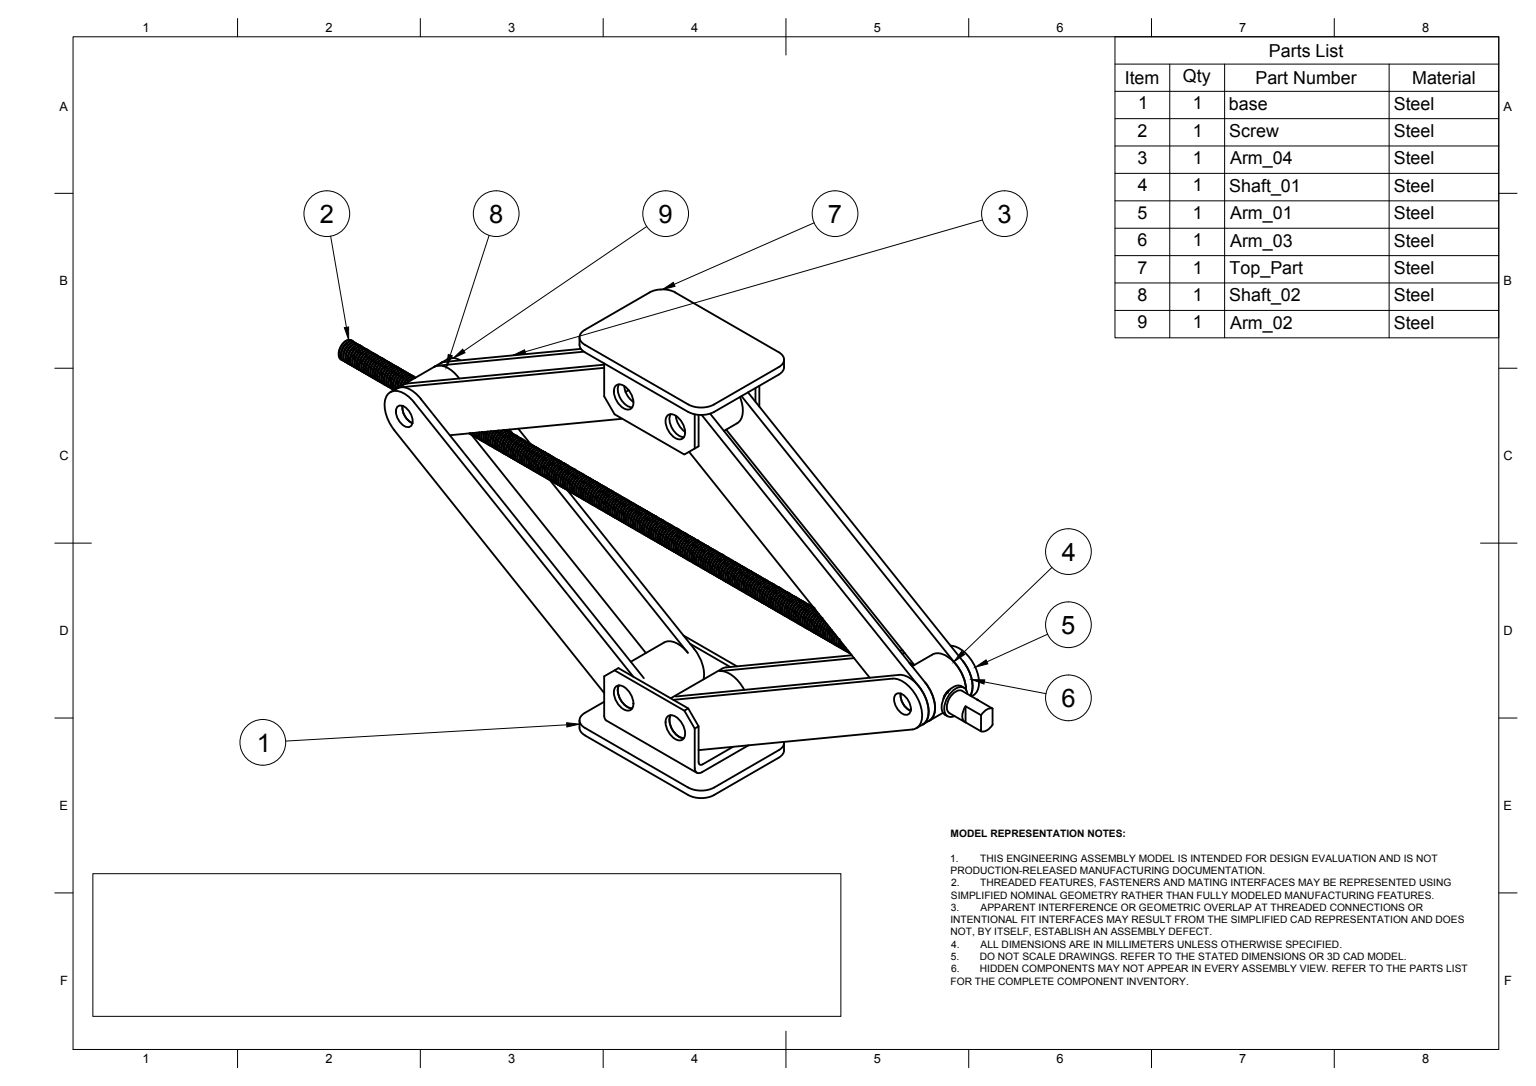
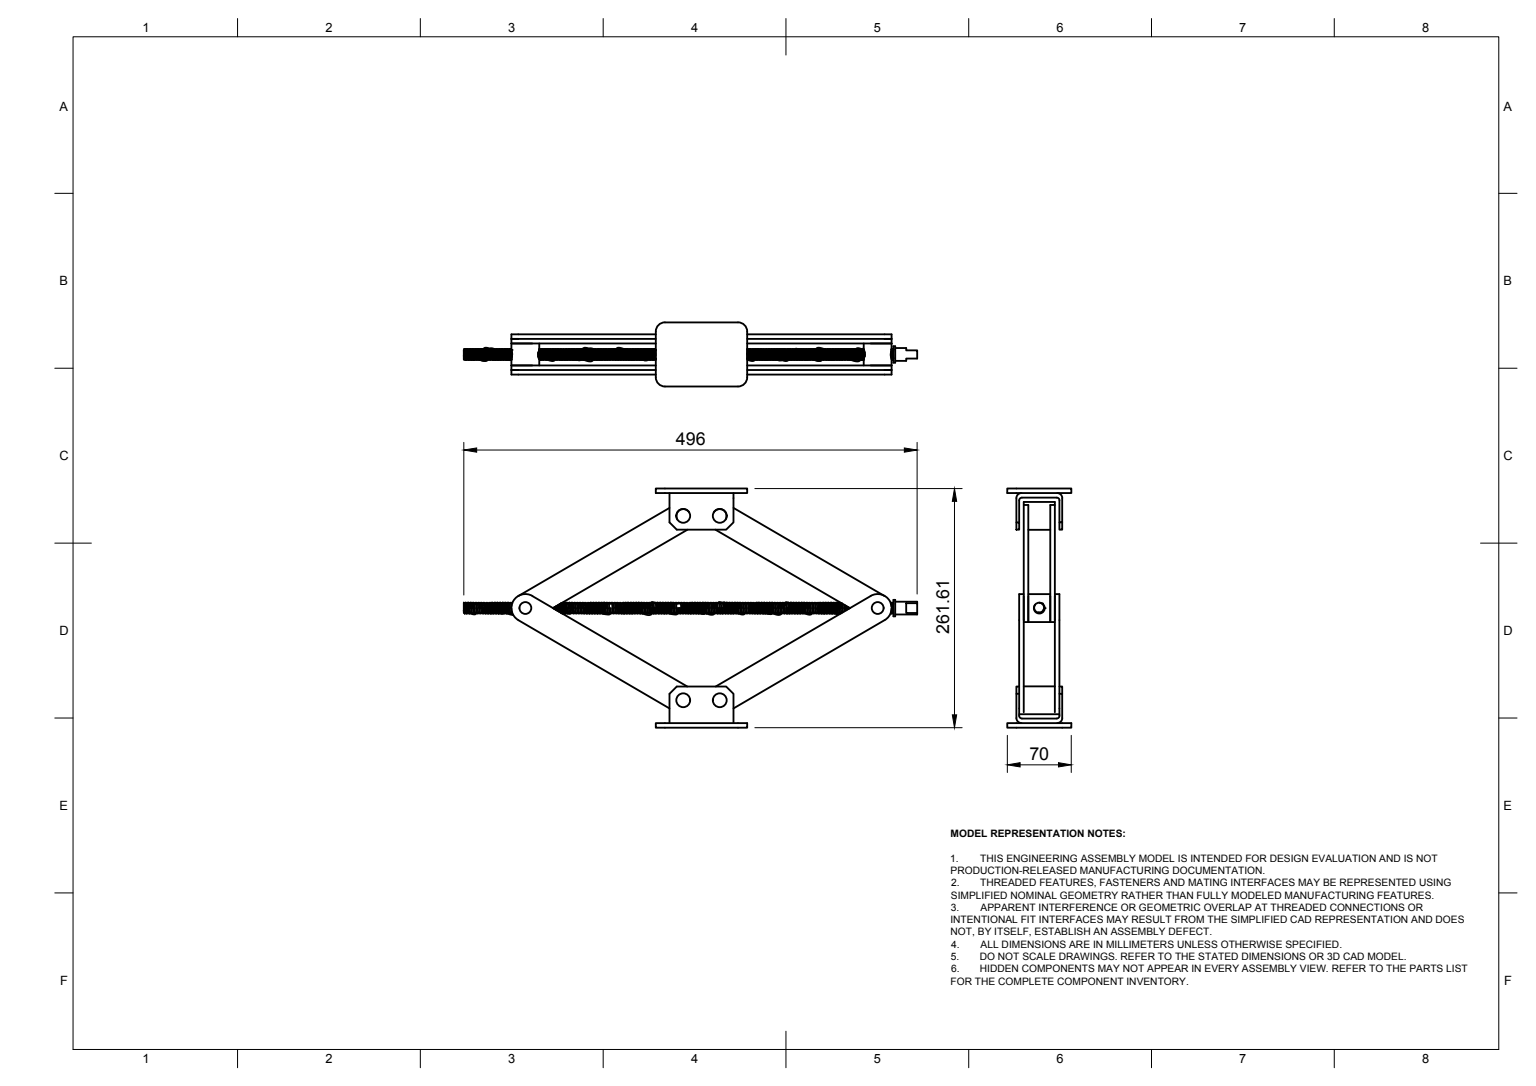
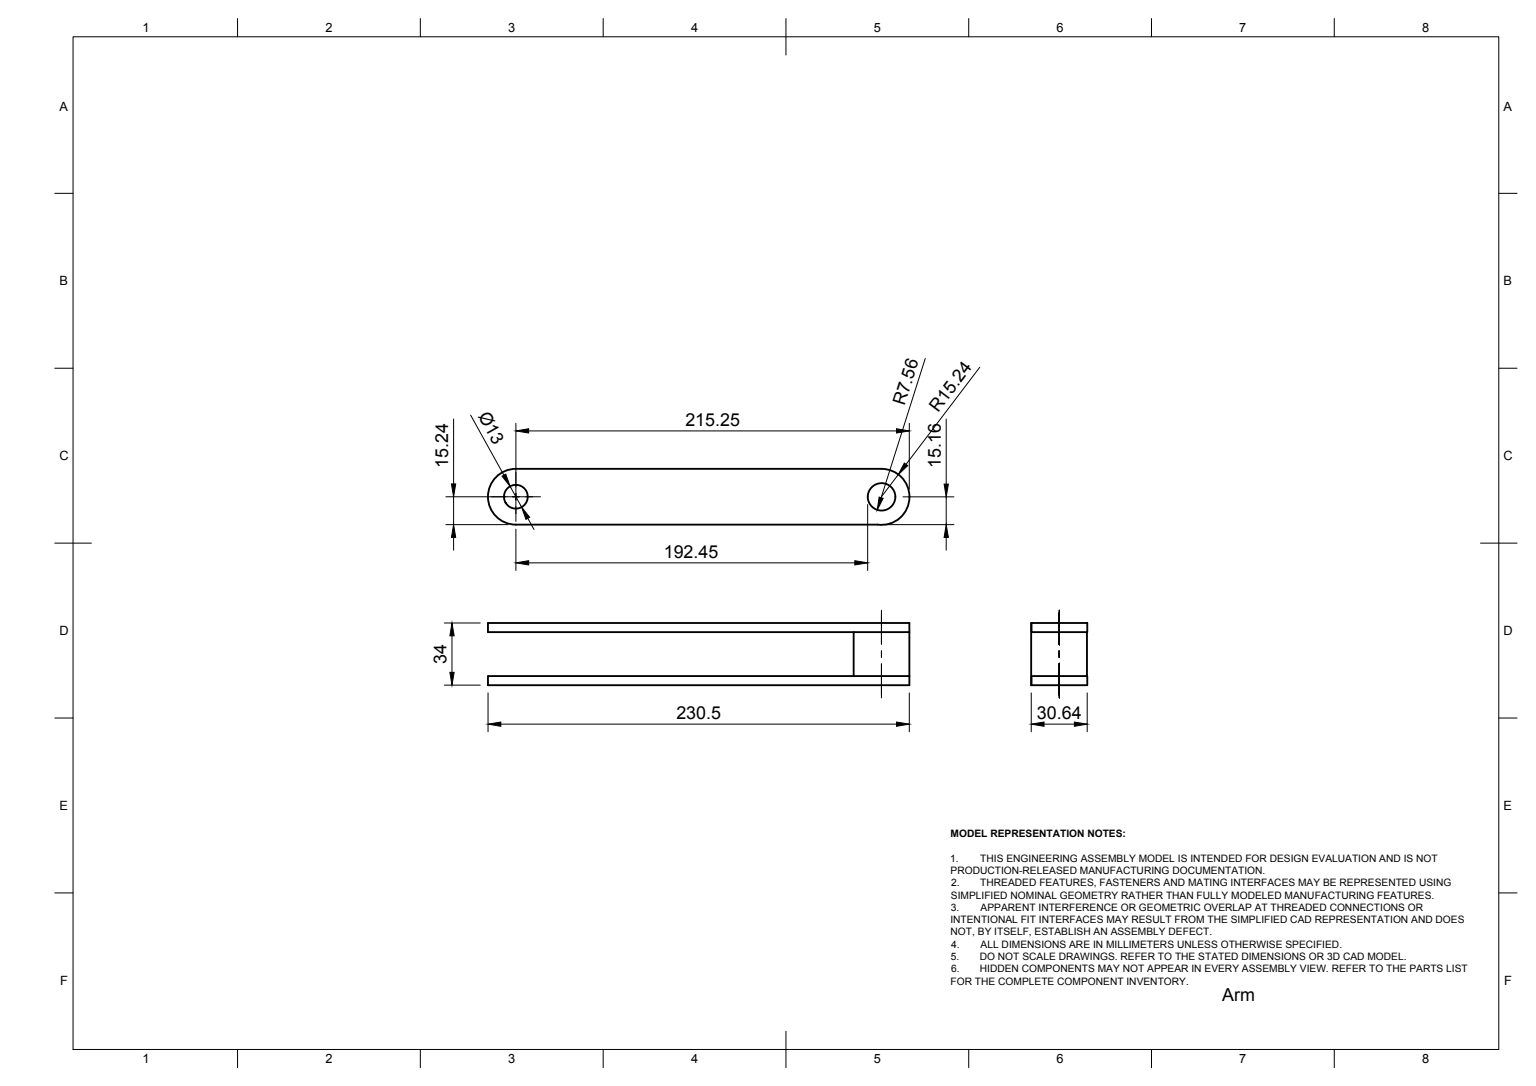
ISO-10303-21;
HEADER;
/* Generated by software containing ST-Developer
 * from STEP Tools, Inc. (www.steptools.com) 
 */

FILE_DESCRIPTION(
/* description */ (''),
/* implementation_level */ '2;1');

FILE_NAME(
/* name */ 'BR-355',
/* time_stamp */ '2026-10-06T13:41:14-07:00',
/* author */ (''),
/* organization */ (''),
/* preprocessor_version */ 'ST-DEVELOPER v20.2',
/* originating_system */ 'Autodesk Translation Framework v15.15.0.0',
/* authorisation */ '');

FILE_SCHEMA (('AUTOMOTIVE_DESIGN { 1 0 10303 214 3 1 1 }'));
ENDSEC;

DATA;
#10=MECHANICAL_DESIGN_GEOMETRIC_PRESENTATION_REPRESENTATION('',(#1960,#1961,
#1962,#1963,#1964,#1965,#1966,#1967,#1968),#279266);
#11=ITEM_DEFINED_TRANSFORMATION($,$,#15048,#15665);
#12=ITEM_DEFINED_TRANSFORMATION($,$,#15104,#15666);
#13=ITEM_DEFINED_TRANSFORMATION($,$,#15397,#15667);
#14=ITEM_DEFINED_TRANSFORMATION($,$,#15446,#15668);
#15=ITEM_DEFINED_TRANSFORMATION($,$,#15474,#15669);
#16=ITEM_DEFINED_TRANSFORMATION($,$,#15503,#15670);
#17=ITEM_DEFINED_TRANSFORMATION($,$,#15552,#15671);
#18=ITEM_DEFINED_TRANSFORMATION($,$,#15608,#15672);
#19=ITEM_DEFINED_TRANSFORMATION($,$,#15636,#15673);
#20=(
REPRESENTATION_RELATIONSHIP($,$,#279301,#279300)
REPRESENTATION_RELATIONSHIP_WITH_TRANSFORMATION(#11)
SHAPE_REPRESENTATION_RELATIONSHIP()
);
#21=(
REPRESENTATION_RELATIONSHIP($,$,#279302,#279300)
REPRESENTATION_RELATIONSHIP_WITH_TRANSFORMATION(#12)
SHAPE_REPRESENTATION_RELATIONSHIP()
);
#22=(
REPRESENTATION_RELATIONSHIP($,$,#279303,#279300)
REPRESENTATION_RELATIONSHIP_WITH_TRANSFORMATION(#13)
SHAPE_REPRESENTATION_RELATIONSHIP()
);
#23=(
REPRESENTATION_RELATIONSHIP($,$,#279304,#279300)
REPRESENTATION_RELATIONSHIP_WITH_TRANSFORMATION(#14)
SHAPE_REPRESENTATION_RELATIONSHIP()
);
#24=(
REPRESENTATION_RELATIONSHIP($,$,#279305,#279300)
REPRESENTATION_RELATIONSHIP_WITH_TRANSFORMATION(#15)
SHAPE_REPRESENTATION_RELATIONSHIP()
);
#25=(
REPRESENTATION_RELATIONSHIP($,$,#279306,#279300)
REPRESENTATION_RELATIONSHIP_WITH_TRANSFORMATION(#16)
SHAPE_REPRESENTATION_RELATIONSHIP()
);
#26=(
REPRESENTATION_RELATIONSHIP($,$,#279307,#279300)
REPRESENTATION_RELATIONSHIP_WITH_TRANSFORMATION(#17)
SHAPE_REPRESENTATION_RELATIONSHIP()
);
#27=(
REPRESENTATION_RELATIONSHIP($,$,#279308,#279300)
REPRESENTATION_RELATIONSHIP_WITH_TRANSFORMATION(#18)
SHAPE_REPRESENTATION_RELATIONSHIP()
);
#28=(
REPRESENTATION_RELATIONSHIP($,$,#279309,#279300)
REPRESENTATION_RELATIONSHIP_WITH_TRANSFORMATION(#19)
SHAPE_REPRESENTATION_RELATIONSHIP()
);
#29=CONTEXT_DEPENDENT_SHAPE_REPRESENTATION(#20,#279291);
#30=CONTEXT_DEPENDENT_SHAPE_REPRESENTATION(#21,#279292);
#31=CONTEXT_DEPENDENT_SHAPE_REPRESENTATION(#22,#279293);
#32=CONTEXT_DEPENDENT_SHAPE_REPRESENTATION(#23,#279294);
#33=CONTEXT_DEPENDENT_SHAPE_REPRESENTATION(#24,#279295);
#34=CONTEXT_DEPENDENT_SHAPE_REPRESENTATION(#25,#279296);
#35=CONTEXT_DEPENDENT_SHAPE_REPRESENTATION(#26,#279297);
#36=CONTEXT_DEPENDENT_SHAPE_REPRESENTATION(#27,#279298);
#37=CONTEXT_DEPENDENT_SHAPE_REPRESENTATION(#28,#279299);
#38=NEXT_ASSEMBLY_USAGE_OCCURRENCE('Base:1','Base:1','Base:1',#279311,#279312,
'Base:1');
#39=NEXT_ASSEMBLY_USAGE_OCCURRENCE('Screw:1','Screw:1','Screw:1',#279311,
#279313,'Screw:1');
#40=NEXT_ASSEMBLY_USAGE_OCCURRENCE('Arm_04:1','Arm_04:1','Arm_04:1',#279311,
#279314,'Arm_04:1');
#41=NEXT_ASSEMBLY_USAGE_OCCURRENCE('Shaft_01:1','Shaft_01:1',
'Shaft_01:1',#279311,#279315,'Shaft_01:1');
#42=NEXT_ASSEMBLY_USAGE_OCCURRENCE('Arm_01:1','Arm_01:1','Arm_01:1',#279311,
#279316,'Arm_01:1');
#43=NEXT_ASSEMBLY_USAGE_OCCURRENCE('Arm_03:1','Arm_03:1','Arm_03:1',#279311,
#279317,'Arm_03:1');
#44=NEXT_ASSEMBLY_USAGE_OCCURRENCE('Top_Part:1','Top_Part:1',
'Top_Part:1',#279311,#279318,'Top_Part:1');
#45=NEXT_ASSEMBLY_USAGE_OCCURRENCE('Shaft_02:1','Shaft_02:1',
'Shaft_02:1',#279311,#279319,'Shaft_02:1');
#46=NEXT_ASSEMBLY_USAGE_OCCURRENCE('Arm_02:1','Arm_02:1','Arm_02:1',#279311,
#279320,'Arm_02:1');
#47=B_SPLINE_SURFACE_WITH_KNOTS('',3,3,((#188642,#188643,#188644,#188645,
#188646,#188647,#188648,#188649,#188650,#188651,#188652,#188653,#188654,
#188655,#188656,#188657,#188658,#188659,#188660,#188661,#188662,#188663,
#188664,#188665,#188666,#188667,#188668,#188669,#188670,#188671,#188672,
#188673,#188674,#188675,#188676,#188677,#188678,#188679,#188680,#188681,
#188682,#188683,#188684,#188685,#188686,#188687,#188688,#188689,#188690,
#188691,#188692,#188693,#188694,#188695,#188696,#188697,#188698,#188699,
#188700,#188701,#188702,#188703,#188704,#188705,#188706,#188707,#188708,
#188709,#188710,#188711,#188712,#188713,#188714,#188715,#188716,#188717,
#188718,#188719,#188720,#188721,#188722,#188723,#188724,#188725,#188726,
#188727,#188728,#188729,#188730,#188731,#188732,#188733,#188734,#188735,
#188736,#188737,#188738,#188739,#188740,#188741,#188742,#188743,#188744,
#188745,#188746,#188747,#188748,#188749,#188750,#188751,#188752,#188753,
#188754,#188755,#188756,#188757,#188758,#188759,#188760,#188761,#188762,
#188763,#188764,#188765,#188766,#188767,#188768,#188769,#188770,#188771,
#188772,#188773,#188774,#188775,#188776,#188777,#188778,#188779,#188780,
#188781,#188782,#188783,#188784,#188785,#188786,#188787,#188788,#188789,
#188790,#188791,#188792,#188793,#188794,#188795,#188796,#188797,#188798,
#188799,#188800,#188801,#188802,#188803,#188804,#188805,#188806,#188807,
#188808,#188809,#188810,#188811,#188812,#188813,#188814,#188815,#188816,
#188817,#188818,#188819,#188820,#188821,#188822,#188823,#188824,#188825,
#188826,#188827,#188828,#188829,#188830,#188831,#188832,#188833,#188834,
#188835,#188836,#188837,#188838,#188839,#188840,#188841,#188842,#188843,
#188844,#188845,#188846,#188847,#188848,#188849,#188850,#188851,#188852,
#188853,#188854,#188855,#188856,#188857,#188858,#188859,#188860,#188861,
#188862,#188863,#188864,#188865,#188866,#188867,#188868,#188869,#188870,
#188871,#188872,#188873,#188874,#188875,#188876,#188877,#188878,#188879,
#188880,#188881,#188882,#188883,#188884,#188885,#188886,#188887,#188888,
#188889,#188890,#188891,#188892,#188893,#188894,#188895,#188896,#188897,
#188898,#188899,#188900,#188901,#188902,#188903,#188904,#188905,#188906,
#188907,#188908,#188909,#188910,#188911,#188912,#188913,#188914,#188915,
#188916,#188917,#188918,#188919,#188920,#188921,#188922,#188923,#188924,
#188925,#188926,#188927,#188928,#188929,#188930,#188931,#188932,#188933,
#188934,#188935,#188936,#188937,#188938,#188939,#188940,#188941,#188942,
#188943,#188944,#188945,#188946,#188947,#188948,#188949,#188950,#188951,
#188952,#188953,#188954,#188955,#188956,#188957,#188958,#188959,#188960,
#188961,#188962,#188963,#188964,#188965,#188966,#188967,#188968,#188969,
#188970,#188971,#188972,#188973,#188974,#188975,#188976,#188977,#188978,
#188979,#188980,#188981,#188982,#188983,#188984,#188985,#188986,#188987,
#188988,#188989,#188990,#188991,#188992,#188993,#188994,#188995,#188996,
#188997,#188998,#188999,#189000,#189001,#189002,#189003,#189004,#189005,
#189006,#189007,#189008,#189009,#189010,#189011,#189012,#189013,#189014,
#189015,#189016,#189017,#189018,#189019,#189020,#189021,#189022,#189023,
#189024,#189025,#189026,#189027,#189028,#189029,#189030,#189031,#189032,
#189033,#189034,#189035,#189036,#189037,#189038,#189039,#189040,#189041,
#189042,#189043,#189044,#189045,#189046,#189047,#189048,#189049,#189050,
#189051,#189052,#189053,#189054,#189055,#189056,#189057,#189058,#189059,
#189060,#189061,#189062,#189063,#189064,#189065,#189066,#189067,#189068,
#189069,#189070,#189071,#189072,#189073,#189074,#189075,#189076,#189077,
#189078,#189079,#189080,#189081,#189082,#189083,#189084,#189085,#189086,
#189087,#189088,#189089,#189090,#189091,#189092,#189093,#189094,#189095,
#189096,#189097,#189098,#189099,#189100,#189101,#189102,#189103,#189104,
#189105,#189106,#189107,#189108,#189109,#189110,#189111,#189112,#189113,
#189114,#189115,#189116,#189117,#189118,#189119,#189120,#189121,#189122,
#189123,#189124,#189125,#189126,#189127,#189128,#189129,#189130,#189131,
#189132,#189133,#189134,#189135,#189136,#189137,#189138,#189139,#189140,
#189141,#189142,#189143,#189144,#189145,#189146,#189147,#189148,#189149,
#189150,#189151,#189152,#189153,#189154,#189155,#189156,#189157,#189158,
#189159,#189160,#189161,#189162,#189163,#189164,#189165,#189166,#189167,
#189168,#189169,#189170,#189171,#189172,#189173,#189174,#189175,#189176,
#189177,#189178,#189179,#189180,#189181,#189182,#189183,#189184,#189185,
#189186,#189187,#189188,#189189,#189190,#189191,#189192,#189193,#189194,
#189195,#189196,#189197,#189198,#189199,#189200,#189201,#189202,#189203,
#189204,#189205,#189206,#189207,#189208,#189209,#189210,#189211,#189212,
#189213,#189214,#189215,#189216,#189217,#189218,#189219,#189220,#189221,
#189222,#189223,#189224,#189225,#189226,#189227,#189228,#189229,#189230,
#189231,#189232,#189233,#189234,#189235,#189236,#189237,#189238,#189239,
#189240,#189241,#189242,#189243,#189244,#189245,#189246,#189247,#189248,
#189249,#189250,#189251,#189252,#189253,#189254,#189255,#189256,#189257,
#189258,#189259,#189260,#189261,#189262,#189263,#189264,#189265,#189266,
#189267,#189268,#189269,#189270,#189271,#189272,#189273,#189274,#189275,
#189276,#189277,#189278,#189279,#189280,#189281,#189282,#189283,#189284,
#189285,#189286,#189287,#189288,#189289,#189290,#189291,#189292,#189293,
#189294,#189295,#189296,#189297,#189298,#189299,#189300,#189301,#189302,
#189303,#189304,#189305,#189306,#189307,#189308,#189309,#189310,#189311,
#189312,#189313,#189314,#189315,#189316,#189317,#189318,#189319,#189320,
#189321,#189322,#189323,#189324,#189325,#189326,#189327,#189328,#189329,
#189330,#189331,#189332,#189333,#189334,#189335,#189336,#189337,#189338,
#189339,#189340,#189341,#189342,#189343,#189344,#189345,#189346,#189347,
#189348,#189349,#189350,#189351,#189352,#189353,#189354,#189355,#189356,
#189357,#189358,#189359,#189360,#189361,#189362,#189363,#189364,#189365,
#189366,#189367,#189368,#189369,#189370,#189371,#189372,#189373,#189374,
#189375,#189376,#189377,#189378,#189379,#189380,#189381,#189382,#189383,
#189384,#189385,#189386,#189387,#189388,#189389,#189390,#189391,#189392,
#189393,#189394,#189395,#189396,#189397,#189398,#189399,#189400,#189401,
#189402,#189403,#189404,#189405,#189406,#189407,#189408,#189409,#189410,
#189411,#189412,#189413,#189414,#189415,#189416,#189417,#189418,#189419,
#189420,#189421,#189422,#189423,#189424,#189425,#189426,#189427,#189428,
#189429,#189430,#189431,#189432,#189433,#189434,#189435,#189436,#189437,
#189438,#189439,#189440,#189441,#189442,#189443,#189444,#189445,#189446,
#189447,#189448,#189449,#189450,#189451,#189452,#189453,#189454,#189455,
#189456,#189457,#189458,#189459,#189460,#189461,#189462,#189463,#189464,
#189465,#189466,#189467,#189468,#189469,#189470,#189471,#189472,#189473,
#189474,#189475,#189476,#189477,#189478,#189479,#189480,#189481,#189482,
#189483,#189484,#189485,#189486,#189487,#189488,#189489,#189490,#189491,
#189492,#189493,#189494,#189495,#189496,#189497,#189498,#189499,#189500,
#189501,#189502,#189503,#189504,#189505,#189506,#189507,#189508,#189509,
#189510,#189511,#189512,#189513,#189514,#189515,#189516,#189517,#189518,
#189519,#189520,#189521,#189522,#189523,#189524,#189525,#189526,#189527,
#189528,#189529,#189530,#189531,#189532,#189533,#189534,#189535,#189536,
#189537,#189538,#189539,#189540,#189541,#189542,#189543,#189544,#189545,
#189546,#189547,#189548,#189549,#189550,#189551,#189552,#189553,#189554,
#189555,#189556,#189557,#189558,#189559,#189560,#189561,#189562,#189563,
#189564,#189565,#189566,#189567,#189568,#189569,#189570,#189571,#189572,
#189573,#189574,#189575,#189576,#189577,#189578,#189579,#189580,#189581,
#189582,#189583,#189584,#189585,#189586,#189587,#189588,#189589,#189590,
#189591,#189592,#189593,#189594,#189595,#189596,#189597,#189598,#189599,
#189600,#189601,#189602,#189603,#189604,#189605,#189606,#189607,#189608,
#189609,#189610,#189611,#189612,#189613,#189614,#189615,#189616,#189617,
#189618,#189619,#189620,#189621,#189622,#189623,#189624,#189625,#189626,
#189627,#189628,#189629,#189630,#189631,#189632,#189633,#189634,#189635,
#189636,#189637,#189638,#189639,#189640,#189641,#189642,#189643,#189644,
#189645,#189646,#189647,#189648,#189649,#189650,#189651,#189652,#189653,
#189654,#189655,#189656,#189657,#189658,#189659,#189660,#189661,#189662,
#189663,#189664,#189665,#189666,#189667,#189668,#189669,#189670,#189671,
#189672,#189673,#189674,#189675,#189676,#189677,#189678,#189679,#189680,
#189681,#189682,#189683,#189684,#189685,#189686,#189687,#189688,#189689,
#189690,#189691,#189692,#189693,#189694,#189695,#189696,#189697,#189698,
#189699,#189700,#189701,#189702,#189703,#189704,#189705,#189706,#189707,
#189708,#189709,#189710,#189711,#189712,#189713,#189714,#189715,#189716,
#189717,#189718,#189719,#189720,#189721,#189722,#189723,#189724,#189725,
#189726,#189727,#189728,#189729,#189730,#189731,#189732,#189733,#189734,
#189735,#189736,#189737,#189738,#189739,#189740,#189741,#189742,#189743,
#189744,#189745,#189746,#189747,#189748,#189749,#189750,#189751,#189752,
#189753,#189754,#189755,#189756,#189757,#189758,#189759,#189760,#189761,
#189762,#189763,#189764,#189765,#189766,#189767,#189768,#189769,#189770,
#189771,#189772,#189773,#189774,#189775,#189776,#189777,#189778,#189779,
#189780,#189781,#189782,#189783,#189784,#189785,#189786,#189787,#189788,
#189789,#189790,#189791,#189792,#189793,#189794,#189795,#189796,#189797,
#189798,#189799,#189800,#189801,#189802,#189803,#189804,#189805,#189806,
#189807,#189808,#189809,#189810,#189811,#189812,#189813,#189814,#189815,
#189816,#189817,#189818,#189819,#189820,#189821,#189822,#189823,#189824,
#189825,#189826,#189827,#189828,#189829,#189830,#189831,#189832,#189833,
#189834,#189835,#189836,#189837,#189838,#189839,#189840,#189841,#189842,
#189843,#189844,#189845,#189846,#189847,#189848,#189849,#189850,#189851,
#189852,#189853,#189854,#189855,#189856,#189857,#189858,#189859,#189860,
#189861,#189862,#189863,#189864,#189865,#189866,#189867,#189868,#189869,
#189870,#189871,#189872,#189873,#189874,#189875,#189876,#189877,#189878,
#189879,#189880,#189881,#189882,#189883,#189884,#189885,#189886,#189887,
#189888,#189889,#189890,#189891,#189892,#189893,#189894,#189895,#189896,
#189897,#189898,#189899,#189900,#189901,#189902,#189903,#189904,#189905,
#189906,#189907,#189908,#189909,#189910,#189911,#189912,#189913,#189914,
#189915,#189916,#189917,#189918,#189919,#189920,#189921,#189922,#189923,
#189924,#189925,#189926,#189927,#189928,#189929,#189930,#189931,#189932,
#189933,#189934,#189935,#189936,#189937,#189938,#189939,#189940,#189941,
#189942,#189943,#189944,#189945,#189946,#189947,#189948,#189949,#189950,
#189951,#189952,#189953,#189954,#189955,#189956,#189957,#189958,#189959,
#189960,#189961,#189962,#189963,#189964,#189965,#189966,#189967,#189968,
#189969,#189970,#189971,#189972,#189973,#189974,#189975,#189976,#189977,
#189978,#189979,#189980,#189981,#189982,#189983,#189984,#189985,#189986,
#189987,#189988,#189989,#189990,#189991,#189992,#189993,#189994,#189995,
#189996,#189997,#189998,#189999,#190000,#190001,#190002,#190003,#190004,
#190005,#190006,#190007,#190008,#190009,#190010,#190011,#190012,#190013,
#190014,#190015,#190016,#190017,#190018,#190019,#190020,#190021,#190022,
#190023,#190024,#190025,#190026,#190027,#190028,#190029,#190030,#190031,
#190032,#190033,#190034,#190035,#190036,#190037,#190038,#190039,#190040,
#190041,#190042,#190043,#190044,#190045,#190046,#190047,#190048,#190049,
#190050,#190051,#190052,#190053,#190054,#190055,#190056,#190057,#190058,
#190059,#190060,#190061,#190062,#190063,#190064,#190065,#190066,#190067,
#190068,#190069,#190070,#190071,#190072,#190073,#190074,#190075,#190076,
#190077,#190078,#190079,#190080,#190081,#190082,#190083,#190084,#190085,
#190086,#190087,#190088,#190089,#190090,#190091,#190092,#190093,#190094,
#190095,#190096,#190097,#190098,#190099,#190100,#190101,#190102,#190103,
#190104,#190105,#190106,#190107,#190108,#190109,#190110,#190111,#190112,
#190113,#190114,#190115,#190116,#190117,#190118,#190119,#190120,#190121,
#190122,#190123,#190124,#190125,#190126,#190127,#190128,#190129,#190130,
#190131,#190132,#190133,#190134,#190135,#190136,#190137,#190138,#190139,
#190140,#190141,#190142,#190143,#190144,#190145,#190146,#190147,#190148,
#190149,#190150,#190151,#190152,#190153,#190154,#190155,#190156,#190157,
#190158,#190159,#190160,#190161,#190162,#190163,#190164,#190165,#190166,
#190167,#190168,#190169,#190170,#190171,#190172,#190173,#190174,#190175,
#190176,#190177,#190178,#190179,#190180,#190181,#190182,#190183,#190184,
#190185,#190186,#190187,#190188,#190189,#190190,#190191,#190192,#190193,
#190194,#190195,#190196,#190197,#190198,#190199,#190200,#190201,#190202,
#190203,#190204,#190205,#190206,#190207,#190208,#190209,#190210,#190211,
#190212,#190213,#190214,#190215,#190216,#190217,#190218,#190219,#190220,
#190221,#190222,#190223,#190224,#190225,#190226,#190227,#190228,#190229,
#190230,#190231,#190232,#190233,#190234,#190235,#190236,#190237,#190238,
#190239,#190240,#190241,#190242,#190243,#190244,#190245,#190246,#190247,
#190248,#190249,#190250,#190251,#190252,#190253,#190254,#190255,#190256,
#190257,#190258,#190259,#190260,#190261,#190262,#190263,#190264,#190265,
#190266,#190267,#190268,#190269,#190270,#190271,#190272,#190273,#190274,
#190275,#190276,#190277,#190278,#190279,#190280,#190281,#190282,#190283,
#190284,#190285,#190286,#190287,#190288,#190289,#190290,#190291,#190292,
#190293,#190294,#190295,#190296,#190297,#190298,#190299,#190300,#190301,
#190302,#190303,#190304,#190305,#190306,#190307,#190308,#190309,#190310,
#190311,#190312,#190313,#190314,#190315,#190316,#190317,#190318,#190319,
#190320,#190321,#190322,#190323,#190324,#190325,#190326,#190327,#190328,
#190329,#190330,#190331,#190332,#190333,#190334,#190335,#190336),(#190337,
#190338,#190339,#190340,#190341,#190342,#190343,#190344,#190345,#190346,
#190347,#190348,#190349,#190350,#190351,#190352,#190353,#190354,#190355,
#190356,#190357,#190358,#190359,#190360,#190361,#190362,#190363,#190364,
#190365,#190366,#190367,#190368,#190369,#190370,#190371,#190372,#190373,
#190374,#190375,#190376,#190377,#190378,#190379,#190380,#190381,#190382,
#190383,#190384,#190385,#190386,#190387,#190388,#190389,#190390,#190391,
#190392,#190393,#190394,#190395,#190396,#190397,#190398,#190399,#190400,
#190401,#190402,#190403,#190404,#190405,#190406,#190407,#190408,#190409,
#190410,#190411,#190412,#190413,#190414,#190415,#190416,#190417,#190418,
#190419,#190420,#190421,#190422,#190423,#190424,#190425,#190426,#190427,
#190428,#190429,#190430,#190431,#190432,#190433,#190434,#190435,#190436,
#190437,#190438,#190439,#190440,#190441,#190442,#190443,#190444,#190445,
#190446,#190447,#190448,#190449,#190450,#190451,#190452,#190453,#190454,
#190455,#190456,#190457,#190458,#190459,#190460,#190461,#190462,#190463,
#190464,#190465,#190466,#190467,#190468,#190469,#190470,#190471,#190472,
#190473,#190474,#190475,#190476,#190477,#190478,#190479,#190480,#190481,
#190482,#190483,#190484,#190485,#190486,#190487,#190488,#190489,#190490,
#190491,#190492,#190493,#190494,#190495,#190496,#190497,#190498,#190499,
#190500,#190501,#190502,#190503,#190504,#190505,#190506,#190507,#190508,
#190509,#190510,#190511,#190512,#190513,#190514,#190515,#190516,#190517,
#190518,#190519,#190520,#190521,#190522,#190523,#190524,#190525,#190526,
#190527,#190528,#190529,#190530,#190531,#190532,#190533,#190534,#190535,
#190536,#190537,#190538,#190539,#190540,#190541,#190542,#190543,#190544,
#190545,#190546,#190547,#190548,#190549,#190550,#190551,#190552,#190553,
#190554,#190555,#190556,#190557,#190558,#190559,#190560,#190561,#190562,
#190563,#190564,#190565,#190566,#190567,#190568,#190569,#190570,#190571,
#190572,#190573,#190574,#190575,#190576,#190577,#190578,#190579,#190580,
#190581,#190582,#190583,#190584,#190585,#190586,#190587,#190588,#190589,
#190590,#190591,#190592,#190593,#190594,#190595,#190596,#190597,#190598,
#190599,#190600,#190601,#190602,#190603,#190604,#190605,#190606,#190607,
#190608,#190609,#190610,#190611,#190612,#190613,#190614,#190615,#190616,
#190617,#190618,#190619,#190620,#190621,#190622,#190623,#190624,#190625,
#190626,#190627,#190628,#190629,#190630,#190631,#190632,#190633,#190634,
#190635,#190636,#190637,#190638,#190639,#190640,#190641,#190642,#190643,
#190644,#190645,#190646,#190647,#190648,#190649,#190650,#190651,#190652,
#190653,#190654,#190655,#190656,#190657,#190658,#190659,#190660,#190661,
#190662,#190663,#190664,#190665,#190666,#190667,#190668,#190669,#190670,
#190671,#190672,#190673,#190674,#190675,#190676,#190677,#190678,#190679,
#190680,#190681,#190682,#190683,#190684,#190685,#190686,#190687,#190688,
#190689,#190690,#190691,#190692,#190693,#190694,#190695,#190696,#190697,
#190698,#190699,#190700,#190701,#190702,#190703,#190704,#190705,#190706,
#190707,#190708,#190709,#190710,#190711,#190712,#190713,#190714,#190715,
#190716,#190717,#190718,#190719,#190720,#190721,#190722,#190723,#190724,
#190725,#190726,#190727,#190728,#190729,#190730,#190731,#190732,#190733,
#190734,#190735,#190736,#190737,#190738,#190739,#190740,#190741,#190742,
#190743,#190744,#190745,#190746,#190747,#190748,#190749,#190750,#190751,
#190752,#190753,#190754,#190755,#190756,#190757,#190758,#190759,#190760,
#190761,#190762,#190763,#190764,#190765,#190766,#190767,#190768,#190769,
#190770,#190771,#190772,#190773,#190774,#190775,#190776,#190777,#190778,
#190779,#190780,#190781,#190782,#190783,#190784,#190785,#190786,#190787,
#190788,#190789,#190790,#190791,#190792,#190793,#190794,#190795,#190796,
#190797,#190798,#190799,#190800,#190801,#190802,#190803,#190804,#190805,
#190806,#190807,#190808,#190809,#190810,#190811,#190812,#190813,#190814,
#190815,#190816,#190817,#190818,#190819,#190820,#190821,#190822,#190823,
#190824,#190825,#190826,#190827,#190828,#190829,#190830,#190831,#190832,
#190833,#190834,#190835,#190836,#190837,#190838,#190839,#190840,#190841,
#190842,#190843,#190844,#190845,#190846,#190847,#190848,#190849,#190850,
#190851,#190852,#190853,#190854,#190855,#190856,#190857,#190858,#190859,
#190860,#190861,#190862,#190863,#190864,#190865,#190866,#190867,#190868,
#190869,#190870,#190871,#190872,#190873,#190874,#190875,#190876,#190877,
#190878,#190879,#190880,#190881,#190882,#190883,#190884,#190885,#190886,
#190887,#190888,#190889,#190890,#190891,#190892,#190893,#190894,#190895,
#190896,#190897,#190898,#190899,#190900,#190901,#190902,#190903,#190904,
#190905,#190906,#190907,#190908,#190909,#190910,#190911,#190912,#190913,
#190914,#190915,#190916,#190917,#190918,#190919,#190920,#190921,#190922,
#190923,#190924,#190925,#190926,#190927,#190928,#190929,#190930,#190931,
#190932,#190933,#190934,#190935,#190936,#190937,#190938,#190939,#190940,
#190941,#190942,#190943,#190944,#190945,#190946,#190947,#190948,#190949,
#190950,#190951,#190952,#190953,#190954,#190955,#190956,#190957,#190958,
#190959,#190960,#190961,#190962,#190963,#190964,#190965,#190966,#190967,
#190968,#190969,#190970,#190971,#190972,#190973,#190974,#190975,#190976,
#190977,#190978,#190979,#190980,#190981,#190982,#190983,#190984,#190985,
#190986,#190987,#190988,#190989,#190990,#190991,#190992,#190993,#190994,
#190995,#190996,#190997,#190998,#190999,#191000,#191001,#191002,#191003,
#191004,#191005,#191006,#191007,#191008,#191009,#191010,#191011,#191012,
#191013,#191014,#191015,#191016,#191017,#191018,#191019,#191020,#191021,
#191022,#191023,#191024,#191025,#191026,#191027,#191028,#191029,#191030,
#191031,#191032,#191033,#191034,#191035,#191036,#191037,#191038,#191039,
#191040,#191041,#191042,#191043,#191044,#191045,#191046,#191047,#191048,
#191049,#191050,#191051,#191052,#191053,#191054,#191055,#191056,#191057,
#191058,#191059,#191060,#191061,#191062,#191063,#191064,#191065,#191066,
#191067,#191068,#191069,#191070,#191071,#191072,#191073,#191074,#191075,
#191076,#191077,#191078,#191079,#191080,#191081,#191082,#191083,#191084,
#191085,#191086,#191087,#191088,#191089,#191090,#191091,#191092,#191093,
#191094,#191095,#191096,#191097,#191098,#191099,#191100,#191101,#191102,
#191103,#191104,#191105,#191106,#191107,#191108,#191109,#191110,#191111,
#191112,#191113,#191114,#191115,#191116,#191117,#191118,#191119,#191120,
#191121,#191122,#191123,#191124,#191125,#191126,#191127,#191128,#191129,
#191130,#191131,#191132,#191133,#191134,#191135,#191136,#191137,#191138,
#191139,#191140,#191141,#191142,#191143,#191144,#191145,#191146,#191147,
#191148,#191149,#191150,#191151,#191152,#191153,#191154,#191155,#191156,
#191157,#191158,#191159,#191160,#191161,#191162,#191163,#191164,#191165,
#191166,#191167,#191168,#191169,#191170,#191171,#191172,#191173,#191174,
#191175,#191176,#191177,#191178,#191179,#191180,#191181,#191182,#191183,
#191184,#191185,#191186,#191187,#191188,#191189,#191190,#191191,#191192,
#191193,#191194,#191195,#191196,#191197,#191198,#191199,#191200,#191201,
#191202,#191203,#191204,#191205,#191206,#191207,#191208,#191209,#191210,
#191211,#191212,#191213,#191214,#191215,#191216,#191217,#191218,#191219,
#191220,#191221,#191222,#191223,#191224,#191225,#191226,#191227,#191228,
#191229,#191230,#191231,#191232,#191233,#191234,#191235,#191236,#191237,
#191238,#191239,#191240,#191241,#191242,#191243,#191244,#191245,#191246,
#191247,#191248,#191249,#191250,#191251,#191252,#191253,#191254,#191255,
#191256,#191257,#191258,#191259,#191260,#191261,#191262,#191263,#191264,
#191265,#191266,#191267,#191268,#191269,#191270,#191271,#191272,#191273,
#191274,#191275,#191276,#191277,#191278,#191279,#191280,#191281,#191282,
#191283,#191284,#191285,#191286,#191287,#191288,#191289,#191290,#191291,
#191292,#191293,#191294,#191295,#191296,#191297,#191298,#191299,#191300,
#191301,#191302,#191303,#191304,#191305,#191306,#191307,#191308,#191309,
#191310,#191311,#191312,#191313,#191314,#191315,#191316,#191317,#191318,
#191319,#191320,#191321,#191322,#191323,#191324,#191325,#191326,#191327,
#191328,#191329,#191330,#191331,#191332,#191333,#191334,#191335,#191336,
#191337,#191338,#191339,#191340,#191341,#191342,#191343,#191344,#191345,
#191346,#191347,#191348,#191349,#191350,#191351,#191352,#191353,#191354,
#191355,#191356,#191357,#191358,#191359,#191360,#191361,#191362,#191363,
#191364,#191365,#191366,#191367,#191368,#191369,#191370,#191371,#191372,
#191373,#191374,#191375,#191376,#191377,#191378,#191379,#191380,#191381,
#191382,#191383,#191384,#191385,#191386,#191387,#191388,#191389,#191390,
#191391,#191392,#191393,#191394,#191395,#191396,#191397,#191398,#191399,
#191400,#191401,#191402,#191403,#191404,#191405,#191406,#191407,#191408,
#191409,#191410,#191411,#191412,#191413,#191414,#191415,#191416,#191417,
#191418,#191419,#191420,#191421,#191422,#191423,#191424,#191425,#191426,
#191427,#191428,#191429,#191430,#191431,#191432,#191433,#191434,#191435,
#191436,#191437,#191438,#191439,#191440,#191441,#191442,#191443,#191444,
#191445,#191446,#191447,#191448,#191449,#191450,#191451,#191452,#191453,
#191454,#191455,#191456,#191457,#191458,#191459,#191460,#191461,#191462,
#191463,#191464,#191465,#191466,#191467,#191468,#191469,#191470,#191471,
#191472,#191473,#191474,#191475,#191476,#191477,#191478,#191479,#191480,
#191481,#191482,#191483,#191484,#191485,#191486,#191487,#191488,#191489,
#191490,#191491,#191492,#191493,#191494,#191495,#191496,#191497,#191498,
#191499,#191500,#191501,#191502,#191503,#191504,#191505,#191506,#191507,
#191508,#191509,#191510,#191511,#191512,#191513,#191514,#191515,#191516,
#191517,#191518,#191519,#191520,#191521,#191522,#191523,#191524,#191525,
#191526,#191527,#191528,#191529,#191530,#191531,#191532,#191533,#191534,
#191535,#191536,#191537,#191538,#191539,#191540,#191541,#191542,#191543,
#191544,#191545,#191546,#191547,#191548,#191549,#191550,#191551,#191552,
#191553,#191554,#191555,#191556,#191557,#191558,#191559,#191560,#191561,
#191562,#191563,#191564,#191565,#191566,#191567,#191568,#191569,#191570,
#191571,#191572,#191573,#191574,#191575,#191576,#191577,#191578,#191579,
#191580,#191581,#191582,#191583,#191584,#191585,#191586,#191587,#191588,
#191589,#191590,#191591,#191592,#191593,#191594,#191595,#191596,#191597,
#191598,#191599,#191600,#191601,#191602,#191603,#191604,#191605,#191606,
#191607,#191608,#191609,#191610,#191611,#191612,#191613,#191614,#191615,
#191616,#191617,#191618,#191619,#191620,#191621,#191622,#191623,#191624,
#191625,#191626,#191627,#191628,#191629,#191630,#191631,#191632,#191633,
#191634,#191635,#191636,#191637,#191638,#191639,#191640,#191641,#191642,
#191643,#191644,#191645,#191646,#191647,#191648,#191649,#191650,#191651,
#191652,#191653,#191654,#191655,#191656,#191657,#191658,#191659,#191660,
#191661,#191662,#191663,#191664,#191665,#191666,#191667,#191668,#191669,
#191670,#191671,#191672,#191673,#191674,#191675,#191676,#191677,#191678,
#191679,#191680,#191681,#191682,#191683,#191684,#191685,#191686,#191687,
#191688,#191689,#191690,#191691,#191692,#191693,#191694,#191695,#191696,
#191697,#191698,#191699,#191700,#191701,#191702,#191703,#191704,#191705,
#191706,#191707,#191708,#191709,#191710,#191711,#191712,#191713,#191714,
#191715,#191716,#191717,#191718,#191719,#191720,#191721,#191722,#191723,
#191724,#191725,#191726,#191727,#191728,#191729,#191730,#191731,#191732,
#191733,#191734,#191735,#191736,#191737,#191738,#191739,#191740,#191741,
#191742,#191743,#191744,#191745,#191746,#191747,#191748,#191749,#191750,
#191751,#191752,#191753,#191754,#191755,#191756,#191757,#191758,#191759,
#191760,#191761,#191762,#191763,#191764,#191765,#191766,#191767,#191768,
#191769,#191770,#191771,#191772,#191773,#191774,#191775,#191776,#191777,
#191778,#191779,#191780,#191781,#191782,#191783,#191784,#191785,#191786,
#191787,#191788,#191789,#191790,#191791,#191792,#191793,#191794,#191795,
#191796,#191797,#191798,#191799,#191800,#191801,#191802,#191803,#191804,
#191805,#191806,#191807,#191808,#191809,#191810,#191811,#191812,#191813,
#191814,#191815,#191816,#191817,#191818,#191819,#191820,#191821,#191822,
#191823,#191824,#191825,#191826,#191827,#191828,#191829,#191830,#191831,
#191832,#191833,#191834,#191835,#191836,#191837,#191838,#191839,#191840,
#191841,#191842,#191843,#191844,#191845,#191846,#191847,#191848,#191849,
#191850,#191851,#191852,#191853,#191854,#191855,#191856,#191857,#191858,
#191859,#191860,#191861,#191862,#191863,#191864,#191865,#191866,#191867,
#191868,#191869,#191870,#191871,#191872,#191873,#191874,#191875,#191876,
#191877,#191878,#191879,#191880,#191881,#191882,#191883,#191884,#191885,
#191886,#191887,#191888,#191889,#191890,#191891,#191892,#191893,#191894,
#191895,#191896,#191897,#191898,#191899,#191900,#191901,#191902,#191903,
#191904,#191905,#191906,#191907,#191908,#191909,#191910,#191911,#191912,
#191913,#191914,#191915,#191916,#191917,#191918,#191919,#191920,#191921,
#191922,#191923,#191924,#191925,#191926,#191927,#191928,#191929,#191930,
#191931,#191932,#191933,#191934,#191935,#191936,#191937,#191938,#191939,
#191940,#191941,#191942,#191943,#191944,#191945,#191946,#191947,#191948,
#191949,#191950,#191951,#191952,#191953,#191954,#191955,#191956,#191957,
#191958,#191959,#191960,#191961,#191962,#191963,#191964,#191965,#191966,
#191967,#191968,#191969,#191970,#191971,#191972,#191973,#191974,#191975,
#191976,#191977,#191978,#191979,#191980,#191981,#191982,#191983,#191984,
#191985,#191986,#191987,#191988,#191989,#191990,#191991,#191992,#191993,
#191994,#191995,#191996,#191997,#191998,#191999,#192000,#192001,#192002,
#192003,#192004,#192005,#192006,#192007,#192008,#192009,#192010,#192011,
#192012,#192013,#192014,#192015,#192016,#192017,#192018,#192019,#192020,
#192021,#192022,#192023,#192024,#192025,#192026,#192027,#192028,#192029,
#192030,#192031),(#192032,#192033,#192034,#192035,#192036,#192037,#192038,
#192039,#192040,#192041,#192042,#192043,#192044,#192045,#192046,#192047,
#192048,#192049,#192050,#192051,#192052,#192053,#192054,#192055,#192056,
#192057,#192058,#192059,#192060,#192061,#192062,#192063,#192064,#192065,
#192066,#192067,#192068,#192069,#192070,#192071,#192072,#192073,#192074,
#192075,#192076,#192077,#192078,#192079,#192080,#192081,#192082,#192083,
#192084,#192085,#192086,#192087,#192088,#192089,#192090,#192091,#192092,
#192093,#192094,#192095,#192096,#192097,#192098,#192099,#192100,#192101,
#192102,#192103,#192104,#192105,#192106,#192107,#192108,#192109,#192110,
#192111,#192112,#192113,#192114,#192115,#192116,#192117,#192118,#192119,
#192120,#192121,#192122,#192123,#192124,#192125,#192126,#192127,#192128,
#192129,#192130,#192131,#192132,#192133,#192134,#192135,#192136,#192137,
#192138,#192139,#192140,#192141,#192142,#192143,#192144,#192145,#192146,
#192147,#192148,#192149,#192150,#192151,#192152,#192153,#192154,#192155,
#192156,#192157,#192158,#192159,#192160,#192161,#192162,#192163,#192164,
#192165,#192166,#192167,#192168,#192169,#192170,#192171,#192172,#192173,
#192174,#192175,#192176,#192177,#192178,#192179,#192180,#192181,#192182,
#192183,#192184,#192185,#192186,#192187,#192188,#192189,#192190,#192191,
#192192,#192193,#192194,#192195,#192196,#192197,#192198,#192199,#192200,
#192201,#192202,#192203,#192204,#192205,#192206,#192207,#192208,#192209,
#192210,#192211,#192212,#192213,#192214,#192215,#192216,#192217,#192218,
#192219,#192220,#192221,#192222,#192223,#192224,#192225,#192226,#192227,
#192228,#192229,#192230,#192231,#192232,#192233,#192234,#192235,#192236,
#192237,#192238,#192239,#192240,#192241,#192242,#192243,#192244,#192245,
#192246,#192247,#192248,#192249,#192250,#192251,#192252,#192253,#192254,
#192255,#192256,#192257,#192258,#192259,#192260,#192261,#192262,#192263,
#192264,#192265,#192266,#192267,#192268,#192269,#192270,#192271,#192272,
#192273,#192274,#192275,#192276,#192277,#192278,#192279,#192280,#192281,
#192282,#192283,#192284,#192285,#192286,#192287,#192288,#192289,#192290,
#192291,#192292,#192293,#192294,#192295,#192296,#192297,#192298,#192299,
#192300,#192301,#192302,#192303,#192304,#192305,#192306,#192307,#192308,
#192309,#192310,#192311,#192312,#192313,#192314,#192315,#192316,#192317,
#192318,#192319,#192320,#192321,#192322,#192323,#192324,#192325,#192326,
#192327,#192328,#192329,#192330,#192331,#192332,#192333,#192334,#192335,
#192336,#192337,#192338,#192339,#192340,#192341,#192342,#192343,#192344,
#192345,#192346,#192347,#192348,#192349,#192350,#192351,#192352,#192353,
#192354,#192355,#192356,#192357,#192358,#192359,#192360,#192361,#192362,
#192363,#192364,#192365,#192366,#192367,#192368,#192369,#192370,#192371,
#192372,#192373,#192374,#192375,#192376,#192377,#192378,#192379,#192380,
#192381,#192382,#192383,#192384,#192385,#192386,#192387,#192388,#192389,
#192390,#192391,#192392,#192393,#192394,#192395,#192396,#192397,#192398,
#192399,#192400,#192401,#192402,#192403,#192404,#192405,#192406,#192407,
#192408,#192409,#192410,#192411,#192412,#192413,#192414,#192415,#192416,
#192417,#192418,#192419,#192420,#192421,#192422,#192423,#192424,#192425,
#192426,#192427,#192428,#192429,#192430,#192431,#192432,#192433,#192434,
#192435,#192436,#192437,#192438,#192439,#192440,#192441,#192442,#192443,
#192444,#192445,#192446,#192447,#192448,#192449,#192450,#192451,#192452,
#192453,#192454,#192455,#192456,#192457,#192458,#192459,#192460,#192461,
#192462,#192463,#192464,#192465,#192466,#192467,#192468,#192469,#192470,
#192471,#192472,#192473,#192474,#192475,#192476,#192477,#192478,#192479,
#192480,#192481,#192482,#192483,#192484,#192485,#192486,#192487,#192488,
#192489,#192490,#192491,#192492,#192493,#192494,#192495,#192496,#192497,
#192498,#192499,#192500,#192501,#192502,#192503,#192504,#192505,#192506,
#192507,#192508,#192509,#192510,#192511,#192512,#192513,#192514,#192515,
#192516,#192517,#192518,#192519,#192520,#192521,#192522,#192523,#192524,
#192525,#192526,#192527,#192528,#192529,#192530,#192531,#192532,#192533,
#192534,#192535,#192536,#192537,#192538,#192539,#192540,#192541,#192542,
#192543,#192544,#192545,#192546,#192547,#192548,#192549,#192550,#192551,
#192552,#192553,#192554,#192555,#192556,#192557,#192558,#192559,#192560,
#192561,#192562,#192563,#192564,#192565,#192566,#192567,#192568,#192569,
#192570,#192571,#192572,#192573,#192574,#192575,#192576,#192577,#192578,
#192579,#192580,#192581,#192582,#192583,#192584,#192585,#192586,#192587,
#192588,#192589,#192590,#192591,#192592,#192593,#192594,#192595,#192596,
#192597,#192598,#192599,#192600,#192601,#192602,#192603,#192604,#192605,
#192606,#192607,#192608,#192609,#192610,#192611,#192612,#192613,#192614,
#192615,#192616,#192617,#192618,#192619,#192620,#192621,#192622,#192623,
#192624,#192625,#192626,#192627,#192628,#192629,#192630,#192631,#192632,
#192633,#192634,#192635,#192636,#192637,#192638,#192639,#192640,#192641,
#192642,#192643,#192644,#192645,#192646,#192647,#192648,#192649,#192650,
#192651,#192652,#192653,#192654,#192655,#192656,#192657,#192658,#192659,
#192660,#192661,#192662,#192663,#192664,#192665,#192666,#192667,#192668,
#192669,#192670,#192671,#192672,#192673,#192674,#192675,#192676,#192677,
#192678,#192679,#192680,#192681,#192682,#192683,#192684,#192685,#192686,
#192687,#192688,#192689,#192690,#192691,#192692,#192693,#192694,#192695,
#192696,#192697,#192698,#192699,#192700,#192701,#192702,#192703,#192704,
#192705,#192706,#192707,#192708,#192709,#192710,#192711,#192712,#192713,
#192714,#192715,#192716,#192717,#192718,#192719,#192720,#192721,#192722,
#192723,#192724,#192725,#192726,#192727,#192728,#192729,#192730,#192731,
#192732,#192733,#192734,#192735,#192736,#192737,#192738,#192739,#192740,
#192741,#192742,#192743,#192744,#192745,#192746,#192747,#192748,#192749,
#192750,#192751,#192752,#192753,#192754,#192755,#192756,#192757,#192758,
#192759,#192760,#192761,#192762,#192763,#192764,#192765,#192766,#192767,
#192768,#192769,#192770,#192771,#192772,#192773,#192774,#192775,#192776,
#192777,#192778,#192779,#192780,#192781,#192782,#192783,#192784,#192785,
#192786,#192787,#192788,#192789,#192790,#192791,#192792,#192793,#192794,
#192795,#192796,#192797,#192798,#192799,#192800,#192801,#192802,#192803,
#192804,#192805,#192806,#192807,#192808,#192809,#192810,#192811,#192812,
#192813,#192814,#192815,#192816,#192817,#192818,#192819,#192820,#192821,
#192822,#192823,#192824,#192825,#192826,#192827,#192828,#192829,#192830,
#192831,#192832,#192833,#192834,#192835,#192836,#192837,#192838,#192839,
#192840,#192841,#192842,#192843,#192844,#192845,#192846,#192847,#192848,
#192849,#192850,#192851,#192852,#192853,#192854,#192855,#192856,#192857,
#192858,#192859,#192860,#192861,#192862,#192863,#192864,#192865,#192866,
#192867,#192868,#192869,#192870,#192871,#192872,#192873,#192874,#192875,
#192876,#192877,#192878,#192879,#192880,#192881,#192882,#192883,#192884,
#192885,#192886,#192887,#192888,#192889,#192890,#192891,#192892,#192893,
#192894,#192895,#192896,#192897,#192898,#192899,#192900,#192901,#192902,
#192903,#192904,#192905,#192906,#192907,#192908,#192909,#192910,#192911,
#192912,#192913,#192914,#192915,#192916,#192917,#192918,#192919,#192920,
#192921,#192922,#192923,#192924,#192925,#192926,#192927,#192928,#192929,
#192930,#192931,#192932,#192933,#192934,#192935,#192936,#192937,#192938,
#192939,#192940,#192941,#192942,#192943,#192944,#192945,#192946,#192947,
#192948,#192949,#192950,#192951,#192952,#192953,#192954,#192955,#192956,
#192957,#192958,#192959,#192960,#192961,#192962,#192963,#192964,#192965,
#192966,#192967,#192968,#192969,#192970,#192971,#192972,#192973,#192974,
#192975,#192976,#192977,#192978,#192979,#192980,#192981,#192982,#192983,
#192984,#192985,#192986,#192987,#192988,#192989,#192990,#192991,#192992,
#192993,#192994,#192995,#192996,#192997,#192998,#192999,#193000,#193001,
#193002,#193003,#193004,#193005,#193006,#193007,#193008,#193009,#193010,
#193011,#193012,#193013,#193014,#193015,#193016,#193017,#193018,#193019,
#193020,#193021,#193022,#193023,#193024,#193025,#193026,#193027,#193028,
#193029,#193030,#193031,#193032,#193033,#193034,#193035,#193036,#193037,
#193038,#193039,#193040,#193041,#193042,#193043,#193044,#193045,#193046,
#193047,#193048,#193049,#193050,#193051,#193052,#193053,#193054,#193055,
#193056,#193057,#193058,#193059,#193060,#193061,#193062,#193063,#193064,
#193065,#193066,#193067,#193068,#193069,#193070,#193071,#193072,#193073,
#193074,#193075,#193076,#193077,#193078,#193079,#193080,#193081,#193082,
#193083,#193084,#193085,#193086,#193087,#193088,#193089,#193090,#193091,
#193092,#193093,#193094,#193095,#193096,#193097,#193098,#193099,#193100,
#193101,#193102,#193103,#193104,#193105,#193106,#193107,#193108,#193109,
#193110,#193111,#193112,#193113,#193114,#193115,#193116,#193117,#193118,
#193119,#193120,#193121,#193122,#193123,#193124,#193125,#193126,#193127,
#193128,#193129,#193130,#193131,#193132,#193133,#193134,#193135,#193136,
#193137,#193138,#193139,#193140,#193141,#193142,#193143,#193144,#193145,
#193146,#193147,#193148,#193149,#193150,#193151,#193152,#193153,#193154,
#193155,#193156,#193157,#193158,#193159,#193160,#193161,#193162,#193163,
#193164,#193165,#193166,#193167,#193168,#193169,#193170,#193171,#193172,
#193173,#193174,#193175,#193176,#193177,#193178,#193179,#193180,#193181,
#193182,#193183,#193184,#193185,#193186,#193187,#193188,#193189,#193190,
#193191,#193192,#193193,#193194,#193195,#193196,#193197,#193198,#193199,
#193200,#193201,#193202,#193203,#193204,#193205,#193206,#193207,#193208,
#193209,#193210,#193211,#193212,#193213,#193214,#193215,#193216,#193217,
#193218,#193219,#193220,#193221,#193222,#193223,#193224,#193225,#193226,
#193227,#193228,#193229,#193230,#193231,#193232,#193233,#193234,#193235,
#193236,#193237,#193238,#193239,#193240,#193241,#193242,#193243,#193244,
#193245,#193246,#193247,#193248,#193249,#193250,#193251,#193252,#193253,
#193254,#193255,#193256,#193257,#193258,#193259,#193260,#193261,#193262,
#193263,#193264,#193265,#193266,#193267,#193268,#193269,#193270,#193271,
#193272,#193273,#193274,#193275,#193276,#193277,#193278,#193279,#193280,
#193281,#193282,#193283,#193284,#193285,#193286,#193287,#193288,#193289,
#193290,#193291,#193292,#193293,#193294,#193295,#193296,#193297,#193298,
#193299,#193300,#193301,#193302,#193303,#193304,#193305,#193306,#193307,
#193308,#193309,#193310,#193311,#193312,#193313,#193314,#193315,#193316,
#193317,#193318,#193319,#193320,#193321,#193322,#193323,#193324,#193325,
#193326,#193327,#193328,#193329,#193330,#193331,#193332,#193333,#193334,
#193335,#193336,#193337,#193338,#193339,#193340,#193341,#193342,#193343,
#193344,#193345,#193346,#193347,#193348,#193349,#193350,#193351,#193352,
#193353,#193354,#193355,#193356,#193357,#193358,#193359,#193360,#193361,
#193362,#193363,#193364,#193365,#193366,#193367,#193368,#193369,#193370,
#193371,#193372,#193373,#193374,#193375,#193376,#193377,#193378,#193379,
#193380,#193381,#193382,#193383,#193384,#193385,#193386,#193387,#193388,
#193389,#193390,#193391,#193392,#193393,#193394,#193395,#193396,#193397,
#193398,#193399,#193400,#193401,#193402,#193403,#193404,#193405,#193406,
#193407,#193408,#193409,#193410,#193411,#193412,#193413,#193414,#193415,
#193416,#193417,#193418,#193419,#193420,#193421,#193422,#193423,#193424,
#193425,#193426,#193427,#193428,#193429,#193430,#193431,#193432,#193433,
#193434,#193435,#193436,#193437,#193438,#193439,#193440,#193441,#193442,
#193443,#193444,#193445,#193446,#193447,#193448,#193449,#193450,#193451,
#193452,#193453,#193454,#193455,#193456,#193457,#193458,#193459,#193460,
#193461,#193462,#193463,#193464,#193465,#193466,#193467,#193468,#193469,
#193470,#193471,#193472,#193473,#193474,#193475,#193476,#193477,#193478,
#193479,#193480,#193481,#193482,#193483,#193484,#193485,#193486,#193487,
#193488,#193489,#193490,#193491,#193492,#193493,#193494,#193495,#193496,
#193497,#193498,#193499,#193500,#193501,#193502,#193503,#193504,#193505,
#193506,#193507,#193508,#193509,#193510,#193511,#193512,#193513,#193514,
#193515,#193516,#193517,#193518,#193519,#193520,#193521,#193522,#193523,
#193524,#193525,#193526,#193527,#193528,#193529,#193530,#193531,#193532,
#193533,#193534,#193535,#193536,#193537,#193538,#193539,#193540,#193541,
#193542,#193543,#193544,#193545,#193546,#193547,#193548,#193549,#193550,
#193551,#193552,#193553,#193554,#193555,#193556,#193557,#193558,#193559,
#193560,#193561,#193562,#193563,#193564,#193565,#193566,#193567,#193568,
#193569,#193570,#193571,#193572,#193573,#193574,#193575,#193576,#193577,
#193578,#193579,#193580,#193581,#193582,#193583,#193584,#193585,#193586,
#193587,#193588,#193589,#193590,#193591,#193592,#193593,#193594,#193595,
#193596,#193597,#193598,#193599,#193600,#193601,#193602,#193603,#193604,
#193605,#193606,#193607,#193608,#193609,#193610,#193611,#193612,#193613,
#193614,#193615,#193616,#193617,#193618,#193619,#193620,#193621,#193622,
#193623,#193624,#193625,#193626,#193627,#193628,#193629,#193630,#193631,
#193632,#193633,#193634,#193635,#193636,#193637,#193638,#193639,#193640,
#193641,#193642,#193643,#193644,#193645,#193646,#193647,#193648,#193649,
#193650,#193651,#193652,#193653,#193654,#193655,#193656,#193657,#193658,
#193659,#193660,#193661,#193662,#193663,#193664,#193665,#193666,#193667,
#193668,#193669,#193670,#193671,#193672,#193673,#193674,#193675,#193676,
#193677,#193678,#193679,#193680,#193681,#193682,#193683,#193684,#193685,
#193686,#193687,#193688,#193689,#193690,#193691,#193692,#193693,#193694,
#193695,#193696,#193697,#193698,#193699,#193700,#193701,#193702,#193703,
#193704,#193705,#193706,#193707,#193708,#193709,#193710,#193711,#193712,
#193713,#193714,#193715,#193716,#193717,#193718,#193719,#193720,#193721,
#193722,#193723,#193724,#193725,#193726),(#193727,#193728,#193729,#193730,
#193731,#193732,#193733,#193734,#193735,#193736,#193737,#193738,#193739,
#193740,#193741,#193742,#193743,#193744,#193745,#193746,#193747,#193748,
#193749,#193750,#193751,#193752,#193753,#193754,#193755,#193756,#193757,
#193758,#193759,#193760,#193761,#193762,#193763,#193764,#193765,#193766,
#193767,#193768,#193769,#193770,#193771,#193772,#193773,#193774,#193775,
#193776,#193777,#193778,#193779,#193780,#193781,#193782,#193783,#193784,
#193785,#193786,#193787,#193788,#193789,#193790,#193791,#193792,#193793,
#193794,#193795,#193796,#193797,#193798,#193799,#193800,#193801,#193802,
#193803,#193804,#193805,#193806,#193807,#193808,#193809,#193810,#193811,
#193812,#193813,#193814,#193815,#193816,#193817,#193818,#193819,#193820,
#193821,#193822,#193823,#193824,#193825,#193826,#193827,#193828,#193829,
#193830,#193831,#193832,#193833,#193834,#193835,#193836,#193837,#193838,
#193839,#193840,#193841,#193842,#193843,#193844,#193845,#193846,#193847,
#193848,#193849,#193850,#193851,#193852,#193853,#193854,#193855,#193856,
#193857,#193858,#193859,#193860,#193861,#193862,#193863,#193864,#193865,
#193866,#193867,#193868,#193869,#193870,#193871,#193872,#193873,#193874,
#193875,#193876,#193877,#193878,#193879,#193880,#193881,#193882,#193883,
#193884,#193885,#193886,#193887,#193888,#193889,#193890,#193891,#193892,
#193893,#193894,#193895,#193896,#193897,#193898,#193899,#193900,#193901,
#193902,#193903,#193904,#193905,#193906,#193907,#193908,#193909,#193910,
#193911,#193912,#193913,#193914,#193915,#193916,#193917,#193918,#193919,
#193920,#193921,#193922,#193923,#193924,#193925,#193926,#193927,#193928,
#193929,#193930,#193931,#193932,#193933,#193934,#193935,#193936,#193937,
#193938,#193939,#193940,#193941,#193942,#193943,#193944,#193945,#193946,
#193947,#193948,#193949,#193950,#193951,#193952,#193953,#193954,#193955,
#193956,#193957,#193958,#193959,#193960,#193961,#193962,#193963,#193964,
#193965,#193966,#193967,#193968,#193969,#193970,#193971,#193972,#193973,
#193974,#193975,#193976,#193977,#193978,#193979,#193980,#193981,#193982,
#193983,#193984,#193985,#193986,#193987,#193988,#193989,#193990,#193991,
#193992,#193993,#193994,#193995,#193996,#193997,#193998,#193999,#194000,
#194001,#194002,#194003,#194004,#194005,#194006,#194007,#194008,#194009,
#194010,#194011,#194012,#194013,#194014,#194015,#194016,#194017,#194018,
#194019,#194020,#194021,#194022,#194023,#194024,#194025,#194026,#194027,
#194028,#194029,#194030,#194031,#194032,#194033,#194034,#194035,#194036,
#194037,#194038,#194039,#194040,#194041,#194042,#194043,#194044,#194045,
#194046,#194047,#194048,#194049,#194050,#194051,#194052,#194053,#194054,
#194055,#194056,#194057,#194058,#194059,#194060,#194061,#194062,#194063,
#194064,#194065,#194066,#194067,#194068,#194069,#194070,#194071,#194072,
#194073,#194074,#194075,#194076,#194077,#194078,#194079,#194080,#194081,
#194082,#194083,#194084,#194085,#194086,#194087,#194088,#194089,#194090,
#194091,#194092,#194093,#194094,#194095,#194096,#194097,#194098,#194099,
#194100,#194101,#194102,#194103,#194104,#194105,#194106,#194107,#194108,
#194109,#194110,#194111,#194112,#194113,#194114,#194115,#194116,#194117,
#194118,#194119,#194120,#194121,#194122,#194123,#194124,#194125,#194126,
#194127,#194128,#194129,#194130,#194131,#194132,#194133,#194134,#194135,
#194136,#194137,#194138,#194139,#194140,#194141,#194142,#194143,#194144,
#194145,#194146,#194147,#194148,#194149,#194150,#194151,#194152,#194153,
#194154,#194155,#194156,#194157,#194158,#194159,#194160,#194161,#194162,
#194163,#194164,#194165,#194166,#194167,#194168,#194169,#194170,#194171,
#194172,#194173,#194174,#194175,#194176,#194177,#194178,#194179,#194180,
#194181,#194182,#194183,#194184,#194185,#194186,#194187,#194188,#194189,
#194190,#194191,#194192,#194193,#194194,#194195,#194196,#194197,#194198,
#194199,#194200,#194201,#194202,#194203,#194204,#194205,#194206,#194207,
#194208,#194209,#194210,#194211,#194212,#194213,#194214,#194215,#194216,
#194217,#194218,#194219,#194220,#194221,#194222,#194223,#194224,#194225,
#194226,#194227,#194228,#194229,#194230,#194231,#194232,#194233,#194234,
#194235,#194236,#194237,#194238,#194239,#194240,#194241,#194242,#194243,
#194244,#194245,#194246,#194247,#194248,#194249,#194250,#194251,#194252,
#194253,#194254,#194255,#194256,#194257,#194258,#194259,#194260,#194261,
#194262,#194263,#194264,#194265,#194266,#194267,#194268,#194269,#194270,
#194271,#194272,#194273,#194274,#194275,#194276,#194277,#194278,#194279,
#194280,#194281,#194282,#194283,#194284,#194285,#194286,#194287,#194288,
#194289,#194290,#194291,#194292,#194293,#194294,#194295,#194296,#194297,
#194298,#194299,#194300,#194301,#194302,#194303,#194304,#194305,#194306,
#194307,#194308,#194309,#194310,#194311,#194312,#194313,#194314,#194315,
#194316,#194317,#194318,#194319,#194320,#194321,#194322,#194323,#194324,
#194325,#194326,#194327,#194328,#194329,#194330,#194331,#194332,#194333,
#194334,#194335,#194336,#194337,#194338,#194339,#194340,#194341,#194342,
#194343,#194344,#194345,#194346,#194347,#194348,#194349,#194350,#194351,
#194352,#194353,#194354,#194355,#194356,#194357,#194358,#194359,#194360,
#194361,#194362,#194363,#194364,#194365,#194366,#194367,#194368,#194369,
#194370,#194371,#194372,#194373,#194374,#194375,#194376,#194377,#194378,
#194379,#194380,#194381,#194382,#194383,#194384,#194385,#194386,#194387,
#194388,#194389,#194390,#194391,#194392,#194393,#194394,#194395,#194396,
#194397,#194398,#194399,#194400,#194401,#194402,#194403,#194404,#194405,
#194406,#194407,#194408,#194409,#194410,#194411,#194412,#194413,#194414,
#194415,#194416,#194417,#194418,#194419,#194420,#194421,#194422,#194423,
#194424,#194425,#194426,#194427,#194428,#194429,#194430,#194431,#194432,
#194433,#194434,#194435,#194436,#194437,#194438,#194439,#194440,#194441,
#194442,#194443,#194444,#194445,#194446,#194447,#194448,#194449,#194450,
#194451,#194452,#194453,#194454,#194455,#194456,#194457,#194458,#194459,
#194460,#194461,#194462,#194463,#194464,#194465,#194466,#194467,#194468,
#194469,#194470,#194471,#194472,#194473,#194474,#194475,#194476,#194477,
#194478,#194479,#194480,#194481,#194482,#194483,#194484,#194485,#194486,
#194487,#194488,#194489,#194490,#194491,#194492,#194493,#194494,#194495,
#194496,#194497,#194498,#194499,#194500,#194501,#194502,#194503,#194504,
#194505,#194506,#194507,#194508,#194509,#194510,#194511,#194512,#194513,
#194514,#194515,#194516,#194517,#194518,#194519,#194520,#194521,#194522,
#194523,#194524,#194525,#194526,#194527,#194528,#194529,#194530,#194531,
#194532,#194533,#194534,#194535,#194536,#194537,#194538,#194539,#194540,
#194541,#194542,#194543,#194544,#194545,#194546,#194547,#194548,#194549,
#194550,#194551,#194552,#194553,#194554,#194555,#194556,#194557,#194558,
#194559,#194560,#194561,#194562,#194563,#194564,#194565,#194566,#194567,
#194568,#194569,#194570,#194571,#194572,#194573,#194574,#194575,#194576,
#194577,#194578,#194579,#194580,#194581,#194582,#194583,#194584,#194585,
#194586,#194587,#194588,#194589,#194590,#194591,#194592,#194593,#194594,
#194595,#194596,#194597,#194598,#194599,#194600,#194601,#194602,#194603,
#194604,#194605,#194606,#194607,#194608,#194609,#194610,#194611,#194612,
#194613,#194614,#194615,#194616,#194617,#194618,#194619,#194620,#194621,
#194622,#194623,#194624,#194625,#194626,#194627,#194628,#194629,#194630,
#194631,#194632,#194633,#194634,#194635,#194636,#194637,#194638,#194639,
#194640,#194641,#194642,#194643,#194644,#194645,#194646,#194647,#194648,
#194649,#194650,#194651,#194652,#194653,#194654,#194655,#194656,#194657,
#194658,#194659,#194660,#194661,#194662,#194663,#194664,#194665,#194666,
#194667,#194668,#194669,#194670,#194671,#194672,#194673,#194674,#194675,
#194676,#194677,#194678,#194679,#194680,#194681,#194682,#194683,#194684,
#194685,#194686,#194687,#194688,#194689,#194690,#194691,#194692,#194693,
#194694,#194695,#194696,#194697,#194698,#194699,#194700,#194701,#194702,
#194703,#194704,#194705,#194706,#194707,#194708,#194709,#194710,#194711,
#194712,#194713,#194714,#194715,#194716,#194717,#194718,#194719,#194720,
#194721,#194722,#194723,#194724,#194725,#194726,#194727,#194728,#194729,
#194730,#194731,#194732,#194733,#194734,#194735,#194736,#194737,#194738,
#194739,#194740,#194741,#194742,#194743,#194744,#194745,#194746,#194747,
#194748,#194749,#194750,#194751,#194752,#194753,#194754,#194755,#194756,
#194757,#194758,#194759,#194760,#194761,#194762,#194763,#194764,#194765,
#194766,#194767,#194768,#194769,#194770,#194771,#194772,#194773,#194774,
#194775,#194776,#194777,#194778,#194779,#194780,#194781,#194782,#194783,
#194784,#194785,#194786,#194787,#194788,#194789,#194790,#194791,#194792,
#194793,#194794,#194795,#194796,#194797,#194798,#194799,#194800,#194801,
#194802,#194803,#194804,#194805,#194806,#194807,#194808,#194809,#194810,
#194811,#194812,#194813,#194814,#194815,#194816,#194817,#194818,#194819,
#194820,#194821,#194822,#194823,#194824,#194825,#194826,#194827,#194828,
#194829,#194830,#194831,#194832,#194833,#194834,#194835,#194836,#194837,
#194838,#194839,#194840,#194841,#194842,#194843,#194844,#194845,#194846,
#194847,#194848,#194849,#194850,#194851,#194852,#194853,#194854,#194855,
#194856,#194857,#194858,#194859,#194860,#194861,#194862,#194863,#194864,
#194865,#194866,#194867,#194868,#194869,#194870,#194871,#194872,#194873,
#194874,#194875,#194876,#194877,#194878,#194879,#194880,#194881,#194882,
#194883,#194884,#194885,#194886,#194887,#194888,#194889,#194890,#194891,
#194892,#194893,#194894,#194895,#194896,#194897,#194898,#194899,#194900,
#194901,#194902,#194903,#194904,#194905,#194906,#194907,#194908,#194909,
#194910,#194911,#194912,#194913,#194914,#194915,#194916,#194917,#194918,
#194919,#194920,#194921,#194922,#194923,#194924,#194925,#194926,#194927,
#194928,#194929,#194930,#194931,#194932,#194933,#194934,#194935,#194936,
#194937,#194938,#194939,#194940,#194941,#194942,#194943,#194944,#194945,
#194946,#194947,#194948,#194949,#194950,#194951,#194952,#194953,#194954,
#194955,#194956,#194957,#194958,#194959,#194960,#194961,#194962,#194963,
#194964,#194965,#194966,#194967,#194968,#194969,#194970,#194971,#194972,
#194973,#194974,#194975,#194976,#194977,#194978,#194979,#194980,#194981,
#194982,#194983,#194984,#194985,#194986,#194987,#194988,#194989,#194990,
#194991,#194992,#194993,#194994,#194995,#194996,#194997,#194998,#194999,
#195000,#195001,#195002,#195003,#195004,#195005,#195006,#195007,#195008,
#195009,#195010,#195011,#195012,#195013,#195014,#195015,#195016,#195017,
#195018,#195019,#195020,#195021,#195022,#195023,#195024,#195025,#195026,
#195027,#195028,#195029,#195030,#195031,#195032,#195033,#195034,#195035,
#195036,#195037,#195038,#195039,#195040,#195041,#195042,#195043,#195044,
#195045,#195046,#195047,#195048,#195049,#195050,#195051,#195052,#195053,
#195054,#195055,#195056,#195057,#195058,#195059,#195060,#195061,#195062,
#195063,#195064,#195065,#195066,#195067,#195068,#195069,#195070,#195071,
#195072,#195073,#195074,#195075,#195076,#195077,#195078,#195079,#195080,
#195081,#195082,#195083,#195084,#195085,#195086,#195087,#195088,#195089,
#195090,#195091,#195092,#195093,#195094,#195095,#195096,#195097,#195098,
#195099,#195100,#195101,#195102,#195103,#195104,#195105,#195106,#195107,
#195108,#195109,#195110,#195111,#195112,#195113,#195114,#195115,#195116,
#195117,#195118,#195119,#195120,#195121,#195122,#195123,#195124,#195125,
#195126,#195127,#195128,#195129,#195130,#195131,#195132,#195133,#195134,
#195135,#195136,#195137,#195138,#195139,#195140,#195141,#195142,#195143,
#195144,#195145,#195146,#195147,#195148,#195149,#195150,#195151,#195152,
#195153,#195154,#195155,#195156,#195157,#195158,#195159,#195160,#195161,
#195162,#195163,#195164,#195165,#195166,#195167,#195168,#195169,#195170,
#195171,#195172,#195173,#195174,#195175,#195176,#195177,#195178,#195179,
#195180,#195181,#195182,#195183,#195184,#195185,#195186,#195187,#195188,
#195189,#195190,#195191,#195192,#195193,#195194,#195195,#195196,#195197,
#195198,#195199,#195200,#195201,#195202,#195203,#195204,#195205,#195206,
#195207,#195208,#195209,#195210,#195211,#195212,#195213,#195214,#195215,
#195216,#195217,#195218,#195219,#195220,#195221,#195222,#195223,#195224,
#195225,#195226,#195227,#195228,#195229,#195230,#195231,#195232,#195233,
#195234,#195235,#195236,#195237,#195238,#195239,#195240,#195241,#195242,
#195243,#195244,#195245,#195246,#195247,#195248,#195249,#195250,#195251,
#195252,#195253,#195254,#195255,#195256,#195257,#195258,#195259,#195260,
#195261,#195262,#195263,#195264,#195265,#195266,#195267,#195268,#195269,
#195270,#195271,#195272,#195273,#195274,#195275,#195276,#195277,#195278,
#195279,#195280,#195281,#195282,#195283,#195284,#195285,#195286,#195287,
#195288,#195289,#195290,#195291,#195292,#195293,#195294,#195295,#195296,
#195297,#195298,#195299,#195300,#195301,#195302,#195303,#195304,#195305,
#195306,#195307,#195308,#195309,#195310,#195311,#195312,#195313,#195314,
#195315,#195316,#195317,#195318,#195319,#195320,#195321,#195322,#195323,
#195324,#195325,#195326,#195327,#195328,#195329,#195330,#195331,#195332,
#195333,#195334,#195335,#195336,#195337,#195338,#195339,#195340,#195341,
#195342,#195343,#195344,#195345,#195346,#195347,#195348,#195349,#195350,
#195351,#195352,#195353,#195354,#195355,#195356,#195357,#195358,#195359,
#195360,#195361,#195362,#195363,#195364,#195365,#195366,#195367,#195368,
#195369,#195370,#195371,#195372,#195373,#195374,#195375,#195376,#195377,
#195378,#195379,#195380,#195381,#195382,#195383,#195384,#195385,#195386,
#195387,#195388,#195389,#195390,#195391,#195392,#195393,#195394,#195395,
#195396,#195397,#195398,#195399,#195400,#195401,#195402,#195403,#195404,
#195405,#195406,#195407,#195408,#195409,#195410,#195411,#195412,#195413,
#195414,#195415,#195416,#195417,#195418,#195419,#195420,#195421)),
 .UNSPECIFIED.,.F.,.F.,.F.,(4,4),(4,1,1,1,1,1,1,1,1,1,1,1,1,1,1,1,1,1,1,
1,1,1,1,1,1,1,1,1,1,1,1,1,1,1,1,1,1,1,1,1,1,1,1,1,1,1,1,1,1,1,1,1,1,1,1,
1,1,1,1,1,1,1,1,1,1,1,1,1,1,1,1,1,1,1,1,1,1,1,1,1,1,1,1,1,1,1,1,1,1,1,1,
1,1,1,1,1,1,1,1,1,1,1,1,1,1,1,1,1,1,1,1,1,1,1,1,1,1,1,1,1,1,1,1,1,1,1,1,
1,1,1,1,1,1,1,1,1,1,1,1,1,1,1,1,1,1,1,1,1,1,1,1,1,1,1,1,1,1,1,1,1,1,1,1,
1,1,1,1,1,1,1,1,1,1,1,1,1,1,1,1,1,1,1,1,1,1,1,1,1,1,1,1,1,1,1,1,1,1,1,1,
1,1,1,1,1,1,1,1,1,1,1,1,1,1,1,1,1,1,1,1,1,1,1,1,1,1,1,1,1,1,1,1,1,1,1,1,
1,1,1,1,1,1,1,1,1,1,1,1,1,1,1,1,1,1,1,1,1,1,1,1,1,1,1,1,1,1,1,1,1,1,1,1,
1,1,1,1,1,1,1,1,1,1,1,1,1,1,1,1,1,1,1,1,1,1,1,1,1,1,1,1,1,1,1,1,1,1,1,1,
1,1,1,1,1,1,1,1,1,1,1,1,1,1,1,1,1,1,1,1,1,1,1,1,1,1,1,1,1,1,1,1,1,1,1,1,
1,1,1,1,1,1,1,1,1,1,1,1,1,1,1,1,1,1,1,1,1,1,1,1,1,1,1,1,1,1,1,1,1,1,1,1,
1,1,1,1,1,1,1,1,1,1,1,1,1,1,1,1,1,1,1,1,1,1,1,1,1,1,1,1,1,1,1,1,1,1,1,1,
1,1,1,1,1,1,1,1,1,1,1,1,1,1,1,1,1,1,1,1,1,1,1,1,1,1,1,1,1,1,1,1,1,1,1,1,
1,1,1,1,1,1,1,1,1,1,1,1,1,1,1,1,1,1,1,1,1,1,1,1,1,1,1,1,1,1,1,1,1,1,1,1,
1,1,1,1,1,1,1,1,1,1,1,1,1,1,1,1,1,1,1,1,1,1,1,1,1,1,1,1,1,1,1,1,1,1,1,1,
1,1,1,1,1,1,1,1,1,1,1,1,1,1,1,1,1,1,1,1,1,1,1,1,1,1,1,1,1,1,1,1,1,1,1,1,
1,1,1,1,1,1,1,1,1,1,1,1,1,1,1,1,1,1,1,1,1,1,1,1,1,1,1,1,1,1,1,1,1,1,1,1,
1,1,1,1,1,1,1,1,1,1,1,1,1,1,1,1,1,1,1,1,1,1,1,1,1,1,1,1,1,1,1,1,1,1,1,1,
1,1,1,1,1,1,1,1,1,1,1,1,1,1,1,1,1,1,1,1,1,1,1,1,1,1,1,1,1,1,1,1,1,1,1,1,
1,1,1,1,1,1,1,1,1,1,1,1,1,1,1,1,1,1,1,1,1,1,1,1,1,1,1,1,1,1,1,1,1,1,1,1,
1,1,1,1,1,1,1,1,1,1,1,1,1,1,1,1,1,1,1,1,1,1,1,1,1,1,1,1,1,1,1,1,1,1,1,1,
1,1,1,1,1,1,1,1,1,1,1,1,1,1,1,1,1,1,1,1,1,1,1,1,1,1,1,1,1,1,1,1,1,1,1,1,
1,1,1,1,1,1,1,1,1,1,1,1,1,1,1,1,1,1,1,1,1,1,1,1,1,1,1,1,1,1,1,1,1,1,1,1,
1,1,1,1,1,1,1,1,1,1,1,1,1,1,1,1,1,1,1,1,1,1,1,1,1,1,1,1,1,1,1,1,1,1,1,1,
1,1,1,1,1,1,1,1,1,1,1,1,1,1,1,1,1,1,1,1,1,1,1,1,1,1,1,1,1,1,1,1,1,1,1,1,
1,1,1,1,1,1,1,1,1,1,1,1,1,1,1,1,1,1,1,1,1,1,1,1,1,1,1,1,1,1,1,1,1,1,1,1,
1,1,1,1,1,1,1,1,1,1,1,1,1,1,1,1,1,1,1,1,1,1,1,1,1,1,1,1,1,1,1,1,1,1,1,1,
1,1,1,1,1,1,1,1,1,1,1,1,1,1,1,1,1,1,1,1,1,1,1,1,1,1,1,1,1,1,1,1,1,1,1,1,
1,1,1,1,1,1,1,1,1,1,1,1,1,1,1,1,1,1,1,1,1,1,1,1,1,1,1,1,1,1,1,1,1,1,1,1,
1,1,1,1,1,1,1,1,1,1,1,1,1,1,1,1,1,1,1,1,1,1,1,1,1,1,1,1,1,1,1,1,1,1,1,1,
1,1,1,1,1,1,1,1,1,1,1,1,1,1,1,1,1,1,1,1,1,1,1,1,1,1,1,1,1,1,1,1,1,1,1,1,
1,1,1,1,1,1,1,1,1,1,1,1,1,1,1,1,1,1,1,1,1,1,1,1,1,1,1,1,1,1,1,1,1,1,1,1,
1,1,1,1,1,1,1,1,1,1,1,1,1,1,1,1,1,1,1,1,1,1,1,1,1,1,1,1,1,1,1,1,1,1,1,1,
1,1,1,1,1,1,1,1,1,1,1,1,1,1,1,1,1,1,1,1,1,1,1,1,1,1,1,1,1,1,1,1,1,1,1,1,
1,1,1,1,1,1,1,1,1,1,1,1,1,1,1,1,1,1,1,1,1,1,1,1,1,1,1,1,1,1,1,1,1,1,1,1,
1,1,1,1,1,1,1,1,1,1,1,1,1,1,1,1,1,1,1,1,1,1,1,1,1,1,1,1,1,1,1,1,1,1,1,1,
1,1,1,1,1,1,1,1,1,1,1,1,1,1,1,1,1,1,1,1,1,1,1,1,1,1,1,1,1,1,1,1,1,1,1,1,
1,1,1,1,1,1,1,1,1,1,1,1,1,1,1,1,1,1,1,1,1,1,1,1,1,1,1,1,1,1,1,1,1,1,1,1,
1,1,1,1,1,1,1,1,1,1,1,1,1,1,1,1,1,1,1,1,1,1,1,1,1,1,1,1,1,1,1,1,1,1,1,1,
1,1,1,1,1,1,1,1,1,1,1,1,1,1,1,1,1,1,1,1,1,1,1,1,1,1,1,1,1,1,1,1,1,1,1,1,
1,1,1,1,1,1,1,1,1,1,1,1,1,1,1,1,1,1,1,1,1,1,1,1,1,1,1,1,1,1,1,1,1,1,1,1,
1,1,1,1,1,1,1,1,1,1,1,1,1,1,1,1,1,1,1,1,1,1,1,1,1,1,1,1,1,1,1,1,1,1,1,1,
1,1,1,1,1,1,1,1,1,1,1,1,1,1,1,1,1,1,1,1,1,1,1,1,1,1,1,1,1,1,1,1,1,1,1,1,
1,1,1,1,1,1,1,1,1,1,1,1,1,1,1,1,1,1,1,1,1,1,1,1,1,1,1,1,1,1,1,1,1,1,1,1,
1,1,1,1,1,1,1,1,1,1,1,1,1,1,1,1,1,1,1,1,1,1,1,1,1,1,1,1,1,1,1,1,1,1,1,1,
1,1,1,1,1,1,1,1,1,1,1,1,1,1,1,1,1,1,1,1,1,1,1,1,1,1,1,1,1,1,1,1,1,1,1,1,
1,1,1,1,1,1,1,1,1,1,1,1,1,1,1,1,1,1,1,1,1,1,1,1,1,1,1,1,1,1,1,1,1,1,1,1,
1,1,1,1,1,1,1,1,1,1,1,1,1,1,1,1,1,4),(-0.000587328099657093,0.1157205948422),
(8.30590413559005,8.80579087257276,9.30565887793282,10.305394888653,11.3051308993731,
12.3048669100932,13.3046029208133,14.3043389315335,15.3040749422536,16.3038109529737,
17.3035469636939,18.303282974414,19.3030189851341,20.3027549958542,21.3024910065744,
22.3022270172945,23.3019630280146,24.3016990387348,25.3014350494549,26.301171060175,
27.3009070708951,28.3006430816153,29.3003790923354,30.3001151030555,31.2998511137757,
32.2995871244958,33.2993231352159,34.299059145936,35.2987951566562,36.2985311673763,
37.2982671780964,38.2980031888166,39.2977391995367,40.2974752102568,41.2972112209769,
42.2969472316971,43.2966832424172,44.2964192531373,45.2961552638575,46.2958912745776,
47.2956272852977,48.2953632960178,49.295099306738,50.2948353174581,51.2945713281782,
52.2943073388984,53.2940433496185,54.2937793603386,55.2935153710587,56.2932513817789,
57.292987392499,58.2927234032191,59.2924594139393,60.2921954246594,61.2919314353795,
62.2916674460996,63.2914034568198,64.2911394675399,65.29087547826,66.2906114889802,
67.2903474997003,68.2900835104204,69.2898195211405,70.2895555318607,71.2892915425808,
72.2890275533009,73.2887635640211,74.2884995747412,75.2882355854613,76.2879715961814,
77.2877076069016,78.2874436176217,79.2871796283418,80.286915639062,81.2866516497821,
82.2863876605022,83.2861236712224,84.2858596819425,85.2855956926626,86.2853317033827,
87.2850677141029,88.284803724823,89.2845397355431,90.2842757462633,91.2840117569834,
92.2837477677035,93.2834837784236,94.2832197891438,95.2829557998639,96.282691810584,
97.2824278213041,98.2821638320243,99.2818998427444,100.281635853465,101.281371864185,
102.281107874905,103.280843885625,104.280579896345,105.280315907065,106.280051917785,
107.279787928505,108.279523939226,109.279259949946,110.278995960666,111.278731971386,
112.278467982106,113.278203992826,114.277940003546,115.277676014266,116.277412024987,
117.277148035707,118.276884046427,119.276620057147,120.276356067867,121.276092078587,
122.275828089307,123.275564100028,124.275300110748,125.275036121468,126.274772132188,
127.274508142908,128.274244153628,129.273980164348,130.273716175068,131.273452185789,
132.273188196509,133.272924207229,134.272660217949,135.272396228669,136.272132239389,
137.271868250109,138.271604260829,139.27134027155,140.27107628227,141.27081229299,
142.27054830371,143.27028431443,144.27002032515,145.26975633587,146.26949234659,
147.269228357311,148.268964368031,149.268700378751,150.268436389471,151.268172400191,
152.267908410911,153.267644421631,154.267380432352,155.267116443072,156.266852453792,
157.266588464512,158.266324475232,159.266060485952,160.265796496672,161.265532507392,
162.265268518113,163.265004528833,164.264740539553,165.264476550273,166.264212560993,
167.263948571713,168.263684582433,169.263420593153,170.263156603874,171.262892614594,
172.262628625314,173.262364636034,174.262100646754,175.261836657474,176.261572668194,
177.261308678914,178.261044689635,179.260780700355,180.260516711075,181.260252721795,
182.259988732515,183.259724743235,184.259460753955,185.259196764675,186.258932775396,
187.258668786116,188.258404796836,189.258140807556,190.257876818276,191.257612828996,
192.257348839716,193.257084850437,194.256820861157,195.256556871877,196.256292882597,
197.256028893317,198.255764904037,199.255500914757,200.255236925477,201.254972936198,
202.254708946918,203.254444957638,204.254180968358,205.253916979078,206.253652989798,
207.253389000518,208.253125011238,209.252861021959,210.252597032679,211.252333043399,
212.252069054119,213.251805064839,214.251541075559,215.251277086279,216.251013096999,
217.25074910772,218.25048511844,219.25022112916,220.24995713988,221.2496931506,
222.24942916132,223.24916517204,224.248901182761,225.248637193481,226.248373204201,
227.248109214921,228.247845225641,229.247581236361,230.247317247081,231.247053257801,
232.246789268522,233.246525279242,234.246261289962,235.245997300682,236.245733311402,
237.245469322122,238.245205332842,239.244941343562,240.244677354283,241.244413365003,
242.244149375723,243.243885386443,244.243621397163,245.243357407883,246.243093418603,
247.242829429323,248.242565440044,249.242301450764,250.242037461484,251.241773472204,
252.241509482924,253.241245493644,254.240981504364,255.240717515084,256.240453525805,
257.240189536525,258.239925547245,259.239661557965,260.239397568685,261.239133579405,
262.238869590125,263.238605600846,264.238341611566,265.238077622286,266.237813633006,
267.237549643726,268.237285654446,269.237021665166,270.236757675886,271.236493686607,
272.236229697327,273.235965708047,274.235701718767,275.235437729487,276.235173740207,
277.234909750927,278.234645761647,279.234381772368,280.234117783088,281.233853793808,
282.233589804528,283.233325815248,284.233061825968,285.232797836688,286.232533847408,
287.232269858129,288.232005868849,289.231741879569,290.231477890289,291.231213901009,
292.230949911729,293.230685922449,294.23042193317,295.23015794389,296.22989395461,
297.22962996533,298.22936597605,299.22910198677,300.22883799749,301.22857400821,
302.228310018931,303.228046029651,304.227782040371,305.227518051091,306.227254061811,
307.226990072531,308.226726083251,309.226462093971,310.226198104692,311.225934115412,
312.225670126132,313.225406136852,314.225142147572,315.224878158292,316.224614169012,
317.224350179732,318.224086190453,319.223822201173,320.223558211893,321.223294222613,
322.223030233333,323.222766244053,324.222502254773,325.222238265494,326.221974276214,
327.221710286934,328.221446297654,329.221182308374,330.220918319094,331.220654329814,
332.220390340534,333.220126351255,334.219862361975,335.219598372695,336.219334383415,
337.219070394135,338.218806404855,339.218542415575,340.218278426295,341.218014437016,
342.217750447736,343.217486458456,344.217222469176,345.216958479896,346.216694490616,
347.216430501336,348.216166512056,349.215902522777,350.215638533497,351.215374544217,
352.215110554937,353.214846565657,354.214582576377,355.214318587097,356.214054597817,
357.213790608538,358.213526619258,359.213262629978,360.212998640698,361.212734651418,
362.212470662138,363.212206672858,364.211942683579,365.211678694299,366.211414705019,
367.211150715739,368.210886726459,369.210622737179,370.210358747899,371.210094758619,
372.20983076934,373.20956678006,374.20930279078,375.2090388015,376.20877481222,
377.20851082294,378.20824683366,379.20798284438,380.207718855101,381.207454865821,
382.207190876541,383.206926887261,384.206662897981,385.206398908701,386.206134919421,
387.205870930141,388.205606940862,389.205342951582,390.205078962302,391.204814973022,
392.204550983742,393.204286994462,394.204023005182,395.203759015903,396.203495026623,
397.203231037343,398.202967048063,399.202703058783,400.202439069503,401.202175080223,
402.201911090943,403.201647101664,404.201383112384,405.201119123104,406.200855133824,
407.200591144544,408.200327155264,409.200063165984,410.199799176704,411.199535187425,
412.199271198145,413.199007208865,414.198743219585,415.198479230305,416.198215241025,
417.197951251745,418.197687262465,419.197423273186,420.197159283906,421.196895294626,
422.196631305346,423.196367316066,424.196103326786,425.195839337506,426.195575348226,
427.195311358947,428.195047369667,429.194783380387,430.194519391107,431.194255401827,
432.193991412547,433.193727423267,434.193463433988,435.193199444708,436.192935455428,
437.192671466148,438.192407476868,439.192143487588,440.191879498308,441.191615509028,
442.191351519749,443.191087530469,444.190823541189,445.190559551909,446.190295562629,
447.190031573349,448.189767584069,449.189503594789,450.18923960551,451.18897561623,
452.18871162695,453.18844763767,454.18818364839,455.18791965911,456.18765566983,
457.18739168055,458.187127691271,459.186863701991,460.186599712711,461.186335723431,
462.186071734151,463.185807744871,464.185543755591,465.185279766312,466.185015777032,
467.184751787752,468.184487798472,469.184223809192,470.183959819912,471.183695830632,
472.183431841352,473.183167852073,474.182903862793,475.182639873513,476.182375884233,
477.182111894953,478.181847905673,479.181583916393,480.181319927113,481.181055937834,
482.180791948554,483.180527959274,484.180263969994,485.179999980714,486.179735991434,
487.179472002154,488.179208012874,489.178944023595,490.178680034315,491.178416045035,
492.178152055755,493.177888066475,494.177624077195,495.177360087915,496.177096098636,
497.176832109356,498.176568120076,499.176304130796,500.176040141516,501.175776152236,
502.175512162956,503.175248173676,504.174984184397,505.174720195117,506.174456205837,
507.174192216557,508.173928227277,509.173664237997,510.173400248717,511.173136259437,
512.172872270158,513.172608280878,514.172344291598,515.172080302318,516.171816313038,
517.171552323758,518.171288334478,519.171024345198,520.170760355919,521.170496366639,
522.170232377359,523.169968388079,524.169704398799,525.169440409519,526.169176420239,
527.168912430959,528.16864844168,529.1683844524,530.16812046312,531.16785647384,
532.16759248456,533.16732849528,534.167064506,535.166800516721,536.166536527441,
537.166272538161,538.166008548881,539.165744559601,540.165480570321,541.165216581041,
542.164952591761,543.164688602482,544.164424613202,545.164160623922,546.163896634642,
547.163632645362,548.163368656082,549.163104666802,550.162840677522,551.162576688243,
552.162312698963,553.162048709683,554.161784720403,555.161520731123,556.161256741843,
557.160992752563,558.160728763283,559.160464774004,560.160200784724,561.159936795444,
562.159672806164,563.159408816884,564.159144827604,565.158880838324,566.158616849045,
567.158352859765,568.158088870485,569.157824881205,570.157560891925,571.157296902645,
572.157032913365,573.156768924085,574.156504934806,575.156240945526,576.155976956246,
577.155712966966,578.155448977686,579.155184988406,580.154920999126,581.154657009846,
582.154393020567,583.154129031287,584.153865042007,585.153601052727,586.153337063447,
587.153073074167,588.152809084887,589.152545095607,590.152281106328,591.152017117048,
592.151753127768,593.151489138488,594.151225149208,595.150961159928,596.150697170648,
597.150433181368,598.150169192089,599.149905202809,600.149641213529,601.149377224249,
602.149113234969,603.148849245689,604.148585256409,605.14832126713,606.14805727785,
607.14779328857,608.14752929929,609.14726531001,610.14700132073,611.14673733145,
612.14647334217,613.146209352891,614.145945363611,615.145681374331,616.145417385051,
617.145153395771,618.144889406491,619.144625417211,620.144361427931,621.144097438652,
622.143833449372,623.143569460092,624.143305470812,625.143041481532,626.142777492252,
627.142513502972,628.142249513692,629.141985524413,630.141721535133,631.141457545853,
632.141193556573,633.140929567293,634.140665578013,635.140401588733,636.140137599454,
637.139873610174,638.139609620894,639.139345631614,640.139081642334,641.138817653054,
642.138553663774,643.138289674494,644.138025685215,645.137761695935,646.137497706655,
647.137233717375,648.136969728095,649.136705738815,650.136441749535,651.136177760255,
652.135913770976,653.135649781696,654.135385792416,655.135121803136,656.134857813856,
657.134593824576,658.134329835296,659.134065846016,660.133801856737,661.133537867457,
662.133273878177,663.133009888897,664.132745899617,665.132481910337,666.132217921057,
667.131953931778,668.131689942498,669.131425953218,670.131161963938,671.130897974658,
672.130633985378,673.130369996098,674.130106006818,675.129842017539,676.129578028259,
677.129314038979,678.129050049699,679.128786060419,680.128522071139,681.128258081859,
682.127994092579,683.1277301033,684.12746611402,685.12720212474,686.12693813546,
687.12667414618,688.1264101569,689.12614616762,690.12588217834,691.125618189061,
692.125354199781,693.125090210501,694.124826221221,695.124562231941,696.124298242661,
697.124034253381,698.123770264101,699.123506274822,700.123242285542,701.122978296262,
702.122714306982,703.122450317702,704.122186328422,705.121922339142,706.121658349863,
707.121394360583,708.121130371303,709.120866382023,710.120602392743,711.120338403463,
712.120074414183,713.119810424903,714.119546435624,715.119282446344,716.119018457064,
717.118754467784,718.118490478504,719.118226489224,720.117962499944,721.117698510664,
722.117434521385,723.117170532105,724.116906542825,725.116642553545,726.116378564265,
727.116114574985,728.115850585705,729.115586596425,730.115322607146,731.115058617866,
732.114794628586,733.114530639306,734.114266650026,735.114002660746,736.113738671466,
737.113474682187,738.113210692907,739.112946703627,740.112682714347,741.112418725067,
742.112154735787,743.111890746507,744.111626757227,745.111362767948,746.111098778668,
747.110834789388,748.110570800108,749.110306810828,750.110042821548,751.109778832268,
752.109514842988,753.109250853709,754.108986864429,755.108722875149,756.108458885869,
757.108194896589,758.107930907309,759.107666918029,760.107402928749,761.10713893947,
762.10687495019,763.10661096091,764.10634697163,765.10608298235,766.10581899307,
767.10555500379,768.10529101451,769.105027025231,770.104763035951,771.104499046671,
772.104235057391,773.103971068111,774.103707078831,775.103443089551,776.103179100272,
777.102915110992,778.102651121712,779.102387132432,780.102123143152,781.101859153872,
782.101595164592,783.101331175312,784.101067186033,785.100803196753,786.100539207473,
787.100275218193,788.100011228913,789.099747239633,790.099483250353,791.099219261073,
792.098955271794,793.098691282514,794.098427293234,795.098163303954,796.097899314674,
797.097635325394,798.097371336114,799.097107346834,800.096843357555,801.096579368275,
802.096315378995,803.096051389715,804.095787400435,805.095523411155,806.095259421875,
807.094995432596,808.094731443316,809.094467454036,810.094203464756,811.093939475476,
812.093675486196,813.093411496916,814.093147507636,815.092883518357,816.092619529077,
817.092355539797,818.092091550517,819.091827561237,820.091563571957,821.091299582677,
822.091035593397,823.090771604118,824.090507614838,825.090243625558,826.089979636278,
827.089715646998,828.089451657718,829.089187668438,830.088923679158,831.088659689879,
832.088395700599,833.088131711319,834.087867722039,835.087603732759,836.087339743479,
837.087075754199,838.08681176492,839.08654777564,840.08628378636,841.08601979708,
842.0857558078,843.08549181852,844.08522782924,845.08496383996,846.084699850681,
847.084435861401,848.084171872121,849.083907882841,850.083643893561,851.083379904281,
852.083115915001,853.082851925721,854.082587936442,855.082323947162,856.082059957882,
857.081795968602,858.081531979322,859.081267990042,860.081004000762,861.080740011482,
862.080476022203,863.080212032923,864.079948043643,865.079684054363,866.079420065083,
867.079156075803,868.078892086523,869.078628097243,870.078364107964,871.078100118684,
872.077836129404,873.077572140124,874.077308150844,875.077044161564,876.076780172284,
877.076516183005,878.076252193725,879.075988204445,880.075724215165,881.075460225885,
882.075196236605,883.074932247325,884.074668258045,885.074404268766,886.074140279486,
887.073876290206,888.073612300926,889.073348311646,890.073084322366,891.072820333086,
892.072556343806,893.072292354527,894.072028365247,895.071764375967,896.071500386687,
897.071236397407,898.070972408127,899.070708418847,900.070444429567,901.070180440288,
902.069916451008,903.069652461728,904.069388472448,905.069124483168,906.068860493888,
907.068596504608,908.068332515329,909.068068526049,910.067804536769,911.067540547489,
912.067276558209,913.067012568929,914.066748579649,915.066484590369,916.06622060109,
917.06595661181,918.06569262253,919.06542863325,920.06516464397,921.06490065469,
922.06463666541,923.06437267613,924.064108686851,925.063844697571,926.063580708291,
927.063316719011,928.063052729731,929.062788740451,930.062524751171,931.062260761891,
932.061996772612,933.061732783332,934.061468794052,935.061204804772,936.060940815492,
937.060676826212,938.060412836932,939.060148847652,940.059884858373,941.059620869093,
942.059356879813,943.059092890533,944.058828901253,945.058564911973,946.058300922693,
947.058036933414,948.057772944134,949.057508954854,950.057244965574,951.056980976294,
952.056716987014,953.056452997734,954.056189008454,955.055925019175,956.055661029895,
957.055397040615,958.055133051335,959.054869062055,960.054605072775,961.054341083495,
962.054077094215,963.053813104936,964.053549115656,965.053285126376,966.053021137096,
967.052757147816,968.052493158536,969.052229169256,970.051965179976,971.051701190697,
972.051437201417,973.051173212137,974.050909222857,975.050645233577,976.050381244297,
977.050117255017,978.049853265738,979.049589276458,980.049325287178,981.049061297898,
982.048797308618,983.048533319338,984.048269330058,985.048005340778,986.047741351499,
987.047477362219,988.047213372939,989.046949383659,990.046685394379,991.046421405099,
992.046157415819,993.045893426539,994.04562943726,995.04536544798,996.0451014587,
997.04483746942,998.04457348014,999.04430949086,1000.04404550158,1001.0437815123,
1002.04351752302,1003.04325353374,1004.04298954446,1005.04272555518,1006.0424615659,
1007.04219757662,1008.04193358734,1009.04166959806,1010.04140560878,1011.0411416195,
1012.04087763022,1013.04061364094,1014.04034965166,1015.04008566238,1016.0398216731,
1017.03955768382,1018.03929369454,1019.03902970526,1020.03876571598,1021.0385017267,
1022.03823773742,1023.03797374814,1024.03770975886,1025.03744576958,1026.0371817803,
1027.03691779102,1028.03665380174,1029.03638981246,1030.03612582318,1031.0358618339,
1032.03559784462,1033.03533385534,1034.03506986606,1035.03480587678,1036.03454188751,
1037.03427789823,1038.03401390895,1039.03374991967,1040.03348593039,1041.03322194111,
1042.03295795183,1043.03269396255,1044.03242997327,1045.03216598399,1046.03190199471,
1047.03163800543,1048.03137401615,1049.03111002687,1050.03084603759,1051.03058204831,
1052.03031805903,1053.03005406975,1054.02979008047,1055.02952609119,1056.02926210191,
1057.02899811263,1058.02873412335,1059.02847013407,1060.02820614479,1061.02794215551,
1062.02767816623,1063.02741417695,1064.02715018767,1065.02688619839,1066.02662220911,
1067.02635821983,1068.02609423055,1069.02583024127,1070.02556625199,1071.02530226271,
1072.02503827343,1073.02477428415,1074.02451029487,1075.02424630559,1076.02398231631,
1077.02371832703,1078.02345433775,1079.02319034847,1080.02292635919,1081.02266236991,
1082.02239838063,1083.02213439135,1084.02187040207,1085.02160641279,1086.02134242351,
1087.02107843423,1088.02081444495,1089.02055045567,1090.02028646639,1091.02002247711,
1092.01975848783,1093.01949449855,1094.01923050927,1095.01896651999,1096.01870253071,
1097.01843854143,1098.01817455215,1099.01791056287,1100.01764657359,1101.01738258431,
1102.01711859503,1103.01685460575,1104.01659061647,1105.01632662719,1106.01606263791,
1107.01579864863,1108.01553465935,1109.01527067007,1110.01500668079,1111.01474269151,
1112.01447870223,1113.01421471295,1114.01395072368,1115.0136867344,1116.01342274512,
1117.01315875584,1118.01289476656,1119.01263077728,1120.012366788,1121.01210279872,
1122.01183880944,1123.01157482016,1124.01131083088,1125.0110468416,1126.01078285232,
1127.01051886304,1128.01025487376,1129.00999088448,1130.0097268952,1131.00946290592,
1132.00919891664,1133.00893492736,1134.00867093808,1135.0084069488,1136.00814295952,
1137.00787897024,1138.00761498096,1139.00735099168,1140.0070870024,1141.00682301312,
1142.00655902384,1143.00629503456,1144.00603104528,1145.005767056,1146.00550306672,
1147.00523907744,1148.00497508816,1149.00471109888,1150.0044471096,1151.00418312032,
1152.00391913104,1153.00365514176,1154.00339115248,1155.0031271632,1156.00286317392,
1157.00259918464,1158.00233519536,1159.00207120608,1160.0018072168,1161.00154322752,
1162.00127923824,1163.00101524896,1164.00075125968,1165.0004872704,1166.00022328112,
1166.99995929184,1167.99969530256,1168.99943131328,1169.999167324,1170.99890333472,
1171.99863934544,1172.99837535616,1173.99811136688,1174.9978473776,1175.99758338832,
1176.99731939904,1177.99705540976,1178.99679142048,1179.9965274312,1180.99626344192,
1181.99599945264,1182.99573546336,1183.99547147408,1184.9952074848,1185.99494349552,
1186.99467950624,1187.99441551696,1188.99415152768,1189.99388753841,1190.99362354913,
1191.99335955985,1192.99309557057,1193.99283158129,1194.99256759201,1195.99230360273,
1196.99203961345,1197.99177562417,1198.99151163489,1199.99124764561,1200.99098365633,
1201.99071966705,1202.99045567777,1203.99019168849,1204.98992769921,1205.98966370993,
1206.98939972065,1207.98913573137,1208.98887174209,1209.98860775281,1210.98834376353,
1211.98807977425,1212.98781578497,1213.98755179569,1214.98728780641,1215.98702381713,
1216.98675982785,1217.98649583857,1218.98623184929,1219.98596786001,1220.98570387073,
1221.98543988145,1222.98517589217,1223.98491190289,1224.98464791361,1225.98438392433,
1226.98411993505,1227.98385594577,1228.98359195649,1229.98332796721,1230.98306397793,
1231.98279998865,1232.98253599937,1233.98227201009,1234.98200802081,1235.98174403153,
1236.98148004225,1237.98121605297,1238.98095206369,1239.98068807441,1240.98042408513,
1241.98016009585,1242.97989610657,1243.97963211729,1244.97936812801,1245.97910413873,
1246.97884014945,1247.97857616017,1248.97831217089,1249.97804818161,1250.97778419233,
1251.97752020305,1252.97725621377,1253.97699222449,1254.97672823521,1255.97646424593,
1256.97620025665,1257.97593626737,1258.97567227809,1259.97540828881,1260.97514429953,
1261.97488031025,1262.97461632097,1263.97435233169,1264.97408834241,1265.97382435313,
1266.97356036385,1267.97329637458,1268.9730323853,1269.97276839602,1270.97250440674,
1271.97224041746,1272.97197642818,1273.9717124389,1274.97144844962,1275.97118446034,
1276.97092047106,1277.97065648178,1278.9703924925,1279.97012850322,1280.96986451394,
1281.96960052466,1282.96933653538,1283.9690725461,1284.96880855682,1285.96854456754,
1286.96828057826,1287.96801658898,1288.9677525997,1289.96748861042,1290.96722462114,
1291.96696063186,1292.96669664258,1293.9664326533,1294.96616866402,1295.96590467474,
1296.96564068546,1297.96537669618,1298.9651127069,1299.96484871762,1300.96458472834,
1301.96432073906,1302.96405674978,1303.9637927605,1304.96352877122,1305.96326478194,
1306.96300079266,1307.96273680338,1308.9624728141,1309.96220882482,1310.96194483554,
1311.96168084626,1312.96141685698,1313.9611528677,1314.96088887842,1315.96062488914,
1316.96036089986,1317.96009691058,1318.9598329213,1319.95956893202,1320.95930494274,
1321.95904095346,1322.95877696418,1323.9585129749,1324.95824898562,1325.95798499634,
1326.95772100706,1327.95745701778,1328.9571930285,1329.95692903922,1330.95666504994,
1331.95640106066,1332.95613707138,1333.9558730821,1334.95560909282,1335.95534510354,
1336.95508111426,1337.95481712498,1338.9545531357,1339.95428914642,1340.95402515714,
1341.95376116786,1342.95349717858,1343.9532331893,1344.95296920002,1345.95270521075,
1346.95244122147,1347.95217723219,1348.95191324291,1349.95164925363,1350.95138526435,
1351.95112127507,1352.95085728579,1353.95059329651,1354.95032930723,1355.95006531795,
1356.94980132867,1357.94953733939,1358.94927335011,1359.94900936083,1360.94874537155,
1361.94848138227,1362.94821739299,1363.94795340371,1364.94768941443,1365.94742542515,
1366.94716143587,1367.94689744659,1368.94663345731,1369.94636946803,1370.94610547875,
1371.94584148947,1372.94557750019,1373.94531351091,1374.94504952163,1375.94478553235,
1376.94452154307,1377.94425755379,1378.94399356451,1379.94372957523,1380.94346558595,
1381.94320159667,1382.94293760739,1383.94267361811,1384.94240962883,1385.94214563955,
1386.94188165027,1387.94161766099,1388.94135367171,1389.94108968243,1390.94082569315,
1391.94056170387,1392.94029771459,1393.94003372531,1394.93976973603,1395.93950574675,
1396.93924175747,1397.93897776819,1398.93871377891,1399.93844978963,1400.93818580035,
1401.93792181107,1402.93765782179,1403.93739383251,1404.93712984323,1405.93686585395,
1406.93660186467,1407.93633787539,1408.93607388611,1409.93580989683,1410.93554590755,
1411.93528191827,1412.93501792899,1413.93475393971,1414.93448995043,1415.93422596115,
1416.93396197187,1417.93369798259,1418.93343399331,1419.93317000403,1420.93290601475,
1421.93264202547,1422.93237803619,1423.93211404692,1424.93185005764,1425.93158606836,
1426.93132207908,1427.9310580898,1428.93079410052,1429.93053011124,1430.93026612196,
1431.93000213268,1432.9297381434,1433.92947415412,1434.92921016484,1435.92894617556,
1436.92868218628,1437.928418197,1438.92815420772,1439.92789021844,1440.92762622916,
1441.92736223988,1442.9270982506,1443.92683426132,1444.92657027204,1445.92630628276,
1446.92604229348,1447.9257783042,1448.92551431492,1449.92525032564,1450.92498633636,
1451.92472234708,1452.9244583578,1453.92419436852,1454.92393037924,1455.92366638996,
1456.92340240068,1457.9231384114,1458.92287442212,1459.92261043284,1460.92234644356,
1461.92208245428,1462.921818465,1463.92155447572,1464.92129048644,1465.92102649716,
1466.92076250788,1467.9204985186,1468.92023452932,1469.91997054004,1470.91970655076,
1471.91944256148,1472.9191785722,1473.91891458292,1474.91865059364,1475.91838660436,
1476.91812261508,1477.9178586258,1478.91759463652,1479.91733064724,1480.91706665796,
1481.91680266868,1482.9165386794,1483.91627469012,1484.91601070084,1485.91574671156,
1486.91548272228,1487.915218733,1488.91495474372,1489.91469075444,1490.91442676516,
1491.91416277588,1492.9138987866,1493.91363479732,1494.91337080804,1495.91310681876,
1496.91284282948,1497.9125788402,1498.91231485092,1499.91205086164,1500.91178687236,
1501.91152288309,1502.91125889381,1503.91099490453,1504.91073091525,1505.91046692597,
1506.91020293669,1507.90993894741,1508.90967495813,1509.90941096885,1510.90914697957,
1511.90888299029,1512.90861900101,1513.90835501173,1514.90809102245,1515.90782703317,
1516.90756304389,1517.90729905461,1518.90703506533,1519.90677107605,1520.90650708677,
1521.90624309749,1522.90597910821,1523.90571511893,1524.90545112965,1525.90518714037,
1526.90492315109,1527.90465916181,1528.90439517253,1529.90413118325,1530.90386719397,
1531.90360320469,1532.90333921541,1533.90307522613,1534.90281123685,1535.90254724757,
1536.90228325829,1537.90201926901,1538.90175527973,1539.90149129045,1540.90122730117,
1541.90096331189,1542.90069932261,1543.90043533333,1544.90017134405,1545.89990735477,
1546.89964336549,1547.89937937621,1548.89911538693,1549.89885139765,1550.89858740837,
1551.89832341909,1552.89805942981,1553.89779544053,1554.89753145125,1555.89726746197,
1556.89700347269,1557.89673948341,1558.89647549413,1559.89621150485,1560.89594751557,
1561.89568352629,1562.89541953701,1563.89515554773,1564.89489155845,1565.89462756917,
1566.89436357989,1567.89409959061,1568.89383560133,1569.89357161205,1570.89330762277,
1571.89304363349,1572.89277964421,1573.89251565493,1574.89225166565,1575.89198767637,
1576.89172368709,1577.89145969781,1578.89119570853,1579.89093171926,1580.89066772998,
1581.8904037407,1582.89013975142,1583.88987576214,1584.88961177286,1585.88934778358,
1586.8890837943,1587.88881980502,1588.88855581574,1589.88829182646,1590.88802783718,
1591.8877638479,1592.88749985862,1593.88723586934,1594.88697188006,1595.88670789078,
1596.8864439015,1597.88617991222,1598.88591592294,1599.88565193366,1600.88538794438,
1601.8851239551,1602.88485996582,1603.88459597654,1604.88433198726,1605.88406799798,
1606.8838040087,1607.88354001942,1608.88327603014,1609.88301204086,1610.88274805158,
1611.8824840623,1612.88222007302,1613.88195608374,1614.88169209446,1615.88142810518,
1616.8811641159,1617.88090012662,1618.88063613734,1619.88037214806,1620.88010815878,
1621.8798441695,1622.87958018022,1623.87931619094,1624.87905220166,1625.87878821238,
1626.8785242231,1627.87826023382,1628.87799624454,1629.87773225526,1630.87746826598,
1631.8772042767,1632.87694028742,1633.87667629814,1634.87641230886,1635.87614831958,
1636.8758843303,1637.87562034102,1638.87535635174,1639.87509236246,1640.87482837318,
1641.8745643839,1642.87430039462,1643.87403640534,1644.87377241606,1645.87350842678,
1646.8732444375,1647.87298044822,1648.87271645894,1649.87245246966,1650.87218848038,
1651.8719244911,1652.87166050182,1653.87139651254,1654.87113252326,1655.87086853399,
1656.8706045447,1657.87034055543,1658.87007656615,1659.86981257687,1660.86954858759,
1661.86928459831,1662.86902060903,1663.86875661975,1664.86849263047,1665.86822864119,
1666.86796465191,1667.86770066263,1668.86743667335,1669.86717268407,1670.86690869479,
1671.86664470551,1672.86638071623,1673.86611672695,1674.86585273767,1675.86558874839,
1676.86532475911,1677.86506076983,1678.86479678055,1679.86453279127,1680.86426880199,
1681.86400481271,1682.86374082343,1683.86347683415,1684.86321284487,1685.86294885559,
1686.86268486631,1687.86242087703,1688.86215688775,1689.86189289847,1690.86162890919,
1691.86136491991,1692.86110093063,1693.86083694135,1694.86057295207,1695.86030896279,
1696.86004497351,1697.35991297887,1697.85988790214),.UNSPECIFIED.);
#48=B_SPLINE_SURFACE_WITH_KNOTS('',3,3,((#195534,#195535,#195536,#195537,
#195538,#195539,#195540,#195541,#195542,#195543,#195544,#195545,#195546,
#195547,#195548,#195549,#195550,#195551,#195552,#195553,#195554,#195555,
#195556,#195557,#195558,#195559,#195560,#195561,#195562,#195563,#195564,
#195565,#195566,#195567,#195568,#195569,#195570,#195571,#195572,#195573,
#195574,#195575,#195576,#195577,#195578,#195579,#195580,#195581,#195582,
#195583,#195584,#195585,#195586,#195587,#195588,#195589,#195590,#195591,
#195592,#195593,#195594,#195595,#195596,#195597,#195598,#195599,#195600,
#195601,#195602,#195603,#195604,#195605,#195606,#195607,#195608,#195609,
#195610,#195611,#195612,#195613,#195614,#195615,#195616,#195617,#195618,
#195619,#195620,#195621,#195622,#195623,#195624,#195625,#195626,#195627,
#195628,#195629,#195630,#195631,#195632,#195633,#195634,#195635,#195636,
#195637,#195638,#195639,#195640,#195641,#195642,#195643,#195644,#195645,
#195646,#195647,#195648,#195649,#195650,#195651,#195652,#195653,#195654,
#195655,#195656,#195657,#195658,#195659,#195660,#195661,#195662,#195663,
#195664,#195665,#195666,#195667,#195668,#195669,#195670,#195671,#195672,
#195673,#195674,#195675,#195676,#195677,#195678,#195679,#195680,#195681,
#195682,#195683,#195684,#195685,#195686,#195687,#195688,#195689,#195690,
#195691,#195692,#195693,#195694,#195695,#195696,#195697,#195698,#195699,
#195700,#195701,#195702,#195703,#195704,#195705,#195706,#195707,#195708,
#195709,#195710,#195711,#195712,#195713,#195714,#195715,#195716,#195717,
#195718,#195719,#195720,#195721,#195722,#195723,#195724,#195725,#195726,
#195727,#195728,#195729,#195730,#195731,#195732,#195733,#195734,#195735,
#195736,#195737,#195738,#195739,#195740,#195741,#195742,#195743,#195744,
#195745,#195746,#195747,#195748,#195749,#195750,#195751,#195752,#195753,
#195754,#195755,#195756,#195757,#195758,#195759,#195760,#195761,#195762,
#195763,#195764,#195765,#195766,#195767,#195768,#195769,#195770,#195771,
#195772,#195773,#195774,#195775,#195776,#195777,#195778,#195779,#195780,
#195781,#195782,#195783,#195784,#195785,#195786,#195787,#195788,#195789,
#195790,#195791,#195792,#195793,#195794,#195795,#195796,#195797,#195798,
#195799,#195800,#195801,#195802,#195803,#195804,#195805,#195806,#195807,
#195808,#195809,#195810,#195811,#195812,#195813,#195814,#195815,#195816,
#195817,#195818,#195819,#195820,#195821,#195822,#195823,#195824,#195825,
#195826,#195827,#195828,#195829,#195830,#195831,#195832,#195833,#195834,
#195835,#195836,#195837,#195838,#195839,#195840,#195841,#195842,#195843,
#195844,#195845,#195846,#195847,#195848,#195849,#195850,#195851,#195852,
#195853,#195854,#195855,#195856,#195857,#195858,#195859,#195860,#195861,
#195862,#195863,#195864,#195865,#195866,#195867,#195868,#195869,#195870,
#195871,#195872,#195873,#195874,#195875,#195876,#195877,#195878,#195879,
#195880,#195881,#195882,#195883,#195884,#195885,#195886,#195887,#195888,
#195889,#195890,#195891,#195892,#195893,#195894,#195895,#195896,#195897,
#195898,#195899,#195900,#195901,#195902,#195903,#195904,#195905,#195906,
#195907,#195908,#195909,#195910,#195911,#195912,#195913,#195914,#195915,
#195916,#195917,#195918,#195919,#195920,#195921,#195922,#195923,#195924,
#195925,#195926,#195927,#195928,#195929,#195930,#195931,#195932,#195933,
#195934,#195935,#195936,#195937,#195938,#195939,#195940,#195941,#195942,
#195943,#195944,#195945,#195946,#195947,#195948,#195949,#195950,#195951,
#195952,#195953,#195954,#195955,#195956,#195957,#195958,#195959,#195960,
#195961,#195962,#195963,#195964,#195965,#195966,#195967,#195968,#195969,
#195970,#195971,#195972,#195973,#195974,#195975,#195976,#195977,#195978,
#195979,#195980,#195981,#195982,#195983,#195984,#195985,#195986,#195987,
#195988,#195989,#195990,#195991,#195992,#195993,#195994,#195995,#195996,
#195997,#195998,#195999,#196000,#196001,#196002,#196003,#196004,#196005,
#196006,#196007,#196008,#196009,#196010,#196011,#196012,#196013,#196014,
#196015,#196016,#196017,#196018,#196019,#196020,#196021,#196022,#196023,
#196024,#196025,#196026,#196027,#196028,#196029,#196030,#196031,#196032,
#196033,#196034,#196035,#196036,#196037,#196038,#196039,#196040,#196041,
#196042,#196043,#196044,#196045,#196046,#196047,#196048,#196049,#196050,
#196051,#196052,#196053,#196054,#196055,#196056,#196057,#196058,#196059,
#196060,#196061,#196062,#196063,#196064,#196065,#196066,#196067,#196068,
#196069,#196070,#196071,#196072,#196073,#196074,#196075,#196076,#196077,
#196078,#196079,#196080,#196081,#196082,#196083,#196084,#196085,#196086,
#196087,#196088,#196089,#196090,#196091,#196092,#196093,#196094,#196095,
#196096,#196097,#196098,#196099,#196100,#196101,#196102,#196103,#196104,
#196105,#196106,#196107,#196108,#196109,#196110,#196111,#196112,#196113,
#196114,#196115,#196116,#196117,#196118,#196119,#196120,#196121,#196122,
#196123,#196124,#196125,#196126,#196127,#196128,#196129,#196130,#196131,
#196132,#196133,#196134,#196135,#196136,#196137,#196138,#196139,#196140,
#196141,#196142,#196143,#196144,#196145,#196146,#196147,#196148,#196149,
#196150,#196151,#196152,#196153,#196154,#196155,#196156,#196157,#196158,
#196159,#196160,#196161,#196162,#196163,#196164,#196165,#196166,#196167,
#196168,#196169,#196170,#196171,#196172,#196173,#196174,#196175,#196176,
#196177,#196178,#196179,#196180,#196181,#196182,#196183,#196184,#196185,
#196186,#196187,#196188,#196189,#196190,#196191,#196192,#196193,#196194,
#196195,#196196,#196197,#196198,#196199,#196200,#196201,#196202,#196203,
#196204,#196205,#196206,#196207,#196208,#196209,#196210,#196211,#196212,
#196213,#196214,#196215,#196216,#196217,#196218,#196219,#196220,#196221,
#196222,#196223,#196224,#196225,#196226,#196227,#196228,#196229,#196230,
#196231,#196232,#196233,#196234,#196235,#196236,#196237,#196238,#196239,
#196240,#196241,#196242,#196243,#196244,#196245,#196246,#196247,#196248,
#196249,#196250,#196251,#196252,#196253,#196254,#196255,#196256,#196257,
#196258,#196259,#196260,#196261,#196262,#196263,#196264,#196265,#196266,
#196267,#196268,#196269,#196270,#196271,#196272,#196273,#196274,#196275,
#196276,#196277,#196278,#196279,#196280,#196281,#196282,#196283,#196284,
#196285,#196286,#196287,#196288,#196289,#196290,#196291,#196292,#196293,
#196294,#196295,#196296,#196297,#196298,#196299,#196300,#196301,#196302,
#196303,#196304,#196305,#196306,#196307,#196308,#196309,#196310,#196311,
#196312,#196313,#196314,#196315,#196316,#196317,#196318,#196319,#196320,
#196321,#196322,#196323,#196324,#196325,#196326,#196327,#196328,#196329,
#196330,#196331,#196332,#196333,#196334,#196335,#196336,#196337,#196338,
#196339,#196340,#196341,#196342,#196343,#196344,#196345,#196346,#196347,
#196348,#196349,#196350,#196351,#196352,#196353,#196354,#196355,#196356,
#196357,#196358,#196359,#196360,#196361,#196362,#196363,#196364,#196365,
#196366,#196367,#196368,#196369,#196370,#196371,#196372,#196373,#196374,
#196375,#196376,#196377,#196378,#196379,#196380,#196381,#196382,#196383,
#196384,#196385,#196386,#196387,#196388,#196389,#196390,#196391,#196392,
#196393,#196394,#196395,#196396,#196397,#196398,#196399,#196400,#196401,
#196402,#196403,#196404,#196405,#196406,#196407,#196408,#196409,#196410,
#196411,#196412,#196413,#196414,#196415,#196416,#196417,#196418,#196419,
#196420,#196421,#196422,#196423,#196424,#196425,#196426,#196427,#196428,
#196429,#196430,#196431,#196432,#196433,#196434,#196435,#196436,#196437,
#196438,#196439,#196440,#196441,#196442,#196443,#196444,#196445,#196446,
#196447,#196448,#196449,#196450,#196451,#196452,#196453,#196454,#196455,
#196456,#196457,#196458,#196459,#196460,#196461,#196462,#196463,#196464,
#196465,#196466,#196467,#196468,#196469,#196470,#196471,#196472,#196473,
#196474,#196475,#196476,#196477,#196478,#196479,#196480,#196481,#196482,
#196483,#196484,#196485,#196486,#196487,#196488,#196489,#196490,#196491,
#196492,#196493,#196494,#196495,#196496,#196497,#196498,#196499,#196500,
#196501,#196502,#196503,#196504,#196505,#196506,#196507,#196508,#196509,
#196510,#196511,#196512,#196513,#196514,#196515,#196516,#196517,#196518,
#196519,#196520,#196521,#196522,#196523,#196524,#196525,#196526,#196527,
#196528,#196529,#196530,#196531,#196532,#196533,#196534,#196535,#196536,
#196537,#196538,#196539,#196540,#196541,#196542,#196543,#196544,#196545,
#196546,#196547,#196548,#196549,#196550,#196551,#196552,#196553,#196554,
#196555,#196556,#196557,#196558,#196559,#196560,#196561,#196562,#196563,
#196564,#196565,#196566,#196567,#196568,#196569,#196570,#196571,#196572,
#196573,#196574,#196575,#196576,#196577,#196578,#196579,#196580,#196581,
#196582,#196583,#196584,#196585,#196586,#196587,#196588,#196589,#196590,
#196591,#196592,#196593,#196594,#196595,#196596,#196597,#196598,#196599,
#196600,#196601,#196602,#196603,#196604,#196605,#196606,#196607,#196608,
#196609,#196610,#196611,#196612,#196613,#196614,#196615,#196616,#196617,
#196618,#196619,#196620,#196621,#196622,#196623,#196624,#196625,#196626,
#196627,#196628,#196629,#196630,#196631,#196632,#196633,#196634,#196635,
#196636,#196637,#196638,#196639,#196640,#196641,#196642,#196643,#196644,
#196645,#196646,#196647,#196648,#196649,#196650,#196651,#196652,#196653,
#196654,#196655,#196656,#196657,#196658,#196659,#196660,#196661,#196662,
#196663,#196664,#196665,#196666,#196667,#196668,#196669,#196670,#196671,
#196672,#196673,#196674,#196675,#196676,#196677,#196678,#196679,#196680,
#196681,#196682,#196683,#196684,#196685,#196686,#196687,#196688,#196689,
#196690,#196691,#196692,#196693,#196694,#196695,#196696,#196697,#196698,
#196699,#196700,#196701,#196702,#196703,#196704,#196705,#196706,#196707,
#196708,#196709,#196710,#196711,#196712,#196713,#196714,#196715,#196716,
#196717,#196718,#196719,#196720,#196721,#196722,#196723,#196724,#196725,
#196726,#196727,#196728,#196729,#196730,#196731,#196732,#196733,#196734,
#196735,#196736,#196737,#196738,#196739,#196740,#196741,#196742,#196743,
#196744,#196745,#196746,#196747,#196748,#196749,#196750,#196751,#196752,
#196753,#196754,#196755,#196756,#196757,#196758,#196759,#196760,#196761,
#196762,#196763,#196764,#196765,#196766,#196767,#196768,#196769,#196770,
#196771,#196772,#196773,#196774,#196775,#196776,#196777,#196778,#196779,
#196780,#196781,#196782,#196783,#196784,#196785,#196786,#196787,#196788,
#196789,#196790,#196791,#196792,#196793,#196794,#196795,#196796,#196797,
#196798,#196799,#196800,#196801,#196802,#196803,#196804,#196805,#196806,
#196807,#196808,#196809,#196810,#196811,#196812,#196813,#196814,#196815,
#196816,#196817,#196818,#196819,#196820,#196821,#196822,#196823,#196824,
#196825,#196826,#196827,#196828,#196829,#196830,#196831,#196832,#196833,
#196834,#196835,#196836,#196837,#196838,#196839,#196840,#196841,#196842,
#196843,#196844,#196845,#196846,#196847,#196848,#196849,#196850,#196851,
#196852,#196853,#196854,#196855,#196856,#196857,#196858,#196859,#196860,
#196861,#196862,#196863,#196864,#196865,#196866,#196867,#196868,#196869,
#196870,#196871,#196872,#196873,#196874,#196875,#196876,#196877,#196878,
#196879,#196880,#196881,#196882,#196883,#196884,#196885,#196886,#196887,
#196888,#196889,#196890,#196891,#196892,#196893,#196894,#196895,#196896,
#196897,#196898,#196899,#196900,#196901,#196902,#196903,#196904,#196905,
#196906,#196907,#196908,#196909,#196910,#196911,#196912,#196913,#196914,
#196915,#196916,#196917,#196918,#196919,#196920,#196921,#196922,#196923,
#196924,#196925,#196926,#196927,#196928,#196929,#196930,#196931,#196932,
#196933,#196934,#196935,#196936,#196937,#196938,#196939,#196940,#196941,
#196942,#196943,#196944,#196945,#196946,#196947,#196948,#196949,#196950,
#196951,#196952,#196953,#196954,#196955,#196956,#196957,#196958,#196959,
#196960,#196961,#196962,#196963,#196964,#196965,#196966,#196967,#196968,
#196969,#196970,#196971,#196972,#196973,#196974,#196975,#196976,#196977,
#196978,#196979,#196980,#196981,#196982,#196983,#196984,#196985,#196986,
#196987,#196988,#196989,#196990,#196991,#196992,#196993,#196994,#196995,
#196996,#196997,#196998,#196999,#197000,#197001,#197002,#197003,#197004,
#197005,#197006,#197007,#197008,#197009,#197010,#197011,#197012,#197013,
#197014,#197015,#197016,#197017,#197018,#197019,#197020,#197021,#197022,
#197023,#197024,#197025,#197026,#197027,#197028,#197029,#197030,#197031,
#197032,#197033,#197034,#197035,#197036,#197037,#197038,#197039,#197040,
#197041,#197042,#197043,#197044,#197045,#197046,#197047,#197048,#197049,
#197050,#197051,#197052,#197053,#197054,#197055,#197056,#197057,#197058,
#197059,#197060,#197061,#197062,#197063,#197064,#197065,#197066,#197067,
#197068,#197069,#197070,#197071,#197072,#197073,#197074,#197075,#197076,
#197077,#197078,#197079,#197080,#197081,#197082,#197083,#197084,#197085,
#197086,#197087,#197088,#197089,#197090,#197091,#197092,#197093,#197094,
#197095,#197096,#197097,#197098,#197099,#197100,#197101,#197102,#197103,
#197104,#197105,#197106,#197107,#197108,#197109,#197110,#197111,#197112,
#197113,#197114,#197115,#197116,#197117,#197118,#197119,#197120,#197121,
#197122,#197123,#197124,#197125,#197126,#197127,#197128,#197129,#197130,
#197131,#197132,#197133,#197134,#197135,#197136,#197137,#197138,#197139,
#197140,#197141,#197142,#197143,#197144,#197145,#197146,#197147,#197148,
#197149,#197150,#197151,#197152,#197153,#197154,#197155,#197156,#197157,
#197158,#197159,#197160,#197161,#197162,#197163,#197164,#197165,#197166,
#197167,#197168,#197169,#197170,#197171,#197172,#197173,#197174,#197175,
#197176,#197177,#197178,#197179,#197180,#197181,#197182,#197183,#197184,
#197185,#197186,#197187,#197188,#197189,#197190,#197191,#197192,#197193,
#197194,#197195,#197196,#197197,#197198,#197199,#197200,#197201,#197202,
#197203,#197204,#197205,#197206,#197207,#197208,#197209,#197210,#197211,
#197212,#197213,#197214,#197215,#197216,#197217,#197218,#197219,#197220,
#197221,#197222,#197223,#197224,#197225,#197226,#197227,#197228),(#197229,
#197230,#197231,#197232,#197233,#197234,#197235,#197236,#197237,#197238,
#197239,#197240,#197241,#197242,#197243,#197244,#197245,#197246,#197247,
#197248,#197249,#197250,#197251,#197252,#197253,#197254,#197255,#197256,
#197257,#197258,#197259,#197260,#197261,#197262,#197263,#197264,#197265,
#197266,#197267,#197268,#197269,#197270,#197271,#197272,#197273,#197274,
#197275,#197276,#197277,#197278,#197279,#197280,#197281,#197282,#197283,
#197284,#197285,#197286,#197287,#197288,#197289,#197290,#197291,#197292,
#197293,#197294,#197295,#197296,#197297,#197298,#197299,#197300,#197301,
#197302,#197303,#197304,#197305,#197306,#197307,#197308,#197309,#197310,
#197311,#197312,#197313,#197314,#197315,#197316,#197317,#197318,#197319,
#197320,#197321,#197322,#197323,#197324,#197325,#197326,#197327,#197328,
#197329,#197330,#197331,#197332,#197333,#197334,#197335,#197336,#197337,
#197338,#197339,#197340,#197341,#197342,#197343,#197344,#197345,#197346,
#197347,#197348,#197349,#197350,#197351,#197352,#197353,#197354,#197355,
#197356,#197357,#197358,#197359,#197360,#197361,#197362,#197363,#197364,
#197365,#197366,#197367,#197368,#197369,#197370,#197371,#197372,#197373,
#197374,#197375,#197376,#197377,#197378,#197379,#197380,#197381,#197382,
#197383,#197384,#197385,#197386,#197387,#197388,#197389,#197390,#197391,
#197392,#197393,#197394,#197395,#197396,#197397,#197398,#197399,#197400,
#197401,#197402,#197403,#197404,#197405,#197406,#197407,#197408,#197409,
#197410,#197411,#197412,#197413,#197414,#197415,#197416,#197417,#197418,
#197419,#197420,#197421,#197422,#197423,#197424,#197425,#197426,#197427,
#197428,#197429,#197430,#197431,#197432,#197433,#197434,#197435,#197436,
#197437,#197438,#197439,#197440,#197441,#197442,#197443,#197444,#197445,
#197446,#197447,#197448,#197449,#197450,#197451,#197452,#197453,#197454,
#197455,#197456,#197457,#197458,#197459,#197460,#197461,#197462,#197463,
#197464,#197465,#197466,#197467,#197468,#197469,#197470,#197471,#197472,
#197473,#197474,#197475,#197476,#197477,#197478,#197479,#197480,#197481,
#197482,#197483,#197484,#197485,#197486,#197487,#197488,#197489,#197490,
#197491,#197492,#197493,#197494,#197495,#197496,#197497,#197498,#197499,
#197500,#197501,#197502,#197503,#197504,#197505,#197506,#197507,#197508,
#197509,#197510,#197511,#197512,#197513,#197514,#197515,#197516,#197517,
#197518,#197519,#197520,#197521,#197522,#197523,#197524,#197525,#197526,
#197527,#197528,#197529,#197530,#197531,#197532,#197533,#197534,#197535,
#197536,#197537,#197538,#197539,#197540,#197541,#197542,#197543,#197544,
#197545,#197546,#197547,#197548,#197549,#197550,#197551,#197552,#197553,
#197554,#197555,#197556,#197557,#197558,#197559,#197560,#197561,#197562,
#197563,#197564,#197565,#197566,#197567,#197568,#197569,#197570,#197571,
#197572,#197573,#197574,#197575,#197576,#197577,#197578,#197579,#197580,
#197581,#197582,#197583,#197584,#197585,#197586,#197587,#197588,#197589,
#197590,#197591,#197592,#197593,#197594,#197595,#197596,#197597,#197598,
#197599,#197600,#197601,#197602,#197603,#197604,#197605,#197606,#197607,
#197608,#197609,#197610,#197611,#197612,#197613,#197614,#197615,#197616,
#197617,#197618,#197619,#197620,#197621,#197622,#197623,#197624,#197625,
#197626,#197627,#197628,#197629,#197630,#197631,#197632,#197633,#197634,
#197635,#197636,#197637,#197638,#197639,#197640,#197641,#197642,#197643,
#197644,#197645,#197646,#197647,#197648,#197649,#197650,#197651,#197652,
#197653,#197654,#197655,#197656,#197657,#197658,#197659,#197660,#197661,
#197662,#197663,#197664,#197665,#197666,#197667,#197668,#197669,#197670,
#197671,#197672,#197673,#197674,#197675,#197676,#197677,#197678,#197679,
#197680,#197681,#197682,#197683,#197684,#197685,#197686,#197687,#197688,
#197689,#197690,#197691,#197692,#197693,#197694,#197695,#197696,#197697,
#197698,#197699,#197700,#197701,#197702,#197703,#197704,#197705,#197706,
#197707,#197708,#197709,#197710,#197711,#197712,#197713,#197714,#197715,
#197716,#197717,#197718,#197719,#197720,#197721,#197722,#197723,#197724,
#197725,#197726,#197727,#197728,#197729,#197730,#197731,#197732,#197733,
#197734,#197735,#197736,#197737,#197738,#197739,#197740,#197741,#197742,
#197743,#197744,#197745,#197746,#197747,#197748,#197749,#197750,#197751,
#197752,#197753,#197754,#197755,#197756,#197757,#197758,#197759,#197760,
#197761,#197762,#197763,#197764,#197765,#197766,#197767,#197768,#197769,
#197770,#197771,#197772,#197773,#197774,#197775,#197776,#197777,#197778,
#197779,#197780,#197781,#197782,#197783,#197784,#197785,#197786,#197787,
#197788,#197789,#197790,#197791,#197792,#197793,#197794,#197795,#197796,
#197797,#197798,#197799,#197800,#197801,#197802,#197803,#197804,#197805,
#197806,#197807,#197808,#197809,#197810,#197811,#197812,#197813,#197814,
#197815,#197816,#197817,#197818,#197819,#197820,#197821,#197822,#197823,
#197824,#197825,#197826,#197827,#197828,#197829,#197830,#197831,#197832,
#197833,#197834,#197835,#197836,#197837,#197838,#197839,#197840,#197841,
#197842,#197843,#197844,#197845,#197846,#197847,#197848,#197849,#197850,
#197851,#197852,#197853,#197854,#197855,#197856,#197857,#197858,#197859,
#197860,#197861,#197862,#197863,#197864,#197865,#197866,#197867,#197868,
#197869,#197870,#197871,#197872,#197873,#197874,#197875,#197876,#197877,
#197878,#197879,#197880,#197881,#197882,#197883,#197884,#197885,#197886,
#197887,#197888,#197889,#197890,#197891,#197892,#197893,#197894,#197895,
#197896,#197897,#197898,#197899,#197900,#197901,#197902,#197903,#197904,
#197905,#197906,#197907,#197908,#197909,#197910,#197911,#197912,#197913,
#197914,#197915,#197916,#197917,#197918,#197919,#197920,#197921,#197922,
#197923,#197924,#197925,#197926,#197927,#197928,#197929,#197930,#197931,
#197932,#197933,#197934,#197935,#197936,#197937,#197938,#197939,#197940,
#197941,#197942,#197943,#197944,#197945,#197946,#197947,#197948,#197949,
#197950,#197951,#197952,#197953,#197954,#197955,#197956,#197957,#197958,
#197959,#197960,#197961,#197962,#197963,#197964,#197965,#197966,#197967,
#197968,#197969,#197970,#197971,#197972,#197973,#197974,#197975,#197976,
#197977,#197978,#197979,#197980,#197981,#197982,#197983,#197984,#197985,
#197986,#197987,#197988,#197989,#197990,#197991,#197992,#197993,#197994,
#197995,#197996,#197997,#197998,#197999,#198000,#198001,#198002,#198003,
#198004,#198005,#198006,#198007,#198008,#198009,#198010,#198011,#198012,
#198013,#198014,#198015,#198016,#198017,#198018,#198019,#198020,#198021,
#198022,#198023,#198024,#198025,#198026,#198027,#198028,#198029,#198030,
#198031,#198032,#198033,#198034,#198035,#198036,#198037,#198038,#198039,
#198040,#198041,#198042,#198043,#198044,#198045,#198046,#198047,#198048,
#198049,#198050,#198051,#198052,#198053,#198054,#198055,#198056,#198057,
#198058,#198059,#198060,#198061,#198062,#198063,#198064,#198065,#198066,
#198067,#198068,#198069,#198070,#198071,#198072,#198073,#198074,#198075,
#198076,#198077,#198078,#198079,#198080,#198081,#198082,#198083,#198084,
#198085,#198086,#198087,#198088,#198089,#198090,#198091,#198092,#198093,
#198094,#198095,#198096,#198097,#198098,#198099,#198100,#198101,#198102,
#198103,#198104,#198105,#198106,#198107,#198108,#198109,#198110,#198111,
#198112,#198113,#198114,#198115,#198116,#198117,#198118,#198119,#198120,
#198121,#198122,#198123,#198124,#198125,#198126,#198127,#198128,#198129,
#198130,#198131,#198132,#198133,#198134,#198135,#198136,#198137,#198138,
#198139,#198140,#198141,#198142,#198143,#198144,#198145,#198146,#198147,
#198148,#198149,#198150,#198151,#198152,#198153,#198154,#198155,#198156,
#198157,#198158,#198159,#198160,#198161,#198162,#198163,#198164,#198165,
#198166,#198167,#198168,#198169,#198170,#198171,#198172,#198173,#198174,
#198175,#198176,#198177,#198178,#198179,#198180,#198181,#198182,#198183,
#198184,#198185,#198186,#198187,#198188,#198189,#198190,#198191,#198192,
#198193,#198194,#198195,#198196,#198197,#198198,#198199,#198200,#198201,
#198202,#198203,#198204,#198205,#198206,#198207,#198208,#198209,#198210,
#198211,#198212,#198213,#198214,#198215,#198216,#198217,#198218,#198219,
#198220,#198221,#198222,#198223,#198224,#198225,#198226,#198227,#198228,
#198229,#198230,#198231,#198232,#198233,#198234,#198235,#198236,#198237,
#198238,#198239,#198240,#198241,#198242,#198243,#198244,#198245,#198246,
#198247,#198248,#198249,#198250,#198251,#198252,#198253,#198254,#198255,
#198256,#198257,#198258,#198259,#198260,#198261,#198262,#198263,#198264,
#198265,#198266,#198267,#198268,#198269,#198270,#198271,#198272,#198273,
#198274,#198275,#198276,#198277,#198278,#198279,#198280,#198281,#198282,
#198283,#198284,#198285,#198286,#198287,#198288,#198289,#198290,#198291,
#198292,#198293,#198294,#198295,#198296,#198297,#198298,#198299,#198300,
#198301,#198302,#198303,#198304,#198305,#198306,#198307,#198308,#198309,
#198310,#198311,#198312,#198313,#198314,#198315,#198316,#198317,#198318,
#198319,#198320,#198321,#198322,#198323,#198324,#198325,#198326,#198327,
#198328,#198329,#198330,#198331,#198332,#198333,#198334,#198335,#198336,
#198337,#198338,#198339,#198340,#198341,#198342,#198343,#198344,#198345,
#198346,#198347,#198348,#198349,#198350,#198351,#198352,#198353,#198354,
#198355,#198356,#198357,#198358,#198359,#198360,#198361,#198362,#198363,
#198364,#198365,#198366,#198367,#198368,#198369,#198370,#198371,#198372,
#198373,#198374,#198375,#198376,#198377,#198378,#198379,#198380,#198381,
#198382,#198383,#198384,#198385,#198386,#198387,#198388,#198389,#198390,
#198391,#198392,#198393,#198394,#198395,#198396,#198397,#198398,#198399,
#198400,#198401,#198402,#198403,#198404,#198405,#198406,#198407,#198408,
#198409,#198410,#198411,#198412,#198413,#198414,#198415,#198416,#198417,
#198418,#198419,#198420,#198421,#198422,#198423,#198424,#198425,#198426,
#198427,#198428,#198429,#198430,#198431,#198432,#198433,#198434,#198435,
#198436,#198437,#198438,#198439,#198440,#198441,#198442,#198443,#198444,
#198445,#198446,#198447,#198448,#198449,#198450,#198451,#198452,#198453,
#198454,#198455,#198456,#198457,#198458,#198459,#198460,#198461,#198462,
#198463,#198464,#198465,#198466,#198467,#198468,#198469,#198470,#198471,
#198472,#198473,#198474,#198475,#198476,#198477,#198478,#198479,#198480,
#198481,#198482,#198483,#198484,#198485,#198486,#198487,#198488,#198489,
#198490,#198491,#198492,#198493,#198494,#198495,#198496,#198497,#198498,
#198499,#198500,#198501,#198502,#198503,#198504,#198505,#198506,#198507,
#198508,#198509,#198510,#198511,#198512,#198513,#198514,#198515,#198516,
#198517,#198518,#198519,#198520,#198521,#198522,#198523,#198524,#198525,
#198526,#198527,#198528,#198529,#198530,#198531,#198532,#198533,#198534,
#198535,#198536,#198537,#198538,#198539,#198540,#198541,#198542,#198543,
#198544,#198545,#198546,#198547,#198548,#198549,#198550,#198551,#198552,
#198553,#198554,#198555,#198556,#198557,#198558,#198559,#198560,#198561,
#198562,#198563,#198564,#198565,#198566,#198567,#198568,#198569,#198570,
#198571,#198572,#198573,#198574,#198575,#198576,#198577,#198578,#198579,
#198580,#198581,#198582,#198583,#198584,#198585,#198586,#198587,#198588,
#198589,#198590,#198591,#198592,#198593,#198594,#198595,#198596,#198597,
#198598,#198599,#198600,#198601,#198602,#198603,#198604,#198605,#198606,
#198607,#198608,#198609,#198610,#198611,#198612,#198613,#198614,#198615,
#198616,#198617,#198618,#198619,#198620,#198621,#198622,#198623,#198624,
#198625,#198626,#198627,#198628,#198629,#198630,#198631,#198632,#198633,
#198634,#198635,#198636,#198637,#198638,#198639,#198640,#198641,#198642,
#198643,#198644,#198645,#198646,#198647,#198648,#198649,#198650,#198651,
#198652,#198653,#198654,#198655,#198656,#198657,#198658,#198659,#198660,
#198661,#198662,#198663,#198664,#198665,#198666,#198667,#198668,#198669,
#198670,#198671,#198672,#198673,#198674,#198675,#198676,#198677,#198678,
#198679,#198680,#198681,#198682,#198683,#198684,#198685,#198686,#198687,
#198688,#198689,#198690,#198691,#198692,#198693,#198694,#198695,#198696,
#198697,#198698,#198699,#198700,#198701,#198702,#198703,#198704,#198705,
#198706,#198707,#198708,#198709,#198710,#198711,#198712,#198713,#198714,
#198715,#198716,#198717,#198718,#198719,#198720,#198721,#198722,#198723,
#198724,#198725,#198726,#198727,#198728,#198729,#198730,#198731,#198732,
#198733,#198734,#198735,#198736,#198737,#198738,#198739,#198740,#198741,
#198742,#198743,#198744,#198745,#198746,#198747,#198748,#198749,#198750,
#198751,#198752,#198753,#198754,#198755,#198756,#198757,#198758,#198759,
#198760,#198761,#198762,#198763,#198764,#198765,#198766,#198767,#198768,
#198769,#198770,#198771,#198772,#198773,#198774,#198775,#198776,#198777,
#198778,#198779,#198780,#198781,#198782,#198783,#198784,#198785,#198786,
#198787,#198788,#198789,#198790,#198791,#198792,#198793,#198794,#198795,
#198796,#198797,#198798,#198799,#198800,#198801,#198802,#198803,#198804,
#198805,#198806,#198807,#198808,#198809,#198810,#198811,#198812,#198813,
#198814,#198815,#198816,#198817,#198818,#198819,#198820,#198821,#198822,
#198823,#198824,#198825,#198826,#198827,#198828,#198829,#198830,#198831,
#198832,#198833,#198834,#198835,#198836,#198837,#198838,#198839,#198840,
#198841,#198842,#198843,#198844,#198845,#198846,#198847,#198848,#198849,
#198850,#198851,#198852,#198853,#198854,#198855,#198856,#198857,#198858,
#198859,#198860,#198861,#198862,#198863,#198864,#198865,#198866,#198867,
#198868,#198869,#198870,#198871,#198872,#198873,#198874,#198875,#198876,
#198877,#198878,#198879,#198880,#198881,#198882,#198883,#198884,#198885,
#198886,#198887,#198888,#198889,#198890,#198891,#198892,#198893,#198894,
#198895,#198896,#198897,#198898,#198899,#198900,#198901,#198902,#198903,
#198904,#198905,#198906,#198907,#198908,#198909,#198910,#198911,#198912,
#198913,#198914,#198915,#198916,#198917,#198918,#198919,#198920,#198921,
#198922,#198923),(#198924,#198925,#198926,#198927,#198928,#198929,#198930,
#198931,#198932,#198933,#198934,#198935,#198936,#198937,#198938,#198939,
#198940,#198941,#198942,#198943,#198944,#198945,#198946,#198947,#198948,
#198949,#198950,#198951,#198952,#198953,#198954,#198955,#198956,#198957,
#198958,#198959,#198960,#198961,#198962,#198963,#198964,#198965,#198966,
#198967,#198968,#198969,#198970,#198971,#198972,#198973,#198974,#198975,
#198976,#198977,#198978,#198979,#198980,#198981,#198982,#198983,#198984,
#198985,#198986,#198987,#198988,#198989,#198990,#198991,#198992,#198993,
#198994,#198995,#198996,#198997,#198998,#198999,#199000,#199001,#199002,
#199003,#199004,#199005,#199006,#199007,#199008,#199009,#199010,#199011,
#199012,#199013,#199014,#199015,#199016,#199017,#199018,#199019,#199020,
#199021,#199022,#199023,#199024,#199025,#199026,#199027,#199028,#199029,
#199030,#199031,#199032,#199033,#199034,#199035,#199036,#199037,#199038,
#199039,#199040,#199041,#199042,#199043,#199044,#199045,#199046,#199047,
#199048,#199049,#199050,#199051,#199052,#199053,#199054,#199055,#199056,
#199057,#199058,#199059,#199060,#199061,#199062,#199063,#199064,#199065,
#199066,#199067,#199068,#199069,#199070,#199071,#199072,#199073,#199074,
#199075,#199076,#199077,#199078,#199079,#199080,#199081,#199082,#199083,
#199084,#199085,#199086,#199087,#199088,#199089,#199090,#199091,#199092,
#199093,#199094,#199095,#199096,#199097,#199098,#199099,#199100,#199101,
#199102,#199103,#199104,#199105,#199106,#199107,#199108,#199109,#199110,
#199111,#199112,#199113,#199114,#199115,#199116,#199117,#199118,#199119,
#199120,#199121,#199122,#199123,#199124,#199125,#199126,#199127,#199128,
#199129,#199130,#199131,#199132,#199133,#199134,#199135,#199136,#199137,
#199138,#199139,#199140,#199141,#199142,#199143,#199144,#199145,#199146,
#199147,#199148,#199149,#199150,#199151,#199152,#199153,#199154,#199155,
#199156,#199157,#199158,#199159,#199160,#199161,#199162,#199163,#199164,
#199165,#199166,#199167,#199168,#199169,#199170,#199171,#199172,#199173,
#199174,#199175,#199176,#199177,#199178,#199179,#199180,#199181,#199182,
#199183,#199184,#199185,#199186,#199187,#199188,#199189,#199190,#199191,
#199192,#199193,#199194,#199195,#199196,#199197,#199198,#199199,#199200,
#199201,#199202,#199203,#199204,#199205,#199206,#199207,#199208,#199209,
#199210,#199211,#199212,#199213,#199214,#199215,#199216,#199217,#199218,
#199219,#199220,#199221,#199222,#199223,#199224,#199225,#199226,#199227,
#199228,#199229,#199230,#199231,#199232,#199233,#199234,#199235,#199236,
#199237,#199238,#199239,#199240,#199241,#199242,#199243,#199244,#199245,
#199246,#199247,#199248,#199249,#199250,#199251,#199252,#199253,#199254,
#199255,#199256,#199257,#199258,#199259,#199260,#199261,#199262,#199263,
#199264,#199265,#199266,#199267,#199268,#199269,#199270,#199271,#199272,
#199273,#199274,#199275,#199276,#199277,#199278,#199279,#199280,#199281,
#199282,#199283,#199284,#199285,#199286,#199287,#199288,#199289,#199290,
#199291,#199292,#199293,#199294,#199295,#199296,#199297,#199298,#199299,
#199300,#199301,#199302,#199303,#199304,#199305,#199306,#199307,#199308,
#199309,#199310,#199311,#199312,#199313,#199314,#199315,#199316,#199317,
#199318,#199319,#199320,#199321,#199322,#199323,#199324,#199325,#199326,
#199327,#199328,#199329,#199330,#199331,#199332,#199333,#199334,#199335,
#199336,#199337,#199338,#199339,#199340,#199341,#199342,#199343,#199344,
#199345,#199346,#199347,#199348,#199349,#199350,#199351,#199352,#199353,
#199354,#199355,#199356,#199357,#199358,#199359,#199360,#199361,#199362,
#199363,#199364,#199365,#199366,#199367,#199368,#199369,#199370,#199371,
#199372,#199373,#199374,#199375,#199376,#199377,#199378,#199379,#199380,
#199381,#199382,#199383,#199384,#199385,#199386,#199387,#199388,#199389,
#199390,#199391,#199392,#199393,#199394,#199395,#199396,#199397,#199398,
#199399,#199400,#199401,#199402,#199403,#199404,#199405,#199406,#199407,
#199408,#199409,#199410,#199411,#199412,#199413,#199414,#199415,#199416,
#199417,#199418,#199419,#199420,#199421,#199422,#199423,#199424,#199425,
#199426,#199427,#199428,#199429,#199430,#199431,#199432,#199433,#199434,
#199435,#199436,#199437,#199438,#199439,#199440,#199441,#199442,#199443,
#199444,#199445,#199446,#199447,#199448,#199449,#199450,#199451,#199452,
#199453,#199454,#199455,#199456,#199457,#199458,#199459,#199460,#199461,
#199462,#199463,#199464,#199465,#199466,#199467,#199468,#199469,#199470,
#199471,#199472,#199473,#199474,#199475,#199476,#199477,#199478,#199479,
#199480,#199481,#199482,#199483,#199484,#199485,#199486,#199487,#199488,
#199489,#199490,#199491,#199492,#199493,#199494,#199495,#199496,#199497,
#199498,#199499,#199500,#199501,#199502,#199503,#199504,#199505,#199506,
#199507,#199508,#199509,#199510,#199511,#199512,#199513,#199514,#199515,
#199516,#199517,#199518,#199519,#199520,#199521,#199522,#199523,#199524,
#199525,#199526,#199527,#199528,#199529,#199530,#199531,#199532,#199533,
#199534,#199535,#199536,#199537,#199538,#199539,#199540,#199541,#199542,
#199543,#199544,#199545,#199546,#199547,#199548,#199549,#199550,#199551,
#199552,#199553,#199554,#199555,#199556,#199557,#199558,#199559,#199560,
#199561,#199562,#199563,#199564,#199565,#199566,#199567,#199568,#199569,
#199570,#199571,#199572,#199573,#199574,#199575,#199576,#199577,#199578,
#199579,#199580,#199581,#199582,#199583,#199584,#199585,#199586,#199587,
#199588,#199589,#199590,#199591,#199592,#199593,#199594,#199595,#199596,
#199597,#199598,#199599,#199600,#199601,#199602,#199603,#199604,#199605,
#199606,#199607,#199608,#199609,#199610,#199611,#199612,#199613,#199614,
#199615,#199616,#199617,#199618,#199619,#199620,#199621,#199622,#199623,
#199624,#199625,#199626,#199627,#199628,#199629,#199630,#199631,#199632,
#199633,#199634,#199635,#199636,#199637,#199638,#199639,#199640,#199641,
#199642,#199643,#199644,#199645,#199646,#199647,#199648,#199649,#199650,
#199651,#199652,#199653,#199654,#199655,#199656,#199657,#199658,#199659,
#199660,#199661,#199662,#199663,#199664,#199665,#199666,#199667,#199668,
#199669,#199670,#199671,#199672,#199673,#199674,#199675,#199676,#199677,
#199678,#199679,#199680,#199681,#199682,#199683,#199684,#199685,#199686,
#199687,#199688,#199689,#199690,#199691,#199692,#199693,#199694,#199695,
#199696,#199697,#199698,#199699,#199700,#199701,#199702,#199703,#199704,
#199705,#199706,#199707,#199708,#199709,#199710,#199711,#199712,#199713,
#199714,#199715,#199716,#199717,#199718,#199719,#199720,#199721,#199722,
#199723,#199724,#199725,#199726,#199727,#199728,#199729,#199730,#199731,
#199732,#199733,#199734,#199735,#199736,#199737,#199738,#199739,#199740,
#199741,#199742,#199743,#199744,#199745,#199746,#199747,#199748,#199749,
#199750,#199751,#199752,#199753,#199754,#199755,#199756,#199757,#199758,
#199759,#199760,#199761,#199762,#199763,#199764,#199765,#199766,#199767,
#199768,#199769,#199770,#199771,#199772,#199773,#199774,#199775,#199776,
#199777,#199778,#199779,#199780,#199781,#199782,#199783,#199784,#199785,
#199786,#199787,#199788,#199789,#199790,#199791,#199792,#199793,#199794,
#199795,#199796,#199797,#199798,#199799,#199800,#199801,#199802,#199803,
#199804,#199805,#199806,#199807,#199808,#199809,#199810,#199811,#199812,
#199813,#199814,#199815,#199816,#199817,#199818,#199819,#199820,#199821,
#199822,#199823,#199824,#199825,#199826,#199827,#199828,#199829,#199830,
#199831,#199832,#199833,#199834,#199835,#199836,#199837,#199838,#199839,
#199840,#199841,#199842,#199843,#199844,#199845,#199846,#199847,#199848,
#199849,#199850,#199851,#199852,#199853,#199854,#199855,#199856,#199857,
#199858,#199859,#199860,#199861,#199862,#199863,#199864,#199865,#199866,
#199867,#199868,#199869,#199870,#199871,#199872,#199873,#199874,#199875,
#199876,#199877,#199878,#199879,#199880,#199881,#199882,#199883,#199884,
#199885,#199886,#199887,#199888,#199889,#199890,#199891,#199892,#199893,
#199894,#199895,#199896,#199897,#199898,#199899,#199900,#199901,#199902,
#199903,#199904,#199905,#199906,#199907,#199908,#199909,#199910,#199911,
#199912,#199913,#199914,#199915,#199916,#199917,#199918,#199919,#199920,
#199921,#199922,#199923,#199924,#199925,#199926,#199927,#199928,#199929,
#199930,#199931,#199932,#199933,#199934,#199935,#199936,#199937,#199938,
#199939,#199940,#199941,#199942,#199943,#199944,#199945,#199946,#199947,
#199948,#199949,#199950,#199951,#199952,#199953,#199954,#199955,#199956,
#199957,#199958,#199959,#199960,#199961,#199962,#199963,#199964,#199965,
#199966,#199967,#199968,#199969,#199970,#199971,#199972,#199973,#199974,
#199975,#199976,#199977,#199978,#199979,#199980,#199981,#199982,#199983,
#199984,#199985,#199986,#199987,#199988,#199989,#199990,#199991,#199992,
#199993,#199994,#199995,#199996,#199997,#199998,#199999,#200000,#200001,
#200002,#200003,#200004,#200005,#200006,#200007,#200008,#200009,#200010,
#200011,#200012,#200013,#200014,#200015,#200016,#200017,#200018,#200019,
#200020,#200021,#200022,#200023,#200024,#200025,#200026,#200027,#200028,
#200029,#200030,#200031,#200032,#200033,#200034,#200035,#200036,#200037,
#200038,#200039,#200040,#200041,#200042,#200043,#200044,#200045,#200046,
#200047,#200048,#200049,#200050,#200051,#200052,#200053,#200054,#200055,
#200056,#200057,#200058,#200059,#200060,#200061,#200062,#200063,#200064,
#200065,#200066,#200067,#200068,#200069,#200070,#200071,#200072,#200073,
#200074,#200075,#200076,#200077,#200078,#200079,#200080,#200081,#200082,
#200083,#200084,#200085,#200086,#200087,#200088,#200089,#200090,#200091,
#200092,#200093,#200094,#200095,#200096,#200097,#200098,#200099,#200100,
#200101,#200102,#200103,#200104,#200105,#200106,#200107,#200108,#200109,
#200110,#200111,#200112,#200113,#200114,#200115,#200116,#200117,#200118,
#200119,#200120,#200121,#200122,#200123,#200124,#200125,#200126,#200127,
#200128,#200129,#200130,#200131,#200132,#200133,#200134,#200135,#200136,
#200137,#200138,#200139,#200140,#200141,#200142,#200143,#200144,#200145,
#200146,#200147,#200148,#200149,#200150,#200151,#200152,#200153,#200154,
#200155,#200156,#200157,#200158,#200159,#200160,#200161,#200162,#200163,
#200164,#200165,#200166,#200167,#200168,#200169,#200170,#200171,#200172,
#200173,#200174,#200175,#200176,#200177,#200178,#200179,#200180,#200181,
#200182,#200183,#200184,#200185,#200186,#200187,#200188,#200189,#200190,
#200191,#200192,#200193,#200194,#200195,#200196,#200197,#200198,#200199,
#200200,#200201,#200202,#200203,#200204,#200205,#200206,#200207,#200208,
#200209,#200210,#200211,#200212,#200213,#200214,#200215,#200216,#200217,
#200218,#200219,#200220,#200221,#200222,#200223,#200224,#200225,#200226,
#200227,#200228,#200229,#200230,#200231,#200232,#200233,#200234,#200235,
#200236,#200237,#200238,#200239,#200240,#200241,#200242,#200243,#200244,
#200245,#200246,#200247,#200248,#200249,#200250,#200251,#200252,#200253,
#200254,#200255,#200256,#200257,#200258,#200259,#200260,#200261,#200262,
#200263,#200264,#200265,#200266,#200267,#200268,#200269,#200270,#200271,
#200272,#200273,#200274,#200275,#200276,#200277,#200278,#200279,#200280,
#200281,#200282,#200283,#200284,#200285,#200286,#200287,#200288,#200289,
#200290,#200291,#200292,#200293,#200294,#200295,#200296,#200297,#200298,
#200299,#200300,#200301,#200302,#200303,#200304,#200305,#200306,#200307,
#200308,#200309,#200310,#200311,#200312,#200313,#200314,#200315,#200316,
#200317,#200318,#200319,#200320,#200321,#200322,#200323,#200324,#200325,
#200326,#200327,#200328,#200329,#200330,#200331,#200332,#200333,#200334,
#200335,#200336,#200337,#200338,#200339,#200340,#200341,#200342,#200343,
#200344,#200345,#200346,#200347,#200348,#200349,#200350,#200351,#200352,
#200353,#200354,#200355,#200356,#200357,#200358,#200359,#200360,#200361,
#200362,#200363,#200364,#200365,#200366,#200367,#200368,#200369,#200370,
#200371,#200372,#200373,#200374,#200375,#200376,#200377,#200378,#200379,
#200380,#200381,#200382,#200383,#200384,#200385,#200386,#200387,#200388,
#200389,#200390,#200391,#200392,#200393,#200394,#200395,#200396,#200397,
#200398,#200399,#200400,#200401,#200402,#200403,#200404,#200405,#200406,
#200407,#200408,#200409,#200410,#200411,#200412,#200413,#200414,#200415,
#200416,#200417,#200418,#200419,#200420,#200421,#200422,#200423,#200424,
#200425,#200426,#200427,#200428,#200429,#200430,#200431,#200432,#200433,
#200434,#200435,#200436,#200437,#200438,#200439,#200440,#200441,#200442,
#200443,#200444,#200445,#200446,#200447,#200448,#200449,#200450,#200451,
#200452,#200453,#200454,#200455,#200456,#200457,#200458,#200459,#200460,
#200461,#200462,#200463,#200464,#200465,#200466,#200467,#200468,#200469,
#200470,#200471,#200472,#200473,#200474,#200475,#200476,#200477,#200478,
#200479,#200480,#200481,#200482,#200483,#200484,#200485,#200486,#200487,
#200488,#200489,#200490,#200491,#200492,#200493,#200494,#200495,#200496,
#200497,#200498,#200499,#200500,#200501,#200502,#200503,#200504,#200505,
#200506,#200507,#200508,#200509,#200510,#200511,#200512,#200513,#200514,
#200515,#200516,#200517,#200518,#200519,#200520,#200521,#200522,#200523,
#200524,#200525,#200526,#200527,#200528,#200529,#200530,#200531,#200532,
#200533,#200534,#200535,#200536,#200537,#200538,#200539,#200540,#200541,
#200542,#200543,#200544,#200545,#200546,#200547,#200548,#200549,#200550,
#200551,#200552,#200553,#200554,#200555,#200556,#200557,#200558,#200559,
#200560,#200561,#200562,#200563,#200564,#200565,#200566,#200567,#200568,
#200569,#200570,#200571,#200572,#200573,#200574,#200575,#200576,#200577,
#200578,#200579,#200580,#200581,#200582,#200583,#200584,#200585,#200586,
#200587,#200588,#200589,#200590,#200591,#200592,#200593,#200594,#200595,
#200596,#200597,#200598,#200599,#200600,#200601,#200602,#200603,#200604,
#200605,#200606,#200607,#200608,#200609,#200610,#200611,#200612,#200613,
#200614,#200615,#200616,#200617,#200618),(#200619,#200620,#200621,#200622,
#200623,#200624,#200625,#200626,#200627,#200628,#200629,#200630,#200631,
#200632,#200633,#200634,#200635,#200636,#200637,#200638,#200639,#200640,
#200641,#200642,#200643,#200644,#200645,#200646,#200647,#200648,#200649,
#200650,#200651,#200652,#200653,#200654,#200655,#200656,#200657,#200658,
#200659,#200660,#200661,#200662,#200663,#200664,#200665,#200666,#200667,
#200668,#200669,#200670,#200671,#200672,#200673,#200674,#200675,#200676,
#200677,#200678,#200679,#200680,#200681,#200682,#200683,#200684,#200685,
#200686,#200687,#200688,#200689,#200690,#200691,#200692,#200693,#200694,
#200695,#200696,#200697,#200698,#200699,#200700,#200701,#200702,#200703,
#200704,#200705,#200706,#200707,#200708,#200709,#200710,#200711,#200712,
#200713,#200714,#200715,#200716,#200717,#200718,#200719,#200720,#200721,
#200722,#200723,#200724,#200725,#200726,#200727,#200728,#200729,#200730,
#200731,#200732,#200733,#200734,#200735,#200736,#200737,#200738,#200739,
#200740,#200741,#200742,#200743,#200744,#200745,#200746,#200747,#200748,
#200749,#200750,#200751,#200752,#200753,#200754,#200755,#200756,#200757,
#200758,#200759,#200760,#200761,#200762,#200763,#200764,#200765,#200766,
#200767,#200768,#200769,#200770,#200771,#200772,#200773,#200774,#200775,
#200776,#200777,#200778,#200779,#200780,#200781,#200782,#200783,#200784,
#200785,#200786,#200787,#200788,#200789,#200790,#200791,#200792,#200793,
#200794,#200795,#200796,#200797,#200798,#200799,#200800,#200801,#200802,
#200803,#200804,#200805,#200806,#200807,#200808,#200809,#200810,#200811,
#200812,#200813,#200814,#200815,#200816,#200817,#200818,#200819,#200820,
#200821,#200822,#200823,#200824,#200825,#200826,#200827,#200828,#200829,
#200830,#200831,#200832,#200833,#200834,#200835,#200836,#200837,#200838,
#200839,#200840,#200841,#200842,#200843,#200844,#200845,#200846,#200847,
#200848,#200849,#200850,#200851,#200852,#200853,#200854,#200855,#200856,
#200857,#200858,#200859,#200860,#200861,#200862,#200863,#200864,#200865,
#200866,#200867,#200868,#200869,#200870,#200871,#200872,#200873,#200874,
#200875,#200876,#200877,#200878,#200879,#200880,#200881,#200882,#200883,
#200884,#200885,#200886,#200887,#200888,#200889,#200890,#200891,#200892,
#200893,#200894,#200895,#200896,#200897,#200898,#200899,#200900,#200901,
#200902,#200903,#200904,#200905,#200906,#200907,#200908,#200909,#200910,
#200911,#200912,#200913,#200914,#200915,#200916,#200917,#200918,#200919,
#200920,#200921,#200922,#200923,#200924,#200925,#200926,#200927,#200928,
#200929,#200930,#200931,#200932,#200933,#200934,#200935,#200936,#200937,
#200938,#200939,#200940,#200941,#200942,#200943,#200944,#200945,#200946,
#200947,#200948,#200949,#200950,#200951,#200952,#200953,#200954,#200955,
#200956,#200957,#200958,#200959,#200960,#200961,#200962,#200963,#200964,
#200965,#200966,#200967,#200968,#200969,#200970,#200971,#200972,#200973,
#200974,#200975,#200976,#200977,#200978,#200979,#200980,#200981,#200982,
#200983,#200984,#200985,#200986,#200987,#200988,#200989,#200990,#200991,
#200992,#200993,#200994,#200995,#200996,#200997,#200998,#200999,#201000,
#201001,#201002,#201003,#201004,#201005,#201006,#201007,#201008,#201009,
#201010,#201011,#201012,#201013,#201014,#201015,#201016,#201017,#201018,
#201019,#201020,#201021,#201022,#201023,#201024,#201025,#201026,#201027,
#201028,#201029,#201030,#201031,#201032,#201033,#201034,#201035,#201036,
#201037,#201038,#201039,#201040,#201041,#201042,#201043,#201044,#201045,
#201046,#201047,#201048,#201049,#201050,#201051,#201052,#201053,#201054,
#201055,#201056,#201057,#201058,#201059,#201060,#201061,#201062,#201063,
#201064,#201065,#201066,#201067,#201068,#201069,#201070,#201071,#201072,
#201073,#201074,#201075,#201076,#201077,#201078,#201079,#201080,#201081,
#201082,#201083,#201084,#201085,#201086,#201087,#201088,#201089,#201090,
#201091,#201092,#201093,#201094,#201095,#201096,#201097,#201098,#201099,
#201100,#201101,#201102,#201103,#201104,#201105,#201106,#201107,#201108,
#201109,#201110,#201111,#201112,#201113,#201114,#201115,#201116,#201117,
#201118,#201119,#201120,#201121,#201122,#201123,#201124,#201125,#201126,
#201127,#201128,#201129,#201130,#201131,#201132,#201133,#201134,#201135,
#201136,#201137,#201138,#201139,#201140,#201141,#201142,#201143,#201144,
#201145,#201146,#201147,#201148,#201149,#201150,#201151,#201152,#201153,
#201154,#201155,#201156,#201157,#201158,#201159,#201160,#201161,#201162,
#201163,#201164,#201165,#201166,#201167,#201168,#201169,#201170,#201171,
#201172,#201173,#201174,#201175,#201176,#201177,#201178,#201179,#201180,
#201181,#201182,#201183,#201184,#201185,#201186,#201187,#201188,#201189,
#201190,#201191,#201192,#201193,#201194,#201195,#201196,#201197,#201198,
#201199,#201200,#201201,#201202,#201203,#201204,#201205,#201206,#201207,
#201208,#201209,#201210,#201211,#201212,#201213,#201214,#201215,#201216,
#201217,#201218,#201219,#201220,#201221,#201222,#201223,#201224,#201225,
#201226,#201227,#201228,#201229,#201230,#201231,#201232,#201233,#201234,
#201235,#201236,#201237,#201238,#201239,#201240,#201241,#201242,#201243,
#201244,#201245,#201246,#201247,#201248,#201249,#201250,#201251,#201252,
#201253,#201254,#201255,#201256,#201257,#201258,#201259,#201260,#201261,
#201262,#201263,#201264,#201265,#201266,#201267,#201268,#201269,#201270,
#201271,#201272,#201273,#201274,#201275,#201276,#201277,#201278,#201279,
#201280,#201281,#201282,#201283,#201284,#201285,#201286,#201287,#201288,
#201289,#201290,#201291,#201292,#201293,#201294,#201295,#201296,#201297,
#201298,#201299,#201300,#201301,#201302,#201303,#201304,#201305,#201306,
#201307,#201308,#201309,#201310,#201311,#201312,#201313,#201314,#201315,
#201316,#201317,#201318,#201319,#201320,#201321,#201322,#201323,#201324,
#201325,#201326,#201327,#201328,#201329,#201330,#201331,#201332,#201333,
#201334,#201335,#201336,#201337,#201338,#201339,#201340,#201341,#201342,
#201343,#201344,#201345,#201346,#201347,#201348,#201349,#201350,#201351,
#201352,#201353,#201354,#201355,#201356,#201357,#201358,#201359,#201360,
#201361,#201362,#201363,#201364,#201365,#201366,#201367,#201368,#201369,
#201370,#201371,#201372,#201373,#201374,#201375,#201376,#201377,#201378,
#201379,#201380,#201381,#201382,#201383,#201384,#201385,#201386,#201387,
#201388,#201389,#201390,#201391,#201392,#201393,#201394,#201395,#201396,
#201397,#201398,#201399,#201400,#201401,#201402,#201403,#201404,#201405,
#201406,#201407,#201408,#201409,#201410,#201411,#201412,#201413,#201414,
#201415,#201416,#201417,#201418,#201419,#201420,#201421,#201422,#201423,
#201424,#201425,#201426,#201427,#201428,#201429,#201430,#201431,#201432,
#201433,#201434,#201435,#201436,#201437,#201438,#201439,#201440,#201441,
#201442,#201443,#201444,#201445,#201446,#201447,#201448,#201449,#201450,
#201451,#201452,#201453,#201454,#201455,#201456,#201457,#201458,#201459,
#201460,#201461,#201462,#201463,#201464,#201465,#201466,#201467,#201468,
#201469,#201470,#201471,#201472,#201473,#201474,#201475,#201476,#201477,
#201478,#201479,#201480,#201481,#201482,#201483,#201484,#201485,#201486,
#201487,#201488,#201489,#201490,#201491,#201492,#201493,#201494,#201495,
#201496,#201497,#201498,#201499,#201500,#201501,#201502,#201503,#201504,
#201505,#201506,#201507,#201508,#201509,#201510,#201511,#201512,#201513,
#201514,#201515,#201516,#201517,#201518,#201519,#201520,#201521,#201522,
#201523,#201524,#201525,#201526,#201527,#201528,#201529,#201530,#201531,
#201532,#201533,#201534,#201535,#201536,#201537,#201538,#201539,#201540,
#201541,#201542,#201543,#201544,#201545,#201546,#201547,#201548,#201549,
#201550,#201551,#201552,#201553,#201554,#201555,#201556,#201557,#201558,
#201559,#201560,#201561,#201562,#201563,#201564,#201565,#201566,#201567,
#201568,#201569,#201570,#201571,#201572,#201573,#201574,#201575,#201576,
#201577,#201578,#201579,#201580,#201581,#201582,#201583,#201584,#201585,
#201586,#201587,#201588,#201589,#201590,#201591,#201592,#201593,#201594,
#201595,#201596,#201597,#201598,#201599,#201600,#201601,#201602,#201603,
#201604,#201605,#201606,#201607,#201608,#201609,#201610,#201611,#201612,
#201613,#201614,#201615,#201616,#201617,#201618,#201619,#201620,#201621,
#201622,#201623,#201624,#201625,#201626,#201627,#201628,#201629,#201630,
#201631,#201632,#201633,#201634,#201635,#201636,#201637,#201638,#201639,
#201640,#201641,#201642,#201643,#201644,#201645,#201646,#201647,#201648,
#201649,#201650,#201651,#201652,#201653,#201654,#201655,#201656,#201657,
#201658,#201659,#201660,#201661,#201662,#201663,#201664,#201665,#201666,
#201667,#201668,#201669,#201670,#201671,#201672,#201673,#201674,#201675,
#201676,#201677,#201678,#201679,#201680,#201681,#201682,#201683,#201684,
#201685,#201686,#201687,#201688,#201689,#201690,#201691,#201692,#201693,
#201694,#201695,#201696,#201697,#201698,#201699,#201700,#201701,#201702,
#201703,#201704,#201705,#201706,#201707,#201708,#201709,#201710,#201711,
#201712,#201713,#201714,#201715,#201716,#201717,#201718,#201719,#201720,
#201721,#201722,#201723,#201724,#201725,#201726,#201727,#201728,#201729,
#201730,#201731,#201732,#201733,#201734,#201735,#201736,#201737,#201738,
#201739,#201740,#201741,#201742,#201743,#201744,#201745,#201746,#201747,
#201748,#201749,#201750,#201751,#201752,#201753,#201754,#201755,#201756,
#201757,#201758,#201759,#201760,#201761,#201762,#201763,#201764,#201765,
#201766,#201767,#201768,#201769,#201770,#201771,#201772,#201773,#201774,
#201775,#201776,#201777,#201778,#201779,#201780,#201781,#201782,#201783,
#201784,#201785,#201786,#201787,#201788,#201789,#201790,#201791,#201792,
#201793,#201794,#201795,#201796,#201797,#201798,#201799,#201800,#201801,
#201802,#201803,#201804,#201805,#201806,#201807,#201808,#201809,#201810,
#201811,#201812,#201813,#201814,#201815,#201816,#201817,#201818,#201819,
#201820,#201821,#201822,#201823,#201824,#201825,#201826,#201827,#201828,
#201829,#201830,#201831,#201832,#201833,#201834,#201835,#201836,#201837,
#201838,#201839,#201840,#201841,#201842,#201843,#201844,#201845,#201846,
#201847,#201848,#201849,#201850,#201851,#201852,#201853,#201854,#201855,
#201856,#201857,#201858,#201859,#201860,#201861,#201862,#201863,#201864,
#201865,#201866,#201867,#201868,#201869,#201870,#201871,#201872,#201873,
#201874,#201875,#201876,#201877,#201878,#201879,#201880,#201881,#201882,
#201883,#201884,#201885,#201886,#201887,#201888,#201889,#201890,#201891,
#201892,#201893,#201894,#201895,#201896,#201897,#201898,#201899,#201900,
#201901,#201902,#201903,#201904,#201905,#201906,#201907,#201908,#201909,
#201910,#201911,#201912,#201913,#201914,#201915,#201916,#201917,#201918,
#201919,#201920,#201921,#201922,#201923,#201924,#201925,#201926,#201927,
#201928,#201929,#201930,#201931,#201932,#201933,#201934,#201935,#201936,
#201937,#201938,#201939,#201940,#201941,#201942,#201943,#201944,#201945,
#201946,#201947,#201948,#201949,#201950,#201951,#201952,#201953,#201954,
#201955,#201956,#201957,#201958,#201959,#201960,#201961,#201962,#201963,
#201964,#201965,#201966,#201967,#201968,#201969,#201970,#201971,#201972,
#201973,#201974,#201975,#201976,#201977,#201978,#201979,#201980,#201981,
#201982,#201983,#201984,#201985,#201986,#201987,#201988,#201989,#201990,
#201991,#201992,#201993,#201994,#201995,#201996,#201997,#201998,#201999,
#202000,#202001,#202002,#202003,#202004,#202005,#202006,#202007,#202008,
#202009,#202010,#202011,#202012,#202013,#202014,#202015,#202016,#202017,
#202018,#202019,#202020,#202021,#202022,#202023,#202024,#202025,#202026,
#202027,#202028,#202029,#202030,#202031,#202032,#202033,#202034,#202035,
#202036,#202037,#202038,#202039,#202040,#202041,#202042,#202043,#202044,
#202045,#202046,#202047,#202048,#202049,#202050,#202051,#202052,#202053,
#202054,#202055,#202056,#202057,#202058,#202059,#202060,#202061,#202062,
#202063,#202064,#202065,#202066,#202067,#202068,#202069,#202070,#202071,
#202072,#202073,#202074,#202075,#202076,#202077,#202078,#202079,#202080,
#202081,#202082,#202083,#202084,#202085,#202086,#202087,#202088,#202089,
#202090,#202091,#202092,#202093,#202094,#202095,#202096,#202097,#202098,
#202099,#202100,#202101,#202102,#202103,#202104,#202105,#202106,#202107,
#202108,#202109,#202110,#202111,#202112,#202113,#202114,#202115,#202116,
#202117,#202118,#202119,#202120,#202121,#202122,#202123,#202124,#202125,
#202126,#202127,#202128,#202129,#202130,#202131,#202132,#202133,#202134,
#202135,#202136,#202137,#202138,#202139,#202140,#202141,#202142,#202143,
#202144,#202145,#202146,#202147,#202148,#202149,#202150,#202151,#202152,
#202153,#202154,#202155,#202156,#202157,#202158,#202159,#202160,#202161,
#202162,#202163,#202164,#202165,#202166,#202167,#202168,#202169,#202170,
#202171,#202172,#202173,#202174,#202175,#202176,#202177,#202178,#202179,
#202180,#202181,#202182,#202183,#202184,#202185,#202186,#202187,#202188,
#202189,#202190,#202191,#202192,#202193,#202194,#202195,#202196,#202197,
#202198,#202199,#202200,#202201,#202202,#202203,#202204,#202205,#202206,
#202207,#202208,#202209,#202210,#202211,#202212,#202213,#202214,#202215,
#202216,#202217,#202218,#202219,#202220,#202221,#202222,#202223,#202224,
#202225,#202226,#202227,#202228,#202229,#202230,#202231,#202232,#202233,
#202234,#202235,#202236,#202237,#202238,#202239,#202240,#202241,#202242,
#202243,#202244,#202245,#202246,#202247,#202248,#202249,#202250,#202251,
#202252,#202253,#202254,#202255,#202256,#202257,#202258,#202259,#202260,
#202261,#202262,#202263,#202264,#202265,#202266,#202267,#202268,#202269,
#202270,#202271,#202272,#202273,#202274,#202275,#202276,#202277,#202278,
#202279,#202280,#202281,#202282,#202283,#202284,#202285,#202286,#202287,
#202288,#202289,#202290,#202291,#202292,#202293,#202294,#202295,#202296,
#202297,#202298,#202299,#202300,#202301,#202302,#202303,#202304,#202305,
#202306,#202307,#202308,#202309,#202310,#202311,#202312,#202313)),
 .UNSPECIFIED.,.F.,.F.,.F.,(4,4),(4,1,1,1,1,1,1,1,1,1,1,1,1,1,1,1,1,1,1,
1,1,1,1,1,1,1,1,1,1,1,1,1,1,1,1,1,1,1,1,1,1,1,1,1,1,1,1,1,1,1,1,1,1,1,1,
1,1,1,1,1,1,1,1,1,1,1,1,1,1,1,1,1,1,1,1,1,1,1,1,1,1,1,1,1,1,1,1,1,1,1,1,
1,1,1,1,1,1,1,1,1,1,1,1,1,1,1,1,1,1,1,1,1,1,1,1,1,1,1,1,1,1,1,1,1,1,1,1,
1,1,1,1,1,1,1,1,1,1,1,1,1,1,1,1,1,1,1,1,1,1,1,1,1,1,1,1,1,1,1,1,1,1,1,1,
1,1,1,1,1,1,1,1,1,1,1,1,1,1,1,1,1,1,1,1,1,1,1,1,1,1,1,1,1,1,1,1,1,1,1,1,
1,1,1,1,1,1,1,1,1,1,1,1,1,1,1,1,1,1,1,1,1,1,1,1,1,1,1,1,1,1,1,1,1,1,1,1,
1,1,1,1,1,1,1,1,1,1,1,1,1,1,1,1,1,1,1,1,1,1,1,1,1,1,1,1,1,1,1,1,1,1,1,1,
1,1,1,1,1,1,1,1,1,1,1,1,1,1,1,1,1,1,1,1,1,1,1,1,1,1,1,1,1,1,1,1,1,1,1,1,
1,1,1,1,1,1,1,1,1,1,1,1,1,1,1,1,1,1,1,1,1,1,1,1,1,1,1,1,1,1,1,1,1,1,1,1,
1,1,1,1,1,1,1,1,1,1,1,1,1,1,1,1,1,1,1,1,1,1,1,1,1,1,1,1,1,1,1,1,1,1,1,1,
1,1,1,1,1,1,1,1,1,1,1,1,1,1,1,1,1,1,1,1,1,1,1,1,1,1,1,1,1,1,1,1,1,1,1,1,
1,1,1,1,1,1,1,1,1,1,1,1,1,1,1,1,1,1,1,1,1,1,1,1,1,1,1,1,1,1,1,1,1,1,1,1,
1,1,1,1,1,1,1,1,1,1,1,1,1,1,1,1,1,1,1,1,1,1,1,1,1,1,1,1,1,1,1,1,1,1,1,1,
1,1,1,1,1,1,1,1,1,1,1,1,1,1,1,1,1,1,1,1,1,1,1,1,1,1,1,1,1,1,1,1,1,1,1,1,
1,1,1,1,1,1,1,1,1,1,1,1,1,1,1,1,1,1,1,1,1,1,1,1,1,1,1,1,1,1,1,1,1,1,1,1,
1,1,1,1,1,1,1,1,1,1,1,1,1,1,1,1,1,1,1,1,1,1,1,1,1,1,1,1,1,1,1,1,1,1,1,1,
1,1,1,1,1,1,1,1,1,1,1,1,1,1,1,1,1,1,1,1,1,1,1,1,1,1,1,1,1,1,1,1,1,1,1,1,
1,1,1,1,1,1,1,1,1,1,1,1,1,1,1,1,1,1,1,1,1,1,1,1,1,1,1,1,1,1,1,1,1,1,1,1,
1,1,1,1,1,1,1,1,1,1,1,1,1,1,1,1,1,1,1,1,1,1,1,1,1,1,1,1,1,1,1,1,1,1,1,1,
1,1,1,1,1,1,1,1,1,1,1,1,1,1,1,1,1,1,1,1,1,1,1,1,1,1,1,1,1,1,1,1,1,1,1,1,
1,1,1,1,1,1,1,1,1,1,1,1,1,1,1,1,1,1,1,1,1,1,1,1,1,1,1,1,1,1,1,1,1,1,1,1,
1,1,1,1,1,1,1,1,1,1,1,1,1,1,1,1,1,1,1,1,1,1,1,1,1,1,1,1,1,1,1,1,1,1,1,1,
1,1,1,1,1,1,1,1,1,1,1,1,1,1,1,1,1,1,1,1,1,1,1,1,1,1,1,1,1,1,1,1,1,1,1,1,
1,1,1,1,1,1,1,1,1,1,1,1,1,1,1,1,1,1,1,1,1,1,1,1,1,1,1,1,1,1,1,1,1,1,1,1,
1,1,1,1,1,1,1,1,1,1,1,1,1,1,1,1,1,1,1,1,1,1,1,1,1,1,1,1,1,1,1,1,1,1,1,1,
1,1,1,1,1,1,1,1,1,1,1,1,1,1,1,1,1,1,1,1,1,1,1,1,1,1,1,1,1,1,1,1,1,1,1,1,
1,1,1,1,1,1,1,1,1,1,1,1,1,1,1,1,1,1,1,1,1,1,1,1,1,1,1,1,1,1,1,1,1,1,1,1,
1,1,1,1,1,1,1,1,1,1,1,1,1,1,1,1,1,1,1,1,1,1,1,1,1,1,1,1,1,1,1,1,1,1,1,1,
1,1,1,1,1,1,1,1,1,1,1,1,1,1,1,1,1,1,1,1,1,1,1,1,1,1,1,1,1,1,1,1,1,1,1,1,
1,1,1,1,1,1,1,1,1,1,1,1,1,1,1,1,1,1,1,1,1,1,1,1,1,1,1,1,1,1,1,1,1,1,1,1,
1,1,1,1,1,1,1,1,1,1,1,1,1,1,1,1,1,1,1,1,1,1,1,1,1,1,1,1,1,1,1,1,1,1,1,1,
1,1,1,1,1,1,1,1,1,1,1,1,1,1,1,1,1,1,1,1,1,1,1,1,1,1,1,1,1,1,1,1,1,1,1,1,
1,1,1,1,1,1,1,1,1,1,1,1,1,1,1,1,1,1,1,1,1,1,1,1,1,1,1,1,1,1,1,1,1,1,1,1,
1,1,1,1,1,1,1,1,1,1,1,1,1,1,1,1,1,1,1,1,1,1,1,1,1,1,1,1,1,1,1,1,1,1,1,1,
1,1,1,1,1,1,1,1,1,1,1,1,1,1,1,1,1,1,1,1,1,1,1,1,1,1,1,1,1,1,1,1,1,1,1,1,
1,1,1,1,1,1,1,1,1,1,1,1,1,1,1,1,1,1,1,1,1,1,1,1,1,1,1,1,1,1,1,1,1,1,1,1,
1,1,1,1,1,1,1,1,1,1,1,1,1,1,1,1,1,1,1,1,1,1,1,1,1,1,1,1,1,1,1,1,1,1,1,1,
1,1,1,1,1,1,1,1,1,1,1,1,1,1,1,1,1,1,1,1,1,1,1,1,1,1,1,1,1,1,1,1,1,1,1,1,
1,1,1,1,1,1,1,1,1,1,1,1,1,1,1,1,1,1,1,1,1,1,1,1,1,1,1,1,1,1,1,1,1,1,1,1,
1,1,1,1,1,1,1,1,1,1,1,1,1,1,1,1,1,1,1,1,1,1,1,1,1,1,1,1,1,1,1,1,1,1,1,1,
1,1,1,1,1,1,1,1,1,1,1,1,1,1,1,1,1,1,1,1,1,1,1,1,1,1,1,1,1,1,1,1,1,1,1,1,
1,1,1,1,1,1,1,1,1,1,1,1,1,1,1,1,1,1,1,1,1,1,1,1,1,1,1,1,1,1,1,1,1,1,1,1,
1,1,1,1,1,1,1,1,1,1,1,1,1,1,1,1,1,1,1,1,1,1,1,1,1,1,1,1,1,1,1,1,1,1,1,1,
1,1,1,1,1,1,1,1,1,1,1,1,1,1,1,1,1,1,1,1,1,1,1,1,1,1,1,1,1,1,1,1,1,1,1,1,
1,1,1,1,1,1,1,1,1,1,1,1,1,1,1,1,1,1,1,1,1,1,1,1,1,1,1,1,1,1,1,1,1,1,1,1,
1,1,1,1,1,1,1,1,1,1,1,1,1,1,1,1,1,1,1,1,1,1,1,1,1,1,1,1,1,1,1,1,1,1,1,1,
1,1,1,1,1,1,1,1,1,1,1,1,1,1,1,1,1,4),(-0.000423095957202541,0.115881565465356),
(11.6153146011728,12.1152895244478,12.6151575298078,13.614893540528,14.6146295512481,
15.6143655619682,16.6141015726884,17.6138375834085,18.6135735941286,19.6133096048488,
20.6130456155689,21.612781626289,22.6125176370092,23.6122536477293,24.6119896584494,
25.6117256691696,26.6114616798897,27.6111976906098,28.6109337013299,29.6106697120501,
30.6104057227702,31.6101417334903,32.6098777442105,33.6096137549306,34.6093497656507,
35.6090857763709,36.608821787091,37.6085577978111,38.6082938085313,39.6080298192514,
40.6077658299715,41.6075018406916,42.6072378514118,43.6069738621319,44.606709872852,
45.6064458835722,46.6061818942923,47.6059179050124,48.6056539157326,49.6053899264527,
50.6051259371728,51.604861947893,52.6045979586131,53.6043339693332,54.6040699800534,
55.6038059907735,56.6035420014936,57.6032780122137,58.6030140229339,59.602750033654,
60.6024860443741,61.6022220550943,62.6019580658144,63.6016940765345,64.6014300872547,
65.6011660979748,66.6009021086949,67.6006381194151,68.6003741301352,69.6001101408553,
70.5998461515754,71.5995821622956,72.5993181730157,73.5990541837358,74.598790194456,
75.5985262051761,76.5982622158962,77.5979982266164,78.5977342373365,79.5974702480566,
80.5972062587768,81.5969422694969,82.596678280217,83.5964142909372,84.5961503016573,
85.5958863123774,86.5956223230975,87.5953583338177,88.5950943445378,89.5948303552579,
90.5945663659781,91.5943023766982,92.5940383874183,93.5937743981385,94.5935104088586,
95.5932464195787,96.5929824302989,97.592718441019,98.5924544517391,99.5921904624593,
100.591926473179,101.5916624839,102.59139849462,103.59113450534,104.59087051606,
105.59060652678,106.5903425375,107.59007854822,108.58981455894,109.589550569661,
110.589286580381,111.589022591101,112.588758601821,113.588494612541,114.588230623261,
115.587966633981,116.587702644701,117.587438655422,118.587174666142,119.586910676862,
120.586646687582,121.586382698302,122.586118709022,123.585854719742,124.585590730463,
125.585326741183,126.585062751903,127.584798762623,128.584534773343,129.584270784063,
130.584006794783,131.583742805503,132.583478816224,133.583214826944,134.582950837664,
135.582686848384,136.582422859104,137.582158869824,138.581894880544,139.581630891264,
140.581366901985,141.581102912705,142.580838923425,143.580574934145,144.580310944865,
145.580046955585,146.579782966305,147.579518977026,148.579254987746,149.578990998466,
150.578727009186,151.578463019906,152.578199030626,153.577935041346,154.577671052066,
155.577407062787,156.577143073507,157.576879084227,158.576615094947,159.576351105667,
160.576087116387,161.575823127107,162.575559137827,163.575295148548,164.575031159268,
165.574767169988,166.574503180708,167.574239191428,168.573975202148,169.573711212868,
170.573447223589,171.573183234309,172.572919245029,173.572655255749,174.572391266469,
175.572127277189,176.571863287909,177.571599298629,178.57133530935,179.57107132007,
180.57080733079,181.57054334151,182.57027935223,183.57001536295,184.56975137367,
185.56948738439,186.569223395111,187.568959405831,188.568695416551,189.568431427271,
190.568167437991,191.567903448711,192.567639459431,193.567375470152,194.567111480872,
195.566847491592,196.566583502312,197.566319513032,198.566055523752,199.565791534472,
200.565527545192,201.565263555913,202.564999566633,203.564735577353,204.564471588073,
205.564207598793,206.563943609513,207.563679620233,208.563415630954,209.563151641674,
210.562887652394,211.562623663114,212.562359673834,213.562095684554,214.561831695274,
215.561567705994,216.561303716715,217.561039727435,218.560775738155,219.560511748875,
220.560247759595,221.559983770315,222.559719781035,223.559455791755,224.559191802476,
225.558927813196,226.558663823916,227.558399834636,228.558135845356,229.557871856076,
230.557607866796,231.557343877517,232.557079888237,233.556815898957,234.556551909677,
235.556287920397,236.556023931117,237.555759941837,238.555495952557,239.555231963278,
240.554967973998,241.554703984718,242.554439995438,243.554176006158,244.553912016878,
245.553648027598,246.553384038319,247.553120049039,248.552856059759,249.552592070479,
250.552328081199,251.552064091919,252.551800102639,253.551536113359,254.55127212408,
255.5510081348,256.55074414552,257.55048015624,258.55021616696,259.54995217768,
260.5496881884,261.54942419912,262.549160209841,263.548896220561,264.548632231281,
265.548368242001,266.548104252721,267.547840263441,268.547576274161,269.547312284882,
270.547048295602,271.546784306322,272.546520317042,273.546256327762,274.545992338482,
275.545728349202,276.545464359922,277.545200370643,278.544936381363,279.544672392083,
280.544408402803,281.544144413523,282.543880424243,283.543616434963,284.543352445683,
285.543088456404,286.542824467124,287.542560477844,288.542296488564,289.542032499284,
290.541768510004,291.541504520724,292.541240531445,293.540976542165,294.540712552885,
295.540448563605,296.540184574325,297.539920585045,298.539656595765,299.539392606485,
300.539128617206,301.538864627926,302.538600638646,303.538336649366,304.538072660086,
305.537808670806,306.537544681526,307.537280692246,308.537016702967,309.536752713687,
310.536488724407,311.536224735127,312.535960745847,313.535696756567,314.535432767287,
315.535168778008,316.534904788728,317.534640799448,318.534376810168,319.534112820888,
320.533848831608,321.533584842328,322.533320853048,323.533056863769,324.532792874489,
325.532528885209,326.532264895929,327.532000906649,328.531736917369,329.531472928089,
330.53120893881,331.53094494953,332.53068096025,333.53041697097,334.53015298169,
335.52988899241,336.52962500313,337.52936101385,338.529097024571,339.528833035291,
340.528569046011,341.528305056731,342.528041067451,343.527777078171,344.527513088891,
345.527249099611,346.526985110332,347.526721121052,348.526457131772,349.526193142492,
350.525929153212,351.525665163932,352.525401174652,353.525137185373,354.524873196093,
355.524609206813,356.524345217533,357.524081228253,358.523817238973,359.523553249693,
360.523289260413,361.523025271134,362.522761281854,363.522497292574,364.522233303294,
365.521969314014,366.521705324734,367.521441335454,368.521177346175,369.520913356895,
370.520649367615,371.520385378335,372.520121389055,373.519857399775,374.519593410495,
375.519329421215,376.519065431936,377.518801442656,378.518537453376,379.518273464096,
380.518009474816,381.517745485536,382.517481496256,383.517217506976,384.516953517697,
385.516689528417,386.516425539137,387.516161549857,388.515897560577,389.515633571297,
390.515369582017,391.515105592737,392.514841603458,393.514577614178,394.514313624898,
395.514049635618,396.513785646338,397.513521657058,398.513257667778,399.512993678499,
400.512729689219,401.512465699939,402.512201710659,403.511937721379,404.511673732099,
405.511409742819,406.511145753539,407.51088176426,408.51061777498,409.5103537857,
410.51008979642,411.50982580714,412.50956181786,413.50929782858,414.509033839301,
415.508769850021,416.508505860741,417.508241871461,418.507977882181,419.507713892901,
420.507449903621,421.507185914341,422.506921925062,423.506657935782,424.506393946502,
425.506129957222,426.505865967942,427.505601978662,428.505337989382,429.505074000102,
430.504810010823,431.504546021543,432.504282032263,433.504018042983,434.503754053703,
435.503490064423,436.503226075143,437.502962085864,438.502698096584,439.502434107304,
440.502170118024,441.501906128744,442.501642139464,443.501378150184,444.501114160904,
445.500850171625,446.500586182345,447.500322193065,448.500058203785,449.499794214505,
450.499530225225,451.499266235945,452.499002246665,453.498738257386,454.498474268106,
455.498210278826,456.497946289546,457.497682300266,458.497418310986,459.497154321706,
460.496890332427,461.496626343147,462.496362353867,463.496098364587,464.495834375307,
465.495570386027,466.495306396747,467.495042407467,468.494778418188,469.494514428908,
470.494250439628,471.493986450348,472.493722461068,473.493458471788,474.493194482508,
475.492930493229,476.492666503949,477.492402514669,478.492138525389,479.491874536109,
480.491610546829,481.491346557549,482.491082568269,483.49081857899,484.49055458971,
485.49029060043,486.49002661115,487.48976262187,488.48949863259,489.48923464331,
490.48897065403,491.488706664751,492.488442675471,493.488178686191,494.487914696911,
495.487650707631,496.487386718351,497.487122729071,498.486858739792,499.486594750512,
500.486330761232,501.486066771952,502.485802782672,503.485538793392,504.485274804112,
505.485010814832,506.484746825553,507.484482836273,508.484218846993,509.483954857713,
510.483690868433,511.483426879153,512.483162889873,513.482898900594,514.482634911314,
515.482370922034,516.482106932754,517.481842943474,518.481578954194,519.481314964914,
520.481050975635,521.480786986355,522.480522997075,523.480259007795,524.479995018515,
525.479731029235,526.479467039955,527.479203050675,528.478939061396,529.478675072116,
530.478411082836,531.478147093556,532.477883104276,533.477619114996,534.477355125716,
535.477091136436,536.476827147157,537.476563157877,538.476299168597,539.476035179317,
540.475771190037,541.475507200757,542.475243211477,543.474979222197,544.474715232918,
545.474451243638,546.474187254358,547.473923265078,548.473659275798,549.473395286518,
550.473131297238,551.472867307958,552.472603318679,553.472339329399,554.472075340119,
555.471811350839,556.471547361559,557.471283372279,558.471019382999,559.47075539372,
560.47049140444,561.47022741516,562.46996342588,563.4696994366,564.46943544732,
565.46917145804,566.46890746876,567.468643479481,568.468379490201,569.468115500921,
570.467851511641,571.467587522361,572.467323533081,573.467059543801,574.466795554521,
575.466531565242,576.466267575962,577.466003586682,578.465739597402,579.465475608122,
580.465211618842,581.464947629562,582.464683640283,583.464419651003,584.464155661723,
585.463891672443,586.463627683163,587.463363693883,588.463099704603,589.462835715323,
590.462571726044,591.462307736764,592.462043747484,593.461779758204,594.461515768924,
595.461251779644,596.460987790364,597.460723801085,598.460459811805,599.460195822525,
600.459931833245,601.459667843965,602.459403854685,603.459139865405,604.458875876125,
605.458611886846,606.458347897566,607.458083908286,608.457819919006,609.457555929726,
610.457291940446,611.457027951166,612.456763961887,613.456499972607,614.456235983327,
615.455971994047,616.455708004767,617.455444015487,618.455180026207,619.454916036927,
620.454652047648,621.454388058368,622.454124069088,623.453860079808,624.453596090528,
625.453332101248,626.453068111968,627.452804122688,628.452540133409,629.452276144129,
630.452012154849,631.451748165569,632.451484176289,633.451220187009,634.450956197729,
635.450692208449,636.45042821917,637.45016422989,638.44990024061,639.44963625133,
640.44937226205,641.44910827277,642.44884428349,643.448580294211,644.448316304931,
645.448052315651,646.447788326371,647.447524337091,648.447260347811,649.446996358531,
650.446732369251,651.446468379972,652.446204390692,653.445940401412,654.445676412132,
655.445412422852,656.445148433572,657.444884444292,658.444620455012,659.444356465733,
660.444092476453,661.443828487173,662.443564497893,663.443300508613,664.443036519333,
665.442772530053,666.442508540774,667.442244551494,668.441980562214,669.441716572934,
670.441452583654,671.441188594374,672.440924605094,673.440660615815,674.440396626535,
675.440132637255,676.439868647975,677.439604658695,678.439340669415,679.439076680135,
680.438812690855,681.438548701576,682.438284712296,683.438020723016,684.437756733736,
685.437492744456,686.437228755176,687.436964765896,688.436700776616,689.436436787337,
690.436172798057,691.435908808777,692.435644819497,693.435380830217,694.435116840937,
695.434852851657,696.434588862377,697.434324873098,698.434060883818,699.433796894538,
700.433532905258,701.433268915978,702.433004926698,703.432740937418,704.432476948139,
705.432212958859,706.431948969579,707.431684980299,708.431420991019,709.431157001739,
710.430893012459,711.430629023179,712.4303650339,713.43010104462,714.42983705534,
715.42957306606,716.42930907678,717.4290450875,718.42878109822,719.42851710894,
720.428253119661,721.427989130381,722.427725141101,723.427461151821,724.427197162541,
725.426933173261,726.426669183981,727.426405194702,728.426141205422,729.425877216142,
730.425613226862,731.425349237582,732.425085248302,733.424821259022,734.424557269742,
735.424293280463,736.424029291183,737.423765301903,738.423501312623,739.423237323343,
740.422973334063,741.422709344783,742.422445355504,743.422181366224,744.421917376944,
745.421653387664,746.421389398384,747.421125409104,748.420861419824,749.420597430544,
750.420333441265,751.420069451985,752.419805462705,753.419541473425,754.419277484145,
755.419013494865,756.418749505585,757.418485516306,758.418221527026,759.417957537746,
760.417693548466,761.417429559186,762.417165569906,763.416901580626,764.416637591346,
765.416373602067,766.416109612787,767.415845623507,768.415581634227,769.415317644947,
770.415053655667,771.414789666387,772.414525677107,773.414261687828,774.413997698548,
775.413733709268,776.413469719988,777.413205730708,778.412941741428,779.412677752148,
780.412413762868,781.412149773589,782.411885784309,783.411621795029,784.411357805749,
785.411093816469,786.410829827189,787.410565837909,788.41030184863,789.41003785935,
790.40977387007,791.40950988079,792.40924589151,793.40898190223,794.40871791295,
795.40845392367,796.408189934391,797.407925945111,798.407661955831,799.407397966551,
800.407133977271,801.406869987991,802.406605998711,803.406342009432,804.406078020152,
805.405814030872,806.405550041592,807.405286052312,808.405022063032,809.404758073752,
810.404494084472,811.404230095193,812.403966105913,813.403702116633,814.403438127353,
815.403174138073,816.402910148793,817.402646159513,818.402382170234,819.402118180954,
820.401854191674,821.401590202394,822.401326213114,823.401062223834,824.400798234554,
825.400534245274,826.400270255995,827.400006266715,828.399742277435,829.399478288155,
830.399214298875,831.398950309595,832.398686320315,833.398422331035,834.398158341756,
835.397894352476,836.397630363196,837.397366373916,838.397102384636,839.396838395356,
840.396574406076,841.396310416796,842.396046427517,843.395782438237,844.395518448957,
845.395254459677,846.394990470397,847.394726481117,848.394462491837,849.394198502558,
850.393934513278,851.393670523998,852.393406534718,853.393142545438,854.392878556158,
855.392614566878,856.392350577598,857.392086588319,858.391822599039,859.391558609759,
860.391294620479,861.391030631199,862.390766641919,863.390502652639,864.390238663359,
865.38997467408,866.3897106848,867.38944669552,868.38918270624,869.38891871696,
870.38865472768,871.3883907384,872.388126749121,873.387862759841,874.387598770561,
875.387334781281,876.387070792001,877.386806802721,878.386542813441,879.386278824161,
880.386014834882,881.385750845602,882.385486856322,883.385222867042,884.384958877762,
885.384694888482,886.384430899202,887.384166909923,888.383902920643,889.383638931363,
890.383374942083,891.383110952803,892.382846963523,893.382582974243,894.382318984963,
895.382054995684,896.381791006404,897.381527017124,898.381263027844,899.380999038564,
900.380735049284,901.380471060004,902.380207070725,903.379943081445,904.379679092165,
905.379415102885,906.379151113605,907.378887124325,908.378623135045,909.378359145765,
910.378095156486,911.377831167206,912.377567177926,913.377303188646,914.377039199366,
915.376775210086,916.376511220806,917.376247231526,918.375983242247,919.375719252967,
920.375455263687,921.375191274407,922.374927285127,923.374663295847,924.374399306567,
925.374135317287,926.373871328008,927.373607338728,928.373343349448,929.373079360168,
930.372815370888,931.372551381608,932.372287392328,933.372023403049,934.371759413769,
935.371495424489,936.371231435209,937.370967445929,938.370703456649,939.370439467369,
940.370175478089,941.36991148881,942.36964749953,943.36938351025,944.36911952097,
945.36885553169,946.36859154241,947.36832755313,948.368063563851,949.367799574571,
950.367535585291,951.367271596011,952.367007606731,953.366743617451,954.366479628171,
955.366215638891,956.365951649612,957.365687660332,958.365423671052,959.365159681772,
960.364895692492,961.364631703212,962.364367713932,963.364103724653,964.363839735373,
965.363575746093,966.363311756813,967.363047767533,968.362783778253,969.362519788973,
970.362255799693,971.361991810414,972.361727821134,973.361463831854,974.361199842574,
975.360935853294,976.360671864014,977.360407874734,978.360143885454,979.359879896175,
980.359615906895,981.359351917615,982.359087928335,983.358823939055,984.358559949775,
985.358295960495,986.358031971215,987.357767981936,988.357503992656,989.357240003376,
990.356976014096,991.356712024816,992.356448035536,993.356184046256,994.355920056977,
995.355656067697,996.355392078417,997.355128089137,998.354864099857,999.354600110577,
1000.3543361213,1001.35407213202,1002.35380814274,1003.35354415346,1004.35328016418,
1005.3530161749,1006.35275218562,1007.35248819634,1008.35222420706,1009.35196021778,
1010.3516962285,1011.35143223922,1012.35116824994,1013.35090426066,1014.35064027138,
1015.3503762821,1016.35011229282,1017.34984830354,1018.34958431426,1019.34932032498,
1020.3490563357,1021.34879234642,1022.34852835714,1023.34826436786,1024.34800037858,
1025.3477363893,1026.34747240002,1027.34720841074,1028.34694442146,1029.34668043218,
1030.3464164429,1031.34615245362,1032.34588846434,1033.34562447506,1034.34536048578,
1035.3450964965,1036.34483250722,1037.34456851794,1038.34430452866,1039.34404053938,
1040.3437765501,1041.34351256082,1042.34324857154,1043.34298458226,1044.34272059298,
1045.3424566037,1046.34219261442,1047.34192862514,1048.34166463586,1049.34140064658,
1050.3411366573,1051.34087266802,1052.34060867874,1053.34034468946,1054.34008070018,
1055.3398167109,1056.33955272162,1057.33928873234,1058.33902474307,1059.33876075378,
1060.33849676451,1061.33823277523,1062.33796878595,1063.33770479667,1064.33744080739,
1065.33717681811,1066.33691282883,1067.33664883955,1068.33638485027,1069.33612086099,
1070.33585687171,1071.33559288243,1072.33532889315,1073.33506490387,1074.33480091459,
1075.33453692531,1076.33427293603,1077.33400894675,1078.33374495747,1079.33348096819,
1080.33321697891,1081.33295298963,1082.33268900035,1083.33242501107,1084.33216102179,
1085.33189703251,1086.33163304323,1087.33136905395,1088.33110506467,1089.33084107539,
1090.33057708611,1091.33031309683,1092.33004910755,1093.32978511827,1094.32952112899,
1095.32925713971,1096.32899315043,1097.32872916115,1098.32846517187,1099.32820118259,
1100.32793719331,1101.32767320403,1102.32740921475,1103.32714522547,1104.32688123619,
1105.32661724691,1106.32635325763,1107.32608926835,1108.32582527907,1109.32556128979,
1110.32529730051,1111.32503331123,1112.32476932195,1113.32450533267,1114.32424134339,
1115.32397735411,1116.32371336483,1117.32344937555,1118.32318538627,1119.32292139699,
1120.32265740771,1121.32239341843,1122.32212942915,1123.32186543987,1124.32160145059,
1125.32133746131,1126.32107347203,1127.32080948275,1128.32054549347,1129.32028150419,
1130.32001751491,1131.31975352563,1132.31948953635,1133.31922554707,1134.31896155779,
1135.31869756852,1136.31843357924,1137.31816958996,1138.31790560068,1139.3176416114,
1140.31737762212,1141.31711363284,1142.31684964356,1143.31658565428,1144.316321665,
1145.31605767572,1146.31579368644,1147.31552969716,1148.31526570788,1149.3150017186,
1150.31473772932,1151.31447374004,1152.31420975076,1153.31394576148,1154.3136817722,
1155.31341778292,1156.31315379364,1157.31288980436,1158.31262581508,1159.3123618258,
1160.31209783652,1161.31183384724,1162.31156985796,1163.31130586868,1164.3110418794,
1165.31077789012,1166.31051390084,1167.31024991156,1168.30998592228,1169.309721933,
1170.30945794372,1171.30919395444,1172.30892996516,1173.30866597588,1174.3084019866,
1175.30813799732,1176.30787400804,1177.30761001876,1178.30734602948,1179.3070820402,
1180.30681805092,1181.30655406164,1182.30629007236,1183.30602608308,1184.3057620938,
1185.30549810452,1186.30523411524,1187.30497012596,1188.30470613668,1189.3044421474,
1190.30417815812,1191.30391416884,1192.30365017956,1193.30338619028,1194.303122201,
1195.30285821172,1196.30259422244,1197.30233023316,1198.30206624388,1199.3018022546,
1200.30153826532,1201.30127427604,1202.30101028676,1203.30074629748,1204.3004823082,
1205.30021831892,1206.29995432964,1207.29969034036,1208.29942635108,1209.2991623618,
1210.29889837252,1211.29863438324,1212.29837039397,1213.29810640469,1214.29784241541,
1215.29757842613,1216.29731443685,1217.29705044757,1218.29678645829,1219.29652246901,
1220.29625847973,1221.29599449045,1222.29573050117,1223.29546651189,1224.29520252261,
1225.29493853333,1226.29467454405,1227.29441055477,1228.29414656549,1229.29388257621,
1230.29361858693,1231.29335459765,1232.29309060837,1233.29282661909,1234.29256262981,
1235.29229864053,1236.29203465125,1237.29177066197,1238.29150667269,1239.29124268341,
1240.29097869413,1241.29071470485,1242.29045071557,1243.29018672629,1244.28992273701,
1245.28965874773,1246.28939475845,1247.28913076917,1248.28886677989,1249.28860279061,
1250.28833880133,1251.28807481205,1252.28781082277,1253.28754683349,1254.28728284421,
1255.28701885493,1256.28675486565,1257.28649087637,1258.28622688709,1259.28596289781,
1260.28569890853,1261.28543491925,1262.28517092997,1263.28490694069,1264.28464295141,
1265.28437896213,1266.28411497285,1267.28385098357,1268.28358699429,1269.28332300501,
1270.28305901573,1271.28279502645,1272.28253103717,1273.28226704789,1274.28200305861,
1275.28173906933,1276.28147508005,1277.28121109077,1278.28094710149,1279.28068311221,
1280.28041912293,1281.28015513365,1282.27989114437,1283.27962715509,1284.27936316581,
1285.27909917653,1286.27883518725,1287.27857119797,1288.2783072087,1289.27804321942,
1290.27777923014,1291.27751524086,1292.27725125158,1293.2769872623,1294.27672327302,
1295.27645928374,1296.27619529446,1297.27593130518,1298.2756673159,1299.27540332662,
1300.27513933734,1301.27487534806,1302.27461135878,1303.2743473695,1304.27408338022,
1305.27381939094,1306.27355540166,1307.27329141238,1308.2730274231,1309.27276343382,
1310.27249944454,1311.27223545526,1312.27197146598,1313.2717074767,1314.27144348742,
1315.27117949814,1316.27091550886,1317.27065151958,1318.2703875303,1319.27012354102,
1320.26985955174,1321.26959556246,1322.26933157318,1323.2690675839,1324.26880359462,
1325.26853960534,1326.26827561606,1327.26801162678,1328.2677476375,1329.26748364822,
1330.26721965894,1331.26695566966,1332.26669168038,1333.2664276911,1334.26616370182,
1335.26589971254,1336.26563572326,1337.26537173398,1338.2651077447,1339.26484375542,
1340.26457976614,1341.26431577686,1342.26405178758,1343.2637877983,1344.26352380902,
1345.26325981974,1346.26299583046,1347.26273184118,1348.2624678519,1349.26220386262,
1350.26193987334,1351.26167588406,1352.26141189478,1353.2611479055,1354.26088391622,
1355.26061992694,1356.26035593766,1357.26009194838,1358.2598279591,1359.25956396982,
1360.25929998054,1361.25903599126,1362.25877200198,1363.2585080127,1364.25824402343,
1365.25798003415,1366.25771604487,1367.25745205559,1368.25718806631,1369.25692407703,
1370.25666008775,1371.25639609847,1372.25613210919,1373.25586811991,1374.25560413063,
1375.25534014135,1376.25507615207,1377.25481216279,1378.25454817351,1379.25428418423,
1380.25402019495,1381.25375620567,1382.25349221639,1383.25322822711,1384.25296423783,
1385.25270024855,1386.25243625927,1387.25217226999,1388.25190828071,1389.25164429143,
1390.25138030215,1391.25111631287,1392.25085232359,1393.25058833431,1394.25032434503,
1395.25006035575,1396.24979636647,1397.24953237719,1398.24926838791,1399.24900439863,
1400.24874040935,1401.24847642007,1402.24821243079,1403.24794844151,1404.24768445223,
1405.24742046295,1406.24715647367,1407.24689248439,1408.24662849511,1409.24636450583,
1410.24610051655,1411.24583652727,1412.24557253799,1413.24530854871,1414.24504455943,
1415.24478057015,1416.24451658087,1417.24425259159,1418.24398860231,1419.24372461303,
1420.24346062375,1421.24319663447,1422.24293264519,1423.24266865591,1424.24240466663,
1425.24214067735,1426.24187668807,1427.24161269879,1428.24134870951,1429.24108472023,
1430.24082073095,1431.24055674167,1432.24029275239,1433.24002876311,1434.23976477383,
1435.23950078455,1436.23923679527,1437.23897280599,1438.23870881671,1439.23844482743,
1440.23818083815,1441.23791684888,1442.2376528596,1443.23738887032,1444.23712488104,
1445.23686089176,1446.23659690248,1447.2363329132,1448.23606892392,1449.23580493464,
1450.23554094536,1451.23527695608,1452.2350129668,1453.23474897752,1454.23448498824,
1455.23422099896,1456.23395700968,1457.2336930204,1458.23342903112,1459.23316504184,
1460.23290105256,1461.23263706328,1462.232373074,1463.23210908472,1464.23184509544,
1465.23158110616,1466.23131711688,1467.2310531276,1468.23078913832,1469.23052514904,
1470.23026115976,1471.22999717048,1472.2297331812,1473.22946919192,1474.22920520264,
1475.22894121336,1476.22867722408,1477.2284132348,1478.22814924552,1479.22788525624,
1480.22762126696,1481.22735727768,1482.2270932884,1483.22682929912,1484.22656530984,
1485.22630132056,1486.22603733128,1487.225773342,1488.22550935272,1489.22524536344,
1490.22498137416,1491.22471738488,1492.2244533956,1493.22418940632,1494.22392541704,
1495.22366142776,1496.22339743848,1497.2231334492,1498.22286945992,1499.22260547064,
1500.22234148136,1501.22207749208,1502.2218135028,1503.22154951352,1504.22128552424,
1505.22102153496,1506.22075754568,1507.2204935564,1508.22022956712,1509.21996557784,
1510.21970158856,1511.21943759928,1512.21917361,1513.21890962072,1514.21864563144,
1515.21838164216,1516.21811765288,1517.21785366361,1518.21758967433,1519.21732568505,
1520.21706169577,1521.21679770649,1522.21653371721,1523.21626972793,1524.21600573865,
1525.21574174937,1526.21547776009,1527.21521377081,1528.21494978153,1529.21468579225,
1530.21442180297,1531.21415781369,1532.21389382441,1533.21362983513,1534.21336584585,
1535.21310185657,1536.21283786729,1537.21257387801,1538.21230988873,1539.21204589945,
1540.21178191017,1541.21151792089,1542.21125393161,1543.21098994233,1544.21072595305,
1545.21046196377,1546.21019797449,1547.20993398521,1548.20966999593,1549.20940600665,
1550.20914201737,1551.20887802809,1552.20861403881,1553.20835004953,1554.20808606025,
1555.20782207097,1556.20755808169,1557.20729409241,1558.20703010313,1559.20676611385,
1560.20650212457,1561.20623813529,1562.20597414601,1563.20571015673,1564.20544616745,
1565.20518217817,1566.20491818889,1567.20465419961,1568.20439021033,1569.20412622105,
1570.20386223177,1571.20359824249,1572.20333425321,1573.20307026393,1574.20280627465,
1575.20254228537,1576.20227829609,1577.20201430681,1578.20175031753,1579.20148632825,
1580.20122233897,1581.20095834969,1582.20069436041,1583.20043037113,1584.20016638185,
1585.19990239257,1586.19963840329,1587.19937441401,1588.19911042473,1589.19884643545,
1590.19858244617,1591.19831845689,1592.19805446761,1593.19779047834,1594.19752648906,
1595.19726249978,1596.1969985105,1597.19673452122,1598.19647053194,1599.19620654266,
1600.19594255338,1601.1956785641,1602.19541457482,1603.19515058554,1604.19488659626,
1605.19462260698,1606.1943586177,1607.19409462842,1608.19383063914,1609.19356664986,
1610.19330266058,1611.1930386713,1612.19277468202,1613.19251069274,1614.19224670346,
1615.19198271418,1616.1917187249,1617.19145473562,1618.19119074634,1619.19092675706,
1620.19066276778,1621.1903987785,1622.19013478922,1623.18987079994,1624.18960681066,
1625.18934282138,1626.1890788321,1627.18881484282,1628.18855085354,1629.18828686426,
1630.18802287498,1631.1877588857,1632.18749489642,1633.18723090714,1634.18696691786,
1635.18670292858,1636.1864389393,1637.18617495002,1638.18591096074,1639.18564697146,
1640.18538298218,1641.1851189929,1642.18485500362,1643.18459101434,1644.18432702506,
1645.18406303578,1646.1837990465,1647.18353505722,1648.18327106794,1649.18300707866,
1650.18274308938,1651.1824791001,1652.18221511082,1653.18195112154,1654.18168713226,
1655.18142314298,1656.1811591537,1657.18089516442,1658.18063117514,1659.18036718586,
1660.18010319658,1661.1798392073,1662.17957521802,1663.17931122874,1664.17904723946,
1665.17878325018,1666.1785192609,1667.17825527162,1668.17799128234,1669.17772729307,
1670.17746330379,1671.17719931451,1672.17693532523,1673.17667133595,1674.17640734667,
1675.17614335739,1676.17587936811,1677.17561537883,1678.17535138955,1679.17508740027,
1680.17482341099,1681.17455942171,1682.17429543243,1683.17403144315,1684.17376745387,
1685.17350346459,1686.17323947531,1687.17297548603,1688.17271149675,1689.17244750747,
1690.17218351819,1691.17191952891,1692.17165553963,1693.17139155035,1694.17112756107,
1695.17086357179,1696.17059958251,1697.17033559323,1698.17007160395,1699.16980761467,
1700.16954362539,1700.66941163075,1701.16959429301),.UNSPECIFIED.);
#49=B_SPLINE_SURFACE_WITH_KNOTS('',3,3,((#209501,#209502,#209503,#209504,
#209505,#209506,#209507,#209508,#209509,#209510,#209511,#209512,#209513,
#209514,#209515,#209516,#209517,#209518,#209519,#209520,#209521,#209522,
#209523,#209524,#209525,#209526,#209527,#209528,#209529,#209530,#209531,
#209532,#209533,#209534,#209535,#209536,#209537,#209538,#209539,#209540,
#209541,#209542,#209543,#209544,#209545,#209546,#209547,#209548,#209549,
#209550,#209551,#209552,#209553,#209554,#209555,#209556,#209557,#209558,
#209559,#209560,#209561,#209562,#209563,#209564,#209565,#209566,#209567,
#209568,#209569,#209570,#209571,#209572,#209573,#209574,#209575,#209576,
#209577,#209578,#209579,#209580,#209581,#209582,#209583,#209584,#209585,
#209586,#209587,#209588,#209589,#209590,#209591,#209592,#209593,#209594,
#209595,#209596,#209597,#209598,#209599,#209600,#209601,#209602,#209603,
#209604,#209605,#209606,#209607,#209608,#209609,#209610,#209611,#209612,
#209613,#209614,#209615,#209616,#209617,#209618,#209619,#209620,#209621,
#209622,#209623,#209624,#209625,#209626,#209627,#209628,#209629,#209630,
#209631,#209632,#209633,#209634,#209635,#209636,#209637,#209638,#209639,
#209640,#209641,#209642,#209643,#209644,#209645,#209646,#209647,#209648,
#209649,#209650,#209651,#209652,#209653,#209654,#209655,#209656,#209657,
#209658,#209659,#209660,#209661,#209662,#209663,#209664,#209665,#209666,
#209667,#209668,#209669,#209670,#209671,#209672,#209673,#209674,#209675,
#209676,#209677,#209678,#209679,#209680,#209681,#209682,#209683,#209684,
#209685,#209686,#209687,#209688,#209689,#209690,#209691,#209692,#209693,
#209694,#209695,#209696,#209697,#209698,#209699,#209700,#209701,#209702,
#209703,#209704,#209705,#209706,#209707,#209708,#209709,#209710,#209711,
#209712,#209713,#209714,#209715,#209716,#209717,#209718,#209719,#209720,
#209721,#209722,#209723,#209724,#209725,#209726,#209727,#209728,#209729,
#209730,#209731,#209732,#209733,#209734,#209735,#209736,#209737,#209738,
#209739,#209740,#209741,#209742,#209743,#209744,#209745,#209746,#209747,
#209748,#209749,#209750,#209751,#209752,#209753,#209754,#209755,#209756,
#209757,#209758,#209759,#209760,#209761,#209762,#209763,#209764,#209765,
#209766,#209767,#209768,#209769,#209770,#209771,#209772,#209773,#209774,
#209775,#209776,#209777,#209778,#209779,#209780,#209781,#209782,#209783,
#209784,#209785,#209786,#209787,#209788,#209789,#209790,#209791,#209792,
#209793,#209794,#209795,#209796,#209797,#209798,#209799,#209800,#209801,
#209802,#209803,#209804,#209805,#209806,#209807,#209808,#209809,#209810,
#209811,#209812,#209813,#209814,#209815,#209816,#209817,#209818,#209819,
#209820,#209821,#209822,#209823,#209824,#209825,#209826,#209827,#209828,
#209829,#209830,#209831,#209832,#209833,#209834,#209835,#209836,#209837,
#209838,#209839,#209840,#209841,#209842,#209843,#209844,#209845,#209846,
#209847,#209848,#209849,#209850,#209851,#209852,#209853,#209854,#209855,
#209856,#209857,#209858,#209859,#209860,#209861,#209862,#209863,#209864,
#209865,#209866,#209867,#209868,#209869,#209870,#209871,#209872,#209873,
#209874,#209875,#209876,#209877,#209878,#209879,#209880,#209881,#209882,
#209883,#209884,#209885,#209886,#209887,#209888,#209889,#209890,#209891,
#209892,#209893,#209894,#209895,#209896,#209897,#209898,#209899,#209900,
#209901,#209902,#209903,#209904,#209905,#209906,#209907,#209908,#209909,
#209910,#209911,#209912,#209913,#209914,#209915,#209916,#209917,#209918,
#209919,#209920,#209921,#209922,#209923,#209924,#209925,#209926,#209927,
#209928,#209929,#209930,#209931,#209932,#209933,#209934,#209935,#209936,
#209937,#209938,#209939,#209940,#209941,#209942,#209943,#209944,#209945,
#209946,#209947,#209948,#209949,#209950,#209951,#209952,#209953,#209954,
#209955,#209956,#209957,#209958,#209959,#209960,#209961,#209962,#209963,
#209964,#209965,#209966,#209967,#209968,#209969,#209970,#209971,#209972,
#209973,#209974,#209975,#209976,#209977,#209978,#209979,#209980,#209981,
#209982,#209983,#209984,#209985,#209986,#209987,#209988,#209989,#209990,
#209991,#209992,#209993,#209994,#209995,#209996,#209997,#209998,#209999,
#210000,#210001,#210002,#210003,#210004,#210005,#210006,#210007,#210008,
#210009,#210010,#210011,#210012,#210013,#210014,#210015,#210016,#210017,
#210018,#210019,#210020,#210021,#210022,#210023,#210024,#210025,#210026,
#210027,#210028,#210029,#210030,#210031,#210032,#210033,#210034,#210035,
#210036,#210037,#210038,#210039,#210040,#210041,#210042,#210043,#210044,
#210045,#210046,#210047,#210048,#210049,#210050,#210051,#210052,#210053,
#210054,#210055,#210056,#210057,#210058,#210059,#210060,#210061,#210062,
#210063,#210064,#210065,#210066,#210067,#210068,#210069,#210070,#210071,
#210072,#210073,#210074,#210075,#210076,#210077,#210078,#210079,#210080,
#210081,#210082,#210083,#210084,#210085,#210086,#210087,#210088,#210089,
#210090,#210091,#210092,#210093,#210094,#210095,#210096,#210097,#210098,
#210099,#210100,#210101,#210102,#210103,#210104,#210105,#210106,#210107,
#210108,#210109,#210110,#210111,#210112,#210113,#210114,#210115,#210116,
#210117,#210118,#210119,#210120,#210121,#210122,#210123,#210124,#210125,
#210126,#210127,#210128,#210129,#210130,#210131,#210132,#210133,#210134,
#210135,#210136,#210137,#210138,#210139,#210140,#210141,#210142,#210143,
#210144,#210145,#210146,#210147,#210148,#210149,#210150,#210151,#210152,
#210153,#210154,#210155,#210156,#210157,#210158,#210159,#210160,#210161,
#210162,#210163,#210164,#210165,#210166,#210167,#210168,#210169,#210170,
#210171,#210172,#210173,#210174,#210175,#210176,#210177,#210178,#210179,
#210180,#210181,#210182,#210183,#210184,#210185,#210186,#210187,#210188,
#210189,#210190,#210191,#210192,#210193,#210194,#210195,#210196,#210197,
#210198,#210199,#210200,#210201,#210202,#210203,#210204,#210205,#210206,
#210207,#210208,#210209,#210210,#210211,#210212,#210213,#210214,#210215,
#210216,#210217,#210218,#210219,#210220,#210221,#210222,#210223,#210224,
#210225,#210226,#210227,#210228,#210229,#210230,#210231,#210232,#210233,
#210234,#210235,#210236,#210237,#210238,#210239,#210240,#210241,#210242,
#210243,#210244,#210245,#210246,#210247,#210248,#210249,#210250,#210251,
#210252,#210253,#210254,#210255,#210256,#210257,#210258,#210259,#210260,
#210261,#210262,#210263,#210264,#210265,#210266,#210267,#210268,#210269,
#210270,#210271,#210272,#210273,#210274,#210275,#210276,#210277,#210278,
#210279,#210280,#210281,#210282,#210283,#210284,#210285,#210286,#210287,
#210288,#210289,#210290,#210291,#210292,#210293,#210294,#210295,#210296,
#210297,#210298,#210299,#210300,#210301,#210302,#210303,#210304,#210305,
#210306,#210307,#210308,#210309,#210310,#210311,#210312,#210313,#210314,
#210315,#210316,#210317,#210318,#210319,#210320,#210321,#210322,#210323,
#210324,#210325,#210326,#210327,#210328,#210329,#210330,#210331,#210332,
#210333,#210334,#210335,#210336,#210337,#210338,#210339,#210340,#210341,
#210342,#210343,#210344,#210345,#210346,#210347,#210348,#210349,#210350,
#210351,#210352,#210353,#210354,#210355,#210356,#210357,#210358,#210359,
#210360,#210361,#210362,#210363,#210364,#210365,#210366,#210367,#210368,
#210369,#210370,#210371,#210372,#210373,#210374,#210375,#210376,#210377,
#210378,#210379,#210380,#210381,#210382,#210383,#210384,#210385,#210386,
#210387,#210388,#210389,#210390,#210391,#210392,#210393,#210394,#210395,
#210396,#210397,#210398,#210399,#210400,#210401,#210402,#210403,#210404,
#210405,#210406,#210407,#210408,#210409,#210410,#210411,#210412,#210413,
#210414,#210415,#210416,#210417,#210418,#210419,#210420,#210421,#210422,
#210423,#210424,#210425,#210426,#210427,#210428,#210429,#210430,#210431,
#210432,#210433,#210434,#210435,#210436,#210437,#210438,#210439,#210440,
#210441,#210442,#210443,#210444,#210445,#210446,#210447,#210448,#210449,
#210450,#210451,#210452,#210453,#210454,#210455,#210456,#210457,#210458,
#210459,#210460,#210461,#210462,#210463,#210464,#210465,#210466,#210467,
#210468,#210469,#210470,#210471,#210472,#210473,#210474,#210475,#210476,
#210477,#210478,#210479,#210480,#210481,#210482,#210483,#210484,#210485,
#210486,#210487,#210488,#210489,#210490,#210491,#210492,#210493,#210494,
#210495,#210496,#210497,#210498,#210499,#210500,#210501,#210502,#210503,
#210504,#210505,#210506,#210507,#210508,#210509,#210510,#210511,#210512,
#210513,#210514,#210515,#210516,#210517,#210518,#210519,#210520,#210521,
#210522,#210523,#210524,#210525,#210526,#210527,#210528,#210529,#210530,
#210531,#210532,#210533,#210534,#210535,#210536,#210537,#210538,#210539,
#210540,#210541,#210542,#210543,#210544,#210545,#210546,#210547,#210548,
#210549,#210550,#210551,#210552,#210553,#210554,#210555,#210556,#210557,
#210558,#210559,#210560,#210561,#210562,#210563,#210564,#210565,#210566,
#210567,#210568,#210569,#210570,#210571,#210572,#210573,#210574,#210575,
#210576,#210577,#210578,#210579,#210580,#210581,#210582,#210583,#210584,
#210585,#210586,#210587,#210588,#210589,#210590,#210591,#210592,#210593,
#210594,#210595,#210596,#210597,#210598,#210599,#210600,#210601,#210602,
#210603,#210604,#210605,#210606,#210607,#210608,#210609,#210610,#210611,
#210612,#210613,#210614,#210615,#210616,#210617,#210618,#210619,#210620,
#210621,#210622,#210623,#210624,#210625,#210626,#210627,#210628,#210629,
#210630,#210631,#210632,#210633,#210634,#210635,#210636,#210637,#210638,
#210639,#210640,#210641,#210642,#210643,#210644,#210645,#210646,#210647,
#210648,#210649,#210650,#210651,#210652,#210653,#210654,#210655,#210656,
#210657,#210658,#210659,#210660,#210661,#210662,#210663,#210664,#210665,
#210666,#210667,#210668,#210669,#210670,#210671,#210672,#210673,#210674,
#210675,#210676,#210677,#210678,#210679,#210680,#210681,#210682,#210683,
#210684,#210685,#210686,#210687,#210688,#210689,#210690,#210691,#210692,
#210693,#210694,#210695,#210696,#210697,#210698,#210699,#210700,#210701,
#210702,#210703,#210704,#210705,#210706,#210707,#210708,#210709,#210710,
#210711,#210712,#210713,#210714,#210715,#210716,#210717,#210718,#210719,
#210720,#210721,#210722,#210723,#210724,#210725,#210726,#210727,#210728,
#210729,#210730,#210731,#210732,#210733,#210734,#210735,#210736,#210737,
#210738,#210739,#210740,#210741,#210742,#210743,#210744,#210745,#210746,
#210747,#210748,#210749,#210750,#210751,#210752,#210753,#210754,#210755,
#210756,#210757,#210758,#210759,#210760,#210761,#210762,#210763,#210764,
#210765,#210766,#210767,#210768,#210769,#210770,#210771,#210772,#210773,
#210774,#210775,#210776,#210777,#210778,#210779,#210780,#210781,#210782,
#210783,#210784,#210785,#210786,#210787,#210788,#210789,#210790,#210791,
#210792,#210793,#210794,#210795,#210796,#210797,#210798,#210799,#210800,
#210801,#210802,#210803,#210804,#210805,#210806,#210807,#210808,#210809,
#210810,#210811,#210812,#210813,#210814,#210815,#210816,#210817,#210818,
#210819,#210820,#210821,#210822,#210823,#210824,#210825,#210826,#210827,
#210828,#210829,#210830,#210831,#210832,#210833,#210834,#210835,#210836,
#210837,#210838,#210839,#210840,#210841,#210842,#210843,#210844,#210845,
#210846,#210847,#210848,#210849,#210850,#210851,#210852,#210853,#210854,
#210855,#210856,#210857,#210858,#210859,#210860,#210861,#210862,#210863,
#210864,#210865,#210866,#210867,#210868,#210869,#210870,#210871,#210872,
#210873,#210874,#210875,#210876,#210877,#210878,#210879,#210880,#210881,
#210882,#210883,#210884,#210885,#210886,#210887,#210888,#210889,#210890,
#210891,#210892,#210893,#210894,#210895,#210896,#210897,#210898,#210899,
#210900,#210901,#210902,#210903,#210904,#210905,#210906,#210907,#210908,
#210909,#210910,#210911,#210912,#210913,#210914,#210915,#210916,#210917,
#210918,#210919,#210920,#210921,#210922,#210923,#210924,#210925,#210926,
#210927,#210928,#210929,#210930,#210931,#210932,#210933,#210934,#210935,
#210936,#210937,#210938,#210939,#210940,#210941,#210942,#210943,#210944,
#210945,#210946,#210947,#210948,#210949,#210950,#210951,#210952,#210953,
#210954,#210955,#210956,#210957,#210958,#210959,#210960,#210961,#210962,
#210963,#210964,#210965,#210966,#210967,#210968,#210969,#210970,#210971,
#210972,#210973,#210974,#210975,#210976,#210977,#210978,#210979,#210980,
#210981,#210982,#210983,#210984,#210985,#210986,#210987,#210988,#210989,
#210990,#210991,#210992,#210993,#210994,#210995,#210996,#210997,#210998,
#210999,#211000,#211001,#211002,#211003,#211004,#211005,#211006,#211007,
#211008,#211009,#211010,#211011,#211012,#211013,#211014,#211015,#211016,
#211017,#211018,#211019,#211020,#211021,#211022,#211023,#211024,#211025,
#211026,#211027,#211028,#211029,#211030,#211031,#211032,#211033,#211034,
#211035,#211036,#211037,#211038,#211039,#211040,#211041,#211042,#211043,
#211044,#211045,#211046,#211047,#211048,#211049,#211050,#211051,#211052,
#211053,#211054,#211055,#211056,#211057,#211058,#211059,#211060,#211061,
#211062,#211063,#211064,#211065,#211066,#211067,#211068,#211069,#211070,
#211071,#211072,#211073,#211074,#211075,#211076,#211077,#211078,#211079,
#211080,#211081,#211082,#211083,#211084,#211085,#211086,#211087,#211088,
#211089,#211090,#211091,#211092,#211093,#211094,#211095,#211096,#211097,
#211098,#211099,#211100,#211101,#211102,#211103,#211104,#211105,#211106,
#211107,#211108,#211109,#211110,#211111,#211112,#211113,#211114,#211115,
#211116,#211117,#211118,#211119,#211120,#211121,#211122,#211123,#211124,
#211125,#211126,#211127,#211128,#211129,#211130,#211131,#211132,#211133,
#211134,#211135,#211136,#211137,#211138,#211139,#211140,#211141,#211142,
#211143,#211144,#211145,#211146,#211147,#211148,#211149,#211150,#211151,
#211152,#211153,#211154,#211155,#211156,#211157,#211158,#211159,#211160,
#211161,#211162,#211163,#211164,#211165,#211166,#211167,#211168,#211169,
#211170,#211171,#211172,#211173,#211174,#211175,#211176,#211177,#211178,
#211179,#211180,#211181,#211182,#211183,#211184,#211185,#211186,#211187,
#211188,#211189,#211190,#211191,#211192,#211193,#211194,#211195),(#211196,
#211197,#211198,#211199,#211200,#211201,#211202,#211203,#211204,#211205,
#211206,#211207,#211208,#211209,#211210,#211211,#211212,#211213,#211214,
#211215,#211216,#211217,#211218,#211219,#211220,#211221,#211222,#211223,
#211224,#211225,#211226,#211227,#211228,#211229,#211230,#211231,#211232,
#211233,#211234,#211235,#211236,#211237,#211238,#211239,#211240,#211241,
#211242,#211243,#211244,#211245,#211246,#211247,#211248,#211249,#211250,
#211251,#211252,#211253,#211254,#211255,#211256,#211257,#211258,#211259,
#211260,#211261,#211262,#211263,#211264,#211265,#211266,#211267,#211268,
#211269,#211270,#211271,#211272,#211273,#211274,#211275,#211276,#211277,
#211278,#211279,#211280,#211281,#211282,#211283,#211284,#211285,#211286,
#211287,#211288,#211289,#211290,#211291,#211292,#211293,#211294,#211295,
#211296,#211297,#211298,#211299,#211300,#211301,#211302,#211303,#211304,
#211305,#211306,#211307,#211308,#211309,#211310,#211311,#211312,#211313,
#211314,#211315,#211316,#211317,#211318,#211319,#211320,#211321,#211322,
#211323,#211324,#211325,#211326,#211327,#211328,#211329,#211330,#211331,
#211332,#211333,#211334,#211335,#211336,#211337,#211338,#211339,#211340,
#211341,#211342,#211343,#211344,#211345,#211346,#211347,#211348,#211349,
#211350,#211351,#211352,#211353,#211354,#211355,#211356,#211357,#211358,
#211359,#211360,#211361,#211362,#211363,#211364,#211365,#211366,#211367,
#211368,#211369,#211370,#211371,#211372,#211373,#211374,#211375,#211376,
#211377,#211378,#211379,#211380,#211381,#211382,#211383,#211384,#211385,
#211386,#211387,#211388,#211389,#211390,#211391,#211392,#211393,#211394,
#211395,#211396,#211397,#211398,#211399,#211400,#211401,#211402,#211403,
#211404,#211405,#211406,#211407,#211408,#211409,#211410,#211411,#211412,
#211413,#211414,#211415,#211416,#211417,#211418,#211419,#211420,#211421,
#211422,#211423,#211424,#211425,#211426,#211427,#211428,#211429,#211430,
#211431,#211432,#211433,#211434,#211435,#211436,#211437,#211438,#211439,
#211440,#211441,#211442,#211443,#211444,#211445,#211446,#211447,#211448,
#211449,#211450,#211451,#211452,#211453,#211454,#211455,#211456,#211457,
#211458,#211459,#211460,#211461,#211462,#211463,#211464,#211465,#211466,
#211467,#211468,#211469,#211470,#211471,#211472,#211473,#211474,#211475,
#211476,#211477,#211478,#211479,#211480,#211481,#211482,#211483,#211484,
#211485,#211486,#211487,#211488,#211489,#211490,#211491,#211492,#211493,
#211494,#211495,#211496,#211497,#211498,#211499,#211500,#211501,#211502,
#211503,#211504,#211505,#211506,#211507,#211508,#211509,#211510,#211511,
#211512,#211513,#211514,#211515,#211516,#211517,#211518,#211519,#211520,
#211521,#211522,#211523,#211524,#211525,#211526,#211527,#211528,#211529,
#211530,#211531,#211532,#211533,#211534,#211535,#211536,#211537,#211538,
#211539,#211540,#211541,#211542,#211543,#211544,#211545,#211546,#211547,
#211548,#211549,#211550,#211551,#211552,#211553,#211554,#211555,#211556,
#211557,#211558,#211559,#211560,#211561,#211562,#211563,#211564,#211565,
#211566,#211567,#211568,#211569,#211570,#211571,#211572,#211573,#211574,
#211575,#211576,#211577,#211578,#211579,#211580,#211581,#211582,#211583,
#211584,#211585,#211586,#211587,#211588,#211589,#211590,#211591,#211592,
#211593,#211594,#211595,#211596,#211597,#211598,#211599,#211600,#211601,
#211602,#211603,#211604,#211605,#211606,#211607,#211608,#211609,#211610,
#211611,#211612,#211613,#211614,#211615,#211616,#211617,#211618,#211619,
#211620,#211621,#211622,#211623,#211624,#211625,#211626,#211627,#211628,
#211629,#211630,#211631,#211632,#211633,#211634,#211635,#211636,#211637,
#211638,#211639,#211640,#211641,#211642,#211643,#211644,#211645,#211646,
#211647,#211648,#211649,#211650,#211651,#211652,#211653,#211654,#211655,
#211656,#211657,#211658,#211659,#211660,#211661,#211662,#211663,#211664,
#211665,#211666,#211667,#211668,#211669,#211670,#211671,#211672,#211673,
#211674,#211675,#211676,#211677,#211678,#211679,#211680,#211681,#211682,
#211683,#211684,#211685,#211686,#211687,#211688,#211689,#211690,#211691,
#211692,#211693,#211694,#211695,#211696,#211697,#211698,#211699,#211700,
#211701,#211702,#211703,#211704,#211705,#211706,#211707,#211708,#211709,
#211710,#211711,#211712,#211713,#211714,#211715,#211716,#211717,#211718,
#211719,#211720,#211721,#211722,#211723,#211724,#211725,#211726,#211727,
#211728,#211729,#211730,#211731,#211732,#211733,#211734,#211735,#211736,
#211737,#211738,#211739,#211740,#211741,#211742,#211743,#211744,#211745,
#211746,#211747,#211748,#211749,#211750,#211751,#211752,#211753,#211754,
#211755,#211756,#211757,#211758,#211759,#211760,#211761,#211762,#211763,
#211764,#211765,#211766,#211767,#211768,#211769,#211770,#211771,#211772,
#211773,#211774,#211775,#211776,#211777,#211778,#211779,#211780,#211781,
#211782,#211783,#211784,#211785,#211786,#211787,#211788,#211789,#211790,
#211791,#211792,#211793,#211794,#211795,#211796,#211797,#211798,#211799,
#211800,#211801,#211802,#211803,#211804,#211805,#211806,#211807,#211808,
#211809,#211810,#211811,#211812,#211813,#211814,#211815,#211816,#211817,
#211818,#211819,#211820,#211821,#211822,#211823,#211824,#211825,#211826,
#211827,#211828,#211829,#211830,#211831,#211832,#211833,#211834,#211835,
#211836,#211837,#211838,#211839,#211840,#211841,#211842,#211843,#211844,
#211845,#211846,#211847,#211848,#211849,#211850,#211851,#211852,#211853,
#211854,#211855,#211856,#211857,#211858,#211859,#211860,#211861,#211862,
#211863,#211864,#211865,#211866,#211867,#211868,#211869,#211870,#211871,
#211872,#211873,#211874,#211875,#211876,#211877,#211878,#211879,#211880,
#211881,#211882,#211883,#211884,#211885,#211886,#211887,#211888,#211889,
#211890,#211891,#211892,#211893,#211894,#211895,#211896,#211897,#211898,
#211899,#211900,#211901,#211902,#211903,#211904,#211905,#211906,#211907,
#211908,#211909,#211910,#211911,#211912,#211913,#211914,#211915,#211916,
#211917,#211918,#211919,#211920,#211921,#211922,#211923,#211924,#211925,
#211926,#211927,#211928,#211929,#211930,#211931,#211932,#211933,#211934,
#211935,#211936,#211937,#211938,#211939,#211940,#211941,#211942,#211943,
#211944,#211945,#211946,#211947,#211948,#211949,#211950,#211951,#211952,
#211953,#211954,#211955,#211956,#211957,#211958,#211959,#211960,#211961,
#211962,#211963,#211964,#211965,#211966,#211967,#211968,#211969,#211970,
#211971,#211972,#211973,#211974,#211975,#211976,#211977,#211978,#211979,
#211980,#211981,#211982,#211983,#211984,#211985,#211986,#211987,#211988,
#211989,#211990,#211991,#211992,#211993,#211994,#211995,#211996,#211997,
#211998,#211999,#212000,#212001,#212002,#212003,#212004,#212005,#212006,
#212007,#212008,#212009,#212010,#212011,#212012,#212013,#212014,#212015,
#212016,#212017,#212018,#212019,#212020,#212021,#212022,#212023,#212024,
#212025,#212026,#212027,#212028,#212029,#212030,#212031,#212032,#212033,
#212034,#212035,#212036,#212037,#212038,#212039,#212040,#212041,#212042,
#212043,#212044,#212045,#212046,#212047,#212048,#212049,#212050,#212051,
#212052,#212053,#212054,#212055,#212056,#212057,#212058,#212059,#212060,
#212061,#212062,#212063,#212064,#212065,#212066,#212067,#212068,#212069,
#212070,#212071,#212072,#212073,#212074,#212075,#212076,#212077,#212078,
#212079,#212080,#212081,#212082,#212083,#212084,#212085,#212086,#212087,
#212088,#212089,#212090,#212091,#212092,#212093,#212094,#212095,#212096,
#212097,#212098,#212099,#212100,#212101,#212102,#212103,#212104,#212105,
#212106,#212107,#212108,#212109,#212110,#212111,#212112,#212113,#212114,
#212115,#212116,#212117,#212118,#212119,#212120,#212121,#212122,#212123,
#212124,#212125,#212126,#212127,#212128,#212129,#212130,#212131,#212132,
#212133,#212134,#212135,#212136,#212137,#212138,#212139,#212140,#212141,
#212142,#212143,#212144,#212145,#212146,#212147,#212148,#212149,#212150,
#212151,#212152,#212153,#212154,#212155,#212156,#212157,#212158,#212159,
#212160,#212161,#212162,#212163,#212164,#212165,#212166,#212167,#212168,
#212169,#212170,#212171,#212172,#212173,#212174,#212175,#212176,#212177,
#212178,#212179,#212180,#212181,#212182,#212183,#212184,#212185,#212186,
#212187,#212188,#212189,#212190,#212191,#212192,#212193,#212194,#212195,
#212196,#212197,#212198,#212199,#212200,#212201,#212202,#212203,#212204,
#212205,#212206,#212207,#212208,#212209,#212210,#212211,#212212,#212213,
#212214,#212215,#212216,#212217,#212218,#212219,#212220,#212221,#212222,
#212223,#212224,#212225,#212226,#212227,#212228,#212229,#212230,#212231,
#212232,#212233,#212234,#212235,#212236,#212237,#212238,#212239,#212240,
#212241,#212242,#212243,#212244,#212245,#212246,#212247,#212248,#212249,
#212250,#212251,#212252,#212253,#212254,#212255,#212256,#212257,#212258,
#212259,#212260,#212261,#212262,#212263,#212264,#212265,#212266,#212267,
#212268,#212269,#212270,#212271,#212272,#212273,#212274,#212275,#212276,
#212277,#212278,#212279,#212280,#212281,#212282,#212283,#212284,#212285,
#212286,#212287,#212288,#212289,#212290,#212291,#212292,#212293,#212294,
#212295,#212296,#212297,#212298,#212299,#212300,#212301,#212302,#212303,
#212304,#212305,#212306,#212307,#212308,#212309,#212310,#212311,#212312,
#212313,#212314,#212315,#212316,#212317,#212318,#212319,#212320,#212321,
#212322,#212323,#212324,#212325,#212326,#212327,#212328,#212329,#212330,
#212331,#212332,#212333,#212334,#212335,#212336,#212337,#212338,#212339,
#212340,#212341,#212342,#212343,#212344,#212345,#212346,#212347,#212348,
#212349,#212350,#212351,#212352,#212353,#212354,#212355,#212356,#212357,
#212358,#212359,#212360,#212361,#212362,#212363,#212364,#212365,#212366,
#212367,#212368,#212369,#212370,#212371,#212372,#212373,#212374,#212375,
#212376,#212377,#212378,#212379,#212380,#212381,#212382,#212383,#212384,
#212385,#212386,#212387,#212388,#212389,#212390,#212391,#212392,#212393,
#212394,#212395,#212396,#212397,#212398,#212399,#212400,#212401,#212402,
#212403,#212404,#212405,#212406,#212407,#212408,#212409,#212410,#212411,
#212412,#212413,#212414,#212415,#212416,#212417,#212418,#212419,#212420,
#212421,#212422,#212423,#212424,#212425,#212426,#212427,#212428,#212429,
#212430,#212431,#212432,#212433,#212434,#212435,#212436,#212437,#212438,
#212439,#212440,#212441,#212442,#212443,#212444,#212445,#212446,#212447,
#212448,#212449,#212450,#212451,#212452,#212453,#212454,#212455,#212456,
#212457,#212458,#212459,#212460,#212461,#212462,#212463,#212464,#212465,
#212466,#212467,#212468,#212469,#212470,#212471,#212472,#212473,#212474,
#212475,#212476,#212477,#212478,#212479,#212480,#212481,#212482,#212483,
#212484,#212485,#212486,#212487,#212488,#212489,#212490,#212491,#212492,
#212493,#212494,#212495,#212496,#212497,#212498,#212499,#212500,#212501,
#212502,#212503,#212504,#212505,#212506,#212507,#212508,#212509,#212510,
#212511,#212512,#212513,#212514,#212515,#212516,#212517,#212518,#212519,
#212520,#212521,#212522,#212523,#212524,#212525,#212526,#212527,#212528,
#212529,#212530,#212531,#212532,#212533,#212534,#212535,#212536,#212537,
#212538,#212539,#212540,#212541,#212542,#212543,#212544,#212545,#212546,
#212547,#212548,#212549,#212550,#212551,#212552,#212553,#212554,#212555,
#212556,#212557,#212558,#212559,#212560,#212561,#212562,#212563,#212564,
#212565,#212566,#212567,#212568,#212569,#212570,#212571,#212572,#212573,
#212574,#212575,#212576,#212577,#212578,#212579,#212580,#212581,#212582,
#212583,#212584,#212585,#212586,#212587,#212588,#212589,#212590,#212591,
#212592,#212593,#212594,#212595,#212596,#212597,#212598,#212599,#212600,
#212601,#212602,#212603,#212604,#212605,#212606,#212607,#212608,#212609,
#212610,#212611,#212612,#212613,#212614,#212615,#212616,#212617,#212618,
#212619,#212620,#212621,#212622,#212623,#212624,#212625,#212626,#212627,
#212628,#212629,#212630,#212631,#212632,#212633,#212634,#212635,#212636,
#212637,#212638,#212639,#212640,#212641,#212642,#212643,#212644,#212645,
#212646,#212647,#212648,#212649,#212650,#212651,#212652,#212653,#212654,
#212655,#212656,#212657,#212658,#212659,#212660,#212661,#212662,#212663,
#212664,#212665,#212666,#212667,#212668,#212669,#212670,#212671,#212672,
#212673,#212674,#212675,#212676,#212677,#212678,#212679,#212680,#212681,
#212682,#212683,#212684,#212685,#212686,#212687,#212688,#212689,#212690,
#212691,#212692,#212693,#212694,#212695,#212696,#212697,#212698,#212699,
#212700,#212701,#212702,#212703,#212704,#212705,#212706,#212707,#212708,
#212709,#212710,#212711,#212712,#212713,#212714,#212715,#212716,#212717,
#212718,#212719,#212720,#212721,#212722,#212723,#212724,#212725,#212726,
#212727,#212728,#212729,#212730,#212731,#212732,#212733,#212734,#212735,
#212736,#212737,#212738,#212739,#212740,#212741,#212742,#212743,#212744,
#212745,#212746,#212747,#212748,#212749,#212750,#212751,#212752,#212753,
#212754,#212755,#212756,#212757,#212758,#212759,#212760,#212761,#212762,
#212763,#212764,#212765,#212766,#212767,#212768,#212769,#212770,#212771,
#212772,#212773,#212774,#212775,#212776,#212777,#212778,#212779,#212780,
#212781,#212782,#212783,#212784,#212785,#212786,#212787,#212788,#212789,
#212790,#212791,#212792,#212793,#212794,#212795,#212796,#212797,#212798,
#212799,#212800,#212801,#212802,#212803,#212804,#212805,#212806,#212807,
#212808,#212809,#212810,#212811,#212812,#212813,#212814,#212815,#212816,
#212817,#212818,#212819,#212820,#212821,#212822,#212823,#212824,#212825,
#212826,#212827,#212828,#212829,#212830,#212831,#212832,#212833,#212834,
#212835,#212836,#212837,#212838,#212839,#212840,#212841,#212842,#212843,
#212844,#212845,#212846,#212847,#212848,#212849,#212850,#212851,#212852,
#212853,#212854,#212855,#212856,#212857,#212858,#212859,#212860,#212861,
#212862,#212863,#212864,#212865,#212866,#212867,#212868,#212869,#212870,
#212871,#212872,#212873,#212874,#212875,#212876,#212877,#212878,#212879,
#212880,#212881,#212882,#212883,#212884,#212885,#212886,#212887,#212888,
#212889,#212890),(#212891,#212892,#212893,#212894,#212895,#212896,#212897,
#212898,#212899,#212900,#212901,#212902,#212903,#212904,#212905,#212906,
#212907,#212908,#212909,#212910,#212911,#212912,#212913,#212914,#212915,
#212916,#212917,#212918,#212919,#212920,#212921,#212922,#212923,#212924,
#212925,#212926,#212927,#212928,#212929,#212930,#212931,#212932,#212933,
#212934,#212935,#212936,#212937,#212938,#212939,#212940,#212941,#212942,
#212943,#212944,#212945,#212946,#212947,#212948,#212949,#212950,#212951,
#212952,#212953,#212954,#212955,#212956,#212957,#212958,#212959,#212960,
#212961,#212962,#212963,#212964,#212965,#212966,#212967,#212968,#212969,
#212970,#212971,#212972,#212973,#212974,#212975,#212976,#212977,#212978,
#212979,#212980,#212981,#212982,#212983,#212984,#212985,#212986,#212987,
#212988,#212989,#212990,#212991,#212992,#212993,#212994,#212995,#212996,
#212997,#212998,#212999,#213000,#213001,#213002,#213003,#213004,#213005,
#213006,#213007,#213008,#213009,#213010,#213011,#213012,#213013,#213014,
#213015,#213016,#213017,#213018,#213019,#213020,#213021,#213022,#213023,
#213024,#213025,#213026,#213027,#213028,#213029,#213030,#213031,#213032,
#213033,#213034,#213035,#213036,#213037,#213038,#213039,#213040,#213041,
#213042,#213043,#213044,#213045,#213046,#213047,#213048,#213049,#213050,
#213051,#213052,#213053,#213054,#213055,#213056,#213057,#213058,#213059,
#213060,#213061,#213062,#213063,#213064,#213065,#213066,#213067,#213068,
#213069,#213070,#213071,#213072,#213073,#213074,#213075,#213076,#213077,
#213078,#213079,#213080,#213081,#213082,#213083,#213084,#213085,#213086,
#213087,#213088,#213089,#213090,#213091,#213092,#213093,#213094,#213095,
#213096,#213097,#213098,#213099,#213100,#213101,#213102,#213103,#213104,
#213105,#213106,#213107,#213108,#213109,#213110,#213111,#213112,#213113,
#213114,#213115,#213116,#213117,#213118,#213119,#213120,#213121,#213122,
#213123,#213124,#213125,#213126,#213127,#213128,#213129,#213130,#213131,
#213132,#213133,#213134,#213135,#213136,#213137,#213138,#213139,#213140,
#213141,#213142,#213143,#213144,#213145,#213146,#213147,#213148,#213149,
#213150,#213151,#213152,#213153,#213154,#213155,#213156,#213157,#213158,
#213159,#213160,#213161,#213162,#213163,#213164,#213165,#213166,#213167,
#213168,#213169,#213170,#213171,#213172,#213173,#213174,#213175,#213176,
#213177,#213178,#213179,#213180,#213181,#213182,#213183,#213184,#213185,
#213186,#213187,#213188,#213189,#213190,#213191,#213192,#213193,#213194,
#213195,#213196,#213197,#213198,#213199,#213200,#213201,#213202,#213203,
#213204,#213205,#213206,#213207,#213208,#213209,#213210,#213211,#213212,
#213213,#213214,#213215,#213216,#213217,#213218,#213219,#213220,#213221,
#213222,#213223,#213224,#213225,#213226,#213227,#213228,#213229,#213230,
#213231,#213232,#213233,#213234,#213235,#213236,#213237,#213238,#213239,
#213240,#213241,#213242,#213243,#213244,#213245,#213246,#213247,#213248,
#213249,#213250,#213251,#213252,#213253,#213254,#213255,#213256,#213257,
#213258,#213259,#213260,#213261,#213262,#213263,#213264,#213265,#213266,
#213267,#213268,#213269,#213270,#213271,#213272,#213273,#213274,#213275,
#213276,#213277,#213278,#213279,#213280,#213281,#213282,#213283,#213284,
#213285,#213286,#213287,#213288,#213289,#213290,#213291,#213292,#213293,
#213294,#213295,#213296,#213297,#213298,#213299,#213300,#213301,#213302,
#213303,#213304,#213305,#213306,#213307,#213308,#213309,#213310,#213311,
#213312,#213313,#213314,#213315,#213316,#213317,#213318,#213319,#213320,
#213321,#213322,#213323,#213324,#213325,#213326,#213327,#213328,#213329,
#213330,#213331,#213332,#213333,#213334,#213335,#213336,#213337,#213338,
#213339,#213340,#213341,#213342,#213343,#213344,#213345,#213346,#213347,
#213348,#213349,#213350,#213351,#213352,#213353,#213354,#213355,#213356,
#213357,#213358,#213359,#213360,#213361,#213362,#213363,#213364,#213365,
#213366,#213367,#213368,#213369,#213370,#213371,#213372,#213373,#213374,
#213375,#213376,#213377,#213378,#213379,#213380,#213381,#213382,#213383,
#213384,#213385,#213386,#213387,#213388,#213389,#213390,#213391,#213392,
#213393,#213394,#213395,#213396,#213397,#213398,#213399,#213400,#213401,
#213402,#213403,#213404,#213405,#213406,#213407,#213408,#213409,#213410,
#213411,#213412,#213413,#213414,#213415,#213416,#213417,#213418,#213419,
#213420,#213421,#213422,#213423,#213424,#213425,#213426,#213427,#213428,
#213429,#213430,#213431,#213432,#213433,#213434,#213435,#213436,#213437,
#213438,#213439,#213440,#213441,#213442,#213443,#213444,#213445,#213446,
#213447,#213448,#213449,#213450,#213451,#213452,#213453,#213454,#213455,
#213456,#213457,#213458,#213459,#213460,#213461,#213462,#213463,#213464,
#213465,#213466,#213467,#213468,#213469,#213470,#213471,#213472,#213473,
#213474,#213475,#213476,#213477,#213478,#213479,#213480,#213481,#213482,
#213483,#213484,#213485,#213486,#213487,#213488,#213489,#213490,#213491,
#213492,#213493,#213494,#213495,#213496,#213497,#213498,#213499,#213500,
#213501,#213502,#213503,#213504,#213505,#213506,#213507,#213508,#213509,
#213510,#213511,#213512,#213513,#213514,#213515,#213516,#213517,#213518,
#213519,#213520,#213521,#213522,#213523,#213524,#213525,#213526,#213527,
#213528,#213529,#213530,#213531,#213532,#213533,#213534,#213535,#213536,
#213537,#213538,#213539,#213540,#213541,#213542,#213543,#213544,#213545,
#213546,#213547,#213548,#213549,#213550,#213551,#213552,#213553,#213554,
#213555,#213556,#213557,#213558,#213559,#213560,#213561,#213562,#213563,
#213564,#213565,#213566,#213567,#213568,#213569,#213570,#213571,#213572,
#213573,#213574,#213575,#213576,#213577,#213578,#213579,#213580,#213581,
#213582,#213583,#213584,#213585,#213586,#213587,#213588,#213589,#213590,
#213591,#213592,#213593,#213594,#213595,#213596,#213597,#213598,#213599,
#213600,#213601,#213602,#213603,#213604,#213605,#213606,#213607,#213608,
#213609,#213610,#213611,#213612,#213613,#213614,#213615,#213616,#213617,
#213618,#213619,#213620,#213621,#213622,#213623,#213624,#213625,#213626,
#213627,#213628,#213629,#213630,#213631,#213632,#213633,#213634,#213635,
#213636,#213637,#213638,#213639,#213640,#213641,#213642,#213643,#213644,
#213645,#213646,#213647,#213648,#213649,#213650,#213651,#213652,#213653,
#213654,#213655,#213656,#213657,#213658,#213659,#213660,#213661,#213662,
#213663,#213664,#213665,#213666,#213667,#213668,#213669,#213670,#213671,
#213672,#213673,#213674,#213675,#213676,#213677,#213678,#213679,#213680,
#213681,#213682,#213683,#213684,#213685,#213686,#213687,#213688,#213689,
#213690,#213691,#213692,#213693,#213694,#213695,#213696,#213697,#213698,
#213699,#213700,#213701,#213702,#213703,#213704,#213705,#213706,#213707,
#213708,#213709,#213710,#213711,#213712,#213713,#213714,#213715,#213716,
#213717,#213718,#213719,#213720,#213721,#213722,#213723,#213724,#213725,
#213726,#213727,#213728,#213729,#213730,#213731,#213732,#213733,#213734,
#213735,#213736,#213737,#213738,#213739,#213740,#213741,#213742,#213743,
#213744,#213745,#213746,#213747,#213748,#213749,#213750,#213751,#213752,
#213753,#213754,#213755,#213756,#213757,#213758,#213759,#213760,#213761,
#213762,#213763,#213764,#213765,#213766,#213767,#213768,#213769,#213770,
#213771,#213772,#213773,#213774,#213775,#213776,#213777,#213778,#213779,
#213780,#213781,#213782,#213783,#213784,#213785,#213786,#213787,#213788,
#213789,#213790,#213791,#213792,#213793,#213794,#213795,#213796,#213797,
#213798,#213799,#213800,#213801,#213802,#213803,#213804,#213805,#213806,
#213807,#213808,#213809,#213810,#213811,#213812,#213813,#213814,#213815,
#213816,#213817,#213818,#213819,#213820,#213821,#213822,#213823,#213824,
#213825,#213826,#213827,#213828,#213829,#213830,#213831,#213832,#213833,
#213834,#213835,#213836,#213837,#213838,#213839,#213840,#213841,#213842,
#213843,#213844,#213845,#213846,#213847,#213848,#213849,#213850,#213851,
#213852,#213853,#213854,#213855,#213856,#213857,#213858,#213859,#213860,
#213861,#213862,#213863,#213864,#213865,#213866,#213867,#213868,#213869,
#213870,#213871,#213872,#213873,#213874,#213875,#213876,#213877,#213878,
#213879,#213880,#213881,#213882,#213883,#213884,#213885,#213886,#213887,
#213888,#213889,#213890,#213891,#213892,#213893,#213894,#213895,#213896,
#213897,#213898,#213899,#213900,#213901,#213902,#213903,#213904,#213905,
#213906,#213907,#213908,#213909,#213910,#213911,#213912,#213913,#213914,
#213915,#213916,#213917,#213918,#213919,#213920,#213921,#213922,#213923,
#213924,#213925,#213926,#213927,#213928,#213929,#213930,#213931,#213932,
#213933,#213934,#213935,#213936,#213937,#213938,#213939,#213940,#213941,
#213942,#213943,#213944,#213945,#213946,#213947,#213948,#213949,#213950,
#213951,#213952,#213953,#213954,#213955,#213956,#213957,#213958,#213959,
#213960,#213961,#213962,#213963,#213964,#213965,#213966,#213967,#213968,
#213969,#213970,#213971,#213972,#213973,#213974,#213975,#213976,#213977,
#213978,#213979,#213980,#213981,#213982,#213983,#213984,#213985,#213986,
#213987,#213988,#213989,#213990,#213991,#213992,#213993,#213994,#213995,
#213996,#213997,#213998,#213999,#214000,#214001,#214002,#214003,#214004,
#214005,#214006,#214007,#214008,#214009,#214010,#214011,#214012,#214013,
#214014,#214015,#214016,#214017,#214018,#214019,#214020,#214021,#214022,
#214023,#214024,#214025,#214026,#214027,#214028,#214029,#214030,#214031,
#214032,#214033,#214034,#214035,#214036,#214037,#214038,#214039,#214040,
#214041,#214042,#214043,#214044,#214045,#214046,#214047,#214048,#214049,
#214050,#214051,#214052,#214053,#214054,#214055,#214056,#214057,#214058,
#214059,#214060,#214061,#214062,#214063,#214064,#214065,#214066,#214067,
#214068,#214069,#214070,#214071,#214072,#214073,#214074,#214075,#214076,
#214077,#214078,#214079,#214080,#214081,#214082,#214083,#214084,#214085,
#214086,#214087,#214088,#214089,#214090,#214091,#214092,#214093,#214094,
#214095,#214096,#214097,#214098,#214099,#214100,#214101,#214102,#214103,
#214104,#214105,#214106,#214107,#214108,#214109,#214110,#214111,#214112,
#214113,#214114,#214115,#214116,#214117,#214118,#214119,#214120,#214121,
#214122,#214123,#214124,#214125,#214126,#214127,#214128,#214129,#214130,
#214131,#214132,#214133,#214134,#214135,#214136,#214137,#214138,#214139,
#214140,#214141,#214142,#214143,#214144,#214145,#214146,#214147,#214148,
#214149,#214150,#214151,#214152,#214153,#214154,#214155,#214156,#214157,
#214158,#214159,#214160,#214161,#214162,#214163,#214164,#214165,#214166,
#214167,#214168,#214169,#214170,#214171,#214172,#214173,#214174,#214175,
#214176,#214177,#214178,#214179,#214180,#214181,#214182,#214183,#214184,
#214185,#214186,#214187,#214188,#214189,#214190,#214191,#214192,#214193,
#214194,#214195,#214196,#214197,#214198,#214199,#214200,#214201,#214202,
#214203,#214204,#214205,#214206,#214207,#214208,#214209,#214210,#214211,
#214212,#214213,#214214,#214215,#214216,#214217,#214218,#214219,#214220,
#214221,#214222,#214223,#214224,#214225,#214226,#214227,#214228,#214229,
#214230,#214231,#214232,#214233,#214234,#214235,#214236,#214237,#214238,
#214239,#214240,#214241,#214242,#214243,#214244,#214245,#214246,#214247,
#214248,#214249,#214250,#214251,#214252,#214253,#214254,#214255,#214256,
#214257,#214258,#214259,#214260,#214261,#214262,#214263,#214264,#214265,
#214266,#214267,#214268,#214269,#214270,#214271,#214272,#214273,#214274,
#214275,#214276,#214277,#214278,#214279,#214280,#214281,#214282,#214283,
#214284,#214285,#214286,#214287,#214288,#214289,#214290,#214291,#214292,
#214293,#214294,#214295,#214296,#214297,#214298,#214299,#214300,#214301,
#214302,#214303,#214304,#214305,#214306,#214307,#214308,#214309,#214310,
#214311,#214312,#214313,#214314,#214315,#214316,#214317,#214318,#214319,
#214320,#214321,#214322,#214323,#214324,#214325,#214326,#214327,#214328,
#214329,#214330,#214331,#214332,#214333,#214334,#214335,#214336,#214337,
#214338,#214339,#214340,#214341,#214342,#214343,#214344,#214345,#214346,
#214347,#214348,#214349,#214350,#214351,#214352,#214353,#214354,#214355,
#214356,#214357,#214358,#214359,#214360,#214361,#214362,#214363,#214364,
#214365,#214366,#214367,#214368,#214369,#214370,#214371,#214372,#214373,
#214374,#214375,#214376,#214377,#214378,#214379,#214380,#214381,#214382,
#214383,#214384,#214385,#214386,#214387,#214388,#214389,#214390,#214391,
#214392,#214393,#214394,#214395,#214396,#214397,#214398,#214399,#214400,
#214401,#214402,#214403,#214404,#214405,#214406,#214407,#214408,#214409,
#214410,#214411,#214412,#214413,#214414,#214415,#214416,#214417,#214418,
#214419,#214420,#214421,#214422,#214423,#214424,#214425,#214426,#214427,
#214428,#214429,#214430,#214431,#214432,#214433,#214434,#214435,#214436,
#214437,#214438,#214439,#214440,#214441,#214442,#214443,#214444,#214445,
#214446,#214447,#214448,#214449,#214450,#214451,#214452,#214453,#214454,
#214455,#214456,#214457,#214458,#214459,#214460,#214461,#214462,#214463,
#214464,#214465,#214466,#214467,#214468,#214469,#214470,#214471,#214472,
#214473,#214474,#214475,#214476,#214477,#214478,#214479,#214480,#214481,
#214482,#214483,#214484,#214485,#214486,#214487,#214488,#214489,#214490,
#214491,#214492,#214493,#214494,#214495,#214496,#214497,#214498,#214499,
#214500,#214501,#214502,#214503,#214504,#214505,#214506,#214507,#214508,
#214509,#214510,#214511,#214512,#214513,#214514,#214515,#214516,#214517,
#214518,#214519,#214520,#214521,#214522,#214523,#214524,#214525,#214526,
#214527,#214528,#214529,#214530,#214531,#214532,#214533,#214534,#214535,
#214536,#214537,#214538,#214539,#214540,#214541,#214542,#214543,#214544,
#214545,#214546,#214547,#214548,#214549,#214550,#214551,#214552,#214553,
#214554,#214555,#214556,#214557,#214558,#214559,#214560,#214561,#214562,
#214563,#214564,#214565,#214566,#214567,#214568,#214569,#214570,#214571,
#214572,#214573,#214574,#214575,#214576,#214577,#214578,#214579,#214580,
#214581,#214582,#214583,#214584,#214585),(#214586,#214587,#214588,#214589,
#214590,#214591,#214592,#214593,#214594,#214595,#214596,#214597,#214598,
#214599,#214600,#214601,#214602,#214603,#214604,#214605,#214606,#214607,
#214608,#214609,#214610,#214611,#214612,#214613,#214614,#214615,#214616,
#214617,#214618,#214619,#214620,#214621,#214622,#214623,#214624,#214625,
#214626,#214627,#214628,#214629,#214630,#214631,#214632,#214633,#214634,
#214635,#214636,#214637,#214638,#214639,#214640,#214641,#214642,#214643,
#214644,#214645,#214646,#214647,#214648,#214649,#214650,#214651,#214652,
#214653,#214654,#214655,#214656,#214657,#214658,#214659,#214660,#214661,
#214662,#214663,#214664,#214665,#214666,#214667,#214668,#214669,#214670,
#214671,#214672,#214673,#214674,#214675,#214676,#214677,#214678,#214679,
#214680,#214681,#214682,#214683,#214684,#214685,#214686,#214687,#214688,
#214689,#214690,#214691,#214692,#214693,#214694,#214695,#214696,#214697,
#214698,#214699,#214700,#214701,#214702,#214703,#214704,#214705,#214706,
#214707,#214708,#214709,#214710,#214711,#214712,#214713,#214714,#214715,
#214716,#214717,#214718,#214719,#214720,#214721,#214722,#214723,#214724,
#214725,#214726,#214727,#214728,#214729,#214730,#214731,#214732,#214733,
#214734,#214735,#214736,#214737,#214738,#214739,#214740,#214741,#214742,
#214743,#214744,#214745,#214746,#214747,#214748,#214749,#214750,#214751,
#214752,#214753,#214754,#214755,#214756,#214757,#214758,#214759,#214760,
#214761,#214762,#214763,#214764,#214765,#214766,#214767,#214768,#214769,
#214770,#214771,#214772,#214773,#214774,#214775,#214776,#214777,#214778,
#214779,#214780,#214781,#214782,#214783,#214784,#214785,#214786,#214787,
#214788,#214789,#214790,#214791,#214792,#214793,#214794,#214795,#214796,
#214797,#214798,#214799,#214800,#214801,#214802,#214803,#214804,#214805,
#214806,#214807,#214808,#214809,#214810,#214811,#214812,#214813,#214814,
#214815,#214816,#214817,#214818,#214819,#214820,#214821,#214822,#214823,
#214824,#214825,#214826,#214827,#214828,#214829,#214830,#214831,#214832,
#214833,#214834,#214835,#214836,#214837,#214838,#214839,#214840,#214841,
#214842,#214843,#214844,#214845,#214846,#214847,#214848,#214849,#214850,
#214851,#214852,#214853,#214854,#214855,#214856,#214857,#214858,#214859,
#214860,#214861,#214862,#214863,#214864,#214865,#214866,#214867,#214868,
#214869,#214870,#214871,#214872,#214873,#214874,#214875,#214876,#214877,
#214878,#214879,#214880,#214881,#214882,#214883,#214884,#214885,#214886,
#214887,#214888,#214889,#214890,#214891,#214892,#214893,#214894,#214895,
#214896,#214897,#214898,#214899,#214900,#214901,#214902,#214903,#214904,
#214905,#214906,#214907,#214908,#214909,#214910,#214911,#214912,#214913,
#214914,#214915,#214916,#214917,#214918,#214919,#214920,#214921,#214922,
#214923,#214924,#214925,#214926,#214927,#214928,#214929,#214930,#214931,
#214932,#214933,#214934,#214935,#214936,#214937,#214938,#214939,#214940,
#214941,#214942,#214943,#214944,#214945,#214946,#214947,#214948,#214949,
#214950,#214951,#214952,#214953,#214954,#214955,#214956,#214957,#214958,
#214959,#214960,#214961,#214962,#214963,#214964,#214965,#214966,#214967,
#214968,#214969,#214970,#214971,#214972,#214973,#214974,#214975,#214976,
#214977,#214978,#214979,#214980,#214981,#214982,#214983,#214984,#214985,
#214986,#214987,#214988,#214989,#214990,#214991,#214992,#214993,#214994,
#214995,#214996,#214997,#214998,#214999,#215000,#215001,#215002,#215003,
#215004,#215005,#215006,#215007,#215008,#215009,#215010,#215011,#215012,
#215013,#215014,#215015,#215016,#215017,#215018,#215019,#215020,#215021,
#215022,#215023,#215024,#215025,#215026,#215027,#215028,#215029,#215030,
#215031,#215032,#215033,#215034,#215035,#215036,#215037,#215038,#215039,
#215040,#215041,#215042,#215043,#215044,#215045,#215046,#215047,#215048,
#215049,#215050,#215051,#215052,#215053,#215054,#215055,#215056,#215057,
#215058,#215059,#215060,#215061,#215062,#215063,#215064,#215065,#215066,
#215067,#215068,#215069,#215070,#215071,#215072,#215073,#215074,#215075,
#215076,#215077,#215078,#215079,#215080,#215081,#215082,#215083,#215084,
#215085,#215086,#215087,#215088,#215089,#215090,#215091,#215092,#215093,
#215094,#215095,#215096,#215097,#215098,#215099,#215100,#215101,#215102,
#215103,#215104,#215105,#215106,#215107,#215108,#215109,#215110,#215111,
#215112,#215113,#215114,#215115,#215116,#215117,#215118,#215119,#215120,
#215121,#215122,#215123,#215124,#215125,#215126,#215127,#215128,#215129,
#215130,#215131,#215132,#215133,#215134,#215135,#215136,#215137,#215138,
#215139,#215140,#215141,#215142,#215143,#215144,#215145,#215146,#215147,
#215148,#215149,#215150,#215151,#215152,#215153,#215154,#215155,#215156,
#215157,#215158,#215159,#215160,#215161,#215162,#215163,#215164,#215165,
#215166,#215167,#215168,#215169,#215170,#215171,#215172,#215173,#215174,
#215175,#215176,#215177,#215178,#215179,#215180,#215181,#215182,#215183,
#215184,#215185,#215186,#215187,#215188,#215189,#215190,#215191,#215192,
#215193,#215194,#215195,#215196,#215197,#215198,#215199,#215200,#215201,
#215202,#215203,#215204,#215205,#215206,#215207,#215208,#215209,#215210,
#215211,#215212,#215213,#215214,#215215,#215216,#215217,#215218,#215219,
#215220,#215221,#215222,#215223,#215224,#215225,#215226,#215227,#215228,
#215229,#215230,#215231,#215232,#215233,#215234,#215235,#215236,#215237,
#215238,#215239,#215240,#215241,#215242,#215243,#215244,#215245,#215246,
#215247,#215248,#215249,#215250,#215251,#215252,#215253,#215254,#215255,
#215256,#215257,#215258,#215259,#215260,#215261,#215262,#215263,#215264,
#215265,#215266,#215267,#215268,#215269,#215270,#215271,#215272,#215273,
#215274,#215275,#215276,#215277,#215278,#215279,#215280,#215281,#215282,
#215283,#215284,#215285,#215286,#215287,#215288,#215289,#215290,#215291,
#215292,#215293,#215294,#215295,#215296,#215297,#215298,#215299,#215300,
#215301,#215302,#215303,#215304,#215305,#215306,#215307,#215308,#215309,
#215310,#215311,#215312,#215313,#215314,#215315,#215316,#215317,#215318,
#215319,#215320,#215321,#215322,#215323,#215324,#215325,#215326,#215327,
#215328,#215329,#215330,#215331,#215332,#215333,#215334,#215335,#215336,
#215337,#215338,#215339,#215340,#215341,#215342,#215343,#215344,#215345,
#215346,#215347,#215348,#215349,#215350,#215351,#215352,#215353,#215354,
#215355,#215356,#215357,#215358,#215359,#215360,#215361,#215362,#215363,
#215364,#215365,#215366,#215367,#215368,#215369,#215370,#215371,#215372,
#215373,#215374,#215375,#215376,#215377,#215378,#215379,#215380,#215381,
#215382,#215383,#215384,#215385,#215386,#215387,#215388,#215389,#215390,
#215391,#215392,#215393,#215394,#215395,#215396,#215397,#215398,#215399,
#215400,#215401,#215402,#215403,#215404,#215405,#215406,#215407,#215408,
#215409,#215410,#215411,#215412,#215413,#215414,#215415,#215416,#215417,
#215418,#215419,#215420,#215421,#215422,#215423,#215424,#215425,#215426,
#215427,#215428,#215429,#215430,#215431,#215432,#215433,#215434,#215435,
#215436,#215437,#215438,#215439,#215440,#215441,#215442,#215443,#215444,
#215445,#215446,#215447,#215448,#215449,#215450,#215451,#215452,#215453,
#215454,#215455,#215456,#215457,#215458,#215459,#215460,#215461,#215462,
#215463,#215464,#215465,#215466,#215467,#215468,#215469,#215470,#215471,
#215472,#215473,#215474,#215475,#215476,#215477,#215478,#215479,#215480,
#215481,#215482,#215483,#215484,#215485,#215486,#215487,#215488,#215489,
#215490,#215491,#215492,#215493,#215494,#215495,#215496,#215497,#215498,
#215499,#215500,#215501,#215502,#215503,#215504,#215505,#215506,#215507,
#215508,#215509,#215510,#215511,#215512,#215513,#215514,#215515,#215516,
#215517,#215518,#215519,#215520,#215521,#215522,#215523,#215524,#215525,
#215526,#215527,#215528,#215529,#215530,#215531,#215532,#215533,#215534,
#215535,#215536,#215537,#215538,#215539,#215540,#215541,#215542,#215543,
#215544,#215545,#215546,#215547,#215548,#215549,#215550,#215551,#215552,
#215553,#215554,#215555,#215556,#215557,#215558,#215559,#215560,#215561,
#215562,#215563,#215564,#215565,#215566,#215567,#215568,#215569,#215570,
#215571,#215572,#215573,#215574,#215575,#215576,#215577,#215578,#215579,
#215580,#215581,#215582,#215583,#215584,#215585,#215586,#215587,#215588,
#215589,#215590,#215591,#215592,#215593,#215594,#215595,#215596,#215597,
#215598,#215599,#215600,#215601,#215602,#215603,#215604,#215605,#215606,
#215607,#215608,#215609,#215610,#215611,#215612,#215613,#215614,#215615,
#215616,#215617,#215618,#215619,#215620,#215621,#215622,#215623,#215624,
#215625,#215626,#215627,#215628,#215629,#215630,#215631,#215632,#215633,
#215634,#215635,#215636,#215637,#215638,#215639,#215640,#215641,#215642,
#215643,#215644,#215645,#215646,#215647,#215648,#215649,#215650,#215651,
#215652,#215653,#215654,#215655,#215656,#215657,#215658,#215659,#215660,
#215661,#215662,#215663,#215664,#215665,#215666,#215667,#215668,#215669,
#215670,#215671,#215672,#215673,#215674,#215675,#215676,#215677,#215678,
#215679,#215680,#215681,#215682,#215683,#215684,#215685,#215686,#215687,
#215688,#215689,#215690,#215691,#215692,#215693,#215694,#215695,#215696,
#215697,#215698,#215699,#215700,#215701,#215702,#215703,#215704,#215705,
#215706,#215707,#215708,#215709,#215710,#215711,#215712,#215713,#215714,
#215715,#215716,#215717,#215718,#215719,#215720,#215721,#215722,#215723,
#215724,#215725,#215726,#215727,#215728,#215729,#215730,#215731,#215732,
#215733,#215734,#215735,#215736,#215737,#215738,#215739,#215740,#215741,
#215742,#215743,#215744,#215745,#215746,#215747,#215748,#215749,#215750,
#215751,#215752,#215753,#215754,#215755,#215756,#215757,#215758,#215759,
#215760,#215761,#215762,#215763,#215764,#215765,#215766,#215767,#215768,
#215769,#215770,#215771,#215772,#215773,#215774,#215775,#215776,#215777,
#215778,#215779,#215780,#215781,#215782,#215783,#215784,#215785,#215786,
#215787,#215788,#215789,#215790,#215791,#215792,#215793,#215794,#215795,
#215796,#215797,#215798,#215799,#215800,#215801,#215802,#215803,#215804,
#215805,#215806,#215807,#215808,#215809,#215810,#215811,#215812,#215813,
#215814,#215815,#215816,#215817,#215818,#215819,#215820,#215821,#215822,
#215823,#215824,#215825,#215826,#215827,#215828,#215829,#215830,#215831,
#215832,#215833,#215834,#215835,#215836,#215837,#215838,#215839,#215840,
#215841,#215842,#215843,#215844,#215845,#215846,#215847,#215848,#215849,
#215850,#215851,#215852,#215853,#215854,#215855,#215856,#215857,#215858,
#215859,#215860,#215861,#215862,#215863,#215864,#215865,#215866,#215867,
#215868,#215869,#215870,#215871,#215872,#215873,#215874,#215875,#215876,
#215877,#215878,#215879,#215880,#215881,#215882,#215883,#215884,#215885,
#215886,#215887,#215888,#215889,#215890,#215891,#215892,#215893,#215894,
#215895,#215896,#215897,#215898,#215899,#215900,#215901,#215902,#215903,
#215904,#215905,#215906,#215907,#215908,#215909,#215910,#215911,#215912,
#215913,#215914,#215915,#215916,#215917,#215918,#215919,#215920,#215921,
#215922,#215923,#215924,#215925,#215926,#215927,#215928,#215929,#215930,
#215931,#215932,#215933,#215934,#215935,#215936,#215937,#215938,#215939,
#215940,#215941,#215942,#215943,#215944,#215945,#215946,#215947,#215948,
#215949,#215950,#215951,#215952,#215953,#215954,#215955,#215956,#215957,
#215958,#215959,#215960,#215961,#215962,#215963,#215964,#215965,#215966,
#215967,#215968,#215969,#215970,#215971,#215972,#215973,#215974,#215975,
#215976,#215977,#215978,#215979,#215980,#215981,#215982,#215983,#215984,
#215985,#215986,#215987,#215988,#215989,#215990,#215991,#215992,#215993,
#215994,#215995,#215996,#215997,#215998,#215999,#216000,#216001,#216002,
#216003,#216004,#216005,#216006,#216007,#216008,#216009,#216010,#216011,
#216012,#216013,#216014,#216015,#216016,#216017,#216018,#216019,#216020,
#216021,#216022,#216023,#216024,#216025,#216026,#216027,#216028,#216029,
#216030,#216031,#216032,#216033,#216034,#216035,#216036,#216037,#216038,
#216039,#216040,#216041,#216042,#216043,#216044,#216045,#216046,#216047,
#216048,#216049,#216050,#216051,#216052,#216053,#216054,#216055,#216056,
#216057,#216058,#216059,#216060,#216061,#216062,#216063,#216064,#216065,
#216066,#216067,#216068,#216069,#216070,#216071,#216072,#216073,#216074,
#216075,#216076,#216077,#216078,#216079,#216080,#216081,#216082,#216083,
#216084,#216085,#216086,#216087,#216088,#216089,#216090,#216091,#216092,
#216093,#216094,#216095,#216096,#216097,#216098,#216099,#216100,#216101,
#216102,#216103,#216104,#216105,#216106,#216107,#216108,#216109,#216110,
#216111,#216112,#216113,#216114,#216115,#216116,#216117,#216118,#216119,
#216120,#216121,#216122,#216123,#216124,#216125,#216126,#216127,#216128,
#216129,#216130,#216131,#216132,#216133,#216134,#216135,#216136,#216137,
#216138,#216139,#216140,#216141,#216142,#216143,#216144,#216145,#216146,
#216147,#216148,#216149,#216150,#216151,#216152,#216153,#216154,#216155,
#216156,#216157,#216158,#216159,#216160,#216161,#216162,#216163,#216164,
#216165,#216166,#216167,#216168,#216169,#216170,#216171,#216172,#216173,
#216174,#216175,#216176,#216177,#216178,#216179,#216180,#216181,#216182,
#216183,#216184,#216185,#216186,#216187,#216188,#216189,#216190,#216191,
#216192,#216193,#216194,#216195,#216196,#216197,#216198,#216199,#216200,
#216201,#216202,#216203,#216204,#216205,#216206,#216207,#216208,#216209,
#216210,#216211,#216212,#216213,#216214,#216215,#216216,#216217,#216218,
#216219,#216220,#216221,#216222,#216223,#216224,#216225,#216226,#216227,
#216228,#216229,#216230,#216231,#216232,#216233,#216234,#216235,#216236,
#216237,#216238,#216239,#216240,#216241,#216242,#216243,#216244,#216245,
#216246,#216247,#216248,#216249,#216250,#216251,#216252,#216253,#216254,
#216255,#216256,#216257,#216258,#216259,#216260,#216261,#216262,#216263,
#216264,#216265,#216266,#216267,#216268,#216269,#216270,#216271,#216272,
#216273,#216274,#216275,#216276,#216277,#216278,#216279,#216280)),
 .UNSPECIFIED.,.F.,.F.,.F.,(4,4),(4,1,1,1,1,1,1,1,1,1,1,1,1,1,1,1,1,1,1,
1,1,1,1,1,1,1,1,1,1,1,1,1,1,1,1,1,1,1,1,1,1,1,1,1,1,1,1,1,1,1,1,1,1,1,1,
1,1,1,1,1,1,1,1,1,1,1,1,1,1,1,1,1,1,1,1,1,1,1,1,1,1,1,1,1,1,1,1,1,1,1,1,
1,1,1,1,1,1,1,1,1,1,1,1,1,1,1,1,1,1,1,1,1,1,1,1,1,1,1,1,1,1,1,1,1,1,1,1,
1,1,1,1,1,1,1,1,1,1,1,1,1,1,1,1,1,1,1,1,1,1,1,1,1,1,1,1,1,1,1,1,1,1,1,1,
1,1,1,1,1,1,1,1,1,1,1,1,1,1,1,1,1,1,1,1,1,1,1,1,1,1,1,1,1,1,1,1,1,1,1,1,
1,1,1,1,1,1,1,1,1,1,1,1,1,1,1,1,1,1,1,1,1,1,1,1,1,1,1,1,1,1,1,1,1,1,1,1,
1,1,1,1,1,1,1,1,1,1,1,1,1,1,1,1,1,1,1,1,1,1,1,1,1,1,1,1,1,1,1,1,1,1,1,1,
1,1,1,1,1,1,1,1,1,1,1,1,1,1,1,1,1,1,1,1,1,1,1,1,1,1,1,1,1,1,1,1,1,1,1,1,
1,1,1,1,1,1,1,1,1,1,1,1,1,1,1,1,1,1,1,1,1,1,1,1,1,1,1,1,1,1,1,1,1,1,1,1,
1,1,1,1,1,1,1,1,1,1,1,1,1,1,1,1,1,1,1,1,1,1,1,1,1,1,1,1,1,1,1,1,1,1,1,1,
1,1,1,1,1,1,1,1,1,1,1,1,1,1,1,1,1,1,1,1,1,1,1,1,1,1,1,1,1,1,1,1,1,1,1,1,
1,1,1,1,1,1,1,1,1,1,1,1,1,1,1,1,1,1,1,1,1,1,1,1,1,1,1,1,1,1,1,1,1,1,1,1,
1,1,1,1,1,1,1,1,1,1,1,1,1,1,1,1,1,1,1,1,1,1,1,1,1,1,1,1,1,1,1,1,1,1,1,1,
1,1,1,1,1,1,1,1,1,1,1,1,1,1,1,1,1,1,1,1,1,1,1,1,1,1,1,1,1,1,1,1,1,1,1,1,
1,1,1,1,1,1,1,1,1,1,1,1,1,1,1,1,1,1,1,1,1,1,1,1,1,1,1,1,1,1,1,1,1,1,1,1,
1,1,1,1,1,1,1,1,1,1,1,1,1,1,1,1,1,1,1,1,1,1,1,1,1,1,1,1,1,1,1,1,1,1,1,1,
1,1,1,1,1,1,1,1,1,1,1,1,1,1,1,1,1,1,1,1,1,1,1,1,1,1,1,1,1,1,1,1,1,1,1,1,
1,1,1,1,1,1,1,1,1,1,1,1,1,1,1,1,1,1,1,1,1,1,1,1,1,1,1,1,1,1,1,1,1,1,1,1,
1,1,1,1,1,1,1,1,1,1,1,1,1,1,1,1,1,1,1,1,1,1,1,1,1,1,1,1,1,1,1,1,1,1,1,1,
1,1,1,1,1,1,1,1,1,1,1,1,1,1,1,1,1,1,1,1,1,1,1,1,1,1,1,1,1,1,1,1,1,1,1,1,
1,1,1,1,1,1,1,1,1,1,1,1,1,1,1,1,1,1,1,1,1,1,1,1,1,1,1,1,1,1,1,1,1,1,1,1,
1,1,1,1,1,1,1,1,1,1,1,1,1,1,1,1,1,1,1,1,1,1,1,1,1,1,1,1,1,1,1,1,1,1,1,1,
1,1,1,1,1,1,1,1,1,1,1,1,1,1,1,1,1,1,1,1,1,1,1,1,1,1,1,1,1,1,1,1,1,1,1,1,
1,1,1,1,1,1,1,1,1,1,1,1,1,1,1,1,1,1,1,1,1,1,1,1,1,1,1,1,1,1,1,1,1,1,1,1,
1,1,1,1,1,1,1,1,1,1,1,1,1,1,1,1,1,1,1,1,1,1,1,1,1,1,1,1,1,1,1,1,1,1,1,1,
1,1,1,1,1,1,1,1,1,1,1,1,1,1,1,1,1,1,1,1,1,1,1,1,1,1,1,1,1,1,1,1,1,1,1,1,
1,1,1,1,1,1,1,1,1,1,1,1,1,1,1,1,1,1,1,1,1,1,1,1,1,1,1,1,1,1,1,1,1,1,1,1,
1,1,1,1,1,1,1,1,1,1,1,1,1,1,1,1,1,1,1,1,1,1,1,1,1,1,1,1,1,1,1,1,1,1,1,1,
1,1,1,1,1,1,1,1,1,1,1,1,1,1,1,1,1,1,1,1,1,1,1,1,1,1,1,1,1,1,1,1,1,1,1,1,
1,1,1,1,1,1,1,1,1,1,1,1,1,1,1,1,1,1,1,1,1,1,1,1,1,1,1,1,1,1,1,1,1,1,1,1,
1,1,1,1,1,1,1,1,1,1,1,1,1,1,1,1,1,1,1,1,1,1,1,1,1,1,1,1,1,1,1,1,1,1,1,1,
1,1,1,1,1,1,1,1,1,1,1,1,1,1,1,1,1,1,1,1,1,1,1,1,1,1,1,1,1,1,1,1,1,1,1,1,
1,1,1,1,1,1,1,1,1,1,1,1,1,1,1,1,1,1,1,1,1,1,1,1,1,1,1,1,1,1,1,1,1,1,1,1,
1,1,1,1,1,1,1,1,1,1,1,1,1,1,1,1,1,1,1,1,1,1,1,1,1,1,1,1,1,1,1,1,1,1,1,1,
1,1,1,1,1,1,1,1,1,1,1,1,1,1,1,1,1,1,1,1,1,1,1,1,1,1,1,1,1,1,1,1,1,1,1,1,
1,1,1,1,1,1,1,1,1,1,1,1,1,1,1,1,1,1,1,1,1,1,1,1,1,1,1,1,1,1,1,1,1,1,1,1,
1,1,1,1,1,1,1,1,1,1,1,1,1,1,1,1,1,1,1,1,1,1,1,1,1,1,1,1,1,1,1,1,1,1,1,1,
1,1,1,1,1,1,1,1,1,1,1,1,1,1,1,1,1,1,1,1,1,1,1,1,1,1,1,1,1,1,1,1,1,1,1,1,
1,1,1,1,1,1,1,1,1,1,1,1,1,1,1,1,1,1,1,1,1,1,1,1,1,1,1,1,1,1,1,1,1,1,1,1,
1,1,1,1,1,1,1,1,1,1,1,1,1,1,1,1,1,1,1,1,1,1,1,1,1,1,1,1,1,1,1,1,1,1,1,1,
1,1,1,1,1,1,1,1,1,1,1,1,1,1,1,1,1,1,1,1,1,1,1,1,1,1,1,1,1,1,1,1,1,1,1,1,
1,1,1,1,1,1,1,1,1,1,1,1,1,1,1,1,1,1,1,1,1,1,1,1,1,1,1,1,1,1,1,1,1,1,1,1,
1,1,1,1,1,1,1,1,1,1,1,1,1,1,1,1,1,1,1,1,1,1,1,1,1,1,1,1,1,1,1,1,1,1,1,1,
1,1,1,1,1,1,1,1,1,1,1,1,1,1,1,1,1,1,1,1,1,1,1,1,1,1,1,1,1,1,1,1,1,1,1,1,
1,1,1,1,1,1,1,1,1,1,1,1,1,1,1,1,1,1,1,1,1,1,1,1,1,1,1,1,1,1,1,1,1,1,1,1,
1,1,1,1,1,1,1,1,1,1,1,1,1,1,1,1,1,1,1,1,1,1,1,1,1,1,1,1,1,1,1,1,1,1,1,1,
1,1,1,1,1,1,1,1,1,1,1,1,1,1,1,1,1,4),(-0.000423095957202541,0.115881565465356),
(11.6153146011728,12.1152895244478,12.6151575298078,13.614893540528,14.6146295512481,
15.6143655619682,16.6141015726884,17.6138375834085,18.6135735941286,19.6133096048488,
20.6130456155689,21.612781626289,22.6125176370092,23.6122536477293,24.6119896584494,
25.6117256691696,26.6114616798897,27.6111976906098,28.6109337013299,29.6106697120501,
30.6104057227702,31.6101417334903,32.6098777442105,33.6096137549306,34.6093497656507,
35.6090857763709,36.608821787091,37.6085577978111,38.6082938085313,39.6080298192514,
40.6077658299715,41.6075018406916,42.6072378514118,43.6069738621319,44.606709872852,
45.6064458835722,46.6061818942923,47.6059179050124,48.6056539157326,49.6053899264527,
50.6051259371728,51.604861947893,52.6045979586131,53.6043339693332,54.6040699800534,
55.6038059907735,56.6035420014936,57.6032780122137,58.6030140229339,59.602750033654,
60.6024860443741,61.6022220550943,62.6019580658144,63.6016940765345,64.6014300872547,
65.6011660979748,66.6009021086949,67.6006381194151,68.6003741301352,69.6001101408553,
70.5998461515754,71.5995821622956,72.5993181730157,73.5990541837358,74.598790194456,
75.5985262051761,76.5982622158962,77.5979982266164,78.5977342373365,79.5974702480566,
80.5972062587768,81.5969422694969,82.596678280217,83.5964142909372,84.5961503016573,
85.5958863123774,86.5956223230975,87.5953583338177,88.5950943445378,89.5948303552579,
90.5945663659781,91.5943023766982,92.5940383874183,93.5937743981385,94.5935104088586,
95.5932464195787,96.5929824302989,97.592718441019,98.5924544517391,99.5921904624593,
100.591926473179,101.5916624839,102.59139849462,103.59113450534,104.59087051606,
105.59060652678,106.5903425375,107.59007854822,108.58981455894,109.589550569661,
110.589286580381,111.589022591101,112.588758601821,113.588494612541,114.588230623261,
115.587966633981,116.587702644701,117.587438655422,118.587174666142,119.586910676862,
120.586646687582,121.586382698302,122.586118709022,123.585854719742,124.585590730463,
125.585326741183,126.585062751903,127.584798762623,128.584534773343,129.584270784063,
130.584006794783,131.583742805503,132.583478816224,133.583214826944,134.582950837664,
135.582686848384,136.582422859104,137.582158869824,138.581894880544,139.581630891264,
140.581366901985,141.581102912705,142.580838923425,143.580574934145,144.580310944865,
145.580046955585,146.579782966305,147.579518977026,148.579254987746,149.578990998466,
150.578727009186,151.578463019906,152.578199030626,153.577935041346,154.577671052066,
155.577407062787,156.577143073507,157.576879084227,158.576615094947,159.576351105667,
160.576087116387,161.575823127107,162.575559137827,163.575295148548,164.575031159268,
165.574767169988,166.574503180708,167.574239191428,168.573975202148,169.573711212868,
170.573447223589,171.573183234309,172.572919245029,173.572655255749,174.572391266469,
175.572127277189,176.571863287909,177.571599298629,178.57133530935,179.57107132007,
180.57080733079,181.57054334151,182.57027935223,183.57001536295,184.56975137367,
185.56948738439,186.569223395111,187.568959405831,188.568695416551,189.568431427271,
190.568167437991,191.567903448711,192.567639459431,193.567375470152,194.567111480872,
195.566847491592,196.566583502312,197.566319513032,198.566055523752,199.565791534472,
200.565527545192,201.565263555913,202.564999566633,203.564735577353,204.564471588073,
205.564207598793,206.563943609513,207.563679620233,208.563415630954,209.563151641674,
210.562887652394,211.562623663114,212.562359673834,213.562095684554,214.561831695274,
215.561567705994,216.561303716715,217.561039727435,218.560775738155,219.560511748875,
220.560247759595,221.559983770315,222.559719781035,223.559455791755,224.559191802476,
225.558927813196,226.558663823916,227.558399834636,228.558135845356,229.557871856076,
230.557607866796,231.557343877517,232.557079888237,233.556815898957,234.556551909677,
235.556287920397,236.556023931117,237.555759941837,238.555495952557,239.555231963278,
240.554967973998,241.554703984718,242.554439995438,243.554176006158,244.553912016878,
245.553648027598,246.553384038319,247.553120049039,248.552856059759,249.552592070479,
250.552328081199,251.552064091919,252.551800102639,253.551536113359,254.55127212408,
255.5510081348,256.55074414552,257.55048015624,258.55021616696,259.54995217768,
260.5496881884,261.54942419912,262.549160209841,263.548896220561,264.548632231281,
265.548368242001,266.548104252721,267.547840263441,268.547576274161,269.547312284882,
270.547048295602,271.546784306322,272.546520317042,273.546256327762,274.545992338482,
275.545728349202,276.545464359922,277.545200370643,278.544936381363,279.544672392083,
280.544408402803,281.544144413523,282.543880424243,283.543616434963,284.543352445683,
285.543088456404,286.542824467124,287.542560477844,288.542296488564,289.542032499284,
290.541768510004,291.541504520724,292.541240531445,293.540976542165,294.540712552885,
295.540448563605,296.540184574325,297.539920585045,298.539656595765,299.539392606485,
300.539128617206,301.538864627926,302.538600638646,303.538336649366,304.538072660086,
305.537808670806,306.537544681526,307.537280692246,308.537016702967,309.536752713687,
310.536488724407,311.536224735127,312.535960745847,313.535696756567,314.535432767287,
315.535168778008,316.534904788728,317.534640799448,318.534376810168,319.534112820888,
320.533848831608,321.533584842328,322.533320853048,323.533056863769,324.532792874489,
325.532528885209,326.532264895929,327.532000906649,328.531736917369,329.531472928089,
330.53120893881,331.53094494953,332.53068096025,333.53041697097,334.53015298169,
335.52988899241,336.52962500313,337.52936101385,338.529097024571,339.528833035291,
340.528569046011,341.528305056731,342.528041067451,343.527777078171,344.527513088891,
345.527249099611,346.526985110332,347.526721121052,348.526457131772,349.526193142492,
350.525929153212,351.525665163932,352.525401174652,353.525137185373,354.524873196093,
355.524609206813,356.524345217533,357.524081228253,358.523817238973,359.523553249693,
360.523289260413,361.523025271134,362.522761281854,363.522497292574,364.522233303294,
365.521969314014,366.521705324734,367.521441335454,368.521177346175,369.520913356895,
370.520649367615,371.520385378335,372.520121389055,373.519857399775,374.519593410495,
375.519329421215,376.519065431936,377.518801442656,378.518537453376,379.518273464096,
380.518009474816,381.517745485536,382.517481496256,383.517217506976,384.516953517697,
385.516689528417,386.516425539137,387.516161549857,388.515897560577,389.515633571297,
390.515369582017,391.515105592737,392.514841603458,393.514577614178,394.514313624898,
395.514049635618,396.513785646338,397.513521657058,398.513257667778,399.512993678499,
400.512729689219,401.512465699939,402.512201710659,403.511937721379,404.511673732099,
405.511409742819,406.511145753539,407.51088176426,408.51061777498,409.5103537857,
410.51008979642,411.50982580714,412.50956181786,413.50929782858,414.509033839301,
415.508769850021,416.508505860741,417.508241871461,418.507977882181,419.507713892901,
420.507449903621,421.507185914341,422.506921925062,423.506657935782,424.506393946502,
425.506129957222,426.505865967942,427.505601978662,428.505337989382,429.505074000102,
430.504810010823,431.504546021543,432.504282032263,433.504018042983,434.503754053703,
435.503490064423,436.503226075143,437.502962085864,438.502698096584,439.502434107304,
440.502170118024,441.501906128744,442.501642139464,443.501378150184,444.501114160904,
445.500850171625,446.500586182345,447.500322193065,448.500058203785,449.499794214505,
450.499530225225,451.499266235945,452.499002246665,453.498738257386,454.498474268106,
455.498210278826,456.497946289546,457.497682300266,458.497418310986,459.497154321706,
460.496890332427,461.496626343147,462.496362353867,463.496098364587,464.495834375307,
465.495570386027,466.495306396747,467.495042407467,468.494778418188,469.494514428908,
470.494250439628,471.493986450348,472.493722461068,473.493458471788,474.493194482508,
475.492930493229,476.492666503949,477.492402514669,478.492138525389,479.491874536109,
480.491610546829,481.491346557549,482.491082568269,483.49081857899,484.49055458971,
485.49029060043,486.49002661115,487.48976262187,488.48949863259,489.48923464331,
490.48897065403,491.488706664751,492.488442675471,493.488178686191,494.487914696911,
495.487650707631,496.487386718351,497.487122729071,498.486858739792,499.486594750512,
500.486330761232,501.486066771952,502.485802782672,503.485538793392,504.485274804112,
505.485010814832,506.484746825553,507.484482836273,508.484218846993,509.483954857713,
510.483690868433,511.483426879153,512.483162889873,513.482898900594,514.482634911314,
515.482370922034,516.482106932754,517.481842943474,518.481578954194,519.481314964914,
520.481050975635,521.480786986355,522.480522997075,523.480259007795,524.479995018515,
525.479731029235,526.479467039955,527.479203050675,528.478939061396,529.478675072116,
530.478411082836,531.478147093556,532.477883104276,533.477619114996,534.477355125716,
535.477091136436,536.476827147157,537.476563157877,538.476299168597,539.476035179317,
540.475771190037,541.475507200757,542.475243211477,543.474979222197,544.474715232918,
545.474451243638,546.474187254358,547.473923265078,548.473659275798,549.473395286518,
550.473131297238,551.472867307958,552.472603318679,553.472339329399,554.472075340119,
555.471811350839,556.471547361559,557.471283372279,558.471019382999,559.47075539372,
560.47049140444,561.47022741516,562.46996342588,563.4696994366,564.46943544732,
565.46917145804,566.46890746876,567.468643479481,568.468379490201,569.468115500921,
570.467851511641,571.467587522361,572.467323533081,573.467059543801,574.466795554521,
575.466531565242,576.466267575962,577.466003586682,578.465739597402,579.465475608122,
580.465211618842,581.464947629562,582.464683640283,583.464419651003,584.464155661723,
585.463891672443,586.463627683163,587.463363693883,588.463099704603,589.462835715323,
590.462571726044,591.462307736764,592.462043747484,593.461779758204,594.461515768924,
595.461251779644,596.460987790364,597.460723801085,598.460459811805,599.460195822525,
600.459931833245,601.459667843965,602.459403854685,603.459139865405,604.458875876125,
605.458611886846,606.458347897566,607.458083908286,608.457819919006,609.457555929726,
610.457291940446,611.457027951166,612.456763961887,613.456499972607,614.456235983327,
615.455971994047,616.455708004767,617.455444015487,618.455180026207,619.454916036927,
620.454652047648,621.454388058368,622.454124069088,623.453860079808,624.453596090528,
625.453332101248,626.453068111968,627.452804122688,628.452540133409,629.452276144129,
630.452012154849,631.451748165569,632.451484176289,633.451220187009,634.450956197729,
635.450692208449,636.45042821917,637.45016422989,638.44990024061,639.44963625133,
640.44937226205,641.44910827277,642.44884428349,643.448580294211,644.448316304931,
645.448052315651,646.447788326371,647.447524337091,648.447260347811,649.446996358531,
650.446732369251,651.446468379972,652.446204390692,653.445940401412,654.445676412132,
655.445412422852,656.445148433572,657.444884444292,658.444620455012,659.444356465733,
660.444092476453,661.443828487173,662.443564497893,663.443300508613,664.443036519333,
665.442772530053,666.442508540774,667.442244551494,668.441980562214,669.441716572934,
670.441452583654,671.441188594374,672.440924605094,673.440660615815,674.440396626535,
675.440132637255,676.439868647975,677.439604658695,678.439340669415,679.439076680135,
680.438812690855,681.438548701576,682.438284712296,683.438020723016,684.437756733736,
685.437492744456,686.437228755176,687.436964765896,688.436700776616,689.436436787337,
690.436172798057,691.435908808777,692.435644819497,693.435380830217,694.435116840937,
695.434852851657,696.434588862377,697.434324873098,698.434060883818,699.433796894538,
700.433532905258,701.433268915978,702.433004926698,703.432740937418,704.432476948139,
705.432212958859,706.431948969579,707.431684980299,708.431420991019,709.431157001739,
710.430893012459,711.430629023179,712.4303650339,713.43010104462,714.42983705534,
715.42957306606,716.42930907678,717.4290450875,718.42878109822,719.42851710894,
720.428253119661,721.427989130381,722.427725141101,723.427461151821,724.427197162541,
725.426933173261,726.426669183981,727.426405194702,728.426141205422,729.425877216142,
730.425613226862,731.425349237582,732.425085248302,733.424821259022,734.424557269742,
735.424293280463,736.424029291183,737.423765301903,738.423501312623,739.423237323343,
740.422973334063,741.422709344783,742.422445355504,743.422181366224,744.421917376944,
745.421653387664,746.421389398384,747.421125409104,748.420861419824,749.420597430544,
750.420333441265,751.420069451985,752.419805462705,753.419541473425,754.419277484145,
755.419013494865,756.418749505585,757.418485516306,758.418221527026,759.417957537746,
760.417693548466,761.417429559186,762.417165569906,763.416901580626,764.416637591346,
765.416373602067,766.416109612787,767.415845623507,768.415581634227,769.415317644947,
770.415053655667,771.414789666387,772.414525677107,773.414261687828,774.413997698548,
775.413733709268,776.413469719988,777.413205730708,778.412941741428,779.412677752148,
780.412413762868,781.412149773589,782.411885784309,783.411621795029,784.411357805749,
785.411093816469,786.410829827189,787.410565837909,788.41030184863,789.41003785935,
790.40977387007,791.40950988079,792.40924589151,793.40898190223,794.40871791295,
795.40845392367,796.408189934391,797.407925945111,798.407661955831,799.407397966551,
800.407133977271,801.406869987991,802.406605998711,803.406342009432,804.406078020152,
805.405814030872,806.405550041592,807.405286052312,808.405022063032,809.404758073752,
810.404494084472,811.404230095193,812.403966105913,813.403702116633,814.403438127353,
815.403174138073,816.402910148793,817.402646159513,818.402382170234,819.402118180954,
820.401854191674,821.401590202394,822.401326213114,823.401062223834,824.400798234554,
825.400534245274,826.400270255995,827.400006266715,828.399742277435,829.399478288155,
830.399214298875,831.398950309595,832.398686320315,833.398422331035,834.398158341756,
835.397894352476,836.397630363196,837.397366373916,838.397102384636,839.396838395356,
840.396574406076,841.396310416796,842.396046427517,843.395782438237,844.395518448957,
845.395254459677,846.394990470397,847.394726481117,848.394462491837,849.394198502558,
850.393934513278,851.393670523998,852.393406534718,853.393142545438,854.392878556158,
855.392614566878,856.392350577598,857.392086588319,858.391822599039,859.391558609759,
860.391294620479,861.391030631199,862.390766641919,863.390502652639,864.390238663359,
865.38997467408,866.3897106848,867.38944669552,868.38918270624,869.38891871696,
870.38865472768,871.3883907384,872.388126749121,873.387862759841,874.387598770561,
875.387334781281,876.387070792001,877.386806802721,878.386542813441,879.386278824161,
880.386014834882,881.385750845602,882.385486856322,883.385222867042,884.384958877762,
885.384694888482,886.384430899202,887.384166909923,888.383902920643,889.383638931363,
890.383374942083,891.383110952803,892.382846963523,893.382582974243,894.382318984963,
895.382054995684,896.381791006404,897.381527017124,898.381263027844,899.380999038564,
900.380735049284,901.380471060004,902.380207070725,903.379943081445,904.379679092165,
905.379415102885,906.379151113605,907.378887124325,908.378623135045,909.378359145765,
910.378095156486,911.377831167206,912.377567177926,913.377303188646,914.377039199366,
915.376775210086,916.376511220806,917.376247231526,918.375983242247,919.375719252967,
920.375455263687,921.375191274407,922.374927285127,923.374663295847,924.374399306567,
925.374135317287,926.373871328008,927.373607338728,928.373343349448,929.373079360168,
930.372815370888,931.372551381608,932.372287392328,933.372023403049,934.371759413769,
935.371495424489,936.371231435209,937.370967445929,938.370703456649,939.370439467369,
940.370175478089,941.36991148881,942.36964749953,943.36938351025,944.36911952097,
945.36885553169,946.36859154241,947.36832755313,948.368063563851,949.367799574571,
950.367535585291,951.367271596011,952.367007606731,953.366743617451,954.366479628171,
955.366215638891,956.365951649612,957.365687660332,958.365423671052,959.365159681772,
960.364895692492,961.364631703212,962.364367713932,963.364103724653,964.363839735373,
965.363575746093,966.363311756813,967.363047767533,968.362783778253,969.362519788973,
970.362255799693,971.361991810414,972.361727821134,973.361463831854,974.361199842574,
975.360935853294,976.360671864014,977.360407874734,978.360143885454,979.359879896175,
980.359615906895,981.359351917615,982.359087928335,983.358823939055,984.358559949775,
985.358295960495,986.358031971215,987.357767981936,988.357503992656,989.357240003376,
990.356976014096,991.356712024816,992.356448035536,993.356184046256,994.355920056977,
995.355656067697,996.355392078417,997.355128089137,998.354864099857,999.354600110577,
1000.3543361213,1001.35407213202,1002.35380814274,1003.35354415346,1004.35328016418,
1005.3530161749,1006.35275218562,1007.35248819634,1008.35222420706,1009.35196021778,
1010.3516962285,1011.35143223922,1012.35116824994,1013.35090426066,1014.35064027138,
1015.3503762821,1016.35011229282,1017.34984830354,1018.34958431426,1019.34932032498,
1020.3490563357,1021.34879234642,1022.34852835714,1023.34826436786,1024.34800037858,
1025.3477363893,1026.34747240002,1027.34720841074,1028.34694442146,1029.34668043218,
1030.3464164429,1031.34615245362,1032.34588846434,1033.34562447506,1034.34536048578,
1035.3450964965,1036.34483250722,1037.34456851794,1038.34430452866,1039.34404053938,
1040.3437765501,1041.34351256082,1042.34324857154,1043.34298458226,1044.34272059298,
1045.3424566037,1046.34219261442,1047.34192862514,1048.34166463586,1049.34140064658,
1050.3411366573,1051.34087266802,1052.34060867874,1053.34034468946,1054.34008070018,
1055.3398167109,1056.33955272162,1057.33928873234,1058.33902474307,1059.33876075378,
1060.33849676451,1061.33823277523,1062.33796878595,1063.33770479667,1064.33744080739,
1065.33717681811,1066.33691282883,1067.33664883955,1068.33638485027,1069.33612086099,
1070.33585687171,1071.33559288243,1072.33532889315,1073.33506490387,1074.33480091459,
1075.33453692531,1076.33427293603,1077.33400894675,1078.33374495747,1079.33348096819,
1080.33321697891,1081.33295298963,1082.33268900035,1083.33242501107,1084.33216102179,
1085.33189703251,1086.33163304323,1087.33136905395,1088.33110506467,1089.33084107539,
1090.33057708611,1091.33031309683,1092.33004910755,1093.32978511827,1094.32952112899,
1095.32925713971,1096.32899315043,1097.32872916115,1098.32846517187,1099.32820118259,
1100.32793719331,1101.32767320403,1102.32740921475,1103.32714522547,1104.32688123619,
1105.32661724691,1106.32635325763,1107.32608926835,1108.32582527907,1109.32556128979,
1110.32529730051,1111.32503331123,1112.32476932195,1113.32450533267,1114.32424134339,
1115.32397735411,1116.32371336483,1117.32344937555,1118.32318538627,1119.32292139699,
1120.32265740771,1121.32239341843,1122.32212942915,1123.32186543987,1124.32160145059,
1125.32133746131,1126.32107347203,1127.32080948275,1128.32054549347,1129.32028150419,
1130.32001751491,1131.31975352563,1132.31948953635,1133.31922554707,1134.31896155779,
1135.31869756852,1136.31843357924,1137.31816958996,1138.31790560068,1139.3176416114,
1140.31737762212,1141.31711363284,1142.31684964356,1143.31658565428,1144.316321665,
1145.31605767572,1146.31579368644,1147.31552969716,1148.31526570788,1149.3150017186,
1150.31473772932,1151.31447374004,1152.31420975076,1153.31394576148,1154.3136817722,
1155.31341778292,1156.31315379364,1157.31288980436,1158.31262581508,1159.3123618258,
1160.31209783652,1161.31183384724,1162.31156985796,1163.31130586868,1164.3110418794,
1165.31077789012,1166.31051390084,1167.31024991156,1168.30998592228,1169.309721933,
1170.30945794372,1171.30919395444,1172.30892996516,1173.30866597588,1174.3084019866,
1175.30813799732,1176.30787400804,1177.30761001876,1178.30734602948,1179.3070820402,
1180.30681805092,1181.30655406164,1182.30629007236,1183.30602608308,1184.3057620938,
1185.30549810452,1186.30523411524,1187.30497012596,1188.30470613668,1189.3044421474,
1190.30417815812,1191.30391416884,1192.30365017956,1193.30338619028,1194.303122201,
1195.30285821172,1196.30259422244,1197.30233023316,1198.30206624388,1199.3018022546,
1200.30153826532,1201.30127427604,1202.30101028676,1203.30074629748,1204.3004823082,
1205.30021831892,1206.29995432964,1207.29969034036,1208.29942635108,1209.2991623618,
1210.29889837252,1211.29863438324,1212.29837039397,1213.29810640469,1214.29784241541,
1215.29757842613,1216.29731443685,1217.29705044757,1218.29678645829,1219.29652246901,
1220.29625847973,1221.29599449045,1222.29573050117,1223.29546651189,1224.29520252261,
1225.29493853333,1226.29467454405,1227.29441055477,1228.29414656549,1229.29388257621,
1230.29361858693,1231.29335459765,1232.29309060837,1233.29282661909,1234.29256262981,
1235.29229864053,1236.29203465125,1237.29177066197,1238.29150667269,1239.29124268341,
1240.29097869413,1241.29071470485,1242.29045071557,1243.29018672629,1244.28992273701,
1245.28965874773,1246.28939475845,1247.28913076917,1248.28886677989,1249.28860279061,
1250.28833880133,1251.28807481205,1252.28781082277,1253.28754683349,1254.28728284421,
1255.28701885493,1256.28675486565,1257.28649087637,1258.28622688709,1259.28596289781,
1260.28569890853,1261.28543491925,1262.28517092997,1263.28490694069,1264.28464295141,
1265.28437896213,1266.28411497285,1267.28385098357,1268.28358699429,1269.28332300501,
1270.28305901573,1271.28279502645,1272.28253103717,1273.28226704789,1274.28200305861,
1275.28173906933,1276.28147508005,1277.28121109077,1278.28094710149,1279.28068311221,
1280.28041912293,1281.28015513365,1282.27989114437,1283.27962715509,1284.27936316581,
1285.27909917653,1286.27883518725,1287.27857119797,1288.2783072087,1289.27804321942,
1290.27777923014,1291.27751524086,1292.27725125158,1293.2769872623,1294.27672327302,
1295.27645928374,1296.27619529446,1297.27593130518,1298.2756673159,1299.27540332662,
1300.27513933734,1301.27487534806,1302.27461135878,1303.2743473695,1304.27408338022,
1305.27381939094,1306.27355540166,1307.27329141238,1308.2730274231,1309.27276343382,
1310.27249944454,1311.27223545526,1312.27197146598,1313.2717074767,1314.27144348742,
1315.27117949814,1316.27091550886,1317.27065151958,1318.2703875303,1319.27012354102,
1320.26985955174,1321.26959556246,1322.26933157318,1323.2690675839,1324.26880359462,
1325.26853960534,1326.26827561606,1327.26801162678,1328.2677476375,1329.26748364822,
1330.26721965894,1331.26695566966,1332.26669168038,1333.2664276911,1334.26616370182,
1335.26589971254,1336.26563572326,1337.26537173398,1338.2651077447,1339.26484375542,
1340.26457976614,1341.26431577686,1342.26405178758,1343.2637877983,1344.26352380902,
1345.26325981974,1346.26299583046,1347.26273184118,1348.2624678519,1349.26220386262,
1350.26193987334,1351.26167588406,1352.26141189478,1353.2611479055,1354.26088391622,
1355.26061992694,1356.26035593766,1357.26009194838,1358.2598279591,1359.25956396982,
1360.25929998054,1361.25903599126,1362.25877200198,1363.2585080127,1364.25824402343,
1365.25798003415,1366.25771604487,1367.25745205559,1368.25718806631,1369.25692407703,
1370.25666008775,1371.25639609847,1372.25613210919,1373.25586811991,1374.25560413063,
1375.25534014135,1376.25507615207,1377.25481216279,1378.25454817351,1379.25428418423,
1380.25402019495,1381.25375620567,1382.25349221639,1383.25322822711,1384.25296423783,
1385.25270024855,1386.25243625927,1387.25217226999,1388.25190828071,1389.25164429143,
1390.25138030215,1391.25111631287,1392.25085232359,1393.25058833431,1394.25032434503,
1395.25006035575,1396.24979636647,1397.24953237719,1398.24926838791,1399.24900439863,
1400.24874040935,1401.24847642007,1402.24821243079,1403.24794844151,1404.24768445223,
1405.24742046295,1406.24715647367,1407.24689248439,1408.24662849511,1409.24636450583,
1410.24610051655,1411.24583652727,1412.24557253799,1413.24530854871,1414.24504455943,
1415.24478057015,1416.24451658087,1417.24425259159,1418.24398860231,1419.24372461303,
1420.24346062375,1421.24319663447,1422.24293264519,1423.24266865591,1424.24240466663,
1425.24214067735,1426.24187668807,1427.24161269879,1428.24134870951,1429.24108472023,
1430.24082073095,1431.24055674167,1432.24029275239,1433.24002876311,1434.23976477383,
1435.23950078455,1436.23923679527,1437.23897280599,1438.23870881671,1439.23844482743,
1440.23818083815,1441.23791684888,1442.2376528596,1443.23738887032,1444.23712488104,
1445.23686089176,1446.23659690248,1447.2363329132,1448.23606892392,1449.23580493464,
1450.23554094536,1451.23527695608,1452.2350129668,1453.23474897752,1454.23448498824,
1455.23422099896,1456.23395700968,1457.2336930204,1458.23342903112,1459.23316504184,
1460.23290105256,1461.23263706328,1462.232373074,1463.23210908472,1464.23184509544,
1465.23158110616,1466.23131711688,1467.2310531276,1468.23078913832,1469.23052514904,
1470.23026115976,1471.22999717048,1472.2297331812,1473.22946919192,1474.22920520264,
1475.22894121336,1476.22867722408,1477.2284132348,1478.22814924552,1479.22788525624,
1480.22762126696,1481.22735727768,1482.2270932884,1483.22682929912,1484.22656530984,
1485.22630132056,1486.22603733128,1487.225773342,1488.22550935272,1489.22524536344,
1490.22498137416,1491.22471738488,1492.2244533956,1493.22418940632,1494.22392541704,
1495.22366142776,1496.22339743848,1497.2231334492,1498.22286945992,1499.22260547064,
1500.22234148136,1501.22207749208,1502.2218135028,1503.22154951352,1504.22128552424,
1505.22102153496,1506.22075754568,1507.2204935564,1508.22022956712,1509.21996557784,
1510.21970158856,1511.21943759928,1512.21917361,1513.21890962072,1514.21864563144,
1515.21838164216,1516.21811765288,1517.21785366361,1518.21758967433,1519.21732568505,
1520.21706169577,1521.21679770649,1522.21653371721,1523.21626972793,1524.21600573865,
1525.21574174937,1526.21547776009,1527.21521377081,1528.21494978153,1529.21468579225,
1530.21442180297,1531.21415781369,1532.21389382441,1533.21362983513,1534.21336584585,
1535.21310185657,1536.21283786729,1537.21257387801,1538.21230988873,1539.21204589945,
1540.21178191017,1541.21151792089,1542.21125393161,1543.21098994233,1544.21072595305,
1545.21046196377,1546.21019797449,1547.20993398521,1548.20966999593,1549.20940600665,
1550.20914201737,1551.20887802809,1552.20861403881,1553.20835004953,1554.20808606025,
1555.20782207097,1556.20755808169,1557.20729409241,1558.20703010313,1559.20676611385,
1560.20650212457,1561.20623813529,1562.20597414601,1563.20571015673,1564.20544616745,
1565.20518217817,1566.20491818889,1567.20465419961,1568.20439021033,1569.20412622105,
1570.20386223177,1571.20359824249,1572.20333425321,1573.20307026393,1574.20280627465,
1575.20254228537,1576.20227829609,1577.20201430681,1578.20175031753,1579.20148632825,
1580.20122233897,1581.20095834969,1582.20069436041,1583.20043037113,1584.20016638185,
1585.19990239257,1586.19963840329,1587.19937441401,1588.19911042473,1589.19884643545,
1590.19858244617,1591.19831845689,1592.19805446761,1593.19779047834,1594.19752648906,
1595.19726249978,1596.1969985105,1597.19673452122,1598.19647053194,1599.19620654266,
1600.19594255338,1601.1956785641,1602.19541457482,1603.19515058554,1604.19488659626,
1605.19462260698,1606.1943586177,1607.19409462842,1608.19383063914,1609.19356664986,
1610.19330266058,1611.1930386713,1612.19277468202,1613.19251069274,1614.19224670346,
1615.19198271418,1616.1917187249,1617.19145473562,1618.19119074634,1619.19092675706,
1620.19066276778,1621.1903987785,1622.19013478922,1623.18987079994,1624.18960681066,
1625.18934282138,1626.1890788321,1627.18881484282,1628.18855085354,1629.18828686426,
1630.18802287498,1631.1877588857,1632.18749489642,1633.18723090714,1634.18696691786,
1635.18670292858,1636.1864389393,1637.18617495002,1638.18591096074,1639.18564697146,
1640.18538298218,1641.1851189929,1642.18485500362,1643.18459101434,1644.18432702506,
1645.18406303578,1646.1837990465,1647.18353505722,1648.18327106794,1649.18300707866,
1650.18274308938,1651.1824791001,1652.18221511082,1653.18195112154,1654.18168713226,
1655.18142314298,1656.1811591537,1657.18089516442,1658.18063117514,1659.18036718586,
1660.18010319658,1661.1798392073,1662.17957521802,1663.17931122874,1664.17904723946,
1665.17878325018,1666.1785192609,1667.17825527162,1668.17799128234,1669.17772729307,
1670.17746330379,1671.17719931451,1672.17693532523,1673.17667133595,1674.17640734667,
1675.17614335739,1676.17587936811,1677.17561537883,1678.17535138955,1679.17508740027,
1680.17482341099,1681.17455942171,1682.17429543243,1683.17403144315,1684.17376745387,
1685.17350346459,1686.17323947531,1687.17297548603,1688.17271149675,1689.17244750747,
1690.17218351819,1691.17191952891,1692.17165553963,1693.17139155035,1694.17112756107,
1695.17086357179,1696.17059958251,1697.17033559323,1698.17007160395,1699.16980761467,
1700.16954362539,1700.66941163075,1701.16959429301),.UNSPECIFIED.);
#50=B_SPLINE_SURFACE_WITH_KNOTS('',3,3,((#218357,#218358,#218359,#218360,
#218361,#218362,#218363,#218364,#218365,#218366,#218367,#218368,#218369,
#218370,#218371,#218372,#218373,#218374,#218375,#218376,#218377,#218378,
#218379,#218380,#218381,#218382,#218383,#218384,#218385,#218386,#218387,
#218388,#218389,#218390,#218391,#218392,#218393,#218394,#218395,#218396,
#218397,#218398,#218399,#218400,#218401,#218402,#218403,#218404,#218405,
#218406,#218407,#218408,#218409,#218410,#218411,#218412,#218413,#218414,
#218415,#218416,#218417,#218418,#218419,#218420,#218421,#218422,#218423,
#218424,#218425,#218426,#218427,#218428,#218429,#218430,#218431,#218432,
#218433,#218434,#218435,#218436,#218437,#218438,#218439,#218440,#218441,
#218442,#218443,#218444,#218445,#218446,#218447,#218448,#218449,#218450,
#218451,#218452,#218453,#218454,#218455,#218456,#218457,#218458,#218459,
#218460,#218461,#218462,#218463,#218464,#218465,#218466,#218467,#218468,
#218469,#218470,#218471,#218472,#218473,#218474,#218475,#218476,#218477,
#218478,#218479,#218480,#218481,#218482,#218483,#218484,#218485,#218486,
#218487,#218488,#218489,#218490,#218491,#218492,#218493,#218494,#218495,
#218496,#218497,#218498,#218499,#218500,#218501,#218502,#218503,#218504,
#218505,#218506,#218507,#218508,#218509,#218510,#218511,#218512,#218513,
#218514,#218515,#218516,#218517,#218518,#218519,#218520,#218521,#218522,
#218523,#218524,#218525,#218526,#218527,#218528,#218529,#218530,#218531,
#218532,#218533,#218534,#218535,#218536,#218537,#218538,#218539,#218540,
#218541,#218542,#218543,#218544,#218545,#218546,#218547,#218548,#218549,
#218550,#218551,#218552,#218553,#218554,#218555,#218556,#218557,#218558,
#218559,#218560,#218561,#218562,#218563,#218564,#218565,#218566,#218567,
#218568,#218569,#218570,#218571,#218572,#218573,#218574,#218575,#218576,
#218577,#218578,#218579,#218580,#218581,#218582,#218583,#218584,#218585,
#218586,#218587,#218588,#218589,#218590,#218591,#218592,#218593,#218594,
#218595,#218596,#218597,#218598,#218599,#218600,#218601,#218602,#218603,
#218604,#218605,#218606,#218607,#218608,#218609,#218610,#218611,#218612,
#218613,#218614,#218615,#218616,#218617,#218618,#218619,#218620,#218621,
#218622,#218623,#218624,#218625,#218626,#218627,#218628,#218629,#218630,
#218631,#218632,#218633,#218634,#218635,#218636,#218637,#218638,#218639,
#218640,#218641,#218642,#218643,#218644,#218645,#218646,#218647,#218648,
#218649,#218650,#218651,#218652,#218653,#218654,#218655,#218656,#218657,
#218658,#218659,#218660,#218661,#218662,#218663,#218664,#218665,#218666,
#218667,#218668,#218669,#218670,#218671,#218672,#218673,#218674,#218675,
#218676,#218677,#218678,#218679,#218680,#218681,#218682,#218683,#218684,
#218685,#218686,#218687,#218688,#218689,#218690,#218691,#218692,#218693,
#218694,#218695,#218696,#218697,#218698,#218699,#218700,#218701,#218702,
#218703,#218704,#218705,#218706,#218707,#218708,#218709,#218710,#218711,
#218712,#218713,#218714,#218715,#218716,#218717,#218718,#218719,#218720,
#218721,#218722,#218723,#218724,#218725,#218726,#218727,#218728,#218729,
#218730,#218731,#218732,#218733,#218734,#218735,#218736,#218737,#218738,
#218739,#218740,#218741,#218742,#218743,#218744,#218745,#218746,#218747,
#218748,#218749,#218750,#218751,#218752,#218753,#218754,#218755,#218756,
#218757,#218758,#218759,#218760,#218761,#218762,#218763,#218764,#218765,
#218766,#218767,#218768,#218769,#218770,#218771,#218772,#218773,#218774,
#218775,#218776,#218777,#218778,#218779,#218780,#218781,#218782,#218783,
#218784,#218785,#218786,#218787,#218788,#218789,#218790,#218791,#218792,
#218793,#218794,#218795,#218796,#218797,#218798,#218799,#218800,#218801,
#218802,#218803,#218804,#218805,#218806,#218807,#218808,#218809,#218810,
#218811,#218812,#218813,#218814,#218815,#218816,#218817,#218818,#218819,
#218820,#218821,#218822,#218823,#218824,#218825,#218826,#218827,#218828,
#218829,#218830,#218831,#218832,#218833,#218834,#218835,#218836,#218837,
#218838,#218839,#218840,#218841,#218842,#218843,#218844,#218845,#218846,
#218847,#218848,#218849,#218850,#218851,#218852,#218853,#218854,#218855,
#218856,#218857,#218858,#218859,#218860,#218861,#218862,#218863,#218864,
#218865,#218866,#218867,#218868,#218869,#218870,#218871,#218872,#218873,
#218874,#218875,#218876,#218877,#218878,#218879,#218880,#218881,#218882,
#218883,#218884,#218885,#218886,#218887,#218888,#218889,#218890,#218891,
#218892,#218893,#218894,#218895,#218896,#218897,#218898,#218899,#218900,
#218901,#218902,#218903,#218904,#218905,#218906,#218907,#218908,#218909,
#218910,#218911,#218912,#218913,#218914,#218915,#218916,#218917,#218918,
#218919,#218920,#218921,#218922,#218923,#218924,#218925,#218926,#218927,
#218928,#218929,#218930,#218931,#218932,#218933,#218934,#218935,#218936,
#218937,#218938,#218939,#218940,#218941,#218942,#218943,#218944,#218945,
#218946,#218947,#218948,#218949,#218950,#218951,#218952,#218953,#218954,
#218955,#218956,#218957,#218958,#218959,#218960,#218961,#218962,#218963,
#218964,#218965,#218966,#218967,#218968,#218969,#218970,#218971,#218972,
#218973,#218974,#218975,#218976,#218977,#218978,#218979,#218980,#218981,
#218982,#218983,#218984,#218985,#218986,#218987,#218988,#218989,#218990,
#218991,#218992,#218993,#218994,#218995,#218996,#218997,#218998,#218999,
#219000,#219001,#219002,#219003,#219004,#219005,#219006,#219007,#219008,
#219009,#219010,#219011,#219012,#219013,#219014,#219015,#219016,#219017,
#219018,#219019,#219020,#219021,#219022,#219023,#219024,#219025,#219026,
#219027,#219028,#219029,#219030,#219031,#219032,#219033,#219034,#219035,
#219036,#219037,#219038,#219039,#219040,#219041,#219042,#219043,#219044,
#219045,#219046,#219047,#219048,#219049,#219050,#219051,#219052,#219053,
#219054,#219055,#219056,#219057,#219058,#219059,#219060,#219061,#219062,
#219063,#219064,#219065,#219066,#219067,#219068,#219069,#219070,#219071,
#219072,#219073,#219074,#219075,#219076,#219077,#219078,#219079,#219080,
#219081,#219082,#219083,#219084,#219085,#219086,#219087,#219088,#219089,
#219090,#219091,#219092,#219093,#219094,#219095,#219096,#219097,#219098,
#219099,#219100,#219101,#219102,#219103,#219104,#219105,#219106,#219107,
#219108,#219109,#219110,#219111,#219112,#219113,#219114,#219115,#219116,
#219117,#219118,#219119,#219120,#219121,#219122,#219123,#219124,#219125,
#219126,#219127,#219128,#219129,#219130,#219131,#219132,#219133,#219134,
#219135,#219136,#219137,#219138,#219139,#219140,#219141,#219142,#219143,
#219144,#219145,#219146,#219147,#219148,#219149,#219150,#219151,#219152,
#219153,#219154,#219155,#219156,#219157,#219158,#219159,#219160,#219161,
#219162,#219163,#219164,#219165,#219166,#219167,#219168,#219169,#219170,
#219171,#219172,#219173,#219174,#219175,#219176,#219177,#219178,#219179,
#219180,#219181,#219182,#219183,#219184,#219185,#219186,#219187,#219188,
#219189,#219190,#219191,#219192,#219193,#219194,#219195,#219196,#219197,
#219198,#219199,#219200,#219201,#219202,#219203,#219204,#219205,#219206,
#219207,#219208,#219209,#219210,#219211,#219212,#219213,#219214,#219215,
#219216,#219217,#219218,#219219,#219220,#219221,#219222,#219223,#219224,
#219225,#219226,#219227,#219228,#219229,#219230,#219231,#219232,#219233,
#219234,#219235,#219236,#219237,#219238,#219239,#219240,#219241,#219242,
#219243,#219244,#219245,#219246,#219247,#219248,#219249,#219250,#219251,
#219252,#219253,#219254,#219255,#219256,#219257,#219258,#219259,#219260,
#219261,#219262,#219263,#219264,#219265,#219266,#219267,#219268,#219269,
#219270,#219271,#219272,#219273,#219274,#219275,#219276,#219277,#219278,
#219279,#219280,#219281,#219282,#219283,#219284,#219285,#219286,#219287,
#219288,#219289,#219290,#219291,#219292,#219293,#219294,#219295,#219296,
#219297,#219298,#219299,#219300,#219301,#219302,#219303,#219304,#219305,
#219306,#219307,#219308,#219309,#219310,#219311,#219312,#219313,#219314,
#219315,#219316,#219317,#219318,#219319,#219320,#219321,#219322,#219323,
#219324,#219325,#219326,#219327,#219328,#219329,#219330,#219331,#219332,
#219333,#219334,#219335,#219336,#219337,#219338,#219339,#219340,#219341,
#219342,#219343,#219344,#219345,#219346,#219347,#219348,#219349,#219350,
#219351,#219352,#219353,#219354,#219355,#219356,#219357,#219358,#219359,
#219360,#219361,#219362,#219363,#219364,#219365,#219366,#219367,#219368,
#219369,#219370,#219371,#219372,#219373,#219374,#219375,#219376,#219377,
#219378,#219379,#219380,#219381,#219382,#219383,#219384,#219385,#219386,
#219387,#219388,#219389,#219390,#219391,#219392,#219393,#219394,#219395,
#219396,#219397,#219398,#219399,#219400,#219401,#219402,#219403,#219404,
#219405,#219406,#219407,#219408,#219409,#219410,#219411,#219412,#219413,
#219414,#219415,#219416,#219417,#219418,#219419,#219420,#219421,#219422,
#219423,#219424,#219425,#219426,#219427,#219428,#219429,#219430,#219431,
#219432,#219433,#219434,#219435,#219436,#219437,#219438,#219439,#219440,
#219441,#219442,#219443,#219444,#219445,#219446,#219447,#219448,#219449,
#219450,#219451,#219452,#219453,#219454,#219455,#219456,#219457,#219458,
#219459,#219460,#219461,#219462,#219463,#219464,#219465,#219466,#219467,
#219468,#219469,#219470,#219471,#219472,#219473,#219474,#219475,#219476,
#219477,#219478,#219479,#219480,#219481,#219482,#219483,#219484,#219485,
#219486,#219487,#219488,#219489,#219490,#219491,#219492,#219493,#219494,
#219495,#219496,#219497,#219498,#219499,#219500,#219501,#219502,#219503,
#219504,#219505,#219506,#219507,#219508,#219509,#219510,#219511,#219512,
#219513,#219514,#219515,#219516,#219517,#219518,#219519,#219520,#219521,
#219522,#219523,#219524,#219525,#219526,#219527,#219528,#219529,#219530,
#219531,#219532,#219533,#219534,#219535,#219536,#219537,#219538,#219539,
#219540,#219541,#219542,#219543,#219544,#219545,#219546,#219547,#219548,
#219549,#219550,#219551,#219552,#219553,#219554,#219555,#219556,#219557,
#219558,#219559,#219560,#219561,#219562,#219563,#219564,#219565,#219566,
#219567,#219568,#219569,#219570,#219571,#219572,#219573,#219574,#219575,
#219576,#219577,#219578,#219579,#219580,#219581,#219582,#219583,#219584,
#219585,#219586,#219587,#219588,#219589,#219590,#219591,#219592,#219593,
#219594,#219595,#219596,#219597,#219598,#219599,#219600,#219601,#219602,
#219603,#219604,#219605,#219606,#219607,#219608,#219609,#219610,#219611,
#219612,#219613,#219614,#219615,#219616,#219617,#219618,#219619,#219620,
#219621,#219622,#219623,#219624,#219625,#219626,#219627,#219628,#219629,
#219630,#219631,#219632,#219633,#219634,#219635,#219636,#219637,#219638,
#219639,#219640,#219641,#219642,#219643,#219644,#219645,#219646,#219647,
#219648,#219649,#219650,#219651,#219652,#219653,#219654,#219655,#219656,
#219657,#219658,#219659,#219660,#219661,#219662,#219663,#219664,#219665,
#219666,#219667,#219668,#219669,#219670,#219671,#219672,#219673,#219674,
#219675,#219676,#219677,#219678,#219679,#219680,#219681,#219682,#219683,
#219684,#219685,#219686,#219687,#219688,#219689,#219690,#219691,#219692,
#219693,#219694,#219695,#219696,#219697,#219698,#219699,#219700,#219701,
#219702,#219703,#219704,#219705,#219706,#219707,#219708,#219709,#219710,
#219711,#219712,#219713,#219714,#219715,#219716,#219717,#219718,#219719,
#219720,#219721,#219722,#219723,#219724,#219725,#219726,#219727,#219728,
#219729,#219730,#219731,#219732,#219733,#219734,#219735,#219736,#219737,
#219738,#219739,#219740,#219741,#219742,#219743,#219744,#219745,#219746,
#219747,#219748,#219749,#219750,#219751,#219752,#219753,#219754,#219755,
#219756,#219757,#219758,#219759,#219760,#219761,#219762,#219763,#219764,
#219765,#219766,#219767,#219768,#219769,#219770,#219771,#219772,#219773,
#219774,#219775,#219776,#219777,#219778,#219779,#219780,#219781,#219782,
#219783,#219784,#219785,#219786,#219787,#219788,#219789,#219790,#219791,
#219792,#219793,#219794,#219795,#219796,#219797,#219798,#219799,#219800,
#219801,#219802,#219803,#219804,#219805,#219806,#219807,#219808,#219809,
#219810,#219811,#219812,#219813,#219814,#219815,#219816,#219817,#219818,
#219819,#219820,#219821,#219822,#219823,#219824,#219825,#219826,#219827,
#219828,#219829,#219830,#219831,#219832,#219833,#219834,#219835,#219836,
#219837,#219838,#219839,#219840,#219841,#219842,#219843,#219844,#219845,
#219846,#219847,#219848,#219849,#219850,#219851,#219852,#219853,#219854,
#219855,#219856,#219857,#219858,#219859,#219860,#219861,#219862,#219863,
#219864,#219865,#219866,#219867,#219868,#219869,#219870,#219871,#219872,
#219873,#219874,#219875,#219876,#219877,#219878,#219879,#219880,#219881,
#219882,#219883,#219884,#219885,#219886,#219887,#219888,#219889,#219890,
#219891,#219892,#219893,#219894,#219895,#219896,#219897,#219898,#219899,
#219900,#219901,#219902,#219903,#219904,#219905,#219906,#219907,#219908,
#219909,#219910,#219911,#219912,#219913,#219914,#219915,#219916,#219917,
#219918,#219919,#219920,#219921,#219922,#219923,#219924,#219925,#219926,
#219927,#219928,#219929,#219930,#219931,#219932,#219933,#219934,#219935,
#219936,#219937,#219938,#219939,#219940,#219941,#219942,#219943,#219944,
#219945,#219946,#219947,#219948,#219949,#219950,#219951,#219952,#219953,
#219954,#219955,#219956,#219957,#219958,#219959,#219960,#219961,#219962,
#219963,#219964,#219965,#219966,#219967,#219968,#219969,#219970,#219971,
#219972,#219973,#219974,#219975,#219976,#219977,#219978,#219979,#219980,
#219981,#219982,#219983,#219984,#219985,#219986,#219987,#219988,#219989,
#219990,#219991,#219992,#219993,#219994,#219995,#219996,#219997,#219998,
#219999,#220000,#220001,#220002,#220003,#220004,#220005,#220006,#220007,
#220008,#220009,#220010,#220011,#220012,#220013,#220014,#220015,#220016,
#220017,#220018,#220019,#220020,#220021,#220022,#220023,#220024,#220025,
#220026,#220027,#220028,#220029,#220030,#220031,#220032,#220033,#220034,
#220035,#220036,#220037,#220038,#220039,#220040,#220041,#220042,#220043,
#220044,#220045,#220046,#220047,#220048,#220049,#220050,#220051),(#220052,
#220053,#220054,#220055,#220056,#220057,#220058,#220059,#220060,#220061,
#220062,#220063,#220064,#220065,#220066,#220067,#220068,#220069,#220070,
#220071,#220072,#220073,#220074,#220075,#220076,#220077,#220078,#220079,
#220080,#220081,#220082,#220083,#220084,#220085,#220086,#220087,#220088,
#220089,#220090,#220091,#220092,#220093,#220094,#220095,#220096,#220097,
#220098,#220099,#220100,#220101,#220102,#220103,#220104,#220105,#220106,
#220107,#220108,#220109,#220110,#220111,#220112,#220113,#220114,#220115,
#220116,#220117,#220118,#220119,#220120,#220121,#220122,#220123,#220124,
#220125,#220126,#220127,#220128,#220129,#220130,#220131,#220132,#220133,
#220134,#220135,#220136,#220137,#220138,#220139,#220140,#220141,#220142,
#220143,#220144,#220145,#220146,#220147,#220148,#220149,#220150,#220151,
#220152,#220153,#220154,#220155,#220156,#220157,#220158,#220159,#220160,
#220161,#220162,#220163,#220164,#220165,#220166,#220167,#220168,#220169,
#220170,#220171,#220172,#220173,#220174,#220175,#220176,#220177,#220178,
#220179,#220180,#220181,#220182,#220183,#220184,#220185,#220186,#220187,
#220188,#220189,#220190,#220191,#220192,#220193,#220194,#220195,#220196,
#220197,#220198,#220199,#220200,#220201,#220202,#220203,#220204,#220205,
#220206,#220207,#220208,#220209,#220210,#220211,#220212,#220213,#220214,
#220215,#220216,#220217,#220218,#220219,#220220,#220221,#220222,#220223,
#220224,#220225,#220226,#220227,#220228,#220229,#220230,#220231,#220232,
#220233,#220234,#220235,#220236,#220237,#220238,#220239,#220240,#220241,
#220242,#220243,#220244,#220245,#220246,#220247,#220248,#220249,#220250,
#220251,#220252,#220253,#220254,#220255,#220256,#220257,#220258,#220259,
#220260,#220261,#220262,#220263,#220264,#220265,#220266,#220267,#220268,
#220269,#220270,#220271,#220272,#220273,#220274,#220275,#220276,#220277,
#220278,#220279,#220280,#220281,#220282,#220283,#220284,#220285,#220286,
#220287,#220288,#220289,#220290,#220291,#220292,#220293,#220294,#220295,
#220296,#220297,#220298,#220299,#220300,#220301,#220302,#220303,#220304,
#220305,#220306,#220307,#220308,#220309,#220310,#220311,#220312,#220313,
#220314,#220315,#220316,#220317,#220318,#220319,#220320,#220321,#220322,
#220323,#220324,#220325,#220326,#220327,#220328,#220329,#220330,#220331,
#220332,#220333,#220334,#220335,#220336,#220337,#220338,#220339,#220340,
#220341,#220342,#220343,#220344,#220345,#220346,#220347,#220348,#220349,
#220350,#220351,#220352,#220353,#220354,#220355,#220356,#220357,#220358,
#220359,#220360,#220361,#220362,#220363,#220364,#220365,#220366,#220367,
#220368,#220369,#220370,#220371,#220372,#220373,#220374,#220375,#220376,
#220377,#220378,#220379,#220380,#220381,#220382,#220383,#220384,#220385,
#220386,#220387,#220388,#220389,#220390,#220391,#220392,#220393,#220394,
#220395,#220396,#220397,#220398,#220399,#220400,#220401,#220402,#220403,
#220404,#220405,#220406,#220407,#220408,#220409,#220410,#220411,#220412,
#220413,#220414,#220415,#220416,#220417,#220418,#220419,#220420,#220421,
#220422,#220423,#220424,#220425,#220426,#220427,#220428,#220429,#220430,
#220431,#220432,#220433,#220434,#220435,#220436,#220437,#220438,#220439,
#220440,#220441,#220442,#220443,#220444,#220445,#220446,#220447,#220448,
#220449,#220450,#220451,#220452,#220453,#220454,#220455,#220456,#220457,
#220458,#220459,#220460,#220461,#220462,#220463,#220464,#220465,#220466,
#220467,#220468,#220469,#220470,#220471,#220472,#220473,#220474,#220475,
#220476,#220477,#220478,#220479,#220480,#220481,#220482,#220483,#220484,
#220485,#220486,#220487,#220488,#220489,#220490,#220491,#220492,#220493,
#220494,#220495,#220496,#220497,#220498,#220499,#220500,#220501,#220502,
#220503,#220504,#220505,#220506,#220507,#220508,#220509,#220510,#220511,
#220512,#220513,#220514,#220515,#220516,#220517,#220518,#220519,#220520,
#220521,#220522,#220523,#220524,#220525,#220526,#220527,#220528,#220529,
#220530,#220531,#220532,#220533,#220534,#220535,#220536,#220537,#220538,
#220539,#220540,#220541,#220542,#220543,#220544,#220545,#220546,#220547,
#220548,#220549,#220550,#220551,#220552,#220553,#220554,#220555,#220556,
#220557,#220558,#220559,#220560,#220561,#220562,#220563,#220564,#220565,
#220566,#220567,#220568,#220569,#220570,#220571,#220572,#220573,#220574,
#220575,#220576,#220577,#220578,#220579,#220580,#220581,#220582,#220583,
#220584,#220585,#220586,#220587,#220588,#220589,#220590,#220591,#220592,
#220593,#220594,#220595,#220596,#220597,#220598,#220599,#220600,#220601,
#220602,#220603,#220604,#220605,#220606,#220607,#220608,#220609,#220610,
#220611,#220612,#220613,#220614,#220615,#220616,#220617,#220618,#220619,
#220620,#220621,#220622,#220623,#220624,#220625,#220626,#220627,#220628,
#220629,#220630,#220631,#220632,#220633,#220634,#220635,#220636,#220637,
#220638,#220639,#220640,#220641,#220642,#220643,#220644,#220645,#220646,
#220647,#220648,#220649,#220650,#220651,#220652,#220653,#220654,#220655,
#220656,#220657,#220658,#220659,#220660,#220661,#220662,#220663,#220664,
#220665,#220666,#220667,#220668,#220669,#220670,#220671,#220672,#220673,
#220674,#220675,#220676,#220677,#220678,#220679,#220680,#220681,#220682,
#220683,#220684,#220685,#220686,#220687,#220688,#220689,#220690,#220691,
#220692,#220693,#220694,#220695,#220696,#220697,#220698,#220699,#220700,
#220701,#220702,#220703,#220704,#220705,#220706,#220707,#220708,#220709,
#220710,#220711,#220712,#220713,#220714,#220715,#220716,#220717,#220718,
#220719,#220720,#220721,#220722,#220723,#220724,#220725,#220726,#220727,
#220728,#220729,#220730,#220731,#220732,#220733,#220734,#220735,#220736,
#220737,#220738,#220739,#220740,#220741,#220742,#220743,#220744,#220745,
#220746,#220747,#220748,#220749,#220750,#220751,#220752,#220753,#220754,
#220755,#220756,#220757,#220758,#220759,#220760,#220761,#220762,#220763,
#220764,#220765,#220766,#220767,#220768,#220769,#220770,#220771,#220772,
#220773,#220774,#220775,#220776,#220777,#220778,#220779,#220780,#220781,
#220782,#220783,#220784,#220785,#220786,#220787,#220788,#220789,#220790,
#220791,#220792,#220793,#220794,#220795,#220796,#220797,#220798,#220799,
#220800,#220801,#220802,#220803,#220804,#220805,#220806,#220807,#220808,
#220809,#220810,#220811,#220812,#220813,#220814,#220815,#220816,#220817,
#220818,#220819,#220820,#220821,#220822,#220823,#220824,#220825,#220826,
#220827,#220828,#220829,#220830,#220831,#220832,#220833,#220834,#220835,
#220836,#220837,#220838,#220839,#220840,#220841,#220842,#220843,#220844,
#220845,#220846,#220847,#220848,#220849,#220850,#220851,#220852,#220853,
#220854,#220855,#220856,#220857,#220858,#220859,#220860,#220861,#220862,
#220863,#220864,#220865,#220866,#220867,#220868,#220869,#220870,#220871,
#220872,#220873,#220874,#220875,#220876,#220877,#220878,#220879,#220880,
#220881,#220882,#220883,#220884,#220885,#220886,#220887,#220888,#220889,
#220890,#220891,#220892,#220893,#220894,#220895,#220896,#220897,#220898,
#220899,#220900,#220901,#220902,#220903,#220904,#220905,#220906,#220907,
#220908,#220909,#220910,#220911,#220912,#220913,#220914,#220915,#220916,
#220917,#220918,#220919,#220920,#220921,#220922,#220923,#220924,#220925,
#220926,#220927,#220928,#220929,#220930,#220931,#220932,#220933,#220934,
#220935,#220936,#220937,#220938,#220939,#220940,#220941,#220942,#220943,
#220944,#220945,#220946,#220947,#220948,#220949,#220950,#220951,#220952,
#220953,#220954,#220955,#220956,#220957,#220958,#220959,#220960,#220961,
#220962,#220963,#220964,#220965,#220966,#220967,#220968,#220969,#220970,
#220971,#220972,#220973,#220974,#220975,#220976,#220977,#220978,#220979,
#220980,#220981,#220982,#220983,#220984,#220985,#220986,#220987,#220988,
#220989,#220990,#220991,#220992,#220993,#220994,#220995,#220996,#220997,
#220998,#220999,#221000,#221001,#221002,#221003,#221004,#221005,#221006,
#221007,#221008,#221009,#221010,#221011,#221012,#221013,#221014,#221015,
#221016,#221017,#221018,#221019,#221020,#221021,#221022,#221023,#221024,
#221025,#221026,#221027,#221028,#221029,#221030,#221031,#221032,#221033,
#221034,#221035,#221036,#221037,#221038,#221039,#221040,#221041,#221042,
#221043,#221044,#221045,#221046,#221047,#221048,#221049,#221050,#221051,
#221052,#221053,#221054,#221055,#221056,#221057,#221058,#221059,#221060,
#221061,#221062,#221063,#221064,#221065,#221066,#221067,#221068,#221069,
#221070,#221071,#221072,#221073,#221074,#221075,#221076,#221077,#221078,
#221079,#221080,#221081,#221082,#221083,#221084,#221085,#221086,#221087,
#221088,#221089,#221090,#221091,#221092,#221093,#221094,#221095,#221096,
#221097,#221098,#221099,#221100,#221101,#221102,#221103,#221104,#221105,
#221106,#221107,#221108,#221109,#221110,#221111,#221112,#221113,#221114,
#221115,#221116,#221117,#221118,#221119,#221120,#221121,#221122,#221123,
#221124,#221125,#221126,#221127,#221128,#221129,#221130,#221131,#221132,
#221133,#221134,#221135,#221136,#221137,#221138,#221139,#221140,#221141,
#221142,#221143,#221144,#221145,#221146,#221147,#221148,#221149,#221150,
#221151,#221152,#221153,#221154,#221155,#221156,#221157,#221158,#221159,
#221160,#221161,#221162,#221163,#221164,#221165,#221166,#221167,#221168,
#221169,#221170,#221171,#221172,#221173,#221174,#221175,#221176,#221177,
#221178,#221179,#221180,#221181,#221182,#221183,#221184,#221185,#221186,
#221187,#221188,#221189,#221190,#221191,#221192,#221193,#221194,#221195,
#221196,#221197,#221198,#221199,#221200,#221201,#221202,#221203,#221204,
#221205,#221206,#221207,#221208,#221209,#221210,#221211,#221212,#221213,
#221214,#221215,#221216,#221217,#221218,#221219,#221220,#221221,#221222,
#221223,#221224,#221225,#221226,#221227,#221228,#221229,#221230,#221231,
#221232,#221233,#221234,#221235,#221236,#221237,#221238,#221239,#221240,
#221241,#221242,#221243,#221244,#221245,#221246,#221247,#221248,#221249,
#221250,#221251,#221252,#221253,#221254,#221255,#221256,#221257,#221258,
#221259,#221260,#221261,#221262,#221263,#221264,#221265,#221266,#221267,
#221268,#221269,#221270,#221271,#221272,#221273,#221274,#221275,#221276,
#221277,#221278,#221279,#221280,#221281,#221282,#221283,#221284,#221285,
#221286,#221287,#221288,#221289,#221290,#221291,#221292,#221293,#221294,
#221295,#221296,#221297,#221298,#221299,#221300,#221301,#221302,#221303,
#221304,#221305,#221306,#221307,#221308,#221309,#221310,#221311,#221312,
#221313,#221314,#221315,#221316,#221317,#221318,#221319,#221320,#221321,
#221322,#221323,#221324,#221325,#221326,#221327,#221328,#221329,#221330,
#221331,#221332,#221333,#221334,#221335,#221336,#221337,#221338,#221339,
#221340,#221341,#221342,#221343,#221344,#221345,#221346,#221347,#221348,
#221349,#221350,#221351,#221352,#221353,#221354,#221355,#221356,#221357,
#221358,#221359,#221360,#221361,#221362,#221363,#221364,#221365,#221366,
#221367,#221368,#221369,#221370,#221371,#221372,#221373,#221374,#221375,
#221376,#221377,#221378,#221379,#221380,#221381,#221382,#221383,#221384,
#221385,#221386,#221387,#221388,#221389,#221390,#221391,#221392,#221393,
#221394,#221395,#221396,#221397,#221398,#221399,#221400,#221401,#221402,
#221403,#221404,#221405,#221406,#221407,#221408,#221409,#221410,#221411,
#221412,#221413,#221414,#221415,#221416,#221417,#221418,#221419,#221420,
#221421,#221422,#221423,#221424,#221425,#221426,#221427,#221428,#221429,
#221430,#221431,#221432,#221433,#221434,#221435,#221436,#221437,#221438,
#221439,#221440,#221441,#221442,#221443,#221444,#221445,#221446,#221447,
#221448,#221449,#221450,#221451,#221452,#221453,#221454,#221455,#221456,
#221457,#221458,#221459,#221460,#221461,#221462,#221463,#221464,#221465,
#221466,#221467,#221468,#221469,#221470,#221471,#221472,#221473,#221474,
#221475,#221476,#221477,#221478,#221479,#221480,#221481,#221482,#221483,
#221484,#221485,#221486,#221487,#221488,#221489,#221490,#221491,#221492,
#221493,#221494,#221495,#221496,#221497,#221498,#221499,#221500,#221501,
#221502,#221503,#221504,#221505,#221506,#221507,#221508,#221509,#221510,
#221511,#221512,#221513,#221514,#221515,#221516,#221517,#221518,#221519,
#221520,#221521,#221522,#221523,#221524,#221525,#221526,#221527,#221528,
#221529,#221530,#221531,#221532,#221533,#221534,#221535,#221536,#221537,
#221538,#221539,#221540,#221541,#221542,#221543,#221544,#221545,#221546,
#221547,#221548,#221549,#221550,#221551,#221552,#221553,#221554,#221555,
#221556,#221557,#221558,#221559,#221560,#221561,#221562,#221563,#221564,
#221565,#221566,#221567,#221568,#221569,#221570,#221571,#221572,#221573,
#221574,#221575,#221576,#221577,#221578,#221579,#221580,#221581,#221582,
#221583,#221584,#221585,#221586,#221587,#221588,#221589,#221590,#221591,
#221592,#221593,#221594,#221595,#221596,#221597,#221598,#221599,#221600,
#221601,#221602,#221603,#221604,#221605,#221606,#221607,#221608,#221609,
#221610,#221611,#221612,#221613,#221614,#221615,#221616,#221617,#221618,
#221619,#221620,#221621,#221622,#221623,#221624,#221625,#221626,#221627,
#221628,#221629,#221630,#221631,#221632,#221633,#221634,#221635,#221636,
#221637,#221638,#221639,#221640,#221641,#221642,#221643,#221644,#221645,
#221646,#221647,#221648,#221649,#221650,#221651,#221652,#221653,#221654,
#221655,#221656,#221657,#221658,#221659,#221660,#221661,#221662,#221663,
#221664,#221665,#221666,#221667,#221668,#221669,#221670,#221671,#221672,
#221673,#221674,#221675,#221676,#221677,#221678,#221679,#221680,#221681,
#221682,#221683,#221684,#221685,#221686,#221687,#221688,#221689,#221690,
#221691,#221692,#221693,#221694,#221695,#221696,#221697,#221698,#221699,
#221700,#221701,#221702,#221703,#221704,#221705,#221706,#221707,#221708,
#221709,#221710,#221711,#221712,#221713,#221714,#221715,#221716,#221717,
#221718,#221719,#221720,#221721,#221722,#221723,#221724,#221725,#221726,
#221727,#221728,#221729,#221730,#221731,#221732,#221733,#221734,#221735,
#221736,#221737,#221738,#221739,#221740,#221741,#221742,#221743,#221744,
#221745,#221746),(#221747,#221748,#221749,#221750,#221751,#221752,#221753,
#221754,#221755,#221756,#221757,#221758,#221759,#221760,#221761,#221762,
#221763,#221764,#221765,#221766,#221767,#221768,#221769,#221770,#221771,
#221772,#221773,#221774,#221775,#221776,#221777,#221778,#221779,#221780,
#221781,#221782,#221783,#221784,#221785,#221786,#221787,#221788,#221789,
#221790,#221791,#221792,#221793,#221794,#221795,#221796,#221797,#221798,
#221799,#221800,#221801,#221802,#221803,#221804,#221805,#221806,#221807,
#221808,#221809,#221810,#221811,#221812,#221813,#221814,#221815,#221816,
#221817,#221818,#221819,#221820,#221821,#221822,#221823,#221824,#221825,
#221826,#221827,#221828,#221829,#221830,#221831,#221832,#221833,#221834,
#221835,#221836,#221837,#221838,#221839,#221840,#221841,#221842,#221843,
#221844,#221845,#221846,#221847,#221848,#221849,#221850,#221851,#221852,
#221853,#221854,#221855,#221856,#221857,#221858,#221859,#221860,#221861,
#221862,#221863,#221864,#221865,#221866,#221867,#221868,#221869,#221870,
#221871,#221872,#221873,#221874,#221875,#221876,#221877,#221878,#221879,
#221880,#221881,#221882,#221883,#221884,#221885,#221886,#221887,#221888,
#221889,#221890,#221891,#221892,#221893,#221894,#221895,#221896,#221897,
#221898,#221899,#221900,#221901,#221902,#221903,#221904,#221905,#221906,
#221907,#221908,#221909,#221910,#221911,#221912,#221913,#221914,#221915,
#221916,#221917,#221918,#221919,#221920,#221921,#221922,#221923,#221924,
#221925,#221926,#221927,#221928,#221929,#221930,#221931,#221932,#221933,
#221934,#221935,#221936,#221937,#221938,#221939,#221940,#221941,#221942,
#221943,#221944,#221945,#221946,#221947,#221948,#221949,#221950,#221951,
#221952,#221953,#221954,#221955,#221956,#221957,#221958,#221959,#221960,
#221961,#221962,#221963,#221964,#221965,#221966,#221967,#221968,#221969,
#221970,#221971,#221972,#221973,#221974,#221975,#221976,#221977,#221978,
#221979,#221980,#221981,#221982,#221983,#221984,#221985,#221986,#221987,
#221988,#221989,#221990,#221991,#221992,#221993,#221994,#221995,#221996,
#221997,#221998,#221999,#222000,#222001,#222002,#222003,#222004,#222005,
#222006,#222007,#222008,#222009,#222010,#222011,#222012,#222013,#222014,
#222015,#222016,#222017,#222018,#222019,#222020,#222021,#222022,#222023,
#222024,#222025,#222026,#222027,#222028,#222029,#222030,#222031,#222032,
#222033,#222034,#222035,#222036,#222037,#222038,#222039,#222040,#222041,
#222042,#222043,#222044,#222045,#222046,#222047,#222048,#222049,#222050,
#222051,#222052,#222053,#222054,#222055,#222056,#222057,#222058,#222059,
#222060,#222061,#222062,#222063,#222064,#222065,#222066,#222067,#222068,
#222069,#222070,#222071,#222072,#222073,#222074,#222075,#222076,#222077,
#222078,#222079,#222080,#222081,#222082,#222083,#222084,#222085,#222086,
#222087,#222088,#222089,#222090,#222091,#222092,#222093,#222094,#222095,
#222096,#222097,#222098,#222099,#222100,#222101,#222102,#222103,#222104,
#222105,#222106,#222107,#222108,#222109,#222110,#222111,#222112,#222113,
#222114,#222115,#222116,#222117,#222118,#222119,#222120,#222121,#222122,
#222123,#222124,#222125,#222126,#222127,#222128,#222129,#222130,#222131,
#222132,#222133,#222134,#222135,#222136,#222137,#222138,#222139,#222140,
#222141,#222142,#222143,#222144,#222145,#222146,#222147,#222148,#222149,
#222150,#222151,#222152,#222153,#222154,#222155,#222156,#222157,#222158,
#222159,#222160,#222161,#222162,#222163,#222164,#222165,#222166,#222167,
#222168,#222169,#222170,#222171,#222172,#222173,#222174,#222175,#222176,
#222177,#222178,#222179,#222180,#222181,#222182,#222183,#222184,#222185,
#222186,#222187,#222188,#222189,#222190,#222191,#222192,#222193,#222194,
#222195,#222196,#222197,#222198,#222199,#222200,#222201,#222202,#222203,
#222204,#222205,#222206,#222207,#222208,#222209,#222210,#222211,#222212,
#222213,#222214,#222215,#222216,#222217,#222218,#222219,#222220,#222221,
#222222,#222223,#222224,#222225,#222226,#222227,#222228,#222229,#222230,
#222231,#222232,#222233,#222234,#222235,#222236,#222237,#222238,#222239,
#222240,#222241,#222242,#222243,#222244,#222245,#222246,#222247,#222248,
#222249,#222250,#222251,#222252,#222253,#222254,#222255,#222256,#222257,
#222258,#222259,#222260,#222261,#222262,#222263,#222264,#222265,#222266,
#222267,#222268,#222269,#222270,#222271,#222272,#222273,#222274,#222275,
#222276,#222277,#222278,#222279,#222280,#222281,#222282,#222283,#222284,
#222285,#222286,#222287,#222288,#222289,#222290,#222291,#222292,#222293,
#222294,#222295,#222296,#222297,#222298,#222299,#222300,#222301,#222302,
#222303,#222304,#222305,#222306,#222307,#222308,#222309,#222310,#222311,
#222312,#222313,#222314,#222315,#222316,#222317,#222318,#222319,#222320,
#222321,#222322,#222323,#222324,#222325,#222326,#222327,#222328,#222329,
#222330,#222331,#222332,#222333,#222334,#222335,#222336,#222337,#222338,
#222339,#222340,#222341,#222342,#222343,#222344,#222345,#222346,#222347,
#222348,#222349,#222350,#222351,#222352,#222353,#222354,#222355,#222356,
#222357,#222358,#222359,#222360,#222361,#222362,#222363,#222364,#222365,
#222366,#222367,#222368,#222369,#222370,#222371,#222372,#222373,#222374,
#222375,#222376,#222377,#222378,#222379,#222380,#222381,#222382,#222383,
#222384,#222385,#222386,#222387,#222388,#222389,#222390,#222391,#222392,
#222393,#222394,#222395,#222396,#222397,#222398,#222399,#222400,#222401,
#222402,#222403,#222404,#222405,#222406,#222407,#222408,#222409,#222410,
#222411,#222412,#222413,#222414,#222415,#222416,#222417,#222418,#222419,
#222420,#222421,#222422,#222423,#222424,#222425,#222426,#222427,#222428,
#222429,#222430,#222431,#222432,#222433,#222434,#222435,#222436,#222437,
#222438,#222439,#222440,#222441,#222442,#222443,#222444,#222445,#222446,
#222447,#222448,#222449,#222450,#222451,#222452,#222453,#222454,#222455,
#222456,#222457,#222458,#222459,#222460,#222461,#222462,#222463,#222464,
#222465,#222466,#222467,#222468,#222469,#222470,#222471,#222472,#222473,
#222474,#222475,#222476,#222477,#222478,#222479,#222480,#222481,#222482,
#222483,#222484,#222485,#222486,#222487,#222488,#222489,#222490,#222491,
#222492,#222493,#222494,#222495,#222496,#222497,#222498,#222499,#222500,
#222501,#222502,#222503,#222504,#222505,#222506,#222507,#222508,#222509,
#222510,#222511,#222512,#222513,#222514,#222515,#222516,#222517,#222518,
#222519,#222520,#222521,#222522,#222523,#222524,#222525,#222526,#222527,
#222528,#222529,#222530,#222531,#222532,#222533,#222534,#222535,#222536,
#222537,#222538,#222539,#222540,#222541,#222542,#222543,#222544,#222545,
#222546,#222547,#222548,#222549,#222550,#222551,#222552,#222553,#222554,
#222555,#222556,#222557,#222558,#222559,#222560,#222561,#222562,#222563,
#222564,#222565,#222566,#222567,#222568,#222569,#222570,#222571,#222572,
#222573,#222574,#222575,#222576,#222577,#222578,#222579,#222580,#222581,
#222582,#222583,#222584,#222585,#222586,#222587,#222588,#222589,#222590,
#222591,#222592,#222593,#222594,#222595,#222596,#222597,#222598,#222599,
#222600,#222601,#222602,#222603,#222604,#222605,#222606,#222607,#222608,
#222609,#222610,#222611,#222612,#222613,#222614,#222615,#222616,#222617,
#222618,#222619,#222620,#222621,#222622,#222623,#222624,#222625,#222626,
#222627,#222628,#222629,#222630,#222631,#222632,#222633,#222634,#222635,
#222636,#222637,#222638,#222639,#222640,#222641,#222642,#222643,#222644,
#222645,#222646,#222647,#222648,#222649,#222650,#222651,#222652,#222653,
#222654,#222655,#222656,#222657,#222658,#222659,#222660,#222661,#222662,
#222663,#222664,#222665,#222666,#222667,#222668,#222669,#222670,#222671,
#222672,#222673,#222674,#222675,#222676,#222677,#222678,#222679,#222680,
#222681,#222682,#222683,#222684,#222685,#222686,#222687,#222688,#222689,
#222690,#222691,#222692,#222693,#222694,#222695,#222696,#222697,#222698,
#222699,#222700,#222701,#222702,#222703,#222704,#222705,#222706,#222707,
#222708,#222709,#222710,#222711,#222712,#222713,#222714,#222715,#222716,
#222717,#222718,#222719,#222720,#222721,#222722,#222723,#222724,#222725,
#222726,#222727,#222728,#222729,#222730,#222731,#222732,#222733,#222734,
#222735,#222736,#222737,#222738,#222739,#222740,#222741,#222742,#222743,
#222744,#222745,#222746,#222747,#222748,#222749,#222750,#222751,#222752,
#222753,#222754,#222755,#222756,#222757,#222758,#222759,#222760,#222761,
#222762,#222763,#222764,#222765,#222766,#222767,#222768,#222769,#222770,
#222771,#222772,#222773,#222774,#222775,#222776,#222777,#222778,#222779,
#222780,#222781,#222782,#222783,#222784,#222785,#222786,#222787,#222788,
#222789,#222790,#222791,#222792,#222793,#222794,#222795,#222796,#222797,
#222798,#222799,#222800,#222801,#222802,#222803,#222804,#222805,#222806,
#222807,#222808,#222809,#222810,#222811,#222812,#222813,#222814,#222815,
#222816,#222817,#222818,#222819,#222820,#222821,#222822,#222823,#222824,
#222825,#222826,#222827,#222828,#222829,#222830,#222831,#222832,#222833,
#222834,#222835,#222836,#222837,#222838,#222839,#222840,#222841,#222842,
#222843,#222844,#222845,#222846,#222847,#222848,#222849,#222850,#222851,
#222852,#222853,#222854,#222855,#222856,#222857,#222858,#222859,#222860,
#222861,#222862,#222863,#222864,#222865,#222866,#222867,#222868,#222869,
#222870,#222871,#222872,#222873,#222874,#222875,#222876,#222877,#222878,
#222879,#222880,#222881,#222882,#222883,#222884,#222885,#222886,#222887,
#222888,#222889,#222890,#222891,#222892,#222893,#222894,#222895,#222896,
#222897,#222898,#222899,#222900,#222901,#222902,#222903,#222904,#222905,
#222906,#222907,#222908,#222909,#222910,#222911,#222912,#222913,#222914,
#222915,#222916,#222917,#222918,#222919,#222920,#222921,#222922,#222923,
#222924,#222925,#222926,#222927,#222928,#222929,#222930,#222931,#222932,
#222933,#222934,#222935,#222936,#222937,#222938,#222939,#222940,#222941,
#222942,#222943,#222944,#222945,#222946,#222947,#222948,#222949,#222950,
#222951,#222952,#222953,#222954,#222955,#222956,#222957,#222958,#222959,
#222960,#222961,#222962,#222963,#222964,#222965,#222966,#222967,#222968,
#222969,#222970,#222971,#222972,#222973,#222974,#222975,#222976,#222977,
#222978,#222979,#222980,#222981,#222982,#222983,#222984,#222985,#222986,
#222987,#222988,#222989,#222990,#222991,#222992,#222993,#222994,#222995,
#222996,#222997,#222998,#222999,#223000,#223001,#223002,#223003,#223004,
#223005,#223006,#223007,#223008,#223009,#223010,#223011,#223012,#223013,
#223014,#223015,#223016,#223017,#223018,#223019,#223020,#223021,#223022,
#223023,#223024,#223025,#223026,#223027,#223028,#223029,#223030,#223031,
#223032,#223033,#223034,#223035,#223036,#223037,#223038,#223039,#223040,
#223041,#223042,#223043,#223044,#223045,#223046,#223047,#223048,#223049,
#223050,#223051,#223052,#223053,#223054,#223055,#223056,#223057,#223058,
#223059,#223060,#223061,#223062,#223063,#223064,#223065,#223066,#223067,
#223068,#223069,#223070,#223071,#223072,#223073,#223074,#223075,#223076,
#223077,#223078,#223079,#223080,#223081,#223082,#223083,#223084,#223085,
#223086,#223087,#223088,#223089,#223090,#223091,#223092,#223093,#223094,
#223095,#223096,#223097,#223098,#223099,#223100,#223101,#223102,#223103,
#223104,#223105,#223106,#223107,#223108,#223109,#223110,#223111,#223112,
#223113,#223114,#223115,#223116,#223117,#223118,#223119,#223120,#223121,
#223122,#223123,#223124,#223125,#223126,#223127,#223128,#223129,#223130,
#223131,#223132,#223133,#223134,#223135,#223136,#223137,#223138,#223139,
#223140,#223141,#223142,#223143,#223144,#223145,#223146,#223147,#223148,
#223149,#223150,#223151,#223152,#223153,#223154,#223155,#223156,#223157,
#223158,#223159,#223160,#223161,#223162,#223163,#223164,#223165,#223166,
#223167,#223168,#223169,#223170,#223171,#223172,#223173,#223174,#223175,
#223176,#223177,#223178,#223179,#223180,#223181,#223182,#223183,#223184,
#223185,#223186,#223187,#223188,#223189,#223190,#223191,#223192,#223193,
#223194,#223195,#223196,#223197,#223198,#223199,#223200,#223201,#223202,
#223203,#223204,#223205,#223206,#223207,#223208,#223209,#223210,#223211,
#223212,#223213,#223214,#223215,#223216,#223217,#223218,#223219,#223220,
#223221,#223222,#223223,#223224,#223225,#223226,#223227,#223228,#223229,
#223230,#223231,#223232,#223233,#223234,#223235,#223236,#223237,#223238,
#223239,#223240,#223241,#223242,#223243,#223244,#223245,#223246,#223247,
#223248,#223249,#223250,#223251,#223252,#223253,#223254,#223255,#223256,
#223257,#223258,#223259,#223260,#223261,#223262,#223263,#223264,#223265,
#223266,#223267,#223268,#223269,#223270,#223271,#223272,#223273,#223274,
#223275,#223276,#223277,#223278,#223279,#223280,#223281,#223282,#223283,
#223284,#223285,#223286,#223287,#223288,#223289,#223290,#223291,#223292,
#223293,#223294,#223295,#223296,#223297,#223298,#223299,#223300,#223301,
#223302,#223303,#223304,#223305,#223306,#223307,#223308,#223309,#223310,
#223311,#223312,#223313,#223314,#223315,#223316,#223317,#223318,#223319,
#223320,#223321,#223322,#223323,#223324,#223325,#223326,#223327,#223328,
#223329,#223330,#223331,#223332,#223333,#223334,#223335,#223336,#223337,
#223338,#223339,#223340,#223341,#223342,#223343,#223344,#223345,#223346,
#223347,#223348,#223349,#223350,#223351,#223352,#223353,#223354,#223355,
#223356,#223357,#223358,#223359,#223360,#223361,#223362,#223363,#223364,
#223365,#223366,#223367,#223368,#223369,#223370,#223371,#223372,#223373,
#223374,#223375,#223376,#223377,#223378,#223379,#223380,#223381,#223382,
#223383,#223384,#223385,#223386,#223387,#223388,#223389,#223390,#223391,
#223392,#223393,#223394,#223395,#223396,#223397,#223398,#223399,#223400,
#223401,#223402,#223403,#223404,#223405,#223406,#223407,#223408,#223409,
#223410,#223411,#223412,#223413,#223414,#223415,#223416,#223417,#223418,
#223419,#223420,#223421,#223422,#223423,#223424,#223425,#223426,#223427,
#223428,#223429,#223430,#223431,#223432,#223433,#223434,#223435,#223436,
#223437,#223438,#223439,#223440,#223441),(#223442,#223443,#223444,#223445,
#223446,#223447,#223448,#223449,#223450,#223451,#223452,#223453,#223454,
#223455,#223456,#223457,#223458,#223459,#223460,#223461,#223462,#223463,
#223464,#223465,#223466,#223467,#223468,#223469,#223470,#223471,#223472,
#223473,#223474,#223475,#223476,#223477,#223478,#223479,#223480,#223481,
#223482,#223483,#223484,#223485,#223486,#223487,#223488,#223489,#223490,
#223491,#223492,#223493,#223494,#223495,#223496,#223497,#223498,#223499,
#223500,#223501,#223502,#223503,#223504,#223505,#223506,#223507,#223508,
#223509,#223510,#223511,#223512,#223513,#223514,#223515,#223516,#223517,
#223518,#223519,#223520,#223521,#223522,#223523,#223524,#223525,#223526,
#223527,#223528,#223529,#223530,#223531,#223532,#223533,#223534,#223535,
#223536,#223537,#223538,#223539,#223540,#223541,#223542,#223543,#223544,
#223545,#223546,#223547,#223548,#223549,#223550,#223551,#223552,#223553,
#223554,#223555,#223556,#223557,#223558,#223559,#223560,#223561,#223562,
#223563,#223564,#223565,#223566,#223567,#223568,#223569,#223570,#223571,
#223572,#223573,#223574,#223575,#223576,#223577,#223578,#223579,#223580,
#223581,#223582,#223583,#223584,#223585,#223586,#223587,#223588,#223589,
#223590,#223591,#223592,#223593,#223594,#223595,#223596,#223597,#223598,
#223599,#223600,#223601,#223602,#223603,#223604,#223605,#223606,#223607,
#223608,#223609,#223610,#223611,#223612,#223613,#223614,#223615,#223616,
#223617,#223618,#223619,#223620,#223621,#223622,#223623,#223624,#223625,
#223626,#223627,#223628,#223629,#223630,#223631,#223632,#223633,#223634,
#223635,#223636,#223637,#223638,#223639,#223640,#223641,#223642,#223643,
#223644,#223645,#223646,#223647,#223648,#223649,#223650,#223651,#223652,
#223653,#223654,#223655,#223656,#223657,#223658,#223659,#223660,#223661,
#223662,#223663,#223664,#223665,#223666,#223667,#223668,#223669,#223670,
#223671,#223672,#223673,#223674,#223675,#223676,#223677,#223678,#223679,
#223680,#223681,#223682,#223683,#223684,#223685,#223686,#223687,#223688,
#223689,#223690,#223691,#223692,#223693,#223694,#223695,#223696,#223697,
#223698,#223699,#223700,#223701,#223702,#223703,#223704,#223705,#223706,
#223707,#223708,#223709,#223710,#223711,#223712,#223713,#223714,#223715,
#223716,#223717,#223718,#223719,#223720,#223721,#223722,#223723,#223724,
#223725,#223726,#223727,#223728,#223729,#223730,#223731,#223732,#223733,
#223734,#223735,#223736,#223737,#223738,#223739,#223740,#223741,#223742,
#223743,#223744,#223745,#223746,#223747,#223748,#223749,#223750,#223751,
#223752,#223753,#223754,#223755,#223756,#223757,#223758,#223759,#223760,
#223761,#223762,#223763,#223764,#223765,#223766,#223767,#223768,#223769,
#223770,#223771,#223772,#223773,#223774,#223775,#223776,#223777,#223778,
#223779,#223780,#223781,#223782,#223783,#223784,#223785,#223786,#223787,
#223788,#223789,#223790,#223791,#223792,#223793,#223794,#223795,#223796,
#223797,#223798,#223799,#223800,#223801,#223802,#223803,#223804,#223805,
#223806,#223807,#223808,#223809,#223810,#223811,#223812,#223813,#223814,
#223815,#223816,#223817,#223818,#223819,#223820,#223821,#223822,#223823,
#223824,#223825,#223826,#223827,#223828,#223829,#223830,#223831,#223832,
#223833,#223834,#223835,#223836,#223837,#223838,#223839,#223840,#223841,
#223842,#223843,#223844,#223845,#223846,#223847,#223848,#223849,#223850,
#223851,#223852,#223853,#223854,#223855,#223856,#223857,#223858,#223859,
#223860,#223861,#223862,#223863,#223864,#223865,#223866,#223867,#223868,
#223869,#223870,#223871,#223872,#223873,#223874,#223875,#223876,#223877,
#223878,#223879,#223880,#223881,#223882,#223883,#223884,#223885,#223886,
#223887,#223888,#223889,#223890,#223891,#223892,#223893,#223894,#223895,
#223896,#223897,#223898,#223899,#223900,#223901,#223902,#223903,#223904,
#223905,#223906,#223907,#223908,#223909,#223910,#223911,#223912,#223913,
#223914,#223915,#223916,#223917,#223918,#223919,#223920,#223921,#223922,
#223923,#223924,#223925,#223926,#223927,#223928,#223929,#223930,#223931,
#223932,#223933,#223934,#223935,#223936,#223937,#223938,#223939,#223940,
#223941,#223942,#223943,#223944,#223945,#223946,#223947,#223948,#223949,
#223950,#223951,#223952,#223953,#223954,#223955,#223956,#223957,#223958,
#223959,#223960,#223961,#223962,#223963,#223964,#223965,#223966,#223967,
#223968,#223969,#223970,#223971,#223972,#223973,#223974,#223975,#223976,
#223977,#223978,#223979,#223980,#223981,#223982,#223983,#223984,#223985,
#223986,#223987,#223988,#223989,#223990,#223991,#223992,#223993,#223994,
#223995,#223996,#223997,#223998,#223999,#224000,#224001,#224002,#224003,
#224004,#224005,#224006,#224007,#224008,#224009,#224010,#224011,#224012,
#224013,#224014,#224015,#224016,#224017,#224018,#224019,#224020,#224021,
#224022,#224023,#224024,#224025,#224026,#224027,#224028,#224029,#224030,
#224031,#224032,#224033,#224034,#224035,#224036,#224037,#224038,#224039,
#224040,#224041,#224042,#224043,#224044,#224045,#224046,#224047,#224048,
#224049,#224050,#224051,#224052,#224053,#224054,#224055,#224056,#224057,
#224058,#224059,#224060,#224061,#224062,#224063,#224064,#224065,#224066,
#224067,#224068,#224069,#224070,#224071,#224072,#224073,#224074,#224075,
#224076,#224077,#224078,#224079,#224080,#224081,#224082,#224083,#224084,
#224085,#224086,#224087,#224088,#224089,#224090,#224091,#224092,#224093,
#224094,#224095,#224096,#224097,#224098,#224099,#224100,#224101,#224102,
#224103,#224104,#224105,#224106,#224107,#224108,#224109,#224110,#224111,
#224112,#224113,#224114,#224115,#224116,#224117,#224118,#224119,#224120,
#224121,#224122,#224123,#224124,#224125,#224126,#224127,#224128,#224129,
#224130,#224131,#224132,#224133,#224134,#224135,#224136,#224137,#224138,
#224139,#224140,#224141,#224142,#224143,#224144,#224145,#224146,#224147,
#224148,#224149,#224150,#224151,#224152,#224153,#224154,#224155,#224156,
#224157,#224158,#224159,#224160,#224161,#224162,#224163,#224164,#224165,
#224166,#224167,#224168,#224169,#224170,#224171,#224172,#224173,#224174,
#224175,#224176,#224177,#224178,#224179,#224180,#224181,#224182,#224183,
#224184,#224185,#224186,#224187,#224188,#224189,#224190,#224191,#224192,
#224193,#224194,#224195,#224196,#224197,#224198,#224199,#224200,#224201,
#224202,#224203,#224204,#224205,#224206,#224207,#224208,#224209,#224210,
#224211,#224212,#224213,#224214,#224215,#224216,#224217,#224218,#224219,
#224220,#224221,#224222,#224223,#224224,#224225,#224226,#224227,#224228,
#224229,#224230,#224231,#224232,#224233,#224234,#224235,#224236,#224237,
#224238,#224239,#224240,#224241,#224242,#224243,#224244,#224245,#224246,
#224247,#224248,#224249,#224250,#224251,#224252,#224253,#224254,#224255,
#224256,#224257,#224258,#224259,#224260,#224261,#224262,#224263,#224264,
#224265,#224266,#224267,#224268,#224269,#224270,#224271,#224272,#224273,
#224274,#224275,#224276,#224277,#224278,#224279,#224280,#224281,#224282,
#224283,#224284,#224285,#224286,#224287,#224288,#224289,#224290,#224291,
#224292,#224293,#224294,#224295,#224296,#224297,#224298,#224299,#224300,
#224301,#224302,#224303,#224304,#224305,#224306,#224307,#224308,#224309,
#224310,#224311,#224312,#224313,#224314,#224315,#224316,#224317,#224318,
#224319,#224320,#224321,#224322,#224323,#224324,#224325,#224326,#224327,
#224328,#224329,#224330,#224331,#224332,#224333,#224334,#224335,#224336,
#224337,#224338,#224339,#224340,#224341,#224342,#224343,#224344,#224345,
#224346,#224347,#224348,#224349,#224350,#224351,#224352,#224353,#224354,
#224355,#224356,#224357,#224358,#224359,#224360,#224361,#224362,#224363,
#224364,#224365,#224366,#224367,#224368,#224369,#224370,#224371,#224372,
#224373,#224374,#224375,#224376,#224377,#224378,#224379,#224380,#224381,
#224382,#224383,#224384,#224385,#224386,#224387,#224388,#224389,#224390,
#224391,#224392,#224393,#224394,#224395,#224396,#224397,#224398,#224399,
#224400,#224401,#224402,#224403,#224404,#224405,#224406,#224407,#224408,
#224409,#224410,#224411,#224412,#224413,#224414,#224415,#224416,#224417,
#224418,#224419,#224420,#224421,#224422,#224423,#224424,#224425,#224426,
#224427,#224428,#224429,#224430,#224431,#224432,#224433,#224434,#224435,
#224436,#224437,#224438,#224439,#224440,#224441,#224442,#224443,#224444,
#224445,#224446,#224447,#224448,#224449,#224450,#224451,#224452,#224453,
#224454,#224455,#224456,#224457,#224458,#224459,#224460,#224461,#224462,
#224463,#224464,#224465,#224466,#224467,#224468,#224469,#224470,#224471,
#224472,#224473,#224474,#224475,#224476,#224477,#224478,#224479,#224480,
#224481,#224482,#224483,#224484,#224485,#224486,#224487,#224488,#224489,
#224490,#224491,#224492,#224493,#224494,#224495,#224496,#224497,#224498,
#224499,#224500,#224501,#224502,#224503,#224504,#224505,#224506,#224507,
#224508,#224509,#224510,#224511,#224512,#224513,#224514,#224515,#224516,
#224517,#224518,#224519,#224520,#224521,#224522,#224523,#224524,#224525,
#224526,#224527,#224528,#224529,#224530,#224531,#224532,#224533,#224534,
#224535,#224536,#224537,#224538,#224539,#224540,#224541,#224542,#224543,
#224544,#224545,#224546,#224547,#224548,#224549,#224550,#224551,#224552,
#224553,#224554,#224555,#224556,#224557,#224558,#224559,#224560,#224561,
#224562,#224563,#224564,#224565,#224566,#224567,#224568,#224569,#224570,
#224571,#224572,#224573,#224574,#224575,#224576,#224577,#224578,#224579,
#224580,#224581,#224582,#224583,#224584,#224585,#224586,#224587,#224588,
#224589,#224590,#224591,#224592,#224593,#224594,#224595,#224596,#224597,
#224598,#224599,#224600,#224601,#224602,#224603,#224604,#224605,#224606,
#224607,#224608,#224609,#224610,#224611,#224612,#224613,#224614,#224615,
#224616,#224617,#224618,#224619,#224620,#224621,#224622,#224623,#224624,
#224625,#224626,#224627,#224628,#224629,#224630,#224631,#224632,#224633,
#224634,#224635,#224636,#224637,#224638,#224639,#224640,#224641,#224642,
#224643,#224644,#224645,#224646,#224647,#224648,#224649,#224650,#224651,
#224652,#224653,#224654,#224655,#224656,#224657,#224658,#224659,#224660,
#224661,#224662,#224663,#224664,#224665,#224666,#224667,#224668,#224669,
#224670,#224671,#224672,#224673,#224674,#224675,#224676,#224677,#224678,
#224679,#224680,#224681,#224682,#224683,#224684,#224685,#224686,#224687,
#224688,#224689,#224690,#224691,#224692,#224693,#224694,#224695,#224696,
#224697,#224698,#224699,#224700,#224701,#224702,#224703,#224704,#224705,
#224706,#224707,#224708,#224709,#224710,#224711,#224712,#224713,#224714,
#224715,#224716,#224717,#224718,#224719,#224720,#224721,#224722,#224723,
#224724,#224725,#224726,#224727,#224728,#224729,#224730,#224731,#224732,
#224733,#224734,#224735,#224736,#224737,#224738,#224739,#224740,#224741,
#224742,#224743,#224744,#224745,#224746,#224747,#224748,#224749,#224750,
#224751,#224752,#224753,#224754,#224755,#224756,#224757,#224758,#224759,
#224760,#224761,#224762,#224763,#224764,#224765,#224766,#224767,#224768,
#224769,#224770,#224771,#224772,#224773,#224774,#224775,#224776,#224777,
#224778,#224779,#224780,#224781,#224782,#224783,#224784,#224785,#224786,
#224787,#224788,#224789,#224790,#224791,#224792,#224793,#224794,#224795,
#224796,#224797,#224798,#224799,#224800,#224801,#224802,#224803,#224804,
#224805,#224806,#224807,#224808,#224809,#224810,#224811,#224812,#224813,
#224814,#224815,#224816,#224817,#224818,#224819,#224820,#224821,#224822,
#224823,#224824,#224825,#224826,#224827,#224828,#224829,#224830,#224831,
#224832,#224833,#224834,#224835,#224836,#224837,#224838,#224839,#224840,
#224841,#224842,#224843,#224844,#224845,#224846,#224847,#224848,#224849,
#224850,#224851,#224852,#224853,#224854,#224855,#224856,#224857,#224858,
#224859,#224860,#224861,#224862,#224863,#224864,#224865,#224866,#224867,
#224868,#224869,#224870,#224871,#224872,#224873,#224874,#224875,#224876,
#224877,#224878,#224879,#224880,#224881,#224882,#224883,#224884,#224885,
#224886,#224887,#224888,#224889,#224890,#224891,#224892,#224893,#224894,
#224895,#224896,#224897,#224898,#224899,#224900,#224901,#224902,#224903,
#224904,#224905,#224906,#224907,#224908,#224909,#224910,#224911,#224912,
#224913,#224914,#224915,#224916,#224917,#224918,#224919,#224920,#224921,
#224922,#224923,#224924,#224925,#224926,#224927,#224928,#224929,#224930,
#224931,#224932,#224933,#224934,#224935,#224936,#224937,#224938,#224939,
#224940,#224941,#224942,#224943,#224944,#224945,#224946,#224947,#224948,
#224949,#224950,#224951,#224952,#224953,#224954,#224955,#224956,#224957,
#224958,#224959,#224960,#224961,#224962,#224963,#224964,#224965,#224966,
#224967,#224968,#224969,#224970,#224971,#224972,#224973,#224974,#224975,
#224976,#224977,#224978,#224979,#224980,#224981,#224982,#224983,#224984,
#224985,#224986,#224987,#224988,#224989,#224990,#224991,#224992,#224993,
#224994,#224995,#224996,#224997,#224998,#224999,#225000,#225001,#225002,
#225003,#225004,#225005,#225006,#225007,#225008,#225009,#225010,#225011,
#225012,#225013,#225014,#225015,#225016,#225017,#225018,#225019,#225020,
#225021,#225022,#225023,#225024,#225025,#225026,#225027,#225028,#225029,
#225030,#225031,#225032,#225033,#225034,#225035,#225036,#225037,#225038,
#225039,#225040,#225041,#225042,#225043,#225044,#225045,#225046,#225047,
#225048,#225049,#225050,#225051,#225052,#225053,#225054,#225055,#225056,
#225057,#225058,#225059,#225060,#225061,#225062,#225063,#225064,#225065,
#225066,#225067,#225068,#225069,#225070,#225071,#225072,#225073,#225074,
#225075,#225076,#225077,#225078,#225079,#225080,#225081,#225082,#225083,
#225084,#225085,#225086,#225087,#225088,#225089,#225090,#225091,#225092,
#225093,#225094,#225095,#225096,#225097,#225098,#225099,#225100,#225101,
#225102,#225103,#225104,#225105,#225106,#225107,#225108,#225109,#225110,
#225111,#225112,#225113,#225114,#225115,#225116,#225117,#225118,#225119,
#225120,#225121,#225122,#225123,#225124,#225125,#225126,#225127,#225128,
#225129,#225130,#225131,#225132,#225133,#225134,#225135,#225136)),
 .UNSPECIFIED.,.F.,.F.,.F.,(4,4),(4,1,1,1,1,1,1,1,1,1,1,1,1,1,1,1,1,1,1,
1,1,1,1,1,1,1,1,1,1,1,1,1,1,1,1,1,1,1,1,1,1,1,1,1,1,1,1,1,1,1,1,1,1,1,1,
1,1,1,1,1,1,1,1,1,1,1,1,1,1,1,1,1,1,1,1,1,1,1,1,1,1,1,1,1,1,1,1,1,1,1,1,
1,1,1,1,1,1,1,1,1,1,1,1,1,1,1,1,1,1,1,1,1,1,1,1,1,1,1,1,1,1,1,1,1,1,1,1,
1,1,1,1,1,1,1,1,1,1,1,1,1,1,1,1,1,1,1,1,1,1,1,1,1,1,1,1,1,1,1,1,1,1,1,1,
1,1,1,1,1,1,1,1,1,1,1,1,1,1,1,1,1,1,1,1,1,1,1,1,1,1,1,1,1,1,1,1,1,1,1,1,
1,1,1,1,1,1,1,1,1,1,1,1,1,1,1,1,1,1,1,1,1,1,1,1,1,1,1,1,1,1,1,1,1,1,1,1,
1,1,1,1,1,1,1,1,1,1,1,1,1,1,1,1,1,1,1,1,1,1,1,1,1,1,1,1,1,1,1,1,1,1,1,1,
1,1,1,1,1,1,1,1,1,1,1,1,1,1,1,1,1,1,1,1,1,1,1,1,1,1,1,1,1,1,1,1,1,1,1,1,
1,1,1,1,1,1,1,1,1,1,1,1,1,1,1,1,1,1,1,1,1,1,1,1,1,1,1,1,1,1,1,1,1,1,1,1,
1,1,1,1,1,1,1,1,1,1,1,1,1,1,1,1,1,1,1,1,1,1,1,1,1,1,1,1,1,1,1,1,1,1,1,1,
1,1,1,1,1,1,1,1,1,1,1,1,1,1,1,1,1,1,1,1,1,1,1,1,1,1,1,1,1,1,1,1,1,1,1,1,
1,1,1,1,1,1,1,1,1,1,1,1,1,1,1,1,1,1,1,1,1,1,1,1,1,1,1,1,1,1,1,1,1,1,1,1,
1,1,1,1,1,1,1,1,1,1,1,1,1,1,1,1,1,1,1,1,1,1,1,1,1,1,1,1,1,1,1,1,1,1,1,1,
1,1,1,1,1,1,1,1,1,1,1,1,1,1,1,1,1,1,1,1,1,1,1,1,1,1,1,1,1,1,1,1,1,1,1,1,
1,1,1,1,1,1,1,1,1,1,1,1,1,1,1,1,1,1,1,1,1,1,1,1,1,1,1,1,1,1,1,1,1,1,1,1,
1,1,1,1,1,1,1,1,1,1,1,1,1,1,1,1,1,1,1,1,1,1,1,1,1,1,1,1,1,1,1,1,1,1,1,1,
1,1,1,1,1,1,1,1,1,1,1,1,1,1,1,1,1,1,1,1,1,1,1,1,1,1,1,1,1,1,1,1,1,1,1,1,
1,1,1,1,1,1,1,1,1,1,1,1,1,1,1,1,1,1,1,1,1,1,1,1,1,1,1,1,1,1,1,1,1,1,1,1,
1,1,1,1,1,1,1,1,1,1,1,1,1,1,1,1,1,1,1,1,1,1,1,1,1,1,1,1,1,1,1,1,1,1,1,1,
1,1,1,1,1,1,1,1,1,1,1,1,1,1,1,1,1,1,1,1,1,1,1,1,1,1,1,1,1,1,1,1,1,1,1,1,
1,1,1,1,1,1,1,1,1,1,1,1,1,1,1,1,1,1,1,1,1,1,1,1,1,1,1,1,1,1,1,1,1,1,1,1,
1,1,1,1,1,1,1,1,1,1,1,1,1,1,1,1,1,1,1,1,1,1,1,1,1,1,1,1,1,1,1,1,1,1,1,1,
1,1,1,1,1,1,1,1,1,1,1,1,1,1,1,1,1,1,1,1,1,1,1,1,1,1,1,1,1,1,1,1,1,1,1,1,
1,1,1,1,1,1,1,1,1,1,1,1,1,1,1,1,1,1,1,1,1,1,1,1,1,1,1,1,1,1,1,1,1,1,1,1,
1,1,1,1,1,1,1,1,1,1,1,1,1,1,1,1,1,1,1,1,1,1,1,1,1,1,1,1,1,1,1,1,1,1,1,1,
1,1,1,1,1,1,1,1,1,1,1,1,1,1,1,1,1,1,1,1,1,1,1,1,1,1,1,1,1,1,1,1,1,1,1,1,
1,1,1,1,1,1,1,1,1,1,1,1,1,1,1,1,1,1,1,1,1,1,1,1,1,1,1,1,1,1,1,1,1,1,1,1,
1,1,1,1,1,1,1,1,1,1,1,1,1,1,1,1,1,1,1,1,1,1,1,1,1,1,1,1,1,1,1,1,1,1,1,1,
1,1,1,1,1,1,1,1,1,1,1,1,1,1,1,1,1,1,1,1,1,1,1,1,1,1,1,1,1,1,1,1,1,1,1,1,
1,1,1,1,1,1,1,1,1,1,1,1,1,1,1,1,1,1,1,1,1,1,1,1,1,1,1,1,1,1,1,1,1,1,1,1,
1,1,1,1,1,1,1,1,1,1,1,1,1,1,1,1,1,1,1,1,1,1,1,1,1,1,1,1,1,1,1,1,1,1,1,1,
1,1,1,1,1,1,1,1,1,1,1,1,1,1,1,1,1,1,1,1,1,1,1,1,1,1,1,1,1,1,1,1,1,1,1,1,
1,1,1,1,1,1,1,1,1,1,1,1,1,1,1,1,1,1,1,1,1,1,1,1,1,1,1,1,1,1,1,1,1,1,1,1,
1,1,1,1,1,1,1,1,1,1,1,1,1,1,1,1,1,1,1,1,1,1,1,1,1,1,1,1,1,1,1,1,1,1,1,1,
1,1,1,1,1,1,1,1,1,1,1,1,1,1,1,1,1,1,1,1,1,1,1,1,1,1,1,1,1,1,1,1,1,1,1,1,
1,1,1,1,1,1,1,1,1,1,1,1,1,1,1,1,1,1,1,1,1,1,1,1,1,1,1,1,1,1,1,1,1,1,1,1,
1,1,1,1,1,1,1,1,1,1,1,1,1,1,1,1,1,1,1,1,1,1,1,1,1,1,1,1,1,1,1,1,1,1,1,1,
1,1,1,1,1,1,1,1,1,1,1,1,1,1,1,1,1,1,1,1,1,1,1,1,1,1,1,1,1,1,1,1,1,1,1,1,
1,1,1,1,1,1,1,1,1,1,1,1,1,1,1,1,1,1,1,1,1,1,1,1,1,1,1,1,1,1,1,1,1,1,1,1,
1,1,1,1,1,1,1,1,1,1,1,1,1,1,1,1,1,1,1,1,1,1,1,1,1,1,1,1,1,1,1,1,1,1,1,1,
1,1,1,1,1,1,1,1,1,1,1,1,1,1,1,1,1,1,1,1,1,1,1,1,1,1,1,1,1,1,1,1,1,1,1,1,
1,1,1,1,1,1,1,1,1,1,1,1,1,1,1,1,1,1,1,1,1,1,1,1,1,1,1,1,1,1,1,1,1,1,1,1,
1,1,1,1,1,1,1,1,1,1,1,1,1,1,1,1,1,1,1,1,1,1,1,1,1,1,1,1,1,1,1,1,1,1,1,1,
1,1,1,1,1,1,1,1,1,1,1,1,1,1,1,1,1,1,1,1,1,1,1,1,1,1,1,1,1,1,1,1,1,1,1,1,
1,1,1,1,1,1,1,1,1,1,1,1,1,1,1,1,1,1,1,1,1,1,1,1,1,1,1,1,1,1,1,1,1,1,1,1,
1,1,1,1,1,1,1,1,1,1,1,1,1,1,1,1,1,1,1,1,1,1,1,1,1,1,1,1,1,1,1,1,1,1,1,1,
1,1,1,1,1,1,1,1,1,1,1,1,1,1,1,1,1,4),(-0.000423095957202541,0.115881565465356),
(11.6153146011728,12.1152895244478,12.6151575298078,13.614893540528,14.6146295512481,
15.6143655619682,16.6141015726884,17.6138375834085,18.6135735941286,19.6133096048488,
20.6130456155689,21.612781626289,22.6125176370092,23.6122536477293,24.6119896584494,
25.6117256691696,26.6114616798897,27.6111976906098,28.6109337013299,29.6106697120501,
30.6104057227702,31.6101417334903,32.6098777442105,33.6096137549306,34.6093497656507,
35.6090857763709,36.608821787091,37.6085577978111,38.6082938085313,39.6080298192514,
40.6077658299715,41.6075018406916,42.6072378514118,43.6069738621319,44.606709872852,
45.6064458835722,46.6061818942923,47.6059179050124,48.6056539157326,49.6053899264527,
50.6051259371728,51.604861947893,52.6045979586131,53.6043339693332,54.6040699800534,
55.6038059907735,56.6035420014936,57.6032780122137,58.6030140229339,59.602750033654,
60.6024860443741,61.6022220550943,62.6019580658144,63.6016940765345,64.6014300872547,
65.6011660979748,66.6009021086949,67.6006381194151,68.6003741301352,69.6001101408553,
70.5998461515754,71.5995821622956,72.5993181730157,73.5990541837358,74.598790194456,
75.5985262051761,76.5982622158962,77.5979982266164,78.5977342373365,79.5974702480566,
80.5972062587768,81.5969422694969,82.596678280217,83.5964142909372,84.5961503016573,
85.5958863123774,86.5956223230975,87.5953583338177,88.5950943445378,89.5948303552579,
90.5945663659781,91.5943023766982,92.5940383874183,93.5937743981385,94.5935104088586,
95.5932464195787,96.5929824302989,97.592718441019,98.5924544517391,99.5921904624593,
100.591926473179,101.5916624839,102.59139849462,103.59113450534,104.59087051606,
105.59060652678,106.5903425375,107.59007854822,108.58981455894,109.589550569661,
110.589286580381,111.589022591101,112.588758601821,113.588494612541,114.588230623261,
115.587966633981,116.587702644701,117.587438655422,118.587174666142,119.586910676862,
120.586646687582,121.586382698302,122.586118709022,123.585854719742,124.585590730463,
125.585326741183,126.585062751903,127.584798762623,128.584534773343,129.584270784063,
130.584006794783,131.583742805503,132.583478816224,133.583214826944,134.582950837664,
135.582686848384,136.582422859104,137.582158869824,138.581894880544,139.581630891264,
140.581366901985,141.581102912705,142.580838923425,143.580574934145,144.580310944865,
145.580046955585,146.579782966305,147.579518977026,148.579254987746,149.578990998466,
150.578727009186,151.578463019906,152.578199030626,153.577935041346,154.577671052066,
155.577407062787,156.577143073507,157.576879084227,158.576615094947,159.576351105667,
160.576087116387,161.575823127107,162.575559137827,163.575295148548,164.575031159268,
165.574767169988,166.574503180708,167.574239191428,168.573975202148,169.573711212868,
170.573447223589,171.573183234309,172.572919245029,173.572655255749,174.572391266469,
175.572127277189,176.571863287909,177.571599298629,178.57133530935,179.57107132007,
180.57080733079,181.57054334151,182.57027935223,183.57001536295,184.56975137367,
185.56948738439,186.569223395111,187.568959405831,188.568695416551,189.568431427271,
190.568167437991,191.567903448711,192.567639459431,193.567375470152,194.567111480872,
195.566847491592,196.566583502312,197.566319513032,198.566055523752,199.565791534472,
200.565527545192,201.565263555913,202.564999566633,203.564735577353,204.564471588073,
205.564207598793,206.563943609513,207.563679620233,208.563415630954,209.563151641674,
210.562887652394,211.562623663114,212.562359673834,213.562095684554,214.561831695274,
215.561567705994,216.561303716715,217.561039727435,218.560775738155,219.560511748875,
220.560247759595,221.559983770315,222.559719781035,223.559455791755,224.559191802476,
225.558927813196,226.558663823916,227.558399834636,228.558135845356,229.557871856076,
230.557607866796,231.557343877517,232.557079888237,233.556815898957,234.556551909677,
235.556287920397,236.556023931117,237.555759941837,238.555495952557,239.555231963278,
240.554967973998,241.554703984718,242.554439995438,243.554176006158,244.553912016878,
245.553648027598,246.553384038319,247.553120049039,248.552856059759,249.552592070479,
250.552328081199,251.552064091919,252.551800102639,253.551536113359,254.55127212408,
255.5510081348,256.55074414552,257.55048015624,258.55021616696,259.54995217768,
260.5496881884,261.54942419912,262.549160209841,263.548896220561,264.548632231281,
265.548368242001,266.548104252721,267.547840263441,268.547576274161,269.547312284882,
270.547048295602,271.546784306322,272.546520317042,273.546256327762,274.545992338482,
275.545728349202,276.545464359922,277.545200370643,278.544936381363,279.544672392083,
280.544408402803,281.544144413523,282.543880424243,283.543616434963,284.543352445683,
285.543088456404,286.542824467124,287.542560477844,288.542296488564,289.542032499284,
290.541768510004,291.541504520724,292.541240531445,293.540976542165,294.540712552885,
295.540448563605,296.540184574325,297.539920585045,298.539656595765,299.539392606485,
300.539128617206,301.538864627926,302.538600638646,303.538336649366,304.538072660086,
305.537808670806,306.537544681526,307.537280692246,308.537016702967,309.536752713687,
310.536488724407,311.536224735127,312.535960745847,313.535696756567,314.535432767287,
315.535168778008,316.534904788728,317.534640799448,318.534376810168,319.534112820888,
320.533848831608,321.533584842328,322.533320853048,323.533056863769,324.532792874489,
325.532528885209,326.532264895929,327.532000906649,328.531736917369,329.531472928089,
330.53120893881,331.53094494953,332.53068096025,333.53041697097,334.53015298169,
335.52988899241,336.52962500313,337.52936101385,338.529097024571,339.528833035291,
340.528569046011,341.528305056731,342.528041067451,343.527777078171,344.527513088891,
345.527249099611,346.526985110332,347.526721121052,348.526457131772,349.526193142492,
350.525929153212,351.525665163932,352.525401174652,353.525137185373,354.524873196093,
355.524609206813,356.524345217533,357.524081228253,358.523817238973,359.523553249693,
360.523289260413,361.523025271134,362.522761281854,363.522497292574,364.522233303294,
365.521969314014,366.521705324734,367.521441335454,368.521177346175,369.520913356895,
370.520649367615,371.520385378335,372.520121389055,373.519857399775,374.519593410495,
375.519329421215,376.519065431936,377.518801442656,378.518537453376,379.518273464096,
380.518009474816,381.517745485536,382.517481496256,383.517217506976,384.516953517697,
385.516689528417,386.516425539137,387.516161549857,388.515897560577,389.515633571297,
390.515369582017,391.515105592737,392.514841603458,393.514577614178,394.514313624898,
395.514049635618,396.513785646338,397.513521657058,398.513257667778,399.512993678499,
400.512729689219,401.512465699939,402.512201710659,403.511937721379,404.511673732099,
405.511409742819,406.511145753539,407.51088176426,408.51061777498,409.5103537857,
410.51008979642,411.50982580714,412.50956181786,413.50929782858,414.509033839301,
415.508769850021,416.508505860741,417.508241871461,418.507977882181,419.507713892901,
420.507449903621,421.507185914341,422.506921925062,423.506657935782,424.506393946502,
425.506129957222,426.505865967942,427.505601978662,428.505337989382,429.505074000102,
430.504810010823,431.504546021543,432.504282032263,433.504018042983,434.503754053703,
435.503490064423,436.503226075143,437.502962085864,438.502698096584,439.502434107304,
440.502170118024,441.501906128744,442.501642139464,443.501378150184,444.501114160904,
445.500850171625,446.500586182345,447.500322193065,448.500058203785,449.499794214505,
450.499530225225,451.499266235945,452.499002246665,453.498738257386,454.498474268106,
455.498210278826,456.497946289546,457.497682300266,458.497418310986,459.497154321706,
460.496890332427,461.496626343147,462.496362353867,463.496098364587,464.495834375307,
465.495570386027,466.495306396747,467.495042407467,468.494778418188,469.494514428908,
470.494250439628,471.493986450348,472.493722461068,473.493458471788,474.493194482508,
475.492930493229,476.492666503949,477.492402514669,478.492138525389,479.491874536109,
480.491610546829,481.491346557549,482.491082568269,483.49081857899,484.49055458971,
485.49029060043,486.49002661115,487.48976262187,488.48949863259,489.48923464331,
490.48897065403,491.488706664751,492.488442675471,493.488178686191,494.487914696911,
495.487650707631,496.487386718351,497.487122729071,498.486858739792,499.486594750512,
500.486330761232,501.486066771952,502.485802782672,503.485538793392,504.485274804112,
505.485010814832,506.484746825553,507.484482836273,508.484218846993,509.483954857713,
510.483690868433,511.483426879153,512.483162889873,513.482898900594,514.482634911314,
515.482370922034,516.482106932754,517.481842943474,518.481578954194,519.481314964914,
520.481050975635,521.480786986355,522.480522997075,523.480259007795,524.479995018515,
525.479731029235,526.479467039955,527.479203050675,528.478939061396,529.478675072116,
530.478411082836,531.478147093556,532.477883104276,533.477619114996,534.477355125716,
535.477091136436,536.476827147157,537.476563157877,538.476299168597,539.476035179317,
540.475771190037,541.475507200757,542.475243211477,543.474979222197,544.474715232918,
545.474451243638,546.474187254358,547.473923265078,548.473659275798,549.473395286518,
550.473131297238,551.472867307958,552.472603318679,553.472339329399,554.472075340119,
555.471811350839,556.471547361559,557.471283372279,558.471019382999,559.47075539372,
560.47049140444,561.47022741516,562.46996342588,563.4696994366,564.46943544732,
565.46917145804,566.46890746876,567.468643479481,568.468379490201,569.468115500921,
570.467851511641,571.467587522361,572.467323533081,573.467059543801,574.466795554521,
575.466531565242,576.466267575962,577.466003586682,578.465739597402,579.465475608122,
580.465211618842,581.464947629562,582.464683640283,583.464419651003,584.464155661723,
585.463891672443,586.463627683163,587.463363693883,588.463099704603,589.462835715323,
590.462571726044,591.462307736764,592.462043747484,593.461779758204,594.461515768924,
595.461251779644,596.460987790364,597.460723801085,598.460459811805,599.460195822525,
600.459931833245,601.459667843965,602.459403854685,603.459139865405,604.458875876125,
605.458611886846,606.458347897566,607.458083908286,608.457819919006,609.457555929726,
610.457291940446,611.457027951166,612.456763961887,613.456499972607,614.456235983327,
615.455971994047,616.455708004767,617.455444015487,618.455180026207,619.454916036927,
620.454652047648,621.454388058368,622.454124069088,623.453860079808,624.453596090528,
625.453332101248,626.453068111968,627.452804122688,628.452540133409,629.452276144129,
630.452012154849,631.451748165569,632.451484176289,633.451220187009,634.450956197729,
635.450692208449,636.45042821917,637.45016422989,638.44990024061,639.44963625133,
640.44937226205,641.44910827277,642.44884428349,643.448580294211,644.448316304931,
645.448052315651,646.447788326371,647.447524337091,648.447260347811,649.446996358531,
650.446732369251,651.446468379972,652.446204390692,653.445940401412,654.445676412132,
655.445412422852,656.445148433572,657.444884444292,658.444620455012,659.444356465733,
660.444092476453,661.443828487173,662.443564497893,663.443300508613,664.443036519333,
665.442772530053,666.442508540774,667.442244551494,668.441980562214,669.441716572934,
670.441452583654,671.441188594374,672.440924605094,673.440660615815,674.440396626535,
675.440132637255,676.439868647975,677.439604658695,678.439340669415,679.439076680135,
680.438812690855,681.438548701576,682.438284712296,683.438020723016,684.437756733736,
685.437492744456,686.437228755176,687.436964765896,688.436700776616,689.436436787337,
690.436172798057,691.435908808777,692.435644819497,693.435380830217,694.435116840937,
695.434852851657,696.434588862377,697.434324873098,698.434060883818,699.433796894538,
700.433532905258,701.433268915978,702.433004926698,703.432740937418,704.432476948139,
705.432212958859,706.431948969579,707.431684980299,708.431420991019,709.431157001739,
710.430893012459,711.430629023179,712.4303650339,713.43010104462,714.42983705534,
715.42957306606,716.42930907678,717.4290450875,718.42878109822,719.42851710894,
720.428253119661,721.427989130381,722.427725141101,723.427461151821,724.427197162541,
725.426933173261,726.426669183981,727.426405194702,728.426141205422,729.425877216142,
730.425613226862,731.425349237582,732.425085248302,733.424821259022,734.424557269742,
735.424293280463,736.424029291183,737.423765301903,738.423501312623,739.423237323343,
740.422973334063,741.422709344783,742.422445355504,743.422181366224,744.421917376944,
745.421653387664,746.421389398384,747.421125409104,748.420861419824,749.420597430544,
750.420333441265,751.420069451985,752.419805462705,753.419541473425,754.419277484145,
755.419013494865,756.418749505585,757.418485516306,758.418221527026,759.417957537746,
760.417693548466,761.417429559186,762.417165569906,763.416901580626,764.416637591346,
765.416373602067,766.416109612787,767.415845623507,768.415581634227,769.415317644947,
770.415053655667,771.414789666387,772.414525677107,773.414261687828,774.413997698548,
775.413733709268,776.413469719988,777.413205730708,778.412941741428,779.412677752148,
780.412413762868,781.412149773589,782.411885784309,783.411621795029,784.411357805749,
785.411093816469,786.410829827189,787.410565837909,788.41030184863,789.41003785935,
790.40977387007,791.40950988079,792.40924589151,793.40898190223,794.40871791295,
795.40845392367,796.408189934391,797.407925945111,798.407661955831,799.407397966551,
800.407133977271,801.406869987991,802.406605998711,803.406342009432,804.406078020152,
805.405814030872,806.405550041592,807.405286052312,808.405022063032,809.404758073752,
810.404494084472,811.404230095193,812.403966105913,813.403702116633,814.403438127353,
815.403174138073,816.402910148793,817.402646159513,818.402382170234,819.402118180954,
820.401854191674,821.401590202394,822.401326213114,823.401062223834,824.400798234554,
825.400534245274,826.400270255995,827.400006266715,828.399742277435,829.399478288155,
830.399214298875,831.398950309595,832.398686320315,833.398422331035,834.398158341756,
835.397894352476,836.397630363196,837.397366373916,838.397102384636,839.396838395356,
840.396574406076,841.396310416796,842.396046427517,843.395782438237,844.395518448957,
845.395254459677,846.394990470397,847.394726481117,848.394462491837,849.394198502558,
850.393934513278,851.393670523998,852.393406534718,853.393142545438,854.392878556158,
855.392614566878,856.392350577598,857.392086588319,858.391822599039,859.391558609759,
860.391294620479,861.391030631199,862.390766641919,863.390502652639,864.390238663359,
865.38997467408,866.3897106848,867.38944669552,868.38918270624,869.38891871696,
870.38865472768,871.3883907384,872.388126749121,873.387862759841,874.387598770561,
875.387334781281,876.387070792001,877.386806802721,878.386542813441,879.386278824161,
880.386014834882,881.385750845602,882.385486856322,883.385222867042,884.384958877762,
885.384694888482,886.384430899202,887.384166909923,888.383902920643,889.383638931363,
890.383374942083,891.383110952803,892.382846963523,893.382582974243,894.382318984963,
895.382054995684,896.381791006404,897.381527017124,898.381263027844,899.380999038564,
900.380735049284,901.380471060004,902.380207070725,903.379943081445,904.379679092165,
905.379415102885,906.379151113605,907.378887124325,908.378623135045,909.378359145765,
910.378095156486,911.377831167206,912.377567177926,913.377303188646,914.377039199366,
915.376775210086,916.376511220806,917.376247231526,918.375983242247,919.375719252967,
920.375455263687,921.375191274407,922.374927285127,923.374663295847,924.374399306567,
925.374135317287,926.373871328008,927.373607338728,928.373343349448,929.373079360168,
930.372815370888,931.372551381608,932.372287392328,933.372023403049,934.371759413769,
935.371495424489,936.371231435209,937.370967445929,938.370703456649,939.370439467369,
940.370175478089,941.36991148881,942.36964749953,943.36938351025,944.36911952097,
945.36885553169,946.36859154241,947.36832755313,948.368063563851,949.367799574571,
950.367535585291,951.367271596011,952.367007606731,953.366743617451,954.366479628171,
955.366215638891,956.365951649612,957.365687660332,958.365423671052,959.365159681772,
960.364895692492,961.364631703212,962.364367713932,963.364103724653,964.363839735373,
965.363575746093,966.363311756813,967.363047767533,968.362783778253,969.362519788973,
970.362255799693,971.361991810414,972.361727821134,973.361463831854,974.361199842574,
975.360935853294,976.360671864014,977.360407874734,978.360143885454,979.359879896175,
980.359615906895,981.359351917615,982.359087928335,983.358823939055,984.358559949775,
985.358295960495,986.358031971215,987.357767981936,988.357503992656,989.357240003376,
990.356976014096,991.356712024816,992.356448035536,993.356184046256,994.355920056977,
995.355656067697,996.355392078417,997.355128089137,998.354864099857,999.354600110577,
1000.3543361213,1001.35407213202,1002.35380814274,1003.35354415346,1004.35328016418,
1005.3530161749,1006.35275218562,1007.35248819634,1008.35222420706,1009.35196021778,
1010.3516962285,1011.35143223922,1012.35116824994,1013.35090426066,1014.35064027138,
1015.3503762821,1016.35011229282,1017.34984830354,1018.34958431426,1019.34932032498,
1020.3490563357,1021.34879234642,1022.34852835714,1023.34826436786,1024.34800037858,
1025.3477363893,1026.34747240002,1027.34720841074,1028.34694442146,1029.34668043218,
1030.3464164429,1031.34615245362,1032.34588846434,1033.34562447506,1034.34536048578,
1035.3450964965,1036.34483250722,1037.34456851794,1038.34430452866,1039.34404053938,
1040.3437765501,1041.34351256082,1042.34324857154,1043.34298458226,1044.34272059298,
1045.3424566037,1046.34219261442,1047.34192862514,1048.34166463586,1049.34140064658,
1050.3411366573,1051.34087266802,1052.34060867874,1053.34034468946,1054.34008070018,
1055.3398167109,1056.33955272162,1057.33928873234,1058.33902474307,1059.33876075378,
1060.33849676451,1061.33823277523,1062.33796878595,1063.33770479667,1064.33744080739,
1065.33717681811,1066.33691282883,1067.33664883955,1068.33638485027,1069.33612086099,
1070.33585687171,1071.33559288243,1072.33532889315,1073.33506490387,1074.33480091459,
1075.33453692531,1076.33427293603,1077.33400894675,1078.33374495747,1079.33348096819,
1080.33321697891,1081.33295298963,1082.33268900035,1083.33242501107,1084.33216102179,
1085.33189703251,1086.33163304323,1087.33136905395,1088.33110506467,1089.33084107539,
1090.33057708611,1091.33031309683,1092.33004910755,1093.32978511827,1094.32952112899,
1095.32925713971,1096.32899315043,1097.32872916115,1098.32846517187,1099.32820118259,
1100.32793719331,1101.32767320403,1102.32740921475,1103.32714522547,1104.32688123619,
1105.32661724691,1106.32635325763,1107.32608926835,1108.32582527907,1109.32556128979,
1110.32529730051,1111.32503331123,1112.32476932195,1113.32450533267,1114.32424134339,
1115.32397735411,1116.32371336483,1117.32344937555,1118.32318538627,1119.32292139699,
1120.32265740771,1121.32239341843,1122.32212942915,1123.32186543987,1124.32160145059,
1125.32133746131,1126.32107347203,1127.32080948275,1128.32054549347,1129.32028150419,
1130.32001751491,1131.31975352563,1132.31948953635,1133.31922554707,1134.31896155779,
1135.31869756852,1136.31843357924,1137.31816958996,1138.31790560068,1139.3176416114,
1140.31737762212,1141.31711363284,1142.31684964356,1143.31658565428,1144.316321665,
1145.31605767572,1146.31579368644,1147.31552969716,1148.31526570788,1149.3150017186,
1150.31473772932,1151.31447374004,1152.31420975076,1153.31394576148,1154.3136817722,
1155.31341778292,1156.31315379364,1157.31288980436,1158.31262581508,1159.3123618258,
1160.31209783652,1161.31183384724,1162.31156985796,1163.31130586868,1164.3110418794,
1165.31077789012,1166.31051390084,1167.31024991156,1168.30998592228,1169.309721933,
1170.30945794372,1171.30919395444,1172.30892996516,1173.30866597588,1174.3084019866,
1175.30813799732,1176.30787400804,1177.30761001876,1178.30734602948,1179.3070820402,
1180.30681805092,1181.30655406164,1182.30629007236,1183.30602608308,1184.3057620938,
1185.30549810452,1186.30523411524,1187.30497012596,1188.30470613668,1189.3044421474,
1190.30417815812,1191.30391416884,1192.30365017956,1193.30338619028,1194.303122201,
1195.30285821172,1196.30259422244,1197.30233023316,1198.30206624388,1199.3018022546,
1200.30153826532,1201.30127427604,1202.30101028676,1203.30074629748,1204.3004823082,
1205.30021831892,1206.29995432964,1207.29969034036,1208.29942635108,1209.2991623618,
1210.29889837252,1211.29863438324,1212.29837039397,1213.29810640469,1214.29784241541,
1215.29757842613,1216.29731443685,1217.29705044757,1218.29678645829,1219.29652246901,
1220.29625847973,1221.29599449045,1222.29573050117,1223.29546651189,1224.29520252261,
1225.29493853333,1226.29467454405,1227.29441055477,1228.29414656549,1229.29388257621,
1230.29361858693,1231.29335459765,1232.29309060837,1233.29282661909,1234.29256262981,
1235.29229864053,1236.29203465125,1237.29177066197,1238.29150667269,1239.29124268341,
1240.29097869413,1241.29071470485,1242.29045071557,1243.29018672629,1244.28992273701,
1245.28965874773,1246.28939475845,1247.28913076917,1248.28886677989,1249.28860279061,
1250.28833880133,1251.28807481205,1252.28781082277,1253.28754683349,1254.28728284421,
1255.28701885493,1256.28675486565,1257.28649087637,1258.28622688709,1259.28596289781,
1260.28569890853,1261.28543491925,1262.28517092997,1263.28490694069,1264.28464295141,
1265.28437896213,1266.28411497285,1267.28385098357,1268.28358699429,1269.28332300501,
1270.28305901573,1271.28279502645,1272.28253103717,1273.28226704789,1274.28200305861,
1275.28173906933,1276.28147508005,1277.28121109077,1278.28094710149,1279.28068311221,
1280.28041912293,1281.28015513365,1282.27989114437,1283.27962715509,1284.27936316581,
1285.27909917653,1286.27883518725,1287.27857119797,1288.2783072087,1289.27804321942,
1290.27777923014,1291.27751524086,1292.27725125158,1293.2769872623,1294.27672327302,
1295.27645928374,1296.27619529446,1297.27593130518,1298.2756673159,1299.27540332662,
1300.27513933734,1301.27487534806,1302.27461135878,1303.2743473695,1304.27408338022,
1305.27381939094,1306.27355540166,1307.27329141238,1308.2730274231,1309.27276343382,
1310.27249944454,1311.27223545526,1312.27197146598,1313.2717074767,1314.27144348742,
1315.27117949814,1316.27091550886,1317.27065151958,1318.2703875303,1319.27012354102,
1320.26985955174,1321.26959556246,1322.26933157318,1323.2690675839,1324.26880359462,
1325.26853960534,1326.26827561606,1327.26801162678,1328.2677476375,1329.26748364822,
1330.26721965894,1331.26695566966,1332.26669168038,1333.2664276911,1334.26616370182,
1335.26589971254,1336.26563572326,1337.26537173398,1338.2651077447,1339.26484375542,
1340.26457976614,1341.26431577686,1342.26405178758,1343.2637877983,1344.26352380902,
1345.26325981974,1346.26299583046,1347.26273184118,1348.2624678519,1349.26220386262,
1350.26193987334,1351.26167588406,1352.26141189478,1353.2611479055,1354.26088391622,
1355.26061992694,1356.26035593766,1357.26009194838,1358.2598279591,1359.25956396982,
1360.25929998054,1361.25903599126,1362.25877200198,1363.2585080127,1364.25824402343,
1365.25798003415,1366.25771604487,1367.25745205559,1368.25718806631,1369.25692407703,
1370.25666008775,1371.25639609847,1372.25613210919,1373.25586811991,1374.25560413063,
1375.25534014135,1376.25507615207,1377.25481216279,1378.25454817351,1379.25428418423,
1380.25402019495,1381.25375620567,1382.25349221639,1383.25322822711,1384.25296423783,
1385.25270024855,1386.25243625927,1387.25217226999,1388.25190828071,1389.25164429143,
1390.25138030215,1391.25111631287,1392.25085232359,1393.25058833431,1394.25032434503,
1395.25006035575,1396.24979636647,1397.24953237719,1398.24926838791,1399.24900439863,
1400.24874040935,1401.24847642007,1402.24821243079,1403.24794844151,1404.24768445223,
1405.24742046295,1406.24715647367,1407.24689248439,1408.24662849511,1409.24636450583,
1410.24610051655,1411.24583652727,1412.24557253799,1413.24530854871,1414.24504455943,
1415.24478057015,1416.24451658087,1417.24425259159,1418.24398860231,1419.24372461303,
1420.24346062375,1421.24319663447,1422.24293264519,1423.24266865591,1424.24240466663,
1425.24214067735,1426.24187668807,1427.24161269879,1428.24134870951,1429.24108472023,
1430.24082073095,1431.24055674167,1432.24029275239,1433.24002876311,1434.23976477383,
1435.23950078455,1436.23923679527,1437.23897280599,1438.23870881671,1439.23844482743,
1440.23818083815,1441.23791684888,1442.2376528596,1443.23738887032,1444.23712488104,
1445.23686089176,1446.23659690248,1447.2363329132,1448.23606892392,1449.23580493464,
1450.23554094536,1451.23527695608,1452.2350129668,1453.23474897752,1454.23448498824,
1455.23422099896,1456.23395700968,1457.2336930204,1458.23342903112,1459.23316504184,
1460.23290105256,1461.23263706328,1462.232373074,1463.23210908472,1464.23184509544,
1465.23158110616,1466.23131711688,1467.2310531276,1468.23078913832,1469.23052514904,
1470.23026115976,1471.22999717048,1472.2297331812,1473.22946919192,1474.22920520264,
1475.22894121336,1476.22867722408,1477.2284132348,1478.22814924552,1479.22788525624,
1480.22762126696,1481.22735727768,1482.2270932884,1483.22682929912,1484.22656530984,
1485.22630132056,1486.22603733128,1487.225773342,1488.22550935272,1489.22524536344,
1490.22498137416,1491.22471738488,1492.2244533956,1493.22418940632,1494.22392541704,
1495.22366142776,1496.22339743848,1497.2231334492,1498.22286945992,1499.22260547064,
1500.22234148136,1501.22207749208,1502.2218135028,1503.22154951352,1504.22128552424,
1505.22102153496,1506.22075754568,1507.2204935564,1508.22022956712,1509.21996557784,
1510.21970158856,1511.21943759928,1512.21917361,1513.21890962072,1514.21864563144,
1515.21838164216,1516.21811765288,1517.21785366361,1518.21758967433,1519.21732568505,
1520.21706169577,1521.21679770649,1522.21653371721,1523.21626972793,1524.21600573865,
1525.21574174937,1526.21547776009,1527.21521377081,1528.21494978153,1529.21468579225,
1530.21442180297,1531.21415781369,1532.21389382441,1533.21362983513,1534.21336584585,
1535.21310185657,1536.21283786729,1537.21257387801,1538.21230988873,1539.21204589945,
1540.21178191017,1541.21151792089,1542.21125393161,1543.21098994233,1544.21072595305,
1545.21046196377,1546.21019797449,1547.20993398521,1548.20966999593,1549.20940600665,
1550.20914201737,1551.20887802809,1552.20861403881,1553.20835004953,1554.20808606025,
1555.20782207097,1556.20755808169,1557.20729409241,1558.20703010313,1559.20676611385,
1560.20650212457,1561.20623813529,1562.20597414601,1563.20571015673,1564.20544616745,
1565.20518217817,1566.20491818889,1567.20465419961,1568.20439021033,1569.20412622105,
1570.20386223177,1571.20359824249,1572.20333425321,1573.20307026393,1574.20280627465,
1575.20254228537,1576.20227829609,1577.20201430681,1578.20175031753,1579.20148632825,
1580.20122233897,1581.20095834969,1582.20069436041,1583.20043037113,1584.20016638185,
1585.19990239257,1586.19963840329,1587.19937441401,1588.19911042473,1589.19884643545,
1590.19858244617,1591.19831845689,1592.19805446761,1593.19779047834,1594.19752648906,
1595.19726249978,1596.1969985105,1597.19673452122,1598.19647053194,1599.19620654266,
1600.19594255338,1601.1956785641,1602.19541457482,1603.19515058554,1604.19488659626,
1605.19462260698,1606.1943586177,1607.19409462842,1608.19383063914,1609.19356664986,
1610.19330266058,1611.1930386713,1612.19277468202,1613.19251069274,1614.19224670346,
1615.19198271418,1616.1917187249,1617.19145473562,1618.19119074634,1619.19092675706,
1620.19066276778,1621.1903987785,1622.19013478922,1623.18987079994,1624.18960681066,
1625.18934282138,1626.1890788321,1627.18881484282,1628.18855085354,1629.18828686426,
1630.18802287498,1631.1877588857,1632.18749489642,1633.18723090714,1634.18696691786,
1635.18670292858,1636.1864389393,1637.18617495002,1638.18591096074,1639.18564697146,
1640.18538298218,1641.1851189929,1642.18485500362,1643.18459101434,1644.18432702506,
1645.18406303578,1646.1837990465,1647.18353505722,1648.18327106794,1649.18300707866,
1650.18274308938,1651.1824791001,1652.18221511082,1653.18195112154,1654.18168713226,
1655.18142314298,1656.1811591537,1657.18089516442,1658.18063117514,1659.18036718586,
1660.18010319658,1661.1798392073,1662.17957521802,1663.17931122874,1664.17904723946,
1665.17878325018,1666.1785192609,1667.17825527162,1668.17799128234,1669.17772729307,
1670.17746330379,1671.17719931451,1672.17693532523,1673.17667133595,1674.17640734667,
1675.17614335739,1676.17587936811,1677.17561537883,1678.17535138955,1679.17508740027,
1680.17482341099,1681.17455942171,1682.17429543243,1683.17403144315,1684.17376745387,
1685.17350346459,1686.17323947531,1687.17297548603,1688.17271149675,1689.17244750747,
1690.17218351819,1691.17191952891,1692.17165553963,1693.17139155035,1694.17112756107,
1695.17086357179,1696.17059958251,1697.17033559323,1698.17007160395,1699.16980761467,
1700.16954362539,1700.66941163075,1701.16959429301),.UNSPECIFIED.);
#51=B_SPLINE_SURFACE_WITH_KNOTS('',3,3,((#226317,#226318,#226319,#226320,
#226321,#226322,#226323,#226324,#226325,#226326,#226327,#226328,#226329,
#226330,#226331,#226332,#226333,#226334,#226335,#226336,#226337,#226338,
#226339,#226340,#226341,#226342,#226343,#226344,#226345,#226346,#226347,
#226348,#226349,#226350,#226351,#226352,#226353,#226354,#226355,#226356,
#226357,#226358,#226359,#226360,#226361,#226362,#226363,#226364,#226365,
#226366,#226367,#226368,#226369,#226370,#226371,#226372,#226373,#226374,
#226375,#226376,#226377,#226378,#226379,#226380,#226381,#226382,#226383,
#226384,#226385,#226386,#226387,#226388,#226389,#226390,#226391,#226392,
#226393,#226394,#226395,#226396,#226397,#226398,#226399,#226400,#226401,
#226402,#226403,#226404,#226405,#226406,#226407,#226408,#226409,#226410,
#226411,#226412,#226413,#226414,#226415,#226416,#226417,#226418,#226419,
#226420,#226421,#226422,#226423,#226424,#226425,#226426,#226427,#226428,
#226429,#226430,#226431,#226432,#226433,#226434,#226435,#226436,#226437,
#226438,#226439,#226440,#226441,#226442,#226443,#226444,#226445,#226446,
#226447,#226448,#226449,#226450,#226451,#226452,#226453,#226454,#226455,
#226456,#226457,#226458,#226459,#226460,#226461,#226462,#226463,#226464,
#226465,#226466,#226467,#226468,#226469,#226470,#226471,#226472,#226473,
#226474,#226475,#226476,#226477,#226478,#226479,#226480,#226481,#226482,
#226483,#226484,#226485,#226486,#226487,#226488,#226489,#226490,#226491,
#226492,#226493,#226494,#226495,#226496,#226497,#226498,#226499,#226500,
#226501,#226502,#226503,#226504,#226505,#226506,#226507,#226508,#226509,
#226510,#226511,#226512,#226513,#226514,#226515,#226516,#226517,#226518,
#226519,#226520,#226521,#226522,#226523,#226524,#226525,#226526,#226527,
#226528,#226529,#226530,#226531,#226532,#226533,#226534,#226535,#226536,
#226537,#226538,#226539,#226540,#226541,#226542,#226543,#226544,#226545,
#226546,#226547,#226548,#226549,#226550,#226551,#226552,#226553,#226554,
#226555,#226556,#226557,#226558,#226559,#226560,#226561,#226562,#226563,
#226564,#226565,#226566,#226567,#226568,#226569,#226570,#226571,#226572,
#226573,#226574,#226575,#226576,#226577,#226578,#226579,#226580,#226581,
#226582,#226583,#226584,#226585,#226586,#226587,#226588,#226589,#226590,
#226591,#226592,#226593,#226594,#226595,#226596,#226597,#226598,#226599,
#226600,#226601,#226602,#226603,#226604,#226605,#226606,#226607,#226608,
#226609,#226610,#226611,#226612,#226613,#226614,#226615,#226616,#226617,
#226618,#226619,#226620,#226621,#226622,#226623,#226624,#226625,#226626,
#226627,#226628,#226629,#226630,#226631,#226632,#226633,#226634,#226635,
#226636,#226637,#226638,#226639,#226640,#226641,#226642,#226643,#226644,
#226645,#226646,#226647,#226648,#226649,#226650,#226651,#226652,#226653,
#226654,#226655,#226656,#226657,#226658,#226659,#226660,#226661,#226662,
#226663,#226664,#226665,#226666,#226667,#226668,#226669,#226670,#226671,
#226672,#226673,#226674,#226675,#226676,#226677,#226678,#226679,#226680,
#226681,#226682,#226683,#226684,#226685,#226686,#226687,#226688,#226689,
#226690,#226691,#226692,#226693,#226694,#226695,#226696,#226697,#226698,
#226699,#226700,#226701,#226702,#226703,#226704,#226705,#226706,#226707,
#226708,#226709,#226710,#226711,#226712,#226713,#226714,#226715,#226716,
#226717,#226718,#226719,#226720,#226721,#226722,#226723,#226724,#226725,
#226726,#226727,#226728,#226729,#226730,#226731,#226732,#226733,#226734,
#226735,#226736,#226737,#226738,#226739,#226740,#226741,#226742,#226743,
#226744,#226745,#226746,#226747,#226748,#226749,#226750,#226751,#226752,
#226753,#226754,#226755,#226756,#226757,#226758,#226759,#226760,#226761,
#226762,#226763,#226764,#226765,#226766,#226767,#226768,#226769,#226770,
#226771,#226772,#226773,#226774,#226775,#226776,#226777,#226778,#226779,
#226780,#226781,#226782,#226783,#226784,#226785,#226786,#226787,#226788,
#226789,#226790,#226791,#226792,#226793,#226794,#226795,#226796,#226797,
#226798,#226799,#226800,#226801,#226802,#226803,#226804,#226805,#226806,
#226807,#226808,#226809,#226810,#226811,#226812,#226813,#226814,#226815,
#226816,#226817,#226818,#226819,#226820,#226821,#226822,#226823,#226824,
#226825,#226826,#226827,#226828,#226829,#226830,#226831,#226832,#226833,
#226834,#226835,#226836,#226837,#226838,#226839,#226840,#226841,#226842,
#226843,#226844,#226845,#226846,#226847,#226848,#226849,#226850,#226851,
#226852,#226853,#226854,#226855,#226856,#226857,#226858,#226859,#226860,
#226861,#226862,#226863,#226864,#226865,#226866,#226867,#226868,#226869,
#226870,#226871,#226872,#226873,#226874,#226875,#226876,#226877,#226878,
#226879,#226880,#226881,#226882,#226883,#226884,#226885,#226886,#226887,
#226888,#226889,#226890,#226891,#226892,#226893,#226894,#226895,#226896,
#226897,#226898,#226899,#226900,#226901,#226902,#226903,#226904,#226905,
#226906,#226907,#226908,#226909,#226910,#226911,#226912,#226913,#226914,
#226915,#226916,#226917,#226918,#226919,#226920,#226921,#226922,#226923,
#226924,#226925,#226926,#226927,#226928,#226929,#226930,#226931,#226932,
#226933,#226934,#226935,#226936,#226937,#226938,#226939,#226940,#226941,
#226942,#226943,#226944,#226945,#226946,#226947,#226948,#226949,#226950,
#226951,#226952,#226953,#226954,#226955,#226956,#226957,#226958,#226959,
#226960,#226961,#226962,#226963,#226964,#226965,#226966,#226967,#226968,
#226969,#226970,#226971,#226972,#226973,#226974,#226975,#226976,#226977,
#226978,#226979,#226980,#226981,#226982,#226983,#226984,#226985,#226986,
#226987,#226988,#226989,#226990,#226991,#226992,#226993,#226994,#226995,
#226996,#226997,#226998,#226999,#227000,#227001,#227002,#227003,#227004,
#227005,#227006,#227007,#227008,#227009,#227010,#227011,#227012,#227013,
#227014,#227015,#227016,#227017,#227018,#227019,#227020,#227021,#227022,
#227023,#227024,#227025,#227026,#227027,#227028,#227029,#227030,#227031,
#227032,#227033,#227034,#227035,#227036,#227037,#227038,#227039,#227040,
#227041,#227042,#227043,#227044,#227045,#227046,#227047,#227048,#227049,
#227050,#227051,#227052,#227053,#227054,#227055,#227056,#227057,#227058,
#227059,#227060,#227061,#227062,#227063,#227064,#227065,#227066,#227067,
#227068,#227069,#227070,#227071,#227072,#227073,#227074,#227075,#227076,
#227077,#227078,#227079,#227080,#227081,#227082,#227083,#227084,#227085,
#227086,#227087,#227088,#227089,#227090,#227091,#227092,#227093,#227094,
#227095,#227096,#227097,#227098,#227099,#227100,#227101,#227102,#227103,
#227104,#227105,#227106,#227107,#227108,#227109,#227110,#227111,#227112,
#227113,#227114,#227115,#227116,#227117,#227118,#227119,#227120,#227121,
#227122,#227123,#227124,#227125,#227126,#227127,#227128,#227129,#227130,
#227131,#227132,#227133,#227134,#227135,#227136,#227137,#227138,#227139,
#227140,#227141,#227142,#227143,#227144,#227145,#227146,#227147,#227148,
#227149,#227150,#227151,#227152,#227153,#227154,#227155,#227156,#227157,
#227158,#227159,#227160,#227161,#227162,#227163,#227164,#227165,#227166,
#227167,#227168,#227169,#227170,#227171,#227172,#227173,#227174,#227175,
#227176,#227177,#227178,#227179,#227180,#227181,#227182,#227183,#227184,
#227185,#227186,#227187,#227188,#227189,#227190,#227191,#227192,#227193,
#227194,#227195,#227196,#227197,#227198,#227199,#227200,#227201,#227202,
#227203,#227204,#227205,#227206,#227207,#227208,#227209,#227210,#227211,
#227212,#227213,#227214,#227215,#227216,#227217,#227218,#227219,#227220,
#227221,#227222,#227223,#227224,#227225,#227226,#227227,#227228,#227229,
#227230,#227231,#227232,#227233,#227234,#227235,#227236,#227237,#227238,
#227239,#227240,#227241,#227242,#227243,#227244,#227245,#227246,#227247,
#227248,#227249,#227250,#227251,#227252,#227253,#227254,#227255,#227256,
#227257,#227258,#227259,#227260,#227261,#227262,#227263,#227264,#227265,
#227266,#227267,#227268,#227269,#227270,#227271,#227272,#227273,#227274,
#227275,#227276,#227277,#227278,#227279,#227280,#227281,#227282,#227283,
#227284,#227285,#227286,#227287,#227288,#227289,#227290,#227291,#227292,
#227293,#227294,#227295,#227296,#227297,#227298,#227299,#227300,#227301,
#227302,#227303,#227304,#227305,#227306,#227307,#227308,#227309,#227310,
#227311,#227312,#227313,#227314,#227315,#227316,#227317,#227318,#227319,
#227320,#227321,#227322,#227323,#227324,#227325,#227326,#227327,#227328,
#227329,#227330,#227331,#227332,#227333,#227334,#227335,#227336,#227337,
#227338,#227339,#227340,#227341,#227342,#227343,#227344,#227345,#227346,
#227347,#227348,#227349,#227350,#227351,#227352,#227353,#227354,#227355,
#227356,#227357,#227358,#227359,#227360,#227361,#227362,#227363,#227364,
#227365,#227366,#227367,#227368,#227369,#227370,#227371,#227372,#227373,
#227374,#227375,#227376,#227377,#227378,#227379,#227380,#227381,#227382,
#227383,#227384,#227385,#227386,#227387,#227388,#227389,#227390,#227391,
#227392,#227393,#227394,#227395,#227396,#227397,#227398,#227399,#227400,
#227401,#227402,#227403,#227404,#227405,#227406,#227407,#227408,#227409,
#227410,#227411,#227412,#227413,#227414,#227415,#227416,#227417,#227418,
#227419,#227420,#227421,#227422,#227423,#227424,#227425,#227426,#227427,
#227428,#227429,#227430,#227431,#227432,#227433,#227434,#227435,#227436,
#227437,#227438,#227439,#227440,#227441,#227442,#227443,#227444,#227445,
#227446,#227447,#227448,#227449,#227450,#227451,#227452,#227453,#227454,
#227455,#227456,#227457,#227458,#227459,#227460,#227461,#227462,#227463,
#227464,#227465,#227466,#227467,#227468,#227469,#227470,#227471,#227472,
#227473,#227474,#227475,#227476,#227477,#227478,#227479,#227480,#227481,
#227482,#227483,#227484,#227485,#227486,#227487,#227488,#227489,#227490,
#227491,#227492,#227493,#227494,#227495,#227496,#227497,#227498,#227499,
#227500,#227501,#227502,#227503,#227504,#227505,#227506,#227507,#227508,
#227509,#227510,#227511,#227512,#227513,#227514,#227515,#227516,#227517,
#227518,#227519,#227520,#227521,#227522,#227523,#227524,#227525,#227526,
#227527,#227528,#227529,#227530,#227531,#227532,#227533,#227534,#227535,
#227536,#227537,#227538,#227539,#227540,#227541,#227542,#227543,#227544,
#227545,#227546,#227547,#227548,#227549,#227550,#227551,#227552,#227553,
#227554,#227555,#227556,#227557,#227558,#227559,#227560,#227561,#227562,
#227563,#227564,#227565,#227566,#227567,#227568,#227569,#227570,#227571,
#227572,#227573,#227574,#227575,#227576,#227577,#227578,#227579,#227580,
#227581,#227582,#227583,#227584,#227585,#227586,#227587,#227588,#227589,
#227590,#227591,#227592,#227593,#227594,#227595,#227596,#227597,#227598,
#227599,#227600,#227601,#227602,#227603,#227604,#227605,#227606,#227607,
#227608,#227609,#227610,#227611,#227612,#227613,#227614,#227615,#227616,
#227617,#227618,#227619,#227620,#227621,#227622,#227623,#227624,#227625,
#227626,#227627,#227628,#227629,#227630,#227631,#227632,#227633,#227634,
#227635,#227636,#227637,#227638,#227639,#227640,#227641,#227642,#227643,
#227644,#227645,#227646,#227647,#227648,#227649,#227650,#227651,#227652,
#227653,#227654,#227655,#227656,#227657,#227658,#227659,#227660,#227661,
#227662,#227663,#227664,#227665,#227666,#227667,#227668,#227669,#227670,
#227671,#227672,#227673,#227674,#227675,#227676,#227677,#227678,#227679,
#227680,#227681,#227682,#227683,#227684,#227685,#227686,#227687,#227688,
#227689,#227690,#227691,#227692,#227693,#227694,#227695,#227696,#227697,
#227698,#227699,#227700,#227701,#227702,#227703,#227704,#227705,#227706,
#227707,#227708,#227709,#227710,#227711,#227712,#227713,#227714,#227715,
#227716,#227717,#227718,#227719,#227720,#227721,#227722,#227723,#227724,
#227725,#227726,#227727,#227728,#227729,#227730,#227731,#227732,#227733,
#227734,#227735,#227736,#227737,#227738,#227739,#227740,#227741,#227742,
#227743,#227744,#227745,#227746,#227747,#227748,#227749,#227750,#227751,
#227752,#227753,#227754,#227755,#227756,#227757,#227758,#227759,#227760,
#227761,#227762,#227763,#227764,#227765,#227766,#227767,#227768,#227769,
#227770,#227771,#227772,#227773,#227774,#227775,#227776,#227777,#227778,
#227779,#227780,#227781,#227782,#227783,#227784,#227785,#227786,#227787,
#227788,#227789,#227790,#227791,#227792,#227793,#227794,#227795,#227796,
#227797,#227798,#227799,#227800,#227801,#227802,#227803,#227804,#227805,
#227806,#227807,#227808,#227809,#227810,#227811,#227812,#227813,#227814,
#227815,#227816,#227817,#227818,#227819,#227820,#227821,#227822,#227823,
#227824,#227825,#227826,#227827,#227828,#227829,#227830,#227831,#227832,
#227833,#227834,#227835,#227836,#227837,#227838,#227839,#227840,#227841,
#227842,#227843,#227844,#227845,#227846,#227847,#227848,#227849,#227850,
#227851,#227852,#227853,#227854,#227855,#227856,#227857,#227858,#227859,
#227860,#227861,#227862,#227863,#227864,#227865,#227866,#227867,#227868,
#227869,#227870,#227871,#227872,#227873,#227874,#227875,#227876,#227877,
#227878,#227879,#227880,#227881,#227882,#227883,#227884,#227885,#227886,
#227887,#227888,#227889,#227890,#227891,#227892,#227893,#227894,#227895,
#227896,#227897,#227898,#227899,#227900,#227901,#227902,#227903,#227904,
#227905,#227906,#227907,#227908,#227909,#227910,#227911,#227912,#227913,
#227914,#227915,#227916,#227917,#227918,#227919,#227920,#227921,#227922,
#227923,#227924,#227925,#227926,#227927,#227928,#227929,#227930,#227931,
#227932,#227933,#227934,#227935,#227936,#227937,#227938,#227939,#227940,
#227941,#227942,#227943,#227944,#227945,#227946,#227947,#227948,#227949,
#227950,#227951,#227952,#227953,#227954,#227955,#227956,#227957,#227958,
#227959,#227960,#227961,#227962,#227963,#227964,#227965,#227966,#227967,
#227968,#227969,#227970,#227971,#227972,#227973,#227974,#227975,#227976,
#227977,#227978,#227979,#227980,#227981,#227982,#227983,#227984,#227985,
#227986,#227987,#227988,#227989,#227990,#227991,#227992,#227993,#227994,
#227995,#227996,#227997,#227998,#227999,#228000,#228001,#228002,#228003,
#228004,#228005,#228006,#228007,#228008,#228009,#228010,#228011),(#228012,
#228013,#228014,#228015,#228016,#228017,#228018,#228019,#228020,#228021,
#228022,#228023,#228024,#228025,#228026,#228027,#228028,#228029,#228030,
#228031,#228032,#228033,#228034,#228035,#228036,#228037,#228038,#228039,
#228040,#228041,#228042,#228043,#228044,#228045,#228046,#228047,#228048,
#228049,#228050,#228051,#228052,#228053,#228054,#228055,#228056,#228057,
#228058,#228059,#228060,#228061,#228062,#228063,#228064,#228065,#228066,
#228067,#228068,#228069,#228070,#228071,#228072,#228073,#228074,#228075,
#228076,#228077,#228078,#228079,#228080,#228081,#228082,#228083,#228084,
#228085,#228086,#228087,#228088,#228089,#228090,#228091,#228092,#228093,
#228094,#228095,#228096,#228097,#228098,#228099,#228100,#228101,#228102,
#228103,#228104,#228105,#228106,#228107,#228108,#228109,#228110,#228111,
#228112,#228113,#228114,#228115,#228116,#228117,#228118,#228119,#228120,
#228121,#228122,#228123,#228124,#228125,#228126,#228127,#228128,#228129,
#228130,#228131,#228132,#228133,#228134,#228135,#228136,#228137,#228138,
#228139,#228140,#228141,#228142,#228143,#228144,#228145,#228146,#228147,
#228148,#228149,#228150,#228151,#228152,#228153,#228154,#228155,#228156,
#228157,#228158,#228159,#228160,#228161,#228162,#228163,#228164,#228165,
#228166,#228167,#228168,#228169,#228170,#228171,#228172,#228173,#228174,
#228175,#228176,#228177,#228178,#228179,#228180,#228181,#228182,#228183,
#228184,#228185,#228186,#228187,#228188,#228189,#228190,#228191,#228192,
#228193,#228194,#228195,#228196,#228197,#228198,#228199,#228200,#228201,
#228202,#228203,#228204,#228205,#228206,#228207,#228208,#228209,#228210,
#228211,#228212,#228213,#228214,#228215,#228216,#228217,#228218,#228219,
#228220,#228221,#228222,#228223,#228224,#228225,#228226,#228227,#228228,
#228229,#228230,#228231,#228232,#228233,#228234,#228235,#228236,#228237,
#228238,#228239,#228240,#228241,#228242,#228243,#228244,#228245,#228246,
#228247,#228248,#228249,#228250,#228251,#228252,#228253,#228254,#228255,
#228256,#228257,#228258,#228259,#228260,#228261,#228262,#228263,#228264,
#228265,#228266,#228267,#228268,#228269,#228270,#228271,#228272,#228273,
#228274,#228275,#228276,#228277,#228278,#228279,#228280,#228281,#228282,
#228283,#228284,#228285,#228286,#228287,#228288,#228289,#228290,#228291,
#228292,#228293,#228294,#228295,#228296,#228297,#228298,#228299,#228300,
#228301,#228302,#228303,#228304,#228305,#228306,#228307,#228308,#228309,
#228310,#228311,#228312,#228313,#228314,#228315,#228316,#228317,#228318,
#228319,#228320,#228321,#228322,#228323,#228324,#228325,#228326,#228327,
#228328,#228329,#228330,#228331,#228332,#228333,#228334,#228335,#228336,
#228337,#228338,#228339,#228340,#228341,#228342,#228343,#228344,#228345,
#228346,#228347,#228348,#228349,#228350,#228351,#228352,#228353,#228354,
#228355,#228356,#228357,#228358,#228359,#228360,#228361,#228362,#228363,
#228364,#228365,#228366,#228367,#228368,#228369,#228370,#228371,#228372,
#228373,#228374,#228375,#228376,#228377,#228378,#228379,#228380,#228381,
#228382,#228383,#228384,#228385,#228386,#228387,#228388,#228389,#228390,
#228391,#228392,#228393,#228394,#228395,#228396,#228397,#228398,#228399,
#228400,#228401,#228402,#228403,#228404,#228405,#228406,#228407,#228408,
#228409,#228410,#228411,#228412,#228413,#228414,#228415,#228416,#228417,
#228418,#228419,#228420,#228421,#228422,#228423,#228424,#228425,#228426,
#228427,#228428,#228429,#228430,#228431,#228432,#228433,#228434,#228435,
#228436,#228437,#228438,#228439,#228440,#228441,#228442,#228443,#228444,
#228445,#228446,#228447,#228448,#228449,#228450,#228451,#228452,#228453,
#228454,#228455,#228456,#228457,#228458,#228459,#228460,#228461,#228462,
#228463,#228464,#228465,#228466,#228467,#228468,#228469,#228470,#228471,
#228472,#228473,#228474,#228475,#228476,#228477,#228478,#228479,#228480,
#228481,#228482,#228483,#228484,#228485,#228486,#228487,#228488,#228489,
#228490,#228491,#228492,#228493,#228494,#228495,#228496,#228497,#228498,
#228499,#228500,#228501,#228502,#228503,#228504,#228505,#228506,#228507,
#228508,#228509,#228510,#228511,#228512,#228513,#228514,#228515,#228516,
#228517,#228518,#228519,#228520,#228521,#228522,#228523,#228524,#228525,
#228526,#228527,#228528,#228529,#228530,#228531,#228532,#228533,#228534,
#228535,#228536,#228537,#228538,#228539,#228540,#228541,#228542,#228543,
#228544,#228545,#228546,#228547,#228548,#228549,#228550,#228551,#228552,
#228553,#228554,#228555,#228556,#228557,#228558,#228559,#228560,#228561,
#228562,#228563,#228564,#228565,#228566,#228567,#228568,#228569,#228570,
#228571,#228572,#228573,#228574,#228575,#228576,#228577,#228578,#228579,
#228580,#228581,#228582,#228583,#228584,#228585,#228586,#228587,#228588,
#228589,#228590,#228591,#228592,#228593,#228594,#228595,#228596,#228597,
#228598,#228599,#228600,#228601,#228602,#228603,#228604,#228605,#228606,
#228607,#228608,#228609,#228610,#228611,#228612,#228613,#228614,#228615,
#228616,#228617,#228618,#228619,#228620,#228621,#228622,#228623,#228624,
#228625,#228626,#228627,#228628,#228629,#228630,#228631,#228632,#228633,
#228634,#228635,#228636,#228637,#228638,#228639,#228640,#228641,#228642,
#228643,#228644,#228645,#228646,#228647,#228648,#228649,#228650,#228651,
#228652,#228653,#228654,#228655,#228656,#228657,#228658,#228659,#228660,
#228661,#228662,#228663,#228664,#228665,#228666,#228667,#228668,#228669,
#228670,#228671,#228672,#228673,#228674,#228675,#228676,#228677,#228678,
#228679,#228680,#228681,#228682,#228683,#228684,#228685,#228686,#228687,
#228688,#228689,#228690,#228691,#228692,#228693,#228694,#228695,#228696,
#228697,#228698,#228699,#228700,#228701,#228702,#228703,#228704,#228705,
#228706,#228707,#228708,#228709,#228710,#228711,#228712,#228713,#228714,
#228715,#228716,#228717,#228718,#228719,#228720,#228721,#228722,#228723,
#228724,#228725,#228726,#228727,#228728,#228729,#228730,#228731,#228732,
#228733,#228734,#228735,#228736,#228737,#228738,#228739,#228740,#228741,
#228742,#228743,#228744,#228745,#228746,#228747,#228748,#228749,#228750,
#228751,#228752,#228753,#228754,#228755,#228756,#228757,#228758,#228759,
#228760,#228761,#228762,#228763,#228764,#228765,#228766,#228767,#228768,
#228769,#228770,#228771,#228772,#228773,#228774,#228775,#228776,#228777,
#228778,#228779,#228780,#228781,#228782,#228783,#228784,#228785,#228786,
#228787,#228788,#228789,#228790,#228791,#228792,#228793,#228794,#228795,
#228796,#228797,#228798,#228799,#228800,#228801,#228802,#228803,#228804,
#228805,#228806,#228807,#228808,#228809,#228810,#228811,#228812,#228813,
#228814,#228815,#228816,#228817,#228818,#228819,#228820,#228821,#228822,
#228823,#228824,#228825,#228826,#228827,#228828,#228829,#228830,#228831,
#228832,#228833,#228834,#228835,#228836,#228837,#228838,#228839,#228840,
#228841,#228842,#228843,#228844,#228845,#228846,#228847,#228848,#228849,
#228850,#228851,#228852,#228853,#228854,#228855,#228856,#228857,#228858,
#228859,#228860,#228861,#228862,#228863,#228864,#228865,#228866,#228867,
#228868,#228869,#228870,#228871,#228872,#228873,#228874,#228875,#228876,
#228877,#228878,#228879,#228880,#228881,#228882,#228883,#228884,#228885,
#228886,#228887,#228888,#228889,#228890,#228891,#228892,#228893,#228894,
#228895,#228896,#228897,#228898,#228899,#228900,#228901,#228902,#228903,
#228904,#228905,#228906,#228907,#228908,#228909,#228910,#228911,#228912,
#228913,#228914,#228915,#228916,#228917,#228918,#228919,#228920,#228921,
#228922,#228923,#228924,#228925,#228926,#228927,#228928,#228929,#228930,
#228931,#228932,#228933,#228934,#228935,#228936,#228937,#228938,#228939,
#228940,#228941,#228942,#228943,#228944,#228945,#228946,#228947,#228948,
#228949,#228950,#228951,#228952,#228953,#228954,#228955,#228956,#228957,
#228958,#228959,#228960,#228961,#228962,#228963,#228964,#228965,#228966,
#228967,#228968,#228969,#228970,#228971,#228972,#228973,#228974,#228975,
#228976,#228977,#228978,#228979,#228980,#228981,#228982,#228983,#228984,
#228985,#228986,#228987,#228988,#228989,#228990,#228991,#228992,#228993,
#228994,#228995,#228996,#228997,#228998,#228999,#229000,#229001,#229002,
#229003,#229004,#229005,#229006,#229007,#229008,#229009,#229010,#229011,
#229012,#229013,#229014,#229015,#229016,#229017,#229018,#229019,#229020,
#229021,#229022,#229023,#229024,#229025,#229026,#229027,#229028,#229029,
#229030,#229031,#229032,#229033,#229034,#229035,#229036,#229037,#229038,
#229039,#229040,#229041,#229042,#229043,#229044,#229045,#229046,#229047,
#229048,#229049,#229050,#229051,#229052,#229053,#229054,#229055,#229056,
#229057,#229058,#229059,#229060,#229061,#229062,#229063,#229064,#229065,
#229066,#229067,#229068,#229069,#229070,#229071,#229072,#229073,#229074,
#229075,#229076,#229077,#229078,#229079,#229080,#229081,#229082,#229083,
#229084,#229085,#229086,#229087,#229088,#229089,#229090,#229091,#229092,
#229093,#229094,#229095,#229096,#229097,#229098,#229099,#229100,#229101,
#229102,#229103,#229104,#229105,#229106,#229107,#229108,#229109,#229110,
#229111,#229112,#229113,#229114,#229115,#229116,#229117,#229118,#229119,
#229120,#229121,#229122,#229123,#229124,#229125,#229126,#229127,#229128,
#229129,#229130,#229131,#229132,#229133,#229134,#229135,#229136,#229137,
#229138,#229139,#229140,#229141,#229142,#229143,#229144,#229145,#229146,
#229147,#229148,#229149,#229150,#229151,#229152,#229153,#229154,#229155,
#229156,#229157,#229158,#229159,#229160,#229161,#229162,#229163,#229164,
#229165,#229166,#229167,#229168,#229169,#229170,#229171,#229172,#229173,
#229174,#229175,#229176,#229177,#229178,#229179,#229180,#229181,#229182,
#229183,#229184,#229185,#229186,#229187,#229188,#229189,#229190,#229191,
#229192,#229193,#229194,#229195,#229196,#229197,#229198,#229199,#229200,
#229201,#229202,#229203,#229204,#229205,#229206,#229207,#229208,#229209,
#229210,#229211,#229212,#229213,#229214,#229215,#229216,#229217,#229218,
#229219,#229220,#229221,#229222,#229223,#229224,#229225,#229226,#229227,
#229228,#229229,#229230,#229231,#229232,#229233,#229234,#229235,#229236,
#229237,#229238,#229239,#229240,#229241,#229242,#229243,#229244,#229245,
#229246,#229247,#229248,#229249,#229250,#229251,#229252,#229253,#229254,
#229255,#229256,#229257,#229258,#229259,#229260,#229261,#229262,#229263,
#229264,#229265,#229266,#229267,#229268,#229269,#229270,#229271,#229272,
#229273,#229274,#229275,#229276,#229277,#229278,#229279,#229280,#229281,
#229282,#229283,#229284,#229285,#229286,#229287,#229288,#229289,#229290,
#229291,#229292,#229293,#229294,#229295,#229296,#229297,#229298,#229299,
#229300,#229301,#229302,#229303,#229304,#229305,#229306,#229307,#229308,
#229309,#229310,#229311,#229312,#229313,#229314,#229315,#229316,#229317,
#229318,#229319,#229320,#229321,#229322,#229323,#229324,#229325,#229326,
#229327,#229328,#229329,#229330,#229331,#229332,#229333,#229334,#229335,
#229336,#229337,#229338,#229339,#229340,#229341,#229342,#229343,#229344,
#229345,#229346,#229347,#229348,#229349,#229350,#229351,#229352,#229353,
#229354,#229355,#229356,#229357,#229358,#229359,#229360,#229361,#229362,
#229363,#229364,#229365,#229366,#229367,#229368,#229369,#229370,#229371,
#229372,#229373,#229374,#229375,#229376,#229377,#229378,#229379,#229380,
#229381,#229382,#229383,#229384,#229385,#229386,#229387,#229388,#229389,
#229390,#229391,#229392,#229393,#229394,#229395,#229396,#229397,#229398,
#229399,#229400,#229401,#229402,#229403,#229404,#229405,#229406,#229407,
#229408,#229409,#229410,#229411,#229412,#229413,#229414,#229415,#229416,
#229417,#229418,#229419,#229420,#229421,#229422,#229423,#229424,#229425,
#229426,#229427,#229428,#229429,#229430,#229431,#229432,#229433,#229434,
#229435,#229436,#229437,#229438,#229439,#229440,#229441,#229442,#229443,
#229444,#229445,#229446,#229447,#229448,#229449,#229450,#229451,#229452,
#229453,#229454,#229455,#229456,#229457,#229458,#229459,#229460,#229461,
#229462,#229463,#229464,#229465,#229466,#229467,#229468,#229469,#229470,
#229471,#229472,#229473,#229474,#229475,#229476,#229477,#229478,#229479,
#229480,#229481,#229482,#229483,#229484,#229485,#229486,#229487,#229488,
#229489,#229490,#229491,#229492,#229493,#229494,#229495,#229496,#229497,
#229498,#229499,#229500,#229501,#229502,#229503,#229504,#229505,#229506,
#229507,#229508,#229509,#229510,#229511,#229512,#229513,#229514,#229515,
#229516,#229517,#229518,#229519,#229520,#229521,#229522,#229523,#229524,
#229525,#229526,#229527,#229528,#229529,#229530,#229531,#229532,#229533,
#229534,#229535,#229536,#229537,#229538,#229539,#229540,#229541,#229542,
#229543,#229544,#229545,#229546,#229547,#229548,#229549,#229550,#229551,
#229552,#229553,#229554,#229555,#229556,#229557,#229558,#229559,#229560,
#229561,#229562,#229563,#229564,#229565,#229566,#229567,#229568,#229569,
#229570,#229571,#229572,#229573,#229574,#229575,#229576,#229577,#229578,
#229579,#229580,#229581,#229582,#229583,#229584,#229585,#229586,#229587,
#229588,#229589,#229590,#229591,#229592,#229593,#229594,#229595,#229596,
#229597,#229598,#229599,#229600,#229601,#229602,#229603,#229604,#229605,
#229606,#229607,#229608,#229609,#229610,#229611,#229612,#229613,#229614,
#229615,#229616,#229617,#229618,#229619,#229620,#229621,#229622,#229623,
#229624,#229625,#229626,#229627,#229628,#229629,#229630,#229631,#229632,
#229633,#229634,#229635,#229636,#229637,#229638,#229639,#229640,#229641,
#229642,#229643,#229644,#229645,#229646,#229647,#229648,#229649,#229650,
#229651,#229652,#229653,#229654,#229655,#229656,#229657,#229658,#229659,
#229660,#229661,#229662,#229663,#229664,#229665,#229666,#229667,#229668,
#229669,#229670,#229671,#229672,#229673,#229674,#229675,#229676,#229677,
#229678,#229679,#229680,#229681,#229682,#229683,#229684,#229685,#229686,
#229687,#229688,#229689,#229690,#229691,#229692,#229693,#229694,#229695,
#229696,#229697,#229698,#229699,#229700,#229701,#229702,#229703,#229704,
#229705,#229706),(#229707,#229708,#229709,#229710,#229711,#229712,#229713,
#229714,#229715,#229716,#229717,#229718,#229719,#229720,#229721,#229722,
#229723,#229724,#229725,#229726,#229727,#229728,#229729,#229730,#229731,
#229732,#229733,#229734,#229735,#229736,#229737,#229738,#229739,#229740,
#229741,#229742,#229743,#229744,#229745,#229746,#229747,#229748,#229749,
#229750,#229751,#229752,#229753,#229754,#229755,#229756,#229757,#229758,
#229759,#229760,#229761,#229762,#229763,#229764,#229765,#229766,#229767,
#229768,#229769,#229770,#229771,#229772,#229773,#229774,#229775,#229776,
#229777,#229778,#229779,#229780,#229781,#229782,#229783,#229784,#229785,
#229786,#229787,#229788,#229789,#229790,#229791,#229792,#229793,#229794,
#229795,#229796,#229797,#229798,#229799,#229800,#229801,#229802,#229803,
#229804,#229805,#229806,#229807,#229808,#229809,#229810,#229811,#229812,
#229813,#229814,#229815,#229816,#229817,#229818,#229819,#229820,#229821,
#229822,#229823,#229824,#229825,#229826,#229827,#229828,#229829,#229830,
#229831,#229832,#229833,#229834,#229835,#229836,#229837,#229838,#229839,
#229840,#229841,#229842,#229843,#229844,#229845,#229846,#229847,#229848,
#229849,#229850,#229851,#229852,#229853,#229854,#229855,#229856,#229857,
#229858,#229859,#229860,#229861,#229862,#229863,#229864,#229865,#229866,
#229867,#229868,#229869,#229870,#229871,#229872,#229873,#229874,#229875,
#229876,#229877,#229878,#229879,#229880,#229881,#229882,#229883,#229884,
#229885,#229886,#229887,#229888,#229889,#229890,#229891,#229892,#229893,
#229894,#229895,#229896,#229897,#229898,#229899,#229900,#229901,#229902,
#229903,#229904,#229905,#229906,#229907,#229908,#229909,#229910,#229911,
#229912,#229913,#229914,#229915,#229916,#229917,#229918,#229919,#229920,
#229921,#229922,#229923,#229924,#229925,#229926,#229927,#229928,#229929,
#229930,#229931,#229932,#229933,#229934,#229935,#229936,#229937,#229938,
#229939,#229940,#229941,#229942,#229943,#229944,#229945,#229946,#229947,
#229948,#229949,#229950,#229951,#229952,#229953,#229954,#229955,#229956,
#229957,#229958,#229959,#229960,#229961,#229962,#229963,#229964,#229965,
#229966,#229967,#229968,#229969,#229970,#229971,#229972,#229973,#229974,
#229975,#229976,#229977,#229978,#229979,#229980,#229981,#229982,#229983,
#229984,#229985,#229986,#229987,#229988,#229989,#229990,#229991,#229992,
#229993,#229994,#229995,#229996,#229997,#229998,#229999,#230000,#230001,
#230002,#230003,#230004,#230005,#230006,#230007,#230008,#230009,#230010,
#230011,#230012,#230013,#230014,#230015,#230016,#230017,#230018,#230019,
#230020,#230021,#230022,#230023,#230024,#230025,#230026,#230027,#230028,
#230029,#230030,#230031,#230032,#230033,#230034,#230035,#230036,#230037,
#230038,#230039,#230040,#230041,#230042,#230043,#230044,#230045,#230046,
#230047,#230048,#230049,#230050,#230051,#230052,#230053,#230054,#230055,
#230056,#230057,#230058,#230059,#230060,#230061,#230062,#230063,#230064,
#230065,#230066,#230067,#230068,#230069,#230070,#230071,#230072,#230073,
#230074,#230075,#230076,#230077,#230078,#230079,#230080,#230081,#230082,
#230083,#230084,#230085,#230086,#230087,#230088,#230089,#230090,#230091,
#230092,#230093,#230094,#230095,#230096,#230097,#230098,#230099,#230100,
#230101,#230102,#230103,#230104,#230105,#230106,#230107,#230108,#230109,
#230110,#230111,#230112,#230113,#230114,#230115,#230116,#230117,#230118,
#230119,#230120,#230121,#230122,#230123,#230124,#230125,#230126,#230127,
#230128,#230129,#230130,#230131,#230132,#230133,#230134,#230135,#230136,
#230137,#230138,#230139,#230140,#230141,#230142,#230143,#230144,#230145,
#230146,#230147,#230148,#230149,#230150,#230151,#230152,#230153,#230154,
#230155,#230156,#230157,#230158,#230159,#230160,#230161,#230162,#230163,
#230164,#230165,#230166,#230167,#230168,#230169,#230170,#230171,#230172,
#230173,#230174,#230175,#230176,#230177,#230178,#230179,#230180,#230181,
#230182,#230183,#230184,#230185,#230186,#230187,#230188,#230189,#230190,
#230191,#230192,#230193,#230194,#230195,#230196,#230197,#230198,#230199,
#230200,#230201,#230202,#230203,#230204,#230205,#230206,#230207,#230208,
#230209,#230210,#230211,#230212,#230213,#230214,#230215,#230216,#230217,
#230218,#230219,#230220,#230221,#230222,#230223,#230224,#230225,#230226,
#230227,#230228,#230229,#230230,#230231,#230232,#230233,#230234,#230235,
#230236,#230237,#230238,#230239,#230240,#230241,#230242,#230243,#230244,
#230245,#230246,#230247,#230248,#230249,#230250,#230251,#230252,#230253,
#230254,#230255,#230256,#230257,#230258,#230259,#230260,#230261,#230262,
#230263,#230264,#230265,#230266,#230267,#230268,#230269,#230270,#230271,
#230272,#230273,#230274,#230275,#230276,#230277,#230278,#230279,#230280,
#230281,#230282,#230283,#230284,#230285,#230286,#230287,#230288,#230289,
#230290,#230291,#230292,#230293,#230294,#230295,#230296,#230297,#230298,
#230299,#230300,#230301,#230302,#230303,#230304,#230305,#230306,#230307,
#230308,#230309,#230310,#230311,#230312,#230313,#230314,#230315,#230316,
#230317,#230318,#230319,#230320,#230321,#230322,#230323,#230324,#230325,
#230326,#230327,#230328,#230329,#230330,#230331,#230332,#230333,#230334,
#230335,#230336,#230337,#230338,#230339,#230340,#230341,#230342,#230343,
#230344,#230345,#230346,#230347,#230348,#230349,#230350,#230351,#230352,
#230353,#230354,#230355,#230356,#230357,#230358,#230359,#230360,#230361,
#230362,#230363,#230364,#230365,#230366,#230367,#230368,#230369,#230370,
#230371,#230372,#230373,#230374,#230375,#230376,#230377,#230378,#230379,
#230380,#230381,#230382,#230383,#230384,#230385,#230386,#230387,#230388,
#230389,#230390,#230391,#230392,#230393,#230394,#230395,#230396,#230397,
#230398,#230399,#230400,#230401,#230402,#230403,#230404,#230405,#230406,
#230407,#230408,#230409,#230410,#230411,#230412,#230413,#230414,#230415,
#230416,#230417,#230418,#230419,#230420,#230421,#230422,#230423,#230424,
#230425,#230426,#230427,#230428,#230429,#230430,#230431,#230432,#230433,
#230434,#230435,#230436,#230437,#230438,#230439,#230440,#230441,#230442,
#230443,#230444,#230445,#230446,#230447,#230448,#230449,#230450,#230451,
#230452,#230453,#230454,#230455,#230456,#230457,#230458,#230459,#230460,
#230461,#230462,#230463,#230464,#230465,#230466,#230467,#230468,#230469,
#230470,#230471,#230472,#230473,#230474,#230475,#230476,#230477,#230478,
#230479,#230480,#230481,#230482,#230483,#230484,#230485,#230486,#230487,
#230488,#230489,#230490,#230491,#230492,#230493,#230494,#230495,#230496,
#230497,#230498,#230499,#230500,#230501,#230502,#230503,#230504,#230505,
#230506,#230507,#230508,#230509,#230510,#230511,#230512,#230513,#230514,
#230515,#230516,#230517,#230518,#230519,#230520,#230521,#230522,#230523,
#230524,#230525,#230526,#230527,#230528,#230529,#230530,#230531,#230532,
#230533,#230534,#230535,#230536,#230537,#230538,#230539,#230540,#230541,
#230542,#230543,#230544,#230545,#230546,#230547,#230548,#230549,#230550,
#230551,#230552,#230553,#230554,#230555,#230556,#230557,#230558,#230559,
#230560,#230561,#230562,#230563,#230564,#230565,#230566,#230567,#230568,
#230569,#230570,#230571,#230572,#230573,#230574,#230575,#230576,#230577,
#230578,#230579,#230580,#230581,#230582,#230583,#230584,#230585,#230586,
#230587,#230588,#230589,#230590,#230591,#230592,#230593,#230594,#230595,
#230596,#230597,#230598,#230599,#230600,#230601,#230602,#230603,#230604,
#230605,#230606,#230607,#230608,#230609,#230610,#230611,#230612,#230613,
#230614,#230615,#230616,#230617,#230618,#230619,#230620,#230621,#230622,
#230623,#230624,#230625,#230626,#230627,#230628,#230629,#230630,#230631,
#230632,#230633,#230634,#230635,#230636,#230637,#230638,#230639,#230640,
#230641,#230642,#230643,#230644,#230645,#230646,#230647,#230648,#230649,
#230650,#230651,#230652,#230653,#230654,#230655,#230656,#230657,#230658,
#230659,#230660,#230661,#230662,#230663,#230664,#230665,#230666,#230667,
#230668,#230669,#230670,#230671,#230672,#230673,#230674,#230675,#230676,
#230677,#230678,#230679,#230680,#230681,#230682,#230683,#230684,#230685,
#230686,#230687,#230688,#230689,#230690,#230691,#230692,#230693,#230694,
#230695,#230696,#230697,#230698,#230699,#230700,#230701,#230702,#230703,
#230704,#230705,#230706,#230707,#230708,#230709,#230710,#230711,#230712,
#230713,#230714,#230715,#230716,#230717,#230718,#230719,#230720,#230721,
#230722,#230723,#230724,#230725,#230726,#230727,#230728,#230729,#230730,
#230731,#230732,#230733,#230734,#230735,#230736,#230737,#230738,#230739,
#230740,#230741,#230742,#230743,#230744,#230745,#230746,#230747,#230748,
#230749,#230750,#230751,#230752,#230753,#230754,#230755,#230756,#230757,
#230758,#230759,#230760,#230761,#230762,#230763,#230764,#230765,#230766,
#230767,#230768,#230769,#230770,#230771,#230772,#230773,#230774,#230775,
#230776,#230777,#230778,#230779,#230780,#230781,#230782,#230783,#230784,
#230785,#230786,#230787,#230788,#230789,#230790,#230791,#230792,#230793,
#230794,#230795,#230796,#230797,#230798,#230799,#230800,#230801,#230802,
#230803,#230804,#230805,#230806,#230807,#230808,#230809,#230810,#230811,
#230812,#230813,#230814,#230815,#230816,#230817,#230818,#230819,#230820,
#230821,#230822,#230823,#230824,#230825,#230826,#230827,#230828,#230829,
#230830,#230831,#230832,#230833,#230834,#230835,#230836,#230837,#230838,
#230839,#230840,#230841,#230842,#230843,#230844,#230845,#230846,#230847,
#230848,#230849,#230850,#230851,#230852,#230853,#230854,#230855,#230856,
#230857,#230858,#230859,#230860,#230861,#230862,#230863,#230864,#230865,
#230866,#230867,#230868,#230869,#230870,#230871,#230872,#230873,#230874,
#230875,#230876,#230877,#230878,#230879,#230880,#230881,#230882,#230883,
#230884,#230885,#230886,#230887,#230888,#230889,#230890,#230891,#230892,
#230893,#230894,#230895,#230896,#230897,#230898,#230899,#230900,#230901,
#230902,#230903,#230904,#230905,#230906,#230907,#230908,#230909,#230910,
#230911,#230912,#230913,#230914,#230915,#230916,#230917,#230918,#230919,
#230920,#230921,#230922,#230923,#230924,#230925,#230926,#230927,#230928,
#230929,#230930,#230931,#230932,#230933,#230934,#230935,#230936,#230937,
#230938,#230939,#230940,#230941,#230942,#230943,#230944,#230945,#230946,
#230947,#230948,#230949,#230950,#230951,#230952,#230953,#230954,#230955,
#230956,#230957,#230958,#230959,#230960,#230961,#230962,#230963,#230964,
#230965,#230966,#230967,#230968,#230969,#230970,#230971,#230972,#230973,
#230974,#230975,#230976,#230977,#230978,#230979,#230980,#230981,#230982,
#230983,#230984,#230985,#230986,#230987,#230988,#230989,#230990,#230991,
#230992,#230993,#230994,#230995,#230996,#230997,#230998,#230999,#231000,
#231001,#231002,#231003,#231004,#231005,#231006,#231007,#231008,#231009,
#231010,#231011,#231012,#231013,#231014,#231015,#231016,#231017,#231018,
#231019,#231020,#231021,#231022,#231023,#231024,#231025,#231026,#231027,
#231028,#231029,#231030,#231031,#231032,#231033,#231034,#231035,#231036,
#231037,#231038,#231039,#231040,#231041,#231042,#231043,#231044,#231045,
#231046,#231047,#231048,#231049,#231050,#231051,#231052,#231053,#231054,
#231055,#231056,#231057,#231058,#231059,#231060,#231061,#231062,#231063,
#231064,#231065,#231066,#231067,#231068,#231069,#231070,#231071,#231072,
#231073,#231074,#231075,#231076,#231077,#231078,#231079,#231080,#231081,
#231082,#231083,#231084,#231085,#231086,#231087,#231088,#231089,#231090,
#231091,#231092,#231093,#231094,#231095,#231096,#231097,#231098,#231099,
#231100,#231101,#231102,#231103,#231104,#231105,#231106,#231107,#231108,
#231109,#231110,#231111,#231112,#231113,#231114,#231115,#231116,#231117,
#231118,#231119,#231120,#231121,#231122,#231123,#231124,#231125,#231126,
#231127,#231128,#231129,#231130,#231131,#231132,#231133,#231134,#231135,
#231136,#231137,#231138,#231139,#231140,#231141,#231142,#231143,#231144,
#231145,#231146,#231147,#231148,#231149,#231150,#231151,#231152,#231153,
#231154,#231155,#231156,#231157,#231158,#231159,#231160,#231161,#231162,
#231163,#231164,#231165,#231166,#231167,#231168,#231169,#231170,#231171,
#231172,#231173,#231174,#231175,#231176,#231177,#231178,#231179,#231180,
#231181,#231182,#231183,#231184,#231185,#231186,#231187,#231188,#231189,
#231190,#231191,#231192,#231193,#231194,#231195,#231196,#231197,#231198,
#231199,#231200,#231201,#231202,#231203,#231204,#231205,#231206,#231207,
#231208,#231209,#231210,#231211,#231212,#231213,#231214,#231215,#231216,
#231217,#231218,#231219,#231220,#231221,#231222,#231223,#231224,#231225,
#231226,#231227,#231228,#231229,#231230,#231231,#231232,#231233,#231234,
#231235,#231236,#231237,#231238,#231239,#231240,#231241,#231242,#231243,
#231244,#231245,#231246,#231247,#231248,#231249,#231250,#231251,#231252,
#231253,#231254,#231255,#231256,#231257,#231258,#231259,#231260,#231261,
#231262,#231263,#231264,#231265,#231266,#231267,#231268,#231269,#231270,
#231271,#231272,#231273,#231274,#231275,#231276,#231277,#231278,#231279,
#231280,#231281,#231282,#231283,#231284,#231285,#231286,#231287,#231288,
#231289,#231290,#231291,#231292,#231293,#231294,#231295,#231296,#231297,
#231298,#231299,#231300,#231301,#231302,#231303,#231304,#231305,#231306,
#231307,#231308,#231309,#231310,#231311,#231312,#231313,#231314,#231315,
#231316,#231317,#231318,#231319,#231320,#231321,#231322,#231323,#231324,
#231325,#231326,#231327,#231328,#231329,#231330,#231331,#231332,#231333,
#231334,#231335,#231336,#231337,#231338,#231339,#231340,#231341,#231342,
#231343,#231344,#231345,#231346,#231347,#231348,#231349,#231350,#231351,
#231352,#231353,#231354,#231355,#231356,#231357,#231358,#231359,#231360,
#231361,#231362,#231363,#231364,#231365,#231366,#231367,#231368,#231369,
#231370,#231371,#231372,#231373,#231374,#231375,#231376,#231377,#231378,
#231379,#231380,#231381,#231382,#231383,#231384,#231385,#231386,#231387,
#231388,#231389,#231390,#231391,#231392,#231393,#231394,#231395,#231396,
#231397,#231398,#231399,#231400,#231401),(#231402,#231403,#231404,#231405,
#231406,#231407,#231408,#231409,#231410,#231411,#231412,#231413,#231414,
#231415,#231416,#231417,#231418,#231419,#231420,#231421,#231422,#231423,
#231424,#231425,#231426,#231427,#231428,#231429,#231430,#231431,#231432,
#231433,#231434,#231435,#231436,#231437,#231438,#231439,#231440,#231441,
#231442,#231443,#231444,#231445,#231446,#231447,#231448,#231449,#231450,
#231451,#231452,#231453,#231454,#231455,#231456,#231457,#231458,#231459,
#231460,#231461,#231462,#231463,#231464,#231465,#231466,#231467,#231468,
#231469,#231470,#231471,#231472,#231473,#231474,#231475,#231476,#231477,
#231478,#231479,#231480,#231481,#231482,#231483,#231484,#231485,#231486,
#231487,#231488,#231489,#231490,#231491,#231492,#231493,#231494,#231495,
#231496,#231497,#231498,#231499,#231500,#231501,#231502,#231503,#231504,
#231505,#231506,#231507,#231508,#231509,#231510,#231511,#231512,#231513,
#231514,#231515,#231516,#231517,#231518,#231519,#231520,#231521,#231522,
#231523,#231524,#231525,#231526,#231527,#231528,#231529,#231530,#231531,
#231532,#231533,#231534,#231535,#231536,#231537,#231538,#231539,#231540,
#231541,#231542,#231543,#231544,#231545,#231546,#231547,#231548,#231549,
#231550,#231551,#231552,#231553,#231554,#231555,#231556,#231557,#231558,
#231559,#231560,#231561,#231562,#231563,#231564,#231565,#231566,#231567,
#231568,#231569,#231570,#231571,#231572,#231573,#231574,#231575,#231576,
#231577,#231578,#231579,#231580,#231581,#231582,#231583,#231584,#231585,
#231586,#231587,#231588,#231589,#231590,#231591,#231592,#231593,#231594,
#231595,#231596,#231597,#231598,#231599,#231600,#231601,#231602,#231603,
#231604,#231605,#231606,#231607,#231608,#231609,#231610,#231611,#231612,
#231613,#231614,#231615,#231616,#231617,#231618,#231619,#231620,#231621,
#231622,#231623,#231624,#231625,#231626,#231627,#231628,#231629,#231630,
#231631,#231632,#231633,#231634,#231635,#231636,#231637,#231638,#231639,
#231640,#231641,#231642,#231643,#231644,#231645,#231646,#231647,#231648,
#231649,#231650,#231651,#231652,#231653,#231654,#231655,#231656,#231657,
#231658,#231659,#231660,#231661,#231662,#231663,#231664,#231665,#231666,
#231667,#231668,#231669,#231670,#231671,#231672,#231673,#231674,#231675,
#231676,#231677,#231678,#231679,#231680,#231681,#231682,#231683,#231684,
#231685,#231686,#231687,#231688,#231689,#231690,#231691,#231692,#231693,
#231694,#231695,#231696,#231697,#231698,#231699,#231700,#231701,#231702,
#231703,#231704,#231705,#231706,#231707,#231708,#231709,#231710,#231711,
#231712,#231713,#231714,#231715,#231716,#231717,#231718,#231719,#231720,
#231721,#231722,#231723,#231724,#231725,#231726,#231727,#231728,#231729,
#231730,#231731,#231732,#231733,#231734,#231735,#231736,#231737,#231738,
#231739,#231740,#231741,#231742,#231743,#231744,#231745,#231746,#231747,
#231748,#231749,#231750,#231751,#231752,#231753,#231754,#231755,#231756,
#231757,#231758,#231759,#231760,#231761,#231762,#231763,#231764,#231765,
#231766,#231767,#231768,#231769,#231770,#231771,#231772,#231773,#231774,
#231775,#231776,#231777,#231778,#231779,#231780,#231781,#231782,#231783,
#231784,#231785,#231786,#231787,#231788,#231789,#231790,#231791,#231792,
#231793,#231794,#231795,#231796,#231797,#231798,#231799,#231800,#231801,
#231802,#231803,#231804,#231805,#231806,#231807,#231808,#231809,#231810,
#231811,#231812,#231813,#231814,#231815,#231816,#231817,#231818,#231819,
#231820,#231821,#231822,#231823,#231824,#231825,#231826,#231827,#231828,
#231829,#231830,#231831,#231832,#231833,#231834,#231835,#231836,#231837,
#231838,#231839,#231840,#231841,#231842,#231843,#231844,#231845,#231846,
#231847,#231848,#231849,#231850,#231851,#231852,#231853,#231854,#231855,
#231856,#231857,#231858,#231859,#231860,#231861,#231862,#231863,#231864,
#231865,#231866,#231867,#231868,#231869,#231870,#231871,#231872,#231873,
#231874,#231875,#231876,#231877,#231878,#231879,#231880,#231881,#231882,
#231883,#231884,#231885,#231886,#231887,#231888,#231889,#231890,#231891,
#231892,#231893,#231894,#231895,#231896,#231897,#231898,#231899,#231900,
#231901,#231902,#231903,#231904,#231905,#231906,#231907,#231908,#231909,
#231910,#231911,#231912,#231913,#231914,#231915,#231916,#231917,#231918,
#231919,#231920,#231921,#231922,#231923,#231924,#231925,#231926,#231927,
#231928,#231929,#231930,#231931,#231932,#231933,#231934,#231935,#231936,
#231937,#231938,#231939,#231940,#231941,#231942,#231943,#231944,#231945,
#231946,#231947,#231948,#231949,#231950,#231951,#231952,#231953,#231954,
#231955,#231956,#231957,#231958,#231959,#231960,#231961,#231962,#231963,
#231964,#231965,#231966,#231967,#231968,#231969,#231970,#231971,#231972,
#231973,#231974,#231975,#231976,#231977,#231978,#231979,#231980,#231981,
#231982,#231983,#231984,#231985,#231986,#231987,#231988,#231989,#231990,
#231991,#231992,#231993,#231994,#231995,#231996,#231997,#231998,#231999,
#232000,#232001,#232002,#232003,#232004,#232005,#232006,#232007,#232008,
#232009,#232010,#232011,#232012,#232013,#232014,#232015,#232016,#232017,
#232018,#232019,#232020,#232021,#232022,#232023,#232024,#232025,#232026,
#232027,#232028,#232029,#232030,#232031,#232032,#232033,#232034,#232035,
#232036,#232037,#232038,#232039,#232040,#232041,#232042,#232043,#232044,
#232045,#232046,#232047,#232048,#232049,#232050,#232051,#232052,#232053,
#232054,#232055,#232056,#232057,#232058,#232059,#232060,#232061,#232062,
#232063,#232064,#232065,#232066,#232067,#232068,#232069,#232070,#232071,
#232072,#232073,#232074,#232075,#232076,#232077,#232078,#232079,#232080,
#232081,#232082,#232083,#232084,#232085,#232086,#232087,#232088,#232089,
#232090,#232091,#232092,#232093,#232094,#232095,#232096,#232097,#232098,
#232099,#232100,#232101,#232102,#232103,#232104,#232105,#232106,#232107,
#232108,#232109,#232110,#232111,#232112,#232113,#232114,#232115,#232116,
#232117,#232118,#232119,#232120,#232121,#232122,#232123,#232124,#232125,
#232126,#232127,#232128,#232129,#232130,#232131,#232132,#232133,#232134,
#232135,#232136,#232137,#232138,#232139,#232140,#232141,#232142,#232143,
#232144,#232145,#232146,#232147,#232148,#232149,#232150,#232151,#232152,
#232153,#232154,#232155,#232156,#232157,#232158,#232159,#232160,#232161,
#232162,#232163,#232164,#232165,#232166,#232167,#232168,#232169,#232170,
#232171,#232172,#232173,#232174,#232175,#232176,#232177,#232178,#232179,
#232180,#232181,#232182,#232183,#232184,#232185,#232186,#232187,#232188,
#232189,#232190,#232191,#232192,#232193,#232194,#232195,#232196,#232197,
#232198,#232199,#232200,#232201,#232202,#232203,#232204,#232205,#232206,
#232207,#232208,#232209,#232210,#232211,#232212,#232213,#232214,#232215,
#232216,#232217,#232218,#232219,#232220,#232221,#232222,#232223,#232224,
#232225,#232226,#232227,#232228,#232229,#232230,#232231,#232232,#232233,
#232234,#232235,#232236,#232237,#232238,#232239,#232240,#232241,#232242,
#232243,#232244,#232245,#232246,#232247,#232248,#232249,#232250,#232251,
#232252,#232253,#232254,#232255,#232256,#232257,#232258,#232259,#232260,
#232261,#232262,#232263,#232264,#232265,#232266,#232267,#232268,#232269,
#232270,#232271,#232272,#232273,#232274,#232275,#232276,#232277,#232278,
#232279,#232280,#232281,#232282,#232283,#232284,#232285,#232286,#232287,
#232288,#232289,#232290,#232291,#232292,#232293,#232294,#232295,#232296,
#232297,#232298,#232299,#232300,#232301,#232302,#232303,#232304,#232305,
#232306,#232307,#232308,#232309,#232310,#232311,#232312,#232313,#232314,
#232315,#232316,#232317,#232318,#232319,#232320,#232321,#232322,#232323,
#232324,#232325,#232326,#232327,#232328,#232329,#232330,#232331,#232332,
#232333,#232334,#232335,#232336,#232337,#232338,#232339,#232340,#232341,
#232342,#232343,#232344,#232345,#232346,#232347,#232348,#232349,#232350,
#232351,#232352,#232353,#232354,#232355,#232356,#232357,#232358,#232359,
#232360,#232361,#232362,#232363,#232364,#232365,#232366,#232367,#232368,
#232369,#232370,#232371,#232372,#232373,#232374,#232375,#232376,#232377,
#232378,#232379,#232380,#232381,#232382,#232383,#232384,#232385,#232386,
#232387,#232388,#232389,#232390,#232391,#232392,#232393,#232394,#232395,
#232396,#232397,#232398,#232399,#232400,#232401,#232402,#232403,#232404,
#232405,#232406,#232407,#232408,#232409,#232410,#232411,#232412,#232413,
#232414,#232415,#232416,#232417,#232418,#232419,#232420,#232421,#232422,
#232423,#232424,#232425,#232426,#232427,#232428,#232429,#232430,#232431,
#232432,#232433,#232434,#232435,#232436,#232437,#232438,#232439,#232440,
#232441,#232442,#232443,#232444,#232445,#232446,#232447,#232448,#232449,
#232450,#232451,#232452,#232453,#232454,#232455,#232456,#232457,#232458,
#232459,#232460,#232461,#232462,#232463,#232464,#232465,#232466,#232467,
#232468,#232469,#232470,#232471,#232472,#232473,#232474,#232475,#232476,
#232477,#232478,#232479,#232480,#232481,#232482,#232483,#232484,#232485,
#232486,#232487,#232488,#232489,#232490,#232491,#232492,#232493,#232494,
#232495,#232496,#232497,#232498,#232499,#232500,#232501,#232502,#232503,
#232504,#232505,#232506,#232507,#232508,#232509,#232510,#232511,#232512,
#232513,#232514,#232515,#232516,#232517,#232518,#232519,#232520,#232521,
#232522,#232523,#232524,#232525,#232526,#232527,#232528,#232529,#232530,
#232531,#232532,#232533,#232534,#232535,#232536,#232537,#232538,#232539,
#232540,#232541,#232542,#232543,#232544,#232545,#232546,#232547,#232548,
#232549,#232550,#232551,#232552,#232553,#232554,#232555,#232556,#232557,
#232558,#232559,#232560,#232561,#232562,#232563,#232564,#232565,#232566,
#232567,#232568,#232569,#232570,#232571,#232572,#232573,#232574,#232575,
#232576,#232577,#232578,#232579,#232580,#232581,#232582,#232583,#232584,
#232585,#232586,#232587,#232588,#232589,#232590,#232591,#232592,#232593,
#232594,#232595,#232596,#232597,#232598,#232599,#232600,#232601,#232602,
#232603,#232604,#232605,#232606,#232607,#232608,#232609,#232610,#232611,
#232612,#232613,#232614,#232615,#232616,#232617,#232618,#232619,#232620,
#232621,#232622,#232623,#232624,#232625,#232626,#232627,#232628,#232629,
#232630,#232631,#232632,#232633,#232634,#232635,#232636,#232637,#232638,
#232639,#232640,#232641,#232642,#232643,#232644,#232645,#232646,#232647,
#232648,#232649,#232650,#232651,#232652,#232653,#232654,#232655,#232656,
#232657,#232658,#232659,#232660,#232661,#232662,#232663,#232664,#232665,
#232666,#232667,#232668,#232669,#232670,#232671,#232672,#232673,#232674,
#232675,#232676,#232677,#232678,#232679,#232680,#232681,#232682,#232683,
#232684,#232685,#232686,#232687,#232688,#232689,#232690,#232691,#232692,
#232693,#232694,#232695,#232696,#232697,#232698,#232699,#232700,#232701,
#232702,#232703,#232704,#232705,#232706,#232707,#232708,#232709,#232710,
#232711,#232712,#232713,#232714,#232715,#232716,#232717,#232718,#232719,
#232720,#232721,#232722,#232723,#232724,#232725,#232726,#232727,#232728,
#232729,#232730,#232731,#232732,#232733,#232734,#232735,#232736,#232737,
#232738,#232739,#232740,#232741,#232742,#232743,#232744,#232745,#232746,
#232747,#232748,#232749,#232750,#232751,#232752,#232753,#232754,#232755,
#232756,#232757,#232758,#232759,#232760,#232761,#232762,#232763,#232764,
#232765,#232766,#232767,#232768,#232769,#232770,#232771,#232772,#232773,
#232774,#232775,#232776,#232777,#232778,#232779,#232780,#232781,#232782,
#232783,#232784,#232785,#232786,#232787,#232788,#232789,#232790,#232791,
#232792,#232793,#232794,#232795,#232796,#232797,#232798,#232799,#232800,
#232801,#232802,#232803,#232804,#232805,#232806,#232807,#232808,#232809,
#232810,#232811,#232812,#232813,#232814,#232815,#232816,#232817,#232818,
#232819,#232820,#232821,#232822,#232823,#232824,#232825,#232826,#232827,
#232828,#232829,#232830,#232831,#232832,#232833,#232834,#232835,#232836,
#232837,#232838,#232839,#232840,#232841,#232842,#232843,#232844,#232845,
#232846,#232847,#232848,#232849,#232850,#232851,#232852,#232853,#232854,
#232855,#232856,#232857,#232858,#232859,#232860,#232861,#232862,#232863,
#232864,#232865,#232866,#232867,#232868,#232869,#232870,#232871,#232872,
#232873,#232874,#232875,#232876,#232877,#232878,#232879,#232880,#232881,
#232882,#232883,#232884,#232885,#232886,#232887,#232888,#232889,#232890,
#232891,#232892,#232893,#232894,#232895,#232896,#232897,#232898,#232899,
#232900,#232901,#232902,#232903,#232904,#232905,#232906,#232907,#232908,
#232909,#232910,#232911,#232912,#232913,#232914,#232915,#232916,#232917,
#232918,#232919,#232920,#232921,#232922,#232923,#232924,#232925,#232926,
#232927,#232928,#232929,#232930,#232931,#232932,#232933,#232934,#232935,
#232936,#232937,#232938,#232939,#232940,#232941,#232942,#232943,#232944,
#232945,#232946,#232947,#232948,#232949,#232950,#232951,#232952,#232953,
#232954,#232955,#232956,#232957,#232958,#232959,#232960,#232961,#232962,
#232963,#232964,#232965,#232966,#232967,#232968,#232969,#232970,#232971,
#232972,#232973,#232974,#232975,#232976,#232977,#232978,#232979,#232980,
#232981,#232982,#232983,#232984,#232985,#232986,#232987,#232988,#232989,
#232990,#232991,#232992,#232993,#232994,#232995,#232996,#232997,#232998,
#232999,#233000,#233001,#233002,#233003,#233004,#233005,#233006,#233007,
#233008,#233009,#233010,#233011,#233012,#233013,#233014,#233015,#233016,
#233017,#233018,#233019,#233020,#233021,#233022,#233023,#233024,#233025,
#233026,#233027,#233028,#233029,#233030,#233031,#233032,#233033,#233034,
#233035,#233036,#233037,#233038,#233039,#233040,#233041,#233042,#233043,
#233044,#233045,#233046,#233047,#233048,#233049,#233050,#233051,#233052,
#233053,#233054,#233055,#233056,#233057,#233058,#233059,#233060,#233061,
#233062,#233063,#233064,#233065,#233066,#233067,#233068,#233069,#233070,
#233071,#233072,#233073,#233074,#233075,#233076,#233077,#233078,#233079,
#233080,#233081,#233082,#233083,#233084,#233085,#233086,#233087,#233088,
#233089,#233090,#233091,#233092,#233093,#233094,#233095,#233096)),
 .UNSPECIFIED.,.F.,.F.,.F.,(4,4),(4,1,1,1,1,1,1,1,1,1,1,1,1,1,1,1,1,1,1,
1,1,1,1,1,1,1,1,1,1,1,1,1,1,1,1,1,1,1,1,1,1,1,1,1,1,1,1,1,1,1,1,1,1,1,1,
1,1,1,1,1,1,1,1,1,1,1,1,1,1,1,1,1,1,1,1,1,1,1,1,1,1,1,1,1,1,1,1,1,1,1,1,
1,1,1,1,1,1,1,1,1,1,1,1,1,1,1,1,1,1,1,1,1,1,1,1,1,1,1,1,1,1,1,1,1,1,1,1,
1,1,1,1,1,1,1,1,1,1,1,1,1,1,1,1,1,1,1,1,1,1,1,1,1,1,1,1,1,1,1,1,1,1,1,1,
1,1,1,1,1,1,1,1,1,1,1,1,1,1,1,1,1,1,1,1,1,1,1,1,1,1,1,1,1,1,1,1,1,1,1,1,
1,1,1,1,1,1,1,1,1,1,1,1,1,1,1,1,1,1,1,1,1,1,1,1,1,1,1,1,1,1,1,1,1,1,1,1,
1,1,1,1,1,1,1,1,1,1,1,1,1,1,1,1,1,1,1,1,1,1,1,1,1,1,1,1,1,1,1,1,1,1,1,1,
1,1,1,1,1,1,1,1,1,1,1,1,1,1,1,1,1,1,1,1,1,1,1,1,1,1,1,1,1,1,1,1,1,1,1,1,
1,1,1,1,1,1,1,1,1,1,1,1,1,1,1,1,1,1,1,1,1,1,1,1,1,1,1,1,1,1,1,1,1,1,1,1,
1,1,1,1,1,1,1,1,1,1,1,1,1,1,1,1,1,1,1,1,1,1,1,1,1,1,1,1,1,1,1,1,1,1,1,1,
1,1,1,1,1,1,1,1,1,1,1,1,1,1,1,1,1,1,1,1,1,1,1,1,1,1,1,1,1,1,1,1,1,1,1,1,
1,1,1,1,1,1,1,1,1,1,1,1,1,1,1,1,1,1,1,1,1,1,1,1,1,1,1,1,1,1,1,1,1,1,1,1,
1,1,1,1,1,1,1,1,1,1,1,1,1,1,1,1,1,1,1,1,1,1,1,1,1,1,1,1,1,1,1,1,1,1,1,1,
1,1,1,1,1,1,1,1,1,1,1,1,1,1,1,1,1,1,1,1,1,1,1,1,1,1,1,1,1,1,1,1,1,1,1,1,
1,1,1,1,1,1,1,1,1,1,1,1,1,1,1,1,1,1,1,1,1,1,1,1,1,1,1,1,1,1,1,1,1,1,1,1,
1,1,1,1,1,1,1,1,1,1,1,1,1,1,1,1,1,1,1,1,1,1,1,1,1,1,1,1,1,1,1,1,1,1,1,1,
1,1,1,1,1,1,1,1,1,1,1,1,1,1,1,1,1,1,1,1,1,1,1,1,1,1,1,1,1,1,1,1,1,1,1,1,
1,1,1,1,1,1,1,1,1,1,1,1,1,1,1,1,1,1,1,1,1,1,1,1,1,1,1,1,1,1,1,1,1,1,1,1,
1,1,1,1,1,1,1,1,1,1,1,1,1,1,1,1,1,1,1,1,1,1,1,1,1,1,1,1,1,1,1,1,1,1,1,1,
1,1,1,1,1,1,1,1,1,1,1,1,1,1,1,1,1,1,1,1,1,1,1,1,1,1,1,1,1,1,1,1,1,1,1,1,
1,1,1,1,1,1,1,1,1,1,1,1,1,1,1,1,1,1,1,1,1,1,1,1,1,1,1,1,1,1,1,1,1,1,1,1,
1,1,1,1,1,1,1,1,1,1,1,1,1,1,1,1,1,1,1,1,1,1,1,1,1,1,1,1,1,1,1,1,1,1,1,1,
1,1,1,1,1,1,1,1,1,1,1,1,1,1,1,1,1,1,1,1,1,1,1,1,1,1,1,1,1,1,1,1,1,1,1,1,
1,1,1,1,1,1,1,1,1,1,1,1,1,1,1,1,1,1,1,1,1,1,1,1,1,1,1,1,1,1,1,1,1,1,1,1,
1,1,1,1,1,1,1,1,1,1,1,1,1,1,1,1,1,1,1,1,1,1,1,1,1,1,1,1,1,1,1,1,1,1,1,1,
1,1,1,1,1,1,1,1,1,1,1,1,1,1,1,1,1,1,1,1,1,1,1,1,1,1,1,1,1,1,1,1,1,1,1,1,
1,1,1,1,1,1,1,1,1,1,1,1,1,1,1,1,1,1,1,1,1,1,1,1,1,1,1,1,1,1,1,1,1,1,1,1,
1,1,1,1,1,1,1,1,1,1,1,1,1,1,1,1,1,1,1,1,1,1,1,1,1,1,1,1,1,1,1,1,1,1,1,1,
1,1,1,1,1,1,1,1,1,1,1,1,1,1,1,1,1,1,1,1,1,1,1,1,1,1,1,1,1,1,1,1,1,1,1,1,
1,1,1,1,1,1,1,1,1,1,1,1,1,1,1,1,1,1,1,1,1,1,1,1,1,1,1,1,1,1,1,1,1,1,1,1,
1,1,1,1,1,1,1,1,1,1,1,1,1,1,1,1,1,1,1,1,1,1,1,1,1,1,1,1,1,1,1,1,1,1,1,1,
1,1,1,1,1,1,1,1,1,1,1,1,1,1,1,1,1,1,1,1,1,1,1,1,1,1,1,1,1,1,1,1,1,1,1,1,
1,1,1,1,1,1,1,1,1,1,1,1,1,1,1,1,1,1,1,1,1,1,1,1,1,1,1,1,1,1,1,1,1,1,1,1,
1,1,1,1,1,1,1,1,1,1,1,1,1,1,1,1,1,1,1,1,1,1,1,1,1,1,1,1,1,1,1,1,1,1,1,1,
1,1,1,1,1,1,1,1,1,1,1,1,1,1,1,1,1,1,1,1,1,1,1,1,1,1,1,1,1,1,1,1,1,1,1,1,
1,1,1,1,1,1,1,1,1,1,1,1,1,1,1,1,1,1,1,1,1,1,1,1,1,1,1,1,1,1,1,1,1,1,1,1,
1,1,1,1,1,1,1,1,1,1,1,1,1,1,1,1,1,1,1,1,1,1,1,1,1,1,1,1,1,1,1,1,1,1,1,1,
1,1,1,1,1,1,1,1,1,1,1,1,1,1,1,1,1,1,1,1,1,1,1,1,1,1,1,1,1,1,1,1,1,1,1,1,
1,1,1,1,1,1,1,1,1,1,1,1,1,1,1,1,1,1,1,1,1,1,1,1,1,1,1,1,1,1,1,1,1,1,1,1,
1,1,1,1,1,1,1,1,1,1,1,1,1,1,1,1,1,1,1,1,1,1,1,1,1,1,1,1,1,1,1,1,1,1,1,1,
1,1,1,1,1,1,1,1,1,1,1,1,1,1,1,1,1,1,1,1,1,1,1,1,1,1,1,1,1,1,1,1,1,1,1,1,
1,1,1,1,1,1,1,1,1,1,1,1,1,1,1,1,1,1,1,1,1,1,1,1,1,1,1,1,1,1,1,1,1,1,1,1,
1,1,1,1,1,1,1,1,1,1,1,1,1,1,1,1,1,1,1,1,1,1,1,1,1,1,1,1,1,1,1,1,1,1,1,1,
1,1,1,1,1,1,1,1,1,1,1,1,1,1,1,1,1,1,1,1,1,1,1,1,1,1,1,1,1,1,1,1,1,1,1,1,
1,1,1,1,1,1,1,1,1,1,1,1,1,1,1,1,1,1,1,1,1,1,1,1,1,1,1,1,1,1,1,1,1,1,1,1,
1,1,1,1,1,1,1,1,1,1,1,1,1,1,1,1,1,1,1,1,1,1,1,1,1,1,1,1,1,1,1,1,1,1,1,1,
1,1,1,1,1,1,1,1,1,1,1,1,1,1,1,1,1,4),(-0.000587328099657093,0.1157205948422),
(8.30590413559005,8.80579087257276,9.30565887793282,10.305394888653,11.3051308993731,
12.3048669100932,13.3046029208133,14.3043389315335,15.3040749422536,16.3038109529737,
17.3035469636939,18.303282974414,19.3030189851341,20.3027549958542,21.3024910065744,
22.3022270172945,23.3019630280146,24.3016990387348,25.3014350494549,26.301171060175,
27.3009070708951,28.3006430816153,29.3003790923354,30.3001151030555,31.2998511137757,
32.2995871244958,33.2993231352159,34.299059145936,35.2987951566562,36.2985311673763,
37.2982671780964,38.2980031888166,39.2977391995367,40.2974752102568,41.2972112209769,
42.2969472316971,43.2966832424172,44.2964192531373,45.2961552638575,46.2958912745776,
47.2956272852977,48.2953632960178,49.295099306738,50.2948353174581,51.2945713281782,
52.2943073388984,53.2940433496185,54.2937793603386,55.2935153710587,56.2932513817789,
57.292987392499,58.2927234032191,59.2924594139393,60.2921954246594,61.2919314353795,
62.2916674460996,63.2914034568198,64.2911394675399,65.29087547826,66.2906114889802,
67.2903474997003,68.2900835104204,69.2898195211405,70.2895555318607,71.2892915425808,
72.2890275533009,73.2887635640211,74.2884995747412,75.2882355854613,76.2879715961814,
77.2877076069016,78.2874436176217,79.2871796283418,80.286915639062,81.2866516497821,
82.2863876605022,83.2861236712224,84.2858596819425,85.2855956926626,86.2853317033827,
87.2850677141029,88.284803724823,89.2845397355431,90.2842757462633,91.2840117569834,
92.2837477677035,93.2834837784236,94.2832197891438,95.2829557998639,96.282691810584,
97.2824278213041,98.2821638320243,99.2818998427444,100.281635853465,101.281371864185,
102.281107874905,103.280843885625,104.280579896345,105.280315907065,106.280051917785,
107.279787928505,108.279523939226,109.279259949946,110.278995960666,111.278731971386,
112.278467982106,113.278203992826,114.277940003546,115.277676014266,116.277412024987,
117.277148035707,118.276884046427,119.276620057147,120.276356067867,121.276092078587,
122.275828089307,123.275564100028,124.275300110748,125.275036121468,126.274772132188,
127.274508142908,128.274244153628,129.273980164348,130.273716175068,131.273452185789,
132.273188196509,133.272924207229,134.272660217949,135.272396228669,136.272132239389,
137.271868250109,138.271604260829,139.27134027155,140.27107628227,141.27081229299,
142.27054830371,143.27028431443,144.27002032515,145.26975633587,146.26949234659,
147.269228357311,148.268964368031,149.268700378751,150.268436389471,151.268172400191,
152.267908410911,153.267644421631,154.267380432352,155.267116443072,156.266852453792,
157.266588464512,158.266324475232,159.266060485952,160.265796496672,161.265532507392,
162.265268518113,163.265004528833,164.264740539553,165.264476550273,166.264212560993,
167.263948571713,168.263684582433,169.263420593153,170.263156603874,171.262892614594,
172.262628625314,173.262364636034,174.262100646754,175.261836657474,176.261572668194,
177.261308678914,178.261044689635,179.260780700355,180.260516711075,181.260252721795,
182.259988732515,183.259724743235,184.259460753955,185.259196764675,186.258932775396,
187.258668786116,188.258404796836,189.258140807556,190.257876818276,191.257612828996,
192.257348839716,193.257084850437,194.256820861157,195.256556871877,196.256292882597,
197.256028893317,198.255764904037,199.255500914757,200.255236925477,201.254972936198,
202.254708946918,203.254444957638,204.254180968358,205.253916979078,206.253652989798,
207.253389000518,208.253125011238,209.252861021959,210.252597032679,211.252333043399,
212.252069054119,213.251805064839,214.251541075559,215.251277086279,216.251013096999,
217.25074910772,218.25048511844,219.25022112916,220.24995713988,221.2496931506,
222.24942916132,223.24916517204,224.248901182761,225.248637193481,226.248373204201,
227.248109214921,228.247845225641,229.247581236361,230.247317247081,231.247053257801,
232.246789268522,233.246525279242,234.246261289962,235.245997300682,236.245733311402,
237.245469322122,238.245205332842,239.244941343562,240.244677354283,241.244413365003,
242.244149375723,243.243885386443,244.243621397163,245.243357407883,246.243093418603,
247.242829429323,248.242565440044,249.242301450764,250.242037461484,251.241773472204,
252.241509482924,253.241245493644,254.240981504364,255.240717515084,256.240453525805,
257.240189536525,258.239925547245,259.239661557965,260.239397568685,261.239133579405,
262.238869590125,263.238605600846,264.238341611566,265.238077622286,266.237813633006,
267.237549643726,268.237285654446,269.237021665166,270.236757675886,271.236493686607,
272.236229697327,273.235965708047,274.235701718767,275.235437729487,276.235173740207,
277.234909750927,278.234645761647,279.234381772368,280.234117783088,281.233853793808,
282.233589804528,283.233325815248,284.233061825968,285.232797836688,286.232533847408,
287.232269858129,288.232005868849,289.231741879569,290.231477890289,291.231213901009,
292.230949911729,293.230685922449,294.23042193317,295.23015794389,296.22989395461,
297.22962996533,298.22936597605,299.22910198677,300.22883799749,301.22857400821,
302.228310018931,303.228046029651,304.227782040371,305.227518051091,306.227254061811,
307.226990072531,308.226726083251,309.226462093971,310.226198104692,311.225934115412,
312.225670126132,313.225406136852,314.225142147572,315.224878158292,316.224614169012,
317.224350179732,318.224086190453,319.223822201173,320.223558211893,321.223294222613,
322.223030233333,323.222766244053,324.222502254773,325.222238265494,326.221974276214,
327.221710286934,328.221446297654,329.221182308374,330.220918319094,331.220654329814,
332.220390340534,333.220126351255,334.219862361975,335.219598372695,336.219334383415,
337.219070394135,338.218806404855,339.218542415575,340.218278426295,341.218014437016,
342.217750447736,343.217486458456,344.217222469176,345.216958479896,346.216694490616,
347.216430501336,348.216166512056,349.215902522777,350.215638533497,351.215374544217,
352.215110554937,353.214846565657,354.214582576377,355.214318587097,356.214054597817,
357.213790608538,358.213526619258,359.213262629978,360.212998640698,361.212734651418,
362.212470662138,363.212206672858,364.211942683579,365.211678694299,366.211414705019,
367.211150715739,368.210886726459,369.210622737179,370.210358747899,371.210094758619,
372.20983076934,373.20956678006,374.20930279078,375.2090388015,376.20877481222,
377.20851082294,378.20824683366,379.20798284438,380.207718855101,381.207454865821,
382.207190876541,383.206926887261,384.206662897981,385.206398908701,386.206134919421,
387.205870930141,388.205606940862,389.205342951582,390.205078962302,391.204814973022,
392.204550983742,393.204286994462,394.204023005182,395.203759015903,396.203495026623,
397.203231037343,398.202967048063,399.202703058783,400.202439069503,401.202175080223,
402.201911090943,403.201647101664,404.201383112384,405.201119123104,406.200855133824,
407.200591144544,408.200327155264,409.200063165984,410.199799176704,411.199535187425,
412.199271198145,413.199007208865,414.198743219585,415.198479230305,416.198215241025,
417.197951251745,418.197687262465,419.197423273186,420.197159283906,421.196895294626,
422.196631305346,423.196367316066,424.196103326786,425.195839337506,426.195575348226,
427.195311358947,428.195047369667,429.194783380387,430.194519391107,431.194255401827,
432.193991412547,433.193727423267,434.193463433988,435.193199444708,436.192935455428,
437.192671466148,438.192407476868,439.192143487588,440.191879498308,441.191615509028,
442.191351519749,443.191087530469,444.190823541189,445.190559551909,446.190295562629,
447.190031573349,448.189767584069,449.189503594789,450.18923960551,451.18897561623,
452.18871162695,453.18844763767,454.18818364839,455.18791965911,456.18765566983,
457.18739168055,458.187127691271,459.186863701991,460.186599712711,461.186335723431,
462.186071734151,463.185807744871,464.185543755591,465.185279766312,466.185015777032,
467.184751787752,468.184487798472,469.184223809192,470.183959819912,471.183695830632,
472.183431841352,473.183167852073,474.182903862793,475.182639873513,476.182375884233,
477.182111894953,478.181847905673,479.181583916393,480.181319927113,481.181055937834,
482.180791948554,483.180527959274,484.180263969994,485.179999980714,486.179735991434,
487.179472002154,488.179208012874,489.178944023595,490.178680034315,491.178416045035,
492.178152055755,493.177888066475,494.177624077195,495.177360087915,496.177096098636,
497.176832109356,498.176568120076,499.176304130796,500.176040141516,501.175776152236,
502.175512162956,503.175248173676,504.174984184397,505.174720195117,506.174456205837,
507.174192216557,508.173928227277,509.173664237997,510.173400248717,511.173136259437,
512.172872270158,513.172608280878,514.172344291598,515.172080302318,516.171816313038,
517.171552323758,518.171288334478,519.171024345198,520.170760355919,521.170496366639,
522.170232377359,523.169968388079,524.169704398799,525.169440409519,526.169176420239,
527.168912430959,528.16864844168,529.1683844524,530.16812046312,531.16785647384,
532.16759248456,533.16732849528,534.167064506,535.166800516721,536.166536527441,
537.166272538161,538.166008548881,539.165744559601,540.165480570321,541.165216581041,
542.164952591761,543.164688602482,544.164424613202,545.164160623922,546.163896634642,
547.163632645362,548.163368656082,549.163104666802,550.162840677522,551.162576688243,
552.162312698963,553.162048709683,554.161784720403,555.161520731123,556.161256741843,
557.160992752563,558.160728763283,559.160464774004,560.160200784724,561.159936795444,
562.159672806164,563.159408816884,564.159144827604,565.158880838324,566.158616849045,
567.158352859765,568.158088870485,569.157824881205,570.157560891925,571.157296902645,
572.157032913365,573.156768924085,574.156504934806,575.156240945526,576.155976956246,
577.155712966966,578.155448977686,579.155184988406,580.154920999126,581.154657009846,
582.154393020567,583.154129031287,584.153865042007,585.153601052727,586.153337063447,
587.153073074167,588.152809084887,589.152545095607,590.152281106328,591.152017117048,
592.151753127768,593.151489138488,594.151225149208,595.150961159928,596.150697170648,
597.150433181368,598.150169192089,599.149905202809,600.149641213529,601.149377224249,
602.149113234969,603.148849245689,604.148585256409,605.14832126713,606.14805727785,
607.14779328857,608.14752929929,609.14726531001,610.14700132073,611.14673733145,
612.14647334217,613.146209352891,614.145945363611,615.145681374331,616.145417385051,
617.145153395771,618.144889406491,619.144625417211,620.144361427931,621.144097438652,
622.143833449372,623.143569460092,624.143305470812,625.143041481532,626.142777492252,
627.142513502972,628.142249513692,629.141985524413,630.141721535133,631.141457545853,
632.141193556573,633.140929567293,634.140665578013,635.140401588733,636.140137599454,
637.139873610174,638.139609620894,639.139345631614,640.139081642334,641.138817653054,
642.138553663774,643.138289674494,644.138025685215,645.137761695935,646.137497706655,
647.137233717375,648.136969728095,649.136705738815,650.136441749535,651.136177760255,
652.135913770976,653.135649781696,654.135385792416,655.135121803136,656.134857813856,
657.134593824576,658.134329835296,659.134065846016,660.133801856737,661.133537867457,
662.133273878177,663.133009888897,664.132745899617,665.132481910337,666.132217921057,
667.131953931778,668.131689942498,669.131425953218,670.131161963938,671.130897974658,
672.130633985378,673.130369996098,674.130106006818,675.129842017539,676.129578028259,
677.129314038979,678.129050049699,679.128786060419,680.128522071139,681.128258081859,
682.127994092579,683.1277301033,684.12746611402,685.12720212474,686.12693813546,
687.12667414618,688.1264101569,689.12614616762,690.12588217834,691.125618189061,
692.125354199781,693.125090210501,694.124826221221,695.124562231941,696.124298242661,
697.124034253381,698.123770264101,699.123506274822,700.123242285542,701.122978296262,
702.122714306982,703.122450317702,704.122186328422,705.121922339142,706.121658349863,
707.121394360583,708.121130371303,709.120866382023,710.120602392743,711.120338403463,
712.120074414183,713.119810424903,714.119546435624,715.119282446344,716.119018457064,
717.118754467784,718.118490478504,719.118226489224,720.117962499944,721.117698510664,
722.117434521385,723.117170532105,724.116906542825,725.116642553545,726.116378564265,
727.116114574985,728.115850585705,729.115586596425,730.115322607146,731.115058617866,
732.114794628586,733.114530639306,734.114266650026,735.114002660746,736.113738671466,
737.113474682187,738.113210692907,739.112946703627,740.112682714347,741.112418725067,
742.112154735787,743.111890746507,744.111626757227,745.111362767948,746.111098778668,
747.110834789388,748.110570800108,749.110306810828,750.110042821548,751.109778832268,
752.109514842988,753.109250853709,754.108986864429,755.108722875149,756.108458885869,
757.108194896589,758.107930907309,759.107666918029,760.107402928749,761.10713893947,
762.10687495019,763.10661096091,764.10634697163,765.10608298235,766.10581899307,
767.10555500379,768.10529101451,769.105027025231,770.104763035951,771.104499046671,
772.104235057391,773.103971068111,774.103707078831,775.103443089551,776.103179100272,
777.102915110992,778.102651121712,779.102387132432,780.102123143152,781.101859153872,
782.101595164592,783.101331175312,784.101067186033,785.100803196753,786.100539207473,
787.100275218193,788.100011228913,789.099747239633,790.099483250353,791.099219261073,
792.098955271794,793.098691282514,794.098427293234,795.098163303954,796.097899314674,
797.097635325394,798.097371336114,799.097107346834,800.096843357555,801.096579368275,
802.096315378995,803.096051389715,804.095787400435,805.095523411155,806.095259421875,
807.094995432596,808.094731443316,809.094467454036,810.094203464756,811.093939475476,
812.093675486196,813.093411496916,814.093147507636,815.092883518357,816.092619529077,
817.092355539797,818.092091550517,819.091827561237,820.091563571957,821.091299582677,
822.091035593397,823.090771604118,824.090507614838,825.090243625558,826.089979636278,
827.089715646998,828.089451657718,829.089187668438,830.088923679158,831.088659689879,
832.088395700599,833.088131711319,834.087867722039,835.087603732759,836.087339743479,
837.087075754199,838.08681176492,839.08654777564,840.08628378636,841.08601979708,
842.0857558078,843.08549181852,844.08522782924,845.08496383996,846.084699850681,
847.084435861401,848.084171872121,849.083907882841,850.083643893561,851.083379904281,
852.083115915001,853.082851925721,854.082587936442,855.082323947162,856.082059957882,
857.081795968602,858.081531979322,859.081267990042,860.081004000762,861.080740011482,
862.080476022203,863.080212032923,864.079948043643,865.079684054363,866.079420065083,
867.079156075803,868.078892086523,869.078628097243,870.078364107964,871.078100118684,
872.077836129404,873.077572140124,874.077308150844,875.077044161564,876.076780172284,
877.076516183005,878.076252193725,879.075988204445,880.075724215165,881.075460225885,
882.075196236605,883.074932247325,884.074668258045,885.074404268766,886.074140279486,
887.073876290206,888.073612300926,889.073348311646,890.073084322366,891.072820333086,
892.072556343806,893.072292354527,894.072028365247,895.071764375967,896.071500386687,
897.071236397407,898.070972408127,899.070708418847,900.070444429567,901.070180440288,
902.069916451008,903.069652461728,904.069388472448,905.069124483168,906.068860493888,
907.068596504608,908.068332515329,909.068068526049,910.067804536769,911.067540547489,
912.067276558209,913.067012568929,914.066748579649,915.066484590369,916.06622060109,
917.06595661181,918.06569262253,919.06542863325,920.06516464397,921.06490065469,
922.06463666541,923.06437267613,924.064108686851,925.063844697571,926.063580708291,
927.063316719011,928.063052729731,929.062788740451,930.062524751171,931.062260761891,
932.061996772612,933.061732783332,934.061468794052,935.061204804772,936.060940815492,
937.060676826212,938.060412836932,939.060148847652,940.059884858373,941.059620869093,
942.059356879813,943.059092890533,944.058828901253,945.058564911973,946.058300922693,
947.058036933414,948.057772944134,949.057508954854,950.057244965574,951.056980976294,
952.056716987014,953.056452997734,954.056189008454,955.055925019175,956.055661029895,
957.055397040615,958.055133051335,959.054869062055,960.054605072775,961.054341083495,
962.054077094215,963.053813104936,964.053549115656,965.053285126376,966.053021137096,
967.052757147816,968.052493158536,969.052229169256,970.051965179976,971.051701190697,
972.051437201417,973.051173212137,974.050909222857,975.050645233577,976.050381244297,
977.050117255017,978.049853265738,979.049589276458,980.049325287178,981.049061297898,
982.048797308618,983.048533319338,984.048269330058,985.048005340778,986.047741351499,
987.047477362219,988.047213372939,989.046949383659,990.046685394379,991.046421405099,
992.046157415819,993.045893426539,994.04562943726,995.04536544798,996.0451014587,
997.04483746942,998.04457348014,999.04430949086,1000.04404550158,1001.0437815123,
1002.04351752302,1003.04325353374,1004.04298954446,1005.04272555518,1006.0424615659,
1007.04219757662,1008.04193358734,1009.04166959806,1010.04140560878,1011.0411416195,
1012.04087763022,1013.04061364094,1014.04034965166,1015.04008566238,1016.0398216731,
1017.03955768382,1018.03929369454,1019.03902970526,1020.03876571598,1021.0385017267,
1022.03823773742,1023.03797374814,1024.03770975886,1025.03744576958,1026.0371817803,
1027.03691779102,1028.03665380174,1029.03638981246,1030.03612582318,1031.0358618339,
1032.03559784462,1033.03533385534,1034.03506986606,1035.03480587678,1036.03454188751,
1037.03427789823,1038.03401390895,1039.03374991967,1040.03348593039,1041.03322194111,
1042.03295795183,1043.03269396255,1044.03242997327,1045.03216598399,1046.03190199471,
1047.03163800543,1048.03137401615,1049.03111002687,1050.03084603759,1051.03058204831,
1052.03031805903,1053.03005406975,1054.02979008047,1055.02952609119,1056.02926210191,
1057.02899811263,1058.02873412335,1059.02847013407,1060.02820614479,1061.02794215551,
1062.02767816623,1063.02741417695,1064.02715018767,1065.02688619839,1066.02662220911,
1067.02635821983,1068.02609423055,1069.02583024127,1070.02556625199,1071.02530226271,
1072.02503827343,1073.02477428415,1074.02451029487,1075.02424630559,1076.02398231631,
1077.02371832703,1078.02345433775,1079.02319034847,1080.02292635919,1081.02266236991,
1082.02239838063,1083.02213439135,1084.02187040207,1085.02160641279,1086.02134242351,
1087.02107843423,1088.02081444495,1089.02055045567,1090.02028646639,1091.02002247711,
1092.01975848783,1093.01949449855,1094.01923050927,1095.01896651999,1096.01870253071,
1097.01843854143,1098.01817455215,1099.01791056287,1100.01764657359,1101.01738258431,
1102.01711859503,1103.01685460575,1104.01659061647,1105.01632662719,1106.01606263791,
1107.01579864863,1108.01553465935,1109.01527067007,1110.01500668079,1111.01474269151,
1112.01447870223,1113.01421471295,1114.01395072368,1115.0136867344,1116.01342274512,
1117.01315875584,1118.01289476656,1119.01263077728,1120.012366788,1121.01210279872,
1122.01183880944,1123.01157482016,1124.01131083088,1125.0110468416,1126.01078285232,
1127.01051886304,1128.01025487376,1129.00999088448,1130.0097268952,1131.00946290592,
1132.00919891664,1133.00893492736,1134.00867093808,1135.0084069488,1136.00814295952,
1137.00787897024,1138.00761498096,1139.00735099168,1140.0070870024,1141.00682301312,
1142.00655902384,1143.00629503456,1144.00603104528,1145.005767056,1146.00550306672,
1147.00523907744,1148.00497508816,1149.00471109888,1150.0044471096,1151.00418312032,
1152.00391913104,1153.00365514176,1154.00339115248,1155.0031271632,1156.00286317392,
1157.00259918464,1158.00233519536,1159.00207120608,1160.0018072168,1161.00154322752,
1162.00127923824,1163.00101524896,1164.00075125968,1165.0004872704,1166.00022328112,
1166.99995929184,1167.99969530256,1168.99943131328,1169.999167324,1170.99890333472,
1171.99863934544,1172.99837535616,1173.99811136688,1174.9978473776,1175.99758338832,
1176.99731939904,1177.99705540976,1178.99679142048,1179.9965274312,1180.99626344192,
1181.99599945264,1182.99573546336,1183.99547147408,1184.9952074848,1185.99494349552,
1186.99467950624,1187.99441551696,1188.99415152768,1189.99388753841,1190.99362354913,
1191.99335955985,1192.99309557057,1193.99283158129,1194.99256759201,1195.99230360273,
1196.99203961345,1197.99177562417,1198.99151163489,1199.99124764561,1200.99098365633,
1201.99071966705,1202.99045567777,1203.99019168849,1204.98992769921,1205.98966370993,
1206.98939972065,1207.98913573137,1208.98887174209,1209.98860775281,1210.98834376353,
1211.98807977425,1212.98781578497,1213.98755179569,1214.98728780641,1215.98702381713,
1216.98675982785,1217.98649583857,1218.98623184929,1219.98596786001,1220.98570387073,
1221.98543988145,1222.98517589217,1223.98491190289,1224.98464791361,1225.98438392433,
1226.98411993505,1227.98385594577,1228.98359195649,1229.98332796721,1230.98306397793,
1231.98279998865,1232.98253599937,1233.98227201009,1234.98200802081,1235.98174403153,
1236.98148004225,1237.98121605297,1238.98095206369,1239.98068807441,1240.98042408513,
1241.98016009585,1242.97989610657,1243.97963211729,1244.97936812801,1245.97910413873,
1246.97884014945,1247.97857616017,1248.97831217089,1249.97804818161,1250.97778419233,
1251.97752020305,1252.97725621377,1253.97699222449,1254.97672823521,1255.97646424593,
1256.97620025665,1257.97593626737,1258.97567227809,1259.97540828881,1260.97514429953,
1261.97488031025,1262.97461632097,1263.97435233169,1264.97408834241,1265.97382435313,
1266.97356036385,1267.97329637458,1268.9730323853,1269.97276839602,1270.97250440674,
1271.97224041746,1272.97197642818,1273.9717124389,1274.97144844962,1275.97118446034,
1276.97092047106,1277.97065648178,1278.9703924925,1279.97012850322,1280.96986451394,
1281.96960052466,1282.96933653538,1283.9690725461,1284.96880855682,1285.96854456754,
1286.96828057826,1287.96801658898,1288.9677525997,1289.96748861042,1290.96722462114,
1291.96696063186,1292.96669664258,1293.9664326533,1294.96616866402,1295.96590467474,
1296.96564068546,1297.96537669618,1298.9651127069,1299.96484871762,1300.96458472834,
1301.96432073906,1302.96405674978,1303.9637927605,1304.96352877122,1305.96326478194,
1306.96300079266,1307.96273680338,1308.9624728141,1309.96220882482,1310.96194483554,
1311.96168084626,1312.96141685698,1313.9611528677,1314.96088887842,1315.96062488914,
1316.96036089986,1317.96009691058,1318.9598329213,1319.95956893202,1320.95930494274,
1321.95904095346,1322.95877696418,1323.9585129749,1324.95824898562,1325.95798499634,
1326.95772100706,1327.95745701778,1328.9571930285,1329.95692903922,1330.95666504994,
1331.95640106066,1332.95613707138,1333.9558730821,1334.95560909282,1335.95534510354,
1336.95508111426,1337.95481712498,1338.9545531357,1339.95428914642,1340.95402515714,
1341.95376116786,1342.95349717858,1343.9532331893,1344.95296920002,1345.95270521075,
1346.95244122147,1347.95217723219,1348.95191324291,1349.95164925363,1350.95138526435,
1351.95112127507,1352.95085728579,1353.95059329651,1354.95032930723,1355.95006531795,
1356.94980132867,1357.94953733939,1358.94927335011,1359.94900936083,1360.94874537155,
1361.94848138227,1362.94821739299,1363.94795340371,1364.94768941443,1365.94742542515,
1366.94716143587,1367.94689744659,1368.94663345731,1369.94636946803,1370.94610547875,
1371.94584148947,1372.94557750019,1373.94531351091,1374.94504952163,1375.94478553235,
1376.94452154307,1377.94425755379,1378.94399356451,1379.94372957523,1380.94346558595,
1381.94320159667,1382.94293760739,1383.94267361811,1384.94240962883,1385.94214563955,
1386.94188165027,1387.94161766099,1388.94135367171,1389.94108968243,1390.94082569315,
1391.94056170387,1392.94029771459,1393.94003372531,1394.93976973603,1395.93950574675,
1396.93924175747,1397.93897776819,1398.93871377891,1399.93844978963,1400.93818580035,
1401.93792181107,1402.93765782179,1403.93739383251,1404.93712984323,1405.93686585395,
1406.93660186467,1407.93633787539,1408.93607388611,1409.93580989683,1410.93554590755,
1411.93528191827,1412.93501792899,1413.93475393971,1414.93448995043,1415.93422596115,
1416.93396197187,1417.93369798259,1418.93343399331,1419.93317000403,1420.93290601475,
1421.93264202547,1422.93237803619,1423.93211404692,1424.93185005764,1425.93158606836,
1426.93132207908,1427.9310580898,1428.93079410052,1429.93053011124,1430.93026612196,
1431.93000213268,1432.9297381434,1433.92947415412,1434.92921016484,1435.92894617556,
1436.92868218628,1437.928418197,1438.92815420772,1439.92789021844,1440.92762622916,
1441.92736223988,1442.9270982506,1443.92683426132,1444.92657027204,1445.92630628276,
1446.92604229348,1447.9257783042,1448.92551431492,1449.92525032564,1450.92498633636,
1451.92472234708,1452.9244583578,1453.92419436852,1454.92393037924,1455.92366638996,
1456.92340240068,1457.9231384114,1458.92287442212,1459.92261043284,1460.92234644356,
1461.92208245428,1462.921818465,1463.92155447572,1464.92129048644,1465.92102649716,
1466.92076250788,1467.9204985186,1468.92023452932,1469.91997054004,1470.91970655076,
1471.91944256148,1472.9191785722,1473.91891458292,1474.91865059364,1475.91838660436,
1476.91812261508,1477.9178586258,1478.91759463652,1479.91733064724,1480.91706665796,
1481.91680266868,1482.9165386794,1483.91627469012,1484.91601070084,1485.91574671156,
1486.91548272228,1487.915218733,1488.91495474372,1489.91469075444,1490.91442676516,
1491.91416277588,1492.9138987866,1493.91363479732,1494.91337080804,1495.91310681876,
1496.91284282948,1497.9125788402,1498.91231485092,1499.91205086164,1500.91178687236,
1501.91152288309,1502.91125889381,1503.91099490453,1504.91073091525,1505.91046692597,
1506.91020293669,1507.90993894741,1508.90967495813,1509.90941096885,1510.90914697957,
1511.90888299029,1512.90861900101,1513.90835501173,1514.90809102245,1515.90782703317,
1516.90756304389,1517.90729905461,1518.90703506533,1519.90677107605,1520.90650708677,
1521.90624309749,1522.90597910821,1523.90571511893,1524.90545112965,1525.90518714037,
1526.90492315109,1527.90465916181,1528.90439517253,1529.90413118325,1530.90386719397,
1531.90360320469,1532.90333921541,1533.90307522613,1534.90281123685,1535.90254724757,
1536.90228325829,1537.90201926901,1538.90175527973,1539.90149129045,1540.90122730117,
1541.90096331189,1542.90069932261,1543.90043533333,1544.90017134405,1545.89990735477,
1546.89964336549,1547.89937937621,1548.89911538693,1549.89885139765,1550.89858740837,
1551.89832341909,1552.89805942981,1553.89779544053,1554.89753145125,1555.89726746197,
1556.89700347269,1557.89673948341,1558.89647549413,1559.89621150485,1560.89594751557,
1561.89568352629,1562.89541953701,1563.89515554773,1564.89489155845,1565.89462756917,
1566.89436357989,1567.89409959061,1568.89383560133,1569.89357161205,1570.89330762277,
1571.89304363349,1572.89277964421,1573.89251565493,1574.89225166565,1575.89198767637,
1576.89172368709,1577.89145969781,1578.89119570853,1579.89093171926,1580.89066772998,
1581.8904037407,1582.89013975142,1583.88987576214,1584.88961177286,1585.88934778358,
1586.8890837943,1587.88881980502,1588.88855581574,1589.88829182646,1590.88802783718,
1591.8877638479,1592.88749985862,1593.88723586934,1594.88697188006,1595.88670789078,
1596.8864439015,1597.88617991222,1598.88591592294,1599.88565193366,1600.88538794438,
1601.8851239551,1602.88485996582,1603.88459597654,1604.88433198726,1605.88406799798,
1606.8838040087,1607.88354001942,1608.88327603014,1609.88301204086,1610.88274805158,
1611.8824840623,1612.88222007302,1613.88195608374,1614.88169209446,1615.88142810518,
1616.8811641159,1617.88090012662,1618.88063613734,1619.88037214806,1620.88010815878,
1621.8798441695,1622.87958018022,1623.87931619094,1624.87905220166,1625.87878821238,
1626.8785242231,1627.87826023382,1628.87799624454,1629.87773225526,1630.87746826598,
1631.8772042767,1632.87694028742,1633.87667629814,1634.87641230886,1635.87614831958,
1636.8758843303,1637.87562034102,1638.87535635174,1639.87509236246,1640.87482837318,
1641.8745643839,1642.87430039462,1643.87403640534,1644.87377241606,1645.87350842678,
1646.8732444375,1647.87298044822,1648.87271645894,1649.87245246966,1650.87218848038,
1651.8719244911,1652.87166050182,1653.87139651254,1654.87113252326,1655.87086853399,
1656.8706045447,1657.87034055543,1658.87007656615,1659.86981257687,1660.86954858759,
1661.86928459831,1662.86902060903,1663.86875661975,1664.86849263047,1665.86822864119,
1666.86796465191,1667.86770066263,1668.86743667335,1669.86717268407,1670.86690869479,
1671.86664470551,1672.86638071623,1673.86611672695,1674.86585273767,1675.86558874839,
1676.86532475911,1677.86506076983,1678.86479678055,1679.86453279127,1680.86426880199,
1681.86400481271,1682.86374082343,1683.86347683415,1684.86321284487,1685.86294885559,
1686.86268486631,1687.86242087703,1688.86215688775,1689.86189289847,1690.86162890919,
1691.86136491991,1692.86110093063,1693.86083694135,1694.86057295207,1695.86030896279,
1696.86004497351,1697.35991297887,1697.85988790214),.UNSPECIFIED.);
#52=B_SPLINE_SURFACE_WITH_KNOTS('',3,3,((#233503,#233504,#233505,#233506,
#233507,#233508,#233509,#233510,#233511,#233512,#233513,#233514,#233515,
#233516,#233517,#233518,#233519,#233520,#233521,#233522,#233523,#233524,
#233525,#233526,#233527,#233528,#233529,#233530,#233531,#233532,#233533,
#233534,#233535,#233536,#233537,#233538,#233539,#233540,#233541,#233542,
#233543,#233544,#233545,#233546,#233547,#233548,#233549,#233550,#233551,
#233552,#233553,#233554,#233555,#233556,#233557,#233558,#233559,#233560,
#233561,#233562,#233563,#233564,#233565,#233566,#233567,#233568,#233569,
#233570,#233571,#233572,#233573,#233574,#233575,#233576,#233577,#233578,
#233579,#233580,#233581,#233582,#233583,#233584,#233585,#233586,#233587,
#233588,#233589,#233590,#233591,#233592,#233593,#233594,#233595,#233596,
#233597,#233598,#233599,#233600,#233601,#233602,#233603,#233604,#233605,
#233606,#233607,#233608,#233609,#233610,#233611,#233612,#233613,#233614,
#233615,#233616,#233617,#233618,#233619,#233620,#233621,#233622,#233623,
#233624,#233625,#233626,#233627,#233628,#233629,#233630,#233631,#233632,
#233633,#233634,#233635,#233636,#233637,#233638,#233639,#233640,#233641,
#233642,#233643,#233644,#233645,#233646,#233647,#233648,#233649,#233650,
#233651,#233652,#233653,#233654,#233655,#233656,#233657,#233658,#233659,
#233660,#233661,#233662,#233663,#233664,#233665,#233666,#233667,#233668,
#233669,#233670,#233671,#233672,#233673,#233674,#233675,#233676,#233677,
#233678,#233679,#233680,#233681,#233682,#233683,#233684,#233685,#233686,
#233687,#233688,#233689,#233690,#233691,#233692,#233693,#233694,#233695,
#233696,#233697,#233698,#233699,#233700,#233701,#233702,#233703,#233704,
#233705,#233706,#233707,#233708,#233709,#233710,#233711,#233712,#233713,
#233714,#233715,#233716,#233717,#233718,#233719,#233720,#233721,#233722,
#233723,#233724,#233725,#233726,#233727,#233728,#233729,#233730,#233731,
#233732,#233733,#233734,#233735,#233736,#233737,#233738,#233739,#233740,
#233741,#233742,#233743,#233744,#233745,#233746,#233747,#233748,#233749,
#233750,#233751,#233752,#233753,#233754,#233755,#233756,#233757,#233758,
#233759,#233760,#233761,#233762,#233763,#233764,#233765,#233766,#233767,
#233768,#233769,#233770,#233771,#233772,#233773,#233774,#233775,#233776,
#233777,#233778,#233779,#233780,#233781,#233782,#233783,#233784,#233785,
#233786,#233787,#233788,#233789,#233790,#233791,#233792,#233793,#233794,
#233795,#233796,#233797,#233798,#233799,#233800,#233801,#233802,#233803,
#233804,#233805,#233806,#233807,#233808,#233809,#233810,#233811,#233812,
#233813,#233814,#233815,#233816,#233817,#233818,#233819,#233820,#233821,
#233822,#233823,#233824,#233825,#233826,#233827,#233828,#233829,#233830,
#233831,#233832,#233833,#233834,#233835,#233836,#233837,#233838,#233839,
#233840,#233841,#233842,#233843,#233844,#233845,#233846,#233847,#233848,
#233849,#233850,#233851,#233852,#233853,#233854,#233855,#233856,#233857,
#233858,#233859,#233860,#233861,#233862,#233863,#233864,#233865,#233866,
#233867,#233868,#233869,#233870,#233871,#233872,#233873,#233874,#233875,
#233876,#233877,#233878,#233879,#233880,#233881,#233882,#233883,#233884,
#233885,#233886,#233887,#233888,#233889,#233890,#233891,#233892,#233893,
#233894,#233895,#233896,#233897,#233898,#233899,#233900,#233901,#233902,
#233903,#233904,#233905,#233906,#233907,#233908,#233909,#233910,#233911,
#233912,#233913,#233914,#233915,#233916,#233917,#233918,#233919,#233920,
#233921,#233922,#233923,#233924,#233925,#233926,#233927,#233928,#233929,
#233930,#233931,#233932,#233933,#233934,#233935,#233936,#233937,#233938,
#233939,#233940,#233941,#233942,#233943,#233944,#233945,#233946,#233947,
#233948,#233949,#233950,#233951,#233952,#233953,#233954,#233955,#233956,
#233957,#233958,#233959,#233960,#233961,#233962,#233963,#233964,#233965,
#233966,#233967,#233968,#233969,#233970,#233971,#233972,#233973,#233974,
#233975,#233976,#233977,#233978,#233979,#233980,#233981,#233982,#233983,
#233984,#233985,#233986,#233987,#233988,#233989,#233990,#233991,#233992,
#233993,#233994,#233995,#233996,#233997,#233998,#233999,#234000,#234001,
#234002,#234003,#234004,#234005,#234006,#234007,#234008,#234009,#234010,
#234011,#234012,#234013,#234014,#234015,#234016,#234017,#234018,#234019,
#234020,#234021,#234022,#234023,#234024,#234025,#234026,#234027,#234028,
#234029,#234030,#234031,#234032,#234033,#234034,#234035,#234036,#234037,
#234038,#234039,#234040,#234041,#234042,#234043,#234044,#234045,#234046,
#234047,#234048,#234049,#234050,#234051,#234052,#234053,#234054,#234055,
#234056,#234057,#234058,#234059,#234060,#234061,#234062,#234063,#234064,
#234065,#234066,#234067,#234068,#234069,#234070,#234071,#234072,#234073,
#234074,#234075,#234076,#234077,#234078,#234079,#234080,#234081,#234082,
#234083,#234084,#234085,#234086,#234087,#234088,#234089,#234090,#234091,
#234092,#234093,#234094,#234095,#234096,#234097,#234098,#234099,#234100,
#234101,#234102,#234103,#234104,#234105,#234106,#234107,#234108,#234109,
#234110,#234111,#234112,#234113,#234114,#234115,#234116,#234117,#234118,
#234119,#234120,#234121,#234122,#234123,#234124,#234125,#234126,#234127,
#234128,#234129,#234130,#234131,#234132,#234133,#234134,#234135,#234136,
#234137,#234138,#234139,#234140,#234141,#234142,#234143,#234144,#234145,
#234146,#234147,#234148,#234149,#234150,#234151,#234152,#234153,#234154,
#234155,#234156,#234157,#234158,#234159,#234160,#234161,#234162,#234163,
#234164,#234165,#234166,#234167,#234168,#234169,#234170,#234171,#234172,
#234173,#234174,#234175,#234176,#234177,#234178,#234179,#234180,#234181,
#234182,#234183,#234184,#234185,#234186,#234187,#234188,#234189,#234190,
#234191,#234192,#234193,#234194,#234195,#234196,#234197,#234198,#234199,
#234200,#234201,#234202,#234203,#234204,#234205,#234206,#234207,#234208,
#234209,#234210,#234211,#234212,#234213,#234214,#234215,#234216,#234217,
#234218,#234219,#234220,#234221,#234222,#234223,#234224,#234225,#234226,
#234227,#234228,#234229,#234230,#234231,#234232,#234233,#234234,#234235,
#234236,#234237,#234238,#234239,#234240,#234241,#234242,#234243,#234244,
#234245,#234246,#234247,#234248,#234249,#234250,#234251,#234252,#234253,
#234254,#234255,#234256,#234257,#234258,#234259,#234260,#234261,#234262,
#234263,#234264,#234265,#234266,#234267,#234268,#234269,#234270,#234271,
#234272,#234273,#234274,#234275,#234276,#234277,#234278,#234279,#234280,
#234281,#234282,#234283,#234284,#234285,#234286,#234287,#234288,#234289,
#234290,#234291,#234292,#234293,#234294,#234295,#234296,#234297,#234298,
#234299,#234300,#234301,#234302,#234303,#234304,#234305,#234306,#234307,
#234308,#234309,#234310,#234311,#234312,#234313,#234314,#234315,#234316,
#234317,#234318,#234319,#234320,#234321,#234322,#234323,#234324,#234325,
#234326,#234327,#234328,#234329,#234330,#234331,#234332,#234333,#234334,
#234335,#234336,#234337,#234338,#234339,#234340,#234341,#234342,#234343,
#234344,#234345,#234346,#234347,#234348,#234349,#234350,#234351,#234352,
#234353,#234354,#234355,#234356,#234357,#234358,#234359,#234360,#234361,
#234362,#234363,#234364,#234365,#234366,#234367,#234368,#234369,#234370,
#234371,#234372,#234373,#234374,#234375,#234376,#234377,#234378,#234379,
#234380,#234381,#234382,#234383,#234384,#234385,#234386,#234387,#234388,
#234389,#234390,#234391,#234392,#234393,#234394,#234395,#234396,#234397,
#234398,#234399,#234400,#234401,#234402,#234403,#234404,#234405,#234406,
#234407,#234408,#234409,#234410,#234411,#234412,#234413,#234414,#234415,
#234416,#234417,#234418,#234419,#234420,#234421,#234422,#234423,#234424,
#234425,#234426,#234427,#234428,#234429,#234430,#234431,#234432,#234433,
#234434,#234435,#234436,#234437,#234438,#234439,#234440,#234441,#234442,
#234443,#234444,#234445,#234446,#234447,#234448,#234449,#234450,#234451,
#234452,#234453,#234454,#234455,#234456,#234457,#234458,#234459,#234460,
#234461,#234462,#234463,#234464,#234465,#234466,#234467,#234468,#234469,
#234470,#234471,#234472,#234473,#234474,#234475,#234476,#234477,#234478,
#234479,#234480,#234481,#234482,#234483,#234484,#234485,#234486,#234487,
#234488,#234489,#234490,#234491,#234492,#234493,#234494,#234495,#234496,
#234497,#234498,#234499,#234500,#234501,#234502,#234503,#234504,#234505,
#234506,#234507,#234508,#234509,#234510,#234511,#234512,#234513,#234514,
#234515,#234516,#234517,#234518,#234519,#234520,#234521,#234522,#234523,
#234524,#234525,#234526,#234527,#234528,#234529,#234530,#234531,#234532,
#234533,#234534,#234535,#234536,#234537,#234538,#234539,#234540,#234541,
#234542,#234543,#234544,#234545,#234546,#234547,#234548,#234549,#234550,
#234551,#234552,#234553,#234554,#234555,#234556,#234557,#234558,#234559,
#234560,#234561,#234562,#234563,#234564,#234565,#234566,#234567,#234568,
#234569,#234570,#234571,#234572,#234573,#234574,#234575,#234576,#234577,
#234578,#234579,#234580,#234581,#234582,#234583,#234584,#234585,#234586,
#234587,#234588,#234589,#234590,#234591,#234592,#234593,#234594,#234595,
#234596,#234597,#234598,#234599,#234600,#234601,#234602,#234603,#234604,
#234605,#234606,#234607,#234608,#234609,#234610,#234611,#234612,#234613,
#234614,#234615,#234616,#234617,#234618,#234619,#234620,#234621,#234622,
#234623,#234624,#234625,#234626,#234627,#234628,#234629,#234630,#234631,
#234632,#234633,#234634,#234635,#234636,#234637,#234638,#234639,#234640,
#234641,#234642,#234643,#234644,#234645,#234646,#234647,#234648,#234649,
#234650,#234651,#234652,#234653,#234654,#234655,#234656,#234657,#234658,
#234659,#234660,#234661,#234662,#234663,#234664,#234665,#234666,#234667,
#234668,#234669,#234670,#234671,#234672,#234673,#234674,#234675,#234676,
#234677,#234678,#234679,#234680,#234681,#234682,#234683,#234684,#234685,
#234686,#234687,#234688,#234689,#234690,#234691,#234692,#234693,#234694,
#234695,#234696,#234697,#234698,#234699,#234700,#234701,#234702,#234703,
#234704,#234705,#234706,#234707,#234708,#234709,#234710,#234711,#234712,
#234713,#234714,#234715,#234716,#234717,#234718,#234719,#234720,#234721,
#234722,#234723,#234724,#234725,#234726,#234727,#234728,#234729,#234730,
#234731,#234732,#234733,#234734,#234735,#234736,#234737,#234738,#234739,
#234740,#234741,#234742,#234743,#234744,#234745,#234746,#234747,#234748,
#234749,#234750,#234751,#234752,#234753,#234754,#234755,#234756,#234757,
#234758,#234759,#234760,#234761,#234762,#234763,#234764,#234765,#234766,
#234767,#234768,#234769,#234770,#234771,#234772,#234773,#234774,#234775,
#234776,#234777,#234778,#234779,#234780,#234781,#234782,#234783,#234784,
#234785,#234786,#234787,#234788,#234789,#234790,#234791,#234792,#234793,
#234794,#234795,#234796,#234797,#234798,#234799,#234800,#234801,#234802,
#234803,#234804,#234805,#234806,#234807,#234808,#234809,#234810,#234811,
#234812,#234813,#234814,#234815,#234816,#234817,#234818,#234819,#234820,
#234821,#234822,#234823,#234824,#234825,#234826,#234827,#234828,#234829,
#234830,#234831,#234832,#234833,#234834,#234835,#234836,#234837,#234838,
#234839,#234840,#234841,#234842,#234843,#234844,#234845,#234846,#234847,
#234848,#234849,#234850,#234851,#234852,#234853,#234854,#234855,#234856,
#234857,#234858,#234859,#234860,#234861,#234862,#234863,#234864,#234865,
#234866,#234867,#234868,#234869,#234870,#234871,#234872,#234873,#234874,
#234875,#234876,#234877,#234878,#234879,#234880,#234881,#234882,#234883,
#234884,#234885,#234886,#234887,#234888,#234889,#234890,#234891,#234892,
#234893,#234894,#234895,#234896,#234897,#234898,#234899,#234900,#234901,
#234902,#234903,#234904,#234905,#234906,#234907,#234908,#234909,#234910,
#234911,#234912,#234913,#234914,#234915,#234916,#234917,#234918,#234919,
#234920,#234921,#234922,#234923,#234924,#234925,#234926,#234927,#234928,
#234929,#234930,#234931,#234932,#234933,#234934,#234935,#234936,#234937,
#234938,#234939,#234940,#234941,#234942,#234943,#234944,#234945,#234946,
#234947,#234948,#234949,#234950,#234951,#234952,#234953,#234954,#234955,
#234956,#234957,#234958,#234959,#234960,#234961,#234962,#234963,#234964,
#234965,#234966,#234967,#234968,#234969,#234970,#234971,#234972,#234973,
#234974,#234975,#234976,#234977,#234978,#234979,#234980,#234981,#234982,
#234983,#234984,#234985,#234986,#234987,#234988,#234989,#234990,#234991,
#234992,#234993,#234994,#234995,#234996,#234997,#234998,#234999,#235000,
#235001,#235002,#235003,#235004,#235005,#235006,#235007,#235008,#235009,
#235010,#235011,#235012,#235013,#235014,#235015,#235016,#235017,#235018,
#235019,#235020,#235021,#235022,#235023,#235024,#235025,#235026,#235027,
#235028,#235029,#235030,#235031,#235032,#235033,#235034,#235035,#235036,
#235037,#235038,#235039,#235040,#235041,#235042,#235043,#235044,#235045,
#235046,#235047,#235048,#235049,#235050,#235051,#235052,#235053,#235054,
#235055,#235056,#235057,#235058,#235059,#235060,#235061,#235062,#235063,
#235064,#235065,#235066,#235067,#235068,#235069,#235070,#235071,#235072,
#235073,#235074,#235075,#235076,#235077,#235078,#235079,#235080,#235081,
#235082,#235083,#235084,#235085,#235086,#235087,#235088,#235089,#235090,
#235091,#235092,#235093,#235094,#235095,#235096,#235097,#235098,#235099,
#235100,#235101,#235102,#235103,#235104,#235105,#235106,#235107,#235108,
#235109,#235110,#235111,#235112,#235113,#235114,#235115,#235116,#235117,
#235118,#235119,#235120,#235121,#235122,#235123,#235124,#235125,#235126,
#235127,#235128,#235129,#235130,#235131,#235132,#235133,#235134,#235135,
#235136,#235137,#235138,#235139,#235140,#235141,#235142,#235143,#235144,
#235145,#235146,#235147,#235148,#235149,#235150,#235151,#235152,#235153,
#235154,#235155,#235156,#235157,#235158,#235159,#235160,#235161,#235162,
#235163,#235164,#235165,#235166,#235167,#235168,#235169,#235170,#235171,
#235172,#235173,#235174,#235175,#235176,#235177,#235178,#235179,#235180,
#235181,#235182,#235183,#235184,#235185,#235186,#235187,#235188,#235189,
#235190,#235191,#235192,#235193,#235194,#235195,#235196,#235197),(#235198,
#235199,#235200,#235201,#235202,#235203,#235204,#235205,#235206,#235207,
#235208,#235209,#235210,#235211,#235212,#235213,#235214,#235215,#235216,
#235217,#235218,#235219,#235220,#235221,#235222,#235223,#235224,#235225,
#235226,#235227,#235228,#235229,#235230,#235231,#235232,#235233,#235234,
#235235,#235236,#235237,#235238,#235239,#235240,#235241,#235242,#235243,
#235244,#235245,#235246,#235247,#235248,#235249,#235250,#235251,#235252,
#235253,#235254,#235255,#235256,#235257,#235258,#235259,#235260,#235261,
#235262,#235263,#235264,#235265,#235266,#235267,#235268,#235269,#235270,
#235271,#235272,#235273,#235274,#235275,#235276,#235277,#235278,#235279,
#235280,#235281,#235282,#235283,#235284,#235285,#235286,#235287,#235288,
#235289,#235290,#235291,#235292,#235293,#235294,#235295,#235296,#235297,
#235298,#235299,#235300,#235301,#235302,#235303,#235304,#235305,#235306,
#235307,#235308,#235309,#235310,#235311,#235312,#235313,#235314,#235315,
#235316,#235317,#235318,#235319,#235320,#235321,#235322,#235323,#235324,
#235325,#235326,#235327,#235328,#235329,#235330,#235331,#235332,#235333,
#235334,#235335,#235336,#235337,#235338,#235339,#235340,#235341,#235342,
#235343,#235344,#235345,#235346,#235347,#235348,#235349,#235350,#235351,
#235352,#235353,#235354,#235355,#235356,#235357,#235358,#235359,#235360,
#235361,#235362,#235363,#235364,#235365,#235366,#235367,#235368,#235369,
#235370,#235371,#235372,#235373,#235374,#235375,#235376,#235377,#235378,
#235379,#235380,#235381,#235382,#235383,#235384,#235385,#235386,#235387,
#235388,#235389,#235390,#235391,#235392,#235393,#235394,#235395,#235396,
#235397,#235398,#235399,#235400,#235401,#235402,#235403,#235404,#235405,
#235406,#235407,#235408,#235409,#235410,#235411,#235412,#235413,#235414,
#235415,#235416,#235417,#235418,#235419,#235420,#235421,#235422,#235423,
#235424,#235425,#235426,#235427,#235428,#235429,#235430,#235431,#235432,
#235433,#235434,#235435,#235436,#235437,#235438,#235439,#235440,#235441,
#235442,#235443,#235444,#235445,#235446,#235447,#235448,#235449,#235450,
#235451,#235452,#235453,#235454,#235455,#235456,#235457,#235458,#235459,
#235460,#235461,#235462,#235463,#235464,#235465,#235466,#235467,#235468,
#235469,#235470,#235471,#235472,#235473,#235474,#235475,#235476,#235477,
#235478,#235479,#235480,#235481,#235482,#235483,#235484,#235485,#235486,
#235487,#235488,#235489,#235490,#235491,#235492,#235493,#235494,#235495,
#235496,#235497,#235498,#235499,#235500,#235501,#235502,#235503,#235504,
#235505,#235506,#235507,#235508,#235509,#235510,#235511,#235512,#235513,
#235514,#235515,#235516,#235517,#235518,#235519,#235520,#235521,#235522,
#235523,#235524,#235525,#235526,#235527,#235528,#235529,#235530,#235531,
#235532,#235533,#235534,#235535,#235536,#235537,#235538,#235539,#235540,
#235541,#235542,#235543,#235544,#235545,#235546,#235547,#235548,#235549,
#235550,#235551,#235552,#235553,#235554,#235555,#235556,#235557,#235558,
#235559,#235560,#235561,#235562,#235563,#235564,#235565,#235566,#235567,
#235568,#235569,#235570,#235571,#235572,#235573,#235574,#235575,#235576,
#235577,#235578,#235579,#235580,#235581,#235582,#235583,#235584,#235585,
#235586,#235587,#235588,#235589,#235590,#235591,#235592,#235593,#235594,
#235595,#235596,#235597,#235598,#235599,#235600,#235601,#235602,#235603,
#235604,#235605,#235606,#235607,#235608,#235609,#235610,#235611,#235612,
#235613,#235614,#235615,#235616,#235617,#235618,#235619,#235620,#235621,
#235622,#235623,#235624,#235625,#235626,#235627,#235628,#235629,#235630,
#235631,#235632,#235633,#235634,#235635,#235636,#235637,#235638,#235639,
#235640,#235641,#235642,#235643,#235644,#235645,#235646,#235647,#235648,
#235649,#235650,#235651,#235652,#235653,#235654,#235655,#235656,#235657,
#235658,#235659,#235660,#235661,#235662,#235663,#235664,#235665,#235666,
#235667,#235668,#235669,#235670,#235671,#235672,#235673,#235674,#235675,
#235676,#235677,#235678,#235679,#235680,#235681,#235682,#235683,#235684,
#235685,#235686,#235687,#235688,#235689,#235690,#235691,#235692,#235693,
#235694,#235695,#235696,#235697,#235698,#235699,#235700,#235701,#235702,
#235703,#235704,#235705,#235706,#235707,#235708,#235709,#235710,#235711,
#235712,#235713,#235714,#235715,#235716,#235717,#235718,#235719,#235720,
#235721,#235722,#235723,#235724,#235725,#235726,#235727,#235728,#235729,
#235730,#235731,#235732,#235733,#235734,#235735,#235736,#235737,#235738,
#235739,#235740,#235741,#235742,#235743,#235744,#235745,#235746,#235747,
#235748,#235749,#235750,#235751,#235752,#235753,#235754,#235755,#235756,
#235757,#235758,#235759,#235760,#235761,#235762,#235763,#235764,#235765,
#235766,#235767,#235768,#235769,#235770,#235771,#235772,#235773,#235774,
#235775,#235776,#235777,#235778,#235779,#235780,#235781,#235782,#235783,
#235784,#235785,#235786,#235787,#235788,#235789,#235790,#235791,#235792,
#235793,#235794,#235795,#235796,#235797,#235798,#235799,#235800,#235801,
#235802,#235803,#235804,#235805,#235806,#235807,#235808,#235809,#235810,
#235811,#235812,#235813,#235814,#235815,#235816,#235817,#235818,#235819,
#235820,#235821,#235822,#235823,#235824,#235825,#235826,#235827,#235828,
#235829,#235830,#235831,#235832,#235833,#235834,#235835,#235836,#235837,
#235838,#235839,#235840,#235841,#235842,#235843,#235844,#235845,#235846,
#235847,#235848,#235849,#235850,#235851,#235852,#235853,#235854,#235855,
#235856,#235857,#235858,#235859,#235860,#235861,#235862,#235863,#235864,
#235865,#235866,#235867,#235868,#235869,#235870,#235871,#235872,#235873,
#235874,#235875,#235876,#235877,#235878,#235879,#235880,#235881,#235882,
#235883,#235884,#235885,#235886,#235887,#235888,#235889,#235890,#235891,
#235892,#235893,#235894,#235895,#235896,#235897,#235898,#235899,#235900,
#235901,#235902,#235903,#235904,#235905,#235906,#235907,#235908,#235909,
#235910,#235911,#235912,#235913,#235914,#235915,#235916,#235917,#235918,
#235919,#235920,#235921,#235922,#235923,#235924,#235925,#235926,#235927,
#235928,#235929,#235930,#235931,#235932,#235933,#235934,#235935,#235936,
#235937,#235938,#235939,#235940,#235941,#235942,#235943,#235944,#235945,
#235946,#235947,#235948,#235949,#235950,#235951,#235952,#235953,#235954,
#235955,#235956,#235957,#235958,#235959,#235960,#235961,#235962,#235963,
#235964,#235965,#235966,#235967,#235968,#235969,#235970,#235971,#235972,
#235973,#235974,#235975,#235976,#235977,#235978,#235979,#235980,#235981,
#235982,#235983,#235984,#235985,#235986,#235987,#235988,#235989,#235990,
#235991,#235992,#235993,#235994,#235995,#235996,#235997,#235998,#235999,
#236000,#236001,#236002,#236003,#236004,#236005,#236006,#236007,#236008,
#236009,#236010,#236011,#236012,#236013,#236014,#236015,#236016,#236017,
#236018,#236019,#236020,#236021,#236022,#236023,#236024,#236025,#236026,
#236027,#236028,#236029,#236030,#236031,#236032,#236033,#236034,#236035,
#236036,#236037,#236038,#236039,#236040,#236041,#236042,#236043,#236044,
#236045,#236046,#236047,#236048,#236049,#236050,#236051,#236052,#236053,
#236054,#236055,#236056,#236057,#236058,#236059,#236060,#236061,#236062,
#236063,#236064,#236065,#236066,#236067,#236068,#236069,#236070,#236071,
#236072,#236073,#236074,#236075,#236076,#236077,#236078,#236079,#236080,
#236081,#236082,#236083,#236084,#236085,#236086,#236087,#236088,#236089,
#236090,#236091,#236092,#236093,#236094,#236095,#236096,#236097,#236098,
#236099,#236100,#236101,#236102,#236103,#236104,#236105,#236106,#236107,
#236108,#236109,#236110,#236111,#236112,#236113,#236114,#236115,#236116,
#236117,#236118,#236119,#236120,#236121,#236122,#236123,#236124,#236125,
#236126,#236127,#236128,#236129,#236130,#236131,#236132,#236133,#236134,
#236135,#236136,#236137,#236138,#236139,#236140,#236141,#236142,#236143,
#236144,#236145,#236146,#236147,#236148,#236149,#236150,#236151,#236152,
#236153,#236154,#236155,#236156,#236157,#236158,#236159,#236160,#236161,
#236162,#236163,#236164,#236165,#236166,#236167,#236168,#236169,#236170,
#236171,#236172,#236173,#236174,#236175,#236176,#236177,#236178,#236179,
#236180,#236181,#236182,#236183,#236184,#236185,#236186,#236187,#236188,
#236189,#236190,#236191,#236192,#236193,#236194,#236195,#236196,#236197,
#236198,#236199,#236200,#236201,#236202,#236203,#236204,#236205,#236206,
#236207,#236208,#236209,#236210,#236211,#236212,#236213,#236214,#236215,
#236216,#236217,#236218,#236219,#236220,#236221,#236222,#236223,#236224,
#236225,#236226,#236227,#236228,#236229,#236230,#236231,#236232,#236233,
#236234,#236235,#236236,#236237,#236238,#236239,#236240,#236241,#236242,
#236243,#236244,#236245,#236246,#236247,#236248,#236249,#236250,#236251,
#236252,#236253,#236254,#236255,#236256,#236257,#236258,#236259,#236260,
#236261,#236262,#236263,#236264,#236265,#236266,#236267,#236268,#236269,
#236270,#236271,#236272,#236273,#236274,#236275,#236276,#236277,#236278,
#236279,#236280,#236281,#236282,#236283,#236284,#236285,#236286,#236287,
#236288,#236289,#236290,#236291,#236292,#236293,#236294,#236295,#236296,
#236297,#236298,#236299,#236300,#236301,#236302,#236303,#236304,#236305,
#236306,#236307,#236308,#236309,#236310,#236311,#236312,#236313,#236314,
#236315,#236316,#236317,#236318,#236319,#236320,#236321,#236322,#236323,
#236324,#236325,#236326,#236327,#236328,#236329,#236330,#236331,#236332,
#236333,#236334,#236335,#236336,#236337,#236338,#236339,#236340,#236341,
#236342,#236343,#236344,#236345,#236346,#236347,#236348,#236349,#236350,
#236351,#236352,#236353,#236354,#236355,#236356,#236357,#236358,#236359,
#236360,#236361,#236362,#236363,#236364,#236365,#236366,#236367,#236368,
#236369,#236370,#236371,#236372,#236373,#236374,#236375,#236376,#236377,
#236378,#236379,#236380,#236381,#236382,#236383,#236384,#236385,#236386,
#236387,#236388,#236389,#236390,#236391,#236392,#236393,#236394,#236395,
#236396,#236397,#236398,#236399,#236400,#236401,#236402,#236403,#236404,
#236405,#236406,#236407,#236408,#236409,#236410,#236411,#236412,#236413,
#236414,#236415,#236416,#236417,#236418,#236419,#236420,#236421,#236422,
#236423,#236424,#236425,#236426,#236427,#236428,#236429,#236430,#236431,
#236432,#236433,#236434,#236435,#236436,#236437,#236438,#236439,#236440,
#236441,#236442,#236443,#236444,#236445,#236446,#236447,#236448,#236449,
#236450,#236451,#236452,#236453,#236454,#236455,#236456,#236457,#236458,
#236459,#236460,#236461,#236462,#236463,#236464,#236465,#236466,#236467,
#236468,#236469,#236470,#236471,#236472,#236473,#236474,#236475,#236476,
#236477,#236478,#236479,#236480,#236481,#236482,#236483,#236484,#236485,
#236486,#236487,#236488,#236489,#236490,#236491,#236492,#236493,#236494,
#236495,#236496,#236497,#236498,#236499,#236500,#236501,#236502,#236503,
#236504,#236505,#236506,#236507,#236508,#236509,#236510,#236511,#236512,
#236513,#236514,#236515,#236516,#236517,#236518,#236519,#236520,#236521,
#236522,#236523,#236524,#236525,#236526,#236527,#236528,#236529,#236530,
#236531,#236532,#236533,#236534,#236535,#236536,#236537,#236538,#236539,
#236540,#236541,#236542,#236543,#236544,#236545,#236546,#236547,#236548,
#236549,#236550,#236551,#236552,#236553,#236554,#236555,#236556,#236557,
#236558,#236559,#236560,#236561,#236562,#236563,#236564,#236565,#236566,
#236567,#236568,#236569,#236570,#236571,#236572,#236573,#236574,#236575,
#236576,#236577,#236578,#236579,#236580,#236581,#236582,#236583,#236584,
#236585,#236586,#236587,#236588,#236589,#236590,#236591,#236592,#236593,
#236594,#236595,#236596,#236597,#236598,#236599,#236600,#236601,#236602,
#236603,#236604,#236605,#236606,#236607,#236608,#236609,#236610,#236611,
#236612,#236613,#236614,#236615,#236616,#236617,#236618,#236619,#236620,
#236621,#236622,#236623,#236624,#236625,#236626,#236627,#236628,#236629,
#236630,#236631,#236632,#236633,#236634,#236635,#236636,#236637,#236638,
#236639,#236640,#236641,#236642,#236643,#236644,#236645,#236646,#236647,
#236648,#236649,#236650,#236651,#236652,#236653,#236654,#236655,#236656,
#236657,#236658,#236659,#236660,#236661,#236662,#236663,#236664,#236665,
#236666,#236667,#236668,#236669,#236670,#236671,#236672,#236673,#236674,
#236675,#236676,#236677,#236678,#236679,#236680,#236681,#236682,#236683,
#236684,#236685,#236686,#236687,#236688,#236689,#236690,#236691,#236692,
#236693,#236694,#236695,#236696,#236697,#236698,#236699,#236700,#236701,
#236702,#236703,#236704,#236705,#236706,#236707,#236708,#236709,#236710,
#236711,#236712,#236713,#236714,#236715,#236716,#236717,#236718,#236719,
#236720,#236721,#236722,#236723,#236724,#236725,#236726,#236727,#236728,
#236729,#236730,#236731,#236732,#236733,#236734,#236735,#236736,#236737,
#236738,#236739,#236740,#236741,#236742,#236743,#236744,#236745,#236746,
#236747,#236748,#236749,#236750,#236751,#236752,#236753,#236754,#236755,
#236756,#236757,#236758,#236759,#236760,#236761,#236762,#236763,#236764,
#236765,#236766,#236767,#236768,#236769,#236770,#236771,#236772,#236773,
#236774,#236775,#236776,#236777,#236778,#236779,#236780,#236781,#236782,
#236783,#236784,#236785,#236786,#236787,#236788,#236789,#236790,#236791,
#236792,#236793,#236794,#236795,#236796,#236797,#236798,#236799,#236800,
#236801,#236802,#236803,#236804,#236805,#236806,#236807,#236808,#236809,
#236810,#236811,#236812,#236813,#236814,#236815,#236816,#236817,#236818,
#236819,#236820,#236821,#236822,#236823,#236824,#236825,#236826,#236827,
#236828,#236829,#236830,#236831,#236832,#236833,#236834,#236835,#236836,
#236837,#236838,#236839,#236840,#236841,#236842,#236843,#236844,#236845,
#236846,#236847,#236848,#236849,#236850,#236851,#236852,#236853,#236854,
#236855,#236856,#236857,#236858,#236859,#236860,#236861,#236862,#236863,
#236864,#236865,#236866,#236867,#236868,#236869,#236870,#236871,#236872,
#236873,#236874,#236875,#236876,#236877,#236878,#236879,#236880,#236881,
#236882,#236883,#236884,#236885,#236886,#236887,#236888,#236889,#236890,
#236891,#236892),(#236893,#236894,#236895,#236896,#236897,#236898,#236899,
#236900,#236901,#236902,#236903,#236904,#236905,#236906,#236907,#236908,
#236909,#236910,#236911,#236912,#236913,#236914,#236915,#236916,#236917,
#236918,#236919,#236920,#236921,#236922,#236923,#236924,#236925,#236926,
#236927,#236928,#236929,#236930,#236931,#236932,#236933,#236934,#236935,
#236936,#236937,#236938,#236939,#236940,#236941,#236942,#236943,#236944,
#236945,#236946,#236947,#236948,#236949,#236950,#236951,#236952,#236953,
#236954,#236955,#236956,#236957,#236958,#236959,#236960,#236961,#236962,
#236963,#236964,#236965,#236966,#236967,#236968,#236969,#236970,#236971,
#236972,#236973,#236974,#236975,#236976,#236977,#236978,#236979,#236980,
#236981,#236982,#236983,#236984,#236985,#236986,#236987,#236988,#236989,
#236990,#236991,#236992,#236993,#236994,#236995,#236996,#236997,#236998,
#236999,#237000,#237001,#237002,#237003,#237004,#237005,#237006,#237007,
#237008,#237009,#237010,#237011,#237012,#237013,#237014,#237015,#237016,
#237017,#237018,#237019,#237020,#237021,#237022,#237023,#237024,#237025,
#237026,#237027,#237028,#237029,#237030,#237031,#237032,#237033,#237034,
#237035,#237036,#237037,#237038,#237039,#237040,#237041,#237042,#237043,
#237044,#237045,#237046,#237047,#237048,#237049,#237050,#237051,#237052,
#237053,#237054,#237055,#237056,#237057,#237058,#237059,#237060,#237061,
#237062,#237063,#237064,#237065,#237066,#237067,#237068,#237069,#237070,
#237071,#237072,#237073,#237074,#237075,#237076,#237077,#237078,#237079,
#237080,#237081,#237082,#237083,#237084,#237085,#237086,#237087,#237088,
#237089,#237090,#237091,#237092,#237093,#237094,#237095,#237096,#237097,
#237098,#237099,#237100,#237101,#237102,#237103,#237104,#237105,#237106,
#237107,#237108,#237109,#237110,#237111,#237112,#237113,#237114,#237115,
#237116,#237117,#237118,#237119,#237120,#237121,#237122,#237123,#237124,
#237125,#237126,#237127,#237128,#237129,#237130,#237131,#237132,#237133,
#237134,#237135,#237136,#237137,#237138,#237139,#237140,#237141,#237142,
#237143,#237144,#237145,#237146,#237147,#237148,#237149,#237150,#237151,
#237152,#237153,#237154,#237155,#237156,#237157,#237158,#237159,#237160,
#237161,#237162,#237163,#237164,#237165,#237166,#237167,#237168,#237169,
#237170,#237171,#237172,#237173,#237174,#237175,#237176,#237177,#237178,
#237179,#237180,#237181,#237182,#237183,#237184,#237185,#237186,#237187,
#237188,#237189,#237190,#237191,#237192,#237193,#237194,#237195,#237196,
#237197,#237198,#237199,#237200,#237201,#237202,#237203,#237204,#237205,
#237206,#237207,#237208,#237209,#237210,#237211,#237212,#237213,#237214,
#237215,#237216,#237217,#237218,#237219,#237220,#237221,#237222,#237223,
#237224,#237225,#237226,#237227,#237228,#237229,#237230,#237231,#237232,
#237233,#237234,#237235,#237236,#237237,#237238,#237239,#237240,#237241,
#237242,#237243,#237244,#237245,#237246,#237247,#237248,#237249,#237250,
#237251,#237252,#237253,#237254,#237255,#237256,#237257,#237258,#237259,
#237260,#237261,#237262,#237263,#237264,#237265,#237266,#237267,#237268,
#237269,#237270,#237271,#237272,#237273,#237274,#237275,#237276,#237277,
#237278,#237279,#237280,#237281,#237282,#237283,#237284,#237285,#237286,
#237287,#237288,#237289,#237290,#237291,#237292,#237293,#237294,#237295,
#237296,#237297,#237298,#237299,#237300,#237301,#237302,#237303,#237304,
#237305,#237306,#237307,#237308,#237309,#237310,#237311,#237312,#237313,
#237314,#237315,#237316,#237317,#237318,#237319,#237320,#237321,#237322,
#237323,#237324,#237325,#237326,#237327,#237328,#237329,#237330,#237331,
#237332,#237333,#237334,#237335,#237336,#237337,#237338,#237339,#237340,
#237341,#237342,#237343,#237344,#237345,#237346,#237347,#237348,#237349,
#237350,#237351,#237352,#237353,#237354,#237355,#237356,#237357,#237358,
#237359,#237360,#237361,#237362,#237363,#237364,#237365,#237366,#237367,
#237368,#237369,#237370,#237371,#237372,#237373,#237374,#237375,#237376,
#237377,#237378,#237379,#237380,#237381,#237382,#237383,#237384,#237385,
#237386,#237387,#237388,#237389,#237390,#237391,#237392,#237393,#237394,
#237395,#237396,#237397,#237398,#237399,#237400,#237401,#237402,#237403,
#237404,#237405,#237406,#237407,#237408,#237409,#237410,#237411,#237412,
#237413,#237414,#237415,#237416,#237417,#237418,#237419,#237420,#237421,
#237422,#237423,#237424,#237425,#237426,#237427,#237428,#237429,#237430,
#237431,#237432,#237433,#237434,#237435,#237436,#237437,#237438,#237439,
#237440,#237441,#237442,#237443,#237444,#237445,#237446,#237447,#237448,
#237449,#237450,#237451,#237452,#237453,#237454,#237455,#237456,#237457,
#237458,#237459,#237460,#237461,#237462,#237463,#237464,#237465,#237466,
#237467,#237468,#237469,#237470,#237471,#237472,#237473,#237474,#237475,
#237476,#237477,#237478,#237479,#237480,#237481,#237482,#237483,#237484,
#237485,#237486,#237487,#237488,#237489,#237490,#237491,#237492,#237493,
#237494,#237495,#237496,#237497,#237498,#237499,#237500,#237501,#237502,
#237503,#237504,#237505,#237506,#237507,#237508,#237509,#237510,#237511,
#237512,#237513,#237514,#237515,#237516,#237517,#237518,#237519,#237520,
#237521,#237522,#237523,#237524,#237525,#237526,#237527,#237528,#237529,
#237530,#237531,#237532,#237533,#237534,#237535,#237536,#237537,#237538,
#237539,#237540,#237541,#237542,#237543,#237544,#237545,#237546,#237547,
#237548,#237549,#237550,#237551,#237552,#237553,#237554,#237555,#237556,
#237557,#237558,#237559,#237560,#237561,#237562,#237563,#237564,#237565,
#237566,#237567,#237568,#237569,#237570,#237571,#237572,#237573,#237574,
#237575,#237576,#237577,#237578,#237579,#237580,#237581,#237582,#237583,
#237584,#237585,#237586,#237587,#237588,#237589,#237590,#237591,#237592,
#237593,#237594,#237595,#237596,#237597,#237598,#237599,#237600,#237601,
#237602,#237603,#237604,#237605,#237606,#237607,#237608,#237609,#237610,
#237611,#237612,#237613,#237614,#237615,#237616,#237617,#237618,#237619,
#237620,#237621,#237622,#237623,#237624,#237625,#237626,#237627,#237628,
#237629,#237630,#237631,#237632,#237633,#237634,#237635,#237636,#237637,
#237638,#237639,#237640,#237641,#237642,#237643,#237644,#237645,#237646,
#237647,#237648,#237649,#237650,#237651,#237652,#237653,#237654,#237655,
#237656,#237657,#237658,#237659,#237660,#237661,#237662,#237663,#237664,
#237665,#237666,#237667,#237668,#237669,#237670,#237671,#237672,#237673,
#237674,#237675,#237676,#237677,#237678,#237679,#237680,#237681,#237682,
#237683,#237684,#237685,#237686,#237687,#237688,#237689,#237690,#237691,
#237692,#237693,#237694,#237695,#237696,#237697,#237698,#237699,#237700,
#237701,#237702,#237703,#237704,#237705,#237706,#237707,#237708,#237709,
#237710,#237711,#237712,#237713,#237714,#237715,#237716,#237717,#237718,
#237719,#237720,#237721,#237722,#237723,#237724,#237725,#237726,#237727,
#237728,#237729,#237730,#237731,#237732,#237733,#237734,#237735,#237736,
#237737,#237738,#237739,#237740,#237741,#237742,#237743,#237744,#237745,
#237746,#237747,#237748,#237749,#237750,#237751,#237752,#237753,#237754,
#237755,#237756,#237757,#237758,#237759,#237760,#237761,#237762,#237763,
#237764,#237765,#237766,#237767,#237768,#237769,#237770,#237771,#237772,
#237773,#237774,#237775,#237776,#237777,#237778,#237779,#237780,#237781,
#237782,#237783,#237784,#237785,#237786,#237787,#237788,#237789,#237790,
#237791,#237792,#237793,#237794,#237795,#237796,#237797,#237798,#237799,
#237800,#237801,#237802,#237803,#237804,#237805,#237806,#237807,#237808,
#237809,#237810,#237811,#237812,#237813,#237814,#237815,#237816,#237817,
#237818,#237819,#237820,#237821,#237822,#237823,#237824,#237825,#237826,
#237827,#237828,#237829,#237830,#237831,#237832,#237833,#237834,#237835,
#237836,#237837,#237838,#237839,#237840,#237841,#237842,#237843,#237844,
#237845,#237846,#237847,#237848,#237849,#237850,#237851,#237852,#237853,
#237854,#237855,#237856,#237857,#237858,#237859,#237860,#237861,#237862,
#237863,#237864,#237865,#237866,#237867,#237868,#237869,#237870,#237871,
#237872,#237873,#237874,#237875,#237876,#237877,#237878,#237879,#237880,
#237881,#237882,#237883,#237884,#237885,#237886,#237887,#237888,#237889,
#237890,#237891,#237892,#237893,#237894,#237895,#237896,#237897,#237898,
#237899,#237900,#237901,#237902,#237903,#237904,#237905,#237906,#237907,
#237908,#237909,#237910,#237911,#237912,#237913,#237914,#237915,#237916,
#237917,#237918,#237919,#237920,#237921,#237922,#237923,#237924,#237925,
#237926,#237927,#237928,#237929,#237930,#237931,#237932,#237933,#237934,
#237935,#237936,#237937,#237938,#237939,#237940,#237941,#237942,#237943,
#237944,#237945,#237946,#237947,#237948,#237949,#237950,#237951,#237952,
#237953,#237954,#237955,#237956,#237957,#237958,#237959,#237960,#237961,
#237962,#237963,#237964,#237965,#237966,#237967,#237968,#237969,#237970,
#237971,#237972,#237973,#237974,#237975,#237976,#237977,#237978,#237979,
#237980,#237981,#237982,#237983,#237984,#237985,#237986,#237987,#237988,
#237989,#237990,#237991,#237992,#237993,#237994,#237995,#237996,#237997,
#237998,#237999,#238000,#238001,#238002,#238003,#238004,#238005,#238006,
#238007,#238008,#238009,#238010,#238011,#238012,#238013,#238014,#238015,
#238016,#238017,#238018,#238019,#238020,#238021,#238022,#238023,#238024,
#238025,#238026,#238027,#238028,#238029,#238030,#238031,#238032,#238033,
#238034,#238035,#238036,#238037,#238038,#238039,#238040,#238041,#238042,
#238043,#238044,#238045,#238046,#238047,#238048,#238049,#238050,#238051,
#238052,#238053,#238054,#238055,#238056,#238057,#238058,#238059,#238060,
#238061,#238062,#238063,#238064,#238065,#238066,#238067,#238068,#238069,
#238070,#238071,#238072,#238073,#238074,#238075,#238076,#238077,#238078,
#238079,#238080,#238081,#238082,#238083,#238084,#238085,#238086,#238087,
#238088,#238089,#238090,#238091,#238092,#238093,#238094,#238095,#238096,
#238097,#238098,#238099,#238100,#238101,#238102,#238103,#238104,#238105,
#238106,#238107,#238108,#238109,#238110,#238111,#238112,#238113,#238114,
#238115,#238116,#238117,#238118,#238119,#238120,#238121,#238122,#238123,
#238124,#238125,#238126,#238127,#238128,#238129,#238130,#238131,#238132,
#238133,#238134,#238135,#238136,#238137,#238138,#238139,#238140,#238141,
#238142,#238143,#238144,#238145,#238146,#238147,#238148,#238149,#238150,
#238151,#238152,#238153,#238154,#238155,#238156,#238157,#238158,#238159,
#238160,#238161,#238162,#238163,#238164,#238165,#238166,#238167,#238168,
#238169,#238170,#238171,#238172,#238173,#238174,#238175,#238176,#238177,
#238178,#238179,#238180,#238181,#238182,#238183,#238184,#238185,#238186,
#238187,#238188,#238189,#238190,#238191,#238192,#238193,#238194,#238195,
#238196,#238197,#238198,#238199,#238200,#238201,#238202,#238203,#238204,
#238205,#238206,#238207,#238208,#238209,#238210,#238211,#238212,#238213,
#238214,#238215,#238216,#238217,#238218,#238219,#238220,#238221,#238222,
#238223,#238224,#238225,#238226,#238227,#238228,#238229,#238230,#238231,
#238232,#238233,#238234,#238235,#238236,#238237,#238238,#238239,#238240,
#238241,#238242,#238243,#238244,#238245,#238246,#238247,#238248,#238249,
#238250,#238251,#238252,#238253,#238254,#238255,#238256,#238257,#238258,
#238259,#238260,#238261,#238262,#238263,#238264,#238265,#238266,#238267,
#238268,#238269,#238270,#238271,#238272,#238273,#238274,#238275,#238276,
#238277,#238278,#238279,#238280,#238281,#238282,#238283,#238284,#238285,
#238286,#238287,#238288,#238289,#238290,#238291,#238292,#238293,#238294,
#238295,#238296,#238297,#238298,#238299,#238300,#238301,#238302,#238303,
#238304,#238305,#238306,#238307,#238308,#238309,#238310,#238311,#238312,
#238313,#238314,#238315,#238316,#238317,#238318,#238319,#238320,#238321,
#238322,#238323,#238324,#238325,#238326,#238327,#238328,#238329,#238330,
#238331,#238332,#238333,#238334,#238335,#238336,#238337,#238338,#238339,
#238340,#238341,#238342,#238343,#238344,#238345,#238346,#238347,#238348,
#238349,#238350,#238351,#238352,#238353,#238354,#238355,#238356,#238357,
#238358,#238359,#238360,#238361,#238362,#238363,#238364,#238365,#238366,
#238367,#238368,#238369,#238370,#238371,#238372,#238373,#238374,#238375,
#238376,#238377,#238378,#238379,#238380,#238381,#238382,#238383,#238384,
#238385,#238386,#238387,#238388,#238389,#238390,#238391,#238392,#238393,
#238394,#238395,#238396,#238397,#238398,#238399,#238400,#238401,#238402,
#238403,#238404,#238405,#238406,#238407,#238408,#238409,#238410,#238411,
#238412,#238413,#238414,#238415,#238416,#238417,#238418,#238419,#238420,
#238421,#238422,#238423,#238424,#238425,#238426,#238427,#238428,#238429,
#238430,#238431,#238432,#238433,#238434,#238435,#238436,#238437,#238438,
#238439,#238440,#238441,#238442,#238443,#238444,#238445,#238446,#238447,
#238448,#238449,#238450,#238451,#238452,#238453,#238454,#238455,#238456,
#238457,#238458,#238459,#238460,#238461,#238462,#238463,#238464,#238465,
#238466,#238467,#238468,#238469,#238470,#238471,#238472,#238473,#238474,
#238475,#238476,#238477,#238478,#238479,#238480,#238481,#238482,#238483,
#238484,#238485,#238486,#238487,#238488,#238489,#238490,#238491,#238492,
#238493,#238494,#238495,#238496,#238497,#238498,#238499,#238500,#238501,
#238502,#238503,#238504,#238505,#238506,#238507,#238508,#238509,#238510,
#238511,#238512,#238513,#238514,#238515,#238516,#238517,#238518,#238519,
#238520,#238521,#238522,#238523,#238524,#238525,#238526,#238527,#238528,
#238529,#238530,#238531,#238532,#238533,#238534,#238535,#238536,#238537,
#238538,#238539,#238540,#238541,#238542,#238543,#238544,#238545,#238546,
#238547,#238548,#238549,#238550,#238551,#238552,#238553,#238554,#238555,
#238556,#238557,#238558,#238559,#238560,#238561,#238562,#238563,#238564,
#238565,#238566,#238567,#238568,#238569,#238570,#238571,#238572,#238573,
#238574,#238575,#238576,#238577,#238578,#238579,#238580,#238581,#238582,
#238583,#238584,#238585,#238586,#238587),(#238588,#238589,#238590,#238591,
#238592,#238593,#238594,#238595,#238596,#238597,#238598,#238599,#238600,
#238601,#238602,#238603,#238604,#238605,#238606,#238607,#238608,#238609,
#238610,#238611,#238612,#238613,#238614,#238615,#238616,#238617,#238618,
#238619,#238620,#238621,#238622,#238623,#238624,#238625,#238626,#238627,
#238628,#238629,#238630,#238631,#238632,#238633,#238634,#238635,#238636,
#238637,#238638,#238639,#238640,#238641,#238642,#238643,#238644,#238645,
#238646,#238647,#238648,#238649,#238650,#238651,#238652,#238653,#238654,
#238655,#238656,#238657,#238658,#238659,#238660,#238661,#238662,#238663,
#238664,#238665,#238666,#238667,#238668,#238669,#238670,#238671,#238672,
#238673,#238674,#238675,#238676,#238677,#238678,#238679,#238680,#238681,
#238682,#238683,#238684,#238685,#238686,#238687,#238688,#238689,#238690,
#238691,#238692,#238693,#238694,#238695,#238696,#238697,#238698,#238699,
#238700,#238701,#238702,#238703,#238704,#238705,#238706,#238707,#238708,
#238709,#238710,#238711,#238712,#238713,#238714,#238715,#238716,#238717,
#238718,#238719,#238720,#238721,#238722,#238723,#238724,#238725,#238726,
#238727,#238728,#238729,#238730,#238731,#238732,#238733,#238734,#238735,
#238736,#238737,#238738,#238739,#238740,#238741,#238742,#238743,#238744,
#238745,#238746,#238747,#238748,#238749,#238750,#238751,#238752,#238753,
#238754,#238755,#238756,#238757,#238758,#238759,#238760,#238761,#238762,
#238763,#238764,#238765,#238766,#238767,#238768,#238769,#238770,#238771,
#238772,#238773,#238774,#238775,#238776,#238777,#238778,#238779,#238780,
#238781,#238782,#238783,#238784,#238785,#238786,#238787,#238788,#238789,
#238790,#238791,#238792,#238793,#238794,#238795,#238796,#238797,#238798,
#238799,#238800,#238801,#238802,#238803,#238804,#238805,#238806,#238807,
#238808,#238809,#238810,#238811,#238812,#238813,#238814,#238815,#238816,
#238817,#238818,#238819,#238820,#238821,#238822,#238823,#238824,#238825,
#238826,#238827,#238828,#238829,#238830,#238831,#238832,#238833,#238834,
#238835,#238836,#238837,#238838,#238839,#238840,#238841,#238842,#238843,
#238844,#238845,#238846,#238847,#238848,#238849,#238850,#238851,#238852,
#238853,#238854,#238855,#238856,#238857,#238858,#238859,#238860,#238861,
#238862,#238863,#238864,#238865,#238866,#238867,#238868,#238869,#238870,
#238871,#238872,#238873,#238874,#238875,#238876,#238877,#238878,#238879,
#238880,#238881,#238882,#238883,#238884,#238885,#238886,#238887,#238888,
#238889,#238890,#238891,#238892,#238893,#238894,#238895,#238896,#238897,
#238898,#238899,#238900,#238901,#238902,#238903,#238904,#238905,#238906,
#238907,#238908,#238909,#238910,#238911,#238912,#238913,#238914,#238915,
#238916,#238917,#238918,#238919,#238920,#238921,#238922,#238923,#238924,
#238925,#238926,#238927,#238928,#238929,#238930,#238931,#238932,#238933,
#238934,#238935,#238936,#238937,#238938,#238939,#238940,#238941,#238942,
#238943,#238944,#238945,#238946,#238947,#238948,#238949,#238950,#238951,
#238952,#238953,#238954,#238955,#238956,#238957,#238958,#238959,#238960,
#238961,#238962,#238963,#238964,#238965,#238966,#238967,#238968,#238969,
#238970,#238971,#238972,#238973,#238974,#238975,#238976,#238977,#238978,
#238979,#238980,#238981,#238982,#238983,#238984,#238985,#238986,#238987,
#238988,#238989,#238990,#238991,#238992,#238993,#238994,#238995,#238996,
#238997,#238998,#238999,#239000,#239001,#239002,#239003,#239004,#239005,
#239006,#239007,#239008,#239009,#239010,#239011,#239012,#239013,#239014,
#239015,#239016,#239017,#239018,#239019,#239020,#239021,#239022,#239023,
#239024,#239025,#239026,#239027,#239028,#239029,#239030,#239031,#239032,
#239033,#239034,#239035,#239036,#239037,#239038,#239039,#239040,#239041,
#239042,#239043,#239044,#239045,#239046,#239047,#239048,#239049,#239050,
#239051,#239052,#239053,#239054,#239055,#239056,#239057,#239058,#239059,
#239060,#239061,#239062,#239063,#239064,#239065,#239066,#239067,#239068,
#239069,#239070,#239071,#239072,#239073,#239074,#239075,#239076,#239077,
#239078,#239079,#239080,#239081,#239082,#239083,#239084,#239085,#239086,
#239087,#239088,#239089,#239090,#239091,#239092,#239093,#239094,#239095,
#239096,#239097,#239098,#239099,#239100,#239101,#239102,#239103,#239104,
#239105,#239106,#239107,#239108,#239109,#239110,#239111,#239112,#239113,
#239114,#239115,#239116,#239117,#239118,#239119,#239120,#239121,#239122,
#239123,#239124,#239125,#239126,#239127,#239128,#239129,#239130,#239131,
#239132,#239133,#239134,#239135,#239136,#239137,#239138,#239139,#239140,
#239141,#239142,#239143,#239144,#239145,#239146,#239147,#239148,#239149,
#239150,#239151,#239152,#239153,#239154,#239155,#239156,#239157,#239158,
#239159,#239160,#239161,#239162,#239163,#239164,#239165,#239166,#239167,
#239168,#239169,#239170,#239171,#239172,#239173,#239174,#239175,#239176,
#239177,#239178,#239179,#239180,#239181,#239182,#239183,#239184,#239185,
#239186,#239187,#239188,#239189,#239190,#239191,#239192,#239193,#239194,
#239195,#239196,#239197,#239198,#239199,#239200,#239201,#239202,#239203,
#239204,#239205,#239206,#239207,#239208,#239209,#239210,#239211,#239212,
#239213,#239214,#239215,#239216,#239217,#239218,#239219,#239220,#239221,
#239222,#239223,#239224,#239225,#239226,#239227,#239228,#239229,#239230,
#239231,#239232,#239233,#239234,#239235,#239236,#239237,#239238,#239239,
#239240,#239241,#239242,#239243,#239244,#239245,#239246,#239247,#239248,
#239249,#239250,#239251,#239252,#239253,#239254,#239255,#239256,#239257,
#239258,#239259,#239260,#239261,#239262,#239263,#239264,#239265,#239266,
#239267,#239268,#239269,#239270,#239271,#239272,#239273,#239274,#239275,
#239276,#239277,#239278,#239279,#239280,#239281,#239282,#239283,#239284,
#239285,#239286,#239287,#239288,#239289,#239290,#239291,#239292,#239293,
#239294,#239295,#239296,#239297,#239298,#239299,#239300,#239301,#239302,
#239303,#239304,#239305,#239306,#239307,#239308,#239309,#239310,#239311,
#239312,#239313,#239314,#239315,#239316,#239317,#239318,#239319,#239320,
#239321,#239322,#239323,#239324,#239325,#239326,#239327,#239328,#239329,
#239330,#239331,#239332,#239333,#239334,#239335,#239336,#239337,#239338,
#239339,#239340,#239341,#239342,#239343,#239344,#239345,#239346,#239347,
#239348,#239349,#239350,#239351,#239352,#239353,#239354,#239355,#239356,
#239357,#239358,#239359,#239360,#239361,#239362,#239363,#239364,#239365,
#239366,#239367,#239368,#239369,#239370,#239371,#239372,#239373,#239374,
#239375,#239376,#239377,#239378,#239379,#239380,#239381,#239382,#239383,
#239384,#239385,#239386,#239387,#239388,#239389,#239390,#239391,#239392,
#239393,#239394,#239395,#239396,#239397,#239398,#239399,#239400,#239401,
#239402,#239403,#239404,#239405,#239406,#239407,#239408,#239409,#239410,
#239411,#239412,#239413,#239414,#239415,#239416,#239417,#239418,#239419,
#239420,#239421,#239422,#239423,#239424,#239425,#239426,#239427,#239428,
#239429,#239430,#239431,#239432,#239433,#239434,#239435,#239436,#239437,
#239438,#239439,#239440,#239441,#239442,#239443,#239444,#239445,#239446,
#239447,#239448,#239449,#239450,#239451,#239452,#239453,#239454,#239455,
#239456,#239457,#239458,#239459,#239460,#239461,#239462,#239463,#239464,
#239465,#239466,#239467,#239468,#239469,#239470,#239471,#239472,#239473,
#239474,#239475,#239476,#239477,#239478,#239479,#239480,#239481,#239482,
#239483,#239484,#239485,#239486,#239487,#239488,#239489,#239490,#239491,
#239492,#239493,#239494,#239495,#239496,#239497,#239498,#239499,#239500,
#239501,#239502,#239503,#239504,#239505,#239506,#239507,#239508,#239509,
#239510,#239511,#239512,#239513,#239514,#239515,#239516,#239517,#239518,
#239519,#239520,#239521,#239522,#239523,#239524,#239525,#239526,#239527,
#239528,#239529,#239530,#239531,#239532,#239533,#239534,#239535,#239536,
#239537,#239538,#239539,#239540,#239541,#239542,#239543,#239544,#239545,
#239546,#239547,#239548,#239549,#239550,#239551,#239552,#239553,#239554,
#239555,#239556,#239557,#239558,#239559,#239560,#239561,#239562,#239563,
#239564,#239565,#239566,#239567,#239568,#239569,#239570,#239571,#239572,
#239573,#239574,#239575,#239576,#239577,#239578,#239579,#239580,#239581,
#239582,#239583,#239584,#239585,#239586,#239587,#239588,#239589,#239590,
#239591,#239592,#239593,#239594,#239595,#239596,#239597,#239598,#239599,
#239600,#239601,#239602,#239603,#239604,#239605,#239606,#239607,#239608,
#239609,#239610,#239611,#239612,#239613,#239614,#239615,#239616,#239617,
#239618,#239619,#239620,#239621,#239622,#239623,#239624,#239625,#239626,
#239627,#239628,#239629,#239630,#239631,#239632,#239633,#239634,#239635,
#239636,#239637,#239638,#239639,#239640,#239641,#239642,#239643,#239644,
#239645,#239646,#239647,#239648,#239649,#239650,#239651,#239652,#239653,
#239654,#239655,#239656,#239657,#239658,#239659,#239660,#239661,#239662,
#239663,#239664,#239665,#239666,#239667,#239668,#239669,#239670,#239671,
#239672,#239673,#239674,#239675,#239676,#239677,#239678,#239679,#239680,
#239681,#239682,#239683,#239684,#239685,#239686,#239687,#239688,#239689,
#239690,#239691,#239692,#239693,#239694,#239695,#239696,#239697,#239698,
#239699,#239700,#239701,#239702,#239703,#239704,#239705,#239706,#239707,
#239708,#239709,#239710,#239711,#239712,#239713,#239714,#239715,#239716,
#239717,#239718,#239719,#239720,#239721,#239722,#239723,#239724,#239725,
#239726,#239727,#239728,#239729,#239730,#239731,#239732,#239733,#239734,
#239735,#239736,#239737,#239738,#239739,#239740,#239741,#239742,#239743,
#239744,#239745,#239746,#239747,#239748,#239749,#239750,#239751,#239752,
#239753,#239754,#239755,#239756,#239757,#239758,#239759,#239760,#239761,
#239762,#239763,#239764,#239765,#239766,#239767,#239768,#239769,#239770,
#239771,#239772,#239773,#239774,#239775,#239776,#239777,#239778,#239779,
#239780,#239781,#239782,#239783,#239784,#239785,#239786,#239787,#239788,
#239789,#239790,#239791,#239792,#239793,#239794,#239795,#239796,#239797,
#239798,#239799,#239800,#239801,#239802,#239803,#239804,#239805,#239806,
#239807,#239808,#239809,#239810,#239811,#239812,#239813,#239814,#239815,
#239816,#239817,#239818,#239819,#239820,#239821,#239822,#239823,#239824,
#239825,#239826,#239827,#239828,#239829,#239830,#239831,#239832,#239833,
#239834,#239835,#239836,#239837,#239838,#239839,#239840,#239841,#239842,
#239843,#239844,#239845,#239846,#239847,#239848,#239849,#239850,#239851,
#239852,#239853,#239854,#239855,#239856,#239857,#239858,#239859,#239860,
#239861,#239862,#239863,#239864,#239865,#239866,#239867,#239868,#239869,
#239870,#239871,#239872,#239873,#239874,#239875,#239876,#239877,#239878,
#239879,#239880,#239881,#239882,#239883,#239884,#239885,#239886,#239887,
#239888,#239889,#239890,#239891,#239892,#239893,#239894,#239895,#239896,
#239897,#239898,#239899,#239900,#239901,#239902,#239903,#239904,#239905,
#239906,#239907,#239908,#239909,#239910,#239911,#239912,#239913,#239914,
#239915,#239916,#239917,#239918,#239919,#239920,#239921,#239922,#239923,
#239924,#239925,#239926,#239927,#239928,#239929,#239930,#239931,#239932,
#239933,#239934,#239935,#239936,#239937,#239938,#239939,#239940,#239941,
#239942,#239943,#239944,#239945,#239946,#239947,#239948,#239949,#239950,
#239951,#239952,#239953,#239954,#239955,#239956,#239957,#239958,#239959,
#239960,#239961,#239962,#239963,#239964,#239965,#239966,#239967,#239968,
#239969,#239970,#239971,#239972,#239973,#239974,#239975,#239976,#239977,
#239978,#239979,#239980,#239981,#239982,#239983,#239984,#239985,#239986,
#239987,#239988,#239989,#239990,#239991,#239992,#239993,#239994,#239995,
#239996,#239997,#239998,#239999,#240000,#240001,#240002,#240003,#240004,
#240005,#240006,#240007,#240008,#240009,#240010,#240011,#240012,#240013,
#240014,#240015,#240016,#240017,#240018,#240019,#240020,#240021,#240022,
#240023,#240024,#240025,#240026,#240027,#240028,#240029,#240030,#240031,
#240032,#240033,#240034,#240035,#240036,#240037,#240038,#240039,#240040,
#240041,#240042,#240043,#240044,#240045,#240046,#240047,#240048,#240049,
#240050,#240051,#240052,#240053,#240054,#240055,#240056,#240057,#240058,
#240059,#240060,#240061,#240062,#240063,#240064,#240065,#240066,#240067,
#240068,#240069,#240070,#240071,#240072,#240073,#240074,#240075,#240076,
#240077,#240078,#240079,#240080,#240081,#240082,#240083,#240084,#240085,
#240086,#240087,#240088,#240089,#240090,#240091,#240092,#240093,#240094,
#240095,#240096,#240097,#240098,#240099,#240100,#240101,#240102,#240103,
#240104,#240105,#240106,#240107,#240108,#240109,#240110,#240111,#240112,
#240113,#240114,#240115,#240116,#240117,#240118,#240119,#240120,#240121,
#240122,#240123,#240124,#240125,#240126,#240127,#240128,#240129,#240130,
#240131,#240132,#240133,#240134,#240135,#240136,#240137,#240138,#240139,
#240140,#240141,#240142,#240143,#240144,#240145,#240146,#240147,#240148,
#240149,#240150,#240151,#240152,#240153,#240154,#240155,#240156,#240157,
#240158,#240159,#240160,#240161,#240162,#240163,#240164,#240165,#240166,
#240167,#240168,#240169,#240170,#240171,#240172,#240173,#240174,#240175,
#240176,#240177,#240178,#240179,#240180,#240181,#240182,#240183,#240184,
#240185,#240186,#240187,#240188,#240189,#240190,#240191,#240192,#240193,
#240194,#240195,#240196,#240197,#240198,#240199,#240200,#240201,#240202,
#240203,#240204,#240205,#240206,#240207,#240208,#240209,#240210,#240211,
#240212,#240213,#240214,#240215,#240216,#240217,#240218,#240219,#240220,
#240221,#240222,#240223,#240224,#240225,#240226,#240227,#240228,#240229,
#240230,#240231,#240232,#240233,#240234,#240235,#240236,#240237,#240238,
#240239,#240240,#240241,#240242,#240243,#240244,#240245,#240246,#240247,
#240248,#240249,#240250,#240251,#240252,#240253,#240254,#240255,#240256,
#240257,#240258,#240259,#240260,#240261,#240262,#240263,#240264,#240265,
#240266,#240267,#240268,#240269,#240270,#240271,#240272,#240273,#240274,
#240275,#240276,#240277,#240278,#240279,#240280,#240281,#240282)),
 .UNSPECIFIED.,.F.,.F.,.F.,(4,4),(4,1,1,1,1,1,1,1,1,1,1,1,1,1,1,1,1,1,1,
1,1,1,1,1,1,1,1,1,1,1,1,1,1,1,1,1,1,1,1,1,1,1,1,1,1,1,1,1,1,1,1,1,1,1,1,
1,1,1,1,1,1,1,1,1,1,1,1,1,1,1,1,1,1,1,1,1,1,1,1,1,1,1,1,1,1,1,1,1,1,1,1,
1,1,1,1,1,1,1,1,1,1,1,1,1,1,1,1,1,1,1,1,1,1,1,1,1,1,1,1,1,1,1,1,1,1,1,1,
1,1,1,1,1,1,1,1,1,1,1,1,1,1,1,1,1,1,1,1,1,1,1,1,1,1,1,1,1,1,1,1,1,1,1,1,
1,1,1,1,1,1,1,1,1,1,1,1,1,1,1,1,1,1,1,1,1,1,1,1,1,1,1,1,1,1,1,1,1,1,1,1,
1,1,1,1,1,1,1,1,1,1,1,1,1,1,1,1,1,1,1,1,1,1,1,1,1,1,1,1,1,1,1,1,1,1,1,1,
1,1,1,1,1,1,1,1,1,1,1,1,1,1,1,1,1,1,1,1,1,1,1,1,1,1,1,1,1,1,1,1,1,1,1,1,
1,1,1,1,1,1,1,1,1,1,1,1,1,1,1,1,1,1,1,1,1,1,1,1,1,1,1,1,1,1,1,1,1,1,1,1,
1,1,1,1,1,1,1,1,1,1,1,1,1,1,1,1,1,1,1,1,1,1,1,1,1,1,1,1,1,1,1,1,1,1,1,1,
1,1,1,1,1,1,1,1,1,1,1,1,1,1,1,1,1,1,1,1,1,1,1,1,1,1,1,1,1,1,1,1,1,1,1,1,
1,1,1,1,1,1,1,1,1,1,1,1,1,1,1,1,1,1,1,1,1,1,1,1,1,1,1,1,1,1,1,1,1,1,1,1,
1,1,1,1,1,1,1,1,1,1,1,1,1,1,1,1,1,1,1,1,1,1,1,1,1,1,1,1,1,1,1,1,1,1,1,1,
1,1,1,1,1,1,1,1,1,1,1,1,1,1,1,1,1,1,1,1,1,1,1,1,1,1,1,1,1,1,1,1,1,1,1,1,
1,1,1,1,1,1,1,1,1,1,1,1,1,1,1,1,1,1,1,1,1,1,1,1,1,1,1,1,1,1,1,1,1,1,1,1,
1,1,1,1,1,1,1,1,1,1,1,1,1,1,1,1,1,1,1,1,1,1,1,1,1,1,1,1,1,1,1,1,1,1,1,1,
1,1,1,1,1,1,1,1,1,1,1,1,1,1,1,1,1,1,1,1,1,1,1,1,1,1,1,1,1,1,1,1,1,1,1,1,
1,1,1,1,1,1,1,1,1,1,1,1,1,1,1,1,1,1,1,1,1,1,1,1,1,1,1,1,1,1,1,1,1,1,1,1,
1,1,1,1,1,1,1,1,1,1,1,1,1,1,1,1,1,1,1,1,1,1,1,1,1,1,1,1,1,1,1,1,1,1,1,1,
1,1,1,1,1,1,1,1,1,1,1,1,1,1,1,1,1,1,1,1,1,1,1,1,1,1,1,1,1,1,1,1,1,1,1,1,
1,1,1,1,1,1,1,1,1,1,1,1,1,1,1,1,1,1,1,1,1,1,1,1,1,1,1,1,1,1,1,1,1,1,1,1,
1,1,1,1,1,1,1,1,1,1,1,1,1,1,1,1,1,1,1,1,1,1,1,1,1,1,1,1,1,1,1,1,1,1,1,1,
1,1,1,1,1,1,1,1,1,1,1,1,1,1,1,1,1,1,1,1,1,1,1,1,1,1,1,1,1,1,1,1,1,1,1,1,
1,1,1,1,1,1,1,1,1,1,1,1,1,1,1,1,1,1,1,1,1,1,1,1,1,1,1,1,1,1,1,1,1,1,1,1,
1,1,1,1,1,1,1,1,1,1,1,1,1,1,1,1,1,1,1,1,1,1,1,1,1,1,1,1,1,1,1,1,1,1,1,1,
1,1,1,1,1,1,1,1,1,1,1,1,1,1,1,1,1,1,1,1,1,1,1,1,1,1,1,1,1,1,1,1,1,1,1,1,
1,1,1,1,1,1,1,1,1,1,1,1,1,1,1,1,1,1,1,1,1,1,1,1,1,1,1,1,1,1,1,1,1,1,1,1,
1,1,1,1,1,1,1,1,1,1,1,1,1,1,1,1,1,1,1,1,1,1,1,1,1,1,1,1,1,1,1,1,1,1,1,1,
1,1,1,1,1,1,1,1,1,1,1,1,1,1,1,1,1,1,1,1,1,1,1,1,1,1,1,1,1,1,1,1,1,1,1,1,
1,1,1,1,1,1,1,1,1,1,1,1,1,1,1,1,1,1,1,1,1,1,1,1,1,1,1,1,1,1,1,1,1,1,1,1,
1,1,1,1,1,1,1,1,1,1,1,1,1,1,1,1,1,1,1,1,1,1,1,1,1,1,1,1,1,1,1,1,1,1,1,1,
1,1,1,1,1,1,1,1,1,1,1,1,1,1,1,1,1,1,1,1,1,1,1,1,1,1,1,1,1,1,1,1,1,1,1,1,
1,1,1,1,1,1,1,1,1,1,1,1,1,1,1,1,1,1,1,1,1,1,1,1,1,1,1,1,1,1,1,1,1,1,1,1,
1,1,1,1,1,1,1,1,1,1,1,1,1,1,1,1,1,1,1,1,1,1,1,1,1,1,1,1,1,1,1,1,1,1,1,1,
1,1,1,1,1,1,1,1,1,1,1,1,1,1,1,1,1,1,1,1,1,1,1,1,1,1,1,1,1,1,1,1,1,1,1,1,
1,1,1,1,1,1,1,1,1,1,1,1,1,1,1,1,1,1,1,1,1,1,1,1,1,1,1,1,1,1,1,1,1,1,1,1,
1,1,1,1,1,1,1,1,1,1,1,1,1,1,1,1,1,1,1,1,1,1,1,1,1,1,1,1,1,1,1,1,1,1,1,1,
1,1,1,1,1,1,1,1,1,1,1,1,1,1,1,1,1,1,1,1,1,1,1,1,1,1,1,1,1,1,1,1,1,1,1,1,
1,1,1,1,1,1,1,1,1,1,1,1,1,1,1,1,1,1,1,1,1,1,1,1,1,1,1,1,1,1,1,1,1,1,1,1,
1,1,1,1,1,1,1,1,1,1,1,1,1,1,1,1,1,1,1,1,1,1,1,1,1,1,1,1,1,1,1,1,1,1,1,1,
1,1,1,1,1,1,1,1,1,1,1,1,1,1,1,1,1,1,1,1,1,1,1,1,1,1,1,1,1,1,1,1,1,1,1,1,
1,1,1,1,1,1,1,1,1,1,1,1,1,1,1,1,1,1,1,1,1,1,1,1,1,1,1,1,1,1,1,1,1,1,1,1,
1,1,1,1,1,1,1,1,1,1,1,1,1,1,1,1,1,1,1,1,1,1,1,1,1,1,1,1,1,1,1,1,1,1,1,1,
1,1,1,1,1,1,1,1,1,1,1,1,1,1,1,1,1,1,1,1,1,1,1,1,1,1,1,1,1,1,1,1,1,1,1,1,
1,1,1,1,1,1,1,1,1,1,1,1,1,1,1,1,1,1,1,1,1,1,1,1,1,1,1,1,1,1,1,1,1,1,1,1,
1,1,1,1,1,1,1,1,1,1,1,1,1,1,1,1,1,1,1,1,1,1,1,1,1,1,1,1,1,1,1,1,1,1,1,1,
1,1,1,1,1,1,1,1,1,1,1,1,1,1,1,1,1,1,1,1,1,1,1,1,1,1,1,1,1,1,1,1,1,1,1,1,
1,1,1,1,1,1,1,1,1,1,1,1,1,1,1,1,1,4),(-0.000587328099657093,0.1157205948422),
(8.30590413559005,8.80579087257276,9.30565887793282,10.305394888653,11.3051308993731,
12.3048669100932,13.3046029208133,14.3043389315335,15.3040749422536,16.3038109529737,
17.3035469636939,18.303282974414,19.3030189851341,20.3027549958542,21.3024910065744,
22.3022270172945,23.3019630280146,24.3016990387348,25.3014350494549,26.301171060175,
27.3009070708951,28.3006430816153,29.3003790923354,30.3001151030555,31.2998511137757,
32.2995871244958,33.2993231352159,34.299059145936,35.2987951566562,36.2985311673763,
37.2982671780964,38.2980031888166,39.2977391995367,40.2974752102568,41.2972112209769,
42.2969472316971,43.2966832424172,44.2964192531373,45.2961552638575,46.2958912745776,
47.2956272852977,48.2953632960178,49.295099306738,50.2948353174581,51.2945713281782,
52.2943073388984,53.2940433496185,54.2937793603386,55.2935153710587,56.2932513817789,
57.292987392499,58.2927234032191,59.2924594139393,60.2921954246594,61.2919314353795,
62.2916674460996,63.2914034568198,64.2911394675399,65.29087547826,66.2906114889802,
67.2903474997003,68.2900835104204,69.2898195211405,70.2895555318607,71.2892915425808,
72.2890275533009,73.2887635640211,74.2884995747412,75.2882355854613,76.2879715961814,
77.2877076069016,78.2874436176217,79.2871796283418,80.286915639062,81.2866516497821,
82.2863876605022,83.2861236712224,84.2858596819425,85.2855956926626,86.2853317033827,
87.2850677141029,88.284803724823,89.2845397355431,90.2842757462633,91.2840117569834,
92.2837477677035,93.2834837784236,94.2832197891438,95.2829557998639,96.282691810584,
97.2824278213041,98.2821638320243,99.2818998427444,100.281635853465,101.281371864185,
102.281107874905,103.280843885625,104.280579896345,105.280315907065,106.280051917785,
107.279787928505,108.279523939226,109.279259949946,110.278995960666,111.278731971386,
112.278467982106,113.278203992826,114.277940003546,115.277676014266,116.277412024987,
117.277148035707,118.276884046427,119.276620057147,120.276356067867,121.276092078587,
122.275828089307,123.275564100028,124.275300110748,125.275036121468,126.274772132188,
127.274508142908,128.274244153628,129.273980164348,130.273716175068,131.273452185789,
132.273188196509,133.272924207229,134.272660217949,135.272396228669,136.272132239389,
137.271868250109,138.271604260829,139.27134027155,140.27107628227,141.27081229299,
142.27054830371,143.27028431443,144.27002032515,145.26975633587,146.26949234659,
147.269228357311,148.268964368031,149.268700378751,150.268436389471,151.268172400191,
152.267908410911,153.267644421631,154.267380432352,155.267116443072,156.266852453792,
157.266588464512,158.266324475232,159.266060485952,160.265796496672,161.265532507392,
162.265268518113,163.265004528833,164.264740539553,165.264476550273,166.264212560993,
167.263948571713,168.263684582433,169.263420593153,170.263156603874,171.262892614594,
172.262628625314,173.262364636034,174.262100646754,175.261836657474,176.261572668194,
177.261308678914,178.261044689635,179.260780700355,180.260516711075,181.260252721795,
182.259988732515,183.259724743235,184.259460753955,185.259196764675,186.258932775396,
187.258668786116,188.258404796836,189.258140807556,190.257876818276,191.257612828996,
192.257348839716,193.257084850437,194.256820861157,195.256556871877,196.256292882597,
197.256028893317,198.255764904037,199.255500914757,200.255236925477,201.254972936198,
202.254708946918,203.254444957638,204.254180968358,205.253916979078,206.253652989798,
207.253389000518,208.253125011238,209.252861021959,210.252597032679,211.252333043399,
212.252069054119,213.251805064839,214.251541075559,215.251277086279,216.251013096999,
217.25074910772,218.25048511844,219.25022112916,220.24995713988,221.2496931506,
222.24942916132,223.24916517204,224.248901182761,225.248637193481,226.248373204201,
227.248109214921,228.247845225641,229.247581236361,230.247317247081,231.247053257801,
232.246789268522,233.246525279242,234.246261289962,235.245997300682,236.245733311402,
237.245469322122,238.245205332842,239.244941343562,240.244677354283,241.244413365003,
242.244149375723,243.243885386443,244.243621397163,245.243357407883,246.243093418603,
247.242829429323,248.242565440044,249.242301450764,250.242037461484,251.241773472204,
252.241509482924,253.241245493644,254.240981504364,255.240717515084,256.240453525805,
257.240189536525,258.239925547245,259.239661557965,260.239397568685,261.239133579405,
262.238869590125,263.238605600846,264.238341611566,265.238077622286,266.237813633006,
267.237549643726,268.237285654446,269.237021665166,270.236757675886,271.236493686607,
272.236229697327,273.235965708047,274.235701718767,275.235437729487,276.235173740207,
277.234909750927,278.234645761647,279.234381772368,280.234117783088,281.233853793808,
282.233589804528,283.233325815248,284.233061825968,285.232797836688,286.232533847408,
287.232269858129,288.232005868849,289.231741879569,290.231477890289,291.231213901009,
292.230949911729,293.230685922449,294.23042193317,295.23015794389,296.22989395461,
297.22962996533,298.22936597605,299.22910198677,300.22883799749,301.22857400821,
302.228310018931,303.228046029651,304.227782040371,305.227518051091,306.227254061811,
307.226990072531,308.226726083251,309.226462093971,310.226198104692,311.225934115412,
312.225670126132,313.225406136852,314.225142147572,315.224878158292,316.224614169012,
317.224350179732,318.224086190453,319.223822201173,320.223558211893,321.223294222613,
322.223030233333,323.222766244053,324.222502254773,325.222238265494,326.221974276214,
327.221710286934,328.221446297654,329.221182308374,330.220918319094,331.220654329814,
332.220390340534,333.220126351255,334.219862361975,335.219598372695,336.219334383415,
337.219070394135,338.218806404855,339.218542415575,340.218278426295,341.218014437016,
342.217750447736,343.217486458456,344.217222469176,345.216958479896,346.216694490616,
347.216430501336,348.216166512056,349.215902522777,350.215638533497,351.215374544217,
352.215110554937,353.214846565657,354.214582576377,355.214318587097,356.214054597817,
357.213790608538,358.213526619258,359.213262629978,360.212998640698,361.212734651418,
362.212470662138,363.212206672858,364.211942683579,365.211678694299,366.211414705019,
367.211150715739,368.210886726459,369.210622737179,370.210358747899,371.210094758619,
372.20983076934,373.20956678006,374.20930279078,375.2090388015,376.20877481222,
377.20851082294,378.20824683366,379.20798284438,380.207718855101,381.207454865821,
382.207190876541,383.206926887261,384.206662897981,385.206398908701,386.206134919421,
387.205870930141,388.205606940862,389.205342951582,390.205078962302,391.204814973022,
392.204550983742,393.204286994462,394.204023005182,395.203759015903,396.203495026623,
397.203231037343,398.202967048063,399.202703058783,400.202439069503,401.202175080223,
402.201911090943,403.201647101664,404.201383112384,405.201119123104,406.200855133824,
407.200591144544,408.200327155264,409.200063165984,410.199799176704,411.199535187425,
412.199271198145,413.199007208865,414.198743219585,415.198479230305,416.198215241025,
417.197951251745,418.197687262465,419.197423273186,420.197159283906,421.196895294626,
422.196631305346,423.196367316066,424.196103326786,425.195839337506,426.195575348226,
427.195311358947,428.195047369667,429.194783380387,430.194519391107,431.194255401827,
432.193991412547,433.193727423267,434.193463433988,435.193199444708,436.192935455428,
437.192671466148,438.192407476868,439.192143487588,440.191879498308,441.191615509028,
442.191351519749,443.191087530469,444.190823541189,445.190559551909,446.190295562629,
447.190031573349,448.189767584069,449.189503594789,450.18923960551,451.18897561623,
452.18871162695,453.18844763767,454.18818364839,455.18791965911,456.18765566983,
457.18739168055,458.187127691271,459.186863701991,460.186599712711,461.186335723431,
462.186071734151,463.185807744871,464.185543755591,465.185279766312,466.185015777032,
467.184751787752,468.184487798472,469.184223809192,470.183959819912,471.183695830632,
472.183431841352,473.183167852073,474.182903862793,475.182639873513,476.182375884233,
477.182111894953,478.181847905673,479.181583916393,480.181319927113,481.181055937834,
482.180791948554,483.180527959274,484.180263969994,485.179999980714,486.179735991434,
487.179472002154,488.179208012874,489.178944023595,490.178680034315,491.178416045035,
492.178152055755,493.177888066475,494.177624077195,495.177360087915,496.177096098636,
497.176832109356,498.176568120076,499.176304130796,500.176040141516,501.175776152236,
502.175512162956,503.175248173676,504.174984184397,505.174720195117,506.174456205837,
507.174192216557,508.173928227277,509.173664237997,510.173400248717,511.173136259437,
512.172872270158,513.172608280878,514.172344291598,515.172080302318,516.171816313038,
517.171552323758,518.171288334478,519.171024345198,520.170760355919,521.170496366639,
522.170232377359,523.169968388079,524.169704398799,525.169440409519,526.169176420239,
527.168912430959,528.16864844168,529.1683844524,530.16812046312,531.16785647384,
532.16759248456,533.16732849528,534.167064506,535.166800516721,536.166536527441,
537.166272538161,538.166008548881,539.165744559601,540.165480570321,541.165216581041,
542.164952591761,543.164688602482,544.164424613202,545.164160623922,546.163896634642,
547.163632645362,548.163368656082,549.163104666802,550.162840677522,551.162576688243,
552.162312698963,553.162048709683,554.161784720403,555.161520731123,556.161256741843,
557.160992752563,558.160728763283,559.160464774004,560.160200784724,561.159936795444,
562.159672806164,563.159408816884,564.159144827604,565.158880838324,566.158616849045,
567.158352859765,568.158088870485,569.157824881205,570.157560891925,571.157296902645,
572.157032913365,573.156768924085,574.156504934806,575.156240945526,576.155976956246,
577.155712966966,578.155448977686,579.155184988406,580.154920999126,581.154657009846,
582.154393020567,583.154129031287,584.153865042007,585.153601052727,586.153337063447,
587.153073074167,588.152809084887,589.152545095607,590.152281106328,591.152017117048,
592.151753127768,593.151489138488,594.151225149208,595.150961159928,596.150697170648,
597.150433181368,598.150169192089,599.149905202809,600.149641213529,601.149377224249,
602.149113234969,603.148849245689,604.148585256409,605.14832126713,606.14805727785,
607.14779328857,608.14752929929,609.14726531001,610.14700132073,611.14673733145,
612.14647334217,613.146209352891,614.145945363611,615.145681374331,616.145417385051,
617.145153395771,618.144889406491,619.144625417211,620.144361427931,621.144097438652,
622.143833449372,623.143569460092,624.143305470812,625.143041481532,626.142777492252,
627.142513502972,628.142249513692,629.141985524413,630.141721535133,631.141457545853,
632.141193556573,633.140929567293,634.140665578013,635.140401588733,636.140137599454,
637.139873610174,638.139609620894,639.139345631614,640.139081642334,641.138817653054,
642.138553663774,643.138289674494,644.138025685215,645.137761695935,646.137497706655,
647.137233717375,648.136969728095,649.136705738815,650.136441749535,651.136177760255,
652.135913770976,653.135649781696,654.135385792416,655.135121803136,656.134857813856,
657.134593824576,658.134329835296,659.134065846016,660.133801856737,661.133537867457,
662.133273878177,663.133009888897,664.132745899617,665.132481910337,666.132217921057,
667.131953931778,668.131689942498,669.131425953218,670.131161963938,671.130897974658,
672.130633985378,673.130369996098,674.130106006818,675.129842017539,676.129578028259,
677.129314038979,678.129050049699,679.128786060419,680.128522071139,681.128258081859,
682.127994092579,683.1277301033,684.12746611402,685.12720212474,686.12693813546,
687.12667414618,688.1264101569,689.12614616762,690.12588217834,691.125618189061,
692.125354199781,693.125090210501,694.124826221221,695.124562231941,696.124298242661,
697.124034253381,698.123770264101,699.123506274822,700.123242285542,701.122978296262,
702.122714306982,703.122450317702,704.122186328422,705.121922339142,706.121658349863,
707.121394360583,708.121130371303,709.120866382023,710.120602392743,711.120338403463,
712.120074414183,713.119810424903,714.119546435624,715.119282446344,716.119018457064,
717.118754467784,718.118490478504,719.118226489224,720.117962499944,721.117698510664,
722.117434521385,723.117170532105,724.116906542825,725.116642553545,726.116378564265,
727.116114574985,728.115850585705,729.115586596425,730.115322607146,731.115058617866,
732.114794628586,733.114530639306,734.114266650026,735.114002660746,736.113738671466,
737.113474682187,738.113210692907,739.112946703627,740.112682714347,741.112418725067,
742.112154735787,743.111890746507,744.111626757227,745.111362767948,746.111098778668,
747.110834789388,748.110570800108,749.110306810828,750.110042821548,751.109778832268,
752.109514842988,753.109250853709,754.108986864429,755.108722875149,756.108458885869,
757.108194896589,758.107930907309,759.107666918029,760.107402928749,761.10713893947,
762.10687495019,763.10661096091,764.10634697163,765.10608298235,766.10581899307,
767.10555500379,768.10529101451,769.105027025231,770.104763035951,771.104499046671,
772.104235057391,773.103971068111,774.103707078831,775.103443089551,776.103179100272,
777.102915110992,778.102651121712,779.102387132432,780.102123143152,781.101859153872,
782.101595164592,783.101331175312,784.101067186033,785.100803196753,786.100539207473,
787.100275218193,788.100011228913,789.099747239633,790.099483250353,791.099219261073,
792.098955271794,793.098691282514,794.098427293234,795.098163303954,796.097899314674,
797.097635325394,798.097371336114,799.097107346834,800.096843357555,801.096579368275,
802.096315378995,803.096051389715,804.095787400435,805.095523411155,806.095259421875,
807.094995432596,808.094731443316,809.094467454036,810.094203464756,811.093939475476,
812.093675486196,813.093411496916,814.093147507636,815.092883518357,816.092619529077,
817.092355539797,818.092091550517,819.091827561237,820.091563571957,821.091299582677,
822.091035593397,823.090771604118,824.090507614838,825.090243625558,826.089979636278,
827.089715646998,828.089451657718,829.089187668438,830.088923679158,831.088659689879,
832.088395700599,833.088131711319,834.087867722039,835.087603732759,836.087339743479,
837.087075754199,838.08681176492,839.08654777564,840.08628378636,841.08601979708,
842.0857558078,843.08549181852,844.08522782924,845.08496383996,846.084699850681,
847.084435861401,848.084171872121,849.083907882841,850.083643893561,851.083379904281,
852.083115915001,853.082851925721,854.082587936442,855.082323947162,856.082059957882,
857.081795968602,858.081531979322,859.081267990042,860.081004000762,861.080740011482,
862.080476022203,863.080212032923,864.079948043643,865.079684054363,866.079420065083,
867.079156075803,868.078892086523,869.078628097243,870.078364107964,871.078100118684,
872.077836129404,873.077572140124,874.077308150844,875.077044161564,876.076780172284,
877.076516183005,878.076252193725,879.075988204445,880.075724215165,881.075460225885,
882.075196236605,883.074932247325,884.074668258045,885.074404268766,886.074140279486,
887.073876290206,888.073612300926,889.073348311646,890.073084322366,891.072820333086,
892.072556343806,893.072292354527,894.072028365247,895.071764375967,896.071500386687,
897.071236397407,898.070972408127,899.070708418847,900.070444429567,901.070180440288,
902.069916451008,903.069652461728,904.069388472448,905.069124483168,906.068860493888,
907.068596504608,908.068332515329,909.068068526049,910.067804536769,911.067540547489,
912.067276558209,913.067012568929,914.066748579649,915.066484590369,916.06622060109,
917.06595661181,918.06569262253,919.06542863325,920.06516464397,921.06490065469,
922.06463666541,923.06437267613,924.064108686851,925.063844697571,926.063580708291,
927.063316719011,928.063052729731,929.062788740451,930.062524751171,931.062260761891,
932.061996772612,933.061732783332,934.061468794052,935.061204804772,936.060940815492,
937.060676826212,938.060412836932,939.060148847652,940.059884858373,941.059620869093,
942.059356879813,943.059092890533,944.058828901253,945.058564911973,946.058300922693,
947.058036933414,948.057772944134,949.057508954854,950.057244965574,951.056980976294,
952.056716987014,953.056452997734,954.056189008454,955.055925019175,956.055661029895,
957.055397040615,958.055133051335,959.054869062055,960.054605072775,961.054341083495,
962.054077094215,963.053813104936,964.053549115656,965.053285126376,966.053021137096,
967.052757147816,968.052493158536,969.052229169256,970.051965179976,971.051701190697,
972.051437201417,973.051173212137,974.050909222857,975.050645233577,976.050381244297,
977.050117255017,978.049853265738,979.049589276458,980.049325287178,981.049061297898,
982.048797308618,983.048533319338,984.048269330058,985.048005340778,986.047741351499,
987.047477362219,988.047213372939,989.046949383659,990.046685394379,991.046421405099,
992.046157415819,993.045893426539,994.04562943726,995.04536544798,996.0451014587,
997.04483746942,998.04457348014,999.04430949086,1000.04404550158,1001.0437815123,
1002.04351752302,1003.04325353374,1004.04298954446,1005.04272555518,1006.0424615659,
1007.04219757662,1008.04193358734,1009.04166959806,1010.04140560878,1011.0411416195,
1012.04087763022,1013.04061364094,1014.04034965166,1015.04008566238,1016.0398216731,
1017.03955768382,1018.03929369454,1019.03902970526,1020.03876571598,1021.0385017267,
1022.03823773742,1023.03797374814,1024.03770975886,1025.03744576958,1026.0371817803,
1027.03691779102,1028.03665380174,1029.03638981246,1030.03612582318,1031.0358618339,
1032.03559784462,1033.03533385534,1034.03506986606,1035.03480587678,1036.03454188751,
1037.03427789823,1038.03401390895,1039.03374991967,1040.03348593039,1041.03322194111,
1042.03295795183,1043.03269396255,1044.03242997327,1045.03216598399,1046.03190199471,
1047.03163800543,1048.03137401615,1049.03111002687,1050.03084603759,1051.03058204831,
1052.03031805903,1053.03005406975,1054.02979008047,1055.02952609119,1056.02926210191,
1057.02899811263,1058.02873412335,1059.02847013407,1060.02820614479,1061.02794215551,
1062.02767816623,1063.02741417695,1064.02715018767,1065.02688619839,1066.02662220911,
1067.02635821983,1068.02609423055,1069.02583024127,1070.02556625199,1071.02530226271,
1072.02503827343,1073.02477428415,1074.02451029487,1075.02424630559,1076.02398231631,
1077.02371832703,1078.02345433775,1079.02319034847,1080.02292635919,1081.02266236991,
1082.02239838063,1083.02213439135,1084.02187040207,1085.02160641279,1086.02134242351,
1087.02107843423,1088.02081444495,1089.02055045567,1090.02028646639,1091.02002247711,
1092.01975848783,1093.01949449855,1094.01923050927,1095.01896651999,1096.01870253071,
1097.01843854143,1098.01817455215,1099.01791056287,1100.01764657359,1101.01738258431,
1102.01711859503,1103.01685460575,1104.01659061647,1105.01632662719,1106.01606263791,
1107.01579864863,1108.01553465935,1109.01527067007,1110.01500668079,1111.01474269151,
1112.01447870223,1113.01421471295,1114.01395072368,1115.0136867344,1116.01342274512,
1117.01315875584,1118.01289476656,1119.01263077728,1120.012366788,1121.01210279872,
1122.01183880944,1123.01157482016,1124.01131083088,1125.0110468416,1126.01078285232,
1127.01051886304,1128.01025487376,1129.00999088448,1130.0097268952,1131.00946290592,
1132.00919891664,1133.00893492736,1134.00867093808,1135.0084069488,1136.00814295952,
1137.00787897024,1138.00761498096,1139.00735099168,1140.0070870024,1141.00682301312,
1142.00655902384,1143.00629503456,1144.00603104528,1145.005767056,1146.00550306672,
1147.00523907744,1148.00497508816,1149.00471109888,1150.0044471096,1151.00418312032,
1152.00391913104,1153.00365514176,1154.00339115248,1155.0031271632,1156.00286317392,
1157.00259918464,1158.00233519536,1159.00207120608,1160.0018072168,1161.00154322752,
1162.00127923824,1163.00101524896,1164.00075125968,1165.0004872704,1166.00022328112,
1166.99995929184,1167.99969530256,1168.99943131328,1169.999167324,1170.99890333472,
1171.99863934544,1172.99837535616,1173.99811136688,1174.9978473776,1175.99758338832,
1176.99731939904,1177.99705540976,1178.99679142048,1179.9965274312,1180.99626344192,
1181.99599945264,1182.99573546336,1183.99547147408,1184.9952074848,1185.99494349552,
1186.99467950624,1187.99441551696,1188.99415152768,1189.99388753841,1190.99362354913,
1191.99335955985,1192.99309557057,1193.99283158129,1194.99256759201,1195.99230360273,
1196.99203961345,1197.99177562417,1198.99151163489,1199.99124764561,1200.99098365633,
1201.99071966705,1202.99045567777,1203.99019168849,1204.98992769921,1205.98966370993,
1206.98939972065,1207.98913573137,1208.98887174209,1209.98860775281,1210.98834376353,
1211.98807977425,1212.98781578497,1213.98755179569,1214.98728780641,1215.98702381713,
1216.98675982785,1217.98649583857,1218.98623184929,1219.98596786001,1220.98570387073,
1221.98543988145,1222.98517589217,1223.98491190289,1224.98464791361,1225.98438392433,
1226.98411993505,1227.98385594577,1228.98359195649,1229.98332796721,1230.98306397793,
1231.98279998865,1232.98253599937,1233.98227201009,1234.98200802081,1235.98174403153,
1236.98148004225,1237.98121605297,1238.98095206369,1239.98068807441,1240.98042408513,
1241.98016009585,1242.97989610657,1243.97963211729,1244.97936812801,1245.97910413873,
1246.97884014945,1247.97857616017,1248.97831217089,1249.97804818161,1250.97778419233,
1251.97752020305,1252.97725621377,1253.97699222449,1254.97672823521,1255.97646424593,
1256.97620025665,1257.97593626737,1258.97567227809,1259.97540828881,1260.97514429953,
1261.97488031025,1262.97461632097,1263.97435233169,1264.97408834241,1265.97382435313,
1266.97356036385,1267.97329637458,1268.9730323853,1269.97276839602,1270.97250440674,
1271.97224041746,1272.97197642818,1273.9717124389,1274.97144844962,1275.97118446034,
1276.97092047106,1277.97065648178,1278.9703924925,1279.97012850322,1280.96986451394,
1281.96960052466,1282.96933653538,1283.9690725461,1284.96880855682,1285.96854456754,
1286.96828057826,1287.96801658898,1288.9677525997,1289.96748861042,1290.96722462114,
1291.96696063186,1292.96669664258,1293.9664326533,1294.96616866402,1295.96590467474,
1296.96564068546,1297.96537669618,1298.9651127069,1299.96484871762,1300.96458472834,
1301.96432073906,1302.96405674978,1303.9637927605,1304.96352877122,1305.96326478194,
1306.96300079266,1307.96273680338,1308.9624728141,1309.96220882482,1310.96194483554,
1311.96168084626,1312.96141685698,1313.9611528677,1314.96088887842,1315.96062488914,
1316.96036089986,1317.96009691058,1318.9598329213,1319.95956893202,1320.95930494274,
1321.95904095346,1322.95877696418,1323.9585129749,1324.95824898562,1325.95798499634,
1326.95772100706,1327.95745701778,1328.9571930285,1329.95692903922,1330.95666504994,
1331.95640106066,1332.95613707138,1333.9558730821,1334.95560909282,1335.95534510354,
1336.95508111426,1337.95481712498,1338.9545531357,1339.95428914642,1340.95402515714,
1341.95376116786,1342.95349717858,1343.9532331893,1344.95296920002,1345.95270521075,
1346.95244122147,1347.95217723219,1348.95191324291,1349.95164925363,1350.95138526435,
1351.95112127507,1352.95085728579,1353.95059329651,1354.95032930723,1355.95006531795,
1356.94980132867,1357.94953733939,1358.94927335011,1359.94900936083,1360.94874537155,
1361.94848138227,1362.94821739299,1363.94795340371,1364.94768941443,1365.94742542515,
1366.94716143587,1367.94689744659,1368.94663345731,1369.94636946803,1370.94610547875,
1371.94584148947,1372.94557750019,1373.94531351091,1374.94504952163,1375.94478553235,
1376.94452154307,1377.94425755379,1378.94399356451,1379.94372957523,1380.94346558595,
1381.94320159667,1382.94293760739,1383.94267361811,1384.94240962883,1385.94214563955,
1386.94188165027,1387.94161766099,1388.94135367171,1389.94108968243,1390.94082569315,
1391.94056170387,1392.94029771459,1393.94003372531,1394.93976973603,1395.93950574675,
1396.93924175747,1397.93897776819,1398.93871377891,1399.93844978963,1400.93818580035,
1401.93792181107,1402.93765782179,1403.93739383251,1404.93712984323,1405.93686585395,
1406.93660186467,1407.93633787539,1408.93607388611,1409.93580989683,1410.93554590755,
1411.93528191827,1412.93501792899,1413.93475393971,1414.93448995043,1415.93422596115,
1416.93396197187,1417.93369798259,1418.93343399331,1419.93317000403,1420.93290601475,
1421.93264202547,1422.93237803619,1423.93211404692,1424.93185005764,1425.93158606836,
1426.93132207908,1427.9310580898,1428.93079410052,1429.93053011124,1430.93026612196,
1431.93000213268,1432.9297381434,1433.92947415412,1434.92921016484,1435.92894617556,
1436.92868218628,1437.928418197,1438.92815420772,1439.92789021844,1440.92762622916,
1441.92736223988,1442.9270982506,1443.92683426132,1444.92657027204,1445.92630628276,
1446.92604229348,1447.9257783042,1448.92551431492,1449.92525032564,1450.92498633636,
1451.92472234708,1452.9244583578,1453.92419436852,1454.92393037924,1455.92366638996,
1456.92340240068,1457.9231384114,1458.92287442212,1459.92261043284,1460.92234644356,
1461.92208245428,1462.921818465,1463.92155447572,1464.92129048644,1465.92102649716,
1466.92076250788,1467.9204985186,1468.92023452932,1469.91997054004,1470.91970655076,
1471.91944256148,1472.9191785722,1473.91891458292,1474.91865059364,1475.91838660436,
1476.91812261508,1477.9178586258,1478.91759463652,1479.91733064724,1480.91706665796,
1481.91680266868,1482.9165386794,1483.91627469012,1484.91601070084,1485.91574671156,
1486.91548272228,1487.915218733,1488.91495474372,1489.91469075444,1490.91442676516,
1491.91416277588,1492.9138987866,1493.91363479732,1494.91337080804,1495.91310681876,
1496.91284282948,1497.9125788402,1498.91231485092,1499.91205086164,1500.91178687236,
1501.91152288309,1502.91125889381,1503.91099490453,1504.91073091525,1505.91046692597,
1506.91020293669,1507.90993894741,1508.90967495813,1509.90941096885,1510.90914697957,
1511.90888299029,1512.90861900101,1513.90835501173,1514.90809102245,1515.90782703317,
1516.90756304389,1517.90729905461,1518.90703506533,1519.90677107605,1520.90650708677,
1521.90624309749,1522.90597910821,1523.90571511893,1524.90545112965,1525.90518714037,
1526.90492315109,1527.90465916181,1528.90439517253,1529.90413118325,1530.90386719397,
1531.90360320469,1532.90333921541,1533.90307522613,1534.90281123685,1535.90254724757,
1536.90228325829,1537.90201926901,1538.90175527973,1539.90149129045,1540.90122730117,
1541.90096331189,1542.90069932261,1543.90043533333,1544.90017134405,1545.89990735477,
1546.89964336549,1547.89937937621,1548.89911538693,1549.89885139765,1550.89858740837,
1551.89832341909,1552.89805942981,1553.89779544053,1554.89753145125,1555.89726746197,
1556.89700347269,1557.89673948341,1558.89647549413,1559.89621150485,1560.89594751557,
1561.89568352629,1562.89541953701,1563.89515554773,1564.89489155845,1565.89462756917,
1566.89436357989,1567.89409959061,1568.89383560133,1569.89357161205,1570.89330762277,
1571.89304363349,1572.89277964421,1573.89251565493,1574.89225166565,1575.89198767637,
1576.89172368709,1577.89145969781,1578.89119570853,1579.89093171926,1580.89066772998,
1581.8904037407,1582.89013975142,1583.88987576214,1584.88961177286,1585.88934778358,
1586.8890837943,1587.88881980502,1588.88855581574,1589.88829182646,1590.88802783718,
1591.8877638479,1592.88749985862,1593.88723586934,1594.88697188006,1595.88670789078,
1596.8864439015,1597.88617991222,1598.88591592294,1599.88565193366,1600.88538794438,
1601.8851239551,1602.88485996582,1603.88459597654,1604.88433198726,1605.88406799798,
1606.8838040087,1607.88354001942,1608.88327603014,1609.88301204086,1610.88274805158,
1611.8824840623,1612.88222007302,1613.88195608374,1614.88169209446,1615.88142810518,
1616.8811641159,1617.88090012662,1618.88063613734,1619.88037214806,1620.88010815878,
1621.8798441695,1622.87958018022,1623.87931619094,1624.87905220166,1625.87878821238,
1626.8785242231,1627.87826023382,1628.87799624454,1629.87773225526,1630.87746826598,
1631.8772042767,1632.87694028742,1633.87667629814,1634.87641230886,1635.87614831958,
1636.8758843303,1637.87562034102,1638.87535635174,1639.87509236246,1640.87482837318,
1641.8745643839,1642.87430039462,1643.87403640534,1644.87377241606,1645.87350842678,
1646.8732444375,1647.87298044822,1648.87271645894,1649.87245246966,1650.87218848038,
1651.8719244911,1652.87166050182,1653.87139651254,1654.87113252326,1655.87086853399,
1656.8706045447,1657.87034055543,1658.87007656615,1659.86981257687,1660.86954858759,
1661.86928459831,1662.86902060903,1663.86875661975,1664.86849263047,1665.86822864119,
1666.86796465191,1667.86770066263,1668.86743667335,1669.86717268407,1670.86690869479,
1671.86664470551,1672.86638071623,1673.86611672695,1674.86585273767,1675.86558874839,
1676.86532475911,1677.86506076983,1678.86479678055,1679.86453279127,1680.86426880199,
1681.86400481271,1682.86374082343,1683.86347683415,1684.86321284487,1685.86294885559,
1686.86268486631,1687.86242087703,1688.86215688775,1689.86189289847,1690.86162890919,
1691.86136491991,1692.86110093063,1693.86083694135,1694.86057295207,1695.86030896279,
1696.86004497351,1697.35991297887,1697.85988790214),.UNSPECIFIED.);
#53=B_SPLINE_SURFACE_WITH_KNOTS('',3,3,((#247756,#247757,#247758,#247759,
#247760,#247761,#247762,#247763,#247764,#247765,#247766,#247767,#247768,
#247769,#247770,#247771,#247772,#247773,#247774,#247775,#247776,#247777,
#247778,#247779,#247780,#247781,#247782,#247783,#247784,#247785,#247786,
#247787,#247788,#247789,#247790,#247791,#247792,#247793,#247794,#247795,
#247796,#247797,#247798,#247799,#247800,#247801,#247802,#247803,#247804,
#247805,#247806,#247807,#247808,#247809,#247810,#247811,#247812,#247813,
#247814,#247815,#247816,#247817,#247818,#247819,#247820,#247821,#247822,
#247823,#247824,#247825,#247826,#247827,#247828,#247829,#247830,#247831,
#247832,#247833,#247834,#247835,#247836,#247837,#247838,#247839,#247840,
#247841,#247842,#247843,#247844,#247845,#247846,#247847,#247848,#247849,
#247850,#247851,#247852,#247853,#247854,#247855,#247856,#247857,#247858,
#247859,#247860,#247861,#247862,#247863,#247864,#247865,#247866,#247867,
#247868,#247869,#247870,#247871,#247872,#247873,#247874,#247875,#247876,
#247877,#247878,#247879,#247880,#247881,#247882,#247883,#247884,#247885,
#247886,#247887,#247888,#247889,#247890,#247891,#247892,#247893,#247894,
#247895,#247896,#247897,#247898,#247899,#247900,#247901,#247902,#247903,
#247904,#247905,#247906,#247907,#247908,#247909,#247910,#247911,#247912,
#247913,#247914,#247915,#247916,#247917,#247918,#247919,#247920,#247921,
#247922,#247923,#247924,#247925,#247926,#247927,#247928,#247929,#247930,
#247931,#247932,#247933,#247934,#247935,#247936,#247937,#247938,#247939,
#247940,#247941,#247942,#247943,#247944,#247945,#247946,#247947,#247948,
#247949,#247950,#247951,#247952,#247953,#247954,#247955,#247956,#247957,
#247958,#247959,#247960,#247961,#247962,#247963,#247964,#247965,#247966,
#247967,#247968,#247969,#247970,#247971,#247972,#247973,#247974,#247975,
#247976,#247977,#247978,#247979,#247980,#247981,#247982,#247983,#247984,
#247985,#247986,#247987,#247988,#247989,#247990,#247991,#247992,#247993,
#247994,#247995,#247996,#247997,#247998,#247999,#248000,#248001,#248002,
#248003,#248004,#248005,#248006,#248007,#248008,#248009,#248010,#248011,
#248012,#248013,#248014,#248015,#248016,#248017,#248018,#248019,#248020,
#248021,#248022,#248023,#248024,#248025,#248026,#248027,#248028,#248029,
#248030,#248031,#248032,#248033,#248034,#248035,#248036,#248037,#248038,
#248039,#248040,#248041,#248042,#248043,#248044,#248045,#248046,#248047,
#248048,#248049,#248050,#248051,#248052,#248053,#248054,#248055,#248056,
#248057,#248058,#248059,#248060,#248061,#248062,#248063,#248064,#248065,
#248066,#248067,#248068,#248069,#248070,#248071,#248072,#248073,#248074,
#248075,#248076,#248077,#248078,#248079,#248080,#248081,#248082,#248083,
#248084,#248085,#248086,#248087,#248088,#248089,#248090,#248091,#248092,
#248093,#248094,#248095,#248096,#248097,#248098,#248099,#248100,#248101,
#248102,#248103,#248104,#248105,#248106,#248107,#248108,#248109,#248110,
#248111,#248112,#248113,#248114,#248115,#248116,#248117,#248118,#248119,
#248120,#248121,#248122,#248123,#248124,#248125,#248126,#248127,#248128,
#248129,#248130,#248131,#248132,#248133,#248134,#248135,#248136,#248137,
#248138,#248139,#248140,#248141,#248142,#248143,#248144,#248145,#248146,
#248147,#248148,#248149,#248150,#248151,#248152,#248153,#248154,#248155,
#248156,#248157,#248158,#248159,#248160,#248161,#248162,#248163,#248164,
#248165,#248166,#248167,#248168,#248169,#248170,#248171,#248172,#248173,
#248174,#248175,#248176,#248177,#248178,#248179,#248180,#248181,#248182,
#248183,#248184,#248185,#248186,#248187,#248188,#248189,#248190,#248191,
#248192,#248193,#248194,#248195,#248196,#248197,#248198,#248199,#248200,
#248201,#248202,#248203,#248204,#248205,#248206,#248207,#248208,#248209,
#248210,#248211,#248212,#248213,#248214,#248215,#248216,#248217,#248218,
#248219,#248220,#248221,#248222,#248223,#248224,#248225,#248226,#248227,
#248228,#248229,#248230,#248231,#248232,#248233,#248234,#248235,#248236,
#248237,#248238,#248239,#248240,#248241,#248242,#248243,#248244,#248245,
#248246,#248247,#248248,#248249,#248250,#248251,#248252,#248253,#248254,
#248255,#248256,#248257,#248258,#248259,#248260,#248261,#248262,#248263,
#248264,#248265,#248266,#248267,#248268,#248269,#248270,#248271,#248272,
#248273,#248274,#248275,#248276,#248277,#248278,#248279,#248280,#248281,
#248282,#248283,#248284,#248285,#248286,#248287,#248288,#248289,#248290,
#248291,#248292,#248293,#248294,#248295,#248296,#248297,#248298,#248299,
#248300,#248301,#248302,#248303,#248304,#248305,#248306,#248307,#248308,
#248309,#248310,#248311,#248312,#248313,#248314,#248315,#248316,#248317,
#248318,#248319,#248320,#248321,#248322,#248323,#248324,#248325,#248326,
#248327,#248328,#248329,#248330,#248331,#248332,#248333,#248334,#248335,
#248336,#248337,#248338,#248339,#248340,#248341,#248342,#248343,#248344,
#248345,#248346,#248347,#248348,#248349,#248350,#248351,#248352,#248353,
#248354,#248355,#248356,#248357,#248358,#248359,#248360,#248361,#248362,
#248363,#248364,#248365,#248366,#248367,#248368,#248369,#248370,#248371,
#248372,#248373,#248374,#248375,#248376,#248377,#248378,#248379,#248380,
#248381,#248382,#248383,#248384,#248385,#248386,#248387,#248388,#248389,
#248390,#248391,#248392,#248393,#248394,#248395,#248396,#248397,#248398,
#248399,#248400,#248401,#248402,#248403,#248404,#248405,#248406,#248407,
#248408,#248409,#248410,#248411,#248412,#248413,#248414,#248415,#248416,
#248417,#248418,#248419,#248420,#248421,#248422,#248423,#248424,#248425,
#248426,#248427,#248428,#248429,#248430,#248431,#248432,#248433,#248434,
#248435,#248436,#248437,#248438,#248439,#248440,#248441,#248442,#248443,
#248444,#248445,#248446,#248447,#248448,#248449,#248450,#248451,#248452,
#248453,#248454,#248455,#248456,#248457,#248458,#248459,#248460,#248461,
#248462,#248463,#248464,#248465,#248466,#248467,#248468,#248469,#248470,
#248471,#248472,#248473,#248474,#248475,#248476,#248477,#248478,#248479,
#248480,#248481,#248482,#248483,#248484,#248485,#248486,#248487,#248488,
#248489,#248490,#248491,#248492,#248493,#248494,#248495,#248496,#248497,
#248498,#248499,#248500,#248501,#248502,#248503,#248504,#248505,#248506,
#248507,#248508,#248509,#248510,#248511,#248512,#248513,#248514,#248515,
#248516,#248517,#248518,#248519,#248520,#248521,#248522,#248523,#248524,
#248525,#248526,#248527,#248528,#248529,#248530,#248531,#248532,#248533,
#248534,#248535,#248536,#248537,#248538,#248539,#248540,#248541,#248542,
#248543,#248544,#248545,#248546,#248547,#248548,#248549,#248550,#248551,
#248552,#248553,#248554,#248555,#248556,#248557,#248558,#248559,#248560,
#248561,#248562,#248563,#248564,#248565,#248566,#248567,#248568,#248569,
#248570,#248571,#248572,#248573,#248574,#248575,#248576,#248577,#248578,
#248579,#248580,#248581,#248582,#248583,#248584,#248585,#248586,#248587,
#248588,#248589,#248590,#248591,#248592,#248593,#248594,#248595,#248596,
#248597,#248598,#248599,#248600,#248601,#248602,#248603,#248604,#248605,
#248606,#248607,#248608,#248609,#248610,#248611,#248612,#248613,#248614,
#248615,#248616,#248617,#248618,#248619,#248620,#248621,#248622,#248623,
#248624,#248625,#248626,#248627,#248628,#248629,#248630,#248631,#248632,
#248633,#248634,#248635,#248636,#248637,#248638,#248639,#248640,#248641,
#248642,#248643,#248644,#248645,#248646,#248647,#248648,#248649,#248650,
#248651,#248652,#248653,#248654,#248655,#248656,#248657,#248658,#248659,
#248660,#248661,#248662,#248663,#248664,#248665,#248666,#248667,#248668,
#248669,#248670,#248671,#248672,#248673,#248674,#248675,#248676,#248677,
#248678,#248679,#248680,#248681,#248682,#248683,#248684,#248685,#248686,
#248687,#248688,#248689,#248690,#248691,#248692,#248693,#248694,#248695,
#248696,#248697,#248698,#248699,#248700,#248701,#248702,#248703,#248704,
#248705,#248706,#248707,#248708,#248709,#248710,#248711,#248712,#248713,
#248714,#248715,#248716,#248717,#248718,#248719,#248720,#248721,#248722,
#248723,#248724,#248725,#248726,#248727,#248728,#248729,#248730,#248731,
#248732,#248733,#248734,#248735,#248736,#248737,#248738,#248739,#248740,
#248741,#248742,#248743,#248744,#248745,#248746,#248747,#248748,#248749,
#248750,#248751,#248752,#248753,#248754,#248755,#248756,#248757,#248758,
#248759,#248760,#248761,#248762,#248763,#248764,#248765,#248766,#248767,
#248768,#248769,#248770,#248771,#248772,#248773,#248774,#248775,#248776,
#248777,#248778,#248779,#248780,#248781,#248782,#248783,#248784,#248785,
#248786,#248787,#248788,#248789,#248790,#248791,#248792,#248793,#248794,
#248795,#248796,#248797,#248798,#248799,#248800,#248801,#248802,#248803,
#248804,#248805,#248806,#248807,#248808,#248809,#248810,#248811,#248812,
#248813,#248814,#248815,#248816,#248817,#248818,#248819,#248820,#248821,
#248822,#248823,#248824,#248825,#248826,#248827,#248828,#248829,#248830,
#248831,#248832,#248833,#248834,#248835,#248836,#248837,#248838,#248839,
#248840,#248841,#248842,#248843,#248844,#248845,#248846,#248847,#248848,
#248849,#248850,#248851,#248852,#248853,#248854,#248855,#248856,#248857,
#248858,#248859,#248860,#248861,#248862,#248863,#248864,#248865,#248866,
#248867,#248868,#248869,#248870,#248871,#248872,#248873,#248874,#248875,
#248876,#248877,#248878,#248879,#248880,#248881,#248882,#248883,#248884,
#248885,#248886,#248887,#248888,#248889,#248890,#248891,#248892,#248893,
#248894,#248895,#248896,#248897,#248898,#248899,#248900,#248901,#248902,
#248903,#248904,#248905,#248906,#248907,#248908,#248909,#248910,#248911,
#248912,#248913,#248914,#248915,#248916,#248917,#248918,#248919,#248920,
#248921,#248922,#248923,#248924,#248925,#248926,#248927,#248928,#248929,
#248930,#248931,#248932,#248933,#248934,#248935,#248936,#248937,#248938,
#248939,#248940,#248941,#248942,#248943,#248944,#248945,#248946,#248947,
#248948,#248949,#248950,#248951,#248952,#248953,#248954,#248955,#248956,
#248957,#248958,#248959,#248960,#248961,#248962,#248963,#248964,#248965,
#248966,#248967,#248968,#248969,#248970,#248971,#248972,#248973,#248974,
#248975,#248976,#248977,#248978,#248979,#248980,#248981,#248982,#248983,
#248984,#248985,#248986,#248987,#248988,#248989,#248990,#248991,#248992,
#248993,#248994,#248995,#248996,#248997,#248998,#248999,#249000,#249001,
#249002,#249003,#249004,#249005,#249006,#249007,#249008,#249009,#249010,
#249011,#249012,#249013,#249014,#249015,#249016,#249017,#249018,#249019,
#249020,#249021,#249022,#249023,#249024,#249025,#249026,#249027,#249028,
#249029,#249030,#249031,#249032,#249033,#249034,#249035,#249036,#249037,
#249038,#249039,#249040,#249041,#249042,#249043,#249044,#249045,#249046,
#249047,#249048,#249049,#249050,#249051,#249052,#249053,#249054,#249055,
#249056,#249057,#249058,#249059,#249060,#249061,#249062,#249063,#249064,
#249065,#249066,#249067,#249068,#249069,#249070,#249071,#249072,#249073,
#249074,#249075,#249076,#249077,#249078,#249079,#249080,#249081,#249082,
#249083,#249084,#249085,#249086,#249087,#249088,#249089,#249090,#249091,
#249092,#249093,#249094,#249095,#249096,#249097,#249098,#249099,#249100,
#249101,#249102,#249103,#249104,#249105,#249106,#249107,#249108,#249109,
#249110,#249111,#249112,#249113,#249114,#249115,#249116,#249117,#249118,
#249119,#249120,#249121,#249122,#249123,#249124,#249125,#249126,#249127,
#249128,#249129,#249130,#249131,#249132,#249133,#249134,#249135,#249136,
#249137,#249138,#249139,#249140,#249141,#249142,#249143,#249144,#249145,
#249146,#249147,#249148,#249149,#249150,#249151,#249152,#249153,#249154,
#249155,#249156,#249157,#249158,#249159,#249160,#249161,#249162,#249163,
#249164,#249165,#249166,#249167,#249168,#249169,#249170,#249171,#249172,
#249173,#249174,#249175,#249176,#249177,#249178,#249179,#249180,#249181,
#249182,#249183,#249184,#249185,#249186,#249187,#249188,#249189,#249190,
#249191,#249192,#249193,#249194,#249195,#249196,#249197,#249198,#249199,
#249200,#249201,#249202,#249203,#249204,#249205,#249206,#249207,#249208,
#249209,#249210,#249211,#249212,#249213,#249214,#249215,#249216,#249217,
#249218,#249219,#249220,#249221,#249222,#249223,#249224,#249225,#249226,
#249227,#249228,#249229,#249230,#249231,#249232,#249233,#249234,#249235,
#249236,#249237,#249238,#249239,#249240,#249241,#249242,#249243,#249244,
#249245,#249246,#249247,#249248,#249249,#249250,#249251,#249252,#249253,
#249254,#249255,#249256,#249257,#249258,#249259,#249260,#249261,#249262,
#249263,#249264,#249265,#249266,#249267,#249268,#249269,#249270,#249271,
#249272,#249273,#249274,#249275,#249276,#249277,#249278,#249279,#249280,
#249281,#249282,#249283,#249284,#249285,#249286,#249287,#249288,#249289,
#249290,#249291,#249292,#249293,#249294,#249295,#249296,#249297,#249298,
#249299,#249300,#249301,#249302,#249303,#249304,#249305,#249306,#249307,
#249308,#249309,#249310,#249311,#249312,#249313,#249314,#249315,#249316,
#249317,#249318,#249319,#249320,#249321,#249322,#249323,#249324,#249325,
#249326,#249327,#249328,#249329,#249330,#249331,#249332,#249333,#249334,
#249335,#249336,#249337,#249338,#249339,#249340,#249341,#249342,#249343,
#249344,#249345,#249346,#249347,#249348,#249349,#249350,#249351,#249352,
#249353,#249354,#249355,#249356,#249357,#249358,#249359,#249360,#249361,
#249362,#249363,#249364,#249365,#249366,#249367,#249368,#249369,#249370,
#249371,#249372,#249373,#249374,#249375,#249376,#249377,#249378,#249379,
#249380,#249381,#249382,#249383,#249384,#249385,#249386,#249387,#249388,
#249389,#249390,#249391,#249392,#249393,#249394,#249395,#249396,#249397,
#249398,#249399,#249400,#249401,#249402,#249403,#249404,#249405,#249406,
#249407,#249408,#249409,#249410,#249411,#249412,#249413,#249414,#249415,
#249416,#249417,#249418,#249419,#249420,#249421,#249422,#249423,#249424,
#249425,#249426,#249427,#249428,#249429,#249430,#249431,#249432,#249433,
#249434,#249435,#249436,#249437,#249438,#249439,#249440,#249441,#249442,
#249443,#249444,#249445,#249446,#249447,#249448,#249449,#249450),(#249451,
#249452,#249453,#249454,#249455,#249456,#249457,#249458,#249459,#249460,
#249461,#249462,#249463,#249464,#249465,#249466,#249467,#249468,#249469,
#249470,#249471,#249472,#249473,#249474,#249475,#249476,#249477,#249478,
#249479,#249480,#249481,#249482,#249483,#249484,#249485,#249486,#249487,
#249488,#249489,#249490,#249491,#249492,#249493,#249494,#249495,#249496,
#249497,#249498,#249499,#249500,#249501,#249502,#249503,#249504,#249505,
#249506,#249507,#249508,#249509,#249510,#249511,#249512,#249513,#249514,
#249515,#249516,#249517,#249518,#249519,#249520,#249521,#249522,#249523,
#249524,#249525,#249526,#249527,#249528,#249529,#249530,#249531,#249532,
#249533,#249534,#249535,#249536,#249537,#249538,#249539,#249540,#249541,
#249542,#249543,#249544,#249545,#249546,#249547,#249548,#249549,#249550,
#249551,#249552,#249553,#249554,#249555,#249556,#249557,#249558,#249559,
#249560,#249561,#249562,#249563,#249564,#249565,#249566,#249567,#249568,
#249569,#249570,#249571,#249572,#249573,#249574,#249575,#249576,#249577,
#249578,#249579,#249580,#249581,#249582,#249583,#249584,#249585,#249586,
#249587,#249588,#249589,#249590,#249591,#249592,#249593,#249594,#249595,
#249596,#249597,#249598,#249599,#249600,#249601,#249602,#249603,#249604,
#249605,#249606,#249607,#249608,#249609,#249610,#249611,#249612,#249613,
#249614,#249615,#249616,#249617,#249618,#249619,#249620,#249621,#249622,
#249623,#249624,#249625,#249626,#249627,#249628,#249629,#249630,#249631,
#249632,#249633,#249634,#249635,#249636,#249637,#249638,#249639,#249640,
#249641,#249642,#249643,#249644,#249645,#249646,#249647,#249648,#249649,
#249650,#249651,#249652,#249653,#249654,#249655,#249656,#249657,#249658,
#249659,#249660,#249661,#249662,#249663,#249664,#249665,#249666,#249667,
#249668,#249669,#249670,#249671,#249672,#249673,#249674,#249675,#249676,
#249677,#249678,#249679,#249680,#249681,#249682,#249683,#249684,#249685,
#249686,#249687,#249688,#249689,#249690,#249691,#249692,#249693,#249694,
#249695,#249696,#249697,#249698,#249699,#249700,#249701,#249702,#249703,
#249704,#249705,#249706,#249707,#249708,#249709,#249710,#249711,#249712,
#249713,#249714,#249715,#249716,#249717,#249718,#249719,#249720,#249721,
#249722,#249723,#249724,#249725,#249726,#249727,#249728,#249729,#249730,
#249731,#249732,#249733,#249734,#249735,#249736,#249737,#249738,#249739,
#249740,#249741,#249742,#249743,#249744,#249745,#249746,#249747,#249748,
#249749,#249750,#249751,#249752,#249753,#249754,#249755,#249756,#249757,
#249758,#249759,#249760,#249761,#249762,#249763,#249764,#249765,#249766,
#249767,#249768,#249769,#249770,#249771,#249772,#249773,#249774,#249775,
#249776,#249777,#249778,#249779,#249780,#249781,#249782,#249783,#249784,
#249785,#249786,#249787,#249788,#249789,#249790,#249791,#249792,#249793,
#249794,#249795,#249796,#249797,#249798,#249799,#249800,#249801,#249802,
#249803,#249804,#249805,#249806,#249807,#249808,#249809,#249810,#249811,
#249812,#249813,#249814,#249815,#249816,#249817,#249818,#249819,#249820,
#249821,#249822,#249823,#249824,#249825,#249826,#249827,#249828,#249829,
#249830,#249831,#249832,#249833,#249834,#249835,#249836,#249837,#249838,
#249839,#249840,#249841,#249842,#249843,#249844,#249845,#249846,#249847,
#249848,#249849,#249850,#249851,#249852,#249853,#249854,#249855,#249856,
#249857,#249858,#249859,#249860,#249861,#249862,#249863,#249864,#249865,
#249866,#249867,#249868,#249869,#249870,#249871,#249872,#249873,#249874,
#249875,#249876,#249877,#249878,#249879,#249880,#249881,#249882,#249883,
#249884,#249885,#249886,#249887,#249888,#249889,#249890,#249891,#249892,
#249893,#249894,#249895,#249896,#249897,#249898,#249899,#249900,#249901,
#249902,#249903,#249904,#249905,#249906,#249907,#249908,#249909,#249910,
#249911,#249912,#249913,#249914,#249915,#249916,#249917,#249918,#249919,
#249920,#249921,#249922,#249923,#249924,#249925,#249926,#249927,#249928,
#249929,#249930,#249931,#249932,#249933,#249934,#249935,#249936,#249937,
#249938,#249939,#249940,#249941,#249942,#249943,#249944,#249945,#249946,
#249947,#249948,#249949,#249950,#249951,#249952,#249953,#249954,#249955,
#249956,#249957,#249958,#249959,#249960,#249961,#249962,#249963,#249964,
#249965,#249966,#249967,#249968,#249969,#249970,#249971,#249972,#249973,
#249974,#249975,#249976,#249977,#249978,#249979,#249980,#249981,#249982,
#249983,#249984,#249985,#249986,#249987,#249988,#249989,#249990,#249991,
#249992,#249993,#249994,#249995,#249996,#249997,#249998,#249999,#250000,
#250001,#250002,#250003,#250004,#250005,#250006,#250007,#250008,#250009,
#250010,#250011,#250012,#250013,#250014,#250015,#250016,#250017,#250018,
#250019,#250020,#250021,#250022,#250023,#250024,#250025,#250026,#250027,
#250028,#250029,#250030,#250031,#250032,#250033,#250034,#250035,#250036,
#250037,#250038,#250039,#250040,#250041,#250042,#250043,#250044,#250045,
#250046,#250047,#250048,#250049,#250050,#250051,#250052,#250053,#250054,
#250055,#250056,#250057,#250058,#250059,#250060,#250061,#250062,#250063,
#250064,#250065,#250066,#250067,#250068,#250069,#250070,#250071,#250072,
#250073,#250074,#250075,#250076,#250077,#250078,#250079,#250080,#250081,
#250082,#250083,#250084,#250085,#250086,#250087,#250088,#250089,#250090,
#250091,#250092,#250093,#250094,#250095,#250096,#250097,#250098,#250099,
#250100,#250101,#250102,#250103,#250104,#250105,#250106,#250107,#250108,
#250109,#250110,#250111,#250112,#250113,#250114,#250115,#250116,#250117,
#250118,#250119,#250120,#250121,#250122,#250123,#250124,#250125,#250126,
#250127,#250128,#250129,#250130,#250131,#250132,#250133,#250134,#250135,
#250136,#250137,#250138,#250139,#250140,#250141,#250142,#250143,#250144,
#250145,#250146,#250147,#250148,#250149,#250150,#250151,#250152,#250153,
#250154,#250155,#250156,#250157,#250158,#250159,#250160,#250161,#250162,
#250163,#250164,#250165,#250166,#250167,#250168,#250169,#250170,#250171,
#250172,#250173,#250174,#250175,#250176,#250177,#250178,#250179,#250180,
#250181,#250182,#250183,#250184,#250185,#250186,#250187,#250188,#250189,
#250190,#250191,#250192,#250193,#250194,#250195,#250196,#250197,#250198,
#250199,#250200,#250201,#250202,#250203,#250204,#250205,#250206,#250207,
#250208,#250209,#250210,#250211,#250212,#250213,#250214,#250215,#250216,
#250217,#250218,#250219,#250220,#250221,#250222,#250223,#250224,#250225,
#250226,#250227,#250228,#250229,#250230,#250231,#250232,#250233,#250234,
#250235,#250236,#250237,#250238,#250239,#250240,#250241,#250242,#250243,
#250244,#250245,#250246,#250247,#250248,#250249,#250250,#250251,#250252,
#250253,#250254,#250255,#250256,#250257,#250258,#250259,#250260,#250261,
#250262,#250263,#250264,#250265,#250266,#250267,#250268,#250269,#250270,
#250271,#250272,#250273,#250274,#250275,#250276,#250277,#250278,#250279,
#250280,#250281,#250282,#250283,#250284,#250285,#250286,#250287,#250288,
#250289,#250290,#250291,#250292,#250293,#250294,#250295,#250296,#250297,
#250298,#250299,#250300,#250301,#250302,#250303,#250304,#250305,#250306,
#250307,#250308,#250309,#250310,#250311,#250312,#250313,#250314,#250315,
#250316,#250317,#250318,#250319,#250320,#250321,#250322,#250323,#250324,
#250325,#250326,#250327,#250328,#250329,#250330,#250331,#250332,#250333,
#250334,#250335,#250336,#250337,#250338,#250339,#250340,#250341,#250342,
#250343,#250344,#250345,#250346,#250347,#250348,#250349,#250350,#250351,
#250352,#250353,#250354,#250355,#250356,#250357,#250358,#250359,#250360,
#250361,#250362,#250363,#250364,#250365,#250366,#250367,#250368,#250369,
#250370,#250371,#250372,#250373,#250374,#250375,#250376,#250377,#250378,
#250379,#250380,#250381,#250382,#250383,#250384,#250385,#250386,#250387,
#250388,#250389,#250390,#250391,#250392,#250393,#250394,#250395,#250396,
#250397,#250398,#250399,#250400,#250401,#250402,#250403,#250404,#250405,
#250406,#250407,#250408,#250409,#250410,#250411,#250412,#250413,#250414,
#250415,#250416,#250417,#250418,#250419,#250420,#250421,#250422,#250423,
#250424,#250425,#250426,#250427,#250428,#250429,#250430,#250431,#250432,
#250433,#250434,#250435,#250436,#250437,#250438,#250439,#250440,#250441,
#250442,#250443,#250444,#250445,#250446,#250447,#250448,#250449,#250450,
#250451,#250452,#250453,#250454,#250455,#250456,#250457,#250458,#250459,
#250460,#250461,#250462,#250463,#250464,#250465,#250466,#250467,#250468,
#250469,#250470,#250471,#250472,#250473,#250474,#250475,#250476,#250477,
#250478,#250479,#250480,#250481,#250482,#250483,#250484,#250485,#250486,
#250487,#250488,#250489,#250490,#250491,#250492,#250493,#250494,#250495,
#250496,#250497,#250498,#250499,#250500,#250501,#250502,#250503,#250504,
#250505,#250506,#250507,#250508,#250509,#250510,#250511,#250512,#250513,
#250514,#250515,#250516,#250517,#250518,#250519,#250520,#250521,#250522,
#250523,#250524,#250525,#250526,#250527,#250528,#250529,#250530,#250531,
#250532,#250533,#250534,#250535,#250536,#250537,#250538,#250539,#250540,
#250541,#250542,#250543,#250544,#250545,#250546,#250547,#250548,#250549,
#250550,#250551,#250552,#250553,#250554,#250555,#250556,#250557,#250558,
#250559,#250560,#250561,#250562,#250563,#250564,#250565,#250566,#250567,
#250568,#250569,#250570,#250571,#250572,#250573,#250574,#250575,#250576,
#250577,#250578,#250579,#250580,#250581,#250582,#250583,#250584,#250585,
#250586,#250587,#250588,#250589,#250590,#250591,#250592,#250593,#250594,
#250595,#250596,#250597,#250598,#250599,#250600,#250601,#250602,#250603,
#250604,#250605,#250606,#250607,#250608,#250609,#250610,#250611,#250612,
#250613,#250614,#250615,#250616,#250617,#250618,#250619,#250620,#250621,
#250622,#250623,#250624,#250625,#250626,#250627,#250628,#250629,#250630,
#250631,#250632,#250633,#250634,#250635,#250636,#250637,#250638,#250639,
#250640,#250641,#250642,#250643,#250644,#250645,#250646,#250647,#250648,
#250649,#250650,#250651,#250652,#250653,#250654,#250655,#250656,#250657,
#250658,#250659,#250660,#250661,#250662,#250663,#250664,#250665,#250666,
#250667,#250668,#250669,#250670,#250671,#250672,#250673,#250674,#250675,
#250676,#250677,#250678,#250679,#250680,#250681,#250682,#250683,#250684,
#250685,#250686,#250687,#250688,#250689,#250690,#250691,#250692,#250693,
#250694,#250695,#250696,#250697,#250698,#250699,#250700,#250701,#250702,
#250703,#250704,#250705,#250706,#250707,#250708,#250709,#250710,#250711,
#250712,#250713,#250714,#250715,#250716,#250717,#250718,#250719,#250720,
#250721,#250722,#250723,#250724,#250725,#250726,#250727,#250728,#250729,
#250730,#250731,#250732,#250733,#250734,#250735,#250736,#250737,#250738,
#250739,#250740,#250741,#250742,#250743,#250744,#250745,#250746,#250747,
#250748,#250749,#250750,#250751,#250752,#250753,#250754,#250755,#250756,
#250757,#250758,#250759,#250760,#250761,#250762,#250763,#250764,#250765,
#250766,#250767,#250768,#250769,#250770,#250771,#250772,#250773,#250774,
#250775,#250776,#250777,#250778,#250779,#250780,#250781,#250782,#250783,
#250784,#250785,#250786,#250787,#250788,#250789,#250790,#250791,#250792,
#250793,#250794,#250795,#250796,#250797,#250798,#250799,#250800,#250801,
#250802,#250803,#250804,#250805,#250806,#250807,#250808,#250809,#250810,
#250811,#250812,#250813,#250814,#250815,#250816,#250817,#250818,#250819,
#250820,#250821,#250822,#250823,#250824,#250825,#250826,#250827,#250828,
#250829,#250830,#250831,#250832,#250833,#250834,#250835,#250836,#250837,
#250838,#250839,#250840,#250841,#250842,#250843,#250844,#250845,#250846,
#250847,#250848,#250849,#250850,#250851,#250852,#250853,#250854,#250855,
#250856,#250857,#250858,#250859,#250860,#250861,#250862,#250863,#250864,
#250865,#250866,#250867,#250868,#250869,#250870,#250871,#250872,#250873,
#250874,#250875,#250876,#250877,#250878,#250879,#250880,#250881,#250882,
#250883,#250884,#250885,#250886,#250887,#250888,#250889,#250890,#250891,
#250892,#250893,#250894,#250895,#250896,#250897,#250898,#250899,#250900,
#250901,#250902,#250903,#250904,#250905,#250906,#250907,#250908,#250909,
#250910,#250911,#250912,#250913,#250914,#250915,#250916,#250917,#250918,
#250919,#250920,#250921,#250922,#250923,#250924,#250925,#250926,#250927,
#250928,#250929,#250930,#250931,#250932,#250933,#250934,#250935,#250936,
#250937,#250938,#250939,#250940,#250941,#250942,#250943,#250944,#250945,
#250946,#250947,#250948,#250949,#250950,#250951,#250952,#250953,#250954,
#250955,#250956,#250957,#250958,#250959,#250960,#250961,#250962,#250963,
#250964,#250965,#250966,#250967,#250968,#250969,#250970,#250971,#250972,
#250973,#250974,#250975,#250976,#250977,#250978,#250979,#250980,#250981,
#250982,#250983,#250984,#250985,#250986,#250987,#250988,#250989,#250990,
#250991,#250992,#250993,#250994,#250995,#250996,#250997,#250998,#250999,
#251000,#251001,#251002,#251003,#251004,#251005,#251006,#251007,#251008,
#251009,#251010,#251011,#251012,#251013,#251014,#251015,#251016,#251017,
#251018,#251019,#251020,#251021,#251022,#251023,#251024,#251025,#251026,
#251027,#251028,#251029,#251030,#251031,#251032,#251033,#251034,#251035,
#251036,#251037,#251038,#251039,#251040,#251041,#251042,#251043,#251044,
#251045,#251046,#251047,#251048,#251049,#251050,#251051,#251052,#251053,
#251054,#251055,#251056,#251057,#251058,#251059,#251060,#251061,#251062,
#251063,#251064,#251065,#251066,#251067,#251068,#251069,#251070,#251071,
#251072,#251073,#251074,#251075,#251076,#251077,#251078,#251079,#251080,
#251081,#251082,#251083,#251084,#251085,#251086,#251087,#251088,#251089,
#251090,#251091,#251092,#251093,#251094,#251095,#251096,#251097,#251098,
#251099,#251100,#251101,#251102,#251103,#251104,#251105,#251106,#251107,
#251108,#251109,#251110,#251111,#251112,#251113,#251114,#251115,#251116,
#251117,#251118,#251119,#251120,#251121,#251122,#251123,#251124,#251125,
#251126,#251127,#251128,#251129,#251130,#251131,#251132,#251133,#251134,
#251135,#251136,#251137,#251138,#251139,#251140,#251141,#251142,#251143,
#251144,#251145),(#251146,#251147,#251148,#251149,#251150,#251151,#251152,
#251153,#251154,#251155,#251156,#251157,#251158,#251159,#251160,#251161,
#251162,#251163,#251164,#251165,#251166,#251167,#251168,#251169,#251170,
#251171,#251172,#251173,#251174,#251175,#251176,#251177,#251178,#251179,
#251180,#251181,#251182,#251183,#251184,#251185,#251186,#251187,#251188,
#251189,#251190,#251191,#251192,#251193,#251194,#251195,#251196,#251197,
#251198,#251199,#251200,#251201,#251202,#251203,#251204,#251205,#251206,
#251207,#251208,#251209,#251210,#251211,#251212,#251213,#251214,#251215,
#251216,#251217,#251218,#251219,#251220,#251221,#251222,#251223,#251224,
#251225,#251226,#251227,#251228,#251229,#251230,#251231,#251232,#251233,
#251234,#251235,#251236,#251237,#251238,#251239,#251240,#251241,#251242,
#251243,#251244,#251245,#251246,#251247,#251248,#251249,#251250,#251251,
#251252,#251253,#251254,#251255,#251256,#251257,#251258,#251259,#251260,
#251261,#251262,#251263,#251264,#251265,#251266,#251267,#251268,#251269,
#251270,#251271,#251272,#251273,#251274,#251275,#251276,#251277,#251278,
#251279,#251280,#251281,#251282,#251283,#251284,#251285,#251286,#251287,
#251288,#251289,#251290,#251291,#251292,#251293,#251294,#251295,#251296,
#251297,#251298,#251299,#251300,#251301,#251302,#251303,#251304,#251305,
#251306,#251307,#251308,#251309,#251310,#251311,#251312,#251313,#251314,
#251315,#251316,#251317,#251318,#251319,#251320,#251321,#251322,#251323,
#251324,#251325,#251326,#251327,#251328,#251329,#251330,#251331,#251332,
#251333,#251334,#251335,#251336,#251337,#251338,#251339,#251340,#251341,
#251342,#251343,#251344,#251345,#251346,#251347,#251348,#251349,#251350,
#251351,#251352,#251353,#251354,#251355,#251356,#251357,#251358,#251359,
#251360,#251361,#251362,#251363,#251364,#251365,#251366,#251367,#251368,
#251369,#251370,#251371,#251372,#251373,#251374,#251375,#251376,#251377,
#251378,#251379,#251380,#251381,#251382,#251383,#251384,#251385,#251386,
#251387,#251388,#251389,#251390,#251391,#251392,#251393,#251394,#251395,
#251396,#251397,#251398,#251399,#251400,#251401,#251402,#251403,#251404,
#251405,#251406,#251407,#251408,#251409,#251410,#251411,#251412,#251413,
#251414,#251415,#251416,#251417,#251418,#251419,#251420,#251421,#251422,
#251423,#251424,#251425,#251426,#251427,#251428,#251429,#251430,#251431,
#251432,#251433,#251434,#251435,#251436,#251437,#251438,#251439,#251440,
#251441,#251442,#251443,#251444,#251445,#251446,#251447,#251448,#251449,
#251450,#251451,#251452,#251453,#251454,#251455,#251456,#251457,#251458,
#251459,#251460,#251461,#251462,#251463,#251464,#251465,#251466,#251467,
#251468,#251469,#251470,#251471,#251472,#251473,#251474,#251475,#251476,
#251477,#251478,#251479,#251480,#251481,#251482,#251483,#251484,#251485,
#251486,#251487,#251488,#251489,#251490,#251491,#251492,#251493,#251494,
#251495,#251496,#251497,#251498,#251499,#251500,#251501,#251502,#251503,
#251504,#251505,#251506,#251507,#251508,#251509,#251510,#251511,#251512,
#251513,#251514,#251515,#251516,#251517,#251518,#251519,#251520,#251521,
#251522,#251523,#251524,#251525,#251526,#251527,#251528,#251529,#251530,
#251531,#251532,#251533,#251534,#251535,#251536,#251537,#251538,#251539,
#251540,#251541,#251542,#251543,#251544,#251545,#251546,#251547,#251548,
#251549,#251550,#251551,#251552,#251553,#251554,#251555,#251556,#251557,
#251558,#251559,#251560,#251561,#251562,#251563,#251564,#251565,#251566,
#251567,#251568,#251569,#251570,#251571,#251572,#251573,#251574,#251575,
#251576,#251577,#251578,#251579,#251580,#251581,#251582,#251583,#251584,
#251585,#251586,#251587,#251588,#251589,#251590,#251591,#251592,#251593,
#251594,#251595,#251596,#251597,#251598,#251599,#251600,#251601,#251602,
#251603,#251604,#251605,#251606,#251607,#251608,#251609,#251610,#251611,
#251612,#251613,#251614,#251615,#251616,#251617,#251618,#251619,#251620,
#251621,#251622,#251623,#251624,#251625,#251626,#251627,#251628,#251629,
#251630,#251631,#251632,#251633,#251634,#251635,#251636,#251637,#251638,
#251639,#251640,#251641,#251642,#251643,#251644,#251645,#251646,#251647,
#251648,#251649,#251650,#251651,#251652,#251653,#251654,#251655,#251656,
#251657,#251658,#251659,#251660,#251661,#251662,#251663,#251664,#251665,
#251666,#251667,#251668,#251669,#251670,#251671,#251672,#251673,#251674,
#251675,#251676,#251677,#251678,#251679,#251680,#251681,#251682,#251683,
#251684,#251685,#251686,#251687,#251688,#251689,#251690,#251691,#251692,
#251693,#251694,#251695,#251696,#251697,#251698,#251699,#251700,#251701,
#251702,#251703,#251704,#251705,#251706,#251707,#251708,#251709,#251710,
#251711,#251712,#251713,#251714,#251715,#251716,#251717,#251718,#251719,
#251720,#251721,#251722,#251723,#251724,#251725,#251726,#251727,#251728,
#251729,#251730,#251731,#251732,#251733,#251734,#251735,#251736,#251737,
#251738,#251739,#251740,#251741,#251742,#251743,#251744,#251745,#251746,
#251747,#251748,#251749,#251750,#251751,#251752,#251753,#251754,#251755,
#251756,#251757,#251758,#251759,#251760,#251761,#251762,#251763,#251764,
#251765,#251766,#251767,#251768,#251769,#251770,#251771,#251772,#251773,
#251774,#251775,#251776,#251777,#251778,#251779,#251780,#251781,#251782,
#251783,#251784,#251785,#251786,#251787,#251788,#251789,#251790,#251791,
#251792,#251793,#251794,#251795,#251796,#251797,#251798,#251799,#251800,
#251801,#251802,#251803,#251804,#251805,#251806,#251807,#251808,#251809,
#251810,#251811,#251812,#251813,#251814,#251815,#251816,#251817,#251818,
#251819,#251820,#251821,#251822,#251823,#251824,#251825,#251826,#251827,
#251828,#251829,#251830,#251831,#251832,#251833,#251834,#251835,#251836,
#251837,#251838,#251839,#251840,#251841,#251842,#251843,#251844,#251845,
#251846,#251847,#251848,#251849,#251850,#251851,#251852,#251853,#251854,
#251855,#251856,#251857,#251858,#251859,#251860,#251861,#251862,#251863,
#251864,#251865,#251866,#251867,#251868,#251869,#251870,#251871,#251872,
#251873,#251874,#251875,#251876,#251877,#251878,#251879,#251880,#251881,
#251882,#251883,#251884,#251885,#251886,#251887,#251888,#251889,#251890,
#251891,#251892,#251893,#251894,#251895,#251896,#251897,#251898,#251899,
#251900,#251901,#251902,#251903,#251904,#251905,#251906,#251907,#251908,
#251909,#251910,#251911,#251912,#251913,#251914,#251915,#251916,#251917,
#251918,#251919,#251920,#251921,#251922,#251923,#251924,#251925,#251926,
#251927,#251928,#251929,#251930,#251931,#251932,#251933,#251934,#251935,
#251936,#251937,#251938,#251939,#251940,#251941,#251942,#251943,#251944,
#251945,#251946,#251947,#251948,#251949,#251950,#251951,#251952,#251953,
#251954,#251955,#251956,#251957,#251958,#251959,#251960,#251961,#251962,
#251963,#251964,#251965,#251966,#251967,#251968,#251969,#251970,#251971,
#251972,#251973,#251974,#251975,#251976,#251977,#251978,#251979,#251980,
#251981,#251982,#251983,#251984,#251985,#251986,#251987,#251988,#251989,
#251990,#251991,#251992,#251993,#251994,#251995,#251996,#251997,#251998,
#251999,#252000,#252001,#252002,#252003,#252004,#252005,#252006,#252007,
#252008,#252009,#252010,#252011,#252012,#252013,#252014,#252015,#252016,
#252017,#252018,#252019,#252020,#252021,#252022,#252023,#252024,#252025,
#252026,#252027,#252028,#252029,#252030,#252031,#252032,#252033,#252034,
#252035,#252036,#252037,#252038,#252039,#252040,#252041,#252042,#252043,
#252044,#252045,#252046,#252047,#252048,#252049,#252050,#252051,#252052,
#252053,#252054,#252055,#252056,#252057,#252058,#252059,#252060,#252061,
#252062,#252063,#252064,#252065,#252066,#252067,#252068,#252069,#252070,
#252071,#252072,#252073,#252074,#252075,#252076,#252077,#252078,#252079,
#252080,#252081,#252082,#252083,#252084,#252085,#252086,#252087,#252088,
#252089,#252090,#252091,#252092,#252093,#252094,#252095,#252096,#252097,
#252098,#252099,#252100,#252101,#252102,#252103,#252104,#252105,#252106,
#252107,#252108,#252109,#252110,#252111,#252112,#252113,#252114,#252115,
#252116,#252117,#252118,#252119,#252120,#252121,#252122,#252123,#252124,
#252125,#252126,#252127,#252128,#252129,#252130,#252131,#252132,#252133,
#252134,#252135,#252136,#252137,#252138,#252139,#252140,#252141,#252142,
#252143,#252144,#252145,#252146,#252147,#252148,#252149,#252150,#252151,
#252152,#252153,#252154,#252155,#252156,#252157,#252158,#252159,#252160,
#252161,#252162,#252163,#252164,#252165,#252166,#252167,#252168,#252169,
#252170,#252171,#252172,#252173,#252174,#252175,#252176,#252177,#252178,
#252179,#252180,#252181,#252182,#252183,#252184,#252185,#252186,#252187,
#252188,#252189,#252190,#252191,#252192,#252193,#252194,#252195,#252196,
#252197,#252198,#252199,#252200,#252201,#252202,#252203,#252204,#252205,
#252206,#252207,#252208,#252209,#252210,#252211,#252212,#252213,#252214,
#252215,#252216,#252217,#252218,#252219,#252220,#252221,#252222,#252223,
#252224,#252225,#252226,#252227,#252228,#252229,#252230,#252231,#252232,
#252233,#252234,#252235,#252236,#252237,#252238,#252239,#252240,#252241,
#252242,#252243,#252244,#252245,#252246,#252247,#252248,#252249,#252250,
#252251,#252252,#252253,#252254,#252255,#252256,#252257,#252258,#252259,
#252260,#252261,#252262,#252263,#252264,#252265,#252266,#252267,#252268,
#252269,#252270,#252271,#252272,#252273,#252274,#252275,#252276,#252277,
#252278,#252279,#252280,#252281,#252282,#252283,#252284,#252285,#252286,
#252287,#252288,#252289,#252290,#252291,#252292,#252293,#252294,#252295,
#252296,#252297,#252298,#252299,#252300,#252301,#252302,#252303,#252304,
#252305,#252306,#252307,#252308,#252309,#252310,#252311,#252312,#252313,
#252314,#252315,#252316,#252317,#252318,#252319,#252320,#252321,#252322,
#252323,#252324,#252325,#252326,#252327,#252328,#252329,#252330,#252331,
#252332,#252333,#252334,#252335,#252336,#252337,#252338,#252339,#252340,
#252341,#252342,#252343,#252344,#252345,#252346,#252347,#252348,#252349,
#252350,#252351,#252352,#252353,#252354,#252355,#252356,#252357,#252358,
#252359,#252360,#252361,#252362,#252363,#252364,#252365,#252366,#252367,
#252368,#252369,#252370,#252371,#252372,#252373,#252374,#252375,#252376,
#252377,#252378,#252379,#252380,#252381,#252382,#252383,#252384,#252385,
#252386,#252387,#252388,#252389,#252390,#252391,#252392,#252393,#252394,
#252395,#252396,#252397,#252398,#252399,#252400,#252401,#252402,#252403,
#252404,#252405,#252406,#252407,#252408,#252409,#252410,#252411,#252412,
#252413,#252414,#252415,#252416,#252417,#252418,#252419,#252420,#252421,
#252422,#252423,#252424,#252425,#252426,#252427,#252428,#252429,#252430,
#252431,#252432,#252433,#252434,#252435,#252436,#252437,#252438,#252439,
#252440,#252441,#252442,#252443,#252444,#252445,#252446,#252447,#252448,
#252449,#252450,#252451,#252452,#252453,#252454,#252455,#252456,#252457,
#252458,#252459,#252460,#252461,#252462,#252463,#252464,#252465,#252466,
#252467,#252468,#252469,#252470,#252471,#252472,#252473,#252474,#252475,
#252476,#252477,#252478,#252479,#252480,#252481,#252482,#252483,#252484,
#252485,#252486,#252487,#252488,#252489,#252490,#252491,#252492,#252493,
#252494,#252495,#252496,#252497,#252498,#252499,#252500,#252501,#252502,
#252503,#252504,#252505,#252506,#252507,#252508,#252509,#252510,#252511,
#252512,#252513,#252514,#252515,#252516,#252517,#252518,#252519,#252520,
#252521,#252522,#252523,#252524,#252525,#252526,#252527,#252528,#252529,
#252530,#252531,#252532,#252533,#252534,#252535,#252536,#252537,#252538,
#252539,#252540,#252541,#252542,#252543,#252544,#252545,#252546,#252547,
#252548,#252549,#252550,#252551,#252552,#252553,#252554,#252555,#252556,
#252557,#252558,#252559,#252560,#252561,#252562,#252563,#252564,#252565,
#252566,#252567,#252568,#252569,#252570,#252571,#252572,#252573,#252574,
#252575,#252576,#252577,#252578,#252579,#252580,#252581,#252582,#252583,
#252584,#252585,#252586,#252587,#252588,#252589,#252590,#252591,#252592,
#252593,#252594,#252595,#252596,#252597,#252598,#252599,#252600,#252601,
#252602,#252603,#252604,#252605,#252606,#252607,#252608,#252609,#252610,
#252611,#252612,#252613,#252614,#252615,#252616,#252617,#252618,#252619,
#252620,#252621,#252622,#252623,#252624,#252625,#252626,#252627,#252628,
#252629,#252630,#252631,#252632,#252633,#252634,#252635,#252636,#252637,
#252638,#252639,#252640,#252641,#252642,#252643,#252644,#252645,#252646,
#252647,#252648,#252649,#252650,#252651,#252652,#252653,#252654,#252655,
#252656,#252657,#252658,#252659,#252660,#252661,#252662,#252663,#252664,
#252665,#252666,#252667,#252668,#252669,#252670,#252671,#252672,#252673,
#252674,#252675,#252676,#252677,#252678,#252679,#252680,#252681,#252682,
#252683,#252684,#252685,#252686,#252687,#252688,#252689,#252690,#252691,
#252692,#252693,#252694,#252695,#252696,#252697,#252698,#252699,#252700,
#252701,#252702,#252703,#252704,#252705,#252706,#252707,#252708,#252709,
#252710,#252711,#252712,#252713,#252714,#252715,#252716,#252717,#252718,
#252719,#252720,#252721,#252722,#252723,#252724,#252725,#252726,#252727,
#252728,#252729,#252730,#252731,#252732,#252733,#252734,#252735,#252736,
#252737,#252738,#252739,#252740,#252741,#252742,#252743,#252744,#252745,
#252746,#252747,#252748,#252749,#252750,#252751,#252752,#252753,#252754,
#252755,#252756,#252757,#252758,#252759,#252760,#252761,#252762,#252763,
#252764,#252765,#252766,#252767,#252768,#252769,#252770,#252771,#252772,
#252773,#252774,#252775,#252776,#252777,#252778,#252779,#252780,#252781,
#252782,#252783,#252784,#252785,#252786,#252787,#252788,#252789,#252790,
#252791,#252792,#252793,#252794,#252795,#252796,#252797,#252798,#252799,
#252800,#252801,#252802,#252803,#252804,#252805,#252806,#252807,#252808,
#252809,#252810,#252811,#252812,#252813,#252814,#252815,#252816,#252817,
#252818,#252819,#252820,#252821,#252822,#252823,#252824,#252825,#252826,
#252827,#252828,#252829,#252830,#252831,#252832,#252833,#252834,#252835,
#252836,#252837,#252838,#252839,#252840),(#252841,#252842,#252843,#252844,
#252845,#252846,#252847,#252848,#252849,#252850,#252851,#252852,#252853,
#252854,#252855,#252856,#252857,#252858,#252859,#252860,#252861,#252862,
#252863,#252864,#252865,#252866,#252867,#252868,#252869,#252870,#252871,
#252872,#252873,#252874,#252875,#252876,#252877,#252878,#252879,#252880,
#252881,#252882,#252883,#252884,#252885,#252886,#252887,#252888,#252889,
#252890,#252891,#252892,#252893,#252894,#252895,#252896,#252897,#252898,
#252899,#252900,#252901,#252902,#252903,#252904,#252905,#252906,#252907,
#252908,#252909,#252910,#252911,#252912,#252913,#252914,#252915,#252916,
#252917,#252918,#252919,#252920,#252921,#252922,#252923,#252924,#252925,
#252926,#252927,#252928,#252929,#252930,#252931,#252932,#252933,#252934,
#252935,#252936,#252937,#252938,#252939,#252940,#252941,#252942,#252943,
#252944,#252945,#252946,#252947,#252948,#252949,#252950,#252951,#252952,
#252953,#252954,#252955,#252956,#252957,#252958,#252959,#252960,#252961,
#252962,#252963,#252964,#252965,#252966,#252967,#252968,#252969,#252970,
#252971,#252972,#252973,#252974,#252975,#252976,#252977,#252978,#252979,
#252980,#252981,#252982,#252983,#252984,#252985,#252986,#252987,#252988,
#252989,#252990,#252991,#252992,#252993,#252994,#252995,#252996,#252997,
#252998,#252999,#253000,#253001,#253002,#253003,#253004,#253005,#253006,
#253007,#253008,#253009,#253010,#253011,#253012,#253013,#253014,#253015,
#253016,#253017,#253018,#253019,#253020,#253021,#253022,#253023,#253024,
#253025,#253026,#253027,#253028,#253029,#253030,#253031,#253032,#253033,
#253034,#253035,#253036,#253037,#253038,#253039,#253040,#253041,#253042,
#253043,#253044,#253045,#253046,#253047,#253048,#253049,#253050,#253051,
#253052,#253053,#253054,#253055,#253056,#253057,#253058,#253059,#253060,
#253061,#253062,#253063,#253064,#253065,#253066,#253067,#253068,#253069,
#253070,#253071,#253072,#253073,#253074,#253075,#253076,#253077,#253078,
#253079,#253080,#253081,#253082,#253083,#253084,#253085,#253086,#253087,
#253088,#253089,#253090,#253091,#253092,#253093,#253094,#253095,#253096,
#253097,#253098,#253099,#253100,#253101,#253102,#253103,#253104,#253105,
#253106,#253107,#253108,#253109,#253110,#253111,#253112,#253113,#253114,
#253115,#253116,#253117,#253118,#253119,#253120,#253121,#253122,#253123,
#253124,#253125,#253126,#253127,#253128,#253129,#253130,#253131,#253132,
#253133,#253134,#253135,#253136,#253137,#253138,#253139,#253140,#253141,
#253142,#253143,#253144,#253145,#253146,#253147,#253148,#253149,#253150,
#253151,#253152,#253153,#253154,#253155,#253156,#253157,#253158,#253159,
#253160,#253161,#253162,#253163,#253164,#253165,#253166,#253167,#253168,
#253169,#253170,#253171,#253172,#253173,#253174,#253175,#253176,#253177,
#253178,#253179,#253180,#253181,#253182,#253183,#253184,#253185,#253186,
#253187,#253188,#253189,#253190,#253191,#253192,#253193,#253194,#253195,
#253196,#253197,#253198,#253199,#253200,#253201,#253202,#253203,#253204,
#253205,#253206,#253207,#253208,#253209,#253210,#253211,#253212,#253213,
#253214,#253215,#253216,#253217,#253218,#253219,#253220,#253221,#253222,
#253223,#253224,#253225,#253226,#253227,#253228,#253229,#253230,#253231,
#253232,#253233,#253234,#253235,#253236,#253237,#253238,#253239,#253240,
#253241,#253242,#253243,#253244,#253245,#253246,#253247,#253248,#253249,
#253250,#253251,#253252,#253253,#253254,#253255,#253256,#253257,#253258,
#253259,#253260,#253261,#253262,#253263,#253264,#253265,#253266,#253267,
#253268,#253269,#253270,#253271,#253272,#253273,#253274,#253275,#253276,
#253277,#253278,#253279,#253280,#253281,#253282,#253283,#253284,#253285,
#253286,#253287,#253288,#253289,#253290,#253291,#253292,#253293,#253294,
#253295,#253296,#253297,#253298,#253299,#253300,#253301,#253302,#253303,
#253304,#253305,#253306,#253307,#253308,#253309,#253310,#253311,#253312,
#253313,#253314,#253315,#253316,#253317,#253318,#253319,#253320,#253321,
#253322,#253323,#253324,#253325,#253326,#253327,#253328,#253329,#253330,
#253331,#253332,#253333,#253334,#253335,#253336,#253337,#253338,#253339,
#253340,#253341,#253342,#253343,#253344,#253345,#253346,#253347,#253348,
#253349,#253350,#253351,#253352,#253353,#253354,#253355,#253356,#253357,
#253358,#253359,#253360,#253361,#253362,#253363,#253364,#253365,#253366,
#253367,#253368,#253369,#253370,#253371,#253372,#253373,#253374,#253375,
#253376,#253377,#253378,#253379,#253380,#253381,#253382,#253383,#253384,
#253385,#253386,#253387,#253388,#253389,#253390,#253391,#253392,#253393,
#253394,#253395,#253396,#253397,#253398,#253399,#253400,#253401,#253402,
#253403,#253404,#253405,#253406,#253407,#253408,#253409,#253410,#253411,
#253412,#253413,#253414,#253415,#253416,#253417,#253418,#253419,#253420,
#253421,#253422,#253423,#253424,#253425,#253426,#253427,#253428,#253429,
#253430,#253431,#253432,#253433,#253434,#253435,#253436,#253437,#253438,
#253439,#253440,#253441,#253442,#253443,#253444,#253445,#253446,#253447,
#253448,#253449,#253450,#253451,#253452,#253453,#253454,#253455,#253456,
#253457,#253458,#253459,#253460,#253461,#253462,#253463,#253464,#253465,
#253466,#253467,#253468,#253469,#253470,#253471,#253472,#253473,#253474,
#253475,#253476,#253477,#253478,#253479,#253480,#253481,#253482,#253483,
#253484,#253485,#253486,#253487,#253488,#253489,#253490,#253491,#253492,
#253493,#253494,#253495,#253496,#253497,#253498,#253499,#253500,#253501,
#253502,#253503,#253504,#253505,#253506,#253507,#253508,#253509,#253510,
#253511,#253512,#253513,#253514,#253515,#253516,#253517,#253518,#253519,
#253520,#253521,#253522,#253523,#253524,#253525,#253526,#253527,#253528,
#253529,#253530,#253531,#253532,#253533,#253534,#253535,#253536,#253537,
#253538,#253539,#253540,#253541,#253542,#253543,#253544,#253545,#253546,
#253547,#253548,#253549,#253550,#253551,#253552,#253553,#253554,#253555,
#253556,#253557,#253558,#253559,#253560,#253561,#253562,#253563,#253564,
#253565,#253566,#253567,#253568,#253569,#253570,#253571,#253572,#253573,
#253574,#253575,#253576,#253577,#253578,#253579,#253580,#253581,#253582,
#253583,#253584,#253585,#253586,#253587,#253588,#253589,#253590,#253591,
#253592,#253593,#253594,#253595,#253596,#253597,#253598,#253599,#253600,
#253601,#253602,#253603,#253604,#253605,#253606,#253607,#253608,#253609,
#253610,#253611,#253612,#253613,#253614,#253615,#253616,#253617,#253618,
#253619,#253620,#253621,#253622,#253623,#253624,#253625,#253626,#253627,
#253628,#253629,#253630,#253631,#253632,#253633,#253634,#253635,#253636,
#253637,#253638,#253639,#253640,#253641,#253642,#253643,#253644,#253645,
#253646,#253647,#253648,#253649,#253650,#253651,#253652,#253653,#253654,
#253655,#253656,#253657,#253658,#253659,#253660,#253661,#253662,#253663,
#253664,#253665,#253666,#253667,#253668,#253669,#253670,#253671,#253672,
#253673,#253674,#253675,#253676,#253677,#253678,#253679,#253680,#253681,
#253682,#253683,#253684,#253685,#253686,#253687,#253688,#253689,#253690,
#253691,#253692,#253693,#253694,#253695,#253696,#253697,#253698,#253699,
#253700,#253701,#253702,#253703,#253704,#253705,#253706,#253707,#253708,
#253709,#253710,#253711,#253712,#253713,#253714,#253715,#253716,#253717,
#253718,#253719,#253720,#253721,#253722,#253723,#253724,#253725,#253726,
#253727,#253728,#253729,#253730,#253731,#253732,#253733,#253734,#253735,
#253736,#253737,#253738,#253739,#253740,#253741,#253742,#253743,#253744,
#253745,#253746,#253747,#253748,#253749,#253750,#253751,#253752,#253753,
#253754,#253755,#253756,#253757,#253758,#253759,#253760,#253761,#253762,
#253763,#253764,#253765,#253766,#253767,#253768,#253769,#253770,#253771,
#253772,#253773,#253774,#253775,#253776,#253777,#253778,#253779,#253780,
#253781,#253782,#253783,#253784,#253785,#253786,#253787,#253788,#253789,
#253790,#253791,#253792,#253793,#253794,#253795,#253796,#253797,#253798,
#253799,#253800,#253801,#253802,#253803,#253804,#253805,#253806,#253807,
#253808,#253809,#253810,#253811,#253812,#253813,#253814,#253815,#253816,
#253817,#253818,#253819,#253820,#253821,#253822,#253823,#253824,#253825,
#253826,#253827,#253828,#253829,#253830,#253831,#253832,#253833,#253834,
#253835,#253836,#253837,#253838,#253839,#253840,#253841,#253842,#253843,
#253844,#253845,#253846,#253847,#253848,#253849,#253850,#253851,#253852,
#253853,#253854,#253855,#253856,#253857,#253858,#253859,#253860,#253861,
#253862,#253863,#253864,#253865,#253866,#253867,#253868,#253869,#253870,
#253871,#253872,#253873,#253874,#253875,#253876,#253877,#253878,#253879,
#253880,#253881,#253882,#253883,#253884,#253885,#253886,#253887,#253888,
#253889,#253890,#253891,#253892,#253893,#253894,#253895,#253896,#253897,
#253898,#253899,#253900,#253901,#253902,#253903,#253904,#253905,#253906,
#253907,#253908,#253909,#253910,#253911,#253912,#253913,#253914,#253915,
#253916,#253917,#253918,#253919,#253920,#253921,#253922,#253923,#253924,
#253925,#253926,#253927,#253928,#253929,#253930,#253931,#253932,#253933,
#253934,#253935,#253936,#253937,#253938,#253939,#253940,#253941,#253942,
#253943,#253944,#253945,#253946,#253947,#253948,#253949,#253950,#253951,
#253952,#253953,#253954,#253955,#253956,#253957,#253958,#253959,#253960,
#253961,#253962,#253963,#253964,#253965,#253966,#253967,#253968,#253969,
#253970,#253971,#253972,#253973,#253974,#253975,#253976,#253977,#253978,
#253979,#253980,#253981,#253982,#253983,#253984,#253985,#253986,#253987,
#253988,#253989,#253990,#253991,#253992,#253993,#253994,#253995,#253996,
#253997,#253998,#253999,#254000,#254001,#254002,#254003,#254004,#254005,
#254006,#254007,#254008,#254009,#254010,#254011,#254012,#254013,#254014,
#254015,#254016,#254017,#254018,#254019,#254020,#254021,#254022,#254023,
#254024,#254025,#254026,#254027,#254028,#254029,#254030,#254031,#254032,
#254033,#254034,#254035,#254036,#254037,#254038,#254039,#254040,#254041,
#254042,#254043,#254044,#254045,#254046,#254047,#254048,#254049,#254050,
#254051,#254052,#254053,#254054,#254055,#254056,#254057,#254058,#254059,
#254060,#254061,#254062,#254063,#254064,#254065,#254066,#254067,#254068,
#254069,#254070,#254071,#254072,#254073,#254074,#254075,#254076,#254077,
#254078,#254079,#254080,#254081,#254082,#254083,#254084,#254085,#254086,
#254087,#254088,#254089,#254090,#254091,#254092,#254093,#254094,#254095,
#254096,#254097,#254098,#254099,#254100,#254101,#254102,#254103,#254104,
#254105,#254106,#254107,#254108,#254109,#254110,#254111,#254112,#254113,
#254114,#254115,#254116,#254117,#254118,#254119,#254120,#254121,#254122,
#254123,#254124,#254125,#254126,#254127,#254128,#254129,#254130,#254131,
#254132,#254133,#254134,#254135,#254136,#254137,#254138,#254139,#254140,
#254141,#254142,#254143,#254144,#254145,#254146,#254147,#254148,#254149,
#254150,#254151,#254152,#254153,#254154,#254155,#254156,#254157,#254158,
#254159,#254160,#254161,#254162,#254163,#254164,#254165,#254166,#254167,
#254168,#254169,#254170,#254171,#254172,#254173,#254174,#254175,#254176,
#254177,#254178,#254179,#254180,#254181,#254182,#254183,#254184,#254185,
#254186,#254187,#254188,#254189,#254190,#254191,#254192,#254193,#254194,
#254195,#254196,#254197,#254198,#254199,#254200,#254201,#254202,#254203,
#254204,#254205,#254206,#254207,#254208,#254209,#254210,#254211,#254212,
#254213,#254214,#254215,#254216,#254217,#254218,#254219,#254220,#254221,
#254222,#254223,#254224,#254225,#254226,#254227,#254228,#254229,#254230,
#254231,#254232,#254233,#254234,#254235,#254236,#254237,#254238,#254239,
#254240,#254241,#254242,#254243,#254244,#254245,#254246,#254247,#254248,
#254249,#254250,#254251,#254252,#254253,#254254,#254255,#254256,#254257,
#254258,#254259,#254260,#254261,#254262,#254263,#254264,#254265,#254266,
#254267,#254268,#254269,#254270,#254271,#254272,#254273,#254274,#254275,
#254276,#254277,#254278,#254279,#254280,#254281,#254282,#254283,#254284,
#254285,#254286,#254287,#254288,#254289,#254290,#254291,#254292,#254293,
#254294,#254295,#254296,#254297,#254298,#254299,#254300,#254301,#254302,
#254303,#254304,#254305,#254306,#254307,#254308,#254309,#254310,#254311,
#254312,#254313,#254314,#254315,#254316,#254317,#254318,#254319,#254320,
#254321,#254322,#254323,#254324,#254325,#254326,#254327,#254328,#254329,
#254330,#254331,#254332,#254333,#254334,#254335,#254336,#254337,#254338,
#254339,#254340,#254341,#254342,#254343,#254344,#254345,#254346,#254347,
#254348,#254349,#254350,#254351,#254352,#254353,#254354,#254355,#254356,
#254357,#254358,#254359,#254360,#254361,#254362,#254363,#254364,#254365,
#254366,#254367,#254368,#254369,#254370,#254371,#254372,#254373,#254374,
#254375,#254376,#254377,#254378,#254379,#254380,#254381,#254382,#254383,
#254384,#254385,#254386,#254387,#254388,#254389,#254390,#254391,#254392,
#254393,#254394,#254395,#254396,#254397,#254398,#254399,#254400,#254401,
#254402,#254403,#254404,#254405,#254406,#254407,#254408,#254409,#254410,
#254411,#254412,#254413,#254414,#254415,#254416,#254417,#254418,#254419,
#254420,#254421,#254422,#254423,#254424,#254425,#254426,#254427,#254428,
#254429,#254430,#254431,#254432,#254433,#254434,#254435,#254436,#254437,
#254438,#254439,#254440,#254441,#254442,#254443,#254444,#254445,#254446,
#254447,#254448,#254449,#254450,#254451,#254452,#254453,#254454,#254455,
#254456,#254457,#254458,#254459,#254460,#254461,#254462,#254463,#254464,
#254465,#254466,#254467,#254468,#254469,#254470,#254471,#254472,#254473,
#254474,#254475,#254476,#254477,#254478,#254479,#254480,#254481,#254482,
#254483,#254484,#254485,#254486,#254487,#254488,#254489,#254490,#254491,
#254492,#254493,#254494,#254495,#254496,#254497,#254498,#254499,#254500,
#254501,#254502,#254503,#254504,#254505,#254506,#254507,#254508,#254509,
#254510,#254511,#254512,#254513,#254514,#254515,#254516,#254517,#254518,
#254519,#254520,#254521,#254522,#254523,#254524,#254525,#254526,#254527,
#254528,#254529,#254530,#254531,#254532,#254533,#254534,#254535)),
 .UNSPECIFIED.,.F.,.F.,.F.,(4,4),(4,1,1,1,1,1,1,1,1,1,1,1,1,1,1,1,1,1,1,
1,1,1,1,1,1,1,1,1,1,1,1,1,1,1,1,1,1,1,1,1,1,1,1,1,1,1,1,1,1,1,1,1,1,1,1,
1,1,1,1,1,1,1,1,1,1,1,1,1,1,1,1,1,1,1,1,1,1,1,1,1,1,1,1,1,1,1,1,1,1,1,1,
1,1,1,1,1,1,1,1,1,1,1,1,1,1,1,1,1,1,1,1,1,1,1,1,1,1,1,1,1,1,1,1,1,1,1,1,
1,1,1,1,1,1,1,1,1,1,1,1,1,1,1,1,1,1,1,1,1,1,1,1,1,1,1,1,1,1,1,1,1,1,1,1,
1,1,1,1,1,1,1,1,1,1,1,1,1,1,1,1,1,1,1,1,1,1,1,1,1,1,1,1,1,1,1,1,1,1,1,1,
1,1,1,1,1,1,1,1,1,1,1,1,1,1,1,1,1,1,1,1,1,1,1,1,1,1,1,1,1,1,1,1,1,1,1,1,
1,1,1,1,1,1,1,1,1,1,1,1,1,1,1,1,1,1,1,1,1,1,1,1,1,1,1,1,1,1,1,1,1,1,1,1,
1,1,1,1,1,1,1,1,1,1,1,1,1,1,1,1,1,1,1,1,1,1,1,1,1,1,1,1,1,1,1,1,1,1,1,1,
1,1,1,1,1,1,1,1,1,1,1,1,1,1,1,1,1,1,1,1,1,1,1,1,1,1,1,1,1,1,1,1,1,1,1,1,
1,1,1,1,1,1,1,1,1,1,1,1,1,1,1,1,1,1,1,1,1,1,1,1,1,1,1,1,1,1,1,1,1,1,1,1,
1,1,1,1,1,1,1,1,1,1,1,1,1,1,1,1,1,1,1,1,1,1,1,1,1,1,1,1,1,1,1,1,1,1,1,1,
1,1,1,1,1,1,1,1,1,1,1,1,1,1,1,1,1,1,1,1,1,1,1,1,1,1,1,1,1,1,1,1,1,1,1,1,
1,1,1,1,1,1,1,1,1,1,1,1,1,1,1,1,1,1,1,1,1,1,1,1,1,1,1,1,1,1,1,1,1,1,1,1,
1,1,1,1,1,1,1,1,1,1,1,1,1,1,1,1,1,1,1,1,1,1,1,1,1,1,1,1,1,1,1,1,1,1,1,1,
1,1,1,1,1,1,1,1,1,1,1,1,1,1,1,1,1,1,1,1,1,1,1,1,1,1,1,1,1,1,1,1,1,1,1,1,
1,1,1,1,1,1,1,1,1,1,1,1,1,1,1,1,1,1,1,1,1,1,1,1,1,1,1,1,1,1,1,1,1,1,1,1,
1,1,1,1,1,1,1,1,1,1,1,1,1,1,1,1,1,1,1,1,1,1,1,1,1,1,1,1,1,1,1,1,1,1,1,1,
1,1,1,1,1,1,1,1,1,1,1,1,1,1,1,1,1,1,1,1,1,1,1,1,1,1,1,1,1,1,1,1,1,1,1,1,
1,1,1,1,1,1,1,1,1,1,1,1,1,1,1,1,1,1,1,1,1,1,1,1,1,1,1,1,1,1,1,1,1,1,1,1,
1,1,1,1,1,1,1,1,1,1,1,1,1,1,1,1,1,1,1,1,1,1,1,1,1,1,1,1,1,1,1,1,1,1,1,1,
1,1,1,1,1,1,1,1,1,1,1,1,1,1,1,1,1,1,1,1,1,1,1,1,1,1,1,1,1,1,1,1,1,1,1,1,
1,1,1,1,1,1,1,1,1,1,1,1,1,1,1,1,1,1,1,1,1,1,1,1,1,1,1,1,1,1,1,1,1,1,1,1,
1,1,1,1,1,1,1,1,1,1,1,1,1,1,1,1,1,1,1,1,1,1,1,1,1,1,1,1,1,1,1,1,1,1,1,1,
1,1,1,1,1,1,1,1,1,1,1,1,1,1,1,1,1,1,1,1,1,1,1,1,1,1,1,1,1,1,1,1,1,1,1,1,
1,1,1,1,1,1,1,1,1,1,1,1,1,1,1,1,1,1,1,1,1,1,1,1,1,1,1,1,1,1,1,1,1,1,1,1,
1,1,1,1,1,1,1,1,1,1,1,1,1,1,1,1,1,1,1,1,1,1,1,1,1,1,1,1,1,1,1,1,1,1,1,1,
1,1,1,1,1,1,1,1,1,1,1,1,1,1,1,1,1,1,1,1,1,1,1,1,1,1,1,1,1,1,1,1,1,1,1,1,
1,1,1,1,1,1,1,1,1,1,1,1,1,1,1,1,1,1,1,1,1,1,1,1,1,1,1,1,1,1,1,1,1,1,1,1,
1,1,1,1,1,1,1,1,1,1,1,1,1,1,1,1,1,1,1,1,1,1,1,1,1,1,1,1,1,1,1,1,1,1,1,1,
1,1,1,1,1,1,1,1,1,1,1,1,1,1,1,1,1,1,1,1,1,1,1,1,1,1,1,1,1,1,1,1,1,1,1,1,
1,1,1,1,1,1,1,1,1,1,1,1,1,1,1,1,1,1,1,1,1,1,1,1,1,1,1,1,1,1,1,1,1,1,1,1,
1,1,1,1,1,1,1,1,1,1,1,1,1,1,1,1,1,1,1,1,1,1,1,1,1,1,1,1,1,1,1,1,1,1,1,1,
1,1,1,1,1,1,1,1,1,1,1,1,1,1,1,1,1,1,1,1,1,1,1,1,1,1,1,1,1,1,1,1,1,1,1,1,
1,1,1,1,1,1,1,1,1,1,1,1,1,1,1,1,1,1,1,1,1,1,1,1,1,1,1,1,1,1,1,1,1,1,1,1,
1,1,1,1,1,1,1,1,1,1,1,1,1,1,1,1,1,1,1,1,1,1,1,1,1,1,1,1,1,1,1,1,1,1,1,1,
1,1,1,1,1,1,1,1,1,1,1,1,1,1,1,1,1,1,1,1,1,1,1,1,1,1,1,1,1,1,1,1,1,1,1,1,
1,1,1,1,1,1,1,1,1,1,1,1,1,1,1,1,1,1,1,1,1,1,1,1,1,1,1,1,1,1,1,1,1,1,1,1,
1,1,1,1,1,1,1,1,1,1,1,1,1,1,1,1,1,1,1,1,1,1,1,1,1,1,1,1,1,1,1,1,1,1,1,1,
1,1,1,1,1,1,1,1,1,1,1,1,1,1,1,1,1,1,1,1,1,1,1,1,1,1,1,1,1,1,1,1,1,1,1,1,
1,1,1,1,1,1,1,1,1,1,1,1,1,1,1,1,1,1,1,1,1,1,1,1,1,1,1,1,1,1,1,1,1,1,1,1,
1,1,1,1,1,1,1,1,1,1,1,1,1,1,1,1,1,1,1,1,1,1,1,1,1,1,1,1,1,1,1,1,1,1,1,1,
1,1,1,1,1,1,1,1,1,1,1,1,1,1,1,1,1,1,1,1,1,1,1,1,1,1,1,1,1,1,1,1,1,1,1,1,
1,1,1,1,1,1,1,1,1,1,1,1,1,1,1,1,1,1,1,1,1,1,1,1,1,1,1,1,1,1,1,1,1,1,1,1,
1,1,1,1,1,1,1,1,1,1,1,1,1,1,1,1,1,1,1,1,1,1,1,1,1,1,1,1,1,1,1,1,1,1,1,1,
1,1,1,1,1,1,1,1,1,1,1,1,1,1,1,1,1,1,1,1,1,1,1,1,1,1,1,1,1,1,1,1,1,1,1,1,
1,1,1,1,1,1,1,1,1,1,1,1,1,1,1,1,1,1,1,1,1,1,1,1,1,1,1,1,1,1,1,1,1,1,1,1,
1,1,1,1,1,1,1,1,1,1,1,1,1,1,1,1,1,4),(-0.000587328099657093,0.1157205948422),
(8.30590413559005,8.80579087257276,9.30565887793282,10.305394888653,11.3051308993731,
12.3048669100932,13.3046029208133,14.3043389315335,15.3040749422536,16.3038109529737,
17.3035469636939,18.303282974414,19.3030189851341,20.3027549958542,21.3024910065744,
22.3022270172945,23.3019630280146,24.3016990387348,25.3014350494549,26.301171060175,
27.3009070708951,28.3006430816153,29.3003790923354,30.3001151030555,31.2998511137757,
32.2995871244958,33.2993231352159,34.299059145936,35.2987951566562,36.2985311673763,
37.2982671780964,38.2980031888166,39.2977391995367,40.2974752102568,41.2972112209769,
42.2969472316971,43.2966832424172,44.2964192531373,45.2961552638575,46.2958912745776,
47.2956272852977,48.2953632960178,49.295099306738,50.2948353174581,51.2945713281782,
52.2943073388984,53.2940433496185,54.2937793603386,55.2935153710587,56.2932513817789,
57.292987392499,58.2927234032191,59.2924594139393,60.2921954246594,61.2919314353795,
62.2916674460996,63.2914034568198,64.2911394675399,65.29087547826,66.2906114889802,
67.2903474997003,68.2900835104204,69.2898195211405,70.2895555318607,71.2892915425808,
72.2890275533009,73.2887635640211,74.2884995747412,75.2882355854613,76.2879715961814,
77.2877076069016,78.2874436176217,79.2871796283418,80.286915639062,81.2866516497821,
82.2863876605022,83.2861236712224,84.2858596819425,85.2855956926626,86.2853317033827,
87.2850677141029,88.284803724823,89.2845397355431,90.2842757462633,91.2840117569834,
92.2837477677035,93.2834837784236,94.2832197891438,95.2829557998639,96.282691810584,
97.2824278213041,98.2821638320243,99.2818998427444,100.281635853465,101.281371864185,
102.281107874905,103.280843885625,104.280579896345,105.280315907065,106.280051917785,
107.279787928505,108.279523939226,109.279259949946,110.278995960666,111.278731971386,
112.278467982106,113.278203992826,114.277940003546,115.277676014266,116.277412024987,
117.277148035707,118.276884046427,119.276620057147,120.276356067867,121.276092078587,
122.275828089307,123.275564100028,124.275300110748,125.275036121468,126.274772132188,
127.274508142908,128.274244153628,129.273980164348,130.273716175068,131.273452185789,
132.273188196509,133.272924207229,134.272660217949,135.272396228669,136.272132239389,
137.271868250109,138.271604260829,139.27134027155,140.27107628227,141.27081229299,
142.27054830371,143.27028431443,144.27002032515,145.26975633587,146.26949234659,
147.269228357311,148.268964368031,149.268700378751,150.268436389471,151.268172400191,
152.267908410911,153.267644421631,154.267380432352,155.267116443072,156.266852453792,
157.266588464512,158.266324475232,159.266060485952,160.265796496672,161.265532507392,
162.265268518113,163.265004528833,164.264740539553,165.264476550273,166.264212560993,
167.263948571713,168.263684582433,169.263420593153,170.263156603874,171.262892614594,
172.262628625314,173.262364636034,174.262100646754,175.261836657474,176.261572668194,
177.261308678914,178.261044689635,179.260780700355,180.260516711075,181.260252721795,
182.259988732515,183.259724743235,184.259460753955,185.259196764675,186.258932775396,
187.258668786116,188.258404796836,189.258140807556,190.257876818276,191.257612828996,
192.257348839716,193.257084850437,194.256820861157,195.256556871877,196.256292882597,
197.256028893317,198.255764904037,199.255500914757,200.255236925477,201.254972936198,
202.254708946918,203.254444957638,204.254180968358,205.253916979078,206.253652989798,
207.253389000518,208.253125011238,209.252861021959,210.252597032679,211.252333043399,
212.252069054119,213.251805064839,214.251541075559,215.251277086279,216.251013096999,
217.25074910772,218.25048511844,219.25022112916,220.24995713988,221.2496931506,
222.24942916132,223.24916517204,224.248901182761,225.248637193481,226.248373204201,
227.248109214921,228.247845225641,229.247581236361,230.247317247081,231.247053257801,
232.246789268522,233.246525279242,234.246261289962,235.245997300682,236.245733311402,
237.245469322122,238.245205332842,239.244941343562,240.244677354283,241.244413365003,
242.244149375723,243.243885386443,244.243621397163,245.243357407883,246.243093418603,
247.242829429323,248.242565440044,249.242301450764,250.242037461484,251.241773472204,
252.241509482924,253.241245493644,254.240981504364,255.240717515084,256.240453525805,
257.240189536525,258.239925547245,259.239661557965,260.239397568685,261.239133579405,
262.238869590125,263.238605600846,264.238341611566,265.238077622286,266.237813633006,
267.237549643726,268.237285654446,269.237021665166,270.236757675886,271.236493686607,
272.236229697327,273.235965708047,274.235701718767,275.235437729487,276.235173740207,
277.234909750927,278.234645761647,279.234381772368,280.234117783088,281.233853793808,
282.233589804528,283.233325815248,284.233061825968,285.232797836688,286.232533847408,
287.232269858129,288.232005868849,289.231741879569,290.231477890289,291.231213901009,
292.230949911729,293.230685922449,294.23042193317,295.23015794389,296.22989395461,
297.22962996533,298.22936597605,299.22910198677,300.22883799749,301.22857400821,
302.228310018931,303.228046029651,304.227782040371,305.227518051091,306.227254061811,
307.226990072531,308.226726083251,309.226462093971,310.226198104692,311.225934115412,
312.225670126132,313.225406136852,314.225142147572,315.224878158292,316.224614169012,
317.224350179732,318.224086190453,319.223822201173,320.223558211893,321.223294222613,
322.223030233333,323.222766244053,324.222502254773,325.222238265494,326.221974276214,
327.221710286934,328.221446297654,329.221182308374,330.220918319094,331.220654329814,
332.220390340534,333.220126351255,334.219862361975,335.219598372695,336.219334383415,
337.219070394135,338.218806404855,339.218542415575,340.218278426295,341.218014437016,
342.217750447736,343.217486458456,344.217222469176,345.216958479896,346.216694490616,
347.216430501336,348.216166512056,349.215902522777,350.215638533497,351.215374544217,
352.215110554937,353.214846565657,354.214582576377,355.214318587097,356.214054597817,
357.213790608538,358.213526619258,359.213262629978,360.212998640698,361.212734651418,
362.212470662138,363.212206672858,364.211942683579,365.211678694299,366.211414705019,
367.211150715739,368.210886726459,369.210622737179,370.210358747899,371.210094758619,
372.20983076934,373.20956678006,374.20930279078,375.2090388015,376.20877481222,
377.20851082294,378.20824683366,379.20798284438,380.207718855101,381.207454865821,
382.207190876541,383.206926887261,384.206662897981,385.206398908701,386.206134919421,
387.205870930141,388.205606940862,389.205342951582,390.205078962302,391.204814973022,
392.204550983742,393.204286994462,394.204023005182,395.203759015903,396.203495026623,
397.203231037343,398.202967048063,399.202703058783,400.202439069503,401.202175080223,
402.201911090943,403.201647101664,404.201383112384,405.201119123104,406.200855133824,
407.200591144544,408.200327155264,409.200063165984,410.199799176704,411.199535187425,
412.199271198145,413.199007208865,414.198743219585,415.198479230305,416.198215241025,
417.197951251745,418.197687262465,419.197423273186,420.197159283906,421.196895294626,
422.196631305346,423.196367316066,424.196103326786,425.195839337506,426.195575348226,
427.195311358947,428.195047369667,429.194783380387,430.194519391107,431.194255401827,
432.193991412547,433.193727423267,434.193463433988,435.193199444708,436.192935455428,
437.192671466148,438.192407476868,439.192143487588,440.191879498308,441.191615509028,
442.191351519749,443.191087530469,444.190823541189,445.190559551909,446.190295562629,
447.190031573349,448.189767584069,449.189503594789,450.18923960551,451.18897561623,
452.18871162695,453.18844763767,454.18818364839,455.18791965911,456.18765566983,
457.18739168055,458.187127691271,459.186863701991,460.186599712711,461.186335723431,
462.186071734151,463.185807744871,464.185543755591,465.185279766312,466.185015777032,
467.184751787752,468.184487798472,469.184223809192,470.183959819912,471.183695830632,
472.183431841352,473.183167852073,474.182903862793,475.182639873513,476.182375884233,
477.182111894953,478.181847905673,479.181583916393,480.181319927113,481.181055937834,
482.180791948554,483.180527959274,484.180263969994,485.179999980714,486.179735991434,
487.179472002154,488.179208012874,489.178944023595,490.178680034315,491.178416045035,
492.178152055755,493.177888066475,494.177624077195,495.177360087915,496.177096098636,
497.176832109356,498.176568120076,499.176304130796,500.176040141516,501.175776152236,
502.175512162956,503.175248173676,504.174984184397,505.174720195117,506.174456205837,
507.174192216557,508.173928227277,509.173664237997,510.173400248717,511.173136259437,
512.172872270158,513.172608280878,514.172344291598,515.172080302318,516.171816313038,
517.171552323758,518.171288334478,519.171024345198,520.170760355919,521.170496366639,
522.170232377359,523.169968388079,524.169704398799,525.169440409519,526.169176420239,
527.168912430959,528.16864844168,529.1683844524,530.16812046312,531.16785647384,
532.16759248456,533.16732849528,534.167064506,535.166800516721,536.166536527441,
537.166272538161,538.166008548881,539.165744559601,540.165480570321,541.165216581041,
542.164952591761,543.164688602482,544.164424613202,545.164160623922,546.163896634642,
547.163632645362,548.163368656082,549.163104666802,550.162840677522,551.162576688243,
552.162312698963,553.162048709683,554.161784720403,555.161520731123,556.161256741843,
557.160992752563,558.160728763283,559.160464774004,560.160200784724,561.159936795444,
562.159672806164,563.159408816884,564.159144827604,565.158880838324,566.158616849045,
567.158352859765,568.158088870485,569.157824881205,570.157560891925,571.157296902645,
572.157032913365,573.156768924085,574.156504934806,575.156240945526,576.155976956246,
577.155712966966,578.155448977686,579.155184988406,580.154920999126,581.154657009846,
582.154393020567,583.154129031287,584.153865042007,585.153601052727,586.153337063447,
587.153073074167,588.152809084887,589.152545095607,590.152281106328,591.152017117048,
592.151753127768,593.151489138488,594.151225149208,595.150961159928,596.150697170648,
597.150433181368,598.150169192089,599.149905202809,600.149641213529,601.149377224249,
602.149113234969,603.148849245689,604.148585256409,605.14832126713,606.14805727785,
607.14779328857,608.14752929929,609.14726531001,610.14700132073,611.14673733145,
612.14647334217,613.146209352891,614.145945363611,615.145681374331,616.145417385051,
617.145153395771,618.144889406491,619.144625417211,620.144361427931,621.144097438652,
622.143833449372,623.143569460092,624.143305470812,625.143041481532,626.142777492252,
627.142513502972,628.142249513692,629.141985524413,630.141721535133,631.141457545853,
632.141193556573,633.140929567293,634.140665578013,635.140401588733,636.140137599454,
637.139873610174,638.139609620894,639.139345631614,640.139081642334,641.138817653054,
642.138553663774,643.138289674494,644.138025685215,645.137761695935,646.137497706655,
647.137233717375,648.136969728095,649.136705738815,650.136441749535,651.136177760255,
652.135913770976,653.135649781696,654.135385792416,655.135121803136,656.134857813856,
657.134593824576,658.134329835296,659.134065846016,660.133801856737,661.133537867457,
662.133273878177,663.133009888897,664.132745899617,665.132481910337,666.132217921057,
667.131953931778,668.131689942498,669.131425953218,670.131161963938,671.130897974658,
672.130633985378,673.130369996098,674.130106006818,675.129842017539,676.129578028259,
677.129314038979,678.129050049699,679.128786060419,680.128522071139,681.128258081859,
682.127994092579,683.1277301033,684.12746611402,685.12720212474,686.12693813546,
687.12667414618,688.1264101569,689.12614616762,690.12588217834,691.125618189061,
692.125354199781,693.125090210501,694.124826221221,695.124562231941,696.124298242661,
697.124034253381,698.123770264101,699.123506274822,700.123242285542,701.122978296262,
702.122714306982,703.122450317702,704.122186328422,705.121922339142,706.121658349863,
707.121394360583,708.121130371303,709.120866382023,710.120602392743,711.120338403463,
712.120074414183,713.119810424903,714.119546435624,715.119282446344,716.119018457064,
717.118754467784,718.118490478504,719.118226489224,720.117962499944,721.117698510664,
722.117434521385,723.117170532105,724.116906542825,725.116642553545,726.116378564265,
727.116114574985,728.115850585705,729.115586596425,730.115322607146,731.115058617866,
732.114794628586,733.114530639306,734.114266650026,735.114002660746,736.113738671466,
737.113474682187,738.113210692907,739.112946703627,740.112682714347,741.112418725067,
742.112154735787,743.111890746507,744.111626757227,745.111362767948,746.111098778668,
747.110834789388,748.110570800108,749.110306810828,750.110042821548,751.109778832268,
752.109514842988,753.109250853709,754.108986864429,755.108722875149,756.108458885869,
757.108194896589,758.107930907309,759.107666918029,760.107402928749,761.10713893947,
762.10687495019,763.10661096091,764.10634697163,765.10608298235,766.10581899307,
767.10555500379,768.10529101451,769.105027025231,770.104763035951,771.104499046671,
772.104235057391,773.103971068111,774.103707078831,775.103443089551,776.103179100272,
777.102915110992,778.102651121712,779.102387132432,780.102123143152,781.101859153872,
782.101595164592,783.101331175312,784.101067186033,785.100803196753,786.100539207473,
787.100275218193,788.100011228913,789.099747239633,790.099483250353,791.099219261073,
792.098955271794,793.098691282514,794.098427293234,795.098163303954,796.097899314674,
797.097635325394,798.097371336114,799.097107346834,800.096843357555,801.096579368275,
802.096315378995,803.096051389715,804.095787400435,805.095523411155,806.095259421875,
807.094995432596,808.094731443316,809.094467454036,810.094203464756,811.093939475476,
812.093675486196,813.093411496916,814.093147507636,815.092883518357,816.092619529077,
817.092355539797,818.092091550517,819.091827561237,820.091563571957,821.091299582677,
822.091035593397,823.090771604118,824.090507614838,825.090243625558,826.089979636278,
827.089715646998,828.089451657718,829.089187668438,830.088923679158,831.088659689879,
832.088395700599,833.088131711319,834.087867722039,835.087603732759,836.087339743479,
837.087075754199,838.08681176492,839.08654777564,840.08628378636,841.08601979708,
842.0857558078,843.08549181852,844.08522782924,845.08496383996,846.084699850681,
847.084435861401,848.084171872121,849.083907882841,850.083643893561,851.083379904281,
852.083115915001,853.082851925721,854.082587936442,855.082323947162,856.082059957882,
857.081795968602,858.081531979322,859.081267990042,860.081004000762,861.080740011482,
862.080476022203,863.080212032923,864.079948043643,865.079684054363,866.079420065083,
867.079156075803,868.078892086523,869.078628097243,870.078364107964,871.078100118684,
872.077836129404,873.077572140124,874.077308150844,875.077044161564,876.076780172284,
877.076516183005,878.076252193725,879.075988204445,880.075724215165,881.075460225885,
882.075196236605,883.074932247325,884.074668258045,885.074404268766,886.074140279486,
887.073876290206,888.073612300926,889.073348311646,890.073084322366,891.072820333086,
892.072556343806,893.072292354527,894.072028365247,895.071764375967,896.071500386687,
897.071236397407,898.070972408127,899.070708418847,900.070444429567,901.070180440288,
902.069916451008,903.069652461728,904.069388472448,905.069124483168,906.068860493888,
907.068596504608,908.068332515329,909.068068526049,910.067804536769,911.067540547489,
912.067276558209,913.067012568929,914.066748579649,915.066484590369,916.06622060109,
917.06595661181,918.06569262253,919.06542863325,920.06516464397,921.06490065469,
922.06463666541,923.06437267613,924.064108686851,925.063844697571,926.063580708291,
927.063316719011,928.063052729731,929.062788740451,930.062524751171,931.062260761891,
932.061996772612,933.061732783332,934.061468794052,935.061204804772,936.060940815492,
937.060676826212,938.060412836932,939.060148847652,940.059884858373,941.059620869093,
942.059356879813,943.059092890533,944.058828901253,945.058564911973,946.058300922693,
947.058036933414,948.057772944134,949.057508954854,950.057244965574,951.056980976294,
952.056716987014,953.056452997734,954.056189008454,955.055925019175,956.055661029895,
957.055397040615,958.055133051335,959.054869062055,960.054605072775,961.054341083495,
962.054077094215,963.053813104936,964.053549115656,965.053285126376,966.053021137096,
967.052757147816,968.052493158536,969.052229169256,970.051965179976,971.051701190697,
972.051437201417,973.051173212137,974.050909222857,975.050645233577,976.050381244297,
977.050117255017,978.049853265738,979.049589276458,980.049325287178,981.049061297898,
982.048797308618,983.048533319338,984.048269330058,985.048005340778,986.047741351499,
987.047477362219,988.047213372939,989.046949383659,990.046685394379,991.046421405099,
992.046157415819,993.045893426539,994.04562943726,995.04536544798,996.0451014587,
997.04483746942,998.04457348014,999.04430949086,1000.04404550158,1001.0437815123,
1002.04351752302,1003.04325353374,1004.04298954446,1005.04272555518,1006.0424615659,
1007.04219757662,1008.04193358734,1009.04166959806,1010.04140560878,1011.0411416195,
1012.04087763022,1013.04061364094,1014.04034965166,1015.04008566238,1016.0398216731,
1017.03955768382,1018.03929369454,1019.03902970526,1020.03876571598,1021.0385017267,
1022.03823773742,1023.03797374814,1024.03770975886,1025.03744576958,1026.0371817803,
1027.03691779102,1028.03665380174,1029.03638981246,1030.03612582318,1031.0358618339,
1032.03559784462,1033.03533385534,1034.03506986606,1035.03480587678,1036.03454188751,
1037.03427789823,1038.03401390895,1039.03374991967,1040.03348593039,1041.03322194111,
1042.03295795183,1043.03269396255,1044.03242997327,1045.03216598399,1046.03190199471,
1047.03163800543,1048.03137401615,1049.03111002687,1050.03084603759,1051.03058204831,
1052.03031805903,1053.03005406975,1054.02979008047,1055.02952609119,1056.02926210191,
1057.02899811263,1058.02873412335,1059.02847013407,1060.02820614479,1061.02794215551,
1062.02767816623,1063.02741417695,1064.02715018767,1065.02688619839,1066.02662220911,
1067.02635821983,1068.02609423055,1069.02583024127,1070.02556625199,1071.02530226271,
1072.02503827343,1073.02477428415,1074.02451029487,1075.02424630559,1076.02398231631,
1077.02371832703,1078.02345433775,1079.02319034847,1080.02292635919,1081.02266236991,
1082.02239838063,1083.02213439135,1084.02187040207,1085.02160641279,1086.02134242351,
1087.02107843423,1088.02081444495,1089.02055045567,1090.02028646639,1091.02002247711,
1092.01975848783,1093.01949449855,1094.01923050927,1095.01896651999,1096.01870253071,
1097.01843854143,1098.01817455215,1099.01791056287,1100.01764657359,1101.01738258431,
1102.01711859503,1103.01685460575,1104.01659061647,1105.01632662719,1106.01606263791,
1107.01579864863,1108.01553465935,1109.01527067007,1110.01500668079,1111.01474269151,
1112.01447870223,1113.01421471295,1114.01395072368,1115.0136867344,1116.01342274512,
1117.01315875584,1118.01289476656,1119.01263077728,1120.012366788,1121.01210279872,
1122.01183880944,1123.01157482016,1124.01131083088,1125.0110468416,1126.01078285232,
1127.01051886304,1128.01025487376,1129.00999088448,1130.0097268952,1131.00946290592,
1132.00919891664,1133.00893492736,1134.00867093808,1135.0084069488,1136.00814295952,
1137.00787897024,1138.00761498096,1139.00735099168,1140.0070870024,1141.00682301312,
1142.00655902384,1143.00629503456,1144.00603104528,1145.005767056,1146.00550306672,
1147.00523907744,1148.00497508816,1149.00471109888,1150.0044471096,1151.00418312032,
1152.00391913104,1153.00365514176,1154.00339115248,1155.0031271632,1156.00286317392,
1157.00259918464,1158.00233519536,1159.00207120608,1160.0018072168,1161.00154322752,
1162.00127923824,1163.00101524896,1164.00075125968,1165.0004872704,1166.00022328112,
1166.99995929184,1167.99969530256,1168.99943131328,1169.999167324,1170.99890333472,
1171.99863934544,1172.99837535616,1173.99811136688,1174.9978473776,1175.99758338832,
1176.99731939904,1177.99705540976,1178.99679142048,1179.9965274312,1180.99626344192,
1181.99599945264,1182.99573546336,1183.99547147408,1184.9952074848,1185.99494349552,
1186.99467950624,1187.99441551696,1188.99415152768,1189.99388753841,1190.99362354913,
1191.99335955985,1192.99309557057,1193.99283158129,1194.99256759201,1195.99230360273,
1196.99203961345,1197.99177562417,1198.99151163489,1199.99124764561,1200.99098365633,
1201.99071966705,1202.99045567777,1203.99019168849,1204.98992769921,1205.98966370993,
1206.98939972065,1207.98913573137,1208.98887174209,1209.98860775281,1210.98834376353,
1211.98807977425,1212.98781578497,1213.98755179569,1214.98728780641,1215.98702381713,
1216.98675982785,1217.98649583857,1218.98623184929,1219.98596786001,1220.98570387073,
1221.98543988145,1222.98517589217,1223.98491190289,1224.98464791361,1225.98438392433,
1226.98411993505,1227.98385594577,1228.98359195649,1229.98332796721,1230.98306397793,
1231.98279998865,1232.98253599937,1233.98227201009,1234.98200802081,1235.98174403153,
1236.98148004225,1237.98121605297,1238.98095206369,1239.98068807441,1240.98042408513,
1241.98016009585,1242.97989610657,1243.97963211729,1244.97936812801,1245.97910413873,
1246.97884014945,1247.97857616017,1248.97831217089,1249.97804818161,1250.97778419233,
1251.97752020305,1252.97725621377,1253.97699222449,1254.97672823521,1255.97646424593,
1256.97620025665,1257.97593626737,1258.97567227809,1259.97540828881,1260.97514429953,
1261.97488031025,1262.97461632097,1263.97435233169,1264.97408834241,1265.97382435313,
1266.97356036385,1267.97329637458,1268.9730323853,1269.97276839602,1270.97250440674,
1271.97224041746,1272.97197642818,1273.9717124389,1274.97144844962,1275.97118446034,
1276.97092047106,1277.97065648178,1278.9703924925,1279.97012850322,1280.96986451394,
1281.96960052466,1282.96933653538,1283.9690725461,1284.96880855682,1285.96854456754,
1286.96828057826,1287.96801658898,1288.9677525997,1289.96748861042,1290.96722462114,
1291.96696063186,1292.96669664258,1293.9664326533,1294.96616866402,1295.96590467474,
1296.96564068546,1297.96537669618,1298.9651127069,1299.96484871762,1300.96458472834,
1301.96432073906,1302.96405674978,1303.9637927605,1304.96352877122,1305.96326478194,
1306.96300079266,1307.96273680338,1308.9624728141,1309.96220882482,1310.96194483554,
1311.96168084626,1312.96141685698,1313.9611528677,1314.96088887842,1315.96062488914,
1316.96036089986,1317.96009691058,1318.9598329213,1319.95956893202,1320.95930494274,
1321.95904095346,1322.95877696418,1323.9585129749,1324.95824898562,1325.95798499634,
1326.95772100706,1327.95745701778,1328.9571930285,1329.95692903922,1330.95666504994,
1331.95640106066,1332.95613707138,1333.9558730821,1334.95560909282,1335.95534510354,
1336.95508111426,1337.95481712498,1338.9545531357,1339.95428914642,1340.95402515714,
1341.95376116786,1342.95349717858,1343.9532331893,1344.95296920002,1345.95270521075,
1346.95244122147,1347.95217723219,1348.95191324291,1349.95164925363,1350.95138526435,
1351.95112127507,1352.95085728579,1353.95059329651,1354.95032930723,1355.95006531795,
1356.94980132867,1357.94953733939,1358.94927335011,1359.94900936083,1360.94874537155,
1361.94848138227,1362.94821739299,1363.94795340371,1364.94768941443,1365.94742542515,
1366.94716143587,1367.94689744659,1368.94663345731,1369.94636946803,1370.94610547875,
1371.94584148947,1372.94557750019,1373.94531351091,1374.94504952163,1375.94478553235,
1376.94452154307,1377.94425755379,1378.94399356451,1379.94372957523,1380.94346558595,
1381.94320159667,1382.94293760739,1383.94267361811,1384.94240962883,1385.94214563955,
1386.94188165027,1387.94161766099,1388.94135367171,1389.94108968243,1390.94082569315,
1391.94056170387,1392.94029771459,1393.94003372531,1394.93976973603,1395.93950574675,
1396.93924175747,1397.93897776819,1398.93871377891,1399.93844978963,1400.93818580035,
1401.93792181107,1402.93765782179,1403.93739383251,1404.93712984323,1405.93686585395,
1406.93660186467,1407.93633787539,1408.93607388611,1409.93580989683,1410.93554590755,
1411.93528191827,1412.93501792899,1413.93475393971,1414.93448995043,1415.93422596115,
1416.93396197187,1417.93369798259,1418.93343399331,1419.93317000403,1420.93290601475,
1421.93264202547,1422.93237803619,1423.93211404692,1424.93185005764,1425.93158606836,
1426.93132207908,1427.9310580898,1428.93079410052,1429.93053011124,1430.93026612196,
1431.93000213268,1432.9297381434,1433.92947415412,1434.92921016484,1435.92894617556,
1436.92868218628,1437.928418197,1438.92815420772,1439.92789021844,1440.92762622916,
1441.92736223988,1442.9270982506,1443.92683426132,1444.92657027204,1445.92630628276,
1446.92604229348,1447.9257783042,1448.92551431492,1449.92525032564,1450.92498633636,
1451.92472234708,1452.9244583578,1453.92419436852,1454.92393037924,1455.92366638996,
1456.92340240068,1457.9231384114,1458.92287442212,1459.92261043284,1460.92234644356,
1461.92208245428,1462.921818465,1463.92155447572,1464.92129048644,1465.92102649716,
1466.92076250788,1467.9204985186,1468.92023452932,1469.91997054004,1470.91970655076,
1471.91944256148,1472.9191785722,1473.91891458292,1474.91865059364,1475.91838660436,
1476.91812261508,1477.9178586258,1478.91759463652,1479.91733064724,1480.91706665796,
1481.91680266868,1482.9165386794,1483.91627469012,1484.91601070084,1485.91574671156,
1486.91548272228,1487.915218733,1488.91495474372,1489.91469075444,1490.91442676516,
1491.91416277588,1492.9138987866,1493.91363479732,1494.91337080804,1495.91310681876,
1496.91284282948,1497.9125788402,1498.91231485092,1499.91205086164,1500.91178687236,
1501.91152288309,1502.91125889381,1503.91099490453,1504.91073091525,1505.91046692597,
1506.91020293669,1507.90993894741,1508.90967495813,1509.90941096885,1510.90914697957,
1511.90888299029,1512.90861900101,1513.90835501173,1514.90809102245,1515.90782703317,
1516.90756304389,1517.90729905461,1518.90703506533,1519.90677107605,1520.90650708677,
1521.90624309749,1522.90597910821,1523.90571511893,1524.90545112965,1525.90518714037,
1526.90492315109,1527.90465916181,1528.90439517253,1529.90413118325,1530.90386719397,
1531.90360320469,1532.90333921541,1533.90307522613,1534.90281123685,1535.90254724757,
1536.90228325829,1537.90201926901,1538.90175527973,1539.90149129045,1540.90122730117,
1541.90096331189,1542.90069932261,1543.90043533333,1544.90017134405,1545.89990735477,
1546.89964336549,1547.89937937621,1548.89911538693,1549.89885139765,1550.89858740837,
1551.89832341909,1552.89805942981,1553.89779544053,1554.89753145125,1555.89726746197,
1556.89700347269,1557.89673948341,1558.89647549413,1559.89621150485,1560.89594751557,
1561.89568352629,1562.89541953701,1563.89515554773,1564.89489155845,1565.89462756917,
1566.89436357989,1567.89409959061,1568.89383560133,1569.89357161205,1570.89330762277,
1571.89304363349,1572.89277964421,1573.89251565493,1574.89225166565,1575.89198767637,
1576.89172368709,1577.89145969781,1578.89119570853,1579.89093171926,1580.89066772998,
1581.8904037407,1582.89013975142,1583.88987576214,1584.88961177286,1585.88934778358,
1586.8890837943,1587.88881980502,1588.88855581574,1589.88829182646,1590.88802783718,
1591.8877638479,1592.88749985862,1593.88723586934,1594.88697188006,1595.88670789078,
1596.8864439015,1597.88617991222,1598.88591592294,1599.88565193366,1600.88538794438,
1601.8851239551,1602.88485996582,1603.88459597654,1604.88433198726,1605.88406799798,
1606.8838040087,1607.88354001942,1608.88327603014,1609.88301204086,1610.88274805158,
1611.8824840623,1612.88222007302,1613.88195608374,1614.88169209446,1615.88142810518,
1616.8811641159,1617.88090012662,1618.88063613734,1619.88037214806,1620.88010815878,
1621.8798441695,1622.87958018022,1623.87931619094,1624.87905220166,1625.87878821238,
1626.8785242231,1627.87826023382,1628.87799624454,1629.87773225526,1630.87746826598,
1631.8772042767,1632.87694028742,1633.87667629814,1634.87641230886,1635.87614831958,
1636.8758843303,1637.87562034102,1638.87535635174,1639.87509236246,1640.87482837318,
1641.8745643839,1642.87430039462,1643.87403640534,1644.87377241606,1645.87350842678,
1646.8732444375,1647.87298044822,1648.87271645894,1649.87245246966,1650.87218848038,
1651.8719244911,1652.87166050182,1653.87139651254,1654.87113252326,1655.87086853399,
1656.8706045447,1657.87034055543,1658.87007656615,1659.86981257687,1660.86954858759,
1661.86928459831,1662.86902060903,1663.86875661975,1664.86849263047,1665.86822864119,
1666.86796465191,1667.86770066263,1668.86743667335,1669.86717268407,1670.86690869479,
1671.86664470551,1672.86638071623,1673.86611672695,1674.86585273767,1675.86558874839,
1676.86532475911,1677.86506076983,1678.86479678055,1679.86453279127,1680.86426880199,
1681.86400481271,1682.86374082343,1683.86347683415,1684.86321284487,1685.86294885559,
1686.86268486631,1687.86242087703,1688.86215688775,1689.86189289847,1690.86162890919,
1691.86136491991,1692.86110093063,1693.86083694135,1694.86057295207,1695.86030896279,
1696.86004497351,1697.35991297887,1697.85988790214),.UNSPECIFIED.);
#54=B_SPLINE_SURFACE_WITH_KNOTS('',3,3,((#254642,#254643,#254644,#254645,
#254646,#254647,#254648,#254649,#254650,#254651,#254652,#254653,#254654,
#254655,#254656,#254657,#254658,#254659,#254660,#254661,#254662,#254663,
#254664,#254665,#254666,#254667,#254668,#254669,#254670,#254671,#254672,
#254673,#254674,#254675,#254676,#254677,#254678,#254679,#254680,#254681,
#254682,#254683,#254684,#254685,#254686,#254687,#254688,#254689,#254690,
#254691,#254692,#254693,#254694,#254695,#254696,#254697,#254698,#254699,
#254700,#254701,#254702,#254703,#254704,#254705,#254706,#254707,#254708,
#254709,#254710,#254711,#254712,#254713,#254714,#254715,#254716,#254717,
#254718,#254719,#254720,#254721,#254722,#254723,#254724,#254725,#254726,
#254727,#254728,#254729,#254730,#254731,#254732,#254733,#254734,#254735,
#254736,#254737,#254738,#254739,#254740,#254741,#254742,#254743,#254744,
#254745,#254746,#254747,#254748,#254749,#254750,#254751,#254752,#254753,
#254754,#254755,#254756,#254757,#254758,#254759,#254760,#254761,#254762,
#254763,#254764,#254765,#254766,#254767,#254768,#254769,#254770,#254771,
#254772,#254773,#254774,#254775,#254776,#254777,#254778,#254779,#254780,
#254781,#254782,#254783,#254784,#254785,#254786,#254787,#254788,#254789,
#254790,#254791,#254792,#254793,#254794,#254795,#254796,#254797,#254798,
#254799,#254800,#254801,#254802,#254803,#254804,#254805,#254806,#254807,
#254808,#254809,#254810,#254811,#254812,#254813,#254814,#254815,#254816,
#254817,#254818,#254819,#254820,#254821,#254822,#254823,#254824,#254825,
#254826,#254827,#254828,#254829,#254830,#254831,#254832,#254833,#254834,
#254835,#254836,#254837,#254838,#254839,#254840,#254841,#254842,#254843,
#254844,#254845,#254846,#254847,#254848,#254849,#254850,#254851,#254852,
#254853,#254854,#254855,#254856,#254857,#254858,#254859,#254860,#254861,
#254862,#254863,#254864,#254865,#254866,#254867,#254868,#254869,#254870,
#254871,#254872,#254873,#254874,#254875,#254876,#254877,#254878,#254879,
#254880,#254881,#254882,#254883,#254884,#254885,#254886,#254887,#254888,
#254889,#254890,#254891,#254892,#254893,#254894,#254895,#254896,#254897,
#254898,#254899,#254900,#254901,#254902,#254903,#254904,#254905,#254906,
#254907,#254908,#254909,#254910,#254911,#254912,#254913,#254914,#254915,
#254916,#254917,#254918,#254919,#254920,#254921,#254922,#254923,#254924,
#254925,#254926,#254927,#254928,#254929,#254930,#254931,#254932,#254933,
#254934,#254935,#254936,#254937,#254938,#254939,#254940,#254941,#254942,
#254943,#254944,#254945,#254946,#254947,#254948,#254949,#254950,#254951,
#254952,#254953,#254954,#254955,#254956,#254957,#254958,#254959,#254960,
#254961,#254962,#254963,#254964,#254965,#254966,#254967,#254968,#254969,
#254970,#254971,#254972,#254973,#254974,#254975,#254976,#254977,#254978,
#254979,#254980,#254981,#254982,#254983,#254984,#254985,#254986,#254987,
#254988,#254989,#254990,#254991,#254992,#254993,#254994,#254995,#254996,
#254997,#254998,#254999,#255000,#255001,#255002,#255003,#255004,#255005,
#255006,#255007,#255008,#255009,#255010,#255011,#255012,#255013,#255014,
#255015,#255016,#255017,#255018,#255019,#255020,#255021,#255022,#255023,
#255024,#255025,#255026,#255027,#255028,#255029,#255030,#255031,#255032,
#255033,#255034,#255035,#255036,#255037,#255038,#255039,#255040,#255041,
#255042,#255043,#255044,#255045,#255046,#255047,#255048,#255049,#255050,
#255051,#255052,#255053,#255054,#255055,#255056,#255057,#255058,#255059,
#255060,#255061,#255062,#255063,#255064,#255065,#255066,#255067,#255068,
#255069,#255070,#255071,#255072,#255073,#255074,#255075,#255076,#255077,
#255078,#255079,#255080,#255081,#255082,#255083,#255084,#255085,#255086,
#255087,#255088,#255089,#255090,#255091,#255092,#255093,#255094,#255095,
#255096,#255097,#255098,#255099,#255100,#255101,#255102,#255103,#255104,
#255105,#255106,#255107,#255108,#255109,#255110,#255111,#255112,#255113,
#255114,#255115,#255116,#255117,#255118,#255119,#255120,#255121,#255122,
#255123,#255124,#255125,#255126,#255127,#255128,#255129,#255130,#255131,
#255132,#255133,#255134,#255135,#255136,#255137,#255138,#255139,#255140,
#255141,#255142,#255143,#255144,#255145,#255146,#255147,#255148,#255149,
#255150,#255151,#255152,#255153,#255154,#255155,#255156,#255157,#255158,
#255159,#255160,#255161,#255162,#255163,#255164,#255165,#255166,#255167,
#255168,#255169,#255170,#255171,#255172,#255173,#255174,#255175,#255176,
#255177,#255178,#255179,#255180,#255181,#255182,#255183,#255184,#255185,
#255186,#255187,#255188,#255189,#255190,#255191,#255192,#255193,#255194,
#255195,#255196,#255197,#255198,#255199,#255200,#255201,#255202,#255203,
#255204,#255205,#255206,#255207,#255208,#255209,#255210,#255211,#255212,
#255213,#255214,#255215,#255216,#255217,#255218,#255219,#255220,#255221,
#255222,#255223,#255224,#255225,#255226,#255227,#255228,#255229,#255230,
#255231,#255232,#255233,#255234,#255235,#255236,#255237,#255238,#255239,
#255240,#255241,#255242,#255243,#255244,#255245,#255246,#255247,#255248,
#255249,#255250,#255251,#255252,#255253,#255254,#255255,#255256,#255257,
#255258,#255259,#255260,#255261,#255262,#255263,#255264,#255265,#255266,
#255267,#255268,#255269,#255270,#255271,#255272,#255273,#255274,#255275,
#255276,#255277,#255278,#255279,#255280,#255281,#255282,#255283,#255284,
#255285,#255286,#255287,#255288,#255289,#255290,#255291,#255292,#255293,
#255294,#255295,#255296,#255297,#255298,#255299,#255300,#255301,#255302,
#255303,#255304,#255305,#255306,#255307,#255308,#255309,#255310,#255311,
#255312,#255313,#255314,#255315,#255316,#255317,#255318,#255319,#255320,
#255321,#255322,#255323,#255324,#255325,#255326,#255327,#255328,#255329,
#255330,#255331,#255332,#255333,#255334,#255335,#255336,#255337,#255338,
#255339,#255340,#255341,#255342,#255343,#255344,#255345,#255346,#255347,
#255348,#255349,#255350,#255351,#255352,#255353,#255354,#255355,#255356,
#255357,#255358,#255359,#255360,#255361,#255362,#255363,#255364,#255365,
#255366,#255367,#255368,#255369,#255370,#255371,#255372,#255373,#255374,
#255375,#255376,#255377,#255378,#255379,#255380,#255381,#255382,#255383,
#255384,#255385,#255386,#255387,#255388,#255389,#255390,#255391,#255392,
#255393,#255394,#255395,#255396,#255397,#255398,#255399,#255400,#255401,
#255402,#255403,#255404,#255405,#255406,#255407,#255408,#255409,#255410,
#255411,#255412,#255413,#255414,#255415,#255416,#255417,#255418,#255419,
#255420,#255421,#255422,#255423,#255424,#255425,#255426,#255427,#255428,
#255429,#255430,#255431,#255432,#255433,#255434,#255435,#255436,#255437,
#255438,#255439,#255440,#255441,#255442,#255443,#255444,#255445,#255446,
#255447,#255448,#255449,#255450,#255451,#255452,#255453,#255454,#255455,
#255456,#255457,#255458,#255459,#255460,#255461,#255462,#255463,#255464,
#255465,#255466,#255467,#255468,#255469,#255470,#255471,#255472,#255473,
#255474,#255475,#255476,#255477,#255478,#255479,#255480,#255481,#255482,
#255483,#255484,#255485,#255486,#255487,#255488,#255489,#255490,#255491,
#255492,#255493,#255494,#255495,#255496,#255497,#255498,#255499,#255500,
#255501,#255502,#255503,#255504,#255505,#255506,#255507,#255508,#255509,
#255510,#255511,#255512,#255513,#255514,#255515,#255516,#255517,#255518,
#255519,#255520,#255521,#255522,#255523,#255524,#255525,#255526,#255527,
#255528,#255529,#255530,#255531,#255532,#255533,#255534,#255535,#255536,
#255537,#255538,#255539,#255540,#255541,#255542,#255543,#255544,#255545,
#255546,#255547,#255548,#255549,#255550,#255551,#255552,#255553,#255554,
#255555,#255556,#255557,#255558,#255559,#255560,#255561,#255562,#255563,
#255564,#255565,#255566,#255567,#255568,#255569,#255570,#255571,#255572,
#255573,#255574,#255575,#255576,#255577,#255578,#255579,#255580,#255581,
#255582,#255583,#255584,#255585,#255586,#255587,#255588,#255589,#255590,
#255591,#255592,#255593,#255594,#255595,#255596,#255597,#255598,#255599,
#255600,#255601,#255602,#255603,#255604,#255605,#255606,#255607,#255608,
#255609,#255610,#255611,#255612,#255613,#255614,#255615,#255616,#255617,
#255618,#255619,#255620,#255621,#255622,#255623,#255624,#255625,#255626,
#255627,#255628,#255629,#255630,#255631,#255632,#255633,#255634,#255635,
#255636,#255637,#255638,#255639,#255640,#255641,#255642,#255643,#255644,
#255645,#255646,#255647,#255648,#255649,#255650,#255651,#255652,#255653,
#255654,#255655,#255656,#255657,#255658,#255659,#255660,#255661,#255662,
#255663,#255664,#255665,#255666,#255667,#255668,#255669,#255670,#255671,
#255672,#255673,#255674,#255675,#255676,#255677,#255678,#255679,#255680,
#255681,#255682,#255683,#255684,#255685,#255686,#255687,#255688,#255689,
#255690,#255691,#255692,#255693,#255694,#255695,#255696,#255697,#255698,
#255699,#255700,#255701,#255702,#255703,#255704,#255705,#255706,#255707,
#255708,#255709,#255710,#255711,#255712,#255713,#255714,#255715,#255716,
#255717,#255718,#255719,#255720,#255721,#255722,#255723,#255724,#255725,
#255726,#255727,#255728,#255729,#255730,#255731,#255732,#255733,#255734,
#255735,#255736,#255737,#255738,#255739,#255740,#255741,#255742,#255743,
#255744,#255745,#255746,#255747,#255748,#255749,#255750,#255751,#255752,
#255753,#255754,#255755,#255756,#255757,#255758,#255759,#255760,#255761,
#255762,#255763,#255764,#255765,#255766,#255767,#255768,#255769,#255770,
#255771,#255772,#255773,#255774,#255775,#255776,#255777,#255778,#255779,
#255780,#255781,#255782,#255783,#255784,#255785,#255786,#255787,#255788,
#255789,#255790,#255791,#255792,#255793,#255794,#255795,#255796,#255797,
#255798,#255799,#255800,#255801,#255802,#255803,#255804,#255805,#255806,
#255807,#255808,#255809,#255810,#255811,#255812,#255813,#255814,#255815,
#255816,#255817,#255818,#255819,#255820,#255821,#255822,#255823,#255824,
#255825,#255826,#255827,#255828,#255829,#255830,#255831,#255832,#255833,
#255834,#255835,#255836,#255837,#255838,#255839,#255840,#255841,#255842,
#255843,#255844,#255845,#255846,#255847,#255848,#255849,#255850,#255851,
#255852,#255853,#255854,#255855,#255856,#255857,#255858,#255859,#255860,
#255861,#255862,#255863,#255864,#255865,#255866,#255867,#255868,#255869,
#255870,#255871,#255872,#255873,#255874,#255875,#255876,#255877,#255878,
#255879,#255880,#255881,#255882,#255883,#255884,#255885,#255886,#255887,
#255888,#255889,#255890,#255891,#255892,#255893,#255894,#255895,#255896,
#255897,#255898,#255899,#255900,#255901,#255902,#255903,#255904,#255905,
#255906,#255907,#255908,#255909,#255910,#255911,#255912,#255913,#255914,
#255915,#255916,#255917,#255918,#255919,#255920,#255921,#255922,#255923,
#255924,#255925,#255926,#255927,#255928,#255929,#255930,#255931,#255932,
#255933,#255934,#255935,#255936,#255937,#255938,#255939,#255940,#255941,
#255942,#255943,#255944,#255945,#255946,#255947,#255948,#255949,#255950,
#255951,#255952,#255953,#255954,#255955,#255956,#255957,#255958,#255959,
#255960,#255961,#255962,#255963,#255964,#255965,#255966,#255967,#255968,
#255969,#255970,#255971,#255972,#255973,#255974,#255975,#255976,#255977,
#255978,#255979,#255980,#255981,#255982,#255983,#255984,#255985,#255986,
#255987,#255988,#255989,#255990,#255991,#255992,#255993,#255994,#255995,
#255996,#255997,#255998,#255999,#256000,#256001,#256002,#256003,#256004,
#256005,#256006,#256007,#256008,#256009,#256010,#256011,#256012,#256013,
#256014,#256015,#256016,#256017,#256018,#256019,#256020,#256021,#256022,
#256023,#256024,#256025,#256026,#256027,#256028,#256029,#256030,#256031,
#256032,#256033,#256034,#256035,#256036,#256037,#256038,#256039,#256040,
#256041,#256042,#256043,#256044,#256045,#256046,#256047,#256048,#256049,
#256050,#256051,#256052,#256053,#256054,#256055,#256056,#256057,#256058,
#256059,#256060,#256061,#256062,#256063,#256064,#256065,#256066,#256067,
#256068,#256069,#256070,#256071,#256072,#256073,#256074,#256075,#256076,
#256077,#256078,#256079,#256080,#256081,#256082,#256083,#256084,#256085,
#256086,#256087,#256088,#256089,#256090,#256091,#256092,#256093,#256094,
#256095,#256096,#256097,#256098,#256099,#256100,#256101,#256102,#256103,
#256104,#256105,#256106,#256107,#256108,#256109,#256110,#256111,#256112,
#256113,#256114,#256115,#256116,#256117,#256118,#256119,#256120,#256121,
#256122,#256123,#256124,#256125,#256126,#256127,#256128,#256129,#256130,
#256131,#256132,#256133,#256134,#256135,#256136,#256137,#256138,#256139,
#256140,#256141,#256142,#256143,#256144,#256145,#256146,#256147,#256148,
#256149,#256150,#256151,#256152,#256153,#256154,#256155,#256156,#256157,
#256158,#256159,#256160,#256161,#256162,#256163,#256164,#256165,#256166,
#256167,#256168,#256169,#256170,#256171,#256172,#256173,#256174,#256175,
#256176,#256177,#256178,#256179,#256180,#256181,#256182,#256183,#256184,
#256185,#256186,#256187,#256188,#256189,#256190,#256191,#256192,#256193,
#256194,#256195,#256196,#256197,#256198,#256199,#256200,#256201,#256202,
#256203,#256204,#256205,#256206,#256207,#256208,#256209,#256210,#256211,
#256212,#256213,#256214,#256215,#256216,#256217,#256218,#256219,#256220,
#256221,#256222,#256223,#256224,#256225,#256226,#256227,#256228,#256229,
#256230,#256231,#256232,#256233,#256234,#256235,#256236,#256237,#256238,
#256239,#256240,#256241,#256242,#256243,#256244,#256245,#256246,#256247,
#256248,#256249,#256250,#256251,#256252,#256253,#256254,#256255,#256256,
#256257,#256258,#256259,#256260,#256261,#256262,#256263,#256264,#256265,
#256266,#256267,#256268,#256269,#256270,#256271,#256272,#256273,#256274,
#256275,#256276,#256277,#256278,#256279,#256280,#256281,#256282,#256283,
#256284,#256285,#256286,#256287,#256288,#256289,#256290,#256291,#256292,
#256293,#256294,#256295,#256296,#256297,#256298,#256299,#256300,#256301,
#256302,#256303,#256304,#256305,#256306,#256307,#256308,#256309,#256310,
#256311,#256312,#256313,#256314,#256315,#256316,#256317,#256318,#256319,
#256320,#256321,#256322,#256323,#256324,#256325,#256326,#256327,#256328,
#256329,#256330,#256331,#256332,#256333,#256334,#256335,#256336),(#256337,
#256338,#256339,#256340,#256341,#256342,#256343,#256344,#256345,#256346,
#256347,#256348,#256349,#256350,#256351,#256352,#256353,#256354,#256355,
#256356,#256357,#256358,#256359,#256360,#256361,#256362,#256363,#256364,
#256365,#256366,#256367,#256368,#256369,#256370,#256371,#256372,#256373,
#256374,#256375,#256376,#256377,#256378,#256379,#256380,#256381,#256382,
#256383,#256384,#256385,#256386,#256387,#256388,#256389,#256390,#256391,
#256392,#256393,#256394,#256395,#256396,#256397,#256398,#256399,#256400,
#256401,#256402,#256403,#256404,#256405,#256406,#256407,#256408,#256409,
#256410,#256411,#256412,#256413,#256414,#256415,#256416,#256417,#256418,
#256419,#256420,#256421,#256422,#256423,#256424,#256425,#256426,#256427,
#256428,#256429,#256430,#256431,#256432,#256433,#256434,#256435,#256436,
#256437,#256438,#256439,#256440,#256441,#256442,#256443,#256444,#256445,
#256446,#256447,#256448,#256449,#256450,#256451,#256452,#256453,#256454,
#256455,#256456,#256457,#256458,#256459,#256460,#256461,#256462,#256463,
#256464,#256465,#256466,#256467,#256468,#256469,#256470,#256471,#256472,
#256473,#256474,#256475,#256476,#256477,#256478,#256479,#256480,#256481,
#256482,#256483,#256484,#256485,#256486,#256487,#256488,#256489,#256490,
#256491,#256492,#256493,#256494,#256495,#256496,#256497,#256498,#256499,
#256500,#256501,#256502,#256503,#256504,#256505,#256506,#256507,#256508,
#256509,#256510,#256511,#256512,#256513,#256514,#256515,#256516,#256517,
#256518,#256519,#256520,#256521,#256522,#256523,#256524,#256525,#256526,
#256527,#256528,#256529,#256530,#256531,#256532,#256533,#256534,#256535,
#256536,#256537,#256538,#256539,#256540,#256541,#256542,#256543,#256544,
#256545,#256546,#256547,#256548,#256549,#256550,#256551,#256552,#256553,
#256554,#256555,#256556,#256557,#256558,#256559,#256560,#256561,#256562,
#256563,#256564,#256565,#256566,#256567,#256568,#256569,#256570,#256571,
#256572,#256573,#256574,#256575,#256576,#256577,#256578,#256579,#256580,
#256581,#256582,#256583,#256584,#256585,#256586,#256587,#256588,#256589,
#256590,#256591,#256592,#256593,#256594,#256595,#256596,#256597,#256598,
#256599,#256600,#256601,#256602,#256603,#256604,#256605,#256606,#256607,
#256608,#256609,#256610,#256611,#256612,#256613,#256614,#256615,#256616,
#256617,#256618,#256619,#256620,#256621,#256622,#256623,#256624,#256625,
#256626,#256627,#256628,#256629,#256630,#256631,#256632,#256633,#256634,
#256635,#256636,#256637,#256638,#256639,#256640,#256641,#256642,#256643,
#256644,#256645,#256646,#256647,#256648,#256649,#256650,#256651,#256652,
#256653,#256654,#256655,#256656,#256657,#256658,#256659,#256660,#256661,
#256662,#256663,#256664,#256665,#256666,#256667,#256668,#256669,#256670,
#256671,#256672,#256673,#256674,#256675,#256676,#256677,#256678,#256679,
#256680,#256681,#256682,#256683,#256684,#256685,#256686,#256687,#256688,
#256689,#256690,#256691,#256692,#256693,#256694,#256695,#256696,#256697,
#256698,#256699,#256700,#256701,#256702,#256703,#256704,#256705,#256706,
#256707,#256708,#256709,#256710,#256711,#256712,#256713,#256714,#256715,
#256716,#256717,#256718,#256719,#256720,#256721,#256722,#256723,#256724,
#256725,#256726,#256727,#256728,#256729,#256730,#256731,#256732,#256733,
#256734,#256735,#256736,#256737,#256738,#256739,#256740,#256741,#256742,
#256743,#256744,#256745,#256746,#256747,#256748,#256749,#256750,#256751,
#256752,#256753,#256754,#256755,#256756,#256757,#256758,#256759,#256760,
#256761,#256762,#256763,#256764,#256765,#256766,#256767,#256768,#256769,
#256770,#256771,#256772,#256773,#256774,#256775,#256776,#256777,#256778,
#256779,#256780,#256781,#256782,#256783,#256784,#256785,#256786,#256787,
#256788,#256789,#256790,#256791,#256792,#256793,#256794,#256795,#256796,
#256797,#256798,#256799,#256800,#256801,#256802,#256803,#256804,#256805,
#256806,#256807,#256808,#256809,#256810,#256811,#256812,#256813,#256814,
#256815,#256816,#256817,#256818,#256819,#256820,#256821,#256822,#256823,
#256824,#256825,#256826,#256827,#256828,#256829,#256830,#256831,#256832,
#256833,#256834,#256835,#256836,#256837,#256838,#256839,#256840,#256841,
#256842,#256843,#256844,#256845,#256846,#256847,#256848,#256849,#256850,
#256851,#256852,#256853,#256854,#256855,#256856,#256857,#256858,#256859,
#256860,#256861,#256862,#256863,#256864,#256865,#256866,#256867,#256868,
#256869,#256870,#256871,#256872,#256873,#256874,#256875,#256876,#256877,
#256878,#256879,#256880,#256881,#256882,#256883,#256884,#256885,#256886,
#256887,#256888,#256889,#256890,#256891,#256892,#256893,#256894,#256895,
#256896,#256897,#256898,#256899,#256900,#256901,#256902,#256903,#256904,
#256905,#256906,#256907,#256908,#256909,#256910,#256911,#256912,#256913,
#256914,#256915,#256916,#256917,#256918,#256919,#256920,#256921,#256922,
#256923,#256924,#256925,#256926,#256927,#256928,#256929,#256930,#256931,
#256932,#256933,#256934,#256935,#256936,#256937,#256938,#256939,#256940,
#256941,#256942,#256943,#256944,#256945,#256946,#256947,#256948,#256949,
#256950,#256951,#256952,#256953,#256954,#256955,#256956,#256957,#256958,
#256959,#256960,#256961,#256962,#256963,#256964,#256965,#256966,#256967,
#256968,#256969,#256970,#256971,#256972,#256973,#256974,#256975,#256976,
#256977,#256978,#256979,#256980,#256981,#256982,#256983,#256984,#256985,
#256986,#256987,#256988,#256989,#256990,#256991,#256992,#256993,#256994,
#256995,#256996,#256997,#256998,#256999,#257000,#257001,#257002,#257003,
#257004,#257005,#257006,#257007,#257008,#257009,#257010,#257011,#257012,
#257013,#257014,#257015,#257016,#257017,#257018,#257019,#257020,#257021,
#257022,#257023,#257024,#257025,#257026,#257027,#257028,#257029,#257030,
#257031,#257032,#257033,#257034,#257035,#257036,#257037,#257038,#257039,
#257040,#257041,#257042,#257043,#257044,#257045,#257046,#257047,#257048,
#257049,#257050,#257051,#257052,#257053,#257054,#257055,#257056,#257057,
#257058,#257059,#257060,#257061,#257062,#257063,#257064,#257065,#257066,
#257067,#257068,#257069,#257070,#257071,#257072,#257073,#257074,#257075,
#257076,#257077,#257078,#257079,#257080,#257081,#257082,#257083,#257084,
#257085,#257086,#257087,#257088,#257089,#257090,#257091,#257092,#257093,
#257094,#257095,#257096,#257097,#257098,#257099,#257100,#257101,#257102,
#257103,#257104,#257105,#257106,#257107,#257108,#257109,#257110,#257111,
#257112,#257113,#257114,#257115,#257116,#257117,#257118,#257119,#257120,
#257121,#257122,#257123,#257124,#257125,#257126,#257127,#257128,#257129,
#257130,#257131,#257132,#257133,#257134,#257135,#257136,#257137,#257138,
#257139,#257140,#257141,#257142,#257143,#257144,#257145,#257146,#257147,
#257148,#257149,#257150,#257151,#257152,#257153,#257154,#257155,#257156,
#257157,#257158,#257159,#257160,#257161,#257162,#257163,#257164,#257165,
#257166,#257167,#257168,#257169,#257170,#257171,#257172,#257173,#257174,
#257175,#257176,#257177,#257178,#257179,#257180,#257181,#257182,#257183,
#257184,#257185,#257186,#257187,#257188,#257189,#257190,#257191,#257192,
#257193,#257194,#257195,#257196,#257197,#257198,#257199,#257200,#257201,
#257202,#257203,#257204,#257205,#257206,#257207,#257208,#257209,#257210,
#257211,#257212,#257213,#257214,#257215,#257216,#257217,#257218,#257219,
#257220,#257221,#257222,#257223,#257224,#257225,#257226,#257227,#257228,
#257229,#257230,#257231,#257232,#257233,#257234,#257235,#257236,#257237,
#257238,#257239,#257240,#257241,#257242,#257243,#257244,#257245,#257246,
#257247,#257248,#257249,#257250,#257251,#257252,#257253,#257254,#257255,
#257256,#257257,#257258,#257259,#257260,#257261,#257262,#257263,#257264,
#257265,#257266,#257267,#257268,#257269,#257270,#257271,#257272,#257273,
#257274,#257275,#257276,#257277,#257278,#257279,#257280,#257281,#257282,
#257283,#257284,#257285,#257286,#257287,#257288,#257289,#257290,#257291,
#257292,#257293,#257294,#257295,#257296,#257297,#257298,#257299,#257300,
#257301,#257302,#257303,#257304,#257305,#257306,#257307,#257308,#257309,
#257310,#257311,#257312,#257313,#257314,#257315,#257316,#257317,#257318,
#257319,#257320,#257321,#257322,#257323,#257324,#257325,#257326,#257327,
#257328,#257329,#257330,#257331,#257332,#257333,#257334,#257335,#257336,
#257337,#257338,#257339,#257340,#257341,#257342,#257343,#257344,#257345,
#257346,#257347,#257348,#257349,#257350,#257351,#257352,#257353,#257354,
#257355,#257356,#257357,#257358,#257359,#257360,#257361,#257362,#257363,
#257364,#257365,#257366,#257367,#257368,#257369,#257370,#257371,#257372,
#257373,#257374,#257375,#257376,#257377,#257378,#257379,#257380,#257381,
#257382,#257383,#257384,#257385,#257386,#257387,#257388,#257389,#257390,
#257391,#257392,#257393,#257394,#257395,#257396,#257397,#257398,#257399,
#257400,#257401,#257402,#257403,#257404,#257405,#257406,#257407,#257408,
#257409,#257410,#257411,#257412,#257413,#257414,#257415,#257416,#257417,
#257418,#257419,#257420,#257421,#257422,#257423,#257424,#257425,#257426,
#257427,#257428,#257429,#257430,#257431,#257432,#257433,#257434,#257435,
#257436,#257437,#257438,#257439,#257440,#257441,#257442,#257443,#257444,
#257445,#257446,#257447,#257448,#257449,#257450,#257451,#257452,#257453,
#257454,#257455,#257456,#257457,#257458,#257459,#257460,#257461,#257462,
#257463,#257464,#257465,#257466,#257467,#257468,#257469,#257470,#257471,
#257472,#257473,#257474,#257475,#257476,#257477,#257478,#257479,#257480,
#257481,#257482,#257483,#257484,#257485,#257486,#257487,#257488,#257489,
#257490,#257491,#257492,#257493,#257494,#257495,#257496,#257497,#257498,
#257499,#257500,#257501,#257502,#257503,#257504,#257505,#257506,#257507,
#257508,#257509,#257510,#257511,#257512,#257513,#257514,#257515,#257516,
#257517,#257518,#257519,#257520,#257521,#257522,#257523,#257524,#257525,
#257526,#257527,#257528,#257529,#257530,#257531,#257532,#257533,#257534,
#257535,#257536,#257537,#257538,#257539,#257540,#257541,#257542,#257543,
#257544,#257545,#257546,#257547,#257548,#257549,#257550,#257551,#257552,
#257553,#257554,#257555,#257556,#257557,#257558,#257559,#257560,#257561,
#257562,#257563,#257564,#257565,#257566,#257567,#257568,#257569,#257570,
#257571,#257572,#257573,#257574,#257575,#257576,#257577,#257578,#257579,
#257580,#257581,#257582,#257583,#257584,#257585,#257586,#257587,#257588,
#257589,#257590,#257591,#257592,#257593,#257594,#257595,#257596,#257597,
#257598,#257599,#257600,#257601,#257602,#257603,#257604,#257605,#257606,
#257607,#257608,#257609,#257610,#257611,#257612,#257613,#257614,#257615,
#257616,#257617,#257618,#257619,#257620,#257621,#257622,#257623,#257624,
#257625,#257626,#257627,#257628,#257629,#257630,#257631,#257632,#257633,
#257634,#257635,#257636,#257637,#257638,#257639,#257640,#257641,#257642,
#257643,#257644,#257645,#257646,#257647,#257648,#257649,#257650,#257651,
#257652,#257653,#257654,#257655,#257656,#257657,#257658,#257659,#257660,
#257661,#257662,#257663,#257664,#257665,#257666,#257667,#257668,#257669,
#257670,#257671,#257672,#257673,#257674,#257675,#257676,#257677,#257678,
#257679,#257680,#257681,#257682,#257683,#257684,#257685,#257686,#257687,
#257688,#257689,#257690,#257691,#257692,#257693,#257694,#257695,#257696,
#257697,#257698,#257699,#257700,#257701,#257702,#257703,#257704,#257705,
#257706,#257707,#257708,#257709,#257710,#257711,#257712,#257713,#257714,
#257715,#257716,#257717,#257718,#257719,#257720,#257721,#257722,#257723,
#257724,#257725,#257726,#257727,#257728,#257729,#257730,#257731,#257732,
#257733,#257734,#257735,#257736,#257737,#257738,#257739,#257740,#257741,
#257742,#257743,#257744,#257745,#257746,#257747,#257748,#257749,#257750,
#257751,#257752,#257753,#257754,#257755,#257756,#257757,#257758,#257759,
#257760,#257761,#257762,#257763,#257764,#257765,#257766,#257767,#257768,
#257769,#257770,#257771,#257772,#257773,#257774,#257775,#257776,#257777,
#257778,#257779,#257780,#257781,#257782,#257783,#257784,#257785,#257786,
#257787,#257788,#257789,#257790,#257791,#257792,#257793,#257794,#257795,
#257796,#257797,#257798,#257799,#257800,#257801,#257802,#257803,#257804,
#257805,#257806,#257807,#257808,#257809,#257810,#257811,#257812,#257813,
#257814,#257815,#257816,#257817,#257818,#257819,#257820,#257821,#257822,
#257823,#257824,#257825,#257826,#257827,#257828,#257829,#257830,#257831,
#257832,#257833,#257834,#257835,#257836,#257837,#257838,#257839,#257840,
#257841,#257842,#257843,#257844,#257845,#257846,#257847,#257848,#257849,
#257850,#257851,#257852,#257853,#257854,#257855,#257856,#257857,#257858,
#257859,#257860,#257861,#257862,#257863,#257864,#257865,#257866,#257867,
#257868,#257869,#257870,#257871,#257872,#257873,#257874,#257875,#257876,
#257877,#257878,#257879,#257880,#257881,#257882,#257883,#257884,#257885,
#257886,#257887,#257888,#257889,#257890,#257891,#257892,#257893,#257894,
#257895,#257896,#257897,#257898,#257899,#257900,#257901,#257902,#257903,
#257904,#257905,#257906,#257907,#257908,#257909,#257910,#257911,#257912,
#257913,#257914,#257915,#257916,#257917,#257918,#257919,#257920,#257921,
#257922,#257923,#257924,#257925,#257926,#257927,#257928,#257929,#257930,
#257931,#257932,#257933,#257934,#257935,#257936,#257937,#257938,#257939,
#257940,#257941,#257942,#257943,#257944,#257945,#257946,#257947,#257948,
#257949,#257950,#257951,#257952,#257953,#257954,#257955,#257956,#257957,
#257958,#257959,#257960,#257961,#257962,#257963,#257964,#257965,#257966,
#257967,#257968,#257969,#257970,#257971,#257972,#257973,#257974,#257975,
#257976,#257977,#257978,#257979,#257980,#257981,#257982,#257983,#257984,
#257985,#257986,#257987,#257988,#257989,#257990,#257991,#257992,#257993,
#257994,#257995,#257996,#257997,#257998,#257999,#258000,#258001,#258002,
#258003,#258004,#258005,#258006,#258007,#258008,#258009,#258010,#258011,
#258012,#258013,#258014,#258015,#258016,#258017,#258018,#258019,#258020,
#258021,#258022,#258023,#258024,#258025,#258026,#258027,#258028,#258029,
#258030,#258031),(#258032,#258033,#258034,#258035,#258036,#258037,#258038,
#258039,#258040,#258041,#258042,#258043,#258044,#258045,#258046,#258047,
#258048,#258049,#258050,#258051,#258052,#258053,#258054,#258055,#258056,
#258057,#258058,#258059,#258060,#258061,#258062,#258063,#258064,#258065,
#258066,#258067,#258068,#258069,#258070,#258071,#258072,#258073,#258074,
#258075,#258076,#258077,#258078,#258079,#258080,#258081,#258082,#258083,
#258084,#258085,#258086,#258087,#258088,#258089,#258090,#258091,#258092,
#258093,#258094,#258095,#258096,#258097,#258098,#258099,#258100,#258101,
#258102,#258103,#258104,#258105,#258106,#258107,#258108,#258109,#258110,
#258111,#258112,#258113,#258114,#258115,#258116,#258117,#258118,#258119,
#258120,#258121,#258122,#258123,#258124,#258125,#258126,#258127,#258128,
#258129,#258130,#258131,#258132,#258133,#258134,#258135,#258136,#258137,
#258138,#258139,#258140,#258141,#258142,#258143,#258144,#258145,#258146,
#258147,#258148,#258149,#258150,#258151,#258152,#258153,#258154,#258155,
#258156,#258157,#258158,#258159,#258160,#258161,#258162,#258163,#258164,
#258165,#258166,#258167,#258168,#258169,#258170,#258171,#258172,#258173,
#258174,#258175,#258176,#258177,#258178,#258179,#258180,#258181,#258182,
#258183,#258184,#258185,#258186,#258187,#258188,#258189,#258190,#258191,
#258192,#258193,#258194,#258195,#258196,#258197,#258198,#258199,#258200,
#258201,#258202,#258203,#258204,#258205,#258206,#258207,#258208,#258209,
#258210,#258211,#258212,#258213,#258214,#258215,#258216,#258217,#258218,
#258219,#258220,#258221,#258222,#258223,#258224,#258225,#258226,#258227,
#258228,#258229,#258230,#258231,#258232,#258233,#258234,#258235,#258236,
#258237,#258238,#258239,#258240,#258241,#258242,#258243,#258244,#258245,
#258246,#258247,#258248,#258249,#258250,#258251,#258252,#258253,#258254,
#258255,#258256,#258257,#258258,#258259,#258260,#258261,#258262,#258263,
#258264,#258265,#258266,#258267,#258268,#258269,#258270,#258271,#258272,
#258273,#258274,#258275,#258276,#258277,#258278,#258279,#258280,#258281,
#258282,#258283,#258284,#258285,#258286,#258287,#258288,#258289,#258290,
#258291,#258292,#258293,#258294,#258295,#258296,#258297,#258298,#258299,
#258300,#258301,#258302,#258303,#258304,#258305,#258306,#258307,#258308,
#258309,#258310,#258311,#258312,#258313,#258314,#258315,#258316,#258317,
#258318,#258319,#258320,#258321,#258322,#258323,#258324,#258325,#258326,
#258327,#258328,#258329,#258330,#258331,#258332,#258333,#258334,#258335,
#258336,#258337,#258338,#258339,#258340,#258341,#258342,#258343,#258344,
#258345,#258346,#258347,#258348,#258349,#258350,#258351,#258352,#258353,
#258354,#258355,#258356,#258357,#258358,#258359,#258360,#258361,#258362,
#258363,#258364,#258365,#258366,#258367,#258368,#258369,#258370,#258371,
#258372,#258373,#258374,#258375,#258376,#258377,#258378,#258379,#258380,
#258381,#258382,#258383,#258384,#258385,#258386,#258387,#258388,#258389,
#258390,#258391,#258392,#258393,#258394,#258395,#258396,#258397,#258398,
#258399,#258400,#258401,#258402,#258403,#258404,#258405,#258406,#258407,
#258408,#258409,#258410,#258411,#258412,#258413,#258414,#258415,#258416,
#258417,#258418,#258419,#258420,#258421,#258422,#258423,#258424,#258425,
#258426,#258427,#258428,#258429,#258430,#258431,#258432,#258433,#258434,
#258435,#258436,#258437,#258438,#258439,#258440,#258441,#258442,#258443,
#258444,#258445,#258446,#258447,#258448,#258449,#258450,#258451,#258452,
#258453,#258454,#258455,#258456,#258457,#258458,#258459,#258460,#258461,
#258462,#258463,#258464,#258465,#258466,#258467,#258468,#258469,#258470,
#258471,#258472,#258473,#258474,#258475,#258476,#258477,#258478,#258479,
#258480,#258481,#258482,#258483,#258484,#258485,#258486,#258487,#258488,
#258489,#258490,#258491,#258492,#258493,#258494,#258495,#258496,#258497,
#258498,#258499,#258500,#258501,#258502,#258503,#258504,#258505,#258506,
#258507,#258508,#258509,#258510,#258511,#258512,#258513,#258514,#258515,
#258516,#258517,#258518,#258519,#258520,#258521,#258522,#258523,#258524,
#258525,#258526,#258527,#258528,#258529,#258530,#258531,#258532,#258533,
#258534,#258535,#258536,#258537,#258538,#258539,#258540,#258541,#258542,
#258543,#258544,#258545,#258546,#258547,#258548,#258549,#258550,#258551,
#258552,#258553,#258554,#258555,#258556,#258557,#258558,#258559,#258560,
#258561,#258562,#258563,#258564,#258565,#258566,#258567,#258568,#258569,
#258570,#258571,#258572,#258573,#258574,#258575,#258576,#258577,#258578,
#258579,#258580,#258581,#258582,#258583,#258584,#258585,#258586,#258587,
#258588,#258589,#258590,#258591,#258592,#258593,#258594,#258595,#258596,
#258597,#258598,#258599,#258600,#258601,#258602,#258603,#258604,#258605,
#258606,#258607,#258608,#258609,#258610,#258611,#258612,#258613,#258614,
#258615,#258616,#258617,#258618,#258619,#258620,#258621,#258622,#258623,
#258624,#258625,#258626,#258627,#258628,#258629,#258630,#258631,#258632,
#258633,#258634,#258635,#258636,#258637,#258638,#258639,#258640,#258641,
#258642,#258643,#258644,#258645,#258646,#258647,#258648,#258649,#258650,
#258651,#258652,#258653,#258654,#258655,#258656,#258657,#258658,#258659,
#258660,#258661,#258662,#258663,#258664,#258665,#258666,#258667,#258668,
#258669,#258670,#258671,#258672,#258673,#258674,#258675,#258676,#258677,
#258678,#258679,#258680,#258681,#258682,#258683,#258684,#258685,#258686,
#258687,#258688,#258689,#258690,#258691,#258692,#258693,#258694,#258695,
#258696,#258697,#258698,#258699,#258700,#258701,#258702,#258703,#258704,
#258705,#258706,#258707,#258708,#258709,#258710,#258711,#258712,#258713,
#258714,#258715,#258716,#258717,#258718,#258719,#258720,#258721,#258722,
#258723,#258724,#258725,#258726,#258727,#258728,#258729,#258730,#258731,
#258732,#258733,#258734,#258735,#258736,#258737,#258738,#258739,#258740,
#258741,#258742,#258743,#258744,#258745,#258746,#258747,#258748,#258749,
#258750,#258751,#258752,#258753,#258754,#258755,#258756,#258757,#258758,
#258759,#258760,#258761,#258762,#258763,#258764,#258765,#258766,#258767,
#258768,#258769,#258770,#258771,#258772,#258773,#258774,#258775,#258776,
#258777,#258778,#258779,#258780,#258781,#258782,#258783,#258784,#258785,
#258786,#258787,#258788,#258789,#258790,#258791,#258792,#258793,#258794,
#258795,#258796,#258797,#258798,#258799,#258800,#258801,#258802,#258803,
#258804,#258805,#258806,#258807,#258808,#258809,#258810,#258811,#258812,
#258813,#258814,#258815,#258816,#258817,#258818,#258819,#258820,#258821,
#258822,#258823,#258824,#258825,#258826,#258827,#258828,#258829,#258830,
#258831,#258832,#258833,#258834,#258835,#258836,#258837,#258838,#258839,
#258840,#258841,#258842,#258843,#258844,#258845,#258846,#258847,#258848,
#258849,#258850,#258851,#258852,#258853,#258854,#258855,#258856,#258857,
#258858,#258859,#258860,#258861,#258862,#258863,#258864,#258865,#258866,
#258867,#258868,#258869,#258870,#258871,#258872,#258873,#258874,#258875,
#258876,#258877,#258878,#258879,#258880,#258881,#258882,#258883,#258884,
#258885,#258886,#258887,#258888,#258889,#258890,#258891,#258892,#258893,
#258894,#258895,#258896,#258897,#258898,#258899,#258900,#258901,#258902,
#258903,#258904,#258905,#258906,#258907,#258908,#258909,#258910,#258911,
#258912,#258913,#258914,#258915,#258916,#258917,#258918,#258919,#258920,
#258921,#258922,#258923,#258924,#258925,#258926,#258927,#258928,#258929,
#258930,#258931,#258932,#258933,#258934,#258935,#258936,#258937,#258938,
#258939,#258940,#258941,#258942,#258943,#258944,#258945,#258946,#258947,
#258948,#258949,#258950,#258951,#258952,#258953,#258954,#258955,#258956,
#258957,#258958,#258959,#258960,#258961,#258962,#258963,#258964,#258965,
#258966,#258967,#258968,#258969,#258970,#258971,#258972,#258973,#258974,
#258975,#258976,#258977,#258978,#258979,#258980,#258981,#258982,#258983,
#258984,#258985,#258986,#258987,#258988,#258989,#258990,#258991,#258992,
#258993,#258994,#258995,#258996,#258997,#258998,#258999,#259000,#259001,
#259002,#259003,#259004,#259005,#259006,#259007,#259008,#259009,#259010,
#259011,#259012,#259013,#259014,#259015,#259016,#259017,#259018,#259019,
#259020,#259021,#259022,#259023,#259024,#259025,#259026,#259027,#259028,
#259029,#259030,#259031,#259032,#259033,#259034,#259035,#259036,#259037,
#259038,#259039,#259040,#259041,#259042,#259043,#259044,#259045,#259046,
#259047,#259048,#259049,#259050,#259051,#259052,#259053,#259054,#259055,
#259056,#259057,#259058,#259059,#259060,#259061,#259062,#259063,#259064,
#259065,#259066,#259067,#259068,#259069,#259070,#259071,#259072,#259073,
#259074,#259075,#259076,#259077,#259078,#259079,#259080,#259081,#259082,
#259083,#259084,#259085,#259086,#259087,#259088,#259089,#259090,#259091,
#259092,#259093,#259094,#259095,#259096,#259097,#259098,#259099,#259100,
#259101,#259102,#259103,#259104,#259105,#259106,#259107,#259108,#259109,
#259110,#259111,#259112,#259113,#259114,#259115,#259116,#259117,#259118,
#259119,#259120,#259121,#259122,#259123,#259124,#259125,#259126,#259127,
#259128,#259129,#259130,#259131,#259132,#259133,#259134,#259135,#259136,
#259137,#259138,#259139,#259140,#259141,#259142,#259143,#259144,#259145,
#259146,#259147,#259148,#259149,#259150,#259151,#259152,#259153,#259154,
#259155,#259156,#259157,#259158,#259159,#259160,#259161,#259162,#259163,
#259164,#259165,#259166,#259167,#259168,#259169,#259170,#259171,#259172,
#259173,#259174,#259175,#259176,#259177,#259178,#259179,#259180,#259181,
#259182,#259183,#259184,#259185,#259186,#259187,#259188,#259189,#259190,
#259191,#259192,#259193,#259194,#259195,#259196,#259197,#259198,#259199,
#259200,#259201,#259202,#259203,#259204,#259205,#259206,#259207,#259208,
#259209,#259210,#259211,#259212,#259213,#259214,#259215,#259216,#259217,
#259218,#259219,#259220,#259221,#259222,#259223,#259224,#259225,#259226,
#259227,#259228,#259229,#259230,#259231,#259232,#259233,#259234,#259235,
#259236,#259237,#259238,#259239,#259240,#259241,#259242,#259243,#259244,
#259245,#259246,#259247,#259248,#259249,#259250,#259251,#259252,#259253,
#259254,#259255,#259256,#259257,#259258,#259259,#259260,#259261,#259262,
#259263,#259264,#259265,#259266,#259267,#259268,#259269,#259270,#259271,
#259272,#259273,#259274,#259275,#259276,#259277,#259278,#259279,#259280,
#259281,#259282,#259283,#259284,#259285,#259286,#259287,#259288,#259289,
#259290,#259291,#259292,#259293,#259294,#259295,#259296,#259297,#259298,
#259299,#259300,#259301,#259302,#259303,#259304,#259305,#259306,#259307,
#259308,#259309,#259310,#259311,#259312,#259313,#259314,#259315,#259316,
#259317,#259318,#259319,#259320,#259321,#259322,#259323,#259324,#259325,
#259326,#259327,#259328,#259329,#259330,#259331,#259332,#259333,#259334,
#259335,#259336,#259337,#259338,#259339,#259340,#259341,#259342,#259343,
#259344,#259345,#259346,#259347,#259348,#259349,#259350,#259351,#259352,
#259353,#259354,#259355,#259356,#259357,#259358,#259359,#259360,#259361,
#259362,#259363,#259364,#259365,#259366,#259367,#259368,#259369,#259370,
#259371,#259372,#259373,#259374,#259375,#259376,#259377,#259378,#259379,
#259380,#259381,#259382,#259383,#259384,#259385,#259386,#259387,#259388,
#259389,#259390,#259391,#259392,#259393,#259394,#259395,#259396,#259397,
#259398,#259399,#259400,#259401,#259402,#259403,#259404,#259405,#259406,
#259407,#259408,#259409,#259410,#259411,#259412,#259413,#259414,#259415,
#259416,#259417,#259418,#259419,#259420,#259421,#259422,#259423,#259424,
#259425,#259426,#259427,#259428,#259429,#259430,#259431,#259432,#259433,
#259434,#259435,#259436,#259437,#259438,#259439,#259440,#259441,#259442,
#259443,#259444,#259445,#259446,#259447,#259448,#259449,#259450,#259451,
#259452,#259453,#259454,#259455,#259456,#259457,#259458,#259459,#259460,
#259461,#259462,#259463,#259464,#259465,#259466,#259467,#259468,#259469,
#259470,#259471,#259472,#259473,#259474,#259475,#259476,#259477,#259478,
#259479,#259480,#259481,#259482,#259483,#259484,#259485,#259486,#259487,
#259488,#259489,#259490,#259491,#259492,#259493,#259494,#259495,#259496,
#259497,#259498,#259499,#259500,#259501,#259502,#259503,#259504,#259505,
#259506,#259507,#259508,#259509,#259510,#259511,#259512,#259513,#259514,
#259515,#259516,#259517,#259518,#259519,#259520,#259521,#259522,#259523,
#259524,#259525,#259526,#259527,#259528,#259529,#259530,#259531,#259532,
#259533,#259534,#259535,#259536,#259537,#259538,#259539,#259540,#259541,
#259542,#259543,#259544,#259545,#259546,#259547,#259548,#259549,#259550,
#259551,#259552,#259553,#259554,#259555,#259556,#259557,#259558,#259559,
#259560,#259561,#259562,#259563,#259564,#259565,#259566,#259567,#259568,
#259569,#259570,#259571,#259572,#259573,#259574,#259575,#259576,#259577,
#259578,#259579,#259580,#259581,#259582,#259583,#259584,#259585,#259586,
#259587,#259588,#259589,#259590,#259591,#259592,#259593,#259594,#259595,
#259596,#259597,#259598,#259599,#259600,#259601,#259602,#259603,#259604,
#259605,#259606,#259607,#259608,#259609,#259610,#259611,#259612,#259613,
#259614,#259615,#259616,#259617,#259618,#259619,#259620,#259621,#259622,
#259623,#259624,#259625,#259626,#259627,#259628,#259629,#259630,#259631,
#259632,#259633,#259634,#259635,#259636,#259637,#259638,#259639,#259640,
#259641,#259642,#259643,#259644,#259645,#259646,#259647,#259648,#259649,
#259650,#259651,#259652,#259653,#259654,#259655,#259656,#259657,#259658,
#259659,#259660,#259661,#259662,#259663,#259664,#259665,#259666,#259667,
#259668,#259669,#259670,#259671,#259672,#259673,#259674,#259675,#259676,
#259677,#259678,#259679,#259680,#259681,#259682,#259683,#259684,#259685,
#259686,#259687,#259688,#259689,#259690,#259691,#259692,#259693,#259694,
#259695,#259696,#259697,#259698,#259699,#259700,#259701,#259702,#259703,
#259704,#259705,#259706,#259707,#259708,#259709,#259710,#259711,#259712,
#259713,#259714,#259715,#259716,#259717,#259718,#259719,#259720,#259721,
#259722,#259723,#259724,#259725,#259726),(#259727,#259728,#259729,#259730,
#259731,#259732,#259733,#259734,#259735,#259736,#259737,#259738,#259739,
#259740,#259741,#259742,#259743,#259744,#259745,#259746,#259747,#259748,
#259749,#259750,#259751,#259752,#259753,#259754,#259755,#259756,#259757,
#259758,#259759,#259760,#259761,#259762,#259763,#259764,#259765,#259766,
#259767,#259768,#259769,#259770,#259771,#259772,#259773,#259774,#259775,
#259776,#259777,#259778,#259779,#259780,#259781,#259782,#259783,#259784,
#259785,#259786,#259787,#259788,#259789,#259790,#259791,#259792,#259793,
#259794,#259795,#259796,#259797,#259798,#259799,#259800,#259801,#259802,
#259803,#259804,#259805,#259806,#259807,#259808,#259809,#259810,#259811,
#259812,#259813,#259814,#259815,#259816,#259817,#259818,#259819,#259820,
#259821,#259822,#259823,#259824,#259825,#259826,#259827,#259828,#259829,
#259830,#259831,#259832,#259833,#259834,#259835,#259836,#259837,#259838,
#259839,#259840,#259841,#259842,#259843,#259844,#259845,#259846,#259847,
#259848,#259849,#259850,#259851,#259852,#259853,#259854,#259855,#259856,
#259857,#259858,#259859,#259860,#259861,#259862,#259863,#259864,#259865,
#259866,#259867,#259868,#259869,#259870,#259871,#259872,#259873,#259874,
#259875,#259876,#259877,#259878,#259879,#259880,#259881,#259882,#259883,
#259884,#259885,#259886,#259887,#259888,#259889,#259890,#259891,#259892,
#259893,#259894,#259895,#259896,#259897,#259898,#259899,#259900,#259901,
#259902,#259903,#259904,#259905,#259906,#259907,#259908,#259909,#259910,
#259911,#259912,#259913,#259914,#259915,#259916,#259917,#259918,#259919,
#259920,#259921,#259922,#259923,#259924,#259925,#259926,#259927,#259928,
#259929,#259930,#259931,#259932,#259933,#259934,#259935,#259936,#259937,
#259938,#259939,#259940,#259941,#259942,#259943,#259944,#259945,#259946,
#259947,#259948,#259949,#259950,#259951,#259952,#259953,#259954,#259955,
#259956,#259957,#259958,#259959,#259960,#259961,#259962,#259963,#259964,
#259965,#259966,#259967,#259968,#259969,#259970,#259971,#259972,#259973,
#259974,#259975,#259976,#259977,#259978,#259979,#259980,#259981,#259982,
#259983,#259984,#259985,#259986,#259987,#259988,#259989,#259990,#259991,
#259992,#259993,#259994,#259995,#259996,#259997,#259998,#259999,#260000,
#260001,#260002,#260003,#260004,#260005,#260006,#260007,#260008,#260009,
#260010,#260011,#260012,#260013,#260014,#260015,#260016,#260017,#260018,
#260019,#260020,#260021,#260022,#260023,#260024,#260025,#260026,#260027,
#260028,#260029,#260030,#260031,#260032,#260033,#260034,#260035,#260036,
#260037,#260038,#260039,#260040,#260041,#260042,#260043,#260044,#260045,
#260046,#260047,#260048,#260049,#260050,#260051,#260052,#260053,#260054,
#260055,#260056,#260057,#260058,#260059,#260060,#260061,#260062,#260063,
#260064,#260065,#260066,#260067,#260068,#260069,#260070,#260071,#260072,
#260073,#260074,#260075,#260076,#260077,#260078,#260079,#260080,#260081,
#260082,#260083,#260084,#260085,#260086,#260087,#260088,#260089,#260090,
#260091,#260092,#260093,#260094,#260095,#260096,#260097,#260098,#260099,
#260100,#260101,#260102,#260103,#260104,#260105,#260106,#260107,#260108,
#260109,#260110,#260111,#260112,#260113,#260114,#260115,#260116,#260117,
#260118,#260119,#260120,#260121,#260122,#260123,#260124,#260125,#260126,
#260127,#260128,#260129,#260130,#260131,#260132,#260133,#260134,#260135,
#260136,#260137,#260138,#260139,#260140,#260141,#260142,#260143,#260144,
#260145,#260146,#260147,#260148,#260149,#260150,#260151,#260152,#260153,
#260154,#260155,#260156,#260157,#260158,#260159,#260160,#260161,#260162,
#260163,#260164,#260165,#260166,#260167,#260168,#260169,#260170,#260171,
#260172,#260173,#260174,#260175,#260176,#260177,#260178,#260179,#260180,
#260181,#260182,#260183,#260184,#260185,#260186,#260187,#260188,#260189,
#260190,#260191,#260192,#260193,#260194,#260195,#260196,#260197,#260198,
#260199,#260200,#260201,#260202,#260203,#260204,#260205,#260206,#260207,
#260208,#260209,#260210,#260211,#260212,#260213,#260214,#260215,#260216,
#260217,#260218,#260219,#260220,#260221,#260222,#260223,#260224,#260225,
#260226,#260227,#260228,#260229,#260230,#260231,#260232,#260233,#260234,
#260235,#260236,#260237,#260238,#260239,#260240,#260241,#260242,#260243,
#260244,#260245,#260246,#260247,#260248,#260249,#260250,#260251,#260252,
#260253,#260254,#260255,#260256,#260257,#260258,#260259,#260260,#260261,
#260262,#260263,#260264,#260265,#260266,#260267,#260268,#260269,#260270,
#260271,#260272,#260273,#260274,#260275,#260276,#260277,#260278,#260279,
#260280,#260281,#260282,#260283,#260284,#260285,#260286,#260287,#260288,
#260289,#260290,#260291,#260292,#260293,#260294,#260295,#260296,#260297,
#260298,#260299,#260300,#260301,#260302,#260303,#260304,#260305,#260306,
#260307,#260308,#260309,#260310,#260311,#260312,#260313,#260314,#260315,
#260316,#260317,#260318,#260319,#260320,#260321,#260322,#260323,#260324,
#260325,#260326,#260327,#260328,#260329,#260330,#260331,#260332,#260333,
#260334,#260335,#260336,#260337,#260338,#260339,#260340,#260341,#260342,
#260343,#260344,#260345,#260346,#260347,#260348,#260349,#260350,#260351,
#260352,#260353,#260354,#260355,#260356,#260357,#260358,#260359,#260360,
#260361,#260362,#260363,#260364,#260365,#260366,#260367,#260368,#260369,
#260370,#260371,#260372,#260373,#260374,#260375,#260376,#260377,#260378,
#260379,#260380,#260381,#260382,#260383,#260384,#260385,#260386,#260387,
#260388,#260389,#260390,#260391,#260392,#260393,#260394,#260395,#260396,
#260397,#260398,#260399,#260400,#260401,#260402,#260403,#260404,#260405,
#260406,#260407,#260408,#260409,#260410,#260411,#260412,#260413,#260414,
#260415,#260416,#260417,#260418,#260419,#260420,#260421,#260422,#260423,
#260424,#260425,#260426,#260427,#260428,#260429,#260430,#260431,#260432,
#260433,#260434,#260435,#260436,#260437,#260438,#260439,#260440,#260441,
#260442,#260443,#260444,#260445,#260446,#260447,#260448,#260449,#260450,
#260451,#260452,#260453,#260454,#260455,#260456,#260457,#260458,#260459,
#260460,#260461,#260462,#260463,#260464,#260465,#260466,#260467,#260468,
#260469,#260470,#260471,#260472,#260473,#260474,#260475,#260476,#260477,
#260478,#260479,#260480,#260481,#260482,#260483,#260484,#260485,#260486,
#260487,#260488,#260489,#260490,#260491,#260492,#260493,#260494,#260495,
#260496,#260497,#260498,#260499,#260500,#260501,#260502,#260503,#260504,
#260505,#260506,#260507,#260508,#260509,#260510,#260511,#260512,#260513,
#260514,#260515,#260516,#260517,#260518,#260519,#260520,#260521,#260522,
#260523,#260524,#260525,#260526,#260527,#260528,#260529,#260530,#260531,
#260532,#260533,#260534,#260535,#260536,#260537,#260538,#260539,#260540,
#260541,#260542,#260543,#260544,#260545,#260546,#260547,#260548,#260549,
#260550,#260551,#260552,#260553,#260554,#260555,#260556,#260557,#260558,
#260559,#260560,#260561,#260562,#260563,#260564,#260565,#260566,#260567,
#260568,#260569,#260570,#260571,#260572,#260573,#260574,#260575,#260576,
#260577,#260578,#260579,#260580,#260581,#260582,#260583,#260584,#260585,
#260586,#260587,#260588,#260589,#260590,#260591,#260592,#260593,#260594,
#260595,#260596,#260597,#260598,#260599,#260600,#260601,#260602,#260603,
#260604,#260605,#260606,#260607,#260608,#260609,#260610,#260611,#260612,
#260613,#260614,#260615,#260616,#260617,#260618,#260619,#260620,#260621,
#260622,#260623,#260624,#260625,#260626,#260627,#260628,#260629,#260630,
#260631,#260632,#260633,#260634,#260635,#260636,#260637,#260638,#260639,
#260640,#260641,#260642,#260643,#260644,#260645,#260646,#260647,#260648,
#260649,#260650,#260651,#260652,#260653,#260654,#260655,#260656,#260657,
#260658,#260659,#260660,#260661,#260662,#260663,#260664,#260665,#260666,
#260667,#260668,#260669,#260670,#260671,#260672,#260673,#260674,#260675,
#260676,#260677,#260678,#260679,#260680,#260681,#260682,#260683,#260684,
#260685,#260686,#260687,#260688,#260689,#260690,#260691,#260692,#260693,
#260694,#260695,#260696,#260697,#260698,#260699,#260700,#260701,#260702,
#260703,#260704,#260705,#260706,#260707,#260708,#260709,#260710,#260711,
#260712,#260713,#260714,#260715,#260716,#260717,#260718,#260719,#260720,
#260721,#260722,#260723,#260724,#260725,#260726,#260727,#260728,#260729,
#260730,#260731,#260732,#260733,#260734,#260735,#260736,#260737,#260738,
#260739,#260740,#260741,#260742,#260743,#260744,#260745,#260746,#260747,
#260748,#260749,#260750,#260751,#260752,#260753,#260754,#260755,#260756,
#260757,#260758,#260759,#260760,#260761,#260762,#260763,#260764,#260765,
#260766,#260767,#260768,#260769,#260770,#260771,#260772,#260773,#260774,
#260775,#260776,#260777,#260778,#260779,#260780,#260781,#260782,#260783,
#260784,#260785,#260786,#260787,#260788,#260789,#260790,#260791,#260792,
#260793,#260794,#260795,#260796,#260797,#260798,#260799,#260800,#260801,
#260802,#260803,#260804,#260805,#260806,#260807,#260808,#260809,#260810,
#260811,#260812,#260813,#260814,#260815,#260816,#260817,#260818,#260819,
#260820,#260821,#260822,#260823,#260824,#260825,#260826,#260827,#260828,
#260829,#260830,#260831,#260832,#260833,#260834,#260835,#260836,#260837,
#260838,#260839,#260840,#260841,#260842,#260843,#260844,#260845,#260846,
#260847,#260848,#260849,#260850,#260851,#260852,#260853,#260854,#260855,
#260856,#260857,#260858,#260859,#260860,#260861,#260862,#260863,#260864,
#260865,#260866,#260867,#260868,#260869,#260870,#260871,#260872,#260873,
#260874,#260875,#260876,#260877,#260878,#260879,#260880,#260881,#260882,
#260883,#260884,#260885,#260886,#260887,#260888,#260889,#260890,#260891,
#260892,#260893,#260894,#260895,#260896,#260897,#260898,#260899,#260900,
#260901,#260902,#260903,#260904,#260905,#260906,#260907,#260908,#260909,
#260910,#260911,#260912,#260913,#260914,#260915,#260916,#260917,#260918,
#260919,#260920,#260921,#260922,#260923,#260924,#260925,#260926,#260927,
#260928,#260929,#260930,#260931,#260932,#260933,#260934,#260935,#260936,
#260937,#260938,#260939,#260940,#260941,#260942,#260943,#260944,#260945,
#260946,#260947,#260948,#260949,#260950,#260951,#260952,#260953,#260954,
#260955,#260956,#260957,#260958,#260959,#260960,#260961,#260962,#260963,
#260964,#260965,#260966,#260967,#260968,#260969,#260970,#260971,#260972,
#260973,#260974,#260975,#260976,#260977,#260978,#260979,#260980,#260981,
#260982,#260983,#260984,#260985,#260986,#260987,#260988,#260989,#260990,
#260991,#260992,#260993,#260994,#260995,#260996,#260997,#260998,#260999,
#261000,#261001,#261002,#261003,#261004,#261005,#261006,#261007,#261008,
#261009,#261010,#261011,#261012,#261013,#261014,#261015,#261016,#261017,
#261018,#261019,#261020,#261021,#261022,#261023,#261024,#261025,#261026,
#261027,#261028,#261029,#261030,#261031,#261032,#261033,#261034,#261035,
#261036,#261037,#261038,#261039,#261040,#261041,#261042,#261043,#261044,
#261045,#261046,#261047,#261048,#261049,#261050,#261051,#261052,#261053,
#261054,#261055,#261056,#261057,#261058,#261059,#261060,#261061,#261062,
#261063,#261064,#261065,#261066,#261067,#261068,#261069,#261070,#261071,
#261072,#261073,#261074,#261075,#261076,#261077,#261078,#261079,#261080,
#261081,#261082,#261083,#261084,#261085,#261086,#261087,#261088,#261089,
#261090,#261091,#261092,#261093,#261094,#261095,#261096,#261097,#261098,
#261099,#261100,#261101,#261102,#261103,#261104,#261105,#261106,#261107,
#261108,#261109,#261110,#261111,#261112,#261113,#261114,#261115,#261116,
#261117,#261118,#261119,#261120,#261121,#261122,#261123,#261124,#261125,
#261126,#261127,#261128,#261129,#261130,#261131,#261132,#261133,#261134,
#261135,#261136,#261137,#261138,#261139,#261140,#261141,#261142,#261143,
#261144,#261145,#261146,#261147,#261148,#261149,#261150,#261151,#261152,
#261153,#261154,#261155,#261156,#261157,#261158,#261159,#261160,#261161,
#261162,#261163,#261164,#261165,#261166,#261167,#261168,#261169,#261170,
#261171,#261172,#261173,#261174,#261175,#261176,#261177,#261178,#261179,
#261180,#261181,#261182,#261183,#261184,#261185,#261186,#261187,#261188,
#261189,#261190,#261191,#261192,#261193,#261194,#261195,#261196,#261197,
#261198,#261199,#261200,#261201,#261202,#261203,#261204,#261205,#261206,
#261207,#261208,#261209,#261210,#261211,#261212,#261213,#261214,#261215,
#261216,#261217,#261218,#261219,#261220,#261221,#261222,#261223,#261224,
#261225,#261226,#261227,#261228,#261229,#261230,#261231,#261232,#261233,
#261234,#261235,#261236,#261237,#261238,#261239,#261240,#261241,#261242,
#261243,#261244,#261245,#261246,#261247,#261248,#261249,#261250,#261251,
#261252,#261253,#261254,#261255,#261256,#261257,#261258,#261259,#261260,
#261261,#261262,#261263,#261264,#261265,#261266,#261267,#261268,#261269,
#261270,#261271,#261272,#261273,#261274,#261275,#261276,#261277,#261278,
#261279,#261280,#261281,#261282,#261283,#261284,#261285,#261286,#261287,
#261288,#261289,#261290,#261291,#261292,#261293,#261294,#261295,#261296,
#261297,#261298,#261299,#261300,#261301,#261302,#261303,#261304,#261305,
#261306,#261307,#261308,#261309,#261310,#261311,#261312,#261313,#261314,
#261315,#261316,#261317,#261318,#261319,#261320,#261321,#261322,#261323,
#261324,#261325,#261326,#261327,#261328,#261329,#261330,#261331,#261332,
#261333,#261334,#261335,#261336,#261337,#261338,#261339,#261340,#261341,
#261342,#261343,#261344,#261345,#261346,#261347,#261348,#261349,#261350,
#261351,#261352,#261353,#261354,#261355,#261356,#261357,#261358,#261359,
#261360,#261361,#261362,#261363,#261364,#261365,#261366,#261367,#261368,
#261369,#261370,#261371,#261372,#261373,#261374,#261375,#261376,#261377,
#261378,#261379,#261380,#261381,#261382,#261383,#261384,#261385,#261386,
#261387,#261388,#261389,#261390,#261391,#261392,#261393,#261394,#261395,
#261396,#261397,#261398,#261399,#261400,#261401,#261402,#261403,#261404,
#261405,#261406,#261407,#261408,#261409,#261410,#261411,#261412,#261413,
#261414,#261415,#261416,#261417,#261418,#261419,#261420,#261421)),
 .UNSPECIFIED.,.F.,.F.,.F.,(4,4),(4,1,1,1,1,1,1,1,1,1,1,1,1,1,1,1,1,1,1,
1,1,1,1,1,1,1,1,1,1,1,1,1,1,1,1,1,1,1,1,1,1,1,1,1,1,1,1,1,1,1,1,1,1,1,1,
1,1,1,1,1,1,1,1,1,1,1,1,1,1,1,1,1,1,1,1,1,1,1,1,1,1,1,1,1,1,1,1,1,1,1,1,
1,1,1,1,1,1,1,1,1,1,1,1,1,1,1,1,1,1,1,1,1,1,1,1,1,1,1,1,1,1,1,1,1,1,1,1,
1,1,1,1,1,1,1,1,1,1,1,1,1,1,1,1,1,1,1,1,1,1,1,1,1,1,1,1,1,1,1,1,1,1,1,1,
1,1,1,1,1,1,1,1,1,1,1,1,1,1,1,1,1,1,1,1,1,1,1,1,1,1,1,1,1,1,1,1,1,1,1,1,
1,1,1,1,1,1,1,1,1,1,1,1,1,1,1,1,1,1,1,1,1,1,1,1,1,1,1,1,1,1,1,1,1,1,1,1,
1,1,1,1,1,1,1,1,1,1,1,1,1,1,1,1,1,1,1,1,1,1,1,1,1,1,1,1,1,1,1,1,1,1,1,1,
1,1,1,1,1,1,1,1,1,1,1,1,1,1,1,1,1,1,1,1,1,1,1,1,1,1,1,1,1,1,1,1,1,1,1,1,
1,1,1,1,1,1,1,1,1,1,1,1,1,1,1,1,1,1,1,1,1,1,1,1,1,1,1,1,1,1,1,1,1,1,1,1,
1,1,1,1,1,1,1,1,1,1,1,1,1,1,1,1,1,1,1,1,1,1,1,1,1,1,1,1,1,1,1,1,1,1,1,1,
1,1,1,1,1,1,1,1,1,1,1,1,1,1,1,1,1,1,1,1,1,1,1,1,1,1,1,1,1,1,1,1,1,1,1,1,
1,1,1,1,1,1,1,1,1,1,1,1,1,1,1,1,1,1,1,1,1,1,1,1,1,1,1,1,1,1,1,1,1,1,1,1,
1,1,1,1,1,1,1,1,1,1,1,1,1,1,1,1,1,1,1,1,1,1,1,1,1,1,1,1,1,1,1,1,1,1,1,1,
1,1,1,1,1,1,1,1,1,1,1,1,1,1,1,1,1,1,1,1,1,1,1,1,1,1,1,1,1,1,1,1,1,1,1,1,
1,1,1,1,1,1,1,1,1,1,1,1,1,1,1,1,1,1,1,1,1,1,1,1,1,1,1,1,1,1,1,1,1,1,1,1,
1,1,1,1,1,1,1,1,1,1,1,1,1,1,1,1,1,1,1,1,1,1,1,1,1,1,1,1,1,1,1,1,1,1,1,1,
1,1,1,1,1,1,1,1,1,1,1,1,1,1,1,1,1,1,1,1,1,1,1,1,1,1,1,1,1,1,1,1,1,1,1,1,
1,1,1,1,1,1,1,1,1,1,1,1,1,1,1,1,1,1,1,1,1,1,1,1,1,1,1,1,1,1,1,1,1,1,1,1,
1,1,1,1,1,1,1,1,1,1,1,1,1,1,1,1,1,1,1,1,1,1,1,1,1,1,1,1,1,1,1,1,1,1,1,1,
1,1,1,1,1,1,1,1,1,1,1,1,1,1,1,1,1,1,1,1,1,1,1,1,1,1,1,1,1,1,1,1,1,1,1,1,
1,1,1,1,1,1,1,1,1,1,1,1,1,1,1,1,1,1,1,1,1,1,1,1,1,1,1,1,1,1,1,1,1,1,1,1,
1,1,1,1,1,1,1,1,1,1,1,1,1,1,1,1,1,1,1,1,1,1,1,1,1,1,1,1,1,1,1,1,1,1,1,1,
1,1,1,1,1,1,1,1,1,1,1,1,1,1,1,1,1,1,1,1,1,1,1,1,1,1,1,1,1,1,1,1,1,1,1,1,
1,1,1,1,1,1,1,1,1,1,1,1,1,1,1,1,1,1,1,1,1,1,1,1,1,1,1,1,1,1,1,1,1,1,1,1,
1,1,1,1,1,1,1,1,1,1,1,1,1,1,1,1,1,1,1,1,1,1,1,1,1,1,1,1,1,1,1,1,1,1,1,1,
1,1,1,1,1,1,1,1,1,1,1,1,1,1,1,1,1,1,1,1,1,1,1,1,1,1,1,1,1,1,1,1,1,1,1,1,
1,1,1,1,1,1,1,1,1,1,1,1,1,1,1,1,1,1,1,1,1,1,1,1,1,1,1,1,1,1,1,1,1,1,1,1,
1,1,1,1,1,1,1,1,1,1,1,1,1,1,1,1,1,1,1,1,1,1,1,1,1,1,1,1,1,1,1,1,1,1,1,1,
1,1,1,1,1,1,1,1,1,1,1,1,1,1,1,1,1,1,1,1,1,1,1,1,1,1,1,1,1,1,1,1,1,1,1,1,
1,1,1,1,1,1,1,1,1,1,1,1,1,1,1,1,1,1,1,1,1,1,1,1,1,1,1,1,1,1,1,1,1,1,1,1,
1,1,1,1,1,1,1,1,1,1,1,1,1,1,1,1,1,1,1,1,1,1,1,1,1,1,1,1,1,1,1,1,1,1,1,1,
1,1,1,1,1,1,1,1,1,1,1,1,1,1,1,1,1,1,1,1,1,1,1,1,1,1,1,1,1,1,1,1,1,1,1,1,
1,1,1,1,1,1,1,1,1,1,1,1,1,1,1,1,1,1,1,1,1,1,1,1,1,1,1,1,1,1,1,1,1,1,1,1,
1,1,1,1,1,1,1,1,1,1,1,1,1,1,1,1,1,1,1,1,1,1,1,1,1,1,1,1,1,1,1,1,1,1,1,1,
1,1,1,1,1,1,1,1,1,1,1,1,1,1,1,1,1,1,1,1,1,1,1,1,1,1,1,1,1,1,1,1,1,1,1,1,
1,1,1,1,1,1,1,1,1,1,1,1,1,1,1,1,1,1,1,1,1,1,1,1,1,1,1,1,1,1,1,1,1,1,1,1,
1,1,1,1,1,1,1,1,1,1,1,1,1,1,1,1,1,1,1,1,1,1,1,1,1,1,1,1,1,1,1,1,1,1,1,1,
1,1,1,1,1,1,1,1,1,1,1,1,1,1,1,1,1,1,1,1,1,1,1,1,1,1,1,1,1,1,1,1,1,1,1,1,
1,1,1,1,1,1,1,1,1,1,1,1,1,1,1,1,1,1,1,1,1,1,1,1,1,1,1,1,1,1,1,1,1,1,1,1,
1,1,1,1,1,1,1,1,1,1,1,1,1,1,1,1,1,1,1,1,1,1,1,1,1,1,1,1,1,1,1,1,1,1,1,1,
1,1,1,1,1,1,1,1,1,1,1,1,1,1,1,1,1,1,1,1,1,1,1,1,1,1,1,1,1,1,1,1,1,1,1,1,
1,1,1,1,1,1,1,1,1,1,1,1,1,1,1,1,1,1,1,1,1,1,1,1,1,1,1,1,1,1,1,1,1,1,1,1,
1,1,1,1,1,1,1,1,1,1,1,1,1,1,1,1,1,1,1,1,1,1,1,1,1,1,1,1,1,1,1,1,1,1,1,1,
1,1,1,1,1,1,1,1,1,1,1,1,1,1,1,1,1,1,1,1,1,1,1,1,1,1,1,1,1,1,1,1,1,1,1,1,
1,1,1,1,1,1,1,1,1,1,1,1,1,1,1,1,1,1,1,1,1,1,1,1,1,1,1,1,1,1,1,1,1,1,1,1,
1,1,1,1,1,1,1,1,1,1,1,1,1,1,1,1,1,1,1,1,1,1,1,1,1,1,1,1,1,1,1,1,1,1,1,1,
1,1,1,1,1,1,1,1,1,1,1,1,1,1,1,1,1,4),(-0.000587328099657093,0.1157205948422),
(8.30590413559005,8.80579087257276,9.30565887793282,10.305394888653,11.3051308993731,
12.3048669100932,13.3046029208133,14.3043389315335,15.3040749422536,16.3038109529737,
17.3035469636939,18.303282974414,19.3030189851341,20.3027549958542,21.3024910065744,
22.3022270172945,23.3019630280146,24.3016990387348,25.3014350494549,26.301171060175,
27.3009070708951,28.3006430816153,29.3003790923354,30.3001151030555,31.2998511137757,
32.2995871244958,33.2993231352159,34.299059145936,35.2987951566562,36.2985311673763,
37.2982671780964,38.2980031888166,39.2977391995367,40.2974752102568,41.2972112209769,
42.2969472316971,43.2966832424172,44.2964192531373,45.2961552638575,46.2958912745776,
47.2956272852977,48.2953632960178,49.295099306738,50.2948353174581,51.2945713281782,
52.2943073388984,53.2940433496185,54.2937793603386,55.2935153710587,56.2932513817789,
57.292987392499,58.2927234032191,59.2924594139393,60.2921954246594,61.2919314353795,
62.2916674460996,63.2914034568198,64.2911394675399,65.29087547826,66.2906114889802,
67.2903474997003,68.2900835104204,69.2898195211405,70.2895555318607,71.2892915425808,
72.2890275533009,73.2887635640211,74.2884995747412,75.2882355854613,76.2879715961814,
77.2877076069016,78.2874436176217,79.2871796283418,80.286915639062,81.2866516497821,
82.2863876605022,83.2861236712224,84.2858596819425,85.2855956926626,86.2853317033827,
87.2850677141029,88.284803724823,89.2845397355431,90.2842757462633,91.2840117569834,
92.2837477677035,93.2834837784236,94.2832197891438,95.2829557998639,96.282691810584,
97.2824278213041,98.2821638320243,99.2818998427444,100.281635853465,101.281371864185,
102.281107874905,103.280843885625,104.280579896345,105.280315907065,106.280051917785,
107.279787928505,108.279523939226,109.279259949946,110.278995960666,111.278731971386,
112.278467982106,113.278203992826,114.277940003546,115.277676014266,116.277412024987,
117.277148035707,118.276884046427,119.276620057147,120.276356067867,121.276092078587,
122.275828089307,123.275564100028,124.275300110748,125.275036121468,126.274772132188,
127.274508142908,128.274244153628,129.273980164348,130.273716175068,131.273452185789,
132.273188196509,133.272924207229,134.272660217949,135.272396228669,136.272132239389,
137.271868250109,138.271604260829,139.27134027155,140.27107628227,141.27081229299,
142.27054830371,143.27028431443,144.27002032515,145.26975633587,146.26949234659,
147.269228357311,148.268964368031,149.268700378751,150.268436389471,151.268172400191,
152.267908410911,153.267644421631,154.267380432352,155.267116443072,156.266852453792,
157.266588464512,158.266324475232,159.266060485952,160.265796496672,161.265532507392,
162.265268518113,163.265004528833,164.264740539553,165.264476550273,166.264212560993,
167.263948571713,168.263684582433,169.263420593153,170.263156603874,171.262892614594,
172.262628625314,173.262364636034,174.262100646754,175.261836657474,176.261572668194,
177.261308678914,178.261044689635,179.260780700355,180.260516711075,181.260252721795,
182.259988732515,183.259724743235,184.259460753955,185.259196764675,186.258932775396,
187.258668786116,188.258404796836,189.258140807556,190.257876818276,191.257612828996,
192.257348839716,193.257084850437,194.256820861157,195.256556871877,196.256292882597,
197.256028893317,198.255764904037,199.255500914757,200.255236925477,201.254972936198,
202.254708946918,203.254444957638,204.254180968358,205.253916979078,206.253652989798,
207.253389000518,208.253125011238,209.252861021959,210.252597032679,211.252333043399,
212.252069054119,213.251805064839,214.251541075559,215.251277086279,216.251013096999,
217.25074910772,218.25048511844,219.25022112916,220.24995713988,221.2496931506,
222.24942916132,223.24916517204,224.248901182761,225.248637193481,226.248373204201,
227.248109214921,228.247845225641,229.247581236361,230.247317247081,231.247053257801,
232.246789268522,233.246525279242,234.246261289962,235.245997300682,236.245733311402,
237.245469322122,238.245205332842,239.244941343562,240.244677354283,241.244413365003,
242.244149375723,243.243885386443,244.243621397163,245.243357407883,246.243093418603,
247.242829429323,248.242565440044,249.242301450764,250.242037461484,251.241773472204,
252.241509482924,253.241245493644,254.240981504364,255.240717515084,256.240453525805,
257.240189536525,258.239925547245,259.239661557965,260.239397568685,261.239133579405,
262.238869590125,263.238605600846,264.238341611566,265.238077622286,266.237813633006,
267.237549643726,268.237285654446,269.237021665166,270.236757675886,271.236493686607,
272.236229697327,273.235965708047,274.235701718767,275.235437729487,276.235173740207,
277.234909750927,278.234645761647,279.234381772368,280.234117783088,281.233853793808,
282.233589804528,283.233325815248,284.233061825968,285.232797836688,286.232533847408,
287.232269858129,288.232005868849,289.231741879569,290.231477890289,291.231213901009,
292.230949911729,293.230685922449,294.23042193317,295.23015794389,296.22989395461,
297.22962996533,298.22936597605,299.22910198677,300.22883799749,301.22857400821,
302.228310018931,303.228046029651,304.227782040371,305.227518051091,306.227254061811,
307.226990072531,308.226726083251,309.226462093971,310.226198104692,311.225934115412,
312.225670126132,313.225406136852,314.225142147572,315.224878158292,316.224614169012,
317.224350179732,318.224086190453,319.223822201173,320.223558211893,321.223294222613,
322.223030233333,323.222766244053,324.222502254773,325.222238265494,326.221974276214,
327.221710286934,328.221446297654,329.221182308374,330.220918319094,331.220654329814,
332.220390340534,333.220126351255,334.219862361975,335.219598372695,336.219334383415,
337.219070394135,338.218806404855,339.218542415575,340.218278426295,341.218014437016,
342.217750447736,343.217486458456,344.217222469176,345.216958479896,346.216694490616,
347.216430501336,348.216166512056,349.215902522777,350.215638533497,351.215374544217,
352.215110554937,353.214846565657,354.214582576377,355.214318587097,356.214054597817,
357.213790608538,358.213526619258,359.213262629978,360.212998640698,361.212734651418,
362.212470662138,363.212206672858,364.211942683579,365.211678694299,366.211414705019,
367.211150715739,368.210886726459,369.210622737179,370.210358747899,371.210094758619,
372.20983076934,373.20956678006,374.20930279078,375.2090388015,376.20877481222,
377.20851082294,378.20824683366,379.20798284438,380.207718855101,381.207454865821,
382.207190876541,383.206926887261,384.206662897981,385.206398908701,386.206134919421,
387.205870930141,388.205606940862,389.205342951582,390.205078962302,391.204814973022,
392.204550983742,393.204286994462,394.204023005182,395.203759015903,396.203495026623,
397.203231037343,398.202967048063,399.202703058783,400.202439069503,401.202175080223,
402.201911090943,403.201647101664,404.201383112384,405.201119123104,406.200855133824,
407.200591144544,408.200327155264,409.200063165984,410.199799176704,411.199535187425,
412.199271198145,413.199007208865,414.198743219585,415.198479230305,416.198215241025,
417.197951251745,418.197687262465,419.197423273186,420.197159283906,421.196895294626,
422.196631305346,423.196367316066,424.196103326786,425.195839337506,426.195575348226,
427.195311358947,428.195047369667,429.194783380387,430.194519391107,431.194255401827,
432.193991412547,433.193727423267,434.193463433988,435.193199444708,436.192935455428,
437.192671466148,438.192407476868,439.192143487588,440.191879498308,441.191615509028,
442.191351519749,443.191087530469,444.190823541189,445.190559551909,446.190295562629,
447.190031573349,448.189767584069,449.189503594789,450.18923960551,451.18897561623,
452.18871162695,453.18844763767,454.18818364839,455.18791965911,456.18765566983,
457.18739168055,458.187127691271,459.186863701991,460.186599712711,461.186335723431,
462.186071734151,463.185807744871,464.185543755591,465.185279766312,466.185015777032,
467.184751787752,468.184487798472,469.184223809192,470.183959819912,471.183695830632,
472.183431841352,473.183167852073,474.182903862793,475.182639873513,476.182375884233,
477.182111894953,478.181847905673,479.181583916393,480.181319927113,481.181055937834,
482.180791948554,483.180527959274,484.180263969994,485.179999980714,486.179735991434,
487.179472002154,488.179208012874,489.178944023595,490.178680034315,491.178416045035,
492.178152055755,493.177888066475,494.177624077195,495.177360087915,496.177096098636,
497.176832109356,498.176568120076,499.176304130796,500.176040141516,501.175776152236,
502.175512162956,503.175248173676,504.174984184397,505.174720195117,506.174456205837,
507.174192216557,508.173928227277,509.173664237997,510.173400248717,511.173136259437,
512.172872270158,513.172608280878,514.172344291598,515.172080302318,516.171816313038,
517.171552323758,518.171288334478,519.171024345198,520.170760355919,521.170496366639,
522.170232377359,523.169968388079,524.169704398799,525.169440409519,526.169176420239,
527.168912430959,528.16864844168,529.1683844524,530.16812046312,531.16785647384,
532.16759248456,533.16732849528,534.167064506,535.166800516721,536.166536527441,
537.166272538161,538.166008548881,539.165744559601,540.165480570321,541.165216581041,
542.164952591761,543.164688602482,544.164424613202,545.164160623922,546.163896634642,
547.163632645362,548.163368656082,549.163104666802,550.162840677522,551.162576688243,
552.162312698963,553.162048709683,554.161784720403,555.161520731123,556.161256741843,
557.160992752563,558.160728763283,559.160464774004,560.160200784724,561.159936795444,
562.159672806164,563.159408816884,564.159144827604,565.158880838324,566.158616849045,
567.158352859765,568.158088870485,569.157824881205,570.157560891925,571.157296902645,
572.157032913365,573.156768924085,574.156504934806,575.156240945526,576.155976956246,
577.155712966966,578.155448977686,579.155184988406,580.154920999126,581.154657009846,
582.154393020567,583.154129031287,584.153865042007,585.153601052727,586.153337063447,
587.153073074167,588.152809084887,589.152545095607,590.152281106328,591.152017117048,
592.151753127768,593.151489138488,594.151225149208,595.150961159928,596.150697170648,
597.150433181368,598.150169192089,599.149905202809,600.149641213529,601.149377224249,
602.149113234969,603.148849245689,604.148585256409,605.14832126713,606.14805727785,
607.14779328857,608.14752929929,609.14726531001,610.14700132073,611.14673733145,
612.14647334217,613.146209352891,614.145945363611,615.145681374331,616.145417385051,
617.145153395771,618.144889406491,619.144625417211,620.144361427931,621.144097438652,
622.143833449372,623.143569460092,624.143305470812,625.143041481532,626.142777492252,
627.142513502972,628.142249513692,629.141985524413,630.141721535133,631.141457545853,
632.141193556573,633.140929567293,634.140665578013,635.140401588733,636.140137599454,
637.139873610174,638.139609620894,639.139345631614,640.139081642334,641.138817653054,
642.138553663774,643.138289674494,644.138025685215,645.137761695935,646.137497706655,
647.137233717375,648.136969728095,649.136705738815,650.136441749535,651.136177760255,
652.135913770976,653.135649781696,654.135385792416,655.135121803136,656.134857813856,
657.134593824576,658.134329835296,659.134065846016,660.133801856737,661.133537867457,
662.133273878177,663.133009888897,664.132745899617,665.132481910337,666.132217921057,
667.131953931778,668.131689942498,669.131425953218,670.131161963938,671.130897974658,
672.130633985378,673.130369996098,674.130106006818,675.129842017539,676.129578028259,
677.129314038979,678.129050049699,679.128786060419,680.128522071139,681.128258081859,
682.127994092579,683.1277301033,684.12746611402,685.12720212474,686.12693813546,
687.12667414618,688.1264101569,689.12614616762,690.12588217834,691.125618189061,
692.125354199781,693.125090210501,694.124826221221,695.124562231941,696.124298242661,
697.124034253381,698.123770264101,699.123506274822,700.123242285542,701.122978296262,
702.122714306982,703.122450317702,704.122186328422,705.121922339142,706.121658349863,
707.121394360583,708.121130371303,709.120866382023,710.120602392743,711.120338403463,
712.120074414183,713.119810424903,714.119546435624,715.119282446344,716.119018457064,
717.118754467784,718.118490478504,719.118226489224,720.117962499944,721.117698510664,
722.117434521385,723.117170532105,724.116906542825,725.116642553545,726.116378564265,
727.116114574985,728.115850585705,729.115586596425,730.115322607146,731.115058617866,
732.114794628586,733.114530639306,734.114266650026,735.114002660746,736.113738671466,
737.113474682187,738.113210692907,739.112946703627,740.112682714347,741.112418725067,
742.112154735787,743.111890746507,744.111626757227,745.111362767948,746.111098778668,
747.110834789388,748.110570800108,749.110306810828,750.110042821548,751.109778832268,
752.109514842988,753.109250853709,754.108986864429,755.108722875149,756.108458885869,
757.108194896589,758.107930907309,759.107666918029,760.107402928749,761.10713893947,
762.10687495019,763.10661096091,764.10634697163,765.10608298235,766.10581899307,
767.10555500379,768.10529101451,769.105027025231,770.104763035951,771.104499046671,
772.104235057391,773.103971068111,774.103707078831,775.103443089551,776.103179100272,
777.102915110992,778.102651121712,779.102387132432,780.102123143152,781.101859153872,
782.101595164592,783.101331175312,784.101067186033,785.100803196753,786.100539207473,
787.100275218193,788.100011228913,789.099747239633,790.099483250353,791.099219261073,
792.098955271794,793.098691282514,794.098427293234,795.098163303954,796.097899314674,
797.097635325394,798.097371336114,799.097107346834,800.096843357555,801.096579368275,
802.096315378995,803.096051389715,804.095787400435,805.095523411155,806.095259421875,
807.094995432596,808.094731443316,809.094467454036,810.094203464756,811.093939475476,
812.093675486196,813.093411496916,814.093147507636,815.092883518357,816.092619529077,
817.092355539797,818.092091550517,819.091827561237,820.091563571957,821.091299582677,
822.091035593397,823.090771604118,824.090507614838,825.090243625558,826.089979636278,
827.089715646998,828.089451657718,829.089187668438,830.088923679158,831.088659689879,
832.088395700599,833.088131711319,834.087867722039,835.087603732759,836.087339743479,
837.087075754199,838.08681176492,839.08654777564,840.08628378636,841.08601979708,
842.0857558078,843.08549181852,844.08522782924,845.08496383996,846.084699850681,
847.084435861401,848.084171872121,849.083907882841,850.083643893561,851.083379904281,
852.083115915001,853.082851925721,854.082587936442,855.082323947162,856.082059957882,
857.081795968602,858.081531979322,859.081267990042,860.081004000762,861.080740011482,
862.080476022203,863.080212032923,864.079948043643,865.079684054363,866.079420065083,
867.079156075803,868.078892086523,869.078628097243,870.078364107964,871.078100118684,
872.077836129404,873.077572140124,874.077308150844,875.077044161564,876.076780172284,
877.076516183005,878.076252193725,879.075988204445,880.075724215165,881.075460225885,
882.075196236605,883.074932247325,884.074668258045,885.074404268766,886.074140279486,
887.073876290206,888.073612300926,889.073348311646,890.073084322366,891.072820333086,
892.072556343806,893.072292354527,894.072028365247,895.071764375967,896.071500386687,
897.071236397407,898.070972408127,899.070708418847,900.070444429567,901.070180440288,
902.069916451008,903.069652461728,904.069388472448,905.069124483168,906.068860493888,
907.068596504608,908.068332515329,909.068068526049,910.067804536769,911.067540547489,
912.067276558209,913.067012568929,914.066748579649,915.066484590369,916.06622060109,
917.06595661181,918.06569262253,919.06542863325,920.06516464397,921.06490065469,
922.06463666541,923.06437267613,924.064108686851,925.063844697571,926.063580708291,
927.063316719011,928.063052729731,929.062788740451,930.062524751171,931.062260761891,
932.061996772612,933.061732783332,934.061468794052,935.061204804772,936.060940815492,
937.060676826212,938.060412836932,939.060148847652,940.059884858373,941.059620869093,
942.059356879813,943.059092890533,944.058828901253,945.058564911973,946.058300922693,
947.058036933414,948.057772944134,949.057508954854,950.057244965574,951.056980976294,
952.056716987014,953.056452997734,954.056189008454,955.055925019175,956.055661029895,
957.055397040615,958.055133051335,959.054869062055,960.054605072775,961.054341083495,
962.054077094215,963.053813104936,964.053549115656,965.053285126376,966.053021137096,
967.052757147816,968.052493158536,969.052229169256,970.051965179976,971.051701190697,
972.051437201417,973.051173212137,974.050909222857,975.050645233577,976.050381244297,
977.050117255017,978.049853265738,979.049589276458,980.049325287178,981.049061297898,
982.048797308618,983.048533319338,984.048269330058,985.048005340778,986.047741351499,
987.047477362219,988.047213372939,989.046949383659,990.046685394379,991.046421405099,
992.046157415819,993.045893426539,994.04562943726,995.04536544798,996.0451014587,
997.04483746942,998.04457348014,999.04430949086,1000.04404550158,1001.0437815123,
1002.04351752302,1003.04325353374,1004.04298954446,1005.04272555518,1006.0424615659,
1007.04219757662,1008.04193358734,1009.04166959806,1010.04140560878,1011.0411416195,
1012.04087763022,1013.04061364094,1014.04034965166,1015.04008566238,1016.0398216731,
1017.03955768382,1018.03929369454,1019.03902970526,1020.03876571598,1021.0385017267,
1022.03823773742,1023.03797374814,1024.03770975886,1025.03744576958,1026.0371817803,
1027.03691779102,1028.03665380174,1029.03638981246,1030.03612582318,1031.0358618339,
1032.03559784462,1033.03533385534,1034.03506986606,1035.03480587678,1036.03454188751,
1037.03427789823,1038.03401390895,1039.03374991967,1040.03348593039,1041.03322194111,
1042.03295795183,1043.03269396255,1044.03242997327,1045.03216598399,1046.03190199471,
1047.03163800543,1048.03137401615,1049.03111002687,1050.03084603759,1051.03058204831,
1052.03031805903,1053.03005406975,1054.02979008047,1055.02952609119,1056.02926210191,
1057.02899811263,1058.02873412335,1059.02847013407,1060.02820614479,1061.02794215551,
1062.02767816623,1063.02741417695,1064.02715018767,1065.02688619839,1066.02662220911,
1067.02635821983,1068.02609423055,1069.02583024127,1070.02556625199,1071.02530226271,
1072.02503827343,1073.02477428415,1074.02451029487,1075.02424630559,1076.02398231631,
1077.02371832703,1078.02345433775,1079.02319034847,1080.02292635919,1081.02266236991,
1082.02239838063,1083.02213439135,1084.02187040207,1085.02160641279,1086.02134242351,
1087.02107843423,1088.02081444495,1089.02055045567,1090.02028646639,1091.02002247711,
1092.01975848783,1093.01949449855,1094.01923050927,1095.01896651999,1096.01870253071,
1097.01843854143,1098.01817455215,1099.01791056287,1100.01764657359,1101.01738258431,
1102.01711859503,1103.01685460575,1104.01659061647,1105.01632662719,1106.01606263791,
1107.01579864863,1108.01553465935,1109.01527067007,1110.01500668079,1111.01474269151,
1112.01447870223,1113.01421471295,1114.01395072368,1115.0136867344,1116.01342274512,
1117.01315875584,1118.01289476656,1119.01263077728,1120.012366788,1121.01210279872,
1122.01183880944,1123.01157482016,1124.01131083088,1125.0110468416,1126.01078285232,
1127.01051886304,1128.01025487376,1129.00999088448,1130.0097268952,1131.00946290592,
1132.00919891664,1133.00893492736,1134.00867093808,1135.0084069488,1136.00814295952,
1137.00787897024,1138.00761498096,1139.00735099168,1140.0070870024,1141.00682301312,
1142.00655902384,1143.00629503456,1144.00603104528,1145.005767056,1146.00550306672,
1147.00523907744,1148.00497508816,1149.00471109888,1150.0044471096,1151.00418312032,
1152.00391913104,1153.00365514176,1154.00339115248,1155.0031271632,1156.00286317392,
1157.00259918464,1158.00233519536,1159.00207120608,1160.0018072168,1161.00154322752,
1162.00127923824,1163.00101524896,1164.00075125968,1165.0004872704,1166.00022328112,
1166.99995929184,1167.99969530256,1168.99943131328,1169.999167324,1170.99890333472,
1171.99863934544,1172.99837535616,1173.99811136688,1174.9978473776,1175.99758338832,
1176.99731939904,1177.99705540976,1178.99679142048,1179.9965274312,1180.99626344192,
1181.99599945264,1182.99573546336,1183.99547147408,1184.9952074848,1185.99494349552,
1186.99467950624,1187.99441551696,1188.99415152768,1189.99388753841,1190.99362354913,
1191.99335955985,1192.99309557057,1193.99283158129,1194.99256759201,1195.99230360273,
1196.99203961345,1197.99177562417,1198.99151163489,1199.99124764561,1200.99098365633,
1201.99071966705,1202.99045567777,1203.99019168849,1204.98992769921,1205.98966370993,
1206.98939972065,1207.98913573137,1208.98887174209,1209.98860775281,1210.98834376353,
1211.98807977425,1212.98781578497,1213.98755179569,1214.98728780641,1215.98702381713,
1216.98675982785,1217.98649583857,1218.98623184929,1219.98596786001,1220.98570387073,
1221.98543988145,1222.98517589217,1223.98491190289,1224.98464791361,1225.98438392433,
1226.98411993505,1227.98385594577,1228.98359195649,1229.98332796721,1230.98306397793,
1231.98279998865,1232.98253599937,1233.98227201009,1234.98200802081,1235.98174403153,
1236.98148004225,1237.98121605297,1238.98095206369,1239.98068807441,1240.98042408513,
1241.98016009585,1242.97989610657,1243.97963211729,1244.97936812801,1245.97910413873,
1246.97884014945,1247.97857616017,1248.97831217089,1249.97804818161,1250.97778419233,
1251.97752020305,1252.97725621377,1253.97699222449,1254.97672823521,1255.97646424593,
1256.97620025665,1257.97593626737,1258.97567227809,1259.97540828881,1260.97514429953,
1261.97488031025,1262.97461632097,1263.97435233169,1264.97408834241,1265.97382435313,
1266.97356036385,1267.97329637458,1268.9730323853,1269.97276839602,1270.97250440674,
1271.97224041746,1272.97197642818,1273.9717124389,1274.97144844962,1275.97118446034,
1276.97092047106,1277.97065648178,1278.9703924925,1279.97012850322,1280.96986451394,
1281.96960052466,1282.96933653538,1283.9690725461,1284.96880855682,1285.96854456754,
1286.96828057826,1287.96801658898,1288.9677525997,1289.96748861042,1290.96722462114,
1291.96696063186,1292.96669664258,1293.9664326533,1294.96616866402,1295.96590467474,
1296.96564068546,1297.96537669618,1298.9651127069,1299.96484871762,1300.96458472834,
1301.96432073906,1302.96405674978,1303.9637927605,1304.96352877122,1305.96326478194,
1306.96300079266,1307.96273680338,1308.9624728141,1309.96220882482,1310.96194483554,
1311.96168084626,1312.96141685698,1313.9611528677,1314.96088887842,1315.96062488914,
1316.96036089986,1317.96009691058,1318.9598329213,1319.95956893202,1320.95930494274,
1321.95904095346,1322.95877696418,1323.9585129749,1324.95824898562,1325.95798499634,
1326.95772100706,1327.95745701778,1328.9571930285,1329.95692903922,1330.95666504994,
1331.95640106066,1332.95613707138,1333.9558730821,1334.95560909282,1335.95534510354,
1336.95508111426,1337.95481712498,1338.9545531357,1339.95428914642,1340.95402515714,
1341.95376116786,1342.95349717858,1343.9532331893,1344.95296920002,1345.95270521075,
1346.95244122147,1347.95217723219,1348.95191324291,1349.95164925363,1350.95138526435,
1351.95112127507,1352.95085728579,1353.95059329651,1354.95032930723,1355.95006531795,
1356.94980132867,1357.94953733939,1358.94927335011,1359.94900936083,1360.94874537155,
1361.94848138227,1362.94821739299,1363.94795340371,1364.94768941443,1365.94742542515,
1366.94716143587,1367.94689744659,1368.94663345731,1369.94636946803,1370.94610547875,
1371.94584148947,1372.94557750019,1373.94531351091,1374.94504952163,1375.94478553235,
1376.94452154307,1377.94425755379,1378.94399356451,1379.94372957523,1380.94346558595,
1381.94320159667,1382.94293760739,1383.94267361811,1384.94240962883,1385.94214563955,
1386.94188165027,1387.94161766099,1388.94135367171,1389.94108968243,1390.94082569315,
1391.94056170387,1392.94029771459,1393.94003372531,1394.93976973603,1395.93950574675,
1396.93924175747,1397.93897776819,1398.93871377891,1399.93844978963,1400.93818580035,
1401.93792181107,1402.93765782179,1403.93739383251,1404.93712984323,1405.93686585395,
1406.93660186467,1407.93633787539,1408.93607388611,1409.93580989683,1410.93554590755,
1411.93528191827,1412.93501792899,1413.93475393971,1414.93448995043,1415.93422596115,
1416.93396197187,1417.93369798259,1418.93343399331,1419.93317000403,1420.93290601475,
1421.93264202547,1422.93237803619,1423.93211404692,1424.93185005764,1425.93158606836,
1426.93132207908,1427.9310580898,1428.93079410052,1429.93053011124,1430.93026612196,
1431.93000213268,1432.9297381434,1433.92947415412,1434.92921016484,1435.92894617556,
1436.92868218628,1437.928418197,1438.92815420772,1439.92789021844,1440.92762622916,
1441.92736223988,1442.9270982506,1443.92683426132,1444.92657027204,1445.92630628276,
1446.92604229348,1447.9257783042,1448.92551431492,1449.92525032564,1450.92498633636,
1451.92472234708,1452.9244583578,1453.92419436852,1454.92393037924,1455.92366638996,
1456.92340240068,1457.9231384114,1458.92287442212,1459.92261043284,1460.92234644356,
1461.92208245428,1462.921818465,1463.92155447572,1464.92129048644,1465.92102649716,
1466.92076250788,1467.9204985186,1468.92023452932,1469.91997054004,1470.91970655076,
1471.91944256148,1472.9191785722,1473.91891458292,1474.91865059364,1475.91838660436,
1476.91812261508,1477.9178586258,1478.91759463652,1479.91733064724,1480.91706665796,
1481.91680266868,1482.9165386794,1483.91627469012,1484.91601070084,1485.91574671156,
1486.91548272228,1487.915218733,1488.91495474372,1489.91469075444,1490.91442676516,
1491.91416277588,1492.9138987866,1493.91363479732,1494.91337080804,1495.91310681876,
1496.91284282948,1497.9125788402,1498.91231485092,1499.91205086164,1500.91178687236,
1501.91152288309,1502.91125889381,1503.91099490453,1504.91073091525,1505.91046692597,
1506.91020293669,1507.90993894741,1508.90967495813,1509.90941096885,1510.90914697957,
1511.90888299029,1512.90861900101,1513.90835501173,1514.90809102245,1515.90782703317,
1516.90756304389,1517.90729905461,1518.90703506533,1519.90677107605,1520.90650708677,
1521.90624309749,1522.90597910821,1523.90571511893,1524.90545112965,1525.90518714037,
1526.90492315109,1527.90465916181,1528.90439517253,1529.90413118325,1530.90386719397,
1531.90360320469,1532.90333921541,1533.90307522613,1534.90281123685,1535.90254724757,
1536.90228325829,1537.90201926901,1538.90175527973,1539.90149129045,1540.90122730117,
1541.90096331189,1542.90069932261,1543.90043533333,1544.90017134405,1545.89990735477,
1546.89964336549,1547.89937937621,1548.89911538693,1549.89885139765,1550.89858740837,
1551.89832341909,1552.89805942981,1553.89779544053,1554.89753145125,1555.89726746197,
1556.89700347269,1557.89673948341,1558.89647549413,1559.89621150485,1560.89594751557,
1561.89568352629,1562.89541953701,1563.89515554773,1564.89489155845,1565.89462756917,
1566.89436357989,1567.89409959061,1568.89383560133,1569.89357161205,1570.89330762277,
1571.89304363349,1572.89277964421,1573.89251565493,1574.89225166565,1575.89198767637,
1576.89172368709,1577.89145969781,1578.89119570853,1579.89093171926,1580.89066772998,
1581.8904037407,1582.89013975142,1583.88987576214,1584.88961177286,1585.88934778358,
1586.8890837943,1587.88881980502,1588.88855581574,1589.88829182646,1590.88802783718,
1591.8877638479,1592.88749985862,1593.88723586934,1594.88697188006,1595.88670789078,
1596.8864439015,1597.88617991222,1598.88591592294,1599.88565193366,1600.88538794438,
1601.8851239551,1602.88485996582,1603.88459597654,1604.88433198726,1605.88406799798,
1606.8838040087,1607.88354001942,1608.88327603014,1609.88301204086,1610.88274805158,
1611.8824840623,1612.88222007302,1613.88195608374,1614.88169209446,1615.88142810518,
1616.8811641159,1617.88090012662,1618.88063613734,1619.88037214806,1620.88010815878,
1621.8798441695,1622.87958018022,1623.87931619094,1624.87905220166,1625.87878821238,
1626.8785242231,1627.87826023382,1628.87799624454,1629.87773225526,1630.87746826598,
1631.8772042767,1632.87694028742,1633.87667629814,1634.87641230886,1635.87614831958,
1636.8758843303,1637.87562034102,1638.87535635174,1639.87509236246,1640.87482837318,
1641.8745643839,1642.87430039462,1643.87403640534,1644.87377241606,1645.87350842678,
1646.8732444375,1647.87298044822,1648.87271645894,1649.87245246966,1650.87218848038,
1651.8719244911,1652.87166050182,1653.87139651254,1654.87113252326,1655.87086853399,
1656.8706045447,1657.87034055543,1658.87007656615,1659.86981257687,1660.86954858759,
1661.86928459831,1662.86902060903,1663.86875661975,1664.86849263047,1665.86822864119,
1666.86796465191,1667.86770066263,1668.86743667335,1669.86717268407,1670.86690869479,
1671.86664470551,1672.86638071623,1673.86611672695,1674.86585273767,1675.86558874839,
1676.86532475911,1677.86506076983,1678.86479678055,1679.86453279127,1680.86426880199,
1681.86400481271,1682.86374082343,1683.86347683415,1684.86321284487,1685.86294885559,
1686.86268486631,1687.86242087703,1688.86215688775,1689.86189289847,1690.86162890919,
1691.86136491991,1692.86110093063,1693.86083694135,1694.86057295207,1695.86030896279,
1696.86004497351,1697.35991297887,1697.85988790214),.UNSPECIFIED.);
#55=B_SPLINE_SURFACE_WITH_KNOTS('',3,3,((#265391,#265392,#265393,#265394,
#265395,#265396,#265397,#265398,#265399,#265400,#265401,#265402,#265403,
#265404,#265405,#265406,#265407,#265408,#265409,#265410,#265411,#265412,
#265413,#265414,#265415,#265416,#265417,#265418,#265419,#265420,#265421,
#265422,#265423,#265424,#265425,#265426,#265427,#265428,#265429,#265430,
#265431,#265432,#265433,#265434,#265435,#265436,#265437,#265438,#265439,
#265440,#265441,#265442,#265443,#265444,#265445,#265446,#265447,#265448,
#265449,#265450,#265451,#265452,#265453,#265454,#265455,#265456,#265457,
#265458,#265459,#265460,#265461,#265462,#265463,#265464,#265465,#265466,
#265467,#265468,#265469,#265470,#265471,#265472,#265473,#265474,#265475,
#265476,#265477,#265478,#265479,#265480,#265481,#265482,#265483,#265484,
#265485,#265486,#265487,#265488,#265489,#265490,#265491,#265492,#265493,
#265494,#265495,#265496,#265497,#265498,#265499,#265500,#265501,#265502,
#265503,#265504,#265505,#265506,#265507,#265508,#265509,#265510,#265511,
#265512,#265513,#265514,#265515,#265516,#265517,#265518,#265519,#265520,
#265521,#265522,#265523,#265524,#265525,#265526,#265527,#265528,#265529,
#265530,#265531,#265532,#265533,#265534,#265535,#265536,#265537,#265538,
#265539,#265540,#265541,#265542,#265543,#265544,#265545,#265546,#265547,
#265548,#265549,#265550,#265551,#265552,#265553,#265554,#265555,#265556,
#265557,#265558,#265559,#265560,#265561,#265562,#265563,#265564,#265565,
#265566,#265567,#265568,#265569,#265570,#265571,#265572,#265573,#265574,
#265575,#265576,#265577,#265578,#265579,#265580,#265581,#265582,#265583,
#265584,#265585,#265586,#265587,#265588,#265589,#265590,#265591,#265592,
#265593,#265594,#265595,#265596,#265597,#265598,#265599,#265600,#265601,
#265602,#265603,#265604,#265605,#265606,#265607,#265608,#265609,#265610,
#265611,#265612,#265613,#265614,#265615,#265616,#265617,#265618,#265619,
#265620,#265621,#265622,#265623,#265624,#265625,#265626,#265627,#265628,
#265629,#265630,#265631,#265632,#265633,#265634,#265635,#265636,#265637,
#265638,#265639,#265640,#265641,#265642,#265643,#265644,#265645,#265646,
#265647,#265648,#265649,#265650,#265651,#265652,#265653,#265654,#265655,
#265656,#265657,#265658,#265659,#265660,#265661,#265662,#265663,#265664,
#265665,#265666,#265667,#265668,#265669,#265670,#265671,#265672,#265673,
#265674,#265675,#265676,#265677,#265678,#265679,#265680,#265681,#265682,
#265683,#265684,#265685,#265686,#265687,#265688,#265689,#265690,#265691,
#265692,#265693,#265694,#265695,#265696,#265697,#265698,#265699,#265700,
#265701,#265702,#265703,#265704,#265705,#265706,#265707,#265708,#265709,
#265710,#265711,#265712,#265713,#265714,#265715,#265716,#265717,#265718,
#265719,#265720,#265721,#265722,#265723,#265724,#265725,#265726,#265727,
#265728,#265729,#265730,#265731,#265732,#265733,#265734,#265735,#265736,
#265737,#265738,#265739,#265740,#265741,#265742,#265743,#265744,#265745,
#265746,#265747,#265748,#265749,#265750,#265751,#265752,#265753,#265754,
#265755,#265756,#265757,#265758,#265759,#265760,#265761,#265762,#265763,
#265764,#265765,#265766,#265767,#265768,#265769,#265770,#265771,#265772,
#265773,#265774,#265775,#265776,#265777,#265778,#265779,#265780,#265781,
#265782,#265783,#265784,#265785,#265786,#265787,#265788,#265789,#265790,
#265791,#265792,#265793,#265794,#265795,#265796,#265797,#265798,#265799,
#265800,#265801,#265802,#265803,#265804,#265805,#265806,#265807,#265808,
#265809,#265810,#265811,#265812,#265813,#265814,#265815,#265816,#265817,
#265818,#265819,#265820,#265821,#265822,#265823,#265824,#265825,#265826,
#265827,#265828,#265829,#265830,#265831,#265832,#265833,#265834,#265835,
#265836,#265837,#265838,#265839,#265840,#265841,#265842,#265843,#265844,
#265845,#265846,#265847,#265848,#265849,#265850,#265851,#265852,#265853,
#265854,#265855,#265856,#265857,#265858,#265859,#265860,#265861,#265862,
#265863,#265864,#265865,#265866,#265867,#265868,#265869,#265870,#265871,
#265872,#265873,#265874,#265875,#265876,#265877,#265878,#265879,#265880,
#265881,#265882,#265883,#265884,#265885,#265886,#265887,#265888,#265889,
#265890,#265891,#265892,#265893,#265894,#265895,#265896,#265897,#265898,
#265899,#265900,#265901,#265902,#265903,#265904,#265905,#265906,#265907,
#265908,#265909,#265910,#265911,#265912,#265913,#265914,#265915,#265916,
#265917,#265918,#265919,#265920,#265921,#265922,#265923,#265924,#265925,
#265926,#265927,#265928,#265929,#265930,#265931,#265932,#265933,#265934,
#265935,#265936,#265937,#265938,#265939,#265940,#265941,#265942,#265943,
#265944,#265945,#265946,#265947,#265948,#265949,#265950,#265951,#265952,
#265953,#265954,#265955,#265956,#265957,#265958,#265959,#265960,#265961,
#265962,#265963,#265964,#265965,#265966,#265967,#265968,#265969,#265970,
#265971,#265972,#265973,#265974,#265975,#265976,#265977,#265978,#265979,
#265980,#265981,#265982,#265983,#265984,#265985,#265986,#265987,#265988,
#265989,#265990,#265991,#265992,#265993,#265994,#265995,#265996,#265997,
#265998,#265999,#266000,#266001,#266002,#266003,#266004,#266005,#266006,
#266007,#266008,#266009,#266010,#266011,#266012,#266013,#266014,#266015,
#266016,#266017,#266018,#266019,#266020,#266021,#266022,#266023,#266024,
#266025,#266026,#266027,#266028,#266029,#266030,#266031,#266032,#266033,
#266034,#266035,#266036,#266037,#266038,#266039,#266040,#266041,#266042,
#266043,#266044,#266045,#266046,#266047,#266048,#266049,#266050,#266051,
#266052,#266053,#266054,#266055,#266056,#266057,#266058,#266059,#266060,
#266061,#266062,#266063,#266064,#266065,#266066,#266067,#266068,#266069,
#266070,#266071,#266072,#266073,#266074,#266075,#266076,#266077,#266078,
#266079,#266080,#266081,#266082,#266083,#266084,#266085,#266086,#266087,
#266088,#266089,#266090,#266091,#266092,#266093,#266094,#266095,#266096,
#266097,#266098,#266099,#266100,#266101,#266102,#266103,#266104,#266105,
#266106,#266107,#266108,#266109,#266110,#266111,#266112,#266113,#266114,
#266115,#266116,#266117,#266118,#266119,#266120,#266121,#266122,#266123,
#266124,#266125,#266126,#266127,#266128,#266129,#266130,#266131,#266132,
#266133,#266134,#266135,#266136,#266137,#266138,#266139,#266140,#266141,
#266142,#266143,#266144,#266145,#266146,#266147,#266148,#266149,#266150,
#266151,#266152,#266153,#266154,#266155,#266156,#266157,#266158,#266159,
#266160,#266161,#266162,#266163,#266164,#266165,#266166,#266167,#266168,
#266169,#266170,#266171,#266172,#266173,#266174,#266175,#266176,#266177,
#266178,#266179,#266180,#266181,#266182,#266183,#266184,#266185,#266186,
#266187,#266188,#266189,#266190,#266191,#266192,#266193,#266194,#266195,
#266196,#266197,#266198,#266199,#266200,#266201,#266202,#266203,#266204,
#266205,#266206,#266207,#266208,#266209,#266210,#266211,#266212,#266213,
#266214,#266215,#266216,#266217,#266218,#266219,#266220,#266221,#266222,
#266223,#266224,#266225,#266226,#266227,#266228,#266229,#266230,#266231,
#266232,#266233,#266234,#266235,#266236,#266237,#266238,#266239,#266240,
#266241,#266242,#266243,#266244,#266245,#266246,#266247,#266248,#266249,
#266250,#266251,#266252,#266253,#266254,#266255,#266256,#266257,#266258,
#266259,#266260,#266261,#266262,#266263,#266264,#266265,#266266,#266267,
#266268,#266269,#266270,#266271,#266272,#266273,#266274,#266275,#266276,
#266277,#266278,#266279,#266280,#266281,#266282,#266283,#266284,#266285,
#266286,#266287,#266288,#266289,#266290,#266291,#266292,#266293,#266294,
#266295,#266296,#266297,#266298,#266299,#266300,#266301,#266302,#266303,
#266304,#266305,#266306,#266307,#266308,#266309,#266310,#266311,#266312,
#266313,#266314,#266315,#266316,#266317,#266318,#266319,#266320,#266321,
#266322,#266323,#266324,#266325,#266326,#266327,#266328,#266329,#266330,
#266331,#266332,#266333,#266334,#266335,#266336,#266337,#266338,#266339,
#266340,#266341,#266342,#266343,#266344,#266345,#266346,#266347,#266348,
#266349,#266350,#266351,#266352,#266353,#266354,#266355,#266356,#266357,
#266358,#266359,#266360,#266361,#266362,#266363,#266364,#266365,#266366,
#266367,#266368,#266369,#266370,#266371,#266372,#266373,#266374,#266375,
#266376,#266377,#266378,#266379,#266380,#266381,#266382,#266383,#266384,
#266385,#266386,#266387,#266388,#266389,#266390,#266391,#266392,#266393,
#266394,#266395,#266396,#266397,#266398,#266399,#266400,#266401,#266402,
#266403,#266404,#266405,#266406,#266407,#266408,#266409,#266410,#266411,
#266412,#266413,#266414,#266415,#266416,#266417,#266418,#266419,#266420,
#266421,#266422,#266423,#266424,#266425,#266426,#266427,#266428,#266429,
#266430,#266431,#266432,#266433,#266434,#266435,#266436,#266437,#266438,
#266439,#266440,#266441,#266442,#266443,#266444,#266445,#266446,#266447,
#266448,#266449,#266450,#266451,#266452,#266453,#266454,#266455,#266456,
#266457,#266458,#266459,#266460,#266461,#266462,#266463,#266464,#266465,
#266466,#266467,#266468,#266469,#266470,#266471,#266472,#266473,#266474,
#266475,#266476,#266477,#266478,#266479,#266480,#266481,#266482,#266483,
#266484,#266485,#266486,#266487,#266488,#266489,#266490,#266491,#266492,
#266493,#266494,#266495,#266496,#266497,#266498,#266499,#266500,#266501,
#266502,#266503,#266504,#266505,#266506,#266507,#266508,#266509,#266510,
#266511,#266512,#266513,#266514,#266515,#266516,#266517,#266518,#266519,
#266520,#266521,#266522,#266523,#266524,#266525,#266526,#266527,#266528,
#266529,#266530,#266531,#266532,#266533,#266534,#266535,#266536,#266537,
#266538,#266539,#266540,#266541,#266542,#266543,#266544,#266545,#266546,
#266547,#266548,#266549,#266550,#266551,#266552,#266553,#266554,#266555,
#266556,#266557,#266558,#266559,#266560,#266561,#266562,#266563,#266564,
#266565,#266566,#266567,#266568,#266569,#266570,#266571,#266572,#266573,
#266574,#266575,#266576,#266577,#266578,#266579,#266580,#266581,#266582,
#266583,#266584,#266585,#266586,#266587,#266588,#266589,#266590,#266591,
#266592,#266593,#266594,#266595,#266596,#266597,#266598,#266599,#266600,
#266601,#266602,#266603,#266604,#266605,#266606,#266607,#266608,#266609,
#266610,#266611,#266612,#266613,#266614,#266615,#266616,#266617,#266618,
#266619,#266620,#266621,#266622,#266623,#266624,#266625,#266626,#266627,
#266628,#266629,#266630,#266631,#266632,#266633,#266634,#266635,#266636,
#266637,#266638,#266639,#266640,#266641,#266642,#266643,#266644,#266645,
#266646,#266647,#266648,#266649,#266650,#266651,#266652,#266653,#266654,
#266655,#266656,#266657,#266658,#266659,#266660,#266661,#266662,#266663,
#266664,#266665,#266666,#266667,#266668,#266669,#266670,#266671,#266672,
#266673,#266674,#266675,#266676,#266677,#266678,#266679,#266680,#266681,
#266682,#266683,#266684,#266685,#266686,#266687,#266688,#266689,#266690,
#266691,#266692,#266693,#266694,#266695,#266696,#266697,#266698,#266699,
#266700,#266701,#266702,#266703,#266704,#266705,#266706,#266707,#266708,
#266709,#266710,#266711,#266712,#266713,#266714,#266715,#266716,#266717,
#266718,#266719,#266720,#266721,#266722,#266723,#266724,#266725,#266726,
#266727,#266728,#266729,#266730,#266731,#266732,#266733,#266734,#266735,
#266736,#266737,#266738,#266739,#266740,#266741,#266742,#266743,#266744,
#266745,#266746,#266747,#266748,#266749,#266750,#266751,#266752,#266753,
#266754,#266755,#266756,#266757,#266758,#266759,#266760,#266761,#266762,
#266763,#266764,#266765,#266766,#266767,#266768,#266769,#266770,#266771,
#266772,#266773,#266774,#266775,#266776,#266777,#266778,#266779,#266780,
#266781,#266782,#266783,#266784,#266785,#266786,#266787,#266788,#266789,
#266790,#266791,#266792,#266793,#266794,#266795,#266796,#266797,#266798,
#266799,#266800,#266801,#266802,#266803,#266804,#266805,#266806,#266807,
#266808,#266809,#266810,#266811,#266812,#266813,#266814,#266815,#266816,
#266817,#266818,#266819,#266820,#266821,#266822,#266823,#266824,#266825,
#266826,#266827,#266828,#266829,#266830,#266831,#266832,#266833,#266834,
#266835,#266836,#266837,#266838,#266839,#266840,#266841,#266842,#266843,
#266844,#266845,#266846,#266847,#266848,#266849,#266850,#266851,#266852,
#266853,#266854,#266855,#266856,#266857,#266858,#266859,#266860,#266861,
#266862,#266863,#266864,#266865,#266866,#266867,#266868,#266869,#266870,
#266871,#266872,#266873,#266874,#266875,#266876,#266877,#266878,#266879,
#266880,#266881,#266882,#266883,#266884,#266885,#266886,#266887,#266888,
#266889,#266890,#266891,#266892,#266893,#266894,#266895,#266896,#266897,
#266898,#266899,#266900,#266901,#266902,#266903,#266904,#266905,#266906,
#266907,#266908,#266909,#266910,#266911,#266912,#266913,#266914,#266915,
#266916,#266917,#266918,#266919,#266920,#266921,#266922,#266923,#266924,
#266925,#266926,#266927,#266928,#266929,#266930,#266931,#266932,#266933,
#266934,#266935,#266936,#266937,#266938,#266939,#266940,#266941,#266942,
#266943,#266944,#266945,#266946,#266947,#266948,#266949,#266950,#266951,
#266952,#266953,#266954,#266955,#266956,#266957,#266958,#266959,#266960,
#266961,#266962,#266963,#266964,#266965,#266966,#266967,#266968,#266969,
#266970,#266971,#266972,#266973,#266974,#266975,#266976,#266977,#266978,
#266979,#266980,#266981,#266982,#266983,#266984,#266985,#266986,#266987,
#266988,#266989,#266990,#266991,#266992,#266993,#266994,#266995,#266996,
#266997,#266998,#266999,#267000,#267001,#267002,#267003,#267004,#267005,
#267006,#267007,#267008,#267009,#267010,#267011,#267012,#267013,#267014,
#267015,#267016,#267017,#267018,#267019,#267020,#267021,#267022,#267023,
#267024,#267025,#267026,#267027,#267028,#267029,#267030,#267031,#267032,
#267033,#267034,#267035,#267036,#267037,#267038,#267039,#267040,#267041,
#267042,#267043,#267044,#267045,#267046,#267047,#267048,#267049,#267050,
#267051,#267052,#267053,#267054,#267055,#267056,#267057,#267058,#267059,
#267060,#267061,#267062,#267063,#267064,#267065,#267066,#267067,#267068,
#267069,#267070,#267071,#267072,#267073,#267074,#267075,#267076,#267077,
#267078,#267079,#267080,#267081,#267082,#267083,#267084,#267085),(#267086,
#267087,#267088,#267089,#267090,#267091,#267092,#267093,#267094,#267095,
#267096,#267097,#267098,#267099,#267100,#267101,#267102,#267103,#267104,
#267105,#267106,#267107,#267108,#267109,#267110,#267111,#267112,#267113,
#267114,#267115,#267116,#267117,#267118,#267119,#267120,#267121,#267122,
#267123,#267124,#267125,#267126,#267127,#267128,#267129,#267130,#267131,
#267132,#267133,#267134,#267135,#267136,#267137,#267138,#267139,#267140,
#267141,#267142,#267143,#267144,#267145,#267146,#267147,#267148,#267149,
#267150,#267151,#267152,#267153,#267154,#267155,#267156,#267157,#267158,
#267159,#267160,#267161,#267162,#267163,#267164,#267165,#267166,#267167,
#267168,#267169,#267170,#267171,#267172,#267173,#267174,#267175,#267176,
#267177,#267178,#267179,#267180,#267181,#267182,#267183,#267184,#267185,
#267186,#267187,#267188,#267189,#267190,#267191,#267192,#267193,#267194,
#267195,#267196,#267197,#267198,#267199,#267200,#267201,#267202,#267203,
#267204,#267205,#267206,#267207,#267208,#267209,#267210,#267211,#267212,
#267213,#267214,#267215,#267216,#267217,#267218,#267219,#267220,#267221,
#267222,#267223,#267224,#267225,#267226,#267227,#267228,#267229,#267230,
#267231,#267232,#267233,#267234,#267235,#267236,#267237,#267238,#267239,
#267240,#267241,#267242,#267243,#267244,#267245,#267246,#267247,#267248,
#267249,#267250,#267251,#267252,#267253,#267254,#267255,#267256,#267257,
#267258,#267259,#267260,#267261,#267262,#267263,#267264,#267265,#267266,
#267267,#267268,#267269,#267270,#267271,#267272,#267273,#267274,#267275,
#267276,#267277,#267278,#267279,#267280,#267281,#267282,#267283,#267284,
#267285,#267286,#267287,#267288,#267289,#267290,#267291,#267292,#267293,
#267294,#267295,#267296,#267297,#267298,#267299,#267300,#267301,#267302,
#267303,#267304,#267305,#267306,#267307,#267308,#267309,#267310,#267311,
#267312,#267313,#267314,#267315,#267316,#267317,#267318,#267319,#267320,
#267321,#267322,#267323,#267324,#267325,#267326,#267327,#267328,#267329,
#267330,#267331,#267332,#267333,#267334,#267335,#267336,#267337,#267338,
#267339,#267340,#267341,#267342,#267343,#267344,#267345,#267346,#267347,
#267348,#267349,#267350,#267351,#267352,#267353,#267354,#267355,#267356,
#267357,#267358,#267359,#267360,#267361,#267362,#267363,#267364,#267365,
#267366,#267367,#267368,#267369,#267370,#267371,#267372,#267373,#267374,
#267375,#267376,#267377,#267378,#267379,#267380,#267381,#267382,#267383,
#267384,#267385,#267386,#267387,#267388,#267389,#267390,#267391,#267392,
#267393,#267394,#267395,#267396,#267397,#267398,#267399,#267400,#267401,
#267402,#267403,#267404,#267405,#267406,#267407,#267408,#267409,#267410,
#267411,#267412,#267413,#267414,#267415,#267416,#267417,#267418,#267419,
#267420,#267421,#267422,#267423,#267424,#267425,#267426,#267427,#267428,
#267429,#267430,#267431,#267432,#267433,#267434,#267435,#267436,#267437,
#267438,#267439,#267440,#267441,#267442,#267443,#267444,#267445,#267446,
#267447,#267448,#267449,#267450,#267451,#267452,#267453,#267454,#267455,
#267456,#267457,#267458,#267459,#267460,#267461,#267462,#267463,#267464,
#267465,#267466,#267467,#267468,#267469,#267470,#267471,#267472,#267473,
#267474,#267475,#267476,#267477,#267478,#267479,#267480,#267481,#267482,
#267483,#267484,#267485,#267486,#267487,#267488,#267489,#267490,#267491,
#267492,#267493,#267494,#267495,#267496,#267497,#267498,#267499,#267500,
#267501,#267502,#267503,#267504,#267505,#267506,#267507,#267508,#267509,
#267510,#267511,#267512,#267513,#267514,#267515,#267516,#267517,#267518,
#267519,#267520,#267521,#267522,#267523,#267524,#267525,#267526,#267527,
#267528,#267529,#267530,#267531,#267532,#267533,#267534,#267535,#267536,
#267537,#267538,#267539,#267540,#267541,#267542,#267543,#267544,#267545,
#267546,#267547,#267548,#267549,#267550,#267551,#267552,#267553,#267554,
#267555,#267556,#267557,#267558,#267559,#267560,#267561,#267562,#267563,
#267564,#267565,#267566,#267567,#267568,#267569,#267570,#267571,#267572,
#267573,#267574,#267575,#267576,#267577,#267578,#267579,#267580,#267581,
#267582,#267583,#267584,#267585,#267586,#267587,#267588,#267589,#267590,
#267591,#267592,#267593,#267594,#267595,#267596,#267597,#267598,#267599,
#267600,#267601,#267602,#267603,#267604,#267605,#267606,#267607,#267608,
#267609,#267610,#267611,#267612,#267613,#267614,#267615,#267616,#267617,
#267618,#267619,#267620,#267621,#267622,#267623,#267624,#267625,#267626,
#267627,#267628,#267629,#267630,#267631,#267632,#267633,#267634,#267635,
#267636,#267637,#267638,#267639,#267640,#267641,#267642,#267643,#267644,
#267645,#267646,#267647,#267648,#267649,#267650,#267651,#267652,#267653,
#267654,#267655,#267656,#267657,#267658,#267659,#267660,#267661,#267662,
#267663,#267664,#267665,#267666,#267667,#267668,#267669,#267670,#267671,
#267672,#267673,#267674,#267675,#267676,#267677,#267678,#267679,#267680,
#267681,#267682,#267683,#267684,#267685,#267686,#267687,#267688,#267689,
#267690,#267691,#267692,#267693,#267694,#267695,#267696,#267697,#267698,
#267699,#267700,#267701,#267702,#267703,#267704,#267705,#267706,#267707,
#267708,#267709,#267710,#267711,#267712,#267713,#267714,#267715,#267716,
#267717,#267718,#267719,#267720,#267721,#267722,#267723,#267724,#267725,
#267726,#267727,#267728,#267729,#267730,#267731,#267732,#267733,#267734,
#267735,#267736,#267737,#267738,#267739,#267740,#267741,#267742,#267743,
#267744,#267745,#267746,#267747,#267748,#267749,#267750,#267751,#267752,
#267753,#267754,#267755,#267756,#267757,#267758,#267759,#267760,#267761,
#267762,#267763,#267764,#267765,#267766,#267767,#267768,#267769,#267770,
#267771,#267772,#267773,#267774,#267775,#267776,#267777,#267778,#267779,
#267780,#267781,#267782,#267783,#267784,#267785,#267786,#267787,#267788,
#267789,#267790,#267791,#267792,#267793,#267794,#267795,#267796,#267797,
#267798,#267799,#267800,#267801,#267802,#267803,#267804,#267805,#267806,
#267807,#267808,#267809,#267810,#267811,#267812,#267813,#267814,#267815,
#267816,#267817,#267818,#267819,#267820,#267821,#267822,#267823,#267824,
#267825,#267826,#267827,#267828,#267829,#267830,#267831,#267832,#267833,
#267834,#267835,#267836,#267837,#267838,#267839,#267840,#267841,#267842,
#267843,#267844,#267845,#267846,#267847,#267848,#267849,#267850,#267851,
#267852,#267853,#267854,#267855,#267856,#267857,#267858,#267859,#267860,
#267861,#267862,#267863,#267864,#267865,#267866,#267867,#267868,#267869,
#267870,#267871,#267872,#267873,#267874,#267875,#267876,#267877,#267878,
#267879,#267880,#267881,#267882,#267883,#267884,#267885,#267886,#267887,
#267888,#267889,#267890,#267891,#267892,#267893,#267894,#267895,#267896,
#267897,#267898,#267899,#267900,#267901,#267902,#267903,#267904,#267905,
#267906,#267907,#267908,#267909,#267910,#267911,#267912,#267913,#267914,
#267915,#267916,#267917,#267918,#267919,#267920,#267921,#267922,#267923,
#267924,#267925,#267926,#267927,#267928,#267929,#267930,#267931,#267932,
#267933,#267934,#267935,#267936,#267937,#267938,#267939,#267940,#267941,
#267942,#267943,#267944,#267945,#267946,#267947,#267948,#267949,#267950,
#267951,#267952,#267953,#267954,#267955,#267956,#267957,#267958,#267959,
#267960,#267961,#267962,#267963,#267964,#267965,#267966,#267967,#267968,
#267969,#267970,#267971,#267972,#267973,#267974,#267975,#267976,#267977,
#267978,#267979,#267980,#267981,#267982,#267983,#267984,#267985,#267986,
#267987,#267988,#267989,#267990,#267991,#267992,#267993,#267994,#267995,
#267996,#267997,#267998,#267999,#268000,#268001,#268002,#268003,#268004,
#268005,#268006,#268007,#268008,#268009,#268010,#268011,#268012,#268013,
#268014,#268015,#268016,#268017,#268018,#268019,#268020,#268021,#268022,
#268023,#268024,#268025,#268026,#268027,#268028,#268029,#268030,#268031,
#268032,#268033,#268034,#268035,#268036,#268037,#268038,#268039,#268040,
#268041,#268042,#268043,#268044,#268045,#268046,#268047,#268048,#268049,
#268050,#268051,#268052,#268053,#268054,#268055,#268056,#268057,#268058,
#268059,#268060,#268061,#268062,#268063,#268064,#268065,#268066,#268067,
#268068,#268069,#268070,#268071,#268072,#268073,#268074,#268075,#268076,
#268077,#268078,#268079,#268080,#268081,#268082,#268083,#268084,#268085,
#268086,#268087,#268088,#268089,#268090,#268091,#268092,#268093,#268094,
#268095,#268096,#268097,#268098,#268099,#268100,#268101,#268102,#268103,
#268104,#268105,#268106,#268107,#268108,#268109,#268110,#268111,#268112,
#268113,#268114,#268115,#268116,#268117,#268118,#268119,#268120,#268121,
#268122,#268123,#268124,#268125,#268126,#268127,#268128,#268129,#268130,
#268131,#268132,#268133,#268134,#268135,#268136,#268137,#268138,#268139,
#268140,#268141,#268142,#268143,#268144,#268145,#268146,#268147,#268148,
#268149,#268150,#268151,#268152,#268153,#268154,#268155,#268156,#268157,
#268158,#268159,#268160,#268161,#268162,#268163,#268164,#268165,#268166,
#268167,#268168,#268169,#268170,#268171,#268172,#268173,#268174,#268175,
#268176,#268177,#268178,#268179,#268180,#268181,#268182,#268183,#268184,
#268185,#268186,#268187,#268188,#268189,#268190,#268191,#268192,#268193,
#268194,#268195,#268196,#268197,#268198,#268199,#268200,#268201,#268202,
#268203,#268204,#268205,#268206,#268207,#268208,#268209,#268210,#268211,
#268212,#268213,#268214,#268215,#268216,#268217,#268218,#268219,#268220,
#268221,#268222,#268223,#268224,#268225,#268226,#268227,#268228,#268229,
#268230,#268231,#268232,#268233,#268234,#268235,#268236,#268237,#268238,
#268239,#268240,#268241,#268242,#268243,#268244,#268245,#268246,#268247,
#268248,#268249,#268250,#268251,#268252,#268253,#268254,#268255,#268256,
#268257,#268258,#268259,#268260,#268261,#268262,#268263,#268264,#268265,
#268266,#268267,#268268,#268269,#268270,#268271,#268272,#268273,#268274,
#268275,#268276,#268277,#268278,#268279,#268280,#268281,#268282,#268283,
#268284,#268285,#268286,#268287,#268288,#268289,#268290,#268291,#268292,
#268293,#268294,#268295,#268296,#268297,#268298,#268299,#268300,#268301,
#268302,#268303,#268304,#268305,#268306,#268307,#268308,#268309,#268310,
#268311,#268312,#268313,#268314,#268315,#268316,#268317,#268318,#268319,
#268320,#268321,#268322,#268323,#268324,#268325,#268326,#268327,#268328,
#268329,#268330,#268331,#268332,#268333,#268334,#268335,#268336,#268337,
#268338,#268339,#268340,#268341,#268342,#268343,#268344,#268345,#268346,
#268347,#268348,#268349,#268350,#268351,#268352,#268353,#268354,#268355,
#268356,#268357,#268358,#268359,#268360,#268361,#268362,#268363,#268364,
#268365,#268366,#268367,#268368,#268369,#268370,#268371,#268372,#268373,
#268374,#268375,#268376,#268377,#268378,#268379,#268380,#268381,#268382,
#268383,#268384,#268385,#268386,#268387,#268388,#268389,#268390,#268391,
#268392,#268393,#268394,#268395,#268396,#268397,#268398,#268399,#268400,
#268401,#268402,#268403,#268404,#268405,#268406,#268407,#268408,#268409,
#268410,#268411,#268412,#268413,#268414,#268415,#268416,#268417,#268418,
#268419,#268420,#268421,#268422,#268423,#268424,#268425,#268426,#268427,
#268428,#268429,#268430,#268431,#268432,#268433,#268434,#268435,#268436,
#268437,#268438,#268439,#268440,#268441,#268442,#268443,#268444,#268445,
#268446,#268447,#268448,#268449,#268450,#268451,#268452,#268453,#268454,
#268455,#268456,#268457,#268458,#268459,#268460,#268461,#268462,#268463,
#268464,#268465,#268466,#268467,#268468,#268469,#268470,#268471,#268472,
#268473,#268474,#268475,#268476,#268477,#268478,#268479,#268480,#268481,
#268482,#268483,#268484,#268485,#268486,#268487,#268488,#268489,#268490,
#268491,#268492,#268493,#268494,#268495,#268496,#268497,#268498,#268499,
#268500,#268501,#268502,#268503,#268504,#268505,#268506,#268507,#268508,
#268509,#268510,#268511,#268512,#268513,#268514,#268515,#268516,#268517,
#268518,#268519,#268520,#268521,#268522,#268523,#268524,#268525,#268526,
#268527,#268528,#268529,#268530,#268531,#268532,#268533,#268534,#268535,
#268536,#268537,#268538,#268539,#268540,#268541,#268542,#268543,#268544,
#268545,#268546,#268547,#268548,#268549,#268550,#268551,#268552,#268553,
#268554,#268555,#268556,#268557,#268558,#268559,#268560,#268561,#268562,
#268563,#268564,#268565,#268566,#268567,#268568,#268569,#268570,#268571,
#268572,#268573,#268574,#268575,#268576,#268577,#268578,#268579,#268580,
#268581,#268582,#268583,#268584,#268585,#268586,#268587,#268588,#268589,
#268590,#268591,#268592,#268593,#268594,#268595,#268596,#268597,#268598,
#268599,#268600,#268601,#268602,#268603,#268604,#268605,#268606,#268607,
#268608,#268609,#268610,#268611,#268612,#268613,#268614,#268615,#268616,
#268617,#268618,#268619,#268620,#268621,#268622,#268623,#268624,#268625,
#268626,#268627,#268628,#268629,#268630,#268631,#268632,#268633,#268634,
#268635,#268636,#268637,#268638,#268639,#268640,#268641,#268642,#268643,
#268644,#268645,#268646,#268647,#268648,#268649,#268650,#268651,#268652,
#268653,#268654,#268655,#268656,#268657,#268658,#268659,#268660,#268661,
#268662,#268663,#268664,#268665,#268666,#268667,#268668,#268669,#268670,
#268671,#268672,#268673,#268674,#268675,#268676,#268677,#268678,#268679,
#268680,#268681,#268682,#268683,#268684,#268685,#268686,#268687,#268688,
#268689,#268690,#268691,#268692,#268693,#268694,#268695,#268696,#268697,
#268698,#268699,#268700,#268701,#268702,#268703,#268704,#268705,#268706,
#268707,#268708,#268709,#268710,#268711,#268712,#268713,#268714,#268715,
#268716,#268717,#268718,#268719,#268720,#268721,#268722,#268723,#268724,
#268725,#268726,#268727,#268728,#268729,#268730,#268731,#268732,#268733,
#268734,#268735,#268736,#268737,#268738,#268739,#268740,#268741,#268742,
#268743,#268744,#268745,#268746,#268747,#268748,#268749,#268750,#268751,
#268752,#268753,#268754,#268755,#268756,#268757,#268758,#268759,#268760,
#268761,#268762,#268763,#268764,#268765,#268766,#268767,#268768,#268769,
#268770,#268771,#268772,#268773,#268774,#268775,#268776,#268777,#268778,
#268779,#268780),(#268781,#268782,#268783,#268784,#268785,#268786,#268787,
#268788,#268789,#268790,#268791,#268792,#268793,#268794,#268795,#268796,
#268797,#268798,#268799,#268800,#268801,#268802,#268803,#268804,#268805,
#268806,#268807,#268808,#268809,#268810,#268811,#268812,#268813,#268814,
#268815,#268816,#268817,#268818,#268819,#268820,#268821,#268822,#268823,
#268824,#268825,#268826,#268827,#268828,#268829,#268830,#268831,#268832,
#268833,#268834,#268835,#268836,#268837,#268838,#268839,#268840,#268841,
#268842,#268843,#268844,#268845,#268846,#268847,#268848,#268849,#268850,
#268851,#268852,#268853,#268854,#268855,#268856,#268857,#268858,#268859,
#268860,#268861,#268862,#268863,#268864,#268865,#268866,#268867,#268868,
#268869,#268870,#268871,#268872,#268873,#268874,#268875,#268876,#268877,
#268878,#268879,#268880,#268881,#268882,#268883,#268884,#268885,#268886,
#268887,#268888,#268889,#268890,#268891,#268892,#268893,#268894,#268895,
#268896,#268897,#268898,#268899,#268900,#268901,#268902,#268903,#268904,
#268905,#268906,#268907,#268908,#268909,#268910,#268911,#268912,#268913,
#268914,#268915,#268916,#268917,#268918,#268919,#268920,#268921,#268922,
#268923,#268924,#268925,#268926,#268927,#268928,#268929,#268930,#268931,
#268932,#268933,#268934,#268935,#268936,#268937,#268938,#268939,#268940,
#268941,#268942,#268943,#268944,#268945,#268946,#268947,#268948,#268949,
#268950,#268951,#268952,#268953,#268954,#268955,#268956,#268957,#268958,
#268959,#268960,#268961,#268962,#268963,#268964,#268965,#268966,#268967,
#268968,#268969,#268970,#268971,#268972,#268973,#268974,#268975,#268976,
#268977,#268978,#268979,#268980,#268981,#268982,#268983,#268984,#268985,
#268986,#268987,#268988,#268989,#268990,#268991,#268992,#268993,#268994,
#268995,#268996,#268997,#268998,#268999,#269000,#269001,#269002,#269003,
#269004,#269005,#269006,#269007,#269008,#269009,#269010,#269011,#269012,
#269013,#269014,#269015,#269016,#269017,#269018,#269019,#269020,#269021,
#269022,#269023,#269024,#269025,#269026,#269027,#269028,#269029,#269030,
#269031,#269032,#269033,#269034,#269035,#269036,#269037,#269038,#269039,
#269040,#269041,#269042,#269043,#269044,#269045,#269046,#269047,#269048,
#269049,#269050,#269051,#269052,#269053,#269054,#269055,#269056,#269057,
#269058,#269059,#269060,#269061,#269062,#269063,#269064,#269065,#269066,
#269067,#269068,#269069,#269070,#269071,#269072,#269073,#269074,#269075,
#269076,#269077,#269078,#269079,#269080,#269081,#269082,#269083,#269084,
#269085,#269086,#269087,#269088,#269089,#269090,#269091,#269092,#269093,
#269094,#269095,#269096,#269097,#269098,#269099,#269100,#269101,#269102,
#269103,#269104,#269105,#269106,#269107,#269108,#269109,#269110,#269111,
#269112,#269113,#269114,#269115,#269116,#269117,#269118,#269119,#269120,
#269121,#269122,#269123,#269124,#269125,#269126,#269127,#269128,#269129,
#269130,#269131,#269132,#269133,#269134,#269135,#269136,#269137,#269138,
#269139,#269140,#269141,#269142,#269143,#269144,#269145,#269146,#269147,
#269148,#269149,#269150,#269151,#269152,#269153,#269154,#269155,#269156,
#269157,#269158,#269159,#269160,#269161,#269162,#269163,#269164,#269165,
#269166,#269167,#269168,#269169,#269170,#269171,#269172,#269173,#269174,
#269175,#269176,#269177,#269178,#269179,#269180,#269181,#269182,#269183,
#269184,#269185,#269186,#269187,#269188,#269189,#269190,#269191,#269192,
#269193,#269194,#269195,#269196,#269197,#269198,#269199,#269200,#269201,
#269202,#269203,#269204,#269205,#269206,#269207,#269208,#269209,#269210,
#269211,#269212,#269213,#269214,#269215,#269216,#269217,#269218,#269219,
#269220,#269221,#269222,#269223,#269224,#269225,#269226,#269227,#269228,
#269229,#269230,#269231,#269232,#269233,#269234,#269235,#269236,#269237,
#269238,#269239,#269240,#269241,#269242,#269243,#269244,#269245,#269246,
#269247,#269248,#269249,#269250,#269251,#269252,#269253,#269254,#269255,
#269256,#269257,#269258,#269259,#269260,#269261,#269262,#269263,#269264,
#269265,#269266,#269267,#269268,#269269,#269270,#269271,#269272,#269273,
#269274,#269275,#269276,#269277,#269278,#269279,#269280,#269281,#269282,
#269283,#269284,#269285,#269286,#269287,#269288,#269289,#269290,#269291,
#269292,#269293,#269294,#269295,#269296,#269297,#269298,#269299,#269300,
#269301,#269302,#269303,#269304,#269305,#269306,#269307,#269308,#269309,
#269310,#269311,#269312,#269313,#269314,#269315,#269316,#269317,#269318,
#269319,#269320,#269321,#269322,#269323,#269324,#269325,#269326,#269327,
#269328,#269329,#269330,#269331,#269332,#269333,#269334,#269335,#269336,
#269337,#269338,#269339,#269340,#269341,#269342,#269343,#269344,#269345,
#269346,#269347,#269348,#269349,#269350,#269351,#269352,#269353,#269354,
#269355,#269356,#269357,#269358,#269359,#269360,#269361,#269362,#269363,
#269364,#269365,#269366,#269367,#269368,#269369,#269370,#269371,#269372,
#269373,#269374,#269375,#269376,#269377,#269378,#269379,#269380,#269381,
#269382,#269383,#269384,#269385,#269386,#269387,#269388,#269389,#269390,
#269391,#269392,#269393,#269394,#269395,#269396,#269397,#269398,#269399,
#269400,#269401,#269402,#269403,#269404,#269405,#269406,#269407,#269408,
#269409,#269410,#269411,#269412,#269413,#269414,#269415,#269416,#269417,
#269418,#269419,#269420,#269421,#269422,#269423,#269424,#269425,#269426,
#269427,#269428,#269429,#269430,#269431,#269432,#269433,#269434,#269435,
#269436,#269437,#269438,#269439,#269440,#269441,#269442,#269443,#269444,
#269445,#269446,#269447,#269448,#269449,#269450,#269451,#269452,#269453,
#269454,#269455,#269456,#269457,#269458,#269459,#269460,#269461,#269462,
#269463,#269464,#269465,#269466,#269467,#269468,#269469,#269470,#269471,
#269472,#269473,#269474,#269475,#269476,#269477,#269478,#269479,#269480,
#269481,#269482,#269483,#269484,#269485,#269486,#269487,#269488,#269489,
#269490,#269491,#269492,#269493,#269494,#269495,#269496,#269497,#269498,
#269499,#269500,#269501,#269502,#269503,#269504,#269505,#269506,#269507,
#269508,#269509,#269510,#269511,#269512,#269513,#269514,#269515,#269516,
#269517,#269518,#269519,#269520,#269521,#269522,#269523,#269524,#269525,
#269526,#269527,#269528,#269529,#269530,#269531,#269532,#269533,#269534,
#269535,#269536,#269537,#269538,#269539,#269540,#269541,#269542,#269543,
#269544,#269545,#269546,#269547,#269548,#269549,#269550,#269551,#269552,
#269553,#269554,#269555,#269556,#269557,#269558,#269559,#269560,#269561,
#269562,#269563,#269564,#269565,#269566,#269567,#269568,#269569,#269570,
#269571,#269572,#269573,#269574,#269575,#269576,#269577,#269578,#269579,
#269580,#269581,#269582,#269583,#269584,#269585,#269586,#269587,#269588,
#269589,#269590,#269591,#269592,#269593,#269594,#269595,#269596,#269597,
#269598,#269599,#269600,#269601,#269602,#269603,#269604,#269605,#269606,
#269607,#269608,#269609,#269610,#269611,#269612,#269613,#269614,#269615,
#269616,#269617,#269618,#269619,#269620,#269621,#269622,#269623,#269624,
#269625,#269626,#269627,#269628,#269629,#269630,#269631,#269632,#269633,
#269634,#269635,#269636,#269637,#269638,#269639,#269640,#269641,#269642,
#269643,#269644,#269645,#269646,#269647,#269648,#269649,#269650,#269651,
#269652,#269653,#269654,#269655,#269656,#269657,#269658,#269659,#269660,
#269661,#269662,#269663,#269664,#269665,#269666,#269667,#269668,#269669,
#269670,#269671,#269672,#269673,#269674,#269675,#269676,#269677,#269678,
#269679,#269680,#269681,#269682,#269683,#269684,#269685,#269686,#269687,
#269688,#269689,#269690,#269691,#269692,#269693,#269694,#269695,#269696,
#269697,#269698,#269699,#269700,#269701,#269702,#269703,#269704,#269705,
#269706,#269707,#269708,#269709,#269710,#269711,#269712,#269713,#269714,
#269715,#269716,#269717,#269718,#269719,#269720,#269721,#269722,#269723,
#269724,#269725,#269726,#269727,#269728,#269729,#269730,#269731,#269732,
#269733,#269734,#269735,#269736,#269737,#269738,#269739,#269740,#269741,
#269742,#269743,#269744,#269745,#269746,#269747,#269748,#269749,#269750,
#269751,#269752,#269753,#269754,#269755,#269756,#269757,#269758,#269759,
#269760,#269761,#269762,#269763,#269764,#269765,#269766,#269767,#269768,
#269769,#269770,#269771,#269772,#269773,#269774,#269775,#269776,#269777,
#269778,#269779,#269780,#269781,#269782,#269783,#269784,#269785,#269786,
#269787,#269788,#269789,#269790,#269791,#269792,#269793,#269794,#269795,
#269796,#269797,#269798,#269799,#269800,#269801,#269802,#269803,#269804,
#269805,#269806,#269807,#269808,#269809,#269810,#269811,#269812,#269813,
#269814,#269815,#269816,#269817,#269818,#269819,#269820,#269821,#269822,
#269823,#269824,#269825,#269826,#269827,#269828,#269829,#269830,#269831,
#269832,#269833,#269834,#269835,#269836,#269837,#269838,#269839,#269840,
#269841,#269842,#269843,#269844,#269845,#269846,#269847,#269848,#269849,
#269850,#269851,#269852,#269853,#269854,#269855,#269856,#269857,#269858,
#269859,#269860,#269861,#269862,#269863,#269864,#269865,#269866,#269867,
#269868,#269869,#269870,#269871,#269872,#269873,#269874,#269875,#269876,
#269877,#269878,#269879,#269880,#269881,#269882,#269883,#269884,#269885,
#269886,#269887,#269888,#269889,#269890,#269891,#269892,#269893,#269894,
#269895,#269896,#269897,#269898,#269899,#269900,#269901,#269902,#269903,
#269904,#269905,#269906,#269907,#269908,#269909,#269910,#269911,#269912,
#269913,#269914,#269915,#269916,#269917,#269918,#269919,#269920,#269921,
#269922,#269923,#269924,#269925,#269926,#269927,#269928,#269929,#269930,
#269931,#269932,#269933,#269934,#269935,#269936,#269937,#269938,#269939,
#269940,#269941,#269942,#269943,#269944,#269945,#269946,#269947,#269948,
#269949,#269950,#269951,#269952,#269953,#269954,#269955,#269956,#269957,
#269958,#269959,#269960,#269961,#269962,#269963,#269964,#269965,#269966,
#269967,#269968,#269969,#269970,#269971,#269972,#269973,#269974,#269975,
#269976,#269977,#269978,#269979,#269980,#269981,#269982,#269983,#269984,
#269985,#269986,#269987,#269988,#269989,#269990,#269991,#269992,#269993,
#269994,#269995,#269996,#269997,#269998,#269999,#270000,#270001,#270002,
#270003,#270004,#270005,#270006,#270007,#270008,#270009,#270010,#270011,
#270012,#270013,#270014,#270015,#270016,#270017,#270018,#270019,#270020,
#270021,#270022,#270023,#270024,#270025,#270026,#270027,#270028,#270029,
#270030,#270031,#270032,#270033,#270034,#270035,#270036,#270037,#270038,
#270039,#270040,#270041,#270042,#270043,#270044,#270045,#270046,#270047,
#270048,#270049,#270050,#270051,#270052,#270053,#270054,#270055,#270056,
#270057,#270058,#270059,#270060,#270061,#270062,#270063,#270064,#270065,
#270066,#270067,#270068,#270069,#270070,#270071,#270072,#270073,#270074,
#270075,#270076,#270077,#270078,#270079,#270080,#270081,#270082,#270083,
#270084,#270085,#270086,#270087,#270088,#270089,#270090,#270091,#270092,
#270093,#270094,#270095,#270096,#270097,#270098,#270099,#270100,#270101,
#270102,#270103,#270104,#270105,#270106,#270107,#270108,#270109,#270110,
#270111,#270112,#270113,#270114,#270115,#270116,#270117,#270118,#270119,
#270120,#270121,#270122,#270123,#270124,#270125,#270126,#270127,#270128,
#270129,#270130,#270131,#270132,#270133,#270134,#270135,#270136,#270137,
#270138,#270139,#270140,#270141,#270142,#270143,#270144,#270145,#270146,
#270147,#270148,#270149,#270150,#270151,#270152,#270153,#270154,#270155,
#270156,#270157,#270158,#270159,#270160,#270161,#270162,#270163,#270164,
#270165,#270166,#270167,#270168,#270169,#270170,#270171,#270172,#270173,
#270174,#270175,#270176,#270177,#270178,#270179,#270180,#270181,#270182,
#270183,#270184,#270185,#270186,#270187,#270188,#270189,#270190,#270191,
#270192,#270193,#270194,#270195,#270196,#270197,#270198,#270199,#270200,
#270201,#270202,#270203,#270204,#270205,#270206,#270207,#270208,#270209,
#270210,#270211,#270212,#270213,#270214,#270215,#270216,#270217,#270218,
#270219,#270220,#270221,#270222,#270223,#270224,#270225,#270226,#270227,
#270228,#270229,#270230,#270231,#270232,#270233,#270234,#270235,#270236,
#270237,#270238,#270239,#270240,#270241,#270242,#270243,#270244,#270245,
#270246,#270247,#270248,#270249,#270250,#270251,#270252,#270253,#270254,
#270255,#270256,#270257,#270258,#270259,#270260,#270261,#270262,#270263,
#270264,#270265,#270266,#270267,#270268,#270269,#270270,#270271,#270272,
#270273,#270274,#270275,#270276,#270277,#270278,#270279,#270280,#270281,
#270282,#270283,#270284,#270285,#270286,#270287,#270288,#270289,#270290,
#270291,#270292,#270293,#270294,#270295,#270296,#270297,#270298,#270299,
#270300,#270301,#270302,#270303,#270304,#270305,#270306,#270307,#270308,
#270309,#270310,#270311,#270312,#270313,#270314,#270315,#270316,#270317,
#270318,#270319,#270320,#270321,#270322,#270323,#270324,#270325,#270326,
#270327,#270328,#270329,#270330,#270331,#270332,#270333,#270334,#270335,
#270336,#270337,#270338,#270339,#270340,#270341,#270342,#270343,#270344,
#270345,#270346,#270347,#270348,#270349,#270350,#270351,#270352,#270353,
#270354,#270355,#270356,#270357,#270358,#270359,#270360,#270361,#270362,
#270363,#270364,#270365,#270366,#270367,#270368,#270369,#270370,#270371,
#270372,#270373,#270374,#270375,#270376,#270377,#270378,#270379,#270380,
#270381,#270382,#270383,#270384,#270385,#270386,#270387,#270388,#270389,
#270390,#270391,#270392,#270393,#270394,#270395,#270396,#270397,#270398,
#270399,#270400,#270401,#270402,#270403,#270404,#270405,#270406,#270407,
#270408,#270409,#270410,#270411,#270412,#270413,#270414,#270415,#270416,
#270417,#270418,#270419,#270420,#270421,#270422,#270423,#270424,#270425,
#270426,#270427,#270428,#270429,#270430,#270431,#270432,#270433,#270434,
#270435,#270436,#270437,#270438,#270439,#270440,#270441,#270442,#270443,
#270444,#270445,#270446,#270447,#270448,#270449,#270450,#270451,#270452,
#270453,#270454,#270455,#270456,#270457,#270458,#270459,#270460,#270461,
#270462,#270463,#270464,#270465,#270466,#270467,#270468,#270469,#270470,
#270471,#270472,#270473,#270474,#270475),(#270476,#270477,#270478,#270479,
#270480,#270481,#270482,#270483,#270484,#270485,#270486,#270487,#270488,
#270489,#270490,#270491,#270492,#270493,#270494,#270495,#270496,#270497,
#270498,#270499,#270500,#270501,#270502,#270503,#270504,#270505,#270506,
#270507,#270508,#270509,#270510,#270511,#270512,#270513,#270514,#270515,
#270516,#270517,#270518,#270519,#270520,#270521,#270522,#270523,#270524,
#270525,#270526,#270527,#270528,#270529,#270530,#270531,#270532,#270533,
#270534,#270535,#270536,#270537,#270538,#270539,#270540,#270541,#270542,
#270543,#270544,#270545,#270546,#270547,#270548,#270549,#270550,#270551,
#270552,#270553,#270554,#270555,#270556,#270557,#270558,#270559,#270560,
#270561,#270562,#270563,#270564,#270565,#270566,#270567,#270568,#270569,
#270570,#270571,#270572,#270573,#270574,#270575,#270576,#270577,#270578,
#270579,#270580,#270581,#270582,#270583,#270584,#270585,#270586,#270587,
#270588,#270589,#270590,#270591,#270592,#270593,#270594,#270595,#270596,
#270597,#270598,#270599,#270600,#270601,#270602,#270603,#270604,#270605,
#270606,#270607,#270608,#270609,#270610,#270611,#270612,#270613,#270614,
#270615,#270616,#270617,#270618,#270619,#270620,#270621,#270622,#270623,
#270624,#270625,#270626,#270627,#270628,#270629,#270630,#270631,#270632,
#270633,#270634,#270635,#270636,#270637,#270638,#270639,#270640,#270641,
#270642,#270643,#270644,#270645,#270646,#270647,#270648,#270649,#270650,
#270651,#270652,#270653,#270654,#270655,#270656,#270657,#270658,#270659,
#270660,#270661,#270662,#270663,#270664,#270665,#270666,#270667,#270668,
#270669,#270670,#270671,#270672,#270673,#270674,#270675,#270676,#270677,
#270678,#270679,#270680,#270681,#270682,#270683,#270684,#270685,#270686,
#270687,#270688,#270689,#270690,#270691,#270692,#270693,#270694,#270695,
#270696,#270697,#270698,#270699,#270700,#270701,#270702,#270703,#270704,
#270705,#270706,#270707,#270708,#270709,#270710,#270711,#270712,#270713,
#270714,#270715,#270716,#270717,#270718,#270719,#270720,#270721,#270722,
#270723,#270724,#270725,#270726,#270727,#270728,#270729,#270730,#270731,
#270732,#270733,#270734,#270735,#270736,#270737,#270738,#270739,#270740,
#270741,#270742,#270743,#270744,#270745,#270746,#270747,#270748,#270749,
#270750,#270751,#270752,#270753,#270754,#270755,#270756,#270757,#270758,
#270759,#270760,#270761,#270762,#270763,#270764,#270765,#270766,#270767,
#270768,#270769,#270770,#270771,#270772,#270773,#270774,#270775,#270776,
#270777,#270778,#270779,#270780,#270781,#270782,#270783,#270784,#270785,
#270786,#270787,#270788,#270789,#270790,#270791,#270792,#270793,#270794,
#270795,#270796,#270797,#270798,#270799,#270800,#270801,#270802,#270803,
#270804,#270805,#270806,#270807,#270808,#270809,#270810,#270811,#270812,
#270813,#270814,#270815,#270816,#270817,#270818,#270819,#270820,#270821,
#270822,#270823,#270824,#270825,#270826,#270827,#270828,#270829,#270830,
#270831,#270832,#270833,#270834,#270835,#270836,#270837,#270838,#270839,
#270840,#270841,#270842,#270843,#270844,#270845,#270846,#270847,#270848,
#270849,#270850,#270851,#270852,#270853,#270854,#270855,#270856,#270857,
#270858,#270859,#270860,#270861,#270862,#270863,#270864,#270865,#270866,
#270867,#270868,#270869,#270870,#270871,#270872,#270873,#270874,#270875,
#270876,#270877,#270878,#270879,#270880,#270881,#270882,#270883,#270884,
#270885,#270886,#270887,#270888,#270889,#270890,#270891,#270892,#270893,
#270894,#270895,#270896,#270897,#270898,#270899,#270900,#270901,#270902,
#270903,#270904,#270905,#270906,#270907,#270908,#270909,#270910,#270911,
#270912,#270913,#270914,#270915,#270916,#270917,#270918,#270919,#270920,
#270921,#270922,#270923,#270924,#270925,#270926,#270927,#270928,#270929,
#270930,#270931,#270932,#270933,#270934,#270935,#270936,#270937,#270938,
#270939,#270940,#270941,#270942,#270943,#270944,#270945,#270946,#270947,
#270948,#270949,#270950,#270951,#270952,#270953,#270954,#270955,#270956,
#270957,#270958,#270959,#270960,#270961,#270962,#270963,#270964,#270965,
#270966,#270967,#270968,#270969,#270970,#270971,#270972,#270973,#270974,
#270975,#270976,#270977,#270978,#270979,#270980,#270981,#270982,#270983,
#270984,#270985,#270986,#270987,#270988,#270989,#270990,#270991,#270992,
#270993,#270994,#270995,#270996,#270997,#270998,#270999,#271000,#271001,
#271002,#271003,#271004,#271005,#271006,#271007,#271008,#271009,#271010,
#271011,#271012,#271013,#271014,#271015,#271016,#271017,#271018,#271019,
#271020,#271021,#271022,#271023,#271024,#271025,#271026,#271027,#271028,
#271029,#271030,#271031,#271032,#271033,#271034,#271035,#271036,#271037,
#271038,#271039,#271040,#271041,#271042,#271043,#271044,#271045,#271046,
#271047,#271048,#271049,#271050,#271051,#271052,#271053,#271054,#271055,
#271056,#271057,#271058,#271059,#271060,#271061,#271062,#271063,#271064,
#271065,#271066,#271067,#271068,#271069,#271070,#271071,#271072,#271073,
#271074,#271075,#271076,#271077,#271078,#271079,#271080,#271081,#271082,
#271083,#271084,#271085,#271086,#271087,#271088,#271089,#271090,#271091,
#271092,#271093,#271094,#271095,#271096,#271097,#271098,#271099,#271100,
#271101,#271102,#271103,#271104,#271105,#271106,#271107,#271108,#271109,
#271110,#271111,#271112,#271113,#271114,#271115,#271116,#271117,#271118,
#271119,#271120,#271121,#271122,#271123,#271124,#271125,#271126,#271127,
#271128,#271129,#271130,#271131,#271132,#271133,#271134,#271135,#271136,
#271137,#271138,#271139,#271140,#271141,#271142,#271143,#271144,#271145,
#271146,#271147,#271148,#271149,#271150,#271151,#271152,#271153,#271154,
#271155,#271156,#271157,#271158,#271159,#271160,#271161,#271162,#271163,
#271164,#271165,#271166,#271167,#271168,#271169,#271170,#271171,#271172,
#271173,#271174,#271175,#271176,#271177,#271178,#271179,#271180,#271181,
#271182,#271183,#271184,#271185,#271186,#271187,#271188,#271189,#271190,
#271191,#271192,#271193,#271194,#271195,#271196,#271197,#271198,#271199,
#271200,#271201,#271202,#271203,#271204,#271205,#271206,#271207,#271208,
#271209,#271210,#271211,#271212,#271213,#271214,#271215,#271216,#271217,
#271218,#271219,#271220,#271221,#271222,#271223,#271224,#271225,#271226,
#271227,#271228,#271229,#271230,#271231,#271232,#271233,#271234,#271235,
#271236,#271237,#271238,#271239,#271240,#271241,#271242,#271243,#271244,
#271245,#271246,#271247,#271248,#271249,#271250,#271251,#271252,#271253,
#271254,#271255,#271256,#271257,#271258,#271259,#271260,#271261,#271262,
#271263,#271264,#271265,#271266,#271267,#271268,#271269,#271270,#271271,
#271272,#271273,#271274,#271275,#271276,#271277,#271278,#271279,#271280,
#271281,#271282,#271283,#271284,#271285,#271286,#271287,#271288,#271289,
#271290,#271291,#271292,#271293,#271294,#271295,#271296,#271297,#271298,
#271299,#271300,#271301,#271302,#271303,#271304,#271305,#271306,#271307,
#271308,#271309,#271310,#271311,#271312,#271313,#271314,#271315,#271316,
#271317,#271318,#271319,#271320,#271321,#271322,#271323,#271324,#271325,
#271326,#271327,#271328,#271329,#271330,#271331,#271332,#271333,#271334,
#271335,#271336,#271337,#271338,#271339,#271340,#271341,#271342,#271343,
#271344,#271345,#271346,#271347,#271348,#271349,#271350,#271351,#271352,
#271353,#271354,#271355,#271356,#271357,#271358,#271359,#271360,#271361,
#271362,#271363,#271364,#271365,#271366,#271367,#271368,#271369,#271370,
#271371,#271372,#271373,#271374,#271375,#271376,#271377,#271378,#271379,
#271380,#271381,#271382,#271383,#271384,#271385,#271386,#271387,#271388,
#271389,#271390,#271391,#271392,#271393,#271394,#271395,#271396,#271397,
#271398,#271399,#271400,#271401,#271402,#271403,#271404,#271405,#271406,
#271407,#271408,#271409,#271410,#271411,#271412,#271413,#271414,#271415,
#271416,#271417,#271418,#271419,#271420,#271421,#271422,#271423,#271424,
#271425,#271426,#271427,#271428,#271429,#271430,#271431,#271432,#271433,
#271434,#271435,#271436,#271437,#271438,#271439,#271440,#271441,#271442,
#271443,#271444,#271445,#271446,#271447,#271448,#271449,#271450,#271451,
#271452,#271453,#271454,#271455,#271456,#271457,#271458,#271459,#271460,
#271461,#271462,#271463,#271464,#271465,#271466,#271467,#271468,#271469,
#271470,#271471,#271472,#271473,#271474,#271475,#271476,#271477,#271478,
#271479,#271480,#271481,#271482,#271483,#271484,#271485,#271486,#271487,
#271488,#271489,#271490,#271491,#271492,#271493,#271494,#271495,#271496,
#271497,#271498,#271499,#271500,#271501,#271502,#271503,#271504,#271505,
#271506,#271507,#271508,#271509,#271510,#271511,#271512,#271513,#271514,
#271515,#271516,#271517,#271518,#271519,#271520,#271521,#271522,#271523,
#271524,#271525,#271526,#271527,#271528,#271529,#271530,#271531,#271532,
#271533,#271534,#271535,#271536,#271537,#271538,#271539,#271540,#271541,
#271542,#271543,#271544,#271545,#271546,#271547,#271548,#271549,#271550,
#271551,#271552,#271553,#271554,#271555,#271556,#271557,#271558,#271559,
#271560,#271561,#271562,#271563,#271564,#271565,#271566,#271567,#271568,
#271569,#271570,#271571,#271572,#271573,#271574,#271575,#271576,#271577,
#271578,#271579,#271580,#271581,#271582,#271583,#271584,#271585,#271586,
#271587,#271588,#271589,#271590,#271591,#271592,#271593,#271594,#271595,
#271596,#271597,#271598,#271599,#271600,#271601,#271602,#271603,#271604,
#271605,#271606,#271607,#271608,#271609,#271610,#271611,#271612,#271613,
#271614,#271615,#271616,#271617,#271618,#271619,#271620,#271621,#271622,
#271623,#271624,#271625,#271626,#271627,#271628,#271629,#271630,#271631,
#271632,#271633,#271634,#271635,#271636,#271637,#271638,#271639,#271640,
#271641,#271642,#271643,#271644,#271645,#271646,#271647,#271648,#271649,
#271650,#271651,#271652,#271653,#271654,#271655,#271656,#271657,#271658,
#271659,#271660,#271661,#271662,#271663,#271664,#271665,#271666,#271667,
#271668,#271669,#271670,#271671,#271672,#271673,#271674,#271675,#271676,
#271677,#271678,#271679,#271680,#271681,#271682,#271683,#271684,#271685,
#271686,#271687,#271688,#271689,#271690,#271691,#271692,#271693,#271694,
#271695,#271696,#271697,#271698,#271699,#271700,#271701,#271702,#271703,
#271704,#271705,#271706,#271707,#271708,#271709,#271710,#271711,#271712,
#271713,#271714,#271715,#271716,#271717,#271718,#271719,#271720,#271721,
#271722,#271723,#271724,#271725,#271726,#271727,#271728,#271729,#271730,
#271731,#271732,#271733,#271734,#271735,#271736,#271737,#271738,#271739,
#271740,#271741,#271742,#271743,#271744,#271745,#271746,#271747,#271748,
#271749,#271750,#271751,#271752,#271753,#271754,#271755,#271756,#271757,
#271758,#271759,#271760,#271761,#271762,#271763,#271764,#271765,#271766,
#271767,#271768,#271769,#271770,#271771,#271772,#271773,#271774,#271775,
#271776,#271777,#271778,#271779,#271780,#271781,#271782,#271783,#271784,
#271785,#271786,#271787,#271788,#271789,#271790,#271791,#271792,#271793,
#271794,#271795,#271796,#271797,#271798,#271799,#271800,#271801,#271802,
#271803,#271804,#271805,#271806,#271807,#271808,#271809,#271810,#271811,
#271812,#271813,#271814,#271815,#271816,#271817,#271818,#271819,#271820,
#271821,#271822,#271823,#271824,#271825,#271826,#271827,#271828,#271829,
#271830,#271831,#271832,#271833,#271834,#271835,#271836,#271837,#271838,
#271839,#271840,#271841,#271842,#271843,#271844,#271845,#271846,#271847,
#271848,#271849,#271850,#271851,#271852,#271853,#271854,#271855,#271856,
#271857,#271858,#271859,#271860,#271861,#271862,#271863,#271864,#271865,
#271866,#271867,#271868,#271869,#271870,#271871,#271872,#271873,#271874,
#271875,#271876,#271877,#271878,#271879,#271880,#271881,#271882,#271883,
#271884,#271885,#271886,#271887,#271888,#271889,#271890,#271891,#271892,
#271893,#271894,#271895,#271896,#271897,#271898,#271899,#271900,#271901,
#271902,#271903,#271904,#271905,#271906,#271907,#271908,#271909,#271910,
#271911,#271912,#271913,#271914,#271915,#271916,#271917,#271918,#271919,
#271920,#271921,#271922,#271923,#271924,#271925,#271926,#271927,#271928,
#271929,#271930,#271931,#271932,#271933,#271934,#271935,#271936,#271937,
#271938,#271939,#271940,#271941,#271942,#271943,#271944,#271945,#271946,
#271947,#271948,#271949,#271950,#271951,#271952,#271953,#271954,#271955,
#271956,#271957,#271958,#271959,#271960,#271961,#271962,#271963,#271964,
#271965,#271966,#271967,#271968,#271969,#271970,#271971,#271972,#271973,
#271974,#271975,#271976,#271977,#271978,#271979,#271980,#271981,#271982,
#271983,#271984,#271985,#271986,#271987,#271988,#271989,#271990,#271991,
#271992,#271993,#271994,#271995,#271996,#271997,#271998,#271999,#272000,
#272001,#272002,#272003,#272004,#272005,#272006,#272007,#272008,#272009,
#272010,#272011,#272012,#272013,#272014,#272015,#272016,#272017,#272018,
#272019,#272020,#272021,#272022,#272023,#272024,#272025,#272026,#272027,
#272028,#272029,#272030,#272031,#272032,#272033,#272034,#272035,#272036,
#272037,#272038,#272039,#272040,#272041,#272042,#272043,#272044,#272045,
#272046,#272047,#272048,#272049,#272050,#272051,#272052,#272053,#272054,
#272055,#272056,#272057,#272058,#272059,#272060,#272061,#272062,#272063,
#272064,#272065,#272066,#272067,#272068,#272069,#272070,#272071,#272072,
#272073,#272074,#272075,#272076,#272077,#272078,#272079,#272080,#272081,
#272082,#272083,#272084,#272085,#272086,#272087,#272088,#272089,#272090,
#272091,#272092,#272093,#272094,#272095,#272096,#272097,#272098,#272099,
#272100,#272101,#272102,#272103,#272104,#272105,#272106,#272107,#272108,
#272109,#272110,#272111,#272112,#272113,#272114,#272115,#272116,#272117,
#272118,#272119,#272120,#272121,#272122,#272123,#272124,#272125,#272126,
#272127,#272128,#272129,#272130,#272131,#272132,#272133,#272134,#272135,
#272136,#272137,#272138,#272139,#272140,#272141,#272142,#272143,#272144,
#272145,#272146,#272147,#272148,#272149,#272150,#272151,#272152,#272153,
#272154,#272155,#272156,#272157,#272158,#272159,#272160,#272161,#272162,
#272163,#272164,#272165,#272166,#272167,#272168,#272169,#272170)),
 .UNSPECIFIED.,.F.,.F.,.F.,(4,4),(4,1,1,1,1,1,1,1,1,1,1,1,1,1,1,1,1,1,1,
1,1,1,1,1,1,1,1,1,1,1,1,1,1,1,1,1,1,1,1,1,1,1,1,1,1,1,1,1,1,1,1,1,1,1,1,
1,1,1,1,1,1,1,1,1,1,1,1,1,1,1,1,1,1,1,1,1,1,1,1,1,1,1,1,1,1,1,1,1,1,1,1,
1,1,1,1,1,1,1,1,1,1,1,1,1,1,1,1,1,1,1,1,1,1,1,1,1,1,1,1,1,1,1,1,1,1,1,1,
1,1,1,1,1,1,1,1,1,1,1,1,1,1,1,1,1,1,1,1,1,1,1,1,1,1,1,1,1,1,1,1,1,1,1,1,
1,1,1,1,1,1,1,1,1,1,1,1,1,1,1,1,1,1,1,1,1,1,1,1,1,1,1,1,1,1,1,1,1,1,1,1,
1,1,1,1,1,1,1,1,1,1,1,1,1,1,1,1,1,1,1,1,1,1,1,1,1,1,1,1,1,1,1,1,1,1,1,1,
1,1,1,1,1,1,1,1,1,1,1,1,1,1,1,1,1,1,1,1,1,1,1,1,1,1,1,1,1,1,1,1,1,1,1,1,
1,1,1,1,1,1,1,1,1,1,1,1,1,1,1,1,1,1,1,1,1,1,1,1,1,1,1,1,1,1,1,1,1,1,1,1,
1,1,1,1,1,1,1,1,1,1,1,1,1,1,1,1,1,1,1,1,1,1,1,1,1,1,1,1,1,1,1,1,1,1,1,1,
1,1,1,1,1,1,1,1,1,1,1,1,1,1,1,1,1,1,1,1,1,1,1,1,1,1,1,1,1,1,1,1,1,1,1,1,
1,1,1,1,1,1,1,1,1,1,1,1,1,1,1,1,1,1,1,1,1,1,1,1,1,1,1,1,1,1,1,1,1,1,1,1,
1,1,1,1,1,1,1,1,1,1,1,1,1,1,1,1,1,1,1,1,1,1,1,1,1,1,1,1,1,1,1,1,1,1,1,1,
1,1,1,1,1,1,1,1,1,1,1,1,1,1,1,1,1,1,1,1,1,1,1,1,1,1,1,1,1,1,1,1,1,1,1,1,
1,1,1,1,1,1,1,1,1,1,1,1,1,1,1,1,1,1,1,1,1,1,1,1,1,1,1,1,1,1,1,1,1,1,1,1,
1,1,1,1,1,1,1,1,1,1,1,1,1,1,1,1,1,1,1,1,1,1,1,1,1,1,1,1,1,1,1,1,1,1,1,1,
1,1,1,1,1,1,1,1,1,1,1,1,1,1,1,1,1,1,1,1,1,1,1,1,1,1,1,1,1,1,1,1,1,1,1,1,
1,1,1,1,1,1,1,1,1,1,1,1,1,1,1,1,1,1,1,1,1,1,1,1,1,1,1,1,1,1,1,1,1,1,1,1,
1,1,1,1,1,1,1,1,1,1,1,1,1,1,1,1,1,1,1,1,1,1,1,1,1,1,1,1,1,1,1,1,1,1,1,1,
1,1,1,1,1,1,1,1,1,1,1,1,1,1,1,1,1,1,1,1,1,1,1,1,1,1,1,1,1,1,1,1,1,1,1,1,
1,1,1,1,1,1,1,1,1,1,1,1,1,1,1,1,1,1,1,1,1,1,1,1,1,1,1,1,1,1,1,1,1,1,1,1,
1,1,1,1,1,1,1,1,1,1,1,1,1,1,1,1,1,1,1,1,1,1,1,1,1,1,1,1,1,1,1,1,1,1,1,1,
1,1,1,1,1,1,1,1,1,1,1,1,1,1,1,1,1,1,1,1,1,1,1,1,1,1,1,1,1,1,1,1,1,1,1,1,
1,1,1,1,1,1,1,1,1,1,1,1,1,1,1,1,1,1,1,1,1,1,1,1,1,1,1,1,1,1,1,1,1,1,1,1,
1,1,1,1,1,1,1,1,1,1,1,1,1,1,1,1,1,1,1,1,1,1,1,1,1,1,1,1,1,1,1,1,1,1,1,1,
1,1,1,1,1,1,1,1,1,1,1,1,1,1,1,1,1,1,1,1,1,1,1,1,1,1,1,1,1,1,1,1,1,1,1,1,
1,1,1,1,1,1,1,1,1,1,1,1,1,1,1,1,1,1,1,1,1,1,1,1,1,1,1,1,1,1,1,1,1,1,1,1,
1,1,1,1,1,1,1,1,1,1,1,1,1,1,1,1,1,1,1,1,1,1,1,1,1,1,1,1,1,1,1,1,1,1,1,1,
1,1,1,1,1,1,1,1,1,1,1,1,1,1,1,1,1,1,1,1,1,1,1,1,1,1,1,1,1,1,1,1,1,1,1,1,
1,1,1,1,1,1,1,1,1,1,1,1,1,1,1,1,1,1,1,1,1,1,1,1,1,1,1,1,1,1,1,1,1,1,1,1,
1,1,1,1,1,1,1,1,1,1,1,1,1,1,1,1,1,1,1,1,1,1,1,1,1,1,1,1,1,1,1,1,1,1,1,1,
1,1,1,1,1,1,1,1,1,1,1,1,1,1,1,1,1,1,1,1,1,1,1,1,1,1,1,1,1,1,1,1,1,1,1,1,
1,1,1,1,1,1,1,1,1,1,1,1,1,1,1,1,1,1,1,1,1,1,1,1,1,1,1,1,1,1,1,1,1,1,1,1,
1,1,1,1,1,1,1,1,1,1,1,1,1,1,1,1,1,1,1,1,1,1,1,1,1,1,1,1,1,1,1,1,1,1,1,1,
1,1,1,1,1,1,1,1,1,1,1,1,1,1,1,1,1,1,1,1,1,1,1,1,1,1,1,1,1,1,1,1,1,1,1,1,
1,1,1,1,1,1,1,1,1,1,1,1,1,1,1,1,1,1,1,1,1,1,1,1,1,1,1,1,1,1,1,1,1,1,1,1,
1,1,1,1,1,1,1,1,1,1,1,1,1,1,1,1,1,1,1,1,1,1,1,1,1,1,1,1,1,1,1,1,1,1,1,1,
1,1,1,1,1,1,1,1,1,1,1,1,1,1,1,1,1,1,1,1,1,1,1,1,1,1,1,1,1,1,1,1,1,1,1,1,
1,1,1,1,1,1,1,1,1,1,1,1,1,1,1,1,1,1,1,1,1,1,1,1,1,1,1,1,1,1,1,1,1,1,1,1,
1,1,1,1,1,1,1,1,1,1,1,1,1,1,1,1,1,1,1,1,1,1,1,1,1,1,1,1,1,1,1,1,1,1,1,1,
1,1,1,1,1,1,1,1,1,1,1,1,1,1,1,1,1,1,1,1,1,1,1,1,1,1,1,1,1,1,1,1,1,1,1,1,
1,1,1,1,1,1,1,1,1,1,1,1,1,1,1,1,1,1,1,1,1,1,1,1,1,1,1,1,1,1,1,1,1,1,1,1,
1,1,1,1,1,1,1,1,1,1,1,1,1,1,1,1,1,1,1,1,1,1,1,1,1,1,1,1,1,1,1,1,1,1,1,1,
1,1,1,1,1,1,1,1,1,1,1,1,1,1,1,1,1,1,1,1,1,1,1,1,1,1,1,1,1,1,1,1,1,1,1,1,
1,1,1,1,1,1,1,1,1,1,1,1,1,1,1,1,1,1,1,1,1,1,1,1,1,1,1,1,1,1,1,1,1,1,1,1,
1,1,1,1,1,1,1,1,1,1,1,1,1,1,1,1,1,1,1,1,1,1,1,1,1,1,1,1,1,1,1,1,1,1,1,1,
1,1,1,1,1,1,1,1,1,1,1,1,1,1,1,1,1,1,1,1,1,1,1,1,1,1,1,1,1,1,1,1,1,1,1,1,
1,1,1,1,1,1,1,1,1,1,1,1,1,1,1,1,1,4),(-0.000423095957202541,0.115881565465356),
(11.6153146011728,12.1152895244478,12.6151575298078,13.614893540528,14.6146295512481,
15.6143655619682,16.6141015726884,17.6138375834085,18.6135735941286,19.6133096048488,
20.6130456155689,21.612781626289,22.6125176370092,23.6122536477293,24.6119896584494,
25.6117256691696,26.6114616798897,27.6111976906098,28.6109337013299,29.6106697120501,
30.6104057227702,31.6101417334903,32.6098777442105,33.6096137549306,34.6093497656507,
35.6090857763709,36.608821787091,37.6085577978111,38.6082938085313,39.6080298192514,
40.6077658299715,41.6075018406916,42.6072378514118,43.6069738621319,44.606709872852,
45.6064458835722,46.6061818942923,47.6059179050124,48.6056539157326,49.6053899264527,
50.6051259371728,51.604861947893,52.6045979586131,53.6043339693332,54.6040699800534,
55.6038059907735,56.6035420014936,57.6032780122137,58.6030140229339,59.602750033654,
60.6024860443741,61.6022220550943,62.6019580658144,63.6016940765345,64.6014300872547,
65.6011660979748,66.6009021086949,67.6006381194151,68.6003741301352,69.6001101408553,
70.5998461515754,71.5995821622956,72.5993181730157,73.5990541837358,74.598790194456,
75.5985262051761,76.5982622158962,77.5979982266164,78.5977342373365,79.5974702480566,
80.5972062587768,81.5969422694969,82.596678280217,83.5964142909372,84.5961503016573,
85.5958863123774,86.5956223230975,87.5953583338177,88.5950943445378,89.5948303552579,
90.5945663659781,91.5943023766982,92.5940383874183,93.5937743981385,94.5935104088586,
95.5932464195787,96.5929824302989,97.592718441019,98.5924544517391,99.5921904624593,
100.591926473179,101.5916624839,102.59139849462,103.59113450534,104.59087051606,
105.59060652678,106.5903425375,107.59007854822,108.58981455894,109.589550569661,
110.589286580381,111.589022591101,112.588758601821,113.588494612541,114.588230623261,
115.587966633981,116.587702644701,117.587438655422,118.587174666142,119.586910676862,
120.586646687582,121.586382698302,122.586118709022,123.585854719742,124.585590730463,
125.585326741183,126.585062751903,127.584798762623,128.584534773343,129.584270784063,
130.584006794783,131.583742805503,132.583478816224,133.583214826944,134.582950837664,
135.582686848384,136.582422859104,137.582158869824,138.581894880544,139.581630891264,
140.581366901985,141.581102912705,142.580838923425,143.580574934145,144.580310944865,
145.580046955585,146.579782966305,147.579518977026,148.579254987746,149.578990998466,
150.578727009186,151.578463019906,152.578199030626,153.577935041346,154.577671052066,
155.577407062787,156.577143073507,157.576879084227,158.576615094947,159.576351105667,
160.576087116387,161.575823127107,162.575559137827,163.575295148548,164.575031159268,
165.574767169988,166.574503180708,167.574239191428,168.573975202148,169.573711212868,
170.573447223589,171.573183234309,172.572919245029,173.572655255749,174.572391266469,
175.572127277189,176.571863287909,177.571599298629,178.57133530935,179.57107132007,
180.57080733079,181.57054334151,182.57027935223,183.57001536295,184.56975137367,
185.56948738439,186.569223395111,187.568959405831,188.568695416551,189.568431427271,
190.568167437991,191.567903448711,192.567639459431,193.567375470152,194.567111480872,
195.566847491592,196.566583502312,197.566319513032,198.566055523752,199.565791534472,
200.565527545192,201.565263555913,202.564999566633,203.564735577353,204.564471588073,
205.564207598793,206.563943609513,207.563679620233,208.563415630954,209.563151641674,
210.562887652394,211.562623663114,212.562359673834,213.562095684554,214.561831695274,
215.561567705994,216.561303716715,217.561039727435,218.560775738155,219.560511748875,
220.560247759595,221.559983770315,222.559719781035,223.559455791755,224.559191802476,
225.558927813196,226.558663823916,227.558399834636,228.558135845356,229.557871856076,
230.557607866796,231.557343877517,232.557079888237,233.556815898957,234.556551909677,
235.556287920397,236.556023931117,237.555759941837,238.555495952557,239.555231963278,
240.554967973998,241.554703984718,242.554439995438,243.554176006158,244.553912016878,
245.553648027598,246.553384038319,247.553120049039,248.552856059759,249.552592070479,
250.552328081199,251.552064091919,252.551800102639,253.551536113359,254.55127212408,
255.5510081348,256.55074414552,257.55048015624,258.55021616696,259.54995217768,
260.5496881884,261.54942419912,262.549160209841,263.548896220561,264.548632231281,
265.548368242001,266.548104252721,267.547840263441,268.547576274161,269.547312284882,
270.547048295602,271.546784306322,272.546520317042,273.546256327762,274.545992338482,
275.545728349202,276.545464359922,277.545200370643,278.544936381363,279.544672392083,
280.544408402803,281.544144413523,282.543880424243,283.543616434963,284.543352445683,
285.543088456404,286.542824467124,287.542560477844,288.542296488564,289.542032499284,
290.541768510004,291.541504520724,292.541240531445,293.540976542165,294.540712552885,
295.540448563605,296.540184574325,297.539920585045,298.539656595765,299.539392606485,
300.539128617206,301.538864627926,302.538600638646,303.538336649366,304.538072660086,
305.537808670806,306.537544681526,307.537280692246,308.537016702967,309.536752713687,
310.536488724407,311.536224735127,312.535960745847,313.535696756567,314.535432767287,
315.535168778008,316.534904788728,317.534640799448,318.534376810168,319.534112820888,
320.533848831608,321.533584842328,322.533320853048,323.533056863769,324.532792874489,
325.532528885209,326.532264895929,327.532000906649,328.531736917369,329.531472928089,
330.53120893881,331.53094494953,332.53068096025,333.53041697097,334.53015298169,
335.52988899241,336.52962500313,337.52936101385,338.529097024571,339.528833035291,
340.528569046011,341.528305056731,342.528041067451,343.527777078171,344.527513088891,
345.527249099611,346.526985110332,347.526721121052,348.526457131772,349.526193142492,
350.525929153212,351.525665163932,352.525401174652,353.525137185373,354.524873196093,
355.524609206813,356.524345217533,357.524081228253,358.523817238973,359.523553249693,
360.523289260413,361.523025271134,362.522761281854,363.522497292574,364.522233303294,
365.521969314014,366.521705324734,367.521441335454,368.521177346175,369.520913356895,
370.520649367615,371.520385378335,372.520121389055,373.519857399775,374.519593410495,
375.519329421215,376.519065431936,377.518801442656,378.518537453376,379.518273464096,
380.518009474816,381.517745485536,382.517481496256,383.517217506976,384.516953517697,
385.516689528417,386.516425539137,387.516161549857,388.515897560577,389.515633571297,
390.515369582017,391.515105592737,392.514841603458,393.514577614178,394.514313624898,
395.514049635618,396.513785646338,397.513521657058,398.513257667778,399.512993678499,
400.512729689219,401.512465699939,402.512201710659,403.511937721379,404.511673732099,
405.511409742819,406.511145753539,407.51088176426,408.51061777498,409.5103537857,
410.51008979642,411.50982580714,412.50956181786,413.50929782858,414.509033839301,
415.508769850021,416.508505860741,417.508241871461,418.507977882181,419.507713892901,
420.507449903621,421.507185914341,422.506921925062,423.506657935782,424.506393946502,
425.506129957222,426.505865967942,427.505601978662,428.505337989382,429.505074000102,
430.504810010823,431.504546021543,432.504282032263,433.504018042983,434.503754053703,
435.503490064423,436.503226075143,437.502962085864,438.502698096584,439.502434107304,
440.502170118024,441.501906128744,442.501642139464,443.501378150184,444.501114160904,
445.500850171625,446.500586182345,447.500322193065,448.500058203785,449.499794214505,
450.499530225225,451.499266235945,452.499002246665,453.498738257386,454.498474268106,
455.498210278826,456.497946289546,457.497682300266,458.497418310986,459.497154321706,
460.496890332427,461.496626343147,462.496362353867,463.496098364587,464.495834375307,
465.495570386027,466.495306396747,467.495042407467,468.494778418188,469.494514428908,
470.494250439628,471.493986450348,472.493722461068,473.493458471788,474.493194482508,
475.492930493229,476.492666503949,477.492402514669,478.492138525389,479.491874536109,
480.491610546829,481.491346557549,482.491082568269,483.49081857899,484.49055458971,
485.49029060043,486.49002661115,487.48976262187,488.48949863259,489.48923464331,
490.48897065403,491.488706664751,492.488442675471,493.488178686191,494.487914696911,
495.487650707631,496.487386718351,497.487122729071,498.486858739792,499.486594750512,
500.486330761232,501.486066771952,502.485802782672,503.485538793392,504.485274804112,
505.485010814832,506.484746825553,507.484482836273,508.484218846993,509.483954857713,
510.483690868433,511.483426879153,512.483162889873,513.482898900594,514.482634911314,
515.482370922034,516.482106932754,517.481842943474,518.481578954194,519.481314964914,
520.481050975635,521.480786986355,522.480522997075,523.480259007795,524.479995018515,
525.479731029235,526.479467039955,527.479203050675,528.478939061396,529.478675072116,
530.478411082836,531.478147093556,532.477883104276,533.477619114996,534.477355125716,
535.477091136436,536.476827147157,537.476563157877,538.476299168597,539.476035179317,
540.475771190037,541.475507200757,542.475243211477,543.474979222197,544.474715232918,
545.474451243638,546.474187254358,547.473923265078,548.473659275798,549.473395286518,
550.473131297238,551.472867307958,552.472603318679,553.472339329399,554.472075340119,
555.471811350839,556.471547361559,557.471283372279,558.471019382999,559.47075539372,
560.47049140444,561.47022741516,562.46996342588,563.4696994366,564.46943544732,
565.46917145804,566.46890746876,567.468643479481,568.468379490201,569.468115500921,
570.467851511641,571.467587522361,572.467323533081,573.467059543801,574.466795554521,
575.466531565242,576.466267575962,577.466003586682,578.465739597402,579.465475608122,
580.465211618842,581.464947629562,582.464683640283,583.464419651003,584.464155661723,
585.463891672443,586.463627683163,587.463363693883,588.463099704603,589.462835715323,
590.462571726044,591.462307736764,592.462043747484,593.461779758204,594.461515768924,
595.461251779644,596.460987790364,597.460723801085,598.460459811805,599.460195822525,
600.459931833245,601.459667843965,602.459403854685,603.459139865405,604.458875876125,
605.458611886846,606.458347897566,607.458083908286,608.457819919006,609.457555929726,
610.457291940446,611.457027951166,612.456763961887,613.456499972607,614.456235983327,
615.455971994047,616.455708004767,617.455444015487,618.455180026207,619.454916036927,
620.454652047648,621.454388058368,622.454124069088,623.453860079808,624.453596090528,
625.453332101248,626.453068111968,627.452804122688,628.452540133409,629.452276144129,
630.452012154849,631.451748165569,632.451484176289,633.451220187009,634.450956197729,
635.450692208449,636.45042821917,637.45016422989,638.44990024061,639.44963625133,
640.44937226205,641.44910827277,642.44884428349,643.448580294211,644.448316304931,
645.448052315651,646.447788326371,647.447524337091,648.447260347811,649.446996358531,
650.446732369251,651.446468379972,652.446204390692,653.445940401412,654.445676412132,
655.445412422852,656.445148433572,657.444884444292,658.444620455012,659.444356465733,
660.444092476453,661.443828487173,662.443564497893,663.443300508613,664.443036519333,
665.442772530053,666.442508540774,667.442244551494,668.441980562214,669.441716572934,
670.441452583654,671.441188594374,672.440924605094,673.440660615815,674.440396626535,
675.440132637255,676.439868647975,677.439604658695,678.439340669415,679.439076680135,
680.438812690855,681.438548701576,682.438284712296,683.438020723016,684.437756733736,
685.437492744456,686.437228755176,687.436964765896,688.436700776616,689.436436787337,
690.436172798057,691.435908808777,692.435644819497,693.435380830217,694.435116840937,
695.434852851657,696.434588862377,697.434324873098,698.434060883818,699.433796894538,
700.433532905258,701.433268915978,702.433004926698,703.432740937418,704.432476948139,
705.432212958859,706.431948969579,707.431684980299,708.431420991019,709.431157001739,
710.430893012459,711.430629023179,712.4303650339,713.43010104462,714.42983705534,
715.42957306606,716.42930907678,717.4290450875,718.42878109822,719.42851710894,
720.428253119661,721.427989130381,722.427725141101,723.427461151821,724.427197162541,
725.426933173261,726.426669183981,727.426405194702,728.426141205422,729.425877216142,
730.425613226862,731.425349237582,732.425085248302,733.424821259022,734.424557269742,
735.424293280463,736.424029291183,737.423765301903,738.423501312623,739.423237323343,
740.422973334063,741.422709344783,742.422445355504,743.422181366224,744.421917376944,
745.421653387664,746.421389398384,747.421125409104,748.420861419824,749.420597430544,
750.420333441265,751.420069451985,752.419805462705,753.419541473425,754.419277484145,
755.419013494865,756.418749505585,757.418485516306,758.418221527026,759.417957537746,
760.417693548466,761.417429559186,762.417165569906,763.416901580626,764.416637591346,
765.416373602067,766.416109612787,767.415845623507,768.415581634227,769.415317644947,
770.415053655667,771.414789666387,772.414525677107,773.414261687828,774.413997698548,
775.413733709268,776.413469719988,777.413205730708,778.412941741428,779.412677752148,
780.412413762868,781.412149773589,782.411885784309,783.411621795029,784.411357805749,
785.411093816469,786.410829827189,787.410565837909,788.41030184863,789.41003785935,
790.40977387007,791.40950988079,792.40924589151,793.40898190223,794.40871791295,
795.40845392367,796.408189934391,797.407925945111,798.407661955831,799.407397966551,
800.407133977271,801.406869987991,802.406605998711,803.406342009432,804.406078020152,
805.405814030872,806.405550041592,807.405286052312,808.405022063032,809.404758073752,
810.404494084472,811.404230095193,812.403966105913,813.403702116633,814.403438127353,
815.403174138073,816.402910148793,817.402646159513,818.402382170234,819.402118180954,
820.401854191674,821.401590202394,822.401326213114,823.401062223834,824.400798234554,
825.400534245274,826.400270255995,827.400006266715,828.399742277435,829.399478288155,
830.399214298875,831.398950309595,832.398686320315,833.398422331035,834.398158341756,
835.397894352476,836.397630363196,837.397366373916,838.397102384636,839.396838395356,
840.396574406076,841.396310416796,842.396046427517,843.395782438237,844.395518448957,
845.395254459677,846.394990470397,847.394726481117,848.394462491837,849.394198502558,
850.393934513278,851.393670523998,852.393406534718,853.393142545438,854.392878556158,
855.392614566878,856.392350577598,857.392086588319,858.391822599039,859.391558609759,
860.391294620479,861.391030631199,862.390766641919,863.390502652639,864.390238663359,
865.38997467408,866.3897106848,867.38944669552,868.38918270624,869.38891871696,
870.38865472768,871.3883907384,872.388126749121,873.387862759841,874.387598770561,
875.387334781281,876.387070792001,877.386806802721,878.386542813441,879.386278824161,
880.386014834882,881.385750845602,882.385486856322,883.385222867042,884.384958877762,
885.384694888482,886.384430899202,887.384166909923,888.383902920643,889.383638931363,
890.383374942083,891.383110952803,892.382846963523,893.382582974243,894.382318984963,
895.382054995684,896.381791006404,897.381527017124,898.381263027844,899.380999038564,
900.380735049284,901.380471060004,902.380207070725,903.379943081445,904.379679092165,
905.379415102885,906.379151113605,907.378887124325,908.378623135045,909.378359145765,
910.378095156486,911.377831167206,912.377567177926,913.377303188646,914.377039199366,
915.376775210086,916.376511220806,917.376247231526,918.375983242247,919.375719252967,
920.375455263687,921.375191274407,922.374927285127,923.374663295847,924.374399306567,
925.374135317287,926.373871328008,927.373607338728,928.373343349448,929.373079360168,
930.372815370888,931.372551381608,932.372287392328,933.372023403049,934.371759413769,
935.371495424489,936.371231435209,937.370967445929,938.370703456649,939.370439467369,
940.370175478089,941.36991148881,942.36964749953,943.36938351025,944.36911952097,
945.36885553169,946.36859154241,947.36832755313,948.368063563851,949.367799574571,
950.367535585291,951.367271596011,952.367007606731,953.366743617451,954.366479628171,
955.366215638891,956.365951649612,957.365687660332,958.365423671052,959.365159681772,
960.364895692492,961.364631703212,962.364367713932,963.364103724653,964.363839735373,
965.363575746093,966.363311756813,967.363047767533,968.362783778253,969.362519788973,
970.362255799693,971.361991810414,972.361727821134,973.361463831854,974.361199842574,
975.360935853294,976.360671864014,977.360407874734,978.360143885454,979.359879896175,
980.359615906895,981.359351917615,982.359087928335,983.358823939055,984.358559949775,
985.358295960495,986.358031971215,987.357767981936,988.357503992656,989.357240003376,
990.356976014096,991.356712024816,992.356448035536,993.356184046256,994.355920056977,
995.355656067697,996.355392078417,997.355128089137,998.354864099857,999.354600110577,
1000.3543361213,1001.35407213202,1002.35380814274,1003.35354415346,1004.35328016418,
1005.3530161749,1006.35275218562,1007.35248819634,1008.35222420706,1009.35196021778,
1010.3516962285,1011.35143223922,1012.35116824994,1013.35090426066,1014.35064027138,
1015.3503762821,1016.35011229282,1017.34984830354,1018.34958431426,1019.34932032498,
1020.3490563357,1021.34879234642,1022.34852835714,1023.34826436786,1024.34800037858,
1025.3477363893,1026.34747240002,1027.34720841074,1028.34694442146,1029.34668043218,
1030.3464164429,1031.34615245362,1032.34588846434,1033.34562447506,1034.34536048578,
1035.3450964965,1036.34483250722,1037.34456851794,1038.34430452866,1039.34404053938,
1040.3437765501,1041.34351256082,1042.34324857154,1043.34298458226,1044.34272059298,
1045.3424566037,1046.34219261442,1047.34192862514,1048.34166463586,1049.34140064658,
1050.3411366573,1051.34087266802,1052.34060867874,1053.34034468946,1054.34008070018,
1055.3398167109,1056.33955272162,1057.33928873234,1058.33902474307,1059.33876075378,
1060.33849676451,1061.33823277523,1062.33796878595,1063.33770479667,1064.33744080739,
1065.33717681811,1066.33691282883,1067.33664883955,1068.33638485027,1069.33612086099,
1070.33585687171,1071.33559288243,1072.33532889315,1073.33506490387,1074.33480091459,
1075.33453692531,1076.33427293603,1077.33400894675,1078.33374495747,1079.33348096819,
1080.33321697891,1081.33295298963,1082.33268900035,1083.33242501107,1084.33216102179,
1085.33189703251,1086.33163304323,1087.33136905395,1088.33110506467,1089.33084107539,
1090.33057708611,1091.33031309683,1092.33004910755,1093.32978511827,1094.32952112899,
1095.32925713971,1096.32899315043,1097.32872916115,1098.32846517187,1099.32820118259,
1100.32793719331,1101.32767320403,1102.32740921475,1103.32714522547,1104.32688123619,
1105.32661724691,1106.32635325763,1107.32608926835,1108.32582527907,1109.32556128979,
1110.32529730051,1111.32503331123,1112.32476932195,1113.32450533267,1114.32424134339,
1115.32397735411,1116.32371336483,1117.32344937555,1118.32318538627,1119.32292139699,
1120.32265740771,1121.32239341843,1122.32212942915,1123.32186543987,1124.32160145059,
1125.32133746131,1126.32107347203,1127.32080948275,1128.32054549347,1129.32028150419,
1130.32001751491,1131.31975352563,1132.31948953635,1133.31922554707,1134.31896155779,
1135.31869756852,1136.31843357924,1137.31816958996,1138.31790560068,1139.3176416114,
1140.31737762212,1141.31711363284,1142.31684964356,1143.31658565428,1144.316321665,
1145.31605767572,1146.31579368644,1147.31552969716,1148.31526570788,1149.3150017186,
1150.31473772932,1151.31447374004,1152.31420975076,1153.31394576148,1154.3136817722,
1155.31341778292,1156.31315379364,1157.31288980436,1158.31262581508,1159.3123618258,
1160.31209783652,1161.31183384724,1162.31156985796,1163.31130586868,1164.3110418794,
1165.31077789012,1166.31051390084,1167.31024991156,1168.30998592228,1169.309721933,
1170.30945794372,1171.30919395444,1172.30892996516,1173.30866597588,1174.3084019866,
1175.30813799732,1176.30787400804,1177.30761001876,1178.30734602948,1179.3070820402,
1180.30681805092,1181.30655406164,1182.30629007236,1183.30602608308,1184.3057620938,
1185.30549810452,1186.30523411524,1187.30497012596,1188.30470613668,1189.3044421474,
1190.30417815812,1191.30391416884,1192.30365017956,1193.30338619028,1194.303122201,
1195.30285821172,1196.30259422244,1197.30233023316,1198.30206624388,1199.3018022546,
1200.30153826532,1201.30127427604,1202.30101028676,1203.30074629748,1204.3004823082,
1205.30021831892,1206.29995432964,1207.29969034036,1208.29942635108,1209.2991623618,
1210.29889837252,1211.29863438324,1212.29837039397,1213.29810640469,1214.29784241541,
1215.29757842613,1216.29731443685,1217.29705044757,1218.29678645829,1219.29652246901,
1220.29625847973,1221.29599449045,1222.29573050117,1223.29546651189,1224.29520252261,
1225.29493853333,1226.29467454405,1227.29441055477,1228.29414656549,1229.29388257621,
1230.29361858693,1231.29335459765,1232.29309060837,1233.29282661909,1234.29256262981,
1235.29229864053,1236.29203465125,1237.29177066197,1238.29150667269,1239.29124268341,
1240.29097869413,1241.29071470485,1242.29045071557,1243.29018672629,1244.28992273701,
1245.28965874773,1246.28939475845,1247.28913076917,1248.28886677989,1249.28860279061,
1250.28833880133,1251.28807481205,1252.28781082277,1253.28754683349,1254.28728284421,
1255.28701885493,1256.28675486565,1257.28649087637,1258.28622688709,1259.28596289781,
1260.28569890853,1261.28543491925,1262.28517092997,1263.28490694069,1264.28464295141,
1265.28437896213,1266.28411497285,1267.28385098357,1268.28358699429,1269.28332300501,
1270.28305901573,1271.28279502645,1272.28253103717,1273.28226704789,1274.28200305861,
1275.28173906933,1276.28147508005,1277.28121109077,1278.28094710149,1279.28068311221,
1280.28041912293,1281.28015513365,1282.27989114437,1283.27962715509,1284.27936316581,
1285.27909917653,1286.27883518725,1287.27857119797,1288.2783072087,1289.27804321942,
1290.27777923014,1291.27751524086,1292.27725125158,1293.2769872623,1294.27672327302,
1295.27645928374,1296.27619529446,1297.27593130518,1298.2756673159,1299.27540332662,
1300.27513933734,1301.27487534806,1302.27461135878,1303.2743473695,1304.27408338022,
1305.27381939094,1306.27355540166,1307.27329141238,1308.2730274231,1309.27276343382,
1310.27249944454,1311.27223545526,1312.27197146598,1313.2717074767,1314.27144348742,
1315.27117949814,1316.27091550886,1317.27065151958,1318.2703875303,1319.27012354102,
1320.26985955174,1321.26959556246,1322.26933157318,1323.2690675839,1324.26880359462,
1325.26853960534,1326.26827561606,1327.26801162678,1328.2677476375,1329.26748364822,
1330.26721965894,1331.26695566966,1332.26669168038,1333.2664276911,1334.26616370182,
1335.26589971254,1336.26563572326,1337.26537173398,1338.2651077447,1339.26484375542,
1340.26457976614,1341.26431577686,1342.26405178758,1343.2637877983,1344.26352380902,
1345.26325981974,1346.26299583046,1347.26273184118,1348.2624678519,1349.26220386262,
1350.26193987334,1351.26167588406,1352.26141189478,1353.2611479055,1354.26088391622,
1355.26061992694,1356.26035593766,1357.26009194838,1358.2598279591,1359.25956396982,
1360.25929998054,1361.25903599126,1362.25877200198,1363.2585080127,1364.25824402343,
1365.25798003415,1366.25771604487,1367.25745205559,1368.25718806631,1369.25692407703,
1370.25666008775,1371.25639609847,1372.25613210919,1373.25586811991,1374.25560413063,
1375.25534014135,1376.25507615207,1377.25481216279,1378.25454817351,1379.25428418423,
1380.25402019495,1381.25375620567,1382.25349221639,1383.25322822711,1384.25296423783,
1385.25270024855,1386.25243625927,1387.25217226999,1388.25190828071,1389.25164429143,
1390.25138030215,1391.25111631287,1392.25085232359,1393.25058833431,1394.25032434503,
1395.25006035575,1396.24979636647,1397.24953237719,1398.24926838791,1399.24900439863,
1400.24874040935,1401.24847642007,1402.24821243079,1403.24794844151,1404.24768445223,
1405.24742046295,1406.24715647367,1407.24689248439,1408.24662849511,1409.24636450583,
1410.24610051655,1411.24583652727,1412.24557253799,1413.24530854871,1414.24504455943,
1415.24478057015,1416.24451658087,1417.24425259159,1418.24398860231,1419.24372461303,
1420.24346062375,1421.24319663447,1422.24293264519,1423.24266865591,1424.24240466663,
1425.24214067735,1426.24187668807,1427.24161269879,1428.24134870951,1429.24108472023,
1430.24082073095,1431.24055674167,1432.24029275239,1433.24002876311,1434.23976477383,
1435.23950078455,1436.23923679527,1437.23897280599,1438.23870881671,1439.23844482743,
1440.23818083815,1441.23791684888,1442.2376528596,1443.23738887032,1444.23712488104,
1445.23686089176,1446.23659690248,1447.2363329132,1448.23606892392,1449.23580493464,
1450.23554094536,1451.23527695608,1452.2350129668,1453.23474897752,1454.23448498824,
1455.23422099896,1456.23395700968,1457.2336930204,1458.23342903112,1459.23316504184,
1460.23290105256,1461.23263706328,1462.232373074,1463.23210908472,1464.23184509544,
1465.23158110616,1466.23131711688,1467.2310531276,1468.23078913832,1469.23052514904,
1470.23026115976,1471.22999717048,1472.2297331812,1473.22946919192,1474.22920520264,
1475.22894121336,1476.22867722408,1477.2284132348,1478.22814924552,1479.22788525624,
1480.22762126696,1481.22735727768,1482.2270932884,1483.22682929912,1484.22656530984,
1485.22630132056,1486.22603733128,1487.225773342,1488.22550935272,1489.22524536344,
1490.22498137416,1491.22471738488,1492.2244533956,1493.22418940632,1494.22392541704,
1495.22366142776,1496.22339743848,1497.2231334492,1498.22286945992,1499.22260547064,
1500.22234148136,1501.22207749208,1502.2218135028,1503.22154951352,1504.22128552424,
1505.22102153496,1506.22075754568,1507.2204935564,1508.22022956712,1509.21996557784,
1510.21970158856,1511.21943759928,1512.21917361,1513.21890962072,1514.21864563144,
1515.21838164216,1516.21811765288,1517.21785366361,1518.21758967433,1519.21732568505,
1520.21706169577,1521.21679770649,1522.21653371721,1523.21626972793,1524.21600573865,
1525.21574174937,1526.21547776009,1527.21521377081,1528.21494978153,1529.21468579225,
1530.21442180297,1531.21415781369,1532.21389382441,1533.21362983513,1534.21336584585,
1535.21310185657,1536.21283786729,1537.21257387801,1538.21230988873,1539.21204589945,
1540.21178191017,1541.21151792089,1542.21125393161,1543.21098994233,1544.21072595305,
1545.21046196377,1546.21019797449,1547.20993398521,1548.20966999593,1549.20940600665,
1550.20914201737,1551.20887802809,1552.20861403881,1553.20835004953,1554.20808606025,
1555.20782207097,1556.20755808169,1557.20729409241,1558.20703010313,1559.20676611385,
1560.20650212457,1561.20623813529,1562.20597414601,1563.20571015673,1564.20544616745,
1565.20518217817,1566.20491818889,1567.20465419961,1568.20439021033,1569.20412622105,
1570.20386223177,1571.20359824249,1572.20333425321,1573.20307026393,1574.20280627465,
1575.20254228537,1576.20227829609,1577.20201430681,1578.20175031753,1579.20148632825,
1580.20122233897,1581.20095834969,1582.20069436041,1583.20043037113,1584.20016638185,
1585.19990239257,1586.19963840329,1587.19937441401,1588.19911042473,1589.19884643545,
1590.19858244617,1591.19831845689,1592.19805446761,1593.19779047834,1594.19752648906,
1595.19726249978,1596.1969985105,1597.19673452122,1598.19647053194,1599.19620654266,
1600.19594255338,1601.1956785641,1602.19541457482,1603.19515058554,1604.19488659626,
1605.19462260698,1606.1943586177,1607.19409462842,1608.19383063914,1609.19356664986,
1610.19330266058,1611.1930386713,1612.19277468202,1613.19251069274,1614.19224670346,
1615.19198271418,1616.1917187249,1617.19145473562,1618.19119074634,1619.19092675706,
1620.19066276778,1621.1903987785,1622.19013478922,1623.18987079994,1624.18960681066,
1625.18934282138,1626.1890788321,1627.18881484282,1628.18855085354,1629.18828686426,
1630.18802287498,1631.1877588857,1632.18749489642,1633.18723090714,1634.18696691786,
1635.18670292858,1636.1864389393,1637.18617495002,1638.18591096074,1639.18564697146,
1640.18538298218,1641.1851189929,1642.18485500362,1643.18459101434,1644.18432702506,
1645.18406303578,1646.1837990465,1647.18353505722,1648.18327106794,1649.18300707866,
1650.18274308938,1651.1824791001,1652.18221511082,1653.18195112154,1654.18168713226,
1655.18142314298,1656.1811591537,1657.18089516442,1658.18063117514,1659.18036718586,
1660.18010319658,1661.1798392073,1662.17957521802,1663.17931122874,1664.17904723946,
1665.17878325018,1666.1785192609,1667.17825527162,1668.17799128234,1669.17772729307,
1670.17746330379,1671.17719931451,1672.17693532523,1673.17667133595,1674.17640734667,
1675.17614335739,1676.17587936811,1677.17561537883,1678.17535138955,1679.17508740027,
1680.17482341099,1681.17455942171,1682.17429543243,1683.17403144315,1684.17376745387,
1685.17350346459,1686.17323947531,1687.17297548603,1688.17271149675,1689.17244750747,
1690.17218351819,1691.17191952891,1692.17165553963,1693.17139155035,1694.17112756107,
1695.17086357179,1696.17059958251,1697.17033559323,1698.17007160395,1699.16980761467,
1700.16954362539,1700.66941163075,1701.16959429301),.UNSPECIFIED.);
#56=B_SPLINE_SURFACE_WITH_KNOTS('',3,3,((#272352,#272353,#272354,#272355,
#272356,#272357,#272358,#272359,#272360,#272361,#272362,#272363,#272364,
#272365,#272366,#272367,#272368,#272369,#272370,#272371,#272372,#272373,
#272374,#272375,#272376,#272377,#272378,#272379,#272380,#272381,#272382,
#272383,#272384,#272385,#272386,#272387,#272388,#272389,#272390,#272391,
#272392,#272393,#272394,#272395,#272396,#272397,#272398,#272399,#272400,
#272401,#272402,#272403,#272404,#272405,#272406,#272407,#272408,#272409,
#272410,#272411,#272412,#272413,#272414,#272415,#272416,#272417,#272418,
#272419,#272420,#272421,#272422,#272423,#272424,#272425,#272426,#272427,
#272428,#272429,#272430,#272431,#272432,#272433,#272434,#272435,#272436,
#272437,#272438,#272439,#272440,#272441,#272442,#272443,#272444,#272445,
#272446,#272447,#272448,#272449,#272450,#272451,#272452,#272453,#272454,
#272455,#272456,#272457,#272458,#272459,#272460,#272461,#272462,#272463,
#272464,#272465,#272466,#272467,#272468,#272469,#272470,#272471,#272472,
#272473,#272474,#272475,#272476,#272477,#272478,#272479,#272480,#272481,
#272482,#272483,#272484,#272485,#272486,#272487,#272488,#272489,#272490,
#272491,#272492,#272493,#272494,#272495,#272496,#272497,#272498,#272499,
#272500,#272501,#272502,#272503,#272504,#272505,#272506,#272507,#272508,
#272509,#272510,#272511,#272512,#272513,#272514,#272515,#272516,#272517,
#272518,#272519,#272520,#272521,#272522,#272523,#272524,#272525,#272526,
#272527,#272528,#272529,#272530,#272531,#272532,#272533,#272534,#272535,
#272536,#272537,#272538,#272539,#272540,#272541,#272542,#272543,#272544,
#272545,#272546,#272547,#272548,#272549,#272550,#272551,#272552,#272553,
#272554,#272555,#272556,#272557,#272558,#272559,#272560,#272561,#272562,
#272563,#272564,#272565,#272566,#272567,#272568,#272569,#272570,#272571,
#272572,#272573,#272574,#272575,#272576,#272577,#272578,#272579,#272580,
#272581,#272582,#272583,#272584,#272585,#272586,#272587,#272588,#272589,
#272590,#272591,#272592,#272593,#272594,#272595,#272596,#272597,#272598,
#272599,#272600,#272601,#272602,#272603,#272604,#272605,#272606,#272607,
#272608,#272609,#272610,#272611,#272612,#272613,#272614,#272615,#272616,
#272617,#272618,#272619,#272620,#272621,#272622,#272623,#272624,#272625,
#272626,#272627,#272628,#272629,#272630,#272631,#272632,#272633,#272634,
#272635,#272636,#272637,#272638,#272639,#272640,#272641,#272642,#272643,
#272644,#272645,#272646,#272647,#272648,#272649,#272650,#272651,#272652,
#272653,#272654,#272655,#272656,#272657,#272658,#272659,#272660,#272661,
#272662,#272663,#272664,#272665,#272666,#272667,#272668,#272669,#272670,
#272671,#272672,#272673,#272674,#272675,#272676,#272677,#272678,#272679,
#272680,#272681,#272682,#272683,#272684,#272685,#272686,#272687,#272688,
#272689,#272690,#272691,#272692,#272693,#272694,#272695,#272696,#272697,
#272698,#272699,#272700,#272701,#272702,#272703,#272704,#272705,#272706,
#272707,#272708,#272709,#272710,#272711,#272712,#272713,#272714,#272715,
#272716,#272717,#272718,#272719,#272720,#272721,#272722,#272723,#272724,
#272725,#272726,#272727,#272728,#272729,#272730,#272731,#272732,#272733,
#272734,#272735,#272736,#272737,#272738,#272739,#272740,#272741,#272742,
#272743,#272744,#272745,#272746,#272747,#272748,#272749,#272750,#272751,
#272752,#272753,#272754,#272755,#272756,#272757,#272758,#272759,#272760,
#272761,#272762,#272763,#272764,#272765,#272766,#272767,#272768,#272769,
#272770,#272771,#272772,#272773,#272774,#272775,#272776,#272777,#272778,
#272779,#272780,#272781,#272782,#272783,#272784,#272785,#272786,#272787,
#272788,#272789,#272790,#272791,#272792,#272793,#272794,#272795,#272796,
#272797,#272798,#272799,#272800,#272801,#272802,#272803,#272804,#272805,
#272806,#272807,#272808,#272809,#272810,#272811,#272812,#272813,#272814,
#272815,#272816,#272817,#272818,#272819,#272820,#272821,#272822,#272823,
#272824,#272825,#272826,#272827,#272828,#272829,#272830,#272831,#272832,
#272833,#272834,#272835,#272836,#272837,#272838,#272839,#272840,#272841,
#272842,#272843,#272844,#272845,#272846,#272847,#272848,#272849,#272850,
#272851,#272852,#272853,#272854,#272855,#272856,#272857,#272858,#272859,
#272860,#272861,#272862,#272863,#272864,#272865,#272866,#272867,#272868,
#272869,#272870,#272871,#272872,#272873,#272874,#272875,#272876,#272877,
#272878,#272879,#272880,#272881,#272882,#272883,#272884,#272885,#272886,
#272887,#272888,#272889,#272890,#272891,#272892,#272893,#272894,#272895,
#272896,#272897,#272898,#272899,#272900,#272901,#272902,#272903,#272904,
#272905,#272906,#272907,#272908,#272909,#272910,#272911,#272912,#272913,
#272914,#272915,#272916,#272917,#272918,#272919,#272920,#272921,#272922,
#272923,#272924,#272925,#272926,#272927,#272928,#272929,#272930,#272931,
#272932,#272933,#272934,#272935,#272936,#272937,#272938,#272939,#272940,
#272941,#272942,#272943,#272944,#272945,#272946,#272947,#272948,#272949,
#272950,#272951,#272952,#272953,#272954,#272955,#272956,#272957,#272958,
#272959,#272960,#272961,#272962,#272963,#272964,#272965,#272966,#272967,
#272968,#272969,#272970,#272971,#272972,#272973,#272974,#272975,#272976,
#272977,#272978,#272979,#272980,#272981,#272982,#272983,#272984,#272985,
#272986,#272987,#272988,#272989,#272990,#272991,#272992,#272993,#272994,
#272995,#272996,#272997,#272998,#272999,#273000,#273001,#273002,#273003,
#273004,#273005,#273006,#273007,#273008,#273009,#273010,#273011,#273012,
#273013,#273014,#273015,#273016,#273017,#273018,#273019,#273020,#273021,
#273022,#273023,#273024,#273025,#273026,#273027,#273028,#273029,#273030,
#273031,#273032,#273033,#273034,#273035,#273036,#273037,#273038,#273039,
#273040,#273041,#273042,#273043,#273044,#273045,#273046,#273047,#273048,
#273049,#273050,#273051,#273052,#273053,#273054,#273055,#273056,#273057,
#273058,#273059,#273060,#273061,#273062,#273063,#273064,#273065,#273066,
#273067,#273068,#273069,#273070,#273071,#273072,#273073,#273074,#273075,
#273076,#273077,#273078,#273079,#273080,#273081,#273082,#273083,#273084,
#273085,#273086,#273087,#273088,#273089,#273090,#273091,#273092,#273093,
#273094,#273095,#273096,#273097,#273098,#273099,#273100,#273101,#273102,
#273103,#273104,#273105,#273106,#273107,#273108,#273109,#273110,#273111,
#273112,#273113,#273114,#273115,#273116,#273117,#273118,#273119,#273120,
#273121,#273122,#273123,#273124,#273125,#273126,#273127,#273128,#273129,
#273130,#273131,#273132,#273133,#273134,#273135,#273136,#273137,#273138,
#273139,#273140,#273141,#273142,#273143,#273144,#273145,#273146,#273147,
#273148,#273149,#273150,#273151,#273152,#273153,#273154,#273155,#273156,
#273157,#273158,#273159,#273160,#273161,#273162,#273163,#273164,#273165,
#273166,#273167,#273168,#273169,#273170,#273171,#273172,#273173,#273174,
#273175,#273176,#273177,#273178,#273179,#273180,#273181,#273182,#273183,
#273184,#273185,#273186,#273187,#273188,#273189,#273190,#273191,#273192,
#273193,#273194,#273195,#273196,#273197,#273198,#273199,#273200,#273201,
#273202,#273203,#273204,#273205,#273206,#273207,#273208,#273209,#273210,
#273211,#273212,#273213,#273214,#273215,#273216,#273217,#273218,#273219,
#273220,#273221,#273222,#273223,#273224,#273225,#273226,#273227,#273228,
#273229,#273230,#273231,#273232,#273233,#273234,#273235,#273236,#273237,
#273238,#273239,#273240,#273241,#273242,#273243,#273244,#273245,#273246,
#273247,#273248,#273249,#273250,#273251,#273252,#273253,#273254,#273255,
#273256,#273257,#273258,#273259,#273260,#273261,#273262,#273263,#273264,
#273265,#273266,#273267,#273268,#273269,#273270,#273271,#273272,#273273,
#273274,#273275,#273276,#273277,#273278,#273279,#273280,#273281,#273282,
#273283,#273284,#273285,#273286,#273287,#273288,#273289,#273290,#273291,
#273292,#273293,#273294,#273295,#273296,#273297,#273298,#273299,#273300,
#273301,#273302,#273303,#273304,#273305,#273306,#273307,#273308,#273309,
#273310,#273311,#273312,#273313,#273314,#273315,#273316,#273317,#273318,
#273319,#273320,#273321,#273322,#273323,#273324,#273325,#273326,#273327,
#273328,#273329,#273330,#273331,#273332,#273333,#273334,#273335,#273336,
#273337,#273338,#273339,#273340,#273341,#273342,#273343,#273344,#273345,
#273346,#273347,#273348,#273349,#273350,#273351,#273352,#273353,#273354,
#273355,#273356,#273357,#273358,#273359,#273360,#273361,#273362,#273363,
#273364,#273365,#273366,#273367,#273368,#273369,#273370,#273371,#273372,
#273373,#273374,#273375,#273376,#273377,#273378,#273379,#273380,#273381,
#273382,#273383,#273384,#273385,#273386,#273387,#273388,#273389,#273390,
#273391,#273392,#273393,#273394,#273395,#273396,#273397,#273398,#273399,
#273400,#273401,#273402,#273403,#273404,#273405,#273406,#273407,#273408,
#273409,#273410,#273411,#273412,#273413,#273414,#273415,#273416,#273417,
#273418,#273419,#273420,#273421,#273422,#273423,#273424,#273425,#273426,
#273427,#273428,#273429,#273430,#273431,#273432,#273433,#273434,#273435,
#273436,#273437,#273438,#273439,#273440,#273441,#273442,#273443,#273444,
#273445,#273446,#273447,#273448,#273449,#273450,#273451,#273452,#273453,
#273454,#273455,#273456,#273457,#273458,#273459,#273460,#273461,#273462,
#273463,#273464,#273465,#273466,#273467,#273468,#273469,#273470,#273471,
#273472,#273473,#273474,#273475,#273476,#273477,#273478,#273479,#273480,
#273481,#273482,#273483,#273484,#273485,#273486,#273487,#273488,#273489,
#273490,#273491,#273492,#273493,#273494,#273495,#273496,#273497,#273498,
#273499,#273500,#273501,#273502,#273503,#273504,#273505,#273506,#273507,
#273508,#273509,#273510,#273511,#273512,#273513,#273514,#273515,#273516,
#273517,#273518,#273519,#273520,#273521,#273522,#273523,#273524,#273525,
#273526,#273527,#273528,#273529,#273530,#273531,#273532,#273533,#273534,
#273535,#273536,#273537,#273538,#273539,#273540,#273541,#273542,#273543,
#273544,#273545,#273546,#273547,#273548,#273549,#273550,#273551,#273552,
#273553,#273554,#273555,#273556,#273557,#273558,#273559,#273560,#273561,
#273562,#273563,#273564,#273565,#273566,#273567,#273568,#273569,#273570,
#273571,#273572,#273573,#273574,#273575,#273576,#273577,#273578,#273579,
#273580,#273581,#273582,#273583,#273584,#273585,#273586,#273587,#273588,
#273589,#273590,#273591,#273592,#273593,#273594,#273595,#273596,#273597,
#273598,#273599,#273600,#273601,#273602,#273603,#273604,#273605,#273606,
#273607,#273608,#273609,#273610,#273611,#273612,#273613,#273614,#273615,
#273616,#273617,#273618,#273619,#273620,#273621,#273622,#273623,#273624,
#273625,#273626,#273627,#273628,#273629,#273630,#273631,#273632,#273633,
#273634,#273635,#273636,#273637,#273638,#273639,#273640,#273641,#273642,
#273643,#273644,#273645,#273646,#273647,#273648,#273649,#273650,#273651,
#273652,#273653,#273654,#273655,#273656,#273657,#273658,#273659,#273660,
#273661,#273662,#273663,#273664,#273665,#273666,#273667,#273668,#273669,
#273670,#273671,#273672,#273673,#273674,#273675,#273676,#273677,#273678,
#273679,#273680,#273681,#273682,#273683,#273684,#273685,#273686,#273687,
#273688,#273689,#273690,#273691,#273692,#273693,#273694,#273695,#273696,
#273697,#273698,#273699,#273700,#273701,#273702,#273703,#273704,#273705,
#273706,#273707,#273708,#273709,#273710,#273711,#273712,#273713,#273714,
#273715,#273716,#273717,#273718,#273719,#273720,#273721,#273722,#273723,
#273724,#273725,#273726,#273727,#273728,#273729,#273730,#273731,#273732,
#273733,#273734,#273735,#273736,#273737,#273738,#273739,#273740,#273741,
#273742,#273743,#273744,#273745,#273746,#273747,#273748,#273749,#273750,
#273751,#273752,#273753,#273754,#273755,#273756,#273757,#273758,#273759,
#273760,#273761,#273762,#273763,#273764,#273765,#273766,#273767,#273768,
#273769,#273770,#273771,#273772,#273773,#273774,#273775,#273776,#273777,
#273778,#273779,#273780,#273781,#273782,#273783,#273784,#273785,#273786,
#273787,#273788,#273789,#273790,#273791,#273792,#273793,#273794,#273795,
#273796,#273797,#273798,#273799,#273800,#273801,#273802,#273803,#273804,
#273805,#273806,#273807,#273808,#273809,#273810,#273811,#273812,#273813,
#273814,#273815,#273816,#273817,#273818,#273819,#273820,#273821,#273822,
#273823,#273824,#273825,#273826,#273827,#273828,#273829,#273830,#273831,
#273832,#273833,#273834,#273835,#273836,#273837,#273838,#273839,#273840,
#273841,#273842,#273843,#273844,#273845,#273846,#273847,#273848,#273849,
#273850,#273851,#273852,#273853,#273854,#273855,#273856,#273857,#273858,
#273859,#273860,#273861,#273862,#273863,#273864,#273865,#273866,#273867,
#273868,#273869,#273870,#273871,#273872,#273873,#273874,#273875,#273876,
#273877,#273878,#273879,#273880,#273881,#273882,#273883,#273884,#273885,
#273886,#273887,#273888,#273889,#273890,#273891,#273892,#273893,#273894,
#273895,#273896,#273897,#273898,#273899,#273900,#273901,#273902,#273903,
#273904,#273905,#273906,#273907,#273908,#273909,#273910,#273911,#273912,
#273913,#273914,#273915,#273916,#273917,#273918,#273919,#273920,#273921,
#273922,#273923,#273924,#273925,#273926,#273927,#273928,#273929,#273930,
#273931,#273932,#273933,#273934,#273935,#273936,#273937,#273938,#273939,
#273940,#273941,#273942,#273943,#273944,#273945,#273946,#273947,#273948,
#273949,#273950,#273951,#273952,#273953,#273954,#273955,#273956,#273957,
#273958,#273959,#273960,#273961,#273962,#273963,#273964,#273965,#273966,
#273967,#273968,#273969,#273970,#273971,#273972,#273973,#273974,#273975,
#273976,#273977,#273978,#273979,#273980,#273981,#273982,#273983,#273984,
#273985,#273986,#273987,#273988,#273989,#273990,#273991,#273992,#273993,
#273994,#273995,#273996,#273997,#273998,#273999,#274000,#274001,#274002,
#274003,#274004,#274005,#274006,#274007,#274008,#274009,#274010,#274011,
#274012,#274013,#274014,#274015,#274016,#274017,#274018,#274019,#274020,
#274021,#274022,#274023,#274024,#274025,#274026,#274027,#274028,#274029,
#274030,#274031,#274032,#274033,#274034,#274035,#274036,#274037,#274038,
#274039,#274040,#274041,#274042,#274043,#274044,#274045,#274046),(#274047,
#274048,#274049,#274050,#274051,#274052,#274053,#274054,#274055,#274056,
#274057,#274058,#274059,#274060,#274061,#274062,#274063,#274064,#274065,
#274066,#274067,#274068,#274069,#274070,#274071,#274072,#274073,#274074,
#274075,#274076,#274077,#274078,#274079,#274080,#274081,#274082,#274083,
#274084,#274085,#274086,#274087,#274088,#274089,#274090,#274091,#274092,
#274093,#274094,#274095,#274096,#274097,#274098,#274099,#274100,#274101,
#274102,#274103,#274104,#274105,#274106,#274107,#274108,#274109,#274110,
#274111,#274112,#274113,#274114,#274115,#274116,#274117,#274118,#274119,
#274120,#274121,#274122,#274123,#274124,#274125,#274126,#274127,#274128,
#274129,#274130,#274131,#274132,#274133,#274134,#274135,#274136,#274137,
#274138,#274139,#274140,#274141,#274142,#274143,#274144,#274145,#274146,
#274147,#274148,#274149,#274150,#274151,#274152,#274153,#274154,#274155,
#274156,#274157,#274158,#274159,#274160,#274161,#274162,#274163,#274164,
#274165,#274166,#274167,#274168,#274169,#274170,#274171,#274172,#274173,
#274174,#274175,#274176,#274177,#274178,#274179,#274180,#274181,#274182,
#274183,#274184,#274185,#274186,#274187,#274188,#274189,#274190,#274191,
#274192,#274193,#274194,#274195,#274196,#274197,#274198,#274199,#274200,
#274201,#274202,#274203,#274204,#274205,#274206,#274207,#274208,#274209,
#274210,#274211,#274212,#274213,#274214,#274215,#274216,#274217,#274218,
#274219,#274220,#274221,#274222,#274223,#274224,#274225,#274226,#274227,
#274228,#274229,#274230,#274231,#274232,#274233,#274234,#274235,#274236,
#274237,#274238,#274239,#274240,#274241,#274242,#274243,#274244,#274245,
#274246,#274247,#274248,#274249,#274250,#274251,#274252,#274253,#274254,
#274255,#274256,#274257,#274258,#274259,#274260,#274261,#274262,#274263,
#274264,#274265,#274266,#274267,#274268,#274269,#274270,#274271,#274272,
#274273,#274274,#274275,#274276,#274277,#274278,#274279,#274280,#274281,
#274282,#274283,#274284,#274285,#274286,#274287,#274288,#274289,#274290,
#274291,#274292,#274293,#274294,#274295,#274296,#274297,#274298,#274299,
#274300,#274301,#274302,#274303,#274304,#274305,#274306,#274307,#274308,
#274309,#274310,#274311,#274312,#274313,#274314,#274315,#274316,#274317,
#274318,#274319,#274320,#274321,#274322,#274323,#274324,#274325,#274326,
#274327,#274328,#274329,#274330,#274331,#274332,#274333,#274334,#274335,
#274336,#274337,#274338,#274339,#274340,#274341,#274342,#274343,#274344,
#274345,#274346,#274347,#274348,#274349,#274350,#274351,#274352,#274353,
#274354,#274355,#274356,#274357,#274358,#274359,#274360,#274361,#274362,
#274363,#274364,#274365,#274366,#274367,#274368,#274369,#274370,#274371,
#274372,#274373,#274374,#274375,#274376,#274377,#274378,#274379,#274380,
#274381,#274382,#274383,#274384,#274385,#274386,#274387,#274388,#274389,
#274390,#274391,#274392,#274393,#274394,#274395,#274396,#274397,#274398,
#274399,#274400,#274401,#274402,#274403,#274404,#274405,#274406,#274407,
#274408,#274409,#274410,#274411,#274412,#274413,#274414,#274415,#274416,
#274417,#274418,#274419,#274420,#274421,#274422,#274423,#274424,#274425,
#274426,#274427,#274428,#274429,#274430,#274431,#274432,#274433,#274434,
#274435,#274436,#274437,#274438,#274439,#274440,#274441,#274442,#274443,
#274444,#274445,#274446,#274447,#274448,#274449,#274450,#274451,#274452,
#274453,#274454,#274455,#274456,#274457,#274458,#274459,#274460,#274461,
#274462,#274463,#274464,#274465,#274466,#274467,#274468,#274469,#274470,
#274471,#274472,#274473,#274474,#274475,#274476,#274477,#274478,#274479,
#274480,#274481,#274482,#274483,#274484,#274485,#274486,#274487,#274488,
#274489,#274490,#274491,#274492,#274493,#274494,#274495,#274496,#274497,
#274498,#274499,#274500,#274501,#274502,#274503,#274504,#274505,#274506,
#274507,#274508,#274509,#274510,#274511,#274512,#274513,#274514,#274515,
#274516,#274517,#274518,#274519,#274520,#274521,#274522,#274523,#274524,
#274525,#274526,#274527,#274528,#274529,#274530,#274531,#274532,#274533,
#274534,#274535,#274536,#274537,#274538,#274539,#274540,#274541,#274542,
#274543,#274544,#274545,#274546,#274547,#274548,#274549,#274550,#274551,
#274552,#274553,#274554,#274555,#274556,#274557,#274558,#274559,#274560,
#274561,#274562,#274563,#274564,#274565,#274566,#274567,#274568,#274569,
#274570,#274571,#274572,#274573,#274574,#274575,#274576,#274577,#274578,
#274579,#274580,#274581,#274582,#274583,#274584,#274585,#274586,#274587,
#274588,#274589,#274590,#274591,#274592,#274593,#274594,#274595,#274596,
#274597,#274598,#274599,#274600,#274601,#274602,#274603,#274604,#274605,
#274606,#274607,#274608,#274609,#274610,#274611,#274612,#274613,#274614,
#274615,#274616,#274617,#274618,#274619,#274620,#274621,#274622,#274623,
#274624,#274625,#274626,#274627,#274628,#274629,#274630,#274631,#274632,
#274633,#274634,#274635,#274636,#274637,#274638,#274639,#274640,#274641,
#274642,#274643,#274644,#274645,#274646,#274647,#274648,#274649,#274650,
#274651,#274652,#274653,#274654,#274655,#274656,#274657,#274658,#274659,
#274660,#274661,#274662,#274663,#274664,#274665,#274666,#274667,#274668,
#274669,#274670,#274671,#274672,#274673,#274674,#274675,#274676,#274677,
#274678,#274679,#274680,#274681,#274682,#274683,#274684,#274685,#274686,
#274687,#274688,#274689,#274690,#274691,#274692,#274693,#274694,#274695,
#274696,#274697,#274698,#274699,#274700,#274701,#274702,#274703,#274704,
#274705,#274706,#274707,#274708,#274709,#274710,#274711,#274712,#274713,
#274714,#274715,#274716,#274717,#274718,#274719,#274720,#274721,#274722,
#274723,#274724,#274725,#274726,#274727,#274728,#274729,#274730,#274731,
#274732,#274733,#274734,#274735,#274736,#274737,#274738,#274739,#274740,
#274741,#274742,#274743,#274744,#274745,#274746,#274747,#274748,#274749,
#274750,#274751,#274752,#274753,#274754,#274755,#274756,#274757,#274758,
#274759,#274760,#274761,#274762,#274763,#274764,#274765,#274766,#274767,
#274768,#274769,#274770,#274771,#274772,#274773,#274774,#274775,#274776,
#274777,#274778,#274779,#274780,#274781,#274782,#274783,#274784,#274785,
#274786,#274787,#274788,#274789,#274790,#274791,#274792,#274793,#274794,
#274795,#274796,#274797,#274798,#274799,#274800,#274801,#274802,#274803,
#274804,#274805,#274806,#274807,#274808,#274809,#274810,#274811,#274812,
#274813,#274814,#274815,#274816,#274817,#274818,#274819,#274820,#274821,
#274822,#274823,#274824,#274825,#274826,#274827,#274828,#274829,#274830,
#274831,#274832,#274833,#274834,#274835,#274836,#274837,#274838,#274839,
#274840,#274841,#274842,#274843,#274844,#274845,#274846,#274847,#274848,
#274849,#274850,#274851,#274852,#274853,#274854,#274855,#274856,#274857,
#274858,#274859,#274860,#274861,#274862,#274863,#274864,#274865,#274866,
#274867,#274868,#274869,#274870,#274871,#274872,#274873,#274874,#274875,
#274876,#274877,#274878,#274879,#274880,#274881,#274882,#274883,#274884,
#274885,#274886,#274887,#274888,#274889,#274890,#274891,#274892,#274893,
#274894,#274895,#274896,#274897,#274898,#274899,#274900,#274901,#274902,
#274903,#274904,#274905,#274906,#274907,#274908,#274909,#274910,#274911,
#274912,#274913,#274914,#274915,#274916,#274917,#274918,#274919,#274920,
#274921,#274922,#274923,#274924,#274925,#274926,#274927,#274928,#274929,
#274930,#274931,#274932,#274933,#274934,#274935,#274936,#274937,#274938,
#274939,#274940,#274941,#274942,#274943,#274944,#274945,#274946,#274947,
#274948,#274949,#274950,#274951,#274952,#274953,#274954,#274955,#274956,
#274957,#274958,#274959,#274960,#274961,#274962,#274963,#274964,#274965,
#274966,#274967,#274968,#274969,#274970,#274971,#274972,#274973,#274974,
#274975,#274976,#274977,#274978,#274979,#274980,#274981,#274982,#274983,
#274984,#274985,#274986,#274987,#274988,#274989,#274990,#274991,#274992,
#274993,#274994,#274995,#274996,#274997,#274998,#274999,#275000,#275001,
#275002,#275003,#275004,#275005,#275006,#275007,#275008,#275009,#275010,
#275011,#275012,#275013,#275014,#275015,#275016,#275017,#275018,#275019,
#275020,#275021,#275022,#275023,#275024,#275025,#275026,#275027,#275028,
#275029,#275030,#275031,#275032,#275033,#275034,#275035,#275036,#275037,
#275038,#275039,#275040,#275041,#275042,#275043,#275044,#275045,#275046,
#275047,#275048,#275049,#275050,#275051,#275052,#275053,#275054,#275055,
#275056,#275057,#275058,#275059,#275060,#275061,#275062,#275063,#275064,
#275065,#275066,#275067,#275068,#275069,#275070,#275071,#275072,#275073,
#275074,#275075,#275076,#275077,#275078,#275079,#275080,#275081,#275082,
#275083,#275084,#275085,#275086,#275087,#275088,#275089,#275090,#275091,
#275092,#275093,#275094,#275095,#275096,#275097,#275098,#275099,#275100,
#275101,#275102,#275103,#275104,#275105,#275106,#275107,#275108,#275109,
#275110,#275111,#275112,#275113,#275114,#275115,#275116,#275117,#275118,
#275119,#275120,#275121,#275122,#275123,#275124,#275125,#275126,#275127,
#275128,#275129,#275130,#275131,#275132,#275133,#275134,#275135,#275136,
#275137,#275138,#275139,#275140,#275141,#275142,#275143,#275144,#275145,
#275146,#275147,#275148,#275149,#275150,#275151,#275152,#275153,#275154,
#275155,#275156,#275157,#275158,#275159,#275160,#275161,#275162,#275163,
#275164,#275165,#275166,#275167,#275168,#275169,#275170,#275171,#275172,
#275173,#275174,#275175,#275176,#275177,#275178,#275179,#275180,#275181,
#275182,#275183,#275184,#275185,#275186,#275187,#275188,#275189,#275190,
#275191,#275192,#275193,#275194,#275195,#275196,#275197,#275198,#275199,
#275200,#275201,#275202,#275203,#275204,#275205,#275206,#275207,#275208,
#275209,#275210,#275211,#275212,#275213,#275214,#275215,#275216,#275217,
#275218,#275219,#275220,#275221,#275222,#275223,#275224,#275225,#275226,
#275227,#275228,#275229,#275230,#275231,#275232,#275233,#275234,#275235,
#275236,#275237,#275238,#275239,#275240,#275241,#275242,#275243,#275244,
#275245,#275246,#275247,#275248,#275249,#275250,#275251,#275252,#275253,
#275254,#275255,#275256,#275257,#275258,#275259,#275260,#275261,#275262,
#275263,#275264,#275265,#275266,#275267,#275268,#275269,#275270,#275271,
#275272,#275273,#275274,#275275,#275276,#275277,#275278,#275279,#275280,
#275281,#275282,#275283,#275284,#275285,#275286,#275287,#275288,#275289,
#275290,#275291,#275292,#275293,#275294,#275295,#275296,#275297,#275298,
#275299,#275300,#275301,#275302,#275303,#275304,#275305,#275306,#275307,
#275308,#275309,#275310,#275311,#275312,#275313,#275314,#275315,#275316,
#275317,#275318,#275319,#275320,#275321,#275322,#275323,#275324,#275325,
#275326,#275327,#275328,#275329,#275330,#275331,#275332,#275333,#275334,
#275335,#275336,#275337,#275338,#275339,#275340,#275341,#275342,#275343,
#275344,#275345,#275346,#275347,#275348,#275349,#275350,#275351,#275352,
#275353,#275354,#275355,#275356,#275357,#275358,#275359,#275360,#275361,
#275362,#275363,#275364,#275365,#275366,#275367,#275368,#275369,#275370,
#275371,#275372,#275373,#275374,#275375,#275376,#275377,#275378,#275379,
#275380,#275381,#275382,#275383,#275384,#275385,#275386,#275387,#275388,
#275389,#275390,#275391,#275392,#275393,#275394,#275395,#275396,#275397,
#275398,#275399,#275400,#275401,#275402,#275403,#275404,#275405,#275406,
#275407,#275408,#275409,#275410,#275411,#275412,#275413,#275414,#275415,
#275416,#275417,#275418,#275419,#275420,#275421,#275422,#275423,#275424,
#275425,#275426,#275427,#275428,#275429,#275430,#275431,#275432,#275433,
#275434,#275435,#275436,#275437,#275438,#275439,#275440,#275441,#275442,
#275443,#275444,#275445,#275446,#275447,#275448,#275449,#275450,#275451,
#275452,#275453,#275454,#275455,#275456,#275457,#275458,#275459,#275460,
#275461,#275462,#275463,#275464,#275465,#275466,#275467,#275468,#275469,
#275470,#275471,#275472,#275473,#275474,#275475,#275476,#275477,#275478,
#275479,#275480,#275481,#275482,#275483,#275484,#275485,#275486,#275487,
#275488,#275489,#275490,#275491,#275492,#275493,#275494,#275495,#275496,
#275497,#275498,#275499,#275500,#275501,#275502,#275503,#275504,#275505,
#275506,#275507,#275508,#275509,#275510,#275511,#275512,#275513,#275514,
#275515,#275516,#275517,#275518,#275519,#275520,#275521,#275522,#275523,
#275524,#275525,#275526,#275527,#275528,#275529,#275530,#275531,#275532,
#275533,#275534,#275535,#275536,#275537,#275538,#275539,#275540,#275541,
#275542,#275543,#275544,#275545,#275546,#275547,#275548,#275549,#275550,
#275551,#275552,#275553,#275554,#275555,#275556,#275557,#275558,#275559,
#275560,#275561,#275562,#275563,#275564,#275565,#275566,#275567,#275568,
#275569,#275570,#275571,#275572,#275573,#275574,#275575,#275576,#275577,
#275578,#275579,#275580,#275581,#275582,#275583,#275584,#275585,#275586,
#275587,#275588,#275589,#275590,#275591,#275592,#275593,#275594,#275595,
#275596,#275597,#275598,#275599,#275600,#275601,#275602,#275603,#275604,
#275605,#275606,#275607,#275608,#275609,#275610,#275611,#275612,#275613,
#275614,#275615,#275616,#275617,#275618,#275619,#275620,#275621,#275622,
#275623,#275624,#275625,#275626,#275627,#275628,#275629,#275630,#275631,
#275632,#275633,#275634,#275635,#275636,#275637,#275638,#275639,#275640,
#275641,#275642,#275643,#275644,#275645,#275646,#275647,#275648,#275649,
#275650,#275651,#275652,#275653,#275654,#275655,#275656,#275657,#275658,
#275659,#275660,#275661,#275662,#275663,#275664,#275665,#275666,#275667,
#275668,#275669,#275670,#275671,#275672,#275673,#275674,#275675,#275676,
#275677,#275678,#275679,#275680,#275681,#275682,#275683,#275684,#275685,
#275686,#275687,#275688,#275689,#275690,#275691,#275692,#275693,#275694,
#275695,#275696,#275697,#275698,#275699,#275700,#275701,#275702,#275703,
#275704,#275705,#275706,#275707,#275708,#275709,#275710,#275711,#275712,
#275713,#275714,#275715,#275716,#275717,#275718,#275719,#275720,#275721,
#275722,#275723,#275724,#275725,#275726,#275727,#275728,#275729,#275730,
#275731,#275732,#275733,#275734,#275735,#275736,#275737,#275738,#275739,
#275740,#275741),(#275742,#275743,#275744,#275745,#275746,#275747,#275748,
#275749,#275750,#275751,#275752,#275753,#275754,#275755,#275756,#275757,
#275758,#275759,#275760,#275761,#275762,#275763,#275764,#275765,#275766,
#275767,#275768,#275769,#275770,#275771,#275772,#275773,#275774,#275775,
#275776,#275777,#275778,#275779,#275780,#275781,#275782,#275783,#275784,
#275785,#275786,#275787,#275788,#275789,#275790,#275791,#275792,#275793,
#275794,#275795,#275796,#275797,#275798,#275799,#275800,#275801,#275802,
#275803,#275804,#275805,#275806,#275807,#275808,#275809,#275810,#275811,
#275812,#275813,#275814,#275815,#275816,#275817,#275818,#275819,#275820,
#275821,#275822,#275823,#275824,#275825,#275826,#275827,#275828,#275829,
#275830,#275831,#275832,#275833,#275834,#275835,#275836,#275837,#275838,
#275839,#275840,#275841,#275842,#275843,#275844,#275845,#275846,#275847,
#275848,#275849,#275850,#275851,#275852,#275853,#275854,#275855,#275856,
#275857,#275858,#275859,#275860,#275861,#275862,#275863,#275864,#275865,
#275866,#275867,#275868,#275869,#275870,#275871,#275872,#275873,#275874,
#275875,#275876,#275877,#275878,#275879,#275880,#275881,#275882,#275883,
#275884,#275885,#275886,#275887,#275888,#275889,#275890,#275891,#275892,
#275893,#275894,#275895,#275896,#275897,#275898,#275899,#275900,#275901,
#275902,#275903,#275904,#275905,#275906,#275907,#275908,#275909,#275910,
#275911,#275912,#275913,#275914,#275915,#275916,#275917,#275918,#275919,
#275920,#275921,#275922,#275923,#275924,#275925,#275926,#275927,#275928,
#275929,#275930,#275931,#275932,#275933,#275934,#275935,#275936,#275937,
#275938,#275939,#275940,#275941,#275942,#275943,#275944,#275945,#275946,
#275947,#275948,#275949,#275950,#275951,#275952,#275953,#275954,#275955,
#275956,#275957,#275958,#275959,#275960,#275961,#275962,#275963,#275964,
#275965,#275966,#275967,#275968,#275969,#275970,#275971,#275972,#275973,
#275974,#275975,#275976,#275977,#275978,#275979,#275980,#275981,#275982,
#275983,#275984,#275985,#275986,#275987,#275988,#275989,#275990,#275991,
#275992,#275993,#275994,#275995,#275996,#275997,#275998,#275999,#276000,
#276001,#276002,#276003,#276004,#276005,#276006,#276007,#276008,#276009,
#276010,#276011,#276012,#276013,#276014,#276015,#276016,#276017,#276018,
#276019,#276020,#276021,#276022,#276023,#276024,#276025,#276026,#276027,
#276028,#276029,#276030,#276031,#276032,#276033,#276034,#276035,#276036,
#276037,#276038,#276039,#276040,#276041,#276042,#276043,#276044,#276045,
#276046,#276047,#276048,#276049,#276050,#276051,#276052,#276053,#276054,
#276055,#276056,#276057,#276058,#276059,#276060,#276061,#276062,#276063,
#276064,#276065,#276066,#276067,#276068,#276069,#276070,#276071,#276072,
#276073,#276074,#276075,#276076,#276077,#276078,#276079,#276080,#276081,
#276082,#276083,#276084,#276085,#276086,#276087,#276088,#276089,#276090,
#276091,#276092,#276093,#276094,#276095,#276096,#276097,#276098,#276099,
#276100,#276101,#276102,#276103,#276104,#276105,#276106,#276107,#276108,
#276109,#276110,#276111,#276112,#276113,#276114,#276115,#276116,#276117,
#276118,#276119,#276120,#276121,#276122,#276123,#276124,#276125,#276126,
#276127,#276128,#276129,#276130,#276131,#276132,#276133,#276134,#276135,
#276136,#276137,#276138,#276139,#276140,#276141,#276142,#276143,#276144,
#276145,#276146,#276147,#276148,#276149,#276150,#276151,#276152,#276153,
#276154,#276155,#276156,#276157,#276158,#276159,#276160,#276161,#276162,
#276163,#276164,#276165,#276166,#276167,#276168,#276169,#276170,#276171,
#276172,#276173,#276174,#276175,#276176,#276177,#276178,#276179,#276180,
#276181,#276182,#276183,#276184,#276185,#276186,#276187,#276188,#276189,
#276190,#276191,#276192,#276193,#276194,#276195,#276196,#276197,#276198,
#276199,#276200,#276201,#276202,#276203,#276204,#276205,#276206,#276207,
#276208,#276209,#276210,#276211,#276212,#276213,#276214,#276215,#276216,
#276217,#276218,#276219,#276220,#276221,#276222,#276223,#276224,#276225,
#276226,#276227,#276228,#276229,#276230,#276231,#276232,#276233,#276234,
#276235,#276236,#276237,#276238,#276239,#276240,#276241,#276242,#276243,
#276244,#276245,#276246,#276247,#276248,#276249,#276250,#276251,#276252,
#276253,#276254,#276255,#276256,#276257,#276258,#276259,#276260,#276261,
#276262,#276263,#276264,#276265,#276266,#276267,#276268,#276269,#276270,
#276271,#276272,#276273,#276274,#276275,#276276,#276277,#276278,#276279,
#276280,#276281,#276282,#276283,#276284,#276285,#276286,#276287,#276288,
#276289,#276290,#276291,#276292,#276293,#276294,#276295,#276296,#276297,
#276298,#276299,#276300,#276301,#276302,#276303,#276304,#276305,#276306,
#276307,#276308,#276309,#276310,#276311,#276312,#276313,#276314,#276315,
#276316,#276317,#276318,#276319,#276320,#276321,#276322,#276323,#276324,
#276325,#276326,#276327,#276328,#276329,#276330,#276331,#276332,#276333,
#276334,#276335,#276336,#276337,#276338,#276339,#276340,#276341,#276342,
#276343,#276344,#276345,#276346,#276347,#276348,#276349,#276350,#276351,
#276352,#276353,#276354,#276355,#276356,#276357,#276358,#276359,#276360,
#276361,#276362,#276363,#276364,#276365,#276366,#276367,#276368,#276369,
#276370,#276371,#276372,#276373,#276374,#276375,#276376,#276377,#276378,
#276379,#276380,#276381,#276382,#276383,#276384,#276385,#276386,#276387,
#276388,#276389,#276390,#276391,#276392,#276393,#276394,#276395,#276396,
#276397,#276398,#276399,#276400,#276401,#276402,#276403,#276404,#276405,
#276406,#276407,#276408,#276409,#276410,#276411,#276412,#276413,#276414,
#276415,#276416,#276417,#276418,#276419,#276420,#276421,#276422,#276423,
#276424,#276425,#276426,#276427,#276428,#276429,#276430,#276431,#276432,
#276433,#276434,#276435,#276436,#276437,#276438,#276439,#276440,#276441,
#276442,#276443,#276444,#276445,#276446,#276447,#276448,#276449,#276450,
#276451,#276452,#276453,#276454,#276455,#276456,#276457,#276458,#276459,
#276460,#276461,#276462,#276463,#276464,#276465,#276466,#276467,#276468,
#276469,#276470,#276471,#276472,#276473,#276474,#276475,#276476,#276477,
#276478,#276479,#276480,#276481,#276482,#276483,#276484,#276485,#276486,
#276487,#276488,#276489,#276490,#276491,#276492,#276493,#276494,#276495,
#276496,#276497,#276498,#276499,#276500,#276501,#276502,#276503,#276504,
#276505,#276506,#276507,#276508,#276509,#276510,#276511,#276512,#276513,
#276514,#276515,#276516,#276517,#276518,#276519,#276520,#276521,#276522,
#276523,#276524,#276525,#276526,#276527,#276528,#276529,#276530,#276531,
#276532,#276533,#276534,#276535,#276536,#276537,#276538,#276539,#276540,
#276541,#276542,#276543,#276544,#276545,#276546,#276547,#276548,#276549,
#276550,#276551,#276552,#276553,#276554,#276555,#276556,#276557,#276558,
#276559,#276560,#276561,#276562,#276563,#276564,#276565,#276566,#276567,
#276568,#276569,#276570,#276571,#276572,#276573,#276574,#276575,#276576,
#276577,#276578,#276579,#276580,#276581,#276582,#276583,#276584,#276585,
#276586,#276587,#276588,#276589,#276590,#276591,#276592,#276593,#276594,
#276595,#276596,#276597,#276598,#276599,#276600,#276601,#276602,#276603,
#276604,#276605,#276606,#276607,#276608,#276609,#276610,#276611,#276612,
#276613,#276614,#276615,#276616,#276617,#276618,#276619,#276620,#276621,
#276622,#276623,#276624,#276625,#276626,#276627,#276628,#276629,#276630,
#276631,#276632,#276633,#276634,#276635,#276636,#276637,#276638,#276639,
#276640,#276641,#276642,#276643,#276644,#276645,#276646,#276647,#276648,
#276649,#276650,#276651,#276652,#276653,#276654,#276655,#276656,#276657,
#276658,#276659,#276660,#276661,#276662,#276663,#276664,#276665,#276666,
#276667,#276668,#276669,#276670,#276671,#276672,#276673,#276674,#276675,
#276676,#276677,#276678,#276679,#276680,#276681,#276682,#276683,#276684,
#276685,#276686,#276687,#276688,#276689,#276690,#276691,#276692,#276693,
#276694,#276695,#276696,#276697,#276698,#276699,#276700,#276701,#276702,
#276703,#276704,#276705,#276706,#276707,#276708,#276709,#276710,#276711,
#276712,#276713,#276714,#276715,#276716,#276717,#276718,#276719,#276720,
#276721,#276722,#276723,#276724,#276725,#276726,#276727,#276728,#276729,
#276730,#276731,#276732,#276733,#276734,#276735,#276736,#276737,#276738,
#276739,#276740,#276741,#276742,#276743,#276744,#276745,#276746,#276747,
#276748,#276749,#276750,#276751,#276752,#276753,#276754,#276755,#276756,
#276757,#276758,#276759,#276760,#276761,#276762,#276763,#276764,#276765,
#276766,#276767,#276768,#276769,#276770,#276771,#276772,#276773,#276774,
#276775,#276776,#276777,#276778,#276779,#276780,#276781,#276782,#276783,
#276784,#276785,#276786,#276787,#276788,#276789,#276790,#276791,#276792,
#276793,#276794,#276795,#276796,#276797,#276798,#276799,#276800,#276801,
#276802,#276803,#276804,#276805,#276806,#276807,#276808,#276809,#276810,
#276811,#276812,#276813,#276814,#276815,#276816,#276817,#276818,#276819,
#276820,#276821,#276822,#276823,#276824,#276825,#276826,#276827,#276828,
#276829,#276830,#276831,#276832,#276833,#276834,#276835,#276836,#276837,
#276838,#276839,#276840,#276841,#276842,#276843,#276844,#276845,#276846,
#276847,#276848,#276849,#276850,#276851,#276852,#276853,#276854,#276855,
#276856,#276857,#276858,#276859,#276860,#276861,#276862,#276863,#276864,
#276865,#276866,#276867,#276868,#276869,#276870,#276871,#276872,#276873,
#276874,#276875,#276876,#276877,#276878,#276879,#276880,#276881,#276882,
#276883,#276884,#276885,#276886,#276887,#276888,#276889,#276890,#276891,
#276892,#276893,#276894,#276895,#276896,#276897,#276898,#276899,#276900,
#276901,#276902,#276903,#276904,#276905,#276906,#276907,#276908,#276909,
#276910,#276911,#276912,#276913,#276914,#276915,#276916,#276917,#276918,
#276919,#276920,#276921,#276922,#276923,#276924,#276925,#276926,#276927,
#276928,#276929,#276930,#276931,#276932,#276933,#276934,#276935,#276936,
#276937,#276938,#276939,#276940,#276941,#276942,#276943,#276944,#276945,
#276946,#276947,#276948,#276949,#276950,#276951,#276952,#276953,#276954,
#276955,#276956,#276957,#276958,#276959,#276960,#276961,#276962,#276963,
#276964,#276965,#276966,#276967,#276968,#276969,#276970,#276971,#276972,
#276973,#276974,#276975,#276976,#276977,#276978,#276979,#276980,#276981,
#276982,#276983,#276984,#276985,#276986,#276987,#276988,#276989,#276990,
#276991,#276992,#276993,#276994,#276995,#276996,#276997,#276998,#276999,
#277000,#277001,#277002,#277003,#277004,#277005,#277006,#277007,#277008,
#277009,#277010,#277011,#277012,#277013,#277014,#277015,#277016,#277017,
#277018,#277019,#277020,#277021,#277022,#277023,#277024,#277025,#277026,
#277027,#277028,#277029,#277030,#277031,#277032,#277033,#277034,#277035,
#277036,#277037,#277038,#277039,#277040,#277041,#277042,#277043,#277044,
#277045,#277046,#277047,#277048,#277049,#277050,#277051,#277052,#277053,
#277054,#277055,#277056,#277057,#277058,#277059,#277060,#277061,#277062,
#277063,#277064,#277065,#277066,#277067,#277068,#277069,#277070,#277071,
#277072,#277073,#277074,#277075,#277076,#277077,#277078,#277079,#277080,
#277081,#277082,#277083,#277084,#277085,#277086,#277087,#277088,#277089,
#277090,#277091,#277092,#277093,#277094,#277095,#277096,#277097,#277098,
#277099,#277100,#277101,#277102,#277103,#277104,#277105,#277106,#277107,
#277108,#277109,#277110,#277111,#277112,#277113,#277114,#277115,#277116,
#277117,#277118,#277119,#277120,#277121,#277122,#277123,#277124,#277125,
#277126,#277127,#277128,#277129,#277130,#277131,#277132,#277133,#277134,
#277135,#277136,#277137,#277138,#277139,#277140,#277141,#277142,#277143,
#277144,#277145,#277146,#277147,#277148,#277149,#277150,#277151,#277152,
#277153,#277154,#277155,#277156,#277157,#277158,#277159,#277160,#277161,
#277162,#277163,#277164,#277165,#277166,#277167,#277168,#277169,#277170,
#277171,#277172,#277173,#277174,#277175,#277176,#277177,#277178,#277179,
#277180,#277181,#277182,#277183,#277184,#277185,#277186,#277187,#277188,
#277189,#277190,#277191,#277192,#277193,#277194,#277195,#277196,#277197,
#277198,#277199,#277200,#277201,#277202,#277203,#277204,#277205,#277206,
#277207,#277208,#277209,#277210,#277211,#277212,#277213,#277214,#277215,
#277216,#277217,#277218,#277219,#277220,#277221,#277222,#277223,#277224,
#277225,#277226,#277227,#277228,#277229,#277230,#277231,#277232,#277233,
#277234,#277235,#277236,#277237,#277238,#277239,#277240,#277241,#277242,
#277243,#277244,#277245,#277246,#277247,#277248,#277249,#277250,#277251,
#277252,#277253,#277254,#277255,#277256,#277257,#277258,#277259,#277260,
#277261,#277262,#277263,#277264,#277265,#277266,#277267,#277268,#277269,
#277270,#277271,#277272,#277273,#277274,#277275,#277276,#277277,#277278,
#277279,#277280,#277281,#277282,#277283,#277284,#277285,#277286,#277287,
#277288,#277289,#277290,#277291,#277292,#277293,#277294,#277295,#277296,
#277297,#277298,#277299,#277300,#277301,#277302,#277303,#277304,#277305,
#277306,#277307,#277308,#277309,#277310,#277311,#277312,#277313,#277314,
#277315,#277316,#277317,#277318,#277319,#277320,#277321,#277322,#277323,
#277324,#277325,#277326,#277327,#277328,#277329,#277330,#277331,#277332,
#277333,#277334,#277335,#277336,#277337,#277338,#277339,#277340,#277341,
#277342,#277343,#277344,#277345,#277346,#277347,#277348,#277349,#277350,
#277351,#277352,#277353,#277354,#277355,#277356,#277357,#277358,#277359,
#277360,#277361,#277362,#277363,#277364,#277365,#277366,#277367,#277368,
#277369,#277370,#277371,#277372,#277373,#277374,#277375,#277376,#277377,
#277378,#277379,#277380,#277381,#277382,#277383,#277384,#277385,#277386,
#277387,#277388,#277389,#277390,#277391,#277392,#277393,#277394,#277395,
#277396,#277397,#277398,#277399,#277400,#277401,#277402,#277403,#277404,
#277405,#277406,#277407,#277408,#277409,#277410,#277411,#277412,#277413,
#277414,#277415,#277416,#277417,#277418,#277419,#277420,#277421,#277422,
#277423,#277424,#277425,#277426,#277427,#277428,#277429,#277430,#277431,
#277432,#277433,#277434,#277435,#277436),(#277437,#277438,#277439,#277440,
#277441,#277442,#277443,#277444,#277445,#277446,#277447,#277448,#277449,
#277450,#277451,#277452,#277453,#277454,#277455,#277456,#277457,#277458,
#277459,#277460,#277461,#277462,#277463,#277464,#277465,#277466,#277467,
#277468,#277469,#277470,#277471,#277472,#277473,#277474,#277475,#277476,
#277477,#277478,#277479,#277480,#277481,#277482,#277483,#277484,#277485,
#277486,#277487,#277488,#277489,#277490,#277491,#277492,#277493,#277494,
#277495,#277496,#277497,#277498,#277499,#277500,#277501,#277502,#277503,
#277504,#277505,#277506,#277507,#277508,#277509,#277510,#277511,#277512,
#277513,#277514,#277515,#277516,#277517,#277518,#277519,#277520,#277521,
#277522,#277523,#277524,#277525,#277526,#277527,#277528,#277529,#277530,
#277531,#277532,#277533,#277534,#277535,#277536,#277537,#277538,#277539,
#277540,#277541,#277542,#277543,#277544,#277545,#277546,#277547,#277548,
#277549,#277550,#277551,#277552,#277553,#277554,#277555,#277556,#277557,
#277558,#277559,#277560,#277561,#277562,#277563,#277564,#277565,#277566,
#277567,#277568,#277569,#277570,#277571,#277572,#277573,#277574,#277575,
#277576,#277577,#277578,#277579,#277580,#277581,#277582,#277583,#277584,
#277585,#277586,#277587,#277588,#277589,#277590,#277591,#277592,#277593,
#277594,#277595,#277596,#277597,#277598,#277599,#277600,#277601,#277602,
#277603,#277604,#277605,#277606,#277607,#277608,#277609,#277610,#277611,
#277612,#277613,#277614,#277615,#277616,#277617,#277618,#277619,#277620,
#277621,#277622,#277623,#277624,#277625,#277626,#277627,#277628,#277629,
#277630,#277631,#277632,#277633,#277634,#277635,#277636,#277637,#277638,
#277639,#277640,#277641,#277642,#277643,#277644,#277645,#277646,#277647,
#277648,#277649,#277650,#277651,#277652,#277653,#277654,#277655,#277656,
#277657,#277658,#277659,#277660,#277661,#277662,#277663,#277664,#277665,
#277666,#277667,#277668,#277669,#277670,#277671,#277672,#277673,#277674,
#277675,#277676,#277677,#277678,#277679,#277680,#277681,#277682,#277683,
#277684,#277685,#277686,#277687,#277688,#277689,#277690,#277691,#277692,
#277693,#277694,#277695,#277696,#277697,#277698,#277699,#277700,#277701,
#277702,#277703,#277704,#277705,#277706,#277707,#277708,#277709,#277710,
#277711,#277712,#277713,#277714,#277715,#277716,#277717,#277718,#277719,
#277720,#277721,#277722,#277723,#277724,#277725,#277726,#277727,#277728,
#277729,#277730,#277731,#277732,#277733,#277734,#277735,#277736,#277737,
#277738,#277739,#277740,#277741,#277742,#277743,#277744,#277745,#277746,
#277747,#277748,#277749,#277750,#277751,#277752,#277753,#277754,#277755,
#277756,#277757,#277758,#277759,#277760,#277761,#277762,#277763,#277764,
#277765,#277766,#277767,#277768,#277769,#277770,#277771,#277772,#277773,
#277774,#277775,#277776,#277777,#277778,#277779,#277780,#277781,#277782,
#277783,#277784,#277785,#277786,#277787,#277788,#277789,#277790,#277791,
#277792,#277793,#277794,#277795,#277796,#277797,#277798,#277799,#277800,
#277801,#277802,#277803,#277804,#277805,#277806,#277807,#277808,#277809,
#277810,#277811,#277812,#277813,#277814,#277815,#277816,#277817,#277818,
#277819,#277820,#277821,#277822,#277823,#277824,#277825,#277826,#277827,
#277828,#277829,#277830,#277831,#277832,#277833,#277834,#277835,#277836,
#277837,#277838,#277839,#277840,#277841,#277842,#277843,#277844,#277845,
#277846,#277847,#277848,#277849,#277850,#277851,#277852,#277853,#277854,
#277855,#277856,#277857,#277858,#277859,#277860,#277861,#277862,#277863,
#277864,#277865,#277866,#277867,#277868,#277869,#277870,#277871,#277872,
#277873,#277874,#277875,#277876,#277877,#277878,#277879,#277880,#277881,
#277882,#277883,#277884,#277885,#277886,#277887,#277888,#277889,#277890,
#277891,#277892,#277893,#277894,#277895,#277896,#277897,#277898,#277899,
#277900,#277901,#277902,#277903,#277904,#277905,#277906,#277907,#277908,
#277909,#277910,#277911,#277912,#277913,#277914,#277915,#277916,#277917,
#277918,#277919,#277920,#277921,#277922,#277923,#277924,#277925,#277926,
#277927,#277928,#277929,#277930,#277931,#277932,#277933,#277934,#277935,
#277936,#277937,#277938,#277939,#277940,#277941,#277942,#277943,#277944,
#277945,#277946,#277947,#277948,#277949,#277950,#277951,#277952,#277953,
#277954,#277955,#277956,#277957,#277958,#277959,#277960,#277961,#277962,
#277963,#277964,#277965,#277966,#277967,#277968,#277969,#277970,#277971,
#277972,#277973,#277974,#277975,#277976,#277977,#277978,#277979,#277980,
#277981,#277982,#277983,#277984,#277985,#277986,#277987,#277988,#277989,
#277990,#277991,#277992,#277993,#277994,#277995,#277996,#277997,#277998,
#277999,#278000,#278001,#278002,#278003,#278004,#278005,#278006,#278007,
#278008,#278009,#278010,#278011,#278012,#278013,#278014,#278015,#278016,
#278017,#278018,#278019,#278020,#278021,#278022,#278023,#278024,#278025,
#278026,#278027,#278028,#278029,#278030,#278031,#278032,#278033,#278034,
#278035,#278036,#278037,#278038,#278039,#278040,#278041,#278042,#278043,
#278044,#278045,#278046,#278047,#278048,#278049,#278050,#278051,#278052,
#278053,#278054,#278055,#278056,#278057,#278058,#278059,#278060,#278061,
#278062,#278063,#278064,#278065,#278066,#278067,#278068,#278069,#278070,
#278071,#278072,#278073,#278074,#278075,#278076,#278077,#278078,#278079,
#278080,#278081,#278082,#278083,#278084,#278085,#278086,#278087,#278088,
#278089,#278090,#278091,#278092,#278093,#278094,#278095,#278096,#278097,
#278098,#278099,#278100,#278101,#278102,#278103,#278104,#278105,#278106,
#278107,#278108,#278109,#278110,#278111,#278112,#278113,#278114,#278115,
#278116,#278117,#278118,#278119,#278120,#278121,#278122,#278123,#278124,
#278125,#278126,#278127,#278128,#278129,#278130,#278131,#278132,#278133,
#278134,#278135,#278136,#278137,#278138,#278139,#278140,#278141,#278142,
#278143,#278144,#278145,#278146,#278147,#278148,#278149,#278150,#278151,
#278152,#278153,#278154,#278155,#278156,#278157,#278158,#278159,#278160,
#278161,#278162,#278163,#278164,#278165,#278166,#278167,#278168,#278169,
#278170,#278171,#278172,#278173,#278174,#278175,#278176,#278177,#278178,
#278179,#278180,#278181,#278182,#278183,#278184,#278185,#278186,#278187,
#278188,#278189,#278190,#278191,#278192,#278193,#278194,#278195,#278196,
#278197,#278198,#278199,#278200,#278201,#278202,#278203,#278204,#278205,
#278206,#278207,#278208,#278209,#278210,#278211,#278212,#278213,#278214,
#278215,#278216,#278217,#278218,#278219,#278220,#278221,#278222,#278223,
#278224,#278225,#278226,#278227,#278228,#278229,#278230,#278231,#278232,
#278233,#278234,#278235,#278236,#278237,#278238,#278239,#278240,#278241,
#278242,#278243,#278244,#278245,#278246,#278247,#278248,#278249,#278250,
#278251,#278252,#278253,#278254,#278255,#278256,#278257,#278258,#278259,
#278260,#278261,#278262,#278263,#278264,#278265,#278266,#278267,#278268,
#278269,#278270,#278271,#278272,#278273,#278274,#278275,#278276,#278277,
#278278,#278279,#278280,#278281,#278282,#278283,#278284,#278285,#278286,
#278287,#278288,#278289,#278290,#278291,#278292,#278293,#278294,#278295,
#278296,#278297,#278298,#278299,#278300,#278301,#278302,#278303,#278304,
#278305,#278306,#278307,#278308,#278309,#278310,#278311,#278312,#278313,
#278314,#278315,#278316,#278317,#278318,#278319,#278320,#278321,#278322,
#278323,#278324,#278325,#278326,#278327,#278328,#278329,#278330,#278331,
#278332,#278333,#278334,#278335,#278336,#278337,#278338,#278339,#278340,
#278341,#278342,#278343,#278344,#278345,#278346,#278347,#278348,#278349,
#278350,#278351,#278352,#278353,#278354,#278355,#278356,#278357,#278358,
#278359,#278360,#278361,#278362,#278363,#278364,#278365,#278366,#278367,
#278368,#278369,#278370,#278371,#278372,#278373,#278374,#278375,#278376,
#278377,#278378,#278379,#278380,#278381,#278382,#278383,#278384,#278385,
#278386,#278387,#278388,#278389,#278390,#278391,#278392,#278393,#278394,
#278395,#278396,#278397,#278398,#278399,#278400,#278401,#278402,#278403,
#278404,#278405,#278406,#278407,#278408,#278409,#278410,#278411,#278412,
#278413,#278414,#278415,#278416,#278417,#278418,#278419,#278420,#278421,
#278422,#278423,#278424,#278425,#278426,#278427,#278428,#278429,#278430,
#278431,#278432,#278433,#278434,#278435,#278436,#278437,#278438,#278439,
#278440,#278441,#278442,#278443,#278444,#278445,#278446,#278447,#278448,
#278449,#278450,#278451,#278452,#278453,#278454,#278455,#278456,#278457,
#278458,#278459,#278460,#278461,#278462,#278463,#278464,#278465,#278466,
#278467,#278468,#278469,#278470,#278471,#278472,#278473,#278474,#278475,
#278476,#278477,#278478,#278479,#278480,#278481,#278482,#278483,#278484,
#278485,#278486,#278487,#278488,#278489,#278490,#278491,#278492,#278493,
#278494,#278495,#278496,#278497,#278498,#278499,#278500,#278501,#278502,
#278503,#278504,#278505,#278506,#278507,#278508,#278509,#278510,#278511,
#278512,#278513,#278514,#278515,#278516,#278517,#278518,#278519,#278520,
#278521,#278522,#278523,#278524,#278525,#278526,#278527,#278528,#278529,
#278530,#278531,#278532,#278533,#278534,#278535,#278536,#278537,#278538,
#278539,#278540,#278541,#278542,#278543,#278544,#278545,#278546,#278547,
#278548,#278549,#278550,#278551,#278552,#278553,#278554,#278555,#278556,
#278557,#278558,#278559,#278560,#278561,#278562,#278563,#278564,#278565,
#278566,#278567,#278568,#278569,#278570,#278571,#278572,#278573,#278574,
#278575,#278576,#278577,#278578,#278579,#278580,#278581,#278582,#278583,
#278584,#278585,#278586,#278587,#278588,#278589,#278590,#278591,#278592,
#278593,#278594,#278595,#278596,#278597,#278598,#278599,#278600,#278601,
#278602,#278603,#278604,#278605,#278606,#278607,#278608,#278609,#278610,
#278611,#278612,#278613,#278614,#278615,#278616,#278617,#278618,#278619,
#278620,#278621,#278622,#278623,#278624,#278625,#278626,#278627,#278628,
#278629,#278630,#278631,#278632,#278633,#278634,#278635,#278636,#278637,
#278638,#278639,#278640,#278641,#278642,#278643,#278644,#278645,#278646,
#278647,#278648,#278649,#278650,#278651,#278652,#278653,#278654,#278655,
#278656,#278657,#278658,#278659,#278660,#278661,#278662,#278663,#278664,
#278665,#278666,#278667,#278668,#278669,#278670,#278671,#278672,#278673,
#278674,#278675,#278676,#278677,#278678,#278679,#278680,#278681,#278682,
#278683,#278684,#278685,#278686,#278687,#278688,#278689,#278690,#278691,
#278692,#278693,#278694,#278695,#278696,#278697,#278698,#278699,#278700,
#278701,#278702,#278703,#278704,#278705,#278706,#278707,#278708,#278709,
#278710,#278711,#278712,#278713,#278714,#278715,#278716,#278717,#278718,
#278719,#278720,#278721,#278722,#278723,#278724,#278725,#278726,#278727,
#278728,#278729,#278730,#278731,#278732,#278733,#278734,#278735,#278736,
#278737,#278738,#278739,#278740,#278741,#278742,#278743,#278744,#278745,
#278746,#278747,#278748,#278749,#278750,#278751,#278752,#278753,#278754,
#278755,#278756,#278757,#278758,#278759,#278760,#278761,#278762,#278763,
#278764,#278765,#278766,#278767,#278768,#278769,#278770,#278771,#278772,
#278773,#278774,#278775,#278776,#278777,#278778,#278779,#278780,#278781,
#278782,#278783,#278784,#278785,#278786,#278787,#278788,#278789,#278790,
#278791,#278792,#278793,#278794,#278795,#278796,#278797,#278798,#278799,
#278800,#278801,#278802,#278803,#278804,#278805,#278806,#278807,#278808,
#278809,#278810,#278811,#278812,#278813,#278814,#278815,#278816,#278817,
#278818,#278819,#278820,#278821,#278822,#278823,#278824,#278825,#278826,
#278827,#278828,#278829,#278830,#278831,#278832,#278833,#278834,#278835,
#278836,#278837,#278838,#278839,#278840,#278841,#278842,#278843,#278844,
#278845,#278846,#278847,#278848,#278849,#278850,#278851,#278852,#278853,
#278854,#278855,#278856,#278857,#278858,#278859,#278860,#278861,#278862,
#278863,#278864,#278865,#278866,#278867,#278868,#278869,#278870,#278871,
#278872,#278873,#278874,#278875,#278876,#278877,#278878,#278879,#278880,
#278881,#278882,#278883,#278884,#278885,#278886,#278887,#278888,#278889,
#278890,#278891,#278892,#278893,#278894,#278895,#278896,#278897,#278898,
#278899,#278900,#278901,#278902,#278903,#278904,#278905,#278906,#278907,
#278908,#278909,#278910,#278911,#278912,#278913,#278914,#278915,#278916,
#278917,#278918,#278919,#278920,#278921,#278922,#278923,#278924,#278925,
#278926,#278927,#278928,#278929,#278930,#278931,#278932,#278933,#278934,
#278935,#278936,#278937,#278938,#278939,#278940,#278941,#278942,#278943,
#278944,#278945,#278946,#278947,#278948,#278949,#278950,#278951,#278952,
#278953,#278954,#278955,#278956,#278957,#278958,#278959,#278960,#278961,
#278962,#278963,#278964,#278965,#278966,#278967,#278968,#278969,#278970,
#278971,#278972,#278973,#278974,#278975,#278976,#278977,#278978,#278979,
#278980,#278981,#278982,#278983,#278984,#278985,#278986,#278987,#278988,
#278989,#278990,#278991,#278992,#278993,#278994,#278995,#278996,#278997,
#278998,#278999,#279000,#279001,#279002,#279003,#279004,#279005,#279006,
#279007,#279008,#279009,#279010,#279011,#279012,#279013,#279014,#279015,
#279016,#279017,#279018,#279019,#279020,#279021,#279022,#279023,#279024,
#279025,#279026,#279027,#279028,#279029,#279030,#279031,#279032,#279033,
#279034,#279035,#279036,#279037,#279038,#279039,#279040,#279041,#279042,
#279043,#279044,#279045,#279046,#279047,#279048,#279049,#279050,#279051,
#279052,#279053,#279054,#279055,#279056,#279057,#279058,#279059,#279060,
#279061,#279062,#279063,#279064,#279065,#279066,#279067,#279068,#279069,
#279070,#279071,#279072,#279073,#279074,#279075,#279076,#279077,#279078,
#279079,#279080,#279081,#279082,#279083,#279084,#279085,#279086,#279087,
#279088,#279089,#279090,#279091,#279092,#279093,#279094,#279095,#279096,
#279097,#279098,#279099,#279100,#279101,#279102,#279103,#279104,#279105,
#279106,#279107,#279108,#279109,#279110,#279111,#279112,#279113,#279114,
#279115,#279116,#279117,#279118,#279119,#279120,#279121,#279122,#279123,
#279124,#279125,#279126,#279127,#279128,#279129,#279130,#279131)),
 .UNSPECIFIED.,.F.,.F.,.F.,(4,4),(4,1,1,1,1,1,1,1,1,1,1,1,1,1,1,1,1,1,1,
1,1,1,1,1,1,1,1,1,1,1,1,1,1,1,1,1,1,1,1,1,1,1,1,1,1,1,1,1,1,1,1,1,1,1,1,
1,1,1,1,1,1,1,1,1,1,1,1,1,1,1,1,1,1,1,1,1,1,1,1,1,1,1,1,1,1,1,1,1,1,1,1,
1,1,1,1,1,1,1,1,1,1,1,1,1,1,1,1,1,1,1,1,1,1,1,1,1,1,1,1,1,1,1,1,1,1,1,1,
1,1,1,1,1,1,1,1,1,1,1,1,1,1,1,1,1,1,1,1,1,1,1,1,1,1,1,1,1,1,1,1,1,1,1,1,
1,1,1,1,1,1,1,1,1,1,1,1,1,1,1,1,1,1,1,1,1,1,1,1,1,1,1,1,1,1,1,1,1,1,1,1,
1,1,1,1,1,1,1,1,1,1,1,1,1,1,1,1,1,1,1,1,1,1,1,1,1,1,1,1,1,1,1,1,1,1,1,1,
1,1,1,1,1,1,1,1,1,1,1,1,1,1,1,1,1,1,1,1,1,1,1,1,1,1,1,1,1,1,1,1,1,1,1,1,
1,1,1,1,1,1,1,1,1,1,1,1,1,1,1,1,1,1,1,1,1,1,1,1,1,1,1,1,1,1,1,1,1,1,1,1,
1,1,1,1,1,1,1,1,1,1,1,1,1,1,1,1,1,1,1,1,1,1,1,1,1,1,1,1,1,1,1,1,1,1,1,1,
1,1,1,1,1,1,1,1,1,1,1,1,1,1,1,1,1,1,1,1,1,1,1,1,1,1,1,1,1,1,1,1,1,1,1,1,
1,1,1,1,1,1,1,1,1,1,1,1,1,1,1,1,1,1,1,1,1,1,1,1,1,1,1,1,1,1,1,1,1,1,1,1,
1,1,1,1,1,1,1,1,1,1,1,1,1,1,1,1,1,1,1,1,1,1,1,1,1,1,1,1,1,1,1,1,1,1,1,1,
1,1,1,1,1,1,1,1,1,1,1,1,1,1,1,1,1,1,1,1,1,1,1,1,1,1,1,1,1,1,1,1,1,1,1,1,
1,1,1,1,1,1,1,1,1,1,1,1,1,1,1,1,1,1,1,1,1,1,1,1,1,1,1,1,1,1,1,1,1,1,1,1,
1,1,1,1,1,1,1,1,1,1,1,1,1,1,1,1,1,1,1,1,1,1,1,1,1,1,1,1,1,1,1,1,1,1,1,1,
1,1,1,1,1,1,1,1,1,1,1,1,1,1,1,1,1,1,1,1,1,1,1,1,1,1,1,1,1,1,1,1,1,1,1,1,
1,1,1,1,1,1,1,1,1,1,1,1,1,1,1,1,1,1,1,1,1,1,1,1,1,1,1,1,1,1,1,1,1,1,1,1,
1,1,1,1,1,1,1,1,1,1,1,1,1,1,1,1,1,1,1,1,1,1,1,1,1,1,1,1,1,1,1,1,1,1,1,1,
1,1,1,1,1,1,1,1,1,1,1,1,1,1,1,1,1,1,1,1,1,1,1,1,1,1,1,1,1,1,1,1,1,1,1,1,
1,1,1,1,1,1,1,1,1,1,1,1,1,1,1,1,1,1,1,1,1,1,1,1,1,1,1,1,1,1,1,1,1,1,1,1,
1,1,1,1,1,1,1,1,1,1,1,1,1,1,1,1,1,1,1,1,1,1,1,1,1,1,1,1,1,1,1,1,1,1,1,1,
1,1,1,1,1,1,1,1,1,1,1,1,1,1,1,1,1,1,1,1,1,1,1,1,1,1,1,1,1,1,1,1,1,1,1,1,
1,1,1,1,1,1,1,1,1,1,1,1,1,1,1,1,1,1,1,1,1,1,1,1,1,1,1,1,1,1,1,1,1,1,1,1,
1,1,1,1,1,1,1,1,1,1,1,1,1,1,1,1,1,1,1,1,1,1,1,1,1,1,1,1,1,1,1,1,1,1,1,1,
1,1,1,1,1,1,1,1,1,1,1,1,1,1,1,1,1,1,1,1,1,1,1,1,1,1,1,1,1,1,1,1,1,1,1,1,
1,1,1,1,1,1,1,1,1,1,1,1,1,1,1,1,1,1,1,1,1,1,1,1,1,1,1,1,1,1,1,1,1,1,1,1,
1,1,1,1,1,1,1,1,1,1,1,1,1,1,1,1,1,1,1,1,1,1,1,1,1,1,1,1,1,1,1,1,1,1,1,1,
1,1,1,1,1,1,1,1,1,1,1,1,1,1,1,1,1,1,1,1,1,1,1,1,1,1,1,1,1,1,1,1,1,1,1,1,
1,1,1,1,1,1,1,1,1,1,1,1,1,1,1,1,1,1,1,1,1,1,1,1,1,1,1,1,1,1,1,1,1,1,1,1,
1,1,1,1,1,1,1,1,1,1,1,1,1,1,1,1,1,1,1,1,1,1,1,1,1,1,1,1,1,1,1,1,1,1,1,1,
1,1,1,1,1,1,1,1,1,1,1,1,1,1,1,1,1,1,1,1,1,1,1,1,1,1,1,1,1,1,1,1,1,1,1,1,
1,1,1,1,1,1,1,1,1,1,1,1,1,1,1,1,1,1,1,1,1,1,1,1,1,1,1,1,1,1,1,1,1,1,1,1,
1,1,1,1,1,1,1,1,1,1,1,1,1,1,1,1,1,1,1,1,1,1,1,1,1,1,1,1,1,1,1,1,1,1,1,1,
1,1,1,1,1,1,1,1,1,1,1,1,1,1,1,1,1,1,1,1,1,1,1,1,1,1,1,1,1,1,1,1,1,1,1,1,
1,1,1,1,1,1,1,1,1,1,1,1,1,1,1,1,1,1,1,1,1,1,1,1,1,1,1,1,1,1,1,1,1,1,1,1,
1,1,1,1,1,1,1,1,1,1,1,1,1,1,1,1,1,1,1,1,1,1,1,1,1,1,1,1,1,1,1,1,1,1,1,1,
1,1,1,1,1,1,1,1,1,1,1,1,1,1,1,1,1,1,1,1,1,1,1,1,1,1,1,1,1,1,1,1,1,1,1,1,
1,1,1,1,1,1,1,1,1,1,1,1,1,1,1,1,1,1,1,1,1,1,1,1,1,1,1,1,1,1,1,1,1,1,1,1,
1,1,1,1,1,1,1,1,1,1,1,1,1,1,1,1,1,1,1,1,1,1,1,1,1,1,1,1,1,1,1,1,1,1,1,1,
1,1,1,1,1,1,1,1,1,1,1,1,1,1,1,1,1,1,1,1,1,1,1,1,1,1,1,1,1,1,1,1,1,1,1,1,
1,1,1,1,1,1,1,1,1,1,1,1,1,1,1,1,1,1,1,1,1,1,1,1,1,1,1,1,1,1,1,1,1,1,1,1,
1,1,1,1,1,1,1,1,1,1,1,1,1,1,1,1,1,1,1,1,1,1,1,1,1,1,1,1,1,1,1,1,1,1,1,1,
1,1,1,1,1,1,1,1,1,1,1,1,1,1,1,1,1,1,1,1,1,1,1,1,1,1,1,1,1,1,1,1,1,1,1,1,
1,1,1,1,1,1,1,1,1,1,1,1,1,1,1,1,1,1,1,1,1,1,1,1,1,1,1,1,1,1,1,1,1,1,1,1,
1,1,1,1,1,1,1,1,1,1,1,1,1,1,1,1,1,1,1,1,1,1,1,1,1,1,1,1,1,1,1,1,1,1,1,1,
1,1,1,1,1,1,1,1,1,1,1,1,1,1,1,1,1,1,1,1,1,1,1,1,1,1,1,1,1,1,1,1,1,1,1,1,
1,1,1,1,1,1,1,1,1,1,1,1,1,1,1,1,1,4),(-0.000423095957202541,0.115881565465356),
(11.6153146011728,12.1152895244478,12.6151575298078,13.614893540528,14.6146295512481,
15.6143655619682,16.6141015726884,17.6138375834085,18.6135735941286,19.6133096048488,
20.6130456155689,21.612781626289,22.6125176370092,23.6122536477293,24.6119896584494,
25.6117256691696,26.6114616798897,27.6111976906098,28.6109337013299,29.6106697120501,
30.6104057227702,31.6101417334903,32.6098777442105,33.6096137549306,34.6093497656507,
35.6090857763709,36.608821787091,37.6085577978111,38.6082938085313,39.6080298192514,
40.6077658299715,41.6075018406916,42.6072378514118,43.6069738621319,44.606709872852,
45.6064458835722,46.6061818942923,47.6059179050124,48.6056539157326,49.6053899264527,
50.6051259371728,51.604861947893,52.6045979586131,53.6043339693332,54.6040699800534,
55.6038059907735,56.6035420014936,57.6032780122137,58.6030140229339,59.602750033654,
60.6024860443741,61.6022220550943,62.6019580658144,63.6016940765345,64.6014300872547,
65.6011660979748,66.6009021086949,67.6006381194151,68.6003741301352,69.6001101408553,
70.5998461515754,71.5995821622956,72.5993181730157,73.5990541837358,74.598790194456,
75.5985262051761,76.5982622158962,77.5979982266164,78.5977342373365,79.5974702480566,
80.5972062587768,81.5969422694969,82.596678280217,83.5964142909372,84.5961503016573,
85.5958863123774,86.5956223230975,87.5953583338177,88.5950943445378,89.5948303552579,
90.5945663659781,91.5943023766982,92.5940383874183,93.5937743981385,94.5935104088586,
95.5932464195787,96.5929824302989,97.592718441019,98.5924544517391,99.5921904624593,
100.591926473179,101.5916624839,102.59139849462,103.59113450534,104.59087051606,
105.59060652678,106.5903425375,107.59007854822,108.58981455894,109.589550569661,
110.589286580381,111.589022591101,112.588758601821,113.588494612541,114.588230623261,
115.587966633981,116.587702644701,117.587438655422,118.587174666142,119.586910676862,
120.586646687582,121.586382698302,122.586118709022,123.585854719742,124.585590730463,
125.585326741183,126.585062751903,127.584798762623,128.584534773343,129.584270784063,
130.584006794783,131.583742805503,132.583478816224,133.583214826944,134.582950837664,
135.582686848384,136.582422859104,137.582158869824,138.581894880544,139.581630891264,
140.581366901985,141.581102912705,142.580838923425,143.580574934145,144.580310944865,
145.580046955585,146.579782966305,147.579518977026,148.579254987746,149.578990998466,
150.578727009186,151.578463019906,152.578199030626,153.577935041346,154.577671052066,
155.577407062787,156.577143073507,157.576879084227,158.576615094947,159.576351105667,
160.576087116387,161.575823127107,162.575559137827,163.575295148548,164.575031159268,
165.574767169988,166.574503180708,167.574239191428,168.573975202148,169.573711212868,
170.573447223589,171.573183234309,172.572919245029,173.572655255749,174.572391266469,
175.572127277189,176.571863287909,177.571599298629,178.57133530935,179.57107132007,
180.57080733079,181.57054334151,182.57027935223,183.57001536295,184.56975137367,
185.56948738439,186.569223395111,187.568959405831,188.568695416551,189.568431427271,
190.568167437991,191.567903448711,192.567639459431,193.567375470152,194.567111480872,
195.566847491592,196.566583502312,197.566319513032,198.566055523752,199.565791534472,
200.565527545192,201.565263555913,202.564999566633,203.564735577353,204.564471588073,
205.564207598793,206.563943609513,207.563679620233,208.563415630954,209.563151641674,
210.562887652394,211.562623663114,212.562359673834,213.562095684554,214.561831695274,
215.561567705994,216.561303716715,217.561039727435,218.560775738155,219.560511748875,
220.560247759595,221.559983770315,222.559719781035,223.559455791755,224.559191802476,
225.558927813196,226.558663823916,227.558399834636,228.558135845356,229.557871856076,
230.557607866796,231.557343877517,232.557079888237,233.556815898957,234.556551909677,
235.556287920397,236.556023931117,237.555759941837,238.555495952557,239.555231963278,
240.554967973998,241.554703984718,242.554439995438,243.554176006158,244.553912016878,
245.553648027598,246.553384038319,247.553120049039,248.552856059759,249.552592070479,
250.552328081199,251.552064091919,252.551800102639,253.551536113359,254.55127212408,
255.5510081348,256.55074414552,257.55048015624,258.55021616696,259.54995217768,
260.5496881884,261.54942419912,262.549160209841,263.548896220561,264.548632231281,
265.548368242001,266.548104252721,267.547840263441,268.547576274161,269.547312284882,
270.547048295602,271.546784306322,272.546520317042,273.546256327762,274.545992338482,
275.545728349202,276.545464359922,277.545200370643,278.544936381363,279.544672392083,
280.544408402803,281.544144413523,282.543880424243,283.543616434963,284.543352445683,
285.543088456404,286.542824467124,287.542560477844,288.542296488564,289.542032499284,
290.541768510004,291.541504520724,292.541240531445,293.540976542165,294.540712552885,
295.540448563605,296.540184574325,297.539920585045,298.539656595765,299.539392606485,
300.539128617206,301.538864627926,302.538600638646,303.538336649366,304.538072660086,
305.537808670806,306.537544681526,307.537280692246,308.537016702967,309.536752713687,
310.536488724407,311.536224735127,312.535960745847,313.535696756567,314.535432767287,
315.535168778008,316.534904788728,317.534640799448,318.534376810168,319.534112820888,
320.533848831608,321.533584842328,322.533320853048,323.533056863769,324.532792874489,
325.532528885209,326.532264895929,327.532000906649,328.531736917369,329.531472928089,
330.53120893881,331.53094494953,332.53068096025,333.53041697097,334.53015298169,
335.52988899241,336.52962500313,337.52936101385,338.529097024571,339.528833035291,
340.528569046011,341.528305056731,342.528041067451,343.527777078171,344.527513088891,
345.527249099611,346.526985110332,347.526721121052,348.526457131772,349.526193142492,
350.525929153212,351.525665163932,352.525401174652,353.525137185373,354.524873196093,
355.524609206813,356.524345217533,357.524081228253,358.523817238973,359.523553249693,
360.523289260413,361.523025271134,362.522761281854,363.522497292574,364.522233303294,
365.521969314014,366.521705324734,367.521441335454,368.521177346175,369.520913356895,
370.520649367615,371.520385378335,372.520121389055,373.519857399775,374.519593410495,
375.519329421215,376.519065431936,377.518801442656,378.518537453376,379.518273464096,
380.518009474816,381.517745485536,382.517481496256,383.517217506976,384.516953517697,
385.516689528417,386.516425539137,387.516161549857,388.515897560577,389.515633571297,
390.515369582017,391.515105592737,392.514841603458,393.514577614178,394.514313624898,
395.514049635618,396.513785646338,397.513521657058,398.513257667778,399.512993678499,
400.512729689219,401.512465699939,402.512201710659,403.511937721379,404.511673732099,
405.511409742819,406.511145753539,407.51088176426,408.51061777498,409.5103537857,
410.51008979642,411.50982580714,412.50956181786,413.50929782858,414.509033839301,
415.508769850021,416.508505860741,417.508241871461,418.507977882181,419.507713892901,
420.507449903621,421.507185914341,422.506921925062,423.506657935782,424.506393946502,
425.506129957222,426.505865967942,427.505601978662,428.505337989382,429.505074000102,
430.504810010823,431.504546021543,432.504282032263,433.504018042983,434.503754053703,
435.503490064423,436.503226075143,437.502962085864,438.502698096584,439.502434107304,
440.502170118024,441.501906128744,442.501642139464,443.501378150184,444.501114160904,
445.500850171625,446.500586182345,447.500322193065,448.500058203785,449.499794214505,
450.499530225225,451.499266235945,452.499002246665,453.498738257386,454.498474268106,
455.498210278826,456.497946289546,457.497682300266,458.497418310986,459.497154321706,
460.496890332427,461.496626343147,462.496362353867,463.496098364587,464.495834375307,
465.495570386027,466.495306396747,467.495042407467,468.494778418188,469.494514428908,
470.494250439628,471.493986450348,472.493722461068,473.493458471788,474.493194482508,
475.492930493229,476.492666503949,477.492402514669,478.492138525389,479.491874536109,
480.491610546829,481.491346557549,482.491082568269,483.49081857899,484.49055458971,
485.49029060043,486.49002661115,487.48976262187,488.48949863259,489.48923464331,
490.48897065403,491.488706664751,492.488442675471,493.488178686191,494.487914696911,
495.487650707631,496.487386718351,497.487122729071,498.486858739792,499.486594750512,
500.486330761232,501.486066771952,502.485802782672,503.485538793392,504.485274804112,
505.485010814832,506.484746825553,507.484482836273,508.484218846993,509.483954857713,
510.483690868433,511.483426879153,512.483162889873,513.482898900594,514.482634911314,
515.482370922034,516.482106932754,517.481842943474,518.481578954194,519.481314964914,
520.481050975635,521.480786986355,522.480522997075,523.480259007795,524.479995018515,
525.479731029235,526.479467039955,527.479203050675,528.478939061396,529.478675072116,
530.478411082836,531.478147093556,532.477883104276,533.477619114996,534.477355125716,
535.477091136436,536.476827147157,537.476563157877,538.476299168597,539.476035179317,
540.475771190037,541.475507200757,542.475243211477,543.474979222197,544.474715232918,
545.474451243638,546.474187254358,547.473923265078,548.473659275798,549.473395286518,
550.473131297238,551.472867307958,552.472603318679,553.472339329399,554.472075340119,
555.471811350839,556.471547361559,557.471283372279,558.471019382999,559.47075539372,
560.47049140444,561.47022741516,562.46996342588,563.4696994366,564.46943544732,
565.46917145804,566.46890746876,567.468643479481,568.468379490201,569.468115500921,
570.467851511641,571.467587522361,572.467323533081,573.467059543801,574.466795554521,
575.466531565242,576.466267575962,577.466003586682,578.465739597402,579.465475608122,
580.465211618842,581.464947629562,582.464683640283,583.464419651003,584.464155661723,
585.463891672443,586.463627683163,587.463363693883,588.463099704603,589.462835715323,
590.462571726044,591.462307736764,592.462043747484,593.461779758204,594.461515768924,
595.461251779644,596.460987790364,597.460723801085,598.460459811805,599.460195822525,
600.459931833245,601.459667843965,602.459403854685,603.459139865405,604.458875876125,
605.458611886846,606.458347897566,607.458083908286,608.457819919006,609.457555929726,
610.457291940446,611.457027951166,612.456763961887,613.456499972607,614.456235983327,
615.455971994047,616.455708004767,617.455444015487,618.455180026207,619.454916036927,
620.454652047648,621.454388058368,622.454124069088,623.453860079808,624.453596090528,
625.453332101248,626.453068111968,627.452804122688,628.452540133409,629.452276144129,
630.452012154849,631.451748165569,632.451484176289,633.451220187009,634.450956197729,
635.450692208449,636.45042821917,637.45016422989,638.44990024061,639.44963625133,
640.44937226205,641.44910827277,642.44884428349,643.448580294211,644.448316304931,
645.448052315651,646.447788326371,647.447524337091,648.447260347811,649.446996358531,
650.446732369251,651.446468379972,652.446204390692,653.445940401412,654.445676412132,
655.445412422852,656.445148433572,657.444884444292,658.444620455012,659.444356465733,
660.444092476453,661.443828487173,662.443564497893,663.443300508613,664.443036519333,
665.442772530053,666.442508540774,667.442244551494,668.441980562214,669.441716572934,
670.441452583654,671.441188594374,672.440924605094,673.440660615815,674.440396626535,
675.440132637255,676.439868647975,677.439604658695,678.439340669415,679.439076680135,
680.438812690855,681.438548701576,682.438284712296,683.438020723016,684.437756733736,
685.437492744456,686.437228755176,687.436964765896,688.436700776616,689.436436787337,
690.436172798057,691.435908808777,692.435644819497,693.435380830217,694.435116840937,
695.434852851657,696.434588862377,697.434324873098,698.434060883818,699.433796894538,
700.433532905258,701.433268915978,702.433004926698,703.432740937418,704.432476948139,
705.432212958859,706.431948969579,707.431684980299,708.431420991019,709.431157001739,
710.430893012459,711.430629023179,712.4303650339,713.43010104462,714.42983705534,
715.42957306606,716.42930907678,717.4290450875,718.42878109822,719.42851710894,
720.428253119661,721.427989130381,722.427725141101,723.427461151821,724.427197162541,
725.426933173261,726.426669183981,727.426405194702,728.426141205422,729.425877216142,
730.425613226862,731.425349237582,732.425085248302,733.424821259022,734.424557269742,
735.424293280463,736.424029291183,737.423765301903,738.423501312623,739.423237323343,
740.422973334063,741.422709344783,742.422445355504,743.422181366224,744.421917376944,
745.421653387664,746.421389398384,747.421125409104,748.420861419824,749.420597430544,
750.420333441265,751.420069451985,752.419805462705,753.419541473425,754.419277484145,
755.419013494865,756.418749505585,757.418485516306,758.418221527026,759.417957537746,
760.417693548466,761.417429559186,762.417165569906,763.416901580626,764.416637591346,
765.416373602067,766.416109612787,767.415845623507,768.415581634227,769.415317644947,
770.415053655667,771.414789666387,772.414525677107,773.414261687828,774.413997698548,
775.413733709268,776.413469719988,777.413205730708,778.412941741428,779.412677752148,
780.412413762868,781.412149773589,782.411885784309,783.411621795029,784.411357805749,
785.411093816469,786.410829827189,787.410565837909,788.41030184863,789.41003785935,
790.40977387007,791.40950988079,792.40924589151,793.40898190223,794.40871791295,
795.40845392367,796.408189934391,797.407925945111,798.407661955831,799.407397966551,
800.407133977271,801.406869987991,802.406605998711,803.406342009432,804.406078020152,
805.405814030872,806.405550041592,807.405286052312,808.405022063032,809.404758073752,
810.404494084472,811.404230095193,812.403966105913,813.403702116633,814.403438127353,
815.403174138073,816.402910148793,817.402646159513,818.402382170234,819.402118180954,
820.401854191674,821.401590202394,822.401326213114,823.401062223834,824.400798234554,
825.400534245274,826.400270255995,827.400006266715,828.399742277435,829.399478288155,
830.399214298875,831.398950309595,832.398686320315,833.398422331035,834.398158341756,
835.397894352476,836.397630363196,837.397366373916,838.397102384636,839.396838395356,
840.396574406076,841.396310416796,842.396046427517,843.395782438237,844.395518448957,
845.395254459677,846.394990470397,847.394726481117,848.394462491837,849.394198502558,
850.393934513278,851.393670523998,852.393406534718,853.393142545438,854.392878556158,
855.392614566878,856.392350577598,857.392086588319,858.391822599039,859.391558609759,
860.391294620479,861.391030631199,862.390766641919,863.390502652639,864.390238663359,
865.38997467408,866.3897106848,867.38944669552,868.38918270624,869.38891871696,
870.38865472768,871.3883907384,872.388126749121,873.387862759841,874.387598770561,
875.387334781281,876.387070792001,877.386806802721,878.386542813441,879.386278824161,
880.386014834882,881.385750845602,882.385486856322,883.385222867042,884.384958877762,
885.384694888482,886.384430899202,887.384166909923,888.383902920643,889.383638931363,
890.383374942083,891.383110952803,892.382846963523,893.382582974243,894.382318984963,
895.382054995684,896.381791006404,897.381527017124,898.381263027844,899.380999038564,
900.380735049284,901.380471060004,902.380207070725,903.379943081445,904.379679092165,
905.379415102885,906.379151113605,907.378887124325,908.378623135045,909.378359145765,
910.378095156486,911.377831167206,912.377567177926,913.377303188646,914.377039199366,
915.376775210086,916.376511220806,917.376247231526,918.375983242247,919.375719252967,
920.375455263687,921.375191274407,922.374927285127,923.374663295847,924.374399306567,
925.374135317287,926.373871328008,927.373607338728,928.373343349448,929.373079360168,
930.372815370888,931.372551381608,932.372287392328,933.372023403049,934.371759413769,
935.371495424489,936.371231435209,937.370967445929,938.370703456649,939.370439467369,
940.370175478089,941.36991148881,942.36964749953,943.36938351025,944.36911952097,
945.36885553169,946.36859154241,947.36832755313,948.368063563851,949.367799574571,
950.367535585291,951.367271596011,952.367007606731,953.366743617451,954.366479628171,
955.366215638891,956.365951649612,957.365687660332,958.365423671052,959.365159681772,
960.364895692492,961.364631703212,962.364367713932,963.364103724653,964.363839735373,
965.363575746093,966.363311756813,967.363047767533,968.362783778253,969.362519788973,
970.362255799693,971.361991810414,972.361727821134,973.361463831854,974.361199842574,
975.360935853294,976.360671864014,977.360407874734,978.360143885454,979.359879896175,
980.359615906895,981.359351917615,982.359087928335,983.358823939055,984.358559949775,
985.358295960495,986.358031971215,987.357767981936,988.357503992656,989.357240003376,
990.356976014096,991.356712024816,992.356448035536,993.356184046256,994.355920056977,
995.355656067697,996.355392078417,997.355128089137,998.354864099857,999.354600110577,
1000.3543361213,1001.35407213202,1002.35380814274,1003.35354415346,1004.35328016418,
1005.3530161749,1006.35275218562,1007.35248819634,1008.35222420706,1009.35196021778,
1010.3516962285,1011.35143223922,1012.35116824994,1013.35090426066,1014.35064027138,
1015.3503762821,1016.35011229282,1017.34984830354,1018.34958431426,1019.34932032498,
1020.3490563357,1021.34879234642,1022.34852835714,1023.34826436786,1024.34800037858,
1025.3477363893,1026.34747240002,1027.34720841074,1028.34694442146,1029.34668043218,
1030.3464164429,1031.34615245362,1032.34588846434,1033.34562447506,1034.34536048578,
1035.3450964965,1036.34483250722,1037.34456851794,1038.34430452866,1039.34404053938,
1040.3437765501,1041.34351256082,1042.34324857154,1043.34298458226,1044.34272059298,
1045.3424566037,1046.34219261442,1047.34192862514,1048.34166463586,1049.34140064658,
1050.3411366573,1051.34087266802,1052.34060867874,1053.34034468946,1054.34008070018,
1055.3398167109,1056.33955272162,1057.33928873234,1058.33902474307,1059.33876075378,
1060.33849676451,1061.33823277523,1062.33796878595,1063.33770479667,1064.33744080739,
1065.33717681811,1066.33691282883,1067.33664883955,1068.33638485027,1069.33612086099,
1070.33585687171,1071.33559288243,1072.33532889315,1073.33506490387,1074.33480091459,
1075.33453692531,1076.33427293603,1077.33400894675,1078.33374495747,1079.33348096819,
1080.33321697891,1081.33295298963,1082.33268900035,1083.33242501107,1084.33216102179,
1085.33189703251,1086.33163304323,1087.33136905395,1088.33110506467,1089.33084107539,
1090.33057708611,1091.33031309683,1092.33004910755,1093.32978511827,1094.32952112899,
1095.32925713971,1096.32899315043,1097.32872916115,1098.32846517187,1099.32820118259,
1100.32793719331,1101.32767320403,1102.32740921475,1103.32714522547,1104.32688123619,
1105.32661724691,1106.32635325763,1107.32608926835,1108.32582527907,1109.32556128979,
1110.32529730051,1111.32503331123,1112.32476932195,1113.32450533267,1114.32424134339,
1115.32397735411,1116.32371336483,1117.32344937555,1118.32318538627,1119.32292139699,
1120.32265740771,1121.32239341843,1122.32212942915,1123.32186543987,1124.32160145059,
1125.32133746131,1126.32107347203,1127.32080948275,1128.32054549347,1129.32028150419,
1130.32001751491,1131.31975352563,1132.31948953635,1133.31922554707,1134.31896155779,
1135.31869756852,1136.31843357924,1137.31816958996,1138.31790560068,1139.3176416114,
1140.31737762212,1141.31711363284,1142.31684964356,1143.31658565428,1144.316321665,
1145.31605767572,1146.31579368644,1147.31552969716,1148.31526570788,1149.3150017186,
1150.31473772932,1151.31447374004,1152.31420975076,1153.31394576148,1154.3136817722,
1155.31341778292,1156.31315379364,1157.31288980436,1158.31262581508,1159.3123618258,
1160.31209783652,1161.31183384724,1162.31156985796,1163.31130586868,1164.3110418794,
1165.31077789012,1166.31051390084,1167.31024991156,1168.30998592228,1169.309721933,
1170.30945794372,1171.30919395444,1172.30892996516,1173.30866597588,1174.3084019866,
1175.30813799732,1176.30787400804,1177.30761001876,1178.30734602948,1179.3070820402,
1180.30681805092,1181.30655406164,1182.30629007236,1183.30602608308,1184.3057620938,
1185.30549810452,1186.30523411524,1187.30497012596,1188.30470613668,1189.3044421474,
1190.30417815812,1191.30391416884,1192.30365017956,1193.30338619028,1194.303122201,
1195.30285821172,1196.30259422244,1197.30233023316,1198.30206624388,1199.3018022546,
1200.30153826532,1201.30127427604,1202.30101028676,1203.30074629748,1204.3004823082,
1205.30021831892,1206.29995432964,1207.29969034036,1208.29942635108,1209.2991623618,
1210.29889837252,1211.29863438324,1212.29837039397,1213.29810640469,1214.29784241541,
1215.29757842613,1216.29731443685,1217.29705044757,1218.29678645829,1219.29652246901,
1220.29625847973,1221.29599449045,1222.29573050117,1223.29546651189,1224.29520252261,
1225.29493853333,1226.29467454405,1227.29441055477,1228.29414656549,1229.29388257621,
1230.29361858693,1231.29335459765,1232.29309060837,1233.29282661909,1234.29256262981,
1235.29229864053,1236.29203465125,1237.29177066197,1238.29150667269,1239.29124268341,
1240.29097869413,1241.29071470485,1242.29045071557,1243.29018672629,1244.28992273701,
1245.28965874773,1246.28939475845,1247.28913076917,1248.28886677989,1249.28860279061,
1250.28833880133,1251.28807481205,1252.28781082277,1253.28754683349,1254.28728284421,
1255.28701885493,1256.28675486565,1257.28649087637,1258.28622688709,1259.28596289781,
1260.28569890853,1261.28543491925,1262.28517092997,1263.28490694069,1264.28464295141,
1265.28437896213,1266.28411497285,1267.28385098357,1268.28358699429,1269.28332300501,
1270.28305901573,1271.28279502645,1272.28253103717,1273.28226704789,1274.28200305861,
1275.28173906933,1276.28147508005,1277.28121109077,1278.28094710149,1279.28068311221,
1280.28041912293,1281.28015513365,1282.27989114437,1283.27962715509,1284.27936316581,
1285.27909917653,1286.27883518725,1287.27857119797,1288.2783072087,1289.27804321942,
1290.27777923014,1291.27751524086,1292.27725125158,1293.2769872623,1294.27672327302,
1295.27645928374,1296.27619529446,1297.27593130518,1298.2756673159,1299.27540332662,
1300.27513933734,1301.27487534806,1302.27461135878,1303.2743473695,1304.27408338022,
1305.27381939094,1306.27355540166,1307.27329141238,1308.2730274231,1309.27276343382,
1310.27249944454,1311.27223545526,1312.27197146598,1313.2717074767,1314.27144348742,
1315.27117949814,1316.27091550886,1317.27065151958,1318.2703875303,1319.27012354102,
1320.26985955174,1321.26959556246,1322.26933157318,1323.2690675839,1324.26880359462,
1325.26853960534,1326.26827561606,1327.26801162678,1328.2677476375,1329.26748364822,
1330.26721965894,1331.26695566966,1332.26669168038,1333.2664276911,1334.26616370182,
1335.26589971254,1336.26563572326,1337.26537173398,1338.2651077447,1339.26484375542,
1340.26457976614,1341.26431577686,1342.26405178758,1343.2637877983,1344.26352380902,
1345.26325981974,1346.26299583046,1347.26273184118,1348.2624678519,1349.26220386262,
1350.26193987334,1351.26167588406,1352.26141189478,1353.2611479055,1354.26088391622,
1355.26061992694,1356.26035593766,1357.26009194838,1358.2598279591,1359.25956396982,
1360.25929998054,1361.25903599126,1362.25877200198,1363.2585080127,1364.25824402343,
1365.25798003415,1366.25771604487,1367.25745205559,1368.25718806631,1369.25692407703,
1370.25666008775,1371.25639609847,1372.25613210919,1373.25586811991,1374.25560413063,
1375.25534014135,1376.25507615207,1377.25481216279,1378.25454817351,1379.25428418423,
1380.25402019495,1381.25375620567,1382.25349221639,1383.25322822711,1384.25296423783,
1385.25270024855,1386.25243625927,1387.25217226999,1388.25190828071,1389.25164429143,
1390.25138030215,1391.25111631287,1392.25085232359,1393.25058833431,1394.25032434503,
1395.25006035575,1396.24979636647,1397.24953237719,1398.24926838791,1399.24900439863,
1400.24874040935,1401.24847642007,1402.24821243079,1403.24794844151,1404.24768445223,
1405.24742046295,1406.24715647367,1407.24689248439,1408.24662849511,1409.24636450583,
1410.24610051655,1411.24583652727,1412.24557253799,1413.24530854871,1414.24504455943,
1415.24478057015,1416.24451658087,1417.24425259159,1418.24398860231,1419.24372461303,
1420.24346062375,1421.24319663447,1422.24293264519,1423.24266865591,1424.24240466663,
1425.24214067735,1426.24187668807,1427.24161269879,1428.24134870951,1429.24108472023,
1430.24082073095,1431.24055674167,1432.24029275239,1433.24002876311,1434.23976477383,
1435.23950078455,1436.23923679527,1437.23897280599,1438.23870881671,1439.23844482743,
1440.23818083815,1441.23791684888,1442.2376528596,1443.23738887032,1444.23712488104,
1445.23686089176,1446.23659690248,1447.2363329132,1448.23606892392,1449.23580493464,
1450.23554094536,1451.23527695608,1452.2350129668,1453.23474897752,1454.23448498824,
1455.23422099896,1456.23395700968,1457.2336930204,1458.23342903112,1459.23316504184,
1460.23290105256,1461.23263706328,1462.232373074,1463.23210908472,1464.23184509544,
1465.23158110616,1466.23131711688,1467.2310531276,1468.23078913832,1469.23052514904,
1470.23026115976,1471.22999717048,1472.2297331812,1473.22946919192,1474.22920520264,
1475.22894121336,1476.22867722408,1477.2284132348,1478.22814924552,1479.22788525624,
1480.22762126696,1481.22735727768,1482.2270932884,1483.22682929912,1484.22656530984,
1485.22630132056,1486.22603733128,1487.225773342,1488.22550935272,1489.22524536344,
1490.22498137416,1491.22471738488,1492.2244533956,1493.22418940632,1494.22392541704,
1495.22366142776,1496.22339743848,1497.2231334492,1498.22286945992,1499.22260547064,
1500.22234148136,1501.22207749208,1502.2218135028,1503.22154951352,1504.22128552424,
1505.22102153496,1506.22075754568,1507.2204935564,1508.22022956712,1509.21996557784,
1510.21970158856,1511.21943759928,1512.21917361,1513.21890962072,1514.21864563144,
1515.21838164216,1516.21811765288,1517.21785366361,1518.21758967433,1519.21732568505,
1520.21706169577,1521.21679770649,1522.21653371721,1523.21626972793,1524.21600573865,
1525.21574174937,1526.21547776009,1527.21521377081,1528.21494978153,1529.21468579225,
1530.21442180297,1531.21415781369,1532.21389382441,1533.21362983513,1534.21336584585,
1535.21310185657,1536.21283786729,1537.21257387801,1538.21230988873,1539.21204589945,
1540.21178191017,1541.21151792089,1542.21125393161,1543.21098994233,1544.21072595305,
1545.21046196377,1546.21019797449,1547.20993398521,1548.20966999593,1549.20940600665,
1550.20914201737,1551.20887802809,1552.20861403881,1553.20835004953,1554.20808606025,
1555.20782207097,1556.20755808169,1557.20729409241,1558.20703010313,1559.20676611385,
1560.20650212457,1561.20623813529,1562.20597414601,1563.20571015673,1564.20544616745,
1565.20518217817,1566.20491818889,1567.20465419961,1568.20439021033,1569.20412622105,
1570.20386223177,1571.20359824249,1572.20333425321,1573.20307026393,1574.20280627465,
1575.20254228537,1576.20227829609,1577.20201430681,1578.20175031753,1579.20148632825,
1580.20122233897,1581.20095834969,1582.20069436041,1583.20043037113,1584.20016638185,
1585.19990239257,1586.19963840329,1587.19937441401,1588.19911042473,1589.19884643545,
1590.19858244617,1591.19831845689,1592.19805446761,1593.19779047834,1594.19752648906,
1595.19726249978,1596.1969985105,1597.19673452122,1598.19647053194,1599.19620654266,
1600.19594255338,1601.1956785641,1602.19541457482,1603.19515058554,1604.19488659626,
1605.19462260698,1606.1943586177,1607.19409462842,1608.19383063914,1609.19356664986,
1610.19330266058,1611.1930386713,1612.19277468202,1613.19251069274,1614.19224670346,
1615.19198271418,1616.1917187249,1617.19145473562,1618.19119074634,1619.19092675706,
1620.19066276778,1621.1903987785,1622.19013478922,1623.18987079994,1624.18960681066,
1625.18934282138,1626.1890788321,1627.18881484282,1628.18855085354,1629.18828686426,
1630.18802287498,1631.1877588857,1632.18749489642,1633.18723090714,1634.18696691786,
1635.18670292858,1636.1864389393,1637.18617495002,1638.18591096074,1639.18564697146,
1640.18538298218,1641.1851189929,1642.18485500362,1643.18459101434,1644.18432702506,
1645.18406303578,1646.1837990465,1647.18353505722,1648.18327106794,1649.18300707866,
1650.18274308938,1651.1824791001,1652.18221511082,1653.18195112154,1654.18168713226,
1655.18142314298,1656.1811591537,1657.18089516442,1658.18063117514,1659.18036718586,
1660.18010319658,1661.1798392073,1662.17957521802,1663.17931122874,1664.17904723946,
1665.17878325018,1666.1785192609,1667.17825527162,1668.17799128234,1669.17772729307,
1670.17746330379,1671.17719931451,1672.17693532523,1673.17667133595,1674.17640734667,
1675.17614335739,1676.17587936811,1677.17561537883,1678.17535138955,1679.17508740027,
1680.17482341099,1681.17455942171,1682.17429543243,1683.17403144315,1684.17376745387,
1685.17350346459,1686.17323947531,1687.17297548603,1688.17271149675,1689.17244750747,
1690.17218351819,1691.17191952891,1692.17165553963,1693.17139155035,1694.17112756107,
1695.17086357179,1696.17059958251,1697.17033559323,1698.17007160395,1699.16980761467,
1700.16954362539,1700.66941163075,1701.16959429301),.UNSPECIFIED.);
#57=B_SPLINE_CURVE_WITH_KNOTS('',3,(#17635,#17636,#17637,#17638,#17639,
#17640,#17641,#17642,#17643,#17644,#17645,#17646,#17647,#17648,#17649,#17650,
#17651,#17652,#17653,#17654,#17655,#17656,#17657,#17658,#17659,#17660,#17661,
#17662,#17663,#17664,#17665,#17666,#17667,#17668,#17669,#17670,#17671,#17672,
#17673,#17674,#17675,#17676,#17677,#17678,#17679,#17680,#17681,#17682,#17683,
#17684,#17685,#17686,#17687,#17688,#17689,#17690,#17691,#17692,#17693,#17694,
#17695,#17696,#17697,#17698,#17699,#17700,#17701,#17702,#17703,#17704,#17705,
#17706,#17707,#17708,#17709,#17710,#17711,#17712,#17713,#17714,#17715,#17716,
#17717,#17718,#17719,#17720,#17721,#17722,#17723,#17724,#17725,#17726,#17727,
#17728,#17729,#17730,#17731,#17732,#17733,#17734,#17735,#17736,#17737,#17738,
#17739,#17740,#17741,#17742,#17743,#17744,#17745,#17746,#17747,#17748,#17749,
#17750,#17751,#17752,#17753,#17754,#17755,#17756,#17757,#17758,#17759,#17760,
#17761,#17762,#17763,#17764,#17765,#17766,#17767,#17768,#17769,#17770,#17771,
#17772,#17773,#17774,#17775,#17776,#17777,#17778,#17779,#17780,#17781,#17782,
#17783,#17784,#17785,#17786,#17787,#17788,#17789,#17790,#17791,#17792,#17793,
#17794,#17795,#17796,#17797,#17798,#17799,#17800,#17801,#17802,#17803,#17804,
#17805,#17806,#17807,#17808,#17809,#17810,#17811,#17812,#17813,#17814,#17815,
#17816,#17817,#17818,#17819,#17820,#17821),.UNSPECIFIED.,.F.,.F.,(4,3,3,
3,3,3,3,3,3,3,3,3,3,3,3,3,3,3,3,3,3,3,3,3,3,3,3,3,3,3,3,3,3,3,3,3,3,3,3,
3,3,3,3,3,3,3,3,3,3,3,3,3,3,3,3,3,3,3,3,3,3,3,4),(10.376533854396,10.4587496980149,
10.5408628620149,10.6228947330942,10.708174253879,10.7901150713661,10.8720441195327,
10.9539805511138,11.0359435241432,11.1179969429654,11.2001039925654,11.2823284670145,
11.3051308993731,11.3890132354057,11.4727929338235,11.5564899638666,11.6401242241457,
11.7237228276305,11.8073038438104,11.8908852014556,11.9744848256528,12.0581716556972,
12.1419024849746,12.2257650432031,12.3048669100932,12.3887095503942,12.4724509163694,
12.556111015579,12.6397097858981,12.7232752401318,12.8068245416396,12.8903756577647,
12.9739465531604,13.0576072322501,13.1413132752236,13.2251536490027,13.3046029208133,
13.3882436530409,13.4717799864317,13.5552321639106,13.6386203543971,13.7219719209224,
13.8053053499079,13.8886388083069,13.9719904593266,14.0554306107815,14.1389150776764,
14.2225343171068,14.3043389315335,14.3881048144593,14.4717676646521,14.5553475841518,
14.638864603264,14.7223462009019,14.8058103764429,14.8892751759554,14.9727586420724,
15.0563306187544,15.1399471272635,15.2236974410639,15.3040749422536,15.3969223262202,
15.4575905445046),.UNSPECIFIED.);
#58=B_SPLINE_CURVE_WITH_KNOTS('',3,(#17824,#17825,#17826,#17827,#17828,
#17829,#17830,#17831,#17832,#17833,#17834,#17835,#17836,#17837,#17838,#17839,
#17840,#17841,#17842,#17843,#17844,#17845,#17846,#17847,#17848,#17849,#17850,
#17851,#17852,#17853,#17854,#17855,#17856,#17857,#17858,#17859,#17860,#17861,
#17862,#17863,#17864,#17865,#17866,#17867,#17868,#17869,#17870,#17871,#17872,
#17873,#17874,#17875,#17876,#17877,#17878,#17879,#17880,#17881,#17882,#17883,
#17884,#17885,#17886,#17887,#17888,#17889,#17890,#17891,#17892,#17893,#17894,
#17895,#17896,#17897,#17898,#17899,#17900,#17901,#17902,#17903,#17904,#17905,
#17906,#17907,#17908,#17909,#17910,#17911,#17912,#17913,#17914,#17915,#17916,
#17917,#17918,#17919,#17920,#17921,#17922,#17923,#17924,#17925,#17926,#17927,
#17928,#17929,#17930,#17931,#17932,#17933,#17934,#17935,#17936,#17937,#17938,
#17939,#17940,#17941,#17942,#17943,#17944,#17945,#17946,#17947,#17948,#17949,
#17950,#17951,#17952,#17953,#17954,#17955,#17956,#17957,#17958,#17959),
 .UNSPECIFIED.,.F.,.F.,(4,3,3,3,3,3,3,3,3,3,3,3,3,3,3,3,3,3,3,3,3,3,3,3,
3,3,3,3,3,3,3,3,3,3,3,3,3,3,3,3,3,3,3,3,3,4),(11.6154215190877,11.7134290666772,
11.8138941811199,11.9120721012973,12.0136808128725,12.1152895244478,12.1990316872646,
12.2827632483713,12.3665368506524,12.4503294937948,12.5342132456109,12.6151575298078,
12.6999655671363,12.7846980365675,12.8693733302146,12.9540097909809,13.0386424107133,
13.1232764318659,13.2079284449498,13.2926150490975,13.3774076283761,13.4622560147635,
13.5472444041499,13.614893540528,13.6979395377845,13.7808742160161,13.8637184213379,
13.9464929096598,14.0300099898584,14.1127187343178,14.1954240856934,14.2781447082332,
14.362265918987,14.4451170212129,14.5298732862305,14.6146295512481,14.6985212370077,
14.7823082215908,14.8665574653667,14.9501883058671,15.0337808140819,15.117352935138,
15.2020902443029,15.2857015431039,15.3710018574507,15.4563021717976),
 .UNSPECIFIED.);
#59=B_SPLINE_CURVE_WITH_KNOTS('',3,(#17965,#17966,#17967,#17968,#17969,
#17970,#17971,#17972,#17973,#17974,#17975,#17976,#17977,#17978,#17979,#17980,
#17981,#17982,#17983,#17984,#17985,#17986,#17987,#17988,#17989,#17990,#17991,
#17992,#17993,#17994,#17995,#17996,#17997,#17998,#17999,#18000,#18001,#18002,
#18003,#18004,#18005,#18006,#18007,#18008,#18009,#18010,#18011,#18012,#18013,
#18014,#18015,#18016,#18017,#18018,#18019,#18020,#18021,#18022,#18023,#18024,
#18025,#18026,#18027,#18028,#18029,#18030,#18031,#18032,#18033,#18034,#18035,
#18036,#18037,#18038,#18039,#18040,#18041,#18042,#18043,#18044,#18045,#18046,
#18047,#18048,#18049,#18050,#18051,#18052,#18053,#18054,#18055,#18056,#18057,
#18058,#18059,#18060,#18061,#18062,#18063,#18064,#18065,#18066,#18067,#18068,
#18069,#18070,#18071,#18072,#18073,#18074,#18075,#18076,#18077,#18078,#18079,
#18080,#18081,#18082,#18083,#18084,#18085,#18086,#18087,#18088,#18089,#18090,
#18091,#18092,#18093,#18094,#18095,#18096,#18097,#18098,#18099,#18100,#18101,
#18102,#18103,#18104,#18105,#18106,#18107,#18108,#18109,#18110,#18111,#18112,
#18113,#18114,#18115,#18116,#18117,#18118,#18119,#18120,#18121,#18122,#18123,
#18124,#18125,#18126,#18127,#18128,#18129,#18130,#18131,#18132,#18133,#18134,
#18135,#18136,#18137,#18138,#18139,#18140,#18141,#18142,#18143,#18144,#18145,
#18146,#18147,#18148,#18149,#18150,#18151,#18152,#18153,#18154,#18155,#18156,
#18157,#18158,#18159,#18160,#18161,#18162,#18163,#18164,#18165,#18166,#18167,
#18168,#18169,#18170,#18171,#18172,#18173,#18174,#18175,#18176,#18177,#18178,
#18179,#18180,#18181,#18182,#18183,#18184),.UNSPECIFIED.,.F.,.F.,(4,3,3,
3,3,3,3,3,3,3,3,3,3,3,3,3,3,3,3,3,3,3,3,3,3,3,3,3,3,3,3,3,3,3,3,3,3,3,3,
3,3,3,3,3,3,3,3,3,3,3,3,3,3,3,3,3,3,3,3,3,3,3,3,3,3,3,3,3,3,3,3,3,3,4),
(15.7079632679298,15.7926435804918,15.8773492161091,15.9620963337644,16.0475249885667,
16.132453607754,16.2181322803638,16.3038109529737,16.3875351972687,16.471156054379,
16.5546936734092,16.6381681310957,16.7216069220662,16.805028147841,16.8884498952704,
16.9718902477285,17.0554192578422,17.138992811707,17.2227006276309,17.3035469636939,
17.3872906015743,17.4709310773888,17.5544885181045,17.6379829786723,17.7214419777467,
17.804883533783,17.8883257146451,17.9717865847761,18.0553361303936,18.1389302620967,
18.2226585200042,18.303282974414,18.3870229255899,18.4706597068039,18.5542134490663,
18.6377042113358,18.7211595257893,18.8045974060827,18.8880359236554,18.9714931465372,
19.0550390912698,19.1386296415935,19.222354388209,19.3030189851341,19.3867556060725,
19.4703889983084,19.5539392967613,19.6374265642217,19.7208783183761,19.8043125989766,
19.8877474807551,19.9712010350115,20.0547432795759,20.1383301067002,20.2220511281309,
20.3027549958542,20.3864945572802,20.4701309258356,20.5536842330696,20.6371745384566,
20.7206293641871,20.8040667364236,20.8875047270122,20.9709614043765,21.0545067771072,
21.1380967401163,21.2218208789181,21.3024910065744,21.3858830961904,21.469172262834,
21.5523598572504,21.6354890394002,21.7185738574777,21.7400988072349),
 .UNSPECIFIED.);
#60=B_SPLINE_CURVE_WITH_KNOTS('',3,(#18185,#18186,#18187,#18188,#18189,
#18190,#18191,#18192,#18193,#18194),.UNSPECIFIED.,.F.,.F.,(4,3,3,4),(15.4575905445046,
15.5499665865835,15.6419244349656,15.7079632677523),.UNSPECIFIED.);
#61=B_SPLINE_CURVE_WITH_KNOTS('',3,(#18196,#18197,#18198,#18199,#18200,
#18201,#18202,#18203,#18204,#18205),.UNSPECIFIED.,.F.,.F.,(4,3,3,4),(15.4563021717976,
15.5401663906876,15.6143655619682,15.7079632679337),.UNSPECIFIED.);
#62=B_SPLINE_CURVE_WITH_KNOTS('',3,(#18206,#18207,#18208,#18209,#18210,
#18211,#18212,#18213,#18214,#18215,#18216,#18217,#18218,#18219,#18220,#18221,
#18222,#18223,#18224,#18225,#18226,#18227,#18228,#18229,#18230,#18231,#18232,
#18233,#18234,#18235,#18236,#18237,#18238,#18239,#18240,#18241,#18242,#18243,
#18244,#18245,#18246,#18247,#18248,#18249,#18250,#18251,#18252,#18253,#18254,
#18255,#18256,#18257,#18258,#18259,#18260,#18261,#18262,#18263,#18264,#18265,
#18266,#18267,#18268,#18269,#18270,#18271,#18272,#18273,#18274,#18275,#18276,
#18277,#18278,#18279,#18280,#18281,#18282,#18283,#18284,#18285,#18286,#18287,
#18288,#18289,#18290,#18291,#18292,#18293,#18294,#18295,#18296,#18297,#18298,
#18299,#18300,#18301,#18302,#18303,#18304,#18305,#18306,#18307,#18308,#18309,
#18310,#18311,#18312,#18313,#18314,#18315,#18316,#18317,#18318,#18319,#18320,
#18321,#18322,#18323,#18324,#18325,#18326,#18327,#18328,#18329,#18330,#18331,
#18332,#18333,#18334,#18335,#18336,#18337,#18338,#18339,#18340,#18341,#18342,
#18343,#18344,#18345,#18346,#18347,#18348,#18349,#18350,#18351,#18352,#18353,
#18354,#18355,#18356,#18357,#18358,#18359,#18360,#18361,#18362,#18363,#18364,
#18365,#18366,#18367,#18368,#18369,#18370,#18371,#18372,#18373,#18374,#18375,
#18376,#18377,#18378,#18379,#18380,#18381,#18382,#18383,#18384,#18385,#18386,
#18387,#18388,#18389,#18390,#18391,#18392,#18393,#18394,#18395,#18396,#18397,
#18398,#18399,#18400,#18401,#18402,#18403,#18404,#18405,#18406,#18407,#18408,
#18409,#18410,#18411,#18412,#18413,#18414,#18415,#18416,#18417,#18418,#18419,
#18420,#18421,#18422,#18423,#18424,#18425),.UNSPECIFIED.,.F.,.F.,(4,3,3,
3,3,3,3,3,3,3,3,3,3,3,3,3,3,3,3,3,3,3,3,3,3,3,3,3,3,3,3,3,3,3,3,3,3,3,3,
3,3,3,3,3,3,3,3,3,3,3,3,3,3,3,3,3,3,3,3,3,3,3,3,3,3,3,3,3,3,3,3,3,3,4),
(15.7079632680592,15.7907745344394,15.8734936731201,15.956141602808,16.0387439060103,
16.1213228371711,16.2038972033411,16.2864858052991,16.3691583325617,16.4518728357758,
16.5347192332603,16.6141015726884,16.697742304916,16.781278638307,16.8647308157857,
16.9481190062724,17.0314705727976,17.1148040017831,17.1981374601819,17.2814891112015,
17.3649292626563,17.4484137295512,17.5320329689815,17.6138375834085,17.6976034663343,
17.781266316527,17.8648462360265,17.9483632551386,18.0318448527766,18.1153090283176,
18.19877382783,18.2822572939469,18.365829270629,18.449445779138,18.5331960929383,
18.6135735941286,18.6973242901216,18.7809720312271,18.86453693568,18.9480390499362,
19.0315059660048,19.1149555983376,19.1984060076848,19.2818752514727,19.365433354798,
19.44903615789,19.5327731955315,19.6133096048488,19.6970338491438,19.780654706254,
19.8641923252842,19.9476667829708,20.0311055739413,20.1145267997161,20.1979485471458,
20.2813888996038,20.3649179097175,20.4484914635823,20.5321992795062,20.6130456155689,
20.6967892534494,20.7804297292639,20.8639871699793,20.9474816305479,21.0309406296223,
21.1143821856589,21.1978243665211,21.2812852366525,21.3648347822701,21.4484289139732,
21.5321571718807,21.612781626289,21.7074539497444,21.740715980233),
 .UNSPECIFIED.);
#63=B_SPLINE_CURVE_WITH_KNOTS('',3,(#18431,#18432,#18433,#18434,#18435,
#18436,#18437,#18438,#18439,#18440,#18441,#18442,#18443,#18444,#18445,#18446,
#18447,#18448,#18449,#18450,#18451,#18452,#18453,#18454,#18455,#18456,#18457,
#18458,#18459,#18460,#18461,#18462,#18463,#18464,#18465,#18466,#18467,#18468,
#18469,#18470,#18471,#18472,#18473,#18474,#18475,#18476,#18477,#18478,#18479,
#18480,#18481,#18482,#18483,#18484,#18485,#18486,#18487,#18488,#18489,#18490,
#18491,#18492,#18493,#18494,#18495,#18496,#18497,#18498,#18499,#18500,#18501,
#18502,#18503,#18504,#18505,#18506,#18507,#18508,#18509,#18510,#18511,#18512,
#18513,#18514,#18515,#18516,#18517,#18518,#18519,#18520,#18521,#18522,#18523,
#18524,#18525,#18526,#18527,#18528,#18529,#18530,#18531,#18532,#18533,#18534,
#18535,#18536,#18537,#18538,#18539,#18540,#18541,#18542,#18543,#18544,#18545,
#18546,#18547,#18548,#18549,#18550,#18551,#18552,#18553,#18554,#18555,#18556,
#18557,#18558,#18559,#18560,#18561,#18562,#18563,#18564,#18565,#18566,#18567,
#18568,#18569,#18570,#18571,#18572,#18573,#18574,#18575,#18576,#18577,#18578,
#18579,#18580,#18581,#18582,#18583,#18584,#18585,#18586,#18587,#18588,#18589,
#18590,#18591,#18592,#18593,#18594,#18595,#18596,#18597,#18598,#18599,#18600,
#18601,#18602,#18603,#18604,#18605,#18606,#18607,#18608,#18609,#18610,#18611,
#18612,#18613,#18614,#18615,#18616,#18617,#18618,#18619,#18620,#18621,#18622,
#18623,#18624,#18625,#18626,#18627,#18628,#18629,#18630,#18631,#18632,#18633,
#18634,#18635,#18636,#18637,#18638,#18639,#18640,#18641,#18642,#18643,#18644,
#18645,#18646,#18647,#18648,#18649,#18650),.UNSPECIFIED.,.F.,.F.,(4,3,3,
3,3,3,3,3,3,3,3,3,3,3,3,3,3,3,3,3,3,3,3,3,3,3,3,3,3,3,3,3,3,3,3,3,3,3,3,
3,3,3,3,3,3,3,3,3,3,3,3,3,3,3,3,3,3,3,3,3,3,3,3,3,3,3,3,3,3,3,3,3,3,4),
(21.9911485752722,22.0905199443307,22.1906522436346,22.2915864234119,22.3022270172945,
22.3859654335529,22.4696006451592,22.5531527849645,22.6366419137261,22.7200955530059,
22.8035317329769,22.8869685266068,22.9704240034381,23.0539681767605,23.1375569390688,
23.2212798871326,23.3019630280146,23.385701881021,23.4693375349391,23.5528901221183,
23.6363797028221,23.719833799406,23.8032704398822,23.8867076967894,23.9701636392423,
24.0537082792805,24.1372975096405,24.2210209233106,24.3016990387348,24.3854377526698,
24.4690732665012,24.5526257127343,24.6361151517867,24.7195691061525,24.803005604086,
24.8864427182613,24.9698985179291,25.0534430159093,25.1370321043811,25.2207553778982,
25.3014350494549,25.3851737205122,25.4688091904866,25.5523615919349,25.6358509853249,
25.7193048928488,25.8027413432284,25.8861784091806,25.9696341599982,26.0531786084049,
26.1367676468314,26.2204908699956,26.301171060175,26.3849097947876,26.4685453291628,
26.5520977957841,26.6355872550472,26.7190412292786,26.8024777468644,26.8859148804588,
26.9693706992928,27.052915215926,27.1365043228015,27.2202276141041,27.3009070708951,
27.3842944828408,27.4675500501445,27.550729511587,27.633851366961,27.7169340711784,
27.8000126126222,27.8830868940955,27.9662056561429,28.0225858316167),
 .UNSPECIFIED.);
#64=B_SPLINE_CURVE_WITH_KNOTS('',3,(#18651,#18652,#18653,#18654,#18655,
#18656,#18657,#18658,#18659,#18660),.UNSPECIFIED.,.F.,.F.,(4,3,3,4),(21.7400988072349,
21.8231667809187,21.907157678014,21.9911485751093),.UNSPECIFIED.);
#65=B_SPLINE_CURVE_WITH_KNOTS('',3,(#18662,#18663,#18664,#18665,#18666,
#18667,#18668,#18669,#18670,#18671),.UNSPECIFIED.,.F.,.F.,(4,3,3,4),(21.740715980233,
21.8348722215429,21.9284884766943,21.9911485749198),.UNSPECIFIED.);
#66=B_SPLINE_CURVE_WITH_KNOTS('',3,(#18672,#18673,#18674,#18675,#18676,
#18677,#18678,#18679,#18680,#18681,#18682,#18683,#18684,#18685,#18686,#18687,
#18688,#18689,#18690,#18691,#18692,#18693,#18694,#18695,#18696,#18697,#18698,
#18699,#18700,#18701,#18702,#18703,#18704,#18705,#18706,#18707,#18708,#18709,
#18710,#18711,#18712,#18713,#18714,#18715,#18716,#18717,#18718,#18719,#18720,
#18721,#18722,#18723,#18724,#18725,#18726,#18727,#18728,#18729,#18730,#18731,
#18732,#18733,#18734,#18735,#18736,#18737,#18738,#18739,#18740,#18741,#18742,
#18743,#18744,#18745,#18746,#18747,#18748,#18749,#18750,#18751,#18752,#18753,
#18754,#18755,#18756,#18757,#18758,#18759,#18760,#18761,#18762,#18763,#18764,
#18765,#18766,#18767,#18768,#18769,#18770,#18771,#18772,#18773,#18774,#18775,
#18776,#18777,#18778,#18779,#18780,#18781,#18782,#18783,#18784,#18785,#18786,
#18787,#18788,#18789,#18790,#18791,#18792,#18793,#18794,#18795,#18796,#18797,
#18798,#18799,#18800,#18801,#18802,#18803,#18804,#18805,#18806,#18807,#18808,
#18809,#18810,#18811,#18812,#18813,#18814,#18815,#18816,#18817,#18818,#18819,
#18820,#18821,#18822,#18823,#18824,#18825,#18826,#18827,#18828,#18829,#18830,
#18831,#18832,#18833,#18834,#18835,#18836,#18837,#18838,#18839,#18840,#18841,
#18842,#18843,#18844,#18845,#18846,#18847,#18848,#18849,#18850,#18851,#18852,
#18853,#18854,#18855,#18856,#18857,#18858,#18859,#18860,#18861,#18862,#18863,
#18864,#18865,#18866,#18867,#18868,#18869,#18870,#18871,#18872,#18873,#18874,
#18875,#18876,#18877,#18878,#18879,#18880,#18881,#18882,#18883,#18884,#18885,
#18886,#18887,#18888,#18889,#18890,#18891),.UNSPECIFIED.,.F.,.F.,(4,3,3,
3,3,3,3,3,3,3,3,3,3,3,3,3,3,3,3,3,3,3,3,3,3,3,3,3,3,3,3,3,3,3,3,3,3,3,3,
3,3,3,3,3,3,3,3,3,3,3,3,3,3,3,3,3,3,3,3,3,3,3,3,3,3,3,3,3,3,3,3,3,3,4),
(21.9911485751133,22.0752803066499,22.1594213519125,22.2435887880297,22.327799705763,
22.412122635211,22.496510193649,22.5810312627201,22.6125176370092,22.6962542579476,
22.7798876501835,22.8634379486364,22.9469252160963,23.0303769702507,23.1138112508511,
23.1972461326295,23.2806996868859,23.3642419314503,23.4478287585743,23.531549780005,
23.6122536477293,23.6959932091553,23.7796295777105,23.8631828849443,23.946673190331,
24.0301280160616,24.113565388298,24.1970033788866,24.2804600562506,24.3640054289813,
24.4475953919903,24.5313195307922,24.6119896584494,24.6957284703853,24.7793640854067,
24.8629166358964,24.9464061821532,25.0298602478526,25.11329685962,25.1967340900312,
25.2801900082394,25.3637346277638,25.4473238396068,25.5310472383997,25.6117256691696,
25.6954640854281,25.7790992970342,25.8626514368397,25.9461405656013,26.0295942048811,
26.1130303848521,26.196467178482,26.2799226553132,26.3634668286356,26.4470555909439,
26.5307785390076,26.6114616798897,26.6952005328961,26.7788361868141,26.8623887739932,
26.9458783546974,27.0293324512814,27.1127690917577,27.1962063486646,27.2796622911176,
27.3632069311557,27.4467961615158,27.530519575186,27.6111976906098,27.6949624620804,
27.7785925584211,27.8621451536583,27.9456293039383,28.0234162092491),
 .UNSPECIFIED.);
#67=B_SPLINE_CURVE_WITH_KNOTS('',3,(#18897,#18898,#18899,#18900,#18901,
#18902,#18903,#18904,#18905,#18906,#18907,#18908,#18909,#18910,#18911,#18912,
#18913,#18914,#18915,#18916,#18917,#18918,#18919,#18920,#18921,#18922,#18923,
#18924,#18925,#18926,#18927,#18928,#18929,#18930,#18931,#18932,#18933,#18934,
#18935,#18936,#18937,#18938,#18939,#18940,#18941,#18942,#18943,#18944,#18945,
#18946,#18947,#18948,#18949,#18950,#18951,#18952,#18953,#18954,#18955,#18956,
#18957,#18958,#18959,#18960,#18961,#18962,#18963,#18964,#18965,#18966,#18967,
#18968,#18969,#18970,#18971,#18972,#18973,#18974,#18975,#18976,#18977,#18978,
#18979,#18980,#18981,#18982,#18983,#18984,#18985,#18986,#18987,#18988,#18989,
#18990,#18991,#18992,#18993,#18994,#18995,#18996,#18997,#18998,#18999,#19000,
#19001,#19002,#19003,#19004,#19005,#19006,#19007,#19008,#19009,#19010,#19011,
#19012,#19013,#19014,#19015,#19016,#19017,#19018,#19019,#19020,#19021,#19022,
#19023,#19024,#19025,#19026,#19027,#19028,#19029,#19030,#19031,#19032,#19033,
#19034,#19035,#19036,#19037,#19038,#19039,#19040,#19041,#19042,#19043,#19044,
#19045,#19046,#19047,#19048,#19049,#19050,#19051,#19052,#19053,#19054,#19055,
#19056,#19057,#19058,#19059,#19060,#19061,#19062,#19063,#19064,#19065,#19066,
#19067,#19068,#19069,#19070,#19071,#19072,#19073,#19074,#19075,#19076,#19077,
#19078,#19079,#19080,#19081,#19082,#19083,#19084,#19085,#19086,#19087,#19088,
#19089,#19090,#19091,#19092,#19093,#19094,#19095,#19096,#19097,#19098,#19099,
#19100,#19101,#19102,#19103,#19104,#19105,#19106,#19107,#19108,#19109,#19110,
#19111,#19112,#19113,#19114,#19115,#19116,#19117,#19118,#19119),
 .UNSPECIFIED.,.F.,.F.,(4,3,3,3,3,3,3,3,3,3,3,3,3,3,3,3,3,3,3,3,3,3,3,3,
3,3,3,3,3,3,3,3,3,3,3,3,3,3,3,3,3,3,3,3,3,3,3,3,3,3,3,3,3,3,3,3,3,3,3,3,
3,3,3,3,3,3,3,3,3,3,3,3,3,3,4),(28.2743338822889,28.3006430816153,28.3843817879882,
28.468017293797,28.5515697315575,28.6350591616976,28.7185131065089,28.8019495944981,
28.8853866983471,28.9688424873144,29.0523869740573,29.1359760509821,29.2196993125341,
29.3003790923354,29.3841178077619,29.4677533227502,29.5513057698054,29.6347952093454,
29.7182491636837,29.801685661276,29.8851227747951,29.9685785734908,30.0521230699997,
30.1357121567266,30.2194354280432,30.3001151030555,30.3838538143865,30.4674893252401,
30.5510417681263,30.6345312034672,30.7179851535757,30.80142164692,30.8848587561773,
30.9683145506009,31.051859042846,31.1354481253068,31.2191713923966,31.2998511137757,
31.3835898249122,31.4672253355584,31.5507777782246,31.6342672133331,31.7177211631913,
31.8011576562743,31.8845947652594,31.9680505594003,32.0515950513474,32.1351841335015,
32.2189074002725,32.2995871244958,32.3833258368923,32.466961348817,32.5505137927785,
32.6340032291978,32.7174571803857,32.8008936748098,32.884330785146,32.967786580647,
33.0513310739606,33.1349201574868,33.2186434256259,33.2993231352159,33.3830618469456,
33.4666973581966,33.5502498014783,33.6337392372124,33.7171931877092,33.8006296814388,
33.8840667910778,33.9675225858795,34.0510670784944,34.1346561613211,34.2183794287664,
34.299059145936,34.3065000825424),.UNSPECIFIED.);
#68=B_SPLINE_CURVE_WITH_KNOTS('',3,(#19120,#19121,#19122,#19123,#19124,
#19125,#19126,#19127,#19128,#19129),.UNSPECIFIED.,.F.,.F.,(4,3,3,4),(28.0225858316167,
28.1058018123903,28.1900678472803,28.2743338821704),.UNSPECIFIED.);
#69=B_SPLINE_CURVE_WITH_KNOTS('',3,(#19131,#19132,#19133,#19134,#19135,
#19136,#19137,#19138,#19139,#19140),.UNSPECIFIED.,.F.,.F.,(4,3,3,4),(28.0234162092491,
28.1068355155373,28.190584698915,28.2743338822928),.UNSPECIFIED.);
#70=B_SPLINE_CURVE_WITH_KNOTS('',3,(#19141,#19142,#19143,#19144,#19145,
#19146,#19147,#19148,#19149,#19150,#19151,#19152,#19153,#19154,#19155,#19156,
#19157,#19158,#19159,#19160,#19161,#19162,#19163,#19164,#19165,#19166,#19167,
#19168,#19169,#19170,#19171,#19172,#19173,#19174,#19175,#19176,#19177,#19178,
#19179,#19180,#19181,#19182,#19183,#19184,#19185,#19186,#19187,#19188,#19189,
#19190,#19191,#19192,#19193,#19194,#19195,#19196,#19197,#19198,#19199,#19200,
#19201,#19202,#19203,#19204,#19205,#19206,#19207,#19208,#19209,#19210,#19211,
#19212,#19213,#19214,#19215,#19216,#19217,#19218,#19219,#19220,#19221,#19222,
#19223,#19224,#19225,#19226,#19227,#19228,#19229,#19230,#19231,#19232,#19233,
#19234,#19235,#19236,#19237,#19238,#19239,#19240,#19241,#19242,#19243,#19244,
#19245,#19246,#19247,#19248,#19249,#19250,#19251,#19252,#19253,#19254,#19255,
#19256,#19257,#19258,#19259,#19260,#19261,#19262,#19263,#19264,#19265,#19266,
#19267,#19268,#19269,#19270,#19271,#19272,#19273,#19274,#19275,#19276,#19277,
#19278,#19279,#19280,#19281,#19282,#19283,#19284,#19285,#19286,#19287,#19288,
#19289,#19290,#19291,#19292,#19293,#19294,#19295,#19296,#19297,#19298,#19299,
#19300,#19301,#19302,#19303,#19304,#19305,#19306,#19307,#19308,#19309,#19310,
#19311,#19312,#19313,#19314,#19315,#19316,#19317,#19318,#19319,#19320,#19321,
#19322,#19323,#19324,#19325,#19326,#19327,#19328,#19329,#19330,#19331,#19332,
#19333,#19334,#19335,#19336,#19337,#19338,#19339,#19340,#19341,#19342,#19343,
#19344,#19345,#19346,#19347,#19348,#19349,#19350,#19351,#19352,#19353,#19354,
#19355,#19356,#19357,#19358,#19359,#19360),.UNSPECIFIED.,.F.,.F.,(4,3,3,
3,3,3,3,3,3,3,3,3,3,3,3,3,3,3,3,3,3,3,3,3,3,3,3,3,3,3,3,3,3,3,3,3,3,3,3,
3,3,3,3,3,3,3,3,3,3,3,3,3,3,3,3,3,3,3,3,3,3,3,3,3,3,3,3,3,3,3,3,3,3,4),
(28.2743338824827,28.3712824055307,28.4687879362423,28.5669577034657,28.6109337013299,
28.6946723723872,28.7783078423616,28.8618602438099,28.9453496371999,29.0288035447238,
29.1122399951033,29.1956770610554,29.2791328118729,29.3626772602797,29.4462662987062,
29.5299895218703,29.6106697120501,29.6944084466627,29.7780439810379,29.8615964476591,
29.9450859069223,30.0285398811537,30.1119763987395,30.1954135323339,30.2788693511678,
30.362413867801,30.4460029746765,30.5297262659791,30.6104057227702,30.694144433022,
30.777779942827,30.8613323846962,30.9448218190526,31.0282757682304,31.1117122606767,
31.1951493690697,31.2786051626639,31.3621496541399,31.4457387358632,31.5294620022777,
31.6101417334903,31.6938804398633,31.7775159456722,31.8610683834328,31.9445578135729,
32.0280117583843,32.1114482463736,32.1948853502228,32.2783411391901,32.3618856259331,
32.4454747028581,32.5291979644102,32.6098777442105,32.693616459637,32.7772519746252,
32.8608044216806,32.9442938612206,33.0277478155589,33.1111843131511,33.1946214266703,
33.2780772253658,33.3616217218747,33.4452108086016,33.5289340799181,33.6096137549306,
33.696625903061,33.7795858721787,33.8624709514653,33.9452998737482,34.0280913257695,
34.1108784301918,34.1936633276373,34.2764866832596,34.3057109399742),
 .UNSPECIFIED.);
#71=B_SPLINE_CURVE_WITH_KNOTS('',3,(#19366,#19367,#19368,#19369,#19370,
#19371,#19372,#19373,#19374,#19375,#19376,#19377,#19378,#19379,#19380,#19381,
#19382,#19383,#19384,#19385,#19386,#19387,#19388,#19389,#19390,#19391,#19392,
#19393,#19394,#19395,#19396,#19397,#19398,#19399,#19400,#19401,#19402,#19403,
#19404,#19405,#19406,#19407,#19408,#19409,#19410,#19411,#19412,#19413,#19414,
#19415,#19416,#19417,#19418,#19419,#19420,#19421,#19422,#19423,#19424,#19425,
#19426,#19427,#19428,#19429,#19430,#19431,#19432,#19433,#19434,#19435,#19436,
#19437,#19438,#19439,#19440,#19441,#19442,#19443,#19444,#19445,#19446,#19447,
#19448,#19449,#19450,#19451,#19452,#19453,#19454,#19455,#19456,#19457,#19458,
#19459,#19460,#19461,#19462,#19463,#19464,#19465,#19466,#19467,#19468,#19469,
#19470,#19471,#19472,#19473,#19474,#19475,#19476,#19477,#19478,#19479,#19480,
#19481,#19482,#19483,#19484,#19485,#19486,#19487,#19488,#19489,#19490,#19491,
#19492,#19493,#19494,#19495,#19496,#19497,#19498,#19499,#19500,#19501,#19502,
#19503,#19504,#19505,#19506,#19507,#19508,#19509,#19510,#19511,#19512,#19513,
#19514,#19515,#19516,#19517,#19518,#19519,#19520,#19521,#19522,#19523,#19524,
#19525,#19526,#19527,#19528,#19529,#19530,#19531,#19532,#19533,#19534,#19535,
#19536,#19537,#19538,#19539,#19540,#19541,#19542,#19543,#19544,#19545,#19546,
#19547,#19548,#19549,#19550,#19551,#19552,#19553,#19554,#19555,#19556,#19557,
#19558,#19559,#19560,#19561,#19562,#19563,#19564,#19565,#19566,#19567,#19568,
#19569,#19570,#19571,#19572,#19573,#19574,#19575,#19576,#19577,#19578,#19579,
#19580,#19581,#19582,#19583,#19584,#19585),.UNSPECIFIED.,.F.,.F.,(4,3,3,
3,3,3,3,3,3,3,3,3,3,3,3,3,3,3,3,3,3,3,3,3,3,3,3,3,3,3,3,3,3,3,3,3,3,3,3,
3,3,3,3,3,3,3,3,3,3,3,3,3,3,3,3,3,3,3,3,3,3,3,3,3,3,3,3,3,3,3,3,3,3,4),
(34.5575191894685,34.6401346660436,34.7227049790521,34.8052521817043,34.8877950853622,
34.9703524953451,35.0529944964819,35.1356787053279,35.2184958070966,35.2987951566562,
35.3825338685851,35.4661693800365,35.5497218235198,35.6332112594563,35.7166652101566,
35.8001017040901,35.8835388139334,35.9669946089394,36.0505391017574,36.134128184787,
36.2178514524327,36.2985311673763,36.3822698791994,36.465905390544,36.5494578339196,
36.6329472697474,36.7164012203379,36.7998377141608,36.8832748238929,36.9667306187873,
37.0502751114939,37.1338641944118,37.2175874619467,37.2982671780964,37.3820058899321,
37.4656414012895,37.5491938446774,37.632683280518,37.7161372311207,37.7995737249558,
37.8830108347001,37.9664666296065,38.0500111223246,38.1336002052539,38.2173234727998,
38.2980031888166,38.3817419006748,38.4653774120547,38.548929855466,38.6324192913301,
38.7158732419566,38.7993097358158,38.8827468455844,38.9662026405151,39.049747133258,
39.133336216212,39.2170594837827,39.2977391995367,39.3814779113784,39.4651134227418,
39.5486658661357,39.6321553019831,39.7156092525924,39.7990457464345,39.8824828561857,
39.9659386510992,40.0494831438246,40.1330722267613,40.2167954943148,40.2974752102568,
40.3839889562121,40.4703860712489,40.5566452121474,40.5902857429648),
 .UNSPECIFIED.);
#72=B_SPLINE_CURVE_WITH_KNOTS('',3,(#19586,#19587,#19588,#19589,#19590,
#19591,#19592,#19593,#19594,#19595),.UNSPECIFIED.,.F.,.F.,(4,3,3,4),(34.3065000825424,
34.4146795617861,34.5207421559751,34.557519189341),.UNSPECIFIED.);
#73=B_SPLINE_CURVE_WITH_KNOTS('',3,(#19597,#19598,#19599,#19600,#19601,
#19602,#19603,#19604,#19605,#19606),.UNSPECIFIED.,.F.,.F.,(4,3,3,4),(34.3057109399742,
34.3886262459297,34.4730727175991,34.5575191892685),.UNSPECIFIED.);
#74=B_SPLINE_CURVE_WITH_KNOTS('',3,(#19607,#19608,#19609,#19610,#19611,
#19612,#19613,#19614,#19615,#19616,#19617,#19618,#19619,#19620,#19621,#19622,
#19623,#19624,#19625,#19626,#19627,#19628,#19629,#19630,#19631,#19632,#19633,
#19634,#19635,#19636,#19637,#19638,#19639,#19640,#19641,#19642,#19643,#19644,
#19645,#19646,#19647,#19648,#19649,#19650,#19651,#19652,#19653,#19654,#19655,
#19656,#19657,#19658,#19659,#19660,#19661,#19662,#19663,#19664,#19665,#19666,
#19667,#19668,#19669,#19670,#19671,#19672,#19673,#19674,#19675,#19676,#19677,
#19678,#19679,#19680,#19681,#19682,#19683,#19684,#19685,#19686,#19687,#19688,
#19689,#19690,#19691,#19692,#19693,#19694,#19695,#19696,#19697,#19698,#19699,
#19700,#19701,#19702,#19703,#19704,#19705,#19706,#19707,#19708,#19709,#19710,
#19711,#19712,#19713,#19714,#19715,#19716,#19717,#19718,#19719,#19720,#19721,
#19722,#19723,#19724,#19725,#19726,#19727,#19728,#19729,#19730,#19731,#19732,
#19733,#19734,#19735,#19736,#19737,#19738,#19739,#19740,#19741,#19742,#19743,
#19744,#19745,#19746,#19747,#19748,#19749,#19750,#19751,#19752,#19753,#19754,
#19755,#19756,#19757,#19758,#19759,#19760,#19761,#19762,#19763,#19764,#19765,
#19766,#19767,#19768,#19769,#19770,#19771,#19772,#19773,#19774,#19775,#19776,
#19777,#19778,#19779,#19780,#19781,#19782,#19783,#19784,#19785,#19786,#19787,
#19788,#19789,#19790,#19791,#19792,#19793,#19794,#19795,#19796,#19797,#19798,
#19799,#19800,#19801,#19802,#19803,#19804,#19805,#19806,#19807,#19808,#19809,
#19810,#19811,#19812,#19813,#19814,#19815,#19816,#19817,#19818,#19819,#19820,
#19821,#19822,#19823,#19824,#19825,#19826),.UNSPECIFIED.,.F.,.F.,(4,3,3,
3,3,3,3,3,3,3,3,3,3,3,3,3,3,3,3,3,3,3,3,3,3,3,3,3,3,3,3,3,3,3,3,3,3,3,3,
3,3,3,3,3,3,3,3,3,3,3,3,3,3,3,3,3,3,3,3,3,3,3,3,3,3,3,3,3,3,3,3,3,3,4),
(34.5575191894724,34.6093497656507,34.6930884767872,34.7767239874333,34.8602764300995,
34.9437658652082,35.0272198150664,35.1106563081493,35.1940934171344,35.2775492112753,
35.3610937032224,35.4446827853765,35.5284060521475,35.6090857763709,35.6928244887674,
35.776460000692,35.8600124446535,35.9435018810726,36.0269558322605,36.1103923266845,
36.1938294370208,36.2772852325218,36.3608297258354,36.4444188093616,36.5281420775006,
36.608821787091,36.6925604988207,36.7761960100715,36.8597484533532,36.9432378890873,
37.0266918395841,37.1101283333137,37.1935654429527,37.2770212377544,37.3605657303692,
37.4441548131959,37.5278780806412,37.6085577978111,37.6922965095691,37.7759320208472,
37.8594844641547,37.9429738999134,38.0264278504329,38.1098643441839,38.1933014538431,
38.2767572486637,38.3603017412953,38.4438908241376,38.5276140915964,38.6082938085313,
38.6920325204602,38.7756680319116,38.859220475395,38.9427099113317,39.026163862032,
39.1096003559656,39.1930374658088,39.2764932608146,39.3600377536327,39.4436268366622,
39.5273501043079,39.6080298192514,39.6917695595991,39.7754058589717,39.8589588508911,
39.9424485965472,40.0259016212374,40.109336849158,40.1927723527529,40.2762262007468,
40.3597640184065,40.4433462857643,40.5270516189311,40.5895313989693),
 .UNSPECIFIED.);
#75=B_SPLINE_CURVE_WITH_KNOTS('',3,(#19832,#19833,#19834,#19835,#19836,
#19837,#19838,#19839,#19840,#19841,#19842,#19843,#19844,#19845,#19846,#19847,
#19848,#19849,#19850,#19851,#19852,#19853,#19854,#19855,#19856,#19857,#19858,
#19859,#19860,#19861,#19862,#19863,#19864,#19865,#19866,#19867,#19868,#19869,
#19870,#19871,#19872,#19873,#19874,#19875,#19876,#19877,#19878,#19879,#19880,
#19881,#19882,#19883,#19884,#19885,#19886,#19887,#19888,#19889,#19890,#19891,
#19892,#19893,#19894,#19895,#19896,#19897,#19898,#19899,#19900,#19901,#19902,
#19903,#19904,#19905,#19906,#19907,#19908,#19909,#19910,#19911,#19912,#19913,
#19914,#19915,#19916,#19917,#19918,#19919,#19920,#19921,#19922,#19923,#19924,
#19925,#19926,#19927,#19928,#19929,#19930,#19931,#19932,#19933,#19934,#19935,
#19936,#19937,#19938,#19939,#19940,#19941,#19942,#19943,#19944,#19945,#19946,
#19947,#19948,#19949,#19950,#19951,#19952,#19953,#19954,#19955,#19956,#19957,
#19958,#19959,#19960,#19961,#19962,#19963,#19964,#19965,#19966,#19967,#19968,
#19969,#19970,#19971,#19972,#19973,#19974,#19975,#19976,#19977,#19978,#19979,
#19980,#19981,#19982,#19983,#19984,#19985,#19986,#19987,#19988,#19989,#19990,
#19991,#19992,#19993,#19994,#19995,#19996,#19997,#19998,#19999,#20000,#20001,
#20002,#20003,#20004,#20005,#20006,#20007,#20008,#20009,#20010,#20011,#20012,
#20013,#20014,#20015,#20016,#20017,#20018,#20019,#20020,#20021,#20022,#20023,
#20024,#20025,#20026,#20027,#20028,#20029,#20030,#20031,#20032,#20033,#20034,
#20035,#20036,#20037,#20038,#20039,#20040,#20041,#20042,#20043,#20044,#20045,
#20046,#20047,#20048),.UNSPECIFIED.,.F.,.F.,(4,3,3,3,3,3,3,3,3,3,3,3,3,
3,3,3,3,3,3,3,3,3,3,3,3,3,3,3,3,3,3,3,3,3,3,3,3,3,3,3,3,3,3,3,3,3,3,3,3,
3,3,3,3,3,3,3,3,3,3,3,3,3,3,3,3,3,3,3,3,3,3,3,4),(40.8407044968307,40.9298601171088,
41.0216978930758,41.1113188688309,41.2042650449039,41.2972112209769,41.3809499328246,
41.4645854441938,41.5481378875942,41.631627323447,41.7150812740625,41.7985177679105,
41.8819548776678,41.9654106725873,42.0489551653189,42.1325442482617,42.2162675158211,
42.2969472316971,42.3806859435423,42.4643214549091,42.547873898307,42.6313633341573,
42.7148172847703,42.7982537786158,42.8816908883705,42.9651466832875,43.0486911760164,
43.1322802589567,43.2160035265135,43.2966832424172,43.380421954263,43.4640574656304,
43.5476099090288,43.6310993448798,43.7145532954933,43.7979897893395,43.8814268990948,
43.9648826940124,44.0484271867419,44.1320162696828,44.2157395372403,44.2964192531373,
44.3801579649835,44.4637934763512,44.54734591975,44.6308353556013,44.7142893062153,
44.7977258000618,44.8811629098175,44.9646187047355,45.0481631974655,45.1317522804067,
45.2154755479646,45.2961552638575,45.3798939757033,45.4635294870707,45.5470819304692,
45.6305713663201,45.7140253169337,45.7974618107799,45.8808989205352,45.9643547154527,
46.0478992081823,46.1314882911231,46.2152115586806,46.2958912745776,46.3783624320973,
46.4607382036819,46.5430378108789,46.625328127725,46.7075361957602,46.7898676370116,
46.872199078263),.UNSPECIFIED.);
#76=B_SPLINE_CURVE_WITH_KNOTS('',3,(#20049,#20050,#20051,#20052,#20053,
#20054,#20055,#20056,#20057,#20058),.UNSPECIFIED.,.F.,.F.,(4,3,3,4),(40.5902857429648,
40.6763925853647,40.7624026469278,40.8407044966482),.UNSPECIFIED.);
#77=B_SPLINE_CURVE_WITH_KNOTS('',3,(#20060,#20061,#20062,#20063,#20064,
#20065,#20066,#20067,#20068,#20069,#20070,#20071,#20072),.UNSPECIFIED.,
 .F.,.F.,(4,3,3,3,4),(40.5895313989693,40.6077658299715,40.7242351632557,
40.8344463524574,40.8407044965399),.UNSPECIFIED.);
#78=B_SPLINE_CURVE_WITH_KNOTS('',3,(#20073,#20074,#20075,#20076,#20077,
#20078,#20079,#20080,#20081,#20082,#20083,#20084,#20085,#20086,#20087,#20088,
#20089,#20090,#20091,#20092,#20093,#20094,#20095,#20096,#20097,#20098,#20099,
#20100,#20101,#20102,#20103,#20104,#20105,#20106,#20107,#20108,#20109,#20110,
#20111,#20112,#20113,#20114,#20115,#20116,#20117,#20118,#20119,#20120,#20121,
#20122,#20123,#20124,#20125,#20126,#20127,#20128,#20129,#20130,#20131,#20132,
#20133,#20134,#20135,#20136,#20137,#20138,#20139,#20140,#20141,#20142,#20143,
#20144,#20145,#20146,#20147,#20148,#20149,#20150,#20151,#20152,#20153,#20154,
#20155,#20156,#20157,#20158,#20159,#20160,#20161,#20162,#20163,#20164,#20165,
#20166,#20167,#20168,#20169,#20170,#20171,#20172,#20173,#20174,#20175,#20176,
#20177,#20178,#20179,#20180,#20181,#20182,#20183,#20184,#20185,#20186,#20187,
#20188,#20189,#20190,#20191,#20192,#20193,#20194,#20195,#20196,#20197,#20198,
#20199,#20200,#20201,#20202,#20203,#20204,#20205,#20206,#20207,#20208,#20209,
#20210,#20211,#20212,#20213,#20214,#20215,#20216,#20217,#20218,#20219,#20220,
#20221,#20222,#20223,#20224,#20225,#20226,#20227,#20228,#20229,#20230,#20231,
#20232,#20233,#20234,#20235,#20236,#20237,#20238,#20239,#20240,#20241,#20242,
#20243,#20244,#20245,#20246,#20247,#20248,#20249,#20250,#20251,#20252,#20253,
#20254,#20255,#20256,#20257,#20258,#20259,#20260,#20261,#20262,#20263,#20264,
#20265,#20266,#20267,#20268,#20269,#20270,#20271,#20272,#20273,#20274,#20275,
#20276,#20277,#20278,#20279,#20280,#20281,#20282,#20283,#20284,#20285,#20286,
#20287,#20288,#20289,#20290,#20291,#20292),.UNSPECIFIED.,.F.,.F.,(4,3,3,
3,3,3,3,3,3,3,3,3,3,3,3,3,3,3,3,3,3,3,3,3,3,3,3,3,3,3,3,3,3,3,3,3,3,3,3,
3,3,3,3,3,3,3,3,3,3,3,3,3,3,3,3,3,3,3,3,3,3,3,3,3,3,3,3,3,3,3,3,3,3,4),
(40.840704496652,40.9231791511788,41.0087194873679,41.0911052472321,41.1734797508196,
41.2558619211434,41.3382706848019,41.4207689799329,41.5033205891009,41.5859878354084,
41.6075018406916,41.6912405525498,41.7748760639297,41.8584285073409,41.9419179432047,
42.0253718938312,42.1088083876904,42.1922454974588,42.2757012923896,42.3592457851324,
42.4428348680864,42.526558135657,42.6072378514118,42.6909765632536,42.7746120746171,
42.8581645180118,42.9416539538587,43.0251079044681,43.1085443983101,43.1919815080613,
43.2754373029746,43.3589817957001,43.4425708786367,43.5262941461901,43.6069738621319,
43.6907125739767,43.774348085343,43.8579005287403,43.9413899645904,44.0248439152029,
44.1082804090481,44.1917175188026,44.2751733137188,44.3587178064472,44.442306889387,
44.5260301569433,44.606709872852,44.6904485846998,44.7740840960691,44.8576365394695,
44.9411259753222,45.0245799259379,45.1080164197859,45.191453529543,45.2749093244626,
45.3584538171943,45.4420429001373,45.5257661676968,45.6064458835722,45.6901845954174,
45.7738201067842,45.8573725501822,45.9408619860327,46.0243159366455,46.1077524304912,
46.1911895402463,46.2746453351632,46.3581898278923,46.4417789108326,46.5255021783895,
46.6061818942923,46.6935617353949,46.7835468238829,46.873531912371),
 .UNSPECIFIED.);
#79=B_SPLINE_CURVE_WITH_KNOTS('',3,(#20298,#20299,#20300,#20301,#20302,
#20303,#20304,#20305,#20306,#20307,#20308,#20309,#20310,#20311,#20312,#20313,
#20314,#20315,#20316,#20317,#20318,#20319,#20320,#20321,#20322,#20323,#20324,
#20325,#20326,#20327,#20328,#20329,#20330,#20331,#20332,#20333,#20334,#20335,
#20336,#20337,#20338,#20339,#20340,#20341,#20342,#20343,#20344,#20345,#20346,
#20347,#20348,#20349,#20350,#20351,#20352,#20353,#20354,#20355,#20356,#20357,
#20358,#20359,#20360,#20361,#20362,#20363,#20364,#20365,#20366,#20367,#20368,
#20369,#20370,#20371,#20372,#20373,#20374,#20375,#20376,#20377,#20378,#20379,
#20380,#20381,#20382,#20383,#20384,#20385,#20386,#20387,#20388,#20389,#20390,
#20391,#20392,#20393,#20394,#20395,#20396,#20397,#20398,#20399,#20400,#20401,
#20402,#20403,#20404,#20405,#20406,#20407,#20408,#20409,#20410,#20411,#20412,
#20413,#20414,#20415,#20416,#20417,#20418,#20419,#20420,#20421,#20422,#20423,
#20424,#20425,#20426,#20427,#20428,#20429,#20430,#20431,#20432,#20433,#20434,
#20435,#20436,#20437,#20438,#20439,#20440,#20441,#20442,#20443,#20444,#20445,
#20446,#20447,#20448,#20449,#20450,#20451,#20452,#20453,#20454,#20455,#20456,
#20457,#20458,#20459,#20460,#20461,#20462,#20463,#20464,#20465,#20466,#20467,
#20468,#20469,#20470,#20471,#20472,#20473,#20474,#20475,#20476,#20477,#20478,
#20479,#20480,#20481,#20482,#20483,#20484,#20485,#20486,#20487,#20488,#20489,
#20490,#20491,#20492,#20493,#20494,#20495,#20496,#20497,#20498,#20499,#20500,
#20501,#20502,#20503,#20504,#20505,#20506,#20507,#20508,#20509,#20510,#20511,
#20512,#20513,#20514,#20515,#20516,#20517),.UNSPECIFIED.,.F.,.F.,(4,3,3,
3,3,3,3,3,3,3,3,3,3,3,3,3,3,3,3,3,3,3,3,3,3,3,3,3,3,3,3,3,3,3,3,3,3,3,3,
3,3,3,3,3,3,3,3,3,3,3,3,3,3,3,3,3,3,3,3,3,3,3,3,3,3,3,3,3,3,3,3,3,3,4),
(47.1238898038278,47.2546038085429,47.2956272852977,47.3793659971438,47.4630015085113,
47.54655395191,47.6300433877611,47.7134973383749,47.7969338322212,47.8803709419768,
47.9638267368945,48.0473712296243,48.1309603125654,48.2146835801231,48.2953632960178,
48.3791020078637,48.4627375192312,48.5462899626297,48.6297793984807,48.7132333490943,
48.7966698429405,48.880106952696,48.9635627476137,49.0471072403433,49.1306963232843,
49.2144195908419,49.295099306738,49.3788380185839,49.4624735299514,49.54602597335,
49.6295154092011,49.7129693598147,49.796405853661,49.8798429634164,49.9632987583341,
50.0468432510638,50.1304323340048,50.2141556015624,50.2948353174581,50.3785740293041,
50.4622095406716,50.5457619840702,50.6292514199212,50.7127053705349,50.7961418643812,
50.8795789741367,50.9630347690544,51.0465792617841,51.1301683447251,51.2138916122827,
51.2945713281782,51.3783100400241,51.4619455513916,51.5454979947902,51.6289874306412,
51.7124413812548,51.795877875101,51.8793149848565,51.9627707797741,52.0463152725038,
52.1299043554448,52.2136276230024,52.2943073388984,52.3780542392129,52.4616961110549,
52.548417940162,52.6319027033865,52.7153500216485,52.7987779830063,52.8822046585315,
52.9656778285902,53.0491789172906,53.1327580827016,53.1554707439118),
 .UNSPECIFIED.);
#80=B_SPLINE_CURVE_WITH_KNOTS('',3,(#20518,#20519,#20520,#20521,#20522,
#20523,#20524,#20525,#20526,#20527),.UNSPECIFIED.,.F.,.F.,(4,3,3,4),(46.872199078263,
46.9544540684318,47.039171936041,47.1238898036503),.UNSPECIFIED.);
#81=B_SPLINE_CURVE_WITH_KNOTS('',3,(#20529,#20530,#20531,#20532,#20533,
#20534,#20535,#20536,#20537,#20538),.UNSPECIFIED.,.F.,.F.,(4,3,3,4),(46.873531912371,
46.960478001365,47.047291421921,47.1238898038316),.UNSPECIFIED.);
#82=B_SPLINE_CURVE_WITH_KNOTS('',3,(#20539,#20540,#20541,#20542,#20543,
#20544,#20545,#20546,#20547,#20548,#20549,#20550,#20551,#20552,#20553,#20554,
#20555,#20556,#20557,#20558,#20559,#20560,#20561,#20562,#20563,#20564,#20565,
#20566,#20567,#20568,#20569,#20570,#20571,#20572,#20573,#20574,#20575,#20576,
#20577,#20578,#20579,#20580,#20581,#20582,#20583,#20584,#20585,#20586,#20587,
#20588,#20589,#20590,#20591,#20592,#20593,#20594,#20595,#20596,#20597,#20598,
#20599,#20600,#20601,#20602,#20603,#20604,#20605,#20606,#20607,#20608,#20609,
#20610,#20611,#20612,#20613,#20614,#20615,#20616,#20617,#20618,#20619,#20620,
#20621,#20622,#20623,#20624,#20625,#20626,#20627,#20628,#20629,#20630,#20631,
#20632,#20633,#20634,#20635,#20636,#20637,#20638,#20639,#20640,#20641,#20642,
#20643,#20644,#20645,#20646,#20647,#20648,#20649,#20650,#20651,#20652,#20653,
#20654,#20655,#20656,#20657,#20658,#20659,#20660,#20661,#20662,#20663,#20664,
#20665,#20666,#20667,#20668,#20669,#20670,#20671,#20672,#20673,#20674,#20675,
#20676,#20677,#20678,#20679,#20680,#20681,#20682,#20683,#20684,#20685,#20686,
#20687,#20688,#20689,#20690,#20691,#20692,#20693,#20694,#20695,#20696,#20697,
#20698,#20699,#20700,#20701,#20702,#20703,#20704,#20705,#20706,#20707,#20708,
#20709,#20710,#20711,#20712,#20713,#20714,#20715,#20716,#20717,#20718,#20719,
#20720,#20721,#20722,#20723,#20724,#20725,#20726,#20727,#20728,#20729,#20730,
#20731,#20732,#20733,#20734,#20735,#20736,#20737,#20738,#20739,#20740,#20741,
#20742,#20743,#20744,#20745,#20746,#20747,#20748,#20749,#20750,#20751,#20752,
#20753,#20754,#20755,#20756,#20757,#20758),.UNSPECIFIED.,.F.,.F.,(4,3,3,
3,3,3,3,3,3,3,3,3,3,3,3,3,3,3,3,3,3,3,3,3,3,3,3,3,3,3,3,3,3,3,3,3,3,3,3,
3,3,3,3,3,3,3,3,3,3,3,3,3,3,3,3,3,3,3,3,3,3,3,3,3,3,3,3,3,3,3,3,3,3,4),
(47.123889804,47.2119695169777,47.3001901238871,47.3886427955167,47.4772210930821,
47.5660058086749,47.6059179050124,47.6896566168586,47.7732921282264,47.8568445716251,
47.9403340074762,48.0237879580902,48.1072244519367,48.1906615616924,48.2741173566102,
48.3576618493402,48.4412509322814,48.5249741998393,48.6056539157326,48.6893926275784,
48.7730281389457,48.8565805823441,48.940070018195,49.0235239688085,49.1069604626546,
49.1903975724099,49.2738533673274,49.3573978600569,49.4409869429977,49.5247102105551,
49.6053899264527,49.6891286382987,49.7727641496662,49.8563165930648,49.9398060289159,
50.0232599795296,50.1066964733759,50.1901335831314,50.2735893780492,50.3571338707789,
50.4407229537199,50.5244462212776,50.6051259371728,50.6888646490187,50.7725001603863,
50.8560526037849,50.9395420396359,51.0229959902495,51.1064324840958,51.1898695938513,
51.273325388769,51.3568698814987,51.4404589644397,51.5241822319973,51.604861947893,
51.688600659739,51.7722361711065,51.8557886145051,51.939278050356,52.0227320009698,
52.1061684948161,52.1896056045716,52.2730613994893,52.356605892219,52.44019497516,
52.5239182427177,52.6045979586131,52.6871060320478,52.7695180670308,52.8518532668798,
52.934128908709,53.0163690882775,53.0986070875677,53.1554762266557),
 .UNSPECIFIED.);
#83=B_SPLINE_CURVE_WITH_KNOTS('',3,(#20764,#20765,#20766,#20767,#20768,
#20769,#20770,#20771,#20772,#20773,#20774,#20775,#20776,#20777,#20778,#20779,
#20780,#20781,#20782,#20783,#20784,#20785,#20786,#20787,#20788,#20789,#20790,
#20791,#20792,#20793,#20794,#20795,#20796,#20797,#20798,#20799,#20800,#20801,
#20802,#20803,#20804,#20805,#20806,#20807,#20808,#20809,#20810,#20811,#20812,
#20813,#20814,#20815,#20816,#20817,#20818,#20819,#20820,#20821,#20822,#20823,
#20824,#20825,#20826,#20827,#20828,#20829,#20830,#20831,#20832,#20833,#20834,
#20835,#20836,#20837,#20838,#20839,#20840,#20841,#20842,#20843,#20844,#20845,
#20846,#20847,#20848,#20849,#20850,#20851,#20852,#20853,#20854,#20855,#20856,
#20857,#20858,#20859,#20860,#20861,#20862,#20863,#20864,#20865,#20866,#20867,
#20868,#20869,#20870,#20871,#20872,#20873,#20874,#20875,#20876,#20877,#20878,
#20879,#20880,#20881,#20882,#20883,#20884,#20885,#20886,#20887,#20888,#20889,
#20890,#20891,#20892,#20893,#20894,#20895,#20896,#20897,#20898,#20899,#20900,
#20901,#20902,#20903,#20904,#20905,#20906,#20907,#20908,#20909,#20910,#20911,
#20912,#20913,#20914,#20915,#20916,#20917,#20918,#20919,#20920,#20921,#20922,
#20923,#20924,#20925,#20926,#20927,#20928,#20929,#20930,#20931,#20932,#20933,
#20934,#20935,#20936,#20937,#20938,#20939,#20940,#20941,#20942,#20943,#20944,
#20945,#20946,#20947,#20948,#20949,#20950,#20951,#20952,#20953,#20954,#20955,
#20956,#20957,#20958,#20959,#20960,#20961,#20962,#20963,#20964,#20965,#20966,
#20967,#20968,#20969,#20970,#20971,#20972,#20973,#20974,#20975,#20976,#20977,
#20978,#20979,#20980,#20981,#20982,#20983),.UNSPECIFIED.,.F.,.F.,(4,3,3,
3,3,3,3,3,3,3,3,3,3,3,3,3,3,3,3,3,3,3,3,3,3,3,3,3,3,3,3,3,3,3,3,3,3,3,3,
3,3,3,3,3,3,3,3,3,3,3,3,3,3,3,3,3,3,3,3,3,3,3,3,3,3,3,3,3,3,3,3,3,3,4),
(53.4070751111425,53.4896343762135,53.5721034786018,53.6545035043015,53.7368608751334,
53.819197084156,53.9015310878447,53.9838818385131,54.066316941824,54.1487965694145,
54.2314023405145,54.2937793603386,54.3775180721845,54.4611535835521,54.5447060269508,
54.6281954628017,54.7116494134154,54.7950859072616,54.8785230170172,54.9619788119348,
55.0455233046645,55.1291123876056,55.2128356551632,55.2935153710587,55.3772540829047,
55.4608895942722,55.5444420376709,55.627931473522,55.7113854241356,55.7948219179819,
55.8782590277374,55.961714822655,56.0452593153847,56.1288483983257,56.2125716658834,
56.2932513817789,56.3769900936248,56.4606256049923,56.5441780483911,56.6276674842419,
56.7111214348556,56.7945579287019,56.8779950384574,56.9614508333752,57.0449953261048,
57.1285844090459,57.2123076766035,57.292987392499,57.376726104345,57.4603616157126,
57.5439140591111,57.6274034949616,57.7108574455754,57.7942939394216,57.8777310491771,
57.9611868440946,58.0447313368243,58.1283204197652,58.2120436873228,58.2927234032191,
58.3764621150651,58.4600976264325,58.5436500698315,58.6271395056821,58.7105934562957,
58.7940299501419,58.8774670598972,58.9609228548147,59.0444673475445,59.1280564304858,
59.2117796980434,59.2924594139393,59.3857393267099,59.4398822683535),
 .UNSPECIFIED.);
#84=B_SPLINE_CURVE_WITH_KNOTS('',3,(#20984,#20985,#20986,#20987,#20988,
#20989,#20990,#20991,#20992,#20993),.UNSPECIFIED.,.F.,.F.,(4,3,3,4),(53.1554707439118,
53.2392036250967,53.2940433496185,53.4070751110074),.UNSPECIFIED.);
#85=B_SPLINE_CURVE_WITH_KNOTS('',3,(#20995,#20996,#20997,#20998,#20999,
#21000,#21001,#21002,#21003,#21004),.UNSPECIFIED.,.F.,.F.,(4,3,3,4),(53.1554762266557,
53.2377493943412,53.3224122526225,53.4070751109039),.UNSPECIFIED.);
#86=B_SPLINE_CURVE_WITH_KNOTS('',3,(#21005,#21006,#21007,#21008,#21009,
#21010,#21011,#21012,#21013,#21014,#21015,#21016,#21017,#21018,#21019,#21020,
#21021,#21022,#21023,#21024,#21025,#21026,#21027,#21028,#21029,#21030,#21031,
#21032,#21033,#21034,#21035,#21036,#21037,#21038,#21039,#21040,#21041,#21042,
#21043,#21044,#21045,#21046,#21047,#21048,#21049,#21050,#21051,#21052,#21053,
#21054,#21055,#21056,#21057,#21058,#21059,#21060,#21061,#21062,#21063,#21064,
#21065,#21066,#21067,#21068,#21069,#21070,#21071,#21072,#21073,#21074,#21075,
#21076,#21077,#21078,#21079,#21080,#21081,#21082,#21083,#21084,#21085,#21086,
#21087,#21088,#21089,#21090,#21091,#21092,#21093,#21094,#21095,#21096,#21097,
#21098,#21099,#21100,#21101,#21102,#21103,#21104,#21105,#21106,#21107,#21108,
#21109,#21110,#21111,#21112,#21113,#21114,#21115,#21116,#21117,#21118,#21119,
#21120,#21121,#21122,#21123,#21124,#21125,#21126,#21127,#21128,#21129,#21130,
#21131,#21132,#21133,#21134,#21135,#21136,#21137,#21138,#21139,#21140,#21141,
#21142,#21143,#21144,#21145,#21146,#21147,#21148,#21149,#21150,#21151,#21152,
#21153,#21154,#21155,#21156,#21157,#21158,#21159,#21160,#21161,#21162,#21163,
#21164,#21165,#21166,#21167,#21168,#21169,#21170,#21171,#21172,#21173,#21174,
#21175,#21176,#21177,#21178,#21179,#21180,#21181,#21182,#21183,#21184,#21185,
#21186,#21187,#21188,#21189,#21190,#21191,#21192,#21193,#21194,#21195,#21196,
#21197,#21198,#21199,#21200,#21201,#21202,#21203,#21204,#21205,#21206,#21207,
#21208,#21209,#21210,#21211,#21212,#21213,#21214,#21215,#21216,#21217,#21218,
#21219,#21220,#21221),.UNSPECIFIED.,.F.,.F.,(4,3,3,3,3,3,3,3,3,3,3,3,3,
3,3,3,3,3,3,3,3,3,3,3,3,3,3,3,3,3,3,3,3,3,3,3,3,3,3,3,3,3,3,3,3,3,3,3,3,
3,3,3,3,3,3,3,3,3,3,3,3,3,3,3,3,3,3,3,3,3,3,3,4),(53.4070751110112,53.5281266875687,
53.6043339693332,53.6880726811791,53.7717081925466,53.8552606359451,53.9387500717959,
54.0222040224095,54.1056405162557,54.1890776260112,54.2725334209287,54.3560779136583,
54.4396669965993,54.5233902641568,54.6040699800534,54.6878086918993,54.7714442032668,
54.8549966466653,54.9384860825163,55.02194003313,55.1053765269762,55.1888136367316,
55.2722694316493,55.3558139243789,55.4394030073199,55.5231262748775,55.6038059907735,
55.6875447026194,55.771180213987,55.8547326573855,55.9382220932365,56.0216760438502,
56.1051125376965,56.188549647452,56.2720054423696,56.3555499350993,56.4391390180403,
56.522862285598,56.6035420014936,56.6872807133395,56.7709162247071,56.8544686681056,
56.9379581039566,57.0214120545703,57.1048485484165,57.188285658172,57.2717414530897,
57.3552859458194,57.4388750287604,57.522598296318,57.6032780122137,57.6870167240596,
57.7706522354271,57.8542046788257,57.9376941146768,58.0211480652904,58.1045845591367,
58.1880216688921,58.2714774638097,58.3550219565394,58.4386110394804,58.522334307038,
58.6030140229339,58.6867625271259,58.7704056656083,58.8539487725955,58.9374351492175,
59.0208829145339,59.1043101578345,59.1878874695081,59.2713533662358,59.3549863853822,
59.4386194045287),.UNSPECIFIED.);
#87=B_SPLINE_CURVE_WITH_KNOTS('',3,(#21227,#21228,#21229,#21230,#21231,
#21232,#21233,#21234,#21235,#21236,#21237,#21238,#21239,#21240,#21241,#21242,
#21243,#21244,#21245,#21246,#21247,#21248,#21249,#21250,#21251,#21252,#21253,
#21254,#21255,#21256,#21257,#21258,#21259,#21260,#21261,#21262,#21263,#21264,
#21265,#21266,#21267,#21268,#21269,#21270,#21271,#21272,#21273,#21274,#21275,
#21276,#21277,#21278,#21279,#21280,#21281,#21282,#21283,#21284,#21285,#21286,
#21287,#21288,#21289,#21290,#21291,#21292,#21293,#21294,#21295,#21296,#21297,
#21298,#21299,#21300,#21301,#21302,#21303,#21304,#21305,#21306,#21307,#21308,
#21309,#21310,#21311,#21312,#21313,#21314,#21315,#21316,#21317,#21318,#21319,
#21320,#21321,#21322,#21323,#21324,#21325,#21326,#21327,#21328,#21329,#21330,
#21331,#21332,#21333,#21334,#21335,#21336,#21337,#21338,#21339,#21340,#21341,
#21342,#21343,#21344,#21345,#21346,#21347,#21348,#21349,#21350,#21351,#21352,
#21353,#21354,#21355,#21356,#21357,#21358,#21359,#21360,#21361,#21362,#21363,
#21364,#21365,#21366,#21367,#21368,#21369,#21370,#21371,#21372,#21373,#21374,
#21375,#21376,#21377,#21378,#21379,#21380,#21381,#21382,#21383,#21384,#21385,
#21386,#21387,#21388,#21389,#21390,#21391,#21392,#21393,#21394,#21395,#21396,
#21397,#21398,#21399,#21400,#21401,#21402,#21403,#21404,#21405,#21406,#21407,
#21408,#21409,#21410,#21411,#21412,#21413,#21414,#21415,#21416,#21417,#21418,
#21419,#21420,#21421,#21422,#21423,#21424,#21425,#21426,#21427,#21428,#21429,
#21430,#21431,#21432,#21433,#21434,#21435,#21436,#21437,#21438,#21439,#21440,
#21441,#21442,#21443,#21444,#21445,#21446),.UNSPECIFIED.,.F.,.F.,(4,3,3,
3,3,3,3,3,3,3,3,3,3,3,3,3,3,3,3,3,3,3,3,3,3,3,3,3,3,3,3,3,3,3,3,3,3,3,3,
3,3,3,3,3,3,3,3,3,3,3,3,3,3,3,3,3,3,3,3,3,3,3,3,3,3,3,3,3,3,3,3,3,3,4),
(59.6902604181869,59.7747787530522,59.8593179788568,59.9438945410883,60.0309697619811,
60.1157222054673,60.2039588150634,60.2921954246594,60.3759341365053,60.4595696478729,
60.5431220912715,60.6266115271223,60.710065477736,60.7935019715823,60.8769390813379,
60.9603948762555,61.0439393689852,61.1275284519262,61.2112517194837,61.2919314353795,
61.3756701472254,61.4593056585929,61.5428581019914,61.6263475378422,61.7098014884559,
61.7932379823021,61.8766750920576,61.9601308869752,62.0436753797049,62.1272644626459,
62.2109877302035,62.2916674460996,62.3754061579455,62.459041669313,62.5425941127115,
62.6260835485626,62.7095374991762,62.7929739930223,62.8764111027777,62.959866897695,
63.0434113904248,63.1270004733656,63.2107237409232,63.2914034568198,63.3751421686657,
63.4587776800333,63.5423301234322,63.6258195592835,63.7092735098971,63.7927100037433,
63.8761471134986,63.9596029084161,64.0431474011459,64.1267364840869,64.2104597516445,
64.2911394675399,64.3748781793858,64.4585136907535,64.5420661341521,64.625555570003,
64.7090095206166,64.792446014463,64.8758831242186,64.9593389191362,65.0428834118659,
65.1264724948068,65.2101957623644,65.29087547826,65.3743504055609,65.4613697556974,
65.544635511258,65.6278429630006,65.7110052807257,65.7224278061069),
 .UNSPECIFIED.);
#88=B_SPLINE_CURVE_WITH_KNOTS('',3,(#21447,#21448,#21449,#21450,#21451,
#21452,#21453,#21454,#21455,#21456),.UNSPECIFIED.,.F.,.F.,(4,3,3,4),(59.4398822683535,
59.5326783695403,59.6250277789513,59.6902604180037),.UNSPECIFIED.);
#89=B_SPLINE_CURVE_WITH_KNOTS('',3,(#21458,#21459,#21460,#21461,#21462,
#21463,#21464,#21465,#21466,#21467),.UNSPECIFIED.,.F.,.F.,(4,3,3,4),(59.4386194045287,
59.5223427634998,59.602750033654,59.6902604181908),.UNSPECIFIED.);
#90=B_SPLINE_CURVE_WITH_KNOTS('',3,(#21468,#21469,#21470,#21471,#21472,
#21473,#21474,#21475,#21476,#21477,#21478,#21479,#21480,#21481,#21482,#21483,
#21484,#21485,#21486,#21487,#21488,#21489,#21490,#21491,#21492,#21493,#21494,
#21495,#21496,#21497,#21498,#21499,#21500,#21501,#21502,#21503,#21504,#21505,
#21506,#21507,#21508,#21509,#21510,#21511,#21512,#21513,#21514,#21515,#21516,
#21517,#21518,#21519,#21520,#21521,#21522,#21523,#21524,#21525,#21526,#21527,
#21528,#21529,#21530,#21531,#21532,#21533,#21534,#21535,#21536,#21537,#21538,
#21539,#21540,#21541,#21542,#21543,#21544,#21545,#21546,#21547,#21548,#21549,
#21550,#21551,#21552,#21553,#21554,#21555,#21556,#21557,#21558,#21559,#21560,
#21561,#21562,#21563,#21564,#21565,#21566,#21567,#21568,#21569,#21570,#21571,
#21572,#21573,#21574,#21575,#21576,#21577,#21578,#21579,#21580,#21581,#21582,
#21583,#21584,#21585,#21586,#21587,#21588,#21589,#21590,#21591,#21592,#21593,
#21594,#21595,#21596,#21597,#21598,#21599,#21600,#21601,#21602,#21603,#21604,
#21605,#21606,#21607,#21608,#21609,#21610,#21611,#21612,#21613,#21614,#21615,
#21616,#21617,#21618,#21619,#21620,#21621,#21622,#21623,#21624,#21625,#21626,
#21627,#21628,#21629,#21630,#21631,#21632,#21633,#21634,#21635,#21636,#21637,
#21638,#21639,#21640,#21641,#21642,#21643,#21644,#21645,#21646,#21647,#21648,
#21649,#21650,#21651,#21652,#21653,#21654,#21655,#21656,#21657,#21658,#21659,
#21660,#21661,#21662,#21663,#21664,#21665,#21666,#21667,#21668,#21669,#21670,
#21671,#21672,#21673,#21674,#21675,#21676,#21677,#21678,#21679,#21680,#21681,
#21682,#21683,#21684,#21685,#21686,#21687),.UNSPECIFIED.,.F.,.F.,(4,3,3,
3,3,3,3,3,3,3,3,3,3,3,3,3,3,3,3,3,3,3,3,3,3,3,3,3,3,3,3,3,3,3,3,3,3,3,3,
3,3,3,3,3,3,3,3,3,3,3,3,3,3,3,3,3,3,3,3,3,3,3,3,3,3,3,3,3,3,3,3,3,3,4),
(59.690260418325,59.7729922509435,59.8556292811794,59.9381925013212,60.0212291942028,
60.1037176127869,60.1861993999656,60.2686934103523,60.3521415688578,60.4347588661806,
60.5186224552774,60.6024860443741,60.68622475622,60.7698602675875,60.8534127109862,
60.936902146837,61.0203560974506,61.1037925912969,61.1872297010523,61.2706854959699,
61.3542299886996,61.4378190716406,61.5215423391982,61.6022220550943,61.6859607669403,
61.7695962783077,61.8531487217063,61.9366381575571,62.0200921081707,62.1035286020169,
62.1869657117725,62.2704215066901,62.3539659994198,62.4375550823607,62.5212783499182,
62.6019580658144,62.6856967776603,62.7693322890281,62.8528847324265,62.9363741682772,
63.0198281188909,63.1032646127372,63.1867017224929,63.2701575174107,63.3537020101404,
63.4372910930814,63.521014360639,63.6016940765345,63.6854327883804,63.7690682997479,
63.8526207431468,63.9361101789976,64.0195641296113,64.1030006234575,64.1864377332125,
64.2698935281301,64.3534380208598,64.4370271038007,64.5207503713583,64.6014300872547,
64.6851687991007,64.7688043104682,64.8523567538665,64.9358461897175,65.0193001403312,
65.1027366341774,65.186173743933,65.269629538851,65.3531740315807,65.4367631145216,
65.5204863820792,65.6011660979748,65.6963168570349,65.7229944280855),
 .UNSPECIFIED.);
#91=B_SPLINE_CURVE_WITH_KNOTS('',3,(#21693,#21694,#21695,#21696,#21697,
#21698,#21699,#21700,#21701,#21702,#21703,#21704,#21705,#21706,#21707,#21708,
#21709,#21710,#21711,#21712,#21713,#21714,#21715,#21716,#21717,#21718,#21719,
#21720,#21721,#21722,#21723,#21724,#21725,#21726,#21727,#21728,#21729,#21730,
#21731,#21732,#21733,#21734,#21735,#21736,#21737,#21738,#21739,#21740,#21741,
#21742,#21743,#21744,#21745,#21746,#21747,#21748,#21749,#21750,#21751,#21752,
#21753,#21754,#21755,#21756,#21757,#21758,#21759,#21760,#21761,#21762,#21763,
#21764,#21765,#21766,#21767,#21768,#21769,#21770,#21771,#21772,#21773,#21774,
#21775,#21776,#21777,#21778,#21779,#21780,#21781,#21782,#21783,#21784,#21785,
#21786,#21787,#21788,#21789,#21790,#21791,#21792,#21793,#21794,#21795,#21796,
#21797,#21798,#21799,#21800,#21801,#21802,#21803,#21804,#21805,#21806,#21807,
#21808,#21809,#21810,#21811,#21812,#21813,#21814,#21815,#21816,#21817,#21818,
#21819,#21820,#21821,#21822,#21823,#21824,#21825,#21826,#21827,#21828,#21829,
#21830,#21831,#21832,#21833,#21834,#21835,#21836,#21837,#21838,#21839,#21840,
#21841,#21842,#21843,#21844,#21845,#21846,#21847,#21848,#21849,#21850,#21851,
#21852,#21853,#21854,#21855,#21856,#21857,#21858,#21859,#21860,#21861,#21862,
#21863,#21864,#21865,#21866,#21867,#21868,#21869,#21870,#21871,#21872,#21873,
#21874,#21875,#21876,#21877,#21878,#21879,#21880,#21881,#21882,#21883,#21884,
#21885,#21886,#21887,#21888,#21889,#21890,#21891,#21892,#21893,#21894,#21895,
#21896,#21897,#21898,#21899,#21900,#21901,#21902,#21903,#21904,#21905,#21906,
#21907,#21908,#21909,#21910,#21911,#21912),.UNSPECIFIED.,.F.,.F.,(4,3,3,
3,3,3,3,3,3,3,3,3,3,3,3,3,3,3,3,3,3,3,3,3,3,3,3,3,3,3,3,3,3,3,3,3,3,3,3,
3,3,3,3,3,3,3,3,3,3,3,3,3,3,3,3,3,3,3,3,3,3,3,3,3,3,3,3,3,3,3,3,3,3,4),
(65.973445725537,66.0722016376632,66.1716623230831,66.2718883360919,66.2906114889802,
66.3743502008262,66.4579857121937,66.5415381555923,66.6250275914434,66.7084815420572,
66.7919180359034,66.875355145659,66.9588109405769,67.0423554333066,67.1259445162477,
67.2096677838053,67.2903474997003,67.3740862115462,67.4577217229137,67.5412741663122,
67.6247636021632,67.7082175527769,67.7916540466231,67.8750911563786,67.9585469512962,
68.0420914440259,68.1256805269669,68.2094037945244,68.2900835104204,68.3738222222663,
68.4574577336338,68.5410101770324,68.6244996128835,68.7079535634972,68.7913900573434,
68.8748271670989,68.9582829620166,69.0418274547463,69.1254165376873,69.2091398052449,
69.2898195211405,69.3735582329864,69.4571937443539,69.5407461877524,69.6242356236035,
69.7076895742171,69.7911260680634,69.8745631778188,69.9580189727365,70.0415634654662,
70.1251525484071,70.2088758159647,70.2895555318607,70.3732942437067,70.4569297550742,
70.5404821984727,70.6239716343238,70.7074255849375,70.7908620787838,70.8742991885393,
70.957754983457,71.0412994761868,71.1248885591278,71.2086118266854,71.2892915425808,
71.3726036548392,71.4557840971122,71.5388885214543,71.6219354908015,71.7049435228024,
71.7879472022301,71.8709469547149,71.9539898147039,72.0048655224089),
 .UNSPECIFIED.);
#92=B_SPLINE_CURVE_WITH_KNOTS('',3,(#21913,#21914,#21915,#21916,#21917,
#21918,#21919,#21920,#21921,#21922),.UNSPECIFIED.,.F.,.F.,(4,3,3,4),(65.7224278061069,
65.8055735571319,65.8895096412492,65.9734457253665),.UNSPECIFIED.);
#93=B_SPLINE_CURVE_WITH_KNOTS('',3,(#21924,#21925,#21926,#21927,#21928,
#21929,#21930,#21931,#21932,#21933),.UNSPECIFIED.,.F.,.F.,(4,3,3,4),(65.7229944280855,
65.8176176411345,65.9116665109351,65.9734457253704),.UNSPECIFIED.);
#94=B_SPLINE_CURVE_WITH_KNOTS('',3,(#21934,#21935,#21936,#21937,#21938,
#21939,#21940,#21941,#21942,#21943),.UNSPECIFIED.,.F.,.F.,(4,1,1,1,1,1,
1,4),(65.9734457253704,66.6009021086949,67.6006381194151,68.6003741301352,
69.6001101408553,70.5998461515754,71.5995821622956,72.0060503087704),
 .UNSPECIFIED.);
#95=B_SPLINE_CURVE_WITH_KNOTS('',3,(#21949,#21950,#21951,#21952,#21953,
#21954,#21955,#21956,#21957,#21958,#21959,#21960,#21961,#21962,#21963,#21964,
#21965,#21966,#21967,#21968,#21969,#21970,#21971,#21972,#21973,#21974,#21975,
#21976,#21977,#21978,#21979,#21980,#21981,#21982,#21983,#21984,#21985,#21986,
#21987,#21988,#21989,#21990,#21991,#21992,#21993,#21994,#21995,#21996,#21997,
#21998,#21999,#22000,#22001,#22002,#22003,#22004,#22005,#22006,#22007,#22008,
#22009,#22010,#22011,#22012,#22013,#22014,#22015,#22016,#22017,#22018,#22019,
#22020,#22021,#22022,#22023,#22024,#22025,#22026,#22027,#22028,#22029,#22030,
#22031,#22032,#22033,#22034,#22035,#22036,#22037,#22038,#22039,#22040,#22041,
#22042,#22043,#22044,#22045,#22046,#22047,#22048,#22049,#22050,#22051,#22052,
#22053,#22054,#22055,#22056,#22057,#22058,#22059,#22060,#22061,#22062,#22063,
#22064,#22065,#22066,#22067,#22068,#22069,#22070,#22071,#22072,#22073,#22074,
#22075,#22076,#22077,#22078,#22079,#22080,#22081,#22082,#22083,#22084,#22085,
#22086,#22087,#22088,#22089,#22090,#22091,#22092,#22093,#22094,#22095,#22096,
#22097,#22098,#22099,#22100,#22101,#22102,#22103,#22104,#22105,#22106,#22107,
#22108,#22109,#22110,#22111,#22112,#22113,#22114,#22115,#22116,#22117,#22118,
#22119,#22120,#22121,#22122,#22123,#22124,#22125,#22126,#22127,#22128,#22129,
#22130,#22131,#22132,#22133,#22134,#22135,#22136,#22137,#22138,#22139,#22140,
#22141,#22142,#22143,#22144,#22145,#22146,#22147,#22148,#22149,#22150,#22151,
#22152,#22153,#22154,#22155,#22156,#22157,#22158,#22159,#22160,#22161,#22162,
#22163,#22164,#22165,#22166,#22167,#22168,#22169,#22170,#22171),
 .UNSPECIFIED.,.F.,.F.,(4,3,3,3,3,3,3,3,3,3,3,3,3,3,3,3,3,3,3,3,3,3,3,3,
3,3,3,3,3,3,3,3,3,3,3,3,3,3,3,3,3,3,3,3,3,3,3,3,3,3,3,3,3,3,3,3,3,3,3,3,
3,3,3,3,3,3,3,3,3,3,3,3,3,3,4),(72.2566310325461,72.2890275533009,72.3727662651468,
72.4564017765142,72.5399542199127,72.6234436557635,72.7068976063771,72.7903341002233,
72.8737712099786,72.9572270048961,73.0407714976257,73.1243605805666,73.2080838481241,
73.2887635640211,73.372502275867,73.4561377872345,73.539690230633,73.6231796664841,
73.7066336170977,73.790070110944,73.8735072206994,73.956963015617,74.0405075083467,
74.1240965912877,74.2078198588453,74.2884995747412,74.3722382865871,74.4558737979546,
74.5394262413532,74.6229156772043,74.7063696278179,74.7898061216642,74.8732432314197,
74.9566990263373,75.0402435190669,75.1238326020079,75.2075558695655,75.2882355854613,
75.3719742973073,75.4556098086748,75.5391622520734,75.6226516879244,75.7061056385381,
75.7895421323844,75.87297924214,75.9564350370577,76.0399795297874,76.1235686127284,
76.207291880286,76.2879715961814,76.3717103080273,76.4553458193948,76.5388982627933,
76.6223876986444,76.7058416492581,76.7892781431043,76.8727152528598,76.9561710477774,
77.0397155405071,77.1233046234481,77.2070278910057,77.2877076069016,77.3714463187476,
77.4550818301151,77.5386342735135,77.6221237093646,77.7055776599783,77.7890141538246,
77.8724512635801,77.9559070584978,78.0394515512275,78.1230406341685,78.2067639017261,
78.2874436176217,78.2887592231474),.UNSPECIFIED.);
#96=B_SPLINE_CURVE_WITH_KNOTS('',3,(#22172,#22173,#22174,#22175,#22176,
#22177,#22178,#22179,#22180,#22181),.UNSPECIFIED.,.F.,.F.,(4,3,3,4),(72.0048655224089,
72.0880045572239,72.172317794814,72.256631032404),.UNSPECIFIED.);
#97=B_SPLINE_CURVE_WITH_KNOTS('',3,(#22183,#22184,#22185,#22186),
 .UNSPECIFIED.,.F.,.F.,(4,4),(72.0060503087704,72.2566310325499),
 .UNSPECIFIED.);
#98=B_SPLINE_CURVE_WITH_KNOTS('',3,(#22187,#22188,#22189,#22190,#22191,
#22192,#22193,#22194,#22195,#22196),.UNSPECIFIED.,.F.,.F.,(4,1,1,1,1,1,
1,4),(72.2566310325499,72.5993181730157,73.5990541837358,74.598790194456,
75.5985262051761,76.5982622158962,77.5979982266164,78.2879140477243),
 .UNSPECIFIED.);
#99=B_SPLINE_CURVE_WITH_KNOTS('',3,(#22202,#22203,#22204,#22205,#22206,
#22207,#22208,#22209,#22210,#22211,#22212,#22213,#22214,#22215,#22216,#22217,
#22218,#22219,#22220,#22221,#22222,#22223,#22224,#22225,#22226,#22227,#22228,
#22229,#22230,#22231,#22232,#22233,#22234,#22235,#22236,#22237,#22238,#22239,
#22240,#22241,#22242,#22243,#22244,#22245,#22246,#22247,#22248,#22249,#22250,
#22251,#22252,#22253,#22254,#22255,#22256,#22257,#22258,#22259,#22260,#22261,
#22262,#22263,#22264,#22265,#22266,#22267,#22268,#22269,#22270,#22271,#22272,
#22273,#22274,#22275,#22276,#22277,#22278,#22279,#22280,#22281,#22282,#22283,
#22284,#22285,#22286,#22287,#22288,#22289,#22290,#22291,#22292,#22293,#22294,
#22295,#22296,#22297,#22298,#22299,#22300,#22301,#22302,#22303,#22304,#22305,
#22306,#22307,#22308,#22309,#22310,#22311,#22312,#22313,#22314,#22315,#22316,
#22317,#22318,#22319,#22320,#22321,#22322,#22323,#22324,#22325,#22326,#22327,
#22328,#22329,#22330,#22331,#22332,#22333,#22334,#22335,#22336,#22337,#22338,
#22339,#22340,#22341,#22342,#22343,#22344,#22345,#22346,#22347,#22348,#22349,
#22350,#22351,#22352,#22353,#22354,#22355,#22356,#22357,#22358,#22359,#22360,
#22361,#22362,#22363,#22364,#22365,#22366,#22367,#22368,#22369,#22370,#22371,
#22372,#22373,#22374,#22375,#22376,#22377,#22378,#22379,#22380,#22381,#22382,
#22383,#22384,#22385,#22386,#22387,#22388,#22389,#22390,#22391,#22392,#22393,
#22394,#22395,#22396,#22397,#22398,#22399,#22400,#22401,#22402,#22403,#22404,
#22405,#22406,#22407,#22408,#22409,#22410,#22411,#22412,#22413,#22414,#22415,
#22416,#22417,#22418,#22419,#22420,#22421),.UNSPECIFIED.,.F.,.F.,(4,3,3,
3,3,3,3,3,3,3,3,3,3,3,3,3,3,3,3,3,3,3,3,3,3,3,3,3,3,3,3,3,3,3,3,3,3,3,3,
3,3,3,3,3,3,3,3,3,3,3,3,3,3,3,3,3,3,3,3,3,3,3,3,3,3,3,3,3,3,3,3,3,3,4),
(78.5398163397257,78.62239295459,78.705491288809,78.7879946449525,78.8704919407165,
78.9530020139644,79.0365464175588,79.1191811714259,79.2031803998838,79.2871796283418,
79.3709183401877,79.4545538515552,79.5381062949538,79.6215957308051,79.7050496814187,
79.788486175265,79.8719232850204,79.955379079938,80.0389235726677,80.1225126556086,
80.2062359231661,80.286915639062,80.3706543509079,80.4542898622755,80.5378423056737,
80.6213317415248,80.7047856921384,80.7882221859847,80.8716592957401,80.9551150906578,
81.0386595833875,81.1222486663285,81.2059719338861,81.2866516497821,81.370390361628,
81.4540258729957,81.5375783163942,81.6210677522452,81.7045217028589,81.7879581967051,
81.8713953064607,81.9548511013783,82.038395594108,82.121984677049,82.2057079446065,
82.2863876605022,82.3701263723481,82.4537618837154,82.5373143271138,82.6208037629648,
82.7042577135786,82.787694207425,82.8711313171803,82.9545871120976,83.0381316048273,
83.1217206877683,83.2054439553258,83.2861236712224,83.3698623830682,83.4534978944356,
83.5370503378342,83.6205397736848,83.7039937242985,83.7874302181448,83.8708673279002,
83.9543231228179,84.0378676155475,84.1214566984884,84.2051799660461,84.2858596819425,
84.3725698184977,84.4591613046955,84.5456123157065,84.5725992439732),
 .UNSPECIFIED.);
#100=B_SPLINE_CURVE_WITH_KNOTS('',3,(#22422,#22423,#22424,#22425,#22426,
#22427,#22428,#22429,#22430,#22431),.UNSPECIFIED.,.F.,.F.,(4,3,3,4),(78.2887592231474,
78.3981054868849,78.5051444124938,78.5398163395285),.UNSPECIFIED.);
#101=B_SPLINE_CURVE_WITH_KNOTS('',3,(#22433,#22434,#22435,#22436),
 .UNSPECIFIED.,.F.,.F.,(4,4),(78.2879140477243,78.5398092039209),
 .UNSPECIFIED.);
#102=B_SPLINE_CURVE_WITH_KNOTS('',3,(#22437,#22438,#22439,#22440,#22441,
#22442,#22443,#22444,#22445,#22446,#22447,#22448,#22449,#22450,#22451,#22452,
#22453,#22454,#22455,#22456,#22457,#22458,#22459,#22460,#22461,#22462,#22463,
#22464,#22465,#22466,#22467,#22468,#22469,#22470,#22471,#22472,#22473,#22474,
#22475,#22476,#22477,#22478,#22479,#22480,#22481,#22482,#22483,#22484,#22485,
#22486,#22487,#22488,#22489,#22490,#22491,#22492,#22493,#22494,#22495,#22496,
#22497,#22498,#22499,#22500,#22501,#22502,#22503,#22504,#22505,#22506,#22507,
#22508,#22509,#22510,#22511,#22512,#22513,#22514,#22515,#22516,#22517,#22518,
#22519,#22520,#22521,#22522,#22523,#22524,#22525,#22526,#22527,#22528,#22529,
#22530,#22531,#22532,#22533,#22534,#22535,#22536,#22537,#22538,#22539,#22540,
#22541,#22542,#22543,#22544,#22545,#22546,#22547,#22548,#22549,#22550,#22551,
#22552,#22553,#22554,#22555,#22556,#22557,#22558,#22559,#22560,#22561,#22562,
#22563,#22564,#22565,#22566,#22567,#22568,#22569,#22570,#22571,#22572,#22573,
#22574,#22575,#22576,#22577,#22578,#22579,#22580,#22581,#22582,#22583,#22584,
#22585,#22586,#22587,#22588,#22589,#22590,#22591,#22592,#22593,#22594,#22595,
#22596,#22597,#22598,#22599,#22600,#22601,#22602,#22603,#22604,#22605,#22606,
#22607,#22608,#22609,#22610,#22611,#22612,#22613,#22614,#22615,#22616,#22617,
#22618,#22619,#22620,#22621,#22622,#22623,#22624,#22625,#22626,#22627,#22628,
#22629,#22630,#22631,#22632,#22633,#22634,#22635,#22636,#22637,#22638,#22639,
#22640,#22641,#22642,#22643,#22644,#22645,#22646,#22647,#22648,#22649,#22650,
#22651,#22652,#22653,#22654,#22655,#22656),.UNSPECIFIED.,.F.,.F.,(4,3,3,
3,3,3,3,3,3,3,3,3,3,3,3,3,3,3,3,3,3,3,3,3,3,3,3,3,3,3,3,3,3,3,3,3,3,3,3,
3,3,3,3,3,3,3,3,3,3,3,3,3,3,3,3,3,3,3,3,3,3,3,3,3,3,3,3,3,3,3,3,3,3,4),
(78.5398163397295,78.5977342373365,78.6814729491824,78.7651084605499,78.8486609039486,
78.9321503397996,79.0156042904133,79.0990407842595,79.1824778940149,79.2659336889324,
79.3494781816621,79.4330672646031,79.5167905321606,79.5974702480566,79.6812089599025,
79.76484447127,79.8483969146685,79.9318863505195,80.0153403011332,80.0987767949795,
80.1822139047349,80.2656696996526,80.3492141923823,80.4328032753233,80.5165265428808,
80.5972062587768,80.6809449706228,80.7645804819903,80.8481329253889,80.93162236124,
81.0150763118536,81.0985128056999,81.1819499154554,81.2654057103731,81.3489502031028,
81.4325392860438,81.5162625536014,81.5969422694969,81.6806809813428,81.7643164927103,
81.8478689361088,81.9313583719598,82.0148123225734,82.0982488164197,82.1816859261751,
82.2651417210928,82.3486862138224,82.4322752967634,82.5159985643209,82.596678280217,
82.680416992063,82.7640525034305,82.8476049468291,82.9310943826802,83.0145483332938,
83.0979848271401,83.1814219368956,83.2648777318133,83.348422224543,83.432011307484,
83.5157345750416,83.5964142909372,83.6801543798819,83.7637909471208,83.847344126517,
83.9308339795196,84.0142867067674,84.0977215231147,84.1811565009327,84.264609708774,
84.3481453391041,84.4317253719729,84.5154248974244,84.571795089726),
 .UNSPECIFIED.);
#103=B_SPLINE_CURVE_WITH_KNOTS('',3,(#22662,#22663,#22664,#22665,#22666,
#22667,#22668,#22669,#22670,#22671,#22672,#22673,#22674,#22675,#22676,#22677,
#22678,#22679,#22680,#22681,#22682,#22683,#22684,#22685,#22686,#22687,#22688,
#22689,#22690,#22691,#22692,#22693,#22694,#22695,#22696,#22697,#22698,#22699,
#22700,#22701,#22702,#22703,#22704,#22705,#22706,#22707,#22708,#22709,#22710,
#22711,#22712,#22713,#22714,#22715,#22716,#22717,#22718,#22719,#22720,#22721,
#22722,#22723,#22724,#22725,#22726,#22727,#22728,#22729,#22730,#22731,#22732,
#22733,#22734,#22735,#22736,#22737,#22738,#22739,#22740,#22741,#22742,#22743,
#22744,#22745,#22746,#22747,#22748,#22749,#22750,#22751,#22752,#22753,#22754,
#22755,#22756,#22757,#22758,#22759,#22760,#22761,#22762,#22763,#22764,#22765,
#22766,#22767,#22768,#22769,#22770,#22771,#22772,#22773,#22774,#22775,#22776,
#22777,#22778,#22779,#22780,#22781,#22782,#22783,#22784,#22785,#22786,#22787,
#22788,#22789,#22790,#22791,#22792,#22793,#22794,#22795,#22796,#22797,#22798,
#22799,#22800,#22801,#22802,#22803,#22804,#22805,#22806,#22807,#22808,#22809,
#22810,#22811,#22812,#22813,#22814,#22815,#22816,#22817,#22818,#22819,#22820,
#22821,#22822,#22823,#22824,#22825,#22826,#22827,#22828,#22829,#22830,#22831,
#22832,#22833,#22834,#22835,#22836,#22837,#22838,#22839,#22840,#22841,#22842,
#22843,#22844,#22845,#22846,#22847,#22848,#22849,#22850,#22851,#22852,#22853,
#22854,#22855,#22856,#22857,#22858,#22859,#22860,#22861,#22862,#22863,#22864,
#22865,#22866,#22867,#22868,#22869,#22870,#22871,#22872,#22873,#22874,#22875,
#22876,#22877,#22878,#22879,#22880,#22881),.UNSPECIFIED.,.F.,.F.,(4,3,3,
3,3,3,3,3,3,3,3,3,3,3,3,3,3,3,3,3,3,3,3,3,3,3,3,3,3,3,3,3,3,3,3,3,3,3,3,
3,3,3,3,3,3,3,3,3,3,3,3,3,3,3,3,3,3,3,3,3,3,3,3,3,3,3,3,3,3,3,3,3,3,4),
(84.8230016470632,84.9118882294179,85.0053150952291,85.0946470022648,85.1841250841541,
85.2738132970661,85.2855956926626,85.3693344045085,85.452969915876,85.5365223592745,
85.6200117951256,85.7034657457393,85.7869022395855,85.8703393493409,85.9537951442584,
86.0373396369881,86.1209287199291,86.2046519874867,86.2853317033827,86.3690704152286,
86.4527059265962,86.5362583699947,86.6197478058457,86.7032017564594,86.7866382503057,
86.8700753600612,86.9535311549789,87.0370756477086,87.1206647306495,87.2043879982071,
87.2850677141029,87.3688064259488,87.4524419373163,87.5359943807148,87.6194838165659,
87.7029377671795,87.7863742610257,87.8698113707812,87.9532671656989,88.0368116584285,
88.1204007413695,88.2041240089271,88.284803724823,88.368542436669,88.4521779480365,
88.535730391435,88.619219827286,88.7026737778997,88.786110271746,88.8695473815015,
88.9530031764193,89.036547669149,89.12013675209,89.2038600196476,89.2845397355431,
89.368278447389,89.4519139587565,89.5354664021551,89.6189558380062,89.7024097886198,
89.7858462824661,89.8692833922215,89.9527391871391,90.0362836798687,90.1198727628097,
90.2035960303673,90.2842757462633,90.3667505459319,90.4491298248377,90.5314328034189,
90.6136786176278,90.69588927706,90.7781041156691,90.8545165002977),
 .UNSPECIFIED.);
#104=B_SPLINE_CURVE_WITH_KNOTS('',3,(#22882,#22883,#22884,#22885,#22886,
#22887,#22888,#22889,#22890,#22891),.UNSPECIFIED.,.F.,.F.,(4,3,3,4),(84.5725992439732,
84.6588962802708,84.7450885344468,84.8230016469053),.UNSPECIFIED.);
#105=B_SPLINE_CURVE_WITH_KNOTS('',3,(#22893,#22894,#22895,#22896,#22897,
#22898,#22899,#22900,#22901,#22902),.UNSPECIFIED.,.F.,.F.,(4,3,3,4),(84.571795089726,
84.5961503016573,84.7095759742832,84.8230016469091),.UNSPECIFIED.);
#106=B_SPLINE_CURVE_WITH_KNOTS('',3,(#22903,#22904,#22905,#22906,#22907,
#22908,#22909,#22910,#22911,#22912,#22913,#22914,#22915,#22916,#22917,#22918,
#22919,#22920,#22921,#22922,#22923,#22924,#22925,#22926,#22927,#22928,#22929,
#22930,#22931,#22932,#22933,#22934,#22935,#22936,#22937,#22938,#22939,#22940,
#22941,#22942,#22943,#22944,#22945,#22946,#22947,#22948,#22949,#22950,#22951,
#22952,#22953,#22954,#22955,#22956,#22957,#22958,#22959,#22960,#22961,#22962,
#22963,#22964,#22965,#22966,#22967,#22968,#22969,#22970,#22971,#22972,#22973,
#22974,#22975,#22976,#22977,#22978,#22979,#22980,#22981,#22982,#22983,#22984,
#22985,#22986,#22987,#22988,#22989,#22990,#22991,#22992,#22993,#22994,#22995,
#22996,#22997,#22998,#22999,#23000,#23001,#23002,#23003,#23004,#23005,#23006,
#23007,#23008,#23009,#23010,#23011,#23012,#23013,#23014,#23015,#23016,#23017,
#23018,#23019,#23020,#23021,#23022,#23023,#23024,#23025,#23026,#23027,#23028,
#23029,#23030,#23031,#23032,#23033,#23034,#23035,#23036,#23037,#23038,#23039,
#23040,#23041,#23042,#23043,#23044,#23045,#23046,#23047,#23048,#23049,#23050,
#23051,#23052,#23053,#23054,#23055,#23056,#23057,#23058,#23059,#23060,#23061,
#23062,#23063,#23064,#23065,#23066,#23067,#23068,#23069,#23070,#23071,#23072,
#23073,#23074,#23075,#23076,#23077,#23078,#23079,#23080,#23081,#23082,#23083,
#23084,#23085,#23086,#23087,#23088,#23089,#23090,#23091,#23092,#23093,#23094,
#23095,#23096,#23097,#23098,#23099,#23100,#23101,#23102,#23103,#23104,#23105,
#23106,#23107,#23108,#23109,#23110,#23111,#23112,#23113,#23114,#23115,#23116,
#23117,#23118,#23119,#23120,#23121,#23122),.UNSPECIFIED.,.F.,.F.,(4,3,3,
3,3,3,3,3,3,3,3,3,3,3,3,3,3,3,3,3,3,3,3,3,3,3,3,3,3,3,3,3,3,3,3,3,3,3,3,
3,3,3,3,3,3,3,3,3,3,3,3,3,3,3,3,3,3,3,3,3,3,3,3,3,3,3,3,3,3,3,3,3,3,4),
(84.8230016470494,84.9054512045182,84.9917555930006,85.0741114802006,85.1564545594353,
85.2388037750452,85.3211780738551,85.4036410329863,85.4861559906397,85.5687878473739,
85.5958863123774,85.6796250242234,85.763260535591,85.8468129789896,85.9303024148405,
86.0137563654542,86.0971928593005,86.180629969056,86.2640857639739,86.3476302567036,
86.4312193396445,86.5149426072021,86.5956223230975,86.6793610349434,86.762996546311,
86.8465489897096,86.9300384255609,87.0134923761746,87.0969288700208,87.1803659797762,
87.2638217746938,87.3473662674234,87.4309553503644,87.514678617922,87.5953583338177,
87.6790970456637,87.7627325570311,87.8462850004296,87.9297744362802,88.0132283868939,
88.0966648807401,88.1801019904954,88.2635577854131,88.3471022781427,88.4306913610839,
88.5144146286414,88.5950943445378,88.6788330563837,88.7624685677512,88.8460210111494,
88.9295104470006,89.0129643976143,89.0964008914605,89.1798380012159,89.2632937961336,
89.3468382888634,89.4304273718043,89.5141506393619,89.5948303552579,89.6785690671039,
89.7622045784714,89.8457570218702,89.929246457721,90.0127004083347,90.0961369021807,
90.1795740119362,90.2630298068536,90.3465742995832,90.430163382524,90.5138866500815,
90.5945663659781,90.6821700263414,90.7695849001495,90.8558404966185),
 .UNSPECIFIED.);
#107=B_SPLINE_CURVE_WITH_KNOTS('',3,(#23128,#23129,#23130,#23131,#23132,
#23133,#23134,#23135,#23136,#23137,#23138,#23139,#23140,#23141,#23142,#23143,
#23144,#23145,#23146,#23147,#23148,#23149,#23150,#23151,#23152,#23153,#23154,
#23155,#23156,#23157,#23158,#23159,#23160,#23161,#23162,#23163,#23164,#23165,
#23166,#23167,#23168,#23169,#23170,#23171,#23172,#23173,#23174,#23175,#23176,
#23177,#23178,#23179,#23180,#23181,#23182,#23183,#23184,#23185,#23186,#23187,
#23188,#23189,#23190,#23191,#23192,#23193,#23194,#23195,#23196,#23197,#23198,
#23199,#23200,#23201,#23202,#23203,#23204,#23205,#23206,#23207,#23208,#23209,
#23210,#23211,#23212,#23213,#23214,#23215,#23216,#23217,#23218,#23219,#23220,
#23221,#23222,#23223,#23224,#23225,#23226,#23227,#23228,#23229,#23230,#23231,
#23232,#23233,#23234,#23235,#23236,#23237,#23238,#23239,#23240,#23241,#23242,
#23243,#23244,#23245,#23246,#23247,#23248,#23249,#23250,#23251,#23252,#23253,
#23254,#23255,#23256,#23257,#23258,#23259,#23260,#23261,#23262,#23263,#23264,
#23265,#23266,#23267,#23268,#23269,#23270,#23271,#23272,#23273,#23274,#23275,
#23276,#23277,#23278,#23279,#23280,#23281,#23282,#23283,#23284,#23285,#23286,
#23287,#23288,#23289,#23290,#23291,#23292,#23293,#23294,#23295,#23296,#23297,
#23298,#23299,#23300,#23301,#23302,#23303,#23304,#23305,#23306,#23307,#23308,
#23309,#23310,#23311,#23312,#23313,#23314,#23315,#23316,#23317,#23318,#23319,
#23320,#23321,#23322,#23323,#23324,#23325,#23326,#23327,#23328,#23329,#23330,
#23331,#23332,#23333,#23334,#23335,#23336,#23337,#23338,#23339,#23340,#23341,
#23342,#23343,#23344,#23345,#23346,#23347),.UNSPECIFIED.,.F.,.F.,(4,3,3,
3,3,3,3,3,3,3,3,3,3,3,3,3,3,3,3,3,3,3,3,3,3,3,3,3,3,3,3,3,3,3,3,3,3,3,3,
3,3,3,3,3,3,3,3,3,3,3,3,3,3,3,3,3,3,3,3,3,3,3,3,3,3,3,3,3,3,3,3,3,3,4),
(91.1061869540849,91.2342698388801,91.2840117569834,91.3677504688293,91.4513859801969,
91.5349384235956,91.6184278594466,91.7018818100603,91.7853183039066,91.8687554136621,
91.95221120858,92.0357557013097,92.1193447842506,92.2030680518082,92.2837477677035,
92.3674864795494,92.4511219909169,92.5346744343155,92.6181638701666,92.7016178207802,
92.7850543146265,92.8684914243819,92.9519472192995,93.0354917120292,93.1190807949702,
93.2028040625277,93.2834837784236,93.3672224902695,93.450858001637,93.5344104450355,
93.6178998808865,93.7013538315002,93.7847903253464,93.8682274351018,93.9516832300195,
94.0352277227491,94.1188168056901,94.2025400732476,94.2832197891438,94.3669585009898,
94.4505940123573,94.5341464557559,94.6176358916069,94.7010898422206,94.7845263360669,
94.8679634458224,94.9514192407401,95.0349637334698,95.1185528164108,95.2022760839684,
95.2829557998639,95.3666945117099,95.4503300230774,95.5338824664759,95.6173719023269,
95.7008258529406,95.7842623467869,95.8676994565424,95.9511552514601,96.0346997441898,
96.1182888271308,96.2020120946884,96.282691810584,96.3664390909035,96.4500812622947,
96.5360408032565,96.6195259372999,96.7029733472777,96.7864011215343,96.8698273312194,
96.9532987109112,97.0367978149355,97.120372459563,97.1377575899893),
 .UNSPECIFIED.);
#108=B_SPLINE_CURVE_WITH_KNOTS('',3,(#23348,#23349,#23350,#23351,#23352,
#23353,#23354,#23355,#23356,#23357),.UNSPECIFIED.,.F.,.F.,(4,3,3,4),(90.8545165002977,
90.9367707195664,91.0214788367447,91.106186953923),.UNSPECIFIED.);
#109=B_SPLINE_CURVE_WITH_KNOTS('',3,(#23359,#23360,#23361,#23362,#23363,
#23364,#23365,#23366,#23367,#23368),.UNSPECIFIED.,.F.,.F.,(4,3,3,4),(90.8558404966185,
90.943003649067,91.0300245809721,91.1061869540887),.UNSPECIFIED.);
#110=B_SPLINE_CURVE_WITH_KNOTS('',3,(#23369,#23370,#23371,#23372,#23373,
#23374,#23375,#23376,#23377,#23378,#23379,#23380,#23381,#23382,#23383,#23384,
#23385,#23386,#23387,#23388,#23389,#23390,#23391,#23392,#23393,#23394,#23395,
#23396,#23397,#23398,#23399,#23400,#23401,#23402,#23403,#23404,#23405,#23406,
#23407,#23408,#23409,#23410,#23411,#23412,#23413,#23414,#23415,#23416,#23417,
#23418,#23419,#23420,#23421,#23422,#23423,#23424,#23425,#23426,#23427,#23428,
#23429,#23430,#23431,#23432,#23433,#23434,#23435,#23436,#23437,#23438,#23439,
#23440,#23441,#23442,#23443,#23444,#23445,#23446,#23447,#23448,#23449,#23450,
#23451,#23452,#23453,#23454,#23455,#23456,#23457,#23458,#23459,#23460,#23461,
#23462,#23463,#23464,#23465,#23466,#23467,#23468,#23469,#23470,#23471,#23472,
#23473,#23474,#23475,#23476,#23477,#23478,#23479,#23480,#23481,#23482,#23483,
#23484,#23485,#23486,#23487,#23488,#23489,#23490,#23491,#23492,#23493,#23494,
#23495,#23496,#23497,#23498,#23499,#23500,#23501,#23502,#23503,#23504,#23505,
#23506,#23507,#23508,#23509,#23510,#23511,#23512,#23513,#23514,#23515,#23516,
#23517,#23518,#23519,#23520,#23521,#23522,#23523,#23524,#23525,#23526,#23527,
#23528,#23529,#23530,#23531,#23532,#23533,#23534,#23535,#23536,#23537,#23538,
#23539,#23540,#23541,#23542,#23543,#23544,#23545,#23546,#23547,#23548,#23549,
#23550,#23551,#23552,#23553,#23554,#23555,#23556,#23557,#23558,#23559,#23560,
#23561,#23562,#23563,#23564,#23565,#23566,#23567,#23568,#23569,#23570,#23571,
#23572,#23573,#23574,#23575,#23576,#23577,#23578,#23579,#23580,#23581,#23582,
#23583,#23584,#23585,#23586,#23587,#23588),.UNSPECIFIED.,.F.,.F.,(4,3,3,
3,3,3,3,3,3,3,3,3,3,3,3,3,3,3,3,3,3,3,3,3,3,3,3,3,3,3,3,3,3,3,3,3,3,3,3,
3,3,3,3,3,3,3,3,3,3,3,3,3,3,3,3,3,3,3,3,3,3,3,3,3,3,3,3,3,3,3,3,3,3,4),
(91.1061869542033,91.1940293877261,91.2820034417824,91.3702005362681,91.4585174044926,
91.5470388628258,91.5943023766982,91.6780410885441,91.7616765999115,91.8452290433101,
91.9287184791611,92.0121724297747,92.095608923621,92.1790460333764,92.262501828294,
92.3460463210237,92.4296354039646,92.5133586715222,92.5940383874183,92.6777770992642,
92.7614126106318,92.8449650540303,92.9284544898813,93.011908440495,93.0953449343413,
93.1787820440968,93.2622378390145,93.3457823317442,93.4293714146852,93.5130946822428,
93.5937743981385,93.6775131099844,93.7611486213519,93.8447010647504,93.9281905006014,
94.0116444512151,94.0950809450613,94.1785180548168,94.2619738497344,94.3455183424641,
94.429107425405,94.5128306929626,94.5935104088586,94.6772491207046,94.7608846320721,
94.8444370754706,94.9279265113217,95.0113804619354,95.0948169557816,95.1782540655371,
95.2617098604549,95.3452543531846,95.4288434361256,95.5125667036832,95.5932464195787,
95.6769851314246,95.7606206427921,95.8441730861908,95.927662522042,96.0111164726556,
96.0945529665019,96.1779900762574,96.2614458711751,96.3449903639048,96.4285794468458,
96.5123027144034,96.5929824302989,96.6755077426029,96.7579368247763,96.8402888703964,
96.9225805906639,97.0048367170366,97.0870887865323,97.1377977613825),
 .UNSPECIFIED.);
#111=B_SPLINE_CURVE_WITH_KNOTS('',3,(#23594,#23595,#23596,#23597,#23598,
#23599,#23600,#23601,#23602,#23603,#23604,#23605,#23606,#23607,#23608,#23609,
#23610,#23611,#23612,#23613,#23614,#23615,#23616,#23617,#23618,#23619,#23620,
#23621,#23622,#23623,#23624,#23625,#23626,#23627,#23628,#23629,#23630,#23631,
#23632,#23633,#23634,#23635,#23636,#23637,#23638,#23639,#23640,#23641,#23642,
#23643,#23644,#23645,#23646,#23647,#23648,#23649,#23650,#23651,#23652,#23653,
#23654,#23655,#23656,#23657,#23658,#23659,#23660,#23661,#23662,#23663,#23664,
#23665,#23666,#23667,#23668,#23669,#23670,#23671,#23672,#23673,#23674,#23675,
#23676,#23677,#23678,#23679,#23680,#23681,#23682,#23683,#23684,#23685,#23686,
#23687,#23688,#23689,#23690,#23691,#23692,#23693,#23694,#23695,#23696,#23697,
#23698,#23699,#23700,#23701,#23702,#23703,#23704,#23705,#23706,#23707,#23708,
#23709,#23710,#23711,#23712,#23713,#23714,#23715,#23716,#23717,#23718,#23719,
#23720,#23721,#23722,#23723,#23724,#23725,#23726,#23727,#23728,#23729,#23730,
#23731,#23732,#23733,#23734,#23735,#23736,#23737,#23738,#23739,#23740,#23741,
#23742,#23743,#23744,#23745,#23746,#23747,#23748,#23749,#23750,#23751,#23752,
#23753,#23754,#23755,#23756,#23757,#23758,#23759,#23760,#23761,#23762,#23763,
#23764,#23765,#23766,#23767,#23768,#23769,#23770,#23771,#23772,#23773,#23774,
#23775,#23776,#23777,#23778,#23779,#23780,#23781,#23782,#23783,#23784,#23785,
#23786,#23787,#23788,#23789,#23790,#23791,#23792,#23793,#23794,#23795,#23796,
#23797,#23798,#23799,#23800,#23801,#23802,#23803,#23804,#23805,#23806,#23807,
#23808,#23809,#23810,#23811,#23812,#23813),.UNSPECIFIED.,.F.,.F.,(4,3,3,
3,3,3,3,3,3,3,3,3,3,3,3,3,3,3,3,3,3,3,3,3,3,3,3,3,3,3,3,3,3,3,3,3,3,3,3,
3,3,3,3,3,3,3,3,3,3,3,3,3,3,3,3,3,3,3,3,3,3,3,3,3,3,3,3,3,3,3,3,3,3,4),
(97.3893722614005,97.4719677846863,97.5544719674218,97.6369058779297,97.7192955269354,
97.8016628999257,97.884026934726,97.9664065640542,98.0488700592945,98.1313770056035,
98.2140118307161,98.2821638320243,98.3659025438702,98.4495380552377,98.5330904986362,
98.6165799344873,98.7000338851009,98.7834703789472,98.8669074887027,98.9503632836207,
99.0339077763503,99.1174968592912,99.2012201268488,99.2818998427444,99.3656385545902,
99.449274065958,99.5328265093568,99.6163159452077,99.6997698958214,99.7832063896676,
99.8666434994231,99.9500992943405,100.03364378707,100.117232870011,100.200956137569,
100.281635853465,100.365374565311,100.449010076678,100.532562520077,100.616051955928,
100.699505906542,100.782942400388,100.866379510144,100.949835305062,101.033379797791,
101.116968880732,101.20069214829,101.281371864185,101.365110576031,101.448746087398,
101.532298530797,101.615787966648,101.699241917262,101.782678411108,101.866115520863,
101.949571315781,102.033115808511,102.116704891452,102.200428159009,102.281107874905,
102.364846586751,102.448482098118,102.532034541517,102.615523977367,102.698977927981,
102.782414421827,102.865851531583,102.949307326501,103.03285181923,103.116440902171,
103.200164169729,103.280843885625,103.374544855062,103.422164115585),
 .UNSPECIFIED.);
#112=B_SPLINE_CURVE_WITH_KNOTS('',3,(#23814,#23815,#23816,#23817,#23818,
#23819,#23820,#23821,#23822,#23823),.UNSPECIFIED.,.F.,.F.,(4,3,3,4),(97.1377575899893,
97.2214880297379,97.2824278213041,97.3893722612645),.UNSPECIFIED.);
#113=B_SPLINE_CURVE_WITH_KNOTS('',3,(#23825,#23826,#23827,#23828,#23829,
#23830,#23831,#23832,#23833,#23834),.UNSPECIFIED.,.F.,.F.,(4,3,3,4),(97.1377977613825,
97.2200836147453,97.3047279379176,97.3893722610898),.UNSPECIFIED.);
#114=B_SPLINE_CURVE_WITH_KNOTS('',3,(#23835,#23836,#23837,#23838,#23839,
#23840,#23841,#23842,#23843,#23844,#23845,#23846,#23847,#23848,#23849,#23850,
#23851,#23852,#23853,#23854,#23855,#23856,#23857,#23858,#23859,#23860,#23861,
#23862,#23863,#23864,#23865,#23866,#23867,#23868,#23869,#23870,#23871,#23872,
#23873,#23874,#23875,#23876,#23877,#23878,#23879,#23880,#23881,#23882,#23883,
#23884,#23885,#23886,#23887,#23888,#23889,#23890,#23891,#23892,#23893,#23894,
#23895,#23896,#23897,#23898,#23899,#23900,#23901,#23902,#23903,#23904,#23905,
#23906,#23907,#23908,#23909,#23910,#23911,#23912,#23913,#23914,#23915,#23916,
#23917,#23918,#23919,#23920,#23921,#23922,#23923,#23924,#23925,#23926,#23927,
#23928,#23929,#23930,#23931,#23932,#23933,#23934,#23935,#23936,#23937,#23938,
#23939,#23940,#23941,#23942,#23943,#23944,#23945,#23946,#23947,#23948,#23949,
#23950,#23951,#23952,#23953,#23954,#23955,#23956,#23957,#23958,#23959,#23960,
#23961,#23962,#23963,#23964,#23965,#23966,#23967,#23968,#23969,#23970,#23971,
#23972,#23973,#23974,#23975,#23976,#23977,#23978,#23979,#23980,#23981,#23982,
#23983,#23984,#23985,#23986,#23987,#23988,#23989,#23990,#23991,#23992,#23993,
#23994,#23995,#23996,#23997,#23998,#23999,#24000,#24001,#24002,#24003,#24004,
#24005,#24006,#24007,#24008,#24009,#24010,#24011,#24012,#24013,#24014,#24015,
#24016,#24017,#24018,#24019,#24020,#24021,#24022,#24023,#24024,#24025,#24026,
#24027,#24028,#24029,#24030,#24031,#24032,#24033,#24034,#24035,#24036,#24037,
#24038,#24039,#24040,#24041,#24042,#24043,#24044,#24045,#24046,#24047,#24048,
#24049,#24050,#24051),.UNSPECIFIED.,.F.,.F.,(4,3,3,3,3,3,3,3,3,3,3,3,3,
3,3,3,3,3,3,3,3,3,3,3,3,3,3,3,3,3,3,3,3,3,3,3,3,3,3,3,3,3,3,3,3,3,3,3,3,
3,3,3,3,3,3,3,3,3,3,3,3,3,3,3,3,3,3,3,3,3,3,3,4),(97.3893722612683,97.5085709008744,
97.592718441019,97.676457152865,97.7600926642325,97.8436451076312,97.9271345434824,
98.0105884940961,98.0940249879424,98.177462097698,98.2609178926158,98.3444623853455,
98.4280514682866,98.5117747358442,98.5924544517391,98.676193163585,98.7598286749525,
98.843381118351,98.926870554202,99.0103245048157,99.0937609986619,99.1771981084174,
99.2606539033351,99.3441983960647,99.4277874790057,99.5115107465633,99.5921904624593,
99.6759291743052,99.7595646856727,99.8431171290711,99.9266065649221,100.010060515536,
100.093497009382,100.176934119137,100.260389914055,100.343934406785,100.427523489726,
100.511246757283,100.591926473179,100.675665185025,100.759300696393,100.842853139791,
100.926342575642,101.009796526256,101.093233020102,101.176670129858,101.260125924776,
101.343670417505,101.427259500446,101.510982768004,101.5916624839,101.675401195746,
101.759036707114,101.842589150512,101.926078586363,102.009532536977,102.092969030823,
102.176406140579,102.259861935497,102.343406428226,102.426995511167,102.510718778725,
102.59139849462,102.675147385514,102.758790830291,102.84233402803,102.925820381412,
103.009268009692,103.09269500225,103.176148517115,103.2596128892,103.3431540916,
103.420910293148),.UNSPECIFIED.);
#115=B_SPLINE_CURVE_WITH_KNOTS('',3,(#24057,#24058,#24059,#24060,#24061,
#24062,#24063,#24064,#24065,#24066,#24067,#24068,#24069,#24070,#24071,#24072,
#24073,#24074,#24075,#24076,#24077,#24078,#24079,#24080,#24081,#24082,#24083,
#24084,#24085,#24086,#24087,#24088,#24089,#24090,#24091,#24092,#24093,#24094,
#24095,#24096,#24097,#24098,#24099,#24100,#24101,#24102,#24103,#24104,#24105,
#24106,#24107,#24108,#24109,#24110,#24111,#24112,#24113,#24114,#24115,#24116,
#24117,#24118,#24119,#24120,#24121,#24122,#24123,#24124,#24125,#24126,#24127,
#24128,#24129,#24130,#24131,#24132,#24133,#24134,#24135,#24136,#24137,#24138,
#24139,#24140,#24141,#24142,#24143,#24144,#24145,#24146,#24147,#24148,#24149,
#24150,#24151,#24152,#24153,#24154,#24155,#24156,#24157,#24158,#24159,#24160,
#24161,#24162,#24163,#24164,#24165,#24166,#24167,#24168,#24169,#24170,#24171,
#24172,#24173,#24174,#24175,#24176,#24177,#24178,#24179,#24180,#24181,#24182,
#24183,#24184,#24185,#24186,#24187,#24188,#24189,#24190,#24191,#24192,#24193,
#24194,#24195,#24196,#24197,#24198,#24199,#24200,#24201,#24202,#24203,#24204,
#24205,#24206,#24207,#24208,#24209,#24210,#24211,#24212,#24213,#24214,#24215,
#24216,#24217,#24218,#24219,#24220,#24221,#24222,#24223,#24224,#24225,#24226,
#24227,#24228,#24229,#24230,#24231,#24232,#24233,#24234,#24235,#24236,#24237,
#24238,#24239,#24240,#24241,#24242,#24243,#24244,#24245,#24246,#24247,#24248,
#24249,#24250,#24251,#24252,#24253,#24254,#24255,#24256,#24257,#24258,#24259,
#24260,#24261,#24262,#24263,#24264,#24265,#24266,#24267,#24268,#24269,#24270,
#24271,#24272,#24273,#24274,#24275,#24276),.UNSPECIFIED.,.F.,.F.,(4,3,3,
3,3,3,3,3,3,3,3,3,3,3,3,3,3,3,3,3,3,3,3,3,3,3,3,3,3,3,3,3,3,3,3,3,3,3,3,
3,3,3,3,3,3,3,3,3,3,3,3,3,3,3,3,3,3,3,3,3,3,3,3,3,3,3,3,3,3,3,3,3,3,4),
(103.672557568444,103.756948747136,103.841357026278,103.925799068812,104.014494275695,
104.099107419003,104.18379133639,104.268605737223,104.280579896345,104.364318608191,
104.447954119558,104.531506562957,104.614995998808,104.698449949422,104.781886443268,
104.865323553023,104.948779347941,105.03232384067,105.115912923611,105.199636191169,
105.280315907065,105.364054618911,105.447690130278,105.531242573677,105.614732009527,
105.698185960141,105.781622453987,105.865059563743,105.94851535866,106.03205985139,
106.115648934331,106.199372201889,106.280051917785,106.363790629631,106.447426140998,
106.530978584397,106.614468020248,106.697921970862,106.781358464708,106.864795574464,
106.948251369382,107.031795862111,107.115384945052,107.19910821261,107.279787928505,
107.363526640351,107.447162151719,107.530714595117,107.614204030968,107.697657981582,
107.781094475428,107.864531585183,107.947987380101,108.031531872831,108.115120955772,
108.198844223329,108.279523939226,108.363262651072,108.44689816244,108.530450605838,
108.613940041689,108.697393992303,108.780830486149,108.864267595905,108.947723390823,
109.031267883552,109.114856966493,109.198580234051,109.279259949946,109.362821357527,
109.448305160013,109.531656885119,109.618206726296,109.704756567473),
 .UNSPECIFIED.);
#116=B_SPLINE_CURVE_WITH_KNOTS('',3,(#24277,#24278,#24279,#24280,#24281,
#24282,#24283,#24284,#24285,#24286),.UNSPECIFIED.,.F.,.F.,(4,3,3,4),(103.422164115585,
103.515371370637,103.608104590454,103.672557568256),.UNSPECIFIED.);
#117=B_SPLINE_CURVE_WITH_KNOTS('',3,(#24288,#24289,#24290,#24291,#24292,
#24293,#24294,#24295,#24296,#24297),.UNSPECIFIED.,.F.,.F.,(4,3,3,4),(103.420910293148,
103.506022399244,103.59113450534,103.672557568448),.UNSPECIFIED.);
#118=B_SPLINE_CURVE_WITH_KNOTS('',3,(#24298,#24299,#24300,#24301,#24302,
#24303,#24304,#24305,#24306,#24307,#24308,#24309,#24310,#24311,#24312,#24313,
#24314,#24315,#24316,#24317,#24318,#24319,#24320,#24321,#24322,#24323,#24324,
#24325,#24326,#24327,#24328,#24329,#24330,#24331,#24332,#24333,#24334,#24335,
#24336,#24337,#24338,#24339,#24340,#24341,#24342,#24343,#24344,#24345,#24346,
#24347,#24348,#24349,#24350,#24351,#24352,#24353,#24354,#24355,#24356,#24357,
#24358,#24359,#24360,#24361,#24362,#24363,#24364,#24365,#24366,#24367,#24368,
#24369,#24370,#24371,#24372,#24373,#24374,#24375,#24376,#24377,#24378,#24379,
#24380,#24381,#24382,#24383,#24384,#24385,#24386,#24387,#24388,#24389,#24390,
#24391,#24392,#24393,#24394,#24395,#24396,#24397,#24398,#24399,#24400,#24401,
#24402,#24403,#24404,#24405,#24406,#24407,#24408,#24409,#24410,#24411,#24412,
#24413,#24414,#24415,#24416,#24417,#24418,#24419,#24420,#24421,#24422,#24423,
#24424,#24425,#24426,#24427,#24428,#24429,#24430,#24431,#24432,#24433,#24434,
#24435,#24436,#24437,#24438,#24439,#24440,#24441,#24442,#24443,#24444,#24445,
#24446,#24447,#24448,#24449,#24450,#24451,#24452,#24453,#24454,#24455,#24456,
#24457,#24458,#24459,#24460,#24461,#24462,#24463,#24464,#24465,#24466,#24467,
#24468,#24469,#24470,#24471,#24472,#24473,#24474,#24475,#24476,#24477,#24478,
#24479,#24480,#24481,#24482,#24483,#24484,#24485,#24486,#24487,#24488,#24489,
#24490,#24491,#24492,#24493,#24494,#24495,#24496,#24497,#24498,#24499,#24500,
#24501,#24502,#24503,#24504,#24505,#24506,#24507,#24508,#24509,#24510,#24511,
#24512,#24513,#24514,#24515,#24516,#24517),.UNSPECIFIED.,.F.,.F.,(4,3,3,
3,3,3,3,3,3,3,3,3,3,3,3,3,3,3,3,3,3,3,3,3,3,3,3,3,3,3,3,3,3,3,3,3,3,3,3,
3,3,3,3,3,3,3,3,3,3,3,3,3,3,3,3,3,3,3,3,3,3,3,3,3,3,3,3,3,3,3,3,3,3,4),
(103.672557568579,103.755338549975,103.838023743102,103.920634109801,104.004413660583,
104.086946693849,104.169472251958,104.252009159745,104.336724498823,104.419384236231,
104.505127376145,104.59087051606,104.674609227906,104.758244739273,104.841797182672,
104.925286618523,105.008740569137,105.092177062983,105.175614172739,105.259069967657,
105.342614460386,105.426203543327,105.509926810885,105.59060652678,105.674345238626,
105.757980749993,105.841533193392,105.925022629242,106.008476579856,106.091913073702,
106.175350183458,106.258805978375,106.342350471105,106.425939554046,106.509662821604,
106.5903425375,106.674081249346,106.757716760713,106.841269204112,106.924758639964,
107.008212590577,107.091649084424,107.175086194179,107.258541989097,107.342086481826,
107.425675564767,107.509398832325,107.59007854822,107.673817260066,107.757452771433,
107.841005214832,107.924494650683,108.007948601297,108.091385095143,108.174822204899,
108.258277999817,108.341822492546,108.425411575487,108.509134843045,108.58981455894,
108.673553270786,108.757188782154,108.840741225552,108.924230661404,109.007684612017,
109.091121105864,109.174558215619,109.258014010538,109.341558503267,109.425147586208,
109.508870853766,109.589550569661,109.68519153841,109.705270710528),
 .UNSPECIFIED.);
#119=B_SPLINE_CURVE_WITH_KNOTS('',3,(#24523,#24524,#24525,#24526,#24527,
#24528,#24529,#24530,#24531,#24532,#24533,#24534,#24535,#24536,#24537,#24538,
#24539,#24540,#24541,#24542,#24543,#24544,#24545,#24546,#24547,#24548,#24549,
#24550,#24551,#24552,#24553,#24554,#24555,#24556,#24557,#24558,#24559,#24560,
#24561,#24562,#24563,#24564,#24565,#24566,#24567,#24568,#24569,#24570,#24571,
#24572,#24573,#24574,#24575,#24576,#24577,#24578,#24579,#24580,#24581,#24582,
#24583,#24584,#24585,#24586,#24587,#24588,#24589,#24590,#24591,#24592,#24593,
#24594,#24595,#24596,#24597,#24598,#24599,#24600,#24601,#24602,#24603,#24604,
#24605,#24606,#24607,#24608,#24609,#24610,#24611,#24612,#24613,#24614,#24615,
#24616,#24617,#24618,#24619,#24620,#24621,#24622,#24623,#24624,#24625,#24626,
#24627,#24628,#24629,#24630,#24631,#24632,#24633,#24634,#24635,#24636,#24637,
#24638,#24639,#24640,#24641,#24642,#24643,#24644,#24645,#24646,#24647,#24648,
#24649,#24650,#24651,#24652,#24653,#24654,#24655,#24656,#24657,#24658,#24659,
#24660,#24661,#24662,#24663,#24664,#24665,#24666,#24667,#24668,#24669,#24670,
#24671,#24672,#24673,#24674,#24675,#24676,#24677,#24678,#24679,#24680,#24681,
#24682,#24683,#24684,#24685,#24686,#24687,#24688,#24689,#24690,#24691,#24692,
#24693,#24694,#24695,#24696,#24697,#24698,#24699,#24700,#24701,#24702,#24703,
#24704,#24705,#24706,#24707,#24708,#24709,#24710,#24711,#24712,#24713,#24714,
#24715,#24716,#24717,#24718,#24719,#24720,#24721,#24722,#24723,#24724,#24725,
#24726,#24727,#24728,#24729,#24730,#24731,#24732,#24733,#24734,#24735,#24736,
#24737,#24738,#24739,#24740,#24741,#24742),.UNSPECIFIED.,.F.,.F.,(4,3,3,
3,3,3,3,3,3,3,3,3,3,3,3,3,3,3,3,3,3,3,3,3,3,3,3,3,3,3,3,3,3,3,3,3,3,3,3,
3,3,3,3,3,3,3,3,3,3,3,3,3,3,3,3,3,3,3,3,3,3,3,3,3,3,3,3,3,3,3,3,3,3,4),
(109.955742875801,110.053908632085,110.152728187028,110.252279042651,110.278995960666,
110.362734672512,110.446370183879,110.529922627278,110.613412063129,110.696866013743,
110.780302507589,110.863739617344,110.947195412262,111.030739904991,111.114328987932,
111.19805225549,111.278731971386,111.362470683232,111.446106194599,111.529658637998,
111.613148073849,111.696602024463,111.780038518309,111.863475628064,111.946931422982,
112.030475915712,112.114064998653,112.19778826621,112.278467982106,112.362206693952,
112.445842205319,112.529394648718,112.612884084569,112.696338035182,112.779774529029,
112.863211638784,112.946667433702,113.030211926431,113.113801009372,113.19752427693,
113.278203992826,113.361942704672,113.445578216039,113.529130659438,113.612620095289,
113.696074045903,113.779510539749,113.862947649505,113.946403444422,114.029947937152,
114.113537020093,114.197260287651,114.277940003546,114.361678715392,114.44531422676,
114.528866670158,114.612356106009,114.695810056623,114.779246550469,114.862683660225,
114.946139455142,115.029683947872,115.113273030813,115.196996298371,115.277676014266,
115.360916343682,115.444025174985,115.527058070878,115.610033652872,115.692970496751,
115.775902763453,115.858831416099,115.94180178495,115.987147173825),
 .UNSPECIFIED.);
#120=B_SPLINE_CURVE_WITH_KNOTS('',3,(#24743,#24744,#24745,#24746,#24747,
#24748,#24749,#24750,#24751,#24752),.UNSPECIFIED.,.F.,.F.,(4,3,3,4),(109.704756567473,
109.787983735154,109.871863305389,109.955742875624),.UNSPECIFIED.);
#121=B_SPLINE_CURVE_WITH_KNOTS('',3,(#24754,#24755,#24756,#24757,#24758,
#24759,#24760,#24761,#24762,#24763),.UNSPECIFIED.,.F.,.F.,(4,3,3,4),(109.705270710528,
109.800372858636,109.894864507288,109.955742875431),.UNSPECIFIED.);
#122=B_SPLINE_CURVE_WITH_KNOTS('',3,(#24764,#24765,#24766,#24767,#24768,
#24769,#24770,#24771,#24772,#24773,#24774,#24775,#24776,#24777,#24778,#24779,
#24780,#24781,#24782,#24783,#24784,#24785,#24786,#24787,#24788,#24789,#24790,
#24791,#24792,#24793,#24794,#24795,#24796,#24797,#24798,#24799,#24800,#24801,
#24802,#24803,#24804,#24805,#24806,#24807,#24808,#24809,#24810,#24811,#24812,
#24813,#24814,#24815,#24816,#24817,#24818,#24819,#24820,#24821,#24822,#24823,
#24824,#24825,#24826,#24827,#24828,#24829,#24830,#24831,#24832,#24833,#24834,
#24835,#24836,#24837,#24838,#24839,#24840,#24841,#24842,#24843,#24844,#24845,
#24846,#24847,#24848,#24849,#24850,#24851,#24852,#24853,#24854,#24855,#24856,
#24857,#24858,#24859,#24860,#24861,#24862,#24863,#24864,#24865,#24866,#24867,
#24868,#24869,#24870,#24871,#24872,#24873,#24874,#24875,#24876,#24877,#24878,
#24879,#24880,#24881,#24882,#24883,#24884,#24885,#24886,#24887,#24888,#24889,
#24890,#24891,#24892,#24893,#24894,#24895,#24896,#24897,#24898,#24899,#24900,
#24901,#24902,#24903,#24904,#24905,#24906,#24907,#24908,#24909,#24910,#24911,
#24912,#24913,#24914,#24915,#24916,#24917,#24918,#24919,#24920,#24921,#24922,
#24923,#24924,#24925,#24926,#24927,#24928,#24929,#24930,#24931,#24932,#24933,
#24934,#24935,#24936,#24937,#24938,#24939,#24940,#24941,#24942,#24943,#24944,
#24945,#24946,#24947,#24948,#24949,#24950,#24951,#24952,#24953,#24954,#24955,
#24956,#24957,#24958,#24959,#24960,#24961,#24962,#24963,#24964,#24965,#24966,
#24967,#24968,#24969,#24970,#24971,#24972,#24973,#24974,#24975,#24976,#24977,
#24978,#24979,#24980,#24981,#24982,#24983),.UNSPECIFIED.,.F.,.F.,(4,3,3,
3,3,3,3,3,3,3,3,3,3,3,3,3,3,3,3,3,3,3,3,3,3,3,3,3,3,3,3,3,3,3,3,3,3,3,3,
3,3,3,3,3,3,3,3,3,3,3,3,3,3,3,3,3,3,3,3,3,3,3,3,3,3,3,3,3,3,3,3,3,3,4),
(109.955742875628,110.039648469011,110.123556652528,110.207484832012,110.291450422462,
110.375523162037,110.459655763239,110.543923584594,110.589286580381,110.673025292227,
110.756660803595,110.840213246993,110.923702682844,111.007156633458,111.090593127304,
111.17403023706,111.257486031977,111.341030524707,111.424619607648,111.508342875206,
111.589022591101,111.672761302947,111.756396814314,111.839949257713,111.923438693564,
112.006892644178,112.090329138024,112.173766247779,112.257222042697,112.340766535426,
112.424355618367,112.508078885925,112.588758601821,112.672497313667,112.756132825034,
112.839685268433,112.923174704284,113.006628654898,113.090065148744,113.173502258499,
113.256958053417,113.340502546147,113.424091629088,113.507814896646,113.588494612541,
113.672233324387,113.755868835754,113.839421279153,113.922910715004,114.006364665617,
114.089801159464,114.173238269219,114.256694064136,114.340238556866,114.423827639807,
114.507550907365,114.588230623261,114.671969335107,114.755604846474,114.839157289873,
114.922646725724,115.006100676337,115.089537170184,115.172974279939,115.256430074857,
115.339974567586,115.423563650527,115.507286918084,115.587966633981,115.671933979496,
115.755764025857,115.839515095663,115.923193376346,115.988071988884),
 .UNSPECIFIED.);
#123=B_SPLINE_CURVE_WITH_KNOTS('',3,(#24989,#24990,#24991,#24992,#24993,
#24994,#24995,#24996,#24997,#24998,#24999,#25000,#25001,#25002,#25003,#25004,
#25005,#25006,#25007,#25008,#25009,#25010,#25011,#25012,#25013,#25014,#25015,
#25016,#25017,#25018,#25019,#25020,#25021,#25022,#25023,#25024,#25025,#25026,
#25027,#25028,#25029,#25030,#25031,#25032,#25033,#25034,#25035,#25036,#25037,
#25038,#25039,#25040,#25041,#25042,#25043,#25044,#25045,#25046,#25047,#25048,
#25049,#25050,#25051,#25052,#25053,#25054,#25055,#25056,#25057,#25058,#25059,
#25060,#25061,#25062,#25063,#25064,#25065,#25066,#25067,#25068,#25069,#25070,
#25071,#25072,#25073,#25074,#25075,#25076,#25077,#25078,#25079,#25080,#25081,
#25082,#25083,#25084,#25085,#25086,#25087,#25088,#25089,#25090,#25091,#25092,
#25093,#25094,#25095,#25096,#25097,#25098,#25099,#25100,#25101,#25102,#25103,
#25104,#25105,#25106,#25107,#25108,#25109,#25110,#25111,#25112,#25113,#25114,
#25115,#25116,#25117,#25118,#25119,#25120,#25121,#25122,#25123,#25124,#25125,
#25126,#25127,#25128,#25129,#25130,#25131,#25132,#25133,#25134,#25135,#25136,
#25137,#25138,#25139,#25140,#25141,#25142,#25143,#25144,#25145,#25146,#25147,
#25148,#25149,#25150,#25151,#25152,#25153,#25154,#25155,#25156,#25157,#25158,
#25159,#25160,#25161,#25162,#25163,#25164,#25165,#25166,#25167,#25168,#25169,
#25170,#25171,#25172,#25173,#25174,#25175,#25176,#25177,#25178,#25179,#25180,
#25181,#25182,#25183,#25184,#25185,#25186,#25187,#25188,#25189,#25190,#25191,
#25192,#25193,#25194,#25195,#25196,#25197,#25198,#25199,#25200,#25201,#25202,
#25203,#25204,#25205,#25206,#25207,#25208),.UNSPECIFIED.,.F.,.F.,(4,3,3,
3,3,3,3,3,3,3,3,3,3,3,3,3,3,3,3,3,3,3,3,3,3,3,3,3,3,3,3,3,3,3,3,3,3,3,3,
3,3,3,3,3,3,3,3,3,3,3,3,3,3,3,3,3,3,3,3,3,3,3,3,3,3,3,3,3,3,3,3,3,3,4),
(116.238928182803,116.277412024987,116.361150736833,116.4447862482,116.528338691599,
116.61182812745,116.695282078063,116.778718571909,116.862155681664,116.945611476582,
117.029155969311,117.112745052252,117.19646831981,117.277148035707,117.360886747553,
117.44452225892,117.528074702319,117.61156413817,117.695018088784,117.77845458263,
117.861891692385,117.945347487303,118.028891980033,118.112481062974,118.196204330531,
118.276884046427,118.360622758273,118.44425826964,118.527810713039,118.61130014889,
118.694754099503,118.77819059335,118.861627703105,118.945083498023,119.028627990752,
119.112217073693,119.195940341251,119.276620057147,119.360358768993,119.44399428036,
119.527546723759,119.61103615961,119.694490110224,119.77792660407,119.861363713826,
119.944819508743,120.028364001473,120.111953084414,120.195676351972,120.276356067867,
120.360094779713,120.44373029108,120.527282734479,120.61077217033,120.694226120944,
120.77766261479,120.861099724545,120.944555519463,121.028100012192,121.111689095133,
121.195412362691,121.276092078587,121.359831060277,121.443466778056,121.5270193647,
121.610508880833,121.693962581455,121.77739873563,121.860835415973,121.944290691593,
122.027833400628,122.111420662809,122.195139108014,122.271018544109),
 .UNSPECIFIED.);
#124=B_SPLINE_CURVE_WITH_KNOTS('',3,(#25209,#25210,#25211,#25212,#25213,
#25214,#25215,#25216,#25217,#25218),.UNSPECIFIED.,.F.,.F.,(4,3,3,4),(115.987147173825,
116.070212549419,116.154570366029,116.238928182639),.UNSPECIFIED.);
#125=B_SPLINE_CURVE_WITH_KNOTS('',3,(#25220,#25221,#25222,#25223,#25224,
#25225,#25226,#25227,#25228,#25229),.UNSPECIFIED.,.F.,.F.,(4,3,3,4),(115.988071988884,
116.071683453257,116.155305818032,116.238928182807),.UNSPECIFIED.);
#126=B_SPLINE_CURVE_WITH_KNOTS('',3,(#25230,#25231,#25232,#25233,#25234,
#25235,#25236,#25237,#25238,#25239,#25240,#25241,#25242,#25243,#25244,#25245,
#25246,#25247,#25248,#25249,#25250,#25251,#25252,#25253,#25254,#25255,#25256,
#25257,#25258,#25259,#25260,#25261,#25262,#25263,#25264,#25265,#25266,#25267,
#25268,#25269,#25270,#25271,#25272,#25273,#25274,#25275,#25276,#25277,#25278,
#25279,#25280,#25281,#25282,#25283,#25284,#25285,#25286,#25287,#25288,#25289,
#25290,#25291,#25292,#25293,#25294,#25295,#25296,#25297,#25298,#25299,#25300,
#25301,#25302,#25303,#25304,#25305,#25306,#25307,#25308,#25309,#25310,#25311,
#25312,#25313,#25314,#25315,#25316,#25317,#25318,#25319,#25320,#25321,#25322,
#25323,#25324,#25325,#25326,#25327,#25328,#25329,#25330,#25331,#25332,#25333,
#25334,#25335,#25336,#25337,#25338,#25339,#25340,#25341,#25342,#25343,#25344,
#25345,#25346,#25347,#25348,#25349,#25350,#25351,#25352,#25353,#25354,#25355,
#25356,#25357,#25358,#25359,#25360,#25361,#25362,#25363,#25364,#25365,#25366,
#25367,#25368,#25369,#25370,#25371,#25372,#25373,#25374,#25375,#25376,#25377,
#25378,#25379,#25380,#25381,#25382,#25383,#25384,#25385,#25386,#25387,#25388,
#25389,#25390,#25391,#25392,#25393,#25394,#25395,#25396,#25397,#25398,#25399,
#25400,#25401,#25402,#25403,#25404,#25405,#25406,#25407,#25408,#25409,#25410,
#25411,#25412,#25413,#25414,#25415,#25416,#25417,#25418,#25419,#25420,#25421,
#25422,#25423,#25424,#25425,#25426,#25427,#25428,#25429,#25430,#25431,#25432,
#25433,#25434,#25435,#25436,#25437,#25438,#25439,#25440,#25441,#25442,#25443,
#25444,#25445,#25446,#25447,#25448,#25449),.UNSPECIFIED.,.F.,.F.,(4,3,3,
3,3,3,3,3,3,3,3,3,3,3,3,3,3,3,3,3,3,3,3,3,3,3,3,3,3,3,3,3,3,3,3,3,3,3,3,
3,3,3,3,3,3,3,3,3,3,3,3,3,3,3,3,3,3,3,3,3,3,3,3,3,3,3,3,3,3,3,3,3,3,4),
(116.238928183003,116.334849321083,116.431253899856,116.528269407277,116.587702644701,
116.671441356547,116.755076867914,116.838629311313,116.922118747164,117.005572697778,
117.089009191624,117.17244630138,117.255902096297,117.339446589027,117.423035671968,
117.506758939526,117.587438655422,117.671177367268,117.754812878636,117.838365322034,
117.921854757885,118.005308708499,118.088745202345,118.172182312101,118.255638107018,
118.339182599748,118.422771682689,118.506494950247,118.587174666142,118.670913377988,
118.754548889355,118.838101332754,118.921590768605,119.005044719218,119.088481213064,
119.17191832282,119.255374117737,119.338918610467,119.422507693408,119.506230960966,
119.586910676862,119.670649388708,119.754284900075,119.837837343474,119.921326779325,
120.004780729939,120.088217223785,120.17165433354,120.255110128458,120.338654621188,
120.422243704129,120.505966971687,120.586646687582,120.670385399428,120.754020910795,
120.837573354194,120.921062790045,121.004516740659,121.087953234505,121.17139034426,
121.254846139178,121.338390631908,121.421979714849,121.505702982407,121.586382698302,
121.671870895413,121.754714488921,121.837482997203,121.920195242189,122.002869998466,
122.085539448033,122.168206900628,122.250910091201,122.27028827519),
 .UNSPECIFIED.);
#127=B_SPLINE_CURVE_WITH_KNOTS('',3,(#25455,#25456,#25457,#25458,#25459,
#25460,#25461,#25462,#25463,#25464,#25465,#25466,#25467,#25468,#25469,#25470,
#25471,#25472,#25473,#25474,#25475,#25476,#25477,#25478,#25479,#25480,#25481,
#25482,#25483,#25484,#25485,#25486,#25487,#25488,#25489,#25490,#25491,#25492,
#25493,#25494,#25495,#25496,#25497,#25498,#25499,#25500,#25501,#25502,#25503,
#25504,#25505,#25506,#25507,#25508,#25509,#25510,#25511,#25512,#25513,#25514,
#25515,#25516,#25517,#25518,#25519,#25520,#25521,#25522,#25523,#25524,#25525,
#25526,#25527,#25528,#25529,#25530,#25531,#25532,#25533,#25534,#25535,#25536,
#25537,#25538,#25539,#25540,#25541,#25542,#25543,#25544,#25545,#25546,#25547,
#25548,#25549,#25550,#25551,#25552,#25553,#25554,#25555,#25556,#25557,#25558,
#25559,#25560,#25561,#25562,#25563,#25564,#25565,#25566,#25567,#25568,#25569,
#25570,#25571,#25572,#25573,#25574,#25575,#25576,#25577,#25578,#25579,#25580,
#25581,#25582,#25583,#25584,#25585,#25586,#25587,#25588,#25589,#25590,#25591,
#25592,#25593,#25594,#25595,#25596,#25597,#25598,#25599,#25600,#25601,#25602,
#25603,#25604,#25605,#25606,#25607,#25608,#25609,#25610,#25611,#25612,#25613,
#25614,#25615,#25616,#25617,#25618,#25619,#25620,#25621,#25622,#25623,#25624,
#25625,#25626,#25627,#25628,#25629,#25630,#25631,#25632,#25633,#25634,#25635,
#25636,#25637,#25638,#25639,#25640,#25641,#25642,#25643,#25644,#25645,#25646,
#25647,#25648,#25649,#25650,#25651,#25652,#25653,#25654,#25655,#25656,#25657,
#25658,#25659,#25660,#25661,#25662,#25663,#25664,#25665,#25666,#25667,#25668,
#25669,#25670,#25671,#25672,#25673,#25674),.UNSPECIFIED.,.F.,.F.,(4,3,3,
3,3,3,3,3,3,3,3,3,3,3,3,3,3,3,3,3,3,3,3,3,3,3,3,3,3,3,3,3,3,3,3,3,3,3,3,
3,3,3,3,3,3,3,3,3,3,3,3,3,3,3,3,3,3,3,3,3,3,3,3,3,3,3,3,3,3,3,3,3,3,4),
(122.522113489983,122.604654564358,122.688518256317,122.770981109149,122.853436233243,
122.93590249609,123.020817897075,123.103407097541,123.189485598785,123.275564100028,
123.359302811874,123.442938323242,123.52649076664,123.609980202491,123.693434153104,
123.77687064695,123.860307756706,123.943763551624,124.027308044353,124.110897127294,
124.194620394852,124.275300110748,124.359038822594,124.442674333961,124.52622677736,
124.609716213211,124.693170163825,124.776606657671,124.860043767427,124.943499562344,
125.027044055074,125.110633138015,125.194356405572,125.275036121468,125.358774833314,
125.442410344681,125.52596278808,125.609452223931,125.692906174545,125.776342668391,
125.859779778146,125.943235573064,126.026780065794,126.110369148735,126.194092416292,
126.274772132188,126.358510844034,126.442146355402,126.5256987988,126.609188234651,
126.692642185265,126.776078679111,126.859515788866,126.942971583784,127.026516076514,
127.110105159455,127.193828427013,127.274508142908,127.358246854754,127.441882366121,
127.525434809519,127.60892424537,127.692378195984,127.77581468983,127.859251799586,
127.942707594504,128.026252087233,128.109841170174,128.193564437732,128.274244153628,
128.361156935022,128.44794892309,128.534597940399,128.554911617023),
 .UNSPECIFIED.);
#128=B_SPLINE_CURVE_WITH_KNOTS('',3,(#25675,#25676,#25677,#25678,#25679,
#25680,#25681,#25682,#25683,#25684,#25685,#25686,#25687),.UNSPECIFIED.,
 .F.,.F.,(4,3,3,3,4),(122.271018544109,122.275828089307,122.386363683307,
122.494373601401,122.522113489845),.UNSPECIFIED.);
#129=B_SPLINE_CURVE_WITH_KNOTS('',3,(#25689,#25690,#25691,#25692,#25693,
#25694,#25695,#25696,#25697,#25698),.UNSPECIFIED.,.F.,.F.,(4,3,3,4),(122.27028827519,
122.35308028165,122.43759688576,122.52211348987),.UNSPECIFIED.);
#130=B_SPLINE_CURVE_WITH_KNOTS('',3,(#25699,#25700,#25701,#25702,#25703,
#25704,#25705,#25706,#25707,#25708,#25709,#25710,#25711,#25712,#25713,#25714,
#25715,#25716,#25717,#25718,#25719,#25720,#25721,#25722,#25723,#25724,#25725,
#25726,#25727,#25728,#25729,#25730,#25731,#25732,#25733,#25734,#25735,#25736,
#25737,#25738,#25739,#25740,#25741,#25742,#25743,#25744,#25745,#25746,#25747,
#25748,#25749,#25750,#25751,#25752,#25753,#25754,#25755,#25756,#25757,#25758,
#25759,#25760,#25761,#25762,#25763,#25764,#25765,#25766,#25767,#25768,#25769,
#25770,#25771,#25772,#25773,#25774,#25775,#25776,#25777,#25778,#25779,#25780,
#25781,#25782,#25783,#25784,#25785,#25786,#25787,#25788,#25789,#25790,#25791,
#25792,#25793,#25794,#25795,#25796,#25797,#25798,#25799,#25800,#25801,#25802,
#25803,#25804,#25805,#25806,#25807,#25808,#25809,#25810,#25811,#25812,#25813,
#25814,#25815,#25816,#25817,#25818,#25819,#25820,#25821,#25822,#25823,#25824,
#25825,#25826,#25827,#25828,#25829,#25830,#25831,#25832,#25833,#25834,#25835,
#25836,#25837,#25838,#25839,#25840,#25841,#25842,#25843,#25844,#25845,#25846,
#25847,#25848,#25849,#25850,#25851,#25852,#25853,#25854,#25855,#25856,#25857,
#25858,#25859,#25860,#25861,#25862,#25863,#25864,#25865,#25866,#25867,#25868,
#25869,#25870,#25871,#25872,#25873,#25874,#25875,#25876,#25877,#25878,#25879,
#25880,#25881,#25882,#25883,#25884,#25885,#25886,#25887,#25888,#25889,#25890,
#25891,#25892,#25893,#25894,#25895,#25896,#25897,#25898,#25899,#25900,#25901,
#25902,#25903,#25904,#25905,#25906,#25907,#25908,#25909,#25910,#25911,#25912,
#25913,#25914,#25915,#25916,#25917,#25918),.UNSPECIFIED.,.F.,.F.,(4,3,3,
3,3,3,3,3,3,3,3,3,3,3,3,3,3,3,3,3,3,3,3,3,3,3,3,3,3,3,3,3,3,3,3,3,3,3,3,
3,3,3,3,3,3,3,3,3,3,3,3,3,3,3,3,3,3,3,3,3,3,3,3,3,3,3,3,3,3,3,3,3,3,4),
(122.522113489987,122.586118709022,122.669857420868,122.753492932236,122.837045375634,
122.920534811485,123.003988762099,123.087425255945,123.170862365701,123.254318160619,
123.337862653349,123.42145173629,123.505175003848,123.585854719742,123.669593431588,
123.753228942956,123.836781386354,123.920270822205,124.003724772819,124.087161266665,
124.170598376421,124.254054171338,124.337598664068,124.421187747009,124.504911014567,
124.585590730463,124.669329442309,124.752964953677,124.836517397075,124.920006832926,
125.00346078354,125.086897277386,125.170334387142,125.25379018206,125.337334674789,
125.42092375773,125.504647025288,125.585326741183,125.669065453029,125.752700964396,
125.836253407795,125.919742843646,126.003196794259,126.086633288106,126.170070397861,
126.253526192779,126.337070685508,126.420659768449,126.504383036007,126.585062751903,
126.668801463749,126.752436975116,126.835989418515,126.919478854366,127.00293280498,
127.086369298826,127.169806408581,127.253262203499,127.336806696229,127.42039577917,
127.504119046727,127.584798762623,127.668539201737,127.752176038431,127.835729406909,
127.919219368881,128.002671805427,128.086106216966,128.169540675799,128.252993250309,
128.336526720534,128.420104546152,128.503798371839,128.554060123745),
 .UNSPECIFIED.);
#131=B_SPLINE_CURVE_WITH_KNOTS('',3,(#25924,#25925,#25926,#25927,#25928,
#25929,#25930,#25931,#25932,#25933,#25934,#25935,#25936,#25937,#25938,#25939,
#25940,#25941,#25942,#25943,#25944,#25945,#25946,#25947,#25948,#25949,#25950,
#25951,#25952,#25953,#25954,#25955,#25956,#25957,#25958,#25959,#25960,#25961,
#25962,#25963,#25964,#25965,#25966,#25967,#25968,#25969,#25970,#25971,#25972,
#25973,#25974,#25975,#25976,#25977,#25978,#25979,#25980,#25981,#25982,#25983,
#25984,#25985,#25986,#25987,#25988,#25989,#25990,#25991,#25992,#25993,#25994,
#25995,#25996,#25997,#25998,#25999,#26000,#26001,#26002,#26003,#26004,#26005,
#26006,#26007,#26008,#26009,#26010,#26011,#26012,#26013,#26014,#26015,#26016,
#26017,#26018,#26019,#26020,#26021,#26022,#26023,#26024,#26025,#26026,#26027,
#26028,#26029,#26030,#26031,#26032,#26033,#26034,#26035,#26036,#26037,#26038,
#26039,#26040,#26041,#26042,#26043,#26044,#26045,#26046,#26047,#26048,#26049,
#26050,#26051,#26052,#26053,#26054,#26055,#26056,#26057,#26058,#26059,#26060,
#26061,#26062,#26063,#26064,#26065,#26066,#26067,#26068,#26069,#26070,#26071,
#26072,#26073,#26074,#26075,#26076,#26077,#26078,#26079,#26080,#26081,#26082,
#26083,#26084,#26085,#26086,#26087,#26088,#26089,#26090,#26091,#26092,#26093,
#26094,#26095,#26096,#26097,#26098,#26099,#26100,#26101,#26102,#26103,#26104,
#26105,#26106,#26107,#26108,#26109,#26110,#26111,#26112,#26113,#26114,#26115,
#26116,#26117,#26118,#26119,#26120,#26121,#26122,#26123,#26124,#26125,#26126,
#26127,#26128,#26129,#26130,#26131,#26132,#26133,#26134,#26135,#26136,#26137,
#26138,#26139,#26140,#26141,#26142,#26143),.UNSPECIFIED.,.F.,.F.,(4,3,3,
3,3,3,3,3,3,3,3,3,3,3,3,3,3,3,3,3,3,3,3,3,3,3,3,3,3,3,3,3,3,3,3,3,3,3,3,
3,3,3,3,3,3,3,3,3,3,3,3,3,3,3,3,3,3,3,3,3,3,3,3,3,3,3,3,3,3,3,3,3,3,4),
(128.805298797295,128.8939242966,128.982712920427,129.07175499949,129.160936434563,
129.250328626049,129.273980164348,129.357718876194,129.441354387561,129.52490683096,
129.608396266811,129.691850217425,129.775286711271,129.858723821027,129.942179615945,
130.025724108675,130.109313191616,130.193036459173,130.273716175068,130.357454886914,
130.441090398282,130.52464284168,130.608132277531,130.691586228145,130.775022721991,
130.858459831747,130.941915626664,131.025460119394,131.109049202335,131.192772469893,
131.273452185789,131.357190897635,131.440826409003,131.524378852401,131.607868288252,
131.691322238866,131.774758732712,131.858195842468,131.941651637385,132.025196130115,
132.108785213056,132.192508480614,132.273188196509,132.356926908355,132.440562419722,
132.524114863121,132.607604298972,132.691058249585,132.774494743432,132.857931853187,
132.941387648105,133.024932140834,133.108521223775,133.192244491333,133.272924207229,
133.356662919075,133.440298430442,133.523850873841,133.607340309692,133.690794260306,
133.774230754152,133.857667863907,133.941123658825,134.024668151555,134.108257234496,
134.191980502053,134.272660217949,134.355141887779,134.43752788941,134.519837440161,
134.602089086034,134.684305498508,134.766524040057,134.836834981773),
 .UNSPECIFIED.);
#132=B_SPLINE_CURVE_WITH_KNOTS('',3,(#26144,#26145,#26146,#26147,#26148,
#26149,#26150,#26151,#26152,#26153),.UNSPECIFIED.,.F.,.F.,(4,3,3,4),(128.554911617023,
128.641404974725,128.727785214999,128.805298797162),.UNSPECIFIED.);
#133=B_SPLINE_CURVE_WITH_KNOTS('',3,(#26155,#26156,#26157,#26158,#26159,
#26160,#26161,#26162,#26163,#26164),.UNSPECIFIED.,.F.,.F.,(4,3,3,4),(128.554060123745,
128.584534773343,128.699129012509,128.805298797166),.UNSPECIFIED.);
#134=B_SPLINE_CURVE_WITH_KNOTS('',3,(#26165,#26166,#26167,#26168,#26169,
#26170,#26171,#26172,#26173,#26174,#26175,#26176,#26177,#26178,#26179,#26180,
#26181,#26182,#26183,#26184,#26185,#26186,#26187,#26188,#26189,#26190,#26191,
#26192,#26193,#26194,#26195,#26196,#26197,#26198,#26199,#26200,#26201,#26202,
#26203,#26204,#26205,#26206,#26207,#26208,#26209,#26210,#26211,#26212,#26213,
#26214,#26215,#26216,#26217,#26218,#26219,#26220,#26221,#26222,#26223,#26224,
#26225,#26226,#26227,#26228,#26229,#26230,#26231,#26232,#26233,#26234,#26235,
#26236,#26237,#26238,#26239,#26240,#26241,#26242,#26243,#26244,#26245,#26246,
#26247,#26248,#26249,#26250,#26251,#26252,#26253,#26254,#26255,#26256,#26257,
#26258,#26259,#26260,#26261,#26262,#26263,#26264,#26265,#26266,#26267,#26268,
#26269,#26270,#26271,#26272,#26273,#26274,#26275,#26276,#26277,#26278,#26279,
#26280,#26281,#26282,#26283,#26284,#26285,#26286,#26287,#26288,#26289,#26290,
#26291,#26292,#26293,#26294,#26295,#26296,#26297,#26298,#26299,#26300,#26301,
#26302,#26303,#26304,#26305,#26306,#26307,#26308,#26309,#26310,#26311,#26312,
#26313,#26314,#26315,#26316,#26317,#26318,#26319,#26320,#26321,#26322,#26323,
#26324,#26325,#26326,#26327,#26328,#26329,#26330,#26331,#26332,#26333,#26334,
#26335,#26336,#26337,#26338,#26339,#26340,#26341,#26342,#26343,#26344,#26345,
#26346,#26347,#26348,#26349,#26350,#26351,#26352,#26353,#26354,#26355,#26356,
#26357,#26358,#26359,#26360,#26361,#26362,#26363,#26364,#26365,#26366,#26367,
#26368,#26369,#26370,#26371,#26372,#26373,#26374,#26375,#26376,#26377,#26378,
#26379,#26380,#26381,#26382,#26383,#26384),.UNSPECIFIED.,.F.,.F.,(4,3,3,
3,3,3,3,3,3,3,3,3,3,3,3,3,3,3,3,3,3,3,3,3,3,3,3,3,3,3,3,3,3,3,3,3,3,3,3,
3,3,3,3,3,3,3,3,3,3,3,3,3,3,3,3,3,3,3,3,3,3,3,3,3,3,3,3,3,3,3,3,3,3,4),
(128.805298797311,128.887726483839,128.970091451098,129.052422139225,129.134737418886,
129.217056253792,129.299397608162,129.381826252758,129.464304627651,129.546902434122,
129.584270784063,129.668009495909,129.751645007276,129.835197450675,129.918686886526,
130.002140837139,130.085577330985,130.169014440741,130.252470235658,130.336014728388,
130.419603811329,130.503327078886,130.584006794783,130.667745506629,130.751381017996,
130.834933461395,130.918422897246,131.00187684786,131.085313341706,131.168750451462,
131.252206246379,131.335750739109,131.41933982205,131.503063089608,131.583742805503,
131.667481517349,131.751117028716,131.834669472115,131.918158907966,132.00161285858,
132.085049352426,132.168486462181,132.251942257099,132.335486749829,132.41907583277,
132.502799100327,132.583478816224,132.66721752807,132.750853039438,132.834405482836,
132.917894918687,133.001348869301,133.084785363147,133.168222472903,133.25167826782,
133.33522276055,133.418811843492,133.502535111049,133.583214826944,133.66695353879,
133.750589050157,133.834141493555,133.917630929406,134.00108488002,134.084521373866,
134.167958483622,134.251414278539,134.334958771269,134.41854785421,134.502271121768,
134.582950837664,134.670785363976,134.758427403399,134.838147840597),
 .UNSPECIFIED.);
#135=B_SPLINE_CURVE_WITH_KNOTS('',3,(#26390,#26391,#26392,#26393,#26394,
#26395,#26396,#26397,#26398,#26399,#26400,#26401,#26402,#26403,#26404,#26405,
#26406,#26407,#26408,#26409,#26410,#26411,#26412,#26413,#26414,#26415,#26416,
#26417,#26418,#26419,#26420,#26421,#26422,#26423,#26424,#26425,#26426,#26427,
#26428,#26429,#26430,#26431,#26432,#26433,#26434,#26435,#26436,#26437,#26438,
#26439,#26440,#26441,#26442,#26443,#26444,#26445,#26446,#26447,#26448,#26449,
#26450,#26451,#26452,#26453,#26454,#26455,#26456,#26457,#26458,#26459,#26460,
#26461,#26462,#26463,#26464,#26465,#26466,#26467,#26468,#26469,#26470,#26471,
#26472,#26473,#26474,#26475,#26476,#26477,#26478,#26479,#26480,#26481,#26482,
#26483,#26484,#26485,#26486,#26487,#26488,#26489,#26490,#26491,#26492,#26493,
#26494,#26495,#26496,#26497,#26498,#26499,#26500,#26501,#26502,#26503,#26504,
#26505,#26506,#26507,#26508,#26509,#26510,#26511,#26512,#26513,#26514,#26515,
#26516,#26517,#26518,#26519,#26520,#26521,#26522,#26523,#26524,#26525,#26526,
#26527,#26528,#26529,#26530,#26531,#26532,#26533,#26534,#26535,#26536,#26537,
#26538,#26539,#26540,#26541,#26542,#26543,#26544,#26545,#26546,#26547,#26548,
#26549,#26550,#26551,#26552,#26553,#26554,#26555,#26556,#26557,#26558,#26559,
#26560,#26561,#26562,#26563,#26564,#26565,#26566,#26567,#26568,#26569,#26570,
#26571,#26572,#26573,#26574,#26575,#26576,#26577,#26578,#26579,#26580,#26581,
#26582,#26583,#26584,#26585,#26586,#26587,#26588,#26589,#26590,#26591,#26592,
#26593,#26594,#26595,#26596,#26597,#26598,#26599,#26600,#26601,#26602,#26603,
#26604,#26605,#26606,#26607,#26608,#26609),.UNSPECIFIED.,.F.,.F.,(4,3,3,
3,3,3,3,3,3,3,3,3,3,3,3,3,3,3,3,3,3,3,3,3,3,3,3,3,3,3,3,3,3,3,3,3,3,3,3,
3,3,3,3,3,3,3,3,3,3,3,3,3,3,3,3,3,3,3,3,3,3,3,3,3,3,3,3,3,3,3,3,3,3,4),
(135.088484104342,135.214157566306,135.272396228669,135.356134940515,135.439770451882,
135.523322895281,135.606812331132,135.690266281746,135.773702775592,135.857139885347,
135.940595680265,136.024140172995,136.107729255936,136.191452523493,136.272132239389,
136.355870951235,136.439506462602,136.523058906001,136.606548341852,136.690002292465,
136.773438786311,136.856875896067,136.940331690984,137.023876183714,137.107465266655,
137.191188534212,137.271868250109,137.355606961955,137.439242473323,137.522794916721,
137.606284352572,137.689738303186,137.773174797032,137.856611906788,137.940067701705,
138.023612194435,138.107201277376,138.190924544934,138.271604260829,138.355342972675,
138.438978484043,138.522530927441,138.606020363292,138.689474313906,138.772910807752,
138.856347917508,138.939803712425,139.023348205155,139.106937288096,139.190660555654,
139.27134027155,139.355078983396,139.438714494763,139.522266938162,139.605756374013,
139.689210324627,139.772646818473,139.856083928229,139.939539723146,140.023084215876,
140.106673298817,140.190396566375,140.27107628227,140.354823944191,140.43846641674,
140.523663793172,140.607149308209,140.690596820117,140.774024417531,140.860529670196,
140.944000016269,141.027498490743,141.111069615446,141.120045428192),
 .UNSPECIFIED.);
#136=B_SPLINE_CURVE_WITH_KNOTS('',3,(#26610,#26611,#26612,#26613,#26614,
#26615,#26616,#26617,#26618,#26619),.UNSPECIFIED.,.F.,.F.,(4,3,3,4),(134.836834981773,
134.919091621056,135.003787862626,135.088484104197),.UNSPECIFIED.);
#137=B_SPLINE_CURVE_WITH_KNOTS('',3,(#26621,#26622,#26623,#26624,#26625,
#26626,#26627,#26628,#26629,#26630),.UNSPECIFIED.,.F.,.F.,(4,3,3,4),(134.838147840597,
134.925534959382,135.012769870911,135.088484104346),.UNSPECIFIED.);
#138=B_SPLINE_CURVE_WITH_KNOTS('',3,(#26631,#26632,#26633,#26634,#26635,
#26636,#26637,#26638,#26639,#26640,#26641,#26642,#26643,#26644,#26645,#26646,
#26647,#26648,#26649,#26650,#26651,#26652,#26653,#26654,#26655,#26656,#26657,
#26658,#26659,#26660,#26661,#26662,#26663,#26664,#26665,#26666,#26667,#26668,
#26669,#26670,#26671,#26672,#26673,#26674,#26675,#26676,#26677,#26678,#26679,
#26680,#26681,#26682,#26683,#26684,#26685,#26686,#26687,#26688,#26689,#26690,
#26691,#26692,#26693,#26694,#26695,#26696,#26697,#26698,#26699,#26700,#26701,
#26702,#26703,#26704,#26705,#26706,#26707,#26708,#26709,#26710,#26711,#26712,
#26713,#26714,#26715,#26716,#26717,#26718,#26719,#26720,#26721,#26722,#26723,
#26724,#26725,#26726,#26727,#26728,#26729,#26730,#26731,#26732,#26733,#26734,
#26735,#26736,#26737,#26738,#26739,#26740,#26741,#26742,#26743,#26744,#26745,
#26746,#26747,#26748,#26749,#26750,#26751,#26752,#26753,#26754,#26755,#26756,
#26757,#26758,#26759,#26760,#26761,#26762,#26763,#26764,#26765,#26766,#26767,
#26768,#26769,#26770,#26771,#26772,#26773,#26774,#26775,#26776,#26777,#26778,
#26779,#26780,#26781,#26782,#26783,#26784,#26785,#26786,#26787,#26788,#26789,
#26790,#26791,#26792,#26793,#26794,#26795,#26796,#26797,#26798,#26799,#26800,
#26801,#26802,#26803,#26804,#26805,#26806,#26807,#26808,#26809,#26810,#26811,
#26812,#26813,#26814,#26815,#26816,#26817,#26818,#26819,#26820,#26821,#26822,
#26823,#26824,#26825,#26826,#26827,#26828,#26829,#26830,#26831,#26832,#26833,
#26834,#26835,#26836,#26837,#26838,#26839,#26840,#26841,#26842,#26843,#26844,
#26845,#26846,#26847,#26848,#26849,#26850),.UNSPECIFIED.,.F.,.F.,(4,3,3,
3,3,3,3,3,3,3,3,3,3,3,3,3,3,3,3,3,3,3,3,3,3,3,3,3,3,3,3,3,3,3,3,3,3,3,3,
3,3,3,3,3,3,3,3,3,3,3,3,3,3,3,3,3,3,3,3,3,3,3,3,3,3,3,3,3,3,3,3,3,3,4),
(135.088484104467,135.176096259964,135.26383125192,135.351780680477,135.439844267785,
135.52811071901,135.582686848384,135.66642556023,135.750061071597,135.833613514996,
135.917102950847,136.00055690146,136.083993395307,136.167430505062,136.25088629998,
136.334430792709,136.41801987565,136.501743143208,136.582422859104,136.66616157095,
136.749797082317,136.833349525716,136.916838961567,137.000292912181,137.083729406027,
137.167166515782,137.2506223107,137.33416680343,137.417755886371,137.501479153928,
137.582158869824,137.66589758167,137.749533093037,137.833085536436,137.916574972287,
138.000028922901,138.083465416747,138.166902526502,138.25035832142,138.33390281415,
138.417491897091,138.501215164648,138.581894880544,138.66563359239,138.749269103757,
138.832821547156,138.916310983007,138.999764933621,139.083201427467,139.166638537223,
139.25009433214,139.33363882487,139.417227907811,139.500951175369,139.581630891264,
139.66536960311,139.749005114477,139.832557557876,139.916046993727,139.999500944341,
140.082937438187,140.166374547942,140.24983034286,140.33337483559,140.416963918531,
140.500687186089,140.581366901985,140.6639127266,140.7463621142,140.82873424645,
140.911045277623,140.993320565168,141.075589977367,141.120120147634),
 .UNSPECIFIED.);
#139=B_SPLINE_CURVE_WITH_KNOTS('',3,(#26856,#26857,#26858,#26859,#26860,
#26861,#26862,#26863,#26864,#26865,#26866,#26867,#26868,#26869,#26870,#26871,
#26872,#26873,#26874,#26875,#26876,#26877,#26878,#26879,#26880,#26881,#26882,
#26883,#26884,#26885,#26886,#26887,#26888,#26889,#26890,#26891,#26892,#26893,
#26894,#26895,#26896,#26897,#26898,#26899,#26900,#26901,#26902,#26903,#26904,
#26905,#26906,#26907,#26908,#26909,#26910,#26911,#26912,#26913,#26914,#26915,
#26916,#26917,#26918,#26919,#26920,#26921,#26922,#26923,#26924,#26925,#26926,
#26927,#26928,#26929,#26930,#26931,#26932,#26933,#26934,#26935,#26936,#26937,
#26938,#26939,#26940,#26941,#26942,#26943,#26944,#26945,#26946,#26947,#26948,
#26949,#26950,#26951,#26952,#26953,#26954,#26955,#26956,#26957,#26958,#26959,
#26960,#26961,#26962,#26963,#26964,#26965,#26966,#26967,#26968,#26969,#26970,
#26971,#26972,#26973,#26974,#26975,#26976,#26977,#26978,#26979,#26980,#26981,
#26982,#26983,#26984,#26985,#26986,#26987,#26988,#26989,#26990,#26991,#26992,
#26993,#26994,#26995,#26996,#26997,#26998,#26999,#27000,#27001,#27002,#27003,
#27004,#27005,#27006,#27007,#27008,#27009,#27010,#27011,#27012,#27013,#27014,
#27015,#27016,#27017,#27018,#27019,#27020,#27021,#27022,#27023,#27024,#27025,
#27026,#27027,#27028,#27029,#27030,#27031,#27032,#27033,#27034,#27035,#27036,
#27037,#27038,#27039,#27040,#27041,#27042,#27043,#27044,#27045,#27046,#27047,
#27048,#27049,#27050,#27051,#27052,#27053,#27054,#27055,#27056,#27057,#27058,
#27059,#27060,#27061,#27062,#27063,#27064,#27065,#27066,#27067,#27068,#27069,
#27070,#27071,#27072,#27073,#27074,#27075),.UNSPECIFIED.,.F.,.F.,(4,3,3,
3,3,3,3,3,3,3,3,3,3,3,3,3,3,3,3,3,3,3,3,3,3,3,3,3,3,3,3,3,3,3,3,3,3,3,3,
3,3,3,3,3,3,3,3,3,3,3,3,3,3,3,3,3,3,3,3,3,3,3,3,3,3,3,3,3,3,3,3,3,3,4),
(141.371669411658,141.454304261838,141.536846637303,141.619317585863,141.701742710514,
141.784144477249,141.866541802964,141.948953598539,142.031448791127,142.113986382401,
142.196653608407,142.27054830371,142.354287015556,142.437922526923,142.521474970322,
142.604964406173,142.688418356786,142.771854850632,142.855291960388,142.938747755305,
143.022292248035,143.105881330976,143.189604598533,143.27028431443,143.354023026276,
143.437658537643,143.521210981042,143.604700416893,143.688154367507,143.771590861353,
143.855027971109,143.938483766026,144.022028258756,144.105617341697,144.189340609254,
144.27002032515,144.353759036996,144.437394548363,144.520946991762,144.604436427613,
144.687890378227,144.771326872073,144.854763981828,144.938219776746,145.021764269475,
145.105353352416,145.189076619974,145.26975633587,145.353495047716,145.437130559084,
145.520683002482,145.604172438333,145.687626388947,145.771062882794,145.854499992549,
145.937955787467,146.021500280197,146.105089363138,146.188812630696,146.26949234659,
146.353231058436,146.436866569804,146.520419013202,146.603908449053,146.687362399667,
146.770798893513,146.854236003269,146.937691798186,147.021236290916,147.104825373857,
147.188548641414,147.269228357311,147.363365580996,147.404444607709),
 .UNSPECIFIED.);
#140=B_SPLINE_CURVE_WITH_KNOTS('',3,(#27076,#27077,#27078,#27079,#27080,
#27081,#27082,#27083,#27084,#27085),.UNSPECIFIED.,.F.,.F.,(4,3,3,4),(141.120045428192,
141.203773533166,141.27081229299,141.371669411522),.UNSPECIFIED.);
#141=B_SPLINE_CURVE_WITH_KNOTS('',3,(#27087,#27088,#27089,#27090,#27091,
#27092,#27093,#27094,#27095,#27096),.UNSPECIFIED.,.F.,.F.,(4,3,3,4),(141.120120147634,
141.20242193175,141.287045671566,141.371669411383),.UNSPECIFIED.);
#142=B_SPLINE_CURVE_WITH_KNOTS('',3,(#27097,#27098,#27099,#27100,#27101,
#27102,#27103,#27104,#27105,#27106,#27107,#27108,#27109,#27110,#27111,#27112,
#27113,#27114,#27115,#27116,#27117,#27118,#27119,#27120,#27121,#27122,#27123,
#27124,#27125,#27126,#27127,#27128,#27129,#27130,#27131,#27132,#27133,#27134,
#27135,#27136,#27137,#27138,#27139,#27140,#27141,#27142,#27143,#27144,#27145,
#27146,#27147,#27148,#27149,#27150,#27151,#27152,#27153,#27154,#27155,#27156,
#27157,#27158,#27159,#27160,#27161,#27162,#27163,#27164,#27165,#27166,#27167,
#27168,#27169,#27170,#27171,#27172,#27173,#27174,#27175,#27176,#27177,#27178,
#27179,#27180,#27181,#27182,#27183,#27184,#27185,#27186,#27187,#27188,#27189,
#27190,#27191,#27192,#27193,#27194,#27195,#27196,#27197,#27198,#27199,#27200,
#27201,#27202,#27203,#27204,#27205,#27206,#27207,#27208,#27209,#27210,#27211,
#27212,#27213,#27214,#27215,#27216,#27217,#27218,#27219,#27220,#27221,#27222,
#27223,#27224,#27225,#27226,#27227,#27228,#27229,#27230,#27231,#27232,#27233,
#27234,#27235,#27236,#27237,#27238,#27239,#27240,#27241,#27242,#27243,#27244,
#27245,#27246,#27247,#27248,#27249,#27250,#27251,#27252,#27253,#27254,#27255,
#27256,#27257,#27258,#27259,#27260,#27261,#27262,#27263,#27264,#27265,#27266,
#27267,#27268,#27269,#27270,#27271,#27272,#27273,#27274,#27275,#27276,#27277,
#27278,#27279,#27280,#27281,#27282,#27283,#27284,#27285,#27286,#27287,#27288,
#27289,#27290,#27291,#27292,#27293,#27294,#27295,#27296,#27297,#27298,#27299,
#27300,#27301,#27302,#27303,#27304,#27305,#27306,#27307,#27308,#27309,#27310,
#27311,#27312,#27313),.UNSPECIFIED.,.F.,.F.,(4,3,3,3,3,3,3,3,3,3,3,3,3,
3,3,3,3,3,3,3,3,3,3,3,3,3,3,3,3,3,3,3,3,3,3,3,3,3,3,3,3,3,3,3,3,3,3,3,3,
3,3,3,3,3,3,3,3,3,3,3,3,3,3,3,3,3,3,3,3,3,3,3,4),(141.371669411525,141.489150236208,
141.581102912705,141.664841624551,141.748477135919,141.832029579317,141.915519015168,
141.998972965782,142.082409459628,142.165846569383,142.249302364301,142.332846857031,
142.416435939972,142.50015920753,142.580838923425,142.664577635271,142.748213146638,
142.831765590037,142.915255025888,142.998708976501,143.082145470347,143.165582580103,
143.24903837502,143.33258286775,143.416171950691,143.499895218248,143.580574934145,
143.664313645991,143.747949157358,143.831501600757,143.914991036608,143.998444987222,
144.081881481068,144.165318590823,144.248774385741,144.332318878471,144.415907961412,
144.499631228969,144.580310944865,144.664049656711,144.747685168078,144.831237611477,
144.914727047328,144.998180997942,145.081617491788,145.165054601543,145.248510396461,
145.332054889191,145.415643972132,145.499367239689,145.580046955585,145.663785667431,
145.747421178799,145.830973622197,145.914463058048,145.997917008662,146.081353502508,
146.164790612264,146.248246407181,146.331790899911,146.415379982852,146.49910325041,
146.579782966305,146.6635322455,146.747175998179,146.830719293296,146.914205630078,
146.997653127976,147.081079876464,147.164531967087,147.247994869194,147.331531662987,
147.403202100703),.UNSPECIFIED.);
#143=B_SPLINE_CURVE_WITH_KNOTS('',3,(#27319,#27320,#27321,#27322,#27323,
#27324,#27325,#27326,#27327,#27328,#27329,#27330,#27331,#27332,#27333,#27334,
#27335,#27336,#27337,#27338,#27339,#27340,#27341,#27342,#27343,#27344,#27345,
#27346,#27347,#27348,#27349,#27350,#27351,#27352,#27353,#27354,#27355,#27356,
#27357,#27358,#27359,#27360,#27361,#27362,#27363,#27364,#27365,#27366,#27367,
#27368,#27369,#27370,#27371,#27372,#27373,#27374,#27375,#27376,#27377,#27378,
#27379,#27380,#27381,#27382,#27383,#27384,#27385,#27386,#27387,#27388,#27389,
#27390,#27391,#27392,#27393,#27394,#27395,#27396,#27397,#27398,#27399,#27400,
#27401,#27402,#27403,#27404,#27405,#27406,#27407,#27408,#27409,#27410,#27411,
#27412,#27413,#27414,#27415,#27416,#27417,#27418,#27419,#27420,#27421,#27422,
#27423,#27424,#27425,#27426,#27427,#27428,#27429,#27430,#27431,#27432,#27433,
#27434,#27435,#27436,#27437,#27438,#27439,#27440,#27441,#27442,#27443,#27444,
#27445,#27446,#27447,#27448,#27449,#27450,#27451,#27452,#27453,#27454,#27455,
#27456,#27457,#27458,#27459,#27460,#27461,#27462,#27463,#27464,#27465,#27466,
#27467,#27468,#27469,#27470,#27471,#27472,#27473,#27474,#27475,#27476,#27477,
#27478,#27479,#27480,#27481,#27482,#27483,#27484,#27485,#27486,#27487,#27488,
#27489,#27490,#27491,#27492,#27493,#27494,#27495,#27496,#27497,#27498,#27499,
#27500,#27501,#27502,#27503,#27504,#27505,#27506,#27507,#27508,#27509,#27510,
#27511,#27512,#27513,#27514,#27515,#27516,#27517,#27518,#27519,#27520,#27521,
#27522,#27523,#27524,#27525,#27526,#27527,#27528,#27529,#27530,#27531,#27532,
#27533,#27534,#27535,#27536,#27537,#27538),.UNSPECIFIED.,.F.,.F.,(4,3,3,
3,3,3,3,3,3,3,3,3,3,3,3,3,3,3,3,3,3,3,3,3,3,3,3,3,3,3,3,3,3,3,3,3,3,3,3,
3,3,3,3,3,3,3,3,3,3,3,3,3,3,3,3,3,3,3,3,3,3,3,3,3,3,3,3,3,3,3,3,3,3,4),
(147.654854718701,147.739123187276,147.823405100597,147.907717322165,147.992076731998,
148.07655108834,148.161092958481,148.245767361688,148.268964368031,148.352703079877,
148.436338591245,148.519891034643,148.603380470494,148.686834421108,148.770270914954,
148.85370802471,148.937163819627,149.020708312357,149.104297395298,149.188020662856,
149.268700378751,149.352439090597,149.436074601964,149.519627045363,149.603116481214,
149.686570431827,149.770006925673,149.853444035429,149.936899830347,150.020444323076,
150.104033406017,150.187756673575,150.268436389471,150.352175101317,150.435810612684,
150.519363056083,150.602852491934,150.686306442548,150.769742936394,150.85318004615,
150.936635841067,151.020180333797,151.103769416738,151.187492684296,151.268172400191,
151.351911112037,151.435546623404,151.519099066803,151.602588502654,151.686042453268,
151.769478947114,151.85291605687,151.936371851788,152.019916344517,152.103505427458,
152.187228695016,152.267908410911,152.351647122757,152.435282634124,152.518835077523,
152.602324513373,152.685778463987,152.769214957833,152.852652067589,152.936107862506,
153.019652355236,153.103241438177,153.186964705735,153.267644421631,153.351296231555,
153.435243463639,153.518685048359,153.602885104126,153.687085159892),
 .UNSPECIFIED.);
#144=B_SPLINE_CURVE_WITH_KNOTS('',3,(#27539,#27540,#27541,#27542,#27543,
#27544,#27545,#27546,#27547,#27548),.UNSPECIFIED.,.F.,.F.,(4,3,3,4),(147.404444607709,
147.498077880791,147.591207952791,147.654854718509),.UNSPECIFIED.);
#145=B_SPLINE_CURVE_WITH_KNOTS('',3,(#27550,#27551,#27552,#27553,#27554,
#27555,#27556,#27557,#27558,#27559,#27560,#27561,#27562),.UNSPECIFIED.,
 .F.,.F.,(4,3,3,3,4),(147.403202100703,147.486842374459,147.570597041304,
147.579518977026,147.654854718705),.UNSPECIFIED.);
#146=B_SPLINE_CURVE_WITH_KNOTS('',3,(#27563,#27564,#27565,#27566,#27567,
#27568,#27569,#27570,#27571,#27572,#27573,#27574,#27575,#27576,#27577,#27578,
#27579,#27580,#27581,#27582,#27583,#27584,#27585,#27586,#27587,#27588,#27589,
#27590,#27591,#27592,#27593,#27594,#27595,#27596,#27597,#27598,#27599,#27600,
#27601,#27602,#27603,#27604,#27605,#27606,#27607,#27608,#27609,#27610,#27611,
#27612,#27613,#27614,#27615,#27616,#27617,#27618,#27619,#27620,#27621,#27622,
#27623,#27624,#27625,#27626,#27627,#27628,#27629,#27630,#27631,#27632,#27633,
#27634,#27635,#27636,#27637,#27638,#27639,#27640,#27641,#27642,#27643,#27644,
#27645,#27646,#27647,#27648,#27649,#27650,#27651,#27652,#27653,#27654,#27655,
#27656,#27657,#27658,#27659,#27660,#27661,#27662,#27663,#27664,#27665,#27666,
#27667,#27668,#27669,#27670,#27671,#27672,#27673,#27674,#27675,#27676,#27677,
#27678,#27679,#27680,#27681,#27682,#27683,#27684,#27685,#27686,#27687,#27688,
#27689,#27690,#27691,#27692,#27693,#27694,#27695,#27696,#27697,#27698,#27699,
#27700,#27701,#27702,#27703,#27704,#27705,#27706,#27707,#27708,#27709,#27710,
#27711,#27712,#27713,#27714,#27715,#27716,#27717,#27718,#27719,#27720,#27721,
#27722,#27723,#27724,#27725,#27726,#27727,#27728,#27729,#27730,#27731,#27732,
#27733,#27734,#27735,#27736,#27737,#27738,#27739,#27740,#27741,#27742,#27743,
#27744,#27745,#27746,#27747,#27748,#27749,#27750,#27751,#27752,#27753,#27754,
#27755,#27756,#27757,#27758,#27759,#27760,#27761,#27762,#27763,#27764,#27765,
#27766,#27767,#27768,#27769,#27770,#27771,#27772,#27773,#27774,#27775,#27776,
#27777,#27778,#27779,#27780,#27781,#27782,#27783,#27784,#27785),
 .UNSPECIFIED.,.F.,.F.,(4,3,3,3,3,3,3,3,3,3,3,3,3,3,3,3,3,3,3,3,3,3,3,3,
3,3,3,3,3,3,3,3,3,3,3,3,3,3,3,3,3,3,3,3,3,3,3,3,3,3,3,3,3,3,3,3,3,3,3,3,
3,3,3,3,3,3,3,3,3,3,3,3,3,3,4),(147.654854718832,147.737687936593,147.820424429939,
147.903085126839,147.987606359453,148.070187266232,148.15275988548,148.235343009465,
148.321321004035,148.404026515879,148.486788223612,148.569662852917,148.579254987746,
148.662993699592,148.746629210959,148.830181654358,148.913671090209,148.997125040823,
149.080561534669,149.163998644425,149.247454439342,149.330998932072,149.414588015013,
149.498311282571,149.578990998466,149.662729710312,149.746365221679,149.829917665078,
149.913407100929,149.996861051543,150.080297545389,150.163734655145,150.247190450062,
150.330734942792,150.414324025733,150.498047293291,150.578727009186,150.662465721032,
150.746101232399,150.829653675798,150.913143111649,150.996597062262,151.080033556109,
151.163470665864,151.246926460781,151.330470953511,151.414060036452,151.497783304009,
151.578463019906,151.662201731752,151.745837243119,151.829389686518,151.91287912237,
151.996333072983,152.079769566829,152.163206676585,152.246662471503,152.330206964232,
152.413796047173,152.497519314731,152.578199030626,152.661937742472,152.745573253839,
152.829125697238,152.912615133089,152.996069083703,153.079505577549,153.162942687305,
153.246398482222,153.329942974952,153.413532057893,153.497255325451,153.577935041346,
153.674085070861,153.687545719545),.UNSPECIFIED.);
#147=B_SPLINE_CURVE_WITH_KNOTS('',3,(#27791,#27792,#27793,#27794,#27795,
#27796,#27797,#27798,#27799,#27800,#27801,#27802,#27803,#27804,#27805,#27806,
#27807,#27808,#27809,#27810,#27811,#27812,#27813,#27814,#27815,#27816,#27817,
#27818,#27819,#27820,#27821,#27822,#27823,#27824,#27825,#27826,#27827,#27828,
#27829,#27830,#27831,#27832,#27833,#27834,#27835,#27836,#27837,#27838,#27839,
#27840,#27841,#27842,#27843,#27844,#27845,#27846,#27847,#27848,#27849,#27850,
#27851,#27852,#27853,#27854,#27855,#27856,#27857,#27858,#27859,#27860,#27861,
#27862,#27863,#27864,#27865,#27866,#27867,#27868,#27869,#27870,#27871,#27872,
#27873,#27874,#27875,#27876,#27877,#27878,#27879,#27880,#27881,#27882,#27883,
#27884,#27885,#27886,#27887,#27888,#27889,#27890,#27891,#27892,#27893,#27894,
#27895,#27896,#27897,#27898,#27899,#27900,#27901,#27902,#27903,#27904,#27905,
#27906,#27907,#27908,#27909,#27910,#27911,#27912,#27913,#27914,#27915,#27916,
#27917,#27918,#27919,#27920,#27921,#27922,#27923,#27924,#27925,#27926,#27927,
#27928,#27929,#27930,#27931,#27932,#27933,#27934,#27935,#27936,#27937,#27938,
#27939,#27940,#27941,#27942,#27943,#27944,#27945,#27946,#27947,#27948,#27949,
#27950,#27951,#27952,#27953,#27954,#27955,#27956,#27957,#27958,#27959,#27960,
#27961,#27962,#27963,#27964,#27965,#27966,#27967,#27968,#27969,#27970,#27971,
#27972,#27973,#27974,#27975,#27976,#27977,#27978,#27979,#27980,#27981,#27982,
#27983,#27984,#27985,#27986,#27987,#27988,#27989,#27990,#27991,#27992,#27993,
#27994,#27995,#27996,#27997,#27998,#27999,#28000,#28001,#28002,#28003,#28004,
#28005,#28006,#28007,#28008,#28009,#28010),.UNSPECIFIED.,.F.,.F.,(4,3,3,
3,3,3,3,3,3,3,3,3,3,3,3,3,3,3,3,3,3,3,3,3,3,3,3,3,3,3,3,3,3,3,3,3,3,3,3,
3,3,3,3,3,3,3,3,3,3,3,3,3,3,3,3,3,3,3,3,3,3,3,3,3,3,3,3,3,3,3,3,3,3,4),
(153.938040026064,154.035637973361,154.133843211017,154.232747939408,154.267380432352,
154.351119144198,154.434754655565,154.518307098964,154.601796534815,154.685250485428,
154.768686979275,154.85212408903,154.935579883948,155.019124376677,155.102713459618,
155.186436727176,155.267116443072,155.350855154918,155.434490666285,155.518043109684,
155.601532545535,155.684986496149,155.768422989995,155.85186009975,155.935315894668,
156.018860387398,156.102449470339,156.186172737896,156.266852453792,156.350591165638,
156.434226677005,156.517779120404,156.601268556255,156.684722506869,156.768159000715,
156.85159611047,156.935051905388,157.018596398118,157.102185481059,157.185908748616,
157.266588464512,157.350327176358,157.433962687725,157.517515131124,157.601004566975,
157.684458517588,157.767895011435,157.85133212119,157.934787916108,158.018332408837,
158.101921491778,158.185644759336,158.266324475232,158.350063187078,158.433698698445,
158.517251141844,158.600740577695,158.684194528309,158.767631022155,158.85106813191,
158.934523926828,159.018068419558,159.101657502499,159.185380770056,159.266060485952,
159.349232519083,159.432273222354,159.515238066942,159.598145728663,159.681014837138,
159.76387911148,159.846740065297,159.929641331942,159.96943076146),
 .UNSPECIFIED.);
#148=B_SPLINE_CURVE_WITH_KNOTS('',3,(#28011,#28012,#28013,#28014,#28015,
#28016,#28017,#28018,#28019,#28020),.UNSPECIFIED.,.F.,.F.,(4,3,3,4),(153.687085159892,
153.770397630781,153.854218828331,153.938040025881),.UNSPECIFIED.);
#149=B_SPLINE_CURVE_WITH_KNOTS('',3,(#28022,#28023,#28024,#28025,#28026,
#28027,#28028,#28029,#28030,#28031),.UNSPECIFIED.,.F.,.F.,(4,3,3,4),(153.687545719545,
153.783145344568,153.87809568214,153.938040025688),.UNSPECIFIED.);
#150=B_SPLINE_CURVE_WITH_KNOTS('',3,(#28032,#28033,#28034,#28035,#28036,
#28037,#28038,#28039,#28040,#28041,#28042,#28043,#28044,#28045,#28046,#28047,
#28048,#28049,#28050,#28051,#28052,#28053,#28054,#28055,#28056,#28057,#28058,
#28059,#28060,#28061,#28062,#28063,#28064,#28065,#28066,#28067,#28068,#28069,
#28070,#28071,#28072,#28073,#28074,#28075,#28076,#28077,#28078,#28079,#28080,
#28081,#28082,#28083,#28084,#28085,#28086,#28087,#28088,#28089,#28090,#28091,
#28092,#28093,#28094,#28095,#28096,#28097,#28098,#28099,#28100,#28101,#28102,
#28103,#28104,#28105,#28106,#28107,#28108,#28109,#28110,#28111,#28112,#28113,
#28114,#28115,#28116,#28117,#28118,#28119,#28120,#28121,#28122,#28123,#28124,
#28125,#28126,#28127,#28128,#28129,#28130,#28131,#28132,#28133,#28134,#28135,
#28136,#28137,#28138,#28139,#28140,#28141,#28142,#28143,#28144,#28145,#28146,
#28147,#28148,#28149,#28150,#28151,#28152,#28153,#28154,#28155,#28156,#28157,
#28158,#28159,#28160,#28161,#28162,#28163,#28164,#28165,#28166,#28167,#28168,
#28169,#28170,#28171,#28172,#28173,#28174,#28175,#28176,#28177,#28178,#28179,
#28180,#28181,#28182,#28183,#28184,#28185,#28186,#28187,#28188,#28189,#28190,
#28191,#28192,#28193,#28194,#28195,#28196,#28197,#28198,#28199,#28200,#28201,
#28202,#28203,#28204,#28205,#28206,#28207,#28208,#28209,#28210,#28211,#28212,
#28213,#28214,#28215,#28216,#28217,#28218,#28219,#28220,#28221,#28222,#28223,
#28224,#28225,#28226,#28227,#28228,#28229,#28230,#28231,#28232,#28233,#28234,
#28235,#28236,#28237,#28238,#28239,#28240,#28241,#28242,#28243,#28244,#28245,
#28246,#28247,#28248,#28249,#28250,#28251),.UNSPECIFIED.,.F.,.F.,(4,3,3,
3,3,3,3,3,3,3,3,3,3,3,3,3,3,3,3,3,3,3,3,3,3,3,3,3,3,3,3,3,3,3,3,3,3,3,3,
3,3,3,3,3,3,3,3,3,3,3,3,3,3,3,3,3,3,3,3,3,3,3,3,3,3,3,3,3,3,3,3,3,3,4),
(153.938040025885,154.021840747954,154.105640891805,154.189458006602,154.273309648661,
154.357266132484,154.441280186974,154.525430396561,154.577671052066,154.661409763912,
154.745045275279,154.828597718678,154.912087154529,154.995541105143,155.078977598989,
155.162414708745,155.245870503662,155.329414996392,155.413004079333,155.496727346891,
155.577407062787,155.661145774633,155.744781286001,155.828333729399,155.91182316525,
155.995277115864,156.07871360971,156.162150719466,156.245606514383,156.329151007113,
156.412740090054,156.496463357612,156.577143073507,156.660881785353,156.74451729672,
156.828069740119,156.91155917597,156.995013126584,157.07844962043,157.161886730185,
157.245342525102,157.328887017832,157.412476100773,157.496199368331,157.576879084227,
157.660617796073,157.74425330744,157.827805750839,157.911295186691,157.994749137304,
158.078185631151,158.161622740906,158.245078535824,158.328623028554,158.412212111495,
158.495935379053,158.576615094947,158.660353806793,158.74398931816,158.827541761559,
158.91103119741,158.994485148024,159.07792164187,159.161358751626,159.244814546543,
159.328359039273,159.411948122214,159.495671389771,159.576351105667,159.660425946794,
159.744362130889,159.828218528182,159.91200005122,159.970399332816),
 .UNSPECIFIED.);
#151=B_SPLINE_CURVE_WITH_KNOTS('',3,(#28257,#28258,#28259,#28260,#28261,
#28262,#28263,#28264,#28265,#28266,#28267,#28268,#28269,#28270,#28271,#28272,
#28273,#28274,#28275,#28276,#28277,#28278,#28279,#28280,#28281,#28282,#28283,
#28284,#28285,#28286,#28287,#28288,#28289,#28290,#28291,#28292,#28293,#28294,
#28295,#28296,#28297,#28298,#28299,#28300,#28301,#28302,#28303,#28304,#28305,
#28306,#28307,#28308,#28309,#28310,#28311,#28312,#28313,#28314,#28315,#28316,
#28317,#28318,#28319,#28320,#28321,#28322,#28323,#28324,#28325,#28326,#28327,
#28328,#28329,#28330,#28331,#28332,#28333,#28334,#28335,#28336,#28337,#28338,
#28339,#28340,#28341,#28342,#28343,#28344,#28345,#28346,#28347,#28348,#28349,
#28350,#28351,#28352,#28353,#28354,#28355,#28356,#28357,#28358,#28359,#28360,
#28361,#28362,#28363,#28364,#28365,#28366,#28367,#28368,#28369,#28370,#28371,
#28372,#28373,#28374,#28375,#28376,#28377,#28378,#28379,#28380,#28381,#28382,
#28383,#28384,#28385,#28386,#28387,#28388,#28389,#28390,#28391,#28392,#28393,
#28394,#28395,#28396,#28397,#28398,#28399,#28400,#28401,#28402,#28403,#28404,
#28405,#28406,#28407,#28408,#28409,#28410,#28411,#28412,#28413,#28414,#28415,
#28416,#28417,#28418,#28419,#28420,#28421,#28422,#28423,#28424,#28425,#28426,
#28427,#28428,#28429,#28430,#28431,#28432,#28433,#28434,#28435,#28436,#28437,
#28438,#28439,#28440,#28441,#28442,#28443,#28444,#28445,#28446,#28447,#28448,
#28449,#28450,#28451,#28452,#28453,#28454,#28455,#28456,#28457,#28458,#28459,
#28460,#28461,#28462,#28463,#28464,#28465,#28466,#28467,#28468,#28469,#28470,
#28471,#28472,#28473,#28474,#28475,#28476),.UNSPECIFIED.,.F.,.F.,(4,3,3,
3,3,3,3,3,3,3,3,3,3,3,3,3,3,3,3,3,3,3,3,3,3,3,3,3,3,3,3,3,3,3,3,3,3,3,3,
3,3,3,3,3,3,3,3,3,3,3,3,3,3,3,3,3,3,3,3,3,3,3,3,3,3,3,3,3,3,3,3,3,3,4),
(160.22122533306,160.265796496672,160.349535208518,160.433170719886,160.516723163284,
160.600212599136,160.683666549749,160.767103043596,160.850540153351,160.933995948269,
161.017540440999,161.10112952394,161.184852791498,161.265532507392,161.349271219238,
161.432906730605,161.516459174004,161.599948609855,161.683402560469,161.766839054315,
161.85027616407,161.933731958988,162.017276451718,162.100865534659,162.184588802216,
162.265268518113,162.349007229959,162.432642741327,162.516195184725,162.599684620576,
162.68313857119,162.766575065036,162.850012174792,162.933467969709,163.017012462439,
163.10060154538,163.184324812938,163.265004528833,163.348743240679,163.432378752046,
163.515931195445,163.599420631296,163.68287458191,163.766311075756,163.849748185511,
163.933203980429,164.016748473159,164.1003375561,164.184060823657,164.264740539553,
164.348479251399,164.432114762766,164.515667206165,164.599156642016,164.68261059263,
164.766047086476,164.849484196231,164.932939991149,165.016484483878,165.100073566819,
165.183796834377,165.264476550273,165.348215877039,165.431851859126,165.515404629652,
165.598894249496,165.682347637802,165.765783365477,165.849219505055,165.932674125469,
166.016214587326,166.09979955514,166.183511955595,166.253279225986),
 .UNSPECIFIED.);
#152=B_SPLINE_CURVE_WITH_KNOTS('',3,(#28477,#28478,#28479,#28480,#28481,
#28482,#28483,#28484,#28485,#28486),.UNSPECIFIED.,.F.,.F.,(4,3,3,4),(159.96943076146,
160.052425750303,160.13682554159,160.221225332876),.UNSPECIFIED.);
#153=B_SPLINE_CURVE_WITH_KNOTS('',3,(#28488,#28489,#28490,#28491,#28492,
#28493,#28494,#28495,#28496,#28497),.UNSPECIFIED.,.F.,.F.,(4,3,3,4),(159.970399332816,
160.054113020307,160.137828429699,160.221225333064),.UNSPECIFIED.);
#154=B_SPLINE_CURVE_WITH_KNOTS('',3,(#28498,#28499,#28500,#28501,#28502,
#28503,#28504,#28505,#28506,#28507,#28508,#28509,#28510,#28511,#28512,#28513,
#28514,#28515,#28516,#28517,#28518,#28519,#28520,#28521,#28522,#28523,#28524,
#28525,#28526,#28527,#28528,#28529,#28530,#28531,#28532,#28533,#28534,#28535,
#28536,#28537,#28538,#28539,#28540,#28541,#28542,#28543,#28544,#28545,#28546,
#28547,#28548,#28549,#28550,#28551,#28552,#28553,#28554,#28555,#28556,#28557,
#28558,#28559,#28560,#28561,#28562,#28563,#28564,#28565,#28566,#28567,#28568,
#28569,#28570,#28571,#28572,#28573,#28574,#28575,#28576,#28577,#28578,#28579,
#28580,#28581,#28582,#28583,#28584,#28585,#28586,#28587,#28588,#28589,#28590,
#28591,#28592,#28593,#28594,#28595,#28596,#28597,#28598,#28599,#28600,#28601,
#28602,#28603,#28604,#28605,#28606,#28607,#28608,#28609,#28610,#28611,#28612,
#28613,#28614,#28615,#28616,#28617,#28618,#28619,#28620,#28621,#28622,#28623,
#28624,#28625,#28626,#28627,#28628,#28629,#28630,#28631,#28632,#28633,#28634,
#28635,#28636,#28637,#28638,#28639,#28640,#28641,#28642,#28643,#28644,#28645,
#28646,#28647,#28648,#28649,#28650,#28651,#28652,#28653,#28654,#28655,#28656,
#28657,#28658,#28659,#28660,#28661,#28662,#28663,#28664,#28665,#28666,#28667,
#28668,#28669,#28670,#28671,#28672,#28673,#28674,#28675,#28676,#28677,#28678,
#28679,#28680,#28681,#28682,#28683,#28684,#28685,#28686,#28687,#28688,#28689,
#28690,#28691,#28692,#28693,#28694,#28695,#28696,#28697,#28698,#28699,#28700,
#28701,#28702,#28703,#28704,#28705,#28706,#28707,#28708,#28709,#28710,#28711,
#28712,#28713,#28714,#28715,#28716,#28717),.UNSPECIFIED.,.F.,.F.,(4,3,3,
3,3,3,3,3,3,3,3,3,3,3,3,3,3,3,3,3,3,3,3,3,3,3,3,3,3,3,3,3,3,3,3,3,3,3,3,
3,3,3,3,3,3,3,3,3,3,3,3,3,3,3,3,3,3,3,3,3,3,3,3,3,3,3,3,3,3,3,3,3,3,4),
(160.221225333262,160.316660060154,160.412545812793,160.509018326866,160.576087116387,
160.659825828233,160.7434613396,160.827013782999,160.91050321885,160.993957169463,
161.077393663309,161.160830773065,161.244286567983,161.327831060712,161.411420143653,
161.495143411211,161.575823127107,161.659561838953,161.74319735032,161.826749793719,
161.91023922957,161.993693180184,162.07712967403,162.160566783786,162.244022578703,
162.327567071433,162.411156154374,162.494879421932,162.575559137827,162.659297849673,
162.74293336104,162.826485804439,162.90997524029,162.993429190904,163.07686568475,
163.160302794506,163.243758589423,163.327303082153,163.410892165094,163.494615432652,
163.575295148548,163.659033860394,163.742669371762,163.82622181516,163.909711251011,
163.993165201625,164.076601695471,164.160038805227,164.243494600144,164.327039092874,
164.410628175815,164.494351443373,164.575031159268,164.658769871114,164.742405382481,
164.82595782588,164.909447261731,164.992901212345,165.076337706191,165.159774815947,
165.243230610864,165.326775103594,165.410364186535,165.494087454093,165.574767169988,
165.659493734827,165.742284208432,165.824999485849,165.907658428563,165.993888743597,
166.076503904695,166.159117880116,166.241766148672,166.252579688701),
 .UNSPECIFIED.);
#155=B_SPLINE_CURVE_WITH_KNOTS('',3,(#28723,#28724,#28725,#28726,#28727,
#28728,#28729,#28730,#28731,#28732,#28733,#28734,#28735,#28736,#28737,#28738,
#28739,#28740,#28741,#28742,#28743,#28744,#28745,#28746,#28747,#28748,#28749,
#28750,#28751,#28752,#28753,#28754,#28755,#28756,#28757,#28758,#28759,#28760,
#28761,#28762,#28763,#28764,#28765,#28766,#28767,#28768,#28769,#28770,#28771,
#28772,#28773,#28774,#28775,#28776,#28777,#28778,#28779,#28780,#28781,#28782,
#28783,#28784,#28785,#28786,#28787,#28788,#28789,#28790,#28791,#28792,#28793,
#28794,#28795,#28796,#28797,#28798,#28799,#28800,#28801,#28802,#28803,#28804,
#28805,#28806,#28807,#28808,#28809,#28810,#28811,#28812,#28813,#28814,#28815,
#28816,#28817,#28818,#28819,#28820,#28821,#28822,#28823,#28824,#28825,#28826,
#28827,#28828,#28829,#28830,#28831,#28832,#28833,#28834,#28835,#28836,#28837,
#28838,#28839,#28840,#28841,#28842,#28843,#28844,#28845,#28846,#28847,#28848,
#28849,#28850,#28851,#28852,#28853,#28854,#28855,#28856,#28857,#28858,#28859,
#28860,#28861,#28862,#28863,#28864,#28865,#28866,#28867,#28868,#28869,#28870,
#28871,#28872,#28873,#28874,#28875,#28876,#28877,#28878,#28879,#28880,#28881,
#28882,#28883,#28884,#28885,#28886,#28887,#28888,#28889,#28890,#28891,#28892,
#28893,#28894,#28895,#28896,#28897,#28898,#28899,#28900,#28901,#28902,#28903,
#28904,#28905,#28906,#28907,#28908,#28909,#28910,#28911,#28912,#28913,#28914,
#28915,#28916,#28917,#28918,#28919,#28920,#28921,#28922,#28923,#28924,#28925,
#28926,#28927,#28928,#28929,#28930,#28931,#28932,#28933,#28934,#28935,#28936,
#28937,#28938,#28939,#28940,#28941,#28942,#28943,#28944,#28945),
 .UNSPECIFIED.,.F.,.F.,(4,3,3,3,3,3,3,3,3,3,3,3,3,3,3,3,3,3,3,3,3,3,3,3,
3,3,3,3,3,3,3,3,3,3,3,3,3,3,3,3,3,3,3,3,3,3,3,3,3,3,3,3,3,3,3,3,3,3,3,3,
3,3,3,3,3,3,3,3,3,3,3,3,3,3,4),(166.50441064024,166.5869194705,166.671548108151,
166.753973814019,166.836390160482,166.918816041903,167.005099174355,167.087646260185,
167.170249047393,167.252965034704,167.263948571713,167.347687283559,167.431322794926,
167.514875238325,167.598364674176,167.68181862479,167.765255118636,167.848692228391,
167.932148023309,168.015692516039,168.09928159898,168.183004866537,168.263684582433,
168.347423294279,168.431058805647,168.514611249045,168.598100684896,168.68155463551,
168.764991129356,168.848428239112,168.931884034029,169.015428526759,169.0990176097,
169.182740877258,169.263420593153,169.347159304999,169.430794816366,169.514347259765,
169.597836695616,169.68129064623,169.764727140076,169.848164249832,169.93162004475,
170.015164537479,170.09875362042,170.182476887978,170.263156603874,170.34689531572,
170.430530827087,170.514083270486,170.597572706337,170.681026656951,170.764463150797,
170.847900260553,170.931356055471,171.014900548201,171.098489631142,171.182212898699,
171.262892614594,171.34663132644,171.430266837807,171.513819281205,171.597308717056,
171.68076266767,171.764199161516,171.847636271271,171.931092066188,172.014636558918,
172.098225641859,172.181948909417,172.262628625314,172.349750479316,172.436749265431,
172.523602585952,172.537222833018),.UNSPECIFIED.);
#156=B_SPLINE_CURVE_WITH_KNOTS('',3,(#28946,#28947,#28948,#28949,#28950,
#28951,#28952,#28953,#28954,#28955,#28956,#28957,#28958),.UNSPECIFIED.,
 .F.,.F.,(4,3,3,3,4),(166.253279225986,166.264212560993,166.375998781252,
166.485008013926,166.504410640086),.UNSPECIFIED.);
#157=B_SPLINE_CURVE_WITH_KNOTS('',3,(#28960,#28961,#28962,#28963,#28964,
#28965,#28966,#28967,#28968,#28969),.UNSPECIFIED.,.F.,.F.,(4,3,3,4),(166.252579688701,
166.33531487359,166.419862756856,166.504410640121),.UNSPECIFIED.);
#158=B_SPLINE_CURVE_WITH_KNOTS('',3,(#28970,#28971,#28972,#28973,#28974,
#28975,#28976,#28977,#28978,#28979,#28980,#28981,#28982,#28983,#28984,#28985,
#28986,#28987,#28988,#28989,#28990,#28991,#28992,#28993,#28994,#28995,#28996,
#28997,#28998,#28999,#29000,#29001,#29002,#29003,#29004,#29005,#29006,#29007,
#29008,#29009,#29010,#29011,#29012,#29013,#29014,#29015,#29016,#29017,#29018,
#29019,#29020,#29021,#29022,#29023,#29024,#29025,#29026,#29027,#29028,#29029,
#29030,#29031,#29032,#29033,#29034,#29035,#29036,#29037,#29038,#29039,#29040,
#29041,#29042,#29043,#29044,#29045,#29046,#29047,#29048,#29049,#29050,#29051,
#29052,#29053,#29054,#29055,#29056,#29057,#29058,#29059,#29060,#29061,#29062,
#29063,#29064,#29065,#29066,#29067,#29068,#29069,#29070,#29071,#29072,#29073,
#29074,#29075,#29076,#29077,#29078,#29079,#29080,#29081,#29082,#29083,#29084,
#29085,#29086,#29087,#29088,#29089,#29090,#29091,#29092,#29093,#29094,#29095,
#29096,#29097,#29098,#29099,#29100,#29101,#29102,#29103,#29104,#29105,#29106,
#29107,#29108,#29109,#29110,#29111,#29112,#29113,#29114,#29115,#29116,#29117,
#29118,#29119,#29120,#29121,#29122,#29123,#29124,#29125,#29126,#29127,#29128,
#29129,#29130,#29131,#29132,#29133,#29134,#29135,#29136,#29137,#29138,#29139,
#29140,#29141,#29142,#29143,#29144,#29145,#29146,#29147,#29148,#29149,#29150,
#29151,#29152,#29153,#29154,#29155,#29156,#29157,#29158,#29159,#29160,#29161,
#29162,#29163,#29164,#29165,#29166,#29167,#29168,#29169,#29170,#29171,#29172,
#29173,#29174,#29175,#29176,#29177,#29178,#29179,#29180,#29181,#29182,#29183,
#29184,#29185,#29186,#29187,#29188,#29189),.UNSPECIFIED.,.F.,.F.,(4,3,3,
3,3,3,3,3,3,3,3,3,3,3,3,3,3,3,3,3,3,3,3,3,3,3,3,3,3,3,3,3,3,3,3,3,3,3,3,
3,3,3,3,3,3,3,3,3,3,3,3,3,3,3,3,3,3,3,3,3,3,3,3,3,3,3,3,3,3,3,3,3,3,4),
(166.504410640244,166.574503180708,166.658241892554,166.741877403921,166.82542984732,
166.908919283171,166.992373233784,167.075809727631,167.159246837386,167.242702632304,
167.326247125034,167.409836207974,167.493559475532,167.574239191428,167.657977903274,
167.741613414641,167.82516585804,167.908655293891,167.992109244504,168.075545738351,
168.158982848106,168.242438643024,168.325983135753,168.409572218694,168.493295486252,
168.573975202148,168.657713913994,168.741349425361,168.82490186876,168.908391304611,
168.991845255225,169.075281749071,169.158718858827,169.242174653744,169.325719146474,
169.409308229415,169.493031496973,169.573711212868,169.657449924714,169.741085436082,
169.82463787948,169.908127315331,169.991581265945,170.075017759791,170.158454869547,
170.241910664464,170.325455157194,170.409044240135,170.492767507693,170.573447223589,
170.657185935435,170.740821446803,170.824373890201,170.907863326052,170.991317276666,
171.074753770512,171.158190880268,171.241646675186,171.325191167915,171.408780250856,
171.492503518414,171.573183234309,171.656924025188,171.740561132948,171.824114692136,
171.907604764723,171.991056917326,172.07449093084,172.157924877497,172.241376825514,
172.324908162857,172.408483808463,172.492172042282,172.536326482869),
 .UNSPECIFIED.);
#159=B_SPLINE_CURVE_WITH_KNOTS('',3,(#29195,#29196,#29197,#29198,#29199,
#29200,#29201,#29202,#29203,#29204,#29205,#29206,#29207,#29208,#29209,#29210,
#29211,#29212,#29213,#29214,#29215,#29216,#29217,#29218,#29219,#29220,#29221,
#29222,#29223,#29224,#29225,#29226,#29227,#29228,#29229,#29230,#29231,#29232,
#29233,#29234,#29235,#29236,#29237,#29238,#29239,#29240,#29241,#29242,#29243,
#29244,#29245,#29246,#29247,#29248,#29249,#29250,#29251,#29252,#29253,#29254,
#29255,#29256,#29257,#29258,#29259,#29260,#29261,#29262,#29263,#29264,#29265,
#29266,#29267,#29268,#29269,#29270,#29271,#29272,#29273,#29274,#29275,#29276,
#29277,#29278,#29279,#29280,#29281,#29282,#29283,#29284,#29285,#29286,#29287,
#29288,#29289,#29290,#29291,#29292,#29293,#29294,#29295,#29296,#29297,#29298,
#29299,#29300,#29301,#29302,#29303,#29304,#29305,#29306,#29307,#29308,#29309,
#29310,#29311,#29312,#29313,#29314,#29315,#29316,#29317,#29318,#29319,#29320,
#29321,#29322,#29323,#29324,#29325,#29326,#29327,#29328,#29329,#29330,#29331,
#29332,#29333,#29334,#29335,#29336,#29337,#29338,#29339,#29340,#29341,#29342,
#29343,#29344,#29345,#29346,#29347,#29348,#29349,#29350,#29351,#29352,#29353,
#29354,#29355,#29356,#29357,#29358,#29359,#29360,#29361,#29362,#29363,#29364,
#29365,#29366,#29367,#29368,#29369,#29370,#29371,#29372,#29373,#29374,#29375,
#29376,#29377,#29378,#29379,#29380,#29381,#29382,#29383,#29384,#29385,#29386,
#29387,#29388,#29389,#29390,#29391,#29392,#29393,#29394,#29395,#29396,#29397,
#29398,#29399,#29400,#29401,#29402,#29403,#29404,#29405,#29406,#29407,#29408,
#29409,#29410,#29411,#29412,#29413,#29414),.UNSPECIFIED.,.F.,.F.,(4,3,3,
3,3,3,3,3,3,3,3,3,3,3,3,3,3,3,3,3,3,3,3,3,3,3,3,3,3,3,3,3,3,3,3,3,3,3,3,
3,3,3,3,3,3,3,3,3,3,3,3,3,3,3,3,3,3,3,3,3,3,3,3,3,3,3,3,3,3,3,3,3,3,4),
(172.787595947525,172.875968071268,172.964492839275,173.053261020649,173.142162136332,
173.231271976019,173.262364636034,173.34610334788,173.429738859247,173.513291302646,
173.596780738497,173.680234689111,173.763671182957,173.847108292712,173.93056408763,
174.01410858036,174.097697663301,174.181420930858,174.262100646754,174.3458393586,
174.429474869967,174.513027313366,174.596516749217,174.67997069983,174.763407193677,
174.846844303432,174.93030009835,175.01384459108,175.09743367402,175.181156941578,
175.261836657474,175.34557536932,175.429210880687,175.512763324086,175.596252759937,
175.67970671055,175.763143204397,175.846580314152,175.93003610907,176.013580601799,
176.09716968474,176.180892952298,176.261572668194,176.34531138004,176.428946891407,
176.512499334806,176.595988770657,176.679442721271,176.762879215117,176.846316324873,
176.92977211979,177.01331661252,177.096905695461,177.180628963019,177.261308678914,
177.34504739076,177.428682902128,177.512235345526,177.595724781377,177.679178731991,
177.762615225837,177.846052335593,177.92950813051,178.01305262324,178.096641706181,
178.180364973739,178.261044689635,178.343536465897,178.425932413336,178.50825174412,
178.590512421042,178.672737770061,178.754963250308,178.819154473902),
 .UNSPECIFIED.);
#160=B_SPLINE_CURVE_WITH_KNOTS('',3,(#29415,#29416,#29417,#29418,#29419,
#29420,#29421,#29422,#29423,#29424),.UNSPECIFIED.,.F.,.F.,(4,3,3,4),(172.537222833018,
172.623918808965,172.710492976874,172.787595947419),.UNSPECIFIED.);
#161=B_SPLINE_CURVE_WITH_KNOTS('',3,(#29426,#29427,#29428,#29429,#29430,
#29431,#29432,#29433,#29434,#29435),.UNSPECIFIED.,.F.,.F.,(4,3,3,4),(172.536326482869,
172.572919245029,172.689017473637,172.787595947423),.UNSPECIFIED.);
#162=B_SPLINE_CURVE_WITH_KNOTS('',3,(#29436,#29437,#29438,#29439,#29440,
#29441,#29442,#29443,#29444,#29445,#29446,#29447,#29448,#29449,#29450,#29451,
#29452,#29453,#29454,#29455,#29456,#29457,#29458,#29459,#29460,#29461,#29462,
#29463,#29464,#29465,#29466,#29467,#29468,#29469,#29470,#29471,#29472,#29473,
#29474,#29475,#29476,#29477,#29478,#29479,#29480,#29481,#29482,#29483,#29484,
#29485,#29486,#29487,#29488,#29489,#29490,#29491,#29492,#29493,#29494,#29495,
#29496,#29497,#29498,#29499,#29500,#29501,#29502,#29503,#29504,#29505,#29506,
#29507,#29508,#29509,#29510,#29511,#29512,#29513,#29514,#29515,#29516,#29517,
#29518,#29519,#29520,#29521,#29522,#29523,#29524,#29525,#29526,#29527,#29528,
#29529,#29530,#29531,#29532,#29533,#29534,#29535,#29536,#29537,#29538,#29539,
#29540,#29541,#29542,#29543,#29544,#29545,#29546,#29547,#29548,#29549,#29550,
#29551,#29552,#29553,#29554,#29555,#29556,#29557,#29558,#29559,#29560,#29561,
#29562,#29563,#29564,#29565,#29566,#29567,#29568,#29569,#29570,#29571,#29572,
#29573,#29574,#29575,#29576,#29577,#29578,#29579,#29580,#29581,#29582,#29583,
#29584,#29585,#29586,#29587,#29588,#29589,#29590,#29591,#29592,#29593,#29594,
#29595,#29596,#29597,#29598,#29599,#29600,#29601,#29602,#29603,#29604,#29605,
#29606,#29607,#29608,#29609,#29610,#29611,#29612,#29613,#29614,#29615,#29616,
#29617,#29618,#29619,#29620,#29621,#29622,#29623,#29624,#29625,#29626,#29627,
#29628,#29629,#29630,#29631,#29632,#29633,#29634,#29635,#29636,#29637,#29638,
#29639,#29640,#29641,#29642,#29643,#29644,#29645,#29646,#29647,#29648,#29649,
#29650,#29651,#29652,#29653,#29654,#29655),.UNSPECIFIED.,.F.,.F.,(4,3,3,
3,3,3,3,3,3,3,3,3,3,3,3,3,3,3,3,3,3,3,3,3,3,3,3,3,3,3,3,3,3,3,3,3,3,3,3,
3,3,3,3,3,3,3,3,3,3,3,3,3,3,3,3,3,3,3,3,3,3,3,3,3,3,3,3,3,3,3,3,3,3,4),
(172.787595947533,172.870004970122,172.952349393634,173.034657092611,173.116947717683,
173.199240249463,173.281553667809,173.363953449252,173.446401525226,173.528970574567,
173.572655255749,173.656393967595,173.740029478962,173.823581922361,173.907071358212,
173.990525308826,174.073961802672,174.157398912427,174.240854707345,174.324399200075,
174.407988283016,174.491711550574,174.572391266469,174.656129978315,174.739765489682,
174.823317933081,174.906807368932,174.990261319546,175.073697813392,175.157134923148,
175.240590718065,175.324135210795,175.407724293736,175.491447561294,175.572127277189,
175.655865989035,175.739501500402,175.823053943801,175.906543379652,175.989997330266,
176.073433824112,176.156870933867,176.240326728785,176.323871221514,176.407460304455,
176.491183572013,176.571863287909,176.655601999755,176.739237511123,176.822789954522,
176.906279390372,176.989733340986,177.073169834833,177.156606944588,177.240062739506,
177.323607232235,177.407196315176,177.490919582734,177.571599298629,177.655338010475,
177.738973521842,177.822525965241,177.906015401092,177.989469351706,178.072905845552,
178.156342955308,178.239798750226,178.323343242955,178.406932325897,178.490655593454,
178.57133530935,178.659407964876,178.747284406029,178.820453921422),
 .UNSPECIFIED.);
#163=B_SPLINE_CURVE_WITH_KNOTS('',3,(#29661,#29662,#29663,#29664,#29665,
#29666,#29667,#29668,#29669,#29670,#29671,#29672,#29673,#29674,#29675,#29676,
#29677,#29678,#29679,#29680,#29681,#29682,#29683,#29684,#29685,#29686,#29687,
#29688,#29689,#29690,#29691,#29692,#29693,#29694,#29695,#29696,#29697,#29698,
#29699,#29700,#29701,#29702,#29703,#29704,#29705,#29706,#29707,#29708,#29709,
#29710,#29711,#29712,#29713,#29714,#29715,#29716,#29717,#29718,#29719,#29720,
#29721,#29722,#29723,#29724,#29725,#29726,#29727,#29728,#29729,#29730,#29731,
#29732,#29733,#29734,#29735,#29736,#29737,#29738,#29739,#29740,#29741,#29742,
#29743,#29744,#29745,#29746,#29747,#29748,#29749,#29750,#29751,#29752,#29753,
#29754,#29755,#29756,#29757,#29758,#29759,#29760,#29761,#29762,#29763,#29764,
#29765,#29766,#29767,#29768,#29769,#29770,#29771,#29772,#29773,#29774,#29775,
#29776,#29777,#29778,#29779,#29780,#29781,#29782,#29783,#29784,#29785,#29786,
#29787,#29788,#29789,#29790,#29791,#29792,#29793,#29794,#29795,#29796,#29797,
#29798,#29799,#29800,#29801,#29802,#29803,#29804,#29805,#29806,#29807,#29808,
#29809,#29810,#29811,#29812,#29813,#29814,#29815,#29816,#29817,#29818,#29819,
#29820,#29821,#29822,#29823,#29824,#29825,#29826,#29827,#29828,#29829,#29830,
#29831,#29832,#29833,#29834,#29835,#29836,#29837,#29838,#29839,#29840,#29841,
#29842,#29843,#29844,#29845,#29846,#29847,#29848,#29849,#29850,#29851,#29852,
#29853,#29854,#29855,#29856,#29857,#29858,#29859,#29860,#29861,#29862,#29863,
#29864,#29865,#29866,#29867,#29868,#29869,#29870,#29871,#29872,#29873,#29874,
#29875,#29876,#29877),.UNSPECIFIED.,.F.,.F.,(4,3,3,3,3,3,3,3,3,3,3,3,3,
3,3,3,3,3,3,3,3,3,3,3,3,3,3,3,3,3,3,3,3,3,3,3,3,3,3,3,3,3,3,3,3,3,3,3,3,
3,3,3,3,3,3,3,3,3,3,3,3,3,3,3,3,3,3,3,3,3,3,3,4),(179.070781254599,179.194242909084,
179.260780700355,179.344519412201,179.428154923568,179.511707366967,179.595196802818,
179.678650753431,179.762087247277,179.845524357033,179.928980151951,180.01252464468,
180.096113727621,180.179836995179,180.260516711075,180.344255422921,180.427890934288,
180.511443377687,180.594932813538,180.678386764152,180.761823257998,180.845260367753,
180.928716162671,181.012260655401,181.095849738342,181.179573005899,181.260252721795,
181.343991433641,181.427626945008,181.511179388407,181.594668824258,181.678122774871,
181.761559268718,181.844996378473,181.928452173391,182.01199666612,182.095585749061,
182.179309016619,182.259988732515,182.343727444361,182.427362955728,182.510915399127,
182.594404834978,182.677858785592,182.761295279438,182.844732389193,182.928188184111,
183.011732676841,183.095321759782,183.179045027339,183.259724743235,183.343463455081,
183.427098966448,183.510651409847,183.594140845698,183.677594796312,183.761031290158,
183.844468399913,183.927924194831,184.01146868756,184.095057770501,184.178781038059,
184.259460753955,184.343208799076,184.426851574391,184.51128690772,184.594772813922,
184.678220437969,184.761647868793,184.84681946185,184.93028775386,185.016310997439,
185.102334241018),.UNSPECIFIED.);
#164=B_SPLINE_CURVE_WITH_KNOTS('',3,(#29878,#29879,#29880,#29881,#29882,
#29883,#29884,#29885,#29886,#29887),.UNSPECIFIED.,.F.,.F.,(4,3,3,4),(178.819154473902,
178.901416734859,178.986098994665,179.070781254471),.UNSPECIFIED.);
#165=B_SPLINE_CURVE_WITH_KNOTS('',3,(#29889,#29890,#29891,#29892,#29893,
#29894,#29895,#29896,#29897,#29898),.UNSPECIFIED.,.F.,.F.,(4,3,3,4),(178.820453921422,
178.908072122234,178.995527665515,179.070781254524),.UNSPECIFIED.);
#166=B_SPLINE_CURVE_WITH_KNOTS('',3,(#29899,#29900,#29901,#29902,#29903,
#29904,#29905,#29906,#29907,#29908,#29909,#29910,#29911,#29912,#29913,#29914,
#29915,#29916,#29917,#29918,#29919,#29920,#29921,#29922,#29923,#29924,#29925,
#29926,#29927,#29928,#29929,#29930,#29931,#29932,#29933,#29934,#29935,#29936,
#29937,#29938,#29939,#29940,#29941,#29942,#29943,#29944,#29945,#29946,#29947,
#29948,#29949,#29950,#29951,#29952,#29953,#29954,#29955,#29956,#29957,#29958,
#29959,#29960,#29961,#29962,#29963,#29964,#29965,#29966,#29967,#29968,#29969,
#29970,#29971,#29972,#29973,#29974,#29975,#29976,#29977,#29978,#29979,#29980,
#29981,#29982,#29983,#29984,#29985,#29986,#29987,#29988,#29989,#29990,#29991,
#29992,#29993,#29994,#29995,#29996,#29997,#29998,#29999,#30000,#30001,#30002,
#30003,#30004,#30005,#30006,#30007,#30008,#30009,#30010,#30011,#30012,#30013,
#30014,#30015,#30016,#30017,#30018,#30019,#30020,#30021,#30022,#30023,#30024,
#30025,#30026,#30027,#30028,#30029,#30030,#30031,#30032,#30033,#30034,#30035,
#30036,#30037,#30038,#30039,#30040,#30041,#30042,#30043,#30044,#30045,#30046,
#30047,#30048,#30049,#30050,#30051,#30052,#30053,#30054,#30055,#30056,#30057,
#30058,#30059,#30060,#30061,#30062,#30063,#30064,#30065,#30066,#30067,#30068,
#30069,#30070,#30071,#30072,#30073,#30074,#30075,#30076,#30077,#30078,#30079,
#30080,#30081,#30082,#30083,#30084,#30085,#30086,#30087,#30088,#30089,#30090,
#30091,#30092,#30093,#30094,#30095,#30096,#30097,#30098,#30099,#30100,#30101,
#30102,#30103,#30104,#30105,#30106,#30107,#30108,#30109,#30110,#30111,#30112,
#30113,#30114,#30115,#30116,#30117,#30118),.UNSPECIFIED.,.F.,.F.,(4,3,3,
3,3,3,3,3,3,3,3,3,3,3,3,3,3,3,3,3,3,3,3,3,3,3,3,3,3,3,3,3,3,3,3,3,3,3,3,
3,3,3,3,3,3,3,3,3,3,3,3,3,3,3,3,3,3,3,3,3,3,3,3,3,3,3,3,3,3,3,3,3,3,4),
(179.070781254603,179.158169935777,179.245673124652,179.333382542047,179.421200727411,
179.509220156274,179.57107132007,179.654810031916,179.738445543283,179.821997986682,
179.905487422533,179.988941373147,180.072377866993,180.155814976749,180.239270771666,
180.322815264396,180.406404347337,180.490127614894,180.57080733079,180.654546042636,
180.738181554003,180.821733997402,180.905223433253,180.988677383867,181.072113877713,
181.155550987468,181.239006782386,181.322551275116,181.406140358057,181.489863625614,
181.57054334151,181.654282053356,181.737917564723,181.821470008122,181.904959443973,
181.988413394587,182.071849888433,182.155286998188,182.238742793106,182.322287285835,
182.405876368776,182.489599636334,182.57027935223,182.654018064076,182.737653575443,
182.821206018842,182.904695454694,182.988149405307,183.071585899154,183.155023008909,
183.238478803827,183.322023296557,183.405612379498,183.489335647055,183.57001536295,
183.653754074796,183.737389586164,183.820942029562,183.904431465413,183.987885416027,
184.071321909873,184.154759019628,184.238214814546,184.321759307275,184.405348390217,
184.489071657774,184.56975137367,184.652320999124,184.73479396478,184.817189438157,
184.899523026234,184.981820702053,185.064110743829,185.102443334662),
 .UNSPECIFIED.);
#167=B_SPLINE_CURVE_WITH_KNOTS('',3,(#30124,#30125,#30126,#30127,#30128,
#30129,#30130,#30131,#30132,#30133,#30134,#30135,#30136,#30137,#30138,#30139,
#30140,#30141,#30142,#30143,#30144,#30145,#30146,#30147,#30148,#30149,#30150,
#30151,#30152,#30153,#30154,#30155,#30156,#30157,#30158,#30159,#30160,#30161,
#30162,#30163,#30164,#30165,#30166,#30167,#30168,#30169,#30170,#30171,#30172,
#30173,#30174,#30175,#30176,#30177,#30178,#30179,#30180,#30181,#30182,#30183,
#30184,#30185,#30186,#30187,#30188,#30189,#30190,#30191,#30192,#30193,#30194,
#30195,#30196,#30197,#30198,#30199,#30200,#30201,#30202,#30203,#30204,#30205,
#30206,#30207,#30208,#30209,#30210,#30211,#30212,#30213,#30214,#30215,#30216,
#30217,#30218,#30219,#30220,#30221,#30222,#30223,#30224,#30225,#30226,#30227,
#30228,#30229,#30230,#30231,#30232,#30233,#30234,#30235,#30236,#30237,#30238,
#30239,#30240,#30241,#30242,#30243,#30244,#30245,#30246,#30247,#30248,#30249,
#30250,#30251,#30252,#30253,#30254,#30255,#30256,#30257,#30258,#30259,#30260,
#30261,#30262,#30263,#30264,#30265,#30266,#30267,#30268,#30269,#30270,#30271,
#30272,#30273,#30274,#30275,#30276,#30277,#30278,#30279,#30280,#30281,#30282,
#30283,#30284,#30285,#30286,#30287,#30288,#30289,#30290,#30291,#30292,#30293,
#30294,#30295,#30296,#30297,#30298,#30299,#30300,#30301,#30302,#30303,#30304,
#30305,#30306,#30307,#30308,#30309,#30310,#30311,#30312,#30313,#30314,#30315,
#30316,#30317,#30318,#30319,#30320,#30321,#30322,#30323,#30324,#30325,#30326,
#30327,#30328,#30329,#30330,#30331,#30332,#30333,#30334,#30335,#30336,#30337,
#30338,#30339,#30340,#30341,#30342,#30343),.UNSPECIFIED.,.F.,.F.,(4,3,3,
3,3,3,3,3,3,3,3,3,3,3,3,3,3,3,3,3,3,3,3,3,3,3,3,3,3,3,3,3,3,3,3,3,3,3,3,
3,3,3,3,3,3,3,3,3,3,3,3,3,3,3,3,3,3,3,3,3,3,3,3,3,3,3,3,3,3,3,3,3,3,4),
(185.353966561914,185.436643810729,185.519227495568,185.601738640769,185.684202445595,
185.766641843628,185.849075728445,185.93152298674,186.0140531916,186.096624763862,
186.179327746526,186.258932775396,186.342671487242,186.426306998609,186.509859442008,
186.593348877859,186.676802828473,186.760239322319,186.843676432075,186.927132226992,
187.010676719722,187.094265802663,187.17798907022,187.258668786116,187.342407497962,
187.42604300933,187.509595452728,187.593084888579,187.676538839193,187.759975333039,
187.843412442794,187.926868237712,188.010412730442,188.094001813383,188.177725080941,
188.258404796836,188.342143508682,188.425779020049,188.509331463448,188.592820899299,
188.676274849913,188.759711343759,188.843148453515,188.926604248432,189.010148741162,
189.093737824103,189.177461091661,189.258140807556,189.341879519402,189.425515030769,
189.509067474168,189.592556910019,189.676010860633,189.759447354479,189.842884464234,
189.926340259152,190.009884751882,190.093473834823,190.17719710238,190.257876818276,
190.341615530122,190.425251041489,190.508803484888,190.592292920739,190.675746871353,
190.759183365199,190.842620474954,190.926076269872,191.009620762602,191.093209845543,
191.1769331131,191.257612828996,191.352202270869,191.386723760419),
 .UNSPECIFIED.);
#168=B_SPLINE_CURVE_WITH_KNOTS('',3,(#30344,#30345,#30346,#30347,#30348,
#30349,#30350,#30351,#30352,#30353),.UNSPECIFIED.,.F.,.F.,(4,3,3,4),(185.102334241018,
185.186060117836,185.259196764675,185.353966561779),.UNSPECIFIED.);
#169=B_SPLINE_CURVE_WITH_KNOTS('',3,(#30355,#30356,#30357,#30358,#30359,
#30360,#30361,#30362,#30363,#30364),.UNSPECIFIED.,.F.,.F.,(4,3,3,4),(185.102443334662,
185.184764311148,185.269365436413,185.353966561677),.UNSPECIFIED.);
#170=B_SPLINE_CURVE_WITH_KNOTS('',3,(#30365,#30366,#30367,#30368,#30369,
#30370,#30371,#30372,#30373,#30374,#30375,#30376,#30377,#30378,#30379,#30380,
#30381,#30382,#30383,#30384,#30385,#30386,#30387,#30388,#30389,#30390,#30391,
#30392,#30393,#30394,#30395,#30396,#30397,#30398,#30399,#30400,#30401,#30402,
#30403,#30404,#30405,#30406,#30407,#30408,#30409,#30410,#30411,#30412,#30413,
#30414,#30415,#30416,#30417,#30418,#30419,#30420,#30421,#30422,#30423,#30424,
#30425,#30426,#30427,#30428,#30429,#30430,#30431,#30432,#30433,#30434,#30435,
#30436,#30437,#30438,#30439,#30440,#30441,#30442,#30443,#30444,#30445,#30446,
#30447,#30448,#30449,#30450,#30451,#30452,#30453,#30454,#30455,#30456,#30457,
#30458,#30459,#30460,#30461,#30462,#30463,#30464,#30465,#30466,#30467,#30468,
#30469,#30470,#30471,#30472,#30473,#30474,#30475,#30476,#30477,#30478,#30479,
#30480,#30481,#30482,#30483,#30484,#30485,#30486,#30487,#30488,#30489,#30490,
#30491,#30492,#30493,#30494,#30495,#30496,#30497,#30498,#30499,#30500,#30501,
#30502,#30503,#30504,#30505,#30506,#30507,#30508,#30509,#30510,#30511,#30512,
#30513,#30514,#30515,#30516,#30517,#30518,#30519,#30520,#30521,#30522,#30523,
#30524,#30525,#30526,#30527,#30528,#30529,#30530,#30531,#30532,#30533,#30534,
#30535,#30536,#30537,#30538,#30539,#30540,#30541,#30542,#30543,#30544,#30545,
#30546,#30547,#30548,#30549,#30550,#30551,#30552,#30553,#30554,#30555,#30556,
#30557,#30558,#30559,#30560,#30561,#30562,#30563,#30564,#30565,#30566,#30567,
#30568,#30569,#30570,#30571,#30572,#30573,#30574,#30575,#30576,#30577,#30578,
#30579,#30580,#30581),.UNSPECIFIED.,.F.,.F.,(4,3,3,3,3,3,3,3,3,3,3,3,3,
3,3,3,3,3,3,3,3,3,3,3,3,3,3,3,3,3,3,3,3,3,3,3,3,3,3,3,3,3,3,3,3,3,3,3,3,
3,3,3,3,3,3,3,3,3,3,3,3,3,3,3,3,3,3,3,3,3,3,3,4),(185.353966561782,185.469849979115,
185.56948738439,185.653226096236,185.736861607603,185.820414051002,185.903903486853,
185.987357437466,186.070793931313,186.154231041068,186.237686835986,186.321231328715,
186.404820411656,186.488543679214,186.569223395111,186.652962106957,186.736597618325,
186.820150061723,186.903639497574,186.987093448188,187.070529942034,187.15396705179,
187.237422846707,187.320967339437,187.404556422378,187.488279689936,187.568959405831,
187.652698117677,187.736333629044,187.819886072443,187.903375508294,187.986829458907,
188.070265952754,188.153703062509,188.237158857427,188.320703350156,188.404292433097,
188.488015700655,188.568695416551,188.652434128397,188.736069639764,188.819622083163,
188.903111519014,188.986565469628,189.070001963474,189.153439073229,189.236894868147,
189.320439360877,189.404028443818,189.487751711375,189.568431427271,189.652170139117,
189.735805650484,189.819358093883,189.902847529734,189.986301480348,190.069737974194,
190.153175083949,190.236630878867,190.320175371597,190.403764454538,190.487487722095,
190.568167437991,190.651917107085,190.735561169276,190.819104568393,190.90259089521,
190.986038269379,191.069464780467,191.152915473613,191.236376932508,191.319909424351,
191.385494809803),.UNSPECIFIED.);
#171=B_SPLINE_CURVE_WITH_KNOTS('',3,(#30587,#30588,#30589,#30590,#30591,
#30592,#30593,#30594,#30595,#30596,#30597,#30598,#30599,#30600,#30601,#30602,
#30603,#30604,#30605,#30606,#30607,#30608,#30609,#30610,#30611,#30612,#30613,
#30614,#30615,#30616,#30617,#30618,#30619,#30620,#30621,#30622,#30623,#30624,
#30625,#30626,#30627,#30628,#30629,#30630,#30631,#30632,#30633,#30634,#30635,
#30636,#30637,#30638,#30639,#30640,#30641,#30642,#30643,#30644,#30645,#30646,
#30647,#30648,#30649,#30650,#30651,#30652,#30653,#30654,#30655,#30656,#30657,
#30658,#30659,#30660,#30661,#30662,#30663,#30664,#30665,#30666,#30667,#30668,
#30669,#30670,#30671,#30672,#30673,#30674,#30675,#30676,#30677,#30678,#30679,
#30680,#30681,#30682,#30683,#30684,#30685,#30686,#30687,#30688,#30689,#30690,
#30691,#30692,#30693,#30694,#30695,#30696,#30697,#30698,#30699,#30700,#30701,
#30702,#30703,#30704,#30705,#30706,#30707,#30708,#30709,#30710,#30711,#30712,
#30713,#30714,#30715,#30716,#30717,#30718,#30719,#30720,#30721,#30722,#30723,
#30724,#30725,#30726,#30727,#30728,#30729,#30730,#30731,#30732,#30733,#30734,
#30735,#30736,#30737,#30738,#30739,#30740,#30741,#30742,#30743,#30744,#30745,
#30746,#30747,#30748,#30749,#30750,#30751,#30752,#30753,#30754,#30755,#30756,
#30757,#30758,#30759,#30760,#30761,#30762,#30763,#30764,#30765,#30766,#30767,
#30768,#30769,#30770,#30771,#30772,#30773,#30774,#30775,#30776,#30777,#30778,
#30779,#30780,#30781,#30782,#30783,#30784,#30785,#30786,#30787,#30788,#30789,
#30790,#30791,#30792,#30793,#30794,#30795,#30796,#30797,#30798,#30799,#30800,
#30801,#30802,#30803,#30804,#30805,#30806),.UNSPECIFIED.,.F.,.F.,(4,3,3,
3,3,3,3,3,3,3,3,3,3,3,3,3,3,3,3,3,3,3,3,3,3,3,3,3,3,3,3,3,3,3,3,3,3,3,3,
3,3,3,3,3,3,3,3,3,3,3,3,3,3,3,3,3,3,3,3,3,3,3,3,3,3,3,3,3,3,3,3,3,3,4),
(191.637151868958,191.72130199631,191.805462039817,191.889649048006,191.973880083454,
192.058223549659,192.14263207536,192.227173928829,192.257348839716,192.341087551562,
192.424723062929,192.508275506328,192.591764942179,192.675218892793,192.758655386639,
192.842092496395,192.925548291313,193.009092784042,193.092681866983,193.176405134541,
193.257084850437,193.340823562283,193.42445907365,193.508011517049,193.5915009529,
193.674954903514,193.75839139736,193.841828507116,193.925284302033,194.008828794763,
194.092417877704,194.176141145262,194.256820861157,194.340559573003,194.42419508437,
194.507747527769,194.59123696362,194.674690914234,194.75812740808,194.841564517836,
194.925020312753,195.008564805483,195.092153888424,195.175877155981,195.256556871877,
195.340295583723,195.42393109509,195.507483538489,195.59097297434,195.674426924954,
195.7578634188,195.841300528555,195.924756323473,196.008300816203,196.091889899144,
196.175613166701,196.256292882597,196.340031594443,196.423667105811,196.507219549209,
196.59070898506,196.674162935674,196.75759942952,196.841036539275,196.924492334193,
197.008036826923,197.091625909864,197.175349177421,197.256028893317,197.339775084216,
197.423386845421,197.506921237328,197.590387613573,197.669413533224),
 .UNSPECIFIED.);
#172=B_SPLINE_CURVE_WITH_KNOTS('',3,(#30807,#30808,#30809,#30810,#30811,
#30812,#30813,#30814,#30815,#30816),.UNSPECIFIED.,.F.,.F.,(4,3,3,4),(191.386723760419,
191.480798684565,191.574339257805,191.637151868763),.UNSPECIFIED.);
#173=B_SPLINE_CURVE_WITH_KNOTS('',3,(#30818,#30819,#30820,#30821,#30822,
#30823,#30824,#30825,#30826,#30827,#30828,#30829,#30830),.UNSPECIFIED.,
 .F.,.F.,(4,3,3,3,4),(191.385494809803,191.469130268462,191.552881694883,
191.567903448711,191.637151868962),.UNSPECIFIED.);
#174=B_SPLINE_CURVE_WITH_KNOTS('',3,(#30831,#30832,#30833,#30834,#30835,
#30836,#30837,#30838,#30839,#30840,#30841,#30842,#30843,#30844,#30845,#30846,
#30847,#30848,#30849,#30850,#30851,#30852,#30853,#30854,#30855,#30856,#30857,
#30858,#30859,#30860,#30861,#30862,#30863,#30864,#30865,#30866,#30867,#30868,
#30869,#30870,#30871,#30872,#30873,#30874,#30875,#30876,#30877,#30878,#30879,
#30880,#30881,#30882,#30883,#30884,#30885,#30886,#30887,#30888,#30889,#30890,
#30891,#30892,#30893,#30894,#30895,#30896,#30897,#30898,#30899,#30900,#30901,
#30902,#30903,#30904,#30905,#30906,#30907,#30908,#30909,#30910,#30911,#30912,
#30913,#30914,#30915,#30916,#30917,#30918,#30919,#30920,#30921,#30922,#30923,
#30924,#30925,#30926,#30927,#30928,#30929,#30930,#30931,#30932,#30933,#30934,
#30935,#30936,#30937,#30938,#30939,#30940,#30941,#30942,#30943,#30944,#30945,
#30946,#30947,#30948,#30949,#30950,#30951,#30952,#30953,#30954,#30955,#30956,
#30957,#30958,#30959,#30960,#30961,#30962,#30963,#30964,#30965,#30966,#30967,
#30968,#30969,#30970,#30971,#30972,#30973,#30974,#30975,#30976,#30977,#30978,
#30979,#30980,#30981,#30982,#30983,#30984,#30985,#30986,#30987,#30988,#30989,
#30990,#30991,#30992,#30993,#30994,#30995,#30996,#30997,#30998,#30999,#31000,
#31001,#31002,#31003,#31004,#31005,#31006,#31007,#31008,#31009,#31010,#31011,
#31012,#31013,#31014,#31015,#31016,#31017,#31018,#31019,#31020,#31021,#31022,
#31023,#31024,#31025,#31026,#31027,#31028,#31029,#31030,#31031,#31032,#31033,
#31034,#31035,#31036,#31037,#31038,#31039,#31040,#31041,#31042,#31043,#31044,
#31045,#31046,#31047,#31048,#31049,#31050,#31051,#31052,#31053),
 .UNSPECIFIED.,.F.,.F.,(4,3,3,3,3,3,3,3,3,3,3,3,3,3,3,3,3,3,3,3,3,3,3,3,
3,3,3,3,3,3,3,3,3,3,3,3,3,3,3,3,3,3,3,3,3,3,3,3,3,3,3,3,3,3,3,3,3,3,3,3,
3,3,3,3,3,3,3,3,3,3,3,3,3,3,4),(191.637151869084,191.720040417558,191.802831357082,
191.885545578145,191.970807313306,192.053439367496,192.136062354038,192.218695029689,
192.30135615543,192.384108212342,192.466914941915,192.5498368084,192.567639459431,
192.651378171277,192.735013682644,192.818566126043,192.902055561894,192.985509512508,
193.068946006354,193.15238311611,193.235838911027,193.319383403757,193.402972486698,
193.486695754256,193.567375470152,193.651114181998,193.734749693366,193.818302136764,
193.901791572616,193.985245523229,194.068682017076,194.152119126831,194.235574921749,
194.319119414479,194.40270849742,194.486431764978,194.567111480872,194.650850192718,
194.734485704085,194.818038147484,194.901527583335,194.984981533949,195.068418027795,
195.151855137551,195.235310932468,195.318855425198,195.402444508139,195.486167775696,
195.566847491592,195.650586203438,195.734221714805,195.817774158204,195.901263594055,
195.984717544669,196.068154038515,196.151591148271,196.235046943188,196.318591435918,
196.402180518859,196.485903786417,196.566583502312,196.650322214158,196.733957725526,
196.817510168924,196.900999604776,196.984453555389,197.067890049236,197.151327158991,
197.234782953909,197.318327446638,197.401916529579,197.485639797137,197.566319513032,
197.662998523347,197.669819480909),.UNSPECIFIED.);
#175=B_SPLINE_CURVE_WITH_KNOTS('',3,(#31059,#31060,#31061,#31062,#31063,
#31064,#31065,#31066,#31067,#31068,#31069,#31070,#31071,#31072,#31073,#31074,
#31075,#31076,#31077,#31078,#31079,#31080,#31081,#31082,#31083,#31084,#31085,
#31086,#31087,#31088,#31089,#31090,#31091,#31092,#31093,#31094,#31095,#31096,
#31097,#31098,#31099,#31100,#31101,#31102,#31103,#31104,#31105,#31106,#31107,
#31108,#31109,#31110,#31111,#31112,#31113,#31114,#31115,#31116,#31117,#31118,
#31119,#31120,#31121,#31122,#31123,#31124,#31125,#31126,#31127,#31128,#31129,
#31130,#31131,#31132,#31133,#31134,#31135,#31136,#31137,#31138,#31139,#31140,
#31141,#31142,#31143,#31144,#31145,#31146,#31147,#31148,#31149,#31150,#31151,
#31152,#31153,#31154,#31155,#31156,#31157,#31158,#31159,#31160,#31161,#31162,
#31163,#31164,#31165,#31166,#31167,#31168,#31169,#31170,#31171,#31172,#31173,
#31174,#31175,#31176,#31177,#31178,#31179,#31180,#31181,#31182,#31183,#31184,
#31185,#31186,#31187,#31188,#31189,#31190,#31191,#31192,#31193,#31194,#31195,
#31196,#31197,#31198,#31199,#31200,#31201,#31202,#31203,#31204,#31205,#31206,
#31207,#31208,#31209,#31210,#31211,#31212,#31213,#31214,#31215,#31216,#31217,
#31218,#31219,#31220,#31221,#31222,#31223,#31224,#31225,#31226,#31227,#31228,
#31229,#31230,#31231,#31232,#31233,#31234,#31235,#31236,#31237,#31238,#31239,
#31240,#31241,#31242,#31243,#31244,#31245,#31246,#31247,#31248,#31249,#31250,
#31251,#31252,#31253,#31254,#31255,#31256,#31257,#31258,#31259,#31260,#31261,
#31262,#31263,#31264,#31265,#31266,#31267,#31268,#31269,#31270,#31271,#31272,
#31273,#31274,#31275,#31276,#31277,#31278),.UNSPECIFIED.,.F.,.F.,(4,3,3,
3,3,3,3,3,3,3,3,3,3,3,3,3,3,3,3,3,3,3,3,3,3,3,3,3,3,3,3,3,3,3,3,3,3,3,3,
3,3,3,3,3,3,3,3,3,3,3,3,3,3,3,3,3,3,3,3,3,3,3,3,3,3,3,3,3,3,3,3,3,3,4),
(197.920337176326,198.017388435386,198.115004455218,198.213290205117,198.255764904037,
198.339503615883,198.42313912725,198.506691570649,198.5901810065,198.673634957114,
198.75707145096,198.840508560715,198.923964355633,199.007508848363,199.091097931304,
199.174821198861,199.255500914757,199.339239626603,199.42287513797,199.506427581369,
199.58991701722,199.673370967834,199.75680746168,199.840244571436,199.923700366353,
200.007244859083,200.090833942024,200.174557209581,200.255236925477,200.338975637323,
200.422611148691,200.506163592089,200.58965302794,200.673106978554,200.7565434724,
200.839980582156,200.923436377074,201.006980869803,201.090569952744,201.174293220302,
201.254972936198,201.338711648044,201.422347159412,201.50589960281,201.589389038661,
201.672842989275,201.756279483121,201.839716592877,201.923172387794,202.006716880524,
202.090305963465,202.174029231023,202.254708946918,202.338447658764,202.422083170131,
202.50563561353,202.589125049381,202.672578999995,202.756015493841,202.839452603596,
202.922908398514,203.006452891243,203.090041974184,203.173765241742,203.254444957638,
203.341603870439,203.424575763055,203.507472782828,203.590313653258,203.673117051873,
203.755916189265,203.838713095402,203.921548720593,203.95171626005),
 .UNSPECIFIED.);
#176=B_SPLINE_CURVE_WITH_KNOTS('',3,(#31279,#31280,#31281,#31282,#31283,
#31284,#31285,#31286,#31287,#31288),.UNSPECIFIED.,.F.,.F.,(4,3,3,4),(197.669413533224,
197.75281524834,197.836576212239,197.920337176138),.UNSPECIFIED.);
#177=B_SPLINE_CURVE_WITH_KNOTS('',3,(#31290,#31291,#31292,#31293,#31294,
#31295,#31296,#31297,#31298,#31299),.UNSPECIFIED.,.F.,.F.,(4,3,3,4),(197.669819480909,
197.765936206161,197.861361969395,197.920337175945),.UNSPECIFIED.);
#178=B_SPLINE_CURVE_WITH_KNOTS('',3,(#31300,#31301,#31302,#31303,#31304,
#31305,#31306,#31307,#31308,#31309,#31310,#31311,#31312,#31313,#31314,#31315,
#31316,#31317,#31318,#31319,#31320,#31321,#31322,#31323,#31324,#31325,#31326,
#31327,#31328,#31329,#31330,#31331,#31332,#31333,#31334,#31335,#31336,#31337,
#31338,#31339,#31340,#31341,#31342,#31343,#31344,#31345,#31346,#31347,#31348,
#31349,#31350,#31351,#31352,#31353,#31354,#31355,#31356,#31357,#31358,#31359,
#31360,#31361,#31362,#31363,#31364,#31365,#31366,#31367,#31368,#31369,#31370,
#31371,#31372,#31373,#31374,#31375,#31376,#31377,#31378,#31379,#31380,#31381,
#31382,#31383,#31384,#31385,#31386,#31387,#31388,#31389,#31390,#31391,#31392,
#31393,#31394,#31395,#31396,#31397,#31398,#31399,#31400,#31401,#31402,#31403,
#31404,#31405,#31406,#31407,#31408,#31409,#31410,#31411,#31412,#31413,#31414,
#31415,#31416,#31417,#31418,#31419,#31420,#31421,#31422,#31423,#31424,#31425,
#31426,#31427,#31428,#31429,#31430,#31431,#31432,#31433,#31434,#31435,#31436,
#31437,#31438,#31439,#31440,#31441,#31442,#31443,#31444,#31445,#31446,#31447,
#31448,#31449,#31450,#31451,#31452,#31453,#31454,#31455,#31456,#31457,#31458,
#31459,#31460,#31461,#31462,#31463,#31464,#31465,#31466,#31467,#31468,#31469,
#31470,#31471,#31472,#31473,#31474,#31475,#31476,#31477,#31478,#31479,#31480,
#31481,#31482,#31483,#31484,#31485,#31486,#31487,#31488,#31489,#31490,#31491,
#31492,#31493,#31494,#31495,#31496,#31497,#31498,#31499,#31500,#31501,#31502,
#31503,#31504,#31505,#31506,#31507,#31508,#31509,#31510,#31511,#31512,#31513,
#31514,#31515,#31516,#31517,#31518,#31519),.UNSPECIFIED.,.F.,.F.,(4,3,3,
3,3,3,3,3,3,3,3,3,3,3,3,3,3,3,3,3,3,3,3,3,3,3,3,3,3,3,3,3,3,3,3,3,3,3,3,
3,3,3,3,3,3,3,3,3,3,3,3,3,3,3,3,3,3,3,3,3,3,3,3,3,3,3,3,3,3,3,3,3,3,4),
(197.920337176141,198.004037107572,198.087733392622,198.171443712856,198.255185755071,
198.339030392134,198.422930356544,198.506967457774,198.566055523752,198.649794235598,
198.733429746965,198.816982190364,198.900471626215,198.983925576829,199.067362070675,
199.15079918043,199.234254975348,199.317799468078,199.401388551019,199.485111818576,
199.565791534472,199.649530246318,199.733165757685,199.816718201084,199.900207636935,
199.983661587549,200.067098081395,200.150535191151,200.233990986069,200.317535478798,
200.401124561739,200.484847829297,200.565527545192,200.649266257038,200.732901768406,
200.816454211804,200.899943647655,200.983397598269,201.066834092115,201.150271201871,
201.233726996788,201.317271489518,201.400860572459,201.484583840017,201.565263555913,
201.649002267759,201.732637779126,201.816190222525,201.899679658377,201.98313360899,
202.066570102837,202.150007212592,202.23346300751,202.31700750024,202.40059658318,
202.484319850738,202.564999566633,202.648738278479,202.732373789846,202.815926233245,
202.899415669096,202.98286961971,203.066306113556,203.149743223311,203.233199018228,
203.316743510958,203.400332593899,203.484055861457,203.564735577353,203.648922162625,
203.732968699384,203.816934586732,203.900823571561,203.952726252955),
 .UNSPECIFIED.);
#179=B_SPLINE_CURVE_WITH_KNOTS('',3,(#31525,#31526,#31527,#31528,#31529,
#31530,#31531,#31532,#31533,#31534,#31535,#31536,#31537,#31538,#31539,#31540,
#31541,#31542,#31543,#31544,#31545,#31546,#31547,#31548,#31549,#31550,#31551,
#31552,#31553,#31554,#31555,#31556,#31557,#31558,#31559,#31560,#31561,#31562,
#31563,#31564,#31565,#31566,#31567,#31568,#31569,#31570,#31571,#31572,#31573,
#31574,#31575,#31576,#31577,#31578,#31579,#31580,#31581,#31582,#31583,#31584,
#31585,#31586,#31587,#31588,#31589,#31590,#31591,#31592,#31593,#31594,#31595,
#31596,#31597,#31598,#31599,#31600,#31601,#31602,#31603,#31604,#31605,#31606,
#31607,#31608,#31609,#31610,#31611,#31612,#31613,#31614,#31615,#31616,#31617,
#31618,#31619,#31620,#31621,#31622,#31623,#31624,#31625,#31626,#31627,#31628,
#31629,#31630,#31631,#31632,#31633,#31634,#31635,#31636,#31637,#31638,#31639,
#31640,#31641,#31642,#31643,#31644,#31645,#31646,#31647,#31648,#31649,#31650,
#31651,#31652,#31653,#31654,#31655,#31656,#31657,#31658,#31659,#31660,#31661,
#31662,#31663,#31664,#31665,#31666,#31667,#31668,#31669,#31670,#31671,#31672,
#31673,#31674,#31675,#31676,#31677,#31678,#31679,#31680,#31681,#31682,#31683,
#31684,#31685,#31686,#31687,#31688,#31689,#31690,#31691,#31692,#31693,#31694,
#31695,#31696,#31697,#31698,#31699,#31700,#31701,#31702,#31703,#31704,#31705,
#31706,#31707,#31708,#31709,#31710,#31711,#31712,#31713,#31714,#31715,#31716,
#31717,#31718,#31719,#31720,#31721,#31722,#31723,#31724,#31725,#31726,#31727,
#31728,#31729,#31730,#31731,#31732,#31733,#31734,#31735,#31736,#31737,#31738,
#31739,#31740,#31741,#31742,#31743,#31744),.UNSPECIFIED.,.F.,.F.,(4,3,3,
3,3,3,3,3,3,3,3,3,3,3,3,3,3,3,3,3,3,3,3,3,3,3,3,3,3,3,3,3,3,3,3,3,3,3,3,
3,3,3,3,3,3,3,3,3,3,3,3,3,3,3,3,3,3,3,3,3,3,3,3,3,3,3,3,3,3,3,3,3,3,4),
(204.203522483317,204.254180968358,204.337919680204,204.421555191571,204.50510763497,
204.588597070821,204.672051021435,204.755487515281,204.838924625037,204.922380419955,
205.005924912684,205.089513995625,205.173237263183,205.253916979078,205.337655690924,
205.421291202291,205.50484364569,205.588333081541,205.671787032155,205.755223526001,
205.838660635756,205.922116430674,206.005660923404,206.089250006344,206.172973273902,
206.253652989798,206.337391701644,206.421027213011,206.50457965641,206.588069092261,
206.671523042874,206.75495953672,206.838396646476,206.921852441393,207.005396934123,
207.088986017064,207.172709284621,207.253389000518,207.337127712364,207.420763223732,
207.50431566713,207.587805102981,207.671259053595,207.754695547441,207.838132657197,
207.921588452115,208.005132944845,208.088722027786,208.172445295343,208.253125011238,
208.336863723084,208.420499234451,208.50405167785,208.587541113701,208.670995064315,
208.754431558161,208.837868667916,208.921324462834,209.004868955564,209.088458038505,
209.172181306062,209.252861021959,209.336600695396,209.420236943405,209.503789899441,
209.587279624644,209.670732707411,209.754168015386,209.837603621028,209.921057593095,
210.004595835075,210.088178535835,210.171884999686,210.235541291062),
 .UNSPECIFIED.);
#180=B_SPLINE_CURVE_WITH_KNOTS('',3,(#31745,#31746,#31747,#31748,#31749,
#31750,#31751,#31752,#31753,#31754),.UNSPECIFIED.,.F.,.F.,(4,3,3,4),(203.95171626005,
204.034644119421,204.119083301269,204.203522483116),.UNSPECIFIED.);
#181=B_SPLINE_CURVE_WITH_KNOTS('',3,(#31756,#31757,#31758,#31759,#31760,
#31761,#31762,#31763,#31764,#31765),.UNSPECIFIED.,.F.,.F.,(4,3,3,4),(203.952726252955,
204.036546364182,204.120363659949,204.203522483321),.UNSPECIFIED.);
#182=B_SPLINE_CURVE_WITH_KNOTS('',3,(#31766,#31767,#31768,#31769,#31770,
#31771,#31772,#31773,#31774,#31775,#31776,#31777,#31778,#31779,#31780,#31781,
#31782,#31783,#31784,#31785,#31786,#31787,#31788,#31789,#31790,#31791,#31792,
#31793,#31794,#31795,#31796,#31797,#31798,#31799,#31800,#31801,#31802,#31803,
#31804,#31805,#31806,#31807,#31808,#31809,#31810,#31811,#31812,#31813,#31814,
#31815,#31816,#31817,#31818,#31819,#31820,#31821,#31822,#31823,#31824,#31825,
#31826,#31827,#31828,#31829,#31830,#31831,#31832,#31833,#31834,#31835,#31836,
#31837,#31838,#31839,#31840,#31841,#31842,#31843,#31844,#31845,#31846,#31847,
#31848,#31849,#31850,#31851,#31852,#31853,#31854,#31855,#31856,#31857,#31858,
#31859,#31860,#31861,#31862,#31863,#31864,#31865,#31866,#31867,#31868,#31869,
#31870,#31871,#31872,#31873,#31874,#31875,#31876,#31877,#31878,#31879,#31880,
#31881,#31882,#31883,#31884,#31885,#31886,#31887,#31888,#31889,#31890,#31891,
#31892,#31893,#31894,#31895,#31896,#31897,#31898,#31899,#31900,#31901,#31902,
#31903,#31904,#31905,#31906,#31907,#31908,#31909,#31910,#31911,#31912,#31913,
#31914,#31915,#31916,#31917,#31918,#31919,#31920,#31921,#31922,#31923,#31924,
#31925,#31926,#31927,#31928,#31929,#31930,#31931,#31932,#31933,#31934,#31935,
#31936,#31937,#31938,#31939,#31940,#31941,#31942,#31943,#31944,#31945,#31946,
#31947,#31948,#31949,#31950,#31951,#31952,#31953,#31954,#31955,#31956,#31957,
#31958,#31959,#31960,#31961,#31962,#31963,#31964,#31965,#31966,#31967,#31968,
#31969,#31970,#31971,#31972,#31973,#31974,#31975,#31976,#31977,#31978,#31979,
#31980,#31981,#31982),.UNSPECIFIED.,.F.,.F.,(4,3,3,3,3,3,3,3,3,3,3,3,3,
3,3,3,3,3,3,3,3,3,3,3,3,3,3,3,3,3,3,3,3,3,3,3,3,3,3,3,3,3,3,3,3,3,3,3,3,
3,3,3,3,3,3,3,3,3,3,3,3,3,3,3,3,3,3,3,3,3,3,3,4),(204.20352248352,204.298487723003,
204.393874096607,204.489824564911,204.564471588073,204.648210299919,204.731845811287,
204.815398254685,204.898887690536,204.98234164115,205.065778134996,205.149215244751,
205.232671039669,205.316215532399,205.39980461534,205.483527882897,205.564207598793,
205.647946310639,205.731581822006,205.815134265405,205.898623701256,205.982077651869,
206.065514145716,206.148951255471,206.232407050389,206.315951543118,206.399540626059,
206.483263893617,206.563943609513,206.647682321359,206.731317832726,206.814870276125,
206.898359711976,206.98181366259,207.065250156436,207.148687266191,207.232143061109,
207.315687553839,207.39927663678,207.482999904337,207.563679620233,207.647418332079,
207.731053843447,207.814606286845,207.898095722696,207.98154967331,208.064986167156,
208.148423276912,208.23187907183,208.31542356456,208.399012647501,208.482735915058,
208.563415630954,208.6471543428,208.730789854168,208.814342297566,208.897831733417,
208.981285684031,209.064722177877,209.148159287633,209.23161508255,209.31515957528,
209.398748658221,209.482471925779,209.563151641674,209.647116797923,209.729857499283,
209.812522884371,209.89513185114,209.980067111272,210.062631853633,210.148752372651,
210.234872891669),.UNSPECIFIED.);
#183=B_SPLINE_CURVE_WITH_KNOTS('',3,(#31988,#31989,#31990,#31991,#31992,
#31993,#31994,#31995,#31996,#31997,#31998,#31999,#32000,#32001,#32002,#32003,
#32004,#32005,#32006,#32007,#32008,#32009,#32010,#32011,#32012,#32013,#32014,
#32015,#32016,#32017,#32018,#32019,#32020,#32021,#32022,#32023,#32024,#32025,
#32026,#32027,#32028,#32029,#32030,#32031,#32032,#32033,#32034,#32035,#32036,
#32037,#32038,#32039,#32040,#32041,#32042,#32043,#32044,#32045,#32046,#32047,
#32048,#32049,#32050,#32051,#32052,#32053,#32054,#32055,#32056,#32057,#32058,
#32059,#32060,#32061,#32062,#32063,#32064,#32065,#32066,#32067,#32068,#32069,
#32070,#32071,#32072,#32073,#32074,#32075,#32076,#32077,#32078,#32079,#32080,
#32081,#32082,#32083,#32084,#32085,#32086,#32087,#32088,#32089,#32090,#32091,
#32092,#32093,#32094,#32095,#32096,#32097,#32098,#32099,#32100,#32101,#32102,
#32103,#32104,#32105,#32106,#32107,#32108,#32109,#32110,#32111,#32112,#32113,
#32114,#32115,#32116,#32117,#32118,#32119,#32120,#32121,#32122,#32123,#32124,
#32125,#32126,#32127,#32128,#32129,#32130,#32131,#32132,#32133,#32134,#32135,
#32136,#32137,#32138,#32139,#32140,#32141,#32142,#32143,#32144,#32145,#32146,
#32147,#32148,#32149,#32150,#32151,#32152,#32153,#32154,#32155,#32156,#32157,
#32158,#32159,#32160,#32161,#32162,#32163,#32164,#32165,#32166,#32167,#32168,
#32169,#32170,#32171,#32172,#32173,#32174,#32175,#32176,#32177,#32178,#32179,
#32180,#32181,#32182,#32183,#32184,#32185,#32186,#32187,#32188,#32189,#32190,
#32191,#32192,#32193,#32194,#32195,#32196,#32197,#32198,#32199,#32200,#32201,
#32202,#32203,#32204,#32205,#32206,#32207),.UNSPECIFIED.,.F.,.F.,(4,3,3,
3,3,3,3,3,3,3,3,3,3,3,3,3,3,3,3,3,3,3,3,3,3,3,3,3,3,3,3,3,3,3,3,3,3,3,3,
3,3,3,3,3,3,3,3,3,3,3,3,3,3,3,3,3,3,3,3,3,3,3,3,3,3,3,3,3,3,3,3,3,3,4),
(210.486707790497,210.569187649479,210.654580823719,210.736972714126,210.819353651069,
210.901742553176,210.984158342872,211.066663834264,211.149222895521,211.231897354181,
211.252333043399,211.336071755245,211.419707266612,211.503259710011,211.586749145862,
211.670203096476,211.753639590322,211.837076700078,211.920532494996,212.004076987725,
212.087666070666,212.171389338224,212.252069054119,212.335807765965,212.419443277332,
212.502995720731,212.586485156582,212.669939107196,212.753375601042,212.836812710797,
212.920268505715,213.003812998444,213.087402081385,213.171125348943,213.251805064839,
213.335543776685,213.419179288052,213.502731731451,213.586221167302,213.669675117916,
213.753111611762,213.836548721517,213.920004516435,214.003549009165,214.087138092106,
214.170861359663,214.251541075559,214.335279787405,214.418915298773,214.502467742171,
214.585957178022,214.669411128636,214.752847622482,214.836284732238,214.919740527155,
215.003285019885,215.086874102826,215.170597370384,215.251277086279,215.335015798125,
215.418651309492,215.502203752891,215.585693188742,215.669147139356,215.752583633203,
215.836020742958,215.919476537876,216.003021030605,216.086610113546,216.170333381104,
216.251013096999,216.338350634161,216.428941749218,216.519532864276),
 .UNSPECIFIED.);
#184=B_SPLINE_CURVE_WITH_KNOTS('',3,(#32208,#32209,#32210,#32211,#32212,
#32213,#32214,#32215,#32216,#32217,#32218,#32219,#32220),.UNSPECIFIED.,
 .F.,.F.,(4,3,3,3,4),(210.235541291062,210.252597032679,210.369652411526,
210.479644992553,210.486707790373),.UNSPECIFIED.);
#185=B_SPLINE_CURVE_WITH_KNOTS('',3,(#32222,#32223,#32224,#32225,#32226,
#32227,#32228,#32229,#32230,#32231),.UNSPECIFIED.,.F.,.F.,(4,3,3,4),(210.234872891669,
210.317554458692,210.402131124533,210.486707790373),.UNSPECIFIED.);
#186=B_SPLINE_CURVE_WITH_KNOTS('',3,(#32232,#32233,#32234,#32235,#32236,
#32237,#32238,#32239,#32240,#32241,#32242,#32243,#32244,#32245,#32246,#32247,
#32248,#32249,#32250,#32251,#32252,#32253,#32254,#32255,#32256,#32257,#32258,
#32259,#32260,#32261,#32262,#32263,#32264,#32265,#32266,#32267,#32268,#32269,
#32270,#32271,#32272,#32273,#32274,#32275,#32276,#32277,#32278,#32279,#32280,
#32281,#32282,#32283,#32284,#32285,#32286,#32287,#32288,#32289,#32290,#32291,
#32292,#32293,#32294,#32295,#32296,#32297,#32298,#32299,#32300,#32301,#32302,
#32303,#32304,#32305,#32306,#32307,#32308,#32309,#32310,#32311,#32312,#32313,
#32314,#32315,#32316,#32317,#32318,#32319,#32320,#32321,#32322,#32323,#32324,
#32325,#32326,#32327,#32328,#32329,#32330,#32331,#32332,#32333,#32334,#32335,
#32336,#32337,#32338,#32339,#32340,#32341,#32342,#32343,#32344,#32345,#32346,
#32347,#32348,#32349,#32350,#32351,#32352,#32353,#32354,#32355,#32356,#32357,
#32358,#32359,#32360,#32361,#32362,#32363,#32364,#32365,#32366,#32367,#32368,
#32369,#32370,#32371,#32372,#32373,#32374,#32375,#32376,#32377,#32378,#32379,
#32380,#32381,#32382,#32383,#32384,#32385,#32386,#32387,#32388,#32389,#32390,
#32391,#32392,#32393,#32394,#32395,#32396,#32397,#32398,#32399,#32400,#32401,
#32402,#32403,#32404,#32405,#32406,#32407,#32408,#32409,#32410,#32411,#32412,
#32413,#32414,#32415,#32416,#32417,#32418,#32419,#32420,#32421,#32422,#32423,
#32424,#32425,#32426,#32427,#32428,#32429,#32430,#32431,#32432,#32433,#32434,
#32435,#32436,#32437,#32438,#32439,#32440,#32441,#32442,#32443,#32444,#32445,
#32446,#32447,#32448,#32449,#32450,#32451),.UNSPECIFIED.,.F.,.F.,(4,3,3,
3,3,3,3,3,3,3,3,3,3,3,3,3,3,3,3,3,3,3,3,3,3,3,3,3,3,3,3,3,3,3,3,3,3,3,3,
3,3,3,3,3,3,3,3,3,3,3,3,3,3,3,3,3,3,3,3,3,3,3,3,3,3,3,3,3,3,3,3,3,3,4),
(210.486707790501,210.562887652394,210.64662636424,210.730261875607,210.813814319006,
210.897303754857,210.98075770547,211.064194199317,211.147631309072,211.23108710399,
211.31463159672,211.398220679661,211.481943947218,211.562623663114,211.64636237496,
211.729997886327,211.813550329726,211.897039765577,211.980493716191,212.063930210037,
212.147367319792,212.23082311471,212.31436760744,212.397956690381,212.481679957938,
212.562359673834,212.64609838568,212.729733897047,212.813286340446,212.896775776297,
212.98022972691,213.063666220757,213.147103330512,213.23055912543,213.314103618159,
213.3976927011,213.481415968658,213.562095684554,213.6458343964,213.729469907767,
213.813022351166,213.896511787017,213.979965737631,214.063402231477,214.146839341232,
214.23029513615,214.313839628879,214.39742871182,214.481151979378,214.561831695274,
214.64557040712,214.729205918488,214.812758361886,214.896247797737,214.979701748351,
215.063138242197,215.146575351953,215.230031146871,215.3135756396,215.397164722542,
215.480887990099,215.561567705994,215.645308850233,215.72894623067,215.812499982196,
215.895990167042,215.979442042456,216.062875664721,216.146309106006,216.229760434362,
216.313289666024,216.396863158832,216.480545908606,216.518594148983),
 .UNSPECIFIED.);
#187=B_SPLINE_CURVE_WITH_KNOTS('',3,(#32457,#32458,#32459,#32460,#32461,
#32462,#32463,#32464,#32465,#32466,#32467,#32468,#32469,#32470,#32471,#32472,
#32473,#32474,#32475,#32476,#32477,#32478,#32479,#32480,#32481,#32482,#32483,
#32484,#32485,#32486,#32487,#32488,#32489,#32490,#32491,#32492,#32493,#32494,
#32495,#32496,#32497,#32498,#32499,#32500,#32501,#32502,#32503,#32504,#32505,
#32506,#32507,#32508,#32509,#32510,#32511,#32512,#32513,#32514,#32515,#32516,
#32517,#32518,#32519,#32520,#32521,#32522,#32523,#32524,#32525,#32526,#32527,
#32528,#32529,#32530,#32531,#32532,#32533,#32534,#32535,#32536,#32537,#32538,
#32539,#32540,#32541,#32542,#32543,#32544,#32545,#32546,#32547,#32548,#32549,
#32550,#32551,#32552,#32553,#32554,#32555,#32556,#32557,#32558,#32559,#32560,
#32561,#32562,#32563,#32564,#32565,#32566,#32567,#32568,#32569,#32570,#32571,
#32572,#32573,#32574,#32575,#32576,#32577,#32578,#32579,#32580,#32581,#32582,
#32583,#32584,#32585,#32586,#32587,#32588,#32589,#32590,#32591,#32592,#32593,
#32594,#32595,#32596,#32597,#32598,#32599,#32600,#32601,#32602,#32603,#32604,
#32605,#32606,#32607,#32608,#32609,#32610,#32611,#32612,#32613,#32614,#32615,
#32616,#32617,#32618,#32619,#32620,#32621,#32622,#32623,#32624,#32625,#32626,
#32627,#32628,#32629,#32630,#32631,#32632,#32633,#32634,#32635,#32636,#32637,
#32638,#32639,#32640,#32641,#32642,#32643,#32644,#32645,#32646,#32647,#32648,
#32649,#32650,#32651,#32652,#32653,#32654,#32655,#32656,#32657,#32658,#32659,
#32660,#32661,#32662,#32663,#32664,#32665,#32666,#32667,#32668,#32669,#32670,
#32671,#32672,#32673,#32674,#32675,#32676),.UNSPECIFIED.,.F.,.F.,(4,3,3,
3,3,3,3,3,3,3,3,3,3,3,3,3,3,3,3,3,3,3,3,3,3,3,3,3,3,3,3,3,3,3,3,3,3,3,3,
3,3,3,3,3,3,3,3,3,3,3,3,3,3,3,3,3,3,3,3,3,3,3,3,3,3,3,3,3,3,3,3,3,3,4),
(216.769893097836,216.858019319225,216.946288279332,217.034791092222,217.123420686244,
217.212257061535,217.25074910772,217.334487819566,217.418123330933,217.501675774332,
217.585165210183,217.668619160797,217.752055654643,217.835492764398,217.918948559316,
218.002493052046,218.086082134987,218.169805402545,218.25048511844,218.334223830286,
218.417859341653,218.501411785052,218.584901220903,218.668355171516,218.751791665363,
218.835228775118,218.918684570036,219.002229062765,219.085818145706,219.169541413264,
219.25022112916,219.333959841006,219.417595352373,219.501147795772,219.584637231623,
219.668091182237,219.751527676083,219.834964785838,219.918420580756,220.001965073486,
220.085554156426,220.169277423984,220.24995713988,220.333695851726,220.417331363093,
220.500883806492,220.584373242343,220.667827192957,220.751263686803,220.834700796558,
220.918156591476,221.001701084206,221.085290167147,221.169013434704,221.2496931506,
221.333431862446,221.417067373813,221.500619817212,221.584109253063,221.667563203677,
221.750999697523,221.834436807278,221.917892602196,222.001437094926,222.085026177867,
222.168749445424,222.24942916132,222.331934290144,222.414343415733,222.496675743037,
222.578948659109,222.661186136252,222.743421800978,222.801474927361),
 .UNSPECIFIED.);
#188=B_SPLINE_CURVE_WITH_KNOTS('',3,(#32677,#32678,#32679,#32680,#32681,
#32682,#32683,#32684,#32685,#32686),.UNSPECIFIED.,.F.,.F.,(4,3,3,4),(216.519532864276,
216.606437933948,216.693212126797,216.769893097676),.UNSPECIFIED.);
#189=B_SPLINE_CURVE_WITH_KNOTS('',3,(#32688,#32689,#32690,#32691,#32692,
#32693,#32694,#32695,#32696,#32697),.UNSPECIFIED.,.F.,.F.,(4,3,3,4),(216.518594148983,
216.561303716715,216.679015246047,216.76989309768),.UNSPECIFIED.);
#190=B_SPLINE_CURVE_WITH_KNOTS('',3,(#32698,#32699,#32700,#32701,#32702,
#32703,#32704,#32705,#32706,#32707,#32708,#32709,#32710,#32711,#32712,#32713,
#32714,#32715,#32716,#32717,#32718,#32719,#32720,#32721,#32722,#32723,#32724,
#32725,#32726,#32727,#32728,#32729,#32730,#32731,#32732,#32733,#32734,#32735,
#32736,#32737,#32738,#32739,#32740,#32741,#32742,#32743,#32744,#32745,#32746,
#32747,#32748,#32749,#32750,#32751,#32752,#32753,#32754,#32755,#32756,#32757,
#32758,#32759,#32760,#32761,#32762,#32763,#32764,#32765,#32766,#32767,#32768,
#32769,#32770,#32771,#32772,#32773,#32774,#32775,#32776,#32777,#32778,#32779,
#32780,#32781,#32782,#32783,#32784,#32785,#32786,#32787,#32788,#32789,#32790,
#32791,#32792,#32793,#32794,#32795,#32796,#32797,#32798,#32799,#32800,#32801,
#32802,#32803,#32804,#32805,#32806,#32807,#32808,#32809,#32810,#32811,#32812,
#32813,#32814,#32815,#32816,#32817,#32818,#32819,#32820,#32821,#32822,#32823,
#32824,#32825,#32826,#32827,#32828,#32829,#32830,#32831,#32832,#32833,#32834,
#32835,#32836,#32837,#32838,#32839,#32840,#32841,#32842,#32843,#32844,#32845,
#32846,#32847,#32848,#32849,#32850,#32851,#32852,#32853,#32854,#32855,#32856,
#32857,#32858,#32859,#32860,#32861,#32862,#32863,#32864,#32865,#32866,#32867,
#32868,#32869,#32870,#32871,#32872,#32873,#32874,#32875,#32876,#32877,#32878,
#32879,#32880,#32881,#32882,#32883,#32884,#32885,#32886,#32887,#32888,#32889,
#32890,#32891,#32892,#32893,#32894,#32895,#32896,#32897,#32898,#32899,#32900,
#32901,#32902,#32903,#32904,#32905,#32906,#32907,#32908,#32909,#32910,#32911,
#32912,#32913,#32914,#32915,#32916,#32917),.UNSPECIFIED.,.F.,.F.,(4,3,3,
3,3,3,3,3,3,3,3,3,3,3,3,3,3,3,3,3,3,3,3,3,3,3,3,3,3,3,3,3,3,3,3,3,3,3,3,
3,3,3,3,3,3,3,3,3,3,3,3,3,3,3,3,3,3,3,3,3,3,3,3,3,3,3,3,3,3,3,3,3,3,4),
(216.769893097827,216.852286645666,216.934613755932,217.016901737036,217.099171012457,
217.181440577583,217.263729425788,217.34610372829,217.428524911439,217.511068641655,
217.561039727435,217.644778439281,217.728413950648,217.811966394047,217.895455829898,
217.978909780512,218.062346274358,218.145783384114,218.229239179031,218.312783671761,
218.396372754702,218.48009602226,218.560775738155,218.644514450001,218.728149961368,
218.811702404767,218.895191840618,218.978645791232,219.062082285078,219.145519394833,
219.228975189751,219.31251968248,219.396108765421,219.479832032979,219.560511748875,
219.644250460721,219.727885972088,219.811438415487,219.894927851338,219.978381801952,
220.061818295798,220.145255405553,220.228711200471,220.312255693201,220.395844776142,
220.4795680437,220.560247759595,220.643986471441,220.727621982808,220.811174426207,
220.894663862058,220.978117812672,221.061554306518,221.144991416273,221.228447211191,
221.31199170392,221.395580786861,221.479304054419,221.559983770315,221.643722482161,
221.727357993528,221.810910436927,221.894399872779,221.977853823392,222.061290317239,
222.144727426994,222.228183221912,222.311727714642,222.395316797583,222.479040065141,
222.559719781035,222.648038057741,222.736156359061,222.802758717798),
 .UNSPECIFIED.);
#191=B_SPLINE_CURVE_WITH_KNOTS('',3,(#32923,#32924,#32925,#32926,#32927,
#32928,#32929,#32930,#32931,#32932,#32933,#32934,#32935,#32936,#32937,#32938,
#32939,#32940,#32941,#32942,#32943,#32944,#32945,#32946,#32947,#32948,#32949,
#32950,#32951,#32952,#32953,#32954,#32955,#32956,#32957,#32958,#32959,#32960,
#32961,#32962,#32963,#32964,#32965,#32966,#32967,#32968,#32969,#32970,#32971,
#32972,#32973,#32974,#32975,#32976,#32977,#32978,#32979,#32980,#32981,#32982,
#32983,#32984,#32985,#32986,#32987,#32988,#32989,#32990,#32991,#32992,#32993,
#32994,#32995,#32996,#32997,#32998,#32999,#33000,#33001,#33002,#33003,#33004,
#33005,#33006,#33007,#33008,#33009,#33010,#33011,#33012,#33013,#33014,#33015,
#33016,#33017,#33018,#33019,#33020,#33021,#33022,#33023,#33024,#33025,#33026,
#33027,#33028,#33029,#33030,#33031,#33032,#33033,#33034,#33035,#33036,#33037,
#33038,#33039,#33040,#33041,#33042,#33043,#33044,#33045,#33046,#33047,#33048,
#33049,#33050,#33051,#33052,#33053,#33054,#33055,#33056,#33057,#33058,#33059,
#33060,#33061,#33062,#33063,#33064,#33065,#33066,#33067,#33068,#33069,#33070,
#33071,#33072,#33073,#33074,#33075,#33076,#33077,#33078,#33079,#33080,#33081,
#33082,#33083,#33084,#33085,#33086,#33087,#33088,#33089,#33090,#33091,#33092,
#33093,#33094,#33095,#33096,#33097,#33098,#33099,#33100,#33101,#33102,#33103,
#33104,#33105,#33106,#33107,#33108,#33109,#33110,#33111,#33112,#33113,#33114,
#33115,#33116,#33117,#33118,#33119,#33120,#33121,#33122,#33123,#33124,#33125,
#33126,#33127,#33128,#33129,#33130,#33131,#33132,#33133,#33134,#33135,#33136,
#33137,#33138,#33139),.UNSPECIFIED.,.F.,.F.,(4,3,3,3,3,3,3,3,3,3,3,3,3,
3,3,3,3,3,3,3,3,3,3,3,3,3,3,3,3,3,3,3,3,3,3,3,3,3,3,3,3,3,3,3,3,3,3,3,3,
3,3,3,3,3,3,3,3,3,3,3,3,3,3,3,3,3,3,3,3,3,3,3,4),(223.053078404856,223.174503651388,
223.24916517204,223.332903883886,223.416539395254,223.500091838652,223.583581274503,
223.667035225117,223.750471718963,223.833908828718,223.917364623636,224.000909116366,
224.084498199307,224.168221466864,224.248901182761,224.332639894607,224.416275405974,
224.499827849373,224.583317285224,224.666771235838,224.750207729684,224.83364483944,
224.917100634357,225.000645127087,225.084234210028,225.167957477586,225.248637193481,
225.332375905327,225.416011416694,225.499563860093,225.583053295944,225.666507246557,
225.749943740404,225.833380850159,225.916836645077,226.000381137806,226.083970220747,
226.167693488305,226.248373204201,226.332111916047,226.415747427414,226.499299870813,
226.582789306664,226.666243257278,226.749679751124,226.833116860879,226.916572655797,
227.000117148527,227.083706231468,227.167429499025,227.248109214921,227.331847926767,
227.415483438134,227.499035881533,227.582525317384,227.665979267998,227.749415761844,
227.832852871599,227.916308666517,227.999853159247,228.083442242188,228.167165509745,
228.247845225641,228.331593655558,228.41523673525,228.498910144718,228.582396452253,
228.665844198643,228.749271473125,228.833109607593,228.916575884921,229.000599947959,
229.084624010996),.UNSPECIFIED.);
#192=B_SPLINE_CURVE_WITH_KNOTS('',3,(#33140,#33141,#33142,#33143,#33144,
#33145,#33146,#33147,#33148,#33149),.UNSPECIFIED.,.F.,.F.,(4,3,3,4),(222.801474927361,
222.883746023741,222.968412214243,223.053078404745),.UNSPECIFIED.);
#193=B_SPLINE_CURVE_WITH_KNOTS('',3,(#33151,#33152,#33153,#33154,#33155,
#33156,#33157,#33158,#33159,#33160),.UNSPECIFIED.,.F.,.F.,(4,3,3,4),(222.802758717798,
222.890615341441,222.978298362488,223.053078404664),.UNSPECIFIED.);
#194=B_SPLINE_CURVE_WITH_KNOTS('',3,(#33161,#33162,#33163,#33164,#33165,
#33166,#33167,#33168,#33169,#33170,#33171,#33172,#33173,#33174,#33175,#33176,
#33177,#33178,#33179,#33180,#33181,#33182,#33183,#33184,#33185,#33186,#33187,
#33188,#33189,#33190,#33191,#33192,#33193,#33194,#33195,#33196,#33197,#33198,
#33199,#33200,#33201,#33202,#33203,#33204,#33205,#33206,#33207,#33208,#33209,
#33210,#33211,#33212,#33213,#33214,#33215,#33216,#33217,#33218,#33219,#33220,
#33221,#33222,#33223,#33224,#33225,#33226,#33227,#33228,#33229,#33230,#33231,
#33232,#33233,#33234,#33235,#33236,#33237,#33238,#33239,#33240,#33241,#33242,
#33243,#33244,#33245,#33246,#33247,#33248,#33249,#33250,#33251,#33252,#33253,
#33254,#33255,#33256,#33257,#33258,#33259,#33260,#33261,#33262,#33263,#33264,
#33265,#33266,#33267,#33268,#33269,#33270,#33271,#33272,#33273,#33274,#33275,
#33276,#33277,#33278,#33279,#33280,#33281,#33282,#33283,#33284,#33285,#33286,
#33287,#33288,#33289,#33290,#33291,#33292,#33293,#33294,#33295,#33296,#33297,
#33298,#33299,#33300,#33301,#33302,#33303,#33304,#33305,#33306,#33307,#33308,
#33309,#33310,#33311,#33312,#33313,#33314,#33315,#33316,#33317,#33318,#33319,
#33320,#33321,#33322,#33323,#33324,#33325,#33326,#33327,#33328,#33329,#33330,
#33331,#33332,#33333,#33334,#33335,#33336,#33337,#33338,#33339,#33340,#33341,
#33342,#33343,#33344,#33345,#33346,#33347,#33348,#33349,#33350,#33351,#33352,
#33353,#33354,#33355,#33356,#33357,#33358,#33359,#33360,#33361,#33362,#33363,
#33364,#33365,#33366,#33367,#33368,#33369,#33370,#33371,#33372,#33373,#33374,
#33375,#33376,#33377,#33378,#33379,#33380),.UNSPECIFIED.,.F.,.F.,(4,3,3,
3,3,3,3,3,3,3,3,3,3,3,3,3,3,3,3,3,3,3,3,3,3,3,3,3,3,3,3,3,3,3,3,3,3,3,3,
3,3,3,3,3,3,3,3,3,3,3,3,3,3,3,3,3,3,3,3,3,3,3,3,3,3,3,3,3,3,3,3,3,3,4),
(223.05307840486,223.140250227663,223.227528653432,223.315005472342,223.402585880388,
223.490366020583,223.559455791755,223.643194503601,223.726830014968,223.810382458367,
223.893871894218,223.977325844832,224.060762338678,224.144199448433,224.227655243351,
224.31119973608,224.394788819021,224.478512086579,224.559191802476,224.642930514322,
224.726566025689,224.810118469088,224.893607904939,224.977061855553,225.060498349399,
225.143935459155,225.227391254073,225.310935746803,225.394524829744,225.478248097301,
225.558927813196,225.642666525042,225.726302036409,225.809854479808,225.893343915659,
225.976797866273,226.060234360119,226.143671469874,226.227127264792,226.310671757522,
226.394260840463,226.47798410802,226.558663823916,226.642402535762,226.726038047129,
226.809590490528,226.893079926379,226.976533876993,227.059970370839,227.143407480594,
227.226863275512,227.310407768241,227.393996851182,227.47772011874,227.558399834636,
227.642138546482,227.725774057849,227.809326501248,227.892815937099,227.976269887713,
228.059706381559,228.143143491315,228.226599286233,228.310143778962,228.393732861904,
228.477456129461,228.558135845356,228.640732576949,228.72323240933,228.805654493565,
228.888013899624,228.970337205032,229.052651179031,229.084767271361),
 .UNSPECIFIED.);
#195=B_SPLINE_CURVE_WITH_KNOTS('',3,(#33386,#33387,#33388,#33389,#33390,
#33391,#33392,#33393,#33394,#33395,#33396,#33397,#33398,#33399,#33400,#33401,
#33402,#33403,#33404,#33405,#33406,#33407,#33408,#33409,#33410,#33411,#33412,
#33413,#33414,#33415,#33416,#33417,#33418,#33419,#33420,#33421,#33422,#33423,
#33424,#33425,#33426,#33427,#33428,#33429,#33430,#33431,#33432,#33433,#33434,
#33435,#33436,#33437,#33438,#33439,#33440,#33441,#33442,#33443,#33444,#33445,
#33446,#33447,#33448,#33449,#33450,#33451,#33452,#33453,#33454,#33455,#33456,
#33457,#33458,#33459,#33460,#33461,#33462,#33463,#33464,#33465,#33466,#33467,
#33468,#33469,#33470,#33471,#33472,#33473,#33474,#33475,#33476,#33477,#33478,
#33479,#33480,#33481,#33482,#33483,#33484,#33485,#33486,#33487,#33488,#33489,
#33490,#33491,#33492,#33493,#33494,#33495,#33496,#33497,#33498,#33499,#33500,
#33501,#33502,#33503,#33504,#33505,#33506,#33507,#33508,#33509,#33510,#33511,
#33512,#33513,#33514,#33515,#33516,#33517,#33518,#33519,#33520,#33521,#33522,
#33523,#33524,#33525,#33526,#33527,#33528,#33529,#33530,#33531,#33532,#33533,
#33534,#33535,#33536,#33537,#33538,#33539,#33540,#33541,#33542,#33543,#33544,
#33545,#33546,#33547,#33548,#33549,#33550,#33551,#33552,#33553,#33554,#33555,
#33556,#33557,#33558,#33559,#33560,#33561,#33562,#33563,#33564,#33565,#33566,
#33567,#33568,#33569,#33570,#33571,#33572,#33573,#33574,#33575,#33576,#33577,
#33578,#33579,#33580,#33581,#33582,#33583,#33584,#33585,#33586,#33587,#33588,
#33589,#33590,#33591,#33592,#33593,#33594,#33595,#33596,#33597,#33598,#33599,
#33600,#33601,#33602,#33603,#33604,#33605),.UNSPECIFIED.,.F.,.F.,(4,3,3,
3,3,3,3,3,3,3,3,3,3,3,3,3,3,3,3,3,3,3,3,3,3,3,3,3,3,3,3,3,3,3,3,3,3,3,3,
3,3,3,3,3,3,3,3,3,3,3,3,3,3,3,3,3,3,3,3,3,3,3,3,3,3,3,3,3,3,3,3,3,3,4),
(229.33626371217,229.418986435348,229.501614551539,229.584169058513,229.667062582084,
229.749542783262,229.83201651903,229.914502649429,229.997706298842,230.080315805856,
230.163816526468,230.247317247081,230.331055958927,230.414691470294,230.498243913693,
230.581733349544,230.665187300158,230.748623794004,230.83206090376,230.915516698677,
230.999061191407,231.082650274348,231.166373541906,231.247053257801,231.330791969647,
231.414427481015,231.497979924413,231.581469360264,231.664923310878,231.748359804724,
231.83179691448,231.915252709397,231.998797202127,232.082386285068,232.166109552626,
232.246789268522,232.330527980368,232.414163491736,232.497715935134,232.581205370985,
232.664659321599,232.748095815445,232.831532925201,232.914988720119,232.998533212848,
233.082122295789,233.165845563347,233.246525279242,233.330263991088,233.413899502455,
233.497451945854,233.580941381706,233.664395332319,233.747831826166,233.831268935921,
233.914724730839,233.998269223568,234.081858306509,234.165581574067,234.246261289962,
234.330000001808,234.413635513175,234.497187956574,234.580677392425,234.664131343039,
234.747567836885,234.83100494664,234.914460741557,234.998005234287,235.081594317228,
235.165317584785,235.245997300682,235.341055752039,235.369001591755),
 .UNSPECIFIED.);
#196=B_SPLINE_CURVE_WITH_KNOTS('',3,(#33606,#33607,#33608,#33609,#33610,
#33611,#33612,#33613,#33614,#33615),.UNSPECIFIED.,.F.,.F.,(4,3,3,4),(229.084624010996,
229.168347766236,229.247581236361,229.336263712035),.UNSPECIFIED.);
#197=B_SPLINE_CURVE_WITH_KNOTS('',3,(#33617,#33618,#33619,#33620,#33621,
#33622,#33623,#33624,#33625,#33626),.UNSPECIFIED.,.F.,.F.,(4,3,3,4),(229.084767271361,
229.167110719834,229.251687215869,229.336263711905),.UNSPECIFIED.);
#198=B_SPLINE_CURVE_WITH_KNOTS('',3,(#33627,#33628,#33629,#33630,#33631,
#33632,#33633,#33634,#33635,#33636,#33637,#33638,#33639,#33640,#33641,#33642,
#33643,#33644,#33645,#33646,#33647,#33648,#33649,#33650,#33651,#33652,#33653,
#33654,#33655,#33656,#33657,#33658,#33659,#33660,#33661,#33662,#33663,#33664,
#33665,#33666,#33667,#33668,#33669,#33670,#33671,#33672,#33673,#33674,#33675,
#33676,#33677,#33678,#33679,#33680,#33681,#33682,#33683,#33684,#33685,#33686,
#33687,#33688,#33689,#33690,#33691,#33692,#33693,#33694,#33695,#33696,#33697,
#33698,#33699,#33700,#33701,#33702,#33703,#33704,#33705,#33706,#33707,#33708,
#33709,#33710,#33711,#33712,#33713,#33714,#33715,#33716,#33717,#33718,#33719,
#33720,#33721,#33722,#33723,#33724,#33725,#33726,#33727,#33728,#33729,#33730,
#33731,#33732,#33733,#33734,#33735,#33736,#33737,#33738,#33739,#33740,#33741,
#33742,#33743,#33744,#33745,#33746,#33747,#33748,#33749,#33750,#33751,#33752,
#33753,#33754,#33755,#33756,#33757,#33758,#33759,#33760,#33761,#33762,#33763,
#33764,#33765,#33766,#33767,#33768,#33769,#33770,#33771,#33772,#33773,#33774,
#33775,#33776,#33777,#33778,#33779,#33780,#33781,#33782,#33783,#33784,#33785,
#33786,#33787,#33788,#33789,#33790,#33791,#33792,#33793,#33794,#33795,#33796,
#33797,#33798,#33799,#33800,#33801,#33802,#33803,#33804,#33805,#33806,#33807,
#33808,#33809,#33810,#33811,#33812,#33813,#33814,#33815,#33816,#33817,#33818,
#33819,#33820,#33821,#33822,#33823,#33824,#33825,#33826,#33827,#33828,#33829,
#33830,#33831,#33832,#33833,#33834,#33835,#33836,#33837,#33838,#33839,#33840,
#33841,#33842,#33843),.UNSPECIFIED.,.F.,.F.,(4,3,3,3,3,3,3,3,3,3,3,3,3,
3,3,3,3,3,3,3,3,3,3,3,3,3,3,3,3,3,3,3,3,3,3,3,3,3,3,3,3,3,3,3,3,3,3,3,3,
3,3,3,3,3,3,3,3,3,3,3,3,3,3,3,3,3,3,3,3,3,3,3,4),(229.336263712039,229.450657371009,
229.557871856076,229.641610567922,229.725246079289,229.808798522688,229.892287958539,
229.975741909153,230.059178402999,230.142615512755,230.226071307672,230.309615800402,
230.393204883343,230.476928150901,230.557607866796,230.641346578642,230.72498209001,
230.808534533408,230.892023969259,230.975477919873,231.058914413719,231.142351523475,
231.225807318393,231.309351811122,231.392940894063,231.476664161621,231.557343877517,
231.641082589363,231.72471810073,231.808270544129,231.89175997998,231.975213930594,
232.05865042444,232.142087534196,232.225543329113,232.309087821843,232.392676904784,
232.476400172341,232.557079888237,232.640818600083,232.72445411145,232.808006554849,
232.8914959907,232.974949941314,233.05838643516,233.141823544915,233.225279339833,
233.308823832563,233.392412915504,233.476136183061,233.556815898957,233.640554610803,
233.72419012217,233.807742565569,233.89123200142,233.974685952034,234.05812244588,
234.141559555635,234.225015350553,234.308559843283,234.392148926224,234.475872193781,
234.556551909677,234.640301970269,234.723946343581,234.807489853318,234.890976176804,
234.97442343389,235.057849714245,235.141299036663,235.224759079097,235.308287375594,
235.367788403087),.UNSPECIFIED.);
#199=B_SPLINE_CURVE_WITH_KNOTS('',3,(#33849,#33850,#33851,#33852,#33853,
#33854,#33855,#33856,#33857,#33858,#33859,#33860,#33861,#33862,#33863,#33864,
#33865,#33866,#33867,#33868,#33869,#33870,#33871,#33872,#33873,#33874,#33875,
#33876,#33877,#33878,#33879,#33880,#33881,#33882,#33883,#33884,#33885,#33886,
#33887,#33888,#33889,#33890,#33891,#33892,#33893,#33894,#33895,#33896,#33897,
#33898,#33899,#33900,#33901,#33902,#33903,#33904,#33905,#33906,#33907,#33908,
#33909,#33910,#33911,#33912,#33913,#33914,#33915,#33916,#33917,#33918,#33919,
#33920,#33921,#33922,#33923,#33924,#33925,#33926,#33927,#33928,#33929,#33930,
#33931,#33932,#33933,#33934,#33935,#33936,#33937,#33938,#33939,#33940,#33941,
#33942,#33943,#33944,#33945,#33946,#33947,#33948,#33949,#33950,#33951,#33952,
#33953,#33954,#33955,#33956,#33957,#33958,#33959,#33960,#33961,#33962,#33963,
#33964,#33965,#33966,#33967,#33968,#33969,#33970,#33971,#33972,#33973,#33974,
#33975,#33976,#33977,#33978,#33979,#33980,#33981,#33982,#33983,#33984,#33985,
#33986,#33987,#33988,#33989,#33990,#33991,#33992,#33993,#33994,#33995,#33996,
#33997,#33998,#33999,#34000,#34001,#34002,#34003,#34004,#34005,#34006,#34007,
#34008,#34009,#34010,#34011,#34012,#34013,#34014,#34015,#34016,#34017,#34018,
#34019,#34020,#34021,#34022,#34023,#34024,#34025,#34026,#34027,#34028,#34029,
#34030,#34031,#34032,#34033,#34034,#34035,#34036,#34037,#34038,#34039,#34040,
#34041,#34042,#34043,#34044,#34045,#34046,#34047,#34048,#34049,#34050,#34051,
#34052,#34053,#34054,#34055,#34056,#34057,#34058,#34059,#34060,#34061,#34062,
#34063,#34064,#34065,#34066,#34067,#34068),.UNSPECIFIED.,.F.,.F.,(4,3,3,
3,3,3,3,3,3,3,3,3,3,3,3,3,3,3,3,3,3,3,3,3,3,3,3,3,3,3,3,3,3,3,3,3,3,3,3,
3,3,3,3,3,3,3,3,3,3,3,3,3,3,3,3,3,3,3,3,3,3,3,3,3,3,3,3,3,3,3,3,3,3,4),
(235.619449019215,235.703485100474,235.787527689251,235.871594004824,235.955701278211,
236.039918534502,236.124198449062,236.208612528274,236.245733311402,236.329472023248,
236.413107534615,236.496659978014,236.580149413865,236.663603364479,236.747039858325,
236.83047696808,236.913932762998,236.997477255727,237.081066338668,237.164789606226,
237.245469322122,237.329208033968,237.412843545335,237.496395988734,237.579885424585,
237.663339375198,237.746775869045,237.8302129788,237.913668773717,237.997213266447,
238.080802349388,238.164525616946,238.245205332842,238.328944044688,238.412579556055,
238.496131999454,238.579621435305,238.663075385919,238.746511879765,238.829948989521,
238.913404784439,238.996949277169,239.080538360109,239.164261627667,239.244941343562,
239.328680055408,239.412315566775,239.495868010174,239.579357446025,239.662811396639,
239.746247890485,239.829685000241,239.913140795158,239.996685287888,240.080274370829,
240.163997638387,240.244677354283,240.328416066129,240.412051577497,240.495604020896,
240.579093456746,240.66254740736,240.745983901207,240.829421010962,240.91287680588,
240.99642129861,241.08001038155,241.163733649108,241.244413365003,241.328257974956,
241.411966864006,241.495597678354,241.579158265343,241.651741637788),
 .UNSPECIFIED.);
#200=B_SPLINE_CURVE_WITH_KNOTS('',3,(#34069,#34070,#34071,#34072,#34073,
#34074,#34075,#34076,#34077,#34078),.UNSPECIFIED.,.F.,.F.,(4,3,3,4),(235.369001591755,
235.463534631651,235.557500007405,235.619449019017),.UNSPECIFIED.);
#201=B_SPLINE_CURVE_WITH_KNOTS('',3,(#34080,#34081,#34082,#34083,#34084,
#34085,#34086,#34087,#34088,#34089,#34090,#34091,#34092),.UNSPECIFIED.,
 .F.,.F.,(4,3,3,3,4),(235.367788403087,235.451419133571,235.535167426197,
235.556287920397,235.619449019219),.UNSPECIFIED.);
#202=B_SPLINE_CURVE_WITH_KNOTS('',3,(#34093,#34094,#34095,#34096,#34097,
#34098,#34099,#34100,#34101,#34102,#34103,#34104,#34105,#34106,#34107,#34108,
#34109,#34110,#34111,#34112,#34113,#34114,#34115,#34116,#34117,#34118,#34119,
#34120,#34121,#34122,#34123,#34124,#34125,#34126,#34127,#34128,#34129,#34130,
#34131,#34132,#34133,#34134,#34135,#34136,#34137,#34138,#34139,#34140,#34141,
#34142,#34143,#34144,#34145,#34146,#34147,#34148,#34149,#34150,#34151,#34152,
#34153,#34154,#34155,#34156,#34157,#34158,#34159,#34160,#34161,#34162,#34163,
#34164,#34165,#34166,#34167,#34168,#34169,#34170,#34171,#34172,#34173,#34174,
#34175,#34176,#34177,#34178,#34179,#34180,#34181,#34182,#34183,#34184,#34185,
#34186,#34187,#34188,#34189,#34190,#34191,#34192,#34193,#34194,#34195,#34196,
#34197,#34198,#34199,#34200,#34201,#34202,#34203,#34204,#34205,#34206,#34207,
#34208,#34209,#34210,#34211,#34212,#34213,#34214,#34215,#34216,#34217,#34218,
#34219,#34220,#34221,#34222,#34223,#34224,#34225,#34226,#34227,#34228,#34229,
#34230,#34231,#34232,#34233,#34234,#34235,#34236,#34237,#34238,#34239,#34240,
#34241,#34242,#34243,#34244,#34245,#34246,#34247,#34248,#34249,#34250,#34251,
#34252,#34253,#34254,#34255,#34256,#34257,#34258,#34259,#34260,#34261,#34262,
#34263,#34264,#34265,#34266,#34267,#34268,#34269,#34270,#34271,#34272,#34273,
#34274,#34275,#34276,#34277,#34278,#34279,#34280,#34281,#34282,#34283,#34284,
#34285,#34286,#34287,#34288,#34289,#34290,#34291,#34292,#34293,#34294,#34295,
#34296,#34297,#34298,#34299,#34300,#34301,#34302,#34303,#34304,#34305,#34306,
#34307,#34308,#34309,#34310,#34311,#34312),.UNSPECIFIED.,.F.,.F.,(4,3,3,
3,3,3,3,3,3,3,3,3,3,3,3,3,3,3,3,3,3,3,3,3,3,3,3,3,3,3,3,3,3,3,3,3,3,3,3,
3,3,3,3,3,3,3,3,3,3,3,3,3,3,3,3,3,3,3,3,3,3,3,3,3,3,3,3,3,3,3,3,3,3,4),
(235.619449019335,235.702396000431,235.785244541703,235.868015492367,235.95401654721,
236.036703039314,236.119379716895,236.202065298067,236.284778504414,236.367582433388,
236.450440219168,236.533414519597,236.556023931117,236.639762642963,236.72339815433,
236.806950597729,236.89044003358,236.973893984194,237.05733047804,237.140767587795,
237.224223382713,237.307767875443,237.391356958383,237.475080225941,237.555759941837,
237.639498653683,237.723134165051,237.806686608449,237.8901760443,237.973629994914,
238.05706648876,238.140503598516,238.223959393434,238.307503886163,238.391092969104,
238.474816236662,238.555495952557,238.639234664403,238.72287017577,238.806422619169,
238.88991205502,238.973366005633,239.05680249948,239.140239609235,239.223695404152,
239.307239896882,239.390828979823,239.474552247381,239.555231963278,239.638970675124,
239.722606186492,239.80615862989,239.889648065741,239.973102016355,240.056538510201,
240.139975619957,240.223431414875,240.306975907605,240.390564990546,240.474288258103,
240.554967973998,240.638706685844,240.722342197211,240.805894640609,240.88938407646,
240.972838027074,241.05627452092,241.139711630676,241.223167425593,241.306711918323,
241.390301001264,241.474024268822,241.554703984718,241.652092022884),
 .UNSPECIFIED.);
#203=B_SPLINE_CURVE_WITH_KNOTS('',3,(#34318,#34319,#34320,#34321,#34322,
#34323,#34324,#34325,#34326,#34327,#34328,#34329,#34330,#34331,#34332,#34333,
#34334,#34335,#34336,#34337,#34338,#34339,#34340,#34341,#34342,#34343,#34344,
#34345,#34346,#34347,#34348,#34349,#34350,#34351,#34352,#34353,#34354,#34355,
#34356,#34357,#34358,#34359,#34360,#34361,#34362,#34363,#34364,#34365,#34366,
#34367,#34368,#34369,#34370,#34371,#34372,#34373,#34374,#34375,#34376,#34377,
#34378,#34379,#34380,#34381,#34382,#34383,#34384,#34385,#34386,#34387,#34388,
#34389,#34390,#34391,#34392,#34393,#34394,#34395,#34396,#34397,#34398,#34399,
#34400,#34401,#34402,#34403,#34404,#34405,#34406,#34407,#34408,#34409,#34410,
#34411,#34412,#34413,#34414,#34415,#34416,#34417,#34418,#34419,#34420,#34421,
#34422,#34423,#34424,#34425,#34426,#34427,#34428,#34429,#34430,#34431,#34432,
#34433,#34434,#34435,#34436,#34437,#34438,#34439,#34440,#34441,#34442,#34443,
#34444,#34445,#34446,#34447,#34448,#34449,#34450,#34451,#34452,#34453,#34454,
#34455,#34456,#34457,#34458,#34459,#34460,#34461,#34462,#34463,#34464,#34465,
#34466,#34467,#34468,#34469,#34470,#34471,#34472,#34473,#34474,#34475,#34476,
#34477,#34478,#34479,#34480,#34481,#34482,#34483,#34484,#34485,#34486,#34487,
#34488,#34489,#34490,#34491,#34492,#34493,#34494,#34495,#34496,#34497,#34498,
#34499,#34500,#34501,#34502,#34503,#34504,#34505,#34506,#34507,#34508,#34509,
#34510,#34511,#34512,#34513,#34514,#34515,#34516,#34517,#34518,#34519,#34520,
#34521,#34522,#34523,#34524,#34525,#34526,#34527,#34528,#34529,#34530,#34531,
#34532,#34533,#34534,#34535,#34536,#34537),.UNSPECIFIED.,.F.,.F.,(4,3,3,
3,3,3,3,3,3,3,3,3,3,3,3,3,3,3,3,3,3,3,3,3,3,3,3,3,3,3,3,3,3,3,3,3,3,3,3,
3,3,3,3,3,3,3,3,3,3,3,3,3,3,3,3,3,3,3,3,3,3,3,3,3,3,3,3,3,3,3,3,3,3,4),
(241.902634326587,241.999158887911,242.096209234875,242.193901448682,242.244149375723,
242.327888087569,242.411523598936,242.495076042335,242.578565478186,242.6620194288,
242.745455922646,242.828893032401,242.912348827319,242.995893320048,243.079482402989,
243.163205670547,243.243885386443,243.327624098289,243.411259609656,243.494812053055,
243.578301488906,243.66175543952,243.745191933366,243.828629043121,243.912084838039,
243.995629330769,244.07921841371,244.162941681267,244.243621397163,244.327360109009,
244.410995620376,244.494548063775,244.578037499626,244.661491450239,244.744927944086,
244.828365053841,244.911820848759,244.995365341488,245.078954424429,245.162677691987,
245.243357407883,245.327096119729,245.410731631096,245.494284074495,245.577773510346,
245.66122746096,245.744663954806,245.828101064562,245.911556859479,245.995101352209,
246.07869043515,246.162413702708,246.243093418603,246.326832130449,246.410467641816,
246.494020085215,246.577509521066,246.66096347168,246.744399965526,246.827837075282,
246.911292870199,246.994837362929,247.07842644587,247.162149713428,247.242829429323,
247.329226206015,247.412137556038,247.494973941528,247.577754132961,247.660496854229,
247.743234853931,247.82597074059,247.908743988731,247.934003642858),
 .UNSPECIFIED.);
#204=B_SPLINE_CURVE_WITH_KNOTS('',3,(#34538,#34539,#34540,#34541,#34542,
#34543,#34544,#34545,#34546,#34547),.UNSPECIFIED.,.F.,.F.,(4,3,3,4),(241.651741637788,
241.735236595357,241.818935460876,241.902634326395),.UNSPECIFIED.);
#205=B_SPLINE_CURVE_WITH_KNOTS('',3,(#34549,#34550,#34551,#34552,#34553,
#34554,#34555,#34556,#34557,#34558),.UNSPECIFIED.,.F.,.F.,(4,3,3,4),(241.652092022884,
241.748746650711,241.844665469492,241.902634326203),.UNSPECIFIED.);
#206=B_SPLINE_CURVE_WITH_KNOTS('',3,(#34559,#34560,#34561,#34562,#34563,
#34564,#34565,#34566,#34567,#34568,#34569,#34570,#34571,#34572,#34573,#34574,
#34575,#34576,#34577,#34578,#34579,#34580,#34581,#34582,#34583,#34584,#34585,
#34586,#34587,#34588,#34589,#34590,#34591,#34592,#34593,#34594,#34595,#34596,
#34597,#34598,#34599,#34600,#34601,#34602,#34603,#34604,#34605,#34606,#34607,
#34608,#34609,#34610,#34611,#34612,#34613,#34614,#34615,#34616,#34617,#34618,
#34619,#34620,#34621,#34622,#34623,#34624,#34625,#34626,#34627,#34628,#34629,
#34630,#34631,#34632,#34633,#34634,#34635,#34636,#34637,#34638,#34639,#34640,
#34641,#34642,#34643,#34644,#34645,#34646,#34647,#34648,#34649,#34650,#34651,
#34652,#34653,#34654,#34655,#34656,#34657,#34658,#34659,#34660,#34661,#34662,
#34663,#34664,#34665,#34666,#34667,#34668,#34669,#34670,#34671,#34672,#34673,
#34674,#34675,#34676,#34677,#34678,#34679,#34680,#34681,#34682,#34683,#34684,
#34685,#34686,#34687,#34688,#34689,#34690,#34691,#34692,#34693,#34694,#34695,
#34696,#34697,#34698,#34699,#34700,#34701,#34702,#34703,#34704,#34705,#34706,
#34707,#34708,#34709,#34710,#34711,#34712,#34713,#34714,#34715,#34716,#34717,
#34718,#34719,#34720,#34721,#34722,#34723,#34724,#34725,#34726,#34727,#34728,
#34729,#34730,#34731,#34732,#34733,#34734,#34735,#34736,#34737,#34738,#34739,
#34740,#34741,#34742,#34743,#34744,#34745,#34746,#34747,#34748,#34749,#34750,
#34751,#34752,#34753,#34754,#34755,#34756,#34757,#34758,#34759,#34760,#34761,
#34762,#34763,#34764,#34765,#34766,#34767,#34768,#34769,#34770,#34771,#34772,
#34773,#34774,#34775,#34776,#34777,#34778),.UNSPECIFIED.,.F.,.F.,(4,3,3,
3,3,3,3,3,3,3,3,3,3,3,3,3,3,3,3,3,3,3,3,3,3,3,3,3,3,3,3,3,3,3,3,3,3,3,3,
3,3,3,3,3,3,3,3,3,3,3,3,3,3,3,3,3,3,3,3,3,3,3,3,3,3,3,3,3,3,3,3,3,3,4),
(241.902634326398,241.986237486797,242.069834027506,242.153441752423,242.237078468855,
242.320815591498,242.404605844241,242.488534263311,242.554439995438,242.638178707284,
242.721814218652,242.80536666205,242.888856097901,242.972310048515,243.055746542361,
243.139183652116,243.222639447034,243.306183939764,243.389773022705,243.473496290262,
243.554176006158,243.637914718004,243.721550229371,243.80510267277,243.888592108621,
243.972046059235,244.055482553081,244.138919662837,244.222375457754,244.305919950484,
244.389509033425,244.473232300982,244.553912016878,244.637650728724,244.721286240092,
244.80483868349,244.888328119341,244.971782069955,245.055218563801,245.138655673557,
245.222111468475,245.305655961205,245.389245044146,245.472968311703,245.553648027598,
245.637386739444,245.721022250812,245.80457469421,245.888064130061,245.971518080675,
246.054954574521,246.138391684277,246.221847479194,246.305391971924,246.388981054865,
246.472704322423,246.553384038319,246.637122750165,246.720758261533,246.804310704931,
246.887800140782,246.971254091396,247.054690585242,247.138127694997,247.221583489915,
247.305127982644,247.388717065586,247.472440333143,247.553120049039,247.637422699873,
247.721583874919,247.805663482454,247.889664215379,247.935052702017),
 .UNSPECIFIED.);
#207=B_SPLINE_CURVE_WITH_KNOTS('',3,(#34784,#34785,#34786,#34787,#34788,
#34789,#34790,#34791,#34792,#34793,#34794,#34795,#34796,#34797,#34798,#34799,
#34800,#34801,#34802,#34803,#34804,#34805,#34806,#34807,#34808,#34809,#34810,
#34811,#34812,#34813,#34814,#34815,#34816,#34817,#34818,#34819,#34820,#34821,
#34822,#34823,#34824,#34825,#34826,#34827,#34828,#34829,#34830,#34831,#34832,
#34833,#34834,#34835,#34836,#34837,#34838,#34839,#34840,#34841,#34842,#34843,
#34844,#34845,#34846,#34847,#34848,#34849,#34850,#34851,#34852,#34853,#34854,
#34855,#34856,#34857,#34858,#34859,#34860,#34861,#34862,#34863,#34864,#34865,
#34866,#34867,#34868,#34869,#34870,#34871,#34872,#34873,#34874,#34875,#34876,
#34877,#34878,#34879,#34880,#34881,#34882,#34883,#34884,#34885,#34886,#34887,
#34888,#34889,#34890,#34891,#34892,#34893,#34894,#34895,#34896,#34897,#34898,
#34899,#34900,#34901,#34902,#34903,#34904,#34905,#34906,#34907,#34908,#34909,
#34910,#34911,#34912,#34913,#34914,#34915,#34916,#34917,#34918,#34919,#34920,
#34921,#34922,#34923,#34924,#34925,#34926,#34927,#34928,#34929,#34930,#34931,
#34932,#34933,#34934,#34935,#34936,#34937,#34938,#34939,#34940,#34941,#34942,
#34943,#34944,#34945,#34946,#34947,#34948,#34949,#34950,#34951,#34952,#34953,
#34954,#34955,#34956,#34957,#34958,#34959,#34960,#34961,#34962,#34963,#34964,
#34965,#34966,#34967,#34968,#34969,#34970,#34971,#34972,#34973,#34974,#34975,
#34976,#34977,#34978,#34979,#34980,#34981,#34982,#34983,#34984,#34985,#34986,
#34987,#34988,#34989,#34990,#34991,#34992,#34993,#34994,#34995,#34996,#34997,
#34998,#34999,#35000,#35001,#35002,#35003),.UNSPECIFIED.,.F.,.F.,(4,3,3,
3,3,3,3,3,3,3,3,3,3,3,3,3,3,3,3,3,3,3,3,3,3,3,3,3,3,3,3,3,3,3,3,3,3,3,3,
3,3,3,3,3,3,3,3,3,3,3,3,3,3,3,3,3,3,3,3,3,3,3,3,3,3,3,3,3,3,3,3,3,3,4),
(248.185819633574,248.242565440044,248.32630415189,248.409939663257,248.493492106656,
248.576981542507,248.66043549312,248.743871986967,248.827309096722,248.91076489164,
248.994309384369,249.07789846731,249.161621734868,249.242301450764,249.32604016261,
249.409675673977,249.493228117376,249.576717553227,249.660171503841,249.743607997687,
249.827045107442,249.91050090236,249.99404539509,250.077634478031,250.161357745588,
250.242037461484,250.32577617333,250.409411684697,250.492964128096,250.576453563947,
250.65990751456,250.743344008406,250.826781118162,250.910236913079,250.993781405809,
251.07737048875,251.161093756307,251.241773472204,251.32551218405,251.409147695417,
251.492700138816,251.576189574667,251.659643525281,251.743080019127,251.826517128883,
251.9099729238,251.99351741653,252.077106499471,252.160829767029,252.241509482924,
252.32524819477,252.408883706137,252.492436149536,252.575925585387,252.659379536001,
252.742816029847,252.826253139602,252.90970893452,252.993253427249,253.07684251019,
253.160565777748,253.241245493644,253.324985515348,253.408622030889,253.492175174065,
253.575665006275,253.659117790273,253.742552685343,253.825987763872,253.909441094444,
253.992977143822,254.076557604818,254.160258240132,254.217804721095),
 .UNSPECIFIED.);
#208=B_SPLINE_CURVE_WITH_KNOTS('',3,(#35004,#35005,#35006,#35007,#35008,
#35009,#35010,#35011,#35012,#35013),.UNSPECIFIED.,.F.,.F.,(4,3,3,4),(247.934003642858,
248.016867615733,248.101343624599,248.185819633466),.UNSPECIFIED.);
#209=B_SPLINE_CURVE_WITH_KNOTS('',3,(#35015,#35016,#35017,#35018,#35019,
#35020,#35021,#35022,#35023,#35024),.UNSPECIFIED.,.F.,.F.,(4,3,3,4),(247.935052702017,
248.018983507691,248.102906829926,248.185819633578),.UNSPECIFIED.);
#210=B_SPLINE_CURVE_WITH_KNOTS('',3,(#35025,#35026,#35027,#35028,#35029,
#35030,#35031,#35032,#35033,#35034,#35035,#35036,#35037,#35038,#35039,#35040,
#35041,#35042,#35043,#35044,#35045,#35046,#35047,#35048,#35049,#35050,#35051,
#35052,#35053,#35054,#35055,#35056,#35057,#35058,#35059,#35060,#35061,#35062,
#35063,#35064,#35065,#35066,#35067,#35068,#35069,#35070,#35071,#35072,#35073,
#35074,#35075,#35076,#35077,#35078,#35079,#35080,#35081,#35082,#35083,#35084,
#35085,#35086,#35087,#35088,#35089,#35090,#35091,#35092,#35093,#35094,#35095,
#35096,#35097,#35098,#35099,#35100,#35101,#35102,#35103,#35104,#35105,#35106,
#35107,#35108,#35109,#35110,#35111,#35112,#35113,#35114,#35115,#35116,#35117,
#35118,#35119,#35120,#35121,#35122,#35123,#35124,#35125,#35126,#35127,#35128,
#35129,#35130,#35131,#35132,#35133,#35134,#35135,#35136,#35137,#35138,#35139,
#35140,#35141,#35142,#35143,#35144,#35145,#35146,#35147,#35148,#35149,#35150,
#35151,#35152,#35153,#35154,#35155,#35156,#35157,#35158,#35159,#35160,#35161,
#35162,#35163,#35164,#35165,#35166,#35167,#35168,#35169,#35170,#35171,#35172,
#35173,#35174,#35175,#35176,#35177,#35178,#35179,#35180,#35181,#35182,#35183,
#35184,#35185,#35186,#35187,#35188,#35189,#35190,#35191,#35192,#35193,#35194,
#35195,#35196,#35197,#35198,#35199,#35200,#35201,#35202,#35203,#35204,#35205,
#35206,#35207,#35208,#35209,#35210,#35211,#35212,#35213,#35214,#35215,#35216,
#35217,#35218,#35219,#35220,#35221,#35222,#35223,#35224,#35225,#35226,#35227,
#35228,#35229,#35230,#35231,#35232,#35233,#35234,#35235,#35236,#35237,#35238,
#35239,#35240,#35241),.UNSPECIFIED.,.F.,.F.,(4,3,3,3,3,3,3,3,3,3,3,3,3,
3,3,3,3,3,3,3,3,3,3,3,3,3,3,3,3,3,3,3,3,3,3,3,3,3,3,3,3,3,3,3,3,3,3,3,3,
3,3,3,3,3,3,3,3,3,3,3,3,3,3,3,3,3,3,3,3,3,3,3,4),(248.185819633777,248.280331492552,
248.375236871607,248.470685077426,248.552856059759,248.636594771605,248.720230282972,
248.803782726371,248.887272162222,248.970726112836,249.054162606682,249.137599716437,
249.221055511355,249.304600004085,249.388189087026,249.471912354583,249.552592070479,
249.636330782325,249.719966293692,249.803518737091,249.887008172942,249.970462123556,
250.053898617402,250.137335727157,250.220791522075,250.304336014805,250.387925097746,
250.471648365303,250.552328081199,250.636066793045,250.719702304412,250.803254747811,
250.886744183662,250.970198134275,251.053634628122,251.137071737877,251.220527532795,
251.304072025524,251.387661108465,251.471384376023,251.552064091919,251.635802803765,
251.719438315132,251.802990758531,251.886480194382,251.969934144996,252.053370638842,
252.136807748597,252.220263543515,252.303808036245,252.387397119186,252.471120386743,
252.551800102639,252.635538814485,252.719174325852,252.802726769251,252.886216205102,
252.969670155716,253.053106649562,253.136543759317,253.219999554235,253.303544046965,
253.387133129906,253.470856397463,253.551536113359,253.63474008064,253.717434336362,
253.800053146387,253.882615442224,253.966253544571,254.048771139043,254.132969495327,
254.217167851611),.UNSPECIFIED.);
#211=B_SPLINE_CURVE_WITH_KNOTS('',3,(#35247,#35248,#35249,#35250,#35251,
#35252,#35253,#35254,#35255,#35256,#35257,#35258,#35259,#35260,#35261,#35262,
#35263,#35264,#35265,#35266,#35267,#35268,#35269,#35270,#35271,#35272,#35273,
#35274,#35275,#35276,#35277,#35278,#35279,#35280,#35281,#35282,#35283,#35284,
#35285,#35286,#35287,#35288,#35289,#35290,#35291,#35292,#35293,#35294,#35295,
#35296,#35297,#35298,#35299,#35300,#35301,#35302,#35303,#35304,#35305,#35306,
#35307,#35308,#35309,#35310,#35311,#35312,#35313,#35314,#35315,#35316,#35317,
#35318,#35319,#35320,#35321,#35322,#35323,#35324,#35325,#35326,#35327,#35328,
#35329,#35330,#35331,#35332,#35333,#35334,#35335,#35336,#35337,#35338,#35339,
#35340,#35341,#35342,#35343,#35344,#35345,#35346,#35347,#35348,#35349,#35350,
#35351,#35352,#35353,#35354,#35355,#35356,#35357,#35358,#35359,#35360,#35361,
#35362,#35363,#35364,#35365,#35366,#35367,#35368,#35369,#35370,#35371,#35372,
#35373,#35374,#35375,#35376,#35377,#35378,#35379,#35380,#35381,#35382,#35383,
#35384,#35385,#35386,#35387,#35388,#35389,#35390,#35391,#35392,#35393,#35394,
#35395,#35396,#35397,#35398,#35399,#35400,#35401,#35402,#35403,#35404,#35405,
#35406,#35407,#35408,#35409,#35410,#35411,#35412,#35413,#35414,#35415,#35416,
#35417,#35418,#35419,#35420,#35421,#35422,#35423,#35424,#35425,#35426,#35427,
#35428,#35429,#35430,#35431,#35432,#35433,#35434,#35435,#35436,#35437,#35438,
#35439,#35440,#35441,#35442,#35443,#35444,#35445,#35446,#35447,#35448,#35449,
#35450,#35451,#35452,#35453,#35454,#35455,#35456,#35457,#35458,#35459,#35460,
#35461,#35462,#35463,#35464,#35465,#35466),.UNSPECIFIED.,.F.,.F.,(4,3,3,
3,3,3,3,3,3,3,3,3,3,3,3,3,3,3,3,3,3,3,3,3,3,3,3,3,3,3,3,3,3,3,3,3,3,3,3,
3,3,3,3,3,3,3,3,3,3,3,3,3,3,3,3,3,3,3,3,3,3,3,3,3,3,3,3,3,3,3,3,3,3,4),
(254.469004940866,254.551459079282,254.637616383758,254.719977767009,254.802326638354,
254.884681938213,254.967062609701,255.049532107573,255.132053855559,255.214692257449,
255.240717515084,255.32445622693,255.408091738297,255.491644181696,255.575133617547,
255.658587568161,255.742024062007,255.825461171763,255.90891696668,255.99246145941,
256.076050542351,256.159773809909,256.240453525805,256.324192237651,256.407827749019,
256.491380192417,256.574869628268,256.658323578882,256.741760072729,256.825197182484,
256.908652977402,256.992197470132,257.075786553073,257.15950982063,257.240189536525,
257.323928248371,257.407563759738,257.491116203137,257.574605638988,257.658059589601,
257.741496083448,257.824933193203,257.90838898812,257.99193348085,258.075522563791,
258.159245831348,258.239925547245,258.323664259091,258.407299770458,258.490852213857,
258.574341649707,258.657795600321,258.741232094167,258.824669203923,258.908124998841,
258.991669491571,259.075258574512,259.158981842069,259.239661557965,259.323400269811,
259.407035781179,259.490588224577,259.574077660428,259.657531611042,259.740968104888,
259.824405214644,259.907861009562,259.991405502292,260.074994585232,260.15871785279,
260.239397568685,260.326957592193,260.414399638384,260.501841684575),
 .UNSPECIFIED.);
#212=B_SPLINE_CURVE_WITH_KNOTS('',3,(#35467,#35468,#35469,#35470,#35471,
#35472,#35473,#35474,#35475,#35476),.UNSPECIFIED.,.F.,.F.,(4,3,3,4),(254.217804721095,
254.240981504364,254.354993222559,254.469004940754),.UNSPECIFIED.);
#213=B_SPLINE_CURVE_WITH_KNOTS('',3,(#35478,#35479,#35480,#35481,#35482,
#35483,#35484,#35485,#35486,#35487),.UNSPECIFIED.,.F.,.F.,(4,3,3,4),(254.217167851611,
254.29979899428,254.384401967453,254.469004940626),.UNSPECIFIED.);
#214=B_SPLINE_CURVE_WITH_KNOTS('',3,(#35488,#35489,#35490,#35491,#35492,
#35493,#35494,#35495,#35496,#35497,#35498,#35499,#35500,#35501,#35502,#35503,
#35504,#35505,#35506,#35507,#35508,#35509,#35510,#35511,#35512,#35513,#35514,
#35515,#35516,#35517,#35518,#35519,#35520,#35521,#35522,#35523,#35524,#35525,
#35526,#35527,#35528,#35529,#35530,#35531,#35532,#35533,#35534,#35535,#35536,
#35537,#35538,#35539,#35540,#35541,#35542,#35543,#35544,#35545,#35546,#35547,
#35548,#35549,#35550,#35551,#35552,#35553,#35554,#35555,#35556,#35557,#35558,
#35559,#35560,#35561,#35562,#35563,#35564,#35565,#35566,#35567,#35568,#35569,
#35570,#35571,#35572,#35573,#35574,#35575,#35576,#35577,#35578,#35579,#35580,
#35581,#35582,#35583,#35584,#35585,#35586,#35587,#35588,#35589,#35590,#35591,
#35592,#35593,#35594,#35595,#35596,#35597,#35598,#35599,#35600,#35601,#35602,
#35603,#35604,#35605,#35606,#35607,#35608,#35609,#35610,#35611,#35612,#35613,
#35614,#35615,#35616,#35617,#35618,#35619,#35620,#35621,#35622,#35623,#35624,
#35625,#35626,#35627,#35628,#35629,#35630,#35631,#35632,#35633,#35634,#35635,
#35636,#35637,#35638,#35639,#35640,#35641,#35642,#35643,#35644,#35645,#35646,
#35647,#35648,#35649,#35650,#35651,#35652,#35653,#35654,#35655,#35656,#35657,
#35658,#35659,#35660,#35661,#35662,#35663,#35664,#35665,#35666,#35667,#35668,
#35669,#35670,#35671,#35672,#35673,#35674,#35675,#35676,#35677,#35678,#35679,
#35680,#35681,#35682,#35683,#35684,#35685,#35686,#35687,#35688,#35689,#35690,
#35691,#35692,#35693,#35694,#35695,#35696,#35697,#35698,#35699,#35700,#35701,
#35702,#35703,#35704,#35705,#35706,#35707),.UNSPECIFIED.,.F.,.F.,(4,3,3,
3,3,3,3,3,3,3,3,3,3,3,3,3,3,3,3,3,3,3,3,3,3,3,3,3,3,3,3,3,3,3,3,3,3,3,3,
3,3,3,3,3,3,3,3,3,3,3,3,3,3,3,3,3,3,3,3,3,3,3,3,3,3,3,3,3,3,3,3,3,3,4),
(254.469004940758,254.55127212408,254.635010835926,254.718646347293,254.802198790692,
254.885688226543,254.969142177157,255.052578671003,255.136015780759,255.219471575676,
255.303016068406,255.386605151347,255.470328418905,255.5510081348,255.634746846646,
255.718382358013,255.801934801412,255.885424237263,255.968878187876,256.052314681723,
256.135751791478,256.219207586396,256.302752079125,256.386341162066,256.470064429624,
256.55074414552,256.634482857366,256.718118368733,256.801670812132,256.885160247983,
256.968614198597,257.052050692443,257.135487802199,257.218943597116,257.302488089846,
257.386077172787,257.469800440344,257.55048015624,257.634218868086,257.717854379453,
257.801406822852,257.884896258703,257.968350209317,258.051786703163,258.135223812918,
258.218679607836,258.302224100566,258.385813183507,258.469536451064,258.55021616696,
258.633954878806,258.717590390173,258.801142833572,258.884632269423,258.968086220037,
259.051522713883,259.134959823638,259.218415618556,259.301960111286,259.385549194227,
259.469272461784,259.54995217768,259.633693676875,259.7173313316,259.80088527709,
259.888382505455,259.971832815521,260.055265626256,260.138699009296,260.222151032625,
260.305679936236,260.389253833429,260.472932818464,260.50086310401),
 .UNSPECIFIED.);
#215=B_SPLINE_CURVE_WITH_KNOTS('',3,(#35713,#35714,#35715,#35716,#35717,
#35718,#35719,#35720,#35721,#35722,#35723,#35724,#35725,#35726,#35727,#35728,
#35729,#35730,#35731,#35732,#35733,#35734,#35735,#35736,#35737,#35738,#35739,
#35740,#35741,#35742,#35743,#35744,#35745,#35746,#35747,#35748,#35749,#35750,
#35751,#35752,#35753,#35754,#35755,#35756,#35757,#35758,#35759,#35760,#35761,
#35762,#35763,#35764,#35765,#35766,#35767,#35768,#35769,#35770,#35771,#35772,
#35773,#35774,#35775,#35776,#35777,#35778,#35779,#35780,#35781,#35782,#35783,
#35784,#35785,#35786,#35787,#35788,#35789,#35790,#35791,#35792,#35793,#35794,
#35795,#35796,#35797,#35798,#35799,#35800,#35801,#35802,#35803,#35804,#35805,
#35806,#35807,#35808,#35809,#35810,#35811,#35812,#35813,#35814,#35815,#35816,
#35817,#35818,#35819,#35820,#35821,#35822,#35823,#35824,#35825,#35826,#35827,
#35828,#35829,#35830,#35831,#35832,#35833,#35834,#35835,#35836,#35837,#35838,
#35839,#35840,#35841,#35842,#35843,#35844,#35845,#35846,#35847,#35848,#35849,
#35850,#35851,#35852,#35853,#35854,#35855,#35856,#35857,#35858,#35859,#35860,
#35861,#35862,#35863,#35864,#35865,#35866,#35867,#35868,#35869,#35870,#35871,
#35872,#35873,#35874,#35875,#35876,#35877,#35878,#35879,#35880,#35881,#35882,
#35883,#35884,#35885,#35886,#35887,#35888,#35889,#35890,#35891,#35892,#35893,
#35894,#35895,#35896,#35897,#35898,#35899,#35900,#35901,#35902,#35903,#35904,
#35905,#35906,#35907,#35908,#35909,#35910,#35911,#35912,#35913,#35914,#35915,
#35916,#35917,#35918,#35919,#35920,#35921,#35922,#35923,#35924,#35925,#35926,
#35927,#35928,#35929,#35930,#35931,#35932),.UNSPECIFIED.,.F.,.F.,(4,3,3,
3,3,3,3,3,3,3,3,3,3,3,3,3,3,3,3,3,3,3,3,3,3,3,3,3,3,3,3,3,3,3,3,3,3,3,3,
3,3,3,3,3,3,3,3,3,3,3,3,3,3,3,3,3,3,3,3,3,3,3,3,3,3,3,3,3,3,3,3,3,3,4),
(260.752190248039,260.840077818288,260.928098755491,261.016344437238,261.104711000688,
261.193282498438,261.239133579405,261.322872291251,261.406507802619,261.490060246017,
261.573549681868,261.657003632482,261.740440126328,261.823877236084,261.907333031002,
261.990877523732,262.074466606673,262.15818987423,262.238869590125,262.322608301971,
262.406243813339,262.489796256737,262.573285692588,262.656739643202,262.740176137048,
262.823613246804,262.907069041721,262.990613534451,263.074202617392,263.15792588495,
263.238605600846,263.322344312692,263.405979824059,263.489532267458,263.573021703309,
263.656475653923,263.739912147769,263.823349257524,263.906805052442,263.990349545172,
264.073938628113,264.15766189567,264.238341611566,264.322080323412,264.405715834779,
264.489268278178,264.572757714029,264.656211664643,264.739648158489,264.823085268244,
264.906541063162,264.990085555892,265.073674638833,265.15739790639,265.238077622286,
265.321816334132,265.405451845499,265.489004288898,265.572493724749,265.655947675363,
265.739384169209,265.822821278965,265.906277073882,265.989821566612,266.073410649553,
266.157133917111,266.237813633006,266.320335372003,266.402760918938,266.48510946943,
266.567397842967,266.649650649338,266.731899755698,266.783796292336),
 .UNSPECIFIED.);
#216=B_SPLINE_CURVE_WITH_KNOTS('',3,(#35933,#35934,#35935,#35936,#35937,
#35938,#35939,#35940,#35941,#35942),.UNSPECIFIED.,.F.,.F.,(4,3,3,4),(260.501841684575,
260.588962512034,260.675942991099,260.752190247933),.UNSPECIFIED.);
#217=B_SPLINE_CURVE_WITH_KNOTS('',3,(#35944,#35945,#35946,#35947,#35948,
#35949,#35950,#35951,#35952,#35953),.UNSPECIFIED.,.F.,.F.,(4,3,3,4),(260.50086310401,
260.5496881884,260.669135343435,260.752190247937),.UNSPECIFIED.);
#218=B_SPLINE_CURVE_WITH_KNOTS('',3,(#35954,#35955,#35956,#35957,#35958,
#35959,#35960,#35961,#35962,#35963,#35964,#35965,#35966,#35967,#35968,#35969,
#35970,#35971,#35972,#35973,#35974,#35975,#35976,#35977,#35978,#35979,#35980,
#35981,#35982,#35983,#35984,#35985,#35986,#35987,#35988,#35989,#35990,#35991,
#35992,#35993,#35994,#35995,#35996,#35997,#35998,#35999,#36000,#36001,#36002,
#36003,#36004,#36005,#36006,#36007,#36008,#36009,#36010,#36011,#36012,#36013,
#36014,#36015,#36016,#36017,#36018,#36019,#36020,#36021,#36022,#36023,#36024,
#36025,#36026,#36027,#36028,#36029,#36030,#36031,#36032,#36033,#36034,#36035,
#36036,#36037,#36038,#36039,#36040,#36041,#36042,#36043,#36044,#36045,#36046,
#36047,#36048,#36049,#36050,#36051,#36052,#36053,#36054,#36055,#36056,#36057,
#36058,#36059,#36060,#36061,#36062,#36063,#36064,#36065,#36066,#36067,#36068,
#36069,#36070,#36071,#36072,#36073,#36074,#36075,#36076,#36077,#36078,#36079,
#36080,#36081,#36082,#36083,#36084,#36085,#36086,#36087,#36088,#36089,#36090,
#36091,#36092,#36093,#36094,#36095,#36096,#36097,#36098,#36099,#36100,#36101,
#36102,#36103,#36104,#36105,#36106,#36107,#36108,#36109,#36110,#36111,#36112,
#36113,#36114,#36115,#36116,#36117,#36118,#36119,#36120,#36121,#36122,#36123,
#36124,#36125,#36126,#36127,#36128,#36129,#36130,#36131,#36132,#36133,#36134,
#36135,#36136,#36137,#36138,#36139,#36140,#36141,#36142,#36143,#36144,#36145,
#36146,#36147,#36148,#36149,#36150,#36151,#36152,#36153,#36154,#36155,#36156,
#36157,#36158,#36159,#36160,#36161,#36162,#36163,#36164,#36165,#36166,#36167,
#36168,#36169,#36170,#36171,#36172,#36173),.UNSPECIFIED.,.F.,.F.,(4,3,3,
3,3,3,3,3,3,3,3,3,3,3,3,3,3,3,3,3,3,3,3,3,3,3,3,3,3,3,3,3,3,3,3,3,3,3,3,
3,3,3,3,3,3,3,3,3,3,3,3,3,3,3,3,3,3,3,3,3,3,3,3,3,3,3,3,3,3,3,3,3,3,4),
(260.752190248121,260.834571493874,260.916884504121,260.999156020819,261.081407233152,
261.163657149231,261.245924773897,261.328276962325,261.410674639221,261.493196468606,
261.54942419912,261.633162910966,261.716798422334,261.800350865732,261.883840301583,
261.967294252197,262.050730746043,262.134167855798,262.217623650716,262.301168143446,
262.384757226387,262.468480493944,262.549160209841,262.632898921687,262.716534433055,
262.800086876454,262.883576312304,262.967030262918,263.050466756764,263.13390386652,
263.217359661438,263.300904154168,263.384493237109,263.468216504666,263.548896220561,
263.632634932407,263.716270443774,263.799822887173,263.883312323024,263.966766273637,
264.050202767484,264.133639877239,264.217095672156,264.300640164886,264.384229247827,
264.467952515385,264.548632231281,264.632370943127,264.716006454494,264.799558897893,
264.883048333744,264.966502284357,265.049938778204,265.133375887959,265.216831682877,
265.300376175607,265.383965258548,265.467688526105,265.548368242001,265.632106953847,
265.715742465215,265.799294908613,265.882784344464,265.966238295078,266.049674788924,
266.13311189868,266.216567693597,266.300112186327,266.383701269268,266.467424536826,
266.548104252721,266.636675884245,266.725043738978,266.785062210057),
 .UNSPECIFIED.);
#219=B_SPLINE_CURVE_WITH_KNOTS('',3,(#36179,#36180,#36181,#36182,#36183,
#36184,#36185,#36186,#36187,#36188,#36189,#36190,#36191,#36192,#36193,#36194,
#36195,#36196,#36197,#36198,#36199,#36200,#36201,#36202,#36203,#36204,#36205,
#36206,#36207,#36208,#36209,#36210,#36211,#36212,#36213,#36214,#36215,#36216,
#36217,#36218,#36219,#36220,#36221,#36222,#36223,#36224,#36225,#36226,#36227,
#36228,#36229,#36230,#36231,#36232,#36233,#36234,#36235,#36236,#36237,#36238,
#36239,#36240,#36241,#36242,#36243,#36244,#36245,#36246,#36247,#36248,#36249,
#36250,#36251,#36252,#36253,#36254,#36255,#36256,#36257,#36258,#36259,#36260,
#36261,#36262,#36263,#36264,#36265,#36266,#36267,#36268,#36269,#36270,#36271,
#36272,#36273,#36274,#36275,#36276,#36277,#36278,#36279,#36280,#36281,#36282,
#36283,#36284,#36285,#36286,#36287,#36288,#36289,#36290,#36291,#36292,#36293,
#36294,#36295,#36296,#36297,#36298,#36299,#36300,#36301,#36302,#36303,#36304,
#36305,#36306,#36307,#36308,#36309,#36310,#36311,#36312,#36313,#36314,#36315,
#36316,#36317,#36318,#36319,#36320,#36321,#36322,#36323,#36324,#36325,#36326,
#36327,#36328,#36329,#36330,#36331,#36332,#36333,#36334,#36335,#36336,#36337,
#36338,#36339,#36340,#36341,#36342,#36343,#36344,#36345,#36346,#36347,#36348,
#36349,#36350,#36351,#36352,#36353,#36354,#36355,#36356,#36357,#36358,#36359,
#36360,#36361,#36362,#36363,#36364,#36365,#36366,#36367,#36368,#36369,#36370,
#36371,#36372,#36373,#36374,#36375,#36376,#36377,#36378,#36379,#36380,#36381,
#36382,#36383,#36384,#36385,#36386,#36387,#36388,#36389,#36390,#36391,#36392,
#36393,#36394,#36395),.UNSPECIFIED.,.F.,.F.,(4,3,3,3,3,3,3,3,3,3,3,3,3,
3,3,3,3,3,3,3,3,3,3,3,3,3,3,3,3,3,3,3,3,3,3,3,3,3,3,3,3,3,3,3,3,3,3,3,3,
3,3,3,3,3,3,3,3,3,3,3,3,3,3,3,3,3,3,3,3,3,3,3,4),(267.035375555113,267.154919976287,
267.237549643726,267.321288355572,267.404923866939,267.488476310338,267.571965746189,
267.655419696803,267.738856190649,267.822293300404,267.905749095322,267.989293588052,
268.072882670993,268.156605938551,268.237285654446,268.321024366292,268.404659877659,
268.488212321058,268.571701756909,268.655155707522,268.738592201369,268.822029311124,
268.905485106042,268.989029598771,269.072618681712,269.15634194927,269.237021665166,
269.320760377012,269.404395888379,269.487948331778,269.571437767629,269.654891718243,
269.738328212089,269.821765321845,269.905221116762,269.988765609492,270.072354692433,
270.156077959991,270.236757675886,270.320496387732,270.4041318991,270.487684342498,
270.571173778349,270.654627728963,270.738064222809,270.821501332565,270.904957127483,
270.988501620212,271.072090703153,271.155813970711,271.236493686607,271.320232398453,
271.403867909821,271.487420353219,271.57090978907,271.654363739684,271.73780023353,
271.821237343286,271.904693138204,271.988237630933,272.071826713874,272.155549981432,
272.236229697327,272.319978513639,272.403621899315,272.487165079065,272.570651436406,
272.654099090554,272.737526130872,272.820979923044,272.904444581242,272.987986644754,
273.06691472068),.UNSPECIFIED.);
#220=B_SPLINE_CURVE_WITH_KNOTS('',3,(#36396,#36397,#36398,#36399,#36400,
#36401,#36402,#36403,#36404,#36405),.UNSPECIFIED.,.F.,.F.,(4,3,3,4),(266.783796292336,
266.866079451347,266.950727503137,267.035375554927),.UNSPECIFIED.);
#221=B_SPLINE_CURVE_WITH_KNOTS('',3,(#36407,#36408,#36409,#36410,#36411,
#36412,#36413,#36414,#36415,#36416),.UNSPECIFIED.,.F.,.F.,(4,3,3,4),(266.785062210057,
266.873164835651,266.961082385074,267.035375555014),.UNSPECIFIED.);
#222=B_SPLINE_CURVE_WITH_KNOTS('',3,(#36417,#36418,#36419,#36420,#36421,
#36422,#36423,#36424,#36425,#36426,#36427,#36428,#36429,#36430,#36431,#36432,
#36433,#36434,#36435,#36436,#36437,#36438,#36439,#36440,#36441,#36442,#36443,
#36444,#36445,#36446,#36447,#36448,#36449,#36450,#36451,#36452,#36453,#36454,
#36455,#36456,#36457,#36458,#36459,#36460,#36461,#36462,#36463,#36464,#36465,
#36466,#36467,#36468,#36469,#36470,#36471,#36472,#36473,#36474,#36475,#36476,
#36477,#36478,#36479,#36480,#36481,#36482,#36483,#36484,#36485,#36486,#36487,
#36488,#36489,#36490,#36491,#36492,#36493,#36494,#36495,#36496,#36497,#36498,
#36499,#36500,#36501,#36502,#36503,#36504,#36505,#36506,#36507,#36508,#36509,
#36510,#36511,#36512,#36513,#36514,#36515,#36516,#36517,#36518,#36519,#36520,
#36521,#36522,#36523,#36524,#36525,#36526,#36527,#36528,#36529,#36530,#36531,
#36532,#36533,#36534,#36535,#36536,#36537,#36538,#36539,#36540,#36541,#36542,
#36543,#36544,#36545,#36546,#36547,#36548,#36549,#36550,#36551,#36552,#36553,
#36554,#36555,#36556,#36557,#36558,#36559,#36560,#36561,#36562,#36563,#36564,
#36565,#36566,#36567,#36568,#36569,#36570,#36571,#36572,#36573,#36574,#36575,
#36576,#36577,#36578,#36579,#36580,#36581,#36582,#36583,#36584,#36585,#36586,
#36587,#36588,#36589,#36590,#36591,#36592,#36593,#36594,#36595,#36596,#36597,
#36598,#36599,#36600,#36601,#36602,#36603,#36604,#36605,#36606,#36607,#36608,
#36609,#36610,#36611,#36612,#36613,#36614,#36615,#36616,#36617,#36618,#36619,
#36620,#36621,#36622,#36623,#36624,#36625,#36626,#36627,#36628,#36629,#36630,
#36631,#36632,#36633,#36634,#36635,#36636),.UNSPECIFIED.,.F.,.F.,(4,3,3,
3,3,3,3,3,3,3,3,3,3,3,3,3,3,3,3,3,3,3,3,3,3,3,3,3,3,3,3,3,3,3,3,3,3,3,3,
3,3,3,3,3,3,3,3,3,3,3,3,3,3,3,3,3,3,3,3,3,3,3,3,3,3,3,3,3,3,3,3,3,3,4),
(267.035375555117,267.122336957127,267.209397452547,267.296648856939,267.383998872037,
267.47154721962,267.547840263441,267.631578975287,267.715214486655,267.798766930053,
267.882256365904,267.965710316518,268.049146810364,268.13258392012,268.216039715037,
268.299584207767,268.383173290708,268.466896558266,268.547576274161,268.631314986007,
268.714950497375,268.798502940773,268.881992376624,268.965446327238,269.048882821084,
269.13231993084,269.215775725758,269.299320218487,269.382909301429,269.466632568986,
269.547312284882,269.631050996728,269.714686508096,269.798238951494,269.881728387345,
269.965182337959,270.048618831805,270.132055941561,270.215511736478,270.299056229208,
270.382645312149,270.466368579707,270.547048295602,270.630787007448,270.714422518815,
270.797974962214,270.881464398065,270.964918348679,271.048354842525,271.13179195228,
271.215247747198,271.298792239928,271.382381322868,271.466104590426,271.546784306322,
271.630523018168,271.714158529536,271.797710972934,271.881200408785,271.964654359398,
272.048090853245,272.131527963,272.214983757918,272.298528250647,272.382117333588,
272.465840601146,272.546520317042,272.629147478544,272.71167748403,272.794129465717,
272.876517967464,272.958870159486,273.041211385537,273.067091906304),
 .UNSPECIFIED.);
#223=B_SPLINE_CURVE_WITH_KNOTS('',3,(#36642,#36643,#36644,#36645,#36646,
#36647,#36648,#36649,#36650,#36651,#36652,#36653,#36654,#36655,#36656,#36657,
#36658,#36659,#36660,#36661,#36662,#36663,#36664,#36665,#36666,#36667,#36668,
#36669,#36670,#36671,#36672,#36673,#36674,#36675,#36676,#36677,#36678,#36679,
#36680,#36681,#36682,#36683,#36684,#36685,#36686,#36687,#36688,#36689,#36690,
#36691,#36692,#36693,#36694,#36695,#36696,#36697,#36698,#36699,#36700,#36701,
#36702,#36703,#36704,#36705,#36706,#36707,#36708,#36709,#36710,#36711,#36712,
#36713,#36714,#36715,#36716,#36717,#36718,#36719,#36720,#36721,#36722,#36723,
#36724,#36725,#36726,#36727,#36728,#36729,#36730,#36731,#36732,#36733,#36734,
#36735,#36736,#36737,#36738,#36739,#36740,#36741,#36742,#36743,#36744,#36745,
#36746,#36747,#36748,#36749,#36750,#36751,#36752,#36753,#36754,#36755,#36756,
#36757,#36758,#36759,#36760,#36761,#36762,#36763,#36764,#36765,#36766,#36767,
#36768,#36769,#36770,#36771,#36772,#36773,#36774,#36775,#36776,#36777,#36778,
#36779,#36780,#36781,#36782,#36783,#36784,#36785,#36786,#36787,#36788,#36789,
#36790,#36791,#36792,#36793,#36794,#36795,#36796,#36797,#36798,#36799,#36800,
#36801,#36802,#36803,#36804,#36805,#36806,#36807,#36808,#36809,#36810,#36811,
#36812,#36813,#36814,#36815,#36816,#36817,#36818,#36819,#36820,#36821,#36822,
#36823,#36824,#36825,#36826,#36827,#36828,#36829,#36830,#36831,#36832,#36833,
#36834,#36835,#36836,#36837,#36838,#36839,#36840,#36841,#36842,#36843,#36844,
#36845,#36846,#36847,#36848,#36849,#36850,#36851,#36852,#36853,#36854,#36855,
#36856,#36857,#36858,#36859,#36860,#36861),.UNSPECIFIED.,.F.,.F.,(4,3,3,
3,3,3,3,3,3,3,3,3,3,3,3,3,3,3,3,3,3,3,3,3,3,3,3,3,3,3,3,3,3,3,3,3,3,3,3,
3,3,3,3,3,3,3,3,3,3,3,3,3,3,3,3,3,3,3,3,3,3,3,3,3,3,3,3,3,3,3,3,3,3,4),
(273.318560862424,273.401332140583,273.48400781649,273.566608858109,273.650245465692,
273.732769655677,273.815286530553,273.8978149211,273.982286620517,274.06493792759,
274.150319823179,274.235701718767,274.319440430613,274.403075941981,274.486628385379,
274.57011782123,274.653571771844,274.73700826569,274.820445375445,274.903901170363,
274.987445663092,275.071034746033,275.154758013591,275.235437729487,275.319176441333,
275.4028119527,275.486364396099,275.56985383195,275.653307782563,275.73674427641,
275.820181386165,275.903637181083,275.987181673812,276.070770756753,276.154494024311,
276.235173740207,276.318912452053,276.40254796342,276.486100406819,276.569589842671,
276.653043793284,276.736480287131,276.819917396886,276.903373191804,276.986917684533,
277.070506767474,277.154230035032,277.234909750927,277.318648462773,277.40228397414,
277.485836417539,277.56932585339,277.652779804003,277.73621629785,277.819653407605,
277.903109202523,277.986653695253,278.070242778194,278.153966045751,278.234645761647,
278.318384473493,278.402019984861,278.48557242826,278.569061864111,278.652515814725,
278.735952308571,278.819389418327,278.902845213245,278.986389705974,279.069978788915,
279.153702056473,279.234381772368,279.329926919196,279.351278122143),
 .UNSPECIFIED.);
#224=B_SPLINE_CURVE_WITH_KNOTS('',3,(#36862,#36863,#36864,#36865,#36866,
#36867,#36868,#36869,#36870,#36871),.UNSPECIFIED.,.F.,.F.,(4,3,3,4),(273.06691472068,
273.151440214363,273.235965708047,273.318560862292),.UNSPECIFIED.);
#225=B_SPLINE_CURVE_WITH_KNOTS('',3,(#36873,#36874,#36875,#36876,#36877,
#36878,#36879,#36880,#36881,#36882),.UNSPECIFIED.,.F.,.F.,(4,3,3,4),(273.067091906304,
273.149461125864,273.23401099402,273.318560862176),.UNSPECIFIED.);
#226=B_SPLINE_CURVE_WITH_KNOTS('',3,(#36883,#36884,#36885,#36886,#36887,
#36888,#36889,#36890,#36891,#36892,#36893,#36894,#36895,#36896,#36897,#36898,
#36899,#36900,#36901,#36902,#36903,#36904,#36905,#36906,#36907,#36908,#36909,
#36910,#36911,#36912,#36913,#36914,#36915,#36916,#36917,#36918,#36919,#36920,
#36921,#36922,#36923,#36924,#36925,#36926,#36927,#36928,#36929,#36930,#36931,
#36932,#36933,#36934,#36935,#36936,#36937,#36938,#36939,#36940,#36941,#36942,
#36943,#36944,#36945,#36946,#36947,#36948,#36949,#36950,#36951,#36952,#36953,
#36954,#36955,#36956,#36957,#36958,#36959,#36960,#36961,#36962,#36963,#36964,
#36965,#36966,#36967,#36968,#36969,#36970,#36971,#36972,#36973,#36974,#36975,
#36976,#36977,#36978,#36979,#36980,#36981,#36982,#36983,#36984,#36985,#36986,
#36987,#36988,#36989,#36990,#36991,#36992,#36993,#36994,#36995,#36996,#36997,
#36998,#36999,#37000,#37001,#37002,#37003,#37004,#37005,#37006,#37007,#37008,
#37009,#37010,#37011,#37012,#37013,#37014,#37015,#37016,#37017,#37018,#37019,
#37020,#37021,#37022,#37023,#37024,#37025,#37026,#37027,#37028,#37029,#37030,
#37031,#37032,#37033,#37034,#37035,#37036,#37037,#37038,#37039,#37040,#37041,
#37042,#37043,#37044,#37045,#37046,#37047,#37048,#37049,#37050,#37051,#37052,
#37053,#37054,#37055,#37056,#37057,#37058,#37059,#37060,#37061,#37062,#37063,
#37064,#37065,#37066,#37067,#37068,#37069,#37070,#37071,#37072,#37073,#37074,
#37075,#37076,#37077,#37078,#37079,#37080,#37081,#37082,#37083,#37084,#37085,
#37086,#37087,#37088,#37089,#37090,#37091,#37092,#37093,#37094,#37095,#37096,
#37097,#37098,#37099),.UNSPECIFIED.,.F.,.F.,(4,3,3,3,3,3,3,3,3,3,3,3,3,
3,3,3,3,3,3,3,3,3,3,3,3,3,3,3,3,3,3,3,3,3,3,3,3,3,3,3,3,3,3,3,3,3,3,3,3,
3,3,3,3,3,3,3,3,3,3,3,3,3,3,3,3,3,3,3,3,3,3,3,4),(273.318560862296,273.432408595029,
273.546256327762,273.629995039608,273.713630550976,273.797182994374,273.880672430225,
273.964126380839,274.047562874685,274.130999984441,274.214455779359,274.298000272089,
274.38158935503,274.465312622587,274.545992338482,274.629731050328,274.713366561695,
274.796919005094,274.880408440945,274.963862391558,275.047298885404,275.13073599516,
275.214191790077,275.297736282807,275.381325365748,275.465048633305,275.545728349202,
275.629467061048,275.713102572415,275.796655015814,275.880144451665,275.963598402279,
276.047034896125,276.130472005881,276.213927800798,276.297472293528,276.381061376469,
276.464784644027,276.545464359922,276.629203071768,276.712838583136,276.796391026534,
276.879880462385,276.963334412999,277.046770906845,277.130208016601,277.213663811519,
277.297208304248,277.380797387189,277.464520654747,277.545200370643,277.628939082489,
277.712574593856,277.796127037255,277.879616473106,277.96307042372,278.046506917566,
278.129944027322,278.213399822239,278.296944314969,278.38053339791,278.464256665468,
278.544936381363,278.628686835053,278.712331521095,278.795875148069,278.879361474852,
278.962808621501,279.046234677786,279.129682656208,279.213141308916,279.296665516618,
279.350082863217),.UNSPECIFIED.);
#227=B_SPLINE_CURVE_WITH_KNOTS('',3,(#37105,#37106,#37107,#37108,#37109,
#37110,#37111,#37112,#37113,#37114,#37115,#37116,#37117,#37118,#37119,#37120,
#37121,#37122,#37123,#37124,#37125,#37126,#37127,#37128,#37129,#37130,#37131,
#37132,#37133,#37134,#37135,#37136,#37137,#37138,#37139,#37140,#37141,#37142,
#37143,#37144,#37145,#37146,#37147,#37148,#37149,#37150,#37151,#37152,#37153,
#37154,#37155,#37156,#37157,#37158,#37159,#37160,#37161,#37162,#37163,#37164,
#37165,#37166,#37167,#37168,#37169,#37170,#37171,#37172,#37173,#37174,#37175,
#37176,#37177,#37178,#37179,#37180,#37181,#37182,#37183,#37184,#37185,#37186,
#37187,#37188,#37189,#37190,#37191,#37192,#37193,#37194,#37195,#37196,#37197,
#37198,#37199,#37200,#37201,#37202,#37203,#37204,#37205,#37206,#37207,#37208,
#37209,#37210,#37211,#37212,#37213,#37214,#37215,#37216,#37217,#37218,#37219,
#37220,#37221,#37222,#37223,#37224,#37225,#37226,#37227,#37228,#37229,#37230,
#37231,#37232,#37233,#37234,#37235,#37236,#37237,#37238,#37239,#37240,#37241,
#37242,#37243,#37244,#37245,#37246,#37247,#37248,#37249,#37250,#37251,#37252,
#37253,#37254,#37255,#37256,#37257,#37258,#37259,#37260,#37261,#37262,#37263,
#37264,#37265,#37266,#37267,#37268,#37269,#37270,#37271,#37272,#37273,#37274,
#37275,#37276,#37277,#37278,#37279,#37280,#37281,#37282,#37283,#37284,#37285,
#37286,#37287,#37288,#37289,#37290,#37291,#37292,#37293,#37294,#37295,#37296,
#37297,#37298,#37299,#37300,#37301,#37302,#37303,#37304,#37305,#37306,#37307,
#37308,#37309,#37310,#37311,#37312,#37313,#37314,#37315,#37316,#37317,#37318,
#37319,#37320,#37321,#37322,#37323,#37324),.UNSPECIFIED.,.F.,.F.,(4,3,3,
3,3,3,3,3,3,3,3,3,3,3,3,3,3,3,3,3,3,3,3,3,3,3,3,3,3,3,3,3,3,3,3,3,3,3,3,
3,3,3,3,3,3,3,3,3,3,3,3,3,3,3,3,3,3,3,3,3,3,3,3,3,3,3,3,3,3,3,3,3,3,4),
(279.601746169472,279.685672429252,279.769601901197,279.853551962208,279.937539998755,
280.021635635826,280.105791581247,280.190082572072,280.234117783088,280.317856494934,
280.401492006301,280.4850444497,280.568533885551,280.651987836165,280.735424330011,
280.818861439766,280.902317234684,280.985861727414,281.069450810355,281.153174077913,
281.233853793808,281.317592505654,281.401228017021,281.48478046042,281.568269896271,
281.651723846884,281.735160340731,281.818597450486,281.902053245403,281.985597738133,
282.069186821074,282.152910088631,282.233589804528,282.317328516374,282.400964027741,
282.48451647114,282.56800590699,282.651459857604,282.734896351451,282.818333461206,
282.901789256124,282.985333748854,283.068922831795,283.152646099352,283.233325815248,
283.317064527094,283.400700038461,283.48425248186,283.567741917711,283.651195868325,
283.734632362171,283.818069471927,283.901525266845,283.985069759574,284.068658842515,
284.152382110073,284.233061825968,284.316800537814,284.400436049181,284.48398849258,
284.567477928431,284.650931879045,284.734368372891,284.817805482646,284.901261277563,
284.984805770293,285.068394853234,285.152118120792,285.232797836688,285.316744966212,
285.400555054353,285.484286316186,285.56794519696,285.634069424409),
 .UNSPECIFIED.);
#228=B_SPLINE_CURVE_WITH_KNOTS('',3,(#37325,#37326,#37327,#37328,#37329,
#37330,#37331,#37332,#37333,#37334),.UNSPECIFIED.,.F.,.F.,(4,3,3,4),(279.351278122143,
279.446286643589,279.540691824518,279.601746169273),.UNSPECIFIED.);
#229=B_SPLINE_CURVE_WITH_KNOTS('',3,(#37336,#37337,#37338,#37339,#37340,
#37341,#37342,#37343,#37344,#37345,#37346,#37347,#37348),.UNSPECIFIED.,
 .F.,.F.,(4,3,3,3,4),(279.350082863217,279.433708952402,279.517454217818,
279.544672392083,279.601746169476),.UNSPECIFIED.);
#230=B_SPLINE_CURVE_WITH_KNOTS('',3,(#37349,#37350,#37351,#37352,#37353,
#37354,#37355,#37356,#37357,#37358,#37359,#37360,#37361,#37362,#37363,#37364,
#37365,#37366,#37367,#37368,#37369,#37370,#37371,#37372,#37373,#37374,#37375,
#37376,#37377,#37378,#37379,#37380,#37381,#37382,#37383,#37384,#37385,#37386,
#37387,#37388,#37389,#37390,#37391,#37392,#37393,#37394,#37395,#37396,#37397,
#37398,#37399,#37400,#37401,#37402,#37403,#37404,#37405,#37406,#37407,#37408,
#37409,#37410,#37411,#37412,#37413,#37414,#37415,#37416,#37417,#37418,#37419,
#37420,#37421,#37422,#37423,#37424,#37425,#37426,#37427,#37428,#37429,#37430,
#37431,#37432,#37433,#37434,#37435,#37436,#37437,#37438,#37439,#37440,#37441,
#37442,#37443,#37444,#37445,#37446,#37447,#37448,#37449,#37450,#37451,#37452,
#37453,#37454,#37455,#37456,#37457,#37458,#37459,#37460,#37461,#37462,#37463,
#37464,#37465,#37466,#37467,#37468,#37469,#37470,#37471,#37472,#37473,#37474,
#37475,#37476,#37477,#37478,#37479,#37480,#37481,#37482,#37483,#37484,#37485,
#37486,#37487,#37488,#37489,#37490,#37491,#37492,#37493,#37494,#37495,#37496,
#37497,#37498,#37499,#37500,#37501,#37502,#37503,#37504,#37505,#37506,#37507,
#37508,#37509,#37510,#37511,#37512,#37513,#37514,#37515,#37516,#37517,#37518,
#37519,#37520,#37521,#37522,#37523,#37524,#37525,#37526,#37527,#37528,#37529,
#37530,#37531,#37532,#37533,#37534,#37535,#37536,#37537,#37538,#37539,#37540,
#37541,#37542,#37543,#37544,#37545,#37546,#37547,#37548,#37549,#37550,#37551,
#37552,#37553,#37554,#37555,#37556,#37557,#37558,#37559,#37560,#37561,#37562,
#37563,#37564,#37565,#37566,#37567,#37568),.UNSPECIFIED.,.F.,.F.,(4,3,3,
3,3,3,3,3,3,3,3,3,3,3,3,3,3,3,3,3,3,3,3,3,3,3,3,3,3,3,3,3,3,3,3,3,3,3,3,
3,3,3,3,3,3,3,3,3,3,3,3,3,3,3,3,3,3,3,3,3,3,3,3,3,3,3,3,3,3,3,3,3,3,4),
(279.601746169585,279.684754693531,279.767664002698,279.850494901022,279.937234088745,
280.019978327433,280.102712039047,280.185453899734,280.268222588391,280.351081808708,
280.433994088779,280.517024272122,280.544408402803,280.628147114649,280.711782626016,
280.795335069415,280.878824505266,280.96227845588,281.045714949726,281.129152059481,
281.212607854399,281.296152347129,281.37974143007,281.463464697627,281.544144413523,
281.627883125369,281.711518636736,281.795071080135,281.878560515986,281.9620144666,
282.045450960446,282.128888070201,282.212343865119,282.295888357849,282.379477440789,
282.463200708347,282.543880424243,282.627619136089,282.711254647456,282.794807090855,
282.878296526706,282.96175047732,283.045186971166,283.128624080921,283.212079875839,
283.295624368568,283.379213451509,283.462936719067,283.543616434963,283.627355146809,
283.710990658177,283.794543101575,283.878032537427,283.96148648804,284.044922981887,
284.128360091642,284.21181588656,284.29536037929,284.378949462231,284.462672729788,
284.543352445683,284.627091157529,284.710726668896,284.794279112295,284.877768548146,
284.96122249876,285.044658992606,285.128096102361,285.211551897279,285.295096390009,
285.37868547295,285.462408740508,285.543088456404,285.63436337626),
 .UNSPECIFIED.);
#231=B_SPLINE_CURVE_WITH_KNOTS('',3,(#37574,#37575,#37576,#37577,#37578,
#37579,#37580,#37581,#37582,#37583,#37584,#37585,#37586,#37587,#37588,#37589,
#37590,#37591,#37592,#37593,#37594,#37595,#37596,#37597,#37598,#37599,#37600,
#37601,#37602,#37603,#37604,#37605,#37606,#37607,#37608,#37609,#37610,#37611,
#37612,#37613,#37614,#37615,#37616,#37617,#37618,#37619,#37620,#37621,#37622,
#37623,#37624,#37625,#37626,#37627,#37628,#37629,#37630,#37631,#37632,#37633,
#37634,#37635,#37636,#37637,#37638,#37639,#37640,#37641,#37642,#37643,#37644,
#37645,#37646,#37647,#37648,#37649,#37650,#37651,#37652,#37653,#37654,#37655,
#37656,#37657,#37658,#37659,#37660,#37661,#37662,#37663,#37664,#37665,#37666,
#37667,#37668,#37669,#37670,#37671,#37672,#37673,#37674,#37675,#37676,#37677,
#37678,#37679,#37680,#37681,#37682,#37683,#37684,#37685,#37686,#37687,#37688,
#37689,#37690,#37691,#37692,#37693,#37694,#37695,#37696,#37697,#37698,#37699,
#37700,#37701,#37702,#37703,#37704,#37705,#37706,#37707,#37708,#37709,#37710,
#37711,#37712,#37713,#37714,#37715,#37716,#37717,#37718,#37719,#37720,#37721,
#37722,#37723,#37724,#37725,#37726,#37727,#37728,#37729,#37730,#37731,#37732,
#37733,#37734,#37735,#37736,#37737,#37738,#37739,#37740,#37741,#37742,#37743,
#37744,#37745,#37746,#37747,#37748,#37749,#37750,#37751,#37752,#37753,#37754,
#37755,#37756,#37757,#37758,#37759,#37760,#37761,#37762,#37763,#37764,#37765,
#37766,#37767,#37768,#37769,#37770,#37771,#37772,#37773,#37774,#37775,#37776,
#37777,#37778,#37779,#37780,#37781,#37782,#37783,#37784,#37785,#37786,#37787,
#37788,#37789,#37790,#37791,#37792,#37793),.UNSPECIFIED.,.F.,.F.,(4,3,3,
3,3,3,3,3,3,3,3,3,3,3,3,3,3,3,3,3,3,3,3,3,3,3,3,3,3,3,3,3,3,3,3,3,3,3,3,
3,3,3,3,3,3,3,3,3,3,3,3,3,3,3,3,3,3,3,3,3,3,3,3,3,3,3,3,3,3,3,3,3,3,4),
(285.884931476846,285.98094828738,286.077455092432,286.174577660897,286.232533847408,
286.316272559254,286.399908070621,286.48346051402,286.566949949871,286.650403900485,
286.733840394331,286.817277504086,286.900733299004,286.984277791734,287.067866874675,
287.151590142232,287.232269858129,287.316008569975,287.399644081342,287.483196524741,
287.566685960592,287.650139911206,287.733576405052,287.817013514808,287.900469309725,
287.984013802455,288.067602885396,288.151326152954,288.232005868849,288.315744580695,
288.399380092062,288.482932535461,288.566421971312,288.649875921926,288.733312415772,
288.816749525527,288.900205320445,288.983749813175,289.067338896116,289.151062163673,
289.231741879569,289.315480591415,289.399116102782,289.482668546181,289.566157982032,
289.649611932645,289.733048426492,289.816485536247,289.899941331165,289.983485823894,
290.067074906835,290.150798174393,290.231477890289,290.315216602135,290.398852113502,
290.482404556901,290.565893992752,290.649347943366,290.732784437212,290.816221546968,
290.899677341886,290.983221834615,291.066810917556,291.150534185114,291.231213901009,
291.316848773597,291.39970298138,291.482482124273,291.565205016221,291.64789042395,
291.730570621983,291.813248806099,291.895962990363,291.916292881714),
 .UNSPECIFIED.);
#232=B_SPLINE_CURVE_WITH_KNOTS('',3,(#37794,#37795,#37796,#37797,#37798,
#37799,#37800,#37801,#37802,#37803),.UNSPECIFIED.,.F.,.F.,(4,3,3,4),(285.634069424409,
285.717661682716,285.801296579684,285.884931476652),.UNSPECIFIED.);
#233=B_SPLINE_CURVE_WITH_KNOTS('',3,(#37805,#37806,#37807,#37808,#37809,
#37810,#37811,#37812,#37813,#37814),.UNSPECIFIED.,.F.,.F.,(4,3,3,4),(285.63436337626,
285.731577997215,285.828008467893,285.884931476463),.UNSPECIFIED.);
#234=B_SPLINE_CURVE_WITH_KNOTS('',3,(#37815,#37816,#37817,#37818,#37819,
#37820,#37821,#37822,#37823,#37824,#37825,#37826,#37827,#37828,#37829,#37830,
#37831,#37832,#37833,#37834,#37835,#37836,#37837,#37838,#37839,#37840,#37841,
#37842,#37843,#37844,#37845,#37846,#37847,#37848,#37849,#37850,#37851,#37852,
#37853,#37854,#37855,#37856,#37857,#37858,#37859,#37860,#37861,#37862,#37863,
#37864,#37865,#37866,#37867,#37868,#37869,#37870,#37871,#37872,#37873,#37874,
#37875,#37876,#37877,#37878,#37879,#37880,#37881,#37882,#37883,#37884,#37885,
#37886,#37887,#37888,#37889,#37890,#37891,#37892,#37893,#37894,#37895,#37896,
#37897,#37898,#37899,#37900,#37901,#37902,#37903,#37904,#37905,#37906,#37907,
#37908,#37909,#37910,#37911,#37912,#37913,#37914,#37915,#37916,#37917,#37918,
#37919,#37920,#37921,#37922,#37923,#37924,#37925,#37926,#37927,#37928,#37929,
#37930,#37931,#37932,#37933,#37934,#37935,#37936,#37937,#37938,#37939,#37940,
#37941,#37942,#37943,#37944,#37945,#37946,#37947,#37948,#37949,#37950,#37951,
#37952,#37953,#37954,#37955,#37956,#37957,#37958,#37959,#37960,#37961,#37962,
#37963,#37964,#37965,#37966,#37967,#37968,#37969,#37970,#37971,#37972,#37973,
#37974,#37975,#37976,#37977,#37978,#37979,#37980,#37981,#37982,#37983,#37984,
#37985,#37986,#37987,#37988,#37989,#37990,#37991,#37992,#37993,#37994,#37995,
#37996,#37997,#37998,#37999,#38000,#38001,#38002,#38003,#38004,#38005,#38006,
#38007,#38008,#38009,#38010,#38011,#38012,#38013,#38014,#38015,#38016,#38017,
#38018,#38019,#38020,#38021,#38022,#38023,#38024,#38025,#38026,#38027,#38028,
#38029,#38030,#38031,#38032,#38033,#38034),.UNSPECIFIED.,.F.,.F.,(4,3,3,
3,3,3,3,3,3,3,3,3,3,3,3,3,3,3,3,3,3,3,3,3,3,3,3,3,3,3,3,3,3,3,3,3,3,3,3,
3,3,3,3,3,3,3,3,3,3,3,3,3,3,3,3,3,3,3,3,3,3,3,3,3,3,3,3,3,3,3,3,3,3,4),
(285.884931476655,285.968441827263,286.051942674745,286.135451936067,286.218987529848,
286.302621397412,286.386306242386,286.470130331817,286.542824467124,286.62656317897,
286.710198690337,286.793751133736,286.877240569587,286.9606945202,287.044131014047,
287.127568123802,287.21102391872,287.29456841145,287.378157494391,287.461880761948,
287.542560477844,287.62629918969,287.709934701057,287.793487144456,287.876976580307,
287.960430530921,288.043867024767,288.127304134522,288.21075992944,288.294304422169,
288.37789350511,288.461616772668,288.542296488564,288.62603520041,288.709670711777,
288.793223155176,288.876712591027,288.96016654164,289.043603035487,289.127040145242,
289.21049594016,289.29404043289,289.377629515831,289.461352783388,289.542032499284,
289.62577121113,289.709406722497,289.792959165896,289.876448601746,289.95990255236,
290.043339046206,290.126776155962,290.21023195088,290.29377644361,290.377365526551,
290.461088794108,290.541768510004,290.62550722185,290.709142733218,290.792695176616,
290.876184612467,290.95963856308,291.043075056927,291.126512166682,291.2099679616,
291.29351245433,291.37710153727,291.460824804828,291.541504520724,291.625927635,
291.710207808076,291.794405436709,291.878522273998,291.917378633395),
 .UNSPECIFIED.);
#235=B_SPLINE_CURVE_WITH_KNOTS('',3,(#38040,#38041,#38042,#38043,#38044,
#38045,#38046,#38047,#38048,#38049,#38050,#38051,#38052,#38053,#38054,#38055,
#38056,#38057,#38058,#38059,#38060,#38061,#38062,#38063,#38064,#38065,#38066,
#38067,#38068,#38069,#38070,#38071,#38072,#38073,#38074,#38075,#38076,#38077,
#38078,#38079,#38080,#38081,#38082,#38083,#38084,#38085,#38086,#38087,#38088,
#38089,#38090,#38091,#38092,#38093,#38094,#38095,#38096,#38097,#38098,#38099,
#38100,#38101,#38102,#38103,#38104,#38105,#38106,#38107,#38108,#38109,#38110,
#38111,#38112,#38113,#38114,#38115,#38116,#38117,#38118,#38119,#38120,#38121,
#38122,#38123,#38124,#38125,#38126,#38127,#38128,#38129,#38130,#38131,#38132,
#38133,#38134,#38135,#38136,#38137,#38138,#38139,#38140,#38141,#38142,#38143,
#38144,#38145,#38146,#38147,#38148,#38149,#38150,#38151,#38152,#38153,#38154,
#38155,#38156,#38157,#38158,#38159,#38160,#38161,#38162,#38163,#38164,#38165,
#38166,#38167,#38168,#38169,#38170,#38171,#38172,#38173,#38174,#38175,#38176,
#38177,#38178,#38179,#38180,#38181,#38182,#38183,#38184,#38185,#38186,#38187,
#38188,#38189,#38190,#38191,#38192,#38193,#38194,#38195,#38196,#38197,#38198,
#38199,#38200,#38201,#38202,#38203,#38204,#38205,#38206,#38207,#38208,#38209,
#38210,#38211,#38212,#38213,#38214,#38215,#38216,#38217,#38218,#38219,#38220,
#38221,#38222,#38223,#38224,#38225,#38226,#38227,#38228,#38229,#38230,#38231,
#38232,#38233,#38234,#38235,#38236,#38237,#38238,#38239,#38240,#38241,#38242,
#38243,#38244,#38245,#38246,#38247,#38248,#38249,#38250,#38251,#38252,#38253,
#38254,#38255,#38256,#38257,#38258,#38259),.UNSPECIFIED.,.F.,.F.,(4,3,3,
3,3,3,3,3,3,3,3,3,3,3,3,3,3,3,3,3,3,3,3,3,3,3,3,3,3,3,3,3,3,3,3,3,3,3,3,
3,3,3,3,3,3,3,3,3,3,3,3,3,3,3,3,3,3,3,3,3,3,3,3,3,3,3,3,3,3,3,3,3,3,4),
(292.168116783831,292.230949911729,292.314688623575,292.398324134942,292.481876578341,
292.565366014192,292.648819964806,292.732256458652,292.815693568407,292.899149363325,
292.982693856055,293.066282938996,293.150006206554,293.230685922449,293.314424634295,
293.398060145663,293.481612589061,293.565102024912,293.648555975526,293.731992469372,
293.815429579128,293.898885374045,293.982429866775,294.066018949716,294.149742217274,
294.23042193317,294.314160645016,294.397796156383,294.481348599782,294.564838035633,
294.648291986247,294.731728480093,294.815165589849,294.898621384766,294.982165877496,
295.065754960437,295.149478227995,295.23015794389,295.313896655736,295.397532167103,
295.481084610502,295.564574046353,295.648027996967,295.731464490813,295.814901600568,
295.898357395486,295.981901888216,296.065490971157,296.149214238714,296.22989395461,
296.313632666456,296.397268177823,296.480820621222,296.564310057073,296.647764007687,
296.731200501533,296.814637611289,296.898093406206,296.981637898936,297.065226981877,
297.148950249435,297.22962996533,297.313370336896,297.397007121582,297.480560453526,
297.564050394389,297.647502886383,297.730937375339,297.814371933571,297.897824629494,
297.981358513522,298.06493676202,298.148631676786,298.200069497888),
 .UNSPECIFIED.);
#236=B_SPLINE_CURVE_WITH_KNOTS('',3,(#38260,#38261,#38262,#38263,#38264,
#38265,#38266,#38267,#38268,#38269),.UNSPECIFIED.,.F.,.F.,(4,3,3,4),(291.916292881714,
291.999096197699,292.083606490707,292.168116783716),.UNSPECIFIED.);
#237=B_SPLINE_CURVE_WITH_KNOTS('',3,(#38271,#38272,#38273,#38274,#38275,
#38276,#38277,#38278,#38279,#38280),.UNSPECIFIED.,.F.,.F.,(4,3,3,4),(291.917378633395,
292.001424477781,292.085458033319,292.168116783835),.UNSPECIFIED.);
#238=B_SPLINE_CURVE_WITH_KNOTS('',3,(#38281,#38282,#38283,#38284,#38285,
#38286,#38287,#38288,#38289,#38290,#38291,#38292,#38293,#38294,#38295,#38296,
#38297,#38298,#38299,#38300,#38301,#38302,#38303,#38304,#38305,#38306,#38307,
#38308,#38309,#38310,#38311,#38312,#38313,#38314,#38315,#38316,#38317,#38318,
#38319,#38320,#38321,#38322,#38323,#38324,#38325,#38326,#38327,#38328,#38329,
#38330,#38331,#38332,#38333,#38334,#38335,#38336,#38337,#38338,#38339,#38340,
#38341,#38342,#38343,#38344,#38345,#38346,#38347,#38348,#38349,#38350,#38351,
#38352,#38353,#38354,#38355,#38356,#38357,#38358,#38359,#38360,#38361,#38362,
#38363,#38364,#38365,#38366,#38367,#38368,#38369,#38370,#38371,#38372,#38373,
#38374,#38375,#38376,#38377,#38378,#38379,#38380,#38381,#38382,#38383,#38384,
#38385,#38386,#38387,#38388,#38389,#38390,#38391,#38392,#38393,#38394,#38395,
#38396,#38397,#38398,#38399,#38400,#38401,#38402,#38403,#38404,#38405,#38406,
#38407,#38408,#38409,#38410,#38411,#38412,#38413,#38414,#38415,#38416,#38417,
#38418,#38419,#38420,#38421,#38422,#38423,#38424,#38425,#38426,#38427,#38428,
#38429,#38430,#38431,#38432,#38433,#38434,#38435,#38436,#38437,#38438,#38439,
#38440,#38441,#38442,#38443,#38444,#38445,#38446,#38447,#38448,#38449,#38450,
#38451,#38452,#38453,#38454,#38455,#38456,#38457,#38458,#38459,#38460,#38461,
#38462,#38463,#38464,#38465,#38466,#38467,#38468,#38469,#38470,#38471,#38472,
#38473,#38474,#38475,#38476,#38477,#38478,#38479,#38480,#38481,#38482,#38483,
#38484,#38485,#38486,#38487,#38488,#38489,#38490,#38491,#38492,#38493,#38494,
#38495,#38496,#38497),.UNSPECIFIED.,.F.,.F.,(4,3,3,3,3,3,3,3,3,3,3,3,3,
3,3,3,3,3,3,3,3,3,3,3,3,3,3,3,3,3,3,3,3,3,3,3,3,3,3,3,3,3,3,3,3,3,3,3,3,
3,3,3,3,3,3,3,3,3,3,3,3,3,3,3,3,3,3,3,3,3,3,3,4),(292.168116784033,292.262190609695,
292.356632402376,292.451597059885,292.541240531445,292.624979243291,292.708614754658,
292.792167198057,292.875656633908,292.959110584522,293.042547078368,293.125984188123,
293.209439983041,293.292984475771,293.376573558712,293.460296826269,293.540976542165,
293.624715254011,293.708350765378,293.791903208777,293.875392644628,293.958846595242,
294.042283089088,294.125720198843,294.209175993761,294.292720486491,294.376309569432,
294.460032836989,294.540712552885,294.624451264731,294.708086776098,294.791639219497,
294.875128655348,294.958582605961,295.042019099808,295.125456209563,295.208912004481,
295.29245649721,295.376045580151,295.459768847709,295.540448563605,295.624187275451,
295.707822786818,295.791375230217,295.874864666068,295.958318616682,296.041755110528,
296.125192220283,296.208648015201,296.292192507931,296.375781590872,296.459504858429,
296.540184574325,296.623923286171,296.707558797538,296.791111240937,296.874600676788,
296.958054627402,297.041491121248,297.124928231003,297.208384025921,297.291928518651,
297.375517601592,297.459240869149,297.539920585045,297.622665935703,297.70531674218,
297.787892033416,297.870410771497,297.952903044171,298.035376688061,298.117882955238,
298.199464534781),.UNSPECIFIED.);
#239=B_SPLINE_CURVE_WITH_KNOTS('',3,(#38503,#38504,#38505,#38506,#38507,
#38508,#38509,#38510,#38511,#38512,#38513,#38514,#38515,#38516,#38517,#38518,
#38519,#38520,#38521,#38522,#38523,#38524,#38525,#38526,#38527,#38528,#38529,
#38530,#38531,#38532,#38533,#38534,#38535,#38536,#38537,#38538,#38539,#38540,
#38541,#38542,#38543,#38544,#38545,#38546,#38547,#38548,#38549,#38550,#38551,
#38552,#38553,#38554,#38555,#38556,#38557,#38558,#38559,#38560,#38561,#38562,
#38563,#38564,#38565,#38566,#38567,#38568,#38569,#38570,#38571,#38572,#38573,
#38574,#38575,#38576,#38577,#38578,#38579,#38580,#38581,#38582,#38583,#38584,
#38585,#38586,#38587,#38588,#38589,#38590,#38591,#38592,#38593,#38594,#38595,
#38596,#38597,#38598,#38599,#38600,#38601,#38602,#38603,#38604,#38605,#38606,
#38607,#38608,#38609,#38610,#38611,#38612,#38613,#38614,#38615,#38616,#38617,
#38618,#38619,#38620,#38621,#38622,#38623,#38624,#38625,#38626,#38627,#38628,
#38629,#38630,#38631,#38632,#38633,#38634,#38635,#38636,#38637,#38638,#38639,
#38640,#38641,#38642,#38643,#38644,#38645,#38646,#38647,#38648,#38649,#38650,
#38651,#38652,#38653,#38654,#38655,#38656,#38657,#38658,#38659,#38660,#38661,
#38662,#38663,#38664,#38665,#38666,#38667,#38668,#38669,#38670,#38671,#38672,
#38673,#38674,#38675,#38676,#38677,#38678,#38679,#38680,#38681,#38682,#38683,
#38684,#38685,#38686,#38687,#38688,#38689,#38690,#38691,#38692,#38693,#38694,
#38695,#38696,#38697,#38698,#38699,#38700,#38701,#38702,#38703,#38704,#38705,
#38706,#38707,#38708,#38709,#38710,#38711,#38712,#38713,#38714,#38715,#38716,
#38717,#38718,#38719,#38720,#38721,#38722),.UNSPECIFIED.,.F.,.F.,(4,3,3,
3,3,3,3,3,3,3,3,3,3,3,3,3,3,3,3,3,3,3,3,3,3,3,3,3,3,3,3,3,3,3,3,3,3,3,3,
3,3,3,3,3,3,3,3,3,3,3,3,3,3,3,3,3,3,3,3,3,3,3,3,3,3,3,3,3,3,3,3,3,3,4),
(298.451302091141,298.533733738966,298.616103034285,298.698438526061,298.780758933961,
298.863083218192,298.945430339711,299.027864932082,299.110349533729,299.192953273766,
299.22910198677,299.312840698616,299.396476209983,299.480028653382,299.563518089232,
299.646972039846,299.730408533692,299.813845643448,299.897301438365,299.980845931095,
300.064435014036,300.148158281593,300.22883799749,300.312576709336,300.396212220703,
300.479764664102,300.563254099953,300.646708050567,300.730144544413,300.813581654168,
300.897037449086,300.980581941816,301.064171024757,301.147894292314,301.22857400821,
301.312312720056,301.395948231423,301.479500674822,301.562990110673,301.646444061287,
301.729880555133,301.813317664889,301.896773459806,301.980317952536,302.063907035477,
302.147630303035,302.228310018931,302.312048730777,302.395684242145,302.479236685543,
302.562726121394,302.646180072008,302.729616565854,302.81305367561,302.896509470527,
302.980053963257,303.063643046198,303.147366313756,303.228046029651,303.311784741497,
303.395420252864,303.478972696263,303.562462132114,303.645916082727,303.729352576573,
303.812789686329,303.896245481247,303.979789973976,304.063379056917,304.147102324475,
304.227782040371,304.315571556541,304.40316930023,304.48414926919),
 .UNSPECIFIED.);
#240=B_SPLINE_CURVE_WITH_KNOTS('',3,(#38723,#38724,#38725,#38726,#38727,
#38728,#38729,#38730,#38731,#38732),.UNSPECIFIED.,.F.,.F.,(4,3,3,4),(298.200069497888,
298.22936597605,298.343682204307,298.451302091011),.UNSPECIFIED.);
#241=B_SPLINE_CURVE_WITH_KNOTS('',3,(#38734,#38735,#38736,#38737,#38738,
#38739,#38740,#38741,#38742,#38743),.UNSPECIFIED.,.F.,.F.,(4,3,3,4),(298.199464534781,
298.28204843746,298.36667526417,298.45130209088),.UNSPECIFIED.);
#242=B_SPLINE_CURVE_WITH_KNOTS('',3,(#38744,#38745,#38746,#38747,#38748,
#38749,#38750,#38751,#38752,#38753,#38754,#38755,#38756,#38757,#38758,#38759,
#38760,#38761,#38762,#38763,#38764,#38765,#38766,#38767,#38768,#38769,#38770,
#38771,#38772,#38773,#38774,#38775,#38776,#38777,#38778,#38779,#38780,#38781,
#38782,#38783,#38784,#38785,#38786,#38787,#38788,#38789,#38790,#38791,#38792,
#38793,#38794,#38795,#38796,#38797,#38798,#38799,#38800,#38801,#38802,#38803,
#38804,#38805,#38806,#38807,#38808,#38809,#38810,#38811,#38812,#38813,#38814,
#38815,#38816,#38817,#38818,#38819,#38820,#38821,#38822,#38823,#38824,#38825,
#38826,#38827,#38828,#38829,#38830,#38831,#38832,#38833,#38834,#38835,#38836,
#38837,#38838,#38839,#38840,#38841,#38842,#38843,#38844,#38845,#38846,#38847,
#38848,#38849,#38850,#38851,#38852,#38853,#38854,#38855,#38856,#38857,#38858,
#38859,#38860,#38861,#38862,#38863,#38864,#38865,#38866,#38867,#38868,#38869,
#38870,#38871,#38872,#38873,#38874,#38875,#38876,#38877,#38878,#38879,#38880,
#38881,#38882,#38883,#38884,#38885,#38886,#38887,#38888,#38889,#38890,#38891,
#38892,#38893,#38894,#38895,#38896,#38897,#38898,#38899,#38900,#38901,#38902,
#38903,#38904,#38905,#38906,#38907,#38908,#38909,#38910,#38911,#38912,#38913,
#38914,#38915,#38916,#38917,#38918,#38919,#38920,#38921,#38922,#38923,#38924,
#38925,#38926,#38927,#38928,#38929,#38930,#38931,#38932,#38933,#38934,#38935,
#38936,#38937,#38938,#38939,#38940,#38941,#38942,#38943,#38944,#38945,#38946,
#38947,#38948,#38949,#38950,#38951,#38952,#38953,#38954,#38955,#38956,#38957,
#38958,#38959,#38960,#38961,#38962,#38963),.UNSPECIFIED.,.F.,.F.,(4,3,3,
3,3,3,3,3,3,3,3,3,3,3,3,3,3,3,3,3,3,3,3,3,3,3,3,3,3,3,3,3,3,3,3,3,3,3,3,
3,3,3,3,3,3,3,3,3,3,3,3,3,3,3,3,3,3,3,3,3,3,3,3,3,3,3,3,3,3,3,3,3,3,4),
(298.451302091015,298.539656595765,298.623395307611,298.707030818978,298.790583262377,
298.874072698228,298.957526648842,299.040963142688,299.124400252444,299.207856047361,
299.291400540091,299.374989623032,299.45871289059,299.539392606485,299.623131318331,
299.706766829699,299.790319273097,299.873808708948,299.957262659562,300.040699153408,
300.124136263164,300.207592058082,300.291136550811,300.374725633752,300.45844890131,
300.539128617206,300.622867329052,300.706502840419,300.790055283818,300.873544719669,
300.956998670283,301.040435164129,301.123872273884,301.207328068802,301.290872561532,
301.374461644473,301.458184912031,301.538864627926,301.622603339772,301.706238851139,
301.789791294538,301.873280730389,301.956734681003,302.040171174849,302.123608284604,
302.207064079522,302.290608572252,302.374197655193,302.45792092275,302.538600638646,
302.622339350492,302.70597486186,302.789527305258,302.873016741109,302.956470691723,
303.039907185569,303.123344295325,303.206800090242,303.290344582972,303.373933665913,
303.45765693347,303.538336649366,303.622078505112,303.705716435735,303.789270576816,
303.876003420953,303.959453706735,304.042886213594,304.12631901319,304.209770173324,
304.293296686938,304.376867998284,304.460541428353,304.483133329908),
 .UNSPECIFIED.);
#243=B_SPLINE_CURVE_WITH_KNOTS('',3,(#38969,#38970,#38971,#38972,#38973,
#38974,#38975,#38976,#38977,#38978,#38979,#38980,#38981,#38982,#38983,#38984,
#38985,#38986,#38987,#38988,#38989,#38990,#38991,#38992,#38993,#38994,#38995,
#38996,#38997,#38998,#38999,#39000,#39001,#39002,#39003,#39004,#39005,#39006,
#39007,#39008,#39009,#39010,#39011,#39012,#39013,#39014,#39015,#39016,#39017,
#39018,#39019,#39020,#39021,#39022,#39023,#39024,#39025,#39026,#39027,#39028,
#39029,#39030,#39031,#39032,#39033,#39034,#39035,#39036,#39037,#39038,#39039,
#39040,#39041,#39042,#39043,#39044,#39045,#39046,#39047,#39048,#39049,#39050,
#39051,#39052,#39053,#39054,#39055,#39056,#39057,#39058,#39059,#39060,#39061,
#39062,#39063,#39064,#39065,#39066,#39067,#39068,#39069,#39070,#39071,#39072,
#39073,#39074,#39075,#39076,#39077,#39078,#39079,#39080,#39081,#39082,#39083,
#39084,#39085,#39086,#39087,#39088,#39089,#39090,#39091,#39092,#39093,#39094,
#39095,#39096,#39097,#39098,#39099,#39100,#39101,#39102,#39103,#39104,#39105,
#39106,#39107,#39108,#39109,#39110,#39111,#39112,#39113,#39114,#39115,#39116,
#39117,#39118,#39119,#39120,#39121,#39122,#39123,#39124,#39125,#39126,#39127,
#39128,#39129,#39130,#39131,#39132,#39133,#39134,#39135,#39136,#39137,#39138,
#39139,#39140,#39141,#39142,#39143,#39144,#39145,#39146,#39147,#39148,#39149,
#39150,#39151,#39152,#39153,#39154,#39155,#39156,#39157,#39158,#39159,#39160,
#39161,#39162,#39163,#39164,#39165,#39166,#39167,#39168,#39169,#39170,#39171,
#39172,#39173,#39174,#39175,#39176,#39177,#39178,#39179,#39180,#39181,#39182,
#39183,#39184,#39185,#39186,#39187,#39188),.UNSPECIFIED.,.F.,.F.,(4,3,3,
3,3,3,3,3,3,3,3,3,3,3,3,3,3,3,3,3,3,3,3,3,3,3,3,3,3,3,3,3,3,3,3,3,3,3,3,
3,3,3,3,3,3,3,3,3,3,3,3,3,3,3,3,3,3,3,3,3,3,3,3,3,3,3,3,3,3,3,3,3,3,4),
(304.734487398294,304.822143358111,304.90992380932,304.997920322264,305.086032057283,
305.174346980483,305.227518051091,305.311256762937,305.394892274304,305.478444717703,
305.561934153554,305.645388104167,305.728824598013,305.812261707769,305.895717502687,
305.979261995416,306.062851078357,306.146574345915,306.227254061811,306.310992773657,
306.394628285024,306.478180728423,306.561670164274,306.645124114888,306.728560608734,
306.811997718489,306.895453513407,306.978998006137,307.062587089078,307.146310356635,
307.226990072531,307.310728784377,307.394364295744,307.477916739143,307.561406174994,
307.644860125607,307.728296619454,307.811733729209,307.895189524127,307.978734016856,
308.062323099797,308.146046367355,308.226726083251,308.310464795097,308.394100306465,
308.477652749863,308.561142185714,308.644596136328,308.728032630174,308.81146973993,
308.894925534847,308.978470027577,309.062059110518,309.145782378076,309.226462093971,
309.310200805817,309.393836317185,309.477388760583,309.560878196434,309.644332147048,
309.727768640895,309.81120575065,309.894661545568,309.978206038298,310.061795121239,
310.145518388796,310.226198104692,310.308739724589,310.391184948521,310.473552960617,
310.555860021654,310.638131369339,310.720397187219,310.766118518563),
 .UNSPECIFIED.);
#244=B_SPLINE_CURVE_WITH_KNOTS('',3,(#39189,#39190,#39191,#39192,#39193,
#39194,#39195,#39196,#39197,#39198),.UNSPECIFIED.,.F.,.F.,(4,3,3,4),(304.48414926919,
304.571492717686,304.658685916941,304.73448739819),.UNSPECIFIED.);
#245=B_SPLINE_CURVE_WITH_KNOTS('',3,(#39200,#39201,#39202,#39203,#39204,
#39205,#39206,#39207,#39208,#39209),.UNSPECIFIED.,.F.,.F.,(4,3,3,4),(304.483133329908,
304.538072660086,304.659392772604,304.734487398194),.UNSPECIFIED.);
#246=B_SPLINE_CURVE_WITH_KNOTS('',3,(#39210,#39211,#39212,#39213,#39214,
#39215,#39216,#39217,#39218,#39219,#39220,#39221,#39222,#39223,#39224,#39225,
#39226,#39227,#39228,#39229,#39230,#39231,#39232,#39233,#39234,#39235,#39236,
#39237,#39238,#39239,#39240,#39241,#39242,#39243,#39244,#39245,#39246,#39247,
#39248,#39249,#39250,#39251,#39252,#39253,#39254,#39255,#39256,#39257,#39258,
#39259,#39260,#39261,#39262,#39263,#39264,#39265,#39266,#39267,#39268,#39269,
#39270,#39271,#39272,#39273,#39274,#39275,#39276,#39277,#39278,#39279,#39280,
#39281,#39282,#39283,#39284,#39285,#39286,#39287,#39288,#39289,#39290,#39291,
#39292,#39293,#39294,#39295,#39296,#39297,#39298,#39299,#39300,#39301,#39302,
#39303,#39304,#39305,#39306,#39307,#39308,#39309,#39310,#39311,#39312,#39313,
#39314,#39315,#39316,#39317,#39318,#39319,#39320,#39321,#39322,#39323,#39324,
#39325,#39326,#39327,#39328,#39329,#39330,#39331,#39332,#39333,#39334,#39335,
#39336,#39337,#39338,#39339,#39340,#39341,#39342,#39343,#39344,#39345,#39346,
#39347,#39348,#39349,#39350,#39351,#39352,#39353,#39354,#39355,#39356,#39357,
#39358,#39359,#39360,#39361,#39362,#39363,#39364,#39365,#39366,#39367,#39368,
#39369,#39370,#39371,#39372,#39373,#39374,#39375,#39376,#39377,#39378,#39379,
#39380,#39381,#39382,#39383,#39384,#39385,#39386,#39387,#39388,#39389,#39390,
#39391,#39392,#39393,#39394,#39395,#39396,#39397,#39398,#39399,#39400,#39401,
#39402,#39403,#39404,#39405,#39406,#39407,#39408,#39409,#39410,#39411,#39412,
#39413,#39414,#39415,#39416,#39417,#39418,#39419,#39420,#39421,#39422,#39423,
#39424,#39425,#39426,#39427,#39428,#39429),.UNSPECIFIED.,.F.,.F.,(4,3,3,
3,3,3,3,3,3,3,3,3,3,3,3,3,3,3,3,3,3,3,3,3,3,3,3,3,3,3,3,3,3,3,3,3,3,3,3,
3,3,3,3,3,3,3,3,3,3,3,3,3,3,3,3,3,3,3,3,3,3,3,3,3,3,3,3,3,3,3,3,3,3,4),
(304.734487398304,304.816859499383,304.89916160694,304.98141989639,305.063656315399,
305.145889882814,305.228139612957,305.310473034548,305.392850573995,305.475353902802,
305.537808670806,305.621547382652,305.705182894019,305.788735337418,305.872224773269,
305.955678723882,306.039115217729,306.122552327484,306.206008122402,306.289552615131,
306.373141698072,306.45686496563,306.537544681526,306.621283393372,306.70491890474,
306.788471348138,306.871960783989,306.955414734603,307.038851228449,307.122288338205,
307.205744133122,307.289288625852,307.372877708793,307.45660097635,307.537280692246,
307.621019404092,307.70465491546,307.788207358858,307.871696794709,307.955150745323,
308.038587239169,308.122024348925,308.205480143842,308.289024636572,308.372613719513,
308.456336987071,308.537016702967,308.620755414813,308.70439092618,308.787943369579,
308.871432805429,308.954886756043,309.03832324989,309.121760359645,309.205216154563,
309.288760647293,309.372349730234,309.456072997791,309.536752713687,309.620491425533,
309.7041269369,309.787679380299,309.87116881615,309.954622766763,310.03805926061,
310.121496370365,310.204952165282,310.288496658012,310.372085740952,310.45580900851,
310.536488724407,310.625321699943,310.713947049508,310.767364380203),
 .UNSPECIFIED.);
#247=B_SPLINE_CURVE_WITH_KNOTS('',3,(#39435,#39436,#39437,#39438,#39439,
#39440,#39441,#39442,#39443,#39444,#39445,#39446,#39447,#39448,#39449,#39450,
#39451,#39452,#39453,#39454,#39455,#39456,#39457,#39458,#39459,#39460,#39461,
#39462,#39463,#39464,#39465,#39466,#39467,#39468,#39469,#39470,#39471,#39472,
#39473,#39474,#39475,#39476,#39477,#39478,#39479,#39480,#39481,#39482,#39483,
#39484,#39485,#39486,#39487,#39488,#39489,#39490,#39491,#39492,#39493,#39494,
#39495,#39496,#39497,#39498,#39499,#39500,#39501,#39502,#39503,#39504,#39505,
#39506,#39507,#39508,#39509,#39510,#39511,#39512,#39513,#39514,#39515,#39516,
#39517,#39518,#39519,#39520,#39521,#39522,#39523,#39524,#39525,#39526,#39527,
#39528,#39529,#39530,#39531,#39532,#39533,#39534,#39535,#39536,#39537,#39538,
#39539,#39540,#39541,#39542,#39543,#39544,#39545,#39546,#39547,#39548,#39549,
#39550,#39551,#39552,#39553,#39554,#39555,#39556,#39557,#39558,#39559,#39560,
#39561,#39562,#39563,#39564,#39565,#39566,#39567,#39568,#39569,#39570,#39571,
#39572,#39573,#39574,#39575,#39576,#39577,#39578,#39579,#39580,#39581,#39582,
#39583,#39584,#39585,#39586,#39587,#39588,#39589,#39590,#39591,#39592,#39593,
#39594,#39595,#39596,#39597,#39598,#39599,#39600,#39601,#39602,#39603,#39604,
#39605,#39606,#39607,#39608,#39609,#39610,#39611,#39612,#39613,#39614,#39615,
#39616,#39617,#39618,#39619,#39620,#39621,#39622,#39623,#39624,#39625,#39626,
#39627,#39628,#39629,#39630,#39631,#39632,#39633,#39634,#39635,#39636,#39637,
#39638,#39639,#39640,#39641,#39642,#39643,#39644,#39645,#39646,#39647,#39648,
#39649,#39650,#39651),.UNSPECIFIED.,.F.,.F.,(4,3,3,3,3,3,3,3,3,3,3,3,3,
3,3,3,3,3,3,3,3,3,3,3,3,3,3,3,3,3,3,3,3,3,3,3,3,3,3,3,3,3,3,3,3,3,3,3,3,
3,3,3,3,3,3,3,3,3,3,3,3,3,3,3,3,3,3,3,3,3,3,3,4),(311.01767270537,311.135474503209,
311.225934115412,311.309672827258,311.393308338626,311.476860782024,311.560350217875,
311.643804168489,311.727240662335,311.810677772091,311.894133567009,311.977678059738,
312.061267142679,312.144990410237,312.225670126132,312.309408837978,312.393044349345,
312.476596792744,312.560086228595,312.643540179209,312.726976673055,312.81041378281,
312.893869577728,312.977414070458,313.061003153399,313.144726420956,313.225406136852,
313.309144848698,313.392780360065,313.476332803464,313.559822239315,313.643276189928,
313.726712683775,313.81014979353,313.893605588448,313.977150081177,314.060739164118,
314.144462431676,314.225142147572,314.308880859418,314.392516370785,314.476068814184,
314.559558250035,314.643012200649,314.726448694495,314.809885804251,314.893341599168,
314.976886091898,315.060475174839,315.144198442397,315.224878158292,315.308616870138,
315.392252381505,315.475804824904,315.559294260755,315.642748211369,315.726184705215,
315.80962181497,315.893077609888,315.976622102618,316.060211185559,316.143934453116,
316.224614169012,316.308363373317,316.392007066586,316.475550342438,316.5590366819,
316.642484204386,316.725910999349,316.809363362124,316.892826545189,316.97636417955,
317.049206352649),.UNSPECIFIED.);
#248=B_SPLINE_CURVE_WITH_KNOTS('',3,(#39652,#39653,#39654,#39655,#39656,
#39657,#39658,#39659,#39660,#39661),.UNSPECIFIED.,.F.,.F.,(4,3,3,4),(310.766118518563,
310.848416982258,310.933044843739,311.017672705221),.UNSPECIFIED.);
#249=B_SPLINE_CURVE_WITH_KNOTS('',3,(#39663,#39664,#39665,#39666,#39667,
#39668,#39669,#39670,#39671,#39672),.UNSPECIFIED.,.F.,.F.,(4,3,3,4),(310.767364380203,
310.855720839339,310.943880183788,311.017672705217),.UNSPECIFIED.);
#250=B_SPLINE_CURVE_WITH_KNOTS('',3,(#39673,#39674,#39675,#39676,#39677,
#39678,#39679,#39680,#39681,#39682,#39683,#39684,#39685,#39686,#39687,#39688,
#39689,#39690,#39691,#39692,#39693,#39694,#39695,#39696,#39697,#39698,#39699,
#39700,#39701,#39702,#39703,#39704,#39705,#39706,#39707,#39708,#39709,#39710,
#39711,#39712,#39713,#39714,#39715,#39716,#39717,#39718,#39719,#39720,#39721,
#39722,#39723,#39724,#39725,#39726,#39727,#39728,#39729,#39730,#39731,#39732,
#39733,#39734,#39735,#39736,#39737,#39738,#39739,#39740,#39741,#39742,#39743,
#39744,#39745,#39746,#39747,#39748,#39749,#39750,#39751,#39752,#39753,#39754,
#39755,#39756,#39757,#39758,#39759,#39760,#39761,#39762,#39763,#39764,#39765,
#39766,#39767,#39768,#39769,#39770,#39771,#39772,#39773,#39774,#39775,#39776,
#39777,#39778,#39779,#39780,#39781,#39782,#39783,#39784,#39785,#39786,#39787,
#39788,#39789,#39790,#39791,#39792,#39793,#39794,#39795,#39796,#39797,#39798,
#39799,#39800,#39801,#39802,#39803,#39804,#39805,#39806,#39807,#39808,#39809,
#39810,#39811,#39812,#39813,#39814,#39815,#39816,#39817,#39818,#39819,#39820,
#39821,#39822,#39823,#39824,#39825,#39826,#39827,#39828,#39829,#39830,#39831,
#39832,#39833,#39834,#39835,#39836,#39837,#39838,#39839,#39840,#39841,#39842,
#39843,#39844,#39845,#39846,#39847,#39848,#39849,#39850,#39851,#39852,#39853,
#39854,#39855,#39856,#39857,#39858,#39859,#39860,#39861,#39862,#39863,#39864,
#39865,#39866,#39867,#39868,#39869,#39870,#39871,#39872,#39873,#39874,#39875,
#39876,#39877,#39878,#39879,#39880,#39881,#39882,#39883,#39884,#39885,#39886,
#39887,#39888,#39889,#39890,#39891,#39892),.UNSPECIFIED.,.F.,.F.,(4,3,3,
3,3,3,3,3,3,3,3,3,3,3,3,3,3,3,3,3,3,3,3,3,3,3,3,3,3,3,3,3,3,3,3,3,3,3,3,
3,3,3,3,3,3,3,3,3,3,3,3,3,3,3,3,3,3,3,3,3,3,3,3,3,3,3,3,3,3,3,3,3,3,4),
(311.017672705374,311.104429954621,311.191279156298,311.278312113916,311.365438893343,
311.452762719316,311.536224735127,311.619963446973,311.70359895834,311.787151401739,
311.87064083759,311.954094788204,312.03753128205,312.120968391805,312.204424186723,
312.287968679453,312.371557762394,312.455281029951,312.535960745847,312.619699457693,
312.70333496906,312.786887412459,312.870376848309,312.953830798923,313.037267292769,
313.120704402525,313.204160197442,313.287704690172,313.371293773113,313.45501704067,
313.535696756567,313.619435468413,313.703070979781,313.786623423179,313.87011285903,
313.953566809644,314.03700330349,314.120440413246,314.203896208163,314.287440700893,
314.371029783834,314.454753051392,314.535432767287,314.619171479133,314.702806990501,
314.786359433899,314.869848869751,314.953302820365,315.036739314211,315.120176423966,
315.203632218884,315.287176711614,315.370765794554,315.454489062112,315.535168778008,
315.618907489854,315.702543001222,315.78609544462,315.869584880471,315.953038831085,
316.036475324931,316.119912434686,316.203368229605,316.286912722334,316.370501805276,
316.454225072833,316.534904788728,316.617565724114,316.700129228481,316.782614412715,
316.865035306066,316.947419658952,317.029791475497,317.049417187792),
 .UNSPECIFIED.);
#251=B_SPLINE_CURVE_WITH_KNOTS('',3,(#39898,#39899,#39900,#39901,#39902,
#39903,#39904,#39905,#39906,#39907,#39908,#39909,#39910,#39911,#39912,#39913,
#39914,#39915,#39916,#39917,#39918,#39919,#39920,#39921,#39922,#39923,#39924,
#39925,#39926,#39927,#39928,#39929,#39930,#39931,#39932,#39933,#39934,#39935,
#39936,#39937,#39938,#39939,#39940,#39941,#39942,#39943,#39944,#39945,#39946,
#39947,#39948,#39949,#39950,#39951,#39952,#39953,#39954,#39955,#39956,#39957,
#39958,#39959,#39960,#39961,#39962,#39963,#39964,#39965,#39966,#39967,#39968,
#39969,#39970,#39971,#39972,#39973,#39974,#39975,#39976,#39977,#39978,#39979,
#39980,#39981,#39982,#39983,#39984,#39985,#39986,#39987,#39988,#39989,#39990,
#39991,#39992,#39993,#39994,#39995,#39996,#39997,#39998,#39999,#40000,#40001,
#40002,#40003,#40004,#40005,#40006,#40007,#40008,#40009,#40010,#40011,#40012,
#40013,#40014,#40015,#40016,#40017,#40018,#40019,#40020,#40021,#40022,#40023,
#40024,#40025,#40026,#40027,#40028,#40029,#40030,#40031,#40032,#40033,#40034,
#40035,#40036,#40037,#40038,#40039,#40040,#40041,#40042,#40043,#40044,#40045,
#40046,#40047,#40048,#40049,#40050,#40051,#40052,#40053,#40054,#40055,#40056,
#40057,#40058,#40059,#40060,#40061,#40062,#40063,#40064,#40065,#40066,#40067,
#40068,#40069,#40070,#40071,#40072,#40073,#40074,#40075,#40076,#40077,#40078,
#40079,#40080,#40081,#40082,#40083,#40084,#40085,#40086,#40087,#40088,#40089,
#40090,#40091,#40092,#40093,#40094,#40095,#40096,#40097,#40098,#40099,#40100,
#40101,#40102,#40103,#40104,#40105,#40106,#40107,#40108,#40109,#40110,#40111,
#40112,#40113,#40114,#40115,#40116,#40117,#40118,#40119,#40120),
 .UNSPECIFIED.,.F.,.F.,(4,3,3,3,3,3,3,3,3,3,3,3,3,3,3,3,3,3,3,3,3,3,3,3,
3,3,3,3,3,3,3,3,3,3,3,3,3,3,3,3,3,3,3,3,3,3,3,3,3,3,3,3,3,3,3,3,3,3,3,3,
3,3,3,3,3,3,3,3,3,3,3,3,3,3,4),(317.300858012677,317.383680932198,317.466407303603,
317.549058061659,317.633436577758,317.716008012657,317.798571313966,317.881145280446,
317.966880507947,318.049576946045,318.132329695274,318.215195165216,318.224086190453,
318.307824902299,318.391460413666,318.475012857065,318.558502292916,318.64195624353,
318.725392737376,318.808829847132,318.892285642049,318.975830134779,319.05941921772,
319.143142485278,319.223822201173,319.307560913019,319.391196424386,319.474748867785,
319.558238303635,319.641692254249,319.725128748095,319.808565857851,319.892021652768,
319.975566145498,320.059155228439,320.142878495996,320.223558211893,320.307296923739,
320.390932435106,320.474484878505,320.557974314356,320.64142826497,320.724864758816,
320.808301868572,320.891757663489,320.975302156219,321.05889123916,321.142614506718,
321.223294222613,321.307032934459,321.390668445827,321.474220889225,321.557710325076,
321.64116427569,321.724600769536,321.808037879292,321.89149367421,321.975038166939,
322.05862724988,322.142350517438,322.223030233333,322.306768945179,322.390404456546,
322.473956899945,322.557446335796,322.64090028641,322.724336780256,322.807773890012,
322.891229684929,322.974774177659,323.0583632606,323.142086528158,323.222766244053,
323.318816741582,323.333553374426),.UNSPECIFIED.);
#252=B_SPLINE_CURVE_WITH_KNOTS('',3,(#40121,#40122,#40123,#40124,#40125,
#40126,#40127,#40128,#40129,#40130),.UNSPECIFIED.,.F.,.F.,(4,3,3,4),(317.049206352649,
317.13677826619,317.224350179732,317.300858012549),.UNSPECIFIED.);
#253=B_SPLINE_CURVE_WITH_KNOTS('',3,(#40132,#40133,#40134,#40135,#40136,
#40137,#40138,#40139,#40140,#40141),.UNSPECIFIED.,.F.,.F.,(4,3,3,4),(317.049417187792,
317.131815498541,317.216336755547,317.300858012553),.UNSPECIFIED.);
#254=B_SPLINE_CURVE_WITH_KNOTS('',3,(#40142,#40143,#40144,#40145,#40146,
#40147,#40148,#40149,#40150,#40151,#40152,#40153,#40154,#40155,#40156,#40157,
#40158,#40159,#40160,#40161,#40162,#40163,#40164,#40165,#40166,#40167,#40168,
#40169,#40170,#40171,#40172,#40173,#40174,#40175,#40176,#40177,#40178,#40179,
#40180,#40181,#40182,#40183,#40184,#40185,#40186,#40187,#40188,#40189,#40190,
#40191,#40192,#40193,#40194,#40195,#40196,#40197,#40198,#40199,#40200,#40201,
#40202,#40203,#40204,#40205,#40206,#40207,#40208,#40209,#40210,#40211,#40212,
#40213,#40214,#40215,#40216,#40217,#40218,#40219,#40220,#40221,#40222,#40223,
#40224,#40225,#40226,#40227,#40228,#40229,#40230,#40231,#40232,#40233,#40234,
#40235,#40236,#40237,#40238,#40239,#40240,#40241,#40242,#40243,#40244,#40245,
#40246,#40247,#40248,#40249,#40250,#40251,#40252,#40253,#40254,#40255,#40256,
#40257,#40258,#40259,#40260,#40261,#40262,#40263,#40264,#40265,#40266,#40267,
#40268,#40269,#40270,#40271,#40272,#40273,#40274,#40275,#40276,#40277,#40278,
#40279,#40280,#40281,#40282,#40283,#40284,#40285,#40286,#40287,#40288,#40289,
#40290,#40291,#40292,#40293,#40294,#40295,#40296,#40297,#40298,#40299,#40300,
#40301,#40302,#40303,#40304,#40305,#40306,#40307,#40308,#40309,#40310,#40311,
#40312,#40313,#40314,#40315,#40316,#40317,#40318,#40319,#40320,#40321,#40322,
#40323,#40324,#40325,#40326,#40327,#40328,#40329,#40330,#40331,#40332,#40333,
#40334,#40335,#40336,#40337,#40338,#40339,#40340,#40341,#40342,#40343,#40344,
#40345,#40346,#40347,#40348,#40349,#40350,#40351,#40352,#40353,#40354,#40355,
#40356,#40357,#40358,#40359,#40360,#40361),.UNSPECIFIED.,.F.,.F.,(4,3,3,
3,3,3,3,3,3,3,3,3,3,3,3,3,3,3,3,3,3,3,3,3,3,3,3,3,3,3,3,3,3,3,3,3,3,3,3,
3,3,3,3,3,3,3,3,3,3,3,3,3,3,3,3,3,3,3,3,3,3,3,3,3,3,3,3,3,3,3,3,3,3,4),
(317.300858012747,317.410911531517,317.524033175183,317.534640799448,317.618379511294,
317.702015022661,317.78556746606,317.869056901911,317.952510852525,318.035947346371,
318.119384456126,318.202840251044,318.286384743774,318.369973826715,318.453697094272,
318.534376810168,318.618115522014,318.701751033381,318.78530347678,318.868792912631,
318.952246863245,319.035683357091,319.119120466846,319.202576261764,319.286120754493,
319.369709837434,319.453433104992,319.534112820888,319.617851532734,319.701487044101,
319.7850394875,319.868528923351,319.951982873965,320.035419367811,320.118856477566,
320.202312272484,320.285856765214,320.369445848155,320.453169115712,320.533848831608,
320.617587543454,320.701223054821,320.78477549822,320.868264934071,320.951718884684,
321.035155378531,321.118592488286,321.202048283204,321.285592775933,321.369181858874,
321.452905126432,321.533584842328,321.617323554174,321.700959065542,321.78451150894,
321.868000944791,321.951454895405,322.034891389251,322.118328499007,322.201784293925,
322.285328786654,322.368917869595,322.452641137153,322.533320853048,322.617071701435,
322.700716701817,322.784260452642,322.867746789349,322.951193832203,323.034619671076,
323.118066332219,323.201523621922,323.285043847328,323.332378172878),
 .UNSPECIFIED.);
#255=B_SPLINE_CURVE_WITH_KNOTS('',3,(#40367,#40368,#40369,#40370,#40371,
#40372,#40373,#40374,#40375,#40376,#40377,#40378,#40379,#40380,#40381,#40382,
#40383,#40384,#40385,#40386,#40387,#40388,#40389,#40390,#40391,#40392,#40393,
#40394,#40395,#40396,#40397,#40398,#40399,#40400,#40401,#40402,#40403,#40404,
#40405,#40406,#40407,#40408,#40409,#40410,#40411,#40412,#40413,#40414,#40415,
#40416,#40417,#40418,#40419,#40420,#40421,#40422,#40423,#40424,#40425,#40426,
#40427,#40428,#40429,#40430,#40431,#40432,#40433,#40434,#40435,#40436,#40437,
#40438,#40439,#40440,#40441,#40442,#40443,#40444,#40445,#40446,#40447,#40448,
#40449,#40450,#40451,#40452,#40453,#40454,#40455,#40456,#40457,#40458,#40459,
#40460,#40461,#40462,#40463,#40464,#40465,#40466,#40467,#40468,#40469,#40470,
#40471,#40472,#40473,#40474,#40475,#40476,#40477,#40478,#40479,#40480,#40481,
#40482,#40483,#40484,#40485,#40486,#40487,#40488,#40489,#40490,#40491,#40492,
#40493,#40494,#40495,#40496,#40497,#40498,#40499,#40500,#40501,#40502,#40503,
#40504,#40505,#40506,#40507,#40508,#40509,#40510,#40511,#40512,#40513,#40514,
#40515,#40516,#40517,#40518,#40519,#40520,#40521,#40522,#40523,#40524,#40525,
#40526,#40527,#40528,#40529,#40530,#40531,#40532,#40533,#40534,#40535,#40536,
#40537,#40538,#40539,#40540,#40541,#40542,#40543,#40544,#40545,#40546,#40547,
#40548,#40549,#40550,#40551,#40552,#40553,#40554,#40555,#40556,#40557,#40558,
#40559,#40560,#40561,#40562,#40563,#40564,#40565,#40566,#40567,#40568,#40569,
#40570,#40571,#40572,#40573,#40574,#40575,#40576,#40577,#40578,#40579,#40580,
#40581,#40582,#40583,#40584,#40585,#40586),.UNSPECIFIED.,.F.,.F.,(4,3,3,
3,3,3,3,3,3,3,3,3,3,3,3,3,3,3,3,3,3,3,3,3,3,3,3,3,3,3,3,3,3,3,3,3,3,3,3,
3,3,3,3,3,3,3,3,3,3,3,3,3,3,3,3,3,3,3,3,3,3,3,3,3,3,3,3,3,3,3,3,3,3,4),
(323.584043319729,323.66786391523,323.751684534608,323.835522700307,323.919395942302,
324.003374465569,324.087410996865,324.171583499636,324.222502254773,324.306240966619,
324.389876477986,324.473428921385,324.556918357236,324.64037230785,324.723808801696,
324.807245911452,324.890701706369,324.974246199099,325.05783528204,325.141558549598,
325.222238265494,325.30597697734,325.389612488707,325.473164932106,325.556654367957,
325.640108318571,325.723544812417,325.806981922173,325.89043771709,325.97398220982,
326.057571292761,326.141294560319,326.221974276214,326.30571298806,326.389348499427,
326.472900942826,326.556390378677,326.63984432929,326.723280823137,326.806717932892,
326.89017372781,326.97371822054,327.057307303481,327.141030571038,327.221710286934,
327.30544899878,327.389084510147,327.472636953546,327.556126389397,327.63958034001,
327.723016833856,327.806453943612,327.889909738529,327.973454231259,328.0570433142,
328.140766581757,328.221446297654,328.3051850095,328.388820520867,328.472372964266,
328.555862400117,328.63931635073,328.722752844577,328.806189954332,328.88964574925,
328.97319024198,329.056779324921,329.140502592479,329.221182308374,329.305236123548,
329.389151545692,329.472987341021,329.55674865914,329.616396844457),
 .UNSPECIFIED.);
#256=B_SPLINE_CURVE_WITH_KNOTS('',3,(#40587,#40588,#40589,#40590,#40591,
#40592,#40593,#40594,#40595,#40596),.UNSPECIFIED.,.F.,.F.,(4,3,3,4),(323.333553374426,
323.429055721388,323.523916465494,323.58404331953),.UNSPECIFIED.);
#257=B_SPLINE_CURVE_WITH_KNOTS('',3,(#40598,#40599,#40600,#40601,#40602,
#40603,#40604,#40605,#40606,#40607,#40608,#40609,#40610),.UNSPECIFIED.,
 .F.,.F.,(4,3,3,3,4),(323.332378172878,323.415999707598,323.499742052346,
323.533056863769,323.584043319733),.UNSPECIFIED.);
#258=B_SPLINE_CURVE_WITH_KNOTS('',3,(#40611,#40612,#40613,#40614,#40615,
#40616,#40617,#40618,#40619,#40620,#40621,#40622,#40623,#40624,#40625,#40626,
#40627,#40628,#40629,#40630,#40631,#40632,#40633,#40634,#40635,#40636,#40637,
#40638,#40639,#40640,#40641,#40642,#40643,#40644,#40645,#40646,#40647,#40648,
#40649,#40650,#40651,#40652,#40653,#40654,#40655,#40656,#40657,#40658,#40659,
#40660,#40661,#40662,#40663,#40664,#40665,#40666,#40667,#40668,#40669,#40670,
#40671,#40672,#40673,#40674,#40675,#40676,#40677,#40678,#40679,#40680,#40681,
#40682,#40683,#40684,#40685,#40686,#40687,#40688,#40689,#40690,#40691,#40692,
#40693,#40694,#40695,#40696,#40697,#40698,#40699,#40700,#40701,#40702,#40703,
#40704,#40705,#40706,#40707,#40708,#40709,#40710,#40711,#40712,#40713,#40714,
#40715,#40716,#40717,#40718,#40719,#40720,#40721,#40722,#40723,#40724,#40725,
#40726,#40727,#40728,#40729,#40730,#40731,#40732,#40733,#40734,#40735,#40736,
#40737,#40738,#40739,#40740,#40741,#40742,#40743,#40744,#40745,#40746,#40747,
#40748,#40749,#40750,#40751,#40752,#40753,#40754,#40755,#40756,#40757,#40758,
#40759,#40760,#40761,#40762,#40763,#40764,#40765,#40766,#40767,#40768,#40769,
#40770,#40771,#40772,#40773,#40774,#40775,#40776,#40777,#40778,#40779,#40780,
#40781,#40782,#40783,#40784,#40785,#40786,#40787,#40788,#40789,#40790,#40791,
#40792,#40793,#40794,#40795,#40796,#40797,#40798,#40799,#40800,#40801,#40802,
#40803,#40804,#40805,#40806,#40807,#40808,#40809,#40810,#40811,#40812,#40813,
#40814,#40815,#40816,#40817,#40818,#40819,#40820,#40821,#40822,#40823,#40824,
#40825,#40826,#40827,#40828,#40829,#40830),.UNSPECIFIED.,.F.,.F.,(4,3,3,
3,3,3,3,3,3,3,3,3,3,3,3,3,3,3,3,3,3,3,3,3,3,3,3,3,3,3,3,3,3,3,3,3,3,3,3,
3,3,3,3,3,3,3,3,3,3,3,3,3,3,3,3,3,3,3,3,3,3,3,3,3,3,3,3,3,3,3,3,3,3,4),
(323.584043319934,323.667116505993,323.75008976071,323.83298383851,323.91581941661,
323.99862590948,324.081420154102,324.164220781389,324.247046423578,324.32996194568,
324.412928810753,324.496016216833,324.532792874489,324.616531586335,324.700167097702,
324.783719541101,324.867208976952,324.950662927566,325.034099421412,325.117536531168,
325.200992326085,325.284536818815,325.368125901756,325.451849169314,325.532528885209,
325.616267597055,325.699903108422,325.783455551821,325.866944987672,325.950398938286,
326.033835432132,326.117272541887,326.200728336805,326.284272829535,326.367861912476,
326.451585180034,326.532264895929,326.616003607775,326.699639119142,326.783191562541,
326.866680998392,326.950134949006,327.033571442852,327.117008552607,327.200464347524,
327.284008840254,327.367597923195,327.451321190753,327.532000906649,327.615739618495,
327.699375129863,327.782927573261,327.866417009112,327.949870959726,328.033307453572,
328.116744563328,328.200200358245,328.283744850975,328.367333933916,328.451057201474,
328.531736917369,328.615475629215,328.699111140582,328.782663583981,328.866153019832,
328.949606970446,329.033043464292,329.116480574048,329.199936368965,329.283480861695,
329.367069944636,329.450793212194,329.531472928089,329.61663357438),
 .UNSPECIFIED.);
#259=B_SPLINE_CURVE_WITH_KNOTS('',3,(#40836,#40837,#40838,#40839,#40840,
#40841,#40842,#40843,#40844,#40845,#40846,#40847,#40848,#40849,#40850,#40851,
#40852,#40853,#40854,#40855,#40856,#40857,#40858,#40859,#40860,#40861,#40862,
#40863,#40864,#40865,#40866,#40867,#40868,#40869,#40870,#40871,#40872,#40873,
#40874,#40875,#40876,#40877,#40878,#40879,#40880,#40881,#40882,#40883,#40884,
#40885,#40886,#40887,#40888,#40889,#40890,#40891,#40892,#40893,#40894,#40895,
#40896,#40897,#40898,#40899,#40900,#40901,#40902,#40903,#40904,#40905,#40906,
#40907,#40908,#40909,#40910,#40911,#40912,#40913,#40914,#40915,#40916,#40917,
#40918,#40919,#40920,#40921,#40922,#40923,#40924,#40925,#40926,#40927,#40928,
#40929,#40930,#40931,#40932,#40933,#40934,#40935,#40936,#40937,#40938,#40939,
#40940,#40941,#40942,#40943,#40944,#40945,#40946,#40947,#40948,#40949,#40950,
#40951,#40952,#40953,#40954,#40955,#40956,#40957,#40958,#40959,#40960,#40961,
#40962,#40963,#40964,#40965,#40966,#40967,#40968,#40969,#40970,#40971,#40972,
#40973,#40974,#40975,#40976,#40977,#40978,#40979,#40980,#40981,#40982,#40983,
#40984,#40985,#40986,#40987,#40988,#40989,#40990,#40991,#40992,#40993,#40994,
#40995,#40996,#40997,#40998,#40999,#41000,#41001,#41002,#41003,#41004,#41005,
#41006,#41007,#41008,#41009,#41010,#41011,#41012,#41013,#41014,#41015,#41016,
#41017,#41018,#41019,#41020,#41021,#41022,#41023,#41024,#41025,#41026,#41027,
#41028,#41029,#41030,#41031,#41032,#41033,#41034,#41035,#41036,#41037,#41038,
#41039,#41040,#41041,#41042,#41043,#41044,#41045,#41046,#41047,#41048,#41049,
#41050,#41051,#41052,#41053,#41054,#41055),.UNSPECIFIED.,.F.,.F.,(4,3,3,
3,3,3,3,3,3,3,3,3,3,3,3,3,3,3,3,3,3,3,3,3,3,3,3,3,3,3,3,3,3,3,3,3,3,3,3,
3,3,3,3,3,3,3,3,3,3,3,3,3,3,3,3,3,3,3,3,3,3,3,3,3,3,3,3,3,3,3,3,3,3,4),
(329.867228627105,329.962755668786,330.058739773327,330.155315172663,330.220918319094,
330.30465703094,330.388292542307,330.471844985706,330.555334421557,330.63878837217,
330.722224866016,330.805661975772,330.889117770689,330.972662263419,331.05625134636,
331.139974613917,331.220654329814,331.30439304166,331.388028553027,331.471580996426,
331.555070432277,331.638524382891,331.721960876737,331.805397986493,331.88885378141,
331.97239827414,332.055987357081,332.139710624639,332.220390340534,332.30412905238,
332.387764563748,332.471317007146,332.554806442997,332.638260393611,332.721696887457,
332.805133997213,332.88858979213,332.97213428486,333.055723367801,333.139446635359,
333.220126351255,333.303865063101,333.387500574469,333.471053017867,333.554542453718,
333.637996404332,333.721432898178,333.804870007934,333.888325802852,333.971870295581,
334.055459378522,334.13918264608,334.219862361975,334.303601073821,334.387236585188,
334.470789028587,334.554278464438,334.637732415052,334.721168908898,334.804606018653,
334.888061813571,334.971606306301,335.055195389242,335.138918656799,335.219598372695,
335.30447156949,335.387272010219,335.469997276829,335.552666223432,335.639145654337,
335.721770900446,335.804394995688,335.88705363544,335.898583947052),
 .UNSPECIFIED.);
#260=B_SPLINE_CURVE_WITH_KNOTS('',3,(#41056,#41057,#41058,#41059,#41060,
#41061,#41062,#41063,#41064,#41065),.UNSPECIFIED.,.F.,.F.,(4,3,3,4),(329.616396844457,
329.700090524835,329.783786786313,329.867228626909),.UNSPECIFIED.);
#261=B_SPLINE_CURVE_WITH_KNOTS('',3,(#41067,#41068,#41069,#41070,#41071,
#41072,#41073,#41074,#41075,#41076),.UNSPECIFIED.,.F.,.F.,(4,3,3,4),(329.61663357438,
329.714431689665,329.811393456063,329.867228626724),.UNSPECIFIED.);
#262=B_SPLINE_CURVE_WITH_KNOTS('',3,(#41077,#41078,#41079,#41080,#41081,
#41082,#41083,#41084,#41085,#41086,#41087,#41088,#41089,#41090,#41091,#41092,
#41093,#41094,#41095,#41096,#41097,#41098,#41099,#41100,#41101,#41102,#41103,
#41104,#41105,#41106,#41107,#41108,#41109,#41110,#41111,#41112,#41113,#41114,
#41115,#41116,#41117,#41118,#41119,#41120,#41121,#41122,#41123,#41124,#41125,
#41126,#41127,#41128,#41129,#41130,#41131,#41132,#41133,#41134,#41135,#41136,
#41137,#41138,#41139,#41140,#41141,#41142,#41143,#41144,#41145,#41146,#41147,
#41148,#41149,#41150,#41151,#41152,#41153,#41154,#41155,#41156,#41157,#41158,
#41159,#41160,#41161,#41162,#41163,#41164,#41165,#41166,#41167,#41168,#41169,
#41170,#41171,#41172,#41173,#41174,#41175,#41176,#41177,#41178,#41179,#41180,
#41181,#41182,#41183,#41184,#41185,#41186,#41187,#41188,#41189,#41190,#41191,
#41192,#41193,#41194,#41195,#41196,#41197,#41198,#41199,#41200,#41201,#41202,
#41203,#41204,#41205,#41206,#41207,#41208,#41209,#41210,#41211,#41212,#41213,
#41214,#41215,#41216,#41217,#41218,#41219,#41220,#41221,#41222,#41223,#41224,
#41225,#41226,#41227,#41228,#41229,#41230,#41231,#41232,#41233,#41234,#41235,
#41236,#41237,#41238,#41239,#41240,#41241,#41242,#41243,#41244,#41245,#41246,
#41247,#41248,#41249,#41250,#41251,#41252,#41253,#41254,#41255,#41256,#41257,
#41258,#41259,#41260,#41261,#41262,#41263,#41264,#41265,#41266,#41267,#41268,
#41269,#41270,#41271,#41272,#41273,#41274,#41275,#41276,#41277,#41278,#41279,
#41280,#41281,#41282,#41283,#41284,#41285,#41286,#41287,#41288,#41289,#41290,
#41291,#41292,#41293,#41294,#41295,#41296),.UNSPECIFIED.,.F.,.F.,(4,3,3,
3,3,3,3,3,3,3,3,3,3,3,3,3,3,3,3,3,3,3,3,3,3,3,3,3,3,3,3,3,3,3,3,3,3,3,3,
3,3,3,3,3,3,3,3,3,3,3,3,3,3,3,3,3,3,3,3,3,3,3,3,3,3,3,3,3,3,3,3,3,3,4),
(329.867228626912,329.950650073194,330.034059218144,330.117474083261,330.200912690001,
330.284447492303,330.368031162443,330.451755204459,330.53120893881,330.614947650656,
330.698583162023,330.782135605422,330.865625041273,330.949078991886,331.032515485733,
331.115952595488,331.199408390406,331.282952883136,331.366541966077,331.450265233634,
331.53094494953,331.614683661376,331.698319172744,331.781871616142,331.865361051993,
331.948815002607,332.032251496453,332.115688606209,332.199144401126,332.282688893856,
332.366277976797,332.450001244354,332.53068096025,332.614419672096,332.698055183463,
332.781607626861,332.865097062713,332.948551013326,333.031987507172,333.115424616928,
333.198880411846,333.282424904576,333.366013987517,333.449737255074,333.53041697097,
333.614155682816,333.697791194183,333.781343637582,333.864833073433,333.948287024047,
334.031723517893,334.115160627648,334.198616422565,334.282160915295,334.365749998236,
334.449473265794,334.53015298169,334.613891693536,334.697527204904,334.781079648302,
334.864569084154,334.948023034767,335.031459528614,335.114896638369,335.198352433287,
335.281896926017,335.365486008958,335.449209276515,335.52988899241,335.61443704822,
335.698840656777,335.783160681546,335.867398052658,335.899704001206),
 .UNSPECIFIED.);
#263=B_SPLINE_CURVE_WITH_KNOTS('',3,(#41302,#41303,#41304,#41305,#41306,
#41307,#41308,#41309,#41310,#41311,#41312,#41313,#41314,#41315,#41316,#41317,
#41318,#41319,#41320,#41321,#41322,#41323,#41324,#41325,#41326,#41327,#41328,
#41329,#41330,#41331,#41332,#41333,#41334,#41335,#41336,#41337,#41338,#41339,
#41340,#41341,#41342,#41343,#41344,#41345,#41346,#41347,#41348,#41349,#41350,
#41351,#41352,#41353,#41354,#41355,#41356,#41357,#41358,#41359,#41360,#41361,
#41362,#41363,#41364,#41365,#41366,#41367,#41368,#41369,#41370,#41371,#41372,
#41373,#41374,#41375,#41376,#41377,#41378,#41379,#41380,#41381,#41382,#41383,
#41384,#41385,#41386,#41387,#41388,#41389,#41390,#41391,#41392,#41393,#41394,
#41395,#41396,#41397,#41398,#41399,#41400,#41401,#41402,#41403,#41404,#41405,
#41406,#41407,#41408,#41409,#41410,#41411,#41412,#41413,#41414,#41415,#41416,
#41417,#41418,#41419,#41420,#41421,#41422,#41423,#41424,#41425,#41426,#41427,
#41428,#41429,#41430,#41431,#41432,#41433,#41434,#41435,#41436,#41437,#41438,
#41439,#41440,#41441,#41442,#41443,#41444,#41445,#41446,#41447,#41448,#41449,
#41450,#41451,#41452,#41453,#41454,#41455,#41456,#41457,#41458,#41459,#41460,
#41461,#41462,#41463,#41464,#41465,#41466,#41467,#41468,#41469,#41470,#41471,
#41472,#41473,#41474,#41475,#41476,#41477,#41478,#41479,#41480,#41481,#41482,
#41483,#41484,#41485,#41486,#41487,#41488,#41489,#41490,#41491,#41492,#41493,
#41494,#41495,#41496,#41497,#41498,#41499,#41500,#41501,#41502,#41503,#41504,
#41505,#41506,#41507,#41508,#41509,#41510,#41511,#41512,#41513,#41514,#41515,
#41516,#41517,#41518,#41519,#41520,#41521),.UNSPECIFIED.,.F.,.F.,(4,3,3,
3,3,3,3,3,3,3,3,3,3,3,3,3,3,3,3,3,3,3,3,3,3,3,3,3,3,3,3,3,3,3,3,3,3,3,3,
3,3,3,3,3,3,3,3,3,3,3,3,3,3,3,3,3,3,3,3,3,3,3,3,3,3,3,3,3,3,3,3,3,3,4),
(336.150413934088,336.219334383415,336.303073095261,336.386708606628,336.470261050027,
336.553750485878,336.637204436491,336.720640930337,336.804078040093,336.88753383501,
336.97107832774,337.054667410681,337.138390678238,337.219070394135,337.302809105981,
337.386444617348,337.469997060747,337.553486496598,337.636940447212,337.720376941058,
337.803814050813,337.887269845731,337.970814338461,338.054403421402,338.138126688959,
338.218806404855,338.302545116701,338.386180628068,338.469733071467,338.553222507318,
338.636676457931,338.720112951778,338.803550061533,338.887005856451,338.97055034918,
339.054139432121,339.137862699679,339.218542415575,339.302281127421,339.385916638788,
339.469469082187,339.552958518038,339.636412468652,339.719848962498,339.803286072254,
339.886741867171,339.970286359901,340.053875442842,340.137598710399,340.218278426295,
340.302017138141,340.385652649509,340.469205092907,340.552694528758,340.636148479372,
340.719584973218,340.803022082974,340.886477877892,340.970022370621,341.053611453562,
341.13733472112,341.218014437016,341.30175516004,341.385392215482,341.468945737824,
341.552435788984,341.635887995735,341.71932208536,341.802756130105,341.88620819822,
341.969739944127,342.05331600737,342.137005309499,342.182335603278),
 .UNSPECIFIED.);
#264=B_SPLINE_CURVE_WITH_KNOTS('',3,(#41522,#41523,#41524,#41525,#41526,
#41527,#41528,#41529,#41530,#41531),.UNSPECIFIED.,.F.,.F.,(4,3,3,4),(335.898583947052,
335.981329823347,336.065871878657,336.150413933966),.UNSPECIFIED.);
#265=B_SPLINE_CURVE_WITH_KNOTS('',3,(#41533,#41534,#41535,#41536,#41537,
#41538,#41539,#41540,#41541,#41542),.UNSPECIFIED.,.F.,.F.,(4,3,3,4),(335.899704001206,
335.983869305751,336.06801737133,336.150413934092),.UNSPECIFIED.);
#266=B_SPLINE_CURVE_WITH_KNOTS('',3,(#41543,#41544,#41545,#41546,#41547,
#41548,#41549,#41550,#41551,#41552,#41553,#41554,#41555,#41556,#41557,#41558,
#41559,#41560,#41561,#41562,#41563,#41564,#41565,#41566,#41567,#41568,#41569,
#41570,#41571,#41572,#41573,#41574,#41575,#41576,#41577,#41578,#41579,#41580,
#41581,#41582,#41583,#41584,#41585,#41586,#41587,#41588,#41589,#41590,#41591,
#41592,#41593,#41594,#41595,#41596,#41597,#41598,#41599,#41600,#41601,#41602,
#41603,#41604,#41605,#41606,#41607,#41608,#41609,#41610,#41611,#41612,#41613,
#41614,#41615,#41616,#41617,#41618,#41619,#41620,#41621,#41622,#41623,#41624,
#41625,#41626,#41627,#41628,#41629,#41630,#41631,#41632,#41633,#41634,#41635,
#41636,#41637,#41638,#41639,#41640,#41641,#41642,#41643,#41644,#41645,#41646,
#41647,#41648,#41649,#41650,#41651,#41652,#41653,#41654,#41655,#41656,#41657,
#41658,#41659,#41660,#41661,#41662,#41663,#41664,#41665,#41666,#41667,#41668,
#41669,#41670,#41671,#41672,#41673,#41674,#41675,#41676,#41677,#41678,#41679,
#41680,#41681,#41682,#41683,#41684,#41685,#41686,#41687,#41688,#41689,#41690,
#41691,#41692,#41693,#41694,#41695,#41696,#41697,#41698,#41699,#41700,#41701,
#41702,#41703,#41704,#41705,#41706,#41707,#41708,#41709,#41710,#41711,#41712,
#41713,#41714,#41715,#41716,#41717,#41718,#41719,#41720,#41721,#41722,#41723,
#41724,#41725,#41726,#41727,#41728,#41729,#41730,#41731,#41732,#41733,#41734,
#41735,#41736,#41737,#41738,#41739,#41740,#41741,#41742,#41743,#41744,#41745,
#41746,#41747,#41748,#41749,#41750,#41751,#41752,#41753,#41754,#41755,#41756,
#41757,#41758,#41759),.UNSPECIFIED.,.F.,.F.,(4,3,3,3,3,3,3,3,3,3,3,3,3,
3,3,3,3,3,3,3,3,3,3,3,3,3,3,3,3,3,3,3,3,3,3,3,3,3,3,3,3,3,3,3,3,3,3,3,3,
3,3,3,3,3,3,3,3,3,3,3,3,3,3,3,3,3,3,3,3,3,3,3,4),(336.150413934288,336.245216701498,
336.339215446596,336.434420224863,336.52962500313,336.613363714976,336.696999226343,
336.780551669742,336.864041105593,336.947495056207,337.030931550053,337.114368659809,
337.197824454726,337.281368947456,337.364958030397,337.448681297955,337.52936101385,
337.613099725696,337.696735237064,337.780287680462,337.863777116313,337.947231066927,
338.030667560773,338.114104670529,338.197560465446,338.281104958176,338.364694041117,
338.448417308675,338.529097024571,338.612835736417,338.696471247784,338.780023691183,
338.863513127034,338.946967077648,339.030403571494,339.113840681249,339.197296476167,
339.280840968897,339.364430051838,339.448153319396,339.528833035291,339.612571747137,
339.696207258504,339.779759701903,339.863249137754,339.946703088367,340.030139582214,
340.113576691969,340.197032486887,340.280576979616,340.364166062557,340.447889330115,
340.528569046011,340.612307757857,340.695943269225,340.779495712623,340.862985148474,
340.946439099088,341.029875592934,341.11331270269,341.196768497607,341.280312990337,
341.363902073278,341.447625340836,341.528305056731,341.611009828143,341.693620044045,
341.776154761799,341.858632971129,341.941084209395,342.023516950066,342.105980397765,
342.181762906209),.UNSPECIFIED.);
#267=B_SPLINE_CURVE_WITH_KNOTS('',3,(#41765,#41766,#41767,#41768,#41769,
#41770,#41771,#41772,#41773,#41774,#41775,#41776,#41777,#41778,#41779,#41780,
#41781,#41782,#41783,#41784,#41785,#41786,#41787,#41788,#41789,#41790,#41791,
#41792,#41793,#41794,#41795,#41796,#41797,#41798,#41799,#41800,#41801,#41802,
#41803,#41804,#41805,#41806,#41807,#41808,#41809,#41810,#41811,#41812,#41813,
#41814,#41815,#41816,#41817,#41818,#41819,#41820,#41821,#41822,#41823,#41824,
#41825,#41826,#41827,#41828,#41829,#41830,#41831,#41832,#41833,#41834,#41835,
#41836,#41837,#41838,#41839,#41840,#41841,#41842,#41843,#41844,#41845,#41846,
#41847,#41848,#41849,#41850,#41851,#41852,#41853,#41854,#41855,#41856,#41857,
#41858,#41859,#41860,#41861,#41862,#41863,#41864,#41865,#41866,#41867,#41868,
#41869,#41870,#41871,#41872,#41873,#41874,#41875,#41876,#41877,#41878,#41879,
#41880,#41881,#41882,#41883,#41884,#41885,#41886,#41887,#41888,#41889,#41890,
#41891,#41892,#41893,#41894,#41895,#41896,#41897,#41898,#41899,#41900,#41901,
#41902,#41903,#41904,#41905,#41906,#41907,#41908,#41909,#41910,#41911,#41912,
#41913,#41914,#41915,#41916,#41917,#41918,#41919,#41920,#41921,#41922,#41923,
#41924,#41925,#41926,#41927,#41928,#41929,#41930,#41931,#41932,#41933,#41934,
#41935,#41936,#41937,#41938,#41939,#41940,#41941,#41942,#41943,#41944,#41945,
#41946,#41947,#41948,#41949,#41950,#41951,#41952,#41953,#41954,#41955,#41956,
#41957,#41958,#41959,#41960,#41961,#41962,#41963,#41964,#41965,#41966,#41967,
#41968,#41969,#41970,#41971,#41972,#41973,#41974,#41975,#41976,#41977,#41978,
#41979,#41980,#41981,#41982,#41983,#41984),.UNSPECIFIED.,.F.,.F.,(4,3,3,
3,3,3,3,3,3,3,3,3,3,3,3,3,3,3,3,3,3,3,3,3,3,3,3,3,3,3,3,3,3,3,3,3,3,3,3,
3,3,3,3,3,3,3,3,3,3,3,3,3,3,3,3,3,3,3,3,3,3,3,3,3,3,3,3,3,3,3,3,3,3,4),
(342.433599241371,342.516011609185,342.598359736635,342.680671607215,342.762966721928,
342.845264058301,342.927582593349,343.009987668582,343.092441313092,343.175015631616,
343.217486458456,343.301225170302,343.384860681669,343.468413125068,343.551902560919,
343.635356511532,343.718793005379,343.802230115134,343.885685910052,343.969230402782,
344.052819485723,344.13654275328,344.217222469176,344.300961181022,344.384596692389,
344.468149135788,344.551638571639,344.635092522253,344.718529016099,344.801966125855,
344.885421920772,344.968966413502,345.052555496443,345.136278764001,345.216958479896,
345.300697191742,345.384332703109,345.467885146508,345.551374582359,345.634828532972,
345.718265026819,345.801702136574,345.885157931492,345.968702424222,346.052291507163,
346.13601477472,346.216694490616,346.300433202462,346.384068713829,346.467621157228,
346.551110593079,346.634564543693,346.718001037539,346.801438147294,346.884893942212,
346.968438434941,347.052027517882,347.13575078544,347.216430501336,347.300169213182,
347.38380472455,347.467357167948,347.550846603799,347.634300554413,347.71773704826,
347.801174158015,347.884629952933,347.968174445662,348.051763528603,348.135486796161,
348.216166512056,348.304192741535,348.392023476754,348.466455594936),
 .UNSPECIFIED.);
#268=B_SPLINE_CURVE_WITH_KNOTS('',3,(#41985,#41986,#41987,#41988,#41989,
#41990,#41991,#41992,#41993,#41994),.UNSPECIFIED.,.F.,.F.,(4,3,3,4),(342.182335603278,
342.217750447736,342.333550962604,342.433599241268),.UNSPECIFIED.);
#269=B_SPLINE_CURVE_WITH_KNOTS('',3,(#41996,#41997,#41998,#41999,#42000,
#42001,#42002,#42003,#42004,#42005),.UNSPECIFIED.,.F.,.F.,(4,3,3,4),(342.181762906209,
342.26430274518,342.348950993158,342.433599241137),.UNSPECIFIED.);
#270=B_SPLINE_CURVE_WITH_KNOTS('',3,(#42006,#42007,#42008,#42009,#42010,
#42011,#42012,#42013,#42014,#42015,#42016,#42017,#42018,#42019,#42020,#42021,
#42022,#42023,#42024,#42025,#42026,#42027,#42028,#42029,#42030,#42031,#42032,
#42033,#42034,#42035,#42036,#42037,#42038,#42039,#42040,#42041,#42042,#42043,
#42044,#42045,#42046,#42047,#42048,#42049,#42050,#42051,#42052,#42053,#42054,
#42055,#42056,#42057,#42058,#42059,#42060,#42061,#42062,#42063,#42064,#42065,
#42066,#42067,#42068,#42069,#42070,#42071,#42072,#42073,#42074,#42075,#42076,
#42077,#42078,#42079,#42080,#42081,#42082,#42083,#42084,#42085,#42086,#42087,
#42088,#42089,#42090,#42091,#42092,#42093,#42094,#42095,#42096,#42097,#42098,
#42099,#42100,#42101,#42102,#42103,#42104,#42105,#42106,#42107,#42108,#42109,
#42110,#42111,#42112,#42113,#42114,#42115,#42116,#42117,#42118,#42119,#42120,
#42121,#42122,#42123,#42124,#42125,#42126,#42127,#42128,#42129,#42130,#42131,
#42132,#42133,#42134,#42135,#42136,#42137,#42138,#42139,#42140,#42141,#42142,
#42143,#42144,#42145,#42146,#42147,#42148,#42149,#42150,#42151,#42152,#42153,
#42154,#42155,#42156,#42157,#42158,#42159,#42160,#42161,#42162,#42163,#42164,
#42165,#42166,#42167,#42168,#42169,#42170,#42171,#42172,#42173,#42174,#42175,
#42176,#42177,#42178,#42179,#42180,#42181,#42182,#42183,#42184,#42185,#42186,
#42187,#42188,#42189,#42190,#42191,#42192,#42193,#42194,#42195,#42196,#42197,
#42198,#42199,#42200,#42201,#42202,#42203,#42204,#42205,#42206,#42207,#42208,
#42209,#42210,#42211,#42212,#42213,#42214,#42215,#42216,#42217,#42218,#42219,
#42220,#42221,#42222,#42223,#42224,#42225),.UNSPECIFIED.,.F.,.F.,(4,3,3,
3,3,3,3,3,3,3,3,3,3,3,3,3,3,3,3,3,3,3,3,3,3,3,3,3,3,3,3,3,3,3,3,3,3,3,3,
3,3,3,3,3,3,3,3,3,3,3,3,3,3,3,3,3,3,3,3,3,3,3,3,3,3,3,3,3,3,3,3,3,3,4),
(342.433599241272,342.528041067451,342.611779779297,342.695415290664,342.778967734063,
342.862457169914,342.945911120527,343.029347614374,343.112784724129,343.196240519047,
343.279785011776,343.363374094717,343.447097362275,343.527777078171,343.611515790017,
343.695151301384,343.778703744783,343.862193180634,343.945647131247,344.029083625094,
344.112520734849,344.195976529767,344.279521022497,344.363110105437,344.446833372995,
344.527513088891,344.611251800737,344.694887312104,344.778439755503,344.861929191354,
344.945383141968,345.028819635814,345.11225674557,345.195712540487,345.279257033217,
345.362846116158,345.446569383716,345.527249099611,345.610987811457,345.694623322825,
345.778175766223,345.861665202074,345.945119152688,346.028555646534,346.11199275629,
346.195448551207,346.278993043937,346.362582126878,346.446305394436,346.526985110332,
346.610723822178,346.694359333545,346.777911776944,346.861401212795,346.944855163409,
347.028291657255,347.111728767011,347.195184561928,347.278729054658,347.362318137599,
347.446041405157,347.526721121052,347.610463334944,347.694101543076,347.777655881374,
347.863624497286,347.94707476908,348.030506982412,348.113939208974,348.19738951639,
348.28091366941,348.364482424372,348.448150397174,348.465404808675),
 .UNSPECIFIED.);
#271=B_SPLINE_CURVE_WITH_KNOTS('',3,(#42231,#42232,#42233,#42234,#42235,
#42236,#42237,#42238,#42239,#42240,#42241,#42242,#42243,#42244,#42245,#42246,
#42247,#42248,#42249,#42250,#42251,#42252,#42253,#42254,#42255,#42256,#42257,
#42258,#42259,#42260,#42261,#42262,#42263,#42264,#42265,#42266,#42267,#42268,
#42269,#42270,#42271,#42272,#42273,#42274,#42275,#42276,#42277,#42278,#42279,
#42280,#42281,#42282,#42283,#42284,#42285,#42286,#42287,#42288,#42289,#42290,
#42291,#42292,#42293,#42294,#42295,#42296,#42297,#42298,#42299,#42300,#42301,
#42302,#42303,#42304,#42305,#42306,#42307,#42308,#42309,#42310,#42311,#42312,
#42313,#42314,#42315,#42316,#42317,#42318,#42319,#42320,#42321,#42322,#42323,
#42324,#42325,#42326,#42327,#42328,#42329,#42330,#42331,#42332,#42333,#42334,
#42335,#42336,#42337,#42338,#42339,#42340,#42341,#42342,#42343,#42344,#42345,
#42346,#42347,#42348,#42349,#42350,#42351,#42352,#42353,#42354,#42355,#42356,
#42357,#42358,#42359,#42360,#42361,#42362,#42363,#42364,#42365,#42366,#42367,
#42368,#42369,#42370,#42371,#42372,#42373,#42374,#42375,#42376,#42377,#42378,
#42379,#42380,#42381,#42382,#42383,#42384,#42385,#42386,#42387,#42388,#42389,
#42390,#42391,#42392,#42393,#42394,#42395,#42396,#42397,#42398,#42399,#42400,
#42401,#42402,#42403,#42404,#42405,#42406,#42407,#42408,#42409,#42410,#42411,
#42412,#42413,#42414,#42415,#42416,#42417,#42418,#42419,#42420,#42421,#42422,
#42423,#42424,#42425,#42426,#42427,#42428,#42429,#42430,#42431,#42432,#42433,
#42434,#42435,#42436,#42437,#42438,#42439,#42440,#42441,#42442,#42443,#42444,
#42445,#42446,#42447,#42448,#42449,#42450),.UNSPECIFIED.,.F.,.F.,(4,3,3,
3,3,3,3,3,3,3,3,3,3,3,3,3,3,3,3,3,3,3,3,3,3,3,3,3,3,3,3,3,3,3,3,3,3,3,3,
3,3,3,3,3,3,3,3,3,3,3,3,3,3,3,3,3,3,3,3,3,3,3,3,3,3,3,3,3,3,3,3,3,3,4),
(348.716784548596,348.804215738956,348.891763006794,348.979518053926,349.067382890157,
349.155449273507,349.215902522777,349.299641234623,349.38327674599,349.466829189389,
349.55031862524,349.633772575854,349.7172090697,349.800646179455,349.884101974373,
349.967646467103,350.051235550044,350.134958817601,350.215638533497,350.299377245343,
350.38301275671,350.466565200109,350.55005463596,350.633508586573,350.71694508042,
350.800382190175,350.883837985093,350.967382477822,351.050971560763,351.134694828321,
351.215374544217,351.299113256063,351.38274876743,351.466301210829,351.54979064668,
351.633244597294,351.71668109114,351.800118200895,351.883573995813,351.967118488543,
352.050707571484,352.134430839041,352.215110554937,352.298849266783,352.38248477815,
352.466037221549,352.5495266574,352.632980608014,352.71641710186,352.799854211615,
352.883310006533,352.966854499263,353.050443582204,353.134166849761,353.214846565657,
353.298585277503,353.382220788871,353.465773232269,353.54926266812,353.632716618734,
353.71615311258,353.799590222336,353.883046017254,353.966590509983,354.050179592924,
354.133902860482,354.214582576377,354.297147362669,354.379615533327,354.462006258773,
354.544335250586,354.626628364119,354.708914177518,354.748441555367),
 .UNSPECIFIED.);
#272=B_SPLINE_CURVE_WITH_KNOTS('',3,(#42451,#42452,#42453,#42454,#42455,
#42456,#42457,#42458,#42459,#42460),.UNSPECIFIED.,.F.,.F.,(4,3,3,4),(348.466455594936,
348.55402873825,348.641441273661,348.716784548447),.UNSPECIFIED.);
#273=B_SPLINE_CURVE_WITH_KNOTS('',3,(#42462,#42463,#42464,#42465,#42466,
#42467,#42468,#42469,#42470,#42471),.UNSPECIFIED.,.F.,.F.,(4,3,3,4),(348.465404808675,
348.526457131772,348.649804787013,348.716784548451),.UNSPECIFIED.);
#274=B_SPLINE_CURVE_WITH_KNOTS('',3,(#42472,#42473,#42474,#42475,#42476,
#42477,#42478,#42479,#42480,#42481,#42482,#42483,#42484,#42485,#42486,#42487,
#42488,#42489,#42490,#42491,#42492,#42493,#42494,#42495,#42496,#42497,#42498,
#42499,#42500,#42501,#42502,#42503,#42504,#42505,#42506,#42507,#42508,#42509,
#42510,#42511,#42512,#42513,#42514,#42515,#42516,#42517,#42518,#42519,#42520,
#42521,#42522,#42523,#42524,#42525,#42526,#42527,#42528,#42529,#42530,#42531,
#42532,#42533,#42534,#42535,#42536,#42537,#42538,#42539,#42540,#42541,#42542,
#42543,#42544,#42545,#42546,#42547,#42548,#42549,#42550,#42551,#42552,#42553,
#42554,#42555,#42556,#42557,#42558,#42559,#42560,#42561,#42562,#42563,#42564,
#42565,#42566,#42567,#42568,#42569,#42570,#42571,#42572,#42573,#42574,#42575,
#42576,#42577,#42578,#42579,#42580,#42581,#42582,#42583,#42584,#42585,#42586,
#42587,#42588,#42589,#42590,#42591,#42592,#42593,#42594,#42595,#42596,#42597,
#42598,#42599,#42600,#42601,#42602,#42603,#42604,#42605,#42606,#42607,#42608,
#42609,#42610,#42611,#42612,#42613,#42614,#42615,#42616,#42617,#42618,#42619,
#42620,#42621,#42622,#42623,#42624,#42625,#42626,#42627,#42628,#42629,#42630,
#42631,#42632,#42633,#42634,#42635,#42636,#42637,#42638,#42639,#42640,#42641,
#42642,#42643,#42644,#42645,#42646,#42647,#42648,#42649,#42650,#42651,#42652,
#42653,#42654,#42655,#42656,#42657,#42658,#42659,#42660,#42661,#42662,#42663,
#42664,#42665,#42666,#42667,#42668,#42669,#42670,#42671,#42672,#42673,#42674,
#42675,#42676,#42677,#42678,#42679,#42680,#42681,#42682,#42683,#42684,#42685,
#42686,#42687,#42688,#42689,#42690,#42691),.UNSPECIFIED.,.F.,.F.,(4,3,3,
3,3,3,3,3,3,3,3,3,3,3,3,3,3,3,3,3,3,3,3,3,3,3,3,3,3,3,3,3,3,3,3,3,3,3,3,
3,3,3,3,3,3,3,3,3,3,3,3,3,3,3,3,3,3,3,3,3,3,3,3,3,3,3,3,3,3,3,3,3,3,4),
(348.716784548578,348.799150648385,348.881445036037,348.963693320568,349.045918200772,
349.128138704293,349.210373853009,349.292691839066,349.375052593812,349.457540805916,
349.526193142492,349.609931854338,349.693567365705,349.777119809104,349.860609244955,
349.944063195568,350.027499689415,350.11093679917,350.194392594088,350.277937086818,
350.361526169759,350.445249437316,350.525929153212,350.609667865058,350.693303376425,
350.776855819824,350.860345255674,350.943799206288,351.027235700134,351.11067280989,
351.194128604807,351.277673097537,351.361262180478,351.444985448035,351.525665163932,
351.609403875778,351.693039387146,351.776591830545,351.860081266395,351.943535217009,
352.026971710855,352.11040882061,352.193864615528,352.277409108258,352.360998191199,
352.444721458757,352.525401174652,352.609139886498,352.692775397865,352.776327841264,
352.859817277115,352.943271227728,353.026707721574,353.11014483133,353.193600626247,
353.277145118977,353.360734201918,353.444457469476,353.525137185373,353.608875897219,
353.692511408586,353.776063851985,353.859553287836,353.94300723845,354.026443732296,
354.109880842052,354.193336636969,354.276881129699,354.36047021264,354.444193480197,
354.524873196093,354.613975775307,354.702866823617,354.749665211946),
 .UNSPECIFIED.);
#275=B_SPLINE_CURVE_WITH_KNOTS('',3,(#42697,#42698,#42699,#42700,#42701,
#42702,#42703,#42704,#42705,#42706,#42707,#42708,#42709,#42710,#42711,#42712,
#42713,#42714,#42715,#42716,#42717,#42718,#42719,#42720,#42721,#42722,#42723,
#42724,#42725,#42726,#42727,#42728,#42729,#42730,#42731,#42732,#42733,#42734,
#42735,#42736,#42737,#42738,#42739,#42740,#42741,#42742,#42743,#42744,#42745,
#42746,#42747,#42748,#42749,#42750,#42751,#42752,#42753,#42754,#42755,#42756,
#42757,#42758,#42759,#42760,#42761,#42762,#42763,#42764,#42765,#42766,#42767,
#42768,#42769,#42770,#42771,#42772,#42773,#42774,#42775,#42776,#42777,#42778,
#42779,#42780,#42781,#42782,#42783,#42784,#42785,#42786,#42787,#42788,#42789,
#42790,#42791,#42792,#42793,#42794,#42795,#42796,#42797,#42798,#42799,#42800,
#42801,#42802,#42803,#42804,#42805,#42806,#42807,#42808,#42809,#42810,#42811,
#42812,#42813,#42814,#42815,#42816,#42817,#42818,#42819,#42820,#42821,#42822,
#42823,#42824,#42825,#42826,#42827,#42828,#42829,#42830,#42831,#42832,#42833,
#42834,#42835,#42836,#42837,#42838,#42839,#42840,#42841,#42842,#42843,#42844,
#42845,#42846,#42847,#42848,#42849,#42850,#42851,#42852,#42853,#42854,#42855,
#42856,#42857,#42858,#42859,#42860,#42861,#42862,#42863,#42864,#42865,#42866,
#42867,#42868,#42869,#42870,#42871,#42872,#42873,#42874,#42875,#42876,#42877,
#42878,#42879,#42880,#42881,#42882,#42883,#42884,#42885,#42886,#42887,#42888,
#42889,#42890,#42891,#42892,#42893,#42894,#42895,#42896,#42897,#42898,#42899,
#42900,#42901,#42902,#42903,#42904,#42905,#42906,#42907,#42908,#42909,#42910,
#42911,#42912,#42913),.UNSPECIFIED.,.F.,.F.,(4,3,3,3,3,3,3,3,3,3,3,3,3,
3,3,3,3,3,3,3,3,3,3,3,3,3,3,3,3,3,3,3,3,3,3,3,3,3,3,3,3,3,3,3,3,3,3,3,3,
3,3,3,3,3,3,3,3,3,3,3,3,3,3,3,3,3,3,3,3,3,3,3,4),(354.999969855627,355.116152110623,
355.214318587097,355.298057298943,355.38169281031,355.465245253709,355.54873468956,
355.632188640174,355.71562513402,355.799062243776,355.882518038693,355.966062531423,
356.049651614364,356.133374881922,356.214054597817,356.297793309663,356.381428821031,
356.464981264429,356.54847070028,356.631924650894,356.71536114474,356.798798254496,
356.882254049414,356.965798542143,357.049387625084,357.133110892642,357.213790608538,
357.297529320384,357.381164831751,357.46471727515,357.548206711001,357.631660661615,
357.715097155461,357.798534265216,357.881990060134,357.965534552864,358.049123635805,
358.132846903362,358.213526619258,358.297265331104,358.380900842471,358.46445328587,
358.547942721721,358.631396672335,358.714833166181,358.798270275936,358.881726070854,
358.965270563584,359.048859646525,359.132582914082,359.213262629978,359.297001341824,
359.380636853192,359.46418929659,359.547678732441,359.631132683055,359.714569176901,
359.798006286657,359.881462081574,359.965006574304,360.048595657245,360.132318924803,
360.212998640698,360.296748234594,360.380392237065,360.463935615642,360.547421943862,
360.630869341337,360.714295897617,360.797746857763,360.881208592463,360.964741904342,
361.031498889511),.UNSPECIFIED.);
#276=B_SPLINE_CURVE_WITH_KNOTS('',3,(#42914,#42915,#42916,#42917,#42918,
#42919,#42920,#42921,#42922,#42923),.UNSPECIFIED.,.F.,.F.,(4,3,3,4),(354.748441555367,
354.830758582066,354.915364218791,354.999969855515),.UNSPECIFIED.);
#277=B_SPLINE_CURVE_WITH_KNOTS('',3,(#42925,#42926,#42927,#42928,#42929,
#42930,#42931,#42932,#42933,#42934),.UNSPECIFIED.,.F.,.F.,(4,3,3,4),(354.749665211946,
354.838283603898,354.926692238297,354.999969855526),.UNSPECIFIED.);
#278=B_SPLINE_CURVE_WITH_KNOTS('',3,(#42935,#42936,#42937,#42938,#42939,
#42940,#42941,#42942,#42943,#42944,#42945,#42946,#42947,#42948,#42949,#42950,
#42951,#42952,#42953,#42954,#42955,#42956,#42957,#42958,#42959,#42960,#42961,
#42962,#42963,#42964,#42965,#42966,#42967,#42968,#42969,#42970,#42971,#42972,
#42973,#42974,#42975,#42976,#42977,#42978,#42979,#42980,#42981,#42982,#42983,
#42984,#42985,#42986,#42987,#42988,#42989,#42990,#42991,#42992,#42993,#42994,
#42995,#42996,#42997,#42998,#42999,#43000,#43001,#43002,#43003,#43004,#43005,
#43006,#43007,#43008,#43009,#43010,#43011,#43012,#43013,#43014,#43015,#43016,
#43017,#43018,#43019,#43020,#43021,#43022,#43023,#43024,#43025,#43026,#43027,
#43028,#43029,#43030,#43031,#43032,#43033,#43034,#43035,#43036,#43037,#43038,
#43039,#43040,#43041,#43042,#43043,#43044,#43045,#43046,#43047,#43048,#43049,
#43050,#43051,#43052,#43053,#43054,#43055,#43056,#43057,#43058,#43059,#43060,
#43061,#43062,#43063,#43064,#43065,#43066,#43067,#43068,#43069,#43070,#43071,
#43072,#43073,#43074,#43075,#43076,#43077,#43078,#43079,#43080,#43081,#43082,
#43083,#43084,#43085,#43086,#43087,#43088,#43089,#43090,#43091,#43092,#43093,
#43094,#43095,#43096,#43097,#43098,#43099,#43100,#43101,#43102,#43103,#43104,
#43105,#43106,#43107,#43108,#43109,#43110,#43111,#43112,#43113,#43114,#43115,
#43116,#43117,#43118,#43119,#43120,#43121,#43122,#43123,#43124,#43125,#43126,
#43127,#43128,#43129,#43130,#43131,#43132,#43133,#43134,#43135,#43136,#43137,
#43138,#43139,#43140,#43141,#43142,#43143,#43144,#43145,#43146,#43147,#43148,
#43149,#43150,#43151,#43152,#43153,#43154),.UNSPECIFIED.,.F.,.F.,(4,3,3,
3,3,3,3,3,3,3,3,3,3,3,3,3,3,3,3,3,3,3,3,3,3,3,3,3,3,3,3,3,3,3,3,3,3,3,3,
3,3,3,3,3,3,3,3,3,3,3,3,3,3,3,3,3,3,3,3,3,3,3,3,3,3,3,3,3,3,3,3,3,3,4),
(354.999969855631,355.086529058888,355.173173417606,355.261032364908,355.347943982277,
355.436276594545,355.524609206813,355.608347918659,355.691983430026,355.775535873425,
355.859025309276,355.94247925989,356.025915753736,356.109352863491,356.192808658409,
356.276353151138,356.359942234079,356.443665501637,356.524345217533,356.608083929379,
356.691719440746,356.775271884145,356.858761319996,356.942215270609,357.025651764456,
357.109088874211,357.192544669129,357.276089161858,357.359678244799,357.443401512357,
357.524081228253,357.607819940099,357.691455451466,357.775007894865,357.858497330716,
357.94195128133,358.025387775176,358.108824884931,358.192280679848,358.275825172578,
358.359414255519,358.443137523077,358.523817238973,358.607555950819,358.691191462187,
358.774743905585,358.858233341436,358.94168729205,359.025123785896,359.108560895652,
359.192016690569,359.275561183299,359.35915026624,359.442873533798,359.523553249693,
359.607291961539,359.690927472906,359.774479916305,359.857969352156,359.94142330277,
360.024859796616,360.108296906372,360.19175270129,360.275297194019,360.358886276961,
360.442609544518,360.523289260413,360.605987335625,360.688587685776,360.774376530304,
360.856831350972,360.939250049255,361.021655093284,361.031743063889),
 .UNSPECIFIED.);
#279=B_SPLINE_CURVE_WITH_KNOTS('',3,(#43160,#43161,#43162,#43163,#43164,
#43165,#43166,#43167,#43168,#43169,#43170,#43171,#43172,#43173,#43174,#43175,
#43176,#43177,#43178,#43179,#43180,#43181,#43182,#43183,#43184,#43185,#43186,
#43187,#43188,#43189,#43190,#43191,#43192,#43193,#43194,#43195,#43196,#43197,
#43198,#43199,#43200,#43201,#43202,#43203,#43204,#43205,#43206,#43207,#43208,
#43209,#43210,#43211,#43212,#43213,#43214,#43215,#43216,#43217,#43218,#43219,
#43220,#43221,#43222,#43223,#43224,#43225,#43226,#43227,#43228,#43229,#43230,
#43231,#43232,#43233,#43234,#43235,#43236,#43237,#43238,#43239,#43240,#43241,
#43242,#43243,#43244,#43245,#43246,#43247,#43248,#43249,#43250,#43251,#43252,
#43253,#43254,#43255,#43256,#43257,#43258,#43259,#43260,#43261,#43262,#43263,
#43264,#43265,#43266,#43267,#43268,#43269,#43270,#43271,#43272,#43273,#43274,
#43275,#43276,#43277,#43278,#43279,#43280,#43281,#43282,#43283,#43284,#43285,
#43286,#43287,#43288,#43289,#43290,#43291,#43292,#43293,#43294,#43295,#43296,
#43297,#43298,#43299,#43300,#43301,#43302,#43303,#43304,#43305,#43306,#43307,
#43308,#43309,#43310,#43311,#43312,#43313,#43314,#43315,#43316,#43317,#43318,
#43319,#43320,#43321,#43322,#43323,#43324,#43325,#43326,#43327,#43328,#43329,
#43330,#43331,#43332,#43333,#43334,#43335,#43336,#43337,#43338,#43339,#43340,
#43341,#43342,#43343,#43344,#43345,#43346,#43347,#43348,#43349,#43350,#43351,
#43352,#43353,#43354,#43355,#43356,#43357,#43358,#43359,#43360,#43361,#43362,
#43363,#43364,#43365,#43366,#43367,#43368,#43369,#43370,#43371,#43372,#43373,
#43374,#43375,#43376,#43377,#43378,#43379,#43380,#43381,#43382),
 .UNSPECIFIED.,.F.,.F.,(4,3,3,3,3,3,3,3,3,3,3,3,3,3,3,3,3,3,3,3,3,3,3,3,
3,3,3,3,3,3,3,3,3,3,3,3,3,3,3,3,3,3,3,3,3,3,3,3,3,3,3,3,3,3,3,3,3,3,3,3,
3,3,3,3,3,3,3,3,3,3,3,3,3,3,4),(361.283155162929,361.366032816794,361.448813027917,
361.531516694294,361.616635940275,361.699257890964,361.781870921663,361.864493796201,
361.951488012686,362.034232931093,362.117033568309,362.199947972622,362.212470662138,
362.296209373984,362.379844885351,362.46339732875,362.546886764601,362.630340715215,
362.713777209061,362.797214318817,362.880670113734,362.964214606464,363.047803689405,
363.131526956963,363.212206672858,363.295945384704,363.379580896072,363.46313333947,
363.546622775321,363.630076725934,363.713513219781,363.796950329536,363.880406124454,
363.963950617184,364.047539700125,364.131262967682,364.211942683579,364.295681395425,
364.379316906793,364.462869350191,364.546358786043,364.629812736656,364.713249230503,
364.796686340258,364.880142135176,364.963686627905,365.047275710846,365.130998978404,
365.211678694299,365.295417406145,365.379052917512,365.462605360911,365.546094796762,
365.629548747375,365.712985241222,365.796422350977,365.879878145895,365.963422638625,
366.047011721566,366.130734989123,366.211414705019,366.295153416865,366.378788928233,
366.462341371631,366.545830807482,366.629284758095,366.712721251942,366.796158361697,
366.879614156615,366.963158649344,367.046747732285,367.130470999843,367.211150715739,
367.307726271185,367.315827373902),.UNSPECIFIED.);
#280=B_SPLINE_CURVE_WITH_KNOTS('',3,(#43383,#43384,#43385,#43386,#43387,
#43388,#43389,#43390,#43391,#43392,#43393,#43394,#43395),.UNSPECIFIED.,
 .F.,.F.,(4,3,3,3,4),(361.031498889511,361.115135268541,361.198887310602,
361.212734651418,361.283155162806),.UNSPECIFIED.);
#281=B_SPLINE_CURVE_WITH_KNOTS('',3,(#43397,#43398,#43399,#43400,#43401,
#43402,#43403,#43404,#43405,#43406),.UNSPECIFIED.,.F.,.F.,(4,3,3,4),(361.031743063889,
361.114173808488,361.198664485649,361.28315516281),.UNSPECIFIED.);
#282=B_SPLINE_CURVE_WITH_KNOTS('',3,(#43407,#43408,#43409,#43410,#43411,
#43412,#43413,#43414,#43415,#43416,#43417,#43418,#43419,#43420,#43421,#43422,
#43423,#43424,#43425,#43426,#43427,#43428,#43429,#43430,#43431,#43432,#43433,
#43434,#43435,#43436,#43437,#43438,#43439,#43440,#43441,#43442,#43443,#43444,
#43445,#43446,#43447,#43448,#43449,#43450,#43451,#43452,#43453,#43454,#43455,
#43456,#43457,#43458,#43459,#43460,#43461,#43462,#43463,#43464,#43465,#43466,
#43467,#43468,#43469,#43470,#43471,#43472,#43473,#43474,#43475,#43476,#43477,
#43478,#43479,#43480,#43481,#43482,#43483,#43484,#43485,#43486,#43487,#43488,
#43489,#43490,#43491,#43492,#43493,#43494,#43495,#43496,#43497,#43498,#43499,
#43500,#43501,#43502,#43503,#43504,#43505,#43506,#43507,#43508,#43509,#43510,
#43511,#43512,#43513,#43514,#43515,#43516,#43517,#43518,#43519,#43520,#43521,
#43522,#43523,#43524,#43525,#43526,#43527,#43528,#43529,#43530,#43531,#43532,
#43533,#43534,#43535,#43536,#43537,#43538,#43539,#43540,#43541,#43542,#43543,
#43544,#43545,#43546,#43547,#43548,#43549,#43550,#43551,#43552,#43553,#43554,
#43555,#43556,#43557,#43558,#43559,#43560,#43561,#43562,#43563,#43564,#43565,
#43566,#43567,#43568,#43569,#43570,#43571,#43572,#43573,#43574,#43575,#43576,
#43577,#43578,#43579,#43580,#43581,#43582,#43583,#43584,#43585,#43586,#43587,
#43588,#43589,#43590,#43591,#43592,#43593,#43594,#43595,#43596,#43597,#43598,
#43599,#43600,#43601,#43602,#43603,#43604,#43605,#43606,#43607,#43608,#43609,
#43610,#43611,#43612,#43613,#43614,#43615,#43616,#43617,#43618,#43619,#43620,
#43621,#43622,#43623,#43624,#43625,#43626),.UNSPECIFIED.,.F.,.F.,(4,3,3,
3,3,3,3,3,3,3,3,3,3,3,3,3,3,3,3,3,3,3,3,3,3,3,3,3,3,3,3,3,3,3,3,3,3,3,3,
3,3,3,3,3,3,3,3,3,3,3,3,3,3,3,3,3,3,3,3,3,3,3,3,3,3,3,3,3,3,3,3,3,3,4),
(361.283155162958,361.392106189189,361.503854892668,361.523025271134,361.60676398298,
361.690399494347,361.773951937746,361.857441373597,361.940895324211,362.024331818057,
362.107768927812,362.19122472273,362.27476921546,362.358358298401,362.442081565958,
362.522761281854,362.6064999937,362.690135505067,362.773687948466,362.857177384317,
362.94063133493,363.024067828777,363.107504938532,363.19096073345,363.274505226179,
363.35809430912,363.441817576678,363.522497292574,363.60623600442,363.689871515787,
363.773423959186,363.856913395037,363.940367345651,364.023803839497,364.107240949252,
364.19069674417,364.2742412369,364.357830319841,364.441553587398,364.522233303294,
364.60597201514,364.689607526507,364.773159969906,364.856649405757,364.940103356371,
365.023539850217,365.106976959972,365.19043275489,365.27397724762,365.357566330561,
365.441289598119,365.521969314014,365.60570802586,365.689343537227,365.772895980626,
365.856385416477,365.93983936709,366.023275860937,366.106712970692,366.19016876561,
366.27371325834,366.35730234128,366.441025608838,366.521705324734,366.605456569419,
366.689101885749,366.772645767038,366.856132120293,366.939579065989,367.023004694106,
367.106450064674,367.189906018076,367.273422367636,367.31467431478),
 .UNSPECIFIED.);
#283=B_SPLINE_CURVE_WITH_KNOTS('',3,(#43632,#43633,#43634,#43635,#43636,
#43637,#43638,#43639,#43640,#43641,#43642,#43643,#43644,#43645,#43646,#43647,
#43648,#43649,#43650,#43651,#43652,#43653,#43654,#43655,#43656,#43657,#43658,
#43659,#43660,#43661,#43662,#43663,#43664,#43665,#43666,#43667,#43668,#43669,
#43670,#43671,#43672,#43673,#43674,#43675,#43676,#43677,#43678,#43679,#43680,
#43681,#43682,#43683,#43684,#43685,#43686,#43687,#43688,#43689,#43690,#43691,
#43692,#43693,#43694,#43695,#43696,#43697,#43698,#43699,#43700,#43701,#43702,
#43703,#43704,#43705,#43706,#43707,#43708,#43709,#43710,#43711,#43712,#43713,
#43714,#43715,#43716,#43717,#43718,#43719,#43720,#43721,#43722,#43723,#43724,
#43725,#43726,#43727,#43728,#43729,#43730,#43731,#43732,#43733,#43734,#43735,
#43736,#43737,#43738,#43739,#43740,#43741,#43742,#43743,#43744,#43745,#43746,
#43747,#43748,#43749,#43750,#43751,#43752,#43753,#43754,#43755,#43756,#43757,
#43758,#43759,#43760,#43761,#43762,#43763,#43764,#43765,#43766,#43767,#43768,
#43769,#43770,#43771,#43772,#43773,#43774,#43775,#43776,#43777,#43778,#43779,
#43780,#43781,#43782,#43783,#43784,#43785,#43786,#43787,#43788,#43789,#43790,
#43791,#43792,#43793,#43794,#43795,#43796,#43797,#43798,#43799,#43800,#43801,
#43802,#43803,#43804,#43805,#43806,#43807,#43808,#43809,#43810,#43811,#43812,
#43813,#43814,#43815,#43816,#43817,#43818,#43819,#43820,#43821,#43822,#43823,
#43824,#43825,#43826,#43827,#43828,#43829,#43830,#43831,#43832,#43833,#43834,
#43835,#43836,#43837,#43838,#43839,#43840,#43841,#43842,#43843,#43844,#43845,
#43846,#43847,#43848,#43849,#43850,#43851),.UNSPECIFIED.,.F.,.F.,(4,3,3,
3,3,3,3,3,3,3,3,3,3,3,3,3,3,3,3,3,3,3,3,3,3,3,3,3,3,3,3,3,3,3,3,3,3,3,3,
3,3,3,3,3,3,3,3,3,3,3,3,3,3,3,3,3,3,3,3,3,3,3,3,3,3,3,3,3,3,3,3,3,3,4),
(367.566340469986,367.650059493962,367.733775454788,367.817506009342,367.9012688201,
367.985134653745,368.069056243052,368.153114776464,368.210886726459,368.294625438305,
368.378260949673,368.461813393071,368.545302828922,368.628756779536,368.712193273382,
368.795630383138,368.879086178055,368.962630670785,369.046219753726,369.129943021284,
369.210622737179,369.294361449025,369.377996960392,369.461549403791,369.545038839641,
369.628492790255,369.711929284101,369.795366393857,369.878822188774,369.962366681504,
370.045955764445,370.129679032002,370.210358747899,370.294097459745,370.377732971112,
370.461285414511,370.544774850362,370.628228800976,370.711665294822,370.795102404578,
370.878558199495,370.962102692225,371.045691775166,371.129415042724,371.210094758619,
371.293833470465,371.377468981833,371.461021425232,371.544510861083,371.627964811697,
371.711401305543,371.794838415299,371.878294210217,371.961838702947,372.045427785888,
372.129151053445,372.20983076934,372.293569481186,372.377204992554,372.460757435952,
372.544246871803,372.627700822417,372.711137316264,372.794574426019,372.878030220937,
372.961574713667,373.045163796608,373.128887064166,373.20956678006,373.293731515783,
373.377756473631,373.461700952373,373.545568914742,373.598723849892),
 .UNSPECIFIED.);
#284=B_SPLINE_CURVE_WITH_KNOTS('',3,(#43852,#43853,#43854,#43855,#43856,
#43857,#43858,#43859,#43860,#43861),.UNSPECIFIED.,.F.,.F.,(4,3,3,4),(367.315827373902,
367.411842954212,367.507175834098,367.566340469788),.UNSPECIFIED.);
#285=B_SPLINE_CURVE_WITH_KNOTS('',3,(#43863,#43864,#43865,#43866,#43867,
#43868,#43869,#43870,#43871,#43872,#43873,#43874,#43875),.UNSPECIFIED.,
 .F.,.F.,(4,3,3,3,4),(367.31467431478,367.398291381823,367.482030912403,
367.521441335454,367.56634046999),.UNSPECIFIED.);
#286=B_SPLINE_CURVE_WITH_KNOTS('',3,(#43876,#43877,#43878,#43879,#43880,
#43881,#43882,#43883,#43884,#43885,#43886,#43887,#43888,#43889,#43890,#43891,
#43892,#43893,#43894,#43895,#43896,#43897,#43898,#43899,#43900,#43901,#43902,
#43903,#43904,#43905,#43906,#43907,#43908,#43909,#43910,#43911,#43912,#43913,
#43914,#43915,#43916,#43917,#43918,#43919,#43920,#43921,#43922,#43923,#43924,
#43925,#43926,#43927,#43928,#43929,#43930,#43931,#43932,#43933,#43934,#43935,
#43936,#43937,#43938,#43939,#43940,#43941,#43942,#43943,#43944,#43945,#43946,
#43947,#43948,#43949,#43950,#43951,#43952,#43953,#43954,#43955,#43956,#43957,
#43958,#43959,#43960,#43961,#43962,#43963,#43964,#43965,#43966,#43967,#43968,
#43969,#43970,#43971,#43972,#43973,#43974,#43975,#43976,#43977,#43978,#43979,
#43980,#43981,#43982,#43983,#43984,#43985,#43986,#43987,#43988,#43989,#43990,
#43991,#43992,#43993,#43994,#43995,#43996,#43997,#43998,#43999,#44000,#44001,
#44002,#44003,#44004,#44005,#44006,#44007,#44008,#44009,#44010,#44011,#44012,
#44013,#44014,#44015,#44016,#44017,#44018,#44019,#44020,#44021,#44022,#44023,
#44024,#44025,#44026,#44027,#44028,#44029,#44030,#44031,#44032,#44033,#44034,
#44035,#44036,#44037,#44038,#44039,#44040,#44041,#44042,#44043,#44044,#44045,
#44046,#44047,#44048,#44049,#44050,#44051,#44052,#44053,#44054,#44055,#44056,
#44057,#44058,#44059,#44060,#44061,#44062,#44063,#44064,#44065,#44066,#44067,
#44068,#44069,#44070,#44071,#44072,#44073,#44074,#44075,#44076,#44077,#44078,
#44079,#44080,#44081,#44082,#44083,#44084,#44085,#44086,#44087,#44088,#44089,
#44090,#44091,#44092,#44093,#44094,#44095),.UNSPECIFIED.,.F.,.F.,(4,3,3,
3,3,3,3,3,3,3,3,3,3,3,3,3,3,3,3,3,3,3,3,3,3,3,3,3,3,3,3,3,3,3,3,3,3,3,3,
3,3,3,3,3,3,3,3,3,3,3,3,3,3,3,3,3,3,3,3,3,3,3,3,3,3,3,3,3,3,3,3,3,3,4),
(367.566340470175,367.649481447308,367.732521837641,367.815482341599,367.898383582848,
367.981254713856,368.064112809716,368.146976452127,368.229864223374,368.312841649614,
368.395869528455,368.479019551326,368.521177346175,368.604916058021,368.688551569388,
368.772104012787,368.855593448637,368.939047399251,369.022483893097,369.105921002853,
369.189376797771,369.2729212905,369.356510373441,369.440233640999,369.520913356895,
369.604652068741,369.688287580108,369.771840023507,369.855329459358,369.938783409972,
370.022219903818,370.105657013573,370.189112808491,370.272657301221,370.356246384162,
370.439969651719,370.520649367615,370.604388079461,370.688023590828,370.771576034227,
370.855065470078,370.938519420692,371.021955914538,371.105393024293,371.18884881921,
371.27239331194,371.355982394881,371.439705662439,371.520385378335,371.604124090181,
371.687759601548,371.771312044947,371.854801480797,371.938255431411,372.021691925257,
372.105129035013,372.188584829931,372.272129322661,372.355718405602,372.439441673159,
372.520121389055,372.603860100901,372.687495612268,372.771048055667,372.854537491519,
372.937991442132,373.021427935979,373.104865045735,373.188320840653,373.271865333382,
373.355454416323,373.439177683881,373.519857399775,373.598902653178),
 .UNSPECIFIED.);
#287=B_SPLINE_CURVE_WITH_KNOTS('',3,(#44101,#44102,#44103,#44104,#44105,
#44106,#44107,#44108,#44109,#44110,#44111,#44112,#44113,#44114,#44115,#44116,
#44117,#44118,#44119,#44120,#44121,#44122,#44123,#44124,#44125,#44126,#44127,
#44128,#44129,#44130,#44131,#44132,#44133,#44134,#44135,#44136,#44137,#44138,
#44139,#44140,#44141,#44142,#44143,#44144,#44145,#44146,#44147,#44148,#44149,
#44150,#44151,#44152,#44153,#44154,#44155,#44156,#44157,#44158,#44159,#44160,
#44161,#44162,#44163,#44164,#44165,#44166,#44167,#44168,#44169,#44170,#44171,
#44172,#44173,#44174,#44175,#44176,#44177,#44178,#44179,#44180,#44181,#44182,
#44183,#44184,#44185,#44186,#44187,#44188,#44189,#44190,#44191,#44192,#44193,
#44194,#44195,#44196,#44197,#44198,#44199,#44200,#44201,#44202,#44203,#44204,
#44205,#44206,#44207,#44208,#44209,#44210,#44211,#44212,#44213,#44214,#44215,
#44216,#44217,#44218,#44219,#44220,#44221,#44222,#44223,#44224,#44225,#44226,
#44227,#44228,#44229,#44230,#44231,#44232,#44233,#44234,#44235,#44236,#44237,
#44238,#44239,#44240,#44241,#44242,#44243,#44244,#44245,#44246,#44247,#44248,
#44249,#44250,#44251,#44252,#44253,#44254,#44255,#44256,#44257,#44258,#44259,
#44260,#44261,#44262,#44263,#44264,#44265,#44266,#44267,#44268,#44269,#44270,
#44271,#44272,#44273,#44274,#44275,#44276,#44277,#44278,#44279,#44280,#44281,
#44282,#44283,#44284,#44285,#44286,#44287,#44288,#44289,#44290,#44291,#44292,
#44293,#44294,#44295,#44296,#44297,#44298,#44299,#44300,#44301,#44302,#44303,
#44304,#44305,#44306,#44307,#44308,#44309,#44310,#44311,#44312,#44313,#44314,
#44315,#44316,#44317),.UNSPECIFIED.,.F.,.F.,(4,3,3,3,3,3,3,3,3,3,3,3,3,
3,3,3,3,3,3,3,3,3,3,3,3,3,3,3,3,3,3,3,3,3,3,3,3,3,3,3,3,3,3,3,3,3,3,3,3,
3,3,3,3,3,3,3,3,3,3,3,3,3,3,3,3,3,3,3,3,3,3,3,4),(373.849525777362,373.944580138424,
374.040061204896,374.136110618714,374.20930279078,374.293041502626,374.376677013994,
374.460229457392,374.543718893243,374.627172843857,374.710609337703,374.794046447459,
374.877502242376,374.961046735106,375.044635818047,375.128359085605,375.2090388015,
375.292777513346,375.376413024713,375.459965468112,375.543454903963,375.626908854576,
375.710345348423,375.793782458178,375.877238253096,375.960782745825,376.044371828766,
376.128095096324,376.20877481222,376.292513524066,376.376149035433,376.459701478832,
376.543190914683,376.626644865296,376.710081359143,376.793518468898,376.876974263816,
376.960518756545,377.044107839486,377.127831107044,377.20851082294,377.292249534786,
377.375885046153,377.459437489552,377.542926925403,377.626380876017,377.709817369863,
377.793254479618,377.876710274536,377.960254767266,378.043843850207,378.127567117764,
378.20824683366,378.291985545506,378.375621056873,378.459173500272,378.542662936123,
378.626116886737,378.709553380583,378.792990490338,378.876446285256,378.959990777986,
379.043579860927,379.127303128484,379.20798284438,379.292094589826,379.374844615425,
379.457519348592,379.540137680491,379.625322462356,379.707896657838,379.794386732894,
379.880876807951),.UNSPECIFIED.);
#288=B_SPLINE_CURVE_WITH_KNOTS('',3,(#44318,#44319,#44320,#44321,#44322,
#44323,#44324,#44325,#44326,#44327),.UNSPECIFIED.,.F.,.F.,(4,3,3,4),(373.598723849892,
373.682523139848,373.766320497947,373.849525777165),.UNSPECIFIED.);
#289=B_SPLINE_CURVE_WITH_KNOTS('',3,(#44329,#44330,#44331,#44332,#44333,
#44334,#44335,#44336,#44337,#44338),.UNSPECIFIED.,.F.,.F.,(4,3,3,4),(373.598902653178,
373.697309312522,373.794823155724,373.849525776986),.UNSPECIFIED.);
#290=B_SPLINE_CURVE_WITH_KNOTS('',3,(#44339,#44340,#44341,#44342,#44343,
#44344,#44345,#44346,#44347,#44348,#44349,#44350,#44351,#44352,#44353,#44354,
#44355,#44356,#44357,#44358,#44359,#44360,#44361,#44362,#44363,#44364,#44365,
#44366,#44367,#44368,#44369,#44370,#44371,#44372,#44373,#44374,#44375,#44376,
#44377,#44378,#44379,#44380,#44381,#44382,#44383,#44384,#44385,#44386,#44387,
#44388,#44389,#44390,#44391,#44392,#44393,#44394,#44395,#44396,#44397,#44398,
#44399,#44400,#44401,#44402,#44403,#44404,#44405,#44406,#44407,#44408,#44409,
#44410,#44411,#44412,#44413,#44414,#44415,#44416,#44417,#44418,#44419,#44420,
#44421,#44422,#44423,#44424,#44425,#44426,#44427,#44428,#44429,#44430,#44431,
#44432,#44433,#44434,#44435,#44436,#44437,#44438,#44439,#44440,#44441,#44442,
#44443,#44444,#44445,#44446,#44447,#44448,#44449,#44450,#44451,#44452,#44453,
#44454,#44455,#44456,#44457,#44458,#44459,#44460,#44461,#44462,#44463,#44464,
#44465,#44466,#44467,#44468,#44469,#44470,#44471,#44472,#44473,#44474,#44475,
#44476,#44477,#44478,#44479,#44480,#44481,#44482,#44483,#44484,#44485,#44486,
#44487,#44488,#44489,#44490,#44491,#44492,#44493,#44494,#44495,#44496,#44497,
#44498,#44499,#44500,#44501,#44502,#44503,#44504,#44505,#44506,#44507,#44508,
#44509,#44510,#44511,#44512,#44513,#44514,#44515,#44516,#44517,#44518,#44519,
#44520,#44521,#44522,#44523,#44524,#44525,#44526,#44527,#44528,#44529,#44530,
#44531,#44532,#44533,#44534,#44535,#44536,#44537,#44538,#44539,#44540,#44541,
#44542,#44543,#44544,#44545,#44546,#44547,#44548,#44549,#44550,#44551,#44552,
#44553,#44554,#44555,#44556,#44557,#44558),.UNSPECIFIED.,.F.,.F.,(4,3,3,
3,3,3,3,3,3,3,3,3,3,3,3,3,3,3,3,3,3,3,3,3,3,3,3,3,3,3,3,3,3,3,3,3,3,3,3,
3,3,3,3,3,3,3,3,3,3,3,3,3,3,3,3,3,3,3,3,3,3,3,3,3,3,3,3,3,3,3,3,3,3,4),
(373.849525777169,373.933284231335,374.016605576888,374.099930113727,374.183275958349,
374.267355321385,374.350842682452,374.435218046474,374.519593410495,374.603332122341,
374.686967633709,374.770520077107,374.854009512958,374.937463463572,375.020899957418,
375.104337067174,375.187792862091,375.271337354821,375.354926437762,375.43864970532,
375.519329421215,375.603068133061,375.686703644428,375.770256087827,375.853745523678,
375.937199474292,376.020635968138,376.104073077894,376.187528872811,376.271073365541,
376.354662448482,376.43838571604,376.519065431936,376.602804143782,376.686439655149,
376.769992098548,376.853481534399,376.936935485012,377.020371978859,377.103809088614,
377.187264883532,377.270809376262,377.354398459203,377.43812172676,377.518801442656,
377.602540154502,377.686175665869,377.769728109268,377.853217545119,377.936671495733,
378.020107989579,378.103545099334,378.187000894251,378.270545386981,378.354134469922,
378.437857737479,378.518537453376,378.602276165222,378.68591167659,378.769464119989,
378.85295355584,378.936407506454,379.0198440003,379.103281110055,379.186736904973,
379.270281397703,379.353870480644,379.437593748202,379.518273464096,379.602951023663,
379.687482586612,379.771929460174,379.856291871132,379.882028760327),
 .UNSPECIFIED.);
#291=B_SPLINE_CURVE_WITH_KNOTS('',3,(#44564,#44565,#44566,#44567,#44568,
#44569,#44570,#44571,#44572,#44573,#44574,#44575,#44576,#44577,#44578,#44579,
#44580,#44581,#44582,#44583,#44584,#44585,#44586,#44587,#44588,#44589,#44590,
#44591,#44592,#44593,#44594,#44595,#44596,#44597,#44598,#44599,#44600,#44601,
#44602,#44603,#44604,#44605,#44606,#44607,#44608,#44609,#44610,#44611,#44612,
#44613,#44614,#44615,#44616,#44617,#44618,#44619,#44620,#44621,#44622,#44623,
#44624,#44625,#44626,#44627,#44628,#44629,#44630,#44631,#44632,#44633,#44634,
#44635,#44636,#44637,#44638,#44639,#44640,#44641,#44642,#44643,#44644,#44645,
#44646,#44647,#44648,#44649,#44650,#44651,#44652,#44653,#44654,#44655,#44656,
#44657,#44658,#44659,#44660,#44661,#44662,#44663,#44664,#44665,#44666,#44667,
#44668,#44669,#44670,#44671,#44672,#44673,#44674,#44675,#44676,#44677,#44678,
#44679,#44680,#44681,#44682,#44683,#44684,#44685,#44686,#44687,#44688,#44689,
#44690,#44691,#44692,#44693,#44694,#44695,#44696,#44697,#44698,#44699,#44700,
#44701,#44702,#44703,#44704,#44705,#44706,#44707,#44708,#44709,#44710,#44711,
#44712,#44713,#44714,#44715,#44716,#44717,#44718,#44719,#44720,#44721,#44722,
#44723,#44724,#44725,#44726,#44727,#44728,#44729,#44730,#44731,#44732,#44733,
#44734,#44735,#44736,#44737,#44738,#44739,#44740,#44741,#44742,#44743,#44744,
#44745,#44746,#44747,#44748,#44749,#44750,#44751,#44752,#44753,#44754,#44755,
#44756,#44757,#44758,#44759,#44760,#44761,#44762,#44763,#44764,#44765,#44766,
#44767,#44768,#44769,#44770,#44771,#44772,#44773,#44774,#44775,#44776,#44777,
#44778,#44779,#44780,#44781,#44782,#44783),.UNSPECIFIED.,.F.,.F.,(4,3,3,
3,3,3,3,3,3,3,3,3,3,3,3,3,3,3,3,3,3,3,3,3,3,3,3,3,3,3,3,3,3,3,3,3,3,3,3,
3,3,3,3,3,3,3,3,3,3,3,3,3,3,3,3,3,3,3,3,3,3,3,3,3,3,3,3,3,3,3,3,3,3,4),
(380.132711084345,380.207718855101,380.291457566947,380.375093078314,380.458645521713,
380.542134957564,380.625588908178,380.709025402024,380.792462511779,380.875918306697,
380.959462799426,381.043051882367,381.126775149925,381.207454865821,381.291193577667,
381.374829089034,381.458381532433,381.541870968284,381.625324918898,381.708761412744,
381.792198522499,381.875654317417,381.959198810147,382.042787893087,382.126511160645,
382.207190876541,382.290929588387,382.374565099754,382.458117543153,382.541606979004,
382.625060929618,382.708497423464,382.791934533219,382.875390328137,382.958934820867,
383.042523903807,383.126247171365,383.206926887261,383.290665599107,383.374301110474,
383.457853553873,383.541342989724,383.624796940338,383.708233434184,383.791670543939,
383.875126338857,383.958670831587,384.042259914528,384.125983182085,384.206662897981,
384.290401609827,384.374037121194,384.457589564593,384.541079000444,384.624532951058,
384.707969444904,384.791406554659,384.874862349577,384.958406842306,385.041995925247,
385.125719192805,385.206398908701,385.290139984778,385.373777312587,385.457331026953,
385.540821190055,385.624273118317,385.707706815389,385.791140353452,385.874591800591,
385.958121435581,386.041695340788,386.125379138116,386.164603019142),
 .UNSPECIFIED.);
#292=B_SPLINE_CURVE_WITH_KNOTS('',3,(#44784,#44785,#44786,#44787,#44788,
#44789,#44790,#44791,#44792,#44793),.UNSPECIFIED.,.F.,.F.,(4,3,3,4),(379.880876807951,
379.963568450344,380.048139767281,380.132711084218),.UNSPECIFIED.);
#293=B_SPLINE_CURVE_WITH_KNOTS('',3,(#44795,#44796,#44797,#44798,#44799,
#44800,#44801,#44802,#44803,#44804),.UNSPECIFIED.,.F.,.F.,(4,3,3,4),(379.882028760327,
379.966318027482,380.050584953051,380.132711084349),.UNSPECIFIED.);
#294=B_SPLINE_CURVE_WITH_KNOTS('',3,(#44805,#44806,#44807,#44808,#44809,
#44810,#44811,#44812,#44813,#44814,#44815,#44816,#44817,#44818,#44819,#44820,
#44821,#44822,#44823,#44824,#44825,#44826,#44827,#44828,#44829,#44830,#44831,
#44832,#44833,#44834,#44835,#44836,#44837,#44838,#44839,#44840,#44841,#44842,
#44843,#44844,#44845,#44846,#44847,#44848,#44849,#44850,#44851,#44852,#44853,
#44854,#44855,#44856,#44857,#44858,#44859,#44860,#44861,#44862,#44863,#44864,
#44865,#44866,#44867,#44868,#44869,#44870,#44871,#44872,#44873,#44874,#44875,
#44876,#44877,#44878,#44879,#44880,#44881,#44882,#44883,#44884,#44885,#44886,
#44887,#44888,#44889,#44890,#44891,#44892,#44893,#44894,#44895,#44896,#44897,
#44898,#44899,#44900,#44901,#44902,#44903,#44904,#44905,#44906,#44907,#44908,
#44909,#44910,#44911,#44912,#44913,#44914,#44915,#44916,#44917,#44918,#44919,
#44920,#44921,#44922,#44923,#44924,#44925,#44926,#44927,#44928,#44929,#44930,
#44931,#44932,#44933,#44934,#44935,#44936,#44937,#44938,#44939,#44940,#44941,
#44942,#44943,#44944,#44945,#44946,#44947,#44948,#44949,#44950,#44951,#44952,
#44953,#44954,#44955,#44956,#44957,#44958,#44959,#44960,#44961,#44962,#44963,
#44964,#44965,#44966,#44967,#44968,#44969,#44970,#44971,#44972,#44973,#44974,
#44975,#44976,#44977,#44978,#44979,#44980,#44981,#44982,#44983,#44984,#44985,
#44986,#44987,#44988,#44989,#44990,#44991,#44992,#44993,#44994,#44995,#44996,
#44997,#44998,#44999,#45000,#45001,#45002,#45003,#45004,#45005,#45006,#45007,
#45008,#45009,#45010,#45011,#45012,#45013,#45014,#45015,#45016,#45017,#45018,
#45019,#45020,#45021),.UNSPECIFIED.,.F.,.F.,(4,3,3,3,3,3,3,3,3,3,3,3,3,
3,3,3,3,3,3,3,3,3,3,3,3,3,3,3,3,3,3,3,3,3,3,3,3,3,3,3,3,3,3,3,3,3,3,3,3,
3,3,3,3,3,3,3,3,3,3,3,3,3,3,3,3,3,3,3,3,3,3,3,4),(380.132711084541,380.22903568211,
380.322609168171,380.420309321493,380.518009474816,380.601748186662,380.685383698029,
380.768936141428,380.852425577279,380.935879527893,381.019316021739,381.102753131494,
381.186208926412,381.269753419141,381.353342502082,381.43706576964,381.517745485536,
381.601484197382,381.685119708749,381.768672152148,381.852161587999,381.935615538612,
382.019052032458,382.102489142214,382.185944937131,382.269489429861,382.353078512802,
382.43680178036,382.517481496256,382.601220208102,382.68485571947,382.768408162868,
382.851897598719,382.935351549333,383.018788043179,383.102225152935,383.185680947853,
383.269225440583,383.352814523524,383.436537791081,383.517217506976,383.600956218822,
383.684591730189,383.768144173588,383.851633609439,383.935087560053,384.018524053899,
384.101961163654,384.185416958572,384.268961451302,384.352550534243,384.4362738018,
384.516953517697,384.600692229543,384.684327740911,384.767880184309,384.85136962016,
384.934823570774,385.01826006462,385.101697174376,385.185152969293,385.268697462023,
385.352286544964,385.436009812522,385.516689528417,385.599356995582,385.681929889722,
385.764427294063,385.846868223446,385.929281659743,386.011676716368,386.094100583877,
386.16406292974),.UNSPECIFIED.);
#295=B_SPLINE_CURVE_WITH_KNOTS('',3,(#45027,#45028,#45029,#45030,#45031,
#45032,#45033,#45034,#45035,#45036,#45037,#45038,#45039,#45040,#45041,#45042,
#45043,#45044,#45045,#45046,#45047,#45048,#45049,#45050,#45051,#45052,#45053,
#45054,#45055,#45056,#45057,#45058,#45059,#45060,#45061,#45062,#45063,#45064,
#45065,#45066,#45067,#45068,#45069,#45070,#45071,#45072,#45073,#45074,#45075,
#45076,#45077,#45078,#45079,#45080,#45081,#45082,#45083,#45084,#45085,#45086,
#45087,#45088,#45089,#45090,#45091,#45092,#45093,#45094,#45095,#45096,#45097,
#45098,#45099,#45100,#45101,#45102,#45103,#45104,#45105,#45106,#45107,#45108,
#45109,#45110,#45111,#45112,#45113,#45114,#45115,#45116,#45117,#45118,#45119,
#45120,#45121,#45122,#45123,#45124,#45125,#45126,#45127,#45128,#45129,#45130,
#45131,#45132,#45133,#45134,#45135,#45136,#45137,#45138,#45139,#45140,#45141,
#45142,#45143,#45144,#45145,#45146,#45147,#45148,#45149,#45150,#45151,#45152,
#45153,#45154,#45155,#45156,#45157,#45158,#45159,#45160,#45161,#45162,#45163,
#45164,#45165,#45166,#45167,#45168,#45169,#45170,#45171,#45172,#45173,#45174,
#45175,#45176,#45177,#45178,#45179,#45180,#45181,#45182,#45183,#45184,#45185,
#45186,#45187,#45188,#45189,#45190,#45191,#45192,#45193,#45194,#45195,#45196,
#45197,#45198,#45199,#45200,#45201,#45202,#45203,#45204,#45205,#45206,#45207,
#45208,#45209,#45210,#45211,#45212,#45213,#45214,#45215,#45216,#45217,#45218,
#45219,#45220,#45221,#45222,#45223,#45224,#45225,#45226,#45227,#45228,#45229,
#45230,#45231,#45232,#45233,#45234,#45235,#45236,#45237,#45238,#45239,#45240,
#45241,#45242,#45243,#45244,#45245,#45246),.UNSPECIFIED.,.F.,.F.,(4,3,3,
3,3,3,3,3,3,3,3,3,3,3,3,3,3,3,3,3,3,3,3,3,3,3,3,3,3,3,3,3,3,3,3,3,3,3,3,
3,3,3,3,3,3,3,3,3,3,3,3,3,3,3,3,3,3,3,3,3,3,3,3,3,3,3,3,3,3,3,3,3,3,4),
(386.415896391665,386.498292671986,386.580622865556,386.662914389823,386.74518752001,
386.827461248823,386.909754567193,386.992133513426,387.074559610852,387.157107949862,
387.205870930141,387.289609641987,387.373245153355,387.456797596753,387.540287032604,
387.623740983218,387.707177477064,387.790614586819,387.874070381737,387.957614874467,
388.041203957408,388.124927224965,388.205606940862,388.289345652708,388.372981164076,
388.456533607474,388.540023043325,388.623476993939,388.706913487785,388.790350597541,
388.873806392459,388.957350885188,389.04093996813,389.124663235687,389.205342951582,
389.289081663428,389.372717174795,389.456269618194,389.539759054044,389.623213004658,
389.706649498504,389.790086608259,389.873542403177,389.957086895907,390.040675978848,
390.124399246405,390.205078962302,390.288817674148,390.372453185516,390.456005628914,
390.539495064766,390.622949015379,390.706385509225,390.789822618981,390.873278413898,
390.956822906628,391.040411989569,391.124135257126,391.204814973022,391.288553684868,
391.372189196236,391.455741639634,391.539231075485,391.622685026098,391.706121519945,
391.7895586297,391.873014424618,391.956558917348,392.040148000289,392.123871267847,
392.204550983742,392.292821373478,392.380892514915,392.448760640207),
 .UNSPECIFIED.);
#296=B_SPLINE_CURVE_WITH_KNOTS('',3,(#45247,#45248,#45249,#45250,#45251,
#45252,#45253,#45254,#45255,#45256),.UNSPECIFIED.,.F.,.F.,(4,3,3,4),(386.164603019142,
386.206134919421,386.323526732866,386.415896391525),.UNSPECIFIED.);
#297=B_SPLINE_CURVE_WITH_KNOTS('',3,(#45258,#45259,#45260,#45261,#45262,
#45263,#45264,#45265,#45266,#45267),.UNSPECIFIED.,.F.,.F.,(4,3,3,4),(386.16406292974,
386.246561874291,386.331229132842,386.415896391393),.UNSPECIFIED.);
#298=B_SPLINE_CURVE_WITH_KNOTS('',3,(#45268,#45269,#45270,#45271,#45272,
#45273,#45274,#45275,#45276,#45277,#45278,#45279,#45280,#45281,#45282,#45283,
#45284,#45285,#45286,#45287,#45288,#45289,#45290,#45291,#45292,#45293,#45294,
#45295,#45296,#45297,#45298,#45299,#45300,#45301,#45302,#45303,#45304,#45305,
#45306,#45307,#45308,#45309,#45310,#45311,#45312,#45313,#45314,#45315,#45316,
#45317,#45318,#45319,#45320,#45321,#45322,#45323,#45324,#45325,#45326,#45327,
#45328,#45329,#45330,#45331,#45332,#45333,#45334,#45335,#45336,#45337,#45338,
#45339,#45340,#45341,#45342,#45343,#45344,#45345,#45346,#45347,#45348,#45349,
#45350,#45351,#45352,#45353,#45354,#45355,#45356,#45357,#45358,#45359,#45360,
#45361,#45362,#45363,#45364,#45365,#45366,#45367,#45368,#45369,#45370,#45371,
#45372,#45373,#45374,#45375,#45376,#45377,#45378,#45379,#45380,#45381,#45382,
#45383,#45384,#45385,#45386,#45387,#45388,#45389,#45390,#45391,#45392,#45393,
#45394,#45395,#45396,#45397,#45398,#45399,#45400,#45401,#45402,#45403,#45404,
#45405,#45406,#45407,#45408,#45409,#45410,#45411,#45412,#45413,#45414,#45415,
#45416,#45417,#45418,#45419,#45420,#45421,#45422,#45423,#45424,#45425,#45426,
#45427,#45428,#45429,#45430,#45431,#45432,#45433,#45434,#45435,#45436,#45437,
#45438,#45439,#45440,#45441,#45442,#45443,#45444,#45445,#45446,#45447,#45448,
#45449,#45450,#45451,#45452,#45453,#45454,#45455,#45456,#45457,#45458,#45459,
#45460,#45461,#45462,#45463,#45464,#45465,#45466,#45467,#45468,#45469,#45470,
#45471,#45472,#45473,#45474,#45475,#45476,#45477,#45478,#45479,#45480,#45481,
#45482,#45483,#45484,#45485,#45486,#45487),.UNSPECIFIED.,.F.,.F.,(4,3,3,
3,3,3,3,3,3,3,3,3,3,3,3,3,3,3,3,3,3,3,3,3,3,3,3,3,3,3,3,3,3,3,3,3,3,3,3,
3,3,3,3,3,3,3,3,3,3,3,3,3,3,3,3,3,3,3,3,3,3,3,3,3,3,3,3,3,3,3,3,3,3,4),
(386.415896391529,386.516425539137,386.600164250983,386.68379976235,386.767352205749,
386.8508416416,386.934295592214,387.01773208606,387.101169195815,387.184624990733,
387.268169483463,387.351758566404,387.435481833961,387.516161549857,387.599900261703,
387.68353577307,387.767088216469,387.85057765232,387.934031602934,388.01746809678,
388.100905206535,388.184361001453,388.267905494183,388.351494577124,388.435217844681,
388.515897560577,388.599636272423,388.68327178379,388.766824227189,388.85031366304,
388.933767613654,389.0172041075,389.100641217255,389.184097012173,389.267641504903,
389.351230587844,389.434953855401,389.515633571297,389.599372283143,389.68300779451,
389.766560237909,389.85004967376,389.933503624373,390.01694011822,390.100377227975,
390.183833022893,390.267377515622,390.350966598563,390.434689866121,390.515369582017,
390.599108293863,390.682743805231,390.766296248629,390.84978568448,390.933239635094,
391.01667612894,391.100113238696,391.183569033614,391.267113526343,391.350702609284,
391.434425876842,391.515105592737,391.59884816637,391.682486653621,391.76604119076,
391.851245732208,391.934696000301,392.01812793045,392.101559594379,392.18808907637,
392.271612247594,392.355180424172,392.438844357499,392.447677522342),
 .UNSPECIFIED.);
#299=B_SPLINE_CURVE_WITH_KNOTS('',3,(#45493,#45494,#45495,#45496,#45497,
#45498,#45499,#45500,#45501,#45502,#45503,#45504,#45505,#45506,#45507,#45508,
#45509,#45510,#45511,#45512,#45513,#45514,#45515,#45516,#45517,#45518,#45519,
#45520,#45521,#45522,#45523,#45524,#45525,#45526,#45527,#45528,#45529,#45530,
#45531,#45532,#45533,#45534,#45535,#45536,#45537,#45538,#45539,#45540,#45541,
#45542,#45543,#45544,#45545,#45546,#45547,#45548,#45549,#45550,#45551,#45552,
#45553,#45554,#45555,#45556,#45557,#45558,#45559,#45560,#45561,#45562,#45563,
#45564,#45565,#45566,#45567,#45568,#45569,#45570,#45571,#45572,#45573,#45574,
#45575,#45576,#45577,#45578,#45579,#45580,#45581,#45582,#45583,#45584,#45585,
#45586,#45587,#45588,#45589,#45590,#45591,#45592,#45593,#45594,#45595,#45596,
#45597,#45598,#45599,#45600,#45601,#45602,#45603,#45604,#45605,#45606,#45607,
#45608,#45609,#45610,#45611,#45612,#45613,#45614,#45615,#45616,#45617,#45618,
#45619,#45620,#45621,#45622,#45623,#45624,#45625,#45626,#45627,#45628,#45629,
#45630,#45631,#45632,#45633,#45634,#45635,#45636,#45637,#45638,#45639,#45640,
#45641,#45642,#45643,#45644,#45645,#45646,#45647,#45648,#45649,#45650,#45651,
#45652,#45653,#45654,#45655,#45656,#45657,#45658,#45659,#45660,#45661,#45662,
#45663,#45664,#45665,#45666,#45667,#45668,#45669,#45670,#45671,#45672,#45673,
#45674,#45675,#45676,#45677,#45678,#45679,#45680,#45681,#45682,#45683,#45684,
#45685,#45686,#45687,#45688,#45689,#45690,#45691,#45692,#45693,#45694,#45695,
#45696,#45697,#45698,#45699,#45700,#45701,#45702,#45703,#45704,#45705,#45706,
#45707,#45708,#45709,#45710,#45711,#45712),.UNSPECIFIED.,.F.,.F.,(4,3,3,
3,3,3,3,3,3,3,3,3,3,3,3,3,3,3,3,3,3,3,3,3,3,3,3,3,3,3,3,3,3,3,3,3,3,3,3,
3,3,3,3,3,3,3,3,3,3,3,3,3,3,3,3,3,3,3,3,3,3,3,3,3,3,3,3,3,3,3,3,3,3,4),
(392.699081698704,392.786294770962,392.873615936636,392.961136976178,393.048762586095,
393.136588210556,393.204286994462,393.288025706308,393.371661217676,393.455213661074,
393.538703096925,393.622157047539,393.705593541386,393.789030651141,393.872486446059,
393.956030938789,394.03962002173,394.123343289288,394.204023005182,394.287761717028,
394.371397228395,394.454949671794,394.538439107645,394.621893058259,394.705329552105,
394.78876666186,394.872222456778,394.955766949508,395.039356032449,395.123079300006,
395.203759015903,395.287497727749,395.371133239117,395.454685682515,395.538175118366,
395.62162906898,395.705065562826,395.788502672582,395.871958467499,395.955502960229,
396.03909204317,396.122815310728,396.203495026623,396.287233738469,396.370869249836,
396.454421693235,396.537911129085,396.621365079699,396.704801573545,396.7882386833,
396.871694478217,396.955238970947,397.038828053888,397.122551321445,397.203231037343,
397.286969749189,397.370605260557,397.454157703955,397.537647139806,397.62110109042,
397.704537584266,397.787974694022,397.871430488939,397.954974981669,398.03856406461,
398.122287332168,398.202967048063,398.285558302687,398.368052705527,398.450469410997,
398.532823591639,398.615141709484,398.697450817903,398.730765351708),
 .UNSPECIFIED.);
#300=B_SPLINE_CURVE_WITH_KNOTS('',3,(#45713,#45714,#45715,#45716,#45717,
#45718,#45719,#45720,#45721,#45722),.UNSPECIFIED.,.F.,.F.,(4,3,3,4),(392.448760640207,
392.536570774805,392.624209454243,392.699081698589),.UNSPECIFIED.);
#301=B_SPLINE_CURVE_WITH_KNOTS('',3,(#45724,#45725,#45726,#45727,#45728,
#45729,#45730,#45731,#45732,#45733),.UNSPECIFIED.,.F.,.F.,(4,3,3,4),(392.447677522342,
392.514841603458,392.64039107027,392.699081698708),.UNSPECIFIED.);
#302=B_SPLINE_CURVE_WITH_KNOTS('',3,(#45734,#45735,#45736,#45737,#45738,
#45739,#45740,#45741,#45742,#45743,#45744,#45745,#45746,#45747,#45748,#45749,
#45750,#45751,#45752,#45753,#45754,#45755,#45756,#45757,#45758,#45759,#45760,
#45761,#45762,#45763,#45764,#45765,#45766,#45767,#45768,#45769,#45770,#45771,
#45772,#45773,#45774,#45775,#45776,#45777,#45778,#45779,#45780,#45781,#45782,
#45783,#45784,#45785,#45786,#45787,#45788,#45789,#45790,#45791,#45792,#45793,
#45794,#45795,#45796,#45797,#45798,#45799,#45800,#45801,#45802,#45803,#45804,
#45805,#45806,#45807,#45808,#45809,#45810,#45811,#45812,#45813,#45814,#45815,
#45816,#45817,#45818,#45819,#45820,#45821,#45822,#45823,#45824,#45825,#45826,
#45827,#45828,#45829,#45830,#45831,#45832,#45833,#45834,#45835,#45836,#45837,
#45838,#45839,#45840,#45841,#45842,#45843,#45844,#45845,#45846,#45847,#45848,
#45849,#45850,#45851,#45852,#45853,#45854,#45855,#45856,#45857,#45858,#45859,
#45860,#45861,#45862,#45863,#45864,#45865,#45866,#45867,#45868,#45869,#45870,
#45871,#45872,#45873,#45874,#45875,#45876,#45877,#45878,#45879,#45880,#45881,
#45882,#45883,#45884,#45885,#45886,#45887,#45888,#45889,#45890,#45891,#45892,
#45893,#45894,#45895,#45896,#45897,#45898,#45899,#45900,#45901,#45902,#45903,
#45904,#45905,#45906,#45907,#45908,#45909,#45910,#45911,#45912,#45913,#45914,
#45915,#45916,#45917,#45918,#45919,#45920,#45921,#45922,#45923,#45924,#45925,
#45926,#45927,#45928,#45929,#45930,#45931,#45932,#45933,#45934,#45935,#45936,
#45937,#45938,#45939,#45940,#45941,#45942,#45943,#45944,#45945,#45946,#45947,
#45948,#45949,#45950,#45951,#45952,#45953),.UNSPECIFIED.,.F.,.F.,(4,3,3,
3,3,3,3,3,3,3,3,3,3,3,3,3,3,3,3,3,3,3,3,3,3,3,3,3,3,3,3,3,3,3,3,3,3,3,3,
3,3,3,3,3,3,3,3,3,3,3,3,3,3,3,3,3,3,3,3,3,3,3,3,3,3,3,3,3,3,3,3,3,3,4),
(392.699081698853,392.781444927998,392.863734765316,392.945976253879,393.028192836073,
393.110403546445,393.192627412544,393.274933280105,393.357280588535,393.439757053061,
393.514577614178,393.598316326024,393.681951837391,393.76550428079,393.848993716641,
393.932447667255,394.015884161101,394.099321270857,394.182777065774,394.266321558504,
394.349910641445,394.433633909003,394.514313624898,394.598052336744,394.681687848111,
394.76524029151,394.848729727361,394.932183677975,395.015620171821,395.099057281577,
395.182513076495,395.266057569224,395.349646652165,395.433369919723,395.514049635618,
395.597788347464,395.681423858831,395.76497630223,395.84846573808,395.931919688694,
396.01535618254,396.098793292295,396.182249087213,396.265793579943,396.349382662884,
396.433105930441,396.513785646338,396.597524358184,396.681159869552,396.76471231295,
396.848201748802,396.931655699415,397.015092193261,397.098529303017,397.181985097934,
397.265529590664,397.349118673605,397.432841941162,397.513521657058,397.597260368904,
397.680895880271,397.76444832367,397.847937759521,397.931391710135,398.014828203981,
398.098265313736,398.181721108654,398.265265601384,398.348854684324,398.432577951882,
398.513257667778,398.602638396779,398.691803625613,398.731964690749),
 .UNSPECIFIED.);
#303=B_SPLINE_CURVE_WITH_KNOTS('',3,(#45959,#45960,#45961,#45962,#45963,
#45964,#45965,#45966,#45967,#45968,#45969,#45970,#45971,#45972,#45973,#45974,
#45975,#45976,#45977,#45978,#45979,#45980,#45981,#45982,#45983,#45984,#45985,
#45986,#45987,#45988,#45989,#45990,#45991,#45992,#45993,#45994,#45995,#45996,
#45997,#45998,#45999,#46000,#46001,#46002,#46003,#46004,#46005,#46006,#46007,
#46008,#46009,#46010,#46011,#46012,#46013,#46014,#46015,#46016,#46017,#46018,
#46019,#46020,#46021,#46022,#46023,#46024,#46025,#46026,#46027,#46028,#46029,
#46030,#46031,#46032,#46033,#46034,#46035,#46036,#46037,#46038,#46039,#46040,
#46041,#46042,#46043,#46044,#46045,#46046,#46047,#46048,#46049,#46050,#46051,
#46052,#46053,#46054,#46055,#46056,#46057,#46058,#46059,#46060,#46061,#46062,
#46063,#46064,#46065,#46066,#46067,#46068,#46069,#46070,#46071,#46072,#46073,
#46074,#46075,#46076,#46077,#46078,#46079,#46080,#46081,#46082,#46083,#46084,
#46085,#46086,#46087,#46088,#46089,#46090,#46091,#46092,#46093,#46094,#46095,
#46096,#46097,#46098,#46099,#46100,#46101,#46102,#46103,#46104,#46105,#46106,
#46107,#46108,#46109,#46110,#46111,#46112,#46113,#46114,#46115,#46116,#46117,
#46118,#46119,#46120,#46121,#46122,#46123,#46124,#46125,#46126,#46127,#46128,
#46129,#46130,#46131,#46132,#46133,#46134,#46135,#46136,#46137,#46138,#46139,
#46140,#46141,#46142,#46143,#46144,#46145,#46146,#46147,#46148,#46149,#46150,
#46151,#46152,#46153,#46154,#46155,#46156,#46157,#46158,#46159,#46160,#46161,
#46162,#46163,#46164,#46165,#46166,#46167,#46168,#46169,#46170,#46171,#46172,
#46173,#46174,#46175),.UNSPECIFIED.,.F.,.F.,(4,3,3,3,3,3,3,3,3,3,3,3,3,
3,3,3,3,3,3,3,3,3,3,3,3,3,3,3,3,3,3,3,3,3,3,3,3,3,3,3,3,3,3,3,3,3,3,3,3,
3,3,3,3,3,3,3,3,3,3,3,3,3,3,3,3,3,3,3,3,3,3,3,4),(398.982267005884,399.096939683955,
399.202703058783,399.286441770629,399.370077281996,399.453629725395,399.537119161246,
399.62057311186,399.704009605706,399.787446715462,399.870902510379,399.954447003109,
400.03803608605,400.121759353607,400.202439069503,400.286177781349,400.369813292716,
400.453365736115,400.536855171966,400.620309122579,400.703745616426,400.787182726181,
400.870638521099,400.954183013828,401.037772096769,401.121495364327,401.202175080223,
401.285913792069,401.369549303436,401.453101746835,401.536591182686,401.6200451333,
401.703481627146,401.786918736901,401.870374531819,401.953919024549,402.03750810749,
402.121231375048,402.201911090943,402.285649802789,402.369285314157,402.452837757555,
402.536327193406,402.61978114402,402.703217637866,402.786654747622,402.870110542539,
402.953655035269,403.03724411821,403.120967385768,403.201647101664,403.28538581351,
403.369021324878,403.452573768276,403.536063204127,403.619517154741,403.702953648587,
403.786390758343,403.869846553261,403.95339104599,404.036980128931,404.120703396489,
404.201383112384,404.285133097471,404.368777410752,404.452320898675,404.535807222286,
404.619254501399,404.702680825663,404.786130409931,404.86959072302,404.953119819031,
405.013792313897),.UNSPECIFIED.);
#304=B_SPLINE_CURVE_WITH_KNOTS('',3,(#46176,#46177,#46178,#46179,#46180,
#46181,#46182,#46183,#46184,#46185),.UNSPECIFIED.,.F.,.F.,(4,3,3,4),(398.730765351708,
398.813104217448,398.897685611592,398.982267005735),.UNSPECIFIED.);
#305=B_SPLINE_CURVE_WITH_KNOTS('',3,(#46187,#46188,#46189,#46190,#46191,
#46192,#46193,#46194,#46195,#46196),.UNSPECIFIED.,.F.,.F.,(4,3,3,4),(398.731964690749,
398.820853398844,398.909519059497,398.982267005757),.UNSPECIFIED.);
#306=B_SPLINE_CURVE_WITH_KNOTS('',3,(#46197,#46198,#46199,#46200,#46201,
#46202,#46203,#46204,#46205,#46206,#46207,#46208,#46209,#46210,#46211,#46212,
#46213,#46214,#46215,#46216,#46217,#46218,#46219,#46220,#46221,#46222,#46223,
#46224,#46225,#46226,#46227,#46228,#46229,#46230,#46231,#46232,#46233,#46234,
#46235,#46236,#46237,#46238,#46239,#46240,#46241,#46242,#46243,#46244,#46245,
#46246,#46247,#46248,#46249,#46250,#46251,#46252,#46253,#46254,#46255,#46256,
#46257,#46258,#46259,#46260,#46261,#46262,#46263,#46264,#46265,#46266,#46267,
#46268,#46269,#46270,#46271,#46272,#46273,#46274,#46275,#46276,#46277,#46278,
#46279,#46280,#46281,#46282,#46283,#46284,#46285,#46286,#46287,#46288,#46289,
#46290,#46291,#46292,#46293,#46294,#46295,#46296,#46297,#46298,#46299,#46300,
#46301,#46302,#46303,#46304,#46305,#46306,#46307,#46308,#46309,#46310,#46311,
#46312,#46313,#46314,#46315,#46316,#46317,#46318,#46319,#46320,#46321,#46322,
#46323,#46324,#46325,#46326,#46327,#46328,#46329,#46330,#46331,#46332,#46333,
#46334,#46335,#46336,#46337,#46338,#46339,#46340,#46341,#46342,#46343,#46344,
#46345,#46346,#46347,#46348,#46349,#46350,#46351,#46352,#46353,#46354,#46355,
#46356,#46357,#46358,#46359,#46360,#46361,#46362,#46363,#46364,#46365,#46366,
#46367,#46368,#46369,#46370,#46371,#46372,#46373,#46374,#46375,#46376,#46377,
#46378,#46379,#46380,#46381,#46382,#46383,#46384,#46385,#46386,#46387,#46388,
#46389,#46390,#46391,#46392,#46393,#46394,#46395,#46396,#46397,#46398,#46399,
#46400,#46401,#46402,#46403,#46404,#46405,#46406,#46407,#46408,#46409,#46410,
#46411,#46412,#46413),.UNSPECIFIED.,.F.,.F.,(4,3,3,3,3,3,3,3,3,3,3,3,3,
3,3,3,3,3,3,3,3,3,3,3,3,3,3,3,3,3,3,3,3,3,3,3,3,3,3,3,3,3,3,3,3,3,3,3,3,
3,3,3,3,3,3,3,3,3,3,3,3,3,3,3,3,3,3,3,3,3,3,3,4),(398.982267005888,399.068634116483,
399.15507990689,399.244558349792,399.331262275071,399.422127976785,399.512993678499,
399.596732390345,399.680367901713,399.763920345111,399.847409780962,399.930863731576,
400.014300225422,400.097737335178,400.181193130095,400.264737622825,400.348326705766,
400.432049973324,400.512729689219,400.596468401065,400.680103912432,400.763656355831,
400.847145791682,400.930599742295,401.014036236142,401.097473345897,401.180929140815,
401.264473633545,401.348062716486,401.431785984043,401.512465699939,401.596204411785,
401.679839923152,401.763392366551,401.846881802402,401.930335753016,402.013772246862,
402.097209356618,402.180665151535,402.264209644265,402.347798727206,402.431521994764,
402.512201710659,402.595940422505,402.679575933872,402.763128377271,402.846617813121,
402.930071763735,403.013508257581,403.096945367337,403.180401162255,403.263945654985,
403.347534737926,403.431258005483,403.511937721379,403.595676433225,403.679311944592,
403.762864387991,403.846353823842,403.929807774456,404.013244268302,404.096681378057,
404.180137172975,404.263681665705,404.347270748646,404.430994016203,404.511673732099,
404.594412336844,404.677052902557,404.761307047535,404.84380176223,404.92893562235,
405.014069482469),.UNSPECIFIED.);
#307=B_SPLINE_CURVE_WITH_KNOTS('',3,(#46419,#46420,#46421,#46422,#46423,
#46424,#46425,#46426,#46427,#46428,#46429,#46430,#46431,#46432,#46433,#46434,
#46435,#46436,#46437,#46438,#46439,#46440,#46441,#46442,#46443,#46444,#46445,
#46446,#46447,#46448,#46449,#46450,#46451,#46452,#46453,#46454,#46455,#46456,
#46457,#46458,#46459,#46460,#46461,#46462,#46463,#46464,#46465,#46466,#46467,
#46468,#46469,#46470,#46471,#46472,#46473,#46474,#46475,#46476,#46477,#46478,
#46479,#46480,#46481,#46482,#46483,#46484,#46485,#46486,#46487,#46488,#46489,
#46490,#46491,#46492,#46493,#46494,#46495,#46496,#46497,#46498,#46499,#46500,
#46501,#46502,#46503,#46504,#46505,#46506,#46507,#46508,#46509,#46510,#46511,
#46512,#46513,#46514,#46515,#46516,#46517,#46518,#46519,#46520,#46521,#46522,
#46523,#46524,#46525,#46526,#46527,#46528,#46529,#46530,#46531,#46532,#46533,
#46534,#46535,#46536,#46537,#46538,#46539,#46540,#46541,#46542,#46543,#46544,
#46545,#46546,#46547,#46548,#46549,#46550,#46551,#46552,#46553,#46554,#46555,
#46556,#46557,#46558,#46559,#46560,#46561,#46562,#46563,#46564,#46565,#46566,
#46567,#46568,#46569,#46570,#46571,#46572,#46573,#46574,#46575,#46576,#46577,
#46578,#46579,#46580,#46581,#46582,#46583,#46584,#46585,#46586,#46587,#46588,
#46589,#46590,#46591,#46592,#46593,#46594,#46595,#46596,#46597,#46598,#46599,
#46600,#46601,#46602,#46603,#46604,#46605,#46606,#46607,#46608,#46609,#46610,
#46611,#46612,#46613,#46614,#46615,#46616,#46617,#46618,#46619,#46620,#46621,
#46622,#46623,#46624,#46625,#46626,#46627,#46628,#46629,#46630,#46631,#46632,
#46633,#46634,#46635,#46636,#46637,#46638),.UNSPECIFIED.,.F.,.F.,(4,3,3,
3,3,3,3,3,3,3,3,3,3,3,3,3,3,3,3,3,3,3,3,3,3,3,3,3,3,3,3,3,3,3,3,3,3,3,3,
3,3,3,3,3,3,3,3,3,3,3,3,3,3,3,3,3,3,3,3,3,3,3,3,3,3,3,3,3,3,3,3,3,3,4),
(405.26545231318,405.348387801783,405.431225006267,405.513984784103,405.599843577818,
405.682519331484,405.765185411802,405.847860544578,405.930563459232,406.01335713532,
406.096204823849,406.179168760872,406.200855133824,406.28459384567,406.368229357037,
406.451781800436,406.535271236287,406.618725186901,406.702161680747,406.785598790502,
406.869054585419,406.952599078149,407.03618816109,407.119911428648,407.200591144544,
407.28432985639,407.367965367757,407.451517811156,407.535007247006,407.61846119762,
407.701897691466,407.785334801222,407.868790596139,407.952335088869,408.03592417181,
408.119647439367,408.200327155264,408.28406586711,408.367701378477,408.451253821876,
408.534743257727,408.61819720834,408.701633702187,408.785070811942,408.86852660686,
408.952071099589,409.03566018253,409.119383450088,409.200063165984,409.28380187783,
409.367437389197,409.450989832596,409.534479268446,409.61793321906,409.701369712907,
409.784806822662,409.86826261758,409.951807110309,410.03539619325,410.119119460808,
410.199799176704,410.28353788855,410.367173399917,410.450725843316,410.534215279167,
410.61766922978,410.701105723627,410.784542833382,410.867998628299,410.951543121029,
411.03513220397,411.118855471527,411.199535187425,411.298100148351),
 .UNSPECIFIED.);
#308=B_SPLINE_CURVE_WITH_KNOTS('',3,(#46639,#46640,#46641,#46642,#46643,
#46644,#46645,#46646,#46647,#46648,#46649,#46650,#46651),.UNSPECIFIED.,
 .F.,.F.,(4,3,3,3,4),(405.013792313897,405.097423948019,405.181172835758,
405.201119123104,405.265452313063),.UNSPECIFIED.);
#309=B_SPLINE_CURVE_WITH_KNOTS('',3,(#46653,#46654,#46655,#46656,#46657,
#46658,#46659,#46660,#46661,#46662),.UNSPECIFIED.,.F.,.F.,(4,3,3,4),(405.014069482469,
405.096536027737,405.180994170402,405.265452313067),.UNSPECIFIED.);
#310=B_SPLINE_CURVE_WITH_KNOTS('',3,(#46663,#46664,#46665,#46666,#46667,
#46668,#46669,#46670,#46671,#46672,#46673,#46674,#46675,#46676,#46677,#46678,
#46679,#46680,#46681,#46682,#46683,#46684,#46685,#46686,#46687,#46688,#46689,
#46690,#46691,#46692,#46693,#46694,#46695,#46696,#46697,#46698,#46699,#46700,
#46701,#46702,#46703,#46704,#46705,#46706,#46707,#46708,#46709,#46710,#46711,
#46712,#46713,#46714,#46715,#46716,#46717,#46718,#46719,#46720,#46721,#46722,
#46723,#46724,#46725,#46726,#46727,#46728,#46729,#46730,#46731,#46732,#46733,
#46734,#46735,#46736,#46737,#46738,#46739,#46740,#46741,#46742,#46743,#46744,
#46745,#46746,#46747,#46748,#46749,#46750,#46751,#46752,#46753,#46754,#46755,
#46756,#46757,#46758,#46759,#46760,#46761,#46762,#46763,#46764,#46765,#46766,
#46767,#46768,#46769,#46770,#46771,#46772,#46773,#46774,#46775,#46776,#46777,
#46778,#46779,#46780,#46781,#46782,#46783,#46784,#46785,#46786,#46787,#46788,
#46789,#46790,#46791,#46792,#46793,#46794,#46795,#46796,#46797,#46798,#46799,
#46800,#46801,#46802,#46803,#46804,#46805,#46806,#46807,#46808,#46809,#46810,
#46811,#46812,#46813,#46814,#46815,#46816,#46817,#46818,#46819,#46820,#46821,
#46822,#46823,#46824,#46825,#46826,#46827,#46828,#46829,#46830,#46831,#46832,
#46833,#46834,#46835,#46836,#46837,#46838,#46839,#46840,#46841,#46842,#46843,
#46844,#46845,#46846,#46847,#46848,#46849,#46850,#46851,#46852,#46853,#46854,
#46855,#46856,#46857,#46858,#46859,#46860,#46861,#46862,#46863,#46864,#46865,
#46866,#46867,#46868,#46869,#46870,#46871,#46872,#46873,#46874,#46875,#46876,
#46877,#46878,#46879,#46880,#46881,#46882),.UNSPECIFIED.,.F.,.F.,(4,3,3,
3,3,3,3,3,3,3,3,3,3,3,3,3,3,3,3,3,3,3,3,3,3,3,3,3,3,3,3,3,3,3,3,3,3,3,3,
3,3,3,3,3,3,3,3,3,3,3,3,3,3,3,3,3,3,3,3,3,3,3,3,3,3,3,3,3,3,3,3,3,3,4),
(405.265452313201,405.373358109382,405.483824806747,405.511409742819,405.595148454665,
405.678783966033,405.762336409431,405.845825845283,405.929279795896,406.012716289743,
406.096153399498,406.179609194416,406.263153687146,406.346742770087,406.430466037645,
406.511145753539,406.594884465385,406.678519976753,406.762072420151,406.845561856002,
406.929015806616,407.012452300462,407.095889410218,407.179345205135,407.262889697865,
407.346478780806,407.430202048364,407.51088176426,407.594620476106,407.678255987474,
407.761808430872,407.845297866723,407.928751817337,408.012188311183,408.095625420938,
408.179081215856,408.262625708586,408.346214791527,408.429938059084,408.51061777498,
408.594356486826,408.677991998193,408.761544441592,408.845033877443,408.928487828057,
409.011924321903,409.095361431658,409.178817226576,409.262361719306,409.345950802247,
409.429674069804,409.5103537857,409.594092497546,409.677728008913,409.761280452312,
409.844769888163,409.928223838776,410.011660332623,410.095097442378,410.178553237296,
410.262097730026,410.345686812966,410.429410080524,410.51008979642,410.593841439003,
410.681732668085,410.765273320821,410.848757253055,410.932202583627,411.015627401392,
411.099071652666,411.182527263906,411.266040390765,411.296971271658),
 .UNSPECIFIED.);
#311=B_SPLINE_CURVE_WITH_KNOTS('',3,(#46888,#46889,#46890,#46891,#46892,
#46893,#46894,#46895,#46896,#46897,#46898,#46899,#46900,#46901,#46902,#46903,
#46904,#46905,#46906,#46907,#46908,#46909,#46910,#46911,#46912,#46913,#46914,
#46915,#46916,#46917,#46918,#46919,#46920,#46921,#46922,#46923,#46924,#46925,
#46926,#46927,#46928,#46929,#46930,#46931,#46932,#46933,#46934,#46935,#46936,
#46937,#46938,#46939,#46940,#46941,#46942,#46943,#46944,#46945,#46946,#46947,
#46948,#46949,#46950,#46951,#46952,#46953,#46954,#46955,#46956,#46957,#46958,
#46959,#46960,#46961,#46962,#46963,#46964,#46965,#46966,#46967,#46968,#46969,
#46970,#46971,#46972,#46973,#46974,#46975,#46976,#46977,#46978,#46979,#46980,
#46981,#46982,#46983,#46984,#46985,#46986,#46987,#46988,#46989,#46990,#46991,
#46992,#46993,#46994,#46995,#46996,#46997,#46998,#46999,#47000,#47001,#47002,
#47003,#47004,#47005,#47006,#47007,#47008,#47009,#47010,#47011,#47012,#47013,
#47014,#47015,#47016,#47017,#47018,#47019,#47020,#47021,#47022,#47023,#47024,
#47025,#47026,#47027,#47028,#47029,#47030,#47031,#47032,#47033,#47034,#47035,
#47036,#47037,#47038,#47039,#47040,#47041,#47042,#47043,#47044,#47045,#47046,
#47047,#47048,#47049,#47050,#47051,#47052,#47053,#47054,#47055,#47056,#47057,
#47058,#47059,#47060,#47061,#47062,#47063,#47064,#47065,#47066,#47067,#47068,
#47069,#47070,#47071,#47072,#47073,#47074,#47075,#47076,#47077,#47078,#47079,
#47080,#47081,#47082,#47083,#47084,#47085,#47086,#47087,#47088,#47089,#47090,
#47091,#47092,#47093,#47094,#47095,#47096,#47097,#47098,#47099,#47100,#47101,
#47102,#47103,#47104,#47105,#47106,#47107),.UNSPECIFIED.,.F.,.F.,(4,3,3,
3,3,3,3,3,3,3,3,3,3,3,3,3,3,3,3,3,3,3,3,3,3,3,3,3,3,3,3,3,3,3,3,3,3,3,3,
3,3,3,3,3,3,3,3,3,3,3,3,3,3,3,3,3,3,3,3,3,3,3,3,3,3,3,3,3,3,3,3,3,3,4),
(411.548637620243,411.632259103847,411.715874533125,411.799501689164,411.883158356806,
411.966915847641,412.050726888138,412.134675892978,412.199271198145,412.283009909991,
412.366645421358,412.450197864757,412.533687300608,412.617141251222,412.700577745068,
412.784014854823,412.867470649741,412.95101514247,413.034604225411,413.118327492969,
413.199007208865,413.282745920711,413.366381432078,413.449933875477,413.533423311328,
413.616877261941,413.700313755788,413.783750865543,413.867206660461,413.95075115319,
414.034340236131,414.118063503689,414.198743219585,414.282481931431,414.366117442798,
414.449669886197,414.533159322048,414.616613272662,414.700049766508,414.783486876264,
414.866942671182,414.950487163911,415.034076246852,415.11779951441,415.198479230305,
415.282217942151,415.365853453518,415.449405896917,415.532895332768,415.616349283381,
415.699785777228,415.783222886983,415.866678681901,415.950223174631,416.033812257572,
416.117535525129,416.198215241025,416.281953952871,416.365589464238,416.449141907637,
416.532631343488,416.616085294102,416.699521787948,416.782958897703,416.866414692621,
416.94995918535,417.033548268291,417.117271535849,417.197951251745,417.282231215125,
417.366369980425,417.450427359457,417.534406239268,417.581050393302),
 .UNSPECIFIED.);
#312=B_SPLINE_CURVE_WITH_KNOTS('',3,(#47108,#47109,#47110,#47111,#47112,
#47113,#47114,#47115,#47116,#47117),.UNSPECIFIED.,.F.,.F.,(4,3,3,4),(411.298100148351,
411.394649529236,411.490471997343,411.548637620046),.UNSPECIFIED.);
#313=B_SPLINE_CURVE_WITH_KNOTS('',3,(#47119,#47120,#47121,#47122,#47123,
#47124,#47125,#47126,#47127,#47128,#47129,#47130,#47131),.UNSPECIFIED.,
 .F.,.F.,(4,3,3,3,4),(411.296971271658,411.380583957771,411.464320780643,
411.50982580714,411.548637620247),.UNSPECIFIED.);
#314=B_SPLINE_CURVE_WITH_KNOTS('',3,(#47132,#47133,#47134,#47135,#47136,
#47137,#47138,#47139,#47140,#47141,#47142,#47143,#47144,#47145,#47146,#47147,
#47148,#47149,#47150,#47151,#47152,#47153,#47154,#47155,#47156,#47157,#47158,
#47159,#47160,#47161,#47162,#47163,#47164,#47165,#47166,#47167,#47168,#47169,
#47170,#47171,#47172,#47173,#47174,#47175,#47176,#47177,#47178,#47179,#47180,
#47181,#47182,#47183,#47184,#47185,#47186,#47187,#47188,#47189,#47190,#47191,
#47192,#47193,#47194,#47195,#47196,#47197,#47198,#47199,#47200,#47201,#47202,
#47203,#47204,#47205,#47206,#47207,#47208,#47209,#47210,#47211,#47212,#47213,
#47214,#47215,#47216,#47217,#47218,#47219,#47220,#47221,#47222,#47223,#47224,
#47225,#47226,#47227,#47228,#47229,#47230,#47231,#47232,#47233,#47234,#47235,
#47236,#47237,#47238,#47239,#47240,#47241,#47242,#47243,#47244,#47245,#47246,
#47247,#47248,#47249,#47250,#47251,#47252,#47253,#47254,#47255,#47256,#47257,
#47258,#47259,#47260,#47261,#47262,#47263,#47264,#47265,#47266,#47267,#47268,
#47269,#47270,#47271,#47272,#47273,#47274,#47275,#47276,#47277,#47278,#47279,
#47280,#47281,#47282,#47283,#47284,#47285,#47286,#47287,#47288,#47289,#47290,
#47291,#47292,#47293,#47294,#47295,#47296,#47297,#47298,#47299,#47300,#47301,
#47302,#47303,#47304,#47305,#47306,#47307,#47308,#47309,#47310,#47311,#47312,
#47313,#47314,#47315,#47316,#47317,#47318,#47319,#47320,#47321,#47322,#47323,
#47324,#47325,#47326,#47327,#47328,#47329,#47330,#47331,#47332,#47333,#47334,
#47335,#47336,#47337,#47338,#47339,#47340,#47341,#47342,#47343,#47344,#47345,
#47346,#47347,#47348,#47349,#47350,#47351),.UNSPECIFIED.,.F.,.F.,(4,3,3,
3,3,3,3,3,3,3,3,3,3,3,3,3,3,3,3,3,3,3,3,3,3,3,3,3,3,3,3,3,3,3,3,3,3,3,3,
3,3,3,3,3,3,3,3,3,3,3,3,3,3,3,3,3,3,3,3,3,3,3,3,3,3,3,3,3,3,3,3,3,3,4),
(411.548637620412,411.631849527888,411.714960257177,411.797990449943,411.880960671604,
411.963899820013,412.04682518702,412.129755301074,412.212708690519,412.295751530242,
412.378843954004,412.462060135133,412.50956181786,412.593300529706,412.676936041073,
412.760488484472,412.843977920323,412.927431870936,413.010868364783,413.094305474538,
413.177761269456,413.261305762185,413.344894845126,413.428618112684,413.50929782858,
413.593036540426,413.676672051794,413.760224495192,413.843713931043,413.927167881657,
414.010604375504,414.094041485259,414.177497280177,414.261041772907,414.344630855848,
414.428354123405,414.509033839301,414.592772551147,414.676408062515,414.759960505913,
414.843449941764,414.926903892378,415.010340386224,415.09377749598,415.177233290898,
415.260777783627,415.344366866568,415.428090134126,415.508769850021,415.592508561867,
415.676144073234,415.759696516633,415.843185952484,415.926639903097,416.010076396944,
416.093513506699,416.176969301617,416.260513794347,416.344102877288,416.427826144845,
416.508505860741,416.592244572587,416.675880083955,416.759432527353,416.842921963204,
416.926375913817,417.009812407664,417.093249517419,417.176705312336,417.260249805066,
417.343838888007,417.427562155565,417.508241871461,417.581170651204),
 .UNSPECIFIED.);
#315=B_SPLINE_CURVE_WITH_KNOTS('',3,(#47357,#47358,#47359,#47360,#47361,
#47362,#47363,#47364,#47365,#47366,#47367,#47368,#47369,#47370,#47371,#47372,
#47373,#47374,#47375,#47376,#47377,#47378,#47379,#47380,#47381,#47382,#47383,
#47384,#47385,#47386,#47387,#47388,#47389,#47390,#47391,#47392,#47393,#47394,
#47395,#47396,#47397,#47398,#47399,#47400,#47401,#47402,#47403,#47404,#47405,
#47406,#47407,#47408,#47409,#47410,#47411,#47412,#47413,#47414,#47415,#47416,
#47417,#47418,#47419,#47420,#47421,#47422,#47423,#47424,#47425,#47426,#47427,
#47428,#47429,#47430,#47431,#47432,#47433,#47434,#47435,#47436,#47437,#47438,
#47439,#47440,#47441,#47442,#47443,#47444,#47445,#47446,#47447,#47448,#47449,
#47450,#47451,#47452,#47453,#47454,#47455,#47456,#47457,#47458,#47459,#47460,
#47461,#47462,#47463,#47464,#47465,#47466,#47467,#47468,#47469,#47470,#47471,
#47472,#47473,#47474,#47475,#47476,#47477,#47478,#47479,#47480,#47481,#47482,
#47483,#47484,#47485,#47486,#47487,#47488,#47489,#47490,#47491,#47492,#47493,
#47494,#47495,#47496,#47497,#47498,#47499,#47500,#47501,#47502,#47503,#47504,
#47505,#47506,#47507,#47508,#47509,#47510,#47511,#47512,#47513,#47514,#47515,
#47516,#47517,#47518,#47519,#47520,#47521,#47522,#47523,#47524,#47525,#47526,
#47527,#47528,#47529,#47530,#47531,#47532,#47533,#47534,#47535,#47536,#47537,
#47538,#47539,#47540,#47541,#47542,#47543,#47544,#47545,#47546,#47547,#47548,
#47549,#47550,#47551,#47552,#47553,#47554,#47555,#47556,#47557,#47558,#47559,
#47560,#47561,#47562,#47563,#47564,#47565,#47566,#47567,#47568,#47569,#47570,
#47571,#47572,#47573),.UNSPECIFIED.,.F.,.F.,(4,3,3,3,3,3,3,3,3,3,3,3,3,
3,3,3,3,3,3,3,3,3,3,3,3,3,3,3,3,3,3,3,3,3,3,3,3,3,3,3,3,3,3,3,3,3,3,3,3,
3,3,3,3,3,3,3,3,3,3,3,3,3,3,3,3,3,3,3,3,3,3,3,4),(417.831822927619,417.926420867418,
418.021417477909,418.116960905954,418.197687262465,418.281425974311,418.365061485678,
418.448613929077,418.532103364928,418.615557315542,418.698993809388,418.782430919143,
418.865886714061,418.949431206791,419.033020289732,419.116743557289,419.197423273186,
419.281161985032,419.364797496399,419.448349939798,419.531839375649,419.615293326263,
419.698729820109,419.782166929864,419.865622724782,419.949167217512,420.032756300453,
420.116479568011,420.197159283906,420.280897995752,420.364533507119,420.448085950518,
420.531575386369,420.615029336983,420.698465830829,420.781902940584,420.865358735502,
420.948903228232,421.032492311173,421.11621557873,421.196895294626,421.280634006472,
421.364269517839,421.447821961238,421.531311397089,421.614765347703,421.698201841549,
421.781638951304,421.865094746222,421.948639238952,422.032228321893,422.11595158945,
422.196631305346,422.280370017192,422.364005528559,422.447557971958,422.531047407809,
422.614501358423,422.697937852269,422.781374962024,422.864830756942,422.948375249672,
423.031964332613,423.11568760017,423.196367316066,423.27971783058,423.362420771565,
423.445048292511,423.527619318683,423.611507347057,423.694033766242,423.77860259921,
423.863171432179),.UNSPECIFIED.);
#316=B_SPLINE_CURVE_WITH_KNOTS('',3,(#47574,#47575,#47576,#47577,#47578,
#47579,#47580,#47581,#47582,#47583),.UNSPECIFIED.,.F.,.F.,(4,3,3,4),(417.581050393302,
417.664959549787,417.748862132102,417.831822927422),.UNSPECIFIED.);
#317=B_SPLINE_CURVE_WITH_KNOTS('',3,(#47585,#47586,#47587,#47588,#47589,
#47590,#47591,#47592,#47593,#47594),.UNSPECIFIED.,.F.,.F.,(4,3,3,4),(417.581170651204,
417.680212608396,417.778300546283,417.831822927248),.UNSPECIFIED.);
#318=B_SPLINE_CURVE_WITH_KNOTS('',3,(#47595,#47596,#47597,#47598,#47599,
#47600,#47601,#47602,#47603,#47604,#47605,#47606,#47607,#47608,#47609,#47610,
#47611,#47612,#47613,#47614,#47615,#47616,#47617,#47618,#47619,#47620,#47621,
#47622,#47623,#47624,#47625,#47626,#47627,#47628,#47629,#47630,#47631,#47632,
#47633,#47634,#47635,#47636,#47637,#47638,#47639,#47640,#47641,#47642,#47643,
#47644,#47645,#47646,#47647,#47648,#47649,#47650,#47651,#47652,#47653,#47654,
#47655,#47656,#47657,#47658,#47659,#47660,#47661,#47662,#47663,#47664,#47665,
#47666,#47667,#47668,#47669,#47670,#47671,#47672,#47673,#47674,#47675,#47676,
#47677,#47678,#47679,#47680,#47681,#47682,#47683,#47684,#47685,#47686,#47687,
#47688,#47689,#47690,#47691,#47692,#47693,#47694,#47695,#47696,#47697,#47698,
#47699,#47700,#47701,#47702,#47703,#47704,#47705,#47706,#47707,#47708,#47709,
#47710,#47711,#47712,#47713,#47714,#47715,#47716,#47717,#47718,#47719,#47720,
#47721,#47722,#47723,#47724,#47725,#47726,#47727,#47728,#47729,#47730,#47731,
#47732,#47733,#47734,#47735,#47736,#47737,#47738,#47739,#47740,#47741,#47742,
#47743,#47744,#47745,#47746,#47747,#47748,#47749,#47750,#47751,#47752,#47753,
#47754,#47755,#47756,#47757,#47758,#47759,#47760,#47761,#47762,#47763,#47764,
#47765,#47766,#47767,#47768,#47769,#47770,#47771,#47772,#47773,#47774,#47775,
#47776,#47777,#47778,#47779,#47780,#47781,#47782,#47783,#47784,#47785,#47786,
#47787,#47788,#47789,#47790,#47791,#47792,#47793,#47794,#47795,#47796,#47797,
#47798,#47799,#47800,#47801,#47802,#47803,#47804,#47805,#47806,#47807,#47808,
#47809,#47810,#47811,#47812,#47813,#47814),.UNSPECIFIED.,.F.,.F.,(4,3,3,
3,3,3,3,3,3,3,3,3,3,3,3,3,3,3,3,3,3,3,3,3,3,3,3,3,3,3,3,3,3,3,3,3,3,3,3,
3,3,3,3,3,3,3,3,3,3,3,3,3,3,3,3,3,3,3,3,3,3,3,3,3,3,3,3,3,3,3,3,3,3,4),
(417.831822927426,417.91634229677,417.999579653168,418.082817834537,418.166075045188,
418.251550754437,418.334946674687,418.421462278434,418.507977882181,418.591716594027,
418.675352105395,418.758904548793,418.842393984644,418.925847935258,419.009284429104,
419.09272153886,419.176177333777,419.259721826507,419.343310909448,419.427034177006,
419.507713892901,419.591452604747,419.675088116114,419.758640559513,419.842129995364,
419.925583945977,420.009020439824,420.092457549579,420.175913344497,420.259457837226,
420.343046920168,420.426770187725,420.507449903621,420.591188615467,420.674824126834,
420.758376570233,420.841866006084,420.925319956698,421.008756450544,421.092193560299,
421.175649355217,421.259193847946,421.342782930887,421.426506198445,421.507185914341,
421.590924626187,421.674560137555,421.758112580953,421.841602016804,421.925055967418,
422.008492461264,422.09192957102,422.175385365938,422.258929858667,422.342518941608,
422.426242209166,422.506921925062,422.590660636908,422.674296148276,422.757848591675,
422.841338027526,422.924791978139,423.008228471986,423.091665581741,423.175121376659,
423.258665869388,423.34225495233,423.425978219887,423.506657935782,423.591469649572,
423.676133771211,423.760712027502,423.845204064411,423.864352866444),
 .UNSPECIFIED.);
#319=B_SPLINE_CURVE_WITH_KNOTS('',3,(#47820,#47821,#47822,#47823,#47824,
#47825,#47826,#47827,#47828,#47829,#47830,#47831,#47832,#47833,#47834,#47835,
#47836,#47837,#47838,#47839,#47840,#47841,#47842,#47843,#47844,#47845,#47846,
#47847,#47848,#47849,#47850,#47851,#47852,#47853,#47854,#47855,#47856,#47857,
#47858,#47859,#47860,#47861,#47862,#47863,#47864,#47865,#47866,#47867,#47868,
#47869,#47870,#47871,#47872,#47873,#47874,#47875,#47876,#47877,#47878,#47879,
#47880,#47881,#47882,#47883,#47884,#47885,#47886,#47887,#47888,#47889,#47890,
#47891,#47892,#47893,#47894,#47895,#47896,#47897,#47898,#47899,#47900,#47901,
#47902,#47903,#47904,#47905,#47906,#47907,#47908,#47909,#47910,#47911,#47912,
#47913,#47914,#47915,#47916,#47917,#47918,#47919,#47920,#47921,#47922,#47923,
#47924,#47925,#47926,#47927,#47928,#47929,#47930,#47931,#47932,#47933,#47934,
#47935,#47936,#47937,#47938,#47939,#47940,#47941,#47942,#47943,#47944,#47945,
#47946,#47947,#47948,#47949,#47950,#47951,#47952,#47953,#47954,#47955,#47956,
#47957,#47958,#47959,#47960,#47961,#47962,#47963,#47964,#47965,#47966,#47967,
#47968,#47969,#47970,#47971,#47972,#47973,#47974,#47975,#47976,#47977,#47978,
#47979,#47980,#47981,#47982,#47983,#47984,#47985,#47986,#47987,#47988,#47989,
#47990,#47991,#47992,#47993,#47994,#47995,#47996,#47997,#47998,#47999,#48000,
#48001,#48002,#48003,#48004,#48005,#48006,#48007,#48008,#48009,#48010,#48011,
#48012,#48013,#48014,#48015,#48016,#48017,#48018,#48019,#48020,#48021,#48022,
#48023,#48024,#48025,#48026,#48027,#48028,#48029,#48030,#48031,#48032,#48033,
#48034,#48035,#48036,#48037,#48038,#48039),.UNSPECIFIED.,.F.,.F.,(4,3,3,
3,3,3,3,3,3,3,3,3,3,3,3,3,3,3,3,3,3,3,3,3,3,3,3,3,3,3,3,3,3,3,3,3,3,3,3,
3,3,3,3,3,3,3,3,3,3,3,3,3,3,3,3,3,3,3,3,3,3,3,3,3,3,3,3,3,3,3,3,3,3,4),
(424.115008234602,424.196103326786,424.279842038632,424.363477549999,424.447029993398,
424.530519429249,424.613973379863,424.697409873709,424.780846983465,424.864302778382,
424.947847271112,425.031436354053,425.115159621611,425.195839337506,425.279578049352,
425.363213560719,425.446766004118,425.530255439969,425.613709390583,425.697145884429,
425.780582994185,425.864038789102,425.947583281832,426.031172364773,426.114895632331,
426.195575348226,426.279314060072,426.36294957144,426.446502014838,426.529991450689,
426.613445401303,426.696881895149,426.780319004905,426.863774799822,426.947319292552,
427.030908375493,427.114631643051,427.195311358947,427.279050070793,427.36268558216,
427.446238025559,427.52972746141,427.613181412024,427.69661790587,427.780055015626,
427.863510810543,427.947055303273,428.030644386214,428.114367653771,428.195047369667,
428.278786081513,428.36242159288,428.445974036279,428.52946347213,428.612917422744,
428.69635391659,428.779791026345,428.863246821263,428.946791313993,429.030380396934,
429.114103664491,429.194783380387,429.278524811112,429.362162412899,429.445716320916,
429.533360746726,429.616811062651,429.700243933085,429.783677429661,429.867129620398,
429.950658987571,430.034233386045,430.11791345189,430.146871727396),
 .UNSPECIFIED.);
#320=B_SPLINE_CURVE_WITH_KNOTS('',3,(#48040,#48041,#48042,#48043,#48044,
#48045,#48046,#48047,#48048,#48049),.UNSPECIFIED.,.F.,.F.,(4,3,3,4),(423.863171432179,
423.945812036063,424.030410135267,424.115008234471),.UNSPECIFIED.);
#321=B_SPLINE_CURVE_WITH_KNOTS('',3,(#48051,#48052,#48053,#48054,#48055,
#48056,#48057,#48058,#48059,#48060),.UNSPECIFIED.,.F.,.F.,(4,3,3,4),(423.864352866444,
423.948770683666,424.033160895861,424.115008234606),.UNSPECIFIED.);
#322=B_SPLINE_CURVE_WITH_KNOTS('',3,(#48061,#48062,#48063,#48064,#48065,
#48066,#48067,#48068,#48069,#48070,#48071,#48072,#48073,#48074,#48075,#48076,
#48077,#48078,#48079,#48080,#48081,#48082,#48083,#48084,#48085,#48086,#48087,
#48088,#48089,#48090,#48091,#48092,#48093,#48094,#48095,#48096,#48097,#48098,
#48099,#48100,#48101,#48102,#48103,#48104,#48105,#48106,#48107,#48108,#48109,
#48110,#48111,#48112,#48113,#48114,#48115,#48116,#48117,#48118,#48119,#48120,
#48121,#48122,#48123,#48124,#48125,#48126,#48127,#48128,#48129,#48130,#48131,
#48132,#48133,#48134,#48135,#48136,#48137,#48138,#48139,#48140,#48141,#48142,
#48143,#48144,#48145,#48146,#48147,#48148,#48149,#48150,#48151,#48152,#48153,
#48154,#48155,#48156,#48157,#48158,#48159,#48160,#48161,#48162,#48163,#48164,
#48165,#48166,#48167,#48168,#48169,#48170,#48171,#48172,#48173,#48174,#48175,
#48176,#48177,#48178,#48179,#48180,#48181,#48182,#48183,#48184,#48185,#48186,
#48187,#48188,#48189,#48190,#48191,#48192,#48193,#48194,#48195,#48196,#48197,
#48198,#48199,#48200,#48201,#48202,#48203,#48204,#48205,#48206,#48207,#48208,
#48209,#48210,#48211,#48212,#48213,#48214,#48215,#48216,#48217,#48218,#48219,
#48220,#48221,#48222,#48223,#48224,#48225,#48226,#48227,#48228,#48229,#48230,
#48231,#48232,#48233,#48234,#48235,#48236,#48237,#48238,#48239,#48240,#48241,
#48242,#48243,#48244,#48245,#48246,#48247,#48248,#48249,#48250,#48251,#48252,
#48253,#48254,#48255,#48256,#48257,#48258,#48259,#48260,#48261,#48262,#48263,
#48264,#48265,#48266,#48267,#48268,#48269,#48270,#48271,#48272,#48273,#48274,
#48275,#48276,#48277,#48278,#48279,#48280),.UNSPECIFIED.,.F.,.F.,(4,3,3,
3,3,3,3,3,3,3,3,3,3,3,3,3,3,3,3,3,3,3,3,3,3,3,3,3,3,3,3,3,3,3,3,3,3,3,3,
3,3,3,3,3,3,3,3,3,3,3,3,3,3,3,3,3,3,3,3,3,3,3,3,3,3,3,3,3,3,3,3,3,3,4),
(424.115008234794,424.2076199709,424.300766079146,424.394189860388,424.487960336065,
424.506393946502,424.590132658348,424.673768169715,424.757320613114,424.840810048965,
424.924263999578,425.007700493424,425.09113760318,425.174593398097,425.258137890827,
425.341726973768,425.425450241325,425.506129957222,425.589868669068,425.673504180435,
425.757056623834,425.840546059685,425.924000010298,426.007436504145,426.0908736139,
426.174329408818,426.257873901547,426.341462984488,426.425186252046,426.505865967942,
426.589604679788,426.673240191155,426.756792634554,426.840282070405,426.923736021019,
427.007172514865,427.090609624621,427.174065419538,427.257609912268,427.341198995209,
427.424922262767,427.505601978662,427.589340690508,427.672976201875,427.756528645274,
427.840018081125,427.923472031739,428.006908525585,428.09034563534,428.173801430258,
428.257345922988,428.340935005929,428.424658273486,428.505337989382,428.589076701228,
428.672712212595,428.756264655994,428.839754091845,428.923208042459,429.006644536305,
429.090081646061,429.173537440978,429.257081933708,429.340671016649,429.424394284206,
429.505074000102,429.587707424315,429.670246251362,429.752709587891,429.835116471439,
429.917495324619,429.999855902794,430.082243419595,430.146364568078),
 .UNSPECIFIED.);
#323=B_SPLINE_CURVE_WITH_KNOTS('',3,(#48286,#48287,#48288,#48289,#48290,
#48291,#48292,#48293,#48294,#48295,#48296,#48297,#48298,#48299,#48300,#48301,
#48302,#48303,#48304,#48305,#48306,#48307,#48308,#48309,#48310,#48311,#48312,
#48313,#48314,#48315,#48316,#48317,#48318,#48319,#48320,#48321,#48322,#48323,
#48324,#48325,#48326,#48327,#48328,#48329,#48330,#48331,#48332,#48333,#48334,
#48335,#48336,#48337,#48338,#48339,#48340,#48341,#48342,#48343,#48344,#48345,
#48346,#48347,#48348,#48349,#48350,#48351,#48352,#48353,#48354,#48355,#48356,
#48357,#48358,#48359,#48360,#48361,#48362,#48363,#48364,#48365,#48366,#48367,
#48368,#48369,#48370,#48371,#48372,#48373,#48374,#48375,#48376,#48377,#48378,
#48379,#48380,#48381,#48382,#48383,#48384,#48385,#48386,#48387,#48388,#48389,
#48390,#48391,#48392,#48393,#48394,#48395,#48396,#48397,#48398,#48399,#48400,
#48401,#48402,#48403,#48404,#48405,#48406,#48407,#48408,#48409,#48410,#48411,
#48412,#48413,#48414,#48415,#48416,#48417,#48418,#48419,#48420,#48421,#48422,
#48423,#48424,#48425,#48426,#48427,#48428,#48429,#48430,#48431,#48432,#48433,
#48434,#48435,#48436,#48437,#48438,#48439,#48440,#48441,#48442,#48443,#48444,
#48445,#48446,#48447,#48448,#48449,#48450,#48451,#48452,#48453,#48454,#48455,
#48456,#48457,#48458,#48459,#48460,#48461,#48462,#48463,#48464,#48465,#48466,
#48467,#48468,#48469,#48470,#48471,#48472,#48473,#48474,#48475,#48476,#48477,
#48478,#48479,#48480,#48481,#48482,#48483,#48484,#48485,#48486,#48487,#48488,
#48489,#48490,#48491,#48492,#48493,#48494,#48495,#48496,#48497,#48498,#48499,
#48500,#48501,#48502,#48503,#48504,#48505),.UNSPECIFIED.,.F.,.F.,(4,3,3,
3,3,3,3,3,3,3,3,3,3,3,3,3,3,3,3,3,3,3,3,3,3,3,3,3,3,3,3,3,3,3,3,3,3,3,3,
3,3,3,3,3,3,3,3,3,3,3,3,3,3,3,3,3,3,3,3,3,3,3,3,3,3,3,3,3,3,3,3,3,3,4),
(430.398193541959,430.480576910534,430.562892386668,430.645166821398,430.727421257035,
430.809674699398,430.891946151272,430.97430233696,431.056704277496,431.139230058947,
431.194255401827,431.277994113673,431.36162962504,431.445182068439,431.52867150429,
431.612125454903,431.695561948749,431.778999058505,431.862454853423,431.945999346153,
432.029588429093,432.113311696651,432.193991412547,432.277730124393,432.361365635761,
432.444918079159,432.52840751501,432.611861465624,432.69529795947,432.778735069225,
432.862190864143,432.945735356873,433.029324439814,433.113047707372,433.193727423267,
433.277466135113,433.361101646481,433.444654089879,433.52814352573,433.611597476344,
433.69503397019,433.778471079946,433.861926874863,433.945471367593,434.029060450534,
434.112783718092,434.193463433988,434.277202145834,434.360837657202,434.4443901006,
434.527879536451,434.611333487065,434.694769980912,434.778207090667,434.861662885585,
434.945207378315,435.028796461256,435.112519728813,435.193199444708,435.276938156554,
435.360573667921,435.44412611132,435.527615547171,435.611069497785,435.694505991631,
435.777943101386,435.861398896304,435.944943389034,436.028532471975,436.112255739532,
436.192935455428,436.281457691473,436.369776886151,436.431064385021),
 .UNSPECIFIED.);
#324=B_SPLINE_CURVE_WITH_KNOTS('',3,(#48506,#48507,#48508,#48509,#48510,
#48511,#48512,#48513,#48514,#48515),.UNSPECIFIED.,.F.,.F.,(4,3,3,4),(430.146871727396,
430.194519391107,430.313622175814,430.398193541782),.UNSPECIFIED.);
#325=B_SPLINE_CURVE_WITH_KNOTS('',3,(#48517,#48518,#48519,#48520,#48521,
#48522,#48523,#48524,#48525,#48526),.UNSPECIFIED.,.F.,.F.,(4,3,3,4),(430.146364568078,
430.228825781605,430.313509661627,430.398193541649),.UNSPECIFIED.);
#326=B_SPLINE_CURVE_WITH_KNOTS('',3,(#48527,#48528,#48529,#48530,#48531,
#48532,#48533,#48534,#48535,#48536,#48537,#48538,#48539,#48540,#48541,#48542,
#48543,#48544,#48545,#48546,#48547,#48548,#48549,#48550,#48551,#48552,#48553,
#48554,#48555,#48556,#48557,#48558,#48559,#48560,#48561,#48562,#48563,#48564,
#48565,#48566,#48567,#48568,#48569,#48570,#48571,#48572,#48573,#48574,#48575,
#48576,#48577,#48578,#48579,#48580,#48581,#48582,#48583,#48584,#48585,#48586,
#48587,#48588,#48589,#48590,#48591,#48592,#48593,#48594,#48595,#48596,#48597,
#48598,#48599,#48600,#48601,#48602,#48603,#48604,#48605,#48606,#48607,#48608,
#48609,#48610,#48611,#48612,#48613,#48614,#48615,#48616,#48617,#48618,#48619,
#48620,#48621,#48622,#48623,#48624,#48625,#48626,#48627,#48628,#48629,#48630,
#48631,#48632,#48633,#48634,#48635,#48636,#48637,#48638,#48639,#48640,#48641,
#48642,#48643,#48644,#48645,#48646,#48647,#48648,#48649,#48650,#48651,#48652,
#48653,#48654,#48655,#48656,#48657,#48658,#48659,#48660,#48661,#48662,#48663,
#48664,#48665,#48666,#48667,#48668,#48669,#48670,#48671,#48672,#48673,#48674,
#48675,#48676,#48677,#48678,#48679,#48680,#48681,#48682,#48683,#48684,#48685,
#48686,#48687,#48688,#48689,#48690,#48691,#48692,#48693,#48694,#48695,#48696,
#48697,#48698,#48699,#48700,#48701,#48702,#48703,#48704,#48705,#48706,#48707,
#48708,#48709,#48710,#48711,#48712,#48713,#48714,#48715,#48716,#48717,#48718,
#48719,#48720,#48721,#48722,#48723,#48724,#48725,#48726,#48727,#48728,#48729,
#48730,#48731,#48732,#48733,#48734,#48735,#48736,#48737,#48738,#48739,#48740,
#48741,#48742,#48743),.UNSPECIFIED.,.F.,.F.,(4,3,3,3,3,3,3,3,3,3,3,3,3,
3,3,3,3,3,3,3,3,3,3,3,3,3,3,3,3,3,3,3,3,3,3,3,3,3,3,3,3,3,3,3,3,3,3,3,3,
3,3,3,3,3,3,3,3,3,3,3,3,3,3,3,3,3,3,3,3,3,3,3,4),(430.398193541785,430.504810010823,
430.588548722669,430.672184234036,430.755736677435,430.839226113286,430.922680063899,
431.006116557746,431.089553667501,431.173009462419,431.256553955148,431.340143038089,
431.423866305647,431.504546021543,431.588284733389,431.671920244756,431.755472688155,
431.838962124006,431.922416074619,432.005852568466,432.089289678221,432.172745473139,
432.256289965868,432.339879048809,432.423602316367,432.504282032263,432.588020744109,
432.671656255476,432.755208698875,432.838698134726,432.92215208534,433.005588579186,
433.089025688941,433.172481483859,433.256025976589,433.33961505953,433.423338327087,
433.504018042983,433.587756754829,433.671392266196,433.754944709595,433.838434145446,
433.92188809606,434.005324589906,434.088761699661,434.172217494579,434.255761987309,
434.33935107025,434.423074337807,434.503754053703,434.587492765549,434.671128276916,
434.754680720315,434.838170156166,434.92162410678,435.005060600626,435.088497710381,
435.171953505299,435.255497998029,435.33908708097,435.422810348527,435.503490064423,
435.587232999392,435.670871767371,435.754426504978,435.838867123478,435.922317398153,
436.005749055453,436.089180167143,436.174372988602,436.257893265946,436.343922359462,
436.429951452978),.UNSPECIFIED.);
#327=B_SPLINE_CURVE_WITH_KNOTS('',3,(#48749,#48750,#48751,#48752,#48753,
#48754,#48755,#48756,#48757,#48758,#48759,#48760,#48761,#48762,#48763,#48764,
#48765,#48766,#48767,#48768,#48769,#48770,#48771,#48772,#48773,#48774,#48775,
#48776,#48777,#48778,#48779,#48780,#48781,#48782,#48783,#48784,#48785,#48786,
#48787,#48788,#48789,#48790,#48791,#48792,#48793,#48794,#48795,#48796,#48797,
#48798,#48799,#48800,#48801,#48802,#48803,#48804,#48805,#48806,#48807,#48808,
#48809,#48810,#48811,#48812,#48813,#48814,#48815,#48816,#48817,#48818,#48819,
#48820,#48821,#48822,#48823,#48824,#48825,#48826,#48827,#48828,#48829,#48830,
#48831,#48832,#48833,#48834,#48835,#48836,#48837,#48838,#48839,#48840,#48841,
#48842,#48843,#48844,#48845,#48846,#48847,#48848,#48849,#48850,#48851,#48852,
#48853,#48854,#48855,#48856,#48857,#48858,#48859,#48860,#48861,#48862,#48863,
#48864,#48865,#48866,#48867,#48868,#48869,#48870,#48871,#48872,#48873,#48874,
#48875,#48876,#48877,#48878,#48879,#48880,#48881,#48882,#48883,#48884,#48885,
#48886,#48887,#48888,#48889,#48890,#48891,#48892,#48893,#48894,#48895,#48896,
#48897,#48898,#48899,#48900,#48901,#48902,#48903,#48904,#48905,#48906,#48907,
#48908,#48909,#48910,#48911,#48912,#48913,#48914,#48915,#48916,#48917,#48918,
#48919,#48920,#48921,#48922,#48923,#48924,#48925,#48926,#48927,#48928,#48929,
#48930,#48931,#48932,#48933,#48934,#48935,#48936,#48937,#48938,#48939,#48940,
#48941,#48942,#48943,#48944,#48945,#48946,#48947,#48948,#48949,#48950,#48951,
#48952,#48953,#48954,#48955,#48956,#48957,#48958,#48959,#48960,#48961,#48962,
#48963,#48964,#48965,#48966,#48967,#48968),.UNSPECIFIED.,.F.,.F.,(4,3,3,
3,3,3,3,3,3,3,3,3,3,3,3,3,3,3,3,3,3,3,3,3,3,3,3,3,3,3,3,3,3,3,3,3,3,3,3,
3,3,3,3,3,3,3,3,3,3,3,3,3,3,3,3,3,3,3,3,3,3,3,3,3,3,3,3,3,3,3,3,3,3,4),
(436.681378848961,436.76838027434,436.855482209621,436.942776468581,437.030170281766,
437.117762688149,437.192671466148,437.276410177994,437.360045689362,437.44359813276,
437.527087568611,437.610541519225,437.693978013071,437.777415122827,437.860870917744,
437.944415410474,438.028004493415,438.111727760972,438.192407476868,438.276146188714,
438.359781700081,438.44333414348,438.526823579331,438.610277529944,438.693714023791,
438.777151133546,438.860606928463,438.944151421193,439.027740504134,439.111463771692,
439.192143487588,439.275882199434,439.359517710801,439.4430701542,439.526559590051,
439.610013540665,439.693450034511,439.776887144266,439.860342939184,439.943887431914,
440.027476514855,440.111199782413,440.191879498308,440.275618210154,440.359253721522,
440.44280616492,440.526295600771,440.609749551385,440.693186045231,440.776623154987,
440.860078949904,440.943623442634,441.027212525575,441.110935793133,441.191615509028,
441.275354220874,441.358989732241,441.44254217564,441.526031611491,441.609485562105,
441.692922055951,441.776359165707,441.859814960624,441.943359453354,442.026948536295,
442.110671803853,442.191351519749,442.273972562786,442.356496500643,442.438942469356,
442.52132511321,442.603671489248,442.686007209095,442.713089856218),
 .UNSPECIFIED.);
#328=B_SPLINE_CURVE_WITH_KNOTS('',3,(#48969,#48970,#48971,#48972,#48973,
#48974,#48975,#48976,#48977,#48978),.UNSPECIFIED.,.F.,.F.,(4,3,3,4),(436.431064385021,
436.519119043064,436.606990876881,436.681378848849),.UNSPECIFIED.);
#329=B_SPLINE_CURVE_WITH_KNOTS('',3,(#48980,#48981,#48982,#48983,#48984,
#48985,#48986,#48987,#48988,#48989),.UNSPECIFIED.,.F.,.F.,(4,3,3,4),(436.429951452978,
436.503226075143,436.631173716165,436.681378848965),.UNSPECIFIED.);
#330=B_SPLINE_CURVE_WITH_KNOTS('',3,(#48990,#48991,#48992,#48993,#48994,
#48995,#48996,#48997,#48998,#48999,#49000,#49001,#49002,#49003,#49004,#49005,
#49006,#49007,#49008,#49009,#49010,#49011,#49012,#49013,#49014,#49015,#49016,
#49017,#49018,#49019,#49020,#49021,#49022,#49023,#49024,#49025,#49026,#49027,
#49028,#49029,#49030,#49031,#49032,#49033,#49034,#49035,#49036,#49037,#49038,
#49039,#49040,#49041,#49042,#49043,#49044,#49045,#49046,#49047,#49048,#49049,
#49050,#49051,#49052,#49053,#49054,#49055,#49056,#49057,#49058,#49059,#49060,
#49061,#49062,#49063,#49064,#49065,#49066,#49067,#49068,#49069,#49070,#49071,
#49072,#49073,#49074,#49075,#49076,#49077,#49078,#49079,#49080,#49081,#49082,
#49083,#49084,#49085,#49086,#49087,#49088,#49089,#49090,#49091,#49092,#49093,
#49094,#49095,#49096,#49097,#49098,#49099,#49100,#49101,#49102,#49103,#49104,
#49105,#49106,#49107,#49108,#49109,#49110,#49111,#49112,#49113,#49114,#49115,
#49116,#49117,#49118,#49119,#49120,#49121,#49122,#49123,#49124,#49125,#49126,
#49127,#49128,#49129,#49130,#49131,#49132,#49133,#49134,#49135,#49136,#49137,
#49138,#49139,#49140,#49141,#49142,#49143,#49144,#49145,#49146,#49147,#49148,
#49149,#49150,#49151,#49152,#49153,#49154,#49155,#49156,#49157,#49158,#49159,
#49160,#49161,#49162,#49163,#49164,#49165,#49166,#49167,#49168,#49169,#49170,
#49171,#49172,#49173,#49174,#49175,#49176,#49177,#49178,#49179,#49180,#49181,
#49182,#49183,#49184,#49185,#49186,#49187,#49188,#49189,#49190,#49191,#49192,
#49193,#49194,#49195,#49196,#49197,#49198,#49199,#49200,#49201,#49202,#49203,
#49204,#49205,#49206,#49207,#49208,#49209),.UNSPECIFIED.,.F.,.F.,(4,3,3,
3,3,3,3,3,3,3,3,3,3,3,3,3,3,3,3,3,3,3,3,3,3,3,3,3,3,3,3,3,3,3,3,3,3,3,3,
3,3,3,3,3,3,3,3,3,3,3,3,3,3,3,3,3,3,3,3,3,3,3,3,3,3,3,3,3,3,3,3,3,3,4),
(436.681378849126,436.763742326637,436.846030771284,436.928268660878,437.010480173638,
437.092684349144,437.174900218767,437.257197272248,437.339534460059,437.422002532994,
437.502962085864,437.58670079771,437.670336309077,437.753888752476,437.837378188327,
437.92083213894,438.004268632787,438.087705742542,438.17116153746,438.254706030189,
438.33829511313,438.422018380688,438.502698096584,438.58643680843,438.670072319797,
438.753624763196,438.837114199047,438.92056814966,439.004004643507,439.087441753262,
439.170897548179,439.254442040909,439.33803112385,439.421754391407,439.502434107304,
439.58617281915,439.669808330517,439.753360773916,439.836850209767,439.920304160381,
440.003740654227,440.087177763983,440.1706335589,440.25417805163,440.337767134571,
440.421490402129,440.502170118024,440.58590882987,440.669544341237,440.753096784636,
440.836586220487,440.920040171101,441.003476664947,441.086913774703,441.17036956962,
441.25391406235,441.337503145291,441.421226412849,441.501906128744,441.58564484059,
441.669280351958,441.752832795356,441.836322231208,441.919776181822,442.003212675668,
442.086649785423,442.170105580341,442.253650073071,442.337239156012,442.42096242357,
442.501642139464,442.591309868028,442.680758053547,442.714262803867),
 .UNSPECIFIED.);
#331=B_SPLINE_CURVE_WITH_KNOTS('',3,(#49215,#49216,#49217,#49218,#49219,
#49220,#49221,#49222,#49223,#49224,#49225,#49226,#49227,#49228,#49229,#49230,
#49231,#49232,#49233,#49234,#49235,#49236,#49237,#49238,#49239,#49240,#49241,
#49242,#49243,#49244,#49245,#49246,#49247,#49248,#49249,#49250,#49251,#49252,
#49253,#49254,#49255,#49256,#49257,#49258,#49259,#49260,#49261,#49262,#49263,
#49264,#49265,#49266,#49267,#49268,#49269,#49270,#49271,#49272,#49273,#49274,
#49275,#49276,#49277,#49278,#49279,#49280,#49281,#49282,#49283,#49284,#49285,
#49286,#49287,#49288,#49289,#49290,#49291,#49292,#49293,#49294,#49295,#49296,
#49297,#49298,#49299,#49300,#49301,#49302,#49303,#49304,#49305,#49306,#49307,
#49308,#49309,#49310,#49311,#49312,#49313,#49314,#49315,#49316,#49317,#49318,
#49319,#49320,#49321,#49322,#49323,#49324,#49325,#49326,#49327,#49328,#49329,
#49330,#49331,#49332,#49333,#49334,#49335,#49336,#49337,#49338,#49339,#49340,
#49341,#49342,#49343,#49344,#49345,#49346,#49347,#49348,#49349,#49350,#49351,
#49352,#49353,#49354,#49355,#49356,#49357,#49358,#49359,#49360,#49361,#49362,
#49363,#49364,#49365,#49366,#49367,#49368,#49369,#49370,#49371,#49372,#49373,
#49374,#49375,#49376,#49377,#49378,#49379,#49380,#49381,#49382,#49383,#49384,
#49385,#49386,#49387,#49388,#49389,#49390,#49391,#49392,#49393,#49394,#49395,
#49396,#49397,#49398,#49399,#49400,#49401,#49402,#49403,#49404,#49405,#49406,
#49407,#49408,#49409,#49410,#49411,#49412,#49413,#49414,#49415,#49416,#49417,
#49418,#49419,#49420,#49421,#49422,#49423,#49424,#49425,#49426,#49427,#49428,
#49429,#49430,#49431),.UNSPECIFIED.,.F.,.F.,(4,3,3,3,3,3,3,3,3,3,3,3,3,
3,3,3,3,3,3,3,3,3,3,3,3,3,3,3,3,3,3,3,3,3,3,3,3,3,3,3,3,3,3,3,3,3,3,3,3,
3,3,3,3,3,3,3,3,3,3,3,3,3,3,3,3,3,3,3,3,3,3,3,4),(442.964564156141,443.07782585304,
443.191087530469,443.274826242315,443.358461753682,443.442014197081,443.525503632932,
443.608957583545,443.692394077392,443.775831187147,443.859286982065,443.942831474795,
444.026420557736,444.110143825293,444.190823541189,444.274562253035,444.358197764402,
444.441750207801,444.525239643652,444.608693594266,444.692130088112,444.775567197867,
444.859022992785,444.942567485515,445.026156568456,445.109879836013,445.190559551909,
445.274298263755,445.357933775122,445.441486218521,445.524975654372,445.608429604986,
445.691866098832,445.775303208587,445.858759003505,445.942303496235,446.025892579176,
446.109615846733,446.190295562629,446.274034274475,446.357669785842,446.441222229241,
446.524711665092,446.608165615706,446.691602109552,446.775039219307,446.858495014225,
446.942039506955,447.025628589896,447.109351857453,447.190031573349,447.273770285195,
447.357405796562,447.440958239961,447.524447675812,447.607901626426,447.691338120272,
447.774775230027,447.858231024945,447.941775517675,448.025364600616,448.109087868173,
448.189767584069,448.273517961945,448.357162587647,448.440706191533,448.524192517166,
448.607639684563,448.691065783473,448.774514018599,448.857972936816,448.94149792352,
448.996086608465),.UNSPECIFIED.);
#332=B_SPLINE_CURVE_WITH_KNOTS('',3,(#49432,#49433,#49434,#49435,#49436,
#49437,#49438,#49439,#49440,#49441),.UNSPECIFIED.,.F.,.F.,(4,3,3,4),(442.713089856218,
442.795453856229,442.880009006111,442.964564155993),.UNSPECIFIED.);
#333=B_SPLINE_CURVE_WITH_KNOTS('',3,(#49443,#49444,#49445,#49446,#49447,
#49448,#49449,#49450,#49451,#49452),.UNSPECIFIED.,.F.,.F.,(4,3,3,4),(442.714262803867,
442.803430513116,442.892361191748,442.964564155987),.UNSPECIFIED.);
#334=B_SPLINE_CURVE_WITH_KNOTS('',3,(#49453,#49454,#49455,#49456,#49457,
#49458,#49459,#49460,#49461,#49462,#49463,#49464,#49465,#49466,#49467,#49468,
#49469,#49470,#49471,#49472,#49473,#49474,#49475,#49476,#49477,#49478,#49479,
#49480,#49481,#49482,#49483,#49484,#49485,#49486,#49487,#49488,#49489,#49490,
#49491,#49492,#49493,#49494,#49495,#49496,#49497,#49498,#49499,#49500,#49501,
#49502,#49503,#49504,#49505,#49506,#49507,#49508,#49509,#49510,#49511,#49512,
#49513,#49514,#49515,#49516,#49517,#49518,#49519,#49520,#49521,#49522,#49523,
#49524,#49525,#49526,#49527,#49528,#49529,#49530,#49531,#49532,#49533,#49534,
#49535,#49536,#49537,#49538,#49539,#49540,#49541,#49542,#49543,#49544,#49545,
#49546,#49547,#49548,#49549,#49550,#49551,#49552,#49553,#49554,#49555,#49556,
#49557,#49558,#49559,#49560,#49561,#49562,#49563,#49564,#49565,#49566,#49567,
#49568,#49569,#49570,#49571,#49572,#49573,#49574,#49575,#49576,#49577,#49578,
#49579,#49580,#49581,#49582,#49583,#49584,#49585,#49586,#49587,#49588,#49589,
#49590,#49591,#49592,#49593,#49594,#49595,#49596,#49597,#49598,#49599,#49600,
#49601,#49602,#49603,#49604,#49605,#49606,#49607,#49608,#49609,#49610,#49611,
#49612,#49613,#49614,#49615,#49616,#49617,#49618,#49619,#49620,#49621,#49622,
#49623,#49624,#49625,#49626,#49627,#49628,#49629,#49630,#49631,#49632,#49633,
#49634,#49635,#49636,#49637,#49638,#49639,#49640,#49641,#49642,#49643,#49644,
#49645,#49646,#49647,#49648,#49649,#49650,#49651,#49652,#49653,#49654,#49655,
#49656,#49657,#49658,#49659,#49660,#49661,#49662,#49663,#49664,#49665,#49666,
#49667,#49668,#49669,#49670,#49671,#49672),.UNSPECIFIED.,.F.,.F.,(4,3,3,
3,3,3,3,3,3,3,3,3,3,3,3,3,3,3,3,3,3,3,3,3,3,3,3,3,3,3,3,3,3,3,3,3,3,3,3,
3,3,3,3,3,3,3,3,3,3,3,3,3,3,3,3,3,3,3,3,3,3,3,3,3,3,3,3,3,3,3,3,3,3,4),
(442.964564156144,443.050744981324,443.136998310996,443.223336707115,443.309834552856,
443.396424672269,443.483172125001,443.501378150184,443.58511686203,443.668752373397,
443.752304816796,443.835794252647,443.91924820326,444.002684697107,444.086121806862,
444.16957760178,444.253122094509,444.33671117745,444.420434445008,444.501114160904,
444.58485287275,444.668488384117,444.752040827516,444.835530263367,444.918984213981,
445.002420707827,445.085857817583,445.169313612501,445.25285810523,445.336447188171,
445.420170455729,445.500850171625,445.584588883471,445.668224394839,445.751776838237,
445.835266274088,445.918720224702,446.002156718549,446.085593828304,446.169049623222,
446.252594115951,446.336183198893,446.41990646645,446.500586182345,446.584324894191,
446.667960405559,446.751512848957,446.835002284809,446.918456235422,447.001892729268,
447.085329839024,447.168785633942,447.252330126671,447.335919209612,447.41964247717,
447.500322193065,447.584060904911,447.667696416278,447.751248859677,447.834738295528,
447.918192246142,448.001628739988,448.085065849744,448.168521644661,448.252066137391,
448.335655220332,448.41937848789,448.500058203785,448.582840753366,448.665524929084,
448.748242794626,448.830780781812,448.913588586533,448.996396391254),
 .UNSPECIFIED.);
#335=B_SPLINE_CURVE_WITH_KNOTS('',3,(#49678,#49679,#49680,#49681,#49682,
#49683,#49684,#49685,#49686,#49687),.UNSPECIFIED.,.F.,.F.,(4,1,1,1,1,1,
1,4),(449.247756624963,450.18923960551,451.18897561623,452.18871162695,
453.18844763767,454.18818364839,455.18791965911,455.280414679422),
 .UNSPECIFIED.);
#336=B_SPLINE_CURVE_WITH_KNOTS('',3,(#49688,#49689,#49690,#49691,#49692,
#49693,#49694,#49695,#49696,#49697,#49698,#49699,#49700),.UNSPECIFIED.,
 .F.,.F.,(4,3,3,3,4),(448.996086608465,449.079713584564,449.163459424575,
449.189503594789,449.24774946332),.UNSPECIFIED.);
#337=B_SPLINE_CURVE_WITH_KNOTS('',3,(#49702,#49703,#49704,#49705,#49706,
#49707,#49708,#49709,#49710,#49711),.UNSPECIFIED.,.F.,.F.,(4,3,3,4),(448.996396391254,
449.078902129801,449.163325796563,449.247749463324),.UNSPECIFIED.);
#338=B_SPLINE_CURVE_WITH_KNOTS('',3,(#49712,#49713,#49714,#49715,#49716,
#49717,#49718,#49719,#49720,#49721,#49722,#49723,#49724,#49725,#49726,#49727,
#49728,#49729,#49730,#49731,#49732,#49733,#49734,#49735,#49736,#49737,#49738,
#49739,#49740,#49741,#49742,#49743,#49744,#49745,#49746,#49747,#49748,#49749,
#49750,#49751,#49752,#49753,#49754,#49755,#49756,#49757,#49758,#49759,#49760,
#49761,#49762,#49763,#49764,#49765,#49766,#49767,#49768,#49769,#49770,#49771,
#49772,#49773,#49774,#49775,#49776,#49777,#49778,#49779,#49780,#49781,#49782,
#49783,#49784,#49785,#49786,#49787,#49788,#49789,#49790,#49791,#49792,#49793,
#49794,#49795,#49796,#49797,#49798,#49799,#49800,#49801,#49802,#49803,#49804,
#49805,#49806,#49807,#49808,#49809,#49810,#49811,#49812,#49813,#49814,#49815,
#49816,#49817,#49818,#49819,#49820,#49821,#49822,#49823,#49824,#49825,#49826,
#49827,#49828,#49829,#49830,#49831,#49832,#49833,#49834,#49835,#49836,#49837,
#49838,#49839,#49840,#49841,#49842,#49843,#49844,#49845,#49846,#49847,#49848,
#49849,#49850,#49851,#49852,#49853,#49854,#49855,#49856,#49857,#49858,#49859,
#49860,#49861,#49862,#49863,#49864,#49865,#49866,#49867,#49868,#49869,#49870,
#49871,#49872,#49873,#49874,#49875,#49876,#49877,#49878,#49879,#49880,#49881,
#49882,#49883,#49884,#49885,#49886,#49887,#49888,#49889,#49890,#49891,#49892,
#49893,#49894,#49895,#49896,#49897,#49898,#49899,#49900,#49901,#49902,#49903,
#49904,#49905,#49906,#49907,#49908,#49909,#49910,#49911,#49912,#49913,#49914,
#49915,#49916,#49917,#49918,#49919,#49920,#49921,#49922,#49923,#49924,#49925,
#49926,#49927,#49928,#49929,#49930,#49931),.UNSPECIFIED.,.F.,.F.,(4,3,3,
3,3,3,3,3,3,3,3,3,3,3,3,3,3,3,3,3,3,3,3,3,3,3,3,3,3,3,3,3,3,3,3,3,3,3,3,
3,3,3,3,3,3,3,3,3,3,3,3,3,3,3,3,3,3,3,3,3,3,3,3,3,3,3,3,3,3,3,3,3,3,4),
(449.247749463518,449.354662883124,449.463928728413,449.499794214505,449.583532926351,
449.667168437718,449.750720881117,449.834210316968,449.917664267582,450.001100761428,
450.084537871183,450.167993666101,450.251538158831,450.335127241772,450.41885050933,
450.499530225225,450.583268937071,450.666904448438,450.750456891837,450.833946327688,
450.917400278301,451.000836772148,451.084273881903,451.16772967682,451.25127416955,
451.334863252491,451.418586520049,451.499266235945,451.583004947791,451.666640459158,
451.750192902557,451.833682338408,451.917136289022,452.000572782868,452.084009892624,
452.167465687541,452.251010180271,452.334599263212,452.41832253077,452.499002246665,
452.582740958511,452.666376469879,452.749928913277,452.833418349128,452.916872299742,
453.000308793588,453.083745903344,453.167201698261,453.250746190991,453.334335273932,
453.41805854149,453.498738257386,453.582476969232,453.666112480599,453.749664923998,
453.833154359849,453.916608310463,454.000044804309,454.083481914064,454.166937708982,
454.250482201712,454.334071284653,454.41779455221,454.498474268106,454.582226310188,
454.669356649698,454.752898041365,454.836382433444,454.919827945315,455.00325266616,
455.086695649327,455.170149799188,455.253659187583,455.279269026268),
 .UNSPECIFIED.);
#339=B_SPLINE_CURVE_WITH_KNOTS('',3,(#49937,#49938,#49939,#49940,#49941,
#49942,#49943,#49944,#49945,#49946),.UNSPECIFIED.,.F.,.F.,(4,1,1,1,1,1,
1,4),(455.5309347705,456.18765566983,457.18739168055,458.187127691271,459.186863701991,
460.186599712711,461.186335723431,461.563668011779),.UNSPECIFIED.);
#340=B_SPLINE_CURVE_WITH_KNOTS('',3,(#49947,#49948,#49949,#49950),
 .UNSPECIFIED.,.F.,.F.,(4,4),(455.280414679422,455.5309347705),
 .UNSPECIFIED.);
#341=B_SPLINE_CURVE_WITH_KNOTS('',3,(#49952,#49953,#49954,#49955,#49956,
#49957,#49958,#49959,#49960,#49961,#49962,#49963,#49964),.UNSPECIFIED.,
 .F.,.F.,(4,3,3,3,4),(455.279269026268,455.362877418155,455.44661163974,
455.498210278826,455.530934770504),.UNSPECIFIED.);
#342=B_SPLINE_CURVE_WITH_KNOTS('',3,(#49965,#49966,#49967,#49968,#49969,
#49970,#49971,#49972,#49973,#49974,#49975,#49976,#49977,#49978,#49979,#49980,
#49981,#49982,#49983,#49984,#49985,#49986,#49987,#49988,#49989,#49990,#49991,
#49992,#49993,#49994,#49995,#49996,#49997,#49998,#49999,#50000,#50001,#50002,
#50003,#50004,#50005,#50006,#50007,#50008,#50009,#50010,#50011,#50012,#50013,
#50014,#50015,#50016,#50017,#50018,#50019,#50020,#50021,#50022,#50023,#50024,
#50025,#50026,#50027,#50028,#50029,#50030,#50031,#50032,#50033,#50034,#50035,
#50036,#50037,#50038,#50039,#50040,#50041,#50042,#50043,#50044,#50045,#50046,
#50047,#50048,#50049,#50050,#50051,#50052,#50053,#50054,#50055,#50056,#50057,
#50058,#50059,#50060,#50061,#50062,#50063,#50064,#50065,#50066,#50067,#50068,
#50069,#50070,#50071,#50072,#50073,#50074,#50075,#50076,#50077,#50078,#50079,
#50080,#50081,#50082,#50083,#50084,#50085,#50086,#50087,#50088,#50089,#50090,
#50091,#50092,#50093,#50094,#50095,#50096,#50097,#50098,#50099,#50100,#50101,
#50102,#50103,#50104,#50105,#50106,#50107,#50108,#50109,#50110,#50111,#50112,
#50113,#50114,#50115,#50116,#50117,#50118,#50119,#50120,#50121,#50122,#50123,
#50124,#50125,#50126,#50127,#50128,#50129,#50130,#50131,#50132,#50133,#50134,
#50135,#50136,#50137,#50138,#50139,#50140,#50141,#50142,#50143,#50144,#50145,
#50146,#50147,#50148,#50149,#50150,#50151,#50152,#50153,#50154,#50155,#50156,
#50157,#50158,#50159,#50160,#50161,#50162,#50163,#50164,#50165,#50166,#50167,
#50168,#50169,#50170,#50171,#50172,#50173,#50174,#50175,#50176,#50177,#50178,
#50179,#50180,#50181,#50182,#50183,#50184),.UNSPECIFIED.,.F.,.F.,(4,3,3,
3,3,3,3,3,3,3,3,3,3,3,3,3,3,3,3,3,3,3,3,3,3,3,3,3,3,3,3,3,3,3,3,3,3,3,3,
3,3,3,3,3,3,3,3,3,3,3,3,3,3,3,3,3,3,3,3,3,3,3,3,3,3,3,3,3,3,3,3,3,3,4),
(455.530934770647,455.614220758589,455.697405044271,455.780508205535,455.863550744547,
455.94656131294,456.029557396033,456.112557464698,456.195579989061,456.278691780244,
456.361852309144,456.445138217639,456.497946289546,456.581685001392,456.665320512759,
456.748872956158,456.832362392009,456.915816342623,456.999252836469,457.082689946224,
457.166145741142,457.249690233872,457.333279316813,457.41700258437,457.497682300266,
457.581421012112,457.665056523479,457.748608966878,457.832098402729,457.915552353342,
457.998988847189,458.082425956944,458.165881751862,458.249426244592,458.333015327533,
458.41673859509,458.497418310986,458.581157022832,458.664792534199,458.748344977598,
458.831834413449,458.915288364063,458.99872485791,459.082161967665,459.165617762583,
459.249162255312,459.332751338254,459.416474605811,459.497154321706,459.580893033552,
459.66452854492,459.748080988318,459.83157042417,459.915024374783,459.99846086863,
460.081897978385,460.165353773303,460.248898266033,460.332487348974,460.416210616532,
460.496890332427,460.580629044273,460.66426455564,460.747816999039,460.83130643489,
460.914760385504,460.99819687935,461.081633989105,461.165089784023,461.248634276753,
461.332223359694,461.415946627251,461.496626343147,461.563437609655),
 .UNSPECIFIED.);
#343=B_SPLINE_CURVE_WITH_KNOTS('',3,(#50190,#50191,#50192,#50193,#50194,
#50195,#50196,#50197,#50198,#50199,#50200,#50201,#50202,#50203,#50204,#50205,
#50206,#50207,#50208,#50209,#50210,#50211,#50212,#50213,#50214,#50215,#50216,
#50217,#50218,#50219,#50220,#50221,#50222,#50223,#50224,#50225,#50226,#50227,
#50228,#50229,#50230,#50231,#50232,#50233,#50234,#50235,#50236,#50237,#50238,
#50239,#50240,#50241,#50242,#50243,#50244,#50245,#50246,#50247,#50248,#50249,
#50250,#50251,#50252,#50253,#50254,#50255,#50256,#50257,#50258,#50259,#50260,
#50261,#50262,#50263,#50264,#50265,#50266,#50267,#50268,#50269,#50270,#50271,
#50272,#50273,#50274,#50275,#50276,#50277,#50278,#50279,#50280,#50281,#50282,
#50283,#50284,#50285,#50286,#50287,#50288,#50289,#50290,#50291,#50292,#50293,
#50294,#50295,#50296,#50297,#50298,#50299,#50300,#50301,#50302,#50303,#50304,
#50305,#50306,#50307,#50308,#50309,#50310,#50311,#50312,#50313,#50314,#50315,
#50316,#50317,#50318,#50319,#50320,#50321,#50322,#50323,#50324,#50325,#50326,
#50327,#50328,#50329,#50330,#50331,#50332,#50333,#50334,#50335,#50336,#50337,
#50338,#50339,#50340,#50341,#50342,#50343,#50344,#50345,#50346,#50347,#50348,
#50349,#50350,#50351,#50352,#50353,#50354,#50355,#50356,#50357,#50358,#50359,
#50360,#50361,#50362,#50363,#50364,#50365,#50366,#50367,#50368,#50369,#50370,
#50371,#50372,#50373,#50374,#50375,#50376,#50377,#50378,#50379,#50380,#50381,
#50382,#50383,#50384,#50385,#50386,#50387,#50388,#50389,#50390,#50391,#50392,
#50393,#50394,#50395,#50396,#50397,#50398,#50399,#50400,#50401,#50402,#50403,
#50404,#50405,#50406),.UNSPECIFIED.,.F.,.F.,(4,3,3,3,3,3,3,3,3,3,3,3,3,
3,3,3,3,3,3,3,3,3,3,3,3,3,3,3,3,3,3,3,3,3,3,3,3,3,3,3,3,3,3,3,3,3,3,3,3,
3,3,3,3,3,3,3,3,3,3,3,3,3,3,3,3,3,3,3,3,3,3,3,4),(461.814120077679,461.908277085704,
462.002806830092,462.09786318546,462.186071734151,462.269810445997,462.353445957364,
462.436998400763,462.520487836614,462.603941787228,462.687378281074,462.77081539083,
462.854271185747,462.937815678477,463.021404761418,463.105128028975,463.185807744871,
463.269546456717,463.353181968084,463.436734411483,463.520223847334,463.603677797948,
463.687114291794,463.77055140155,463.854007196467,463.937551689197,464.021140772138,
464.104864039696,464.185543755591,464.269282467437,464.352917978804,464.436470422203,
464.519959858054,464.603413808668,464.686850302514,464.77028741227,464.853743207187,
464.937287699917,465.020876782858,465.104600050416,465.185279766312,465.269018478158,
465.352653989526,465.436206432924,465.519695868775,465.603149819389,465.686586313236,
465.770023422991,465.853479217909,465.937023710639,466.02061279358,466.104336061137,
466.185015777032,466.268754488878,466.352390000245,466.435942443644,466.519431879495,
466.602885830109,466.686322323955,466.76975943371,466.853215228628,466.936759721357,
467.020348804298,467.104072071856,467.184751787752,467.26750532906,467.350164327694,
467.432747806821,467.515274722903,467.597822988734,467.680304873322,467.762886329776,
467.845467786229),.UNSPECIFIED.);
#344=B_SPLINE_CURVE_WITH_KNOTS('',3,(#50407,#50408,#50409,#50410),
 .UNSPECIFIED.,.F.,.F.,(4,4),(461.563668011779,461.814120077679),
 .UNSPECIFIED.);
#345=B_SPLINE_CURVE_WITH_KNOTS('',3,(#50412,#50413,#50414,#50415,#50416,
#50417,#50418,#50419,#50420,#50421),.UNSPECIFIED.,.F.,.F.,(4,3,3,4),(461.563437609655,
461.663143498821,461.761828896827,461.814120077512),.UNSPECIFIED.);
#346=B_SPLINE_CURVE_WITH_KNOTS('',3,(#50422,#50423,#50424,#50425,#50426,
#50427,#50428,#50429,#50430,#50431,#50432,#50433,#50434,#50435,#50436,#50437,
#50438,#50439,#50440,#50441,#50442,#50443,#50444,#50445,#50446,#50447,#50448,
#50449,#50450,#50451,#50452,#50453,#50454,#50455,#50456,#50457,#50458,#50459,
#50460,#50461,#50462,#50463,#50464,#50465,#50466,#50467,#50468,#50469,#50470,
#50471,#50472,#50473,#50474,#50475,#50476,#50477,#50478,#50479,#50480,#50481,
#50482,#50483,#50484,#50485,#50486,#50487,#50488,#50489,#50490,#50491,#50492,
#50493,#50494,#50495,#50496,#50497,#50498,#50499,#50500,#50501,#50502,#50503,
#50504,#50505,#50506,#50507,#50508,#50509,#50510,#50511,#50512,#50513,#50514,
#50515,#50516,#50517,#50518,#50519,#50520,#50521,#50522,#50523,#50524,#50525,
#50526,#50527,#50528,#50529,#50530,#50531,#50532,#50533,#50534,#50535,#50536,
#50537,#50538,#50539,#50540,#50541,#50542,#50543,#50544,#50545,#50546,#50547,
#50548,#50549,#50550,#50551,#50552,#50553,#50554,#50555,#50556,#50557,#50558,
#50559,#50560,#50561,#50562,#50563,#50564,#50565,#50566,#50567,#50568,#50569,
#50570,#50571,#50572,#50573,#50574,#50575,#50576,#50577,#50578,#50579,#50580,
#50581,#50582,#50583,#50584,#50585,#50586,#50587,#50588,#50589,#50590,#50591,
#50592,#50593,#50594,#50595,#50596,#50597,#50598,#50599,#50600,#50601,#50602,
#50603,#50604,#50605,#50606,#50607,#50608,#50609,#50610,#50611,#50612,#50613,
#50614,#50615,#50616,#50617,#50618,#50619,#50620,#50621,#50622,#50623,#50624,
#50625,#50626,#50627,#50628,#50629,#50630,#50631,#50632,#50633,#50634,#50635,
#50636,#50637,#50638,#50639,#50640,#50641,#50642,#50643,#50644),
 .UNSPECIFIED.,.F.,.F.,(4,3,3,3,3,3,3,3,3,3,3,3,3,3,3,3,3,3,3,3,3,3,3,3,
3,3,3,3,3,3,3,3,3,3,3,3,3,3,3,3,3,3,3,3,3,3,3,3,3,3,3,3,3,3,3,3,3,3,3,3,
3,3,3,3,3,3,3,3,3,3,3,3,3,3,4),(461.814120077683,461.899400362206,461.982557506644,
462.065713177296,462.148885659595,462.235754833163,462.319063252884,462.402432042527,
462.485918963466,462.496362353867,462.580101065713,462.66373657708,462.747289020479,
462.83077845633,462.914232406944,462.99766890079,463.081106010546,463.164561805463,
463.248106298193,463.331695381134,463.415418648691,463.496098364587,463.579837076433,
463.6634725878,463.747025031199,463.830514467049,463.913968417663,463.997404911509,
464.080842021265,464.164297816183,464.247842308912,464.331431391853,464.415154659411,
464.495834375307,464.579573087153,464.66320859852,464.746761041919,464.83025047777,
464.913704428384,464.99714092223,465.080578031985,465.164033826903,465.247578319632,
465.331167402573,465.414890670131,465.495570386027,465.579309097873,465.66294460924,
465.746497052639,465.82998648849,465.913440439103,465.99687693295,466.080314042705,
466.163769837623,466.247314330353,466.330903413294,466.414626680851,466.495306396747,
466.579045108593,466.662680619961,466.746233063359,466.82972249921,466.913176449824,
466.99661294367,467.080050053425,467.163505848343,467.247050341073,467.330639424014,
467.414362691571,467.495042407467,467.582950874621,467.667748959495,467.752460450876,
467.837084945233,467.846676276085),.UNSPECIFIED.);
#347=B_SPLINE_CURVE_WITH_KNOTS('',3,(#50650,#50651,#50652,#50653,#50654,
#50655,#50656,#50657,#50658,#50659,#50660,#50661,#50662,#50663,#50664,#50665,
#50666,#50667,#50668,#50669,#50670,#50671,#50672,#50673,#50674,#50675,#50676,
#50677,#50678,#50679,#50680,#50681,#50682,#50683,#50684,#50685,#50686,#50687,
#50688,#50689,#50690,#50691,#50692,#50693,#50694,#50695,#50696,#50697,#50698,
#50699,#50700,#50701,#50702,#50703,#50704,#50705,#50706,#50707,#50708,#50709,
#50710,#50711,#50712,#50713,#50714,#50715,#50716,#50717,#50718,#50719,#50720,
#50721,#50722,#50723,#50724,#50725,#50726,#50727,#50728,#50729,#50730,#50731,
#50732,#50733,#50734,#50735,#50736,#50737,#50738,#50739,#50740,#50741,#50742,
#50743,#50744,#50745,#50746,#50747,#50748,#50749,#50750,#50751,#50752,#50753,
#50754,#50755,#50756,#50757,#50758,#50759,#50760,#50761,#50762,#50763,#50764,
#50765,#50766,#50767,#50768,#50769,#50770,#50771,#50772,#50773,#50774,#50775,
#50776,#50777,#50778,#50779,#50780,#50781,#50782,#50783,#50784,#50785,#50786,
#50787,#50788,#50789,#50790,#50791,#50792,#50793,#50794,#50795,#50796,#50797,
#50798,#50799,#50800,#50801,#50802,#50803,#50804,#50805,#50806,#50807,#50808,
#50809,#50810,#50811,#50812,#50813,#50814,#50815,#50816,#50817,#50818,#50819,
#50820,#50821,#50822,#50823,#50824,#50825,#50826,#50827,#50828,#50829,#50830,
#50831,#50832,#50833,#50834,#50835,#50836,#50837,#50838,#50839,#50840,#50841,
#50842,#50843,#50844,#50845,#50846,#50847,#50848,#50849,#50850,#50851,#50852,
#50853,#50854,#50855,#50856,#50857,#50858,#50859,#50860,#50861,#50862,#50863,
#50864,#50865,#50866,#50867,#50868,#50869),.UNSPECIFIED.,.F.,.F.,(4,3,3,
3,3,3,3,3,3,3,3,3,3,3,3,3,3,3,3,3,3,3,3,3,3,3,3,3,3,3,3,3,3,3,3,3,3,3,3,
3,3,3,3,3,3,3,3,3,3,3,3,3,3,3,3,3,3,3,3,3,3,3,3,3,3,3,3,3,3,3,3,3,3,4),
(468.097305384859,468.184487798472,468.268226510318,468.351862021685,468.435414465084,
468.518903900935,468.602357851549,468.685794345395,468.76923145515,468.852687250068,
468.936231742798,469.019820825739,469.103544093296,469.184223809192,469.267962521038,
469.351598032405,469.435150475804,469.518639911655,469.602093862269,469.685530356115,
469.76896746587,469.852423260788,469.935967753518,470.019556836459,470.103280104016,
470.183959819912,470.267698531758,470.351334043125,470.434886486524,470.518375922375,
470.601829872989,470.685266366835,470.76870347659,470.852159271508,470.935703764237,
471.019292847178,471.103016114736,471.183695830632,471.267434542478,471.351070053845,
471.434622497244,471.518111933095,471.601565883709,471.685002377555,471.768439487311,
471.851895282228,471.935439774958,472.019028857899,472.102752125457,472.183431841352,
472.267170553198,472.350806064566,472.434358507964,472.517847943815,472.601301894429,
472.684738388275,472.768175498031,472.851631292948,472.935175785678,473.018764868619,
473.102488136177,473.183167852073,473.266909639042,473.350547516417,473.434101619712,
473.520981630997,473.604431920655,473.68786448522,473.771297396346,473.854748721871,
473.938275693383,474.021847500333,474.105521992394,474.129141709994),
 .UNSPECIFIED.);
#348=B_SPLINE_CURVE_WITH_KNOTS('',3,(#50870,#50871,#50872,#50873,#50874,
#50875,#50876,#50877,#50878,#50879),.UNSPECIFIED.,.F.,.F.,(4,3,3,4),(467.845467786229,
467.928060537647,468.012682961186,468.097305384725),.UNSPECIFIED.);
#349=B_SPLINE_CURVE_WITH_KNOTS('',3,(#50881,#50882,#50883,#50884,#50885,
#50886,#50887,#50888,#50889,#50890),.UNSPECIFIED.,.F.,.F.,(4,3,3,4),(467.846676276085,
467.931227320063,468.015745325857,468.097305384863),.UNSPECIFIED.);
#350=B_SPLINE_CURVE_WITH_KNOTS('',3,(#50891,#50892,#50893,#50894,#50895,
#50896,#50897,#50898,#50899,#50900,#50901,#50902,#50903,#50904,#50905,#50906,
#50907,#50908,#50909,#50910,#50911,#50912,#50913,#50914,#50915,#50916,#50917,
#50918,#50919,#50920,#50921,#50922,#50923,#50924,#50925,#50926,#50927,#50928,
#50929,#50930,#50931,#50932,#50933,#50934,#50935,#50936,#50937,#50938,#50939,
#50940,#50941,#50942,#50943,#50944,#50945,#50946,#50947,#50948,#50949,#50950,
#50951,#50952,#50953,#50954,#50955,#50956,#50957,#50958,#50959,#50960,#50961,
#50962,#50963,#50964,#50965,#50966,#50967,#50968,#50969,#50970,#50971,#50972,
#50973,#50974,#50975,#50976,#50977,#50978,#50979,#50980,#50981,#50982,#50983,
#50984,#50985,#50986,#50987,#50988,#50989,#50990,#50991,#50992,#50993,#50994,
#50995,#50996,#50997,#50998,#50999,#51000,#51001,#51002,#51003,#51004,#51005,
#51006,#51007,#51008,#51009,#51010,#51011,#51012,#51013,#51014,#51015,#51016,
#51017,#51018,#51019,#51020,#51021,#51022,#51023,#51024,#51025,#51026,#51027,
#51028,#51029,#51030,#51031,#51032,#51033,#51034,#51035,#51036,#51037,#51038,
#51039,#51040,#51041,#51042,#51043,#51044,#51045,#51046,#51047,#51048,#51049,
#51050,#51051,#51052,#51053,#51054,#51055,#51056,#51057,#51058,#51059,#51060,
#51061,#51062,#51063,#51064,#51065,#51066,#51067,#51068,#51069,#51070,#51071,
#51072,#51073,#51074,#51075,#51076,#51077,#51078,#51079,#51080,#51081,#51082,
#51083,#51084,#51085,#51086,#51087,#51088,#51089,#51090,#51091,#51092,#51093,
#51094,#51095,#51096,#51097,#51098,#51099,#51100,#51101,#51102,#51103,#51104,
#51105,#51106,#51107,#51108,#51109,#51110),.UNSPECIFIED.,.F.,.F.,(4,3,3,
3,3,3,3,3,3,3,3,3,3,3,3,3,3,3,3,3,3,3,3,3,3,3,3,3,3,3,3,3,3,3,3,3,3,3,3,
3,3,3,3,3,3,3,3,3,3,3,3,3,3,3,3,3,3,3,3,3,3,3,3,3,3,3,3,3,3,3,3,3,3,4),
(468.097305385047,468.189543032656,468.282286929498,468.375293080407,468.468637906394,
468.494778418188,468.578517130034,468.662152641401,468.7457050848,468.829194520651,
468.912648471265,468.996084965111,469.079522074867,469.162977869784,469.246522362514,
469.330111445455,469.413834713013,469.494514428908,469.578253140754,469.661888652121,
469.74544109552,469.828930531371,469.912384481985,469.995820975831,470.079258085586,
470.162713880504,470.246258373234,470.329847456174,470.413570723732,470.494250439628,
470.577989151474,470.661624662841,470.74517710624,470.828666542091,470.912120492705,
470.995556986551,471.078994096307,471.162449891224,471.245994383954,471.329583466895,
471.413306734453,471.493986450348,471.577725162194,471.661360673561,471.74491311696,
471.828402552811,471.911856503425,471.995292997271,472.078730107026,472.162185901944,
472.245730394673,472.329319477614,472.413042745172,472.493722461068,472.577461172914,
472.661096684282,472.74464912768,472.828138563531,472.911592514145,472.995029007991,
473.078466117747,473.161921912664,473.245466405394,473.329055488335,473.412778755893,
473.493458471788,473.57606110231,473.658569104472,473.741001605987,473.823377664764,
473.905725141663,473.988054434924,474.070408822026,474.128667782826),
 .UNSPECIFIED.);
#351=B_SPLINE_CURVE_WITH_KNOTS('',3,(#51116,#51117,#51118,#51119,#51120,
#51121,#51122,#51123,#51124,#51125,#51126,#51127,#51128,#51129,#51130,#51131,
#51132,#51133,#51134,#51135,#51136,#51137,#51138,#51139,#51140,#51141,#51142,
#51143,#51144,#51145,#51146,#51147,#51148,#51149,#51150,#51151,#51152,#51153,
#51154,#51155,#51156,#51157,#51158,#51159,#51160,#51161,#51162,#51163,#51164,
#51165,#51166,#51167,#51168,#51169,#51170,#51171,#51172,#51173,#51174,#51175,
#51176,#51177,#51178,#51179,#51180,#51181,#51182,#51183,#51184,#51185,#51186,
#51187,#51188,#51189,#51190,#51191,#51192,#51193,#51194,#51195,#51196,#51197,
#51198,#51199,#51200,#51201,#51202,#51203,#51204,#51205,#51206,#51207,#51208,
#51209,#51210,#51211,#51212,#51213,#51214,#51215,#51216,#51217,#51218,#51219,
#51220,#51221,#51222,#51223,#51224,#51225,#51226,#51227,#51228,#51229,#51230,
#51231,#51232,#51233,#51234,#51235,#51236,#51237,#51238,#51239,#51240,#51241,
#51242,#51243,#51244,#51245,#51246,#51247,#51248,#51249,#51250,#51251,#51252,
#51253,#51254,#51255,#51256,#51257,#51258,#51259,#51260,#51261,#51262,#51263,
#51264,#51265,#51266,#51267,#51268,#51269,#51270,#51271,#51272,#51273,#51274,
#51275,#51276,#51277,#51278,#51279,#51280,#51281,#51282,#51283,#51284,#51285,
#51286,#51287,#51288,#51289,#51290,#51291,#51292,#51293,#51294,#51295,#51296,
#51297,#51298,#51299,#51300,#51301,#51302,#51303,#51304,#51305,#51306,#51307,
#51308,#51309,#51310,#51311,#51312,#51313,#51314,#51315,#51316,#51317,#51318,
#51319,#51320,#51321,#51322,#51323,#51324,#51325,#51326,#51327,#51328,#51329,
#51330,#51331,#51332,#51333,#51334,#51335),.UNSPECIFIED.,.F.,.F.,(4,3,3,
3,3,3,3,3,3,3,3,3,3,3,3,3,3,3,3,3,3,3,3,3,3,3,3,3,3,3,3,3,3,3,3,3,3,3,3,
3,3,3,3,3,3,3,3,3,3,3,3,3,3,3,3,3,3,3,3,3,3,3,3,3,3,3,3,3,3,3,3,3,3,4),
(474.380490692145,474.462864309227,474.545168268208,474.627428853586,474.709667867551,
474.791904327036,474.874157244687,474.95649402033,475.038875176067,475.121381803559,
475.182639873513,475.266378585359,475.350014096726,475.433566540125,475.517055975976,
475.60050992659,475.683946420436,475.767383530192,475.850839325109,475.934383817839,
476.01797290078,476.101696168337,476.182375884233,476.266114596079,476.349750107446,
476.433302550845,476.516791986696,476.60024593731,476.683682431156,476.767119540911,
476.850575335829,476.934119828559,477.0177089115,477.101432179057,477.182111894953,
477.265850606799,477.349486118166,477.433038561565,477.516527997415,477.599981948029,
477.683418441875,477.766855551631,477.850311346548,477.933855839278,478.017444922219,
478.101168189777,478.181847905673,478.265586617519,478.349222128886,478.432774572285,
478.516264008136,478.59971795875,478.683154452596,478.766591562351,478.850047357269,
478.933591849999,479.01718093294,479.100904200497,479.181583916393,479.265322628239,
479.348958139607,479.432510583006,479.516000018856,479.59945396947,479.682890463316,
479.766327573071,479.849783367989,479.933327860719,480.01691694366,480.100640211218,
480.181319927113,480.27010194833,480.358677088798,480.413366811053),
 .UNSPECIFIED.);
#352=B_SPLINE_CURVE_WITH_KNOTS('',3,(#51336,#51337,#51338,#51339,#51340,
#51341,#51342,#51343,#51344,#51345),.UNSPECIFIED.,.F.,.F.,(4,3,3,4),(474.129141709994,
474.182903862793,474.30385189376,474.380490692039),.UNSPECIFIED.);
#353=B_SPLINE_CURVE_WITH_KNOTS('',3,(#51347,#51348,#51349,#51350,#51351,
#51352,#51353,#51354,#51355,#51356),.UNSPECIFIED.,.F.,.F.,(4,3,3,4),(474.128667782826,
474.211094423954,474.29579255793,474.380490691907),.UNSPECIFIED.);
#354=B_SPLINE_CURVE_WITH_KNOTS('',3,(#51357,#51358,#51359,#51360,#51361,
#51362,#51363,#51364,#51365,#51366,#51367,#51368,#51369,#51370,#51371,#51372,
#51373,#51374,#51375,#51376,#51377,#51378,#51379,#51380,#51381,#51382,#51383,
#51384,#51385,#51386,#51387,#51388,#51389,#51390,#51391,#51392,#51393,#51394,
#51395,#51396,#51397,#51398,#51399,#51400,#51401,#51402,#51403,#51404,#51405,
#51406,#51407,#51408,#51409,#51410,#51411,#51412,#51413,#51414,#51415,#51416,
#51417,#51418,#51419,#51420,#51421,#51422,#51423,#51424,#51425,#51426,#51427,
#51428,#51429,#51430,#51431,#51432,#51433,#51434,#51435,#51436,#51437,#51438,
#51439,#51440,#51441,#51442,#51443,#51444,#51445,#51446,#51447,#51448,#51449,
#51450,#51451,#51452,#51453,#51454,#51455,#51456,#51457,#51458,#51459,#51460,
#51461,#51462,#51463,#51464,#51465,#51466,#51467,#51468,#51469,#51470,#51471,
#51472,#51473,#51474,#51475,#51476,#51477,#51478,#51479,#51480,#51481,#51482,
#51483,#51484,#51485,#51486,#51487,#51488,#51489,#51490,#51491,#51492,#51493,
#51494,#51495,#51496,#51497,#51498,#51499,#51500,#51501,#51502,#51503,#51504,
#51505,#51506,#51507,#51508,#51509,#51510,#51511,#51512,#51513,#51514,#51515,
#51516,#51517,#51518,#51519,#51520,#51521,#51522,#51523,#51524,#51525,#51526,
#51527,#51528,#51529,#51530,#51531,#51532,#51533,#51534,#51535,#51536,#51537,
#51538,#51539,#51540,#51541,#51542,#51543,#51544,#51545,#51546,#51547,#51548,
#51549,#51550,#51551,#51552,#51553,#51554,#51555,#51556,#51557,#51558,#51559,
#51560,#51561,#51562,#51563,#51564,#51565,#51566,#51567,#51568,#51569,#51570,
#51571,#51572,#51573),.UNSPECIFIED.,.F.,.F.,(4,3,3,3,3,3,3,3,3,3,3,3,3,
3,3,3,3,3,3,3,3,3,3,3,3,3,3,3,3,3,3,3,3,3,3,3,3,3,3,3,3,3,3,3,3,3,3,3,3,
3,3,3,3,3,3,3,3,3,3,3,3,3,3,3,3,3,3,3,3,3,3,3,4),(474.380490692042,474.493194482508,
474.576933194354,474.660568705722,474.74412114912,474.827610584971,474.911064535585,
474.994501029431,475.077938139187,475.161393934104,475.244938426834,475.328527509775,
475.412250777333,475.492930493229,475.576669205075,475.660304716442,475.743857159841,
475.827346595692,475.910800546306,475.994237040152,476.077674149907,476.161129944825,
476.244674437555,476.328263520496,476.411986788053,476.492666503949,476.576405215795,
476.660040727162,476.743593170561,476.827082606412,476.910536557026,476.993973050872,
477.077410160627,477.160865955545,477.244410448275,477.327999531216,477.411722798773,
477.492402514669,477.576141226515,477.659776737882,477.743329181281,477.826818617132,
477.910272567746,477.993709061592,478.077146171347,478.160601966265,478.244146458995,
478.327735541936,478.411458809493,478.492138525389,478.575877237235,478.659512748602,
478.743065192001,478.826554627852,478.910008578466,478.993445072312,479.076882182067,
479.160337976985,479.243882469715,479.327471552656,479.411194820213,479.491874536109,
479.57561783401,479.659256884327,479.742811824025,479.826488668858,479.909938960391,
479.99337035517,480.076800925009,480.160657339428,480.244174762693,480.328200672689,
480.412226582686),.UNSPECIFIED.);
#355=B_SPLINE_CURVE_WITH_KNOTS('',3,(#51579,#51580,#51581,#51582,#51583,
#51584,#51585,#51586,#51587,#51588,#51589,#51590,#51591,#51592,#51593,#51594,
#51595,#51596,#51597,#51598,#51599,#51600,#51601,#51602,#51603,#51604,#51605,
#51606,#51607,#51608,#51609,#51610,#51611,#51612,#51613,#51614,#51615,#51616,
#51617,#51618,#51619,#51620,#51621,#51622,#51623,#51624,#51625,#51626,#51627,
#51628,#51629,#51630,#51631,#51632,#51633,#51634,#51635,#51636,#51637,#51638,
#51639,#51640,#51641,#51642,#51643,#51644,#51645,#51646,#51647,#51648,#51649,
#51650,#51651,#51652,#51653,#51654,#51655,#51656,#51657,#51658,#51659,#51660,
#51661,#51662,#51663,#51664,#51665,#51666,#51667,#51668,#51669,#51670,#51671,
#51672,#51673,#51674,#51675,#51676,#51677,#51678,#51679,#51680,#51681,#51682,
#51683,#51684,#51685,#51686,#51687,#51688,#51689,#51690,#51691,#51692,#51693,
#51694,#51695,#51696,#51697,#51698,#51699,#51700,#51701,#51702,#51703,#51704,
#51705,#51706,#51707,#51708,#51709,#51710,#51711,#51712,#51713,#51714,#51715,
#51716,#51717,#51718,#51719,#51720,#51721,#51722,#51723,#51724,#51725,#51726,
#51727,#51728,#51729,#51730,#51731,#51732,#51733,#51734,#51735,#51736,#51737,
#51738,#51739,#51740,#51741,#51742,#51743,#51744,#51745,#51746,#51747,#51748,
#51749,#51750,#51751,#51752,#51753,#51754,#51755,#51756,#51757,#51758,#51759,
#51760,#51761,#51762,#51763,#51764,#51765,#51766,#51767,#51768,#51769,#51770,
#51771,#51772,#51773,#51774,#51775,#51776,#51777,#51778,#51779,#51780,#51781,
#51782,#51783,#51784,#51785,#51786,#51787,#51788,#51789,#51790,#51791,#51792,
#51793,#51794,#51795,#51796,#51797,#51798),.UNSPECIFIED.,.F.,.F.,(4,3,3,
3,3,3,3,3,3,3,3,3,3,3,3,3,3,3,3,3,3,3,3,3,3,3,3,3,3,3,3,3,3,3,3,3,3,3,3,
3,3,3,3,3,3,3,3,3,3,3,3,3,3,3,3,3,3,3,3,3,3,3,3,3,3,3,3,3,3,3,3,3,3,4),
(480.663675999218,480.750472077734,480.837361456173,480.924435942999,481.011605159472,
481.098971661175,481.181055937834,481.26479464968,481.348430161048,481.431982604446,
481.515472040297,481.598925990911,481.682362484757,481.765799594513,481.84925538943,
481.93279988216,482.016388965101,482.100112232659,482.180791948554,482.2645306604,
482.348166171767,482.431718615166,482.515208051016,482.59866200163,482.682098495476,
482.765535605232,482.848991400149,482.932535892879,483.01612497582,483.099848243377,
483.180527959274,483.26426667112,483.347902182487,483.431454625886,483.514944061737,
483.598398012351,483.681834506197,483.765271615952,483.84872741087,483.932271903599,
484.01586098654,484.099584254098,484.180263969994,484.26400268184,484.347638193207,
484.431190636606,484.514680072456,484.59813402307,484.681570516916,484.765007626672,
484.848463421589,484.932007914319,485.01559699726,485.099320264818,485.179999980714,
485.26373869256,485.347374203927,485.430926647326,485.514416083177,485.597870033791,
485.681306527637,485.764743637392,485.84819943231,485.93174392504,486.015333007981,
486.099056275539,486.179735991434,486.262390162833,486.344946957616,486.427425490976,
486.509839890327,486.592217795374,486.674583461396,486.695415017246),
 .UNSPECIFIED.);
#356=B_SPLINE_CURVE_WITH_KNOTS('',3,(#51799,#51800,#51801,#51802,#51803,
#51804,#51805,#51806,#51807,#51808),.UNSPECIFIED.,.F.,.F.,(4,3,3,4),(480.413366811053,
480.50167377437,480.589785986689,480.663675999053),.UNSPECIFIED.);
#357=B_SPLINE_CURVE_WITH_KNOTS('',3,(#51810,#51811,#51812,#51813,#51814,
#51815,#51816,#51817,#51818,#51819),.UNSPECIFIED.,.F.,.F.,(4,3,3,4),(480.412226582686,
480.491610546829,480.622176733975,480.663675999222),.UNSPECIFIED.);
#358=B_SPLINE_CURVE_WITH_KNOTS('',3,(#51820,#51821,#51822,#51823,#51824,
#51825,#51826,#51827,#51828,#51829,#51830,#51831,#51832,#51833,#51834,#51835,
#51836,#51837,#51838,#51839,#51840,#51841,#51842,#51843,#51844,#51845,#51846,
#51847,#51848,#51849,#51850,#51851,#51852,#51853,#51854,#51855,#51856,#51857,
#51858,#51859,#51860,#51861,#51862,#51863,#51864,#51865,#51866,#51867,#51868,
#51869,#51870,#51871,#51872,#51873,#51874,#51875,#51876,#51877,#51878,#51879,
#51880,#51881,#51882,#51883,#51884,#51885,#51886,#51887,#51888,#51889,#51890,
#51891,#51892,#51893,#51894,#51895,#51896,#51897,#51898,#51899,#51900,#51901,
#51902,#51903,#51904,#51905,#51906,#51907,#51908,#51909,#51910,#51911,#51912,
#51913,#51914,#51915,#51916,#51917,#51918,#51919,#51920,#51921,#51922,#51923,
#51924,#51925,#51926,#51927,#51928,#51929,#51930,#51931,#51932,#51933,#51934,
#51935,#51936,#51937,#51938,#51939,#51940,#51941,#51942,#51943,#51944,#51945,
#51946,#51947,#51948,#51949,#51950,#51951,#51952,#51953,#51954,#51955,#51956,
#51957,#51958,#51959,#51960,#51961,#51962,#51963,#51964,#51965,#51966,#51967,
#51968,#51969,#51970,#51971,#51972,#51973,#51974,#51975,#51976,#51977,#51978,
#51979,#51980,#51981,#51982,#51983,#51984,#51985,#51986,#51987,#51988,#51989,
#51990,#51991,#51992,#51993,#51994,#51995,#51996,#51997,#51998,#51999,#52000,
#52001,#52002,#52003,#52004,#52005,#52006,#52007,#52008,#52009,#52010,#52011,
#52012,#52013,#52014,#52015,#52016,#52017,#52018,#52019,#52020,#52021,#52022,
#52023,#52024,#52025,#52026,#52027,#52028,#52029,#52030,#52031,#52032,#52033,
#52034,#52035,#52036,#52037,#52038,#52039),.UNSPECIFIED.,.F.,.F.,(4,3,3,
3,3,3,3,3,3,3,3,3,3,3,3,3,3,3,3,3,3,3,3,3,3,3,3,3,3,3,3,3,3,3,3,3,3,3,3,
3,3,3,3,3,3,3,3,3,3,3,3,3,3,3,3,3,3,3,3,3,3,3,3,3,3,3,3,3,3,3,3,3,3,4),
(480.663675999399,480.746042833896,480.828333032913,480.911209723492,480.993419243018,
481.075620137376,481.15783143992,481.241210219328,481.323541599451,481.4074440785,
481.491346557549,481.575085269395,481.658720780763,481.742273224161,481.825762660012,
481.909216610626,481.992653104472,482.076090214228,482.159546009145,482.243090501875,
482.326679584816,482.410402852374,482.491082568269,482.574821280115,482.658456791482,
482.742009234881,482.825498670732,482.908952621346,482.992389115192,483.075826224948,
483.159282019866,483.242826512595,483.326415595536,483.410138863094,483.49081857899,
483.574557290836,483.658192802204,483.741745245602,483.825234681453,483.908688632067,
483.992125125913,484.075562235669,484.159018030587,484.242562523316,484.326151606257,
484.409874873815,484.49055458971,484.574293301556,484.657928812923,484.741481256322,
484.824970692172,484.908424642786,484.991861136632,485.075298246387,485.158754041305,
485.242298534034,485.325887616975,485.409610884532,485.49029060043,485.574029312276,
485.657664823644,485.741217267042,485.824706702892,485.908160653506,485.991597147352,
486.075034257108,486.158490052025,486.242034544755,486.325623627696,486.409346895254,
486.49002661115,486.579990511233,486.669730741741,486.696559540383),
 .UNSPECIFIED.);
#359=B_SPLINE_CURVE_WITH_KNOTS('',3,(#52045,#52046,#52047,#52048,#52049,
#52050,#52051,#52052,#52053,#52054,#52055,#52056,#52057,#52058,#52059,#52060,
#52061,#52062,#52063,#52064,#52065,#52066,#52067,#52068,#52069,#52070,#52071,
#52072,#52073,#52074,#52075,#52076,#52077,#52078,#52079,#52080,#52081,#52082,
#52083,#52084,#52085,#52086,#52087,#52088,#52089,#52090,#52091,#52092,#52093,
#52094,#52095,#52096,#52097,#52098,#52099,#52100,#52101,#52102,#52103,#52104,
#52105,#52106,#52107,#52108,#52109,#52110,#52111,#52112,#52113,#52114,#52115,
#52116,#52117,#52118,#52119,#52120,#52121,#52122,#52123,#52124,#52125,#52126,
#52127,#52128,#52129,#52130,#52131,#52132,#52133,#52134,#52135,#52136,#52137,
#52138,#52139,#52140,#52141,#52142,#52143,#52144,#52145,#52146,#52147,#52148,
#52149,#52150,#52151,#52152,#52153,#52154,#52155,#52156,#52157,#52158,#52159,
#52160,#52161,#52162,#52163,#52164,#52165,#52166,#52167,#52168,#52169,#52170,
#52171,#52172,#52173,#52174,#52175,#52176,#52177,#52178,#52179,#52180,#52181,
#52182,#52183,#52184,#52185,#52186,#52187,#52188,#52189,#52190,#52191,#52192,
#52193,#52194,#52195,#52196,#52197,#52198,#52199,#52200,#52201,#52202,#52203,
#52204,#52205,#52206,#52207,#52208,#52209,#52210,#52211,#52212,#52213,#52214,
#52215,#52216,#52217,#52218,#52219,#52220,#52221,#52222,#52223,#52224,#52225,
#52226,#52227,#52228,#52229,#52230,#52231,#52232,#52233,#52234,#52235,#52236,
#52237,#52238,#52239,#52240,#52241,#52242,#52243,#52244,#52245,#52246,#52247,
#52248,#52249,#52250,#52251,#52252,#52253,#52254,#52255,#52256,#52257,#52258,
#52259,#52260,#52261,#52262,#52263,#52264),.UNSPECIFIED.,.F.,.F.,(4,3,3,
3,3,3,3,3,3,3,3,3,3,3,3,3,3,3,3,3,3,3,3,3,3,3,3,3,3,3,3,3,3,3,3,3,3,3,3,
3,3,3,3,3,3,3,3,3,3,3,3,3,3,3,3,3,3,3,3,3,3,3,3,3,3,3,3,3,3,3,3,3,3,4),
(486.946861306398,487.057134081218,487.170531457197,487.179472002154,487.263210714,
487.346846225367,487.430398668766,487.513888104617,487.597342055231,487.680778549077,
487.764215658832,487.84767145375,487.93121594648,488.014805029421,488.098528296979,
488.179208012874,488.26294672472,488.346582236088,488.430134679486,488.513624115337,
488.597078065951,488.680514559797,488.763951669553,488.84740746447,488.9309519572,
489.014541040141,489.098264307699,489.178944023595,489.262682735441,489.346318246809,
489.429870690207,489.513360126058,489.596814076672,489.680250570518,489.763687680274,
489.847143475192,489.930687967921,490.014277050862,490.09800031842,490.178680034315,
490.262418746161,490.346054257528,490.429606700927,490.513096136778,490.596550087391,
490.679986581237,490.763423690993,490.846879485911,490.93042397864,491.014013061581,
491.097736329139,491.178416045035,491.262154756881,491.345790268248,491.429342711647,
491.512832147498,491.596286098112,491.679722591958,491.763159701714,491.846615496631,
491.930159989361,492.013749072302,492.09747233986,492.178152055755,492.26190282802,
492.345547767752,492.429091494216,492.512577828497,492.59602489082,492.679450771037,
492.762897683742,492.84635523381,492.929876217716,492.978381755897),
 .UNSPECIFIED.);
#360=B_SPLINE_CURVE_WITH_KNOTS('',3,(#52265,#52266,#52267,#52268,#52269,
#52270,#52271,#52272,#52273,#52274),.UNSPECIFIED.,.F.,.F.,(4,3,3,4),(486.695415017246,
486.777807467469,486.862334386933,486.946861306398),.UNSPECIFIED.);
#361=B_SPLINE_CURVE_WITH_KNOTS('',3,(#52276,#52277,#52278,#52279,#52280,
#52281,#52282,#52283,#52284,#52285),.UNSPECIFIED.,.F.,.F.,(4,3,3,4),(486.696559540383,
486.786015256491,486.875219215317,486.946861306221),.UNSPECIFIED.);
#362=B_SPLINE_CURVE_WITH_KNOTS('',3,(#52286,#52287,#52288,#52289,#52290,
#52291,#52292,#52293,#52294,#52295,#52296,#52297,#52298,#52299,#52300,#52301,
#52302,#52303,#52304,#52305,#52306,#52307,#52308,#52309,#52310,#52311,#52312,
#52313,#52314,#52315,#52316,#52317,#52318,#52319,#52320,#52321,#52322,#52323,
#52324,#52325,#52326,#52327,#52328,#52329,#52330,#52331,#52332,#52333,#52334,
#52335,#52336,#52337,#52338,#52339,#52340,#52341,#52342,#52343,#52344,#52345,
#52346,#52347,#52348,#52349,#52350,#52351,#52352,#52353,#52354,#52355,#52356,
#52357,#52358,#52359,#52360,#52361,#52362,#52363,#52364,#52365,#52366,#52367,
#52368,#52369,#52370,#52371,#52372,#52373,#52374,#52375,#52376,#52377,#52378,
#52379,#52380,#52381,#52382,#52383,#52384,#52385,#52386,#52387,#52388,#52389,
#52390,#52391,#52392,#52393,#52394,#52395,#52396,#52397,#52398,#52399,#52400,
#52401,#52402,#52403,#52404,#52405,#52406,#52407,#52408,#52409,#52410,#52411,
#52412,#52413,#52414,#52415,#52416,#52417,#52418,#52419,#52420,#52421,#52422,
#52423,#52424,#52425,#52426,#52427,#52428,#52429,#52430,#52431,#52432,#52433,
#52434,#52435,#52436,#52437,#52438,#52439,#52440,#52441,#52442,#52443,#52444,
#52445,#52446,#52447,#52448,#52449,#52450,#52451,#52452,#52453,#52454,#52455,
#52456,#52457,#52458,#52459,#52460,#52461,#52462,#52463,#52464,#52465,#52466,
#52467,#52468,#52469,#52470,#52471,#52472,#52473,#52474,#52475,#52476,#52477,
#52478,#52479,#52480,#52481,#52482,#52483,#52484,#52485,#52486,#52487,#52488,
#52489,#52490,#52491,#52492,#52493,#52494,#52495,#52496,#52497,#52498,#52499,
#52500,#52501,#52502,#52503,#52504,#52505),.UNSPECIFIED.,.F.,.F.,(4,3,3,
3,3,3,3,3,3,3,3,3,3,3,3,3,3,3,3,3,3,3,3,3,3,3,3,3,3,3,3,3,3,3,3,3,3,3,3,
3,3,3,3,3,3,3,3,3,3,3,3,3,3,3,3,3,3,3,3,3,3,3,3,3,3,3,3,3,3,3,3,3,3,4),
(486.946861306402,487.032861514281,487.118928332231,487.20507484832,487.291376054737,
487.377765824186,487.464312824274,487.48976262187,487.573501333716,487.657136845083,
487.740689288482,487.824178724332,487.907632674946,487.991069168792,488.074506278548,
488.157962073465,488.241506566195,488.325095649136,488.408818916693,488.48949863259,
488.573237344436,488.656872855803,488.740425299202,488.823914735053,488.907368685667,
488.990805179513,489.074242289269,489.157698084186,489.241242576916,489.324831659857,
489.408554927414,489.48923464331,489.572973355156,489.656608866524,489.740161309922,
489.823650745774,489.907104696387,489.990541190234,490.073978299989,490.157434094907,
490.240978587637,490.324567670578,490.408290938135,490.48897065403,490.572709365876,
490.656344877243,490.739897320642,490.823386756494,490.906840707107,490.990277200954,
491.073714310709,491.157170105627,491.240714598357,491.324303681298,491.408026948855,
491.488706664751,491.572445376597,491.656080887964,491.739633331363,491.823122767214,
491.906576717828,491.990013211674,492.07345032143,492.156906116347,492.240450609077,
492.324039692018,492.407762959576,492.488442675471,492.571272612664,492.654003819318,
492.736642260717,492.819226107672,492.901781529493,492.978723737855),
 .UNSPECIFIED.);
#363=B_SPLINE_CURVE_WITH_KNOTS('',3,(#52511,#52512,#52513,#52514,#52515,
#52516,#52517,#52518,#52519,#52520,#52521,#52522,#52523,#52524,#52525,#52526,
#52527,#52528,#52529,#52530,#52531,#52532,#52533,#52534,#52535,#52536,#52537,
#52538,#52539,#52540,#52541,#52542,#52543,#52544,#52545,#52546,#52547,#52548,
#52549,#52550,#52551,#52552,#52553,#52554,#52555,#52556,#52557,#52558,#52559,
#52560,#52561,#52562,#52563,#52564,#52565,#52566,#52567,#52568,#52569,#52570,
#52571,#52572,#52573,#52574,#52575,#52576,#52577,#52578,#52579,#52580,#52581,
#52582,#52583,#52584,#52585,#52586,#52587,#52588,#52589,#52590,#52591,#52592,
#52593,#52594,#52595,#52596,#52597,#52598,#52599,#52600,#52601,#52602,#52603,
#52604,#52605,#52606,#52607,#52608,#52609,#52610,#52611,#52612,#52613,#52614,
#52615,#52616,#52617,#52618,#52619,#52620,#52621,#52622,#52623,#52624,#52625,
#52626,#52627,#52628,#52629,#52630,#52631,#52632,#52633,#52634,#52635,#52636,
#52637,#52638,#52639,#52640,#52641,#52642,#52643,#52644,#52645,#52646,#52647,
#52648,#52649,#52650,#52651,#52652,#52653,#52654,#52655,#52656,#52657,#52658,
#52659,#52660,#52661,#52662,#52663,#52664,#52665,#52666,#52667,#52668,#52669,
#52670,#52671,#52672,#52673,#52674,#52675,#52676,#52677,#52678,#52679,#52680,
#52681,#52682,#52683,#52684,#52685,#52686,#52687,#52688,#52689,#52690,#52691,
#52692,#52693,#52694,#52695,#52696,#52697,#52698,#52699,#52700,#52701,#52702,
#52703,#52704,#52705,#52706,#52707,#52708,#52709,#52710,#52711,#52712,#52713,
#52714,#52715,#52716,#52717,#52718,#52719,#52720,#52721,#52722,#52723,#52724,
#52725,#52726,#52727,#52728,#52729,#52730),.UNSPECIFIED.,.F.,.F.,(4,3,3,
3,3,3,3,3,3,3,3,3,3,3,3,3,3,3,3,3,3,3,3,3,3,3,3,3,3,3,3,3,3,3,3,3,3,3,3,
3,3,3,3,3,3,3,3,3,3,3,3,3,3,3,3,3,3,3,3,3,3,3,3,3,3,3,3,3,3,3,3,3,3,4),
(493.230046613679,493.313107106364,493.396067801015,493.478949461932,493.561772776128,
493.644567209288,493.727349550249,493.810138438958,493.892952516834,493.975856520167,
494.058812040378,494.141887794238,494.177624077195,494.261362789041,494.344998300409,
494.428550743807,494.512040179658,494.595494130272,494.678930624118,494.762367733873,
494.845823528791,494.929368021521,495.012957104462,495.096680372019,495.177360087915,
495.261098799761,495.344734311128,495.428286754527,495.511776190378,495.595230140992,
495.678666634838,495.762103744594,495.845559539511,495.929104032241,496.012693115182,
496.09641638274,496.177096098636,496.260834810482,496.34447032185,496.428022765248,
496.511512201099,496.594966151713,496.678402645559,496.761839755315,496.845295550233,
496.928840042962,497.012429125903,497.096152393461,497.176832109356,497.260570821202,
497.344206332569,497.427758775968,497.511248211818,497.594702162432,497.678138656279,
497.761575766034,497.845031560952,497.928576053682,498.012165136622,498.09588840418,
498.176568120076,498.260306831922,498.343942343289,498.427494786688,498.510984222539,
498.594438173153,498.677874666999,498.761311776754,498.844767571672,498.928312064401,
499.011901147342,499.095624414899,499.176304130796,499.262642145922),
 .UNSPECIFIED.);
#364=B_SPLINE_CURVE_WITH_KNOTS('',3,(#52731,#52732,#52733,#52734,#52735,
#52736,#52737,#52738,#52739,#52740,#52741,#52742,#52743),.UNSPECIFIED.,
 .F.,.F.,(4,3,3,3,4),(492.978381755897,493.062004160814,493.145747059646,
493.177888066475,493.230046613577),.UNSPECIFIED.);
#365=B_SPLINE_CURVE_WITH_KNOTS('',3,(#52745,#52746,#52747,#52748,#52749,
#52750,#52751,#52752,#52753,#52754),.UNSPECIFIED.,.F.,.F.,(4,3,3,4),(492.978723737855,
493.061272089773,493.145659351677,493.230046613581),.UNSPECIFIED.);
#366=B_SPLINE_CURVE_WITH_KNOTS('',3,(#52755,#52756,#52757,#52758,#52759,
#52760,#52761,#52762,#52763,#52764,#52765,#52766,#52767,#52768,#52769,#52770,
#52771,#52772,#52773,#52774,#52775,#52776,#52777,#52778,#52779,#52780,#52781,
#52782,#52783,#52784,#52785,#52786,#52787,#52788,#52789,#52790,#52791,#52792,
#52793,#52794,#52795,#52796,#52797,#52798,#52799,#52800,#52801,#52802,#52803,
#52804,#52805,#52806,#52807,#52808,#52809,#52810,#52811,#52812,#52813,#52814,
#52815,#52816,#52817,#52818,#52819,#52820,#52821,#52822,#52823,#52824,#52825,
#52826,#52827,#52828,#52829,#52830,#52831,#52832,#52833,#52834,#52835,#52836,
#52837,#52838,#52839,#52840,#52841,#52842,#52843,#52844,#52845,#52846,#52847,
#52848,#52849,#52850,#52851,#52852,#52853,#52854,#52855,#52856,#52857,#52858,
#52859,#52860,#52861,#52862,#52863,#52864,#52865,#52866,#52867,#52868,#52869,
#52870,#52871,#52872,#52873,#52874,#52875,#52876,#52877,#52878,#52879,#52880,
#52881,#52882,#52883,#52884,#52885,#52886,#52887,#52888,#52889,#52890,#52891,
#52892,#52893,#52894,#52895,#52896,#52897,#52898,#52899,#52900,#52901,#52902,
#52903,#52904,#52905,#52906,#52907,#52908,#52909,#52910,#52911,#52912,#52913,
#52914,#52915,#52916,#52917,#52918,#52919,#52920,#52921,#52922,#52923,#52924,
#52925,#52926,#52927,#52928,#52929,#52930,#52931,#52932,#52933,#52934,#52935,
#52936,#52937,#52938,#52939,#52940,#52941,#52942,#52943,#52944,#52945,#52946,
#52947,#52948,#52949,#52950,#52951,#52952,#52953,#52954,#52955,#52956,#52957,
#52958,#52959,#52960,#52961,#52962,#52963,#52964,#52965,#52966,#52967,#52968,
#52969,#52970,#52971,#52972,#52973,#52974),.UNSPECIFIED.,.F.,.F.,(4,3,3,
3,3,3,3,3,3,3,3,3,3,3,3,3,3,3,3,3,3,3,3,3,3,3,3,3,3,3,3,3,3,3,3,3,3,3,3,
3,3,3,3,3,3,3,3,3,3,3,3,3,3,3,3,3,3,3,3,3,3,3,3,3,3,3,3,3,3,3,3,3,3,4),
(493.230046613707,493.336016526352,493.444154354458,493.488178686191,493.571917398037,
493.655552909404,493.739105352803,493.822594788654,493.906048739268,493.989485233114,
494.072922342869,494.156378137787,494.239922630517,494.323511713458,494.407234981015,
494.487914696911,494.571653408757,494.655288920124,494.738841363523,494.822330799374,
494.905784749988,494.989221243834,495.072658353589,495.156114148507,495.239658641237,
495.323247724178,495.406970991735,495.487650707631,495.571389419477,495.655024930844,
495.738577374243,495.822066810094,495.905520760707,495.988957254554,496.072394364309,
496.155850159227,496.239394651956,496.322983734897,496.406707002455,496.487386718351,
496.571125430197,496.654760941565,496.738313384963,496.821802820814,496.905256771428,
496.988693265274,497.07213037503,497.155586169947,497.239130662677,497.322719745618,
497.406443013176,497.487122729071,497.570861440917,497.654496952284,497.738049395683,
497.821538831534,497.904992782148,497.988429275994,498.07186638575,498.155322180667,
498.238866673397,498.322455756338,498.406179023896,498.486858739792,498.570611182974,
498.656980730276,498.740522870978,498.824007733033,498.907453436365,498.990878070489,
499.074319814382,499.157772531728,499.241278278077,499.261567561389),
 .UNSPECIFIED.);
#367=B_SPLINE_CURVE_WITH_KNOTS('',3,(#52980,#52981,#52982,#52983,#52984,
#52985,#52986,#52987,#52988,#52989,#52990,#52991,#52992,#52993,#52994,#52995,
#52996,#52997,#52998,#52999,#53000,#53001,#53002,#53003,#53004,#53005,#53006,
#53007,#53008,#53009,#53010,#53011,#53012,#53013,#53014,#53015,#53016,#53017,
#53018,#53019,#53020,#53021,#53022,#53023,#53024,#53025,#53026,#53027,#53028,
#53029,#53030,#53031,#53032,#53033,#53034,#53035,#53036,#53037,#53038,#53039,
#53040,#53041,#53042,#53043,#53044,#53045,#53046,#53047,#53048,#53049,#53050,
#53051,#53052,#53053,#53054,#53055,#53056,#53057,#53058,#53059,#53060,#53061,
#53062,#53063,#53064,#53065,#53066,#53067,#53068,#53069,#53070,#53071,#53072,
#53073,#53074,#53075,#53076,#53077,#53078,#53079,#53080,#53081,#53082,#53083,
#53084,#53085,#53086,#53087,#53088,#53089,#53090,#53091,#53092,#53093,#53094,
#53095,#53096,#53097,#53098,#53099,#53100,#53101,#53102,#53103,#53104,#53105,
#53106,#53107,#53108,#53109,#53110,#53111,#53112,#53113,#53114,#53115,#53116,
#53117,#53118,#53119,#53120,#53121,#53122,#53123,#53124,#53125,#53126,#53127,
#53128,#53129,#53130,#53131,#53132,#53133,#53134,#53135,#53136,#53137,#53138,
#53139,#53140,#53141,#53142,#53143,#53144,#53145,#53146,#53147,#53148,#53149,
#53150,#53151,#53152,#53153,#53154,#53155,#53156,#53157,#53158,#53159,#53160,
#53161,#53162,#53163,#53164,#53165,#53166,#53167,#53168,#53169,#53170,#53171,
#53172,#53173,#53174,#53175,#53176,#53177,#53178,#53179,#53180,#53181,#53182,
#53183,#53184,#53185,#53186,#53187,#53188,#53189,#53190,#53191,#53192,#53193,
#53194,#53195,#53196,#53197,#53198,#53199),.UNSPECIFIED.,.F.,.F.,(4,3,3,
3,3,3,3,3,3,3,3,3,3,3,3,3,3,3,3,3,3,3,3,3,3,3,3,3,3,3,3,3,3,3,3,3,3,3,3,
3,3,3,3,3,3,3,3,3,3,3,3,3,3,3,3,3,3,3,3,3,3,3,3,3,3,3,3,3,3,3,3,3,3,4),
(499.513231920757,499.596670184171,499.680096678619,499.763529406103,499.846986368907,
499.930539923303,500.014142748441,500.097885724517,500.176040141516,500.259778853362,
500.343414364729,500.426966808128,500.510456243979,500.593910194592,500.677346688439,
500.760783798194,500.844239593111,500.927784085841,501.011373168782,501.09509643634,
501.175776152236,501.259514864082,501.343150375449,501.426702818848,501.510192254698,
501.593646205312,501.677082699158,501.760519808914,501.843975603832,501.927520096562,
502.011109179503,502.09483244706,502.175512162956,502.259250874802,502.342886386169,
502.426438829568,502.509928265419,502.593382216033,502.676818709879,502.760255819634,
502.843711614552,502.927256107281,503.010845190222,503.09456845778,503.175248173676,
503.258986885522,503.342622396889,503.426174840288,503.509664276139,503.593118226753,
503.676554720599,503.759991830355,503.843447625273,503.926992118002,504.010581200943,
504.094304468501,504.174984184397,504.258722896243,504.342358407611,504.42591085101,
504.509400286861,504.592854237474,504.676290731321,504.759727841076,504.843183635994,
504.926728128724,505.010317211665,505.094040479223,505.174720195117,505.259243841905,
505.343623334706,505.427919448869,505.512133263776,505.545701907803),
 .UNSPECIFIED.);
#368=B_SPLINE_CURVE_WITH_KNOTS('',3,(#53200,#53201,#53202,#53203,#53204,
#53205,#53206,#53207,#53208,#53209),.UNSPECIFIED.,.F.,.F.,(4,3,3,4),(499.262642145922,
499.360326014176,499.457183902584,499.513231920567),.UNSPECIFIED.);
#369=B_SPLINE_CURVE_WITH_KNOTS('',3,(#53211,#53212,#53213,#53214,#53215,
#53216,#53217,#53218,#53219,#53220,#53221,#53222,#53223),.UNSPECIFIED.,
 .F.,.F.,(4,3,3,3,4),(499.261567561389,499.345171745714,499.428903472395,
499.486594750512,499.513231920761),.UNSPECIFIED.);
#370=B_SPLINE_CURVE_WITH_KNOTS('',3,(#53224,#53225,#53226,#53227,#53228,
#53229,#53230,#53231,#53232,#53233,#53234,#53235,#53236,#53237,#53238,#53239,
#53240,#53241,#53242,#53243,#53244,#53245,#53246,#53247,#53248,#53249,#53250,
#53251,#53252,#53253,#53254,#53255,#53256,#53257,#53258,#53259,#53260,#53261,
#53262,#53263,#53264,#53265,#53266,#53267,#53268,#53269,#53270,#53271,#53272,
#53273,#53274,#53275,#53276,#53277,#53278,#53279,#53280,#53281,#53282,#53283,
#53284,#53285,#53286,#53287,#53288,#53289,#53290,#53291,#53292,#53293,#53294,
#53295,#53296,#53297,#53298,#53299,#53300,#53301,#53302,#53303,#53304,#53305,
#53306,#53307,#53308,#53309,#53310,#53311,#53312,#53313,#53314,#53315,#53316,
#53317,#53318,#53319,#53320,#53321,#53322,#53323,#53324,#53325,#53326,#53327,
#53328,#53329,#53330,#53331,#53332,#53333,#53334,#53335,#53336,#53337,#53338,
#53339,#53340,#53341,#53342,#53343,#53344,#53345,#53346,#53347,#53348,#53349,
#53350,#53351,#53352,#53353,#53354,#53355,#53356,#53357,#53358,#53359,#53360,
#53361,#53362,#53363,#53364,#53365,#53366,#53367,#53368,#53369,#53370,#53371,
#53372,#53373,#53374,#53375,#53376,#53377,#53378,#53379,#53380,#53381,#53382,
#53383,#53384,#53385,#53386,#53387,#53388,#53389,#53390,#53391,#53392,#53393,
#53394,#53395,#53396,#53397,#53398,#53399,#53400,#53401,#53402,#53403,#53404,
#53405,#53406,#53407,#53408,#53409,#53410,#53411,#53412,#53413,#53414,#53415,
#53416,#53417,#53418,#53419,#53420,#53421,#53422,#53423,#53424,#53425,#53426,
#53427,#53428,#53429,#53430,#53431,#53432,#53433,#53434,#53435,#53436,#53437,
#53438,#53439,#53440,#53441,#53442,#53443),.UNSPECIFIED.,.F.,.F.,(4,3,3,
3,3,3,3,3,3,3,3,3,3,3,3,3,3,3,3,3,3,3,3,3,3,3,3,3,3,3,3,3,3,3,3,3,3,3,3,
3,3,3,3,3,3,3,3,3,3,3,3,3,3,3,3,3,3,3,3,3,3,3,3,3,3,3,3,3,3,3,3,3,3,4),
(499.513231920881,499.596595150741,499.679856225129,499.763035652673,499.84615386694,
499.92923928284,500.012309553756,500.095383088349,500.178478293937,500.261662605286,
500.344894830732,500.428254065379,500.486330761232,500.570069473078,500.653704984445,
500.737257427844,500.820746863695,500.904200814309,500.987637308155,501.07107441791,
501.154530212828,501.238074705558,501.321663788499,501.405387056056,501.486066771952,
501.569805483798,501.653440995165,501.736993438563,501.820482874414,501.903936825028,
501.987373318874,502.07081042863,502.154266223547,502.237810716277,502.321399799218,
502.405123066775,502.485802782672,502.569541494518,502.653177005886,502.736729449284,
502.820218885135,502.903672835749,502.987109329595,503.070546439351,503.154002234268,
503.237546726998,503.321135809939,503.404859077496,503.485538793392,503.569277505238,
503.652913016605,503.736465460004,503.819954895854,503.903408846468,503.986845340314,
504.07028245007,504.153738244987,504.237282737717,504.320871820658,504.404595088216,
504.485274804112,504.569013515958,504.652649027325,504.736201470724,504.819690906575,
504.903144857189,504.986581351035,505.070018460791,505.153474255708,505.237018748438,
505.320607831379,505.404331098937,505.485010814832,505.545703572404),
 .UNSPECIFIED.);
#371=B_SPLINE_CURVE_WITH_KNOTS('',3,(#53449,#53450,#53451,#53452,#53453,
#53454,#53455,#53456,#53457,#53458,#53459,#53460,#53461,#53462,#53463,#53464,
#53465,#53466,#53467,#53468,#53469,#53470,#53471,#53472,#53473,#53474,#53475,
#53476,#53477,#53478,#53479,#53480,#53481,#53482,#53483,#53484,#53485,#53486,
#53487,#53488,#53489,#53490,#53491,#53492,#53493,#53494,#53495,#53496,#53497,
#53498,#53499,#53500,#53501,#53502,#53503,#53504,#53505,#53506,#53507,#53508,
#53509,#53510,#53511,#53512,#53513,#53514,#53515,#53516,#53517,#53518,#53519,
#53520,#53521,#53522,#53523,#53524,#53525,#53526,#53527,#53528,#53529,#53530,
#53531,#53532,#53533,#53534,#53535,#53536,#53537,#53538,#53539,#53540,#53541,
#53542,#53543,#53544,#53545,#53546,#53547,#53548,#53549,#53550,#53551,#53552,
#53553,#53554,#53555,#53556,#53557,#53558,#53559,#53560,#53561,#53562,#53563,
#53564,#53565,#53566,#53567,#53568,#53569,#53570,#53571,#53572,#53573,#53574,
#53575,#53576,#53577,#53578,#53579,#53580,#53581,#53582,#53583,#53584,#53585,
#53586,#53587,#53588,#53589,#53590,#53591,#53592,#53593,#53594,#53595,#53596,
#53597,#53598,#53599,#53600,#53601,#53602,#53603,#53604,#53605,#53606,#53607,
#53608,#53609,#53610,#53611,#53612,#53613,#53614,#53615,#53616,#53617,#53618,
#53619,#53620,#53621,#53622,#53623,#53624,#53625,#53626,#53627,#53628,#53629,
#53630,#53631,#53632,#53633,#53634,#53635,#53636,#53637,#53638,#53639,#53640,
#53641,#53642,#53643,#53644,#53645,#53646,#53647,#53648,#53649,#53650,#53651,
#53652,#53653,#53654,#53655,#53656,#53657,#53658,#53659,#53660,#53661,#53662,
#53663,#53664,#53665),.UNSPECIFIED.,.F.,.F.,(4,3,3,3,3,3,3,3,3,3,3,3,3,
3,3,3,3,3,3,3,3,3,3,3,3,3,3,3,3,3,3,3,3,3,3,3,3,3,3,3,3,3,3,3,3,3,3,3,3,
3,3,3,3,3,3,3,3,3,3,3,3,3,3,3,3,3,3,3,3,3,3,3,4),(505.79641722813,505.890926972556,
505.985009282388,506.079732744112,506.174456205837,506.258194917683,506.34183042905,
506.425382872449,506.5088723083,506.592326258913,506.675762752759,506.759199862515,
506.842655657432,506.926200150162,507.009789233103,507.09351250066,507.174192216557,
507.257930928403,507.34156643977,507.425118883169,507.50860831902,507.592062269633,
507.67549876348,507.758935873235,507.842391668153,507.925936160882,508.009525243823,
508.093248511381,508.173928227277,508.257666939123,508.34130245049,508.424854893889,
508.50834432974,508.591798280354,508.6752347742,508.758671883955,508.842127678873,
508.925672171603,509.009261254544,509.092984522101,509.173664237997,509.257402949843,
509.34103846121,509.424590904609,509.50808034046,509.591534291074,509.67497078492,
509.758407894675,509.841863689593,509.925408182323,510.008997265264,510.092720532821,
510.173400248717,510.257138960563,510.34077447193,510.424326915329,510.50781635118,
510.591270301794,510.67470679564,510.758143905396,510.841599700313,510.925144193043,
511.008733275984,511.092456543541,511.173136259437,511.255848589194,511.338466366091,
511.421008642217,511.503494402176,511.585953289741,511.668393655483,511.750865095778,
511.827765835364),.UNSPECIFIED.);
#372=B_SPLINE_CURVE_WITH_KNOTS('',3,(#53666,#53667,#53668,#53669,#53670,
#53671,#53672,#53673,#53674,#53675),.UNSPECIFIED.,.F.,.F.,(4,3,3,4),(505.545701907803,
505.629843863293,505.713969544551,505.796417227936),.UNSPECIFIED.);
#373=B_SPLINE_CURVE_WITH_KNOTS('',3,(#53677,#53678,#53679,#53680,#53681,
#53682,#53683,#53684,#53685,#53686),.UNSPECIFIED.,.F.,.F.,(4,3,3,4),(505.545703572404,
505.646104108299,505.745411802745,505.796417227777),.UNSPECIFIED.);
#374=B_SPLINE_CURVE_WITH_KNOTS('',3,(#53687,#53688,#53689,#53690,#53691,
#53692,#53693,#53694,#53695,#53696,#53697,#53698,#53699,#53700,#53701,#53702,
#53703,#53704,#53705,#53706,#53707,#53708,#53709,#53710,#53711,#53712,#53713,
#53714,#53715,#53716,#53717,#53718,#53719,#53720,#53721,#53722,#53723,#53724,
#53725,#53726,#53727,#53728,#53729,#53730,#53731,#53732,#53733,#53734,#53735,
#53736,#53737,#53738,#53739,#53740,#53741,#53742,#53743,#53744,#53745,#53746,
#53747,#53748,#53749,#53750,#53751,#53752,#53753,#53754,#53755,#53756,#53757,
#53758,#53759,#53760,#53761,#53762,#53763,#53764,#53765,#53766,#53767,#53768,
#53769,#53770,#53771,#53772,#53773,#53774,#53775,#53776,#53777,#53778,#53779,
#53780,#53781,#53782,#53783,#53784,#53785,#53786,#53787,#53788,#53789,#53790,
#53791,#53792,#53793,#53794,#53795,#53796,#53797,#53798,#53799,#53800,#53801,
#53802,#53803,#53804,#53805,#53806,#53807,#53808,#53809,#53810,#53811,#53812,
#53813,#53814,#53815,#53816,#53817,#53818,#53819,#53820,#53821,#53822,#53823,
#53824,#53825,#53826,#53827,#53828,#53829,#53830,#53831,#53832,#53833,#53834,
#53835,#53836,#53837,#53838,#53839,#53840,#53841,#53842,#53843,#53844,#53845,
#53846,#53847,#53848,#53849,#53850,#53851,#53852,#53853,#53854,#53855,#53856,
#53857,#53858,#53859,#53860,#53861,#53862,#53863,#53864,#53865,#53866,#53867,
#53868,#53869,#53870,#53871,#53872,#53873,#53874,#53875,#53876,#53877,#53878,
#53879,#53880,#53881,#53882,#53883,#53884,#53885,#53886,#53887,#53888,#53889,
#53890,#53891,#53892,#53893,#53894,#53895,#53896,#53897,#53898,#53899,#53900,
#53901,#53902,#53903,#53904,#53905,#53906),.UNSPECIFIED.,.F.,.F.,(4,3,3,
3,3,3,3,3,3,3,3,3,3,3,3,3,3,3,3,3,3,3,3,3,3,3,3,3,3,3,3,3,3,3,3,3,3,3,3,
3,3,3,3,3,3,3,3,3,3,3,3,3,3,3,3,3,3,3,3,3,3,3,3,3,3,3,3,3,3,3,3,3,3,4),
(505.79641722794,505.882458427642,505.965539089651,506.048616043483,506.131707649494,
506.21483227441,506.298053982271,506.381333616868,506.464733332468,506.484746825553,
506.568485537399,506.652121048766,506.735673492165,506.819162928016,506.90261687863,
506.986053372476,507.069490482231,507.152946277149,507.236490769879,507.32007985282,
507.403803120377,507.484482836273,507.568221548119,507.651857059486,507.735409502885,
507.818898938736,507.90235288935,507.985789383196,508.069226492952,508.152682287869,
508.236226780599,508.31981586354,508.403539131097,508.484218846993,508.567957558839,
508.651593070206,508.735145513605,508.818634949455,508.902088900069,508.985525393915,
509.06896250367,509.152418298588,509.235962791318,509.319551874259,509.403275141816,
509.483954857713,509.567693569559,509.651329080926,509.734881524325,509.818370960176,
509.90182491079,509.985261404636,510.068698514392,510.152154309309,510.235698802039,
510.31928788498,510.403011152537,510.483690868433,510.567429580279,510.651065091646,
510.734617535045,510.818106970896,510.901560921509,510.984997415356,511.068434525111,
511.151890320029,511.235434812759,511.3190238957,511.402747163258,511.483426879153,
511.569819896032,511.654761847421,511.741880397046,511.82899894667),
 .UNSPECIFIED.);
#375=B_SPLINE_CURVE_WITH_KNOTS('',3,(#53912,#53913,#53914,#53915,#53916,
#53917,#53918,#53919,#53920,#53921,#53922,#53923,#53924,#53925,#53926,#53927,
#53928,#53929,#53930,#53931,#53932,#53933,#53934,#53935,#53936,#53937,#53938,
#53939,#53940,#53941,#53942,#53943,#53944,#53945,#53946,#53947,#53948,#53949,
#53950,#53951,#53952,#53953,#53954,#53955,#53956,#53957,#53958,#53959,#53960,
#53961,#53962,#53963,#53964,#53965,#53966,#53967,#53968,#53969,#53970,#53971,
#53972,#53973,#53974,#53975,#53976,#53977,#53978,#53979,#53980,#53981,#53982,
#53983,#53984,#53985,#53986,#53987,#53988,#53989,#53990,#53991,#53992,#53993,
#53994,#53995,#53996,#53997,#53998,#53999,#54000,#54001,#54002,#54003,#54004,
#54005,#54006,#54007,#54008,#54009,#54010,#54011,#54012,#54013,#54014,#54015,
#54016,#54017,#54018,#54019,#54020,#54021,#54022,#54023,#54024,#54025,#54026,
#54027,#54028,#54029,#54030,#54031,#54032,#54033,#54034,#54035,#54036,#54037,
#54038,#54039,#54040,#54041,#54042,#54043,#54044,#54045,#54046,#54047,#54048,
#54049,#54050,#54051,#54052,#54053,#54054,#54055,#54056,#54057,#54058,#54059,
#54060,#54061,#54062,#54063,#54064,#54065,#54066,#54067,#54068,#54069,#54070,
#54071,#54072,#54073,#54074,#54075,#54076,#54077,#54078,#54079,#54080,#54081,
#54082,#54083,#54084,#54085,#54086,#54087,#54088,#54089,#54090,#54091,#54092,
#54093,#54094,#54095,#54096,#54097,#54098,#54099,#54100,#54101,#54102,#54103,
#54104,#54105,#54106,#54107,#54108,#54109,#54110,#54111,#54112,#54113,#54114,
#54115,#54116,#54117,#54118,#54119,#54120,#54121,#54122,#54123,#54124,#54125,
#54126,#54127,#54128,#54129,#54130,#54131),.UNSPECIFIED.,.F.,.F.,(4,3,3,
3,3,3,3,3,3,3,3,3,3,3,3,3,3,3,3,3,3,3,3,3,3,3,3,3,3,3,3,3,3,3,3,3,3,3,3,
3,3,3,3,3,3,3,3,3,3,3,3,3,3,3,3,3,3,3,3,3,3,3,3,3,3,3,3,3,3,3,3,3,3,4),
(512.079602535116,512.172872270158,512.256610982004,512.340246493371,512.42379893677,
512.507288372621,512.590742323234,512.67417881708,512.757615926836,512.841071721753,
512.924616214483,513.008205297423,513.091928564981,513.172608280878,513.256346992724,
513.339982504091,513.42353494749,513.507024383341,513.590478333954,513.673914827801,
513.757351937556,513.840807732474,513.924352225203,514.007941308144,514.091664575702,
514.172344291598,514.256083003444,514.339718514812,514.42327095821,514.506760394061,
514.590214344675,514.673650838521,514.757087948277,514.840543743195,514.924088235924,
515.007677318865,515.091400586423,515.172080302318,515.255819014164,515.339454525531,
515.42300696893,515.506496404781,515.589950355395,515.673386849241,515.756823958996,
515.840279753914,515.923824246643,516.007413329584,516.091136597142,516.171816313038,
516.255555024884,516.339190536252,516.42274297965,516.506232415501,516.589686366115,
516.673122859961,516.756559969716,516.840015764634,516.923560257364,517.007149340305,
517.090872607862,517.171552323758,517.255294468566,517.338932623139,517.422486923337,
517.508602676535,517.592052950222,517.675485219268,517.758917555356,517.842368026146,
517.925892631405,518.0094618763,518.093130892287,518.111412948922),
 .UNSPECIFIED.);
#376=B_SPLINE_CURVE_WITH_KNOTS('',3,(#54132,#54133,#54134,#54135,#54136,
#54137,#54138,#54139,#54140,#54141),.UNSPECIFIED.,.F.,.F.,(4,3,3,4),(511.827765835364,
511.910313912069,511.994958223525,512.079602534982),.UNSPECIFIED.);
#377=B_SPLINE_CURVE_WITH_KNOTS('',3,(#54143,#54144,#54145,#54146,#54147,
#54148,#54149,#54150,#54151,#54152),.UNSPECIFIED.,.F.,.F.,(4,3,3,4),(511.82899894667,
511.913687987766,511.99833837829,512.07960253512),.UNSPECIFIED.);
#378=B_SPLINE_CURVE_WITH_KNOTS('',3,(#54153,#54154,#54155,#54156,#54157,
#54158,#54159,#54160,#54161,#54162,#54163,#54164,#54165,#54166,#54167,#54168,
#54169,#54170,#54171,#54172,#54173,#54174,#54175,#54176,#54177,#54178,#54179,
#54180,#54181,#54182,#54183,#54184,#54185,#54186,#54187,#54188,#54189,#54190,
#54191,#54192,#54193,#54194,#54195,#54196,#54197,#54198,#54199,#54200,#54201,
#54202,#54203,#54204,#54205,#54206,#54207,#54208,#54209,#54210,#54211,#54212,
#54213,#54214,#54215,#54216,#54217,#54218,#54219,#54220,#54221,#54222,#54223,
#54224,#54225,#54226,#54227,#54228,#54229,#54230,#54231,#54232,#54233,#54234,
#54235,#54236,#54237,#54238,#54239,#54240,#54241,#54242,#54243,#54244,#54245,
#54246,#54247,#54248,#54249,#54250,#54251,#54252,#54253,#54254,#54255,#54256,
#54257,#54258,#54259,#54260,#54261,#54262,#54263,#54264,#54265,#54266,#54267,
#54268,#54269,#54270,#54271,#54272,#54273,#54274,#54275,#54276,#54277,#54278,
#54279,#54280,#54281,#54282,#54283,#54284,#54285,#54286,#54287,#54288,#54289,
#54290,#54291,#54292,#54293,#54294,#54295,#54296,#54297,#54298,#54299,#54300,
#54301,#54302,#54303,#54304,#54305,#54306,#54307,#54308,#54309,#54310,#54311,
#54312,#54313,#54314,#54315,#54316,#54317,#54318,#54319,#54320,#54321,#54322,
#54323,#54324,#54325,#54326,#54327,#54328,#54329,#54330,#54331,#54332,#54333,
#54334,#54335,#54336,#54337,#54338,#54339,#54340,#54341,#54342,#54343,#54344,
#54345,#54346,#54347,#54348,#54349,#54350,#54351,#54352,#54353,#54354,#54355,
#54356,#54357,#54358,#54359,#54360,#54361,#54362,#54363,#54364,#54365,#54366,
#54367,#54368,#54369,#54370,#54371,#54372),.UNSPECIFIED.,.F.,.F.,(4,3,3,
3,3,3,3,3,3,3,3,3,3,3,3,3,3,3,3,3,3,3,3,3,3,3,3,3,3,3,3,3,3,3,3,3,3,3,3,
3,3,3,3,3,3,3,3,3,3,3,3,3,3,3,3,3,3,3,3,3,3,3,3,3,3,3,3,3,3,3,3,3,3,4),
(512.079602535298,512.171477821645,512.263833046544,512.356436043018,512.449370007146,
512.483162889873,512.566901601719,512.650537113087,512.734089556487,512.817578992338,
512.901032942952,512.984469436799,513.067906546555,513.151362341473,513.234906834204,
513.318495917145,513.402219184703,513.482898900594,513.56663761244,513.650273123808,
513.733825567206,513.817315003057,513.900768953671,513.984205447517,514.067642557272,
514.15109835219,514.23464284492,514.318231927861,514.401955195418,514.482634911314,
514.56637362316,514.650009134527,514.733561577925,514.817051013776,514.900504964389,
514.983941458236,515.067378567991,515.150834362908,515.234378855638,515.317967938579,
515.401691206136,515.482370922034,515.56610963388,515.649745145248,515.733297588646,
515.816787024497,515.900240975111,515.983677468958,516.067114578713,516.150570373631,
516.234114866361,516.317703949302,516.40142721686,516.482106932754,516.5658456446,
516.649481155967,516.733033599366,516.816523035217,516.89997698583,516.983413479677,
517.066850589432,517.15030638435,517.233850877079,517.31743996002,517.401163227578,
517.481842943474,517.564418019187,517.646898427861,517.729303315999,517.811651759644,
517.893971056624,517.976272247947,518.058596719203,518.110972534525),
 .UNSPECIFIED.);
#379=B_SPLINE_CURVE_WITH_KNOTS('',3,(#54378,#54379,#54380,#54381,#54382,
#54383,#54384,#54385,#54386,#54387,#54388,#54389,#54390,#54391,#54392,#54393,
#54394,#54395,#54396,#54397,#54398,#54399,#54400,#54401,#54402,#54403,#54404,
#54405,#54406,#54407,#54408,#54409,#54410,#54411,#54412,#54413,#54414,#54415,
#54416,#54417,#54418,#54419,#54420,#54421,#54422,#54423,#54424,#54425,#54426,
#54427,#54428,#54429,#54430,#54431,#54432,#54433,#54434,#54435,#54436,#54437,
#54438,#54439,#54440,#54441,#54442,#54443,#54444,#54445,#54446,#54447,#54448,
#54449,#54450,#54451,#54452,#54453,#54454,#54455,#54456,#54457,#54458,#54459,
#54460,#54461,#54462,#54463,#54464,#54465,#54466,#54467,#54468,#54469,#54470,
#54471,#54472,#54473,#54474,#54475,#54476,#54477,#54478,#54479,#54480,#54481,
#54482,#54483,#54484,#54485,#54486,#54487,#54488,#54489,#54490,#54491,#54492,
#54493,#54494,#54495,#54496,#54497,#54498,#54499,#54500,#54501,#54502,#54503,
#54504,#54505,#54506,#54507,#54508,#54509,#54510,#54511,#54512,#54513,#54514,
#54515,#54516,#54517,#54518,#54519,#54520,#54521,#54522,#54523,#54524,#54525,
#54526,#54527,#54528,#54529,#54530,#54531,#54532,#54533,#54534,#54535,#54536,
#54537,#54538,#54539,#54540,#54541,#54542,#54543,#54544,#54545,#54546,#54547,
#54548,#54549,#54550,#54551,#54552,#54553,#54554,#54555,#54556,#54557,#54558,
#54559,#54560,#54561,#54562,#54563,#54564,#54565,#54566,#54567,#54568,#54569,
#54570,#54571,#54572,#54573,#54574,#54575,#54576,#54577,#54578,#54579,#54580,
#54581,#54582,#54583,#54584,#54585,#54586,#54587,#54588,#54589,#54590,#54591,
#54592,#54593,#54594,#54595,#54596,#54597),.UNSPECIFIED.,.F.,.F.,(4,3,3,
3,3,3,3,3,3,3,3,3,3,3,3,3,3,3,3,3,3,3,3,3,3,3,3,3,3,3,3,3,3,3,3,3,3,3,3,
3,3,3,3,3,3,3,3,3,3,3,3,3,3,3,3,3,3,3,3,3,3,3,3,3,3,3,3,3,3,3,3,3,3,4),
(518.362787842419,518.445154854009,518.52745048132,518.609700442417,518.691927292045,
518.774150056304,518.856387755764,518.938708455605,519.021072182249,519.103563042683,
519.171024345199,519.254763057045,519.338398568412,519.421951011811,519.505440447662,
519.588894398276,519.672330892122,519.755768001877,519.839223796794,519.922768289524,
520.006357372465,520.090080640023,520.170760355919,520.254499067765,520.338134579132,
520.42168702253,520.505176458381,520.588630408995,520.672066902841,520.755504012596,
520.838959807513,520.922504300243,521.006093383184,521.089816650741,521.170496366639,
521.254235078485,521.337870589853,521.421423033251,521.504912469102,521.588366419715,
521.671802913562,521.755240023317,521.838695818235,521.922240310965,522.005829393906,
522.089552661463,522.170232377359,522.253971089205,522.337606600572,522.421159043971,
522.504648479823,522.588102430436,522.671538924282,522.754976034038,522.838431828956,
522.921976321685,523.005565404627,523.089288672184,523.169968388079,523.253707099925,
523.337342611292,523.42089505469,523.504384490541,523.587838441154,523.671274935001,
523.754712044756,523.838167839673,523.921712332403,524.005301415344,524.089024682901,
524.169704398799,524.25875441157,524.347593650043,524.395667901685),
 .UNSPECIFIED.);
#380=B_SPLINE_CURVE_WITH_KNOTS('',3,(#54598,#54599,#54600,#54601,#54602,
#54603,#54604,#54605,#54606,#54607),.UNSPECIFIED.,.F.,.F.,(4,3,3,4),(518.111412948922,
518.171288334478,518.294232689854,518.362787842295),.UNSPECIFIED.);
#381=B_SPLINE_CURVE_WITH_KNOTS('',3,(#54609,#54610,#54611,#54612,#54613,
#54614,#54615,#54616,#54617,#54618),.UNSPECIFIED.,.F.,.F.,(4,3,3,4),(518.110972534525,
518.193367758242,518.278077800204,518.362787842165),.UNSPECIFIED.);
#382=B_SPLINE_CURVE_WITH_KNOTS('',3,(#54619,#54620,#54621,#54622,#54623,
#54624,#54625,#54626,#54627,#54628,#54629,#54630,#54631,#54632,#54633,#54634,
#54635,#54636,#54637,#54638,#54639,#54640,#54641,#54642,#54643,#54644,#54645,
#54646,#54647,#54648,#54649,#54650,#54651,#54652,#54653,#54654,#54655,#54656,
#54657,#54658,#54659,#54660,#54661,#54662,#54663,#54664,#54665,#54666,#54667,
#54668,#54669,#54670,#54671,#54672,#54673,#54674,#54675,#54676,#54677,#54678,
#54679,#54680,#54681,#54682,#54683,#54684,#54685,#54686,#54687,#54688,#54689,
#54690,#54691,#54692,#54693,#54694,#54695,#54696,#54697,#54698,#54699,#54700,
#54701,#54702,#54703,#54704,#54705,#54706,#54707,#54708,#54709,#54710,#54711,
#54712,#54713,#54714,#54715,#54716,#54717,#54718,#54719,#54720,#54721,#54722,
#54723,#54724,#54725,#54726,#54727,#54728,#54729,#54730,#54731,#54732,#54733,
#54734,#54735,#54736,#54737,#54738,#54739,#54740,#54741,#54742,#54743,#54744,
#54745,#54746,#54747,#54748,#54749,#54750,#54751,#54752,#54753,#54754,#54755,
#54756,#54757,#54758,#54759,#54760,#54761,#54762,#54763,#54764,#54765,#54766,
#54767,#54768,#54769,#54770,#54771,#54772,#54773,#54774,#54775,#54776,#54777,
#54778,#54779,#54780,#54781,#54782,#54783,#54784,#54785,#54786,#54787,#54788,
#54789,#54790,#54791,#54792,#54793,#54794,#54795,#54796,#54797,#54798,#54799,
#54800,#54801,#54802,#54803,#54804,#54805,#54806,#54807,#54808,#54809,#54810,
#54811,#54812,#54813,#54814,#54815,#54816,#54817,#54818,#54819,#54820,#54821,
#54822,#54823,#54824,#54825,#54826,#54827,#54828,#54829,#54830,#54831,#54832,
#54833,#54834,#54835),.UNSPECIFIED.,.F.,.F.,(4,3,3,3,3,3,3,3,3,3,3,3,3,
3,3,3,3,3,3,3,3,3,3,3,3,3,3,3,3,3,3,3,3,3,3,3,3,3,3,3,3,3,3,3,3,3,3,3,3,
3,3,3,3,3,3,3,3,3,3,3,3,3,3,3,3,3,3,3,3,3,3,3,4),(518.362787842299,518.481578954194,
518.56531766604,518.648953177408,518.732505620807,518.815995056658,518.899449007272,
518.982885501119,519.066322610875,519.149778405793,519.233322898523,519.316911981464,
519.400635249022,519.481314964914,519.56505367676,519.648689188128,519.732241631526,
519.815731067378,519.899185017991,519.982621511838,520.066058621593,520.149514416511,
520.233058909241,520.316647992182,520.40037125974,520.481050975635,520.564789687481,
520.648425198848,520.731977642247,520.815467078098,520.898921028711,520.982357522557,
521.065794632313,521.14925042723,521.23279491996,521.3163840029,521.400107270458,
521.480786986355,521.564525698201,521.648161209569,521.731713652967,521.815203088818,
521.898657039432,521.982093533278,522.065530643034,522.148986437952,522.232530930681,
522.316120013622,522.39984328118,522.480522997075,522.564261708921,522.647897220288,
522.731449663687,522.814939099538,522.898393050152,522.981829543998,523.065266653753,
523.148722448671,523.232266941401,523.315856024342,523.399579291899,523.480259007795,
523.564002670223,523.647642004487,523.731197147901,523.814684413027,523.898134538052,
523.981565611332,524.064995704658,524.148483264892,524.231998532224,524.315618988745,
524.394502893603),.UNSPECIFIED.);
#383=B_SPLINE_CURVE_WITH_KNOTS('',3,(#54841,#54842,#54843,#54844,#54845,
#54846,#54847,#54848,#54849,#54850,#54851,#54852,#54853,#54854,#54855,#54856,
#54857,#54858,#54859,#54860,#54861,#54862,#54863,#54864,#54865,#54866,#54867,
#54868,#54869,#54870,#54871,#54872,#54873,#54874,#54875,#54876,#54877,#54878,
#54879,#54880,#54881,#54882,#54883,#54884,#54885,#54886,#54887,#54888,#54889,
#54890,#54891,#54892,#54893,#54894,#54895,#54896,#54897,#54898,#54899,#54900,
#54901,#54902,#54903,#54904,#54905,#54906,#54907,#54908,#54909,#54910,#54911,
#54912,#54913,#54914,#54915,#54916,#54917,#54918,#54919,#54920,#54921,#54922,
#54923,#54924,#54925,#54926,#54927,#54928,#54929,#54930,#54931,#54932,#54933,
#54934,#54935,#54936,#54937,#54938,#54939,#54940,#54941,#54942,#54943,#54944,
#54945,#54946,#54947,#54948,#54949,#54950,#54951,#54952,#54953,#54954,#54955,
#54956,#54957,#54958,#54959,#54960,#54961,#54962,#54963,#54964,#54965,#54966,
#54967,#54968,#54969,#54970,#54971,#54972,#54973,#54974,#54975,#54976,#54977,
#54978,#54979,#54980,#54981,#54982,#54983,#54984,#54985,#54986,#54987,#54988,
#54989,#54990,#54991,#54992,#54993,#54994,#54995,#54996,#54997,#54998,#54999,
#55000,#55001,#55002,#55003,#55004,#55005,#55006,#55007,#55008,#55009,#55010,
#55011,#55012,#55013,#55014,#55015,#55016,#55017,#55018,#55019,#55020,#55021,
#55022,#55023,#55024,#55025,#55026,#55027,#55028,#55029,#55030,#55031,#55032,
#55033,#55034,#55035,#55036,#55037,#55038,#55039,#55040,#55041,#55042,#55043,
#55044,#55045,#55046,#55047,#55048,#55049,#55050,#55051,#55052,#55053,#55054,
#55055,#55056,#55057,#55058,#55059,#55060),.UNSPECIFIED.,.F.,.F.,(4,3,3,
3,3,3,3,3,3,3,3,3,3,3,3,3,3,3,3,3,3,3,3,3,3,3,3,3,3,3,3,3,3,3,3,3,3,3,3,
3,3,3,3,3,3,3,3,3,3,3,3,3,3,3,3,3,3,3,3,3,3,3,3,3,3,3,3,3,3,3,3,3,3,4),
(524.645973149475,524.732570018328,524.819253325717,524.906800096668,524.993752452295,
525.081596430907,525.169440409519,525.253179121365,525.336814632732,525.420367076131,
525.503856511982,525.587310462595,525.670746956442,525.754184066197,525.837639861115,
525.921184353845,526.004773436786,526.088496704343,526.169176420239,526.252915132085,
526.336550643452,526.420103086851,526.503592522703,526.587046473316,526.670482967162,
526.753920076918,526.837375871836,526.920920364565,527.004509447506,527.088232715064,
527.168912430959,527.252651142805,527.336286654173,527.419839097571,527.503328533422,
527.586782484036,527.670218977882,527.753656087637,527.837111882555,527.920656375285,
528.004245458226,528.087968725783,528.16864844168,528.252387153526,528.336022664894,
528.419575108292,528.503064544143,528.586518494757,528.669954988603,528.753392098358,
528.836847893276,528.920392386006,529.003981468947,529.087704736504,529.1683844524,
529.252123164246,529.335758675613,529.419311119012,529.502800554863,529.586254505477,
529.669690999323,529.753128109078,529.836583903995,529.920128396725,530.003717479666,
530.087440747223,530.16812046312,530.250811124454,530.333404118865,530.419488284874,
530.501935809903,530.58434732562,530.666745501053,530.677740782901),
 .UNSPECIFIED.);
#384=B_SPLINE_CURVE_WITH_KNOTS('',3,(#55061,#55062,#55063,#55064,#55065,
#55066,#55067,#55068,#55069,#55070),.UNSPECIFIED.,.F.,.F.,(4,3,3,4),(524.395667901685,
524.484235216775,524.57259525758,524.645973149366),.UNSPECIFIED.);
#385=B_SPLINE_CURVE_WITH_KNOTS('',3,(#55072,#55073,#55074,#55075,#55076,
#55077,#55078,#55079,#55080,#55081),.UNSPECIFIED.,.F.,.F.,(4,3,3,4),(524.394502893603,
524.479995018515,524.613424523667,524.645973149479),.UNSPECIFIED.);
#386=B_SPLINE_CURVE_WITH_KNOTS('',3,(#55082,#55083,#55084,#55085,#55086,
#55087,#55088,#55089,#55090,#55091,#55092,#55093,#55094,#55095,#55096,#55097,
#55098,#55099,#55100,#55101,#55102,#55103,#55104,#55105,#55106,#55107,#55108,
#55109,#55110,#55111,#55112,#55113,#55114,#55115,#55116,#55117,#55118,#55119,
#55120,#55121,#55122,#55123,#55124,#55125,#55126,#55127,#55128,#55129,#55130,
#55131,#55132,#55133,#55134,#55135,#55136,#55137,#55138,#55139,#55140,#55141,
#55142,#55143,#55144,#55145,#55146,#55147,#55148,#55149,#55150,#55151,#55152,
#55153,#55154,#55155,#55156,#55157,#55158,#55159,#55160,#55161,#55162,#55163,
#55164,#55165,#55166,#55167,#55168,#55169,#55170,#55171,#55172,#55173,#55174,
#55175,#55176,#55177,#55178,#55179,#55180,#55181,#55182,#55183,#55184,#55185,
#55186,#55187,#55188,#55189,#55190,#55191,#55192,#55193,#55194,#55195,#55196,
#55197,#55198,#55199,#55200,#55201,#55202,#55203,#55204,#55205,#55206,#55207,
#55208,#55209,#55210,#55211,#55212,#55213,#55214,#55215,#55216,#55217,#55218,
#55219,#55220,#55221,#55222,#55223,#55224,#55225,#55226,#55227,#55228,#55229,
#55230,#55231,#55232,#55233,#55234,#55235,#55236,#55237,#55238,#55239,#55240,
#55241,#55242,#55243,#55244,#55245,#55246,#55247,#55248,#55249,#55250,#55251,
#55252,#55253,#55254,#55255,#55256,#55257,#55258,#55259,#55260,#55261,#55262,
#55263,#55264,#55265,#55266,#55267,#55268,#55269,#55270,#55271,#55272,#55273,
#55274,#55275,#55276,#55277,#55278,#55279,#55280,#55281,#55282,#55283,#55284,
#55285,#55286,#55287,#55288,#55289,#55290,#55291,#55292,#55293,#55294,#55295,
#55296,#55297,#55298,#55299,#55300,#55301),.UNSPECIFIED.,.F.,.F.,(4,3,3,
3,3,3,3,3,3,3,3,3,3,3,3,3,3,3,3,3,3,3,3,3,3,3,3,3,3,3,3,3,3,3,3,3,3,3,3,
3,3,3,3,3,3,3,3,3,3,3,3,3,3,3,3,3,3,3,3,3,3,3,3,3,3,3,3,3,3,3,3,3,3,4),
(524.645973149671,524.728346440534,524.810641531603,524.894277718807,524.97648840522,
525.058689235174,525.140899242172,525.225607188938,525.307936227225,525.39383362823,
525.479731029235,525.563469741081,525.647105252449,525.730657695847,525.814147131698,
525.897601082312,525.981037576158,526.064474685913,526.147930480831,526.23147497356,
526.315064056501,526.398787324059,526.479467039955,526.563205751801,526.646841263168,
526.730393706567,526.813883142418,526.897337093032,526.980773586878,527.064210696633,
527.147666491551,527.231210984281,527.314800067222,527.398523334779,527.479203050675,
527.562941762521,527.646577273889,527.730129717287,527.813619153138,527.897073103752,
527.980509597598,528.063946707353,528.147402502271,528.230946995001,528.314536077942,
528.3982593455,528.478939061396,528.562677773242,528.64631328461,528.729865728008,
528.813355163859,528.896809114473,528.980245608319,529.063682718075,529.147138512993,
529.230683005722,529.314272088664,529.397995356221,529.478675072116,529.562413783962,
529.646049295329,529.729601738727,529.813091174578,529.896545125192,529.979981619038,
530.063418728794,530.146874523711,530.230419016441,530.314008099382,530.397731366939,
530.478411082836,530.568680668526,530.6587223636,530.67885489125),
 .UNSPECIFIED.);
#387=B_SPLINE_CURVE_WITH_KNOTS('',3,(#55307,#55308,#55309,#55310,#55311,
#55312,#55313,#55314,#55315,#55316,#55317,#55318,#55319,#55320,#55321,#55322,
#55323,#55324,#55325,#55326,#55327,#55328,#55329,#55330,#55331,#55332,#55333,
#55334,#55335,#55336,#55337,#55338,#55339,#55340,#55341,#55342,#55343,#55344,
#55345,#55346,#55347,#55348,#55349,#55350,#55351,#55352,#55353,#55354,#55355,
#55356,#55357,#55358,#55359,#55360,#55361,#55362,#55363,#55364,#55365,#55366,
#55367,#55368,#55369,#55370,#55371,#55372,#55373,#55374,#55375,#55376,#55377,
#55378,#55379,#55380,#55381,#55382,#55383,#55384,#55385,#55386,#55387,#55388,
#55389,#55390,#55391,#55392,#55393,#55394,#55395,#55396,#55397,#55398,#55399,
#55400,#55401,#55402,#55403,#55404,#55405,#55406,#55407,#55408,#55409,#55410,
#55411,#55412,#55413,#55414,#55415,#55416,#55417,#55418,#55419,#55420,#55421,
#55422,#55423,#55424,#55425,#55426,#55427,#55428,#55429,#55430,#55431,#55432,
#55433,#55434,#55435,#55436,#55437,#55438,#55439,#55440,#55441,#55442,#55443,
#55444,#55445,#55446,#55447,#55448,#55449,#55450,#55451,#55452,#55453,#55454,
#55455,#55456,#55457,#55458,#55459,#55460,#55461,#55462,#55463,#55464,#55465,
#55466,#55467,#55468,#55469,#55470,#55471,#55472,#55473,#55474,#55475,#55476,
#55477,#55478,#55479,#55480,#55481,#55482,#55483,#55484,#55485,#55486,#55487,
#55488,#55489,#55490,#55491,#55492,#55493,#55494,#55495,#55496,#55497,#55498,
#55499,#55500,#55501,#55502,#55503,#55504,#55505,#55506,#55507,#55508,#55509,
#55510,#55511,#55512,#55513,#55514,#55515,#55516,#55517,#55518,#55519,#55520,
#55521,#55522,#55523,#55524,#55525,#55526),.UNSPECIFIED.,.F.,.F.,(4,3,3,
3,3,3,3,3,3,3,3,3,3,3,3,3,3,3,3,3,3,3,3,3,3,3,3,3,3,3,3,3,3,3,3,3,3,3,3,
3,3,3,3,3,3,3,3,3,3,3,3,3,3,3,3,3,3,3,3,3,3,3,3,3,3,3,3,3,3,3,3,3,3,4),
(530.929158456779,531.038317168575,531.150322827254,531.16785647384,531.251595185686,
531.335230697053,531.418783140452,531.502272576303,531.585726526917,531.669163020763,
531.752600130519,531.836055925437,531.919600418166,532.003189501107,532.086912768665,
532.16759248456,532.251331196406,532.334966707774,532.418519151172,532.502008587023,
532.585462537637,532.668899031483,532.752336141238,532.835791936156,532.919336428886,
533.002925511826,533.086648779384,533.16732849528,533.251067207126,533.334702718494,
533.418255161892,533.501744597743,533.585198548357,533.668635042203,533.752072151958,
533.835527946876,533.919072439606,534.002661522547,534.086384790104,534.167064506,
534.250803217846,534.334438729214,534.417991172612,534.501480608463,534.584934559077,
534.668371052923,534.751808162679,534.835263957596,534.918808450326,535.002397533267,
535.086120800825,535.166800516721,535.250539228567,535.334174739934,535.417727183333,
535.501216619184,535.584670569798,535.668107063644,535.7515441734,535.834999968318,
535.918544461047,536.002133543988,536.085856811546,536.166536527441,536.250287695696,
536.333932951066,536.41747680672,536.500963156274,536.584410120162,536.667835788342,
536.75128140533,536.834737613956,536.918254701524,536.960677738898),
 .UNSPECIFIED.);
#388=B_SPLINE_CURVE_WITH_KNOTS('',3,(#55527,#55528,#55529,#55530,#55531,
#55532,#55533,#55534,#55535,#55536),.UNSPECIFIED.,.F.,.F.,(4,3,3,4),(530.677740782901,
530.760165021528,530.844661739092,530.929158456655),.UNSPECIFIED.);
#389=B_SPLINE_CURVE_WITH_KNOTS('',3,(#55538,#55539,#55540,#55541,#55542,
#55543,#55544,#55545,#55546,#55547),.UNSPECIFIED.,.F.,.F.,(4,3,3,4),(530.67885489125,
530.768607961165,530.858093749068,530.929158456555),.UNSPECIFIED.);
#390=B_SPLINE_CURVE_WITH_KNOTS('',3,(#55548,#55549,#55550,#55551,#55552,
#55553,#55554,#55555,#55556,#55557,#55558,#55559,#55560,#55561,#55562,#55563,
#55564,#55565,#55566,#55567,#55568,#55569,#55570,#55571,#55572,#55573,#55574,
#55575,#55576,#55577,#55578,#55579,#55580,#55581,#55582,#55583,#55584,#55585,
#55586,#55587,#55588,#55589,#55590,#55591,#55592,#55593,#55594,#55595,#55596,
#55597,#55598,#55599,#55600,#55601,#55602,#55603,#55604,#55605,#55606,#55607,
#55608,#55609,#55610,#55611,#55612,#55613,#55614,#55615,#55616,#55617,#55618,
#55619,#55620,#55621,#55622,#55623,#55624,#55625,#55626,#55627,#55628,#55629,
#55630,#55631,#55632,#55633,#55634,#55635,#55636,#55637,#55638,#55639,#55640,
#55641,#55642,#55643,#55644,#55645,#55646,#55647,#55648,#55649,#55650,#55651,
#55652,#55653,#55654,#55655,#55656,#55657,#55658,#55659,#55660,#55661,#55662,
#55663,#55664,#55665,#55666,#55667,#55668,#55669,#55670,#55671,#55672,#55673,
#55674,#55675,#55676,#55677,#55678,#55679,#55680,#55681,#55682,#55683,#55684,
#55685,#55686,#55687,#55688,#55689,#55690,#55691,#55692,#55693,#55694,#55695,
#55696,#55697,#55698,#55699,#55700,#55701,#55702,#55703,#55704,#55705,#55706,
#55707,#55708,#55709,#55710,#55711,#55712,#55713,#55714,#55715,#55716,#55717,
#55718,#55719,#55720,#55721,#55722,#55723,#55724,#55725,#55726,#55727,#55728,
#55729,#55730,#55731,#55732,#55733,#55734,#55735,#55736,#55737,#55738,#55739,
#55740,#55741,#55742,#55743,#55744,#55745,#55746,#55747,#55748,#55749,#55750,
#55751,#55752,#55753,#55754,#55755,#55756,#55757,#55758,#55759,#55760,#55761,
#55762,#55763,#55764,#55765,#55766,#55767),.UNSPECIFIED.,.F.,.F.,(4,3,3,
3,3,3,3,3,3,3,3,3,3,3,3,3,3,3,3,3,3,3,3,3,3,3,3,3,3,3,3,3,3,3,3,3,3,3,3,
3,3,3,3,3,3,3,3,3,3,3,3,3,3,3,3,3,3,3,3,3,3,3,3,3,3,3,3,3,3,3,3,3,3,4),
(530.929158456658,531.014983582773,531.100869687444,531.186830342444,531.272941100469,
531.35913682173,531.445489719647,531.478147093556,531.561885805402,531.645521316769,
531.729073760168,531.812563196019,531.896017146633,531.979453640479,532.062890750234,
532.146346545152,532.229891037881,532.313480120822,532.39720338838,532.477883104276,
532.561621816122,532.64525732749,532.728809770888,532.812299206739,532.895753157353,
532.979189651199,533.062626760954,533.146082555872,533.229627048602,533.313216131543,
533.3969393991,533.477619114996,533.561357826842,533.644993338209,533.728545781608,
533.812035217459,533.895489168073,533.978925661919,534.062362771674,534.145818566592,
534.229363059321,534.312952142262,534.39667540982,534.477355125716,534.561093837562,
534.64472934893,534.728281792328,534.811771228179,534.895225178793,534.978661672639,
535.062098782395,535.145554577312,535.229099070042,535.312688152983,535.396411420541,
535.477091136436,535.560829848282,535.644465359649,535.728017803047,535.811507238898,
535.894961189512,535.978397683358,536.061834793114,536.145290588032,536.228835080762,
536.312424163703,536.39614743126,536.476827147157,536.559707944129,536.642489631007,
536.725177599064,536.807810647652,536.890413189107,536.96105146982),
 .UNSPECIFIED.);
#391=B_SPLINE_CURVE_WITH_KNOTS('',3,(#55773,#55774,#55775,#55776,#55777,
#55778,#55779,#55780,#55781,#55782,#55783,#55784,#55785,#55786,#55787,#55788,
#55789,#55790,#55791,#55792,#55793,#55794,#55795,#55796,#55797,#55798,#55799,
#55800,#55801,#55802,#55803,#55804,#55805,#55806,#55807,#55808,#55809,#55810,
#55811,#55812,#55813,#55814,#55815,#55816,#55817,#55818,#55819,#55820,#55821,
#55822,#55823,#55824,#55825,#55826,#55827,#55828,#55829,#55830,#55831,#55832,
#55833,#55834,#55835,#55836,#55837,#55838,#55839,#55840,#55841,#55842,#55843,
#55844,#55845,#55846,#55847,#55848,#55849,#55850,#55851,#55852,#55853,#55854,
#55855,#55856,#55857,#55858,#55859,#55860,#55861,#55862,#55863,#55864,#55865,
#55866,#55867,#55868,#55869,#55870,#55871,#55872,#55873,#55874,#55875,#55876,
#55877,#55878,#55879,#55880,#55881,#55882,#55883,#55884,#55885,#55886,#55887,
#55888,#55889,#55890,#55891,#55892,#55893,#55894,#55895,#55896,#55897,#55898,
#55899,#55900,#55901,#55902,#55903,#55904,#55905,#55906,#55907,#55908,#55909,
#55910,#55911,#55912,#55913,#55914,#55915,#55916,#55917,#55918,#55919,#55920,
#55921,#55922,#55923,#55924,#55925,#55926,#55927,#55928,#55929,#55930,#55931,
#55932,#55933,#55934,#55935,#55936,#55937,#55938,#55939,#55940,#55941,#55942,
#55943,#55944,#55945,#55946,#55947,#55948,#55949,#55950,#55951,#55952,#55953,
#55954,#55955,#55956,#55957,#55958,#55959,#55960,#55961,#55962,#55963,#55964,
#55965,#55966,#55967,#55968,#55969,#55970,#55971,#55972,#55973,#55974,#55975,
#55976,#55977,#55978,#55979,#55980,#55981,#55982,#55983,#55984,#55985,#55986,
#55987,#55988,#55989,#55990,#55991,#55992),.UNSPECIFIED.,.F.,.F.,(4,3,3,
3,3,3,3,3,3,3,3,3,3,3,3,3,3,3,3,3,3,3,3,3,3,3,3,3,3,3,3,3,3,3,3,3,3,3,3,
3,3,3,3,3,3,3,3,3,3,3,3,3,3,3,3,3,3,3,3,3,3,3,3,3,3,3,3,3,3,3,3,3,3,4),
(537.212343764021,537.295471444526,537.378498659553,537.461446120284,537.544334461052,
537.627192884229,537.710038420663,537.792889661834,537.875765199949,537.958730434824,
538.041746292055,538.124883983816,538.166008548881,538.249747260727,538.333382772094,
538.416935215493,538.500424651344,538.583878601958,538.667315095804,538.750752205559,
538.834208000477,538.917752493206,539.001341576147,539.085064843705,539.165744559601,
539.249483271447,539.333118782814,539.416671226213,539.500160662064,539.583614612678,
539.667051106524,539.750488216279,539.833944011197,539.917488503927,540.001077586868,
540.084800854425,540.165480570321,540.249219282167,540.332854793534,540.416407236933,
540.499896672783,540.583350623397,540.666787117243,540.750224226999,540.833680021917,
540.917224514646,541.000813597587,541.084536865145,541.165216581041,541.248955292887,
541.332590804255,541.416143247653,541.499632683504,541.583086634118,541.666523127965,
541.74996023772,541.833416032638,541.916960525368,542.000549608309,542.084272875866,
542.164952591761,542.248691303607,542.332326814974,542.415879258372,542.499368694223,
542.582822644836,542.666259138682,542.749696248438,542.833152043356,542.916696536085,
543.000285619026,543.084008886584,543.164688602482,543.244911437326),
 .UNSPECIFIED.);
#392=B_SPLINE_CURVE_WITH_KNOTS('',3,(#55993,#55994,#55995,#55996,#55997,
#55998,#55999,#56000,#56001,#56002,#56003,#56004,#56005),.UNSPECIFIED.,
 .F.,.F.,(4,3,3,3,4),(536.960677738898,537.044295659432,537.128035723592,
537.166272538161,537.212343763834),.UNSPECIFIED.);
#393=B_SPLINE_CURVE_WITH_KNOTS('',3,(#56007,#56008,#56009,#56010,#56011,
#56012,#56013,#56014,#56015,#56016),.UNSPECIFIED.,.F.,.F.,(4,3,3,4),(536.96105146982,
537.043645884405,537.127994824122,537.212343763838),.UNSPECIFIED.);
#394=B_SPLINE_CURVE_WITH_KNOTS('',3,(#56017,#56018,#56019,#56020,#56021,
#56022,#56023,#56024,#56025,#56026,#56027,#56028,#56029,#56030,#56031,#56032,
#56033,#56034,#56035,#56036,#56037,#56038,#56039,#56040,#56041,#56042,#56043,
#56044,#56045,#56046,#56047,#56048,#56049,#56050,#56051,#56052,#56053,#56054,
#56055,#56056,#56057,#56058,#56059,#56060,#56061,#56062,#56063,#56064,#56065,
#56066,#56067,#56068,#56069,#56070,#56071,#56072,#56073,#56074,#56075,#56076,
#56077,#56078,#56079,#56080,#56081,#56082,#56083,#56084,#56085,#56086,#56087,
#56088,#56089,#56090,#56091,#56092,#56093,#56094,#56095,#56096,#56097,#56098,
#56099,#56100,#56101,#56102,#56103,#56104,#56105,#56106,#56107,#56108,#56109,
#56110,#56111,#56112,#56113,#56114,#56115,#56116,#56117,#56118,#56119,#56120,
#56121,#56122,#56123,#56124,#56125,#56126,#56127,#56128,#56129,#56130,#56131,
#56132,#56133,#56134,#56135,#56136,#56137,#56138,#56139,#56140,#56141,#56142,
#56143,#56144,#56145,#56146,#56147,#56148,#56149,#56150,#56151,#56152,#56153,
#56154,#56155,#56156,#56157,#56158,#56159,#56160,#56161,#56162,#56163,#56164,
#56165,#56166,#56167,#56168,#56169,#56170,#56171,#56172,#56173,#56174,#56175,
#56176,#56177,#56178,#56179,#56180,#56181,#56182,#56183,#56184,#56185,#56186,
#56187,#56188,#56189,#56190,#56191,#56192,#56193,#56194,#56195,#56196,#56197,
#56198,#56199,#56200,#56201,#56202,#56203,#56204,#56205,#56206,#56207,#56208,
#56209,#56210,#56211,#56212,#56213,#56214,#56215,#56216,#56217,#56218,#56219,
#56220,#56221,#56222,#56223,#56224,#56225,#56226,#56227,#56228,#56229,#56230,
#56231,#56232,#56233,#56234,#56235,#56236),.UNSPECIFIED.,.F.,.F.,(4,3,3,
3,3,3,3,3,3,3,3,3,3,3,3,3,3,3,3,3,3,3,3,3,3,3,3,3,3,3,3,3,3,3,3,3,3,3,3,
3,3,3,3,3,3,3,3,3,3,3,3,3,3,3,3,3,3,3,3,3,3,3,3,3,3,3,3,3,3,3,3,3,3,4),
(537.212343763992,537.317415438732,537.424490953973,537.476563157877,537.560301869723,
537.64393738109,537.727489824489,537.81097926034,537.894433210954,537.9778697048,
538.061306814556,538.144762609473,538.228307102203,538.311896185144,538.395619452702,
538.476299168597,538.560037880443,538.643673391811,538.727225835209,538.81071527106,
538.894169221674,538.97760571552,539.061042825275,539.144498620193,539.228043112923,
539.311632195864,539.395355463421,539.476035179317,539.559773891163,539.64340940253,
539.726961845929,539.81045128178,539.893905232393,539.97734172624,540.060778835995,
540.144234630913,540.227779123642,540.311368206583,540.395091474141,540.475771190037,
540.559509901883,540.643145413251,540.726697856649,540.8101872925,540.893641243114,
540.97707773696,541.060514846715,541.143970641633,541.227515134363,541.311104217304,
541.394827484861,541.475507200757,541.559245912603,541.64288142397,541.726433867369,
541.80992330322,541.893377253834,541.97681374768,542.060250857435,542.143706652353,
542.227251145083,542.310840228024,542.394563495581,542.475243211477,542.558996057361,
542.644604907669,542.728147807509,542.811633149667,542.895079054618,542.982276005919,
543.06571667707,543.149168860928,543.232671653005,543.24386685982),
 .UNSPECIFIED.);
#395=B_SPLINE_CURVE_WITH_KNOTS('',3,(#56242,#56243,#56244,#56245,#56246,
#56247,#56248,#56249,#56250,#56251,#56252,#56253,#56254,#56255,#56256,#56257,
#56258,#56259,#56260,#56261,#56262,#56263,#56264,#56265,#56266,#56267,#56268,
#56269,#56270,#56271,#56272,#56273,#56274,#56275,#56276,#56277,#56278,#56279,
#56280,#56281,#56282,#56283,#56284,#56285,#56286,#56287,#56288,#56289,#56290,
#56291,#56292,#56293,#56294,#56295,#56296,#56297,#56298,#56299,#56300,#56301,
#56302,#56303,#56304,#56305,#56306,#56307,#56308,#56309,#56310,#56311,#56312,
#56313,#56314,#56315,#56316,#56317,#56318,#56319,#56320,#56321,#56322,#56323,
#56324,#56325,#56326,#56327,#56328,#56329,#56330,#56331,#56332,#56333,#56334,
#56335,#56336,#56337,#56338,#56339,#56340,#56341,#56342,#56343,#56344,#56345,
#56346,#56347,#56348,#56349,#56350,#56351,#56352,#56353,#56354,#56355,#56356,
#56357,#56358,#56359,#56360,#56361,#56362,#56363,#56364,#56365,#56366,#56367,
#56368,#56369,#56370,#56371,#56372,#56373,#56374,#56375,#56376,#56377,#56378,
#56379,#56380,#56381,#56382,#56383,#56384,#56385,#56386,#56387,#56388,#56389,
#56390,#56391,#56392,#56393,#56394,#56395,#56396,#56397,#56398,#56399,#56400,
#56401,#56402,#56403,#56404,#56405,#56406,#56407,#56408,#56409,#56410,#56411,
#56412,#56413,#56414,#56415,#56416,#56417,#56418,#56419,#56420,#56421,#56422,
#56423,#56424,#56425,#56426,#56427,#56428,#56429,#56430,#56431,#56432,#56433,
#56434,#56435,#56436,#56437,#56438,#56439,#56440,#56441,#56442,#56443,#56444,
#56445,#56446,#56447,#56448,#56449,#56450,#56451,#56452,#56453,#56454,#56455,
#56456,#56457,#56458,#56459,#56460,#56461),.UNSPECIFIED.,.F.,.F.,(4,3,3,
3,3,3,3,3,3,3,3,3,3,3,3,3,3,3,3,3,3,3,3,3,3,3,3,3,3,3,3,3,3,3,3,3,3,3,3,
3,3,3,3,3,3,3,3,3,3,3,3,3,3,3,3,3,3,3,3,3,3,3,3,3,3,3,3,3,3,3,3,3,3,4),
(543.495529071014,543.579141013787,543.662478968956,543.745820579077,543.829183942922,
543.912994110492,543.996499535333,544.080462074267,544.164424613202,544.248163325048,
544.331798836415,544.415351279814,544.498840715664,544.582294666278,544.665731160124,
544.749168269879,544.832624064797,544.916168557526,544.999757640467,545.083480908025,
545.164160623922,545.247899335768,545.331534847135,545.415087290534,545.498576726385,
545.582030676999,545.665467170845,545.7489042806,545.832360075518,545.915904568247,
545.999493651188,546.083216918746,546.163896634642,546.247635346488,546.331270857856,
546.414823301254,546.498312737105,546.581766687719,546.665203181565,546.748640291321,
546.832096086239,546.915640578968,546.99922966191,547.082952929467,547.163632645362,
547.247371357208,547.331006868575,547.414559311973,547.498048747824,547.581502698438,
547.664939192284,547.748376302039,547.831832096956,547.915376589686,547.998965672627,
548.082688940184,548.163368656082,548.247107367928,548.330742879295,548.414295322694,
548.497784758545,548.581238709159,548.664675203005,548.74811231276,548.831568107678,
548.915112600408,548.998701683349,549.082424950906,549.163104666802,549.247756932178,
549.332263502758,549.41668560217,549.50102358319,549.528026787596),
 .UNSPECIFIED.);
#396=B_SPLINE_CURVE_WITH_KNOTS('',3,(#56462,#56463,#56464,#56465,#56466,
#56467,#56468,#56469,#56470,#56471),.UNSPECIFIED.,.F.,.F.,(4,3,3,4),(543.244911437326,
543.343198899028,543.440604770004,543.495529070829),.UNSPECIFIED.);
#397=B_SPLINE_CURVE_WITH_KNOTS('',3,(#56473,#56474,#56475,#56476,#56477,
#56478,#56479,#56480,#56481,#56482,#56483,#56484,#56485),.UNSPECIFIED.,
 .F.,.F.,(4,3,3,3,4),(543.24386685982,543.327466923206,543.41119626133,
543.474979222197,543.495529071018),.UNSPECIFIED.);
#398=B_SPLINE_CURVE_WITH_KNOTS('',3,(#56486,#56487,#56488,#56489,#56490,
#56491,#56492,#56493,#56494,#56495,#56496,#56497,#56498,#56499,#56500,#56501,
#56502,#56503,#56504,#56505,#56506,#56507,#56508,#56509,#56510,#56511,#56512,
#56513,#56514,#56515,#56516,#56517,#56518,#56519,#56520,#56521,#56522,#56523,
#56524,#56525,#56526,#56527,#56528,#56529,#56530,#56531,#56532,#56533,#56534,
#56535,#56536,#56537,#56538,#56539,#56540,#56541,#56542,#56543,#56544,#56545,
#56546,#56547,#56548,#56549,#56550,#56551,#56552,#56553,#56554,#56555,#56556,
#56557,#56558,#56559,#56560,#56561,#56562,#56563,#56564,#56565,#56566,#56567,
#56568,#56569,#56570,#56571,#56572,#56573,#56574,#56575,#56576,#56577,#56578,
#56579,#56580,#56581,#56582,#56583,#56584,#56585,#56586,#56587,#56588,#56589,
#56590,#56591,#56592,#56593,#56594,#56595,#56596,#56597,#56598,#56599,#56600,
#56601,#56602,#56603,#56604,#56605,#56606,#56607,#56608,#56609,#56610,#56611,
#56612,#56613,#56614,#56615,#56616,#56617,#56618,#56619,#56620,#56621,#56622,
#56623,#56624,#56625,#56626,#56627,#56628,#56629,#56630,#56631,#56632,#56633,
#56634,#56635,#56636,#56637,#56638,#56639,#56640,#56641,#56642,#56643,#56644,
#56645,#56646,#56647,#56648,#56649,#56650,#56651,#56652,#56653,#56654,#56655,
#56656,#56657,#56658,#56659,#56660,#56661,#56662,#56663,#56664,#56665,#56666,
#56667,#56668,#56669,#56670,#56671,#56672,#56673,#56674,#56675,#56676,#56677,
#56678,#56679,#56680,#56681,#56682,#56683,#56684,#56685,#56686,#56687,#56688,
#56689,#56690,#56691,#56692,#56693,#56694,#56695,#56696,#56697,#56698,#56699,
#56700,#56701,#56702,#56703,#56704,#56705),.UNSPECIFIED.,.F.,.F.,(4,3,3,
3,3,3,3,3,3,3,3,3,3,3,3,3,3,3,3,3,3,3,3,3,3,3,3,3,3,3,3,3,3,3,3,3,3,3,3,
3,3,3,3,3,3,3,3,3,3,3,3,3,3,3,3,3,3,3,3,3,3,3,3,3,3,3,3,3,3,3,3,3,3,4),
(543.495529071208,543.578972716166,543.662313827173,543.745572837891,543.82877010757,
543.911933825072,543.995081784154,544.078232326288,544.161403791053,544.244664224159,
544.327971770939,544.411407962298,544.474715232918,544.558453944764,544.642089456131,
544.72564189953,544.809131335381,544.892585285995,544.976021779841,545.059458889596,
545.142914684514,545.226459177244,545.310048260185,545.393771527742,545.474451243638,
545.558189955484,545.641825466851,545.72537791025,545.808867346101,545.892321296714,
545.975757790561,546.059194900316,546.142650695233,546.226195187963,546.309784270904,
546.393507538462,546.474187254358,546.557925966204,546.641561477571,546.72511392097,
546.808603356822,546.892057307435,546.975493801281,547.058930911037,547.142386705955,
547.225931198684,547.309520281625,547.393243549183,547.473923265078,547.557661976924,
547.641297488292,547.72484993169,547.808339367541,547.891793318155,547.975229812001,
548.058666921756,548.142122716674,548.225667209403,548.309256292344,548.392979559902,
548.473659275798,548.557397987644,548.641033499012,548.72458594241,548.808075378261,
548.891529328875,548.974965822721,549.058402932477,549.141858727395,549.225403220124,
549.308992303066,549.392715570623,549.473395286518,549.52796858603),
 .UNSPECIFIED.);
#399=B_SPLINE_CURVE_WITH_KNOTS('',3,(#56711,#56712,#56713,#56714,#56715,
#56716,#56717,#56718,#56719,#56720,#56721,#56722,#56723,#56724,#56725,#56726,
#56727,#56728,#56729,#56730,#56731,#56732,#56733,#56734,#56735,#56736,#56737,
#56738,#56739,#56740,#56741,#56742,#56743,#56744,#56745,#56746,#56747,#56748,
#56749,#56750,#56751,#56752,#56753,#56754,#56755,#56756,#56757,#56758,#56759,
#56760,#56761,#56762,#56763,#56764,#56765,#56766,#56767,#56768,#56769,#56770,
#56771,#56772,#56773,#56774,#56775,#56776,#56777,#56778,#56779,#56780,#56781,
#56782,#56783,#56784,#56785,#56786,#56787,#56788,#56789,#56790,#56791,#56792,
#56793,#56794,#56795,#56796,#56797,#56798,#56799,#56800,#56801,#56802,#56803,
#56804,#56805,#56806,#56807,#56808,#56809,#56810,#56811,#56812,#56813,#56814,
#56815,#56816,#56817,#56818,#56819,#56820,#56821,#56822,#56823,#56824,#56825,
#56826,#56827,#56828,#56829,#56830,#56831,#56832,#56833,#56834,#56835,#56836,
#56837,#56838,#56839,#56840,#56841,#56842,#56843,#56844,#56845,#56846,#56847,
#56848,#56849,#56850,#56851,#56852,#56853,#56854,#56855,#56856,#56857,#56858,
#56859,#56860,#56861,#56862,#56863,#56864,#56865,#56866,#56867,#56868,#56869,
#56870,#56871,#56872,#56873,#56874,#56875,#56876,#56877,#56878,#56879,#56880,
#56881,#56882,#56883,#56884,#56885,#56886,#56887,#56888,#56889,#56890,#56891,
#56892,#56893,#56894,#56895,#56896,#56897,#56898,#56899,#56900,#56901,#56902,
#56903,#56904,#56905,#56906,#56907,#56908,#56909,#56910,#56911,#56912,#56913,
#56914,#56915,#56916,#56917,#56918,#56919,#56920,#56921,#56922,#56923,#56924,
#56925,#56926,#56927),.UNSPECIFIED.,.F.,.F.,(4,3,3,3,3,3,3,3,3,3,3,3,3,
3,3,3,3,3,3,3,3,3,3,3,3,3,3,3,3,3,3,3,3,3,3,3,3,3,3,3,3,3,3,3,3,3,3,3,3,
3,3,3,3,3,3,3,3,3,3,3,3,3,3,3,3,3,3,3,3,3,3,3,4),(549.778714378383,549.874745953168,
549.96840019969,550.065620438607,550.162840677523,550.246579389368,550.330214900735,
550.413767344133,550.497256779984,550.580710730597,550.664147224443,550.747584334197,
550.831040129114,550.914584621843,550.998173704784,551.081896972341,551.162576688243,
551.246315400089,551.329950911457,551.413503354855,551.496992790706,551.58044674132,
551.663883235166,551.747320344921,551.830776139839,551.914320632569,551.99790971551,
552.081632983067,552.162312698963,552.246051410809,552.329686922177,552.413239365575,
552.496728801426,552.58018275204,552.663619245886,552.747056355642,552.830512150559,
552.914056643289,552.99764572623,553.081368993788,553.162048709683,553.245787421529,
553.329422932896,553.412975376295,553.496464812146,553.579918762759,553.663355256606,
553.746792366361,553.830248161279,553.913792654008,553.997381736949,554.081105004507,
554.161784720403,554.245523432249,554.329158943616,554.412711387015,554.496200822866,
554.57965477348,554.663091267326,554.746528377081,554.829984171999,554.913528664729,
554.99711774767,555.080841015227,555.161520731123,555.244195127162,555.32677495405,
555.409279290226,555.491727145886,555.574147610193,555.656549673153,555.738980910349,
555.810065543653),.UNSPECIFIED.);
#400=B_SPLINE_CURVE_WITH_KNOTS('',3,(#56928,#56929,#56930,#56931,#56932,
#56933,#56934,#56935,#56936,#56937),.UNSPECIFIED.,.F.,.F.,(4,3,3,4),(549.528026787596,
549.612291832284,549.696535530113,549.778714378193),.UNSPECIFIED.);
#401=B_SPLINE_CURVE_WITH_KNOTS('',3,(#56939,#56940,#56941,#56942,#56943,
#56944,#56945,#56946,#56947,#56948),.UNSPECIFIED.,.F.,.F.,(4,3,3,4),(549.52796858603,
549.629096792747,549.729053228591,549.778714378042),.UNSPECIFIED.);
#402=B_SPLINE_CURVE_WITH_KNOTS('',3,(#56949,#56950,#56951,#56952,#56953,
#56954,#56955,#56956,#56957,#56958,#56959,#56960,#56961,#56962,#56963,#56964,
#56965,#56966,#56967,#56968,#56969,#56970,#56971,#56972,#56973,#56974,#56975,
#56976,#56977,#56978,#56979,#56980,#56981,#56982,#56983,#56984,#56985,#56986,
#56987,#56988,#56989,#56990,#56991,#56992,#56993,#56994,#56995,#56996,#56997,
#56998,#56999,#57000,#57001,#57002,#57003,#57004,#57005,#57006,#57007,#57008,
#57009,#57010,#57011,#57012,#57013,#57014,#57015,#57016,#57017,#57018,#57019,
#57020,#57021,#57022,#57023,#57024,#57025,#57026,#57027,#57028,#57029,#57030,
#57031,#57032,#57033,#57034,#57035,#57036,#57037,#57038,#57039,#57040,#57041,
#57042,#57043,#57044,#57045,#57046,#57047,#57048,#57049,#57050,#57051,#57052,
#57053,#57054,#57055,#57056,#57057,#57058,#57059,#57060,#57061,#57062,#57063,
#57064,#57065,#57066,#57067,#57068,#57069,#57070,#57071,#57072,#57073,#57074,
#57075,#57076,#57077,#57078,#57079,#57080,#57081,#57082,#57083,#57084,#57085,
#57086,#57087,#57088,#57089,#57090,#57091,#57092,#57093,#57094,#57095,#57096,
#57097,#57098,#57099,#57100,#57101,#57102,#57103,#57104,#57105,#57106,#57107,
#57108,#57109,#57110,#57111,#57112,#57113,#57114,#57115,#57116,#57117,#57118,
#57119,#57120,#57121,#57122,#57123,#57124,#57125,#57126,#57127,#57128,#57129,
#57130,#57131,#57132,#57133,#57134,#57135,#57136,#57137,#57138,#57139,#57140,
#57141,#57142,#57143,#57144,#57145,#57146,#57147,#57148,#57149,#57150,#57151,
#57152,#57153,#57154,#57155,#57156,#57157,#57158,#57159,#57160,#57161,#57162,
#57163,#57164,#57165,#57166,#57167,#57168),.UNSPECIFIED.,.F.,.F.,(4,3,3,
3,3,3,3,3,3,3,3,3,3,3,3,3,3,3,3,3,3,3,3,3,3,3,3,3,3,3,3,3,3,3,3,3,3,3,3,
3,3,3,3,3,3,3,3,3,3,3,3,3,3,3,3,3,3,3,3,3,3,3,3,3,3,3,3,3,3,3,3,3,3,4),
(549.778714378197,549.865516493077,549.948524356781,550.031526339296,550.114540870175,
550.197586384082,550.280727545981,550.363924948296,550.447243433877,550.473131297238,
550.556870009084,550.640505520451,550.724057963849,550.8075473997,550.891001350314,
550.97443784416,551.057874953916,551.141330748833,551.224875241563,551.308464324503,
551.392187592061,551.472867307958,551.556606019804,551.640241531172,551.723793974571,
551.807283410422,551.890737361036,551.974173854882,552.057610964638,552.141066759556,
552.224611252286,552.308200335227,552.391923602785,552.472603318679,552.556342030525,
552.639977541893,552.723529985291,552.807019421142,552.890473371756,552.973909865602,
553.057346975358,553.140802770276,553.224347263005,553.307936345947,553.391659613504,
553.472339329399,553.556078041245,553.639713552612,553.723265996011,553.806755431861,
553.890209382475,553.973645876321,554.057082986076,554.140538780993,554.224083273723,
554.307672356664,554.391395624221,554.472075340119,554.555814051965,554.639449563332,
554.723002006731,554.806491442581,554.889945393195,554.973381887041,555.056818996797,
555.140274791715,555.223819284444,555.307408367385,555.391131634943,555.471811350839,
555.557006243862,555.642096639219,555.727068916262,555.811320836548),
 .UNSPECIFIED.);
#403=B_SPLINE_CURVE_WITH_KNOTS('',3,(#57174,#57175,#57176,#57177,#57178,
#57179,#57180,#57181,#57182,#57183,#57184,#57185,#57186,#57187,#57188,#57189,
#57190,#57191,#57192,#57193,#57194,#57195,#57196,#57197,#57198,#57199,#57200,
#57201,#57202,#57203,#57204,#57205,#57206,#57207,#57208,#57209,#57210,#57211,
#57212,#57213,#57214,#57215,#57216,#57217,#57218,#57219,#57220,#57221,#57222,
#57223,#57224,#57225,#57226,#57227,#57228,#57229,#57230,#57231,#57232,#57233,
#57234,#57235,#57236,#57237,#57238,#57239,#57240,#57241,#57242,#57243,#57244,
#57245,#57246,#57247,#57248,#57249,#57250,#57251,#57252,#57253,#57254,#57255,
#57256,#57257,#57258,#57259,#57260,#57261,#57262,#57263,#57264,#57265,#57266,
#57267,#57268,#57269,#57270,#57271,#57272,#57273,#57274,#57275,#57276,#57277,
#57278,#57279,#57280,#57281,#57282,#57283,#57284,#57285,#57286,#57287,#57288,
#57289,#57290,#57291,#57292,#57293,#57294,#57295,#57296,#57297,#57298,#57299,
#57300,#57301,#57302,#57303,#57304,#57305,#57306,#57307,#57308,#57309,#57310,
#57311,#57312,#57313,#57314,#57315,#57316,#57317,#57318,#57319,#57320,#57321,
#57322,#57323,#57324,#57325,#57326,#57327,#57328,#57329,#57330,#57331,#57332,
#57333,#57334,#57335,#57336,#57337,#57338,#57339,#57340,#57341,#57342,#57343,
#57344,#57345,#57346,#57347,#57348,#57349,#57350,#57351,#57352,#57353,#57354,
#57355,#57356,#57357,#57358,#57359,#57360,#57361,#57362,#57363,#57364,#57365,
#57366,#57367,#57368,#57369,#57370,#57371,#57372,#57373,#57374,#57375,#57376,
#57377,#57378,#57379,#57380,#57381,#57382,#57383,#57384,#57385,#57386,#57387,
#57388,#57389,#57390,#57391,#57392,#57393),.UNSPECIFIED.,.F.,.F.,(4,3,3,
3,3,3,3,3,3,3,3,3,3,3,3,3,3,3,3,3,3,3,3,3,3,3,3,3,3,3,3,3,3,3,3,3,3,3,3,
3,3,3,3,3,3,3,3,3,3,3,3,3,3,3,3,3,3,3,3,3,3,3,3,3,3,3,3,3,3,3,3,3,3,4),
(556.061899685373,556.161256741843,556.244995453689,556.328630965056,556.412183408455,
556.495672844306,556.579126794919,556.662563288766,556.746000398521,556.829456193439,
556.913000686169,556.996589769109,557.080313036667,557.160992752563,557.244731464409,
557.328366975777,557.411919419175,557.495408855027,557.57886280564,557.662299299487,
557.745736409242,557.82919220416,557.91273669689,557.996325779831,558.080049047389,
558.160728763284,558.24446747513,558.328102986498,558.411655429896,558.495144865747,
558.578598816361,558.662035310207,558.745472419963,558.828928214881,558.91247270761,
558.996061790551,559.079785058109,559.160464774004,559.24420348585,559.327838997217,
559.411391440616,559.494880876467,559.57833482708,559.661771320926,559.745208430682,
559.828664225599,559.912208718329,559.99579780127,560.079521068827,560.160200784724,
560.24393949657,560.327575007937,560.411127451336,560.494616887187,560.578070837801,
560.661507331647,560.744944441402,560.82840023632,560.911944729049,560.99553381199,
561.079257079548,561.159936795444,561.243679299686,561.327317733069,561.410872231796,
561.496223881097,561.579674149104,561.663106132975,561.746537904429,561.833324784874,
561.916848517875,562.000417343959,562.084082409679,562.093685426209),
 .UNSPECIFIED.);
#404=B_SPLINE_CURVE_WITH_KNOTS('',3,(#57394,#57395,#57396,#57397,#57398,
#57399,#57400,#57401,#57402,#57403),.UNSPECIFIED.,.F.,.F.,(4,3,3,4),(555.810065543653,
555.892572116197,555.977235900717,556.061899685237),.UNSPECIFIED.);
#405=B_SPLINE_CURVE_WITH_KNOTS('',3,(#57405,#57406,#57407,#57408,#57409,
#57410,#57411,#57412,#57413,#57414),.UNSPECIFIED.,.F.,.F.,(4,3,3,4),(555.811320836548,
555.896152743485,555.980940198063,556.061899685377),.UNSPECIFIED.);
#406=B_SPLINE_CURVE_WITH_KNOTS('',3,(#57415,#57416,#57417,#57418,#57419,
#57420,#57421,#57422,#57423,#57424,#57425,#57426,#57427,#57428,#57429,#57430,
#57431,#57432,#57433,#57434,#57435,#57436,#57437,#57438,#57439,#57440,#57441,
#57442,#57443,#57444,#57445,#57446,#57447,#57448,#57449,#57450,#57451,#57452,
#57453,#57454,#57455,#57456,#57457,#57458,#57459,#57460,#57461,#57462,#57463,
#57464,#57465,#57466,#57467,#57468,#57469,#57470,#57471,#57472,#57473,#57474,
#57475,#57476,#57477,#57478,#57479,#57480,#57481,#57482,#57483,#57484,#57485,
#57486,#57487,#57488,#57489,#57490,#57491,#57492,#57493,#57494,#57495,#57496,
#57497,#57498,#57499,#57500,#57501,#57502,#57503,#57504,#57505,#57506,#57507,
#57508,#57509,#57510,#57511,#57512,#57513,#57514,#57515,#57516,#57517,#57518,
#57519,#57520,#57521,#57522,#57523,#57524,#57525,#57526,#57527,#57528,#57529,
#57530,#57531,#57532,#57533,#57534,#57535,#57536,#57537,#57538,#57539,#57540,
#57541,#57542,#57543,#57544,#57545,#57546,#57547,#57548,#57549,#57550,#57551,
#57552,#57553,#57554,#57555,#57556,#57557,#57558,#57559,#57560,#57561,#57562,
#57563,#57564,#57565,#57566,#57567,#57568,#57569,#57570,#57571,#57572,#57573,
#57574,#57575,#57576,#57577,#57578,#57579,#57580,#57581,#57582,#57583,#57584,
#57585,#57586,#57587,#57588,#57589,#57590,#57591,#57592,#57593,#57594,#57595,
#57596,#57597,#57598,#57599,#57600,#57601,#57602,#57603,#57604,#57605,#57606,
#57607,#57608,#57609,#57610,#57611,#57612,#57613,#57614,#57615,#57616,#57617,
#57618,#57619,#57620,#57621,#57622,#57623,#57624,#57625,#57626,#57627,#57628,
#57629,#57630,#57631,#57632,#57633,#57634),.UNSPECIFIED.,.F.,.F.,(4,3,3,
3,3,3,3,3,3,3,3,3,3,3,3,3,3,3,3,3,3,3,3,3,3,3,3,3,3,3,3,3,3,3,3,3,3,3,3,
3,3,3,3,3,3,3,3,3,3,3,3,3,3,3,3,3,3,3,3,3,3,3,3,3,3,3,3,3,3,3,3,3,3,4),
(556.061899685548,556.153423872283,556.245403354288,556.337616989708,556.430154199635,
556.471547361559,556.555286073405,556.638921584773,556.722474028172,556.805963464024,
556.889417414637,556.972853908484,557.05629101824,557.139746813158,557.223291305888,
557.306880388829,557.390603656387,557.471283372279,557.555022084125,557.638657595493,
557.722210038891,557.805699474743,557.889153425356,557.972589919203,558.056027028959,
558.139482823876,558.223027316606,558.306616399547,558.390339667105,558.471019383,
558.554758094846,558.638393606213,558.721946049612,558.805435485463,558.888889436077,
558.972325929923,559.055763039678,559.139218834596,559.222763327325,559.306352410266,
559.390075677824,559.47075539372,559.554494105566,559.638129616933,559.721682060332,
559.805171496183,559.888625446796,559.972061940643,560.055499050398,560.138954845316,
560.222499338045,560.306088420986,560.389811688544,560.47049140444,560.554230116286,
560.637865627654,560.721418071052,560.804907506903,560.888361457517,560.971797951363,
561.055235061119,561.138690856037,561.222235348767,561.305824431708,561.389547699265,
561.47022741516,561.552778166199,561.635234203606,561.717614690464,561.799938718783,
561.882233023257,561.96450928654,562.046807049963,562.093278782699),
 .UNSPECIFIED.);
#407=B_SPLINE_CURVE_WITH_KNOTS('',3,(#57640,#57641,#57642,#57643,#57644,
#57645,#57646,#57647,#57648,#57649,#57650,#57651,#57652,#57653,#57654,#57655,
#57656,#57657,#57658,#57659,#57660,#57661,#57662,#57663,#57664,#57665,#57666,
#57667,#57668,#57669,#57670,#57671,#57672,#57673,#57674,#57675,#57676,#57677,
#57678,#57679,#57680,#57681,#57682,#57683,#57684,#57685,#57686,#57687,#57688,
#57689,#57690,#57691,#57692,#57693,#57694,#57695,#57696,#57697,#57698,#57699,
#57700,#57701,#57702,#57703,#57704,#57705,#57706,#57707,#57708,#57709,#57710,
#57711,#57712,#57713,#57714,#57715,#57716,#57717,#57718,#57719,#57720,#57721,
#57722,#57723,#57724,#57725,#57726,#57727,#57728,#57729,#57730,#57731,#57732,
#57733,#57734,#57735,#57736,#57737,#57738,#57739,#57740,#57741,#57742,#57743,
#57744,#57745,#57746,#57747,#57748,#57749,#57750,#57751,#57752,#57753,#57754,
#57755,#57756,#57757,#57758,#57759,#57760,#57761,#57762,#57763,#57764,#57765,
#57766,#57767,#57768,#57769,#57770,#57771,#57772,#57773,#57774,#57775,#57776,
#57777,#57778,#57779,#57780,#57781,#57782,#57783,#57784,#57785,#57786,#57787,
#57788,#57789,#57790,#57791,#57792,#57793,#57794,#57795,#57796,#57797,#57798,
#57799,#57800,#57801,#57802,#57803,#57804,#57805,#57806,#57807,#57808,#57809,
#57810,#57811,#57812,#57813,#57814,#57815,#57816,#57817,#57818,#57819,#57820,
#57821,#57822,#57823,#57824,#57825,#57826,#57827,#57828,#57829,#57830,#57831,
#57832,#57833,#57834,#57835,#57836,#57837,#57838,#57839,#57840,#57841,#57842,
#57843,#57844,#57845,#57846,#57847,#57848,#57849,#57850,#57851,#57852,#57853,
#57854,#57855,#57856,#57857,#57858,#57859),.UNSPECIFIED.,.F.,.F.,(4,3,3,
3,3,3,3,3,3,3,3,3,3,3,3,3,3,3,3,3,3,3,3,3,3,3,3,3,3,3,3,3,3,3,3,3,3,3,3,
3,3,3,3,3,3,3,3,3,3,3,3,3,3,3,3,3,3,3,3,3,3,3,3,3,3,3,3,3,3,3,3,3,3,4),
(562.345084992693,562.427448531772,562.509738999425,562.591981547654,562.674199476266,
562.756411818623,562.838637601327,562.92094554502,563.003295183593,563.085773648807,
563.159408816884,563.24314752873,563.326783040097,563.410335483496,563.493824919347,
563.577278869961,563.660715363807,563.744152473562,563.82760826848,563.91115276121,
563.994741844151,564.078465111708,564.159144827604,564.24288353945,564.326519050818,
564.410071494216,564.493560930067,564.57701488068,564.660451374527,564.743888484282,
564.8273442792,564.91088877193,564.994477854871,565.078201122428,565.158880838324,
565.24261955017,565.326255061537,565.409807504936,565.493296940786,565.5767508914,
565.660187385246,565.743624495002,565.827080289919,565.910624782649,565.99421386559,
566.077937133148,566.158616849045,566.242355560891,566.325991072258,566.409543515657,
566.493032951509,566.576486902122,566.659923395969,566.743360505724,566.826816300642,
566.910360793372,566.993949876313,567.07767314387,567.158352859765,567.242091571611,
567.325727082978,567.409279526377,567.492768962228,567.576222912842,567.659659406688,
567.743096516444,567.826552311361,567.910096804091,567.993685887032,568.077409154589,
568.158088870485,568.247415364467,568.336527127973,568.37796764204),
 .UNSPECIFIED.);
#408=B_SPLINE_CURVE_WITH_KNOTS('',3,(#57860,#57861,#57862,#57863,#57864,
#57865,#57866,#57867,#57868,#57869),.UNSPECIFIED.,.F.,.F.,(4,3,3,4),(562.093685426209,
562.159672806164,562.284783772402,562.345084992552),.UNSPECIFIED.);
#409=B_SPLINE_CURVE_WITH_KNOTS('',3,(#57871,#57872,#57873,#57874,#57875,
#57876,#57877,#57878,#57879,#57880),.UNSPECIFIED.,.F.,.F.,(4,3,3,4),(562.093278782699,
562.175645741503,562.260365366964,562.345084992425),.UNSPECIFIED.);
#410=B_SPLINE_CURVE_WITH_KNOTS('',3,(#57881,#57882,#57883,#57884,#57885,
#57886,#57887,#57888,#57889,#57890,#57891,#57892,#57893,#57894,#57895,#57896,
#57897,#57898,#57899,#57900,#57901,#57902,#57903,#57904,#57905,#57906,#57907,
#57908,#57909,#57910,#57911,#57912,#57913,#57914,#57915,#57916,#57917,#57918,
#57919,#57920,#57921,#57922,#57923,#57924,#57925,#57926,#57927,#57928,#57929,
#57930,#57931,#57932,#57933,#57934,#57935,#57936,#57937,#57938,#57939,#57940,
#57941,#57942,#57943,#57944,#57945,#57946,#57947,#57948,#57949,#57950,#57951,
#57952,#57953,#57954,#57955,#57956,#57957,#57958,#57959,#57960,#57961,#57962,
#57963,#57964,#57965,#57966,#57967,#57968,#57969,#57970,#57971,#57972,#57973,
#57974,#57975,#57976,#57977,#57978,#57979,#57980,#57981,#57982,#57983,#57984,
#57985,#57986,#57987,#57988,#57989,#57990,#57991,#57992,#57993,#57994,#57995,
#57996,#57997,#57998,#57999,#58000,#58001,#58002,#58003,#58004,#58005,#58006,
#58007,#58008,#58009,#58010,#58011,#58012,#58013,#58014,#58015,#58016,#58017,
#58018,#58019,#58020,#58021,#58022,#58023,#58024,#58025,#58026,#58027,#58028,
#58029,#58030,#58031,#58032,#58033,#58034,#58035,#58036,#58037,#58038,#58039,
#58040,#58041,#58042,#58043,#58044,#58045,#58046,#58047,#58048,#58049,#58050,
#58051,#58052,#58053,#58054,#58055,#58056,#58057,#58058,#58059,#58060,#58061,
#58062,#58063,#58064,#58065,#58066,#58067,#58068,#58069,#58070,#58071,#58072,
#58073,#58074,#58075,#58076,#58077,#58078,#58079,#58080,#58081,#58082,#58083,
#58084,#58085,#58086,#58087,#58088,#58089,#58090,#58091,#58092,#58093,#58094,
#58095,#58096,#58097),.UNSPECIFIED.,.F.,.F.,(4,3,3,3,3,3,3,3,3,3,3,3,3,
3,3,3,3,3,3,3,3,3,3,3,3,3,3,3,3,3,3,3,3,3,3,3,3,3,3,3,3,3,3,3,3,3,3,3,3,
3,3,3,3,3,3,3,3,3,3,3,3,3,3,3,3,3,3,3,3,3,3,3,4),(562.345084992556,562.46996342588,
562.553702137726,562.637337649093,562.720890092492,562.804379528343,562.887833478956,
562.971269972802,563.054707082558,563.138162877476,563.221707370205,563.305296453146,
563.389019720704,563.4696994366,563.553438148446,563.637073659813,563.720626103212,
563.804115539063,563.887569489677,563.971005983523,564.054443093278,564.137898888196,
564.221443380925,564.305032463866,564.388755731424,564.46943544732,564.553174159166,
564.636809670533,564.720362113932,564.803851549783,564.887305500397,564.970741994243,
565.054179103998,565.137634898916,565.221179391645,565.304768474586,565.388491742144,
565.46917145804,565.552910169886,565.636545681254,565.720098124652,565.803587560503,
565.887041511117,565.970478004963,566.053915114719,566.137370909636,566.220915402366,
566.304504485307,566.388227752865,566.46890746876,566.552646180606,566.636281691974,
566.719834135372,566.803323571223,566.886777521837,566.970214015683,567.053651125439,
567.137106920357,567.220651413086,567.304240496028,567.387963763585,567.468643479481,
567.552387508031,567.636027127852,567.719582476606,567.803069632465,567.886519534233,
567.969950270323,568.053379912481,568.136865629516,568.220379007305,568.303994204407,
568.3767803679),.UNSPECIFIED.);
#411=B_SPLINE_CURVE_WITH_KNOTS('',3,(#58103,#58104,#58105,#58106,#58107,
#58108,#58109,#58110,#58111,#58112,#58113,#58114,#58115,#58116,#58117,#58118,
#58119,#58120,#58121,#58122,#58123,#58124,#58125,#58126,#58127,#58128,#58129,
#58130,#58131,#58132,#58133,#58134,#58135,#58136,#58137,#58138,#58139,#58140,
#58141,#58142,#58143,#58144,#58145,#58146,#58147,#58148,#58149,#58150,#58151,
#58152,#58153,#58154,#58155,#58156,#58157,#58158,#58159,#58160,#58161,#58162,
#58163,#58164,#58165,#58166,#58167,#58168,#58169,#58170,#58171,#58172,#58173,
#58174,#58175,#58176,#58177,#58178,#58179,#58180,#58181,#58182,#58183,#58184,
#58185,#58186,#58187,#58188,#58189,#58190,#58191,#58192,#58193,#58194,#58195,
#58196,#58197,#58198,#58199,#58200,#58201,#58202,#58203,#58204,#58205,#58206,
#58207,#58208,#58209,#58210,#58211,#58212,#58213,#58214,#58215,#58216,#58217,
#58218,#58219,#58220,#58221,#58222,#58223,#58224,#58225,#58226,#58227,#58228,
#58229,#58230,#58231,#58232,#58233,#58234,#58235,#58236,#58237,#58238,#58239,
#58240,#58241,#58242,#58243,#58244,#58245,#58246,#58247,#58248,#58249,#58250,
#58251,#58252,#58253,#58254,#58255,#58256,#58257,#58258,#58259,#58260,#58261,
#58262,#58263,#58264,#58265,#58266,#58267,#58268,#58269,#58270,#58271,#58272,
#58273,#58274,#58275,#58276,#58277,#58278,#58279,#58280,#58281,#58282,#58283,
#58284,#58285,#58286,#58287,#58288,#58289,#58290,#58291,#58292,#58293,#58294,
#58295,#58296,#58297,#58298,#58299,#58300,#58301,#58302,#58303,#58304,#58305,
#58306,#58307,#58308,#58309,#58310,#58311,#58312,#58313,#58314,#58315,#58316,
#58317,#58318,#58319),.UNSPECIFIED.,.F.,.F.,(4,3,3,3,3,3,3,3,3,3,3,3,3,
3,3,3,3,3,3,3,3,3,3,3,3,3,3,3,3,3,3,3,3,3,3,3,3,3,3,3,3,3,3,3,3,3,3,3,3,
3,3,3,3,3,3,3,3,3,3,3,3,3,3,3,3,3,3,3,3,3,3,3,4),(568.628270299732,568.714673941208,
568.801157485386,568.890324334341,568.977067748322,569.067446314764,569.157824881205,
569.241563593051,569.325199104419,569.408751547817,569.492240983668,569.575694934282,
569.659131428128,569.742568537883,569.826024332801,569.909568825531,569.993157908472,
570.07688117603,570.157560891925,570.241299603771,570.324935115138,570.408487558537,
570.491976994388,570.575430945002,570.658867438848,570.742304548603,570.825760343521,
570.90930483625,570.992893919191,571.076617186749,571.157296902645,571.241035614491,
571.324671125859,571.408223569257,571.491713005108,571.575166955722,571.658603449568,
571.742040559324,571.825496354241,571.909040846971,571.992629929912,572.07635319747,
572.157032913365,572.240771625211,572.324407136578,572.407959579977,572.491449015828,
572.574902966442,572.658339460288,572.741776570043,572.825232364961,572.908776857691,
572.992365940632,573.076089208189,573.156768924085,573.240507635931,573.324143147299,
573.407695590697,573.491185026548,573.574638977162,573.658075471008,573.741512580764,
573.824968375682,573.908512868411,573.992101951352,574.07582521891,574.156504934806,
574.239235471064,574.321868030338,574.406417798025,574.488904569422,574.574485835255,
574.660067101088),.UNSPECIFIED.);
#412=B_SPLINE_CURVE_WITH_KNOTS('',3,(#58320,#58321,#58322,#58323,#58324,
#58325,#58326,#58327,#58328,#58329),.UNSPECIFIED.,.F.,.F.,(4,3,3,4),(568.37796764204,
568.466803636206,568.555419194261,568.628270299597),.UNSPECIFIED.);
#413=B_SPLINE_CURVE_WITH_KNOTS('',3,(#58331,#58332,#58333,#58334,#58335,
#58336,#58337,#58338,#58339,#58340,#58341,#58342,#58343),.UNSPECIFIED.,
 .F.,.F.,(4,3,3,3,4),(568.3767803679,568.460535618476,568.468379490201,
568.604938226218,568.628270299736),.UNSPECIFIED.);
#414=B_SPLINE_CURVE_WITH_KNOTS('',3,(#58344,#58345,#58346,#58347,#58348,
#58349,#58350,#58351,#58352,#58353,#58354,#58355,#58356,#58357,#58358,#58359,
#58360,#58361,#58362,#58363,#58364,#58365,#58366,#58367,#58368,#58369,#58370,
#58371,#58372,#58373,#58374,#58375,#58376,#58377,#58378,#58379,#58380,#58381,
#58382,#58383,#58384,#58385,#58386,#58387,#58388,#58389,#58390,#58391,#58392,
#58393,#58394,#58395,#58396,#58397,#58398,#58399,#58400,#58401,#58402,#58403,
#58404,#58405,#58406,#58407,#58408,#58409,#58410,#58411,#58412,#58413,#58414,
#58415,#58416,#58417,#58418,#58419,#58420,#58421,#58422,#58423,#58424,#58425,
#58426,#58427,#58428,#58429,#58430,#58431,#58432,#58433,#58434,#58435,#58436,
#58437,#58438,#58439,#58440,#58441,#58442,#58443,#58444,#58445,#58446,#58447,
#58448,#58449,#58450,#58451,#58452,#58453,#58454,#58455,#58456,#58457,#58458,
#58459,#58460,#58461,#58462,#58463,#58464,#58465,#58466,#58467,#58468,#58469,
#58470,#58471,#58472,#58473,#58474,#58475,#58476,#58477,#58478,#58479,#58480,
#58481,#58482,#58483,#58484,#58485,#58486,#58487,#58488,#58489,#58490,#58491,
#58492,#58493,#58494,#58495,#58496,#58497,#58498,#58499,#58500,#58501,#58502,
#58503,#58504,#58505,#58506,#58507,#58508,#58509,#58510,#58511,#58512,#58513,
#58514,#58515,#58516,#58517,#58518,#58519,#58520,#58521,#58522,#58523,#58524,
#58525,#58526,#58527,#58528,#58529,#58530,#58531,#58532,#58533,#58534,#58535,
#58536,#58537,#58538,#58539,#58540,#58541,#58542,#58543,#58544,#58545,#58546,
#58547,#58548,#58549,#58550,#58551,#58552,#58553,#58554,#58555,#58556,#58557,
#58558,#58559,#58560,#58561,#58562,#58563,#58564,#58565,#58566),
 .UNSPECIFIED.,.F.,.F.,(4,3,3,3,3,3,3,3,3,3,3,3,3,3,3,3,3,3,3,3,3,3,3,3,
3,3,3,3,3,3,3,3,3,3,3,3,3,3,3,3,3,3,3,3,3,3,3,3,3,3,3,3,3,3,3,3,3,3,3,3,
3,3,3,3,3,3,3,3,3,3,3,3,3,3,4),(568.628270299839,568.710653138352,568.792956251044,
568.877351157279,568.959566188819,569.041770160988,569.12398210561,569.210015454438,
569.292345390399,569.374730026394,569.457226730502,569.468115500921,569.551854212767,
569.635489724134,569.719042167533,569.802531603384,569.885985553998,569.969422047844,
570.052859157599,570.136314952517,570.219859445246,570.303448528187,570.387171795745,
570.467851511641,570.551590223487,570.635225734855,570.718778178253,570.802267614104,
570.885721564718,570.969158058564,571.052595168319,571.136050963237,571.219595455967,
571.303184538908,571.386907806466,571.467587522361,571.551326234207,571.634961745575,
571.718514188973,571.802003624824,571.885457575438,571.968894069284,572.05233117904,
572.135786973957,572.219331466687,572.302920549628,572.386643817186,572.467323533081,
572.551062244927,572.634697756294,572.718250199692,572.801739635544,572.885193586158,
572.968630080004,573.05206718976,573.135522984677,573.219067477407,573.302656560348,
573.386379827905,573.467059543801,573.550798255647,573.634433767015,573.717986210413,
573.801475646264,573.884929596878,573.968366090724,574.05180320048,574.135258995397,
574.218803488127,574.302392571068,574.386115838625,574.466795554521,574.557380703572,
574.647733634699,574.661148849332),.UNSPECIFIED.);
#415=B_SPLINE_CURVE_WITH_KNOTS('',3,(#58572,#58573,#58574,#58575,#58576,
#58577,#58578,#58579,#58580,#58581,#58582,#58583,#58584,#58585,#58586,#58587,
#58588,#58589,#58590,#58591,#58592,#58593,#58594,#58595,#58596,#58597,#58598,
#58599,#58600,#58601,#58602,#58603,#58604,#58605,#58606,#58607,#58608,#58609,
#58610,#58611,#58612,#58613,#58614,#58615,#58616,#58617,#58618,#58619,#58620,
#58621,#58622,#58623,#58624,#58625,#58626,#58627,#58628,#58629,#58630,#58631,
#58632,#58633,#58634,#58635,#58636,#58637,#58638,#58639,#58640,#58641,#58642,
#58643,#58644,#58645,#58646,#58647,#58648,#58649,#58650,#58651,#58652,#58653,
#58654,#58655,#58656,#58657,#58658,#58659,#58660,#58661,#58662,#58663,#58664,
#58665,#58666,#58667,#58668,#58669,#58670,#58671,#58672,#58673,#58674,#58675,
#58676,#58677,#58678,#58679,#58680,#58681,#58682,#58683,#58684,#58685,#58686,
#58687,#58688,#58689,#58690,#58691,#58692,#58693,#58694,#58695,#58696,#58697,
#58698,#58699,#58700,#58701,#58702,#58703,#58704,#58705,#58706,#58707,#58708,
#58709,#58710,#58711,#58712,#58713,#58714,#58715,#58716,#58717,#58718,#58719,
#58720,#58721,#58722,#58723,#58724,#58725,#58726,#58727,#58728,#58729,#58730,
#58731,#58732,#58733,#58734,#58735,#58736,#58737,#58738,#58739,#58740,#58741,
#58742,#58743,#58744,#58745,#58746,#58747,#58748,#58749,#58750,#58751,#58752,
#58753,#58754,#58755,#58756,#58757,#58758,#58759,#58760,#58761,#58762,#58763,
#58764,#58765,#58766,#58767,#58768,#58769,#58770,#58771,#58772,#58773,#58774,
#58775,#58776,#58777,#58778,#58779,#58780,#58781,#58782,#58783,#58784,#58785,
#58786,#58787,#58788,#58789,#58790,#58791),.UNSPECIFIED.,.F.,.F.,(4,3,3,
3,3,3,3,3,3,3,3,3,3,3,3,3,3,3,3,3,3,3,3,3,3,3,3,3,3,3,3,3,3,3,3,3,3,3,3,
3,3,3,3,3,3,3,3,3,3,3,3,3,3,3,3,3,3,3,3,3,3,3,3,3,3,3,3,3,3,3,3,3,3,4),
(574.911455607035,575.019558419726,575.130265374109,575.156240945526,575.239979657372,
575.323615168739,575.407167612138,575.490657047989,575.574110998603,575.657547492449,
575.740984602205,575.824440397122,575.907984889852,575.991573972793,576.075297240351,
576.155976956246,576.239715668092,576.32335117946,576.406903622858,576.490393058709,
576.573847009323,576.657283503169,576.740720612924,576.824176407842,576.907720900572,
576.991309983512,577.07503325107,577.155712966966,577.239451678812,577.323087190179,
577.406639633578,577.490129069429,577.573583020042,577.657019513889,577.740456623644,
577.823912418562,577.907456911291,577.991045994232,578.07476926179,578.155448977686,
578.239187689532,578.3228232009,578.406375644298,578.489865080149,578.573319030763,
578.656755524609,578.740192634365,578.823648429282,578.907192922012,578.990782004953,
579.074505272511,579.155184988406,579.238923700252,579.322559211619,579.406111655018,
579.489601090869,579.573055041483,579.656491535329,579.739928645084,579.823384440002,
579.906928932732,579.990518015673,580.07424128323,580.154920999126,580.238672564971,
580.326710311874,580.410250823492,580.493734668348,580.577179965179,580.660604802776,
580.744049301531,580.82750519747,580.91101905523,580.942974540196),
 .UNSPECIFIED.);
#416=B_SPLINE_CURVE_WITH_KNOTS('',3,(#58792,#58793,#58794,#58795,#58796,
#58797,#58798,#58799,#58800,#58801),.UNSPECIFIED.,.F.,.F.,(4,3,3,4),(574.660067101088,
574.742526490161,574.826991048537,574.911455606912),.UNSPECIFIED.);
#417=B_SPLINE_CURVE_WITH_KNOTS('',3,(#58803,#58804,#58805,#58806,#58807,
#58808,#58809,#58810,#58811,#58812),.UNSPECIFIED.,.F.,.F.,(4,3,3,4),(574.661148849332,
574.751208983431,574.840985453372,574.911455606801),.UNSPECIFIED.);
#418=B_SPLINE_CURVE_WITH_KNOTS('',3,(#58813,#58814,#58815,#58816,#58817,
#58818,#58819,#58820,#58821,#58822,#58823,#58824,#58825,#58826,#58827,#58828,
#58829,#58830,#58831,#58832,#58833,#58834,#58835,#58836,#58837,#58838,#58839,
#58840,#58841,#58842,#58843,#58844,#58845,#58846,#58847,#58848,#58849,#58850,
#58851,#58852,#58853,#58854,#58855,#58856,#58857,#58858,#58859,#58860,#58861,
#58862,#58863,#58864,#58865,#58866,#58867,#58868,#58869,#58870,#58871,#58872,
#58873,#58874,#58875,#58876,#58877,#58878,#58879,#58880,#58881,#58882,#58883,
#58884,#58885,#58886,#58887,#58888,#58889,#58890,#58891,#58892,#58893,#58894,
#58895,#58896,#58897,#58898,#58899,#58900,#58901,#58902,#58903,#58904,#58905,
#58906,#58907,#58908,#58909,#58910,#58911,#58912,#58913,#58914,#58915,#58916,
#58917,#58918,#58919,#58920,#58921,#58922,#58923,#58924,#58925,#58926,#58927,
#58928,#58929,#58930,#58931,#58932,#58933,#58934,#58935,#58936,#58937,#58938,
#58939,#58940,#58941,#58942,#58943,#58944,#58945,#58946,#58947,#58948,#58949,
#58950,#58951,#58952,#58953,#58954,#58955,#58956,#58957,#58958,#58959,#58960,
#58961,#58962,#58963,#58964,#58965,#58966,#58967,#58968,#58969,#58970,#58971,
#58972,#58973,#58974,#58975,#58976,#58977,#58978,#58979,#58980,#58981,#58982,
#58983,#58984,#58985,#58986,#58987,#58988,#58989,#58990,#58991,#58992,#58993,
#58994,#58995,#58996,#58997,#58998,#58999,#59000,#59001,#59002,#59003,#59004,
#59005,#59006,#59007,#59008,#59009,#59010,#59011,#59012,#59013,#59014,#59015,
#59016,#59017,#59018,#59019,#59020,#59021,#59022,#59023,#59024,#59025,#59026,
#59027,#59028,#59029,#59030,#59031,#59032),.UNSPECIFIED.,.F.,.F.,(4,3,3,
3,3,3,3,3,3,3,3,3,3,3,3,3,3,3,3,3,3,3,3,3,3,3,3,3,3,3,3,3,3,3,3,3,3,3,3,
3,3,3,3,3,3,3,3,3,3,3,3,3,3,3,3,3,3,3,3,3,3,3,3,3,3,3,3,3,3,3,3,3,3,4),
(574.911455606915,574.997111060428,575.082822107205,575.168602763877,575.254529100318,
575.340536906395,575.426701887711,575.466531565242,575.550270277088,575.633905788455,
575.717458231854,575.800947667705,575.884401618319,575.967838112165,576.05127522192,
576.134731016837,576.218275509567,576.301864592508,576.385587860065,576.466267575962,
576.550006287808,576.633641799176,576.717194242574,576.800683678425,576.884137629039,
576.967574122885,577.051011232641,577.134467027558,577.218011520288,577.301600603229,
577.385323870787,577.466003586682,577.549742298528,577.633377809895,577.716930253294,
577.800419689145,577.883873639758,577.967310133604,578.05074724336,578.134203038277,
578.217747531007,578.301336613948,578.385059881506,578.465739597402,578.549478309248,
578.633113820615,578.716666264014,578.800155699865,578.883609650479,578.967046144325,
579.05048325408,579.133939048997,579.217483541727,579.301072624668,579.384795892226,
579.465475608122,579.549214319968,579.632849831336,579.716402274735,579.799891710585,
579.883345661199,579.966782155046,580.050219264801,580.133675059718,580.217219552448,
580.300808635389,580.384531902946,580.465211618842,580.548146779117,580.630982425771,
580.713723386536,580.796409076522,580.879062240394,580.943379534668),
 .UNSPECIFIED.);
#419=B_SPLINE_CURVE_WITH_KNOTS('',3,(#59038,#59039,#59040,#59041,#59042,
#59043,#59044,#59045,#59046,#59047,#59048,#59049,#59050,#59051,#59052,#59053,
#59054,#59055,#59056,#59057,#59058,#59059,#59060,#59061,#59062,#59063,#59064,
#59065,#59066,#59067,#59068,#59069,#59070,#59071,#59072,#59073,#59074,#59075,
#59076,#59077,#59078,#59079,#59080,#59081,#59082,#59083,#59084,#59085,#59086,
#59087,#59088,#59089,#59090,#59091,#59092,#59093,#59094,#59095,#59096,#59097,
#59098,#59099,#59100,#59101,#59102,#59103,#59104,#59105,#59106,#59107,#59108,
#59109,#59110,#59111,#59112,#59113,#59114,#59115,#59116,#59117,#59118,#59119,
#59120,#59121,#59122,#59123,#59124,#59125,#59126,#59127,#59128,#59129,#59130,
#59131,#59132,#59133,#59134,#59135,#59136,#59137,#59138,#59139,#59140,#59141,
#59142,#59143,#59144,#59145,#59146,#59147,#59148,#59149,#59150,#59151,#59152,
#59153,#59154,#59155,#59156,#59157,#59158,#59159,#59160,#59161,#59162,#59163,
#59164,#59165,#59166,#59167,#59168,#59169,#59170,#59171,#59172,#59173,#59174,
#59175,#59176,#59177,#59178,#59179,#59180,#59181,#59182,#59183,#59184,#59185,
#59186,#59187,#59188,#59189,#59190,#59191,#59192,#59193,#59194,#59195,#59196,
#59197,#59198,#59199,#59200,#59201,#59202,#59203,#59204,#59205,#59206,#59207,
#59208,#59209,#59210,#59211,#59212,#59213,#59214,#59215,#59216,#59217,#59218,
#59219,#59220,#59221,#59222,#59223,#59224,#59225,#59226,#59227,#59228,#59229,
#59230,#59231,#59232,#59233,#59234,#59235,#59236,#59237,#59238,#59239,#59240,
#59241,#59242,#59243,#59244,#59245,#59246,#59247,#59248,#59249,#59250,#59251,
#59252,#59253,#59254,#59255,#59256,#59257),.UNSPECIFIED.,.F.,.F.,(4,3,3,
3,3,3,3,3,3,3,3,3,3,3,3,3,3,3,3,3,3,3,3,3,3,3,3,3,3,3,3,3,3,3,3,3,3,3,3,
3,3,3,3,3,3,3,3,3,3,3,3,3,3,3,3,3,3,3,3,3,3,3,3,3,3,3,3,3,3,3,3,3,3,4),
(581.19464091426,581.277838919826,581.360935855946,581.443952375982,581.526909056947,
581.609834845097,581.692746992297,581.775664037574,581.858604519983,581.941634490468,
582.024714210515,582.107917376551,582.154393020567,582.238131732413,582.321767243781,
582.405319687179,582.48880912303,582.572263073644,582.65569956749,582.739136677245,
582.822592472162,582.906136964892,582.989726047833,583.073449315391,583.154129031287,
583.237867743133,583.3215032545,583.405055697899,583.48854513375,583.571999084363,
583.655435578209,583.738872687965,583.822328482882,583.905872975611,583.989462058552,
584.07318532611,584.153865042007,584.237603753853,584.321239265221,584.404791708619,
584.48828114447,584.571735095084,584.65517158893,584.738608698686,584.822064493604,
584.905608986333,584.989198069274,585.072921336832,585.153601052727,585.237339764573,
585.32097527594,585.404527719338,585.488017155189,585.571471105803,585.654907599649,
585.738344709405,585.821800504322,585.905344997052,585.988934079993,586.07265734755,
586.153337063447,586.237075775293,586.32071128666,586.404263730059,586.487753165909,
586.571207116523,586.654643610369,586.738080720125,586.821536515042,586.905081007772,
586.988670090713,587.07239335827,587.153073074167,587.227179640329),
 .UNSPECIFIED.);
#420=B_SPLINE_CURVE_WITH_KNOTS('',3,(#59258,#59259,#59260,#59261,#59262,
#59263,#59264,#59265,#59266,#59267,#59268,#59269,#59270),.UNSPECIFIED.,
 .F.,.F.,(4,3,3,3,4),(580.942974540196,581.0265880631,581.110325399057,
581.154657009846,581.194640914091),.UNSPECIFIED.);
#421=B_SPLINE_CURVE_WITH_KNOTS('',3,(#59272,#59273,#59274,#59275,#59276,
#59277,#59278,#59279,#59280,#59281),.UNSPECIFIED.,.F.,.F.,(4,3,3,4),(580.943379534668,
581.026023492215,581.110332203155,581.194640914095),.UNSPECIFIED.);
#422=B_SPLINE_CURVE_WITH_KNOTS('',3,(#59282,#59283,#59284,#59285,#59286,
#59287,#59288,#59289,#59290,#59291,#59292,#59293,#59294,#59295,#59296,#59297,
#59298,#59299,#59300,#59301,#59302,#59303,#59304,#59305,#59306,#59307,#59308,
#59309,#59310,#59311,#59312,#59313,#59314,#59315,#59316,#59317,#59318,#59319,
#59320,#59321,#59322,#59323,#59324,#59325,#59326,#59327,#59328,#59329,#59330,
#59331,#59332,#59333,#59334,#59335,#59336,#59337,#59338,#59339,#59340,#59341,
#59342,#59343,#59344,#59345,#59346,#59347,#59348,#59349,#59350,#59351,#59352,
#59353,#59354,#59355,#59356,#59357,#59358,#59359,#59360,#59361,#59362,#59363,
#59364,#59365,#59366,#59367,#59368,#59369,#59370,#59371,#59372,#59373,#59374,
#59375,#59376,#59377,#59378,#59379,#59380,#59381,#59382,#59383,#59384,#59385,
#59386,#59387,#59388,#59389,#59390,#59391,#59392,#59393,#59394,#59395,#59396,
#59397,#59398,#59399,#59400,#59401,#59402,#59403,#59404,#59405,#59406,#59407,
#59408,#59409,#59410,#59411,#59412,#59413,#59414,#59415,#59416,#59417,#59418,
#59419,#59420,#59421,#59422,#59423,#59424,#59425,#59426,#59427,#59428,#59429,
#59430,#59431,#59432,#59433,#59434,#59435,#59436,#59437,#59438,#59439,#59440,
#59441,#59442,#59443,#59444,#59445,#59446,#59447,#59448,#59449,#59450,#59451,
#59452,#59453,#59454,#59455,#59456,#59457,#59458,#59459,#59460,#59461,#59462,
#59463,#59464,#59465,#59466,#59467,#59468,#59469,#59470,#59471,#59472,#59473,
#59474,#59475,#59476,#59477,#59478,#59479,#59480,#59481,#59482,#59483,#59484,
#59485,#59486,#59487,#59488,#59489,#59490,#59491,#59492,#59493,#59494,#59495,
#59496,#59497,#59498),.UNSPECIFIED.,.F.,.F.,(4,3,3,3,3,3,3,3,3,3,3,3,3,
3,3,3,3,3,3,3,3,3,3,3,3,3,3,3,3,3,3,3,3,3,3,3,3,3,3,3,3,3,3,3,3,3,3,3,3,
3,3,3,3,3,3,3,3,3,3,3,3,3,3,3,3,3,3,3,3,3,3,3,4),(581.194640914276,581.298856363405,
581.404929115638,581.464947629562,581.548686341409,581.632321852777,581.715874296177,
581.799363732029,581.882817682644,581.966254176491,582.049691286248,582.133147081167,
582.216691573897,582.30028065684,582.384003924398,582.464683640283,582.548422352129,
582.632057863496,582.715610306895,582.799099742746,582.882553693359,582.965990187205,
583.04942729696,583.132883091878,583.216427584607,583.300016667548,583.383739935106,
583.464419651003,583.548158362849,583.631793874216,583.715346317615,583.798835753466,
583.882289704079,583.965726197925,584.04916330768,584.132619102598,584.216163595328,
584.299752678268,584.383475945826,584.464155661723,584.547894373569,584.631529884937,
584.715082328335,584.798571764186,584.8820257148,584.965462208646,585.048899318402,
585.13235511332,585.215899606049,585.29948868899,585.383211956548,585.463891672443,
585.547630384289,585.631265895656,585.714818339055,585.798307774906,585.88176172552,
585.965198219366,586.048635329122,586.13209112404,586.215635616769,586.29922469971,
586.382947967268,586.463627683163,586.547380933352,586.632229179731,586.71577284881,
586.799258681196,586.882704797921,586.968570324537,587.05200975601,587.139088330197,
587.226166904384),.UNSPECIFIED.);
#423=B_SPLINE_CURVE_WITH_KNOTS('',3,(#59504,#59505,#59506,#59507,#59508,
#59509,#59510,#59511,#59512,#59513,#59514,#59515,#59516,#59517,#59518,#59519,
#59520,#59521,#59522,#59523,#59524,#59525,#59526,#59527,#59528,#59529,#59530,
#59531,#59532,#59533,#59534,#59535,#59536,#59537,#59538,#59539,#59540,#59541,
#59542,#59543,#59544,#59545,#59546,#59547,#59548,#59549,#59550,#59551,#59552,
#59553,#59554,#59555,#59556,#59557,#59558,#59559,#59560,#59561,#59562,#59563,
#59564,#59565,#59566,#59567,#59568,#59569,#59570,#59571,#59572,#59573,#59574,
#59575,#59576,#59577,#59578,#59579,#59580,#59581,#59582,#59583,#59584,#59585,
#59586,#59587,#59588,#59589,#59590,#59591,#59592,#59593,#59594,#59595,#59596,
#59597,#59598,#59599,#59600,#59601,#59602,#59603,#59604,#59605,#59606,#59607,
#59608,#59609,#59610,#59611,#59612,#59613,#59614,#59615,#59616,#59617,#59618,
#59619,#59620,#59621,#59622,#59623,#59624,#59625,#59626,#59627,#59628,#59629,
#59630,#59631,#59632,#59633,#59634,#59635,#59636,#59637,#59638,#59639,#59640,
#59641,#59642,#59643,#59644,#59645,#59646,#59647,#59648,#59649,#59650,#59651,
#59652,#59653,#59654,#59655,#59656,#59657,#59658,#59659,#59660,#59661,#59662,
#59663,#59664,#59665,#59666,#59667,#59668,#59669,#59670,#59671,#59672,#59673,
#59674,#59675,#59676,#59677,#59678,#59679,#59680,#59681,#59682,#59683,#59684,
#59685,#59686,#59687,#59688,#59689,#59690,#59691,#59692,#59693,#59694,#59695,
#59696,#59697,#59698,#59699,#59700,#59701,#59702,#59703,#59704,#59705,#59706,
#59707,#59708,#59709,#59710,#59711,#59712,#59713,#59714,#59715,#59716,#59717,
#59718,#59719,#59720,#59721,#59722,#59723),.UNSPECIFIED.,.F.,.F.,(4,3,3,
3,3,3,3,3,3,3,3,3,3,3,3,3,3,3,3,3,3,3,3,3,3,3,3,3,3,3,3,3,3,3,3,3,3,3,3,
3,3,3,3,3,3,3,3,3,3,3,3,3,3,3,3,3,3,3,3,3,3,3,3,3,3,3,3,3,3,3,3,3,3,4),
(587.477826221271,587.562199079223,587.645452312285,587.728706820588,587.811980792074,
587.897187865277,587.98060108407,588.066705084478,588.152809084887,588.236547796733,
588.320183308101,588.403735751499,588.48722518735,588.570679137964,588.65411563181,
588.737552741565,588.821008536483,588.904553029213,588.988142112154,589.071865379711,
589.152545095607,589.236283807453,589.319919318821,589.40347176222,589.486961198071,
589.570415148684,589.653851642531,589.737288752287,589.820744547204,589.904289039934,
589.987878122875,590.071601390433,590.152281106328,590.236019818174,590.319655329541,
590.40320777294,590.486697208792,590.570151159405,590.653587653252,590.737024763007,
590.820480557925,590.904025050655,590.987614133596,591.071337401153,591.152017117048,
591.235755828894,591.319391340261,591.40294378366,591.48643321951,591.569887170124,
591.65332366397,591.736760773726,591.820216568643,591.903761061373,591.987350144314,
592.071073411871,592.151753127768,592.235491839614,592.319127350981,592.40267979438,
592.486169230231,592.569623180845,592.653059674691,592.736496784446,592.819952579364,
592.903497072094,592.987086155035,593.070809422592,593.151489138488,593.236274655599,
593.320912891502,593.405465494156,593.489932211694,593.510351022852),
 .UNSPECIFIED.);
#424=B_SPLINE_CURVE_WITH_KNOTS('',3,(#59724,#59725,#59726,#59727,#59728,
#59729,#59730,#59731,#59732,#59733),.UNSPECIFIED.,.F.,.F.,(4,3,3,4),(587.227179640329,
587.32609710812,587.424072733153,587.477826221091),.UNSPECIFIED.);
#425=B_SPLINE_CURVE_WITH_KNOTS('',3,(#59735,#59736,#59737,#59738,#59739,
#59740,#59741,#59742,#59743,#59744,#59745,#59746,#59747),.UNSPECIFIED.,
 .F.,.F.,(4,3,3,3,4),(587.226166904384,587.309762933416,587.393489989296,
587.463363693883,587.477826221275),.UNSPECIFIED.);
#426=B_SPLINE_CURVE_WITH_KNOTS('',3,(#59748,#59749,#59750,#59751,#59752,
#59753,#59754,#59755,#59756,#59757,#59758,#59759,#59760,#59761,#59762,#59763,
#59764,#59765,#59766,#59767,#59768,#59769,#59770,#59771,#59772,#59773,#59774,
#59775,#59776,#59777,#59778,#59779,#59780,#59781,#59782,#59783,#59784,#59785,
#59786,#59787,#59788,#59789,#59790,#59791,#59792,#59793,#59794,#59795,#59796,
#59797,#59798,#59799,#59800,#59801,#59802,#59803,#59804,#59805,#59806,#59807,
#59808,#59809,#59810,#59811,#59812,#59813,#59814,#59815,#59816,#59817,#59818,
#59819,#59820,#59821,#59822,#59823,#59824,#59825,#59826,#59827,#59828,#59829,
#59830,#59831,#59832,#59833,#59834,#59835,#59836,#59837,#59838,#59839,#59840,
#59841,#59842,#59843,#59844,#59845,#59846,#59847,#59848,#59849,#59850,#59851,
#59852,#59853,#59854,#59855,#59856,#59857,#59858,#59859,#59860,#59861,#59862,
#59863,#59864,#59865,#59866,#59867,#59868,#59869,#59870,#59871,#59872,#59873,
#59874,#59875,#59876,#59877,#59878,#59879,#59880,#59881,#59882,#59883,#59884,
#59885,#59886,#59887,#59888,#59889,#59890,#59891,#59892,#59893,#59894,#59895,
#59896,#59897,#59898,#59899,#59900,#59901,#59902,#59903,#59904,#59905,#59906,
#59907,#59908,#59909,#59910,#59911,#59912,#59913,#59914,#59915,#59916,#59917,
#59918,#59919,#59920,#59921,#59922,#59923,#59924,#59925,#59926,#59927,#59928,
#59929,#59930,#59931,#59932,#59933,#59934,#59935,#59936,#59937,#59938,#59939,
#59940,#59941,#59942,#59943,#59944,#59945,#59946,#59947,#59948,#59949,#59950,
#59951,#59952,#59953,#59954,#59955,#59956,#59957,#59958,#59959,#59960,#59961,
#59962,#59963,#59964,#59965,#59966,#59967),.UNSPECIFIED.,.F.,.F.,(4,3,3,
3,3,3,3,3,3,3,3,3,3,3,3,3,3,3,3,3,3,3,3,3,3,3,3,3,3,3,3,3,3,3,3,3,3,3,3,
3,3,3,3,3,3,3,3,3,3,3,3,3,3,3,3,3,3,3,3,3,3,3,3,3,3,3,3,3,3,3,3,3,3,4),
(587.477826221412,587.56135346668,587.644777878487,587.728119809374,587.81139953815,
587.894645039578,587.977874217614,588.061105341191,588.14435667684,588.227696868397,
588.311083396933,588.394600209494,588.463099704603,588.546838416449,588.630473927817,
588.714026371216,588.797515807067,588.880969757681,588.964406251527,589.047843361283,
589.131299156201,589.214843648931,589.298432731872,589.38215599943,589.462835715324,
589.54657442717,589.630209938538,589.713762381936,589.797251817787,589.880705768401,
589.964142262248,590.047579372003,590.131035166921,590.214579659651,590.298168742592,
590.38189201015,590.462571726044,590.54631043789,590.629945949257,590.713498392655,
590.796987828507,590.88044177912,590.963878272966,591.047315382721,591.130771177639,
591.214315670369,591.297904753309,591.381628020867,591.462307736764,591.54604644861,
591.629681959978,591.713234403376,591.796723839227,591.880177789841,591.963614283687,
592.047051393443,592.130507188361,592.21405168109,592.297640764032,592.381364031589,
592.462043747484,592.54578245933,592.629417970697,592.712970414096,592.796459849947,
592.879913800561,592.963350294408,593.046787404163,593.130243199081,593.21378769181,
593.297376774751,593.381100042309,593.461779758204,593.510232699841),
 .UNSPECIFIED.);
#427=B_SPLINE_CURVE_WITH_KNOTS('',3,(#59973,#59974,#59975,#59976,#59977,
#59978,#59979,#59980,#59981,#59982,#59983,#59984,#59985,#59986,#59987,#59988,
#59989,#59990,#59991,#59992,#59993,#59994,#59995,#59996,#59997,#59998,#59999,
#60000,#60001,#60002,#60003,#60004,#60005,#60006,#60007,#60008,#60009,#60010,
#60011,#60012,#60013,#60014,#60015,#60016,#60017,#60018,#60019,#60020,#60021,
#60022,#60023,#60024,#60025,#60026,#60027,#60028,#60029,#60030,#60031,#60032,
#60033,#60034,#60035,#60036,#60037,#60038,#60039,#60040,#60041,#60042,#60043,
#60044,#60045,#60046,#60047,#60048,#60049,#60050,#60051,#60052,#60053,#60054,
#60055,#60056,#60057,#60058,#60059,#60060,#60061,#60062,#60063,#60064,#60065,
#60066,#60067,#60068,#60069,#60070,#60071,#60072,#60073,#60074,#60075,#60076,
#60077,#60078,#60079,#60080,#60081,#60082,#60083,#60084,#60085,#60086,#60087,
#60088,#60089,#60090,#60091,#60092,#60093,#60094,#60095,#60096,#60097,#60098,
#60099,#60100,#60101,#60102,#60103,#60104,#60105,#60106,#60107,#60108,#60109,
#60110,#60111,#60112,#60113,#60114,#60115,#60116,#60117,#60118,#60119,#60120,
#60121,#60122,#60123,#60124,#60125,#60126,#60127,#60128,#60129,#60130,#60131,
#60132,#60133,#60134,#60135,#60136,#60137,#60138,#60139,#60140,#60141,#60142,
#60143,#60144,#60145,#60146,#60147,#60148,#60149,#60150,#60151,#60152,#60153,
#60154,#60155,#60156,#60157,#60158,#60159,#60160,#60161,#60162,#60163,#60164,
#60165,#60166,#60167,#60168,#60169,#60170,#60171,#60172,#60173,#60174,#60175,
#60176,#60177,#60178,#60179,#60180,#60181,#60182,#60183,#60184,#60185,#60186,
#60187,#60188,#60189,#60190,#60191,#60192),.UNSPECIFIED.,.F.,.F.,(4,3,3,
3,3,3,3,3,3,3,3,3,3,3,3,3,3,3,3,3,3,3,3,3,3,3,3,3,3,3,3,3,3,3,3,3,3,3,3,
3,3,3,3,3,3,3,3,3,3,3,3,3,3,3,3,3,3,3,3,3,3,3,3,3,3,3,3,3,3,3,3,3,3,4),
(593.761011528636,593.858564933779,593.951805410787,594.045325295478,594.139187343676,
594.151225149208,594.234963861054,594.318599372422,594.40215181582,594.485641251671,
594.569095202285,594.652531696131,594.735968805886,594.819424600804,594.902969093533,
594.986558176474,595.070281444032,595.150961159928,595.234699871774,595.318335383141,
595.40188782654,595.485377262391,595.568831213004,595.65226770685,595.735704816606,
595.819160611524,595.902705104253,595.986294187194,596.070017454752,596.150697170648,
596.234435882494,596.318071393861,596.40162383726,596.485113273111,596.568567223725,
596.652003717571,596.735440827327,596.818896622245,596.902441114974,596.986030197915,
597.069753465473,597.150433181368,597.234171893214,597.317807404581,597.40135984798,
597.484849283831,597.568303234445,597.651739728291,597.735176838047,597.818632632964,
597.902177125694,597.985766208635,598.069489476193,598.150169192089,598.233907903935,
598.317543415303,598.401095858701,598.484585294552,598.568039245166,598.651475739012,
598.734912848768,598.818368643686,598.901913136415,598.985502219356,599.069225486914,
599.149905202809,599.232544928932,599.315090063073,599.397559707556,599.479972895729,
599.562358158123,599.644725126391,599.727119391754,599.792366874018),
 .UNSPECIFIED.);
#428=B_SPLINE_CURVE_WITH_KNOTS('',3,(#60193,#60194,#60195,#60196,#60197,
#60198,#60199,#60200,#60201,#60202),.UNSPECIFIED.,.F.,.F.,(4,3,3,4),(593.510351022852,
593.594743727506,593.679109853501,593.76101152845),.UNSPECIFIED.);
#429=B_SPLINE_CURVE_WITH_KNOTS('',3,(#60204,#60205,#60206,#60207,#60208,
#60209,#60210,#60211,#60212,#60213),.UNSPECIFIED.,.F.,.F.,(4,3,3,4),(593.510232699841,
593.612124172686,593.712757557617,593.761011528308),.UNSPECIFIED.);
#430=B_SPLINE_CURVE_WITH_KNOTS('',3,(#60214,#60215,#60216,#60217,#60218,
#60219,#60220,#60221,#60222,#60223,#60224,#60225,#60226,#60227,#60228,#60229,
#60230,#60231,#60232,#60233,#60234,#60235,#60236,#60237,#60238,#60239,#60240,
#60241,#60242,#60243,#60244,#60245,#60246,#60247,#60248,#60249,#60250,#60251,
#60252,#60253,#60254,#60255,#60256,#60257,#60258,#60259,#60260,#60261,#60262,
#60263,#60264,#60265,#60266,#60267,#60268,#60269,#60270,#60271,#60272,#60273,
#60274,#60275,#60276,#60277,#60278,#60279,#60280,#60281,#60282,#60283,#60284,
#60285,#60286,#60287,#60288,#60289,#60290,#60291,#60292,#60293,#60294,#60295,
#60296,#60297,#60298,#60299,#60300,#60301,#60302,#60303,#60304,#60305,#60306,
#60307,#60308,#60309,#60310,#60311,#60312,#60313,#60314,#60315,#60316,#60317,
#60318,#60319,#60320,#60321,#60322,#60323,#60324,#60325,#60326,#60327,#60328,
#60329,#60330,#60331,#60332,#60333,#60334,#60335,#60336,#60337,#60338,#60339,
#60340,#60341,#60342,#60343,#60344,#60345,#60346,#60347,#60348,#60349,#60350,
#60351,#60352,#60353,#60354,#60355,#60356,#60357,#60358,#60359,#60360,#60361,
#60362,#60363,#60364,#60365,#60366,#60367,#60368,#60369,#60370,#60371,#60372,
#60373,#60374,#60375,#60376,#60377,#60378,#60379,#60380,#60381,#60382,#60383,
#60384,#60385,#60386,#60387,#60388,#60389,#60390,#60391,#60392,#60393,#60394,
#60395,#60396,#60397,#60398,#60399,#60400,#60401,#60402,#60403,#60404,#60405,
#60406,#60407,#60408,#60409,#60410,#60411,#60412,#60413,#60414,#60415,#60416,
#60417,#60418,#60419,#60420,#60421,#60422,#60423,#60424,#60425,#60426,#60427,
#60428,#60429,#60430,#60431,#60432,#60433),.UNSPECIFIED.,.F.,.F.,(4,3,3,
3,3,3,3,3,3,3,3,3,3,3,3,3,3,3,3,3,3,3,3,3,3,3,3,3,3,3,3,3,3,3,3,3,3,3,3,
3,3,3,3,3,3,3,3,3,3,3,3,3,3,3,3,3,3,3,3,3,3,3,3,3,3,3,3,3,3,3,3,3,3,4),
(593.761011528454,593.843975061803,593.926914752704,594.009845422425,594.09278556456,
594.175753675864,594.258815591675,594.341931170951,594.425170135204,594.461515768924,
594.54525448077,594.628889992137,594.712442435536,594.795931871387,594.879385822,
594.962822315846,595.046259425602,595.129715220519,595.213259713249,595.29684879619,
595.380572063748,595.461251779644,595.54499049149,595.628626002857,595.712178446256,
595.795667882107,595.879121832721,595.962558326567,596.045995436323,596.129451231241,
596.21299572397,596.296584806911,596.380308074469,596.460987790364,596.54472650221,
596.628362013578,596.711914456976,596.795403892827,596.878857843441,596.962294337287,
597.045731447042,597.12918724196,597.21273173469,597.296320817631,597.380044085189,
597.460723801085,597.544462512931,597.628098024298,597.711650467697,597.795139903548,
597.878593854162,597.962030348008,598.045467457764,598.128923252681,598.212467745411,
598.296056828352,598.37978009591,598.460459811805,598.544198523651,598.627834035018,
598.711386478417,598.794875914268,598.878329864882,598.961766358728,599.045203468484,
599.128659263401,599.212203756131,599.295792839072,599.379516106629,599.460195822525,
599.545543916236,599.630786228184,599.715907753929,599.793641905039),
 .UNSPECIFIED.);
#431=B_SPLINE_CURVE_WITH_KNOTS('',3,(#60439,#60440,#60441,#60442,#60443,
#60444,#60445,#60446,#60447,#60448,#60449,#60450,#60451,#60452,#60453,#60454,
#60455,#60456,#60457,#60458,#60459,#60460,#60461,#60462,#60463,#60464,#60465,
#60466,#60467,#60468,#60469,#60470,#60471,#60472,#60473,#60474,#60475,#60476,
#60477,#60478,#60479,#60480,#60481,#60482,#60483,#60484,#60485,#60486,#60487,
#60488,#60489,#60490,#60491,#60492,#60493,#60494,#60495,#60496,#60497,#60498,
#60499,#60500,#60501,#60502,#60503,#60504,#60505,#60506,#60507,#60508,#60509,
#60510,#60511,#60512,#60513,#60514,#60515,#60516,#60517,#60518,#60519,#60520,
#60521,#60522,#60523,#60524,#60525,#60526,#60527,#60528,#60529,#60530,#60531,
#60532,#60533,#60534,#60535,#60536,#60537,#60538,#60539,#60540,#60541,#60542,
#60543,#60544,#60545,#60546,#60547,#60548,#60549,#60550,#60551,#60552,#60553,
#60554,#60555,#60556,#60557,#60558,#60559,#60560,#60561,#60562,#60563,#60564,
#60565,#60566,#60567,#60568,#60569,#60570,#60571,#60572,#60573,#60574,#60575,
#60576,#60577,#60578,#60579,#60580,#60581,#60582,#60583,#60584,#60585,#60586,
#60587,#60588,#60589,#60590,#60591,#60592,#60593,#60594,#60595,#60596,#60597,
#60598,#60599,#60600,#60601,#60602,#60603,#60604,#60605,#60606,#60607,#60608,
#60609,#60610,#60611,#60612,#60613,#60614,#60615,#60616,#60617,#60618,#60619,
#60620,#60621,#60622,#60623,#60624,#60625,#60626,#60627,#60628,#60629,#60630,
#60631,#60632,#60633,#60634,#60635,#60636,#60637,#60638,#60639,#60640,#60641,
#60642,#60643,#60644,#60645,#60646,#60647,#60648,#60649,#60650,#60651,#60652,
#60653,#60654,#60655),.UNSPECIFIED.,.F.,.F.,(4,3,3,3,3,3,3,3,3,3,3,3,3,
3,3,3,3,3,3,3,3,3,3,3,3,3,3,3,3,3,3,3,3,3,3,3,3,3,3,3,3,3,3,3,3,3,3,3,3,
3,3,3,3,3,3,3,3,3,3,3,3,3,3,3,3,3,3,3,3,3,3,3,4),(600.04419683563,600.149641213529,
600.233379925375,600.317015436743,600.400567880141,600.484057315992,600.567511266605,
600.650947760452,600.734384870207,600.817840665125,600.901385157854,600.984974240795,
601.068697508353,601.149377224249,601.233115936095,601.316751447462,601.400303890861,
601.483793326712,601.567247277326,601.650683771172,601.734120880928,601.817576675845,
601.901121168575,601.984710251516,602.068433519073,602.149113234969,602.232851946815,
602.316487458182,602.400039901581,602.483529337432,602.566983288045,602.650419781892,
602.733856891647,602.817312686564,602.900857179294,602.984446262235,603.068169529793,
603.148849245689,603.232587957535,603.316223468903,603.399775912301,603.483265348152,
603.566719298766,603.650155792612,603.733592902368,603.817048697286,603.900593190015,
603.984182272956,604.067905540514,604.148585256409,604.232323968255,604.315959479622,
604.399511923021,604.483001358872,604.566455309486,604.649891803332,604.733328913088,
604.816784708005,604.900329200735,604.983918283676,605.067641551234,605.14832126713,
605.232064132401,605.315702846202,605.399257545084,605.483845242438,605.567295515047,
605.650727224079,605.734158441295,605.81960861195,605.903129443405,605.98954428366,
606.075959123915),.UNSPECIFIED.);
#432=B_SPLINE_CURVE_WITH_KNOTS('',3,(#60656,#60657,#60658,#60659,#60660,
#60661,#60662,#60663,#60664,#60665),.UNSPECIFIED.,.F.,.F.,(4,3,3,4),(599.792366874018,
599.874835106843,599.959515971168,600.044196835494),.UNSPECIFIED.);
#433=B_SPLINE_CURVE_WITH_KNOTS('',3,(#60667,#60668,#60669,#60670,#60671,
#60672,#60673,#60674,#60675,#60676),.UNSPECIFIED.,.F.,.F.,(4,3,3,4),(599.793641905039,
599.878621649841,599.963550940226,600.044196835634),.UNSPECIFIED.);
#434=B_SPLINE_CURVE_WITH_KNOTS('',3,(#60677,#60678,#60679,#60680,#60681,
#60682,#60683,#60684,#60685,#60686,#60687,#60688,#60689,#60690,#60691,#60692,
#60693,#60694,#60695,#60696,#60697,#60698,#60699,#60700,#60701,#60702,#60703,
#60704,#60705,#60706,#60707,#60708,#60709,#60710,#60711,#60712,#60713,#60714,
#60715,#60716,#60717,#60718,#60719,#60720,#60721,#60722,#60723,#60724,#60725,
#60726,#60727,#60728,#60729,#60730,#60731,#60732,#60733,#60734,#60735,#60736,
#60737,#60738,#60739,#60740,#60741,#60742,#60743,#60744,#60745,#60746,#60747,
#60748,#60749,#60750,#60751,#60752,#60753,#60754,#60755,#60756,#60757,#60758,
#60759,#60760,#60761,#60762,#60763,#60764,#60765,#60766,#60767,#60768,#60769,
#60770,#60771,#60772,#60773,#60774,#60775,#60776,#60777,#60778,#60779,#60780,
#60781,#60782,#60783,#60784,#60785,#60786,#60787,#60788,#60789,#60790,#60791,
#60792,#60793,#60794,#60795,#60796,#60797,#60798,#60799,#60800,#60801,#60802,
#60803,#60804,#60805,#60806,#60807,#60808,#60809,#60810,#60811,#60812,#60813,
#60814,#60815,#60816,#60817,#60818,#60819,#60820,#60821,#60822,#60823,#60824,
#60825,#60826,#60827,#60828,#60829,#60830,#60831,#60832,#60833,#60834,#60835,
#60836,#60837,#60838,#60839,#60840,#60841,#60842,#60843,#60844,#60845,#60846,
#60847,#60848,#60849,#60850,#60851,#60852,#60853,#60854,#60855,#60856,#60857,
#60858,#60859,#60860,#60861,#60862,#60863,#60864,#60865,#60866,#60867,#60868,
#60869,#60870,#60871,#60872,#60873,#60874,#60875,#60876,#60877,#60878,#60879,
#60880,#60881,#60882,#60883,#60884,#60885,#60886,#60887,#60888,#60889,#60890,
#60891,#60892,#60893,#60894,#60895,#60896),.UNSPECIFIED.,.F.,.F.,(4,3,3,
3,3,3,3,3,3,3,3,3,3,3,3,3,3,3,3,3,3,3,3,3,3,3,3,3,3,3,3,3,3,3,3,3,3,3,3,
3,3,3,3,3,3,3,3,3,3,3,3,3,3,3,3,3,3,3,3,3,3,3,3,3,3,3,3,3,3,3,3,3,3,4),
(600.044196835797,600.135380747604,600.226996847853,600.31883428202,600.410988212238,
600.459931833245,600.543670545091,600.627306056459,600.710858499857,600.794347935708,
600.877801886322,600.961238380168,601.044675489923,601.128131284841,601.211675777571,
601.295264860512,601.378988128069,601.459667843965,601.543406555811,601.627042067178,
601.710594510577,601.794083946428,601.877537897041,601.960974390888,602.044411500643,
602.127867295561,602.21141178829,602.295000871231,602.378724138789,602.459403854685,
602.543142566531,602.626778077898,602.710330521297,602.793819957148,602.877273907761,
602.960710401608,603.044147511363,603.127603306281,603.211147799011,603.294736881952,
603.378460149509,603.459139865405,603.542878577251,603.626514088618,603.710066532017,
603.793555967868,603.877009918482,603.960446412328,604.043883522084,604.127339317002,
604.210883809731,604.294472892672,604.37819616023,604.458875876125,604.542614587971,
604.626250099339,604.709802542737,604.793291978588,604.876745929202,604.960182423048,
605.043619532804,605.127075327721,605.210619820451,605.294208903392,605.37793217095,
605.458611886846,605.54114153622,605.623576417017,605.705935706753,605.788238511302,
605.870511003234,605.952765504759,606.03503976382,606.075586485893),
 .UNSPECIFIED.);
#435=B_SPLINE_CURVE_WITH_KNOTS('',3,(#60902,#60903,#60904,#60905,#60906,
#60907,#60908,#60909,#60910,#60911,#60912,#60913,#60914,#60915,#60916,#60917,
#60918,#60919,#60920,#60921,#60922,#60923,#60924,#60925,#60926,#60927,#60928,
#60929,#60930,#60931,#60932,#60933,#60934,#60935,#60936,#60937,#60938,#60939,
#60940,#60941,#60942,#60943,#60944,#60945,#60946,#60947,#60948,#60949,#60950,
#60951,#60952,#60953,#60954,#60955,#60956,#60957,#60958,#60959,#60960,#60961,
#60962,#60963,#60964,#60965,#60966,#60967,#60968,#60969,#60970,#60971,#60972,
#60973,#60974,#60975,#60976,#60977,#60978,#60979,#60980,#60981,#60982,#60983,
#60984,#60985,#60986,#60987,#60988,#60989,#60990,#60991,#60992,#60993,#60994,
#60995,#60996,#60997,#60998,#60999,#61000,#61001,#61002,#61003,#61004,#61005,
#61006,#61007,#61008,#61009,#61010,#61011,#61012,#61013,#61014,#61015,#61016,
#61017,#61018,#61019,#61020,#61021,#61022,#61023,#61024,#61025,#61026,#61027,
#61028,#61029,#61030,#61031,#61032,#61033,#61034,#61035,#61036,#61037,#61038,
#61039,#61040,#61041,#61042,#61043,#61044,#61045,#61046,#61047,#61048,#61049,
#61050,#61051,#61052,#61053,#61054,#61055,#61056,#61057,#61058,#61059,#61060,
#61061,#61062,#61063,#61064,#61065,#61066,#61067,#61068,#61069,#61070,#61071,
#61072,#61073,#61074,#61075,#61076,#61077,#61078,#61079,#61080,#61081,#61082,
#61083,#61084,#61085,#61086,#61087,#61088,#61089,#61090,#61091,#61092,#61093,
#61094,#61095,#61096,#61097,#61098,#61099,#61100,#61101,#61102,#61103,#61104,
#61105,#61106,#61107,#61108,#61109,#61110,#61111,#61112,#61113,#61114,#61115,
#61116,#61117,#61118,#61119,#61120,#61121),.UNSPECIFIED.,.F.,.F.,(4,3,3,
3,3,3,3,3,3,3,3,3,3,3,3,3,3,3,3,3,3,3,3,3,3,3,3,3,3,3,3,3,3,3,3,3,3,3,3,
3,3,3,3,3,3,3,3,3,3,3,3,3,3,3,3,3,3,3,3,3,3,3,3,3,3,3,3,3,3,3,3,3,3,4),
(606.327382142967,606.409745330699,606.49203379855,606.574272133103,606.65648437151,
606.738689552527,606.820906706931,606.903205201195,606.985544079707,607.068013508093,
607.14779328857,607.231532000416,607.315167511784,607.398719955182,607.482209391033,
607.565663341647,607.649099835493,607.732536945249,607.815992740166,607.899537232896,
607.983126315837,608.066849583395,608.14752929929,608.231268011136,608.314903522503,
608.398455965902,608.481945401753,608.565399352367,608.648835846213,608.732272955968,
608.815728750886,608.899273243616,608.982862326557,609.066585594114,609.14726531001,
609.231004021856,609.314639533223,609.398191976622,609.481681412473,609.565135363087,
609.648571856933,609.732008966689,609.815464761606,609.899009254336,609.982598337277,
610.066321604835,610.14700132073,610.230740032576,610.314375543943,610.397927987342,
610.481417423193,610.564871373807,610.648307867653,610.731744977409,610.815200772326,
610.898745265056,610.982334347997,611.066057615554,611.14673733145,611.230476043296,
611.314111554663,611.397663998062,611.481153433913,611.564607384527,611.648043878373,
611.731480988128,611.814936783046,611.898481275776,611.982070358717,612.065793626274,
612.14647334217,612.236085107274,612.325478113949,612.360266019021),
 .UNSPECIFIED.);
#436=B_SPLINE_CURVE_WITH_KNOTS('',3,(#61122,#61123,#61124,#61125,#61126,
#61127,#61128,#61129,#61130,#61131),.UNSPECIFIED.,.F.,.F.,(4,3,3,4),(606.075959123915,
606.14805727785,606.275526789432,606.327382142809),.UNSPECIFIED.);
#437=B_SPLINE_CURVE_WITH_KNOTS('',3,(#61133,#61134,#61135,#61136,#61137,
#61138,#61139,#61140,#61141,#61142),.UNSPECIFIED.,.F.,.F.,(4,3,3,4),(606.075586485893,
606.157928330959,606.242655236822,606.327382142685),.UNSPECIFIED.);
#438=B_SPLINE_CURVE_WITH_KNOTS('',3,(#61143,#61144,#61145,#61146,#61147,
#61148,#61149,#61150,#61151,#61152,#61153,#61154,#61155,#61156,#61157,#61158,
#61159,#61160,#61161,#61162,#61163,#61164,#61165,#61166,#61167,#61168,#61169,
#61170,#61171,#61172,#61173,#61174,#61175,#61176,#61177,#61178,#61179,#61180,
#61181,#61182,#61183,#61184,#61185,#61186,#61187,#61188,#61189,#61190,#61191,
#61192,#61193,#61194,#61195,#61196,#61197,#61198,#61199,#61200,#61201,#61202,
#61203,#61204,#61205,#61206,#61207,#61208,#61209,#61210,#61211,#61212,#61213,
#61214,#61215,#61216,#61217,#61218,#61219,#61220,#61221,#61222,#61223,#61224,
#61225,#61226,#61227,#61228,#61229,#61230,#61231,#61232,#61233,#61234,#61235,
#61236,#61237,#61238,#61239,#61240,#61241,#61242,#61243,#61244,#61245,#61246,
#61247,#61248,#61249,#61250,#61251,#61252,#61253,#61254,#61255,#61256,#61257,
#61258,#61259,#61260,#61261,#61262,#61263,#61264,#61265,#61266,#61267,#61268,
#61269,#61270,#61271,#61272,#61273,#61274,#61275,#61276,#61277,#61278,#61279,
#61280,#61281,#61282,#61283,#61284,#61285,#61286,#61287,#61288,#61289,#61290,
#61291,#61292,#61293,#61294,#61295,#61296,#61297,#61298,#61299,#61300,#61301,
#61302,#61303,#61304,#61305,#61306,#61307,#61308,#61309,#61310,#61311,#61312,
#61313,#61314,#61315,#61316,#61317,#61318,#61319,#61320,#61321,#61322,#61323,
#61324,#61325,#61326,#61327,#61328,#61329,#61330,#61331,#61332,#61333,#61334,
#61335,#61336,#61337,#61338,#61339,#61340,#61341,#61342,#61343,#61344,#61345,
#61346,#61347,#61348,#61349,#61350,#61351,#61352,#61353,#61354,#61355,#61356,
#61357,#61358,#61359),.UNSPECIFIED.,.F.,.F.,(4,3,3,3,3,3,3,3,3,3,3,3,3,
3,3,3,3,3,3,3,3,3,3,3,3,3,3,3,3,3,3,3,3,3,3,3,3,3,3,3,3,3,3,3,3,3,3,3,3,
3,3,3,3,3,3,3,3,3,3,3,3,3,3,3,3,3,3,3,3,3,3,3,4),(606.327382142813,606.458347897566,
606.542086609412,606.62572212078,606.709274564178,606.792764000029,606.876217950643,
606.959654444489,607.043091554244,607.126547349162,607.210091841892,607.293680924833,
607.37740419239,607.458083908286,607.541822620132,607.625458131499,607.709010574898,
607.792500010749,607.875953961362,607.959390455209,608.042827564964,608.126283359882,
608.209827852611,608.293416935552,608.37714020311,608.457819919006,608.541558630852,
608.62519414222,608.708746585618,608.792236021469,608.875689972083,608.959126465929,
609.042563575685,609.126019370602,609.209563863332,609.293152946273,609.376876213831,
609.457555929726,609.541294641572,609.624930152939,609.708482596338,609.791972032189,
609.875425982802,609.958862476649,610.042299586404,610.125755381321,610.209299874051,
610.292888956992,610.376612224549,610.457291940446,610.541030652292,610.62466616366,
610.708218607058,610.791708042909,610.875161993523,610.958598487369,611.042035597125,
611.125491392042,611.209035884772,611.292624967713,611.376348235271,611.457027951166,
611.540772347434,611.624412254421,611.707967810137,611.791454863418,611.874904548639,
611.958334954268,612.041764152013,612.125248052861,612.208759568125,612.292369613153,
612.359058987781),.UNSPECIFIED.);
#439=B_SPLINE_CURVE_WITH_KNOTS('',3,(#61365,#61366,#61367,#61368,#61369,
#61370,#61371,#61372,#61373,#61374,#61375,#61376,#61377,#61378,#61379,#61380,
#61381,#61382,#61383,#61384,#61385,#61386,#61387,#61388,#61389,#61390,#61391,
#61392,#61393,#61394,#61395,#61396,#61397,#61398,#61399,#61400,#61401,#61402,
#61403,#61404,#61405,#61406,#61407,#61408,#61409,#61410,#61411,#61412,#61413,
#61414,#61415,#61416,#61417,#61418,#61419,#61420,#61421,#61422,#61423,#61424,
#61425,#61426,#61427,#61428,#61429,#61430,#61431,#61432,#61433,#61434,#61435,
#61436,#61437,#61438,#61439,#61440,#61441,#61442,#61443,#61444,#61445,#61446,
#61447,#61448,#61449,#61450,#61451,#61452,#61453,#61454,#61455,#61456,#61457,
#61458,#61459,#61460,#61461,#61462,#61463,#61464,#61465,#61466,#61467,#61468,
#61469,#61470,#61471,#61472,#61473,#61474,#61475,#61476,#61477,#61478,#61479,
#61480,#61481,#61482,#61483,#61484,#61485,#61486,#61487,#61488,#61489,#61490,
#61491,#61492,#61493,#61494,#61495,#61496,#61497,#61498,#61499,#61500,#61501,
#61502,#61503,#61504,#61505,#61506,#61507,#61508,#61509,#61510,#61511,#61512,
#61513,#61514,#61515,#61516,#61517,#61518,#61519,#61520,#61521,#61522,#61523,
#61524,#61525,#61526,#61527,#61528,#61529,#61530,#61531,#61532,#61533,#61534,
#61535,#61536,#61537,#61538,#61539,#61540,#61541,#61542,#61543,#61544,#61545,
#61546,#61547,#61548,#61549,#61550,#61551,#61552,#61553,#61554,#61555,#61556,
#61557,#61558,#61559,#61560,#61561,#61562,#61563,#61564,#61565,#61566,#61567,
#61568,#61569,#61570,#61571,#61572,#61573,#61574,#61575,#61576,#61577,#61578,
#61579,#61580,#61581,#61582,#61583,#61584),.UNSPECIFIED.,.F.,.F.,(4,3,3,
3,3,3,3,3,3,3,3,3,3,3,3,3,3,3,3,3,3,3,3,3,3,3,3,3,3,3,3,3,3,3,3,3,3,3,3,
3,3,3,3,3,3,3,3,3,3,3,3,3,3,3,3,3,3,3,3,3,3,3,3,3,3,3,3,3,3,3,3,3,3,4),
(612.610567449989,612.696783698912,612.783073618945,612.873857552431,612.960398441322,
613.047032929598,613.133823015052,613.146209352891,613.229948064737,613.313583576104,
613.397136019502,613.480625455353,613.564079405967,613.647515899813,613.730953009568,
613.814408804486,613.897953297216,613.981542380156,614.065265647714,614.145945363611,
614.229684075457,614.313319586824,614.396872030223,614.480361466074,614.563815416687,
614.647251910534,614.730689020289,614.814144815207,614.897689307937,614.981278390877,
615.065001658435,615.145681374331,615.229420086177,615.313055597545,615.396608040944,
615.480097476794,615.563551427408,615.646987921254,615.73042503101,615.813880825928,
615.897425318657,615.981014401598,616.064737669156,616.145417385051,616.229156096897,
616.312791608264,616.396344051663,616.479833487514,616.563287438128,616.646723931974,
616.730161041729,616.813616836646,616.897161329376,616.980750412317,617.064473679875,
617.145153395771,617.228892107617,617.312527618985,617.396080062383,617.479569498234,
617.563023448848,617.646459942694,617.729897052449,617.813352847367,617.896897340096,
617.980486423037,618.064209690595,618.144889406491,618.227663227904,618.310338741592,
618.393352536083,618.475881927484,618.559137923519,618.642393919554),
 .UNSPECIFIED.);
#440=B_SPLINE_CURVE_WITH_KNOTS('',3,(#61585,#61586,#61587,#61588,#61589,
#61590,#61591,#61592,#61593,#61594),.UNSPECIFIED.,.F.,.F.,(4,3,3,4),(612.360266019021,
612.449379317751,612.538258334461,612.610567449828),.UNSPECIFIED.);
#441=B_SPLINE_CURVE_WITH_KNOTS('',3,(#61596,#61597,#61598,#61599,#61600,
#61601,#61602,#61603,#61604,#61605,#61606,#61607,#61608),.UNSPECIFIED.,
 .F.,.F.,(4,3,3,3,4),(612.359058987781,612.442810974301,612.456763961887,
612.596727833402,612.610567449993),.UNSPECIFIED.);
#442=B_SPLINE_CURVE_WITH_KNOTS('',3,(#61609,#61610,#61611,#61612,#61613,
#61614,#61615,#61616,#61617,#61618,#61619,#61620,#61621,#61622,#61623,#61624,
#61625,#61626,#61627,#61628,#61629,#61630,#61631,#61632,#61633,#61634,#61635,
#61636,#61637,#61638,#61639,#61640,#61641,#61642,#61643,#61644,#61645,#61646,
#61647,#61648,#61649,#61650,#61651,#61652,#61653,#61654,#61655,#61656,#61657,
#61658,#61659,#61660,#61661,#61662,#61663,#61664,#61665,#61666,#61667,#61668,
#61669,#61670,#61671,#61672,#61673,#61674,#61675,#61676,#61677,#61678,#61679,
#61680,#61681,#61682,#61683,#61684,#61685,#61686,#61687,#61688,#61689,#61690,
#61691,#61692,#61693,#61694,#61695,#61696,#61697,#61698,#61699,#61700,#61701,
#61702,#61703,#61704,#61705,#61706,#61707,#61708,#61709,#61710,#61711,#61712,
#61713,#61714,#61715,#61716,#61717,#61718,#61719,#61720,#61721,#61722,#61723,
#61724,#61725,#61726,#61727,#61728,#61729,#61730,#61731,#61732,#61733,#61734,
#61735,#61736,#61737,#61738,#61739,#61740,#61741,#61742,#61743,#61744,#61745,
#61746,#61747,#61748,#61749,#61750,#61751,#61752,#61753,#61754,#61755,#61756,
#61757,#61758,#61759,#61760,#61761,#61762,#61763,#61764,#61765,#61766,#61767,
#61768,#61769,#61770,#61771,#61772,#61773,#61774,#61775,#61776,#61777,#61778,
#61779,#61780,#61781,#61782,#61783,#61784,#61785,#61786,#61787,#61788,#61789,
#61790,#61791,#61792,#61793,#61794,#61795,#61796,#61797,#61798,#61799,#61800,
#61801,#61802,#61803,#61804,#61805,#61806,#61807,#61808,#61809,#61810,#61811,
#61812,#61813,#61814,#61815,#61816,#61817,#61818,#61819,#61820,#61821,#61822,
#61823,#61824,#61825,#61826,#61827,#61828),.UNSPECIFIED.,.F.,.F.,(4,3,3,
3,3,3,3,3,3,3,3,3,3,3,3,3,3,3,3,3,3,3,3,3,3,3,3,3,3,3,3,3,3,3,3,3,3,3,3,
3,3,3,3,3,3,3,3,3,3,3,3,3,3,3,3,3,3,3,3,3,3,3,3,3,3,3,3,3,3,3,3,3,3,4),
(612.610567450102,612.692962920578,612.775277177584,612.860430026961,612.942652576491,
613.024862892056,613.107080001966,613.189322938079,613.271654224329,613.354038348432,
613.436536843195,613.456499972607,613.540238684453,613.62387419582,613.707426639219,
613.79091607507,613.874370025683,613.95780651953,614.041243629285,614.124699424203,
614.208243916932,614.291832999873,614.375556267431,614.456235983327,614.539974695173,
614.623610206541,614.707162649939,614.79065208579,614.874106036404,614.95754253025,
615.040979640006,615.124435434923,615.207979927653,615.291569010594,615.375292278152,
615.455971994047,615.539710705893,615.62334621726,615.706898660659,615.79038809651,
615.873842047124,615.95727854097,616.040715650726,616.124171445643,616.207715938373,
616.291305021314,616.375028288872,616.455708004767,616.539446716613,616.62308222798,
616.706634671378,616.79012410723,616.873578057843,616.957014551689,617.040451661445,
617.123907456363,617.207451949092,617.291041032033,617.374764299591,617.455444015487,
617.539182727333,617.6228182387,617.706370682099,617.78986011795,617.873314068564,
617.95675056241,618.040187672165,618.123643467082,618.207187959812,618.290777042753,
618.37450031031,618.455180026207,618.549310717824,618.643441409442),
 .UNSPECIFIED.);
#443=B_SPLINE_CURVE_WITH_KNOTS('',3,(#61834,#61835,#61836,#61837,#61838,
#61839,#61840,#61841,#61842,#61843,#61844,#61845,#61846,#61847,#61848,#61849,
#61850,#61851,#61852,#61853,#61854,#61855,#61856,#61857,#61858,#61859,#61860,
#61861,#61862,#61863,#61864,#61865,#61866,#61867,#61868,#61869,#61870,#61871,
#61872,#61873,#61874,#61875,#61876,#61877,#61878,#61879,#61880,#61881,#61882,
#61883,#61884,#61885,#61886,#61887,#61888,#61889,#61890,#61891,#61892,#61893,
#61894,#61895,#61896,#61897,#61898,#61899,#61900,#61901,#61902,#61903,#61904,
#61905,#61906,#61907,#61908,#61909,#61910,#61911,#61912,#61913,#61914,#61915,
#61916,#61917,#61918,#61919,#61920,#61921,#61922,#61923,#61924,#61925,#61926,
#61927,#61928,#61929,#61930,#61931,#61932,#61933,#61934,#61935,#61936,#61937,
#61938,#61939,#61940,#61941,#61942,#61943,#61944,#61945,#61946,#61947,#61948,
#61949,#61950,#61951,#61952,#61953,#61954,#61955,#61956,#61957,#61958,#61959,
#61960,#61961,#61962,#61963,#61964,#61965,#61966,#61967,#61968,#61969,#61970,
#61971,#61972,#61973,#61974,#61975,#61976,#61977,#61978,#61979,#61980,#61981,
#61982,#61983,#61984,#61985,#61986,#61987,#61988,#61989,#61990,#61991,#61992,
#61993,#61994,#61995,#61996,#61997,#61998,#61999,#62000,#62001,#62002,#62003,
#62004,#62005,#62006,#62007,#62008,#62009,#62010,#62011,#62012,#62013,#62014,
#62015,#62016,#62017,#62018,#62019,#62020,#62021,#62022,#62023,#62024,#62025,
#62026,#62027,#62028,#62029,#62030,#62031,#62032,#62033,#62034,#62035,#62036,
#62037,#62038,#62039,#62040,#62041,#62042,#62043,#62044,#62045,#62046,#62047,
#62048,#62049,#62050,#62051,#62052,#62053),.UNSPECIFIED.,.F.,.F.,(4,3,3,
3,3,3,3,3,3,3,3,3,3,3,3,3,3,3,3,3,3,3,3,3,3,3,3,3,3,3,3,3,3,3,3,3,3,3,3,
3,3,3,3,3,3,3,3,3,3,3,3,3,3,3,3,3,3,3,3,3,3,3,3,3,3,3,3,3,3,3,3,3,3,4),
(618.893752757351,619.000853338961,619.110344502978,619.144625417211,619.228364129057,
619.311999640424,619.395552083822,619.479041519673,619.562495470287,619.645931964133,
619.729369073888,619.812824868806,619.896369361535,619.979958444476,620.063681712033,
620.144361427932,620.228100139778,620.311735651146,620.395288094544,620.478777530395,
620.562231481009,620.645667974855,620.729105084611,620.812560879528,620.896105372258,
620.979694455199,621.063417722757,621.144097438652,621.227836150498,621.311471661865,
621.395024105264,621.478513541115,621.561967491728,621.645403985574,621.72884109533,
621.812296890247,621.895841382977,621.979430465918,622.063153733475,622.143833449372,
622.227572161218,622.311207672586,622.394760115984,622.478249551835,622.561703502449,
622.645139996295,622.728577106051,622.812032900968,622.895577393698,622.979166476639,
623.062889744197,623.143569460092,623.227308171938,623.310943683305,623.394496126704,
623.477985562555,623.561439513169,623.644876007015,623.728313116771,623.811768911688,
623.895313404418,623.978902487359,624.062625754917,624.143305470812,624.227057435847,
624.314334274184,624.397875522788,624.481359825538,624.564805301711,624.648230040424,
624.731673265519,624.815127694519,624.898637795245,624.925272142545),
 .UNSPECIFIED.);
#444=B_SPLINE_CURVE_WITH_KNOTS('',3,(#62054,#62055,#62056,#62057,#62058,
#62059,#62060,#62061,#62062,#62063),.UNSPECIFIED.,.F.,.F.,(4,3,3,4),(618.642393919554,
618.72489184659,618.809322301879,618.893752757168),.UNSPECIFIED.);
#445=B_SPLINE_CURVE_WITH_KNOTS('',3,(#62065,#62066,#62067,#62068,#62069,
#62070,#62071,#62072,#62073,#62074),.UNSPECIFIED.,.F.,.F.,(4,3,3,4),(618.643441409442,
618.733818705617,618.823895033376,618.893752757047),.UNSPECIFIED.);
#446=B_SPLINE_CURVE_WITH_KNOTS('',3,(#62075,#62076,#62077,#62078,#62079,
#62080,#62081,#62082,#62083,#62084,#62085,#62086,#62087,#62088,#62089,#62090,
#62091,#62092,#62093,#62094,#62095,#62096,#62097,#62098,#62099,#62100,#62101,
#62102,#62103,#62104,#62105,#62106,#62107,#62108,#62109,#62110,#62111,#62112,
#62113,#62114,#62115,#62116,#62117,#62118,#62119,#62120,#62121,#62122,#62123,
#62124,#62125,#62126,#62127,#62128,#62129,#62130,#62131,#62132,#62133,#62134,
#62135,#62136,#62137,#62138,#62139,#62140,#62141,#62142,#62143,#62144,#62145,
#62146,#62147,#62148,#62149,#62150,#62151,#62152,#62153,#62154,#62155,#62156,
#62157,#62158,#62159,#62160,#62161,#62162,#62163,#62164,#62165,#62166,#62167,
#62168,#62169,#62170,#62171,#62172,#62173,#62174,#62175,#62176,#62177,#62178,
#62179,#62180,#62181,#62182,#62183,#62184,#62185,#62186,#62187,#62188,#62189,
#62190,#62191,#62192,#62193,#62194,#62195,#62196,#62197,#62198,#62199,#62200,
#62201,#62202,#62203,#62204,#62205,#62206,#62207,#62208,#62209,#62210,#62211,
#62212,#62213,#62214,#62215,#62216,#62217,#62218,#62219,#62220,#62221,#62222,
#62223,#62224,#62225,#62226,#62227,#62228,#62229,#62230,#62231,#62232,#62233,
#62234,#62235,#62236,#62237,#62238,#62239,#62240,#62241,#62242,#62243,#62244,
#62245,#62246,#62247,#62248,#62249,#62250,#62251,#62252,#62253,#62254,#62255,
#62256,#62257,#62258,#62259,#62260,#62261,#62262,#62263,#62264,#62265,#62266,
#62267,#62268,#62269,#62270,#62271,#62272,#62273,#62274,#62275,#62276,#62277,
#62278,#62279,#62280,#62281,#62282,#62283,#62284,#62285,#62286,#62287,#62288,
#62289,#62290,#62291,#62292,#62293,#62294),.UNSPECIFIED.,.F.,.F.,(4,3,3,
3,3,3,3,3,3,3,3,3,3,3,3,3,3,3,3,3,3,3,3,3,3,3,3,3,3,3,3,3,3,3,3,3,3,3,3,
3,3,3,3,3,3,3,3,3,3,3,3,3,3,3,3,3,3,3,3,3,3,3,3,3,3,3,3,3,3,3,3,3,3,4),
(618.893752757172,618.979243826729,619.064785335007,619.150391707895,619.236139493783,
619.321965357415,619.407948450812,619.454916036928,619.538654748774,619.622290260141,
619.70584270354,619.78933213939,619.872786090004,619.95622258385,620.039659693606,
620.123115488524,620.206659981253,620.290249064194,620.373972331751,620.454652047648,
620.538390759494,620.622026270862,620.70557871426,620.789068150111,620.872522100725,
620.955958594571,621.039395704327,621.122851499244,621.206395991974,621.289985074915,
621.373708342473,621.454388058368,621.538126770214,621.621762281581,621.70531472498,
621.788804160831,621.872258111445,621.955694605291,622.039131715046,622.122587509964,
622.206132002693,622.289721085634,622.373444353192,622.454124069088,622.537862780934,
622.621498292301,622.7050507357,622.788540171551,622.871994122165,622.955430616011,
623.038867725766,623.122323520684,623.205868013413,623.289457096354,623.373180363912,
623.453860079808,623.537598791654,623.621234303022,623.70478674642,623.788276182272,
623.871730132886,623.955166626732,624.038603736487,624.122059531405,624.205604024135,
624.289193107076,624.372916374633,624.453596090528,624.536589151006,624.619482269218,
624.702279720181,624.785021521373,624.867728841325,624.925707879934),
 .UNSPECIFIED.);
#447=B_SPLINE_CURVE_WITH_KNOTS('',3,(#62300,#62301,#62302,#62303,#62304,
#62305,#62306,#62307,#62308,#62309,#62310,#62311,#62312,#62313,#62314,#62315,
#62316,#62317,#62318,#62319,#62320,#62321,#62322,#62323,#62324,#62325,#62326,
#62327,#62328,#62329,#62330,#62331,#62332,#62333,#62334,#62335,#62336,#62337,
#62338,#62339,#62340,#62341,#62342,#62343,#62344,#62345,#62346,#62347,#62348,
#62349,#62350,#62351,#62352,#62353,#62354,#62355,#62356,#62357,#62358,#62359,
#62360,#62361,#62362,#62363,#62364,#62365,#62366,#62367,#62368,#62369,#62370,
#62371,#62372,#62373,#62374,#62375,#62376,#62377,#62378,#62379,#62380,#62381,
#62382,#62383,#62384,#62385,#62386,#62387,#62388,#62389,#62390,#62391,#62392,
#62393,#62394,#62395,#62396,#62397,#62398,#62399,#62400,#62401,#62402,#62403,
#62404,#62405,#62406,#62407,#62408,#62409,#62410,#62411,#62412,#62413,#62414,
#62415,#62416,#62417,#62418,#62419,#62420,#62421,#62422,#62423,#62424,#62425,
#62426,#62427,#62428,#62429,#62430,#62431,#62432,#62433,#62434,#62435,#62436,
#62437,#62438,#62439,#62440,#62441,#62442,#62443,#62444,#62445,#62446,#62447,
#62448,#62449,#62450,#62451,#62452,#62453,#62454,#62455,#62456,#62457,#62458,
#62459,#62460,#62461,#62462,#62463,#62464,#62465,#62466,#62467,#62468,#62469,
#62470,#62471,#62472,#62473,#62474,#62475,#62476,#62477,#62478,#62479,#62480,
#62481,#62482,#62483,#62484,#62485,#62486,#62487,#62488,#62489,#62490,#62491,
#62492,#62493,#62494,#62495,#62496,#62497,#62498,#62499,#62500,#62501,#62502,
#62503,#62504,#62505,#62506,#62507,#62508,#62509,#62510,#62511,#62512,#62513,
#62514,#62515,#62516,#62517,#62518,#62519),.UNSPECIFIED.,.F.,.F.,(4,3,3,
3,3,3,3,3,3,3,3,3,3,3,3,3,3,3,3,3,3,3,3,3,3,3,3,3,3,3,3,3,3,3,3,3,3,3,3,
3,3,3,3,3,3,3,3,3,3,3,3,3,3,3,3,3,3,3,3,3,3,3,3,3,3,3,3,3,3,3,3,3,3,4),
(625.176938064496,625.260209543116,625.34337941499,625.426468270658,625.509496624868,
625.59249317596,625.675475373907,625.758461701018,625.841470638977,625.924568877374,
626.007716014695,626.090988218634,626.142777492252,626.226516204098,626.310151715465,
626.393704158864,626.477193594715,626.560647545328,626.644084039175,626.72752114893,
626.810976943847,626.894521436577,626.978110519518,627.061833787075,627.142513502972,
627.226252214818,627.309887726185,627.393440169584,627.476929605435,627.560383556049,
627.643820049895,627.72725715965,627.810712954568,627.894257447297,627.977846530238,
628.061569797796,628.142249513692,628.225988225538,628.309623736906,628.393176180304,
628.476665616155,628.560119566769,628.643556060615,628.726993170371,628.810448965288,
628.893993458018,628.977582540959,629.061305808517,629.141985524413,629.225724236259,
629.309359747627,629.392912191025,629.476401626876,629.55985557749,629.643292071336,
629.726729181092,629.810184976009,629.893729468739,629.97731855168,630.061041819238,
630.141721535133,630.225460246979,630.309095758346,630.392648201745,630.476137637597,
630.55959158821,630.643028082057,630.726465191812,630.809920986729,630.893465479459,
630.9770545624,631.060777829957,631.141457545853,631.209446795619),
 .UNSPECIFIED.);
#448=B_SPLINE_CURVE_WITH_KNOTS('',3,(#62520,#62521,#62522,#62523,#62524,
#62525,#62526,#62527,#62528,#62529,#62530,#62531,#62532),.UNSPECIFIED.,
 .F.,.F.,(4,3,3,3,4),(624.925272142545,625.008881354531,625.092616068713,
625.143041481532,625.176938064348),.UNSPECIFIED.);
#449=B_SPLINE_CURVE_WITH_KNOTS('',3,(#62534,#62535,#62536,#62537,#62538,
#62539,#62540,#62541,#62542,#62543),.UNSPECIFIED.,.F.,.F.,(4,3,3,4),(624.925707879934,
625.008404893569,625.09267147896,625.176938064352),.UNSPECIFIED.);
#450=B_SPLINE_CURVE_WITH_KNOTS('',3,(#62544,#62545,#62546,#62547,#62548,
#62549,#62550,#62551,#62552,#62553,#62554,#62555,#62556,#62557,#62558,#62559,
#62560,#62561,#62562,#62563,#62564,#62565,#62566,#62567,#62568,#62569,#62570,
#62571,#62572,#62573,#62574,#62575,#62576,#62577,#62578,#62579,#62580,#62581,
#62582,#62583,#62584,#62585,#62586,#62587,#62588,#62589,#62590,#62591,#62592,
#62593,#62594,#62595,#62596,#62597,#62598,#62599,#62600,#62601,#62602,#62603,
#62604,#62605,#62606,#62607,#62608,#62609,#62610,#62611,#62612,#62613,#62614,
#62615,#62616,#62617,#62618,#62619,#62620,#62621,#62622,#62623,#62624,#62625,
#62626,#62627,#62628,#62629,#62630,#62631,#62632,#62633,#62634,#62635,#62636,
#62637,#62638,#62639,#62640,#62641,#62642,#62643,#62644,#62645,#62646,#62647,
#62648,#62649,#62650,#62651,#62652,#62653,#62654,#62655,#62656,#62657,#62658,
#62659,#62660,#62661,#62662,#62663,#62664,#62665,#62666,#62667,#62668,#62669,
#62670,#62671,#62672,#62673,#62674,#62675,#62676,#62677,#62678,#62679,#62680,
#62681,#62682,#62683,#62684,#62685,#62686,#62687,#62688,#62689,#62690,#62691,
#62692,#62693,#62694,#62695,#62696,#62697,#62698,#62699,#62700,#62701,#62702,
#62703,#62704,#62705,#62706,#62707,#62708,#62709,#62710,#62711,#62712,#62713,
#62714,#62715,#62716,#62717,#62718,#62719,#62720,#62721,#62722,#62723,#62724,
#62725,#62726,#62727,#62728,#62729,#62730,#62731,#62732,#62733,#62734,#62735,
#62736,#62737,#62738,#62739,#62740,#62741,#62742,#62743,#62744,#62745,#62746,
#62747,#62748,#62749,#62750,#62751,#62752,#62753,#62754,#62755,#62756,#62757,
#62758,#62759,#62760),.UNSPECIFIED.,.F.,.F.,(4,3,3,3,3,3,3,3,3,3,3,3,3,
3,3,3,3,3,3,3,3,3,3,3,3,3,3,3,3,3,3,3,3,3,3,3,3,3,3,3,3,3,3,3,3,3,3,3,3,
3,3,3,3,3,3,3,3,3,3,3,3,3,3,3,3,3,3,3,3,3,3,3,4),(625.176938064455,625.280336351129,
625.385460544446,625.453332101248,625.537070813094,625.620706324461,625.70425876786,
625.787748203711,625.871202154325,625.954638648171,626.038075757926,626.121531552844,
626.205076045573,626.288665128514,626.372388396072,626.453068111968,626.536806823814,
626.620442335182,626.70399477858,626.787484214431,626.870938165045,626.954374658891,
627.037811768647,627.121267563564,627.204812056294,627.288401139235,627.372124406793,
627.452804122688,627.536542834534,627.620178345902,627.7037307893,627.787220225151,
627.870674175765,627.954110669611,628.037547779367,628.121003574284,628.204548067014,
628.288137149955,628.371860417513,628.452540133409,628.536278845255,628.619914356623,
628.703466800021,628.786956235872,628.870410186486,628.953846680332,629.037283790087,
629.120739585005,629.204284077735,629.287873160676,629.371596428233,629.452276144129,
629.536014855975,629.619650367343,629.703202810741,629.786692246592,629.870146197206,
629.953582691052,630.037019800807,630.120475595725,630.204020088455,630.287609171396,
630.371332438953,630.452012154849,630.535765810946,630.619853544318,630.703397992737,
630.786884325473,630.870330664123,630.954864917574,631.038303148445,631.123385413185,
631.208467677925),.UNSPECIFIED.);
#451=B_SPLINE_CURVE_WITH_KNOTS('',3,(#62766,#62767,#62768,#62769,#62770,
#62771,#62772,#62773,#62774,#62775,#62776,#62777,#62778,#62779,#62780,#62781,
#62782,#62783,#62784,#62785,#62786,#62787,#62788,#62789,#62790,#62791,#62792,
#62793,#62794,#62795,#62796,#62797,#62798,#62799,#62800,#62801,#62802,#62803,
#62804,#62805,#62806,#62807,#62808,#62809,#62810,#62811,#62812,#62813,#62814,
#62815,#62816,#62817,#62818,#62819,#62820,#62821,#62822,#62823,#62824,#62825,
#62826,#62827,#62828,#62829,#62830,#62831,#62832,#62833,#62834,#62835,#62836,
#62837,#62838,#62839,#62840,#62841,#62842,#62843,#62844,#62845,#62846,#62847,
#62848,#62849,#62850,#62851,#62852,#62853,#62854,#62855,#62856,#62857,#62858,
#62859,#62860,#62861,#62862,#62863,#62864,#62865,#62866,#62867,#62868,#62869,
#62870,#62871,#62872,#62873,#62874,#62875,#62876,#62877,#62878,#62879,#62880,
#62881,#62882,#62883,#62884,#62885,#62886,#62887,#62888,#62889,#62890,#62891,
#62892,#62893,#62894,#62895,#62896,#62897,#62898,#62899,#62900,#62901,#62902,
#62903,#62904,#62905,#62906,#62907,#62908,#62909,#62910,#62911,#62912,#62913,
#62914,#62915,#62916,#62917,#62918,#62919,#62920,#62921,#62922,#62923,#62924,
#62925,#62926,#62927,#62928,#62929,#62930,#62931,#62932,#62933,#62934,#62935,
#62936,#62937,#62938,#62939,#62940,#62941,#62942,#62943,#62944,#62945,#62946,
#62947,#62948,#62949,#62950,#62951,#62952,#62953,#62954,#62955,#62956,#62957,
#62958,#62959,#62960,#62961,#62962,#62963,#62964,#62965,#62966,#62967,#62968,
#62969,#62970,#62971,#62972,#62973,#62974,#62975,#62976,#62977,#62978,#62979,
#62980,#62981,#62982,#62983,#62984,#62985,#62986,#62987,#62988),
 .UNSPECIFIED.,.F.,.F.,(4,3,3,3,3,3,3,3,3,3,3,3,3,3,3,3,3,3,3,3,3,3,3,3,
3,3,3,3,3,3,3,3,3,3,3,3,3,3,3,3,3,3,3,3,3,3,3,3,3,3,3,3,3,3,3,3,3,3,3,3,
3,3,3,3,3,3,3,3,3,3,3,3,3,3,4),(631.460123371528,631.545257144659,631.628429442251,
631.711600703576,631.794789198943,631.88139028835,631.964715252283,632.048100864044,
632.131604501457,632.141193556573,632.224932268419,632.308567779786,632.392120223185,
632.475609659036,632.55906360965,632.642500103496,632.725937213251,632.809393008169,
632.892937500899,632.97652658384,633.060249851397,633.140929567293,633.224668279139,
633.308303790506,633.391856233905,633.475345669756,633.55879962037,633.642236114216,
633.725673223971,633.809129018888,633.892673511618,633.976262594559,634.059985862116,
634.140665578013,634.224404289859,634.308039801227,634.391592244625,634.475081680476,
634.55853563109,634.641972124936,634.725409234691,634.808865029609,634.892409522339,
634.97599860528,635.059721872837,635.140401588733,635.224140300579,635.307775811946,
635.391328255345,635.474817691196,635.55827164181,635.641708135656,635.725145245412,
635.80860104033,635.892145533059,635.975734616,636.059457883558,636.140137599454,
636.2238763113,636.307511822667,636.391064266066,636.474553701917,636.55800765253,
636.641444146377,636.724881256132,636.80833705105,636.89188154378,636.975470626721,
637.059193894279,637.139873610174,637.228073850114,637.31284479252,637.397529446154,
637.482127520008,637.492674569935),.UNSPECIFIED.);
#452=B_SPLINE_CURVE_WITH_KNOTS('',3,(#62989,#62990,#62991,#62992,#62993,
#62994,#62995,#62996,#62997,#62998),.UNSPECIFIED.,.F.,.F.,(4,3,3,4),(631.209446795619,
631.309022526793,631.407591002671,631.460123371355),.UNSPECIFIED.);
#453=B_SPLINE_CURVE_WITH_KNOTS('',3,(#63000,#63001,#63002,#63003,#63004,
#63005,#63006,#63007,#63008,#63009,#63010,#63011,#63012),.UNSPECIFIED.,
 .F.,.F.,(4,3,3,3,4),(631.208467677925,631.292059759149,631.375784639063,
631.451748165569,631.460123371531),.UNSPECIFIED.);
#454=B_SPLINE_CURVE_WITH_KNOTS('',3,(#63013,#63014,#63015,#63016,#63017,
#63018,#63019,#63020,#63021,#63022,#63023,#63024,#63025,#63026,#63027,#63028,
#63029,#63030,#63031,#63032,#63033,#63034,#63035,#63036,#63037,#63038,#63039,
#63040,#63041,#63042,#63043,#63044,#63045,#63046,#63047,#63048,#63049,#63050,
#63051,#63052,#63053,#63054,#63055,#63056,#63057,#63058,#63059,#63060,#63061,
#63062,#63063,#63064,#63065,#63066,#63067,#63068,#63069,#63070,#63071,#63072,
#63073,#63074,#63075,#63076,#63077,#63078,#63079,#63080,#63081,#63082,#63083,
#63084,#63085,#63086,#63087,#63088,#63089,#63090,#63091,#63092,#63093,#63094,
#63095,#63096,#63097,#63098,#63099,#63100,#63101,#63102,#63103,#63104,#63105,
#63106,#63107,#63108,#63109,#63110,#63111,#63112,#63113,#63114,#63115,#63116,
#63117,#63118,#63119,#63120,#63121,#63122,#63123,#63124,#63125,#63126,#63127,
#63128,#63129,#63130,#63131,#63132,#63133,#63134,#63135,#63136,#63137,#63138,
#63139,#63140,#63141,#63142,#63143,#63144,#63145,#63146,#63147,#63148,#63149,
#63150,#63151,#63152,#63153,#63154,#63155,#63156,#63157,#63158,#63159,#63160,
#63161,#63162,#63163,#63164,#63165,#63166,#63167,#63168,#63169,#63170,#63171,
#63172,#63173,#63174,#63175,#63176,#63177,#63178,#63179,#63180,#63181,#63182,
#63183,#63184,#63185,#63186,#63187,#63188,#63189,#63190,#63191,#63192,#63193,
#63194,#63195,#63196,#63197,#63198,#63199,#63200,#63201,#63202,#63203,#63204,
#63205,#63206,#63207,#63208,#63209,#63210,#63211,#63212,#63213,#63214,#63215,
#63216,#63217,#63218,#63219,#63220,#63221,#63222,#63223,#63224,#63225,#63226,
#63227,#63228,#63229,#63230,#63231,#63232),.UNSPECIFIED.,.F.,.F.,(4,3,3,
3,3,3,3,3,3,3,3,3,3,3,3,3,3,3,3,3,3,3,3,3,3,3,3,3,3,3,3,3,3,3,3,3,3,3,3,
3,3,3,3,3,3,3,3,3,3,3,3,3,3,3,3,3,3,3,3,3,3,3,3,3,3,3,3,3,3,3,3,3,3,4),
(631.460123371693,631.54373741473,631.627248408381,631.710676617484,631.794042233833,
631.87737303142,631.96068699152,632.04400230477,632.127337158942,632.21076078304,
632.294229991713,632.377831126119,632.451484176289,632.535222888135,632.618858399503,
632.702410842901,632.785900278752,632.869354229366,632.952790723213,633.036227832968,
633.119683627886,633.203228120616,633.286817203557,633.370540471114,633.451220187009,
633.534958898855,633.618594410222,633.702146853621,633.785636289472,633.869090240085,
633.952526733931,634.035963843687,634.119419638604,634.202964131333,634.286553214274,
634.370276481832,634.450956197729,634.534694909575,634.618330420943,634.701882864341,
634.785372300192,634.868826250806,634.952262744652,635.035699854407,635.119155649325,
635.202700142055,635.286289224996,635.370012492554,635.450692208449,635.534430920295,
635.618066431662,635.701618875061,635.785108310911,635.868562261525,635.951998755371,
636.035435865127,636.118891660045,636.202436152775,636.286025235716,636.369748503273,
636.45042821917,636.534166931016,636.617802442384,636.701354885782,636.784844321633,
636.868298272247,636.951734766093,637.035171875849,637.118627670766,637.202172163496,
637.285761246437,637.369484513995,637.45016422989,637.492495965904),
 .UNSPECIFIED.);
#455=B_SPLINE_CURVE_WITH_KNOTS('',3,(#63238,#63239,#63240,#63241,#63242,
#63243,#63244,#63245,#63246,#63247,#63248,#63249,#63250,#63251,#63252,#63253,
#63254,#63255,#63256,#63257,#63258,#63259,#63260,#63261,#63262,#63263,#63264,
#63265,#63266,#63267,#63268,#63269,#63270,#63271,#63272,#63273,#63274,#63275,
#63276,#63277,#63278,#63279,#63280,#63281,#63282,#63283,#63284,#63285,#63286,
#63287,#63288,#63289,#63290,#63291,#63292,#63293,#63294,#63295,#63296,#63297,
#63298,#63299,#63300,#63301,#63302,#63303,#63304,#63305,#63306,#63307,#63308,
#63309,#63310,#63311,#63312,#63313,#63314,#63315,#63316,#63317,#63318,#63319,
#63320,#63321,#63322,#63323,#63324,#63325,#63326,#63327,#63328,#63329,#63330,
#63331,#63332,#63333,#63334,#63335,#63336,#63337,#63338,#63339,#63340,#63341,
#63342,#63343,#63344,#63345,#63346,#63347,#63348,#63349,#63350,#63351,#63352,
#63353,#63354,#63355,#63356,#63357,#63358,#63359,#63360,#63361,#63362,#63363,
#63364,#63365,#63366,#63367,#63368,#63369,#63370,#63371,#63372,#63373,#63374,
#63375,#63376,#63377,#63378,#63379,#63380,#63381,#63382,#63383,#63384,#63385,
#63386,#63387,#63388,#63389,#63390,#63391,#63392,#63393,#63394,#63395,#63396,
#63397,#63398,#63399,#63400,#63401,#63402,#63403,#63404,#63405,#63406,#63407,
#63408,#63409,#63410,#63411,#63412,#63413,#63414,#63415,#63416,#63417,#63418,
#63419,#63420,#63421,#63422,#63423,#63424,#63425,#63426,#63427,#63428,#63429,
#63430,#63431,#63432,#63433,#63434,#63435,#63436,#63437,#63438,#63439,#63440,
#63441,#63442,#63443,#63444,#63445,#63446,#63447,#63448,#63449,#63450,#63451,
#63452,#63453,#63454,#63455,#63456,#63457),.UNSPECIFIED.,.F.,.F.,(4,3,3,
3,3,3,3,3,3,3,3,3,3,3,3,3,3,3,3,3,3,3,3,3,3,3,3,3,3,3,3,3,3,3,3,3,3,3,3,
3,3,3,3,3,3,3,3,3,3,3,3,3,3,3,3,3,3,3,3,3,3,3,3,3,3,3,3,3,3,3,3,3,3,4),
(637.743308678889,637.835617429321,637.928437698344,638.02152311515,638.114948726993,
638.139609620894,638.22334833274,638.306983844108,638.390536287506,638.474025723357,
638.557479673971,638.640916167817,638.724353277572,638.80780907249,638.89135356522,
638.97494264816,639.058665915718,639.139345631614,639.22308434346,639.306719854827,
639.390272298226,639.473761734077,639.55721568469,639.640652178537,639.724089288292,
639.80754508321,639.891089575939,639.97467865888,640.058401926438,640.139081642334,
640.22282035418,640.306455865547,640.390008308946,640.473497744797,640.556951695411,
640.640388189257,640.723825299012,640.80728109393,640.89082558666,640.974414669601,
641.058137937158,641.138817653054,641.2225563649,641.306191876267,641.389744319666,
641.473233755517,641.55668770613,641.640124199977,641.723561309732,641.80701710465,
641.890561597379,641.97415068032,642.057873947878,642.138553663774,642.22229237562,
642.305927886988,642.389480330386,642.472969766237,642.556423716851,642.639860210697,
642.723297320453,642.80675311537,642.8902976081,642.973886691041,643.057609958599,
643.138289674494,643.220897982151,643.303411668023,643.385849855946,643.468231600083,
643.550584869593,643.63291993891,643.715280454977,643.774669788269),
 .UNSPECIFIED.);
#456=B_SPLINE_CURVE_WITH_KNOTS('',3,(#63458,#63459,#63460,#63461,#63462,
#63463,#63464,#63465,#63466,#63467),.UNSPECIFIED.,.F.,.F.,(4,3,3,4),(637.492674569935,
637.577199593725,637.661692639095,637.743308678707),.UNSPECIFIED.);
#457=B_SPLINE_CURVE_WITH_KNOTS('',3,(#63469,#63470,#63471,#63472,#63473,
#63474,#63475,#63476,#63477,#63478),.UNSPECIFIED.,.F.,.F.,(4,3,3,4),(637.492495965904,
637.595189172829,637.696529649985,637.743308678576),.UNSPECIFIED.);
#458=B_SPLINE_CURVE_WITH_KNOTS('',3,(#63479,#63480,#63481,#63482,#63483,
#63484,#63485,#63486,#63487,#63488,#63489,#63490,#63491,#63492,#63493,#63494,
#63495,#63496,#63497,#63498,#63499,#63500,#63501,#63502,#63503,#63504,#63505,
#63506,#63507,#63508,#63509,#63510,#63511,#63512,#63513,#63514,#63515,#63516,
#63517,#63518,#63519,#63520,#63521,#63522,#63523,#63524,#63525,#63526,#63527,
#63528,#63529,#63530,#63531,#63532,#63533,#63534,#63535,#63536,#63537,#63538,
#63539,#63540,#63541,#63542,#63543,#63544,#63545,#63546,#63547,#63548,#63549,
#63550,#63551,#63552,#63553,#63554,#63555,#63556,#63557,#63558,#63559,#63560,
#63561,#63562,#63563,#63564,#63565,#63566,#63567,#63568,#63569,#63570,#63571,
#63572,#63573,#63574,#63575,#63576,#63577,#63578,#63579,#63580,#63581,#63582,
#63583,#63584,#63585,#63586,#63587,#63588,#63589,#63590,#63591,#63592,#63593,
#63594,#63595,#63596,#63597,#63598,#63599,#63600,#63601,#63602,#63603,#63604,
#63605,#63606,#63607,#63608,#63609,#63610,#63611,#63612,#63613,#63614,#63615,
#63616,#63617,#63618,#63619,#63620,#63621,#63622,#63623,#63624,#63625,#63626,
#63627,#63628,#63629,#63630,#63631,#63632,#63633,#63634,#63635,#63636,#63637,
#63638,#63639,#63640,#63641,#63642,#63643,#63644,#63645,#63646,#63647,#63648,
#63649,#63650,#63651,#63652,#63653,#63654,#63655,#63656,#63657,#63658,#63659,
#63660,#63661,#63662,#63663,#63664,#63665,#63666,#63667,#63668,#63669,#63670,
#63671,#63672,#63673,#63674,#63675,#63676,#63677,#63678,#63679,#63680,#63681,
#63682,#63683,#63684,#63685,#63686,#63687,#63688,#63689,#63690,#63691,#63692,
#63693,#63694,#63695,#63696,#63697,#63698),.UNSPECIFIED.,.F.,.F.,(4,3,3,
3,3,3,3,3,3,3,3,3,3,3,3,3,3,3,3,3,3,3,3,3,3,3,3,3,3,3,3,3,3,3,3,3,3,3,3,
3,3,3,3,3,3,3,3,3,3,3,3,3,3,3,3,3,3,3,3,3,3,3,3,3,3,3,3,3,3,3,3,3,3,4),
(637.743308678711,637.826210344786,637.909084797821,637.991947982986,638.074818452954,
638.157714762192,638.240703416289,638.323743941136,638.406909159978,638.44990024061,
638.533638952456,638.617274463823,638.700826907222,638.784316343073,638.867770293687,
638.951206787533,639.034643897288,639.118099692206,639.201644184936,639.285233267877,
639.368956535434,639.44963625133,639.533374963176,639.617010474544,639.700562917942,
639.784052353793,639.867506304406,639.950942798253,640.034379908008,640.117835702925,
640.201380195655,640.284969278596,640.368692546154,640.44937226205,640.533110973896,
640.616746485263,640.700298928662,640.783788364513,640.867242315127,640.950678808973,
641.034115918728,641.117571713646,641.201116206376,641.284705289317,641.368428556874,
641.44910827277,641.532846984616,641.616482495984,641.700034939382,641.783524375233,
641.866978325847,641.950414819693,642.033851929448,642.117307724366,642.200852217096,
642.284441300037,642.368164567595,642.44884428349,642.532582995336,642.616218506703,
642.699770950101,642.783260385952,642.866714336566,642.950150830412,643.033587940168,
643.117043735085,643.200588227815,643.284177310756,643.367900578314,643.448580294211,
643.534086763533,643.619486089427,643.704761993063,643.775962112477),
 .UNSPECIFIED.);
#459=B_SPLINE_CURVE_WITH_KNOTS('',3,(#63704,#63705,#63706,#63707,#63708,
#63709,#63710,#63711,#63712,#63713,#63714,#63715,#63716,#63717,#63718,#63719,
#63720,#63721,#63722,#63723,#63724,#63725,#63726,#63727,#63728,#63729,#63730,
#63731,#63732,#63733,#63734,#63735,#63736,#63737,#63738,#63739,#63740,#63741,
#63742,#63743,#63744,#63745,#63746,#63747,#63748,#63749,#63750,#63751,#63752,
#63753,#63754,#63755,#63756,#63757,#63758,#63759,#63760,#63761,#63762,#63763,
#63764,#63765,#63766,#63767,#63768,#63769,#63770,#63771,#63772,#63773,#63774,
#63775,#63776,#63777,#63778,#63779,#63780,#63781,#63782,#63783,#63784,#63785,
#63786,#63787,#63788,#63789,#63790,#63791,#63792,#63793,#63794,#63795,#63796,
#63797,#63798,#63799,#63800,#63801,#63802,#63803,#63804,#63805,#63806,#63807,
#63808,#63809,#63810,#63811,#63812,#63813,#63814,#63815,#63816,#63817,#63818,
#63819,#63820,#63821,#63822,#63823,#63824,#63825,#63826,#63827,#63828,#63829,
#63830,#63831,#63832,#63833,#63834,#63835,#63836,#63837,#63838,#63839,#63840,
#63841,#63842,#63843,#63844,#63845,#63846,#63847,#63848,#63849,#63850,#63851,
#63852,#63853,#63854,#63855,#63856,#63857,#63858,#63859,#63860,#63861,#63862,
#63863,#63864,#63865,#63866,#63867,#63868,#63869,#63870,#63871,#63872,#63873,
#63874,#63875,#63876,#63877,#63878,#63879,#63880,#63881,#63882,#63883,#63884,
#63885,#63886,#63887,#63888,#63889,#63890,#63891,#63892,#63893,#63894,#63895,
#63896,#63897,#63898,#63899,#63900,#63901,#63902,#63903,#63904,#63905,#63906,
#63907,#63908,#63909,#63910,#63911,#63912,#63913,#63914,#63915,#63916,#63917,
#63918,#63919,#63920),.UNSPECIFIED.,.F.,.F.,(4,3,3,3,3,3,3,3,3,3,3,3,3,
3,3,3,3,3,3,3,3,3,3,3,3,3,3,3,3,3,3,3,3,3,3,3,3,3,3,3,3,3,3,3,3,3,3,3,3,
3,3,3,3,3,3,3,3,3,3,3,3,3,3,3,3,3,3,3,3,3,3,3,4),(644.026493985887,644.138025685215,
644.22176439706,644.305399908426,644.388952351823,644.472441787673,644.555895738286,
644.639332232131,644.722769341885,644.806225136801,644.88976962953,644.97335871247,
645.057081980026,645.137761695935,645.221500407781,645.305135919149,645.388688362548,
645.472177798399,645.555631749013,645.639068242859,645.722505352615,645.805961147533,
645.889505640263,645.973094723204,646.056817990762,646.137497706655,646.221236418501,
646.304871929869,646.388424373267,646.471913809118,646.555367759732,646.638804253578,
646.722241363334,646.805697158252,646.889241650981,646.972830733922,647.05655400148,
647.137233717375,647.220972429221,647.304607940588,647.388160383987,647.471649819838,
647.555103770451,647.638540264297,647.721977374053,647.80543316897,647.8889776617,
647.972566744641,648.056290012198,648.136969728095,648.220708439941,648.304343951309,
648.387896394707,648.471385830558,648.554839781172,648.638276275018,648.721713384774,
648.805169179691,648.888713672421,648.972302755362,649.05602602292,649.136705738815,
649.220448966711,649.30408796254,649.3876428632,649.471466758317,649.554917045806,
649.63834849033,649.721779163694,649.805892878804,649.889410848519,649.973822436327,
650.058234024135),.UNSPECIFIED.);
#460=B_SPLINE_CURVE_WITH_KNOTS('',3,(#63921,#63922,#63923,#63924,#63925,
#63926,#63927,#63928,#63929,#63930),.UNSPECIFIED.,.F.,.F.,(4,3,3,4),(643.774669788269,
643.857102840832,643.941798413292,644.026493985751),.UNSPECIFIED.);
#461=B_SPLINE_CURVE_WITH_KNOTS('',3,(#63932,#63933,#63934,#63935,#63936,
#63937,#63938,#63939,#63940,#63941),.UNSPECIFIED.,.F.,.F.,(4,3,3,4),(643.775962112477,
643.861094775698,643.946170770531,644.026493985891),.UNSPECIFIED.);
#462=B_SPLINE_CURVE_WITH_KNOTS('',3,(#63942,#63943,#63944,#63945,#63946,
#63947,#63948,#63949,#63950,#63951,#63952,#63953,#63954,#63955,#63956,#63957,
#63958,#63959,#63960,#63961,#63962,#63963,#63964,#63965,#63966,#63967,#63968,
#63969,#63970,#63971,#63972,#63973,#63974,#63975,#63976,#63977,#63978,#63979,
#63980,#63981,#63982,#63983,#63984,#63985,#63986,#63987,#63988,#63989,#63990,
#63991,#63992,#63993,#63994,#63995,#63996,#63997,#63998,#63999,#64000,#64001,
#64002,#64003,#64004,#64005,#64006,#64007,#64008,#64009,#64010,#64011,#64012,
#64013,#64014,#64015,#64016,#64017,#64018,#64019,#64020,#64021,#64022,#64023,
#64024,#64025,#64026,#64027,#64028,#64029,#64030,#64031,#64032,#64033,#64034,
#64035,#64036,#64037,#64038,#64039,#64040,#64041,#64042,#64043,#64044,#64045,
#64046,#64047,#64048,#64049,#64050,#64051,#64052,#64053,#64054,#64055,#64056,
#64057,#64058,#64059,#64060,#64061,#64062,#64063,#64064,#64065,#64066,#64067,
#64068,#64069,#64070,#64071,#64072,#64073,#64074,#64075,#64076,#64077,#64078,
#64079,#64080,#64081,#64082,#64083,#64084,#64085,#64086,#64087,#64088,#64089,
#64090,#64091,#64092,#64093,#64094,#64095,#64096,#64097,#64098,#64099,#64100,
#64101,#64102,#64103,#64104,#64105,#64106,#64107,#64108,#64109,#64110,#64111,
#64112,#64113,#64114,#64115,#64116,#64117,#64118,#64119,#64120,#64121,#64122,
#64123,#64124,#64125,#64126,#64127,#64128,#64129,#64130,#64131,#64132,#64133,
#64134,#64135,#64136,#64137,#64138,#64139,#64140,#64141,#64142,#64143,#64144,
#64145,#64146,#64147,#64148,#64149,#64150,#64151,#64152,#64153,#64154,#64155,
#64156,#64157,#64158,#64159,#64160,#64161),.UNSPECIFIED.,.F.,.F.,(4,3,3,
3,3,3,3,3,3,3,3,3,3,3,3,3,3,3,3,3,3,3,3,3,3,3,3,3,3,3,3,3,3,3,3,3,3,3,3,
3,3,3,3,3,3,3,3,3,3,3,3,3,3,3,3,3,3,3,3,3,3,3,3,3,3,3,3,3,3,3,3,3,3,4),
(644.026493986046,644.117348037072,644.208612587543,644.300086391216,644.391869926028,
644.448316304931,644.532055016777,644.615690528145,644.699242971544,644.782732407395,
644.866186358009,644.949622851855,645.033059961611,645.116515756529,645.200060249259,
645.2836493322,645.367372599758,645.448052315651,645.531791027497,645.615426538864,
645.698978982263,645.782468418114,645.865922368727,645.949358862573,646.032795972329,
646.116251767246,646.199796259976,646.283385342917,646.367108610474,646.447788326371,
646.531527038217,646.615162549584,646.698714992983,646.782204428834,646.865658379447,
646.949094873294,647.032531983049,647.115987777967,647.199532270696,647.283121353637,
647.366844621195,647.447524337091,647.531263048937,647.614898560304,647.698451003703,
647.781940439554,647.865394390168,647.948830884014,648.03226799377,648.115723788688,
648.199268281417,648.282857364358,648.366580631916,648.447260347811,648.530999059657,
648.614634571024,648.698187014423,648.781676450274,648.865130400887,648.948566894734,
649.032004004489,649.115459799406,649.199004292136,649.282593375077,649.366316642635,
649.446996358531,649.529508123726,649.611925056606,649.694266347022,649.776551112661,
649.858804966058,649.941040865934,650.023294820861,650.057895601715),
 .UNSPECIFIED.);
#463=B_SPLINE_CURVE_WITH_KNOTS('',3,(#64167,#64168,#64169,#64170,#64171,
#64172,#64173,#64174,#64175,#64176,#64177,#64178,#64179,#64180,#64181,#64182,
#64183,#64184,#64185,#64186,#64187,#64188,#64189,#64190,#64191,#64192,#64193,
#64194,#64195,#64196,#64197,#64198,#64199,#64200,#64201,#64202,#64203,#64204,
#64205,#64206,#64207,#64208,#64209,#64210,#64211,#64212,#64213,#64214,#64215,
#64216,#64217,#64218,#64219,#64220,#64221,#64222,#64223,#64224,#64225,#64226,
#64227,#64228,#64229,#64230,#64231,#64232,#64233,#64234,#64235,#64236,#64237,
#64238,#64239,#64240,#64241,#64242,#64243,#64244,#64245,#64246,#64247,#64248,
#64249,#64250,#64251,#64252,#64253,#64254,#64255,#64256,#64257,#64258,#64259,
#64260,#64261,#64262,#64263,#64264,#64265,#64266,#64267,#64268,#64269,#64270,
#64271,#64272,#64273,#64274,#64275,#64276,#64277,#64278,#64279,#64280,#64281,
#64282,#64283,#64284,#64285,#64286,#64287,#64288,#64289,#64290,#64291,#64292,
#64293,#64294,#64295,#64296,#64297,#64298,#64299,#64300,#64301,#64302,#64303,
#64304,#64305,#64306,#64307,#64308,#64309,#64310,#64311,#64312,#64313,#64314,
#64315,#64316,#64317,#64318,#64319,#64320,#64321,#64322,#64323,#64324,#64325,
#64326,#64327,#64328,#64329,#64330,#64331,#64332,#64333,#64334,#64335,#64336,
#64337,#64338,#64339,#64340,#64341,#64342,#64343,#64344,#64345,#64346,#64347,
#64348,#64349,#64350,#64351,#64352,#64353,#64354,#64355,#64356,#64357,#64358,
#64359,#64360,#64361,#64362,#64363,#64364,#64365,#64366,#64367,#64368,#64369,
#64370,#64371,#64372,#64373,#64374,#64375,#64376,#64377,#64378,#64379,#64380,
#64381,#64382,#64383,#64384,#64385,#64386),.UNSPECIFIED.,.F.,.F.,(4,3,3,
3,3,3,3,3,3,3,3,3,3,3,3,3,3,3,3,3,3,3,3,3,3,3,3,3,3,3,3,3,3,3,3,3,3,3,3,
3,3,3,3,3,3,3,3,3,3,3,3,3,3,3,3,3,3,3,3,3,3,3,3,3,3,3,3,3,3,3,3,3,3,4),
(650.30967929324,650.392045240159,650.474334857195,650.557065220078,650.639274880365,
650.721476155833,650.803688079595,650.88681049976,650.969142703203,651.052660231729,
651.136177760256,651.219916472102,651.303551983469,651.387104426868,651.470593862719,
651.554047813333,651.637484307179,651.720921416934,651.804377211852,651.887921704582,
651.971510787523,652.05523405508,652.135913770976,652.219652482822,652.303287994189,
652.386840437588,652.470329873438,652.553783824052,652.637220317898,652.720657427653,
652.804113222571,652.887657715301,652.971246798242,653.054970065799,653.135649781696,
653.219388493542,653.30302400491,653.386576448308,653.470065884159,653.553519834773,
653.636956328619,653.720393438375,653.803849233292,653.887393726022,653.970982808963,
654.054706076521,654.135385792416,654.219124504262,654.302760015629,654.386312459028,
654.469801894879,654.553255845492,654.636692339339,654.720129449094,654.803585244012,
654.887129736742,654.970718819683,655.05444208724,655.135121803136,655.218860514982,
655.30249602635,655.386048469748,655.469537905599,655.552991856213,655.636428350059,
655.719865459815,655.803321254733,655.886865747462,655.970454830404,656.054178097961,
656.134857813856,656.224763958492,656.314447235095,656.342563021358),
 .UNSPECIFIED.);
#464=B_SPLINE_CURVE_WITH_KNOTS('',3,(#64387,#64388,#64389,#64390,#64391,
#64392,#64393,#64394,#64395,#64396),.UNSPECIFIED.,.F.,.F.,(4,3,3,4),(650.058234024135,
650.136441749535,650.266485457141,650.309679293066),.UNSPECIFIED.);
#465=B_SPLINE_CURVE_WITH_KNOTS('',3,(#64398,#64399,#64400,#64401,#64402,
#64403,#64404,#64405,#64406,#64407),.UNSPECIFIED.,.F.,.F.,(4,3,3,4),(650.057895601715,
650.140215484069,650.224947388508,650.309679292946),.UNSPECIFIED.);
#466=B_SPLINE_CURVE_WITH_KNOTS('',3,(#64408,#64409,#64410,#64411,#64412,
#64413,#64414,#64415,#64416,#64417,#64418,#64419,#64420,#64421,#64422,#64423,
#64424,#64425,#64426,#64427,#64428,#64429,#64430,#64431,#64432,#64433,#64434,
#64435,#64436,#64437,#64438,#64439,#64440,#64441,#64442,#64443,#64444,#64445,
#64446,#64447,#64448,#64449,#64450,#64451,#64452,#64453,#64454,#64455,#64456,
#64457,#64458,#64459,#64460,#64461,#64462,#64463,#64464,#64465,#64466,#64467,
#64468,#64469,#64470,#64471,#64472,#64473,#64474,#64475,#64476,#64477,#64478,
#64479,#64480,#64481,#64482,#64483,#64484,#64485,#64486,#64487,#64488,#64489,
#64490,#64491,#64492,#64493,#64494,#64495,#64496,#64497,#64498,#64499,#64500,
#64501,#64502,#64503,#64504,#64505,#64506,#64507,#64508,#64509,#64510,#64511,
#64512,#64513,#64514,#64515,#64516,#64517,#64518,#64519,#64520,#64521,#64522,
#64523,#64524,#64525,#64526,#64527,#64528,#64529,#64530,#64531,#64532,#64533,
#64534,#64535,#64536,#64537,#64538,#64539,#64540,#64541,#64542,#64543,#64544,
#64545,#64546,#64547,#64548,#64549,#64550,#64551,#64552,#64553,#64554,#64555,
#64556,#64557,#64558,#64559,#64560,#64561,#64562,#64563,#64564,#64565,#64566,
#64567,#64568,#64569,#64570,#64571,#64572,#64573,#64574,#64575,#64576,#64577,
#64578,#64579,#64580,#64581,#64582,#64583,#64584,#64585,#64586,#64587,#64588,
#64589,#64590,#64591,#64592,#64593,#64594,#64595,#64596,#64597,#64598,#64599,
#64600,#64601,#64602,#64603,#64604,#64605,#64606,#64607,#64608,#64609,#64610,
#64611,#64612,#64613,#64614,#64615,#64616,#64617,#64618,#64619,#64620,#64621,
#64622,#64623,#64624),.UNSPECIFIED.,.F.,.F.,(4,3,3,3,3,3,3,3,3,3,3,3,3,
3,3,3,3,3,3,3,3,3,3,3,3,3,3,3,3,3,3,3,3,3,3,3,3,3,3,3,3,3,3,3,3,3,3,3,3,
3,3,3,3,3,3,3,3,3,3,3,3,3,3,3,3,3,3,3,3,3,3,3,4),(650.30967929307,650.446732369252,
650.530471081096,650.614106592462,650.697659035858,650.781148471707,650.864602422319,
650.948038916163,651.031476025916,651.114931820832,651.198476313559,651.282065396498,
651.365788664054,651.446468379972,651.530207091818,651.613842603186,651.697395046585,
651.780884482436,651.86433843305,651.947774926897,652.031212036653,652.114667831571,
652.198212324301,652.281801407242,652.3655246748,652.446204390692,652.529943102538,
652.613578613906,652.697131057305,652.780620493156,652.86407444377,652.947510937617,
653.030948047372,653.11440384229,653.19794833502,653.281537417961,653.365260685519,
653.445940401412,653.529679113258,653.613314624625,653.696867068023,653.780356503874,
653.863810454487,653.947246948333,654.030684058088,654.114139853006,654.197684345735,
654.281273428676,654.364996696233,654.445676412132,654.529415123978,654.613050635346,
654.696603078744,654.780092514595,654.863546465209,654.946982959055,655.030420068811,
655.113875863729,655.197420356458,655.281009439399,655.364732706957,655.445412422852,
655.529157188434,655.612797384195,655.696353148497,655.779840105885,655.863289581261,
655.946719663156,656.030148423237,656.113630534888,656.197140214626,656.280745214861,
656.341338735484),.UNSPECIFIED.);
#467=B_SPLINE_CURVE_WITH_KNOTS('',3,(#64630,#64631,#64632,#64633,#64634,
#64635,#64636,#64637,#64638,#64639,#64640,#64641,#64642,#64643,#64644,#64645,
#64646,#64647,#64648,#64649,#64650,#64651,#64652,#64653,#64654,#64655,#64656,
#64657,#64658,#64659,#64660,#64661,#64662,#64663,#64664,#64665,#64666,#64667,
#64668,#64669,#64670,#64671,#64672,#64673,#64674,#64675,#64676,#64677,#64678,
#64679,#64680,#64681,#64682,#64683,#64684,#64685,#64686,#64687,#64688,#64689,
#64690,#64691,#64692,#64693,#64694,#64695,#64696,#64697,#64698,#64699,#64700,
#64701,#64702,#64703,#64704,#64705,#64706,#64707,#64708,#64709,#64710,#64711,
#64712,#64713,#64714,#64715,#64716,#64717,#64718,#64719,#64720,#64721,#64722,
#64723,#64724,#64725,#64726,#64727,#64728,#64729,#64730,#64731,#64732,#64733,
#64734,#64735,#64736,#64737,#64738,#64739,#64740,#64741,#64742,#64743,#64744,
#64745,#64746,#64747,#64748,#64749,#64750,#64751,#64752,#64753,#64754,#64755,
#64756,#64757,#64758,#64759,#64760,#64761,#64762,#64763,#64764,#64765,#64766,
#64767,#64768,#64769,#64770,#64771,#64772,#64773,#64774,#64775,#64776,#64777,
#64778,#64779,#64780,#64781,#64782,#64783,#64784,#64785,#64786,#64787,#64788,
#64789,#64790,#64791,#64792,#64793,#64794,#64795,#64796,#64797,#64798,#64799,
#64800,#64801,#64802,#64803,#64804,#64805,#64806,#64807,#64808,#64809,#64810,
#64811,#64812,#64813,#64814,#64815,#64816,#64817,#64818,#64819,#64820,#64821,
#64822,#64823,#64824,#64825,#64826,#64827,#64828,#64829,#64830,#64831,#64832,
#64833,#64834,#64835,#64836,#64837,#64838,#64839,#64840,#64841,#64842,#64843,
#64844,#64845,#64846,#64847,#64848,#64849),.UNSPECIFIED.,.F.,.F.,(4,3,3,
3,3,3,3,3,3,3,3,3,3,3,3,3,3,3,3,3,3,3,3,3,3,3,3,3,3,3,3,3,3,3,3,3,3,3,3,
3,3,3,3,3,3,3,3,3,3,3,3,3,3,3,3,3,3,3,3,3,3,3,3,3,3,3,3,3,3,3,3,3,3,4),
(656.592864600246,656.678899150996,656.765001425791,656.85118441481,656.937522996922,
657.02395084777,657.110535945372,657.134593824576,657.218332536422,657.301968047789,
657.385520491188,657.469009927039,657.552463877653,657.635900371499,657.719337481254,
657.802793276172,657.886337768901,657.969926851842,658.0536501194,658.134329835296,
658.218068547142,658.301704058509,658.385256501908,658.468745937759,658.552199888373,
658.635636382219,658.719073491974,658.802529286892,658.886073779622,658.969662862563,
659.05338613012,659.134065846016,659.217804557862,659.301440069229,659.384992512628,
659.468481948479,659.551935899093,659.635372392939,659.718809502695,659.802265297612,
659.885809790342,659.969398873283,660.053122140841,660.133801856737,660.217540568583,
660.301176079951,660.384728523349,660.4682179592,660.551671909814,660.63510840366,
660.718545513416,660.802001308334,660.885545801063,660.969134884005,661.052858151562,
661.133537867457,661.217276579303,661.300912090671,661.384464534069,661.46795396992,
661.551407920534,661.63484441438,661.718281524136,661.801737319053,661.885281811783,
661.968870894724,662.052594162281,662.133273878177,662.216094422083,662.298816305874,
662.381445606525,662.464020372407,662.546567121197,662.624721185932),
 .UNSPECIFIED.);
#468=B_SPLINE_CURVE_WITH_KNOTS('',3,(#64850,#64851,#64852,#64853,#64854,
#64855,#64856,#64857,#64858,#64859),.UNSPECIFIED.,.F.,.F.,(4,3,3,4),(656.342563021358,
656.431962567064,656.52111325134,656.592864600061),.UNSPECIFIED.);
#469=B_SPLINE_CURVE_WITH_KNOTS('',3,(#64861,#64862,#64863,#64864,#64865,
#64866,#64867,#64868,#64869,#64870),.UNSPECIFIED.,.F.,.F.,(4,3,3,4),(656.341338735484,
656.425087564978,656.445148433572,656.59286460025),.UNSPECIFIED.);
#470=B_SPLINE_CURVE_WITH_KNOTS('',3,(#64871,#64872,#64873,#64874,#64875,
#64876,#64877,#64878,#64879,#64880,#64881,#64882,#64883,#64884,#64885,#64886,
#64887,#64888,#64889,#64890,#64891,#64892,#64893,#64894,#64895,#64896,#64897,
#64898,#64899,#64900,#64901,#64902,#64903,#64904,#64905,#64906,#64907,#64908,
#64909,#64910,#64911,#64912,#64913,#64914,#64915,#64916,#64917,#64918,#64919,
#64920,#64921,#64922,#64923,#64924,#64925,#64926,#64927,#64928,#64929,#64930,
#64931,#64932,#64933,#64934,#64935,#64936,#64937,#64938,#64939,#64940,#64941,
#64942,#64943,#64944,#64945,#64946,#64947,#64948,#64949,#64950,#64951,#64952,
#64953,#64954,#64955,#64956,#64957,#64958,#64959,#64960,#64961,#64962,#64963,
#64964,#64965,#64966,#64967,#64968,#64969,#64970,#64971,#64972,#64973,#64974,
#64975,#64976,#64977,#64978,#64979,#64980,#64981,#64982,#64983,#64984,#64985,
#64986,#64987,#64988,#64989,#64990,#64991,#64992,#64993,#64994,#64995,#64996,
#64997,#64998,#64999,#65000,#65001,#65002,#65003,#65004,#65005,#65006,#65007,
#65008,#65009,#65010,#65011,#65012,#65013,#65014,#65015,#65016,#65017,#65018,
#65019,#65020,#65021,#65022,#65023,#65024,#65025,#65026,#65027,#65028,#65029,
#65030,#65031,#65032,#65033,#65034,#65035,#65036,#65037,#65038,#65039,#65040,
#65041,#65042,#65043,#65044,#65045,#65046,#65047,#65048,#65049,#65050,#65051,
#65052,#65053,#65054,#65055,#65056,#65057,#65058,#65059,#65060,#65061,#65062,
#65063,#65064,#65065,#65066,#65067,#65068,#65069,#65070,#65071,#65072,#65073,
#65074,#65075,#65076,#65077,#65078,#65079,#65080,#65081,#65082,#65083,#65084,
#65085,#65086,#65087,#65088,#65089,#65090),.UNSPECIFIED.,.F.,.F.,(4,3,3,
3,3,3,3,3,3,3,3,3,3,3,3,3,3,3,3,3,3,3,3,3,3,3,3,3,3,3,3,3,3,3,3,3,3,3,3,
3,3,3,3,3,3,3,3,3,3,3,3,3,3,3,3,3,3,3,3,3,3,3,3,3,3,3,3,3,3,3,3,3,3,4),
(656.592864600365,656.675275781259,656.757604299598,656.843514317685,656.925747554104,
657.007967410282,657.090192909171,657.17244307627,657.254781085733,657.337170879931,
657.419676421055,657.444884444292,657.528623156138,657.612258667505,657.695811110904,
657.779300546755,657.862754497369,657.946190991215,658.02962810097,658.113083895888,
658.196628388618,658.280217471559,658.363940739116,658.444620455012,658.528359166858,
658.611994678226,658.695547121624,658.779036557476,658.862490508089,658.945927001936,
659.029364111691,659.112819906609,659.196364399339,659.27995348228,659.363676749838,
659.444356465733,659.528095177579,659.611730688947,659.695283132345,659.778772568196,
659.86222651881,659.945663012656,660.029100122411,660.112555917329,660.196100410059,
660.279689493,660.363412760557,660.444092476453,660.527831188299,660.611466699666,
660.695019143065,660.778508578915,660.861962529529,660.945399023375,661.02883613313,
661.112291928048,661.195836420778,661.279425503719,661.363148771276,661.443828487173,
661.527567199019,661.611202710387,661.694755153785,661.778244589636,661.86169854025,
661.945135034096,662.028572143852,662.112027938769,662.195572431499,662.27916151444,
662.362884781998,662.443564497893,662.534703199586,662.62573256838),
 .UNSPECIFIED.);
#471=B_SPLINE_CURVE_WITH_KNOTS('',3,(#65096,#65097,#65098,#65099,#65100,
#65101,#65102,#65103,#65104,#65105,#65106,#65107,#65108,#65109,#65110,#65111,
#65112,#65113,#65114,#65115,#65116,#65117,#65118,#65119,#65120,#65121,#65122,
#65123,#65124,#65125,#65126,#65127,#65128,#65129,#65130,#65131,#65132,#65133,
#65134,#65135,#65136,#65137,#65138,#65139,#65140,#65141,#65142,#65143,#65144,
#65145,#65146,#65147,#65148,#65149,#65150,#65151,#65152,#65153,#65154,#65155,
#65156,#65157,#65158,#65159,#65160,#65161,#65162,#65163,#65164,#65165,#65166,
#65167,#65168,#65169,#65170,#65171,#65172,#65173,#65174,#65175,#65176,#65177,
#65178,#65179,#65180,#65181,#65182,#65183,#65184,#65185,#65186,#65187,#65188,
#65189,#65190,#65191,#65192,#65193,#65194,#65195,#65196,#65197,#65198,#65199,
#65200,#65201,#65202,#65203,#65204,#65205,#65206,#65207,#65208,#65209,#65210,
#65211,#65212,#65213,#65214,#65215,#65216,#65217,#65218,#65219,#65220,#65221,
#65222,#65223,#65224,#65225,#65226,#65227,#65228,#65229,#65230,#65231,#65232,
#65233,#65234,#65235,#65236,#65237,#65238,#65239,#65240,#65241,#65242,#65243,
#65244,#65245,#65246,#65247,#65248,#65249,#65250,#65251,#65252,#65253,#65254,
#65255,#65256,#65257,#65258,#65259,#65260,#65261,#65262,#65263,#65264,#65265,
#65266,#65267,#65268,#65269,#65270,#65271,#65272,#65273,#65274,#65275,#65276,
#65277,#65278,#65279,#65280,#65281,#65282,#65283,#65284,#65285,#65286,#65287,
#65288,#65289,#65290,#65291,#65292,#65293,#65294,#65295,#65296,#65297,#65298,
#65299,#65300,#65301,#65302,#65303,#65304,#65305,#65306,#65307,#65308,#65309,
#65310,#65311,#65312,#65313,#65314,#65315),.UNSPECIFIED.,.F.,.F.,(4,3,3,
3,3,3,3,3,3,3,3,3,3,3,3,3,3,3,3,3,3,3,3,3,3,3,3,3,3,3,3,3,3,3,3,3,3,3,3,
3,3,3,3,3,3,3,3,3,3,3,3,3,3,3,3,3,3,3,3,3,3,3,3,3,3,3,3,3,3,3,3,3,3,4),
(662.876049907546,662.982197863683,663.09054757415,663.133009888897,663.216748600743,
663.30038411211,663.383936555509,663.46742599136,663.550879941973,663.63431643582,
663.717753545575,663.801209340493,663.884753833222,663.968342916163,664.052066183721,
664.132745899617,664.216484611463,664.30012012283,664.383672566229,664.46716200208,
664.550615952693,664.634052446539,664.717489556295,664.800945351212,664.884489843942,
664.968078926883,665.051802194441,665.132481910337,665.216220622183,665.299856133551,
665.383408576949,665.4668980128,665.550351963414,665.63378845726,665.717225567016,
665.800681361934,665.884225854663,665.967814937604,666.051538205162,666.132217921057,
666.215956632903,666.29959214427,666.383144587669,666.46663402352,666.550087974134,
666.63352446798,666.716961577735,666.800417372653,666.883961865383,666.967550948324,
667.051274215882,667.131953931778,667.215692643624,667.299328154991,667.38288059839,
667.466370034241,667.549823984855,667.633260478701,667.716697588457,667.800153383375,
667.883697876104,667.967286959046,668.051010226603,668.131689942498,668.215442308325,
668.301958335874,668.385500331567,668.468985102343,668.55243076802,668.635855418049,
668.719297398319,668.802750389247,668.886256829366,668.907570528719),
 .UNSPECIFIED.);
#472=B_SPLINE_CURVE_WITH_KNOTS('',3,(#65316,#65317,#65318,#65319,#65320,
#65321,#65322,#65323,#65324,#65325),.UNSPECIFIED.,.F.,.F.,(4,3,3,4),(662.624721185932,
662.707261065595,662.79165548651,662.876049907425),.UNSPECIFIED.);
#473=B_SPLINE_CURVE_WITH_KNOTS('',3,(#65327,#65328,#65329,#65330,#65331,
#65332,#65333,#65334,#65335,#65336),.UNSPECIFIED.,.F.,.F.,(4,3,3,4),(662.62573256838,
662.716437538103,662.806823242474,662.876049907294),.UNSPECIFIED.);
#474=B_SPLINE_CURVE_WITH_KNOTS('',3,(#65337,#65338,#65339,#65340,#65341,
#65342,#65343,#65344,#65345,#65346,#65347,#65348,#65349,#65350,#65351,#65352,
#65353,#65354,#65355,#65356,#65357,#65358,#65359,#65360,#65361,#65362,#65363,
#65364,#65365,#65366,#65367,#65368,#65369,#65370,#65371,#65372,#65373,#65374,
#65375,#65376,#65377,#65378,#65379,#65380,#65381,#65382,#65383,#65384,#65385,
#65386,#65387,#65388,#65389,#65390,#65391,#65392,#65393,#65394,#65395,#65396,
#65397,#65398,#65399,#65400,#65401,#65402,#65403,#65404,#65405,#65406,#65407,
#65408,#65409,#65410,#65411,#65412,#65413,#65414,#65415,#65416,#65417,#65418,
#65419,#65420,#65421,#65422,#65423,#65424,#65425,#65426,#65427,#65428,#65429,
#65430,#65431,#65432,#65433,#65434,#65435,#65436,#65437,#65438,#65439,#65440,
#65441,#65442,#65443,#65444,#65445,#65446,#65447,#65448,#65449,#65450,#65451,
#65452,#65453,#65454,#65455,#65456,#65457,#65458,#65459,#65460,#65461,#65462,
#65463,#65464,#65465,#65466,#65467,#65468,#65469,#65470,#65471,#65472,#65473,
#65474,#65475,#65476,#65477,#65478,#65479,#65480,#65481,#65482,#65483,#65484,
#65485,#65486,#65487,#65488,#65489,#65490,#65491,#65492,#65493,#65494,#65495,
#65496,#65497,#65498,#65499,#65500,#65501,#65502,#65503,#65504,#65505,#65506,
#65507,#65508,#65509,#65510,#65511,#65512,#65513,#65514,#65515,#65516,#65517,
#65518,#65519,#65520,#65521,#65522,#65523,#65524,#65525,#65526,#65527,#65528,
#65529,#65530,#65531,#65532,#65533,#65534,#65535,#65536,#65537,#65538,#65539,
#65540,#65541,#65542,#65543,#65544,#65545,#65546,#65547,#65548,#65549,#65550,
#65551,#65552,#65553,#65554,#65555,#65556),.UNSPECIFIED.,.F.,.F.,(4,3,3,
3,3,3,3,3,3,3,3,3,3,3,3,3,3,3,3,3,3,3,3,3,3,3,3,3,3,3,3,3,3,3,3,3,3,3,3,
3,3,3,3,3,3,3,3,3,3,3,3,3,3,3,3,3,3,3,3,3,3,3,3,3,3,3,3,3,3,3,3,3,3,4),
(662.876049907429,662.961381766709,663.046759126554,663.13219678947,663.217771747914,
663.303421489595,663.389228574437,663.443300508613,663.527039220459,663.610674731827,
663.694227175225,663.777716611076,663.86117056169,663.944607055536,664.028044165291,
664.111499960209,664.195044452939,664.27863353588,664.362356803438,664.443036519333,
664.526775231179,664.610410742546,664.693963185945,664.777452621796,664.860906572409,
664.944343066256,665.027780176011,665.111235970929,665.194780463659,665.2783695466,
665.362092814157,665.442772530053,665.526511241899,665.610146753267,665.693699196665,
665.777188632516,665.86064258313,665.944079076976,666.027516186732,666.11097198165,
666.194516474379,666.27810555732,666.361828824878,666.442508540774,666.52624725262,
666.609882763988,666.693435207386,666.776924643237,666.860378593851,666.943815087697,
667.027252197452,667.11070799237,667.1942524851,667.277841568041,667.361564835599,
667.442244551494,667.52598326334,667.609618774707,667.693171218105,667.776660653956,
667.86011460457,667.943551098416,668.026988208172,668.110444003089,668.193988495819,
668.27757757876,668.361300846318,668.441980562214,668.525035095247,668.607989231031,
668.690846703051,668.773648117135,668.856413159468,668.908036453214),
 .UNSPECIFIED.);
#475=B_SPLINE_CURVE_WITH_KNOTS('',3,(#65562,#65563,#65564,#65565,#65566,
#65567,#65568,#65569,#65570,#65571,#65572,#65573,#65574,#65575,#65576,#65577,
#65578,#65579,#65580,#65581,#65582,#65583,#65584,#65585,#65586,#65587,#65588,
#65589,#65590,#65591,#65592,#65593,#65594,#65595,#65596,#65597,#65598,#65599,
#65600,#65601,#65602,#65603,#65604,#65605,#65606,#65607,#65608,#65609,#65610,
#65611,#65612,#65613,#65614,#65615,#65616,#65617,#65618,#65619,#65620,#65621,
#65622,#65623,#65624,#65625,#65626,#65627,#65628,#65629,#65630,#65631,#65632,
#65633,#65634,#65635,#65636,#65637,#65638,#65639,#65640,#65641,#65642,#65643,
#65644,#65645,#65646,#65647,#65648,#65649,#65650,#65651,#65652,#65653,#65654,
#65655,#65656,#65657,#65658,#65659,#65660,#65661,#65662,#65663,#65664,#65665,
#65666,#65667,#65668,#65669,#65670,#65671,#65672,#65673,#65674,#65675,#65676,
#65677,#65678,#65679,#65680,#65681,#65682,#65683,#65684,#65685,#65686,#65687,
#65688,#65689,#65690,#65691,#65692,#65693,#65694,#65695,#65696,#65697,#65698,
#65699,#65700,#65701,#65702,#65703,#65704,#65705,#65706,#65707,#65708,#65709,
#65710,#65711,#65712,#65713,#65714,#65715,#65716,#65717,#65718,#65719,#65720,
#65721,#65722,#65723,#65724,#65725,#65726,#65727,#65728,#65729,#65730,#65731,
#65732,#65733,#65734,#65735,#65736,#65737,#65738,#65739,#65740,#65741,#65742,
#65743,#65744,#65745,#65746,#65747,#65748,#65749,#65750,#65751,#65752,#65753,
#65754,#65755,#65756,#65757,#65758,#65759,#65760,#65761,#65762,#65763,#65764,
#65765,#65766,#65767,#65768,#65769,#65770,#65771,#65772,#65773,#65774,#65775,
#65776,#65777,#65778,#65779,#65780,#65781),.UNSPECIFIED.,.F.,.F.,(4,3,3,
3,3,3,3,3,3,3,3,3,3,3,3,3,3,3,3,3,3,3,3,3,3,3,3,3,3,3,3,3,3,3,3,3,3,3,3,
3,3,3,3,3,3,3,3,3,3,3,3,3,3,3,3,3,3,3,3,3,3,3,3,3,3,3,3,3,3,3,3,3,3,4),
(669.15923521473,669.242583325641,669.325829362661,669.408993848178,669.492097229402,
669.575167966028,669.65822368116,669.741282795814,669.824363729774,669.907533798707,
669.990751938535,670.07409677329,670.131161963938,670.214900675784,670.298536187151,
670.38208863055,670.465578066401,670.549032017015,670.632468510861,670.715905620616,
670.799361415534,670.882905908263,670.966494991204,671.050218258762,671.130897974658,
671.214636686504,671.298272197871,671.38182464127,671.465314077121,671.548768027735,
671.632204521581,671.715641631337,671.799097426254,671.882641918984,671.966231001925,
672.049954269483,672.130633985378,672.214372697224,672.298008208592,672.38156065199,
672.465050087841,672.548504038455,672.631940532301,672.715377642056,672.798833436974,
672.882377929704,672.965967012645,673.049690280202,673.130369996098,673.214108707944,
673.297744219312,673.38129666271,673.464786098561,673.548240049175,673.631676543021,
673.715113652777,673.798569447694,673.882113940424,673.965703023365,674.049426290923,
674.130106006818,674.213844718664,674.297480230032,674.38103267343,674.464522109281,
674.547976059895,674.631412553741,674.714849663497,674.798305458415,674.881849951144,
674.965439034085,675.049162301643,675.129842017539,675.19171294655),
 .UNSPECIFIED.);
#476=B_SPLINE_CURVE_WITH_KNOTS('',3,(#65782,#65783,#65784,#65785,#65786,
#65787,#65788,#65789,#65790,#65791,#65792,#65793,#65794),.UNSPECIFIED.,
 .F.,.F.,(4,3,3,3,4),(668.907570528719,668.991175516459,669.074907715256,
669.131425953218,669.159235214605),.UNSPECIFIED.);
#477=B_SPLINE_CURVE_WITH_KNOTS('',3,(#65796,#65797,#65798,#65799,#65800,
#65801,#65802,#65803,#65804,#65805),.UNSPECIFIED.,.F.,.F.,(4,3,3,4),(668.908036453214,
668.990790070795,669.075012642702,669.159235214609),.UNSPECIFIED.);
#478=B_SPLINE_CURVE_WITH_KNOTS('',3,(#65806,#65807,#65808,#65809,#65810,
#65811,#65812,#65813,#65814,#65815,#65816,#65817,#65818,#65819,#65820,#65821,
#65822,#65823,#65824,#65825,#65826,#65827,#65828,#65829,#65830,#65831,#65832,
#65833,#65834,#65835,#65836,#65837,#65838,#65839,#65840,#65841,#65842,#65843,
#65844,#65845,#65846,#65847,#65848,#65849,#65850,#65851,#65852,#65853,#65854,
#65855,#65856,#65857,#65858,#65859,#65860,#65861,#65862,#65863,#65864,#65865,
#65866,#65867,#65868,#65869,#65870,#65871,#65872,#65873,#65874,#65875,#65876,
#65877,#65878,#65879,#65880,#65881,#65882,#65883,#65884,#65885,#65886,#65887,
#65888,#65889,#65890,#65891,#65892,#65893,#65894,#65895,#65896,#65897,#65898,
#65899,#65900,#65901,#65902,#65903,#65904,#65905,#65906,#65907,#65908,#65909,
#65910,#65911,#65912,#65913,#65914,#65915,#65916,#65917,#65918,#65919,#65920,
#65921,#65922,#65923,#65924,#65925,#65926,#65927,#65928,#65929,#65930,#65931,
#65932,#65933,#65934,#65935,#65936,#65937,#65938,#65939,#65940,#65941,#65942,
#65943,#65944,#65945,#65946,#65947,#65948,#65949,#65950,#65951,#65952,#65953,
#65954,#65955,#65956,#65957,#65958,#65959,#65960,#65961,#65962,#65963,#65964,
#65965,#65966,#65967,#65968,#65969,#65970,#65971,#65972,#65973,#65974,#65975,
#65976,#65977,#65978,#65979,#65980,#65981,#65982,#65983,#65984,#65985,#65986,
#65987,#65988,#65989,#65990,#65991,#65992,#65993,#65994,#65995,#65996,#65997,
#65998,#65999,#66000,#66001,#66002,#66003,#66004,#66005,#66006,#66007,#66008,
#66009,#66010,#66011,#66012,#66013,#66014,#66015,#66016,#66017,#66018,#66019,
#66020,#66021,#66022),.UNSPECIFIED.,.F.,.F.,(4,3,3,3,3,3,3,3,3,3,3,3,3,
3,3,3,3,3,3,3,3,3,3,3,3,3,3,3,3,3,3,3,3,3,3,3,3,3,3,3,3,3,3,3,3,3,3,3,3,
3,3,3,3,3,3,3,3,3,3,3,3,3,3,3,3,3,3,3,3,3,3,3,4),(669.159235214725,669.261852727765,
669.366077895762,669.441716572934,669.52545528478,669.609090796147,669.692643239546,
669.776132675397,669.85958662601,669.943023119857,670.026460229612,670.10991602453,
670.193460517259,670.2770496002,670.360772867758,670.441452583654,670.5251912955,
670.608826806867,670.692379250266,670.775868686117,670.85932263673,670.942759130577,
671.026196240332,671.10965203525,671.193196527979,671.27678561092,671.360508878478,
671.441188594374,671.52492730622,671.608562817588,671.692115260986,671.775604696837,
671.859058647451,671.942495141297,672.025932251052,672.10938804597,672.1929325387,
672.276521621641,672.360244889198,672.440924605094,672.52466331694,672.608298828308,
672.691851271706,672.775340707557,672.858794658171,672.942231152017,673.025668261773,
673.109124056691,673.19266854942,673.276257632361,673.359980899919,673.440660615815,
673.524399327661,673.608034839029,673.691587282427,673.775076718278,673.858530668892,
673.941967162738,674.025404272494,674.108860067412,674.192404560142,674.275993643083,
674.35971691064,674.440396626535,674.524150690143,674.60777218701,674.691317187497,
674.774803857193,674.858250318129,674.941693339784,675.025130422603,675.108618520543,
675.190769163306),.UNSPECIFIED.);
#479=B_SPLINE_CURVE_WITH_KNOTS('',3,(#66028,#66029,#66030,#66031,#66032,
#66033,#66034,#66035,#66036,#66037,#66038,#66039,#66040,#66041,#66042,#66043,
#66044,#66045,#66046,#66047,#66048,#66049,#66050,#66051,#66052,#66053,#66054,
#66055,#66056,#66057,#66058,#66059,#66060,#66061,#66062,#66063,#66064,#66065,
#66066,#66067,#66068,#66069,#66070,#66071,#66072,#66073,#66074,#66075,#66076,
#66077,#66078,#66079,#66080,#66081,#66082,#66083,#66084,#66085,#66086,#66087,
#66088,#66089,#66090,#66091,#66092,#66093,#66094,#66095,#66096,#66097,#66098,
#66099,#66100,#66101,#66102,#66103,#66104,#66105,#66106,#66107,#66108,#66109,
#66110,#66111,#66112,#66113,#66114,#66115,#66116,#66117,#66118,#66119,#66120,
#66121,#66122,#66123,#66124,#66125,#66126,#66127,#66128,#66129,#66130,#66131,
#66132,#66133,#66134,#66135,#66136,#66137,#66138,#66139,#66140,#66141,#66142,
#66143,#66144,#66145,#66146,#66147,#66148,#66149,#66150,#66151,#66152,#66153,
#66154,#66155,#66156,#66157,#66158,#66159,#66160,#66161,#66162,#66163,#66164,
#66165,#66166,#66167,#66168,#66169,#66170,#66171,#66172,#66173,#66174,#66175,
#66176,#66177,#66178,#66179,#66180,#66181,#66182,#66183,#66184,#66185,#66186,
#66187,#66188,#66189,#66190,#66191,#66192,#66193,#66194,#66195,#66196,#66197,
#66198,#66199,#66200,#66201,#66202,#66203,#66204,#66205,#66206,#66207,#66208,
#66209,#66210,#66211,#66212,#66213,#66214,#66215,#66216,#66217,#66218,#66219,
#66220,#66221,#66222,#66223,#66224,#66225,#66226,#66227,#66228,#66229,#66230,
#66231,#66232,#66233,#66234,#66235,#66236,#66237,#66238,#66239,#66240,#66241,
#66242,#66243,#66244,#66245,#66246,#66247),.UNSPECIFIED.,.F.,.F.,(4,3,3,
3,3,3,3,3,3,3,3,3,3,3,3,3,3,3,3,3,3,3,3,3,3,3,3,3,3,3,3,3,3,3,3,3,3,3,3,
3,3,3,3,3,3,3,3,3,3,3,3,3,3,3,3,3,3,3,3,3,3,3,3,3,3,3,3,3,3,3,3,3,3,4),
(675.442420521784,675.528315210093,675.611410310749,675.694502128589,675.777609010005,
675.860749307999,675.943986969613,676.027282886383,676.110698695133,676.129578028259,
676.213316740105,676.296952251472,676.380504694871,676.463994130722,676.547448081336,
676.630884575182,676.714321684938,676.797777479856,676.881321972585,676.964911055526,
677.048634323084,677.129314038979,677.213052750825,677.296688262192,677.380240705591,
677.463730141442,677.547184092056,677.630620585902,677.714057695657,677.797513490575,
677.881057983305,677.964647066246,678.048370333803,678.129050049699,678.212788761545,
678.296424272913,678.379976716311,678.463466152162,678.546920102776,678.630356596622,
678.713793706377,678.797249501295,678.880793994025,678.964383076966,679.048106344523,
679.128786060419,679.212524772265,679.296160283633,679.379712727031,679.463202162882,
679.546656113496,679.630092607342,679.713529717097,679.796985512015,679.880530004744,
679.964119087685,680.047842355243,680.128522071139,680.212260782985,680.295896294352,
680.379448737751,680.462938173603,680.546392124216,680.629828618062,680.713265727818,
680.796721522735,680.880266015465,680.963855098406,681.047578365964,681.128258081859,
681.214942907917,681.299856777557,681.387427081823,681.47499738609),
 .UNSPECIFIED.);
#480=B_SPLINE_CURVE_WITH_KNOTS('',3,(#66248,#66249,#66250,#66251,#66252,
#66253,#66254,#66255,#66256,#66257),.UNSPECIFIED.,.F.,.F.,(4,3,3,4),(675.19171294655,
675.291977238445,675.391163108053,675.442420521618),.UNSPECIFIED.);
#481=B_SPLINE_CURVE_WITH_KNOTS('',3,(#66259,#66260,#66261,#66262,#66263,
#66264,#66265,#66266,#66267,#66268,#66269,#66270,#66271),.UNSPECIFIED.,
 .F.,.F.,(4,3,3,3,4),(675.190769163306,675.274357383231,675.358080193425,
675.440132637255,675.442420521788),.UNSPECIFIED.);
#482=B_SPLINE_CURVE_WITH_KNOTS('',3,(#66272,#66273,#66274,#66275,#66276,
#66277,#66278,#66279,#66280,#66281,#66282,#66283,#66284,#66285,#66286,#66287,
#66288,#66289,#66290,#66291,#66292,#66293,#66294,#66295,#66296,#66297,#66298,
#66299,#66300,#66301,#66302,#66303,#66304,#66305,#66306,#66307,#66308,#66309,
#66310,#66311,#66312,#66313,#66314,#66315,#66316,#66317,#66318,#66319,#66320,
#66321,#66322,#66323,#66324,#66325,#66326,#66327,#66328,#66329,#66330,#66331,
#66332,#66333,#66334,#66335,#66336,#66337,#66338,#66339,#66340,#66341,#66342,
#66343,#66344,#66345,#66346,#66347,#66348,#66349,#66350,#66351,#66352,#66353,
#66354,#66355,#66356,#66357,#66358,#66359,#66360,#66361,#66362,#66363,#66364,
#66365,#66366,#66367,#66368,#66369,#66370,#66371,#66372,#66373,#66374,#66375,
#66376,#66377,#66378,#66379,#66380,#66381,#66382,#66383,#66384,#66385,#66386,
#66387,#66388,#66389,#66390,#66391,#66392,#66393,#66394,#66395,#66396,#66397,
#66398,#66399,#66400,#66401,#66402,#66403,#66404,#66405,#66406,#66407,#66408,
#66409,#66410,#66411,#66412,#66413,#66414,#66415,#66416,#66417,#66418,#66419,
#66420,#66421,#66422,#66423,#66424,#66425,#66426,#66427,#66428,#66429,#66430,
#66431,#66432,#66433,#66434,#66435,#66436,#66437,#66438,#66439,#66440,#66441,
#66442,#66443,#66444,#66445,#66446,#66447,#66448,#66449,#66450,#66451,#66452,
#66453,#66454,#66455,#66456,#66457,#66458,#66459,#66460,#66461,#66462,#66463,
#66464,#66465,#66466,#66467,#66468,#66469,#66470,#66471,#66472,#66473,#66474,
#66475,#66476,#66477,#66478,#66479,#66480,#66481,#66482,#66483,#66484,#66485,
#66486,#66487,#66488,#66489,#66490,#66491),.UNSPECIFIED.,.F.,.F.,(4,3,3,
3,3,3,3,3,3,3,3,3,3,3,3,3,3,3,3,3,3,3,3,3,3,3,3,3,3,3,3,3,3,3,3,3,3,3,3,
3,3,3,3,3,3,3,3,3,3,3,3,3,3,3,3,3,3,3,3,3,3,3,3,3,3,3,3,3,3,3,3,3,3,4),
(675.442420521969,675.526124572569,675.6097254465,675.693243313824,675.776698272257,
675.860117909839,675.943520249349,676.026923396924,676.110345455421,676.193856225904,
676.277411853459,676.361101048798,676.439868647975,676.523607359821,676.607242871188,
676.690795314587,676.774284750438,676.857738701052,676.941175194898,677.024612304653,
677.10806809957,677.1916125923,677.275201675241,677.358924942799,677.439604658695,
677.523343370541,677.606978881909,677.690531325307,677.774020761158,677.857474711772,
677.940911205618,678.024348315373,678.107804110291,678.191348603021,678.274937685962,
678.358660953519,678.439340669415,678.523079381261,678.606714892628,678.690267336027,
678.773756771878,678.857210722491,678.940647216338,679.024084326093,679.107540121011,
679.191084613741,679.274673696682,679.358396964239,679.439076680135,679.522815391981,
679.606450903349,679.690003346748,679.773492782599,679.856946733213,679.940383227059,
680.023820336815,680.107276131732,680.190820624462,680.274409707403,680.358132974961,
680.438812690855,680.522551402701,680.606186914068,680.689739357467,680.773228793319,
680.856682743933,680.940119237779,681.023556347535,681.107012142452,681.190556635182,
681.274145718123,681.357868985681,681.438548701576,681.474758439067),
 .UNSPECIFIED.);
#483=B_SPLINE_CURVE_WITH_KNOTS('',3,(#66497,#66498,#66499,#66500,#66501,
#66502,#66503,#66504,#66505,#66506,#66507,#66508,#66509,#66510,#66511,#66512,
#66513,#66514,#66515,#66516,#66517,#66518,#66519,#66520,#66521,#66522,#66523,
#66524,#66525,#66526,#66527,#66528,#66529,#66530,#66531,#66532,#66533,#66534,
#66535,#66536,#66537,#66538,#66539,#66540,#66541,#66542,#66543,#66544,#66545,
#66546,#66547,#66548,#66549,#66550,#66551,#66552,#66553,#66554,#66555,#66556,
#66557,#66558,#66559,#66560,#66561,#66562,#66563,#66564,#66565,#66566,#66567,
#66568,#66569,#66570,#66571,#66572,#66573,#66574,#66575,#66576,#66577,#66578,
#66579,#66580,#66581,#66582,#66583,#66584,#66585,#66586,#66587,#66588,#66589,
#66590,#66591,#66592,#66593,#66594,#66595,#66596,#66597,#66598,#66599,#66600,
#66601,#66602,#66603,#66604,#66605,#66606,#66607,#66608,#66609,#66610,#66611,
#66612,#66613,#66614,#66615,#66616,#66617,#66618,#66619,#66620,#66621,#66622,
#66623,#66624,#66625,#66626,#66627,#66628,#66629,#66630,#66631,#66632,#66633,
#66634,#66635,#66636,#66637,#66638,#66639,#66640,#66641,#66642,#66643,#66644,
#66645,#66646,#66647,#66648,#66649,#66650,#66651,#66652,#66653,#66654,#66655,
#66656,#66657,#66658,#66659,#66660,#66661,#66662,#66663,#66664,#66665,#66666,
#66667,#66668,#66669,#66670,#66671,#66672,#66673,#66674,#66675,#66676,#66677,
#66678,#66679,#66680,#66681,#66682,#66683,#66684,#66685,#66686,#66687,#66688,
#66689,#66690,#66691,#66692,#66693,#66694,#66695,#66696,#66697,#66698,#66699,
#66700,#66701,#66702,#66703,#66704,#66705,#66706,#66707,#66708,#66709,#66710,
#66711,#66712,#66713,#66714,#66715,#66716),.UNSPECIFIED.,.F.,.F.,(4,3,3,
3,3,3,3,3,3,3,3,3,3,3,3,3,3,3,3,3,3,3,3,3,3,3,3,3,3,3,3,3,3,3,3,3,3,3,3,
3,3,3,3,3,3,3,3,3,3,3,3,3,3,3,3,3,3,3,3,3,3,3,3,3,3,3,3,3,3,3,3,3,3,4),
(681.72560582914,681.817549997391,681.90997903633,682.00265856607,682.095670523113,
682.127994092579,682.211732804426,682.295368315794,682.378920759193,682.462410195044,
682.545864145659,682.629300639506,682.712737749262,682.79619354418,682.879738036911,
682.963327119852,683.04705038741,683.1277301033,683.211468815146,683.295104326513,
683.378656769912,683.462146205763,683.545600156376,683.629036650223,683.712473759978,
683.795929554896,683.879474047625,683.963063130566,684.046786398124,684.12746611402,
684.211204825866,684.294840337233,684.378392780632,684.461882216483,684.545336167096,
684.628772660942,684.712209770698,684.795665565615,684.879210058345,684.962799141285,
685.046522408843,685.12720212474,685.210940836586,685.294576347954,685.378128791352,
685.461618227203,685.545072177817,685.628508671663,685.711945781419,685.795401576337,
685.878946069066,685.962535152007,686.046258419565,686.12693813546,686.210676847306,
686.294312358673,686.377864802072,686.461354237923,686.544808188536,686.628244682383,
686.711681792138,686.795137587055,686.878682079785,686.962271162726,687.045994430283,
687.12667414618,687.209254276124,687.291739747078,687.374149702101,687.456503213914,
687.538827688801,687.621134044061,687.703464025962,687.75697424715),
 .UNSPECIFIED.);
#484=B_SPLINE_CURVE_WITH_KNOTS('',3,(#66717,#66718,#66719,#66720,#66721,
#66722,#66723,#66724,#66725,#66726),.UNSPECIFIED.,.F.,.F.,(4,3,3,4),(681.47499738609,
681.559659480984,681.64428402035,681.725605828964),.UNSPECIFIED.);
#485=B_SPLINE_CURVE_WITH_KNOTS('',3,(#66728,#66729,#66730,#66731,#66732,
#66733,#66734,#66735,#66736,#66737),.UNSPECIFIED.,.F.,.F.,(4,3,3,4),(681.474758439067,
681.578295068869,681.680374910821,681.725605828844),.UNSPECIFIED.);
#486=B_SPLINE_CURVE_WITH_KNOTS('',3,(#66738,#66739,#66740,#66741,#66742,
#66743,#66744,#66745,#66746,#66747,#66748,#66749,#66750,#66751,#66752,#66753,
#66754,#66755,#66756,#66757,#66758,#66759,#66760,#66761,#66762,#66763,#66764,
#66765,#66766,#66767,#66768,#66769,#66770,#66771,#66772,#66773,#66774,#66775,
#66776,#66777,#66778,#66779,#66780,#66781,#66782,#66783,#66784,#66785,#66786,
#66787,#66788,#66789,#66790,#66791,#66792,#66793,#66794,#66795,#66796,#66797,
#66798,#66799,#66800,#66801,#66802,#66803,#66804,#66805,#66806,#66807,#66808,
#66809,#66810,#66811,#66812,#66813,#66814,#66815,#66816,#66817,#66818,#66819,
#66820,#66821,#66822,#66823,#66824,#66825,#66826,#66827,#66828,#66829,#66830,
#66831,#66832,#66833,#66834,#66835,#66836,#66837,#66838,#66839,#66840,#66841,
#66842,#66843,#66844,#66845,#66846,#66847,#66848,#66849,#66850,#66851,#66852,
#66853,#66854,#66855,#66856,#66857,#66858,#66859,#66860,#66861,#66862,#66863,
#66864,#66865,#66866,#66867,#66868,#66869,#66870,#66871,#66872,#66873,#66874,
#66875,#66876,#66877,#66878,#66879,#66880,#66881,#66882,#66883,#66884,#66885,
#66886,#66887,#66888,#66889,#66890,#66891,#66892,#66893,#66894,#66895,#66896,
#66897,#66898,#66899,#66900,#66901,#66902,#66903,#66904,#66905,#66906,#66907,
#66908,#66909,#66910,#66911,#66912,#66913,#66914,#66915,#66916,#66917,#66918,
#66919,#66920,#66921,#66922,#66923,#66924,#66925,#66926,#66927,#66928,#66929,
#66930,#66931,#66932,#66933,#66934,#66935,#66936,#66937,#66938,#66939,#66940,
#66941,#66942,#66943,#66944,#66945,#66946,#66947,#66948,#66949,#66950,#66951,
#66952,#66953,#66954,#66955,#66956,#66957),.UNSPECIFIED.,.F.,.F.,(4,3,3,
3,3,3,3,3,3,3,3,3,3,3,3,3,3,3,3,3,3,3,3,3,3,3,3,3,3,3,3,3,3,3,3,3,3,3,3,
3,3,3,3,3,3,3,3,3,3,3,3,3,3,3,3,3,3,3,3,3,3,3,3,3,3,3,3,3,3,3,3,3,3,4),
(681.725605828968,681.808449156847,681.891261971294,681.974061324514,682.056865823715,
682.13969407653,682.22261324518,682.305582521765,682.388677839725,682.438284712296,
682.522023424142,682.605658935509,682.689211378908,682.772700814759,682.856154765373,
682.939591259219,683.023028368974,683.106484163892,683.190028656622,683.273617739562,
683.35734100712,683.438020723016,683.521759434862,683.605394946229,683.688947389627,
683.772436825478,683.855890776091,683.939327269938,684.022764379693,684.10622017461,
684.18976466734,684.273353750281,684.357077017838,684.437756733736,684.521495445582,
684.60513095695,684.688683400348,684.772172836199,684.855626786813,684.939063280659,
685.022500390415,685.105956185333,685.189500678062,685.273089761004,685.356813028562,
685.437492744456,685.521231456302,685.604866967669,685.688419411067,685.771908846918,
685.855362797532,685.938799291378,686.022236401133,686.10569219605,686.18923668878,
686.272825771721,686.356549039278,686.437228755176,686.520967467022,686.60460297839,
686.688155421788,686.771644857639,686.855098808253,686.938535302099,687.021972411854,
687.105428206772,687.188972699502,687.272561782443,687.35628505,687.436964765896,
687.52263490387,687.608196454512,687.693631976101,687.758281420251),
 .UNSPECIFIED.);
#487=B_SPLINE_CURVE_WITH_KNOTS('',3,(#66963,#66964,#66965,#66966,#66967,
#66968,#66969,#66970,#66971,#66972,#66973,#66974,#66975,#66976,#66977,#66978,
#66979,#66980,#66981,#66982,#66983,#66984,#66985,#66986,#66987,#66988,#66989,
#66990,#66991,#66992,#66993,#66994,#66995,#66996,#66997,#66998,#66999,#67000,
#67001,#67002,#67003,#67004,#67005,#67006,#67007,#67008,#67009,#67010,#67011,
#67012,#67013,#67014,#67015,#67016,#67017,#67018,#67019,#67020,#67021,#67022,
#67023,#67024,#67025,#67026,#67027,#67028,#67029,#67030,#67031,#67032,#67033,
#67034,#67035,#67036,#67037,#67038,#67039,#67040,#67041,#67042,#67043,#67044,
#67045,#67046,#67047,#67048,#67049,#67050,#67051,#67052,#67053,#67054,#67055,
#67056,#67057,#67058,#67059,#67060,#67061,#67062,#67063,#67064,#67065,#67066,
#67067,#67068,#67069,#67070,#67071,#67072,#67073,#67074,#67075,#67076,#67077,
#67078,#67079,#67080,#67081,#67082,#67083,#67084,#67085,#67086,#67087,#67088,
#67089,#67090,#67091,#67092,#67093,#67094,#67095,#67096,#67097,#67098,#67099,
#67100,#67101,#67102,#67103,#67104,#67105,#67106,#67107,#67108,#67109,#67110,
#67111,#67112,#67113,#67114,#67115,#67116,#67117,#67118,#67119,#67120,#67121,
#67122,#67123,#67124,#67125,#67126,#67127,#67128,#67129,#67130,#67131,#67132,
#67133,#67134,#67135,#67136,#67137,#67138,#67139,#67140,#67141,#67142,#67143,
#67144,#67145,#67146,#67147,#67148,#67149,#67150,#67151,#67152,#67153,#67154,
#67155,#67156,#67157,#67158,#67159,#67160,#67161,#67162,#67163,#67164,#67165,
#67166,#67167,#67168,#67169,#67170,#67171,#67172,#67173,#67174,#67175,#67176,
#67177,#67178,#67179),.UNSPECIFIED.,.F.,.F.,(4,3,3,3,3,3,3,3,3,3,3,3,3,
3,3,3,3,3,3,3,3,3,3,3,3,3,3,3,3,3,3,3,3,3,3,3,3,3,3,3,3,3,3,3,3,3,3,3,3,
3,3,3,3,3,3,3,3,3,3,3,3,3,3,3,3,3,3,3,3,3,3,3,4),(688.008791136144,688.1264101569,
688.210148868748,688.293784380117,688.377336823517,688.460826259369,688.544280209985,
688.627716703833,688.71115381359,688.794609608509,688.87815410124,688.961743184183,
689.045466451742,689.126146167621,689.209884879467,689.293520390834,689.377072834232,
689.460562270083,689.544016220696,689.627452714542,689.710889824298,689.794345619215,
689.877890111945,689.961479194885,690.045202462443,690.125882178341,690.209620890187,
690.293256401554,690.376808844952,690.460298280803,690.543752231416,690.627188725262,
690.710625835017,690.794081629935,690.877626122664,690.961215205605,691.044938473162,
691.125618189061,691.209356900907,691.292992412275,691.376544855673,691.460034291525,
691.543488242138,691.626924735985,691.710361845741,691.793817640658,691.877362133388,
691.960951216329,692.044674483887,692.125354199781,692.209092911627,692.292728422995,
692.376280866393,692.459770302244,692.543224252858,692.626660746704,692.71009785646,
692.793553651377,692.877098144107,692.960687227048,693.044410494605,693.125090210501,
693.208833802616,693.292473082083,693.376028186146,693.459515473079,693.542965641862,
693.62639678084,693.709826961812,693.79331488005,693.87683051431,693.960451995844,
694.040510109002),.UNSPECIFIED.);
#488=B_SPLINE_CURVE_WITH_KNOTS('',3,(#67180,#67181,#67182,#67183,#67184,
#67185,#67186,#67187,#67188,#67189),.UNSPECIFIED.,.F.,.F.,(4,3,3,4),(687.75697424715,
687.839375275049,687.92408320553,688.00879113601),.UNSPECIFIED.);
#489=B_SPLINE_CURVE_WITH_KNOTS('',3,(#67191,#67192,#67193,#67194,#67195,
#67196,#67197,#67198,#67199,#67200),.UNSPECIFIED.,.F.,.F.,(4,3,3,4),(687.758281420251,
687.843572196486,687.928799866004,688.008791136148),.UNSPECIFIED.);
#490=B_SPLINE_CURVE_WITH_KNOTS('',3,(#67201,#67202,#67203,#67204,#67205,
#67206,#67207,#67208,#67209,#67210,#67211,#67212,#67213,#67214,#67215,#67216,
#67217,#67218,#67219,#67220,#67221,#67222,#67223,#67224,#67225,#67226,#67227,
#67228,#67229,#67230,#67231,#67232,#67233,#67234,#67235,#67236,#67237,#67238,
#67239,#67240,#67241,#67242,#67243,#67244,#67245,#67246,#67247,#67248,#67249,
#67250,#67251,#67252,#67253,#67254,#67255,#67256,#67257,#67258,#67259,#67260,
#67261,#67262,#67263,#67264,#67265,#67266,#67267,#67268,#67269,#67270,#67271,
#67272,#67273,#67274,#67275,#67276,#67277,#67278,#67279,#67280,#67281,#67282,
#67283,#67284,#67285,#67286,#67287,#67288,#67289,#67290,#67291,#67292,#67293,
#67294,#67295,#67296,#67297,#67298,#67299,#67300,#67301,#67302,#67303,#67304,
#67305,#67306,#67307,#67308,#67309,#67310,#67311,#67312,#67313,#67314,#67315,
#67316,#67317,#67318,#67319,#67320,#67321,#67322,#67323,#67324,#67325,#67326,
#67327,#67328,#67329,#67330,#67331,#67332,#67333,#67334,#67335,#67336,#67337,
#67338,#67339,#67340,#67341,#67342,#67343,#67344,#67345,#67346,#67347,#67348,
#67349,#67350,#67351,#67352,#67353,#67354,#67355,#67356,#67357,#67358,#67359,
#67360,#67361,#67362,#67363,#67364,#67365,#67366,#67367,#67368,#67369,#67370,
#67371,#67372,#67373,#67374,#67375,#67376,#67377,#67378,#67379,#67380,#67381,
#67382,#67383,#67384,#67385,#67386,#67387,#67388,#67389,#67390,#67391,#67392,
#67393,#67394,#67395,#67396,#67397,#67398,#67399,#67400,#67401,#67402,#67403,
#67404,#67405,#67406,#67407,#67408,#67409,#67410,#67411,#67412,#67413,#67414,
#67415,#67416,#67417,#67418,#67419,#67420),.UNSPECIFIED.,.F.,.F.,(4,3,3,
3,3,3,3,3,3,3,3,3,3,3,3,3,3,3,3,3,3,3,3,3,3,3,3,3,3,3,3,3,3,3,3,3,3,3,3,
3,3,3,3,3,3,3,3,3,3,3,3,3,3,3,3,3,3,3,3,3,3,3,3,3,3,3,3,3,3,3,3,3,3,4),
(688.008791136294,688.099325354651,688.190249693613,688.281371889162,688.372797362083,
688.436700776617,688.520439488463,688.60407499983,688.687627443229,688.77111687908,
688.854570829693,688.93800732354,689.021444433295,689.104900228213,689.188444720942,
689.272033803883,689.355757071441,689.436436787337,689.520175499183,689.60381101055,
689.687363453949,689.7708528898,689.854306840413,689.937743334259,690.021180444015,
690.104636238933,690.188180731662,690.271769814603,690.355493082161,690.436172798057,
690.519911509903,690.603547021271,690.687099464669,690.77058890052,690.854042851134,
690.93747934498,691.020916454735,691.104372249653,691.187916742383,691.271505825324,
691.355229092881,691.435908808777,691.519647520623,691.60328303199,691.686835475389,
691.77032491124,691.853778861854,691.9372153557,692.020652465456,692.104108260373,
692.187652753103,692.271241836044,692.354965103602,692.435644819497,692.519383531343,
692.60301904271,692.686571486109,692.77006092196,692.853514872574,692.93695136642,
693.020388476175,693.103844271093,693.187388763822,693.270977846763,693.354701114321,
693.435380830217,693.517877924792,693.600280114073,693.682606598185,693.76487650462,
693.847114889009,693.929335342606,694.011572191676,694.04020608688),
 .UNSPECIFIED.);
#491=B_SPLINE_CURVE_WITH_KNOTS('',3,(#67426,#67427,#67428,#67429,#67430,
#67431,#67432,#67433,#67434,#67435,#67436,#67437,#67438,#67439,#67440,#67441,
#67442,#67443,#67444,#67445,#67446,#67447,#67448,#67449,#67450,#67451,#67452,
#67453,#67454,#67455,#67456,#67457,#67458,#67459,#67460,#67461,#67462,#67463,
#67464,#67465,#67466,#67467,#67468,#67469,#67470,#67471,#67472,#67473,#67474,
#67475,#67476,#67477,#67478,#67479,#67480,#67481,#67482,#67483,#67484,#67485,
#67486,#67487,#67488,#67489,#67490,#67491,#67492,#67493,#67494,#67495,#67496,
#67497,#67498,#67499,#67500,#67501,#67502,#67503,#67504,#67505,#67506,#67507,
#67508,#67509,#67510,#67511,#67512,#67513,#67514,#67515,#67516,#67517,#67518,
#67519,#67520,#67521,#67522,#67523,#67524,#67525,#67526,#67527,#67528,#67529,
#67530,#67531,#67532,#67533,#67534,#67535,#67536,#67537,#67538,#67539,#67540,
#67541,#67542,#67543,#67544,#67545,#67546,#67547,#67548,#67549,#67550,#67551,
#67552,#67553,#67554,#67555,#67556,#67557,#67558,#67559,#67560,#67561,#67562,
#67563,#67564,#67565,#67566,#67567,#67568,#67569,#67570,#67571,#67572,#67573,
#67574,#67575,#67576,#67577,#67578,#67579,#67580,#67581,#67582,#67583,#67584,
#67585,#67586,#67587,#67588,#67589,#67590,#67591,#67592,#67593,#67594,#67595,
#67596,#67597,#67598,#67599,#67600,#67601,#67602,#67603,#67604,#67605,#67606,
#67607,#67608,#67609,#67610,#67611,#67612,#67613,#67614,#67615,#67616,#67617,
#67618,#67619,#67620,#67621,#67622,#67623,#67624,#67625,#67626,#67627,#67628,
#67629,#67630,#67631,#67632,#67633,#67634,#67635,#67636,#67637,#67638,#67639,
#67640,#67641,#67642,#67643,#67644,#67645),.UNSPECIFIED.,.F.,.F.,(4,3,3,
3,3,3,3,3,3,3,3,3,3,3,3,3,3,3,3,3,3,3,3,3,3,3,3,3,3,3,3,3,3,3,3,3,3,3,3,
3,3,3,3,3,3,3,3,3,3,3,3,3,3,3,3,3,3,3,3,3,3,3,3,3,3,3,3,3,3,3,3,3,3,4),
(694.291976443512,694.374348250688,694.456642156296,694.540132165751,694.62234238023,
694.704542973122,694.786752978043,694.871205291518,694.953534528726,695.039048380334,
695.124562231941,695.208300943787,695.291936455154,695.375488898553,695.458978334404,
695.542432285018,695.625868778864,695.709305888619,695.792761683537,695.876306176267,
695.959895259208,696.043618526765,696.124298242661,696.208036954507,696.291672465874,
696.375224909273,696.458714345123,696.542168295737,696.625604789583,696.709041899339,
696.792497694256,696.876042186986,696.959631269927,697.043354537484,697.124034253381,
697.207772965227,697.291408476594,697.374960919993,697.458450355845,697.541904306458,
697.625340800304,697.70877791006,697.792233704978,697.875778197708,697.959367280649,
698.043090548206,698.123770264101,698.207508975947,698.291144487314,698.374696930713,
698.458186366563,698.541640317177,698.625076811023,698.708513920779,698.791969715697,
698.875514208427,698.959103291368,699.042826558925,699.123506274822,699.207244986668,
699.290880498036,699.374432941434,699.457922377285,699.541376327899,699.624812821745,
699.708249931501,699.791705726419,699.875250219148,699.958839302089,700.042562569647,
700.123242285542,700.213452256298,700.303435157064,700.324858639641),
 .UNSPECIFIED.);
#492=B_SPLINE_CURVE_WITH_KNOTS('',3,(#67646,#67647,#67648,#67649,#67650,
#67651,#67652,#67653,#67654,#67655),.UNSPECIFIED.,.F.,.F.,(4,3,3,4),(694.040510109002,
694.124826221221,694.257684296808,694.291976443323),.UNSPECIFIED.);
#493=B_SPLINE_CURVE_WITH_KNOTS('',3,(#67657,#67658,#67659,#67660,#67661,
#67662,#67663,#67664,#67665,#67666),.UNSPECIFIED.,.F.,.F.,(4,3,3,4),(694.04020608688,
694.122507158593,694.207241800901,694.291976443208),.UNSPECIFIED.);
#494=B_SPLINE_CURVE_WITH_KNOTS('',3,(#67667,#67668,#67669,#67670,#67671,
#67672,#67673,#67674,#67675,#67676,#67677,#67678,#67679,#67680,#67681,#67682,
#67683,#67684,#67685,#67686,#67687,#67688,#67689,#67690,#67691,#67692,#67693,
#67694,#67695,#67696,#67697,#67698,#67699,#67700,#67701,#67702,#67703,#67704,
#67705,#67706,#67707,#67708,#67709,#67710,#67711,#67712,#67713,#67714,#67715,
#67716,#67717,#67718,#67719,#67720,#67721,#67722,#67723,#67724,#67725,#67726,
#67727,#67728,#67729,#67730,#67731,#67732,#67733,#67734,#67735,#67736,#67737,
#67738,#67739,#67740,#67741,#67742,#67743,#67744,#67745,#67746,#67747,#67748,
#67749,#67750,#67751,#67752,#67753,#67754,#67755,#67756,#67757,#67758,#67759,
#67760,#67761,#67762,#67763,#67764,#67765,#67766,#67767,#67768,#67769,#67770,
#67771,#67772,#67773,#67774,#67775,#67776,#67777,#67778,#67779,#67780,#67781,
#67782,#67783,#67784,#67785,#67786,#67787,#67788,#67789,#67790,#67791,#67792,
#67793,#67794,#67795,#67796,#67797,#67798,#67799,#67800,#67801,#67802,#67803,
#67804,#67805,#67806,#67807,#67808,#67809,#67810,#67811,#67812,#67813,#67814,
#67815,#67816,#67817,#67818,#67819,#67820,#67821,#67822,#67823,#67824,#67825,
#67826,#67827,#67828,#67829,#67830,#67831,#67832,#67833,#67834,#67835,#67836,
#67837,#67838,#67839,#67840,#67841,#67842,#67843,#67844,#67845,#67846,#67847,
#67848,#67849,#67850,#67851,#67852,#67853,#67854,#67855,#67856,#67857,#67858,
#67859,#67860,#67861,#67862,#67863,#67864,#67865,#67866,#67867,#67868,#67869,
#67870,#67871,#67872,#67873,#67874,#67875,#67876,#67877,#67878,#67879,#67880,
#67881,#67882,#67883),.UNSPECIFIED.,.F.,.F.,(4,3,3,3,3,3,3,3,3,3,3,3,3,
3,3,3,3,3,3,3,3,3,3,3,3,3,3,3,3,3,3,3,3,3,3,3,3,3,3,3,3,3,3,3,3,3,3,3,3,
3,3,3,3,3,3,3,3,3,3,3,3,3,3,3,3,3,3,3,3,3,3,3,4),(694.291976443327,694.435116840937,
694.518855552783,694.602491064151,694.686043507549,694.7695329434,694.852986894013,
694.93642338786,695.019860497615,695.103316292533,695.186860785263,695.270449868204,
695.354173135761,695.434852851657,695.518591563503,695.60222707487,695.685779518269,
695.76926895412,695.852722904734,695.93615939858,696.019596508335,696.103052303253,
696.186596795983,696.270185878924,696.353909146481,696.434588862377,696.518327574223,
696.601963085591,696.685515528989,696.76900496484,696.852458915454,696.9358954093,
697.019332519056,697.102788313974,697.186332806703,697.269921889645,697.353645157202,
697.434324873098,697.518063584944,697.601699096312,697.68525153971,697.768740975561,
697.852194926175,697.935631420021,698.019068529777,698.102524324694,698.186068817424,
698.269657900365,698.353381167923,698.434060883818,698.517799595664,698.601435107031,
698.68498755043,698.768476986281,698.851930936895,698.935367430741,699.018804540496,
699.102260335414,699.185804828143,699.269393911084,699.353117178642,699.433796894538,
699.517542031029,699.601182517174,699.684738491684,699.768225359862,699.851674632092,
699.935104396973,700.018532726135,700.102013075559,700.18552094675,700.269121009406,
700.323619593279),.UNSPECIFIED.);
#495=B_SPLINE_CURVE_WITH_KNOTS('',3,(#67889,#67890,#67891,#67892,#67893,
#67894,#67895,#67896,#67897,#67898,#67899,#67900,#67901,#67902,#67903,#67904,
#67905,#67906,#67907,#67908,#67909,#67910,#67911,#67912,#67913,#67914,#67915,
#67916,#67917,#67918,#67919,#67920,#67921,#67922,#67923,#67924,#67925,#67926,
#67927,#67928,#67929,#67930,#67931,#67932,#67933,#67934,#67935,#67936,#67937,
#67938,#67939,#67940,#67941,#67942,#67943,#67944,#67945,#67946,#67947,#67948,
#67949,#67950,#67951,#67952,#67953,#67954,#67955,#67956,#67957,#67958,#67959,
#67960,#67961,#67962,#67963,#67964,#67965,#67966,#67967,#67968,#67969,#67970,
#67971,#67972,#67973,#67974,#67975,#67976,#67977,#67978,#67979,#67980,#67981,
#67982,#67983,#67984,#67985,#67986,#67987,#67988,#67989,#67990,#67991,#67992,
#67993,#67994,#67995,#67996,#67997,#67998,#67999,#68000,#68001,#68002,#68003,
#68004,#68005,#68006,#68007,#68008,#68009,#68010,#68011,#68012,#68013,#68014,
#68015,#68016,#68017,#68018,#68019,#68020,#68021,#68022,#68023,#68024,#68025,
#68026,#68027,#68028,#68029,#68030,#68031,#68032,#68033,#68034,#68035,#68036,
#68037,#68038,#68039,#68040,#68041,#68042,#68043,#68044,#68045,#68046,#68047,
#68048,#68049,#68050,#68051,#68052,#68053,#68054,#68055,#68056,#68057,#68058,
#68059,#68060,#68061,#68062,#68063,#68064,#68065,#68066,#68067,#68068,#68069,
#68070,#68071,#68072,#68073,#68074,#68075,#68076,#68077,#68078,#68079,#68080,
#68081,#68082,#68083,#68084,#68085,#68086,#68087,#68088,#68089,#68090,#68091,
#68092,#68093,#68094,#68095,#68096,#68097,#68098,#68099,#68100,#68101,#68102,
#68103,#68104,#68105,#68106,#68107,#68108),.UNSPECIFIED.,.F.,.F.,(4,3,3,
3,3,3,3,3,3,3,3,3,3,3,3,3,3,3,3,3,3,3,3,3,3,3,3,3,3,3,3,3,3,3,3,3,3,3,3,
3,3,3,3,3,3,3,3,3,3,3,3,3,3,3,3,3,3,3,3,3,3,3,3,3,3,3,3,3,3,3,3,3,3,4),
(700.575161750503,700.661020163653,700.746940620048,700.83293660145,700.919083556154,
701.005316158823,701.091705944569,701.122978296262,701.206717008108,701.290352519475,
701.373904962874,701.457394398725,701.540848349338,701.624284843185,701.70772195294,
701.791177747857,701.874722240587,701.958311323528,702.042034591086,702.122714306982,
702.206453018828,702.290088530195,702.373640973594,702.457130409445,702.540584360059,
702.624020853905,702.70745796366,702.790913758578,702.874458251308,702.958047334249,
703.041770601806,703.122450317702,703.206189029548,703.289824540915,703.373376984314,
703.456866420165,703.540320370779,703.623756864625,703.70719397438,703.790649769298,
703.874194262028,703.957783344969,704.041506612527,704.122186328422,704.205925040268,
704.289560551635,704.373112995034,704.456602430885,704.540056381499,704.623492875345,
704.706929985101,704.790385780018,704.873930272748,704.957519355689,705.041242623247,
705.121922339142,705.205661050988,705.289296562355,705.372849005754,705.456338441604,
705.539792392218,705.623228886064,705.70666599582,705.790121790737,705.873666283467,
705.957255366407,706.040978633965,706.121658349863,706.20452908262,706.287300780193,
706.369978943579,706.452602252079,706.535195449455,706.607048847776),
 .UNSPECIFIED.);
#496=B_SPLINE_CURVE_WITH_KNOTS('',3,(#68109,#68110,#68111,#68112,#68113,
#68114,#68115,#68116,#68117,#68118),.UNSPECIFIED.,.F.,.F.,(4,3,3,4),(700.324858639641,
700.414553711888,700.503984556103,700.575161750398),.UNSPECIFIED.);
#497=B_SPLINE_CURVE_WITH_KNOTS('',3,(#68120,#68121,#68122,#68123,#68124,
#68125,#68126,#68127,#68128,#68129),.UNSPECIFIED.,.F.,.F.,(4,3,3,4),(700.323619593279,
700.407365372727,700.433532905258,700.575161750507),.UNSPECIFIED.);
#498=B_SPLINE_CURVE_WITH_KNOTS('',3,(#68130,#68131,#68132,#68133,#68134,
#68135,#68136,#68137,#68138,#68139,#68140,#68141,#68142,#68143,#68144,#68145,
#68146,#68147,#68148,#68149,#68150,#68151,#68152,#68153,#68154,#68155,#68156,
#68157,#68158,#68159,#68160,#68161,#68162,#68163,#68164,#68165,#68166,#68167,
#68168,#68169,#68170,#68171,#68172,#68173,#68174,#68175,#68176,#68177,#68178,
#68179,#68180,#68181,#68182,#68183,#68184,#68185,#68186,#68187,#68188,#68189,
#68190,#68191,#68192,#68193,#68194,#68195,#68196,#68197,#68198,#68199,#68200,
#68201,#68202,#68203,#68204,#68205,#68206,#68207,#68208,#68209,#68210,#68211,
#68212,#68213,#68214,#68215,#68216,#68217,#68218,#68219,#68220,#68221,#68222,
#68223,#68224,#68225,#68226,#68227,#68228,#68229,#68230,#68231,#68232,#68233,
#68234,#68235,#68236,#68237,#68238,#68239,#68240,#68241,#68242,#68243,#68244,
#68245,#68246,#68247,#68248,#68249,#68250,#68251,#68252,#68253,#68254,#68255,
#68256,#68257,#68258,#68259,#68260,#68261,#68262,#68263,#68264,#68265,#68266,
#68267,#68268,#68269,#68270,#68271,#68272,#68273,#68274,#68275,#68276,#68277,
#68278,#68279,#68280,#68281,#68282,#68283,#68284,#68285,#68286,#68287,#68288,
#68289,#68290,#68291,#68292,#68293,#68294,#68295,#68296,#68297,#68298,#68299,
#68300,#68301,#68302,#68303,#68304,#68305,#68306,#68307,#68308,#68309,#68310,
#68311,#68312,#68313,#68314,#68315,#68316,#68317,#68318,#68319,#68320,#68321,
#68322,#68323,#68324,#68325,#68326,#68327,#68328,#68329,#68330,#68331,#68332,
#68333,#68334,#68335,#68336,#68337,#68338,#68339,#68340,#68341,#68342,#68343,
#68344,#68345,#68346,#68347,#68348,#68349),.UNSPECIFIED.,.F.,.F.,(4,3,3,
3,3,3,3,3,3,3,3,3,3,3,3,3,3,3,3,3,3,3,3,3,3,3,3,3,3,3,3,3,3,3,3,3,3,3,3,
3,3,3,3,3,3,3,3,3,3,3,3,3,3,3,3,3,3,3,3,3,3,3,3,3,3,3,3,3,3,3,3,3,3,4),
(700.575161750627,700.657591715628,700.739937607852,700.822220561261,700.904468957315,
700.986701841693,701.068938230475,701.151197140463,701.233542912853,701.315938523513,
701.398452425323,701.433268915978,701.517007627824,701.600643139191,701.68419558259,
701.767685018441,701.851138969054,701.9345754629,702.018012572656,702.101468367573,
702.185012860303,702.268601943244,702.352325210801,702.433004926698,702.516743638544,
702.600379149912,702.68393159331,702.767421029161,702.850874979775,702.934311473621,
703.017748583377,703.101204378294,703.184748871024,703.268337953965,703.352061221523,
703.432740937418,703.516479649264,703.600115160631,703.68366760403,703.76715703988,
703.850610990494,703.93404748434,704.017484594096,704.100940389013,704.184484881743,
704.268073964684,704.351797232242,704.432476948139,704.516215659985,704.599851171352,
704.683403614751,704.766893050603,704.850347001217,704.933783495063,705.017220604818,
705.100676399736,705.184220892466,705.267809975407,705.351533242964,705.432212958859,
705.515951670705,705.599587182072,705.683139625471,705.766629061321,705.850083011935,
705.933519505781,706.016956615537,706.100412410454,706.183956903184,706.267545986125,
706.351269253682,706.431948969579,706.523434315707,706.608022324974),
 .UNSPECIFIED.);
#499=B_SPLINE_CURVE_WITH_KNOTS('',3,(#68355,#68356,#68357,#68358,#68359,
#68360,#68361,#68362,#68363,#68364,#68365,#68366,#68367,#68368,#68369,#68370,
#68371,#68372,#68373,#68374,#68375,#68376,#68377,#68378,#68379,#68380,#68381,
#68382,#68383,#68384,#68385,#68386,#68387,#68388,#68389,#68390,#68391,#68392,
#68393,#68394,#68395,#68396,#68397,#68398,#68399,#68400,#68401,#68402,#68403,
#68404,#68405,#68406,#68407,#68408,#68409,#68410,#68411,#68412,#68413,#68414,
#68415,#68416,#68417,#68418,#68419,#68420,#68421,#68422,#68423,#68424,#68425,
#68426,#68427,#68428,#68429,#68430,#68431,#68432,#68433,#68434,#68435,#68436,
#68437,#68438,#68439,#68440,#68441,#68442,#68443,#68444,#68445,#68446,#68447,
#68448,#68449,#68450,#68451,#68452,#68453,#68454,#68455,#68456,#68457,#68458,
#68459,#68460,#68461,#68462,#68463,#68464,#68465,#68466,#68467,#68468,#68469,
#68470,#68471,#68472,#68473,#68474,#68475,#68476,#68477,#68478,#68479,#68480,
#68481,#68482,#68483,#68484,#68485,#68486,#68487,#68488,#68489,#68490,#68491,
#68492,#68493,#68494,#68495,#68496,#68497,#68498,#68499,#68500,#68501,#68502,
#68503,#68504,#68505,#68506,#68507,#68508,#68509,#68510,#68511,#68512,#68513,
#68514,#68515,#68516,#68517,#68518,#68519,#68520,#68521,#68522,#68523,#68524,
#68525,#68526,#68527,#68528,#68529,#68530,#68531,#68532,#68533,#68534,#68535,
#68536,#68537,#68538,#68539,#68540,#68541,#68542,#68543,#68544,#68545,#68546,
#68547,#68548,#68549,#68550,#68551,#68552,#68553,#68554,#68555,#68556,#68557,
#68558,#68559,#68560,#68561,#68562,#68563,#68564,#68565,#68566,#68567,#68568,
#68569,#68570,#68571,#68572,#68573,#68574),.UNSPECIFIED.,.F.,.F.,(4,3,3,
3,3,3,3,3,3,3,3,3,3,3,3,3,3,3,3,3,3,3,3,3,3,3,3,3,3,3,3,3,3,3,3,3,3,3,3,
3,3,3,3,3,3,3,3,3,3,3,3,3,3,3,3,3,3,3,3,3,3,3,3,3,3,3,3,3,3,3,3,3,3,4),
(706.858347057831,706.963588322933,707.070863575414,707.121394360583,707.205133072429,
707.288768583797,707.372321027195,707.455810463046,707.539264413659,707.622700907506,
707.706138017261,707.789593812179,707.873138304909,707.95672738785,708.040450655407,
708.121130371303,708.204869083149,708.288504594516,708.372057037915,708.455546473766,
708.539000424379,708.622436918226,708.705874027981,708.789329822899,708.872874315628,
708.956463398569,709.040186666127,709.120866382023,709.204605093869,709.288240605237,
709.371793048635,709.455282484486,709.5387364351,709.622172928946,709.705610038701,
709.789065833619,709.872610326349,709.95619940929,710.039922676847,710.120602392743,
710.204341104589,710.287976615956,710.371529059355,710.455018495206,710.53847244582,
710.621908939666,710.705346049421,710.788801844339,710.872346337069,710.955935420009,
711.039658687567,711.120338403463,711.204077115309,711.287712626676,711.371265070075,
711.454754505926,711.53820845654,711.621644950386,711.705082060141,711.788537855059,
711.872082347789,711.955671430729,712.039394698287,712.120074414183,712.203827182404,
712.289582494793,712.373125247679,712.456610496607,712.540056361948,712.62750969184,
712.710950606173,712.794403120195,712.877906624947,712.889869681513),
 .UNSPECIFIED.);
#500=B_SPLINE_CURVE_WITH_KNOTS('',3,(#68575,#68576,#68577,#68578,#68579,
#68580,#68581,#68582,#68583,#68584),.UNSPECIFIED.,.F.,.F.,(4,3,3,4),(706.607048847776,
706.689634123604,706.773990590643,706.858347057682),.UNSPECIFIED.);
#501=B_SPLINE_CURVE_WITH_KNOTS('',3,(#68586,#68587,#68588,#68589,#68590,
#68591,#68592,#68593,#68594,#68595),.UNSPECIFIED.,.F.,.F.,(4,3,3,4),(706.608022324974,
706.69906592166,706.789770886259,706.858347057541),.UNSPECIFIED.);
#502=B_SPLINE_CURVE_WITH_KNOTS('',3,(#68596,#68597,#68598,#68599,#68600,
#68601,#68602,#68603,#68604,#68605,#68606,#68607,#68608,#68609,#68610,#68611,
#68612,#68613,#68614,#68615,#68616,#68617,#68618,#68619,#68620,#68621,#68622,
#68623,#68624,#68625,#68626,#68627,#68628,#68629,#68630,#68631,#68632,#68633,
#68634,#68635,#68636,#68637,#68638,#68639,#68640,#68641,#68642,#68643,#68644,
#68645,#68646,#68647,#68648,#68649,#68650,#68651,#68652,#68653,#68654,#68655,
#68656,#68657,#68658,#68659,#68660,#68661,#68662,#68663,#68664,#68665,#68666,
#68667,#68668,#68669,#68670,#68671,#68672,#68673,#68674,#68675,#68676,#68677,
#68678,#68679,#68680,#68681,#68682,#68683,#68684,#68685,#68686,#68687,#68688,
#68689,#68690,#68691,#68692,#68693,#68694,#68695,#68696,#68697,#68698,#68699,
#68700,#68701,#68702,#68703,#68704,#68705,#68706,#68707,#68708,#68709,#68710,
#68711,#68712,#68713,#68714,#68715,#68716,#68717,#68718,#68719,#68720,#68721,
#68722,#68723,#68724,#68725,#68726,#68727,#68728,#68729,#68730,#68731,#68732,
#68733,#68734,#68735,#68736,#68737,#68738,#68739,#68740,#68741,#68742,#68743,
#68744,#68745,#68746,#68747,#68748,#68749,#68750,#68751,#68752,#68753,#68754,
#68755,#68756,#68757,#68758,#68759,#68760,#68761,#68762,#68763,#68764,#68765,
#68766,#68767,#68768,#68769,#68770,#68771,#68772,#68773,#68774,#68775,#68776,
#68777,#68778,#68779,#68780,#68781,#68782,#68783,#68784,#68785,#68786,#68787,
#68788,#68789,#68790,#68791,#68792,#68793,#68794,#68795,#68796,#68797,#68798,
#68799,#68800,#68801,#68802,#68803,#68804,#68805,#68806,#68807,#68808,#68809,
#68810,#68811,#68812,#68813,#68814,#68815),.UNSPECIFIED.,.F.,.F.,(4,3,3,
3,3,3,3,3,3,3,3,3,3,3,3,3,3,3,3,3,3,3,3,3,3,3,3,3,3,3,3,3,3,3,3,3,3,3,3,
3,3,3,3,3,3,3,3,3,3,3,3,3,3,3,3,3,3,3,3,3,3,3,3,3,3,3,3,3,3,3,3,3,3,4),
(706.858347057686,706.943524770658,707.028743249084,707.114017642153,707.199425355731,
707.284904651278,707.370541464767,707.431684980299,707.515423692145,707.599059203512,
707.682611646911,707.766101082762,707.849555033376,707.932991527222,708.016428636977,
708.099884431894,708.183428924624,708.267018007565,708.350741275123,708.431420991019,
708.515159702865,708.598795214232,708.682347657631,708.765837093482,708.849291044096,
708.932727537942,709.016164647697,709.099620442615,709.183164935344,709.266754018285,
709.350477285843,709.431157001739,709.514895713585,709.598531224952,709.682083668351,
709.765573104202,709.849027054816,709.932463548662,710.015900658418,710.099356453336,
710.182900946065,710.266490029006,710.350213296563,710.430893012459,710.514631724305,
710.598267235673,710.681819679071,710.765309114922,710.848763065536,710.932199559382,
711.015636669138,711.099092464055,711.182636956785,711.266226039726,711.349949307284,
711.430629023179,711.514367735025,711.598003246393,711.681555689791,711.765045125642,
711.848499076256,711.931935570102,712.015372679857,712.098828474775,712.182372967505,
712.265962050446,712.349685318003,712.4303650339,712.513484649423,712.596503385103,
712.67942444439,712.762289006816,712.845115372263,712.890365202201),
 .UNSPECIFIED.);
#503=B_SPLINE_CURVE_WITH_KNOTS('',3,(#68821,#68822,#68823,#68824,#68825,
#68826,#68827,#68828,#68829,#68830,#68831,#68832,#68833,#68834,#68835,#68836,
#68837,#68838,#68839,#68840,#68841,#68842,#68843,#68844,#68845,#68846,#68847,
#68848,#68849,#68850,#68851,#68852,#68853,#68854,#68855,#68856,#68857,#68858,
#68859,#68860,#68861,#68862,#68863,#68864,#68865,#68866,#68867,#68868,#68869,
#68870,#68871,#68872,#68873,#68874,#68875,#68876,#68877,#68878,#68879,#68880,
#68881,#68882,#68883,#68884,#68885,#68886,#68887,#68888,#68889,#68890,#68891,
#68892,#68893,#68894,#68895,#68896,#68897,#68898,#68899,#68900,#68901,#68902,
#68903,#68904,#68905,#68906,#68907,#68908,#68909,#68910,#68911,#68912,#68913,
#68914,#68915,#68916,#68917,#68918,#68919,#68920,#68921,#68922,#68923,#68924,
#68925,#68926,#68927,#68928,#68929,#68930,#68931,#68932,#68933,#68934,#68935,
#68936,#68937,#68938,#68939,#68940,#68941,#68942,#68943,#68944,#68945,#68946,
#68947,#68948,#68949,#68950,#68951,#68952,#68953,#68954,#68955,#68956,#68957,
#68958,#68959,#68960,#68961,#68962,#68963,#68964,#68965,#68966,#68967,#68968,
#68969,#68970,#68971,#68972,#68973,#68974,#68975,#68976,#68977,#68978,#68979,
#68980,#68981,#68982,#68983,#68984,#68985,#68986,#68987,#68988,#68989,#68990,
#68991,#68992,#68993,#68994,#68995,#68996,#68997,#68998,#68999,#69000,#69001,
#69002,#69003,#69004,#69005,#69006,#69007,#69008,#69009,#69010,#69011,#69012,
#69013,#69014,#69015,#69016,#69017,#69018,#69019,#69020,#69021,#69022,#69023,
#69024,#69025,#69026,#69027,#69028,#69029,#69030,#69031,#69032,#69033,#69034,
#69035,#69036,#69037,#69038,#69039,#69040),.UNSPECIFIED.,.F.,.F.,(4,3,3,
3,3,3,3,3,3,3,3,3,3,3,3,3,3,3,3,3,3,3,3,3,3,3,3,3,3,3,3,3,3,3,3,3,3,3,3,
3,3,3,3,3,3,3,3,3,3,3,3,3,3,3,3,3,3,3,3,3,3,3,3,3,3,3,3,3,3,3,3,3,3,4),
(713.141532365062,713.224960279161,713.308285726181,713.391529154684,713.474710938694,
713.557859309706,713.640992036717,713.724127474541,713.807283976197,713.890529470755,
713.973822231279,714.057243321125,714.119546435624,714.20328514747,714.286920658837,
714.370473102236,714.453962538087,714.5374164887,714.620852982547,714.704290092302,
714.787745887219,714.871290379949,714.95487946289,715.038602730447,715.119282446344,
715.20302115819,715.286656669557,715.370209112956,715.453698548807,715.537152499421,
715.620588993267,715.704026103022,715.78748189794,715.871026390669,715.95461547361,
716.038338741168,716.119018457064,716.20275716891,716.286392680278,716.369945123676,
716.453434559527,716.536888510141,716.620325003988,716.703762113743,716.78721790866,
716.87076240139,716.954351484331,717.038074751889,717.118754467784,717.20249317963,
717.286128690997,717.369681134396,717.453170570247,717.536624520861,717.620061014707,
717.703498124462,717.786953919379,717.870498412109,717.95408749505,718.037810762608,
718.118490478504,718.20222919035,718.285864701717,718.369417145116,718.452906580967,
718.536360531581,718.619797025427,718.703234135183,718.7866899301,718.87023442283,
718.953823505771,719.037546773328,719.118226489224,719.173978139178),
 .UNSPECIFIED.);
#504=B_SPLINE_CURVE_WITH_KNOTS('',3,(#69041,#69042,#69043,#69044,#69045,
#69046,#69047,#69048,#69049,#69050,#69051,#69052,#69053),.UNSPECIFIED.,
 .F.,.F.,(4,3,3,3,4),(712.889869681513,712.973470531639,713.057200321406,
713.119810424903,713.141532364862),.UNSPECIFIED.);
#505=B_SPLINE_CURVE_WITH_KNOTS('',3,(#69055,#69056,#69057,#69058,#69059,
#69060,#69061,#69062,#69063,#69064),.UNSPECIFIED.,.F.,.F.,(4,3,3,4),(712.890365202201,
712.973179008283,713.057355686575,713.141532364866),.UNSPECIFIED.);
#506=B_SPLINE_CURVE_WITH_KNOTS('',3,(#69065,#69066,#69067,#69068,#69069,
#69070,#69071,#69072,#69073,#69074,#69075,#69076,#69077,#69078,#69079,#69080,
#69081,#69082,#69083,#69084,#69085,#69086,#69087,#69088,#69089,#69090,#69091,
#69092,#69093,#69094,#69095,#69096,#69097,#69098,#69099,#69100,#69101,#69102,
#69103,#69104,#69105,#69106,#69107,#69108,#69109,#69110,#69111,#69112,#69113,
#69114,#69115,#69116,#69117,#69118,#69119,#69120,#69121,#69122,#69123,#69124,
#69125,#69126,#69127,#69128,#69129,#69130,#69131,#69132,#69133,#69134,#69135,
#69136,#69137,#69138,#69139,#69140,#69141,#69142,#69143,#69144,#69145,#69146,
#69147,#69148,#69149,#69150,#69151,#69152,#69153,#69154,#69155,#69156,#69157,
#69158,#69159,#69160,#69161,#69162,#69163,#69164,#69165,#69166,#69167,#69168,
#69169,#69170,#69171,#69172,#69173,#69174,#69175,#69176,#69177,#69178,#69179,
#69180,#69181,#69182,#69183,#69184,#69185,#69186,#69187,#69188,#69189,#69190,
#69191,#69192,#69193,#69194,#69195,#69196,#69197,#69198,#69199,#69200,#69201,
#69202,#69203,#69204,#69205,#69206,#69207,#69208,#69209,#69210,#69211,#69212,
#69213,#69214,#69215,#69216,#69217,#69218,#69219,#69220,#69221,#69222,#69223,
#69224,#69225,#69226,#69227,#69228,#69229,#69230,#69231,#69232,#69233,#69234,
#69235,#69236,#69237,#69238,#69239,#69240,#69241,#69242,#69243,#69244,#69245,
#69246,#69247,#69248,#69249,#69250,#69251,#69252,#69253,#69254,#69255,#69256,
#69257,#69258,#69259,#69260,#69261,#69262,#69263,#69264,#69265,#69266,#69267,
#69268,#69269,#69270,#69271,#69272,#69273,#69274,#69275,#69276,#69277,#69278,
#69279,#69280,#69281),.UNSPECIFIED.,.F.,.F.,(4,3,3,3,3,3,3,3,3,3,3,3,3,
3,3,3,3,3,3,3,3,3,3,3,3,3,3,3,3,3,3,3,3,3,3,3,3,3,3,3,3,3,3,3,3,3,3,3,3,
3,3,3,3,3,3,3,3,3,3,3,3,3,3,3,3,3,3,3,3,3,3,3,4),(713.141532364993,713.243403064375,
713.346774638295,713.43010104462,713.513839756466,713.597475267833,713.681027711231,
713.764517147082,713.847971097695,713.931407591541,714.014844701296,714.098300496213,
714.181844988943,714.265434071883,714.34915733944,714.42983705534,714.513575767186,
714.597211278553,714.680763721952,714.764253157803,714.847707108416,714.931143602263,
715.014580712018,715.098036506936,715.181580999665,715.265170082606,715.348893350164,
715.42957306606,715.513311777906,715.596947289274,715.680499732673,715.763989168524,
715.847443119138,715.930879612984,716.01431672274,716.097772517657,716.181317010387,
716.264906093328,716.348629360886,716.42930907678,716.513047788626,716.596683299993,
716.680235743392,716.763725179243,716.847179129856,716.930615623702,717.014052733458,
717.097508528375,717.181053021105,717.264642104046,717.348365371603,717.4290450875,
717.512783799346,717.596419310713,717.679971754112,717.763461189963,717.846915140576,
717.930351634423,718.013788744178,718.097244539096,718.180789031825,718.264378114766,
718.348101382324,718.42878109822,718.512478123154,718.596042648195,718.679530701119,
718.762960502754,718.8463502302,718.929736147028,719.013116380725,719.096545899213,
719.173051552182),.UNSPECIFIED.);
#507=B_SPLINE_CURVE_WITH_KNOTS('',3,(#69287,#69288,#69289,#69290,#69291,
#69292,#69293,#69294,#69295,#69296,#69297,#69298,#69299,#69300,#69301,#69302,
#69303,#69304,#69305,#69306,#69307,#69308,#69309,#69310,#69311,#69312,#69313,
#69314,#69315,#69316,#69317,#69318,#69319,#69320,#69321,#69322,#69323,#69324,
#69325,#69326,#69327,#69328,#69329,#69330,#69331,#69332,#69333,#69334,#69335,
#69336,#69337,#69338,#69339,#69340,#69341,#69342,#69343,#69344,#69345,#69346,
#69347,#69348,#69349,#69350,#69351,#69352,#69353,#69354,#69355,#69356,#69357,
#69358,#69359,#69360,#69361,#69362,#69363,#69364,#69365,#69366,#69367,#69368,
#69369,#69370,#69371,#69372,#69373,#69374,#69375,#69376,#69377,#69378,#69379,
#69380,#69381,#69382,#69383,#69384,#69385,#69386,#69387,#69388,#69389,#69390,
#69391,#69392,#69393,#69394,#69395,#69396,#69397,#69398,#69399,#69400,#69401,
#69402,#69403,#69404,#69405,#69406,#69407,#69408,#69409,#69410,#69411,#69412,
#69413,#69414,#69415,#69416,#69417,#69418,#69419,#69420,#69421,#69422,#69423,
#69424,#69425,#69426,#69427,#69428,#69429,#69430,#69431,#69432,#69433,#69434,
#69435,#69436,#69437,#69438,#69439,#69440,#69441,#69442,#69443,#69444,#69445,
#69446,#69447,#69448,#69449,#69450,#69451,#69452,#69453,#69454,#69455,#69456,
#69457,#69458,#69459,#69460,#69461,#69462,#69463,#69464,#69465,#69466,#69467,
#69468,#69469,#69470,#69471,#69472,#69473,#69474,#69475,#69476,#69477,#69478,
#69479,#69480,#69481,#69482,#69483,#69484,#69485,#69486,#69487,#69488,#69489,
#69490,#69491,#69492,#69493,#69494,#69495,#69496,#69497,#69498,#69499,#69500,
#69501,#69502,#69503,#69504,#69505,#69506),.UNSPECIFIED.,.F.,.F.,(4,3,3,
3,3,3,3,3,3,3,3,3,3,3,3,3,3,3,3,3,3,3,3,3,3,3,3,3,3,3,3,3,3,3,3,3,3,3,3,
3,3,3,3,3,3,3,3,3,3,3,3,3,3,3,3,3,3,3,3,3,3,3,3,3,3,3,3,3,3,3,3,3,3,4),
(719.424717672042,719.51137327553,719.594394871942,719.677411000932,719.760440079154,
719.843500528614,719.926656899427,720.009869832851,720.093203653868,720.117962499944,
720.20170121179,720.285336723158,720.368889166556,720.452378602407,720.535832553021,
720.619269046867,720.702706156623,720.78616195154,720.86970644427,720.953295527211,
721.037018794769,721.117698510664,721.20143722251,721.285072733878,721.368625177277,
721.452114613128,721.535568563742,721.619005057588,721.702442167344,721.785897962262,
721.869442454991,721.953031537933,722.036754805491,722.117434521385,722.201173233231,
722.284808744598,722.368361187997,722.451850623848,722.535304574462,722.618741068308,
722.702178178063,722.785633972981,722.869178465711,722.952767548652,723.036490816209,
723.117170532105,723.200909243951,723.284544755318,723.368097198717,723.451586634568,
723.535040585181,723.618477079027,723.701914188783,723.785369983701,723.86891447643,
723.952503559371,724.036226826929,724.116906542825,724.200645254671,724.284280766038,
724.367833209437,724.451322645288,724.534776595901,724.618213089748,724.701650199503,
724.785105994421,724.868650487151,724.952239570092,725.03596283765,725.116642553545,
725.201811772529,725.286873489287,725.372096459385,725.457319429483),
 .UNSPECIFIED.);
#508=B_SPLINE_CURVE_WITH_KNOTS('',3,(#69507,#69508,#69509,#69510,#69511,
#69512,#69513,#69514,#69515,#69516),.UNSPECIFIED.,.F.,.F.,(4,3,3,4),(719.173978139178,
719.274963551938,719.37479293904,719.424717671885),.UNSPECIFIED.);
#509=B_SPLINE_CURVE_WITH_KNOTS('',3,(#69518,#69519,#69520,#69521,#69522,
#69523,#69524,#69525,#69526,#69527),.UNSPECIFIED.,.F.,.F.,(4,3,3,4),(719.173051552182,
719.256580922333,719.340649297114,719.424717671895),.UNSPECIFIED.);
#510=B_SPLINE_CURVE_WITH_KNOTS('',3,(#69528,#69529,#69530,#69531,#69532,
#69533,#69534,#69535,#69536,#69537,#69538,#69539,#69540,#69541,#69542,#69543,
#69544,#69545,#69546,#69547,#69548,#69549,#69550,#69551,#69552,#69553,#69554,
#69555,#69556,#69557,#69558,#69559,#69560,#69561,#69562,#69563,#69564,#69565,
#69566,#69567,#69568,#69569,#69570,#69571,#69572,#69573,#69574,#69575,#69576,
#69577,#69578,#69579,#69580,#69581,#69582,#69583,#69584,#69585,#69586,#69587,
#69588,#69589,#69590,#69591,#69592,#69593,#69594,#69595,#69596,#69597,#69598,
#69599,#69600,#69601,#69602,#69603,#69604,#69605,#69606,#69607,#69608,#69609,
#69610,#69611,#69612,#69613,#69614,#69615,#69616,#69617,#69618,#69619,#69620,
#69621,#69622,#69623,#69624,#69625,#69626,#69627,#69628,#69629,#69630,#69631,
#69632,#69633,#69634,#69635,#69636,#69637,#69638,#69639,#69640,#69641,#69642,
#69643,#69644,#69645,#69646,#69647,#69648,#69649,#69650,#69651,#69652,#69653,
#69654,#69655,#69656,#69657,#69658,#69659,#69660,#69661,#69662,#69663,#69664,
#69665,#69666,#69667,#69668,#69669,#69670,#69671,#69672,#69673,#69674,#69675,
#69676,#69677,#69678,#69679,#69680,#69681,#69682,#69683,#69684,#69685,#69686,
#69687,#69688,#69689,#69690,#69691,#69692,#69693,#69694,#69695,#69696,#69697,
#69698,#69699,#69700,#69701,#69702,#69703,#69704,#69705,#69706,#69707,#69708,
#69709,#69710,#69711,#69712,#69713,#69714,#69715,#69716,#69717,#69718,#69719,
#69720,#69721,#69722,#69723,#69724,#69725,#69726,#69727,#69728,#69729,#69730,
#69731,#69732,#69733,#69734,#69735,#69736,#69737,#69738,#69739,#69740,#69741,
#69742,#69743,#69744,#69745,#69746,#69747,#69748,#69749,#69750),
 .UNSPECIFIED.,.F.,.F.,(4,3,3,3,3,3,3,3,3,3,3,3,3,3,3,3,3,3,3,3,3,3,3,3,
3,3,3,3,3,3,3,3,3,3,3,3,3,3,3,3,3,3,3,3,3,3,3,3,3,3,3,3,3,3,3,3,3,3,3,3,
3,3,3,3,3,3,3,3,3,3,3,3,3,3,4),(719.424717672045,719.428517108941,719.512255820787,
719.595891332154,719.679443775553,719.762933211404,719.846387162017,719.929823655863,
720.013260765619,720.096716560536,720.180261053266,720.263850136207,720.347573403764,
720.428253119661,720.511991831507,720.595627342874,720.679179786273,720.762669222124,
720.846123172737,720.929559666584,721.012996776339,721.096452571257,721.179997063986,
721.263586146927,721.347309414485,721.427989130381,721.511727842227,721.595363353595,
721.678915796993,721.762405232844,721.845859183458,721.929295677304,722.01273278706,
722.096188581977,722.179733074707,722.263322157648,722.347045425206,722.427725141101,
722.511463852947,722.595099364314,722.678651807713,722.762141243564,722.845595194177,
722.929031688023,723.012468797779,723.095924592697,723.179469085426,723.263058168367,
723.346781435925,723.427461151821,723.511199863667,723.594835375035,723.678387818433,
723.761877254284,723.845331204898,723.928767698744,724.0122048085,724.095660603417,
724.179205096147,724.262794179088,724.346517446646,724.427197162541,724.510935874387,
724.594571385754,724.678123829153,724.761613265004,724.845067215618,724.928503709464,
725.011940819219,725.095396614137,725.178941106867,725.262530189808,725.346253457365,
725.426933173261,725.457020176983),.UNSPECIFIED.);
#511=B_SPLINE_CURVE_WITH_KNOTS('',3,(#69756,#69757,#69758,#69759,#69760,
#69761,#69762,#69763,#69764,#69765,#69766,#69767,#69768,#69769,#69770,#69771,
#69772,#69773,#69774,#69775,#69776,#69777,#69778,#69779,#69780,#69781,#69782,
#69783,#69784,#69785,#69786,#69787,#69788,#69789,#69790,#69791,#69792,#69793,
#69794,#69795,#69796,#69797,#69798,#69799,#69800,#69801,#69802,#69803,#69804,
#69805,#69806,#69807,#69808,#69809,#69810,#69811,#69812,#69813,#69814,#69815,
#69816,#69817,#69818,#69819,#69820,#69821,#69822,#69823,#69824,#69825,#69826,
#69827,#69828,#69829,#69830,#69831,#69832,#69833,#69834,#69835,#69836,#69837,
#69838,#69839,#69840,#69841,#69842,#69843,#69844,#69845,#69846,#69847,#69848,
#69849,#69850,#69851,#69852,#69853,#69854,#69855,#69856,#69857,#69858,#69859,
#69860,#69861,#69862,#69863,#69864,#69865,#69866,#69867,#69868,#69869,#69870,
#69871,#69872,#69873,#69874,#69875,#69876,#69877,#69878,#69879,#69880,#69881,
#69882,#69883,#69884,#69885,#69886,#69887,#69888,#69889,#69890,#69891,#69892,
#69893,#69894,#69895,#69896,#69897,#69898,#69899,#69900,#69901,#69902,#69903,
#69904,#69905,#69906,#69907,#69908,#69909,#69910,#69911,#69912,#69913,#69914,
#69915,#69916,#69917,#69918,#69919,#69920,#69921,#69922,#69923,#69924,#69925,
#69926,#69927,#69928,#69929,#69930,#69931,#69932,#69933,#69934,#69935,#69936,
#69937,#69938,#69939,#69940,#69941,#69942,#69943,#69944,#69945,#69946,#69947,
#69948,#69949,#69950,#69951,#69952,#69953,#69954,#69955,#69956,#69957,#69958,
#69959,#69960,#69961,#69962,#69963,#69964,#69965,#69966,#69967,#69968,#69969,
#69970,#69971,#69972,#69973,#69974,#69975),.UNSPECIFIED.,.F.,.F.,(4,3,3,
3,3,3,3,3,3,3,3,3,3,3,3,3,3,3,3,3,3,3,3,3,3,3,3,3,3,3,3,3,3,3,3,3,3,3,3,
3,3,3,3,3,3,3,3,3,3,3,3,3,3,3,3,3,3,3,3,3,3,3,3,3,3,3,3,3,3,3,3,3,3,4),
(725.70790297939,725.799493914464,725.891544766478,725.983832330002,726.076444867083,
726.116378564265,726.200117276111,726.283752787479,726.367305230877,726.450794666728,
726.534248617342,726.617685111188,726.701122220943,726.784578015861,726.868122508591,
726.951711591532,727.035434859089,727.116114574985,727.199853286831,727.283488798198,
727.367041241597,727.450530677448,727.533984628061,727.617421121908,727.700858231663,
727.784314026581,727.867858519311,727.951447602252,728.035170869809,728.115850585705,
728.199589297551,728.283224808918,728.366777252317,728.450266688168,728.533720638782,
728.617157132628,728.700594242383,728.784050037301,728.867594530031,728.951183612972,
729.034906880529,729.115586596425,729.199325308271,729.282960819639,729.366513263037,
729.450002698888,729.533456649502,729.616893143348,729.700330253104,729.783786048022,
729.867330540751,729.950919623692,730.03464289125,730.115322607146,730.199061318992,
730.28269683036,730.366249273758,730.449738709609,730.533192660223,730.616629154069,
730.700066263825,730.783522058743,730.867066551472,730.950655634413,731.034378901971,
731.115058617866,731.197613801789,731.280074281687,731.362459217619,731.444787698686,
731.527086567966,731.609367384702,731.691670041471,731.739280210377),
 .UNSPECIFIED.);
#512=B_SPLINE_CURVE_WITH_KNOTS('',3,(#69976,#69977,#69978,#69979,#69980,
#69981,#69982,#69983,#69984,#69985),.UNSPECIFIED.,.F.,.F.,(4,3,3,4),(725.457319429483,
725.54212344489,725.626884140274,725.707902979221),.UNSPECIFIED.);
#513=B_SPLINE_CURVE_WITH_KNOTS('',3,(#69987,#69988,#69989,#69990,#69991,
#69992,#69993,#69994,#69995,#69996),.UNSPECIFIED.,.F.,.F.,(4,3,3,4),(725.457020176983,
725.561445543817,725.664299370825,725.707902979112),.UNSPECIFIED.);
#514=B_SPLINE_CURVE_WITH_KNOTS('',3,(#69997,#69998,#69999,#70000,#70001,
#70002,#70003,#70004,#70005,#70006,#70007,#70008,#70009,#70010,#70011,#70012,
#70013,#70014,#70015,#70016,#70017,#70018,#70019,#70020,#70021,#70022,#70023,
#70024,#70025,#70026,#70027,#70028,#70029,#70030,#70031,#70032,#70033,#70034,
#70035,#70036,#70037,#70038,#70039,#70040,#70041,#70042,#70043,#70044,#70045,
#70046,#70047,#70048,#70049,#70050,#70051,#70052,#70053,#70054,#70055,#70056,
#70057,#70058,#70059,#70060,#70061,#70062,#70063,#70064,#70065,#70066,#70067,
#70068,#70069,#70070,#70071,#70072,#70073,#70074,#70075,#70076,#70077,#70078,
#70079,#70080,#70081,#70082,#70083,#70084,#70085,#70086,#70087,#70088,#70089,
#70090,#70091,#70092,#70093,#70094,#70095,#70096,#70097,#70098,#70099,#70100,
#70101,#70102,#70103,#70104,#70105,#70106,#70107,#70108,#70109,#70110,#70111,
#70112,#70113,#70114,#70115,#70116,#70117,#70118,#70119,#70120,#70121,#70122,
#70123,#70124,#70125,#70126,#70127,#70128,#70129,#70130,#70131,#70132,#70133,
#70134,#70135,#70136,#70137,#70138,#70139,#70140,#70141,#70142,#70143,#70144,
#70145,#70146,#70147,#70148,#70149,#70150,#70151,#70152,#70153,#70154,#70155,
#70156,#70157,#70158,#70159,#70160,#70161,#70162,#70163,#70164,#70165,#70166,
#70167,#70168,#70169,#70170,#70171,#70172,#70173,#70174,#70175,#70176,#70177,
#70178,#70179,#70180,#70181,#70182,#70183,#70184,#70185,#70186,#70187,#70188,
#70189,#70190,#70191,#70192,#70193,#70194,#70195,#70196,#70197,#70198,#70199,
#70200,#70201,#70202,#70203,#70204,#70205,#70206,#70207,#70208,#70209,#70210,
#70211,#70212,#70213,#70214,#70215,#70216),.UNSPECIFIED.,.F.,.F.,(4,3,3,
3,3,3,3,3,3,3,3,3,3,3,3,3,3,3,3,3,3,3,3,3,3,3,3,3,3,3,3,3,3,3,3,3,3,3,3,
3,3,3,3,3,3,3,3,3,3,3,3,3,3,3,3,3,3,3,3,3,3,3,3,3,3,3,3,3,3,3,3,3,3,4),
(725.707902979225,725.790691462221,725.873446198533,725.956185331489,726.038927518606,
726.121691416454,726.204544830995,726.287446619887,726.370475836275,726.426669183981,
726.510407895827,726.594043407194,726.677595850593,726.761085286444,726.844539237058,
726.927975730904,727.01141284066,727.094868635577,727.178413128307,727.262002211248,
727.345725478806,727.426405194702,727.510143906548,727.593779417915,727.677331861314,
727.760821297165,727.844275247779,727.927711741625,728.011148851381,728.094604646298,
728.178149139028,728.261738221969,728.345461489527,728.426141205422,728.509879917268,
728.593515428635,728.677067872034,728.760557307885,728.844011258499,728.927447752345,
729.0108848621,729.094340657017,729.177885149747,729.261474232688,729.345197500245,
729.425877216142,729.509615927988,729.593251439356,729.676803882754,729.760293318605,
729.843747269219,729.927183763065,730.01062087282,730.094076667738,730.177621160468,
730.261210243409,730.344933510966,730.425613226862,730.509351938708,730.592987450075,
730.676539893474,730.760029329326,730.84348327994,730.926919773786,731.010356883541,
731.093812678459,731.177357171189,731.26094625413,731.344669521687,731.425349237582,
731.511188461276,731.596917566492,731.682518062319,731.740599790848),
 .UNSPECIFIED.);
#515=B_SPLINE_CURVE_WITH_KNOTS('',3,(#70222,#70223,#70224,#70225,#70226,
#70227,#70228,#70229,#70230,#70231,#70232,#70233,#70234,#70235,#70236,#70237,
#70238,#70239,#70240,#70241,#70242,#70243,#70244,#70245,#70246,#70247,#70248,
#70249,#70250,#70251,#70252,#70253,#70254,#70255,#70256,#70257,#70258,#70259,
#70260,#70261,#70262,#70263,#70264,#70265,#70266,#70267,#70268,#70269,#70270,
#70271,#70272,#70273,#70274,#70275,#70276,#70277,#70278,#70279,#70280,#70281,
#70282,#70283,#70284,#70285,#70286,#70287,#70288,#70289,#70290,#70291,#70292,
#70293,#70294,#70295,#70296,#70297,#70298,#70299,#70300,#70301,#70302,#70303,
#70304,#70305,#70306,#70307,#70308,#70309,#70310,#70311,#70312,#70313,#70314,
#70315,#70316,#70317,#70318,#70319,#70320,#70321,#70322,#70323,#70324,#70325,
#70326,#70327,#70328,#70329,#70330,#70331,#70332,#70333,#70334,#70335,#70336,
#70337,#70338,#70339,#70340,#70341,#70342,#70343,#70344,#70345,#70346,#70347,
#70348,#70349,#70350,#70351,#70352,#70353,#70354,#70355,#70356,#70357,#70358,
#70359,#70360,#70361,#70362,#70363,#70364,#70365,#70366,#70367,#70368,#70369,
#70370,#70371,#70372,#70373,#70374,#70375,#70376,#70377,#70378,#70379,#70380,
#70381,#70382,#70383,#70384,#70385,#70386,#70387,#70388,#70389,#70390,#70391,
#70392,#70393,#70394,#70395,#70396,#70397,#70398,#70399,#70400,#70401,#70402,
#70403,#70404,#70405,#70406,#70407,#70408,#70409,#70410,#70411,#70412,#70413,
#70414,#70415,#70416,#70417,#70418,#70419,#70420,#70421,#70422,#70423,#70424,
#70425,#70426,#70427,#70428,#70429,#70430,#70431,#70432,#70433,#70434,#70435,
#70436,#70437,#70438),.UNSPECIFIED.,.F.,.F.,(4,3,3,3,3,3,3,3,3,3,3,3,3,
3,3,3,3,3,3,3,3,3,3,3,3,3,3,3,3,3,3,3,3,3,3,3,3,3,3,3,3,3,3,3,3,3,3,3,3,
3,3,3,3,3,3,3,3,3,3,3,3,3,3,3,3,3,3,3,3,3,3,3,4),(731.991088286401,732.114794628586,
732.198533340432,732.282168851799,732.365721295198,732.449210731049,732.532664681662,
732.616101175508,732.699538285264,732.782994080181,732.866538572911,732.950127655852,
733.033850923409,733.114530639306,733.198269351152,733.28190486252,733.365457305918,
733.448946741769,733.532400692383,733.615837186229,733.699274295985,733.782730090902,
733.866274583632,733.949863666573,734.033586934131,734.114266650026,734.198005361872,
734.281640873239,734.365193316638,734.448682752489,734.532136703102,734.615573196949,
734.699010306704,734.782466101621,734.866010594351,734.949599677292,735.033322944849,
735.114002660746,735.197741372592,735.28137688396,735.364929327358,735.448418763209,
735.531872713823,735.615309207669,735.698746317425,735.782202112342,735.865746605072,
735.949335688013,736.033058955571,736.113738671466,736.197477383312,736.28111289468,
736.364665338078,736.448154773929,736.531608724543,736.615045218389,736.698482328145,
736.781938123063,736.865482615792,736.949071698733,737.032794966291,737.113474682187,
737.197218640118,737.280858204831,737.364413513921,737.447900690298,737.531350634533,
737.614781435024,737.698211163527,737.781697233363,737.865210972875,737.948827174312,
738.022787360679),.UNSPECIFIED.);
#516=B_SPLINE_CURVE_WITH_KNOTS('',3,(#70439,#70440,#70441,#70442,#70443,
#70444,#70445,#70446,#70447,#70448),.UNSPECIFIED.,.F.,.F.,(4,3,3,4),(731.739280210377,
731.8216523665,731.906370326385,731.991088286269),.UNSPECIFIED.);
#517=B_SPLINE_CURVE_WITH_KNOTS('',3,(#70450,#70451,#70452,#70453,#70454,
#70455,#70456,#70457,#70458,#70459),.UNSPECIFIED.,.F.,.F.,(4,3,3,4),(731.740599790848,
731.826053994574,731.911438415576,731.991088286405),.UNSPECIFIED.);
#518=B_SPLINE_CURVE_WITH_KNOTS('',3,(#70460,#70461,#70462,#70463,#70464,
#70465,#70466,#70467,#70468,#70469,#70470,#70471,#70472,#70473,#70474,#70475,
#70476,#70477,#70478,#70479,#70480,#70481,#70482,#70483,#70484,#70485,#70486,
#70487,#70488,#70489,#70490,#70491,#70492,#70493,#70494,#70495,#70496,#70497,
#70498,#70499,#70500,#70501,#70502,#70503,#70504,#70505,#70506,#70507,#70508,
#70509,#70510,#70511,#70512,#70513,#70514,#70515,#70516,#70517,#70518,#70519,
#70520,#70521,#70522,#70523,#70524,#70525,#70526,#70527,#70528,#70529,#70530,
#70531,#70532,#70533,#70534,#70535,#70536,#70537,#70538,#70539,#70540,#70541,
#70542,#70543,#70544,#70545,#70546,#70547,#70548,#70549,#70550,#70551,#70552,
#70553,#70554,#70555,#70556,#70557,#70558,#70559,#70560,#70561,#70562,#70563,
#70564,#70565,#70566,#70567,#70568,#70569,#70570,#70571,#70572,#70573,#70574,
#70575,#70576,#70577,#70578,#70579,#70580,#70581,#70582,#70583,#70584,#70585,
#70586,#70587,#70588,#70589,#70590,#70591,#70592,#70593,#70594,#70595,#70596,
#70597,#70598,#70599,#70600,#70601,#70602,#70603,#70604,#70605,#70606,#70607,
#70608,#70609,#70610,#70611,#70612,#70613,#70614,#70615,#70616,#70617,#70618,
#70619,#70620,#70621,#70622,#70623,#70624,#70625,#70626,#70627,#70628,#70629,
#70630,#70631,#70632,#70633,#70634,#70635,#70636,#70637,#70638,#70639,#70640,
#70641,#70642,#70643,#70644,#70645,#70646,#70647,#70648,#70649,#70650,#70651,
#70652,#70653,#70654,#70655,#70656,#70657,#70658,#70659,#70660,#70661,#70662,
#70663,#70664,#70665,#70666,#70667,#70668,#70669,#70670,#70671,#70672,#70673,
#70674,#70675,#70676,#70677,#70678,#70679),.UNSPECIFIED.,.F.,.F.,(4,3,3,
3,3,3,3,3,3,3,3,3,3,3,3,3,3,3,3,3,3,3,3,3,3,3,3,3,3,3,3,3,3,3,3,3,3,3,3,
3,3,3,3,3,3,3,3,3,3,3,3,3,3,3,3,3,3,3,3,3,3,3,3,3,3,3,3,3,3,3,3,3,3,4),
(731.991088286542,732.081312336988,732.17190734144,732.262689439977,732.35376866986,
732.425085248302,732.508823960148,732.592459471515,732.676011914914,732.759501350765,
732.842955301379,732.926391795225,733.00982890498,733.093284699898,733.176829192628,
733.260418275569,733.344141543127,733.424821259022,733.508559970868,733.592195482236,
733.675747925634,733.759237361485,733.842691312099,733.926127805945,734.0095649157,
734.093020710618,734.176565203348,734.260154286289,734.343877553846,734.424557269742,
734.508295981588,734.591931492955,734.675483936354,734.758973372205,734.842427322819,
734.925863816665,735.009300926421,735.092756721338,735.176301214068,735.259890297009,
735.343613564567,735.424293280463,735.508031992309,735.591667503676,735.675219947075,
735.758709382926,735.84216333354,735.925599827386,736.009036937142,736.09249273206,
736.176037224789,736.25962630773,736.343349575288,736.424029291183,736.507768003029,
736.591403514396,736.674955957795,736.758445393646,736.84189934426,736.925335838106,
737.008772947861,737.092228742779,737.175773235508,737.259362318449,737.343085586007,
737.423765301903,737.506250937077,737.588641584275,737.670956451871,737.753214675185,
737.835440757069,737.91764891644,737.999871857261,738.022517897246),
 .UNSPECIFIED.);
#519=B_SPLINE_CURVE_WITH_KNOTS('',3,(#70685,#70686,#70687,#70688,#70689,
#70690,#70691,#70692,#70693,#70694,#70695,#70696,#70697,#70698,#70699,#70700,
#70701,#70702,#70703,#70704,#70705,#70706,#70707,#70708,#70709,#70710,#70711,
#70712,#70713,#70714,#70715,#70716,#70717,#70718,#70719,#70720,#70721,#70722,
#70723,#70724,#70725,#70726,#70727,#70728,#70729,#70730,#70731,#70732,#70733,
#70734,#70735,#70736,#70737,#70738,#70739,#70740,#70741,#70742,#70743,#70744,
#70745,#70746,#70747,#70748,#70749,#70750,#70751,#70752,#70753,#70754,#70755,
#70756,#70757,#70758,#70759,#70760,#70761,#70762,#70763,#70764,#70765,#70766,
#70767,#70768,#70769,#70770,#70771,#70772,#70773,#70774,#70775,#70776,#70777,
#70778,#70779,#70780,#70781,#70782,#70783,#70784,#70785,#70786,#70787,#70788,
#70789,#70790,#70791,#70792,#70793,#70794,#70795,#70796,#70797,#70798,#70799,
#70800,#70801,#70802,#70803,#70804,#70805,#70806,#70807,#70808,#70809,#70810,
#70811,#70812,#70813,#70814,#70815,#70816,#70817,#70818,#70819,#70820,#70821,
#70822,#70823,#70824,#70825,#70826,#70827,#70828,#70829,#70830,#70831,#70832,
#70833,#70834,#70835,#70836,#70837,#70838,#70839,#70840,#70841,#70842,#70843,
#70844,#70845,#70846,#70847,#70848,#70849,#70850,#70851,#70852,#70853,#70854,
#70855,#70856,#70857,#70858,#70859,#70860,#70861,#70862,#70863,#70864,#70865,
#70866,#70867,#70868,#70869,#70870,#70871,#70872,#70873,#70874,#70875,#70876,
#70877,#70878,#70879,#70880,#70881,#70882,#70883,#70884,#70885,#70886,#70887,
#70888,#70889,#70890,#70891,#70892,#70893,#70894,#70895,#70896,#70897,#70898,
#70899,#70900,#70901,#70902,#70903,#70904,#70905,#70906,#70907),
 .UNSPECIFIED.,.F.,.F.,(4,3,3,3,3,3,3,3,3,3,3,3,3,3,3,3,3,3,3,3,3,3,3,3,
3,3,3,3,3,3,3,3,3,3,3,3,3,3,3,3,3,3,3,3,3,3,3,3,3,3,3,3,3,3,3,3,3,3,3,3,
3,3,3,3,3,3,3,3,3,3,3,3,3,3,4),(738.274273593783,738.356654353969,738.438955679186,
738.523204557241,738.605418505351,738.687621623504,738.769832943989,738.855611383899,
738.937940895418,739.020325262459,739.102821504759,739.112946703627,739.196685415473,
739.280320926841,739.363873370239,739.44736280609,739.530816756704,739.61425325055,
739.697690360305,739.781146155223,739.864690647952,739.948279730893,740.032002998451,
740.112682714347,740.196421426193,740.28005693756,740.363609380959,740.44709881681,
740.530552767424,740.61398926127,740.697426371025,740.780882165943,740.864426658672,
740.948015741613,741.031739009171,741.112418725067,741.196157436913,741.27979294828,
741.363345391679,741.44683482753,741.530288778144,741.61372527199,741.697162381746,
741.780618176663,741.864162669393,741.947751752334,742.031475019892,742.112154735787,
742.195893447633,742.279528959001,742.363081402399,742.44657083825,742.530024788864,
742.61346128271,742.696898392465,742.780354187382,742.863898680112,742.947487763053,
743.031211030611,743.111890746507,743.195629458353,743.279264969721,743.362817413119,
743.44630684897,743.529760799584,743.61319729343,743.696634403185,743.780090198102,
743.863634690832,743.947223773773,744.030947041331,744.111626757227,744.20215036008,
744.292442587059,744.307152866363),.UNSPECIFIED.);
#520=B_SPLINE_CURVE_WITH_KNOTS('',3,(#70908,#70909,#70910,#70911,#70912,
#70913,#70914,#70915,#70916,#70917,#70918,#70919,#70920),.UNSPECIFIED.,
 .F.,.F.,(4,3,3,3,4),(738.022787360679,738.106543252029,738.113210692907,
738.249145518636,738.27427359358),.UNSPECIFIED.);
#521=B_SPLINE_CURVE_WITH_KNOTS('',3,(#70922,#70923,#70924,#70925,#70926,
#70927,#70928,#70929,#70930,#70931),.UNSPECIFIED.,.F.,.F.,(4,3,3,4),(738.022517897246,
738.104803312639,738.189538453055,738.27427359347),.UNSPECIFIED.);
#522=B_SPLINE_CURVE_WITH_KNOTS('',3,(#70932,#70933,#70934,#70935,#70936,
#70937,#70938,#70939,#70940,#70941,#70942,#70943,#70944,#70945,#70946,#70947,
#70948,#70949,#70950,#70951,#70952,#70953,#70954,#70955,#70956,#70957,#70958,
#70959,#70960,#70961,#70962,#70963,#70964,#70965,#70966,#70967,#70968,#70969,
#70970,#70971,#70972,#70973,#70974,#70975,#70976,#70977,#70978,#70979,#70980,
#70981,#70982,#70983,#70984,#70985,#70986,#70987,#70988,#70989,#70990,#70991,
#70992,#70993,#70994,#70995,#70996,#70997,#70998,#70999,#71000,#71001,#71002,
#71003,#71004,#71005,#71006,#71007,#71008,#71009,#71010,#71011,#71012,#71013,
#71014,#71015,#71016,#71017,#71018,#71019,#71020,#71021,#71022,#71023,#71024,
#71025,#71026,#71027,#71028,#71029,#71030,#71031,#71032,#71033,#71034,#71035,
#71036,#71037,#71038,#71039,#71040,#71041,#71042,#71043,#71044,#71045,#71046,
#71047,#71048,#71049,#71050,#71051,#71052,#71053,#71054,#71055,#71056,#71057,
#71058,#71059,#71060,#71061,#71062,#71063,#71064,#71065,#71066,#71067,#71068,
#71069,#71070,#71071,#71072,#71073,#71074,#71075,#71076,#71077,#71078,#71079,
#71080,#71081,#71082,#71083,#71084,#71085,#71086,#71087,#71088,#71089,#71090,
#71091,#71092,#71093,#71094,#71095,#71096,#71097,#71098,#71099,#71100,#71101,
#71102,#71103,#71104,#71105,#71106,#71107,#71108,#71109,#71110,#71111,#71112,
#71113,#71114,#71115,#71116,#71117,#71118,#71119,#71120,#71121,#71122,#71123,
#71124,#71125,#71126,#71127,#71128,#71129,#71130,#71131,#71132,#71133,#71134,
#71135,#71136,#71137,#71138,#71139,#71140,#71141,#71142,#71143,#71144,#71145,
#71146,#71147,#71148),.UNSPECIFIED.,.F.,.F.,(4,3,3,3,3,3,3,3,3,3,3,3,3,
3,3,3,3,3,3,3,3,3,3,3,3,3,3,3,3,3,3,3,3,3,3,3,3,3,3,3,3,3,3,3,3,3,3,3,3,
3,3,3,3,3,3,3,3,3,3,3,3,3,3,3,3,3,3,3,3,3,3,3,4),(738.274273593584,738.423501312623,
738.507240024469,738.590875535836,738.674427979235,738.757917415086,738.841371365699,
738.924807859546,739.008244969301,739.091700764219,739.175245256948,739.258834339889,
739.342557607447,739.423237323343,739.506976035189,739.590611546556,739.674163989955,
739.757653425806,739.84110737642,739.924543870266,740.007980980021,740.091436774939,
740.174981267669,740.25857035061,740.342293618167,740.422973334063,740.506712045909,
740.590347557276,740.673900000675,740.757389436526,740.840843387139,740.924279880986,
741.007716990741,741.091172785659,741.174717278388,741.258306361329,741.342029628887,
741.422709344783,741.506448056629,741.590083567997,741.673636011395,741.757125447246,
741.84057939786,741.924015891707,742.007453001462,742.09090879638,742.17445328911,
742.258042372051,742.341765639608,742.422445355504,742.50618406735,742.589819578718,
742.673372022116,742.756861457967,742.840315408581,742.923751902427,743.007189012183,
743.0906448071,743.17418929983,743.257778382771,743.341501650329,743.422181366224,
743.50592687522,743.589567653357,743.673123839699,743.756610625342,743.840059701123,
743.923489155705,744.006917060688,744.090395674837,744.173901764441,744.257496996667,
744.305901543465),.UNSPECIFIED.);
#523=B_SPLINE_CURVE_WITH_KNOTS('',3,(#71154,#71155,#71156,#71157,#71158,
#71159,#71160,#71161,#71162,#71163,#71164,#71165,#71166,#71167,#71168,#71169,
#71170,#71171,#71172,#71173,#71174,#71175,#71176,#71177,#71178,#71179,#71180,
#71181,#71182,#71183,#71184,#71185,#71186,#71187,#71188,#71189,#71190,#71191,
#71192,#71193,#71194,#71195,#71196,#71197,#71198,#71199,#71200,#71201,#71202,
#71203,#71204,#71205,#71206,#71207,#71208,#71209,#71210,#71211,#71212,#71213,
#71214,#71215,#71216,#71217,#71218,#71219,#71220,#71221,#71222,#71223,#71224,
#71225,#71226,#71227,#71228,#71229,#71230,#71231,#71232,#71233,#71234,#71235,
#71236,#71237,#71238,#71239,#71240,#71241,#71242,#71243,#71244,#71245,#71246,
#71247,#71248,#71249,#71250,#71251,#71252,#71253,#71254,#71255,#71256,#71257,
#71258,#71259,#71260,#71261,#71262,#71263,#71264,#71265,#71266,#71267,#71268,
#71269,#71270,#71271,#71272,#71273,#71274,#71275,#71276,#71277,#71278,#71279,
#71280,#71281,#71282,#71283,#71284,#71285,#71286,#71287,#71288,#71289,#71290,
#71291,#71292,#71293,#71294,#71295,#71296,#71297,#71298,#71299,#71300,#71301,
#71302,#71303,#71304,#71305,#71306,#71307,#71308,#71309,#71310,#71311,#71312,
#71313,#71314,#71315,#71316,#71317,#71318,#71319,#71320,#71321,#71322,#71323,
#71324,#71325,#71326,#71327,#71328,#71329,#71330,#71331,#71332,#71333,#71334,
#71335,#71336,#71337,#71338,#71339,#71340,#71341,#71342,#71343,#71344,#71345,
#71346,#71347,#71348,#71349,#71350,#71351,#71352,#71353,#71354,#71355,#71356,
#71357,#71358,#71359,#71360,#71361,#71362,#71363,#71364,#71365,#71366,#71367,
#71368,#71369,#71370,#71371,#71372,#71373),.UNSPECIFIED.,.F.,.F.,(4,3,3,
3,3,3,3,3,3,3,3,3,3,3,3,3,3,3,3,3,3,3,3,3,3,3,3,3,3,3,3,3,3,3,3,3,3,3,3,
3,3,3,3,3,3,3,3,3,3,3,3,3,3,3,3,3,3,3,3,3,3,3,3,3,3,3,3,3,3,3,3,3,3,4),
(744.55745890076,744.643146609339,744.7288909297,744.814705795683,744.900667180722,
744.986710700036,745.072911390609,745.111362767948,745.195101479794,745.278736991162,
745.36228943456,745.445778870411,745.529232821025,745.612669314871,745.696106424627,
745.779562219544,745.863106712274,745.946695795215,746.030419062773,746.111098778668,
746.194837490514,746.278473001881,746.36202544528,746.445514881131,746.528968831744,
746.612405325591,746.695842435346,746.779298230264,746.862842722994,746.946431805935,
747.030155073492,747.110834789388,747.194573501234,747.278209012601,747.361761456,
747.445250891851,747.528704842465,747.612141336311,747.695578446066,747.779034240983,
747.862578733713,747.946167816654,748.029891084211,748.110570800108,748.194309511954,
748.277945023322,748.36149746672,748.444986902571,748.528440853185,748.611877347031,
748.695314456787,748.778770251704,748.862314744434,748.945903827375,749.029627094933,
749.110306810828,749.194045522674,749.277681034042,749.36123347744,749.444722913291,
749.528176863904,749.61161335775,749.695050467506,749.778506262423,749.862050755153,
749.945639838094,750.029363105652,750.110042821548,750.192967240485,750.275792225416,
750.358522711749,750.441197997053,750.523841140051,750.589376852607),
 .UNSPECIFIED.);
#524=B_SPLINE_CURVE_WITH_KNOTS('',3,(#71374,#71375,#71376,#71377,#71378,
#71379,#71380,#71381,#71382,#71383),.UNSPECIFIED.,.F.,.F.,(4,3,3,4),(744.307152866363,
744.397153103746,744.486872900899,744.557458900644),.UNSPECIFIED.);
#525=B_SPLINE_CURVE_WITH_KNOTS('',3,(#71385,#71386,#71387,#71388,#71389,
#71390,#71391,#71392,#71393,#71394),.UNSPECIFIED.,.F.,.F.,(4,3,3,4),(744.305901543465,
744.389644379796,744.421917376944,744.557458900764),.UNSPECIFIED.);
#526=B_SPLINE_CURVE_WITH_KNOTS('',3,(#71395,#71396,#71397,#71398,#71399,
#71400,#71401,#71402,#71403,#71404,#71405,#71406,#71407,#71408,#71409,#71410,
#71411,#71412,#71413,#71414,#71415,#71416,#71417,#71418,#71419,#71420,#71421,
#71422,#71423,#71424,#71425,#71426,#71427,#71428,#71429,#71430,#71431,#71432,
#71433,#71434,#71435,#71436,#71437,#71438,#71439,#71440,#71441,#71442,#71443,
#71444,#71445,#71446,#71447,#71448,#71449,#71450,#71451,#71452,#71453,#71454,
#71455,#71456,#71457,#71458,#71459,#71460,#71461,#71462,#71463,#71464,#71465,
#71466,#71467,#71468,#71469,#71470,#71471,#71472,#71473,#71474,#71475,#71476,
#71477,#71478,#71479,#71480,#71481,#71482,#71483,#71484,#71485,#71486,#71487,
#71488,#71489,#71490,#71491,#71492,#71493,#71494,#71495,#71496,#71497,#71498,
#71499,#71500,#71501,#71502,#71503,#71504,#71505,#71506,#71507,#71508,#71509,
#71510,#71511,#71512,#71513,#71514,#71515,#71516,#71517,#71518,#71519,#71520,
#71521,#71522,#71523,#71524,#71525,#71526,#71527,#71528,#71529,#71530,#71531,
#71532,#71533,#71534,#71535,#71536,#71537,#71538,#71539,#71540,#71541,#71542,
#71543,#71544,#71545,#71546,#71547,#71548,#71549,#71550,#71551,#71552,#71553,
#71554,#71555,#71556,#71557,#71558,#71559,#71560,#71561,#71562,#71563,#71564,
#71565,#71566,#71567,#71568,#71569,#71570,#71571,#71572,#71573,#71574,#71575,
#71576,#71577,#71578,#71579,#71580,#71581,#71582,#71583,#71584,#71585,#71586,
#71587,#71588,#71589,#71590,#71591,#71592,#71593,#71594,#71595,#71596,#71597,
#71598,#71599,#71600,#71601,#71602,#71603,#71604,#71605,#71606,#71607,#71608,
#71609,#71610,#71611,#71612,#71613,#71614),.UNSPECIFIED.,.F.,.F.,(4,3,3,
3,3,3,3,3,3,3,3,3,3,3,3,3,3,3,3,3,3,3,3,3,3,3,3,3,3,3,3,3,3,3,3,3,3,3,3,
3,3,3,3,3,3,3,3,3,3,3,3,3,3,3,3,3,3,3,3,3,3,3,3,3,3,3,3,3,3,3,3,3,3,4),
(744.557458900889,744.639910719997,744.722277095366,744.804579155342,744.886844861793,
744.969093797692,745.0513449701,745.133617385711,745.215976099959,745.298383484231,
745.380910787678,745.421653387664,745.50539209951,745.589027610877,745.672580054276,
745.756069490127,745.839523440741,745.922959934587,746.006397044343,746.08985283926,
746.17339733199,746.256986414931,746.340709682489,746.421389398384,746.50512811023,
746.588763621597,746.672316064996,746.755805500847,746.839259451461,746.922695945307,
747.006133055062,747.08958884998,747.173133342709,747.25672242565,747.340445693208,
747.421125409104,747.50486412095,747.588499632317,747.672052075716,747.755541511567,
747.83899546218,747.922431956027,748.005869065782,748.0893248607,748.172869353429,
748.25645843637,748.340181703928,748.420861419824,748.50460013167,748.588235643037,
748.671788086436,748.755277522287,748.8387314729,748.922167966747,749.005605076502,
749.08906087142,749.17260536415,749.256194447091,749.339917714648,749.420597430544,
749.50433614239,749.587971653758,749.671524097157,749.755013533008,749.838467483622,
749.921903977468,750.005341087224,750.088796882142,750.172341374872,750.255930457813,
750.339653725371,750.420333441265,750.51217718284,750.590310680117),
 .UNSPECIFIED.);
#527=B_SPLINE_CURVE_WITH_KNOTS('',3,(#71620,#71621,#71622,#71623,#71624,
#71625,#71626,#71627,#71628,#71629,#71630,#71631,#71632,#71633,#71634,#71635,
#71636,#71637,#71638,#71639,#71640,#71641,#71642,#71643,#71644,#71645,#71646,
#71647,#71648,#71649,#71650,#71651,#71652,#71653,#71654,#71655,#71656,#71657,
#71658,#71659,#71660,#71661,#71662,#71663,#71664,#71665,#71666,#71667,#71668,
#71669,#71670,#71671,#71672,#71673,#71674,#71675,#71676,#71677,#71678,#71679,
#71680,#71681,#71682,#71683,#71684,#71685,#71686,#71687,#71688,#71689,#71690,
#71691,#71692,#71693,#71694,#71695,#71696,#71697,#71698,#71699,#71700,#71701,
#71702,#71703,#71704,#71705,#71706,#71707,#71708,#71709,#71710,#71711,#71712,
#71713,#71714,#71715,#71716,#71717,#71718,#71719,#71720,#71721,#71722,#71723,
#71724,#71725,#71726,#71727,#71728,#71729,#71730,#71731,#71732,#71733,#71734,
#71735,#71736,#71737,#71738,#71739,#71740,#71741,#71742,#71743,#71744,#71745,
#71746,#71747,#71748,#71749,#71750,#71751,#71752,#71753,#71754,#71755,#71756,
#71757,#71758,#71759,#71760,#71761,#71762,#71763,#71764,#71765,#71766,#71767,
#71768,#71769,#71770,#71771,#71772,#71773,#71774,#71775,#71776,#71777,#71778,
#71779,#71780,#71781,#71782,#71783,#71784,#71785,#71786,#71787,#71788,#71789,
#71790,#71791,#71792,#71793,#71794,#71795,#71796,#71797,#71798,#71799,#71800,
#71801,#71802,#71803,#71804,#71805,#71806,#71807,#71808,#71809,#71810,#71811,
#71812,#71813,#71814,#71815,#71816,#71817,#71818,#71819,#71820,#71821,#71822,
#71823,#71824,#71825,#71826,#71827,#71828,#71829,#71830,#71831,#71832,#71833,
#71834,#71835,#71836),.UNSPECIFIED.,.F.,.F.,(4,3,3,3,3,3,3,3,3,3,3,3,3,
3,3,3,3,3,3,3,3,3,3,3,3,3,3,3,3,3,3,3,3,3,3,3,3,3,3,3,3,3,3,3,3,3,3,3,3,
3,3,3,3,3,3,3,3,3,3,3,3,3,3,3,3,3,3,3,3,3,3,3,4),(750.840644208115,750.945021396592,
751.051282858485,751.109778832268,751.193517544114,751.277153055482,751.360705498881,
751.444194934733,751.527648885347,751.611085379193,751.694522488949,751.777978283867,
751.861522776597,751.945111859538,752.028835127096,752.109514842989,752.193253554835,
752.276889066202,752.360441509601,752.443930945452,752.527384896065,752.610821389912,
752.694258499667,752.777714294585,752.861258787314,752.944847870255,753.028571137813,
753.109250853709,753.192989565555,753.276625076922,753.360177520321,753.443666956172,
753.527120906785,753.610557400631,753.693994510387,753.777450305304,753.860994798034,
753.944583880975,754.028307148532,754.108986864429,754.192725576275,754.276361087642,
754.359913531041,754.443402966892,754.526856917506,754.610293411352,754.693730521108,
754.777186316025,754.860730808755,754.944319891696,755.028043159254,755.108722875149,
755.192461586995,755.276097098363,755.359649541761,755.443138977612,755.526592928226,
755.610029422072,755.693466531828,755.776922326745,755.860466819475,755.944055902416,
756.027779169974,756.108458885869,756.192212058086,756.277206748794,756.360750268974,
756.444236006182,756.527682081341,756.613803956943,756.697243624074,756.784706603911,
756.872169583747),.UNSPECIFIED.);
#528=B_SPLINE_CURVE_WITH_KNOTS('',3,(#71837,#71838,#71839,#71840,#71841,
#71842,#71843,#71844,#71845,#71846),.UNSPECIFIED.,.F.,.F.,(4,3,3,4),(750.589376852607,
750.672010998785,750.756327603362,750.840644207939),.UNSPECIFIED.);
#529=B_SPLINE_CURVE_WITH_KNOTS('',3,(#71848,#71849,#71850,#71851,#71852,
#71853,#71854,#71855,#71856,#71857),.UNSPECIFIED.,.F.,.F.,(4,3,3,4),(750.590310680117,
750.681704329962,750.772738826785,750.840644207789),.UNSPECIFIED.);
#530=B_SPLINE_CURVE_WITH_KNOTS('',3,(#71858,#71859,#71860,#71861,#71862,
#71863,#71864,#71865,#71866,#71867,#71868,#71869,#71870,#71871,#71872,#71873,
#71874,#71875,#71876,#71877,#71878,#71879,#71880,#71881,#71882,#71883,#71884,
#71885,#71886,#71887,#71888,#71889,#71890,#71891,#71892,#71893,#71894,#71895,
#71896,#71897,#71898,#71899,#71900,#71901,#71902,#71903,#71904,#71905,#71906,
#71907,#71908,#71909,#71910,#71911,#71912,#71913,#71914,#71915,#71916,#71917,
#71918,#71919,#71920,#71921,#71922,#71923,#71924,#71925,#71926,#71927,#71928,
#71929,#71930,#71931,#71932,#71933,#71934,#71935,#71936,#71937,#71938,#71939,
#71940,#71941,#71942,#71943,#71944,#71945,#71946,#71947,#71948,#71949,#71950,
#71951,#71952,#71953,#71954,#71955,#71956,#71957,#71958,#71959,#71960,#71961,
#71962,#71963,#71964,#71965,#71966,#71967,#71968,#71969,#71970,#71971,#71972,
#71973,#71974,#71975,#71976,#71977,#71978,#71979,#71980,#71981,#71982,#71983,
#71984,#71985,#71986,#71987,#71988,#71989,#71990,#71991,#71992,#71993,#71994,
#71995,#71996,#71997,#71998,#71999,#72000,#72001,#72002,#72003,#72004,#72005,
#72006,#72007,#72008,#72009,#72010,#72011,#72012,#72013,#72014,#72015,#72016,
#72017,#72018,#72019,#72020,#72021,#72022,#72023,#72024,#72025,#72026,#72027,
#72028,#72029,#72030,#72031,#72032,#72033,#72034,#72035,#72036,#72037,#72038,
#72039,#72040,#72041,#72042,#72043,#72044,#72045,#72046,#72047,#72048,#72049,
#72050,#72051,#72052,#72053,#72054,#72055,#72056,#72057,#72058,#72059,#72060,
#72061,#72062,#72063,#72064,#72065,#72066,#72067,#72068,#72069,#72070,#72071,
#72072,#72073,#72074,#72075,#72076,#72077),.UNSPECIFIED.,.F.,.F.,(4,3,3,
3,3,3,3,3,3,3,3,3,3,3,3,3,3,3,3,3,3,3,3,3,3,3,3,3,3,3,3,3,3,3,3,3,3,3,3,
3,3,3,3,3,3,3,3,3,3,3,3,3,3,3,3,3,3,3,3,3,3,3,3,3,3,3,3,3,3,3,3,3,3,4),
(750.840644207943,750.925672733848,751.010737480744,751.095853917042,751.181099834772,
751.266414222463,751.351886366408,751.420069451985,751.503808163831,751.587443675199,
751.670996118597,751.754485554448,751.837939505062,751.921375998908,752.004813108663,
752.088268903581,752.17181339631,752.255402479251,752.339125746809,752.419805462705,
752.503544174551,752.587179685918,752.670732129317,752.754221565168,752.837675515782,
752.921112009628,753.004549119384,753.088004914302,753.171549407032,753.255138489973,
753.33886175753,753.419541473425,753.503280185271,753.586915696638,753.670468140037,
753.753957575888,753.837411526502,753.920848020348,754.004285130103,754.087740925021,
754.17128541775,754.254874500691,754.338597768249,754.419277484145,754.503016195991,
754.586651707358,754.670204150757,754.753693586608,754.837147537222,754.920584031068,
755.004021140824,755.087476935742,755.171021428471,755.254610511412,755.33833377897,
755.419013494865,755.502752206711,755.586387718078,755.669940161476,755.753429597327,
755.836883547941,755.920320041787,756.003757151542,756.087212946459,756.170757439189,
756.25434652213,756.338069789687,756.418749505585,756.501937853318,756.585024809647,
756.668013059796,756.750944341703,756.833835667285,756.872694074728),
 .UNSPECIFIED.);
#531=B_SPLINE_CURVE_WITH_KNOTS('',3,(#72083,#72084,#72085,#72086,#72087,
#72088,#72089,#72090,#72091,#72092,#72093,#72094,#72095,#72096,#72097,#72098,
#72099,#72100,#72101,#72102,#72103,#72104,#72105,#72106,#72107,#72108,#72109,
#72110,#72111,#72112,#72113,#72114,#72115,#72116,#72117,#72118,#72119,#72120,
#72121,#72122,#72123,#72124,#72125,#72126,#72127,#72128,#72129,#72130,#72131,
#72132,#72133,#72134,#72135,#72136,#72137,#72138,#72139,#72140,#72141,#72142,
#72143,#72144,#72145,#72146,#72147,#72148,#72149,#72150,#72151,#72152,#72153,
#72154,#72155,#72156,#72157,#72158,#72159,#72160,#72161,#72162,#72163,#72164,
#72165,#72166,#72167,#72168,#72169,#72170,#72171,#72172,#72173,#72174,#72175,
#72176,#72177,#72178,#72179,#72180,#72181,#72182,#72183,#72184,#72185,#72186,
#72187,#72188,#72189,#72190,#72191,#72192,#72193,#72194,#72195,#72196,#72197,
#72198,#72199,#72200,#72201,#72202,#72203,#72204,#72205,#72206,#72207,#72208,
#72209,#72210,#72211,#72212,#72213,#72214,#72215,#72216,#72217,#72218,#72219,
#72220,#72221,#72222,#72223,#72224,#72225,#72226,#72227,#72228,#72229,#72230,
#72231,#72232,#72233,#72234,#72235,#72236,#72237,#72238,#72239,#72240,#72241,
#72242,#72243,#72244,#72245,#72246,#72247,#72248,#72249,#72250,#72251,#72252,
#72253,#72254,#72255,#72256,#72257,#72258,#72259,#72260,#72261,#72262,#72263,
#72264,#72265,#72266,#72267,#72268,#72269,#72270,#72271,#72272,#72273,#72274,
#72275,#72276,#72277,#72278,#72279,#72280,#72281,#72282,#72283,#72284,#72285,
#72286,#72287,#72288,#72289,#72290,#72291,#72292,#72293,#72294,#72295,#72296,
#72297,#72298,#72299,#72300,#72301,#72302),.UNSPECIFIED.,.F.,.F.,(4,3,3,
3,3,3,3,3,3,3,3,3,3,3,3,3,3,3,3,3,3,3,3,3,3,3,3,3,3,3,3,3,3,3,3,3,3,3,3,
3,3,3,3,3,3,3,3,3,3,3,3,3,3,3,3,3,3,3,3,3,3,3,3,3,3,3,3,3,3,3,3,3,3,4),
(757.123829515267,757.207340415428,757.290748533449,757.374074237987,757.457337823838,
757.540567305995,757.623780569666,757.706995898186,757.790231572581,757.873556122523,
757.956927157123,758.040428159847,758.107930907309,758.191669619155,758.275305130522,
758.35885757392,758.442347009771,758.525800960385,758.609237454231,758.692674563986,
758.776130358904,758.859674851634,758.943263934574,759.026987202132,759.107666918029,
759.191405629875,759.275041141243,759.358593584642,759.442083020493,759.525536971107,
759.608973464954,759.69241057471,759.775866369628,759.859410862358,759.942999945299,
760.026723212857,760.10740292875,760.191141640596,760.274777151963,760.358329595362,
760.441819031212,760.525272981826,760.608709475672,760.692146585428,760.775602380345,
760.859146873075,760.942735956016,761.026459223573,761.10713893947,761.190877651316,
761.274513162684,761.358065606082,761.441555041933,761.525008992547,761.608445486393,
761.691882596149,761.775338391067,761.858882883796,761.942471966738,762.026195234295,
762.10687495019,762.190613662036,762.274249173404,762.357801616802,762.441291052653,
762.524745003267,762.608181497114,762.691618606869,762.775074401788,762.858618894518,
762.942207977459,763.025931245016,763.10661096091,763.156242422283),
 .UNSPECIFIED.);
#532=B_SPLINE_CURVE_WITH_KNOTS('',3,(#72303,#72304,#72305,#72306,#72307,
#72308,#72309,#72310,#72311,#72312,#72313,#72314,#72315),.UNSPECIFIED.,
 .F.,.F.,(4,3,3,3,4),(756.872169583747,756.95576638285,757.039493869905,
757.108194896589,757.123829515119),.UNSPECIFIED.);
#533=B_SPLINE_CURVE_WITH_KNOTS('',3,(#72317,#72318,#72319,#72320,#72321,
#72322,#72323,#72324,#72325,#72326),.UNSPECIFIED.,.F.,.F.,(4,3,3,4),(756.872694074728,
756.955571692592,757.039700603857,757.123829515123),.UNSPECIFIED.);
#534=B_SPLINE_CURVE_WITH_KNOTS('',3,(#72327,#72328,#72329,#72330,#72331,
#72332,#72333,#72334,#72335,#72336,#72337,#72338,#72339,#72340,#72341,#72342,
#72343,#72344,#72345,#72346,#72347,#72348,#72349,#72350,#72351,#72352,#72353,
#72354,#72355,#72356,#72357,#72358,#72359,#72360,#72361,#72362,#72363,#72364,
#72365,#72366,#72367,#72368,#72369,#72370,#72371,#72372,#72373,#72374,#72375,
#72376,#72377,#72378,#72379,#72380,#72381,#72382,#72383,#72384,#72385,#72386,
#72387,#72388,#72389,#72390,#72391,#72392,#72393,#72394,#72395,#72396,#72397,
#72398,#72399,#72400,#72401,#72402,#72403,#72404,#72405,#72406,#72407,#72408,
#72409,#72410,#72411,#72412,#72413,#72414,#72415,#72416,#72417,#72418,#72419,
#72420,#72421,#72422,#72423,#72424,#72425,#72426,#72427,#72428,#72429,#72430,
#72431,#72432,#72433,#72434,#72435,#72436,#72437,#72438,#72439,#72440,#72441,
#72442,#72443,#72444,#72445,#72446,#72447,#72448,#72449,#72450,#72451,#72452,
#72453,#72454,#72455,#72456,#72457,#72458,#72459,#72460,#72461,#72462,#72463,
#72464,#72465,#72466,#72467,#72468,#72469,#72470,#72471,#72472,#72473,#72474,
#72475,#72476,#72477,#72478,#72479,#72480,#72481,#72482,#72483,#72484,#72485,
#72486,#72487,#72488,#72489,#72490,#72491,#72492,#72493,#72494,#72495,#72496,
#72497,#72498,#72499,#72500,#72501,#72502,#72503,#72504,#72505,#72506,#72507,
#72508,#72509,#72510,#72511,#72512,#72513,#72514,#72515,#72516,#72517,#72518,
#72519,#72520,#72521,#72522,#72523,#72524,#72525,#72526,#72527,#72528,#72529,
#72530,#72531,#72532,#72533,#72534,#72535,#72536,#72537,#72538,#72539,#72540,
#72541,#72542,#72543),.UNSPECIFIED.,.F.,.F.,(4,3,3,3,3,3,3,3,3,3,3,3,3,
3,3,3,3,3,3,3,3,3,3,3,3,3,3,3,3,3,3,3,3,3,3,3,3,3,3,3,3,3,3,3,3,3,3,3,3,
3,3,3,3,3,3,3,3,3,3,3,3,3,3,3,3,3,3,3,3,3,3,3,4),(757.123829515261,757.224985151375,
757.327544941235,757.418485516306,757.502224228152,757.585859739519,757.669412182918,
757.752901618769,757.836355569382,757.919792063228,758.003229172984,758.086684967901,
758.170229460631,758.253818543572,758.337541811129,758.418221527026,758.501960238872,
758.585595750239,758.669148193638,758.752637629489,758.836091580102,758.919528073949,
759.002965183704,759.086420978622,759.169965471351,759.253554554292,759.33727782185,
759.417957537746,759.501696249592,759.58533176096,759.668884204358,759.752373640209,
759.835827590823,759.919264084669,760.002701194424,760.086156989342,760.169701482072,
760.253290565013,760.33701383257,760.417693548466,760.501432260312,760.585067771679,
760.668620215078,760.752109650929,760.835563601543,760.919000095389,761.002437205144,
761.085893000062,761.169437492791,761.253026575732,761.33674984329,761.417429559186,
761.501168271032,761.584803782399,761.668356225798,761.751845661649,761.835299612263,
761.918736106109,762.002173215865,762.085629010782,762.169173503512,762.252762586453,
762.336485854011,762.417165569906,762.500773963721,762.5842500345,762.667649737885,
762.750991377849,762.834293214392,762.917591204417,763.000883927774,763.084224691449,
763.155323815868),.UNSPECIFIED.);
#535=B_SPLINE_CURVE_WITH_KNOTS('',3,(#72549,#72550,#72551,#72552,#72553,
#72554,#72555,#72556,#72557,#72558,#72559,#72560,#72561,#72562,#72563,#72564,
#72565,#72566,#72567,#72568,#72569,#72570,#72571,#72572,#72573,#72574,#72575,
#72576,#72577,#72578,#72579,#72580,#72581,#72582,#72583,#72584,#72585,#72586,
#72587,#72588,#72589,#72590,#72591,#72592,#72593,#72594,#72595,#72596,#72597,
#72598,#72599,#72600,#72601,#72602,#72603,#72604,#72605,#72606,#72607,#72608,
#72609,#72610,#72611,#72612,#72613,#72614,#72615,#72616,#72617,#72618,#72619,
#72620,#72621,#72622,#72623,#72624,#72625,#72626,#72627,#72628,#72629,#72630,
#72631,#72632,#72633,#72634,#72635,#72636,#72637,#72638,#72639,#72640,#72641,
#72642,#72643,#72644,#72645,#72646,#72647,#72648,#72649,#72650,#72651,#72652,
#72653,#72654,#72655,#72656,#72657,#72658,#72659,#72660,#72661,#72662,#72663,
#72664,#72665,#72666,#72667,#72668,#72669,#72670,#72671,#72672,#72673,#72674,
#72675,#72676,#72677,#72678,#72679,#72680,#72681,#72682,#72683,#72684,#72685,
#72686,#72687,#72688,#72689,#72690,#72691,#72692,#72693,#72694,#72695,#72696,
#72697,#72698,#72699,#72700,#72701,#72702,#72703,#72704,#72705,#72706,#72707,
#72708,#72709,#72710,#72711,#72712,#72713,#72714,#72715,#72716,#72717,#72718,
#72719,#72720,#72721,#72722,#72723,#72724,#72725,#72726,#72727,#72728,#72729,
#72730,#72731,#72732,#72733,#72734,#72735,#72736,#72737,#72738,#72739,#72740,
#72741,#72742,#72743,#72744,#72745,#72746,#72747,#72748,#72749,#72750,#72751,
#72752,#72753,#72754,#72755,#72756,#72757,#72758,#72759,#72760,#72761,#72762,
#72763,#72764,#72765,#72766,#72767,#72768),.UNSPECIFIED.,.F.,.F.,(4,3,3,
3,3,3,3,3,3,3,3,3,3,3,3,3,3,3,3,3,3,3,3,3,3,3,3,3,3,3,3,3,3,3,3,3,3,3,3,
3,3,3,3,3,3,3,3,3,3,3,3,3,3,3,3,3,3,3,3,3,3,3,3,3,3,3,3,3,3,3,3,3,3,4),
(763.407014822298,763.489990676255,763.572943345094,763.655887431654,763.738841417603,
763.821823788036,763.904900247605,763.988030719312,764.071284328313,764.10634697163,
764.190085683476,764.273721194844,764.357273638242,764.440763074093,764.524217024707,
764.607653518553,764.691090628309,764.774546423226,764.858090915956,764.941679998897,
765.025403266455,765.10608298235,765.189821694196,765.273457205564,765.357009648962,
765.440499084813,765.523953035426,765.607389529273,765.690826639028,765.774282433945,
765.857826926675,765.941416009616,766.025139277173,766.10581899307,766.189557704916,
766.273193216284,766.356745659682,766.440235095533,766.523689046147,766.607125539993,
766.690562649748,766.774018444666,766.857562937396,766.941152020337,767.024875287894,
767.10555500379,767.189293715636,767.272929227004,767.356481670402,767.439971106254,
767.523425056867,767.606861550714,767.690298660469,767.773754455387,767.857298948116,
767.940888031058,768.024611298615,768.10529101451,768.189029726356,768.272665237723,
768.356217681122,768.439707116974,768.523161067587,768.606597561434,768.690034671189,
768.773490466107,768.857034958837,768.940624041778,769.024347309336,769.105027025231,
769.190345221994,769.275557890134,769.36065028321,769.439640659244),
 .UNSPECIFIED.);
#536=B_SPLINE_CURVE_WITH_KNOTS('',3,(#72769,#72770,#72771,#72772,#72773,
#72774,#72775,#72776,#72777,#72778),.UNSPECIFIED.,.F.,.F.,(4,3,3,4),(763.156242422283,
763.257984034045,763.358484794115,763.40701482215),.UNSPECIFIED.);
#537=B_SPLINE_CURVE_WITH_KNOTS('',3,(#72780,#72781,#72782,#72783,#72784,
#72785,#72786,#72787,#72788,#72789),.UNSPECIFIED.,.F.,.F.,(4,3,3,4),(763.155323815868,
763.238763926004,763.322889374058,763.407014822111),.UNSPECIFIED.);
#538=B_SPLINE_CURVE_WITH_KNOTS('',3,(#72790,#72791,#72792,#72793,#72794,
#72795,#72796,#72797,#72798,#72799,#72800,#72801,#72802,#72803,#72804,#72805,
#72806,#72807,#72808,#72809,#72810,#72811,#72812,#72813,#72814,#72815,#72816,
#72817,#72818,#72819,#72820,#72821,#72822,#72823,#72824,#72825,#72826,#72827,
#72828,#72829,#72830,#72831,#72832,#72833,#72834,#72835,#72836,#72837,#72838,
#72839,#72840,#72841,#72842,#72843,#72844,#72845,#72846,#72847,#72848,#72849,
#72850,#72851,#72852,#72853,#72854,#72855,#72856,#72857,#72858,#72859,#72860,
#72861,#72862,#72863,#72864,#72865,#72866,#72867,#72868,#72869,#72870,#72871,
#72872,#72873,#72874,#72875,#72876,#72877,#72878,#72879,#72880,#72881,#72882,
#72883,#72884,#72885,#72886,#72887,#72888,#72889,#72890,#72891,#72892,#72893,
#72894,#72895,#72896,#72897,#72898,#72899,#72900,#72901,#72902,#72903,#72904,
#72905,#72906,#72907,#72908,#72909,#72910,#72911,#72912,#72913,#72914,#72915,
#72916,#72917,#72918,#72919,#72920,#72921,#72922,#72923,#72924,#72925,#72926,
#72927,#72928,#72929,#72930,#72931,#72932,#72933,#72934,#72935,#72936,#72937,
#72938,#72939,#72940,#72941,#72942,#72943,#72944,#72945,#72946,#72947,#72948,
#72949,#72950,#72951,#72952,#72953,#72954,#72955,#72956,#72957,#72958,#72959,
#72960,#72961,#72962,#72963,#72964,#72965,#72966,#72967,#72968,#72969,#72970,
#72971,#72972,#72973,#72974,#72975,#72976,#72977,#72978,#72979,#72980,#72981,
#72982,#72983,#72984,#72985,#72986,#72987,#72988,#72989,#72990,#72991,#72992,
#72993,#72994,#72995,#72996,#72997,#72998,#72999,#73000,#73001,#73002,#73003,
#73004,#73005,#73006,#73007,#73008,#73009,#73010,#73011,#73012),
 .UNSPECIFIED.,.F.,.F.,(4,3,3,3,3,3,3,3,3,3,3,3,3,3,3,3,3,3,3,3,3,3,3,3,
3,3,3,3,3,3,3,3,3,3,3,3,3,3,3,3,3,3,3,3,3,3,3,3,3,3,3,3,3,3,3,3,3,3,3,3,
3,3,3,3,3,3,3,3,3,3,3,3,3,3,4),(763.407014822302,763.416901580626,763.500640292472,
763.58427580384,763.667828247238,763.751317683089,763.834771633703,763.918208127549,
764.001645237305,764.085101032222,764.168645524952,764.252234607893,764.335957875451,
764.416637591346,764.500376303192,764.58401181456,764.667564257958,764.751053693809,
764.834507644423,764.917944138269,765.001381248025,765.084837042942,765.168381535672,
765.251970618613,765.335693886171,765.416373602067,765.500112313913,765.583747825281,
765.667300268679,765.75078970453,765.834243655144,765.91768014899,766.001117258746,
766.084573053663,766.168117546393,766.251706629334,766.335429896892,766.416109612787,
766.499848324633,766.583483836,766.667036279399,766.75052571525,766.833979665864,
766.91741615971,767.000853269465,767.084309064383,767.167853557113,767.251442640054,
767.335165907611,767.415845623507,767.499584335353,767.58321984672,767.666772290119,
767.75026172597,767.833715676584,767.91715217043,768.000589280185,768.084045075103,
768.167589567832,768.251178650773,768.334901918331,768.415581634227,768.499320346073,
768.582955857441,768.666508300839,768.74999773669,768.833451687304,768.91688818115,
769.000325290906,769.083781085823,769.167325578553,769.250914661494,769.334637929052,
769.415317644947,769.43928124014),.UNSPECIFIED.);
#539=B_SPLINE_CURVE_WITH_KNOTS('',3,(#73018,#73019,#73020,#73021,#73022,
#73023,#73024,#73025,#73026,#73027,#73028,#73029,#73030,#73031,#73032,#73033,
#73034,#73035,#73036,#73037,#73038,#73039,#73040,#73041,#73042,#73043,#73044,
#73045,#73046,#73047,#73048,#73049,#73050,#73051,#73052,#73053,#73054,#73055,
#73056,#73057,#73058,#73059,#73060,#73061,#73062,#73063,#73064,#73065,#73066,
#73067,#73068,#73069,#73070,#73071,#73072,#73073,#73074,#73075,#73076,#73077,
#73078,#73079,#73080,#73081,#73082,#73083,#73084,#73085,#73086,#73087,#73088,
#73089,#73090,#73091,#73092,#73093,#73094,#73095,#73096,#73097,#73098,#73099,
#73100,#73101,#73102,#73103,#73104,#73105,#73106,#73107,#73108,#73109,#73110,
#73111,#73112,#73113,#73114,#73115,#73116,#73117,#73118,#73119,#73120,#73121,
#73122,#73123,#73124,#73125,#73126,#73127,#73128,#73129,#73130,#73131,#73132,
#73133,#73134,#73135,#73136,#73137,#73138,#73139,#73140,#73141,#73142,#73143,
#73144,#73145,#73146,#73147,#73148,#73149,#73150,#73151,#73152,#73153,#73154,
#73155,#73156,#73157,#73158,#73159,#73160,#73161,#73162,#73163,#73164,#73165,
#73166,#73167,#73168,#73169,#73170,#73171,#73172,#73173,#73174,#73175,#73176,
#73177,#73178,#73179,#73180,#73181,#73182,#73183,#73184,#73185,#73186,#73187,
#73188,#73189,#73190,#73191,#73192,#73193,#73194,#73195,#73196,#73197,#73198,
#73199,#73200,#73201,#73202,#73203,#73204,#73205,#73206,#73207,#73208,#73209,
#73210,#73211,#73212,#73213,#73214,#73215,#73216,#73217,#73218,#73219,#73220,
#73221,#73222,#73223,#73224,#73225,#73226,#73227,#73228,#73229,#73230,#73231,
#73232,#73233,#73234,#73235,#73236,#73237),.UNSPECIFIED.,.F.,.F.,(4,3,3,
3,3,3,3,3,3,3,3,3,3,3,3,3,3,3,3,3,3,3,3,3,3,3,3,3,3,3,3,3,3,3,3,3,3,3,3,
3,3,3,3,3,3,3,3,3,3,3,3,3,3,3,3,3,3,3,3,3,3,3,3,3,3,3,3,3,3,3,3,3,3,4),
(769.690200129639,769.781448738232,769.87313387068,769.965042746187,770.057269456248,
770.104763035951,770.188501747797,770.272137259165,770.355689702563,770.439179138414,
770.522633089028,770.606069582874,770.68950669263,770.772962487548,770.856506980277,
770.940096063218,771.023819330776,771.104499046671,771.188237758517,771.271873269884,
771.355425713283,771.438915149134,771.522369099747,771.605805593594,771.689242703349,
771.772698498267,771.856242990997,771.939832073938,772.023555341495,772.104235057391,
772.187973769237,772.271609280604,772.355161724003,772.438651159854,772.522105110468,
772.605541604314,772.688978714069,772.772434508987,772.855979001717,772.939568084657,
773.023291352215,773.103971068111,773.187709779957,773.271345291324,773.354897734723,
773.438387170574,773.521841121187,773.605277615034,773.688714724789,773.772170519706,
773.855715012436,773.939304095377,774.023027362935,774.103707078831,774.187445790677,
774.271081302045,774.354633745443,774.438123181294,774.521577131908,774.605013625754,
774.68845073551,774.771906530427,774.855451023157,774.939040106098,775.022763373656,
775.103443089551,775.185976551709,775.268415256539,775.350778378943,775.433085022286,
775.515361467243,775.597619913088,775.679898448971,775.721587636679),
 .UNSPECIFIED.);
#540=B_SPLINE_CURVE_WITH_KNOTS('',3,(#73238,#73239,#73240,#73241,#73242,
#73243,#73244,#73245,#73246,#73247),.UNSPECIFIED.,.F.,.F.,(4,3,3,4),(769.439640659244,
769.524591546901,769.609493151917,769.690200129478),.UNSPECIFIED.);
#541=B_SPLINE_CURVE_WITH_KNOTS('',3,(#73249,#73250,#73251,#73252,#73253,
#73254,#73255,#73256,#73257,#73258),.UNSPECIFIED.,.F.,.F.,(4,3,3,4),(769.43928124014,
769.544644755484,769.648309781464,769.690200129282),.UNSPECIFIED.);
#542=B_SPLINE_CURVE_WITH_KNOTS('',3,(#73259,#73260,#73261,#73262,#73263,
#73264,#73265,#73266,#73267,#73268,#73269,#73270,#73271,#73272,#73273,#73274,
#73275,#73276,#73277,#73278,#73279,#73280,#73281,#73282,#73283,#73284,#73285,
#73286,#73287,#73288,#73289,#73290,#73291,#73292,#73293,#73294,#73295,#73296,
#73297,#73298,#73299,#73300,#73301,#73302,#73303,#73304,#73305,#73306,#73307,
#73308,#73309,#73310,#73311,#73312,#73313,#73314,#73315,#73316,#73317,#73318,
#73319,#73320,#73321,#73322,#73323,#73324,#73325,#73326,#73327,#73328,#73329,
#73330,#73331,#73332,#73333,#73334,#73335,#73336,#73337,#73338,#73339,#73340,
#73341,#73342,#73343,#73344,#73345,#73346,#73347,#73348,#73349,#73350,#73351,
#73352,#73353,#73354,#73355,#73356,#73357,#73358,#73359,#73360,#73361,#73362,
#73363,#73364,#73365,#73366,#73367,#73368,#73369,#73370,#73371,#73372,#73373,
#73374,#73375,#73376,#73377,#73378,#73379,#73380,#73381,#73382,#73383,#73384,
#73385,#73386,#73387,#73388,#73389,#73390,#73391,#73392,#73393,#73394,#73395,
#73396,#73397,#73398,#73399,#73400,#73401,#73402,#73403,#73404,#73405,#73406,
#73407,#73408,#73409,#73410,#73411,#73412,#73413,#73414,#73415,#73416,#73417,
#73418,#73419,#73420,#73421,#73422,#73423,#73424,#73425,#73426,#73427,#73428,
#73429,#73430,#73431,#73432,#73433,#73434,#73435,#73436,#73437,#73438,#73439,
#73440,#73441,#73442,#73443,#73444,#73445,#73446,#73447,#73448,#73449,#73450,
#73451,#73452,#73453,#73454,#73455,#73456,#73457,#73458,#73459,#73460,#73461,
#73462,#73463,#73464,#73465,#73466,#73467,#73468,#73469,#73470,#73471,#73472,
#73473,#73474,#73475,#73476,#73477,#73478),.UNSPECIFIED.,.F.,.F.,(4,3,3,
3,3,3,3,3,3,3,3,3,3,3,3,3,3,3,3,3,3,3,3,3,3,3,3,3,3,3,3,3,3,3,3,3,3,3,3,
3,3,3,3,3,3,3,3,3,3,3,3,3,3,3,3,3,3,3,3,3,3,3,3,3,3,3,3,3,3,3,3,3,3,4),
(769.690200129482,769.77293722689,769.855637408681,769.938319894256,770.021003387505,
770.103706590002,770.186497939218,770.269335957804,770.352302829011,770.415053655667,
770.498792367513,770.58242787888,770.665980322279,770.74946975813,770.832923708743,
770.91636020259,770.999797312345,771.083253107263,771.166797599992,771.250386682933,
771.334109950491,771.414789666387,771.498528378233,771.582163889601,771.665716332999,
771.74920576885,771.832659719464,771.916096213311,771.999533323066,772.082989117984,
772.166533610713,772.250122693655,772.333845961212,772.414525677107,772.498264388953,
772.58189990032,772.665452343718,772.748941779569,772.832395730183,772.915832224029,
772.999269333785,773.082725128702,773.166269621432,773.249858704373,773.333581971931,
773.414261687828,773.498000399674,773.581635911042,773.66518835444,773.748677790291,
773.832131740905,773.915568234752,773.999005344507,774.082461139425,774.166005632155,
774.249594715096,774.333317982653,774.413997698548,774.497736410394,774.581371921762,
774.66492436516,774.748413801012,774.831867751625,774.915304245472,774.998741355227,
775.082197150145,775.165741642875,775.249330725816,775.333053993373,775.413733709268,
775.499747566005,775.585649680523,775.671420628738,775.722917187892),
 .UNSPECIFIED.);
#543=B_SPLINE_CURVE_WITH_KNOTS('',3,(#73484,#73485,#73486,#73487,#73488,
#73489,#73490,#73491,#73492,#73493,#73494,#73495,#73496,#73497,#73498,#73499,
#73500,#73501,#73502,#73503,#73504,#73505,#73506,#73507,#73508,#73509,#73510,
#73511,#73512,#73513,#73514,#73515,#73516,#73517,#73518,#73519,#73520,#73521,
#73522,#73523,#73524,#73525,#73526,#73527,#73528,#73529,#73530,#73531,#73532,
#73533,#73534,#73535,#73536,#73537,#73538,#73539,#73540,#73541,#73542,#73543,
#73544,#73545,#73546,#73547,#73548,#73549,#73550,#73551,#73552,#73553,#73554,
#73555,#73556,#73557,#73558,#73559,#73560,#73561,#73562,#73563,#73564,#73565,
#73566,#73567,#73568,#73569,#73570,#73571,#73572,#73573,#73574,#73575,#73576,
#73577,#73578,#73579,#73580,#73581,#73582,#73583,#73584,#73585,#73586,#73587,
#73588,#73589,#73590,#73591,#73592,#73593,#73594,#73595,#73596,#73597,#73598,
#73599,#73600,#73601,#73602,#73603,#73604,#73605,#73606,#73607,#73608,#73609,
#73610,#73611,#73612,#73613,#73614,#73615,#73616,#73617,#73618,#73619,#73620,
#73621,#73622,#73623,#73624,#73625,#73626,#73627,#73628,#73629,#73630,#73631,
#73632,#73633,#73634,#73635,#73636,#73637,#73638,#73639,#73640,#73641,#73642,
#73643,#73644,#73645,#73646,#73647,#73648,#73649,#73650,#73651,#73652,#73653,
#73654,#73655,#73656,#73657,#73658,#73659,#73660,#73661,#73662,#73663,#73664,
#73665,#73666,#73667,#73668,#73669,#73670,#73671,#73672,#73673,#73674,#73675,
#73676,#73677,#73678,#73679,#73680,#73681,#73682,#73683,#73684,#73685,#73686,
#73687,#73688,#73689,#73690,#73691,#73692,#73693,#73694,#73695,#73696,#73697,
#73698,#73699,#73700),.UNSPECIFIED.,.F.,.F.,(4,3,3,3,3,3,3,3,3,3,3,3,3,
3,3,3,3,3,3,3,3,3,3,3,3,3,3,3,3,3,3,3,3,3,3,3,3,3,3,3,3,3,3,3,3,3,3,3,3,
3,3,3,3,3,3,3,3,3,3,3,3,3,3,3,3,3,3,3,3,3,3,3,4),(775.973385436658,776.103179100272,
776.186917812118,776.270553323486,776.354105766885,776.437595202736,776.52104915335,
776.604485647197,776.687922756953,776.77137855187,776.8549230446,776.938512127542,
777.0222353951,777.102915110992,777.186653822838,777.270289334205,777.353841777604,
777.437331213455,777.520785164068,777.604221657914,777.68765876767,777.771114562588,
777.854659055317,777.938248138258,778.021971405816,778.102651121712,778.186389833558,
778.270025344926,778.353577788324,778.437067224175,778.520521174789,778.603957668635,
778.687394778391,778.770850573309,778.854395066038,778.937984148979,779.021707416537,
779.102387132432,779.186125844278,779.269761355645,779.353313799044,779.436803234895,
779.520257185508,779.603693679355,779.68713078911,779.770586584028,779.854131076757,
779.937720159698,780.021443427256,780.102123143152,780.185861854998,780.269497366365,
780.353049809764,780.436539245615,780.519993196228,780.603429690075,780.68686679983,
780.770322594748,780.853867087477,780.937456170418,781.021179437976,781.101859153872,
781.185603479214,781.269243330783,781.352798846523,781.436285919035,781.51973564543,
781.603166114165,781.686595396955,781.770079645405,781.853591517192,781.937202545892,
782.005065761364),.UNSPECIFIED.);
#544=B_SPLINE_CURVE_WITH_KNOTS('',3,(#73701,#73702,#73703,#73704,#73705,
#73706,#73707,#73708,#73709,#73710),.UNSPECIFIED.,.F.,.F.,(4,3,3,4),(775.721587636679,
775.803934072365,775.888659754447,775.973385436529),.UNSPECIFIED.);
#545=B_SPLINE_CURVE_WITH_KNOTS('',3,(#73712,#73713,#73714,#73715,#73716,
#73717,#73718,#73719,#73720,#73721),.UNSPECIFIED.,.F.,.F.,(4,3,3,4),(775.722917187892,
775.808540259658,775.894086620738,775.973385436661),.UNSPECIFIED.);
#546=B_SPLINE_CURVE_WITH_KNOTS('',3,(#73722,#73723,#73724,#73725,#73726,
#73727,#73728,#73729,#73730,#73731,#73732,#73733,#73734,#73735,#73736,#73737,
#73738,#73739,#73740,#73741,#73742,#73743,#73744,#73745,#73746,#73747,#73748,
#73749,#73750,#73751,#73752,#73753,#73754,#73755,#73756,#73757,#73758,#73759,
#73760,#73761,#73762,#73763,#73764,#73765,#73766,#73767,#73768,#73769,#73770,
#73771,#73772,#73773,#73774,#73775,#73776,#73777,#73778,#73779,#73780,#73781,
#73782,#73783,#73784,#73785,#73786,#73787,#73788,#73789,#73790,#73791,#73792,
#73793,#73794,#73795,#73796,#73797,#73798,#73799,#73800,#73801,#73802,#73803,
#73804,#73805,#73806,#73807,#73808,#73809,#73810,#73811,#73812,#73813,#73814,
#73815,#73816,#73817,#73818,#73819,#73820,#73821,#73822,#73823,#73824,#73825,
#73826,#73827,#73828,#73829,#73830,#73831,#73832,#73833,#73834,#73835,#73836,
#73837,#73838,#73839,#73840,#73841,#73842,#73843,#73844,#73845,#73846,#73847,
#73848,#73849,#73850,#73851,#73852,#73853,#73854,#73855,#73856,#73857,#73858,
#73859,#73860,#73861,#73862,#73863,#73864,#73865,#73866,#73867,#73868,#73869,
#73870,#73871,#73872,#73873,#73874,#73875,#73876,#73877,#73878,#73879,#73880,
#73881,#73882,#73883,#73884,#73885,#73886,#73887,#73888,#73889,#73890,#73891,
#73892,#73893,#73894,#73895,#73896,#73897,#73898,#73899,#73900,#73901,#73902,
#73903,#73904,#73905,#73906,#73907,#73908,#73909,#73910,#73911,#73912,#73913,
#73914,#73915,#73916,#73917,#73918,#73919,#73920,#73921,#73922,#73923,#73924,
#73925,#73926,#73927,#73928,#73929,#73930,#73931,#73932,#73933,#73934,#73935,
#73936,#73937,#73938,#73939,#73940,#73941),.UNSPECIFIED.,.F.,.F.,(4,3,3,
3,3,3,3,3,3,3,3,3,3,3,3,3,3,3,3,3,3,3,3,3,3,3,3,3,3,3,3,3,3,3,3,3,3,3,3,
3,3,3,3,3,3,3,3,3,3,3,3,3,3,3,3,3,3,3,3,3,3,3,3,3,3,3,3,3,3,3,3,3,3,4),
(775.973385436787,776.06330864179,776.15358475724,776.244037792623,776.334782116871,
776.413469719988,776.497208431834,776.580843943202,776.6643963866,776.747885822451,
776.831339773064,776.914776266911,776.998213376666,777.081669171584,777.165213664314,
777.248802747254,777.332526014812,777.413205730708,777.496944442554,777.580579953921,
777.664132397319,777.74762183317,777.831075783784,777.91451227763,777.997949387385,
778.081405182303,778.164949675032,778.248538757973,778.33226202553,778.412941741428,
778.496680453274,778.580315964642,778.663868408041,778.747357843892,778.830811794506,
778.914248288352,778.997685398108,779.081141193026,779.164685685756,779.248274768697,
779.331998036255,779.412677752149,779.496416463995,779.580051975362,779.663604418761,
779.747093854612,779.830547805226,779.913984299072,779.997421408828,780.080877203746,
780.164421696475,780.248010779416,780.331734046974,780.412413762869,780.496152474715,
780.579787986082,780.663340429481,780.746829865331,780.830283815945,780.913720309791,
780.997157419546,781.080613214464,781.164157707193,781.247746790134,781.331470057691,
781.412149773589,781.494627159821,781.577009465221,781.659315904408,781.745694675271,
781.827910312565,781.910108877223,781.992320812228,782.004830987862),
 .UNSPECIFIED.);
#547=B_SPLINE_CURVE_WITH_KNOTS('',3,(#73947,#73948,#73949,#73950,#73951,
#73952,#73953,#73954,#73955,#73956,#73957,#73958,#73959,#73960,#73961,#73962,
#73963,#73964,#73965,#73966,#73967,#73968,#73969,#73970,#73971,#73972,#73973,
#73974,#73975,#73976,#73977,#73978,#73979,#73980,#73981,#73982,#73983,#73984,
#73985,#73986,#73987,#73988,#73989,#73990,#73991,#73992,#73993,#73994,#73995,
#73996,#73997,#73998,#73999,#74000,#74001,#74002,#74003,#74004,#74005,#74006,
#74007,#74008,#74009,#74010,#74011,#74012,#74013,#74014,#74015,#74016,#74017,
#74018,#74019,#74020,#74021,#74022,#74023,#74024,#74025,#74026,#74027,#74028,
#74029,#74030,#74031,#74032,#74033,#74034,#74035,#74036,#74037,#74038,#74039,
#74040,#74041,#74042,#74043,#74044,#74045,#74046,#74047,#74048,#74049,#74050,
#74051,#74052,#74053,#74054,#74055,#74056,#74057,#74058,#74059,#74060,#74061,
#74062,#74063,#74064,#74065,#74066,#74067,#74068,#74069,#74070,#74071,#74072,
#74073,#74074,#74075,#74076,#74077,#74078,#74079,#74080,#74081,#74082,#74083,
#74084,#74085,#74086,#74087,#74088,#74089,#74090,#74091,#74092,#74093,#74094,
#74095,#74096,#74097,#74098,#74099,#74100,#74101,#74102,#74103,#74104,#74105,
#74106,#74107,#74108,#74109,#74110,#74111,#74112,#74113,#74114,#74115,#74116,
#74117,#74118,#74119,#74120,#74121,#74122,#74123,#74124,#74125,#74126,#74127,
#74128,#74129,#74130,#74131,#74132,#74133,#74134,#74135,#74136,#74137,#74138,
#74139,#74140,#74141,#74142,#74143,#74144,#74145,#74146,#74147,#74148,#74149,
#74150,#74151,#74152,#74153,#74154,#74155,#74156,#74157,#74158,#74159,#74160,
#74161,#74162,#74163,#74164,#74165,#74166),.UNSPECIFIED.,.F.,.F.,(4,3,3,
3,3,3,3,3,3,3,3,3,3,3,3,3,3,3,3,3,3,3,3,3,3,3,3,3,3,3,3,3,3,3,3,3,3,3,3,
3,3,3,3,3,3,3,3,3,3,3,3,3,3,3,3,3,3,3,3,3,3,3,3,3,3,3,3,3,3,3,3,3,3,4),
(782.256570743945,782.338963542711,782.421275411456,782.506282381938,782.588503237466,
782.670712082992,782.752927947646,782.835169864301,782.917500230731,782.999883639915,
783.082381157245,783.101331175313,783.185069887159,783.268705398526,783.352257841925,
783.435747277776,783.519201228389,783.602637722236,783.686074831991,783.769530626909,
783.853075119638,783.936664202579,784.020387470136,784.101067186033,784.184805897879,
784.268441409246,784.351993852645,784.435483288496,784.51893723911,784.602373732956,
784.685810842711,784.769266637628,784.852811130358,784.936400213299,785.020123480856,
785.100803196753,785.184541908599,785.268177419966,785.351729863365,785.435219299217,
785.51867324983,785.602109743676,785.685546853432,785.76900264835,785.852547141079,
785.93613622402,786.019859491578,786.100539207473,786.184277919319,786.267913430686,
786.351465874085,786.434955309936,786.51840926055,786.601845754396,786.685282864151,
786.768738659069,786.852283151799,786.93587223474,787.019595502297,787.100275218193,
787.184013930039,787.267649441406,787.351201884805,787.434691320656,787.51814527127,
787.601581765116,787.685018874872,787.768474669789,787.852019162519,787.93560824546,
788.019331513017,788.100011228913,788.194728462435,788.289445695958),
 .UNSPECIFIED.);
#548=B_SPLINE_CURVE_WITH_KNOTS('',3,(#74167,#74168,#74169,#74170,#74171,
#74172,#74173,#74174,#74175,#74176,#74177,#74178,#74179),.UNSPECIFIED.,
 .F.,.F.,(4,3,3,3,4),(782.005065761364,782.088818368043,782.101595164592,
782.240882181406,782.256570743837),.UNSPECIFIED.);
#549=B_SPLINE_CURVE_WITH_KNOTS('',3,(#74181,#74182,#74183,#74184,#74185,
#74186,#74187,#74188,#74189,#74190),.UNSPECIFIED.,.F.,.F.,(4,3,3,4),(782.004830987862,
782.087103904726,782.17183732423,782.256570743733),.UNSPECIFIED.);
#550=B_SPLINE_CURVE_WITH_KNOTS('',3,(#74191,#74192,#74193,#74194,#74195,
#74196,#74197,#74198,#74199,#74200,#74201,#74202,#74203,#74204,#74205,#74206,
#74207,#74208,#74209,#74210,#74211,#74212,#74213,#74214,#74215,#74216,#74217,
#74218,#74219,#74220,#74221,#74222,#74223,#74224,#74225,#74226,#74227,#74228,
#74229,#74230,#74231,#74232,#74233,#74234,#74235,#74236,#74237,#74238,#74239,
#74240,#74241,#74242,#74243,#74244,#74245,#74246,#74247,#74248,#74249,#74250,
#74251,#74252,#74253,#74254,#74255,#74256,#74257,#74258,#74259,#74260,#74261,
#74262,#74263,#74264,#74265,#74266,#74267,#74268,#74269,#74270,#74271,#74272,
#74273,#74274,#74275,#74276,#74277,#74278,#74279,#74280,#74281,#74282,#74283,
#74284,#74285,#74286,#74287,#74288,#74289,#74290,#74291,#74292,#74293,#74294,
#74295,#74296,#74297,#74298,#74299,#74300,#74301,#74302,#74303,#74304,#74305,
#74306,#74307,#74308,#74309,#74310,#74311,#74312,#74313,#74314,#74315,#74316,
#74317,#74318,#74319,#74320,#74321,#74322,#74323,#74324,#74325,#74326,#74327,
#74328,#74329,#74330,#74331,#74332,#74333,#74334,#74335,#74336,#74337,#74338,
#74339,#74340,#74341,#74342,#74343,#74344,#74345,#74346,#74347,#74348,#74349,
#74350,#74351,#74352,#74353,#74354,#74355,#74356,#74357,#74358,#74359,#74360,
#74361,#74362,#74363,#74364,#74365,#74366,#74367,#74368,#74369,#74370,#74371,
#74372,#74373,#74374,#74375,#74376,#74377,#74378,#74379,#74380,#74381,#74382,
#74383,#74384,#74385,#74386,#74387,#74388,#74389,#74390,#74391,#74392,#74393,
#74394,#74395,#74396,#74397,#74398,#74399,#74400,#74401,#74402,#74403,#74404,
#74405,#74406,#74407,#74408,#74409,#74410),.UNSPECIFIED.,.F.,.F.,(4,3,3,
3,3,3,3,3,3,3,3,3,3,3,3,3,3,3,3,3,3,3,3,3,3,3,3,3,3,3,3,3,3,3,3,3,3,3,3,
3,3,3,3,3,3,3,3,3,3,3,3,3,3,3,3,3,3,3,3,3,3,3,3,3,3,3,3,3,3,3,3,3,3,4),
(782.256570743841,782.395663585156,782.411885784309,782.495624496155,782.579260007523,
782.662812450921,782.746301886772,782.829755837386,782.913192331232,782.996629440987,
783.080085235905,783.163629728635,783.247218811576,783.330942079133,783.411621795029,
783.495360506875,783.578996018242,783.662548461641,783.746037897492,783.829491848105,
783.912928341952,783.996365451707,784.079821246625,784.163365739354,784.246954822295,
784.330678089853,784.411357805749,784.495096517595,784.578732028962,784.662284472361,
784.745773908211,784.829227858825,784.912664352671,784.996101462426,785.079557257344,
785.163101750073,785.246690833014,785.330414100572,785.411093816469,785.494832528315,
785.578468039683,785.662020483082,785.745509918933,785.828963869547,785.912400363393,
785.995837473149,786.079293268067,786.162837760797,786.246426843738,786.330150111296,
786.41082982719,786.494568539036,786.578204050404,786.661756493802,786.745245929653,
786.828699880267,786.912136374113,786.995573483869,787.079029278786,787.162573771516,
787.246162854457,787.329886122015,787.41056583791,787.494311721008,787.577952792745,
787.661509192539,787.744995902321,787.828444788344,787.91187393934,787.995301426878,
788.078778332683,788.16228266764,788.245873176523,788.288184568376),
 .UNSPECIFIED.);
#551=B_SPLINE_CURVE_WITH_KNOTS('',3,(#74416,#74417,#74418,#74419,#74420,
#74421,#74422,#74423,#74424,#74425,#74426,#74427,#74428,#74429,#74430,#74431,
#74432,#74433,#74434,#74435,#74436,#74437,#74438,#74439,#74440,#74441,#74442,
#74443,#74444,#74445,#74446,#74447,#74448,#74449,#74450,#74451,#74452,#74453,
#74454,#74455,#74456,#74457,#74458,#74459,#74460,#74461,#74462,#74463,#74464,
#74465,#74466,#74467,#74468,#74469,#74470,#74471,#74472,#74473,#74474,#74475,
#74476,#74477,#74478,#74479,#74480,#74481,#74482,#74483,#74484,#74485,#74486,
#74487,#74488,#74489,#74490,#74491,#74492,#74493,#74494,#74495,#74496,#74497,
#74498,#74499,#74500,#74501,#74502,#74503,#74504,#74505,#74506,#74507,#74508,
#74509,#74510,#74511,#74512,#74513,#74514,#74515,#74516,#74517,#74518,#74519,
#74520,#74521,#74522,#74523,#74524,#74525,#74526,#74527,#74528,#74529,#74530,
#74531,#74532,#74533,#74534,#74535,#74536,#74537,#74538,#74539,#74540,#74541,
#74542,#74543,#74544,#74545,#74546,#74547,#74548,#74549,#74550,#74551,#74552,
#74553,#74554,#74555,#74556,#74557,#74558,#74559,#74560,#74561,#74562,#74563,
#74564,#74565,#74566,#74567,#74568,#74569,#74570,#74571,#74572,#74573,#74574,
#74575,#74576,#74577,#74578,#74579,#74580,#74581,#74582,#74583,#74584,#74585,
#74586,#74587,#74588,#74589,#74590,#74591,#74592,#74593,#74594,#74595,#74596,
#74597,#74598,#74599,#74600,#74601,#74602,#74603,#74604,#74605,#74606,#74607,
#74608,#74609,#74610,#74611,#74612,#74613,#74614,#74615,#74616,#74617,#74618,
#74619,#74620,#74621,#74622,#74623,#74624,#74625,#74626,#74627,#74628,#74629,
#74630,#74631,#74632,#74633,#74634,#74635),.UNSPECIFIED.,.F.,.F.,(4,3,3,
3,3,3,3,3,3,3,3,3,3,3,3,3,3,3,3,3,3,3,3,3,3,3,3,3,3,3,3,3,3,3,3,3,3,3,3,
3,3,3,3,3,3,3,3,3,3,3,3,3,3,3,3,3,3,3,3,3,3,3,3,3,3,3,3,3,3,3,3,3,3,4),
(788.539756051017,788.625278366436,788.710852095813,788.796491588863,788.88227330464,
788.968133743556,789.054151397246,789.099747239633,789.183485951479,789.267121462846,
789.350673906245,789.434163342096,789.51761729271,789.601053786556,789.684490896311,
789.767946691229,789.851491183959,789.9350802669,790.018803534458,790.099483250353,
790.183221962199,790.266857473567,790.350409916965,790.433899352816,790.51735330343,
790.600789797276,790.684226907031,790.767682701949,790.851227194678,790.934816277619,
791.018539545177,791.099219261073,791.182957972919,791.266593484287,791.350145927685,
791.433635363536,791.51708931415,791.600525807996,791.683962917752,791.76741871267,
791.8509632054,791.934552288341,792.018275555898,792.098955271794,792.18269398364,
792.266329495008,792.349881938406,792.433371374257,792.516825324871,792.600261818717,
792.683698928473,792.76715472339,792.85069921612,792.934288299061,793.018011566619,
793.098691282514,793.18242999436,793.266065505728,793.349617949126,793.433107384977,
793.516561335591,793.599997829437,793.683434939193,793.766890734111,793.85043522684,
793.934024309781,794.017747577339,794.098427293234,794.181408928667,794.264290706377,
794.347077006945,794.429807732937,794.51250434914,794.571705147957),
 .UNSPECIFIED.);
#552=B_SPLINE_CURVE_WITH_KNOTS('',3,(#74636,#74637,#74638,#74639,#74640,
#74641,#74642,#74643,#74644,#74645),.UNSPECIFIED.,.F.,.F.,(4,3,3,4),(788.289445695958,
788.379761119791,788.46977898198,788.53975605089),.UNSPECIFIED.);
#553=B_SPLINE_CURVE_WITH_KNOTS('',3,(#74647,#74648,#74649,#74650,#74651,
#74652,#74653,#74654,#74655,#74656),.UNSPECIFIED.,.F.,.F.,(4,3,3,4),(788.288184568376,
788.371924568467,788.41030184863,788.539756051021),.UNSPECIFIED.);
#554=B_SPLINE_CURVE_WITH_KNOTS('',3,(#74657,#74658,#74659,#74660,#74661,
#74662,#74663,#74664,#74665,#74666,#74667,#74668,#74669,#74670,#74671,#74672,
#74673,#74674,#74675,#74676,#74677,#74678,#74679,#74680,#74681,#74682,#74683,
#74684,#74685,#74686,#74687,#74688,#74689,#74690,#74691,#74692,#74693,#74694,
#74695,#74696,#74697,#74698,#74699,#74700,#74701,#74702,#74703,#74704,#74705,
#74706,#74707,#74708,#74709,#74710,#74711,#74712,#74713,#74714,#74715,#74716,
#74717,#74718,#74719,#74720,#74721,#74722,#74723,#74724,#74725,#74726,#74727,
#74728,#74729,#74730,#74731,#74732,#74733,#74734,#74735,#74736,#74737,#74738,
#74739,#74740,#74741,#74742,#74743,#74744,#74745,#74746,#74747,#74748,#74749,
#74750,#74751,#74752,#74753,#74754,#74755,#74756,#74757,#74758,#74759,#74760,
#74761,#74762,#74763,#74764,#74765,#74766,#74767,#74768,#74769,#74770,#74771,
#74772,#74773,#74774,#74775,#74776,#74777,#74778,#74779,#74780,#74781,#74782,
#74783,#74784,#74785,#74786,#74787,#74788,#74789,#74790,#74791,#74792,#74793,
#74794,#74795,#74796,#74797,#74798,#74799,#74800,#74801,#74802,#74803,#74804,
#74805,#74806,#74807,#74808,#74809,#74810,#74811,#74812,#74813,#74814,#74815,
#74816,#74817,#74818,#74819,#74820,#74821,#74822,#74823,#74824,#74825,#74826,
#74827,#74828,#74829,#74830,#74831,#74832,#74833,#74834,#74835,#74836,#74837,
#74838,#74839,#74840,#74841,#74842,#74843,#74844,#74845,#74846,#74847,#74848,
#74849,#74850,#74851,#74852,#74853,#74854,#74855,#74856,#74857,#74858,#74859,
#74860,#74861,#74862,#74863,#74864,#74865,#74866,#74867,#74868,#74869,#74870,
#74871,#74872,#74873,#74874,#74875,#74876),.UNSPECIFIED.,.F.,.F.,(4,3,3,
3,3,3,3,3,3,3,3,3,3,3,3,3,3,3,3,3,3,3,3,3,3,3,3,3,3,3,3,3,3,3,3,3,3,3,3,
3,3,3,3,3,3,3,3,3,3,3,3,3,3,3,3,3,3,3,3,3,3,3,3,3,3,3,3,3,3,3,3,3,3,4),
(788.53975605115,788.622232791737,788.70462275739,788.786947068423,788.869233268008,
788.951501468204,789.033770665122,789.116059853442,789.198434792231,789.280857252709,
789.363401284496,789.41003785935,789.493776571196,789.577412082563,789.660964525962,
789.744453961813,789.827907912427,789.911344406273,789.994781516028,790.078237310946,
790.161781803676,790.245370886617,790.329094154174,790.40977387007,790.493512581916,
790.577148093283,790.660700536682,790.744189972533,790.827643923146,790.911080416993,
790.994517526748,791.077973321666,791.161517814395,791.245106897336,791.328830164894,
791.40950988079,791.493248592636,791.576884104004,791.660436547402,791.743925983253,
791.827379933867,791.910816427713,791.994253537469,792.077709332387,792.161253825117,
792.244842908058,792.328566175615,792.40924589151,792.492984603356,792.576620114723,
792.660172558122,792.743661993973,792.827115944587,792.910552438433,792.993989548189,
793.077445343106,793.160989835836,793.244578918777,793.328302186335,793.40898190223,
793.492720614076,793.576356125443,793.659908568842,793.743398004692,793.826851955306,
793.910288449152,793.993725558907,794.077181353825,794.160725846555,794.244314929496,
794.328038197053,794.40871791295,794.500932310921,794.572597636804),
 .UNSPECIFIED.);
#555=B_SPLINE_CURVE_WITH_KNOTS('',3,(#74882,#74883,#74884,#74885,#74886,
#74887,#74888,#74889,#74890,#74891,#74892,#74893,#74894,#74895,#74896,#74897,
#74898,#74899,#74900,#74901,#74902,#74903,#74904,#74905,#74906,#74907,#74908,
#74909,#74910,#74911,#74912,#74913,#74914,#74915,#74916,#74917,#74918,#74919,
#74920,#74921,#74922,#74923,#74924,#74925,#74926,#74927,#74928,#74929,#74930,
#74931,#74932,#74933,#74934,#74935,#74936,#74937,#74938,#74939,#74940,#74941,
#74942,#74943,#74944,#74945,#74946,#74947,#74948,#74949,#74950,#74951,#74952,
#74953,#74954,#74955,#74956,#74957,#74958,#74959,#74960,#74961,#74962,#74963,
#74964,#74965,#74966,#74967,#74968,#74969,#74970,#74971,#74972,#74973,#74974,
#74975,#74976,#74977,#74978,#74979,#74980,#74981,#74982,#74983,#74984,#74985,
#74986,#74987,#74988,#74989,#74990,#74991,#74992,#74993,#74994,#74995,#74996,
#74997,#74998,#74999,#75000,#75001,#75002,#75003,#75004,#75005,#75006,#75007,
#75008,#75009,#75010,#75011,#75012,#75013,#75014,#75015,#75016,#75017,#75018,
#75019,#75020,#75021,#75022,#75023,#75024,#75025,#75026,#75027,#75028,#75029,
#75030,#75031,#75032,#75033,#75034,#75035,#75036,#75037,#75038,#75039,#75040,
#75041,#75042,#75043,#75044,#75045,#75046,#75047,#75048,#75049,#75050,#75051,
#75052,#75053,#75054,#75055,#75056,#75057,#75058,#75059,#75060,#75061,#75062,
#75063,#75064,#75065,#75066,#75067,#75068,#75069,#75070,#75071,#75072,#75073,
#75074,#75075,#75076,#75077,#75078,#75079,#75080,#75081,#75082,#75083,#75084,
#75085,#75086,#75087,#75088,#75089,#75090,#75091,#75092,#75093,#75094,#75095,
#75096,#75097,#75098),.UNSPECIFIED.,.F.,.F.,(4,3,3,3,3,3,3,3,3,3,3,3,3,
3,3,3,3,3,3,3,3,3,3,3,3,3,3,3,3,3,3,3,3,3,3,3,3,3,3,3,3,3,3,3,3,3,3,3,3,
3,3,3,3,3,3,3,3,3,3,3,3,3,3,3,3,3,3,3,3,3,3,3,4),(794.822941358398,794.926494078898,
795.031796927361,795.098163303954,795.1819020158,795.265537527167,795.349089970566,
795.432579406417,795.516033357031,795.599469850877,795.682906960633,795.76636275555,
795.84990724828,795.933496331221,796.017219598778,796.097899314674,796.18163802652,
796.265273537887,796.348825981286,796.432315417137,796.515769367751,796.599205861597,
796.682642971352,796.76609876627,796.849643258999,796.93323234194,797.016955609498,
797.097635325394,797.18137403724,797.265009548607,797.348561992006,797.432051427857,
797.51550537847,797.598941872317,797.682378982072,797.76583477699,797.849379269719,
797.93296835266,798.016691620218,798.097371336114,798.18111004796,798.264745559327,
798.348298002726,798.431787438577,798.515241389191,798.598677883037,798.682114992793,
798.765570787711,798.84911528044,798.932704363382,799.016427630939,799.097107346834,
799.18084605868,799.264481570047,799.348034013446,799.431523449297,799.514977399911,
799.598413893757,799.681851003513,799.765306798431,799.84885129116,799.932440374101,
800.016163641659,800.096843357555,800.180596935371,800.264831095732,800.348375393307,
800.431861628916,800.515307924047,800.6000984976,800.683536956606,800.769003587433,
800.85447021826),.UNSPECIFIED.);
#556=B_SPLINE_CURVE_WITH_KNOTS('',3,(#75099,#75100,#75101,#75102,#75103,
#75104,#75105,#75106,#75107,#75108),.UNSPECIFIED.,.F.,.F.,(4,3,3,4),(794.571705147957,
794.654391671142,794.738666514669,794.822941358196),.UNSPECIFIED.);
#557=B_SPLINE_CURVE_WITH_KNOTS('',3,(#75110,#75111,#75112,#75113,#75114,
#75115,#75116,#75117,#75118,#75119),.UNSPECIFIED.,.F.,.F.,(4,3,3,4),(794.572597636804,
794.664353272392,794.755727987324,794.822941358038),.UNSPECIFIED.);
#558=B_SPLINE_CURVE_WITH_KNOTS('',3,(#75120,#75121,#75122,#75123,#75124,
#75125,#75126,#75127,#75128,#75129,#75130,#75131,#75132,#75133,#75134,#75135,
#75136,#75137,#75138,#75139,#75140,#75141,#75142,#75143,#75144,#75145,#75146,
#75147,#75148,#75149,#75150,#75151,#75152,#75153,#75154,#75155,#75156,#75157,
#75158,#75159,#75160,#75161,#75162,#75163,#75164,#75165,#75166,#75167,#75168,
#75169,#75170,#75171,#75172,#75173,#75174,#75175,#75176,#75177,#75178,#75179,
#75180,#75181,#75182,#75183,#75184,#75185,#75186,#75187,#75188,#75189,#75190,
#75191,#75192,#75193,#75194,#75195,#75196,#75197,#75198,#75199,#75200,#75201,
#75202,#75203,#75204,#75205,#75206,#75207,#75208,#75209,#75210,#75211,#75212,
#75213,#75214,#75215,#75216,#75217,#75218,#75219,#75220,#75221,#75222,#75223,
#75224,#75225,#75226,#75227,#75228,#75229,#75230,#75231,#75232,#75233,#75234,
#75235,#75236,#75237,#75238,#75239,#75240,#75241,#75242,#75243,#75244,#75245,
#75246,#75247,#75248,#75249,#75250,#75251,#75252,#75253,#75254,#75255,#75256,
#75257,#75258,#75259,#75260,#75261,#75262,#75263,#75264,#75265,#75266,#75267,
#75268,#75269,#75270,#75271,#75272,#75273,#75274,#75275,#75276,#75277,#75278,
#75279,#75280,#75281,#75282,#75283,#75284,#75285,#75286,#75287,#75288,#75289,
#75290,#75291,#75292,#75293,#75294,#75295,#75296,#75297,#75298,#75299,#75300,
#75301,#75302,#75303,#75304,#75305,#75306,#75307,#75308,#75309,#75310,#75311,
#75312,#75313,#75314,#75315,#75316,#75317,#75318,#75319,#75320,#75321,#75322,
#75323,#75324,#75325,#75326,#75327,#75328,#75329,#75330,#75331,#75332,#75333,
#75334,#75335,#75336,#75337,#75338,#75339),.UNSPECIFIED.,.F.,.F.,(4,3,3,
3,3,3,3,3,3,3,3,3,3,3,3,3,3,3,3,3,3,3,3,3,3,3,3,3,3,3,3,3,3,3,3,3,3,3,3,
3,3,3,3,3,3,3,3,3,3,3,3,3,3,3,3,3,3,3,3,3,3,3,3,3,3,3,3,3,3,3,3,3,3,4),
(794.8229413582,794.90782555628,794.992741610013,795.077705281825,795.162794725737,
795.247949613061,795.333262560284,795.40845392367,795.492192635516,795.575828146884,
795.659380590282,795.742870026133,795.826323976747,795.909760470593,795.993197580348,
796.076653375266,796.160197867996,796.243786950937,796.327510218494,796.408189934391,
796.491928646237,796.575564157605,796.659116601003,796.742606036854,796.826059987468,
796.909496481314,796.992933591069,797.076389385987,797.159933878717,797.243522961658,
797.327246229216,797.407925945111,797.491664656957,797.575300168324,797.658852611723,
797.742342047574,797.825795998188,797.909232492034,797.992669601789,798.076125396707,
798.159669889436,798.243258972377,798.326982239935,798.407661955831,798.491400667677,
798.575036179045,798.658588622443,798.742078058294,798.825532008908,798.908968502754,
798.992405612509,799.075861407427,799.159405900156,799.242994983097,799.326718250655,
799.407397966551,799.491136678397,799.574772189765,799.658324633163,799.741814069014,
799.825268019628,799.908704513474,799.992141623229,800.075597418147,800.159141910877,
800.242730993818,800.326454261375,800.407133977271,800.490394748986,800.573553587345,
800.656612671435,800.739614281639,800.822574242566,800.855023018815),
 .UNSPECIFIED.);
#559=B_SPLINE_CURVE_WITH_KNOTS('',3,(#75345,#75346,#75347,#75348,#75349,
#75350,#75351,#75352,#75353,#75354,#75355,#75356,#75357,#75358,#75359,#75360,
#75361,#75362,#75363,#75364,#75365,#75366,#75367,#75368,#75369,#75370,#75371,
#75372,#75373,#75374,#75375,#75376,#75377,#75378,#75379,#75380,#75381,#75382,
#75383,#75384,#75385,#75386,#75387,#75388,#75389,#75390,#75391,#75392,#75393,
#75394,#75395,#75396,#75397,#75398,#75399,#75400,#75401,#75402,#75403,#75404,
#75405,#75406,#75407,#75408,#75409,#75410,#75411,#75412,#75413,#75414,#75415,
#75416,#75417,#75418,#75419,#75420,#75421,#75422,#75423,#75424,#75425,#75426,
#75427,#75428,#75429,#75430,#75431,#75432,#75433,#75434,#75435,#75436,#75437,
#75438,#75439,#75440,#75441,#75442,#75443,#75444,#75445,#75446,#75447,#75448,
#75449,#75450,#75451,#75452,#75453,#75454,#75455,#75456,#75457,#75458,#75459,
#75460,#75461,#75462,#75463,#75464,#75465,#75466,#75467,#75468,#75469,#75470,
#75471,#75472,#75473,#75474,#75475,#75476,#75477,#75478,#75479,#75480,#75481,
#75482,#75483,#75484,#75485,#75486,#75487,#75488,#75489,#75490,#75491,#75492,
#75493,#75494,#75495,#75496,#75497,#75498,#75499,#75500,#75501,#75502,#75503,
#75504,#75505,#75506,#75507,#75508,#75509,#75510,#75511,#75512,#75513,#75514,
#75515,#75516,#75517,#75518,#75519,#75520,#75521,#75522,#75523,#75524,#75525,
#75526,#75527,#75528,#75529,#75530,#75531,#75532,#75533,#75534,#75535,#75536,
#75537,#75538,#75539,#75540,#75541,#75542,#75543,#75544,#75545,#75546,#75547,
#75548,#75549,#75550,#75551,#75552,#75553,#75554,#75555,#75556,#75557,#75558,
#75559,#75560,#75561,#75562,#75563,#75564),.UNSPECIFIED.,.F.,.F.,(4,3,3,
3,3,3,3,3,3,3,3,3,3,3,3,3,3,3,3,3,3,3,3,3,3,3,3,3,3,3,3,3,3,3,3,3,3,3,3,
3,3,3,3,3,3,3,3,3,3,3,3,3,3,3,3,3,3,3,3,3,3,3,3,3,3,3,3,3,3,3,3,3,3,4),
(801.106126665561,801.189723746874,801.273217813649,801.356629148145,801.439977959442,
801.523292059086,801.606589416156,801.689888236832,801.773206724513,801.856613996548,
801.940066996113,802.023651605219,802.096315378995,802.180054090841,802.263689602208,
802.347242045607,802.430731481458,802.514185432072,802.597621925918,802.681059035674,
802.764514830591,802.848059323321,802.931648406262,803.015371673819,803.096051389715,
803.179790101561,803.263425612928,803.346978056327,803.430467492178,803.513921442791,
803.597357936638,803.680795046393,803.764250841311,803.847795334041,803.931384416982,
804.015107684539,804.095787400435,804.179526112281,804.263161623648,804.346714067047,
804.430203502898,804.513657453512,804.597093947358,804.680531057113,804.76398685203,
804.84753134476,804.931120427701,805.014843695259,805.095523411155,805.179262123001,
805.262897634369,805.346450077767,805.429939513618,805.513393464232,805.596829958078,
805.680267067833,805.763722862751,805.847267355481,805.930856438422,806.014579705979,
806.095259421875,806.178998133721,806.262633645088,806.346186088487,806.429675524338,
806.513129474951,806.596565968798,806.680003078553,806.76345887347,806.8470033662,
806.930592449141,807.014315716699,807.094995432596,807.1385058474),
 .UNSPECIFIED.);
#560=B_SPLINE_CURVE_WITH_KNOTS('',3,(#75565,#75566,#75567,#75568,#75569,
#75570,#75571,#75572,#75573,#75574,#75575,#75576,#75577),.UNSPECIFIED.,
 .F.,.F.,(4,3,3,3,4),(800.85447021826,800.938063052894,801.021788343522,
801.096579368275,801.106126665376),.UNSPECIFIED.);
#561=B_SPLINE_CURVE_WITH_KNOTS('',3,(#75579,#75580,#75581,#75582,#75583,
#75584,#75585,#75586,#75587,#75588),.UNSPECIFIED.,.F.,.F.,(4,3,3,4),(800.855023018815,
800.937968112572,801.022047388976,801.10612666538),.UNSPECIFIED.);
#562=B_SPLINE_CURVE_WITH_KNOTS('',3,(#75589,#75590,#75591,#75592,#75593,
#75594,#75595,#75596,#75597,#75598,#75599,#75600,#75601,#75602,#75603,#75604,
#75605,#75606,#75607,#75608,#75609,#75610,#75611,#75612,#75613,#75614,#75615,
#75616,#75617,#75618,#75619,#75620,#75621,#75622,#75623,#75624,#75625,#75626,
#75627,#75628,#75629,#75630,#75631,#75632,#75633,#75634,#75635,#75636,#75637,
#75638,#75639,#75640,#75641,#75642,#75643,#75644,#75645,#75646,#75647,#75648,
#75649,#75650,#75651,#75652,#75653,#75654,#75655,#75656,#75657,#75658,#75659,
#75660,#75661,#75662,#75663,#75664,#75665,#75666,#75667,#75668,#75669,#75670,
#75671,#75672,#75673,#75674,#75675,#75676,#75677,#75678,#75679,#75680,#75681,
#75682,#75683,#75684,#75685,#75686,#75687,#75688,#75689,#75690,#75691,#75692,
#75693,#75694,#75695,#75696,#75697,#75698,#75699,#75700,#75701,#75702,#75703,
#75704,#75705,#75706,#75707,#75708,#75709,#75710,#75711,#75712,#75713,#75714,
#75715,#75716,#75717,#75718,#75719,#75720,#75721,#75722,#75723,#75724,#75725,
#75726,#75727,#75728,#75729,#75730,#75731,#75732,#75733,#75734,#75735,#75736,
#75737,#75738,#75739,#75740,#75741,#75742,#75743,#75744,#75745,#75746,#75747,
#75748,#75749,#75750,#75751,#75752,#75753,#75754,#75755,#75756,#75757,#75758,
#75759,#75760,#75761,#75762,#75763,#75764,#75765,#75766,#75767,#75768,#75769,
#75770,#75771,#75772,#75773,#75774,#75775,#75776,#75777,#75778,#75779,#75780,
#75781,#75782,#75783,#75784,#75785,#75786,#75787,#75788,#75789,#75790,#75791,
#75792,#75793,#75794,#75795,#75796,#75797,#75798,#75799,#75800,#75801,#75802,
#75803,#75804,#75805),.UNSPECIFIED.,.F.,.F.,(4,3,3,3,3,3,3,3,3,3,3,3,3,
3,3,3,3,3,3,3,3,3,3,3,3,3,3,3,3,3,3,3,3,3,3,3,3,3,3,3,3,3,3,3,3,3,3,3,3,
3,3,3,3,3,3,3,3,3,3,3,3,3,3,3,3,3,3,3,3,3,3,3,4),(801.106126665528,801.206596975234,
801.308383579925,801.406869987991,801.490608699837,801.574244211204,801.657796654603,
801.741286090454,801.824740041068,801.908176534914,801.99161364467,802.075069439587,
802.158613932317,802.242203015258,802.325926282816,802.406605998711,802.490344710557,
802.573980221925,802.657532665323,802.741022101174,802.824476051788,802.907912545634,
802.99134965539,803.074805450308,803.158349943037,803.241939025978,803.325662293536,
803.406342009432,803.490080721278,803.573716232646,803.657268676044,803.740758111895,
803.824212062509,803.907648556355,803.991085666111,804.074541461028,804.158085953758,
804.241675036699,804.325398304257,804.406078020152,804.489816731998,804.573452243366,
804.657004686764,804.740494122615,804.823948073229,804.907384567075,804.99082167683,
805.074277471748,805.157821964478,805.241411047419,805.325134314976,805.405814030872,
805.489552742718,805.573188254085,805.656740697484,805.740230133335,805.823684083949,
805.907120577795,805.99055768755,806.074013482468,806.157557975198,806.241147058139,
806.324870325696,806.405550041592,806.489073461701,806.572464736515,806.655779744683,
806.739036867379,806.822254441502,806.905468087397,806.988676858978,807.071932381418,
807.137598113524),.UNSPECIFIED.);
#563=B_SPLINE_CURVE_WITH_KNOTS('',3,(#75811,#75812,#75813,#75814,#75815,
#75816,#75817,#75818,#75819,#75820,#75821,#75822,#75823,#75824,#75825,#75826,
#75827,#75828,#75829,#75830,#75831,#75832,#75833,#75834,#75835,#75836,#75837,
#75838,#75839,#75840,#75841,#75842,#75843,#75844,#75845,#75846,#75847,#75848,
#75849,#75850,#75851,#75852,#75853,#75854,#75855,#75856,#75857,#75858,#75859,
#75860,#75861,#75862,#75863,#75864,#75865,#75866,#75867,#75868,#75869,#75870,
#75871,#75872,#75873,#75874,#75875,#75876,#75877,#75878,#75879,#75880,#75881,
#75882,#75883,#75884,#75885,#75886,#75887,#75888,#75889,#75890,#75891,#75892,
#75893,#75894,#75895,#75896,#75897,#75898,#75899,#75900,#75901,#75902,#75903,
#75904,#75905,#75906,#75907,#75908,#75909,#75910,#75911,#75912,#75913,#75914,
#75915,#75916,#75917,#75918,#75919,#75920,#75921,#75922,#75923,#75924,#75925,
#75926,#75927,#75928,#75929,#75930,#75931,#75932,#75933,#75934,#75935,#75936,
#75937,#75938,#75939,#75940,#75941,#75942,#75943,#75944,#75945,#75946,#75947,
#75948,#75949,#75950,#75951,#75952,#75953,#75954,#75955,#75956,#75957,#75958,
#75959,#75960,#75961,#75962,#75963,#75964,#75965,#75966,#75967,#75968,#75969,
#75970,#75971,#75972,#75973,#75974,#75975,#75976,#75977,#75978,#75979,#75980,
#75981,#75982,#75983,#75984,#75985,#75986,#75987,#75988,#75989,#75990,#75991,
#75992,#75993,#75994,#75995,#75996,#75997,#75998,#75999,#76000,#76001,#76002,
#76003,#76004,#76005,#76006,#76007,#76008,#76009,#76010,#76011,#76012,#76013,
#76014,#76015,#76016,#76017,#76018,#76019,#76020,#76021,#76022,#76023,#76024,
#76025,#76026,#76027,#76028,#76029,#76030),.UNSPECIFIED.,.F.,.F.,(4,3,3,
3,3,3,3,3,3,3,3,3,3,3,3,3,3,3,3,3,3,3,3,3,3,3,3,3,3,3,3,3,3,3,3,3,3,3,3,
3,3,3,3,3,3,3,3,3,3,3,3,3,3,3,3,3,3,3,3,3,3,3,3,3,3,3,3,3,3,3,3,3,3,4),
(807.389311972555,807.472225275472,807.555112008788,807.637987902611,807.720871498604,
807.803781340485,807.886783805871,807.969838484841,808.053017602792,808.094731443316,
808.178470155162,808.26210566653,808.345658109928,808.429147545779,808.512601496393,
808.596037990239,808.679475099994,808.762930894912,808.846475387642,808.930064470583,
809.01378773814,809.094467454036,809.178206165882,809.261841677249,809.345394120648,
809.428883556499,809.512337507112,809.595774000959,809.679211110714,809.762666905631,
809.846211398361,809.929800481302,810.013523748859,810.094203464756,810.177942176602,
810.26157768797,810.345130131368,810.428619567219,810.512073517833,810.595510011679,
810.678947121434,810.762402916351,810.845947409081,810.929536492022,811.01325975958,
811.093939475476,811.177678187322,811.261313698689,811.344866142088,811.428355577939,
811.511809528552,811.595246022398,811.678683132154,811.762138927072,811.845683419801,
811.929272502743,812.0129957703,812.093675486196,812.177414198042,812.261049709409,
812.344602152808,812.428091588659,812.511545539273,812.594982033119,812.678419142875,
812.761874937793,812.845419430522,812.929008513464,813.012731781021,813.093411496916,
813.178887063871,813.264255755827,813.34950153073,813.421961035509),
 .UNSPECIFIED.);
#564=B_SPLINE_CURVE_WITH_KNOTS('',3,(#76031,#76032,#76033,#76034,#76035,
#76036,#76037,#76038,#76039,#76040),.UNSPECIFIED.,.F.,.F.,(4,3,3,4),(807.1385058474,
807.241041547493,807.342243436622,807.389311972417),.UNSPECIFIED.);
#565=B_SPLINE_CURVE_WITH_KNOTS('',3,(#76042,#76043,#76044,#76045,#76046,
#76047,#76048,#76049,#76050,#76051),.UNSPECIFIED.,.F.,.F.,(4,3,3,4),(807.137598113524,
807.220952318012,807.30513214521,807.389311972408),.UNSPECIFIED.);
#566=B_SPLINE_CURVE_WITH_KNOTS('',3,(#76052,#76053,#76054,#76055,#76056,
#76057,#76058,#76059,#76060,#76061,#76062,#76063,#76064,#76065,#76066,#76067,
#76068,#76069,#76070,#76071,#76072,#76073,#76074,#76075,#76076,#76077,#76078,
#76079,#76080,#76081,#76082,#76083,#76084,#76085,#76086,#76087,#76088,#76089,
#76090,#76091,#76092,#76093,#76094,#76095,#76096,#76097,#76098,#76099,#76100,
#76101,#76102,#76103,#76104,#76105,#76106,#76107,#76108,#76109,#76110,#76111,
#76112,#76113,#76114,#76115,#76116,#76117,#76118,#76119,#76120,#76121,#76122,
#76123,#76124,#76125,#76126,#76127,#76128,#76129,#76130,#76131,#76132,#76133,
#76134,#76135,#76136,#76137,#76138,#76139,#76140,#76141,#76142,#76143,#76144,
#76145,#76146,#76147,#76148,#76149,#76150,#76151,#76152,#76153,#76154,#76155,
#76156,#76157,#76158,#76159,#76160,#76161,#76162,#76163,#76164,#76165,#76166,
#76167,#76168,#76169,#76170,#76171,#76172,#76173,#76174,#76175,#76176,#76177,
#76178,#76179,#76180,#76181,#76182,#76183,#76184,#76185,#76186,#76187,#76188,
#76189,#76190,#76191,#76192,#76193,#76194,#76195,#76196,#76197,#76198,#76199,
#76200,#76201,#76202,#76203,#76204,#76205,#76206,#76207,#76208,#76209,#76210,
#76211,#76212,#76213,#76214,#76215,#76216,#76217,#76218,#76219,#76220,#76221,
#76222,#76223,#76224,#76225,#76226,#76227,#76228,#76229,#76230,#76231,#76232,
#76233,#76234,#76235,#76236,#76237,#76238,#76239,#76240,#76241,#76242,#76243,
#76244,#76245,#76246,#76247,#76248,#76249,#76250,#76251,#76252,#76253,#76254,
#76255,#76256,#76257,#76258,#76259,#76260,#76261,#76262,#76263,#76264,#76265,
#76266,#76267,#76268,#76269,#76270,#76271,#76272,#76273,#76274),
 .UNSPECIFIED.,.F.,.F.,(4,3,3,3,3,3,3,3,3,3,3,3,3,3,3,3,3,3,3,3,3,3,3,3,
3,3,3,3,3,3,3,3,3,3,3,3,3,3,3,3,3,3,3,3,3,3,3,3,3,3,3,3,3,3,3,3,3,3,3,3,
3,3,3,3,3,3,3,3,3,3,3,3,3,3,4),(807.389311972559,807.405286052312,807.489024764158,
807.572660275525,807.656212718924,807.739702154775,807.823156105389,807.906592599235,
807.99002970899,808.073485503908,808.157029996638,808.240619079579,808.324342347136,
808.405022063032,808.488760774878,808.572396286245,808.655948729644,808.739438165495,
808.822892116108,808.906328609955,808.98976571971,809.073221514628,809.156766007357,
809.240355090298,809.324078357856,809.404758073752,809.488496785598,809.572132296965,
809.655684740364,809.739174176215,809.822628126829,809.906064620675,809.989501730431,
810.072957525348,810.156502018078,810.240091101019,810.323814368577,810.404494084472,
810.488232796318,810.571868307686,810.655420751084,810.738910186935,810.822364137549,
810.905800631395,810.989237741151,811.072693536069,811.156238028798,811.239827111739,
811.323550379297,811.404230095193,811.487968807039,811.571604318407,811.655156761805,
811.738646197656,811.82210014827,811.905536642116,811.988973751872,812.07242954679,
812.155974039519,812.23956312246,812.323286390018,812.403966105913,812.487704817759,
812.571340329126,812.654892772525,812.738382208375,812.821836158989,812.905272652835,
812.988709762591,813.072165557508,813.155710050238,813.239299133179,813.323022400736,
813.403702116633,813.421541691872),.UNSPECIFIED.);
#567=B_SPLINE_CURVE_WITH_KNOTS('',3,(#76280,#76281,#76282,#76283,#76284,
#76285,#76286,#76287,#76288,#76289,#76290,#76291,#76292,#76293,#76294,#76295,
#76296,#76297,#76298,#76299,#76300,#76301,#76302,#76303,#76304,#76305,#76306,
#76307,#76308,#76309,#76310,#76311,#76312,#76313,#76314,#76315,#76316,#76317,
#76318,#76319,#76320,#76321,#76322,#76323,#76324,#76325,#76326,#76327,#76328,
#76329,#76330,#76331,#76332,#76333,#76334,#76335,#76336,#76337,#76338,#76339,
#76340,#76341,#76342,#76343,#76344,#76345,#76346,#76347,#76348,#76349,#76350,
#76351,#76352,#76353,#76354,#76355,#76356,#76357,#76358,#76359,#76360,#76361,
#76362,#76363,#76364,#76365,#76366,#76367,#76368,#76369,#76370,#76371,#76372,
#76373,#76374,#76375,#76376,#76377,#76378,#76379,#76380,#76381,#76382,#76383,
#76384,#76385,#76386,#76387,#76388,#76389,#76390,#76391,#76392,#76393,#76394,
#76395,#76396,#76397,#76398,#76399,#76400,#76401,#76402,#76403,#76404,#76405,
#76406,#76407,#76408,#76409,#76410,#76411,#76412,#76413,#76414,#76415,#76416,
#76417,#76418,#76419,#76420,#76421,#76422,#76423,#76424,#76425,#76426,#76427,
#76428,#76429,#76430,#76431,#76432,#76433,#76434,#76435,#76436,#76437,#76438,
#76439,#76440,#76441,#76442,#76443,#76444,#76445,#76446,#76447,#76448,#76449,
#76450,#76451,#76452,#76453,#76454,#76455,#76456,#76457,#76458,#76459,#76460,
#76461,#76462,#76463,#76464,#76465,#76466,#76467,#76468,#76469,#76470,#76471,
#76472,#76473,#76474,#76475,#76476,#76477,#76478,#76479,#76480,#76481,#76482,
#76483,#76484,#76485,#76486,#76487,#76488,#76489,#76490,#76491,#76492,#76493,
#76494,#76495,#76496,#76497,#76498,#76499),.UNSPECIFIED.,.F.,.F.,(4,3,3,
3,3,3,3,3,3,3,3,3,3,3,3,3,3,3,3,3,3,3,3,3,3,3,3,3,3,3,3,3,3,3,3,3,3,3,3,
3,3,3,3,3,3,3,3,3,3,3,3,3,3,3,3,3,3,3,3,3,3,3,3,3,3,3,3,3,3,3,3,3,3,4),
(813.672497279888,813.763414053234,813.854745397129,813.946288265523,814.038142143338,
814.093147507636,814.176886219482,814.26052173085,814.344074174249,814.427563610101,
814.511017560715,814.594454054562,814.677891164318,814.761346959237,814.844891451967,
814.928480534908,815.012203802467,815.092883518357,815.176622230203,815.26025774157,
815.343810184968,815.427299620819,815.510753571433,815.594190065279,815.677627175034,
815.761082969952,815.844627462681,815.928216545622,816.011939813179,816.092619529077,
816.176358240923,816.25999375229,816.343546195689,816.42703563154,816.510489582153,
816.593926076,816.677363185755,816.760818980673,816.844363473402,816.927952556343,
817.011675823901,817.092355539797,817.176094251643,817.259729763011,817.343282206409,
817.42677164226,817.510225592874,817.59366208672,817.677099196476,817.760554991394,
817.844099484123,817.927688567064,818.011411834622,818.092091550517,818.175830262363,
818.25946577373,818.343018217128,818.426507652979,818.509961603593,818.593398097439,
818.676835207194,818.760291002111,818.843835494841,818.927424577782,819.011147845339,
819.091827561237,819.174342520055,819.256762659536,819.339107167316,819.421395158965,
819.503652354638,819.58589159078,819.668149206529,819.703896483842),
 .UNSPECIFIED.);
#568=B_SPLINE_CURVE_WITH_KNOTS('',3,(#76500,#76501,#76502,#76503,#76504,
#76505,#76506,#76507,#76508,#76509),.UNSPECIFIED.,.F.,.F.,(4,3,3,4),(813.421961035509,
813.507063854652,813.592111218928,813.672497279735),.UNSPECIFIED.);
#569=B_SPLINE_CURVE_WITH_KNOTS('',3,(#76511,#76512,#76513,#76514,#76515,
#76516,#76517,#76518,#76519,#76520),.UNSPECIFIED.,.F.,.F.,(4,3,3,4),(813.421541691872,
813.527897418378,813.632413728413,813.672497279565),.UNSPECIFIED.);
#570=B_SPLINE_CURVE_WITH_KNOTS('',3,(#76521,#76522,#76523,#76524,#76525,
#76526,#76527,#76528,#76529,#76530,#76531,#76532,#76533,#76534,#76535,#76536,
#76537,#76538,#76539,#76540,#76541,#76542,#76543,#76544,#76545,#76546,#76547,
#76548,#76549,#76550,#76551,#76552,#76553,#76554,#76555,#76556,#76557,#76558,
#76559,#76560,#76561,#76562,#76563,#76564,#76565,#76566,#76567,#76568,#76569,
#76570,#76571,#76572,#76573,#76574,#76575,#76576,#76577,#76578,#76579,#76580,
#76581,#76582,#76583,#76584,#76585,#76586,#76587,#76588,#76589,#76590,#76591,
#76592,#76593,#76594,#76595,#76596,#76597,#76598,#76599,#76600,#76601,#76602,
#76603,#76604,#76605,#76606,#76607,#76608,#76609,#76610,#76611,#76612,#76613,
#76614,#76615,#76616,#76617,#76618,#76619,#76620,#76621,#76622,#76623,#76624,
#76625,#76626,#76627,#76628,#76629,#76630,#76631,#76632,#76633,#76634,#76635,
#76636,#76637,#76638,#76639,#76640,#76641,#76642,#76643,#76644,#76645,#76646,
#76647,#76648,#76649,#76650,#76651,#76652,#76653,#76654,#76655,#76656,#76657,
#76658,#76659,#76660,#76661,#76662,#76663,#76664,#76665,#76666,#76667,#76668,
#76669,#76670,#76671,#76672,#76673,#76674,#76675,#76676,#76677,#76678,#76679,
#76680,#76681,#76682,#76683,#76684,#76685,#76686,#76687,#76688,#76689,#76690,
#76691,#76692,#76693,#76694,#76695,#76696,#76697,#76698,#76699,#76700,#76701,
#76702,#76703,#76704,#76705,#76706,#76707,#76708,#76709,#76710,#76711,#76712,
#76713,#76714,#76715,#76716,#76717,#76718,#76719,#76720,#76721,#76722,#76723,
#76724,#76725,#76726,#76727,#76728,#76729,#76730,#76731,#76732,#76733,#76734,
#76735,#76736,#76737,#76738,#76739,#76740),.UNSPECIFIED.,.F.,.F.,(4,3,3,
3,3,3,3,3,3,3,3,3,3,3,3,3,3,3,3,3,3,3,3,3,3,3,3,3,3,3,3,3,3,3,3,3,3,3,3,
3,3,3,3,3,3,3,3,3,3,3,3,3,3,3,3,3,3,3,3,3,3,3,3,3,3,3,3,3,3,3,3,3,3,4),
(813.672497279739,813.75518641853,813.837835534489,813.920464908825,814.00309328813,
814.085739415308,814.168472347732,814.251250272538,814.334158514269,814.403438127353,
814.487176839199,814.570812350566,814.654364793965,814.737854229817,814.82130818043,
814.904744674277,814.988181784032,815.07163757895,815.15518207168,815.238771154621,
815.322494422179,815.403174138073,815.486912849919,815.570548361287,815.654100804685,
815.737590240536,815.82104419115,815.904480684996,815.987917794751,816.071373589669,
816.154918082398,816.238507165339,816.322230432897,816.402910148793,816.486648860639,
816.570284372006,816.653836815404,816.737326251255,816.820780201869,816.904216695715,
816.98765380547,817.071109600387,817.154654093117,817.238243176058,817.321966443615,
817.402646159513,817.486384871359,817.570020382727,817.653572826126,817.737062261977,
817.820516212591,817.903952706438,817.987389816194,818.070845611112,818.154390103841,
818.237979186783,818.321702454341,818.402382170234,818.48612088208,818.569756393448,
818.653308836846,818.736798272697,818.820252223311,818.903688717158,818.987125826914,
819.070581621832,819.154126114561,819.237715197503,819.321438465061,819.402118180954,
819.488312354914,819.574393064568,819.660340071141,819.705233576188),
 .UNSPECIFIED.);
#571=B_SPLINE_CURVE_WITH_KNOTS('',3,(#76746,#76747,#76748,#76749,#76750,
#76751,#76752,#76753,#76754,#76755,#76756,#76757,#76758,#76759,#76760,#76761,
#76762,#76763,#76764,#76765,#76766,#76767,#76768,#76769,#76770,#76771,#76772,
#76773,#76774,#76775,#76776,#76777,#76778,#76779,#76780,#76781,#76782,#76783,
#76784,#76785,#76786,#76787,#76788,#76789,#76790,#76791,#76792,#76793,#76794,
#76795,#76796,#76797,#76798,#76799,#76800,#76801,#76802,#76803,#76804,#76805,
#76806,#76807,#76808,#76809,#76810,#76811,#76812,#76813,#76814,#76815,#76816,
#76817,#76818,#76819,#76820,#76821,#76822,#76823,#76824,#76825,#76826,#76827,
#76828,#76829,#76830,#76831,#76832,#76833,#76834,#76835,#76836,#76837,#76838,
#76839,#76840,#76841,#76842,#76843,#76844,#76845,#76846,#76847,#76848,#76849,
#76850,#76851,#76852,#76853,#76854,#76855,#76856,#76857,#76858,#76859,#76860,
#76861,#76862,#76863,#76864,#76865,#76866,#76867,#76868,#76869,#76870,#76871,
#76872,#76873,#76874,#76875,#76876,#76877,#76878,#76879,#76880,#76881,#76882,
#76883,#76884,#76885,#76886,#76887,#76888,#76889,#76890,#76891,#76892,#76893,
#76894,#76895,#76896,#76897,#76898,#76899,#76900,#76901,#76902,#76903,#76904,
#76905,#76906,#76907,#76908,#76909,#76910,#76911,#76912,#76913,#76914,#76915,
#76916,#76917,#76918,#76919,#76920,#76921,#76922,#76923,#76924,#76925,#76926,
#76927,#76928,#76929,#76930,#76931,#76932,#76933,#76934,#76935,#76936,#76937,
#76938,#76939,#76940,#76941,#76942,#76943,#76944,#76945,#76946,#76947,#76948,
#76949,#76950,#76951,#76952,#76953,#76954,#76955,#76956,#76957,#76958,#76959,
#76960,#76961,#76962),.UNSPECIFIED.,.F.,.F.,(4,3,3,3,3,3,3,3,3,3,3,3,3,
3,3,3,3,3,3,3,3,3,3,3,3,3,3,3,3,3,3,3,3,3,3,3,3,3,3,3,3,3,3,3,3,3,3,3,3,
3,3,3,3,3,3,3,3,3,3,3,3,3,3,3,3,3,3,3,3,3,3,3,4),(819.955682586915,820.091563571957,
820.175302283805,820.258937795175,820.342490238576,820.425979674429,820.509433625045,
820.592870118894,820.676307228652,820.759763023573,820.843307516305,820.926896599248,
821.010619866809,821.091299582677,821.175038294523,821.25867380589,821.342226249288,
821.425715685139,821.509169635753,821.592606129598,821.676043239354,821.759499034271,
821.843043527001,821.926632609941,822.010355877499,822.091035593398,822.174774305244,
822.258409816611,822.341962260009,822.42545169586,822.508905646474,822.59234214032,
822.675779250075,822.759235044992,822.842779537722,822.926368620662,823.01009188822,
823.090771604118,823.174510315964,823.258145827332,823.34169827073,823.425187706581,
823.508641657195,823.592078151041,823.675515260797,823.758971055714,823.842515548444,
823.926104631385,824.009827898943,824.090507614838,824.174246326684,824.257881838051,
824.34143428145,824.424923717301,824.508377667914,824.591814161761,824.675251271516,
824.758707066434,824.842251559163,824.925840642104,825.009563909662,825.090243625558,
825.173988319906,825.25762845994,825.341184183953,825.424671159286,825.508120674546,
825.591550818252,825.67497966208,825.758462116136,825.8419721472,825.925578110456,
825.987345293289),.UNSPECIFIED.);
#572=B_SPLINE_CURVE_WITH_KNOTS('',3,(#76963,#76964,#76965,#76966,#76967,
#76968,#76969,#76970,#76971,#76972),.UNSPECIFIED.,.F.,.F.,(4,3,3,4),(819.703896483842,
819.786220350054,819.870951468422,819.95568258679),.UNSPECIFIED.);
#573=B_SPLINE_CURVE_WITH_KNOTS('',3,(#76974,#76975,#76976,#76977,#76978,
#76979,#76980,#76981,#76982,#76983),.UNSPECIFIED.,.F.,.F.,(4,3,3,4),(819.705233576188,
819.79103108917,819.876744696265,819.955682586918),.UNSPECIFIED.);
#574=B_SPLINE_CURVE_WITH_KNOTS('',3,(#76984,#76985,#76986,#76987,#76988,
#76989,#76990,#76991,#76992,#76993,#76994,#76995,#76996,#76997,#76998,#76999,
#77000,#77001,#77002,#77003,#77004,#77005,#77006,#77007,#77008,#77009,#77010,
#77011,#77012,#77013,#77014,#77015,#77016,#77017,#77018,#77019,#77020,#77021,
#77022,#77023,#77024,#77025,#77026,#77027,#77028,#77029,#77030,#77031,#77032,
#77033,#77034,#77035,#77036,#77037,#77038,#77039,#77040,#77041,#77042,#77043,
#77044,#77045,#77046,#77047,#77048,#77049,#77050,#77051,#77052,#77053,#77054,
#77055,#77056,#77057,#77058,#77059,#77060,#77061,#77062,#77063,#77064,#77065,
#77066,#77067,#77068,#77069,#77070,#77071,#77072,#77073,#77074,#77075,#77076,
#77077,#77078,#77079,#77080,#77081,#77082,#77083,#77084,#77085,#77086,#77087,
#77088,#77089,#77090,#77091,#77092,#77093,#77094,#77095,#77096,#77097,#77098,
#77099,#77100,#77101,#77102,#77103,#77104,#77105,#77106,#77107,#77108,#77109,
#77110,#77111,#77112,#77113,#77114,#77115,#77116,#77117,#77118,#77119,#77120,
#77121,#77122,#77123,#77124,#77125,#77126,#77127,#77128,#77129,#77130,#77131,
#77132,#77133,#77134,#77135,#77136,#77137,#77138,#77139,#77140,#77141,#77142,
#77143,#77144,#77145,#77146,#77147,#77148,#77149,#77150,#77151,#77152,#77153,
#77154,#77155,#77156,#77157,#77158,#77159,#77160,#77161,#77162,#77163,#77164,
#77165,#77166,#77167,#77168,#77169,#77170,#77171,#77172,#77173,#77174,#77175,
#77176,#77177,#77178,#77179,#77180,#77181,#77182,#77183,#77184,#77185,#77186,
#77187,#77188,#77189,#77190,#77191,#77192,#77193,#77194,#77195,#77196,#77197,
#77198,#77199,#77200),.UNSPECIFIED.,.F.,.F.,(4,3,3,3,3,3,3,3,3,3,3,3,3,
3,3,3,3,3,3,3,3,3,3,3,3,3,3,3,3,3,3,3,3,3,3,3,3,3,3,3,3,3,3,3,3,3,3,3,3,
3,3,3,3,3,3,3,3,3,3,3,3,3,3,3,3,3,3,3,3,3,3,3,4),(819.955682587033,820.045313946329,
820.135281214152,820.225415774172,820.315836079296,820.401854191674,820.485592903519,
820.569228414886,820.652780858284,820.736270294135,820.819724244748,820.903160738594,
820.986597848349,821.070053643266,821.153598135995,821.237187218935,821.320910486492,
821.401590202394,821.48532891424,821.568964425608,821.652516869006,821.736006304857,
821.819460255471,821.902896749317,821.986333859072,822.06978965399,822.15333414672,
822.236923229661,822.320646497218,822.401326213114,822.48506492496,822.568700436328,
822.652252879726,822.735742315577,822.819196266191,822.902632760037,822.986069869792,
823.06952566471,823.15307015744,823.236659240381,823.320382507938,823.401062223834,
823.48480093568,823.568436447047,823.651988890446,823.735478326297,823.818932276911,
823.902368770757,823.985805880512,824.06926167543,824.15280616816,824.236395251101,
824.320118518658,824.400798234554,824.4845369464,824.568172457768,824.651724901166,
824.735214337017,824.818668287631,824.902104781477,824.985541891233,825.068997686151,
825.15254217888,825.236131261821,825.319854529379,825.400534245274,825.48300659384,
825.565383758059,825.647684956802,825.732550045853,825.814760182079,825.900952747541,
825.987145313003),.UNSPECIFIED.);
#575=B_SPLINE_CURVE_WITH_KNOTS('',3,(#77206,#77207,#77208,#77209,#77210,
#77211,#77212,#77213,#77214,#77215,#77216,#77217,#77218,#77219,#77220,#77221,
#77222,#77223,#77224,#77225,#77226,#77227,#77228,#77229,#77230,#77231,#77232,
#77233,#77234,#77235,#77236,#77237,#77238,#77239,#77240,#77241,#77242,#77243,
#77244,#77245,#77246,#77247,#77248,#77249,#77250,#77251,#77252,#77253,#77254,
#77255,#77256,#77257,#77258,#77259,#77260,#77261,#77262,#77263,#77264,#77265,
#77266,#77267,#77268,#77269,#77270,#77271,#77272,#77273,#77274,#77275,#77276,
#77277,#77278,#77279,#77280,#77281,#77282,#77283,#77284,#77285,#77286,#77287,
#77288,#77289,#77290,#77291,#77292,#77293,#77294,#77295,#77296,#77297,#77298,
#77299,#77300,#77301,#77302,#77303,#77304,#77305,#77306,#77307,#77308,#77309,
#77310,#77311,#77312,#77313,#77314,#77315,#77316,#77317,#77318,#77319,#77320,
#77321,#77322,#77323,#77324,#77325,#77326,#77327,#77328,#77329,#77330,#77331,
#77332,#77333,#77334,#77335,#77336,#77337,#77338,#77339,#77340,#77341,#77342,
#77343,#77344,#77345,#77346,#77347,#77348,#77349,#77350,#77351,#77352,#77353,
#77354,#77355,#77356,#77357,#77358,#77359,#77360,#77361,#77362,#77363,#77364,
#77365,#77366,#77367,#77368,#77369,#77370,#77371,#77372,#77373,#77374,#77375,
#77376,#77377,#77378,#77379,#77380,#77381,#77382,#77383,#77384,#77385,#77386,
#77387,#77388,#77389,#77390,#77391,#77392,#77393,#77394,#77395,#77396,#77397,
#77398,#77399,#77400,#77401,#77402,#77403,#77404,#77405,#77406,#77407,#77408,
#77409,#77410,#77411,#77412,#77413,#77414,#77415,#77416,#77417,#77418,#77419,
#77420,#77421,#77422,#77423,#77424,#77425),.UNSPECIFIED.,.F.,.F.,(4,3,3,
3,3,3,3,3,3,3,3,3,3,3,3,3,3,3,3,3,3,3,3,3,3,3,3,3,3,3,3,3,3,3,3,3,3,3,3,
3,3,3,3,3,3,3,3,3,3,3,3,3,3,3,3,3,3,3,3,3,3,3,3,3,3,3,3,3,3,3,3,3,3,4),
(826.238867894208,826.32127581105,826.403601341344,826.489365629551,826.57159656205,
826.653814332816,826.736037965977,826.818286488398,826.900622949684,826.983011397038,
827.065515324656,827.089715646998,827.173454358844,827.257089870211,827.34064231361,
827.424131749461,827.507585700075,827.591022193921,827.674459303676,827.757915098594,
827.841459591324,827.925048674265,828.008771941822,828.089451657718,828.173190369564,
828.256825880931,828.340378324329,828.42386776018,828.507321710794,828.59075820464,
828.674195314395,828.757651109313,828.841195602043,828.924784684984,829.008507952541,
829.089187668438,829.172926380284,829.256561891651,829.34011433505,829.423603770901,
829.507057721515,829.590494215361,829.673931325117,829.757387120035,829.840931612764,
829.924520695706,830.008243963263,830.088923679158,830.172662391004,830.256297902372,
830.33985034577,830.423339781621,830.506793732235,830.590230226081,830.673667335836,
830.757123130754,830.840667623484,830.924256706425,831.007979973982,831.088659689879,
831.172398401725,831.256033913093,831.339586356492,831.423075792343,831.506529742956,
831.589966236803,831.673403346558,831.756859141476,831.840403634205,831.923992717146,
832.007715984704,832.088395700599,832.18006641272,832.271737124841),
 .UNSPECIFIED.);
#576=B_SPLINE_CURVE_WITH_KNOTS('',3,(#77426,#77427,#77428,#77429,#77430,
#77431,#77432,#77433,#77434,#77435),.UNSPECIFIED.,.F.,.F.,(4,3,3,4),(825.987345293289,
826.071094722339,826.089979636278,826.238867894094),.UNSPECIFIED.);
#577=B_SPLINE_CURVE_WITH_KNOTS('',3,(#77437,#77438,#77439,#77440,#77441,
#77442,#77443,#77444,#77445,#77446),.UNSPECIFIED.,.F.,.F.,(4,3,3,4),(825.987145313003,
826.069408893835,826.154138393866,826.238867893896),.UNSPECIFIED.);
#578=B_SPLINE_CURVE_WITH_KNOTS('',3,(#77447,#77448,#77449,#77450,#77451,
#77452,#77453,#77454,#77455,#77456,#77457,#77458,#77459,#77460,#77461,#77462,
#77463,#77464,#77465,#77466,#77467,#77468,#77469,#77470,#77471,#77472,#77473,
#77474,#77475,#77476,#77477,#77478,#77479,#77480,#77481,#77482,#77483,#77484,
#77485,#77486,#77487,#77488,#77489,#77490,#77491,#77492,#77493,#77494,#77495,
#77496,#77497,#77498,#77499,#77500,#77501,#77502,#77503,#77504,#77505,#77506,
#77507,#77508,#77509,#77510,#77511,#77512,#77513,#77514,#77515,#77516,#77517,
#77518,#77519,#77520,#77521,#77522,#77523,#77524,#77525,#77526,#77527,#77528,
#77529,#77530,#77531,#77532,#77533,#77534,#77535,#77536,#77537,#77538,#77539,
#77540,#77541,#77542,#77543,#77544,#77545,#77546,#77547,#77548,#77549,#77550,
#77551,#77552,#77553,#77554,#77555,#77556,#77557,#77558,#77559,#77560,#77561,
#77562,#77563,#77564,#77565,#77566,#77567,#77568,#77569,#77570,#77571,#77572,
#77573,#77574,#77575,#77576,#77577,#77578,#77579,#77580,#77581,#77582,#77583,
#77584,#77585,#77586,#77587,#77588,#77589,#77590,#77591,#77592,#77593,#77594,
#77595,#77596,#77597,#77598,#77599,#77600,#77601,#77602,#77603,#77604,#77605,
#77606,#77607,#77608,#77609,#77610,#77611,#77612,#77613,#77614,#77615,#77616,
#77617,#77618,#77619,#77620,#77621,#77622,#77623,#77624,#77625,#77626,#77627,
#77628,#77629,#77630,#77631,#77632,#77633,#77634,#77635,#77636,#77637,#77638,
#77639,#77640,#77641,#77642,#77643,#77644,#77645,#77646,#77647,#77648,#77649,
#77650,#77651,#77652,#77653,#77654,#77655,#77656,#77657,#77658,#77659,#77660,
#77661,#77662,#77663,#77664,#77665,#77666),.UNSPECIFIED.,.F.,.F.,(4,3,3,
3,3,3,3,3,3,3,3,3,3,3,3,3,3,3,3,3,3,3,3,3,3,3,3,3,3,3,3,3,3,3,3,3,3,3,3,
3,3,3,3,3,3,3,3,3,3,3,3,3,3,3,3,3,3,3,3,3,3,3,3,3,3,3,3,3,3,3,3,3,3,4),
(826.238867894098,826.374623943545,826.400270255995,826.484008967841,826.567644479209,
826.651196922607,826.734686358458,826.818140309072,826.901576802918,826.985013912674,
827.068469707591,827.152014200321,827.235603283262,827.319326550819,827.400006266715,
827.483744978561,827.567380489928,827.650932933327,827.734422369178,827.817876319791,
827.901312813638,827.984749923393,828.068205718311,828.15175021104,828.235339293981,
828.319062561539,828.399742277435,828.483480989281,828.567116500649,828.650668944047,
828.734158379898,828.817612330512,828.901048824358,828.984485934113,829.067941729031,
829.151486221761,829.235075304702,829.318798572259,829.399478288155,829.483217000001,
829.566852511369,829.650404954767,829.733894390618,829.817348341232,829.900784835078,
829.984221944833,830.067677739751,830.151222232481,830.234811315422,830.318534582979,
830.399214298875,830.482953010721,830.566588522088,830.650140965487,830.733630401338,
830.817084351952,830.900520845798,830.983957955553,831.067413750471,831.150958243201,
831.234547326142,831.318270593699,831.398950309595,831.48269656839,831.566337935338,
831.649894550206,831.733381190797,831.816829893747,831.900258747863,831.983685824687,
832.067161049063,832.150663656295,832.23424954886,832.270468650374),
 .UNSPECIFIED.);
#579=B_SPLINE_CURVE_WITH_KNOTS('',3,(#77672,#77673,#77674,#77675,#77676,
#77677,#77678,#77679,#77680,#77681,#77682,#77683,#77684,#77685,#77686,#77687,
#77688,#77689,#77690,#77691,#77692,#77693,#77694,#77695,#77696,#77697,#77698,
#77699,#77700,#77701,#77702,#77703,#77704,#77705,#77706,#77707,#77708,#77709,
#77710,#77711,#77712,#77713,#77714,#77715,#77716,#77717,#77718,#77719,#77720,
#77721,#77722,#77723,#77724,#77725,#77726,#77727,#77728,#77729,#77730,#77731,
#77732,#77733,#77734,#77735,#77736,#77737,#77738,#77739,#77740,#77741,#77742,
#77743,#77744,#77745,#77746,#77747,#77748,#77749,#77750,#77751,#77752,#77753,
#77754,#77755,#77756,#77757,#77758,#77759,#77760,#77761,#77762,#77763,#77764,
#77765,#77766,#77767,#77768,#77769,#77770,#77771,#77772,#77773,#77774,#77775,
#77776,#77777,#77778,#77779,#77780,#77781,#77782,#77783,#77784,#77785,#77786,
#77787,#77788,#77789,#77790,#77791,#77792,#77793,#77794,#77795,#77796,#77797,
#77798,#77799,#77800,#77801,#77802,#77803,#77804,#77805,#77806,#77807,#77808,
#77809,#77810,#77811,#77812,#77813,#77814,#77815,#77816,#77817,#77818,#77819,
#77820,#77821,#77822,#77823,#77824,#77825,#77826,#77827,#77828,#77829,#77830,
#77831,#77832,#77833,#77834,#77835,#77836,#77837,#77838,#77839,#77840,#77841,
#77842,#77843,#77844,#77845,#77846,#77847,#77848,#77849,#77850,#77851,#77852,
#77853,#77854,#77855,#77856,#77857,#77858,#77859,#77860,#77861,#77862,#77863,
#77864,#77865,#77866,#77867,#77868,#77869,#77870,#77871,#77872,#77873,#77874,
#77875,#77876,#77877,#77878,#77879,#77880,#77881,#77882,#77883,#77884,#77885,
#77886,#77887,#77888,#77889,#77890,#77891),.UNSPECIFIED.,.F.,.F.,(4,3,3,
3,3,3,3,3,3,3,3,3,3,3,3,3,3,3,3,3,3,3,3,3,3,3,3,3,3,3,3,3,3,3,3,3,3,3,3,
3,3,3,3,3,3,3,3,3,3,3,3,3,3,3,3,3,3,3,3,3,3,3,3,3,3,3,3,3,3,3,3,3,3,4),
(832.522053201274,832.60741531893,832.692823871791,832.778293592255,832.863901389771,
832.949584597495,833.035425121847,833.088131711319,833.171870423165,833.255505934532,
833.339058377931,833.422547813782,833.506001764395,833.589438258241,833.672875367997,
833.756331162914,833.839875655643,833.923464738584,834.007188006142,834.087867722039,
834.171606433885,834.255241945253,834.338794388651,834.422283824502,834.505737775116,
834.589174268962,834.672611378717,834.756067173635,834.839611666365,834.923200749306,
835.006924016863,835.087603732759,835.171342444605,835.254977955973,835.338530399371,
835.422019835222,835.505473785836,835.588910279682,835.672347389438,835.755803184355,
835.839347677085,835.922936760026,836.006660027584,836.087339743479,836.171078455325,
836.254713966693,836.338266410091,836.421755845942,836.505209796556,836.588646290402,
836.672083400158,836.755539195075,836.839083687805,836.922672770746,837.006396038303,
837.087075754199,837.170814466045,837.254449977413,837.338002420811,837.421491856662,
837.504945807275,837.588382301122,837.671819410877,837.755275205794,837.838819698524,
837.922408781465,838.006132049023,838.08681176492,838.16985418221,838.252796291963,
838.335641931048,838.41843159313,838.501185242415,838.554033681403),
 .UNSPECIFIED.);
#580=B_SPLINE_CURVE_WITH_KNOTS('',3,(#77892,#77893,#77894,#77895,#77896,
#77897,#77898,#77899,#77900,#77901),.UNSPECIFIED.,.F.,.F.,(4,3,3,4),(832.271737124841,
832.362378164833,832.452703543163,832.522053201137),.UNSPECIFIED.);
#581=B_SPLINE_CURVE_WITH_KNOTS('',3,(#77903,#77904,#77905,#77906,#77907,
#77908,#77909,#77910,#77911,#77912),.UNSPECIFIED.,.F.,.F.,(4,3,3,4),(832.270468650374,
832.354205921054,832.398686320315,832.522053201278),.UNSPECIFIED.);
#582=B_SPLINE_CURVE_WITH_KNOTS('',3,(#77913,#77914,#77915,#77916,#77917,
#77918,#77919,#77920,#77921,#77922,#77923,#77924,#77925,#77926,#77927,#77928,
#77929,#77930,#77931,#77932,#77933,#77934,#77935,#77936,#77937,#77938,#77939,
#77940,#77941,#77942,#77943,#77944,#77945,#77946,#77947,#77948,#77949,#77950,
#77951,#77952,#77953,#77954,#77955,#77956,#77957,#77958,#77959,#77960,#77961,
#77962,#77963,#77964,#77965,#77966,#77967,#77968,#77969,#77970,#77971,#77972,
#77973,#77974,#77975,#77976,#77977,#77978,#77979,#77980,#77981,#77982,#77983,
#77984,#77985,#77986,#77987,#77988,#77989,#77990,#77991,#77992,#77993,#77994,
#77995,#77996,#77997,#77998,#77999,#78000,#78001,#78002,#78003,#78004,#78005,
#78006,#78007,#78008,#78009,#78010,#78011,#78012,#78013,#78014,#78015,#78016,
#78017,#78018,#78019,#78020,#78021,#78022,#78023,#78024,#78025,#78026,#78027,
#78028,#78029,#78030,#78031,#78032,#78033,#78034,#78035,#78036,#78037,#78038,
#78039,#78040,#78041,#78042,#78043,#78044,#78045,#78046,#78047,#78048,#78049,
#78050,#78051,#78052,#78053,#78054,#78055,#78056,#78057,#78058,#78059,#78060,
#78061,#78062,#78063,#78064,#78065,#78066,#78067,#78068,#78069,#78070,#78071,
#78072,#78073,#78074,#78075,#78076,#78077,#78078,#78079,#78080,#78081,#78082,
#78083,#78084,#78085,#78086,#78087,#78088,#78089,#78090,#78091,#78092,#78093,
#78094,#78095,#78096,#78097,#78098,#78099,#78100,#78101,#78102,#78103,#78104,
#78105,#78106,#78107,#78108,#78109,#78110,#78111,#78112,#78113,#78114,#78115,
#78116,#78117,#78118,#78119,#78120,#78121,#78122,#78123,#78124,#78125,#78126,
#78127,#78128,#78129,#78130,#78131,#78132),.UNSPECIFIED.,.F.,.F.,(4,3,3,
3,3,3,3,3,3,3,3,3,3,3,3,3,3,3,3,3,3,3,3,3,3,3,3,3,3,3,3,3,3,3,3,3,3,3,3,
3,3,3,3,3,3,3,3,3,3,3,3,3,3,3,3,3,3,3,3,3,3,3,3,3,3,3,3,3,3,3,3,3,3,4),
(832.52205320141,832.604557929264,832.686974591374,832.76932429753,832.851634173575,
832.933924851774,833.016215315304,833.098524544869,833.180918992729,833.26335983401,
833.345923922194,833.398422331035,833.482161042881,833.565796554248,833.649348997647,
833.732838433498,833.816292384111,833.899728877957,833.983165987713,834.06662178263,
834.15016627536,834.233755358301,834.317478625858,834.398158341756,834.481897053602,
834.56553256497,834.649085008368,834.732574444219,834.816028394833,834.899464888679,
834.982901998434,835.066357793352,835.149902286082,835.233491369023,835.317214636581,
835.397894352476,835.481633064322,835.565268575689,835.648821019088,835.732310454939,
835.815764405553,835.899200899399,835.982638009155,836.066093804072,836.149638296802,
836.233227379743,836.316950647301,836.397630363196,836.481369075042,836.565004586409,
836.648557029808,836.732046465659,836.815500416273,836.898936910119,836.982374019874,
837.065829814792,837.149374307522,837.232963390463,837.31668665802,837.397366373916,
837.481105085762,837.56474059713,837.648293040528,837.731782476379,837.815236426993,
837.898672920839,837.982110030595,838.065565825513,838.149110318242,838.232699401183,
838.316422668741,838.397102384636,838.489700245904,838.554883200175),
 .UNSPECIFIED.);
#583=B_SPLINE_CURVE_WITH_KNOTS('',3,(#78138,#78139,#78140,#78141,#78142,
#78143,#78144,#78145,#78146,#78147,#78148,#78149,#78150,#78151,#78152,#78153,
#78154,#78155,#78156,#78157,#78158,#78159,#78160,#78161,#78162,#78163,#78164,
#78165,#78166,#78167,#78168,#78169,#78170,#78171,#78172,#78173,#78174,#78175,
#78176,#78177,#78178,#78179,#78180,#78181,#78182,#78183,#78184,#78185,#78186,
#78187,#78188,#78189,#78190,#78191,#78192,#78193,#78194,#78195,#78196,#78197,
#78198,#78199,#78200,#78201,#78202,#78203,#78204,#78205,#78206,#78207,#78208,
#78209,#78210,#78211,#78212,#78213,#78214,#78215,#78216,#78217,#78218,#78219,
#78220,#78221,#78222,#78223,#78224,#78225,#78226,#78227,#78228,#78229,#78230,
#78231,#78232,#78233,#78234,#78235,#78236,#78237,#78238,#78239,#78240,#78241,
#78242,#78243,#78244,#78245,#78246,#78247,#78248,#78249,#78250,#78251,#78252,
#78253,#78254,#78255,#78256,#78257,#78258,#78259,#78260,#78261,#78262,#78263,
#78264,#78265,#78266,#78267,#78268,#78269,#78270,#78271,#78272,#78273,#78274,
#78275,#78276,#78277,#78278,#78279,#78280,#78281,#78282,#78283,#78284,#78285,
#78286,#78287,#78288,#78289,#78290,#78291,#78292,#78293,#78294,#78295,#78296,
#78297,#78298,#78299,#78300,#78301,#78302,#78303,#78304,#78305,#78306,#78307,
#78308,#78309,#78310,#78311,#78312,#78313,#78314,#78315,#78316,#78317,#78318,
#78319,#78320,#78321,#78322,#78323,#78324,#78325,#78326,#78327,#78328,#78329,
#78330,#78331,#78332,#78333,#78334,#78335,#78336,#78337,#78338,#78339,#78340,
#78341,#78342,#78343,#78344,#78345,#78346,#78347,#78348,#78349,#78350,#78351,
#78352,#78353,#78354),.UNSPECIFIED.,.F.,.F.,(4,3,3,3,3,3,3,3,3,3,3,3,3,
3,3,3,3,3,3,3,3,3,3,3,3,3,3,3,3,3,3,3,3,3,3,3,3,3,3,3,3,3,3,3,3,3,3,3,3,
3,3,3,3,3,3,3,3,3,3,3,3,3,3,3,3,3,3,3,3,3,3,3,4),(838.805238508566,838.908003644901,
839.012398265655,839.08654777564,839.170286487486,839.253921998854,839.337474442252,
839.420963878103,839.504417828717,839.587854322563,839.671291432319,839.754747227237,
839.838291719966,839.921880802907,840.005604070465,840.08628378636,840.170022498206,
840.253658009573,840.337210452972,840.420699888823,840.504153839436,840.587590333282,
840.671027443038,840.754483237955,840.838027730685,840.921616813626,841.005340081183,
841.08601979708,841.169758508926,841.253394020294,841.336946463692,841.420435899543,
841.503889850157,841.587326344003,841.670763453758,841.754219248676,841.837763741406,
841.921352824347,842.005076091904,842.0857558078,842.169494519646,842.253130031013,
842.336682474412,842.420171910263,842.503625860877,842.587062354723,842.670499464479,
842.753955259396,842.837499752126,842.921088835067,843.004812102625,843.08549181852,
843.169230530366,843.252866041734,843.336418485132,843.419907920983,843.503361871597,
843.586798365443,843.670235475198,843.753691270116,843.837235762846,843.920824845787,
844.004548113344,844.08522782924,844.168981814258,844.252603254596,844.336148220539,
844.419634877612,844.5030813478,844.586524571239,844.669961864576,844.753450679487,
844.836771567909),.UNSPECIFIED.);
#584=B_SPLINE_CURVE_WITH_KNOTS('',3,(#78355,#78356,#78357,#78358,#78359,
#78360,#78361,#78362,#78363,#78364),.UNSPECIFIED.,.F.,.F.,(4,3,3,4),(838.554033681403,
838.636776122618,838.721007315535,838.805238508453),.UNSPECIFIED.);
#585=B_SPLINE_CURVE_WITH_KNOTS('',3,(#78366,#78367,#78368,#78369,#78370,
#78371,#78372,#78373,#78374,#78375),.UNSPECIFIED.,.F.,.F.,(4,3,3,4),(838.554883200175,
838.647013297185,838.738739357629,838.805238508288),.UNSPECIFIED.);
#586=B_SPLINE_CURVE_WITH_KNOTS('',3,(#78376,#78377,#78378,#78379,#78380,
#78381,#78382,#78383,#78384,#78385,#78386,#78387,#78388,#78389,#78390,#78391,
#78392,#78393,#78394,#78395,#78396,#78397,#78398,#78399,#78400,#78401,#78402,
#78403,#78404,#78405,#78406,#78407,#78408,#78409,#78410,#78411,#78412,#78413,
#78414,#78415,#78416,#78417,#78418,#78419,#78420,#78421,#78422,#78423,#78424,
#78425,#78426,#78427,#78428,#78429,#78430,#78431,#78432,#78433,#78434,#78435,
#78436,#78437,#78438,#78439,#78440,#78441,#78442,#78443,#78444,#78445,#78446,
#78447,#78448,#78449,#78450,#78451,#78452,#78453,#78454,#78455,#78456,#78457,
#78458,#78459,#78460,#78461,#78462,#78463,#78464,#78465,#78466,#78467,#78468,
#78469,#78470,#78471,#78472,#78473,#78474,#78475,#78476,#78477,#78478,#78479,
#78480,#78481,#78482,#78483,#78484,#78485,#78486,#78487,#78488,#78489,#78490,
#78491,#78492,#78493,#78494,#78495,#78496,#78497,#78498,#78499,#78500,#78501,
#78502,#78503,#78504,#78505,#78506,#78507,#78508,#78509,#78510,#78511,#78512,
#78513,#78514,#78515,#78516,#78517,#78518,#78519,#78520,#78521,#78522,#78523,
#78524,#78525,#78526,#78527,#78528,#78529,#78530,#78531,#78532,#78533,#78534,
#78535,#78536,#78537,#78538,#78539,#78540,#78541,#78542,#78543,#78544,#78545,
#78546,#78547,#78548,#78549,#78550,#78551,#78552,#78553,#78554,#78555,#78556,
#78557,#78558,#78559,#78560,#78561,#78562,#78563,#78564,#78565,#78566,#78567,
#78568,#78569,#78570,#78571,#78572,#78573,#78574,#78575,#78576,#78577,#78578,
#78579,#78580,#78581,#78582,#78583,#78584,#78585,#78586,#78587,#78588,#78589,
#78590,#78591,#78592,#78593,#78594,#78595),.UNSPECIFIED.,.F.,.F.,(4,3,3,
3,3,3,3,3,3,3,3,3,3,3,3,3,3,3,3,3,3,3,3,3,3,3,3,3,3,3,3,3,3,3,3,3,3,3,3,
3,3,3,3,3,3,3,3,3,3,3,3,3,3,3,3,3,3,3,3,3,3,3,3,3,3,3,3,3,3,3,3,3,3,4),
(838.805238508457,838.889983142447,838.974755435149,839.059571419872,839.144509591216,
839.229510261239,839.314669361647,839.396838395356,839.480577107202,839.564212618569,
839.647765061968,839.731254497819,839.814708448432,839.898144942279,839.981582052034,
840.065037846951,840.148582339681,840.232171422622,840.315894690179,840.396574406076,
840.480313117922,840.56394862929,840.647501072688,840.73099050854,840.814444459153,
840.897880953,840.981318062755,841.064773857673,841.148318350403,841.231907433344,
841.315630700901,841.396310416796,841.480049128642,841.563684640009,841.647237083408,
841.730726519259,841.814180469873,841.897616963719,841.981054073475,842.064509868392,
842.148054361122,842.231643444063,842.315366711621,842.396046427517,842.479785139363,
842.563420650731,842.646973094129,842.73046252998,842.813916480594,842.89735297444,
842.980790084196,843.064245879113,843.147790371843,843.231379454784,843.315102722342,
843.395782438237,843.479521150083,843.56315666145,843.646709104849,843.7301985407,
843.813652491314,843.89708898516,843.980526094916,844.063981889833,844.147526382563,
844.231115465504,844.314838733061,844.395518448957,844.478855380823,844.562089805476,
844.645223408232,844.728298995265,844.811331306897,844.837351982703),
 .UNSPECIFIED.);
#587=B_SPLINE_CURVE_WITH_KNOTS('',3,(#78601,#78602,#78603,#78604,#78605,
#78606,#78607,#78608,#78609,#78610,#78611,#78612,#78613,#78614,#78615,#78616,
#78617,#78618,#78619,#78620,#78621,#78622,#78623,#78624,#78625,#78626,#78627,
#78628,#78629,#78630,#78631,#78632,#78633,#78634,#78635,#78636,#78637,#78638,
#78639,#78640,#78641,#78642,#78643,#78644,#78645,#78646,#78647,#78648,#78649,
#78650,#78651,#78652,#78653,#78654,#78655,#78656,#78657,#78658,#78659,#78660,
#78661,#78662,#78663,#78664,#78665,#78666,#78667,#78668,#78669,#78670,#78671,
#78672,#78673,#78674,#78675,#78676,#78677,#78678,#78679,#78680,#78681,#78682,
#78683,#78684,#78685,#78686,#78687,#78688,#78689,#78690,#78691,#78692,#78693,
#78694,#78695,#78696,#78697,#78698,#78699,#78700,#78701,#78702,#78703,#78704,
#78705,#78706,#78707,#78708,#78709,#78710,#78711,#78712,#78713,#78714,#78715,
#78716,#78717,#78718,#78719,#78720,#78721,#78722,#78723,#78724,#78725,#78726,
#78727,#78728,#78729,#78730,#78731,#78732,#78733,#78734,#78735,#78736,#78737,
#78738,#78739,#78740,#78741,#78742,#78743,#78744,#78745,#78746,#78747,#78748,
#78749,#78750,#78751,#78752,#78753,#78754,#78755,#78756,#78757,#78758,#78759,
#78760,#78761,#78762,#78763,#78764,#78765,#78766,#78767,#78768,#78769,#78770,
#78771,#78772,#78773,#78774,#78775,#78776,#78777,#78778,#78779,#78780,#78781,
#78782,#78783,#78784,#78785,#78786,#78787,#78788,#78789,#78790,#78791,#78792,
#78793,#78794,#78795,#78796,#78797,#78798,#78799,#78800,#78801,#78802,#78803,
#78804,#78805,#78806,#78807,#78808,#78809,#78810,#78811,#78812,#78813,#78814,
#78815,#78816,#78817,#78818,#78819,#78820),.UNSPECIFIED.,.F.,.F.,(4,3,3,
3,3,3,3,3,3,3,3,3,3,3,3,3,3,3,3,3,3,3,3,3,3,3,3,3,3,3,3,3,3,3,3,3,3,3,3,
3,3,3,3,3,3,3,3,3,3,3,3,3,3,3,3,3,3,3,3,3,3,3,3,3,3,3,3,3,3,3,3,3,3,4),
(845.088423815769,845.172110285652,845.255693596232,845.339193936393,845.42263142254,
845.50603367729,845.589418718362,845.672804668667,845.756209647912,845.839703348041,
845.923242043354,846.006913990348,846.084699850681,846.168438562527,846.252074073895,
846.335626517293,846.419115953144,846.502569903758,846.586006397604,846.66944350736,
846.752899302277,846.836443795007,846.920032877948,847.003756145506,847.084435861401,
847.168174573247,847.251810084614,847.335362528013,847.418851963864,847.502305914478,
847.585742408324,847.66917951808,847.752635312998,847.836179805727,847.919768888668,
848.003492156226,848.084171872121,848.167910583967,848.251546095335,848.335098538733,
848.418587974584,848.502041925198,848.585478419044,848.6689155288,848.752371323718,
848.835915816447,848.919504899388,849.003228166946,849.083907882841,849.167646594687,
849.251282106054,849.334834549453,849.418323985304,849.501777935918,849.585214429764,
849.668651539519,849.752107334437,849.835651827166,849.919240910107,850.002964177665,
850.083643893561,850.167382605407,850.251018116774,850.334570560173,850.418059996024,
850.501513946638,850.584950440484,850.66838755024,850.751843345158,850.835387837888,
850.918976920829,851.002700188386,851.083379904281,851.120768468837),
 .UNSPECIFIED.);
#588=B_SPLINE_CURVE_WITH_KNOTS('',3,(#78821,#78822,#78823,#78824,#78825,
#78826,#78827,#78828,#78829,#78830,#78831,#78832,#78833),.UNSPECIFIED.,
 .F.,.F.,(4,3,3,3,4),(844.836771567909,844.92036052459,845.004083725043,
845.08496383996,845.088423815633),.UNSPECIFIED.);
#589=B_SPLINE_CURVE_WITH_KNOTS('',3,(#78835,#78836,#78837,#78838,#78839,
#78840,#78841,#78842,#78843,#78844),.UNSPECIFIED.,.F.,.F.,(4,3,3,4),(844.837351982703,
844.920368259476,845.004396037556,845.088423815637),.UNSPECIFIED.);
#590=B_SPLINE_CURVE_WITH_KNOTS('',3,(#78845,#78846,#78847,#78848,#78849,
#78850,#78851,#78852,#78853,#78854,#78855,#78856,#78857,#78858,#78859,#78860,
#78861,#78862,#78863,#78864,#78865,#78866,#78867,#78868,#78869,#78870,#78871,
#78872,#78873,#78874,#78875,#78876,#78877,#78878,#78879,#78880,#78881,#78882,
#78883,#78884,#78885,#78886,#78887,#78888,#78889,#78890,#78891,#78892,#78893,
#78894,#78895,#78896,#78897,#78898,#78899,#78900,#78901,#78902,#78903,#78904,
#78905,#78906,#78907,#78908,#78909,#78910,#78911,#78912,#78913,#78914,#78915,
#78916,#78917,#78918,#78919,#78920,#78921,#78922,#78923,#78924,#78925,#78926,
#78927,#78928,#78929,#78930,#78931,#78932,#78933,#78934,#78935,#78936,#78937,
#78938,#78939,#78940,#78941,#78942,#78943,#78944,#78945,#78946,#78947,#78948,
#78949,#78950,#78951,#78952,#78953,#78954,#78955,#78956,#78957,#78958,#78959,
#78960,#78961,#78962,#78963,#78964,#78965,#78966,#78967,#78968,#78969,#78970,
#78971,#78972,#78973,#78974,#78975,#78976,#78977,#78978,#78979,#78980,#78981,
#78982,#78983,#78984,#78985,#78986,#78987,#78988,#78989,#78990,#78991,#78992,
#78993,#78994,#78995,#78996,#78997,#78998,#78999,#79000,#79001,#79002,#79003,
#79004,#79005,#79006,#79007,#79008,#79009,#79010,#79011,#79012,#79013,#79014,
#79015,#79016,#79017,#79018,#79019,#79020,#79021,#79022,#79023,#79024,#79025,
#79026,#79027,#79028,#79029,#79030,#79031,#79032,#79033,#79034,#79035,#79036,
#79037,#79038,#79039,#79040,#79041,#79042,#79043,#79044,#79045,#79046,#79047,
#79048,#79049,#79050,#79051,#79052,#79053,#79054,#79055,#79056,#79057,#79058,
#79059,#79060,#79061),.UNSPECIFIED.,.F.,.F.,(4,3,3,3,3,3,3,3,3,3,3,3,3,
3,3,3,3,3,3,3,3,3,3,3,3,3,3,3,3,3,3,3,3,3,3,3,3,3,3,3,3,3,3,3,3,3,3,3,3,
3,3,3,3,3,3,3,3,3,3,3,3,3,3,3,3,3,3,3,3,3,3,3,4),(845.088423815795,845.188236697791,
845.291745578734,845.395254459677,845.478993171523,845.562628682891,845.64618112629,
845.729670562141,845.813124512755,845.896561006601,845.979998116357,846.063453911274,
846.146998404004,846.230587486945,846.314310754503,846.394990470397,846.478729182243,
846.56236469361,846.645917137009,846.72940657286,846.812860523473,846.896297017319,
846.979734127075,847.063189921992,847.146734414722,847.230323497663,847.31404676522,
847.394726481117,847.478465192963,847.562100704331,847.645653147729,847.729142583581,
847.812596534194,847.896033028041,847.979470137797,848.062925932714,848.146470425444,
848.230059508385,848.313782775943,848.394462491838,848.478201203684,848.561836715052,
848.64538915845,848.728878594301,848.812332544915,848.895769038761,848.979206148517,
849.062661943435,849.146206436164,849.229795519105,849.313518786663,849.394198502558,
849.477937214404,849.561572725771,849.64512516917,849.728614605021,849.812068555634,
849.89550504948,849.978942159236,850.062397954153,850.145942446883,850.229531529824,
850.313254797381,850.393934513278,850.477376576719,850.560686672338,850.643920597657,
850.727096805523,850.810233704164,850.893366550294,850.976494891575,851.059668657128,
851.119874427346),.UNSPECIFIED.);
#591=B_SPLINE_CURVE_WITH_KNOTS('',3,(#79067,#79068,#79069,#79070,#79071,
#79072,#79073,#79074,#79075,#79076,#79077,#79078,#79079,#79080,#79081,#79082,
#79083,#79084,#79085,#79086,#79087,#79088,#79089,#79090,#79091,#79092,#79093,
#79094,#79095,#79096,#79097,#79098,#79099,#79100,#79101,#79102,#79103,#79104,
#79105,#79106,#79107,#79108,#79109,#79110,#79111,#79112,#79113,#79114,#79115,
#79116,#79117,#79118,#79119,#79120,#79121,#79122,#79123,#79124,#79125,#79126,
#79127,#79128,#79129,#79130,#79131,#79132,#79133,#79134,#79135,#79136,#79137,
#79138,#79139,#79140,#79141,#79142,#79143,#79144,#79145,#79146,#79147,#79148,
#79149,#79150,#79151,#79152,#79153,#79154,#79155,#79156,#79157,#79158,#79159,
#79160,#79161,#79162,#79163,#79164,#79165,#79166,#79167,#79168,#79169,#79170,
#79171,#79172,#79173,#79174,#79175,#79176,#79177,#79178,#79179,#79180,#79181,
#79182,#79183,#79184,#79185,#79186,#79187,#79188,#79189,#79190,#79191,#79192,
#79193,#79194,#79195,#79196,#79197,#79198,#79199,#79200,#79201,#79202,#79203,
#79204,#79205,#79206,#79207,#79208,#79209,#79210,#79211,#79212,#79213,#79214,
#79215,#79216,#79217,#79218,#79219,#79220,#79221,#79222,#79223,#79224,#79225,
#79226,#79227,#79228,#79229,#79230,#79231,#79232,#79233,#79234,#79235,#79236,
#79237,#79238,#79239,#79240,#79241,#79242,#79243,#79244,#79245,#79246,#79247,
#79248,#79249,#79250,#79251,#79252,#79253,#79254,#79255,#79256,#79257,#79258,
#79259,#79260,#79261,#79262,#79263,#79264,#79265,#79266,#79267,#79268,#79269,
#79270,#79271,#79272,#79273,#79274,#79275,#79276,#79277,#79278,#79279,#79280,
#79281,#79282,#79283,#79284,#79285,#79286),.UNSPECIFIED.,.F.,.F.,(4,3,3,
3,3,3,3,3,3,3,3,3,3,3,3,3,3,3,3,3,3,3,3,3,3,3,3,3,3,3,3,3,3,3,3,3,3,3,3,
3,3,3,3,3,3,3,3,3,3,3,3,3,3,3,3,3,3,3,3,3,3,3,3,3,3,3,3,3,3,3,3,3,3,4),
(851.371609122812,851.454463410857,851.537287815637,851.620099177469,851.702916093396,
851.785757161153,851.868689417554,851.95167211902,852.034780599427,852.083115915001,
852.166854626847,852.250490138214,852.334042581613,852.417532017464,852.500985968077,
852.584422461924,852.667859571679,852.751315366596,852.834859859326,852.918448942267,
853.002172209824,853.082851925721,853.166590637567,853.250226148935,853.333778592334,
853.417268028185,853.500721978799,853.584158472646,853.667595582401,853.751051377319,
853.834595870049,853.91818495299,854.001908220548,854.082587936442,854.166326648288,
854.249962159655,854.333514603054,854.417004038905,854.500457989519,854.583894483365,
854.66733159312,854.750787388038,854.834331880767,854.917920963708,855.001644231265,
855.082323947162,855.166062659008,855.249698170375,855.333250613773,855.416740049625,
855.500194000238,855.583630494085,855.66706760384,855.750523398758,855.834067891488,
855.917656974429,856.001380241986,856.082059957882,856.165798669728,856.249434181096,
856.332986624494,856.416476060346,856.499930010959,856.583366504806,856.666803614561,
856.750259409479,856.833803902209,856.91739298515,857.001116252707,857.081795968602,
857.1674341756,857.252964079907,857.338368454942,857.404280519461),
 .UNSPECIFIED.);
#592=B_SPLINE_CURVE_WITH_KNOTS('',3,(#79287,#79288,#79289,#79290,#79291,
#79292,#79293,#79294,#79295,#79296),.UNSPECIFIED.,.F.,.F.,(4,3,3,4),(851.120768468837,
851.224139296325,851.326074160885,851.371609122685),.UNSPECIFIED.);
#593=B_SPLINE_CURVE_WITH_KNOTS('',3,(#79298,#79299,#79300,#79301,#79302,
#79303,#79304,#79305,#79306,#79307),.UNSPECIFIED.,.F.,.F.,(4,3,3,4),(851.119874427346,
851.203146061834,851.287377592223,851.371609122613),.UNSPECIFIED.);
#594=B_SPLINE_CURVE_WITH_KNOTS('',3,(#79308,#79309,#79310,#79311,#79312,
#79313,#79314,#79315,#79316,#79317,#79318,#79319,#79320,#79321,#79322,#79323,
#79324,#79325,#79326,#79327,#79328,#79329,#79330,#79331,#79332,#79333,#79334,
#79335,#79336,#79337,#79338,#79339,#79340,#79341,#79342,#79343,#79344,#79345,
#79346,#79347,#79348,#79349,#79350,#79351,#79352,#79353,#79354,#79355,#79356,
#79357,#79358,#79359,#79360,#79361,#79362,#79363,#79364,#79365,#79366,#79367,
#79368,#79369,#79370,#79371,#79372,#79373,#79374,#79375,#79376,#79377,#79378,
#79379,#79380,#79381,#79382,#79383,#79384,#79385,#79386,#79387,#79388,#79389,
#79390,#79391,#79392,#79393,#79394,#79395,#79396,#79397,#79398,#79399,#79400,
#79401,#79402,#79403,#79404,#79405,#79406,#79407,#79408,#79409,#79410,#79411,
#79412,#79413,#79414,#79415,#79416,#79417,#79418,#79419,#79420,#79421,#79422,
#79423,#79424,#79425,#79426,#79427,#79428,#79429,#79430,#79431,#79432,#79433,
#79434,#79435,#79436,#79437,#79438,#79439,#79440,#79441,#79442,#79443,#79444,
#79445,#79446,#79447,#79448,#79449,#79450,#79451,#79452,#79453,#79454,#79455,
#79456,#79457,#79458,#79459,#79460,#79461,#79462,#79463,#79464,#79465,#79466,
#79467,#79468,#79469,#79470,#79471,#79472,#79473,#79474,#79475,#79476,#79477,
#79478,#79479,#79480,#79481,#79482,#79483,#79484,#79485,#79486,#79487,#79488,
#79489,#79490,#79491,#79492,#79493,#79494,#79495,#79496,#79497,#79498,#79499,
#79500,#79501,#79502,#79503,#79504,#79505,#79506,#79507,#79508,#79509,#79510,
#79511,#79512,#79513,#79514,#79515,#79516,#79517,#79518,#79519,#79520,#79521,
#79522,#79523,#79524,#79525,#79526,#79527,#79528,#79529,#79530),
 .UNSPECIFIED.,.F.,.F.,(4,3,3,3,3,3,3,3,3,3,3,3,3,3,3,3,3,3,3,3,3,3,3,3,
3,3,3,3,3,3,3,3,3,3,3,3,3,3,3,3,3,3,3,3,3,3,3,3,3,3,3,3,3,3,3,3,3,3,3,3,
3,3,3,3,3,3,3,3,3,3,3,3,3,3,4),(851.371609122816,851.393670523998,851.477409235844,
851.561044747211,851.64459719061,851.728086626461,851.811540577074,851.89497707092,
851.978414180676,852.061869975593,852.145414468323,852.229003551263,852.312726818821,
852.393406534718,852.477145246564,852.560780757931,852.64433320133,852.727822637181,
852.811276587794,852.894713081641,852.978150191396,853.061605986314,853.145150479043,
853.228739561984,853.312462829542,853.393142545438,853.476881257284,853.560516768651,
853.64406921205,853.727558647901,853.811012598515,853.894449092361,853.977886202116,
854.061341997034,854.144886489764,854.228475572705,854.312198840262,854.392878556158,
854.476617268004,854.560252779371,854.64380522277,854.727294658621,854.810748609235,
854.894185103081,854.977622212836,855.061078007754,855.144622500483,855.228211583424,
855.311934850982,855.392614566878,855.476353278724,855.559988790091,855.64354123349,
855.727030669341,855.810484619954,855.893921113801,855.977358223556,856.060814018473,
856.144358511203,856.227947594144,856.311670861701,856.392350577598,856.476089289444,
856.559724800812,856.64327724421,856.726766680061,856.810220630675,856.893657124522,
856.977094234277,857.060550029195,857.144094521925,857.227683604866,857.311406872424,
857.392086588319,857.403801598388),.UNSPECIFIED.);
#595=B_SPLINE_CURVE_WITH_KNOTS('',3,(#79536,#79537,#79538,#79539,#79540,
#79541,#79542,#79543,#79544,#79545,#79546,#79547,#79548,#79549,#79550,#79551,
#79552,#79553,#79554,#79555,#79556,#79557,#79558,#79559,#79560,#79561,#79562,
#79563,#79564,#79565,#79566,#79567,#79568,#79569,#79570,#79571,#79572,#79573,
#79574,#79575,#79576,#79577,#79578,#79579,#79580,#79581,#79582,#79583,#79584,
#79585,#79586,#79587,#79588,#79589,#79590,#79591,#79592,#79593,#79594,#79595,
#79596,#79597,#79598,#79599,#79600,#79601,#79602,#79603,#79604,#79605,#79606,
#79607,#79608,#79609,#79610,#79611,#79612,#79613,#79614,#79615,#79616,#79617,
#79618,#79619,#79620,#79621,#79622,#79623,#79624,#79625,#79626,#79627,#79628,
#79629,#79630,#79631,#79632,#79633,#79634,#79635,#79636,#79637,#79638,#79639,
#79640,#79641,#79642,#79643,#79644,#79645,#79646,#79647,#79648,#79649,#79650,
#79651,#79652,#79653,#79654,#79655,#79656,#79657,#79658,#79659,#79660,#79661,
#79662,#79663,#79664,#79665,#79666,#79667,#79668,#79669,#79670,#79671,#79672,
#79673,#79674,#79675,#79676,#79677,#79678,#79679,#79680,#79681,#79682,#79683,
#79684,#79685,#79686,#79687,#79688,#79689,#79690,#79691,#79692,#79693,#79694,
#79695,#79696,#79697,#79698,#79699,#79700,#79701,#79702,#79703,#79704,#79705,
#79706,#79707,#79708,#79709,#79710,#79711,#79712,#79713,#79714,#79715,#79716,
#79717,#79718,#79719,#79720,#79721,#79722,#79723,#79724,#79725,#79726,#79727,
#79728,#79729,#79730,#79731,#79732,#79733,#79734,#79735,#79736,#79737,#79738,
#79739,#79740,#79741,#79742,#79743,#79744,#79745,#79746,#79747,#79748,#79749,
#79750,#79751,#79752,#79753,#79754,#79755),.UNSPECIFIED.,.F.,.F.,(4,3,3,
3,3,3,3,3,3,3,3,3,3,3,3,3,3,3,3,3,3,3,3,3,3,3,3,3,3,3,3,3,3,3,3,3,3,3,3,
3,3,3,3,3,3,3,3,3,3,3,3,3,3,3,3,3,3,3,3,3,3,3,3,3,3,3,3,3,3,3,3,3,3,4),
(857.654794430136,857.74538946886,857.836378454926,857.927567441179,858.019060923412,
858.081531979322,858.165270691168,858.248906202536,858.332458645934,858.415948081785,
858.499402032399,858.582838526245,858.666275636001,858.749731430919,858.833275923648,
858.916865006589,859.000588274147,859.081267990042,859.165006701888,859.248642213255,
859.332194656654,859.415684092505,859.499138043118,859.582574536965,859.66601164672,
859.749467441638,859.833011934367,859.916601017308,860.000324284866,860.081004000762,
860.164742712608,860.248378223976,860.331930667374,860.415420103225,860.498874053839,
860.582310547685,860.665747657441,860.749203452359,860.832747945088,860.916337028029,
861.000060295587,861.080740011482,861.164478723328,861.248114234695,861.331666678094,
861.415156113945,861.498610064559,861.582046558405,861.665483668161,861.748939463078,
861.832483955808,861.916073038749,861.999796306307,862.080476022203,862.164214734049,
862.247850245417,862.331402688815,862.414892124666,862.49834607528,862.581782569126,
862.665219678882,862.7486754738,862.832219966529,862.91580904947,862.999532317028,
863.080212032923,863.162711702593,863.245116481761,863.327445568733,863.409718089265,
863.491959205929,863.574182388538,863.656422282705,863.68620670875),
 .UNSPECIFIED.);
#596=B_SPLINE_CURVE_WITH_KNOTS('',3,(#79756,#79757,#79758,#79759,#79760,
#79761,#79762,#79763,#79764,#79765),.UNSPECIFIED.,.F.,.F.,(4,3,3,4),(857.404280519461,
857.489540442283,857.574738516118,857.654794429992),.UNSPECIFIED.);
#597=B_SPLINE_CURVE_WITH_KNOTS('',3,(#79767,#79768,#79769,#79770,#79771,
#79772,#79773,#79774,#79775,#79776),.UNSPECIFIED.,.F.,.F.,(4,3,3,4),(857.403801598388,
857.511208903319,857.616619766979,857.654794429849),.UNSPECIFIED.);
#598=B_SPLINE_CURVE_WITH_KNOTS('',3,(#79777,#79778,#79779,#79780,#79781,
#79782,#79783,#79784,#79785,#79786,#79787,#79788,#79789,#79790,#79791,#79792,
#79793,#79794,#79795,#79796,#79797,#79798,#79799,#79800,#79801,#79802,#79803,
#79804,#79805,#79806,#79807,#79808,#79809,#79810,#79811,#79812,#79813,#79814,
#79815,#79816,#79817,#79818,#79819,#79820,#79821,#79822,#79823,#79824,#79825,
#79826,#79827,#79828,#79829,#79830,#79831,#79832,#79833,#79834,#79835,#79836,
#79837,#79838,#79839,#79840,#79841,#79842,#79843,#79844,#79845,#79846,#79847,
#79848,#79849,#79850,#79851,#79852,#79853,#79854,#79855,#79856,#79857,#79858,
#79859,#79860,#79861,#79862,#79863,#79864,#79865,#79866,#79867,#79868,#79869,
#79870,#79871,#79872,#79873,#79874,#79875,#79876,#79877,#79878,#79879,#79880,
#79881,#79882,#79883,#79884,#79885,#79886,#79887,#79888,#79889,#79890,#79891,
#79892,#79893,#79894,#79895,#79896,#79897,#79898,#79899,#79900,#79901,#79902,
#79903,#79904,#79905,#79906,#79907,#79908,#79909,#79910,#79911,#79912,#79913,
#79914,#79915,#79916,#79917,#79918,#79919,#79920,#79921,#79922,#79923,#79924,
#79925,#79926,#79927,#79928,#79929,#79930,#79931,#79932,#79933,#79934,#79935,
#79936,#79937,#79938,#79939,#79940,#79941,#79942,#79943,#79944,#79945,#79946,
#79947,#79948,#79949,#79950,#79951,#79952,#79953,#79954,#79955,#79956,#79957,
#79958,#79959,#79960,#79961,#79962,#79963,#79964,#79965,#79966,#79967,#79968,
#79969,#79970,#79971,#79972,#79973,#79974,#79975,#79976,#79977,#79978,#79979,
#79980,#79981,#79982,#79983,#79984,#79985,#79986,#79987,#79988,#79989,#79990,
#79991,#79992,#79993,#79994,#79995,#79996),.UNSPECIFIED.,.F.,.F.,(4,3,3,
3,3,3,3,3,3,3,3,3,3,3,3,3,3,3,3,3,3,3,3,3,3,3,3,3,3,3,3,3,3,3,3,3,3,3,3,
3,3,3,3,3,3,3,3,3,3,3,3,3,3,3,3,3,3,3,3,3,3,3,3,3,3,3,3,3,3,3,3,3,3,4),
(857.654794429996,857.737439006459,857.820040512216,857.902620276709,857.985197085807,
858.067789720308,858.150467846438,858.233189315394,858.31604260483,858.391822599039,
858.475561310885,858.559196822252,858.642749265651,858.726238701502,858.809692652115,
858.893129145961,858.976566255717,859.060022050635,859.143566543364,859.227155626305,
859.310878893863,859.391558609759,859.475297321605,859.558932832972,859.642485276371,
859.725974712222,859.809428662836,859.892865156682,859.976302266437,860.059758061355,
860.143302554085,860.226891637026,860.310614904583,860.391294620479,860.475033332325,
860.558668843692,860.642221287091,860.725710722942,860.809164673556,860.892601167402,
860.976038277157,861.059494072074,861.143038564804,861.226627647745,861.310350915303,
861.391030631199,861.474769343045,861.558404854412,861.641957297811,861.725446733662,
861.808900684276,861.892337178122,861.975774287878,862.059230082796,862.142774575525,
862.226363658466,862.310086926024,862.390766641919,862.474505353765,862.558140865132,
862.64169330853,862.725182744381,862.808636694995,862.892073188841,862.975510298596,
863.058966093514,863.142510586243,863.226099669184,863.309822936742,863.390502652639,
863.476882971832,863.563148000132,863.649276805144,863.687548921762),
 .UNSPECIFIED.);
#599=B_SPLINE_CURVE_WITH_KNOTS('',3,(#80002,#80003,#80004,#80005,#80006,
#80007,#80008,#80009,#80010,#80011,#80012,#80013,#80014,#80015,#80016,#80017,
#80018,#80019,#80020,#80021,#80022,#80023,#80024,#80025,#80026,#80027,#80028,
#80029,#80030,#80031,#80032,#80033,#80034,#80035,#80036,#80037,#80038,#80039,
#80040,#80041,#80042,#80043,#80044,#80045,#80046,#80047,#80048,#80049,#80050,
#80051,#80052,#80053,#80054,#80055,#80056,#80057,#80058,#80059,#80060,#80061,
#80062,#80063,#80064,#80065,#80066,#80067,#80068,#80069,#80070,#80071,#80072,
#80073,#80074,#80075,#80076,#80077,#80078,#80079,#80080,#80081,#80082,#80083,
#80084,#80085,#80086,#80087,#80088,#80089,#80090,#80091,#80092,#80093,#80094,
#80095,#80096,#80097,#80098,#80099,#80100,#80101,#80102,#80103,#80104,#80105,
#80106,#80107,#80108,#80109,#80110,#80111,#80112,#80113,#80114,#80115,#80116,
#80117,#80118,#80119,#80120,#80121,#80122,#80123,#80124,#80125,#80126,#80127,
#80128,#80129,#80130,#80131,#80132,#80133,#80134,#80135,#80136,#80137,#80138,
#80139,#80140,#80141,#80142,#80143,#80144,#80145,#80146,#80147,#80148,#80149,
#80150,#80151,#80152,#80153,#80154,#80155,#80156,#80157,#80158,#80159,#80160,
#80161,#80162,#80163,#80164,#80165,#80166,#80167,#80168,#80169,#80170,#80171,
#80172,#80173,#80174,#80175,#80176,#80177,#80178,#80179,#80180,#80181,#80182,
#80183,#80184,#80185,#80186,#80187,#80188,#80189,#80190,#80191,#80192,#80193,
#80194,#80195,#80196,#80197,#80198,#80199,#80200,#80201,#80202,#80203,#80204,
#80205,#80206,#80207,#80208,#80209,#80210,#80211,#80212,#80213,#80214,#80215,
#80216,#80217,#80218),.UNSPECIFIED.,.F.,.F.,(4,3,3,3,3,3,3,3,3,3,3,3,3,
3,3,3,3,3,3,3,3,3,3,3,3,3,3,3,3,3,3,3,3,3,3,3,3,3,3,3,3,3,3,3,3,3,3,3,3,
3,3,3,3,3,3,3,3,3,3,3,3,3,3,3,3,3,3,3,3,3,3,3,4),(863.937979737172,864.079948043643,
864.163686755489,864.247322266856,864.330874710255,864.414364146106,864.49781809672,
864.581254590566,864.664691700322,864.748147495239,864.831691987969,864.91528107091,
864.999004338468,865.079684054363,865.163422766209,865.247058277577,865.330610720975,
865.414100156826,865.49755410744,865.580990601286,865.664427711041,865.747883505959,
865.831427998689,865.91501708163,865.998740349187,866.079420065083,866.163158776929,
866.246794288297,866.330346731695,866.413836167546,866.49729011816,866.580726612006,
866.664163721761,866.747619516679,866.831164009409,866.91475309235,866.998476359907,
867.079156075803,867.162894787649,867.246530299016,867.330082742415,867.413572178266,
867.497026128879,867.580462622726,867.663899732481,867.747355527399,867.830900020128,
867.914489103069,867.998212370627,868.078892086523,868.162630798369,868.246266309736,
868.329818753135,868.413308188986,868.4967621396,868.580198633446,868.663635743202,
868.74709153812,868.830636030849,868.91422511379,868.997948381348,869.078628097243,
869.162373162193,869.2460135923,869.32956952621,869.413056411045,869.49650572187,
869.579935547268,869.663363958879,869.746844645517,869.830352862841,869.913953867878,
869.969625938716),.UNSPECIFIED.);
#600=B_SPLINE_CURVE_WITH_KNOTS('',3,(#80219,#80220,#80221,#80222,#80223,
#80224,#80225,#80226,#80227,#80228),.UNSPECIFIED.,.F.,.F.,(4,3,3,4),(863.68620670875,
863.768511157265,863.853245447158,863.937979737052),.UNSPECIFIED.);
#601=B_SPLINE_CURVE_WITH_KNOTS('',3,(#80230,#80231,#80232,#80233,#80234,
#80235,#80236,#80237,#80238,#80239),.UNSPECIFIED.,.F.,.F.,(4,3,3,4),(863.687548921762,
863.773526588714,863.859412870955,863.937979737175),.UNSPECIFIED.);
#602=B_SPLINE_CURVE_WITH_KNOTS('',3,(#80240,#80241,#80242,#80243,#80244,
#80245,#80246,#80247,#80248,#80249,#80250,#80251,#80252,#80253,#80254,#80255,
#80256,#80257,#80258,#80259,#80260,#80261,#80262,#80263,#80264,#80265,#80266,
#80267,#80268,#80269,#80270,#80271,#80272,#80273,#80274,#80275,#80276,#80277,
#80278,#80279,#80280,#80281,#80282,#80283,#80284,#80285,#80286,#80287,#80288,
#80289,#80290,#80291,#80292,#80293,#80294,#80295,#80296,#80297,#80298,#80299,
#80300,#80301,#80302,#80303,#80304,#80305,#80306,#80307,#80308,#80309,#80310,
#80311,#80312,#80313,#80314,#80315,#80316,#80317,#80318,#80319,#80320,#80321,
#80322,#80323,#80324,#80325,#80326,#80327,#80328,#80329,#80330,#80331,#80332,
#80333,#80334,#80335,#80336,#80337,#80338,#80339,#80340,#80341,#80342,#80343,
#80344,#80345,#80346,#80347,#80348,#80349,#80350,#80351,#80352,#80353,#80354,
#80355,#80356,#80357,#80358,#80359,#80360,#80361,#80362,#80363,#80364,#80365,
#80366,#80367,#80368,#80369,#80370,#80371,#80372,#80373,#80374,#80375,#80376,
#80377,#80378,#80379,#80380,#80381,#80382,#80383,#80384,#80385,#80386,#80387,
#80388,#80389,#80390,#80391,#80392,#80393,#80394,#80395,#80396,#80397,#80398,
#80399,#80400,#80401,#80402,#80403,#80404,#80405,#80406,#80407,#80408,#80409,
#80410,#80411,#80412,#80413,#80414,#80415,#80416,#80417,#80418,#80419,#80420,
#80421,#80422,#80423,#80424,#80425,#80426,#80427,#80428,#80429,#80430,#80431,
#80432,#80433,#80434,#80435,#80436,#80437,#80438,#80439,#80440,#80441,#80442,
#80443,#80444,#80445,#80446,#80447,#80448,#80449,#80450,#80451,#80452,#80453,
#80454,#80455,#80456),.UNSPECIFIED.,.F.,.F.,(4,3,3,3,3,3,3,3,3,3,3,3,3,
3,3,3,3,3,3,3,3,3,3,3,3,3,3,3,3,3,3,3,3,3,3,3,3,3,3,3,3,3,3,3,3,3,3,3,3,
3,3,3,3,3,3,3,3,3,3,3,3,3,3,3,3,3,3,3,3,3,3,3,4),(863.937979737279,864.027327946061,
864.118055625386,864.207883747777,864.299061205568,864.390238663359,864.473977375205,
864.557612886573,864.641165329971,864.724654765822,864.808108716436,864.891545210282,
864.974982320037,865.058438114955,865.141982607685,865.225571690626,865.309294958184,
865.38997467408,865.473713385926,865.557348897294,865.640901340692,865.724390776543,
865.807844727157,865.891281221003,865.974718330758,866.058174125676,866.141718618406,
866.225307701347,866.309030968904,866.3897106848,866.473449396646,866.557084908013,
866.640637351412,866.724126787263,866.807580737876,866.891017231723,866.974454341478,
867.057910136396,867.141454629125,867.225043712066,867.308766979624,867.38944669552,
867.473185407366,867.556820918733,867.640373362132,867.723862797983,867.807316748596,
867.890753242443,867.974190352198,868.057646147116,868.141190639845,868.224779722786,
868.308502990344,868.38918270624,868.472921418086,868.556556929454,868.640109372852,
868.723598808703,868.807052759317,868.890489253163,868.973926362918,869.057382157836,
869.140926650566,869.224515733507,869.308239001065,869.38891871696,869.471389241532,
869.553764467079,869.636063614742,869.719412917611,869.801620727064,869.885540776641,
869.969460826219),.UNSPECIFIED.);
#603=B_SPLINE_CURVE_WITH_KNOTS('',3,(#80462,#80463,#80464,#80465,#80466,
#80467,#80468,#80469,#80470,#80471,#80472,#80473,#80474,#80475,#80476,#80477,
#80478,#80479,#80480,#80481,#80482,#80483,#80484,#80485,#80486,#80487,#80488,
#80489,#80490,#80491,#80492,#80493,#80494,#80495,#80496,#80497,#80498,#80499,
#80500,#80501,#80502,#80503,#80504,#80505,#80506,#80507,#80508,#80509,#80510,
#80511,#80512,#80513,#80514,#80515,#80516,#80517,#80518,#80519,#80520,#80521,
#80522,#80523,#80524,#80525,#80526,#80527,#80528,#80529,#80530,#80531,#80532,
#80533,#80534,#80535,#80536,#80537,#80538,#80539,#80540,#80541,#80542,#80543,
#80544,#80545,#80546,#80547,#80548,#80549,#80550,#80551,#80552,#80553,#80554,
#80555,#80556,#80557,#80558,#80559,#80560,#80561,#80562,#80563,#80564,#80565,
#80566,#80567,#80568,#80569,#80570,#80571,#80572,#80573,#80574,#80575,#80576,
#80577,#80578,#80579,#80580,#80581,#80582,#80583,#80584,#80585,#80586,#80587,
#80588,#80589,#80590,#80591,#80592,#80593,#80594,#80595,#80596,#80597,#80598,
#80599,#80600,#80601,#80602,#80603,#80604,#80605,#80606,#80607,#80608,#80609,
#80610,#80611,#80612,#80613,#80614,#80615,#80616,#80617,#80618,#80619,#80620,
#80621,#80622,#80623,#80624,#80625,#80626,#80627,#80628,#80629,#80630,#80631,
#80632,#80633,#80634,#80635,#80636,#80637,#80638,#80639,#80640,#80641,#80642,
#80643,#80644,#80645,#80646,#80647,#80648,#80649,#80650,#80651,#80652,#80653,
#80654,#80655,#80656,#80657,#80658,#80659,#80660,#80661,#80662,#80663,#80664,
#80665,#80666,#80667,#80668,#80669,#80670,#80671,#80672,#80673,#80674,#80675,
#80676,#80677,#80678,#80679,#80680,#80681),.UNSPECIFIED.,.F.,.F.,(4,3,3,
3,3,3,3,3,3,3,3,3,3,3,3,3,3,3,3,3,3,3,3,3,3,3,3,3,3,3,3,3,3,3,3,3,3,3,3,
3,3,3,3,3,3,3,3,3,3,3,3,3,3,3,3,3,3,3,3,3,3,3,3,3,3,3,3,3,3,3,3,3,3,4),
(870.22116504447,870.303591153912,870.385933459072,870.472454291523,870.554698467721,
870.636928358824,870.719162982089,870.80142135653,870.883767175294,870.966163941988,
871.048677582414,871.078100118684,871.16183883053,871.245474341898,871.329026785296,
871.412516221147,871.495970171761,871.579406665607,871.662843775362,871.74629957028,
871.82984406301,871.913433145951,871.997156413508,872.077836129404,872.16157484125,
872.245210352618,872.328762796016,872.412252231867,872.495706182481,872.579142676327,
872.662579786082,872.746035581,872.82958007373,872.913169156671,872.996892424228,
873.077572140124,873.16131085197,873.244946363337,873.328498806736,873.411988242587,
873.495442193201,873.578878687047,873.662315796802,873.74577159172,873.82931608445,
873.912905167391,873.996628434948,874.077308150844,874.16104686269,874.244682374057,
874.328234817456,874.411724253307,874.495178203921,874.578614697767,874.662051807522,
874.74550760244,874.829052095169,874.91264117811,874.996364445668,875.077044161564,
875.16078287341,875.244418384777,875.327970828176,875.411460264028,875.494914214641,
875.578350708488,875.661787818243,875.745243613161,875.828788105891,875.912377188832,
875.996100456389,876.076780172284,876.168197875014,876.254027151446),
 .UNSPECIFIED.);
#604=B_SPLINE_CURVE_WITH_KNOTS('',3,(#80682,#80683,#80684,#80685,#80686,
#80687,#80688,#80689,#80690,#80691),.UNSPECIFIED.,.F.,.F.,(4,3,3,4),(869.969625938716,
870.053372297126,870.078364107964,870.221165044351),.UNSPECIFIED.);
#605=B_SPLINE_CURVE_WITH_KNOTS('',3,(#80693,#80694,#80695,#80696,#80697,
#80698,#80699,#80700,#80701,#80702),.UNSPECIFIED.,.F.,.F.,(4,3,3,4),(869.969460826219,
870.051718239475,870.136441641821,870.221165044167),.UNSPECIFIED.);
#606=B_SPLINE_CURVE_WITH_KNOTS('',3,(#80703,#80704,#80705,#80706,#80707,
#80708,#80709,#80710,#80711,#80712,#80713,#80714,#80715,#80716,#80717,#80718,
#80719,#80720,#80721,#80722,#80723,#80724,#80725,#80726,#80727,#80728,#80729,
#80730,#80731,#80732,#80733,#80734,#80735,#80736,#80737,#80738,#80739,#80740,
#80741,#80742,#80743,#80744,#80745,#80746,#80747,#80748,#80749,#80750,#80751,
#80752,#80753,#80754,#80755,#80756,#80757,#80758,#80759,#80760,#80761,#80762,
#80763,#80764,#80765,#80766,#80767,#80768,#80769,#80770,#80771,#80772,#80773,
#80774,#80775,#80776,#80777,#80778,#80779,#80780,#80781,#80782,#80783,#80784,
#80785,#80786,#80787,#80788,#80789,#80790,#80791,#80792,#80793,#80794,#80795,
#80796,#80797,#80798,#80799,#80800,#80801,#80802,#80803,#80804,#80805,#80806,
#80807,#80808,#80809,#80810,#80811,#80812,#80813,#80814,#80815,#80816,#80817,
#80818,#80819,#80820,#80821,#80822,#80823,#80824,#80825,#80826,#80827,#80828,
#80829,#80830,#80831,#80832,#80833,#80834,#80835,#80836,#80837,#80838,#80839,
#80840,#80841,#80842,#80843,#80844,#80845,#80846,#80847,#80848,#80849,#80850,
#80851,#80852,#80853,#80854,#80855,#80856,#80857,#80858,#80859,#80860,#80861,
#80862,#80863,#80864,#80865,#80866,#80867,#80868,#80869,#80870,#80871,#80872,
#80873,#80874,#80875,#80876,#80877,#80878,#80879,#80880,#80881,#80882,#80883,
#80884,#80885,#80886,#80887,#80888,#80889,#80890,#80891,#80892,#80893,#80894,
#80895,#80896,#80897,#80898,#80899,#80900,#80901,#80902,#80903,#80904,#80905,
#80906,#80907,#80908,#80909,#80910,#80911,#80912,#80913,#80914,#80915,#80916,
#80917,#80918,#80919,#80920,#80921,#80922),.UNSPECIFIED.,.F.,.F.,(4,3,3,
3,3,3,3,3,3,3,3,3,3,3,3,3,3,3,3,3,3,3,3,3,3,3,3,3,3,3,3,3,3,3,3,3,3,3,3,
3,3,3,3,3,3,3,3,3,3,3,3,3,3,3,3,3,3,3,3,3,3,3,3,3,3,3,3,3,3,3,3,3,3,4),
(870.221165044355,870.353859449894,870.38865472768,870.472393439526,870.556028950894,
870.639581394292,870.723070830144,870.806524780757,870.889961274604,870.973398384359,
871.056854179277,871.140398672007,871.223987754948,871.307711022506,871.3883907384,
871.472129450246,871.555764961613,871.639317405012,871.722806840863,871.806260791477,
871.889697285323,871.973134395079,872.056590189996,872.140134682726,872.223723765667,
872.307447033224,872.388126749121,872.471865460967,872.555500972335,872.639053415733,
872.722542851584,872.805996802198,872.889433296044,872.9728704058,873.056326200718,
873.139870693447,873.223459776388,873.307183043946,873.387862759841,873.471601471687,
873.555236983054,873.638789426453,873.722278862304,873.805732812917,873.889169306764,
873.972606416519,874.056062211436,874.139606704166,874.223195787107,874.306919054664,
874.387598770561,874.471337482407,874.554972993774,874.638525437173,874.722014873024,
874.805468823638,874.888905317484,874.972342427239,875.055798222157,875.139342714887,
875.222931797828,875.306655065385,875.387334781281,875.47108141737,875.554723081136,
875.641976917475,875.725461427968,875.808908688283,875.892336786282,875.975763792985,
876.059238229605,876.142740720485,876.226323097985,876.252753771852),
 .UNSPECIFIED.);
#607=B_SPLINE_CURVE_WITH_KNOTS('',3,(#80928,#80929,#80930,#80931,#80932,
#80933,#80934,#80935,#80936,#80937,#80938,#80939,#80940,#80941,#80942,#80943,
#80944,#80945,#80946,#80947,#80948,#80949,#80950,#80951,#80952,#80953,#80954,
#80955,#80956,#80957,#80958,#80959,#80960,#80961,#80962,#80963,#80964,#80965,
#80966,#80967,#80968,#80969,#80970,#80971,#80972,#80973,#80974,#80975,#80976,
#80977,#80978,#80979,#80980,#80981,#80982,#80983,#80984,#80985,#80986,#80987,
#80988,#80989,#80990,#80991,#80992,#80993,#80994,#80995,#80996,#80997,#80998,
#80999,#81000,#81001,#81002,#81003,#81004,#81005,#81006,#81007,#81008,#81009,
#81010,#81011,#81012,#81013,#81014,#81015,#81016,#81017,#81018,#81019,#81020,
#81021,#81022,#81023,#81024,#81025,#81026,#81027,#81028,#81029,#81030,#81031,
#81032,#81033,#81034,#81035,#81036,#81037,#81038,#81039,#81040,#81041,#81042,
#81043,#81044,#81045,#81046,#81047,#81048,#81049,#81050,#81051,#81052,#81053,
#81054,#81055,#81056,#81057,#81058,#81059,#81060,#81061,#81062,#81063,#81064,
#81065,#81066,#81067,#81068,#81069,#81070,#81071,#81072,#81073,#81074,#81075,
#81076,#81077,#81078,#81079,#81080,#81081,#81082,#81083,#81084,#81085,#81086,
#81087,#81088,#81089,#81090,#81091,#81092,#81093,#81094,#81095,#81096,#81097,
#81098,#81099,#81100,#81101,#81102,#81103,#81104,#81105,#81106,#81107,#81108,
#81109,#81110,#81111,#81112,#81113,#81114,#81115,#81116,#81117,#81118,#81119,
#81120,#81121,#81122,#81123,#81124,#81125,#81126,#81127,#81128,#81129,#81130,
#81131,#81132,#81133,#81134,#81135,#81136,#81137,#81138,#81139,#81140,#81141,
#81142,#81143,#81144,#81145,#81146,#81147),.UNSPECIFIED.,.F.,.F.,(4,3,3,
3,3,3,3,3,3,3,3,3,3,3,3,3,3,3,3,3,3,3,3,3,3,3,3,3,3,3,3,3,3,3,3,3,3,3,3,
3,3,3,3,3,3,3,3,3,3,3,3,3,3,3,3,3,3,3,3,3,3,3,3,3,3,3,3,3,3,3,3,3,3,4),
(876.504350351531,876.589557356121,876.674806022702,876.760111435919,876.845550924257,
876.931062603895,877.016731762945,877.076516183005,877.160254894851,877.243890406219,
877.327442849617,877.410932285469,877.494386236082,877.577822729929,877.661259839684,
877.744715634602,877.828260127332,877.911849210273,877.99557247783,878.076252193725,
878.159990905571,878.243626416938,878.327178860337,878.410668296188,878.494122246802,
878.577558740648,878.660995850403,878.744451645321,878.82799613805,878.911585220991,
878.995308488549,879.075988204445,879.159726916291,879.243362427658,879.326914871057,
879.410404306908,879.493858257522,879.577294751368,879.660731861123,879.74418765604,
879.82773214877,879.911321231711,879.995044499269,880.075724215165,880.159462927011,
880.243098438379,880.326650881777,880.410140317628,880.493594268242,880.577030762088,
880.660467871844,880.743923666761,880.827468159491,880.911057242432,880.994780509989,
881.075460225885,881.159198937731,881.242834449098,881.326386892496,881.409876328348,
881.493330278961,881.576766772807,881.660203882563,881.743659677481,881.827204170211,
881.910793253152,881.99451652071,882.075196236605,882.158303038281,882.241309055246,
882.324217592094,882.407069719065,882.489883995394,882.536362400618),
 .UNSPECIFIED.);
#608=B_SPLINE_CURVE_WITH_KNOTS('',3,(#81148,#81149,#81150,#81151,#81152,
#81153,#81154,#81155,#81156,#81157),.UNSPECIFIED.,.F.,.F.,(4,3,3,4),(876.254027151446,
876.345004673597,876.435647379661,876.504350351384),.UNSPECIFIED.);
#609=B_SPLINE_CURVE_WITH_KNOTS('',3,(#81159,#81160,#81161,#81162,#81163,
#81164,#81165,#81166,#81167,#81168),.UNSPECIFIED.,.F.,.F.,(4,3,3,4),(876.252753771852,
876.336488419904,876.387070792001,876.504350351535),.UNSPECIFIED.);
#610=B_SPLINE_CURVE_WITH_KNOTS('',3,(#81169,#81170,#81171,#81172,#81173,
#81174,#81175,#81176,#81177,#81178,#81179,#81180,#81181,#81182,#81183,#81184,
#81185,#81186,#81187,#81188,#81189,#81190,#81191,#81192,#81193,#81194,#81195,
#81196,#81197,#81198,#81199,#81200,#81201,#81202,#81203,#81204,#81205,#81206,
#81207,#81208,#81209,#81210,#81211,#81212,#81213,#81214,#81215,#81216,#81217,
#81218,#81219,#81220,#81221,#81222,#81223,#81224,#81225,#81226,#81227,#81228,
#81229,#81230,#81231,#81232,#81233,#81234,#81235,#81236,#81237,#81238,#81239,
#81240,#81241,#81242,#81243,#81244,#81245,#81246,#81247,#81248,#81249,#81250,
#81251,#81252,#81253,#81254,#81255,#81256,#81257,#81258,#81259,#81260,#81261,
#81262,#81263,#81264,#81265,#81266,#81267,#81268,#81269,#81270,#81271,#81272,
#81273,#81274,#81275,#81276,#81277,#81278,#81279,#81280,#81281,#81282,#81283,
#81284,#81285,#81286,#81287,#81288,#81289,#81290,#81291,#81292,#81293,#81294,
#81295,#81296,#81297,#81298,#81299,#81300,#81301,#81302,#81303,#81304,#81305,
#81306,#81307,#81308,#81309,#81310,#81311,#81312,#81313,#81314,#81315,#81316,
#81317,#81318,#81319,#81320,#81321,#81322,#81323,#81324,#81325,#81326,#81327,
#81328,#81329,#81330,#81331,#81332,#81333,#81334,#81335,#81336,#81337,#81338,
#81339,#81340,#81341,#81342,#81343,#81344,#81345,#81346,#81347,#81348,#81349,
#81350,#81351,#81352,#81353,#81354,#81355,#81356,#81357,#81358,#81359,#81360,
#81361,#81362,#81363,#81364,#81365,#81366,#81367,#81368,#81369,#81370,#81371,
#81372,#81373,#81374,#81375,#81376,#81377,#81378,#81379,#81380,#81381,#81382,
#81383,#81384,#81385,#81386,#81387,#81388),.UNSPECIFIED.,.F.,.F.,(4,3,3,
3,3,3,3,3,3,3,3,3,3,3,3,3,3,3,3,3,3,3,3,3,3,3,3,3,3,3,3,3,3,3,3,3,3,3,3,
3,3,3,3,3,3,3,3,3,3,3,3,3,3,3,3,3,3,3,3,3,3,3,3,3,3,3,3,3,3,3,3,3,3,4),
(876.504350351669,876.586886132016,876.669332596924,876.751710843094,876.83404758089,
876.916363953182,876.998678928157,877.081011470526,877.163428715444,877.245891245748,
877.328478721327,877.386806802721,877.470545514567,877.554181025935,877.637733469333,
877.721222905184,877.804676855798,877.888113349644,877.9715504594,878.055006254318,
878.138550747047,878.222139829988,878.305863097546,878.386542813441,878.470281525287,
878.553917036655,878.637469480054,878.720958915905,878.804412866519,878.887849360365,
878.971286470121,879.054742265039,879.138286757769,879.22187584071,879.305599108268,
879.386278824162,879.470017536008,879.553653047375,879.637205490774,879.720694926625,
879.804148877238,879.887585371085,879.97102248084,880.054478275757,880.138022768487,
880.221611851428,880.305335118986,880.386014834882,880.469753546728,880.553389058095,
880.636941501493,880.720430937344,880.803884887958,880.887321381804,880.970758491559,
881.054214286477,881.137758779206,881.221347862147,881.305071129705,881.385750845602,
881.469489557448,881.553125068816,881.636677512215,881.720166948066,881.80362089868,
881.887057392526,881.970494502282,882.053950297199,882.137494789929,882.22108387287,
882.304807140428,882.385486856322,882.478481573058,882.537167377545),
 .UNSPECIFIED.);
#611=B_SPLINE_CURVE_WITH_KNOTS('',3,(#81394,#81395,#81396,#81397,#81398,
#81399,#81400,#81401,#81402,#81403,#81404,#81405,#81406,#81407,#81408,#81409,
#81410,#81411,#81412,#81413,#81414,#81415,#81416,#81417,#81418,#81419,#81420,
#81421,#81422,#81423,#81424,#81425,#81426,#81427,#81428,#81429,#81430,#81431,
#81432,#81433,#81434,#81435,#81436,#81437,#81438,#81439,#81440,#81441,#81442,
#81443,#81444,#81445,#81446,#81447,#81448,#81449,#81450,#81451,#81452,#81453,
#81454,#81455,#81456,#81457,#81458,#81459,#81460,#81461,#81462,#81463,#81464,
#81465,#81466,#81467,#81468,#81469,#81470,#81471,#81472,#81473,#81474,#81475,
#81476,#81477,#81478,#81479,#81480,#81481,#81482,#81483,#81484,#81485,#81486,
#81487,#81488,#81489,#81490,#81491,#81492,#81493,#81494,#81495,#81496,#81497,
#81498,#81499,#81500,#81501,#81502,#81503,#81504,#81505,#81506,#81507,#81508,
#81509,#81510,#81511,#81512,#81513,#81514,#81515,#81516,#81517,#81518,#81519,
#81520,#81521,#81522,#81523,#81524,#81525,#81526,#81527,#81528,#81529,#81530,
#81531,#81532,#81533,#81534,#81535,#81536,#81537,#81538,#81539,#81540,#81541,
#81542,#81543,#81544,#81545,#81546,#81547,#81548,#81549,#81550,#81551,#81552,
#81553,#81554,#81555,#81556,#81557,#81558,#81559,#81560,#81561,#81562,#81563,
#81564,#81565,#81566,#81567,#81568,#81569,#81570,#81571,#81572,#81573,#81574,
#81575,#81576,#81577,#81578,#81579,#81580,#81581,#81582,#81583,#81584,#81585,
#81586,#81587,#81588,#81589,#81590,#81591,#81592,#81593,#81594,#81595,#81596,
#81597,#81598,#81599,#81600,#81601,#81602,#81603,#81604,#81605,#81606,#81607,
#81608,#81609,#81610),.UNSPECIFIED.,.F.,.F.,(4,3,3,3,3,3,3,3,3,3,3,3,3,
3,3,3,3,3,3,3,3,3,3,3,3,3,3,3,3,3,3,3,3,3,3,3,3,3,3,3,3,3,3,3,3,3,3,3,3,
3,3,3,3,3,3,3,3,3,3,3,3,3,3,3,3,3,3,3,3,3,3,3,4),(882.787535658835,882.889547620838,
882.993080195182,883.074932247325,883.158670959172,883.24230647054,883.325858913939,
883.409348349791,883.492802300405,883.576238794252,883.659675904008,883.743131698927,
883.826676191657,883.910265274599,883.993988542157,884.074668258046,884.158406969892,
884.242042481259,884.325594924658,884.409084360509,884.492538311123,884.575974804969,
884.659411914724,884.742867709642,884.826412202372,884.910001285312,884.99372455287,
885.074404268766,885.158142980612,885.241778491979,885.325330935377,885.408820371228,
885.492274321841,885.575710815687,885.659147925442,885.74260372036,885.826148213089,
885.90973729603,885.993460563587,886.074140279486,886.157878991332,886.2415145027,
886.325066946098,886.40855638195,886.492010332563,886.57544682641,886.658883936165,
886.742339731083,886.825884223813,886.909473306754,886.993196574312,887.073876290206,
887.157615002052,887.241250513419,887.324802956818,887.408292392669,887.491746343283,
887.575182837129,887.658619946884,887.742075741802,887.825620234531,887.909209317472,
887.99293258503,888.073612300926,888.157326814901,888.240908795136,888.324414282672,
888.407861481606,888.491268552351,888.574671813844,888.658069309137,888.74151632298,
888.81905987275),.UNSPECIFIED.);
#612=B_SPLINE_CURVE_WITH_KNOTS('',3,(#81611,#81612,#81613,#81614,#81615,
#81616,#81617,#81618,#81619,#81620),.UNSPECIFIED.,.F.,.F.,(4,3,3,4),(882.536362400618,
882.619164337193,882.703349997951,882.78753565871),.UNSPECIFIED.);
#613=B_SPLINE_CURVE_WITH_KNOTS('',3,(#81622,#81623,#81624,#81625,#81626,
#81627,#81628,#81629,#81630,#81631),.UNSPECIFIED.,.F.,.F.,(4,3,3,4),(882.537167377545,
882.629684994883,882.721773999743,882.787535658538),.UNSPECIFIED.);
#614=B_SPLINE_CURVE_WITH_KNOTS('',3,(#81632,#81633,#81634,#81635,#81636,
#81637,#81638,#81639,#81640,#81641,#81642,#81643,#81644,#81645,#81646,#81647,
#81648,#81649,#81650,#81651,#81652,#81653,#81654,#81655,#81656,#81657,#81658,
#81659,#81660,#81661,#81662,#81663,#81664,#81665,#81666,#81667,#81668,#81669,
#81670,#81671,#81672,#81673,#81674,#81675,#81676,#81677,#81678,#81679,#81680,
#81681,#81682,#81683,#81684,#81685,#81686,#81687,#81688,#81689,#81690,#81691,
#81692,#81693,#81694,#81695,#81696,#81697,#81698,#81699,#81700,#81701,#81702,
#81703,#81704,#81705,#81706,#81707,#81708,#81709,#81710,#81711,#81712,#81713,
#81714,#81715,#81716,#81717,#81718,#81719,#81720,#81721,#81722,#81723,#81724,
#81725,#81726,#81727,#81728,#81729,#81730,#81731,#81732,#81733,#81734,#81735,
#81736,#81737,#81738,#81739,#81740,#81741,#81742,#81743,#81744,#81745,#81746,
#81747,#81748,#81749,#81750,#81751,#81752,#81753,#81754,#81755,#81756,#81757,
#81758,#81759,#81760,#81761,#81762,#81763,#81764,#81765,#81766,#81767,#81768,
#81769,#81770,#81771,#81772,#81773,#81774,#81775,#81776,#81777,#81778,#81779,
#81780,#81781,#81782,#81783,#81784,#81785,#81786,#81787,#81788,#81789,#81790,
#81791,#81792,#81793,#81794,#81795,#81796,#81797,#81798,#81799,#81800,#81801,
#81802,#81803,#81804,#81805,#81806,#81807,#81808,#81809,#81810,#81811,#81812,
#81813,#81814,#81815,#81816,#81817,#81818,#81819,#81820,#81821,#81822,#81823,
#81824,#81825,#81826,#81827,#81828,#81829,#81830,#81831,#81832,#81833,#81834,
#81835,#81836,#81837,#81838,#81839,#81840,#81841,#81842,#81843,#81844,#81845,
#81846,#81847,#81848,#81849,#81850,#81851),.UNSPECIFIED.,.F.,.F.,(4,3,3,
3,3,3,3,3,3,3,3,3,3,3,3,3,3,3,3,3,3,3,3,3,3,3,3,3,3,3,3,3,3,3,3,3,3,3,3,
3,3,3,3,3,3,3,3,3,3,3,3,3,3,3,3,3,3,3,3,3,3,3,3,3,3,3,3,3,3,3,3,3,3,4),
(882.787535658714,882.872145401109,882.956778763697,883.041452029423,883.127394738828,
883.212247266875,883.298735066959,883.385222867042,883.468961578888,883.552597090256,
883.636149533654,883.719638969505,883.803092920119,883.886529413965,883.96996652372,
884.053422318637,884.136966811367,884.220555894308,884.304279161866,884.384958877762,
884.468697589608,884.552333100975,884.635885544374,884.719374980225,884.802828930838,
884.886265424684,884.96970253444,885.053158329357,885.136702822086,885.220291905027,
885.304015172585,885.384694888482,885.468433600328,885.552069111695,885.635621555094,
885.719110990945,885.802564941559,885.886001435405,885.96943854516,886.052894340078,
886.136438832807,886.220027915748,886.303751183306,886.384430899202,886.468169611048,
886.551805122416,886.635357565815,886.718847001666,886.80230095228,886.885737446126,
886.969174555882,887.0526303508,887.13617484353,887.219763926471,887.303487194029,
887.384166909923,887.467905621769,887.551541133137,887.635093576535,887.718583012385,
887.802036962999,887.885473456846,887.968910566601,888.052366361519,888.135910854248,
888.219499937189,888.303223204747,888.383902920643,888.467319795645,888.550633556085,
888.633845406105,888.716998660311,888.800107080176,888.819680914903),
 .UNSPECIFIED.);
#615=B_SPLINE_CURVE_WITH_KNOTS('',3,(#81857,#81858,#81859,#81860,#81861,
#81862,#81863,#81864,#81865,#81866,#81867,#81868,#81869,#81870,#81871,#81872,
#81873,#81874,#81875,#81876,#81877,#81878,#81879,#81880,#81881,#81882,#81883,
#81884,#81885,#81886,#81887,#81888,#81889,#81890,#81891,#81892,#81893,#81894,
#81895,#81896,#81897,#81898,#81899,#81900,#81901,#81902,#81903,#81904,#81905,
#81906,#81907,#81908,#81909,#81910,#81911,#81912,#81913,#81914,#81915,#81916,
#81917,#81918,#81919,#81920,#81921,#81922,#81923,#81924,#81925,#81926,#81927,
#81928,#81929,#81930,#81931,#81932,#81933,#81934,#81935,#81936,#81937,#81938,
#81939,#81940,#81941,#81942,#81943,#81944,#81945,#81946,#81947,#81948,#81949,
#81950,#81951,#81952,#81953,#81954,#81955,#81956,#81957,#81958,#81959,#81960,
#81961,#81962,#81963,#81964,#81965,#81966,#81967,#81968,#81969,#81970,#81971,
#81972,#81973,#81974,#81975,#81976,#81977,#81978,#81979,#81980,#81981,#81982,
#81983,#81984,#81985,#81986,#81987,#81988,#81989,#81990,#81991,#81992,#81993,
#81994,#81995,#81996,#81997,#81998,#81999,#82000,#82001,#82002,#82003,#82004,
#82005,#82006,#82007,#82008,#82009,#82010,#82011,#82012,#82013,#82014,#82015,
#82016,#82017,#82018,#82019,#82020,#82021,#82022,#82023,#82024,#82025,#82026,
#82027,#82028,#82029,#82030,#82031,#82032,#82033,#82034,#82035,#82036,#82037,
#82038,#82039,#82040,#82041,#82042,#82043,#82044,#82045,#82046,#82047,#82048,
#82049,#82050,#82051,#82052,#82053,#82054,#82055,#82056,#82057,#82058,#82059,
#82060,#82061,#82062,#82063,#82064,#82065,#82066,#82067,#82068,#82069,#82070,
#82071,#82072,#82073,#82074,#82075,#82076,#82077,#82078,#82079),
 .UNSPECIFIED.,.F.,.F.,(4,3,3,3,3,3,3,3,3,3,3,3,3,3,3,3,3,3,3,3,3,3,3,3,
3,3,3,3,3,3,3,3,3,3,3,3,3,3,3,3,3,3,3,3,3,3,3,3,3,3,3,3,3,3,3,3,3,3,3,3,
3,3,3,3,3,3,3,3,3,3,3,3,3,3,4),(889.07072096589,889.073348311646,889.157087023492,
889.24072253486,889.324274978258,889.407764414109,889.491218364723,889.574654858569,
889.658091968324,889.741547763242,889.825092255972,889.908681338913,889.99240460647,
890.073084322366,890.156823034212,890.240458545579,890.324010988978,890.407500424829,
890.490954375443,890.574390869289,890.657827979044,890.741283773962,890.824828266692,
890.908417349633,890.99214061719,891.072820333086,891.156559044932,891.240194556299,
891.323746999698,891.407236435548,891.490690386162,891.574126880008,891.657563989763,
891.741019784681,891.82456427741,891.908153360351,891.991876627909,892.072556343806,
892.156295055652,892.23993056702,892.323483010418,892.406972446269,892.490426396883,
892.57386289073,892.657300000485,892.740755795403,892.824300288133,892.907889371074,
892.991612638632,893.072292354527,893.156031066373,893.239666577741,893.323219021139,
893.40670845699,893.490162407604,893.573598901451,893.657036011206,893.740491806124,
893.824036298854,893.907625381795,893.991348649352,894.072028365247,894.155767077093,
894.23940258846,894.322955031859,894.40644446771,894.489898418323,894.573334912169,
894.656772021925,894.740227816842,894.823772309572,894.907361392512,894.99108466007,
895.071764375967,895.103030343709),.UNSPECIFIED.);
#616=B_SPLINE_CURVE_WITH_KNOTS('',3,(#82080,#82081,#82082,#82083,#82084,
#82085,#82086,#82087,#82088,#82089),.UNSPECIFIED.,.F.,.F.,(4,3,3,4),(888.81905987275,
888.902606816309,888.986663891048,889.070720965786),.UNSPECIFIED.);
#617=B_SPLINE_CURVE_WITH_KNOTS('',3,(#82091,#82092,#82093,#82094,#82095,
#82096,#82097,#82098,#82099,#82100),.UNSPECIFIED.,.F.,.F.,(4,3,3,4),(888.819680914903,
888.90277212709,888.986746546492,889.070720965894),.UNSPECIFIED.);
#618=B_SPLINE_CURVE_WITH_KNOTS('',3,(#82101,#82102,#82103,#82104,#82105,
#82106,#82107,#82108,#82109,#82110),.UNSPECIFIED.,.F.,.F.,(4,1,1,1,1,1,
1,4),(889.070727437116,889.383638931363,890.383374942083,891.383110952803,
892.382846963523,893.382582974243,894.382318984963,895.101947493761),
 .UNSPECIFIED.);
#619=B_SPLINE_CURVE_WITH_KNOTS('',3,(#82116,#82117,#82118,#82119,#82120,
#82121,#82122,#82123,#82124,#82125,#82126,#82127,#82128,#82129,#82130,#82131,
#82132,#82133,#82134,#82135,#82136,#82137,#82138,#82139,#82140,#82141,#82142,
#82143,#82144,#82145,#82146,#82147,#82148,#82149,#82150,#82151,#82152,#82153,
#82154,#82155,#82156,#82157,#82158,#82159,#82160,#82161,#82162,#82163,#82164,
#82165,#82166,#82167,#82168,#82169,#82170,#82171,#82172,#82173,#82174,#82175,
#82176,#82177,#82178,#82179,#82180,#82181,#82182,#82183,#82184,#82185,#82186,
#82187,#82188,#82189,#82190,#82191,#82192,#82193,#82194,#82195,#82196,#82197,
#82198,#82199,#82200,#82201,#82202,#82203,#82204,#82205,#82206,#82207,#82208,
#82209,#82210,#82211,#82212,#82213,#82214,#82215,#82216,#82217,#82218,#82219,
#82220,#82221,#82222,#82223,#82224,#82225,#82226,#82227,#82228,#82229,#82230,
#82231,#82232,#82233,#82234,#82235,#82236,#82237,#82238,#82239,#82240,#82241,
#82242,#82243,#82244,#82245,#82246,#82247,#82248,#82249,#82250,#82251,#82252,
#82253,#82254,#82255,#82256,#82257,#82258,#82259,#82260,#82261,#82262,#82263,
#82264,#82265,#82266,#82267,#82268,#82269,#82270,#82271,#82272,#82273,#82274,
#82275,#82276,#82277,#82278,#82279,#82280,#82281,#82282,#82283,#82284,#82285,
#82286,#82287,#82288,#82289,#82290,#82291,#82292,#82293,#82294,#82295,#82296,
#82297,#82298,#82299,#82300,#82301,#82302,#82303,#82304,#82305,#82306,#82307,
#82308,#82309,#82310,#82311,#82312,#82313,#82314,#82315,#82316,#82317,#82318,
#82319,#82320,#82321,#82322,#82323,#82324,#82325,#82326,#82327,#82328,#82329,
#82330,#82331,#82332,#82333,#82334,#82335),.UNSPECIFIED.,.F.,.F.,(4,3,3,
3,3,3,3,3,3,3,3,3,3,3,3,3,3,3,3,3,3,3,3,3,3,3,3,3,3,3,3,3,3,3,3,3,3,3,3,
3,3,3,3,3,3,3,3,3,3,3,3,3,3,3,3,3,3,3,3,3,3,3,3,3,3,3,3,3,3,3,3,3,3,4),
(895.353906273069,895.436705046304,895.519470690322,895.602221139555,895.684975042146,
895.767751045559,895.850616832775,895.933531325895,896.016572976593,896.071500386687,
896.155239098533,896.238874609901,896.322427053299,896.40591648915,896.489370439764,
896.57280693361,896.656244043365,896.739699838282,896.823244331012,896.906833413953,
896.99055668151,897.071236397407,897.154975109253,897.238610620621,897.322163064019,
897.40565249987,897.489106450484,897.57254294433,897.655980054085,897.739435849002,
897.822980341732,897.906569424673,897.99029269223,898.070972408127,898.154711119973,
898.23834663134,898.321899074739,898.40538851059,898.488842461203,898.57227895505,
898.655716064805,898.739171859722,898.822716352452,898.906305435393,898.990028702951,
899.070708418847,899.154447130693,899.23808264206,899.321635085459,899.40512452131,
899.488578471924,899.57201496577,899.655452075525,899.738907870443,899.822452363173,
899.906041446114,899.989764713671,900.070444429567,900.154183141413,900.237818652781,
900.321371096179,900.40486053203,900.488314482643,900.57175097649,900.655188086245,
900.738643881162,900.822188373892,900.905777456833,900.989500724391,901.070180440288,
901.155986680042,901.241683103162,901.327251411809,901.386599073372),
 .UNSPECIFIED.);
#620=B_SPLINE_CURVE_WITH_KNOTS('',3,(#82336,#82337,#82338,#82339,#82340,
#82341,#82342,#82343,#82344,#82345),.UNSPECIFIED.,.F.,.F.,(4,3,3,4),(895.103030343709,
895.207280880286,895.309982870308,895.353906272954),.UNSPECIFIED.);
#621=B_SPLINE_CURVE_WITH_KNOTS('',3,(#82347,#82348,#82349,#82350),
 .UNSPECIFIED.,.F.,.F.,(4,4),(895.101947493761,895.353906273073),
 .UNSPECIFIED.);
#622=B_SPLINE_CURVE_WITH_KNOTS('',3,(#82351,#82352,#82353,#82354,#82355,
#82356,#82357,#82358,#82359,#82360,#82361),.UNSPECIFIED.,.F.,.F.,(4,1,1,
1,1,1,1,1,4),(895.353906273073,895.382054995684,896.381791006404,897.381527017124,
898.381263027844,899.380999038564,900.380735049284,901.380471060004,901.386062069609),
 .UNSPECIFIED.);
#623=B_SPLINE_CURVE_WITH_KNOTS('',3,(#82367,#82368,#82369,#82370,#82371,
#82372,#82373,#82374,#82375,#82376,#82377,#82378,#82379,#82380,#82381,#82382,
#82383,#82384,#82385,#82386,#82387,#82388,#82389,#82390,#82391,#82392,#82393,
#82394,#82395,#82396,#82397,#82398,#82399,#82400,#82401,#82402,#82403,#82404,
#82405,#82406,#82407,#82408,#82409,#82410,#82411,#82412,#82413,#82414,#82415,
#82416,#82417,#82418,#82419,#82420,#82421,#82422,#82423,#82424,#82425,#82426,
#82427,#82428,#82429,#82430,#82431,#82432,#82433,#82434,#82435,#82436,#82437,
#82438,#82439,#82440,#82441,#82442,#82443,#82444,#82445,#82446,#82447,#82448,
#82449,#82450,#82451,#82452,#82453,#82454,#82455,#82456,#82457,#82458,#82459,
#82460,#82461,#82462,#82463,#82464,#82465,#82466,#82467,#82468,#82469,#82470,
#82471,#82472,#82473,#82474,#82475,#82476,#82477,#82478,#82479,#82480,#82481,
#82482,#82483,#82484,#82485,#82486,#82487,#82488,#82489,#82490,#82491,#82492,
#82493,#82494,#82495,#82496,#82497,#82498,#82499,#82500,#82501,#82502,#82503,
#82504,#82505,#82506,#82507,#82508,#82509,#82510,#82511,#82512,#82513,#82514,
#82515,#82516,#82517,#82518,#82519,#82520,#82521,#82522,#82523,#82524,#82525,
#82526,#82527,#82528,#82529,#82530,#82531,#82532,#82533,#82534,#82535,#82536,
#82537,#82538,#82539,#82540,#82541,#82542,#82543,#82544,#82545,#82546,#82547,
#82548,#82549,#82550,#82551,#82552,#82553,#82554,#82555,#82556,#82557,#82558,
#82559,#82560,#82561,#82562,#82563,#82564,#82565,#82566,#82567,#82568,#82569,
#82570,#82571,#82572,#82573,#82574,#82575,#82576,#82577,#82578,#82579,#82580,
#82581,#82582,#82583,#82584,#82585,#82586),.UNSPECIFIED.,.F.,.F.,(4,3,3,
3,3,3,3,3,3,3,3,3,3,3,3,3,3,3,3,3,3,3,3,3,3,3,3,3,3,3,3,3,3,3,3,3,3,3,3,
3,3,3,3,3,3,3,3,3,3,3,3,3,3,3,3,3,3,3,3,3,3,3,3,3,3,3,3,3,3,3,3,3,3,4),
(901.637091580384,901.727374617521,901.818032209178,901.908878920106,902.000023922038,
902.069916451008,902.153655162854,902.237290674222,902.32084311762,902.404332553471,
902.487786504085,902.571222997931,902.654660107686,902.738115902604,902.821660395334,
902.905249478275,902.988972745832,903.069652461728,903.153391173574,903.237026684941,
903.32057912834,903.404068564191,903.487522514805,903.570959008651,903.654396118406,
903.737851913324,903.821396406054,903.904985488995,903.988708756552,904.069388472448,
904.153127184294,904.236762695661,904.32031513906,904.403804574911,904.487258525524,
904.570695019371,904.654132129126,904.737587924044,904.821132416773,904.904721499714,
904.988444767272,905.069124483168,905.152863195014,905.236498706382,905.32005114978,
905.403540585631,905.486994536245,905.570431030091,905.653868139847,905.737323934764,
905.820868427494,905.904457510435,905.988180777993,906.068860493888,906.152599205734,
906.236234717101,906.3197871605,906.403276596351,906.486730546965,906.570167040811,
906.653604150566,906.737059945484,906.820604438213,906.904193521154,906.987916788712,
907.068596504608,907.151084096677,907.233476717466,907.315793573918,907.398053799997,
907.480282004625,907.562492286284,907.644717656506,907.668518267423),
 .UNSPECIFIED.);
#624=B_SPLINE_CURVE_WITH_KNOTS('',3,(#82587,#82588,#82589,#82590,#82591,
#82592,#82593,#82594,#82595,#82596),.UNSPECIFIED.,.F.,.F.,(4,3,3,4),(901.386599073372,
901.4720213908,901.557375230074,901.637091580249),.UNSPECIFIED.);
#625=B_SPLINE_CURVE_WITH_KNOTS('',3,(#82598,#82599,#82600,#82601),
 .UNSPECIFIED.,.F.,.F.,(4,4),(901.386062069609,901.637089254157),
 .UNSPECIFIED.);
#626=B_SPLINE_CURVE_WITH_KNOTS('',3,(#82602,#82603,#82604,#82605,#82606,
#82607,#82608,#82609,#82610,#82611,#82612,#82613,#82614,#82615,#82616,#82617,
#82618,#82619,#82620,#82621,#82622,#82623,#82624,#82625,#82626,#82627,#82628,
#82629,#82630,#82631,#82632,#82633,#82634,#82635,#82636,#82637,#82638,#82639,
#82640,#82641,#82642,#82643,#82644,#82645,#82646,#82647,#82648,#82649,#82650,
#82651,#82652,#82653,#82654,#82655,#82656,#82657,#82658,#82659,#82660,#82661,
#82662,#82663,#82664,#82665,#82666,#82667,#82668,#82669,#82670,#82671,#82672,
#82673,#82674,#82675,#82676,#82677,#82678,#82679,#82680,#82681,#82682,#82683,
#82684,#82685,#82686,#82687,#82688,#82689,#82690,#82691,#82692,#82693,#82694,
#82695,#82696,#82697,#82698,#82699,#82700,#82701,#82702,#82703,#82704,#82705,
#82706,#82707,#82708,#82709,#82710,#82711,#82712,#82713,#82714,#82715,#82716,
#82717,#82718,#82719,#82720,#82721,#82722,#82723,#82724,#82725,#82726,#82727,
#82728,#82729,#82730,#82731,#82732,#82733,#82734,#82735,#82736,#82737,#82738,
#82739,#82740,#82741,#82742,#82743,#82744,#82745,#82746,#82747,#82748,#82749,
#82750,#82751,#82752,#82753,#82754,#82755,#82756,#82757,#82758,#82759,#82760,
#82761,#82762,#82763,#82764,#82765,#82766,#82767,#82768,#82769,#82770,#82771,
#82772,#82773,#82774,#82775,#82776,#82777,#82778,#82779,#82780,#82781,#82782,
#82783,#82784,#82785,#82786,#82787,#82788,#82789,#82790,#82791,#82792,#82793,
#82794,#82795,#82796,#82797,#82798,#82799,#82800,#82801,#82802,#82803,#82804,
#82805,#82806,#82807,#82808,#82809,#82810,#82811,#82812,#82813,#82814,#82815,
#82816,#82817,#82818,#82819,#82820,#82821),.UNSPECIFIED.,.F.,.F.,(4,3,3,
3,3,3,3,3,3,3,3,3,3,3,3,3,3,3,3,3,3,3,3,3,3,3,3,3,3,3,3,3,3,3,3,3,3,3,3,
3,3,3,3,3,3,3,3,3,3,3,3,3,3,3,3,3,3,3,3,3,3,3,3,3,3,3,3,3,3,3,3,3,3,4),
(901.637091580253,901.719694961594,901.802258975235,901.884792597306,901.967321346146,
902.049864037226,902.132490934378,902.215159553066,902.297961533055,902.380207070725,
902.463945782571,902.547581293938,902.631133737337,902.714623173188,902.798077123801,
902.881513617648,902.964950727403,903.048406522321,903.131951015051,903.215540097991,
903.299263365549,903.379943081445,903.463681793291,903.547317304658,903.630869748057,
903.714359183908,903.797813134521,903.881249628368,903.964686738123,904.04814253304,
904.13168702577,904.215276108711,904.298999376268,904.379679092165,904.463417804011,
904.547053315379,904.630605758777,904.714095194628,904.797549145242,904.880985639088,
904.964422748844,905.047878543761,905.131423036491,905.215012119432,905.29873538699,
905.379415102885,905.463153814731,905.546789326099,905.630341769497,905.713831205348,
905.797285155962,905.880721649808,905.964158759564,906.047614554481,906.131159047211,
906.214748130152,906.298471397709,906.379151113605,906.462889825451,906.546525336818,
906.630077780216,906.713567216068,906.797021166681,906.880457660527,906.963894770283,
907.047350565201,907.130895057931,907.214484140871,907.298207408429,907.378887124325,
907.465459567995,907.551914783059,907.638231267352,907.669863191904),
 .UNSPECIFIED.);
#627=B_SPLINE_CURVE_WITH_KNOTS('',3,(#82827,#82828,#82829,#82830,#82831,
#82832,#82833,#82834,#82835,#82836,#82837,#82838,#82839,#82840,#82841,#82842,
#82843,#82844,#82845,#82846,#82847,#82848,#82849,#82850,#82851,#82852,#82853,
#82854,#82855,#82856,#82857,#82858,#82859,#82860,#82861,#82862,#82863,#82864,
#82865,#82866,#82867,#82868,#82869,#82870,#82871,#82872,#82873,#82874,#82875,
#82876,#82877,#82878,#82879,#82880,#82881,#82882,#82883,#82884,#82885,#82886,
#82887,#82888,#82889,#82890,#82891,#82892,#82893,#82894,#82895,#82896,#82897,
#82898,#82899,#82900,#82901,#82902,#82903,#82904,#82905,#82906,#82907,#82908,
#82909,#82910,#82911,#82912,#82913,#82914,#82915,#82916,#82917,#82918,#82919,
#82920,#82921,#82922,#82923,#82924,#82925,#82926,#82927,#82928,#82929,#82930,
#82931,#82932,#82933,#82934,#82935,#82936,#82937,#82938,#82939,#82940,#82941,
#82942,#82943,#82944,#82945,#82946,#82947,#82948,#82949,#82950,#82951,#82952,
#82953,#82954,#82955,#82956,#82957,#82958,#82959,#82960,#82961,#82962,#82963,
#82964,#82965,#82966,#82967,#82968,#82969,#82970,#82971,#82972,#82973,#82974,
#82975,#82976,#82977,#82978,#82979,#82980,#82981,#82982,#82983,#82984,#82985,
#82986,#82987,#82988,#82989,#82990,#82991,#82992,#82993,#82994,#82995,#82996,
#82997,#82998,#82999,#83000,#83001,#83002,#83003,#83004,#83005,#83006,#83007,
#83008,#83009,#83010,#83011,#83012,#83013,#83014,#83015,#83016,#83017,#83018,
#83019,#83020,#83021,#83022,#83023,#83024,#83025,#83026,#83027,#83028,#83029,
#83030,#83031,#83032,#83033,#83034,#83035,#83036,#83037,#83038,#83039,#83040,
#83041,#83042,#83043),.UNSPECIFIED.,.F.,.F.,(4,3,3,3,3,3,3,3,3,3,3,3,3,
3,3,3,3,3,3,3,3,3,3,3,3,3,3,3,3,3,3,3,3,3,3,3,3,3,3,3,3,3,3,3,3,3,3,3,3,
3,3,3,3,3,3,3,3,3,3,3,3,3,3,3,3,3,3,3,3,3,3,3,4),(907.920276887428,908.068332515329,
908.152071227175,908.235706738542,908.319259181941,908.402748617792,908.486202568405,
908.569639062252,908.653076172007,908.736531966925,908.820076459654,908.903665542595,
908.987388810152,909.068068526049,909.151807237895,909.235442749263,909.318995192661,
909.402484628512,909.485938579126,909.569375072972,909.652812182727,909.736267977645,
909.819812470374,909.903401553315,909.987124820873,910.067804536769,910.151543248615,
910.235178759982,910.318731203381,910.402220639232,910.485674589845,910.569111083692,
910.652548193447,910.736003988365,910.819548481094,910.903137564035,910.986860831593,
911.067540547489,911.151279259335,911.234914770703,911.318467214101,911.401956649952,
911.485410600566,911.568847094412,911.652284204167,911.735739999085,911.819284491815,
911.902873574756,911.986596842313,912.067276558209,912.151015270055,912.234650781422,
912.318203224821,912.401692660672,912.485146611285,912.568583105132,912.652020214887,
912.735476009805,912.819020502534,912.902609585475,912.986332853033,913.067012568929,
913.150758006077,913.234398727867,913.317954873295,913.401441674311,913.484890787398,
913.568320301205,913.651748287339,913.735227233515,913.818733664062,913.902329818043,
913.951907679941),.UNSPECIFIED.);
#628=B_SPLINE_CURVE_WITH_KNOTS('',3,(#83044,#83045,#83046,#83047,#83048,
#83049,#83050,#83051,#83052,#83053),.UNSPECIFIED.,.F.,.F.,(4,3,3,4),(907.668518267423,
907.750806452033,907.835541669673,907.920276887313),.UNSPECIFIED.);
#629=B_SPLINE_CURVE_WITH_KNOTS('',3,(#83055,#83056,#83057,#83058,#83059,
#83060,#83061,#83062,#83063,#83064),.UNSPECIFIED.,.F.,.F.,(4,3,3,4),(907.669863191904,
907.756026872551,907.842091388467,907.920276887432),.UNSPECIFIED.);
#630=B_SPLINE_CURVE_WITH_KNOTS('',3,(#83065,#83066,#83067,#83068,#83069,
#83070,#83071,#83072,#83073,#83074,#83075,#83076,#83077,#83078,#83079,#83080,
#83081,#83082,#83083,#83084,#83085,#83086,#83087,#83088,#83089,#83090,#83091,
#83092,#83093,#83094,#83095,#83096,#83097,#83098,#83099,#83100,#83101,#83102,
#83103,#83104,#83105,#83106,#83107,#83108,#83109,#83110,#83111,#83112,#83113,
#83114,#83115,#83116,#83117,#83118,#83119,#83120,#83121,#83122,#83123,#83124,
#83125,#83126,#83127,#83128,#83129,#83130,#83131,#83132,#83133,#83134,#83135,
#83136,#83137,#83138,#83139,#83140,#83141,#83142,#83143,#83144,#83145,#83146,
#83147,#83148,#83149,#83150,#83151,#83152,#83153,#83154,#83155,#83156,#83157,
#83158,#83159,#83160,#83161,#83162,#83163,#83164,#83165,#83166,#83167,#83168,
#83169,#83170,#83171,#83172,#83173,#83174,#83175,#83176,#83177,#83178,#83179,
#83180,#83181,#83182,#83183,#83184,#83185,#83186,#83187,#83188,#83189,#83190,
#83191,#83192,#83193,#83194,#83195,#83196,#83197,#83198,#83199,#83200,#83201,
#83202,#83203,#83204,#83205,#83206,#83207,#83208,#83209,#83210,#83211,#83212,
#83213,#83214,#83215,#83216,#83217,#83218,#83219,#83220,#83221,#83222,#83223,
#83224,#83225,#83226,#83227,#83228,#83229,#83230,#83231,#83232,#83233,#83234,
#83235,#83236,#83237,#83238,#83239,#83240,#83241,#83242,#83243,#83244,#83245,
#83246,#83247,#83248,#83249,#83250,#83251,#83252,#83253,#83254,#83255,#83256,
#83257,#83258,#83259,#83260,#83261,#83262,#83263,#83264,#83265,#83266,#83267,
#83268,#83269,#83270,#83271,#83272,#83273,#83274,#83275,#83276,#83277,#83278,
#83279,#83280,#83281),.UNSPECIFIED.,.F.,.F.,(4,3,3,3,3,3,3,3,3,3,3,3,3,
3,3,3,3,3,3,3,3,3,3,3,3,3,3,3,3,3,3,3,3,3,3,3,3,3,3,3,3,3,3,3,3,3,3,3,3,
3,3,3,3,3,3,3,3,3,3,3,3,3,3,3,3,3,3,3,3,3,3,3,4),(907.920276887616,908.009350353477,
908.101668548869,908.191201216186,908.284912175615,908.378623135045,908.462361846891,
908.545997358259,908.629549801657,908.713039237508,908.796493188122,908.879929681968,
908.963366791724,909.046822586642,909.130367079371,909.213956162312,909.29767942987,
909.378359145765,909.462097857611,909.545733368978,909.629285812377,909.712775248228,
909.796229198842,909.879665692688,909.963102802443,910.046558597361,910.130103090091,
910.213692173032,910.297415440589,910.378095156486,910.461833868332,910.5454693797,
910.629021823098,910.712511258949,910.795965209563,910.879401703409,910.962838813165,
911.046294608083,911.129839100812,911.213428183753,911.297151451311,911.377831167206,
911.461569879052,911.545205390419,911.628757833818,911.712247269669,911.795701220282,
911.879137714129,911.962574823884,912.046030618802,912.129575111531,912.213164194472,
912.29688746203,912.377567177926,912.461305889772,912.54494140114,912.628493844538,
912.711983280389,912.795437231003,912.878873724849,912.962310834605,913.045766629522,
913.129311122252,913.212900205193,913.296623472751,913.377303188646,913.459775106865,
913.542151599702,913.624451888579,913.706695524716,913.788904051849,913.871118218614,
913.951777480369),.UNSPECIFIED.);
#631=B_SPLINE_CURVE_WITH_KNOTS('',3,(#83287,#83288,#83289,#83290,#83291,
#83292,#83293,#83294,#83295,#83296,#83297,#83298,#83299,#83300,#83301,#83302,
#83303,#83304,#83305,#83306,#83307,#83308,#83309,#83310,#83311,#83312,#83313,
#83314,#83315,#83316,#83317,#83318,#83319,#83320,#83321,#83322,#83323,#83324,
#83325,#83326,#83327,#83328,#83329,#83330,#83331,#83332,#83333,#83334,#83335,
#83336,#83337,#83338,#83339,#83340,#83341,#83342,#83343,#83344,#83345,#83346,
#83347,#83348,#83349,#83350,#83351,#83352,#83353,#83354,#83355,#83356,#83357,
#83358,#83359,#83360,#83361,#83362,#83363,#83364,#83365,#83366,#83367,#83368,
#83369,#83370,#83371,#83372,#83373,#83374,#83375,#83376,#83377,#83378,#83379,
#83380,#83381,#83382,#83383,#83384,#83385,#83386,#83387,#83388,#83389,#83390,
#83391,#83392,#83393,#83394,#83395,#83396,#83397,#83398,#83399,#83400,#83401,
#83402,#83403,#83404,#83405,#83406,#83407,#83408,#83409,#83410,#83411,#83412,
#83413,#83414,#83415,#83416,#83417,#83418,#83419,#83420,#83421,#83422,#83423,
#83424,#83425,#83426,#83427,#83428,#83429,#83430,#83431,#83432,#83433,#83434,
#83435,#83436,#83437,#83438,#83439,#83440,#83441,#83442,#83443,#83444,#83445,
#83446,#83447,#83448,#83449,#83450,#83451,#83452,#83453,#83454,#83455,#83456,
#83457,#83458,#83459,#83460,#83461,#83462,#83463,#83464,#83465,#83466,#83467,
#83468,#83469,#83470,#83471,#83472,#83473,#83474,#83475,#83476,#83477,#83478,
#83479,#83480,#83481,#83482,#83483,#83484,#83485,#83486,#83487,#83488,#83489,
#83490,#83491,#83492,#83493,#83494,#83495,#83496,#83497,#83498,#83499,#83500,
#83501,#83502,#83503,#83504,#83505,#83506),.UNSPECIFIED.,.F.,.F.,(4,3,3,
3,3,3,3,3,3,3,3,3,3,3,3,3,3,3,3,3,3,3,3,3,3,3,3,3,3,3,3,3,3,3,3,3,3,3,3,
3,3,3,3,3,3,3,3,3,3,3,3,3,3,3,3,3,3,3,3,3,3,3,3,3,3,3,3,3,3,3,3,3,3,4),
(914.203462194732,914.2859095674,914.368271757229,914.450569893832,914.532832019811,
914.615077615304,914.697325689258,914.779595250459,914.861951217647,914.944356078256,
915.026880542678,915.066484590369,915.150223302215,915.233858813583,915.317411256982,
915.400900692834,915.484354643448,915.567791137294,915.65122824705,915.734684041968,
915.818228534698,915.901817617639,915.985540885197,916.06622060109,916.149959312936,
916.233594824304,916.317147267702,916.400636703553,916.484090654167,916.567527148013,
916.650964257769,916.734420052686,916.817964545416,916.901553628357,916.985276895914,
917.06595661181,917.149695323656,917.233330835023,917.316883278422,917.400372714273,
917.483826664886,917.567263158732,917.650700268488,917.734156063405,917.817700556135,
917.901289639076,917.985012906633,918.06569262253,918.149431334376,918.233066845744,
918.316619289142,918.400108724993,918.483562675607,918.566999169453,918.650436279208,
918.733892074126,918.817436566856,918.901025649797,918.984748917355,919.06542863325,
919.149167345096,919.232802856463,919.316355299862,919.399844735712,919.483298686326,
919.566735180172,919.650172289927,919.733628084845,919.817172577575,919.900761660516,
919.984484928073,920.06516464397,920.156938440952,920.236315776265),
 .UNSPECIFIED.);
#632=B_SPLINE_CURVE_WITH_KNOTS('',3,(#83507,#83508,#83509,#83510,#83511,
#83512,#83513,#83514,#83515,#83516),.UNSPECIFIED.,.F.,.F.,(4,3,3,4),(913.951907679941,
914.035651074648,914.066748579649,914.203462194608),.UNSPECIFIED.);
#633=B_SPLINE_CURVE_WITH_KNOTS('',3,(#83518,#83519,#83520,#83521,#83522,
#83523,#83524,#83525,#83526,#83527),.UNSPECIFIED.,.F.,.F.,(4,3,3,4),(913.951777480369,
914.034031901732,914.118747048086,914.203462194439),.UNSPECIFIED.);
#634=B_SPLINE_CURVE_WITH_KNOTS('',3,(#83528,#83529,#83530,#83531,#83532,
#83533,#83534,#83535,#83536,#83537,#83538,#83539,#83540,#83541,#83542,#83543,
#83544,#83545,#83546,#83547,#83548,#83549,#83550,#83551,#83552,#83553,#83554,
#83555,#83556,#83557,#83558,#83559,#83560,#83561,#83562,#83563,#83564,#83565,
#83566,#83567,#83568,#83569,#83570,#83571,#83572,#83573,#83574,#83575,#83576,
#83577,#83578,#83579,#83580,#83581,#83582,#83583,#83584,#83585,#83586,#83587,
#83588,#83589,#83590,#83591,#83592,#83593,#83594,#83595,#83596,#83597,#83598,
#83599,#83600,#83601,#83602,#83603,#83604,#83605,#83606,#83607,#83608,#83609,
#83610,#83611,#83612,#83613,#83614,#83615,#83616,#83617,#83618,#83619,#83620,
#83621,#83622,#83623,#83624,#83625,#83626,#83627,#83628,#83629,#83630,#83631,
#83632,#83633,#83634,#83635,#83636,#83637,#83638,#83639,#83640,#83641,#83642,
#83643,#83644,#83645,#83646,#83647,#83648,#83649,#83650,#83651,#83652,#83653,
#83654,#83655,#83656,#83657,#83658,#83659,#83660,#83661,#83662,#83663,#83664,
#83665,#83666,#83667,#83668,#83669,#83670,#83671,#83672,#83673,#83674,#83675,
#83676,#83677,#83678,#83679,#83680,#83681,#83682,#83683,#83684,#83685,#83686,
#83687,#83688,#83689,#83690,#83691,#83692,#83693,#83694,#83695,#83696,#83697,
#83698,#83699,#83700,#83701,#83702,#83703,#83704,#83705,#83706,#83707,#83708,
#83709,#83710,#83711,#83712,#83713,#83714,#83715,#83716,#83717,#83718,#83719,
#83720,#83721,#83722,#83723,#83724,#83725,#83726,#83727,#83728,#83729,#83730,
#83731,#83732,#83733,#83734,#83735,#83736,#83737,#83738,#83739,#83740,#83741,
#83742,#83743,#83744,#83745,#83746,#83747),.UNSPECIFIED.,.F.,.F.,(4,3,3,
3,3,3,3,3,3,3,3,3,3,3,3,3,3,3,3,3,3,3,3,3,3,3,3,3,3,3,3,3,3,3,3,3,3,3,3,
3,3,3,3,3,3,3,3,3,3,3,3,3,3,3,3,3,3,3,3,3,3,3,3,3,3,3,3,3,3,3,3,3,3,4),
(914.203462194612,914.333356253278,914.377039199366,914.460777911212,914.54441342258,
914.627965865979,914.71145530183,914.794909252444,914.87834574629,914.961782856046,
915.045238650964,915.128783143694,915.212372226635,915.296095494193,915.376775210086,
915.460513921932,915.544149433299,915.627701876698,915.711191312549,915.794645263162,
915.878081757009,915.961518866764,916.044974661682,916.128519154411,916.212108237352,
916.29583150491,916.376511220806,916.460249932652,916.543885444019,916.627437887418,
916.710927323269,916.794381273882,916.877817767729,916.961254877484,917.044710672402,
917.128255165131,917.211844248072,917.29556751563,917.376247231526,917.459985943372,
917.54362145474,917.627173898138,917.71066333399,917.794117284604,917.87755377845,
917.960990888206,918.044446683124,918.127991175853,918.211580258794,918.295303526352,
918.375983242247,918.459721954093,918.543357465461,918.626909908859,918.71039934471,
918.793853295324,918.87728978917,918.960726898926,919.044182693843,919.127727186573,
919.211316269514,919.295039537072,919.375719252967,919.459466267946,919.543108230139,
919.629599690776,919.713084564985,919.796531909885,919.879959813621,919.963386347286,
920.04685897325,920.130359459133,920.21393724819,920.235039915232),
 .UNSPECIFIED.);
#635=B_SPLINE_CURVE_WITH_KNOTS('',3,(#83753,#83754,#83755,#83756,#83757,
#83758,#83759,#83760,#83761,#83762,#83763,#83764,#83765,#83766,#83767,#83768,
#83769,#83770,#83771,#83772,#83773,#83774,#83775,#83776,#83777,#83778,#83779,
#83780,#83781,#83782,#83783,#83784,#83785,#83786,#83787,#83788,#83789,#83790,
#83791,#83792,#83793,#83794,#83795,#83796,#83797,#83798,#83799,#83800,#83801,
#83802,#83803,#83804,#83805,#83806,#83807,#83808,#83809,#83810,#83811,#83812,
#83813,#83814,#83815,#83816,#83817,#83818,#83819,#83820,#83821,#83822,#83823,
#83824,#83825,#83826,#83827,#83828,#83829,#83830,#83831,#83832,#83833,#83834,
#83835,#83836,#83837,#83838,#83839,#83840,#83841,#83842,#83843,#83844,#83845,
#83846,#83847,#83848,#83849,#83850,#83851,#83852,#83853,#83854,#83855,#83856,
#83857,#83858,#83859,#83860,#83861,#83862,#83863,#83864,#83865,#83866,#83867,
#83868,#83869,#83870,#83871,#83872,#83873,#83874,#83875,#83876,#83877,#83878,
#83879,#83880,#83881,#83882,#83883,#83884,#83885,#83886,#83887,#83888,#83889,
#83890,#83891,#83892,#83893,#83894,#83895,#83896,#83897,#83898,#83899,#83900,
#83901,#83902,#83903,#83904,#83905,#83906,#83907,#83908,#83909,#83910,#83911,
#83912,#83913,#83914,#83915,#83916,#83917,#83918,#83919,#83920,#83921,#83922,
#83923,#83924,#83925,#83926,#83927,#83928,#83929,#83930,#83931,#83932,#83933,
#83934,#83935,#83936,#83937,#83938,#83939,#83940,#83941,#83942,#83943,#83944,
#83945,#83946,#83947,#83948,#83949,#83950,#83951,#83952,#83953,#83954,#83955,
#83956,#83957,#83958,#83959,#83960,#83961,#83962,#83963,#83964,#83965,#83966,
#83967,#83968,#83969,#83970,#83971,#83972),.UNSPECIFIED.,.F.,.F.,(4,3,3,
3,3,3,3,3,3,3,3,3,3,3,3,3,3,3,3,3,3,3,3,3,3,3,3,3,3,3,3,3,3,3,3,3,3,3,3,
3,3,3,3,3,3,3,3,3,3,3,3,3,3,3,3,3,3,3,3,3,3,3,3,3,3,3,3,3,3,3,3,3,3,4),
(920.486647501788,920.571704372344,920.656798324641,920.741944767653,920.827221421023,
920.912567136802,920.998070557921,921.06490065469,921.148639366536,921.232274877904,
921.315827321302,921.399316757153,921.482770707767,921.566207201614,921.649644311369,
921.733100106287,921.816644599017,921.900233681958,921.983956949516,922.06463666541,
922.148375377256,922.232010888624,922.315563332023,922.399052767874,922.482506718488,
922.565943212334,922.64938032209,922.732836117008,922.816380609738,922.899969692679,
922.983692960237,923.064372676131,923.148111387977,923.231746899345,923.315299342743,
923.398788778594,923.482242729208,923.565679223054,923.649116332809,923.732572127726,
923.816116620456,923.899705703397,923.983428970955,924.064108686851,924.147847398697,
924.231482910064,924.315035353463,924.398524789314,924.481978739928,924.565415233774,
924.648852343529,924.732308138447,924.815852631176,924.899441714117,924.983164981675,
925.063844697571,925.147583409417,925.231218920785,925.314771364184,925.398260800035,
925.481714750648,925.565151244495,925.64858835425,925.732044149168,925.815588641898,
925.899177724839,925.982900992397,926.063580708291,926.14675553624,926.229829073602,
926.31280410445,926.395722260427,926.478600793687,926.518691253405),
 .UNSPECIFIED.);
#636=B_SPLINE_CURVE_WITH_KNOTS('',3,(#83973,#83974,#83975,#83976,#83977,
#83978,#83979,#83980,#83981,#83982),.UNSPECIFIED.,.F.,.F.,(4,3,3,4),(920.236315776265,
920.327641113218,920.418611342316,920.486647501632),.UNSPECIFIED.);
#637=B_SPLINE_CURVE_WITH_KNOTS('',3,(#83984,#83985,#83986,#83987,#83988,
#83989,#83990,#83991,#83992,#83993),.UNSPECIFIED.,.F.,.F.,(4,3,3,4),(920.235039915232,
920.318772047392,920.375455263687,920.486647501791),.UNSPECIFIED.);
#638=B_SPLINE_CURVE_WITH_KNOTS('',3,(#83994,#83995,#83996,#83997,#83998,
#83999,#84000,#84001,#84002,#84003,#84004,#84005,#84006,#84007,#84008,#84009,
#84010,#84011,#84012,#84013,#84014,#84015,#84016,#84017,#84018,#84019,#84020,
#84021,#84022,#84023,#84024,#84025,#84026,#84027,#84028,#84029,#84030,#84031,
#84032,#84033,#84034,#84035,#84036,#84037,#84038,#84039,#84040,#84041,#84042,
#84043,#84044,#84045,#84046,#84047,#84048,#84049,#84050,#84051,#84052,#84053,
#84054,#84055,#84056,#84057,#84058,#84059,#84060,#84061,#84062,#84063,#84064,
#84065,#84066,#84067,#84068,#84069,#84070,#84071,#84072,#84073,#84074,#84075,
#84076,#84077,#84078,#84079,#84080,#84081,#84082,#84083,#84084,#84085,#84086,
#84087,#84088,#84089,#84090,#84091,#84092,#84093,#84094,#84095,#84096,#84097,
#84098,#84099,#84100,#84101,#84102,#84103,#84104,#84105,#84106,#84107,#84108,
#84109,#84110,#84111,#84112,#84113,#84114,#84115,#84116,#84117,#84118,#84119,
#84120,#84121,#84122,#84123,#84124,#84125,#84126,#84127,#84128,#84129,#84130,
#84131,#84132,#84133,#84134,#84135,#84136,#84137,#84138,#84139,#84140,#84141,
#84142,#84143,#84144,#84145,#84146,#84147,#84148,#84149,#84150,#84151,#84152,
#84153,#84154,#84155,#84156,#84157,#84158,#84159,#84160,#84161,#84162,#84163,
#84164,#84165,#84166,#84167,#84168,#84169,#84170,#84171,#84172,#84173,#84174,
#84175,#84176,#84177,#84178,#84179,#84180,#84181,#84182,#84183,#84184,#84185,
#84186,#84187,#84188,#84189,#84190,#84191,#84192,#84193,#84194,#84195,#84196,
#84197,#84198,#84199,#84200,#84201,#84202,#84203,#84204,#84205,#84206,#84207,
#84208,#84209,#84210,#84211,#84212,#84213),.UNSPECIFIED.,.F.,.F.,(4,3,3,
3,3,3,3,3,3,3,3,3,3,3,3,3,3,3,3,3,3,3,3,3,3,3,3,3,3,3,3,3,3,3,3,3,3,3,3,
3,3,3,3,3,3,3,3,3,3,3,3,3,3,3,3,3,3,3,3,3,3,3,3,3,3,3,3,3,3,3,3,3,3,4),
(920.486647501927,920.569217400438,920.651696775787,920.73410670892,920.816473497108,
920.89881878342,920.981161518928,921.063520650256,921.145963985295,921.228451518121,
921.311065716616,921.375191274407,921.458929986253,921.54256549762,921.626117941019,
921.70960737687,921.793061327484,921.87649782133,921.959934931086,922.043390726003,
922.126935218733,922.210524301674,922.294247569232,922.374927285127,922.458665996973,
922.542301508341,922.625853951739,922.70934338759,922.792797338203,922.87623383205,
922.959670941805,923.043126736722,923.126671229452,923.210260312393,923.293983579951,
923.374663295847,923.458402007693,923.54203751906,923.625589962459,923.70907939831,
923.792533348923,923.875969842769,923.959406952524,924.042862747442,924.126407240172,
924.209996323113,924.29371959067,924.374399306567,924.458138018413,924.541773529781,
924.62532597318,924.708815409031,924.792269359644,924.875705853491,924.959142963247,
925.042598758165,925.126143250895,925.209732333836,925.293455601394,925.374135317288,
925.457874029134,925.541509540502,925.6250619839,925.708551419751,925.792005370365,
925.875441864211,925.958878973966,926.042334768884,926.125879261614,926.209468344555,
926.293191612113,926.373871328008,926.467276920671,926.519450178445),
 .UNSPECIFIED.);
#639=B_SPLINE_CURVE_WITH_KNOTS('',3,(#84219,#84220,#84221,#84222,#84223,
#84224,#84225,#84226,#84227,#84228,#84229,#84230,#84231,#84232,#84233,#84234,
#84235,#84236,#84237,#84238,#84239,#84240,#84241,#84242,#84243,#84244,#84245,
#84246,#84247,#84248,#84249,#84250,#84251,#84252,#84253,#84254,#84255,#84256,
#84257,#84258,#84259,#84260,#84261,#84262,#84263,#84264,#84265,#84266,#84267,
#84268,#84269,#84270,#84271,#84272,#84273,#84274,#84275,#84276,#84277,#84278,
#84279,#84280,#84281,#84282,#84283,#84284,#84285,#84286,#84287,#84288,#84289,
#84290,#84291,#84292,#84293,#84294,#84295,#84296,#84297,#84298,#84299,#84300,
#84301,#84302,#84303,#84304,#84305,#84306,#84307,#84308,#84309,#84310,#84311,
#84312,#84313,#84314,#84315,#84316,#84317,#84318,#84319,#84320,#84321,#84322,
#84323,#84324,#84325,#84326,#84327,#84328,#84329,#84330,#84331,#84332,#84333,
#84334,#84335,#84336,#84337,#84338,#84339,#84340,#84341,#84342,#84343,#84344,
#84345,#84346,#84347,#84348,#84349,#84350,#84351,#84352,#84353,#84354,#84355,
#84356,#84357,#84358,#84359,#84360,#84361,#84362,#84363,#84364,#84365,#84366,
#84367,#84368,#84369,#84370,#84371,#84372,#84373,#84374,#84375,#84376,#84377,
#84378,#84379,#84380,#84381,#84382,#84383,#84384,#84385,#84386,#84387,#84388,
#84389,#84390,#84391,#84392,#84393,#84394,#84395,#84396,#84397,#84398,#84399,
#84400,#84401,#84402,#84403,#84404,#84405,#84406,#84407,#84408,#84409,#84410,
#84411,#84412,#84413,#84414,#84415,#84416,#84417,#84418,#84419,#84420,#84421,
#84422,#84423,#84424,#84425,#84426,#84427,#84428,#84429,#84430,#84431,#84432,
#84433,#84434,#84435),.UNSPECIFIED.,.F.,.F.,(4,3,3,3,3,3,3,3,3,3,3,3,3,
3,3,3,3,3,3,3,3,3,3,3,3,3,3,3,3,3,3,3,3,3,3,3,3,3,3,3,3,3,3,3,3,3,3,3,3,
3,3,3,3,3,3,3,3,3,3,3,3,3,3,3,3,3,3,3,3,3,3,3,4),(926.769832809103,926.871123756702,
926.973836758034,927.063316719011,927.147055430857,927.230690942225,927.314243385623,
927.397732821475,927.481186772088,927.564623265935,927.64806037569,927.731516170608,
927.815060663338,927.898649746279,927.982373013837,928.063052729731,928.146791441577,
928.230426952944,928.313979396343,928.397468832194,928.480922782807,928.564359276653,
928.647796386409,928.731252181327,928.814796674056,928.898385756997,928.982109024555,
929.062788740451,929.146527452297,929.230162963664,929.313715407063,929.397204842914,
929.480658793528,929.564095287374,929.647532397129,929.730988192047,929.814532684777,
929.898121767718,929.981845035275,930.062524751171,930.146263463017,930.229898974385,
930.313451417783,930.396940853634,930.480394804248,930.563831298094,930.647268407849,
930.730724202767,930.814268695497,930.897857778438,930.981581045995,931.062260761891,
931.145999473737,931.229634985105,931.313187428503,931.396676864354,931.480130814968,
931.563567308814,931.64700441857,931.730460213488,931.814004706217,931.897593789159,
931.981317056716,932.061996772612,932.145621946421,932.229114763035,932.312531192385,
932.395889522913,932.479207999135,932.562522639417,932.645831934757,932.729189513781,
932.8013317429),.UNSPECIFIED.);
#640=B_SPLINE_CURVE_WITH_KNOTS('',3,(#84436,#84437,#84438,#84439,#84440,
#84441,#84442,#84443,#84444,#84445),.UNSPECIFIED.,.F.,.F.,(4,3,3,4),(926.518691253405,
926.601556301005,926.685694554986,926.769832808967),.UNSPECIFIED.);
#641=B_SPLINE_CURVE_WITH_KNOTS('',3,(#84447,#84448,#84449,#84450,#84451,
#84452,#84453,#84454,#84455,#84456),.UNSPECIFIED.,.F.,.F.,(4,3,3,4),(926.519450178445,
926.612369002246,926.704833054526,926.769832808789),.UNSPECIFIED.);
#642=B_SPLINE_CURVE_WITH_KNOTS('',3,(#84457,#84458,#84459,#84460,#84461,
#84462,#84463,#84464,#84465,#84466,#84467,#84468,#84469,#84470,#84471,#84472,
#84473,#84474,#84475,#84476,#84477,#84478,#84479,#84480,#84481,#84482,#84483,
#84484,#84485,#84486,#84487,#84488,#84489,#84490,#84491,#84492,#84493,#84494,
#84495,#84496,#84497,#84498,#84499,#84500,#84501,#84502,#84503,#84504,#84505,
#84506,#84507,#84508,#84509,#84510,#84511,#84512,#84513,#84514,#84515,#84516,
#84517,#84518,#84519,#84520,#84521,#84522,#84523,#84524,#84525,#84526,#84527,
#84528,#84529,#84530,#84531,#84532,#84533,#84534,#84535,#84536,#84537,#84538,
#84539,#84540,#84541,#84542,#84543,#84544,#84545,#84546,#84547,#84548,#84549,
#84550,#84551,#84552,#84553,#84554,#84555,#84556,#84557,#84558,#84559,#84560,
#84561,#84562,#84563,#84564,#84565,#84566,#84567,#84568,#84569,#84570,#84571,
#84572,#84573,#84574,#84575,#84576,#84577,#84578,#84579,#84580,#84581,#84582,
#84583,#84584,#84585,#84586,#84587,#84588,#84589,#84590,#84591,#84592,#84593,
#84594,#84595,#84596,#84597,#84598,#84599,#84600,#84601,#84602,#84603,#84604,
#84605,#84606,#84607,#84608,#84609,#84610,#84611,#84612,#84613,#84614,#84615,
#84616,#84617,#84618,#84619,#84620,#84621,#84622,#84623,#84624,#84625,#84626,
#84627,#84628,#84629,#84630,#84631,#84632,#84633,#84634,#84635,#84636,#84637,
#84638,#84639,#84640,#84641,#84642,#84643,#84644,#84645,#84646,#84647,#84648,
#84649,#84650,#84651,#84652,#84653,#84654,#84655,#84656,#84657,#84658,#84659,
#84660,#84661,#84662,#84663,#84664,#84665,#84666,#84667,#84668,#84669,#84670,
#84671,#84672,#84673,#84674,#84675,#84676),.UNSPECIFIED.,.F.,.F.,(4,3,3,
3,3,3,3,3,3,3,3,3,3,3,3,3,3,3,3,3,3,3,3,3,3,3,3,3,3,3,3,3,3,3,3,3,3,3,3,
3,3,3,3,3,3,3,3,3,3,3,3,3,3,3,3,3,3,3,3,3,3,3,3,3,3,3,3,3,3,3,3,3,3,4),
(926.769832808971,926.854312245086,926.938811412004,927.023346822792,927.110911951776,
927.195621791297,927.284614565012,927.373607338728,927.457346050574,927.540981561942,
927.62453400534,927.708023441191,927.791477391805,927.874913885651,927.958350995407,
928.041806790324,928.125351283054,928.208940365995,928.292663633553,928.373343349448,
928.457082061294,928.540717572661,928.62427001606,928.707759451911,928.791213402524,
928.874649896371,928.958087006126,929.041542801044,929.125087293774,929.208676376715,
929.292399644272,929.373079360168,929.456818072014,929.540453583382,929.62400602678,
929.707495462631,929.790949413245,929.874385907091,929.957823016847,930.041278811764,
930.124823304494,930.208412387435,930.292135654993,930.372815370888,930.456554082734,
930.540189594101,930.6237420375,930.707231473351,930.790685423965,930.874121917811,
930.957559027566,931.041014822483,931.124559315213,931.208148398154,931.291871665712,
931.372551381608,931.456290093454,931.539925604822,931.62347804822,931.706967484071,
931.790421434685,931.873857928531,931.957295038286,932.040750833203,932.124295325933,
932.207884408874,932.291607676431,932.372287392328,932.455788042781,932.542343473143,
932.625634800808,932.708867535087,932.79205460146,932.802009764231),
 .UNSPECIFIED.);
#643=B_SPLINE_CURVE_WITH_KNOTS('',3,(#84682,#84683,#84684,#84685,#84686,
#84687,#84688,#84689,#84690,#84691,#84692,#84693,#84694,#84695,#84696,#84697,
#84698,#84699,#84700,#84701,#84702,#84703,#84704,#84705,#84706,#84707,#84708,
#84709,#84710,#84711,#84712,#84713,#84714,#84715,#84716,#84717,#84718,#84719,
#84720,#84721,#84722,#84723,#84724,#84725,#84726,#84727,#84728,#84729,#84730,
#84731,#84732,#84733,#84734,#84735,#84736,#84737,#84738,#84739,#84740,#84741,
#84742,#84743,#84744,#84745,#84746,#84747,#84748,#84749,#84750,#84751,#84752,
#84753,#84754,#84755,#84756,#84757,#84758,#84759,#84760,#84761,#84762,#84763,
#84764,#84765,#84766,#84767,#84768,#84769,#84770,#84771,#84772,#84773,#84774,
#84775,#84776,#84777,#84778,#84779,#84780,#84781,#84782,#84783,#84784,#84785,
#84786,#84787,#84788,#84789,#84790,#84791,#84792,#84793,#84794,#84795,#84796,
#84797,#84798,#84799,#84800,#84801,#84802,#84803,#84804,#84805,#84806,#84807,
#84808,#84809,#84810,#84811,#84812,#84813,#84814,#84815,#84816,#84817,#84818,
#84819,#84820,#84821,#84822,#84823,#84824,#84825,#84826,#84827,#84828,#84829,
#84830,#84831,#84832,#84833,#84834,#84835,#84836,#84837,#84838,#84839,#84840,
#84841,#84842,#84843,#84844,#84845,#84846,#84847,#84848,#84849,#84850,#84851,
#84852,#84853,#84854,#84855,#84856,#84857,#84858,#84859,#84860,#84861,#84862,
#84863,#84864,#84865,#84866,#84867,#84868,#84869,#84870,#84871,#84872,#84873,
#84874,#84875,#84876,#84877,#84878,#84879,#84880,#84881,#84882,#84883,#84884,
#84885,#84886,#84887,#84888,#84889,#84890,#84891,#84892,#84893,#84894,#84895,
#84896,#84897,#84898,#84899,#84900,#84901,#84902,#84903,#84904),
 .UNSPECIFIED.,.F.,.F.,(4,3,3,3,3,3,3,3,3,3,3,3,3,3,3,3,3,3,3,3,3,3,3,3,
3,3,3,3,3,3,3,3,3,3,3,3,3,3,3,3,3,3,3,3,3,3,3,3,3,3,3,3,3,3,3,3,3,3,3,3,
3,3,3,3,3,3,3,3,3,3,3,3,3,3,4),(933.053018116147,933.061732783332,933.145471495178,
933.229107006546,933.312659449944,933.396148885795,933.479602836409,933.563039330255,
933.64647644001,933.729932234928,933.813476727658,933.897065810599,933.980789078156,
934.061468794052,934.145207505898,934.228843017265,934.312395460664,934.395884896515,
934.479338847128,934.562775340975,934.64621245073,934.729668245648,934.813212738378,
934.896801821318,934.980525088876,935.061204804772,935.144943516618,935.228579027986,
935.312131471384,935.395620907235,935.479074857849,935.562511351695,935.645948461451,
935.729404256368,935.812948749098,935.896537832039,935.980261099597,936.060940815492,
936.144679527338,936.228315038705,936.311867482104,936.395356917955,936.478810868568,
936.562247362415,936.64568447217,936.729140267087,936.812684759817,936.896273842758,
936.979997110315,937.060676826212,937.144415538058,937.228051049426,937.311603492824,
937.395092928675,937.478546879289,937.561983373135,937.64542048289,937.728876277808,
937.812420770538,937.896009853479,937.979733121036,938.060412836932,938.144151548778,
938.227787060145,938.311339503544,938.394828939395,938.478282890009,938.561719383855,
938.64515649361,938.728612288528,938.812156781258,938.895745864199,938.979469131756,
939.060148847652,939.085291531953),.UNSPECIFIED.);
#644=B_SPLINE_CURVE_WITH_KNOTS('',3,(#84905,#84906,#84907,#84908,#84909,
#84910,#84911,#84912,#84913,#84914),.UNSPECIFIED.,.F.,.F.,(4,3,3,4),(932.8013317429,
932.884788778377,932.968903447177,933.053018115978),.UNSPECIFIED.);
#645=B_SPLINE_CURVE_WITH_KNOTS('',3,(#84916,#84917,#84918,#84919,#84920,
#84921,#84922,#84923,#84924,#84925),.UNSPECIFIED.,.F.,.F.,(4,3,3,4),(932.802009764231,
932.88517971186,932.969098914005,933.053018116151),.UNSPECIFIED.);
#646=B_SPLINE_CURVE_WITH_KNOTS('',3,(#84926,#84927,#84928,#84929,#84930,
#84931,#84932,#84933,#84934,#84935,#84936,#84937,#84938,#84939,#84940,#84941,
#84942,#84943,#84944,#84945,#84946,#84947,#84948,#84949,#84950,#84951,#84952,
#84953,#84954,#84955,#84956,#84957,#84958,#84959,#84960,#84961,#84962,#84963,
#84964,#84965,#84966,#84967,#84968,#84969,#84970,#84971,#84972,#84973,#84974,
#84975,#84976,#84977,#84978,#84979,#84980,#84981,#84982,#84983,#84984,#84985,
#84986,#84987,#84988,#84989,#84990,#84991,#84992,#84993,#84994,#84995,#84996,
#84997,#84998,#84999,#85000,#85001,#85002,#85003,#85004,#85005,#85006,#85007,
#85008,#85009,#85010,#85011,#85012,#85013,#85014,#85015,#85016,#85017,#85018,
#85019,#85020,#85021,#85022,#85023,#85024,#85025,#85026,#85027,#85028,#85029,
#85030,#85031,#85032,#85033,#85034,#85035,#85036,#85037,#85038,#85039,#85040,
#85041,#85042,#85043,#85044,#85045,#85046,#85047,#85048,#85049,#85050,#85051,
#85052,#85053,#85054,#85055,#85056,#85057,#85058,#85059,#85060,#85061,#85062,
#85063,#85064,#85065,#85066,#85067,#85068,#85069,#85070,#85071,#85072,#85073,
#85074,#85075,#85076,#85077,#85078,#85079,#85080,#85081,#85082,#85083,#85084,
#85085,#85086,#85087,#85088,#85089,#85090,#85091,#85092,#85093,#85094,#85095,
#85096,#85097,#85098,#85099,#85100,#85101,#85102,#85103,#85104,#85105,#85106,
#85107,#85108,#85109,#85110,#85111,#85112,#85113,#85114,#85115,#85116,#85117,
#85118,#85119,#85120,#85121,#85122,#85123,#85124,#85125,#85126,#85127,#85128,
#85129,#85130,#85131,#85132,#85133,#85134,#85135,#85136,#85137,#85138,#85139,
#85140,#85141,#85142,#85143,#85144,#85145),.UNSPECIFIED.,.F.,.F.,(4,3,3,
3,3,3,3,3,3,3,3,3,3,3,3,3,3,3,3,3,3,3,3,3,3,3,3,3,3,3,3,3,3,3,3,3,3,3,3,
3,3,3,3,3,3,3,3,3,3,3,3,3,3,3,3,3,3,3,3,3,3,3,3,3,3,3,3,3,3,3,3,3,3,4),
(933.053018116324,933.151593256213,933.250857262522,933.350876069408,933.372023403049,
933.455762114895,933.539397626262,933.622950069661,933.706439505512,933.789893456126,
933.873329949972,933.956767059727,934.040222854645,934.123767347375,934.207356430316,
934.291079697873,934.371759413769,934.455498125615,934.539133636983,934.622686080381,
934.706175516232,934.789629466846,934.873065960692,934.956503070447,935.039958865365,
935.123503358095,935.207092441036,935.290815708593,935.371495424489,935.455234136335,
935.538869647702,935.622422091101,935.705911526952,935.789365477565,935.872801971412,
935.956239081167,936.039694876085,936.123239368814,936.206828451755,936.290551719313,
936.371231435209,936.454970147055,936.538605658423,936.622158101821,936.705647537672,
936.789101488286,936.872537982132,936.955975091888,937.039430886805,937.122975379535,
937.206564462476,937.290287730034,937.370967445929,937.454706157775,937.538341669142,
937.621894112541,937.705383548392,937.788837499006,937.872273992852,937.955711102608,
938.039166897525,938.122711390255,938.206300473196,938.290023740754,938.370703456649,
938.453993507398,938.537151940436,938.62023438107,938.703259410404,938.786245564127,
938.86922730096,938.95220520749,939.035225802725,939.084433024015),
 .UNSPECIFIED.);
#647=B_SPLINE_CURVE_WITH_KNOTS('',3,(#85151,#85152,#85153,#85154,#85155,
#85156,#85157,#85158,#85159,#85160,#85161,#85162,#85163,#85164,#85165,#85166,
#85167,#85168,#85169,#85170,#85171,#85172,#85173,#85174,#85175,#85176,#85177,
#85178,#85179,#85180,#85181,#85182,#85183,#85184,#85185,#85186,#85187,#85188,
#85189,#85190,#85191,#85192,#85193,#85194,#85195,#85196,#85197,#85198,#85199,
#85200,#85201,#85202,#85203,#85204,#85205,#85206,#85207,#85208,#85209,#85210,
#85211,#85212,#85213,#85214,#85215,#85216,#85217,#85218,#85219,#85220,#85221,
#85222,#85223,#85224,#85225,#85226,#85227,#85228,#85229,#85230,#85231,#85232,
#85233,#85234,#85235,#85236,#85237,#85238,#85239,#85240,#85241,#85242,#85243,
#85244,#85245,#85246,#85247,#85248,#85249,#85250,#85251,#85252,#85253,#85254,
#85255,#85256,#85257,#85258,#85259,#85260,#85261,#85262,#85263,#85264,#85265,
#85266,#85267,#85268,#85269,#85270,#85271,#85272,#85273,#85274,#85275,#85276,
#85277,#85278,#85279,#85280,#85281,#85282,#85283,#85284,#85285,#85286,#85287,
#85288,#85289,#85290,#85291,#85292,#85293,#85294,#85295,#85296,#85297,#85298,
#85299,#85300,#85301,#85302,#85303,#85304,#85305,#85306,#85307,#85308,#85309,
#85310,#85311,#85312,#85313,#85314,#85315,#85316,#85317,#85318,#85319,#85320,
#85321,#85322,#85323,#85324,#85325,#85326,#85327,#85328,#85329,#85330,#85331,
#85332,#85333,#85334,#85335,#85336,#85337,#85338,#85339,#85340,#85341,#85342,
#85343,#85344,#85345,#85346,#85347,#85348,#85349,#85350,#85351,#85352,#85353,
#85354,#85355,#85356,#85357,#85358,#85359,#85360,#85361,#85362,#85363,#85364,
#85365,#85366,#85367,#85368,#85369,#85370),.UNSPECIFIED.,.F.,.F.,(4,3,3,
3,3,3,3,3,3,3,3,3,3,3,3,3,3,3,3,3,3,3,3,3,3,3,3,3,3,3,3,3,3,3,3,3,3,3,3,
3,3,3,3,3,3,3,3,3,3,3,3,3,3,3,3,3,3,3,3,3,3,3,3,3,3,3,3,3,3,3,3,3,3,4),
(939.336203423326,939.418950147463,939.501660561274,939.584353678099,939.667048193191,
939.749762799753,939.832565814582,939.915415824873,939.998394410342,940.059884858373,
940.143623570219,940.227259081587,940.310811524985,940.394300960836,940.47775491145,
940.561191405296,940.644628515052,940.728084309969,940.811628802699,940.89521788564,
940.978941153198,941.059620869093,941.143359580939,941.226995092306,941.310547535705,
941.394036971556,941.47749092217,941.560927416016,941.644364525771,941.727820320688,
941.811364813418,941.894953896359,941.978677163916,942.059356879813,942.143095591659,
942.226731103027,942.310283546425,942.393772982276,942.477226932889,942.560663426736,
942.644100536491,942.727556331409,942.811100824139,942.89468990708,942.978413174637,
943.059092890533,943.142831602379,943.226467113746,943.310019557145,943.393508992996,
943.47696294361,943.560399437456,943.643836547211,943.727292342129,943.810836834859,
943.8944259178,943.978149185357,944.058828901253,944.142567613099,944.226203124467,
944.309755567865,944.393245003716,944.47669895433,944.560135448176,944.643572557932,
944.727028352849,944.810572845579,944.89416192852,944.977885196078,945.058564911973,
945.144544706224,945.230413078362,945.316150774852,945.368916660643),
 .UNSPECIFIED.);
#648=B_SPLINE_CURVE_WITH_KNOTS('',3,(#85371,#85372,#85373,#85374,#85375,
#85376,#85377,#85378,#85379,#85380),.UNSPECIFIED.,.F.,.F.,(4,3,3,4),(939.085291531953,
939.190470359852,939.293976169291,939.336203423223),.UNSPECIFIED.);
#649=B_SPLINE_CURVE_WITH_KNOTS('',3,(#85382,#85383,#85384,#85385,#85386,
#85387,#85388,#85389,#85390,#85391),.UNSPECIFIED.,.F.,.F.,(4,3,3,4),(939.084433024015,
939.167549453827,939.251876438504,939.336203423181),.UNSPECIFIED.);
#650=B_SPLINE_CURVE_WITH_KNOTS('',3,(#85392,#85393,#85394,#85395,#85396,
#85397,#85398,#85399,#85400,#85401,#85402,#85403,#85404,#85405,#85406,#85407,
#85408,#85409,#85410,#85411,#85412,#85413,#85414,#85415,#85416,#85417,#85418,
#85419,#85420,#85421,#85422,#85423,#85424,#85425,#85426,#85427,#85428,#85429,
#85430,#85431,#85432,#85433,#85434,#85435,#85436,#85437,#85438,#85439,#85440,
#85441,#85442,#85443,#85444,#85445,#85446,#85447,#85448,#85449,#85450,#85451,
#85452,#85453,#85454,#85455,#85456,#85457,#85458,#85459,#85460,#85461,#85462,
#85463,#85464,#85465,#85466,#85467,#85468,#85469,#85470,#85471,#85472,#85473,
#85474,#85475,#85476,#85477,#85478,#85479,#85480,#85481,#85482,#85483,#85484,
#85485,#85486,#85487,#85488,#85489,#85490,#85491,#85492,#85493,#85494,#85495,
#85496,#85497,#85498,#85499,#85500,#85501,#85502,#85503,#85504,#85505,#85506,
#85507,#85508,#85509,#85510,#85511,#85512,#85513,#85514,#85515,#85516,#85517,
#85518,#85519,#85520,#85521,#85522,#85523,#85524,#85525,#85526,#85527,#85528,
#85529,#85530,#85531,#85532,#85533,#85534,#85535,#85536,#85537,#85538,#85539,
#85540,#85541,#85542,#85543,#85544,#85545,#85546,#85547,#85548,#85549,#85550,
#85551,#85552,#85553,#85554,#85555,#85556,#85557,#85558,#85559,#85560,#85561,
#85562,#85563,#85564,#85565,#85566,#85567,#85568,#85569,#85570,#85571,#85572,
#85573,#85574,#85575,#85576,#85577,#85578,#85579,#85580,#85581,#85582,#85583,
#85584,#85585,#85586,#85587,#85588,#85589,#85590,#85591,#85592,#85593,#85594,
#85595,#85596,#85597,#85598,#85599,#85600,#85601,#85602,#85603,#85604,#85605,
#85606,#85607,#85608,#85609,#85610,#85611),.UNSPECIFIED.,.F.,.F.,(4,3,3,
3,3,3,3,3,3,3,3,3,3,3,3,3,3,3,3,3,3,3,3,3,3,3,3,3,3,3,3,3,3,3,3,3,3,3,3,
3,3,3,3,3,3,3,3,3,3,3,3,3,3,3,3,3,3,3,3,3,3,3,3,3,3,3,3,3,3,3,3,3,3,4),
(939.33620342333,939.370439467369,939.454178179215,939.537813690583,939.621366133981,
939.704855569833,939.788309520447,939.871746014293,939.955183124049,940.038638918967,
940.122183411696,940.205772494638,940.289495762195,940.370175478089,940.453914189935,
940.537549701303,940.621102144701,940.704591580552,940.788045531166,940.871482025012,
940.954919134767,941.038374929685,941.121919422415,941.205508505356,941.289231772913,
941.36991148881,941.453650200656,941.537285712024,941.620838155422,941.704327591273,
941.787781541887,941.871218035733,941.954655145489,942.038110940406,942.121655433136,
942.205244516077,942.288967783635,942.36964749953,942.453386211376,942.537021722743,
942.620574166142,942.704063601993,942.787517552607,942.870954046453,942.954391156208,
943.037846951126,943.121391443855,943.204980526796,943.288703794354,943.36938351025,
943.453122222096,943.536757733464,943.620310176862,943.703799612713,943.787253563327,
943.870690057173,943.954127166928,944.037582961846,944.121127454576,944.204716537517,
944.288439805074,944.36911952097,944.452858262808,944.536493797105,944.620046256401,
944.703535701139,944.786989623716,944.87042607954,944.953863141282,945.037318878179,
945.120863171504,945.204452050913,945.288174778316,945.36832006177),
 .UNSPECIFIED.);
#651=B_SPLINE_CURVE_WITH_KNOTS('',3,(#85617,#85618,#85619,#85620,#85621,
#85622,#85623,#85624,#85625,#85626,#85627,#85628,#85629,#85630,#85631,#85632,
#85633,#85634,#85635,#85636,#85637,#85638,#85639,#85640,#85641,#85642,#85643,
#85644,#85645,#85646,#85647,#85648,#85649,#85650,#85651,#85652,#85653,#85654,
#85655,#85656,#85657,#85658,#85659,#85660,#85661,#85662,#85663,#85664,#85665,
#85666,#85667,#85668,#85669,#85670,#85671,#85672,#85673,#85674,#85675,#85676,
#85677,#85678,#85679,#85680,#85681,#85682,#85683,#85684,#85685,#85686,#85687,
#85688,#85689,#85690,#85691,#85692,#85693,#85694,#85695,#85696,#85697,#85698,
#85699,#85700,#85701,#85702,#85703,#85704,#85705,#85706,#85707,#85708,#85709,
#85710,#85711,#85712,#85713,#85714,#85715,#85716,#85717,#85718,#85719,#85720,
#85721,#85722,#85723,#85724,#85725,#85726,#85727,#85728,#85729,#85730,#85731,
#85732,#85733,#85734,#85735,#85736,#85737,#85738,#85739,#85740,#85741,#85742,
#85743,#85744,#85745,#85746,#85747,#85748,#85749,#85750,#85751,#85752,#85753,
#85754,#85755,#85756,#85757,#85758,#85759,#85760,#85761,#85762,#85763,#85764,
#85765,#85766,#85767,#85768,#85769,#85770,#85771,#85772,#85773,#85774,#85775,
#85776,#85777,#85778,#85779,#85780,#85781,#85782,#85783,#85784,#85785,#85786,
#85787,#85788,#85789,#85790,#85791,#85792,#85793,#85794,#85795,#85796,#85797,
#85798,#85799,#85800,#85801,#85802,#85803,#85804,#85805,#85806,#85807,#85808,
#85809,#85810,#85811,#85812,#85813,#85814,#85815,#85816,#85817,#85818,#85819,
#85820,#85821,#85822,#85823,#85824,#85825,#85826,#85827,#85828,#85829,#85830,
#85831,#85832,#85833,#85834,#85835,#85836),.UNSPECIFIED.,.F.,.F.,(4,3,3,
3,3,3,3,3,3,3,3,3,3,3,3,3,3,3,3,3,3,3,3,3,3,3,3,3,3,3,3,3,3,3,3,3,3,3,3,
3,3,3,3,3,3,3,3,3,3,3,3,3,3,3,3,3,3,3,3,3,3,3,3,3,3,3,3,3,3,3,3,3,3,4),
(945.61938873063,945.70936915299,945.799705876632,945.890221435482,945.981029384766,
946.058300922693,946.142039634539,946.225675145907,946.309227589306,946.392717025158,
946.476170975772,946.559607469619,946.643044579375,946.726500374293,946.810044867023,
946.893633949964,946.977357217522,947.058036933414,947.14177564526,947.225411156627,
947.308963600026,947.392453035876,947.47590698649,947.559343480336,947.642780590091,
947.726236385009,947.809780877738,947.893369960679,947.977093228237,948.057772944134,
948.14151165598,948.225147167347,948.308699610746,948.392189046597,948.47564299721,
948.559079491057,948.642516600812,948.72597239573,948.809516888459,948.8931059714,
948.976829238958,949.057508954854,949.1412476667,949.224883178068,949.308435621466,
949.391925057317,949.475379007931,949.558815501777,949.642252611533,949.725708406451,
949.809252899181,949.892841982122,949.976565249679,950.057244965574,950.14098367742,
950.224619188787,950.308171632186,950.391661068037,950.475115018651,950.558551512497,
950.641988622252,950.72544441717,950.808988909899,950.89257799284,950.976301260398,
951.056980976294,951.139459701244,951.221843364055,951.304151178297,951.386402284189,
951.468620741908,951.550821273017,951.633035317302,951.650831115062),
 .UNSPECIFIED.);
#652=B_SPLINE_CURVE_WITH_KNOTS('',3,(#85837,#85838,#85839,#85840,#85841,
#85842,#85843,#85844,#85845,#85846),.UNSPECIFIED.,.F.,.F.,(4,3,3,4),(945.368916660643,
945.454506788451,945.540021559813,945.619388730506),.UNSPECIFIED.);
#653=B_SPLINE_CURVE_WITH_KNOTS('',3,(#85848,#85849,#85850,#85851,#85852,
#85853,#85854,#85855,#85856,#85857,#85858,#85859,#85860),.UNSPECIFIED.,
 .F.,.F.,(4,3,3,3,4),(945.36832006177,945.36885553169,945.478563499207,
945.585901681379,945.61938873033),.UNSPECIFIED.);
#654=B_SPLINE_CURVE_WITH_KNOTS('',3,(#85861,#85862,#85863,#85864,#85865,
#85866,#85867,#85868,#85869,#85870,#85871,#85872,#85873,#85874,#85875,#85876,
#85877,#85878,#85879,#85880,#85881,#85882,#85883,#85884,#85885,#85886,#85887,
#85888,#85889,#85890,#85891,#85892,#85893,#85894,#85895,#85896,#85897,#85898,
#85899,#85900,#85901,#85902,#85903,#85904,#85905,#85906,#85907,#85908,#85909,
#85910,#85911,#85912,#85913,#85914,#85915,#85916,#85917,#85918,#85919,#85920,
#85921,#85922,#85923,#85924,#85925,#85926,#85927,#85928,#85929,#85930,#85931,
#85932,#85933,#85934,#85935,#85936,#85937,#85938,#85939,#85940,#85941,#85942,
#85943,#85944,#85945,#85946,#85947,#85948,#85949,#85950,#85951,#85952,#85953,
#85954,#85955,#85956,#85957,#85958,#85959,#85960,#85961,#85962,#85963,#85964,
#85965,#85966,#85967,#85968,#85969,#85970,#85971,#85972,#85973,#85974,#85975,
#85976,#85977,#85978,#85979,#85980,#85981,#85982,#85983,#85984,#85985,#85986,
#85987,#85988,#85989,#85990,#85991,#85992,#85993,#85994,#85995,#85996,#85997,
#85998,#85999,#86000,#86001,#86002,#86003,#86004,#86005,#86006,#86007,#86008,
#86009,#86010,#86011,#86012,#86013,#86014,#86015,#86016,#86017,#86018,#86019,
#86020,#86021,#86022,#86023,#86024,#86025,#86026,#86027,#86028,#86029,#86030,
#86031,#86032,#86033,#86034,#86035,#86036,#86037,#86038,#86039,#86040,#86041,
#86042,#86043,#86044,#86045,#86046,#86047,#86048,#86049,#86050,#86051,#86052,
#86053,#86054,#86055,#86056,#86057,#86058,#86059,#86060,#86061,#86062,#86063,
#86064,#86065,#86066,#86067,#86068,#86069,#86070,#86071,#86072,#86073,#86074,
#86075,#86076,#86077,#86078,#86079,#86080),.UNSPECIFIED.,.F.,.F.,(4,3,3,
3,3,3,3,3,3,3,3,3,3,3,3,3,3,3,3,3,3,3,3,3,3,3,3,3,3,3,3,3,3,3,3,3,3,3,3,
3,3,3,3,3,3,3,3,3,3,3,3,3,3,3,3,3,3,3,3,3,3,3,3,3,3,3,3,3,3,3,3,3,3,4),
(945.61938873051,945.701954256402,945.785283917153,945.867774678202,945.950258870669,
946.032755341671,946.116714391856,946.199335015738,946.283963279074,946.36859154241,
946.452330254256,946.535965765623,946.619518209021,946.703007644873,946.786461595486,
946.869898089332,946.953335199088,947.036790994005,947.120335486734,947.203924569675,
947.287647837233,947.36832755313,947.452066264976,947.535701776344,947.619254219743,
947.702743655595,947.786197606209,947.869634100055,947.953071209811,948.036527004729,
948.120071497459,948.203660580401,948.287383847958,948.368063563851,948.451802275697,
948.535437787064,948.618990230463,948.702479666314,948.785933616928,948.869370110774,
948.952807220529,949.036263015446,949.119807508176,949.203396591117,949.287119858675,
949.367799574571,949.451538286417,949.535173797784,949.618726241183,949.702215677034,
949.785669627648,949.869106121494,949.952543231249,950.035999026167,950.119543518896,
950.203132601837,950.286855869395,950.367535585291,950.451274297137,950.534909808505,
950.618462251903,950.701951687755,950.785405638368,950.868842132215,950.95227924197,
951.035735036888,951.119279529618,951.202868612559,951.286591880117,951.367271596011,
951.454042302477,951.540693724387,951.627203916606,951.652176355207),
 .UNSPECIFIED.);
#655=B_SPLINE_CURVE_WITH_KNOTS('',3,(#86086,#86087,#86088,#86089,#86090,
#86091,#86092,#86093,#86094,#86095,#86096,#86097,#86098,#86099,#86100,#86101,
#86102,#86103,#86104,#86105,#86106,#86107,#86108,#86109,#86110,#86111,#86112,
#86113,#86114,#86115,#86116,#86117,#86118,#86119,#86120,#86121,#86122,#86123,
#86124,#86125,#86126,#86127,#86128,#86129,#86130,#86131,#86132,#86133,#86134,
#86135,#86136,#86137,#86138,#86139,#86140,#86141,#86142,#86143,#86144,#86145,
#86146,#86147,#86148,#86149,#86150,#86151,#86152,#86153,#86154,#86155,#86156,
#86157,#86158,#86159,#86160,#86161,#86162,#86163,#86164,#86165,#86166,#86167,
#86168,#86169,#86170,#86171,#86172,#86173,#86174,#86175,#86176,#86177,#86178,
#86179,#86180,#86181,#86182,#86183,#86184,#86185,#86186,#86187,#86188,#86189,
#86190,#86191,#86192,#86193,#86194,#86195,#86196,#86197,#86198,#86199,#86200,
#86201,#86202,#86203,#86204,#86205,#86206,#86207,#86208,#86209,#86210,#86211,
#86212,#86213,#86214,#86215,#86216,#86217,#86218,#86219,#86220,#86221,#86222,
#86223,#86224,#86225,#86226,#86227,#86228,#86229,#86230,#86231,#86232,#86233,
#86234,#86235,#86236,#86237,#86238,#86239,#86240,#86241,#86242,#86243,#86244,
#86245,#86246,#86247,#86248,#86249,#86250,#86251,#86252,#86253,#86254,#86255,
#86256,#86257,#86258,#86259,#86260,#86261,#86262,#86263,#86264,#86265,#86266,
#86267,#86268,#86269,#86270,#86271,#86272,#86273,#86274,#86275,#86276,#86277,
#86278,#86279,#86280,#86281,#86282,#86283,#86284,#86285,#86286,#86287,#86288,
#86289,#86290,#86291,#86292,#86293,#86294,#86295,#86296,#86297,#86298,#86299,
#86300,#86301,#86302,#86303,#86304,#86305),.UNSPECIFIED.,.F.,.F.,(4,3,3,
3,3,3,3,3,3,3,3,3,3,3,3,3,3,3,3,3,3,3,3,3,3,3,3,3,3,3,3,3,3,3,3,3,3,3,3,
3,3,3,3,3,3,3,3,3,3,3,3,3,3,3,3,3,3,3,3,3,3,3,3,3,3,3,3,3,3,3,3,3,3,4),
(951.902574037685,952.042340863672,952.056716987014,952.14045569886,952.224091210227,
952.307643653625,952.391133089475,952.474587040089,952.558023533934,952.641460643689,
952.724916438606,952.808460931336,952.892050014276,952.975773281834,953.056452997734,
953.14019170958,953.223827220948,953.307379664347,953.390869100198,953.474323050812,
953.557759544658,953.641196654414,953.724652449332,953.808196942062,953.891786025003,
953.97550929256,954.056189008455,954.139927720301,954.223563231669,954.307115675067,
954.390605110918,954.474059061532,954.557495555378,954.640932665134,954.724388460052,
954.807932952781,954.891522035722,954.97524530328,955.055925019175,955.139663731021,
955.223299242388,955.306851685786,955.390341121637,955.473795072251,955.557231566097,
955.640668675852,955.72412447077,955.807668963499,955.89125804644,955.974981313997,
956.055661029895,956.139399741741,956.223035253109,956.306587696507,956.390077132359,
956.473531082972,956.556967576819,956.640404686574,956.723860481492,956.807404974222,
956.890994057163,956.974717324721,957.055397040615,957.139142851557,957.222783866638,
957.306340225206,957.389826949076,957.473275871116,957.556705080045,957.640132647437,
957.723609880086,957.8071145508,957.890705960823,957.934190499289),
 .UNSPECIFIED.);
#656=B_SPLINE_CURVE_WITH_KNOTS('',3,(#86306,#86307,#86308,#86309,#86310,
#86311,#86312,#86313,#86314,#86315),.UNSPECIFIED.,.F.,.F.,(4,3,3,4),(951.650831115062,
951.733106192795,951.817840115185,951.902574037576),.UNSPECIFIED.);
#657=B_SPLINE_CURVE_WITH_KNOTS('',3,(#86317,#86318,#86319,#86320,#86321,
#86322,#86323,#86324,#86325,#86326),.UNSPECIFIED.,.F.,.F.,(4,3,3,4),(951.652176355207,
951.738532064097,951.824780508187,951.902574037689),.UNSPECIFIED.);
#658=B_SPLINE_CURVE_WITH_KNOTS('',3,(#86327,#86328,#86329,#86330,#86331,
#86332,#86333,#86334,#86335,#86336,#86337,#86338,#86339,#86340,#86341,#86342,
#86343,#86344,#86345,#86346,#86347,#86348,#86349,#86350,#86351,#86352,#86353,
#86354,#86355,#86356,#86357,#86358,#86359,#86360,#86361,#86362,#86363,#86364,
#86365,#86366,#86367,#86368,#86369,#86370,#86371,#86372,#86373,#86374,#86375,
#86376,#86377,#86378,#86379,#86380,#86381,#86382,#86383,#86384,#86385,#86386,
#86387,#86388,#86389,#86390,#86391,#86392,#86393,#86394,#86395,#86396,#86397,
#86398,#86399,#86400,#86401,#86402,#86403,#86404,#86405,#86406,#86407,#86408,
#86409,#86410,#86411,#86412,#86413,#86414,#86415,#86416,#86417,#86418,#86419,
#86420,#86421,#86422,#86423,#86424,#86425,#86426,#86427,#86428,#86429,#86430,
#86431,#86432,#86433,#86434,#86435,#86436,#86437,#86438,#86439,#86440,#86441,
#86442,#86443,#86444,#86445,#86446,#86447,#86448,#86449,#86450,#86451,#86452,
#86453,#86454,#86455,#86456,#86457,#86458,#86459,#86460,#86461,#86462,#86463,
#86464,#86465,#86466,#86467,#86468,#86469,#86470,#86471,#86472,#86473,#86474,
#86475,#86476,#86477,#86478,#86479,#86480,#86481,#86482,#86483,#86484,#86485,
#86486,#86487,#86488,#86489,#86490,#86491,#86492,#86493,#86494,#86495,#86496,
#86497,#86498,#86499,#86500,#86501,#86502,#86503,#86504,#86505,#86506,#86507,
#86508,#86509,#86510,#86511,#86512,#86513,#86514,#86515,#86516,#86517,#86518,
#86519,#86520,#86521,#86522,#86523,#86524,#86525,#86526,#86527,#86528,#86529,
#86530,#86531,#86532,#86533,#86534,#86535,#86536,#86537,#86538,#86539,#86540,
#86541,#86542,#86543,#86544,#86545,#86546),.UNSPECIFIED.,.F.,.F.,(4,3,3,
3,3,3,3,3,3,3,3,3,3,3,3,3,3,3,3,3,3,3,3,3,3,3,3,3,3,3,3,3,3,3,3,3,3,3,3,
3,3,3,3,3,3,3,3,3,3,3,3,3,3,3,3,3,3,3,3,3,3,3,3,3,3,3,3,3,3,3,3,3,3,4),
(951.902574037848,951.991380896566,952.080358557091,952.169596981776,952.258979410966,
952.348574064124,952.367007606731,952.450746318577,952.534381829944,952.617934273341,
952.701423709192,952.784877659805,952.868314153651,952.951751263406,953.035207058323,
953.118751551052,953.202340633993,953.28606390155,953.366743617451,953.450482329297,
953.534117840664,953.617670284063,953.701159719914,953.784613670527,953.868050164373,
953.951487274128,954.034943069046,954.118487561775,954.202076644716,954.285799912274,
954.366479628171,954.450218340017,954.533853851385,954.617406294784,954.700895730636,
954.78434968125,954.867786175096,954.951223284852,955.03467907977,955.1182235725,
955.201812655442,955.285535923,955.366215638892,955.449954350738,955.533589862105,
955.617142305504,955.700631741355,955.784085691969,955.867522185815,955.95095929557,
956.034415090488,956.117959583218,956.201548666159,956.285271933716,956.365951649612,
956.449690361458,956.533325872825,956.616878316224,956.700367752074,956.783821702688,
956.867258196534,956.950695306289,957.034151101207,957.117695593936,957.201284676877,
957.285007944435,957.365687660332,957.448164195396,957.530545166499,957.612849793349,
957.695097032956,957.777309095665,957.859524712643,957.934095227666),
 .UNSPECIFIED.);
#659=B_SPLINE_CURVE_WITH_KNOTS('',3,(#86552,#86553,#86554,#86555,#86556,
#86557,#86558,#86559,#86560,#86561,#86562,#86563,#86564,#86565,#86566,#86567,
#86568,#86569,#86570,#86571,#86572,#86573,#86574,#86575,#86576,#86577,#86578,
#86579,#86580,#86581,#86582,#86583,#86584,#86585,#86586,#86587,#86588,#86589,
#86590,#86591,#86592,#86593,#86594,#86595,#86596,#86597,#86598,#86599,#86600,
#86601,#86602,#86603,#86604,#86605,#86606,#86607,#86608,#86609,#86610,#86611,
#86612,#86613,#86614,#86615,#86616,#86617,#86618,#86619,#86620,#86621,#86622,
#86623,#86624,#86625,#86626,#86627,#86628,#86629,#86630,#86631,#86632,#86633,
#86634,#86635,#86636,#86637,#86638,#86639,#86640,#86641,#86642,#86643,#86644,
#86645,#86646,#86647,#86648,#86649,#86650,#86651,#86652,#86653,#86654,#86655,
#86656,#86657,#86658,#86659,#86660,#86661,#86662,#86663,#86664,#86665,#86666,
#86667,#86668,#86669,#86670,#86671,#86672,#86673,#86674,#86675,#86676,#86677,
#86678,#86679,#86680,#86681,#86682,#86683,#86684,#86685,#86686,#86687,#86688,
#86689,#86690,#86691,#86692,#86693,#86694,#86695,#86696,#86697,#86698,#86699,
#86700,#86701,#86702,#86703,#86704,#86705,#86706,#86707,#86708,#86709,#86710,
#86711,#86712,#86713,#86714,#86715,#86716,#86717,#86718,#86719,#86720,#86721,
#86722,#86723,#86724,#86725,#86726,#86727,#86728,#86729,#86730,#86731,#86732,
#86733,#86734,#86735,#86736,#86737,#86738,#86739,#86740,#86741,#86742,#86743,
#86744,#86745,#86746,#86747,#86748,#86749,#86750,#86751,#86752,#86753,#86754,
#86755,#86756,#86757,#86758,#86759,#86760,#86761,#86762,#86763,#86764,#86765,
#86766,#86767,#86768,#86769,#86770,#86771),.UNSPECIFIED.,.F.,.F.,(4,3,3,
3,3,3,3,3,3,3,3,3,3,3,3,3,3,3,3,3,3,3,3,3,3,3,3,3,3,3,3,3,3,3,3,3,3,3,3,
3,3,3,3,3,3,3,3,3,3,3,3,3,3,3,3,3,3,3,3,3,3,3,3,3,3,3,3,3,3,3,3,3,3,4),
(958.185759344993,958.268231048685,958.350616230641,958.432936012912,958.515218019199,
958.597482260353,958.67974773475,958.76203343953,958.844404999096,958.926824299906,
959.009364852066,959.054869062055,959.138607773901,959.222243285268,959.305795728667,
959.389285164518,959.472739115132,959.556175608978,959.639612718734,959.723068513651,
959.806613006381,959.890202089322,959.973925356879,960.054605072775,960.138343784621,
960.221979295989,960.305531739388,960.389021175239,960.472475125853,960.5559116197,
960.639348729455,960.722804524373,960.806349017103,960.889938100044,960.973661367602,
961.054341083496,961.138079795342,961.221715306709,961.305267750108,961.388757185959,
961.472211136572,961.555647630418,961.639084740174,961.722540535091,961.806085027821,
961.889674110762,961.973397378319,962.054077094216,962.137815806062,962.22145131743,
962.305003760828,962.388493196679,962.471947147293,962.555383641139,962.638820750894,
962.722276545811,962.805821038541,962.889410121482,962.973133389039,963.053813104936,
963.137551816782,963.22118732815,963.304739771548,963.388229207399,963.471683158013,
963.555119651859,963.638556761615,963.722012556532,963.805557049262,963.889146132203,
963.97286939976,964.053549115656,964.145691166955,964.218603001888),
 .UNSPECIFIED.);
#660=B_SPLINE_CURVE_WITH_KNOTS('',3,(#86772,#86773,#86774,#86775,#86776,
#86777,#86778,#86779,#86780,#86781),.UNSPECIFIED.,.F.,.F.,(4,3,3,4),(957.934190499289,
958.017931037181,958.055133051335,958.185759344865),.UNSPECIFIED.);
#661=B_SPLINE_CURVE_WITH_KNOTS('',3,(#86783,#86784,#86785,#86786,#86787,
#86788,#86789,#86790,#86791,#86792),.UNSPECIFIED.,.F.,.F.,(4,3,3,4),(957.934095227666,
958.016349841335,958.101054593024,958.185759344712),.UNSPECIFIED.);
#662=B_SPLINE_CURVE_WITH_KNOTS('',3,(#86793,#86794,#86795,#86796,#86797,
#86798,#86799,#86800,#86801,#86802,#86803,#86804,#86805,#86806,#86807,#86808,
#86809,#86810,#86811,#86812,#86813,#86814,#86815,#86816,#86817,#86818,#86819,
#86820,#86821,#86822,#86823,#86824,#86825,#86826,#86827,#86828,#86829,#86830,
#86831,#86832,#86833,#86834,#86835,#86836,#86837,#86838,#86839,#86840,#86841,
#86842,#86843,#86844,#86845,#86846,#86847,#86848,#86849,#86850,#86851,#86852,
#86853,#86854,#86855,#86856,#86857,#86858,#86859,#86860,#86861,#86862,#86863,
#86864,#86865,#86866,#86867,#86868,#86869,#86870,#86871,#86872,#86873,#86874,
#86875,#86876,#86877,#86878,#86879,#86880,#86881,#86882,#86883,#86884,#86885,
#86886,#86887,#86888,#86889,#86890,#86891,#86892,#86893,#86894,#86895,#86896,
#86897,#86898,#86899,#86900,#86901,#86902,#86903,#86904,#86905,#86906,#86907,
#86908,#86909,#86910,#86911,#86912,#86913,#86914,#86915,#86916,#86917,#86918,
#86919,#86920,#86921,#86922,#86923,#86924,#86925,#86926,#86927,#86928,#86929,
#86930,#86931,#86932,#86933,#86934,#86935,#86936,#86937,#86938,#86939,#86940,
#86941,#86942,#86943,#86944,#86945,#86946,#86947,#86948,#86949,#86950,#86951,
#86952,#86953,#86954,#86955,#86956,#86957,#86958,#86959,#86960,#86961,#86962,
#86963,#86964,#86965,#86966,#86967,#86968,#86969,#86970,#86971,#86972,#86973,
#86974,#86975,#86976,#86977,#86978,#86979,#86980,#86981,#86982,#86983,#86984,
#86985,#86986,#86987,#86988,#86989,#86990,#86991,#86992,#86993,#86994,#86995,
#86996,#86997,#86998,#86999,#87000,#87001,#87002,#87003,#87004,#87005,#87006,
#87007,#87008,#87009,#87010,#87011,#87012),.UNSPECIFIED.,.F.,.F.,(4,3,3,
3,3,3,3,3,3,3,3,3,3,3,3,3,3,3,3,3,3,3,3,3,3,3,3,3,3,3,3,3,3,3,3,3,3,3,3,
3,3,3,3,3,3,3,3,3,3,3,3,3,3,3,3,3,3,3,3,3,3,3,3,3,3,3,3,3,3,3,3,3,3,4),
(958.185759344869,958.31309188077,958.365423671052,958.449162382898,958.532797894266,
958.616350337665,958.699839773516,958.78329372413,958.866730217977,958.950167327733,
959.033623122651,959.117167615381,959.200756698322,959.28447996588,959.365159681772,
959.448898393618,959.532533904985,959.616086348384,959.699575784235,959.783029734848,
959.866466228695,959.94990333845,960.033359133368,960.116903626097,960.200492709038,
960.284215976596,960.364895692492,960.448634404338,960.532269915705,960.615822359104,
960.699311794955,960.782765745568,960.866202239414,960.94963934917,961.033095144087,
961.116639636817,961.200228719758,961.283951987315,961.364631703212,961.448370415058,
961.532005926425,961.615558369824,961.699047805675,961.782501756288,961.865938250135,
961.94937535989,962.032831154807,962.116375647537,962.199964730478,962.283687998035,
962.364367713932,962.448106425778,962.531741937146,962.615294380545,962.698783816396,
962.78223776701,962.865674260857,962.949111370613,963.032567165531,963.11611165826,
963.199700741202,963.28342400876,963.364103724653,963.44785112012,963.531493382349,
963.617222592426,963.700707840529,963.784155280232,963.867582999968,963.955019015717,
964.038490818479,964.121991065998,964.205565530793,964.217327062966),
 .UNSPECIFIED.);
#663=B_SPLINE_CURVE_WITH_KNOTS('',3,(#87018,#87019,#87020,#87021,#87022,
#87023,#87024,#87025,#87026,#87027,#87028,#87029,#87030,#87031,#87032,#87033,
#87034,#87035,#87036,#87037,#87038,#87039,#87040,#87041,#87042,#87043,#87044,
#87045,#87046,#87047,#87048,#87049,#87050,#87051,#87052,#87053,#87054,#87055,
#87056,#87057,#87058,#87059,#87060,#87061,#87062,#87063,#87064,#87065,#87066,
#87067,#87068,#87069,#87070,#87071,#87072,#87073,#87074,#87075,#87076,#87077,
#87078,#87079,#87080,#87081,#87082,#87083,#87084,#87085,#87086,#87087,#87088,
#87089,#87090,#87091,#87092,#87093,#87094,#87095,#87096,#87097,#87098,#87099,
#87100,#87101,#87102,#87103,#87104,#87105,#87106,#87107,#87108,#87109,#87110,
#87111,#87112,#87113,#87114,#87115,#87116,#87117,#87118,#87119,#87120,#87121,
#87122,#87123,#87124,#87125,#87126,#87127,#87128,#87129,#87130,#87131,#87132,
#87133,#87134,#87135,#87136,#87137,#87138,#87139,#87140,#87141,#87142,#87143,
#87144,#87145,#87146,#87147,#87148,#87149,#87150,#87151,#87152,#87153,#87154,
#87155,#87156,#87157,#87158,#87159,#87160,#87161,#87162,#87163,#87164,#87165,
#87166,#87167,#87168,#87169,#87170,#87171,#87172,#87173,#87174,#87175,#87176,
#87177,#87178,#87179,#87180,#87181,#87182,#87183,#87184,#87185,#87186,#87187,
#87188,#87189,#87190,#87191,#87192,#87193,#87194,#87195,#87196,#87197,#87198,
#87199,#87200,#87201,#87202,#87203,#87204,#87205,#87206,#87207,#87208,#87209,
#87210,#87211,#87212,#87213,#87214,#87215,#87216,#87217,#87218,#87219,#87220,
#87221,#87222,#87223,#87224,#87225,#87226,#87227,#87228,#87229,#87230,#87231,
#87232,#87233,#87234,#87235,#87236,#87237),.UNSPECIFIED.,.F.,.F.,(4,3,3,
3,3,3,3,3,3,3,3,3,3,3,3,3,3,3,3,3,3,3,3,3,3,3,3,3,3,3,3,3,3,3,3,3,3,3,3,
3,3,3,3,3,3,3,3,3,3,3,3,3,3,3,3,3,3,3,3,3,3,3,3,3,3,3,3,3,3,3,3,3,3,4),
(964.468944652045,964.553856266707,964.63880056414,964.723793252019,964.80891241641,
964.894097600493,964.979440780856,965.053285126376,965.137023838222,965.220659349589,
965.304211792988,965.387701228839,965.471155179452,965.554591673298,965.638028783054,
965.721484577971,965.805029070701,965.888618153642,965.972341421199,966.053021137096,
966.136759848942,966.22039536031,966.303947803708,966.387437239559,966.470891190173,
966.554327684019,966.637764793774,966.721220588692,966.804765081422,966.888354164363,
966.972077431921,967.052757147816,967.136495859662,967.220131371029,967.303683814428,
967.387173250279,967.470627200893,967.554063694739,967.637500804495,967.720956599413,
967.804501092142,967.888090175083,967.971813442641,968.052493158536,968.136231870382,
968.219867381749,968.303419825148,968.386909260999,968.470363211613,968.553799705459,
968.637236815214,968.720692610132,968.804237102861,968.887826185802,968.97154945336,
969.052229169256,969.135967881102,969.219603392469,969.303155835867,969.386645271719,
969.470099222332,969.553535716179,969.636972825934,969.720428620852,969.803973113582,
969.887562196523,969.97128546408,970.051965179976,970.135211717693,970.218356428836,
970.301401588995,970.38438937538,970.467335833278,970.501020187744),
 .UNSPECIFIED.);
#664=B_SPLINE_CURVE_WITH_KNOTS('',3,(#87238,#87239,#87240,#87241,#87242,
#87243,#87244,#87245,#87246,#87247),.UNSPECIFIED.,.F.,.F.,(4,3,3,4),(964.218603001888,
964.31028798597,964.401596342216,964.468944651881),.UNSPECIFIED.);
#665=B_SPLINE_CURVE_WITH_KNOTS('',3,(#87249,#87250,#87251,#87252,#87253,
#87254,#87255,#87256,#87257,#87258),.UNSPECIFIED.,.F.,.F.,(4,3,3,4),(964.217327062966,
964.301056785927,964.363839735373,964.468944652048),.UNSPECIFIED.);
#666=B_SPLINE_CURVE_WITH_KNOTS('',3,(#87259,#87260,#87261,#87262,#87263,
#87264,#87265,#87266,#87267,#87268,#87269,#87270,#87271,#87272,#87273,#87274,
#87275,#87276,#87277,#87278,#87279,#87280,#87281,#87282,#87283,#87284,#87285,
#87286,#87287,#87288,#87289,#87290,#87291,#87292,#87293,#87294,#87295,#87296,
#87297,#87298,#87299,#87300,#87301,#87302,#87303,#87304,#87305,#87306,#87307,
#87308,#87309,#87310,#87311,#87312,#87313,#87314,#87315,#87316,#87317,#87318,
#87319,#87320,#87321,#87322,#87323,#87324,#87325,#87326,#87327,#87328,#87329,
#87330,#87331,#87332,#87333,#87334,#87335,#87336,#87337,#87338,#87339,#87340,
#87341,#87342,#87343,#87344,#87345,#87346,#87347,#87348,#87349,#87350,#87351,
#87352,#87353,#87354,#87355,#87356,#87357,#87358,#87359,#87360,#87361,#87362,
#87363,#87364,#87365,#87366,#87367,#87368,#87369,#87370,#87371,#87372,#87373,
#87374,#87375,#87376,#87377,#87378,#87379,#87380,#87381,#87382,#87383,#87384,
#87385,#87386,#87387,#87388,#87389,#87390,#87391,#87392,#87393,#87394,#87395,
#87396,#87397,#87398,#87399,#87400,#87401,#87402,#87403,#87404,#87405,#87406,
#87407,#87408,#87409,#87410,#87411,#87412,#87413,#87414,#87415,#87416,#87417,
#87418,#87419,#87420,#87421,#87422,#87423,#87424,#87425,#87426,#87427,#87428,
#87429,#87430,#87431,#87432,#87433,#87434,#87435,#87436,#87437,#87438,#87439,
#87440,#87441,#87442,#87443,#87444,#87445,#87446,#87447,#87448,#87449,#87450,
#87451,#87452,#87453,#87454,#87455,#87456,#87457,#87458,#87459,#87460,#87461,
#87462,#87463,#87464,#87465,#87466,#87467,#87468,#87469,#87470,#87471,#87472,
#87473,#87474,#87475,#87476,#87477,#87478),.UNSPECIFIED.,.F.,.F.,(4,3,3,
3,3,3,3,3,3,3,3,3,3,3,3,3,3,3,3,3,3,3,3,3,3,3,3,3,3,3,3,3,3,3,3,3,3,3,3,
3,3,3,3,3,3,3,3,3,3,3,3,3,3,3,3,3,3,3,3,3,3,3,3,3,3,3,3,3,3,3,3,3,3,4),
(964.468944652184,964.551551735966,964.634067131806,964.716511902131,964.798911934073,
964.881289359624,964.963663110529,965.046052113148,965.128524838076,965.211040693846,
965.293684956907,965.363575746093,965.447314457939,965.530949969307,965.614502412705,
965.697991848556,965.78144579917,965.864882293016,965.948319402772,966.031775197689,
966.115319690419,966.19890877336,966.282632040918,966.363311756813,966.447050468659,
966.530685980026,966.614238423425,966.697727859276,966.78118180989,966.864618303736,
966.948055413491,967.031511208409,967.115055701138,967.198644784079,967.282368051637,
967.363047767533,967.446786479379,967.530421990746,967.613974434145,967.697463869996,
967.780917820609,967.864354314456,967.947791424211,968.031247219128,968.114791711858,
968.198380794799,968.282104062356,968.362783778253,968.446522490099,968.530158001466,
968.613710444865,968.697199880717,968.78065383133,968.864090325176,968.947527434932,
969.03098322985,969.114527722579,969.19811680552,969.281840073078,969.362519788973,
969.446258500819,969.529894012187,969.613446455585,969.696935891436,969.78038984205,
969.863826335896,969.947263445651,970.030719240569,970.114263733299,970.19785281624,
970.281576083798,970.362255799693,970.45608696417,970.501731614662),
 .UNSPECIFIED.);
#667=B_SPLINE_CURVE_WITH_KNOTS('',3,(#87484,#87485,#87486,#87487,#87488,
#87489,#87490,#87491,#87492,#87493,#87494,#87495,#87496,#87497,#87498,#87499,
#87500,#87501,#87502,#87503,#87504,#87505,#87506,#87507,#87508,#87509,#87510,
#87511,#87512,#87513,#87514,#87515,#87516,#87517,#87518,#87519,#87520,#87521,
#87522,#87523,#87524,#87525,#87526,#87527,#87528,#87529,#87530,#87531,#87532,
#87533,#87534,#87535,#87536,#87537,#87538,#87539,#87540,#87541,#87542,#87543,
#87544,#87545,#87546,#87547,#87548,#87549,#87550,#87551,#87552,#87553,#87554,
#87555,#87556,#87557,#87558,#87559,#87560,#87561,#87562,#87563,#87564,#87565,
#87566,#87567,#87568,#87569,#87570,#87571,#87572,#87573,#87574,#87575,#87576,
#87577,#87578,#87579,#87580,#87581,#87582,#87583,#87584,#87585,#87586,#87587,
#87588,#87589,#87590,#87591,#87592,#87593,#87594,#87595,#87596,#87597,#87598,
#87599,#87600,#87601,#87602,#87603,#87604,#87605,#87606,#87607,#87608,#87609,
#87610,#87611,#87612,#87613,#87614,#87615,#87616,#87617,#87618,#87619,#87620,
#87621,#87622,#87623,#87624,#87625,#87626,#87627,#87628,#87629,#87630,#87631,
#87632,#87633,#87634,#87635,#87636,#87637,#87638,#87639,#87640,#87641,#87642,
#87643,#87644,#87645,#87646,#87647,#87648,#87649,#87650,#87651,#87652,#87653,
#87654,#87655,#87656,#87657,#87658,#87659,#87660,#87661,#87662,#87663,#87664,
#87665,#87666,#87667,#87668,#87669,#87670,#87671,#87672,#87673,#87674,#87675,
#87676,#87677,#87678,#87679,#87680,#87681,#87682,#87683,#87684,#87685,#87686,
#87687,#87688,#87689,#87690,#87691,#87692,#87693,#87694,#87695,#87696,#87697,
#87698,#87699,#87700),.UNSPECIFIED.,.F.,.F.,(4,3,3,3,3,3,3,3,3,3,3,3,3,
3,3,3,3,3,3,3,3,3,3,3,3,3,3,3,3,3,3,3,3,3,3,3,3,3,3,3,3,3,3,3,3,3,3,3,3,
3,3,3,3,3,3,3,3,3,3,3,3,3,3,3,3,3,3,3,3,3,3,3,4),(970.75212995937,970.852730002883,
970.954662619401,971.051701190697,971.135439902543,971.219075413911,971.302627857309,
971.38611729316,971.469571243774,971.55300773762,971.636444847375,971.719900642293,
971.803445135023,971.887034217964,971.970757485521,972.051437201417,972.135175913263,
972.21881142463,972.302363868029,972.38585330388,972.469307254493,972.552743748339,
972.636180858095,972.719636653013,972.803181145742,972.886770228683,972.970493496241,
973.051173212137,973.134911923983,973.218547435351,973.302099878749,973.3855893146,
973.469043265214,973.55247975906,973.635916868816,973.719372663734,973.802917156463,
973.886506239404,973.970229506962,974.050909222857,974.134647934703,974.21828344607,
974.301835889469,974.38532532532,974.468779275933,974.55221576978,974.635652879535,
974.719108674453,974.802653167182,974.886242250123,974.969965517681,975.050645233577,
975.134383945423,975.218019456791,975.301571900189,975.38506133604,975.468515286654,
975.5519517805,975.635388890256,975.718844685174,975.802389177903,975.885978260844,
975.969701528402,976.050381244297,976.133920743387,976.217328062945,976.300659096788,
976.383932211667,976.467165730121,976.550395339485,976.633620000805,976.716891664386,
976.783605650254),.UNSPECIFIED.);
#668=B_SPLINE_CURVE_WITH_KNOTS('',3,(#87701,#87702,#87703,#87704,#87705,
#87706,#87707,#87708,#87709,#87710),.UNSPECIFIED.,.F.,.F.,(4,3,3,4),(970.501020187744,
970.583952002451,970.668040980838,970.752129959224),.UNSPECIFIED.);
#669=B_SPLINE_CURVE_WITH_KNOTS('',3,(#87712,#87713,#87714,#87715,#87716,
#87717,#87718,#87719,#87720,#87721),.UNSPECIFIED.,.F.,.F.,(4,3,3,4),(970.501731614662,
970.595066006553,970.687917748817,970.752129959041),.UNSPECIFIED.);
#670=B_SPLINE_CURVE_WITH_KNOTS('',3,(#87722,#87723,#87724,#87725,#87726,
#87727,#87728,#87729,#87730,#87731,#87732,#87733,#87734,#87735,#87736,#87737,
#87738,#87739,#87740,#87741,#87742,#87743,#87744,#87745,#87746,#87747,#87748,
#87749,#87750,#87751,#87752,#87753,#87754,#87755,#87756,#87757,#87758,#87759,
#87760,#87761,#87762,#87763,#87764,#87765,#87766,#87767,#87768,#87769,#87770,
#87771,#87772,#87773,#87774,#87775,#87776,#87777,#87778,#87779,#87780,#87781,
#87782,#87783,#87784,#87785,#87786,#87787,#87788,#87789,#87790,#87791,#87792,
#87793,#87794,#87795,#87796,#87797,#87798,#87799,#87800,#87801,#87802,#87803,
#87804,#87805,#87806,#87807,#87808,#87809,#87810,#87811,#87812,#87813,#87814,
#87815,#87816,#87817,#87818,#87819,#87820,#87821,#87822,#87823,#87824,#87825,
#87826,#87827,#87828,#87829,#87830,#87831,#87832,#87833,#87834,#87835,#87836,
#87837,#87838,#87839,#87840,#87841,#87842,#87843,#87844,#87845,#87846,#87847,
#87848,#87849,#87850,#87851,#87852,#87853,#87854,#87855,#87856,#87857,#87858,
#87859,#87860,#87861,#87862,#87863,#87864,#87865,#87866,#87867,#87868,#87869,
#87870,#87871,#87872,#87873,#87874,#87875,#87876,#87877,#87878,#87879,#87880,
#87881,#87882,#87883,#87884,#87885,#87886,#87887,#87888,#87889,#87890,#87891,
#87892,#87893,#87894,#87895,#87896,#87897,#87898,#87899,#87900,#87901,#87902,
#87903,#87904,#87905,#87906,#87907,#87908,#87909,#87910,#87911,#87912,#87913,
#87914,#87915,#87916,#87917,#87918,#87919,#87920,#87921,#87922,#87923,#87924,
#87925,#87926,#87927,#87928,#87929,#87930,#87931,#87932,#87933,#87934,#87935,
#87936,#87937,#87938,#87939,#87940,#87941),.UNSPECIFIED.,.F.,.F.,(4,3,3,
3,3,3,3,3,3,3,3,3,3,3,3,3,3,3,3,3,3,3,3,3,3,3,3,3,3,3,3,3,3,3,3,3,3,3,3,
3,3,3,3,3,3,3,3,3,3,3,3,3,3,3,3,3,3,3,3,3,3,3,3,3,3,3,3,3,3,3,3,3,3,4),
(970.752129959228,970.836483591065,970.920853204787,971.005255525662,971.089707297296,
971.174275812516,971.258913586583,971.343683363136,971.361991810414,971.44573052226,
971.529366033628,971.612918477026,971.696407912877,971.779861863491,971.863298357337,
971.946735467092,972.03019126201,972.11373575474,972.197324837681,972.281048105238,
972.361727821134,972.44546653298,972.529102044347,972.612654487746,972.696143923597,
972.779597874211,972.863034368057,972.946471477812,973.02992727273,973.11347176546,
973.197060848401,973.280784115958,973.361463831854,973.4452025437,973.528838055067,
973.612390498466,973.695879934317,973.779333884931,973.862770378777,973.946207488532,
974.02966328345,974.113207776179,974.19679685912,974.280520126678,974.361199842574,
974.44493855442,974.528574065787,974.612126509186,974.695615945037,974.779069895651,
974.862506389497,974.945943499252,975.02939929417,975.112943786899,975.19653286984,
975.280256137398,975.360935853294,975.44467456514,975.528310076508,975.611862519906,
975.695351955757,975.778805906371,975.862242400217,975.945679509972,976.02913530489,
976.11267979762,976.196268880561,976.279992148118,976.360671864014,976.444260174154,
976.52927975058,976.612658217677,976.698498348767,976.784338479856),
 .UNSPECIFIED.);
#671=B_SPLINE_CURVE_WITH_KNOTS('',3,(#87947,#87948,#87949,#87950,#87951,
#87952,#87953,#87954,#87955,#87956,#87957,#87958,#87959,#87960,#87961,#87962,
#87963,#87964,#87965,#87966,#87967,#87968,#87969,#87970,#87971,#87972,#87973,
#87974,#87975,#87976,#87977,#87978,#87979,#87980,#87981,#87982,#87983,#87984,
#87985,#87986,#87987,#87988,#87989,#87990,#87991,#87992,#87993,#87994,#87995,
#87996,#87997,#87998,#87999,#88000,#88001,#88002,#88003,#88004,#88005,#88006,
#88007,#88008,#88009,#88010,#88011,#88012,#88013,#88014,#88015,#88016,#88017,
#88018,#88019,#88020,#88021,#88022,#88023,#88024,#88025,#88026,#88027,#88028,
#88029,#88030,#88031,#88032,#88033,#88034,#88035,#88036,#88037,#88038,#88039,
#88040,#88041,#88042,#88043,#88044,#88045,#88046,#88047,#88048,#88049,#88050,
#88051,#88052,#88053,#88054,#88055,#88056,#88057,#88058,#88059,#88060,#88061,
#88062,#88063,#88064,#88065,#88066,#88067,#88068,#88069,#88070,#88071,#88072,
#88073,#88074,#88075,#88076,#88077,#88078,#88079,#88080,#88081,#88082,#88083,
#88084,#88085,#88086,#88087,#88088,#88089,#88090,#88091,#88092,#88093,#88094,
#88095,#88096,#88097,#88098,#88099,#88100,#88101,#88102,#88103,#88104,#88105,
#88106,#88107,#88108,#88109,#88110,#88111,#88112,#88113,#88114,#88115,#88116,
#88117,#88118,#88119,#88120,#88121,#88122,#88123,#88124,#88125,#88126,#88127,
#88128,#88129,#88130,#88131,#88132,#88133,#88134,#88135,#88136,#88137,#88138,
#88139,#88140,#88141,#88142,#88143,#88144,#88145,#88146,#88147,#88148,#88149,
#88150,#88151,#88152,#88153,#88154,#88155,#88156,#88157,#88158,#88159,#88160,
#88161,#88162,#88163,#88164,#88165,#88166,#88167,#88168,#88169),
 .UNSPECIFIED.,.F.,.F.,(4,3,3,3,3,3,3,3,3,3,3,3,3,3,3,3,3,3,3,3,3,3,3,3,
3,3,3,3,3,3,3,3,3,3,3,3,3,3,3,3,3,3,3,3,3,3,3,3,3,3,3,3,3,3,3,3,3,3,3,3,
3,3,3,3,3,3,3,3,3,3,3,3,3,3,4),(977.035315266404,977.050117255017,977.133855966863,
977.217491478231,977.30104392163,977.384533357481,977.467987308095,977.551423801942,
977.634860911698,977.718316706616,977.801861199346,977.885450282287,977.969173549845,
978.049853265738,978.133591977584,978.217227488951,978.30077993235,978.384269368201,
978.467723318814,978.55115981266,978.634596922416,978.718052717333,978.801597210063,
978.885186293004,978.968909560561,979.049589276458,979.133327988304,979.216963499671,
979.30051594307,979.384005378921,979.467459329534,979.55089582338,979.634332933136,
979.717788728053,979.801333220783,979.884922303724,979.968645571281,980.049325287178,
980.133063999024,980.216699510392,980.30025195379,980.383741389641,980.467195340255,
980.550631834101,980.634068943857,980.717524738775,980.801069231504,980.884658314445,
980.968381582003,981.049061297898,981.132800009744,981.216435521112,981.29998796451,
981.383477400361,981.466931350975,981.550367844821,981.633804954576,981.717260749494,
981.800805242224,981.884394325165,981.968117592722,982.048797308618,982.132536020464,
982.216171531831,982.29972397523,982.383213411081,982.466667361694,982.550103855541,
982.633540965296,982.716996760214,982.800541252943,982.884130335884,982.967853603442,
983.048533319338,983.067552096354),.UNSPECIFIED.);
#672=B_SPLINE_CURVE_WITH_KNOTS('',3,(#88170,#88171,#88172,#88173,#88174,
#88175,#88176,#88177,#88178,#88179),.UNSPECIFIED.,.F.,.F.,(4,3,3,4),(976.783605650254,
976.866976135685,976.951145700975,977.035315266264),.UNSPECIFIED.);
#673=B_SPLINE_CURVE_WITH_KNOTS('',3,(#88181,#88182,#88183,#88184,#88185,
#88186,#88187,#88188,#88189,#88190),.UNSPECIFIED.,.F.,.F.,(4,3,3,4),(976.784338479856,
976.867591013031,976.95145313972,977.035315266408),.UNSPECIFIED.);
#674=B_SPLINE_CURVE_WITH_KNOTS('',3,(#88191,#88192,#88193,#88194,#88195,
#88196,#88197,#88198,#88199,#88200,#88201,#88202,#88203,#88204,#88205,#88206,
#88207,#88208,#88209,#88210,#88211,#88212,#88213,#88214,#88215,#88216,#88217,
#88218,#88219,#88220,#88221,#88222,#88223,#88224,#88225,#88226,#88227,#88228,
#88229,#88230,#88231,#88232,#88233,#88234,#88235,#88236,#88237,#88238,#88239,
#88240,#88241,#88242,#88243,#88244,#88245,#88246,#88247,#88248,#88249,#88250,
#88251,#88252,#88253,#88254,#88255,#88256,#88257,#88258,#88259,#88260,#88261,
#88262,#88263,#88264,#88265,#88266,#88267,#88268,#88269,#88270,#88271,#88272,
#88273,#88274,#88275,#88276,#88277,#88278,#88279,#88280,#88281,#88282,#88283,
#88284,#88285,#88286,#88287,#88288,#88289,#88290,#88291,#88292,#88293,#88294,
#88295,#88296,#88297,#88298,#88299,#88300,#88301,#88302,#88303,#88304,#88305,
#88306,#88307,#88308,#88309,#88310,#88311,#88312,#88313,#88314,#88315,#88316,
#88317,#88318,#88319,#88320,#88321,#88322,#88323,#88324,#88325,#88326,#88327,
#88328,#88329,#88330,#88331,#88332,#88333,#88334,#88335,#88336,#88337,#88338,
#88339,#88340,#88341,#88342,#88343,#88344,#88345,#88346,#88347,#88348,#88349,
#88350,#88351,#88352,#88353,#88354,#88355,#88356,#88357,#88358,#88359,#88360,
#88361,#88362,#88363,#88364,#88365,#88366,#88367,#88368,#88369,#88370,#88371,
#88372,#88373,#88374,#88375,#88376,#88377,#88378,#88379,#88380,#88381,#88382,
#88383,#88384,#88385,#88386,#88387,#88388,#88389,#88390,#88391,#88392,#88393,
#88394,#88395,#88396,#88397,#88398,#88399,#88400,#88401,#88402,#88403,#88404,
#88405,#88406,#88407,#88408,#88409,#88410),.UNSPECIFIED.,.F.,.F.,(4,3,3,
3,3,3,3,3,3,3,3,3,3,3,3,3,3,3,3,3,3,3,3,3,3,3,3,3,3,3,3,3,3,3,3,3,3,3,3,
3,3,3,3,3,3,3,3,3,3,3,3,3,3,3,3,3,3,3,3,3,3,3,3,3,3,3,3,3,3,3,3,3,3,4),
(977.035315266588,977.133307139005,977.231938308519,977.331290940343,977.360407874734,
977.444146586581,977.527782097949,977.611334541349,977.694823977201,977.778277927815,
977.861714421662,977.945151531419,978.028607326338,978.112151819068,978.19574090201,
978.279464169569,978.360143885455,978.443882597301,978.527518108668,978.611070552067,
978.694559987918,978.778013938531,978.861450432378,978.944887542133,979.028343337051,
979.11188782978,979.195476912721,979.279200180279,979.359879896175,979.443618608021,
979.527254119388,979.610806562786,979.694295998637,979.777749949251,979.861186443097,
979.944623552852,980.028079347769,980.111623840499,980.19521292344,980.278936190997,
980.359615906895,980.443354618741,980.526990130109,980.610542573507,980.694032009358,
980.777485959972,980.860922453818,980.944359563574,981.027815358491,981.111359851221,
981.194948934162,981.27867220172,981.359351917615,981.443090629461,981.526726140828,
981.610278584227,981.693768020078,981.777221970692,981.860658464538,981.944095574294,
982.027551369211,982.111095861941,982.194684944882,982.27840821244,982.359087928335,
982.442307253171,982.525395131154,982.60840709754,982.691361790686,982.774277803087,
982.857189163963,982.940097001489,983.023046132135,983.06671526311),
 .UNSPECIFIED.);
#675=B_SPLINE_CURVE_WITH_KNOTS('',3,(#88416,#88417,#88418,#88419,#88420,
#88421,#88422,#88423,#88424,#88425,#88426,#88427,#88428,#88429,#88430,#88431,
#88432,#88433,#88434,#88435,#88436,#88437,#88438,#88439,#88440,#88441,#88442,
#88443,#88444,#88445,#88446,#88447,#88448,#88449,#88450,#88451,#88452,#88453,
#88454,#88455,#88456,#88457,#88458,#88459,#88460,#88461,#88462,#88463,#88464,
#88465,#88466,#88467,#88468,#88469,#88470,#88471,#88472,#88473,#88474,#88475,
#88476,#88477,#88478,#88479,#88480,#88481,#88482,#88483,#88484,#88485,#88486,
#88487,#88488,#88489,#88490,#88491,#88492,#88493,#88494,#88495,#88496,#88497,
#88498,#88499,#88500,#88501,#88502,#88503,#88504,#88505,#88506,#88507,#88508,
#88509,#88510,#88511,#88512,#88513,#88514,#88515,#88516,#88517,#88518,#88519,
#88520,#88521,#88522,#88523,#88524,#88525,#88526,#88527,#88528,#88529,#88530,
#88531,#88532,#88533,#88534,#88535,#88536,#88537,#88538,#88539,#88540,#88541,
#88542,#88543,#88544,#88545,#88546,#88547,#88548,#88549,#88550,#88551,#88552,
#88553,#88554,#88555,#88556,#88557,#88558,#88559,#88560,#88561,#88562,#88563,
#88564,#88565,#88566,#88567,#88568,#88569,#88570,#88571,#88572,#88573,#88574,
#88575,#88576,#88577,#88578,#88579,#88580,#88581,#88582,#88583,#88584,#88585,
#88586,#88587,#88588,#88589,#88590,#88591,#88592,#88593,#88594,#88595,#88596,
#88597,#88598,#88599,#88600,#88601,#88602,#88603,#88604,#88605,#88606,#88607,
#88608,#88609,#88610,#88611,#88612,#88613,#88614,#88615,#88616,#88617,#88618,
#88619,#88620,#88621,#88622,#88623,#88624,#88625,#88626,#88627,#88628,#88629,
#88630,#88631,#88632,#88633,#88634,#88635),.UNSPECIFIED.,.F.,.F.,(4,3,3,
3,3,3,3,3,3,3,3,3,3,3,3,3,3,3,3,3,3,3,3,3,3,3,3,3,3,3,3,3,3,3,3,3,3,3,3,
3,3,3,3,3,3,3,3,3,3,3,3,3,3,3,3,3,3,3,3,3,3,3,3,3,3,3,3,3,3,3,3,3,3,4),
(983.318500573583,983.401198681688,983.48385736056,983.566496688037,983.649135402762,
983.731792239955,983.814536138504,983.897325350184,983.980244593793,984.048269330058,
984.132008041904,984.215643553272,984.299195996671,984.382685432522,984.466139383136,
984.549575876982,984.633012986738,984.716468781656,984.800013274386,984.883602357327,
984.967325624885,985.048005340779,985.131744052625,985.215379563992,985.298932007391,
985.382421443242,985.465875393856,985.549311887702,985.632748997458,985.716204792375,
985.799749285105,985.883338368046,985.967061635603,986.047741351499,986.131480063345,
986.215115574712,986.298668018111,986.382157453962,986.465611404576,986.549047898422,
986.632485008177,986.715940803095,986.799485295824,986.883074378765,986.966797646323,
987.047477362219,987.131216074065,987.214851585432,987.298404028831,987.381893464682,
987.465347415296,987.548783909142,987.632221018897,987.715676813815,987.799221306545,
987.882810389486,987.966533657043,988.047213372939,988.130952084785,988.214587596152,
988.298140039551,988.381629475402,988.465083426015,988.548519919862,988.631957029617,
988.715412824534,988.798957317263,988.882546400204,988.966269667762,989.046949383659,
989.133108389705,989.219154270956,989.305066936171,989.351233245849),
 .UNSPECIFIED.);
#676=B_SPLINE_CURVE_WITH_KNOTS('',3,(#88636,#88637,#88638,#88639,#88640,
#88641,#88642,#88643,#88644,#88645),.UNSPECIFIED.,.F.,.F.,(4,3,3,4),(983.067552096354,
983.173712335231,983.278061473153,983.318500573403),.UNSPECIFIED.);
#677=B_SPLINE_CURVE_WITH_KNOTS('',3,(#88647,#88648,#88649,#88650,#88651,
#88652,#88653,#88654,#88655,#88656),.UNSPECIFIED.,.F.,.F.,(4,3,3,4),(983.06671526311,
983.14975902426,983.234129798838,983.318500573417),.UNSPECIFIED.);
#678=B_SPLINE_CURVE_WITH_KNOTS('',3,(#88657,#88658,#88659,#88660,#88661,
#88662,#88663,#88664,#88665,#88666,#88667,#88668,#88669,#88670,#88671,#88672,
#88673,#88674,#88675,#88676,#88677,#88678,#88679,#88680,#88681,#88682,#88683,
#88684,#88685,#88686,#88687,#88688,#88689,#88690,#88691,#88692,#88693,#88694,
#88695,#88696,#88697,#88698,#88699,#88700,#88701,#88702,#88703,#88704,#88705,
#88706,#88707,#88708,#88709,#88710,#88711,#88712,#88713,#88714,#88715,#88716,
#88717,#88718,#88719,#88720,#88721,#88722,#88723,#88724,#88725,#88726,#88727,
#88728,#88729,#88730,#88731,#88732,#88733,#88734,#88735,#88736,#88737,#88738,
#88739,#88740,#88741,#88742,#88743,#88744,#88745,#88746,#88747,#88748,#88749,
#88750,#88751,#88752,#88753,#88754,#88755,#88756,#88757,#88758,#88759,#88760,
#88761,#88762,#88763,#88764,#88765,#88766,#88767,#88768,#88769,#88770,#88771,
#88772,#88773,#88774,#88775,#88776,#88777,#88778,#88779,#88780,#88781,#88782,
#88783,#88784,#88785,#88786,#88787,#88788,#88789,#88790,#88791,#88792,#88793,
#88794,#88795,#88796,#88797,#88798,#88799,#88800,#88801,#88802,#88803,#88804,
#88805,#88806,#88807,#88808,#88809,#88810,#88811,#88812,#88813,#88814,#88815,
#88816,#88817,#88818,#88819,#88820,#88821,#88822,#88823,#88824,#88825,#88826,
#88827,#88828,#88829,#88830,#88831,#88832,#88833,#88834,#88835,#88836,#88837,
#88838,#88839,#88840,#88841,#88842,#88843,#88844,#88845,#88846,#88847,#88848,
#88849,#88850,#88851,#88852,#88853,#88854,#88855,#88856,#88857,#88858,#88859,
#88860,#88861,#88862,#88863,#88864,#88865,#88866,#88867,#88868,#88869,#88870,
#88871,#88872,#88873,#88874,#88875,#88876),.UNSPECIFIED.,.F.,.F.,(4,3,3,
3,3,3,3,3,3,3,3,3,3,3,3,3,3,3,3,3,3,3,3,3,3,3,3,3,3,3,3,3,3,3,3,3,3,3,3,
3,3,3,3,3,3,3,3,3,3,3,3,3,3,3,3,3,3,3,3,3,3,3,3,3,3,3,3,3,3,3,3,3,3,4),
(983.318500573587,983.358823939055,983.442562650901,983.526198162268,983.609750605667,
983.693240041518,983.776693992131,983.860130485977,983.943567595733,984.027023390651,
984.11056788338,984.194156966321,984.277880233879,984.358559949775,984.442298661621,
984.525934172989,984.609486616387,984.692976052239,984.776430002853,984.859866496699,
984.943303606454,985.026759401372,985.110303894102,985.193892977043,985.277616244601,
985.358295960496,985.442034672342,985.525670183709,985.609222627108,985.692712062959,
985.776166013572,985.859602507418,985.943039617174,986.026495412092,986.110039904821,
986.193628987762,986.27735225532,986.358031971216,986.441770683062,986.525406194429,
986.608958637828,986.692448073679,986.775902024293,986.859338518139,986.942775627895,
987.026231422812,987.109775915542,987.193364998483,987.277088266041,987.357767981936,
987.441506693782,987.52514220515,987.608694648548,987.692184084399,987.775638035013,
987.859074528859,987.942511638614,988.025967433532,988.109511926262,988.193101009202,
988.27682427676,988.357503992656,988.441243078456,988.524878875936,988.608431517975,
988.691921065274,988.775374670802,988.858810695376,988.942247211585,989.025702288485,
989.109244315567,989.192830881534,989.276547488672,989.35057976761),
 .UNSPECIFIED.);
#679=B_SPLINE_CURVE_WITH_KNOTS('',3,(#88882,#88883,#88884,#88885,#88886,
#88887,#88888,#88889,#88890,#88891,#88892,#88893,#88894,#88895,#88896,#88897,
#88898,#88899,#88900,#88901,#88902,#88903,#88904,#88905,#88906,#88907,#88908,
#88909,#88910,#88911,#88912,#88913,#88914,#88915,#88916,#88917,#88918,#88919,
#88920,#88921,#88922,#88923,#88924,#88925,#88926,#88927,#88928,#88929,#88930,
#88931,#88932,#88933,#88934,#88935,#88936,#88937,#88938,#88939,#88940,#88941,
#88942,#88943,#88944,#88945,#88946,#88947,#88948,#88949,#88950,#88951,#88952,
#88953,#88954,#88955,#88956,#88957,#88958,#88959,#88960,#88961,#88962,#88963,
#88964,#88965,#88966,#88967,#88968,#88969,#88970,#88971,#88972,#88973,#88974,
#88975,#88976,#88977,#88978,#88979,#88980,#88981,#88982,#88983,#88984,#88985,
#88986,#88987,#88988,#88989,#88990,#88991,#88992,#88993,#88994,#88995,#88996,
#88997,#88998,#88999,#89000,#89001,#89002,#89003,#89004,#89005,#89006,#89007,
#89008,#89009,#89010,#89011,#89012,#89013,#89014,#89015,#89016,#89017,#89018,
#89019,#89020,#89021,#89022,#89023,#89024,#89025,#89026,#89027,#89028,#89029,
#89030,#89031,#89032,#89033,#89034,#89035,#89036,#89037,#89038,#89039,#89040,
#89041,#89042,#89043,#89044,#89045,#89046,#89047,#89048,#89049,#89050,#89051,
#89052,#89053,#89054,#89055,#89056,#89057,#89058,#89059,#89060,#89061,#89062,
#89063,#89064,#89065,#89066,#89067,#89068,#89069,#89070,#89071,#89072,#89073,
#89074,#89075,#89076,#89077,#89078,#89079,#89080,#89081,#89082,#89083,#89084,
#89085,#89086,#89087,#89088,#89089,#89090,#89091,#89092,#89093,#89094,#89095,
#89096,#89097,#89098,#89099,#89100,#89101),.UNSPECIFIED.,.F.,.F.,(4,3,3,
3,3,3,3,3,3,3,3,3,3,3,3,3,3,3,3,3,3,3,3,3,3,3,3,3,3,3,3,3,3,3,3,3,3,3,3,
3,3,3,3,3,3,3,3,3,3,3,3,3,3,3,3,3,3,3,3,3,3,3,3,3,3,3,3,3,3,3,3,3,3,4),
(989.601685880876,989.691372748879,989.781398721669,989.871593799813,989.962075667513,
990.046685394379,990.130424106225,990.214059617593,990.297612060992,990.381101496843,
990.464555447457,990.547991941303,990.631429051059,990.714884845977,990.798429338707,
990.882018421648,990.965741689206,991.046421405099,991.130160116945,991.213795628312,
991.297348071711,991.380837507562,991.464291458175,991.547727952021,991.631165061777,
991.714620856694,991.798165349424,991.881754432365,991.965477699922,992.046157415819,
992.129896127665,992.213531639033,992.297084082431,992.380573518283,992.464027468896,
992.547463962743,992.630901072498,992.714356867416,992.797901360146,992.881490443087,
992.965213710645,993.04589342654,993.129632138386,993.213267649754,993.296820093152,
993.380309529003,993.463763479617,993.547199973463,993.630637083219,993.714092878137,
993.797637370866,993.881226453807,993.964949721365,994.04562943726,994.129368149106,
994.213003660473,994.296556103872,994.380045539723,994.463499490336,994.546935984183,
994.630373093938,994.713828888855,994.797373381585,994.880962464526,994.964685732083,
995.04536544798,995.127838516808,995.210216422072,995.292518381979,995.377675088007,
995.459886036772,995.542079644179,995.624285367826,995.63314520609),
 .UNSPECIFIED.);
#680=B_SPLINE_CURVE_WITH_KNOTS('',3,(#89102,#89103,#89104,#89105,#89106,
#89107,#89108,#89109,#89110,#89111),.UNSPECIFIED.,.F.,.F.,(4,3,3,4),(989.351233245849,
989.436996731148,989.522677717496,989.601685880763),.UNSPECIFIED.);
#681=B_SPLINE_CURVE_WITH_KNOTS('',3,(#89113,#89114,#89115,#89116,#89117,
#89118,#89119,#89120,#89121,#89122,#89123,#89124,#89125),.UNSPECIFIED.,
 .F.,.F.,(4,3,3,3,4),(989.35057976761,989.357240003376,989.468145220993,
989.576452495159,989.601685880647),.UNSPECIFIED.);
#682=B_SPLINE_CURVE_WITH_KNOTS('',3,(#89126,#89127,#89128,#89129,#89130,
#89131,#89132,#89133,#89134,#89135,#89136,#89137,#89138,#89139,#89140,#89141,
#89142,#89143,#89144,#89145,#89146,#89147,#89148,#89149,#89150,#89151,#89152,
#89153,#89154,#89155,#89156,#89157,#89158,#89159,#89160,#89161,#89162,#89163,
#89164,#89165,#89166,#89167,#89168,#89169,#89170,#89171,#89172,#89173,#89174,
#89175,#89176,#89177,#89178,#89179,#89180,#89181,#89182,#89183,#89184,#89185,
#89186,#89187,#89188,#89189,#89190,#89191,#89192,#89193,#89194,#89195,#89196,
#89197,#89198,#89199,#89200,#89201,#89202,#89203,#89204,#89205,#89206,#89207,
#89208,#89209,#89210,#89211,#89212,#89213,#89214,#89215,#89216,#89217,#89218,
#89219,#89220,#89221,#89222,#89223,#89224,#89225,#89226,#89227,#89228,#89229,
#89230,#89231,#89232,#89233,#89234,#89235,#89236,#89237,#89238,#89239,#89240,
#89241,#89242,#89243,#89244,#89245,#89246,#89247,#89248,#89249,#89250,#89251,
#89252,#89253,#89254,#89255,#89256,#89257,#89258,#89259,#89260,#89261,#89262,
#89263,#89264,#89265,#89266,#89267,#89268,#89269,#89270,#89271,#89272,#89273,
#89274,#89275,#89276,#89277,#89278,#89279,#89280,#89281,#89282,#89283,#89284,
#89285,#89286,#89287,#89288,#89289,#89290,#89291,#89292,#89293,#89294,#89295,
#89296,#89297,#89298,#89299,#89300,#89301,#89302,#89303,#89304,#89305,#89306,
#89307,#89308,#89309,#89310,#89311,#89312,#89313,#89314,#89315,#89316,#89317,
#89318,#89319,#89320,#89321,#89322,#89323,#89324,#89325,#89326,#89327,#89328,
#89329,#89330,#89331,#89332,#89333,#89334,#89335,#89336,#89337,#89338,#89339,
#89340,#89341,#89342,#89343,#89344,#89345),.UNSPECIFIED.,.F.,.F.,(4,3,3,
3,3,3,3,3,3,3,3,3,3,3,3,3,3,3,3,3,3,3,3,3,3,3,3,3,3,3,3,3,3,3,3,3,3,3,3,
3,3,3,3,3,3,3,3,3,3,3,3,3,3,3,3,3,3,3,3,3,3,3,3,3,3,3,3,3,3,3,3,3,3,4),
(989.601685880767,989.684216864866,989.768311758519,989.850763033228,989.933206082506,
990.015659782248,990.10098884021,990.183564952774,990.270270483435,990.356976014096,
990.440714725942,990.524350237309,990.607902680708,990.691392116559,990.774846067173,
990.858282561019,990.941719670774,991.025175465692,991.108719958422,991.192309041363,
991.27603230892,991.356712024816,991.440450736662,991.52408624803,991.607638691428,
991.691128127279,991.774582077893,991.858018571739,991.941455681495,992.024911476413,
992.108455969142,992.192045052083,992.275768319641,992.356448035536,992.440186747382,
992.523822258749,992.607374702147,992.690864137998,992.774318088612,992.857754582458,
992.941191692213,993.02464748713,993.10819197986,993.191781062801,993.275504330358,
993.356184046256,993.439922758102,993.52355826947,993.607110712868,993.690600148719,
993.774054099333,993.857490593179,993.940927702935,994.024383497852,994.107927990582,
994.191517073524,994.275240341081,994.355920056977,994.439658768823,994.52329428019,
994.606846723589,994.690336159441,994.773790110055,994.857226603901,994.940663713658,
995.024119508576,995.107664001306,995.191253084247,995.274976351805,995.355656067697,
995.442631342696,995.529485151282,995.616195235346,995.634488381611),
 .UNSPECIFIED.);
#683=B_SPLINE_CURVE_WITH_KNOTS('',3,(#89351,#89352,#89353,#89354,#89355,
#89356,#89357,#89358,#89359,#89360,#89361,#89362,#89363,#89364,#89365,#89366,
#89367,#89368,#89369,#89370,#89371,#89372,#89373,#89374,#89375,#89376,#89377,
#89378,#89379,#89380,#89381,#89382,#89383,#89384,#89385,#89386,#89387,#89388,
#89389,#89390,#89391,#89392,#89393,#89394,#89395,#89396,#89397,#89398,#89399,
#89400,#89401,#89402,#89403,#89404,#89405,#89406,#89407,#89408,#89409,#89410,
#89411,#89412,#89413,#89414,#89415,#89416,#89417,#89418,#89419,#89420,#89421,
#89422,#89423,#89424,#89425,#89426,#89427,#89428,#89429,#89430,#89431,#89432,
#89433,#89434,#89435,#89436,#89437,#89438,#89439,#89440,#89441,#89442,#89443,
#89444,#89445,#89446,#89447,#89448,#89449,#89450,#89451,#89452,#89453,#89454,
#89455,#89456,#89457,#89458,#89459,#89460,#89461,#89462,#89463,#89464,#89465,
#89466,#89467,#89468,#89469,#89470,#89471,#89472,#89473,#89474,#89475,#89476,
#89477,#89478,#89479,#89480,#89481,#89482,#89483,#89484,#89485,#89486,#89487,
#89488,#89489,#89490,#89491,#89492,#89493,#89494,#89495,#89496,#89497,#89498,
#89499,#89500,#89501,#89502,#89503,#89504,#89505,#89506,#89507,#89508,#89509,
#89510,#89511,#89512,#89513,#89514,#89515,#89516,#89517,#89518,#89519,#89520,
#89521,#89522,#89523,#89524,#89525,#89526,#89527,#89528,#89529,#89530,#89531,
#89532,#89533,#89534,#89535,#89536,#89537,#89538,#89539,#89540,#89541,#89542,
#89543,#89544,#89545,#89546,#89547,#89548,#89549,#89550,#89551,#89552,#89553,
#89554,#89555,#89556,#89557,#89558,#89559,#89560,#89561,#89562,#89563,#89564,
#89565,#89566,#89567,#89568,#89569,#89570),.UNSPECIFIED.,.F.,.F.,(4,3,3,
3,3,3,3,3,3,3,3,3,3,3,3,3,3,3,3,3,3,3,3,3,3,3,3,3,3,3,3,3,3,3,3,3,3,3,3,
3,3,3,3,3,3,3,3,3,3,3,3,3,3,3,3,3,3,3,3,3,3,3,3,3,3,3,3,3,3,3,3,3,3,4),
(995.884871187942,996.021248167525,996.0451014587,996.128840170546,996.212475681913,
996.296028125312,996.379517561163,996.462971511777,996.546408005623,996.629845115378,
996.713300910296,996.796845403025,996.880434485966,996.964157753524,997.04483746942,
997.128576181266,997.212211692633,997.295764136032,997.379253571883,997.462707522496,
997.546144016343,997.629581126098,997.713036921016,997.796581413745,997.880170496686,
997.963893764244,998.04457348014,998.128312191986,998.211947703354,998.295500146752,
998.378989582603,998.462443533217,998.545880027063,998.629317136818,998.712772931736,
998.796317424466,998.879906507407,998.963629774964,999.04430949086,999.128048202706,
999.211683714074,999.295236157472,999.378725593323,999.462179543937,999.545616037783,
999.629053147538,999.712508942456,999.796053435186,999.879642518127,999.963365785684,
1000.04404550158,1000.12778421343,1000.21141972479,1000.29497216819,1000.37846160404,
1000.46191555466,1000.5453520485,1000.62878915826,1000.71224495318,1000.79578944591,
1000.87937852885,1000.96310179641,1001.0437815123,1001.12752769863,1001.21116900861,
1001.29472558194,1001.37821223534,1001.46166097302,1001.54508988378,1001.62851703916,
1001.7119925852,1001.79549552301,1001.87908229611,1001.91647437912),
 .UNSPECIFIED.);
#684=B_SPLINE_CURVE_WITH_KNOTS('',3,(#89571,#89572,#89573,#89574,#89575,
#89576,#89577,#89578,#89579,#89580),.UNSPECIFIED.,.F.,.F.,(4,3,3,4),(995.63314520609,
995.715410338439,995.800140763139,995.88487118784),.UNSPECIFIED.);
#685=B_SPLINE_CURVE_WITH_KNOTS('',3,(#89582,#89583,#89584,#89585,#89586,
#89587,#89588,#89589,#89590,#89591),.UNSPECIFIED.,.F.,.F.,(4,3,3,4),(995.634488381611,
995.721042296476,995.807480506179,995.884871187946),.UNSPECIFIED.);
#686=B_SPLINE_CURVE_WITH_KNOTS('',3,(#89592,#89593,#89594,#89595,#89596,
#89597,#89598,#89599,#89600,#89601,#89602,#89603,#89604,#89605,#89606,#89607,
#89608,#89609,#89610,#89611,#89612,#89613,#89614,#89615,#89616,#89617,#89618,
#89619,#89620,#89621,#89622,#89623,#89624,#89625,#89626,#89627,#89628,#89629,
#89630,#89631,#89632,#89633,#89634,#89635,#89636,#89637,#89638,#89639,#89640,
#89641,#89642,#89643,#89644,#89645,#89646,#89647,#89648,#89649,#89650,#89651,
#89652,#89653,#89654,#89655,#89656,#89657,#89658,#89659,#89660,#89661,#89662,
#89663,#89664,#89665,#89666,#89667,#89668,#89669,#89670,#89671,#89672,#89673,
#89674,#89675,#89676,#89677,#89678,#89679,#89680,#89681,#89682,#89683,#89684,
#89685,#89686,#89687,#89688,#89689,#89690,#89691,#89692,#89693,#89694,#89695,
#89696,#89697,#89698,#89699,#89700,#89701,#89702,#89703,#89704,#89705,#89706,
#89707,#89708,#89709,#89710,#89711,#89712,#89713,#89714,#89715,#89716,#89717,
#89718,#89719,#89720,#89721,#89722,#89723,#89724,#89725,#89726,#89727,#89728,
#89729,#89730,#89731,#89732,#89733,#89734,#89735,#89736,#89737,#89738,#89739,
#89740,#89741,#89742,#89743,#89744,#89745,#89746,#89747,#89748,#89749,#89750,
#89751,#89752,#89753,#89754,#89755,#89756,#89757,#89758,#89759,#89760,#89761,
#89762,#89763,#89764,#89765,#89766,#89767,#89768,#89769,#89770,#89771,#89772,
#89773,#89774,#89775,#89776,#89777,#89778,#89779,#89780,#89781,#89782,#89783,
#89784,#89785,#89786,#89787,#89788,#89789,#89790,#89791,#89792,#89793,#89794,
#89795,#89796,#89797,#89798,#89799,#89800,#89801,#89802,#89803,#89804,#89805,
#89806,#89807,#89808,#89809,#89810,#89811),.UNSPECIFIED.,.F.,.F.,(4,3,3,
3,3,3,3,3,3,3,3,3,3,3,3,3,3,3,3,3,3,3,3,3,3,3,3,3,3,3,3,3,3,3,3,3,3,3,3,
3,3,3,3,3,3,3,3,3,3,3,3,3,3,3,3,3,3,3,3,3,3,3,3,3,3,3,3,3,3,3,3,3,3,4),
(995.88487118808,995.973419318332,996.062127342903,996.151085735606,996.240181514523,
996.329487426633,996.355392078417,996.439130790263,996.52276630163,996.606318745029,
996.68980818088,996.773262131493,996.85669862534,996.940135735095,997.023591530013,
997.107136022742,997.190725105683,997.274448373241,997.355128089137,997.438866800983,
997.52250231235,997.606054755749,997.6895441916,997.772998142213,997.856434636059,
997.939871745815,998.023327540733,998.106872033462,998.190461116403,998.274184383961,
998.354864099857,998.438602811703,998.52223832307,998.605790766468,998.689280202319,
998.772734152932,998.856170646778,998.939607756534,999.023063551451,999.106608044181,
999.190197127122,999.273920394679,999.354600110577,999.438338822424,999.521974333792,
999.605526777191,999.689016213043,999.772470163657,999.855906657504,999.93934376726,
1000.02279956218,1000.10634405491,1000.18993313785,1000.27365640541,1000.3543361213,
1000.43807483315,1000.52171034451,1000.60526278791,1000.68875222376,1000.77220617438,
1000.85564266822,1000.93907977798,1001.0225355729,1001.10608006563,1001.18966914857,
1001.27339241612,1001.35407213202,1001.43655651427,1001.51894518119,1001.60125734878,
1001.68351138604,1001.76573016305,1001.8479504598,1001.91641401972),
 .UNSPECIFIED.);
#687=B_SPLINE_CURVE_WITH_KNOTS('',3,(#89817,#89818,#89819,#89820,#89821,
#89822,#89823,#89824,#89825,#89826,#89827,#89828,#89829,#89830,#89831,#89832,
#89833,#89834,#89835,#89836,#89837,#89838,#89839,#89840,#89841,#89842,#89843,
#89844,#89845,#89846,#89847,#89848,#89849,#89850,#89851,#89852,#89853,#89854,
#89855,#89856,#89857,#89858,#89859,#89860,#89861,#89862,#89863,#89864,#89865,
#89866,#89867,#89868,#89869,#89870,#89871,#89872,#89873,#89874,#89875,#89876,
#89877,#89878,#89879,#89880,#89881,#89882,#89883,#89884,#89885,#89886,#89887,
#89888,#89889,#89890,#89891,#89892,#89893,#89894,#89895,#89896,#89897,#89898,
#89899,#89900,#89901,#89902,#89903,#89904,#89905,#89906,#89907,#89908,#89909,
#89910,#89911,#89912,#89913,#89914,#89915,#89916,#89917,#89918,#89919,#89920,
#89921,#89922,#89923,#89924,#89925,#89926,#89927,#89928,#89929,#89930,#89931,
#89932,#89933,#89934,#89935,#89936,#89937,#89938,#89939,#89940,#89941,#89942,
#89943,#89944,#89945,#89946,#89947,#89948,#89949,#89950,#89951,#89952,#89953,
#89954,#89955,#89956,#89957,#89958,#89959,#89960,#89961,#89962,#89963,#89964,
#89965,#89966,#89967,#89968,#89969,#89970,#89971,#89972,#89973,#89974,#89975,
#89976,#89977,#89978,#89979,#89980,#89981,#89982,#89983,#89984,#89985,#89986,
#89987,#89988,#89989,#89990,#89991,#89992,#89993,#89994,#89995,#89996,#89997,
#89998,#89999,#90000,#90001,#90002,#90003,#90004,#90005,#90006,#90007,#90008,
#90009,#90010,#90011,#90012,#90013,#90014,#90015,#90016,#90017,#90018,#90019,
#90020,#90021,#90022,#90023,#90024,#90025,#90026,#90027,#90028,#90029,#90030,
#90031,#90032,#90033,#90034,#90035,#90036),.UNSPECIFIED.,.F.,.F.,(4,3,3,
3,3,3,3,3,3,3,3,3,3,3,3,3,3,3,3,3,3,3,3,3,3,3,3,3,3,3,3,3,3,3,3,3,3,3,3,
3,3,3,3,3,3,3,3,3,3,3,3,3,3,3,3,3,3,3,3,3,3,3,3,3,3,3,3,3,3,3,3,3,3,4),
(1002.16805649525,1002.25055559598,1002.33296687633,1002.41531144832,1002.49761651802,
1002.57990261825,1002.66218873484,1002.74449385133,1002.82688428733,1002.90932133242,
1002.99188129999,1003.04325353374,1003.12699224559,1003.21062775695,1003.29418020035,
1003.3776696362,1003.46112358682,1003.54456008066,1003.62799719042,1003.71145298534,
1003.79499747807,1003.87858656101,1003.96230982856,1004.04298954446,1004.12672825631,
1004.21036376767,1004.29391621107,1004.37740564692,1004.46085959754,1004.54429609138,
1004.62773320114,1004.71118899606,1004.79473348879,1004.87832257173,1004.96204583928,
1005.04272555518,1005.12646426703,1005.21009977839,1005.29365222179,1005.37714165764,
1005.46059560826,1005.5440321021,1005.62746921186,1005.71092500678,1005.79446949951,
1005.87805858245,1005.96178185,1006.0424615659,1006.12620027775,1006.20983578911,
1006.29338823251,1006.37687766836,1006.46033161898,1006.54376811282,1006.62720522258,
1006.7106610175,1006.79420551023,1006.87779459317,1006.96151786072,1007.04219757662,
1007.12593628847,1007.20957179983,1007.29312424323,1007.37661367908,1007.4600676297,
1007.54350412354,1007.6269412333,1007.71039702821,1007.79394152094,1007.87753060389,
1007.96125387144,1008.04193358734,1008.13445659178,1008.20088883303),
 .UNSPECIFIED.);
#688=B_SPLINE_CURVE_WITH_KNOTS('',3,(#90037,#90038,#90039,#90040,#90041,
#90042,#90043,#90044,#90045,#90046),.UNSPECIFIED.,.F.,.F.,(4,3,3,4),(1001.91647437912,
1002.00021216703,1002.04351752302,1002.16805649512),.UNSPECIFIED.);
#689=B_SPLINE_CURVE_WITH_KNOTS('',3,(#90048,#90049,#90050,#90051,#90052,
#90053,#90054,#90055,#90056,#90057),.UNSPECIFIED.,.F.,.F.,(4,3,3,4),(1001.91641401972,
1001.99867201972,1002.08336425735,1002.16805649499),.UNSPECIFIED.);
#690=B_SPLINE_CURVE_WITH_KNOTS('',3,(#90058,#90059,#90060,#90061,#90062,
#90063,#90064,#90065,#90066,#90067,#90068,#90069,#90070,#90071,#90072,#90073,
#90074,#90075,#90076,#90077,#90078,#90079,#90080,#90081,#90082,#90083,#90084,
#90085,#90086,#90087,#90088,#90089,#90090,#90091,#90092,#90093,#90094,#90095,
#90096,#90097,#90098,#90099,#90100,#90101,#90102,#90103,#90104,#90105,#90106,
#90107,#90108,#90109,#90110,#90111,#90112,#90113,#90114,#90115,#90116,#90117,
#90118,#90119,#90120,#90121,#90122,#90123,#90124,#90125,#90126,#90127,#90128,
#90129,#90130,#90131,#90132,#90133,#90134,#90135,#90136,#90137,#90138,#90139,
#90140,#90141,#90142,#90143,#90144,#90145,#90146,#90147,#90148,#90149,#90150,
#90151,#90152,#90153,#90154,#90155,#90156,#90157,#90158,#90159,#90160,#90161,
#90162,#90163,#90164,#90165,#90166,#90167,#90168,#90169,#90170,#90171,#90172,
#90173,#90174,#90175,#90176,#90177,#90178,#90179,#90180,#90181,#90182,#90183,
#90184,#90185,#90186,#90187,#90188,#90189,#90190,#90191,#90192,#90193,#90194,
#90195,#90196,#90197,#90198,#90199,#90200,#90201,#90202,#90203,#90204,#90205,
#90206,#90207,#90208,#90209,#90210,#90211,#90212,#90213,#90214,#90215,#90216,
#90217,#90218,#90219,#90220,#90221,#90222,#90223,#90224,#90225,#90226,#90227,
#90228,#90229,#90230,#90231,#90232,#90233,#90234,#90235,#90236,#90237,#90238,
#90239,#90240,#90241,#90242,#90243,#90244,#90245,#90246,#90247,#90248,#90249,
#90250,#90251,#90252,#90253,#90254,#90255,#90256,#90257,#90258,#90259,#90260,
#90261,#90262,#90263,#90264,#90265,#90266,#90267,#90268,#90269,#90270,#90271,
#90272,#90273,#90274),.UNSPECIFIED.,.F.,.F.,(4,3,3,3,3,3,3,3,3,3,3,3,3,
3,3,3,3,3,3,3,3,3,3,3,3,3,3,3,3,3,3,3,3,3,3,3,3,3,3,3,3,3,3,3,3,3,3,3,3,
3,3,3,3,3,3,3,3,3,3,3,3,3,3,3,3,3,3,3,3,3,3,3,4),(1002.16805649513,1002.29304179767,
1002.35380814274,1002.43754685459,1002.52118236595,1002.60473480935,1002.6882242452,
1002.77167819582,1002.85511468966,1002.93855179942,1003.02200759434,1003.10555208707,
1003.18914117001,1003.27286443756,1003.35354415346,1003.43728286531,1003.52091837667,
1003.60447082007,1003.68796025592,1003.77141420654,1003.85485070038,1003.93828781014,
1004.02174360506,1004.10528809779,1004.18887718073,1004.27260044828,1004.35328016418,
1004.43701887603,1004.52065438739,1004.60420683079,1004.68769626664,1004.77115021726,
1004.8545867111,1004.93802382086,1005.02147961578,1005.10502410851,1005.18861319145,
1005.272336459,1005.3530161749,1005.43675488675,1005.52039039811,1005.60394284151,
1005.68743227736,1005.77088622798,1005.85432272182,1005.93775983158,1006.0212156265,
1006.10476011923,1006.18834920217,1006.27207246972,1006.35275218562,1006.43649089747,
1006.52012640883,1006.60367885223,1006.68716828808,1006.7706222387,1006.85405873254,
1006.9374958423,1007.02095163722,1007.10449612994,1007.18808521289,1007.27180848044,
1007.35248819634,1007.43623597389,1007.51987853776,1007.60484562024,1007.68833125241,
1007.77177879713,1007.85520634312,1007.94130855672,1008.02477827793,1008.11219673773,
1008.19961519754),.UNSPECIFIED.);
#691=B_SPLINE_CURVE_WITH_KNOTS('',3,(#90280,#90281,#90282,#90283,#90284,
#90285,#90286,#90287,#90288,#90289,#90290,#90291,#90292,#90293,#90294,#90295,
#90296,#90297,#90298,#90299,#90300,#90301,#90302,#90303,#90304,#90305,#90306,
#90307,#90308,#90309,#90310,#90311,#90312,#90313,#90314,#90315,#90316,#90317,
#90318,#90319,#90320,#90321,#90322,#90323,#90324,#90325,#90326,#90327,#90328,
#90329,#90330,#90331,#90332,#90333,#90334,#90335,#90336,#90337,#90338,#90339,
#90340,#90341,#90342,#90343,#90344,#90345,#90346,#90347,#90348,#90349,#90350,
#90351,#90352,#90353,#90354,#90355,#90356,#90357,#90358,#90359,#90360,#90361,
#90362,#90363,#90364,#90365,#90366,#90367,#90368,#90369,#90370,#90371,#90372,
#90373,#90374,#90375,#90376,#90377,#90378,#90379,#90380,#90381,#90382,#90383,
#90384,#90385,#90386,#90387,#90388,#90389,#90390,#90391,#90392,#90393,#90394,
#90395,#90396,#90397,#90398,#90399,#90400,#90401,#90402,#90403,#90404,#90405,
#90406,#90407,#90408,#90409,#90410,#90411,#90412,#90413,#90414,#90415,#90416,
#90417,#90418,#90419,#90420,#90421,#90422,#90423,#90424,#90425,#90426,#90427,
#90428,#90429,#90430,#90431,#90432,#90433,#90434,#90435,#90436,#90437,#90438,
#90439,#90440,#90441,#90442,#90443,#90444,#90445,#90446,#90447,#90448,#90449,
#90450,#90451,#90452,#90453,#90454,#90455,#90456,#90457,#90458,#90459,#90460,
#90461,#90462,#90463,#90464,#90465,#90466,#90467,#90468,#90469,#90470,#90471,
#90472,#90473,#90474,#90475,#90476,#90477,#90478,#90479,#90480,#90481,#90482,
#90483,#90484,#90485,#90486,#90487,#90488,#90489,#90490,#90491,#90492,#90493,
#90494,#90495,#90496,#90497,#90498,#90499),.UNSPECIFIED.,.F.,.F.,(4,3,3,
3,3,3,3,3,3,3,3,3,3,3,3,3,3,3,3,3,3,3,3,3,3,3,3,3,3,3,3,3,3,3,3,3,3,3,3,
3,3,3,3,3,3,3,3,3,3,3,3,3,3,3,3,3,3,3,3,3,3,3,3,3,3,3,3,3,3,3,3,3,3,4),
(1008.4512418023,1008.53601294285,1008.62081253761,1008.70565656944,1008.79062346889,
1008.87565342782,1008.96084174054,1009.04166959806,1009.12540830991,1009.20904382127,
1009.29259626467,1009.37608570052,1009.45953965114,1009.54297614498,1009.62641325474,
1009.70986904966,1009.79341354239,1009.87700262533,1009.96072589288,1010.04140560878,
1010.12514432063,1010.20877983199,1010.29233227539,1010.37582171124,1010.45927566186,
1010.5427121557,1010.62614926546,1010.70960506037,1010.7931495531,1010.87673863604,
1010.9604619036,1011.0411416195,1011.12488033135,1011.20851584271,1011.29206828611,
1011.37555772196,1011.45901167258,1011.54244816642,1011.62588527618,1011.7093410711,
1011.79288556383,1011.87647464677,1011.96019791433,1012.04087763022,1012.12461634207,
1012.20825185343,1012.29180429683,1012.37529373268,1012.4587476833,1012.54218417714,
1012.6256212869,1012.70907708182,1012.79262157455,1012.87621065749,1012.95993392504,
1013.04061364094,1013.12435235279,1013.20798786415,1013.29154030755,1013.3750297434,
1013.45848369402,1013.54192018786,1013.62535729762,1013.70881309253,1013.79235758526,
1013.8759466682,1013.95966993576,1014.04034965166,1014.12367162658,1014.20689120733,
1014.29001017334,1014.37307123086,1014.45608932087,1014.48334915183),
 .UNSPECIFIED.);
#692=B_SPLINE_CURVE_WITH_KNOTS('',3,(#90500,#90501,#90502,#90503,#90504,
#90505,#90506,#90507,#90508,#90509),.UNSPECIFIED.,.F.,.F.,(4,3,3,4),(1008.20088883303,
1008.29294583235,1008.38460335587,1008.45124180213),.UNSPECIFIED.);
#693=B_SPLINE_CURVE_WITH_KNOTS('',3,(#90511,#90512,#90513,#90514,#90515,
#90516,#90517,#90518,#90519,#90520),.UNSPECIFIED.,.F.,.F.,(4,3,3,4),(1008.19961519754,
1008.28334261795,1008.35222420706,1008.45124180231),.UNSPECIFIED.);
#694=B_SPLINE_CURVE_WITH_KNOTS('',3,(#90521,#90522,#90523,#90524,#90525,
#90526,#90527,#90528,#90529,#90530,#90531,#90532,#90533,#90534,#90535,#90536,
#90537,#90538,#90539,#90540,#90541,#90542,#90543,#90544,#90545,#90546,#90547,
#90548,#90549,#90550,#90551,#90552,#90553,#90554,#90555,#90556,#90557,#90558,
#90559,#90560,#90561,#90562,#90563,#90564,#90565,#90566,#90567,#90568,#90569,
#90570,#90571,#90572,#90573,#90574,#90575,#90576,#90577,#90578,#90579,#90580,
#90581,#90582,#90583,#90584,#90585,#90586,#90587,#90588,#90589,#90590,#90591,
#90592,#90593,#90594,#90595,#90596,#90597,#90598,#90599,#90600,#90601,#90602,
#90603,#90604,#90605,#90606,#90607,#90608,#90609,#90610,#90611,#90612,#90613,
#90614,#90615,#90616,#90617,#90618,#90619,#90620,#90621,#90622,#90623,#90624,
#90625,#90626,#90627,#90628,#90629,#90630,#90631,#90632,#90633,#90634,#90635,
#90636,#90637,#90638,#90639,#90640,#90641,#90642,#90643,#90644,#90645,#90646,
#90647,#90648,#90649,#90650,#90651,#90652,#90653,#90654,#90655,#90656,#90657,
#90658,#90659,#90660,#90661,#90662,#90663,#90664,#90665,#90666,#90667,#90668,
#90669,#90670,#90671,#90672,#90673,#90674,#90675,#90676,#90677,#90678,#90679,
#90680,#90681,#90682,#90683,#90684,#90685,#90686,#90687,#90688,#90689,#90690,
#90691,#90692,#90693,#90694,#90695,#90696,#90697,#90698,#90699,#90700,#90701,
#90702,#90703,#90704,#90705,#90706,#90707,#90708,#90709,#90710,#90711,#90712,
#90713,#90714,#90715,#90716,#90717,#90718,#90719,#90720,#90721,#90722,#90723,
#90724,#90725,#90726,#90727,#90728,#90729,#90730,#90731,#90732,#90733,#90734,
#90735,#90736,#90737,#90738,#90739,#90740),.UNSPECIFIED.,.F.,.F.,(4,3,3,
3,3,3,3,3,3,3,3,3,3,3,3,3,3,3,3,3,3,3,3,3,3,3,3,3,3,3,3,3,3,3,3,3,3,3,3,
3,3,3,3,3,3,3,3,3,3,3,3,3,3,3,3,3,3,3,3,3,3,3,3,3,3,3,3,3,3,3,3,3,3,4),
(1008.45124180245,1008.533889141,1008.61644367089,1008.69892643314,1008.78136290829,
1008.86377570506,1008.94618373353,1009.02860589755,1009.11111132048,1009.19365882821,
1009.27633650523,1009.35196021778,1009.43569892963,1009.51933444099,1009.60288688439,
1009.68637632024,1009.76983027086,1009.8532667647,1009.93670387446,1010.02015966938,
1010.10370416211,1010.18729324505,1010.27101651261,1010.3516962285,1010.43543494035,
1010.51907045171,1010.60262289511,1010.68611233096,1010.76956628158,1010.85300277543,
1010.93643988518,1011.0198956801,1011.10344017283,1011.18702925577,1011.27075252333,
1011.35143223922,1011.43517095107,1011.51880646243,1011.60235890583,1011.68584834168,
1011.7693022923,1011.85273878614,1011.9361758959,1012.01963169081,1012.10317618354,
1012.18676526648,1012.27048853404,1012.35116824994,1012.43490696179,1012.51854247315,
1012.60209491655,1012.6855843524,1012.76903830302,1012.85247479686,1012.93591190662,
1013.01936770154,1013.10291219427,1013.18650127721,1013.27022454476,1013.35090426066,
1013.43464297251,1013.51827848388,1013.60183092728,1013.68532036313,1013.76877431374,
1013.85221080759,1013.93564791735,1014.01910371226,1014.102648205,1014.18623728794,
1014.2699605555,1014.35064027138,1014.44491243077,1014.48401170027),
 .UNSPECIFIED.);
#695=B_SPLINE_CURVE_WITH_KNOTS('',3,(#90746,#90747,#90748,#90749,#90750,
#90751,#90752,#90753,#90754,#90755,#90756,#90757,#90758,#90759,#90760,#90761,
#90762,#90763,#90764,#90765,#90766,#90767,#90768,#90769,#90770,#90771,#90772,
#90773,#90774,#90775,#90776,#90777,#90778,#90779,#90780,#90781,#90782,#90783,
#90784,#90785,#90786,#90787,#90788,#90789,#90790,#90791,#90792,#90793,#90794,
#90795,#90796,#90797,#90798,#90799,#90800,#90801,#90802,#90803,#90804,#90805,
#90806,#90807,#90808,#90809,#90810,#90811,#90812,#90813,#90814,#90815,#90816,
#90817,#90818,#90819,#90820,#90821,#90822,#90823,#90824,#90825,#90826,#90827,
#90828,#90829,#90830,#90831,#90832,#90833,#90834,#90835,#90836,#90837,#90838,
#90839,#90840,#90841,#90842,#90843,#90844,#90845,#90846,#90847,#90848,#90849,
#90850,#90851,#90852,#90853,#90854,#90855,#90856,#90857,#90858,#90859,#90860,
#90861,#90862,#90863,#90864,#90865,#90866,#90867,#90868,#90869,#90870,#90871,
#90872,#90873,#90874,#90875,#90876,#90877,#90878,#90879,#90880,#90881,#90882,
#90883,#90884,#90885,#90886,#90887,#90888,#90889,#90890,#90891,#90892,#90893,
#90894,#90895,#90896,#90897,#90898,#90899,#90900,#90901,#90902,#90903,#90904,
#90905,#90906,#90907,#90908,#90909,#90910,#90911,#90912,#90913,#90914,#90915,
#90916,#90917,#90918,#90919,#90920,#90921,#90922,#90923,#90924,#90925,#90926,
#90927,#90928,#90929,#90930,#90931,#90932,#90933,#90934,#90935,#90936,#90937,
#90938,#90939,#90940,#90941,#90942,#90943,#90944,#90945,#90946,#90947,#90948,
#90949,#90950,#90951,#90952,#90953,#90954,#90955,#90956,#90957,#90958,#90959,
#90960,#90961,#90962),.UNSPECIFIED.,.F.,.F.,(4,3,3,3,3,3,3,3,3,3,3,3,3,
3,3,3,3,3,3,3,3,3,3,3,3,3,3,3,3,3,3,3,3,3,3,3,3,3,3,3,3,3,3,3,3,3,3,3,3,
3,3,3,3,3,3,3,3,3,3,3,3,3,3,3,3,3,3,3,3,3,3,3,4),(1014.73442710964,1014.83436448893,
1014.93722507566,1015.04008566238,1015.12382437423,1015.2074598856,1015.291012329,
1015.37450176485,1015.45795571546,1015.54139220931,1015.62482931907,1015.70828511399,
1015.79182960672,1015.87541868966,1015.95914195722,1016.0398216731,1016.12356038495,
1016.20719589631,1016.29074833971,1016.37423777556,1016.45769172618,1016.54112822002,
1016.62456532978,1016.7080211247,1016.79156561743,1016.87515470037,1016.95887796792,
1017.03955768382,1017.12329639567,1017.20693190703,1017.29048435043,1017.37397378628,
1017.4574277369,1017.54086423074,1017.6243013405,1017.70775713541,1017.79130162814,
1017.87489071108,1017.95861397864,1018.03929369454,1018.12303240639,1018.20666791775,
1018.29022036115,1018.373709797,1018.45716374762,1018.54060024146,1018.62403735122,
1018.70749314614,1018.79103763887,1018.87462672181,1018.95834998937,1019.03902970526,
1019.12276841711,1019.20640392847,1019.28995637187,1019.37344580772,1019.45689975834,
1019.54033625218,1019.62377336194,1019.70722915685,1019.79077364958,1019.87436273252,
1019.95808600008,1020.03876571598,1020.12222316499,1020.20554861207,1020.28879787067,
1020.37198938023,1020.45514153568,1020.5382896657,1020.62143322146,1020.70462245946,
1020.76588157733),.UNSPECIFIED.);
#696=B_SPLINE_CURVE_WITH_KNOTS('',3,(#90963,#90964,#90965,#90966,#90967,
#90968,#90969,#90970,#90971,#90972),.UNSPECIFIED.,.F.,.F.,(4,3,3,4),(1014.48334915183,
1014.56635143231,1014.6503892709,1014.73442710948),.UNSPECIFIED.);
#697=B_SPLINE_CURVE_WITH_KNOTS('',3,(#90974,#90975,#90976,#90977,#90978,
#90979,#90980,#90981,#90982,#90983),.UNSPECIFIED.,.F.,.F.,(4,3,3,4),(1014.48401170027,
1014.57777675051,1014.67102940355,1014.73442710929),.UNSPECIFIED.);
#698=B_SPLINE_CURVE_WITH_KNOTS('',3,(#90984,#90985,#90986,#90987,#90988,
#90989,#90990,#90991,#90992,#90993,#90994,#90995,#90996,#90997,#90998,#90999,
#91000,#91001,#91002,#91003,#91004,#91005,#91006,#91007,#91008,#91009,#91010,
#91011,#91012,#91013,#91014,#91015,#91016,#91017,#91018,#91019,#91020,#91021,
#91022,#91023,#91024,#91025,#91026,#91027,#91028,#91029,#91030,#91031,#91032,
#91033,#91034,#91035,#91036,#91037,#91038,#91039,#91040,#91041,#91042,#91043,
#91044,#91045,#91046,#91047,#91048,#91049,#91050,#91051,#91052,#91053,#91054,
#91055,#91056,#91057,#91058,#91059,#91060,#91061,#91062,#91063,#91064,#91065,
#91066,#91067,#91068,#91069,#91070,#91071,#91072,#91073,#91074,#91075,#91076,
#91077,#91078,#91079,#91080,#91081,#91082,#91083,#91084,#91085,#91086,#91087,
#91088,#91089,#91090,#91091,#91092,#91093,#91094,#91095,#91096,#91097,#91098,
#91099,#91100,#91101,#91102,#91103,#91104,#91105,#91106,#91107,#91108,#91109,
#91110,#91111,#91112,#91113,#91114,#91115,#91116,#91117,#91118,#91119,#91120,
#91121,#91122,#91123,#91124,#91125,#91126,#91127,#91128,#91129,#91130,#91131,
#91132,#91133,#91134,#91135,#91136,#91137,#91138,#91139,#91140,#91141,#91142,
#91143,#91144,#91145,#91146,#91147,#91148,#91149,#91150,#91151,#91152,#91153,
#91154,#91155,#91156,#91157,#91158,#91159,#91160,#91161,#91162,#91163,#91164,
#91165,#91166,#91167,#91168,#91169,#91170,#91171,#91172,#91173,#91174,#91175,
#91176,#91177,#91178,#91179,#91180,#91181,#91182,#91183,#91184,#91185,#91186,
#91187,#91188,#91189,#91190,#91191,#91192,#91193,#91194,#91195,#91196,#91197,
#91198,#91199,#91200,#91201,#91202,#91203),.UNSPECIFIED.,.F.,.F.,(4,3,3,
3,3,3,3,3,3,3,3,3,3,3,3,3,3,3,3,3,3,3,3,3,3,3,3,3,3,3,3,3,3,3,3,3,3,3,3,
3,3,3,3,3,3,3,3,3,3,3,3,3,3,3,3,3,3,3,3,3,3,3,3,3,3,3,3,3,3,3,3,3,3,4),
(1014.73442710948,1014.81865935941,1014.90290397472,1014.98717787641,1015.07149800121,
1015.15593230497,1015.24043337517,1015.32506721425,1015.3503762821,1015.43411499394,
1015.51775050531,1015.60130294871,1015.68479238456,1015.76824633517,1015.85168282902,
1015.93511993877,1016.01857573369,1016.10212022642,1016.18570930935,1016.26943257691,
1016.35011229282,1016.43385100467,1016.51748651603,1016.60103895943,1016.68452839528,
1016.76798234589,1016.85141883974,1016.93485594949,1017.01831174441,1017.10185623714,
1017.18544532008,1017.26916858764,1017.34984830354,1017.43358701539,1017.51722252675,
1017.60077497015,1017.68426440601,1017.76771835662,1017.85115485047,1017.93459196022,
1018.01804775514,1018.10159224787,1018.18518133081,1018.26890459837,1018.34958431426,
1018.43332302611,1018.51695853747,1018.60051098087,1018.68400041672,1018.76745436734,
1018.85089086118,1018.93432797094,1019.01778376585,1019.10132825858,1019.18491734152,
1019.26864060908,1019.34932032498,1019.43305903683,1019.51669454819,1019.60024699159,
1019.68373642744,1019.76719037806,1019.85062687191,1019.93406398166,1020.01751977658,
1020.10106426931,1020.18465335225,1020.26837661981,1020.3490563357,1020.43273624439,
1020.51628260801,1020.59975206856,1020.68320953995,1020.76666701133),
 .UNSPECIFIED.);
#699=B_SPLINE_CURVE_WITH_KNOTS('',3,(#91209,#91210,#91211,#91212,#91213,
#91214,#91215,#91216,#91217,#91218,#91219,#91220,#91221,#91222,#91223,#91224,
#91225,#91226,#91227,#91228,#91229,#91230,#91231,#91232,#91233,#91234,#91235,
#91236,#91237,#91238,#91239,#91240,#91241,#91242,#91243,#91244,#91245,#91246,
#91247,#91248,#91249,#91250,#91251,#91252,#91253,#91254,#91255,#91256,#91257,
#91258,#91259,#91260,#91261,#91262,#91263,#91264,#91265,#91266,#91267,#91268,
#91269,#91270,#91271,#91272,#91273,#91274,#91275,#91276,#91277,#91278,#91279,
#91280,#91281,#91282,#91283,#91284,#91285,#91286,#91287,#91288,#91289,#91290,
#91291,#91292,#91293,#91294,#91295,#91296,#91297,#91298,#91299,#91300,#91301,
#91302,#91303,#91304,#91305,#91306,#91307,#91308,#91309,#91310,#91311,#91312,
#91313,#91314,#91315,#91316,#91317,#91318,#91319,#91320,#91321,#91322,#91323,
#91324,#91325,#91326,#91327,#91328,#91329,#91330,#91331,#91332,#91333,#91334,
#91335,#91336,#91337,#91338,#91339,#91340,#91341,#91342,#91343,#91344,#91345,
#91346,#91347,#91348,#91349,#91350,#91351,#91352,#91353,#91354,#91355,#91356,
#91357,#91358,#91359,#91360,#91361,#91362,#91363,#91364,#91365,#91366,#91367,
#91368,#91369,#91370,#91371,#91372,#91373,#91374,#91375,#91376,#91377,#91378,
#91379,#91380,#91381,#91382,#91383,#91384,#91385,#91386,#91387,#91388,#91389,
#91390,#91391,#91392,#91393,#91394,#91395,#91396,#91397,#91398,#91399,#91400,
#91401,#91402,#91403,#91404,#91405,#91406,#91407,#91408,#91409,#91410,#91411,
#91412,#91413,#91414,#91415,#91416,#91417,#91418,#91419,#91420,#91421,#91422,
#91423,#91424,#91425,#91426,#91427,#91428,#91429,#91430,#91431),
 .UNSPECIFIED.,.F.,.F.,(4,3,3,3,3,3,3,3,3,3,3,3,3,3,3,3,3,3,3,3,3,3,3,3,
3,3,3,3,3,3,3,3,3,3,3,3,3,3,3,3,3,3,3,3,3,3,3,3,3,3,3,3,3,3,3,3,3,3,3,3,
3,3,3,3,3,3,3,3,3,3,3,3,3,3,4),(1021.01761241666,1021.0385017267,1021.12224043855,
1021.20587594991,1021.28942839331,1021.37291782916,1021.45637177978,1021.53980827363,
1021.62324538338,1021.7067011783,1021.79024567103,1021.87383475397,1021.95755802153,
1022.03823773742,1022.12197644927,1022.20561196063,1022.28916440403,1022.37265383988,
1022.4561077905,1022.53954428434,1022.6229813941,1022.70643718902,1022.78998168175,
1022.87357076469,1022.95729403224,1023.03797374814,1023.12171245999,1023.20534797135,
1023.28890041475,1023.3723898506,1023.45584380122,1023.53928029506,1023.62271740482,
1023.70617319974,1023.78971769246,1023.87330677541,1023.95703004296,1024.03770975886,
1024.12144847071,1024.20508398207,1024.28863642547,1024.37212586132,1024.45557981194,
1024.53901630578,1024.62245341554,1024.70590921046,1024.78945370319,1024.87304278613,
1024.95676605368,1025.03744576958,1025.12118448143,1025.20481999279,1025.28837243619,
1025.37186187204,1025.45531582266,1025.5387523165,1025.62218942626,1025.70564522118,
1025.78918971391,1025.87277879685,1025.9565020644,1026.0371817803,1026.12092049215,
1026.20455600351,1026.28810844691,1026.37159788276,1026.45505183337,1026.53848832722,
1026.62192543697,1026.70538123189,1026.78892572462,1026.87251480756,1026.95623807512,
1027.03691779102,1027.04981210257),.UNSPECIFIED.);
#700=B_SPLINE_CURVE_WITH_KNOTS('',3,(#91432,#91433,#91434,#91435,#91436,
#91437,#91438,#91439,#91440,#91441),.UNSPECIFIED.,.F.,.F.,(4,3,3,4),(1020.76588157733,
1020.84916885192,1020.9333906342,1021.01761241647),.UNSPECIFIED.);
#701=B_SPLINE_CURVE_WITH_KNOTS('',3,(#91443,#91444,#91445,#91446,#91447,
#91448,#91449,#91450,#91451,#91452),.UNSPECIFIED.,.F.,.F.,(4,3,3,4),(1020.76666701133,
1020.85000603278,1020.93380922472,1021.01761241666),.UNSPECIFIED.);
#702=B_SPLINE_CURVE_WITH_KNOTS('',3,(#91453,#91454,#91455,#91456,#91457,
#91458,#91459,#91460,#91461,#91462,#91463,#91464,#91465,#91466,#91467,#91468,
#91469,#91470,#91471,#91472,#91473,#91474,#91475,#91476,#91477,#91478,#91479,
#91480,#91481,#91482,#91483,#91484,#91485,#91486,#91487,#91488,#91489,#91490,
#91491,#91492,#91493,#91494,#91495,#91496,#91497,#91498,#91499,#91500,#91501,
#91502,#91503,#91504,#91505,#91506,#91507,#91508,#91509,#91510,#91511,#91512,
#91513,#91514,#91515,#91516,#91517,#91518,#91519,#91520,#91521,#91522,#91523,
#91524,#91525,#91526,#91527,#91528,#91529,#91530,#91531,#91532,#91533,#91534,
#91535,#91536,#91537,#91538,#91539,#91540,#91541,#91542,#91543,#91544,#91545,
#91546,#91547,#91548,#91549,#91550,#91551,#91552,#91553,#91554,#91555,#91556,
#91557,#91558,#91559,#91560,#91561,#91562,#91563,#91564,#91565,#91566,#91567,
#91568,#91569,#91570,#91571,#91572,#91573,#91574,#91575,#91576,#91577,#91578,
#91579,#91580,#91581,#91582,#91583,#91584,#91585,#91586,#91587,#91588,#91589,
#91590,#91591,#91592,#91593,#91594,#91595,#91596,#91597,#91598,#91599,#91600,
#91601,#91602,#91603,#91604,#91605,#91606,#91607,#91608,#91609,#91610,#91611,
#91612,#91613,#91614,#91615,#91616,#91617,#91618,#91619,#91620,#91621,#91622,
#91623,#91624,#91625,#91626,#91627,#91628,#91629,#91630,#91631,#91632,#91633,
#91634,#91635,#91636,#91637,#91638,#91639,#91640,#91641,#91642,#91643,#91644,
#91645,#91646,#91647,#91648,#91649,#91650,#91651,#91652,#91653,#91654,#91655,
#91656,#91657,#91658,#91659,#91660,#91661,#91662,#91663,#91664,#91665,#91666,
#91667,#91668,#91669,#91670,#91671,#91672),.UNSPECIFIED.,.F.,.F.,(4,3,3,
3,3,3,3,3,3,3,3,3,3,3,3,3,3,3,3,3,3,3,3,3,3,3,3,3,3,3,3,3,3,3,3,3,3,3,3,
3,3,3,3,3,3,3,3,3,3,3,3,3,3,3,3,3,3,3,3,3,3,3,3,3,3,3,3,3,3,3,3,3,3,4),
(1021.01761241685,1021.11504298746,1021.21306759752,1021.31178249612,1021.34879234642,
1021.43253105826,1021.51616656963,1021.59971901302,1021.68320844887,1021.76666239948,
1021.85009889332,1021.93353600308,1022.01699179799,1022.10053629072,1022.18412537365,
1022.26784864121,1022.34852835714,1022.43226706899,1022.51590258035,1022.59945502375,
1022.6829444596,1022.76639841022,1022.84983490406,1022.93327201382,1023.01672780874,
1023.10027230147,1023.18386138441,1023.26758465196,1023.34826436786,1023.43200307971,
1023.51563859107,1023.59919103447,1023.68268047032,1023.76613442094,1023.84957091479,
1023.93300802454,1024.01646381946,1024.10000831219,1024.18359739513,1024.26732066269,
1024.34800037858,1024.43173909043,1024.51537460179,1024.59892704519,1024.68241648104,
1024.76587043166,1024.8493069255,1024.93274403526,1025.01619983017,1025.0997443229,
1025.18333340584,1025.2670566734,1025.3477363893,1025.43147510115,1025.51511061251,
1025.59866305591,1025.68215249176,1025.76560644238,1025.84904293623,1025.93248004598,
1026.0159358409,1026.09948033363,1026.18306941657,1026.26679268413,1026.34747240002,
1026.43062447609,1026.51364527232,1026.59659023187,1026.67947804615,1026.76232736026,
1026.84517175658,1026.92801291739,1027.01089396545,1027.04899943094),
 .UNSPECIFIED.);
#703=B_SPLINE_CURVE_WITH_KNOTS('',3,(#91678,#91679,#91680,#91681,#91682,
#91683,#91684,#91685,#91686,#91687,#91688,#91689,#91690,#91691,#91692,#91693,
#91694,#91695,#91696,#91697,#91698,#91699,#91700,#91701,#91702,#91703,#91704,
#91705,#91706,#91707,#91708,#91709,#91710,#91711,#91712,#91713,#91714,#91715,
#91716,#91717,#91718,#91719,#91720,#91721,#91722,#91723,#91724,#91725,#91726,
#91727,#91728,#91729,#91730,#91731,#91732,#91733,#91734,#91735,#91736,#91737,
#91738,#91739,#91740,#91741,#91742,#91743,#91744,#91745,#91746,#91747,#91748,
#91749,#91750,#91751,#91752,#91753,#91754,#91755,#91756,#91757,#91758,#91759,
#91760,#91761,#91762,#91763,#91764,#91765,#91766,#91767,#91768,#91769,#91770,
#91771,#91772,#91773,#91774,#91775,#91776,#91777,#91778,#91779,#91780,#91781,
#91782,#91783,#91784,#91785,#91786,#91787,#91788,#91789,#91790,#91791,#91792,
#91793,#91794,#91795,#91796,#91797,#91798,#91799,#91800,#91801,#91802,#91803,
#91804,#91805,#91806,#91807,#91808,#91809,#91810,#91811,#91812,#91813,#91814,
#91815,#91816,#91817,#91818,#91819,#91820,#91821,#91822,#91823,#91824,#91825,
#91826,#91827,#91828,#91829,#91830,#91831,#91832,#91833,#91834,#91835,#91836,
#91837,#91838,#91839,#91840,#91841,#91842,#91843,#91844,#91845,#91846,#91847,
#91848,#91849,#91850,#91851,#91852,#91853,#91854,#91855,#91856,#91857,#91858,
#91859,#91860,#91861,#91862,#91863,#91864,#91865,#91866,#91867,#91868,#91869,
#91870,#91871,#91872,#91873,#91874,#91875,#91876,#91877,#91878,#91879,#91880,
#91881,#91882,#91883,#91884,#91885,#91886,#91887,#91888,#91889,#91890,#91891,
#91892,#91893,#91894,#91895,#91896,#91897),.UNSPECIFIED.,.F.,.F.,(4,3,3,
3,3,3,3,3,3,3,3,3,3,3,3,3,3,3,3,3,3,3,3,3,3,3,3,3,3,3,3,3,3,3,3,3,3,3,3,
3,3,3,3,3,3,3,3,3,3,3,3,3,3,3,3,3,3,3,3,3,3,3,3,3,3,3,3,3,3,3,3,3,3,4),
(1027.30079772384,1027.38345061798,1027.46606102377,1027.54865006983,1027.63123653473,
1027.71383919223,1027.79652759215,1027.8792596504,1027.96212323658,1028.03665380174,
1028.12039251359,1028.20402802495,1028.28758046835,1028.3710699042,1028.45452385482,
1028.53796034866,1028.62139745842,1028.70485325334,1028.78839774607,1028.87198682901,
1028.95571009657,1029.03638981246,1029.12012852431,1029.20376403567,1029.28731647907,
1029.37080591492,1029.45425986554,1029.53769635938,1029.62113346914,1029.70458926406,
1029.78813375679,1029.87172283973,1029.95544610729,1030.03612582318,1030.11986453503,
1030.20350004639,1030.28705248979,1030.37054192564,1030.45399587626,1030.5374323701,
1030.62086947986,1030.70432527478,1030.7878697675,1030.87145885045,1030.955182118,
1031.0358618339,1031.11960054575,1031.20323605711,1031.28678850051,1031.37027793636,
1031.45373188697,1031.53716838082,1031.62060549057,1031.70406128549,1031.78760577822,
1031.87119486116,1031.95491812871,1032.03559784462,1032.11933655647,1032.20297206784,
1032.28652451124,1032.37001394709,1032.45346789771,1032.53690439156,1032.62034150132,
1032.70379729624,1032.78734178897,1032.87093087191,1032.95465413947,1033.03533385535,
1033.12167787295,1033.20790695979,1033.29400030748,1033.33354879478),
 .UNSPECIFIED.);
#704=B_SPLINE_CURVE_WITH_KNOTS('',3,(#91898,#91899,#91900,#91901,#91902,
#91903,#91904,#91905,#91906,#91907),.UNSPECIFIED.,.F.,.F.,(4,3,3,4),(1027.04981210257,
1027.15701204208,1027.26224713867,1027.30079772369),.UNSPECIFIED.);
#705=B_SPLINE_CURVE_WITH_KNOTS('',3,(#91909,#91910,#91911,#91912,#91913,
#91914,#91915,#91916,#91917,#91918),.UNSPECIFIED.,.F.,.F.,(4,3,3,4),(1027.04899943094,
1027.13197379122,1027.21638575744,1027.30079772365),.UNSPECIFIED.);
#706=B_SPLINE_CURVE_WITH_KNOTS('',3,(#91919,#91920,#91921,#91922,#91923,
#91924,#91925,#91926,#91927,#91928,#91929,#91930,#91931,#91932,#91933,#91934,
#91935,#91936,#91937,#91938,#91939,#91940,#91941,#91942,#91943,#91944,#91945,
#91946,#91947,#91948,#91949,#91950,#91951,#91952,#91953,#91954,#91955,#91956,
#91957,#91958,#91959,#91960,#91961,#91962,#91963,#91964,#91965,#91966,#91967,
#91968,#91969,#91970,#91971,#91972,#91973,#91974,#91975,#91976,#91977,#91978,
#91979,#91980,#91981,#91982,#91983,#91984,#91985,#91986,#91987,#91988,#91989,
#91990,#91991,#91992,#91993,#91994,#91995,#91996,#91997,#91998,#91999,#92000,
#92001,#92002,#92003,#92004,#92005,#92006,#92007,#92008,#92009,#92010,#92011,
#92012,#92013,#92014,#92015,#92016,#92017,#92018,#92019,#92020,#92021,#92022,
#92023,#92024,#92025,#92026,#92027,#92028,#92029,#92030,#92031,#92032,#92033,
#92034,#92035,#92036,#92037,#92038,#92039,#92040,#92041,#92042,#92043,#92044,
#92045,#92046,#92047,#92048,#92049,#92050,#92051,#92052,#92053,#92054,#92055,
#92056,#92057,#92058,#92059,#92060,#92061,#92062,#92063,#92064,#92065,#92066,
#92067,#92068,#92069,#92070,#92071,#92072,#92073,#92074,#92075,#92076,#92077,
#92078,#92079,#92080,#92081,#92082,#92083,#92084,#92085,#92086,#92087,#92088,
#92089,#92090,#92091,#92092,#92093,#92094,#92095,#92096,#92097,#92098,#92099,
#92100,#92101,#92102,#92103,#92104,#92105,#92106,#92107,#92108,#92109,#92110,
#92111,#92112,#92113,#92114,#92115,#92116,#92117,#92118,#92119,#92120,#92121,
#92122,#92123,#92124,#92125,#92126,#92127,#92128,#92129,#92130,#92131,#92132,
#92133,#92134,#92135,#92136,#92137,#92138),.UNSPECIFIED.,.F.,.F.,(4,3,3,
3,3,3,3,3,3,3,3,3,3,3,3,3,3,3,3,3,3,3,3,3,3,3,3,3,3,3,3,3,3,3,3,3,3,3,3,
3,3,3,3,3,3,3,3,3,3,3,3,3,3,3,3,3,3,3,3,3,3,3,3,3,3,3,3,3,3,3,3,3,3,4),
(1027.30079772384,1027.34720841074,1027.43094712259,1027.51458263395,1027.59813507735,
1027.6816245132,1027.76507846381,1027.84851495766,1027.93195206742,1028.01540786233,
1028.09895235506,1028.182541438,1028.26626470556,1028.34694442146,1028.43068313331,
1028.51431864467,1028.59787108807,1028.68136052392,1028.76481447454,1028.84825096838,
1028.93168807814,1029.01514387306,1029.09868836579,1029.18227744873,1029.26600071628,
1029.34668043218,1029.43041914403,1029.51405465539,1029.59760709879,1029.68109653464,
1029.76455048526,1029.8479869791,1029.93142408886,1030.01487988377,1030.0984243765,
1030.18201345944,1030.265736727,1030.3464164429,1030.43015515475,1030.51379066611,
1030.59734310951,1030.68083254536,1030.76428649598,1030.84772298982,1030.93116009958,
1031.0146158945,1031.09816038723,1031.18174947017,1031.26547273773,1031.34615245362,
1031.42989116547,1031.51352667683,1031.59707912023,1031.68056855608,1031.7640225067,
1031.84745900054,1031.9308961103,1032.01435190522,1032.09789639795,1032.18148548089,
1032.26520874844,1032.34588846434,1032.4296278957,1032.51326395797,1032.59681678439,
1032.6803064359,1032.76375973116,1032.84719533129,1032.9306313088,1033.01408573256,
1033.09762552072,1033.18120980058,1033.26492039566,1033.3328408694),
 .UNSPECIFIED.);
#707=B_SPLINE_CURVE_WITH_KNOTS('',3,(#92144,#92145,#92146,#92147,#92148,
#92149,#92150,#92151,#92152,#92153,#92154,#92155,#92156,#92157,#92158,#92159,
#92160,#92161,#92162,#92163,#92164,#92165,#92166,#92167,#92168,#92169,#92170,
#92171,#92172,#92173,#92174,#92175,#92176,#92177,#92178,#92179,#92180,#92181,
#92182,#92183,#92184,#92185,#92186,#92187,#92188,#92189,#92190,#92191,#92192,
#92193,#92194,#92195,#92196,#92197,#92198,#92199,#92200,#92201,#92202,#92203,
#92204,#92205,#92206,#92207,#92208,#92209,#92210,#92211,#92212,#92213,#92214,
#92215,#92216,#92217,#92218,#92219,#92220,#92221,#92222,#92223,#92224,#92225,
#92226,#92227,#92228,#92229,#92230,#92231,#92232,#92233,#92234,#92235,#92236,
#92237,#92238,#92239,#92240,#92241,#92242,#92243,#92244,#92245,#92246,#92247,
#92248,#92249,#92250,#92251,#92252,#92253,#92254,#92255,#92256,#92257,#92258,
#92259,#92260,#92261,#92262,#92263,#92264,#92265,#92266,#92267,#92268,#92269,
#92270,#92271,#92272,#92273,#92274,#92275,#92276,#92277,#92278,#92279,#92280,
#92281,#92282,#92283,#92284,#92285,#92286,#92287,#92288,#92289,#92290,#92291,
#92292,#92293,#92294,#92295,#92296,#92297,#92298,#92299,#92300,#92301,#92302,
#92303,#92304,#92305,#92306,#92307,#92308,#92309,#92310,#92311,#92312,#92313,
#92314,#92315,#92316,#92317,#92318,#92319,#92320,#92321,#92322,#92323,#92324,
#92325,#92326,#92327,#92328,#92329,#92330,#92331,#92332,#92333,#92334,#92335,
#92336,#92337,#92338,#92339,#92340,#92341,#92342,#92343,#92344,#92345,#92346,
#92347,#92348,#92349,#92350,#92351,#92352,#92353,#92354,#92355,#92356,#92357,
#92358,#92359,#92360),.UNSPECIFIED.,.F.,.F.,(4,3,3,3,3,3,3,3,3,3,3,3,3,
3,3,3,3,3,3,3,3,3,3,3,3,3,3,3,3,3,3,3,3,3,3,3,3,3,3,3,3,3,3,3,3,3,3,3,3,
3,3,3,3,3,3,3,3,3,3,3,3,3,3,3,3,3,3,3,3,3,3,3,4),(1033.58398303112,1033.67338509724,
1033.76380628944,1033.85369237392,1033.94438111999,1034.03506986606,1034.11880857791,
1034.20244408928,1034.28599653269,1034.36948596854,1034.45293991916,1034.53637641301,
1034.61981352278,1034.7032693177,1034.78681381043,1034.87040289338,1034.95412616094,
1035.03480587679,1035.11854458864,1035.2021801,1035.2857325434,1035.36922197925,
1035.45267592987,1035.53611242371,1035.61954953347,1035.70300532839,1035.78654982112,
1035.87013890406,1035.95386217161,1036.03454188751,1036.11828059935,1036.20191611072,
1036.28546855412,1036.36895798997,1036.45241194058,1036.53584843442,1036.61928554418,
1036.70274133909,1036.78628583182,1036.86987491476,1036.95359818232,1037.03427789823,
1037.11801661008,1037.20165212144,1037.28520456484,1037.3686940007,1037.45214795131,
1037.53558444516,1037.61902155491,1037.70247734983,1037.78602184256,1037.8696109255,
1037.95333419306,1038.03401390895,1038.1177526208,1038.20138813216,1038.28494057556,
1038.36843001142,1038.45188396203,1038.53532045588,1038.61875756563,1038.70221336055,
1038.78575785328,1038.86934693622,1038.95307020378,1039.03374991967,1039.11622054546,
1039.1985958952,1039.28089518975,1039.36453651586,1039.44674452642,1039.5311025103,
1039.61546049419),.UNSPECIFIED.);
#708=B_SPLINE_CURVE_WITH_KNOTS('',3,(#92361,#92362,#92363,#92364,#92365,
#92366,#92367,#92368,#92369,#92370),.UNSPECIFIED.,.F.,.F.,(4,3,3,4),(1033.33354879478,
1033.41949132289,1033.50534392917,1033.58398303102),.UNSPECIFIED.);
#709=B_SPLINE_CURVE_WITH_KNOTS('',3,(#92372,#92373,#92374,#92375,#92376,
#92377,#92378,#92379,#92380,#92381,#92382,#92383,#92384),.UNSPECIFIED.,
 .F.,.F.,(4,3,3,3,4),(1033.3328408694,1033.34562447506,1033.45780467658,
1033.56712465127,1033.5839830309),.UNSPECIFIED.);
#710=B_SPLINE_CURVE_WITH_KNOTS('',3,(#92385,#92386,#92387,#92388,#92389,
#92390,#92391,#92392,#92393,#92394,#92395,#92396,#92397,#92398,#92399,#92400,
#92401,#92402,#92403,#92404,#92405,#92406,#92407,#92408,#92409,#92410,#92411,
#92412,#92413,#92414,#92415,#92416,#92417,#92418,#92419,#92420,#92421,#92422,
#92423,#92424,#92425,#92426,#92427,#92428,#92429,#92430,#92431,#92432,#92433,
#92434,#92435,#92436,#92437,#92438,#92439,#92440,#92441,#92442,#92443,#92444,
#92445,#92446,#92447,#92448,#92449,#92450,#92451,#92452,#92453,#92454,#92455,
#92456,#92457,#92458,#92459,#92460,#92461,#92462,#92463,#92464,#92465,#92466,
#92467,#92468,#92469,#92470,#92471,#92472,#92473,#92474,#92475,#92476,#92477,
#92478,#92479,#92480,#92481,#92482,#92483,#92484,#92485,#92486,#92487,#92488,
#92489,#92490,#92491,#92492,#92493,#92494,#92495,#92496,#92497,#92498,#92499,
#92500,#92501,#92502,#92503,#92504,#92505,#92506,#92507,#92508,#92509,#92510,
#92511,#92512,#92513,#92514,#92515,#92516,#92517,#92518,#92519,#92520,#92521,
#92522,#92523,#92524,#92525,#92526,#92527,#92528,#92529,#92530,#92531,#92532,
#92533,#92534,#92535,#92536,#92537,#92538,#92539,#92540,#92541,#92542,#92543,
#92544,#92545,#92546,#92547,#92548,#92549,#92550,#92551,#92552,#92553,#92554,
#92555,#92556,#92557,#92558,#92559,#92560,#92561,#92562,#92563,#92564,#92565,
#92566,#92567,#92568,#92569,#92570,#92571,#92572,#92573,#92574,#92575,#92576,
#92577,#92578,#92579,#92580,#92581,#92582,#92583,#92584,#92585,#92586,#92587,
#92588,#92589,#92590,#92591,#92592,#92593,#92594,#92595,#92596,#92597,#92598,
#92599,#92600,#92601,#92602,#92603,#92604,#92605,#92606,#92607),
 .UNSPECIFIED.,.F.,.F.,(4,3,3,3,3,3,3,3,3,3,3,3,3,3,3,3,3,3,3,3,3,3,3,3,
3,3,3,3,3,3,3,3,3,3,3,3,3,3,3,3,3,3,3,3,3,3,3,3,3,3,3,3,3,3,3,3,3,3,3,3,
3,3,3,3,3,3,3,3,3,3,3,3,3,3,4),(1033.58398303102,1033.66648276244,1033.75134247786,
1033.83375761489,1033.916162907,1033.99857725614,1034.08527306355,1034.1678080953,
1034.25039850859,1034.33310237985,1034.34536048578,1034.42909919763,1034.51273470899,
1034.59628715239,1034.67977658824,1034.76323053885,1034.8466670327,1034.93010414246,
1035.01355993737,1035.0971044301,1035.18069351304,1035.2644167806,1035.3450964965,
1035.42883520835,1035.51247071971,1035.59602316311,1035.67951259896,1035.76296654958,
1035.84640304342,1035.92984015318,1036.0132959481,1036.09684044082,1036.18042952377,
1036.26415279132,1036.34483250722,1036.42857121907,1036.51220673043,1036.59575917383,
1036.67924860968,1036.7627025603,1036.84613905414,1036.9295761639,1037.01303195882,
1037.09657645155,1037.18016553449,1037.26388880205,1037.34456851794,1037.42830722979,
1037.51194274115,1037.59549518455,1037.6789846204,1037.76243857102,1037.84587506486,
1037.92931217462,1038.01276796954,1038.09631246226,1038.17990154521,1038.26362481276,
1038.34430452866,1038.42804324051,1038.51167875187,1038.59523119527,1038.67872063112,
1038.76217458174,1038.84561107558,1038.92904818534,1039.01250398026,1039.09604847299,
1039.17963755593,1039.26336082349,1039.34404053938,1039.43122686491,1039.51828940803,
1039.60520573103,1039.61679924244),.UNSPECIFIED.);
#711=B_SPLINE_CURVE_WITH_KNOTS('',3,(#92613,#92614,#92615,#92616,#92617,
#92618,#92619,#92620,#92621,#92622,#92623,#92624,#92625,#92626,#92627,#92628,
#92629,#92630,#92631,#92632,#92633,#92634,#92635,#92636,#92637,#92638,#92639,
#92640,#92641,#92642,#92643,#92644,#92645,#92646,#92647,#92648,#92649,#92650,
#92651,#92652,#92653,#92654,#92655,#92656,#92657,#92658,#92659,#92660,#92661,
#92662,#92663,#92664,#92665,#92666,#92667,#92668,#92669,#92670,#92671,#92672,
#92673,#92674,#92675,#92676,#92677,#92678,#92679,#92680,#92681,#92682,#92683,
#92684,#92685,#92686,#92687,#92688,#92689,#92690,#92691,#92692,#92693,#92694,
#92695,#92696,#92697,#92698,#92699,#92700,#92701,#92702,#92703,#92704,#92705,
#92706,#92707,#92708,#92709,#92710,#92711,#92712,#92713,#92714,#92715,#92716,
#92717,#92718,#92719,#92720,#92721,#92722,#92723,#92724,#92725,#92726,#92727,
#92728,#92729,#92730,#92731,#92732,#92733,#92734,#92735,#92736,#92737,#92738,
#92739,#92740,#92741,#92742,#92743,#92744,#92745,#92746,#92747,#92748,#92749,
#92750,#92751,#92752,#92753,#92754,#92755,#92756,#92757,#92758,#92759,#92760,
#92761,#92762,#92763,#92764,#92765,#92766,#92767,#92768,#92769,#92770,#92771,
#92772,#92773,#92774,#92775,#92776,#92777,#92778,#92779,#92780,#92781,#92782,
#92783,#92784,#92785,#92786,#92787,#92788,#92789,#92790,#92791,#92792,#92793,
#92794,#92795,#92796,#92797,#92798,#92799,#92800,#92801,#92802,#92803,#92804,
#92805,#92806,#92807,#92808,#92809,#92810,#92811,#92812,#92813,#92814,#92815,
#92816,#92817,#92818,#92819,#92820,#92821,#92822,#92823,#92824,#92825,#92826,
#92827,#92828,#92829,#92830,#92831,#92832),.UNSPECIFIED.,.F.,.F.,(4,3,3,
3,3,3,3,3,3,3,3,3,3,3,3,3,3,3,3,3,3,3,3,3,3,3,3,3,3,3,3,3,3,3,3,3,3,3,3,
3,3,3,3,3,3,3,3,3,3,3,3,3,3,3,3,3,3,3,3,3,3,3,3,3,3,3,3,3,3,3,3,3,3,4),
(1039.8671683382,1040.00043133528,1040.03348593039,1040.11722464224,1040.2008601536,
1040.284412597,1040.36790203285,1040.45135598347,1040.53479247731,1040.61822958707,
1040.70168538198,1040.78522987471,1040.86881895765,1040.95254222521,1041.03322194111,
1041.11696065296,1041.20059616432,1041.28414860772,1041.36763804357,1041.45109199419,
1041.53452848803,1041.61796559779,1041.70142139271,1041.78496588544,1041.86855496838,
1041.95227823593,1042.03295795183,1042.11669666368,1042.20033217504,1042.28388461844,
1042.36737405429,1042.45082800491,1042.53426449875,1042.61770160851,1042.70115740343,
1042.78470189616,1042.8682909791,1042.95201424665,1043.03269396255,1043.1164326744,
1043.20006818576,1043.28362062916,1043.36711006501,1043.45056401563,1043.53400050947,
1043.61743761923,1043.70089341415,1043.78443790688,1043.86802698982,1043.95175025737,
1044.03242997327,1044.11616868512,1044.19980419648,1044.28335663988,1044.36684607573,
1044.45030002635,1044.53373652019,1044.61717362995,1044.70062942487,1044.7841739176,
1044.86776300054,1044.95148626809,1045.03216598399,1045.11591254731,1045.1995541538,
1045.2869547973,1045.37043923893,1045.45388648413,1045.53731462072,1045.62074171969,
1045.70421650828,1045.78771938856,1045.87130266069,1045.89875930182),
 .UNSPECIFIED.);
#712=B_SPLINE_CURVE_WITH_KNOTS('',3,(#92833,#92834,#92835,#92836,#92837,
#92838,#92839,#92840,#92841,#92842),.UNSPECIFIED.,.F.,.F.,(4,3,3,4),(1039.61546049419,
1039.69771884837,1039.78244359319,1039.86716833801),.UNSPECIFIED.);
#713=B_SPLINE_CURVE_WITH_KNOTS('',3,(#92844,#92845,#92846,#92847,#92848,
#92849,#92850,#92851,#92852,#92853),.UNSPECIFIED.,.F.,.F.,(4,3,3,4),(1039.61679924244,
1039.70355771309,1039.79019167618,1039.8671683382),.UNSPECIFIED.);
#714=B_SPLINE_CURVE_WITH_KNOTS('',3,(#92854,#92855,#92856,#92857,#92858,
#92859,#92860,#92861,#92862,#92863,#92864,#92865,#92866,#92867,#92868,#92869,
#92870,#92871,#92872,#92873,#92874,#92875,#92876,#92877,#92878,#92879,#92880,
#92881,#92882,#92883,#92884,#92885,#92886,#92887,#92888,#92889,#92890,#92891,
#92892,#92893,#92894,#92895,#92896,#92897,#92898,#92899,#92900,#92901,#92902,
#92903,#92904,#92905,#92906,#92907,#92908,#92909,#92910,#92911,#92912,#92913,
#92914,#92915,#92916,#92917,#92918,#92919,#92920,#92921,#92922,#92923,#92924,
#92925,#92926,#92927,#92928,#92929,#92930,#92931,#92932,#92933,#92934,#92935,
#92936,#92937,#92938,#92939,#92940,#92941,#92942,#92943,#92944,#92945,#92946,
#92947,#92948,#92949,#92950,#92951,#92952,#92953,#92954,#92955,#92956,#92957,
#92958,#92959,#92960,#92961,#92962,#92963,#92964,#92965,#92966,#92967,#92968,
#92969,#92970,#92971,#92972,#92973,#92974,#92975,#92976,#92977,#92978,#92979,
#92980,#92981,#92982,#92983,#92984,#92985,#92986,#92987,#92988,#92989,#92990,
#92991,#92992,#92993,#92994,#92995,#92996,#92997,#92998,#92999,#93000,#93001,
#93002,#93003,#93004,#93005,#93006,#93007,#93008,#93009,#93010,#93011,#93012,
#93013,#93014,#93015,#93016,#93017,#93018,#93019,#93020,#93021,#93022,#93023,
#93024,#93025,#93026,#93027,#93028,#93029,#93030,#93031,#93032,#93033,#93034,
#93035,#93036,#93037,#93038,#93039,#93040,#93041,#93042,#93043,#93044,#93045,
#93046,#93047,#93048,#93049,#93050,#93051,#93052,#93053,#93054,#93055,#93056,
#93057,#93058,#93059,#93060,#93061,#93062,#93063,#93064,#93065,#93066,#93067,
#93068,#93069,#93070,#93071,#93072,#93073),.UNSPECIFIED.,.F.,.F.,(4,3,3,
3,3,3,3,3,3,3,3,3,3,3,3,3,3,3,3,3,3,3,3,3,3,3,3,3,3,3,3,3,3,3,3,3,3,3,3,
3,3,3,3,3,3,3,3,3,3,3,3,3,3,3,3,3,3,3,3,3,3,3,3,3,3,3,3,3,3,3,3,3,3,4),
(1039.86716833831,1039.95546537544,1040.04391200484,1040.13259910912,1040.22141726067,
1040.31044353939,1040.3437765501,1040.42751526195,1040.51115077331,1040.59470321671,
1040.67819265256,1040.76164660318,1040.84508309702,1040.92852020678,1041.01197600169,
1041.09552049442,1041.17910957736,1041.26283284492,1041.34351256082,1041.42725127267,
1041.51088678403,1041.59443922743,1041.67792866328,1041.7613826139,1041.84481910774,
1041.9282562175,1042.01171201242,1042.09525650515,1042.17884558809,1042.26256885564,
1042.34324857154,1042.42698728339,1042.51062279475,1042.59417523815,1042.677664674,
1042.76111862462,1042.84455511846,1042.92799222822,1043.01144802314,1043.09499251587,
1043.17858159881,1043.26230486636,1043.34298458226,1043.42672329411,1043.51035880547,
1043.59391124887,1043.67740068472,1043.76085463534,1043.84429112918,1043.92772823894,
1044.01118403386,1044.09472852659,1044.17831760953,1044.26204087708,1044.34272059298,
1044.42645930483,1044.51009481619,1044.59364725959,1044.67713669544,1044.76059064606,
1044.8440271399,1044.92746424966,1045.01092004458,1045.09446453731,1045.17805362025,
1045.2617768878,1045.3424566037,1045.42495207221,1045.50735166068,1045.5896745793,
1045.67193861608,1045.75416729317,1045.83639550835,1045.89873380757),
 .UNSPECIFIED.);
#715=B_SPLINE_CURVE_WITH_KNOTS('',3,(#93079,#93080,#93081,#93082,#93083,
#93084,#93085,#93086,#93087,#93088,#93089,#93090,#93091,#93092,#93093,#93094,
#93095,#93096,#93097,#93098,#93099,#93100,#93101,#93102,#93103,#93104,#93105,
#93106,#93107,#93108,#93109,#93110,#93111,#93112,#93113,#93114,#93115,#93116,
#93117,#93118,#93119,#93120,#93121,#93122,#93123,#93124,#93125,#93126,#93127,
#93128,#93129,#93130,#93131,#93132,#93133,#93134,#93135,#93136,#93137,#93138,
#93139,#93140,#93141,#93142,#93143,#93144,#93145,#93146,#93147,#93148,#93149,
#93150,#93151,#93152,#93153,#93154,#93155,#93156,#93157,#93158,#93159,#93160,
#93161,#93162,#93163,#93164,#93165,#93166,#93167,#93168,#93169,#93170,#93171,
#93172,#93173,#93174,#93175,#93176,#93177,#93178,#93179,#93180,#93181,#93182,
#93183,#93184,#93185,#93186,#93187,#93188,#93189,#93190,#93191,#93192,#93193,
#93194,#93195,#93196,#93197,#93198,#93199,#93200,#93201,#93202,#93203,#93204,
#93205,#93206,#93207,#93208,#93209,#93210,#93211,#93212,#93213,#93214,#93215,
#93216,#93217,#93218,#93219,#93220,#93221,#93222,#93223,#93224,#93225,#93226,
#93227,#93228,#93229,#93230,#93231,#93232,#93233,#93234,#93235,#93236,#93237,
#93238,#93239,#93240,#93241,#93242,#93243,#93244,#93245,#93246,#93247,#93248,
#93249,#93250,#93251,#93252,#93253,#93254,#93255,#93256,#93257,#93258,#93259,
#93260,#93261,#93262,#93263,#93264,#93265,#93266,#93267,#93268,#93269,#93270,
#93271,#93272,#93273,#93274,#93275,#93276,#93277,#93278,#93279,#93280,#93281,
#93282,#93283,#93284,#93285,#93286,#93287,#93288,#93289,#93290,#93291,#93292,
#93293,#93294,#93295,#93296,#93297,#93298),.UNSPECIFIED.,.F.,.F.,(4,3,3,
3,3,3,3,3,3,3,3,3,3,3,3,3,3,3,3,3,3,3,3,3,3,3,3,3,3,3,3,3,3,3,3,3,3,3,3,
3,3,3,3,3,3,3,3,3,3,3,3,3,3,3,3,3,3,3,3,3,3,3,3,3,3,3,3,3,3,3,3,3,3,4),
(1046.15035364551,1046.23288320853,1046.3153236935,1046.39769619985,1046.48002751776,
1046.56233869259,1046.64464869556,1046.72697649462,1046.80938909424,1046.89184719101,
1046.9744299043,1047.03163800543,1047.11537671728,1047.19901222864,1047.28256467204,
1047.36605410789,1047.44950805851,1047.53294455235,1047.61638166211,1047.69983745703,
1047.78338194976,1047.8669710327,1047.95069430026,1048.03137401615,1048.115112728,
1048.19874823936,1048.28230068276,1048.36579011861,1048.44924406923,1048.53268056307,
1048.61611767283,1048.69957346774,1048.78311796047,1048.86670704341,1048.95043031097,
1049.03111002687,1049.11484873872,1049.19848425008,1049.28203669348,1049.36552612933,
1049.44898007995,1049.53241657379,1049.61585368355,1049.69930947847,1049.7828539712,
1049.86644305414,1049.95016632169,1050.03084603759,1050.11458474944,1050.1982202608,
1050.2817727042,1050.36526214005,1050.44871609067,1050.53215258451,1050.61558969427,
1050.69904548919,1050.78258998192,1050.86617906486,1050.94990233242,1051.03058204831,
1051.11432076016,1051.19795627152,1051.28150871492,1051.36499815077,1051.44845210139,
1051.53188859523,1051.61532570499,1051.69878149991,1051.78232599264,1051.86591507558,
1051.94963834313,1052.03031805903,1052.12323529288,1052.1831732766),
 .UNSPECIFIED.);
#716=B_SPLINE_CURVE_WITH_KNOTS('',3,(#93299,#93300,#93301,#93302,#93303,
#93304,#93305,#93306,#93307,#93308),.UNSPECIFIED.,.F.,.F.,(4,3,3,4),(1045.89875930182,
1045.98249444655,1046.03190199471,1046.15035364538),.UNSPECIFIED.);
#717=B_SPLINE_CURVE_WITH_KNOTS('',3,(#93310,#93311,#93312,#93313,#93314,
#93315,#93316,#93317,#93318,#93319),.UNSPECIFIED.,.F.,.F.,(4,3,3,4),(1045.89873380757,
1045.98099839907,1046.06567602216,1046.15035364526),.UNSPECIFIED.);
#718=B_SPLINE_CURVE_WITH_KNOTS('',3,(#93320,#93321,#93322,#93323,#93324,
#93325,#93326,#93327,#93328,#93329,#93330,#93331,#93332,#93333,#93334,#93335,
#93336,#93337,#93338,#93339,#93340,#93341,#93342,#93343,#93344,#93345,#93346,
#93347,#93348,#93349,#93350,#93351,#93352,#93353,#93354,#93355,#93356,#93357,
#93358,#93359,#93360,#93361,#93362,#93363,#93364,#93365,#93366,#93367,#93368,
#93369,#93370,#93371,#93372,#93373,#93374,#93375,#93376,#93377,#93378,#93379,
#93380,#93381,#93382,#93383,#93384,#93385,#93386,#93387,#93388,#93389,#93390,
#93391,#93392,#93393,#93394,#93395,#93396,#93397,#93398,#93399,#93400,#93401,
#93402,#93403,#93404,#93405,#93406,#93407,#93408,#93409,#93410,#93411,#93412,
#93413,#93414,#93415,#93416,#93417,#93418,#93419,#93420,#93421,#93422,#93423,
#93424,#93425,#93426,#93427,#93428,#93429,#93430,#93431,#93432,#93433,#93434,
#93435,#93436,#93437,#93438,#93439,#93440,#93441,#93442,#93443,#93444,#93445,
#93446,#93447,#93448,#93449,#93450,#93451,#93452,#93453,#93454,#93455,#93456,
#93457,#93458,#93459,#93460,#93461,#93462,#93463,#93464,#93465,#93466,#93467,
#93468,#93469,#93470,#93471,#93472,#93473,#93474,#93475,#93476,#93477,#93478,
#93479,#93480,#93481,#93482,#93483,#93484,#93485,#93486,#93487,#93488,#93489,
#93490,#93491,#93492,#93493,#93494,#93495,#93496,#93497,#93498,#93499,#93500,
#93501,#93502,#93503,#93504,#93505,#93506,#93507,#93508,#93509,#93510,#93511,
#93512,#93513,#93514,#93515,#93516,#93517,#93518,#93519,#93520,#93521,#93522,
#93523,#93524,#93525,#93526,#93527,#93528,#93529,#93530,#93531,#93532,#93533,
#93534,#93535,#93536),.UNSPECIFIED.,.F.,.F.,(4,3,3,3,3,3,3,3,3,3,3,3,3,
3,3,3,3,3,3,3,3,3,3,3,3,3,3,3,3,3,3,3,3,3,3,3,3,3,3,3,3,3,3,3,3,3,3,3,3,
3,3,3,3,3,3,3,3,3,3,3,3,3,3,3,3,3,3,3,3,3,3,3,4),(1046.15035364538,1046.27318238103,
1046.34219261442,1046.42593132627,1046.50956683763,1046.59311928103,1046.67660871688,
1046.7600626675,1046.84349916134,1046.9269362711,1047.01039206602,1047.09393655875,
1047.17752564169,1047.26124890924,1047.34192862514,1047.42566733699,1047.50930284835,
1047.59285529175,1047.6763447276,1047.75979867822,1047.84323517206,1047.92667228182,
1048.01012807674,1048.09367256947,1048.17726165241,1048.26098491996,1048.34166463586,
1048.42540334771,1048.50903885907,1048.59259130247,1048.67608073832,1048.75953468894,
1048.84297118278,1048.92640829254,1049.00986408746,1049.09340858019,1049.17699766313,
1049.26072093069,1049.34140064658,1049.42513935843,1049.50877486979,1049.59232731319,
1049.67581674904,1049.75927069966,1049.8427071935,1049.92614430326,1050.00960009818,
1050.09314459091,1050.17673367385,1050.2604569414,1050.3411366573,1050.42487536915,
1050.50851088051,1050.59206332391,1050.67555275976,1050.75900671038,1050.84244320422,
1050.92588031398,1051.0093361089,1051.09288060163,1051.17646968457,1051.26019295212,
1051.34087266802,1051.42462082925,1051.50826369638,1051.59246877201,1051.67595479842,
1051.75940245836,1051.84282984086,1051.92759845601,1052.01106613505,1052.09648521824,
1052.18190430144),.UNSPECIFIED.);
#719=B_SPLINE_CURVE_WITH_KNOTS('',3,(#93542,#93543,#93544,#93545,#93546,
#93547,#93548,#93549,#93550,#93551,#93552,#93553,#93554,#93555,#93556,#93557,
#93558,#93559,#93560,#93561,#93562,#93563,#93564,#93565,#93566,#93567,#93568,
#93569,#93570,#93571,#93572,#93573,#93574,#93575,#93576,#93577,#93578,#93579,
#93580,#93581,#93582,#93583,#93584,#93585,#93586,#93587,#93588,#93589,#93590,
#93591,#93592,#93593,#93594,#93595,#93596,#93597,#93598,#93599,#93600,#93601,
#93602,#93603,#93604,#93605,#93606,#93607,#93608,#93609,#93610,#93611,#93612,
#93613,#93614,#93615,#93616,#93617,#93618,#93619,#93620,#93621,#93622,#93623,
#93624,#93625,#93626,#93627,#93628,#93629,#93630,#93631,#93632,#93633,#93634,
#93635,#93636,#93637,#93638,#93639,#93640,#93641,#93642,#93643,#93644,#93645,
#93646,#93647,#93648,#93649,#93650,#93651,#93652,#93653,#93654,#93655,#93656,
#93657,#93658,#93659,#93660,#93661,#93662,#93663,#93664,#93665,#93666,#93667,
#93668,#93669,#93670,#93671,#93672,#93673,#93674,#93675,#93676,#93677,#93678,
#93679,#93680,#93681,#93682,#93683,#93684,#93685,#93686,#93687,#93688,#93689,
#93690,#93691,#93692,#93693,#93694,#93695,#93696,#93697,#93698,#93699,#93700,
#93701,#93702,#93703,#93704,#93705,#93706,#93707,#93708,#93709,#93710,#93711,
#93712,#93713,#93714,#93715,#93716,#93717,#93718,#93719,#93720,#93721,#93722,
#93723,#93724,#93725,#93726,#93727,#93728,#93729,#93730,#93731,#93732,#93733,
#93734,#93735,#93736,#93737,#93738,#93739,#93740,#93741,#93742,#93743,#93744,
#93745,#93746,#93747,#93748,#93749,#93750,#93751,#93752,#93753,#93754,#93755,
#93756,#93757,#93758,#93759,#93760,#93761),.UNSPECIFIED.,.F.,.F.,(4,3,3,
3,3,3,3,3,3,3,3,3,3,3,3,3,3,3,3,3,3,3,3,3,3,3,3,3,3,3,3,3,3,3,3,3,3,3,3,
3,3,3,3,3,3,3,3,3,3,3,3,3,3,3,3,3,3,3,3,3,3,3,3,3,3,3,3,3,3,3,3,3,3,4),
(1052.43353895256,1052.51817430875,1052.60283405086,1052.68753441534,1052.77316432894,
1052.85804489543,1052.94404948259,1053.03005406975,1053.1137927816,1053.19742829296,
1053.28098073636,1053.36447017221,1053.44792412283,1053.53136061667,1053.61479772643,
1053.69825352135,1053.78179801408,1053.86538709702,1053.94911036457,1054.02979008047,
1054.11352879232,1054.19716430368,1054.28071674708,1054.36420618293,1054.44766013355,
1054.53109662739,1054.61453373715,1054.69798953207,1054.78153402479,1054.86512310774,
1054.94884637529,1055.02952609119,1055.11326480304,1055.1969003144,1055.2804527578,
1055.36394219365,1055.44739614427,1055.53083263811,1055.61426974787,1055.69772554279,
1055.78127003552,1055.86485911846,1055.94858238601,1056.02926210191,1056.11300081376,
1056.19663632512,1056.28018876852,1056.36367820437,1056.44713215499,1056.53056864883,
1056.61400575859,1056.69746155351,1056.78100604624,1056.86459512918,1056.94831839673,
1057.02899811263,1057.11273682448,1057.19637233584,1057.27992477924,1057.36341421509,
1057.44686816571,1057.53030465955,1057.61374176931,1057.69719756423,1057.78074205696,
1057.8643311399,1057.94805440745,1058.02873412335,1058.11213530925,1058.19543350021,
1058.27862999203,1058.36176800281,1058.44486147418,1058.46567809412),
 .UNSPECIFIED.);
#720=B_SPLINE_CURVE_WITH_KNOTS('',3,(#93762,#93763,#93764,#93765,#93766,
#93767,#93768,#93769,#93770,#93771),.UNSPECIFIED.,.F.,.F.,(4,3,3,4),(1052.1831732766,
1052.27561523447,1052.36763343095,1052.43353895238),.UNSPECIFIED.);
#721=B_SPLINE_CURVE_WITH_KNOTS('',3,(#93773,#93774,#93775,#93776,#93777,
#93778,#93779,#93780,#93781,#93782),.UNSPECIFIED.,.F.,.F.,(4,3,3,4),(1052.18190430144,
1052.2656295259,1052.34060867874,1052.43353895256),.UNSPECIFIED.);
#722=B_SPLINE_CURVE_WITH_KNOTS('',3,(#93783,#93784,#93785,#93786,#93787,
#93788,#93789,#93790,#93791,#93792,#93793,#93794,#93795,#93796,#93797,#93798,
#93799,#93800,#93801,#93802,#93803,#93804,#93805,#93806,#93807,#93808,#93809,
#93810,#93811,#93812,#93813,#93814,#93815,#93816,#93817,#93818,#93819,#93820,
#93821,#93822,#93823,#93824,#93825,#93826,#93827,#93828,#93829,#93830,#93831,
#93832,#93833,#93834,#93835,#93836,#93837,#93838,#93839,#93840,#93841,#93842,
#93843,#93844,#93845,#93846,#93847,#93848,#93849,#93850,#93851,#93852,#93853,
#93854,#93855,#93856,#93857,#93858,#93859,#93860,#93861,#93862,#93863,#93864,
#93865,#93866,#93867,#93868,#93869,#93870,#93871,#93872,#93873,#93874,#93875,
#93876,#93877,#93878,#93879,#93880,#93881,#93882,#93883,#93884,#93885,#93886,
#93887,#93888,#93889,#93890,#93891,#93892,#93893,#93894,#93895,#93896,#93897,
#93898,#93899,#93900,#93901,#93902,#93903,#93904,#93905,#93906,#93907,#93908,
#93909,#93910,#93911,#93912,#93913,#93914,#93915,#93916,#93917,#93918,#93919,
#93920,#93921,#93922,#93923,#93924,#93925,#93926,#93927,#93928,#93929,#93930,
#93931,#93932,#93933,#93934,#93935,#93936,#93937,#93938,#93939,#93940,#93941,
#93942,#93943,#93944,#93945,#93946,#93947,#93948,#93949,#93950,#93951,#93952,
#93953,#93954,#93955,#93956,#93957,#93958,#93959,#93960,#93961,#93962,#93963,
#93964,#93965,#93966,#93967,#93968,#93969,#93970,#93971,#93972,#93973,#93974,
#93975,#93976,#93977,#93978,#93979,#93980,#93981,#93982,#93983,#93984,#93985,
#93986,#93987,#93988,#93989,#93990,#93991,#93992,#93993,#93994,#93995,#93996,
#93997,#93998,#93999,#94000,#94001,#94002),.UNSPECIFIED.,.F.,.F.,(4,3,3,
3,3,3,3,3,3,3,3,3,3,3,3,3,3,3,3,3,3,3,3,3,3,3,3,3,3,3,3,3,3,3,3,3,3,3,3,
3,3,3,3,3,3,3,3,3,3,3,3,3,3,3,3,3,3,3,3,3,3,3,3,3,3,3,3,3,3,3,3,3,3,4),
(1052.43353895269,1052.51622961888,1052.59882640096,1052.68135031557,1052.76382644087,
1052.84627784904,1052.92872342611,1053.011182051,1053.09372349006,1053.17630598907,
1053.25902043882,1053.34034468946,1053.42408340131,1053.50771891267,1053.59127135607,
1053.67476079192,1053.75821474254,1053.84165123638,1053.92508834614,1054.00854414106,
1054.09208863378,1054.17567771673,1054.25940098428,1054.34008070018,1054.42381941203,
1054.50745492339,1054.59100736679,1054.67449680264,1054.75795075326,1054.8413872471,
1054.92482435686,1055.00828015178,1055.09182464451,1055.17541372745,1055.259136995,
1055.3398167109,1055.42355542275,1055.50719093411,1055.59074337751,1055.67423281336,
1055.75768676398,1055.84112325782,1055.92456036758,1056.00801616249,1056.09156065522,
1056.17514973816,1056.25887300572,1056.33955272162,1056.42329143347,1056.50692694483,
1056.59047938823,1056.67396882409,1056.7574227747,1056.84085926855,1056.9242963783,
1057.00775217322,1057.09129666595,1057.17488574889,1057.25860901645,1057.33928873234,
1057.42302744419,1057.50666295555,1057.59021539895,1057.6737048348,1057.75715878542,
1057.84059527926,1057.92403238902,1058.00748818394,1058.09103267667,1058.17462175961,
1058.25834502717,1058.33902474307,1058.43375410464,1058.46629045166),
 .UNSPECIFIED.);
#723=B_SPLINE_CURVE_WITH_KNOTS('',3,(#94008,#94009,#94010,#94011,#94012,
#94013,#94014,#94015,#94016,#94017,#94018,#94019,#94020,#94021,#94022,#94023,
#94024,#94025,#94026,#94027,#94028,#94029,#94030,#94031,#94032,#94033,#94034,
#94035,#94036,#94037,#94038,#94039,#94040,#94041,#94042,#94043,#94044,#94045,
#94046,#94047,#94048,#94049,#94050,#94051,#94052,#94053,#94054,#94055,#94056,
#94057,#94058,#94059,#94060,#94061,#94062,#94063,#94064,#94065,#94066,#94067,
#94068,#94069,#94070,#94071,#94072,#94073,#94074,#94075,#94076,#94077,#94078,
#94079,#94080,#94081,#94082,#94083,#94084,#94085,#94086,#94087,#94088,#94089,
#94090,#94091,#94092,#94093,#94094,#94095,#94096,#94097,#94098,#94099,#94100,
#94101,#94102,#94103,#94104,#94105,#94106,#94107,#94108,#94109,#94110,#94111,
#94112,#94113,#94114,#94115,#94116,#94117,#94118,#94119,#94120,#94121,#94122,
#94123,#94124,#94125,#94126,#94127,#94128,#94129,#94130,#94131,#94132,#94133,
#94134,#94135,#94136,#94137,#94138,#94139,#94140,#94141,#94142,#94143,#94144,
#94145,#94146,#94147,#94148,#94149,#94150,#94151,#94152,#94153,#94154,#94155,
#94156,#94157,#94158,#94159,#94160,#94161,#94162,#94163,#94164,#94165,#94166,
#94167,#94168,#94169,#94170,#94171,#94172,#94173,#94174,#94175,#94176,#94177,
#94178,#94179,#94180,#94181,#94182,#94183,#94184,#94185,#94186,#94187,#94188,
#94189,#94190,#94191,#94192,#94193,#94194,#94195,#94196,#94197,#94198,#94199,
#94200,#94201,#94202,#94203,#94204,#94205,#94206,#94207,#94208,#94209,#94210,
#94211,#94212,#94213,#94214,#94215,#94216,#94217,#94218,#94219,#94220,#94221,
#94222,#94223,#94224,#94225,#94226,#94227),.UNSPECIFIED.,.F.,.F.,(4,3,3,
3,3,3,3,3,3,3,3,3,3,3,3,3,3,3,3,3,3,3,3,3,3,3,3,3,3,3,3,3,3,3,3,3,3,3,3,
3,3,3,3,3,3,3,3,3,3,3,3,3,3,3,3,3,3,3,3,3,3,3,3,3,3,3,3,3,3,3,3,3,3,4),
(1058.7167242599,1058.81602550497,1058.9160811218,1059.01693437788,1059.02847013407,
1059.11220884592,1059.19584435728,1059.27939680068,1059.36288623653,1059.44634018715,
1059.52977668099,1059.61321379075,1059.69666958567,1059.7802140784,1059.86380316134,
1059.94752642889,1060.02820614479,1060.11194485664,1060.195580368,1060.2791328114,
1060.36262224725,1060.44607619787,1060.52951269171,1060.61294980147,1060.69640559639,
1060.77995008912,1060.86353917206,1060.94726243961,1061.02794215551,1061.11168086736,
1061.19531637872,1061.27886882212,1061.36235825797,1061.44581220859,1061.52924870243,
1061.61268581219,1061.69614160711,1061.77968609984,1061.86327518278,1061.94699845033,
1062.02767816623,1062.11141687808,1062.19505238944,1062.27860483284,1062.36209426869,
1062.44554821931,1062.52898471315,1062.61242182291,1062.69587761783,1062.77942211056,
1062.8630111935,1062.94673446106,1063.02741417695,1063.1111528888,1063.19478840016,
1063.27834084356,1063.36183027941,1063.44528423003,1063.52872072387,1063.61215783363,
1063.69561362855,1063.77915812128,1063.86274720422,1063.94647047177,1064.02715018767,
1064.11052917265,1064.19377633222,1064.27694739578,1064.3600608703,1064.4431352178,
1064.52620538345,1064.60927132662,1064.69238160085,1064.74815950499),
 .UNSPECIFIED.);
#724=B_SPLINE_CURVE_WITH_KNOTS('',3,(#94228,#94229,#94230,#94231,#94232,
#94233,#94234,#94235,#94236,#94237),.UNSPECIFIED.,.F.,.F.,(4,3,3,4),(1058.46567809412,
1058.54875458388,1058.63273942181,1058.71672425974),.UNSPECIFIED.);
#725=B_SPLINE_CURVE_WITH_KNOTS('',3,(#94239,#94240,#94241,#94242,#94243,
#94244,#94245,#94246,#94247,#94248),.UNSPECIFIED.,.F.,.F.,(4,3,3,4),(1058.46629045166,
1058.56050203772,1058.6541694428,1058.71672425955),.UNSPECIFIED.);
#726=B_SPLINE_CURVE_WITH_KNOTS('',3,(#94249,#94250,#94251,#94252,#94253,
#94254,#94255,#94256,#94257,#94258,#94259,#94260,#94261,#94262,#94263,#94264,
#94265,#94266,#94267,#94268,#94269,#94270,#94271,#94272,#94273,#94274,#94275,
#94276,#94277,#94278,#94279,#94280,#94281,#94282,#94283,#94284,#94285,#94286,
#94287,#94288,#94289,#94290,#94291,#94292,#94293,#94294,#94295,#94296,#94297,
#94298,#94299,#94300,#94301,#94302,#94303,#94304,#94305,#94306,#94307,#94308,
#94309,#94310,#94311,#94312,#94313,#94314,#94315,#94316,#94317,#94318,#94319,
#94320,#94321,#94322,#94323,#94324,#94325,#94326,#94327,#94328,#94329,#94330,
#94331,#94332,#94333,#94334,#94335,#94336,#94337,#94338,#94339,#94340,#94341,
#94342,#94343,#94344,#94345,#94346,#94347,#94348,#94349,#94350,#94351,#94352,
#94353,#94354,#94355,#94356,#94357,#94358,#94359,#94360,#94361,#94362,#94363,
#94364,#94365,#94366,#94367,#94368,#94369,#94370,#94371,#94372,#94373,#94374,
#94375,#94376,#94377,#94378,#94379,#94380,#94381,#94382,#94383,#94384,#94385,
#94386,#94387,#94388,#94389,#94390,#94391,#94392,#94393,#94394,#94395,#94396,
#94397,#94398,#94399,#94400,#94401,#94402,#94403,#94404,#94405,#94406,#94407,
#94408,#94409,#94410,#94411,#94412,#94413,#94414,#94415,#94416,#94417,#94418,
#94419,#94420,#94421,#94422,#94423,#94424,#94425,#94426,#94427,#94428,#94429,
#94430,#94431,#94432,#94433,#94434,#94435,#94436,#94437,#94438,#94439,#94440,
#94441,#94442,#94443,#94444,#94445,#94446,#94447,#94448,#94449,#94450,#94451,
#94452,#94453,#94454,#94455,#94456,#94457,#94458,#94459,#94460,#94461,#94462,
#94463,#94464,#94465,#94466,#94467,#94468),.UNSPECIFIED.,.F.,.F.,(4,3,3,
3,3,3,3,3,3,3,3,3,3,3,3,3,3,3,3,3,3,3,3,3,3,3,3,3,3,3,3,3,3,3,3,3,3,3,3,
3,3,3,3,3,3,3,3,3,3,3,3,3,3,3,3,3,3,3,3,3,3,3,3,3,3,3,3,3,3,3,3,3,3,4),
(1058.71672425974,1058.80083947402,1058.88496356206,1058.96911362546,1059.0533067791,
1059.13761161675,1059.22198078275,1059.30648352489,1059.33876075378,1059.42249946563,
1059.50613497699,1059.58968742039,1059.67317685624,1059.75663080686,1059.84006730071,
1059.92350441046,1060.00696020538,1060.09050469811,1060.17409378105,1060.25781704861,
1060.33849676451,1060.42223547636,1060.50587098772,1060.58942343112,1060.67291286697,
1060.75636681759,1060.83980331143,1060.92324042119,1061.00669621611,1061.09024070884,
1061.17382979178,1061.25755305934,1061.33823277523,1061.42197148708,1061.50560699844,
1061.58915944184,1061.67264887769,1061.75610282831,1061.83953932215,1061.92297643191,
1062.00643222682,1062.08997671955,1062.17356580249,1062.25728907005,1062.33796878595,
1062.4217074978,1062.50534300916,1062.58889545256,1062.67238488841,1062.75583883903,
1062.83927533287,1062.92271244263,1063.00616823755,1063.08971273028,1063.17330181322,
1063.25702508078,1063.33770479667,1063.42144350852,1063.50507901988,1063.58863146328,
1063.67212089913,1063.75557484975,1063.83901134359,1063.92244845335,1064.00590424827,
1064.08944874099,1064.17303782394,1064.25676109149,1064.33744080739,1064.42121631092,
1064.50485699754,1064.58842010642,1064.67191452514,1064.74899530866),
 .UNSPECIFIED.);
#727=B_SPLINE_CURVE_WITH_KNOTS('',3,(#94474,#94475,#94476,#94477,#94478,
#94479,#94480,#94481,#94482,#94483,#94484,#94485,#94486,#94487,#94488,#94489,
#94490,#94491,#94492,#94493,#94494,#94495,#94496,#94497,#94498,#94499,#94500,
#94501,#94502,#94503,#94504,#94505,#94506,#94507,#94508,#94509,#94510,#94511,
#94512,#94513,#94514,#94515,#94516,#94517,#94518,#94519,#94520,#94521,#94522,
#94523,#94524,#94525,#94526,#94527,#94528,#94529,#94530,#94531,#94532,#94533,
#94534,#94535,#94536,#94537,#94538,#94539,#94540,#94541,#94542,#94543,#94544,
#94545,#94546,#94547,#94548,#94549,#94550,#94551,#94552,#94553,#94554,#94555,
#94556,#94557,#94558,#94559,#94560,#94561,#94562,#94563,#94564,#94565,#94566,
#94567,#94568,#94569,#94570,#94571,#94572,#94573,#94574,#94575,#94576,#94577,
#94578,#94579,#94580,#94581,#94582,#94583,#94584,#94585,#94586,#94587,#94588,
#94589,#94590,#94591,#94592,#94593,#94594,#94595,#94596,#94597,#94598,#94599,
#94600,#94601,#94602,#94603,#94604,#94605,#94606,#94607,#94608,#94609,#94610,
#94611,#94612,#94613,#94614,#94615,#94616,#94617,#94618,#94619,#94620,#94621,
#94622,#94623,#94624,#94625,#94626,#94627,#94628,#94629,#94630,#94631,#94632,
#94633,#94634,#94635,#94636,#94637,#94638,#94639,#94640,#94641,#94642,#94643,
#94644,#94645,#94646,#94647,#94648,#94649,#94650,#94651,#94652,#94653,#94654,
#94655,#94656,#94657,#94658,#94659,#94660,#94661,#94662,#94663,#94664,#94665,
#94666,#94667,#94668,#94669,#94670,#94671,#94672,#94673,#94674,#94675,#94676,
#94677,#94678,#94679,#94680,#94681,#94682,#94683,#94684,#94685,#94686,#94687,
#94688,#94689,#94690,#94691,#94692,#94693,#94694,#94695,#94696),
 .UNSPECIFIED.,.F.,.F.,(4,3,3,3,3,3,3,3,3,3,3,3,3,3,3,3,3,3,3,3,3,3,3,3,
3,3,3,3,3,3,3,3,3,3,3,3,3,3,3,3,3,3,3,3,3,3,3,3,3,3,3,3,3,3,3,3,3,3,3,3,
3,3,3,3,3,3,3,3,3,3,3,3,3,3,4),(1064.99990956692,1065.02688619839,1065.11062491024,
1065.1942604216,1065.277812865,1065.36130230085,1065.44475625147,1065.52819274531,
1065.61162985507,1065.69508564999,1065.77863014272,1065.86221922566,1065.94594249321,
1066.02662220911,1066.11036092096,1066.19399643232,1066.27754887572,1066.36103831157,
1066.44449226219,1066.52792875603,1066.61136586579,1066.69482166071,1066.77836615343,
1066.86195523638,1066.94567850393,1067.02635821983,1067.11009693168,1067.19373244304,
1067.27728488644,1067.36077432229,1067.44422827291,1067.52766476675,1067.61110187651,
1067.69455767143,1067.77810216416,1067.8616912471,1067.94541451465,1068.02609423055,
1068.1098329424,1068.19346845376,1068.27702089716,1068.36051033301,1068.44396428363,
1068.52740077747,1068.61083788723,1068.69429368215,1068.77783817487,1068.86142725782,
1068.94515052537,1069.02583024127,1069.10956895312,1069.19320446448,1069.27675690788,
1069.36024634373,1069.44370029435,1069.52713678819,1069.61057389795,1069.69402969287,
1069.7775741856,1069.86116326854,1069.94488653609,1070.02556625199,1070.10930496384,
1070.1929404752,1070.2764929186,1070.35998235445,1070.44343630507,1070.52687279891,
1070.61030990867,1070.69376570359,1070.77731019632,1070.86089927926,1070.94462254681,
1071.02530226271,1071.03207161914),.UNSPECIFIED.);
#728=B_SPLINE_CURVE_WITH_KNOTS('',3,(#94697,#94698,#94699,#94700,#94701,
#94702,#94703,#94704,#94705,#94706),.UNSPECIFIED.,.F.,.F.,(4,3,3,4),(1064.74815950499,
1064.83136688974,1064.91563822827,1064.9999095668),.UNSPECIFIED.);
#729=B_SPLINE_CURVE_WITH_KNOTS('',3,(#94708,#94709,#94710,#94711,#94712,
#94713,#94714,#94715,#94716,#94717),.UNSPECIFIED.,.F.,.F.,(4,3,3,4),(1064.74899530866,
1064.8324247764,1064.91616717166,1064.99990956692),.UNSPECIFIED.);
#730=B_SPLINE_CURVE_WITH_KNOTS('',3,(#94718,#94719,#94720,#94721,#94722,
#94723,#94724,#94725,#94726,#94727,#94728,#94729,#94730,#94731,#94732,#94733,
#94734,#94735,#94736,#94737,#94738,#94739,#94740,#94741,#94742,#94743,#94744,
#94745,#94746,#94747,#94748,#94749,#94750,#94751,#94752,#94753,#94754,#94755,
#94756,#94757,#94758,#94759,#94760,#94761,#94762,#94763,#94764,#94765,#94766,
#94767,#94768,#94769,#94770,#94771,#94772,#94773,#94774,#94775,#94776,#94777,
#94778,#94779,#94780,#94781,#94782,#94783,#94784,#94785,#94786,#94787,#94788,
#94789,#94790,#94791,#94792,#94793,#94794,#94795,#94796,#94797,#94798,#94799,
#94800,#94801,#94802,#94803,#94804,#94805,#94806,#94807,#94808,#94809,#94810,
#94811,#94812,#94813,#94814,#94815,#94816,#94817,#94818,#94819,#94820,#94821,
#94822,#94823,#94824,#94825,#94826,#94827,#94828,#94829,#94830,#94831,#94832,
#94833,#94834,#94835,#94836,#94837,#94838,#94839,#94840,#94841,#94842,#94843,
#94844,#94845,#94846,#94847,#94848,#94849,#94850,#94851,#94852,#94853,#94854,
#94855,#94856,#94857,#94858,#94859,#94860,#94861,#94862,#94863,#94864,#94865,
#94866,#94867,#94868,#94869,#94870,#94871,#94872,#94873,#94874,#94875,#94876,
#94877,#94878,#94879,#94880,#94881,#94882,#94883,#94884,#94885,#94886,#94887,
#94888,#94889,#94890,#94891,#94892,#94893,#94894,#94895,#94896,#94897,#94898,
#94899,#94900,#94901,#94902,#94903,#94904,#94905,#94906,#94907,#94908,#94909,
#94910,#94911,#94912,#94913,#94914,#94915,#94916,#94917,#94918,#94919,#94920,
#94921,#94922,#94923,#94924,#94925,#94926,#94927,#94928,#94929,#94930,#94931,
#94932,#94933,#94934,#94935,#94936,#94937),.UNSPECIFIED.,.F.,.F.,(4,3,3,
3,3,3,3,3,3,3,3,3,3,3,3,3,3,3,3,3,3,3,3,3,3,3,3,3,3,3,3,3,3,3,3,3,3,3,3,
3,3,3,3,3,3,3,3,3,3,3,3,3,3,3,3,3,3,3,3,3,3,3,3,3,3,3,3,3,3,3,3,3,3,4),
(1064.99990956711,1065.09679960539,1065.19424226973,1065.29234605066,1065.33717681811,
1065.42091552996,1065.50455104132,1065.58810348472,1065.67159292057,1065.75504687119,
1065.83848336503,1065.92192047479,1066.00537626971,1066.08892076244,1066.17250984538,
1066.25623311294,1066.33691282883,1066.42065154068,1066.50428705204,1066.58783949544,
1066.67132893129,1066.75478288191,1066.83821937575,1066.92165648551,1067.00511228042,
1067.08865677315,1067.17224585609,1067.25596912365,1067.33664883955,1067.4203875514,
1067.50402306276,1067.58757550616,1067.67106494201,1067.75451889263,1067.83795538647,
1067.92139249623,1068.00484829115,1068.08839278387,1068.17198186682,1068.25570513437,
1068.33638485027,1068.42012356212,1068.50375907348,1068.58731151688,1068.67080095273,
1068.75425490335,1068.83769139719,1068.92112850695,1069.00458430187,1069.0881287946,
1069.17171787754,1069.2554411451,1069.33612086099,1069.41985957284,1069.5034950842,
1069.5870475276,1069.67053696345,1069.75399091407,1069.83742740791,1069.92086451767,
1070.00432031259,1070.08786480531,1070.17145388826,1070.25517715581,1070.33585687171,
1070.42278545047,1070.50573868767,1070.58861702522,1070.67143920119,1070.75422390752,
1070.83700421657,1070.91978233213,1071.00259875718,1071.03128550181),
 .UNSPECIFIED.);
#731=B_SPLINE_CURVE_WITH_KNOTS('',3,(#94943,#94944,#94945,#94946,#94947,
#94948,#94949,#94950,#94951,#94952,#94953,#94954,#94955,#94956,#94957,#94958,
#94959,#94960,#94961,#94962,#94963,#94964,#94965,#94966,#94967,#94968,#94969,
#94970,#94971,#94972,#94973,#94974,#94975,#94976,#94977,#94978,#94979,#94980,
#94981,#94982,#94983,#94984,#94985,#94986,#94987,#94988,#94989,#94990,#94991,
#94992,#94993,#94994,#94995,#94996,#94997,#94998,#94999,#95000,#95001,#95002,
#95003,#95004,#95005,#95006,#95007,#95008,#95009,#95010,#95011,#95012,#95013,
#95014,#95015,#95016,#95017,#95018,#95019,#95020,#95021,#95022,#95023,#95024,
#95025,#95026,#95027,#95028,#95029,#95030,#95031,#95032,#95033,#95034,#95035,
#95036,#95037,#95038,#95039,#95040,#95041,#95042,#95043,#95044,#95045,#95046,
#95047,#95048,#95049,#95050,#95051,#95052,#95053,#95054,#95055,#95056,#95057,
#95058,#95059,#95060,#95061,#95062,#95063,#95064,#95065,#95066,#95067,#95068,
#95069,#95070,#95071,#95072,#95073,#95074,#95075,#95076,#95077,#95078,#95079,
#95080,#95081,#95082,#95083,#95084,#95085,#95086,#95087,#95088,#95089,#95090,
#95091,#95092,#95093,#95094,#95095,#95096,#95097,#95098,#95099,#95100,#95101,
#95102,#95103,#95104,#95105,#95106,#95107,#95108,#95109,#95110,#95111,#95112,
#95113,#95114,#95115,#95116,#95117,#95118,#95119,#95120,#95121,#95122,#95123,
#95124,#95125,#95126,#95127,#95128,#95129,#95130,#95131,#95132,#95133,#95134,
#95135,#95136,#95137,#95138,#95139,#95140,#95141,#95142,#95143,#95144,#95145,
#95146,#95147,#95148,#95149,#95150,#95151,#95152,#95153,#95154,#95155,#95156,
#95157,#95158,#95159,#95160,#95161,#95162),.UNSPECIFIED.,.F.,.F.,(4,3,3,
3,3,3,3,3,3,3,3,3,3,3,3,3,3,3,3,3,3,3,3,3,3,3,3,3,3,3,3,3,3,3,3,3,3,3,3,
3,3,3,3,3,3,3,3,3,3,3,3,3,3,3,3,3,3,3,3,3,3,3,3,3,3,3,3,3,3,3,3,3,3,4),
(1071.2830948741,1071.36570592697,1071.44827148991,1071.53081372931,1071.61335146039,
1071.69590349219,1071.77853997485,1071.86121848805,1071.9440300644,1072.02503827343,
1072.10877698528,1072.19241249664,1072.27596494004,1072.35945437589,1072.44290832651,
1072.52634482035,1072.60978193011,1072.69323772503,1072.77678221776,1072.8603713007,
1072.94409456825,1073.02477428415,1073.108512996,1073.19214850736,1073.27570095076,
1073.35919038661,1073.44264433723,1073.52608083107,1073.60951794083,1073.69297373575,
1073.77651822848,1073.86010731142,1073.94383057897,1074.02451029487,1074.10824900672,
1074.19188451808,1074.27543696148,1074.35892639733,1074.44238034795,1074.52581684179,
1074.60925395155,1074.69270974647,1074.7762542392,1074.85984332214,1074.94356658969,
1075.02424630559,1075.10798501744,1075.1916205288,1075.2751729722,1075.35866240805,
1075.44211635867,1075.52555285251,1075.60898996227,1075.69244575718,1075.77599024991,
1075.85957933286,1075.94330260041,1076.02398231631,1076.10772102816,1076.19135653952,
1076.27490898292,1076.35839841877,1076.44185236939,1076.52528886323,1076.60872597299,
1076.69218176791,1076.77572626064,1076.85931534358,1076.94303861114,1077.02371832703,
1077.1102533057,1077.19667143783,1077.2829513212,1077.31586327447),
 .UNSPECIFIED.);
#732=B_SPLINE_CURVE_WITH_KNOTS('',3,(#95163,#95164,#95165,#95166,#95167,
#95168,#95169,#95170,#95171,#95172),.UNSPECIFIED.,.F.,.F.,(4,3,3,4),(1071.03207161914,
1071.14037546939,1071.24654262183,1071.28309487398),.UNSPECIFIED.);
#733=B_SPLINE_CURVE_WITH_KNOTS('',3,(#95174,#95175,#95176,#95177,#95178,
#95179,#95180,#95181,#95182,#95183),.UNSPECIFIED.,.F.,.F.,(4,3,3,4),(1071.03128550181,
1071.11419371407,1071.19864429404,1071.283094874),.UNSPECIFIED.);
#734=B_SPLINE_CURVE_WITH_KNOTS('',3,(#95184,#95185,#95186,#95187,#95188,
#95189,#95190,#95191,#95192,#95193,#95194,#95195,#95196,#95197,#95198,#95199,
#95200,#95201,#95202,#95203,#95204,#95205,#95206,#95207,#95208,#95209,#95210,
#95211,#95212,#95213,#95214,#95215,#95216,#95217,#95218,#95219,#95220,#95221,
#95222,#95223,#95224,#95225,#95226,#95227,#95228,#95229,#95230,#95231,#95232,
#95233,#95234,#95235,#95236,#95237,#95238,#95239,#95240,#95241,#95242,#95243,
#95244,#95245,#95246,#95247,#95248,#95249,#95250,#95251,#95252,#95253,#95254,
#95255,#95256,#95257,#95258,#95259,#95260,#95261,#95262,#95263,#95264,#95265,
#95266,#95267,#95268,#95269,#95270,#95271,#95272,#95273,#95274,#95275,#95276,
#95277,#95278,#95279,#95280,#95281,#95282,#95283,#95284,#95285,#95286,#95287,
#95288,#95289,#95290,#95291,#95292,#95293,#95294,#95295,#95296,#95297,#95298,
#95299,#95300,#95301,#95302,#95303,#95304,#95305,#95306,#95307,#95308,#95309,
#95310,#95311,#95312,#95313,#95314,#95315,#95316,#95317,#95318,#95319,#95320,
#95321,#95322,#95323,#95324,#95325,#95326,#95327,#95328,#95329,#95330,#95331,
#95332,#95333,#95334,#95335,#95336,#95337,#95338,#95339,#95340,#95341,#95342,
#95343,#95344,#95345,#95346,#95347,#95348,#95349,#95350,#95351,#95352,#95353,
#95354,#95355,#95356,#95357,#95358,#95359,#95360,#95361,#95362,#95363,#95364,
#95365,#95366,#95367,#95368,#95369,#95370,#95371,#95372,#95373,#95374,#95375,
#95376,#95377,#95378,#95379,#95380,#95381,#95382,#95383,#95384,#95385,#95386,
#95387,#95388,#95389,#95390,#95391,#95392,#95393,#95394,#95395,#95396,#95397,
#95398,#95399,#95400,#95401,#95402,#95403),.UNSPECIFIED.,.F.,.F.,(4,3,3,
3,3,3,3,3,3,3,3,3,3,3,3,3,3,3,3,3,3,3,3,3,3,3,3,3,3,3,3,3,3,3,3,3,3,3,3,
3,3,3,3,3,3,3,3,3,3,3,3,3,3,3,3,3,3,3,3,3,3,3,3,3,3,3,3,3,3,3,3,3,3,4),
(1071.2830948741,1071.33559288243,1071.41933159428,1071.50296710564,1071.58651954904,
1071.67000898489,1071.75346293551,1071.83689942935,1071.92033653911,1072.00379233403,
1072.08733682676,1072.1709259097,1072.25464917725,1072.33532889315,1072.419067605,
1072.50270311636,1072.58625555976,1072.66974499561,1072.75319894623,1072.83663544007,
1072.92007254983,1073.00352834474,1073.08707283747,1073.17066192041,1073.25438518797,
1073.33506490387,1073.41880361572,1073.50243912708,1073.58599157048,1073.66948100633,
1073.75293495695,1073.83637145079,1073.91980856055,1074.00326435547,1074.0868088482,
1074.17039793114,1074.25412119869,1074.33480091459,1074.41853962644,1074.5021751378,
1074.5857275812,1074.66921701705,1074.75267096767,1074.83610746151,1074.91954457127,
1075.00300036619,1075.08654485892,1075.17013394186,1075.25385720941,1075.33453692531,
1075.41827563716,1075.50191114852,1075.58546359192,1075.66895302777,1075.75240697839,
1075.83584347223,1075.91928058199,1076.00273637691,1076.08628086964,1076.16986995258,
1076.25359322014,1076.33427293603,1076.41801271454,1076.50164904323,1076.58520205564,
1076.66869181301,1076.75214480477,1076.83557998726,1076.91901543289,1077.00246921039,
1077.08600678691,1077.16958880796,1077.2532934991,1077.31510334887),
 .UNSPECIFIED.);
#735=B_SPLINE_CURVE_WITH_KNOTS('',3,(#95409,#95410,#95411,#95412,#95413,
#95414,#95415,#95416,#95417,#95418,#95419,#95420,#95421,#95422,#95423,#95424,
#95425,#95426,#95427,#95428,#95429,#95430,#95431,#95432,#95433,#95434,#95435,
#95436,#95437,#95438,#95439,#95440,#95441,#95442,#95443,#95444,#95445,#95446,
#95447,#95448,#95449,#95450,#95451,#95452,#95453,#95454,#95455,#95456,#95457,
#95458,#95459,#95460,#95461,#95462,#95463,#95464,#95465,#95466,#95467,#95468,
#95469,#95470,#95471,#95472,#95473,#95474,#95475,#95476,#95477,#95478,#95479,
#95480,#95481,#95482,#95483,#95484,#95485,#95486,#95487,#95488,#95489,#95490,
#95491,#95492,#95493,#95494,#95495,#95496,#95497,#95498,#95499,#95500,#95501,
#95502,#95503,#95504,#95505,#95506,#95507,#95508,#95509,#95510,#95511,#95512,
#95513,#95514,#95515,#95516,#95517,#95518,#95519,#95520,#95521,#95522,#95523,
#95524,#95525,#95526,#95527,#95528,#95529,#95530,#95531,#95532,#95533,#95534,
#95535,#95536,#95537,#95538,#95539,#95540,#95541,#95542,#95543,#95544,#95545,
#95546,#95547,#95548,#95549,#95550,#95551,#95552,#95553,#95554,#95555,#95556,
#95557,#95558,#95559,#95560,#95561,#95562,#95563,#95564,#95565,#95566,#95567,
#95568,#95569,#95570,#95571,#95572,#95573,#95574,#95575,#95576,#95577,#95578,
#95579,#95580,#95581,#95582,#95583,#95584,#95585,#95586,#95587,#95588,#95589,
#95590,#95591,#95592,#95593,#95594,#95595,#95596,#95597,#95598,#95599,#95600,
#95601,#95602,#95603,#95604,#95605,#95606,#95607,#95608,#95609,#95610,#95611,
#95612,#95613,#95614,#95615,#95616,#95617,#95618,#95619,#95620,#95621,#95622,
#95623,#95624,#95625),.UNSPECIFIED.,.F.,.F.,(4,3,3,3,3,3,3,3,3,3,3,3,3,
3,3,3,3,3,3,3,3,3,3,3,3,3,3,3,3,3,3,3,3,3,3,3,3,3,3,3,3,3,3,3,3,3,3,3,3,
3,3,3,3,3,3,3,3,3,3,3,3,3,3,3,3,3,3,3,3,3,3,3,4),(1077.56628018146,1077.65540590742,
1077.747418015,1077.83700685327,1077.93023059551,1078.02345433775,1078.1071930496,
1078.19082856096,1078.27438100436,1078.35787044021,1078.44132439083,1078.52476088467,
1078.60819799443,1078.69165378935,1078.77519828208,1078.85878736502,1078.94251063257,
1079.02319034847,1079.10692906032,1079.19056457168,1079.27411701508,1079.35760645093,
1079.44106040155,1079.52449689539,1079.60793400515,1079.69138980007,1079.7749342928,
1079.85852337574,1079.94224664329,1080.02292635919,1080.10666507104,1080.1903005824,
1080.2738530258,1080.35734246165,1080.44079641227,1080.52423290611,1080.60767001587,
1080.69112581079,1080.77467030352,1080.85825938646,1080.94198265401,1081.02266236991,
1081.10640108176,1081.19003659312,1081.27358903652,1081.35707847237,1081.44053242299,
1081.52396891683,1081.60740602659,1081.69086182151,1081.77440631423,1081.85799539718,
1081.94171866473,1082.02239838063,1082.10613709248,1082.18977260384,1082.27332504724,
1082.35681448309,1082.44026843371,1082.52370492755,1082.60714203731,1082.69059783223,
1082.77414232496,1082.8577314079,1082.94145467546,1083.02213439135,1083.10460579086,
1083.18698179026,1083.26928161105,1083.35152491953,1083.43373313036,1083.515947388,
1083.59777693235),.UNSPECIFIED.);
#736=B_SPLINE_CURVE_WITH_KNOTS('',3,(#95626,#95627,#95628,#95629,#95630,
#95631,#95632,#95633,#95634,#95635),.UNSPECIFIED.,.F.,.F.,(4,3,3,4),(1077.31586327447,
1077.40199067622,1077.48802043553,1077.56628018128),.UNSPECIFIED.);
#737=B_SPLINE_CURVE_WITH_KNOTS('',3,(#95637,#95638,#95639,#95640,#95641,
#95642,#95643,#95644,#95645,#95646),.UNSPECIFIED.,.F.,.F.,(4,3,3,4),(1077.31510334887,
1077.33400894675,1077.45014456401,1077.56628018128),.UNSPECIFIED.);
#738=B_SPLINE_CURVE_WITH_KNOTS('',3,(#95647,#95648,#95649,#95650,#95651,
#95652,#95653,#95654,#95655,#95656,#95657,#95658,#95659,#95660,#95661,#95662,
#95663,#95664,#95665,#95666,#95667,#95668,#95669,#95670,#95671,#95672,#95673,
#95674,#95675,#95676,#95677,#95678,#95679,#95680,#95681,#95682,#95683,#95684,
#95685,#95686,#95687,#95688,#95689,#95690,#95691,#95692,#95693,#95694,#95695,
#95696,#95697,#95698,#95699,#95700,#95701,#95702,#95703,#95704,#95705,#95706,
#95707,#95708,#95709,#95710,#95711,#95712,#95713,#95714,#95715,#95716,#95717,
#95718,#95719,#95720,#95721,#95722,#95723,#95724,#95725,#95726,#95727,#95728,
#95729,#95730,#95731,#95732,#95733,#95734,#95735,#95736,#95737,#95738,#95739,
#95740,#95741,#95742,#95743,#95744,#95745,#95746,#95747,#95748,#95749,#95750,
#95751,#95752,#95753,#95754,#95755,#95756,#95757,#95758,#95759,#95760,#95761,
#95762,#95763,#95764,#95765,#95766,#95767,#95768,#95769,#95770,#95771,#95772,
#95773,#95774,#95775,#95776,#95777,#95778,#95779,#95780,#95781,#95782,#95783,
#95784,#95785,#95786,#95787,#95788,#95789,#95790,#95791,#95792,#95793,#95794,
#95795,#95796,#95797,#95798,#95799,#95800,#95801,#95802,#95803,#95804,#95805,
#95806,#95807,#95808,#95809,#95810,#95811,#95812,#95813,#95814,#95815,#95816,
#95817,#95818,#95819,#95820,#95821,#95822,#95823,#95824,#95825,#95826,#95827,
#95828,#95829,#95830,#95831,#95832,#95833,#95834,#95835,#95836,#95837,#95838,
#95839,#95840,#95841,#95842,#95843,#95844,#95845,#95846,#95847,#95848,#95849,
#95850,#95851,#95852,#95853,#95854,#95855,#95856,#95857,#95858,#95859,#95860,
#95861,#95862,#95863,#95864,#95865,#95866),.UNSPECIFIED.,.F.,.F.,(4,3,3,
3,3,3,3,3,3,3,3,3,3,3,3,3,3,3,3,3,3,3,3,3,3,3,3,3,3,3,3,3,3,3,3,3,3,3,3,
3,3,3,3,3,3,3,3,3,3,3,3,3,3,3,3,3,3,3,3,3,3,3,3,3,3,3,3,3,3,3,3,3,3,4),
(1077.5662801814,1077.64875192614,1077.73437605505,1077.81675837873,1077.89912927429,
1077.98150766719,1078.06391248638,1078.14640674046,1078.22895416328,1078.31161736021,
1078.33374495747,1078.41748366932,1078.50111918068,1078.58467162408,1078.66816105993,
1078.75161501055,1078.83505150439,1078.91848861415,1079.00194440907,1079.0854889018,
1079.16907798474,1079.2528012523,1079.33348096819,1079.41721968004,1079.5008551914,
1079.5844076348,1079.66789707065,1079.75135102127,1079.83478751511,1079.91822462487,
1080.00168041978,1080.08522491251,1080.16881399545,1080.25253726301,1080.33321697891,
1080.41695569076,1080.50059120212,1080.58414364552,1080.66763308137,1080.75108703199,
1080.83452352583,1080.91796063559,1081.00141643051,1081.08496092323,1081.16855000618,
1081.25227327373,1081.33295298963,1081.41669170148,1081.50032721284,1081.58387965624,
1081.66736909209,1081.75082304271,1081.83425953655,1081.91769664631,1082.00115244123,
1082.08469693396,1082.1682860169,1082.25200928446,1082.33268900035,1082.4164277122,
1082.50006322356,1082.58361566696,1082.66710510281,1082.75055905343,1082.83399554727,
1082.91743265703,1083.00088845195,1083.08443294467,1083.16802202762,1083.25174529517,
1083.33242501107,1083.41982905484,1083.50946898265,1083.59910891046),
 .UNSPECIFIED.);
#739=B_SPLINE_CURVE_WITH_KNOTS('',3,(#95872,#95873,#95874,#95875,#95876,
#95877,#95878,#95879,#95880,#95881,#95882,#95883,#95884,#95885,#95886,#95887,
#95888,#95889,#95890,#95891,#95892,#95893,#95894,#95895,#95896,#95897,#95898,
#95899,#95900,#95901,#95902,#95903,#95904,#95905,#95906,#95907,#95908,#95909,
#95910,#95911,#95912,#95913,#95914,#95915,#95916,#95917,#95918,#95919,#95920,
#95921,#95922,#95923,#95924,#95925,#95926,#95927,#95928,#95929,#95930,#95931,
#95932,#95933,#95934,#95935,#95936,#95937,#95938,#95939,#95940,#95941,#95942,
#95943,#95944,#95945,#95946,#95947,#95948,#95949,#95950,#95951,#95952,#95953,
#95954,#95955,#95956,#95957,#95958,#95959,#95960,#95961,#95962,#95963,#95964,
#95965,#95966,#95967,#95968,#95969,#95970,#95971,#95972,#95973,#95974,#95975,
#95976,#95977,#95978,#95979,#95980,#95981,#95982,#95983,#95984,#95985,#95986,
#95987,#95988,#95989,#95990,#95991,#95992,#95993,#95994,#95995,#95996,#95997,
#95998,#95999,#96000,#96001,#96002,#96003,#96004,#96005,#96006,#96007,#96008,
#96009,#96010,#96011,#96012,#96013,#96014,#96015,#96016,#96017,#96018,#96019,
#96020,#96021,#96022,#96023,#96024,#96025,#96026,#96027,#96028,#96029,#96030,
#96031,#96032,#96033,#96034,#96035,#96036,#96037,#96038,#96039,#96040,#96041,
#96042,#96043,#96044,#96045,#96046,#96047,#96048,#96049,#96050,#96051,#96052,
#96053,#96054,#96055,#96056,#96057,#96058,#96059,#96060,#96061,#96062,#96063,
#96064,#96065,#96066,#96067,#96068,#96069,#96070,#96071,#96072,#96073,#96074,
#96075,#96076,#96077,#96078,#96079,#96080,#96081,#96082,#96083,#96084,#96085,
#96086,#96087,#96088,#96089,#96090,#96091),.UNSPECIFIED.,.F.,.F.,(4,3,3,
3,3,3,3,3,3,3,3,3,3,3,3,3,3,3,3,3,3,3,3,3,3,3,3,3,3,3,3,3,3,3,3,3,3,3,3,
3,3,3,3,3,3,3,3,3,3,3,3,3,3,3,3,3,3,3,3,3,3,3,3,3,3,3,3,3,3,3,3,3,3,4),
(1083.84946548846,1083.97987942881,1084.02187040207,1084.10560911392,1084.18924462528,
1084.27279706868,1084.35628650453,1084.43974045515,1084.52317694899,1084.60661405875,
1084.69006985367,1084.77361434639,1084.85720342934,1084.94092669689,1085.02160641279,
1085.10534512464,1085.188980636,1085.2725330794,1085.35602251525,1085.43947646587,
1085.52291295971,1085.60635006947,1085.68980586439,1085.77335035712,1085.85693944006,
1085.94066270762,1086.02134242351,1086.10508113536,1086.18871664672,1086.27226909012,
1086.35575852597,1086.43921247659,1086.52264897043,1086.60608608019,1086.68954187511,
1086.77308636784,1086.85667545078,1086.94039871833,1087.02107843423,1087.10481714608,
1087.18845265744,1087.27200510084,1087.35549453669,1087.43894848731,1087.52238498115,
1087.60582209091,1087.68927788583,1087.77282237856,1087.8564114615,1087.94013472905,
1088.02081444495,1088.1045531568,1088.18818866816,1088.27174111156,1088.35523054741,
1088.43868449803,1088.52212099187,1088.60555810163,1088.68901389654,1088.77255838927,
1088.85614747221,1088.93987073977,1089.02055045567,1089.10429739757,1089.18793930218,
1089.27457754563,1089.35806234902,1089.44150967684,1089.52493761718,1089.60836424112,
1089.69183721346,1089.77533808313,1089.85891674814,1089.8810452498),
 .UNSPECIFIED.);
#740=B_SPLINE_CURVE_WITH_KNOTS('',3,(#96092,#96093,#96094,#96095,#96096,
#96097,#96098,#96099,#96100,#96101),.UNSPECIFIED.,.F.,.F.,(4,3,3,4),(1083.59777693235,
1083.68003168255,1083.76474858542,1083.84946548828),.UNSPECIFIED.);
#741=B_SPLINE_CURVE_WITH_KNOTS('',3,(#96103,#96104,#96105,#96106,#96107,
#96108,#96109,#96110,#96111,#96112),.UNSPECIFIED.,.F.,.F.,(4,3,3,4),(1083.59910891046,
1083.68607846829,1083.77291433074,1083.84946548846),.UNSPECIFIED.);
#742=B_SPLINE_CURVE_WITH_KNOTS('',3,(#96113,#96114,#96115,#96116,#96117,
#96118,#96119,#96120,#96121,#96122,#96123,#96124,#96125,#96126,#96127,#96128,
#96129,#96130,#96131,#96132,#96133,#96134,#96135,#96136,#96137,#96138,#96139,
#96140,#96141,#96142,#96143,#96144,#96145,#96146,#96147,#96148,#96149,#96150,
#96151,#96152,#96153,#96154,#96155,#96156,#96157,#96158,#96159,#96160,#96161,
#96162,#96163,#96164,#96165,#96166,#96167,#96168,#96169,#96170,#96171,#96172,
#96173,#96174,#96175,#96176,#96177,#96178,#96179,#96180,#96181,#96182,#96183,
#96184,#96185,#96186,#96187,#96188,#96189,#96190,#96191,#96192,#96193,#96194,
#96195,#96196,#96197,#96198,#96199,#96200,#96201,#96202,#96203,#96204,#96205,
#96206,#96207,#96208,#96209,#96210,#96211,#96212,#96213,#96214,#96215,#96216,
#96217,#96218,#96219,#96220,#96221,#96222,#96223,#96224,#96225,#96226,#96227,
#96228,#96229,#96230,#96231,#96232,#96233,#96234,#96235,#96236,#96237,#96238,
#96239,#96240,#96241,#96242,#96243,#96244,#96245,#96246,#96247,#96248,#96249,
#96250,#96251,#96252,#96253,#96254,#96255,#96256,#96257,#96258,#96259,#96260,
#96261,#96262,#96263,#96264,#96265,#96266,#96267,#96268,#96269,#96270,#96271,
#96272,#96273,#96274,#96275,#96276,#96277,#96278,#96279,#96280,#96281,#96282,
#96283,#96284,#96285,#96286,#96287,#96288,#96289,#96290,#96291,#96292,#96293,
#96294,#96295,#96296,#96297,#96298,#96299,#96300,#96301,#96302,#96303,#96304,
#96305,#96306,#96307,#96308,#96309,#96310,#96311,#96312,#96313,#96314,#96315,
#96316,#96317,#96318,#96319,#96320,#96321,#96322,#96323,#96324,#96325,#96326,
#96327,#96328,#96329,#96330,#96331,#96332),.UNSPECIFIED.,.F.,.F.,(4,3,3,
3,3,3,3,3,3,3,3,3,3,3,3,3,3,3,3,3,3,3,3,3,3,3,3,3,3,3,3,3,3,3,3,3,3,3,3,
3,3,3,3,3,3,3,3,3,3,3,3,3,3,3,3,3,3,3,3,3,3,3,3,3,3,3,3,3,3,3,3,3,3,4),
(1083.84946548862,1083.93751883751,1084.02571203857,1084.11413629358,1084.20268552087,
1084.29144096095,1084.33216102179,1084.41589973364,1084.499535245,1084.5830876884,
1084.66657712425,1084.75003107487,1084.83346756871,1084.91690467847,1085.00036047339,
1085.08390496612,1085.16749404906,1085.25121731662,1085.33189703251,1085.41563574436,
1085.49927125572,1085.58282369912,1085.66631313497,1085.74976708559,1085.83320357943,
1085.91664068919,1086.0000964841,1086.08364097683,1086.16723005978,1086.25095332733,
1086.33163304323,1086.41537175508,1086.49900726644,1086.58255970984,1086.66604914569,
1086.74950309631,1086.83293959015,1086.91637669991,1086.99983249483,1087.08337698756,
1087.1669660705,1087.25068933805,1087.33136905395,1087.4151077658,1087.49874327716,
1087.58229572056,1087.66578515641,1087.74923910703,1087.83267560087,1087.91611271063,
1087.99956850555,1088.08311299828,1088.16670208122,1088.25042534878,1088.33110506467,
1088.41484377652,1088.49847928788,1088.58203173128,1088.66552116713,1088.74897511775,
1088.83241161159,1088.91584872135,1088.99930451627,1089.082849009,1089.16643809194,
1089.25016135949,1089.33084107539,1089.41335087959,1089.49576462505,1089.57810151412,
1089.66037876144,1089.74262053293,1089.82485991559,1089.88105454176),
 .UNSPECIFIED.);
#743=B_SPLINE_CURVE_WITH_KNOTS('',3,(#96338,#96339,#96340,#96341,#96342,
#96343,#96344,#96345,#96346,#96347,#96348,#96349,#96350,#96351,#96352,#96353,
#96354,#96355,#96356,#96357,#96358,#96359,#96360,#96361,#96362,#96363,#96364,
#96365,#96366,#96367,#96368,#96369,#96370,#96371,#96372,#96373,#96374,#96375,
#96376,#96377,#96378,#96379,#96380,#96381,#96382,#96383,#96384,#96385,#96386,
#96387,#96388,#96389,#96390,#96391,#96392,#96393,#96394,#96395,#96396,#96397,
#96398,#96399,#96400,#96401,#96402,#96403,#96404,#96405,#96406,#96407,#96408,
#96409,#96410,#96411,#96412,#96413,#96414,#96415,#96416,#96417,#96418,#96419,
#96420,#96421,#96422,#96423,#96424,#96425,#96426,#96427,#96428,#96429,#96430,
#96431,#96432,#96433,#96434,#96435,#96436,#96437,#96438,#96439,#96440,#96441,
#96442,#96443,#96444,#96445,#96446,#96447,#96448,#96449,#96450,#96451,#96452,
#96453,#96454,#96455,#96456,#96457,#96458,#96459,#96460,#96461,#96462,#96463,
#96464,#96465,#96466,#96467,#96468,#96469,#96470,#96471,#96472,#96473,#96474,
#96475,#96476,#96477,#96478,#96479,#96480,#96481,#96482,#96483,#96484,#96485,
#96486,#96487,#96488,#96489,#96490,#96491,#96492,#96493,#96494,#96495,#96496,
#96497,#96498,#96499,#96500,#96501,#96502,#96503,#96504,#96505,#96506,#96507,
#96508,#96509,#96510,#96511,#96512,#96513,#96514,#96515,#96516,#96517,#96518,
#96519,#96520,#96521,#96522,#96523,#96524,#96525,#96526,#96527,#96528,#96529,
#96530,#96531,#96532,#96533,#96534,#96535,#96536,#96537,#96538,#96539,#96540,
#96541,#96542,#96543,#96544,#96545,#96546,#96547,#96548,#96549,#96550,#96551,
#96552,#96553,#96554,#96555,#96556,#96557),.UNSPECIFIED.,.F.,.F.,(4,3,3,
3,3,3,3,3,3,3,3,3,3,3,3,3,3,3,3,3,3,3,3,3,3,3,3,3,3,3,3,3,3,3,3,3,3,3,3,
3,3,3,3,3,3,3,3,3,3,3,3,3,3,3,3,3,3,3,3,3,3,3,3,3,3,3,3,3,3,3,3,3,3,4),
(1090.13265079578,1090.21521388659,1090.29768668348,1090.38009027064,1090.46245102466,
1090.54479049315,1090.62712763065,1090.70948138743,1090.79191944263,1090.87440190344,
1090.95701069698,1091.02002247711,1091.10376118896,1091.18739670032,1091.27094914372,
1091.35443857957,1091.43789253019,1091.52132902403,1091.60476613379,1091.68822192871,
1091.77176642144,1091.85535550438,1091.93907877194,1092.01975848783,1092.10349719968,
1092.18713271104,1092.27068515444,1092.35417459029,1092.43762854091,1092.52106503476,
1092.60450214451,1092.68795793943,1092.77150243216,1092.8550915151,1092.93881478266,
1093.01949449855,1093.1032332104,1093.18686872176,1093.27042116516,1093.35391060101,
1093.43736455163,1093.52080104547,1093.60423815523,1093.68769395014,1093.77123844287,
1093.85482752581,1093.93855079337,1094.01923050927,1094.10296922112,1094.18660473248,
1094.27015717588,1094.35364661173,1094.43710056235,1094.52053705619,1094.60397416595,
1094.68742996087,1094.7709744536,1094.85456353654,1094.93828680409,1095.01896651999,
1095.10270523184,1095.1863407432,1095.2698931866,1095.35338262245,1095.43683657306,
1095.52027306691,1095.60371017666,1095.68716597158,1095.77071046431,1095.85429954725,
1095.93802281481,1096.01870253071,1096.1120278899,1096.16545634169),
 .UNSPECIFIED.);
#744=B_SPLINE_CURVE_WITH_KNOTS('',3,(#96558,#96559,#96560,#96561,#96562,
#96563,#96564,#96565,#96566,#96567),.UNSPECIFIED.,.F.,.F.,(4,3,3,4),(1089.8810452498,
1089.96477785809,1090.02028646639,1090.13265079564),.UNSPECIFIED.);
#745=B_SPLINE_CURVE_WITH_KNOTS('',3,(#96569,#96570,#96571,#96572,#96573,
#96574,#96575,#96576,#96577,#96578),.UNSPECIFIED.,.F.,.F.,(4,3,3,4),(1089.88105454176,
1089.96332894242,1090.04798986898,1090.13265079553),.UNSPECIFIED.);
#746=B_SPLINE_CURVE_WITH_KNOTS('',3,(#96579,#96580,#96581,#96582,#96583,
#96584,#96585,#96586,#96587,#96588,#96589,#96590,#96591,#96592,#96593,#96594,
#96595,#96596,#96597,#96598,#96599,#96600,#96601,#96602,#96603,#96604,#96605,
#96606,#96607,#96608,#96609,#96610,#96611,#96612,#96613,#96614,#96615,#96616,
#96617,#96618,#96619,#96620,#96621,#96622,#96623,#96624,#96625,#96626,#96627,
#96628,#96629,#96630,#96631,#96632,#96633,#96634,#96635,#96636,#96637,#96638,
#96639,#96640,#96641,#96642,#96643,#96644,#96645,#96646,#96647,#96648,#96649,
#96650,#96651,#96652,#96653,#96654,#96655,#96656,#96657,#96658,#96659,#96660,
#96661,#96662,#96663,#96664,#96665,#96666,#96667,#96668,#96669,#96670,#96671,
#96672,#96673,#96674,#96675,#96676,#96677,#96678,#96679,#96680,#96681,#96682,
#96683,#96684,#96685,#96686,#96687,#96688,#96689,#96690,#96691,#96692,#96693,
#96694,#96695,#96696,#96697,#96698,#96699,#96700,#96701,#96702,#96703,#96704,
#96705,#96706,#96707,#96708,#96709,#96710,#96711,#96712,#96713,#96714,#96715,
#96716,#96717,#96718,#96719,#96720,#96721,#96722,#96723,#96724,#96725,#96726,
#96727,#96728,#96729,#96730,#96731,#96732,#96733,#96734,#96735,#96736,#96737,
#96738,#96739,#96740,#96741,#96742,#96743,#96744,#96745,#96746,#96747,#96748,
#96749,#96750,#96751,#96752,#96753,#96754,#96755,#96756,#96757,#96758,#96759,
#96760,#96761,#96762,#96763,#96764,#96765,#96766,#96767,#96768,#96769,#96770,
#96771,#96772,#96773,#96774,#96775,#96776,#96777,#96778,#96779,#96780,#96781,
#96782,#96783,#96784,#96785,#96786,#96787,#96788,#96789,#96790,#96791,#96792,
#96793,#96794,#96795),.UNSPECIFIED.,.F.,.F.,(4,3,3,3,3,3,3,3,3,3,3,3,3,
3,3,3,3,3,3,3,3,3,3,3,3,3,3,3,3,3,3,3,3,3,3,3,3,3,3,3,3,3,3,3,3,3,3,3,3,
3,3,3,3,3,3,3,3,3,3,3,3,3,3,3,3,3,3,3,3,3,3,3,4),(1090.13265079564,1090.2534921149,
1090.33057708611,1090.41431579796,1090.49795130932,1090.58150375272,1090.66499318857,
1090.74844713919,1090.83188363303,1090.91532074279,1090.9987765377,1091.08232103043,
1091.16591011337,1091.24963338093,1091.33031309683,1091.41405180868,1091.49768732004,
1091.58123976344,1091.66472919929,1091.74818314991,1091.83161964375,1091.91505675351,
1091.99851254843,1092.08205704116,1092.1656461241,1092.24936939165,1092.33004910755,
1092.4137878194,1092.49742333076,1092.58097577416,1092.66446521001,1092.74791916063,
1092.83135565447,1092.91479276423,1092.99824855915,1093.08179305188,1093.16538213482,
1093.24910540237,1093.32978511827,1093.41352383012,1093.49715934148,1093.58071178488,
1093.66420122073,1093.74765517135,1093.83109166519,1093.91452877495,1093.99798456987,
1094.0815290626,1094.16511814554,1094.24884141309,1094.32952112899,1094.41325984084,
1094.4968953522,1094.5804477956,1094.66393723145,1094.74739118207,1094.83082767591,
1094.91426478567,1094.99772058059,1095.08126507332,1095.16485415626,1095.24857742381,
1095.32925713971,1095.41300568622,1095.49664885821,1095.58019197483,1095.66367834858,
1095.74712609854,1095.83055331403,1095.91400811951,1095.99747382294,1096.08101904038,
1096.16419435723),.UNSPECIFIED.);
#747=B_SPLINE_CURVE_WITH_KNOTS('',3,(#96801,#96802,#96803,#96804,#96805,
#96806,#96807,#96808,#96809,#96810,#96811,#96812,#96813,#96814,#96815,#96816,
#96817,#96818,#96819,#96820,#96821,#96822,#96823,#96824,#96825,#96826,#96827,
#96828,#96829,#96830,#96831,#96832,#96833,#96834,#96835,#96836,#96837,#96838,
#96839,#96840,#96841,#96842,#96843,#96844,#96845,#96846,#96847,#96848,#96849,
#96850,#96851,#96852,#96853,#96854,#96855,#96856,#96857,#96858,#96859,#96860,
#96861,#96862,#96863,#96864,#96865,#96866,#96867,#96868,#96869,#96870,#96871,
#96872,#96873,#96874,#96875,#96876,#96877,#96878,#96879,#96880,#96881,#96882,
#96883,#96884,#96885,#96886,#96887,#96888,#96889,#96890,#96891,#96892,#96893,
#96894,#96895,#96896,#96897,#96898,#96899,#96900,#96901,#96902,#96903,#96904,
#96905,#96906,#96907,#96908,#96909,#96910,#96911,#96912,#96913,#96914,#96915,
#96916,#96917,#96918,#96919,#96920,#96921,#96922,#96923,#96924,#96925,#96926,
#96927,#96928,#96929,#96930,#96931,#96932,#96933,#96934,#96935,#96936,#96937,
#96938,#96939,#96940,#96941,#96942,#96943,#96944,#96945,#96946,#96947,#96948,
#96949,#96950,#96951,#96952,#96953,#96954,#96955,#96956,#96957,#96958,#96959,
#96960,#96961,#96962,#96963,#96964,#96965,#96966,#96967,#96968,#96969,#96970,
#96971,#96972,#96973,#96974,#96975,#96976,#96977,#96978,#96979,#96980,#96981,
#96982,#96983,#96984,#96985,#96986,#96987,#96988,#96989,#96990,#96991,#96992,
#96993,#96994,#96995,#96996,#96997,#96998,#96999,#97000,#97001,#97002,#97003,
#97004,#97005,#97006,#97007,#97008,#97009,#97010,#97011,#97012,#97013,#97014,
#97015,#97016,#97017,#97018,#97019,#97020),.UNSPECIFIED.,.F.,.F.,(4,3,3,
3,3,3,3,3,3,3,3,3,3,3,3,3,3,3,3,3,3,3,3,3,3,3,3,3,3,3,3,3,3,3,3,3,3,3,3,
3,3,3,3,3,3,3,3,3,3,3,3,3,3,3,3,3,3,3,3,3,3,3,3,3,3,3,3,3,3,3,3,3,3,4),
(1096.41583610282,1096.50034027643,1096.58486491856,1096.66942649939,1096.7566795099,
1096.84141644417,1096.9299274928,1097.01843854143,1097.10217725328,1097.18581276465,
1097.26936520804,1097.3528546439,1097.43630859451,1097.51974508836,1097.60318219812,
1097.68663799303,1097.77018248577,1097.85377156871,1097.93749483627,1098.01817455215,
1098.101913264,1098.18554877536,1098.26910121876,1098.35259065461,1098.43604460523,
1098.51948109908,1098.60291820883,1098.68637400375,1098.76991849648,1098.85350757942,
1098.93723084698,1099.01791056287,1099.10164927472,1099.18528478608,1099.26883722948,
1099.35232666533,1099.43578061594,1099.51921710979,1099.60265421955,1099.68611001446,
1099.76965450719,1099.85324359013,1099.93696685769,1100.01764657359,1100.10138528544,
1100.1850207968,1100.2685732402,1100.35206267605,1100.43551662667,1100.51895312051,
1100.60239023027,1100.68584602519,1100.76939051792,1100.85297960086,1100.93670286842,
1101.01738258431,1101.10112129616,1101.18475680752,1101.26830925092,1101.35179868677,
1101.43525263738,1101.51868913123,1101.60212624098,1101.6855820359,1101.76912652863,
1101.85271561157,1101.93643887913,1102.01711859503,1102.10060281453,1102.18745385174,
1102.27072884502,1102.35394542984,1102.43711668659,1102.44800696337),
 .UNSPECIFIED.);
#748=B_SPLINE_CURVE_WITH_KNOTS('',3,(#97021,#97022,#97023,#97024,#97025,
#97026,#97027,#97028,#97029,#97030),.UNSPECIFIED.,.F.,.F.,(4,3,3,4),(1096.16545634169,
1096.25829681984,1096.35068769254,1096.41583610264),.UNSPECIFIED.);
#749=B_SPLINE_CURVE_WITH_KNOTS('',3,(#97032,#97033,#97034,#97035,#97036,
#97037,#97038,#97039,#97040,#97041),.UNSPECIFIED.,.F.,.F.,(4,3,3,4),(1096.16419435723,
1096.24791749231,1096.32899315043,1096.41583610282),.UNSPECIFIED.);
#750=B_SPLINE_CURVE_WITH_KNOTS('',3,(#97042,#97043,#97044,#97045,#97046,
#97047,#97048,#97049,#97050,#97051,#97052,#97053,#97054,#97055,#97056,#97057,
#97058,#97059,#97060,#97061,#97062,#97063,#97064,#97065,#97066,#97067,#97068,
#97069,#97070,#97071,#97072,#97073,#97074,#97075,#97076,#97077,#97078,#97079,
#97080,#97081,#97082,#97083,#97084,#97085,#97086,#97087,#97088,#97089,#97090,
#97091,#97092,#97093,#97094,#97095,#97096,#97097,#97098,#97099,#97100,#97101,
#97102,#97103,#97104,#97105,#97106,#97107,#97108,#97109,#97110,#97111,#97112,
#97113,#97114,#97115,#97116,#97117,#97118,#97119,#97120,#97121,#97122,#97123,
#97124,#97125,#97126,#97127,#97128,#97129,#97130,#97131,#97132,#97133,#97134,
#97135,#97136,#97137,#97138,#97139,#97140,#97141,#97142,#97143,#97144,#97145,
#97146,#97147,#97148,#97149,#97150,#97151,#97152,#97153,#97154,#97155,#97156,
#97157,#97158,#97159,#97160,#97161,#97162,#97163,#97164,#97165,#97166,#97167,
#97168,#97169,#97170,#97171,#97172,#97173,#97174,#97175,#97176,#97177,#97178,
#97179,#97180,#97181,#97182,#97183,#97184,#97185,#97186,#97187,#97188,#97189,
#97190,#97191,#97192,#97193,#97194,#97195,#97196,#97197,#97198,#97199,#97200,
#97201,#97202,#97203,#97204,#97205,#97206,#97207,#97208,#97209,#97210,#97211,
#97212,#97213,#97214,#97215,#97216,#97217,#97218,#97219,#97220,#97221,#97222,
#97223,#97224,#97225,#97226,#97227,#97228,#97229,#97230,#97231,#97232,#97233,
#97234,#97235,#97236,#97237,#97238,#97239,#97240,#97241,#97242,#97243,#97244,
#97245,#97246,#97247,#97248,#97249,#97250,#97251,#97252,#97253,#97254,#97255,
#97256,#97257,#97258,#97259,#97260,#97261),.UNSPECIFIED.,.F.,.F.,(4,3,3,
3,3,3,3,3,3,3,3,3,3,3,3,3,3,3,3,3,3,3,3,3,3,3,3,3,3,3,3,3,3,3,3,3,3,3,3,
3,3,3,3,3,3,3,3,3,3,3,3,3,3,3,3,3,3,3,3,3,3,3,3,3,3,3,3,3,3,3,3,3,3,4),
(1096.41583610295,1096.49857317387,1096.58121533194,1096.66378356627,1096.74690176563,
1096.82939491726,1096.91188134348,1096.99437989575,1097.0779672121,1097.16058900046,
1097.2446590808,1097.32872916115,1097.412467873,1097.49610338436,1097.57965582776,
1097.66314526361,1097.74659921423,1097.83003570807,1097.91347281783,1097.99692861274,
1098.08047310547,1098.16406218841,1098.24778545597,1098.32846517187,1098.41220388372,
1098.49583939508,1098.57939183848,1098.66288127433,1098.74633522495,1098.82977171879,
1098.91320882855,1098.99666462346,1099.08020911619,1099.16379819913,1099.24752146669,
1099.32820118259,1099.41193989444,1099.4955754058,1099.5791278492,1099.66261728505,
1099.74607123567,1099.82950772951,1099.91294483927,1099.99640063419,1100.07994512692,
1100.16353420986,1100.24725747742,1100.32793719331,1100.41167590516,1100.49531141652,
1100.57886385992,1100.66235329577,1100.74580724639,1100.82924374023,1100.91268084999,
1100.99613664491,1101.07968113763,1101.16327022058,1101.24699348813,1101.32767320403,
1101.41141191588,1101.49504742724,1101.57859987064,1101.66208930649,1101.74554325711,
1101.82897975095,1101.91241686071,1101.99587265563,1102.07941714836,1102.1630062313,
1102.24672949886,1102.32740921475,1102.4226128327,1102.4485678876),
 .UNSPECIFIED.);
#751=B_SPLINE_CURVE_WITH_KNOTS('',3,(#97267,#97268,#97269,#97270,#97271,
#97272,#97273,#97274,#97275,#97276,#97277,#97278,#97279,#97280,#97281,#97282,
#97283,#97284,#97285,#97286,#97287,#97288,#97289,#97290,#97291,#97292,#97293,
#97294,#97295,#97296,#97297,#97298,#97299,#97300,#97301,#97302,#97303,#97304,
#97305,#97306,#97307,#97308,#97309,#97310,#97311,#97312,#97313,#97314,#97315,
#97316,#97317,#97318,#97319,#97320,#97321,#97322,#97323,#97324,#97325,#97326,
#97327,#97328,#97329,#97330,#97331,#97332,#97333,#97334,#97335,#97336,#97337,
#97338,#97339,#97340,#97341,#97342,#97343,#97344,#97345,#97346,#97347,#97348,
#97349,#97350,#97351,#97352,#97353,#97354,#97355,#97356,#97357,#97358,#97359,
#97360,#97361,#97362,#97363,#97364,#97365,#97366,#97367,#97368,#97369,#97370,
#97371,#97372,#97373,#97374,#97375,#97376,#97377,#97378,#97379,#97380,#97381,
#97382,#97383,#97384,#97385,#97386,#97387,#97388,#97389,#97390,#97391,#97392,
#97393,#97394,#97395,#97396,#97397,#97398,#97399,#97400,#97401,#97402,#97403,
#97404,#97405,#97406,#97407,#97408,#97409,#97410,#97411,#97412,#97413,#97414,
#97415,#97416,#97417,#97418,#97419,#97420,#97421,#97422,#97423,#97424,#97425,
#97426,#97427,#97428,#97429,#97430,#97431,#97432,#97433,#97434,#97435,#97436,
#97437,#97438,#97439,#97440,#97441,#97442,#97443,#97444,#97445,#97446,#97447,
#97448,#97449,#97450,#97451,#97452,#97453,#97454,#97455,#97456,#97457,#97458,
#97459,#97460,#97461,#97462,#97463,#97464,#97465,#97466,#97467,#97468,#97469,
#97470,#97471,#97472,#97473,#97474,#97475,#97476,#97477,#97478,#97479,#97480,
#97481,#97482,#97483,#97484,#97485,#97486),.UNSPECIFIED.,.F.,.F.,(4,3,3,
3,3,3,3,3,3,3,3,3,3,3,3,3,3,3,3,3,3,3,3,3,3,3,3,3,3,3,3,3,3,3,3,3,3,3,3,
3,3,3,3,3,3,3,3,3,3,3,3,3,3,3,3,3,3,3,3,3,3,3,3,3,3,3,3,3,3,3,3,3,3,4),
(1102.69902141017,1102.79771148504,1102.89710050959,1102.99725101716,1103.01685460575,
1103.1005933176,1103.18422882897,1103.26778127237,1103.35127070823,1103.43472465885,
1103.5181611527,1103.60159826246,1103.68505405738,1103.76859855011,1103.85218763306,
1103.93591090062,1104.01659061647,1104.10032932832,1104.18396483968,1104.26751728308,
1104.35100671893,1104.43446066955,1104.51789716339,1104.60133427315,1104.68479006807,
1104.7683345608,1104.85192364374,1104.93564691129,1105.01632662719,1105.10006533904,
1105.1837008504,1105.2672532938,1105.35074272965,1105.43419668026,1105.51763317411,
1105.60107028386,1105.68452607878,1105.76807057151,1105.85165965445,1105.93538292201,
1106.01606263791,1106.09980134976,1106.18343686112,1106.26698930452,1106.35047874037,
1106.43393269099,1106.51736918484,1106.60080629459,1106.68426208951,1106.76780658224,
1106.85139566518,1106.93511893274,1107.01579864863,1107.09953736047,1107.18317287184,
1107.26672531524,1107.35021475109,1107.4336687017,1107.51710519555,1107.6005423053,
1107.68399810022,1107.76754259295,1107.85113167589,1107.93485494345,1108.01553465935,
1108.09883872996,1108.18201114958,1108.2651075606,1108.34814653257,1108.43114658976,
1108.5141422714,1108.59713406137,1108.68016880708,1108.73043941245),
 .UNSPECIFIED.);
#752=B_SPLINE_CURVE_WITH_KNOTS('',3,(#97487,#97488,#97489,#97490,#97491,
#97492,#97493,#97494,#97495,#97496),.UNSPECIFIED.,.F.,.F.,(4,3,3,4),(1102.44800696337,
1102.53116145307,1102.61509143154,1102.69902141),.UNSPECIFIED.);
#753=B_SPLINE_CURVE_WITH_KNOTS('',3,(#97498,#97499,#97500,#97501,#97502,
#97503,#97504,#97505,#97506,#97507),.UNSPECIFIED.,.F.,.F.,(4,3,3,4),(1102.4485678876,
1102.54324273876,1102.63733940364,1102.6990214098),.UNSPECIFIED.);
#754=B_SPLINE_CURVE_WITH_KNOTS('',3,(#97508,#97509,#97510,#97511,#97512,
#97513,#97514,#97515,#97516,#97517,#97518,#97519,#97520,#97521,#97522,#97523,
#97524,#97525,#97526,#97527,#97528,#97529,#97530,#97531,#97532,#97533,#97534,
#97535,#97536,#97537,#97538,#97539,#97540,#97541,#97542,#97543,#97544,#97545,
#97546,#97547,#97548,#97549,#97550,#97551,#97552,#97553,#97554,#97555,#97556,
#97557,#97558,#97559,#97560,#97561,#97562,#97563,#97564,#97565,#97566,#97567,
#97568,#97569,#97570,#97571,#97572,#97573,#97574,#97575,#97576,#97577,#97578,
#97579,#97580,#97581,#97582,#97583,#97584,#97585,#97586,#97587,#97588,#97589,
#97590,#97591,#97592,#97593,#97594,#97595,#97596,#97597,#97598,#97599,#97600,
#97601,#97602,#97603,#97604,#97605,#97606,#97607,#97608,#97609,#97610,#97611,
#97612,#97613,#97614,#97615,#97616,#97617,#97618,#97619,#97620,#97621,#97622,
#97623,#97624,#97625,#97626,#97627,#97628,#97629,#97630,#97631,#97632,#97633,
#97634,#97635,#97636,#97637,#97638,#97639,#97640,#97641,#97642,#97643,#97644,
#97645,#97646,#97647,#97648,#97649,#97650,#97651,#97652,#97653,#97654,#97655,
#97656,#97657,#97658,#97659,#97660,#97661,#97662,#97663,#97664,#97665,#97666,
#97667,#97668,#97669,#97670,#97671,#97672,#97673,#97674,#97675,#97676,#97677,
#97678,#97679,#97680,#97681,#97682,#97683,#97684,#97685,#97686,#97687,#97688,
#97689,#97690,#97691,#97692,#97693,#97694,#97695,#97696,#97697,#97698,#97699,
#97700,#97701,#97702,#97703,#97704,#97705,#97706,#97707,#97708,#97709,#97710,
#97711,#97712,#97713,#97714,#97715,#97716,#97717,#97718,#97719,#97720,#97721,
#97722,#97723,#97724,#97725,#97726,#97727),.UNSPECIFIED.,.F.,.F.,(4,3,3,
3,3,3,3,3,3,3,3,3,3,3,3,3,3,3,3,3,3,3,3,3,3,3,3,3,3,3,3,3,3,3,3,3,3,3,3,
3,3,3,3,3,3,3,3,3,3,3,3,3,3,3,3,3,3,3,3,3,3,3,3,3,3,3,3,3,3,3,3,3,3,4),
(1102.69902141,1102.78302386211,1102.86703181426,1102.9510625347,1103.03513330275,
1103.11931332698,1103.20355529402,1103.28793168718,1103.32714522547,1103.41088393732,
1103.49451944868,1103.57807189208,1103.66156132793,1103.74501527855,1103.82845177239,
1103.91188888215,1103.99534467707,1104.0788891698,1104.16247825274,1104.24620152029,
1104.32688123619,1104.41061994804,1104.4942554594,1104.5778079028,1104.66129733865,
1104.74475128927,1104.82818778311,1104.91162489287,1104.99508068779,1105.07862518051,
1105.16221426346,1105.24593753101,1105.32661724691,1105.41035595876,1105.49399147012,
1105.57754391352,1105.66103334937,1105.74448729999,1105.82792379383,1105.91136090359,
1105.99481669851,1106.07836119124,1106.16195027418,1106.24567354173,1106.32635325763,
1106.41009196948,1106.49372748084,1106.57727992424,1106.66076936009,1106.74422331071,
1106.82765980455,1106.91109691431,1106.99455270923,1107.07809720196,1107.1616862849,
1107.24540955245,1107.32608926835,1107.4098279802,1107.49346349156,1107.57701593496,
1107.66050537081,1107.74395932143,1107.82739581527,1107.91083292503,1107.99428871995,
1108.07783321268,1108.16142229562,1108.24514556317,1108.32582527907,1108.40970043406,
1108.49343947228,1108.57710021367,1108.66069007077,1108.73132332231),
 .UNSPECIFIED.);
#755=B_SPLINE_CURVE_WITH_KNOTS('',3,(#97733,#97734,#97735,#97736,#97737,
#97738,#97739,#97740,#97741,#97742,#97743,#97744,#97745,#97746,#97747,#97748,
#97749,#97750,#97751,#97752,#97753,#97754,#97755,#97756,#97757,#97758,#97759,
#97760,#97761,#97762,#97763,#97764,#97765,#97766,#97767,#97768,#97769,#97770,
#97771,#97772,#97773,#97774,#97775,#97776,#97777,#97778,#97779,#97780,#97781,
#97782,#97783,#97784,#97785,#97786,#97787,#97788,#97789,#97790,#97791,#97792,
#97793,#97794,#97795,#97796,#97797,#97798,#97799,#97800,#97801,#97802,#97803,
#97804,#97805,#97806,#97807,#97808,#97809,#97810,#97811,#97812,#97813,#97814,
#97815,#97816,#97817,#97818,#97819,#97820,#97821,#97822,#97823,#97824,#97825,
#97826,#97827,#97828,#97829,#97830,#97831,#97832,#97833,#97834,#97835,#97836,
#97837,#97838,#97839,#97840,#97841,#97842,#97843,#97844,#97845,#97846,#97847,
#97848,#97849,#97850,#97851,#97852,#97853,#97854,#97855,#97856,#97857,#97858,
#97859,#97860,#97861,#97862,#97863,#97864,#97865,#97866,#97867,#97868,#97869,
#97870,#97871,#97872,#97873,#97874,#97875,#97876,#97877,#97878,#97879,#97880,
#97881,#97882,#97883,#97884,#97885,#97886,#97887,#97888,#97889,#97890,#97891,
#97892,#97893,#97894,#97895,#97896,#97897,#97898,#97899,#97900,#97901,#97902,
#97903,#97904,#97905,#97906,#97907,#97908,#97909,#97910,#97911,#97912,#97913,
#97914,#97915,#97916,#97917,#97918,#97919,#97920,#97921,#97922,#97923,#97924,
#97925,#97926,#97927,#97928,#97929,#97930,#97931,#97932,#97933,#97934,#97935,
#97936,#97937,#97938,#97939,#97940,#97941,#97942,#97943,#97944,#97945,#97946,
#97947,#97948,#97949,#97950,#97951,#97952,#97953,#97954,#97955),
 .UNSPECIFIED.,.F.,.F.,(4,3,3,3,3,3,3,3,3,3,3,3,3,3,3,3,3,3,3,3,3,3,3,3,
3,3,3,3,3,3,3,3,3,3,3,3,3,3,3,3,3,3,3,3,3,3,3,3,3,3,3,3,3,3,3,3,3,3,3,3,
3,3,3,3,3,3,3,3,3,3,3,3,3,3,4),(1108.98220671718,1109.01527067007,1109.09900938192,
1109.18264489328,1109.26619733668,1109.34968677253,1109.43314072315,1109.51657721699,
1109.60001432675,1109.68347012166,1109.76701461439,1109.85060369733,1109.93432696489,
1110.01500668079,1110.09874539264,1110.18238090401,1110.26593334741,1110.34942278327,
1110.43287673388,1110.51631322773,1110.59975033749,1110.68320613241,1110.76675062514,
1110.85033970809,1110.93406297565,1111.01474269152,1111.09848140336,1111.18211691473,
1111.26566935812,1111.34915879397,1111.43261274458,1111.51604923843,1111.59948634818,
1111.6829421431,1111.76648663582,1111.85007571876,1111.93379898632,1112.01447870223,
1112.09821741408,1112.18185292544,1112.26540536884,1112.34889480469,1112.43234875531,
1112.51578524916,1112.59922235891,1112.68267815383,1112.76622264656,1112.8498117295,
1112.93353499706,1113.01421471296,1113.09795342481,1113.18158893618,1113.26514137958,
1113.34863081543,1113.43208476605,1113.51552125989,1113.59895836965,1113.68241416457,
1113.7659586573,1113.84954774025,1113.93327100781,1114.01395072368,1114.09768943552,
1114.18132494689,1114.26487739029,1114.34836682614,1114.43182077675,1114.5152572706,
1114.59869438035,1114.68215017527,1114.76569466799,1114.84928375093,1114.93300701849,
1115.0136867344,1115.01433071751),.UNSPECIFIED.);
#756=B_SPLINE_CURVE_WITH_KNOTS('',3,(#97956,#97957,#97958,#97959,#97960,
#97961,#97962,#97963,#97964,#97965),.UNSPECIFIED.,.F.,.F.,(4,3,3,4),(1108.73043941245,
1108.81357021083,1108.89788846393,1108.98220671704),.UNSPECIFIED.);
#757=B_SPLINE_CURVE_WITH_KNOTS('',3,(#97967,#97968,#97969,#97970,#97971,
#97972,#97973,#97974,#97975,#97976),.UNSPECIFIED.,.F.,.F.,(4,3,3,4),(1108.73132332231,
1108.8148472524,1108.89852698479,1108.98220671718),.UNSPECIFIED.);
#758=B_SPLINE_CURVE_WITH_KNOTS('',3,(#97977,#97978,#97979,#97980,#97981,
#97982,#97983,#97984,#97985,#97986),.UNSPECIFIED.,.F.,.F.,(4,1,1,1,1,1,
1,4),(1108.98221426278,1109.32556128979,1110.32529730051,1111.32503331123,
1112.32476932195,1113.32450533267,1114.32424134339,1115.01349131436),
 .UNSPECIFIED.);
#759=B_SPLINE_CURVE_WITH_KNOTS('',3,(#97992,#97993,#97994,#97995,#97996,
#97997,#97998,#97999,#98000,#98001,#98002,#98003,#98004,#98005,#98006,#98007,
#98008,#98009,#98010,#98011,#98012,#98013,#98014,#98015,#98016,#98017,#98018,
#98019,#98020,#98021,#98022,#98023,#98024,#98025,#98026,#98027,#98028,#98029,
#98030,#98031,#98032,#98033,#98034,#98035,#98036,#98037,#98038,#98039,#98040,
#98041,#98042,#98043,#98044,#98045,#98046,#98047,#98048,#98049,#98050,#98051,
#98052,#98053,#98054,#98055,#98056,#98057,#98058,#98059,#98060,#98061,#98062,
#98063,#98064,#98065,#98066,#98067,#98068,#98069,#98070,#98071,#98072,#98073,
#98074,#98075,#98076,#98077,#98078,#98079,#98080,#98081,#98082,#98083,#98084,
#98085,#98086,#98087,#98088,#98089,#98090,#98091,#98092,#98093,#98094,#98095,
#98096,#98097,#98098,#98099,#98100,#98101,#98102,#98103,#98104,#98105,#98106,
#98107,#98108,#98109,#98110,#98111,#98112,#98113,#98114,#98115,#98116,#98117,
#98118,#98119,#98120,#98121,#98122,#98123,#98124,#98125,#98126,#98127,#98128,
#98129,#98130,#98131,#98132,#98133,#98134,#98135,#98136,#98137,#98138,#98139,
#98140,#98141,#98142,#98143,#98144,#98145,#98146,#98147,#98148,#98149,#98150,
#98151,#98152,#98153,#98154,#98155,#98156,#98157,#98158,#98159,#98160,#98161,
#98162,#98163,#98164,#98165,#98166,#98167,#98168,#98169,#98170,#98171,#98172,
#98173,#98174,#98175,#98176,#98177,#98178,#98179,#98180,#98181,#98182,#98183,
#98184,#98185,#98186,#98187,#98188,#98189,#98190,#98191,#98192,#98193,#98194,
#98195,#98196,#98197,#98198,#98199,#98200,#98201,#98202,#98203,#98204,#98205,
#98206,#98207,#98208,#98209,#98210,#98211),.UNSPECIFIED.,.F.,.F.,(4,3,3,
3,3,3,3,3,3,3,3,3,3,3,3,3,3,3,3,3,3,3,3,3,3,3,3,3,3,3,3,3,3,3,3,3,3,3,3,
3,3,3,3,3,3,3,3,3,3,3,3,3,3,3,3,3,3,3,3,3,3,3,3,3,3,3,3,3,3,3,3,3,3,4),
(1115.26539202436,1115.3479645808,1115.43114685134,1115.51364560196,1115.59613810739,
1115.6786432089,1115.76233809295,1115.8449676835,1115.92919521431,1116.01342274512,
1116.09716145697,1116.18079696833,1116.26434941173,1116.34783884758,1116.4312927982,
1116.51472929204,1116.5981664018,1116.68162219672,1116.76516668945,1116.84875577239,
1116.93247903994,1117.01315875584,1117.09689746769,1117.18053297905,1117.26408542245,
1117.3475748583,1117.43102880892,1117.51446530276,1117.59790241252,1117.68135820744,
1117.76490270017,1117.84849178311,1117.93221505066,1118.01289476656,1118.09663347841,
1118.18026898977,1118.26382143317,1118.34731086902,1118.43076481964,1118.51420131348,
1118.59763842324,1118.68109421816,1118.76463871089,1118.84822779383,1118.93195106138,
1119.01263077728,1119.09636948913,1119.18000500049,1119.26355744389,1119.34704687974,
1119.43050083036,1119.5139373242,1119.59737443396,1119.68083022888,1119.76437472161,
1119.84796380455,1119.9316870721,1120.012366788,1120.09610549985,1120.17974101121,
1120.26329345461,1120.34678289046,1120.43023684108,1120.51367333492,1120.59711044468,
1120.6805662396,1120.76411073233,1120.84769981527,1120.93142308282,1121.01210279872,
1121.09883484553,1121.18544801319,1121.27192043186,1121.29817665327),
 .UNSPECIFIED.);
#760=B_SPLINE_CURVE_WITH_KNOTS('',3,(#98212,#98213,#98214,#98215,#98216,
#98217,#98218,#98219,#98220,#98221),.UNSPECIFIED.,.F.,.F.,(4,3,3,4),(1115.01433071751,
1115.12380950414,1115.23095866677,1115.26539202417),.UNSPECIFIED.);
#761=B_SPLINE_CURVE_WITH_KNOTS('',3,(#98223,#98224,#98225,#98226),
 .UNSPECIFIED.,.F.,.F.,(4,4),(1115.01349131436,1115.26538483617),
 .UNSPECIFIED.);
#762=B_SPLINE_CURVE_WITH_KNOTS('',3,(#98227,#98228,#98229,#98230,#98231,
#98232,#98233,#98234,#98235,#98236,#98237,#98238,#98239,#98240,#98241,#98242,
#98243,#98244,#98245,#98246,#98247,#98248,#98249,#98250,#98251,#98252,#98253,
#98254,#98255,#98256,#98257,#98258,#98259,#98260,#98261,#98262,#98263,#98264,
#98265,#98266,#98267,#98268,#98269,#98270,#98271,#98272,#98273,#98274,#98275,
#98276,#98277,#98278,#98279,#98280,#98281,#98282,#98283,#98284,#98285,#98286,
#98287,#98288,#98289,#98290,#98291,#98292,#98293,#98294,#98295,#98296,#98297,
#98298,#98299,#98300,#98301,#98302,#98303,#98304,#98305,#98306,#98307,#98308,
#98309,#98310,#98311,#98312,#98313,#98314,#98315,#98316,#98317,#98318,#98319,
#98320,#98321,#98322,#98323,#98324,#98325,#98326,#98327,#98328,#98329,#98330,
#98331,#98332,#98333,#98334,#98335,#98336,#98337,#98338,#98339,#98340,#98341,
#98342,#98343,#98344,#98345,#98346,#98347,#98348,#98349,#98350,#98351,#98352,
#98353,#98354,#98355,#98356,#98357,#98358,#98359,#98360,#98361,#98362,#98363,
#98364,#98365,#98366,#98367,#98368,#98369,#98370,#98371,#98372,#98373,#98374,
#98375,#98376,#98377,#98378,#98379,#98380,#98381,#98382,#98383,#98384,#98385,
#98386,#98387,#98388,#98389,#98390,#98391,#98392,#98393,#98394,#98395,#98396,
#98397,#98398,#98399,#98400,#98401,#98402,#98403,#98404,#98405,#98406,#98407,
#98408,#98409,#98410,#98411,#98412,#98413,#98414,#98415,#98416,#98417,#98418,
#98419,#98420,#98421,#98422,#98423,#98424,#98425,#98426,#98427,#98428,#98429,
#98430,#98431,#98432,#98433,#98434,#98435,#98436,#98437,#98438,#98439,#98440,
#98441,#98442,#98443,#98444,#98445,#98446),.UNSPECIFIED.,.F.,.F.,(4,3,3,
3,3,3,3,3,3,3,3,3,3,3,3,3,3,3,3,3,3,3,3,3,3,3,3,3,3,3,3,3,3,3,3,3,3,3,3,
3,3,3,3,3,3,3,3,3,3,3,3,3,3,3,3,3,3,3,3,3,3,3,3,3,3,3,3,3,3,3,3,3,3,4),
(1115.26539202436,1115.32397735411,1115.40771606596,1115.49135157732,1115.57490402072,
1115.65839345657,1115.74184740719,1115.82528390103,1115.90872101079,1115.99217680571,
1116.07572129843,1116.15931038138,1116.24303364893,1116.32371336483,1116.40745207668,
1116.49108758804,1116.57464003144,1116.65812946729,1116.74158341791,1116.82501991175,
1116.90845702151,1116.99191281643,1117.07545730916,1117.1590463921,1117.24276965966,
1117.32344937555,1117.4071880874,1117.49082359876,1117.57437604216,1117.65786547801,
1117.74131942863,1117.82475592247,1117.90819303223,1117.99164882715,1118.07519331987,
1118.15878240282,1118.24250567037,1118.32318538627,1118.40692409812,1118.49055960948,
1118.57411205288,1118.65760148873,1118.74105543935,1118.82449193319,1118.90792904295,
1118.99138483787,1119.0749293306,1119.15851841354,1119.24224168109,1119.32292139699,
1119.40666010884,1119.4902956202,1119.5738480636,1119.65733749945,1119.74079145007,
1119.82422794391,1119.90766505367,1119.99112084859,1120.07466534132,1120.15825442426,
1120.24197769181,1120.32265740771,1120.40639753497,1120.49003413167,1120.57358733172,
1120.65707719659,1120.74052989164,1120.82396466327,1120.90739958385,1120.99085272192,
1121.07438811408,1121.15796790361,1121.24166679885,1121.2973671878),
 .UNSPECIFIED.);
#763=B_SPLINE_CURVE_WITH_KNOTS('',3,(#98452,#98453,#98454,#98455,#98456,
#98457,#98458,#98459,#98460,#98461,#98462,#98463,#98464,#98465,#98466,#98467,
#98468,#98469,#98470,#98471,#98472,#98473,#98474,#98475,#98476,#98477,#98478,
#98479,#98480,#98481,#98482,#98483,#98484,#98485,#98486,#98487,#98488,#98489,
#98490,#98491,#98492,#98493,#98494,#98495,#98496,#98497,#98498,#98499,#98500,
#98501,#98502,#98503,#98504,#98505,#98506,#98507,#98508,#98509,#98510,#98511,
#98512,#98513,#98514,#98515,#98516,#98517,#98518,#98519,#98520,#98521,#98522,
#98523,#98524,#98525,#98526,#98527,#98528,#98529,#98530,#98531,#98532,#98533,
#98534,#98535,#98536,#98537,#98538,#98539,#98540,#98541,#98542,#98543,#98544,
#98545,#98546,#98547,#98548,#98549,#98550,#98551,#98552,#98553,#98554,#98555,
#98556,#98557,#98558,#98559,#98560,#98561,#98562,#98563,#98564,#98565,#98566,
#98567,#98568,#98569,#98570,#98571,#98572,#98573,#98574,#98575,#98576,#98577,
#98578,#98579,#98580,#98581,#98582,#98583,#98584,#98585,#98586,#98587,#98588,
#98589,#98590,#98591,#98592,#98593,#98594,#98595,#98596,#98597,#98598,#98599,
#98600,#98601,#98602,#98603,#98604,#98605,#98606,#98607,#98608,#98609,#98610,
#98611,#98612,#98613,#98614,#98615,#98616,#98617,#98618,#98619,#98620,#98621,
#98622,#98623,#98624,#98625,#98626,#98627,#98628,#98629,#98630,#98631,#98632,
#98633,#98634,#98635,#98636,#98637,#98638,#98639,#98640,#98641,#98642,#98643,
#98644,#98645,#98646,#98647,#98648,#98649,#98650,#98651,#98652,#98653,#98654,
#98655,#98656,#98657,#98658,#98659,#98660,#98661,#98662,#98663,#98664,#98665,
#98666,#98667,#98668,#98669,#98670,#98671),.UNSPECIFIED.,.F.,.F.,(4,3,3,
3,3,3,3,3,3,3,3,3,3,3,3,3,3,3,3,3,3,3,3,3,3,3,3,3,3,3,3,3,3,3,3,3,3,3,3,
3,3,3,3,3,3,3,3,3,3,3,3,3,3,3,3,3,3,3,3,3,3,3,3,3,3,3,3,3,3,3,3,3,3,4),
(1121.5485773317,1121.63743490442,1121.73103588068,1121.82033663901,1121.90978283507,
1121.99943881037,1122.01183880944,1122.09557752129,1122.17921303265,1122.26276547605,
1122.3462549119,1122.42970886252,1122.51314535636,1122.59658246612,1122.68003826104,
1122.76358275377,1122.84717183671,1122.93089510426,1123.01157482016,1123.09531353201,
1123.17894904337,1123.26250148677,1123.34599092262,1123.42944487324,1123.51288136708,
1123.59631847684,1123.67977427176,1123.76331876449,1123.84690784743,1123.93063111498,
1124.01131083088,1124.09504954273,1124.17868505409,1124.26223749749,1124.34572693334,
1124.42918088396,1124.5126173778,1124.59605448756,1124.67951028248,1124.76305477521,
1124.84664385815,1124.9303671257,1125.0110468416,1125.09478555345,1125.17842106481,
1125.26197350821,1125.34546294406,1125.42891689468,1125.51235338852,1125.59579049828,
1125.6792462932,1125.76279078593,1125.84637986887,1125.93010313642,1126.01078285232,
1126.09452156417,1126.17815707553,1126.26170951893,1126.34519895478,1126.4286529054,
1126.51208939924,1126.595526509,1126.67898230392,1126.76252679665,1126.84611587959,
1126.92983914714,1127.01051886304,1127.09299425828,1127.17537411721,1127.25767766004,
1127.33992395772,1127.42213509276,1127.50435017971,1127.58009447292),
 .UNSPECIFIED.);
#764=B_SPLINE_CURVE_WITH_KNOTS('',3,(#98672,#98673,#98674,#98675,#98676,
#98677,#98678,#98679,#98680,#98681),.UNSPECIFIED.,.F.,.F.,(4,3,3,4),(1121.29817665327,
1121.38449491277,1121.47070749291,1121.54857733154),.UNSPECIFIED.);
#765=B_SPLINE_CURVE_WITH_KNOTS('',3,(#98683,#98684,#98685,#98686,#98687,
#98688,#98689,#98690,#98691,#98692),.UNSPECIFIED.,.F.,.F.,(4,3,3,4),(1121.2973671878,
1121.32239341843,1121.43573137779,1121.54857733154),.UNSPECIFIED.);
#766=B_SPLINE_CURVE_WITH_KNOTS('',3,(#98693,#98694,#98695,#98696,#98697,
#98698,#98699,#98700,#98701,#98702,#98703,#98704,#98705,#98706,#98707,#98708,
#98709,#98710,#98711,#98712,#98713,#98714,#98715,#98716,#98717,#98718,#98719,
#98720,#98721,#98722,#98723,#98724,#98725,#98726,#98727,#98728,#98729,#98730,
#98731,#98732,#98733,#98734,#98735,#98736,#98737,#98738,#98739,#98740,#98741,
#98742,#98743,#98744,#98745,#98746,#98747,#98748,#98749,#98750,#98751,#98752,
#98753,#98754,#98755,#98756,#98757,#98758,#98759,#98760,#98761,#98762,#98763,
#98764,#98765,#98766,#98767,#98768,#98769,#98770,#98771,#98772,#98773,#98774,
#98775,#98776,#98777,#98778,#98779,#98780,#98781,#98782,#98783,#98784,#98785,
#98786,#98787,#98788,#98789,#98790,#98791,#98792,#98793,#98794,#98795,#98796,
#98797,#98798,#98799,#98800,#98801,#98802,#98803,#98804,#98805,#98806,#98807,
#98808,#98809,#98810,#98811,#98812,#98813,#98814,#98815,#98816,#98817,#98818,
#98819,#98820,#98821,#98822,#98823,#98824,#98825,#98826,#98827,#98828,#98829,
#98830,#98831,#98832,#98833,#98834,#98835,#98836,#98837,#98838,#98839,#98840,
#98841,#98842,#98843,#98844,#98845,#98846,#98847,#98848,#98849,#98850,#98851,
#98852,#98853,#98854,#98855,#98856,#98857,#98858,#98859,#98860,#98861,#98862,
#98863,#98864,#98865,#98866,#98867,#98868,#98869,#98870,#98871,#98872,#98873,
#98874,#98875,#98876,#98877,#98878,#98879,#98880,#98881,#98882,#98883,#98884,
#98885,#98886,#98887,#98888,#98889,#98890,#98891,#98892,#98893,#98894,#98895,
#98896,#98897,#98898,#98899,#98900,#98901,#98902,#98903,#98904,#98905,#98906,
#98907,#98908,#98909,#98910,#98911,#98912),.UNSPECIFIED.,.F.,.F.,(4,3,3,
3,3,3,3,3,3,3,3,3,3,3,3,3,3,3,3,3,3,3,3,3,3,3,3,3,3,3,3,3,3,3,3,3,3,3,3,
3,3,3,3,3,3,3,3,3,3,3,3,3,3,3,3,3,3,3,3,3,3,3,3,3,3,3,3,3,3,3,3,3,3,4),
(1121.5485773317,1121.63102433406,1121.71741247094,1121.79976528288,1121.88210511884,
1121.96445092535,1122.04682165131,1122.12928094339,1122.21179209108,1122.29442027794,
1122.32212942915,1122.405868141,1122.48950365236,1122.57305609576,1122.65654553161,
1122.73999948223,1122.82343597607,1122.90687308583,1122.99032888075,1123.07387337347,
1123.15746245642,1123.24118572397,1123.32186543987,1123.40560415172,1123.48923966308,
1123.57279210648,1123.65628154233,1123.73973549295,1123.82317198679,1123.90660909655,
1123.99006489147,1124.0736093842,1124.15719846714,1124.24092173469,1124.32160145059,
1124.40534016244,1124.4889756738,1124.5725281172,1124.65601755305,1124.73947150367,
1124.82290799751,1124.90634510727,1124.98980090219,1125.07334539491,1125.15693447786,
1125.24065774541,1125.32133746131,1125.40507617316,1125.48871168452,1125.57226412792,
1125.65575356377,1125.73920751439,1125.82264400823,1125.90608111799,1125.98953691291,
1126.07308140564,1126.15667048858,1126.24039375613,1126.32107347203,1126.40481218388,
1126.48844769524,1126.57200013864,1126.65548957449,1126.73894352511,1126.82238001895,
1126.90581712871,1126.98927292363,1127.07281741636,1127.1564064993,1127.24012976685,
1127.32080948275,1127.40843810818,1127.49587754248,1127.58141735988),
 .UNSPECIFIED.);
#767=B_SPLINE_CURVE_WITH_KNOTS('',3,(#98918,#98919,#98920,#98921,#98922,
#98923,#98924,#98925,#98926,#98927,#98928,#98929,#98930,#98931,#98932,#98933,
#98934,#98935,#98936,#98937,#98938,#98939,#98940,#98941,#98942,#98943,#98944,
#98945,#98946,#98947,#98948,#98949,#98950,#98951,#98952,#98953,#98954,#98955,
#98956,#98957,#98958,#98959,#98960,#98961,#98962,#98963,#98964,#98965,#98966,
#98967,#98968,#98969,#98970,#98971,#98972,#98973,#98974,#98975,#98976,#98977,
#98978,#98979,#98980,#98981,#98982,#98983,#98984,#98985,#98986,#98987,#98988,
#98989,#98990,#98991,#98992,#98993,#98994,#98995,#98996,#98997,#98998,#98999,
#99000,#99001,#99002,#99003,#99004,#99005,#99006,#99007,#99008,#99009,#99010,
#99011,#99012,#99013,#99014,#99015,#99016,#99017,#99018,#99019,#99020,#99021,
#99022,#99023,#99024,#99025,#99026,#99027,#99028,#99029,#99030,#99031,#99032,
#99033,#99034,#99035,#99036,#99037,#99038,#99039,#99040,#99041,#99042,#99043,
#99044,#99045,#99046,#99047,#99048,#99049,#99050,#99051,#99052,#99053,#99054,
#99055,#99056,#99057,#99058,#99059,#99060,#99061,#99062,#99063,#99064,#99065,
#99066,#99067,#99068,#99069,#99070,#99071,#99072,#99073,#99074,#99075,#99076,
#99077,#99078,#99079,#99080,#99081,#99082,#99083,#99084,#99085,#99086,#99087,
#99088,#99089,#99090,#99091,#99092,#99093,#99094,#99095,#99096,#99097,#99098,
#99099,#99100,#99101,#99102,#99103,#99104,#99105,#99106,#99107,#99108,#99109,
#99110,#99111,#99112,#99113,#99114,#99115,#99116,#99117,#99118,#99119,#99120,
#99121,#99122,#99123,#99124,#99125,#99126,#99127,#99128,#99129,#99130,#99131,
#99132,#99133,#99134,#99135,#99136,#99137),.UNSPECIFIED.,.F.,.F.,(4,3,3,
3,3,3,3,3,3,3,3,3,3,3,3,3,3,3,3,3,3,3,3,3,3,3,3,3,3,3,3,3,3,3,3,3,3,3,3,
3,3,3,3,3,3,3,3,3,3,3,3,3,3,3,3,3,3,3,3,3,3,3,3,3,3,3,3,3,3,3,3,3,3,4),
(1127.83176263872,1127.95957097145,1128.01025487376,1128.09399358561,1128.17762909697,
1128.26118154037,1128.34467097622,1128.42812492684,1128.51156142068,1128.59499853044,
1128.67845432536,1128.76199881809,1128.84558790103,1128.92931116858,1129.00999088448,
1129.09372959633,1129.17736510769,1129.26091755109,1129.34440698694,1129.42786093756,
1129.5112974314,1129.59473454116,1129.67819033608,1129.7617348288,1129.84532391175,
1129.9290471793,1130.0097268952,1130.09346560705,1130.17710111841,1130.26065356181,
1130.34414299766,1130.42759694828,1130.51103344212,1130.59447055188,1130.6779263468,
1130.76147083953,1130.84505992247,1130.92878319002,1131.00946290592,1131.09320161777,
1131.17683712913,1131.26038957253,1131.34387900838,1131.427332959,1131.51076945284,
1131.5942065626,1131.67766235752,1131.76120685025,1131.84479593319,1131.92851920074,
1132.00919891664,1132.09293762849,1132.17657313985,1132.26012558325,1132.3436150191,
1132.42706896972,1132.51050546356,1132.59394257332,1132.67739836824,1132.76094286097,
1132.84453194391,1132.92825521146,1133.00893492736,1133.09268224944,1133.17632445377,
1133.26220042274,1133.34568559806,1133.42913301872,1133.51256077308,1133.60025363119,
1133.68372583927,1133.76722657941,1133.85080197334,1133.86333220551),
 .UNSPECIFIED.);
#768=B_SPLINE_CURVE_WITH_KNOTS('',3,(#99138,#99139,#99140,#99141,#99142,
#99143,#99144,#99145,#99146,#99147),.UNSPECIFIED.,.F.,.F.,(4,3,3,4),(1127.58009447292,
1127.66234880159,1127.74705572007,1127.83176263856),.UNSPECIFIED.);
#769=B_SPLINE_CURVE_WITH_KNOTS('',3,(#99149,#99150,#99151,#99152,#99153,
#99154,#99155,#99156,#99157,#99158),.UNSPECIFIED.,.F.,.F.,(4,3,3,4),(1127.58141735988,
1127.668604728,1127.75564880231,1127.83176263872),.UNSPECIFIED.);
#770=B_SPLINE_CURVE_WITH_KNOTS('',3,(#99159,#99160,#99161,#99162,#99163,
#99164,#99165,#99166,#99167,#99168,#99169,#99170,#99171,#99172,#99173,#99174,
#99175,#99176,#99177,#99178,#99179,#99180,#99181,#99182,#99183,#99184,#99185,
#99186,#99187,#99188,#99189,#99190,#99191,#99192,#99193,#99194,#99195,#99196,
#99197,#99198,#99199,#99200,#99201,#99202,#99203,#99204,#99205,#99206,#99207,
#99208,#99209,#99210,#99211,#99212,#99213,#99214,#99215,#99216,#99217,#99218,
#99219,#99220,#99221,#99222,#99223,#99224,#99225,#99226,#99227,#99228,#99229,
#99230,#99231,#99232,#99233,#99234,#99235,#99236,#99237,#99238,#99239,#99240,
#99241,#99242,#99243,#99244,#99245,#99246,#99247,#99248,#99249,#99250,#99251,
#99252,#99253,#99254,#99255,#99256,#99257,#99258,#99259,#99260,#99261,#99262,
#99263,#99264,#99265,#99266,#99267,#99268,#99269,#99270,#99271,#99272,#99273,
#99274,#99275,#99276,#99277,#99278,#99279,#99280,#99281,#99282,#99283,#99284,
#99285,#99286,#99287,#99288,#99289,#99290,#99291,#99292,#99293,#99294,#99295,
#99296,#99297,#99298,#99299,#99300,#99301,#99302,#99303,#99304,#99305,#99306,
#99307,#99308,#99309,#99310,#99311,#99312,#99313,#99314,#99315,#99316,#99317,
#99318,#99319,#99320,#99321,#99322,#99323,#99324,#99325,#99326,#99327,#99328,
#99329,#99330,#99331,#99332,#99333,#99334,#99335,#99336,#99337,#99338,#99339,
#99340,#99341,#99342,#99343,#99344,#99345,#99346,#99347,#99348,#99349,#99350,
#99351,#99352,#99353,#99354,#99355,#99356,#99357,#99358,#99359,#99360,#99361,
#99362,#99363,#99364,#99365,#99366,#99367,#99368,#99369,#99370,#99371,#99372,
#99373,#99374,#99375,#99376,#99377,#99378),.UNSPECIFIED.,.F.,.F.,(4,3,3,
3,3,3,3,3,3,3,3,3,3,3,3,3,3,3,3,3,3,3,3,3,3,3,3,3,3,3,3,3,3,3,3,3,3,3,3,
3,3,3,3,3,3,3,3,3,3,3,3,3,3,3,3,3,3,3,3,3,3,3,3,3,3,3,3,3,3,3,3,3,3,4),
(1127.83176263883,1127.91957948589,1128.00752696713,1128.09569652539,1128.18398523041,
1128.27247833123,1128.32054549347,1128.40428420532,1128.48791971668,1128.57147216008,
1128.65496159593,1128.73841554655,1128.82185204039,1128.90528915015,1128.98874494507,
1129.0722894378,1129.15587852074,1129.23960178829,1129.32028150419,1129.40402021604,
1129.4876557274,1129.5712081708,1129.65469760665,1129.73815155727,1129.82158805111,
1129.90502516087,1129.98848095579,1130.07202544852,1130.15561453146,1130.23933779902,
1130.32001751491,1130.40375622676,1130.48739173812,1130.57094418152,1130.65443361737,
1130.73788756799,1130.82132406183,1130.90476117159,1130.98821696651,1131.07176145923,
1131.15535054218,1131.23907380973,1131.31975352563,1131.40349223748,1131.48712774884,
1131.57068019224,1131.65416962809,1131.73762357871,1131.82106007255,1131.90449718231,
1131.98795297723,1132.07149746995,1132.1550865529,1132.23880982045,1132.31948953635,
1132.4032282482,1132.48686375956,1132.57041620296,1132.65390563881,1132.73735958943,
1132.82079608327,1132.90423319303,1132.98768898795,1133.07123348068,1133.15482256362,
1133.23854583118,1133.31922554707,1133.40175294837,1133.48418409761,1133.56653818716,
1133.64883186673,1133.73108993687,1133.8133437479,1133.86337617231),
 .UNSPECIFIED.);
#771=B_SPLINE_CURVE_WITH_KNOTS('',3,(#99384,#99385,#99386,#99387,#99388,
#99389,#99390,#99391,#99392,#99393,#99394,#99395,#99396,#99397,#99398,#99399,
#99400,#99401,#99402,#99403,#99404,#99405,#99406,#99407,#99408,#99409,#99410,
#99411,#99412,#99413,#99414,#99415,#99416,#99417,#99418,#99419,#99420,#99421,
#99422,#99423,#99424,#99425,#99426,#99427,#99428,#99429,#99430,#99431,#99432,
#99433,#99434,#99435,#99436,#99437,#99438,#99439,#99440,#99441,#99442,#99443,
#99444,#99445,#99446,#99447,#99448,#99449,#99450,#99451,#99452,#99453,#99454,
#99455,#99456,#99457,#99458,#99459,#99460,#99461,#99462,#99463,#99464,#99465,
#99466,#99467,#99468,#99469,#99470,#99471,#99472,#99473,#99474,#99475,#99476,
#99477,#99478,#99479,#99480,#99481,#99482,#99483,#99484,#99485,#99486,#99487,
#99488,#99489,#99490,#99491,#99492,#99493,#99494,#99495,#99496,#99497,#99498,
#99499,#99500,#99501,#99502,#99503,#99504,#99505,#99506,#99507,#99508,#99509,
#99510,#99511,#99512,#99513,#99514,#99515,#99516,#99517,#99518,#99519,#99520,
#99521,#99522,#99523,#99524,#99525,#99526,#99527,#99528,#99529,#99530,#99531,
#99532,#99533,#99534,#99535,#99536,#99537,#99538,#99539,#99540,#99541,#99542,
#99543,#99544,#99545,#99546,#99547,#99548,#99549,#99550,#99551,#99552,#99553,
#99554,#99555,#99556,#99557,#99558,#99559,#99560,#99561,#99562,#99563,#99564,
#99565,#99566,#99567,#99568,#99569,#99570,#99571,#99572,#99573,#99574,#99575,
#99576,#99577,#99578,#99579,#99580,#99581,#99582,#99583,#99584,#99585,#99586,
#99587,#99588,#99589,#99590,#99591,#99592,#99593,#99594,#99595,#99596,#99597,
#99598,#99599,#99600,#99601,#99602,#99603),.UNSPECIFIED.,.F.,.F.,(4,3,3,
3,3,3,3,3,3,3,3,3,3,3,3,3,3,3,3,3,3,3,3,3,3,3,3,3,3,3,3,3,3,3,3,3,3,3,3,
3,3,3,3,3,3,3,3,3,3,3,3,3,3,3,3,3,3,3,3,3,3,3,3,3,3,3,3,3,3,3,3,3,3,4),
(1134.11494794604,1134.19754763141,1134.28005584972,1134.3624936672,1134.44488704967,
1134.52725803592,1134.60962556158,1134.6920085571,1134.77447536623,1134.85698551003,
1134.93962372416,1135.0084069488,1135.09214566065,1135.17578117201,1135.25933361541,
1135.34282305126,1135.42627700188,1135.50971349572,1135.59315060548,1135.6766064004,
1135.76015089313,1135.84373997607,1135.92746324362,1136.00814295952,1136.09188167137,
1136.17551718273,1136.25906962613,1136.34255906198,1136.4260130126,1136.50944950644,
1136.5928866162,1136.67634241112,1136.75988690385,1136.84347598679,1136.92719925434,
1137.00787897024,1137.09161768209,1137.17525319345,1137.25880563685,1137.3422950727,
1137.42574902332,1137.50918551716,1137.59262262692,1137.67607842184,1137.75962291457,
1137.84321199751,1137.92693526506,1138.00761498096,1138.09135369281,1138.17498920417,
1138.25854164757,1138.34203108342,1138.42548503404,1138.50892152788,1138.59235863764,
1138.67581443255,1138.75935892528,1138.84294800823,1138.92667127578,1139.00735099168,
1139.09108970353,1139.17472521489,1139.25827765829,1139.34176709414,1139.42522104476,
1139.5086575386,1139.59209464836,1139.67555044328,1139.75909493601,1139.84268401895,
1139.9264072865,1140.0070870024,1140.1008350489,1140.14773803965),
 .UNSPECIFIED.);
#772=B_SPLINE_CURVE_WITH_KNOTS('',3,(#99604,#99605,#99606,#99607,#99608,
#99609,#99610,#99611,#99612,#99613),.UNSPECIFIED.,.F.,.F.,(4,3,3,4),(1133.86333220551,
1133.94706238406,1134.00867093808,1134.1149479459),.UNSPECIFIED.);
#773=B_SPLINE_CURVE_WITH_KNOTS('',3,(#99615,#99616,#99617,#99618,#99619,
#99620,#99621,#99622,#99623,#99624),.UNSPECIFIED.,.F.,.F.,(4,3,3,4),(1133.86337617231,
1133.94566361369,1134.03030577971,1134.11494794573),.UNSPECIFIED.);
#774=B_SPLINE_CURVE_WITH_KNOTS('',3,(#99625,#99626,#99627,#99628,#99629,
#99630,#99631,#99632,#99633,#99634,#99635,#99636,#99637,#99638,#99639,#99640,
#99641,#99642,#99643,#99644,#99645,#99646,#99647,#99648,#99649,#99650,#99651,
#99652,#99653,#99654,#99655,#99656,#99657,#99658,#99659,#99660,#99661,#99662,
#99663,#99664,#99665,#99666,#99667,#99668,#99669,#99670,#99671,#99672,#99673,
#99674,#99675,#99676,#99677,#99678,#99679,#99680,#99681,#99682,#99683,#99684,
#99685,#99686,#99687,#99688,#99689,#99690,#99691,#99692,#99693,#99694,#99695,
#99696,#99697,#99698,#99699,#99700,#99701,#99702,#99703,#99704,#99705,#99706,
#99707,#99708,#99709,#99710,#99711,#99712,#99713,#99714,#99715,#99716,#99717,
#99718,#99719,#99720,#99721,#99722,#99723,#99724,#99725,#99726,#99727,#99728,
#99729,#99730,#99731,#99732,#99733,#99734,#99735,#99736,#99737,#99738,#99739,
#99740,#99741,#99742,#99743,#99744,#99745,#99746,#99747,#99748,#99749,#99750,
#99751,#99752,#99753,#99754,#99755,#99756,#99757,#99758,#99759,#99760,#99761,
#99762,#99763,#99764,#99765,#99766,#99767,#99768,#99769,#99770,#99771,#99772,
#99773,#99774,#99775,#99776,#99777,#99778,#99779,#99780,#99781,#99782,#99783,
#99784,#99785,#99786,#99787,#99788,#99789,#99790,#99791,#99792,#99793,#99794,
#99795,#99796,#99797,#99798,#99799,#99800,#99801,#99802,#99803,#99804,#99805,
#99806,#99807,#99808,#99809,#99810,#99811,#99812,#99813,#99814,#99815,#99816,
#99817,#99818,#99819,#99820,#99821,#99822,#99823,#99824,#99825,#99826,#99827,
#99828,#99829,#99830,#99831,#99832,#99833,#99834,#99835,#99836,#99837,#99838,
#99839,#99840,#99841),.UNSPECIFIED.,.F.,.F.,(4,3,3,3,3,3,3,3,3,3,3,3,3,
3,3,3,3,3,3,3,3,3,3,3,3,3,3,3,3,3,3,3,3,3,3,3,3,3,3,3,3,3,3,3,3,3,3,3,3,
3,3,3,3,3,3,3,3,3,3,3,3,3,3,3,3,3,3,3,3,3,3,3,4),(1134.1149479459,1134.23395192778,
1134.31896155779,1134.40270026964,1134.486335781,1134.5698882244,1134.65337766025,
1134.73683161087,1134.82026810471,1134.90370521447,1134.98716100939,1135.07070550212,
1135.15429458506,1135.23801785262,1135.31869756852,1135.40243628037,1135.48607179173,
1135.56962423513,1135.65311367099,1135.7365676216,1135.82000411545,1135.9034412252,
1135.98689702012,1136.07044151285,1136.15403059579,1136.23775386335,1136.31843357924,
1136.40217229109,1136.48580780245,1136.56936024585,1136.6528496817,1136.73630363232,
1136.81974012616,1136.90317723592,1136.98663303083,1137.07017752356,1137.1537666065,
1137.23748987406,1137.31816958996,1137.40190830181,1137.48554381317,1137.56909625657,
1137.65258569242,1137.73603964304,1137.81947613688,1137.90291324664,1137.98636904156,
1138.06991353429,1138.15350261723,1138.23722588478,1138.31790560068,1138.40164431253,
1138.48527982389,1138.56883226729,1138.65232170314,1138.73577565376,1138.8192121476,
1138.90264925736,1138.98610505228,1139.06964954501,1139.15323862795,1139.23696189551,
1139.3176416114,1139.40139054479,1139.48503402325,1139.56857723134,1139.65206358258,
1139.73551119624,1139.81893816171,1139.90239151911,1139.98585572871,1140.06939644253,
1140.14648534745),.UNSPECIFIED.);
#775=B_SPLINE_CURVE_WITH_KNOTS('',3,(#99847,#99848,#99849,#99850,#99851,
#99852,#99853,#99854,#99855,#99856,#99857,#99858,#99859,#99860,#99861,#99862,
#99863,#99864,#99865,#99866,#99867,#99868,#99869,#99870,#99871,#99872,#99873,
#99874,#99875,#99876,#99877,#99878,#99879,#99880,#99881,#99882,#99883,#99884,
#99885,#99886,#99887,#99888,#99889,#99890,#99891,#99892,#99893,#99894,#99895,
#99896,#99897,#99898,#99899,#99900,#99901,#99902,#99903,#99904,#99905,#99906,
#99907,#99908,#99909,#99910,#99911,#99912,#99913,#99914,#99915,#99916,#99917,
#99918,#99919,#99920,#99921,#99922,#99923,#99924,#99925,#99926,#99927,#99928,
#99929,#99930,#99931,#99932,#99933,#99934,#99935,#99936,#99937,#99938,#99939,
#99940,#99941,#99942,#99943,#99944,#99945,#99946,#99947,#99948,#99949,#99950,
#99951,#99952,#99953,#99954,#99955,#99956,#99957,#99958,#99959,#99960,#99961,
#99962,#99963,#99964,#99965,#99966,#99967,#99968,#99969,#99970,#99971,#99972,
#99973,#99974,#99975,#99976,#99977,#99978,#99979,#99980,#99981,#99982,#99983,
#99984,#99985,#99986,#99987,#99988,#99989,#99990,#99991,#99992,#99993,#99994,
#99995,#99996,#99997,#99998,#99999,#100000,#100001,#100002,#100003,#100004,
#100005,#100006,#100007,#100008,#100009,#100010,#100011,#100012,#100013,
#100014,#100015,#100016,#100017,#100018,#100019,#100020,#100021,#100022,
#100023,#100024,#100025,#100026,#100027,#100028,#100029,#100030,#100031,
#100032,#100033,#100034,#100035,#100036,#100037,#100038,#100039,#100040,
#100041,#100042,#100043,#100044,#100045,#100046,#100047,#100048,#100049,
#100050,#100051,#100052,#100053,#100054,#100055,#100056,#100057,#100058,
#100059,#100060,#100061,#100062,#100063,#100064,#100065,#100066),
 .UNSPECIFIED.,.F.,.F.,(4,3,3,3,3,3,3,3,3,3,3,3,3,3,3,3,3,3,3,3,3,3,3,3,
3,3,3,3,3,3,3,3,3,3,3,3,3,3,3,3,3,3,3,3,3,3,3,3,3,3,3,3,3,3,3,3,3,3,3,3,
3,3,3,3,3,3,3,3,3,3,3,3,3,4),(1140.39813325308,1140.48251076188,1140.56690496386,
1140.65133254477,1140.74020516186,1140.8248033239,1140.90947201762,1140.99427121713,
1141.00682301312,1141.09056172497,1141.17419723633,1141.25774967973,1141.34123911558,
1141.4246930662,1141.50812956004,1141.5915666698,1141.67502246472,1141.75856695744,
1141.84215604039,1141.92587930794,1142.00655902384,1142.09029773569,1142.17393324705,
1142.25748569045,1142.3409751263,1142.42442907692,1142.50786557076,1142.59130268052,
1142.67475847544,1142.75830296817,1142.84189205111,1142.92561531866,1143.00629503456,
1143.09003374641,1143.17366925777,1143.25722170117,1143.34071113702,1143.42416508764,
1143.50760158148,1143.59103869124,1143.67449448616,1143.75803897888,1143.84162806183,
1143.92535132938,1144.00603104528,1144.08976975713,1144.17340526849,1144.25695771189,
1144.34044714774,1144.42390109836,1144.5073375922,1144.59077470196,1144.67423049688,
1144.75777498961,1144.84136407255,1144.9250873401,1145.005767056,1145.08950576785,
1145.17314127921,1145.25669372261,1145.34018315846,1145.42363710908,1145.50707360292,
1145.59051071268,1145.6739665076,1145.75751100033,1145.84110008327,1145.92482335083,
1146.00550306672,1146.08907419385,1146.17438957255,1146.25775095929,1146.34404333398,
1146.43033570868),.UNSPECIFIED.);
#776=B_SPLINE_CURVE_WITH_KNOTS('',3,(#100067,#100068,#100069,#100070,#100071,
#100072,#100073,#100074,#100075,#100076),.UNSPECIFIED.,.F.,.F.,(4,3,3,4),
(1140.14773803965,1140.24099126569,1140.33376735038,1140.39813325289),
 .UNSPECIFIED.);
#777=B_SPLINE_CURVE_WITH_KNOTS('',3,(#100078,#100079,#100080,#100081,#100082,
#100083,#100084,#100085,#100086,#100087),.UNSPECIFIED.,.F.,.F.,(4,3,3,4),
(1140.14648534745,1140.23193148479,1140.31737762212,1140.39813325308),
 .UNSPECIFIED.);
#778=B_SPLINE_CURVE_WITH_KNOTS('',3,(#100088,#100089,#100090,#100091,#100092,
#100093,#100094,#100095,#100096,#100097,#100098,#100099,#100100,#100101,
#100102,#100103,#100104,#100105,#100106,#100107,#100108,#100109,#100110,
#100111,#100112,#100113,#100114,#100115,#100116,#100117,#100118,#100119,
#100120,#100121,#100122,#100123,#100124,#100125,#100126,#100127,#100128,
#100129,#100130,#100131,#100132,#100133,#100134,#100135,#100136,#100137,
#100138,#100139,#100140,#100141,#100142,#100143,#100144,#100145,#100146,
#100147,#100148,#100149,#100150,#100151,#100152,#100153,#100154,#100155,
#100156,#100157,#100158,#100159,#100160,#100161,#100162,#100163,#100164,
#100165,#100166,#100167,#100168,#100169,#100170,#100171,#100172,#100173,
#100174,#100175,#100176,#100177,#100178,#100179,#100180,#100181,#100182,
#100183,#100184,#100185,#100186,#100187,#100188,#100189,#100190,#100191,
#100192,#100193,#100194,#100195,#100196,#100197,#100198,#100199,#100200,
#100201,#100202,#100203,#100204,#100205,#100206,#100207,#100208,#100209,
#100210,#100211,#100212,#100213,#100214,#100215,#100216,#100217,#100218,
#100219,#100220,#100221,#100222,#100223,#100224,#100225,#100226,#100227,
#100228,#100229,#100230,#100231,#100232,#100233,#100234,#100235,#100236,
#100237,#100238,#100239,#100240,#100241,#100242,#100243,#100244,#100245,
#100246,#100247,#100248,#100249,#100250,#100251,#100252,#100253,#100254,
#100255,#100256,#100257,#100258,#100259,#100260,#100261,#100262,#100263,
#100264,#100265,#100266,#100267,#100268,#100269,#100270,#100271,#100272,
#100273,#100274,#100275,#100276,#100277,#100278,#100279,#100280,#100281,
#100282,#100283,#100284,#100285,#100286,#100287,#100288,#100289,#100290,
#100291,#100292,#100293,#100294,#100295,#100296,#100297,#100298,#100299,
#100300,#100301,#100302,#100303,#100304,#100305,#100306,#100307),
 .UNSPECIFIED.,.F.,.F.,(4,3,3,3,3,3,3,3,3,3,3,3,3,3,3,3,3,3,3,3,3,3,3,3,
3,3,3,3,3,3,3,3,3,3,3,3,3,3,3,3,3,3,3,3,3,3,3,3,3,3,3,3,3,3,3,3,3,3,3,3,
3,3,3,3,3,3,3,3,3,3,3,3,3,4),(1140.39813325321,1140.48091981114,1140.56361047569,
1140.64622620517,1140.73008713363,1140.81262525657,1140.89515581373,1140.97769762652,
1141.0625516281,1141.14521622128,1141.23116492706,1141.31711363284,1141.40085234469,
1141.48448785605,1141.56804029945,1141.6515297353,1141.73498368592,1141.81842017976,
1141.90185728952,1141.98531308444,1142.06885757717,1142.15244666011,1142.23616992767,
1142.31684964356,1142.40058835541,1142.48422386677,1142.56777631017,1142.65126574602,
1142.73471969664,1142.81815619048,1142.90159330024,1142.98504909516,1143.06859358789,
1143.15218267083,1143.23590593838,1143.31658565428,1143.40032436613,1143.48395987749,
1143.56751232089,1143.65100175674,1143.73445570736,1143.8178922012,1143.90132931096,
1143.98478510588,1144.06832959861,1144.15191868155,1144.2356419491,1144.316321665,
1144.40006037685,1144.48369588821,1144.56724833161,1144.65073776746,1144.73419171808,
1144.81762821192,1144.90106532168,1144.9845211166,1145.06806560933,1145.15165469227,
1145.23537795982,1145.31605767572,1145.39979638757,1145.48343189893,1145.56698434233,
1145.65047377818,1145.7339277288,1145.81736422264,1145.9008013324,1145.98425712732,
1146.06780162004,1146.15139070299,1146.23511397054,1146.31579368644,1146.41148953146,
1146.43084402924),.UNSPECIFIED.);
#779=B_SPLINE_CURVE_WITH_KNOTS('',3,(#100313,#100314,#100315,#100316,#100317,
#100318,#100319,#100320,#100321,#100322,#100323,#100324,#100325,#100326,
#100327,#100328,#100329,#100330,#100331,#100332,#100333,#100334,#100335,
#100336,#100337,#100338,#100339,#100340,#100341,#100342,#100343,#100344,
#100345,#100346,#100347,#100348,#100349,#100350,#100351,#100352,#100353,
#100354,#100355,#100356,#100357,#100358,#100359,#100360,#100361,#100362,
#100363,#100364,#100365,#100366,#100367,#100368,#100369,#100370,#100371,
#100372,#100373,#100374,#100375,#100376,#100377,#100378,#100379,#100380,
#100381,#100382,#100383,#100384,#100385,#100386,#100387,#100388,#100389,
#100390,#100391,#100392,#100393,#100394,#100395,#100396,#100397,#100398,
#100399,#100400,#100401,#100402,#100403,#100404,#100405,#100406,#100407,
#100408,#100409,#100410,#100411,#100412,#100413,#100414,#100415,#100416,
#100417,#100418,#100419,#100420,#100421,#100422,#100423,#100424,#100425,
#100426,#100427,#100428,#100429,#100430,#100431,#100432,#100433,#100434,
#100435,#100436,#100437,#100438,#100439,#100440,#100441,#100442,#100443,
#100444,#100445,#100446,#100447,#100448,#100449,#100450,#100451,#100452,
#100453,#100454,#100455,#100456,#100457,#100458,#100459,#100460,#100461,
#100462,#100463,#100464,#100465,#100466,#100467,#100468,#100469,#100470,
#100471,#100472,#100473,#100474,#100475,#100476,#100477,#100478,#100479,
#100480,#100481,#100482,#100483,#100484,#100485,#100486,#100487,#100488,
#100489,#100490,#100491,#100492,#100493,#100494,#100495,#100496,#100497,
#100498,#100499,#100500,#100501,#100502,#100503,#100504,#100505,#100506,
#100507,#100508,#100509,#100510,#100511,#100512,#100513,#100514,#100515,
#100516,#100517,#100518,#100519,#100520,#100521,#100522,#100523,#100524,
#100525,#100526,#100527,#100528,#100529,#100530,#100531,#100532),
 .UNSPECIFIED.,.F.,.F.,(4,3,3,3,3,3,3,3,3,3,3,3,3,3,3,3,3,3,3,3,3,3,3,3,
3,3,3,3,3,3,3,3,3,3,3,3,3,3,3,3,3,3,3,3,3,3,3,3,3,3,3,3,3,3,3,3,3,3,3,3,
3,3,3,3,3,3,3,3,3,3,3,3,3,4),(1146.68131856044,1146.7794209927,1146.87817191571,
1146.97765054662,1147.00523907744,1147.08897778929,1147.17261330065,1147.25616574405,
1147.3396551799,1147.42310913052,1147.50654562436,1147.58998273412,1147.67343852904,
1147.75698302176,1147.84057210471,1147.92429537226,1148.00497508816,1148.08871380001,
1148.17234931137,1148.25590175477,1148.33939119062,1148.42284514124,1148.50628163508,
1148.58971874484,1148.67317453976,1148.75671903249,1148.84030811543,1148.92403138299,
1149.00471109888,1149.08844981073,1149.17208532209,1149.25563776549,1149.33912720134,
1149.42258115196,1149.5060176458,1149.58945475556,1149.67291055048,1149.75645504321,
1149.84004412615,1149.9237673937,1150.0044471096,1150.08818582145,1150.17182133281,
1150.25537377621,1150.33886321206,1150.42231716268,1150.50575365652,1150.58919076628,
1150.67264656119,1150.75619105392,1150.83978013687,1150.92350340442,1151.00418312032,
1151.08792183217,1151.17155734353,1151.25510978693,1151.33859922278,1151.4220531734,
1151.50548966724,1151.588926777,1151.67238257192,1151.75592706465,1151.83951614759,
1151.92323941515,1152.00391913104,1152.08715180263,1152.17025299475,1152.25327826016,
1152.33624622653,1152.41917547575,1152.50210012115,1152.58502118562,1152.6679838129,
1152.71272127735),.UNSPECIFIED.);
#780=B_SPLINE_CURVE_WITH_KNOTS('',3,(#100533,#100534,#100535,#100536,#100537,
#100538,#100539,#100540,#100541,#100542),.UNSPECIFIED.,.F.,.F.,(4,3,3,4),
(1146.43033570868,1146.51357203859,1146.59744529942,1146.68131856026),
 .UNSPECIFIED.);
#781=B_SPLINE_CURVE_WITH_KNOTS('',3,(#100544,#100545,#100546,#100547,#100548,
#100549,#100550,#100551,#100552,#100553),.UNSPECIFIED.,.F.,.F.,(4,3,3,4),
(1146.43084402924,1146.52599979843,1146.62054094815,1146.68131856006),
 .UNSPECIFIED.);
#782=B_SPLINE_CURVE_WITH_KNOTS('',3,(#100554,#100555,#100556,#100557,#100558,
#100559,#100560,#100561,#100562,#100563,#100564,#100565,#100566,#100567,
#100568,#100569,#100570,#100571,#100572,#100573,#100574,#100575,#100576,
#100577,#100578,#100579,#100580,#100581,#100582,#100583,#100584,#100585,
#100586,#100587,#100588,#100589,#100590,#100591,#100592,#100593,#100594,
#100595,#100596,#100597,#100598,#100599,#100600,#100601,#100602,#100603,
#100604,#100605,#100606,#100607,#100608,#100609,#100610,#100611,#100612,
#100613,#100614,#100615,#100616,#100617,#100618,#100619,#100620,#100621,
#100622,#100623,#100624,#100625,#100626,#100627,#100628,#100629,#100630,
#100631,#100632,#100633,#100634,#100635,#100636,#100637,#100638,#100639,
#100640,#100641,#100642,#100643,#100644,#100645,#100646,#100647,#100648,
#100649,#100650,#100651,#100652,#100653,#100654,#100655,#100656,#100657,
#100658,#100659,#100660,#100661,#100662,#100663,#100664,#100665,#100666,
#100667,#100668,#100669,#100670,#100671,#100672,#100673,#100674,#100675,
#100676,#100677,#100678,#100679,#100680,#100681,#100682,#100683,#100684,
#100685,#100686,#100687,#100688,#100689,#100690,#100691,#100692,#100693,
#100694,#100695,#100696,#100697,#100698,#100699,#100700,#100701,#100702,
#100703,#100704,#100705,#100706,#100707,#100708,#100709,#100710,#100711,
#100712,#100713,#100714,#100715,#100716,#100717,#100718,#100719,#100720,
#100721,#100722,#100723,#100724,#100725,#100726,#100727,#100728,#100729,
#100730,#100731,#100732,#100733,#100734,#100735,#100736,#100737,#100738,
#100739,#100740,#100741,#100742,#100743,#100744,#100745,#100746,#100747,
#100748,#100749,#100750,#100751,#100752,#100753,#100754,#100755,#100756,
#100757,#100758,#100759,#100760,#100761,#100762,#100763,#100764,#100765,
#100766,#100767,#100768,#100769,#100770,#100771,#100772,#100773),
 .UNSPECIFIED.,.F.,.F.,(4,3,3,3,3,3,3,3,3,3,3,3,3,3,3,3,3,3,3,3,3,3,3,3,
3,3,3,3,3,3,3,3,3,3,3,3,3,3,3,3,3,3,3,3,3,3,3,3,3,3,3,3,3,3,3,3,3,3,3,3,
3,3,3,3,3,3,3,3,3,3,3,3,3,4),(1146.68131856026,1146.76521245412,1146.84910858566,
1146.93302437699,1147.01697725917,1147.10103703447,1147.18515641783,1147.2694111216,
1147.31552969716,1147.39926840901,1147.48290392037,1147.56645636377,1147.64994579962,
1147.73339975024,1147.81683624408,1147.90027335384,1147.98372914876,1148.06727364149,
1148.15086272443,1148.23458599198,1148.31526570788,1148.39900441973,1148.48263993109,
1148.56619237449,1148.64968181034,1148.73313576096,1148.8165722548,1148.90000936456,
1148.98346515948,1149.0670096522,1149.15059873515,1149.2343220027,1149.3150017186,
1149.39874043045,1149.48237594181,1149.56592838521,1149.64941782106,1149.73287177168,
1149.81630826552,1149.89974537528,1149.9832011702,1150.06674566293,1150.15033474587,
1150.23405801342,1150.31473772932,1150.39847644117,1150.48211195253,1150.56566439593,
1150.64915383178,1150.7326077824,1150.81604427624,1150.899481386,1150.98293718092,
1151.06648167365,1151.15007075659,1151.23379402415,1151.31447374004,1151.39821245189,
1151.48184796325,1151.56540040665,1151.6488898425,1151.73234379312,1151.81578028696,
1151.89921739672,1151.98267319164,1152.06621768437,1152.14980676731,1152.23353003486,
1152.31420975076,1152.39818867721,1152.48203015719,1152.56579257425,1152.64948197077,
1152.71365100326),.UNSPECIFIED.);
#783=B_SPLINE_CURVE_WITH_KNOTS('',3,(#100779,#100780,#100781,#100782,#100783,
#100784,#100785,#100786,#100787,#100788,#100789,#100790,#100791,#100792,
#100793,#100794,#100795,#100796,#100797,#100798,#100799,#100800,#100801,
#100802,#100803,#100804,#100805,#100806,#100807,#100808,#100809,#100810,
#100811,#100812,#100813,#100814,#100815,#100816,#100817,#100818,#100819,
#100820,#100821,#100822,#100823,#100824,#100825,#100826,#100827,#100828,
#100829,#100830,#100831,#100832,#100833,#100834,#100835,#100836,#100837,
#100838,#100839,#100840,#100841,#100842,#100843,#100844,#100845,#100846,
#100847,#100848,#100849,#100850,#100851,#100852,#100853,#100854,#100855,
#100856,#100857,#100858,#100859,#100860,#100861,#100862,#100863,#100864,
#100865,#100866,#100867,#100868,#100869,#100870,#100871,#100872,#100873,
#100874,#100875,#100876,#100877,#100878,#100879,#100880,#100881,#100882,
#100883,#100884,#100885,#100886,#100887,#100888,#100889,#100890,#100891,
#100892,#100893,#100894,#100895,#100896,#100897,#100898,#100899,#100900,
#100901,#100902,#100903,#100904,#100905,#100906,#100907,#100908,#100909,
#100910,#100911,#100912,#100913,#100914,#100915,#100916,#100917,#100918,
#100919,#100920,#100921,#100922,#100923,#100924,#100925,#100926,#100927,
#100928,#100929,#100930,#100931,#100932,#100933,#100934,#100935,#100936,
#100937,#100938,#100939,#100940,#100941,#100942,#100943,#100944,#100945,
#100946,#100947,#100948,#100949,#100950,#100951,#100952,#100953,#100954,
#100955,#100956,#100957,#100958,#100959,#100960,#100961,#100962,#100963,
#100964,#100965,#100966,#100967,#100968,#100969,#100970,#100971,#100972,
#100973,#100974,#100975,#100976,#100977,#100978,#100979,#100980,#100981,
#100982,#100983,#100984,#100985,#100986,#100987,#100988,#100989,#100990,
#100991,#100992,#100993,#100994,#100995,#100996,#100997,#100998),
 .UNSPECIFIED.,.F.,.F.,(4,3,3,3,3,3,3,3,3,3,3,3,3,3,3,3,3,3,3,3,3,3,3,3,
3,3,3,3,3,3,3,3,3,3,3,3,3,3,3,3,3,3,3,3,3,3,3,3,3,3,3,3,3,3,3,3,3,3,3,3,
3,3,3,3,3,3,3,3,3,3,3,3,3,4),(1152.96450386744,1153.00365514176,1153.08739385361,
1153.17102936497,1153.25458180837,1153.33807124422,1153.42152519484,1153.50496168868,
1153.58839879844,1153.67185459336,1153.75539908609,1153.83898816903,1153.92271143658,
1154.00339115248,1154.08712986433,1154.17076537569,1154.25431781909,1154.33780725494,
1154.42126120556,1154.5046976994,1154.58813480916,1154.67159060408,1154.75513509681,
1154.83872417975,1154.92244744731,1155.0031271632,1155.08686587505,1155.17050138641,
1155.25405382981,1155.33754326566,1155.42099721628,1155.50443371012,1155.58787081988,
1155.6713266148,1155.75487110753,1155.83846019047,1155.92218345802,1156.00286317392,
1156.08660188577,1156.17023739713,1156.25378984053,1156.33727927638,1156.420733227,
1156.50416972084,1156.5876068306,1156.67106262552,1156.75460711825,1156.83819620119,
1156.92191946874,1157.00259918464,1157.08633789649,1157.16997340785,1157.25352585125,
1157.3370152871,1157.42046923772,1157.50390573156,1157.58734284132,1157.67079863623,
1157.75434312896,1157.8379322119,1157.92165547946,1158.00233519536,1158.08607421481,
1158.16970996149,1158.25326256821,1158.33675209564,1158.42020576168,1158.50364186877,
1158.58707848948,1158.67053369293,1158.75407615424,1158.83766316353,1158.92138094069,
1158.99659016216),.UNSPECIFIED.);
#784=B_SPLINE_CURVE_WITH_KNOTS('',3,(#100999,#101000,#101001,#101002,#101003,
#101004,#101005,#101006,#101007,#101008),.UNSPECIFIED.,.F.,.F.,(4,3,3,4),
(1152.71272127735,1152.79577877608,1152.88014132168,1152.96450386727),
 .UNSPECIFIED.);
#785=B_SPLINE_CURVE_WITH_KNOTS('',3,(#101010,#101011,#101012,#101013,#101014,
#101015,#101016,#101017,#101018,#101019),.UNSPECIFIED.,.F.,.F.,(4,3,3,4),
(1152.71365100326,1152.79727347273,1152.88090159923,1152.96450386744),
 .UNSPECIFIED.);
#786=B_SPLINE_CURVE_WITH_KNOTS('',3,(#101020,#101021,#101022,#101023,#101024,
#101025,#101026,#101027,#101028,#101029,#101030,#101031,#101032,#101033,
#101034,#101035,#101036,#101037,#101038,#101039,#101040,#101041,#101042,
#101043,#101044,#101045,#101046,#101047,#101048,#101049,#101050,#101051,
#101052,#101053,#101054,#101055,#101056,#101057,#101058,#101059,#101060,
#101061,#101062,#101063,#101064,#101065,#101066,#101067,#101068,#101069,
#101070,#101071,#101072,#101073,#101074,#101075,#101076,#101077,#101078,
#101079,#101080,#101081,#101082,#101083,#101084,#101085,#101086,#101087,
#101088,#101089,#101090,#101091,#101092,#101093,#101094,#101095,#101096,
#101097,#101098,#101099,#101100,#101101,#101102,#101103,#101104,#101105,
#101106,#101107,#101108,#101109,#101110,#101111,#101112,#101113,#101114,
#101115,#101116,#101117,#101118,#101119,#101120,#101121,#101122,#101123,
#101124,#101125,#101126,#101127,#101128,#101129,#101130,#101131,#101132,
#101133,#101134,#101135,#101136,#101137,#101138,#101139,#101140,#101141,
#101142,#101143,#101144,#101145,#101146,#101147,#101148,#101149,#101150,
#101151,#101152,#101153,#101154,#101155,#101156,#101157,#101158,#101159,
#101160,#101161,#101162,#101163,#101164,#101165,#101166,#101167,#101168,
#101169,#101170,#101171,#101172,#101173,#101174,#101175,#101176,#101177,
#101178,#101179,#101180,#101181,#101182,#101183,#101184,#101185,#101186,
#101187,#101188,#101189,#101190,#101191,#101192,#101193,#101194,#101195,
#101196,#101197,#101198,#101199,#101200,#101201,#101202,#101203,#101204,
#101205,#101206,#101207,#101208,#101209,#101210,#101211,#101212,#101213,
#101214,#101215,#101216,#101217,#101218,#101219,#101220,#101221,#101222,
#101223,#101224,#101225,#101226,#101227,#101228,#101229,#101230,#101231,
#101232,#101233,#101234,#101235,#101236,#101237,#101238,#101239),
 .UNSPECIFIED.,.F.,.F.,(4,3,3,3,3,3,3,3,3,3,3,3,3,3,3,3,3,3,3,3,3,3,3,3,
3,3,3,3,3,3,3,3,3,3,3,3,3,3,3,3,3,3,3,3,3,3,3,3,3,3,3,3,3,3,3,3,3,3,3,3,
3,3,3,3,3,3,3,3,3,3,3,3,3,4),(1152.96450386764,1153.06037082155,1153.15671753066,
1153.25367244208,1153.31394576148,1153.39768447333,1153.48131998469,1153.56487242809,
1153.64836186394,1153.73181581456,1153.8152523084,1153.89868941816,1153.98214521308,
1154.06568970581,1154.14927878875,1154.2330020563,1154.3136817722,1154.39742048405,
1154.48105599541,1154.56460843881,1154.64809787466,1154.73155182528,1154.81498831912,
1154.89842542888,1154.9818812238,1155.06542571653,1155.14901479947,1155.23273806702,
1155.31341778292,1155.39715649477,1155.48079200613,1155.56434444953,1155.64783388538,
1155.731287836,1155.81472432984,1155.8981614396,1155.98161723452,1156.06516172725,
1156.14875081019,1156.23247407774,1156.31315379364,1156.39689250549,1156.48052801685,
1156.56408046025,1156.6475698961,1156.73102384672,1156.81446034056,1156.89789745032,
1156.98135324524,1157.06489773797,1157.14848682091,1157.23221008847,1157.31288980436,
1157.39662851621,1157.48026402757,1157.56381647097,1157.64730590682,1157.73075985744,
1157.81419635128,1157.89763346104,1157.98108925596,1158.06463374869,1158.14822283163,
1158.23194609918,1158.31262581508,1158.39803049351,1158.4808680987,1158.56363060694,
1158.64633684465,1158.72900559084,1158.81166897465,1158.89433037083,1158.97702735572,
1158.99586324251),.UNSPECIFIED.);
#787=B_SPLINE_CURVE_WITH_KNOTS('',3,(#101245,#101246,#101247,#101248,#101249,
#101250,#101251,#101252,#101253,#101254,#101255,#101256,#101257,#101258,
#101259,#101260,#101261,#101262,#101263,#101264,#101265,#101266,#101267,
#101268,#101269,#101270,#101271,#101272,#101273,#101274,#101275,#101276,
#101277,#101278,#101279,#101280,#101281,#101282,#101283,#101284,#101285,
#101286,#101287,#101288,#101289,#101290,#101291,#101292,#101293,#101294,
#101295,#101296,#101297,#101298,#101299,#101300,#101301,#101302,#101303,
#101304,#101305,#101306,#101307,#101308,#101309,#101310,#101311,#101312,
#101313,#101314,#101315,#101316,#101317,#101318,#101319,#101320,#101321,
#101322,#101323,#101324,#101325,#101326,#101327,#101328,#101329,#101330,
#101331,#101332,#101333,#101334,#101335,#101336,#101337,#101338,#101339,
#101340,#101341,#101342,#101343,#101344,#101345,#101346,#101347,#101348,
#101349,#101350,#101351,#101352,#101353,#101354,#101355,#101356,#101357,
#101358,#101359,#101360,#101361,#101362,#101363,#101364,#101365,#101366,
#101367,#101368,#101369,#101370,#101371,#101372,#101373,#101374,#101375,
#101376,#101377,#101378,#101379,#101380,#101381,#101382,#101383,#101384,
#101385,#101386,#101387,#101388,#101389,#101390,#101391,#101392,#101393,
#101394,#101395,#101396,#101397,#101398,#101399,#101400,#101401,#101402,
#101403,#101404,#101405,#101406,#101407,#101408,#101409,#101410,#101411,
#101412,#101413,#101414,#101415,#101416,#101417,#101418,#101419,#101420,
#101421,#101422,#101423,#101424,#101425,#101426,#101427,#101428,#101429,
#101430,#101431,#101432,#101433,#101434,#101435,#101436,#101437,#101438,
#101439,#101440,#101441,#101442,#101443,#101444,#101445,#101446,#101447,
#101448,#101449,#101450,#101451,#101452,#101453,#101454,#101455,#101456,
#101457,#101458,#101459,#101460,#101461,#101462,#101463,#101464),
 .UNSPECIFIED.,.F.,.F.,(4,3,3,3,3,3,3,3,3,3,3,3,3,3,3,3,3,3,3,3,3,3,3,3,
3,3,3,3,3,3,3,3,3,3,3,3,3,3,3,3,3,3,3,3,3,3,3,3,3,3,3,3,3,3,3,3,3,3,3,3,
3,3,3,3,3,3,3,3,3,3,3,3,3,4),(1159.24768917462,1159.33022655319,1159.41417413614,
1159.49663275271,1159.57908345992,1159.66154512836,1159.74661065047,1159.82919506601,
1159.9155011414,1160.0018072168,1160.08554592865,1160.16918144001,1160.25273388341,
1160.33622331926,1160.41967726988,1160.50311376373,1160.58655087348,1160.6700066684,
1160.75355116113,1160.83714024407,1160.92086351163,1161.00154322752,1161.08528193937,
1161.16891745073,1161.25246989413,1161.33595932998,1161.4194132806,1161.50284977445,
1161.5862868842,1161.66974267912,1161.75328717185,1161.83687625479,1161.92059952235,
1162.00127923824,1162.08501795009,1162.16865346145,1162.25220590485,1162.3356953407,
1162.41914929132,1162.50258578516,1162.58602289492,1162.66947868983,1162.75302318256,
1162.8366122655,1162.92033553306,1163.00101524896,1163.08475396081,1163.16838947217,
1163.25194191557,1163.33543135142,1163.41888530204,1163.50232179588,1163.58575890564,
1163.66921470056,1163.75275919329,1163.83634827623,1163.92007154378,1164.00075125968,
1164.08448997153,1164.16812548289,1164.25167792629,1164.33516736214,1164.41862131275,
1164.5020578066,1164.58549491635,1164.66895071127,1164.752495204,1164.83608428694,
1164.9198075545,1165.0004872704,1165.08742265818,1165.17423700981,1165.2609081172,
1165.28048890086),.UNSPECIFIED.);
#788=B_SPLINE_CURVE_WITH_KNOTS('',3,(#101465,#101466,#101467,#101468,#101469,
#101470,#101471,#101472,#101473,#101474,#101475,#101476,#101477),
 .UNSPECIFIED.,.F.,.F.,(4,3,3,3,4),(1158.99659016216,1159.00207120608,1159.11274010456,
1159.22085745498,1159.24768917449),.UNSPECIFIED.);
#789=B_SPLINE_CURVE_WITH_KNOTS('',3,(#101479,#101480,#101481,#101482,#101483,
#101484,#101485,#101486,#101487,#101488),.UNSPECIFIED.,.F.,.F.,(4,3,3,4),
(1158.99586324251,1159.07864886217,1159.16316901834,1159.2476891745),
 .UNSPECIFIED.);
#790=B_SPLINE_CURVE_WITH_KNOTS('',3,(#101489,#101490,#101491,#101492,#101493,
#101494,#101495,#101496,#101497,#101498,#101499,#101500,#101501,#101502,
#101503,#101504,#101505,#101506,#101507,#101508,#101509,#101510,#101511,
#101512,#101513,#101514,#101515,#101516,#101517,#101518,#101519,#101520,
#101521,#101522,#101523,#101524,#101525,#101526,#101527,#101528,#101529,
#101530,#101531,#101532,#101533,#101534,#101535,#101536,#101537,#101538,
#101539,#101540,#101541,#101542,#101543,#101544,#101545,#101546,#101547,
#101548,#101549,#101550,#101551,#101552,#101553,#101554,#101555,#101556,
#101557,#101558,#101559,#101560,#101561,#101562,#101563,#101564,#101565,
#101566,#101567,#101568,#101569,#101570,#101571,#101572,#101573,#101574,
#101575,#101576,#101577,#101578,#101579,#101580,#101581,#101582,#101583,
#101584,#101585,#101586,#101587,#101588,#101589,#101590,#101591,#101592,
#101593,#101594,#101595,#101596,#101597,#101598,#101599,#101600,#101601,
#101602,#101603,#101604,#101605,#101606,#101607,#101608,#101609,#101610,
#101611,#101612,#101613,#101614,#101615,#101616,#101617,#101618,#101619,
#101620,#101621,#101622,#101623,#101624,#101625,#101626,#101627,#101628,
#101629,#101630,#101631,#101632,#101633,#101634,#101635,#101636,#101637,
#101638,#101639,#101640,#101641,#101642,#101643,#101644,#101645,#101646,
#101647,#101648,#101649,#101650,#101651,#101652,#101653,#101654,#101655,
#101656,#101657,#101658,#101659,#101660,#101661,#101662,#101663,#101664,
#101665,#101666,#101667,#101668,#101669,#101670,#101671,#101672,#101673,
#101674,#101675,#101676,#101677,#101678,#101679,#101680,#101681,#101682,
#101683,#101684,#101685,#101686,#101687,#101688,#101689,#101690,#101691,
#101692,#101693,#101694,#101695,#101696,#101697,#101698,#101699,#101700,
#101701,#101702,#101703,#101704,#101705,#101706,#101707,#101708),
 .UNSPECIFIED.,.F.,.F.,(4,3,3,3,3,3,3,3,3,3,3,3,3,3,3,3,3,3,3,3,3,3,3,3,
3,3,3,3,3,3,3,3,3,3,3,3,3,3,3,3,3,3,3,3,3,3,3,3,3,3,3,3,3,3,3,3,3,3,3,3,
3,3,3,3,3,3,3,3,3,3,3,3,3,4),(1159.24768917462,1159.3123618258,1159.39610053765,
1159.47973604901,1159.56328849241,1159.64677792826,1159.73023187888,1159.81366837272,
1159.89710548248,1159.9805612774,1160.06410577012,1160.14769485307,1160.23141812062,
1160.31209783652,1160.39583654837,1160.47947205973,1160.56302450313,1160.64651393898,
1160.7299678896,1160.81340438344,1160.8968414932,1160.98029728812,1161.06384178085,
1161.14743086379,1161.23115413134,1161.31183384724,1161.39557255909,1161.47920807045,
1161.56276051385,1161.6462499497,1161.72970390032,1161.81314039416,1161.89657750392,
1161.98003329884,1162.06357779156,1162.14716687451,1162.23089014206,1162.31156985796,
1162.39530856981,1162.47894408117,1162.56249652457,1162.64598596042,1162.72943991104,
1162.81287640488,1162.89631351464,1162.97976930956,1163.06331380229,1163.14690288523,
1163.23062615278,1163.31130586868,1163.39504458053,1163.47868009189,1163.56223253529,
1163.64572197114,1163.72917592176,1163.8126124156,1163.89604952536,1163.97950532028,
1164.06304981301,1164.14663889595,1164.2303621635,1164.3110418794,1164.394782357,
1164.47841922334,1164.56197261265,1164.64546258667,1164.72891499175,1164.81234935932,
1164.89578376167,1164.97923626715,1165.06276950219,1165.14634708746,1165.23004029477,
1165.27963236799),.UNSPECIFIED.);
#791=B_SPLINE_CURVE_WITH_KNOTS('',3,(#101714,#101715,#101716,#101717,#101718,
#101719,#101720,#101721,#101722,#101723,#101724,#101725,#101726,#101727,
#101728,#101729,#101730,#101731,#101732,#101733,#101734,#101735,#101736,
#101737,#101738,#101739,#101740,#101741,#101742,#101743,#101744,#101745,
#101746,#101747,#101748,#101749,#101750,#101751,#101752,#101753,#101754,
#101755,#101756,#101757,#101758,#101759,#101760,#101761,#101762,#101763,
#101764,#101765,#101766,#101767,#101768,#101769,#101770,#101771,#101772,
#101773,#101774,#101775,#101776,#101777,#101778,#101779,#101780,#101781,
#101782,#101783,#101784,#101785,#101786,#101787,#101788,#101789,#101790,
#101791,#101792,#101793,#101794,#101795,#101796,#101797,#101798,#101799,
#101800,#101801,#101802,#101803,#101804,#101805,#101806,#101807,#101808,
#101809,#101810,#101811,#101812,#101813,#101814,#101815,#101816,#101817,
#101818,#101819,#101820,#101821,#101822,#101823,#101824,#101825,#101826,
#101827,#101828,#101829,#101830,#101831,#101832,#101833,#101834,#101835,
#101836,#101837,#101838,#101839,#101840,#101841,#101842,#101843,#101844,
#101845,#101846,#101847,#101848,#101849,#101850,#101851,#101852,#101853,
#101854,#101855,#101856,#101857,#101858,#101859,#101860,#101861,#101862,
#101863,#101864,#101865,#101866,#101867,#101868,#101869,#101870,#101871,
#101872,#101873,#101874,#101875,#101876,#101877,#101878,#101879,#101880,
#101881,#101882,#101883,#101884,#101885,#101886,#101887,#101888,#101889,
#101890,#101891,#101892,#101893,#101894,#101895,#101896,#101897,#101898,
#101899,#101900,#101901,#101902,#101903,#101904,#101905,#101906,#101907,
#101908,#101909,#101910,#101911,#101912,#101913,#101914,#101915,#101916,
#101917,#101918,#101919,#101920,#101921,#101922,#101923,#101924,#101925,
#101926,#101927,#101928,#101929,#101930,#101931,#101932,#101933),
 .UNSPECIFIED.,.F.,.F.,(4,3,3,3,3,3,3,3,3,3,3,3,3,3,3,3,3,3,3,3,3,3,3,3,
3,3,3,3,3,3,3,3,3,3,3,3,3,3,3,3,3,3,3,3,3,3,3,3,3,3,3,3,3,3,3,3,3,3,3,3,
3,3,3,3,3,3,3,3,3,3,3,3,3,4),(1165.53087448193,1165.6194718285,1165.70823112112,
1165.79724274353,1165.88639300426,1165.97575379441,1166.00022328112,1166.08396199297,
1166.16759750434,1166.25114994774,1166.33463938359,1166.41809333421,1166.50152982806,
1166.58496693782,1166.66842273274,1166.75196722547,1166.83555630841,1166.91927957597,
1166.99995929184,1167.08369800369,1167.16733351505,1167.25088595845,1167.3343753943,
1167.41782934492,1167.50126583876,1167.58470294852,1167.66815874344,1167.75170323617,
1167.83529231911,1167.91901558667,1167.99969530256,1168.08343401441,1168.16706952577,
1168.25062196917,1168.33411140502,1168.41756535563,1168.50100184948,1168.58443895923,
1168.66789475415,1168.75143924688,1168.83502832982,1168.91875159738,1168.99943131328,
1169.08317002513,1169.16680553649,1169.25035797989,1169.33384741574,1169.41730136636,
1169.5007378602,1169.58417496996,1169.66763076488,1169.75117525761,1169.83476434055,
1169.91848760811,1169.999167324,1170.08290603585,1170.16654154721,1170.25009399061,
1170.33358342646,1170.41703737707,1170.50047387092,1170.58391098067,1170.66736677559,
1170.75091126832,1170.83450035126,1170.91822361882,1170.99890333472,1171.08138595452,
1171.16377288917,1171.24608335551,1171.32833583527,1171.41055307205,1171.49277221627,
1171.56241306759),.UNSPECIFIED.);
#792=B_SPLINE_CURVE_WITH_KNOTS('',3,(#101934,#101935,#101936,#101937,#101938,
#101939,#101940,#101941,#101942,#101943),.UNSPECIFIED.,.F.,.F.,(4,3,3,4),
(1165.28048890086,1165.36700416373,1165.45340537406,1165.5308744818),
 .UNSPECIFIED.);
#793=B_SPLINE_CURVE_WITH_KNOTS('',3,(#101945,#101946,#101947,#101948,#101949,
#101950,#101951,#101952,#101953,#101954),.UNSPECIFIED.,.F.,.F.,(4,3,3,4),
(1165.27963236799,1165.31077789012,1165.4255320562,1165.5308744818),
 .UNSPECIFIED.);
#794=B_SPLINE_CURVE_WITH_KNOTS('',3,(#101955,#101956,#101957,#101958,#101959,
#101960,#101961,#101962,#101963,#101964,#101965,#101966,#101967,#101968,
#101969,#101970,#101971,#101972,#101973,#101974,#101975,#101976,#101977,
#101978,#101979,#101980,#101981,#101982,#101983,#101984,#101985,#101986,
#101987,#101988,#101989,#101990,#101991,#101992,#101993,#101994,#101995,
#101996,#101997,#101998,#101999,#102000,#102001,#102002,#102003,#102004,
#102005,#102006,#102007,#102008,#102009,#102010,#102011,#102012,#102013,
#102014,#102015,#102016,#102017,#102018,#102019,#102020,#102021,#102022,
#102023,#102024,#102025,#102026,#102027,#102028,#102029,#102030,#102031,
#102032,#102033,#102034,#102035,#102036,#102037,#102038,#102039,#102040,
#102041,#102042,#102043,#102044,#102045,#102046,#102047,#102048,#102049,
#102050,#102051,#102052,#102053,#102054,#102055,#102056,#102057,#102058,
#102059,#102060,#102061,#102062,#102063,#102064,#102065,#102066,#102067,
#102068,#102069,#102070,#102071,#102072,#102073,#102074,#102075,#102076,
#102077,#102078,#102079,#102080,#102081,#102082,#102083,#102084,#102085,
#102086,#102087,#102088,#102089,#102090,#102091,#102092,#102093,#102094,
#102095,#102096,#102097,#102098,#102099,#102100,#102101,#102102,#102103,
#102104,#102105,#102106,#102107,#102108,#102109,#102110,#102111,#102112,
#102113,#102114,#102115,#102116,#102117,#102118,#102119,#102120,#102121,
#102122,#102123,#102124,#102125,#102126,#102127,#102128,#102129,#102130,
#102131,#102132,#102133,#102134,#102135,#102136,#102137,#102138,#102139,
#102140,#102141,#102142,#102143,#102144,#102145,#102146,#102147,#102148,
#102149,#102150,#102151,#102152,#102153,#102154,#102155,#102156,#102157,
#102158,#102159,#102160,#102161,#102162,#102163,#102164,#102165,#102166,
#102167,#102168,#102169,#102170,#102171,#102172,#102173,#102174),
 .UNSPECIFIED.,.F.,.F.,(4,3,3,3,3,3,3,3,3,3,3,3,3,3,3,3,3,3,3,3,3,3,3,3,
3,3,3,3,3,3,3,3,3,3,3,3,3,3,3,3,3,3,3,3,3,3,3,3,3,3,3,3,3,3,3,3,3,3,3,3,
3,3,3,3,3,3,3,3,3,3,3,3,3,4),(1165.53087448195,1165.61329996591,1165.69566252244,
1165.77799052972,1165.86030294426,1165.94261873174,1166.02495685819,1166.10738217233,
1166.18985705826,1166.27245154326,1166.31051390084,1166.39425261269,1166.47788812405,
1166.56144056745,1166.6449300033,1166.72838395392,1166.81182044776,1166.89525755752,
1166.97871335244,1167.06225784517,1167.14584692811,1167.22957019567,1167.31024991156,
1167.39398862341,1167.47762413477,1167.56117657817,1167.64466601402,1167.72811996464,
1167.81155645848,1167.89499356824,1167.97844936316,1168.06199385589,1168.14558293883,
1168.22930620638,1168.30998592228,1168.39372463413,1168.47736014549,1168.56091258889,
1168.64440202474,1168.72785597536,1168.8112924692,1168.89472957896,1168.97818537388,
1169.0617298666,1169.14531894955,1169.2290422171,1169.309721933,1169.39346064485,
1169.47709615621,1169.56064859961,1169.64413803546,1169.72759198608,1169.81102847992,
1169.89446558968,1169.9779213846,1170.06146587733,1170.14505496027,1170.22877822782,
1170.30945794372,1170.39319665557,1170.47683216693,1170.56038461033,1170.64387404618,
1170.7273279968,1170.81076449064,1170.8942016004,1170.97765739531,1171.06120188804,
1171.14479097098,1171.22851423854,1171.30919395444,1171.3970542314,1171.48472161422,
1171.56372456646),.UNSPECIFIED.);
#795=B_SPLINE_CURVE_WITH_KNOTS('',3,(#102180,#102181,#102182,#102183,#102184,
#102185,#102186,#102187,#102188,#102189,#102190,#102191,#102192,#102193,
#102194,#102195,#102196,#102197,#102198,#102199,#102200,#102201,#102202,
#102203,#102204,#102205,#102206,#102207,#102208,#102209,#102210,#102211,
#102212,#102213,#102214,#102215,#102216,#102217,#102218,#102219,#102220,
#102221,#102222,#102223,#102224,#102225,#102226,#102227,#102228,#102229,
#102230,#102231,#102232,#102233,#102234,#102235,#102236,#102237,#102238,
#102239,#102240,#102241,#102242,#102243,#102244,#102245,#102246,#102247,
#102248,#102249,#102250,#102251,#102252,#102253,#102254,#102255,#102256,
#102257,#102258,#102259,#102260,#102261,#102262,#102263,#102264,#102265,
#102266,#102267,#102268,#102269,#102270,#102271,#102272,#102273,#102274,
#102275,#102276,#102277,#102278,#102279,#102280,#102281,#102282,#102283,
#102284,#102285,#102286,#102287,#102288,#102289,#102290,#102291,#102292,
#102293,#102294,#102295,#102296,#102297,#102298,#102299,#102300,#102301,
#102302,#102303,#102304,#102305,#102306,#102307,#102308,#102309,#102310,
#102311,#102312,#102313,#102314,#102315,#102316,#102317,#102318,#102319,
#102320,#102321,#102322,#102323,#102324,#102325,#102326,#102327,#102328,
#102329,#102330,#102331,#102332,#102333,#102334,#102335,#102336,#102337,
#102338,#102339,#102340,#102341,#102342,#102343,#102344,#102345,#102346,
#102347,#102348,#102349,#102350,#102351,#102352,#102353,#102354,#102355,
#102356,#102357,#102358,#102359,#102360,#102361,#102362,#102363,#102364,
#102365,#102366,#102367,#102368,#102369,#102370,#102371,#102372,#102373,
#102374,#102375,#102376,#102377,#102378,#102379,#102380,#102381,#102382,
#102383,#102384,#102385,#102386,#102387,#102388,#102389,#102390,#102391,
#102392,#102393,#102394,#102395,#102396),.UNSPECIFIED.,.F.,.F.,(4,3,3,3,
3,3,3,3,3,3,3,3,3,3,3,3,3,3,3,3,3,3,3,3,3,3,3,3,3,3,3,3,3,3,3,3,3,3,3,3,
3,3,3,3,3,3,3,3,3,3,3,3,3,3,3,3,3,3,3,3,3,3,3,3,3,3,3,3,3,3,3,3,4),(1171.81405978898,
1171.93948151509,1171.99863934544,1172.08237805729,1172.16601356865,1172.24956601205,
1172.33305544791,1172.41650939852,1172.49994589237,1172.58338300212,1172.66683879704,
1172.75038328977,1172.83397237271,1172.91769564027,1172.99837535616,1173.08211406801,
1173.16574957937,1173.24930202277,1173.33279145862,1173.41624540924,1173.49968190308,
1173.58311901284,1173.66657480776,1173.75011930049,1173.83370838343,1173.91743165098,
1173.99811136688,1174.08185007873,1174.16548559009,1174.24903803349,1174.33252746934,
1174.41598141996,1174.4994179138,1174.58285502356,1174.66631081848,1174.74985531121,
1174.83344439415,1174.9171676617,1174.9978473776,1175.08158608945,1175.16522160081,
1175.24877404421,1175.33226348006,1175.41571743068,1175.49915392452,1175.58259103428,
1175.6660468292,1175.74959132193,1175.83318040487,1175.91690367242,1175.99758338832,
1176.08132210017,1176.16495761153,1176.24851005493,1176.33199949078,1176.4154534414,
1176.49888993524,1176.582327045,1176.66578283992,1176.74932733265,1176.83291641559,
1176.91663968314,1176.99731939904,1177.0810671029,1177.16470960856,1177.24982342642,
1177.33330898385,1177.41675650755,1177.5001840862,1177.5865431025,1177.67001322144,
1177.75781668643,1177.84562015143),.UNSPECIFIED.);
#796=B_SPLINE_CURVE_WITH_KNOTS('',3,(#102397,#102398,#102399,#102400,#102401,
#102402,#102403,#102404,#102405,#102406),.UNSPECIFIED.,.F.,.F.,(4,3,3,4),
(1171.56241306759,1171.64467016677,1171.7293649778,1171.81405978884),
 .UNSPECIFIED.);
#797=B_SPLINE_CURVE_WITH_KNOTS('',3,(#102408,#102409,#102410,#102411,#102412,
#102413,#102414,#102415,#102416,#102417),.UNSPECIFIED.,.F.,.F.,(4,3,3,4),
(1171.56372456646,1171.65113667049,1171.73839544464,1171.81405978898),
 .UNSPECIFIED.);
#798=B_SPLINE_CURVE_WITH_KNOTS('',3,(#102418,#102419,#102420,#102421,#102422,
#102423,#102424,#102425,#102426,#102427,#102428,#102429,#102430,#102431,
#102432,#102433,#102434,#102435,#102436,#102437,#102438,#102439,#102440,
#102441,#102442,#102443,#102444,#102445,#102446,#102447,#102448,#102449,
#102450,#102451,#102452,#102453,#102454,#102455,#102456,#102457,#102458,
#102459,#102460,#102461,#102462,#102463,#102464,#102465,#102466,#102467,
#102468,#102469,#102470,#102471,#102472,#102473,#102474,#102475,#102476,
#102477,#102478,#102479,#102480,#102481,#102482,#102483,#102484,#102485,
#102486,#102487,#102488,#102489,#102490,#102491,#102492,#102493,#102494,
#102495,#102496,#102497,#102498,#102499,#102500,#102501,#102502,#102503,
#102504,#102505,#102506,#102507,#102508,#102509,#102510,#102511,#102512,
#102513,#102514,#102515,#102516,#102517,#102518,#102519,#102520,#102521,
#102522,#102523,#102524,#102525,#102526,#102527,#102528,#102529,#102530,
#102531,#102532,#102533,#102534,#102535,#102536,#102537,#102538,#102539,
#102540,#102541,#102542,#102543,#102544,#102545,#102546,#102547,#102548,
#102549,#102550,#102551,#102552,#102553,#102554,#102555,#102556,#102557,
#102558,#102559,#102560,#102561,#102562,#102563,#102564,#102565,#102566,
#102567,#102568,#102569,#102570,#102571,#102572,#102573,#102574,#102575,
#102576,#102577,#102578,#102579,#102580,#102581,#102582,#102583,#102584,
#102585,#102586,#102587,#102588,#102589,#102590,#102591,#102592,#102593,
#102594,#102595,#102596,#102597,#102598,#102599,#102600,#102601,#102602,
#102603,#102604,#102605,#102606,#102607,#102608,#102609,#102610,#102611,
#102612,#102613,#102614,#102615,#102616,#102617,#102618,#102619,#102620,
#102621,#102622,#102623,#102624,#102625,#102626,#102627,#102628,#102629,
#102630,#102631,#102632,#102633,#102634,#102635,#102636,#102637),
 .UNSPECIFIED.,.F.,.F.,(4,3,3,3,3,3,3,3,3,3,3,3,3,3,3,3,3,3,3,3,3,3,3,3,
3,3,3,3,3,3,3,3,3,3,3,3,3,3,3,3,3,3,3,3,3,3,3,3,3,3,3,3,3,3,3,3,3,3,3,3,
3,3,3,3,3,3,3,3,3,3,3,3,3,4),(1171.81405978909,1171.90164711357,1171.98935633969,
1172.07727908356,1172.1653153844,1172.25355436627,1172.30892996516,1172.39266867701,
1172.47630418837,1172.55985663177,1172.64334606762,1172.72680001824,1172.81023651208,
1172.89367362184,1172.97712941676,1173.06067390949,1173.14426299243,1173.22798625999,
1173.30866597588,1173.39240468773,1173.47604019909,1173.55959264249,1173.64308207834,
1173.72653602896,1173.8099725228,1173.89340963256,1173.97686542748,1174.06040992021,
1174.14399900315,1174.22772227071,1174.3084019866,1174.39214069845,1174.47577620981,
1174.55932865321,1174.64281808906,1174.72627203968,1174.80970853352,1174.89314564328,
1174.97660143819,1175.06014593092,1175.14373501386,1175.22745828142,1175.30813799732,
1175.39187670917,1175.47551222053,1175.55906466393,1175.64255409978,1175.7260080504,
1175.80944454424,1175.892881654,1175.97633744892,1176.05988194165,1176.14347102459,
1176.22719429215,1176.30787400804,1176.39161271989,1176.47524823125,1176.55880067465,
1176.6422901105,1176.72574406112,1176.80918055496,1176.89261766472,1176.97607345964,
1177.05961795236,1177.14320703531,1177.22693030286,1177.30761001876,1177.39015829217,
1177.47261010492,1177.55498463725,1177.63729798293,1177.71957556743,1177.80184708081,
1177.84569864885),.UNSPECIFIED.);
#799=B_SPLINE_CURVE_WITH_KNOTS('',3,(#102643,#102644,#102645,#102646,#102647,
#102648,#102649,#102650,#102651,#102652,#102653,#102654,#102655,#102656,
#102657,#102658,#102659,#102660,#102661,#102662,#102663,#102664,#102665,
#102666,#102667,#102668,#102669,#102670,#102671,#102672,#102673,#102674,
#102675,#102676,#102677,#102678,#102679,#102680,#102681,#102682,#102683,
#102684,#102685,#102686,#102687,#102688,#102689,#102690,#102691,#102692,
#102693,#102694,#102695,#102696,#102697,#102698,#102699,#102700,#102701,
#102702,#102703,#102704,#102705,#102706,#102707,#102708,#102709,#102710,
#102711,#102712,#102713,#102714,#102715,#102716,#102717,#102718,#102719,
#102720,#102721,#102722,#102723,#102724,#102725,#102726,#102727,#102728,
#102729,#102730,#102731,#102732,#102733,#102734,#102735,#102736,#102737,
#102738,#102739,#102740,#102741,#102742,#102743,#102744,#102745,#102746,
#102747,#102748,#102749,#102750,#102751,#102752,#102753,#102754,#102755,
#102756,#102757,#102758,#102759,#102760,#102761,#102762,#102763,#102764,
#102765,#102766,#102767,#102768,#102769,#102770,#102771,#102772,#102773,
#102774,#102775,#102776,#102777,#102778,#102779,#102780,#102781,#102782,
#102783,#102784,#102785,#102786,#102787,#102788,#102789,#102790,#102791,
#102792,#102793,#102794,#102795,#102796,#102797,#102798,#102799,#102800,
#102801,#102802,#102803,#102804,#102805,#102806,#102807,#102808,#102809,
#102810,#102811,#102812,#102813,#102814,#102815,#102816,#102817,#102818,
#102819,#102820,#102821,#102822,#102823,#102824,#102825,#102826,#102827,
#102828,#102829,#102830,#102831,#102832,#102833,#102834,#102835,#102836,
#102837,#102838,#102839,#102840,#102841,#102842,#102843,#102844,#102845,
#102846,#102847,#102848,#102849,#102850,#102851,#102852,#102853,#102854,
#102855,#102856,#102857,#102858,#102859,#102860,#102861,#102862),
 .UNSPECIFIED.,.F.,.F.,(4,3,3,3,3,3,3,3,3,3,3,3,3,3,3,3,3,3,3,3,3,3,3,3,
3,3,3,3,3,3,3,3,3,3,3,3,3,3,3,3,3,3,3,3,3,3,3,3,3,3,3,3,3,3,3,3,3,3,3,3,
3,3,3,3,3,3,3,3,3,3,3,3,3,4),(1178.0972450963,1178.17988444519,1178.26243119773,
1178.34490639929,1178.42733560839,1178.50974134295,1178.59214251743,1178.67455804016,
1178.75705690961,1178.83959806364,1178.92226904614,1178.99679142048,1179.08053013233,
1179.16416564369,1179.24771808709,1179.33120752294,1179.41466147356,1179.4980979674,
1179.58153507716,1179.66499087207,1179.7485353648,1179.83212444774,1179.9158477153,
1179.9965274312,1180.08026614305,1180.16390165441,1180.24745409781,1180.33094353366,
1180.41439748428,1180.49783397812,1180.58127108788,1180.6647268828,1180.74827137553,
1180.83186045847,1180.91558372603,1180.99626344192,1181.08000215377,1181.16363766513,
1181.24719010853,1181.33067954438,1181.414133495,1181.49756998884,1181.5810070986,
1181.66446289352,1181.74800738625,1181.83159646919,1181.91531973674,1181.99599945264,
1182.07973816449,1182.16337367585,1182.24692611925,1182.3304155551,1182.41386950571,
1182.49730599956,1182.58074310932,1182.66419890423,1182.74774339696,1182.8313324799,
1182.91505574746,1182.99573546336,1183.07947417521,1183.16310968657,1183.24666212997,
1183.33015156582,1183.41360551644,1183.49704201028,1183.58047912004,1183.66393491496,
1183.74747940769,1183.83106849063,1183.91479175819,1183.99547147408,1184.08965748669,
1184.13001838411),.UNSPECIFIED.);
#800=B_SPLINE_CURVE_WITH_KNOTS('',3,(#102863,#102864,#102865,#102866,#102867,
#102868,#102869,#102870,#102871,#102872),.UNSPECIFIED.,.F.,.F.,(4,3,3,4),
(1177.84562015143,1177.92934800689,1177.99705540976,1178.09724509616),
 .UNSPECIFIED.);
#801=B_SPLINE_CURVE_WITH_KNOTS('',3,(#102874,#102875,#102876,#102877,#102878,
#102879,#102880,#102881,#102882,#102883),.UNSPECIFIED.,.F.,.F.,(4,3,3,4),
(1177.84569864885,1177.92800237776,1178.01262373689,1178.09724509602),
 .UNSPECIFIED.);
#802=B_SPLINE_CURVE_WITH_KNOTS('',3,(#102884,#102885,#102886,#102887,#102888,
#102889,#102890,#102891,#102892,#102893,#102894,#102895,#102896,#102897,
#102898,#102899,#102900,#102901,#102902,#102903,#102904,#102905,#102906,
#102907,#102908,#102909,#102910,#102911,#102912,#102913,#102914,#102915,
#102916,#102917,#102918,#102919,#102920,#102921,#102922,#102923,#102924,
#102925,#102926,#102927,#102928,#102929,#102930,#102931,#102932,#102933,
#102934,#102935,#102936,#102937,#102938,#102939,#102940,#102941,#102942,
#102943,#102944,#102945,#102946,#102947,#102948,#102949,#102950,#102951,
#102952,#102953,#102954,#102955,#102956,#102957,#102958,#102959,#102960,
#102961,#102962,#102963,#102964,#102965,#102966,#102967,#102968,#102969,
#102970,#102971,#102972,#102973,#102974,#102975,#102976,#102977,#102978,
#102979,#102980,#102981,#102982,#102983,#102984,#102985,#102986,#102987,
#102988,#102989,#102990,#102991,#102992,#102993,#102994,#102995,#102996,
#102997,#102998,#102999,#103000,#103001,#103002,#103003,#103004,#103005,
#103006,#103007,#103008,#103009,#103010,#103011,#103012,#103013,#103014,
#103015,#103016,#103017,#103018,#103019,#103020,#103021,#103022,#103023,
#103024,#103025,#103026,#103027,#103028,#103029,#103030,#103031,#103032,
#103033,#103034,#103035,#103036,#103037,#103038,#103039,#103040,#103041,
#103042,#103043,#103044,#103045,#103046,#103047,#103048,#103049,#103050,
#103051,#103052,#103053,#103054,#103055,#103056,#103057,#103058,#103059,
#103060,#103061,#103062,#103063,#103064,#103065,#103066,#103067,#103068,
#103069,#103070,#103071,#103072,#103073,#103074,#103075,#103076,#103077,
#103078,#103079,#103080,#103081,#103082,#103083,#103084,#103085,#103086,
#103087,#103088,#103089,#103090,#103091,#103092,#103093,#103094,#103095,
#103096,#103097,#103098,#103099,#103100),.UNSPECIFIED.,.F.,.F.,(4,3,3,3,
3,3,3,3,3,3,3,3,3,3,3,3,3,3,3,3,3,3,3,3,3,3,3,3,3,3,3,3,3,3,3,3,3,3,3,3,
3,3,3,3,3,3,3,3,3,3,3,3,3,3,3,3,3,3,3,3,3,3,3,3,3,3,3,3,3,3,3,3,4),(1178.09724509616,
1178.2145451453,1178.30734602948,1178.39108474133,1178.47472025269,1178.55827269609,
1178.64176213194,1178.72521608256,1178.8086525764,1178.89208968616,1178.97554548108,
1179.0590899738,1179.14267905675,1179.2264023243,1179.3070820402,1179.39082075205,
1179.47445626341,1179.55800870681,1179.64149814266,1179.72495209328,1179.80838858712,
1179.89182569688,1179.9752814918,1180.05882598453,1180.14241506747,1180.22613833502,
1180.30681805092,1180.39055676277,1180.47419227413,1180.55774471753,1180.64123415338,
1180.724688104,1180.80812459784,1180.8915617076,1180.97501750252,1181.05856199525,
1181.14215107819,1181.22587434574,1181.30655406164,1181.39029277349,1181.47392828485,
1181.55748072825,1181.6409701641,1181.72442411472,1181.80786060856,1181.89129771832,
1181.97475351324,1182.05829800597,1182.14188708891,1182.22561035646,1182.30629007236,
1182.39002878421,1182.47366429557,1182.55721673897,1182.64070617482,1182.72416012544,
1182.80759661928,1182.89103372904,1182.97448952396,1183.05803401669,1183.14162309963,
1183.22534636718,1183.30602608308,1183.38977540495,1183.47341919148,1183.55696249768,
1183.64044883304,1183.72389631705,1183.80732303918,1183.89077497528,1183.97423771784,
1184.05777403475,1184.1287772547),.UNSPECIFIED.);
#803=B_SPLINE_CURVE_WITH_KNOTS('',3,(#103106,#103107,#103108,#103109,#103110,
#103111,#103112,#103113,#103114,#103115,#103116,#103117,#103118,#103119,
#103120,#103121,#103122,#103123,#103124,#103125,#103126,#103127,#103128,
#103129,#103130,#103131,#103132,#103133,#103134,#103135,#103136,#103137,
#103138,#103139,#103140,#103141,#103142,#103143,#103144,#103145,#103146,
#103147,#103148,#103149,#103150,#103151,#103152,#103153,#103154,#103155,
#103156,#103157,#103158,#103159,#103160,#103161,#103162,#103163,#103164,
#103165,#103166,#103167,#103168,#103169,#103170,#103171,#103172,#103173,
#103174,#103175,#103176,#103177,#103178,#103179,#103180,#103181,#103182,
#103183,#103184,#103185,#103186,#103187,#103188,#103189,#103190,#103191,
#103192,#103193,#103194,#103195,#103196,#103197,#103198,#103199,#103200,
#103201,#103202,#103203,#103204,#103205,#103206,#103207,#103208,#103209,
#103210,#103211,#103212,#103213,#103214,#103215,#103216,#103217,#103218,
#103219,#103220,#103221,#103222,#103223,#103224,#103225,#103226,#103227,
#103228,#103229,#103230,#103231,#103232,#103233,#103234,#103235,#103236,
#103237,#103238,#103239,#103240,#103241,#103242,#103243,#103244,#103245,
#103246,#103247,#103248,#103249,#103250,#103251,#103252,#103253,#103254,
#103255,#103256,#103257,#103258,#103259,#103260,#103261,#103262,#103263,
#103264,#103265,#103266,#103267,#103268,#103269,#103270,#103271,#103272,
#103273,#103274,#103275,#103276,#103277,#103278,#103279,#103280,#103281,
#103282,#103283,#103284,#103285,#103286,#103287,#103288,#103289,#103290,
#103291,#103292,#103293,#103294,#103295,#103296,#103297,#103298,#103299,
#103300,#103301,#103302,#103303,#103304,#103305,#103306,#103307,#103308,
#103309,#103310,#103311,#103312,#103313,#103314,#103315,#103316,#103317,
#103318,#103319,#103320,#103321,#103322,#103323,#103324,#103325),
 .UNSPECIFIED.,.F.,.F.,(4,3,3,3,3,3,3,3,3,3,3,3,3,3,3,3,3,3,3,3,3,3,3,3,
3,3,3,3,3,3,3,3,3,3,3,3,3,3,3,3,3,3,3,3,3,3,3,3,3,3,3,3,3,3,3,3,3,3,3,3,
3,3,3,3,3,3,3,3,3,3,3,3,3,4),(1184.38043040334,1184.46468568474,1184.54895401794,
1184.63325228744,1184.71759739402,1184.80205716788,1184.8865841838,1184.97124381791,
1184.9952074848,1185.07894619665,1185.16258170801,1185.24613415141,1185.32962358726,
1185.41307753788,1185.49651403172,1185.57995114148,1185.66340693639,1185.74695142912,
1185.83054051206,1185.91426377962,1185.99494349552,1186.07868220737,1186.16231771873,
1186.24587016213,1186.32935959798,1186.4128135486,1186.49625004244,1186.5796871522,
1186.66314294712,1186.74668743985,1186.83027652279,1186.91399979035,1186.99467950624,
1187.07841821809,1187.16205372945,1187.24560617285,1187.3290956087,1187.41254955932,
1187.49598605316,1187.57942316292,1187.66287895783,1187.74642345056,1187.8300125335,
1187.91373580106,1187.99441551696,1188.07815422881,1188.16178974018,1188.24534218357,
1188.32883161943,1188.41228557004,1188.49572206389,1188.57915917364,1188.66261496856,
1188.74615946129,1188.82974854423,1188.91347181179,1188.99415152768,1189.07789023953,
1189.16152575089,1189.24507819429,1189.32856763014,1189.41202158076,1189.4954580746,
1189.57889518436,1189.66235097928,1189.74589547201,1189.82948455495,1189.91320782251,
1189.99388753841,1190.0775495013,1190.16132819585,1190.24477987203,1190.32872207577,
1190.41266427951),.UNSPECIFIED.);
#804=B_SPLINE_CURVE_WITH_KNOTS('',3,(#103326,#103327,#103328,#103329,#103330,
#103331,#103332,#103333,#103334,#103335),.UNSPECIFIED.,.F.,.F.,(4,3,3,4),
(1184.13001838411,1184.22369930359,1184.31687370656,1184.38043040315),
 .UNSPECIFIED.);
#805=B_SPLINE_CURVE_WITH_KNOTS('',3,(#103337,#103338,#103339,#103340,#103341,
#103342,#103343,#103344,#103345,#103346,#103347,#103348,#103349),
 .UNSPECIFIED.,.F.,.F.,(4,3,3,3,4),(1184.1287772547,1184.21241699627,1184.29617130262,
1184.3057620938,1184.38043040334),.UNSPECIFIED.);
#806=B_SPLINE_CURVE_WITH_KNOTS('',3,(#103350,#103351,#103352,#103353,#103354,
#103355,#103356,#103357,#103358,#103359,#103360,#103361,#103362,#103363,
#103364,#103365,#103366,#103367,#103368,#103369,#103370,#103371,#103372,
#103373,#103374,#103375,#103376,#103377,#103378,#103379,#103380,#103381,
#103382,#103383,#103384,#103385,#103386,#103387,#103388,#103389,#103390,
#103391,#103392,#103393,#103394,#103395,#103396,#103397,#103398,#103399,
#103400,#103401,#103402,#103403,#103404,#103405,#103406,#103407,#103408,
#103409,#103410,#103411,#103412,#103413,#103414,#103415,#103416,#103417,
#103418,#103419,#103420,#103421,#103422,#103423,#103424,#103425,#103426,
#103427,#103428,#103429,#103430,#103431,#103432,#103433,#103434,#103435,
#103436,#103437,#103438,#103439,#103440,#103441,#103442,#103443,#103444,
#103445,#103446,#103447,#103448,#103449,#103450,#103451,#103452,#103453,
#103454,#103455,#103456,#103457,#103458,#103459,#103460,#103461,#103462,
#103463,#103464,#103465,#103466,#103467,#103468,#103469,#103470,#103471,
#103472,#103473,#103474,#103475,#103476,#103477,#103478,#103479,#103480,
#103481,#103482,#103483,#103484,#103485,#103486,#103487,#103488,#103489,
#103490,#103491,#103492,#103493,#103494,#103495,#103496,#103497,#103498,
#103499,#103500,#103501,#103502,#103503,#103504,#103505,#103506,#103507,
#103508,#103509,#103510,#103511,#103512,#103513,#103514,#103515,#103516,
#103517,#103518,#103519,#103520,#103521,#103522,#103523,#103524,#103525,
#103526,#103527,#103528,#103529,#103530,#103531,#103532,#103533,#103534,
#103535,#103536,#103537,#103538,#103539,#103540,#103541,#103542,#103543,
#103544,#103545,#103546,#103547,#103548,#103549,#103550,#103551,#103552,
#103553,#103554,#103555,#103556,#103557,#103558,#103559,#103560,#103561,
#103562,#103563,#103564,#103565,#103566,#103567,#103568,#103569,#103570,
#103571,#103572),.UNSPECIFIED.,.F.,.F.,(4,3,3,3,3,3,3,3,3,3,3,3,3,3,3,3,
3,3,3,3,3,3,3,3,3,3,3,3,3,3,3,3,3,3,3,3,3,3,3,3,3,3,3,3,3,3,3,3,3,3,3,3,
3,3,3,3,3,3,3,3,3,3,3,3,3,3,3,3,3,3,3,3,3,3,4),(1184.38043040347,1184.46326953669,
1184.54601184595,1184.6286782553,1184.71328073646,1184.7958670911,1184.87844507109,
1184.96103346495,1185.04714962484,1185.12986035915,1185.21262722398,1185.29550712489,
1185.30549810452,1185.38923681637,1185.47287232773,1185.55642477113,1185.63991420698,
1185.7233681576,1185.80680465144,1185.8902417612,1185.97369755612,1186.05724204884,
1186.14083113179,1186.22455439934,1186.30523411524,1186.38897282709,1186.47260833845,
1186.55616078185,1186.6396502177,1186.72310416832,1186.80654066216,1186.88997777192,
1186.97343356684,1187.05697805957,1187.14056714251,1187.22429041006,1187.30497012596,
1187.38870883781,1187.47234434917,1187.55589679257,1187.63938622842,1187.72284017904,
1187.80627667288,1187.88971378264,1187.97316957756,1188.05671407029,1188.14030315323,
1188.22402642078,1188.30470613668,1188.38844484853,1188.47208035989,1188.55563280329,
1188.63912223914,1188.72257618976,1188.8060126836,1188.88944979336,1188.97290558827,
1189.056450081,1189.14003916395,1189.2237624315,1189.3044421474,1189.38818085925,
1189.47181637061,1189.55536881401,1189.63885824986,1189.72231220048,1189.80574869432,
1189.88918580408,1189.97264159899,1190.05618609172,1190.13977517467,1190.22349844222,
1190.30417815812,1190.40038519419,1190.41311890016),.UNSPECIFIED.);
#807=B_SPLINE_CURVE_WITH_KNOTS('',3,(#103578,#103579,#103580,#103581,#103582,
#103583,#103584,#103585,#103586,#103587,#103588,#103589,#103590,#103591,
#103592,#103593,#103594,#103595,#103596,#103597,#103598,#103599,#103600,
#103601,#103602,#103603,#103604,#103605,#103606,#103607,#103608,#103609,
#103610,#103611,#103612,#103613,#103614,#103615,#103616,#103617,#103618,
#103619,#103620,#103621,#103622,#103623,#103624,#103625,#103626,#103627,
#103628,#103629,#103630,#103631,#103632,#103633,#103634,#103635,#103636,
#103637,#103638,#103639,#103640,#103641,#103642,#103643,#103644,#103645,
#103646,#103647,#103648,#103649,#103650,#103651,#103652,#103653,#103654,
#103655,#103656,#103657,#103658,#103659,#103660,#103661,#103662,#103663,
#103664,#103665,#103666,#103667,#103668,#103669,#103670,#103671,#103672,
#103673,#103674,#103675,#103676,#103677,#103678,#103679,#103680,#103681,
#103682,#103683,#103684,#103685,#103686,#103687,#103688,#103689,#103690,
#103691,#103692,#103693,#103694,#103695,#103696,#103697,#103698,#103699,
#103700,#103701,#103702,#103703,#103704,#103705,#103706,#103707,#103708,
#103709,#103710,#103711,#103712,#103713,#103714,#103715,#103716,#103717,
#103718,#103719,#103720,#103721,#103722,#103723,#103724,#103725,#103726,
#103727,#103728,#103729,#103730,#103731,#103732,#103733,#103734,#103735,
#103736,#103737,#103738,#103739,#103740,#103741,#103742,#103743,#103744,
#103745,#103746,#103747,#103748,#103749,#103750,#103751,#103752,#103753,
#103754,#103755,#103756,#103757,#103758,#103759,#103760,#103761,#103762,
#103763,#103764,#103765,#103766,#103767,#103768,#103769,#103770,#103771,
#103772,#103773,#103774,#103775,#103776,#103777,#103778,#103779,#103780,
#103781,#103782,#103783,#103784,#103785,#103786,#103787,#103788,#103789,
#103790,#103791,#103792,#103793,#103794,#103795,#103796,#103797),
 .UNSPECIFIED.,.F.,.F.,(4,3,3,3,3,3,3,3,3,3,3,3,3,3,3,3,3,3,3,3,3,3,3,3,
3,3,3,3,3,3,3,3,3,3,3,3,3,3,3,3,3,3,3,3,3,3,3,3,3,3,3,3,3,3,3,3,3,3,3,3,
3,3,3,3,3,3,3,3,3,3,3,3,3,4),(1190.66361571069,1190.76115270768,1190.85929214592,
1190.95812771467,1190.99362354913,1191.07736226098,1191.16099777234,1191.24455021574,
1191.32803965159,1191.41149360221,1191.49493009605,1191.57836720581,1191.66182300073,
1191.74536749346,1191.8289565764,1191.91267984396,1191.99335955985,1192.0770982717,
1192.16073378306,1192.24428622646,1192.32777566231,1192.41122961292,1192.49466610677,
1192.57810321653,1192.66155901144,1192.74510350417,1192.82869258711,1192.91241585467,
1192.99309557057,1193.07683428242,1193.16046979378,1193.24402223718,1193.32751167303,
1193.41096562365,1193.49440211749,1193.57783922725,1193.66129502217,1193.7448395149,
1193.82842859784,1193.91215186539,1193.99283158129,1194.07657029314,1194.1602058045,
1194.2437582479,1194.32724768375,1194.41070163437,1194.49413812821,1194.57757523797,
1194.66103103289,1194.74457552562,1194.82816460856,1194.91188787612,1194.99256759201,
1195.07630630386,1195.15994181522,1195.24349425862,1195.32698369447,1195.41043764509,
1195.49387413893,1195.57731124869,1195.6607670436,1195.74431153633,1195.82790061927,
1195.91162388683,1195.99230360273,1196.07546835843,1196.15850180246,1196.24145939585,
1196.32435982013,1196.40722171057,1196.49007873684,1196.57293247362,1196.65582636887,
1196.69500507576),.UNSPECIFIED.);
#808=B_SPLINE_CURVE_WITH_KNOTS('',3,(#103798,#103799,#103800,#103801,#103802,
#103803,#103804,#103805,#103806,#103807),.UNSPECIFIED.,.F.,.F.,(4,3,3,4),
(1190.41266427951,1190.49598634203,1190.57980102627,1190.66361571051),
 .UNSPECIFIED.);
#809=B_SPLINE_CURVE_WITH_KNOTS('',3,(#103809,#103810,#103811,#103812,#103813,
#103814,#103815,#103816,#103817,#103818),.UNSPECIFIED.,.F.,.F.,(4,3,3,4),
(1190.41311890016,1190.50877424335,1190.60377587554,1190.66361571032),
 .UNSPECIFIED.);
#810=B_SPLINE_CURVE_WITH_KNOTS('',3,(#103819,#103820,#103821,#103822,#103823,
#103824,#103825,#103826,#103827,#103828,#103829,#103830,#103831,#103832,
#103833,#103834,#103835,#103836,#103837,#103838,#103839,#103840,#103841,
#103842,#103843,#103844,#103845,#103846,#103847,#103848,#103849,#103850,
#103851,#103852,#103853,#103854,#103855,#103856,#103857,#103858,#103859,
#103860,#103861,#103862,#103863,#103864,#103865,#103866,#103867,#103868,
#103869,#103870,#103871,#103872,#103873,#103874,#103875,#103876,#103877,
#103878,#103879,#103880,#103881,#103882,#103883,#103884,#103885,#103886,
#103887,#103888,#103889,#103890,#103891,#103892,#103893,#103894,#103895,
#103896,#103897,#103898,#103899,#103900,#103901,#103902,#103903,#103904,
#103905,#103906,#103907,#103908,#103909,#103910,#103911,#103912,#103913,
#103914,#103915,#103916,#103917,#103918,#103919,#103920,#103921,#103922,
#103923,#103924,#103925,#103926,#103927,#103928,#103929,#103930,#103931,
#103932,#103933,#103934,#103935,#103936,#103937,#103938,#103939,#103940,
#103941,#103942,#103943,#103944,#103945,#103946,#103947,#103948,#103949,
#103950,#103951,#103952,#103953,#103954,#103955,#103956,#103957,#103958,
#103959,#103960,#103961,#103962,#103963,#103964,#103965,#103966,#103967,
#103968,#103969,#103970,#103971,#103972,#103973,#103974,#103975,#103976,
#103977,#103978,#103979,#103980,#103981,#103982,#103983,#103984,#103985,
#103986,#103987,#103988,#103989,#103990,#103991,#103992,#103993,#103994,
#103995,#103996,#103997,#103998,#103999,#104000,#104001,#104002,#104003,
#104004,#104005,#104006,#104007,#104008,#104009,#104010,#104011,#104012,
#104013,#104014,#104015,#104016,#104017,#104018,#104019,#104020,#104021,
#104022,#104023,#104024,#104025,#104026,#104027,#104028,#104029,#104030,
#104031,#104032,#104033,#104034,#104035,#104036,#104037,#104038),
 .UNSPECIFIED.,.F.,.F.,(4,3,3,3,3,3,3,3,3,3,3,3,3,3,3,3,3,3,3,3,3,3,3,3,
3,3,3,3,3,3,3,3,3,3,3,3,3,3,3,3,3,3,3,3,3,3,3,3,3,3,3,3,3,3,3,3,3,3,3,3,
3,3,3,3,3,3,3,3,3,3,3,3,3,4),(1190.66361571052,1190.74740518355,1190.83119373716,
1190.91499893557,1190.99883834989,1191.08278235671,1191.16678368594,1191.2509212756,
1191.30391416884,1191.38765288069,1191.47128839205,1191.55484083545,1191.6383302713,
1191.72178422192,1191.80522071576,1191.88865782552,1191.97211362043,1192.05565811316,
1192.1392471961,1192.22297046366,1192.30365017956,1192.38738889141,1192.47102440277,
1192.55457684617,1192.63806628202,1192.72152023264,1192.80495672648,1192.88839383624,
1192.97184963116,1193.05539412389,1193.13898320683,1193.22270647438,1193.30338619028,
1193.38712490213,1193.47076041349,1193.55431285689,1193.63780229274,1193.72125624336,
1193.8046927372,1193.88812984696,1193.97158564188,1194.05513013461,1194.13871921755,
1194.2224424851,1194.303122201,1194.38686091285,1194.47049642421,1194.55404886761,
1194.63753830346,1194.72099225408,1194.80442874792,1194.88786585768,1194.97132165259,
1195.05486614532,1195.13845522826,1195.22217849582,1195.30285821172,1195.38659692357,
1195.47023243493,1195.55378487833,1195.63727431418,1195.7207282648,1195.80416475864,
1195.8876018684,1195.97105766332,1196.05460215605,1196.13819123899,1196.22191450655,
1196.30259422244,1196.38668110687,1196.47062918338,1196.55449738112,1196.63829047945,
1196.69597830305),.UNSPECIFIED.);
#811=B_SPLINE_CURVE_WITH_KNOTS('',3,(#104044,#104045,#104046,#104047,#104048,
#104049,#104050,#104051,#104052,#104053,#104054,#104055,#104056,#104057,
#104058,#104059,#104060,#104061,#104062,#104063,#104064,#104065,#104066,
#104067,#104068,#104069,#104070,#104071,#104072,#104073,#104074,#104075,
#104076,#104077,#104078,#104079,#104080,#104081,#104082,#104083,#104084,
#104085,#104086,#104087,#104088,#104089,#104090,#104091,#104092,#104093,
#104094,#104095,#104096,#104097,#104098,#104099,#104100,#104101,#104102,
#104103,#104104,#104105,#104106,#104107,#104108,#104109,#104110,#104111,
#104112,#104113,#104114,#104115,#104116,#104117,#104118,#104119,#104120,
#104121,#104122,#104123,#104124,#104125,#104126,#104127,#104128,#104129,
#104130,#104131,#104132,#104133,#104134,#104135,#104136,#104137,#104138,
#104139,#104140,#104141,#104142,#104143,#104144,#104145,#104146,#104147,
#104148,#104149,#104150,#104151,#104152,#104153,#104154,#104155,#104156,
#104157,#104158,#104159,#104160,#104161,#104162,#104163,#104164,#104165,
#104166,#104167,#104168,#104169,#104170,#104171,#104172,#104173,#104174,
#104175,#104176,#104177,#104178,#104179,#104180,#104181,#104182,#104183,
#104184,#104185,#104186,#104187,#104188,#104189,#104190,#104191,#104192,
#104193,#104194,#104195,#104196,#104197,#104198,#104199,#104200,#104201,
#104202,#104203,#104204,#104205,#104206,#104207,#104208,#104209,#104210,
#104211,#104212,#104213,#104214,#104215,#104216,#104217,#104218,#104219,
#104220,#104221,#104222,#104223,#104224,#104225,#104226,#104227,#104228,
#104229,#104230,#104231,#104232,#104233,#104234,#104235,#104236,#104237,
#104238,#104239,#104240,#104241,#104242,#104243,#104244,#104245,#104246,
#104247,#104248,#104249,#104250,#104251,#104252,#104253,#104254,#104255,
#104256,#104257,#104258,#104259,#104260,#104261,#104262,#104263),
 .UNSPECIFIED.,.F.,.F.,(4,3,3,3,3,3,3,3,3,3,3,3,3,3,3,3,3,3,3,3,3,3,3,3,
3,3,3,3,3,3,3,3,3,3,3,3,3,3,3,3,3,3,3,3,3,3,3,3,3,3,3,3,3,3,3,3,3,3,3,3,
3,3,3,3,3,3,3,3,3,3,3,3,3,4),(1196.94680101769,1196.99203961345,1197.0757783253,
1197.15941383666,1197.24296628006,1197.32645571591,1197.40990966653,1197.49334616037,
1197.57678327013,1197.66023906505,1197.74378355778,1197.82737264072,1197.91109590827,
1197.99177562417,1198.07551433602,1198.15914984738,1198.24270229078,1198.32619172663,
1198.40964567724,1198.49308217109,1198.57651928085,1198.65997507576,1198.74351956849,
1198.82710865143,1198.91083191899,1198.99151163489,1199.07525034674,1199.1588858581,
1199.2424383015,1199.32592773735,1199.40938168797,1199.49281818181,1199.57625529157,
1199.65971108649,1199.74325557922,1199.82684466216,1199.91056792971,1199.99124764561,
1200.07498635746,1200.15862186882,1200.24217431222,1200.32566374807,1200.40911769869,
1200.49255419253,1200.57599130229,1200.65944709721,1200.74299158994,1200.82658067288,
1200.91030394043,1200.99098365633,1201.07472236818,1201.15835787954,1201.24191032294,
1201.32539975879,1201.40885370941,1201.49229020326,1201.57572731301,1201.65918310793,
1201.74272760066,1201.8263166836,1201.91003995116,1201.99071966705,1202.07445903175,
1202.15809504291,1202.2416478337,1202.32513746501,1202.40859081949,1202.49202650081,
1202.57546258152,1202.65891713051,1202.74245734764,1202.82604206555,1202.90975380982,
1202.97885099659),.UNSPECIFIED.);
#812=B_SPLINE_CURVE_WITH_KNOTS('',3,(#104264,#104265,#104266,#104267,#104268,
#104269,#104270,#104271,#104272,#104273),.UNSPECIFIED.,.F.,.F.,(4,3,3,4),
(1196.69500507576,1196.7779925456,1196.86239678155,1196.9468010175),
 .UNSPECIFIED.);
#813=B_SPLINE_CURVE_WITH_KNOTS('',3,(#104275,#104276,#104277,#104278,#104279,
#104280,#104281,#104282,#104283,#104284),.UNSPECIFIED.,.F.,.F.,(4,3,3,4),
(1196.69597830305,1196.77970345289,1196.86342983331,1196.9468010177),
 .UNSPECIFIED.);
#814=B_SPLINE_CURVE_WITH_KNOTS('',3,(#104285,#104286,#104287,#104288,#104289,
#104290,#104291,#104292,#104293,#104294,#104295,#104296,#104297,#104298,
#104299,#104300,#104301,#104302,#104303,#104304,#104305,#104306,#104307,
#104308,#104309,#104310,#104311,#104312,#104313,#104314,#104315,#104316,
#104317,#104318,#104319,#104320,#104321,#104322,#104323,#104324,#104325,
#104326,#104327,#104328,#104329,#104330,#104331,#104332,#104333,#104334,
#104335,#104336,#104337,#104338,#104339,#104340,#104341,#104342,#104343,
#104344,#104345,#104346,#104347,#104348,#104349,#104350,#104351,#104352,
#104353,#104354,#104355,#104356,#104357,#104358,#104359,#104360,#104361,
#104362,#104363,#104364,#104365,#104366,#104367,#104368,#104369,#104370,
#104371,#104372,#104373,#104374,#104375,#104376,#104377,#104378,#104379,
#104380,#104381,#104382,#104383,#104384,#104385,#104386,#104387,#104388,
#104389,#104390,#104391,#104392,#104393,#104394,#104395,#104396,#104397,
#104398,#104399,#104400,#104401,#104402,#104403,#104404,#104405,#104406,
#104407,#104408,#104409,#104410,#104411,#104412,#104413,#104414,#104415,
#104416,#104417,#104418,#104419,#104420,#104421,#104422,#104423,#104424,
#104425,#104426,#104427,#104428,#104429,#104430,#104431,#104432,#104433,
#104434,#104435,#104436,#104437,#104438,#104439,#104440,#104441,#104442,
#104443,#104444,#104445,#104446,#104447,#104448,#104449,#104450,#104451,
#104452,#104453,#104454,#104455,#104456,#104457,#104458,#104459,#104460,
#104461,#104462,#104463,#104464,#104465,#104466,#104467,#104468,#104469,
#104470,#104471,#104472,#104473,#104474,#104475,#104476,#104477,#104478,
#104479,#104480,#104481,#104482,#104483,#104484,#104485,#104486,#104487,
#104488,#104489,#104490,#104491,#104492,#104493,#104494,#104495,#104496,
#104497,#104498,#104499,#104500,#104501,#104502,#104503,#104504),
 .UNSPECIFIED.,.F.,.F.,(4,3,3,3,3,3,3,3,3,3,3,3,3,3,3,3,3,3,3,3,3,3,3,3,
3,3,3,3,3,3,3,3,3,3,3,3,3,3,3,3,3,3,3,3,3,3,3,3,3,3,3,3,3,3,3,3,3,3,3,3,
3,3,3,3,3,3,3,3,3,3,3,3,3,4),(1196.9468010179,1197.04218345801,1197.13801352799,
1197.23442780283,1197.30233023316,1197.38606894501,1197.46970445637,1197.55325689977,
1197.63674633562,1197.72020028624,1197.80363678008,1197.88707388984,1197.97052968476,
1198.05407417749,1198.13766326043,1198.22138652798,1198.30206624388,1198.38580495573,
1198.46944046709,1198.55299291049,1198.63648234634,1198.71993629696,1198.8033727908,
1198.88680990056,1198.97026569548,1199.05381018821,1199.13739927115,1199.22112253871,
1199.3018022546,1199.38554096645,1199.46917647781,1199.55272892121,1199.63621835706,
1199.71967230768,1199.80310880152,1199.88654591128,1199.9700017062,1200.05354619893,
1200.13713528187,1200.22085854942,1200.30153826532,1200.38527697717,1200.46891248853,
1200.55246493193,1200.63595436778,1200.7194083184,1200.80284481224,1200.886281922,
1200.96973771691,1201.05328220964,1201.13687129258,1201.22059456014,1201.30127427604,
1201.38501298789,1201.46864849925,1201.55220094265,1201.6356903785,1201.71914432912,
1201.80258082296,1201.88601793272,1201.96947372764,1202.05301822037,1202.13660730331,
1202.22033057087,1202.30101028676,1202.38565335764,1202.46843821106,1202.55114785557,
1202.63380115682,1202.71988958105,1202.80249905388,1202.88510732086,1202.96774973769,
1202.97815485377),.UNSPECIFIED.);
#815=B_SPLINE_CURVE_WITH_KNOTS('',3,(#104510,#104511,#104512,#104513,#104514,
#104515,#104516,#104517,#104518,#104519,#104520,#104521,#104522,#104523,
#104524,#104525,#104526,#104527,#104528,#104529,#104530,#104531,#104532,
#104533,#104534,#104535,#104536,#104537,#104538,#104539,#104540,#104541,
#104542,#104543,#104544,#104545,#104546,#104547,#104548,#104549,#104550,
#104551,#104552,#104553,#104554,#104555,#104556,#104557,#104558,#104559,
#104560,#104561,#104562,#104563,#104564,#104565,#104566,#104567,#104568,
#104569,#104570,#104571,#104572,#104573,#104574,#104575,#104576,#104577,
#104578,#104579,#104580,#104581,#104582,#104583,#104584,#104585,#104586,
#104587,#104588,#104589,#104590,#104591,#104592,#104593,#104594,#104595,
#104596,#104597,#104598,#104599,#104600,#104601,#104602,#104603,#104604,
#104605,#104606,#104607,#104608,#104609,#104610,#104611,#104612,#104613,
#104614,#104615,#104616,#104617,#104618,#104619,#104620,#104621,#104622,
#104623,#104624,#104625,#104626,#104627,#104628,#104629,#104630,#104631,
#104632,#104633,#104634,#104635,#104636,#104637,#104638,#104639,#104640,
#104641,#104642,#104643,#104644,#104645,#104646,#104647,#104648,#104649,
#104650,#104651,#104652,#104653,#104654,#104655,#104656,#104657,#104658,
#104659,#104660,#104661,#104662,#104663,#104664,#104665,#104666,#104667,
#104668,#104669,#104670,#104671,#104672,#104673,#104674,#104675,#104676,
#104677,#104678,#104679,#104680,#104681,#104682,#104683,#104684,#104685,
#104686,#104687,#104688,#104689,#104690,#104691,#104692,#104693,#104694,
#104695,#104696,#104697,#104698,#104699,#104700,#104701,#104702,#104703,
#104704,#104705,#104706,#104707,#104708,#104709,#104710,#104711,#104712,
#104713,#104714,#104715,#104716,#104717,#104718,#104719,#104720,#104721,
#104722,#104723,#104724,#104725,#104726,#104727,#104728,#104729,#104730,
#104731,#104732),.UNSPECIFIED.,.F.,.F.,(4,3,3,3,3,3,3,3,3,3,3,3,3,3,3,3,
3,3,3,3,3,3,3,3,3,3,3,3,3,3,3,3,3,3,3,3,3,3,3,3,3,3,3,3,3,3,3,3,3,3,3,3,
3,3,3,3,3,3,3,3,3,3,3,3,3,3,3,3,3,3,3,3,3,3,4),(1203.22998632487,1203.31249181929,
1203.39720430294,1203.479626139,1203.56203843911,1203.64446010042,1203.73089299743,
1203.81343567372,1203.8960339351,1203.9787454899,1203.99019168849,1204.07393040034,
1204.1575659117,1204.2411183551,1204.32460779095,1204.40806174157,1204.49149823541,
1204.57493534517,1204.65839114009,1204.74193563282,1204.82552471576,1204.90924798332,
1204.98992769921,1205.07366641106,1205.15730192242,1205.24085436582,1205.32434380167,
1205.40779775229,1205.49123424613,1205.57467135589,1205.6581271508,1205.74167164353,
1205.82526072647,1205.90898399403,1205.98966370993,1206.07340242178,1206.15703793314,
1206.24059037654,1206.32407981239,1206.40753376301,1206.49097025685,1206.57440736661,
1206.65786316153,1206.74140765426,1206.8249967372,1206.90872000475,1206.98939972065,
1207.0731384325,1207.15677394386,1207.24032638726,1207.32381582311,1207.40726977373,
1207.49070626757,1207.57414337733,1207.65759917225,1207.74114366498,1207.82473274792,
1207.90845601548,1207.98913573137,1208.07287444322,1208.15650995458,1208.24006239798,
1208.32355183383,1208.40700578445,1208.49044227829,1208.57387938805,1208.65733518297,
1208.74087967569,1208.82446875864,1208.90819202619,1208.98887174209,1209.07601691819,
1209.16303876864,1209.24991487978,1209.26279998827),.UNSPECIFIED.);
#816=B_SPLINE_CURVE_WITH_KNOTS('',3,(#104733,#104734,#104735,#104736,#104737,
#104738,#104739,#104740,#104741,#104742,#104743,#104744,#104745),
 .UNSPECIFIED.,.F.,.F.,(4,3,3,3,4),(1202.97885099659,1202.99045567777,1203.10238395014,
1203.21150545175,1203.22998632473),.UNSPECIFIED.);
#817=B_SPLINE_CURVE_WITH_KNOTS('',3,(#104747,#104748,#104749,#104750,#104751,
#104752,#104753,#104754,#104755,#104756),.UNSPECIFIED.,.F.,.F.,(4,3,3,4),
(1202.97815485377,1203.06088400365,1203.14543516421,1203.22998632476),
 .UNSPECIFIED.);
#818=B_SPLINE_CURVE_WITH_KNOTS('',3,(#104757,#104758,#104759,#104760,#104761,
#104762,#104763,#104764,#104765,#104766,#104767,#104768,#104769,#104770,
#104771,#104772,#104773,#104774,#104775,#104776,#104777,#104778,#104779,
#104780,#104781,#104782,#104783,#104784,#104785,#104786,#104787,#104788,
#104789,#104790,#104791,#104792,#104793,#104794,#104795,#104796,#104797,
#104798,#104799,#104800,#104801,#104802,#104803,#104804,#104805,#104806,
#104807,#104808,#104809,#104810,#104811,#104812,#104813,#104814,#104815,
#104816,#104817,#104818,#104819,#104820,#104821,#104822,#104823,#104824,
#104825,#104826,#104827,#104828,#104829,#104830,#104831,#104832,#104833,
#104834,#104835,#104836,#104837,#104838,#104839,#104840,#104841,#104842,
#104843,#104844,#104845,#104846,#104847,#104848,#104849,#104850,#104851,
#104852,#104853,#104854,#104855,#104856,#104857,#104858,#104859,#104860,
#104861,#104862,#104863,#104864,#104865,#104866,#104867,#104868,#104869,
#104870,#104871,#104872,#104873,#104874,#104875,#104876,#104877,#104878,
#104879,#104880,#104881,#104882,#104883,#104884,#104885,#104886,#104887,
#104888,#104889,#104890,#104891,#104892,#104893,#104894,#104895,#104896,
#104897,#104898,#104899,#104900,#104901,#104902,#104903,#104904,#104905,
#104906,#104907,#104908,#104909,#104910,#104911,#104912,#104913,#104914,
#104915,#104916,#104917,#104918,#104919,#104920,#104921,#104922,#104923,
#104924,#104925,#104926,#104927,#104928,#104929,#104930,#104931,#104932,
#104933,#104934,#104935,#104936,#104937,#104938,#104939,#104940,#104941,
#104942,#104943,#104944,#104945,#104946,#104947,#104948,#104949,#104950,
#104951,#104952,#104953,#104954,#104955,#104956,#104957,#104958,#104959,
#104960,#104961,#104962,#104963,#104964,#104965,#104966,#104967,#104968,
#104969,#104970,#104971,#104972,#104973,#104974,#104975,#104976),
 .UNSPECIFIED.,.F.,.F.,(4,3,3,3,3,3,3,3,3,3,3,3,3,3,3,3,3,3,3,3,3,3,3,3,
3,3,3,3,3,3,3,3,3,3,3,3,3,3,3,3,3,3,3,3,3,3,3,3,3,3,3,3,3,3,3,3,3,3,3,3,
3,3,3,3,3,3,3,3,3,3,3,3,3,4),(1203.22998632488,1203.30074629748,1203.38448500933,
1203.46812052069,1203.55167296409,1203.63516239994,1203.71861635056,1203.8020528444,
1203.88548995416,1203.96894574908,1204.05249024181,1204.13607932475,1204.2198025923,
1204.3004823082,1204.38422102005,1204.46785653141,1204.55140897481,1204.63489841066,
1204.71835236128,1204.80178885512,1204.88522596488,1204.9686817598,1205.05222625253,
1205.13581533547,1205.21953860303,1205.30021831892,1205.38395703077,1205.46759254213,
1205.55114498553,1205.63463442138,1205.718088372,1205.80152486584,1205.8849619756,
1205.96841777052,1206.05196226325,1206.13555134619,1206.21927461374,1206.29995432964,
1206.38369304149,1206.46732855285,1206.55088099625,1206.6343704321,1206.71782438272,
1206.80126087656,1206.88469798632,1206.96815378124,1207.05169827397,1207.13528735691,
1207.21901062446,1207.29969034036,1207.38342905221,1207.46706456357,1207.55061700697,
1207.63410644282,1207.71756039344,1207.80099688728,1207.88443399704,1207.96788979195,
1208.05143428468,1208.13502336762,1208.21874663518,1208.29942635108,1208.38316718062,
1208.4668043182,1208.5503578984,1208.63384798321,1208.7173001051,1208.80073407538,
1208.8841679663,1208.96761984604,1209.05115095118,1209.13472635942,1209.21841398669,
1209.2618988713),.UNSPECIFIED.);
#819=B_SPLINE_CURVE_WITH_KNOTS('',3,(#104982,#104983,#104984,#104985,#104986,
#104987,#104988,#104989,#104990,#104991,#104992,#104993,#104994,#104995,
#104996,#104997,#104998,#104999,#105000,#105001,#105002,#105003,#105004,
#105005,#105006,#105007,#105008,#105009,#105010,#105011,#105012,#105013,
#105014,#105015,#105016,#105017,#105018,#105019,#105020,#105021,#105022,
#105023,#105024,#105025,#105026,#105027,#105028,#105029,#105030,#105031,
#105032,#105033,#105034,#105035,#105036,#105037,#105038,#105039,#105040,
#105041,#105042,#105043,#105044,#105045,#105046,#105047,#105048,#105049,
#105050,#105051,#105052,#105053,#105054,#105055,#105056,#105057,#105058,
#105059,#105060,#105061,#105062,#105063,#105064,#105065,#105066,#105067,
#105068,#105069,#105070,#105071,#105072,#105073,#105074,#105075,#105076,
#105077,#105078,#105079,#105080,#105081,#105082,#105083,#105084,#105085,
#105086,#105087,#105088,#105089,#105090,#105091,#105092,#105093,#105094,
#105095,#105096,#105097,#105098,#105099,#105100,#105101,#105102,#105103,
#105104,#105105,#105106,#105107,#105108,#105109,#105110,#105111,#105112,
#105113,#105114,#105115,#105116,#105117,#105118,#105119,#105120,#105121,
#105122,#105123,#105124,#105125,#105126,#105127,#105128,#105129,#105130,
#105131,#105132,#105133,#105134,#105135,#105136,#105137,#105138,#105139,
#105140,#105141,#105142,#105143,#105144,#105145,#105146,#105147,#105148,
#105149,#105150,#105151,#105152,#105153,#105154,#105155,#105156,#105157,
#105158,#105159,#105160,#105161,#105162,#105163,#105164,#105165,#105166,
#105167,#105168,#105169,#105170,#105171,#105172,#105173,#105174,#105175,
#105176,#105177,#105178,#105179,#105180,#105181,#105182,#105183,#105184,
#105185,#105186,#105187,#105188,#105189,#105190,#105191,#105192,#105193,
#105194,#105195,#105196,#105197,#105198,#105199,#105200,#105201),
 .UNSPECIFIED.,.F.,.F.,(4,3,3,3,3,3,3,3,3,3,3,3,3,3,3,3,3,3,3,3,3,3,3,3,
3,3,3,3,3,3,3,3,3,3,3,3,3,3,3,3,3,3,3,3,3,3,3,3,3,3,3,3,3,3,3,3,3,3,3,3,
3,3,3,3,3,3,3,3,3,3,3,3,3,4),(1209.51317163215,1209.60151643376,1209.69001276627,
1209.77875144095,1209.86762236245,1209.95670179045,1209.98860775281,1210.07234646466,
1210.15598197602,1210.23953441942,1210.32302385527,1210.40647780589,1210.48991429973,
1210.57335140949,1210.65680720441,1210.74035169714,1210.82394078008,1210.90766404764,
1210.98834376353,1211.07208247538,1211.15571798674,1211.23927043014,1211.32275986599,
1211.40621381661,1211.48965031045,1211.57308742021,1211.65654321512,1211.74008770785,
1211.82367679079,1211.90740005835,1211.98807977425,1212.0718184861,1212.15545399746,
1212.23900644086,1212.32249587671,1212.40594982733,1212.48938632117,1212.57282343093,
1212.65627922585,1212.73982371858,1212.82341280152,1212.90713606907,1212.98781578497,
1213.07155449682,1213.15519000818,1213.23874245158,1213.32223188743,1213.40568583805,
1213.48912233189,1213.57255944165,1213.65601523657,1213.7395597293,1213.82314881224,
1213.9068720798,1213.98755179569,1214.07129050754,1214.1549260189,1214.2384784623,
1214.32196789815,1214.40542184877,1214.48885834261,1214.57229545237,1214.65575124728,
1214.73929574001,1214.82288482295,1214.90660809051,1214.98728780641,1215.06978088805,
1215.15217812242,1215.23449872101,1215.31676058311,1215.39898710595,1215.48121354423,
1215.54473266754),.UNSPECIFIED.);
#820=B_SPLINE_CURVE_WITH_KNOTS('',3,(#105202,#105203,#105204,#105205,#105206,
#105207,#105208,#105209,#105210,#105211),.UNSPECIFIED.,.F.,.F.,(4,3,3,4),
(1209.26279998827,1209.34951857049,1209.43611436924,1209.51317163205),
 .UNSPECIFIED.);
#821=B_SPLINE_CURVE_WITH_KNOTS('',3,(#105213,#105214,#105215,#105216,#105217,
#105218,#105219,#105220,#105221,#105222),.UNSPECIFIED.,.F.,.F.,(4,3,3,4),
(1209.2618988713,1209.2991623618,1209.41543192236,1209.51317163206),
 .UNSPECIFIED.);
#822=B_SPLINE_CURVE_WITH_KNOTS('',3,(#105223,#105224,#105225,#105226,#105227,
#105228,#105229,#105230,#105231,#105232,#105233,#105234,#105235,#105236,
#105237,#105238,#105239,#105240,#105241,#105242,#105243,#105244,#105245,
#105246,#105247,#105248,#105249,#105250,#105251,#105252,#105253,#105254,
#105255,#105256,#105257,#105258,#105259,#105260,#105261,#105262,#105263,
#105264,#105265,#105266,#105267,#105268,#105269,#105270,#105271,#105272,
#105273,#105274,#105275,#105276,#105277,#105278,#105279,#105280,#105281,
#105282,#105283,#105284,#105285,#105286,#105287,#105288,#105289,#105290,
#105291,#105292,#105293,#105294,#105295,#105296,#105297,#105298,#105299,
#105300,#105301,#105302,#105303,#105304,#105305,#105306,#105307,#105308,
#105309,#105310,#105311,#105312,#105313,#105314,#105315,#105316,#105317,
#105318,#105319,#105320,#105321,#105322,#105323,#105324,#105325,#105326,
#105327,#105328,#105329,#105330,#105331,#105332,#105333,#105334,#105335,
#105336,#105337,#105338,#105339,#105340,#105341,#105342,#105343,#105344,
#105345,#105346,#105347,#105348,#105349,#105350,#105351,#105352,#105353,
#105354,#105355,#105356,#105357,#105358,#105359,#105360,#105361,#105362,
#105363,#105364,#105365,#105366,#105367,#105368,#105369,#105370,#105371,
#105372,#105373,#105374,#105375,#105376,#105377,#105378,#105379,#105380,
#105381,#105382,#105383,#105384,#105385,#105386,#105387,#105388,#105389,
#105390,#105391,#105392,#105393,#105394,#105395,#105396,#105397,#105398,
#105399,#105400,#105401,#105402,#105403,#105404,#105405,#105406,#105407,
#105408,#105409,#105410,#105411,#105412,#105413,#105414,#105415,#105416,
#105417,#105418,#105419,#105420,#105421,#105422,#105423,#105424,#105425,
#105426,#105427,#105428,#105429,#105430,#105431,#105432,#105433,#105434,
#105435,#105436,#105437,#105438,#105439,#105440,#105441,#105442),
 .UNSPECIFIED.,.F.,.F.,(4,3,3,3,3,3,3,3,3,3,3,3,3,3,3,3,3,3,3,3,3,3,3,3,
3,3,3,3,3,3,3,3,3,3,3,3,3,3,3,3,3,3,3,3,3,3,3,3,3,3,3,3,3,3,3,3,3,3,3,3,
3,3,3,3,3,3,3,3,3,3,3,3,3,4),(1209.51317163217,1209.59557880271,1209.67792117058,
1209.7602265483,1209.84251467156,1209.9248045227,1210.00711508318,1210.08951190621,
1210.17195686769,1210.25452297352,1210.29889837252,1210.38263708437,1210.46627259573,
1210.54982503913,1210.63331447498,1210.7167684256,1210.80020491944,1210.8836420292,
1210.96709782412,1211.05064231685,1211.13423139979,1211.21795466735,1211.29863438324,
1211.38237309509,1211.46600860645,1211.54956104985,1211.63305048571,1211.71650443632,
1211.79994093017,1211.88337803992,1211.96683383484,1212.05037832757,1212.13396741051,
1212.21769067807,1212.29837039397,1212.38210910582,1212.46574461718,1212.54929706058,
1212.63278649643,1212.71624044705,1212.79967694089,1212.88311405065,1212.96656984557,
1213.0501143383,1213.13370342124,1213.2174266888,1213.29810640469,1213.38184511654,
1213.4654806279,1213.5490330713,1213.63252250715,1213.71597645777,1213.79941295161,
1213.88285006137,1213.96630585628,1214.04985034901,1214.13343943195,1214.21716269951,
1214.29784241541,1214.38158112726,1214.46521663862,1214.54876908202,1214.63225851787,
1214.71571246849,1214.79914896233,1214.88258607209,1214.96604186701,1215.04958635974,
1215.13317544268,1215.21689871023,1215.29757842613,1215.38567764236,1215.47358023361,
1215.54603050746),.UNSPECIFIED.);
#823=B_SPLINE_CURVE_WITH_KNOTS('',3,(#105448,#105449,#105450,#105451,#105452,
#105453,#105454,#105455,#105456,#105457,#105458,#105459,#105460,#105461,
#105462,#105463,#105464,#105465,#105466,#105467,#105468,#105469,#105470,
#105471,#105472,#105473,#105474,#105475,#105476,#105477,#105478,#105479,
#105480,#105481,#105482,#105483,#105484,#105485,#105486,#105487,#105488,
#105489,#105490,#105491,#105492,#105493,#105494,#105495,#105496,#105497,
#105498,#105499,#105500,#105501,#105502,#105503,#105504,#105505,#105506,
#105507,#105508,#105509,#105510,#105511,#105512,#105513,#105514,#105515,
#105516,#105517,#105518,#105519,#105520,#105521,#105522,#105523,#105524,
#105525,#105526,#105527,#105528,#105529,#105530,#105531,#105532,#105533,
#105534,#105535,#105536,#105537,#105538,#105539,#105540,#105541,#105542,
#105543,#105544,#105545,#105546,#105547,#105548,#105549,#105550,#105551,
#105552,#105553,#105554,#105555,#105556,#105557,#105558,#105559,#105560,
#105561,#105562,#105563,#105564,#105565,#105566,#105567,#105568,#105569,
#105570,#105571,#105572,#105573,#105574,#105575,#105576,#105577,#105578,
#105579,#105580,#105581,#105582,#105583,#105584,#105585,#105586,#105587,
#105588,#105589,#105590,#105591,#105592,#105593,#105594,#105595,#105596,
#105597,#105598,#105599,#105600,#105601,#105602,#105603,#105604,#105605,
#105606,#105607,#105608,#105609,#105610,#105611,#105612,#105613,#105614,
#105615,#105616,#105617,#105618,#105619,#105620,#105621,#105622,#105623,
#105624,#105625,#105626,#105627,#105628,#105629,#105630,#105631,#105632,
#105633,#105634,#105635,#105636,#105637,#105638,#105639,#105640,#105641,
#105642,#105643,#105644,#105645,#105646,#105647,#105648,#105649,#105650,
#105651,#105652,#105653,#105654,#105655,#105656,#105657,#105658,#105659,
#105660,#105661,#105662,#105663,#105664),.UNSPECIFIED.,.F.,.F.,(4,3,3,3,
3,3,3,3,3,3,3,3,3,3,3,3,3,3,3,3,3,3,3,3,3,3,3,3,3,3,3,3,3,3,3,3,3,3,3,3,
3,3,3,3,3,3,3,3,3,3,3,3,3,3,3,3,3,3,3,3,3,3,3,3,3,3,3,3,3,3,3,3,4),(1215.79635693923,
1215.91958713295,1215.98702381713,1216.07076252898,1216.15439804034,1216.23795048374,
1216.32143991959,1216.40489387021,1216.48833036405,1216.57176747381,1216.65522326873,
1216.73876776146,1216.8223568444,1216.90608011196,1216.98675982785,1217.0704985397,
1217.15413405106,1217.23768649446,1217.32117593031,1217.40462988093,1217.48806637477,
1217.57150348453,1217.65495927944,1217.73850377217,1217.82209285511,1217.90581612267,
1217.98649583857,1218.07023455042,1218.15387006178,1218.23742250518,1218.32091194103,
1218.40436589165,1218.48780238549,1218.57123949525,1218.65469529017,1218.7382397829,
1218.82182886584,1218.90555213339,1218.98623184929,1219.06997056114,1219.1536060725,
1219.2371585159,1219.32064795175,1219.40410190237,1219.48753839621,1219.57097550597,
1219.65443130089,1219.73797579362,1219.82156487656,1219.90528814411,1219.98596786001,
1220.06970657186,1220.15334208322,1220.23689452662,1220.32038396247,1220.40383791309,
1220.48727440693,1220.57071151669,1220.65416731161,1220.73771180434,1220.82130088728,
1220.90502415484,1220.98570387073,1221.06945195796,1221.15309476657,1221.23744655451,
1221.32093250422,1221.40438014118,1221.48780755436,1221.57283293328,1221.65630100248,
1221.74210503626,1221.82790907005),.UNSPECIFIED.);
#824=B_SPLINE_CURVE_WITH_KNOTS('',3,(#105665,#105666,#105667,#105668,#105669,
#105670,#105671,#105672,#105673,#105674),.UNSPECIFIED.,.F.,.F.,(4,3,3,4),
(1215.54473266754,1215.62699574014,1215.71167633962,1215.7963569391),
 .UNSPECIFIED.);
#825=B_SPLINE_CURVE_WITH_KNOTS('',3,(#105676,#105677,#105678,#105679,#105680,
#105681,#105682,#105683,#105684,#105685),.UNSPECIFIED.,.F.,.F.,(4,3,3,4),
(1215.54603050746,1215.63367448717,1215.72115463404,1215.796356939),
 .UNSPECIFIED.);
#826=B_SPLINE_CURVE_WITH_KNOTS('',3,(#105686,#105687,#105688,#105689,#105690,
#105691,#105692,#105693,#105694,#105695,#105696,#105697,#105698,#105699,
#105700,#105701,#105702,#105703,#105704,#105705,#105706,#105707,#105708,
#105709,#105710,#105711,#105712,#105713,#105714,#105715,#105716,#105717,
#105718,#105719,#105720,#105721,#105722,#105723,#105724,#105725,#105726,
#105727,#105728,#105729,#105730,#105731,#105732,#105733,#105734,#105735,
#105736,#105737,#105738,#105739,#105740,#105741,#105742,#105743,#105744,
#105745,#105746,#105747,#105748,#105749,#105750,#105751,#105752,#105753,
#105754,#105755,#105756,#105757,#105758,#105759,#105760,#105761,#105762,
#105763,#105764,#105765,#105766,#105767,#105768,#105769,#105770,#105771,
#105772,#105773,#105774,#105775,#105776,#105777,#105778,#105779,#105780,
#105781,#105782,#105783,#105784,#105785,#105786,#105787,#105788,#105789,
#105790,#105791,#105792,#105793,#105794,#105795,#105796,#105797,#105798,
#105799,#105800,#105801,#105802,#105803,#105804,#105805,#105806,#105807,
#105808,#105809,#105810,#105811,#105812,#105813,#105814,#105815,#105816,
#105817,#105818,#105819,#105820,#105821,#105822,#105823,#105824,#105825,
#105826,#105827,#105828,#105829,#105830,#105831,#105832,#105833,#105834,
#105835,#105836,#105837,#105838,#105839,#105840,#105841,#105842,#105843,
#105844,#105845,#105846,#105847,#105848,#105849,#105850,#105851,#105852,
#105853,#105854,#105855,#105856,#105857,#105858,#105859,#105860,#105861,
#105862,#105863,#105864,#105865,#105866,#105867,#105868,#105869,#105870,
#105871,#105872,#105873,#105874,#105875,#105876,#105877,#105878,#105879,
#105880,#105881,#105882,#105883,#105884,#105885,#105886,#105887,#105888,
#105889,#105890,#105891,#105892,#105893,#105894,#105895,#105896,#105897,
#105898,#105899,#105900,#105901,#105902,#105903,#105904,#105905),
 .UNSPECIFIED.,.F.,.F.,(4,3,3,3,3,3,3,3,3,3,3,3,3,3,3,3,3,3,3,3,3,3,3,3,
3,3,3,3,3,3,3,3,3,3,3,3,3,3,3,3,3,3,3,3,3,3,3,3,3,3,3,3,3,3,3,3,3,3,3,3,
3,3,3,3,3,3,3,3,3,3,3,3,3,4),(1215.79635693924,1215.88372152378,1215.97119972917,
1216.05888328619,1216.14667503323,1216.23466785268,1216.29731443685,1216.3810531487,
1216.46468866006,1216.54824110346,1216.63173053931,1216.71518448993,1216.79862098377,
1216.88205809353,1216.96551388845,1217.04905838118,1217.13264746412,1217.21637073167,
1217.29705044757,1217.38078915942,1217.46442467078,1217.54797711418,1217.63146655003,
1217.71492050065,1217.79835699449,1217.88179410425,1217.96524989917,1218.04879439189,
1218.13238347484,1218.21610674239,1218.29678645829,1218.38052517014,1218.4641606815,
1218.5477131249,1218.63120256075,1218.71465651137,1218.79809300521,1218.88153011497,
1218.96498590989,1219.04853040262,1219.13211948556,1219.21584275312,1219.29652246901,
1219.38026118086,1219.46389669222,1219.54744913562,1219.63093857147,1219.71439252209,
1219.79782901593,1219.88126612569,1219.96472192061,1220.04826641334,1220.13185549628,
1220.21557876383,1220.29625847973,1220.37999719158,1220.46363270294,1220.54718514634,
1220.63067458219,1220.71412853281,1220.79756502665,1220.88100213641,1220.96445793133,
1221.04800242406,1221.131591507,1221.21531477455,1221.29599449045,1221.37856692625,
1221.46104267683,1221.54344090801,1221.62577716739,1221.70807749483,1221.7903699991,
1221.82802192058),.UNSPECIFIED.);
#827=B_SPLINE_CURVE_WITH_KNOTS('',3,(#105911,#105912,#105913,#105914,#105915,
#105916,#105917,#105918,#105919,#105920,#105921,#105922,#105923,#105924,
#105925,#105926,#105927,#105928,#105929,#105930,#105931,#105932,#105933,
#105934,#105935,#105936,#105937,#105938,#105939,#105940,#105941,#105942,
#105943,#105944,#105945,#105946,#105947,#105948,#105949,#105950,#105951,
#105952,#105953,#105954,#105955,#105956,#105957,#105958,#105959,#105960,
#105961,#105962,#105963,#105964,#105965,#105966,#105967,#105968,#105969,
#105970,#105971,#105972,#105973,#105974,#105975,#105976,#105977,#105978,
#105979,#105980,#105981,#105982,#105983,#105984,#105985,#105986,#105987,
#105988,#105989,#105990,#105991,#105992,#105993,#105994,#105995,#105996,
#105997,#105998,#105999,#106000,#106001,#106002,#106003,#106004,#106005,
#106006,#106007,#106008,#106009,#106010,#106011,#106012,#106013,#106014,
#106015,#106016,#106017,#106018,#106019,#106020,#106021,#106022,#106023,
#106024,#106025,#106026,#106027,#106028,#106029,#106030,#106031,#106032,
#106033,#106034,#106035,#106036,#106037,#106038,#106039,#106040,#106041,
#106042,#106043,#106044,#106045,#106046,#106047,#106048,#106049,#106050,
#106051,#106052,#106053,#106054,#106055,#106056,#106057,#106058,#106059,
#106060,#106061,#106062,#106063,#106064,#106065,#106066,#106067,#106068,
#106069,#106070,#106071,#106072,#106073,#106074,#106075,#106076,#106077,
#106078,#106079,#106080,#106081,#106082,#106083,#106084,#106085,#106086,
#106087,#106088,#106089,#106090,#106091,#106092,#106093,#106094,#106095,
#106096,#106097,#106098,#106099,#106100,#106101,#106102,#106103,#106104,
#106105,#106106,#106107,#106108,#106109,#106110,#106111,#106112,#106113,
#106114,#106115,#106116,#106117,#106118,#106119,#106120,#106121,#106122,
#106123,#106124,#106125,#106126,#106127,#106128,#106129,#106130),
 .UNSPECIFIED.,.F.,.F.,(4,3,3,3,3,3,3,3,3,3,3,3,3,3,3,3,3,3,3,3,3,3,3,3,
3,3,3,3,3,3,3,3,3,3,3,3,3,3,3,3,3,3,3,3,3,3,3,3,3,3,3,3,3,3,3,3,3,3,3,3,
3,3,3,3,3,3,3,3,3,3,3,3,3,4),(1222.07954224654,1222.1622243311,1222.24481273503,
1222.32732847992,1222.40979672105,1222.49224044242,1222.5746785349,1222.6571298824,
1222.73966412823,1222.82223962968,1222.90494673739,1222.98517589217,1223.06891460402,
1223.15255011538,1223.23610255878,1223.31959199463,1223.40304594525,1223.48648243909,
1223.56991954885,1223.65337534377,1223.7369198365,1223.82050891944,1223.904232187,
1223.98491190289,1224.06865061474,1224.1522861261,1224.2358385695,1224.31932800535,
1224.40278195597,1224.48621844981,1224.56965555957,1224.65311135448,1224.73665584721,
1224.82024493015,1224.90396819771,1224.98464791361,1225.06838662546,1225.15202213682,
1225.23557458022,1225.31906401607,1225.40251796669,1225.48595446053,1225.56939157029,
1225.65284736521,1225.73639185794,1225.81998094088,1225.90370420844,1225.98438392433,
1226.06812263618,1226.15175814754,1226.23531059094,1226.31880002679,1226.40225397741,
1226.48569047125,1226.56912758101,1226.65258337593,1226.73612786866,1226.8197169516,
1226.90344021916,1226.98411993505,1227.0678586469,1227.15149415826,1227.23504660166,
1227.31853603751,1227.40198998813,1227.48542648197,1227.56886359173,1227.65231938665,
1227.73586387938,1227.81945296232,1227.90317622987,1227.98385594577,1228.07849597611,
1228.11229739101),.UNSPECIFIED.);
#828=B_SPLINE_CURVE_WITH_KNOTS('',3,(#106131,#106132,#106133,#106134,#106135,
#106136,#106137,#106138,#106139,#106140),.UNSPECIFIED.,.F.,.F.,(4,3,3,4),
(1221.82790907005,1221.91163470905,1221.98543988145,1222.07954224641),
 .UNSPECIFIED.);
#829=B_SPLINE_CURVE_WITH_KNOTS('',3,(#106142,#106143,#106144,#106145,#106146,
#106147,#106148,#106149,#106150,#106151),.UNSPECIFIED.,.F.,.F.,(4,3,3,4),
(1221.82802192058,1221.91034520054,1221.99494372338,1222.07954224622),
 .UNSPECIFIED.);
#830=B_SPLINE_CURVE_WITH_KNOTS('',3,(#106152,#106153,#106154,#106155,#106156,
#106157,#106158,#106159,#106160,#106161,#106162,#106163,#106164,#106165,
#106166,#106167,#106168,#106169,#106170,#106171,#106172,#106173,#106174,
#106175,#106176,#106177,#106178,#106179,#106180,#106181,#106182,#106183,
#106184,#106185,#106186,#106187,#106188,#106189,#106190,#106191,#106192,
#106193,#106194,#106195,#106196,#106197,#106198,#106199,#106200,#106201,
#106202,#106203,#106204,#106205,#106206,#106207,#106208,#106209,#106210,
#106211,#106212,#106213,#106214,#106215,#106216,#106217,#106218,#106219,
#106220,#106221,#106222,#106223,#106224,#106225,#106226,#106227,#106228,
#106229,#106230,#106231,#106232,#106233,#106234,#106235,#106236,#106237,
#106238,#106239,#106240,#106241,#106242,#106243,#106244,#106245,#106246,
#106247,#106248,#106249,#106250,#106251,#106252,#106253,#106254,#106255,
#106256,#106257,#106258,#106259,#106260,#106261,#106262,#106263,#106264,
#106265,#106266,#106267,#106268,#106269,#106270,#106271,#106272,#106273,
#106274,#106275,#106276,#106277,#106278,#106279,#106280,#106281,#106282,
#106283,#106284,#106285,#106286,#106287,#106288,#106289,#106290,#106291,
#106292,#106293,#106294,#106295,#106296,#106297,#106298,#106299,#106300,
#106301,#106302,#106303,#106304,#106305,#106306,#106307,#106308,#106309,
#106310,#106311,#106312,#106313,#106314,#106315,#106316,#106317,#106318,
#106319,#106320,#106321,#106322,#106323,#106324,#106325,#106326,#106327,
#106328,#106329,#106330,#106331,#106332,#106333,#106334,#106335,#106336,
#106337,#106338,#106339,#106340,#106341,#106342,#106343,#106344,#106345,
#106346,#106347,#106348,#106349,#106350,#106351,#106352,#106353,#106354,
#106355,#106356,#106357,#106358,#106359,#106360,#106361,#106362,#106363,
#106364,#106365,#106366,#106367,#106368),.UNSPECIFIED.,.F.,.F.,(4,3,3,3,
3,3,3,3,3,3,3,3,3,3,3,3,3,3,3,3,3,3,3,3,3,3,3,3,3,3,3,3,3,3,3,3,3,3,3,3,
3,3,3,3,3,3,3,3,3,3,3,3,3,3,3,3,3,3,3,3,3,3,3,3,3,3,3,3,3,3,3,3,4),(1222.07954224642,
1222.19525728097,1222.29573050117,1222.37946921302,1222.46310472438,1222.54665716778,
1222.63014660363,1222.71360055425,1222.79703704809,1222.88047415785,1222.96392995277,
1223.0474744455,1223.13106352844,1223.21478679599,1223.29546651189,1223.37920522374,
1223.4628407351,1223.5463931785,1223.62988261435,1223.71333656497,1223.79677305881,
1223.88021016857,1223.96366596349,1224.04721045621,1224.13079953916,1224.21452280671,
1224.29520252261,1224.37894123446,1224.46257674582,1224.54612918922,1224.62961862507,
1224.71307257569,1224.79650906953,1224.87994617929,1224.96340197421,1225.04694646694,
1225.13053554988,1225.21425881743,1225.29493853333,1225.37867724518,1225.46231275654,
1225.54586519994,1225.62935463579,1225.71280858641,1225.79624508025,1225.87968219001,
1225.96313798493,1226.04668247766,1226.1302715606,1226.21399482815,1226.29467454405,
1226.3784132559,1226.46204876726,1226.54560121066,1226.62909064651,1226.71254459713,
1226.79598109097,1226.87941820073,1226.96287399565,1227.04641848838,1227.13000757132,
1227.21373083887,1227.29441055477,1227.37816026671,1227.46180436294,1227.54534777386,
1227.62883409999,1227.71228146099,1227.79570794646,1227.87915848801,1227.96261979029,
1228.04615181694,1228.1110700616),.UNSPECIFIED.);
#831=B_SPLINE_CURVE_WITH_KNOTS('',3,(#106374,#106375,#106376,#106377,#106378,
#106379,#106380,#106381,#106382,#106383,#106384,#106385,#106386,#106387,
#106388,#106389,#106390,#106391,#106392,#106393,#106394,#106395,#106396,
#106397,#106398,#106399,#106400,#106401,#106402,#106403,#106404,#106405,
#106406,#106407,#106408,#106409,#106410,#106411,#106412,#106413,#106414,
#106415,#106416,#106417,#106418,#106419,#106420,#106421,#106422,#106423,
#106424,#106425,#106426,#106427,#106428,#106429,#106430,#106431,#106432,
#106433,#106434,#106435,#106436,#106437,#106438,#106439,#106440,#106441,
#106442,#106443,#106444,#106445,#106446,#106447,#106448,#106449,#106450,
#106451,#106452,#106453,#106454,#106455,#106456,#106457,#106458,#106459,
#106460,#106461,#106462,#106463,#106464,#106465,#106466,#106467,#106468,
#106469,#106470,#106471,#106472,#106473,#106474,#106475,#106476,#106477,
#106478,#106479,#106480,#106481,#106482,#106483,#106484,#106485,#106486,
#106487,#106488,#106489,#106490,#106491,#106492,#106493,#106494,#106495,
#106496,#106497,#106498,#106499,#106500,#106501,#106502,#106503,#106504,
#106505,#106506,#106507,#106508,#106509,#106510,#106511,#106512,#106513,
#106514,#106515,#106516,#106517,#106518,#106519,#106520,#106521,#106522,
#106523,#106524,#106525,#106526,#106527,#106528,#106529,#106530,#106531,
#106532,#106533,#106534,#106535,#106536,#106537,#106538,#106539,#106540,
#106541,#106542,#106543,#106544,#106545,#106546,#106547,#106548,#106549,
#106550,#106551,#106552,#106553,#106554,#106555,#106556,#106557,#106558,
#106559,#106560,#106561,#106562,#106563,#106564,#106565,#106566,#106567,
#106568,#106569,#106570,#106571,#106572,#106573,#106574,#106575,#106576,
#106577,#106578,#106579,#106580,#106581,#106582,#106583,#106584,#106585,
#106586,#106587,#106588,#106589,#106590,#106591,#106592,#106593),
 .UNSPECIFIED.,.F.,.F.,(4,3,3,3,3,3,3,3,3,3,3,3,3,3,3,3,3,3,3,3,3,3,3,3,
3,3,3,3,3,3,3,3,3,3,3,3,3,3,3,3,3,3,3,3,3,3,3,3,3,3,3,3,3,3,3,3,3,3,3,3,
3,3,3,3,3,3,3,3,3,3,3,3,3,4),(1228.36272755359,1228.44686496824,1228.53101191958,
1228.61518547554,1228.69940271783,1228.78373211921,1228.86812631425,1228.95265392673,
1228.98359195649,1229.06733066834,1229.1509661797,1229.2345186231,1229.31800805895,
1229.40146200956,1229.48489850341,1229.56833561316,1229.65179140808,1229.73533590081,
1229.81892498375,1229.90264825131,1229.98332796721,1230.06706667906,1230.15070219042,
1230.23425463382,1230.31774406967,1230.40119802029,1230.48463451413,1230.56807162389,
1230.6515274188,1230.73507191153,1230.81866099447,1230.90238426203,1230.98306397793,
1231.06680268978,1231.15043820114,1231.23399064454,1231.31748008039,1231.40093403101,
1231.48437052485,1231.56780763461,1231.65126342953,1231.73480792226,1231.8183970052,
1231.90212027276,1231.98279998865,1232.0665387005,1232.15017421186,1232.23372665526,
1232.31721609111,1232.40067004173,1232.48410653557,1232.56754364533,1232.65099944025,
1232.73454393298,1232.81813301592,1232.90185628347,1232.98253599937,1233.06627471122,
1233.14991022258,1233.23346266598,1233.31695210183,1233.40040605245,1233.48384254629,
1233.56727965605,1233.65073545097,1233.7342799437,1233.81786902664,1233.9015922942,
1233.98227201009,1234.06602879375,1234.14965100751,1234.23319577681,1234.3166722851,
1234.39499262579),.UNSPECIFIED.);
#832=B_SPLINE_CURVE_WITH_KNOTS('',3,(#106594,#106595,#106596,#106597,#106598,
#106599,#106600,#106601,#106602,#106603),.UNSPECIFIED.,.F.,.F.,(4,3,3,4),
(1228.11229739101,1228.20642172505,1228.30000816463,1228.36272755339),
 .UNSPECIFIED.);
#833=B_SPLINE_CURVE_WITH_KNOTS('',3,(#106605,#106606,#106607,#106608,#106609,
#106610,#106611,#106612,#106613,#106614,#106615,#106616,#106617),
 .UNSPECIFIED.,.F.,.F.,(4,3,3,3,4),(1228.1110700616,1228.1947049976,1228.27845607522,
1228.29414656549,1228.3627275536),.UNSPECIFIED.);
#834=B_SPLINE_CURVE_WITH_KNOTS('',3,(#106618,#106619,#106620,#106621,#106622,
#106623,#106624,#106625,#106626,#106627,#106628,#106629,#106630,#106631,
#106632,#106633,#106634,#106635,#106636,#106637,#106638,#106639,#106640,
#106641,#106642,#106643,#106644,#106645,#106646,#106647,#106648,#106649,
#106650,#106651,#106652,#106653,#106654,#106655,#106656,#106657,#106658,
#106659,#106660,#106661,#106662,#106663,#106664,#106665,#106666,#106667,
#106668,#106669,#106670,#106671,#106672,#106673,#106674,#106675,#106676,
#106677,#106678,#106679,#106680,#106681,#106682,#106683,#106684,#106685,
#106686,#106687,#106688,#106689,#106690,#106691,#106692,#106693,#106694,
#106695,#106696,#106697,#106698,#106699,#106700,#106701,#106702,#106703,
#106704,#106705,#106706,#106707,#106708,#106709,#106710,#106711,#106712,
#106713,#106714,#106715,#106716,#106717,#106718,#106719,#106720,#106721,
#106722,#106723,#106724,#106725,#106726,#106727,#106728,#106729,#106730,
#106731,#106732,#106733,#106734,#106735,#106736,#106737,#106738,#106739,
#106740,#106741,#106742,#106743,#106744,#106745,#106746,#106747,#106748,
#106749,#106750,#106751,#106752,#106753,#106754,#106755,#106756,#106757,
#106758,#106759,#106760,#106761,#106762,#106763,#106764,#106765,#106766,
#106767,#106768,#106769,#106770,#106771,#106772,#106773,#106774,#106775,
#106776,#106777,#106778,#106779,#106780,#106781,#106782,#106783,#106784,
#106785,#106786,#106787,#106788,#106789,#106790,#106791,#106792,#106793,
#106794,#106795,#106796,#106797,#106798,#106799,#106800,#106801,#106802,
#106803,#106804,#106805,#106806,#106807,#106808,#106809,#106810,#106811,
#106812,#106813,#106814,#106815,#106816,#106817,#106818,#106819,#106820,
#106821,#106822,#106823,#106824,#106825,#106826,#106827,#106828,#106829,
#106830,#106831,#106832,#106833,#106834,#106835,#106836,#106837,#106838,
#106839,#106840),.UNSPECIFIED.,.F.,.F.,(4,3,3,3,3,3,3,3,3,3,3,3,3,3,3,3,
3,3,3,3,3,3,3,3,3,3,3,3,3,3,3,3,3,3,3,3,3,3,3,3,3,3,3,3,3,3,3,3,3,3,3,3,
3,3,3,3,3,3,3,3,3,3,3,3,3,3,3,3,3,3,3,3,3,3,4),(1228.36272755372,1228.44562235737,
1228.52841945832,1228.6111397427,1228.69648259689,1228.77912045889,1228.86174916971,
1228.94438748203,1229.02705415266,1229.10981173076,1229.19262389116,1229.27555133896,
1229.29388257621,1229.37762128806,1229.46125679942,1229.54480924282,1229.62829867867,
1229.71175262929,1229.79518912313,1229.87862623289,1229.96208202781,1230.04562652054,
1230.12921560348,1230.21293887103,1230.29361858693,1230.37735729878,1230.46099281014,
1230.54454525354,1230.62803468939,1230.71148864001,1230.79492513385,1230.87836224361,
1230.96181803853,1231.04536253126,1231.1289516142,1231.21267488175,1231.29335459765,
1231.3770933095,1231.46072882086,1231.54428126426,1231.62777070011,1231.71122465073,
1231.79466114457,1231.87809825433,1231.96155404925,1232.04509854198,1232.12868762492,
1232.21241089247,1232.29309060837,1232.37682932022,1232.46046483158,1232.54401727498,
1232.62750671083,1232.71096066145,1232.79439715529,1232.87783426505,1232.96129005997,
1233.0448345527,1233.12842363564,1233.21214690319,1233.29282661909,1233.37656533094,
1233.4602008423,1233.5437532857,1233.62724272155,1233.71069667216,1233.79413316601,
1233.87757027577,1233.96102607068,1234.04457056341,1234.12815964635,1234.21188291391,
1234.29256262981,1234.38930089973,1234.3953925264),.UNSPECIFIED.);
#835=B_SPLINE_CURVE_WITH_KNOTS('',3,(#106846,#106847,#106848,#106849,#106850,
#106851,#106852,#106853,#106854,#106855,#106856,#106857,#106858,#106859,
#106860,#106861,#106862,#106863,#106864,#106865,#106866,#106867,#106868,
#106869,#106870,#106871,#106872,#106873,#106874,#106875,#106876,#106877,
#106878,#106879,#106880,#106881,#106882,#106883,#106884,#106885,#106886,
#106887,#106888,#106889,#106890,#106891,#106892,#106893,#106894,#106895,
#106896,#106897,#106898,#106899,#106900,#106901,#106902,#106903,#106904,
#106905,#106906,#106907,#106908,#106909,#106910,#106911,#106912,#106913,
#106914,#106915,#106916,#106917,#106918,#106919,#106920,#106921,#106922,
#106923,#106924,#106925,#106926,#106927,#106928,#106929,#106930,#106931,
#106932,#106933,#106934,#106935,#106936,#106937,#106938,#106939,#106940,
#106941,#106942,#106943,#106944,#106945,#106946,#106947,#106948,#106949,
#106950,#106951,#106952,#106953,#106954,#106955,#106956,#106957,#106958,
#106959,#106960,#106961,#106962,#106963,#106964,#106965,#106966,#106967,
#106968,#106969,#106970,#106971,#106972,#106973,#106974,#106975,#106976,
#106977,#106978,#106979,#106980,#106981,#106982,#106983,#106984,#106985,
#106986,#106987,#106988,#106989,#106990,#106991,#106992,#106993,#106994,
#106995,#106996,#106997,#106998,#106999,#107000,#107001,#107002,#107003,
#107004,#107005,#107006,#107007,#107008,#107009,#107010,#107011,#107012,
#107013,#107014,#107015,#107016,#107017,#107018,#107019,#107020,#107021,
#107022,#107023,#107024,#107025,#107026,#107027,#107028,#107029,#107030,
#107031,#107032,#107033,#107034,#107035,#107036,#107037,#107038,#107039,
#107040,#107041,#107042,#107043,#107044,#107045,#107046,#107047,#107048,
#107049,#107050,#107051,#107052,#107053,#107054,#107055,#107056,#107057,
#107058,#107059,#107060,#107061,#107062,#107063,#107064,#107065),
 .UNSPECIFIED.,.F.,.F.,(4,3,3,3,3,3,3,3,3,3,3,3,3,3,3,3,3,3,3,3,3,3,3,3,
3,3,3,3,3,3,3,3,3,3,3,3,3,3,3,3,3,3,3,3,3,3,3,3,3,3,3,3,3,3,3,3,3,3,3,3,
3,3,3,3,3,3,3,3,3,3,3,3,3,4),(1234.64591286096,1234.74290541511,1234.84045829031,
1234.93867775055,1234.98200802081,1235.06574673265,1235.14938224402,1235.23293468742,
1235.31642412327,1235.39987807388,1235.48331456772,1235.56675167748,1235.65020747239,
1235.73375196512,1235.81734104806,1235.90106431562,1235.98174403153,1236.06548274338,
1236.14911825474,1236.23267069814,1236.31616013399,1236.39961408461,1236.48305057845,
1236.56648768821,1236.64994348313,1236.73348797586,1236.8170770588,1236.90080032635,
1236.98148004225,1237.0652187541,1237.14885426546,1237.23240670886,1237.31589614471,
1237.39935009533,1237.48278658917,1237.56622369893,1237.64967949385,1237.73322398658,
1237.81681306952,1237.90053633708,1237.98121605297,1238.06495476482,1238.14859027618,
1238.23214271958,1238.31563215543,1238.39908610605,1238.48252259989,1238.56595970965,
1238.64941550456,1238.73295999729,1238.81654908023,1238.90027234779,1238.98095206369,
1239.06469077554,1239.1483262869,1239.2318787303,1239.31536816615,1239.39882211677,
1239.48225861061,1239.56569572037,1239.64915151529,1239.73269600802,1239.81628509096,
1239.90000835852,1239.98068807441,1240.06776341289,1240.15072850065,1240.23361870592,
1240.31645275755,1240.39924933831,1240.4820416088,1240.56483166194,1240.64766028562,
1240.67729078227),.UNSPECIFIED.);
#836=B_SPLINE_CURVE_WITH_KNOTS('',3,(#107066,#107067,#107068,#107069,#107070,
#107071,#107072,#107073,#107074,#107075),.UNSPECIFIED.,.F.,.F.,(4,3,3,4),
(1234.39499262579,1234.47840436807,1234.56215861442,1234.64591286077),
 .UNSPECIFIED.);
#837=B_SPLINE_CURVE_WITH_KNOTS('',3,(#107077,#107078,#107079,#107080,#107081,
#107082,#107083,#107084,#107085,#107086),.UNSPECIFIED.,.F.,.F.,(4,3,3,4),
(1234.3953925264,1234.49156719124,1234.58704613723,1234.64591286058),
 .UNSPECIFIED.);
#838=B_SPLINE_CURVE_WITH_KNOTS('',3,(#107087,#107088,#107089,#107090,#107091,
#107092,#107093,#107094,#107095,#107096,#107097,#107098,#107099,#107100,
#107101,#107102,#107103,#107104,#107105,#107106,#107107,#107108,#107109,
#107110,#107111,#107112,#107113,#107114,#107115,#107116,#107117,#107118,
#107119,#107120,#107121,#107122,#107123,#107124,#107125,#107126,#107127,
#107128,#107129,#107130,#107131,#107132,#107133,#107134,#107135,#107136,
#107137,#107138,#107139,#107140,#107141,#107142,#107143,#107144,#107145,
#107146,#107147,#107148,#107149,#107150,#107151,#107152,#107153,#107154,
#107155,#107156,#107157,#107158,#107159,#107160,#107161,#107162,#107163,
#107164,#107165,#107166,#107167,#107168,#107169,#107170,#107171,#107172,
#107173,#107174,#107175,#107176,#107177,#107178,#107179,#107180,#107181,
#107182,#107183,#107184,#107185,#107186,#107187,#107188,#107189,#107190,
#107191,#107192,#107193,#107194,#107195,#107196,#107197,#107198,#107199,
#107200,#107201,#107202,#107203,#107204,#107205,#107206,#107207,#107208,
#107209,#107210,#107211,#107212,#107213,#107214,#107215,#107216,#107217,
#107218,#107219,#107220,#107221,#107222,#107223,#107224,#107225,#107226,
#107227,#107228,#107229,#107230,#107231,#107232,#107233,#107234,#107235,
#107236,#107237,#107238,#107239,#107240,#107241,#107242,#107243,#107244,
#107245,#107246,#107247,#107248,#107249,#107250,#107251,#107252,#107253,
#107254,#107255,#107256,#107257,#107258,#107259,#107260,#107261,#107262,
#107263,#107264,#107265,#107266,#107267,#107268,#107269,#107270,#107271,
#107272,#107273,#107274,#107275,#107276,#107277,#107278,#107279,#107280,
#107281,#107282,#107283,#107284,#107285,#107286,#107287,#107288,#107289,
#107290,#107291,#107292,#107293,#107294,#107295,#107296,#107297,#107298,
#107299,#107300,#107301,#107302,#107303,#107304,#107305,#107306),
 .UNSPECIFIED.,.F.,.F.,(4,3,3,3,3,3,3,3,3,3,3,3,3,3,3,3,3,3,3,3,3,3,3,3,
3,3,3,3,3,3,3,3,3,3,3,3,3,3,3,3,3,3,3,3,3,3,3,3,3,3,3,3,3,3,3,3,3,3,3,3,
3,3,3,3,3,3,3,3,3,3,3,3,3,4),(1234.64591286078,1234.72960198682,1234.81328713594,
1234.8969860036,1234.98071629027,1235.06454892901,1235.14843665197,1235.23246162227,
1235.29229864053,1235.37603735238,1235.45967286374,1235.54322530714,1235.62671474299,
1235.71016869361,1235.79360518745,1235.87704229721,1235.96049809213,1236.04404258486,
1236.1276316678,1236.21135493536,1236.29203465125,1236.3757733631,1236.45940887446,
1236.54296131786,1236.62645075371,1236.70990470433,1236.79334119817,1236.87677830793,
1236.96023410285,1237.04377859558,1237.12736767852,1237.21109094607,1237.29177066197,
1237.37550937382,1237.45914488518,1237.54269732858,1237.62618676443,1237.70964071505,
1237.79307720889,1237.87651431865,1237.95997011357,1238.0435146063,1238.12710368924,
1238.2108269568,1238.29150667269,1238.37524538454,1238.4588808959,1238.5424333393,
1238.62592277515,1238.70937672577,1238.79281321961,1238.87625032937,1238.95970612429,
1239.04325061702,1239.12683969996,1239.21056296751,1239.29124268341,1239.37498139526,
1239.45861690662,1239.54216935002,1239.62565878587,1239.70911273649,1239.79254923033,
1239.87598634009,1239.959442135,1240.04298662773,1240.12657571067,1240.21029897823,
1240.29097869413,1240.3751777929,1240.45923668845,1240.54321483669,1240.62711586346,
1240.67830517384),.UNSPECIFIED.);
#839=B_SPLINE_CURVE_WITH_KNOTS('',3,(#107312,#107313,#107314,#107315,#107316,
#107317,#107318,#107319,#107320,#107321,#107322,#107323,#107324,#107325,
#107326,#107327,#107328,#107329,#107330,#107331,#107332,#107333,#107334,
#107335,#107336,#107337,#107338,#107339,#107340,#107341,#107342,#107343,
#107344,#107345,#107346,#107347,#107348,#107349,#107350,#107351,#107352,
#107353,#107354,#107355,#107356,#107357,#107358,#107359,#107360,#107361,
#107362,#107363,#107364,#107365,#107366,#107367,#107368,#107369,#107370,
#107371,#107372,#107373,#107374,#107375,#107376,#107377,#107378,#107379,
#107380,#107381,#107382,#107383,#107384,#107385,#107386,#107387,#107388,
#107389,#107390,#107391,#107392,#107393,#107394,#107395,#107396,#107397,
#107398,#107399,#107400,#107401,#107402,#107403,#107404,#107405,#107406,
#107407,#107408,#107409,#107410,#107411,#107412,#107413,#107414,#107415,
#107416,#107417,#107418,#107419,#107420,#107421,#107422,#107423,#107424,
#107425,#107426,#107427,#107428,#107429,#107430,#107431,#107432,#107433,
#107434,#107435,#107436,#107437,#107438,#107439,#107440,#107441,#107442,
#107443,#107444,#107445,#107446,#107447,#107448,#107449,#107450,#107451,
#107452,#107453,#107454,#107455,#107456,#107457,#107458,#107459,#107460,
#107461,#107462,#107463,#107464,#107465,#107466,#107467,#107468,#107469,
#107470,#107471,#107472,#107473,#107474,#107475,#107476,#107477,#107478,
#107479,#107480,#107481,#107482,#107483,#107484,#107485,#107486,#107487,
#107488,#107489,#107490,#107491,#107492,#107493,#107494,#107495,#107496,
#107497,#107498,#107499,#107500,#107501,#107502,#107503,#107504,#107505,
#107506,#107507,#107508,#107509,#107510,#107511,#107512,#107513,#107514,
#107515,#107516,#107517,#107518,#107519,#107520,#107521,#107522,#107523,
#107524,#107525,#107526,#107527,#107528,#107529,#107530,#107531),
 .UNSPECIFIED.,.F.,.F.,(4,3,3,3,3,3,3,3,3,3,3,3,3,3,3,3,3,3,3,3,3,3,3,3,
3,3,3,3,3,3,3,3,3,3,3,3,3,3,3,3,3,3,3,3,3,3,3,3,3,3,3,3,3,3,3,3,3,3,3,3,
3,3,3,3,3,3,3,3,3,3,3,3,3,4),(1240.92909816795,1240.98042408513,1241.06416279698,
1241.14779830834,1241.23135075174,1241.31484018759,1241.39829413821,1241.48173063205,
1241.56516774181,1241.64862353672,1241.73216802945,1241.8157571124,1241.89948037995,
1241.98016009585,1242.0638988077,1242.14753431906,1242.23108676246,1242.31457619831,
1242.39803014893,1242.48146664277,1242.56490375253,1242.64835954745,1242.73190404018,
1242.81549312312,1242.89921639068,1242.97989610657,1243.06363481842,1243.14727032978,
1243.23082277318,1243.31431220903,1243.39776615965,1243.48120265349,1243.56463976325,
1243.64809555817,1243.7316400509,1243.81522913384,1243.89895240139,1243.97963211729,
1244.06337082914,1244.1470063405,1244.2305587839,1244.31404821975,1244.39750217037,
1244.48093866421,1244.56437577397,1244.64783156889,1244.73137606162,1244.81496514456,
1244.89868841211,1244.97936812801,1245.06310683986,1245.14674235122,1245.23029479462,
1245.31378423047,1245.39723818109,1245.48067467493,1245.56411178469,1245.64756757961,
1245.73111207234,1245.81470115528,1245.89842442283,1245.97910413873,1246.06284385027,
1246.14648012754,1246.23003310401,1246.31352284087,1246.39697589055,1246.48041115292,
1246.56384670043,1246.64730060183,1246.73083860208,1246.81442105593,1246.89812687545,
1246.96111321221),.UNSPECIFIED.);
#840=B_SPLINE_CURVE_WITH_KNOTS('',3,(#107532,#107533,#107534,#107535,#107536,
#107537,#107538,#107539,#107540,#107541),.UNSPECIFIED.,.F.,.F.,(4,3,3,4),
(1240.67729078227,1240.76021147889,1240.84465482332,1240.92909816775),
 .UNSPECIFIED.);
#841=B_SPLINE_CURVE_WITH_KNOTS('',3,(#107543,#107544,#107545,#107546,#107547,
#107548,#107549,#107550,#107551,#107552),.UNSPECIFIED.,.F.,.F.,(4,3,3,4),
(1240.67830517384,1240.76213721218,1240.84596592975,1240.92909816796),
 .UNSPECIFIED.);
#842=B_SPLINE_CURVE_WITH_KNOTS('',3,(#107553,#107554,#107555,#107556,#107557,
#107558,#107559,#107560,#107561,#107562,#107563,#107564,#107565,#107566,
#107567,#107568,#107569,#107570,#107571,#107572,#107573,#107574,#107575,
#107576,#107577,#107578,#107579,#107580,#107581,#107582,#107583,#107584,
#107585,#107586,#107587,#107588,#107589,#107590,#107591,#107592,#107593,
#107594,#107595,#107596,#107597,#107598,#107599,#107600,#107601,#107602,
#107603,#107604,#107605,#107606,#107607,#107608,#107609,#107610,#107611,
#107612,#107613,#107614,#107615,#107616,#107617,#107618,#107619,#107620,
#107621,#107622,#107623,#107624,#107625,#107626,#107627,#107628,#107629,
#107630,#107631,#107632,#107633,#107634,#107635,#107636,#107637,#107638,
#107639,#107640,#107641,#107642,#107643,#107644,#107645,#107646,#107647,
#107648,#107649,#107650,#107651,#107652,#107653,#107654,#107655,#107656,
#107657,#107658,#107659,#107660,#107661,#107662,#107663,#107664,#107665,
#107666,#107667,#107668,#107669,#107670,#107671,#107672,#107673,#107674,
#107675,#107676,#107677,#107678,#107679,#107680,#107681,#107682,#107683,
#107684,#107685,#107686,#107687,#107688,#107689,#107690,#107691,#107692,
#107693,#107694,#107695,#107696,#107697,#107698,#107699,#107700,#107701,
#107702,#107703,#107704,#107705,#107706,#107707,#107708,#107709,#107710,
#107711,#107712,#107713,#107714,#107715,#107716,#107717,#107718,#107719,
#107720,#107721,#107722,#107723,#107724,#107725,#107726,#107727,#107728,
#107729,#107730,#107731,#107732,#107733,#107734,#107735,#107736,#107737,
#107738,#107739,#107740,#107741,#107742,#107743,#107744,#107745,#107746,
#107747,#107748,#107749,#107750,#107751,#107752,#107753,#107754,#107755,
#107756,#107757,#107758,#107759,#107760,#107761,#107762,#107763,#107764,
#107765,#107766,#107767,#107768,#107769),.UNSPECIFIED.,.F.,.F.,(4,3,3,3,
3,3,3,3,3,3,3,3,3,3,3,3,3,3,3,3,3,3,3,3,3,3,3,3,3,3,3,3,3,3,3,3,3,3,3,3,
3,3,3,3,3,3,3,3,3,3,3,3,3,3,3,3,3,3,3,3,3,3,3,3,3,3,3,3,3,3,3,3,4),(1240.92909816816,
1241.02401292562,1241.11934568251,1241.21524013569,1241.29071470485,1241.3744534167,
1241.45808892806,1241.54164137146,1241.62513080732,1241.70858475793,1241.79202125178,
1241.87545836153,1241.95891415645,1242.04245864918,1242.12604773212,1242.20977099968,
1242.29045071557,1242.37418942742,1242.45782493878,1242.54137738218,1242.62486681803,
1242.70832076865,1242.79175726249,1242.87519437225,1242.95865016717,1243.0421946599,
1243.12578374284,1243.2095070104,1243.29018672629,1243.37392543814,1243.4575609495,
1243.5411133929,1243.62460282875,1243.70805677937,1243.79149327321,1243.87493038297,
1243.95838617788,1244.04193067061,1244.12551975356,1244.20924302111,1244.28992273701,
1244.37366144886,1244.45729696022,1244.54084940362,1244.62433883947,1244.70779279009,
1244.79122928393,1244.87466639369,1244.95812218861,1245.04166668134,1245.12525576428,
1245.20897903183,1245.28965874773,1245.37339745958,1245.45703297094,1245.54058541434,
1245.62407485019,1245.70752880081,1245.79096529465,1245.87440240441,1245.95785819932,
1246.04140269205,1246.12499177499,1246.20871504255,1246.28939475845,1246.37327644502,
1246.45601189193,1246.53867200883,1246.62127569751,1246.70606883588,1246.78862824948,
1246.87453825023,1246.96044825099),.UNSPECIFIED.);
#843=B_SPLINE_CURVE_WITH_KNOTS('',3,(#107775,#107776,#107777,#107778,#107779,
#107780,#107781,#107782,#107783,#107784,#107785,#107786,#107787,#107788,
#107789,#107790,#107791,#107792,#107793,#107794,#107795,#107796,#107797,
#107798,#107799,#107800,#107801,#107802,#107803,#107804,#107805,#107806,
#107807,#107808,#107809,#107810,#107811,#107812,#107813,#107814,#107815,
#107816,#107817,#107818,#107819,#107820,#107821,#107822,#107823,#107824,
#107825,#107826,#107827,#107828,#107829,#107830,#107831,#107832,#107833,
#107834,#107835,#107836,#107837,#107838,#107839,#107840,#107841,#107842,
#107843,#107844,#107845,#107846,#107847,#107848,#107849,#107850,#107851,
#107852,#107853,#107854,#107855,#107856,#107857,#107858,#107859,#107860,
#107861,#107862,#107863,#107864,#107865,#107866,#107867,#107868,#107869,
#107870,#107871,#107872,#107873,#107874,#107875,#107876,#107877,#107878,
#107879,#107880,#107881,#107882,#107883,#107884,#107885,#107886,#107887,
#107888,#107889,#107890,#107891,#107892,#107893,#107894,#107895,#107896,
#107897,#107898,#107899,#107900,#107901,#107902,#107903,#107904,#107905,
#107906,#107907,#107908,#107909,#107910,#107911,#107912,#107913,#107914,
#107915,#107916,#107917,#107918,#107919,#107920,#107921,#107922,#107923,
#107924,#107925,#107926,#107927,#107928,#107929,#107930,#107931,#107932,
#107933,#107934,#107935,#107936,#107937,#107938,#107939,#107940,#107941,
#107942,#107943,#107944,#107945,#107946,#107947,#107948,#107949,#107950,
#107951,#107952,#107953,#107954,#107955,#107956,#107957,#107958,#107959,
#107960,#107961,#107962,#107963,#107964,#107965,#107966,#107967,#107968,
#107969,#107970,#107971,#107972,#107973,#107974,#107975,#107976,#107977,
#107978,#107979,#107980,#107981,#107982,#107983,#107984,#107985,#107986,
#107987,#107988,#107989,#107990,#107991,#107992,#107993,#107994),
 .UNSPECIFIED.,.F.,.F.,(4,3,3,3,3,3,3,3,3,3,3,3,3,3,3,3,3,3,3,3,3,3,3,3,
3,3,3,3,3,3,3,3,3,3,3,3,3,3,3,3,3,3,3,3,3,3,3,3,3,3,3,3,3,3,3,3,3,3,3,3,
3,3,3,3,3,3,3,3,3,3,3,3,3,4),(1247.21228347513,1247.29476035575,1247.3802373313,
1247.46262571574,1247.54500297411,1247.62738802756,1247.70979980091,1247.79230117892,
1247.87485598102,1247.9575263169,1247.97857616017,1248.06231487202,1248.14595038338,
1248.22950282678,1248.31299226263,1248.39644621325,1248.47988270709,1248.56331981685,
1248.64677561177,1248.7303201045,1248.81390918744,1248.89763245499,1248.97831217089,
1249.06205088274,1249.1456863941,1249.2292388375,1249.31272827335,1249.39618222397,
1249.47961871781,1249.56305582757,1249.64651162249,1249.73005611522,1249.81364519816,
1249.89736846571,1249.97804818161,1250.06178689346,1250.14542240482,1250.22897484822,
1250.31246428407,1250.39591823469,1250.47935472853,1250.56279183829,1250.64624763321,
1250.72979212594,1250.81338120888,1250.89710447643,1250.97778419233,1251.06152290418,
1251.14515841554,1251.22871085894,1251.31220029479,1251.39565424541,1251.47909073925,
1251.56252784901,1251.64598364393,1251.72952813666,1251.8131172196,1251.89684048716,
1251.97752020305,1252.0612589149,1252.14489442626,1252.22844686966,1252.31193630551,
1252.39539025613,1252.47882674997,1252.56226385973,1252.64571965465,1252.72926414738,
1252.81285323032,1252.89657649787,1252.97725621377,1253.06461780936,1253.15486384868,
1253.24510988801),.UNSPECIFIED.);
#844=B_SPLINE_CURVE_WITH_KNOTS('',3,(#107995,#107996,#107997,#107998,#107999,
#108000,#108001,#108002,#108003,#108004,#108005,#108006,#108007),
 .UNSPECIFIED.,.F.,.F.,(4,3,3,3,4),(1246.96111321221,1246.97884014945,1247.09556181222,
1247.20567859351,1247.21228347499),.UNSPECIFIED.);
#845=B_SPLINE_CURVE_WITH_KNOTS('',3,(#108009,#108010,#108011,#108012,#108013,
#108014,#108015,#108016,#108017,#108018),.UNSPECIFIED.,.F.,.F.,(4,3,3,4),
(1246.96044825099,1247.04312413363,1247.12770380432,1247.21228347501),
 .UNSPECIFIED.);
#846=B_SPLINE_CURVE_WITH_KNOTS('',3,(#108019,#108020,#108021,#108022,#108023,
#108024,#108025,#108026,#108027,#108028,#108029,#108030,#108031,#108032,
#108033,#108034,#108035,#108036,#108037,#108038,#108039,#108040,#108041,
#108042,#108043,#108044,#108045,#108046,#108047,#108048,#108049,#108050,
#108051,#108052,#108053,#108054,#108055,#108056,#108057,#108058,#108059,
#108060,#108061,#108062,#108063,#108064,#108065,#108066,#108067,#108068,
#108069,#108070,#108071,#108072,#108073,#108074,#108075,#108076,#108077,
#108078,#108079,#108080,#108081,#108082,#108083,#108084,#108085,#108086,
#108087,#108088,#108089,#108090,#108091,#108092,#108093,#108094,#108095,
#108096,#108097,#108098,#108099,#108100,#108101,#108102,#108103,#108104,
#108105,#108106,#108107,#108108,#108109,#108110,#108111,#108112,#108113,
#108114,#108115,#108116,#108117,#108118,#108119,#108120,#108121,#108122,
#108123,#108124,#108125,#108126,#108127,#108128,#108129,#108130,#108131,
#108132,#108133,#108134,#108135,#108136,#108137,#108138,#108139,#108140,
#108141,#108142,#108143,#108144,#108145,#108146,#108147,#108148,#108149,
#108150,#108151,#108152,#108153,#108154,#108155,#108156,#108157,#108158,
#108159,#108160,#108161,#108162,#108163,#108164,#108165,#108166,#108167,
#108168,#108169,#108170,#108171,#108172,#108173,#108174,#108175,#108176,
#108177,#108178,#108179,#108180,#108181,#108182,#108183,#108184,#108185,
#108186,#108187,#108188,#108189,#108190,#108191,#108192,#108193,#108194,
#108195,#108196,#108197,#108198,#108199,#108200,#108201,#108202,#108203,
#108204,#108205,#108206,#108207,#108208,#108209,#108210,#108211,#108212,
#108213,#108214,#108215,#108216,#108217,#108218,#108219,#108220,#108221,
#108222,#108223,#108224,#108225,#108226,#108227,#108228,#108229,#108230,
#108231,#108232,#108233,#108234,#108235,#108236,#108237,#108238),
 .UNSPECIFIED.,.F.,.F.,(4,3,3,3,3,3,3,3,3,3,3,3,3,3,3,3,3,3,3,3,3,3,3,3,
3,3,3,3,3,3,3,3,3,3,3,3,3,3,3,3,3,3,3,3,3,3,3,3,3,3,3,3,3,3,3,3,3,3,3,3,
3,3,3,3,3,3,3,3,3,3,3,3,3,4),(1247.21228347514,1247.28913076917,1247.37286948102,
1247.45650499238,1247.54005743578,1247.62354687163,1247.70700082225,1247.79043731609,
1247.87387442585,1247.95733022077,1248.0408747135,1248.12446379644,1248.20818706399,
1248.28886677989,1248.37260549174,1248.4562410031,1248.5397934465,1248.62328288235,
1248.70673683297,1248.79017332681,1248.87361043657,1248.95706623149,1249.04061072422,
1249.12419980716,1249.20792307471,1249.28860279061,1249.37234150246,1249.45597701382,
1249.53952945722,1249.62301889307,1249.70647284369,1249.78990933753,1249.87334644729,
1249.95680224221,1250.04034673494,1250.12393581788,1250.20765908543,1250.28833880133,
1250.37207751318,1250.45571302454,1250.53926546794,1250.62275490379,1250.70620885441,
1250.78964534825,1250.87308245801,1250.95653825293,1251.04008274566,1251.1236718286,
1251.20739509615,1251.28807481205,1251.3718135239,1251.45544903526,1251.53900147866,
1251.62249091451,1251.70594486513,1251.78938135897,1251.87281846873,1251.95627426365,
1252.03981875637,1252.12340783932,1252.20713110687,1252.28781082277,1252.37155200585,
1252.45518941628,1252.538743189,1252.62223338625,1252.70568523168,1252.78911881146,
1252.87255219775,1252.95600345858,1253.03953246102,1253.12310571945,1253.20678787449,
1253.24416667962),.UNSPECIFIED.);
#847=B_SPLINE_CURVE_WITH_KNOTS('',3,(#108244,#108245,#108246,#108247,#108248,
#108249,#108250,#108251,#108252,#108253,#108254,#108255,#108256,#108257,
#108258,#108259,#108260,#108261,#108262,#108263,#108264,#108265,#108266,
#108267,#108268,#108269,#108270,#108271,#108272,#108273,#108274,#108275,
#108276,#108277,#108278,#108279,#108280,#108281,#108282,#108283,#108284,
#108285,#108286,#108287,#108288,#108289,#108290,#108291,#108292,#108293,
#108294,#108295,#108296,#108297,#108298,#108299,#108300,#108301,#108302,
#108303,#108304,#108305,#108306,#108307,#108308,#108309,#108310,#108311,
#108312,#108313,#108314,#108315,#108316,#108317,#108318,#108319,#108320,
#108321,#108322,#108323,#108324,#108325,#108326,#108327,#108328,#108329,
#108330,#108331,#108332,#108333,#108334,#108335,#108336,#108337,#108338,
#108339,#108340,#108341,#108342,#108343,#108344,#108345,#108346,#108347,
#108348,#108349,#108350,#108351,#108352,#108353,#108354,#108355,#108356,
#108357,#108358,#108359,#108360,#108361,#108362,#108363,#108364,#108365,
#108366,#108367,#108368,#108369,#108370,#108371,#108372,#108373,#108374,
#108375,#108376,#108377,#108378,#108379,#108380,#108381,#108382,#108383,
#108384,#108385,#108386,#108387,#108388,#108389,#108390,#108391,#108392,
#108393,#108394,#108395,#108396,#108397,#108398,#108399,#108400,#108401,
#108402,#108403,#108404,#108405,#108406,#108407,#108408,#108409,#108410,
#108411,#108412,#108413,#108414,#108415,#108416,#108417,#108418,#108419,
#108420,#108421,#108422,#108423,#108424,#108425,#108426,#108427,#108428,
#108429,#108430,#108431,#108432,#108433,#108434,#108435,#108436,#108437,
#108438,#108439,#108440,#108441,#108442,#108443,#108444,#108445,#108446,
#108447,#108448,#108449,#108450,#108451,#108452,#108453,#108454,#108455,
#108456,#108457,#108458,#108459,#108460,#108461,#108462,#108463),
 .UNSPECIFIED.,.F.,.F.,(4,3,3,3,3,3,3,3,3,3,3,3,3,3,3,3,3,3,3,3,3,3,3,3,
3,3,3,3,3,3,3,3,3,3,3,3,3,3,3,3,3,3,3,3,3,3,3,3,3,3,3,3,3,3,3,3,3,3,3,3,
3,3,3,3,3,3,3,3,3,3,3,3,3,4),(1253.49546878246,1253.58356848739,1253.67180987813,
1253.76028410143,1253.8488844469,1253.93769136636,1253.97699222449,1254.06073093634,
1254.1443664477,1254.2279188911,1254.31140832695,1254.39486227757,1254.47829877141,
1254.56173588117,1254.64519167609,1254.72873616882,1254.81232525176,1254.89604851931,
1254.97672823521,1255.06046694706,1255.14410245842,1255.22765490182,1255.31114433767,
1255.39459828829,1255.47803478213,1255.56147189189,1255.64492768681,1255.72847217954,
1255.81206126248,1255.89578453003,1255.97646424593,1256.06020295778,1256.14383846914,
1256.22739091254,1256.31088034839,1256.39433429901,1256.47777079285,1256.56120790261,
1256.64466369753,1256.72820819026,1256.8117972732,1256.89552054075,1256.97620025665,
1257.0599389685,1257.14357447986,1257.22712692326,1257.31061635911,1257.39407030973,
1257.47750680357,1257.56094391333,1257.64439970825,1257.72794420098,1257.81153328392,
1257.89525655147,1257.97593626737,1258.05967497922,1258.14331049058,1258.22686293398,
1258.31035236983,1258.39380632045,1258.47724281429,1258.56067992405,1258.64413571897,
1258.7276802117,1258.81126929464,1258.89499256219,1258.97567227809,1259.05817906887,
1259.14058983644,1259.2229237848,1259.30519823839,1259.38743723984,1259.46967421915,
1259.52705322338),.UNSPECIFIED.);
#848=B_SPLINE_CURVE_WITH_KNOTS('',3,(#108464,#108465,#108466,#108467,#108468,
#108469,#108470,#108471,#108472,#108473),.UNSPECIFIED.,.F.,.F.,(4,3,3,4),
(1253.24510988801,1253.33203828523,1253.41883478726,1253.49546878231),
 .UNSPECIFIED.);
#849=B_SPLINE_CURVE_WITH_KNOTS('',3,(#108475,#108476,#108477,#108478,#108479,
#108480,#108481,#108482,#108483,#108484),.UNSPECIFIED.,.F.,.F.,(4,3,3,4),
(1253.24416667962,1253.28754683349,1253.40544243805,1253.49546878232),
 .UNSPECIFIED.);
#850=B_SPLINE_CURVE_WITH_KNOTS('',3,(#108485,#108486,#108487,#108488,#108489,
#108490,#108491,#108492,#108493,#108494,#108495,#108496,#108497,#108498,
#108499,#108500,#108501,#108502,#108503,#108504,#108505,#108506,#108507,
#108508,#108509,#108510,#108511,#108512,#108513,#108514,#108515,#108516,
#108517,#108518,#108519,#108520,#108521,#108522,#108523,#108524,#108525,
#108526,#108527,#108528,#108529,#108530,#108531,#108532,#108533,#108534,
#108535,#108536,#108537,#108538,#108539,#108540,#108541,#108542,#108543,
#108544,#108545,#108546,#108547,#108548,#108549,#108550,#108551,#108552,
#108553,#108554,#108555,#108556,#108557,#108558,#108559,#108560,#108561,
#108562,#108563,#108564,#108565,#108566,#108567,#108568,#108569,#108570,
#108571,#108572,#108573,#108574,#108575,#108576,#108577,#108578,#108579,
#108580,#108581,#108582,#108583,#108584,#108585,#108586,#108587,#108588,
#108589,#108590,#108591,#108592,#108593,#108594,#108595,#108596,#108597,
#108598,#108599,#108600,#108601,#108602,#108603,#108604,#108605,#108606,
#108607,#108608,#108609,#108610,#108611,#108612,#108613,#108614,#108615,
#108616,#108617,#108618,#108619,#108620,#108621,#108622,#108623,#108624,
#108625,#108626,#108627,#108628,#108629,#108630,#108631,#108632,#108633,
#108634,#108635,#108636,#108637,#108638,#108639,#108640,#108641,#108642,
#108643,#108644,#108645,#108646,#108647,#108648,#108649,#108650,#108651,
#108652,#108653,#108654,#108655,#108656,#108657,#108658,#108659,#108660,
#108661,#108662,#108663,#108664,#108665,#108666,#108667,#108668,#108669,
#108670,#108671,#108672,#108673,#108674,#108675,#108676,#108677,#108678,
#108679,#108680,#108681,#108682,#108683,#108684,#108685,#108686,#108687,
#108688,#108689,#108690,#108691,#108692,#108693,#108694,#108695,#108696,
#108697,#108698,#108699,#108700,#108701,#108702,#108703,#108704),
 .UNSPECIFIED.,.F.,.F.,(4,3,3,3,3,3,3,3,3,3,3,3,3,3,3,3,3,3,3,3,3,3,3,3,
3,3,3,3,3,3,3,3,3,3,3,3,3,3,3,3,3,3,3,3,3,3,3,3,3,3,3,3,3,3,3,3,3,3,3,3,
3,3,3,3,3,3,3,3,3,3,3,3,3,4),(1253.49546878247,1253.5778608269,1253.66018623466,
1253.74247225206,1253.82473938688,1253.90700663602,1253.9892929942,1254.07166470814,
1254.15408314902,1254.23662431146,1254.28728284421,1254.37102155606,1254.45465706742,
1254.53820951082,1254.62169894667,1254.70515289729,1254.78858939113,1254.87202650089,
1254.95548229581,1255.03902678854,1255.12261587148,1255.20633913903,1255.28701885493,
1255.37075756678,1255.45439307814,1255.53794552154,1255.62143495739,1255.70488890801,
1255.78832540185,1255.87176251161,1255.95521830653,1256.03876279926,1256.1223518822,
1256.20607514976,1256.28675486565,1256.3704935775,1256.45412908886,1256.53768153226,
1256.62117096811,1256.70462491873,1256.78806141257,1256.87149852233,1256.95495431725,
1257.03849880997,1257.12208789292,1257.20581116047,1257.28649087637,1257.37022958822,
1257.45386509958,1257.53741754298,1257.62090697883,1257.70436092945,1257.78779742329,
1257.87123453305,1257.95469032796,1258.03823482069,1258.12182390363,1258.20554717119,
1258.28622688709,1258.36996559894,1258.4536011103,1258.5371535537,1258.62064298955,
1258.70409694017,1258.78753343401,1258.87097054377,1258.95442633869,1259.03797083142,
1259.12155991436,1259.20528318192,1259.28596289781,1259.37430857112,1259.46245385434,
1259.52833516178),.UNSPECIFIED.);
#851=B_SPLINE_CURVE_WITH_KNOTS('',3,(#108710,#108711,#108712,#108713,#108714,
#108715,#108716,#108717,#108718,#108719,#108720,#108721,#108722,#108723,
#108724,#108725,#108726,#108727,#108728,#108729,#108730,#108731,#108732,
#108733,#108734,#108735,#108736,#108737,#108738,#108739,#108740,#108741,
#108742,#108743,#108744,#108745,#108746,#108747,#108748,#108749,#108750,
#108751,#108752,#108753,#108754,#108755,#108756,#108757,#108758,#108759,
#108760,#108761,#108762,#108763,#108764,#108765,#108766,#108767,#108768,
#108769,#108770,#108771,#108772,#108773,#108774,#108775,#108776,#108777,
#108778,#108779,#108780,#108781,#108782,#108783,#108784,#108785,#108786,
#108787,#108788,#108789,#108790,#108791,#108792,#108793,#108794,#108795,
#108796,#108797,#108798,#108799,#108800,#108801,#108802,#108803,#108804,
#108805,#108806,#108807,#108808,#108809,#108810,#108811,#108812,#108813,
#108814,#108815,#108816,#108817,#108818,#108819,#108820,#108821,#108822,
#108823,#108824,#108825,#108826,#108827,#108828,#108829,#108830,#108831,
#108832,#108833,#108834,#108835,#108836,#108837,#108838,#108839,#108840,
#108841,#108842,#108843,#108844,#108845,#108846,#108847,#108848,#108849,
#108850,#108851,#108852,#108853,#108854,#108855,#108856,#108857,#108858,
#108859,#108860,#108861,#108862,#108863,#108864,#108865,#108866,#108867,
#108868,#108869,#108870,#108871,#108872,#108873,#108874,#108875,#108876,
#108877,#108878,#108879,#108880,#108881,#108882,#108883,#108884,#108885,
#108886,#108887,#108888,#108889,#108890,#108891,#108892,#108893,#108894,
#108895,#108896,#108897,#108898,#108899,#108900,#108901,#108902,#108903,
#108904,#108905,#108906,#108907,#108908,#108909,#108910,#108911,#108912,
#108913,#108914,#108915,#108916,#108917,#108918,#108919,#108920,#108921,
#108922,#108923,#108924,#108925,#108926),.UNSPECIFIED.,.F.,.F.,(4,3,3,3,
3,3,3,3,3,3,3,3,3,3,3,3,3,3,3,3,3,3,3,3,3,3,3,3,3,3,3,3,3,3,3,3,3,3,3,3,
3,3,3,3,3,3,3,3,3,3,3,3,3,3,3,3,3,3,3,3,3,3,3,3,3,3,3,3,3,3,3,3,4),(1259.77865408949,
1259.89986585675,1259.97540828881,1260.05914700066,1260.14278251202,1260.22633495542,
1260.30982439127,1260.39327834189,1260.47671483573,1260.56015194549,1260.64360774041,
1260.72715223314,1260.81074131608,1260.89446458363,1260.97514429953,1261.05888301138,
1261.14251852274,1261.22607096614,1261.30956040199,1261.39301435261,1261.47645084645,
1261.55988795621,1261.64334375113,1261.72688824386,1261.8104773268,1261.89420059435,
1261.97488031025,1262.0586190221,1262.14225453346,1262.22580697686,1262.30929641271,
1262.39275036333,1262.47618685717,1262.55962396693,1262.64307976185,1262.72662425458,
1262.81021333752,1262.89393660507,1262.97461632097,1263.05835503282,1263.14199054418,
1263.22554298758,1263.30903242343,1263.39248637405,1263.47592286789,1263.55935997765,
1263.64281577257,1263.7263602653,1263.80994934824,1263.89367261579,1263.97435233169,
1264.05809104354,1264.1417265549,1264.2252789983,1264.30876843415,1264.39222238477,
1264.47565887861,1264.55909598837,1264.64255178329,1264.72609627602,1264.80968535896,
1264.89340862651,1264.97408834241,1265.05783681461,1265.14147992778,1265.22506980479,
1265.30855615695,1265.39200391737,1265.47543117534,1265.55912311748,1265.64258917631,
1265.72639406011,1265.81019894391),.UNSPECIFIED.);
#852=B_SPLINE_CURVE_WITH_KNOTS('',3,(#108927,#108928,#108929,#108930,#108931,
#108932,#108933,#108934,#108935,#108936),.UNSPECIFIED.,.F.,.F.,(4,3,3,4),
(1259.52705322338,1259.60932548456,1259.69398978697,1259.77865408938),
 .UNSPECIFIED.);
#853=B_SPLINE_CURVE_WITH_KNOTS('',3,(#108938,#108939,#108940,#108941,#108942,
#108943,#108944,#108945,#108946,#108947),.UNSPECIFIED.,.F.,.F.,(4,3,3,4),
(1259.52833516178,1259.61621838343,1259.70392677093,1259.77865408939),
 .UNSPECIFIED.);
#854=B_SPLINE_CURVE_WITH_KNOTS('',3,(#108948,#108949,#108950,#108951,#108952,
#108953,#108954,#108955,#108956,#108957,#108958,#108959,#108960,#108961,
#108962,#108963,#108964,#108965,#108966,#108967,#108968,#108969,#108970,
#108971,#108972,#108973,#108974,#108975,#108976,#108977,#108978,#108979,
#108980,#108981,#108982,#108983,#108984,#108985,#108986,#108987,#108988,
#108989,#108990,#108991,#108992,#108993,#108994,#108995,#108996,#108997,
#108998,#108999,#109000,#109001,#109002,#109003,#109004,#109005,#109006,
#109007,#109008,#109009,#109010,#109011,#109012,#109013,#109014,#109015,
#109016,#109017,#109018,#109019,#109020,#109021,#109022,#109023,#109024,
#109025,#109026,#109027,#109028,#109029,#109030,#109031,#109032,#109033,
#109034,#109035,#109036,#109037,#109038,#109039,#109040,#109041,#109042,
#109043,#109044,#109045,#109046,#109047,#109048,#109049,#109050,#109051,
#109052,#109053,#109054,#109055,#109056,#109057,#109058,#109059,#109060,
#109061,#109062,#109063,#109064,#109065,#109066,#109067,#109068,#109069,
#109070,#109071,#109072,#109073,#109074,#109075,#109076,#109077,#109078,
#109079,#109080,#109081,#109082,#109083,#109084,#109085,#109086,#109087,
#109088,#109089,#109090,#109091,#109092,#109093,#109094,#109095,#109096,
#109097,#109098,#109099,#109100,#109101,#109102,#109103,#109104,#109105,
#109106,#109107,#109108,#109109,#109110,#109111,#109112,#109113,#109114,
#109115,#109116,#109117,#109118,#109119,#109120,#109121,#109122,#109123,
#109124,#109125,#109126,#109127,#109128,#109129,#109130,#109131,#109132,
#109133,#109134,#109135,#109136,#109137,#109138,#109139,#109140,#109141,
#109142,#109143,#109144,#109145,#109146,#109147,#109148,#109149,#109150,
#109151,#109152,#109153,#109154,#109155,#109156,#109157,#109158,#109159,
#109160,#109161,#109162,#109163,#109164,#109165,#109166,#109167),
 .UNSPECIFIED.,.F.,.F.,(4,3,3,3,3,3,3,3,3,3,3,3,3,3,3,3,3,3,3,3,3,3,3,3,
3,3,3,3,3,3,3,3,3,3,3,3,3,3,3,3,3,3,3,3,3,3,3,3,3,3,3,3,3,3,3,3,3,3,3,3,
3,3,3,3,3,3,3,3,3,3,3,3,3,4),(1259.7786540895,1259.86580253005,1259.95305673141,
1260.04050848855,1260.1280632794,1260.21581764344,1260.28569890853,1260.36943762038,
1260.45307313174,1260.53662557514,1260.62011501099,1260.70356896161,1260.78700545545,
1260.87044256521,1260.95389836013,1261.03744285286,1261.1210319358,1261.20475520335,
1261.28543491925,1261.3691736311,1261.45280914246,1261.53636158586,1261.61985102171,
1261.70330497233,1261.78674146617,1261.87017857593,1261.95363437085,1262.03717886358,
1262.12076794652,1262.20449121408,1262.28517092997,1262.36890964182,1262.45254515318,
1262.53609759658,1262.61958703243,1262.70304098305,1262.78647747689,1262.86991458665,
1262.95337038157,1263.0369148743,1263.12050395724,1263.20422722479,1263.28490694069,
1263.36864565254,1263.4522811639,1263.5358336073,1263.61932304315,1263.70277699377,
1263.78621348761,1263.86965059737,1263.95310639228,1264.03665088501,1264.12023996795,
1264.20396323551,1264.28464295141,1264.36838166326,1264.45201717462,1264.53556961802,
1264.61905905387,1264.70251300449,1264.78594949833,1264.86938660809,1264.95284240301,
1265.03638689574,1265.11997597868,1265.20369924624,1265.28437896213,1265.36697886756,
1265.44948184649,1265.53190704803,1265.61426948393,1265.69659579727,1265.7789125969,
1265.81034593635),.UNSPECIFIED.);
#855=B_SPLINE_CURVE_WITH_KNOTS('',3,(#109173,#109174,#109175,#109176,#109177,
#109178,#109179,#109180,#109181,#109182,#109183,#109184,#109185,#109186,
#109187,#109188,#109189,#109190,#109191,#109192,#109193,#109194,#109195,
#109196,#109197,#109198,#109199,#109200,#109201,#109202,#109203,#109204,
#109205,#109206,#109207,#109208,#109209,#109210,#109211,#109212,#109213,
#109214,#109215,#109216,#109217,#109218,#109219,#109220,#109221,#109222,
#109223,#109224,#109225,#109226,#109227,#109228,#109229,#109230,#109231,
#109232,#109233,#109234,#109235,#109236,#109237,#109238,#109239,#109240,
#109241,#109242,#109243,#109244,#109245,#109246,#109247,#109248,#109249,
#109250,#109251,#109252,#109253,#109254,#109255,#109256,#109257,#109258,
#109259,#109260,#109261,#109262,#109263,#109264,#109265,#109266,#109267,
#109268,#109269,#109270,#109271,#109272,#109273,#109274,#109275,#109276,
#109277,#109278,#109279,#109280,#109281,#109282,#109283,#109284,#109285,
#109286,#109287,#109288,#109289,#109290,#109291,#109292,#109293,#109294,
#109295,#109296,#109297,#109298,#109299,#109300,#109301,#109302,#109303,
#109304,#109305,#109306,#109307,#109308,#109309,#109310,#109311,#109312,
#109313,#109314,#109315,#109316,#109317,#109318,#109319,#109320,#109321,
#109322,#109323,#109324,#109325,#109326,#109327,#109328,#109329,#109330,
#109331,#109332,#109333,#109334,#109335,#109336,#109337,#109338,#109339,
#109340,#109341,#109342,#109343,#109344,#109345,#109346,#109347,#109348,
#109349,#109350,#109351,#109352,#109353,#109354,#109355,#109356,#109357,
#109358,#109359,#109360,#109361,#109362,#109363,#109364,#109365,#109366,
#109367,#109368,#109369,#109370,#109371,#109372,#109373,#109374,#109375,
#109376,#109377,#109378,#109379,#109380,#109381,#109382,#109383,#109384,
#109385,#109386,#109387,#109388,#109389,#109390,#109391,#109392),
 .UNSPECIFIED.,.F.,.F.,(4,3,3,3,3,3,3,3,3,3,3,3,3,3,3,3,3,3,3,3,3,3,3,3,
3,3,3,3,3,3,3,3,3,3,3,3,3,3,3,3,3,3,3,3,3,3,3,3,3,3,3,3,3,3,3,3,3,3,3,3,
3,3,3,3,3,3,3,3,3,3,3,3,3,4),(1266.0618393968,1266.14456729323,1266.22720047119,
1266.30975992534,1266.39273498016,1266.47521984589,1266.55769815155,1266.6401887541,
1266.72353165653,1266.80614558457,1266.88985297421,1266.97356036385,1267.0572990757,
1267.14093458706,1267.22448703046,1267.30797646631,1267.39143041693,1267.47486691078,
1267.55830402053,1267.64175981545,1267.72530430818,1267.80889339112,1267.89261665868,
1267.97329637458,1268.05703508643,1268.14067059779,1268.22422304119,1268.30771247704,
1268.39116642766,1268.47460292151,1268.55804003126,1268.64149582618,1268.72504031891,
1268.80862940185,1268.89235266941,1268.9730323853,1269.05677109715,1269.14040660851,
1269.22395905191,1269.30744848776,1269.39090243838,1269.47433893222,1269.55777604198,
1269.64123183689,1269.72477632962,1269.80836541256,1269.89208868012,1269.97276839602,
1270.05650710787,1270.14014261923,1270.22369506263,1270.30718449848,1270.3906384491,
1270.47407494294,1270.5575120527,1270.64096784762,1270.72451234035,1270.80810142329,
1270.89182469085,1270.97250440674,1271.05624311859,1271.13987862995,1271.22343107335,
1271.3069205092,1271.39037445982,1271.47381095366,1271.55724806342,1271.64070385833,
1271.72424835106,1271.80783743401,1271.89156070156,1271.97224041746,1272.06735135149,
1272.09457507867),.UNSPECIFIED.);
#856=B_SPLINE_CURVE_WITH_KNOTS('',3,(#109393,#109394,#109395,#109396,#109397,
#109398,#109399,#109400,#109401,#109402),.UNSPECIFIED.,.F.,.F.,(4,3,3,4),
(1265.81019894391,1265.89392247301,1265.97382435313,1266.06183939667),
 .UNSPECIFIED.);
#857=B_SPLINE_CURVE_WITH_KNOTS('',3,(#109404,#109405,#109406,#109407,#109408,
#109409,#109410,#109411,#109412,#109413),.UNSPECIFIED.,.F.,.F.,(4,3,3,4),
(1265.81034593635,1265.89269204904,1265.9772657228,1266.06183939655),
 .UNSPECIFIED.);
#858=B_SPLINE_CURVE_WITH_KNOTS('',3,(#109414,#109415,#109416,#109417,#109418,
#109419,#109420,#109421,#109422,#109423,#109424,#109425,#109426,#109427,
#109428,#109429,#109430,#109431,#109432,#109433,#109434,#109435,#109436,
#109437,#109438,#109439,#109440,#109441,#109442,#109443,#109444,#109445,
#109446,#109447,#109448,#109449,#109450,#109451,#109452,#109453,#109454,
#109455,#109456,#109457,#109458,#109459,#109460,#109461,#109462,#109463,
#109464,#109465,#109466,#109467,#109468,#109469,#109470,#109471,#109472,
#109473,#109474,#109475,#109476,#109477,#109478,#109479,#109480,#109481,
#109482,#109483,#109484,#109485,#109486,#109487,#109488,#109489,#109490,
#109491,#109492,#109493,#109494,#109495,#109496,#109497,#109498,#109499,
#109500,#109501,#109502,#109503,#109504,#109505,#109506,#109507,#109508,
#109509,#109510,#109511,#109512,#109513,#109514,#109515,#109516,#109517,
#109518,#109519,#109520,#109521,#109522,#109523,#109524,#109525,#109526,
#109527,#109528,#109529,#109530,#109531,#109532,#109533,#109534,#109535,
#109536,#109537,#109538,#109539,#109540,#109541,#109542,#109543,#109544,
#109545,#109546,#109547,#109548,#109549,#109550,#109551,#109552,#109553,
#109554,#109555,#109556,#109557,#109558,#109559,#109560,#109561,#109562,
#109563,#109564,#109565,#109566,#109567,#109568,#109569,#109570,#109571,
#109572,#109573,#109574,#109575,#109576,#109577,#109578,#109579,#109580,
#109581,#109582,#109583,#109584,#109585,#109586,#109587,#109588,#109589,
#109590,#109591,#109592,#109593,#109594,#109595,#109596,#109597,#109598,
#109599,#109600,#109601,#109602,#109603,#109604,#109605,#109606,#109607,
#109608,#109609,#109610,#109611,#109612,#109613,#109614,#109615,#109616,
#109617,#109618,#109619,#109620,#109621,#109622,#109623,#109624,#109625,
#109626,#109627,#109628,#109629,#109630),.UNSPECIFIED.,.F.,.F.,(4,3,3,3,
3,3,3,3,3,3,3,3,3,3,3,3,3,3,3,3,3,3,3,3,3,3,3,3,3,3,3,3,3,3,3,3,3,3,3,3,
3,3,3,3,3,3,3,3,3,3,3,3,3,3,3,3,3,3,3,3,3,3,3,3,3,3,3,3,3,3,3,3,4),(1266.06183939668,
1266.17607577489,1266.28411497285,1266.3678536847,1266.45148919606,1266.53504163946,
1266.61853107531,1266.70198502593,1266.78542151977,1266.86885862953,1266.95231442445,
1267.03585891718,1267.11944800012,1267.20317126767,1267.28385098357,1267.36758969542,
1267.45122520678,1267.53477765018,1267.61826708603,1267.70172103665,1267.78515753049,
1267.86859464025,1267.95205043517,1268.0355949279,1268.11918401084,1268.2029072784,
1268.28358699429,1268.36732570614,1268.4509612175,1268.5345136609,1268.61800309675,
1268.70145704737,1268.78489354121,1268.86833065097,1268.95178644589,1269.03533093862,
1269.11892002156,1269.20264328912,1269.28332300501,1269.36706171686,1269.45069722822,
1269.53424967162,1269.61773910747,1269.70119305809,1269.78462955193,1269.86806666169,
1269.95152245661,1270.03506694934,1270.11865603228,1270.20237929983,1270.28305901573,
1270.36679772758,1270.45043323894,1270.53398568234,1270.61747511819,1270.70092906881,
1270.78436556265,1270.86780267241,1270.95125846732,1271.03480296005,1271.11839204299,
1271.20211531055,1271.28279502645,1271.36654513006,1271.45018953759,1271.53373305985,
1271.61721938338,1271.70066662803,1271.78409288349,1271.86754205725,1271.951001946,
1272.03452978899,1272.09336375077),.UNSPECIFIED.);
#859=B_SPLINE_CURVE_WITH_KNOTS('',3,(#109636,#109637,#109638,#109639,#109640,
#109641,#109642,#109643,#109644,#109645),.UNSPECIFIED.,.F.,.F.,(4,1,1,1,
1,1,1,4),(1272.34502470385,1272.97197642818,1273.9717124389,1274.97144844962,
1275.97118446034,1276.97092047106,1277.97065648178,1278.37762693477),
 .UNSPECIFIED.);
#860=B_SPLINE_CURVE_WITH_KNOTS('',3,(#109646,#109647,#109648,#109649,#109650,
#109651,#109652,#109653,#109654,#109655),.UNSPECIFIED.,.F.,.F.,(4,3,3,4),
(1272.09457507867,1272.1891593872,1272.28317223907,1272.34502470385),
 .UNSPECIFIED.);
#861=B_SPLINE_CURVE_WITH_KNOTS('',3,(#109657,#109658,#109659,#109660,#109661,
#109662,#109663,#109664,#109665,#109666,#109667,#109668,#109669),
 .UNSPECIFIED.,.F.,.F.,(4,3,3,3,4),(1272.09336375077,1272.17699396813,1272.26074192364,
1272.28253103717,1272.34502470386),.UNSPECIFIED.);
#862=B_SPLINE_CURVE_WITH_KNOTS('',3,(#109670,#109671,#109672,#109673,#109674,
#109675,#109676,#109677,#109678,#109679,#109680,#109681,#109682,#109683,
#109684,#109685,#109686,#109687,#109688,#109689,#109690,#109691,#109692,
#109693,#109694,#109695,#109696,#109697,#109698,#109699,#109700,#109701,
#109702,#109703,#109704,#109705,#109706,#109707,#109708,#109709,#109710,
#109711,#109712,#109713,#109714,#109715,#109716,#109717,#109718,#109719,
#109720,#109721,#109722,#109723,#109724,#109725,#109726,#109727,#109728,
#109729,#109730,#109731,#109732,#109733,#109734,#109735,#109736,#109737,
#109738,#109739,#109740,#109741,#109742,#109743,#109744,#109745,#109746,
#109747,#109748,#109749,#109750,#109751,#109752,#109753,#109754,#109755,
#109756,#109757,#109758,#109759,#109760,#109761,#109762,#109763,#109764,
#109765,#109766,#109767,#109768,#109769,#109770,#109771,#109772,#109773,
#109774,#109775,#109776,#109777,#109778,#109779,#109780,#109781,#109782,
#109783,#109784,#109785,#109786,#109787,#109788,#109789,#109790,#109791,
#109792,#109793,#109794,#109795,#109796,#109797,#109798,#109799,#109800,
#109801,#109802,#109803,#109804,#109805,#109806,#109807,#109808,#109809,
#109810,#109811,#109812,#109813,#109814,#109815,#109816,#109817,#109818,
#109819,#109820,#109821,#109822,#109823,#109824,#109825,#109826,#109827,
#109828,#109829,#109830,#109831,#109832,#109833,#109834,#109835,#109836,
#109837,#109838,#109839,#109840,#109841,#109842,#109843,#109844,#109845,
#109846,#109847,#109848,#109849,#109850,#109851,#109852,#109853,#109854,
#109855,#109856,#109857,#109858,#109859,#109860,#109861,#109862,#109863,
#109864,#109865,#109866,#109867,#109868,#109869,#109870,#109871,#109872,
#109873,#109874,#109875,#109876,#109877,#109878,#109879,#109880,#109881,
#109882,#109883,#109884,#109885,#109886,#109887,#109888,#109889),
 .UNSPECIFIED.,.F.,.F.,(4,3,3,3,3,3,3,3,3,3,3,3,3,3,3,3,3,3,3,3,3,3,3,3,
3,3,3,3,3,3,3,3,3,3,3,3,3,3,3,3,3,3,3,3,3,3,3,3,3,3,3,3,3,3,3,3,3,3,3,3,
3,3,3,3,3,3,3,3,3,3,3,3,3,4),(1272.34502470398,1272.42797828084,1272.51083333015,
1272.59361069634,1272.67969274028,1272.76238540205,1272.84506816948,1272.92775975624,
1273.0104788794,1273.09328870338,1273.17615229585,1273.25913255471,1273.28226704789,
1273.36600575974,1273.4496412711,1273.5331937145,1273.61668315035,1273.70013710097,
1273.78357359481,1273.86701070457,1273.95046649948,1274.03401099221,1274.11760007515,
1274.20132334271,1274.28200305861,1274.36574177046,1274.44937728182,1274.53292972522,
1274.61641916107,1274.69987311169,1274.78330960553,1274.86674671529,1274.95020251021,
1275.03374700294,1275.11733608588,1275.20105935344,1275.28173906933,1275.36547778118,
1275.44911329254,1275.53266573594,1275.61615517179,1275.69960912241,1275.78304561625,
1275.86648272601,1275.94993852093,1276.03348301366,1276.1170720966,1276.20079536415,
1276.28147508005,1276.3652137919,1276.44884930326,1276.53240174666,1276.61589118251,
1276.69934513313,1276.78278162697,1276.86621873673,1276.94967453164,1277.03321902437,
1277.11680810731,1277.20053137487,1277.28121109077,1277.36494980262,1277.44858531398,
1277.53213775738,1277.61562719323,1277.69908114385,1277.78251763769,1277.86595474745,
1277.94941054237,1278.0329550351,1278.11654411804,1278.2002673856,1278.28094710149,
1278.37766493651),.UNSPECIFIED.);
#863=B_SPLINE_CURVE_WITH_KNOTS('',3,(#109895,#109896,#109897,#109898,#109899,
#109900,#109901,#109902,#109903,#109904,#109905,#109906,#109907,#109908,
#109909,#109910,#109911,#109912,#109913,#109914,#109915,#109916,#109917,
#109918,#109919,#109920,#109921,#109922,#109923,#109924,#109925,#109926,
#109927,#109928,#109929,#109930,#109931,#109932,#109933,#109934,#109935,
#109936,#109937,#109938,#109939,#109940,#109941,#109942,#109943,#109944,
#109945,#109946,#109947,#109948,#109949,#109950,#109951,#109952,#109953,
#109954,#109955,#109956,#109957,#109958,#109959,#109960,#109961,#109962,
#109963,#109964,#109965,#109966,#109967,#109968,#109969,#109970,#109971,
#109972,#109973,#109974,#109975,#109976,#109977,#109978,#109979,#109980,
#109981,#109982,#109983,#109984,#109985,#109986,#109987,#109988,#109989,
#109990,#109991,#109992,#109993,#109994,#109995,#109996,#109997,#109998,
#109999,#110000,#110001,#110002,#110003,#110004,#110005,#110006,#110007,
#110008,#110009,#110010,#110011,#110012,#110013,#110014,#110015,#110016,
#110017,#110018,#110019,#110020,#110021,#110022,#110023,#110024,#110025,
#110026,#110027,#110028,#110029,#110030,#110031,#110032,#110033,#110034,
#110035,#110036,#110037,#110038,#110039,#110040,#110041,#110042,#110043,
#110044,#110045,#110046,#110047,#110048,#110049,#110050,#110051,#110052,
#110053,#110054,#110055,#110056,#110057,#110058,#110059,#110060,#110061,
#110062,#110063,#110064,#110065,#110066,#110067,#110068,#110069,#110070,
#110071,#110072,#110073,#110074,#110075,#110076,#110077,#110078,#110079,
#110080,#110081,#110082,#110083,#110084,#110085,#110086,#110087,#110088,
#110089,#110090,#110091,#110092,#110093,#110094,#110095,#110096,#110097,
#110098,#110099,#110100,#110101,#110102,#110103,#110104,#110105,#110106,
#110107,#110108,#110109,#110110,#110111,#110112,#110113,#110114),
 .UNSPECIFIED.,.F.,.F.,(4,3,3,3,3,3,3,3,3,3,3,3,3,3,3,3,3,3,3,3,3,3,3,3,
3,3,3,3,3,3,3,3,3,3,3,3,3,3,3,3,3,3,3,3,3,3,3,3,3,3,3,3,3,3,3,3,3,3,3,3,
3,3,3,3,3,3,3,3,3,3,3,3,3,4),(1278.62821001103,1278.72467799427,1278.82166768971,
1278.91929630639,1278.9703924925,1279.05413120435,1279.13776671571,1279.22131915911,
1279.30480859496,1279.38826254558,1279.47169903942,1279.55513614918,1279.6385919441,
1279.72213643683,1279.80572551977,1279.88944878732,1279.97012850322,1280.05386721507,
1280.13750272643,1280.22105516983,1280.30454460568,1280.3879985563,1280.47143505014,
1280.5548721599,1280.63832795481,1280.72187244754,1280.80546153048,1280.88918479804,
1280.96986451394,1281.05360322579,1281.13723873715,1281.22079118055,1281.3042806164,
1281.38773456702,1281.47117106086,1281.55460817062,1281.63806396554,1281.72160845827,
1281.80519754121,1281.88892080876,1281.96960052466,1282.05333923651,1282.13697474787,
1282.22052719127,1282.30401662712,1282.38747057774,1282.47090707158,1282.55434418134,
1282.63779997626,1282.72134446899,1282.80493355193,1282.88865681949,1282.96933653538,
1283.05307524723,1283.13671075859,1283.22026320199,1283.30375263784,1283.38720658846,
1283.4706430823,1283.55408019206,1283.63753598698,1283.7210804797,1283.80466956265,
1283.8883928302,1283.9690725461,1284.05538577409,1284.13829069336,1284.22112063752,
1284.30389438199,1284.38663065551,1284.46936215526,1284.55209155376,1284.63485816459,
1284.65957836999),.UNSPECIFIED.);
#864=B_SPLINE_CURVE_WITH_KNOTS('',3,(#110115,#110116,#110117,#110118),
 .UNSPECIFIED.,.F.,.F.,(4,4),(1278.37762693477,1278.62821001103),
 .UNSPECIFIED.);
#865=B_SPLINE_CURVE_WITH_KNOTS('',3,(#110120,#110121,#110122,#110123,#110124,
#110125,#110126,#110127,#110128,#110129),.UNSPECIFIED.,.F.,.F.,(4,3,3,4),
(1278.37766493651,1278.47437986099,1278.5703538529,1278.62821001085),
 .UNSPECIFIED.);
#866=B_SPLINE_CURVE_WITH_KNOTS('',3,(#110130,#110131,#110132,#110133,#110134,
#110135,#110136,#110137,#110138,#110139,#110140,#110141,#110142,#110143,
#110144,#110145,#110146,#110147,#110148,#110149,#110150,#110151,#110152,
#110153,#110154,#110155,#110156,#110157,#110158,#110159,#110160,#110161,
#110162,#110163,#110164,#110165,#110166,#110167,#110168,#110169,#110170,
#110171,#110172,#110173,#110174,#110175,#110176,#110177,#110178,#110179,
#110180,#110181,#110182,#110183,#110184,#110185,#110186,#110187,#110188,
#110189,#110190,#110191,#110192,#110193,#110194,#110195,#110196,#110197,
#110198,#110199,#110200,#110201,#110202,#110203,#110204,#110205,#110206,
#110207,#110208,#110209,#110210,#110211,#110212,#110213,#110214,#110215,
#110216,#110217,#110218,#110219,#110220,#110221,#110222,#110223,#110224,
#110225,#110226,#110227,#110228,#110229,#110230,#110231,#110232,#110233,
#110234,#110235,#110236,#110237,#110238,#110239,#110240,#110241,#110242,
#110243,#110244,#110245,#110246,#110247,#110248,#110249,#110250,#110251,
#110252,#110253,#110254,#110255,#110256,#110257,#110258,#110259,#110260,
#110261,#110262,#110263,#110264,#110265,#110266,#110267,#110268,#110269,
#110270,#110271,#110272,#110273,#110274,#110275,#110276,#110277,#110278,
#110279,#110280,#110281,#110282,#110283,#110284,#110285,#110286,#110287,
#110288,#110289,#110290,#110291,#110292,#110293,#110294,#110295,#110296,
#110297,#110298,#110299,#110300,#110301,#110302,#110303,#110304,#110305,
#110306,#110307,#110308,#110309,#110310,#110311,#110312,#110313,#110314,
#110315,#110316,#110317,#110318,#110319,#110320,#110321,#110322,#110323,
#110324,#110325,#110326,#110327,#110328,#110329,#110330,#110331,#110332,
#110333,#110334,#110335,#110336,#110337,#110338,#110339,#110340,#110341,
#110342,#110343,#110344,#110345,#110346,#110347,#110348,#110349),
 .UNSPECIFIED.,.F.,.F.,(4,3,3,3,3,3,3,3,3,3,3,3,3,3,3,3,3,3,3,3,3,3,3,3,
3,3,3,3,3,3,3,3,3,3,3,3,3,3,3,3,3,3,3,3,3,3,3,3,3,3,3,3,3,3,3,3,3,3,3,3,
3,3,3,3,3,3,3,3,3,3,3,3,3,4),(1278.62821001104,1278.71180280317,1278.79538865517,
1278.87898538376,1278.96261080889,1279.04633640373,1279.13011489048,1279.21403165939,
1279.28068311221,1279.36442182406,1279.44805733542,1279.53160977882,1279.61509921467,
1279.69855316529,1279.78198965913,1279.86542676889,1279.9488825638,1280.03242705653,
1280.11601613947,1280.19973940703,1280.28041912293,1280.36415783478,1280.44779334614,
1280.53134578954,1280.61483522539,1280.69828917601,1280.78172566985,1280.86516277961,
1280.94861857453,1281.03216306726,1281.1157521502,1281.19947541776,1281.28015513365,
1281.3638938455,1281.44752935686,1281.53108180026,1281.61457123611,1281.69802518673,
1281.78146168057,1281.86489879033,1281.94835458525,1282.03189907798,1282.11548816092,
1282.19921142847,1282.27989114437,1282.36362985622,1282.44726536758,1282.53081781098,
1282.61430724683,1282.69776119744,1282.78119769129,1282.86463480105,1282.94809059596,
1283.03163508869,1283.11522417163,1283.19894743919,1283.27962715509,1283.36336586694,
1283.4470013783,1283.5305538217,1283.61404325755,1283.69749720817,1283.78093370202,
1283.86437081177,1283.94782660669,1284.03137109942,1284.11496018236,1284.19868344992,
1284.27936316581,1284.36367880853,1284.44785281671,1284.53194515319,1284.61595840221,
1284.6606315684),.UNSPECIFIED.);
#867=B_SPLINE_CURVE_WITH_KNOTS('',3,(#110355,#110356,#110357,#110358,#110359,
#110360,#110361,#110362,#110363,#110364,#110365,#110366,#110367,#110368,
#110369,#110370,#110371,#110372,#110373,#110374,#110375,#110376,#110377,
#110378,#110379,#110380,#110381,#110382,#110383,#110384,#110385,#110386,
#110387,#110388,#110389,#110390,#110391,#110392,#110393,#110394,#110395,
#110396,#110397,#110398,#110399,#110400,#110401,#110402,#110403,#110404,
#110405,#110406,#110407,#110408,#110409,#110410,#110411,#110412,#110413,
#110414,#110415,#110416,#110417,#110418,#110419,#110420,#110421,#110422,
#110423,#110424,#110425,#110426,#110427,#110428,#110429,#110430,#110431,
#110432,#110433,#110434,#110435,#110436,#110437,#110438,#110439,#110440,
#110441,#110442,#110443,#110444,#110445,#110446,#110447,#110448,#110449,
#110450,#110451,#110452,#110453,#110454,#110455,#110456,#110457,#110458,
#110459,#110460,#110461,#110462,#110463,#110464,#110465,#110466,#110467,
#110468,#110469,#110470,#110471,#110472,#110473,#110474,#110475,#110476,
#110477,#110478,#110479,#110480,#110481,#110482,#110483,#110484,#110485,
#110486,#110487,#110488,#110489,#110490,#110491,#110492,#110493,#110494,
#110495,#110496,#110497,#110498,#110499,#110500,#110501,#110502,#110503,
#110504,#110505,#110506,#110507,#110508,#110509,#110510,#110511,#110512,
#110513,#110514,#110515,#110516,#110517,#110518,#110519,#110520,#110521,
#110522,#110523,#110524,#110525,#110526,#110527,#110528,#110529,#110530,
#110531,#110532,#110533,#110534,#110535,#110536,#110537,#110538,#110539,
#110540,#110541,#110542,#110543,#110544,#110545,#110546,#110547,#110548,
#110549,#110550,#110551,#110552,#110553,#110554,#110555,#110556,#110557,
#110558,#110559,#110560,#110561,#110562,#110563,#110564,#110565,#110566,
#110567,#110568,#110569,#110570,#110571,#110572,#110573,#110574),
 .UNSPECIFIED.,.F.,.F.,(4,3,3,3,3,3,3,3,3,3,3,3,3,3,3,3,3,3,3,3,3,3,3,3,
3,3,3,3,3,3,3,3,3,3,3,3,3,3,3,3,3,3,3,3,3,3,3,3,3,3,3,3,3,3,3,3,3,3,3,3,
3,3,3,3,3,3,3,3,3,3,3,3,3,4),(1284.91139531821,1284.96880855682,1285.05254726867,
1285.13618278003,1285.21973522343,1285.30322465928,1285.3866786099,1285.47011510374,
1285.5535522135,1285.63700800842,1285.72055250115,1285.80414158409,1285.88786485164,
1285.96854456754,1286.05228327939,1286.13591879075,1286.21947123415,1286.30296067,
1286.38641462062,1286.46985111446,1286.55328822422,1286.63674401913,1286.72028851186,
1286.8038775948,1286.88760086236,1286.96828057826,1287.05201929011,1287.13565480147,
1287.21920724487,1287.30269668072,1287.38615063134,1287.46958712518,1287.55302423494,
1287.63648002986,1287.72002452259,1287.80361360553,1287.88733687308,1287.96801658898,
1288.05175530083,1288.13539081219,1288.21894325559,1288.30243269144,1288.38588664206,
1288.4693231359,1288.55276024566,1288.63621604058,1288.71976053331,1288.80334961625,
1288.8870728838,1288.9677525997,1289.05149131155,1289.13512682291,1289.21867926631,
1289.30216870216,1289.38562265278,1289.46905914662,1289.55249625638,1289.6359520513,
1289.71949654403,1289.80308562697,1289.88680889453,1289.96748861042,1290.05122867041,
1290.13486521538,1290.21841837917,1290.30190822321,1290.38536097487,1290.46879582508,
1290.55223084623,1290.63568410688,1290.71921991751,1290.80280013459,1290.88650013742,
1290.9433767908),.UNSPECIFIED.);
#868=B_SPLINE_CURVE_WITH_KNOTS('',3,(#110575,#110576,#110577,#110578,#110579,
#110580,#110581,#110582,#110583,#110584),.UNSPECIFIED.,.F.,.F.,(4,3,3,4),
(1284.65957836999,1284.74243553485,1284.82691542648,1284.9113953181),
 .UNSPECIFIED.);
#869=B_SPLINE_CURVE_WITH_KNOTS('',3,(#110586,#110587,#110588,#110589,#110590,
#110591,#110592,#110593,#110594,#110595),.UNSPECIFIED.,.F.,.F.,(4,3,3,4),
(1284.6606315684,1284.74457477385,1284.82850997582,1284.91139531822),
 .UNSPECIFIED.);
#870=B_SPLINE_CURVE_WITH_KNOTS('',3,(#110596,#110597,#110598,#110599,#110600,
#110601,#110602,#110603,#110604,#110605,#110606,#110607,#110608,#110609,
#110610,#110611,#110612,#110613,#110614,#110615,#110616,#110617,#110618,
#110619,#110620,#110621,#110622,#110623,#110624,#110625,#110626,#110627,
#110628,#110629,#110630,#110631,#110632,#110633,#110634,#110635,#110636,
#110637,#110638,#110639,#110640,#110641,#110642,#110643,#110644,#110645,
#110646,#110647,#110648,#110649,#110650,#110651,#110652,#110653,#110654,
#110655,#110656,#110657,#110658,#110659,#110660,#110661,#110662,#110663,
#110664,#110665,#110666,#110667,#110668,#110669,#110670,#110671,#110672,
#110673,#110674,#110675,#110676,#110677,#110678,#110679,#110680,#110681,
#110682,#110683,#110684,#110685,#110686,#110687,#110688,#110689,#110690,
#110691,#110692,#110693,#110694,#110695,#110696,#110697,#110698,#110699,
#110700,#110701,#110702,#110703,#110704,#110705,#110706,#110707,#110708,
#110709,#110710,#110711,#110712,#110713,#110714,#110715,#110716,#110717,
#110718,#110719,#110720,#110721,#110722,#110723,#110724,#110725,#110726,
#110727,#110728,#110729,#110730,#110731,#110732,#110733,#110734,#110735,
#110736,#110737,#110738,#110739,#110740,#110741,#110742,#110743,#110744,
#110745,#110746,#110747,#110748,#110749,#110750,#110751,#110752,#110753,
#110754,#110755,#110756,#110757,#110758,#110759,#110760,#110761,#110762,
#110763,#110764,#110765,#110766,#110767,#110768,#110769,#110770,#110771,
#110772,#110773,#110774,#110775,#110776,#110777,#110778,#110779,#110780,
#110781,#110782,#110783,#110784,#110785,#110786,#110787,#110788,#110789,
#110790,#110791,#110792,#110793,#110794,#110795,#110796,#110797,#110798,
#110799,#110800,#110801,#110802,#110803,#110804,#110805,#110806,#110807,
#110808,#110809,#110810,#110811,#110812),.UNSPECIFIED.,.F.,.F.,(4,3,3,3,
3,3,3,3,3,3,3,3,3,3,3,3,3,3,3,3,3,3,3,3,3,3,3,3,3,3,3,3,3,3,3,3,3,3,3,3,
3,3,3,3,3,3,3,3,3,3,3,3,3,3,3,3,3,3,3,3,3,3,3,3,3,3,3,3,3,3,3,3,4),(1284.91139531842,
1285.00585841401,1285.10071213125,1285.19610642442,1285.27909917653,1285.36283788838,
1285.44647339974,1285.53002584314,1285.61351527899,1285.6969692296,1285.78040572345,
1285.86384283321,1285.94729862812,1286.03084312085,1286.11443220379,1286.19815547135,
1286.27883518725,1286.3625738991,1286.44620941046,1286.52976185386,1286.61325128972,
1286.69670524033,1286.78014173418,1286.86357884393,1286.94703463885,1287.03057913158,
1287.11416821452,1287.19789148208,1287.27857119797,1287.36230990982,1287.44594542118,
1287.52949786458,1287.61298730044,1287.69644125105,1287.7798777449,1287.86331485465,
1287.94677064957,1288.0303151423,1288.11390422524,1288.1976274928,1288.2783072087,
1288.36204592055,1288.44568143191,1288.52923387531,1288.61272331116,1288.69617726178,
1288.77961375563,1288.86305086538,1288.9465066603,1289.03005115303,1289.11364023597,
1289.19736350353,1289.27804321942,1289.36178193127,1289.44541744263,1289.52896988603,
1289.61245932188,1289.6959132725,1289.77934976634,1289.8627868761,1289.94624267101,
1290.02978716374,1290.11337624668,1290.19709951424,1290.27777923014,1290.36089975157,
1290.44358911637,1290.52620302072,1290.60876039961,1290.69225615009,1290.77476877336,
1290.85875608745,1290.94274340154),.UNSPECIFIED.);
#871=B_SPLINE_CURVE_WITH_KNOTS('',3,(#110818,#110819,#110820,#110821,#110822,
#110823,#110824,#110825,#110826,#110827,#110828,#110829,#110830,#110831,
#110832,#110833,#110834,#110835,#110836,#110837,#110838,#110839,#110840,
#110841,#110842,#110843,#110844,#110845,#110846,#110847,#110848,#110849,
#110850,#110851,#110852,#110853,#110854,#110855,#110856,#110857,#110858,
#110859,#110860,#110861,#110862,#110863,#110864,#110865,#110866,#110867,
#110868,#110869,#110870,#110871,#110872,#110873,#110874,#110875,#110876,
#110877,#110878,#110879,#110880,#110881,#110882,#110883,#110884,#110885,
#110886,#110887,#110888,#110889,#110890,#110891,#110892,#110893,#110894,
#110895,#110896,#110897,#110898,#110899,#110900,#110901,#110902,#110903,
#110904,#110905,#110906,#110907,#110908,#110909,#110910,#110911,#110912,
#110913,#110914,#110915,#110916,#110917,#110918,#110919,#110920,#110921,
#110922,#110923,#110924,#110925,#110926,#110927,#110928,#110929,#110930,
#110931,#110932,#110933,#110934,#110935,#110936,#110937,#110938,#110939,
#110940,#110941,#110942,#110943,#110944,#110945,#110946,#110947,#110948,
#110949,#110950,#110951,#110952,#110953,#110954,#110955,#110956,#110957,
#110958,#110959,#110960,#110961,#110962,#110963,#110964,#110965,#110966,
#110967,#110968,#110969,#110970,#110971,#110972,#110973,#110974,#110975,
#110976,#110977,#110978,#110979,#110980,#110981,#110982,#110983,#110984,
#110985,#110986,#110987,#110988,#110989,#110990,#110991,#110992,#110993,
#110994,#110995,#110996,#110997,#110998,#110999,#111000,#111001,#111002,
#111003,#111004,#111005,#111006,#111007,#111008,#111009,#111010,#111011,
#111012,#111013,#111014,#111015,#111016,#111017,#111018,#111019,#111020,
#111021,#111022,#111023,#111024,#111025,#111026,#111027,#111028,#111029,
#111030,#111031,#111032,#111033,#111034,#111035,#111036,#111037),
 .UNSPECIFIED.,.F.,.F.,(4,3,3,3,3,3,3,3,3,3,3,3,3,3,3,3,3,3,3,3,3,3,3,3,
3,3,3,3,3,3,3,3,3,3,3,3,3,3,3,3,3,3,3,3,3,3,3,3,3,3,3,3,3,3,3,3,3,3,3,3,
3,3,3,3,3,3,3,3,3,3,3,3,3,4),(1291.19458062552,1291.2770321407,1291.3632732021,
1291.44563144077,1291.52797699879,1291.61032881882,1291.6927058461,1291.77517160511,
1291.85768947086,1291.94032413001,1291.96696063186,1292.05069934371,1292.13433485507,
1292.21788729847,1292.30137673432,1292.38483068493,1292.46826717878,1292.55170428853,
1292.63516008345,1292.71870457618,1292.80229365912,1292.88601692668,1292.96669664258,
1293.05043535443,1293.13407086579,1293.21762330919,1293.30111274504,1293.38456669566,
1293.4680031895,1293.55144029926,1293.63489609417,1293.7184405869,1293.80202966984,
1293.8857529374,1293.9664326533,1294.05017136515,1294.13380687651,1294.21735931991,
1294.30084875576,1294.38430270638,1294.46773920022,1294.55117630998,1294.6346321049,
1294.71817659763,1294.80176568057,1294.88548894813,1294.96616866402,1295.04990737587,
1295.13354288723,1295.21709533063,1295.30058476648,1295.3840387171,1295.46747521094,
1295.5509123207,1295.63436811562,1295.71791260834,1295.80150169129,1295.88522495884,
1295.96590467474,1296.04964338659,1296.13327889795,1296.21683134135,1296.3003207772,
1296.38377472782,1296.46721122166,1296.55064833142,1296.63410412634,1296.71764861907,
1296.80123770201,1296.88496096957,1296.96564068546,1297.05322552547,1297.14062188468,
1297.22741857401),.UNSPECIFIED.);
#872=B_SPLINE_CURVE_WITH_KNOTS('',3,(#111038,#111039,#111040,#111041,#111042,
#111043,#111044,#111045,#111046,#111047),.UNSPECIFIED.,.F.,.F.,(4,3,3,4),
(1290.9433767908,1290.96722462114,1291.08090262327,1291.19458062539),
 .UNSPECIFIED.);
#873=B_SPLINE_CURVE_WITH_KNOTS('',3,(#111049,#111050,#111051,#111052,#111053,
#111054,#111055,#111056,#111057,#111058),.UNSPECIFIED.,.F.,.F.,(4,3,3,4),
(1290.94274340154,1291.0253692094,1291.10997491734,1291.19458062527),
 .UNSPECIFIED.);
#874=B_SPLINE_CURVE_WITH_KNOTS('',3,(#111059,#111060,#111061,#111062,#111063,
#111064,#111065,#111066,#111067,#111068,#111069,#111070,#111071,#111072,
#111073,#111074,#111075,#111076,#111077,#111078,#111079,#111080,#111081,
#111082,#111083,#111084,#111085,#111086,#111087,#111088,#111089,#111090,
#111091,#111092,#111093,#111094,#111095,#111096,#111097,#111098,#111099,
#111100,#111101,#111102,#111103,#111104,#111105,#111106,#111107,#111108,
#111109,#111110,#111111,#111112,#111113,#111114,#111115,#111116,#111117,
#111118,#111119,#111120,#111121,#111122,#111123,#111124,#111125,#111126,
#111127,#111128,#111129,#111130,#111131,#111132,#111133,#111134,#111135,
#111136,#111137,#111138,#111139,#111140,#111141,#111142,#111143,#111144,
#111145,#111146,#111147,#111148,#111149,#111150,#111151,#111152,#111153,
#111154,#111155,#111156,#111157,#111158,#111159,#111160,#111161,#111162,
#111163,#111164,#111165,#111166,#111167,#111168,#111169,#111170,#111171,
#111172,#111173,#111174,#111175,#111176,#111177,#111178,#111179,#111180,
#111181,#111182,#111183,#111184,#111185,#111186,#111187,#111188,#111189,
#111190,#111191,#111192,#111193,#111194,#111195,#111196,#111197,#111198,
#111199,#111200,#111201,#111202,#111203,#111204,#111205,#111206,#111207,
#111208,#111209,#111210,#111211,#111212,#111213,#111214,#111215,#111216,
#111217,#111218,#111219,#111220,#111221,#111222,#111223,#111224,#111225,
#111226,#111227,#111228,#111229,#111230,#111231,#111232,#111233,#111234,
#111235,#111236,#111237,#111238,#111239,#111240,#111241,#111242,#111243,
#111244,#111245,#111246,#111247,#111248,#111249,#111250,#111251,#111252,
#111253,#111254,#111255,#111256,#111257,#111258,#111259,#111260,#111261,
#111262,#111263,#111264,#111265,#111266,#111267,#111268,#111269,#111270,
#111271,#111272,#111273,#111274,#111275,#111276,#111277,#111278),
 .UNSPECIFIED.,.F.,.F.,(4,3,3,3,3,3,3,3,3,3,3,3,3,3,3,3,3,3,3,3,3,3,3,3,
3,3,3,3,3,3,3,3,3,3,3,3,3,3,3,3,3,3,3,3,3,3,3,3,3,3,3,3,3,3,3,3,3,3,3,3,
3,3,3,3,3,3,3,3,3,3,3,3,3,4),(1291.1945806254,1291.27751524086,1291.36125395271,
1291.44488946407,1291.52844190747,1291.61193134332,1291.69538529394,1291.77882178778,
1291.86225889754,1291.94571469246,1292.02925918519,1292.11284826813,1292.19657153568,
1292.27725125158,1292.36098996343,1292.44462547479,1292.52817791819,1292.61166735404,
1292.69512130466,1292.7785577985,1292.86199490826,1292.94545070318,1293.02899519591,
1293.11258427885,1293.1963075464,1293.2769872623,1293.36072597415,1293.44436148551,
1293.52791392891,1293.61140336476,1293.69485731538,1293.77829380922,1293.86173091898,
1293.94518671389,1294.02873120662,1294.11232028956,1294.19604355712,1294.27672327302,
1294.36046198487,1294.44409749623,1294.52764993963,1294.61113937548,1294.6945933261,
1294.77802981994,1294.8614669297,1294.94492272462,1295.02846721735,1295.11205630029,
1295.19577956785,1295.27645928374,1295.36019799559,1295.44383350695,1295.52738595035,
1295.6108753862,1295.69432933682,1295.77776583066,1295.86120294042,1295.94465873534,
1296.02820322807,1296.11179231101,1296.19551557856,1296.27619529446,1296.35993683267,
1296.44357451757,1296.52712848442,1296.61454189573,1296.69799220263,1296.78142497954,
1296.8648582981,1296.94831022628,1297.0318388664,1297.11541247864,1297.19909084984,
1297.22643577487),.UNSPECIFIED.);
#875=B_SPLINE_CURVE_WITH_KNOTS('',3,(#111284,#111285,#111286,#111287,#111288,
#111289,#111290,#111291,#111292,#111293,#111294,#111295,#111296,#111297,
#111298,#111299,#111300,#111301,#111302,#111303,#111304,#111305,#111306,
#111307,#111308,#111309,#111310,#111311,#111312,#111313,#111314,#111315,
#111316,#111317,#111318,#111319,#111320,#111321,#111322,#111323,#111324,
#111325,#111326,#111327,#111328,#111329,#111330,#111331,#111332,#111333,
#111334,#111335,#111336,#111337,#111338,#111339,#111340,#111341,#111342,
#111343,#111344,#111345,#111346,#111347,#111348,#111349,#111350,#111351,
#111352,#111353,#111354,#111355,#111356,#111357,#111358,#111359,#111360,
#111361,#111362,#111363,#111364,#111365,#111366,#111367,#111368,#111369,
#111370,#111371,#111372,#111373,#111374,#111375,#111376,#111377,#111378,
#111379,#111380,#111381,#111382,#111383,#111384,#111385,#111386,#111387,
#111388,#111389,#111390,#111391,#111392,#111393,#111394,#111395,#111396,
#111397,#111398,#111399,#111400,#111401,#111402,#111403,#111404,#111405,
#111406,#111407,#111408,#111409,#111410,#111411,#111412,#111413,#111414,
#111415,#111416,#111417,#111418,#111419,#111420,#111421,#111422,#111423,
#111424,#111425,#111426,#111427,#111428,#111429,#111430,#111431,#111432,
#111433,#111434,#111435,#111436,#111437,#111438,#111439,#111440,#111441,
#111442,#111443,#111444,#111445,#111446,#111447,#111448,#111449,#111450,
#111451,#111452,#111453,#111454,#111455,#111456,#111457,#111458,#111459,
#111460,#111461,#111462,#111463,#111464,#111465,#111466,#111467,#111468,
#111469,#111470,#111471,#111472,#111473,#111474,#111475,#111476,#111477,
#111478,#111479,#111480,#111481,#111482,#111483,#111484,#111485,#111486,
#111487,#111488,#111489,#111490,#111491,#111492,#111493,#111494,#111495,
#111496,#111497,#111498,#111499,#111500,#111501,#111502,#111503),
 .UNSPECIFIED.,.F.,.F.,(4,3,3,3,3,3,3,3,3,3,3,3,3,3,3,3,3,3,3,3,3,3,3,3,
3,3,3,3,3,3,3,3,3,3,3,3,3,3,3,3,3,3,3,3,3,3,3,3,3,3,3,3,3,3,3,3,3,3,3,3,
3,3,3,3,3,3,3,3,3,3,3,3,3,4),(1297.47776593277,1297.5656277686,1297.65362197466,
1297.74183995296,1297.83017818097,1297.91872114682,1297.96537669618,1298.04911540803,
1298.13275091939,1298.21630336279,1298.29979279864,1298.38324674925,1298.4666832431,
1298.55012035285,1298.63357614777,1298.7171206405,1298.80070972344,1298.884432991,
1298.9651127069,1299.04885141875,1299.13248693011,1299.21603937351,1299.29952880936,
1299.38298275998,1299.46641925382,1299.54985636358,1299.6333121585,1299.71685665122,
1299.80044573417,1299.88416900172,1299.96484871762,1300.04858742947,1300.13222294083,
1300.21577538423,1300.29926482008,1300.3827187707,1300.46615526454,1300.5495923743,
1300.63304816922,1300.71659266195,1300.80018174489,1300.88390501245,1300.96458472834,
1301.04832344019,1301.13195895155,1301.21551139495,1301.2990008308,1301.38245478142,
1301.46589127526,1301.54932838502,1301.63278417994,1301.71632867267,1301.79991775561,
1301.88364102316,1301.96432073906,1302.04805945091,1302.13169496227,1302.21524740567,
1302.29873684152,1302.38219079214,1302.46562728598,1302.54906439574,1302.63252019066,
1302.71606468339,1302.79965376633,1302.88337703389,1302.96405674978,1303.04658050868,
1303.12900805391,1303.21135857993,1303.29364884454,1303.37590352684,1303.45815430565,
1303.50937468525),.UNSPECIFIED.);
#876=B_SPLINE_CURVE_WITH_KNOTS('',3,(#111504,#111505,#111506,#111507,#111508,
#111509,#111510,#111511,#111512,#111513),.UNSPECIFIED.,.F.,.F.,(4,3,3,4),
(1297.22741857401,1297.3145634716,1297.4015669567,1297.47776593257),
 .UNSPECIFIED.);
#877=B_SPLINE_CURVE_WITH_KNOTS('',3,(#111515,#111516,#111517,#111518,#111519,
#111520,#111521,#111522,#111523,#111524),.UNSPECIFIED.,.F.,.F.,(4,3,3,4),
(1297.22643577487,1297.27593130518,1297.39557682204,1297.47776593258),
 .UNSPECIFIED.);
#878=B_SPLINE_CURVE_WITH_KNOTS('',3,(#111525,#111526,#111527,#111528,#111529,
#111530,#111531,#111532,#111533,#111534,#111535,#111536,#111537,#111538,
#111539,#111540,#111541,#111542,#111543,#111544,#111545,#111546,#111547,
#111548,#111549,#111550,#111551,#111552,#111553,#111554,#111555,#111556,
#111557,#111558,#111559,#111560,#111561,#111562,#111563,#111564,#111565,
#111566,#111567,#111568,#111569,#111570,#111571,#111572,#111573,#111574,
#111575,#111576,#111577,#111578,#111579,#111580,#111581,#111582,#111583,
#111584,#111585,#111586,#111587,#111588,#111589,#111590,#111591,#111592,
#111593,#111594,#111595,#111596,#111597,#111598,#111599,#111600,#111601,
#111602,#111603,#111604,#111605,#111606,#111607,#111608,#111609,#111610,
#111611,#111612,#111613,#111614,#111615,#111616,#111617,#111618,#111619,
#111620,#111621,#111622,#111623,#111624,#111625,#111626,#111627,#111628,
#111629,#111630,#111631,#111632,#111633,#111634,#111635,#111636,#111637,
#111638,#111639,#111640,#111641,#111642,#111643,#111644,#111645,#111646,
#111647,#111648,#111649,#111650,#111651,#111652,#111653,#111654,#111655,
#111656,#111657,#111658,#111659,#111660,#111661,#111662,#111663,#111664,
#111665,#111666,#111667,#111668,#111669,#111670,#111671,#111672,#111673,
#111674,#111675,#111676,#111677,#111678,#111679,#111680,#111681,#111682,
#111683,#111684,#111685,#111686,#111687,#111688,#111689,#111690,#111691,
#111692,#111693,#111694,#111695,#111696,#111697,#111698,#111699,#111700,
#111701,#111702,#111703,#111704,#111705,#111706,#111707,#111708,#111709,
#111710,#111711,#111712,#111713,#111714,#111715,#111716,#111717,#111718,
#111719,#111720,#111721,#111722,#111723,#111724,#111725,#111726,#111727,
#111728,#111729,#111730,#111731,#111732,#111733,#111734,#111735,#111736,
#111737,#111738,#111739,#111740,#111741,#111742,#111743,#111744),
 .UNSPECIFIED.,.F.,.F.,(4,3,3,3,3,3,3,3,3,3,3,3,3,3,3,3,3,3,3,3,3,3,3,3,
3,3,3,3,3,3,3,3,3,3,3,3,3,3,3,3,3,3,3,3,3,3,3,3,3,3,3,3,3,3,3,3,3,3,3,3,
3,3,3,3,3,3,3,3,3,3,3,3,3,4),(1297.47776593277,1297.56014602202,1297.64245768107,
1297.72472758977,1297.8069770208,1297.88922498357,1297.97149048404,1298.05384045173,
1298.13623575657,1298.21875539183,1298.2756673159,1298.35940602775,1298.44304153911,
1298.52659398251,1298.61008341836,1298.69353736898,1298.77697386282,1298.86041097258,
1298.9438667675,1299.02741126023,1299.11100034317,1299.19472361073,1299.27540332662,
1299.35914203847,1299.44277754983,1299.52632999323,1299.60981942908,1299.6932733797,
1299.77670987354,1299.8601469833,1299.94360277822,1300.02714727095,1300.11073635389,
1300.19445962144,1300.27513933734,1300.35887804919,1300.44251356055,1300.52606600395,
1300.6095554398,1300.69300939042,1300.77644588426,1300.85988299402,1300.94333878894,
1301.02688328167,1301.11047236461,1301.19419563217,1301.27487534806,1301.35861405991,
1301.44224957127,1301.52580201467,1301.60929145052,1301.69274540114,1301.77618189498,
1301.85961900474,1301.94307479966,1302.02661929239,1302.11020837533,1302.19393164289,
1302.27461135878,1302.35835007063,1302.44198558199,1302.52553802539,1302.60902746124,
1302.69248141185,1302.7759179057,1302.85935501546,1302.94281081037,1303.0263553031,
1303.10994438604,1303.1936676536,1303.2743473695,1303.36294726085,1303.45134295585,
1303.51063850993),.UNSPECIFIED.);
#879=B_SPLINE_CURVE_WITH_KNOTS('',3,(#111750,#111751,#111752,#111753,#111754,
#111755,#111756,#111757,#111758,#111759,#111760,#111761,#111762,#111763,
#111764,#111765,#111766,#111767,#111768,#111769,#111770,#111771,#111772,
#111773,#111774,#111775,#111776,#111777,#111778,#111779,#111780,#111781,
#111782,#111783,#111784,#111785,#111786,#111787,#111788,#111789,#111790,
#111791,#111792,#111793,#111794,#111795,#111796,#111797,#111798,#111799,
#111800,#111801,#111802,#111803,#111804,#111805,#111806,#111807,#111808,
#111809,#111810,#111811,#111812,#111813,#111814,#111815,#111816,#111817,
#111818,#111819,#111820,#111821,#111822,#111823,#111824,#111825,#111826,
#111827,#111828,#111829,#111830,#111831,#111832,#111833,#111834,#111835,
#111836,#111837,#111838,#111839,#111840,#111841,#111842,#111843,#111844,
#111845,#111846,#111847,#111848,#111849,#111850,#111851,#111852,#111853,
#111854,#111855,#111856,#111857,#111858,#111859,#111860,#111861,#111862,
#111863,#111864,#111865,#111866,#111867,#111868,#111869,#111870,#111871,
#111872,#111873,#111874,#111875,#111876,#111877,#111878,#111879,#111880,
#111881,#111882,#111883,#111884,#111885,#111886,#111887,#111888,#111889,
#111890,#111891,#111892,#111893,#111894,#111895,#111896,#111897,#111898,
#111899,#111900,#111901,#111902,#111903,#111904,#111905,#111906,#111907,
#111908,#111909,#111910,#111911,#111912,#111913,#111914,#111915,#111916,
#111917,#111918,#111919,#111920,#111921,#111922,#111923,#111924,#111925,
#111926,#111927,#111928,#111929,#111930,#111931,#111932,#111933,#111934,
#111935,#111936,#111937,#111938,#111939,#111940,#111941,#111942,#111943,
#111944,#111945,#111946,#111947,#111948,#111949,#111950,#111951,#111952,
#111953,#111954,#111955,#111956,#111957,#111958,#111959,#111960,#111961,
#111962,#111963,#111964,#111965,#111966),.UNSPECIFIED.,.F.,.F.,(4,3,3,3,
3,3,3,3,3,3,3,3,3,3,3,3,3,3,3,3,3,3,3,3,3,3,3,3,3,3,3,3,3,3,3,3,3,3,3,3,
3,3,3,3,3,3,3,3,3,3,3,3,3,3,3,3,3,3,3,3,3,3,3,3,3,3,3,3,3,3,3,3,4),(1303.76095123975,
1303.88029814022,1303.9637927605,1304.04753147234,1304.13116698371,1304.21471942711,
1304.29820886296,1304.38166281357,1304.46509930742,1304.54853641717,1304.63199221209,
1304.71553670481,1304.79912578775,1304.88284905531,1304.96352877122,1305.04726748307,
1305.13090299443,1305.21445543783,1305.29794487368,1305.3813988243,1305.46483531814,
1305.5482724279,1305.63172822282,1305.71527271555,1305.79886179849,1305.88258506605,
1305.96326478194,1306.04700349379,1306.13063900515,1306.21419144855,1306.2976808844,
1306.38113483502,1306.46457132886,1306.54800843862,1306.63146423354,1306.71500872627,
1306.79859780921,1306.88232107676,1306.96300079266,1307.04673950451,1307.13037501587,
1307.21392745927,1307.29741689512,1307.38087084574,1307.46430733958,1307.54774444934,
1307.63120024426,1307.71474473699,1307.79833381993,1307.88205708748,1307.96273680338,
1308.04647551523,1308.13011102659,1308.21366346999,1308.29715290584,1308.38060685646,
1308.4640433503,1308.54748046006,1308.63093625498,1308.71448074771,1308.79806983065,
1308.8817930982,1308.9624728141,1309.04622167287,1309.1298650922,1309.21340828216,
1309.29689463722,1309.3803422766,1309.4637692897,1309.54722292384,1309.63068741899,
1309.71422899167,1309.79248975557),.UNSPECIFIED.);
#880=B_SPLINE_CURVE_WITH_KNOTS('',3,(#111967,#111968,#111969,#111970,#111971,
#111972,#111973,#111974,#111975,#111976),.UNSPECIFIED.,.F.,.F.,(4,3,3,4),
(1303.50937468525,1303.59165936378,1303.67630530167,1303.76095123957),
 .UNSPECIFIED.);
#881=B_SPLINE_CURVE_WITH_KNOTS('',3,(#111978,#111979,#111980,#111981,#111982,
#111983,#111984,#111985,#111986,#111987),.UNSPECIFIED.,.F.,.F.,(4,3,3,4),
(1303.51063850993,1303.59876857963,1303.68671228148,1303.76095123965),
 .UNSPECIFIED.);
#882=B_SPLINE_CURVE_WITH_KNOTS('',3,(#111988,#111989,#111990,#111991,#111992,
#111993,#111994,#111995,#111996,#111997,#111998,#111999,#112000,#112001,
#112002,#112003,#112004,#112005,#112006,#112007,#112008,#112009,#112010,
#112011,#112012,#112013,#112014,#112015,#112016,#112017,#112018,#112019,
#112020,#112021,#112022,#112023,#112024,#112025,#112026,#112027,#112028,
#112029,#112030,#112031,#112032,#112033,#112034,#112035,#112036,#112037,
#112038,#112039,#112040,#112041,#112042,#112043,#112044,#112045,#112046,
#112047,#112048,#112049,#112050,#112051,#112052,#112053,#112054,#112055,
#112056,#112057,#112058,#112059,#112060,#112061,#112062,#112063,#112064,
#112065,#112066,#112067,#112068,#112069,#112070,#112071,#112072,#112073,
#112074,#112075,#112076,#112077,#112078,#112079,#112080,#112081,#112082,
#112083,#112084,#112085,#112086,#112087,#112088,#112089,#112090,#112091,
#112092,#112093,#112094,#112095,#112096,#112097,#112098,#112099,#112100,
#112101,#112102,#112103,#112104,#112105,#112106,#112107,#112108,#112109,
#112110,#112111,#112112,#112113,#112114,#112115,#112116,#112117,#112118,
#112119,#112120,#112121,#112122,#112123,#112124,#112125,#112126,#112127,
#112128,#112129,#112130,#112131,#112132,#112133,#112134,#112135,#112136,
#112137,#112138,#112139,#112140,#112141,#112142,#112143,#112144,#112145,
#112146,#112147,#112148,#112149,#112150,#112151,#112152,#112153,#112154,
#112155,#112156,#112157,#112158,#112159,#112160,#112161,#112162,#112163,
#112164,#112165,#112166,#112167,#112168,#112169,#112170,#112171,#112172,
#112173,#112174,#112175,#112176,#112177,#112178,#112179,#112180,#112181,
#112182,#112183,#112184,#112185,#112186,#112187,#112188,#112189,#112190,
#112191,#112192,#112193,#112194,#112195,#112196,#112197,#112198,#112199,
#112200,#112201,#112202,#112203,#112204,#112205,#112206,#112207),
 .UNSPECIFIED.,.F.,.F.,(4,3,3,3,3,3,3,3,3,3,3,3,3,3,3,3,3,3,3,3,3,3,3,3,
3,3,3,3,3,3,3,3,3,3,3,3,3,3,3,3,3,3,3,3,3,3,3,3,3,3,3,3,3,3,3,3,3,3,3,3,
3,3,3,3,3,3,3,3,3,3,3,3,3,4),(1303.76095123976,1303.84788995488,1303.93492696292,
1304.02215407985,1304.10947927334,1304.19700265275,1304.27408338022,1304.35782209207,
1304.44145760344,1304.52501004683,1304.60849948269,1304.6919534333,1304.77538992715,
1304.8588270369,1304.94228283182,1305.02582732455,1305.10941640749,1305.19313967505,
1305.27381939094,1305.35755810279,1305.44119361415,1305.52474605755,1305.6082354934,
1305.69168944402,1305.77512593786,1305.85856304762,1305.94201884254,1306.02556333527,
1306.10915241821,1306.19287568576,1306.27355540166,1306.35729411351,1306.44092962487,
1306.52448206827,1306.60797150412,1306.69142545474,1306.77486194858,1306.85829905834,
1306.94175485325,1307.02529934598,1307.10888842892,1307.19261169648,1307.27329141238,
1307.35703012423,1307.44066563559,1307.52421807899,1307.60770751484,1307.69116146546,
1307.7745979593,1307.85803506906,1307.94149086398,1308.02503535671,1308.10862443965,
1308.19234770721,1308.2730274231,1308.35676613495,1308.44040164632,1308.52395408972,
1308.60744352557,1308.69089747618,1308.77433397003,1308.85777107978,1308.9412268747,
1309.02477136743,1309.10836045037,1309.19208371793,1309.27276343382,1309.35539413479,
1309.43792765049,1309.52038311093,1309.60277500297,1309.68513056106,1309.76747497784,
1309.7926706447),.UNSPECIFIED.);
#883=B_SPLINE_CURVE_WITH_KNOTS('',3,(#112213,#112214,#112215,#112216,#112217,
#112218,#112219,#112220,#112221,#112222,#112223,#112224,#112225,#112226,
#112227,#112228,#112229,#112230,#112231,#112232,#112233,#112234,#112235,
#112236,#112237,#112238,#112239,#112240,#112241,#112242,#112243,#112244,
#112245,#112246,#112247,#112248,#112249,#112250,#112251,#112252,#112253,
#112254,#112255,#112256,#112257,#112258,#112259,#112260,#112261,#112262,
#112263,#112264,#112265,#112266,#112267,#112268,#112269,#112270,#112271,
#112272,#112273,#112274,#112275,#112276,#112277,#112278,#112279,#112280,
#112281,#112282,#112283,#112284,#112285,#112286,#112287,#112288,#112289,
#112290,#112291,#112292,#112293,#112294,#112295,#112296,#112297,#112298,
#112299,#112300,#112301,#112302,#112303,#112304,#112305,#112306,#112307,
#112308,#112309,#112310,#112311,#112312,#112313,#112314,#112315,#112316,
#112317,#112318,#112319,#112320,#112321,#112322,#112323,#112324,#112325,
#112326,#112327,#112328,#112329,#112330,#112331,#112332,#112333,#112334,
#112335,#112336,#112337,#112338,#112339,#112340,#112341,#112342,#112343,
#112344,#112345,#112346,#112347,#112348,#112349,#112350,#112351,#112352,
#112353,#112354,#112355,#112356,#112357,#112358,#112359,#112360,#112361,
#112362,#112363,#112364,#112365,#112366,#112367,#112368,#112369,#112370,
#112371,#112372,#112373,#112374,#112375,#112376,#112377,#112378,#112379,
#112380,#112381,#112382,#112383,#112384,#112385,#112386,#112387,#112388,
#112389,#112390,#112391,#112392,#112393,#112394,#112395,#112396,#112397,
#112398,#112399,#112400,#112401,#112402,#112403,#112404,#112405,#112406,
#112407,#112408,#112409,#112410,#112411,#112412,#112413,#112414,#112415,
#112416,#112417,#112418,#112419,#112420,#112421,#112422,#112423,#112424,
#112425,#112426,#112427,#112428,#112429,#112430,#112431,#112432),
 .UNSPECIFIED.,.F.,.F.,(4,3,3,3,3,3,3,3,3,3,3,3,3,3,3,3,3,3,3,3,3,3,3,3,
3,3,3,3,3,3,3,3,3,3,3,3,3,3,3,3,3,3,3,3,3,3,3,3,3,3,3,3,3,3,3,3,3,3,3,3,
3,3,3,3,3,3,3,3,3,3,3,3,3,4),(1310.04413654706,1310.12691333657,1310.20959441768,
1310.29220075488,1310.37591876497,1310.45844797584,1310.54096978032,1310.62350300583,
1310.70811346325,1310.79076955573,1310.87635719563,1310.96194483554,1311.04568354739,
1311.12931905875,1311.21287150215,1311.296360938,1311.37981488862,1311.46325138246,
1311.54668849222,1311.63014428714,1311.71368877987,1311.79727786281,1311.88100113036,
1311.96168084626,1312.04541955811,1312.12905506947,1312.21260751287,1312.29609694872,
1312.37955089934,1312.46298739318,1312.54642450294,1312.62988029785,1312.71342479058,
1312.79701387353,1312.88073714108,1312.96141685698,1313.04515556883,1313.12879108019,
1313.21234352359,1313.29583295944,1313.37928691006,1313.4627234039,1313.54616051366,
1313.62961630858,1313.71316080131,1313.79674988425,1313.8804731518,1313.9611528677,
1314.04489157955,1314.12852709091,1314.21207953431,1314.29556897016,1314.37902292078,
1314.46245941462,1314.54589652438,1314.6293523193,1314.71289681203,1314.79648589497,
1314.88020916253,1314.96088887842,1315.04462759027,1315.12826310163,1315.21181554503,
1315.29530498088,1315.3787589315,1315.46219542534,1315.5456325351,1315.62908833002,
1315.71263282275,1315.79622190569,1315.87994517324,1315.96062488914,1316.0562245153,
1316.07685146776),.UNSPECIFIED.);
#884=B_SPLINE_CURVE_WITH_KNOTS('',3,(#112433,#112434,#112435,#112436,#112437,
#112438,#112439,#112440,#112441,#112442),.UNSPECIFIED.,.F.,.F.,(4,3,3,4),
(1309.79248975557,1309.87734929019,1309.96220882482,1310.04413654693),
 .UNSPECIFIED.);
#885=B_SPLINE_CURVE_WITH_KNOTS('',3,(#112444,#112445,#112446,#112447,#112448,
#112449,#112450,#112451,#112452,#112453),.UNSPECIFIED.,.F.,.F.,(4,3,3,4),
(1309.7926706447,1309.87504289146,1309.95958971914,1310.04413654683),
 .UNSPECIFIED.);
#886=B_SPLINE_CURVE_WITH_KNOTS('',3,(#112454,#112455,#112456,#112457,#112458,
#112459,#112460,#112461,#112462,#112463,#112464,#112465,#112466,#112467,
#112468,#112469,#112470,#112471,#112472,#112473,#112474,#112475,#112476,
#112477,#112478,#112479,#112480,#112481,#112482,#112483,#112484,#112485,
#112486,#112487,#112488,#112489,#112490,#112491,#112492,#112493,#112494,
#112495,#112496,#112497,#112498,#112499,#112500,#112501,#112502,#112503,
#112504,#112505,#112506,#112507,#112508,#112509,#112510,#112511,#112512,
#112513,#112514,#112515,#112516,#112517,#112518,#112519,#112520,#112521,
#112522,#112523,#112524,#112525,#112526,#112527,#112528,#112529,#112530,
#112531,#112532,#112533,#112534,#112535,#112536,#112537,#112538,#112539,
#112540,#112541,#112542,#112543,#112544,#112545,#112546,#112547,#112548,
#112549,#112550,#112551,#112552,#112553,#112554,#112555,#112556,#112557,
#112558,#112559,#112560,#112561,#112562,#112563,#112564,#112565,#112566,
#112567,#112568,#112569,#112570,#112571,#112572,#112573,#112574,#112575,
#112576,#112577,#112578,#112579,#112580,#112581,#112582,#112583,#112584,
#112585,#112586,#112587,#112588,#112589,#112590,#112591,#112592,#112593,
#112594,#112595,#112596,#112597,#112598,#112599,#112600,#112601,#112602,
#112603,#112604,#112605,#112606,#112607,#112608,#112609,#112610,#112611,
#112612,#112613,#112614,#112615,#112616,#112617,#112618,#112619,#112620,
#112621,#112622,#112623,#112624,#112625,#112626,#112627,#112628,#112629,
#112630,#112631,#112632,#112633,#112634,#112635,#112636,#112637,#112638,
#112639,#112640,#112641,#112642,#112643,#112644,#112645,#112646,#112647,
#112648,#112649,#112650,#112651,#112652,#112653,#112654,#112655,#112656,
#112657,#112658,#112659,#112660,#112661,#112662,#112663,#112664,#112665,
#112666,#112667,#112668,#112669,#112670),.UNSPECIFIED.,.F.,.F.,(4,3,3,3,
3,3,3,3,3,3,3,3,3,3,3,3,3,3,3,3,3,3,3,3,3,3,3,3,3,3,3,3,3,3,3,3,3,3,3,3,
3,3,3,3,3,3,3,3,3,3,3,3,3,3,3,3,3,3,3,3,3,3,3,3,3,3,3,3,3,3,3,3,4),(1310.04413654693,
1310.15831799574,1310.27249944454,1310.35623815639,1310.43987366775,1310.52342611115,
1310.606915547,1310.69036949762,1310.77380599146,1310.85724310122,1310.94069889614,
1311.02424338887,1311.10783247181,1311.19155573937,1311.27223545526,1311.35597416711,
1311.43960967847,1311.52316212187,1311.60665155772,1311.69010550834,1311.77354200218,
1311.85697911194,1311.94043490685,1312.02397939958,1312.10756848252,1312.19129175008,
1312.27197146598,1312.35571017783,1312.43934568919,1312.52289813259,1312.60638756844,
1312.68984151906,1312.7732780129,1312.85671512266,1312.94017091758,1313.02371541031,
1313.10730449325,1313.1910277608,1313.2717074767,1313.35544618855,1313.43908169991,
1313.52263414331,1313.60612357916,1313.68957752978,1313.77301402362,1313.85645113338,
1313.9399069283,1314.02345142103,1314.10704050397,1314.19076377152,1314.27144348742,
1314.35518219927,1314.43881771063,1314.52237015403,1314.60585958988,1314.6893135405,
1314.77275003434,1314.8561871441,1314.93964293902,1315.02318743175,1315.10677651469,
1315.19049978225,1315.27117949814,1315.35492999503,1315.43857471546,1315.52211835569,
1315.60560468323,1315.68905181818,1315.7724778503,1315.85592568299,1315.93938418495,
1316.02290795082,1316.07565830488),.UNSPECIFIED.);
#887=B_SPLINE_CURVE_WITH_KNOTS('',3,(#112676,#112677,#112678,#112679,#112680,
#112681,#112682,#112683,#112684,#112685,#112686,#112687,#112688,#112689,
#112690,#112691,#112692,#112693,#112694,#112695,#112696,#112697,#112698,
#112699,#112700,#112701,#112702,#112703,#112704,#112705,#112706,#112707,
#112708,#112709,#112710,#112711,#112712,#112713,#112714,#112715,#112716,
#112717,#112718,#112719,#112720,#112721,#112722,#112723,#112724,#112725,
#112726,#112727,#112728,#112729,#112730,#112731,#112732,#112733,#112734,
#112735,#112736,#112737,#112738,#112739,#112740,#112741,#112742,#112743,
#112744,#112745,#112746,#112747,#112748,#112749,#112750,#112751,#112752,
#112753,#112754,#112755,#112756,#112757,#112758,#112759,#112760,#112761,
#112762,#112763,#112764,#112765,#112766,#112767,#112768,#112769,#112770,
#112771,#112772,#112773,#112774,#112775,#112776,#112777,#112778,#112779,
#112780,#112781,#112782,#112783,#112784,#112785,#112786,#112787,#112788,
#112789,#112790,#112791,#112792,#112793,#112794,#112795,#112796,#112797,
#112798,#112799,#112800,#112801,#112802,#112803,#112804,#112805,#112806,
#112807,#112808,#112809,#112810,#112811,#112812,#112813,#112814,#112815,
#112816,#112817,#112818,#112819,#112820,#112821,#112822,#112823,#112824,
#112825,#112826,#112827,#112828,#112829,#112830,#112831,#112832,#112833,
#112834,#112835,#112836,#112837,#112838,#112839,#112840,#112841,#112842,
#112843,#112844,#112845,#112846,#112847,#112848,#112849,#112850,#112851,
#112852,#112853,#112854,#112855,#112856,#112857,#112858,#112859,#112860,
#112861,#112862,#112863,#112864,#112865,#112866,#112867,#112868,#112869,
#112870,#112871,#112872,#112873,#112874,#112875,#112876,#112877,#112878,
#112879,#112880,#112881,#112882,#112883,#112884,#112885,#112886,#112887,
#112888,#112889,#112890,#112891,#112892,#112893,#112894,#112895),
 .UNSPECIFIED.,.F.,.F.,(4,3,3,3,3,3,3,3,3,3,3,3,3,3,3,3,3,3,3,3,3,3,3,3,
3,3,3,3,3,3,3,3,3,3,3,3,3,3,3,3,3,3,3,3,3,3,3,3,3,3,3,3,3,3,3,3,3,3,3,3,
3,3,3,3,3,3,3,3,3,3,3,3,3,4),(1316.32732185411,1316.41123632682,1316.49515365699,
1316.57909123808,1316.66306647283,1316.74714905078,1316.83129168248,1316.91556945888,
1316.96036089986,1317.04409961171,1317.12773512307,1317.21128756647,1317.29477700232,
1317.37823095294,1317.46166744678,1317.54510455654,1317.62856035146,1317.71210484419,
1317.79569392713,1317.87941719468,1317.96009691058,1318.04383562243,1318.12747113379,
1318.21102357719,1318.29451301304,1318.37796696366,1318.4614034575,1318.54484056726,
1318.62829636218,1318.71184085491,1318.79542993785,1318.8791532054,1318.9598329213,
1319.04357163315,1319.12720714451,1319.21075958791,1319.29424902376,1319.37770297438,
1319.46113946822,1319.54457657798,1319.6280323729,1319.71157686563,1319.79516594857,
1319.87888921612,1319.95956893202,1320.04330764387,1320.12694315523,1320.21049559863,
1320.29398503448,1320.3774389851,1320.46087547894,1320.5443125887,1320.62776838362,
1320.71131287635,1320.79490195929,1320.87862522685,1320.95930494274,1321.04304365459,
1321.12667916595,1321.21023160935,1321.2937210452,1321.37717499582,1321.46061148966,
1321.54404859942,1321.62750439434,1321.71104888707,1321.79463797001,1321.87836123756,
1321.95904095346,1322.04299957575,1322.12682101002,1322.21056353265,1322.29423344159,
1322.35964844668),.UNSPECIFIED.);
#888=B_SPLINE_CURVE_WITH_KNOTS('',3,(#112896,#112897,#112898,#112899,#112900,
#112901,#112902,#112903,#112904,#112905),.UNSPECIFIED.,.F.,.F.,(4,3,3,4),
(1316.07685146776,1316.17191321989,1316.26636756679,1316.32732185391),
 .UNSPECIFIED.);
#889=B_SPLINE_CURVE_WITH_KNOTS('',3,(#112907,#112908,#112909,#112910,#112911,
#112912,#112913,#112914,#112915,#112916,#112917,#112918,#112919),
 .UNSPECIFIED.,.F.,.F.,(4,3,3,3,4),(1316.07565830488,1316.15928389047,1316.24302883045,
1316.27091550886,1316.32732185411),.UNSPECIFIED.);
#890=B_SPLINE_CURVE_WITH_KNOTS('',3,(#112920,#112921,#112922,#112923,#112924,
#112925,#112926,#112927,#112928,#112929,#112930,#112931,#112932,#112933,
#112934,#112935,#112936,#112937,#112938,#112939,#112940,#112941,#112942,
#112943,#112944,#112945,#112946,#112947,#112948,#112949,#112950,#112951,
#112952,#112953,#112954,#112955,#112956,#112957,#112958,#112959,#112960,
#112961,#112962,#112963,#112964,#112965,#112966,#112967,#112968,#112969,
#112970,#112971,#112972,#112973,#112974,#112975,#112976,#112977,#112978,
#112979,#112980,#112981,#112982,#112983,#112984,#112985,#112986,#112987,
#112988,#112989,#112990,#112991,#112992,#112993,#112994,#112995,#112996,
#112997,#112998,#112999,#113000,#113001,#113002,#113003,#113004,#113005,
#113006,#113007,#113008,#113009,#113010,#113011,#113012,#113013,#113014,
#113015,#113016,#113017,#113018,#113019,#113020,#113021,#113022,#113023,
#113024,#113025,#113026,#113027,#113028,#113029,#113030,#113031,#113032,
#113033,#113034,#113035,#113036,#113037,#113038,#113039,#113040,#113041,
#113042,#113043,#113044,#113045,#113046,#113047,#113048,#113049,#113050,
#113051,#113052,#113053,#113054,#113055,#113056,#113057,#113058,#113059,
#113060,#113061,#113062,#113063,#113064,#113065,#113066,#113067,#113068,
#113069,#113070,#113071,#113072,#113073,#113074,#113075,#113076,#113077,
#113078,#113079,#113080,#113081,#113082,#113083,#113084,#113085,#113086,
#113087,#113088,#113089,#113090,#113091,#113092,#113093,#113094,#113095,
#113096,#113097,#113098,#113099,#113100,#113101,#113102,#113103,#113104,
#113105,#113106,#113107,#113108,#113109,#113110,#113111,#113112,#113113,
#113114,#113115,#113116,#113117,#113118,#113119,#113120,#113121,#113122,
#113123,#113124,#113125,#113126,#113127,#113128,#113129,#113130,#113131,
#113132,#113133,#113134,#113135,#113136,#113137,#113138,#113139),
 .UNSPECIFIED.,.F.,.F.,(4,3,3,3,3,3,3,3,3,3,3,3,3,3,3,3,3,3,3,3,3,3,3,3,
3,3,3,3,3,3,3,3,3,3,3,3,3,3,3,3,3,3,3,3,3,3,3,3,3,3,3,3,3,3,3,3,3,3,3,3,
3,3,3,3,3,3,3,3,3,3,3,3,3,4),(1316.32732185422,1316.41033731549,1316.49325348052,
1316.57609114802,1316.66291119447,1316.74566196677,1316.82840213601,1316.91115037352,
1316.9939253533,1317.07679084491,1317.15970931004,1317.2427458313,1317.27065151958,
1317.35439023143,1317.43802574279,1317.52157818619,1317.60506762204,1317.68852157266,
1317.7719580665,1317.85539517626,1317.93885097118,1318.02239546391,1318.10598454685,
1318.18970781441,1318.2703875303,1318.35412624215,1318.43776175351,1318.52131419691,
1318.60480363276,1318.68825758338,1318.77169407722,1318.85513118698,1318.9385869819,
1319.02213147462,1319.10572055757,1319.18944382512,1319.27012354102,1319.35386225287,
1319.43749776423,1319.52105020763,1319.60453964348,1319.6879935941,1319.77143008794,
1319.8548671977,1319.93832299262,1320.02186748535,1320.10545656829,1320.18917983584,
1320.26985955174,1320.35359826359,1320.43723377495,1320.52078621835,1320.6042756542,
1320.68772960482,1320.77116609866,1320.85460320842,1320.93805900334,1321.02160349607,
1321.10519257901,1321.18891584657,1321.26959556246,1321.35333427431,1321.43696978567,
1321.52052222907,1321.60401166492,1321.68746561554,1321.77090210938,1321.85433921914,
1321.93779501405,1322.02133950678,1322.10492858972,1322.18865185728,1322.26933157318,
1322.35993616154),.UNSPECIFIED.);
#891=B_SPLINE_CURVE_WITH_KNOTS('',3,(#113145,#113146,#113147,#113148,#113149,
#113150,#113151,#113152,#113153,#113154,#113155,#113156,#113157,#113158,
#113159,#113160,#113161,#113162,#113163,#113164,#113165,#113166,#113167,
#113168,#113169,#113170,#113171,#113172,#113173,#113174,#113175,#113176,
#113177,#113178,#113179,#113180,#113181,#113182,#113183,#113184,#113185,
#113186,#113187,#113188,#113189,#113190,#113191,#113192,#113193,#113194,
#113195,#113196,#113197,#113198,#113199,#113200,#113201,#113202,#113203,
#113204,#113205,#113206,#113207,#113208,#113209,#113210,#113211,#113212,
#113213,#113214,#113215,#113216,#113217,#113218,#113219,#113220,#113221,
#113222,#113223,#113224,#113225,#113226,#113227,#113228,#113229,#113230,
#113231,#113232,#113233,#113234,#113235,#113236,#113237,#113238,#113239,
#113240,#113241,#113242,#113243,#113244,#113245,#113246,#113247,#113248,
#113249,#113250,#113251,#113252,#113253,#113254,#113255,#113256,#113257,
#113258,#113259,#113260,#113261,#113262,#113263,#113264,#113265,#113266,
#113267,#113268,#113269,#113270,#113271,#113272,#113273,#113274,#113275,
#113276,#113277,#113278,#113279,#113280,#113281,#113282,#113283,#113284,
#113285,#113286,#113287,#113288,#113289,#113290,#113291,#113292,#113293,
#113294,#113295,#113296,#113297,#113298,#113299,#113300,#113301,#113302,
#113303,#113304,#113305,#113306,#113307,#113308,#113309,#113310,#113311,
#113312,#113313,#113314,#113315,#113316,#113317,#113318,#113319,#113320,
#113321,#113322,#113323,#113324,#113325,#113326,#113327,#113328,#113329,
#113330,#113331,#113332,#113333,#113334,#113335,#113336,#113337,#113338,
#113339,#113340,#113341,#113342,#113343,#113344,#113345,#113346,#113347,
#113348,#113349,#113350,#113351,#113352,#113353,#113354,#113355,#113356,
#113357,#113358,#113359,#113360,#113361,#113362,#113363,#113364),
 .UNSPECIFIED.,.F.,.F.,(4,3,3,3,3,3,3,3,3,3,3,3,3,3,3,3,3,3,3,3,3,3,3,3,
3,3,3,3,3,3,3,3,3,3,3,3,3,3,3,3,3,3,3,3,3,3,3,3,3,3,3,3,3,3,3,3,3,3,3,3,
3,3,3,3,3,3,3,3,3,3,3,3,3,4),(1322.61050716148,1322.7064694113,1322.8029179108,
1322.89997941325,1322.95877696418,1323.04251567603,1323.12615118739,1323.20970363079,
1323.29319306664,1323.37664701726,1323.4600835111,1323.54352062086,1323.62697641578,
1323.7105209085,1323.79410999145,1323.877833259,1323.9585129749,1324.04225168675,
1324.12588719811,1324.20943964151,1324.29292907736,1324.37638302798,1324.45981952182,
1324.54325663158,1324.6267124265,1324.71025691923,1324.79384600217,1324.87756926972,
1324.95824898562,1325.04198769747,1325.12562320883,1325.20917565223,1325.29266508808,
1325.3761190387,1325.45955553254,1325.5429926423,1325.62644843722,1325.70999292995,
1325.79358201289,1325.87730528044,1325.95798499634,1326.04172370819,1326.12535921955,
1326.20891166295,1326.2924010988,1326.37585504942,1326.45929154326,1326.54272865302,
1326.62618444794,1326.70972894067,1326.79331802361,1326.87704129116,1326.95772100706,
1327.04145971891,1327.12509523027,1327.20864767367,1327.29213710952,1327.37559106014,
1327.45902755398,1327.54246466374,1327.62592045866,1327.70946495139,1327.79305403433,
1327.87677730188,1327.95745701778,1328.04300836688,1328.12585651517,1328.20862958704,
1328.29134640098,1328.37402572821,1328.45669979063,1328.53937184885,1328.62207975794,
1328.64186781057),.UNSPECIFIED.);
#892=B_SPLINE_CURVE_WITH_KNOTS('',3,(#113365,#113366,#113367,#113368,#113369,
#113370,#113371,#113372,#113373,#113374),.UNSPECIFIED.,.F.,.F.,(4,3,3,4),
(1322.35964844668,1322.44325162287,1322.52687939208,1322.61050716129),
 .UNSPECIFIED.);
#893=B_SPLINE_CURVE_WITH_KNOTS('',3,(#113376,#113377,#113378,#113379,#113380,
#113381,#113382,#113383,#113384,#113385),.UNSPECIFIED.,.F.,.F.,(4,3,3,4),
(1322.35993616154,1322.45721358474,1322.55370132972,1322.6105071611),
 .UNSPECIFIED.);
#894=B_SPLINE_CURVE_WITH_KNOTS('',3,(#113386,#113387,#113388,#113389,#113390,
#113391,#113392,#113393,#113394,#113395,#113396,#113397,#113398,#113399,
#113400,#113401,#113402,#113403,#113404,#113405,#113406,#113407,#113408,
#113409,#113410,#113411,#113412,#113413,#113414,#113415,#113416,#113417,
#113418,#113419,#113420,#113421,#113422,#113423,#113424,#113425,#113426,
#113427,#113428,#113429,#113430,#113431,#113432,#113433,#113434,#113435,
#113436,#113437,#113438,#113439,#113440,#113441,#113442,#113443,#113444,
#113445,#113446,#113447,#113448,#113449,#113450,#113451,#113452,#113453,
#113454,#113455,#113456,#113457,#113458,#113459,#113460,#113461,#113462,
#113463,#113464,#113465,#113466,#113467,#113468,#113469,#113470,#113471,
#113472,#113473,#113474,#113475,#113476,#113477,#113478,#113479,#113480,
#113481,#113482,#113483,#113484,#113485,#113486,#113487,#113488,#113489,
#113490,#113491,#113492,#113493,#113494,#113495,#113496,#113497,#113498,
#113499,#113500,#113501,#113502,#113503,#113504,#113505,#113506,#113507,
#113508,#113509,#113510,#113511,#113512,#113513,#113514,#113515,#113516,
#113517,#113518,#113519,#113520,#113521,#113522,#113523,#113524,#113525,
#113526,#113527,#113528,#113529,#113530,#113531,#113532,#113533,#113534,
#113535,#113536,#113537,#113538,#113539,#113540,#113541,#113542,#113543,
#113544,#113545,#113546,#113547,#113548,#113549,#113550,#113551,#113552,
#113553,#113554,#113555,#113556,#113557,#113558,#113559,#113560,#113561,
#113562,#113563,#113564,#113565,#113566,#113567,#113568,#113569,#113570,
#113571,#113572,#113573,#113574,#113575,#113576,#113577,#113578,#113579,
#113580,#113581,#113582,#113583,#113584,#113585,#113586,#113587,#113588,
#113589,#113590,#113591,#113592,#113593,#113594,#113595,#113596,#113597,
#113598,#113599,#113600,#113601,#113602,#113603,#113604,#113605),
 .UNSPECIFIED.,.F.,.F.,(4,3,3,3,3,3,3,3,3,3,3,3,3,3,3,3,3,3,3,3,3,3,3,3,
3,3,3,3,3,3,3,3,3,3,3,3,3,3,3,3,3,3,3,3,3,3,3,3,3,3,3,3,3,3,3,3,3,3,3,3,
3,3,3,3,3,3,3,3,3,3,3,3,3,4),(1322.61050716129,1322.69400757452,1322.77749817373,
1322.86099688777,1322.94452164693,1323.02814444939,1323.11181799589,1323.19563090804,
1323.2690675839,1323.35280629575,1323.43644180711,1323.51999425051,1323.60348368636,
1323.68693763698,1323.77037413082,1323.85381124058,1323.9372670355,1324.02081152823,
1324.10440061117,1324.18812387873,1324.26880359462,1324.35254230647,1324.43617781783,
1324.51973026123,1324.60321969708,1324.6866736477,1324.77011014154,1324.8535472513,
1324.93700304621,1325.02054753894,1325.10413662188,1325.18785988944,1325.26853960534,
1325.35227831719,1325.43591382855,1325.51946627195,1325.6029557078,1325.68640965842,
1325.76984615226,1325.85328326202,1325.93673905694,1326.02028354967,1326.10387263261,
1326.18759590016,1326.26827561606,1326.35201432791,1326.43564983927,1326.51920228267,
1326.60269171852,1326.68614566914,1326.76958216298,1326.85301927274,1326.93647506766,
1327.02001956039,1327.10360864333,1327.18733191089,1327.26801162678,1327.35175033863,
1327.43538584999,1327.51893829339,1327.60242772924,1327.68588167986,1327.7693181737,
1327.85275528346,1327.93621107838,1328.01975557111,1328.10334465405,1328.1870679216,
1328.2677476375,1328.35218423068,1328.43647771956,1328.52068855315,1328.60481838857,
1328.64295744021),.UNSPECIFIED.);
#895=B_SPLINE_CURVE_WITH_KNOTS('',3,(#113611,#113612,#113613,#113614,#113615,
#113616,#113617,#113618,#113619,#113620,#113621,#113622,#113623,#113624,
#113625,#113626,#113627,#113628,#113629,#113630,#113631,#113632,#113633,
#113634,#113635,#113636,#113637,#113638,#113639,#113640,#113641,#113642,
#113643,#113644,#113645,#113646,#113647,#113648,#113649,#113650,#113651,
#113652,#113653,#113654,#113655,#113656,#113657,#113658,#113659,#113660,
#113661,#113662,#113663,#113664,#113665,#113666,#113667,#113668,#113669,
#113670,#113671,#113672,#113673,#113674,#113675,#113676,#113677,#113678,
#113679,#113680,#113681,#113682,#113683,#113684,#113685,#113686,#113687,
#113688,#113689,#113690,#113691,#113692,#113693,#113694,#113695,#113696,
#113697,#113698,#113699,#113700,#113701,#113702,#113703,#113704,#113705,
#113706,#113707,#113708,#113709,#113710,#113711,#113712,#113713,#113714,
#113715,#113716,#113717,#113718,#113719,#113720,#113721,#113722,#113723,
#113724,#113725,#113726,#113727,#113728,#113729,#113730,#113731,#113732,
#113733,#113734,#113735,#113736,#113737,#113738,#113739,#113740,#113741,
#113742,#113743,#113744,#113745,#113746,#113747,#113748,#113749,#113750,
#113751,#113752,#113753,#113754,#113755,#113756,#113757,#113758,#113759,
#113760,#113761,#113762,#113763,#113764,#113765,#113766,#113767,#113768,
#113769,#113770,#113771,#113772,#113773,#113774,#113775,#113776,#113777,
#113778,#113779,#113780,#113781,#113782,#113783,#113784,#113785,#113786,
#113787,#113788,#113789,#113790,#113791,#113792,#113793,#113794,#113795,
#113796,#113797,#113798,#113799,#113800,#113801,#113802,#113803,#113804,
#113805,#113806,#113807,#113808,#113809,#113810,#113811,#113812,#113813,
#113814,#113815,#113816,#113817,#113818,#113819,#113820,#113821,#113822,
#113823,#113824,#113825,#113826,#113827,#113828,#113829,#113830),
 .UNSPECIFIED.,.F.,.F.,(4,3,3,3,3,3,3,3,3,3,3,3,3,3,3,3,3,3,3,3,3,3,3,3,
3,3,3,3,3,3,3,3,3,3,3,3,3,3,3,3,3,3,3,3,3,3,3,3,3,3,3,3,3,3,3,3,3,3,3,3,
3,3,3,3,3,3,3,3,3,3,3,3,3,4),(1328.89369246847,1328.9571930285,1329.04093174035,
1329.12456725171,1329.20811969511,1329.29160913096,1329.37506308158,1329.45849957542,
1329.54193668518,1329.6253924801,1329.70893697283,1329.79252605577,1329.87624932332,
1329.95692903922,1330.04066775107,1330.12430326243,1330.20785570583,1330.29134514168,
1330.3747990923,1330.45823558614,1330.5416726959,1330.62512849082,1330.70867298355,
1330.79226206649,1330.87598533405,1330.95666504994,1331.04040376179,1331.12403927315,
1331.20759171655,1331.2910811524,1331.37453510302,1331.45797159686,1331.54140870662,
1331.62486450154,1331.70840899427,1331.79199807721,1331.87572134476,1331.95640106066,
1332.04013977251,1332.12377528387,1332.20732772727,1332.29081716312,1332.37427111374,
1332.45770760758,1332.54114471734,1332.62460051226,1332.70814500499,1332.79173408793,
1332.87545735548,1332.95613707138,1333.03987578323,1333.12351129459,1333.20706373799,
1333.29055317384,1333.37400712446,1333.4574436183,1333.54088072806,1333.62433652297,
1333.7078810157,1333.79147009865,1333.8751933662,1333.9558730821,1334.03961349212,
1334.12325030642,1334.20680365916,1334.29029361203,1334.37374607242,1334.45718051726,
1334.54061501886,1334.62406764562,1334.70760129389,1334.79117930146,1334.87487359557,
1334.92564171414),.UNSPECIFIED.);
#896=B_SPLINE_CURVE_WITH_KNOTS('',3,(#113831,#113832,#113833,#113834,#113835,
#113836,#113837,#113838,#113839,#113840),.UNSPECIFIED.,.F.,.F.,(4,3,3,4),
(1328.64186781057,1328.72466467188,1328.80917857012,1328.89369246835),
 .UNSPECIFIED.);
#897=B_SPLINE_CURVE_WITH_KNOTS('',3,(#113842,#113843,#113844,#113845,#113846,
#113847,#113848,#113849,#113850,#113851),.UNSPECIFIED.,.F.,.F.,(4,3,3,4),
(1328.64295744021,1328.72701616532,1328.81106206604,1328.89369246847),
 .UNSPECIFIED.);
#898=B_SPLINE_CURVE_WITH_KNOTS('',3,(#113852,#113853,#113854,#113855,#113856,
#113857,#113858,#113859,#113860,#113861,#113862,#113863,#113864,#113865,
#113866,#113867,#113868,#113869,#113870,#113871,#113872,#113873,#113874,
#113875,#113876,#113877,#113878,#113879,#113880,#113881,#113882,#113883,
#113884,#113885,#113886,#113887,#113888,#113889,#113890,#113891,#113892,
#113893,#113894,#113895,#113896,#113897,#113898,#113899,#113900,#113901,
#113902,#113903,#113904,#113905,#113906,#113907,#113908,#113909,#113910,
#113911,#113912,#113913,#113914,#113915,#113916,#113917,#113918,#113919,
#113920,#113921,#113922,#113923,#113924,#113925,#113926,#113927,#113928,
#113929,#113930,#113931,#113932,#113933,#113934,#113935,#113936,#113937,
#113938,#113939,#113940,#113941,#113942,#113943,#113944,#113945,#113946,
#113947,#113948,#113949,#113950,#113951,#113952,#113953,#113954,#113955,
#113956,#113957,#113958,#113959,#113960,#113961,#113962,#113963,#113964,
#113965,#113966,#113967,#113968,#113969,#113970,#113971,#113972,#113973,
#113974,#113975,#113976,#113977,#113978,#113979,#113980,#113981,#113982,
#113983,#113984,#113985,#113986,#113987,#113988,#113989,#113990,#113991,
#113992,#113993,#113994,#113995,#113996,#113997,#113998,#113999,#114000,
#114001,#114002,#114003,#114004,#114005,#114006,#114007,#114008,#114009,
#114010,#114011,#114012,#114013,#114014,#114015,#114016,#114017,#114018,
#114019,#114020,#114021,#114022,#114023,#114024,#114025,#114026,#114027,
#114028,#114029,#114030,#114031,#114032,#114033,#114034,#114035,#114036,
#114037,#114038,#114039,#114040,#114041,#114042,#114043,#114044,#114045,
#114046,#114047,#114048,#114049,#114050,#114051,#114052,#114053,#114054,
#114055,#114056,#114057,#114058,#114059,#114060,#114061,#114062,#114063,
#114064,#114065,#114066,#114067,#114068),.UNSPECIFIED.,.F.,.F.,(4,3,3,3,
3,3,3,3,3,3,3,3,3,3,3,3,3,3,3,3,3,3,3,3,3,3,3,3,3,3,3,3,3,3,3,3,3,3,3,3,
3,3,3,3,3,3,3,3,3,3,3,3,3,3,3,3,3,3,3,3,3,3,3,3,3,3,3,3,3,3,3,3,4),(1328.89369246867,
1328.98771917001,1329.08211115352,1329.17702388892,1329.26748364822,1329.35122236007,
1329.43485787143,1329.51841031483,1329.60189975068,1329.6853537013,1329.76879019514,
1329.8522273049,1329.93568309982,1330.01922759255,1330.10281667549,1330.18653994305,
1330.26721965894,1330.35095837079,1330.43459388215,1330.51814632555,1330.6016357614,
1330.68508971202,1330.76852620586,1330.85196331562,1330.93541911054,1331.01896360326,
1331.10255268621,1331.18627595376,1331.26695566966,1331.35069438151,1331.43432989287,
1331.51788233627,1331.60137177212,1331.68482572274,1331.76826221658,1331.85169932634,
1331.93515512126,1332.01869961399,1332.10228869693,1332.18601196448,1332.26669168038,
1332.35043039223,1332.43406590359,1332.51761834699,1332.60110778284,1332.68456173346,
1332.7679982273,1332.85143533706,1332.93489113198,1333.01843562471,1333.10202470765,
1333.18574797521,1333.2664276911,1333.35016640295,1333.43380191431,1333.51735435771,
1333.60084379356,1333.68429774418,1333.76773423802,1333.85117134778,1333.9346271427,
1334.01817163543,1334.10176071837,1334.18548398592,1334.26616370182,1334.34890444293,
1334.43155063891,1334.51412132194,1334.59663545726,1334.67912307257,1334.76159207413,
1334.84409348801,1334.92504027154),.UNSPECIFIED.);
#899=B_SPLINE_CURVE_WITH_KNOTS('',3,(#114074,#114075,#114076,#114077,#114078,
#114079,#114080,#114081,#114082,#114083,#114084,#114085,#114086,#114087,
#114088,#114089,#114090,#114091,#114092,#114093,#114094,#114095,#114096,
#114097,#114098,#114099,#114100,#114101,#114102,#114103,#114104,#114105,
#114106,#114107,#114108,#114109,#114110,#114111,#114112,#114113,#114114,
#114115,#114116,#114117,#114118,#114119,#114120,#114121,#114122,#114123,
#114124,#114125,#114126,#114127,#114128,#114129,#114130,#114131,#114132,
#114133,#114134,#114135,#114136,#114137,#114138,#114139,#114140,#114141,
#114142,#114143,#114144,#114145,#114146,#114147,#114148,#114149,#114150,
#114151,#114152,#114153,#114154,#114155,#114156,#114157,#114158,#114159,
#114160,#114161,#114162,#114163,#114164,#114165,#114166,#114167,#114168,
#114169,#114170,#114171,#114172,#114173,#114174,#114175,#114176,#114177,
#114178,#114179,#114180,#114181,#114182,#114183,#114184,#114185,#114186,
#114187,#114188,#114189,#114190,#114191,#114192,#114193,#114194,#114195,
#114196,#114197,#114198,#114199,#114200,#114201,#114202,#114203,#114204,
#114205,#114206,#114207,#114208,#114209,#114210,#114211,#114212,#114213,
#114214,#114215,#114216,#114217,#114218,#114219,#114220,#114221,#114222,
#114223,#114224,#114225,#114226,#114227,#114228,#114229,#114230,#114231,
#114232,#114233,#114234,#114235,#114236,#114237,#114238,#114239,#114240,
#114241,#114242,#114243,#114244,#114245,#114246,#114247,#114248,#114249,
#114250,#114251,#114252,#114253,#114254,#114255,#114256,#114257,#114258,
#114259,#114260,#114261,#114262,#114263,#114264,#114265,#114266,#114267,
#114268,#114269,#114270,#114271,#114272,#114273,#114274,#114275,#114276,
#114277,#114278,#114279,#114280,#114281,#114282,#114283,#114284,#114285,
#114286,#114287,#114288,#114289,#114290,#114291,#114292,#114293),
 .UNSPECIFIED.,.F.,.F.,(4,3,3,3,3,3,3,3,3,3,3,3,3,3,3,3,3,3,3,3,3,3,3,3,
3,3,3,3,3,3,3,3,3,3,3,3,3,3,3,3,3,3,3,3,3,3,3,3,3,3,3,3,3,3,3,3,3,3,3,3,
3,3,3,3,3,3,3,3,3,3,3,3,3,4),(1335.17687777579,1335.25930715332,1335.34167396931,
1335.42400671075,1335.50632418332,1335.58864534924,1335.67098917132,1335.75342036133,
1335.83590140164,1335.91850174716,1335.95534510354,1336.03908381539,1336.12271932675,
1336.20627177015,1336.289761206,1336.37321515662,1336.45665165046,1336.54008876022,
1336.62354455513,1336.70708904786,1336.7906781308,1336.87440139836,1336.95508111426,
1337.03881982611,1337.12245533747,1337.20600778087,1337.28949721672,1337.37295116734,
1337.45638766118,1337.53982477094,1337.62328056586,1337.70682505859,1337.79041414153,
1337.87413740909,1337.95481712498,1338.03855583683,1338.12219134819,1338.20574379159,
1338.28923322744,1338.37268717806,1338.4561236719,1338.53956078166,1338.62301657658,
1338.70656106931,1338.79015015225,1338.8738734198,1338.9545531357,1339.03829184755,
1339.12192735891,1339.20547980231,1339.28896923816,1339.37242318878,1339.45585968262,
1339.53929679238,1339.6227525873,1339.70629708003,1339.78988616297,1339.87360943052,
1339.95428914642,1340.03802785827,1340.12166336963,1340.20521581303,1340.28870524888,
1340.3721591995,1340.45559569334,1340.5390328031,1340.62248859802,1340.70603309075,
1340.78962217369,1340.87334544125,1340.95402515714,1341.04184027084,1341.12946320536,
1341.2097260217),.UNSPECIFIED.);
#900=B_SPLINE_CURVE_WITH_KNOTS('',3,(#114294,#114295,#114296,#114297,#114298,
#114299,#114300,#114301,#114302,#114303),.UNSPECIFIED.,.F.,.F.,(4,3,3,4),
(1334.92564171414,1334.95560909282,1335.07008319006,1335.17687777565),
 .UNSPECIFIED.);
#901=B_SPLINE_CURVE_WITH_KNOTS('',3,(#114305,#114306,#114307,#114308,#114309,
#114310,#114311,#114312,#114313,#114314),.UNSPECIFIED.,.F.,.F.,(4,3,3,4),
(1334.92504027154,1335.00761918804,1335.09224848178,1335.17687777552),
 .UNSPECIFIED.);
#902=B_SPLINE_CURVE_WITH_KNOTS('',3,(#114315,#114316,#114317,#114318,#114319,
#114320,#114321,#114322,#114323,#114324,#114325,#114326,#114327,#114328,
#114329,#114330,#114331,#114332,#114333,#114334,#114335,#114336,#114337,
#114338,#114339,#114340,#114341,#114342,#114343,#114344,#114345,#114346,
#114347,#114348,#114349,#114350,#114351,#114352,#114353,#114354,#114355,
#114356,#114357,#114358,#114359,#114360,#114361,#114362,#114363,#114364,
#114365,#114366,#114367,#114368,#114369,#114370,#114371,#114372,#114373,
#114374,#114375,#114376,#114377,#114378,#114379,#114380,#114381,#114382,
#114383,#114384,#114385,#114386,#114387,#114388,#114389,#114390,#114391,
#114392,#114393,#114394,#114395,#114396,#114397,#114398,#114399,#114400,
#114401,#114402,#114403,#114404,#114405,#114406,#114407,#114408,#114409,
#114410,#114411,#114412,#114413,#114414,#114415,#114416,#114417,#114418,
#114419,#114420,#114421,#114422,#114423,#114424,#114425,#114426,#114427,
#114428,#114429,#114430,#114431,#114432,#114433,#114434,#114435,#114436,
#114437,#114438,#114439,#114440,#114441,#114442,#114443,#114444,#114445,
#114446,#114447,#114448,#114449,#114450,#114451,#114452,#114453,#114454,
#114455,#114456,#114457,#114458,#114459,#114460,#114461,#114462,#114463,
#114464,#114465,#114466,#114467,#114468,#114469,#114470,#114471,#114472,
#114473,#114474,#114475,#114476,#114477,#114478,#114479,#114480,#114481,
#114482,#114483,#114484,#114485,#114486,#114487,#114488,#114489,#114490,
#114491,#114492,#114493,#114494,#114495,#114496,#114497,#114498,#114499,
#114500,#114501,#114502,#114503,#114504,#114505,#114506,#114507,#114508,
#114509,#114510,#114511,#114512,#114513,#114514,#114515,#114516,#114517,
#114518,#114519,#114520,#114521,#114522,#114523,#114524,#114525,#114526,
#114527,#114528,#114529,#114530,#114531,#114532,#114533,#114534),
 .UNSPECIFIED.,.F.,.F.,(4,3,3,3,3,3,3,3,3,3,3,3,3,3,3,3,3,3,3,3,3,3,3,3,
3,3,3,3,3,3,3,3,3,3,3,3,3,3,3,3,3,3,3,3,3,3,3,3,3,3,3,3,3,3,3,3,3,3,3,3,
3,3,3,3,3,3,3,3,3,3,3,3,3,4),(1335.17687777565,1335.26589971254,1335.34963842439,
1335.43327393575,1335.51682637915,1335.600315815,1335.68376976562,1335.76720625946,
1335.85064336922,1335.93409916414,1336.01764365687,1336.10123273981,1336.18495600736,
1336.26563572326,1336.34937443511,1336.43300994647,1336.51656238987,1336.60005182572,
1336.68350577634,1336.76694227018,1336.85037937994,1336.93383517486,1337.01737966758,
1337.10096875053,1337.18469201808,1337.26537173398,1337.34911044583,1337.43274595719,
1337.51629840059,1337.59978783644,1337.68324178706,1337.7666782809,1337.85011539066,
1337.93357118558,1338.01711567831,1338.10070476125,1338.1844280288,1338.2651077447,
1338.34884645655,1338.43248196791,1338.51603441131,1338.59952384716,1338.68297779778,
1338.76641429162,1338.84985140138,1338.9333071963,1339.01685168903,1339.10044077197,
1339.18416403952,1339.26484375542,1339.34858246727,1339.43221797863,1339.51577042203,
1339.59925985788,1339.6827138085,1339.76615030234,1339.8495874121,1339.93304320702,
1340.01658769975,1340.10017678269,1340.18390005025,1340.26457976614,1340.34832166108,
1340.43195962205,1340.51551378467,1340.60216282896,1340.68561311271,1340.76904558688,
1340.85247832314,1340.93592938927,1341.01945564263,1341.10302667224,1341.18669949919,
1341.20870613901),.UNSPECIFIED.);
#903=B_SPLINE_CURVE_WITH_KNOTS('',3,(#114540,#114541,#114542,#114543,#114544,
#114545,#114546,#114547,#114548,#114549,#114550,#114551,#114552,#114553,
#114554,#114555,#114556,#114557,#114558,#114559,#114560,#114561,#114562,
#114563,#114564,#114565,#114566,#114567,#114568,#114569,#114570,#114571,
#114572,#114573,#114574,#114575,#114576,#114577,#114578,#114579,#114580,
#114581,#114582,#114583,#114584,#114585,#114586,#114587,#114588,#114589,
#114590,#114591,#114592,#114593,#114594,#114595,#114596,#114597,#114598,
#114599,#114600,#114601,#114602,#114603,#114604,#114605,#114606,#114607,
#114608,#114609,#114610,#114611,#114612,#114613,#114614,#114615,#114616,
#114617,#114618,#114619,#114620,#114621,#114622,#114623,#114624,#114625,
#114626,#114627,#114628,#114629,#114630,#114631,#114632,#114633,#114634,
#114635,#114636,#114637,#114638,#114639,#114640,#114641,#114642,#114643,
#114644,#114645,#114646,#114647,#114648,#114649,#114650,#114651,#114652,
#114653,#114654,#114655,#114656,#114657,#114658,#114659,#114660,#114661,
#114662,#114663,#114664,#114665,#114666,#114667,#114668,#114669,#114670,
#114671,#114672,#114673,#114674,#114675,#114676,#114677,#114678,#114679,
#114680,#114681,#114682,#114683,#114684,#114685,#114686,#114687,#114688,
#114689,#114690,#114691,#114692,#114693,#114694,#114695,#114696,#114697,
#114698,#114699,#114700,#114701,#114702,#114703,#114704,#114705,#114706,
#114707,#114708,#114709,#114710,#114711,#114712,#114713,#114714,#114715,
#114716,#114717,#114718,#114719,#114720,#114721,#114722,#114723,#114724,
#114725,#114726,#114727,#114728,#114729,#114730,#114731,#114732,#114733,
#114734,#114735,#114736,#114737,#114738,#114739,#114740,#114741,#114742,
#114743,#114744,#114745,#114746,#114747,#114748,#114749,#114750,#114751,
#114752,#114753,#114754,#114755,#114756,#114757,#114758,#114759),
 .UNSPECIFIED.,.F.,.F.,(4,3,3,3,3,3,3,3,3,3,3,3,3,3,3,3,3,3,3,3,3,3,3,3,
3,3,3,3,3,3,3,3,3,3,3,3,3,3,3,3,3,3,3,3,3,3,3,3,3,3,3,3,3,3,3,3,3,3,3,3,
3,3,3,3,3,3,3,3,3,3,3,3,3,4),(1341.46006308301,1341.54769406803,1341.63544859998,
1341.72341826644,1341.81150254846,1341.89978983354,1341.95376116786,1342.03749987971,
1342.12113539107,1342.20468783447,1342.28817727032,1342.37163122094,1342.45506771478,
1342.53850482454,1342.62196061946,1342.70550511219,1342.78909419513,1342.87281746268,
1342.95349717858,1343.03723589043,1343.12087140179,1343.20442384519,1343.28791328104,
1343.37136723166,1343.4548037255,1343.53824083526,1343.62169663017,1343.7052411229,
1343.78883020584,1343.8725534734,1343.9532331893,1344.03697190115,1344.12060741251,
1344.20415985591,1344.28764929176,1344.37110324238,1344.45453973623,1344.53797684598,
1344.6214326409,1344.70497713363,1344.78856621657,1344.87228948413,1344.95296920002,
1345.03670791187,1345.12034342323,1345.20389586663,1345.28738530249,1345.3708392531,
1345.45427574695,1345.5377128567,1345.62116865162,1345.70471314435,1345.78830222729,
1345.87202549485,1345.95270521075,1346.0364439226,1346.12007943396,1346.20363187736,
1346.28712131322,1346.37057526383,1346.45401175768,1346.53744886743,1346.62090466235,
1346.70444915508,1346.78803823802,1346.87176150558,1346.95244122147,1347.03498522075,
1347.11743280076,1347.19980314424,1347.28211245127,1347.3643860278,1347.44665387749,
1347.49169700283),.UNSPECIFIED.);
#904=B_SPLINE_CURVE_WITH_KNOTS('',3,(#114760,#114761,#114762,#114763,#114764,
#114765,#114766,#114767,#114768,#114769),.UNSPECIFIED.,.F.,.F.,(4,3,3,4),
(1341.2097260217,1341.29709430543,1341.38431122704,1341.46006308283),
 .UNSPECIFIED.);
#905=B_SPLINE_CURVE_WITH_KNOTS('',3,(#114771,#114772,#114773,#114774,#114775,
#114776,#114777,#114778,#114779,#114780),.UNSPECIFIED.,.F.,.F.,(4,3,3,4),
(1341.20870613901,1341.26431577686,1341.3858503157,1341.46006308283),
 .UNSPECIFIED.);
#906=B_SPLINE_CURVE_WITH_KNOTS('',3,(#114781,#114782,#114783,#114784,#114785,
#114786,#114787,#114788,#114789,#114790,#114791,#114792,#114793,#114794,
#114795,#114796,#114797,#114798,#114799,#114800,#114801,#114802,#114803,
#114804,#114805,#114806,#114807,#114808,#114809,#114810,#114811,#114812,
#114813,#114814,#114815,#114816,#114817,#114818,#114819,#114820,#114821,
#114822,#114823,#114824,#114825,#114826,#114827,#114828,#114829,#114830,
#114831,#114832,#114833,#114834,#114835,#114836,#114837,#114838,#114839,
#114840,#114841,#114842,#114843,#114844,#114845,#114846,#114847,#114848,
#114849,#114850,#114851,#114852,#114853,#114854,#114855,#114856,#114857,
#114858,#114859,#114860,#114861,#114862,#114863,#114864,#114865,#114866,
#114867,#114868,#114869,#114870,#114871,#114872,#114873,#114874,#114875,
#114876,#114877,#114878,#114879,#114880,#114881,#114882,#114883,#114884,
#114885,#114886,#114887,#114888,#114889,#114890,#114891,#114892,#114893,
#114894,#114895,#114896,#114897,#114898,#114899,#114900,#114901,#114902,
#114903,#114904,#114905,#114906,#114907,#114908,#114909,#114910,#114911,
#114912,#114913,#114914,#114915,#114916,#114917,#114918,#114919,#114920,
#114921,#114922,#114923,#114924,#114925,#114926,#114927,#114928,#114929,
#114930,#114931,#114932,#114933,#114934,#114935,#114936,#114937,#114938,
#114939,#114940,#114941,#114942,#114943,#114944,#114945,#114946,#114947,
#114948,#114949,#114950,#114951,#114952,#114953,#114954,#114955,#114956,
#114957,#114958,#114959,#114960,#114961,#114962,#114963,#114964,#114965,
#114966,#114967,#114968,#114969,#114970,#114971,#114972,#114973,#114974,
#114975,#114976,#114977,#114978,#114979,#114980,#114981,#114982,#114983,
#114984,#114985,#114986,#114987,#114988,#114989,#114990,#114991,#114992,
#114993,#114994,#114995,#114996,#114997,#114998,#114999,#115000),
 .UNSPECIFIED.,.F.,.F.,(4,3,3,3,3,3,3,3,3,3,3,3,3,3,3,3,3,3,3,3,3,3,3,3,
3,3,3,3,3,3,3,3,3,3,3,3,3,3,3,3,3,3,3,3,3,3,3,3,3,3,3,3,3,3,3,3,3,3,3,3,
3,3,3,3,3,3,3,3,3,3,3,3,3,4),(1341.46006308294,1341.54243437283,1341.62473547885,
1341.7069925143,1341.78922750957,1341.87145948455,1341.9537074545,1342.03603902136,
1342.11841455711,1342.20091606359,1342.26405178758,1342.34779049943,1342.43142601079,
1342.51497845419,1342.59846789004,1342.68192184066,1342.7653583345,1342.84879544426,
1342.93225123918,1343.01579573191,1343.09938481485,1343.1831080824,1343.2637877983,
1343.34752651015,1343.43116202151,1343.51471446491,1343.59820390076,1343.68165785138,
1343.76509434522,1343.84853145498,1343.9319872499,1344.01553174262,1344.09912082557,
1344.18284409312,1344.26352380902,1344.34726252087,1344.43089803223,1344.51445047563,
1344.59793991148,1344.6813938621,1344.76483035594,1344.8482674657,1344.93172326062,
1345.01526775335,1345.09885683629,1345.18258010384,1345.26325981974,1345.34699853159,
1345.43063404295,1345.51418648635,1345.5976759222,1345.68112987282,1345.76456636666,
1345.84800347642,1345.93145927134,1346.01500376407,1346.09859284701,1346.18231611456,
1346.26299583046,1346.34673454231,1346.43037005367,1346.51392249707,1346.59741193292,
1346.68086588354,1346.76430237738,1346.84773948714,1346.93119528206,1347.01473977479,
1347.09832885773,1347.18205212529,1347.26273184118,1347.35159396868,1347.44024804493,
1347.49294053409),.UNSPECIFIED.);
#907=B_SPLINE_CURVE_WITH_KNOTS('',3,(#115006,#115007,#115008,#115009,#115010,
#115011,#115012,#115013,#115014,#115015,#115016,#115017,#115018,#115019,
#115020,#115021,#115022,#115023,#115024,#115025,#115026,#115027,#115028,
#115029,#115030,#115031,#115032,#115033,#115034,#115035,#115036,#115037,
#115038,#115039,#115040,#115041,#115042,#115043,#115044,#115045,#115046,
#115047,#115048,#115049,#115050,#115051,#115052,#115053,#115054,#115055,
#115056,#115057,#115058,#115059,#115060,#115061,#115062,#115063,#115064,
#115065,#115066,#115067,#115068,#115069,#115070,#115071,#115072,#115073,
#115074,#115075,#115076,#115077,#115078,#115079,#115080,#115081,#115082,
#115083,#115084,#115085,#115086,#115087,#115088,#115089,#115090,#115091,
#115092,#115093,#115094,#115095,#115096,#115097,#115098,#115099,#115100,
#115101,#115102,#115103,#115104,#115105,#115106,#115107,#115108,#115109,
#115110,#115111,#115112,#115113,#115114,#115115,#115116,#115117,#115118,
#115119,#115120,#115121,#115122,#115123,#115124,#115125,#115126,#115127,
#115128,#115129,#115130,#115131,#115132,#115133,#115134,#115135,#115136,
#115137,#115138,#115139,#115140,#115141,#115142,#115143,#115144,#115145,
#115146,#115147,#115148,#115149,#115150,#115151,#115152,#115153,#115154,
#115155,#115156,#115157,#115158,#115159,#115160,#115161,#115162,#115163,
#115164,#115165,#115166,#115167,#115168,#115169,#115170,#115171,#115172,
#115173,#115174,#115175,#115176,#115177,#115178,#115179,#115180,#115181,
#115182,#115183,#115184,#115185,#115186,#115187,#115188,#115189,#115190,
#115191,#115192,#115193,#115194,#115195,#115196,#115197,#115198,#115199,
#115200,#115201,#115202,#115203,#115204,#115205,#115206,#115207,#115208,
#115209,#115210,#115211,#115212,#115213,#115214,#115215,#115216,#115217,
#115218,#115219,#115220,#115221,#115222),.UNSPECIFIED.,.F.,.F.,(4,3,3,3,
3,3,3,3,3,3,3,3,3,3,3,3,3,3,3,3,3,3,3,3,3,3,3,3,3,3,3,3,3,3,3,3,3,3,3,3,
3,3,3,3,3,3,3,3,3,3,3,3,3,3,3,3,3,3,3,3,3,3,3,3,3,3,3,3,3,3,3,3,4),(1347.74324839001,
1347.86086686141,1347.95217723219,1348.03591594404,1348.1195514554,1348.2031038988,
1348.28659333465,1348.37004728527,1348.45348377911,1348.53692088887,1348.62037668379,
1348.70392117652,1348.78751025946,1348.87123352702,1348.95191324291,1349.03565195476,
1349.11928746612,1349.20283990952,1349.28632934537,1349.36978329599,1349.45321978983,
1349.53665689959,1349.6201126945,1349.70365718723,1349.78724627017,1349.87096953773,
1349.95164925363,1350.03538796548,1350.11902347684,1350.20257592024,1350.28606535609,
1350.36951930671,1350.45295580055,1350.53639291031,1350.61984870523,1350.70339319796,
1350.7869822809,1350.87070554845,1350.95138526435,1351.0351239762,1351.11875948756,
1351.20231193096,1351.28580136681,1351.36925531743,1351.45269181127,1351.53612892103,
1351.61958471595,1351.70312920868,1351.78671829162,1351.87044155917,1351.95112127507,
1352.03485998692,1352.11849549828,1352.20204794168,1352.28553737753,1352.36899132815,
1352.45242782199,1352.53586493175,1352.61932072667,1352.7028652194,1352.78645430234,
1352.8701775699,1352.95085728579,1353.03460653273,1353.11825025982,1353.20179354662,
1353.28527988452,1353.36872739298,1353.45215416144,1353.53560636913,1353.61906939208,
1353.70260654731,1353.7747814876),.UNSPECIFIED.);
#908=B_SPLINE_CURVE_WITH_KNOTS('',3,(#115223,#115224,#115225,#115226,#115227,
#115228,#115229,#115230,#115231,#115232),.UNSPECIFIED.,.F.,.F.,(4,3,3,4),
(1347.49169700283,1347.57399734248,1347.65862286617,1347.74324838987),
 .UNSPECIFIED.);
#909=B_SPLINE_CURVE_WITH_KNOTS('',3,(#115234,#115235,#115236,#115237,#115238,
#115239,#115240,#115241,#115242,#115243),.UNSPECIFIED.,.F.,.F.,(4,3,3,4),
(1347.49294053409,1347.581325312,1347.66951161927,1347.74324838985),
 .UNSPECIFIED.);
#910=B_SPLINE_CURVE_WITH_KNOTS('',3,(#115244,#115245,#115246,#115247,#115248,
#115249,#115250,#115251,#115252,#115253,#115254,#115255,#115256,#115257,
#115258,#115259,#115260,#115261,#115262,#115263,#115264,#115265,#115266,
#115267,#115268,#115269,#115270,#115271,#115272,#115273,#115274,#115275,
#115276,#115277,#115278,#115279,#115280,#115281,#115282,#115283,#115284,
#115285,#115286,#115287,#115288,#115289,#115290,#115291,#115292,#115293,
#115294,#115295,#115296,#115297,#115298,#115299,#115300,#115301,#115302,
#115303,#115304,#115305,#115306,#115307,#115308,#115309,#115310,#115311,
#115312,#115313,#115314,#115315,#115316,#115317,#115318,#115319,#115320,
#115321,#115322,#115323,#115324,#115325,#115326,#115327,#115328,#115329,
#115330,#115331,#115332,#115333,#115334,#115335,#115336,#115337,#115338,
#115339,#115340,#115341,#115342,#115343,#115344,#115345,#115346,#115347,
#115348,#115349,#115350,#115351,#115352,#115353,#115354,#115355,#115356,
#115357,#115358,#115359,#115360,#115361,#115362,#115363,#115364,#115365,
#115366,#115367,#115368,#115369,#115370,#115371,#115372,#115373,#115374,
#115375,#115376,#115377,#115378,#115379,#115380,#115381,#115382,#115383,
#115384,#115385,#115386,#115387,#115388,#115389,#115390,#115391,#115392,
#115393,#115394,#115395,#115396,#115397,#115398,#115399,#115400,#115401,
#115402,#115403,#115404,#115405,#115406,#115407,#115408,#115409,#115410,
#115411,#115412,#115413,#115414,#115415,#115416,#115417,#115418,#115419,
#115420,#115421,#115422,#115423,#115424,#115425,#115426,#115427,#115428,
#115429,#115430,#115431,#115432,#115433,#115434,#115435,#115436,#115437,
#115438,#115439,#115440,#115441,#115442,#115443,#115444,#115445,#115446,
#115447,#115448,#115449,#115450,#115451,#115452,#115453,#115454,#115455,
#115456,#115457,#115458,#115459,#115460,#115461,#115462,#115463),
 .UNSPECIFIED.,.F.,.F.,(4,3,3,3,3,3,3,3,3,3,3,3,3,3,3,3,3,3,3,3,3,3,3,3,
3,3,3,3,3,3,3,3,3,3,3,3,3,3,3,3,3,3,3,3,3,3,3,3,3,3,3,3,3,3,3,3,3,3,3,3,
3,3,3,3,3,3,3,3,3,3,3,3,3,4),(1347.74324839001,1347.82998362966,1347.91681006014,
1348.0038194816,1348.0909222109,1348.17822185273,1348.2624678519,1348.34620656375,
1348.42984207511,1348.51339451851,1348.59688395436,1348.68033790498,1348.76377439882,
1348.84721150858,1348.9306673035,1349.01421179623,1349.09780087917,1349.18152414672,
1349.26220386262,1349.34594257447,1349.42957808583,1349.51313052923,1349.59661996508,
1349.6800739157,1349.76351040954,1349.8469475193,1349.93040331422,1350.01394780694,
1350.09753688989,1350.18126015744,1350.26193987334,1350.34567858519,1350.42931409655,
1350.51286653995,1350.5963559758,1350.67980992642,1350.76324642026,1350.84668353002,
1350.93013932494,1351.01368381766,1351.09727290061,1351.18099616816,1351.26167588406,
1351.34541459591,1351.42905010727,1351.51260255067,1351.59609198652,1351.67954593714,
1351.76298243098,1351.84641954074,1351.92987533566,1352.01341982838,1352.09700891133,
1352.18073217888,1352.26141189478,1352.34515060663,1352.42878611799,1352.51233856139,
1352.59582799724,1352.67928194786,1352.7627184417,1352.84615555146,1352.92961134638,
1353.01315583911,1353.09674492205,1353.1804681896,1353.2611479055,1353.3438127483,
1353.42638012879,1353.50886915535,1353.59129380154,1353.67368188061,1353.75605725512,
1353.77499599392),.UNSPECIFIED.);
#911=B_SPLINE_CURVE_WITH_KNOTS('',3,(#115469,#115470,#115471,#115472,#115473,
#115474,#115475,#115476,#115477,#115478,#115479,#115480,#115481,#115482,
#115483,#115484,#115485,#115486,#115487,#115488,#115489,#115490,#115491,
#115492,#115493,#115494,#115495,#115496,#115497,#115498,#115499,#115500,
#115501,#115502,#115503,#115504,#115505,#115506,#115507,#115508,#115509,
#115510,#115511,#115512,#115513,#115514,#115515,#115516,#115517,#115518,
#115519,#115520,#115521,#115522,#115523,#115524,#115525,#115526,#115527,
#115528,#115529,#115530,#115531,#115532,#115533,#115534,#115535,#115536,
#115537,#115538,#115539,#115540,#115541,#115542,#115543,#115544,#115545,
#115546,#115547,#115548,#115549,#115550,#115551,#115552,#115553,#115554,
#115555,#115556,#115557,#115558,#115559,#115560,#115561,#115562,#115563,
#115564,#115565,#115566,#115567,#115568,#115569,#115570,#115571,#115572,
#115573,#115574,#115575,#115576,#115577,#115578,#115579,#115580,#115581,
#115582,#115583,#115584,#115585,#115586,#115587,#115588,#115589,#115590,
#115591,#115592,#115593,#115594,#115595,#115596,#115597,#115598,#115599,
#115600,#115601,#115602,#115603,#115604,#115605,#115606,#115607,#115608,
#115609,#115610,#115611,#115612,#115613,#115614,#115615,#115616,#115617,
#115618,#115619,#115620,#115621,#115622,#115623,#115624,#115625,#115626,
#115627,#115628,#115629,#115630,#115631,#115632,#115633,#115634,#115635,
#115636,#115637,#115638,#115639,#115640,#115641,#115642,#115643,#115644,
#115645,#115646,#115647,#115648,#115649,#115650,#115651,#115652,#115653,
#115654,#115655,#115656,#115657,#115658,#115659,#115660,#115661,#115662,
#115663,#115664,#115665,#115666,#115667,#115668,#115669,#115670,#115671,
#115672,#115673,#115674,#115675,#115676,#115677,#115678,#115679,#115680,
#115681,#115682,#115683,#115684,#115685,#115686,#115687,#115688,#115689,
#115690,#115691),.UNSPECIFIED.,.F.,.F.,(4,3,3,3,3,3,3,3,3,3,3,3,3,3,3,3,
3,3,3,3,3,3,3,3,3,3,3,3,3,3,3,3,3,3,3,3,3,3,3,3,3,3,3,3,3,3,3,3,3,3,3,3,
3,3,3,3,3,3,3,3,3,3,3,3,3,3,3,3,3,3,3,3,3,3,4),(1354.02643369732,1354.10926246698,
1354.1919945879,1354.27465099099,1354.35911078052,1354.44168759419,1354.52425618646,
1354.60683535241,1354.69270884111,1354.77541043091,1354.85816826614,1354.94103893643,
1354.95032930723,1355.03406801908,1355.11770353044,1355.20125597384,1355.28474540969,
1355.36819936031,1355.45163585415,1355.53507296391,1355.61852875883,1355.70207325156,
1355.7856623345,1355.86938560205,1355.95006531795,1356.0338040298,1356.11743954116,
1356.20099198456,1356.28448142041,1356.36793537103,1356.45137186487,1356.53480897463,
1356.61826476954,1356.70180926227,1356.78539834522,1356.86912161277,1356.94980132867,
1357.03354004052,1357.11717555188,1357.20072799528,1357.28421743113,1357.36767138175,
1357.45110787559,1357.53454498535,1357.61800078027,1357.701545273,1357.78513435594,
1357.86885762349,1357.94953733939,1358.03327605124,1358.1169115626,1358.200464006,
1358.28395344185,1358.36740739247,1358.45084388631,1358.53428099607,1358.61773679099,
1358.70128128372,1358.78487036666,1358.86859363421,1358.94927335011,1359.03301206196,
1359.11664757332,1359.20020001672,1359.28368945257,1359.36714340319,1359.45057989703,
1359.53401700679,1359.6174728017,1359.70101729443,1359.78460637737,1359.86832964493,
1359.94900936083,1360.04511644553,1360.05912658141),.UNSPECIFIED.);
#912=B_SPLINE_CURVE_WITH_KNOTS('',3,(#115692,#115693,#115694,#115695,#115696,
#115697,#115698,#115699,#115700,#115701),.UNSPECIFIED.,.F.,.F.,(4,3,3,4),
(1353.7747814876,1353.86268739206,1353.95059329651,1354.02643369719),
 .UNSPECIFIED.);
#913=B_SPLINE_CURVE_WITH_KNOTS('',3,(#115703,#115704,#115705,#115706,#115707,
#115708,#115709,#115710,#115711,#115712),.UNSPECIFIED.,.F.,.F.,(4,3,3,4),
(1353.77499599392,1353.85739769724,1353.94191569721,1354.02643369719),
 .UNSPECIFIED.);
#914=B_SPLINE_CURVE_WITH_KNOTS('',3,(#115713,#115714,#115715,#115716,#115717,
#115718,#115719,#115720,#115721,#115722,#115723,#115724,#115725,#115726,
#115727,#115728,#115729,#115730,#115731,#115732,#115733,#115734,#115735,
#115736,#115737,#115738,#115739,#115740,#115741,#115742,#115743,#115744,
#115745,#115746,#115747,#115748,#115749,#115750,#115751,#115752,#115753,
#115754,#115755,#115756,#115757,#115758,#115759,#115760,#115761,#115762,
#115763,#115764,#115765,#115766,#115767,#115768,#115769,#115770,#115771,
#115772,#115773,#115774,#115775,#115776,#115777,#115778,#115779,#115780,
#115781,#115782,#115783,#115784,#115785,#115786,#115787,#115788,#115789,
#115790,#115791,#115792,#115793,#115794,#115795,#115796,#115797,#115798,
#115799,#115800,#115801,#115802,#115803,#115804,#115805,#115806,#115807,
#115808,#115809,#115810,#115811,#115812,#115813,#115814,#115815,#115816,
#115817,#115818,#115819,#115820,#115821,#115822,#115823,#115824,#115825,
#115826,#115827,#115828,#115829,#115830,#115831,#115832,#115833,#115834,
#115835,#115836,#115837,#115838,#115839,#115840,#115841,#115842,#115843,
#115844,#115845,#115846,#115847,#115848,#115849,#115850,#115851,#115852,
#115853,#115854,#115855,#115856,#115857,#115858,#115859,#115860,#115861,
#115862,#115863,#115864,#115865,#115866,#115867,#115868,#115869,#115870,
#115871,#115872,#115873,#115874,#115875,#115876,#115877,#115878,#115879,
#115880,#115881,#115882,#115883,#115884,#115885,#115886,#115887,#115888,
#115889,#115890,#115891,#115892,#115893,#115894,#115895,#115896,#115897,
#115898,#115899,#115900,#115901,#115902,#115903,#115904,#115905,#115906,
#115907,#115908,#115909,#115910,#115911,#115912,#115913,#115914,#115915,
#115916,#115917,#115918,#115919,#115920,#115921,#115922,#115923,#115924,
#115925,#115926,#115927,#115928,#115929,#115930,#115931,#115932),
 .UNSPECIFIED.,.F.,.F.,(4,3,3,3,3,3,3,3,3,3,3,3,3,3,3,3,3,3,3,3,3,3,3,3,
3,3,3,3,3,3,3,3,3,3,3,3,3,3,3,3,3,3,3,3,3,3,3,3,3,3,3,3,3,3,3,3,3,3,3,3,
3,3,3,3,3,3,3,3,3,3,3,3,3,4),(1354.02643369734,1354.13636339471,1354.24932972749,
1354.26088391622,1354.34462262807,1354.42825813943,1354.51181058283,1354.59530001868,
1354.6787539693,1354.76219046314,1354.8456275729,1354.92908336782,1355.01262786055,
1355.09621694349,1355.17994021105,1355.26061992694,1355.34435863879,1355.42799415015,
1355.51154659355,1355.5950360294,1355.67848998002,1355.76192647386,1355.84536358362,
1355.92881937854,1356.01236387127,1356.09595295421,1356.17967622176,1356.26035593766,
1356.34409464951,1356.42773016087,1356.51128260427,1356.59477204012,1356.67822599074,
1356.76166248458,1356.84509959434,1356.92855538926,1357.01209988199,1357.09568896493,
1357.17941223248,1357.26009194838,1357.34383066023,1357.42746617159,1357.51101861499,
1357.59450805084,1357.67796200146,1357.7613984953,1357.84483560506,1357.92829139998,
1358.01183589271,1358.09542497565,1358.1791482432,1358.2598279591,1358.34356667095,
1358.42720218231,1358.51075462571,1358.59424406156,1358.67769801218,1358.76113450602,
1358.84457161578,1358.9280274107,1359.01157190343,1359.09516098637,1359.17888425392,
1359.25956396982,1359.34331486158,1359.42695989653,1359.51050366133,1359.59398999953,
1359.67743703141,1359.76086284685,1359.84430936519,1359.92776650707,1360.01128630232,
1360.05795370664),.UNSPECIFIED.);
#915=B_SPLINE_CURVE_WITH_KNOTS('',3,(#115938,#115939,#115940,#115941,#115942,
#115943,#115944,#115945,#115946,#115947,#115948,#115949,#115950,#115951,
#115952,#115953,#115954,#115955,#115956,#115957,#115958,#115959,#115960,
#115961,#115962,#115963,#115964,#115965,#115966,#115967,#115968,#115969,
#115970,#115971,#115972,#115973,#115974,#115975,#115976,#115977,#115978,
#115979,#115980,#115981,#115982,#115983,#115984,#115985,#115986,#115987,
#115988,#115989,#115990,#115991,#115992,#115993,#115994,#115995,#115996,
#115997,#115998,#115999,#116000,#116001,#116002,#116003,#116004,#116005,
#116006,#116007,#116008,#116009,#116010,#116011,#116012,#116013,#116014,
#116015,#116016,#116017,#116018,#116019,#116020,#116021,#116022,#116023,
#116024,#116025,#116026,#116027,#116028,#116029,#116030,#116031,#116032,
#116033,#116034,#116035,#116036,#116037,#116038,#116039,#116040,#116041,
#116042,#116043,#116044,#116045,#116046,#116047,#116048,#116049,#116050,
#116051,#116052,#116053,#116054,#116055,#116056,#116057,#116058,#116059,
#116060,#116061,#116062,#116063,#116064,#116065,#116066,#116067,#116068,
#116069,#116070,#116071,#116072,#116073,#116074,#116075,#116076,#116077,
#116078,#116079,#116080,#116081,#116082,#116083,#116084,#116085,#116086,
#116087,#116088,#116089,#116090,#116091,#116092,#116093,#116094,#116095,
#116096,#116097,#116098,#116099,#116100,#116101,#116102,#116103,#116104,
#116105,#116106,#116107,#116108,#116109,#116110,#116111,#116112,#116113,
#116114,#116115,#116116,#116117,#116118,#116119,#116120,#116121,#116122,
#116123,#116124,#116125,#116126,#116127,#116128,#116129,#116130,#116131,
#116132,#116133,#116134,#116135,#116136,#116137,#116138,#116139,#116140,
#116141,#116142,#116143,#116144,#116145,#116146,#116147,#116148,#116149,
#116150,#116151,#116152,#116153,#116154,#116155,#116156,#116157),
 .UNSPECIFIED.,.F.,.F.,(4,3,3,3,3,3,3,3,3,3,3,3,3,3,3,3,3,3,3,3,3,3,3,3,
3,3,3,3,3,3,3,3,3,3,3,3,3,3,3,3,3,3,3,3,3,3,3,3,3,3,3,3,3,3,3,3,3,3,3,3,
3,3,3,3,3,3,3,3,3,3,3,3,3,4),(1360.30961900437,1360.39342826463,1360.47723720546,
1360.56106336456,1360.64492428695,1360.72889024008,1360.81291395196,1360.89707373967,
1360.94874537155,1361.0324840834,1361.11611959476,1361.19967203816,1361.28316147401,
1361.36661542463,1361.45005191847,1361.53348902823,1361.61694482314,1361.70048931587,
1361.78407839881,1361.86780166637,1361.94848138227,1362.03222009412,1362.11585560548,
1362.19940804888,1362.28289748473,1362.36635143535,1362.44978792919,1362.53322503895,
1362.61668083387,1362.7002253266,1362.78381440954,1362.86753767709,1362.94821739299,
1363.03195610484,1363.1155916162,1363.1991440596,1363.28263349545,1363.36608744607,
1363.44952393991,1363.53296104967,1363.61641684459,1363.69996133732,1363.78355042026,
1363.86727368782,1363.94795340371,1364.03169211556,1364.11532762692,1364.19888007032,
1364.28236950617,1364.36582345679,1364.44925995063,1364.53269706039,1364.61615285531,
1364.69969734804,1364.78328643098,1364.86700969853,1364.94768941443,1365.03142812628,
1365.11506363764,1365.19861608104,1365.28210551689,1365.36555946751,1365.44899596135,
1365.53243307111,1365.61588886603,1365.69943335876,1365.7830224417,1365.86674570925,
1365.94742542515,1366.031491194,1366.11541841964,1366.19926592761,1366.28303873201,
1366.3419758236),.UNSPECIFIED.);
#916=B_SPLINE_CURVE_WITH_KNOTS('',3,(#116158,#116159,#116160,#116161,#116162,
#116163,#116164,#116165,#116166,#116167),.UNSPECIFIED.,.F.,.F.,(4,3,3,4),
(1360.05912658141,1360.15468423343,1360.2495959197,1360.30961900417),
 .UNSPECIFIED.);
#917=B_SPLINE_CURVE_WITH_KNOTS('',3,(#116169,#116170,#116171,#116172,#116173,
#116174,#116175,#116176,#116177,#116178,#116179,#116180,#116181),
 .UNSPECIFIED.,.F.,.F.,(4,3,3,3,4),(1360.05795370664,1360.14157474727,1360.22531677827,
1360.25929998054,1360.30961900437),.UNSPECIFIED.);
#918=B_SPLINE_CURVE_WITH_KNOTS('',3,(#116182,#116183,#116184,#116185,#116186,
#116187,#116188,#116189,#116190,#116191,#116192,#116193,#116194,#116195,
#116196,#116197,#116198,#116199,#116200,#116201,#116202,#116203,#116204,
#116205,#116206,#116207,#116208,#116209,#116210,#116211,#116212,#116213,
#116214,#116215,#116216,#116217,#116218,#116219,#116220,#116221,#116222,
#116223,#116224,#116225,#116226,#116227,#116228,#116229,#116230,#116231,
#116232,#116233,#116234,#116235,#116236,#116237,#116238,#116239,#116240,
#116241,#116242,#116243,#116244,#116245,#116246,#116247,#116248,#116249,
#116250,#116251,#116252,#116253,#116254,#116255,#116256,#116257,#116258,
#116259,#116260,#116261,#116262,#116263,#116264,#116265,#116266,#116267,
#116268,#116269,#116270,#116271,#116272,#116273,#116274,#116275,#116276,
#116277,#116278,#116279,#116280,#116281,#116282,#116283,#116284,#116285,
#116286,#116287,#116288,#116289,#116290,#116291,#116292,#116293,#116294,
#116295,#116296,#116297,#116298,#116299,#116300,#116301,#116302,#116303,
#116304,#116305,#116306,#116307,#116308,#116309,#116310,#116311,#116312,
#116313,#116314,#116315,#116316,#116317,#116318,#116319,#116320,#116321,
#116322,#116323,#116324,#116325,#116326,#116327,#116328,#116329,#116330,
#116331,#116332,#116333,#116334,#116335,#116336,#116337,#116338,#116339,
#116340,#116341,#116342,#116343,#116344,#116345,#116346,#116347,#116348,
#116349,#116350,#116351,#116352,#116353,#116354,#116355,#116356,#116357,
#116358,#116359,#116360,#116361,#116362,#116363,#116364,#116365,#116366,
#116367,#116368,#116369,#116370,#116371,#116372,#116373,#116374,#116375,
#116376,#116377,#116378,#116379,#116380,#116381,#116382,#116383,#116384,
#116385,#116386,#116387,#116388,#116389,#116390,#116391,#116392,#116393,
#116394,#116395,#116396,#116397,#116398,#116399,#116400,#116401),
 .UNSPECIFIED.,.F.,.F.,(4,3,3,3,3,3,3,3,3,3,3,3,3,3,3,3,3,3,3,3,3,3,3,3,
3,3,3,3,3,3,3,3,3,3,3,3,3,3,3,3,3,3,3,3,3,3,3,3,3,3,3,3,3,3,3,3,3,3,3,3,
3,3,3,3,3,3,3,3,3,3,3,3,3,4),(1360.30961900457,1360.39269947054,1360.47567993026,
1360.55858113247,1360.64142374873,1360.72423716446,1360.80703824373,1360.88984561224,
1360.97267789694,1361.05560003594,1361.13857341923,1361.22166751875,1361.25903599126,
1361.3427747031,1361.42641021447,1361.50996265787,1361.59345209372,1361.67690604433,
1361.76034253818,1361.84377964793,1361.92723544285,1362.01077993558,1362.09436901852,
1362.17809228608,1362.25877200198,1362.34251071383,1362.4261462252,1362.5096986686,
1362.59318810445,1362.67664205507,1362.76007854892,1362.84351565867,1362.92697145359,
1363.01051594633,1363.09410502927,1363.17782829683,1363.25850801271,1363.34224672456,
1363.42588223592,1363.50943467932,1363.59292411518,1363.67637806579,1363.75981455964,
1363.84325166939,1363.92670746431,1364.01025195704,1364.09384103998,1364.17756430754,
1364.25824402343,1364.34198273527,1364.42561824664,1364.50917069004,1364.59266012589,
1364.6761140765,1364.75955057035,1364.8429876801,1364.92644347502,1365.00998796774,
1365.09357705068,1365.17730031824,1365.25798003415,1365.341718746,1365.42535425737,
1365.50890670077,1365.59239613662,1365.67585008724,1365.75928658108,1365.84272369084,
1365.92617948576,1366.00972397849,1366.09331306143,1366.17703632899,1366.25771604487,
1366.34220623514),.UNSPECIFIED.);
#919=B_SPLINE_CURVE_WITH_KNOTS('',3,(#116407,#116408,#116409,#116410,#116411,
#116412,#116413,#116414,#116415,#116416,#116417,#116418,#116419,#116420,
#116421,#116422,#116423,#116424,#116425,#116426,#116427,#116428,#116429,
#116430,#116431,#116432,#116433,#116434,#116435,#116436,#116437,#116438,
#116439,#116440,#116441,#116442,#116443,#116444,#116445,#116446,#116447,
#116448,#116449,#116450,#116451,#116452,#116453,#116454,#116455,#116456,
#116457,#116458,#116459,#116460,#116461,#116462,#116463,#116464,#116465,
#116466,#116467,#116468,#116469,#116470,#116471,#116472,#116473,#116474,
#116475,#116476,#116477,#116478,#116479,#116480,#116481,#116482,#116483,
#116484,#116485,#116486,#116487,#116488,#116489,#116490,#116491,#116492,
#116493,#116494,#116495,#116496,#116497,#116498,#116499,#116500,#116501,
#116502,#116503,#116504,#116505,#116506,#116507,#116508,#116509,#116510,
#116511,#116512,#116513,#116514,#116515,#116516,#116517,#116518,#116519,
#116520,#116521,#116522,#116523,#116524,#116525,#116526,#116527,#116528,
#116529,#116530,#116531,#116532,#116533,#116534,#116535,#116536,#116537,
#116538,#116539,#116540,#116541,#116542,#116543,#116544,#116545,#116546,
#116547,#116548,#116549,#116550,#116551,#116552,#116553,#116554,#116555,
#116556,#116557,#116558,#116559,#116560,#116561,#116562,#116563,#116564,
#116565,#116566,#116567,#116568,#116569,#116570,#116571,#116572,#116573,
#116574,#116575,#116576,#116577,#116578,#116579,#116580,#116581,#116582,
#116583,#116584,#116585,#116586,#116587,#116588,#116589,#116590,#116591,
#116592,#116593,#116594,#116595,#116596,#116597,#116598,#116599,#116600,
#116601,#116602,#116603,#116604,#116605,#116606,#116607,#116608,#116609,
#116610,#116611,#116612,#116613,#116614,#116615,#116616,#116617,#116618,
#116619,#116620,#116621,#116622,#116623,#116624,#116625,#116626),
 .UNSPECIFIED.,.F.,.F.,(4,3,3,3,3,3,3,3,3,3,3,3,3,3,3,3,3,3,3,3,3,3,3,3,
3,3,3,3,3,3,3,3,3,3,3,3,3,3,3,3,3,3,3,3,3,3,3,3,3,3,3,3,3,3,3,3,3,3,3,3,
3,3,3,3,3,3,3,3,3,3,3,3,3,4),(1366.59280431175,1366.68827870871,1366.78420671922,
1366.8807234362,1366.94716143587,1367.03090014772,1367.11453565908,1367.19808810248,
1367.28157753833,1367.36503148894,1367.44846798279,1367.53190509255,1367.61536088746,
1367.69890538019,1367.78249446313,1367.86621773069,1367.94689744659,1368.03063615844,
1368.1142716698,1368.1978241132,1368.28131354905,1368.36476749967,1368.44820399351,
1368.53164110327,1368.61509689819,1368.69864139092,1368.78223047386,1368.86595374141,
1368.94663345731,1369.03037216916,1369.11400768052,1369.19756012392,1369.28104955977,
1369.36450351039,1369.44794000423,1369.53137711399,1369.61483290891,1369.69837740164,
1369.78196648458,1369.86568975213,1369.94636946803,1370.03010817988,1370.11374369124,
1370.19729613464,1370.28078557049,1370.36423952111,1370.44767601495,1370.53111312471,
1370.61456891963,1370.69811341236,1370.7817024953,1370.86542576285,1370.94610547875,
1371.0298441906,1371.11347970196,1371.19703214536,1371.28052158121,1371.36397553183,
1371.44741202567,1371.53084913543,1371.61430493035,1371.69784942308,1371.78143850602,
1371.86516177357,1371.94584148947,1372.03063118758,1372.11342593743,1372.19614550064,
1372.27880873553,1372.36514632023,1372.4477658086,1372.53038412638,1372.61303684556,
1372.62415907432),.UNSPECIFIED.);
#920=B_SPLINE_CURVE_WITH_KNOTS('',3,(#116627,#116628,#116629,#116630,#116631,
#116632,#116633,#116634,#116635,#116636),.UNSPECIFIED.,.F.,.F.,(4,3,3,4),
(1366.3419758236,1366.42568087771,1366.50938802422,1366.59280431155),
 .UNSPECIFIED.);
#921=B_SPLINE_CURVE_WITH_KNOTS('',3,(#116638,#116639,#116640,#116641,#116642,
#116643,#116644,#116645,#116646,#116647),.UNSPECIFIED.,.F.,.F.,(4,3,3,4),
(1366.34220623514,1366.44006982097,1366.53709108296,1366.59280431136),
 .UNSPECIFIED.);
#922=B_SPLINE_CURVE_WITH_KNOTS('',3,(#116648,#116649,#116650,#116651,#116652,
#116653,#116654,#116655,#116656,#116657,#116658,#116659,#116660,#116661,
#116662,#116663,#116664,#116665,#116666,#116667,#116668,#116669,#116670,
#116671,#116672,#116673,#116674,#116675,#116676,#116677,#116678,#116679,
#116680,#116681,#116682,#116683,#116684,#116685,#116686,#116687,#116688,
#116689,#116690,#116691,#116692,#116693,#116694,#116695,#116696,#116697,
#116698,#116699,#116700,#116701,#116702,#116703,#116704,#116705,#116706,
#116707,#116708,#116709,#116710,#116711,#116712,#116713,#116714,#116715,
#116716,#116717,#116718,#116719,#116720,#116721,#116722,#116723,#116724,
#116725,#116726,#116727,#116728,#116729,#116730,#116731,#116732,#116733,
#116734,#116735,#116736,#116737,#116738,#116739,#116740,#116741,#116742,
#116743,#116744,#116745,#116746,#116747,#116748,#116749,#116750,#116751,
#116752,#116753,#116754,#116755,#116756,#116757,#116758,#116759,#116760,
#116761,#116762,#116763,#116764,#116765,#116766,#116767,#116768,#116769,
#116770,#116771,#116772,#116773,#116774,#116775,#116776,#116777,#116778,
#116779,#116780,#116781,#116782,#116783,#116784,#116785,#116786,#116787,
#116788,#116789,#116790,#116791,#116792,#116793,#116794,#116795,#116796,
#116797,#116798,#116799,#116800,#116801,#116802,#116803,#116804,#116805,
#116806,#116807,#116808,#116809,#116810,#116811,#116812,#116813,#116814,
#116815,#116816,#116817,#116818,#116819,#116820,#116821,#116822,#116823,
#116824,#116825,#116826,#116827,#116828,#116829,#116830,#116831,#116832,
#116833,#116834,#116835,#116836,#116837,#116838,#116839,#116840,#116841,
#116842,#116843,#116844,#116845,#116846,#116847,#116848,#116849,#116850,
#116851,#116852,#116853,#116854,#116855,#116856,#116857,#116858,#116859,
#116860,#116861,#116862,#116863,#116864,#116865,#116866,#116867),
 .UNSPECIFIED.,.F.,.F.,(4,3,3,3,3,3,3,3,3,3,3,3,3,3,3,3,3,3,3,3,3,3,3,3,
3,3,3,3,3,3,3,3,3,3,3,3,3,3,3,3,3,3,3,3,3,3,3,3,3,3,3,3,3,3,3,3,3,3,3,3,
3,3,3,3,3,3,3,3,3,3,3,3,3,4),(1366.59280431155,1366.67621624537,1366.75961557606,
1366.84302033608,1366.92644855767,1367.00997275018,1367.09354558179,1367.17725891191,
1367.25745205559,1367.34119076743,1367.4248262788,1367.5083787222,1367.59186815805,
1367.67532210866,1367.7587586025,1367.84219571226,1367.92565150718,1368.0091959999,
1368.09278508284,1368.1765083504,1368.25718806631,1368.34092677816,1368.42456228952,
1368.50811473292,1368.59160416877,1368.67505811938,1368.75849461323,1368.84193172298,
1368.9253875179,1369.00893201063,1369.09252109357,1369.17624436113,1369.25692407703,
1369.34066278888,1369.42429830024,1369.50785074364,1369.5913401795,1369.67479413011,
1369.75823062396,1369.84166773371,1369.92512352863,1370.00866802136,1370.0922571043,
1370.17598037186,1370.25666008775,1370.3403987996,1370.42403431096,1370.50758675436,
1370.59107619021,1370.67453014083,1370.75796663467,1370.84140374443,1370.92485953934,
1371.00840403207,1371.09199311501,1371.17571638257,1371.25639609847,1371.34013481032,
1371.42377032168,1371.50732276508,1371.59081220094,1371.67426615155,1371.7577026454,
1371.84113975515,1371.92459555007,1372.0081400428,1372.09172912574,1372.1754523933,
1372.25613210919,1372.34069413994,1372.42511155572,1372.5094452698,1372.59369612929,
1372.62528274347),.UNSPECIFIED.);
#923=B_SPLINE_CURVE_WITH_KNOTS('',3,(#116873,#116874,#116875,#116876,#116877,
#116878,#116879,#116880,#116881,#116882,#116883,#116884,#116885,#116886,
#116887,#116888,#116889,#116890,#116891,#116892,#116893,#116894,#116895,
#116896,#116897,#116898,#116899,#116900,#116901,#116902,#116903,#116904,
#116905,#116906,#116907,#116908,#116909,#116910,#116911,#116912,#116913,
#116914,#116915,#116916,#116917,#116918,#116919,#116920,#116921,#116922,
#116923,#116924,#116925,#116926,#116927,#116928,#116929,#116930,#116931,
#116932,#116933,#116934,#116935,#116936,#116937,#116938,#116939,#116940,
#116941,#116942,#116943,#116944,#116945,#116946,#116947,#116948,#116949,
#116950,#116951,#116952,#116953,#116954,#116955,#116956,#116957,#116958,
#116959,#116960,#116961,#116962,#116963,#116964,#116965,#116966,#116967,
#116968,#116969,#116970,#116971,#116972,#116973,#116974,#116975,#116976,
#116977,#116978,#116979,#116980,#116981,#116982,#116983,#116984,#116985,
#116986,#116987,#116988,#116989,#116990,#116991,#116992,#116993,#116994,
#116995,#116996,#116997,#116998,#116999,#117000,#117001,#117002,#117003,
#117004,#117005,#117006,#117007,#117008,#117009,#117010,#117011,#117012,
#117013,#117014,#117015,#117016,#117017,#117018,#117019,#117020,#117021,
#117022,#117023,#117024,#117025,#117026,#117027,#117028,#117029,#117030,
#117031,#117032,#117033,#117034,#117035,#117036,#117037,#117038,#117039,
#117040,#117041,#117042,#117043,#117044,#117045,#117046,#117047,#117048,
#117049,#117050,#117051,#117052,#117053,#117054,#117055,#117056,#117057,
#117058,#117059,#117060,#117061,#117062,#117063,#117064,#117065,#117066,
#117067,#117068,#117069,#117070,#117071,#117072,#117073,#117074,#117075,
#117076,#117077,#117078,#117079,#117080,#117081,#117082,#117083,#117084,
#117085,#117086,#117087,#117088,#117089,#117090,#117091,#117092),
 .UNSPECIFIED.,.F.,.F.,(4,3,3,3,3,3,3,3,3,3,3,3,3,3,3,3,3,3,3,3,3,3,3,3,
3,3,3,3,3,3,3,3,3,3,3,3,3,3,3,3,3,3,3,3,3,3,3,3,3,3,3,3,3,3,3,3,3,3,3,3,
3,3,3,3,3,3,3,3,3,3,3,3,3,4),(1372.87598961873,1372.94557750019,1373.02931621204,
1373.1129517234,1373.1965041668,1373.27999360265,1373.36344755327,1373.44688404711,
1373.53032115687,1373.61377695179,1373.69732144452,1373.78091052746,1373.86463379502,
1373.94531351091,1374.02905222276,1374.11268773412,1374.19624017752,1374.27972961337,
1374.36318356399,1374.44662005783,1374.53005716759,1374.6135129625,1374.69705745523,
1374.78064653818,1374.86436980573,1374.94504952163,1375.02878823348,1375.11242374484,
1375.19597618824,1375.27946562409,1375.36291957471,1375.44635606855,1375.52979317831,
1375.61324897323,1375.69679346596,1375.7803825489,1375.86410581645,1375.94478553235,
1376.0285242442,1376.11215975556,1376.19571219896,1376.27920163481,1376.36265558543,
1376.44609207927,1376.52952918903,1376.61298498395,1376.69652947668,1376.78011855962,
1376.86384182718,1376.94452154307,1377.02826025492,1377.11189576628,1377.19544820968,
1377.27893764553,1377.36239159615,1377.44582808999,1377.52926519975,1377.61272099467,
1377.6962654874,1377.77985457034,1377.86357783789,1377.94425755379,1378.02799831545,
1378.11163540067,1378.19518894399,1378.27867900734,1378.36213118323,1378.44556522948,
1378.52899921834,1378.61245121803,1378.69598273117,1378.77955855647,1378.86324724977,
1378.9079079641),.UNSPECIFIED.);
#924=B_SPLINE_CURVE_WITH_KNOTS('',3,(#117093,#117094,#117095,#117096,#117097,
#117098,#117099,#117100,#117101,#117102),.UNSPECIFIED.,.F.,.F.,(4,3,3,4),
(1372.62415907432,1372.70689884796,1372.79144423329,1372.87598961861),
 .UNSPECIFIED.);
#925=B_SPLINE_CURVE_WITH_KNOTS('',3,(#117104,#117105,#117106,#117107,#117108,
#117109,#117110,#117111,#117112,#117113),.UNSPECIFIED.,.F.,.F.,(4,3,3,4),
(1372.62528274347,1372.70946141838,1372.79362230245,1372.87598961873),
 .UNSPECIFIED.);
#926=B_SPLINE_CURVE_WITH_KNOTS('',3,(#117114,#117115,#117116,#117117,#117118,
#117119,#117120,#117121,#117122,#117123,#117124,#117125,#117126,#117127,
#117128,#117129,#117130,#117131,#117132,#117133,#117134,#117135,#117136,
#117137,#117138,#117139,#117140,#117141,#117142,#117143,#117144,#117145,
#117146,#117147,#117148,#117149,#117150,#117151,#117152,#117153,#117154,
#117155,#117156,#117157,#117158,#117159,#117160,#117161,#117162,#117163,
#117164,#117165,#117166,#117167,#117168,#117169,#117170,#117171,#117172,
#117173,#117174,#117175,#117176,#117177,#117178,#117179,#117180,#117181,
#117182,#117183,#117184,#117185,#117186,#117187,#117188,#117189,#117190,
#117191,#117192,#117193,#117194,#117195,#117196,#117197,#117198,#117199,
#117200,#117201,#117202,#117203,#117204,#117205,#117206,#117207,#117208,
#117209,#117210,#117211,#117212,#117213,#117214,#117215,#117216,#117217,
#117218,#117219,#117220,#117221,#117222,#117223,#117224,#117225,#117226,
#117227,#117228,#117229,#117230,#117231,#117232,#117233,#117234,#117235,
#117236,#117237,#117238,#117239,#117240,#117241,#117242,#117243,#117244,
#117245,#117246,#117247,#117248,#117249,#117250,#117251,#117252,#117253,
#117254,#117255,#117256,#117257,#117258,#117259,#117260,#117261,#117262,
#117263,#117264,#117265,#117266,#117267,#117268,#117269,#117270,#117271,
#117272,#117273,#117274,#117275,#117276,#117277,#117278,#117279,#117280,
#117281,#117282,#117283,#117284,#117285,#117286,#117287,#117288,#117289,
#117290,#117291,#117292,#117293,#117294,#117295,#117296,#117297,#117298,
#117299,#117300,#117301,#117302,#117303,#117304,#117305,#117306,#117307,
#117308,#117309,#117310,#117311,#117312,#117313,#117314,#117315,#117316,
#117317,#117318,#117319,#117320,#117321,#117322,#117323,#117324,#117325,
#117326,#117327,#117328,#117329,#117330),.UNSPECIFIED.,.F.,.F.,(4,3,3,3,
3,3,3,3,3,3,3,3,3,3,3,3,3,3,3,3,3,3,3,3,3,3,3,3,3,3,3,3,3,3,3,3,3,3,3,3,
3,3,3,3,3,3,3,3,3,3,3,3,3,3,3,3,3,3,3,3,3,3,3,3,3,3,3,3,3,3,3,3,4),(1372.87598961893,
1372.97095924417,1373.06491065064,1373.16038938527,1373.25586811991,1373.33960683175,
1373.42324234312,1373.50679478651,1373.59028422236,1373.67373817297,1373.75717466681,
1373.84061177656,1373.92406757148,1374.0076120642,1374.09120114714,1374.17492441469,
1374.25560413063,1374.33934284248,1374.42297835384,1374.50653079724,1374.59002023309,
1374.67347418371,1374.75691067755,1374.84034778731,1374.92380358223,1375.00734807496,
1375.0909371579,1375.17466042545,1375.25534014135,1375.3390788532,1375.42271436456,
1375.50626680796,1375.58975624382,1375.67321019443,1375.75664668828,1375.84008379803,
1375.92353959295,1376.00708408568,1376.09067316862,1376.17439643618,1376.25507615207,
1376.33881486392,1376.42245037528,1376.50600281868,1376.58949225453,1376.67294620514,
1376.75638269899,1376.83981980874,1376.92327560366,1377.00682009639,1377.09040917933,
1377.17413244689,1377.25481216279,1377.33855087464,1377.422186386,1377.5057388294,
1377.58922826526,1377.67268221587,1377.75611870972,1377.83955581947,1377.92301161439,
1378.00655610712,1378.09014519006,1378.17386845762,1378.25454817351,1378.33724869518,
1378.41985465973,1378.50238512748,1378.58485909102,1378.66730602705,1378.74973447906,
1378.83219342914,1378.9073388259),.UNSPECIFIED.);
#927=B_SPLINE_CURVE_WITH_KNOTS('',3,(#117336,#117337,#117338,#117339,#117340,
#117341,#117342,#117343,#117344,#117345,#117346,#117347,#117348,#117349,
#117350,#117351,#117352,#117353,#117354,#117355,#117356,#117357,#117358,
#117359,#117360,#117361,#117362,#117363,#117364,#117365,#117366,#117367,
#117368,#117369,#117370,#117371,#117372,#117373,#117374,#117375,#117376,
#117377,#117378,#117379,#117380,#117381,#117382,#117383,#117384,#117385,
#117386,#117387,#117388,#117389,#117390,#117391,#117392,#117393,#117394,
#117395,#117396,#117397,#117398,#117399,#117400,#117401,#117402,#117403,
#117404,#117405,#117406,#117407,#117408,#117409,#117410,#117411,#117412,
#117413,#117414,#117415,#117416,#117417,#117418,#117419,#117420,#117421,
#117422,#117423,#117424,#117425,#117426,#117427,#117428,#117429,#117430,
#117431,#117432,#117433,#117434,#117435,#117436,#117437,#117438,#117439,
#117440,#117441,#117442,#117443,#117444,#117445,#117446,#117447,#117448,
#117449,#117450,#117451,#117452,#117453,#117454,#117455,#117456,#117457,
#117458,#117459,#117460,#117461,#117462,#117463,#117464,#117465,#117466,
#117467,#117468,#117469,#117470,#117471,#117472,#117473,#117474,#117475,
#117476,#117477,#117478,#117479,#117480,#117481,#117482,#117483,#117484,
#117485,#117486,#117487,#117488,#117489,#117490,#117491,#117492,#117493,
#117494,#117495,#117496,#117497,#117498,#117499,#117500,#117501,#117502,
#117503,#117504,#117505,#117506,#117507,#117508,#117509,#117510,#117511,
#117512,#117513,#117514,#117515,#117516,#117517,#117518,#117519,#117520,
#117521,#117522,#117523,#117524,#117525,#117526,#117527,#117528,#117529,
#117530,#117531,#117532,#117533,#117534,#117535,#117536,#117537,#117538,
#117539,#117540,#117541,#117542,#117543,#117544,#117545,#117546,#117547,
#117548,#117549,#117550,#117551,#117552,#117553,#117554,#117555),
 .UNSPECIFIED.,.F.,.F.,(4,3,3,3,3,3,3,3,3,3,3,3,3,3,3,3,3,3,3,3,3,3,3,3,
3,3,3,3,3,3,3,3,3,3,3,3,3,3,3,3,3,3,3,3,3,3,3,3,3,3,3,3,3,3,3,3,3,3,3,3,
3,3,3,3,3,3,3,3,3,3,3,3,3,4),(1379.15917492602,1379.24158537443,1379.32393137804,
1379.40624085828,1379.48853340139,1379.57082798668,1379.65314359278,1379.73554563815,
1379.81799609624,1379.90056739866,1379.94372957523,1380.02746828708,1380.11110379844,
1380.19465624184,1380.27814567769,1380.36159962831,1380.44503612215,1380.52847323191,
1380.61192902683,1380.69547351956,1380.7790626025,1380.86278587005,1380.94346558595,
1381.0272042978,1381.11083980916,1381.19439225256,1381.27788168841,1381.36133563903,
1381.44477213287,1381.52820924263,1381.61166503755,1381.69520953028,1381.77879861322,
1381.86252188077,1381.94320159667,1382.02694030852,1382.11057581988,1382.19412826328,
1382.27761769913,1382.36107164975,1382.44450814359,1382.52794525335,1382.61140104827,
1382.694945541,1382.77853462394,1382.86225789149,1382.94293760739,1383.02667631924,
1383.1103118306,1383.193864274,1383.27735370985,1383.36080766047,1383.44424415431,
1383.52768126407,1383.61113705899,1383.69468155172,1383.77827063466,1383.86199390221,
1383.94267361811,1384.02641232996,1384.11004784132,1384.19360028472,1384.27708972057,
1384.36054367119,1384.44398016503,1384.52741727479,1384.61087306971,1384.69441756244,
1384.77800664538,1384.86172991294,1384.94240962883,1385.03046226107,1385.11831898915,
1385.19203220808),.UNSPECIFIED.);
#928=B_SPLINE_CURVE_WITH_KNOTS('',3,(#117556,#117557,#117558,#117559,#117560,
#117561,#117562,#117563,#117564,#117565),.UNSPECIFIED.,.F.,.F.,(4,3,3,4),
(1378.9079079641,1378.94399356451,1379.05996311743,1379.15917492591),
 .UNSPECIFIED.);
#929=B_SPLINE_CURVE_WITH_KNOTS('',3,(#117567,#117568,#117569,#117570,#117571,
#117572,#117573,#117574,#117575,#117576),.UNSPECIFIED.,.F.,.F.,(4,3,3,4),
(1378.9073388259,1378.9898740265,1379.07452447614,1379.15917492578),
 .UNSPECIFIED.);
#930=B_SPLINE_CURVE_WITH_KNOTS('',3,(#117577,#117578,#117579,#117580,#117581,
#117582,#117583,#117584,#117585,#117586,#117587,#117588,#117589,#117590,
#117591,#117592,#117593,#117594,#117595,#117596,#117597,#117598,#117599,
#117600,#117601,#117602,#117603,#117604,#117605,#117606,#117607,#117608,
#117609,#117610,#117611,#117612,#117613,#117614,#117615,#117616,#117617,
#117618,#117619,#117620,#117621,#117622,#117623,#117624,#117625,#117626,
#117627,#117628,#117629,#117630,#117631,#117632,#117633,#117634,#117635,
#117636,#117637,#117638,#117639,#117640,#117641,#117642,#117643,#117644,
#117645,#117646,#117647,#117648,#117649,#117650,#117651,#117652,#117653,
#117654,#117655,#117656,#117657,#117658,#117659,#117660,#117661,#117662,
#117663,#117664,#117665,#117666,#117667,#117668,#117669,#117670,#117671,
#117672,#117673,#117674,#117675,#117676,#117677,#117678,#117679,#117680,
#117681,#117682,#117683,#117684,#117685,#117686,#117687,#117688,#117689,
#117690,#117691,#117692,#117693,#117694,#117695,#117696,#117697,#117698,
#117699,#117700,#117701,#117702,#117703,#117704,#117705,#117706,#117707,
#117708,#117709,#117710,#117711,#117712,#117713,#117714,#117715,#117716,
#117717,#117718,#117719,#117720,#117721,#117722,#117723,#117724,#117725,
#117726,#117727,#117728,#117729,#117730,#117731,#117732,#117733,#117734,
#117735,#117736,#117737,#117738,#117739,#117740,#117741,#117742,#117743,
#117744,#117745,#117746,#117747,#117748,#117749,#117750,#117751,#117752,
#117753,#117754,#117755,#117756,#117757,#117758,#117759,#117760,#117761,
#117762,#117763,#117764,#117765,#117766,#117767,#117768,#117769,#117770,
#117771,#117772,#117773,#117774,#117775,#117776,#117777,#117778,#117779,
#117780,#117781,#117782,#117783,#117784,#117785,#117786,#117787,#117788,
#117789,#117790,#117791,#117792,#117793,#117794,#117795,#117796),
 .UNSPECIFIED.,.F.,.F.,(4,3,3,3,3,3,3,3,3,3,3,3,3,3,3,3,3,3,3,3,3,3,3,3,
3,3,3,3,3,3,3,3,3,3,3,3,3,3,3,3,3,3,3,3,3,3,3,3,3,3,3,3,3,3,3,3,3,3,3,3,
3,3,3,3,3,3,3,3,3,3,3,3,3,4),(1379.15917492591,1379.25428418423,1379.33802289608,
1379.42165840744,1379.50521085084,1379.58870028669,1379.67215423731,1379.75559073115,
1379.83902784091,1379.92248363583,1380.00602812856,1380.0896172115,1380.17334047906,
1380.25402019495,1380.3377589068,1380.42139441816,1380.50494686156,1380.58843629741,
1380.67189024803,1380.75532674187,1380.83876385163,1380.92221964654,1381.00576413927,
1381.08935322221,1381.17307648977,1381.25375620567,1381.33749491752,1381.42113042888,
1381.50468287228,1381.58817230813,1381.67162625875,1381.75506275259,1381.83849986235,
1381.92195565727,1382.00550015,1382.08908923294,1382.17281250049,1382.25349221639,
1382.33723092824,1382.4208664396,1382.504418883,1382.58790831885,1382.67136226947,
1382.75479876331,1382.83823587307,1382.92169166799,1383.00523616072,1383.08882524366,
1383.17254851121,1383.25322822711,1383.33696693896,1383.42060245032,1383.50415489372,
1383.58764432957,1383.67109828019,1383.75453477403,1383.83797188379,1383.92142767871,
1384.00497217144,1384.08856125438,1384.17228452194,1384.25296423783,1384.33670649109,
1384.42034472974,1384.50389908976,1384.5897839228,1384.67323419369,1384.75666637546,
1384.84009853983,1384.92781834339,1385.01134412471,1385.0949153171,1385.17858451418,
1385.19097775405),.UNSPECIFIED.);
#931=B_SPLINE_CURVE_WITH_KNOTS('',3,(#117802,#117803,#117804,#117805,#117806,
#117807,#117808,#117809,#117810,#117811,#117812,#117813,#117814,#117815,
#117816,#117817,#117818,#117819,#117820,#117821,#117822,#117823,#117824,
#117825,#117826,#117827,#117828,#117829,#117830,#117831,#117832,#117833,
#117834,#117835,#117836,#117837,#117838,#117839,#117840,#117841,#117842,
#117843,#117844,#117845,#117846,#117847,#117848,#117849,#117850,#117851,
#117852,#117853,#117854,#117855,#117856,#117857,#117858,#117859,#117860,
#117861,#117862,#117863,#117864,#117865,#117866,#117867,#117868,#117869,
#117870,#117871,#117872,#117873,#117874,#117875,#117876,#117877,#117878,
#117879,#117880,#117881,#117882,#117883,#117884,#117885,#117886,#117887,
#117888,#117889,#117890,#117891,#117892,#117893,#117894,#117895,#117896,
#117897,#117898,#117899,#117900,#117901,#117902,#117903,#117904,#117905,
#117906,#117907,#117908,#117909,#117910,#117911,#117912,#117913,#117914,
#117915,#117916,#117917,#117918,#117919,#117920,#117921,#117922,#117923,
#117924,#117925,#117926,#117927,#117928,#117929,#117930,#117931,#117932,
#117933,#117934,#117935,#117936,#117937,#117938,#117939,#117940,#117941,
#117942,#117943,#117944,#117945,#117946,#117947,#117948,#117949,#117950,
#117951,#117952,#117953,#117954,#117955,#117956,#117957,#117958,#117959,
#117960,#117961,#117962,#117963,#117964,#117965,#117966,#117967,#117968,
#117969,#117970,#117971,#117972,#117973,#117974,#117975,#117976,#117977,
#117978,#117979,#117980,#117981,#117982,#117983,#117984,#117985,#117986,
#117987,#117988,#117989,#117990,#117991,#117992,#117993,#117994,#117995,
#117996,#117997,#117998,#117999,#118000,#118001,#118002,#118003,#118004,
#118005,#118006,#118007,#118008,#118009,#118010,#118011,#118012,#118013,
#118014,#118015,#118016,#118017,#118018,#118019,#118020,#118021),
 .UNSPECIFIED.,.F.,.F.,(4,3,3,3,3,3,3,3,3,3,3,3,3,3,3,3,3,3,3,3,3,3,3,3,
3,3,3,3,3,3,3,3,3,3,3,3,3,3,3,3,3,3,3,3,3,3,3,3,3,3,3,3,3,3,3,3,3,3,3,3,
3,3,3,3,3,3,3,3,3,3,3,3,3,4),(1385.44236023311,1385.52976718702,1385.61728932258,
1385.70501835267,1385.79285658942,1385.8808961999,1385.94214563955,1386.0258843514,
1386.10951986276,1386.19307230616,1386.27656174201,1386.36001569263,1386.44345218647,
1386.52688929623,1386.61034509115,1386.69388958388,1386.77747866682,1386.86120193437,
1386.94188165027,1387.02562036212,1387.10925587348,1387.19280831688,1387.27629775273,
1387.35975170335,1387.44318819719,1387.52662530695,1387.61008110187,1387.6936255946,
1387.77721467754,1387.86093794509,1387.94161766099,1388.02535637284,1388.1089918842,
1388.1925443276,1388.27603376345,1388.35948771407,1388.44292420791,1388.52636131767,
1388.60981711259,1388.69336160532,1388.77695068826,1388.86067395581,1388.94135367171,
1389.02509238356,1389.10872789492,1389.19228033832,1389.27576977417,1389.35922372479,
1389.44266021863,1389.52609732839,1389.6095531233,1389.69309761603,1389.77668669898,
1389.86040996653,1389.94108968243,1390.02482839428,1390.10846390564,1390.19201634904,
1390.27550578489,1390.35895973551,1390.44239622935,1390.52583333911,1390.60928913403,
1390.69283362676,1390.7764227097,1390.86014597725,1390.94082569315,1391.02339322003,
1391.10586410619,1391.18825752044,1391.27058911472,1391.35288481146,1391.43517301765,
1391.47402012541),.UNSPECIFIED.);
#932=B_SPLINE_CURVE_WITH_KNOTS('',3,(#118022,#118023,#118024,#118025,#118026,
#118027,#118028,#118029,#118030,#118031),.UNSPECIFIED.,.F.,.F.,(4,3,3,4),
(1385.19203220808,1385.27963097554,1385.3670679702,1385.44236023309),
 .UNSPECIFIED.);
#933=B_SPLINE_CURVE_WITH_KNOTS('',3,(#118033,#118034,#118035,#118036,#118037,
#118038,#118039,#118040,#118041,#118042),.UNSPECIFIED.,.F.,.F.,(4,3,3,4),
(1385.19097775405,1385.25270024855,1385.37628043219,1385.44236023309),
 .UNSPECIFIED.);
#934=B_SPLINE_CURVE_WITH_KNOTS('',3,(#118043,#118044,#118045,#118046,#118047,
#118048,#118049,#118050,#118051,#118052,#118053,#118054,#118055,#118056,
#118057,#118058,#118059,#118060,#118061,#118062,#118063,#118064,#118065,
#118066,#118067,#118068,#118069,#118070,#118071,#118072,#118073,#118074,
#118075,#118076,#118077,#118078,#118079,#118080,#118081,#118082,#118083,
#118084,#118085,#118086,#118087,#118088,#118089,#118090,#118091,#118092,
#118093,#118094,#118095,#118096,#118097,#118098,#118099,#118100,#118101,
#118102,#118103,#118104,#118105,#118106,#118107,#118108,#118109,#118110,
#118111,#118112,#118113,#118114,#118115,#118116,#118117,#118118,#118119,
#118120,#118121,#118122,#118123,#118124,#118125,#118126,#118127,#118128,
#118129,#118130,#118131,#118132,#118133,#118134,#118135,#118136,#118137,
#118138,#118139,#118140,#118141,#118142,#118143,#118144,#118145,#118146,
#118147,#118148,#118149,#118150,#118151,#118152,#118153,#118154,#118155,
#118156,#118157,#118158,#118159,#118160,#118161,#118162,#118163,#118164,
#118165,#118166,#118167,#118168,#118169,#118170,#118171,#118172,#118173,
#118174,#118175,#118176,#118177,#118178,#118179,#118180,#118181,#118182,
#118183,#118184,#118185,#118186,#118187,#118188,#118189,#118190,#118191,
#118192,#118193,#118194,#118195,#118196,#118197,#118198,#118199,#118200,
#118201,#118202,#118203,#118204,#118205,#118206,#118207,#118208,#118209,
#118210,#118211,#118212,#118213,#118214,#118215,#118216,#118217,#118218,
#118219,#118220,#118221,#118222,#118223,#118224,#118225,#118226,#118227,
#118228,#118229,#118230,#118231,#118232,#118233,#118234,#118235,#118236,
#118237,#118238,#118239,#118240,#118241,#118242,#118243,#118244,#118245,
#118246,#118247,#118248,#118249,#118250,#118251,#118252,#118253,#118254,
#118255,#118256,#118257,#118258,#118259,#118260,#118261,#118262),
 .UNSPECIFIED.,.F.,.F.,(4,3,3,3,3,3,3,3,3,3,3,3,3,3,3,3,3,3,3,3,3,3,3,3,
3,3,3,3,3,3,3,3,3,3,3,3,3,3,3,3,3,3,3,3,3,3,3,3,3,3,3,3,3,3,3,3,3,3,3,3,
3,3,3,3,3,3,3,3,3,3,3,3,3,4),(1385.44236023322,1385.52472586569,1385.60701959995,
1385.68926698294,1385.77149079538,1385.85371006574,1385.93594381662,1386.0182603123,
1386.10061943005,1386.18310618992,1386.25243625927,1386.33617497112,1386.41981048248,
1386.50336292588,1386.58685236173,1386.67030631235,1386.75374280619,1386.83717991595,
1386.92063571087,1387.0041802036,1387.08776928654,1387.17149255409,1387.25217226999,
1387.33591098184,1387.4195464932,1387.5030989366,1387.58658837245,1387.67004232307,
1387.75347881691,1387.83691592667,1387.92037172159,1388.00391621431,1388.08750529726,
1388.17122856481,1388.25190828071,1388.33564699256,1388.41928250392,1388.50283494732,
1388.58632438317,1388.66977833379,1388.75321482763,1388.83665193739,1388.92010773231,
1389.00365222504,1389.08724130798,1389.17096457553,1389.25164429143,1389.33538300328,
1389.41901851464,1389.50257095804,1389.58606039389,1389.66951434451,1389.75295083835,
1389.83638794811,1389.91984374303,1390.00338823576,1390.0869773187,1390.17070058625,
1390.25138030215,1390.335119014,1390.41875452536,1390.50230696876,1390.58579640461,
1390.66925035523,1390.75268684907,1390.83612395883,1390.91957975375,1391.00312424648,
1391.08671332942,1391.17043659697,1391.25111631287,1391.34024896678,1391.4291696579,
1391.47524121817),.UNSPECIFIED.);
#935=B_SPLINE_CURVE_WITH_KNOTS('',3,(#118268,#118269,#118270,#118271,#118272,
#118273,#118274,#118275,#118276,#118277,#118278,#118279,#118280,#118281,
#118282,#118283,#118284,#118285,#118286,#118287,#118288,#118289,#118290,
#118291,#118292,#118293,#118294,#118295,#118296,#118297,#118298,#118299,
#118300,#118301,#118302,#118303,#118304,#118305,#118306,#118307,#118308,
#118309,#118310,#118311,#118312,#118313,#118314,#118315,#118316,#118317,
#118318,#118319,#118320,#118321,#118322,#118323,#118324,#118325,#118326,
#118327,#118328,#118329,#118330,#118331,#118332,#118333,#118334,#118335,
#118336,#118337,#118338,#118339,#118340,#118341,#118342,#118343,#118344,
#118345,#118346,#118347,#118348,#118349,#118350,#118351,#118352,#118353,
#118354,#118355,#118356,#118357,#118358,#118359,#118360,#118361,#118362,
#118363,#118364,#118365,#118366,#118367,#118368,#118369,#118370,#118371,
#118372,#118373,#118374,#118375,#118376,#118377,#118378,#118379,#118380,
#118381,#118382,#118383,#118384,#118385,#118386,#118387,#118388,#118389,
#118390,#118391,#118392,#118393,#118394,#118395,#118396,#118397,#118398,
#118399,#118400,#118401,#118402,#118403,#118404,#118405,#118406,#118407,
#118408,#118409,#118410,#118411,#118412,#118413,#118414,#118415,#118416,
#118417,#118418,#118419,#118420,#118421,#118422,#118423,#118424,#118425,
#118426,#118427,#118428,#118429,#118430,#118431,#118432,#118433,#118434,
#118435,#118436,#118437,#118438,#118439,#118440,#118441,#118442,#118443,
#118444,#118445,#118446,#118447,#118448,#118449,#118450,#118451,#118452,
#118453,#118454,#118455,#118456,#118457,#118458,#118459,#118460,#118461,
#118462,#118463,#118464,#118465,#118466,#118467,#118468,#118469,#118470,
#118471,#118472,#118473,#118474,#118475,#118476,#118477,#118478,#118479,
#118480,#118481,#118482,#118483,#118484),.UNSPECIFIED.,.F.,.F.,(4,3,3,3,
3,3,3,3,3,3,3,3,3,3,3,3,3,3,3,3,3,3,3,3,3,3,3,3,3,3,3,3,3,3,3,3,3,3,3,3,
3,3,3,3,3,3,3,3,3,3,3,3,3,3,3,3,3,3,3,3,3,3,3,3,3,3,3,3,3,3,3,3,4),(1391.72554554027,
1391.84155713252,1391.94056170387,1392.02430041572,1392.10793592708,1392.19148837048,
1392.27497780633,1392.35843175695,1392.44186825079,1392.52530536055,1392.60876115547,
1392.6923056482,1392.77589473114,1392.85961799869,1392.94029771459,1393.02403642644,
1393.1076719378,1393.1912243812,1393.27471381705,1393.35816776767,1393.44160426151,
1393.52504137127,1393.60849716619,1393.69204165892,1393.77563074186,1393.85935400942,
1393.94003372531,1394.02377243716,1394.10740794852,1394.19096039192,1394.27444982777,
1394.35790377839,1394.44134027223,1394.52477738199,1394.60823317691,1394.69177766964,
1394.77536675258,1394.85909002013,1394.93976973603,1395.02350844788,1395.10714395924,
1395.19069640264,1395.27418583849,1395.35763978911,1395.44107628295,1395.52451339271,
1395.60796918763,1395.69151368036,1395.7751027633,1395.85882603085,1395.93950574675,
1396.0232444586,1396.10687996996,1396.19043241336,1396.27392184921,1396.35737579983,
1396.44081229367,1396.52424940343,1396.60770519834,1396.69124969107,1396.77483877401,
1396.85856204157,1396.93924175747,1397.02299139418,1397.10663543065,1397.19017882089,
1397.27366514828,1397.35711253246,1397.44053906297,1397.52398987096,1397.60745144848,
1397.69098429292,1397.75707412262),.UNSPECIFIED.);
#936=B_SPLINE_CURVE_WITH_KNOTS('',3,(#118485,#118486,#118487,#118488,#118489,
#118490,#118491,#118492,#118493,#118494),.UNSPECIFIED.,.F.,.F.,(4,3,3,4),
(1391.47402012541,1391.55633938637,1391.64094246326,1391.72554554016),
 .UNSPECIFIED.);
#937=B_SPLINE_CURVE_WITH_KNOTS('',3,(#118496,#118497,#118498,#118499,#118500,
#118501,#118502,#118503,#118504,#118505),.UNSPECIFIED.,.F.,.F.,(4,3,3,4),
(1391.47524121817,1391.56388883391,1391.65232526733,1391.72554554016),
 .UNSPECIFIED.);
#938=B_SPLINE_CURVE_WITH_KNOTS('',3,(#118506,#118507,#118508,#118509,#118510,
#118511,#118512,#118513,#118514,#118515,#118516,#118517,#118518,#118519,
#118520,#118521,#118522,#118523,#118524,#118525,#118526,#118527,#118528,
#118529,#118530,#118531,#118532,#118533,#118534,#118535,#118536,#118537,
#118538,#118539,#118540,#118541,#118542,#118543,#118544,#118545,#118546,
#118547,#118548,#118549,#118550,#118551,#118552,#118553,#118554,#118555,
#118556,#118557,#118558,#118559,#118560,#118561,#118562,#118563,#118564,
#118565,#118566,#118567,#118568,#118569,#118570,#118571,#118572,#118573,
#118574,#118575,#118576,#118577,#118578,#118579,#118580,#118581,#118582,
#118583,#118584,#118585,#118586,#118587,#118588,#118589,#118590,#118591,
#118592,#118593,#118594,#118595,#118596,#118597,#118598,#118599,#118600,
#118601,#118602,#118603,#118604,#118605,#118606,#118607,#118608,#118609,
#118610,#118611,#118612,#118613,#118614,#118615,#118616,#118617,#118618,
#118619,#118620,#118621,#118622,#118623,#118624,#118625,#118626,#118627,
#118628,#118629,#118630,#118631,#118632,#118633,#118634,#118635,#118636,
#118637,#118638,#118639,#118640,#118641,#118642,#118643,#118644,#118645,
#118646,#118647,#118648,#118649,#118650,#118651,#118652,#118653,#118654,
#118655,#118656,#118657,#118658,#118659,#118660,#118661,#118662,#118663,
#118664,#118665,#118666,#118667,#118668,#118669,#118670,#118671,#118672,
#118673,#118674,#118675,#118676,#118677,#118678,#118679,#118680,#118681,
#118682,#118683,#118684,#118685,#118686,#118687,#118688,#118689,#118690,
#118691,#118692,#118693,#118694,#118695,#118696,#118697,#118698,#118699,
#118700,#118701,#118702,#118703,#118704,#118705,#118706,#118707,#118708,
#118709,#118710,#118711,#118712,#118713,#118714,#118715,#118716,#118717,
#118718,#118719,#118720,#118721,#118722,#118723,#118724,#118725),
 .UNSPECIFIED.,.F.,.F.,(4,3,3,3,3,3,3,3,3,3,3,3,3,3,3,3,3,3,3,3,3,3,3,3,
3,3,3,3,3,3,3,3,3,3,3,3,3,3,3,3,3,3,3,3,3,3,3,3,3,3,3,3,3,3,3,3,3,3,3,3,
3,3,3,3,3,3,3,3,3,3,3,3,3,4),(1391.72554554027,1391.81208339403,1391.89870567794,
1391.98674233935,1392.07363086768,1392.16224159564,1392.25085232359,1392.33459103544,
1392.4182265468,1392.5017789902,1392.58526842605,1392.66872237667,1392.75215887051,
1392.83559598027,1392.91905177519,1393.00259626792,1393.08618535086,1393.16990861841,
1393.25058833431,1393.33432704616,1393.41796255752,1393.50151500092,1393.58500443677,
1393.66845838739,1393.75189488123,1393.83533199099,1393.9187877859,1394.00233227863,
1394.08592136157,1394.16964462913,1394.25032434503,1394.33406305688,1394.41769856824,
1394.50125101164,1394.58474044749,1394.66819439811,1394.75163089195,1394.83506800171,
1394.91852379663,1395.00206828936,1395.0856573723,1395.16938063986,1395.25006035575,
1395.3337990676,1395.41743457896,1395.50098702236,1395.58447645821,1395.66793040883,
1395.75136690267,1395.83480401243,1395.91825980735,1396.00180430008,1396.08539338302,
1396.16911665058,1396.24979636647,1396.33353507832,1396.41717058968,1396.50072303308,
1396.58421246893,1396.66766641955,1396.75110291339,1396.83454002315,1396.91799581807,
1397.0015403108,1397.08512939374,1397.16885266129,1397.24953237719,1397.33223473028,
1397.41483932488,1397.50045997667,1397.5829190073,1397.66534185076,1397.74775086179,
1397.75732193205),.UNSPECIFIED.);
#939=B_SPLINE_CURVE_WITH_KNOTS('',3,(#118731,#118732,#118733,#118734,#118735,
#118736,#118737,#118738,#118739,#118740,#118741,#118742,#118743,#118744,
#118745,#118746,#118747,#118748,#118749,#118750,#118751,#118752,#118753,
#118754,#118755,#118756,#118757,#118758,#118759,#118760,#118761,#118762,
#118763,#118764,#118765,#118766,#118767,#118768,#118769,#118770,#118771,
#118772,#118773,#118774,#118775,#118776,#118777,#118778,#118779,#118780,
#118781,#118782,#118783,#118784,#118785,#118786,#118787,#118788,#118789,
#118790,#118791,#118792,#118793,#118794,#118795,#118796,#118797,#118798,
#118799,#118800,#118801,#118802,#118803,#118804,#118805,#118806,#118807,
#118808,#118809,#118810,#118811,#118812,#118813,#118814,#118815,#118816,
#118817,#118818,#118819,#118820,#118821,#118822,#118823,#118824,#118825,
#118826,#118827,#118828,#118829,#118830,#118831,#118832,#118833,#118834,
#118835,#118836,#118837,#118838,#118839,#118840,#118841,#118842,#118843,
#118844,#118845,#118846,#118847,#118848,#118849,#118850,#118851,#118852,
#118853,#118854,#118855,#118856,#118857,#118858,#118859,#118860,#118861,
#118862,#118863,#118864,#118865,#118866,#118867,#118868,#118869,#118870,
#118871,#118872,#118873,#118874,#118875,#118876,#118877,#118878,#118879,
#118880,#118881,#118882,#118883,#118884,#118885,#118886,#118887,#118888,
#118889,#118890,#118891,#118892,#118893,#118894,#118895,#118896,#118897,
#118898,#118899,#118900,#118901,#118902,#118903,#118904,#118905,#118906,
#118907,#118908,#118909,#118910,#118911,#118912,#118913,#118914,#118915,
#118916,#118917,#118918,#118919,#118920,#118921,#118922,#118923,#118924,
#118925,#118926,#118927,#118928,#118929,#118930,#118931,#118932,#118933,
#118934,#118935,#118936,#118937,#118938,#118939,#118940,#118941,#118942,
#118943,#118944,#118945,#118946,#118947,#118948,#118949,#118950,#118951,
#118952,#118953),.UNSPECIFIED.,.F.,.F.,(4,3,3,3,3,3,3,3,3,3,3,3,3,3,3,3,
3,3,3,3,3,3,3,3,3,3,3,3,3,3,3,3,3,3,3,3,3,3,3,3,3,3,3,3,3,3,3,3,3,3,3,3,
3,3,3,3,3,3,3,3,3,3,3,3,3,3,3,3,3,3,3,3,3,3,4),(1398.00873084757,1398.09161469114,
1398.17440099707,1398.25711065912,1398.34231104909,1398.42493873814,1398.50755742297,
1398.59018586339,1398.67284282351,1398.75559073286,1398.83839338335,1398.92131105705,
1398.93871377891,1399.02245249076,1399.10608800212,1399.18964044552,1399.27312988137,
1399.35658383199,1399.44002032583,1399.52345743559,1399.6069132305,1399.69045772323,
1399.77404680618,1399.85777007373,1399.93844978963,1400.02218850148,1400.10582401284,
1400.18937645624,1400.27286589209,1400.35631984271,1400.43975633655,1400.52319344631,
1400.60664924123,1400.69019373396,1400.7737828169,1400.85750608446,1400.93818580035,
1401.0219245122,1401.10556002356,1401.18911246696,1401.27260190281,1401.35605585343,
1401.43949234727,1401.52292945703,1401.60638525194,1401.68992974467,1401.77351882761,
1401.85724209517,1401.93792181107,1402.02166052292,1402.10529603428,1402.18884847768,
1402.27233791353,1402.35579186415,1402.43922835799,1402.52266546775,1402.60612126267,
1402.6896657554,1402.77325483834,1402.85697810589,1402.93765782179,1403.02139653364,
1403.105032045,1403.1885844884,1403.27207392425,1403.35552787487,1403.43896436871,
1403.52240147847,1403.60585727339,1403.68940176612,1403.77299084906,1403.85671411662,
1403.93739383251,1404.03402820369,1404.04140044517),.UNSPECIFIED.);
#940=B_SPLINE_CURVE_WITH_KNOTS('',3,(#118954,#118955,#118956,#118957,#118958,
#118959,#118960,#118961,#118962,#118963,#118964,#118965,#118966),
 .UNSPECIFIED.,.F.,.F.,(4,3,3,3,4),(1397.75707412262,1397.84070997716,1397.92446166817,
1397.93897776819,1398.00873084745),.UNSPECIFIED.);
#941=B_SPLINE_CURVE_WITH_KNOTS('',3,(#118968,#118969,#118970,#118971,#118972,
#118973,#118974,#118975,#118976,#118977),.UNSPECIFIED.,.F.,.F.,(4,3,3,4),
(1397.75732193205,1397.83975643715,1397.9242436423,1398.00873084745),
 .UNSPECIFIED.);
#942=B_SPLINE_CURVE_WITH_KNOTS('',3,(#118978,#118979,#118980,#118981,#118982,
#118983,#118984,#118985,#118986,#118987,#118988,#118989,#118990,#118991,
#118992,#118993,#118994,#118995,#118996,#118997,#118998,#118999,#119000,
#119001,#119002,#119003,#119004,#119005,#119006,#119007,#119008,#119009,
#119010,#119011,#119012,#119013,#119014,#119015,#119016,#119017,#119018,
#119019,#119020,#119021,#119022,#119023,#119024,#119025,#119026,#119027,
#119028,#119029,#119030,#119031,#119032,#119033,#119034,#119035,#119036,
#119037,#119038,#119039,#119040,#119041,#119042,#119043,#119044,#119045,
#119046,#119047,#119048,#119049,#119050,#119051,#119052,#119053,#119054,
#119055,#119056,#119057,#119058,#119059,#119060,#119061,#119062,#119063,
#119064,#119065,#119066,#119067,#119068,#119069,#119070,#119071,#119072,
#119073,#119074,#119075,#119076,#119077,#119078,#119079,#119080,#119081,
#119082,#119083,#119084,#119085,#119086,#119087,#119088,#119089,#119090,
#119091,#119092,#119093,#119094,#119095,#119096,#119097,#119098,#119099,
#119100,#119101,#119102,#119103,#119104,#119105,#119106,#119107,#119108,
#119109,#119110,#119111,#119112,#119113,#119114,#119115,#119116,#119117,
#119118,#119119,#119120,#119121,#119122,#119123,#119124,#119125,#119126,
#119127,#119128,#119129,#119130,#119131,#119132,#119133,#119134,#119135,
#119136,#119137,#119138,#119139,#119140,#119141,#119142,#119143,#119144,
#119145,#119146,#119147,#119148,#119149,#119150,#119151,#119152,#119153,
#119154,#119155,#119156,#119157,#119158,#119159,#119160,#119161,#119162,
#119163,#119164,#119165,#119166,#119167,#119168,#119169,#119170,#119171,
#119172,#119173,#119174,#119175,#119176,#119177,#119178,#119179,#119180,
#119181,#119182,#119183,#119184,#119185,#119186,#119187,#119188,#119189,
#119190,#119191,#119192,#119193,#119194,#119195,#119196,#119197),
 .UNSPECIFIED.,.F.,.F.,(4,3,3,3,3,3,3,3,3,3,3,3,3,3,3,3,3,3,3,3,3,3,3,3,
3,3,3,3,3,3,3,3,3,3,3,3,3,3,3,3,3,3,3,3,3,3,3,3,3,3,3,3,3,3,3,3,3,3,3,3,
3,3,3,3,3,3,3,3,3,3,3,3,3,4),(1398.00873084761,1398.11756456005,1398.22916845252,
1398.24926838791,1398.33300709976,1398.41664261112,1398.50019505452,1398.58368449037,
1398.66713844099,1398.75057493483,1398.83401204459,1398.91746783951,1399.00101233224,
1399.08460141518,1399.16832468273,1399.24900439863,1399.33274311048,1399.41637862184,
1399.49993106524,1399.58342050109,1399.66687445171,1399.75031094555,1399.83374805531,
1399.91720385023,1400.00074834295,1400.0843374259,1400.16806069345,1400.24874040935,
1400.3324791212,1400.41611463256,1400.49966707596,1400.58315651181,1400.66661046243,
1400.75004695627,1400.83348406603,1400.91693986095,1401.00048435368,1401.08407343662,
1401.16779670417,1401.24847642007,1401.33221513192,1401.41585064328,1401.49940308668,
1401.58289252253,1401.66634647315,1401.74978296699,1401.83322007675,1401.91667587167,
1402.0002203644,1402.08380944734,1402.16753271489,1402.24821243079,1402.33195114264,
1402.415586654,1402.4991390974,1402.58262853325,1402.66608248387,1402.74951897771,
1402.83295608747,1402.91641188239,1402.99995637512,1403.08354545806,1403.16726872562,
1403.24794844151,1403.33169972974,1403.41534508081,1403.49888897681,1403.58237533228,
1403.66582226773,1403.74924787314,1403.83269310383,1403.91614891234,1403.99966484341,
1404.04024993874),.UNSPECIFIED.);
#943=B_SPLINE_CURVE_WITH_KNOTS('',3,(#119203,#119204,#119205,#119206,#119207,
#119208,#119209,#119210,#119211,#119212,#119213,#119214,#119215,#119216,
#119217,#119218,#119219,#119220,#119221,#119222,#119223,#119224,#119225,
#119226,#119227,#119228,#119229,#119230,#119231,#119232,#119233,#119234,
#119235,#119236,#119237,#119238,#119239,#119240,#119241,#119242,#119243,
#119244,#119245,#119246,#119247,#119248,#119249,#119250,#119251,#119252,
#119253,#119254,#119255,#119256,#119257,#119258,#119259,#119260,#119261,
#119262,#119263,#119264,#119265,#119266,#119267,#119268,#119269,#119270,
#119271,#119272,#119273,#119274,#119275,#119276,#119277,#119278,#119279,
#119280,#119281,#119282,#119283,#119284,#119285,#119286,#119287,#119288,
#119289,#119290,#119291,#119292,#119293,#119294,#119295,#119296,#119297,
#119298,#119299,#119300,#119301,#119302,#119303,#119304,#119305,#119306,
#119307,#119308,#119309,#119310,#119311,#119312,#119313,#119314,#119315,
#119316,#119317,#119318,#119319,#119320,#119321,#119322,#119323,#119324,
#119325,#119326,#119327,#119328,#119329,#119330,#119331,#119332,#119333,
#119334,#119335,#119336,#119337,#119338,#119339,#119340,#119341,#119342,
#119343,#119344,#119345,#119346,#119347,#119348,#119349,#119350,#119351,
#119352,#119353,#119354,#119355,#119356,#119357,#119358,#119359,#119360,
#119361,#119362,#119363,#119364,#119365,#119366,#119367,#119368,#119369,
#119370,#119371,#119372,#119373,#119374,#119375,#119376,#119377,#119378,
#119379,#119380,#119381,#119382,#119383,#119384,#119385,#119386,#119387,
#119388,#119389,#119390,#119391,#119392,#119393,#119394,#119395,#119396,
#119397,#119398,#119399,#119400,#119401,#119402,#119403,#119404,#119405,
#119406,#119407,#119408,#119409,#119410,#119411,#119412,#119413,#119414,
#119415,#119416,#119417,#119418,#119419,#119420,#119421,#119422),
 .UNSPECIFIED.,.F.,.F.,(4,3,3,3,3,3,3,3,3,3,3,3,3,3,3,3,3,3,3,3,3,3,3,3,
3,3,3,3,3,3,3,3,3,3,3,3,3,3,3,3,3,3,3,3,3,3,3,3,3,3,3,3,3,3,3,3,3,3,3,3,
3,3,3,3,3,3,3,3,3,3,3,3,3,4),(1404.29191615463,1404.37562428831,1404.4593290263,
1404.54304803957,1404.62679900449,1404.7106527483,1404.79456200366,1404.87860831265,
1404.93712984323,1405.02086855508,1405.10450406644,1405.18805650984,1405.27154594569,
1405.35499989631,1405.43843639015,1405.52187349991,1405.60532929482,1405.68887378755,
1405.7724628705,1405.85618613805,1405.93686585395,1406.0206045658,1406.10424007716,
1406.18779252056,1406.27128195641,1406.35473590703,1406.43817240087,1406.52160951063,
1406.60506530555,1406.68860979828,1406.77219888122,1406.85592214878,1406.93660186467,
1407.02034057652,1407.10397608788,1407.18752853128,1407.27101796713,1407.35447191775,
1407.43790841159,1407.52134552135,1407.60480131627,1407.688345809,1407.77193489194,
1407.85565815949,1407.93633787539,1408.02007658724,1408.1037120986,1408.187264542,
1408.27075397785,1408.35420792847,1408.43764442231,1408.52108153207,1408.60453732698,
1408.68808181971,1408.77167090265,1408.85539417021,1408.93607388611,1409.01981259796,
1409.10344810932,1409.18700055272,1409.27048998857,1409.35394393919,1409.43738043303,
1409.52081754279,1409.60427333771,1409.68781783044,1409.77140691338,1409.85513018094,
1409.93580989683,1410.01998705489,1410.10402428112,1410.18798093152,1410.2718608454,
1410.32430278068),.UNSPECIFIED.);
#944=B_SPLINE_CURVE_WITH_KNOTS('',3,(#119423,#119424,#119425,#119426,#119427,
#119428,#119429,#119430,#119431,#119432),.UNSPECIFIED.,.F.,.F.,(4,3,3,4),
(1404.04140044517,1404.13747352714,1404.23285921852,1404.29191615443),
 .UNSPECIFIED.);
#945=B_SPLINE_CURVE_WITH_KNOTS('',3,(#119434,#119435,#119436,#119437,#119438,
#119439,#119440,#119441,#119442,#119443,#119444,#119445,#119446),
 .UNSPECIFIED.,.F.,.F.,(4,3,3,3,4),(1404.04024993874,1404.12386652121,1404.20760574971,
1404.24768445223,1404.29191615463),.UNSPECIFIED.);
#946=B_SPLINE_CURVE_WITH_KNOTS('',3,(#119447,#119448,#119449,#119450,#119451,
#119452,#119453,#119454,#119455,#119456,#119457,#119458,#119459,#119460,
#119461,#119462,#119463,#119464,#119465,#119466,#119467,#119468,#119469,
#119470,#119471,#119472,#119473,#119474,#119475,#119476,#119477,#119478,
#119479,#119480,#119481,#119482,#119483,#119484,#119485,#119486,#119487,
#119488,#119489,#119490,#119491,#119492,#119493,#119494,#119495,#119496,
#119497,#119498,#119499,#119500,#119501,#119502,#119503,#119504,#119505,
#119506,#119507,#119508,#119509,#119510,#119511,#119512,#119513,#119514,
#119515,#119516,#119517,#119518,#119519,#119520,#119521,#119522,#119523,
#119524,#119525,#119526,#119527,#119528,#119529,#119530,#119531,#119532,
#119533,#119534,#119535,#119536,#119537,#119538,#119539,#119540,#119541,
#119542,#119543,#119544,#119545,#119546,#119547,#119548,#119549,#119550,
#119551,#119552,#119553,#119554,#119555,#119556,#119557,#119558,#119559,
#119560,#119561,#119562,#119563,#119564,#119565,#119566,#119567,#119568,
#119569,#119570,#119571,#119572,#119573,#119574,#119575,#119576,#119577,
#119578,#119579,#119580,#119581,#119582,#119583,#119584,#119585,#119586,
#119587,#119588,#119589,#119590,#119591,#119592,#119593,#119594,#119595,
#119596,#119597,#119598,#119599,#119600,#119601,#119602,#119603,#119604,
#119605,#119606,#119607,#119608,#119609,#119610,#119611,#119612,#119613,
#119614,#119615,#119616,#119617,#119618,#119619,#119620,#119621,#119622,
#119623,#119624,#119625,#119626,#119627,#119628,#119629,#119630,#119631,
#119632,#119633,#119634,#119635,#119636,#119637,#119638,#119639,#119640,
#119641,#119642,#119643,#119644,#119645,#119646,#119647,#119648,#119649,
#119650,#119651,#119652,#119653,#119654,#119655,#119656,#119657,#119658,
#119659,#119660,#119661,#119662,#119663,#119664,#119665,#119666),
 .UNSPECIFIED.,.F.,.F.,(4,3,3,3,3,3,3,3,3,3,3,3,3,3,3,3,3,3,3,3,3,3,3,3,
3,3,3,3,3,3,3,3,3,3,3,3,3,3,3,3,3,3,3,3,3,3,3,3,3,3,3,3,3,3,3,3,3,3,3,3,
3,3,3,3,3,3,3,3,3,3,3,3,3,4),(1404.29191615481,1404.37506475554,1404.45811270144,
1404.54108068674,1404.62398932894,1404.70686775223,1404.78973305654,1404.87260381792,
1404.95549861295,1405.03848303953,1405.1215178224,1405.20467492572,1405.24742046295,
1405.3311591748,1405.41479468616,1405.49834712956,1405.58183656541,1405.66529051603,
1405.74872700987,1405.83216411963,1405.91561991455,1405.99916440728,1406.08275349022,
1406.16647675777,1406.24715647367,1406.33089518552,1406.41453069688,1406.49808314028,
1406.58157257613,1406.66502652675,1406.74846302059,1406.83190013035,1406.91535592527,
1406.998900418,1407.08248950094,1407.16621276849,1407.24689248439,1407.33063119624,
1407.4142667076,1407.497819151,1407.58130858685,1407.66476253747,1407.74819903131,
1407.83163614107,1407.91509193599,1407.99863642872,1408.08222551166,1408.16594877921,
1408.24662849511,1408.33036720696,1408.41400271832,1408.49755516172,1408.58104459757,
1408.66449854819,1408.74793504203,1408.83137215179,1408.91482794671,1408.99837243944,
1409.08196152238,1409.16568478993,1409.24636450583,1409.33010321768,1409.41373872904,
1409.49729117244,1409.58078060829,1409.66423455891,1409.74767105275,1409.83110816251,
1409.91456395743,1409.99810845016,1410.0816975331,1410.16542080065,1410.24610051655,
1410.3244751935),.UNSPECIFIED.);
#947=B_SPLINE_CURVE_WITH_KNOTS('',3,(#119672,#119673,#119674,#119675,#119676,
#119677,#119678,#119679,#119680,#119681,#119682,#119683,#119684,#119685,
#119686,#119687,#119688,#119689,#119690,#119691,#119692,#119693,#119694,
#119695,#119696,#119697,#119698,#119699,#119700,#119701,#119702,#119703,
#119704,#119705,#119706,#119707,#119708,#119709,#119710,#119711,#119712,
#119713,#119714,#119715,#119716,#119717,#119718,#119719,#119720,#119721,
#119722,#119723,#119724,#119725,#119726,#119727,#119728,#119729,#119730,
#119731,#119732,#119733,#119734,#119735,#119736,#119737,#119738,#119739,
#119740,#119741,#119742,#119743,#119744,#119745,#119746,#119747,#119748,
#119749,#119750,#119751,#119752,#119753,#119754,#119755,#119756,#119757,
#119758,#119759,#119760,#119761,#119762,#119763,#119764,#119765,#119766,
#119767,#119768,#119769,#119770,#119771,#119772,#119773,#119774,#119775,
#119776,#119777,#119778,#119779,#119780,#119781,#119782,#119783,#119784,
#119785,#119786,#119787,#119788,#119789,#119790,#119791,#119792,#119793,
#119794,#119795,#119796,#119797,#119798,#119799,#119800,#119801,#119802,
#119803,#119804,#119805,#119806,#119807,#119808,#119809,#119810,#119811,
#119812,#119813,#119814,#119815,#119816,#119817,#119818,#119819,#119820,
#119821,#119822,#119823,#119824,#119825,#119826,#119827,#119828,#119829,
#119830,#119831,#119832,#119833,#119834,#119835,#119836,#119837,#119838,
#119839,#119840,#119841,#119842,#119843,#119844,#119845,#119846,#119847,
#119848,#119849,#119850,#119851,#119852,#119853,#119854,#119855,#119856,
#119857,#119858,#119859,#119860,#119861,#119862,#119863,#119864,#119865,
#119866,#119867,#119868,#119869,#119870,#119871,#119872,#119873,#119874,
#119875,#119876,#119877,#119878,#119879,#119880,#119881,#119882,#119883,
#119884,#119885,#119886,#119887,#119888),.UNSPECIFIED.,.F.,.F.,(4,3,3,3,
3,3,3,3,3,3,3,3,3,3,3,3,3,3,3,3,3,3,3,3,3,3,3,3,3,3,3,3,3,3,3,3,3,3,3,3,
3,3,3,3,3,3,3,3,3,3,3,3,3,3,3,3,3,3,3,3,3,3,3,3,3,3,3,3,3,3,3,3,4),(1410.57510146201,
1410.67010500045,1410.76553206136,1410.86152504162,1410.93554590755,1411.0192846194,
1411.10292013076,1411.18647257416,1411.26996201001,1411.35341596063,1411.43685245447,
1411.52028956423,1411.60374535915,1411.68728985187,1411.77087893482,1411.85460220237,
1411.93528191827,1412.01902063012,1412.10265614148,1412.18620858488,1412.26969802073,
1412.35315197135,1412.43658846519,1412.52002557495,1412.60348136987,1412.6870258626,
1412.77061494554,1412.8543382131,1412.93501792899,1413.01875664084,1413.1023921522,
1413.1859445956,1413.26943403145,1413.35288798207,1413.43632447591,1413.51976158567,
1413.60321738059,1413.68676187332,1413.77035095626,1413.85407422381,1413.93475393971,
1414.01849265156,1414.10212816292,1414.18568060632,1414.26917004217,1414.35262399279,
1414.43606048663,1414.51949759639,1414.6029533913,1414.68649788403,1414.77008696697,
1414.85381023453,1414.93448995043,1415.01822866228,1415.10186417364,1415.18541661704,
1415.26890605289,1415.35236000351,1415.43579649735,1415.51923360711,1415.60268940203,
1415.68623389476,1415.7698229777,1415.85354624526,1415.93422596115,1416.01825423227,
1416.10099893318,1416.18366832812,1416.26628131214,1416.35132401664,1416.43389281429,
1416.52017247222,1416.60645213015),.UNSPECIFIED.);
#948=B_SPLINE_CURVE_WITH_KNOTS('',3,(#119889,#119890,#119891,#119892,#119893,
#119894,#119895,#119896,#119897,#119898),.UNSPECIFIED.,.F.,.F.,(4,3,3,4),
(1410.32430278068,1410.40811390766,1410.49192260022,1410.57510146181),
 .UNSPECIFIED.);
#949=B_SPLINE_CURVE_WITH_KNOTS('',3,(#119900,#119901,#119902,#119903,#119904,
#119905,#119906,#119907,#119908,#119909),.UNSPECIFIED.,.F.,.F.,(4,3,3,4),
(1410.3244751935,1410.42295017058,1410.52052586119,1410.57510146163),
 .UNSPECIFIED.);
#950=B_SPLINE_CURVE_WITH_KNOTS('',3,(#119910,#119911,#119912,#119913,#119914,
#119915,#119916,#119917,#119918,#119919,#119920,#119921,#119922,#119923,
#119924,#119925,#119926,#119927,#119928,#119929,#119930,#119931,#119932,
#119933,#119934,#119935,#119936,#119937,#119938,#119939,#119940,#119941,
#119942,#119943,#119944,#119945,#119946,#119947,#119948,#119949,#119950,
#119951,#119952,#119953,#119954,#119955,#119956,#119957,#119958,#119959,
#119960,#119961,#119962,#119963,#119964,#119965,#119966,#119967,#119968,
#119969,#119970,#119971,#119972,#119973,#119974,#119975,#119976,#119977,
#119978,#119979,#119980,#119981,#119982,#119983,#119984,#119985,#119986,
#119987,#119988,#119989,#119990,#119991,#119992,#119993,#119994,#119995,
#119996,#119997,#119998,#119999,#120000,#120001,#120002,#120003,#120004,
#120005,#120006,#120007,#120008,#120009,#120010,#120011,#120012,#120013,
#120014,#120015,#120016,#120017,#120018,#120019,#120020,#120021,#120022,
#120023,#120024,#120025,#120026,#120027,#120028,#120029,#120030,#120031,
#120032,#120033,#120034,#120035,#120036,#120037,#120038,#120039,#120040,
#120041,#120042,#120043,#120044,#120045,#120046,#120047,#120048,#120049,
#120050,#120051,#120052,#120053,#120054,#120055,#120056,#120057,#120058,
#120059,#120060,#120061,#120062,#120063,#120064,#120065,#120066,#120067,
#120068,#120069,#120070,#120071,#120072,#120073,#120074,#120075,#120076,
#120077,#120078,#120079,#120080,#120081,#120082,#120083,#120084,#120085,
#120086,#120087,#120088,#120089,#120090,#120091,#120092,#120093,#120094,
#120095,#120096,#120097,#120098,#120099,#120100,#120101,#120102,#120103,
#120104,#120105,#120106,#120107,#120108,#120109,#120110,#120111,#120112,
#120113,#120114,#120115,#120116,#120117,#120118,#120119,#120120,#120121,
#120122,#120123,#120124,#120125,#120126,#120127,#120128,#120129),
 .UNSPECIFIED.,.F.,.F.,(4,3,3,3,3,3,3,3,3,3,3,3,3,3,3,3,3,3,3,3,3,3,3,3,
3,3,3,3,3,3,3,3,3,3,3,3,3,3,3,3,3,3,3,3,3,3,3,3,3,3,3,3,3,3,3,3,3,3,3,3,
3,3,3,3,3,3,3,3,3,3,3,3,3,4),(1410.57510146181,1410.65894334499,1410.74225529584,
1410.82557017512,1410.9089061093,1410.9931387138,1411.07661585494,1411.1612261911,
1411.24583652727,1411.32957523912,1411.41321075048,1411.49676319388,1411.58025262973,
1411.66370658035,1411.74714307419,1411.83058018395,1411.91403597887,1411.9975804716,
1412.08116955454,1412.16489282209,1412.24557253799,1412.32931124984,1412.4129467612,
1412.4964992046,1412.57998864045,1412.66344259107,1412.74687908491,1412.83031619467,
1412.91377198959,1412.99731648232,1413.08090556526,1413.16462883281,1413.24530854871,
1413.32904726056,1413.41268277192,1413.49623521532,1413.57972465117,1413.66317860179,
1413.74661509563,1413.83005220539,1413.91350800031,1413.99705249304,1414.08064157598,
1414.16436484353,1414.24504455943,1414.32878327128,1414.41241878264,1414.49597122604,
1414.57946066189,1414.66291461251,1414.74635110635,1414.82978821611,1414.91324401103,
1414.99678850376,1415.0803775867,1415.16410085425,1415.24478057015,1415.328519282,
1415.41215479336,1415.49570723676,1415.57919667261,1415.66265062323,1415.74608711707,
1415.82952422683,1415.91298002175,1415.99652451447,1416.08011359742,1416.16383686497,
1416.24451658087,1416.32920862088,1416.41375449164,1416.49821554759,1416.5825919458,
1416.60760743314),.UNSPECIFIED.);
#951=B_SPLINE_CURVE_WITH_KNOTS('',3,(#120135,#120136,#120137,#120138,#120139,
#120140,#120141,#120142,#120143,#120144,#120145,#120146,#120147,#120148,
#120149,#120150,#120151,#120152,#120153,#120154,#120155,#120156,#120157,
#120158,#120159,#120160,#120161,#120162,#120163,#120164,#120165,#120166,
#120167,#120168,#120169,#120170,#120171,#120172,#120173,#120174,#120175,
#120176,#120177,#120178,#120179,#120180,#120181,#120182,#120183,#120184,
#120185,#120186,#120187,#120188,#120189,#120190,#120191,#120192,#120193,
#120194,#120195,#120196,#120197,#120198,#120199,#120200,#120201,#120202,
#120203,#120204,#120205,#120206,#120207,#120208,#120209,#120210,#120211,
#120212,#120213,#120214,#120215,#120216,#120217,#120218,#120219,#120220,
#120221,#120222,#120223,#120224,#120225,#120226,#120227,#120228,#120229,
#120230,#120231,#120232,#120233,#120234,#120235,#120236,#120237,#120238,
#120239,#120240,#120241,#120242,#120243,#120244,#120245,#120246,#120247,
#120248,#120249,#120250,#120251,#120252,#120253,#120254,#120255,#120256,
#120257,#120258,#120259,#120260,#120261,#120262,#120263,#120264,#120265,
#120266,#120267,#120268,#120269,#120270,#120271,#120272,#120273,#120274,
#120275,#120276,#120277,#120278,#120279,#120280,#120281,#120282,#120283,
#120284,#120285,#120286,#120287,#120288,#120289,#120290,#120291,#120292,
#120293,#120294,#120295,#120296,#120297,#120298,#120299,#120300,#120301,
#120302,#120303,#120304,#120305,#120306,#120307,#120308,#120309,#120310,
#120311,#120312,#120313,#120314,#120315,#120316,#120317,#120318,#120319,
#120320,#120321,#120322,#120323,#120324,#120325,#120326,#120327,#120328,
#120329,#120330,#120331,#120332,#120333,#120334,#120335,#120336,#120337,
#120338,#120339,#120340,#120341,#120342,#120343,#120344,#120345,#120346,
#120347,#120348,#120349,#120350,#120351,#120352,#120353,#120354),
 .UNSPECIFIED.,.F.,.F.,(4,3,3,3,3,3,3,3,3,3,3,3,3,3,3,3,3,3,3,3,3,3,3,3,
3,3,3,3,3,3,3,3,3,3,3,3,3,3,3,3,3,3,3,3,3,3,3,3,3,3,3,3,3,3,3,3,3,3,3,3,
3,3,3,3,3,3,3,3,3,3,3,3,3,4),(1416.85828676899,1416.93396197187,1417.01770068372,
1417.10133619508,1417.18488863848,1417.26837807433,1417.35183202495,1417.43526851879,
1417.51870562855,1417.60216142347,1417.6857059162,1417.76929499914,1417.8530182667,
1417.93369798259,1418.01743669444,1418.1010722058,1418.1846246492,1418.26811408505,
1418.35156803567,1418.43500452951,1418.51844163927,1418.60189743419,1418.68544192692,
1418.76903100986,1418.85275427742,1418.93343399331,1419.01717270516,1419.10080821652,
1419.18436065992,1419.26785009577,1419.35130404639,1419.43474054023,1419.51817764999,
1419.60163344491,1419.68517793764,1419.76876702058,1419.85249028813,1419.93317000403,
1420.01690871588,1420.10054422724,1420.18409667064,1420.26758610649,1420.35104005711,
1420.43447655095,1420.51791366071,1420.60136945563,1420.68491394836,1420.7685030313,
1420.85222629885,1420.93290601475,1421.0166447266,1421.10028023796,1421.18383268136,
1421.26732211721,1421.35077606783,1421.43421256167,1421.51764967143,1421.60110546634,
1421.68464995907,1421.76823904201,1421.85196230957,1421.93264202547,1422.01638314035,
1422.10002049812,1422.18357423364,1422.26706440912,1422.35051630726,1422.4339499617,
1422.51738344462,1422.60083482409,1422.68436422929,1422.76793789954,1422.85162109986,
1422.89017552255),.UNSPECIFIED.);
#952=B_SPLINE_CURVE_WITH_KNOTS('',3,(#120355,#120356,#120357,#120358,#120359,
#120360,#120361,#120362,#120363,#120364),.UNSPECIFIED.,.F.,.F.,(4,3,3,4),
(1416.60645213015,1416.68913802073,1416.7737123948,1416.85828676886),
 .UNSPECIFIED.);
#953=B_SPLINE_CURVE_WITH_KNOTS('',3,(#120366,#120367,#120368,#120369,#120370,
#120371,#120372,#120373,#120374,#120375),.UNSPECIFIED.,.F.,.F.,(4,3,3,4),
(1416.60760743314,1416.69191056942,1416.77619079502,1416.85828676899),
 .UNSPECIFIED.);
#954=B_SPLINE_CURVE_WITH_KNOTS('',3,(#120376,#120377,#120378,#120379,#120380,
#120381,#120382,#120383,#120384,#120385,#120386,#120387,#120388,#120389,
#120390,#120391,#120392,#120393,#120394,#120395,#120396,#120397,#120398,
#120399,#120400,#120401,#120402,#120403,#120404,#120405,#120406,#120407,
#120408,#120409,#120410,#120411,#120412,#120413,#120414,#120415,#120416,
#120417,#120418,#120419,#120420,#120421,#120422,#120423,#120424,#120425,
#120426,#120427,#120428,#120429,#120430,#120431,#120432,#120433,#120434,
#120435,#120436,#120437,#120438,#120439,#120440,#120441,#120442,#120443,
#120444,#120445,#120446,#120447,#120448,#120449,#120450,#120451,#120452,
#120453,#120454,#120455,#120456,#120457,#120458,#120459,#120460,#120461,
#120462,#120463,#120464,#120465,#120466,#120467,#120468,#120469,#120470,
#120471,#120472,#120473,#120474,#120475,#120476,#120477,#120478,#120479,
#120480,#120481,#120482,#120483,#120484,#120485,#120486,#120487,#120488,
#120489,#120490,#120491,#120492,#120493,#120494,#120495,#120496,#120497,
#120498,#120499,#120500,#120501,#120502,#120503,#120504,#120505,#120506,
#120507,#120508,#120509,#120510,#120511,#120512,#120513,#120514,#120515,
#120516,#120517,#120518,#120519,#120520,#120521,#120522,#120523,#120524,
#120525,#120526,#120527,#120528,#120529,#120530,#120531,#120532,#120533,
#120534,#120535,#120536,#120537,#120538,#120539,#120540,#120541,#120542,
#120543,#120544,#120545,#120546,#120547,#120548,#120549,#120550,#120551,
#120552,#120553,#120554,#120555,#120556,#120557,#120558,#120559,#120560,
#120561,#120562,#120563,#120564,#120565,#120566,#120567,#120568,#120569,
#120570,#120571,#120572,#120573,#120574,#120575,#120576,#120577,#120578,
#120579,#120580,#120581,#120582,#120583,#120584,#120585,#120586,#120587,
#120588,#120589,#120590,#120591,#120592),.UNSPECIFIED.,.F.,.F.,(4,3,3,3,
3,3,3,3,3,3,3,3,3,3,3,3,3,3,3,3,3,3,3,3,3,3,3,3,3,3,3,3,3,3,3,3,3,3,3,3,
3,3,3,3,3,3,3,3,3,3,3,3,3,3,3,3,3,3,3,3,3,3,3,3,3,3,3,3,3,3,3,3,4),(1416.85828676918,
1416.95477822478,1417.04830595778,1417.14627927468,1417.24425259159,1417.32799130344,
1417.4116268148,1417.4951792582,1417.57866869405,1417.66212264467,1417.74555913851,
1417.82899624827,1417.91245204319,1417.99599653592,1418.07958561886,1418.16330888641,
1418.24398860231,1418.32772731416,1418.41136282552,1418.49491526892,1418.57840470477,
1418.66185865539,1418.74529514923,1418.82873225899,1418.91218805391,1418.99573254664,
1419.07932162958,1419.16304489713,1419.24372461303,1419.32746332488,1419.41109883624,
1419.49465127964,1419.57814071549,1419.66159466611,1419.74503115995,1419.82846826971,
1419.91192406463,1419.99546855736,1420.0790576403,1420.16278090785,1420.24346062375,
1420.3271993356,1420.41083484696,1420.49438729036,1420.57787672621,1420.66133067683,
1420.74476717067,1420.82820428043,1420.91166007535,1420.99520456808,1421.07879365102,
1421.16251691857,1421.24319663447,1421.32693534632,1421.41057085768,1421.49412330108,
1421.57761273693,1421.66106668755,1421.74450318139,1421.82794029115,1421.91139608607,
1421.9949405788,1422.07852966174,1422.16225292929,1422.24293264519,1422.32559622083,
1422.40816522113,1422.490658732,1422.57309577088,1422.6555052585,1422.73789637857,
1422.82031610301,1422.88963902832),.UNSPECIFIED.);
#955=B_SPLINE_CURVE_WITH_KNOTS('',3,(#120598,#120599,#120600,#120601,#120602,
#120603,#120604,#120605,#120606,#120607,#120608,#120609,#120610,#120611,
#120612,#120613,#120614,#120615,#120616,#120617,#120618,#120619,#120620,
#120621,#120622,#120623,#120624,#120625,#120626,#120627,#120628,#120629,
#120630,#120631,#120632,#120633,#120634,#120635,#120636,#120637,#120638,
#120639,#120640,#120641,#120642,#120643,#120644,#120645,#120646,#120647,
#120648,#120649,#120650,#120651,#120652,#120653,#120654,#120655,#120656,
#120657,#120658,#120659,#120660,#120661,#120662,#120663,#120664,#120665,
#120666,#120667,#120668,#120669,#120670,#120671,#120672,#120673,#120674,
#120675,#120676,#120677,#120678,#120679,#120680,#120681,#120682,#120683,
#120684,#120685,#120686,#120687,#120688,#120689,#120690,#120691,#120692,
#120693,#120694,#120695,#120696,#120697,#120698,#120699,#120700,#120701,
#120702,#120703,#120704,#120705,#120706,#120707,#120708,#120709,#120710,
#120711,#120712,#120713,#120714,#120715,#120716,#120717,#120718,#120719,
#120720,#120721,#120722,#120723,#120724,#120725,#120726,#120727,#120728,
#120729,#120730,#120731,#120732,#120733,#120734,#120735,#120736,#120737,
#120738,#120739,#120740,#120741,#120742,#120743,#120744,#120745,#120746,
#120747,#120748,#120749,#120750,#120751,#120752,#120753,#120754,#120755,
#120756,#120757,#120758,#120759,#120760,#120761,#120762,#120763,#120764,
#120765,#120766,#120767,#120768,#120769,#120770,#120771,#120772,#120773,
#120774,#120775,#120776,#120777,#120778,#120779,#120780,#120781,#120782,
#120783,#120784,#120785,#120786,#120787,#120788,#120789,#120790,#120791,
#120792,#120793,#120794,#120795,#120796,#120797,#120798,#120799,#120800,
#120801,#120802,#120803,#120804,#120805,#120806,#120807,#120808,#120809,
#120810,#120811,#120812,#120813,#120814,#120815,#120816,#120817),
 .UNSPECIFIED.,.F.,.F.,(4,3,3,3,3,3,3,3,3,3,3,3,3,3,3,3,3,3,3,3,3,3,3,3,
3,3,3,3,3,3,3,3,3,3,3,3,3,3,3,3,3,3,3,3,3,3,3,3,3,3,3,3,3,3,3,3,3,3,3,3,
3,3,3,3,3,3,3,3,3,3,3,3,3,4),(1423.14147207631,1423.22386678623,1423.30619520945,
1423.38848470131,1423.47075562151,1423.55302696428,1423.63531772196,1423.71769400858,
1423.80011729223,1423.88266299128,1423.93211404692,1424.01585275877,1424.09948827013,
1424.18304071353,1424.26653014938,1424.3499841,1424.43342059384,1424.5168577036,
1424.60031349852,1424.68385799124,1424.76744707419,1424.85117034174,1424.93185005764,
1425.01558876949,1425.09922428085,1425.18277672425,1425.2662661601,1425.34972011072,
1425.43315660456,1425.51659371432,1425.60004950923,1425.68359400196,1425.7671830849,
1425.85090635246,1425.93158606836,1426.01532478021,1426.09896029157,1426.18251273497,
1426.26600217082,1426.34945612144,1426.43289261528,1426.51632972504,1426.59978551996,
1426.68333001269,1426.76691909563,1426.85064236319,1426.93132207908,1427.01506079093,
1427.09869630229,1427.18224874569,1427.26573818154,1427.34919213216,1427.432628626,
1427.51606573576,1427.59952153068,1427.68306602341,1427.76665510635,1427.85037837391,
1427.9310580898,1428.01479680165,1428.09843231301,1428.18198475641,1428.26547419226,
1428.34892814288,1428.43236463672,1428.51580174648,1428.5992575414,1428.68280203413,
1428.76639111707,1428.85011438462,1428.93079410052,1429.01909172383,1429.10718968499,
1429.17433711171),.UNSPECIFIED.);
#956=B_SPLINE_CURVE_WITH_KNOTS('',3,(#120818,#120819,#120820,#120821,#120822,
#120823,#120824,#120825,#120826,#120827),.UNSPECIFIED.,.F.,.F.,(4,3,3,4),
(1422.89017552255,1422.93237803619,1423.04995135785,1423.14147207617),
 .UNSPECIFIED.);
#957=B_SPLINE_CURVE_WITH_KNOTS('',3,(#120829,#120830,#120831,#120832,#120833,
#120834,#120835,#120836,#120837,#120838),.UNSPECIFIED.,.F.,.F.,(4,3,3,4),
(1422.88963902832,1422.97213368162,1423.05680287883,1423.14147207603),
 .UNSPECIFIED.);
#958=B_SPLINE_CURVE_WITH_KNOTS('',3,(#120839,#120840,#120841,#120842,#120843,
#120844,#120845,#120846,#120847,#120848,#120849,#120850,#120851,#120852,
#120853,#120854,#120855,#120856,#120857,#120858,#120859,#120860,#120861,
#120862,#120863,#120864,#120865,#120866,#120867,#120868,#120869,#120870,
#120871,#120872,#120873,#120874,#120875,#120876,#120877,#120878,#120879,
#120880,#120881,#120882,#120883,#120884,#120885,#120886,#120887,#120888,
#120889,#120890,#120891,#120892,#120893,#120894,#120895,#120896,#120897,
#120898,#120899,#120900,#120901,#120902,#120903,#120904,#120905,#120906,
#120907,#120908,#120909,#120910,#120911,#120912,#120913,#120914,#120915,
#120916,#120917,#120918,#120919,#120920,#120921,#120922,#120923,#120924,
#120925,#120926,#120927,#120928,#120929,#120930,#120931,#120932,#120933,
#120934,#120935,#120936,#120937,#120938,#120939,#120940,#120941,#120942,
#120943,#120944,#120945,#120946,#120947,#120948,#120949,#120950,#120951,
#120952,#120953,#120954,#120955,#120956,#120957,#120958,#120959,#120960,
#120961,#120962,#120963,#120964,#120965,#120966,#120967,#120968,#120969,
#120970,#120971,#120972,#120973,#120974,#120975,#120976,#120977,#120978,
#120979,#120980,#120981,#120982,#120983,#120984,#120985,#120986,#120987,
#120988,#120989,#120990,#120991,#120992,#120993,#120994,#120995,#120996,
#120997,#120998,#120999,#121000,#121001,#121002,#121003,#121004,#121005,
#121006,#121007,#121008,#121009,#121010,#121011,#121012,#121013,#121014,
#121015,#121016,#121017,#121018,#121019,#121020,#121021,#121022,#121023,
#121024,#121025,#121026,#121027,#121028,#121029,#121030,#121031,#121032,
#121033,#121034,#121035,#121036,#121037,#121038,#121039,#121040,#121041,
#121042,#121043,#121044,#121045,#121046,#121047,#121048,#121049,#121050,
#121051,#121052,#121053,#121054,#121055),.UNSPECIFIED.,.F.,.F.,(4,3,3,3,
3,3,3,3,3,3,3,3,3,3,3,3,3,3,3,3,3,3,3,3,3,3,3,3,3,3,3,3,3,3,3,3,3,3,3,3,
3,3,3,3,3,3,3,3,3,3,3,3,3,3,3,3,3,3,3,3,3,3,3,3,3,3,3,3,3,3,3,3,4),(1423.14147207617,
1423.24266865591,1423.32640736776,1423.41004287912,1423.49359532252,1423.57708475837,
1423.66053870899,1423.74397520283,1423.82741231259,1423.91086810751,1423.99441260024,
1424.07800168318,1424.16172495074,1424.24240466663,1424.32614337848,1424.40977888984,
1424.49333133324,1424.57682076909,1424.66027471971,1424.74371121355,1424.82714832331,
1424.91060411823,1424.99414861096,1425.0777376939,1425.16146096146,1425.24214067735,
1425.3258793892,1425.40951490056,1425.49306734396,1425.57655677981,1425.66001073043,
1425.74344722427,1425.82688433403,1425.91034012894,1425.99388462167,1426.07747370462,
1426.16119697217,1426.24187668807,1426.32561539992,1426.40925091128,1426.49280335468,
1426.57629279053,1426.65974674115,1426.74318323499,1426.82662034475,1426.91007613967,
1426.9936206324,1427.07720971534,1427.1609329829,1427.24161269879,1427.32535141064,
1427.408986922,1427.4925393654,1427.57602880125,1427.65948275187,1427.74291924571,
1427.82635635547,1427.90981215039,1427.99335664312,1428.07694572606,1428.16066899361,
1428.24134870951,1428.32509132268,1428.40872984063,1428.49228439967,1428.57740517497,
1428.66085544328,1428.74428734301,1428.82771894588,1428.91410185992,1428.9976247119,
1429.08543765696,1429.17325060202),.UNSPECIFIED.);
#959=B_SPLINE_CURVE_WITH_KNOTS('',3,(#121061,#121062,#121063,#121064,#121065,
#121066,#121067,#121068,#121069,#121070,#121071,#121072,#121073,#121074,
#121075,#121076,#121077,#121078,#121079,#121080,#121081,#121082,#121083,
#121084,#121085,#121086,#121087,#121088,#121089,#121090,#121091,#121092,
#121093,#121094,#121095,#121096,#121097,#121098,#121099,#121100,#121101,
#121102,#121103,#121104,#121105,#121106,#121107,#121108,#121109,#121110,
#121111,#121112,#121113,#121114,#121115,#121116,#121117,#121118,#121119,
#121120,#121121,#121122,#121123,#121124,#121125,#121126,#121127,#121128,
#121129,#121130,#121131,#121132,#121133,#121134,#121135,#121136,#121137,
#121138,#121139,#121140,#121141,#121142,#121143,#121144,#121145,#121146,
#121147,#121148,#121149,#121150,#121151,#121152,#121153,#121154,#121155,
#121156,#121157,#121158,#121159,#121160,#121161,#121162,#121163,#121164,
#121165,#121166,#121167,#121168,#121169,#121170,#121171,#121172,#121173,
#121174,#121175,#121176,#121177,#121178,#121179,#121180,#121181,#121182,
#121183,#121184,#121185,#121186,#121187,#121188,#121189,#121190,#121191,
#121192,#121193,#121194,#121195,#121196,#121197,#121198,#121199,#121200,
#121201,#121202,#121203,#121204,#121205,#121206,#121207,#121208,#121209,
#121210,#121211,#121212,#121213,#121214,#121215,#121216,#121217,#121218,
#121219,#121220,#121221,#121222,#121223,#121224,#121225,#121226,#121227,
#121228,#121229,#121230,#121231,#121232,#121233,#121234,#121235,#121236,
#121237,#121238,#121239,#121240,#121241,#121242,#121243,#121244,#121245,
#121246,#121247,#121248,#121249,#121250,#121251,#121252,#121253,#121254,
#121255,#121256,#121257,#121258,#121259,#121260,#121261,#121262,#121263,
#121264,#121265,#121266,#121267,#121268,#121269,#121270,#121271,#121272,
#121273,#121274,#121275,#121276,#121277,#121278,#121279,#121280),
 .UNSPECIFIED.,.F.,.F.,(4,3,3,3,3,3,3,3,3,3,3,3,3,3,3,3,3,3,3,3,3,3,3,3,
3,3,3,3,3,3,3,3,3,3,3,3,3,3,3,3,3,3,3,3,3,3,3,3,3,3,3,3,3,3,3,3,3,3,3,3,
3,3,3,3,3,3,3,3,3,3,3,3,3,4),(1429.42465738335,1429.51184693731,1429.59914373417,
1429.6866395601,1429.77423939675,1429.86203908662,1429.93053011124,1430.01426882309,
1430.09790433445,1430.18145677785,1430.2649462137,1430.34840016431,1430.43183665816,
1430.51527376791,1430.59872956283,1430.68227405556,1430.7658631385,1430.84958640606,
1430.93026612196,1431.01400483381,1431.09764034517,1431.18119278857,1431.26468222442,
1431.34813617504,1431.43157266888,1431.51500977864,1431.59846557356,1431.68201006629,
1431.76559914923,1431.84932241678,1431.93000213268,1432.01374084453,1432.09737635589,
1432.18092879929,1432.26441823514,1432.34787218576,1432.4313086796,1432.51474578936,
1432.59820158428,1432.68174607701,1432.76533515995,1432.84905842751,1432.9297381434,
1433.01347685525,1433.09711236661,1433.18066481001,1433.26415424586,1433.34760819648,
1433.43104469032,1433.51448180008,1433.597937595,1433.68148208772,1433.76507117067,
1433.84879443822,1433.92947415412,1434.01321286597,1434.09684837733,1434.18040082073,
1434.26389025658,1434.3473442072,1434.43078070104,1434.5142178108,1434.59767360572,
1434.68121809845,1434.76480718139,1434.84853044895,1434.92921016484,1435.01180452316,
1435.09430200276,1435.17672175617,1435.25907889747,1435.34139995451,1435.42371181849,
1435.45634400191),.UNSPECIFIED.);
#960=B_SPLINE_CURVE_WITH_KNOTS('',3,(#121281,#121282,#121283,#121284,#121285,
#121286,#121287,#121288,#121289,#121290),.UNSPECIFIED.,.F.,.F.,(4,3,3,4),
(1429.17433711171,1429.26217368456,1429.3498375818,1429.42465738322),
 .UNSPECIFIED.);
#961=B_SPLINE_CURVE_WITH_KNOTS('',3,(#121292,#121293,#121294,#121295,#121296,
#121297,#121298,#121299,#121300,#121301),.UNSPECIFIED.,.F.,.F.,(4,3,3,4),
(1429.17325060202,1429.24108472023,1429.36688712493,1429.42465738335),
 .UNSPECIFIED.);
#962=B_SPLINE_CURVE_WITH_KNOTS('',3,(#121302,#121303,#121304,#121305,#121306,
#121307,#121308,#121309,#121310,#121311,#121312,#121313,#121314,#121315,
#121316,#121317,#121318,#121319,#121320,#121321,#121322,#121323,#121324,
#121325,#121326,#121327,#121328,#121329,#121330,#121331,#121332,#121333,
#121334,#121335,#121336,#121337,#121338,#121339,#121340,#121341,#121342,
#121343,#121344,#121345,#121346,#121347,#121348,#121349,#121350,#121351,
#121352,#121353,#121354,#121355,#121356,#121357,#121358,#121359,#121360,
#121361,#121362,#121363,#121364,#121365,#121366,#121367,#121368,#121369,
#121370,#121371,#121372,#121373,#121374,#121375,#121376,#121377,#121378,
#121379,#121380,#121381,#121382,#121383,#121384,#121385,#121386,#121387,
#121388,#121389,#121390,#121391,#121392,#121393,#121394,#121395,#121396,
#121397,#121398,#121399,#121400,#121401,#121402,#121403,#121404,#121405,
#121406,#121407,#121408,#121409,#121410,#121411,#121412,#121413,#121414,
#121415,#121416,#121417,#121418,#121419,#121420,#121421,#121422,#121423,
#121424,#121425,#121426,#121427,#121428,#121429,#121430,#121431,#121432,
#121433,#121434,#121435,#121436,#121437,#121438,#121439,#121440,#121441,
#121442,#121443,#121444,#121445,#121446,#121447,#121448,#121449,#121450,
#121451,#121452,#121453,#121454,#121455,#121456,#121457,#121458,#121459,
#121460,#121461,#121462,#121463,#121464,#121465,#121466,#121467,#121468,
#121469,#121470,#121471,#121472,#121473,#121474,#121475,#121476,#121477,
#121478,#121479,#121480,#121481,#121482,#121483,#121484,#121485,#121486,
#121487,#121488,#121489,#121490,#121491,#121492,#121493,#121494,#121495,
#121496,#121497,#121498,#121499,#121500,#121501,#121502,#121503,#121504,
#121505,#121506,#121507,#121508,#121509,#121510,#121511,#121512,#121513,
#121514,#121515,#121516,#121517,#121518,#121519,#121520,#121521),
 .UNSPECIFIED.,.F.,.F.,(4,3,3,3,3,3,3,3,3,3,3,3,3,3,3,3,3,3,3,3,3,3,3,3,
3,3,3,3,3,3,3,3,3,3,3,3,3,3,3,3,3,3,3,3,3,3,3,3,3,3,3,3,3,3,3,3,3,3,3,3,
3,3,3,3,3,3,3,3,3,3,3,3,3,4),(1429.4246573835,1429.50702048783,1429.58931001852,
1429.67155095664,1429.75376682562,1429.83597666066,1429.91819948982,1430.0005042299,
1430.08285026655,1430.16532564741,1430.24082073095,1430.3245594428,1430.40819495416,
1430.49174739756,1430.57523683341,1430.65869078403,1430.74212727787,1430.82556438763,
1430.90902018255,1430.99256467528,1431.07615375822,1431.15987702578,1431.24055674167,
1431.32429545352,1431.40793096488,1431.49148340828,1431.57497284413,1431.65842679475,
1431.74186328859,1431.82530039835,1431.90875619327,1431.992300686,1432.07588976894,
1432.1596130365,1432.24029275239,1432.32403146424,1432.4076669756,1432.491219419,
1432.57470885485,1432.65816280547,1432.74159929931,1432.82503640907,1432.90849220399,
1432.99203669672,1433.07562577966,1433.15934904721,1433.24002876311,1433.32376747496,
1433.40740298632,1433.49095542972,1433.57444486557,1433.65789881619,1433.74133531003,
1433.82477241979,1433.90822821471,1433.99177270744,1434.07536179038,1434.15908505794,
1434.23976477383,1434.32350348568,1434.40713899704,1434.49069144044,1434.57418087629,
1434.6576348269,1434.74107132075,1434.8245084305,1434.90796422542,1434.99150871815,
1435.07509780109,1435.15882106865,1435.23950078455,1435.32891254343,1435.41810836263,
1435.45754054782),.UNSPECIFIED.);
#963=B_SPLINE_CURVE_WITH_KNOTS('',3,(#121527,#121528,#121529,#121530,#121531,
#121532,#121533,#121534,#121535,#121536,#121537,#121538,#121539,#121540,
#121541,#121542,#121543,#121544,#121545,#121546,#121547,#121548,#121549,
#121550,#121551,#121552,#121553,#121554,#121555,#121556,#121557,#121558,
#121559,#121560,#121561,#121562,#121563,#121564,#121565,#121566,#121567,
#121568,#121569,#121570,#121571,#121572,#121573,#121574,#121575,#121576,
#121577,#121578,#121579,#121580,#121581,#121582,#121583,#121584,#121585,
#121586,#121587,#121588,#121589,#121590,#121591,#121592,#121593,#121594,
#121595,#121596,#121597,#121598,#121599,#121600,#121601,#121602,#121603,
#121604,#121605,#121606,#121607,#121608,#121609,#121610,#121611,#121612,
#121613,#121614,#121615,#121616,#121617,#121618,#121619,#121620,#121621,
#121622,#121623,#121624,#121625,#121626,#121627,#121628,#121629,#121630,
#121631,#121632,#121633,#121634,#121635,#121636,#121637,#121638,#121639,
#121640,#121641,#121642,#121643,#121644,#121645,#121646,#121647,#121648,
#121649,#121650,#121651,#121652,#121653,#121654,#121655,#121656,#121657,
#121658,#121659,#121660,#121661,#121662,#121663,#121664,#121665,#121666,
#121667,#121668,#121669,#121670,#121671,#121672,#121673,#121674,#121675,
#121676,#121677,#121678,#121679,#121680,#121681,#121682,#121683,#121684,
#121685,#121686,#121687,#121688,#121689,#121690,#121691,#121692,#121693,
#121694,#121695,#121696,#121697,#121698,#121699,#121700,#121701,#121702,
#121703,#121704,#121705,#121706,#121707,#121708,#121709,#121710,#121711,
#121712,#121713,#121714,#121715,#121716,#121717,#121718,#121719,#121720,
#121721,#121722,#121723,#121724,#121725,#121726,#121727,#121728,#121729,
#121730,#121731,#121732,#121733,#121734,#121735,#121736,#121737,#121738,
#121739,#121740,#121741,#121742,#121743),.UNSPECIFIED.,.F.,.F.,(4,3,3,3,
3,3,3,3,3,3,3,3,3,3,3,3,3,3,3,3,3,3,3,3,3,3,3,3,3,3,3,3,3,3,3,3,3,3,3,3,
3,3,3,3,3,3,3,3,3,3,3,3,3,3,3,3,3,3,3,3,3,3,3,3,3,3,3,3,3,3,3,3,4),(1435.70784269053,
1435.82235604207,1435.92894617556,1436.01268488741,1436.09632039877,1436.17987284217,
1436.26336227802,1436.34681622863,1436.43025272248,1436.51368983223,1436.59714562715,
1436.68069011988,1436.76427920282,1436.84800247038,1436.92868218628,1437.01242089813,
1437.09605640949,1437.17960885289,1437.26309828874,1437.34655223936,1437.4299887332,
1437.51342584296,1437.59688163788,1437.68042613061,1437.76401521355,1437.8477384811,
1437.928418197,1438.01215690885,1438.09579242021,1438.17934486361,1438.26283429946,
1438.34628825008,1438.42972474392,1438.51316185368,1438.5966176486,1438.68016214133,
1438.76375122427,1438.84747449183,1438.92815420772,1439.01189291957,1439.09552843093,
1439.17908087433,1439.26257031018,1439.3460242608,1439.42946075464,1439.5128978644,
1439.59635365932,1439.67989815205,1439.76348723499,1439.84721050254,1439.92789021844,
1440.01162893029,1440.09526444165,1440.17881688505,1440.2623063209,1440.34576027152,
1440.42919676536,1440.51263387512,1440.59608967004,1440.67963416277,1440.76322324571,
1440.84694651326,1440.92762622916,1441.01137625723,1441.09502060469,1441.17856410501,
1441.26205042852,1441.34549769506,1441.42892399429,1441.51237342932,1441.59583358817,
1441.67936222842,1441.73936764326),.UNSPECIFIED.);
#964=B_SPLINE_CURVE_WITH_KNOTS('',3,(#121744,#121745,#121746,#121747,#121748,
#121749,#121750,#121751,#121752,#121753),.UNSPECIFIED.,.F.,.F.,(4,3,3,4),
(1435.45634400191,1435.53868546224,1435.62326407632,1435.70784269039),
 .UNSPECIFIED.);
#965=B_SPLINE_CURVE_WITH_KNOTS('',3,(#121755,#121756,#121757,#121758,#121759,
#121760,#121761,#121762,#121763,#121764),.UNSPECIFIED.,.F.,.F.,(4,3,3,4),
(1435.45754054782,1435.54645941689,1435.63515374008,1435.7078426904),
 .UNSPECIFIED.);
#966=B_SPLINE_CURVE_WITH_KNOTS('',3,(#121765,#121766,#121767,#121768,#121769,
#121770,#121771,#121772,#121773,#121774,#121775,#121776,#121777,#121778,
#121779,#121780,#121781,#121782,#121783,#121784,#121785,#121786,#121787,
#121788,#121789,#121790,#121791,#121792,#121793,#121794,#121795,#121796,
#121797,#121798,#121799,#121800,#121801,#121802,#121803,#121804,#121805,
#121806,#121807,#121808,#121809,#121810,#121811,#121812,#121813,#121814,
#121815,#121816,#121817,#121818,#121819,#121820,#121821,#121822,#121823,
#121824,#121825,#121826,#121827,#121828,#121829,#121830,#121831,#121832,
#121833,#121834,#121835,#121836,#121837,#121838,#121839,#121840,#121841,
#121842,#121843,#121844,#121845,#121846,#121847,#121848,#121849,#121850,
#121851,#121852,#121853,#121854,#121855,#121856,#121857,#121858,#121859,
#121860,#121861,#121862,#121863,#121864,#121865,#121866,#121867,#121868,
#121869,#121870,#121871,#121872,#121873,#121874,#121875,#121876,#121877,
#121878,#121879,#121880,#121881,#121882,#121883,#121884,#121885,#121886,
#121887,#121888,#121889,#121890,#121891,#121892,#121893,#121894,#121895,
#121896,#121897,#121898,#121899,#121900,#121901,#121902,#121903,#121904,
#121905,#121906,#121907,#121908,#121909,#121910,#121911,#121912,#121913,
#121914,#121915,#121916,#121917,#121918,#121919,#121920,#121921,#121922,
#121923,#121924,#121925,#121926,#121927,#121928,#121929,#121930,#121931,
#121932,#121933,#121934,#121935,#121936,#121937,#121938,#121939,#121940,
#121941,#121942,#121943,#121944,#121945,#121946,#121947,#121948,#121949,
#121950,#121951,#121952,#121953,#121954,#121955,#121956,#121957,#121958,
#121959,#121960,#121961,#121962,#121963,#121964,#121965,#121966,#121967,
#121968,#121969,#121970,#121971,#121972,#121973,#121974,#121975,#121976,
#121977,#121978,#121979,#121980,#121981),.UNSPECIFIED.,.F.,.F.,(4,3,3,3,
3,3,3,3,3,3,3,3,3,3,3,3,3,3,3,3,3,3,3,3,3,3,3,3,3,3,3,3,3,3,3,3,3,3,3,3,
3,3,3,3,3,3,3,3,3,3,3,3,3,3,3,3,3,3,3,3,3,3,3,3,3,3,3,3,3,3,3,3,4),(1435.70784269053,
1435.79418909534,1435.8806134886,1435.97026931526,1436.05695086,1436.14809382764,
1436.23923679527,1436.32297550712,1436.40661101849,1436.49016346189,1436.57365289774,
1436.65710684835,1436.7405433422,1436.82398045196,1436.90743624688,1436.99098073961,
1437.07456982255,1437.15829309011,1437.23897280599,1437.32271151783,1437.4063470292,
1437.4898994726,1437.57338890845,1437.65684285906,1437.74027935291,1437.82371646266,
1437.90717225758,1437.99071675031,1438.07430583325,1438.15802910081,1438.23870881671,
1438.32244752856,1438.40608303993,1438.48963548333,1438.57312491918,1438.6565788698,
1438.74001536364,1438.8234524734,1438.90690826832,1438.99045276105,1439.07404184399,
1439.15776511155,1439.23844482744,1439.32218353929,1439.40581905065,1439.48937149405,
1439.57286092991,1439.65631488052,1439.73975137437,1439.82318848412,1439.90664427904,
1439.99018877177,1440.07377785471,1440.15750112227,1440.23818083816,1440.32191955001,
1440.40555506137,1440.48910750477,1440.57259694062,1440.65605089123,1440.73948738508,
1440.82292449483,1440.90638028975,1440.98992478248,1441.07351386542,1441.15723713298,
1441.23791684888,1441.32066010468,1441.40330528578,1441.48739106607,1441.56989035993,
1441.65476938343,1441.73964840693),.UNSPECIFIED.);
#967=B_SPLINE_CURVE_WITH_KNOTS('',3,(#121987,#121988,#121989,#121990,#121991,
#121992,#121993,#121994,#121995,#121996,#121997,#121998,#121999,#122000,
#122001,#122002,#122003,#122004,#122005,#122006,#122007,#122008,#122009,
#122010,#122011,#122012,#122013,#122014,#122015,#122016,#122017,#122018,
#122019,#122020,#122021,#122022,#122023,#122024,#122025,#122026,#122027,
#122028,#122029,#122030,#122031,#122032,#122033,#122034,#122035,#122036,
#122037,#122038,#122039,#122040,#122041,#122042,#122043,#122044,#122045,
#122046,#122047,#122048,#122049,#122050,#122051,#122052,#122053,#122054,
#122055,#122056,#122057,#122058,#122059,#122060,#122061,#122062,#122063,
#122064,#122065,#122066,#122067,#122068,#122069,#122070,#122071,#122072,
#122073,#122074,#122075,#122076,#122077,#122078,#122079,#122080,#122081,
#122082,#122083,#122084,#122085,#122086,#122087,#122088,#122089,#122090,
#122091,#122092,#122093,#122094,#122095,#122096,#122097,#122098,#122099,
#122100,#122101,#122102,#122103,#122104,#122105,#122106,#122107,#122108,
#122109,#122110,#122111,#122112,#122113,#122114,#122115,#122116,#122117,
#122118,#122119,#122120,#122121,#122122,#122123,#122124,#122125,#122126,
#122127,#122128,#122129,#122130,#122131,#122132,#122133,#122134,#122135,
#122136,#122137,#122138,#122139,#122140,#122141,#122142,#122143,#122144,
#122145,#122146,#122147,#122148,#122149,#122150,#122151,#122152,#122153,
#122154,#122155,#122156,#122157,#122158,#122159,#122160,#122161,#122162,
#122163,#122164,#122165,#122166,#122167,#122168,#122169,#122170,#122171,
#122172,#122173,#122174,#122175,#122176,#122177,#122178,#122179,#122180,
#122181,#122182,#122183,#122184,#122185,#122186,#122187,#122188,#122189,
#122190,#122191,#122192,#122193,#122194,#122195,#122196,#122197,#122198,
#122199,#122200,#122201,#122202,#122203,#122204,#122205,#122206),
 .UNSPECIFIED.,.F.,.F.,(4,3,3,3,3,3,3,3,3,3,3,3,3,3,3,3,3,3,3,3,3,3,3,3,
3,3,3,3,3,3,3,3,3,3,3,3,3,3,3,3,3,3,3,3,3,3,3,3,3,3,3,3,3,3,3,3,3,3,3,3,
3,3,3,3,3,3,3,3,3,3,3,3,3,4),(1441.99102799783,1442.07397001655,1442.15681366223,
1442.23957978767,1442.32551959554,1442.40820144904,1442.49087354865,1442.5735546158,
1442.65626337548,1442.73906287441,1442.82191629707,1442.90488611973,1442.9270982506,
1443.01083696245,1443.09447247381,1443.17802491721,1443.26151435306,1443.34496830368,
1443.42840479752,1443.51184190728,1443.5952977022,1443.67884219493,1443.76243127787,
1443.84615454542,1443.92683426132,1444.01057297317,1444.09420848453,1444.17776092793,
1444.26125036378,1444.3447043144,1444.42814080824,1444.511577918,1444.59503371292,
1444.67857820565,1444.76216728859,1444.84589055615,1444.92657027204,1445.01030898389,
1445.09394449525,1445.17749693865,1445.2609863745,1445.34444032512,1445.42787681896,
1445.51131392872,1445.59476972363,1445.67831421636,1445.7619032993,1445.84562656686,
1445.92630628276,1446.01004499461,1446.09368050597,1446.17723294937,1446.26072238522,
1446.34417633584,1446.42761282968,1446.51104993944,1446.59450573436,1446.67805022709,
1446.76163931003,1446.84536257758,1446.92604229348,1447.00978100533,1447.09341651669,
1447.17696896009,1447.26045839594,1447.34391234655,1447.4273488404,1447.51078595016,
1447.59424174507,1447.6777862378,1447.76137532074,1447.8450985883,1447.9257783042,
1448.0236730871),.UNSPECIFIED.);
#968=B_SPLINE_CURVE_WITH_KNOTS('',3,(#122207,#122208,#122209,#122210,#122211,
#122212,#122213,#122214,#122215,#122216,#122217,#122218,#122219),
 .UNSPECIFIED.,.F.,.F.,(4,3,3,3,4),(1441.73936764326,1441.82299876243,1441.9067473108,
1441.92736223988,1441.99102799771),.UNSPECIFIED.);
#969=B_SPLINE_CURVE_WITH_KNOTS('',3,(#122221,#122222,#122223,#122224,#122225,
#122226,#122227,#122228,#122229,#122230),.UNSPECIFIED.,.F.,.F.,(4,3,3,4),
(1441.73964840693,1441.82211908339,1441.90657354055,1441.99102799771),
 .UNSPECIFIED.);
#970=B_SPLINE_CURVE_WITH_KNOTS('',3,(#122231,#122232,#122233,#122234,#122235,
#122236,#122237,#122238,#122239,#122240,#122241,#122242,#122243,#122244,
#122245,#122246,#122247,#122248,#122249,#122250,#122251,#122252,#122253,
#122254,#122255,#122256,#122257,#122258,#122259,#122260,#122261,#122262,
#122263,#122264,#122265,#122266,#122267,#122268,#122269,#122270,#122271,
#122272,#122273,#122274,#122275,#122276,#122277,#122278,#122279,#122280,
#122281,#122282,#122283,#122284,#122285,#122286,#122287,#122288,#122289,
#122290,#122291,#122292,#122293,#122294,#122295,#122296,#122297,#122298,
#122299,#122300,#122301,#122302,#122303,#122304,#122305,#122306,#122307,
#122308,#122309,#122310,#122311,#122312,#122313,#122314,#122315,#122316,
#122317,#122318,#122319,#122320,#122321,#122322,#122323,#122324,#122325,
#122326,#122327,#122328,#122329,#122330,#122331,#122332,#122333,#122334,
#122335,#122336,#122337,#122338,#122339,#122340,#122341,#122342,#122343,
#122344,#122345,#122346,#122347,#122348,#122349,#122350,#122351,#122352,
#122353,#122354,#122355,#122356,#122357,#122358,#122359,#122360,#122361,
#122362,#122363,#122364,#122365,#122366,#122367,#122368,#122369,#122370,
#122371,#122372,#122373,#122374,#122375,#122376,#122377,#122378,#122379,
#122380,#122381,#122382,#122383,#122384,#122385,#122386,#122387,#122388,
#122389,#122390,#122391,#122392,#122393,#122394,#122395,#122396,#122397,
#122398,#122399,#122400,#122401,#122402,#122403,#122404,#122405,#122406,
#122407,#122408,#122409,#122410,#122411,#122412,#122413,#122414,#122415,
#122416,#122417,#122418,#122419,#122420,#122421,#122422,#122423,#122424,
#122425,#122426,#122427,#122428,#122429,#122430,#122431,#122432,#122433,
#122434,#122435,#122436,#122437,#122438,#122439,#122440,#122441,#122442,
#122443,#122444,#122445,#122446,#122447,#122448,#122449,#122450),
 .UNSPECIFIED.,.F.,.F.,(4,3,3,3,3,3,3,3,3,3,3,3,3,3,3,3,3,3,3,3,3,3,3,3,
3,3,3,3,3,3,3,3,3,3,3,3,3,3,3,3,3,3,3,3,3,3,3,3,3,3,3,3,3,3,3,3,3,3,3,3,
3,3,3,3,3,3,3,3,3,3,3,3,3,4),(1441.99102799785,1442.09882248263,1442.20915371554,
1442.2376528596,1442.32139157145,1442.40502708281,1442.48857952621,1442.57206896206,
1442.65552291267,1442.73895940652,1442.82239651628,1442.90585231119,1442.98939680392,
1443.07298588686,1443.15670915442,1443.23738887032,1443.32112758217,1443.40476309353,
1443.48831553693,1443.57180497278,1443.6552589234,1443.73869541724,1443.822132527,
1443.90558832192,1443.98913281465,1444.07272189759,1444.15644516514,1444.23712488104,
1444.32086359289,1444.40449910425,1444.48805154765,1444.5715409835,1444.65499493412,
1444.73843142796,1444.82186853772,1444.90532433264,1444.98886882536,1445.07245790831,
1445.15618117586,1445.23686089176,1445.32059960361,1445.40423511497,1445.48778755837,
1445.57127699422,1445.65473094484,1445.73816743868,1445.82160454844,1445.90506034336,
1445.98860483609,1446.07219391903,1446.15591718658,1446.23659690248,1446.32033561433,
1446.40397112569,1446.48752356909,1446.57101300494,1446.65446695556,1446.7379034494,
1446.82134055916,1446.90479635408,1446.98834084681,1447.07192992975,1447.1556531973,
1447.2363329132,1447.32008459951,1447.40789239756,1447.49143313082,1447.57491711298,
1447.65836246294,1447.74178726958,1447.82523138041,1447.90868683001,1447.99219954226,
1448.02254698393),.UNSPECIFIED.);
#971=B_SPLINE_CURVE_WITH_KNOTS('',3,(#122456,#122457,#122458,#122459,#122460,
#122461,#122462,#122463,#122464,#122465,#122466,#122467,#122468,#122469,
#122470,#122471,#122472,#122473,#122474,#122475,#122476,#122477,#122478,
#122479,#122480,#122481,#122482,#122483,#122484,#122485,#122486,#122487,
#122488,#122489,#122490,#122491,#122492,#122493,#122494,#122495,#122496,
#122497,#122498,#122499,#122500,#122501,#122502,#122503,#122504,#122505,
#122506,#122507,#122508,#122509,#122510,#122511,#122512,#122513,#122514,
#122515,#122516,#122517,#122518,#122519,#122520,#122521,#122522,#122523,
#122524,#122525,#122526,#122527,#122528,#122529,#122530,#122531,#122532,
#122533,#122534,#122535,#122536,#122537,#122538,#122539,#122540,#122541,
#122542,#122543,#122544,#122545,#122546,#122547,#122548,#122549,#122550,
#122551,#122552,#122553,#122554,#122555,#122556,#122557,#122558,#122559,
#122560,#122561,#122562,#122563,#122564,#122565,#122566,#122567,#122568,
#122569,#122570,#122571,#122572,#122573,#122574,#122575,#122576,#122577,
#122578,#122579,#122580,#122581,#122582,#122583,#122584,#122585,#122586,
#122587,#122588,#122589,#122590,#122591,#122592,#122593,#122594,#122595,
#122596,#122597,#122598,#122599,#122600,#122601,#122602,#122603,#122604,
#122605,#122606,#122607,#122608,#122609,#122610,#122611,#122612,#122613,
#122614,#122615,#122616,#122617,#122618,#122619,#122620,#122621,#122622,
#122623,#122624,#122625,#122626,#122627,#122628,#122629,#122630,#122631,
#122632,#122633,#122634,#122635,#122636,#122637,#122638,#122639,#122640,
#122641,#122642,#122643,#122644,#122645,#122646,#122647,#122648,#122649,
#122650,#122651,#122652,#122653,#122654,#122655,#122656,#122657,#122658,
#122659,#122660,#122661,#122662,#122663,#122664,#122665,#122666,#122667,
#122668,#122669,#122670,#122671,#122672,#122673,#122674,#122675),
 .UNSPECIFIED.,.F.,.F.,(4,3,3,3,3,3,3,3,3,3,3,3,3,3,3,3,3,3,3,3,3,3,3,3,
3,3,3,3,3,3,3,3,3,3,3,3,3,3,3,3,3,3,3,3,3,3,3,3,3,3,3,3,3,3,3,3,3,3,3,3,
3,3,3,3,3,3,3,3,3,3,3,3,3,4),(1448.27421330489,1448.35782433656,1448.44142899155,
1448.52504506398,1448.60869035153,1448.69243622458,1448.77623540817,1448.8601726709,
1448.92551431492,1449.00925302677,1449.09288853813,1449.17644098153,1449.25993041738,
1449.343384368,1449.42682086184,1449.5102579716,1449.59371376652,1449.67725825924,
1449.76084734219,1449.84457060974,1449.92525032564,1450.00898903749,1450.09262454885,
1450.17617699225,1450.2596664281,1450.34312037872,1450.42655687256,1450.50999398232,
1450.59344977724,1450.67699426997,1450.76058335291,1450.84430662046,1450.92498633636,
1451.00872504821,1451.09236055957,1451.17591300297,1451.25940243882,1451.34285638944,
1451.42629288328,1451.50972999304,1451.59318578796,1451.67673028069,1451.76031936363,
1451.84404263118,1451.92472234708,1452.00846105893,1452.09209657029,1452.17564901369,
1452.25913844954,1452.34259240016,1452.426028894,1452.50946600376,1452.59292179867,
1452.6764662914,1452.76005537434,1452.8437786419,1452.9244583578,1453.00819706965,
1453.09183258101,1453.17538502441,1453.25887446026,1453.34232841088,1453.42576490472,
1453.50920201448,1453.5926578094,1453.67620230213,1453.75979138507,1453.84351465263,
1453.92419436852,1454.00848723102,1454.09263873748,1454.17670875473,1454.26070005874,
1454.30662927058),.UNSPECIFIED.);
#972=B_SPLINE_CURVE_WITH_KNOTS('',3,(#122676,#122677,#122678,#122679,#122680,
#122681,#122682,#122683,#122684,#122685),.UNSPECIFIED.,.F.,.F.,(4,3,3,4),
(1448.0236730871,1448.12028229969,1448.21615954937,1448.27421330469),
 .UNSPECIFIED.);
#973=B_SPLINE_CURVE_WITH_KNOTS('',3,(#122687,#122688,#122689,#122690,#122691,
#122692,#122693,#122694,#122695,#122696,#122697,#122698,#122699),
 .UNSPECIFIED.,.F.,.F.,(4,3,3,3,4),(1448.02254698393,1448.10615919498,1448.18989572745,
1448.23606892392,1448.27421330489),.UNSPECIFIED.);
#974=B_SPLINE_CURVE_WITH_KNOTS('',3,(#122700,#122701,#122702,#122703,#122704,
#122705,#122706,#122707,#122708,#122709,#122710,#122711,#122712,#122713,
#122714,#122715,#122716,#122717,#122718,#122719,#122720,#122721,#122722,
#122723,#122724,#122725,#122726,#122727,#122728,#122729,#122730,#122731,
#122732,#122733,#122734,#122735,#122736,#122737,#122738,#122739,#122740,
#122741,#122742,#122743,#122744,#122745,#122746,#122747,#122748,#122749,
#122750,#122751,#122752,#122753,#122754,#122755,#122756,#122757,#122758,
#122759,#122760,#122761,#122762,#122763,#122764,#122765,#122766,#122767,
#122768,#122769,#122770,#122771,#122772,#122773,#122774,#122775,#122776,
#122777,#122778,#122779,#122780,#122781,#122782,#122783,#122784,#122785,
#122786,#122787,#122788,#122789,#122790,#122791,#122792,#122793,#122794,
#122795,#122796,#122797,#122798,#122799,#122800,#122801,#122802,#122803,
#122804,#122805,#122806,#122807,#122808,#122809,#122810,#122811,#122812,
#122813,#122814,#122815,#122816,#122817,#122818,#122819,#122820,#122821,
#122822,#122823,#122824,#122825,#122826,#122827,#122828,#122829,#122830,
#122831,#122832,#122833,#122834,#122835,#122836,#122837,#122838,#122839,
#122840,#122841,#122842,#122843,#122844,#122845,#122846,#122847,#122848,
#122849,#122850,#122851,#122852,#122853,#122854,#122855,#122856,#122857,
#122858,#122859,#122860,#122861,#122862,#122863,#122864,#122865,#122866,
#122867,#122868,#122869,#122870,#122871,#122872,#122873,#122874,#122875,
#122876,#122877,#122878,#122879,#122880,#122881,#122882,#122883,#122884,
#122885,#122886,#122887,#122888,#122889,#122890,#122891,#122892,#122893,
#122894,#122895,#122896,#122897,#122898,#122899,#122900,#122901,#122902,
#122903,#122904,#122905,#122906,#122907,#122908,#122909,#122910,#122911,
#122912,#122913,#122914,#122915,#122916,#122917,#122918,#122919),
 .UNSPECIFIED.,.F.,.F.,(4,3,3,3,3,3,3,3,3,3,3,3,3,3,3,3,3,3,3,3,3,3,3,3,
3,3,3,3,3,3,3,3,3,3,3,3,3,3,3,3,3,3,3,3,3,3,3,3,3,3,3,3,3,3,3,3,3,3,3,3,
3,3,3,3,3,3,3,3,3,3,3,3,3,4),(1448.27421330505,1448.35743318097,1448.4405518179,
1448.52358985075,1448.60656783825,1448.68951465084,1448.77244760275,1448.85538521634,
1448.93834601377,1449.02139624031,1449.10449595701,1449.18771960852,1449.23580493464,
1449.31954364649,1449.40317915785,1449.48673160125,1449.5702210371,1449.65367498772,
1449.73711148156,1449.82054859132,1449.90400438624,1449.98754887897,1450.07113796191,
1450.15486122947,1450.23554094536,1450.31927965721,1450.40291516857,1450.48646761197,
1450.56995704782,1450.65341099844,1450.73684749228,1450.82028460204,1450.90374039696,
1450.98728488969,1451.07087397263,1451.15459724018,1451.23527695608,1451.31901566793,
1451.40265117929,1451.48620362269,1451.56969305854,1451.65314700916,1451.736583503,
1451.82002061276,1451.90347640768,1451.98702090041,1452.07060998335,1452.1543332509,
1452.2350129668,1452.31875167865,1452.40238719001,1452.48593963341,1452.56942906926,
1452.65288301988,1452.73631951372,1452.81975662348,1452.9032124184,1452.98675691113,
1453.07034599407,1453.15406926163,1453.23474897752,1453.31848768937,1453.40212320073,
1453.48567564413,1453.56916507998,1453.6526190306,1453.73605552444,1453.8194926342,
1453.90294842912,1453.98649292185,1454.07008200479,1454.15380527234,1454.23448498824,
1454.30674307549),.UNSPECIFIED.);
#975=B_SPLINE_CURVE_WITH_KNOTS('',3,(#122925,#122926,#122927,#122928,#122929,
#122930,#122931,#122932,#122933,#122934,#122935,#122936,#122937,#122938,
#122939,#122940,#122941,#122942,#122943,#122944,#122945,#122946,#122947,
#122948,#122949,#122950,#122951,#122952,#122953,#122954,#122955,#122956,
#122957,#122958,#122959,#122960,#122961,#122962,#122963,#122964,#122965,
#122966,#122967,#122968,#122969,#122970,#122971,#122972,#122973,#122974,
#122975,#122976,#122977,#122978,#122979,#122980,#122981,#122982,#122983,
#122984,#122985,#122986,#122987,#122988,#122989,#122990,#122991,#122992,
#122993,#122994,#122995,#122996,#122997,#122998,#122999,#123000,#123001,
#123002,#123003,#123004,#123005,#123006,#123007,#123008,#123009,#123010,
#123011,#123012,#123013,#123014,#123015,#123016,#123017,#123018,#123019,
#123020,#123021,#123022,#123023,#123024,#123025,#123026,#123027,#123028,
#123029,#123030,#123031,#123032,#123033,#123034,#123035,#123036,#123037,
#123038,#123039,#123040,#123041,#123042,#123043,#123044,#123045,#123046,
#123047,#123048,#123049,#123050,#123051,#123052,#123053,#123054,#123055,
#123056,#123057,#123058,#123059,#123060,#123061,#123062,#123063,#123064,
#123065,#123066,#123067,#123068,#123069,#123070,#123071,#123072,#123073,
#123074,#123075,#123076,#123077,#123078,#123079,#123080,#123081,#123082,
#123083,#123084,#123085,#123086,#123087,#123088,#123089,#123090,#123091,
#123092,#123093,#123094,#123095,#123096,#123097,#123098,#123099,#123100,
#123101,#123102,#123103,#123104,#123105,#123106,#123107,#123108,#123109,
#123110,#123111,#123112,#123113,#123114,#123115,#123116,#123117,#123118,
#123119,#123120,#123121,#123122,#123123,#123124,#123125,#123126,#123127,
#123128,#123129,#123130,#123131,#123132,#123133,#123134,#123135,#123136,
#123137,#123138,#123139,#123140,#123141),.UNSPECIFIED.,.F.,.F.,(4,3,3,3,
3,3,3,3,3,3,3,3,3,3,3,3,3,3,3,3,3,3,3,3,3,3,3,3,3,3,3,3,3,3,3,3,3,3,3,3,
3,3,3,3,3,3,3,3,3,3,3,3,3,3,3,3,3,3,3,3,3,3,3,3,3,3,3,3,3,3,3,3,4),(1454.55739861227,
1454.65194746431,1454.74689204477,1454.84238116431,1454.92393037924,1455.00766909109,
1455.09130460245,1455.17485704585,1455.2583464817,1455.34180043232,1455.42523692616,
1455.50867403592,1455.59212983084,1455.67567432356,1455.75926340651,1455.84298667406,
1455.92366638996,1456.00740510181,1456.09104061317,1456.17459305657,1456.25808249242,
1456.34153644304,1456.42497293688,1456.50841004664,1456.59186584156,1456.67541033429,
1456.75899941723,1456.84272268479,1456.92340240068,1457.00714111253,1457.09077662389,
1457.17432906729,1457.25781850314,1457.34127245376,1457.4247089476,1457.50814605736,
1457.59160185228,1457.67514634501,1457.75873542795,1457.8424586955,1457.9231384114,
1458.00687712325,1458.09051263461,1458.17406507801,1458.25755451386,1458.34100846448,
1458.42444495832,1458.50788206808,1458.591337863,1458.67488235572,1458.75847143867,
1458.84219470622,1458.92287442212,1459.00661313397,1459.09024864533,1459.17380108873,
1459.25729052458,1459.3407444752,1459.42418096904,1459.5076180788,1459.59107387372,
1459.67461836645,1459.75820744939,1459.84193071695,1459.92261043284,1460.00587749695,
1460.08857547718,1460.17119802281,1460.25376406267,1460.33750978343,1460.4200311627,
1460.5043890542,1460.5887469457),.UNSPECIFIED.);
#976=B_SPLINE_CURVE_WITH_KNOTS('',3,(#123142,#123143,#123144,#123145,#123146,
#123147,#123148,#123149,#123150,#123151),.UNSPECIFIED.,.F.,.F.,(4,3,3,4),
(1454.30662927058,1454.3905507352,1454.47446510851,1454.55739861207),
 .UNSPECIFIED.);
#977=B_SPLINE_CURVE_WITH_KNOTS('',3,(#123153,#123154,#123155,#123156,#123157,
#123158,#123159,#123160,#123161,#123162),.UNSPECIFIED.,.F.,.F.,(4,3,3,4),
(1454.30674307549,1454.40585639479,1454.50400867407,1454.55739861189),
 .UNSPECIFIED.);
#978=B_SPLINE_CURVE_WITH_KNOTS('',3,(#123163,#123164,#123165,#123166,#123167,
#123168,#123169,#123170,#123171,#123172,#123173,#123174,#123175,#123176,
#123177,#123178,#123179,#123180,#123181,#123182,#123183,#123184,#123185,
#123186,#123187,#123188,#123189,#123190,#123191,#123192,#123193,#123194,
#123195,#123196,#123197,#123198,#123199,#123200,#123201,#123202,#123203,
#123204,#123205,#123206,#123207,#123208,#123209,#123210,#123211,#123212,
#123213,#123214,#123215,#123216,#123217,#123218,#123219,#123220,#123221,
#123222,#123223,#123224,#123225,#123226,#123227,#123228,#123229,#123230,
#123231,#123232,#123233,#123234,#123235,#123236,#123237,#123238,#123239,
#123240,#123241,#123242,#123243,#123244,#123245,#123246,#123247,#123248,
#123249,#123250,#123251,#123252,#123253,#123254,#123255,#123256,#123257,
#123258,#123259,#123260,#123261,#123262,#123263,#123264,#123265,#123266,
#123267,#123268,#123269,#123270,#123271,#123272,#123273,#123274,#123275,
#123276,#123277,#123278,#123279,#123280,#123281,#123282,#123283,#123284,
#123285,#123286,#123287,#123288,#123289,#123290,#123291,#123292,#123293,
#123294,#123295,#123296,#123297,#123298,#123299,#123300,#123301,#123302,
#123303,#123304,#123305,#123306,#123307,#123308,#123309,#123310,#123311,
#123312,#123313,#123314,#123315,#123316,#123317,#123318,#123319,#123320,
#123321,#123322,#123323,#123324,#123325,#123326,#123327,#123328,#123329,
#123330,#123331,#123332,#123333,#123334,#123335,#123336,#123337,#123338,
#123339,#123340,#123341,#123342,#123343,#123344,#123345,#123346,#123347,
#123348,#123349,#123350,#123351,#123352,#123353,#123354,#123355,#123356,
#123357,#123358,#123359,#123360,#123361,#123362,#123363,#123364,#123365,
#123366,#123367,#123368,#123369,#123370,#123371,#123372,#123373,#123374,
#123375,#123376,#123377,#123378,#123379,#123380,#123381,#123382),
 .UNSPECIFIED.,.F.,.F.,(4,3,3,3,3,3,3,3,3,3,3,3,3,3,3,3,3,3,3,3,3,3,3,3,
3,3,3,3,3,3,3,3,3,3,3,3,3,3,3,3,3,3,3,3,3,3,3,3,3,3,3,3,3,3,3,3,3,3,3,3,
3,3,3,3,3,3,3,3,3,3,3,3,3,4),(1454.55739861207,1454.64200141043,1454.72522978866,
1454.80845873658,1454.89170646772,1454.97733510053,1455.06072123565,1455.1474711173,
1455.23422099896,1455.31795971081,1455.40159522217,1455.48514766557,1455.56863710142,
1455.65209105204,1455.73552754588,1455.81896465564,1455.90242045056,1455.98596494329,
1456.06955402623,1456.15327729378,1456.23395700968,1456.31769572153,1456.40133123289,
1456.48488367629,1456.56837311214,1456.65182706276,1456.7352635566,1456.81870066636,
1456.90215646127,1456.985700954,1457.06929003695,1457.1530133045,1457.2336930204,
1457.31743173225,1457.40106724361,1457.48461968701,1457.56810912286,1457.65156307348,
1457.73499956732,1457.81843667708,1457.901892472,1457.98543696473,1458.06902604767,
1458.15274931522,1458.23342903112,1458.31716774297,1458.40080325433,1458.48435569773,
1458.56784513358,1458.6512990842,1458.73473557804,1458.8181726878,1458.90162848272,
1458.98517297545,1459.06876205839,1459.15248532595,1459.23316504184,1459.31690375369,
1459.40053926505,1459.48409170845,1459.5675811443,1459.65103509492,1459.73447158876,
1459.81790869852,1459.90136449344,1459.98490898617,1460.06849806911,1460.15222133666,
1460.23290105256,1460.32215865567,1460.40683272219,1460.49142158211,1460.57592537746,
1460.58993146501),.UNSPECIFIED.);
#979=B_SPLINE_CURVE_WITH_KNOTS('',3,(#123388,#123389,#123390,#123391,#123392,
#123393,#123394,#123395,#123396,#123397,#123398,#123399,#123400,#123401,
#123402,#123403,#123404,#123405,#123406,#123407,#123408,#123409,#123410,
#123411,#123412,#123413,#123414,#123415,#123416,#123417,#123418,#123419,
#123420,#123421,#123422,#123423,#123424,#123425,#123426,#123427,#123428,
#123429,#123430,#123431,#123432,#123433,#123434,#123435,#123436,#123437,
#123438,#123439,#123440,#123441,#123442,#123443,#123444,#123445,#123446,
#123447,#123448,#123449,#123450,#123451,#123452,#123453,#123454,#123455,
#123456,#123457,#123458,#123459,#123460,#123461,#123462,#123463,#123464,
#123465,#123466,#123467,#123468,#123469,#123470,#123471,#123472,#123473,
#123474,#123475,#123476,#123477,#123478,#123479,#123480,#123481,#123482,
#123483,#123484,#123485,#123486,#123487,#123488,#123489,#123490,#123491,
#123492,#123493,#123494,#123495,#123496,#123497,#123498,#123499,#123500,
#123501,#123502,#123503,#123504,#123505,#123506,#123507,#123508,#123509,
#123510,#123511,#123512,#123513,#123514,#123515,#123516,#123517,#123518,
#123519,#123520,#123521,#123522,#123523,#123524,#123525,#123526,#123527,
#123528,#123529,#123530,#123531,#123532,#123533,#123534,#123535,#123536,
#123537,#123538,#123539,#123540,#123541,#123542,#123543,#123544,#123545,
#123546,#123547,#123548,#123549,#123550,#123551,#123552,#123553,#123554,
#123555,#123556,#123557,#123558,#123559,#123560,#123561,#123562,#123563,
#123564,#123565,#123566,#123567,#123568,#123569,#123570,#123571,#123572,
#123573,#123574,#123575,#123576,#123577,#123578,#123579,#123580,#123581,
#123582,#123583,#123584,#123585,#123586,#123587,#123588,#123589,#123590,
#123591,#123592,#123593,#123594,#123595,#123596,#123597,#123598,#123599,
#123600,#123601,#123602,#123603,#123604,#123605,#123606,#123607),
 .UNSPECIFIED.,.F.,.F.,(4,3,3,3,3,3,3,3,3,3,3,3,3,3,3,3,3,3,3,3,3,3,3,3,
3,3,3,3,3,3,3,3,3,3,3,3,3,3,3,3,3,3,3,3,3,3,3,3,3,3,3,3,3,3,3,3,3,3,3,3,
3,3,3,3,3,3,3,3,3,3,3,3,3,4),(1460.84058391925,1460.92234644356,1461.00608515541,
1461.08972066677,1461.17327311017,1461.25676254602,1461.34021649664,1461.42365299048,
1461.50709010024,1461.59054589516,1461.67409038789,1461.75767947083,1461.84140273838,
1461.92208245428,1462.00582116613,1462.08945667749,1462.17300912089,1462.25649855674,
1462.33995250736,1462.4233890012,1462.50682611096,1462.59028190588,1462.67382639861,
1462.75741548155,1462.84113874911,1462.921818465,1463.00555717685,1463.08919268821,
1463.17274513161,1463.25623456746,1463.33968851808,1463.42312501192,1463.50656212168,
1463.5900179166,1463.67356240933,1463.75715149227,1463.84087475982,1463.92155447572,
1464.00529318757,1464.08892869893,1464.17248114233,1464.25597057818,1464.3394245288,
1464.42286102264,1464.5062981324,1464.58975392732,1464.67329842005,1464.75688750299,
1464.84061077054,1464.92129048644,1465.00502919829,1465.08866470965,1465.17221715305,
1465.2557065889,1465.33916053952,1465.42259703336,1465.50603414312,1465.58948993803,
1465.67303443076,1465.7566235137,1465.84034678126,1465.92102649716,1466.00476796687,
1466.08840559879,1466.17195952814,1466.25952013355,1466.34297044609,1466.42640328248,
1466.50983671436,1466.59328880972,1466.67681791279,1466.76039202568,1466.84407147563,
1466.87244437141),.UNSPECIFIED.);
#980=B_SPLINE_CURVE_WITH_KNOTS('',3,(#123608,#123609,#123610,#123611,#123612,
#123613,#123614,#123615,#123616,#123617),.UNSPECIFIED.,.F.,.F.,(4,3,3,4),
(1460.5887469457,1460.67138214754,1460.75598303333,1460.84058391912),
 .UNSPECIFIED.);
#981=B_SPLINE_CURVE_WITH_KNOTS('',3,(#123619,#123620,#123621,#123622,#123623,
#123624,#123625,#123626,#123627,#123628),.UNSPECIFIED.,.F.,.F.,(4,3,3,4),
(1460.58993146501,1460.67436365968,1460.75876766208,1460.84058391925),
 .UNSPECIFIED.);
#982=B_SPLINE_CURVE_WITH_KNOTS('',3,(#123629,#123630,#123631,#123632,#123633,
#123634,#123635,#123636,#123637,#123638,#123639,#123640,#123641,#123642,
#123643,#123644,#123645,#123646,#123647,#123648,#123649,#123650,#123651,
#123652,#123653,#123654,#123655,#123656,#123657,#123658,#123659,#123660,
#123661,#123662,#123663,#123664,#123665,#123666,#123667,#123668,#123669,
#123670,#123671,#123672,#123673,#123674,#123675,#123676,#123677,#123678,
#123679,#123680,#123681,#123682,#123683,#123684,#123685,#123686,#123687,
#123688,#123689,#123690,#123691,#123692,#123693,#123694,#123695,#123696,
#123697,#123698,#123699,#123700,#123701,#123702,#123703,#123704,#123705,
#123706,#123707,#123708,#123709,#123710,#123711,#123712,#123713,#123714,
#123715,#123716,#123717,#123718,#123719,#123720,#123721,#123722,#123723,
#123724,#123725,#123726,#123727,#123728,#123729,#123730,#123731,#123732,
#123733,#123734,#123735,#123736,#123737,#123738,#123739,#123740,#123741,
#123742,#123743,#123744,#123745,#123746,#123747,#123748,#123749,#123750,
#123751,#123752,#123753,#123754,#123755,#123756,#123757,#123758,#123759,
#123760,#123761,#123762,#123763,#123764,#123765,#123766,#123767,#123768,
#123769,#123770,#123771,#123772,#123773,#123774,#123775,#123776,#123777,
#123778,#123779,#123780,#123781,#123782,#123783,#123784,#123785,#123786,
#123787,#123788,#123789,#123790,#123791,#123792,#123793,#123794,#123795,
#123796,#123797,#123798,#123799,#123800,#123801,#123802,#123803,#123804,
#123805,#123806,#123807,#123808,#123809,#123810,#123811,#123812,#123813,
#123814,#123815,#123816,#123817,#123818,#123819,#123820,#123821,#123822,
#123823,#123824,#123825,#123826,#123827,#123828,#123829,#123830,#123831,
#123832,#123833,#123834,#123835,#123836,#123837,#123838,#123839,#123840,
#123841,#123842,#123843,#123844,#123845,#123846,#123847,#123848),
 .UNSPECIFIED.,.F.,.F.,(4,3,3,3,3,3,3,3,3,3,3,3,3,3,3,3,3,3,3,3,3,3,3,3,
3,3,3,3,3,3,3,3,3,3,3,3,3,3,3,3,3,3,3,3,3,3,3,3,3,3,3,3,3,3,3,3,3,3,3,3,
3,3,3,3,3,3,3,3,3,3,3,3,3,4),(1460.84058391944,1460.93315405195,1461.02625537987,
1461.11963264212,1461.21335570444,1461.23263706328,1461.31637577513,1461.40001128649,
1461.48356372989,1461.56705316574,1461.65050711636,1461.7339436102,1461.81738071996,
1461.90083651488,1461.98438100761,1462.06797009055,1462.1516933581,1462.232373074,
1462.31611178585,1462.39974729721,1462.48329974061,1462.56678917646,1462.65024312708,
1462.73367962092,1462.81711673068,1462.9005725256,1462.98411701832,1463.06770610127,
1463.15142936882,1463.23210908472,1463.31584779657,1463.39948330793,1463.48303575133,
1463.56652518718,1463.6499791378,1463.73341563164,1463.8168527414,1463.90030853632,
1463.98385302905,1464.06744211199,1464.15116537954,1464.23184509544,1464.31558380729,
1464.39921931865,1464.48277176205,1464.5662611979,1464.64971514852,1464.73315164236,
1464.81658875212,1464.90004454704,1464.98358903977,1465.06717812271,1465.15090139026,
1465.23158110616,1465.31531981801,1465.39895532937,1465.48250777277,1465.56599720862,
1465.64945115924,1465.73288765308,1465.81632476284,1465.89978055776,1465.98332505049,
1466.06691413343,1466.15063740098,1466.23131711688,1466.31394700638,1466.39648229565,
1466.47894209376,1466.56134544058,1466.64372069725,1466.72607768958,1466.80846141686,
1466.8719408414),.UNSPECIFIED.);
#983=B_SPLINE_CURVE_WITH_KNOTS('',3,(#123854,#123855,#123856,#123857,#123858,
#123859,#123860,#123861,#123862,#123863,#123864,#123865,#123866,#123867,
#123868,#123869,#123870,#123871,#123872,#123873,#123874,#123875,#123876,
#123877,#123878,#123879,#123880,#123881,#123882,#123883,#123884,#123885,
#123886,#123887,#123888,#123889,#123890,#123891,#123892,#123893,#123894,
#123895,#123896,#123897,#123898,#123899,#123900,#123901,#123902,#123903,
#123904,#123905,#123906,#123907,#123908,#123909,#123910,#123911,#123912,
#123913,#123914,#123915,#123916,#123917,#123918,#123919,#123920,#123921,
#123922,#123923,#123924,#123925,#123926,#123927,#123928,#123929,#123930,
#123931,#123932,#123933,#123934,#123935,#123936,#123937,#123938,#123939,
#123940,#123941,#123942,#123943,#123944,#123945,#123946,#123947,#123948,
#123949,#123950,#123951,#123952,#123953,#123954,#123955,#123956,#123957,
#123958,#123959,#123960,#123961,#123962,#123963,#123964,#123965,#123966,
#123967,#123968,#123969,#123970,#123971,#123972,#123973,#123974,#123975,
#123976,#123977,#123978,#123979,#123980,#123981,#123982,#123983,#123984,
#123985,#123986,#123987,#123988,#123989,#123990,#123991,#123992,#123993,
#123994,#123995,#123996,#123997,#123998,#123999,#124000,#124001,#124002,
#124003,#124004,#124005,#124006,#124007,#124008,#124009,#124010,#124011,
#124012,#124013,#124014,#124015,#124016,#124017,#124018,#124019,#124020,
#124021,#124022,#124023,#124024,#124025,#124026,#124027,#124028,#124029,
#124030,#124031,#124032,#124033,#124034,#124035,#124036,#124037,#124038,
#124039,#124040,#124041,#124042,#124043,#124044,#124045,#124046,#124047,
#124048,#124049,#124050,#124051,#124052,#124053,#124054,#124055,#124056,
#124057,#124058,#124059,#124060,#124061,#124062,#124063,#124064,#124065,
#124066,#124067,#124068,#124069,#124070,#124071,#124072,#124073),
 .UNSPECIFIED.,.F.,.F.,(4,3,3,3,3,3,3,3,3,3,3,3,3,3,3,3,3,3,3,3,3,3,3,3,
3,3,3,3,3,3,3,3,3,3,3,3,3,3,3,3,3,3,3,3,3,3,3,3,3,3,3,3,3,3,3,3,3,3,3,3,
3,3,3,3,3,3,3,3,3,3,3,3,3,4),(1467.12376922661,1467.20615137202,1467.28846542945,
1467.37073818782,1467.45299077312,1467.53524219248,1467.61751144987,1467.69986534415,
1467.78226484149,1467.86478835703,1467.9204985186,1468.00423723045,1468.08787274181,
1468.17142518521,1468.25491462106,1468.33836857168,1468.42180506552,1468.50524217528,
1468.5886979702,1468.67224246292,1468.75583154587,1468.83955481342,1468.92023452932,
1469.00397324117,1469.08760875253,1469.17116119593,1469.25465063178,1469.3381045824,
1469.42154107624,1469.504978186,1469.58843398092,1469.67197847365,1469.75556755659,
1469.83929082415,1469.91997054004,1470.00370925189,1470.08734476325,1470.17089720665,
1470.2543866425,1470.33784059312,1470.42127708696,1470.50471419672,1470.58816999164,
1470.67171448437,1470.75530356731,1470.83902683487,1470.91970655076,1471.00344526261,
1471.08708077397,1471.17063321737,1471.25412265322,1471.33757660384,1471.42101309768,
1471.50445020744,1471.58790600235,1471.67145049508,1471.75503957802,1471.83876284558,
1471.91944256148,1472.00318127333,1472.08681678469,1472.17036922809,1472.25385866394,
1472.33731261456,1472.4207491084,1472.50418621816,1472.58764201308,1472.67118650581,
1472.75477558875,1472.83849885631,1472.9191785722,1473.00772889966,1473.09607576719,
1473.15664071279),.UNSPECIFIED.);
#984=B_SPLINE_CURVE_WITH_KNOTS('',3,(#124074,#124075,#124076,#124077,#124078,
#124079,#124080,#124081,#124082,#124083),.UNSPECIFIED.,.F.,.F.,(4,3,3,4),
(1466.87244437141,1466.92076250788,1467.04006077289,1467.12376922643),
 .UNSPECIFIED.);
#985=B_SPLINE_CURVE_WITH_KNOTS('',3,(#124085,#124086,#124087,#124088,#124089,
#124090,#124091,#124092,#124093,#124094),.UNSPECIFIED.,.F.,.F.,(4,3,3,4),
(1466.8719408414,1466.9543981102,1467.03908366825,1467.12376922629),
 .UNSPECIFIED.);
#986=B_SPLINE_CURVE_WITH_KNOTS('',3,(#124095,#124096,#124097,#124098,#124099,
#124100,#124101,#124102,#124103,#124104,#124105,#124106,#124107,#124108,
#124109,#124110,#124111,#124112,#124113,#124114,#124115,#124116,#124117,
#124118,#124119,#124120,#124121,#124122,#124123,#124124,#124125,#124126,
#124127,#124128,#124129,#124130,#124131,#124132,#124133,#124134,#124135,
#124136,#124137,#124138,#124139,#124140,#124141,#124142,#124143,#124144,
#124145,#124146,#124147,#124148,#124149,#124150,#124151,#124152,#124153,
#124154,#124155,#124156,#124157,#124158,#124159,#124160,#124161,#124162,
#124163,#124164,#124165,#124166,#124167,#124168,#124169,#124170,#124171,
#124172,#124173,#124174,#124175,#124176,#124177,#124178,#124179,#124180,
#124181,#124182,#124183,#124184,#124185,#124186,#124187,#124188,#124189,
#124190,#124191,#124192,#124193,#124194,#124195,#124196,#124197,#124198,
#124199,#124200,#124201,#124202,#124203,#124204,#124205,#124206,#124207,
#124208,#124209,#124210,#124211,#124212,#124213,#124214,#124215,#124216,
#124217,#124218,#124219,#124220,#124221,#124222,#124223,#124224,#124225,
#124226,#124227,#124228,#124229,#124230,#124231,#124232,#124233,#124234,
#124235,#124236,#124237,#124238,#124239,#124240,#124241,#124242,#124243,
#124244,#124245,#124246,#124247,#124248,#124249,#124250,#124251,#124252,
#124253,#124254,#124255,#124256,#124257,#124258,#124259,#124260,#124261,
#124262,#124263,#124264,#124265,#124266,#124267,#124268,#124269,#124270,
#124271,#124272,#124273,#124274,#124275,#124276,#124277,#124278,#124279,
#124280,#124281,#124282,#124283,#124284,#124285,#124286,#124287,#124288,
#124289,#124290,#124291,#124292,#124293,#124294,#124295,#124296,#124297,
#124298,#124299,#124300,#124301,#124302,#124303,#124304,#124305,#124306,
#124307,#124308,#124309,#124310,#124311),.UNSPECIFIED.,.F.,.F.,(4,3,3,3,
3,3,3,3,3,3,3,3,3,3,3,3,3,3,3,3,3,3,3,3,3,3,3,3,3,3,3,3,3,3,3,3,3,3,3,3,
3,3,3,3,3,3,3,3,3,3,3,3,3,3,3,3,3,3,3,3,3,3,3,3,3,3,3,3,3,3,3,3,4),(1467.12376922643,
1467.2310531276,1467.31479183945,1467.39842735081,1467.48197979421,1467.56546923006,
1467.64892318068,1467.73235967452,1467.81579678428,1467.8992525792,1467.98279707193,
1468.06638615487,1468.15010942242,1468.23078913832,1468.31452785017,1468.39816336153,
1468.48171580493,1468.56520524078,1468.6486591914,1468.73209568524,1468.815532795,
1468.89898858992,1468.98253308265,1469.06612216559,1469.14984543314,1469.23052514904,
1469.31426386089,1469.39789937225,1469.48145181565,1469.5649412515,1469.64839520212,
1469.73183169596,1469.81526880572,1469.89872460064,1469.98226909337,1470.06585817631,
1470.14958144386,1470.23026115976,1470.31399987161,1470.39763538297,1470.48118782637,
1470.56467726222,1470.64813121284,1470.73156770668,1470.81500481644,1470.89846061136,
1470.98200510409,1471.06559418703,1471.14931745458,1471.22999717048,1471.31373588233,
1471.39737139369,1471.48092383709,1471.56441327294,1471.64786722356,1471.7313037174,
1471.81474082716,1471.89819662208,1471.98174111481,1472.06533019775,1472.1490534653,
1472.2297331812,1472.31347615588,1472.39711495474,1472.48066971443,1472.56502658325,
1472.64847685927,1472.73190848728,1472.81533953906,1472.90038582054,1472.98390578302,
1473.06971522401,1473.15552466501),.UNSPECIFIED.);
#987=B_SPLINE_CURVE_WITH_KNOTS('',3,(#124317,#124318,#124319,#124320,#124321,
#124322,#124323,#124324,#124325,#124326,#124327,#124328,#124329,#124330,
#124331,#124332,#124333,#124334,#124335,#124336,#124337,#124338,#124339,
#124340,#124341,#124342,#124343,#124344,#124345,#124346,#124347,#124348,
#124349,#124350,#124351,#124352,#124353,#124354,#124355,#124356,#124357,
#124358,#124359,#124360,#124361,#124362,#124363,#124364,#124365,#124366,
#124367,#124368,#124369,#124370,#124371,#124372,#124373,#124374,#124375,
#124376,#124377,#124378,#124379,#124380,#124381,#124382,#124383,#124384,
#124385,#124386,#124387,#124388,#124389,#124390,#124391,#124392,#124393,
#124394,#124395,#124396,#124397,#124398,#124399,#124400,#124401,#124402,
#124403,#124404,#124405,#124406,#124407,#124408,#124409,#124410,#124411,
#124412,#124413,#124414,#124415,#124416,#124417,#124418,#124419,#124420,
#124421,#124422,#124423,#124424,#124425,#124426,#124427,#124428,#124429,
#124430,#124431,#124432,#124433,#124434,#124435,#124436,#124437,#124438,
#124439,#124440,#124441,#124442,#124443,#124444,#124445,#124446,#124447,
#124448,#124449,#124450,#124451,#124452,#124453,#124454,#124455,#124456,
#124457,#124458,#124459,#124460,#124461,#124462,#124463,#124464,#124465,
#124466,#124467,#124468,#124469,#124470,#124471,#124472,#124473,#124474,
#124475,#124476,#124477,#124478,#124479,#124480,#124481,#124482,#124483,
#124484,#124485,#124486,#124487,#124488,#124489,#124490,#124491,#124492,
#124493,#124494,#124495,#124496,#124497,#124498,#124499,#124500,#124501,
#124502,#124503,#124504,#124505,#124506,#124507,#124508,#124509,#124510,
#124511,#124512,#124513,#124514,#124515,#124516,#124517,#124518,#124519,
#124520,#124521,#124522,#124523,#124524,#124525,#124526,#124527,#124528,
#124529,#124530,#124531,#124532,#124533,#124534,#124535,#124536),
 .UNSPECIFIED.,.F.,.F.,(4,3,3,3,3,3,3,3,3,3,3,3,3,3,3,3,3,3,3,3,3,3,3,3,
3,3,3,3,3,3,3,3,3,3,3,3,3,3,3,3,3,3,3,3,3,3,3,3,3,3,3,3,3,3,3,3,3,3,3,3,
3,3,3,3,3,3,3,3,3,3,3,3,3,4),(1473.40695453361,1473.49393313965,1473.5810114473,
1473.66828127154,1473.75565011186,1473.8432173964,1473.91891458292,1474.00265329477,
1474.08628880613,1474.16984124953,1474.25333068538,1474.336784636,1474.42022112984,
1474.5036582396,1474.58711403452,1474.67065852724,1474.75424761019,1474.83797087774,
1474.91865059364,1475.00238930549,1475.08602481685,1475.16957726025,1475.2530666961,
1475.33652064672,1475.41995714056,1475.50339425032,1475.58685004524,1475.67039453797,
1475.75398362091,1475.83770688847,1475.91838660436,1476.00212531621,1476.08576082757,
1476.16931327097,1476.25280270682,1476.33625665744,1476.41969315128,1476.50313026104,
1476.58658605596,1476.67013054869,1476.75371963163,1476.83744289918,1476.91812261508,
1477.00186132693,1477.08549683829,1477.16904928169,1477.25253871754,1477.33599266816,
1477.419429162,1477.50286627176,1477.58632206667,1477.6698665594,1477.75345564234,
1477.8371789099,1477.9178586258,1478.00159733765,1478.08523284901,1478.16878529241,
1478.25227472826,1478.33572867888,1478.41916517272,1478.50260228248,1478.5860580774,
1478.66960257013,1478.75319165307,1478.83691492063,1478.91759463652,1479.00021914845,
1479.08274652633,1479.16519590404,1479.24758186863,1479.32993154163,1479.41227038175,
1479.43866858093),.UNSPECIFIED.);
#988=B_SPLINE_CURVE_WITH_KNOTS('',3,(#124537,#124538,#124539,#124540,#124541,
#124542,#124543,#124544,#124545,#124546),.UNSPECIFIED.,.F.,.F.,(4,3,3,4),
(1473.15664071279,1473.24472264985,1473.3326204829,1473.40695453349),
 .UNSPECIFIED.);
#989=B_SPLINE_CURVE_WITH_KNOTS('',3,(#124548,#124549,#124550,#124551,#124552,
#124553,#124554,#124555,#124556,#124557),.UNSPECIFIED.,.F.,.F.,(4,3,3,4),
(1473.15552466501,1473.22946919192,1473.35769273628,1473.40695453361),
 .UNSPECIFIED.);
#990=B_SPLINE_CURVE_WITH_KNOTS('',3,(#124558,#124559,#124560,#124561,#124562,
#124563,#124564,#124565,#124566,#124567,#124568,#124569,#124570,#124571,
#124572,#124573,#124574,#124575,#124576,#124577,#124578,#124579,#124580,
#124581,#124582,#124583,#124584,#124585,#124586,#124587,#124588,#124589,
#124590,#124591,#124592,#124593,#124594,#124595,#124596,#124597,#124598,
#124599,#124600,#124601,#124602,#124603,#124604,#124605,#124606,#124607,
#124608,#124609,#124610,#124611,#124612,#124613,#124614,#124615,#124616,
#124617,#124618,#124619,#124620,#124621,#124622,#124623,#124624,#124625,
#124626,#124627,#124628,#124629,#124630,#124631,#124632,#124633,#124634,
#124635,#124636,#124637,#124638,#124639,#124640,#124641,#124642,#124643,
#124644,#124645,#124646,#124647,#124648,#124649,#124650,#124651,#124652,
#124653,#124654,#124655,#124656,#124657,#124658,#124659,#124660,#124661,
#124662,#124663,#124664,#124665,#124666,#124667,#124668,#124669,#124670,
#124671,#124672,#124673,#124674,#124675,#124676,#124677,#124678,#124679,
#124680,#124681,#124682,#124683,#124684,#124685,#124686,#124687,#124688,
#124689,#124690,#124691,#124692,#124693,#124694,#124695,#124696,#124697,
#124698,#124699,#124700,#124701,#124702,#124703,#124704,#124705,#124706,
#124707,#124708,#124709,#124710,#124711,#124712,#124713,#124714,#124715,
#124716,#124717,#124718,#124719,#124720,#124721,#124722,#124723,#124724,
#124725,#124726,#124727,#124728,#124729,#124730,#124731,#124732,#124733,
#124734,#124735,#124736,#124737,#124738,#124739,#124740,#124741,#124742,
#124743,#124744,#124745,#124746,#124747,#124748,#124749,#124750,#124751,
#124752,#124753,#124754,#124755,#124756,#124757,#124758,#124759,#124760,
#124761,#124762,#124763,#124764,#124765,#124766,#124767,#124768,#124769,
#124770,#124771,#124772,#124773,#124774,#124775,#124776,#124777),
 .UNSPECIFIED.,.F.,.F.,(4,3,3,3,3,3,3,3,3,3,3,3,3,3,3,3,3,3,3,3,3,3,3,3,
3,3,3,3,3,3,3,3,3,3,3,3,3,3,3,3,3,3,3,3,3,3,3,3,3,3,3,3,3,3,3,3,3,3,3,3,
3,3,3,3,3,3,3,3,3,3,3,3,3,4),(1473.40695453377,1473.4893182278,1473.57160671137,
1473.65384440038,1473.73605555324,1473.81825920997,1473.90047440225,1473.98277068985,
1474.06510696983,1474.14757432633,1474.22920520264,1474.31294391449,1474.39657942585,
1474.48013186925,1474.5636213051,1474.64707525572,1474.73051174956,1474.81394885932,
1474.89740465424,1474.98094914697,1475.06453822991,1475.14826149746,1475.22894121336,
1475.31267992521,1475.39631543657,1475.47986787997,1475.56335731582,1475.64681126644,
1475.73024776028,1475.81368487004,1475.89714066496,1475.98068515769,1476.06427424063,
1476.14799750818,1476.22867722408,1476.31241593593,1476.39605144729,1476.47960389069,
1476.56309332654,1476.64654727716,1476.729983771,1476.81342088076,1476.89687667568,
1476.98042116841,1477.06401025135,1477.1477335189,1477.2284132348,1477.31215194665,
1477.39578745801,1477.47933990141,1477.56282933726,1477.64628328788,1477.72971978172,
1477.81315689148,1477.8966126864,1477.98015717913,1478.06374626207,1478.14746952962,
1478.22814924552,1478.31188795737,1478.39552346873,1478.47907591213,1478.56256534798,
1478.6460192986,1478.72945579244,1478.8128929022,1478.89634869712,1478.97989318985,
1479.06348227279,1479.14720554034,1479.22788525624,1479.31758500425,1479.40706476103,
1479.43983851051),.UNSPECIFIED.);
#991=B_SPLINE_CURVE_WITH_KNOTS('',3,(#124783,#124784,#124785,#124786,#124787,
#124788,#124789,#124790,#124791,#124792,#124793,#124794,#124795,#124796,
#124797,#124798,#124799,#124800,#124801,#124802,#124803,#124804,#124805,
#124806,#124807,#124808,#124809,#124810,#124811,#124812,#124813,#124814,
#124815,#124816,#124817,#124818,#124819,#124820,#124821,#124822,#124823,
#124824,#124825,#124826,#124827,#124828,#124829,#124830,#124831,#124832,
#124833,#124834,#124835,#124836,#124837,#124838,#124839,#124840,#124841,
#124842,#124843,#124844,#124845,#124846,#124847,#124848,#124849,#124850,
#124851,#124852,#124853,#124854,#124855,#124856,#124857,#124858,#124859,
#124860,#124861,#124862,#124863,#124864,#124865,#124866,#124867,#124868,
#124869,#124870,#124871,#124872,#124873,#124874,#124875,#124876,#124877,
#124878,#124879,#124880,#124881,#124882,#124883,#124884,#124885,#124886,
#124887,#124888,#124889,#124890,#124891,#124892,#124893,#124894,#124895,
#124896,#124897,#124898,#124899,#124900,#124901,#124902,#124903,#124904,
#124905,#124906,#124907,#124908,#124909,#124910,#124911,#124912,#124913,
#124914,#124915,#124916,#124917,#124918,#124919,#124920,#124921,#124922,
#124923,#124924,#124925,#124926,#124927,#124928,#124929,#124930,#124931,
#124932,#124933,#124934,#124935,#124936,#124937,#124938,#124939,#124940,
#124941,#124942,#124943,#124944,#124945,#124946,#124947,#124948,#124949,
#124950,#124951,#124952,#124953,#124954,#124955,#124956,#124957,#124958,
#124959,#124960,#124961,#124962,#124963,#124964,#124965,#124966,#124967,
#124968,#124969,#124970,#124971,#124972,#124973,#124974,#124975,#124976,
#124977,#124978,#124979,#124980,#124981,#124982,#124983,#124984,#124985,
#124986,#124987,#124988,#124989,#124990,#124991,#124992,#124993,#124994,
#124995,#124996,#124997,#124998,#124999),.UNSPECIFIED.,.F.,.F.,(4,3,3,3,
3,3,3,3,3,3,3,3,3,3,3,3,3,3,3,3,3,3,3,3,3,3,3,3,3,3,3,3,3,3,3,3,3,3,3,3,
3,3,3,3,3,3,3,3,3,3,3,3,3,3,3,3,3,3,3,3,3,3,3,3,3,3,3,3,3,3,3,3,4),(1479.69013984079,
1479.80373524402,1479.91733064724,1480.00106935909,1480.08470487045,1480.16825731385,
1480.2517467497,1480.33520070032,1480.41863719416,1480.50207430392,1480.58553009884,
1480.66907459157,1480.75266367451,1480.83638694206,1480.91706665796,1481.00080536981,
1481.08444088117,1481.16799332457,1481.25148276042,1481.33493671104,1481.41837320488,
1481.50181031464,1481.58526610956,1481.66881060229,1481.75239968523,1481.83612295279,
1481.91680266868,1482.00054138053,1482.08417689189,1482.16772933529,1482.25121877114,
1482.33467272176,1482.4181092156,1482.50154632536,1482.58500212028,1482.66854661301,
1482.75213569595,1482.8358589635,1482.9165386794,1483.00027739125,1483.08391290261,
1483.16746534601,1483.25095478186,1483.33440873248,1483.41784522632,1483.50128233608,
1483.584738131,1483.66828262373,1483.75187170667,1483.83559497422,1483.91627469012,
1484.00001340197,1484.08364891333,1484.16720135673,1484.25069079258,1484.33414474319,
1484.41758123704,1484.5010183468,1484.58447414171,1484.66801863444,1484.75160771738,
1484.83533098494,1484.91601070084,1484.99976112188,1485.08340578193,1485.16694939894,
1485.25043572519,1485.33388288075,1485.41730895535,1485.50075704418,1485.58421581109,
1485.66774035371,1485.72166203219),.UNSPECIFIED.);
#992=B_SPLINE_CURVE_WITH_KNOTS('',3,(#125000,#125001,#125002,#125003,#125004,
#125005,#125006,#125007,#125008,#125009),.UNSPECIFIED.,.F.,.F.,(4,3,3,4),
(1479.43866858093,1479.52103553806,1479.60558768936,1479.69013984066),
 .UNSPECIFIED.);
#993=B_SPLINE_CURVE_WITH_KNOTS('',3,(#125011,#125012,#125013,#125014,#125015,
#125016,#125017,#125018,#125019,#125020),.UNSPECIFIED.,.F.,.F.,(4,3,3,4),
(1479.43983851051,1479.52903735213,1479.61799758571,1479.69013984063),
 .UNSPECIFIED.);
#994=B_SPLINE_CURVE_WITH_KNOTS('',3,(#125021,#125022,#125023,#125024,#125025,
#125026,#125027,#125028,#125029,#125030,#125031,#125032,#125033,#125034,
#125035,#125036,#125037,#125038,#125039,#125040,#125041,#125042,#125043,
#125044,#125045,#125046,#125047,#125048,#125049,#125050,#125051,#125052,
#125053,#125054,#125055,#125056,#125057,#125058,#125059,#125060,#125061,
#125062,#125063,#125064,#125065,#125066,#125067,#125068,#125069,#125070,
#125071,#125072,#125073,#125074,#125075,#125076,#125077,#125078,#125079,
#125080,#125081,#125082,#125083,#125084,#125085,#125086,#125087,#125088,
#125089,#125090,#125091,#125092,#125093,#125094,#125095,#125096,#125097,
#125098,#125099,#125100,#125101,#125102,#125103,#125104,#125105,#125106,
#125107,#125108,#125109,#125110,#125111,#125112,#125113,#125114,#125115,
#125116,#125117,#125118,#125119,#125120,#125121,#125122,#125123,#125124,
#125125,#125126,#125127,#125128,#125129,#125130,#125131,#125132,#125133,
#125134,#125135,#125136,#125137,#125138,#125139,#125140,#125141,#125142,
#125143,#125144,#125145,#125146,#125147,#125148,#125149,#125150,#125151,
#125152,#125153,#125154,#125155,#125156,#125157,#125158,#125159,#125160,
#125161,#125162,#125163,#125164,#125165,#125166,#125167,#125168,#125169,
#125170,#125171,#125172,#125173,#125174,#125175,#125176,#125177,#125178,
#125179,#125180,#125181,#125182,#125183,#125184,#125185,#125186,#125187,
#125188,#125189,#125190,#125191,#125192,#125193,#125194,#125195,#125196,
#125197,#125198,#125199,#125200,#125201,#125202,#125203,#125204,#125205,
#125206,#125207,#125208,#125209,#125210,#125211,#125212,#125213,#125214,
#125215,#125216,#125217,#125218,#125219,#125220,#125221,#125222,#125223,
#125224,#125225,#125226,#125227,#125228,#125229,#125230,#125231,#125232,
#125233,#125234,#125235,#125236,#125237,#125238,#125239,#125240),
 .UNSPECIFIED.,.F.,.F.,(4,3,3,3,3,3,3,3,3,3,3,3,3,3,3,3,3,3,3,3,3,3,3,3,
3,3,3,3,3,3,3,3,3,3,3,3,3,3,3,3,3,3,3,3,3,3,3,3,3,3,3,3,3,3,3,3,3,3,3,3,
3,3,3,3,3,3,3,3,3,3,3,3,3,4),(1479.69013984079,1479.77630058833,1479.86253318071,
1479.94885023975,1480.03532621794,1480.1218940574,1480.20861921668,1480.22762126696,
1480.31135997881,1480.39499549017,1480.47854793357,1480.56203736942,1480.64549132004,
1480.72892781388,1480.81236492364,1480.89582071856,1480.97936521129,1481.06295429423,
1481.14667756178,1481.22735727768,1481.31109598953,1481.39473150089,1481.47828394429,
1481.56177338014,1481.64522733076,1481.7286638246,1481.81210093436,1481.89555672928,
1481.97910122201,1482.06269030495,1482.1464135725,1482.2270932884,1482.31083200025,
1482.39446751161,1482.47801995501,1482.56150939086,1482.64496334148,1482.72839983532,
1482.81183694508,1482.89529274,1482.97883723273,1483.06242631567,1483.14614958322,
1483.22682929912,1483.31056801097,1483.39420352233,1483.47775596573,1483.56124540158,
1483.6446993522,1483.72813584604,1483.8115729558,1483.89502875072,1483.97857324344,
1484.06216232639,1484.14588559394,1484.22656530984,1484.31030402169,1484.39393953305,
1484.47749197645,1484.5609814123,1484.64443536292,1484.72787185676,1484.81130896652,
1484.89476476144,1484.97830925417,1485.06189833711,1485.14562160467,1485.22630132056,
1485.3090888973,1485.39177806216,1485.47437529998,1485.5569182117,1485.63944678899,
1485.72197536628),.UNSPECIFIED.);
#995=B_SPLINE_CURVE_WITH_KNOTS('',3,(#125246,#125247,#125248,#125249,#125250,
#125251,#125252,#125253,#125254,#125255),.UNSPECIFIED.,.F.,.F.,(4,1,1,1,
1,1,1,4),(1485.97333225685,1486.91548272228,1487.915218733,1488.91495474372,
1489.91469075444,1490.91442676516,1491.91416277588,1492.00598701905),
 .UNSPECIFIED.);
#996=B_SPLINE_CURVE_WITH_KNOTS('',3,(#125256,#125257,#125258,#125259,#125260,
#125261,#125262,#125263,#125264,#125265,#125266,#125267,#125268),
 .UNSPECIFIED.,.F.,.F.,(4,3,3,3,4),(1485.72166203219,1485.80528850285,1485.88903401518,
1485.91574671156,1485.97332514797),.UNSPECIFIED.);
#997=B_SPLINE_CURVE_WITH_KNOTS('',3,(#125270,#125271,#125272,#125273,#125274,
#125275,#125276,#125277,#125278,#125279),.UNSPECIFIED.,.F.,.F.,(4,3,3,4),
(1485.72197536628,1485.80448560964,1485.8889053788,1485.97332514797),
 .UNSPECIFIED.);
#998=B_SPLINE_CURVE_WITH_KNOTS('',3,(#125280,#125281,#125282,#125283,#125284,
#125285,#125286,#125287,#125288,#125289,#125290,#125291,#125292,#125293,
#125294,#125295,#125296,#125297,#125298,#125299,#125300,#125301,#125302,
#125303,#125304,#125305,#125306,#125307,#125308,#125309,#125310,#125311,
#125312,#125313,#125314,#125315,#125316,#125317,#125318,#125319,#125320,
#125321,#125322,#125323,#125324,#125325,#125326,#125327,#125328,#125329,
#125330,#125331,#125332,#125333,#125334,#125335,#125336,#125337,#125338,
#125339,#125340,#125341,#125342,#125343,#125344,#125345,#125346,#125347,
#125348,#125349,#125350,#125351,#125352,#125353,#125354,#125355,#125356,
#125357,#125358,#125359,#125360,#125361,#125362,#125363,#125364,#125365,
#125366,#125367,#125368,#125369,#125370,#125371,#125372,#125373,#125374,
#125375,#125376,#125377,#125378,#125379,#125380,#125381,#125382,#125383,
#125384,#125385,#125386,#125387,#125388,#125389,#125390,#125391,#125392,
#125393,#125394,#125395,#125396,#125397,#125398,#125399,#125400,#125401,
#125402,#125403,#125404,#125405,#125406,#125407,#125408,#125409,#125410,
#125411,#125412,#125413,#125414,#125415,#125416,#125417,#125418,#125419,
#125420,#125421,#125422,#125423,#125424,#125425,#125426,#125427,#125428,
#125429,#125430,#125431,#125432,#125433,#125434,#125435,#125436,#125437,
#125438,#125439,#125440,#125441,#125442,#125443,#125444,#125445,#125446,
#125447,#125448,#125449,#125450,#125451,#125452,#125453,#125454,#125455,
#125456,#125457,#125458,#125459,#125460,#125461,#125462,#125463,#125464,
#125465,#125466,#125467,#125468,#125469,#125470,#125471,#125472,#125473,
#125474,#125475,#125476,#125477,#125478,#125479,#125480,#125481,#125482,
#125483,#125484,#125485,#125486,#125487,#125488,#125489,#125490,#125491,
#125492,#125493,#125494,#125495,#125496,#125497,#125498,#125499),
 .UNSPECIFIED.,.F.,.F.,(4,3,3,3,3,3,3,3,3,3,3,3,3,3,3,3,3,3,3,3,3,3,3,3,
3,3,3,3,3,3,3,3,3,3,3,3,3,3,3,3,3,3,3,3,3,3,3,3,3,3,3,3,3,3,3,3,3,3,3,3,
3,3,3,3,3,3,3,3,3,3,3,3,3,4),(1485.97332514817,1486.08013280166,1486.18927155072,
1486.22603733128,1486.30977604313,1486.39341155449,1486.47696399789,1486.56045343374,
1486.64390738436,1486.7273438782,1486.81078098796,1486.89423678288,1486.97778127561,
1487.06137035855,1487.1450936261,1487.225773342,1487.30951205385,1487.39314756521,
1487.47670000861,1487.56018944446,1487.64364339508,1487.72707988892,1487.81051699868,
1487.8939727936,1487.97751728633,1488.06110636927,1488.14482963682,1488.22550935272,
1488.30924806457,1488.39288357593,1488.47643601933,1488.55992545518,1488.6433794058,
1488.72681589964,1488.8102530094,1488.89370880432,1488.97725329705,1489.06084237999,
1489.14456564755,1489.22524536344,1489.30898407529,1489.39261958665,1489.47617203005,
1489.5596614659,1489.64311541652,1489.72655191036,1489.80998902012,1489.89344481504,
1489.97698930776,1490.06057839071,1490.14430165826,1490.22498137416,1490.30872008601,
1490.39235559737,1490.47590804077,1490.55939747662,1490.64285142724,1490.72628792108,
1490.80972503084,1490.89318082576,1490.97672531848,1491.06031440143,1491.14403766898,
1491.22471738488,1491.30846947086,1491.39551639012,1491.47905786342,1491.56254230654,
1491.64598783891,1491.72941254974,1491.81285539563,1491.89630938701,1491.97981837138,
1492.00484482495),.UNSPECIFIED.);
#999=B_SPLINE_CURVE_WITH_KNOTS('',3,(#125505,#125506,#125507,#125508,#125509,
#125510,#125511,#125512,#125513,#125514),.UNSPECIFIED.,.F.,.F.,(4,1,1,1,
1,1,1,4),(1492.25651045514,1492.9138987866,1493.91363479732,1494.91337080804,
1495.91310681876,1496.91284282948,1497.9125788402,1498.28924643674),
 .UNSPECIFIED.);
#1000=B_SPLINE_CURVE_WITH_KNOTS('',3,(#125515,#125516,#125517,#125518),
 .UNSPECIFIED.,.F.,.F.,(4,4),(1492.00598701905,1492.25651045514),
 .UNSPECIFIED.);
#1001=B_SPLINE_CURVE_WITH_KNOTS('',3,(#125520,#125521,#125522,#125523,#125524,
#125525,#125526,#125527,#125528,#125529,#125530,#125531,#125532),
 .UNSPECIFIED.,.F.,.F.,(4,3,3,3,4),(1492.00484482495,1492.08845275128,1492.17218669413,
1492.2244533956,1492.25651045515),.UNSPECIFIED.);
#1002=B_SPLINE_CURVE_WITH_KNOTS('',3,(#125533,#125534,#125535,#125536,#125537,
#125538,#125539,#125540,#125541,#125542,#125543,#125544,#125545,#125546,
#125547,#125548,#125549,#125550,#125551,#125552,#125553,#125554,#125555,
#125556,#125557,#125558,#125559,#125560,#125561,#125562,#125563,#125564,
#125565,#125566,#125567,#125568,#125569,#125570,#125571,#125572,#125573,
#125574,#125575,#125576,#125577,#125578,#125579,#125580,#125581,#125582,
#125583,#125584,#125585,#125586,#125587,#125588,#125589,#125590,#125591,
#125592,#125593,#125594,#125595,#125596,#125597,#125598,#125599,#125600,
#125601,#125602,#125603,#125604,#125605,#125606,#125607,#125608,#125609,
#125610,#125611,#125612,#125613,#125614,#125615,#125616,#125617,#125618,
#125619,#125620,#125621,#125622,#125623,#125624,#125625,#125626,#125627,
#125628,#125629,#125630,#125631,#125632,#125633,#125634,#125635,#125636,
#125637,#125638,#125639,#125640,#125641,#125642,#125643,#125644,#125645,
#125646,#125647,#125648,#125649,#125650,#125651,#125652,#125653,#125654,
#125655,#125656,#125657,#125658,#125659,#125660,#125661,#125662,#125663,
#125664,#125665,#125666,#125667,#125668,#125669,#125670,#125671,#125672,
#125673,#125674,#125675,#125676,#125677,#125678,#125679,#125680,#125681,
#125682,#125683,#125684,#125685,#125686,#125687,#125688,#125689,#125690,
#125691,#125692,#125693,#125694,#125695,#125696,#125697,#125698,#125699,
#125700,#125701,#125702,#125703,#125704,#125705,#125706,#125707,#125708,
#125709,#125710,#125711,#125712,#125713,#125714,#125715,#125716,#125717,
#125718,#125719,#125720,#125721,#125722,#125723,#125724,#125725,#125726,
#125727,#125728,#125729,#125730,#125731,#125732,#125733,#125734,#125735,
#125736,#125737,#125738,#125739,#125740,#125741,#125742,#125743,#125744,
#125745,#125746,#125747,#125748,#125749,#125750,#125751,#125752),
 .UNSPECIFIED.,.F.,.F.,(4,3,3,3,3,3,3,3,3,3,3,3,3,3,3,3,3,3,3,3,3,3,3,3,
3,3,3,3,3,3,3,3,3,3,3,3,3,3,3,3,3,3,3,3,3,3,3,3,3,3,3,3,3,3,3,3,3,3,3,3,
3,3,3,3,3,3,3,3,3,3,3,3,3,4),(1492.25651045529,1492.33980475775,1492.42299730472,
1492.50610866675,1492.58915933873,1492.67217794586,1492.75518199317,1492.83818994494,
1492.92122026463,1493.00433983238,1493.08750804642,1493.1708018184,1493.22418940632,
1493.30792811817,1493.39156362953,1493.47511607293,1493.55860550878,1493.6420594594,
1493.72549595324,1493.808933063,1493.89238885792,1493.97593335065,1494.05952243359,
1494.14324570114,1494.22392541704,1494.30766412889,1494.39129964025,1494.47485208365,
1494.5583415195,1494.64179547012,1494.72523196396,1494.80866907372,1494.89212486864,
1494.97566936137,1495.05925844431,1495.14298171187,1495.22366142776,1495.30740013961,
1495.39103565097,1495.47458809437,1495.55807753022,1495.64153148084,1495.72496797468,
1495.80840508444,1495.89186087936,1495.97540537209,1496.05899445503,1496.14271772258,
1496.22339743848,1496.30713615033,1496.39077166169,1496.47432410509,1496.55781354094,
1496.64126749156,1496.7247039854,1496.80814109516,1496.89159689008,1496.9751413828,
1497.05873046575,1497.1424537333,1497.2231334492,1497.30687216105,1497.39050767241,
1497.47406011581,1497.55754955166,1497.64100350227,1497.72443999612,1497.80787710587,
1497.89133290079,1497.97487739352,1498.05846647646,1498.14218974402,1498.22286945992,
1498.28900992258),.UNSPECIFIED.);
#1003=B_SPLINE_CURVE_WITH_KNOTS('',3,(#125758,#125759,#125760,#125761,#125762,
#125763,#125764,#125765,#125766,#125767,#125768,#125769,#125770,#125771,
#125772,#125773,#125774,#125775,#125776,#125777,#125778,#125779,#125780,
#125781,#125782,#125783,#125784,#125785,#125786,#125787,#125788,#125789,
#125790,#125791,#125792,#125793,#125794,#125795,#125796,#125797,#125798,
#125799,#125800,#125801,#125802,#125803,#125804,#125805,#125806,#125807,
#125808,#125809,#125810,#125811,#125812,#125813,#125814,#125815,#125816,
#125817,#125818,#125819,#125820,#125821,#125822,#125823,#125824,#125825,
#125826,#125827,#125828,#125829,#125830,#125831,#125832,#125833,#125834,
#125835,#125836,#125837,#125838,#125839,#125840,#125841,#125842,#125843,
#125844,#125845,#125846,#125847,#125848,#125849,#125850,#125851,#125852,
#125853,#125854,#125855,#125856,#125857,#125858,#125859,#125860,#125861,
#125862,#125863,#125864,#125865,#125866,#125867,#125868,#125869,#125870,
#125871,#125872,#125873,#125874,#125875,#125876,#125877,#125878,#125879,
#125880,#125881,#125882,#125883,#125884,#125885,#125886,#125887,#125888,
#125889,#125890,#125891,#125892,#125893,#125894,#125895,#125896,#125897,
#125898,#125899,#125900,#125901,#125902,#125903,#125904,#125905,#125906,
#125907,#125908,#125909,#125910,#125911,#125912,#125913,#125914,#125915,
#125916,#125917,#125918,#125919,#125920,#125921,#125922,#125923,#125924,
#125925,#125926,#125927,#125928,#125929,#125930,#125931,#125932,#125933,
#125934,#125935,#125936,#125937,#125938,#125939,#125940,#125941,#125942,
#125943,#125944,#125945,#125946,#125947,#125948,#125949,#125950,#125951,
#125952,#125953,#125954,#125955,#125956,#125957,#125958,#125959,#125960,
#125961,#125962,#125963,#125964,#125965,#125966,#125967,#125968,#125969,
#125970,#125971,#125972,#125973,#125974),.UNSPECIFIED.,.F.,.F.,(4,3,3,3,
3,3,3,3,3,3,3,3,3,3,3,3,3,3,3,3,3,3,3,3,3,3,3,3,3,3,3,3,3,3,3,3,3,3,3,3,
3,3,3,3,3,3,3,3,3,3,3,3,3,3,3,3,3,3,3,3,3,3,3,3,3,3,3,3,3,3,3,3,4),(1498.53969576232,
1498.63380533641,1498.72828492247,1498.82328898073,1498.91231485092,1498.99605356277,
1499.07968907413,1499.16324151753,1499.24673095338,1499.33018490399,1499.41362139784,
1499.4970585076,1499.58051430251,1499.66405879524,1499.74764787818,1499.83137114574,
1499.91205086164,1499.99578957349,1500.07942508486,1500.16297752826,1500.24646696411,
1500.32992091473,1500.41335740858,1500.49679451833,1500.58025031325,1500.66379480598,
1500.74738388893,1500.83110715649,1500.91178687237,1500.99552558422,1501.07916109558,
1501.16271353898,1501.24620297483,1501.32965692545,1501.41309341929,1501.49653052905,
1501.57998632397,1501.6635308167,1501.74711989964,1501.8308431672,1501.91152288309,
1501.99526159493,1502.0788971063,1502.1624495497,1502.24593898555,1502.32939293616,
1502.41282943001,1502.49626653976,1502.57972233468,1502.66326682741,1502.74685591035,
1502.8305791779,1502.91125889381,1502.99499760566,1503.07863311703,1503.16218556043,
1503.24567499628,1503.32912894689,1503.41256544074,1503.4960025505,1503.57945834542,
1503.66300283815,1503.74659192109,1503.83031518865,1503.91099490453,1503.99374376682,
1504.0763980856,1504.15897688734,1504.24149913172,1504.32399495184,1504.4064721317,
1504.48898209449,1504.57104348731),.UNSPECIFIED.);
#1004=B_SPLINE_CURVE_WITH_KNOTS('',3,(#125975,#125976,#125977,#125978),
 .UNSPECIFIED.,.F.,.F.,(4,4),(1498.28924643674,1498.53969576232),
 .UNSPECIFIED.);
#1005=B_SPLINE_CURVE_WITH_KNOTS('',3,(#125980,#125981,#125982,#125983,#125984,
#125985,#125986,#125987,#125988,#125989),.UNSPECIFIED.,.F.,.F.,(4,3,3,4),
(1498.28900992258,1498.38879043601,1498.48754282435,1498.53969576216),
 .UNSPECIFIED.);
#1006=B_SPLINE_CURVE_WITH_KNOTS('',3,(#125990,#125991,#125992,#125993,#125994,
#125995,#125996,#125997,#125998,#125999,#126000,#126001,#126002,#126003,
#126004,#126005,#126006,#126007,#126008,#126009,#126010,#126011,#126012,
#126013,#126014,#126015,#126016,#126017,#126018,#126019,#126020,#126021,
#126022,#126023,#126024,#126025,#126026,#126027,#126028,#126029,#126030,
#126031,#126032,#126033,#126034,#126035,#126036,#126037,#126038,#126039,
#126040,#126041,#126042,#126043,#126044,#126045,#126046,#126047,#126048,
#126049,#126050,#126051,#126052,#126053,#126054,#126055,#126056,#126057,
#126058,#126059,#126060,#126061,#126062,#126063,#126064,#126065,#126066,
#126067,#126068,#126069,#126070,#126071,#126072,#126073,#126074,#126075,
#126076,#126077,#126078,#126079,#126080,#126081,#126082,#126083,#126084,
#126085,#126086,#126087,#126088,#126089,#126090,#126091,#126092,#126093,
#126094,#126095,#126096,#126097,#126098,#126099,#126100,#126101,#126102,
#126103,#126104,#126105,#126106,#126107,#126108,#126109,#126110,#126111,
#126112,#126113,#126114,#126115,#126116,#126117,#126118,#126119,#126120,
#126121,#126122,#126123,#126124,#126125,#126126,#126127,#126128,#126129,
#126130,#126131,#126132,#126133,#126134,#126135,#126136,#126137,#126138,
#126139,#126140,#126141,#126142,#126143,#126144,#126145,#126146,#126147,
#126148,#126149,#126150,#126151,#126152,#126153,#126154,#126155,#126156,
#126157,#126158,#126159,#126160,#126161,#126162,#126163,#126164,#126165,
#126166,#126167,#126168,#126169,#126170,#126171,#126172,#126173,#126174,
#126175,#126176,#126177,#126178,#126179,#126180,#126181,#126182,#126183,
#126184,#126185,#126186,#126187,#126188,#126189,#126190,#126191,#126192,
#126193,#126194,#126195,#126196,#126197,#126198,#126199,#126200,#126201,
#126202,#126203,#126204,#126205,#126206,#126207,#126208,#126209,#126210,
#126211,#126212),.UNSPECIFIED.,.F.,.F.,(4,3,3,3,3,3,3,3,3,3,3,3,3,3,3,3,
3,3,3,3,3,3,3,3,3,3,3,3,3,3,3,3,3,3,3,3,3,3,3,3,3,3,3,3,3,3,3,3,3,3,3,3,
3,3,3,3,3,3,3,3,3,3,3,3,3,3,3,3,3,3,3,3,3,3,4),(1498.53969576233,1498.62505947587,
1498.70820805334,1498.79135490896,1498.87451833665,1498.96154012015,1499.04483918337,
1499.12819845884,1499.21167592631,1499.22260547064,1499.30634418249,1499.38997969385,
1499.47353213725,1499.55702157311,1499.64047552372,1499.72391201757,1499.80734912732,
1499.89080492224,1499.97434941497,1500.05793849791,1500.14166176547,1500.22234148136,
1500.30608019321,1500.38971570457,1500.47326814797,1500.55675758382,1500.64021153444,
1500.72364802828,1500.80708513804,1500.89054093296,1500.97408542569,1501.05767450863,
1501.14139777619,1501.22207749208,1501.30581620393,1501.38945171529,1501.47300415869,
1501.55649359454,1501.63994754516,1501.723384039,1501.80682114876,1501.89027694367,
1501.9738214364,1502.05741051934,1502.1411337869,1502.2218135028,1502.30555221465,
1502.38918772601,1502.47274016941,1502.55622960526,1502.63968355588,1502.72312004972,
1502.80655715948,1502.8900129544,1502.97355744713,1503.05714653007,1503.14086979762,
1503.22154951352,1503.30528822537,1503.38892373673,1503.47247618013,1503.55596561598,
1503.63941956659,1503.72285606044,1503.80629317019,1503.88974896511,1503.97329345784,
1504.05688254078,1504.14060580834,1504.22128552424,1504.3090278421,1504.39384146299,
1504.47856831567,1504.56320793387,1504.57225479568),.UNSPECIFIED.);
#1007=B_SPLINE_CURVE_WITH_KNOTS('',3,(#126218,#126219,#126220,#126221,#126222,
#126223,#126224,#126225,#126226,#126227,#126228,#126229,#126230,#126231,
#126232,#126233,#126234,#126235,#126236,#126237,#126238,#126239,#126240,
#126241,#126242,#126243,#126244,#126245,#126246,#126247,#126248,#126249,
#126250,#126251,#126252,#126253,#126254,#126255,#126256,#126257,#126258,
#126259,#126260,#126261,#126262,#126263,#126264,#126265,#126266,#126267,
#126268,#126269,#126270,#126271,#126272,#126273,#126274,#126275,#126276,
#126277,#126278,#126279,#126280,#126281,#126282,#126283,#126284,#126285,
#126286,#126287,#126288,#126289,#126290,#126291,#126292,#126293,#126294,
#126295,#126296,#126297,#126298,#126299,#126300,#126301,#126302,#126303,
#126304,#126305,#126306,#126307,#126308,#126309,#126310,#126311,#126312,
#126313,#126314,#126315,#126316,#126317,#126318,#126319,#126320,#126321,
#126322,#126323,#126324,#126325,#126326,#126327,#126328,#126329,#126330,
#126331,#126332,#126333,#126334,#126335,#126336,#126337,#126338,#126339,
#126340,#126341,#126342,#126343,#126344,#126345,#126346,#126347,#126348,
#126349,#126350,#126351,#126352,#126353,#126354,#126355,#126356,#126357,
#126358,#126359,#126360,#126361,#126362,#126363,#126364,#126365,#126366,
#126367,#126368,#126369,#126370,#126371,#126372,#126373,#126374,#126375,
#126376,#126377,#126378,#126379,#126380,#126381,#126382,#126383,#126384,
#126385,#126386,#126387,#126388,#126389,#126390,#126391,#126392,#126393,
#126394,#126395,#126396,#126397,#126398,#126399,#126400,#126401,#126402,
#126403,#126404,#126405,#126406,#126407,#126408,#126409,#126410,#126411,
#126412,#126413,#126414,#126415,#126416,#126417,#126418,#126419,#126420,
#126421,#126422,#126423,#126424,#126425,#126426,#126427,#126428,#126429,
#126430,#126431,#126432,#126433,#126434,#126435,#126436,#126437),
 .UNSPECIFIED.,.F.,.F.,(4,3,3,3,3,3,3,3,3,3,3,3,3,3,3,3,3,3,3,3,3,3,3,3,
3,3,3,3,3,3,3,3,3,3,3,3,3,3,3,3,3,3,3,3,3,3,3,3,3,3,3,3,3,3,3,3,3,3,3,3,
3,3,3,3,3,3,3,3,3,3,3,3,3,4),(1504.8228810695,1504.91073091525,1504.9944696271,
1505.07810513846,1505.16165758186,1505.24514701771,1505.32860096832,1505.41203746217,
1505.49547457192,1505.57893036684,1505.66247485957,1505.74606394251,1505.82978721006,
1505.91046692597,1505.99420563782,1506.07784114918,1506.16139359258,1506.24488302843,
1506.32833697905,1506.41177347289,1506.49521058265,1506.57866637757,1506.6622108703,
1506.74579995324,1506.82952322079,1506.91020293669,1506.99394164854,1507.0775771599,
1507.1611296033,1507.24461903915,1507.32807298977,1507.41150948361,1507.49494659337,
1507.57840238829,1507.66194688102,1507.74553596396,1507.82925923151,1507.90993894741,
1507.99367765926,1508.07731317062,1508.16086561402,1508.24435504987,1508.32780900049,
1508.41124549433,1508.49468260409,1508.57813839901,1508.66168289173,1508.74527197468,
1508.82899524223,1508.90967495813,1508.99341366998,1509.07704918134,1509.16060162474,
1509.24409106059,1509.32754501121,1509.41098150505,1509.49441861481,1509.57787440973,
1509.66141890246,1509.7450079854,1509.82873125295,1509.90941096885,1509.99315279498,
1510.07679070267,1510.16034482747,1510.24714103562,1510.33059132302,1510.41402385468,
1510.49745670225,1510.58090793355,1510.66443464419,1510.74800616879,1510.83168005567,
1510.85471449263),.UNSPECIFIED.);
#1008=B_SPLINE_CURVE_WITH_KNOTS('',3,(#126438,#126439,#126440,#126441,#126442,
#126443,#126444,#126445,#126446,#126447),.UNSPECIFIED.,.F.,.F.,(4,3,3,4),
(1504.57104348731,1504.65363118549,1504.73825612743,1504.82288106937),
 .UNSPECIFIED.);
#1009=B_SPLINE_CURVE_WITH_KNOTS('',3,(#126449,#126450,#126451,#126452,#126453,
#126454,#126455,#126456,#126457,#126458),.UNSPECIFIED.,.F.,.F.,(4,3,3,4),
(1504.57225479568,1504.65682073549,1504.74135303069,1504.82288106951),
 .UNSPECIFIED.);
#1010=B_SPLINE_CURVE_WITH_KNOTS('',3,(#126459,#126460,#126461,#126462,#126463,
#126464,#126465,#126466,#126467,#126468,#126469,#126470,#126471,#126472,
#126473,#126474,#126475,#126476,#126477,#126478,#126479,#126480,#126481,
#126482,#126483,#126484,#126485,#126486,#126487,#126488,#126489,#126490,
#126491,#126492,#126493,#126494,#126495,#126496,#126497,#126498,#126499,
#126500,#126501,#126502,#126503,#126504,#126505,#126506,#126507,#126508,
#126509,#126510,#126511,#126512,#126513,#126514,#126515,#126516,#126517,
#126518,#126519,#126520,#126521,#126522,#126523,#126524,#126525,#126526,
#126527,#126528,#126529,#126530,#126531,#126532,#126533,#126534,#126535,
#126536,#126537,#126538,#126539,#126540,#126541,#126542,#126543,#126544,
#126545,#126546,#126547,#126548,#126549,#126550,#126551,#126552,#126553,
#126554,#126555,#126556,#126557,#126558,#126559,#126560,#126561,#126562,
#126563,#126564,#126565,#126566,#126567,#126568,#126569,#126570,#126571,
#126572,#126573,#126574,#126575,#126576,#126577,#126578,#126579,#126580,
#126581,#126582,#126583,#126584,#126585,#126586,#126587,#126588,#126589,
#126590,#126591,#126592,#126593,#126594,#126595,#126596,#126597,#126598,
#126599,#126600,#126601,#126602,#126603,#126604,#126605,#126606,#126607,
#126608,#126609,#126610,#126611,#126612,#126613,#126614,#126615,#126616,
#126617,#126618,#126619,#126620,#126621,#126622,#126623,#126624,#126625,
#126626,#126627,#126628,#126629,#126630,#126631,#126632,#126633,#126634,
#126635,#126636,#126637,#126638,#126639,#126640,#126641,#126642,#126643,
#126644,#126645,#126646,#126647,#126648,#126649,#126650,#126651,#126652,
#126653,#126654,#126655,#126656,#126657,#126658,#126659,#126660,#126661,
#126662,#126663,#126664,#126665,#126666,#126667,#126668,#126669,#126670,
#126671,#126672,#126673,#126674,#126675,#126676,#126677,#126678),
 .UNSPECIFIED.,.F.,.F.,(4,3,3,3,3,3,3,3,3,3,3,3,3,3,3,3,3,3,3,3,3,3,3,3,
3,3,3,3,3,3,3,3,3,3,3,3,3,3,3,3,3,3,3,3,3,3,3,3,3,3,3,3,3,3,3,3,3,3,3,3,
3,3,3,3,3,3,3,3,3,3,3,3,3,4),(1504.82288106969,1504.91507842316,1505.00777905537,
1505.1007403094,1505.19403937815,1505.22102153496,1505.30476024681,1505.38839575818,
1505.47194820158,1505.55543763743,1505.63889158805,1505.7223280819,1505.80576519166,
1505.88922098658,1505.97276547931,1506.05635456225,1506.14007782982,1506.22075754568,
1506.30449625753,1506.38813176889,1506.47168421229,1506.55517364814,1506.63862759876,
1506.7220640926,1506.80550120236,1506.88895699728,1506.97250149001,1507.05609057295,
1507.13981384051,1507.2204935564,1507.30423226825,1507.38786777961,1507.47142022301,
1507.55490965886,1507.63836360947,1507.72180010332,1507.80523721307,1507.88869300799,
1507.97223750072,1508.05582658366,1508.13954985122,1508.22022956712,1508.30396827897,
1508.38760379033,1508.47115623373,1508.55464566958,1508.6380996202,1508.72153611404,
1508.8049732238,1508.88842901872,1508.97197351145,1509.05556259439,1509.13928586195,
1509.21996557784,1509.30370428969,1509.38733980105,1509.47089224445,1509.5543816803,
1509.63783563091,1509.72127212476,1509.80470923451,1509.88816502943,1509.97170952216,
1510.0552986051,1510.13902187266,1510.21970158856,1510.30230103997,1510.38480585915,
1510.46723517599,1510.54960805049,1510.63195228182,1510.71427833871,1510.796629289,
1510.85424422661),.UNSPECIFIED.);
#1011=B_SPLINE_CURVE_WITH_KNOTS('',3,(#126684,#126685,#126686,#126687,#126688,
#126689,#126690,#126691,#126692,#126693,#126694,#126695,#126696,#126697,
#126698,#126699,#126700,#126701,#126702,#126703,#126704,#126705,#126706,
#126707,#126708,#126709,#126710,#126711,#126712,#126713,#126714,#126715,
#126716,#126717,#126718,#126719,#126720,#126721,#126722,#126723,#126724,
#126725,#126726,#126727,#126728,#126729,#126730,#126731,#126732,#126733,
#126734,#126735,#126736,#126737,#126738,#126739,#126740,#126741,#126742,
#126743,#126744,#126745,#126746,#126747,#126748,#126749,#126750,#126751,
#126752,#126753,#126754,#126755,#126756,#126757,#126758,#126759,#126760,
#126761,#126762,#126763,#126764,#126765,#126766,#126767,#126768,#126769,
#126770,#126771,#126772,#126773,#126774,#126775,#126776,#126777,#126778,
#126779,#126780,#126781,#126782,#126783,#126784,#126785,#126786,#126787,
#126788,#126789,#126790,#126791,#126792,#126793,#126794,#126795,#126796,
#126797,#126798,#126799,#126800,#126801,#126802,#126803,#126804,#126805,
#126806,#126807,#126808,#126809,#126810,#126811,#126812,#126813,#126814,
#126815,#126816,#126817,#126818,#126819,#126820,#126821,#126822,#126823,
#126824,#126825,#126826,#126827,#126828,#126829,#126830,#126831,#126832,
#126833,#126834,#126835,#126836,#126837,#126838,#126839,#126840,#126841,
#126842,#126843,#126844,#126845,#126846,#126847,#126848,#126849,#126850,
#126851,#126852,#126853,#126854,#126855,#126856,#126857,#126858,#126859,
#126860,#126861,#126862,#126863,#126864,#126865,#126866,#126867,#126868,
#126869,#126870,#126871,#126872,#126873,#126874,#126875,#126876,#126877,
#126878,#126879,#126880,#126881,#126882,#126883,#126884,#126885,#126886,
#126887,#126888,#126889,#126890,#126891,#126892,#126893,#126894,#126895,
#126896,#126897,#126898,#126899,#126900,#126901,#126902,#126903),
 .UNSPECIFIED.,.F.,.F.,(4,3,3,3,3,3,3,3,3,3,3,3,3,3,3,3,3,3,3,3,3,3,3,3,
3,3,3,3,3,3,3,3,3,3,3,3,3,3,3,3,3,3,3,3,3,3,3,3,3,3,3,3,3,3,3,3,3,3,3,3,
3,3,3,3,3,3,3,3,3,3,3,3,3,4),(1511.10606637679,1511.18843911631,1511.27074200656,
1511.3530012699,1511.4352387914,1511.51747358911,1511.59972467661,1511.68205952719,
1511.76443860843,1511.84694334215,1511.90888299029,1511.99262170214,1512.0762572135,
1512.1598096569,1512.24329909275,1512.32675304336,1512.41018953721,1512.49362664696,
1512.57708244188,1512.66062693461,1512.74421601755,1512.8279392851,1512.90861900101,
1512.99235771286,1513.07599322422,1513.15954566762,1513.24303510347,1513.32648905408,
1513.40992554793,1513.49336265768,1513.5768184526,1513.66036294533,1513.74395202827,
1513.82767529583,1513.90835501173,1513.99209372358,1514.07572923494,1514.15928167834,
1514.24277111419,1514.32622506481,1514.40966155865,1514.49309866841,1514.57655446333,
1514.66009895606,1514.743688039,1514.82741130656,1514.90809102245,1514.9918297343,
1515.07546524566,1515.15901768906,1515.24250712491,1515.32596107553,1515.40939756937,
1515.49283467913,1515.57629047405,1515.65983496678,1515.74342404972,1515.82714731727,
1515.90782703317,1515.99156574502,1516.07520125639,1516.15875369978,1516.24224313564,
1516.32569708625,1516.4091335801,1516.49257068986,1516.57602648477,1516.6595709775,
1516.74316006045,1516.826883328,1516.90756304389,1516.99637404297,1517.08497773719,
1517.13894299318),.UNSPECIFIED.);
#1012=B_SPLINE_CURVE_WITH_KNOTS('',3,(#126904,#126905,#126906,#126907,#126908,
#126909,#126910,#126911,#126912,#126913),.UNSPECIFIED.,.F.,.F.,(4,3,3,4),
(1510.85471449263,1510.90914697957,1511.03030619401,1511.10606637668),
 .UNSPECIFIED.);
#1013=B_SPLINE_CURVE_WITH_KNOTS('',3,(#126915,#126916,#126917,#126918,#126919,
#126920,#126921,#126922,#126923,#126924),.UNSPECIFIED.,.F.,.F.,(4,3,3,4),
(1510.85424422661,1510.93666726909,1511.02136682282,1511.10606637655),
 .UNSPECIFIED.);
#1014=B_SPLINE_CURVE_WITH_KNOTS('',3,(#126925,#126926,#126927,#126928,#126929,
#126930,#126931,#126932,#126933,#126934,#126935,#126936,#126937,#126938,
#126939,#126940,#126941,#126942,#126943,#126944,#126945,#126946,#126947,
#126948,#126949,#126950,#126951,#126952,#126953,#126954,#126955,#126956,
#126957,#126958,#126959,#126960,#126961,#126962,#126963,#126964,#126965,
#126966,#126967,#126968,#126969,#126970,#126971,#126972,#126973,#126974,
#126975,#126976,#126977,#126978,#126979,#126980,#126981,#126982,#126983,
#126984,#126985,#126986,#126987,#126988,#126989,#126990,#126991,#126992,
#126993,#126994,#126995,#126996,#126997,#126998,#126999,#127000,#127001,
#127002,#127003,#127004,#127005,#127006,#127007,#127008,#127009,#127010,
#127011,#127012,#127013,#127014,#127015,#127016,#127017,#127018,#127019,
#127020,#127021,#127022,#127023,#127024,#127025,#127026,#127027,#127028,
#127029,#127030,#127031,#127032,#127033,#127034,#127035,#127036,#127037,
#127038,#127039,#127040,#127041,#127042,#127043,#127044,#127045,#127046,
#127047,#127048,#127049,#127050,#127051,#127052,#127053,#127054,#127055,
#127056,#127057,#127058,#127059,#127060,#127061,#127062,#127063,#127064,
#127065,#127066,#127067,#127068,#127069,#127070,#127071,#127072,#127073,
#127074,#127075,#127076,#127077,#127078,#127079,#127080,#127081,#127082,
#127083,#127084,#127085,#127086,#127087,#127088,#127089,#127090,#127091,
#127092,#127093,#127094,#127095,#127096,#127097,#127098,#127099,#127100,
#127101,#127102,#127103,#127104,#127105,#127106,#127107,#127108,#127109,
#127110,#127111,#127112,#127113,#127114,#127115,#127116,#127117,#127118,
#127119,#127120,#127121,#127122,#127123,#127124,#127125,#127126,#127127,
#127128,#127129,#127130,#127131,#127132,#127133,#127134,#127135,#127136,
#127137,#127138,#127139,#127140,#127141),.UNSPECIFIED.,.F.,.F.,(4,3,3,3,
3,3,3,3,3,3,3,3,3,3,3,3,3,3,3,3,3,3,3,3,3,3,3,3,3,3,3,3,3,3,3,3,3,3,3,3,
3,3,3,3,3,3,3,3,3,3,3,3,3,3,3,3,3,3,3,3,3,3,3,3,3,3,3,3,3,3,3,3,4),(1511.10606637669,
1511.21943759928,1511.30317631113,1511.38681182249,1511.47036426589,1511.55385370175,
1511.63730765236,1511.72074414621,1511.80418125596,1511.88763705088,1511.97118154361,
1512.05477062655,1512.13849389411,1512.21917361,1512.30291232185,1512.38654783321,
1512.47010027661,1512.55358971246,1512.63704366307,1512.72048015692,1512.80391726667,
1512.88737306159,1512.97091755432,1513.05450663726,1513.13822990481,1513.21890962072,
1513.30264833257,1513.38628384394,1513.46983628734,1513.5533257232,1513.63677967381,
1513.72021616766,1513.80365327742,1513.88710907234,1513.97065356507,1514.05424264802,
1514.13796591558,1514.21864563145,1514.30238434329,1514.38601985466,1514.46957229805,
1514.5530617339,1514.63651568451,1514.71995217836,1514.80338928811,1514.88684508302,
1514.97038957575,1515.05397865869,1515.13770192624,1515.21838164216,1515.30212035401,
1515.38575586537,1515.46930830877,1515.55279774463,1515.63625169524,1515.71968818909,
1515.80312529884,1515.88658109376,1515.97012558649,1516.05371466943,1516.13743793699,
1516.21811765289,1516.30186099068,1516.38550007206,1516.46905503402,1516.5526481454,
1516.63609843941,1516.71952980604,1516.8029603171,1516.8866702191,1516.97018733186,
1517.05399362848,1517.1377999251),.UNSPECIFIED.);
#1015=B_SPLINE_CURVE_WITH_KNOTS('',3,(#127147,#127148,#127149,#127150,#127151,
#127152,#127153,#127154,#127155,#127156,#127157,#127158,#127159,#127160,
#127161,#127162,#127163,#127164,#127165,#127166,#127167,#127168,#127169,
#127170,#127171,#127172,#127173,#127174,#127175,#127176,#127177,#127178,
#127179,#127180,#127181,#127182,#127183,#127184,#127185,#127186,#127187,
#127188,#127189,#127190,#127191,#127192,#127193,#127194,#127195,#127196,
#127197,#127198,#127199,#127200,#127201,#127202,#127203,#127204,#127205,
#127206,#127207,#127208,#127209,#127210,#127211,#127212,#127213,#127214,
#127215,#127216,#127217,#127218,#127219,#127220,#127221,#127222,#127223,
#127224,#127225,#127226,#127227,#127228,#127229,#127230,#127231,#127232,
#127233,#127234,#127235,#127236,#127237,#127238,#127239,#127240,#127241,
#127242,#127243,#127244,#127245,#127246,#127247,#127248,#127249,#127250,
#127251,#127252,#127253,#127254,#127255,#127256,#127257,#127258,#127259,
#127260,#127261,#127262,#127263,#127264,#127265,#127266,#127267,#127268,
#127269,#127270,#127271,#127272,#127273,#127274,#127275,#127276,#127277,
#127278,#127279,#127280,#127281,#127282,#127283,#127284,#127285,#127286,
#127287,#127288,#127289,#127290,#127291,#127292,#127293,#127294,#127295,
#127296,#127297,#127298,#127299,#127300,#127301,#127302,#127303,#127304,
#127305,#127306,#127307,#127308,#127309,#127310,#127311,#127312,#127313,
#127314,#127315,#127316,#127317,#127318,#127319,#127320,#127321,#127322,
#127323,#127324,#127325,#127326,#127327,#127328,#127329,#127330,#127331,
#127332,#127333,#127334,#127335,#127336,#127337,#127338,#127339,#127340,
#127341,#127342,#127343,#127344,#127345,#127346,#127347,#127348,#127349,
#127350,#127351,#127352,#127353,#127354,#127355,#127356,#127357,#127358,
#127359,#127360,#127361,#127362,#127363,#127364,#127365,#127366),
 .UNSPECIFIED.,.F.,.F.,(4,3,3,3,3,3,3,3,3,3,3,3,3,3,3,3,3,3,3,3,3,3,3,3,
3,3,3,3,3,3,3,3,3,3,3,3,3,3,3,3,3,3,3,3,3,3,3,3,3,3,3,3,3,3,3,3,3,3,3,3,
3,3,3,3,3,3,3,3,3,3,3,3,3,4),(1517.38925168386,1517.47602562373,1517.56289209464,
1517.64994290237,1517.73708792198,1517.82443009038,1517.90729905461,1517.99103776646,
1518.07467327782,1518.15822572122,1518.24171515707,1518.32516910769,1518.40860560153,
1518.49204271129,1518.57549850621,1518.65904299894,1518.74263208188,1518.82635534944,
1518.90703506533,1518.99077377718,1519.07440928854,1519.15796173194,1519.24145116779,
1519.32490511841,1519.40834161225,1519.49177872201,1519.57523451692,1519.65877900965,
1519.74236809259,1519.82609136015,1519.90677107605,1519.9905097879,1520.07414529926,
1520.15769774266,1520.24118717851,1520.32464112913,1520.40807762297,1520.49151473273,
1520.57497052765,1520.65851502038,1520.74210410332,1520.82582737088,1520.90650708677,
1520.99024579862,1521.07388130998,1521.15743375338,1521.24092318923,1521.32437713985,
1521.40781363369,1521.49125074345,1521.57470653837,1521.6582510311,1521.74184011404,
1521.8255633816,1521.90624309749,1521.98998180934,1522.0736173207,1522.1571697641,
1522.24065919995,1522.32411315057,1522.40754964441,1522.49098675417,1522.57444254909,
1522.65798704182,1522.74157612476,1522.82529939231,1522.90597910821,1522.98863711599,
1523.07119771625,1523.15368002176,1523.23609810398,1523.31847966571,1523.40084881881,
1523.42099381078),.UNSPECIFIED.);
#1016=B_SPLINE_CURVE_WITH_KNOTS('',3,(#127367,#127368,#127369,#127370,#127371,
#127372,#127373,#127374,#127375,#127376),.UNSPECIFIED.,.F.,.F.,(4,3,3,4),
(1517.13894299318,1517.22727810457,1517.31541712171,1517.38925168369),
 .UNSPECIFIED.);
#1017=B_SPLINE_CURVE_WITH_KNOTS('',3,(#127378,#127379,#127380,#127381,#127382,
#127383,#127384,#127385,#127386,#127387),.UNSPECIFIED.,.F.,.F.,(4,3,3,4),
(1517.1377999251,1517.21785366361,1517.34872141794,1517.38925168387),
 .UNSPECIFIED.);
#1018=B_SPLINE_CURVE_WITH_KNOTS('',3,(#127388,#127389,#127390,#127391,#127392,
#127393,#127394,#127395,#127396,#127397,#127398,#127399,#127400,#127401,
#127402,#127403,#127404,#127405,#127406,#127407,#127408,#127409,#127410,
#127411,#127412,#127413,#127414,#127415,#127416,#127417,#127418,#127419,
#127420,#127421,#127422,#127423,#127424,#127425,#127426,#127427,#127428,
#127429,#127430,#127431,#127432,#127433,#127434,#127435,#127436,#127437,
#127438,#127439,#127440,#127441,#127442,#127443,#127444,#127445,#127446,
#127447,#127448,#127449,#127450,#127451,#127452,#127453,#127454,#127455,
#127456,#127457,#127458,#127459,#127460,#127461,#127462,#127463,#127464,
#127465,#127466,#127467,#127468,#127469,#127470,#127471,#127472,#127473,
#127474,#127475,#127476,#127477,#127478,#127479,#127480,#127481,#127482,
#127483,#127484,#127485,#127486,#127487,#127488,#127489,#127490,#127491,
#127492,#127493,#127494,#127495,#127496,#127497,#127498,#127499,#127500,
#127501,#127502,#127503,#127504,#127505,#127506,#127507,#127508,#127509,
#127510,#127511,#127512,#127513,#127514,#127515,#127516,#127517,#127518,
#127519,#127520,#127521,#127522,#127523,#127524,#127525,#127526,#127527,
#127528,#127529,#127530,#127531,#127532,#127533,#127534,#127535,#127536,
#127537,#127538,#127539,#127540,#127541,#127542,#127543,#127544,#127545,
#127546,#127547,#127548,#127549,#127550,#127551,#127552,#127553,#127554,
#127555,#127556,#127557,#127558,#127559,#127560,#127561,#127562,#127563,
#127564,#127565,#127566,#127567,#127568,#127569,#127570,#127571,#127572,
#127573,#127574,#127575,#127576,#127577,#127578,#127579,#127580,#127581,
#127582,#127583,#127584,#127585,#127586,#127587,#127588,#127589,#127590,
#127591,#127592,#127593,#127594,#127595,#127596,#127597,#127598,#127599,
#127600,#127601,#127602,#127603,#127604,#127605,#127606,#127607),
 .UNSPECIFIED.,.F.,.F.,(4,3,3,3,3,3,3,3,3,3,3,3,3,3,3,3,3,3,3,3,3,3,3,3,
3,3,3,3,3,3,3,3,3,3,3,3,3,3,3,3,3,3,3,3,3,3,3,3,3,3,3,3,3,3,3,3,3,3,3,3,
3,3,3,3,3,3,3,3,3,3,3,3,3,4),(1517.38925168405,1517.47161907531,1517.55390965771,
1517.63686965979,1517.71907915193,1517.80127988251,1517.88349088499,1517.96701558232,
1518.04934654739,1518.13346811086,1518.21758967433,1518.30132838618,1518.38496389754,
1518.46851634094,1518.55200577679,1518.63545972741,1518.71889622125,1518.80233333101,
1518.88578912593,1518.96933361866,1519.0529227016,1519.13664596916,1519.21732568505,
1519.3010643969,1519.38469990826,1519.46825235166,1519.55174178751,1519.63519573813,
1519.71863223197,1519.80206934173,1519.88552513665,1519.96906962938,1520.05265871232,
1520.13638197987,1520.21706169577,1520.30080040762,1520.38443591898,1520.46798836238,
1520.55147779823,1520.63493174885,1520.71836824269,1520.80180535245,1520.88526114737,
1520.9688056401,1521.05239472304,1521.13611799059,1521.21679770649,1521.30053641834,
1521.3841719297,1521.4677243731,1521.55121380895,1521.63466775957,1521.71810425341,
1521.80154136317,1521.88499715809,1521.96854165082,1522.05213073376,1522.13585400131,
1522.21653371721,1522.30027242906,1522.38390794042,1522.46746038382,1522.55094981967,
1522.63440377029,1522.71784026413,1522.80127737389,1522.88473316881,1522.96827766154,
1523.05186674448,1523.13559001203,1523.21626972793,1523.30626667354,1523.39603949157,
1523.42213509551),.UNSPECIFIED.);
#1019=B_SPLINE_CURVE_WITH_KNOTS('',3,(#127613,#127614,#127615,#127616,#127617,
#127618,#127619,#127620,#127621,#127622,#127623,#127624,#127625,#127626,
#127627,#127628,#127629,#127630,#127631,#127632,#127633,#127634,#127635,
#127636,#127637,#127638,#127639,#127640,#127641,#127642,#127643,#127644,
#127645,#127646,#127647,#127648,#127649,#127650,#127651,#127652,#127653,
#127654,#127655,#127656,#127657,#127658,#127659,#127660,#127661,#127662,
#127663,#127664,#127665,#127666,#127667,#127668,#127669,#127670,#127671,
#127672,#127673,#127674,#127675,#127676,#127677,#127678,#127679,#127680,
#127681,#127682,#127683,#127684,#127685,#127686,#127687,#127688,#127689,
#127690,#127691,#127692,#127693,#127694,#127695,#127696,#127697,#127698,
#127699,#127700,#127701,#127702,#127703,#127704,#127705,#127706,#127707,
#127708,#127709,#127710,#127711,#127712,#127713,#127714,#127715,#127716,
#127717,#127718,#127719,#127720,#127721,#127722,#127723,#127724,#127725,
#127726,#127727,#127728,#127729,#127730,#127731,#127732,#127733,#127734,
#127735,#127736,#127737,#127738,#127739,#127740,#127741,#127742,#127743,
#127744,#127745,#127746,#127747,#127748,#127749,#127750,#127751,#127752,
#127753,#127754,#127755,#127756,#127757,#127758,#127759,#127760,#127761,
#127762,#127763,#127764,#127765,#127766,#127767,#127768,#127769,#127770,
#127771,#127772,#127773,#127774,#127775,#127776,#127777,#127778,#127779,
#127780,#127781,#127782,#127783,#127784,#127785,#127786,#127787,#127788,
#127789,#127790,#127791,#127792,#127793,#127794,#127795,#127796,#127797,
#127798,#127799,#127800,#127801,#127802,#127803,#127804,#127805,#127806,
#127807,#127808,#127809,#127810,#127811,#127812,#127813,#127814,#127815,
#127816,#127817,#127818,#127819,#127820,#127821,#127822,#127823,#127824,
#127825,#127826,#127827,#127828,#127829,#127830,#127831,#127832),
 .UNSPECIFIED.,.F.,.F.,(4,3,3,3,3,3,3,3,3,3,3,3,3,3,3,3,3,3,3,3,3,3,3,3,
3,3,3,3,3,3,3,3,3,3,3,3,3,3,3,3,3,3,3,3,3,3,3,3,3,3,3,3,3,3,3,3,3,3,3,3,
3,3,3,3,3,3,3,3,3,3,3,3,3,4),(1523.67243699115,1523.78258462893,1523.89582452207,
1523.90571511893,1523.98945383078,1524.07308934214,1524.15664178554,1524.24013122139,
1524.32358517201,1524.40702166585,1524.49045877561,1524.57391457053,1524.65745906326,
1524.7410481462,1524.82477141375,1524.90545112965,1524.9891898415,1525.07282535286,
1525.15637779626,1525.23986723211,1525.32332118273,1525.40675767657,1525.49019478633,
1525.57365058124,1525.65719507397,1525.74078415691,1525.82450742447,1525.90518714037,
1525.98892585222,1526.07256136358,1526.15611380698,1526.23960324283,1526.32305719345,
1526.40649368729,1526.48993079705,1526.57338659197,1526.6569310847,1526.74052016764,
1526.82424343519,1526.90492315109,1526.98866186294,1527.0722973743,1527.1558498177,
1527.23933925355,1527.32279320417,1527.40622969801,1527.48966680777,1527.57312260269,
1527.65666709542,1527.74025617836,1527.82397944591,1527.90465916181,1527.98839787366,
1528.07203338502,1528.15558582842,1528.23907526427,1528.32252921489,1528.40596570873,
1528.48940281849,1528.57285861341,1528.65640310614,1528.73999218908,1528.82371545664,
1528.90439517253,1528.98814598813,1529.0717909624,1529.1553347027,1529.23882103833,
1529.32226808954,1529.40569394618,1529.48914071552,1529.5725981172,1529.65611866871,
1529.70395727207),.UNSPECIFIED.);
#1020=B_SPLINE_CURVE_WITH_KNOTS('',3,(#127833,#127834,#127835,#127836,#127837,
#127838,#127839,#127840,#127841,#127842),.UNSPECIFIED.,.F.,.F.,(4,3,3,4),
(1523.42099381078,1523.50338958302,1523.58791328703,1523.67243699104),
 .UNSPECIFIED.);
#1021=B_SPLINE_CURVE_WITH_KNOTS('',3,(#127844,#127845,#127846,#127847,#127848,
#127849,#127850,#127851,#127852,#127853),.UNSPECIFIED.,.F.,.F.,(4,3,3,4),
(1523.42213509551,1523.51162295178,1523.60085738858,1523.67243699087),
 .UNSPECIFIED.);
#1022=B_SPLINE_CURVE_WITH_KNOTS('',3,(#127854,#127855,#127856,#127857,#127858,
#127859,#127860,#127861,#127862,#127863,#127864,#127865,#127866,#127867,
#127868,#127869,#127870,#127871,#127872,#127873,#127874,#127875,#127876,
#127877,#127878,#127879,#127880,#127881,#127882,#127883,#127884,#127885,
#127886,#127887,#127888,#127889,#127890,#127891,#127892,#127893,#127894,
#127895,#127896,#127897,#127898,#127899,#127900,#127901,#127902,#127903,
#127904,#127905,#127906,#127907,#127908,#127909,#127910,#127911,#127912,
#127913,#127914,#127915,#127916,#127917,#127918,#127919,#127920,#127921,
#127922,#127923,#127924,#127925,#127926,#127927,#127928,#127929,#127930,
#127931,#127932,#127933,#127934,#127935,#127936,#127937,#127938,#127939,
#127940,#127941,#127942,#127943,#127944,#127945,#127946,#127947,#127948,
#127949,#127950,#127951,#127952,#127953,#127954,#127955,#127956,#127957,
#127958,#127959,#127960,#127961,#127962,#127963,#127964,#127965,#127966,
#127967,#127968,#127969,#127970,#127971,#127972,#127973,#127974,#127975,
#127976,#127977,#127978,#127979,#127980,#127981,#127982,#127983,#127984,
#127985,#127986,#127987,#127988,#127989,#127990,#127991,#127992,#127993,
#127994,#127995,#127996,#127997,#127998,#127999,#128000,#128001,#128002,
#128003,#128004,#128005,#128006,#128007,#128008,#128009,#128010,#128011,
#128012,#128013,#128014,#128015,#128016,#128017,#128018,#128019,#128020,
#128021,#128022,#128023,#128024,#128025,#128026,#128027,#128028,#128029,
#128030,#128031,#128032,#128033,#128034,#128035,#128036,#128037,#128038,
#128039,#128040,#128041,#128042,#128043,#128044,#128045,#128046,#128047,
#128048,#128049,#128050,#128051,#128052,#128053,#128054,#128055,#128056,
#128057,#128058,#128059,#128060,#128061,#128062,#128063,#128064,#128065,
#128066,#128067,#128068,#128069,#128070,#128071,#128072,#128073),
 .UNSPECIFIED.,.F.,.F.,(4,3,3,3,3,3,3,3,3,3,3,3,3,3,3,3,3,3,3,3,3,3,3,3,
3,3,3,3,3,3,3,3,3,3,3,3,3,3,3,3,3,3,3,3,3,3,3,3,3,3,3,3,3,3,3,3,3,3,3,3,
3,3,3,3,3,3,3,3,3,3,3,3,3,4),(1523.67243699105,1523.75841773458,1523.8444644582,
1523.93059030503,1524.01687033097,1524.10323851992,1524.18976393114,1524.21600573865,
1524.2997444505,1524.38337996186,1524.46693240526,1524.55042184111,1524.63387579173,
1524.71731228557,1524.80074939533,1524.88420519025,1524.96774968298,1525.05133876592,
1525.13506203347,1525.21574174937,1525.29948046122,1525.38311597258,1525.46666841598,
1525.55015785183,1525.63361180245,1525.71704829629,1525.80048540605,1525.88394120097,
1525.96748569369,1526.05107477664,1526.13479804419,1526.21547776009,1526.29921647194,
1526.3828519833,1526.4664044267,1526.54989386255,1526.63334781317,1526.71678430701,
1526.80022141677,1526.88367721169,1526.96722170441,1527.05081078736,1527.13453405491,
1527.21521377081,1527.29895248266,1527.38258799402,1527.46614043742,1527.54962987327,
1527.63308382389,1527.71652031773,1527.79995742749,1527.88341322241,1527.96695771514,
1528.05054679808,1528.13427006563,1528.21494978153,1528.29868849338,1528.38232400474,
1528.46587644814,1528.54936588399,1528.63281983461,1528.71625632845,1528.79969343821,
1528.88314923313,1528.96669372586,1529.0502828088,1529.13400607636,1529.21468579225,
1529.29752113583,1529.3802577084,1529.46290141179,1529.54549048635,1529.62805090444,
1529.7043027577),.UNSPECIFIED.);
#1023=B_SPLINE_CURVE_WITH_KNOTS('',3,(#128079,#128080,#128081,#128082,#128083,
#128084,#128085,#128086,#128087,#128088,#128089,#128090,#128091,#128092,
#128093,#128094,#128095,#128096,#128097,#128098,#128099,#128100,#128101,
#128102,#128103,#128104,#128105,#128106,#128107,#128108,#128109,#128110,
#128111,#128112,#128113,#128114,#128115,#128116,#128117,#128118,#128119,
#128120,#128121,#128122,#128123,#128124,#128125,#128126,#128127,#128128,
#128129,#128130,#128131,#128132,#128133,#128134,#128135,#128136,#128137,
#128138,#128139,#128140,#128141,#128142,#128143,#128144,#128145,#128146,
#128147,#128148,#128149,#128150,#128151,#128152,#128153,#128154,#128155,
#128156,#128157,#128158,#128159,#128160,#128161,#128162,#128163,#128164,
#128165,#128166,#128167,#128168,#128169,#128170,#128171,#128172,#128173,
#128174,#128175,#128176,#128177,#128178,#128179,#128180,#128181,#128182,
#128183,#128184,#128185,#128186,#128187,#128188,#128189,#128190,#128191,
#128192,#128193,#128194,#128195,#128196,#128197,#128198,#128199,#128200,
#128201,#128202,#128203,#128204,#128205,#128206,#128207,#128208,#128209,
#128210,#128211,#128212,#128213,#128214,#128215,#128216,#128217,#128218,
#128219,#128220,#128221,#128222,#128223,#128224,#128225,#128226,#128227,
#128228,#128229,#128230,#128231,#128232,#128233,#128234,#128235,#128236,
#128237,#128238,#128239,#128240,#128241,#128242,#128243,#128244,#128245,
#128246,#128247,#128248,#128249,#128250,#128251,#128252,#128253,#128254,
#128255,#128256,#128257,#128258,#128259,#128260,#128261,#128262,#128263,
#128264,#128265,#128266,#128267,#128268,#128269,#128270,#128271,#128272,
#128273,#128274,#128275,#128276,#128277,#128278,#128279,#128280,#128281,
#128282,#128283,#128284,#128285,#128286,#128287,#128288,#128289,#128290,
#128291,#128292,#128293,#128294,#128295,#128296,#128297,#128298),
 .UNSPECIFIED.,.F.,.F.,(4,3,3,3,3,3,3,3,3,3,3,3,3,3,3,3,3,3,3,3,3,3,3,3,
3,3,3,3,3,3,3,3,3,3,3,3,3,3,3,3,3,3,3,3,3,3,3,3,3,3,3,3,3,3,3,3,3,3,3,3,
3,3,3,3,3,3,3,3,3,3,3,3,3,4),(1529.95562229842,1530.03869000497,1530.12165783729,
1530.2045465541,1530.28737683683,1530.37017812198,1530.4529672259,1530.53576278341,
1530.6185834307,1530.70149397743,1530.78445594191,1530.86753831501,1530.90386719397,
1530.98760590582,1531.07124141718,1531.15479386058,1531.23828329643,1531.32173724705,
1531.40517374089,1531.48861085065,1531.57206664557,1531.6556111383,1531.73920022124,
1531.82292348879,1531.90360320469,1531.98734191654,1532.0709774279,1532.1545298713,
1532.23801930715,1532.32147325777,1532.40490975161,1532.48834686137,1532.57180265629,
1532.65534714902,1532.73893623196,1532.82265949951,1532.90333921541,1532.98707792726,
1533.07071343862,1533.15426588202,1533.23775531787,1533.32120926849,1533.40464576233,
1533.48808287209,1533.57153866701,1533.65508315974,1533.73867224268,1533.82239551023,
1533.90307522613,1533.98681393798,1534.07044944934,1534.15400189274,1534.23749132859,
1534.32094527921,1534.40438177305,1534.48781888281,1534.57127467773,1534.65481917046,
1534.7384082534,1534.82213152096,1534.90281123685,1534.9865499487,1535.07018546006,
1535.15373790346,1535.23722733931,1535.32068128993,1535.40411778377,1535.48755489353,
1535.57101068844,1535.65455518117,1535.73814426412,1535.82186753167,1535.90254724757,
1535.98821483034),.UNSPECIFIED.);
#1024=B_SPLINE_CURVE_WITH_KNOTS('',3,(#128299,#128300,#128301,#128302,#128303,
#128304,#128305,#128306,#128307,#128308,#128309,#128310,#128311),
 .UNSPECIFIED.,.F.,.F.,(4,3,3,3,4),(1529.70395727207,1529.78757918107,1529.87132176391,
1529.90413118325,1529.95562229822),.UNSPECIFIED.);
#1025=B_SPLINE_CURVE_WITH_KNOTS('',3,(#128313,#128314,#128315,#128316,#128317,
#128318,#128319,#128320,#128321,#128322),.UNSPECIFIED.,.F.,.F.,(4,3,3,4),
(1529.7043027577,1529.78685599116,1529.87123914469,1529.95562229823),
 .UNSPECIFIED.);
#1026=B_SPLINE_CURVE_WITH_KNOTS('',3,(#128323,#128324,#128325,#128326,#128327,
#128328,#128329,#128330,#128331,#128332,#128333,#128334,#128335,#128336,
#128337,#128338,#128339,#128340,#128341,#128342,#128343,#128344,#128345,
#128346,#128347,#128348,#128349,#128350,#128351,#128352,#128353,#128354,
#128355,#128356,#128357,#128358,#128359,#128360,#128361,#128362,#128363,
#128364,#128365,#128366,#128367,#128368,#128369,#128370,#128371,#128372,
#128373,#128374,#128375,#128376,#128377,#128378,#128379,#128380,#128381,
#128382,#128383,#128384,#128385,#128386,#128387,#128388,#128389,#128390,
#128391,#128392,#128393,#128394,#128395,#128396,#128397,#128398,#128399,
#128400,#128401,#128402,#128403,#128404,#128405,#128406,#128407,#128408,
#128409,#128410,#128411,#128412,#128413,#128414,#128415,#128416,#128417,
#128418,#128419,#128420,#128421,#128422,#128423,#128424,#128425,#128426,
#128427,#128428,#128429,#128430,#128431,#128432,#128433,#128434,#128435,
#128436,#128437,#128438,#128439,#128440,#128441,#128442,#128443,#128444,
#128445,#128446,#128447,#128448,#128449,#128450,#128451,#128452,#128453,
#128454,#128455,#128456,#128457,#128458,#128459,#128460,#128461,#128462,
#128463,#128464,#128465,#128466,#128467,#128468,#128469,#128470,#128471,
#128472,#128473,#128474,#128475,#128476,#128477,#128478,#128479,#128480,
#128481,#128482,#128483,#128484,#128485,#128486,#128487,#128488,#128489,
#128490,#128491,#128492,#128493,#128494,#128495,#128496,#128497,#128498,
#128499,#128500,#128501,#128502,#128503,#128504,#128505,#128506,#128507,
#128508,#128509,#128510,#128511,#128512,#128513,#128514,#128515,#128516,
#128517,#128518,#128519,#128520,#128521,#128522,#128523,#128524,#128525,
#128526,#128527,#128528,#128529,#128530,#128531,#128532,#128533,#128534,
#128535,#128536,#128537,#128538,#128539,#128540,#128541,#128542),
 .UNSPECIFIED.,.F.,.F.,(4,3,3,3,3,3,3,3,3,3,3,3,3,3,3,3,3,3,3,3,3,3,3,3,
3,3,3,3,3,3,3,3,3,3,3,3,3,3,3,3,3,3,3,3,3,3,3,3,3,3,3,3,3,3,3,3,3,3,3,3,
3,3,3,3,3,3,3,3,3,3,3,3,3,4),(1529.95562229836,1530.06149157749,1530.16950984213,
1530.21442180297,1530.29816051482,1530.38179602618,1530.46534846958,1530.54883790543,
1530.63229185605,1530.71572834989,1530.79916545965,1530.88262125457,1530.9661657473,
1531.04975483024,1531.13347809779,1531.21415781369,1531.29789652554,1531.3815320369,
1531.4650844803,1531.54857391615,1531.63202786677,1531.71546436061,1531.79890147037,
1531.88235726529,1531.96590175802,1532.04949084096,1532.13321410851,1532.21389382441,
1532.29763253626,1532.38126804762,1532.46482049102,1532.54830992687,1532.63176387749,
1532.71520037133,1532.79863748109,1532.88209327601,1532.96563776874,1533.04922685168,
1533.13295011923,1533.21362983513,1533.29736854698,1533.38100405834,1533.46455650174,
1533.54804593759,1533.63149988821,1533.71493638205,1533.79837349181,1533.88182928673,
1533.96537377946,1534.0489628624,1534.13268612995,1534.21336584585,1534.2971045577,
1534.38074006906,1534.46429251246,1534.54778194831,1534.63123589893,1534.71467239277,
1534.79810950253,1534.88156529745,1534.96510979018,1535.04869887312,1535.13242214067,
1535.21310185657,1535.29685434383,1535.38314048142,1535.46668270487,1535.55016761907,
1535.63361334401,1535.71703796925,1535.80047957901,1535.88393214105,1535.96743749394,
1535.98714344461),.UNSPECIFIED.);
#1027=B_SPLINE_CURVE_WITH_KNOTS('',3,(#128548,#128549,#128550,#128551,#128552,
#128553,#128554,#128555,#128556,#128557,#128558,#128559,#128560,#128561,
#128562,#128563,#128564,#128565,#128566,#128567,#128568,#128569,#128570,
#128571,#128572,#128573,#128574,#128575,#128576,#128577,#128578,#128579,
#128580,#128581,#128582,#128583,#128584,#128585,#128586,#128587,#128588,
#128589,#128590,#128591,#128592,#128593,#128594,#128595,#128596,#128597,
#128598,#128599,#128600,#128601,#128602,#128603,#128604,#128605,#128606,
#128607,#128608,#128609,#128610,#128611,#128612,#128613,#128614,#128615,
#128616,#128617,#128618,#128619,#128620,#128621,#128622,#128623,#128624,
#128625,#128626,#128627,#128628,#128629,#128630,#128631,#128632,#128633,
#128634,#128635,#128636,#128637,#128638,#128639,#128640,#128641,#128642,
#128643,#128644,#128645,#128646,#128647,#128648,#128649,#128650,#128651,
#128652,#128653,#128654,#128655,#128656,#128657,#128658,#128659,#128660,
#128661,#128662,#128663,#128664,#128665,#128666,#128667,#128668,#128669,
#128670,#128671,#128672,#128673,#128674,#128675,#128676,#128677,#128678,
#128679,#128680,#128681,#128682,#128683,#128684,#128685,#128686,#128687,
#128688,#128689,#128690,#128691,#128692,#128693,#128694,#128695,#128696,
#128697,#128698,#128699,#128700,#128701,#128702,#128703,#128704,#128705,
#128706,#128707,#128708,#128709,#128710,#128711,#128712,#128713,#128714,
#128715,#128716,#128717,#128718,#128719,#128720,#128721,#128722,#128723,
#128724,#128725,#128726,#128727,#128728,#128729,#128730,#128731,#128732,
#128733,#128734,#128735,#128736,#128737,#128738,#128739,#128740,#128741,
#128742,#128743,#128744,#128745,#128746,#128747,#128748,#128749,#128750,
#128751,#128752,#128753,#128754,#128755,#128756,#128757,#128758,#128759,
#128760,#128761,#128762,#128763,#128764,#128765,#128766,#128767),
 .UNSPECIFIED.,.F.,.F.,(4,3,3,3,3,3,3,3,3,3,3,3,3,3,3,3,3,3,3,3,3,3,3,3,
3,3,3,3,3,3,3,3,3,3,3,3,3,3,3,3,3,3,3,3,3,3,3,3,3,3,3,3,3,3,3,3,3,3,3,3,
3,3,3,3,3,3,3,3,3,3,3,3,3,4),(1536.2388076054,1536.32223627499,1536.40565287209,
1536.48907540985,1536.5725219015,1536.65606475899,1536.7396566576,1536.82338883274,
1536.90228325829,1536.98602197014,1537.0696574815,1537.1532099249,1537.23669936075,
1537.32015331137,1537.40358980521,1537.48702691497,1537.57048270989,1537.65402720262,
1537.73761628556,1537.82133955312,1537.90201926901,1537.98575798086,1538.06939349222,
1538.15294593562,1538.23643537147,1538.31988932209,1538.40332581593,1538.48676292569,
1538.57021872061,1538.65376321333,1538.73735229628,1538.82107556383,1538.90175527973,
1538.98549399158,1539.06912950294,1539.15268194634,1539.23617138219,1539.31962533281,
1539.40306182665,1539.48649893641,1539.56995473132,1539.65349922405,1539.737088307,
1539.82081157455,1539.90149129045,1539.9852300023,1540.06886551366,1540.15241795706,
1540.23590739291,1540.31936134353,1540.40279783737,1540.48623494713,1540.56969074205,
1540.65323523478,1540.73682431772,1540.82054758528,1540.90122730117,1540.98496601302,
1541.06860152438,1541.15215396778,1541.23564340363,1541.31909735425,1541.40253384809,
1541.48597095785,1541.56942675276,1541.65297124549,1541.73656032843,1541.82028359599,
1541.90096331189,1541.98550083738,1542.06989404209,1542.15420375164,1542.23843095987,
1542.27128066288),.UNSPECIFIED.);
#1028=B_SPLINE_CURVE_WITH_KNOTS('',3,(#128768,#128769,#128770,#128771,#128772,
#128773,#128774,#128775,#128776,#128777),.UNSPECIFIED.,.F.,.F.,(4,3,3,4),
(1535.98821483034,1536.08596364199,1536.18288058848,1536.23880760521),
 .UNSPECIFIED.);
#1029=B_SPLINE_CURVE_WITH_KNOTS('',3,(#128779,#128780,#128781,#128782,#128783,
#128784,#128785,#128786,#128787,#128788,#128789,#128790,#128791),
 .UNSPECIFIED.,.F.,.F.,(4,3,3,3,4),(1535.98714344461,1536.07074717287,1536.15447863248,
1536.21283786729,1536.23880760541),.UNSPECIFIED.);
#1030=B_SPLINE_CURVE_WITH_KNOTS('',3,(#128792,#128793,#128794,#128795,#128796,
#128797,#128798,#128799,#128800,#128801,#128802,#128803,#128804,#128805,
#128806,#128807,#128808,#128809,#128810,#128811,#128812,#128813,#128814,
#128815,#128816,#128817,#128818,#128819,#128820,#128821,#128822,#128823,
#128824,#128825,#128826,#128827,#128828,#128829,#128830,#128831,#128832,
#128833,#128834,#128835,#128836,#128837,#128838,#128839,#128840,#128841,
#128842,#128843,#128844,#128845,#128846,#128847,#128848,#128849,#128850,
#128851,#128852,#128853,#128854,#128855,#128856,#128857,#128858,#128859,
#128860,#128861,#128862,#128863,#128864,#128865,#128866,#128867,#128868,
#128869,#128870,#128871,#128872,#128873,#128874,#128875,#128876,#128877,
#128878,#128879,#128880,#128881,#128882,#128883,#128884,#128885,#128886,
#128887,#128888,#128889,#128890,#128891,#128892,#128893,#128894,#128895,
#128896,#128897,#128898,#128899,#128900,#128901,#128902,#128903,#128904,
#128905,#128906,#128907,#128908,#128909,#128910,#128911,#128912,#128913,
#128914,#128915,#128916,#128917,#128918,#128919,#128920,#128921,#128922,
#128923,#128924,#128925,#128926,#128927,#128928,#128929,#128930,#128931,
#128932,#128933,#128934,#128935,#128936,#128937,#128938,#128939,#128940,
#128941,#128942,#128943,#128944,#128945,#128946,#128947,#128948,#128949,
#128950,#128951,#128952,#128953,#128954,#128955,#128956,#128957,#128958,
#128959,#128960,#128961,#128962,#128963,#128964,#128965,#128966,#128967,
#128968,#128969,#128970,#128971,#128972,#128973,#128974,#128975,#128976,
#128977,#128978,#128979,#128980,#128981,#128982,#128983,#128984,#128985,
#128986,#128987,#128988,#128989,#128990,#128991,#128992,#128993,#128994,
#128995,#128996,#128997,#128998,#128999,#129000,#129001,#129002,#129003,
#129004,#129005,#129006,#129007,#129008,#129009,#129010,#129011),
 .UNSPECIFIED.,.F.,.F.,(4,3,3,3,3,3,3,3,3,3,3,3,3,3,3,3,3,3,3,3,3,3,3,3,
3,3,3,3,3,3,3,3,3,3,3,3,3,3,3,3,3,3,3,3,3,3,3,3,3,3,3,3,3,3,3,3,3,3,3,3,
3,3,3,3,3,3,3,3,3,3,3,3,3,4),(1536.23880760553,1536.32217949724,1536.40544918826,
1536.48863717929,1536.57176389602,1536.65485772805,1536.73793634554,1536.82101815004,
1536.90412154168,1536.98731402283,1537.07055432919,1537.15392182379,1537.21257387801,
1537.29631258986,1537.37994810122,1537.46350054462,1537.54698998047,1537.63044393109,
1537.71388042493,1537.79731753469,1537.88077332961,1537.96431782234,1538.04790690528,
1538.13163017283,1538.21230988873,1538.29604860058,1538.37968411194,1538.46323655534,
1538.54672599119,1538.63017994181,1538.71361643565,1538.79705354541,1538.88050934033,
1538.96405383306,1539.047642916,1539.13136618355,1539.21204589945,1539.2957846113,
1539.37942012266,1539.46297256606,1539.54646200191,1539.62991595253,1539.71335244637,
1539.79678955613,1539.88024535105,1539.96378984378,1540.04737892672,1540.13110219427,
1540.21178191017,1540.29552062202,1540.37915613338,1540.46270857678,1540.54619801263,
1540.62965196325,1540.71308845709,1540.79652556685,1540.87998136177,1540.96352585449,
1541.04711493744,1541.13083820499,1541.21151792089,1541.29525663274,1541.3788921441,
1541.4624445875,1541.54593402335,1541.62938797397,1541.71282446781,1541.79626157757,
1541.87971737249,1541.96326186522,1542.04685094816,1542.13057421572,1542.21125393161,
1542.27127577894),.UNSPECIFIED.);
#1031=B_SPLINE_CURVE_WITH_KNOTS('',3,(#129017,#129018,#129019,#129020,#129021,
#129022,#129023,#129024,#129025,#129026,#129027,#129028,#129029,#129030,
#129031,#129032,#129033,#129034,#129035,#129036,#129037,#129038,#129039,
#129040,#129041,#129042,#129043,#129044,#129045,#129046,#129047,#129048,
#129049,#129050,#129051,#129052,#129053,#129054,#129055,#129056,#129057,
#129058,#129059,#129060,#129061,#129062,#129063,#129064,#129065,#129066,
#129067,#129068,#129069,#129070,#129071,#129072,#129073,#129074,#129075,
#129076,#129077,#129078,#129079,#129080,#129081,#129082,#129083,#129084,
#129085,#129086,#129087,#129088,#129089,#129090,#129091,#129092,#129093,
#129094,#129095,#129096,#129097,#129098,#129099,#129100,#129101,#129102,
#129103,#129104,#129105,#129106,#129107,#129108,#129109,#129110,#129111,
#129112,#129113,#129114,#129115,#129116,#129117,#129118,#129119,#129120,
#129121,#129122,#129123,#129124,#129125,#129126,#129127,#129128,#129129,
#129130,#129131,#129132,#129133,#129134,#129135,#129136,#129137,#129138,
#129139,#129140,#129141,#129142,#129143,#129144,#129145,#129146,#129147,
#129148,#129149,#129150,#129151,#129152,#129153,#129154,#129155,#129156,
#129157,#129158,#129159,#129160,#129161,#129162,#129163,#129164,#129165,
#129166,#129167,#129168,#129169,#129170,#129171,#129172,#129173,#129174,
#129175,#129176,#129177,#129178,#129179,#129180,#129181,#129182,#129183,
#129184,#129185,#129186,#129187,#129188,#129189,#129190,#129191,#129192,
#129193,#129194,#129195,#129196,#129197,#129198,#129199,#129200,#129201,
#129202,#129203,#129204,#129205,#129206,#129207,#129208,#129209,#129210,
#129211,#129212,#129213,#129214,#129215,#129216,#129217,#129218,#129219,
#129220,#129221,#129222,#129223,#129224,#129225,#129226,#129227,#129228,
#129229,#129230,#129231,#129232,#129233),.UNSPECIFIED.,.F.,.F.,(4,3,3,3,
3,3,3,3,3,3,3,3,3,3,3,3,3,3,3,3,3,3,3,3,3,3,3,3,3,3,3,3,3,3,3,3,3,3,3,3,
3,3,3,3,3,3,3,3,3,3,3,3,3,3,3,3,3,3,3,3,3,3,3,3,3,3,3,3,3,3,3,3,4),(1542.52199291277,
1542.61666951523,1542.71070417245,1542.80570174753,1542.90069932261,1542.98443803446,
1543.06807354582,1543.15162598922,1543.23511542507,1543.31856937569,1543.40200586953,
1543.48544297929,1543.56889877421,1543.65244326694,1543.73603234988,1543.81975561743,
1543.90043533333,1543.98417404518,1544.06780955654,1544.15136199994,1544.23485143579,
1544.31830538641,1544.40174188025,1544.48517899001,1544.56863478492,1544.65217927765,
1544.73576836059,1544.81949162815,1544.90017134405,1544.9839100559,1545.06754556726,
1545.15109801066,1545.23458744651,1545.31804139713,1545.40147789097,1545.48491500073,
1545.56837079565,1545.65191528838,1545.73550437132,1545.81922763887,1545.89990735477,
1545.98364606662,1546.06728157798,1546.15083402138,1546.23432345723,1546.31777740785,
1546.40121390169,1546.48465101145,1546.56810680637,1546.6516512991,1546.73524038204,
1546.81896364959,1546.89964336549,1546.98338207734,1547.0670175887,1547.1505700321,
1547.23405946795,1547.31751341857,1547.40094991241,1547.48438702217,1547.56784281709,
1547.65138730982,1547.73497639276,1547.81869966031,1547.89937937621,1547.98208738707,
1548.0647008436,1548.14723880089,1548.22972024646,1548.31217476354,1548.39461077265,
1548.47707764694,1548.55334172014),.UNSPECIFIED.);
#1032=B_SPLINE_CURVE_WITH_KNOTS('',3,(#129234,#129235,#129236,#129237,#129238,
#129239,#129240,#129241,#129242,#129243),.UNSPECIFIED.,.F.,.F.,(4,3,3,4),
(1542.27128066288,1542.35543589376,1542.43957430175,1542.52199291258),
 .UNSPECIFIED.);
#1033=B_SPLINE_CURVE_WITH_KNOTS('',3,(#129245,#129246,#129247,#129248,#129249,
#129250,#129251,#129252,#129253,#129254),.UNSPECIFIED.,.F.,.F.,(4,3,3,4),
(1542.27127577894,1542.37175444285,1542.47113194599,1542.52199291243),
 .UNSPECIFIED.);
#1034=B_SPLINE_CURVE_WITH_KNOTS('',3,(#129255,#129256,#129257,#129258,#129259,
#129260,#129261,#129262,#129263,#129264,#129265,#129266,#129267,#129268,
#129269,#129270,#129271,#129272,#129273,#129274,#129275,#129276,#129277,
#129278,#129279,#129280,#129281,#129282,#129283,#129284,#129285,#129286,
#129287,#129288,#129289,#129290,#129291,#129292,#129293,#129294,#129295,
#129296,#129297,#129298,#129299,#129300,#129301,#129302,#129303,#129304,
#129305,#129306,#129307,#129308,#129309,#129310,#129311,#129312,#129313,
#129314,#129315,#129316,#129317,#129318,#129319,#129320,#129321,#129322,
#129323,#129324,#129325,#129326,#129327,#129328,#129329,#129330,#129331,
#129332,#129333,#129334,#129335,#129336,#129337,#129338,#129339,#129340,
#129341,#129342,#129343,#129344,#129345,#129346,#129347,#129348,#129349,
#129350,#129351,#129352,#129353,#129354,#129355,#129356,#129357,#129358,
#129359,#129360,#129361,#129362,#129363,#129364,#129365,#129366,#129367,
#129368,#129369,#129370,#129371,#129372,#129373,#129374,#129375,#129376,
#129377,#129378,#129379,#129380,#129381,#129382,#129383,#129384,#129385,
#129386,#129387,#129388,#129389,#129390,#129391,#129392,#129393,#129394,
#129395,#129396,#129397,#129398,#129399,#129400,#129401,#129402,#129403,
#129404,#129405,#129406,#129407,#129408,#129409,#129410,#129411,#129412,
#129413,#129414,#129415,#129416,#129417,#129418,#129419,#129420,#129421,
#129422,#129423,#129424,#129425,#129426,#129427,#129428,#129429,#129430,
#129431,#129432,#129433,#129434,#129435,#129436,#129437,#129438,#129439,
#129440,#129441,#129442,#129443,#129444,#129445,#129446,#129447,#129448,
#129449,#129450,#129451,#129452,#129453,#129454,#129455,#129456,#129457,
#129458,#129459,#129460,#129461,#129462,#129463,#129464,#129465,#129466,
#129467,#129468,#129469,#129470,#129471,#129472,#129473,#129474),
 .UNSPECIFIED.,.F.,.F.,(4,3,3,3,3,3,3,3,3,3,3,3,3,3,3,3,3,3,3,3,3,3,3,3,
3,3,3,3,3,3,3,3,3,3,3,3,3,3,3,3,3,3,3,3,3,3,3,3,3,3,3,3,3,3,3,3,3,3,3,3,
3,3,3,3,3,3,3,3,3,3,3,3,3,4),(1542.52199291259,1542.60811754131,1542.69119004247,
1542.77425859425,1542.85734156487,1542.94045732878,1543.02367001644,1543.10694044436,
1543.19033106149,1543.21098994233,1543.29472865418,1543.37836416554,1543.46191660894,
1543.54540604479,1543.62885999541,1543.71229648925,1543.79573359901,1543.87918939393,
1543.96273388666,1544.0463229696,1544.13004623715,1544.21072595305,1544.2944646649,
1544.37810017626,1544.46165261966,1544.54514205551,1544.62859600613,1544.71203249997,
1544.79546960973,1544.87892540465,1544.96246989738,1545.04605898032,1545.12978224787,
1545.21046196377,1545.29420067562,1545.37783618698,1545.46138863038,1545.54487806623,
1545.62833201685,1545.71176851069,1545.79520562045,1545.87866141537,1545.9622059081,
1546.04579499104,1546.12951825859,1546.21019797449,1546.29393668634,1546.3775721977,
1546.4611246411,1546.54461407695,1546.62806802757,1546.71150452141,1546.79494163117,
1546.87839742609,1546.96194191882,1547.04553100176,1547.12925426931,1547.20993398521,
1547.29367269706,1547.37730820842,1547.46086065182,1547.54435008767,1547.62780403829,
1547.71124053213,1547.79467764189,1547.87813343681,1547.96167792954,1548.04526701248,
1548.12899028003,1548.20966999593,1548.29589684262,1548.38085486658,1548.46771612463,
1548.55457738268),.UNSPECIFIED.);
#1035=B_SPLINE_CURVE_WITH_KNOTS('',3,(#129480,#129481,#129482,#129483,#129484,
#129485,#129486,#129487,#129488,#129489,#129490,#129491,#129492,#129493,
#129494,#129495,#129496,#129497,#129498,#129499,#129500,#129501,#129502,
#129503,#129504,#129505,#129506,#129507,#129508,#129509,#129510,#129511,
#129512,#129513,#129514,#129515,#129516,#129517,#129518,#129519,#129520,
#129521,#129522,#129523,#129524,#129525,#129526,#129527,#129528,#129529,
#129530,#129531,#129532,#129533,#129534,#129535,#129536,#129537,#129538,
#129539,#129540,#129541,#129542,#129543,#129544,#129545,#129546,#129547,
#129548,#129549,#129550,#129551,#129552,#129553,#129554,#129555,#129556,
#129557,#129558,#129559,#129560,#129561,#129562,#129563,#129564,#129565,
#129566,#129567,#129568,#129569,#129570,#129571,#129572,#129573,#129574,
#129575,#129576,#129577,#129578,#129579,#129580,#129581,#129582,#129583,
#129584,#129585,#129586,#129587,#129588,#129589,#129590,#129591,#129592,
#129593,#129594,#129595,#129596,#129597,#129598,#129599,#129600,#129601,
#129602,#129603,#129604,#129605,#129606,#129607,#129608,#129609,#129610,
#129611,#129612,#129613,#129614,#129615,#129616,#129617,#129618,#129619,
#129620,#129621,#129622,#129623,#129624,#129625,#129626,#129627,#129628,
#129629,#129630,#129631,#129632,#129633,#129634,#129635,#129636,#129637,
#129638,#129639,#129640,#129641,#129642,#129643,#129644,#129645,#129646,
#129647,#129648,#129649,#129650,#129651,#129652,#129653,#129654,#129655,
#129656,#129657,#129658,#129659,#129660,#129661,#129662,#129663,#129664,
#129665,#129666,#129667,#129668,#129669,#129670,#129671,#129672,#129673,
#129674,#129675,#129676,#129677,#129678,#129679,#129680,#129681,#129682,
#129683,#129684,#129685,#129686,#129687,#129688,#129689,#129690,#129691,
#129692,#129693,#129694,#129695,#129696,#129697,#129698,#129699),
 .UNSPECIFIED.,.F.,.F.,(4,3,3,3,3,3,3,3,3,3,3,3,3,3,3,3,3,3,3,3,3,3,3,3,
3,3,3,3,3,3,3,3,3,3,3,3,3,3,3,3,3,3,3,3,3,3,3,3,3,3,3,3,3,3,3,3,3,3,3,3,
3,3,3,3,3,3,3,3,3,3,3,3,3,4),(1548.80517821976,1548.89911538693,1548.98285409878,
1549.06648961014,1549.15004205354,1549.23353148939,1549.31698544001,1549.40042193385,
1549.48385904361,1549.56731483853,1549.65085933126,1549.7344484142,1549.81817168175,
1549.89885139765,1549.9825901095,1550.06622562086,1550.14977806426,1550.23326750011,
1550.31672145073,1550.40015794457,1550.48359505433,1550.56705084925,1550.65059534197,
1550.73418442492,1550.81790769247,1550.89858740837,1550.98232612022,1551.06596163158,
1551.14951407498,1551.23300351083,1551.31645746145,1551.39989395529,1551.48333106505,
1551.56678685997,1551.6503313527,1551.73392043564,1551.81764370319,1551.89832341909,
1551.98206213094,1552.0656976423,1552.1492500857,1552.23273952155,1552.31619347217,
1552.39962996601,1552.48306707577,1552.56652287069,1552.65006736342,1552.73365644636,
1552.81737971391,1552.89805942981,1552.98179814166,1553.06543365302,1553.14898609642,
1553.23247553227,1553.31592948289,1553.39936597673,1553.48280308649,1553.56625888141,
1553.64980337414,1553.73339245708,1553.81711572463,1553.89779544053,1553.98153762467,
1554.06517580973,1554.14873013162,1554.23476209869,1554.31821237126,1554.40164460853,
1554.4850768822,1554.56852725991,1554.65205160752,1554.73562057329,1554.81928899481,
1554.83698586821),.UNSPECIFIED.);
#1036=B_SPLINE_CURVE_WITH_KNOTS('',3,(#129700,#129701,#129702,#129703,#129704,
#129705,#129706,#129707,#129708,#129709),.UNSPECIFIED.,.F.,.F.,(4,3,3,4),
(1548.55334172014,1548.63588509157,1548.7205316556,1548.80517821963),
 .UNSPECIFIED.);
#1037=B_SPLINE_CURVE_WITH_KNOTS('',3,(#129711,#129712,#129713,#129714,#129715,
#129716,#129717,#129718,#129719,#129720),.UNSPECIFIED.,.F.,.F.,(4,3,3,4),
(1548.55457738268,1548.63928184855,1548.72394703715,1548.80517821977),
 .UNSPECIFIED.);
#1038=B_SPLINE_CURVE_WITH_KNOTS('',3,(#129721,#129722,#129723,#129724,#129725,
#129726,#129727,#129728,#129729,#129730,#129731,#129732,#129733,#129734,
#129735,#129736,#129737,#129738,#129739,#129740,#129741,#129742,#129743,
#129744,#129745,#129746,#129747,#129748,#129749,#129750,#129751,#129752,
#129753,#129754,#129755,#129756,#129757,#129758,#129759,#129760,#129761,
#129762,#129763,#129764,#129765,#129766,#129767,#129768,#129769,#129770,
#129771,#129772,#129773,#129774,#129775,#129776,#129777,#129778,#129779,
#129780,#129781,#129782,#129783,#129784,#129785,#129786,#129787,#129788,
#129789,#129790,#129791,#129792,#129793,#129794,#129795,#129796,#129797,
#129798,#129799,#129800,#129801,#129802,#129803,#129804,#129805,#129806,
#129807,#129808,#129809,#129810,#129811,#129812,#129813,#129814,#129815,
#129816,#129817,#129818,#129819,#129820,#129821,#129822,#129823,#129824,
#129825,#129826,#129827,#129828,#129829,#129830,#129831,#129832,#129833,
#129834,#129835,#129836,#129837,#129838,#129839,#129840,#129841,#129842,
#129843,#129844,#129845,#129846,#129847,#129848,#129849,#129850,#129851,
#129852,#129853,#129854,#129855,#129856,#129857,#129858,#129859,#129860,
#129861,#129862,#129863,#129864,#129865,#129866,#129867,#129868,#129869,
#129870,#129871,#129872,#129873,#129874,#129875,#129876,#129877,#129878,
#129879,#129880,#129881,#129882,#129883,#129884,#129885,#129886,#129887,
#129888,#129889,#129890,#129891,#129892,#129893,#129894,#129895,#129896,
#129897,#129898,#129899,#129900,#129901,#129902,#129903,#129904,#129905,
#129906,#129907,#129908,#129909,#129910,#129911,#129912,#129913,#129914,
#129915,#129916,#129917,#129918,#129919,#129920,#129921,#129922,#129923,
#129924,#129925,#129926,#129927,#129928,#129929,#129930,#129931,#129932,
#129933,#129934,#129935,#129936,#129937,#129938,#129939,#129940),
 .UNSPECIFIED.,.F.,.F.,(4,3,3,3,3,3,3,3,3,3,3,3,3,3,3,3,3,3,3,3,3,3,3,3,
3,3,3,3,3,3,3,3,3,3,3,3,3,3,3,3,3,3,3,3,3,3,3,3,3,3,3,3,3,3,3,3,3,3,3,3,
3,3,3,3,3,3,3,3,3,3,3,3,3,4),(1548.80517821995,1548.89701446912,1548.98932787598,
1549.08188752032,1549.17477730635,1549.20940600665,1549.2931447185,1549.37678022986,
1549.46033267326,1549.54382210911,1549.62727605973,1549.71071255357,1549.79414966333,
1549.87760545825,1549.96114995098,1550.04473903392,1550.12846230147,1550.20914201737,
1550.29288072922,1550.37651624058,1550.46006868398,1550.54355811983,1550.62701207045,
1550.71044856429,1550.79388567405,1550.87734146897,1550.9608859617,1551.04447504464,
1551.12819831219,1551.20887802809,1551.29261673994,1551.3762522513,1551.4598046947,
1551.54329413055,1551.62674808117,1551.71018457501,1551.79362168477,1551.87707747969,
1551.96062197242,1552.04421105536,1552.12793432291,1552.20861403881,1552.29235275066,
1552.37598826202,1552.45954070542,1552.54303014127,1552.62648409189,1552.70992058573,
1552.79335769549,1552.87681349041,1552.96035798314,1553.04394706608,1553.12767033363,
1553.20835004953,1553.29208876138,1553.37572427274,1553.45927671614,1553.54276615199,
1553.62622010261,1553.70965659645,1553.79309370621,1553.87654950113,1553.96009399386,
1554.0436830768,1554.12740634436,1554.20808606025,1554.29065831141,1554.37313589082,
1554.4555379469,1554.53788355755,1554.62019995884,1554.70249826221,1554.78481964865,
1554.83654914438),.UNSPECIFIED.);
#1039=B_SPLINE_CURVE_WITH_KNOTS('',3,(#129946,#129947,#129948,#129949,#129950,
#129951,#129952,#129953,#129954,#129955,#129956,#129957,#129958,#129959,
#129960,#129961,#129962,#129963,#129964,#129965,#129966,#129967,#129968,
#129969,#129970,#129971,#129972,#129973,#129974,#129975,#129976,#129977,
#129978,#129979,#129980,#129981,#129982,#129983,#129984,#129985,#129986,
#129987,#129988,#129989,#129990,#129991,#129992,#129993,#129994,#129995,
#129996,#129997,#129998,#129999,#130000,#130001,#130002,#130003,#130004,
#130005,#130006,#130007,#130008,#130009,#130010,#130011,#130012,#130013,
#130014,#130015,#130016,#130017,#130018,#130019,#130020,#130021,#130022,
#130023,#130024,#130025,#130026,#130027,#130028,#130029,#130030,#130031,
#130032,#130033,#130034,#130035,#130036,#130037,#130038,#130039,#130040,
#130041,#130042,#130043,#130044,#130045,#130046,#130047,#130048,#130049,
#130050,#130051,#130052,#130053,#130054,#130055,#130056,#130057,#130058,
#130059,#130060,#130061,#130062,#130063,#130064,#130065,#130066,#130067,
#130068,#130069,#130070,#130071,#130072,#130073,#130074,#130075,#130076,
#130077,#130078,#130079,#130080,#130081,#130082,#130083,#130084,#130085,
#130086,#130087,#130088,#130089,#130090,#130091,#130092,#130093,#130094,
#130095,#130096,#130097,#130098,#130099,#130100,#130101,#130102,#130103,
#130104,#130105,#130106,#130107,#130108,#130109,#130110,#130111,#130112,
#130113,#130114,#130115,#130116,#130117,#130118,#130119,#130120,#130121,
#130122,#130123,#130124,#130125,#130126,#130127,#130128,#130129,#130130,
#130131,#130132,#130133,#130134,#130135,#130136,#130137,#130138,#130139,
#130140,#130141,#130142,#130143,#130144,#130145,#130146,#130147,#130148,
#130149,#130150,#130151,#130152,#130153,#130154,#130155,#130156,#130157,
#130158,#130159,#130160,#130161,#130162,#130163,#130164,#130165),
 .UNSPECIFIED.,.F.,.F.,(4,3,3,3,3,3,3,3,3,3,3,3,3,3,3,3,3,3,3,3,3,3,3,3,
3,3,3,3,3,3,3,3,3,3,3,3,3,3,3,3,3,3,3,3,3,3,3,3,3,3,3,3,3,3,3,3,3,3,3,3,
3,3,3,3,3,3,3,3,3,3,3,3,3,4),(1555.08836352707,1555.17073000522,1555.25302491221,
1555.33527390402,1555.41749961745,1555.4997210795,1555.58195731147,1555.6642764509,
1555.74663847006,1555.82912780712,1555.89726746197,1555.98100617382,1556.06464168518,
1556.14819412858,1556.23168356443,1556.31513751505,1556.39857400889,1556.48201111865,
1556.56546691357,1556.64901140629,1556.73260048924,1556.81632375679,1556.89700347269,
1556.98074218454,1557.0643776959,1557.1479301393,1557.23141957515,1557.31487352577,
1557.39831001961,1557.48174712937,1557.56520292428,1557.64874741701,1557.73233649995,
1557.81605976751,1557.89673948341,1557.98047819526,1558.06411370662,1558.14766615002,
1558.23115558587,1558.31460953649,1558.39804603033,1558.48148314009,1558.56493893501,
1558.64848342774,1558.73207251068,1558.81579577824,1558.89647549413,1558.98021420598,
1559.06384971734,1559.14740216074,1559.23089159659,1559.31434554721,1559.39778204105,
1559.48121915081,1559.56467494573,1559.64821943846,1559.7318085214,1559.81553178895,
1559.89621150485,1559.9799502167,1560.06358572806,1560.14713817146,1560.23062760731,
1560.31408155793,1560.39751805177,1560.48095516153,1560.56441095645,1560.64795544918,
1560.73154453212,1560.81526779967,1560.89594751557,1560.9850274229,1561.07389612539,
1561.12124393646),.UNSPECIFIED.);
#1040=B_SPLINE_CURVE_WITH_KNOTS('',3,(#130166,#130167,#130168,#130169,#130170,
#130171,#130172,#130173,#130174,#130175),.UNSPECIFIED.,.F.,.F.,(4,3,3,4),
(1554.83698586821,1554.89753145125,1555.0207046782,1555.08836352694),
 .UNSPECIFIED.);
#1041=B_SPLINE_CURVE_WITH_KNOTS('',3,(#130177,#130178,#130179,#130180,#130181,
#130182,#130183,#130184,#130185,#130186),.UNSPECIFIED.,.F.,.F.,(4,3,3,4),
(1554.83654914438,1554.9189411152,1555.00365232101,1555.08836352682),
 .UNSPECIFIED.);
#1042=B_SPLINE_CURVE_WITH_KNOTS('',3,(#130187,#130188,#130189,#130190,#130191,
#130192,#130193,#130194,#130195,#130196,#130197,#130198,#130199,#130200,
#130201,#130202,#130203,#130204,#130205,#130206,#130207,#130208,#130209,
#130210,#130211,#130212,#130213,#130214,#130215,#130216,#130217,#130218,
#130219,#130220,#130221,#130222,#130223,#130224,#130225,#130226,#130227,
#130228,#130229,#130230,#130231,#130232,#130233,#130234,#130235,#130236,
#130237,#130238,#130239,#130240,#130241,#130242,#130243,#130244,#130245,
#130246,#130247,#130248,#130249,#130250,#130251,#130252,#130253,#130254,
#130255,#130256,#130257,#130258,#130259,#130260,#130261,#130262,#130263,
#130264,#130265,#130266,#130267,#130268,#130269,#130270,#130271,#130272,
#130273,#130274,#130275,#130276,#130277,#130278,#130279,#130280,#130281,
#130282,#130283,#130284,#130285,#130286,#130287,#130288,#130289,#130290,
#130291,#130292,#130293,#130294,#130295,#130296,#130297,#130298,#130299,
#130300,#130301,#130302,#130303,#130304,#130305,#130306,#130307,#130308,
#130309,#130310,#130311,#130312,#130313,#130314,#130315,#130316,#130317,
#130318,#130319,#130320,#130321,#130322,#130323,#130324,#130325,#130326,
#130327,#130328,#130329,#130330,#130331,#130332,#130333,#130334,#130335,
#130336,#130337,#130338,#130339,#130340,#130341,#130342,#130343,#130344,
#130345,#130346,#130347,#130348,#130349,#130350,#130351,#130352,#130353,
#130354,#130355,#130356,#130357,#130358,#130359,#130360,#130361,#130362,
#130363,#130364,#130365,#130366,#130367,#130368,#130369,#130370,#130371,
#130372,#130373,#130374,#130375,#130376,#130377,#130378,#130379,#130380,
#130381,#130382,#130383,#130384,#130385,#130386,#130387,#130388,#130389,
#130390,#130391,#130392,#130393,#130394,#130395,#130396,#130397,#130398,
#130399,#130400,#130401,#130402,#130403),.UNSPECIFIED.,.F.,.F.,(4,3,3,3,
3,3,3,3,3,3,3,3,3,3,3,3,3,3,3,3,3,3,3,3,3,3,3,3,3,3,3,3,3,3,3,3,3,3,3,3,
3,3,3,3,3,3,3,3,3,3,3,3,3,3,3,3,3,3,3,3,3,3,3,3,3,3,3,3,3,3,3,3,4),(1555.08836352695,
1555.20782207097,1555.29156078282,1555.37519629418,1555.45874873758,1555.54223817343,
1555.62569212405,1555.70912861789,1555.79256572765,1555.87602152257,1555.9595660153,
1556.04315509824,1556.12687836579,1556.20755808169,1556.29129679354,1556.3749323049,
1556.4584847483,1556.54197418415,1556.62542813477,1556.70886462861,1556.79230173837,
1556.87575753329,1556.95930202602,1557.04289110896,1557.12661437651,1557.20729409241,
1557.29103280426,1557.37466831562,1557.45822075902,1557.54171019487,1557.62516414549,
1557.70860063933,1557.79203774909,1557.87549354401,1557.95903803674,1558.04262711968,
1558.12635038723,1558.20703010313,1558.29076881498,1558.37440432634,1558.45795676974,
1558.54144620559,1558.62490015621,1558.70833665005,1558.79177375981,1558.87522955473,
1558.95877404746,1559.0423631304,1559.12608639796,1559.20676611385,1559.2905048257,
1559.37414033706,1559.45769278046,1559.54118221631,1559.62463616693,1559.70807266077,
1559.79150977053,1559.87496556544,1559.95851005817,1560.04209914112,1560.12582240867,
1560.20650212457,1560.29024582706,1560.37388519256,1560.4574403584,1560.54092761122,
1560.62437771144,1560.70780874742,1560.79123879095,1560.87472614777,1560.95824120661,
1561.04186108123,1561.12007636444),.UNSPECIFIED.);
#1043=B_SPLINE_CURVE_WITH_KNOTS('',3,(#130409,#130410,#130411,#130412,#130413,
#130414,#130415,#130416,#130417,#130418,#130419,#130420,#130421,#130422,
#130423,#130424,#130425,#130426,#130427,#130428,#130429,#130430,#130431,
#130432,#130433,#130434,#130435,#130436,#130437,#130438,#130439,#130440,
#130441,#130442,#130443,#130444,#130445,#130446,#130447,#130448,#130449,
#130450,#130451,#130452,#130453,#130454,#130455,#130456,#130457,#130458,
#130459,#130460,#130461,#130462,#130463,#130464,#130465,#130466,#130467,
#130468,#130469,#130470,#130471,#130472,#130473,#130474,#130475,#130476,
#130477,#130478,#130479,#130480,#130481,#130482,#130483,#130484,#130485,
#130486,#130487,#130488,#130489,#130490,#130491,#130492,#130493,#130494,
#130495,#130496,#130497,#130498,#130499,#130500,#130501,#130502,#130503,
#130504,#130505,#130506,#130507,#130508,#130509,#130510,#130511,#130512,
#130513,#130514,#130515,#130516,#130517,#130518,#130519,#130520,#130521,
#130522,#130523,#130524,#130525,#130526,#130527,#130528,#130529,#130530,
#130531,#130532,#130533,#130534,#130535,#130536,#130537,#130538,#130539,
#130540,#130541,#130542,#130543,#130544,#130545,#130546,#130547,#130548,
#130549,#130550,#130551,#130552,#130553,#130554,#130555,#130556,#130557,
#130558,#130559,#130560,#130561,#130562,#130563,#130564,#130565,#130566,
#130567,#130568,#130569,#130570,#130571,#130572,#130573,#130574,#130575,
#130576,#130577,#130578,#130579,#130580,#130581,#130582,#130583,#130584,
#130585,#130586,#130587,#130588,#130589,#130590,#130591,#130592,#130593,
#130594,#130595,#130596,#130597,#130598,#130599,#130600,#130601,#130602,
#130603,#130604,#130605,#130606,#130607,#130608,#130609,#130610,#130611,
#130612,#130613,#130614,#130615,#130616,#130617,#130618,#130619,#130620,
#130621,#130622,#130623,#130624,#130625,#130626,#130627,#130628),
 .UNSPECIFIED.,.F.,.F.,(4,3,3,3,3,3,3,3,3,3,3,3,3,3,3,3,3,3,3,3,3,3,3,3,
3,3,3,3,3,3,3,3,3,3,3,3,3,3,3,3,3,3,3,3,3,3,3,3,3,3,3,3,3,3,3,3,3,3,3,3,
3,3,3,3,3,3,3,3,3,3,3,3,3,4),(1561.37154883412,1561.45812422767,1561.54478532766,
1561.63250987732,1561.71943900516,1561.80756126572,1561.89568352629,1561.97942223814,
1562.0630577495,1562.1466101929,1562.23009962875,1562.31355357937,1562.39699007321,
1562.48042718297,1562.56388297789,1562.64742747061,1562.73101655356,1562.81473982111,
1562.89541953701,1562.97915824886,1563.06279376022,1563.14634620362,1563.22983563947,
1563.31328959009,1563.39672608393,1563.48016319369,1563.56361898861,1563.64716348134,
1563.73075256428,1563.81447583183,1563.89515554773,1563.97889425958,1564.06252977094,
1564.14608221434,1564.22957165019,1564.31302560081,1564.39646209465,1564.47989920441,
1564.56335499933,1564.64689949206,1564.730488575,1564.81421184255,1564.89489155845,
1564.9786302703,1565.06226578166,1565.14581822506,1565.22930766091,1565.31276161153,
1565.39619810537,1565.47963521513,1565.56309101005,1565.64663550278,1565.73022458572,
1565.81394785327,1565.89462756917,1565.97836628102,1566.06200179238,1566.14555423578,
1566.22904367163,1566.31249762225,1566.39593411609,1566.47937122585,1566.56282702076,
1566.64637151349,1566.72996059643,1566.81368386399,1566.89436357989,1566.97705844757,
1567.0596556153,1567.14557162137,1567.22802328557,1567.31043887618,1567.39284094755,
1567.40331963956),.UNSPECIFIED.);
#1044=B_SPLINE_CURVE_WITH_KNOTS('',3,(#130629,#130630,#130631,#130632,#130633,
#130634,#130635,#130636,#130637,#130638),.UNSPECIFIED.,.F.,.F.,(4,3,3,4),
(1561.12124393646,1561.20984029863,1561.29822797538,1561.37154883401),
 .UNSPECIFIED.);
#1045=B_SPLINE_CURVE_WITH_KNOTS('',3,(#130640,#130641,#130642,#130643,#130644,
#130645,#130646,#130647,#130648,#130649),.UNSPECIFIED.,.F.,.F.,(4,3,3,4),
(1561.12007636444,1561.20623813529,1561.33999744342,1561.37154883413),
 .UNSPECIFIED.);
#1046=B_SPLINE_CURVE_WITH_KNOTS('',3,(#130650,#130651,#130652,#130653,#130654,
#130655,#130656,#130657,#130658,#130659,#130660,#130661,#130662,#130663,
#130664,#130665,#130666,#130667,#130668,#130669,#130670,#130671,#130672,
#130673,#130674,#130675,#130676,#130677,#130678,#130679,#130680,#130681,
#130682,#130683,#130684,#130685,#130686,#130687,#130688,#130689,#130690,
#130691,#130692,#130693,#130694,#130695,#130696,#130697,#130698,#130699,
#130700,#130701,#130702,#130703,#130704,#130705,#130706,#130707,#130708,
#130709,#130710,#130711,#130712,#130713,#130714,#130715,#130716,#130717,
#130718,#130719,#130720,#130721,#130722,#130723,#130724,#130725,#130726,
#130727,#130728,#130729,#130730,#130731,#130732,#130733,#130734,#130735,
#130736,#130737,#130738,#130739,#130740,#130741,#130742,#130743,#130744,
#130745,#130746,#130747,#130748,#130749,#130750,#130751,#130752,#130753,
#130754,#130755,#130756,#130757,#130758,#130759,#130760,#130761,#130762,
#130763,#130764,#130765,#130766,#130767,#130768,#130769,#130770,#130771,
#130772,#130773,#130774,#130775,#130776,#130777,#130778,#130779,#130780,
#130781,#130782,#130783,#130784,#130785,#130786,#130787,#130788,#130789,
#130790,#130791,#130792,#130793,#130794,#130795,#130796,#130797,#130798,
#130799,#130800,#130801,#130802,#130803,#130804,#130805,#130806,#130807,
#130808,#130809,#130810,#130811,#130812,#130813,#130814,#130815,#130816,
#130817,#130818,#130819,#130820,#130821,#130822,#130823,#130824,#130825,
#130826,#130827,#130828,#130829,#130830,#130831,#130832,#130833,#130834,
#130835,#130836,#130837,#130838,#130839,#130840,#130841,#130842,#130843,
#130844,#130845,#130846,#130847,#130848,#130849,#130850,#130851,#130852,
#130853,#130854,#130855,#130856,#130857,#130858,#130859,#130860,#130861,
#130862,#130863,#130864,#130865,#130866,#130867,#130868,#130869),
 .UNSPECIFIED.,.F.,.F.,(4,3,3,3,3,3,3,3,3,3,3,3,3,3,3,3,3,3,3,3,3,3,3,3,
3,3,3,3,3,3,3,3,3,3,3,3,3,3,3,3,3,3,3,3,3,3,3,3,3,3,3,3,3,3,3,3,3,3,3,3,
3,3,3,3,3,3,3,3,3,3,3,3,3,4),(1561.37154883432,1561.45392302127,1561.53621883923,
1561.61993825257,1561.70214926038,1561.78435027844,1561.86656034019,1561.95141379164,
1562.03374277032,1562.11985845817,1562.20597414601,1562.28971285786,1562.37334836922,
1562.45690081262,1562.54039024847,1562.62384419909,1562.70728069294,1562.79071780269,
1562.87417359761,1562.95771809034,1563.04130717328,1563.12503044084,1563.20571015673,
1563.28944886858,1563.37308437994,1563.45663682334,1563.54012625919,1563.62358020981,
1563.70701670366,1563.79045381341,1563.87390960833,1563.95745410106,1564.041043184,
1564.12476645156,1564.20544616745,1564.2891848793,1564.37282039066,1564.45637283406,
1564.53986226991,1564.62331622053,1564.70675271437,1564.79018982413,1564.87364561904,
1564.95719011177,1565.04077919471,1565.12450246227,1565.20518217817,1565.28892089002,
1565.37255640138,1565.45610884478,1565.53959828063,1565.62305223125,1565.70648872509,
1565.78992583485,1565.87338162976,1565.95692612249,1566.04051520543,1566.12423847299,
1566.20491818889,1566.28865690074,1566.3722924121,1566.4558448555,1566.53933429135,
1566.62278824196,1566.70622473581,1566.78966184557,1566.87311764048,1566.95666213321,
1567.04025121615,1567.12397448371,1567.20465419961,1567.29495789568,1567.38503323209,
1567.40443029398),.UNSPECIFIED.);
#1047=B_SPLINE_CURVE_WITH_KNOTS('',3,(#130875,#130876,#130877,#130878,#130879,
#130880,#130881,#130882,#130883,#130884,#130885,#130886,#130887,#130888,
#130889,#130890,#130891,#130892,#130893,#130894,#130895,#130896,#130897,
#130898,#130899,#130900,#130901,#130902,#130903,#130904,#130905,#130906,
#130907,#130908,#130909,#130910,#130911,#130912,#130913,#130914,#130915,
#130916,#130917,#130918,#130919,#130920,#130921,#130922,#130923,#130924,
#130925,#130926,#130927,#130928,#130929,#130930,#130931,#130932,#130933,
#130934,#130935,#130936,#130937,#130938,#130939,#130940,#130941,#130942,
#130943,#130944,#130945,#130946,#130947,#130948,#130949,#130950,#130951,
#130952,#130953,#130954,#130955,#130956,#130957,#130958,#130959,#130960,
#130961,#130962,#130963,#130964,#130965,#130966,#130967,#130968,#130969,
#130970,#130971,#130972,#130973,#130974,#130975,#130976,#130977,#130978,
#130979,#130980,#130981,#130982,#130983,#130984,#130985,#130986,#130987,
#130988,#130989,#130990,#130991,#130992,#130993,#130994,#130995,#130996,
#130997,#130998,#130999,#131000,#131001,#131002,#131003,#131004,#131005,
#131006,#131007,#131008,#131009,#131010,#131011,#131012,#131013,#131014,
#131015,#131016,#131017,#131018,#131019,#131020,#131021,#131022,#131023,
#131024,#131025,#131026,#131027,#131028,#131029,#131030,#131031,#131032,
#131033,#131034,#131035,#131036,#131037,#131038,#131039,#131040,#131041,
#131042,#131043,#131044,#131045,#131046,#131047,#131048,#131049,#131050,
#131051,#131052,#131053,#131054,#131055,#131056,#131057,#131058,#131059,
#131060,#131061,#131062,#131063,#131064,#131065,#131066,#131067,#131068,
#131069,#131070,#131071,#131072,#131073,#131074,#131075,#131076,#131077,
#131078,#131079,#131080,#131081,#131082,#131083,#131084,#131085,#131086,
#131087,#131088,#131089,#131090,#131091,#131092,#131093,#131094),
 .UNSPECIFIED.,.F.,.F.,(4,3,3,3,3,3,3,3,3,3,3,3,3,3,3,3,3,3,3,3,3,3,3,3,
3,3,3,3,3,3,3,3,3,3,3,3,3,3,3,3,3,3,3,3,3,3,3,3,3,3,3,3,3,3,3,3,3,3,3,3,
3,3,3,3,3,3,3,3,3,3,3,3,3,4),(1567.65473414144,1567.76377432732,1567.87563324908,
1567.89409959061,1567.97783830246,1568.06147381383,1568.14502625723,1568.22851569308,
1568.3119696437,1568.39540613755,1568.4788432473,1568.56229904222,1568.64584353496,
1568.7294326179,1568.81315588546,1568.89383560133,1568.97757431318,1569.06120982454,
1569.14476226794,1569.22825170379,1569.31170565441,1569.39514214825,1569.47857925801,
1569.56203505292,1569.64557954565,1569.7291686286,1569.81289189615,1569.89357161205,
1569.9773103239,1570.06094583526,1570.14449827866,1570.22798771451,1570.31144166512,
1570.39487815897,1570.47831526873,1570.56177106364,1570.64531555637,1570.72890463931,
1570.81262790687,1570.89330762277,1570.97704633462,1571.06068184598,1571.14423428938,
1571.22772372523,1571.31117767585,1571.39461416969,1571.47805127945,1571.56150707437,
1571.6450515671,1571.72864065004,1571.8123639176,1571.89304363349,1571.97678234534,
1572.0604178567,1572.1439703001,1572.22745973595,1572.31091368657,1572.39435018041,
1572.47778729017,1572.56124308509,1572.64478757782,1572.72837666076,1572.81209992831,
1572.89277964421,1572.97653085598,1573.06017614605,1573.14372001628,1573.22720636791,
1573.3106533214,1573.39407896674,1573.47752444329,1573.56098050646,1573.64449717329,
1573.68625334563),.UNSPECIFIED.);
#1048=B_SPLINE_CURVE_WITH_KNOTS('',3,(#131095,#131096,#131097,#131098,#131099,
#131100,#131101,#131102,#131103,#131104),.UNSPECIFIED.,.F.,.F.,(4,3,3,4),
(1567.40331963956,1567.48574756764,1567.57024085447,1567.6547341413),
 .UNSPECIFIED.);
#1049=B_SPLINE_CURVE_WITH_KNOTS('',3,(#131106,#131107,#131108,#131109,#131110,
#131111,#131112,#131113,#131114,#131115),.UNSPECIFIED.,.F.,.F.,(4,3,3,4),
(1567.40443029398,1567.49421655057,1567.58373377193,1567.65473414121),
 .UNSPECIFIED.);
#1050=B_SPLINE_CURVE_WITH_KNOTS('',3,(#131116,#131117,#131118,#131119,#131120,
#131121,#131122,#131123,#131124,#131125,#131126,#131127,#131128,#131129,
#131130,#131131,#131132,#131133,#131134,#131135,#131136,#131137,#131138,
#131139,#131140,#131141,#131142,#131143,#131144,#131145,#131146,#131147,
#131148,#131149,#131150,#131151,#131152,#131153,#131154,#131155,#131156,
#131157,#131158,#131159,#131160,#131161,#131162,#131163,#131164,#131165,
#131166,#131167,#131168,#131169,#131170,#131171,#131172,#131173,#131174,
#131175,#131176,#131177,#131178,#131179,#131180,#131181,#131182,#131183,
#131184,#131185,#131186,#131187,#131188,#131189,#131190,#131191,#131192,
#131193,#131194,#131195,#131196,#131197,#131198,#131199,#131200,#131201,
#131202,#131203,#131204,#131205,#131206,#131207,#131208,#131209,#131210,
#131211,#131212,#131213,#131214,#131215,#131216,#131217,#131218,#131219,
#131220,#131221,#131222,#131223,#131224,#131225,#131226,#131227,#131228,
#131229,#131230,#131231,#131232,#131233,#131234,#131235,#131236,#131237,
#131238,#131239,#131240,#131241,#131242,#131243,#131244,#131245,#131246,
#131247,#131248,#131249,#131250,#131251,#131252,#131253,#131254,#131255,
#131256,#131257,#131258,#131259,#131260,#131261,#131262,#131263,#131264,
#131265,#131266,#131267,#131268,#131269,#131270,#131271,#131272,#131273,
#131274,#131275,#131276,#131277,#131278,#131279,#131280,#131281,#131282,
#131283,#131284,#131285,#131286,#131287,#131288,#131289,#131290,#131291,
#131292,#131293,#131294,#131295,#131296,#131297,#131298,#131299,#131300,
#131301,#131302,#131303,#131304,#131305,#131306,#131307,#131308,#131309,
#131310,#131311,#131312,#131313,#131314,#131315,#131316,#131317,#131318,
#131319,#131320,#131321,#131322,#131323,#131324,#131325,#131326,#131327,
#131328,#131329,#131330,#131331,#131332,#131333,#131334,#131335),
 .UNSPECIFIED.,.F.,.F.,(4,3,3,3,3,3,3,3,3,3,3,3,3,3,3,3,3,3,3,3,3,3,3,3,
3,3,3,3,3,3,3,3,3,3,3,3,3,3,3,3,3,3,3,3,3,3,3,3,3,3,3,3,3,3,3,3,3,3,3,3,
3,3,3,3,3,3,3,3,3,3,3,3,3,4),(1567.65473414131,1567.74054040221,1567.82640703948,
1567.91234767549,1567.99843792169,1568.08461274297,1568.17094473813,1568.20439021033,
1568.28812892218,1568.37176443355,1568.45531687695,1568.5388063128,1568.62226026341,
1568.70569675726,1568.78913386702,1568.87258966194,1568.95613415467,1569.03972323761,
1569.12344650517,1569.20412622105,1569.2878649329,1569.37150044426,1569.45505288766,
1569.53854232351,1569.62199627413,1569.70543276797,1569.78886987773,1569.87232567265,
1569.95587016538,1570.03945924832,1570.12318251588,1570.20386223177,1570.28760094362,
1570.37123645498,1570.45478889838,1570.53827833423,1570.62173228484,1570.70516877869,
1570.78860588845,1570.87206168336,1570.95560617609,1571.03919525903,1571.12291852659,
1571.20359824249,1571.28733695434,1571.3709724657,1571.4545249091,1571.53801434495,
1571.62146829557,1571.70490478941,1571.78834189917,1571.87179769409,1571.95534218682,
1572.03893126976,1572.12265453732,1572.20333425321,1572.28707296506,1572.37070847642,
1572.45426091982,1572.53775035567,1572.62120430628,1572.70464080013,1572.78807790988,
1572.8715337048,1572.95507819753,1573.03866728047,1573.12239054803,1573.20307026393,
1573.28595684986,1573.36874428265,1573.45143789125,1573.53407654318,1573.61668446351,
1573.68663052872),.UNSPECIFIED.);
#1051=B_SPLINE_CURVE_WITH_KNOTS('',3,(#131341,#131342,#131343,#131344,#131345,
#131346,#131347,#131348,#131349,#131350,#131351,#131352,#131353,#131354,
#131355,#131356,#131357,#131358,#131359,#131360,#131361,#131362,#131363,
#131364,#131365,#131366,#131367,#131368,#131369,#131370,#131371,#131372,
#131373,#131374,#131375,#131376,#131377,#131378,#131379,#131380,#131381,
#131382,#131383,#131384,#131385,#131386,#131387,#131388,#131389,#131390,
#131391,#131392,#131393,#131394,#131395,#131396,#131397,#131398,#131399,
#131400,#131401,#131402,#131403,#131404,#131405,#131406,#131407,#131408,
#131409,#131410,#131411,#131412,#131413,#131414,#131415,#131416,#131417,
#131418,#131419,#131420,#131421,#131422,#131423,#131424,#131425,#131426,
#131427,#131428,#131429,#131430,#131431,#131432,#131433,#131434,#131435,
#131436,#131437,#131438,#131439,#131440,#131441,#131442,#131443,#131444,
#131445,#131446,#131447,#131448,#131449,#131450,#131451,#131452,#131453,
#131454,#131455,#131456,#131457,#131458,#131459,#131460,#131461,#131462,
#131463,#131464,#131465,#131466,#131467,#131468,#131469,#131470,#131471,
#131472,#131473,#131474,#131475,#131476,#131477,#131478,#131479,#131480,
#131481,#131482,#131483,#131484,#131485,#131486,#131487,#131488,#131489,
#131490,#131491,#131492,#131493,#131494,#131495,#131496,#131497,#131498,
#131499,#131500,#131501,#131502,#131503,#131504,#131505,#131506,#131507,
#131508,#131509,#131510,#131511,#131512,#131513,#131514,#131515,#131516,
#131517,#131518,#131519,#131520,#131521,#131522,#131523,#131524,#131525,
#131526,#131527,#131528,#131529,#131530,#131531,#131532,#131533,#131534,
#131535,#131536,#131537,#131538,#131539,#131540,#131541,#131542,#131543,
#131544,#131545,#131546,#131547,#131548,#131549,#131550,#131551,#131552,
#131553,#131554,#131555,#131556,#131557,#131558,#131559,#131560),
 .UNSPECIFIED.,.F.,.F.,(4,3,3,3,3,3,3,3,3,3,3,3,3,3,3,3,3,3,3,3,3,3,3,3,
3,3,3,3,3,3,3,3,3,3,3,3,3,3,3,3,3,3,3,3,3,3,3,3,3,3,3,3,3,3,3,3,3,3,3,3,
3,3,3,3,3,3,3,3,3,3,3,3,3,4),(1573.93791944867,1574.0210546865,1574.10408938948,
1574.18704426269,1574.2699399344,1574.35280557854,1574.43565825124,1574.51851653844,
1574.60139902671,1574.68437118786,1574.7673938746,1574.85053857207,1574.89225166565,
1574.9759903775,1575.05962588886,1575.14317833226,1575.22666776811,1575.31012171873,
1575.39355821257,1575.47699532233,1575.56045111725,1575.64399560998,1575.72758469292,
1575.81130796048,1575.89198767637,1575.97572638821,1576.05936189958,1576.14291434298,
1576.22640377883,1576.30985772944,1576.39329422329,1576.47673133304,1576.56018712796,
1576.64373162069,1576.72732070363,1576.81104397118,1576.89172368709,1576.97546239894,
1577.05909791031,1577.14265035371,1577.22613978956,1577.30959374018,1577.39303023403,
1577.47646734378,1577.5599231387,1577.64346763143,1577.72705671438,1577.81077998194,
1577.89145969782,1577.97519840967,1578.05883392103,1578.14238636443,1578.22587580028,
1578.3093297509,1578.39276624475,1578.4762033545,1578.55965914942,1578.64320364215,
1578.72679272509,1578.81051599265,1578.89119570854,1578.97493442039,1579.05856993175,
1579.14212237515,1579.225611811,1579.30906576162,1579.39250225546,1579.47593936522,
1579.55939516013,1579.64293965286,1579.7265287358,1579.81025200336,1579.89093171926,
1579.97048400051),.UNSPECIFIED.);
#1052=B_SPLINE_CURVE_WITH_KNOTS('',3,(#131561,#131562,#131563,#131564,#131565,
#131566,#131567,#131568,#131569,#131570,#131571,#131572,#131573),
 .UNSPECIFIED.,.F.,.F.,(4,3,3,3,4),(1573.68625334563,1573.76987077976,1573.8536105396,
1573.89251565493,1573.93791944848),.UNSPECIFIED.);
#1053=B_SPLINE_CURVE_WITH_KNOTS('',3,(#131575,#131576,#131577,#131578,#131579,
#131580,#131581,#131582,#131583,#131584),.UNSPECIFIED.,.F.,.F.,(4,3,3,4),
(1573.68663052872,1573.76923020489,1573.85357482669,1573.93791944849),
 .UNSPECIFIED.);
#1054=B_SPLINE_CURVE_WITH_KNOTS('',3,(#131585,#131586,#131587,#131588,#131589,
#131590,#131591,#131592,#131593,#131594,#131595,#131596,#131597,#131598,
#131599,#131600,#131601,#131602,#131603,#131604,#131605,#131606,#131607,
#131608,#131609,#131610,#131611,#131612,#131613,#131614,#131615,#131616,
#131617,#131618,#131619,#131620,#131621,#131622,#131623,#131624,#131625,
#131626,#131627,#131628,#131629,#131630,#131631,#131632,#131633,#131634,
#131635,#131636,#131637,#131638,#131639,#131640,#131641,#131642,#131643,
#131644,#131645,#131646,#131647,#131648,#131649,#131650,#131651,#131652,
#131653,#131654,#131655,#131656,#131657,#131658,#131659,#131660,#131661,
#131662,#131663,#131664,#131665,#131666,#131667,#131668,#131669,#131670,
#131671,#131672,#131673,#131674,#131675,#131676,#131677,#131678,#131679,
#131680,#131681,#131682,#131683,#131684,#131685,#131686,#131687,#131688,
#131689,#131690,#131691,#131692,#131693,#131694,#131695,#131696,#131697,
#131698,#131699,#131700,#131701,#131702,#131703,#131704,#131705,#131706,
#131707,#131708,#131709,#131710,#131711,#131712,#131713,#131714,#131715,
#131716,#131717,#131718,#131719,#131720,#131721,#131722,#131723,#131724,
#131725,#131726,#131727,#131728,#131729,#131730,#131731,#131732,#131733,
#131734,#131735,#131736,#131737,#131738,#131739,#131740,#131741,#131742,
#131743,#131744,#131745,#131746,#131747,#131748,#131749,#131750,#131751,
#131752,#131753,#131754,#131755,#131756,#131757,#131758,#131759,#131760,
#131761,#131762,#131763,#131764,#131765,#131766,#131767,#131768,#131769,
#131770,#131771,#131772,#131773,#131774,#131775,#131776,#131777,#131778,
#131779,#131780,#131781,#131782,#131783,#131784,#131785,#131786,#131787,
#131788,#131789,#131790,#131791,#131792,#131793,#131794,#131795,#131796,
#131797,#131798,#131799,#131800,#131801,#131802,#131803,#131804),
 .UNSPECIFIED.,.F.,.F.,(4,3,3,3,3,3,3,3,3,3,3,3,3,3,3,3,3,3,3,3,3,3,3,3,
3,3,3,3,3,3,3,3,3,3,3,3,3,3,3,3,3,3,3,3,3,3,3,3,3,3,3,3,3,3,3,3,3,3,3,3,
3,3,3,3,3,3,3,3,3,3,3,3,3,4),(1573.93791944865,1574.04289524923,1574.14985801462,
1574.20280627465,1574.2865449865,1574.37018049786,1574.45373294126,1574.53722237712,
1574.62067632773,1574.70411282158,1574.78754993133,1574.87100572625,1574.95455021898,
1575.03813930192,1575.12186256948,1575.20254228537,1575.28628099722,1575.36991650858,
1575.45346895198,1575.53695838783,1575.62041233845,1575.70384883229,1575.78728594205,
1575.87074173697,1575.9542862297,1576.03787531264,1576.12159858019,1576.20227829609,
1576.28601700794,1576.3696525193,1576.4532049627,1576.53669439855,1576.62014834917,
1576.70358484301,1576.78702195277,1576.87047774769,1576.95402224041,1577.03761132336,
1577.12133459091,1577.20201430681,1577.28575301866,1577.36938853002,1577.45294097342,
1577.53643040927,1577.61988435989,1577.70332085373,1577.78675796349,1577.87021375841,
1577.95375825114,1578.03734733408,1578.12107060163,1578.20175031753,1578.28548902938,
1578.36912454074,1578.45267698414,1578.53616641999,1578.61962037061,1578.70305686445,
1578.78649397421,1578.86994976913,1578.95349426186,1579.0370833448,1579.12080661235,
1579.20148632825,1579.28523921838,1579.3707646693,1579.45430765298,1579.5377930484,
1579.62123897607,1579.70828993847,1579.79173047179,1579.87518246829,1579.95868485598,
1579.96944282568),.UNSPECIFIED.);
#1055=B_SPLINE_CURVE_WITH_KNOTS('',3,(#131810,#131811,#131812,#131813,#131814,
#131815,#131816,#131817,#131818,#131819,#131820,#131821,#131822,#131823,
#131824,#131825,#131826,#131827,#131828,#131829,#131830,#131831,#131832,
#131833,#131834,#131835,#131836,#131837,#131838,#131839,#131840,#131841,
#131842,#131843,#131844,#131845,#131846,#131847,#131848,#131849,#131850,
#131851,#131852,#131853,#131854,#131855,#131856,#131857,#131858,#131859,
#131860,#131861,#131862,#131863,#131864,#131865,#131866,#131867,#131868,
#131869,#131870,#131871,#131872,#131873,#131874,#131875,#131876,#131877,
#131878,#131879,#131880,#131881,#131882,#131883,#131884,#131885,#131886,
#131887,#131888,#131889,#131890,#131891,#131892,#131893,#131894,#131895,
#131896,#131897,#131898,#131899,#131900,#131901,#131902,#131903,#131904,
#131905,#131906,#131907,#131908,#131909,#131910,#131911,#131912,#131913,
#131914,#131915,#131916,#131917,#131918,#131919,#131920,#131921,#131922,
#131923,#131924,#131925,#131926,#131927,#131928,#131929,#131930,#131931,
#131932,#131933,#131934,#131935,#131936,#131937,#131938,#131939,#131940,
#131941,#131942,#131943,#131944,#131945,#131946,#131947,#131948,#131949,
#131950,#131951,#131952,#131953,#131954,#131955,#131956,#131957,#131958,
#131959,#131960,#131961,#131962,#131963,#131964,#131965,#131966,#131967,
#131968,#131969,#131970,#131971,#131972,#131973,#131974,#131975,#131976,
#131977,#131978,#131979,#131980,#131981,#131982,#131983,#131984,#131985,
#131986,#131987,#131988,#131989,#131990,#131991,#131992,#131993,#131994,
#131995,#131996,#131997,#131998,#131999,#132000,#132001,#132002,#132003,
#132004,#132005,#132006,#132007,#132008,#132009,#132010,#132011,#132012,
#132013,#132014,#132015,#132016,#132017,#132018,#132019,#132020,#132021,
#132022,#132023,#132024,#132025,#132026,#132027,#132028,#132029),
 .UNSPECIFIED.,.F.,.F.,(4,3,3,3,3,3,3,3,3,3,3,3,3,3,3,3,3,3,3,3,3,3,3,3,
3,3,3,3,3,3,3,3,3,3,3,3,3,3,3,3,3,3,3,3,3,3,3,3,3,3,3,3,3,3,3,3,3,3,3,3,
3,3,3,3,3,3,3,3,3,3,3,3,3,4),(1580.22110475566,1580.30480012745,1580.38812860707,
1580.4714604773,1580.55481384701,1580.63877731776,1580.72227243822,1580.8064700841,
1580.89066772998,1580.97440644183,1581.05804195319,1581.14159439659,1581.22508383244,
1581.30853778306,1581.3919742769,1581.47541138666,1581.55886718158,1581.64241167431,
1581.72600075725,1581.80972402481,1581.8904037407,1581.97414245255,1582.05777796391,
1582.14133040731,1582.22481984316,1582.30827379378,1582.39171028762,1582.47514739738,
1582.55860319229,1582.64214768502,1582.72573676796,1582.80946003552,1582.89013975142,
1582.97387846327,1583.05751397463,1583.14106641803,1583.22455585388,1583.3080098045,
1583.39144629834,1583.4748834081,1583.55833920302,1583.64188369575,1583.72547277869,
1583.80919604624,1583.88987576214,1583.97361447399,1584.05724998535,1584.14080242875,
1584.2242918646,1584.30774581522,1584.39118230906,1584.47461941882,1584.55807521374,
1584.64161970647,1584.72520878941,1584.80893205697,1584.88961177286,1584.97335048471,
1585.05698599607,1585.14053843947,1585.22402787532,1585.30748182594,1585.39091831978,
1585.47435542954,1585.55781122445,1585.64135571718,1585.72494480013,1585.80866806768,
1585.88934778358,1585.97401443131,1586.05853521259,1586.14297139875,1586.22732327027,
1586.25360547416),.UNSPECIFIED.);
#1056=B_SPLINE_CURVE_WITH_KNOTS('',3,(#132030,#132031,#132032,#132033,#132034,
#132035,#132036,#132037,#132038,#132039),.UNSPECIFIED.,.F.,.F.,(4,3,3,4),
(1579.97048400051,1580.06883921701,1580.1663064719,1580.22110475548),
 .UNSPECIFIED.);
#1057=B_SPLINE_CURVE_WITH_KNOTS('',3,(#132041,#132042,#132043,#132044,#132045,
#132046,#132047,#132048,#132049,#132050,#132051,#132052,#132053),
 .UNSPECIFIED.,.F.,.F.,(4,3,3,3,4),(1579.96944282568,1580.0530424425,1580.1367715252,
1580.20122233897,1580.22110475567),.UNSPECIFIED.);
#1058=B_SPLINE_CURVE_WITH_KNOTS('',3,(#132054,#132055,#132056,#132057,#132058,
#132059,#132060,#132061,#132062,#132063,#132064,#132065,#132066,#132067,
#132068,#132069,#132070,#132071,#132072,#132073,#132074,#132075,#132076,
#132077,#132078,#132079,#132080,#132081,#132082,#132083,#132084,#132085,
#132086,#132087,#132088,#132089,#132090,#132091,#132092,#132093,#132094,
#132095,#132096,#132097,#132098,#132099,#132100,#132101,#132102,#132103,
#132104,#132105,#132106,#132107,#132108,#132109,#132110,#132111,#132112,
#132113,#132114,#132115,#132116,#132117,#132118,#132119,#132120,#132121,
#132122,#132123,#132124,#132125,#132126,#132127,#132128,#132129,#132130,
#132131,#132132,#132133,#132134,#132135,#132136,#132137,#132138,#132139,
#132140,#132141,#132142,#132143,#132144,#132145,#132146,#132147,#132148,
#132149,#132150,#132151,#132152,#132153,#132154,#132155,#132156,#132157,
#132158,#132159,#132160,#132161,#132162,#132163,#132164,#132165,#132166,
#132167,#132168,#132169,#132170,#132171,#132172,#132173,#132174,#132175,
#132176,#132177,#132178,#132179,#132180,#132181,#132182,#132183,#132184,
#132185,#132186,#132187,#132188,#132189,#132190,#132191,#132192,#132193,
#132194,#132195,#132196,#132197,#132198,#132199,#132200,#132201,#132202,
#132203,#132204,#132205,#132206,#132207,#132208,#132209,#132210,#132211,
#132212,#132213,#132214,#132215,#132216,#132217,#132218,#132219,#132220,
#132221,#132222,#132223,#132224,#132225,#132226,#132227,#132228,#132229,
#132230,#132231,#132232,#132233,#132234,#132235,#132236,#132237,#132238,
#132239,#132240,#132241,#132242,#132243,#132244,#132245,#132246,#132247,
#132248,#132249,#132250,#132251,#132252,#132253,#132254,#132255,#132256,
#132257,#132258,#132259,#132260,#132261,#132262,#132263,#132264,#132265,
#132266,#132267,#132268,#132269,#132270,#132271,#132272,#132273),
 .UNSPECIFIED.,.F.,.F.,(4,3,3,3,3,3,3,3,3,3,3,3,3,3,3,3,3,3,3,3,3,3,3,3,
3,3,3,3,3,3,3,3,3,3,3,3,3,3,3,3,3,3,3,3,3,3,3,3,3,3,3,3,3,3,3,3,3,3,3,3,
3,3,3,3,3,3,3,3,3,3,3,3,3,4),(1580.22110475585,1580.30455741131,1580.38790749604,
1580.47117543512,1580.55438157929,1580.63755409332,1580.72071078458,1580.80386998686,
1580.88705003199,1580.97031903189,1581.05363505913,1581.13707991054,1581.20095834969,
1581.28469706154,1581.3683325729,1581.4518850163,1581.53537445215,1581.61882840277,
1581.70226489661,1581.78570200637,1581.86915780128,1581.95270229401,1582.03629137695,
1582.12001464451,1582.20069436041,1582.28443307226,1582.36806858362,1582.45162102702,
1582.53511046287,1582.61856441349,1582.70200090733,1582.78543801709,1582.86889381201,
1582.95243830474,1583.03602738768,1583.11975065524,1583.20043037113,1583.28416908298,
1583.36780459434,1583.45135703774,1583.53484647359,1583.61830042421,1583.70173691805,
1583.78517402781,1583.86862982273,1583.95217431546,1584.0357633984,1584.11948666596,
1584.20016638185,1584.2839050937,1584.36754060506,1584.45109304846,1584.53458248431,
1584.61803643492,1584.70147292877,1584.78491003853,1584.86836583344,1584.95191032617,
1585.03549940911,1585.11922267667,1585.19990239257,1585.28364110442,1585.36727661578,
1585.45082905918,1585.53431849503,1585.61777244565,1585.70120893949,1585.78464604925,
1585.86810184417,1585.9516463369,1586.03523541984,1586.1189586874,1586.19963840329,
1586.25354069145),.UNSPECIFIED.);
#1059=B_SPLINE_CURVE_WITH_KNOTS('',3,(#132279,#132280,#132281,#132282,#132283,
#132284,#132285,#132286,#132287,#132288,#132289,#132290,#132291,#132292,
#132293,#132294,#132295,#132296,#132297,#132298,#132299,#132300,#132301,
#132302,#132303,#132304,#132305,#132306,#132307,#132308,#132309,#132310,
#132311,#132312,#132313,#132314,#132315,#132316,#132317,#132318,#132319,
#132320,#132321,#132322,#132323,#132324,#132325,#132326,#132327,#132328,
#132329,#132330,#132331,#132332,#132333,#132334,#132335,#132336,#132337,
#132338,#132339,#132340,#132341,#132342,#132343,#132344,#132345,#132346,
#132347,#132348,#132349,#132350,#132351,#132352,#132353,#132354,#132355,
#132356,#132357,#132358,#132359,#132360,#132361,#132362,#132363,#132364,
#132365,#132366,#132367,#132368,#132369,#132370,#132371,#132372,#132373,
#132374,#132375,#132376,#132377,#132378,#132379,#132380,#132381,#132382,
#132383,#132384,#132385,#132386,#132387,#132388,#132389,#132390,#132391,
#132392,#132393,#132394,#132395,#132396,#132397,#132398,#132399,#132400,
#132401,#132402,#132403,#132404,#132405,#132406,#132407,#132408,#132409,
#132410,#132411,#132412,#132413,#132414,#132415,#132416,#132417,#132418,
#132419,#132420,#132421,#132422,#132423,#132424,#132425,#132426,#132427,
#132428,#132429,#132430,#132431,#132432,#132433,#132434,#132435,#132436,
#132437,#132438,#132439,#132440,#132441,#132442,#132443,#132444,#132445,
#132446,#132447,#132448,#132449,#132450,#132451,#132452,#132453,#132454,
#132455,#132456,#132457,#132458,#132459,#132460,#132461,#132462,#132463,
#132464,#132465,#132466,#132467,#132468,#132469,#132470,#132471,#132472,
#132473,#132474,#132475,#132476,#132477,#132478,#132479,#132480,#132481,
#132482,#132483,#132484,#132485,#132486,#132487,#132488,#132489,#132490,
#132491,#132492,#132493,#132494,#132495),.UNSPECIFIED.,.F.,.F.,(4,3,3,3,
3,3,3,3,3,3,3,3,3,3,3,3,3,3,3,3,3,3,3,3,3,3,3,3,3,3,3,3,3,3,3,3,3,3,3,3,
3,3,3,3,3,3,3,3,3,3,3,3,3,3,3,3,3,3,3,3,3,3,3,3,3,3,3,3,3,3,3,3,4),(1586.50429006303,
1586.60048849585,1586.69409668971,1586.79159024201,1586.8890837943,1586.97282250615,
1587.05645801751,1587.14001046091,1587.22349989676,1587.30695384738,1587.39039034122,
1587.47382745098,1587.5572832459,1587.64082773863,1587.72441682157,1587.80814008913,
1587.88881980502,1587.97255851687,1588.05619402823,1588.13974647163,1588.22323590748,
1588.3066898581,1588.39012635194,1588.4735634617,1588.55701925661,1588.64056374934,
1588.72415283228,1588.80787609984,1588.88855581574,1588.97229452759,1589.05593003895,
1589.13948248235,1589.2229719182,1589.30642586882,1589.38986236266,1589.47329947242,
1589.55675526734,1589.64029976007,1589.72388884301,1589.80761211056,1589.88829182646,
1589.97203053831,1590.05566604967,1590.13921849307,1590.22270792892,1590.30616187954,
1590.38959837338,1590.47303548314,1590.55649127806,1590.64003577079,1590.72362485373,
1590.80734812129,1590.88802783718,1590.97176654903,1591.05540206039,1591.13895450379,
1591.22244393964,1591.30589789026,1591.3893343841,1591.47277149386,1591.55622728877,
1591.6397717815,1591.72336086445,1591.807084132,1591.8877638479,1591.97043428355,
1592.05301014788,1592.13551052206,1592.21795441894,1592.3003708666,1592.38276892532,
1592.46519595126,1592.53564160811),.UNSPECIFIED.);
#1060=B_SPLINE_CURVE_WITH_KNOTS('',3,(#132496,#132497,#132498,#132499,#132500,
#132501,#132502,#132503,#132504,#132505),.UNSPECIFIED.,.F.,.F.,(4,3,3,4),
(1586.25360547416,1586.33788429121,1586.42214119569,1586.50429006284),
 .UNSPECIFIED.);
#1061=B_SPLINE_CURVE_WITH_KNOTS('',3,(#132507,#132508,#132509,#132510,#132511,
#132512,#132513,#132514,#132515,#132516),.UNSPECIFIED.,.F.,.F.,(4,3,3,4),
(1586.25354069145,1586.35475079831,1586.45478004659,1586.5042900627),
 .UNSPECIFIED.);
#1062=B_SPLINE_CURVE_WITH_KNOTS('',3,(#132517,#132518,#132519,#132520,#132521,
#132522,#132523,#132524,#132525,#132526,#132527,#132528,#132529,#132530,
#132531,#132532,#132533,#132534,#132535,#132536,#132537,#132538,#132539,
#132540,#132541,#132542,#132543,#132544,#132545,#132546,#132547,#132548,
#132549,#132550,#132551,#132552,#132553,#132554,#132555,#132556,#132557,
#132558,#132559,#132560,#132561,#132562,#132563,#132564,#132565,#132566,
#132567,#132568,#132569,#132570,#132571,#132572,#132573,#132574,#132575,
#132576,#132577,#132578,#132579,#132580,#132581,#132582,#132583,#132584,
#132585,#132586,#132587,#132588,#132589,#132590,#132591,#132592,#132593,
#132594,#132595,#132596,#132597,#132598,#132599,#132600,#132601,#132602,
#132603,#132604,#132605,#132606,#132607,#132608,#132609,#132610,#132611,
#132612,#132613,#132614,#132615,#132616,#132617,#132618,#132619,#132620,
#132621,#132622,#132623,#132624,#132625,#132626,#132627,#132628,#132629,
#132630,#132631,#132632,#132633,#132634,#132635,#132636,#132637,#132638,
#132639,#132640,#132641,#132642,#132643,#132644,#132645,#132646,#132647,
#132648,#132649,#132650,#132651,#132652,#132653,#132654,#132655,#132656,
#132657,#132658,#132659,#132660,#132661,#132662,#132663,#132664,#132665,
#132666,#132667,#132668,#132669,#132670,#132671,#132672,#132673,#132674,
#132675,#132676,#132677,#132678,#132679,#132680,#132681,#132682,#132683,
#132684,#132685,#132686,#132687,#132688,#132689,#132690,#132691,#132692,
#132693,#132694,#132695,#132696,#132697,#132698,#132699,#132700,#132701,
#132702,#132703,#132704,#132705,#132706,#132707,#132708,#132709,#132710,
#132711,#132712,#132713,#132714,#132715,#132716,#132717,#132718,#132719,
#132720,#132721,#132722,#132723,#132724,#132725,#132726,#132727,#132728,
#132729,#132730,#132731,#132732,#132733,#132734,#132735,#132736),
 .UNSPECIFIED.,.F.,.F.,(4,3,3,3,3,3,3,3,3,3,3,3,3,3,3,3,3,3,3,3,3,3,3,3,
3,3,3,3,3,3,3,3,3,3,3,3,3,3,3,3,3,3,3,3,3,3,3,3,3,3,3,3,3,3,3,3,3,3,3,3,
3,3,3,3,3,3,3,3,3,3,3,3,3,4),(1586.50429006285,1586.59117560675,1586.67417571087,
1586.75716969916,1586.84017600843,1586.92321308047,1587.00634564545,1587.08953426791,
1587.17284408563,1587.19937441401,1587.28311312586,1587.36674863722,1587.45030108062,
1587.53379051647,1587.61724446709,1587.70068096093,1587.78411807069,1587.8675738656,
1587.95111835833,1588.03470744127,1588.11843070883,1588.19911042473,1588.28284913658,
1588.36648464794,1588.45003709134,1588.53352652719,1588.61698047781,1588.70041697165,
1588.78385408141,1588.86730987633,1588.95085436906,1589.034443452,1589.11816671956,
1589.19884643545,1589.2825851473,1589.36622065866,1589.44977310206,1589.53326253791,
1589.61671648853,1589.70015298237,1589.78359009213,1589.86704588705,1589.95059037978,
1590.03417946272,1590.11790273027,1590.19858244617,1590.28232115802,1590.36595666938,
1590.44950911278,1590.53299854863,1590.61645249924,1590.69988899309,1590.78332610285,
1590.86678189776,1590.95032639049,1591.03391547343,1591.11763874099,1591.19831845689,
1591.28205716874,1591.3656926801,1591.4492451235,1591.53273455935,1591.61618850997,
1591.69962500381,1591.78306211357,1591.86651790849,1591.95006240122,1592.03365148416,
1592.11737475172,1592.19805446761,1592.28326590893,1592.36837271544,1592.45336110949,
1592.53689918447),.UNSPECIFIED.);
#1063=B_SPLINE_CURVE_WITH_KNOTS('',3,(#132742,#132743,#132744,#132745,#132746,
#132747,#132748,#132749,#132750,#132751,#132752,#132753,#132754,#132755,
#132756,#132757,#132758,#132759,#132760,#132761,#132762,#132763,#132764,
#132765,#132766,#132767,#132768,#132769,#132770,#132771,#132772,#132773,
#132774,#132775,#132776,#132777,#132778,#132779,#132780,#132781,#132782,
#132783,#132784,#132785,#132786,#132787,#132788,#132789,#132790,#132791,
#132792,#132793,#132794,#132795,#132796,#132797,#132798,#132799,#132800,
#132801,#132802,#132803,#132804,#132805,#132806,#132807,#132808,#132809,
#132810,#132811,#132812,#132813,#132814,#132815,#132816,#132817,#132818,
#132819,#132820,#132821,#132822,#132823,#132824,#132825,#132826,#132827,
#132828,#132829,#132830,#132831,#132832,#132833,#132834,#132835,#132836,
#132837,#132838,#132839,#132840,#132841,#132842,#132843,#132844,#132845,
#132846,#132847,#132848,#132849,#132850,#132851,#132852,#132853,#132854,
#132855,#132856,#132857,#132858,#132859,#132860,#132861,#132862,#132863,
#132864,#132865,#132866,#132867,#132868,#132869,#132870,#132871,#132872,
#132873,#132874,#132875,#132876,#132877,#132878,#132879,#132880,#132881,
#132882,#132883,#132884,#132885,#132886,#132887,#132888,#132889,#132890,
#132891,#132892,#132893,#132894,#132895,#132896,#132897,#132898,#132899,
#132900,#132901,#132902,#132903,#132904,#132905,#132906,#132907,#132908,
#132909,#132910,#132911,#132912,#132913,#132914,#132915,#132916,#132917,
#132918,#132919,#132920,#132921,#132922,#132923,#132924,#132925,#132926,
#132927,#132928,#132929,#132930,#132931,#132932,#132933,#132934,#132935,
#132936,#132937,#132938,#132939,#132940,#132941,#132942,#132943,#132944,
#132945,#132946,#132947,#132948,#132949,#132950,#132951,#132952,#132953,
#132954,#132955,#132956,#132957,#132958,#132959,#132960,#132961),
 .UNSPECIFIED.,.F.,.F.,(4,3,3,3,3,3,3,3,3,3,3,3,3,3,3,3,3,3,3,3,3,3,3,3,
3,3,3,3,3,3,3,3,3,3,3,3,3,3,3,3,3,3,3,3,3,3,3,3,3,3,3,3,3,3,3,3,3,3,3,3,
3,3,3,3,3,3,3,3,3,3,3,3,3,4),(1592.78747537002,1592.88749985862,1592.97123857047,
1593.05487408183,1593.13842652523,1593.22191596108,1593.3053699117,1593.38880640554,
1593.4722435153,1593.55569931022,1593.63924380295,1593.72283288589,1593.80655615344,
1593.88723586934,1593.97097458119,1594.05461009255,1594.13816253595,1594.2216519718,
1594.30510592242,1594.38854241626,1594.47197952602,1594.55543532093,1594.63897981366,
1594.7225688966,1594.80629216416,1594.88697188006,1594.97071059191,1595.05434610327,
1595.13789854667,1595.22138798252,1595.30484193314,1595.38827842698,1595.47171553674,
1595.55517133166,1595.63871582439,1595.72230490733,1595.80602817488,1595.88670789078,
1595.97044660263,1596.05408211399,1596.13763455739,1596.22112399324,1596.30457794386,
1596.3880144377,1596.47145154746,1596.55490734238,1596.63845183511,1596.72204091805,
1596.8057641856,1596.8864439015,1596.97018261335,1597.05381812471,1597.13737056811,
1597.22086000396,1597.30431395458,1597.38775044842,1597.47118755818,1597.5546433531,
1597.63818784583,1597.72177692877,1597.80550019633,1597.88617991222,1597.96992245597,
1598.05356092002,1598.13711544061,1598.22238332056,1598.30583358857,1598.3892655418,
1598.47269725198,1598.55933755903,1598.64286097195,1598.726429428,1598.8100938485,
1598.81925848019),.UNSPECIFIED.);
#1064=B_SPLINE_CURVE_WITH_KNOTS('',3,(#132962,#132963,#132964,#132965,#132966,
#132967,#132968,#132969,#132970,#132971),.UNSPECIFIED.,.F.,.F.,(4,3,3,4),
(1592.53564160811,1592.61814382261,1592.70280959625,1592.78747536988),
 .UNSPECIFIED.);
#1065=B_SPLINE_CURVE_WITH_KNOTS('',3,(#132973,#132974,#132975,#132976,#132977,
#132978,#132979,#132980,#132981,#132982),.UNSPECIFIED.,.F.,.F.,(4,3,3,4),
(1592.53689918447,1592.62174705618,1592.70654982744,1592.78747537003),
 .UNSPECIFIED.);
#1066=B_SPLINE_CURVE_WITH_KNOTS('',3,(#132983,#132984,#132985,#132986,#132987,
#132988,#132989,#132990,#132991,#132992,#132993,#132994,#132995,#132996,
#132997,#132998,#132999,#133000,#133001,#133002,#133003,#133004,#133005,
#133006,#133007,#133008,#133009,#133010,#133011,#133012,#133013,#133014,
#133015,#133016,#133017,#133018,#133019,#133020,#133021,#133022,#133023,
#133024,#133025,#133026,#133027,#133028,#133029,#133030,#133031,#133032,
#133033,#133034,#133035,#133036,#133037,#133038,#133039,#133040,#133041,
#133042,#133043,#133044,#133045,#133046,#133047,#133048,#133049,#133050,
#133051,#133052,#133053,#133054,#133055,#133056,#133057,#133058,#133059,
#133060,#133061,#133062,#133063,#133064,#133065,#133066,#133067,#133068,
#133069,#133070,#133071,#133072,#133073,#133074,#133075,#133076,#133077,
#133078,#133079,#133080,#133081,#133082,#133083,#133084,#133085,#133086,
#133087,#133088,#133089,#133090,#133091,#133092,#133093,#133094,#133095,
#133096,#133097,#133098,#133099,#133100,#133101,#133102,#133103,#133104,
#133105,#133106,#133107,#133108,#133109,#133110,#133111,#133112,#133113,
#133114,#133115,#133116,#133117,#133118,#133119,#133120,#133121,#133122,
#133123,#133124,#133125,#133126,#133127,#133128,#133129,#133130,#133131,
#133132,#133133,#133134,#133135,#133136,#133137,#133138,#133139,#133140,
#133141,#133142,#133143,#133144,#133145,#133146,#133147,#133148,#133149,
#133150,#133151,#133152,#133153,#133154,#133155,#133156,#133157,#133158,
#133159,#133160,#133161,#133162,#133163,#133164,#133165,#133166,#133167,
#133168,#133169,#133170,#133171,#133172,#133173,#133174,#133175,#133176,
#133177,#133178,#133179,#133180,#133181,#133182,#133183,#133184,#133185,
#133186,#133187,#133188,#133189,#133190,#133191,#133192,#133193,#133194,
#133195,#133196,#133197,#133198,#133199,#133200,#133201,#133202),
 .UNSPECIFIED.,.F.,.F.,(4,3,3,3,3,3,3,3,3,3,3,3,3,3,3,3,3,3,3,3,3,3,3,3,
3,3,3,3,3,3,3,3,3,3,3,3,3,3,3,3,3,3,3,3,3,3,3,3,3,3,3,3,3,3,3,3,3,3,3,3,
3,3,3,3,3,3,3,3,3,3,3,3,3,4),(1592.7874753702,1592.87896172744,1592.9709007737,
1593.06307252995,1593.15556706926,1593.19779047834,1593.28152919019,1593.36516470155,
1593.44871714495,1593.5322065808,1593.61566053142,1593.69909702526,1593.78253413502,
1593.86598992994,1593.94953442267,1594.03312350561,1594.11684677316,1594.19752648906,
1594.28126520091,1594.36490071227,1594.44845315567,1594.53194259152,1594.61539654214,
1594.69883303598,1594.78227014574,1594.86572594066,1594.94927043339,1595.03285951633,
1595.11658278388,1595.19726249978,1595.28100121163,1595.36463672299,1595.44818916639,
1595.53167860224,1595.61513255286,1595.6985690467,1595.78200615646,1595.86546195138,
1595.94900644411,1596.03259552705,1596.1163187946,1596.1969985105,1596.28073722235,
1596.36437273371,1596.44792517711,1596.53141461296,1596.61486856358,1596.69830505742,
1596.78174216718,1596.8651979621,1596.94874245483,1597.03233153777,1597.11605480532,
1597.19673452122,1597.28047323307,1597.36410874443,1597.44766118783,1597.53115062368,
1597.6146045743,1597.69804106814,1597.7814781779,1597.86493397282,1597.94847846555,
1598.03206754849,1598.11579081604,1598.19647053194,1598.27901881213,1598.36147237307,
1598.44385037954,1598.52617192518,1598.60846368296,1598.6907374058,1598.77303243584,
1598.81885555413),.UNSPECIFIED.);
#1067=B_SPLINE_CURVE_WITH_KNOTS('',3,(#133208,#133209,#133210,#133211,#133212,
#133213,#133214,#133215,#133216,#133217,#133218,#133219,#133220,#133221,
#133222,#133223,#133224,#133225,#133226,#133227,#133228,#133229,#133230,
#133231,#133232,#133233,#133234,#133235,#133236,#133237,#133238,#133239,
#133240,#133241,#133242,#133243,#133244,#133245,#133246,#133247,#133248,
#133249,#133250,#133251,#133252,#133253,#133254,#133255,#133256,#133257,
#133258,#133259,#133260,#133261,#133262,#133263,#133264,#133265,#133266,
#133267,#133268,#133269,#133270,#133271,#133272,#133273,#133274,#133275,
#133276,#133277,#133278,#133279,#133280,#133281,#133282,#133283,#133284,
#133285,#133286,#133287,#133288,#133289,#133290,#133291,#133292,#133293,
#133294,#133295,#133296,#133297,#133298,#133299,#133300,#133301,#133302,
#133303,#133304,#133305,#133306,#133307,#133308,#133309,#133310,#133311,
#133312,#133313,#133314,#133315,#133316,#133317,#133318,#133319,#133320,
#133321,#133322,#133323,#133324,#133325,#133326,#133327,#133328,#133329,
#133330,#133331,#133332,#133333,#133334,#133335,#133336,#133337,#133338,
#133339,#133340,#133341,#133342,#133343,#133344,#133345,#133346,#133347,
#133348,#133349,#133350,#133351,#133352,#133353,#133354,#133355,#133356,
#133357,#133358,#133359,#133360,#133361,#133362,#133363,#133364,#133365,
#133366,#133367,#133368,#133369,#133370,#133371,#133372,#133373,#133374,
#133375,#133376,#133377,#133378,#133379,#133380,#133381,#133382,#133383,
#133384,#133385,#133386,#133387,#133388,#133389,#133390,#133391,#133392,
#133393,#133394,#133395,#133396,#133397,#133398,#133399,#133400,#133401,
#133402,#133403,#133404,#133405,#133406,#133407,#133408,#133409,#133410,
#133411,#133412,#133413,#133414,#133415,#133416,#133417,#133418,#133419,
#133420,#133421,#133422,#133423,#133424,#133425,#133426,#133427),
 .UNSPECIFIED.,.F.,.F.,(4,3,3,3,3,3,3,3,3,3,3,3,3,3,3,3,3,3,3,3,3,3,3,3,
3,3,3,3,3,3,3,3,3,3,3,3,3,3,3,3,3,3,3,3,3,3,3,3,3,3,3,3,3,3,3,3,3,3,3,3,
3,3,3,3,3,3,3,3,3,3,3,3,3,4),(1599.07066067734,1599.15302402575,1599.23531412012,
1599.3175560504,1599.39977319763,1599.48198459586,1599.56420927224,1599.64651601869,
1599.72886431527,1599.81134162596,1599.88565193366,1599.96939064551,1600.05302615687,
1600.13657860027,1600.22006803612,1600.30352198674,1600.38695848058,1600.47039559034,
1600.55385138526,1600.63739587799,1600.72098496093,1600.80470822849,1600.88538794438,
1600.96912665623,1601.05276216759,1601.13631461099,1601.21980404684,1601.30325799746,
1601.3866944913,1601.47013160106,1601.55358739598,1601.6371318887,1601.72072097165,
1601.8044442392,1601.8851239551,1601.96886266695,1602.05249817831,1602.13605062171,
1602.21954005756,1602.30299400818,1602.38643050202,1602.46986761178,1602.5533234067,
1602.63686789943,1602.72045698237,1602.80418024992,1602.88485996582,1602.96859867767,
1603.05223418903,1603.13578663243,1603.21927606828,1603.3027300189,1603.38616651274,
1603.4696036225,1603.55305941742,1603.63660391015,1603.72019299309,1603.80391626064,
1603.88459597654,1603.96833468839,1604.05197019975,1604.13552264315,1604.219012079,
1604.30246602962,1604.38590252346,1604.46933963322,1604.55279542814,1604.63633992087,
1604.71992900381,1604.80365227136,1604.88433198726,1604.97368932459,1605.06283149349,
1605.10354352794),.UNSPECIFIED.);
#1068=B_SPLINE_CURVE_WITH_KNOTS('',3,(#133428,#133429,#133430,#133431,#133432,
#133433,#133434,#133435,#133436,#133437),.UNSPECIFIED.,.F.,.F.,(4,3,3,4),
(1598.81925848019,1598.88591592294,1599.01127570596,1599.0706606772),
 .UNSPECIFIED.);
#1069=B_SPLINE_CURVE_WITH_KNOTS('',3,(#133439,#133440,#133441,#133442,#133443,
#133444,#133445,#133446,#133447,#133448),.UNSPECIFIED.,.F.,.F.,(4,3,3,4),
(1598.81885555413,1598.90121960559,1598.98594014133,1599.07066067708),
 .UNSPECIFIED.);
#1070=B_SPLINE_CURVE_WITH_KNOTS('',3,(#133449,#133450,#133451,#133452,#133453,
#133454,#133455,#133456,#133457,#133458,#133459,#133460,#133461,#133462,
#133463,#133464,#133465,#133466,#133467,#133468,#133469,#133470,#133471,
#133472,#133473,#133474,#133475,#133476,#133477,#133478,#133479,#133480,
#133481,#133482,#133483,#133484,#133485,#133486,#133487,#133488,#133489,
#133490,#133491,#133492,#133493,#133494,#133495,#133496,#133497,#133498,
#133499,#133500,#133501,#133502,#133503,#133504,#133505,#133506,#133507,
#133508,#133509,#133510,#133511,#133512,#133513,#133514,#133515,#133516,
#133517,#133518,#133519,#133520,#133521,#133522,#133523,#133524,#133525,
#133526,#133527,#133528,#133529,#133530,#133531,#133532,#133533,#133534,
#133535,#133536,#133537,#133538,#133539,#133540,#133541,#133542,#133543,
#133544,#133545,#133546,#133547,#133548,#133549,#133550,#133551,#133552,
#133553,#133554,#133555,#133556,#133557,#133558,#133559,#133560,#133561,
#133562,#133563,#133564,#133565,#133566,#133567,#133568,#133569,#133570,
#133571,#133572,#133573,#133574,#133575,#133576,#133577,#133578,#133579,
#133580,#133581,#133582,#133583,#133584,#133585,#133586,#133587,#133588,
#133589,#133590,#133591,#133592,#133593,#133594,#133595,#133596,#133597,
#133598,#133599,#133600,#133601,#133602,#133603,#133604,#133605,#133606,
#133607,#133608,#133609,#133610,#133611,#133612,#133613,#133614,#133615,
#133616,#133617,#133618,#133619,#133620,#133621,#133622,#133623,#133624,
#133625,#133626,#133627,#133628,#133629,#133630,#133631,#133632,#133633,
#133634,#133635,#133636,#133637,#133638,#133639,#133640,#133641,#133642,
#133643,#133644,#133645,#133646,#133647,#133648,#133649,#133650,#133651,
#133652,#133653,#133654,#133655,#133656,#133657,#133658,#133659,#133660,
#133661,#133662,#133663,#133664,#133665),.UNSPECIFIED.,.F.,.F.,(4,3,3,3,
3,3,3,3,3,3,3,3,3,3,3,3,3,3,3,3,3,3,3,3,3,3,3,3,3,3,3,3,3,3,3,3,3,3,3,3,
3,3,3,3,3,3,3,3,3,3,3,3,3,3,3,3,3,3,3,3,3,3,3,3,3,3,3,3,3,3,3,3,4),(1599.07066067721,
1599.19620654266,1599.27994525451,1599.36358076587,1599.44713320927,1599.53062264512,
1599.61407659574,1599.69751308958,1599.78095019934,1599.86440599426,1599.94795048699,
1600.03153956993,1600.11526283748,1600.19594255338,1600.27968126523,1600.36331677659,
1600.44686921999,1600.53035865584,1600.61381260646,1600.6972491003,1600.78068621006,
1600.86414200498,1600.94768649771,1601.03127558065,1601.1149988482,1601.1956785641,
1601.27941727595,1601.36305278731,1601.44660523071,1601.53009466656,1601.61354861718,
1601.69698511102,1601.78042222078,1601.8638780157,1601.94742250843,1602.03101159137,
1602.11473485892,1602.19541457482,1602.27915328667,1602.36278879803,1602.44634124143,
1602.52983067728,1602.6132846279,1602.69672112174,1602.7801582315,1602.86361402642,
1602.94715851915,1603.03074760209,1603.11447086964,1603.19515058554,1603.27888929739,
1603.36252480875,1603.44607725215,1603.529566688,1603.61302063862,1603.69645713246,
1603.77989424222,1603.86335003713,1603.94689452986,1604.03048361281,1604.11420688036,
1604.19488659626,1604.27863066505,1604.36227031628,1604.44582568764,1604.52931283193,
1604.61276270963,1604.69619340916,1604.77962300226,1604.86310851884,1604.9466216911,
1605.03023631808,1605.10235396521),.UNSPECIFIED.);
#1071=B_SPLINE_CURVE_WITH_KNOTS('',3,(#133671,#133672,#133673,#133674,#133675,
#133676,#133677,#133678,#133679,#133680,#133681,#133682,#133683,#133684,
#133685,#133686,#133687,#133688,#133689,#133690,#133691,#133692,#133693,
#133694,#133695,#133696,#133697,#133698,#133699,#133700,#133701,#133702,
#133703,#133704,#133705,#133706,#133707,#133708,#133709,#133710,#133711,
#133712,#133713,#133714,#133715,#133716,#133717,#133718,#133719,#133720,
#133721,#133722,#133723,#133724,#133725,#133726,#133727,#133728,#133729,
#133730,#133731,#133732,#133733,#133734,#133735,#133736,#133737,#133738,
#133739,#133740,#133741,#133742,#133743,#133744,#133745,#133746,#133747,
#133748,#133749,#133750,#133751,#133752,#133753,#133754,#133755,#133756,
#133757,#133758,#133759,#133760,#133761,#133762,#133763,#133764,#133765,
#133766,#133767,#133768,#133769,#133770,#133771,#133772,#133773,#133774,
#133775,#133776,#133777,#133778,#133779,#133780,#133781,#133782,#133783,
#133784,#133785,#133786,#133787,#133788,#133789,#133790,#133791,#133792,
#133793,#133794,#133795,#133796,#133797,#133798,#133799,#133800,#133801,
#133802,#133803,#133804,#133805,#133806,#133807,#133808,#133809,#133810,
#133811,#133812,#133813,#133814,#133815,#133816,#133817,#133818,#133819,
#133820,#133821,#133822,#133823,#133824,#133825,#133826,#133827,#133828,
#133829,#133830,#133831,#133832,#133833,#133834,#133835,#133836,#133837,
#133838,#133839,#133840,#133841,#133842,#133843,#133844,#133845,#133846,
#133847,#133848,#133849,#133850,#133851,#133852,#133853,#133854,#133855,
#133856,#133857,#133858,#133859,#133860,#133861,#133862,#133863,#133864,
#133865,#133866,#133867,#133868,#133869,#133870,#133871,#133872,#133873,
#133874,#133875,#133876,#133877,#133878,#133879,#133880,#133881,#133882,
#133883,#133884,#133885,#133886,#133887),.UNSPECIFIED.,.F.,.F.,(4,3,3,3,
3,3,3,3,3,3,3,3,3,3,3,3,3,3,3,3,3,3,3,3,3,3,3,3,3,3,3,3,3,3,3,3,3,3,3,3,
3,3,3,3,3,3,3,3,3,3,3,3,3,3,3,3,3,3,3,3,3,3,3,3,3,3,3,3,3,3,3,3,4),(1605.35384598438,
1605.44022879737,1605.52669081532,1605.61603511099,1605.70275600956,1605.79341200377,
1605.88406799798,1605.96780670983,1606.05144222119,1606.13499466459,1606.21848410044,
1606.30193805106,1606.3853745449,1606.46881165466,1606.55226744958,1606.63581194231,
1606.71940102525,1606.80312429281,1606.8838040087,1606.96754272055,1607.05117823191,
1607.13473067531,1607.21822011116,1607.30167406178,1607.38511055562,1607.46854766538,
1607.5520034603,1607.63554795302,1607.71913703597,1607.80286030352,1607.88354001942,
1607.96727873127,1608.05091424263,1608.13446668603,1608.21795612188,1608.3014100725,
1608.38484656634,1608.4682836761,1608.55173947102,1608.63528396375,1608.71887304669,
1608.80259631424,1608.88327603014,1608.96701474199,1609.05065025335,1609.13420269675,
1609.2176921326,1609.30114608322,1609.38458257706,1609.46801968682,1609.55147548174,
1609.63501997447,1609.71860905741,1609.80233232497,1609.88301204086,1609.96675075271,
1610.05038626407,1610.13393870747,1610.21742814332,1610.30088209394,1610.38431858778,
1610.46775569754,1610.55121149246,1610.63475598519,1610.71834506813,1610.80206833568,
1610.88274805158,1610.96548316682,1611.04812026984,1611.13250170617,1611.21499298543,
1611.30031950029,1611.38564601516),.UNSPECIFIED.);
#1072=B_SPLINE_CURVE_WITH_KNOTS('',3,(#133888,#133889,#133890,#133891,#133892,
#133893,#133894,#133895,#133896,#133897),.UNSPECIFIED.,.F.,.F.,(4,3,3,4),
(1605.10354352794,1605.19240950004,1605.28105355217,1605.35384598424),
 .UNSPECIFIED.);
#1073=B_SPLINE_CURVE_WITH_KNOTS('',3,(#133899,#133900,#133901,#133902,#133903,
#133904,#133905,#133906,#133907,#133908,#133909,#133910,#133911),
 .UNSPECIFIED.,.F.,.F.,(4,3,3,3,4),(1605.10235396521,1605.18610885268,1605.19462260698,
1605.33154122428,1605.35384598439),.UNSPECIFIED.);
#1074=B_SPLINE_CURVE_WITH_KNOTS('',3,(#133912,#133913,#133914,#133915,#133916,
#133917,#133918,#133919,#133920,#133921,#133922,#133923,#133924,#133925,
#133926,#133927,#133928,#133929,#133930,#133931,#133932,#133933,#133934,
#133935,#133936,#133937,#133938,#133939,#133940,#133941,#133942,#133943,
#133944,#133945,#133946,#133947,#133948,#133949,#133950,#133951,#133952,
#133953,#133954,#133955,#133956,#133957,#133958,#133959,#133960,#133961,
#133962,#133963,#133964,#133965,#133966,#133967,#133968,#133969,#133970,
#133971,#133972,#133973,#133974,#133975,#133976,#133977,#133978,#133979,
#133980,#133981,#133982,#133983,#133984,#133985,#133986,#133987,#133988,
#133989,#133990,#133991,#133992,#133993,#133994,#133995,#133996,#133997,
#133998,#133999,#134000,#134001,#134002,#134003,#134004,#134005,#134006,
#134007,#134008,#134009,#134010,#134011,#134012,#134013,#134014,#134015,
#134016,#134017,#134018,#134019,#134020,#134021,#134022,#134023,#134024,
#134025,#134026,#134027,#134028,#134029,#134030,#134031,#134032,#134033,
#134034,#134035,#134036,#134037,#134038,#134039,#134040,#134041,#134042,
#134043,#134044,#134045,#134046,#134047,#134048,#134049,#134050,#134051,
#134052,#134053,#134054,#134055,#134056,#134057,#134058,#134059,#134060,
#134061,#134062,#134063,#134064,#134065,#134066,#134067,#134068,#134069,
#134070,#134071,#134072,#134073,#134074,#134075,#134076,#134077,#134078,
#134079,#134080,#134081,#134082,#134083,#134084,#134085,#134086,#134087,
#134088,#134089,#134090,#134091,#134092,#134093,#134094,#134095,#134096,
#134097,#134098,#134099,#134100,#134101,#134102,#134103,#134104,#134105,
#134106,#134107,#134108,#134109,#134110,#134111,#134112,#134113,#134114,
#134115,#134116,#134117,#134118,#134119,#134120,#134121,#134122,#134123,
#134124,#134125,#134126,#134127,#134128,#134129,#134130,#134131,#134132,
#134133,#134134),.UNSPECIFIED.,.F.,.F.,(4,3,3,3,3,3,3,3,3,3,3,3,3,3,3,3,
3,3,3,3,3,3,3,3,3,3,3,3,3,3,3,3,3,3,3,3,3,3,3,3,3,3,3,3,3,3,3,3,3,3,3,3,
3,3,3,3,3,3,3,3,3,3,3,3,3,3,3,3,3,3,3,3,3,3,4),(1605.35384598449,1605.43623005758,
1605.51853423986,1605.60301228709,1605.68522798814,1605.76743249965,1605.84964485315,
1605.93582329429,1606.01815352553,1606.10053836855,1606.18303538978,1606.1943586177,
1606.27809732955,1606.36173284091,1606.44528528431,1606.52877472016,1606.61222867078,
1606.69566516462,1606.77910227438,1606.8625580693,1606.94610256203,1607.02969164497,
1607.11341491252,1607.19409462842,1607.27783334027,1607.36146885163,1607.44502129503,
1607.52851073088,1607.6119646815,1607.69540117534,1607.7788382851,1607.86229408002,
1607.94583857275,1608.02942765569,1608.11315092324,1608.19383063914,1608.27756935099,
1608.36120486235,1608.44475730575,1608.5282467416,1608.61170069222,1608.69513718606,
1608.77857429582,1608.86203009074,1608.94557458347,1609.02916366641,1609.11288693397,
1609.19356664986,1609.27730536171,1609.36094087307,1609.44449331647,1609.52798275232,
1609.61143670294,1609.69487319678,1609.77831030654,1609.86176610146,1609.94531059419,
1610.02889967713,1610.11262294469,1610.19330266058,1610.27704137243,1610.36067688379,
1610.44422932719,1610.52771876304,1610.61117271366,1610.6946092075,1610.77804631726,
1610.86150211217,1610.9450466049,1611.02863568784,1611.1123589554,1611.1930386713,
1611.28365903689,1611.37404670308,1611.386724099),.UNSPECIFIED.);
#1075=B_SPLINE_CURVE_WITH_KNOTS('',3,(#134140,#134141,#134142,#134143,#134144,
#134145,#134146,#134147,#134148,#134149,#134150,#134151,#134152,#134153,
#134154,#134155,#134156,#134157,#134158,#134159,#134160,#134161,#134162,
#134163,#134164,#134165,#134166,#134167,#134168,#134169,#134170,#134171,
#134172,#134173,#134174,#134175,#134176,#134177,#134178,#134179,#134180,
#134181,#134182,#134183,#134184,#134185,#134186,#134187,#134188,#134189,
#134190,#134191,#134192,#134193,#134194,#134195,#134196,#134197,#134198,
#134199,#134200,#134201,#134202,#134203,#134204,#134205,#134206,#134207,
#134208,#134209,#134210,#134211,#134212,#134213,#134214,#134215,#134216,
#134217,#134218,#134219,#134220,#134221,#134222,#134223,#134224,#134225,
#134226,#134227,#134228,#134229,#134230,#134231,#134232,#134233,#134234,
#134235,#134236,#134237,#134238,#134239,#134240,#134241,#134242,#134243,
#134244,#134245,#134246,#134247,#134248,#134249,#134250,#134251,#134252,
#134253,#134254,#134255,#134256,#134257,#134258,#134259,#134260,#134261,
#134262,#134263,#134264,#134265,#134266,#134267,#134268,#134269,#134270,
#134271,#134272,#134273,#134274,#134275,#134276,#134277,#134278,#134279,
#134280,#134281,#134282,#134283,#134284,#134285,#134286,#134287,#134288,
#134289,#134290,#134291,#134292,#134293,#134294,#134295,#134296,#134297,
#134298,#134299,#134300,#134301,#134302,#134303,#134304,#134305,#134306,
#134307,#134308,#134309,#134310,#134311,#134312,#134313,#134314,#134315,
#134316,#134317,#134318,#134319,#134320,#134321,#134322,#134323,#134324,
#134325,#134326,#134327,#134328,#134329,#134330,#134331,#134332,#134333,
#134334,#134335,#134336,#134337,#134338,#134339,#134340,#134341,#134342,
#134343,#134344,#134345,#134346,#134347,#134348,#134349,#134350,#134351,
#134352,#134353,#134354,#134355,#134356,#134357,#134358,#134359),
 .UNSPECIFIED.,.F.,.F.,(4,3,3,3,3,3,3,3,3,3,3,3,3,3,3,3,3,3,3,3,3,3,3,3,
3,3,3,3,3,3,3,3,3,3,3,3,3,3,3,3,3,3,3,3,3,3,3,3,3,3,3,3,3,3,3,3,3,3,3,3,
3,3,3,3,3,3,3,3,3,3,3,3,3,4),(1611.63703129169,1611.74502167405,1611.85559144508,
1611.8824840623,1611.96622277415,1612.04985828551,1612.13341072891,1612.21690016476,
1612.30035411538,1612.38379060922,1612.46722771898,1612.5506835139,1612.63422800663,
1612.71781708957,1612.80154035712,1612.88222007302,1612.96595878487,1613.04959429623,
1613.13314673963,1613.21663617548,1613.3000901261,1613.38352661994,1613.4669637297,
1613.55041952462,1613.63396401734,1613.71755310029,1613.80127636784,1613.88195608374,
1613.96569479559,1614.04933030695,1614.13288275035,1614.2163721862,1614.29982613682,
1614.38326263066,1614.46669974042,1614.55015553534,1614.63370002806,1614.71728911101,
1614.80101237856,1614.88169209446,1614.96543080631,1615.04906631767,1615.13261876107,
1615.21610819692,1615.29956214754,1615.38299864138,1615.46643575114,1615.54989154606,
1615.63343603879,1615.71702512173,1615.80074838928,1615.88142810518,1615.96516681703,
1616.04880232839,1616.13235477179,1616.21584420764,1616.29929815826,1616.3827346521,
1616.46617176186,1616.54962755678,1616.63317204951,1616.71676113245,1616.8004844,
1616.8811641159,1616.96491572543,1617.05287003921,1617.13641063114,1617.2198945257,
1617.3033398417,1617.38676466796,1617.47020902566,1617.55366475935,1617.63717820047,
1617.66855023561),.UNSPECIFIED.);
#1076=B_SPLINE_CURVE_WITH_KNOTS('',3,(#134360,#134361,#134362,#134363,#134364,
#134365,#134366,#134367,#134368,#134369),.UNSPECIFIED.,.F.,.F.,(4,3,3,4),
(1611.38564601516,1611.46810946382,1611.55257037769,1611.63703129156),
 .UNSPECIFIED.);
#1077=B_SPLINE_CURVE_WITH_KNOTS('',3,(#134371,#134372,#134373,#134374,#134375,
#134376,#134377,#134378,#134379,#134380),.UNSPECIFIED.,.F.,.F.,(4,3,3,4),
(1611.386724099,1611.47681850758,1611.56662740094,1611.63703129145),
 .UNSPECIFIED.);
#1078=B_SPLINE_CURVE_WITH_KNOTS('',3,(#134381,#134382,#134383,#134384,#134385,
#134386,#134387,#134388,#134389,#134390,#134391,#134392,#134393,#134394,
#134395,#134396,#134397,#134398,#134399,#134400,#134401,#134402,#134403,
#134404,#134405,#134406,#134407,#134408,#134409,#134410,#134411,#134412,
#134413,#134414,#134415,#134416,#134417,#134418,#134419,#134420,#134421,
#134422,#134423,#134424,#134425,#134426,#134427,#134428,#134429,#134430,
#134431,#134432,#134433,#134434,#134435,#134436,#134437,#134438,#134439,
#134440,#134441,#134442,#134443,#134444,#134445,#134446,#134447,#134448,
#134449,#134450,#134451,#134452,#134453,#134454,#134455,#134456,#134457,
#134458,#134459,#134460,#134461,#134462,#134463,#134464,#134465,#134466,
#134467,#134468,#134469,#134470,#134471,#134472,#134473,#134474,#134475,
#134476,#134477,#134478,#134479,#134480,#134481,#134482,#134483,#134484,
#134485,#134486,#134487,#134488,#134489,#134490,#134491,#134492,#134493,
#134494,#134495,#134496,#134497,#134498,#134499,#134500,#134501,#134502,
#134503,#134504,#134505,#134506,#134507,#134508,#134509,#134510,#134511,
#134512,#134513,#134514,#134515,#134516,#134517,#134518,#134519,#134520,
#134521,#134522,#134523,#134524,#134525,#134526,#134527,#134528,#134529,
#134530,#134531,#134532,#134533,#134534,#134535,#134536,#134537,#134538,
#134539,#134540,#134541,#134542,#134543,#134544,#134545,#134546,#134547,
#134548,#134549,#134550,#134551,#134552,#134553,#134554,#134555,#134556,
#134557,#134558,#134559,#134560,#134561,#134562,#134563,#134564,#134565,
#134566,#134567,#134568,#134569,#134570,#134571,#134572,#134573,#134574,
#134575,#134576,#134577,#134578,#134579,#134580,#134581,#134582,#134583,
#134584,#134585,#134586,#134587,#134588,#134589,#134590,#134591,#134592,
#134593,#134594,#134595,#134596,#134597,#134598,#134599,#134600),
 .UNSPECIFIED.,.F.,.F.,(4,3,3,3,3,3,3,3,3,3,3,3,3,3,3,3,3,3,3,3,3,3,3,3,
3,3,3,3,3,3,3,3,3,3,3,3,3,3,3,3,3,3,3,3,3,3,3,3,3,3,3,3,3,3,3,3,3,3,3,3,
3,3,3,3,3,3,3,3,3,3,3,3,3,4),(1611.63703129156,1611.7226684655,1611.80836065655,
1611.8941219279,1611.98002840369,1612.06601597233,1612.1521607194,1612.19277468202,
1612.27651339387,1612.36014890523,1612.44370134863,1612.52719078448,1612.6106447351,
1612.69408122894,1612.7775183387,1612.86097413362,1612.94451862635,1613.02810770929,
1613.11183097685,1613.19251069274,1613.27624940459,1613.35988491595,1613.44343735935,
1613.5269267952,1613.61038074582,1613.69381723966,1613.77725434942,1613.86071014433,
1613.94425463706,1614.02784372,1614.11156698756,1614.19224670346,1614.27598541531,
1614.35962092667,1614.44317337007,1614.52666280592,1614.61011675654,1614.69355325038,
1614.77699036014,1614.86044615506,1614.94399064779,1615.02757973073,1615.11130299828,
1615.19198271418,1615.27572142603,1615.35935693739,1615.44290938079,1615.52639881664,
1615.60985276726,1615.6932892611,1615.77672637086,1615.86018216578,1615.94372665851,
1616.02731574145,1616.11103900901,1616.1917187249,1616.27545743675,1616.35909294811,
1616.44264539151,1616.52613482736,1616.60958877798,1616.69302527182,1616.77646238158,
1616.8599181765,1616.94346266922,1617.02705175217,1617.11077501972,1617.19145473562,
1617.27439607099,1617.35723784698,1617.4399848302,1617.52267650246,1617.60533543112,
1617.66895862687),.UNSPECIFIED.);
#1079=B_SPLINE_CURVE_WITH_KNOTS('',3,(#134606,#134607,#134608,#134609,#134610,
#134611,#134612,#134613,#134614,#134615,#134616,#134617,#134618,#134619,
#134620,#134621,#134622,#134623,#134624,#134625,#134626,#134627,#134628,
#134629,#134630,#134631,#134632,#134633,#134634,#134635,#134636,#134637,
#134638,#134639,#134640,#134641,#134642,#134643,#134644,#134645,#134646,
#134647,#134648,#134649,#134650,#134651,#134652,#134653,#134654,#134655,
#134656,#134657,#134658,#134659,#134660,#134661,#134662,#134663,#134664,
#134665,#134666,#134667,#134668,#134669,#134670,#134671,#134672,#134673,
#134674,#134675,#134676,#134677,#134678,#134679,#134680,#134681,#134682,
#134683,#134684,#134685,#134686,#134687,#134688,#134689,#134690,#134691,
#134692,#134693,#134694,#134695,#134696,#134697,#134698,#134699,#134700,
#134701,#134702,#134703,#134704,#134705,#134706,#134707,#134708,#134709,
#134710,#134711,#134712,#134713,#134714,#134715,#134716,#134717,#134718,
#134719,#134720,#134721,#134722,#134723,#134724,#134725,#134726,#134727,
#134728,#134729,#134730,#134731,#134732,#134733,#134734,#134735,#134736,
#134737,#134738,#134739,#134740,#134741,#134742,#134743,#134744,#134745,
#134746,#134747,#134748,#134749,#134750,#134751,#134752,#134753,#134754,
#134755,#134756,#134757,#134758,#134759,#134760,#134761,#134762,#134763,
#134764,#134765,#134766,#134767,#134768,#134769,#134770,#134771,#134772,
#134773,#134774,#134775,#134776,#134777,#134778,#134779,#134780,#134781,
#134782,#134783,#134784,#134785,#134786,#134787,#134788,#134789,#134790,
#134791,#134792,#134793,#134794,#134795,#134796,#134797,#134798,#134799,
#134800,#134801,#134802,#134803,#134804,#134805,#134806,#134807,#134808,
#134809,#134810,#134811,#134812,#134813,#134814,#134815,#134816,#134817,
#134818,#134819,#134820,#134821,#134822,#134823,#134824,#134825),
 .UNSPECIFIED.,.F.,.F.,(4,3,3,3,3,3,3,3,3,3,3,3,3,3,3,3,3,3,3,3,3,3,3,3,
3,3,3,3,3,3,3,3,3,3,3,3,3,3,3,3,3,3,3,3,3,3,3,3,3,3,3,3,3,3,3,3,3,3,3,3,
3,3,3,3,3,3,3,3,3,3,3,3,3,4),(1617.92021659891,1618.00342250642,1618.08652728227,
1618.16955157317,1618.25251594955,1618.33544933007,1618.41836898947,1618.50129346078,
1618.58424127696,1618.6672785596,1618.75036549745,1618.83357605855,1618.88063613734,
1618.96437484919,1619.04801036055,1619.13156280395,1619.2150522398,1619.29850619042,
1619.38194268426,1619.46537979402,1619.54883558894,1619.63238008167,1619.71596916461,
1619.79969243216,1619.88037214806,1619.96411085991,1620.04774637127,1620.13129881467,
1620.21478825052,1620.29824220114,1620.38167869498,1620.46511580474,1620.54857159966,
1620.63211609239,1620.71570517533,1620.79942844288,1620.88010815878,1620.96384687063,
1621.04748238199,1621.13103482539,1621.21452426124,1621.29797821186,1621.3814147057,
1621.46485181546,1621.54830761038,1621.63185210311,1621.71544118605,1621.7991644536,
1621.8798441695,1621.96358288135,1622.04721839271,1622.13077083611,1622.21426027196,
1622.29771422258,1622.38115071642,1622.46458782618,1622.5480436211,1622.63158811383,
1622.71517719677,1622.79890046433,1622.87958018022,1622.96331889207,1623.04695440343,
1623.13050684683,1623.21399628268,1623.2974502333,1623.38088672714,1623.4643238369,
1623.54777963182,1623.63132412455,1623.71491320749,1623.79863647504,1623.87931619094,
1623.9527520866),.UNSPECIFIED.);
#1080=B_SPLINE_CURVE_WITH_KNOTS('',3,(#134826,#134827,#134828,#134829,#134830,
#134831,#134832,#134833,#134834,#134835,#134836,#134837,#134838),
 .UNSPECIFIED.,.F.,.F.,(4,3,3,3,4),(1617.66855023561,1617.75216328162,1617.83590032492,
1617.88090012662,1617.92021659874),.UNSPECIFIED.);
#1081=B_SPLINE_CURVE_WITH_KNOTS('',3,(#134840,#134841,#134842,#134843,#134844,
#134845,#134846,#134847,#134848,#134849),.UNSPECIFIED.,.F.,.F.,(4,3,3,4),
(1617.66895862687,1617.75160822956,1617.83591241415,1617.92021659874),
 .UNSPECIFIED.);
#1082=B_SPLINE_CURVE_WITH_KNOTS('',3,(#134850,#134851,#134852,#134853,#134854,
#134855,#134856,#134857,#134858,#134859,#134860,#134861,#134862,#134863,
#134864,#134865,#134866,#134867,#134868,#134869,#134870,#134871,#134872,
#134873,#134874,#134875,#134876,#134877,#134878,#134879,#134880,#134881,
#134882,#134883,#134884,#134885,#134886,#134887,#134888,#134889,#134890,
#134891,#134892,#134893,#134894,#134895,#134896,#134897,#134898,#134899,
#134900,#134901,#134902,#134903,#134904,#134905,#134906,#134907,#134908,
#134909,#134910,#134911,#134912,#134913,#134914,#134915,#134916,#134917,
#134918,#134919,#134920,#134921,#134922,#134923,#134924,#134925,#134926,
#134927,#134928,#134929,#134930,#134931,#134932,#134933,#134934,#134935,
#134936,#134937,#134938,#134939,#134940,#134941,#134942,#134943,#134944,
#134945,#134946,#134947,#134948,#134949,#134950,#134951,#134952,#134953,
#134954,#134955,#134956,#134957,#134958,#134959,#134960,#134961,#134962,
#134963,#134964,#134965,#134966,#134967,#134968,#134969,#134970,#134971,
#134972,#134973,#134974,#134975,#134976,#134977,#134978,#134979,#134980,
#134981,#134982,#134983,#134984,#134985,#134986,#134987,#134988,#134989,
#134990,#134991,#134992,#134993,#134994,#134995,#134996,#134997,#134998,
#134999,#135000,#135001,#135002,#135003,#135004,#135005,#135006,#135007,
#135008,#135009,#135010,#135011,#135012,#135013,#135014,#135015,#135016,
#135017,#135018,#135019,#135020,#135021,#135022,#135023,#135024,#135025,
#135026,#135027,#135028,#135029,#135030,#135031,#135032,#135033,#135034,
#135035,#135036,#135037,#135038,#135039,#135040,#135041,#135042,#135043,
#135044,#135045,#135046,#135047,#135048,#135049,#135050,#135051,#135052,
#135053,#135054,#135055,#135056,#135057,#135058,#135059,#135060,#135061,
#135062,#135063,#135064,#135065,#135066),.UNSPECIFIED.,.F.,.F.,(4,3,3,3,
3,3,3,3,3,3,3,3,3,3,3,3,3,3,3,3,3,3,3,3,3,3,3,3,3,3,3,3,3,3,3,3,3,3,3,3,
3,3,3,3,3,3,3,3,3,3,3,3,3,3,3,3,3,3,3,3,3,3,3,3,3,3,3,3,3,3,3,3,4),(1617.92021659892,
1618.02434059583,1618.13030678927,1618.19119074634,1618.27492945819,1618.35856496955,
1618.44211741295,1618.5256068488,1618.60906079941,1618.69249729326,1618.77593440302,
1618.85939019793,1618.94293469066,1619.0265237736,1619.11024704116,1619.19092675706,
1619.27466546891,1619.35830098027,1619.44185342367,1619.52534285952,1619.60879681014,
1619.69223330398,1619.77567041374,1619.85912620866,1619.94267070138,1620.02625978433,
1620.10998305188,1620.19066276778,1620.27440147963,1620.35803699099,1620.44158943439,
1620.52507887024,1620.60853282086,1620.6919693147,1620.77540642446,1620.85886221938,
1620.94240671211,1621.02599579505,1621.10971906261,1621.1903987785,1621.27413749035,
1621.35777300171,1621.44132544511,1621.52481488096,1621.60826883158,1621.69170532542,
1621.77514243518,1621.8585982301,1621.94214272282,1622.02573180577,1622.10945507332,
1622.19013478922,1622.27387350107,1622.35750901243,1622.44106145583,1622.52455089168,
1622.6080048423,1622.69144133614,1622.7748784459,1622.85833424082,1622.94187873355,
1623.02546781649,1623.10919108405,1623.18987079994,1623.27362409456,1623.35838895161,
1623.44193270565,1623.5254185924,1623.60886473297,1623.69458428748,1623.77802358541,
1623.86488326821,1623.95174295101),.UNSPECIFIED.);
#1083=B_SPLINE_CURVE_WITH_KNOTS('',3,(#135072,#135073,#135074,#135075,#135076,
#135077,#135078,#135079,#135080,#135081,#135082,#135083,#135084,#135085,
#135086,#135087,#135088,#135089,#135090,#135091,#135092,#135093,#135094,
#135095,#135096,#135097,#135098,#135099,#135100,#135101,#135102,#135103,
#135104,#135105,#135106,#135107,#135108,#135109,#135110,#135111,#135112,
#135113,#135114,#135115,#135116,#135117,#135118,#135119,#135120,#135121,
#135122,#135123,#135124,#135125,#135126,#135127,#135128,#135129,#135130,
#135131,#135132,#135133,#135134,#135135,#135136,#135137,#135138,#135139,
#135140,#135141,#135142,#135143,#135144,#135145,#135146,#135147,#135148,
#135149,#135150,#135151,#135152,#135153,#135154,#135155,#135156,#135157,
#135158,#135159,#135160,#135161,#135162,#135163,#135164,#135165,#135166,
#135167,#135168,#135169,#135170,#135171,#135172,#135173,#135174,#135175,
#135176,#135177,#135178,#135179,#135180,#135181,#135182,#135183,#135184,
#135185,#135186,#135187,#135188,#135189,#135190,#135191,#135192,#135193,
#135194,#135195,#135196,#135197,#135198,#135199,#135200,#135201,#135202,
#135203,#135204,#135205,#135206,#135207,#135208,#135209,#135210,#135211,
#135212,#135213,#135214,#135215,#135216,#135217,#135218,#135219,#135220,
#135221,#135222,#135223,#135224,#135225,#135226,#135227,#135228,#135229,
#135230,#135231,#135232,#135233,#135234,#135235,#135236,#135237,#135238,
#135239,#135240,#135241,#135242,#135243,#135244,#135245,#135246,#135247,
#135248,#135249,#135250,#135251,#135252,#135253,#135254,#135255,#135256,
#135257,#135258,#135259,#135260,#135261,#135262,#135263,#135264,#135265,
#135266,#135267,#135268,#135269,#135270,#135271,#135272,#135273,#135274,
#135275,#135276,#135277,#135278,#135279,#135280,#135281,#135282,#135283,
#135284,#135285,#135286,#135287,#135288,#135289,#135290,#135291),
 .UNSPECIFIED.,.F.,.F.,(4,3,3,3,3,3,3,3,3,3,3,3,3,3,3,3,3,3,3,3,3,3,3,3,
3,3,3,3,3,3,3,3,3,3,3,3,3,3,3,3,3,3,3,3,3,3,3,3,3,3,3,3,3,3,3,3,3,3,3,3,
3,3,3,3,3,3,3,3,3,3,3,3,3,4),(1624.20340190592,1624.28785819289,1624.371102368,
1624.45434756165,1624.53761197112,1624.62297202876,1624.70637537919,1624.79271379042,
1624.87905220166,1624.96279091351,1625.04642642487,1625.12997886827,1625.21346830412,
1625.29692225474,1625.38035874858,1625.46379585834,1625.54725165326,1625.63079614599,
1625.71438522893,1625.79810849648,1625.87878821238,1625.96252692423,1626.04616243559,
1626.12971487899,1626.21320431484,1626.29665826546,1626.3800947593,1626.46353186906,
1626.54698766398,1626.63053215671,1626.71412123965,1626.79784450721,1626.8785242231,
1626.96226293495,1627.04589844631,1627.12945088971,1627.21294032556,1627.29639427618,
1627.37983077002,1627.46326787978,1627.5467236747,1627.63026816742,1627.71385725037,
1627.79758051792,1627.87826023382,1627.96199894567,1628.04563445703,1628.12918690043,
1628.21267633628,1628.2961302869,1628.37956678074,1628.4630038905,1628.54645968542,
1628.63000417815,1628.71359326109,1628.79731652864,1628.87799624454,1628.96173495639,
1629.04537046775,1629.12892291115,1629.212412347,1629.29586629762,1629.37930279146,
1629.46273990122,1629.54619569613,1629.62974018886,1629.7133292718,1629.79705253936,
1629.87773225526,1629.96253266822,1630.04718562312,1630.13175281295,1630.21623392709,
1630.23592963608),.UNSPECIFIED.);
#1084=B_SPLINE_CURVE_WITH_KNOTS('',3,(#135292,#135293,#135294,#135295,#135296,
#135297,#135298,#135299,#135300,#135301),.UNSPECIFIED.,.F.,.F.,(4,3,3,4),
(1623.9527520866,1624.05174031403,1624.1497797886,1624.20340190574),
 .UNSPECIFIED.);
#1085=B_SPLINE_CURVE_WITH_KNOTS('',3,(#135303,#135304,#135305,#135306,#135307,
#135308,#135309,#135310,#135311,#135312,#135313,#135314,#135315),
 .UNSPECIFIED.,.F.,.F.,(4,3,3,3,4),(1623.95174295101,1624.03533854297,1624.11906535509,
1624.18960681066,1624.20340190592),.UNSPECIFIED.);
#1086=B_SPLINE_CURVE_WITH_KNOTS('',3,(#135316,#135317,#135318,#135319,#135320,
#135321,#135322,#135323,#135324,#135325,#135326,#135327,#135328,#135329,
#135330,#135331,#135332,#135333,#135334,#135335,#135336,#135337,#135338,
#135339,#135340,#135341,#135342,#135343,#135344,#135345,#135346,#135347,
#135348,#135349,#135350,#135351,#135352,#135353,#135354,#135355,#135356,
#135357,#135358,#135359,#135360,#135361,#135362,#135363,#135364,#135365,
#135366,#135367,#135368,#135369,#135370,#135371,#135372,#135373,#135374,
#135375,#135376,#135377,#135378,#135379,#135380,#135381,#135382,#135383,
#135384,#135385,#135386,#135387,#135388,#135389,#135390,#135391,#135392,
#135393,#135394,#135395,#135396,#135397,#135398,#135399,#135400,#135401,
#135402,#135403,#135404,#135405,#135406,#135407,#135408,#135409,#135410,
#135411,#135412,#135413,#135414,#135415,#135416,#135417,#135418,#135419,
#135420,#135421,#135422,#135423,#135424,#135425,#135426,#135427,#135428,
#135429,#135430,#135431,#135432,#135433,#135434,#135435,#135436,#135437,
#135438,#135439,#135440,#135441,#135442,#135443,#135444,#135445,#135446,
#135447,#135448,#135449,#135450,#135451,#135452,#135453,#135454,#135455,
#135456,#135457,#135458,#135459,#135460,#135461,#135462,#135463,#135464,
#135465,#135466,#135467,#135468,#135469,#135470,#135471,#135472,#135473,
#135474,#135475,#135476,#135477,#135478,#135479,#135480,#135481,#135482,
#135483,#135484,#135485,#135486,#135487,#135488,#135489,#135490,#135491,
#135492,#135493,#135494,#135495,#135496,#135497,#135498,#135499,#135500,
#135501,#135502,#135503,#135504,#135505,#135506,#135507,#135508,#135509,
#135510,#135511,#135512,#135513,#135514,#135515,#135516,#135517,#135518,
#135519,#135520,#135521,#135522,#135523,#135524,#135525,#135526,#135527,
#135528,#135529,#135530,#135531,#135532,#135533,#135534,#135535),
 .UNSPECIFIED.,.F.,.F.,(4,3,3,3,3,3,3,3,3,3,3,3,3,3,3,3,3,3,3,3,3,3,3,3,
3,3,3,3,3,3,3,3,3,3,3,3,3,3,3,3,3,3,3,3,3,3,3,3,3,3,3,3,3,3,3,3,3,3,3,3,
3,3,3,3,3,3,3,3,3,3,3,3,3,4),(1624.20340190605,1624.28693851179,1624.37037225623,
1624.45372348263,1624.53701246057,1624.62026714213,1624.70350544141,1624.78674561904,
1624.87000593319,1624.95335509251,1625.03675050512,1625.12027638167,1625.18934282138,
1625.27308153323,1625.35671704459,1625.44026948799,1625.52375892384,1625.60721287446,
1625.6906493683,1625.77408647806,1625.85754227297,1625.9410867657,1626.02467584864,
1626.1083991162,1626.1890788321,1626.27281754395,1626.35645305531,1626.44000549871,
1626.52349493456,1626.60694888517,1626.69038537902,1626.77382248878,1626.85727828369,
1626.94082277642,1627.02441185936,1627.10813512692,1627.18881484282,1627.27255355467,
1627.35618906603,1627.43974150943,1627.52323094528,1627.6066848959,1627.69012138974,
1627.7735584995,1627.85701429442,1627.94055878715,1628.02414787009,1628.10787113765,
1628.18855085354,1628.27228956539,1628.35592507675,1628.43947752015,1628.522966956,
1628.60642090662,1628.68985740046,1628.77329451022,1628.85675030514,1628.94029479787,
1629.02388388081,1629.10760714836,1629.18828686426,1629.27202557611,1629.35566108747,
1629.43921353087,1629.52270296673,1629.60615691734,1629.68959341119,1629.77303052094,
1629.85648631586,1629.94003080859,1630.02361989153,1630.10734315909,1630.18802287498,
1630.23580470972),.UNSPECIFIED.);
#1087=B_SPLINE_CURVE_WITH_KNOTS('',3,(#135541,#135542,#135543,#135544,#135545,
#135546,#135547,#135548,#135549,#135550,#135551,#135552,#135553,#135554,
#135555,#135556,#135557,#135558,#135559,#135560,#135561,#135562,#135563,
#135564,#135565,#135566,#135567,#135568,#135569,#135570,#135571,#135572,
#135573,#135574,#135575,#135576,#135577,#135578,#135579,#135580,#135581,
#135582,#135583,#135584,#135585,#135586,#135587,#135588,#135589,#135590,
#135591,#135592,#135593,#135594,#135595,#135596,#135597,#135598,#135599,
#135600,#135601,#135602,#135603,#135604,#135605,#135606,#135607,#135608,
#135609,#135610,#135611,#135612,#135613,#135614,#135615,#135616,#135617,
#135618,#135619,#135620,#135621,#135622,#135623,#135624,#135625,#135626,
#135627,#135628,#135629,#135630,#135631,#135632,#135633,#135634,#135635,
#135636,#135637,#135638,#135639,#135640,#135641,#135642,#135643,#135644,
#135645,#135646,#135647,#135648,#135649,#135650,#135651,#135652,#135653,
#135654,#135655,#135656,#135657,#135658,#135659,#135660,#135661,#135662,
#135663,#135664,#135665,#135666,#135667,#135668,#135669,#135670,#135671,
#135672,#135673,#135674,#135675,#135676,#135677,#135678,#135679,#135680,
#135681,#135682,#135683,#135684,#135685,#135686,#135687,#135688,#135689,
#135690,#135691,#135692,#135693,#135694,#135695,#135696,#135697,#135698,
#135699,#135700,#135701,#135702,#135703,#135704,#135705,#135706,#135707,
#135708,#135709,#135710,#135711,#135712,#135713,#135714,#135715,#135716,
#135717,#135718,#135719,#135720,#135721,#135722,#135723,#135724,#135725,
#135726,#135727,#135728,#135729,#135730,#135731,#135732,#135733,#135734,
#135735,#135736,#135737,#135738,#135739,#135740,#135741,#135742,#135743,
#135744,#135745,#135746,#135747,#135748,#135749,#135750,#135751,#135752,
#135753,#135754,#135755,#135756,#135757,#135758,#135759,#135760),
 .UNSPECIFIED.,.F.,.F.,(4,3,3,3,3,3,3,3,3,3,3,3,3,3,3,3,3,3,3,3,3,3,3,3,
3,3,3,3,3,3,3,3,3,3,3,3,3,3,3,3,3,3,3,3,3,3,3,3,3,3,3,3,3,3,3,3,3,3,3,3,
3,3,3,3,3,3,3,3,3,3,3,3,3,4),(1630.48658721329,1630.57923050421,1630.67241058499,
1630.76586966149,1630.85967611113,1630.87746826598,1630.96120697783,1631.0448424892,
1631.1283949326,1631.21188436845,1631.29533831906,1631.37877481291,1631.46221192267,
1631.54566771758,1631.62921221032,1631.71280129326,1631.79652456082,1631.8772042767,
1631.96094298855,1632.04457849991,1632.12813094331,1632.21162037916,1632.29507432978,
1632.37851082362,1632.46194793338,1632.5454037283,1632.62894822102,1632.71253730397,
1632.79626057152,1632.87694028742,1632.96067899927,1633.04431451063,1633.12786695403,
1633.21135638988,1633.2948103405,1633.37824683434,1633.4616839441,1633.54513973901,
1633.62868423174,1633.71227331469,1633.79599658224,1633.87667629814,1633.96041500999,
1634.04405052135,1634.12760296475,1634.2110924006,1634.29454635122,1634.37798284506,
1634.46141995482,1634.54487574974,1634.62842024247,1634.71200932541,1634.79573259296,
1634.87641230886,1634.96015102071,1635.04378653207,1635.12733897547,1635.21082841132,
1635.29428236194,1635.37771885578,1635.46115596554,1635.54461176045,1635.62815625318,
1635.71174533612,1635.79546860368,1635.87614831958,1635.95878444239,1636.0413259703,
1636.1237920081,1636.20620159154,1636.28858318972,1636.37094650471,1636.45333691255,
1636.51794311402),.UNSPECIFIED.);
#1088=B_SPLINE_CURVE_WITH_KNOTS('',3,(#135761,#135762,#135763,#135764,#135765,
#135766,#135767,#135768,#135769,#135770),.UNSPECIFIED.,.F.,.F.,(4,3,3,4),
(1630.23592963608,1630.32033661955,1630.40471644067,1630.4865872131),
 .UNSPECIFIED.);
#1089=B_SPLINE_CURVE_WITH_KNOTS('',3,(#135772,#135773,#135774,#135775,#135776,
#135777,#135778,#135779,#135780,#135781),.UNSPECIFIED.,.F.,.F.,(4,3,3,4),
(1630.23580470972,1630.33778215448,1630.43849155912,1630.48658721296),
 .UNSPECIFIED.);
#1090=B_SPLINE_CURVE_WITH_KNOTS('',3,(#135782,#135783,#135784,#135785,#135786,
#135787,#135788,#135789,#135790,#135791,#135792,#135793,#135794,#135795,
#135796,#135797,#135798,#135799,#135800,#135801,#135802,#135803,#135804,
#135805,#135806,#135807,#135808,#135809,#135810,#135811,#135812,#135813,
#135814,#135815,#135816,#135817,#135818,#135819,#135820,#135821,#135822,
#135823,#135824,#135825,#135826,#135827,#135828,#135829,#135830,#135831,
#135832,#135833,#135834,#135835,#135836,#135837,#135838,#135839,#135840,
#135841,#135842,#135843,#135844,#135845,#135846,#135847,#135848,#135849,
#135850,#135851,#135852,#135853,#135854,#135855,#135856,#135857,#135858,
#135859,#135860,#135861,#135862,#135863,#135864,#135865,#135866,#135867,
#135868,#135869,#135870,#135871,#135872,#135873,#135874,#135875,#135876,
#135877,#135878,#135879,#135880,#135881,#135882,#135883,#135884,#135885,
#135886,#135887,#135888,#135889,#135890,#135891,#135892,#135893,#135894,
#135895,#135896,#135897,#135898,#135899,#135900,#135901,#135902,#135903,
#135904,#135905,#135906,#135907,#135908,#135909,#135910,#135911,#135912,
#135913,#135914,#135915,#135916,#135917,#135918,#135919,#135920,#135921,
#135922,#135923,#135924,#135925,#135926,#135927,#135928,#135929,#135930,
#135931,#135932,#135933,#135934,#135935,#135936,#135937,#135938,#135939,
#135940,#135941,#135942,#135943,#135944,#135945,#135946,#135947,#135948,
#135949,#135950,#135951,#135952,#135953,#135954,#135955,#135956,#135957,
#135958,#135959,#135960,#135961,#135962,#135963,#135964,#135965,#135966,
#135967,#135968,#135969,#135970,#135971,#135972,#135973,#135974,#135975,
#135976,#135977,#135978,#135979,#135980,#135981,#135982,#135983,#135984,
#135985,#135986,#135987,#135988,#135989,#135990,#135991,#135992,#135993,
#135994,#135995,#135996,#135997,#135998,#135999,#136000,#136001),
 .UNSPECIFIED.,.F.,.F.,(4,3,3,3,3,3,3,3,3,3,3,3,3,3,3,3,3,3,3,3,3,3,3,3,
3,3,3,3,3,3,3,3,3,3,3,3,3,3,3,3,3,3,3,3,3,3,3,3,3,3,3,3,3,3,3,3,3,3,3,3,
3,3,3,3,3,3,3,3,3,3,3,3,3,4),(1630.4865872131,1630.56954378974,1630.65247615085,
1630.73539924177,1630.8183315628,1630.90129161728,1630.9843453147,1631.06745247754,
1631.15068316703,1631.1877588857,1631.27149759755,1631.35513310891,1631.43868555231,
1631.52217498816,1631.60562893877,1631.68906543262,1631.77250254237,1631.85595833729,
1631.93950283002,1632.02309191296,1632.10681518052,1632.18749489642,1632.27123360827,
1632.35486911963,1632.43842156303,1632.52191099888,1632.6053649495,1632.68880144334,
1632.7722385531,1632.85569434801,1632.93923884074,1633.02282792368,1633.10655119124,
1633.18723090714,1633.27096961899,1633.35460513035,1633.43815757375,1633.5216470096,
1633.60510096022,1633.68853745406,1633.77197456382,1633.85543035874,1633.93897485147,
1634.02256393441,1634.10628720197,1634.18696691786,1634.27070562971,1634.35434114107,
1634.43789358447,1634.52138302032,1634.60483697094,1634.68827346478,1634.77171057454,
1634.85516636946,1634.93871086218,1635.02229994513,1635.10602321268,1635.18670292858,
1635.27044164043,1635.35407715179,1635.43762959519,1635.52111903104,1635.60457298166,
1635.6880094755,1635.77144658526,1635.85490238018,1635.93844687291,1636.02203595585,
1636.10575922341,1636.1864389393,1636.27180414311,1636.35706341973,1636.44220161961,
1636.51922016046),.UNSPECIFIED.);
#1091=B_SPLINE_CURVE_WITH_KNOTS('',3,(#136007,#136008,#136009,#136010,#136011,
#136012,#136013,#136014,#136015,#136016,#136017,#136018,#136019,#136020,
#136021,#136022,#136023,#136024,#136025,#136026,#136027,#136028,#136029,
#136030,#136031,#136032,#136033,#136034,#136035,#136036,#136037,#136038,
#136039,#136040,#136041,#136042,#136043,#136044,#136045,#136046,#136047,
#136048,#136049,#136050,#136051,#136052,#136053,#136054,#136055,#136056,
#136057,#136058,#136059,#136060,#136061,#136062,#136063,#136064,#136065,
#136066,#136067,#136068,#136069,#136070,#136071,#136072,#136073,#136074,
#136075,#136076,#136077,#136078,#136079,#136080,#136081,#136082,#136083,
#136084,#136085,#136086,#136087,#136088,#136089,#136090,#136091,#136092,
#136093,#136094,#136095,#136096,#136097,#136098,#136099,#136100,#136101,
#136102,#136103,#136104,#136105,#136106,#136107,#136108,#136109,#136110,
#136111,#136112,#136113,#136114,#136115,#136116,#136117,#136118,#136119,
#136120,#136121,#136122,#136123,#136124,#136125,#136126,#136127,#136128,
#136129,#136130,#136131,#136132,#136133,#136134,#136135,#136136,#136137,
#136138,#136139,#136140,#136141,#136142,#136143,#136144,#136145,#136146,
#136147,#136148,#136149,#136150,#136151,#136152,#136153,#136154,#136155,
#136156,#136157,#136158,#136159,#136160,#136161,#136162,#136163,#136164,
#136165,#136166,#136167,#136168,#136169,#136170,#136171,#136172,#136173,
#136174,#136175,#136176,#136177,#136178,#136179,#136180,#136181,#136182,
#136183,#136184,#136185,#136186,#136187,#136188,#136189,#136190,#136191,
#136192,#136193,#136194,#136195,#136196,#136197,#136198,#136199,#136200,
#136201,#136202,#136203,#136204,#136205,#136206,#136207,#136208,#136209,
#136210,#136211,#136212,#136213,#136214,#136215,#136216,#136217,#136218,
#136219,#136220,#136221,#136222,#136223),.UNSPECIFIED.,.F.,.F.,(4,3,3,3,
3,3,3,3,3,3,3,3,3,3,3,3,3,3,3,3,3,3,3,3,3,3,3,3,3,3,3,3,3,3,3,3,3,3,3,3,
3,3,3,3,3,3,3,3,3,3,3,3,3,3,3,3,3,3,3,3,3,3,3,3,3,3,3,3,3,3,3,3,4),(1636.76977252028,
1636.8758843303,1636.95962304215,1637.04325855351,1637.12681099691,1637.21030043276,
1637.29375438338,1637.37719087722,1637.46062798698,1637.5440837819,1637.62762827463,
1637.71121735757,1637.79494062513,1637.87562034102,1637.95935905287,1638.04299456423,
1638.12654700763,1638.21003644348,1638.2934903941,1638.37692688794,1638.4603639977,
1638.54381979262,1638.62736428535,1638.71095336829,1638.79467663584,1638.87535635174,
1638.95909506359,1639.04273057495,1639.12628301835,1639.2097724542,1639.29322640482,
1639.37666289866,1639.46010000842,1639.54355580334,1639.62710029607,1639.71068937901,
1639.79441264657,1639.87509236246,1639.95883107431,1640.04246658567,1640.12601902907,
1640.20950846492,1640.29296241554,1640.37639890938,1640.45983601914,1640.54329181406,
1640.62683630679,1640.71042538973,1640.79414865728,1640.87482837318,1640.95856708503,
1641.04220259639,1641.12575503979,1641.20924447564,1641.29269842626,1641.3761349201,
1641.45957202986,1641.54302782478,1641.62657231751,1641.71016140045,1641.793884668,
1641.8745643839,1641.95830728885,1642.0419460335,1642.12550075442,1642.21000469894,
1642.29345497268,1642.37688665221,1642.46031780929,1642.54562143462,1642.62914195036,
1642.71533713049,1642.80153231061),.UNSPECIFIED.);
#1092=B_SPLINE_CURVE_WITH_KNOTS('',3,(#136224,#136225,#136226,#136227,#136228,
#136229,#136230,#136231,#136232,#136233),.UNSPECIFIED.,.F.,.F.,(4,3,3,4),
(1636.51794311402,1636.60040733544,1636.68508992779,1636.76977252014),
 .UNSPECIFIED.);
#1093=B_SPLINE_CURVE_WITH_KNOTS('',3,(#136235,#136236,#136237,#136238,#136239,
#136240,#136241,#136242,#136243,#136244),.UNSPECIFIED.,.F.,.F.,(4,3,3,4),
(1636.51922016046,1636.6042164217,1636.68916155776,1636.76977252028),
 .UNSPECIFIED.);
#1094=B_SPLINE_CURVE_WITH_KNOTS('',3,(#136245,#136246,#136247,#136248,#136249,
#136250,#136251,#136252,#136253,#136254,#136255,#136256,#136257,#136258,
#136259,#136260,#136261,#136262,#136263,#136264,#136265,#136266,#136267,
#136268,#136269,#136270,#136271,#136272,#136273,#136274,#136275,#136276,
#136277,#136278,#136279,#136280,#136281,#136282,#136283,#136284,#136285,
#136286,#136287,#136288,#136289,#136290,#136291,#136292,#136293,#136294,
#136295,#136296,#136297,#136298,#136299,#136300,#136301,#136302,#136303,
#136304,#136305,#136306,#136307,#136308,#136309,#136310,#136311,#136312,
#136313,#136314,#136315,#136316,#136317,#136318,#136319,#136320,#136321,
#136322,#136323,#136324,#136325,#136326,#136327,#136328,#136329,#136330,
#136331,#136332,#136333,#136334,#136335,#136336,#136337,#136338,#136339,
#136340,#136341,#136342,#136343,#136344,#136345,#136346,#136347,#136348,
#136349,#136350,#136351,#136352,#136353,#136354,#136355,#136356,#136357,
#136358,#136359,#136360,#136361,#136362,#136363,#136364,#136365,#136366,
#136367,#136368,#136369,#136370,#136371,#136372,#136373,#136374,#136375,
#136376,#136377,#136378,#136379,#136380,#136381,#136382,#136383,#136384,
#136385,#136386,#136387,#136388,#136389,#136390,#136391,#136392,#136393,
#136394,#136395,#136396,#136397,#136398,#136399,#136400,#136401,#136402,
#136403,#136404,#136405,#136406,#136407,#136408,#136409,#136410,#136411,
#136412,#136413,#136414,#136415,#136416,#136417,#136418,#136419,#136420,
#136421,#136422,#136423,#136424,#136425,#136426,#136427,#136428,#136429,
#136430,#136431,#136432,#136433,#136434,#136435,#136436,#136437,#136438,
#136439,#136440,#136441,#136442,#136443,#136444,#136445,#136446,#136447,
#136448,#136449,#136450,#136451,#136452,#136453,#136454,#136455,#136456,
#136457,#136458,#136459,#136460,#136461,#136462,#136463,#136464),
 .UNSPECIFIED.,.F.,.F.,(4,3,3,3,3,3,3,3,3,3,3,3,3,3,3,3,3,3,3,3,3,3,3,3,
3,3,3,3,3,3,3,3,3,3,3,3,3,3,3,3,3,3,3,3,3,3,3,3,3,3,3,3,3,3,3,3,3,3,3,3,
3,3,3,3,3,3,3,3,3,3,3,3,3,4),(1636.76977252044,1636.86091976418,1636.95249675115,
1637.04429371243,1637.13640641277,1637.18617495002,1637.26991366186,1637.35354917323,
1637.43710161663,1637.52059105248,1637.60404500309,1637.68748149694,1637.77091860669,
1637.85437440161,1637.93791889433,1638.02150797727,1638.10523124483,1638.18591096074,
1638.26964967259,1638.35328518395,1638.43683762735,1638.5203270632,1638.60378101382,
1638.68721750766,1638.77065461742,1638.85411041234,1638.93765490507,1639.02124398801,
1639.10496725556,1639.18564697146,1639.26938568331,1639.35302119467,1639.43657363807,
1639.52006307392,1639.60351702454,1639.68695351838,1639.77039062814,1639.85384642306,
1639.93739091579,1640.02097999873,1640.10470326629,1640.18538298218,1640.26912169403,
1640.35275720539,1640.43630964879,1640.51979908464,1640.60325303526,1640.6866895291,
1640.77012663886,1640.85358243378,1640.93712692651,1641.02071600945,1641.104439277,
1641.1851189929,1641.26885770475,1641.35249321611,1641.43604565951,1641.51953509536,
1641.60298904598,1641.68642553982,1641.76986264958,1641.8533184445,1641.93686293723,
1642.02045202017,1642.10417528773,1642.18485500362,1642.26738253516,1642.34981529156,
1642.43217245181,1642.51447312317,1642.59674341669,1642.67899572452,1642.76126760122,
1642.80116341428),.UNSPECIFIED.);
#1095=B_SPLINE_CURVE_WITH_KNOTS('',3,(#136470,#136471,#136472,#136473,#136474,
#136475,#136476,#136477,#136478,#136479,#136480,#136481,#136482,#136483,
#136484,#136485,#136486,#136487,#136488,#136489,#136490,#136491,#136492,
#136493,#136494,#136495,#136496,#136497,#136498,#136499,#136500,#136501,
#136502,#136503,#136504,#136505,#136506,#136507,#136508,#136509,#136510,
#136511,#136512,#136513,#136514,#136515,#136516,#136517,#136518,#136519,
#136520,#136521,#136522,#136523,#136524,#136525,#136526,#136527,#136528,
#136529,#136530,#136531,#136532,#136533,#136534,#136535,#136536,#136537,
#136538,#136539,#136540,#136541,#136542,#136543,#136544,#136545,#136546,
#136547,#136548,#136549,#136550,#136551,#136552,#136553,#136554,#136555,
#136556,#136557,#136558,#136559,#136560,#136561,#136562,#136563,#136564,
#136565,#136566,#136567,#136568,#136569,#136570,#136571,#136572,#136573,
#136574,#136575,#136576,#136577,#136578,#136579,#136580,#136581,#136582,
#136583,#136584,#136585,#136586,#136587,#136588,#136589,#136590,#136591,
#136592,#136593,#136594,#136595,#136596,#136597,#136598,#136599,#136600,
#136601,#136602,#136603,#136604,#136605,#136606,#136607,#136608,#136609,
#136610,#136611,#136612,#136613,#136614,#136615,#136616,#136617,#136618,
#136619,#136620,#136621,#136622,#136623,#136624,#136625,#136626,#136627,
#136628,#136629,#136630,#136631,#136632,#136633,#136634,#136635,#136636,
#136637,#136638,#136639,#136640,#136641,#136642,#136643,#136644,#136645,
#136646,#136647,#136648,#136649,#136650,#136651,#136652,#136653,#136654,
#136655,#136656,#136657,#136658,#136659,#136660,#136661,#136662,#136663,
#136664,#136665,#136666,#136667,#136668,#136669,#136670,#136671,#136672,
#136673,#136674,#136675,#136676,#136677,#136678,#136679,#136680,#136681,
#136682,#136683,#136684,#136685,#136686,#136687,#136688,#136689),
 .UNSPECIFIED.,.F.,.F.,(4,3,3,3,3,3,3,3,3,3,3,3,3,3,3,3,3,3,3,3,3,3,3,3,
3,3,3,3,3,3,3,3,3,3,3,3,3,3,3,3,3,3,3,3,3,3,3,3,3,3,3,3,3,3,3,3,3,3,3,3,
3,3,3,3,3,3,3,3,3,3,3,3,3,4),(1643.05295782762,1643.13532116623,1643.21760960656,
1643.29984767325,1643.38205948382,1643.4642640775,1643.54648048541,1643.62877814426,
1643.71111604496,1643.79358468629,1643.87403640534,1643.95777511719,1644.04141062855,
1644.12496307195,1644.2084525078,1644.29190645842,1644.37534295227,1644.45878006202,
1644.54223585694,1644.62578034967,1644.70936943261,1644.79309270017,1644.87377241606,
1644.95751112791,1645.04114663927,1645.12469908267,1645.20818851852,1645.29164246914,
1645.37507896298,1645.45851607274,1645.54197186766,1645.62551636039,1645.70910544333,
1645.79282871089,1645.87350842678,1645.95724713863,1646.04088264999,1646.12443509339,
1646.20792452924,1646.29137847986,1646.3748149737,1646.45825208346,1646.54170787837,
1646.6252523711,1646.70884145404,1646.7925647216,1646.8732444375,1646.95698314935,
1647.04061866071,1647.12417110411,1647.20766053996,1647.29111449058,1647.37455098442,
1647.45798809418,1647.5414438891,1647.62498838183,1647.70857746477,1647.79230073233,
1647.87298044822,1647.95671916007,1648.04035467143,1648.12390711483,1648.20739655068,
1648.29085050129,1648.37428699514,1648.45772410489,1648.54117989981,1648.62472439254,
1648.70831347548,1648.79203674304,1648.87271645894,1648.96236005017,1649.05178443656,
1649.08584175472),.UNSPECIFIED.);
#1096=B_SPLINE_CURVE_WITH_KNOTS('',3,(#136690,#136691,#136692,#136693,#136694,
#136695,#136696,#136697,#136698,#136699),.UNSPECIFIED.,.F.,.F.,(4,3,3,4),
(1642.80153231061,1642.87430039462,1643.00204117945,1643.05295782746),
 .UNSPECIFIED.);
#1097=B_SPLINE_CURVE_WITH_KNOTS('',3,(#136701,#136702,#136703,#136704,#136705,
#136706,#136707,#136708,#136709,#136710),.UNSPECIFIED.,.F.,.F.,(4,3,3,4),
(1642.80116341428,1642.88350269748,1642.96823026241,1643.05295782733),
 .UNSPECIFIED.);
#1098=B_SPLINE_CURVE_WITH_KNOTS('',3,(#136711,#136712,#136713,#136714,#136715,
#136716,#136717,#136718,#136719,#136720,#136721,#136722,#136723,#136724,
#136725,#136726,#136727,#136728,#136729,#136730,#136731,#136732,#136733,
#136734,#136735,#136736,#136737,#136738,#136739,#136740,#136741,#136742,
#136743,#136744,#136745,#136746,#136747,#136748,#136749,#136750,#136751,
#136752,#136753,#136754,#136755,#136756,#136757,#136758,#136759,#136760,
#136761,#136762,#136763,#136764,#136765,#136766,#136767,#136768,#136769,
#136770,#136771,#136772,#136773,#136774,#136775,#136776,#136777,#136778,
#136779,#136780,#136781,#136782,#136783,#136784,#136785,#136786,#136787,
#136788,#136789,#136790,#136791,#136792,#136793,#136794,#136795,#136796,
#136797,#136798,#136799,#136800,#136801,#136802,#136803,#136804,#136805,
#136806,#136807,#136808,#136809,#136810,#136811,#136812,#136813,#136814,
#136815,#136816,#136817,#136818,#136819,#136820,#136821,#136822,#136823,
#136824,#136825,#136826,#136827,#136828,#136829,#136830,#136831,#136832,
#136833,#136834,#136835,#136836,#136837,#136838,#136839,#136840,#136841,
#136842,#136843,#136844,#136845,#136846,#136847,#136848,#136849,#136850,
#136851,#136852,#136853,#136854,#136855,#136856,#136857,#136858,#136859,
#136860,#136861,#136862,#136863,#136864,#136865,#136866,#136867,#136868,
#136869,#136870,#136871,#136872,#136873,#136874,#136875,#136876,#136877,
#136878,#136879,#136880,#136881,#136882,#136883,#136884,#136885,#136886,
#136887,#136888,#136889,#136890,#136891,#136892,#136893,#136894,#136895,
#136896,#136897,#136898,#136899,#136900,#136901,#136902,#136903,#136904,
#136905,#136906,#136907,#136908,#136909,#136910,#136911,#136912,#136913,
#136914,#136915,#136916,#136917,#136918,#136919,#136920,#136921,#136922,
#136923,#136924,#136925,#136926,#136927),.UNSPECIFIED.,.F.,.F.,(4,3,3,3,
3,3,3,3,3,3,3,3,3,3,3,3,3,3,3,3,3,3,3,3,3,3,3,3,3,3,3,3,3,3,3,3,3,3,3,3,
3,3,3,3,3,3,3,3,3,3,3,3,3,3,3,3,3,3,3,3,3,3,3,3,3,3,3,3,3,3,3,3,4),(1643.05295782746,
1643.18459101434,1643.26832972619,1643.35196523755,1643.43551768095,1643.5190071168,
1643.60246106742,1643.68589756126,1643.76933467102,1643.85279046593,1643.93633495866,
1644.01992404161,1644.10364730916,1644.18432702506,1644.26806573691,1644.35170124827,
1644.43525369167,1644.51874312752,1644.60219707814,1644.68563357198,1644.76907068174,
1644.85252647666,1644.93607096939,1645.01966005233,1645.10338331988,1645.18406303578,
1645.26780174763,1645.35143725899,1645.43498970239,1645.51847913824,1645.60193308886,
1645.6853695827,1645.76880669246,1645.85226248738,1645.93580698011,1646.01939606305,
1646.1031193306,1646.1837990465,1646.26753775835,1646.35117326971,1646.43472571311,
1646.51821514896,1646.60166909958,1646.68510559342,1646.76854270318,1646.8519984981,
1646.93554299083,1647.01913207377,1647.10285534132,1647.18353505722,1647.26727376907,
1647.35090928043,1647.43446172383,1647.51795115968,1647.6014051103,1647.68484160414,
1647.7682787139,1647.85173450882,1647.93527900155,1648.01886808449,1648.10259135205,
1648.18327106794,1648.26701550462,1648.35065544319,1648.4342110217,1648.51769806414,
1648.60114772603,1648.68457809583,1648.76800724526,1648.85149094862,1648.93500226131,
1649.01861174798,1649.08463270961),.UNSPECIFIED.);
#1099=B_SPLINE_CURVE_WITH_KNOTS('',3,(#136933,#136934,#136935,#136936,#136937,
#136938,#136939,#136940,#136941,#136942,#136943,#136944,#136945,#136946,
#136947,#136948,#136949,#136950,#136951,#136952,#136953,#136954,#136955,
#136956,#136957,#136958,#136959,#136960,#136961,#136962,#136963,#136964,
#136965,#136966,#136967,#136968,#136969,#136970,#136971,#136972,#136973,
#136974,#136975,#136976,#136977,#136978,#136979,#136980,#136981,#136982,
#136983,#136984,#136985,#136986,#136987,#136988,#136989,#136990,#136991,
#136992,#136993,#136994,#136995,#136996,#136997,#136998,#136999,#137000,
#137001,#137002,#137003,#137004,#137005,#137006,#137007,#137008,#137009,
#137010,#137011,#137012,#137013,#137014,#137015,#137016,#137017,#137018,
#137019,#137020,#137021,#137022,#137023,#137024,#137025,#137026,#137027,
#137028,#137029,#137030,#137031,#137032,#137033,#137034,#137035,#137036,
#137037,#137038,#137039,#137040,#137041,#137042,#137043,#137044,#137045,
#137046,#137047,#137048,#137049,#137050,#137051,#137052,#137053,#137054,
#137055,#137056,#137057,#137058,#137059,#137060,#137061,#137062,#137063,
#137064,#137065,#137066,#137067,#137068,#137069,#137070,#137071,#137072,
#137073,#137074,#137075,#137076,#137077,#137078,#137079,#137080,#137081,
#137082,#137083,#137084,#137085,#137086,#137087,#137088,#137089,#137090,
#137091,#137092,#137093,#137094,#137095,#137096,#137097,#137098,#137099,
#137100,#137101,#137102,#137103,#137104,#137105,#137106,#137107,#137108,
#137109,#137110,#137111,#137112,#137113,#137114,#137115,#137116,#137117,
#137118,#137119,#137120,#137121,#137122,#137123,#137124,#137125,#137126,
#137127,#137128,#137129,#137130,#137131,#137132,#137133,#137134,#137135,
#137136,#137137,#137138,#137139,#137140,#137141,#137142,#137143,#137144,
#137145,#137146,#137147,#137148,#137149,#137150,#137151,#137152),
 .UNSPECIFIED.,.F.,.F.,(4,3,3,3,3,3,3,3,3,3,3,3,3,3,3,3,3,3,3,3,3,3,3,3,
3,3,3,3,3,3,3,3,3,3,3,3,3,3,3,3,3,3,3,3,3,3,3,3,3,3,3,3,3,3,3,3,3,3,3,3,
3,3,3,3,3,3,3,3,3,3,3,3,3,4),(1649.33614313464,1649.42233918616,1649.50860824319,
1649.59496282204,1649.68147725306,1649.7680842705,1649.85484863182,1649.87245246966,
1649.95619118151,1650.03982669287,1650.12337913627,1650.20686857212,1650.29032252274,
1650.37375901658,1650.45719612634,1650.54065192126,1650.62419641398,1650.70778549693,
1650.79150876448,1650.87218848038,1650.95592719223,1651.03956270359,1651.12311514699,
1651.20660458284,1651.29005853346,1651.3734950273,1651.45693213706,1651.54038793198,
1651.62393242471,1651.70752150765,1651.79124477521,1651.8719244911,1651.95566320295,
1652.03929871431,1652.12285115771,1652.20634059356,1652.28979454418,1652.37323103802,
1652.45666814778,1652.5401239427,1652.62366843543,1652.70725751837,1652.79098078592,
1652.87166050182,1652.95539921367,1653.03903472503,1653.12258716843,1653.20607660428,
1653.2895305549,1653.37296704874,1653.4564041585,1653.53985995341,1653.62340444614,
1653.70699352908,1653.79071679664,1653.87139651254,1653.95513522439,1654.03877073575,
1654.12232317915,1654.205812615,1654.28926656562,1654.37270305946,1654.45614016922,
1654.53959596414,1654.62314045687,1654.70672953981,1654.79045280737,1654.87113252326,
1654.95391129918,1655.03659172981,1655.11943701868,1655.20197128938,1655.28497208733,
1655.36797288529),.UNSPECIFIED.);
#1100=B_SPLINE_CURVE_WITH_KNOTS('',3,(#137153,#137154,#137155,#137156,#137157,
#137158,#137159,#137160,#137161,#137162),.UNSPECIFIED.,.F.,.F.,(4,3,3,4),
(1649.08584175472,1649.17498599602,1649.26389439352,1649.33614313448),
 .UNSPECIFIED.);
#1101=B_SPLINE_CURVE_WITH_KNOTS('',3,(#137164,#137165,#137166,#137167,#137168,
#137169,#137170,#137171,#137172,#137173,#137174,#137175,#137176),
 .UNSPECIFIED.,.F.,.F.,(4,3,3,3,4),(1649.08463270961,1649.16838434476,1649.18300707866,
1649.32336075287,1649.33614313464),.UNSPECIFIED.);
#1102=B_SPLINE_CURVE_WITH_KNOTS('',3,(#137177,#137178,#137179,#137180,#137181,
#137182,#137183,#137184,#137185,#137186,#137187,#137188,#137189,#137190,
#137191,#137192,#137193,#137194,#137195,#137196,#137197,#137198,#137199,
#137200,#137201,#137202,#137203,#137204,#137205,#137206,#137207,#137208,
#137209,#137210,#137211,#137212,#137213,#137214,#137215,#137216,#137217,
#137218,#137219,#137220,#137221,#137222,#137223,#137224,#137225,#137226,
#137227,#137228,#137229,#137230,#137231,#137232,#137233,#137234,#137235,
#137236,#137237,#137238,#137239,#137240,#137241,#137242,#137243,#137244,
#137245,#137246,#137247,#137248,#137249,#137250,#137251,#137252,#137253,
#137254,#137255,#137256,#137257,#137258,#137259,#137260,#137261,#137262,
#137263,#137264,#137265,#137266,#137267,#137268,#137269,#137270,#137271,
#137272,#137273,#137274,#137275,#137276,#137277,#137278,#137279,#137280,
#137281,#137282,#137283,#137284,#137285,#137286,#137287,#137288,#137289,
#137290,#137291,#137292,#137293,#137294,#137295,#137296,#137297,#137298,
#137299,#137300,#137301,#137302,#137303,#137304,#137305,#137306,#137307,
#137308,#137309,#137310,#137311,#137312,#137313,#137314,#137315,#137316,
#137317,#137318,#137319,#137320,#137321,#137322,#137323,#137324,#137325,
#137326,#137327,#137328,#137329,#137330,#137331,#137332,#137333,#137334,
#137335,#137336,#137337,#137338,#137339,#137340,#137341,#137342,#137343,
#137344,#137345,#137346,#137347,#137348,#137349,#137350,#137351,#137352,
#137353,#137354,#137355,#137356,#137357,#137358,#137359,#137360,#137361,
#137362,#137363,#137364,#137365,#137366,#137367,#137368,#137369,#137370,
#137371,#137372,#137373,#137374,#137375,#137376,#137377,#137378,#137379,
#137380,#137381,#137382,#137383,#137384,#137385,#137386,#137387,#137388,
#137389,#137390,#137391,#137392,#137393,#137394,#137395,#137396),
 .UNSPECIFIED.,.F.,.F.,(4,3,3,3,3,3,3,3,3,3,3,3,3,3,3,3,3,3,3,3,3,3,3,3,
3,3,3,3,3,3,3,3,3,3,3,3,3,3,3,3,3,3,3,3,3,3,3,3,3,3,3,3,3,3,3,3,3,3,3,3,
3,3,3,3,3,3,3,3,3,3,3,3,3,4),(1649.33614313475,1649.4185401776,1649.5008558462,
1649.5860917516,1649.66831531826,1649.75052652388,1649.83274439629,1649.91498796673,
1649.99731983084,1650.07970441643,1650.16220352253,1650.18274308938,1650.26648180123,
1650.35011731259,1650.43366975599,1650.51715919184,1650.60061314246,1650.6840496363,
1650.76748674606,1650.85094254098,1650.93448703371,1651.01807611665,1651.1017993842,
1651.1824791001,1651.26621781195,1651.34985332331,1651.43340576671,1651.51689520256,
1651.60034915318,1651.68378564702,1651.76722275678,1651.8506785517,1651.93422304442,
1652.01781212737,1652.10153539492,1652.18221511082,1652.26595382267,1652.34958933403,
1652.43314177743,1652.51663121328,1652.6000851639,1652.68352165774,1652.7669587675,
1652.85041456242,1652.93395905515,1653.01754813809,1653.10127140564,1653.18195112154,
1653.26568983339,1653.34932534475,1653.43287778815,1653.516367224,1653.59982117462,
1653.68325766846,1653.76669477822,1653.85015057314,1653.93369506587,1654.01728414881,
1654.10100741636,1654.18168713226,1654.26542584411,1654.34906135547,1654.43261379887,
1654.51610323472,1654.59955718534,1654.68299367918,1654.76643078894,1654.84988658386,
1654.93343107659,1655.01702015953,1655.10074342709,1655.18142314298,1655.27521982429,
1655.3690165056),.UNSPECIFIED.);
#1103=B_SPLINE_CURVE_WITH_KNOTS('',3,(#137402,#137403,#137404,#137405,#137406,
#137407,#137408,#137409,#137410,#137411,#137412,#137413,#137414,#137415,
#137416,#137417,#137418,#137419,#137420,#137421,#137422,#137423,#137424,
#137425,#137426,#137427,#137428,#137429,#137430,#137431,#137432,#137433,
#137434,#137435,#137436,#137437,#137438,#137439,#137440,#137441,#137442,
#137443,#137444,#137445,#137446,#137447,#137448,#137449,#137450,#137451,
#137452,#137453,#137454,#137455,#137456,#137457,#137458,#137459,#137460,
#137461,#137462,#137463,#137464,#137465,#137466,#137467,#137468,#137469,
#137470,#137471,#137472,#137473,#137474,#137475,#137476,#137477,#137478,
#137479,#137480,#137481,#137482,#137483,#137484,#137485,#137486,#137487,
#137488,#137489,#137490,#137491,#137492,#137493,#137494,#137495,#137496,
#137497,#137498,#137499,#137500,#137501,#137502,#137503,#137504,#137505,
#137506,#137507,#137508,#137509,#137510,#137511,#137512,#137513,#137514,
#137515,#137516,#137517,#137518,#137519,#137520,#137521,#137522,#137523,
#137524,#137525,#137526,#137527,#137528,#137529,#137530,#137531,#137532,
#137533,#137534,#137535,#137536,#137537,#137538,#137539,#137540,#137541,
#137542,#137543,#137544,#137545,#137546,#137547,#137548,#137549,#137550,
#137551,#137552,#137553,#137554,#137555,#137556,#137557,#137558,#137559,
#137560,#137561,#137562,#137563,#137564,#137565,#137566,#137567,#137568,
#137569,#137570,#137571,#137572,#137573,#137574,#137575,#137576,#137577,
#137578,#137579,#137580,#137581,#137582,#137583,#137584,#137585,#137586,
#137587,#137588,#137589,#137590,#137591,#137592,#137593,#137594,#137595,
#137596,#137597,#137598,#137599,#137600,#137601,#137602,#137603,#137604,
#137605,#137606,#137607,#137608,#137609,#137610,#137611,#137612,#137613,
#137614,#137615,#137616,#137617,#137618,#137619,#137620,#137621),
 .UNSPECIFIED.,.F.,.F.,(4,3,3,3,3,3,3,3,3,3,3,3,3,3,3,3,3,3,3,3,3,3,3,3,
3,3,3,3,3,3,3,3,3,3,3,3,3,3,3,3,3,3,3,3,3,3,3,3,3,3,3,3,3,3,3,3,3,3,3,3,
3,3,3,3,3,3,3,3,3,3,3,3,3,4),(1655.61932844201,1655.72632222295,1655.83568474814,
1655.87086853399,1655.95460724584,1656.0382427572,1656.1217952006,1656.20528463645,
1656.28873858707,1656.37217508092,1656.45561219067,1656.53906798559,1656.62261247832,
1656.70620156126,1656.78992482882,1656.8706045447,1656.95434325655,1657.03797876791,
1657.12153121131,1657.20502064716,1657.28847459778,1657.37191109162,1657.45534820138,
1657.5388039963,1657.62234848903,1657.70593757197,1657.78966083952,1657.87034055543,
1657.95407926728,1658.03771477864,1658.12126722204,1658.2047566579,1658.28821060851,
1658.37164710236,1658.45508421211,1658.53854000703,1658.62208449976,1658.7056735827,
1658.78939685026,1658.87007656615,1658.953815278,1659.03745078936,1659.12100323276,
1659.20449266861,1659.28794661923,1659.37138311307,1659.45482022283,1659.53827601774,
1659.62182051047,1659.70540959341,1659.78913286097,1659.86981257687,1659.95355128872,
1660.03718680008,1660.12073924348,1660.20422867933,1660.28768262995,1660.37111912379,
1660.45455623355,1660.53801202847,1660.6215565212,1660.70514560414,1660.78886887169,
1660.86954858759,1660.95330059649,1661.04049401252,1661.12403534255,1661.20751969612,
1661.29096519257,1661.37438992107,1661.45783300827,1661.54128727818,1661.62479697284,
1661.65084792474),.UNSPECIFIED.);
#1104=B_SPLINE_CURVE_WITH_KNOTS('',3,(#137622,#137623,#137624,#137625,#137626,
#137627,#137628,#137629,#137630,#137631),.UNSPECIFIED.,.F.,.F.,(4,3,3,4),
(1655.36797288529,1655.45047524496,1655.53490184339,1655.61932844182),
 .UNSPECIFIED.);
#1105=B_SPLINE_CURVE_WITH_KNOTS('',3,(#137633,#137634,#137635,#137636,#137637,
#137638,#137639,#137640,#137641,#137642),.UNSPECIFIED.,.F.,.F.,(4,3,3,4),
(1655.3690165056,1655.45942920808,1655.5495389858,1655.61932844169),
 .UNSPECIFIED.);
#1106=B_SPLINE_CURVE_WITH_KNOTS('',3,(#137643,#137644,#137645,#137646,#137647,
#137648,#137649,#137650,#137651,#137652,#137653,#137654,#137655,#137656,
#137657,#137658,#137659,#137660,#137661,#137662,#137663,#137664,#137665,
#137666,#137667,#137668,#137669,#137670,#137671,#137672,#137673,#137674,
#137675,#137676,#137677,#137678,#137679,#137680,#137681,#137682,#137683,
#137684,#137685,#137686,#137687,#137688,#137689,#137690,#137691,#137692,
#137693,#137694,#137695,#137696,#137697,#137698,#137699,#137700,#137701,
#137702,#137703,#137704,#137705,#137706,#137707,#137708,#137709,#137710,
#137711,#137712,#137713,#137714,#137715,#137716,#137717,#137718,#137719,
#137720,#137721,#137722,#137723,#137724,#137725,#137726,#137727,#137728,
#137729,#137730,#137731,#137732,#137733,#137734,#137735,#137736,#137737,
#137738,#137739,#137740,#137741,#137742,#137743,#137744,#137745,#137746,
#137747,#137748,#137749,#137750,#137751,#137752,#137753,#137754,#137755,
#137756,#137757,#137758,#137759,#137760,#137761,#137762,#137763,#137764,
#137765,#137766,#137767,#137768,#137769,#137770,#137771,#137772,#137773,
#137774,#137775,#137776,#137777,#137778,#137779,#137780,#137781,#137782,
#137783,#137784,#137785,#137786,#137787,#137788,#137789,#137790,#137791,
#137792,#137793,#137794,#137795,#137796,#137797,#137798,#137799,#137800,
#137801,#137802,#137803,#137804,#137805,#137806,#137807,#137808,#137809,
#137810,#137811,#137812,#137813,#137814,#137815,#137816,#137817,#137818,
#137819,#137820,#137821,#137822,#137823,#137824,#137825,#137826,#137827,
#137828,#137829,#137830,#137831,#137832,#137833,#137834,#137835,#137836,
#137837,#137838,#137839,#137840,#137841,#137842,#137843,#137844,#137845,
#137846,#137847,#137848,#137849,#137850,#137851,#137852,#137853,#137854,
#137855,#137856,#137857,#137858,#137859,#137860,#137861,#137862),
 .UNSPECIFIED.,.F.,.F.,(4,3,3,3,3,3,3,3,3,3,3,3,3,3,3,3,3,3,3,3,3,3,3,3,
3,3,3,3,3,3,3,3,3,3,3,3,3,3,3,3,3,3,3,3,3,3,3,3,3,3,3,3,3,3,3,3,3,3,3,3,
3,3,3,3,3,3,3,3,3,3,3,3,3,4),(1655.61932844182,1655.70480180458,1655.79032505431,
1655.87591265975,1655.96164121957,1656.04744749123,1656.13341100218,1656.1811591537,
1656.26489786555,1656.34853337691,1656.43208582031,1656.51557525616,1656.59902920678,
1656.68246570062,1656.76590281038,1656.8493586053,1656.93290309803,1657.01649218097,
1657.10021544852,1657.18089516442,1657.26463387627,1657.34826938763,1657.43182183103,
1657.51531126688,1657.5987652175,1657.68220171134,1657.7656388211,1657.84909461602,
1657.93263910875,1658.01622819169,1658.09995145924,1658.18063117514,1658.26436988699,
1658.34800539835,1658.43155784175,1658.5150472776,1658.59850122822,1658.68193772206,
1658.76537483182,1658.84883062674,1658.93237511947,1659.01596420241,1659.09968746996,
1659.18036718586,1659.26410589771,1659.34774140907,1659.43129385247,1659.51478328832,
1659.59823723894,1659.68167373278,1659.76511084254,1659.84856663746,1659.93211113019,
1660.01570021313,1660.09942348068,1660.18010319658,1660.26384190843,1660.34747741979,
1660.43102986319,1660.51451929904,1660.59797324966,1660.6814097435,1660.76484685326,
1660.84830264818,1660.9318471409,1661.01543622385,1661.0991594914,1661.1798392073,
1661.26283883278,1661.34573846742,1661.42854232631,1661.51129049212,1661.59400396625,
1661.65128699969),.UNSPECIFIED.);
#1107=B_SPLINE_CURVE_WITH_KNOTS('',3,(#137868,#137869,#137870,#137871,#137872,
#137873,#137874,#137875,#137876,#137877,#137878,#137879,#137880,#137881,
#137882,#137883,#137884,#137885,#137886,#137887,#137888,#137889,#137890,
#137891,#137892,#137893,#137894,#137895,#137896,#137897,#137898,#137899,
#137900,#137901,#137902,#137903,#137904,#137905,#137906,#137907,#137908,
#137909,#137910,#137911,#137912,#137913,#137914,#137915,#137916,#137917,
#137918,#137919,#137920,#137921,#137922,#137923,#137924,#137925,#137926,
#137927,#137928,#137929,#137930,#137931,#137932,#137933,#137934,#137935,
#137936,#137937,#137938,#137939,#137940,#137941,#137942,#137943,#137944,
#137945,#137946,#137947,#137948,#137949,#137950,#137951,#137952,#137953,
#137954,#137955,#137956,#137957,#137958,#137959,#137960,#137961,#137962,
#137963,#137964,#137965,#137966,#137967,#137968,#137969,#137970,#137971,
#137972,#137973,#137974,#137975,#137976,#137977,#137978,#137979,#137980,
#137981,#137982,#137983,#137984,#137985,#137986,#137987,#137988,#137989,
#137990,#137991,#137992,#137993,#137994,#137995,#137996,#137997,#137998,
#137999,#138000,#138001,#138002,#138003,#138004,#138005,#138006,#138007,
#138008,#138009,#138010,#138011,#138012,#138013,#138014,#138015,#138016,
#138017,#138018,#138019,#138020,#138021,#138022,#138023,#138024,#138025,
#138026,#138027,#138028,#138029,#138030,#138031,#138032,#138033,#138034,
#138035,#138036,#138037,#138038,#138039,#138040,#138041,#138042,#138043,
#138044,#138045,#138046,#138047,#138048,#138049,#138050,#138051,#138052,
#138053,#138054,#138055,#138056,#138057,#138058,#138059,#138060,#138061,
#138062,#138063,#138064,#138065,#138066,#138067,#138068,#138069,#138070,
#138071,#138072,#138073,#138074,#138075,#138076,#138077,#138078,#138079,
#138080,#138081,#138082,#138083,#138084,#138085,#138086,#138087),
 .UNSPECIFIED.,.F.,.F.,(4,3,3,3,3,3,3,3,3,3,3,3,3,3,3,3,3,3,3,3,3,3,3,3,
3,3,3,3,3,3,3,3,3,3,3,3,3,3,3,3,3,3,3,3,3,3,3,3,3,3,3,3,3,3,3,3,3,3,3,3,
3,3,3,3,3,3,3,3,3,3,3,3,3,4),(1661.90251374915,1661.98579347555,1662.06897154049,
1662.15206852732,1662.23510494363,1662.31810946112,1662.40109955002,1662.48409368614,
1662.56711034459,1662.65021628424,1662.73337103092,1662.8166510224,1662.86902060903,
1662.95275932088,1663.03639483224,1663.11994727564,1663.20343671149,1663.2868906621,
1663.37032715595,1663.4537642657,1663.53722006062,1663.62076455335,1663.70435363629,
1663.78807690385,1663.86875661975,1663.9524953316,1664.03613084297,1664.11968328637,
1664.20317272222,1664.28662667284,1664.37006316668,1664.45350027644,1664.53695607136,
1664.62050056409,1664.70408964703,1664.78781291459,1664.86849263047,1664.95223134231,
1665.03586685368,1665.11941929708,1665.20290873293,1665.28636268354,1665.36979917739,
1665.45323628714,1665.53669208206,1665.62023657478,1665.70382565772,1665.78754892528,
1665.86822864119,1665.95196735303,1666.0356028644,1666.11915530779,1666.20264474364,
1666.28609869425,1666.36953518809,1666.45297229784,1666.53642809275,1666.61997258548,
1666.70356166842,1666.78728493597,1666.86796465191,1666.95170336377,1667.03533887515,
1667.11889131856,1667.20238075443,1667.28583470505,1667.36927119891,1667.45270830868,
1667.53616410361,1667.61970859635,1667.70329767931,1667.78702094688,1667.86770066263,
1667.93501912961),.UNSPECIFIED.);
#1108=B_SPLINE_CURVE_WITH_KNOTS('',3,(#138088,#138089,#138090,#138091,#138092,
#138093,#138094,#138095,#138096,#138097,#138098,#138099,#138100),
 .UNSPECIFIED.,.F.,.F.,(4,3,3,3,4),(1661.65084792474,1661.73445666934,1661.81819110253,
1661.86928459831,1661.902513749),.UNSPECIFIED.);
#1109=B_SPLINE_CURVE_WITH_KNOTS('',3,(#138102,#138103,#138104,#138105,#138106,
#138107,#138108,#138109,#138110,#138111),.UNSPECIFIED.,.F.,.F.,(4,3,3,4),
(1661.65128699969,1661.73399004573,1661.81825189737,1661.902513749),
 .UNSPECIFIED.);
#1110=B_SPLINE_CURVE_WITH_KNOTS('',3,(#138112,#138113,#138114,#138115,#138116,
#138117,#138118,#138119,#138120,#138121,#138122,#138123,#138124,#138125,
#138126,#138127,#138128,#138129,#138130,#138131,#138132,#138133,#138134,
#138135,#138136,#138137,#138138,#138139,#138140,#138141,#138142,#138143,
#138144,#138145,#138146,#138147,#138148,#138149,#138150,#138151,#138152,
#138153,#138154,#138155,#138156,#138157,#138158,#138159,#138160,#138161,
#138162,#138163,#138164,#138165,#138166,#138167,#138168,#138169,#138170,
#138171,#138172,#138173,#138174,#138175,#138176,#138177,#138178,#138179,
#138180,#138181,#138182,#138183,#138184,#138185,#138186,#138187,#138188,
#138189,#138190,#138191,#138192,#138193,#138194,#138195,#138196,#138197,
#138198,#138199,#138200,#138201,#138202,#138203,#138204,#138205,#138206,
#138207,#138208,#138209,#138210,#138211,#138212,#138213,#138214,#138215,
#138216,#138217,#138218,#138219,#138220,#138221,#138222,#138223,#138224,
#138225,#138226,#138227,#138228,#138229,#138230,#138231,#138232,#138233,
#138234,#138235,#138236,#138237,#138238,#138239,#138240,#138241,#138242,
#138243,#138244,#138245,#138246,#138247,#138248,#138249,#138250,#138251,
#138252,#138253,#138254,#138255,#138256,#138257,#138258,#138259,#138260,
#138261,#138262,#138263,#138264,#138265,#138266,#138267,#138268,#138269,
#138270,#138271,#138272,#138273,#138274,#138275,#138276,#138277,#138278,
#138279,#138280,#138281,#138282,#138283,#138284,#138285,#138286,#138287,
#138288,#138289,#138290,#138291,#138292,#138293,#138294,#138295,#138296,
#138297,#138298,#138299,#138300,#138301,#138302,#138303,#138304,#138305,
#138306,#138307,#138308,#138309,#138310,#138311,#138312,#138313,#138314,
#138315,#138316,#138317,#138318,#138319,#138320,#138321,#138322,#138323,
#138324,#138325,#138326,#138327,#138328),.UNSPECIFIED.,.F.,.F.,(4,3,3,3,
3,3,3,3,3,3,3,3,3,3,3,3,3,3,3,3,3,3,3,3,3,3,3,3,3,3,3,3,3,3,3,3,3,3,3,3,
3,3,3,3,3,3,3,3,3,3,3,3,3,3,3,3,3,3,3,3,3,3,3,3,3,3,3,3,3,3,3,3,4),(1661.9025137491,
1662.00582469911,1662.11084798141,1662.17957521802,1662.26331392987,1662.34694944123,
1662.43050188463,1662.51399132048,1662.5974452711,1662.68088176494,1662.7643188747,
1662.84777466962,1662.93131916235,1663.01490824529,1663.09863151284,1663.17931122874,
1663.26304994059,1663.34668545195,1663.43023789535,1663.5137273312,1663.59718128182,
1663.68061777566,1663.76405488542,1663.84751068034,1663.93105517306,1664.01464425601,
1664.09836752356,1664.17904723946,1664.26278595131,1664.34642146267,1664.42997390607,
1664.51346334192,1664.59691729254,1664.68035378638,1664.76379089614,1664.84724669106,
1664.93079118379,1665.01438026673,1665.09810353429,1665.17878325018,1665.26252196203,
1665.34615747339,1665.42970991679,1665.51319935264,1665.59665330326,1665.6800897971,
1665.76352690686,1665.84698270178,1665.93052719451,1666.01411627745,1666.097839545,
1666.1785192609,1666.26225797275,1666.34589348411,1666.42944592751,1666.51293536336,
1666.59638931397,1666.67982580782,1666.76326291757,1666.84671871249,1666.93026320522,
1667.01385228816,1667.09757555572,1667.17825527162,1667.26200897232,1667.34601332621,
1667.42955786069,1667.51304424891,1667.59649061251,1667.68087891024,1667.76431701185,
1667.84918040764,1667.93404380343),.UNSPECIFIED.);
#1111=B_SPLINE_CURVE_WITH_KNOTS('',3,(#138334,#138335,#138336,#138337,#138338,
#138339,#138340,#138341,#138342,#138343,#138344,#138345,#138346,#138347,
#138348,#138349,#138350,#138351,#138352,#138353,#138354,#138355,#138356,
#138357,#138358,#138359,#138360,#138361,#138362,#138363,#138364,#138365,
#138366,#138367,#138368,#138369,#138370,#138371,#138372,#138373,#138374,
#138375,#138376,#138377,#138378,#138379,#138380,#138381,#138382,#138383,
#138384,#138385,#138386,#138387,#138388,#138389,#138390,#138391,#138392,
#138393,#138394,#138395,#138396,#138397,#138398,#138399,#138400,#138401,
#138402,#138403,#138404,#138405,#138406,#138407,#138408,#138409,#138410,
#138411,#138412,#138413,#138414,#138415,#138416,#138417,#138418,#138419,
#138420,#138421,#138422,#138423,#138424,#138425,#138426,#138427,#138428,
#138429,#138430,#138431,#138432,#138433,#138434,#138435,#138436,#138437,
#138438,#138439,#138440,#138441,#138442,#138443,#138444,#138445,#138446,
#138447,#138448,#138449,#138450,#138451,#138452,#138453,#138454,#138455,
#138456,#138457,#138458,#138459,#138460,#138461,#138462,#138463,#138464,
#138465,#138466,#138467,#138468,#138469,#138470,#138471,#138472,#138473,
#138474,#138475,#138476,#138477,#138478,#138479,#138480,#138481,#138482,
#138483,#138484,#138485,#138486,#138487,#138488,#138489,#138490,#138491,
#138492,#138493,#138494,#138495,#138496,#138497,#138498,#138499,#138500,
#138501,#138502,#138503,#138504,#138505,#138506,#138507,#138508,#138509,
#138510,#138511,#138512,#138513,#138514,#138515,#138516,#138517,#138518,
#138519,#138520,#138521,#138522,#138523,#138524,#138525,#138526,#138527,
#138528,#138529,#138530,#138531,#138532,#138533,#138534,#138535,#138536,
#138537,#138538,#138539,#138540,#138541,#138542,#138543,#138544,#138545,
#138546,#138547,#138548,#138549,#138550,#138551,#138552,#138553,#138554,
#138555,#138556),.UNSPECIFIED.,.F.,.F.,(4,3,3,3,3,3,3,3,3,3,3,3,3,3,3,3,
3,3,3,3,3,3,3,3,3,3,3,3,3,3,3,3,3,3,3,3,3,3,3,3,3,3,3,3,3,3,3,3,3,3,3,3,
3,3,3,3,3,3,3,3,3,3,3,3,3,3,3,3,3,3,3,3,3,3,4),(1668.18569905618,1668.27091625833,
1668.35407991018,1668.43724227634,1668.52042163574,1668.60717539514,1668.69049092051,
1668.77386693529,1668.85736103574,1668.86743667335,1668.95117538517,1669.03481089652,
1669.11836333989,1669.20185277572,1669.28530672631,1669.36874322014,1669.45218032987,
1669.53563612476,1669.61918061747,1669.70276970039,1669.78649296792,1669.86717268407,
1669.950911396,1670.03454690746,1670.11809935095,1670.20158878688,1670.28504273759,
1670.36847923152,1670.45191634136,1670.53537213637,1670.61891662918,1670.70250571221,
1670.78622897985,1670.86690869479,1670.95064740654,1671.03428291781,1671.11783536111,
1671.20132479686,1671.28477874738,1671.36821524113,1671.45165235079,1671.53510814561,
1671.61865263825,1671.7022417211,1671.78596498857,1671.86664470551,1671.95038341724,
1672.0340189285,1672.11757137178,1672.20106080752,1672.28451475802,1672.36795125175,
1672.45138836139,1672.53484415619,1672.6183886488,1672.70197773162,1672.78570099906,
1672.86638071623,1672.95011942866,1673.0337549406,1673.11730738458,1673.20079682102,
1673.28425077221,1673.36768726663,1673.45112437697,1673.53458017246,1673.61812466576,
1673.70171374926,1673.78543701737,1673.86611672695,1673.95415082145,1674.03893719653,
1674.12363710965,1674.20825020537,1674.21825310493),.UNSPECIFIED.);
#1112=B_SPLINE_CURVE_WITH_KNOTS('',3,(#138557,#138558,#138559,#138560,#138561,
#138562,#138563,#138564,#138565,#138566),.UNSPECIFIED.,.F.,.F.,(4,3,3,4),
(1667.93501912961,1668.03466883892,1668.13330378235,1668.18569905601),
 .UNSPECIFIED.);
#1113=B_SPLINE_CURVE_WITH_KNOTS('',3,(#138568,#138569,#138570,#138571,#138572,
#138573,#138574,#138575,#138576,#138577,#138578,#138579,#138580),
 .UNSPECIFIED.,.F.,.F.,(4,3,3,3,4),(1667.93404380343,1668.01763545707,1668.10136010487,
1668.17799128234,1668.18569905618),.UNSPECIFIED.);
#1114=B_SPLINE_CURVE_WITH_KNOTS('',3,(#138581,#138582,#138583,#138584,#138585,
#138586,#138587,#138588,#138589,#138590,#138591,#138592,#138593,#138594,
#138595,#138596,#138597,#138598,#138599,#138600,#138601,#138602,#138603,
#138604,#138605,#138606,#138607,#138608,#138609,#138610,#138611,#138612,
#138613,#138614,#138615,#138616,#138617,#138618,#138619,#138620,#138621,
#138622,#138623,#138624,#138625,#138626,#138627,#138628,#138629,#138630,
#138631,#138632,#138633,#138634,#138635,#138636,#138637,#138638,#138639,
#138640,#138641,#138642,#138643,#138644,#138645,#138646,#138647,#138648,
#138649,#138650,#138651,#138652,#138653,#138654,#138655,#138656,#138657,
#138658,#138659,#138660,#138661,#138662,#138663,#138664,#138665,#138666,
#138667,#138668,#138669,#138670,#138671,#138672,#138673,#138674,#138675,
#138676,#138677,#138678,#138679,#138680,#138681,#138682,#138683,#138684,
#138685,#138686,#138687,#138688,#138689,#138690,#138691,#138692,#138693,
#138694,#138695,#138696,#138697,#138698,#138699,#138700,#138701,#138702,
#138703,#138704,#138705,#138706,#138707,#138708,#138709,#138710,#138711,
#138712,#138713,#138714,#138715,#138716,#138717,#138718,#138719,#138720,
#138721,#138722,#138723,#138724,#138725,#138726,#138727,#138728,#138729,
#138730,#138731,#138732,#138733,#138734,#138735,#138736,#138737,#138738,
#138739,#138740,#138741,#138742,#138743,#138744,#138745,#138746,#138747,
#138748,#138749,#138750,#138751,#138752,#138753,#138754,#138755,#138756,
#138757,#138758,#138759,#138760,#138761,#138762,#138763,#138764,#138765,
#138766,#138767,#138768,#138769,#138770,#138771,#138772,#138773,#138774,
#138775,#138776,#138777,#138778,#138779,#138780,#138781,#138782,#138783,
#138784,#138785,#138786,#138787,#138788,#138789,#138790,#138791,#138792,
#138793,#138794,#138795,#138796,#138797,#138798,#138799,#138800),
 .UNSPECIFIED.,.F.,.F.,(4,3,3,3,3,3,3,3,3,3,3,3,3,3,3,3,3,3,3,3,3,3,3,3,
3,3,3,3,3,3,3,3,3,3,3,3,3,3,3,3,3,3,3,3,3,3,3,3,3,3,3,3,3,3,3,3,3,3,3,3,
3,3,3,3,3,3,3,3,3,3,3,3,3,4),(1668.18569905633,1668.26932281117,1668.35284349824,
1668.43628137236,1668.51965661534,1668.60299698004,1668.6863204541,1668.76964521919,
1668.85298945409,1668.93642245116,1669.01990095181,1669.10351155826,1669.17772729307,
1669.26146600491,1669.34510151628,1669.42865395967,1669.51214339552,1669.59559734613,
1669.67903383997,1669.76247094972,1669.84592674463,1669.92947123736,1670.0130603203,
1670.09678358785,1670.17746330379,1670.26120201565,1670.34483752703,1670.42838997044,
1670.5118794063,1670.59533335693,1670.67876985079,1670.76220696056,1670.84566275549,
1670.92920724823,1671.01279633118,1671.09651959875,1671.17719931451,1671.26093802634,
1671.3445735377,1671.42812598109,1671.51161541693,1671.59506936753,1671.67850586136,
1671.76194297111,1671.84539876602,1671.92894325873,1672.01253234166,1672.09625560921,
1672.17693532523,1672.26067403705,1672.3443095484,1672.42786199177,1672.5113514276,
1672.59480537819,1672.67824187202,1672.76167898175,1672.84513477664,1672.92867926935,
1673.01226835227,1673.0959916198,1673.17667133595,1673.26041004788,1673.34404555934,
1673.42759800283,1673.51108743876,1673.59454138947,1673.6779778834,1673.76141499324,
1673.84487078825,1673.92841528106,1674.01200436409,1674.09572763173,1674.17640734667,
1674.21806788616),.UNSPECIFIED.);
#1115=B_SPLINE_CURVE_WITH_KNOTS('',3,(#138806,#138807,#138808,#138809,#138810,
#138811,#138812,#138813,#138814,#138815,#138816,#138817,#138818,#138819,
#138820,#138821,#138822,#138823,#138824,#138825,#138826,#138827,#138828,
#138829,#138830,#138831,#138832,#138833,#138834,#138835,#138836,#138837,
#138838,#138839,#138840,#138841,#138842,#138843,#138844,#138845,#138846,
#138847,#138848,#138849,#138850,#138851,#138852,#138853,#138854,#138855,
#138856,#138857,#138858,#138859,#138860,#138861,#138862,#138863,#138864,
#138865,#138866,#138867,#138868,#138869,#138870,#138871,#138872,#138873,
#138874,#138875,#138876,#138877,#138878,#138879,#138880,#138881,#138882,
#138883,#138884,#138885,#138886,#138887,#138888,#138889,#138890,#138891,
#138892,#138893,#138894,#138895,#138896,#138897,#138898,#138899,#138900,
#138901,#138902,#138903,#138904,#138905,#138906,#138907,#138908,#138909,
#138910,#138911,#138912,#138913,#138914,#138915,#138916,#138917,#138918,
#138919,#138920,#138921,#138922,#138923,#138924,#138925,#138926,#138927,
#138928,#138929,#138930,#138931,#138932,#138933,#138934,#138935,#138936,
#138937,#138938,#138939,#138940,#138941,#138942,#138943,#138944,#138945,
#138946,#138947,#138948,#138949,#138950,#138951,#138952,#138953,#138954,
#138955,#138956,#138957,#138958,#138959,#138960,#138961,#138962,#138963,
#138964,#138965,#138966,#138967,#138968,#138969,#138970,#138971,#138972,
#138973,#138974,#138975,#138976,#138977,#138978,#138979,#138980,#138981,
#138982,#138983,#138984,#138985,#138986,#138987,#138988,#138989,#138990,
#138991,#138992,#138993,#138994,#138995,#138996,#138997,#138998,#138999,
#139000,#139001,#139002,#139003,#139004,#139005,#139006,#139007,#139008,
#139009,#139010,#139011,#139012,#139013,#139014,#139015,#139016,#139017,
#139018,#139019,#139020,#139021,#139022,#139023,#139024,#139025),
 .UNSPECIFIED.,.F.,.F.,(4,3,3,3,3,3,3,3,3,3,3,3,3,3,3,3,3,3,3,3,3,3,3,3,
3,3,3,3,3,3,3,3,3,3,3,3,3,3,3,3,3,3,3,3,3,3,3,3,3,3,3,3,3,3,3,3,3,3,3,3,
3,3,3,3,3,3,3,3,3,3,3,3,3,4),(1674.46888436354,1674.56115257197,1674.65392929022,
1674.74696950423,1674.84034904643,1674.86585273767,1674.94959144905,1675.03322695995,
1675.11677940287,1675.20026883823,1675.28372278835,1675.36715928169,1675.45059639094,
1675.53405218535,1675.61759667757,1675.70118575999,1675.78490902703,1675.86558874839,
1675.94932746398,1676.0329629791,1676.11651542627,1676.20000486588,1676.28345882025,
1676.36689531785,1676.45033243134,1676.53378822999,1676.6173327264,1676.70092181301,
1676.78464508417,1676.86532475911,1676.94906346497,1677.03269897035,1677.11625140778,
1677.19974083768,1677.2831947824,1677.36663127038,1677.4500683743,1677.53352416343,
1677.61706865047,1677.70065772776,1677.78438098981,1677.86506076983,1677.94879948055,
1678.03243499074,1678.11598743291,1678.19947686748,1678.28293081675,1678.3663673092,
1678.44980441753,1678.53326021097,1678.61680470218,1678.70039378357,1678.78411704954,
1678.86479678055,1678.94853551605,1679.03217105115,1679.11572351834,1679.19921297802,
1679.28266695241,1679.36610347002,1679.44954060348,1679.53299642204,1679.61654093816,
1679.7001300444,1679.78385333486,1679.86453279127,1679.9471378052,1680.02964819366,
1680.11208308275,1680.19446152879,1680.27681143944,1680.35914315951,1680.44150012559,
1680.50024617582),.UNSPECIFIED.);
#1116=B_SPLINE_CURVE_WITH_KNOTS('',3,(#139026,#139027,#139028,#139029,#139030,
#139031,#139032,#139033,#139034,#139035),.UNSPECIFIED.,.F.,.F.,(4,3,3,4),
(1674.21825310493,1674.30279292267,1674.38730015935,1674.46888436336),
 .UNSPECIFIED.);
#1117=B_SPLINE_CURVE_WITH_KNOTS('',3,(#139037,#139038,#139039,#139040,#139041,
#139042,#139043,#139044,#139045,#139046),.UNSPECIFIED.,.F.,.F.,(4,3,3,4),
(1674.21806788616,1674.32085147138,1674.4222713986,1674.46888436323),
 .UNSPECIFIED.);
#1118=B_SPLINE_CURVE_WITH_KNOTS('',3,(#139047,#139048,#139049,#139050,#139051,
#139052,#139053,#139054,#139055,#139056,#139057,#139058,#139059,#139060,
#139061,#139062,#139063,#139064,#139065,#139066,#139067,#139068,#139069,
#139070,#139071,#139072,#139073,#139074,#139075,#139076,#139077,#139078,
#139079,#139080,#139081,#139082,#139083,#139084,#139085,#139086,#139087,
#139088,#139089,#139090,#139091,#139092,#139093,#139094,#139095,#139096,
#139097,#139098,#139099,#139100,#139101,#139102,#139103,#139104,#139105,
#139106,#139107,#139108,#139109,#139110,#139111,#139112,#139113,#139114,
#139115,#139116,#139117,#139118,#139119,#139120,#139121,#139122,#139123,
#139124,#139125,#139126,#139127,#139128,#139129,#139130,#139131,#139132,
#139133,#139134,#139135,#139136,#139137,#139138,#139139,#139140,#139141,
#139142,#139143,#139144,#139145,#139146,#139147,#139148,#139149,#139150,
#139151,#139152,#139153,#139154,#139155,#139156,#139157,#139158,#139159,
#139160,#139161,#139162,#139163,#139164,#139165,#139166,#139167,#139168,
#139169,#139170,#139171,#139172,#139173,#139174,#139175,#139176,#139177,
#139178,#139179,#139180,#139181,#139182,#139183,#139184,#139185,#139186,
#139187,#139188,#139189,#139190,#139191,#139192,#139193,#139194,#139195,
#139196,#139197,#139198,#139199,#139200,#139201,#139202,#139203,#139204,
#139205,#139206,#139207,#139208,#139209,#139210,#139211,#139212,#139213,
#139214,#139215,#139216,#139217,#139218,#139219,#139220,#139221,#139222,
#139223,#139224,#139225,#139226,#139227,#139228,#139229,#139230,#139231,
#139232,#139233,#139234,#139235,#139236,#139237,#139238,#139239,#139240,
#139241,#139242,#139243,#139244,#139245,#139246,#139247,#139248,#139249,
#139250,#139251,#139252,#139253,#139254,#139255,#139256,#139257,#139258,
#139259,#139260,#139261,#139262,#139263,#139264,#139265,#139266),
 .UNSPECIFIED.,.F.,.F.,(4,3,3,3,3,3,3,3,3,3,3,3,3,3,3,3,3,3,3,3,3,3,3,3,
3,3,3,3,3,3,3,3,3,3,3,3,3,3,3,3,3,3,3,3,3,3,3,3,3,3,3,3,3,3,3,3,3,3,3,3,
3,3,3,3,3,3,3,3,3,3,3,3,3,4),(1674.46888436336,1674.55177946142,1674.63464698122,
1674.71750299009,1674.80036604691,1674.88325471219,1674.96623556418,1675.04926809218,
1675.13242546003,1675.17614335739,1675.25988206912,1675.34351758038,1675.42707002366,
1675.5105594594,1675.5940134099,1675.67744990363,1675.76088701327,1675.84434280807,
1675.92788730068,1676.0114763835,1676.09519965094,1676.17587936811,1676.25961808053,
1676.34325359248,1676.42680603646,1676.5102954729,1676.59374942409,1676.67718591851,
1676.76062302885,1676.84407882434,1676.92762331763,1677.01121240114,1677.09493566925,
1677.17561537883,1677.25935408989,1677.34298960048,1677.42654204309,1677.51003147817,
1677.59348542801,1677.67692192109,1677.76035903009,1677.84381482425,1677.92735931624,
1678.01094839845,1678.09467166529,1678.17535138955,1678.25909010093,1678.34272561183,
1678.42627805475,1678.50976749011,1678.59322144023,1678.67665793357,1678.76009504282,
1678.84355083723,1678.92709532945,1679.01068441187,1679.09440767892,1679.17508740027,
1679.25882611586,1679.34246163098,1679.42601407815,1679.50950351776,1679.59295747213,
1679.67639396973,1679.75983108322,1679.84328688186,1679.92683137828,1680.01042046489,
1680.09414373605,1680.17482341099,1680.26034755561,1680.34576440261,1680.43105754023,
1680.50154027024),.UNSPECIFIED.);
#1119=B_SPLINE_CURVE_WITH_KNOTS('',3,(#139272,#139273,#139274,#139275,#139276,
#139277,#139278,#139279,#139280,#139281,#139282,#139283,#139284,#139285,
#139286,#139287,#139288,#139289,#139290,#139291,#139292,#139293,#139294,
#139295,#139296,#139297,#139298,#139299,#139300,#139301,#139302,#139303,
#139304,#139305,#139306,#139307,#139308,#139309,#139310,#139311,#139312,
#139313,#139314,#139315,#139316,#139317,#139318,#139319,#139320,#139321,
#139322,#139323,#139324,#139325,#139326,#139327,#139328,#139329,#139330,
#139331,#139332,#139333,#139334,#139335,#139336,#139337,#139338,#139339,
#139340,#139341,#139342,#139343,#139344,#139345,#139346,#139347,#139348,
#139349,#139350,#139351,#139352,#139353,#139354,#139355,#139356,#139357,
#139358,#139359,#139360,#139361,#139362,#139363,#139364,#139365,#139366,
#139367,#139368,#139369,#139370,#139371,#139372,#139373,#139374,#139375,
#139376,#139377,#139378,#139379,#139380,#139381,#139382,#139383,#139384,
#139385,#139386,#139387,#139388,#139389,#139390,#139391,#139392,#139393,
#139394,#139395,#139396,#139397,#139398,#139399,#139400,#139401,#139402,
#139403,#139404,#139405,#139406,#139407,#139408,#139409,#139410,#139411,
#139412,#139413,#139414,#139415,#139416,#139417,#139418,#139419,#139420,
#139421,#139422,#139423,#139424,#139425,#139426,#139427,#139428,#139429,
#139430,#139431,#139432,#139433,#139434,#139435,#139436,#139437,#139438,
#139439,#139440,#139441,#139442,#139443,#139444,#139445,#139446,#139447,
#139448,#139449,#139450,#139451,#139452,#139453,#139454,#139455,#139456,
#139457,#139458,#139459,#139460,#139461,#139462,#139463,#139464,#139465,
#139466,#139467,#139468,#139469,#139470,#139471,#139472,#139473,#139474,
#139475,#139476,#139477,#139478,#139479,#139480,#139481,#139482,#139483,
#139484,#139485,#139486,#139487,#139488),.UNSPECIFIED.,.F.,.F.,(4,3,3,3,
3,3,3,3,3,3,3,3,3,3,3,3,3,3,3,3,3,3,3,3,3,3,3,3,3,3,3,3,3,3,3,3,3,3,3,3,
3,3,3,3,3,3,3,3,3,3,3,3,3,3,3,3,3,3,3,3,3,3,3,3,3,3,3,3,3,3,3,3,4),(1680.75206967054,
1680.86426880199,1680.94800751987,1681.03164303693,1681.11519548569,1681.19868492656,
1681.28213888166,1681.36557537968,1681.44901249328,1681.53246829172,1681.61601278743,
1681.69960187308,1681.78332514284,1681.86400481271,1681.94774367009,1682.03137932759,
1682.11493191756,1682.19842150028,1682.28187559768,1682.36531223825,1682.44874949452,
1682.53220543561,1682.61575007314,1682.69933930037,1682.78306270987,1682.86374082343,
1682.94747921671,1683.03111440949,1683.11466653459,1683.19815565276,1683.28160928774,
1683.36504546723,1683.4484822642,1683.5319377482,1683.6154819347,1683.69907071347,
1683.78279368346,1683.86347683415,1683.94721567741,1684.0308513181,1684.11440388863,
1684.19789344933,1684.28134752089,1684.36478413332,1684.44822135917,1684.53167726761,
1684.61522186917,1684.69881105857,1684.78253442747,1684.86321284487,1684.94695242428,
1685.03058880757,1685.11414212632,1685.19763243999,1685.28108726909,1685.3645246417,
1685.44796262968,1685.53141930143,1685.61496466385,1685.69855461397,1685.78227873561,
1685.86294885559,1685.94668988417,1686.03032667021,1686.11387935293,1686.19762019608,
1686.2810682586,1686.36449745582,1686.44792586159,1686.53189592071,1686.61541141165,
1686.69960875486,1686.78380609807),.UNSPECIFIED.);
#1120=B_SPLINE_CURVE_WITH_KNOTS('',3,(#139489,#139490,#139491,#139492,#139493,
#139494,#139495,#139496,#139497,#139498),.UNSPECIFIED.,.F.,.F.,(4,3,3,4),
(1680.50024617582,1680.58267551838,1680.66737259439,1680.7520696704),
 .UNSPECIFIED.);
#1121=B_SPLINE_CURVE_WITH_KNOTS('',3,(#139500,#139501,#139502,#139503,#139504,
#139505,#139506,#139507,#139508,#139509),.UNSPECIFIED.,.F.,.F.,(4,3,3,4),
(1680.50154027024,1680.58669000473,1680.67178237626,1680.75206967054),
 .UNSPECIFIED.);
#1122=B_SPLINE_CURVE_WITH_KNOTS('',3,(#139510,#139511,#139512,#139513,#139514,
#139515,#139516,#139517,#139518,#139519,#139520,#139521,#139522,#139523,
#139524,#139525,#139526,#139527,#139528,#139529,#139530,#139531,#139532,
#139533,#139534,#139535,#139536,#139537,#139538,#139539,#139540,#139541,
#139542,#139543,#139544,#139545,#139546,#139547,#139548,#139549,#139550,
#139551,#139552,#139553,#139554,#139555,#139556,#139557,#139558,#139559,
#139560,#139561,#139562,#139563,#139564,#139565,#139566,#139567,#139568,
#139569,#139570,#139571,#139572,#139573,#139574,#139575,#139576,#139577,
#139578,#139579,#139580,#139581,#139582,#139583,#139584,#139585,#139586,
#139587,#139588,#139589,#139590,#139591,#139592,#139593,#139594,#139595,
#139596,#139597,#139598,#139599,#139600,#139601,#139602,#139603,#139604,
#139605,#139606,#139607,#139608,#139609,#139610,#139611,#139612,#139613,
#139614,#139615,#139616,#139617,#139618,#139619,#139620,#139621,#139622,
#139623,#139624,#139625,#139626,#139627,#139628,#139629,#139630,#139631,
#139632,#139633,#139634,#139635,#139636,#139637,#139638,#139639,#139640,
#139641,#139642,#139643,#139644,#139645,#139646,#139647,#139648,#139649,
#139650,#139651,#139652,#139653,#139654,#139655,#139656,#139657,#139658,
#139659,#139660,#139661,#139662,#139663,#139664,#139665,#139666,#139667,
#139668,#139669,#139670,#139671,#139672,#139673,#139674,#139675,#139676,
#139677,#139678,#139679,#139680,#139681,#139682,#139683,#139684,#139685,
#139686,#139687,#139688,#139689,#139690,#139691,#139692,#139693,#139694,
#139695,#139696,#139697,#139698,#139699,#139700,#139701,#139702,#139703,
#139704,#139705,#139706,#139707,#139708,#139709,#139710,#139711,#139712,
#139713,#139714,#139715,#139716,#139717,#139718,#139719,#139720,#139721,
#139722,#139723,#139724,#139725,#139726,#139727,#139728,#139729),
 .UNSPECIFIED.,.F.,.F.,(4,3,3,3,3,3,3,3,3,3,3,3,3,3,3,3,3,3,3,3,3,3,3,3,
3,3,3,3,3,3,3,3,3,3,3,3,3,3,3,3,3,3,3,3,3,3,3,3,3,3,3,3,3,3,3,3,3,3,3,3,
3,3,3,3,3,3,3,3,3,3,3,3,3,4),(1680.75206967069,1680.84288816935,1680.93411487138,
1681.02554954485,1681.11729322716,1681.17455942171,1681.25829813243,1681.34193364261,
1681.42548608478,1681.50897551935,1681.59242946861,1681.67586596107,1681.75930306939,
1681.84275886284,1681.92630335404,1682.00989243543,1682.09361570139,1682.17429543243,
1682.25803416793,1682.34166970303,1682.42522217022,1682.5087116299,1682.59216560429,
1682.6756021219,1682.75903925536,1682.84249507392,1682.92603959004,1683.00962869628,
1683.09335198674,1683.17403144315,1683.25777011073,1683.34140557785,1683.42495797707,
1683.50844736885,1683.59190127572,1683.67533772603,1683.75877479249,1683.84223054439,
1683.9257749948,1684.00936403572,1684.09308726221,1684.17376745387,1684.25750617175,
1684.34114168881,1684.42469413757,1684.50818357844,1684.59163753354,1684.67507403155,
1684.75851114516,1684.84196694359,1684.92551143931,1685.00910052496,1685.09282379471,
1685.17350346459,1685.25724232197,1685.34087797947,1685.42443056944,1685.50792015216,
1685.59137424956,1685.67481089013,1685.7582481464,1685.84170408749,1685.92524872503,
1686.00883795226,1686.09256136176,1686.17323947531,1686.25574915047,1686.33816398583,
1686.42050317268,1686.50278583004,1686.58503751018,1686.6672712406,1686.74952284399,
1686.7834725217),.UNSPECIFIED.);
#1123=B_SPLINE_CURVE_WITH_KNOTS('',3,(#139735,#139736,#139737,#139738,#139739,
#139740,#139741,#139742,#139743,#139744,#139745,#139746,#139747,#139748,
#139749,#139750,#139751,#139752,#139753,#139754,#139755,#139756,#139757,
#139758,#139759,#139760,#139761,#139762,#139763,#139764,#139765,#139766,
#139767,#139768,#139769,#139770,#139771,#139772,#139773,#139774,#139775,
#139776,#139777,#139778,#139779,#139780,#139781,#139782,#139783,#139784,
#139785,#139786,#139787,#139788,#139789,#139790,#139791,#139792,#139793,
#139794,#139795,#139796,#139797,#139798,#139799,#139800,#139801,#139802,
#139803,#139804,#139805,#139806,#139807,#139808,#139809,#139810,#139811,
#139812,#139813,#139814,#139815,#139816,#139817,#139818,#139819,#139820,
#139821,#139822,#139823,#139824,#139825,#139826,#139827,#139828,#139829,
#139830,#139831,#139832,#139833,#139834,#139835,#139836,#139837,#139838,
#139839,#139840,#139841,#139842,#139843,#139844,#139845,#139846,#139847,
#139848,#139849,#139850,#139851,#139852,#139853,#139854,#139855,#139856,
#139857,#139858,#139859,#139860,#139861,#139862,#139863,#139864,#139865,
#139866,#139867,#139868,#139869,#139870,#139871,#139872,#139873,#139874,
#139875,#139876,#139877,#139878,#139879,#139880,#139881,#139882,#139883,
#139884,#139885,#139886,#139887,#139888,#139889,#139890,#139891,#139892,
#139893,#139894,#139895,#139896,#139897,#139898,#139899,#139900,#139901,
#139902,#139903,#139904,#139905,#139906,#139907,#139908,#139909,#139910,
#139911,#139912,#139913,#139914,#139915,#139916,#139917,#139918,#139919,
#139920,#139921,#139922,#139923,#139924,#139925,#139926,#139927,#139928,
#139929,#139930,#139931,#139932,#139933,#139934,#139935,#139936,#139937,
#139938,#139939,#139940,#139941,#139942,#139943,#139944,#139945,#139946,
#139947,#139948,#139949,#139950,#139951,#139952,#139953,#139954),
 .UNSPECIFIED.,.F.,.F.,(4,3,3,3,3,3,3,3,3,3,3,3,3,3,3,3,3,3,3,3,3,3,3,3,
3,3,3,3,3,3,3,3,3,3,3,3,3,3,3,3,3,3,3,3,3,3,3,3,3,3,3,3,3,3,3,3,3,3,3,3,
3,3,3,3,3,3,3,3,3,3,3,3,3,4),(1687.0352549779,1687.11762183547,1687.19991216208,
1687.28272575145,1687.36493564271,1687.44713698684,1687.52934881702,1687.61261683202,
1687.69494876307,1687.77868482005,1687.86242087703,1687.94616455657,1688.02980506654,
1688.11336253391,1688.19685701369,1688.28031602056,1688.36375757747,1688.44719975227,
1688.5306606094,1688.61421013112,1688.69780423297,1688.78153245111,1688.86215688775,
1688.94588019747,1689.02950028853,1689.11303730936,1689.19651133616,1689.27994995193,
1689.36337115805,1689.44679304129,1689.53023368507,1689.61376323092,1689.69733745427,
1689.78104616198,1689.86189289847,1689.94564535982,1690.02929454784,1690.11286058205,
1690.19636350991,1690.27983075653,1690.3632804255,1690.44673057771,1690.53019927051,
1690.61375636118,1690.69735789888,1690.78109325142,1690.86162890919,1690.94539453213,
1691.02905716924,1691.11263692238,1691.19615382169,1691.27963537068,1691.36309954086,
1691.44656437829,1691.5300479256,1691.61362005147,1691.69723674639,1691.7809873084,
1691.86136491991,1691.94499994849,1692.02853160577,1692.11198013047,1692.19536568823,
1692.27871618166,1692.36204948573,1692.44538376701,1692.52873718895,1692.61218060301,
1692.69566914794,1692.77929382412,1692.86110093063,1692.9513655271,1693.04140261296,
1693.06812991347),.UNSPECIFIED.);
#1124=B_SPLINE_CURVE_WITH_KNOTS('',3,(#139955,#139956,#139957,#139958,#139959,
#139960,#139961,#139962,#139963,#139964),.UNSPECIFIED.,.F.,.F.,(4,3,3,4),
(1686.78380609807,1686.86268486631,1686.99306837669,1687.03525497772),
 .UNSPECIFIED.);
#1125=B_SPLINE_CURVE_WITH_KNOTS('',3,(#139966,#139967,#139968,#139969,#139970,
#139971,#139972,#139973,#139974,#139975),.UNSPECIFIED.,.F.,.F.,(4,3,3,4),
(1686.7834725217,1686.86578987103,1686.95052242432,1687.0352549776),
 .UNSPECIFIED.);
#1126=B_SPLINE_CURVE_WITH_KNOTS('',3,(#139976,#139977,#139978,#139979,#139980,
#139981,#139982,#139983,#139984,#139985,#139986,#139987,#139988,#139989,
#139990,#139991,#139992,#139993,#139994,#139995,#139996,#139997,#139998,
#139999,#140000,#140001,#140002,#140003,#140004,#140005,#140006,#140007,
#140008,#140009,#140010,#140011,#140012,#140013,#140014,#140015,#140016,
#140017,#140018,#140019,#140020,#140021,#140022,#140023,#140024,#140025,
#140026,#140027,#140028,#140029,#140030,#140031,#140032,#140033,#140034,
#140035,#140036,#140037,#140038,#140039,#140040,#140041,#140042,#140043,
#140044,#140045,#140046,#140047,#140048,#140049,#140050,#140051,#140052,
#140053,#140054,#140055,#140056,#140057,#140058,#140059,#140060,#140061,
#140062,#140063,#140064,#140065,#140066,#140067,#140068,#140069,#140070,
#140071,#140072,#140073,#140074,#140075,#140076,#140077,#140078,#140079,
#140080,#140081,#140082,#140083,#140084,#140085,#140086,#140087,#140088,
#140089,#140090,#140091,#140092,#140093,#140094,#140095,#140096,#140097,
#140098,#140099,#140100,#140101,#140102,#140103,#140104,#140105,#140106,
#140107,#140108,#140109,#140110,#140111,#140112,#140113,#140114,#140115,
#140116,#140117,#140118,#140119,#140120,#140121,#140122,#140123,#140124,
#140125,#140126,#140127,#140128,#140129,#140130,#140131,#140132,#140133,
#140134,#140135,#140136,#140137,#140138,#140139,#140140,#140141,#140142,
#140143,#140144,#140145,#140146,#140147,#140148,#140149,#140150,#140151,
#140152,#140153,#140154,#140155,#140156,#140157,#140158,#140159,#140160,
#140161,#140162,#140163,#140164,#140165,#140166,#140167,#140168,#140169,
#140170,#140171,#140172,#140173,#140174,#140175,#140176,#140177,#140178,
#140179,#140180,#140181,#140182,#140183,#140184,#140185,#140186,#140187,
#140188,#140189,#140190,#140191,#140192),.UNSPECIFIED.,.F.,.F.,(4,3,3,3,
3,3,3,3,3,3,3,3,3,3,3,3,3,3,3,3,3,3,3,3,3,3,3,3,3,3,3,3,3,3,3,3,3,3,3,3,
3,3,3,3,3,3,3,3,3,3,3,3,3,3,3,3,3,3,3,3,3,3,3,3,3,3,3,3,3,3,3,3,4),(1687.03525497772,
1687.17297548603,1687.25671432929,1687.34034996998,1687.42390254051,1687.50739210121,
1687.59084617277,1687.67428278519,1687.75772001105,1687.84117591948,1687.92472052105,
1688.00830971045,1688.09203307935,1688.17271149675,1688.25645107616,1688.34008745945,
1688.4236407782,1688.50713109187,1688.59058592097,1688.67402329358,1688.75746128155,
1688.84091795331,1688.92446331573,1689.00805326585,1689.09177738749,1689.17244750747,
1689.25618398008,1689.33981725074,1689.42336745426,1689.50685465334,1689.59030637971,
1689.6737406572,1689.75717556056,1689.84062916108,1689.9241714907,1690.00775842411,
1690.0914795871,1690.17218351819,1690.25592370815,1690.33956068508,1690.42311458017,
1690.5066054525,1690.59006081169,1690.67349869696,1690.75693717979,1690.84039432818,
1690.92394013598,1691.00753051519,1691.09125503391,1691.17191952891,1691.25566320845,
1691.33930371841,1691.42286118579,1691.50635566557,1691.58981467244,1691.67325622935,
1691.75669840415,1691.84015926128,1691.923708783,1692.00730288485,1692.09103110299,
1692.17165553963,1692.25538494486,1692.33900975173,1692.42255011458,1692.5060216795,
1692.5894557807,1692.67287052082,1692.75628398561,1692.83975081521,1692.92324528107,
1693.00683495087,1693.06690371234),.UNSPECIFIED.);
#1127=B_SPLINE_CURVE_WITH_KNOTS('',3,(#140196,#140197,#140198,#140199,#140200,
#140201,#140202,#140203,#140204,#140205,#140206,#140207,#140208,#140209,
#140210,#140211,#140212,#140213,#140214,#140215,#140216,#140217,#140218,
#140219,#140220,#140221,#140222,#140223,#140224,#140225,#140226,#140227,
#140228,#140229,#140230,#140231,#140232,#140233,#140234,#140235,#140236,
#140237,#140238,#140239,#140240,#140241,#140242,#140243,#140244,#140245,
#140246,#140247,#140248,#140249,#140250,#140251,#140252,#140253,#140254,
#140255,#140256,#140257,#140258,#140259,#140260,#140261,#140262,#140263,
#140264,#140265,#140266,#140267,#140268,#140269,#140270,#140271,#140272,
#140273,#140274),.UNSPECIFIED.,.F.,.F.,(4,3,3,3,3,3,3,3,3,3,3,3,3,3,3,3,
3,3,3,3,3,3,3,3,3,3,4),(-4.09254174884206,-3.99894404288052,-3.91885449630764,
-3.83885809227166,-3.75893744803051,-3.67907523956829,-3.59925418855671,
-3.51944544555752,-3.43963967421031,-3.35982126989644,-3.27997462355469,
-3.20004057373489,-3.1200573453262,-3.03996113306838,-2.99920803216039,
-2.9207016395211,-2.84228988317914,-2.76395413880008,-2.68567586928874,
-2.60742974348718,-2.52919913889701,-2.45096738081357,-2.37271779450763,
-2.29438746102101,-2.21601536556249,-2.13752365119797,-2.07058826465548),
 .UNSPECIFIED.);
#1128=B_SPLINE_CURVE_WITH_KNOTS('',3,(#140278,#140279,#140280,#140281,#140282,
#140283,#140284,#140285,#140286,#140287,#140288,#140289,#140290,#140291,
#140292,#140293,#140294,#140295,#140296,#140297,#140298,#140299,#140300,
#140301,#140302,#140303,#140304,#140305,#140306,#140307,#140308,#140309,
#140310,#140311,#140312,#140313,#140314,#140315,#140316,#140317,#140318,
#140319,#140320),.UNSPECIFIED.,.F.,.F.,(4,3,3,3,3,3,3,3,3,3,3,3,3,3,4),
(0.,0.0935817941909758,0.187331892979243,0.281085442661883,0.374720077979815,
0.468011049746007,0.499868005357902,0.579828600624018,0.659779162846936,
0.739735219717809,0.819740648566051,0.899775729107479,0.979885236083813,
0.999736010719684,1.11885509353369),.UNSPECIFIED.);
#1129=B_SPLINE_CURVE_WITH_KNOTS('',3,(#140322,#140323,#140324,#140325,#140326,
#140327,#140328,#140329,#140330,#140331,#140332,#140333,#140334,#140335,
#140336,#140337,#140338,#140339,#140340,#140341,#140342,#140343,#140344,
#140345,#140346,#140347,#140348,#140349,#140350,#140351,#140352,#140353,
#140354,#140355,#140356,#140357,#140358,#140359,#140360,#140361,#140362,
#140363,#140364,#140365,#140366,#140367,#140368,#140369,#140370,#140371,
#140372,#140373,#140374,#140375,#140376,#140377,#140378,#140379,#140380,
#140381,#140382,#140383,#140384,#140385,#140386,#140387,#140388,#140389,
#140390,#140391,#140392,#140393,#140394,#140395,#140396,#140397,#140398,
#140399,#140400,#140401,#140402,#140403,#140404,#140405,#140406,#140407,
#140408,#140409,#140410,#140411,#140412,#140413,#140414,#140415,#140416,
#140417,#140418,#140419,#140420,#140421,#140422,#140423,#140424,#140425,
#140426,#140427,#140428,#140429,#140430,#140431,#140432,#140433,#140434,
#140435,#140436,#140437,#140438,#140439,#140440,#140441,#140442,#140443,
#140444,#140445,#140446,#140447,#140448,#140449,#140450,#140451,#140452,
#140453,#140454,#140455,#140456,#140457,#140458,#140459,#140460,#140461,
#140462,#140463,#140464,#140465,#140466,#140467,#140468,#140469,#140470,
#140471,#140472,#140473,#140474,#140475,#140476,#140477,#140478,#140479,
#140480,#140481,#140482,#140483,#140484,#140485,#140486,#140487,#140488,
#140489,#140490,#140491,#140492,#140493,#140494,#140495,#140496,#140497,
#140498,#140499,#140500,#140501,#140502,#140503,#140504,#140505,#140506,
#140507,#140508,#140509,#140510,#140511,#140512,#140513,#140514,#140515,
#140516,#140517,#140518,#140519,#140520,#140521,#140522,#140523,#140524,
#140525,#140526,#140527,#140528,#140529,#140530,#140531,#140532,#140533,
#140534,#140535,#140536,#140537,#140538,#140539,#140540,#140541,#140542,
#140543,#140544,#140545,#140546,#140547,#140548,#140549,#140550,#140551,
#140552,#140553,#140554,#140555,#140556,#140557,#140558,#140559,#140560,
#140561,#140562,#140563,#140564,#140565),.UNSPECIFIED.,.F.,.F.,(4,3,3,3,
3,3,3,3,3,3,3,3,3,3,3,3,3,3,3,3,3,3,3,3,3,3,3,3,3,3,3,3,3,3,3,3,3,3,3,3,
3,3,3,3,3,3,3,3,3,3,3,3,3,3,3,3,3,3,3,3,3,3,3,3,3,3,3,3,3,3,3,3,3,3,3,3,
3,3,3,3,3,4),(1.11885509365316,1.19890412789216,1.27889220714027,1.35883652401209,
1.43891596119061,1.518840493998,1.59877521794939,1.6787356591488,1.75891974972165,
1.83901897528853,1.919249023072,1.99947202144022,2.07876788808251,2.15796183556404,
2.23707201384114,2.31611649693057,2.39511330010876,2.4740904982881,2.55306021205585,
2.63203868968195,2.71104218287401,2.79013230483545,2.86926983209992,2.94852490788452,
2.99920803216035,3.07930247080208,3.15930292307334,3.23922677491295,3.31909135287532,
3.39891393720777,3.47872295966545,3.55852823188179,3.6383453584131,3.71818994778447,
3.79812076697098,3.8781000941454,3.95819139359745,3.99894404288049,4.07900057834142,
4.15896436952754,4.23885283571627,4.31868333758502,4.39847319032814,4.47825161765034,
4.55802762890995,4.63781686288743,4.71763496319276,4.79754158030628,4.87749796878064,
4.95756851179511,4.99868005360062,5.07854379860577,5.15831194592404,5.23800211985226,
5.31763188244565,5.39721874739824,5.47679146185666,5.5563600875881,5.63594043642507,
5.71554832432581,5.79524375880277,5.87498809798384,5.95484705923799,5.99841606432075,
6.07839930855999,6.15828820346944,6.23810025063035,6.31785289130088,6.39756351983018,
6.4772609324546,6.55695482576828,6.63666090658931,6.71639488600397,6.79621632762634,
6.87608681649885,6.9560710618768,6.99815207504088,7.08687973637244,7.1752513055744,
7.26339298300667,7.35115912867321,7.40204018020966),.UNSPECIFIED.);
#1130=B_SPLINE_CURVE_WITH_KNOTS('',3,(#140567,#140568,#140569,#140570,#140571,
#140572,#140573,#140574,#140575,#140576),.UNSPECIFIED.,.F.,.F.,(4,1,1,1,
1,1,1,4),(7.40204040069455,7.99788808576102,8.99762409648117,9.99736010720132,
10.9970961179215,11.9968321286416,12.9965681393618,13.6852257078742),
 .UNSPECIFIED.);
#1131=B_SPLINE_CURVE_WITH_KNOTS('',3,(#140578,#140579,#140580,#140581,#140582,
#140583,#140584,#140585,#140586,#140587,#140588,#140589,#140590,#140591,
#140592,#140593,#140594,#140595,#140596,#140597,#140598,#140599,#140600,
#140601,#140602,#140603,#140604,#140605,#140606,#140607,#140608,#140609,
#140610,#140611,#140612,#140613,#140614,#140615,#140616,#140617,#140618,
#140619,#140620,#140621,#140622,#140623,#140624,#140625,#140626,#140627,
#140628,#140629,#140630,#140631,#140632,#140633,#140634,#140635,#140636,
#140637,#140638,#140639,#140640,#140641,#140642,#140643,#140644,#140645,
#140646,#140647,#140648,#140649,#140650,#140651,#140652,#140653,#140654,
#140655,#140656,#140657,#140658,#140659,#140660,#140661,#140662,#140663,
#140664,#140665,#140666,#140667,#140668,#140669,#140670,#140671,#140672,
#140673,#140674,#140675,#140676,#140677,#140678,#140679,#140680,#140681,
#140682,#140683,#140684,#140685,#140686,#140687,#140688,#140689,#140690,
#140691,#140692,#140693,#140694,#140695,#140696,#140697,#140698,#140699,
#140700,#140701,#140702,#140703,#140704,#140705,#140706,#140707,#140708,
#140709,#140710,#140711,#140712,#140713,#140714,#140715,#140716,#140717,
#140718,#140719,#140720,#140721,#140722,#140723,#140724,#140725,#140726,
#140727,#140728,#140729,#140730,#140731,#140732,#140733,#140734,#140735,
#140736,#140737,#140738,#140739,#140740,#140741,#140742,#140743,#140744,
#140745,#140746,#140747,#140748,#140749,#140750,#140751,#140752,#140753,
#140754,#140755,#140756,#140757,#140758,#140759,#140760,#140761,#140762,
#140763,#140764,#140765,#140766,#140767,#140768,#140769,#140770,#140771,
#140772,#140773,#140774,#140775,#140776,#140777,#140778,#140779,#140780,
#140781,#140782,#140783,#140784,#140785,#140786,#140787,#140788,#140789,
#140790,#140791,#140792,#140793,#140794,#140795,#140796,#140797,#140798,
#140799,#140800,#140801,#140802,#140803,#140804,#140805,#140806,#140807,
#140808,#140809,#140810,#140811,#140812,#140813,#140814,#140815,#140816,
#140817,#140818,#140819,#140820,#140821,#140822,#140823,#140824),
 .UNSPECIFIED.,.F.,.F.,(4,3,3,3,3,3,3,3,3,3,3,3,3,3,3,3,3,3,3,3,3,3,3,3,
3,3,3,3,3,3,3,3,3,3,3,3,3,3,3,3,3,3,3,3,3,3,3,3,3,3,3,3,3,3,3,3,3,3,3,3,
3,3,3,3,3,3,3,3,3,3,3,3,3,3,3,3,3,3,3,3,3,3,4),(13.6852259127505,13.7801099435782,
13.8756905427146,13.9720376507108,13.9963041500819,14.0762611679736,14.1561236791645,
14.2359092120701,14.3156352344774,14.3953191670501,14.4749898540935,14.5546570063244,
14.6343363539807,14.7140436316013,14.7938385549703,14.8736825899846,14.9536407114316,
14.996040160802,15.0759975957193,15.1558605290186,15.2356464886784,15.3153729420553,
15.3950573093886,15.4747284354873,15.5543960293979,15.6340758209858,15.7137835444186,
15.7935789142272,15.8734233967061,15.9533819633687,15.9957761715221,16.075733473648,
16.1555962732271,16.2353820983737,16.3151084165785,16.3947926482139,16.4744636382654,
16.5541310959256,16.6338107511781,16.7135183383086,16.7933135725563,16.873157919691,
16.9531163525208,16.9955121822422,17.0754694434268,17.1553322011706,17.2351179836328,
17.314844258348,17.3945284457316,17.4741993905267,17.5538668023107,17.633546411104,
17.713253951229,17.7930491378706,17.8728934369877,17.9528518215654,17.9952481929623,
18.0752055148322,18.1550683340336,18.2348541786619,18.3145805161891,18.3942647669683,
18.4739357758324,18.5536032520972,18.6332829257289,18.7129905309957,18.7927857829151,
18.8726301474848,18.9525885972255,18.9949842036824,19.0745911127166,19.1541037254495,
19.2335398970435,19.3129174188851,19.3948541184062,19.4741786590968,19.5535018339292,
19.6328396635326,19.7122081748832,19.7916638055052,19.8711715970075,19.9507856857916,
19.9684110150538),.UNSPECIFIED.);
#1132=B_SPLINE_CURVE_WITH_KNOTS('',3,(#140826,#140827,#140828,#140829,#140830,
#140831,#140832,#140833,#140834,#140835,#140836,#140837),.UNSPECIFIED.,
 .F.,.F.,(4,2,1,1,1,1,1,1,4),(19.9684110150538,19.9947202144025,20.9944562251227,
21.9941922358428,22.9939282465629,23.9936642572831,24.9934002680032,25.9931362787233,
26.2515963222334),.UNSPECIFIED.);
#1133=B_SPLINE_CURVE_WITH_KNOTS('',3,(#140839,#140840,#140841,#140842,#140843,
#140844,#140845,#140846,#140847,#140848),.UNSPECIFIED.,.F.,.F.,(4,1,1,1,
1,1,1,4),(26.2515963222334,26.9928722894435,27.9926083001636,28.9923443108837,
29.9920803216039,30.991816332324,31.9915523430441,32.534781629413),
 .UNSPECIFIED.);
#1134=B_SPLINE_CURVE_WITH_KNOTS('',3,(#140850,#140851,#140852,#140853,#140854,
#140855,#140856,#140857,#140858,#140859),.UNSPECIFIED.,.F.,.F.,(4,1,1,1,
1,1,1,4),(32.534781629413,32.9912883537643,33.9910243644844,34.9907603752045,
35.9904963859246,36.9902323966447,37.9899684073648,38.8179669365925),
 .UNSPECIFIED.);
#1135=B_SPLINE_CURVE_WITH_KNOTS('',3,(#140861,#140862,#140863,#140864,#140865,
#140866,#140867,#140868,#140869,#140870,#140871),.UNSPECIFIED.,.F.,.F.,
(4,1,1,1,1,1,1,1,4),(38.8179669365925,38.9897044180849,39.9894404288051,
40.9891764395252,41.9889124502454,42.9886484609655,43.9883844716856,44.9881204824058,
45.1011522437721),.UNSPECIFIED.);
#1136=B_SPLINE_CURVE_WITH_KNOTS('',3,(#140873,#140874,#140875,#140876,#140877,
#140878,#140879,#140880,#140881,#140882),.UNSPECIFIED.,.F.,.F.,(4,1,1,1,
1,1,1,4),(45.1011522437721,45.9878564931259,46.9875925038461,47.9873285145662,
48.9870645252863,49.9868005360065,50.9865365467266,51.3843375509517),
 .UNSPECIFIED.);
#1137=B_SPLINE_CURVE_WITH_KNOTS('',3,(#140884,#140885,#140886,#140887,#140888,
#140889,#140890,#140891,#140892,#140893),.UNSPECIFIED.,.F.,.F.,(4,1,1,1,
1,1,1,4),(51.3843375509517,51.9862725574467,52.9860085681668,53.9857445788869,
54.985480589607,55.9852166003271,56.9849526110472,57.6675228581313),
 .UNSPECIFIED.);
#1138=B_SPLINE_CURVE_WITH_KNOTS('',3,(#140895,#140896,#140897,#140898,#140899,
#140900,#140901,#140902,#140903,#140904),.UNSPECIFIED.,.F.,.F.,(4,1,1,1,
1,1,1,4),(57.6675228581313,57.9846886217673,58.9844246324875,59.9841606432076,
60.9838966539278,61.983632664648,62.9833686753681,63.9507037176747),
 .UNSPECIFIED.);
#1139=B_SPLINE_CURVE_WITH_KNOTS('',3,(#140906,#140907,#140908,#140909,#140910,
#140911,#140912,#140913,#140914,#140915,#140916,#140917,#140918,#140919,
#140920,#140921,#140922,#140923,#140924,#140925,#140926,#140927,#140928,
#140929,#140930,#140931,#140932,#140933,#140934,#140935,#140936,#140937,
#140938,#140939,#140940,#140941,#140942,#140943,#140944,#140945,#140946,
#140947,#140948,#140949,#140950,#140951,#140952,#140953,#140954,#140955,
#140956,#140957,#140958,#140959,#140960,#140961,#140962,#140963,#140964,
#140965,#140966,#140967,#140968,#140969,#140970,#140971,#140972,#140973,
#140974,#140975,#140976,#140977,#140978,#140979,#140980,#140981,#140982,
#140983,#140984,#140985,#140986,#140987,#140988,#140989,#140990,#140991,
#140992,#140993,#140994,#140995,#140996,#140997,#140998,#140999,#141000,
#141001,#141002,#141003,#141004,#141005,#141006,#141007,#141008,#141009,
#141010,#141011,#141012,#141013,#141014,#141015,#141016,#141017,#141018,
#141019,#141020,#141021,#141022,#141023,#141024,#141025,#141026,#141027,
#141028,#141029,#141030,#141031,#141032,#141033,#141034,#141035,#141036,
#141037,#141038,#141039,#141040,#141041,#141042,#141043,#141044,#141045,
#141046,#141047,#141048,#141049,#141050,#141051,#141052,#141053,#141054,
#141055,#141056,#141057,#141058,#141059,#141060,#141061,#141062,#141063,
#141064,#141065,#141066,#141067,#141068,#141069,#141070,#141071,#141072,
#141073,#141074,#141075,#141076,#141077,#141078,#141079,#141080,#141081,
#141082,#141083,#141084,#141085,#141086,#141087,#141088,#141089,#141090,
#141091,#141092,#141093,#141094,#141095,#141096,#141097,#141098,#141099,
#141100,#141101,#141102,#141103,#141104,#141105,#141106,#141107,#141108,
#141109,#141110,#141111,#141112,#141113,#141114,#141115,#141116,#141117,
#141118,#141119,#141120,#141121,#141122,#141123,#141124,#141125,#141126,
#141127,#141128,#141129,#141130,#141131,#141132,#141133,#141134,#141135,
#141136,#141137,#141138,#141139,#141140,#141141,#141142,#141143,#141144,
#141145,#141146,#141147,#141148,#141149,#141150,#141151,#141152),
 .UNSPECIFIED.,.F.,.F.,(4,3,3,3,3,3,3,3,3,3,3,3,3,3,3,3,3,3,3,3,3,3,3,3,
3,3,3,3,3,3,3,3,3,3,3,3,3,3,3,3,3,3,3,3,3,3,3,3,3,3,3,3,3,3,3,3,3,3,3,3,
3,3,3,3,3,3,3,3,3,3,3,3,3,3,3,3,3,3,3,3,3,3,4),(63.9507081653109,63.9831046860883,
64.0630619862195,64.142924783462,64.2227106059338,64.3024369211289,64.382121149423,
64.4617921356438,64.5414595891696,64.621139239986,64.7008468223806,64.7806420514561,
64.8604863931635,64.9404448202108,64.9828406968084,65.0627979969396,65.1426607941822,
65.2224466166541,65.3021729318493,65.3818571601433,65.4615281463642,65.5411955998901,
65.6208752507066,65.7005828331011,65.7803780621766,65.8602224038843,65.9401808309317,
65.9825767075286,66.0625340076599,66.1423968049025,66.2221826273744,66.3019089425698,
66.381593170864,66.461264157085,66.540931610611,66.6206112614275,66.7003188438221,
66.7801140728977,66.8599584146054,66.9399168416528,66.9823127182487,67.0622700183799,
67.1421328156224,67.2219186380942,67.3016449532894,67.3813291815834,67.4610001678043,
67.5406676213301,67.6203472721465,67.700054854541,67.7798500836165,67.8596944253241,
67.9396528523714,67.9820487289688,68.0620060291001,68.1418688263428,68.2216546488147,
68.30138096401,68.381065192304,68.460736178525,68.540403632051,68.6200832828675,
68.6997908652621,68.7795860943376,68.8594304360453,68.9393888630927,68.9817847396889,
69.0617420398201,69.1416048370627,69.2213906595346,69.3011169747299,69.3808012030239,
69.4604721892448,69.5401396427707,69.6198192935872,69.6995268759819,69.7793221050574,
69.8591664467649,69.9391248738123,69.981520750409,70.0859426319418,70.1882149143938,
70.2338934108873),.UNSPECIFIED.);
#1140=B_SPLINE_CURVE_WITH_KNOTS('',3,(#141154,#141155,#141156,#141157,#141158,
#141159,#141160,#141161,#141162,#141163),.UNSPECIFIED.,.F.,.F.,(4,1,1,1,
1,1,1,4),(70.2338934724905,70.9812567611292,71.9809927718493,72.9807287825695,
73.9804647932896,74.9802008040097,75.9799368147299,76.5170787796701),
 .UNSPECIFIED.);
#1141=B_SPLINE_CURVE_WITH_KNOTS('',3,(#141165,#141166,#141167,#141168,#141169,
#141170,#141171,#141172,#141173,#141174,#141175,#141176,#141177,#141178,
#141179,#141180,#141181,#141182,#141183,#141184,#141185,#141186,#141187,
#141188,#141189,#141190,#141191,#141192,#141193,#141194,#141195,#141196,
#141197,#141198,#141199,#141200,#141201,#141202,#141203,#141204,#141205,
#141206,#141207,#141208,#141209,#141210,#141211,#141212,#141213,#141214,
#141215,#141216,#141217,#141218,#141219,#141220,#141221,#141222,#141223,
#141224,#141225,#141226,#141227,#141228,#141229,#141230,#141231,#141232,
#141233,#141234,#141235,#141236,#141237,#141238,#141239,#141240,#141241,
#141242,#141243,#141244,#141245,#141246,#141247,#141248,#141249,#141250,
#141251,#141252,#141253,#141254,#141255,#141256,#141257,#141258,#141259,
#141260,#141261,#141262,#141263,#141264,#141265,#141266,#141267,#141268,
#141269,#141270,#141271,#141272,#141273,#141274,#141275,#141276,#141277,
#141278,#141279,#141280,#141281,#141282,#141283,#141284,#141285,#141286,
#141287,#141288,#141289,#141290,#141291,#141292,#141293,#141294,#141295,
#141296,#141297,#141298,#141299,#141300,#141301,#141302,#141303,#141304,
#141305,#141306,#141307,#141308,#141309,#141310,#141311,#141312,#141313,
#141314,#141315,#141316,#141317,#141318,#141319,#141320,#141321,#141322,
#141323,#141324,#141325,#141326,#141327,#141328,#141329,#141330,#141331,
#141332,#141333,#141334,#141335,#141336,#141337,#141338,#141339,#141340,
#141341,#141342,#141343,#141344,#141345,#141346,#141347,#141348,#141349,
#141350,#141351,#141352,#141353,#141354,#141355,#141356,#141357,#141358,
#141359,#141360,#141361,#141362,#141363,#141364,#141365,#141366,#141367,
#141368,#141369,#141370,#141371,#141372,#141373,#141374,#141375,#141376,
#141377,#141378,#141379,#141380,#141381,#141382,#141383,#141384,#141385,
#141386,#141387,#141388,#141389,#141390,#141391,#141392,#141393,#141394,
#141395,#141396,#141397,#141398,#141399,#141400,#141401,#141402,#141403,
#141404,#141405,#141406,#141407,#141408,#141409,#141410,#141411),
 .UNSPECIFIED.,.F.,.F.,(4,3,3,3,3,3,3,3,3,3,3,3,3,3,3,3,3,3,3,3,3,3,3,3,
3,3,3,3,3,3,3,3,3,3,3,3,3,3,3,3,3,3,3,3,3,3,3,3,3,3,3,3,3,3,3,3,3,3,3,3,
3,3,3,3,3,3,3,3,3,3,3,3,3,3,3,3,3,3,3,3,3,3,4),(76.5170789829915,76.6019516902264,
76.6869832338072,76.7722619244241,76.8576735508233,76.9432918856119,76.97967282545,
77.0596301255811,77.1394929228235,77.2192787452951,77.2990050604903,77.3786892887841,
77.4583602750048,77.5380277285305,77.6177073793468,77.6974149617411,77.7772101908165,
77.8570545325239,77.9370129595711,77.9794088361701,78.0593661363013,78.1392289335439,
78.2190147560157,78.298741071211,78.3784252995052,78.4580962857261,78.537763739252,
78.6174433900685,78.6971509724629,78.7769462015385,78.8567905432461,78.9367489702935,
78.9791448468902,79.0591021470215,79.1389649442642,79.2187507667361,79.2984770819315,
79.3781613102257,79.4578322964467,79.5374997499727,79.6171794007892,79.6968869831838,
79.7766822122594,79.8565265539671,79.9364849810146,79.9788808576104,80.0588381577416,
80.1387009549841,80.2184867774559,80.2982130926512,80.3778973209452,80.4575683071661,
80.537235760692,80.6169154115085,80.696622993903,80.7764182229785,80.856262564686,
80.9362209917334,80.9786168683304,81.0585741684617,81.1384369657043,81.2182227881762,
81.2979491033716,81.3776333316657,81.4573043178867,81.5369717714127,81.6166514222292,
81.6963590046238,81.7761542336994,81.8559985754071,81.9359570024545,81.9783528790506,
82.0571196435331,82.1357922323713,82.2143891387368,82.2929249535672,82.37142792239,
82.4499146286459,82.5284016410875,82.6069360191478,82.6854971762447,82.764138078185,
82.8002640868496),.UNSPECIFIED.);
#1142=B_SPLINE_CURVE_WITH_KNOTS('',3,(#141413,#141414,#141415,#141416,#141417,
#141418,#141419,#141420,#141421,#141422,#141423),.UNSPECIFIED.,.F.,.F.,
(4,1,1,1,1,1,1,1,4),(82.8002640868496,82.9780888897707,83.9778249004908,
84.977560911211,85.9772969219311,86.9770329326513,87.9767689433714,88.9765049540916,
89.0834493940292),.UNSPECIFIED.);
#1143=B_SPLINE_CURVE_WITH_KNOTS('',3,(#141425,#141426,#141427,#141428,#141429,
#141430,#141431,#141432,#141433,#141434),.UNSPECIFIED.,.F.,.F.,(4,1,1,1,
1,1,1,4),(89.0834493940292,89.9762409648117,90.9759769755319,91.975712986252,
92.9754489969721,93.9751850076922,94.9749210184123,95.3666347012089),
 .UNSPECIFIED.);
#1144=B_SPLINE_CURVE_WITH_KNOTS('',3,(#141436,#141437,#141438,#141439,#141440,
#141441,#141442,#141443,#141444,#141445),.UNSPECIFIED.,.F.,.F.,(4,1,1,1,
1,1,1,4),(95.3666347012089,95.9746570291324,96.9743930398526,97.9741290505727,
98.9738650612928,99.973601072013,100.973337082733,101.649820008388),
 .UNSPECIFIED.);
#1145=B_SPLINE_CURVE_WITH_KNOTS('',3,(#141447,#141448,#141449,#141450,#141451,
#141452,#141453,#141454,#141455,#141456),.UNSPECIFIED.,.F.,.F.,(4,1,1,1,
1,1,1,4),(101.649820008388,101.973073093453,102.972809104173,103.972545114893,
104.972281125613,105.972017136334,106.971753147054,107.93300001923),
 .UNSPECIFIED.);
#1146=B_SPLINE_CURVE_WITH_KNOTS('',3,(#141458,#141459,#141460,#141461,#141462,
#141463,#141464,#141465,#141466,#141467,#141468,#141469,#141470,#141471,
#141472,#141473,#141474,#141475,#141476,#141477,#141478,#141479,#141480,
#141481,#141482,#141483,#141484,#141485,#141486,#141487,#141488,#141489,
#141490,#141491,#141492,#141493,#141494,#141495,#141496,#141497,#141498,
#141499,#141500,#141501,#141502,#141503,#141504,#141505,#141506,#141507,
#141508,#141509,#141510,#141511,#141512,#141513,#141514,#141515,#141516,
#141517,#141518,#141519,#141520,#141521,#141522,#141523,#141524,#141525,
#141526,#141527,#141528,#141529,#141530,#141531,#141532,#141533,#141534,
#141535,#141536,#141537,#141538,#141539,#141540,#141541,#141542,#141543,
#141544,#141545,#141546,#141547,#141548,#141549,#141550,#141551,#141552,
#141553,#141554,#141555,#141556,#141557,#141558,#141559,#141560,#141561,
#141562,#141563,#141564,#141565,#141566,#141567,#141568,#141569,#141570,
#141571,#141572,#141573,#141574,#141575,#141576,#141577,#141578,#141579,
#141580,#141581,#141582,#141583,#141584,#141585,#141586,#141587,#141588,
#141589,#141590,#141591,#141592,#141593,#141594,#141595,#141596,#141597,
#141598,#141599,#141600,#141601,#141602,#141603,#141604,#141605,#141606,
#141607,#141608,#141609,#141610,#141611,#141612,#141613,#141614,#141615,
#141616,#141617,#141618,#141619,#141620,#141621,#141622,#141623,#141624,
#141625,#141626,#141627,#141628,#141629,#141630,#141631,#141632,#141633,
#141634,#141635,#141636,#141637,#141638,#141639,#141640,#141641,#141642,
#141643,#141644,#141645,#141646,#141647,#141648,#141649,#141650,#141651,
#141652,#141653,#141654,#141655,#141656,#141657,#141658,#141659,#141660,
#141661,#141662,#141663,#141664,#141665,#141666,#141667,#141668,#141669,
#141670,#141671,#141672,#141673,#141674,#141675,#141676,#141677,#141678,
#141679,#141680,#141681,#141682,#141683,#141684,#141685,#141686,#141687,
#141688,#141689,#141690,#141691,#141692,#141693,#141694,#141695,#141696,
#141697,#141698,#141699,#141700,#141701,#141702,#141703,#141704),
 .UNSPECIFIED.,.F.,.F.,(4,3,3,3,3,3,3,3,3,3,3,3,3,3,3,3,3,3,3,3,3,3,3,3,
3,3,3,3,3,3,3,3,3,3,3,3,3,3,3,3,3,3,3,3,3,3,3,3,3,3,3,3,3,3,3,3,3,3,3,3,
3,3,3,3,3,3,3,3,3,3,3,3,3,3,3,3,3,3,3,3,3,3,4),(107.933005315568,107.971489157774,
108.051446457905,108.131309255148,108.21109507762,108.290821392815,108.370505621109,
108.45017660733,108.529844060856,108.609523711672,108.689231294067,108.769026523142,
108.84887086485,108.928829291897,108.971225168494,109.051182468625,109.131045265868,
109.21083108834,109.290557403535,109.370241631829,109.44991261805,109.529580071576,
109.609259722392,109.688967304787,109.768762533862,109.84860687557,109.928565302617,
109.970961179214,110.050918479345,110.130781276588,110.21056709906,110.290293414255,
110.369977642549,110.44964862877,110.529316082296,110.608995733112,110.688703315507,
110.768498544582,110.84834288629,110.928301313337,110.970697189934,111.050654490065,
111.130517287308,111.210303109779,111.290029424975,111.369713653269,111.449384639489,
111.529052093015,111.608731743832,111.688439326226,111.768234555301,111.848078897009,
111.928037324056,111.970433200654,112.050390500785,112.130253298028,112.2100391205,
112.289765435696,112.36944966399,112.449120650211,112.528788103737,112.608467754554,
112.688175336949,112.767970566025,112.847814907733,112.92777333478,112.970169211375,
113.050126511506,113.129989308749,113.209775131221,113.289501446416,113.36918567471,
113.448856660931,113.528524114457,113.608203765274,113.687911347668,113.767706576744,
113.847550918451,113.927509345499,113.969905222095,114.075449330656,114.17864104367,
114.216190536642),.UNSPECIFIED.);
#1147=B_SPLINE_CURVE_WITH_KNOTS('',3,(#141706,#141707,#141708,#141709,#141710,
#141711,#141712,#141713,#141714,#141715),.UNSPECIFIED.,.F.,.F.,(4,1,1,1,
1,1,1,4),(114.216190622748,114.969641232815,115.969377243535,116.969113254255,
117.968849264975,118.968585275695,119.968321286416,120.499375929927),
 .UNSPECIFIED.);
#1148=B_SPLINE_CURVE_WITH_KNOTS('',3,(#141717,#141718,#141719,#141720,#141721,
#141722,#141723,#141724,#141725,#141726),.UNSPECIFIED.,.F.,.F.,(4,1,1,1,
1,1,1,4),(120.499375929927,120.968057297136,121.967793307856,122.967529318576,
123.967265329296,124.967001340016,125.966737350736,126.782556444121),
 .UNSPECIFIED.);
#1149=B_SPLINE_CURVE_WITH_KNOTS('',3,(#141728,#141729,#141730,#141731,#141732,
#141733,#141734,#141735,#141736,#141737,#141738,#141739,#141740,#141741,
#141742,#141743,#141744,#141745,#141746,#141747,#141748,#141749,#141750,
#141751,#141752,#141753,#141754,#141755,#141756,#141757,#141758,#141759,
#141760,#141761,#141762,#141763,#141764,#141765,#141766,#141767,#141768,
#141769,#141770,#141771,#141772,#141773,#141774,#141775,#141776,#141777,
#141778,#141779,#141780,#141781,#141782,#141783,#141784,#141785,#141786,
#141787,#141788,#141789,#141790,#141791,#141792,#141793,#141794,#141795,
#141796,#141797,#141798,#141799,#141800,#141801,#141802,#141803,#141804,
#141805,#141806,#141807,#141808,#141809,#141810,#141811,#141812,#141813,
#141814,#141815,#141816,#141817,#141818,#141819,#141820,#141821,#141822,
#141823,#141824,#141825,#141826,#141827,#141828,#141829,#141830,#141831,
#141832,#141833,#141834,#141835,#141836,#141837,#141838,#141839,#141840,
#141841,#141842,#141843,#141844,#141845,#141846,#141847,#141848,#141849,
#141850,#141851,#141852,#141853,#141854,#141855,#141856,#141857,#141858,
#141859,#141860,#141861,#141862,#141863,#141864,#141865,#141866,#141867,
#141868,#141869,#141870,#141871,#141872,#141873,#141874,#141875,#141876,
#141877,#141878,#141879,#141880,#141881,#141882,#141883,#141884,#141885,
#141886,#141887,#141888,#141889,#141890,#141891,#141892,#141893,#141894,
#141895,#141896,#141897,#141898,#141899,#141900,#141901,#141902,#141903,
#141904,#141905,#141906,#141907,#141908,#141909,#141910,#141911,#141912,
#141913,#141914,#141915,#141916,#141917,#141918,#141919,#141920,#141921,
#141922,#141923,#141924,#141925,#141926,#141927,#141928,#141929,#141930,
#141931,#141932,#141933,#141934,#141935,#141936,#141937,#141938,#141939,
#141940,#141941,#141942,#141943,#141944,#141945,#141946,#141947,#141948,
#141949,#141950,#141951,#141952,#141953,#141954,#141955,#141956,#141957,
#141958,#141959,#141960,#141961,#141962,#141963,#141964,#141965,#141966,
#141967,#141968,#141969,#141970,#141971),.UNSPECIFIED.,.F.,.F.,(4,3,3,3,
3,3,3,3,3,3,3,3,3,3,3,3,3,3,3,3,3,3,3,3,3,3,3,3,3,3,3,3,3,3,3,3,3,3,3,3,
3,3,3,3,3,3,3,3,3,3,3,3,3,3,3,3,3,3,3,3,3,3,3,3,3,3,3,3,3,3,3,3,3,3,3,3,
3,3,3,3,3,4),(126.782561237107,126.902559628464,126.966473361456,127.046430661588,
127.126293458831,127.206079281303,127.285805596499,127.365489824793,127.445160811014,
127.524828264541,127.604507915357,127.684215497752,127.764010726828,127.843855068536,
127.923813495584,127.966209372176,128.046166672307,128.12602946955,128.205815292022,
128.285541607217,128.365225835512,128.444896821733,128.524564275259,128.604243926075,
128.68395150847,128.763746737546,128.843591079253,128.923549506301,128.965945382897,
129.045902683028,129.125765480271,129.205551302743,129.285277617938,129.364961846232,
129.444632832453,129.524300285979,129.603979936795,129.68368751919,129.763482748265,
129.843327089973,129.92328551702,129.965681393617,130.045638693748,130.125501490991,
130.205287313463,130.285013628658,130.364697856952,130.444368843173,130.524036296699,
130.603715947515,130.68342352991,130.763218758985,130.843063100693,130.92302152774,
130.965417404337,131.045374704468,131.125237501711,131.205023324183,131.284749639378,
131.364433867672,131.444104853893,131.523772307419,131.603451958235,131.68315954063,
131.762954769705,131.842799111413,131.92275753846,131.965153415057,132.045110715188,
132.124973512431,132.204759334903,132.284485650098,132.364169878393,132.443840864614,
132.52350831814,132.603187968956,132.682895551351,132.762690780427,132.842535122134,
132.922493549182,132.964889425777,133.065746544286),.UNSPECIFIED.);
#1150=B_SPLINE_CURVE_WITH_KNOTS('',3,(#141973,#141974,#141975,#141976,#141977,
#141978,#141979,#141980,#141981,#141982),.UNSPECIFIED.,.F.,.F.,(4,1,1,1,
1,1,1,4),(133.065755642825,133.964625436497,134.964361447218,135.964097457938,
136.963833468658,137.963569479378,138.963305490098,139.34892440658),
 .UNSPECIFIED.);
#1151=B_SPLINE_CURVE_WITH_KNOTS('',3,(#141984,#141985,#141986,#141987,#141988,
#141989,#141990,#141991,#141992,#141993,#141994,#141995,#141996,#141997,
#141998,#141999,#142000,#142001,#142002,#142003,#142004,#142005,#142006,
#142007,#142008,#142009,#142010,#142011,#142012,#142013,#142014,#142015,
#142016,#142017,#142018,#142019,#142020,#142021,#142022,#142023,#142024,
#142025,#142026,#142027,#142028,#142029,#142030,#142031,#142032,#142033,
#142034,#142035,#142036,#142037,#142038,#142039,#142040,#142041,#142042,
#142043,#142044,#142045,#142046,#142047,#142048,#142049,#142050,#142051,
#142052,#142053,#142054,#142055,#142056,#142057,#142058,#142059,#142060,
#142061,#142062,#142063,#142064,#142065,#142066,#142067,#142068,#142069,
#142070,#142071,#142072,#142073,#142074,#142075,#142076,#142077,#142078,
#142079,#142080,#142081,#142082,#142083,#142084,#142085,#142086,#142087,
#142088,#142089,#142090,#142091,#142092,#142093,#142094,#142095,#142096,
#142097,#142098,#142099,#142100,#142101,#142102,#142103,#142104,#142105,
#142106,#142107,#142108,#142109,#142110,#142111,#142112,#142113,#142114,
#142115,#142116,#142117,#142118,#142119,#142120,#142121,#142122,#142123,
#142124,#142125,#142126,#142127,#142128,#142129,#142130,#142131,#142132,
#142133,#142134,#142135,#142136,#142137,#142138,#142139,#142140,#142141,
#142142,#142143,#142144,#142145,#142146,#142147,#142148,#142149,#142150,
#142151,#142152,#142153,#142154,#142155,#142156,#142157,#142158,#142159,
#142160,#142161,#142162,#142163,#142164,#142165,#142166,#142167,#142168,
#142169,#142170,#142171,#142172,#142173,#142174,#142175,#142176,#142177,
#142178,#142179,#142180,#142181,#142182,#142183,#142184,#142185,#142186,
#142187,#142188,#142189,#142190,#142191,#142192,#142193,#142194,#142195,
#142196,#142197,#142198,#142199,#142200,#142201,#142202,#142203,#142204,
#142205,#142206,#142207,#142208,#142209,#142210,#142211,#142212,#142213,
#142214,#142215,#142216,#142217,#142218,#142219,#142220,#142221,#142222,
#142223,#142224,#142225,#142226,#142227,#142228,#142229,#142230),
 .UNSPECIFIED.,.F.,.F.,(4,3,3,3,3,3,3,3,3,3,3,3,3,3,3,3,3,3,3,3,3,3,3,3,
3,3,3,3,3,3,3,3,3,3,3,3,3,3,3,3,3,3,3,3,3,3,3,3,3,3,3,3,3,3,3,3,3,3,3,3,
3,3,3,3,3,3,3,3,3,3,3,3,3,3,3,3,3,3,3,3,3,3,4),(139.348931851466,139.429394985958,
139.509870031329,139.590371667878,139.670914589187,139.751564232921,139.832272604219,
139.913111307842,139.963041500818,140.042998800949,140.122861598192,140.202647420663,
140.282373735859,140.362057964153,140.441728950374,140.521396403899,140.601076054716,
140.68078363711,140.760578866186,140.840423207893,140.92038163494,140.962777511538,
141.042734811669,141.122597608912,141.202383431384,141.282109746579,141.361793974873,
141.441464961094,141.52113241462,141.600812065436,141.680519647831,141.760314876907,
141.840159218614,141.920117645662,141.962513522258,142.042470822389,142.122333619632,
142.202119442103,142.281845757298,142.361529985591,142.441200971812,142.520868425338,
142.600548076154,142.680255658548,142.760050887624,142.839895229331,142.919853656379,
142.962249532978,143.04220683311,143.122069630352,143.201855452824,143.28158176802,
143.361265996314,143.440936982535,143.520604436061,143.600284086878,143.679991669273,
143.759786898348,143.839631240056,143.919589667104,143.961985543699,144.04194284383,
144.121805641073,144.201591463546,144.281317778741,144.361002007036,144.440672993257,
144.520340446783,144.6000200976,144.679727679994,144.75952290907,144.839367250778,
144.919325677825,144.961721554419,145.045521004947,145.125273005645,145.204950022292,
145.284567928792,145.364142558629,145.443696576801,145.523238805001,145.602799540725,
145.632117158645),.UNSPECIFIED.);
#1152=B_SPLINE_CURVE_WITH_KNOTS('',3,(#142232,#142233,#142234,#142235,#142236,
#142237,#142238,#142239,#142240,#142241),.UNSPECIFIED.,.F.,.F.,(4,1,1,1,
1,1,1,4),(145.632124439118,145.961457565139,146.961193575859,147.960929586579,
148.960665597299,149.960401608019,150.960137618739,151.915296521168),
 .UNSPECIFIED.);
#1153=B_SPLINE_CURVE_WITH_KNOTS('',3,(#142243,#142244,#142245,#142246,#142247,
#142248,#142249,#142250,#142251,#142252,#142253,#142254,#142255,#142256,
#142257,#142258,#142259,#142260,#142261,#142262,#142263,#142264,#142265,
#142266,#142267,#142268,#142269,#142270,#142271,#142272,#142273,#142274,
#142275,#142276,#142277,#142278,#142279,#142280,#142281,#142282,#142283,
#142284,#142285,#142286,#142287,#142288,#142289,#142290,#142291,#142292,
#142293,#142294,#142295,#142296,#142297,#142298,#142299,#142300,#142301,
#142302,#142303,#142304,#142305,#142306,#142307,#142308,#142309,#142310,
#142311,#142312,#142313,#142314,#142315,#142316,#142317,#142318,#142319,
#142320,#142321,#142322,#142323,#142324,#142325,#142326,#142327,#142328,
#142329,#142330,#142331,#142332,#142333,#142334,#142335,#142336,#142337,
#142338,#142339,#142340,#142341,#142342,#142343,#142344,#142345,#142346,
#142347,#142348,#142349,#142350,#142351,#142352,#142353,#142354,#142355,
#142356,#142357,#142358,#142359,#142360,#142361,#142362,#142363,#142364,
#142365,#142366,#142367,#142368,#142369,#142370,#142371,#142372,#142373,
#142374,#142375,#142376,#142377,#142378,#142379,#142380,#142381,#142382,
#142383,#142384,#142385,#142386,#142387,#142388,#142389,#142390,#142391,
#142392,#142393,#142394,#142395,#142396,#142397,#142398,#142399,#142400,
#142401,#142402,#142403,#142404,#142405,#142406,#142407,#142408,#142409,
#142410,#142411,#142412,#142413,#142414,#142415,#142416,#142417,#142418,
#142419,#142420,#142421,#142422,#142423,#142424,#142425,#142426,#142427,
#142428,#142429,#142430,#142431,#142432,#142433,#142434,#142435,#142436,
#142437,#142438,#142439,#142440,#142441,#142442,#142443,#142444,#142445,
#142446,#142447,#142448,#142449,#142450,#142451,#142452,#142453,#142454,
#142455,#142456,#142457,#142458,#142459,#142460,#142461,#142462,#142463,
#142464,#142465,#142466,#142467,#142468,#142469,#142470,#142471,#142472,
#142473,#142474,#142475,#142476,#142477,#142478,#142479,#142480,#142481,
#142482,#142483,#142484,#142485,#142486,#142487,#142488,#142489),
 .UNSPECIFIED.,.F.,.F.,(4,3,3,3,3,3,3,3,3,3,3,3,3,3,3,3,3,3,3,3,3,3,3,3,
3,3,3,3,3,3,3,3,3,3,3,3,3,3,3,3,3,3,3,3,3,3,3,3,3,3,3,3,3,3,3,3,3,3,3,3,
3,3,3,3,3,3,3,3,3,3,3,3,3,3,3,3,3,3,3,3,3,3,4),(151.915302465825,151.95987362946,
152.039830929591,152.119693726834,152.199479549306,152.279205864501,152.358890092795,
152.438561079015,152.518228532541,152.597908183358,152.677615765752,152.757410994827,
152.837255336535,152.917213763582,152.95960964018,153.039566940311,153.119429737554,
153.199215560026,153.278941875221,153.358626103515,153.438297089736,153.517964543262,
153.597644194079,153.677351776473,153.757147005549,153.836991347256,153.916949774304,
153.9593456509,154.039302951031,154.119165748274,154.198951570746,154.278677885941,
154.358362114235,154.438033100456,154.517700553982,154.597380204798,154.677087787193,
154.756883016268,154.836727357976,154.916685785023,154.95908166162,155.039038961751,
155.118901758994,155.198687581466,155.278413896661,155.358098124955,155.437769111176,
155.517436564702,155.597116215519,155.676823797913,155.756619026989,155.836463368696,
155.916421795744,155.95881767234,156.038774972471,156.118637769714,156.198423592186,
156.278149907381,156.357834135675,156.437505121896,156.517172575422,156.596852226238,
156.676559808633,156.756355037708,156.836199379416,156.916157806463,156.95855368306,
157.038510983191,157.118373780434,157.198159602905,157.2778859181,157.357570146394,
157.437241132615,157.516908586141,157.596588236957,157.676295819352,157.756091048427,
157.835935390135,157.915893817182,157.95828969378,158.065027953602,158.16918115264,
158.198487725055),.UNSPECIFIED.);
#1154=B_SPLINE_CURVE_WITH_KNOTS('',3,(#142491,#142492,#142493,#142494,#142495,
#142496,#142497,#142498,#142499,#142500),.UNSPECIFIED.,.F.,.F.,(4,1,1,1,
1,1,1,4),(158.198487773005,158.958025704501,159.957761715221,160.957497725941,
161.957233736661,162.956969747381,163.956705758101,164.481673080184),
 .UNSPECIFIED.);
#1155=B_SPLINE_CURVE_WITH_KNOTS('',3,(#142502,#142503,#142504,#142505,#142506,
#142507,#142508,#142509,#142510,#142511),.UNSPECIFIED.,.F.,.F.,(4,1,1,1,
1,1,1,4),(164.481673080184,164.956441768821,165.956177779541,166.955913790262,
167.955649800982,168.955385811702,169.955121822422,170.76485415669),
 .UNSPECIFIED.);
#1156=B_SPLINE_CURVE_WITH_KNOTS('',3,(#142513,#142514,#142515,#142516,#142517,
#142518,#142519,#142520,#142521,#142522,#142523,#142524,#142525,#142526,
#142527,#142528,#142529,#142530,#142531,#142532,#142533,#142534,#142535,
#142536,#142537,#142538,#142539,#142540,#142541,#142542,#142543,#142544,
#142545,#142546,#142547,#142548,#142549,#142550,#142551,#142552,#142553,
#142554,#142555,#142556,#142557,#142558,#142559,#142560,#142561,#142562,
#142563,#142564,#142565,#142566,#142567,#142568,#142569,#142570,#142571,
#142572,#142573,#142574,#142575,#142576,#142577,#142578,#142579,#142580,
#142581,#142582,#142583,#142584,#142585,#142586,#142587,#142588,#142589,
#142590,#142591,#142592,#142593,#142594,#142595,#142596,#142597,#142598,
#142599,#142600,#142601,#142602,#142603,#142604,#142605,#142606,#142607,
#142608,#142609,#142610,#142611,#142612,#142613,#142614,#142615,#142616,
#142617,#142618,#142619,#142620,#142621,#142622,#142623,#142624,#142625,
#142626,#142627,#142628,#142629,#142630,#142631,#142632,#142633,#142634,
#142635,#142636,#142637,#142638,#142639,#142640,#142641,#142642,#142643,
#142644,#142645,#142646,#142647,#142648,#142649,#142650,#142651,#142652,
#142653,#142654,#142655,#142656,#142657,#142658,#142659,#142660,#142661,
#142662,#142663,#142664,#142665,#142666,#142667,#142668,#142669,#142670,
#142671,#142672,#142673,#142674,#142675,#142676,#142677,#142678,#142679,
#142680,#142681,#142682,#142683,#142684,#142685,#142686,#142687,#142688,
#142689,#142690,#142691,#142692,#142693,#142694,#142695,#142696,#142697,
#142698,#142699,#142700,#142701,#142702,#142703,#142704,#142705,#142706,
#142707,#142708,#142709,#142710,#142711,#142712,#142713,#142714,#142715,
#142716,#142717,#142718,#142719,#142720,#142721,#142722,#142723,#142724,
#142725,#142726,#142727,#142728,#142729,#142730,#142731,#142732,#142733,
#142734,#142735,#142736,#142737,#142738,#142739,#142740,#142741,#142742,
#142743,#142744,#142745,#142746,#142747,#142748,#142749,#142750,#142751,
#142752,#142753,#142754,#142755,#142756),.UNSPECIFIED.,.F.,.F.,(4,3,3,3,
3,3,3,3,3,3,3,3,3,3,3,3,3,3,3,3,3,3,3,3,3,3,3,3,3,3,3,3,3,3,3,3,3,3,3,3,
3,3,3,3,3,3,3,3,3,3,3,3,3,3,3,3,3,3,3,3,3,3,3,3,3,3,3,3,3,3,3,3,3,3,3,3,
3,3,3,3,3,4),(170.764858387364,170.882744850471,170.954857833142,171.034815133274,
171.114677930517,171.194463752989,171.274190068185,171.353874296479,171.433545282701,
171.513212736227,171.592892387044,171.672599969439,171.752395198515,171.832239540223,
171.912197967271,171.954593843862,172.034551143993,172.114413941236,172.194199763708,
172.273926078903,172.353610307197,172.433281293418,172.512948746943,172.59262839776,
172.672335980154,172.75213120923,172.831975550937,172.911933977985,172.954329854582,
173.034287154713,173.114149951956,173.193935774427,173.273662089622,173.353346317916,
173.433017304137,173.512684757663,173.592364408479,173.672071990873,173.751867219949,
173.831711561656,173.911669988704,173.954065865302,174.034023165433,174.113885962676,
174.193671785148,174.273398100344,174.353082328638,174.432753314859,174.512420768386,
174.592100419202,174.671808001597,174.751603230673,174.831447572381,174.911405999428,
174.953801876023,175.033759176154,175.113621973397,175.193407795869,175.273134111064,
175.352818339358,175.432489325579,175.512156779105,175.591836429922,175.671544012316,
175.751339241392,175.8311835831,175.911142010147,175.953537886743,176.033495186874,
176.113357984117,176.193143806589,176.272870121784,176.352554350078,176.432225336299,
176.511892789825,176.591572440641,176.671280023036,176.751075252111,176.830919593819,
176.910878020866,176.953273897463,177.048043694543),.UNSPECIFIED.);
#1157=B_SPLINE_CURVE_WITH_KNOTS('',3,(#142758,#142759,#142760,#142761,#142762,
#142763,#142764,#142765,#142766,#142767),.UNSPECIFIED.,.F.,.F.,(4,1,1,1,
1,1,1,4),(177.048052727997,177.953009908183,178.952745918903,179.952481929623,
180.952217940343,181.951953951063,182.951689961784,183.33122142995),
 .UNSPECIFIED.);
#1158=B_SPLINE_CURVE_WITH_KNOTS('',3,(#142769,#142770,#142771,#142772,#142773,
#142774,#142775,#142776,#142777,#142778,#142779,#142780,#142781,#142782,
#142783,#142784,#142785,#142786,#142787,#142788,#142789,#142790,#142791,
#142792,#142793,#142794,#142795,#142796,#142797,#142798,#142799,#142800,
#142801,#142802,#142803,#142804,#142805,#142806,#142807,#142808,#142809,
#142810,#142811,#142812,#142813,#142814,#142815,#142816,#142817,#142818,
#142819,#142820,#142821,#142822,#142823,#142824,#142825,#142826,#142827,
#142828,#142829,#142830,#142831,#142832,#142833,#142834,#142835,#142836,
#142837,#142838,#142839,#142840,#142841,#142842,#142843,#142844,#142845,
#142846,#142847,#142848,#142849,#142850,#142851,#142852,#142853,#142854,
#142855,#142856,#142857,#142858,#142859,#142860,#142861,#142862,#142863,
#142864,#142865,#142866,#142867,#142868,#142869,#142870,#142871,#142872,
#142873,#142874,#142875,#142876,#142877,#142878,#142879,#142880,#142881,
#142882,#142883,#142884,#142885,#142886,#142887,#142888,#142889,#142890,
#142891,#142892,#142893,#142894,#142895,#142896,#142897,#142898,#142899,
#142900,#142901,#142902,#142903,#142904,#142905,#142906,#142907,#142908,
#142909,#142910,#142911,#142912,#142913,#142914,#142915,#142916,#142917,
#142918,#142919,#142920,#142921,#142922,#142923,#142924,#142925,#142926,
#142927,#142928,#142929,#142930,#142931,#142932,#142933,#142934,#142935,
#142936,#142937,#142938,#142939,#142940,#142941,#142942,#142943,#142944,
#142945,#142946,#142947,#142948,#142949,#142950,#142951,#142952,#142953,
#142954,#142955,#142956,#142957,#142958,#142959,#142960,#142961,#142962,
#142963,#142964,#142965,#142966,#142967,#142968,#142969,#142970,#142971,
#142972,#142973,#142974,#142975,#142976,#142977,#142978,#142979,#142980,
#142981,#142982,#142983,#142984,#142985,#142986,#142987,#142988,#142989,
#142990,#142991,#142992,#142993,#142994,#142995,#142996,#142997,#142998,
#142999,#143000,#143001,#143002,#143003,#143004,#143005,#143006,#143007,
#143008,#143009,#143010,#143011,#143012,#143013,#143014,#143015),
 .UNSPECIFIED.,.F.,.F.,(4,3,3,3,3,3,3,3,3,3,3,3,3,3,3,3,3,3,3,3,3,3,3,3,
3,3,3,3,3,3,3,3,3,3,3,3,3,3,3,3,3,3,3,3,3,3,3,3,3,3,3,3,3,3,3,3,3,3,3,3,
3,3,3,3,3,3,3,3,3,3,3,3,3,3,3,3,3,3,3,3,3,3,4),(183.331229001723,183.411579138959,
183.49193796612,183.572320324641,183.65274106719,183.733266169438,183.81384773384,
183.894560468422,183.951425972504,184.031383272635,184.111246069878,184.191031892349,
184.270758207545,184.350442435838,184.430113422059,184.509780875585,184.589460526401,
184.669168108795,184.748963337871,184.828807679578,184.908766106625,184.951161983224,
185.031119283355,185.110982080598,185.190767903069,185.270494218265,185.350178446559,
185.42984943278,185.509516886306,185.589196537122,185.668904119517,185.748699348592,
185.8285436903,185.908502117347,185.950897993944,186.030855294075,186.110718091318,
186.190503913789,186.270230228985,186.349914457279,186.4295854435,186.509252897026,
186.588932547842,186.668640130237,186.748435359312,186.82827970102,186.908238128067,
186.950634004664,187.030591304795,187.110454102038,187.190239924509,187.269966239705,
187.349650467998,187.429321454219,187.508988907745,187.588668558562,187.668376140956,
187.748171370032,187.82801571174,187.907974138787,187.950370015384,188.030327315515,
188.110190112758,188.189975935229,188.269702250425,188.349386478719,188.42905746494,
188.508724918465,188.588404569282,188.668112151676,188.747907380752,188.82775172246,
188.907710149507,188.950106026104,189.033144561454,189.112986258176,189.192752007562,
189.272457603206,189.352118797911,189.431757014182,189.511382385588,189.591023092393,
189.614414308902),.UNSPECIFIED.);
#1159=B_SPLINE_CURVE_WITH_KNOTS('',3,(#143017,#143018,#143019,#143020,#143021,
#143022,#143023,#143024,#143025,#143026),.UNSPECIFIED.,.F.,.F.,(4,1,1,1,
1,1,1,4),(189.614421781537,189.949842036824,190.949578047545,191.949314058265,
192.949050068985,193.948786079705,194.948522090425,195.897599616082),
 .UNSPECIFIED.);
#1160=B_SPLINE_CURVE_WITH_KNOTS('',3,(#143028,#143029,#143030,#143031,#143032,
#143033,#143034,#143035,#143036,#143037,#143038,#143039),.UNSPECIFIED.,
 .F.,.F.,(4,2,1,1,1,1,1,1,4),(195.897599616082,195.948258101145,196.947994111865,
197.947730122585,198.947466133306,199.947202144026,200.946938154746,201.946674165466,
202.180784923262),.UNSPECIFIED.);
#1161=B_SPLINE_CURVE_WITH_KNOTS('',3,(#143041,#143042,#143043,#143044,#143045,
#143046,#143047,#143048,#143049,#143050),.UNSPECIFIED.,.F.,.F.,(4,1,1,1,
1,1,1,4),(202.180784923262,202.946410176186,203.946146186906,204.945882197626,
205.945618208347,206.945354219067,207.945090229787,208.463970230441),
 .UNSPECIFIED.);
#1162=B_SPLINE_CURVE_WITH_KNOTS('',3,(#143052,#143053,#143054,#143055,#143056,
#143057,#143058,#143059,#143060,#143061),.UNSPECIFIED.,.F.,.F.,(4,1,1,1,
1,1,1,4),(208.463970230441,208.944826240507,209.944562251227,210.944298261947,
211.944034272667,212.943770283387,213.943506294108,214.747151886774),
 .UNSPECIFIED.);
#1163=B_SPLINE_CURVE_WITH_KNOTS('',3,(#143063,#143064,#143065,#143066,#143067,
#143068,#143069,#143070,#143071,#143072,#143073,#143074,#143075,#143076,
#143077,#143078,#143079,#143080,#143081,#143082,#143083,#143084,#143085,
#143086,#143087,#143088,#143089,#143090,#143091,#143092,#143093,#143094,
#143095,#143096,#143097,#143098,#143099,#143100,#143101,#143102,#143103,
#143104,#143105,#143106,#143107,#143108,#143109,#143110,#143111,#143112,
#143113,#143114,#143115,#143116,#143117,#143118,#143119,#143120,#143121,
#143122,#143123,#143124,#143125,#143126,#143127,#143128,#143129,#143130,
#143131,#143132,#143133,#143134,#143135,#143136,#143137,#143138,#143139,
#143140,#143141,#143142,#143143,#143144,#143145,#143146,#143147,#143148,
#143149,#143150,#143151,#143152,#143153,#143154,#143155,#143156,#143157,
#143158,#143159,#143160,#143161,#143162,#143163,#143164,#143165,#143166,
#143167,#143168,#143169,#143170,#143171,#143172,#143173,#143174,#143175,
#143176,#143177,#143178,#143179,#143180,#143181,#143182,#143183,#143184,
#143185,#143186,#143187,#143188,#143189,#143190,#143191,#143192,#143193,
#143194,#143195,#143196,#143197,#143198,#143199,#143200,#143201,#143202,
#143203,#143204,#143205,#143206,#143207,#143208,#143209,#143210,#143211,
#143212,#143213,#143214,#143215,#143216,#143217,#143218,#143219,#143220,
#143221,#143222,#143223,#143224,#143225,#143226,#143227,#143228,#143229,
#143230,#143231,#143232,#143233,#143234,#143235,#143236,#143237,#143238,
#143239,#143240,#143241,#143242,#143243,#143244,#143245,#143246,#143247,
#143248,#143249,#143250,#143251,#143252,#143253,#143254,#143255,#143256,
#143257,#143258,#143259,#143260,#143261,#143262,#143263,#143264,#143265,
#143266,#143267,#143268,#143269,#143270,#143271,#143272,#143273,#143274,
#143275,#143276,#143277,#143278,#143279,#143280,#143281,#143282,#143283,
#143284,#143285,#143286,#143287,#143288,#143289,#143290,#143291,#143292,
#143293,#143294,#143295,#143296,#143297,#143298,#143299,#143300,#143301,
#143302,#143303,#143304,#143305,#143306),.UNSPECIFIED.,.F.,.F.,(4,3,3,3,
3,3,3,3,3,3,3,3,3,3,3,3,3,3,3,3,3,3,3,3,3,3,3,3,3,3,3,3,3,3,3,3,3,3,3,3,
3,3,3,3,3,3,3,3,3,3,3,3,3,3,3,3,3,3,3,3,3,3,3,3,3,3,3,3,3,3,3,3,3,3,3,3,
3,3,3,3,3,4),(214.747155537621,214.863097551269,214.943242304828,215.02319960496,
215.103062402203,215.182848224675,215.262574539871,215.342258768165,215.421929754386,
215.501597207913,215.581276858729,215.660984441124,215.7407796702,215.820624011908,
215.900582438956,215.942978315548,216.022935615679,216.102798412922,216.182584235393,
216.262310550589,216.341994778883,216.421665765104,216.501333218629,216.581012869446,
216.66072045184,216.740515680916,216.820360022623,216.900318449671,216.942714326268,
217.022671626399,217.102534423642,217.182320246114,217.262046561309,217.341730789603,
217.421401775824,217.50106922935,217.580748880166,217.660456462561,217.740251691636,
217.820096033344,217.900054460391,217.942450336988,218.022407637119,218.102270434362,
218.182056256834,218.261782572029,218.341466800323,218.421137786544,218.50080524007,
218.580484890887,218.660192473281,218.739987702357,218.819832044064,218.899790471112,
218.942186347708,219.022143647839,219.102006445082,219.181792267553,219.261518582749,
219.341202811043,219.420873797263,219.500541250789,219.580220901606,219.659928484,
219.739723713076,219.819568054783,219.89952648183,219.941922358428,220.02187965856,
220.101742455802,220.181528278274,220.26125459347,220.340938821764,220.420609807986,
220.500277261512,220.579956912329,220.659664494723,220.739459723799,220.819304065507,
220.899262492555,220.941658369149,221.0303408448),.UNSPECIFIED.);
#1164=B_SPLINE_CURVE_WITH_KNOTS('',3,(#143308,#143309,#143310,#143311,#143312,
#143313,#143314,#143315,#143316,#143317),.UNSPECIFIED.,.F.,.F.,(4,1,1,1,
1,1,1,4),(221.030349614055,221.941394379869,222.941130390589,223.940866401309,
224.940602412029,225.940338422749,226.940074433469,227.313518490426),
 .UNSPECIFIED.);
#1165=B_SPLINE_CURVE_WITH_KNOTS('',3,(#143319,#143320,#143321,#143322,#143323,
#143324,#143325,#143326,#143327,#143328,#143329,#143330,#143331,#143332,
#143333,#143334,#143335,#143336,#143337,#143338,#143339,#143340,#143341,
#143342,#143343,#143344,#143345,#143346,#143347,#143348,#143349,#143350,
#143351,#143352,#143353,#143354,#143355,#143356,#143357,#143358,#143359,
#143360,#143361,#143362,#143363,#143364,#143365,#143366,#143367,#143368,
#143369,#143370,#143371,#143372,#143373,#143374,#143375,#143376,#143377,
#143378,#143379,#143380,#143381,#143382,#143383,#143384,#143385,#143386,
#143387,#143388,#143389,#143390,#143391,#143392,#143393,#143394,#143395,
#143396,#143397,#143398,#143399,#143400,#143401,#143402,#143403,#143404,
#143405,#143406,#143407,#143408,#143409,#143410,#143411,#143412,#143413,
#143414,#143415,#143416,#143417,#143418,#143419,#143420,#143421,#143422,
#143423,#143424,#143425,#143426,#143427,#143428,#143429,#143430,#143431,
#143432,#143433,#143434,#143435,#143436,#143437,#143438,#143439,#143440,
#143441,#143442,#143443,#143444,#143445,#143446,#143447,#143448,#143449,
#143450,#143451,#143452,#143453,#143454,#143455,#143456,#143457,#143458,
#143459,#143460,#143461,#143462,#143463,#143464,#143465,#143466,#143467,
#143468,#143469,#143470,#143471,#143472,#143473,#143474,#143475,#143476,
#143477,#143478,#143479,#143480,#143481,#143482,#143483,#143484,#143485,
#143486,#143487,#143488,#143489,#143490,#143491,#143492,#143493,#143494,
#143495,#143496,#143497,#143498,#143499,#143500,#143501,#143502,#143503,
#143504,#143505,#143506,#143507,#143508,#143509,#143510,#143511,#143512,
#143513,#143514,#143515,#143516,#143517,#143518,#143519,#143520,#143521,
#143522,#143523,#143524,#143525,#143526,#143527,#143528,#143529,#143530,
#143531,#143532,#143533,#143534,#143535,#143536,#143537,#143538,#143539,
#143540,#143541,#143542,#143543,#143544,#143545,#143546,#143547,#143548,
#143549,#143550,#143551,#143552,#143553,#143554,#143555,#143556,#143557,
#143558,#143559,#143560,#143561,#143562,#143563,#143564,#143565),
 .UNSPECIFIED.,.F.,.F.,(4,3,3,3,3,3,3,3,3,3,3,3,3,3,3,3,3,3,3,3,3,3,3,3,
3,3,3,3,3,3,3,3,3,3,3,3,3,3,3,3,3,3,3,3,3,3,3,3,3,3,3,3,3,3,3,3,3,3,3,3,
3,3,3,3,3,3,3,3,3,3,3,3,3,3,3,3,3,3,3,3,3,3,4),(227.31352615198,227.393767393133,
227.474014212927,227.554281601494,227.634584558287,227.714989577679,227.795448844244,
227.876040164136,227.939810444189,228.01976774432,228.099630541563,228.179416364034,
228.25914267923,228.338826907524,228.418497893745,228.49816534727,228.577844998087,
228.657552580481,228.737347809557,228.817192151264,228.897150578312,228.939546454909,
229.01950375504,229.099366552283,229.179152374755,229.258878689951,229.338562918246,
229.418233904467,229.497901357993,229.577581008809,229.657288591204,229.73708382028,
229.816928161988,229.896886589035,229.93928246563,230.019239765761,230.099102563004,
230.178888385476,230.258614700671,230.338298928965,230.417969915187,230.497637368713,
230.577317019529,230.657024601924,230.736819831,230.816664172707,230.896622599755,
230.93901847635,231.018975776481,231.098838573724,231.178624396195,231.25835071139,
231.338034939684,231.417705925905,231.497373379431,231.577053030248,231.656760612642,
231.736555841717,231.816400183424,231.896358610472,231.93875448707,232.018711787201,
232.098574584444,232.178360406916,232.258086722111,232.337770950405,232.417441936626,
232.497109390152,232.576789040969,232.656496623363,232.736291852439,232.816136194146,
232.896094621194,232.93849049779,233.020768117961,233.100703328103,233.18056158131,
233.260358584177,233.340110002069,233.419836019979,233.499548074529,233.579272327654,
233.596711459159),.UNSPECIFIED.);
#1166=B_SPLINE_CURVE_WITH_KNOTS('',3,(#143567,#143568,#143569,#143570,#143571,
#143572,#143573,#143574,#143575,#143576),.UNSPECIFIED.,.F.,.F.,(4,1,1,1,
1,1,1,4),(233.596719085091,233.93822650851,234.93796251923,235.93769852995,
236.937434540671,237.937170551391,238.936906562111,239.879896766339),
 .UNSPECIFIED.);
#1167=B_SPLINE_CURVE_WITH_KNOTS('',3,(#143578,#143579,#143580,#143581,#143582,
#143583,#143584,#143585,#143586,#143587,#143588,#143589),.UNSPECIFIED.,
 .F.,.F.,(4,2,1,1,1,1,1,1,4),(239.879896766339,239.936642572831,240.936378583551,
241.936114594271,242.935850604991,243.935586615712,244.935322626432,245.935058637152,
246.163082073519),.UNSPECIFIED.);
#1168=B_SPLINE_CURVE_WITH_KNOTS('',3,(#143591,#143592,#143593,#143594,#143595,
#143596,#143597,#143598,#143599,#143600,#143601,#143602,#143603,#143604,
#143605,#143606,#143607,#143608,#143609,#143610,#143611,#143612,#143613,
#143614,#143615,#143616,#143617,#143618,#143619,#143620,#143621,#143622,
#143623,#143624,#143625,#143626,#143627,#143628,#143629,#143630,#143631,
#143632,#143633,#143634,#143635,#143636,#143637,#143638,#143639,#143640,
#143641,#143642,#143643,#143644,#143645,#143646,#143647,#143648,#143649,
#143650,#143651,#143652,#143653,#143654,#143655,#143656,#143657,#143658,
#143659,#143660,#143661,#143662,#143663,#143664,#143665,#143666,#143667,
#143668,#143669,#143670,#143671,#143672,#143673,#143674,#143675,#143676,
#143677,#143678,#143679,#143680,#143681,#143682,#143683,#143684,#143685,
#143686,#143687,#143688,#143689,#143690,#143691,#143692,#143693,#143694,
#143695,#143696,#143697,#143698,#143699,#143700,#143701,#143702,#143703,
#143704,#143705,#143706,#143707,#143708,#143709,#143710,#143711,#143712,
#143713,#143714,#143715,#143716,#143717,#143718,#143719,#143720,#143721,
#143722,#143723,#143724,#143725,#143726,#143727,#143728,#143729,#143730,
#143731,#143732,#143733,#143734,#143735,#143736,#143737,#143738,#143739,
#143740,#143741,#143742,#143743,#143744,#143745,#143746,#143747,#143748,
#143749,#143750,#143751,#143752,#143753,#143754,#143755,#143756,#143757,
#143758,#143759,#143760,#143761,#143762,#143763,#143764,#143765,#143766,
#143767,#143768,#143769,#143770,#143771,#143772,#143773,#143774,#143775,
#143776,#143777,#143778,#143779,#143780,#143781,#143782,#143783,#143784,
#143785,#143786,#143787,#143788,#143789,#143790,#143791,#143792,#143793,
#143794,#143795,#143796,#143797,#143798,#143799,#143800,#143801,#143802,
#143803,#143804,#143805,#143806,#143807,#143808,#143809,#143810,#143811,
#143812,#143813,#143814,#143815,#143816,#143817,#143818,#143819,#143820,
#143821,#143822,#143823,#143824,#143825,#143826,#143827,#143828,#143829,
#143830,#143831,#143832,#143833,#143834,#143835,#143836,#143837),
 .UNSPECIFIED.,.F.,.F.,(4,3,3,3,3,3,3,3,3,3,3,3,3,3,3,3,3,3,3,3,3,3,3,3,
3,3,3,3,3,3,3,3,3,3,3,3,3,3,3,3,3,3,3,3,3,3,3,3,3,3,3,3,3,3,3,3,3,3,3,3,
3,3,3,3,3,3,3,3,3,3,3,3,3,3,3,3,3,3,3,3,3,3,4),(246.163082073519,246.241812808052,
246.320488022863,246.399133213762,246.477764257754,246.55639764423,246.635049862504,
246.713782865171,246.792558235773,246.871451270532,246.934794647872,247.014751948003,
247.094614745246,247.174400567718,247.254126882913,247.333811111207,247.413482097428,
247.493149550953,247.57282920177,247.652536784164,247.73233201324,247.812176354948,
247.892134781995,247.934530658592,248.014487958723,248.094350755966,248.174136578438,
248.253862893633,248.333547121927,248.413218108148,248.492885561674,248.57256521249,
248.652272794885,248.73206802396,248.811912365668,248.891870792716,248.934266669312,
249.014223969443,249.094086766686,249.173872589157,249.253598904353,249.333283132647,
249.412954118868,249.492621572393,249.57230122321,249.652008805604,249.73180403468,
249.811648376387,249.891606803435,249.934002680032,250.013959980163,250.093822777406,
250.173608599878,250.253334915073,250.333019143366,250.412690129587,250.492357583113,
250.572037233929,250.651744816324,250.7315400454,250.811384387107,250.891342814154,
250.933738690752,251.013695990883,251.093558788126,251.173344610597,251.253070925793,
251.332755154087,251.412426140308,251.492093593834,251.57177324465,251.651480827045,
251.73127605612,251.811120397828,251.891078824876,251.933474701472,252.017082946527,
252.100559235755,252.186986271991,252.270183268191,252.353287967343,252.436284943832,
252.446267380698),.UNSPECIFIED.);
#1169=B_SPLINE_CURVE_WITH_KNOTS('',3,(#143839,#143840,#143841,#143842,#143843,
#143844,#143845,#143846,#143847,#143848,#143849,#143850,#143851,#143852,
#143853,#143854,#143855,#143856,#143857,#143858,#143859,#143860,#143861,
#143862,#143863,#143864,#143865,#143866,#143867,#143868,#143869,#143870,
#143871,#143872,#143873,#143874,#143875,#143876,#143877,#143878,#143879,
#143880,#143881,#143882,#143883,#143884,#143885,#143886,#143887,#143888,
#143889,#143890,#143891,#143892,#143893,#143894,#143895,#143896,#143897,
#143898,#143899,#143900,#143901,#143902,#143903,#143904,#143905,#143906,
#143907,#143908,#143909,#143910,#143911,#143912,#143913,#143914,#143915,
#143916,#143917,#143918,#143919,#143920,#143921,#143922,#143923,#143924,
#143925,#143926,#143927,#143928,#143929,#143930,#143931,#143932,#143933,
#143934,#143935,#143936,#143937,#143938,#143939,#143940,#143941,#143942,
#143943,#143944,#143945,#143946,#143947,#143948,#143949,#143950,#143951,
#143952,#143953,#143954,#143955,#143956,#143957,#143958,#143959,#143960,
#143961,#143962,#143963,#143964,#143965,#143966,#143967,#143968,#143969,
#143970,#143971,#143972,#143973,#143974,#143975,#143976,#143977,#143978,
#143979,#143980,#143981,#143982,#143983,#143984,#143985,#143986,#143987,
#143988,#143989,#143990,#143991,#143992,#143993,#143994,#143995,#143996,
#143997,#143998,#143999,#144000,#144001,#144002,#144003,#144004,#144005,
#144006,#144007,#144008,#144009,#144010,#144011,#144012,#144013,#144014,
#144015,#144016,#144017,#144018,#144019,#144020,#144021,#144022,#144023,
#144024,#144025,#144026,#144027,#144028,#144029,#144030,#144031,#144032,
#144033,#144034,#144035,#144036,#144037,#144038,#144039,#144040,#144041,
#144042,#144043,#144044,#144045,#144046,#144047,#144048,#144049,#144050,
#144051,#144052,#144053,#144054,#144055,#144056,#144057,#144058,#144059,
#144060,#144061,#144062,#144063,#144064,#144065,#144066,#144067,#144068,
#144069,#144070,#144071,#144072,#144073,#144074,#144075,#144076,#144077,
#144078,#144079,#144080,#144081,#144082),.UNSPECIFIED.,.F.,.F.,(4,3,3,3,
3,3,3,3,3,3,3,3,3,3,3,3,3,3,3,3,3,3,3,3,3,3,3,3,3,3,3,3,3,3,3,3,3,3,3,3,
3,3,3,3,3,3,3,3,3,3,3,3,3,3,3,3,3,3,3,3,3,3,3,3,3,3,3,3,3,3,3,3,3,3,3,3,
3,3,3,3,3,4),(252.446267380839,252.530186188249,252.614226469652,252.698477120877,
252.782837309082,252.867396283387,252.933210712193,253.013168012324,253.093030809567,
253.172816632039,253.252542947234,253.332227175528,253.411898161749,253.491565615275,
253.571245266091,253.650952848486,253.730748077561,253.810592419269,253.890550846316,
253.932946722913,254.012904023044,254.092766820287,254.172552642759,254.252278957954,
254.331963186248,254.411634172469,254.491301625995,254.570981276811,254.650688859206,
254.730484088281,254.810328429989,254.890286857036,254.932682733633,255.012640033764,
255.092502831007,255.172288653479,255.252014968674,255.331699196968,255.411370183189,
255.491037636715,255.570717287531,255.650424869926,255.730220099001,255.810064440709,
255.890022867756,255.932418744353,256.012376044484,256.092238841727,256.172024664199,
256.251750979394,256.331435207688,256.411106193909,256.490773647435,256.570453298251,
256.650160880646,256.729956109722,256.809800451429,256.889758878476,256.932154755073,
257.012112055204,257.091974852447,257.171760674918,257.251486990114,257.331171218408,
257.410842204628,257.490509658154,257.570189308971,257.649896891365,257.729692120441,
257.809536462148,257.889494889195,257.931890765793,258.01070166188,258.08941789444,
258.16942224362,258.24799898334,258.326542478408,258.405069289344,258.486165138977,
258.564734604693,258.647093646286,258.729452687878),.UNSPECIFIED.);
#1170=B_SPLINE_CURVE_WITH_KNOTS('',3,(#144084,#144085,#144086,#144087,#144088,
#144089,#144090,#144091,#144092,#144093,#144094),.UNSPECIFIED.,.F.,.F.,
(4,1,1,1,1,1,1,1,4),(258.729452687878,258.931626776513,259.931362787234,
260.931098797954,261.930834808674,262.930570819394,263.930306830114,264.930042840834,
265.012637995057),.UNSPECIFIED.);
#1171=B_SPLINE_CURVE_WITH_KNOTS('',3,(#144096,#144097,#144098,#144099,#144100,
#144101,#144102,#144103,#144104,#144105),.UNSPECIFIED.,.F.,.F.,(4,1,1,1,
1,1,1,4),(265.012637995057,265.929778851554,266.929514862274,267.929250872995,
268.928986883715,269.928722894435,270.928458905155,271.295823302237),
 .UNSPECIFIED.);
#1172=B_SPLINE_CURVE_WITH_KNOTS('',3,(#144107,#144108,#144109,#144110,#144111,
#144112,#144113,#144114,#144115,#144116),.UNSPECIFIED.,.F.,.F.,(4,1,1,1,
1,1,1,4),(271.295823302237,271.928194915875,272.927930926595,273.927666937315,
274.927402948035,275.927138958756,276.926874969476,277.579008609416),
 .UNSPECIFIED.);
#1173=B_SPLINE_CURVE_WITH_KNOTS('',3,(#144118,#144119,#144120,#144121,#144122,
#144123,#144124,#144125,#144126,#144127,#144128,#144129,#144130,#144131,
#144132,#144133,#144134,#144135,#144136,#144137,#144138,#144139,#144140,
#144141,#144142,#144143,#144144,#144145,#144146,#144147,#144148,#144149,
#144150,#144151,#144152,#144153,#144154,#144155,#144156,#144157,#144158,
#144159,#144160,#144161,#144162,#144163,#144164,#144165,#144166,#144167,
#144168,#144169,#144170,#144171,#144172,#144173,#144174,#144175,#144176,
#144177,#144178,#144179,#144180,#144181,#144182,#144183,#144184,#144185,
#144186,#144187,#144188,#144189,#144190,#144191,#144192,#144193,#144194,
#144195,#144196,#144197,#144198,#144199,#144200,#144201,#144202,#144203,
#144204,#144205,#144206,#144207,#144208,#144209,#144210,#144211,#144212,
#144213,#144214,#144215,#144216,#144217,#144218,#144219,#144220,#144221,
#144222,#144223,#144224,#144225,#144226,#144227,#144228,#144229,#144230,
#144231,#144232,#144233,#144234,#144235,#144236,#144237,#144238,#144239,
#144240,#144241,#144242,#144243,#144244,#144245,#144246,#144247,#144248,
#144249,#144250,#144251,#144252,#144253,#144254,#144255,#144256,#144257,
#144258,#144259,#144260,#144261,#144262,#144263,#144264,#144265,#144266,
#144267,#144268,#144269,#144270,#144271,#144272,#144273,#144274,#144275,
#144276,#144277,#144278,#144279,#144280,#144281,#144282,#144283,#144284,
#144285,#144286,#144287,#144288,#144289,#144290,#144291,#144292,#144293,
#144294,#144295,#144296,#144297,#144298,#144299,#144300,#144301,#144302,
#144303,#144304,#144305,#144306,#144307,#144308,#144309,#144310,#144311,
#144312,#144313,#144314,#144315,#144316,#144317,#144318,#144319,#144320,
#144321,#144322,#144323,#144324,#144325,#144326,#144327,#144328,#144329,
#144330,#144331,#144332,#144333,#144334,#144335,#144336,#144337,#144338,
#144339,#144340,#144341,#144342,#144343,#144344,#144345,#144346,#144347,
#144348,#144349,#144350,#144351,#144352,#144353,#144354,#144355,#144356,
#144357,#144358,#144359,#144360,#144361),.UNSPECIFIED.,.F.,.F.,(4,3,3,3,
3,3,3,3,3,3,3,3,3,3,3,3,3,3,3,3,3,3,3,3,3,3,3,3,3,3,3,3,3,3,3,3,3,3,3,3,
3,3,3,3,3,3,3,3,3,3,3,3,3,3,3,3,3,3,3,3,3,3,3,3,3,3,3,3,3,3,3,3,3,3,3,3,
3,3,3,3,3,4),(277.579008731906,277.670689685924,277.762818730233,277.855534755267,
277.926610980196,278.006568280327,278.086431077569,278.166216900041,278.245943215236,
278.325627443529,278.40529842975,278.484965883276,278.564645534092,278.644353116486,
278.724148345561,278.803992687268,278.883951114315,278.926346990916,279.006304291047,
279.08616708829,279.165952910762,279.245679225957,279.325363454251,279.405034440472,
279.484701893998,279.564381544814,279.644089127209,279.723884356284,279.803728697992,
279.883687125039,279.926083001636,280.006040301767,280.08590309901,280.165688921482,
280.245415236677,280.325099464972,280.404770451193,280.484437904719,280.564117555535,
280.64382513793,280.723620367006,280.803464708713,280.883423135761,280.925819012356,
281.005776312487,281.085639109729,281.165424932201,281.245151247396,281.32483547569,
281.404506461911,281.484173915437,281.563853566253,281.643561148647,281.723356377723,
281.80320071943,281.883159146478,281.925555023076,282.005512323207,282.08537512045,
282.165160942922,282.244887258118,282.324571486412,282.404242472633,282.48390992616,
282.563589576976,282.643297159371,282.723092388447,282.802936730155,282.882895157202,
282.925291033797,283.004516126559,283.083647236245,283.162702529059,283.241700101922,
283.32066381893,283.399610922056,283.478557706701,283.557520465671,283.636559775155,
283.715638650542,283.794832188231,283.862193916596),.UNSPECIFIED.);
#1174=B_SPLINE_CURVE_WITH_KNOTS('',3,(#144363,#144364,#144365,#144366,#144367,
#144368,#144369,#144370,#144371,#144372,#144373,#144374),.UNSPECIFIED.,
 .F.,.F.,(4,2,1,1,1,1,1,1,4),(283.862193916596,283.925027044517,284.924763055237,
285.924499065957,286.924235076677,287.923971087397,288.923707098117,289.923443108837,
290.145379223776),.UNSPECIFIED.);
#1175=B_SPLINE_CURVE_WITH_KNOTS('',3,(#144376,#144377,#144378,#144379,#144380,
#144381,#144382,#144383,#144384,#144385,#144386,#144387,#144388,#144389,
#144390,#144391,#144392,#144393,#144394,#144395,#144396,#144397,#144398,
#144399,#144400,#144401,#144402,#144403,#144404,#144405,#144406,#144407,
#144408,#144409,#144410,#144411,#144412,#144413,#144414,#144415,#144416,
#144417,#144418,#144419,#144420,#144421,#144422,#144423,#144424,#144425,
#144426,#144427,#144428,#144429,#144430,#144431,#144432,#144433,#144434,
#144435,#144436,#144437,#144438,#144439,#144440,#144441,#144442,#144443,
#144444,#144445,#144446,#144447,#144448,#144449,#144450,#144451,#144452,
#144453,#144454,#144455,#144456,#144457,#144458,#144459,#144460,#144461,
#144462,#144463,#144464,#144465,#144466,#144467,#144468,#144469,#144470,
#144471,#144472,#144473,#144474,#144475,#144476,#144477,#144478,#144479,
#144480,#144481,#144482,#144483,#144484,#144485,#144486,#144487,#144488,
#144489,#144490,#144491,#144492,#144493,#144494,#144495,#144496,#144497,
#144498,#144499,#144500,#144501,#144502,#144503,#144504,#144505,#144506,
#144507,#144508,#144509,#144510,#144511,#144512,#144513,#144514,#144515,
#144516,#144517,#144518,#144519,#144520,#144521,#144522,#144523,#144524,
#144525,#144526,#144527,#144528,#144529,#144530,#144531,#144532,#144533,
#144534,#144535,#144536,#144537,#144538,#144539,#144540,#144541,#144542,
#144543,#144544,#144545,#144546,#144547,#144548,#144549,#144550,#144551,
#144552,#144553,#144554,#144555,#144556,#144557,#144558,#144559,#144560,
#144561,#144562,#144563,#144564,#144565,#144566,#144567,#144568,#144569,
#144570,#144571,#144572,#144573,#144574,#144575,#144576,#144577,#144578,
#144579,#144580,#144581,#144582,#144583,#144584,#144585,#144586,#144587,
#144588,#144589,#144590,#144591,#144592,#144593,#144594,#144595,#144596,
#144597,#144598,#144599,#144600,#144601,#144602,#144603,#144604,#144605,
#144606,#144607,#144608,#144609,#144610,#144611,#144612,#144613,#144614,
#144615,#144616,#144617,#144618,#144619),.UNSPECIFIED.,.F.,.F.,(4,3,3,3,
3,3,3,3,3,3,3,3,3,3,3,3,3,3,3,3,3,3,3,3,3,3,3,3,3,3,3,3,3,3,3,3,3,3,3,3,
3,3,3,3,3,3,3,3,3,3,3,3,3,3,3,3,3,3,3,3,3,3,3,3,3,3,3,3,3,3,3,3,3,3,3,3,
3,3,3,3,3,4),(290.145379223776,290.22408848333,290.302740462822,290.381360101647,
290.459964035669,290.538568771433,290.617190814347,290.69589275774,290.774635731816,
290.853497957081,290.923179119557,291.003136419688,291.082999216931,291.162785039403,
291.242511354598,291.322195582892,291.401866569113,291.481534022639,291.561213673455,
291.640921255849,291.720716484925,291.800560826633,291.88051925368,291.922915130277,
292.002872430409,292.082735227652,292.162521050124,292.242247365319,292.321931593614,
292.401602579835,292.481270033361,292.560949684178,292.640657266573,292.720452495648,
292.800296837356,292.880255264404,292.922651140998,293.002608441129,293.082471238372,
293.162257060844,293.241983376039,293.321667604333,293.401338590553,293.481006044079,
293.560685694896,293.640393277291,293.720188506366,293.800032848074,293.879991275121,
293.922387151718,294.002344451849,294.082207249092,294.161993071563,294.241719386759,
294.321403615052,294.401074601273,294.480742054799,294.560421705615,294.640129288009,
294.719924517084,294.799768858792,294.87972728584,294.922123162438,295.002080462569,
295.081943259812,295.161729082284,295.241455397479,295.321139625774,295.400810611995,
295.480478065521,295.560157716337,295.639865298731,295.719660527807,295.799504869514,
295.879463296561,295.921859173158,296.005685485794,296.089376747263,296.174173693186,
296.257577841536,296.343071186246,296.428564530955),.UNSPECIFIED.);
#1176=B_SPLINE_CURVE_WITH_KNOTS('',3,(#144621,#144622,#144623,#144624,#144625,
#144626,#144627,#144628,#144629,#144630,#144631,#144632,#144633,#144634,
#144635,#144636,#144637,#144638,#144639,#144640,#144641,#144642,#144643,
#144644,#144645,#144646,#144647,#144648,#144649,#144650,#144651,#144652,
#144653,#144654,#144655,#144656,#144657,#144658,#144659,#144660,#144661,
#144662,#144663,#144664,#144665,#144666,#144667,#144668,#144669,#144670,
#144671,#144672,#144673,#144674,#144675,#144676,#144677,#144678,#144679,
#144680,#144681,#144682,#144683,#144684,#144685,#144686,#144687,#144688,
#144689,#144690,#144691,#144692,#144693,#144694,#144695,#144696,#144697,
#144698,#144699,#144700,#144701,#144702,#144703,#144704,#144705,#144706,
#144707,#144708,#144709,#144710,#144711,#144712,#144713,#144714,#144715,
#144716,#144717,#144718,#144719,#144720,#144721,#144722,#144723,#144724,
#144725,#144726,#144727,#144728,#144729,#144730,#144731,#144732,#144733,
#144734,#144735,#144736,#144737,#144738,#144739,#144740,#144741,#144742,
#144743,#144744,#144745,#144746,#144747,#144748,#144749,#144750,#144751,
#144752,#144753,#144754,#144755,#144756,#144757,#144758,#144759,#144760,
#144761,#144762,#144763,#144764,#144765,#144766,#144767,#144768,#144769,
#144770,#144771,#144772,#144773,#144774,#144775,#144776,#144777,#144778,
#144779,#144780,#144781,#144782,#144783,#144784,#144785,#144786,#144787,
#144788,#144789,#144790,#144791,#144792,#144793,#144794,#144795,#144796,
#144797,#144798,#144799,#144800,#144801,#144802,#144803,#144804,#144805,
#144806,#144807,#144808,#144809,#144810,#144811,#144812,#144813,#144814,
#144815,#144816,#144817,#144818,#144819,#144820,#144821,#144822,#144823,
#144824,#144825,#144826,#144827,#144828,#144829,#144830,#144831,#144832,
#144833,#144834,#144835,#144836,#144837,#144838,#144839,#144840,#144841,
#144842,#144843,#144844,#144845,#144846,#144847,#144848,#144849,#144850,
#144851,#144852,#144853,#144854,#144855,#144856,#144857,#144858,#144859,
#144860,#144861,#144862,#144863,#144864),.UNSPECIFIED.,.F.,.F.,(4,3,3,3,
3,3,3,3,3,3,3,3,3,3,3,3,3,3,3,3,3,3,3,3,3,3,3,3,3,3,3,3,3,3,3,3,3,3,3,3,
3,3,3,3,3,3,3,3,3,3,3,3,3,3,3,3,3,3,3,3,3,3,3,3,3,3,3,3,3,3,3,3,3,3,3,3,
3,3,3,3,3,4),(296.428564531105,296.512262186977,296.59607320243,296.680086462927,
296.764204012982,296.848518636483,296.921595183878,297.001552484009,297.081415281252,
297.161201103724,297.240927418919,297.320611647213,297.400282633434,297.47995008696,
297.559629737777,297.639337320171,297.719132549247,297.798976890955,297.878935318002,
297.921331194598,298.001288494729,298.081151291972,298.160937114443,298.240663429639,
298.320347657933,298.400018644154,298.47968609768,298.559365748496,298.639073330891,
298.718868559966,298.798712901674,298.878671328721,298.921067205318,299.001024505449,
299.080887302692,299.160673125164,299.240399440359,299.320083668654,299.399754654875,
299.479422108401,299.559101759217,299.638809341612,299.718604570687,299.798448912395,
299.878407339443,299.920803216039,300.00076051617,300.080623313413,300.160409135885,
300.24013545108,300.319819679374,300.399490665595,300.479158119121,300.558837769938,
300.638545352333,300.718340581408,300.798184923116,300.878143350163,300.920539226759,
301.00049652689,301.080359324132,301.160145146604,301.239871461799,301.319555690093,
301.399226676314,301.47889412984,301.558573780656,301.63828136305,301.718076592126,
301.797920933833,301.87787936088,301.920275237479,301.999104940712,302.077839823292,
302.157078575147,302.235673780349,302.314235355996,302.392779852823,302.472522349151,
302.551107246514,302.631428542324,302.711749838135),.UNSPECIFIED.);
#1177=B_SPLINE_CURVE_WITH_KNOTS('',3,(#144866,#144867,#144868,#144869,#144870,
#144871,#144872,#144873,#144874,#144875,#144876),.UNSPECIFIED.,.F.,.F.,
(4,1,1,1,1,1,1,1,4),(302.711749838135,302.920011248199,303.919747258919,
304.919483269639,305.919219280359,306.91895529108,307.9186913018,308.91842731252,
308.994935145314),.UNSPECIFIED.);
#1178=B_SPLINE_CURVE_WITH_KNOTS('',3,(#144878,#144879,#144880,#144881,#144882,
#144883,#144884,#144885,#144886,#144887),.UNSPECIFIED.,.F.,.F.,(4,1,1,1,
1,1,1,4),(308.994935145314,309.91816332324,310.91789933396,311.91763534468,
312.9173713554,313.91710736612,314.916843376841,315.278120452494),
 .UNSPECIFIED.);
#1179=B_SPLINE_CURVE_WITH_KNOTS('',3,(#144889,#144890,#144891,#144892,#144893,
#144894,#144895,#144896,#144897,#144898),.UNSPECIFIED.,.F.,.F.,(4,1,1,1,
1,1,1,4),(315.278120452494,315.916579387561,316.916315398281,317.916051409001,
318.915787419721,319.915523430441,320.915259441161,321.561305759673),
 .UNSPECIFIED.);
#1180=B_SPLINE_CURVE_WITH_KNOTS('',3,(#144900,#144901,#144902,#144903,#144904,
#144905,#144906,#144907,#144908,#144909,#144910,#144911,#144912,#144913,
#144914,#144915,#144916,#144917,#144918,#144919,#144920,#144921,#144922,
#144923,#144924,#144925,#144926,#144927,#144928,#144929,#144930,#144931,
#144932,#144933,#144934,#144935,#144936,#144937,#144938,#144939,#144940,
#144941,#144942,#144943,#144944,#144945,#144946,#144947,#144948,#144949,
#144950,#144951,#144952,#144953,#144954,#144955,#144956,#144957,#144958,
#144959,#144960,#144961,#144962,#144963,#144964,#144965,#144966,#144967,
#144968,#144969,#144970,#144971,#144972,#144973,#144974,#144975,#144976,
#144977,#144978,#144979,#144980,#144981,#144982,#144983,#144984,#144985,
#144986,#144987,#144988,#144989,#144990,#144991,#144992,#144993,#144994,
#144995,#144996,#144997,#144998,#144999,#145000,#145001,#145002,#145003,
#145004,#145005,#145006,#145007,#145008,#145009,#145010,#145011,#145012,
#145013,#145014,#145015,#145016,#145017,#145018,#145019,#145020,#145021,
#145022,#145023,#145024,#145025,#145026,#145027,#145028,#145029,#145030,
#145031,#145032,#145033,#145034,#145035,#145036,#145037,#145038,#145039,
#145040,#145041,#145042,#145043,#145044,#145045,#145046,#145047,#145048,
#145049,#145050,#145051,#145052,#145053,#145054,#145055,#145056,#145057,
#145058,#145059,#145060,#145061,#145062,#145063,#145064,#145065,#145066,
#145067,#145068,#145069,#145070,#145071,#145072,#145073,#145074,#145075,
#145076,#145077,#145078,#145079,#145080,#145081,#145082,#145083,#145084,
#145085,#145086,#145087,#145088,#145089,#145090,#145091,#145092,#145093,
#145094,#145095,#145096,#145097,#145098,#145099,#145100,#145101,#145102,
#145103,#145104,#145105,#145106,#145107,#145108,#145109,#145110,#145111,
#145112,#145113,#145114,#145115,#145116,#145117,#145118,#145119,#145120,
#145121,#145122,#145123,#145124,#145125,#145126,#145127,#145128,#145129,
#145130,#145131,#145132,#145133,#145134,#145135,#145136,#145137,#145138,
#145139,#145140,#145141,#145142,#145143),.UNSPECIFIED.,.F.,.F.,(4,3,3,3,
3,3,3,3,3,3,3,3,3,3,3,3,3,3,3,3,3,3,3,3,3,3,3,3,3,3,3,3,3,3,3,3,3,3,3,3,
3,3,3,3,3,3,3,3,3,3,3,3,3,3,3,3,3,3,3,3,3,3,3,3,3,3,3,3,3,3,3,3,3,3,3,3,
3,3,3,3,3,4),(321.561306006896,321.652519309254,321.744150517988,321.836345229445,
321.914995451882,321.994952752013,322.074815549254,322.154601371726,322.23432768692,
322.314011915214,322.393682901434,322.473350354959,322.553030005775,322.632737588169,
322.712532817243,322.79237715895,322.872335585997,322.914731462602,322.994688762733,
323.074551559976,323.154337382448,323.234063697643,323.313747925937,323.393418912158,
323.473086365684,323.5527660165,323.632473598895,323.71226882797,323.792113169678,
323.872071596725,323.914467473322,323.994424773453,324.074287570696,324.154073393168,
324.233799708364,324.313483936658,324.393154922879,324.472822376405,324.552502027222,
324.632209609616,324.712004838692,324.7918491804,324.871807607447,324.914203484042,
324.994160784173,325.074023581416,325.153809403887,325.233535719083,325.313219947377,
325.392890933597,325.472558387123,325.55223803794,325.631945620334,325.71174084941,
325.791585191117,325.871543618164,325.913939494762,325.993896794893,326.073759592136,
326.153545414608,326.233271729803,326.312955958097,326.392626944318,326.472294397844,
326.55197404866,326.631681631054,326.71147686013,326.791321201837,326.871279628885,
326.913675505482,326.99284839066,327.071927338325,327.150930553951,327.229876172782,
327.308787992154,327.387683355991,327.466578593443,327.545490031237,327.624477289976,
327.703504406966,327.78264369027,327.844491066853),.UNSPECIFIED.);
#1181=B_SPLINE_CURVE_WITH_KNOTS('',3,(#145145,#145146,#145147,#145148,#145149,
#145150,#145151,#145152,#145153,#145154,#145155,#145156),.UNSPECIFIED.,
 .F.,.F.,(4,2,1,1,1,1,1,1,4),(327.844491066853,327.913411516202,328.913147526922,
329.912883537642,330.912619548363,331.912355559083,332.912091569803,333.911827580523,
334.127676374032),.UNSPECIFIED.);
#1182=B_SPLINE_CURVE_WITH_KNOTS('',3,(#145158,#145159,#145160,#145161,#145162,
#145163,#145164,#145165,#145166,#145167),.UNSPECIFIED.,.F.,.F.,(4,1,1,1,
1,1,1,4),(334.127676374032,334.911563591243,335.911299601963,336.911035612683,
337.910771623403,338.910507634124,339.910243644844,340.410861681212),
 .UNSPECIFIED.);
#1183=B_SPLINE_CURVE_WITH_KNOTS('',3,(#145169,#145170,#145171,#145172,#145173,
#145174,#145175,#145176,#145177,#145178),.UNSPECIFIED.,.F.,.F.,(4,1,1,1,
1,1,1,4),(340.410861681212,340.909979655564,341.909715666284,342.909451677004,
343.909187687724,344.908923698445,345.908659709165,346.694046988392),
 .UNSPECIFIED.);
#1184=B_SPLINE_CURVE_WITH_KNOTS('',3,(#145180,#145181,#145182,#145183,#145184,
#145185,#145186,#145187,#145188,#145189,#145190),.UNSPECIFIED.,.F.,.F.,
(4,1,1,1,1,1,1,1,4),(346.694046988392,346.908395719885,347.908131730605,
348.907867741325,349.907603752045,350.907339762765,351.907075773485,352.906811784205,
352.977232295571),.UNSPECIFIED.);
#1185=B_SPLINE_CURVE_WITH_KNOTS('',3,(#145192,#145193,#145194,#145195,#145196,
#145197,#145198,#145199,#145200,#145201,#145202,#145203,#145204,#145205,
#145206,#145207,#145208,#145209,#145210,#145211,#145212,#145213,#145214,
#145215,#145216,#145217,#145218,#145219,#145220,#145221,#145222,#145223,
#145224,#145225,#145226,#145227,#145228,#145229,#145230,#145231,#145232,
#145233,#145234,#145235,#145236,#145237,#145238,#145239,#145240,#145241,
#145242,#145243,#145244,#145245,#145246,#145247,#145248,#145249,#145250,
#145251,#145252,#145253,#145254,#145255,#145256,#145257,#145258,#145259,
#145260,#145261,#145262,#145263,#145264,#145265,#145266,#145267,#145268,
#145269,#145270,#145271,#145272,#145273,#145274,#145275,#145276,#145277,
#145278,#145279,#145280,#145281,#145282,#145283,#145284,#145285,#145286,
#145287,#145288,#145289,#145290,#145291,#145292,#145293,#145294,#145295,
#145296,#145297,#145298,#145299,#145300,#145301,#145302,#145303,#145304,
#145305,#145306,#145307,#145308,#145309,#145310,#145311,#145312,#145313,
#145314,#145315,#145316,#145317,#145318,#145319,#145320,#145321,#145322,
#145323,#145324,#145325,#145326,#145327,#145328,#145329,#145330,#145331,
#145332,#145333,#145334,#145335,#145336,#145337,#145338,#145339,#145340,
#145341,#145342,#145343,#145344,#145345,#145346,#145347,#145348,#145349,
#145350,#145351,#145352,#145353,#145354,#145355,#145356,#145357,#145358,
#145359,#145360,#145361,#145362,#145363,#145364,#145365,#145366,#145367,
#145368,#145369,#145370,#145371,#145372,#145373,#145374,#145375,#145376,
#145377,#145378,#145379,#145380,#145381,#145382,#145383,#145384,#145385,
#145386,#145387,#145388,#145389,#145390,#145391,#145392,#145393,#145394,
#145395,#145396,#145397,#145398,#145399,#145400,#145401,#145402,#145403,
#145404,#145405,#145406,#145407,#145408,#145409,#145410,#145411,#145412,
#145413,#145414,#145415,#145416,#145417,#145418,#145419,#145420,#145421,
#145422,#145423,#145424,#145425,#145426,#145427,#145428,#145429,#145430,
#145431,#145432,#145433,#145434,#145435),.UNSPECIFIED.,.F.,.F.,(4,3,3,3,
3,3,3,3,3,3,3,3,3,3,3,3,3,3,3,3,3,3,3,3,3,3,3,3,3,3,3,3,3,3,3,3,3,3,3,3,
3,3,3,3,3,3,3,3,3,3,3,3,3,3,3,3,3,3,3,3,3,3,3,3,3,3,3,3,3,3,3,3,3,3,3,3,
3,3,3,3,3,4),(352.977232295571,353.056367420751,353.135413276433,353.214388057453,
353.293309892804,353.372204939949,353.451087864685,353.529975002706,353.60888269035,
353.687872640281,353.766906214855,353.846057232216,353.906547794926,353.986505095057,
354.0663678923,354.146153714771,354.225880029967,354.305564258261,354.385235244482,
354.464902698008,354.544582348824,354.624289931219,354.704085160294,354.783929502002,
354.863887929049,354.906283805646,354.986241105777,355.06610390302,355.145889725491,
355.225616040687,355.305300268981,355.384971255202,355.464638708728,355.544318359544,
355.624025941938,355.703821171014,355.783665512722,355.863623939769,355.906019816366,
355.985977116497,356.06583991374,356.145625736211,356.225352051406,356.305036279701,
356.384707265921,356.464374719447,356.544054370264,356.623761952658,356.703557181734,
356.783401523441,356.863359950489,356.905755827086,356.985713127217,357.06557592446,
357.145361746932,357.225088062127,357.304772290421,357.384443276641,357.464110730167,
357.543790380984,357.623497963379,357.703293192455,357.783137534163,357.86309596121,
357.905491837806,357.985449137937,358.06531193518,358.145097757652,358.224824072848,
358.304508301142,358.384179287363,358.463846740889,358.543526391705,358.6232339741,
358.703029203175,358.782873544883,358.86283197193,358.905227848526,358.99728591963,
359.089015060361,359.180096318555,359.260417355136),.UNSPECIFIED.);
#1186=B_SPLINE_CURVE_WITH_KNOTS('',3,(#145437,#145438,#145439,#145440,#145441,
#145442,#145443,#145444,#145445,#145446),.UNSPECIFIED.,.F.,.F.,(4,1,1,1,
1,1,1,4),(359.260417602751,359.904963859246,360.904699869967,361.904435880687,
362.904171891407,363.903907902127,364.903643912847,365.54360290993),
 .UNSPECIFIED.);
#1187=B_SPLINE_CURVE_WITH_KNOTS('',3,(#145448,#145449,#145450,#145451,#145452,
#145453,#145454,#145455,#145456,#145457),.UNSPECIFIED.,.F.,.F.,(4,1,1,1,
1,1,1,4),(365.54360290993,365.903379923567,366.903115934287,367.902851945007,
368.902587955728,369.902323966448,370.902059977168,371.82678821711),
 .UNSPECIFIED.);
#1188=B_SPLINE_CURVE_WITH_KNOTS('',3,(#145459,#145460,#145461,#145462,#145463,
#145464,#145465,#145466,#145467,#145468,#145469,#145470),.UNSPECIFIED.,
 .F.,.F.,(4,2,1,1,1,1,1,1,4),(371.82678821711,371.901795987888,372.901531998608,
373.901268009328,374.901004020048,375.900740030769,376.900476041489,377.900212052209,
378.109973524289),.UNSPECIFIED.);
#1189=B_SPLINE_CURVE_WITH_KNOTS('',3,(#145472,#145473,#145474,#145475,#145476,
#145477,#145478,#145479,#145480,#145481,#145482,#145483,#145484,#145485,
#145486,#145487,#145488,#145489,#145490,#145491,#145492,#145493,#145494,
#145495,#145496,#145497,#145498,#145499,#145500,#145501,#145502,#145503,
#145504,#145505,#145506,#145507,#145508,#145509,#145510,#145511,#145512,
#145513,#145514,#145515,#145516,#145517,#145518,#145519,#145520,#145521,
#145522,#145523,#145524,#145525,#145526,#145527,#145528,#145529,#145530,
#145531,#145532,#145533,#145534,#145535,#145536,#145537,#145538,#145539,
#145540,#145541,#145542,#145543,#145544,#145545,#145546,#145547,#145548,
#145549,#145550,#145551,#145552,#145553,#145554,#145555,#145556,#145557,
#145558,#145559,#145560,#145561,#145562,#145563,#145564,#145565,#145566,
#145567,#145568,#145569,#145570,#145571,#145572,#145573,#145574,#145575,
#145576,#145577,#145578,#145579,#145580,#145581,#145582,#145583,#145584,
#145585,#145586,#145587,#145588,#145589,#145590,#145591,#145592,#145593,
#145594,#145595,#145596,#145597,#145598,#145599,#145600,#145601,#145602,
#145603,#145604,#145605,#145606,#145607,#145608,#145609,#145610,#145611,
#145612,#145613,#145614,#145615,#145616,#145617,#145618,#145619,#145620,
#145621,#145622,#145623,#145624,#145625,#145626,#145627,#145628,#145629,
#145630,#145631,#145632,#145633,#145634,#145635,#145636,#145637,#145638,
#145639,#145640,#145641,#145642,#145643,#145644,#145645,#145646,#145647,
#145648,#145649,#145650,#145651,#145652,#145653,#145654,#145655,#145656,
#145657,#145658,#145659,#145660,#145661,#145662,#145663,#145664,#145665,
#145666,#145667,#145668,#145669,#145670,#145671,#145672,#145673,#145674,
#145675,#145676,#145677,#145678,#145679,#145680,#145681,#145682,#145683,
#145684,#145685,#145686,#145687,#145688,#145689,#145690,#145691,#145692,
#145693,#145694,#145695,#145696,#145697,#145698,#145699,#145700,#145701,
#145702,#145703,#145704,#145705,#145706,#145707,#145708,#145709,#145710,
#145711,#145712,#145713,#145714,#145715),.UNSPECIFIED.,.F.,.F.,(4,3,3,3,
3,3,3,3,3,3,3,3,3,3,3,3,3,3,3,3,3,3,3,3,3,3,3,3,3,3,3,3,3,3,3,3,3,3,3,3,
3,3,3,3,3,3,3,3,3,3,3,3,3,3,3,3,3,3,3,3,3,3,3,3,3,3,3,3,3,3,3,3,3,3,3,3,
3,3,3,3,3,4),(378.109973524289,378.18864901344,378.267263817067,378.3463493478,
378.424908498294,378.503465564377,378.582037077905,378.661514824161,378.740203576295,
378.820075819612,378.899948062929,378.97990536306,379.059768160303,379.139553982774,
379.21928029797,379.298964526263,379.378635512484,379.45830296601,379.537982616827,
379.617690199221,379.697485428297,379.777329770004,379.857288197051,379.899684073649,
379.97964137378,380.059504171023,380.139289993494,380.219016308689,380.298700536984,
380.378371523204,380.45803897673,380.537718627547,380.617426209941,380.697221439016,
380.777065780724,380.857024207772,380.899420084369,380.9793773845,381.059240181743,
381.139026004215,381.21875231941,381.298436547704,381.378107533925,381.457774987451,
381.537454638268,381.617162220663,381.696957449738,381.776801791446,381.856760218493,
381.899156095089,381.97911339522,382.058976192463,382.138762014934,382.21848833013,
382.298172558423,382.377843544645,382.457510998171,382.537190648987,382.616898231381,
382.696693460457,382.776537802164,382.856496229212,382.898892105809,382.97884940594,
383.058712203183,383.138498025655,383.21822434085,383.297908569144,383.377579555365,
383.457247008891,383.536926659707,383.616634242102,383.696429471177,383.776273812885,
383.856232239932,383.898628116529,383.98291122769,384.067052492983,384.151000358076,
384.234834447973,384.318511508669,384.393158831352),.UNSPECIFIED.);
#1190=B_SPLINE_CURVE_WITH_KNOTS('',3,(#145717,#145718,#145719,#145720,#145721,
#145722,#145723,#145724,#145725,#145726,#145727,#145728,#145729,#145730,
#145731,#145732,#145733,#145734,#145735,#145736,#145737,#145738,#145739,
#145740,#145741,#145742,#145743,#145744,#145745,#145746,#145747,#145748,
#145749,#145750,#145751,#145752,#145753,#145754,#145755,#145756,#145757,
#145758,#145759,#145760,#145761,#145762,#145763,#145764,#145765,#145766,
#145767,#145768,#145769,#145770,#145771,#145772,#145773,#145774,#145775,
#145776,#145777,#145778,#145779,#145780,#145781,#145782,#145783,#145784,
#145785,#145786,#145787,#145788,#145789,#145790,#145791,#145792,#145793,
#145794,#145795,#145796,#145797,#145798,#145799,#145800,#145801,#145802,
#145803,#145804,#145805,#145806,#145807,#145808,#145809,#145810,#145811,
#145812,#145813,#145814,#145815,#145816,#145817,#145818,#145819,#145820,
#145821,#145822,#145823,#145824,#145825,#145826,#145827,#145828,#145829,
#145830,#145831,#145832,#145833,#145834,#145835,#145836,#145837,#145838,
#145839,#145840,#145841,#145842,#145843,#145844,#145845,#145846,#145847,
#145848,#145849,#145850,#145851,#145852,#145853,#145854,#145855,#145856,
#145857,#145858,#145859,#145860,#145861,#145862,#145863,#145864,#145865,
#145866,#145867,#145868,#145869,#145870,#145871,#145872,#145873,#145874,
#145875,#145876,#145877,#145878,#145879,#145880,#145881,#145882,#145883,
#145884,#145885,#145886,#145887,#145888,#145889,#145890,#145891,#145892,
#145893,#145894,#145895,#145896,#145897,#145898,#145899,#145900,#145901,
#145902,#145903,#145904,#145905,#145906,#145907,#145908,#145909,#145910,
#145911,#145912,#145913,#145914,#145915,#145916,#145917,#145918,#145919,
#145920,#145921,#145922,#145923,#145924,#145925,#145926,#145927,#145928,
#145929,#145930,#145931,#145932,#145933,#145934,#145935,#145936,#145937,
#145938,#145939,#145940,#145941,#145942,#145943,#145944,#145945,#145946,
#145947,#145948,#145949,#145950,#145951,#145952,#145953,#145954,#145955,
#145956,#145957,#145958,#145959,#145960),.UNSPECIFIED.,.F.,.F.,(4,3,3,3,
3,3,3,3,3,3,3,3,3,3,3,3,3,3,3,3,3,3,3,3,3,3,3,3,3,3,3,3,3,3,3,3,3,3,3,3,
3,3,3,3,3,3,3,3,3,3,3,3,3,3,3,3,3,3,3,3,3,3,3,3,3,3,3,3,3,3,3,3,3,3,3,3,
3,3,3,3,3,4),(384.393158831469,384.476433599377,384.559806737166,384.644446084687,
384.72810202294,384.813233075095,384.89836412725,384.978321427381,385.058184224624,
385.137970047095,385.21769636229,385.297380590584,385.377051576805,385.456719030331,
385.536398681147,385.616106263541,385.695901492617,385.775745834324,385.855704261371,
385.89810013797,385.978057438101,386.057920235344,386.137706057815,386.217432373011,
386.297116601305,386.376787587526,386.456455041052,386.536134691868,386.615842274262,
386.695637503338,386.775481845045,386.855440272093,386.89783614869,386.977793448821,
387.057656246064,387.137442068536,387.217168383731,387.296852612025,387.376523598246,
387.456191051772,387.535870702588,387.615578284983,387.695373514059,387.775217855766,
387.855176282814,387.89757215941,387.977529459541,388.057392256784,388.137178079256,
388.216904394451,388.296588622745,388.376259608966,388.455927062492,388.535606713308,
388.615314295703,388.695109524778,388.774953866486,388.854912293533,388.89730817013,
388.977265470261,389.057128267504,389.136914089976,389.216640405171,389.296324633465,
389.375995619686,389.455663073212,389.535342724028,389.615050306422,389.694845535497,
389.774689877205,389.854648304252,389.89704418085,389.975920919647,390.054702476653,
390.133394158125,390.212035029523,390.290641644439,390.369230528185,390.447844999415,
390.526470395101,390.605166603164,390.676344138649),.UNSPECIFIED.);
#1191=B_SPLINE_CURVE_WITH_KNOTS('',3,(#145962,#145963,#145964,#145965,#145966,
#145967,#145968,#145969,#145970,#145971,#145972),.UNSPECIFIED.,.F.,.F.,
(4,1,1,1,1,1,1,1,4),(390.676344138649,390.89678019157,391.896516202291,
392.896252213011,393.895988223731,394.895724234451,395.895460245171,396.895196255891,
396.959529445828),.UNSPECIFIED.);
#1192=B_SPLINE_CURVE_WITH_KNOTS('',3,(#145974,#145975,#145976,#145977,#145978,
#145979,#145980,#145981,#145982,#145983,#145984,#145985,#145986,#145987,
#145988,#145989,#145990,#145991,#145992,#145993,#145994,#145995,#145996,
#145997,#145998,#145999,#146000,#146001,#146002,#146003,#146004,#146005,
#146006,#146007,#146008,#146009,#146010,#146011,#146012,#146013,#146014,
#146015,#146016,#146017,#146018,#146019,#146020,#146021,#146022,#146023,
#146024,#146025,#146026,#146027,#146028,#146029,#146030,#146031,#146032,
#146033,#146034,#146035,#146036,#146037,#146038,#146039,#146040,#146041,
#146042,#146043,#146044,#146045,#146046,#146047,#146048,#146049,#146050,
#146051,#146052,#146053,#146054,#146055,#146056,#146057,#146058,#146059,
#146060,#146061,#146062,#146063,#146064,#146065,#146066,#146067,#146068,
#146069,#146070,#146071,#146072,#146073,#146074,#146075,#146076,#146077,
#146078,#146079,#146080,#146081,#146082,#146083,#146084,#146085,#146086,
#146087,#146088,#146089,#146090,#146091,#146092,#146093,#146094,#146095,
#146096,#146097,#146098,#146099,#146100,#146101,#146102,#146103,#146104,
#146105,#146106,#146107,#146108,#146109,#146110,#146111,#146112,#146113,
#146114,#146115,#146116,#146117,#146118,#146119,#146120,#146121,#146122,
#146123,#146124,#146125,#146126,#146127,#146128,#146129,#146130,#146131,
#146132,#146133,#146134,#146135,#146136,#146137,#146138,#146139,#146140,
#146141,#146142,#146143,#146144,#146145,#146146,#146147,#146148,#146149,
#146150,#146151,#146152,#146153,#146154,#146155,#146156,#146157,#146158,
#146159,#146160,#146161,#146162,#146163,#146164,#146165,#146166,#146167,
#146168,#146169,#146170,#146171,#146172,#146173,#146174,#146175,#146176,
#146177,#146178,#146179,#146180,#146181,#146182,#146183,#146184,#146185,
#146186,#146187,#146188,#146189,#146190,#146191,#146192,#146193,#146194,
#146195,#146196,#146197,#146198,#146199,#146200,#146201,#146202,#146203,
#146204,#146205,#146206,#146207,#146208,#146209,#146210,#146211,#146212,
#146213,#146214,#146215,#146216,#146217),.UNSPECIFIED.,.F.,.F.,(4,3,3,3,
3,3,3,3,3,3,3,3,3,3,3,3,3,3,3,3,3,3,3,3,3,3,3,3,3,3,3,3,3,3,3,3,3,3,3,3,
3,3,3,3,3,3,3,3,3,3,3,3,3,3,3,3,3,3,3,3,3,3,3,3,3,3,3,3,3,3,3,3,3,3,3,3,
3,3,3,3,3,4),(396.959529445828,397.038719794086,397.117820106619,397.196848542962,
397.275823196973,397.354769946268,397.433703753278,397.512640920773,397.591597751488,
397.670636594479,397.749718202142,397.82891891408,397.894932266611,397.974889566742,
398.054752363985,398.134538186457,398.214264501652,398.293948729946,398.373619716167,
398.453287169693,398.532966820509,398.612674402903,398.692469631979,398.772313973687,
398.852272400734,398.894668277331,398.974625577462,399.054488374705,399.134274197176,
399.214000512371,399.293684740665,399.373355726886,399.453023180412,399.532702831229,
399.612410413623,399.692205642699,399.772049984406,399.852008411453,399.894404288051,
399.974361588182,400.054224385425,400.134010207897,400.213736523093,400.293420751387,
400.373091737608,400.452759191135,400.532438841951,400.612146424346,400.691941653422,
400.77178599513,400.851744422178,400.894140298772,400.974097598903,401.053960396146,
401.133746218618,401.213472533813,401.293156762107,401.372827748328,401.452495201854,
401.53217485267,401.611882435065,401.691677664141,401.771522005849,401.851480432896,
401.893876309492,401.973833609623,402.053696406866,402.133482229338,402.213208544533,
402.292892772827,402.372563759048,402.452231212574,402.53191086339,402.611618445785,
402.69141367486,402.771258016568,402.851216443615,402.893612320212,402.986176437499,
403.078390750204,403.169920872596,403.242714630167),.UNSPECIFIED.);
#1193=B_SPLINE_CURVE_WITH_KNOTS('',3,(#146219,#146220,#146221,#146222,#146223,
#146224,#146225,#146226,#146227,#146228),.UNSPECIFIED.,.F.,.F.,(4,1,1,1,
1,1,1,4),(403.242714753008,403.893348330932,404.893084341652,405.892820352372,
406.892556363092,407.892292373813,408.892028384533,409.525900060187),
 .UNSPECIFIED.);
#1194=B_SPLINE_CURVE_WITH_KNOTS('',3,(#146230,#146231,#146232,#146233,#146234,
#146235,#146236,#146237,#146238,#146239),.UNSPECIFIED.,.F.,.F.,(4,1,1,1,
1,1,1,4),(409.525900060187,409.891764395253,410.891500405973,411.891236416693,
412.890972427413,413.890708438133,414.890444448853,415.809085367367),
 .UNSPECIFIED.);
#1195=B_SPLINE_CURVE_WITH_KNOTS('',3,(#146241,#146242,#146243,#146244,#146245,
#146246,#146247,#146248,#146249,#146250,#146251),.UNSPECIFIED.,.F.,.F.,
(4,1,1,1,1,1,1,1,4),(415.809085367367,415.890180459574,416.889916470294,
417.889652481014,418.889388491734,419.889124502454,420.888860513174,421.888596523894,
422.092270674546),.UNSPECIFIED.);
#1196=B_SPLINE_CURVE_WITH_KNOTS('',3,(#146253,#146254,#146255,#146256,#146257,
#146258,#146259,#146260,#146261,#146262,#146263,#146264,#146265,#146266,
#146267,#146268,#146269,#146270,#146271,#146272,#146273,#146274,#146275,
#146276,#146277,#146278,#146279,#146280,#146281,#146282,#146283,#146284,
#146285,#146286,#146287,#146288,#146289,#146290,#146291,#146292,#146293,
#146294,#146295,#146296,#146297,#146298,#146299,#146300,#146301,#146302,
#146303,#146304,#146305,#146306,#146307,#146308,#146309,#146310,#146311,
#146312,#146313,#146314,#146315,#146316,#146317,#146318,#146319,#146320,
#146321,#146322,#146323,#146324,#146325,#146326,#146327,#146328,#146329,
#146330,#146331,#146332,#146333,#146334,#146335,#146336,#146337,#146338,
#146339,#146340,#146341,#146342,#146343,#146344,#146345,#146346,#146347,
#146348,#146349,#146350,#146351,#146352,#146353,#146354,#146355,#146356,
#146357,#146358,#146359,#146360,#146361,#146362,#146363,#146364,#146365,
#146366,#146367,#146368,#146369,#146370,#146371,#146372,#146373,#146374,
#146375,#146376,#146377,#146378,#146379,#146380,#146381,#146382,#146383,
#146384,#146385,#146386,#146387,#146388,#146389,#146390,#146391,#146392,
#146393,#146394,#146395,#146396,#146397,#146398,#146399,#146400,#146401,
#146402,#146403,#146404,#146405,#146406,#146407,#146408,#146409,#146410,
#146411,#146412,#146413,#146414,#146415,#146416,#146417,#146418,#146419,
#146420,#146421,#146422,#146423,#146424,#146425,#146426,#146427,#146428,
#146429,#146430,#146431,#146432,#146433,#146434,#146435,#146436,#146437,
#146438,#146439,#146440,#146441,#146442,#146443,#146444,#146445,#146446,
#146447,#146448,#146449,#146450,#146451,#146452,#146453,#146454,#146455,
#146456,#146457,#146458,#146459,#146460,#146461,#146462,#146463,#146464,
#146465,#146466,#146467,#146468,#146469,#146470,#146471,#146472,#146473,
#146474,#146475,#146476,#146477,#146478,#146479,#146480,#146481,#146482,
#146483,#146484,#146485,#146486,#146487,#146488,#146489,#146490,#146491,
#146492,#146493,#146494,#146495,#146496),.UNSPECIFIED.,.F.,.F.,(4,3,3,3,
3,3,3,3,3,3,3,3,3,3,3,3,3,3,3,3,3,3,3,3,3,3,3,3,3,3,3,3,3,3,3,3,3,3,3,3,
3,3,3,3,3,3,3,3,3,3,3,3,3,3,3,3,3,3,3,3,3,3,3,3,3,3,3,3,3,3,3,3,3,3,3,3,
3,3,3,3,3,4),(422.092270674546,422.170933835011,422.249534663302,422.329384397216,
422.407925778346,422.486463786289,422.565014963407,422.645844356209,422.72451167452,
422.806422104568,422.888332534615,422.968289834746,423.048152631989,423.12793845446,
423.207664769656,423.287348997949,423.36701998417,423.446687437696,423.526367088512,
423.606074670906,423.685869899982,423.765714241689,423.845672668736,423.888068545335,
423.968025845466,424.047888642709,424.12767446518,424.207400780376,424.28708500867,
424.366755994891,424.446423448417,424.526103099233,424.605810681627,424.685605910703,
424.76545025241,424.845408679457,424.887804556055,424.967761856186,425.047624653429,
425.127410475901,425.207136791096,425.28682101939,425.366492005611,425.446159459137,
425.525839109954,425.605546692348,425.685341921424,425.765186263132,425.845144690179,
425.887540566775,425.967497866906,426.047360664149,426.127146486621,426.206872801816,
426.28655703011,426.366228016331,426.445895469857,426.525575120673,426.605282703068,
426.685077932144,426.764922273852,426.844880700899,426.887276577495,426.967233877626,
427.047096674869,427.12688249734,427.206608812536,427.28629304083,427.365964027051,
427.445631480577,427.525311131393,427.605018713787,427.684813942863,427.76465828457,
427.844616711618,427.887012588215,427.971534865699,428.055911567113,428.14008793926,
428.224145636171,428.308038251325,428.375455981601),.UNSPECIFIED.);
#1197=B_SPLINE_CURVE_WITH_KNOTS('',3,(#146498,#146499,#146500,#146501,#146502,
#146503,#146504,#146505,#146506,#146507,#146508,#146509,#146510,#146511,
#146512,#146513,#146514,#146515,#146516,#146517,#146518,#146519,#146520,
#146521,#146522,#146523,#146524,#146525,#146526,#146527,#146528,#146529,
#146530,#146531,#146532,#146533,#146534,#146535,#146536,#146537,#146538,
#146539,#146540,#146541,#146542,#146543,#146544,#146545,#146546,#146547,
#146548,#146549,#146550,#146551,#146552,#146553,#146554,#146555,#146556,
#146557,#146558,#146559,#146560,#146561,#146562,#146563,#146564,#146565,
#146566,#146567,#146568,#146569,#146570,#146571,#146572,#146573,#146574,
#146575,#146576,#146577,#146578,#146579,#146580,#146581,#146582,#146583,
#146584,#146585,#146586,#146587,#146588,#146589,#146590,#146591,#146592,
#146593,#146594,#146595,#146596,#146597,#146598,#146599,#146600,#146601,
#146602,#146603,#146604,#146605,#146606,#146607,#146608,#146609,#146610,
#146611,#146612,#146613,#146614,#146615,#146616,#146617,#146618,#146619,
#146620,#146621,#146622,#146623,#146624,#146625,#146626,#146627,#146628,
#146629,#146630,#146631,#146632,#146633,#146634,#146635,#146636,#146637,
#146638,#146639,#146640,#146641,#146642,#146643,#146644,#146645,#146646,
#146647,#146648,#146649,#146650,#146651,#146652,#146653,#146654,#146655,
#146656,#146657,#146658,#146659,#146660,#146661,#146662,#146663,#146664,
#146665,#146666,#146667,#146668,#146669,#146670,#146671,#146672,#146673,
#146674,#146675,#146676,#146677,#146678,#146679,#146680,#146681,#146682,
#146683,#146684,#146685,#146686,#146687,#146688,#146689,#146690,#146691,
#146692,#146693,#146694,#146695,#146696,#146697,#146698,#146699,#146700,
#146701,#146702,#146703,#146704,#146705,#146706,#146707,#146708,#146709,
#146710,#146711,#146712,#146713,#146714,#146715,#146716,#146717,#146718,
#146719,#146720,#146721,#146722,#146723,#146724,#146725,#146726,#146727,
#146728,#146729,#146730,#146731,#146732,#146733,#146734,#146735,#146736,
#146737,#146738,#146739,#146740,#146741),.UNSPECIFIED.,.F.,.F.,(4,3,3,3,
3,3,3,3,3,3,3,3,3,3,3,3,3,3,3,3,3,3,3,3,3,3,3,3,3,3,3,3,3,3,3,3,3,3,3,3,
3,3,3,3,3,3,3,3,3,3,3,3,3,3,3,3,3,3,3,3,3,3,3,3,3,3,3,3,3,3,3,3,3,3,3,3,
3,3,3,3,3,4),(428.375455981726,428.458528660149,428.541692777151,428.627956732597,
428.711393977797,428.799071288366,428.886748598935,428.966705899066,429.046568696309,
429.126354518781,429.206080833977,429.285765062272,429.365436048493,429.445103502019,
429.524783152836,429.60449073523,429.684285964306,429.764130306014,429.844088733061,
429.886484609655,429.966441909786,430.046304707029,430.1260905295,430.205816844696,
430.28550107299,430.36517205921,430.444839512736,430.524519163553,430.604226745947,
430.684021975022,430.76386631673,430.843824743777,430.886220620375,430.966177920506,
431.046040717749,431.125826540221,431.205552855417,431.285237083711,431.364908069932,
431.444575523458,431.524255174275,431.60396275667,431.683757985745,431.763602327453,
431.843560754501,431.885956631096,431.965913931227,432.04577672847,432.125562550942,
432.205288866137,432.284973094431,432.364644080652,432.444311534178,432.523991184994,
432.603698767389,432.683493996464,432.763338338172,432.84329676522,432.885692641816,
432.965649941947,433.04551273919,433.125298561661,433.205024876856,433.284709105151,
433.364380091372,433.444047544898,433.523727195714,433.603434778108,433.683230007184,
433.763074348891,433.843032775938,433.885428652536,433.964333652462,434.04314326512,
434.121862540956,434.200530738074,434.279164394412,434.357780019542,434.436419696968,
434.515070068844,434.59378794452,434.658641288905),.UNSPECIFIED.);
#1198=B_SPLINE_CURVE_WITH_KNOTS('',3,(#146743,#146744,#146745,#146746,#146747,
#146748,#146749,#146750,#146751,#146752,#146753),.UNSPECIFIED.,.F.,.F.,
(4,1,1,1,1,1,1,1,4),(434.658641288905,434.885164663256,435.884900673976,
436.884636684696,437.884372695416,438.884108706137,439.883844716857,440.883580727577,
440.941826596085),.UNSPECIFIED.);
#1199=B_SPLINE_CURVE_WITH_KNOTS('',3,(#146755,#146756,#146757,#146758,#146759,
#146760,#146761,#146762,#146763,#146764,#146765,#146766,#146767,#146768,
#146769,#146770,#146771,#146772,#146773,#146774,#146775,#146776,#146777,
#146778,#146779,#146780,#146781,#146782,#146783,#146784,#146785,#146786,
#146787,#146788,#146789,#146790,#146791,#146792,#146793,#146794,#146795,
#146796,#146797,#146798,#146799,#146800,#146801,#146802,#146803,#146804,
#146805,#146806,#146807,#146808,#146809,#146810,#146811,#146812,#146813,
#146814,#146815,#146816,#146817,#146818,#146819,#146820,#146821,#146822,
#146823,#146824,#146825,#146826,#146827,#146828,#146829,#146830,#146831,
#146832,#146833,#146834,#146835,#146836,#146837,#146838,#146839,#146840,
#146841,#146842,#146843,#146844,#146845,#146846,#146847,#146848,#146849,
#146850,#146851,#146852,#146853,#146854,#146855,#146856,#146857,#146858,
#146859,#146860,#146861,#146862,#146863,#146864,#146865,#146866,#146867,
#146868,#146869,#146870,#146871,#146872,#146873,#146874,#146875,#146876,
#146877,#146878,#146879,#146880,#146881,#146882,#146883,#146884,#146885,
#146886,#146887,#146888,#146889,#146890,#146891,#146892,#146893,#146894,
#146895,#146896,#146897,#146898,#146899,#146900,#146901,#146902,#146903,
#146904,#146905,#146906,#146907,#146908,#146909,#146910,#146911,#146912,
#146913,#146914,#146915,#146916,#146917,#146918,#146919,#146920,#146921,
#146922,#146923,#146924,#146925,#146926,#146927,#146928,#146929,#146930,
#146931,#146932,#146933,#146934,#146935,#146936,#146937,#146938,#146939,
#146940,#146941,#146942,#146943,#146944,#146945,#146946,#146947,#146948,
#146949,#146950,#146951,#146952,#146953,#146954,#146955,#146956,#146957,
#146958,#146959,#146960,#146961,#146962,#146963,#146964,#146965,#146966,
#146967,#146968,#146969,#146970,#146971,#146972,#146973,#146974,#146975,
#146976,#146977,#146978,#146979,#146980,#146981,#146982,#146983,#146984,
#146985,#146986,#146987,#146988,#146989,#146990,#146991,#146992,#146993,
#146994,#146995,#146996,#146997,#146998),.UNSPECIFIED.,.F.,.F.,(4,3,3,3,
3,3,3,3,3,3,3,3,3,3,3,3,3,3,3,3,3,3,3,3,3,3,3,3,3,3,3,3,3,3,3,3,3,3,3,3,
3,3,3,3,3,3,3,3,3,3,3,3,3,3,3,3,3,3,3,3,3,3,3,3,3,3,3,3,3,3,3,3,3,3,3,3,
3,3,3,3,3,4),(440.941826596085,441.021075135616,441.100232923846,441.179318081556,
441.258348664094,441.337350274657,441.416338156607,441.495328576932,441.574337801935,
441.65342880663,441.732561735784,441.811815443062,441.883316738297,441.963274038428,
442.043136835671,442.122922658143,442.202648973338,442.282333201632,442.362004187853,
442.441671641379,442.521351292195,442.60105887459,442.680854103665,442.760698445373,
442.84065687242,442.883052749017,442.963010049148,443.042872846391,443.122658668863,
443.202384984058,443.282069212352,443.361740198573,443.441407652099,443.521087302915,
443.60079488531,443.680590114385,443.760434456093,443.84039288314,443.882788759737,
443.962746059868,444.042608857111,444.122394679583,444.202120994778,444.281805223072,
444.361476209293,444.441143662819,444.520823313635,444.60053089603,444.680326125105,
444.760170466813,444.84012889386,444.882524770457,444.962482070588,445.042344867831,
445.122130690303,445.201857005498,445.281541233792,445.361212220013,445.440879673539,
445.520559324355,445.600266906749,445.680062135825,445.759906477532,445.83986490458,
445.882260781177,445.962218081308,446.042080878551,446.121866701023,446.201593016219,
446.281277244513,446.360948230734,446.440615684261,446.520295335077,446.600002917472,
446.679798146548,446.759642488256,446.839600915303,446.881996791898,446.9750868076,
447.06780402742,447.159797907512,447.22501190315),.UNSPECIFIED.);
#1200=B_SPLINE_CURVE_WITH_KNOTS('',3,(#147000,#147001,#147002,#147003,#147004,
#147005,#147006,#147007,#147008,#147009,#147010,#147011,#147012,#147013,
#147014,#147015,#147016,#147017,#147018,#147019,#147020,#147021,#147022,
#147023,#147024,#147025,#147026,#147027,#147028,#147029,#147030,#147031,
#147032,#147033,#147034,#147035,#147036,#147037,#147038,#147039,#147040,
#147041,#147042,#147043,#147044,#147045,#147046,#147047,#147048,#147049,
#147050,#147051,#147052,#147053,#147054,#147055,#147056,#147057,#147058,
#147059,#147060,#147061,#147062,#147063,#147064,#147065,#147066,#147067,
#147068,#147069,#147070,#147071,#147072,#147073,#147074,#147075,#147076,
#147077,#147078,#147079,#147080,#147081,#147082,#147083,#147084,#147085,
#147086,#147087,#147088,#147089,#147090,#147091,#147092,#147093,#147094,
#147095,#147096,#147097,#147098,#147099,#147100,#147101,#147102,#147103,
#147104,#147105,#147106,#147107,#147108,#147109,#147110,#147111,#147112,
#147113,#147114,#147115,#147116,#147117,#147118,#147119,#147120,#147121,
#147122,#147123,#147124,#147125,#147126,#147127,#147128,#147129,#147130,
#147131,#147132,#147133,#147134,#147135,#147136,#147137,#147138,#147139,
#147140,#147141,#147142,#147143,#147144,#147145,#147146,#147147,#147148,
#147149,#147150,#147151,#147152,#147153,#147154,#147155,#147156,#147157,
#147158,#147159,#147160,#147161,#147162,#147163,#147164,#147165,#147166,
#147167,#147168,#147169,#147170,#147171,#147172,#147173,#147174,#147175,
#147176,#147177,#147178,#147179,#147180,#147181,#147182,#147183,#147184,
#147185,#147186,#147187,#147188,#147189,#147190,#147191,#147192,#147193,
#147194,#147195,#147196,#147197,#147198,#147199,#147200,#147201,#147202,
#147203,#147204,#147205,#147206,#147207,#147208,#147209,#147210,#147211,
#147212,#147213,#147214,#147215,#147216,#147217,#147218,#147219,#147220,
#147221,#147222,#147223,#147224,#147225,#147226,#147227,#147228,#147229,
#147230,#147231,#147232,#147233,#147234,#147235,#147236,#147237,#147238,
#147239,#147240,#147241,#147242,#147243,#147244,#147245,#147246),
 .UNSPECIFIED.,.F.,.F.,(4,3,3,3,3,3,3,3,3,3,3,3,3,3,3,3,3,3,3,3,3,3,3,3,
3,3,3,3,3,3,3,3,3,3,3,3,3,3,3,3,3,3,3,3,3,3,3,3,3,3,3,3,3,3,3,3,3,3,3,3,
3,3,3,3,3,3,3,3,3,3,3,3,3,3,3,3,3,3,3,3,3,3,4),(447.225011903265,447.307102015684,
447.386849490768,447.466604468513,447.546382529658,447.630220097898,447.710136669819,
447.790112257442,447.8701997552,447.881732802618,447.961690102749,448.041552899992,
448.121338722464,448.201065037659,448.280749265953,448.360420252173,448.440087705699,
448.519767356516,448.59947493891,448.679270167986,448.759114509693,448.83907293674,
448.881468813338,448.961426113469,449.041288910712,449.121074733183,449.200801048379,
449.280485276673,449.360156262894,449.43982371642,449.519503367236,449.599210949631,
449.679006178707,449.758850520414,449.838808947461,449.881204824058,449.961162124189,
450.041024921432,450.120810743904,450.2005370591,450.280221287394,450.359892273615,
450.439559727141,450.519239377957,450.598946960352,450.678742189427,450.758586531135,
450.838544958183,450.880940834778,450.960898134909,451.040760932152,451.120546754624,
451.200273069819,451.279957298114,451.359628284335,451.439295737861,451.518975388677,
451.598682971072,451.678478200147,451.758322541855,451.838280968902,451.880676845498,
451.960634145629,452.040496942872,452.120282765343,452.200009080539,452.279693308832,
452.359364295054,452.43903174858,452.518711399396,452.598418981791,452.678214210866,
452.758058552574,452.838016979622,452.880412856218,452.960970301763,453.041430143191,
453.121807583264,453.202117770593,453.28237162908,453.362591658213,453.442803262859,
453.508197210444),.UNSPECIFIED.);
#1201=B_SPLINE_CURVE_WITH_KNOTS('',3,(#147248,#147249,#147250,#147251,#147252,
#147253,#147254,#147255,#147256,#147257),.UNSPECIFIED.,.F.,.F.,(4,1,1,1,
1,1,1,4),(453.508204888342,453.880148866938,454.879884877659,455.879620888379,
456.879356899099,457.879092909819,458.878828920539,459.791373789161),
 .UNSPECIFIED.);
#1202=B_SPLINE_CURVE_WITH_KNOTS('',3,(#147259,#147260,#147261,#147262,#147263,
#147264,#147265,#147266,#147267,#147268,#147269,#147270,#147271,#147272,
#147273,#147274,#147275,#147276,#147277,#147278,#147279,#147280,#147281,
#147282,#147283,#147284,#147285,#147286,#147287,#147288,#147289,#147290,
#147291,#147292,#147293,#147294,#147295,#147296,#147297,#147298,#147299,
#147300,#147301,#147302,#147303,#147304,#147305,#147306,#147307,#147308,
#147309,#147310,#147311,#147312,#147313,#147314,#147315,#147316,#147317,
#147318,#147319,#147320,#147321,#147322,#147323,#147324,#147325,#147326,
#147327,#147328,#147329,#147330,#147331,#147332,#147333,#147334,#147335,
#147336,#147337,#147338,#147339,#147340,#147341,#147342,#147343,#147344,
#147345,#147346,#147347,#147348,#147349,#147350,#147351,#147352,#147353,
#147354,#147355,#147356,#147357,#147358,#147359,#147360,#147361,#147362,
#147363,#147364,#147365,#147366,#147367,#147368,#147369,#147370,#147371,
#147372,#147373,#147374,#147375,#147376,#147377,#147378,#147379,#147380,
#147381,#147382,#147383,#147384,#147385,#147386,#147387,#147388,#147389,
#147390,#147391,#147392,#147393,#147394,#147395,#147396,#147397,#147398,
#147399,#147400,#147401,#147402,#147403,#147404,#147405,#147406,#147407,
#147408,#147409,#147410,#147411,#147412,#147413,#147414,#147415,#147416,
#147417,#147418,#147419,#147420,#147421,#147422,#147423,#147424,#147425,
#147426,#147427,#147428,#147429,#147430,#147431,#147432,#147433,#147434,
#147435,#147436,#147437,#147438,#147439,#147440,#147441,#147442,#147443,
#147444,#147445,#147446,#147447,#147448,#147449,#147450,#147451,#147452,
#147453,#147454,#147455,#147456,#147457,#147458,#147459,#147460,#147461,
#147462,#147463,#147464,#147465,#147466,#147467,#147468,#147469,#147470,
#147471,#147472,#147473,#147474,#147475,#147476,#147477,#147478,#147479,
#147480,#147481,#147482,#147483,#147484,#147485,#147486,#147487,#147488,
#147489,#147490,#147491,#147492,#147493,#147494,#147495,#147496,#147497,
#147498,#147499,#147500,#147501,#147502),.UNSPECIFIED.,.F.,.F.,(4,3,3,3,
3,3,3,3,3,3,3,3,3,3,3,3,3,3,3,3,3,3,3,3,3,3,3,3,3,3,3,3,3,3,3,3,3,3,3,3,
3,3,3,3,3,3,3,3,3,3,3,3,3,3,3,3,3,3,3,3,3,3,3,3,3,3,3,3,3,3,3,3,3,3,3,3,
3,3,3,3,3,4),(459.791382517624,459.878564931259,459.95852223139,460.038385028633,
460.118170851104,460.1978971663,460.277581394593,460.357252380814,460.43691983434,
460.516599485156,460.596307067551,460.676102296626,460.755946638334,460.835905065381,
460.878300941979,460.95825824211,461.038121039353,461.117906861825,461.19763317702,
461.277317405314,461.356988391535,461.436655845061,461.516335495877,461.596043078271,
461.675838307347,461.755682649054,461.835641076102,461.878036952699,461.95799425283,
462.037857050073,462.117642872545,462.197369187741,462.277053416035,462.356724402256,
462.436391855782,462.516071506599,462.595779088994,462.675574318069,462.755418659777,
462.835377086825,462.87777296342,462.957730263551,463.037593060794,463.117378883266,
463.197105198461,463.276789426755,463.356460412976,463.436127866502,463.515807517319,
463.595515099713,463.675310328789,463.755154670496,463.835113097544,463.87750897414,
463.957466274271,464.037329071514,464.117114893985,464.196841209181,464.276525437475,
464.356196423695,464.435863877221,464.515543528038,464.595251110432,464.675046339507,
464.754890681215,464.834849108262,464.87724498486,464.957202284991,465.037065082234,
465.116850904706,465.196577219901,465.276261448196,465.355932434417,465.435599887943,
465.515279538759,465.594987121154,465.674782350229,465.754626691937,465.834585118985,
465.87698099558,465.99246734354,466.074567824803),.UNSPECIFIED.);
#1203=B_SPLINE_CURVE_WITH_KNOTS('',3,(#147504,#147505,#147506,#147507,#147508,
#147509,#147510,#147511,#147512,#147513),.UNSPECIFIED.,.F.,.F.,(4,1,1,1,
1,1,1,4),(466.074571330478,466.8767170063,467.87645301702,468.87618902774,
469.875925038461,470.875661049181,471.875397059901,472.357753131983),
 .UNSPECIFIED.);
#1204=B_SPLINE_CURVE_WITH_KNOTS('',3,(#147515,#147516,#147517,#147518,#147519,
#147520,#147521,#147522,#147523,#147524),.UNSPECIFIED.,.F.,.F.,(4,1,1,1,
1,1,1,4),(472.357753131983,472.875133070621,473.874869081341,474.874605092061,
475.874341102781,476.874077113501,477.873813124221,478.640938439162),
 .UNSPECIFIED.);
#1205=B_SPLINE_CURVE_WITH_KNOTS('',3,(#147526,#147527,#147528,#147529,#147530,
#147531,#147532,#147533,#147534,#147535,#147536),.UNSPECIFIED.,.F.,.F.,
(4,1,1,1,1,1,1,1,4),(478.640938439162,478.873549134942,479.873285145662,
480.873021156382,481.872757167102,482.872493177822,483.872229188542,484.871965199263,
484.924123746342),.UNSPECIFIED.);
#1206=B_SPLINE_CURVE_WITH_KNOTS('',3,(#147538,#147539,#147540,#147541,#147542,
#147543,#147544,#147545,#147546,#147547),.UNSPECIFIED.,.F.,.F.,(4,1,1,1,
1,1,1,4),(484.924123746342,485.871701209983,486.871437220703,487.871173231423,
488.870909242143,489.870645252863,490.870381263583,491.207301539485),
 .UNSPECIFIED.);
#1207=B_SPLINE_CURVE_WITH_KNOTS('',3,(#147549,#147550,#147551,#147552,#147553,
#147554,#147555,#147556,#147557,#147558,#147559,#147560,#147561,#147562,
#147563,#147564,#147565,#147566,#147567,#147568,#147569,#147570,#147571,
#147572,#147573,#147574,#147575,#147576,#147577,#147578,#147579,#147580,
#147581,#147582,#147583,#147584,#147585,#147586,#147587,#147588,#147589,
#147590,#147591,#147592,#147593,#147594,#147595,#147596,#147597,#147598,
#147599,#147600,#147601,#147602,#147603,#147604,#147605,#147606,#147607,
#147608,#147609,#147610,#147611,#147612,#147613,#147614,#147615,#147616,
#147617,#147618,#147619,#147620,#147621,#147622,#147623,#147624,#147625,
#147626,#147627,#147628,#147629,#147630,#147631,#147632,#147633,#147634,
#147635,#147636,#147637,#147638,#147639,#147640,#147641,#147642,#147643,
#147644,#147645,#147646,#147647,#147648,#147649,#147650,#147651,#147652,
#147653,#147654,#147655,#147656,#147657,#147658,#147659,#147660,#147661,
#147662,#147663,#147664,#147665,#147666,#147667,#147668,#147669,#147670,
#147671,#147672,#147673,#147674,#147675,#147676,#147677,#147678,#147679,
#147680,#147681,#147682,#147683,#147684,#147685,#147686,#147687,#147688,
#147689,#147690,#147691,#147692,#147693,#147694,#147695,#147696,#147697,
#147698,#147699,#147700,#147701,#147702,#147703,#147704,#147705,#147706,
#147707,#147708,#147709,#147710,#147711,#147712,#147713,#147714,#147715,
#147716,#147717,#147718,#147719,#147720,#147721,#147722,#147723,#147724,
#147725,#147726,#147727,#147728,#147729,#147730,#147731,#147732,#147733,
#147734,#147735,#147736,#147737,#147738,#147739,#147740,#147741,#147742,
#147743,#147744,#147745,#147746,#147747,#147748,#147749,#147750,#147751,
#147752,#147753,#147754,#147755,#147756,#147757,#147758,#147759,#147760,
#147761,#147762,#147763,#147764,#147765,#147766,#147767,#147768,#147769,
#147770,#147771,#147772,#147773,#147774,#147775,#147776,#147777,#147778,
#147779,#147780,#147781,#147782,#147783,#147784,#147785,#147786,#147787,
#147788,#147789,#147790,#147791,#147792,#147793,#147794,#147795),
 .UNSPECIFIED.,.F.,.F.,(4,3,3,3,3,3,3,3,3,3,3,3,3,3,3,3,3,3,3,3,3,3,3,3,
3,3,3,3,3,3,3,3,3,3,3,3,3,3,3,3,3,3,3,3,3,3,3,3,3,3,3,3,3,3,3,3,3,3,3,3,
3,3,3,3,3,3,3,3,3,3,3,3,3,3,3,3,3,3,3,3,3,3,4),(491.207309053522,491.29016008112,
491.36981928176,491.449483679156,491.529168945053,491.608890760716,491.688708275316,
491.768582379995,491.848570368169,491.870117274303,491.950074574434,492.029937371677,
492.109723194149,492.189449509344,492.269133737638,492.348804723859,492.428472177385,
492.508151828201,492.587859410595,492.667654639671,492.747498981378,492.827457408426,
492.869853285023,492.949810585154,493.029673382397,493.109459204869,493.189185520065,
493.268869748359,493.34854073458,493.428208188107,493.507887838923,493.587595421318,
493.667390650394,493.747234992102,493.827193419149,493.869589295744,493.949546595875,
494.029409393118,494.109195215589,494.188921530785,494.268605759078,494.348276745299,
494.427944198825,494.507623849641,494.587331432035,494.667126661111,494.746971002818,
494.826929429866,494.869325306464,494.949282606595,495.029145403838,495.108931226309,
495.188657541505,495.268341769799,495.34801275602,495.427680209546,495.507359860362,
495.587067442756,495.666862671832,495.74670701354,495.826665440587,495.869061317184,
495.949018617315,496.028881414558,496.10866723703,496.188393552226,496.268077780519,
496.347748766741,496.427416220267,496.507095871083,496.586803453478,496.666598682554,
496.746443024261,496.826401451308,496.868797327904,496.949472541059,497.030049103338,
497.110542076934,497.190966469049,497.271331757617,497.351661880682,497.431979636697,
497.490494360701),.UNSPECIFIED.);
#1208=B_SPLINE_CURVE_WITH_KNOTS('',3,(#147797,#147798,#147799,#147800,#147801,
#147802,#147803,#147804,#147805,#147806),.UNSPECIFIED.,.F.,.F.,(4,1,1,1,
1,1,1,4),(497.490501958073,497.868533338624,498.868269349344,499.868005360064,
500.867741370785,501.867477381505,502.867213392225,503.773670660106),
 .UNSPECIFIED.);
#1209=B_SPLINE_CURVE_WITH_KNOTS('',3,(#147808,#147809,#147810,#147811,#147812,
#147813,#147814,#147815,#147816,#147817,#147818,#147819,#147820,#147821,
#147822,#147823,#147824,#147825,#147826,#147827,#147828,#147829,#147830,
#147831,#147832,#147833,#147834,#147835,#147836,#147837,#147838,#147839,
#147840,#147841,#147842,#147843,#147844,#147845,#147846,#147847,#147848,
#147849,#147850,#147851,#147852,#147853,#147854,#147855,#147856,#147857,
#147858,#147859,#147860,#147861,#147862,#147863,#147864,#147865,#147866,
#147867,#147868,#147869,#147870,#147871,#147872,#147873,#147874,#147875,
#147876,#147877,#147878,#147879,#147880,#147881,#147882,#147883,#147884,
#147885,#147886,#147887,#147888,#147889,#147890,#147891,#147892,#147893,
#147894,#147895,#147896,#147897,#147898,#147899,#147900,#147901,#147902,
#147903,#147904,#147905,#147906,#147907,#147908,#147909,#147910,#147911,
#147912,#147913,#147914,#147915,#147916,#147917,#147918,#147919,#147920,
#147921,#147922,#147923,#147924,#147925,#147926,#147927,#147928,#147929,
#147930,#147931,#147932,#147933,#147934,#147935,#147936,#147937,#147938,
#147939,#147940,#147941,#147942,#147943,#147944,#147945,#147946,#147947,
#147948,#147949,#147950,#147951,#147952,#147953,#147954,#147955,#147956,
#147957,#147958,#147959,#147960,#147961,#147962,#147963,#147964,#147965,
#147966,#147967,#147968,#147969,#147970,#147971,#147972,#147973,#147974,
#147975,#147976,#147977,#147978,#147979,#147980,#147981,#147982,#147983,
#147984,#147985,#147986,#147987,#147988,#147989,#147990,#147991,#147992,
#147993,#147994,#147995,#147996,#147997,#147998,#147999,#148000,#148001,
#148002,#148003,#148004,#148005,#148006,#148007,#148008,#148009,#148010,
#148011,#148012,#148013,#148014,#148015,#148016,#148017,#148018,#148019,
#148020,#148021,#148022,#148023,#148024,#148025,#148026,#148027,#148028,
#148029,#148030,#148031,#148032,#148033,#148034,#148035,#148036,#148037,
#148038,#148039,#148040,#148041,#148042,#148043,#148044,#148045,#148046,
#148047,#148048,#148049,#148050,#148051),.UNSPECIFIED.,.F.,.F.,(4,3,3,3,
3,3,3,3,3,3,3,3,3,3,3,3,3,3,3,3,3,3,3,3,3,3,3,3,3,3,3,3,3,3,3,3,3,3,3,3,
3,3,3,3,3,3,3,3,3,3,3,3,3,3,3,3,3,3,3,3,3,3,3,3,3,3,3,3,3,3,3,3,3,3,3,3,
3,3,3,3,3,4),(503.773679667881,503.866949402945,503.946906703076,504.026769500319,
504.106555322791,504.186281637986,504.26596586628,504.345636852501,504.425304306027,
504.504983956843,504.584691539238,504.664486768314,504.744331110021,504.824289537068,
504.866685413665,504.946642713796,505.026505511039,505.106291333511,505.186017648706,
505.265701877,505.345372863221,505.425040316747,505.504719967563,505.584427549958,
505.664222779033,505.744067120741,505.824025547788,505.866421424385,505.946378724516,
506.026241521759,506.106027344231,506.185753659426,506.26543788772,506.345108873941,
506.424776327467,506.504455978284,506.584163560678,506.663958789754,506.743803131461,
506.823761558509,506.866157435105,506.946114735236,507.025977532479,507.105763354951,
507.185489670146,507.26517389844,507.344844884661,507.424512338188,507.504191989004,
507.583899571399,507.663694800474,507.743539142182,507.82349756923,507.865893445826,
507.945850745957,508.0257135432,508.105499365672,508.185225680867,508.264909909161,
508.344580895382,508.424248348908,508.503927999725,508.58363558212,508.663430811195,
508.743275152903,508.82323357995,508.865629456546,508.945586756677,509.02544955392,
509.105235376392,509.184961691587,509.264645919881,509.344316906102,509.423984359628,
509.503664010445,509.583371592839,509.663166821915,509.743011163623,509.82296959067,
509.865365467266,509.982757991064,510.05686497506),.UNSPECIFIED.);
#1210=B_SPLINE_CURVE_WITH_KNOTS('',3,(#148053,#148054,#148055,#148056,#148057,
#148058,#148059,#148060,#148061,#148062),.UNSPECIFIED.,.F.,.F.,(4,1,1,1,
1,1,1,4),(510.056869064338,510.865101477986,511.864837488706,512.864573499426,
513.864309510146,514.864045520866,515.863781531586,516.34005028224),
 .UNSPECIFIED.);
#1211=B_SPLINE_CURVE_WITH_KNOTS('',3,(#148064,#148065,#148066,#148067,#148068,
#148069,#148070,#148071,#148072,#148073),.UNSPECIFIED.,.F.,.F.,(4,1,1,1,
1,1,1,4),(516.34005028224,516.863517542307,517.863253553027,518.862989563747,
519.862725574467,520.862461585187,521.862197595907,522.623235589419),
 .UNSPECIFIED.);
#1212=B_SPLINE_CURVE_WITH_KNOTS('',3,(#148075,#148076,#148077,#148078,#148079,
#148080,#148081,#148082,#148083,#148084,#148085),.UNSPECIFIED.,.F.,.F.,
(4,1,1,1,1,1,1,1,4),(522.623235589419,522.861933606627,523.861669617348,
524.861405628068,525.861141638788,526.860877649508,527.860613660228,528.860349670948,
528.906420896599),.UNSPECIFIED.);
#1213=B_SPLINE_CURVE_WITH_KNOTS('',3,(#148087,#148088,#148089,#148090,#148091,
#148092,#148093,#148094,#148095,#148096),.UNSPECIFIED.,.F.,.F.,(4,1,1,1,
1,1,1,4),(528.906420896599,529.860085681668,530.859821692388,531.859557703109,
532.859293713829,533.859029724549,534.858765735269,535.189598872372),
 .UNSPECIFIED.);
#1214=B_SPLINE_CURVE_WITH_KNOTS('',3,(#148098,#148099,#148100,#148101,#148102,
#148103,#148104,#148105,#148106,#148107,#148108,#148109,#148110,#148111,
#148112,#148113,#148114,#148115,#148116,#148117,#148118,#148119,#148120,
#148121,#148122,#148123,#148124,#148125,#148126,#148127,#148128,#148129,
#148130,#148131,#148132,#148133,#148134,#148135,#148136,#148137,#148138,
#148139,#148140,#148141,#148142,#148143,#148144,#148145,#148146,#148147,
#148148,#148149,#148150,#148151,#148152,#148153,#148154,#148155,#148156,
#148157,#148158,#148159,#148160,#148161,#148162,#148163,#148164,#148165,
#148166,#148167,#148168,#148169,#148170,#148171,#148172,#148173,#148174,
#148175,#148176,#148177,#148178,#148179,#148180,#148181,#148182,#148183,
#148184,#148185,#148186,#148187,#148188,#148189,#148190,#148191,#148192,
#148193,#148194,#148195,#148196,#148197,#148198,#148199,#148200,#148201,
#148202,#148203,#148204,#148205,#148206,#148207,#148208,#148209,#148210,
#148211,#148212,#148213,#148214,#148215,#148216,#148217,#148218,#148219,
#148220,#148221,#148222,#148223,#148224,#148225,#148226,#148227,#148228,
#148229,#148230,#148231,#148232,#148233,#148234,#148235,#148236,#148237,
#148238,#148239,#148240,#148241,#148242,#148243,#148244,#148245,#148246,
#148247,#148248,#148249,#148250,#148251,#148252,#148253,#148254,#148255,
#148256,#148257,#148258,#148259,#148260,#148261,#148262,#148263,#148264,
#148265,#148266,#148267,#148268,#148269,#148270,#148271,#148272,#148273,
#148274,#148275,#148276,#148277,#148278,#148279,#148280,#148281,#148282,
#148283,#148284,#148285,#148286,#148287,#148288,#148289,#148290,#148291,
#148292,#148293,#148294,#148295,#148296,#148297,#148298,#148299,#148300,
#148301,#148302,#148303,#148304,#148305,#148306,#148307,#148308,#148309,
#148310,#148311,#148312,#148313,#148314,#148315,#148316,#148317,#148318,
#148319,#148320,#148321,#148322,#148323,#148324,#148325,#148326,#148327,
#148328,#148329,#148330,#148331,#148332,#148333,#148334,#148335,#148336,
#148337,#148338,#148339,#148340,#148341,#148342,#148343,#148344),
 .UNSPECIFIED.,.F.,.F.,(4,3,3,3,3,3,3,3,3,3,3,3,3,3,3,3,3,3,3,3,3,3,3,3,
3,3,3,3,3,3,3,3,3,3,3,3,3,3,3,3,3,3,3,3,3,3,3,3,3,3,3,3,3,3,3,3,3,3,3,3,
3,3,3,3,3,3,3,3,3,3,3,3,3,3,3,3,3,3,3,3,3,3,4),(535.189606203779,535.273218146555,
535.352792787086,535.432370387379,535.511966703241,535.591597498818,535.671322497607,
535.751102402933,535.83099710307,535.858501745989,535.93845904612,536.018321843363,
536.098107665835,536.17783398103,536.257518209324,536.337189195545,536.416856649071,
536.496536299887,536.576243882282,536.656039111357,536.735883453065,536.815841880112,
536.858237756709,536.93819505684,537.018057854083,537.097843676555,537.17756999175,
537.257254220045,537.336925206266,537.416592659792,537.496272310609,537.575979893003,
537.655775122079,537.735619463787,537.815577890834,537.857973767429,537.93793106756,
538.017793864803,538.097579687275,538.17730600247,538.256990230764,538.336661216985,
538.416328670511,538.496008321327,538.575715903721,538.655511132797,538.735355474505,
538.815313901552,538.857709778149,538.93766707828,539.017529875523,539.097315697994,
539.17704201319,539.256726241484,539.336397227705,539.416064681231,539.495744332047,
539.575451914442,539.655247143517,539.735091485225,539.815049912272,539.857445788869,
539.937403089,540.017265886243,540.097051708715,540.176778023911,540.256462252206,
540.336133238427,540.415800691953,540.49548034277,540.575187925165,540.65498315424,
540.734827495948,540.814785922996,540.85718179959,540.937979098972,541.018676641078,
541.099289335752,541.179832036869,541.260312775082,541.340756917768,541.4211847832,
541.472791510958),.UNSPECIFIED.);
#1215=B_SPLINE_CURVE_WITH_KNOTS('',3,(#148346,#148347,#148348,#148349,#148350,
#148351,#148352,#148353,#148354,#148355),.UNSPECIFIED.,.F.,.F.,(4,1,1,1,
1,1,1,4),(541.472798990514,541.85691781031,542.85665382103,543.85638983175,
544.85612584247,545.85586185319,546.85559786391,547.755967729876),
 .UNSPECIFIED.);
#1216=B_SPLINE_CURVE_WITH_KNOTS('',3,(#148357,#148358,#148359,#148360,#148361,
#148362,#148363,#148364,#148365,#148366,#148367,#148368,#148369,#148370,
#148371,#148372,#148373,#148374,#148375,#148376,#148377,#148378,#148379,
#148380,#148381,#148382,#148383,#148384,#148385,#148386,#148387,#148388,
#148389,#148390,#148391,#148392,#148393,#148394,#148395,#148396,#148397,
#148398,#148399,#148400,#148401,#148402,#148403,#148404,#148405,#148406,
#148407,#148408,#148409,#148410,#148411,#148412,#148413,#148414,#148415,
#148416,#148417,#148418,#148419,#148420,#148421,#148422,#148423,#148424,
#148425,#148426,#148427,#148428,#148429,#148430,#148431,#148432,#148433,
#148434,#148435,#148436,#148437,#148438,#148439,#148440,#148441,#148442,
#148443,#148444,#148445,#148446,#148447,#148448,#148449,#148450,#148451,
#148452,#148453,#148454,#148455,#148456,#148457,#148458,#148459,#148460,
#148461,#148462,#148463,#148464,#148465,#148466,#148467,#148468,#148469,
#148470,#148471,#148472,#148473,#148474,#148475,#148476,#148477,#148478,
#148479,#148480,#148481,#148482,#148483,#148484,#148485,#148486,#148487,
#148488,#148489,#148490,#148491,#148492,#148493,#148494,#148495,#148496,
#148497,#148498,#148499,#148500,#148501,#148502,#148503,#148504,#148505,
#148506,#148507,#148508,#148509,#148510,#148511,#148512,#148513,#148514,
#148515,#148516,#148517,#148518,#148519,#148520,#148521,#148522,#148523,
#148524,#148525,#148526,#148527,#148528,#148529,#148530,#148531,#148532,
#148533,#148534,#148535,#148536,#148537,#148538,#148539,#148540,#148541,
#148542,#148543,#148544,#148545,#148546,#148547,#148548,#148549,#148550,
#148551,#148552,#148553,#148554,#148555,#148556,#148557,#148558,#148559,
#148560,#148561,#148562,#148563,#148564,#148565,#148566,#148567,#148568,
#148569,#148570,#148571,#148572,#148573,#148574,#148575,#148576,#148577,
#148578,#148579,#148580,#148581,#148582,#148583,#148584,#148585,#148586,
#148587,#148588,#148589,#148590,#148591,#148592,#148593,#148594,#148595,
#148596,#148597,#148598,#148599,#148600),.UNSPECIFIED.,.F.,.F.,(4,3,3,3,
3,3,3,3,3,3,3,3,3,3,3,3,3,3,3,3,3,3,3,3,3,3,3,3,3,3,3,3,3,3,3,3,3,3,3,3,
3,3,3,3,3,3,3,3,3,3,3,3,3,3,3,3,3,3,3,3,3,3,3,3,3,3,3,3,3,3,3,3,3,3,3,3,
3,3,3,3,3,4),(547.755976818138,547.85533387463,547.935291174761,548.015153972004,
548.094939794476,548.174666109672,548.254350337966,548.334021324187,548.413688777713,
548.49336842853,548.573076010925,548.65287124,548.732715581708,548.812674008755,
548.855069885351,548.935027185482,549.014889982725,549.094675805197,549.174402120392,
549.254086348686,549.333757334907,549.413424788432,549.493104439249,549.572812021643,
549.652607250719,549.732451592426,549.812410019474,549.854805896071,549.934763196202,
550.014625993445,550.094411815916,550.174138131111,550.253822359405,550.333493345626,
550.413160799152,550.492840449969,550.572548032363,550.652343261439,550.732187603146,
550.812146030193,550.854541906791,550.934499206922,551.014362004165,551.094147826637,
551.173874141832,551.253558370126,551.333229356347,551.412896809873,551.49257646069,
551.572284043085,551.65207927216,551.731923613868,551.811882040915,551.854277917511,
551.934235217642,552.014098014885,552.093883837357,552.173610152552,552.253294380846,
552.332965367067,552.412632820593,552.492312471409,552.572020053803,552.651815282879,
552.731659624587,552.811618051634,552.854013928231,552.933971228362,553.013834025605,
553.093619848077,553.173346163272,553.253030391566,553.332701377787,553.412368831313,
553.492048482129,553.571756064523,553.651551293599,553.731395635307,553.811354062354,
553.853749938951,553.973211235292,554.039162125317),.UNSPECIFIED.);
#1217=B_SPLINE_CURVE_WITH_KNOTS('',3,(#148602,#148603,#148604,#148605,#148606,
#148607,#148608,#148609,#148610,#148611),.UNSPECIFIED.,.F.,.F.,(4,1,1,1,
1,1,1,4),(554.039166781551,554.853485949671,555.853221960391,556.852957971112,
557.852693981832,558.852429992552,559.852166003272,560.322347432497),
 .UNSPECIFIED.);
#1218=B_SPLINE_CURVE_WITH_KNOTS('',3,(#148613,#148614,#148615,#148616,#148617,
#148618,#148619,#148620,#148621,#148622),.UNSPECIFIED.,.F.,.F.,(4,1,1,1,
1,1,1,4),(560.322347432497,560.851902013992,561.851638024712,562.851374035433,
563.851110046153,564.850846056873,565.850582067593,566.605532739676),
 .UNSPECIFIED.);
#1219=B_SPLINE_CURVE_WITH_KNOTS('',3,(#148624,#148625,#148626,#148627,#148628,
#148629,#148630,#148631,#148632,#148633,#148634,#148635,#148636,#148637,
#148638,#148639,#148640,#148641,#148642,#148643,#148644,#148645,#148646,
#148647,#148648,#148649,#148650,#148651,#148652,#148653,#148654,#148655,
#148656,#148657,#148658,#148659,#148660,#148661,#148662,#148663,#148664,
#148665,#148666,#148667,#148668,#148669,#148670,#148671,#148672,#148673,
#148674,#148675,#148676,#148677,#148678,#148679,#148680,#148681,#148682,
#148683,#148684,#148685,#148686,#148687,#148688,#148689,#148690,#148691,
#148692,#148693,#148694,#148695,#148696,#148697,#148698,#148699,#148700,
#148701,#148702,#148703,#148704,#148705,#148706,#148707,#148708,#148709,
#148710,#148711,#148712,#148713,#148714,#148715,#148716,#148717,#148718,
#148719,#148720,#148721,#148722,#148723,#148724,#148725,#148726,#148727,
#148728,#148729,#148730,#148731,#148732,#148733,#148734,#148735,#148736,
#148737,#148738,#148739,#148740,#148741,#148742,#148743,#148744,#148745,
#148746,#148747,#148748,#148749,#148750,#148751,#148752,#148753,#148754,
#148755,#148756,#148757,#148758,#148759,#148760,#148761,#148762,#148763,
#148764,#148765,#148766,#148767,#148768,#148769,#148770,#148771,#148772,
#148773,#148774,#148775,#148776,#148777,#148778,#148779,#148780,#148781,
#148782,#148783,#148784,#148785,#148786,#148787,#148788,#148789,#148790,
#148791,#148792,#148793,#148794,#148795,#148796,#148797,#148798,#148799,
#148800,#148801,#148802,#148803,#148804,#148805,#148806,#148807,#148808,
#148809,#148810,#148811,#148812,#148813,#148814,#148815,#148816,#148817,
#148818,#148819,#148820,#148821,#148822,#148823,#148824,#148825,#148826,
#148827,#148828,#148829,#148830,#148831,#148832,#148833,#148834,#148835,
#148836,#148837,#148838,#148839,#148840,#148841,#148842,#148843,#148844,
#148845,#148846,#148847,#148848,#148849,#148850,#148851,#148852,#148853,
#148854,#148855,#148856,#148857,#148858,#148859,#148860,#148861,#148862,
#148863,#148864,#148865,#148866,#148867,#148868,#148869,#148870),
 .UNSPECIFIED.,.F.,.F.,(4,3,3,3,3,3,3,3,3,3,3,3,3,3,3,3,3,3,3,3,3,3,3,3,
3,3,3,3,3,3,3,3,3,3,3,3,3,3,3,3,3,3,3,3,3,3,3,3,3,3,3,3,3,3,3,3,3,3,3,3,
3,3,3,3,3,3,3,3,3,3,3,3,3,3,3,3,3,3,3,3,3,3,4),(566.60553281651,566.708754002674,
566.814418024236,566.850318078313,566.930275378444,567.010138175686,567.089923998157,
567.169650313352,567.249334541646,567.329005527866,567.408672981392,567.488352632208,
567.568060214602,567.647855443677,567.727699785384,567.807658212431,567.850054089033,
567.930011389164,568.009874186407,568.089660008879,568.169386324074,568.249070552368,
568.328741538589,568.408408992115,568.488088642932,568.567796225326,568.647591454402,
568.727435796109,568.807394223157,568.849790099753,568.929747399884,569.009610197127,
569.089396019599,569.169122334794,569.248806563088,569.328477549309,569.408145002835,
569.487824653652,569.567532236047,569.647327465122,569.72717180683,569.807130233877,
569.849526110473,569.929483410604,570.009346207847,570.089132030318,570.168858345514,
570.248542573808,570.328213560028,570.407881013554,570.487560664371,570.567268246765,
570.64706347584,570.726907817548,570.806866244595,570.849262121193,570.929219421324,
571.009082218567,571.088868041039,571.168594356235,571.248278584529,571.32794957075,
571.407617024276,571.487296675093,571.567004257488,571.646799486564,571.726643828271,
571.806602255319,571.848998131914,571.928955432045,572.008818229288,572.08860405176,
572.168330366955,572.24801459525,572.327685581471,572.407353034997,572.487032685813,
572.566740268208,572.646535497284,572.726379838991,572.806338266039,572.848734142634,
572.888718046856),.UNSPECIFIED.);
#1220=B_SPLINE_CURVE_WITH_KNOTS('',3,(#148872,#148873,#148874,#148875,#148876,
#148877,#148878,#148879,#148880,#148881),.UNSPECIFIED.,.F.,.F.,(4,1,1,1,
1,1,1,4),(572.88872350849,573.848470153354,574.848206164074,575.847942174794,
576.847678185514,577.847414196235,578.847150206955,579.171903354036),
 .UNSPECIFIED.);
#1221=B_SPLINE_CURVE_WITH_KNOTS('',3,(#148883,#148884,#148885,#148886,#148887,
#148888,#148889,#148890,#148891,#148892),.UNSPECIFIED.,.F.,.F.,(4,1,1,1,
1,1,1,4),(579.171903354036,579.846886217675,580.846622228395,581.846358239115,
582.846094249835,583.845830260555,584.845566271275,585.455088661215),
 .UNSPECIFIED.);
#1222=B_SPLINE_CURVE_WITH_KNOTS('',3,(#148894,#148895,#148896,#148897,#148898,
#148899,#148900,#148901,#148902,#148903),.UNSPECIFIED.,.F.,.F.,(4,1,1,1,
1,1,1,4),(585.455088661215,585.845302281995,586.845038292716,587.844774303436,
588.844510314156,589.844246324876,590.843982335596,591.738273968395),
 .UNSPECIFIED.);
#1223=B_SPLINE_CURVE_WITH_KNOTS('',3,(#148905,#148906,#148907,#148908,#148909,
#148910,#148911,#148912,#148913,#148914,#148915,#148916),.UNSPECIFIED.,
 .F.,.F.,(4,2,1,1,1,1,1,1,4),(591.738273968395,591.843718346316,592.843454357036,
593.843190367756,594.842926378477,595.842662389197,596.842398399917,597.842134410637,
598.021459275574),.UNSPECIFIED.);
#1224=B_SPLINE_CURVE_WITH_KNOTS('',3,(#148918,#148919,#148920,#148921,#148922,
#148923,#148924,#148925,#148926,#148927,#148928,#148929,#148930,#148931,
#148932,#148933,#148934,#148935,#148936,#148937,#148938,#148939,#148940,
#148941,#148942,#148943,#148944,#148945,#148946,#148947,#148948,#148949,
#148950,#148951,#148952,#148953,#148954,#148955,#148956,#148957,#148958,
#148959,#148960,#148961,#148962,#148963,#148964,#148965,#148966,#148967,
#148968,#148969,#148970,#148971,#148972,#148973,#148974,#148975,#148976,
#148977,#148978,#148979,#148980,#148981,#148982,#148983,#148984,#148985,
#148986,#148987,#148988,#148989,#148990,#148991,#148992,#148993,#148994,
#148995,#148996,#148997,#148998,#148999,#149000,#149001,#149002,#149003,
#149004,#149005,#149006,#149007,#149008,#149009,#149010,#149011,#149012,
#149013,#149014,#149015,#149016,#149017,#149018,#149019,#149020,#149021,
#149022,#149023,#149024,#149025,#149026,#149027,#149028,#149029,#149030,
#149031,#149032,#149033,#149034,#149035,#149036,#149037,#149038,#149039,
#149040,#149041,#149042,#149043,#149044,#149045,#149046,#149047,#149048,
#149049,#149050,#149051,#149052,#149053,#149054,#149055,#149056,#149057,
#149058,#149059,#149060,#149061,#149062,#149063,#149064,#149065,#149066,
#149067,#149068,#149069,#149070,#149071,#149072,#149073,#149074,#149075,
#149076,#149077,#149078,#149079,#149080,#149081,#149082,#149083,#149084,
#149085,#149086,#149087,#149088,#149089,#149090,#149091,#149092,#149093,
#149094,#149095,#149096,#149097,#149098,#149099,#149100,#149101,#149102,
#149103,#149104,#149105,#149106,#149107,#149108,#149109,#149110,#149111,
#149112,#149113,#149114,#149115,#149116,#149117,#149118,#149119,#149120,
#149121,#149122,#149123,#149124,#149125,#149126,#149127,#149128,#149129,
#149130,#149131,#149132,#149133,#149134,#149135,#149136,#149137,#149138,
#149139,#149140,#149141,#149142,#149143,#149144,#149145,#149146,#149147,
#149148,#149149,#149150,#149151,#149152,#149153,#149154,#149155,#149156,
#149157,#149158,#149159,#149160,#149161,#149162,#149163,#149164),
 .UNSPECIFIED.,.F.,.F.,(4,3,3,3,3,3,3,3,3,3,3,3,3,3,3,3,3,3,3,3,3,3,3,3,
3,3,3,3,3,3,3,3,3,3,3,3,3,3,3,3,3,3,3,3,3,3,3,3,3,3,3,3,3,3,3,3,3,3,3,3,
3,3,3,3,3,3,3,3,3,3,3,3,3,3,3,3,3,3,3,3,3,3,4),(598.021459275574,598.100103166507,
598.178678499566,598.257203660822,598.335705731097,598.414198623025,598.492698903982,
598.571223145469,598.649829847877,598.728483691741,598.807246837996,598.841870421357,
598.921827721488,599.001690518731,599.081476341203,599.161202656398,599.240886884692,
599.320557870912,599.400225324438,599.479904975255,599.55961255765,599.639407786725,
599.719252128433,599.79921055548,599.841606432077,599.921563732208,600.001426529451,
600.081212351923,600.160938667118,600.240622895412,600.320293881633,600.399961335159,
600.479640985975,600.55934856837,600.639143797445,600.718988139153,600.7989465662,
600.841342442797,600.921299742928,601.001162540171,601.080948362644,601.160674677839,
601.240358906133,601.320029892354,601.39969734588,601.479376996697,601.559084579092,
601.638879808168,601.718724149876,601.798682576923,601.841078453518,601.921035753649,
602.000898550892,602.080684373364,602.160410688559,602.240094916853,602.319765903074,
602.3994333566,602.479113007416,602.55882058981,602.638615818886,602.718460160594,
602.798418587641,602.840814464238,602.920771764369,603.000634561611,603.080420384083,
603.160146699278,603.239830927572,603.319501913793,603.399169367319,603.478849018135,
603.558556600529,603.638351829605,603.718196171312,603.798154598359,603.840550474958,
603.926106881067,604.011500138433,604.096661221207,604.181679898875,604.26649877441,
604.304644387162),.UNSPECIFIED.);
#1225=B_SPLINE_CURVE_WITH_KNOTS('',3,(#149166,#149167,#149168,#149169,#149170,
#149171,#149172,#149173,#149174,#149175),.UNSPECIFIED.,.F.,.F.,(4,1,1,1,
1,1,1,4),(604.304644582754,604.840286485678,605.840022496398,606.839758507118,
607.839494517838,608.839230528559,609.838966539279,610.587829889933),
 .UNSPECIFIED.);
#1226=B_SPLINE_CURVE_WITH_KNOTS('',3,(#149177,#149178,#149179,#149180,#149181,
#149182,#149183,#149184,#149185,#149186,#149187,#149188,#149189,#149190,
#149191,#149192,#149193,#149194,#149195,#149196,#149197,#149198,#149199,
#149200,#149201,#149202,#149203,#149204,#149205,#149206,#149207,#149208,
#149209,#149210,#149211,#149212,#149213,#149214,#149215,#149216,#149217,
#149218,#149219,#149220,#149221,#149222,#149223,#149224,#149225,#149226,
#149227,#149228,#149229,#149230,#149231,#149232,#149233,#149234,#149235,
#149236,#149237,#149238,#149239,#149240,#149241,#149242,#149243,#149244,
#149245,#149246,#149247,#149248,#149249,#149250,#149251,#149252,#149253,
#149254,#149255,#149256,#149257,#149258,#149259,#149260,#149261,#149262,
#149263,#149264,#149265,#149266,#149267,#149268,#149269,#149270,#149271,
#149272,#149273,#149274,#149275,#149276,#149277,#149278,#149279,#149280,
#149281,#149282,#149283,#149284,#149285,#149286,#149287,#149288,#149289,
#149290,#149291,#149292,#149293,#149294,#149295,#149296,#149297,#149298,
#149299,#149300,#149301,#149302,#149303,#149304,#149305,#149306,#149307,
#149308,#149309,#149310,#149311,#149312,#149313,#149314,#149315,#149316,
#149317,#149318,#149319,#149320,#149321,#149322,#149323,#149324,#149325,
#149326,#149327,#149328,#149329,#149330,#149331,#149332,#149333,#149334,
#149335,#149336,#149337,#149338,#149339,#149340,#149341,#149342,#149343,
#149344,#149345,#149346,#149347,#149348,#149349,#149350,#149351,#149352,
#149353,#149354,#149355,#149356,#149357,#149358,#149359,#149360,#149361,
#149362,#149363,#149364,#149365,#149366,#149367,#149368,#149369,#149370,
#149371,#149372,#149373,#149374,#149375,#149376,#149377,#149378,#149379,
#149380,#149381,#149382,#149383,#149384,#149385,#149386,#149387,#149388,
#149389,#149390,#149391,#149392,#149393,#149394,#149395,#149396,#149397,
#149398,#149399,#149400,#149401,#149402,#149403,#149404,#149405,#149406,
#149407,#149408,#149409,#149410,#149411,#149412,#149413,#149414,#149415,
#149416,#149417,#149418,#149419,#149420,#149421,#149422,#149423),
 .UNSPECIFIED.,.F.,.F.,(4,3,3,3,3,3,3,3,3,3,3,3,3,3,3,3,3,3,3,3,3,3,3,3,
3,3,3,3,3,3,3,3,3,3,3,3,3,3,3,3,3,3,3,3,3,3,3,3,3,3,3,3,3,3,3,3,3,3,3,3,
3,3,3,3,3,3,3,3,3,3,3,3,3,3,3,3,3,3,3,3,3,3,4),(610.587829947008,610.690094159622,
610.794601151968,610.838702549999,610.91865985013,610.998522647371,611.078308469843,
611.158034785037,611.237719013331,611.317389999551,611.397057453076,611.476737103892,
611.556444686285,611.63623991536,611.716084257067,611.796042684113,611.838438560719,
611.91839586085,611.998258658093,612.078044480565,612.15777079576,612.237455024055,
612.317126010276,612.396793463802,612.476473114618,612.556180697013,612.635975926088,
612.715820267796,612.795778694843,612.838174571439,612.91813187157,612.997994668813,
613.077780491285,613.15750680648,613.237191034775,613.316862020996,613.396529474522,
613.476209125338,613.555916707733,613.635711936808,613.715556278516,613.795514705563,
613.837910582159,613.91786788229,613.997730679533,614.077516502004,614.1572428172,
614.236927045494,614.316598031715,614.39626548524,614.475945136057,614.555652718451,
614.635447947527,614.715292289234,614.795250716281,614.837646592879,614.91760389301,
614.997466690253,615.077252512725,615.15697882792,615.236663056215,615.316334042436,
615.396001495962,615.475681146778,615.555388729173,615.635183958249,615.715028299957,
615.794986727004,615.837382603599,615.91733990373,615.997202700973,616.076988523444,
616.15671483864,616.236399066934,616.316070053155,616.395737506681,616.475417157497,
616.555124739891,616.634919968967,616.714764310675,616.794722737722,616.837118614319,
616.871015197113),.UNSPECIFIED.);
#1227=B_SPLINE_CURVE_WITH_KNOTS('',3,(#149425,#149426,#149427,#149428,#149429,
#149430,#149431,#149432,#149433,#149434),.UNSPECIFIED.,.F.,.F.,(4,1,1,1,
1,1,1,4),(616.871019818576,617.836854625039,618.836590635759,619.83632664648,
620.8360626572,621.83579866792,622.83553467864,623.154200504292),
 .UNSPECIFIED.);
#1228=B_SPLINE_CURVE_WITH_KNOTS('',3,(#149436,#149437,#149438,#149439,#149440,
#149441,#149442,#149443,#149444,#149445),.UNSPECIFIED.,.F.,.F.,(4,1,1,1,
1,1,1,4),(623.154200504292,623.83527068936,624.83500670008,625.834742710801,
626.834478721521,627.834214732241,628.833950742961,629.437385811472),
 .UNSPECIFIED.);
#1229=B_SPLINE_CURVE_WITH_KNOTS('',3,(#149447,#149448,#149449,#149450,#149451,
#149452,#149453,#149454,#149455,#149456),.UNSPECIFIED.,.F.,.F.,(4,1,1,1,
1,1,1,4),(629.437385811472,629.833686753681,630.833422764401,631.833158775121,
632.832894785842,633.832630796561,634.832366807282,635.720571118652),
 .UNSPECIFIED.);
#1230=B_SPLINE_CURVE_WITH_KNOTS('',3,(#149458,#149459,#149460,#149461,#149462,
#149463,#149464,#149465,#149466,#149467,#149468),.UNSPECIFIED.,.F.,.F.,
(4,1,1,1,1,1,1,1,4),(635.720571118652,635.832102818002,636.831838828722,
637.831574839442,638.831310850162,639.831046860882,640.830782871603,641.830518882323,
642.003756425831),.UNSPECIFIED.);
#1231=B_SPLINE_CURVE_WITH_KNOTS('',3,(#149470,#149471,#149472,#149473,#149474,
#149475,#149476,#149477,#149478,#149479,#149480,#149481,#149482,#149483,
#149484,#149485,#149486,#149487,#149488,#149489,#149490,#149491,#149492,
#149493,#149494,#149495,#149496,#149497,#149498,#149499,#149500,#149501,
#149502,#149503,#149504,#149505,#149506,#149507,#149508,#149509,#149510,
#149511,#149512,#149513,#149514,#149515,#149516,#149517,#149518,#149519,
#149520,#149521,#149522,#149523,#149524,#149525,#149526,#149527,#149528,
#149529,#149530,#149531,#149532,#149533,#149534,#149535,#149536,#149537,
#149538,#149539,#149540,#149541,#149542,#149543,#149544,#149545,#149546,
#149547,#149548,#149549,#149550,#149551,#149552,#149553,#149554,#149555,
#149556,#149557,#149558,#149559,#149560,#149561,#149562,#149563,#149564,
#149565,#149566,#149567,#149568,#149569,#149570,#149571,#149572,#149573,
#149574,#149575,#149576,#149577,#149578,#149579,#149580,#149581,#149582,
#149583,#149584,#149585,#149586,#149587,#149588,#149589,#149590,#149591,
#149592,#149593,#149594,#149595,#149596,#149597,#149598,#149599,#149600,
#149601,#149602,#149603,#149604,#149605,#149606,#149607,#149608,#149609,
#149610,#149611,#149612,#149613,#149614,#149615,#149616,#149617,#149618,
#149619,#149620,#149621,#149622,#149623,#149624,#149625,#149626,#149627,
#149628,#149629,#149630,#149631,#149632,#149633,#149634,#149635,#149636,
#149637,#149638,#149639,#149640,#149641,#149642,#149643,#149644,#149645,
#149646,#149647,#149648,#149649,#149650,#149651,#149652,#149653,#149654,
#149655,#149656,#149657,#149658,#149659,#149660,#149661,#149662,#149663,
#149664,#149665,#149666,#149667,#149668,#149669,#149670,#149671,#149672,
#149673,#149674,#149675,#149676,#149677,#149678,#149679,#149680,#149681,
#149682,#149683,#149684,#149685,#149686,#149687,#149688,#149689,#149690,
#149691,#149692,#149693,#149694,#149695,#149696,#149697,#149698,#149699,
#149700,#149701,#149702,#149703,#149704,#149705,#149706,#149707,#149708,
#149709,#149710,#149711,#149712,#149713,#149714,#149715,#149716),
 .UNSPECIFIED.,.F.,.F.,(4,3,3,3,3,3,3,3,3,3,3,3,3,3,3,3,3,3,3,3,3,3,3,3,
3,3,3,3,3,3,3,3,3,3,3,3,3,3,3,3,3,3,3,3,3,3,3,3,3,3,3,3,3,3,3,3,3,3,3,3,
3,3,3,3,3,3,3,3,3,3,3,3,3,3,3,3,3,3,3,3,3,3,4),(642.003756425831,642.082402951354,
642.160979450999,642.239504318118,642.318004216256,642.396493621382,642.474989103083,
642.553507234078,642.632107218901,642.710753169526,642.789509990212,642.830254893043,
642.910212193174,642.990074990417,643.069860812889,643.149587128084,643.229271356378,
643.308942342599,643.388609796125,643.468289446942,643.547997029336,643.627792258412,
643.707636600119,643.787595027166,643.829990903763,643.909948203894,643.989811001137,
644.069596823609,644.149323138804,644.229007367098,644.308678353319,644.388345806845,
644.468025457662,644.547733040056,644.627528269132,644.70737261084,644.787331037887,
644.829726914483,644.909684214614,644.989547011857,645.069332834328,645.149059149524,
645.228743377818,645.308414364038,645.388081817564,645.467761468381,645.547469050775,
645.627264279851,645.707108621558,645.787067048606,645.829462925203,645.909420225334,
645.989283022577,646.069068845049,646.148795160244,646.228479388538,646.308150374759,
646.387817828285,646.467497479101,646.547205061496,646.627000290572,646.706844632279,
646.786803059327,646.829198935923,646.909156236054,646.989019033297,647.068804855769,
647.148531170965,647.228215399259,647.30788638548,647.387553839006,647.467233489822,
647.546941072216,647.626736301292,647.706580642999,647.786539070046,647.828934946643,
647.914770615256,648.000437967126,648.08586396628,648.171140400706,648.256207607788,
648.28694150642),.UNSPECIFIED.);
#1232=B_SPLINE_CURVE_WITH_KNOTS('',3,(#149718,#149719,#149720,#149721,#149722,
#149723,#149724,#149725,#149726,#149727),.UNSPECIFIED.,.F.,.F.,(4,1,1,1,
1,1,1,4),(648.286941733011,648.828670957363,649.828406968084,650.828142978804,
651.827878989524,652.827615000244,653.827351010964,654.57012704019),
 .UNSPECIFIED.);
#1233=B_SPLINE_CURVE_WITH_KNOTS('',3,(#149729,#149730,#149731,#149732,#149733,
#149734,#149735,#149736,#149737,#149738,#149739),.UNSPECIFIED.,.F.,.F.,
(4,1,1,1,1,1,1,1,4),(654.57012704019,654.827087021684,655.826823032404,
656.826559043124,657.826295053845,658.826031064565,659.825767075285,660.825503086005,
660.85331234737),.UNSPECIFIED.);
#1234=B_SPLINE_CURVE_WITH_KNOTS('',3,(#149741,#149742,#149743,#149744,#149745,
#149746,#149747,#149748,#149749,#149750,#149751,#149752,#149753,#149754,
#149755,#149756,#149757,#149758,#149759,#149760,#149761,#149762,#149763,
#149764,#149765,#149766,#149767,#149768,#149769,#149770,#149771,#149772,
#149773,#149774,#149775,#149776,#149777,#149778,#149779,#149780,#149781,
#149782,#149783,#149784,#149785,#149786,#149787,#149788,#149789,#149790,
#149791,#149792,#149793,#149794,#149795,#149796,#149797,#149798,#149799,
#149800,#149801,#149802,#149803,#149804,#149805,#149806,#149807,#149808,
#149809,#149810,#149811,#149812,#149813,#149814,#149815,#149816,#149817,
#149818,#149819,#149820,#149821,#149822,#149823,#149824,#149825,#149826,
#149827,#149828,#149829,#149830,#149831,#149832,#149833,#149834,#149835,
#149836,#149837,#149838,#149839,#149840,#149841,#149842,#149843,#149844,
#149845,#149846,#149847,#149848,#149849,#149850,#149851,#149852,#149853,
#149854,#149855,#149856,#149857,#149858,#149859,#149860,#149861,#149862,
#149863,#149864,#149865,#149866,#149867,#149868,#149869,#149870,#149871,
#149872,#149873,#149874,#149875,#149876,#149877,#149878,#149879,#149880,
#149881,#149882,#149883,#149884,#149885,#149886,#149887,#149888,#149889,
#149890,#149891,#149892,#149893,#149894,#149895,#149896,#149897,#149898,
#149899,#149900,#149901,#149902,#149903,#149904,#149905,#149906,#149907,
#149908,#149909,#149910,#149911,#149912,#149913,#149914,#149915,#149916,
#149917,#149918,#149919,#149920,#149921,#149922,#149923,#149924,#149925,
#149926,#149927,#149928,#149929,#149930,#149931,#149932,#149933,#149934,
#149935,#149936,#149937,#149938,#149939,#149940,#149941,#149942,#149943,
#149944,#149945,#149946,#149947,#149948,#149949,#149950,#149951,#149952,
#149953,#149954,#149955,#149956,#149957,#149958,#149959,#149960,#149961,
#149962,#149963,#149964,#149965,#149966,#149967,#149968,#149969,#149970,
#149971,#149972,#149973,#149974,#149975,#149976,#149977,#149978,#149979,
#149980,#149981,#149982,#149983,#149984,#149985,#149986,#149987),
 .UNSPECIFIED.,.F.,.F.,(4,3,3,3,3,3,3,3,3,3,3,3,3,3,3,3,3,3,3,3,3,3,3,3,
3,3,3,3,3,3,3,3,3,3,3,3,3,3,3,3,3,3,3,3,3,3,3,3,3,3,3,3,3,3,3,3,3,3,3,3,
3,3,3,3,3,3,3,3,3,3,3,3,3,3,3,3,3,3,3,3,3,3,4),(660.85331234737,660.93289668504,
661.012387538856,661.09180277648,661.171160202289,661.252920064094,661.332226639779,
661.411532635294,661.490854085283,661.570207031294,661.649648079436,661.729142021672,
661.808742750969,661.825239096725,661.905196396856,661.985059194099,662.06484501657,
662.144571331765,662.224255560059,662.30392654628,662.383593999806,662.463273650622,
662.542981233017,662.622776462092,662.7026208038,662.782579230847,662.824975107445,
662.904932407576,662.984795204819,663.064581027291,663.144307342487,663.223991570781,
663.303662557002,663.383330010528,663.463009661345,663.542717243739,663.622512472815,
663.702356814523,663.782315241571,663.824711118166,663.904668418297,663.98453121554,
664.064317038012,664.144043353207,664.223727581501,664.303398567722,664.383066021248,
664.462745672064,664.542453254459,664.622248483534,664.702092825242,664.78205125229,
664.824447128886,664.904404429017,664.98426722626,665.064053048731,665.143779363927,
665.223463592221,665.303134578442,665.382802031968,665.462481682784,665.542189265178,
665.621984494254,665.701828835961,665.781787263009,665.824183139606,665.904140439737,
665.98400323698,666.063789059453,666.143515374648,666.223199602942,666.302870589163,
666.382538042689,666.462217693506,666.5419252759,666.621720504976,666.701564846683,
666.781523273731,666.823919150326,666.919981952889,667.01551406519,667.110071646987,
667.136497447219),.UNSPECIFIED.);
#1235=B_SPLINE_CURVE_WITH_KNOTS('',3,(#149989,#149990,#149991,#149992,#149993,
#149994,#149995,#149996,#149997,#149998),.UNSPECIFIED.,.F.,.F.,(4,1,1,1,
1,1,1,4),(667.136497654549,667.823655161046,668.823391171766,669.823127182486,
670.822863193206,671.822599203926,672.822335214646,673.419682961729),
 .UNSPECIFIED.);
#1236=B_SPLINE_CURVE_WITH_KNOTS('',3,(#150000,#150001,#150002,#150003,#150004,
#150005,#150006,#150007,#150008,#150009,#150010,#150011,#150012,#150013,
#150014,#150015,#150016,#150017,#150018,#150019,#150020,#150021,#150022,
#150023,#150024,#150025,#150026,#150027,#150028,#150029,#150030,#150031,
#150032,#150033,#150034,#150035,#150036,#150037,#150038,#150039,#150040,
#150041,#150042,#150043,#150044,#150045,#150046,#150047,#150048,#150049,
#150050,#150051,#150052,#150053,#150054,#150055,#150056,#150057,#150058,
#150059,#150060,#150061,#150062,#150063,#150064,#150065,#150066,#150067,
#150068,#150069,#150070,#150071,#150072,#150073,#150074,#150075,#150076,
#150077,#150078,#150079,#150080,#150081,#150082,#150083,#150084,#150085,
#150086,#150087,#150088,#150089,#150090,#150091,#150092,#150093,#150094,
#150095,#150096,#150097,#150098,#150099,#150100,#150101,#150102,#150103,
#150104,#150105,#150106,#150107,#150108,#150109,#150110,#150111,#150112,
#150113,#150114,#150115,#150116,#150117,#150118,#150119,#150120,#150121,
#150122,#150123,#150124,#150125,#150126,#150127,#150128,#150129,#150130,
#150131,#150132,#150133,#150134,#150135,#150136,#150137,#150138,#150139,
#150140,#150141,#150142,#150143,#150144,#150145,#150146,#150147,#150148,
#150149,#150150,#150151,#150152,#150153,#150154,#150155,#150156,#150157,
#150158,#150159,#150160,#150161,#150162,#150163,#150164,#150165,#150166,
#150167,#150168,#150169,#150170,#150171,#150172,#150173,#150174,#150175,
#150176,#150177,#150178,#150179,#150180,#150181,#150182,#150183,#150184,
#150185,#150186,#150187,#150188,#150189,#150190,#150191,#150192,#150193,
#150194,#150195,#150196,#150197,#150198,#150199,#150200,#150201,#150202,
#150203,#150204,#150205,#150206,#150207,#150208,#150209,#150210,#150211,
#150212,#150213,#150214,#150215,#150216,#150217,#150218,#150219,#150220,
#150221,#150222,#150223,#150224,#150225,#150226,#150227,#150228,#150229,
#150230,#150231,#150232,#150233,#150234,#150235,#150236,#150237,#150238,
#150239,#150240,#150241,#150242,#150243,#150244,#150245,#150246),
 .UNSPECIFIED.,.F.,.F.,(4,3,3,3,3,3,3,3,3,3,3,3,3,3,3,3,3,3,3,3,3,3,3,3,
3,3,3,3,3,3,3,3,3,3,3,3,3,3,3,3,3,3,3,3,3,3,3,3,3,3,3,3,3,3,3,3,3,3,3,3,
3,3,3,3,3,3,3,3,3,3,3,3,3,3,3,3,3,3,3,3,3,3,4),(673.419683183978,673.507475405285,
673.595719432381,673.684192986917,673.772987001415,673.822071225367,673.902028525498,
673.981891322741,674.061677145213,674.141403460408,674.221087688703,674.300758674924,
674.38042612845,674.460105779266,674.539813361661,674.619608590737,674.699452932444,
674.779411359492,674.821807236087,674.901764536218,674.981627333461,675.061413155933,
675.141139471128,675.220823699422,675.300494685643,675.380162139169,675.459841789985,
675.53954937238,675.619344601455,675.699188943163,675.77914737021,675.821543246807,
675.901500546938,675.981363344181,676.061149166653,676.140875481848,676.220559710142,
676.300230696363,676.379898149889,676.459577800705,676.539285383099,676.619080612175,
676.698924953882,676.77888338093,676.821279257527,676.901236557658,676.981099354901,
677.060885177373,677.140611492568,677.220295720862,677.299966707083,677.379634160609,
677.459313811426,677.53902139382,677.618816622896,677.698660964603,677.778619391651,
677.821015268247,677.900972568378,677.980835365621,678.060621188092,678.140347503288,
678.220031731582,678.299702717803,678.379370171329,678.459049822145,678.53875740454,
678.618552633615,678.698396975322,678.77835540237,678.820751278967,678.89962025868,
678.978395497203,679.057095415522,679.137817022195,679.216425133687,679.295017936498,
679.373611941843,679.45592602361,679.534608192868,679.613332891335,679.692148113422,
679.702868268909),.UNSPECIFIED.);
#1237=B_SPLINE_CURVE_WITH_KNOTS('',3,(#150248,#150249,#150250,#150251,#150252,
#150253,#150254,#150255,#150256,#150257,#150258,#150259),.UNSPECIFIED.,
 .F.,.F.,(4,2,1,1,1,1,1,1,4),(679.702868268909,679.820487289687,680.820223300408,
681.819959311128,682.819695321848,683.819431332568,684.819167343288,685.818903354008,
685.986053576088),.UNSPECIFIED.);
#1238=B_SPLINE_CURVE_WITH_KNOTS('',3,(#150261,#150262,#150263,#150264,#150265,
#150266,#150267,#150268,#150269,#150270),.UNSPECIFIED.,.F.,.F.,(4,1,1,1,
1,1,1,4),(685.986053576088,686.818639364728,687.818375375449,688.818111386169,
689.817847396889,690.817583407609,691.817319418329,692.269238883268),
 .UNSPECIFIED.);
#1239=B_SPLINE_CURVE_WITH_KNOTS('',3,(#150272,#150273,#150274,#150275,#150276,
#150277,#150278,#150279,#150280,#150281),.UNSPECIFIED.,.F.,.F.,(4,1,1,1,
1,1,1,4),(692.269238883268,692.817055429049,693.816791439769,694.81652745049,
695.81626346121,696.81599947193,697.81573548265,698.552424190447),
 .UNSPECIFIED.);
#1240=B_SPLINE_CURVE_WITH_KNOTS('',3,(#150283,#150284,#150285,#150286,#150287,
#150288,#150289,#150290,#150291,#150292,#150293),.UNSPECIFIED.,.F.,.F.,
(4,1,1,1,1,1,1,1,4),(698.552424190447,698.81547149337,699.81520750409,700.81494351481,
701.81467952553,702.814415536251,703.814151546971,704.813887557691,704.835609497627),
 .UNSPECIFIED.);
#1241=B_SPLINE_CURVE_WITH_KNOTS('',3,(#150295,#150296,#150297,#150298,#150299,
#150300,#150301,#150302,#150303,#150304,#150305,#150306,#150307,#150308,
#150309,#150310,#150311,#150312,#150313,#150314,#150315,#150316,#150317,
#150318,#150319,#150320,#150321,#150322,#150323,#150324,#150325,#150326,
#150327,#150328,#150329,#150330,#150331,#150332,#150333,#150334,#150335,
#150336,#150337,#150338,#150339,#150340,#150341,#150342,#150343,#150344,
#150345,#150346,#150347,#150348,#150349,#150350,#150351,#150352,#150353,
#150354,#150355,#150356,#150357,#150358,#150359,#150360,#150361,#150362,
#150363,#150364,#150365,#150366,#150367,#150368,#150369,#150370,#150371,
#150372,#150373,#150374,#150375,#150376,#150377,#150378,#150379,#150380,
#150381,#150382,#150383,#150384,#150385,#150386,#150387,#150388,#150389,
#150390,#150391,#150392,#150393,#150394,#150395,#150396,#150397,#150398,
#150399,#150400,#150401,#150402,#150403,#150404,#150405,#150406,#150407,
#150408,#150409,#150410,#150411,#150412,#150413,#150414,#150415,#150416,
#150417,#150418,#150419,#150420,#150421,#150422,#150423,#150424,#150425,
#150426,#150427,#150428,#150429,#150430,#150431,#150432,#150433,#150434,
#150435,#150436,#150437,#150438,#150439,#150440,#150441,#150442,#150443,
#150444,#150445,#150446,#150447,#150448,#150449,#150450,#150451,#150452,
#150453,#150454,#150455,#150456,#150457,#150458,#150459,#150460,#150461,
#150462,#150463,#150464,#150465,#150466,#150467,#150468,#150469,#150470,
#150471,#150472,#150473,#150474,#150475,#150476,#150477,#150478,#150479,
#150480,#150481,#150482,#150483,#150484,#150485,#150486,#150487,#150488,
#150489,#150490,#150491,#150492,#150493,#150494,#150495,#150496,#150497,
#150498,#150499,#150500,#150501,#150502,#150503,#150504,#150505,#150506,
#150507,#150508,#150509,#150510,#150511,#150512,#150513,#150514,#150515,
#150516,#150517,#150518,#150519,#150520,#150521,#150522,#150523,#150524,
#150525,#150526,#150527,#150528,#150529,#150530,#150531,#150532,#150533,
#150534,#150535,#150536,#150537,#150538,#150539,#150540,#150541),
 .UNSPECIFIED.,.F.,.F.,(4,3,3,3,3,3,3,3,3,3,3,3,3,3,3,3,3,3,3,3,3,3,3,3,
3,3,3,3,3,3,3,3,3,3,3,3,3,3,3,3,3,3,3,3,3,3,3,3,3,3,3,3,3,3,3,3,3,3,3,3,
3,3,3,3,3,3,3,3,3,3,3,3,3,3,3,3,3,3,3,3,3,3,4),(704.835609497627,704.915270034789,
704.994836731164,705.074327390111,705.153759752259,705.236242729278,705.315622886734,
705.395001979489,705.474395984204,705.553820883933,705.633333846027,705.712899052128,
705.792572327826,705.813623568411,705.893580868542,705.973443665785,706.053229488257,
706.132955803452,706.212640031746,706.292311017967,706.371978471493,706.451658122309,
706.531365704703,706.611160933779,706.691005275486,706.770963702534,706.813359579131,
706.893316879262,706.973179676505,707.052965498977,707.132691814172,707.212376042466,
707.292047028687,707.371714482213,707.451394133029,707.531101715423,707.610896944499,
707.690741286207,707.770699713254,707.813095589851,707.893052889982,707.972915687225,
708.052701509696,708.132427824892,708.212112053186,708.291783039407,708.371450492933,
708.45113014375,708.530837726144,708.61063295522,708.690477296927,708.770435723975,
708.812831600571,708.892788900702,708.972651697945,709.052437520416,709.132163835612,
709.211848063906,709.291519050127,709.371186503653,709.450866154469,709.530573736864,
709.610368965939,709.690213307647,709.770171734694,709.812567611291,709.892524911422,
709.972387708665,710.052173531137,710.131899846332,710.211584074626,710.291255060847,
710.370922514373,710.45060216519,710.530309747585,710.610104976661,710.689949318368,
710.769907745416,710.812303622012,710.909040597874,711.005203662865,711.100327550192,
711.118794607969),.UNSPECIFIED.);
#1242=B_SPLINE_CURVE_WITH_KNOTS('',3,(#150543,#150544,#150545,#150546,#150547,
#150548,#150549,#150550,#150551,#150552),.UNSPECIFIED.,.F.,.F.,(4,1,1,1,
1,1,1,4),(711.118794804806,711.812039632732,712.811775643452,713.811511654172,
714.811247664892,715.810983675612,716.810719686332,717.401980111986),
 .UNSPECIFIED.);
#1243=B_SPLINE_CURVE_WITH_KNOTS('',3,(#150554,#150555,#150556,#150557,#150558,
#150559,#150560,#150561,#150562,#150563,#150564,#150565,#150566,#150567,
#150568,#150569,#150570,#150571,#150572,#150573,#150574,#150575,#150576,
#150577,#150578,#150579,#150580,#150581,#150582,#150583,#150584,#150585,
#150586,#150587,#150588,#150589,#150590,#150591,#150592,#150593,#150594,
#150595,#150596,#150597,#150598,#150599,#150600,#150601,#150602,#150603,
#150604,#150605,#150606,#150607,#150608,#150609,#150610,#150611,#150612,
#150613,#150614,#150615,#150616,#150617,#150618,#150619,#150620,#150621,
#150622,#150623,#150624,#150625,#150626,#150627,#150628,#150629,#150630,
#150631,#150632,#150633,#150634,#150635,#150636,#150637,#150638,#150639,
#150640,#150641,#150642,#150643,#150644,#150645,#150646,#150647,#150648,
#150649,#150650,#150651,#150652,#150653,#150654,#150655,#150656,#150657,
#150658,#150659,#150660,#150661,#150662,#150663,#150664,#150665,#150666,
#150667,#150668,#150669,#150670,#150671,#150672,#150673,#150674,#150675,
#150676,#150677,#150678,#150679,#150680,#150681,#150682,#150683,#150684,
#150685,#150686,#150687,#150688,#150689,#150690,#150691,#150692,#150693,
#150694,#150695,#150696,#150697,#150698,#150699,#150700,#150701,#150702,
#150703,#150704,#150705,#150706,#150707,#150708,#150709,#150710,#150711,
#150712,#150713,#150714,#150715,#150716,#150717,#150718,#150719,#150720,
#150721,#150722,#150723,#150724,#150725,#150726,#150727,#150728,#150729,
#150730,#150731,#150732,#150733,#150734,#150735,#150736,#150737,#150738,
#150739,#150740,#150741,#150742,#150743,#150744,#150745,#150746,#150747,
#150748,#150749,#150750,#150751,#150752,#150753,#150754,#150755,#150756,
#150757,#150758,#150759,#150760,#150761,#150762,#150763,#150764,#150765,
#150766,#150767,#150768,#150769,#150770,#150771,#150772,#150773,#150774,
#150775,#150776,#150777,#150778,#150779,#150780,#150781,#150782,#150783,
#150784,#150785,#150786,#150787,#150788,#150789,#150790,#150791,#150792,
#150793,#150794,#150795,#150796,#150797),.UNSPECIFIED.,.F.,.F.,(4,3,3,3,
3,3,3,3,3,3,3,3,3,3,3,3,3,3,3,3,3,3,3,3,3,3,3,3,3,3,3,3,3,3,3,3,3,3,3,3,
3,3,3,3,3,3,3,3,3,3,3,3,3,3,3,3,3,3,3,3,3,3,3,3,3,3,3,3,3,3,3,3,3,3,3,3,
3,3,3,3,3,4),(717.401980325962,717.489435265062,717.57731884262,717.665419190297,
717.753832653133,717.810455697052,717.890412997183,717.970275794426,718.050061616897,
718.129787932093,718.209472160386,718.289143146607,718.368810600133,718.448490250949,
718.528197833344,718.607993062419,718.687837404127,718.767795831174,718.810191707772,
718.890149007903,718.970011805146,719.049797627618,719.129523942814,719.209208171108,
719.288879157329,719.368546610855,719.448226261672,719.527933844067,719.607729073142,
719.68757341485,719.767531841898,719.809927718493,719.889885018624,719.969747815867,
720.049533638339,720.129259953534,720.208944181828,720.288615168049,720.368282621575,
720.447962272392,720.527669854787,720.607465083862,720.68730942557,720.767267852618,
720.809663729213,720.889621029344,720.969483826587,721.049269649058,721.128995964253,
721.208680192547,721.288351178768,721.368018632294,721.44769828311,721.527405865505,
721.60720109458,721.687045436287,721.767003863335,721.809399739933,721.889357040064,
721.969219837307,722.049005659779,722.128731974974,722.208416203268,722.288087189489,
722.367754643015,722.447434293831,722.527141876226,722.606937105301,722.686781447009,
722.766739874056,722.809135750653,722.887980746099,722.966731996665,723.0454079396,
723.125377624546,723.203961856065,723.282530646254,723.361100519844,723.442116744675,
723.520772986718,723.602969202942,723.685165419166),.UNSPECIFIED.);
#1244=B_SPLINE_CURVE_WITH_KNOTS('',3,(#150799,#150800,#150801,#150802,#150803,
#150804,#150805,#150806,#150807,#150808,#150809),.UNSPECIFIED.,.F.,.F.,
(4,1,1,1,1,1,1,1,4),(723.685165419166,723.808871761373,724.808607772093,
725.808343782813,726.808079793533,727.807815804254,728.807551814974,729.807287825694,
729.968350726345),.UNSPECIFIED.);
#1245=B_SPLINE_CURVE_WITH_KNOTS('',3,(#150811,#150812,#150813,#150814,#150815,
#150816,#150817,#150818,#150819,#150820),.UNSPECIFIED.,.F.,.F.,(4,1,1,1,
1,1,1,4),(729.968350726345,730.807023836414,731.806759847134,732.806495857854,
733.806231868575,734.805967879295,735.805703890015,736.251536033525),
 .UNSPECIFIED.);
#1246=B_SPLINE_CURVE_WITH_KNOTS('',3,(#150822,#150823,#150824,#150825,#150826,
#150827,#150828,#150829,#150830,#150831),.UNSPECIFIED.,.F.,.F.,(4,1,1,1,
1,1,1,4),(736.251536033525,736.805439900735,737.805175911455,738.804911922175,
739.804647932895,740.804383943615,741.804119954336,742.534721340704),
 .UNSPECIFIED.);
#1247=B_SPLINE_CURVE_WITH_KNOTS('',3,(#150833,#150834,#150835,#150836,#150837,
#150838,#150839,#150840,#150841,#150842,#150843),.UNSPECIFIED.,.F.,.F.,
(4,1,1,1,1,1,1,1,4),(742.534721340704,742.803855965056,743.803591975776,
744.803327986496,745.803063997216,746.802800007936,747.802536018656,748.802272029376,
748.817906647884),.UNSPECIFIED.);
#1248=B_SPLINE_CURVE_WITH_KNOTS('',3,(#150845,#150846,#150847,#150848,#150849,
#150850,#150851,#150852,#150853,#150854,#150855,#150856,#150857,#150858,
#150859,#150860,#150861,#150862,#150863,#150864,#150865,#150866,#150867,
#150868,#150869,#150870,#150871,#150872,#150873,#150874,#150875,#150876,
#150877,#150878,#150879,#150880,#150881,#150882,#150883,#150884,#150885,
#150886,#150887,#150888,#150889,#150890,#150891,#150892,#150893,#150894,
#150895,#150896,#150897,#150898,#150899,#150900,#150901,#150902,#150903,
#150904,#150905,#150906,#150907,#150908,#150909,#150910,#150911,#150912,
#150913,#150914,#150915,#150916,#150917,#150918,#150919,#150920,#150921,
#150922,#150923,#150924,#150925,#150926,#150927,#150928,#150929,#150930,
#150931,#150932,#150933,#150934,#150935,#150936,#150937,#150938,#150939,
#150940,#150941,#150942,#150943,#150944,#150945,#150946,#150947,#150948,
#150949,#150950,#150951,#150952,#150953,#150954,#150955,#150956,#150957,
#150958,#150959,#150960,#150961,#150962,#150963,#150964,#150965,#150966,
#150967,#150968,#150969,#150970,#150971,#150972,#150973,#150974,#150975,
#150976,#150977,#150978,#150979,#150980,#150981,#150982,#150983,#150984,
#150985,#150986,#150987,#150988,#150989,#150990,#150991,#150992,#150993,
#150994,#150995,#150996,#150997,#150998,#150999,#151000,#151001,#151002,
#151003,#151004,#151005,#151006,#151007,#151008,#151009,#151010,#151011,
#151012,#151013,#151014,#151015,#151016,#151017,#151018,#151019,#151020,
#151021,#151022,#151023,#151024,#151025,#151026,#151027,#151028,#151029,
#151030,#151031,#151032,#151033,#151034,#151035,#151036,#151037,#151038,
#151039,#151040,#151041,#151042,#151043,#151044,#151045,#151046,#151047,
#151048,#151049,#151050,#151051,#151052,#151053,#151054,#151055,#151056,
#151057,#151058,#151059,#151060,#151061,#151062,#151063,#151064,#151065,
#151066,#151067,#151068,#151069,#151070,#151071,#151072,#151073,#151074,
#151075,#151076,#151077,#151078,#151079,#151080,#151081,#151082,#151083,
#151084,#151085,#151086,#151087,#151088,#151089,#151090,#151091),
 .UNSPECIFIED.,.F.,.F.,(4,3,3,3,3,3,3,3,3,3,3,3,3,3,3,3,3,3,3,3,3,3,3,3,
3,3,3,3,3,3,3,3,3,3,3,3,3,3,3,3,3,3,3,3,3,3,3,3,3,3,3,3,3,3,3,3,3,3,3,3,
3,3,3,3,3,3,3,3,3,3,3,3,3,3,3,3,3,3,3,3,3,3,4),(748.817906647884,748.897646423686,
748.977292073114,749.056861329939,749.136371865781,749.21957638757,749.299033476738,
749.378489054434,749.457959034762,749.537459337759,749.617047679928,749.696687633192,
749.776436940243,749.802008040097,749.881965340228,749.961828137471,750.041613959943,
750.121340275138,750.201024503432,750.280695489653,750.360362943179,750.440042593995,
750.519750176389,750.599545405465,750.679389747172,750.759348174219,750.801744050817,
750.881701350948,750.961564148191,751.041349970662,751.121076285858,751.200760514152,
751.280431500372,751.360098953898,751.439778604715,751.51948618711,751.599281416185,
751.679125757893,751.75908418494,751.801480061537,751.881437361668,751.961300158911,
752.041085981383,752.120812296578,752.200496524872,752.280167511094,752.35983496462,
752.439514615436,752.519222197831,752.599017426906,752.678861768614,752.758820195662,
752.801216072257,752.881173372388,752.961036169631,753.040821992103,753.120548307298,
753.200232535592,753.279903521813,753.359570975339,753.439250626156,753.51895820855,
753.598753437626,753.678597779333,753.75855620638,753.800952082977,753.880909383108,
753.960772180351,754.040558002822,754.120284318017,754.199968546312,754.279639532533,
754.359306986059,754.438986636875,754.518694219269,754.598489448345,754.678333790053,
754.7582922171,754.800688093697,754.89813020414,754.999610987187,755.095292303198,
755.101091770234),.UNSPECIFIED.);
#1249=B_SPLINE_CURVE_WITH_KNOTS('',3,(#151093,#151094,#151095,#151096,#151097,
#151098,#151099,#151100,#151101,#151102),.UNSPECIFIED.,.F.,.F.,(4,1,1,1,
1,1,1,4),(755.101091955063,755.800424104417,756.800160115137,757.799896125858,
758.799632136578,759.799368147298,760.799104158018,761.384277262243),
 .UNSPECIFIED.);
#1250=B_SPLINE_CURVE_WITH_KNOTS('',3,(#151104,#151105,#151106,#151107,#151108,
#151109,#151110,#151111,#151112,#151113,#151114,#151115,#151116,#151117,
#151118,#151119,#151120,#151121,#151122,#151123,#151124,#151125,#151126,
#151127,#151128,#151129,#151130,#151131,#151132,#151133,#151134,#151135,
#151136,#151137,#151138,#151139,#151140,#151141,#151142,#151143,#151144,
#151145,#151146,#151147,#151148,#151149,#151150,#151151,#151152,#151153,
#151154,#151155,#151156,#151157,#151158,#151159,#151160,#151161,#151162,
#151163,#151164,#151165,#151166,#151167,#151168,#151169,#151170,#151171,
#151172,#151173,#151174,#151175,#151176,#151177,#151178,#151179,#151180,
#151181,#151182,#151183,#151184,#151185,#151186,#151187,#151188,#151189,
#151190,#151191,#151192,#151193,#151194,#151195,#151196,#151197,#151198,
#151199,#151200,#151201,#151202,#151203,#151204,#151205,#151206,#151207,
#151208,#151209,#151210,#151211,#151212,#151213,#151214,#151215,#151216,
#151217,#151218,#151219,#151220,#151221,#151222,#151223,#151224,#151225,
#151226,#151227,#151228,#151229,#151230,#151231,#151232,#151233,#151234,
#151235,#151236,#151237,#151238,#151239,#151240,#151241,#151242,#151243,
#151244,#151245,#151246,#151247,#151248,#151249,#151250,#151251,#151252,
#151253,#151254,#151255,#151256,#151257,#151258,#151259,#151260,#151261,
#151262,#151263,#151264,#151265,#151266,#151267,#151268,#151269,#151270,
#151271,#151272,#151273,#151274,#151275,#151276,#151277,#151278,#151279,
#151280,#151281,#151282,#151283,#151284,#151285,#151286,#151287,#151288,
#151289,#151290,#151291,#151292,#151293,#151294,#151295,#151296,#151297,
#151298,#151299,#151300,#151301,#151302,#151303,#151304,#151305,#151306,
#151307,#151308,#151309,#151310,#151311,#151312,#151313,#151314,#151315,
#151316,#151317,#151318,#151319,#151320,#151321,#151322,#151323,#151324,
#151325,#151326,#151327,#151328,#151329,#151330,#151331,#151332,#151333,
#151334,#151335,#151336,#151337,#151338,#151339,#151340,#151341,#151342,
#151343,#151344,#151345,#151346,#151347),.UNSPECIFIED.,.F.,.F.,(4,3,3,3,
3,3,3,3,3,3,3,3,3,3,3,3,3,3,3,3,3,3,3,3,3,3,3,3,3,3,3,3,3,3,3,3,3,3,3,3,
3,3,3,3,3,3,3,3,3,3,3,3,3,3,3,3,3,3,3,3,3,3,3,3,3,3,3,3,3,3,3,3,3,3,3,3,
3,3,3,3,3,4),(761.384277466923,761.471405537994,761.558940529162,761.646680291344,
761.73472615752,761.798840168738,761.87879746887,761.958660266113,762.038446088585,
762.11817240378,762.197856632075,762.277527618296,762.357195071823,762.436874722639,
762.516582305034,762.59637753411,762.676221875818,762.756180302866,762.798576179458,
762.878533479589,762.958396276832,763.038182099303,763.117908414499,763.197592642792,
763.277263629013,763.356931082539,763.436610733355,763.51631831575,763.596113544825,
763.675957886533,763.75591631358,763.798312190178,763.878269490309,763.958132287552,
764.037918110024,764.117644425219,764.197328653514,764.276999639735,764.356667093261,
764.436346744077,764.516054326472,764.595849555547,764.675693897255,764.755652324303,
764.798048200899,764.87800550103,764.957868298273,765.037654120745,765.117380435941,
765.197064664235,765.276735650456,765.356403103982,765.436082754798,765.515790337193,
765.595585566269,765.675429907976,765.755388335024,765.797784211619,765.87774151175,
765.957604308993,766.037390131464,766.11711644666,766.196800674954,766.276471661175,
766.356139114701,766.435818765517,766.515526347911,766.595321576987,766.675165918694,
766.755124345742,766.797520222339,766.876344312258,766.955074645796,767.033729674355,
767.112946286238,767.191509667396,767.270057457799,767.348606193875,767.428320287762,
767.506953550245,767.587208059834,767.667462569422),.UNSPECIFIED.);
#1251=B_SPLINE_CURVE_WITH_KNOTS('',3,(#151349,#151350,#151351,#151352,#151353,
#151354,#151355,#151356,#151357,#151358,#151359),.UNSPECIFIED.,.F.,.F.,
(4,1,1,1,1,1,1,1,4),(767.667462569422,767.797256233059,768.796992243779,
769.796728254499,770.796464265219,771.79620027594,772.79593628666,773.79567229738,
773.950647876602),.UNSPECIFIED.);
#1252=B_SPLINE_CURVE_WITH_KNOTS('',3,(#151361,#151362,#151363,#151364,#151365,
#151366,#151367,#151368,#151369,#151370),.UNSPECIFIED.,.F.,.F.,(4,1,1,1,
1,1,1,4),(773.950647876602,774.7954083081,775.79514431882,776.79488032954,
777.79461634026,778.79435235098,779.794088361701,780.233828319243),
 .UNSPECIFIED.);
#1253=B_SPLINE_CURVE_WITH_KNOTS('',3,(#151372,#151373,#151374,#151375,#151376,
#151377,#151378,#151379,#151380,#151381,#151382,#151383,#151384,#151385,
#151386,#151387,#151388,#151389,#151390,#151391,#151392,#151393,#151394,
#151395,#151396,#151397,#151398,#151399,#151400,#151401,#151402,#151403,
#151404,#151405,#151406,#151407,#151408,#151409,#151410,#151411,#151412,
#151413,#151414,#151415,#151416,#151417,#151418,#151419,#151420,#151421,
#151422,#151423,#151424,#151425,#151426,#151427,#151428,#151429,#151430,
#151431,#151432,#151433,#151434,#151435,#151436,#151437,#151438,#151439,
#151440,#151441,#151442,#151443,#151444,#151445,#151446,#151447,#151448,
#151449,#151450,#151451,#151452,#151453,#151454,#151455,#151456,#151457,
#151458,#151459,#151460,#151461,#151462,#151463,#151464,#151465,#151466,
#151467,#151468,#151469,#151470,#151471,#151472,#151473,#151474,#151475,
#151476,#151477,#151478,#151479,#151480,#151481,#151482,#151483,#151484,
#151485,#151486,#151487,#151488,#151489,#151490,#151491,#151492,#151493,
#151494,#151495,#151496,#151497,#151498,#151499,#151500,#151501,#151502,
#151503,#151504,#151505,#151506,#151507,#151508,#151509,#151510,#151511,
#151512,#151513,#151514,#151515,#151516,#151517,#151518,#151519,#151520,
#151521,#151522,#151523,#151524,#151525,#151526,#151527,#151528,#151529,
#151530,#151531,#151532,#151533,#151534,#151535,#151536,#151537,#151538,
#151539,#151540,#151541,#151542,#151543,#151544,#151545,#151546,#151547,
#151548,#151549,#151550,#151551,#151552,#151553,#151554,#151555,#151556,
#151557,#151558,#151559,#151560,#151561,#151562,#151563,#151564,#151565,
#151566,#151567,#151568,#151569,#151570,#151571,#151572,#151573,#151574,
#151575,#151576,#151577,#151578,#151579,#151580,#151581,#151582,#151583,
#151584,#151585,#151586,#151587,#151588,#151589,#151590,#151591,#151592,
#151593,#151594,#151595,#151596,#151597,#151598,#151599,#151600,#151601,
#151602,#151603,#151604,#151605,#151606,#151607,#151608,#151609,#151610,
#151611,#151612,#151613,#151614,#151615,#151616,#151617,#151618),
 .UNSPECIFIED.,.F.,.F.,(4,3,3,3,3,3,3,3,3,3,3,3,3,3,3,3,3,3,3,3,3,3,3,3,
3,3,3,3,3,3,3,3,3,3,3,3,3,3,3,3,3,3,3,3,3,3,3,3,3,3,3,3,3,3,3,3,3,3,3,3,
3,3,3,3,3,3,3,3,3,3,3,3,3,3,3,3,3,3,3,3,3,3,4),(780.233833183782,780.315493544815,
780.397200486774,780.478966500679,780.560865346708,780.64283406342,780.724956376328,
780.793824372421,780.873781672552,780.953644469795,781.033430292267,781.113156607462,
781.192840835756,781.272511821977,781.352179275503,781.431858926319,781.511566508713,
781.591361737789,781.671206079497,781.751164506544,781.793560383141,781.873517683272,
781.953380480515,782.033166302987,782.112892618182,782.192576846476,782.272247832697,
782.351915286223,782.43159493704,782.511302519434,782.59109774851,782.670942090218,
782.750900517265,782.793296393861,782.873253693992,782.953116491235,783.032902313706,
783.112628628902,783.192312857196,783.271983843416,783.351651296942,783.431330947759,
783.511038530154,783.590833759229,783.670678100936,783.750636527984,783.793032404581,
783.872989704712,783.952852501955,784.032638324427,784.112364639622,784.192048867916,
784.271719854137,784.351387307663,784.43106695848,784.510774540875,784.59056976995,
784.670414111658,784.750372538705,784.792768415301,784.872725715432,784.952588512675,
785.032374335147,785.112100650342,785.191784878636,785.271455864857,785.351123318383,
785.4308029692,785.510510551594,785.590305780669,785.670150122377,785.750108549425,
785.792504426021,785.871752178378,785.952410467451,786.031464250185,786.110464253903,
786.189426805881,786.271324727151,786.350277412381,786.429238753714,786.508242705639,
786.517018490961),.UNSPECIFIED.);
#1254=B_SPLINE_CURVE_WITH_KNOTS('',3,(#151620,#151621,#151622,#151623,#151624,
#151625,#151626,#151627,#151628,#151629,#151630),.UNSPECIFIED.,.F.,.F.,
(4,1,1,1,1,1,1,1,4),(786.517022438603,786.792240436741,787.791976447461,
788.791712458181,789.791448468902,790.791184479622,791.790920490342,792.790656501062,
792.800203798141),.UNSPECIFIED.);
#1255=B_SPLINE_CURVE_WITH_KNOTS('',3,(#151632,#151633,#151634,#151635,#151636,
#151637,#151638,#151639,#151640,#151641,#151642,#151643,#151644,#151645,
#151646,#151647,#151648,#151649,#151650,#151651,#151652,#151653,#151654,
#151655,#151656,#151657,#151658,#151659,#151660,#151661,#151662,#151663,
#151664,#151665,#151666,#151667,#151668,#151669,#151670,#151671,#151672,
#151673,#151674,#151675,#151676,#151677,#151678,#151679,#151680,#151681,
#151682,#151683,#151684,#151685,#151686,#151687,#151688,#151689,#151690,
#151691,#151692,#151693,#151694,#151695,#151696,#151697,#151698,#151699,
#151700,#151701,#151702,#151703,#151704,#151705,#151706,#151707,#151708,
#151709,#151710,#151711,#151712,#151713,#151714,#151715,#151716,#151717,
#151718,#151719,#151720,#151721,#151722,#151723,#151724,#151725,#151726,
#151727,#151728,#151729,#151730,#151731,#151732,#151733,#151734,#151735,
#151736,#151737,#151738,#151739,#151740,#151741,#151742,#151743,#151744,
#151745,#151746,#151747,#151748,#151749,#151750,#151751,#151752,#151753,
#151754,#151755,#151756,#151757,#151758,#151759,#151760,#151761,#151762,
#151763,#151764,#151765,#151766,#151767,#151768,#151769,#151770,#151771,
#151772,#151773,#151774,#151775,#151776,#151777,#151778,#151779,#151780,
#151781,#151782,#151783,#151784,#151785,#151786,#151787,#151788,#151789,
#151790,#151791,#151792,#151793,#151794,#151795,#151796,#151797,#151798,
#151799,#151800,#151801,#151802,#151803,#151804,#151805,#151806,#151807,
#151808,#151809,#151810,#151811,#151812,#151813,#151814,#151815,#151816,
#151817,#151818,#151819,#151820,#151821,#151822,#151823,#151824,#151825,
#151826,#151827,#151828,#151829,#151830,#151831,#151832,#151833,#151834,
#151835,#151836,#151837,#151838,#151839,#151840,#151841,#151842,#151843,
#151844,#151845,#151846,#151847,#151848,#151849,#151850,#151851,#151852,
#151853,#151854,#151855,#151856,#151857,#151858,#151859,#151860,#151861,
#151862,#151863,#151864,#151865,#151866,#151867,#151868,#151869,#151870,
#151871,#151872,#151873,#151874,#151875),.UNSPECIFIED.,.F.,.F.,(4,3,3,3,
3,3,3,3,3,3,3,3,3,3,3,3,3,3,3,3,3,3,3,3,3,3,3,3,3,3,3,3,3,3,3,3,3,3,3,3,
3,3,3,3,3,3,3,3,3,3,3,3,3,3,3,3,3,3,3,3,3,3,3,3,3,3,3,3,3,3,3,3,3,3,3,3,
3,3,3,3,3,4),(792.800203798141,792.880025863388,792.959753592175,793.039404643025,
793.118996612905,793.198547051178,793.278085018463,793.357620195601,793.437168429199,
793.516745570841,793.596410406403,793.676125453485,793.75595229044,793.790392511782,
793.870349811913,793.950212609156,794.029998431628,794.109724746823,794.189408975117,
794.269079961338,794.348747414864,794.428427065681,794.508134648075,794.587929877151,
794.667774218858,794.747732645906,794.790128522502,794.870085822633,794.949948619876,
795.029734442348,795.109460757543,795.189144985837,795.268815972058,795.348483425584,
795.428163076401,795.507870658795,795.587665887871,795.667510229578,795.747468656626,
795.789864533222,795.869821833353,795.949684630596,796.029470453068,796.109196768264,
796.188880996558,796.268551982779,796.348219436305,796.427899087122,796.507606669517,
796.587401898592,796.6672462403,796.747204667347,796.789600543943,796.869557844074,
796.949420641317,797.029206463789,797.108932778984,797.188617007278,797.268287993499,
797.347955447025,797.427635097842,797.507342680236,797.587137909312,797.66698225102,
797.746940678067,797.789336554663,797.869293854794,797.949156652037,798.028942474509,
798.108668789704,798.188353017998,798.268024004219,798.347691457745,798.427371108561,
798.507078690955,798.586873920031,798.666718261738,798.746676688786,798.789072565383,
798.887253081097,798.985321007094,799.083388933091),.UNSPECIFIED.);
#1256=B_SPLINE_CURVE_WITH_KNOTS('',3,(#151877,#151878,#151879,#151880,#151881,
#151882,#151883,#151884,#151885,#151886),.UNSPECIFIED.,.F.,.F.,(4,1,1,1,
1,1,1,4),(799.08338910532,799.788808576103,800.788544586823,801.788280597543,
802.788016608263,803.787752618983,804.787488629703,805.3665744125),
 .UNSPECIFIED.);
#1257=B_SPLINE_CURVE_WITH_KNOTS('',3,(#151888,#151889,#151890,#151891,#151892,
#151893,#151894,#151895,#151896,#151897),.UNSPECIFIED.,.F.,.F.,(4,1,1,1,
1,1,1,4),(805.3665744125,805.787224640424,806.786960651144,807.786696661864,
808.786432672584,809.786168683304,810.785904694024,811.649759719679),
 .UNSPECIFIED.);
#1258=B_SPLINE_CURVE_WITH_KNOTS('',3,(#151899,#151900,#151901,#151902,#151903,
#151904,#151905,#151906,#151907,#151908,#151909),.UNSPECIFIED.,.F.,.F.,
(4,1,1,1,1,1,1,1,4),(811.649759719679,811.785640704745,812.785376715465,
813.785112726185,814.784848736905,815.784584747625,816.784320758345,817.784056769065,
817.932945026859),.UNSPECIFIED.);
#1259=B_SPLINE_CURVE_WITH_KNOTS('',3,(#151911,#151912,#151913,#151914,#151915,
#151916,#151917,#151918,#151919,#151920),.UNSPECIFIED.,.F.,.F.,(4,1,1,1,
1,1,1,4),(817.932945026859,818.783792779785,819.783528790505,820.783264801226,
821.783000811946,822.782736822666,823.782472833386,824.216125065963),
 .UNSPECIFIED.);
#1260=B_SPLINE_CURVE_WITH_KNOTS('',3,(#151922,#151923,#151924,#151925,#151926,
#151927,#151928,#151929,#151930,#151931,#151932,#151933,#151934,#151935,
#151936,#151937,#151938,#151939,#151940,#151941,#151942,#151943,#151944,
#151945,#151946,#151947,#151948,#151949,#151950,#151951,#151952,#151953,
#151954,#151955,#151956,#151957,#151958,#151959,#151960,#151961,#151962,
#151963,#151964,#151965,#151966,#151967,#151968,#151969,#151970,#151971,
#151972,#151973,#151974,#151975,#151976,#151977,#151978,#151979,#151980,
#151981,#151982,#151983,#151984,#151985,#151986,#151987,#151988,#151989,
#151990,#151991,#151992,#151993,#151994,#151995,#151996,#151997,#151998,
#151999,#152000,#152001,#152002,#152003,#152004,#152005,#152006,#152007,
#152008,#152009,#152010,#152011,#152012,#152013,#152014,#152015,#152016,
#152017,#152018,#152019,#152020,#152021,#152022,#152023,#152024,#152025,
#152026,#152027,#152028,#152029,#152030,#152031,#152032,#152033,#152034,
#152035,#152036,#152037,#152038,#152039,#152040,#152041,#152042,#152043,
#152044,#152045,#152046,#152047,#152048,#152049,#152050,#152051,#152052,
#152053,#152054,#152055,#152056,#152057,#152058,#152059,#152060,#152061,
#152062,#152063,#152064,#152065,#152066,#152067,#152068,#152069,#152070,
#152071,#152072,#152073,#152074,#152075,#152076,#152077,#152078,#152079,
#152080,#152081,#152082,#152083,#152084,#152085,#152086,#152087,#152088,
#152089,#152090,#152091,#152092,#152093,#152094,#152095,#152096,#152097,
#152098,#152099,#152100,#152101,#152102,#152103,#152104,#152105,#152106,
#152107,#152108,#152109,#152110,#152111,#152112,#152113,#152114,#152115,
#152116,#152117,#152118,#152119,#152120,#152121,#152122,#152123,#152124,
#152125,#152126,#152127,#152128,#152129,#152130,#152131,#152132,#152133,
#152134,#152135,#152136,#152137,#152138,#152139,#152140,#152141,#152142,
#152143,#152144,#152145,#152146,#152147,#152148,#152149,#152150,#152151,
#152152,#152153,#152154,#152155,#152156,#152157,#152158,#152159,#152160,
#152161,#152162,#152163,#152164,#152165),.UNSPECIFIED.,.F.,.F.,(4,3,3,3,
3,3,3,3,3,3,3,3,3,3,3,3,3,3,3,3,3,3,3,3,3,3,3,3,3,3,3,3,3,3,3,3,3,3,3,3,
3,3,3,3,3,3,3,3,3,3,3,3,3,3,3,3,3,3,3,3,3,3,3,3,3,3,3,3,3,3,3,3,3,3,3,3,
3,3,3,3,3,4),(824.216130334038,824.297637731403,824.379187162414,824.460791451376,
824.542524682942,824.624324720818,824.706278491386,824.782208844106,824.862166144237,
824.94202894148,825.021814763951,825.101541079147,825.181225307441,825.260896293662,
825.340563747188,825.420243398004,825.499950980398,825.579746209474,825.659590551181,
825.739548978228,825.781944854826,825.861902154957,825.9417649522,826.021550774672,
826.101277089867,826.180961318162,826.260632304382,826.340299757908,826.419979408725,
826.499686991119,826.579482220195,826.659326561903,826.73928498895,826.781680865546,
826.861638165677,826.94150096292,827.021286785392,827.101013100587,827.180697328881,
827.260368315102,827.340035768628,827.419715419444,827.499423001839,827.579218230914,
827.659062572622,827.739020999669,827.781416876266,827.861374176397,827.94123697364,
828.021022796112,828.100749111307,828.180433339602,828.260104325823,828.339771779349,
828.419451430166,828.499159012561,828.578954241637,828.658798583344,828.738757010392,
828.781152886987,828.861110187118,828.940972984361,829.020758806833,829.100485122028,
829.180169350322,829.259840336543,829.339507790069,829.419187440885,829.49889502328,
829.578690252356,829.658534594064,829.738493021111,829.780888897707,829.86019447738,
829.94008462286,830.019195745959,830.098252415943,830.177270921403,830.257782101357,
830.336788066053,830.418051853635,830.499315641218),.UNSPECIFIED.);
#1261=B_SPLINE_CURVE_WITH_KNOTS('',3,(#152167,#152168,#152169,#152170,#152171,
#152172,#152173,#152174,#152175,#152176,#152177),.UNSPECIFIED.,.F.,.F.,
(4,1,1,1,1,1,1,1,4),(830.499320072584,830.780624908427,831.780360919147,
832.780096929867,833.779832940587,834.779568951308,835.779304962028,836.779040972748,
836.782500948398),.UNSPECIFIED.);
#1262=B_SPLINE_CURVE_WITH_KNOTS('',3,(#152179,#152180,#152181,#152182,#152183,
#152184,#152185,#152186,#152187,#152188,#152189,#152190,#152191,#152192,
#152193,#152194,#152195,#152196,#152197,#152198,#152199,#152200,#152201,
#152202,#152203,#152204,#152205,#152206,#152207,#152208,#152209,#152210,
#152211,#152212,#152213,#152214,#152215,#152216,#152217,#152218,#152219,
#152220,#152221,#152222,#152223,#152224,#152225,#152226,#152227,#152228,
#152229,#152230,#152231,#152232,#152233,#152234,#152235,#152236,#152237,
#152238,#152239,#152240,#152241,#152242,#152243,#152244,#152245,#152246,
#152247,#152248,#152249,#152250,#152251,#152252,#152253,#152254,#152255,
#152256,#152257,#152258,#152259,#152260,#152261,#152262,#152263,#152264,
#152265,#152266,#152267,#152268,#152269,#152270,#152271,#152272,#152273,
#152274,#152275,#152276,#152277,#152278,#152279,#152280,#152281,#152282,
#152283,#152284,#152285,#152286,#152287,#152288,#152289,#152290,#152291,
#152292,#152293,#152294,#152295,#152296,#152297,#152298,#152299,#152300,
#152301,#152302,#152303,#152304,#152305,#152306,#152307,#152308,#152309,
#152310,#152311,#152312,#152313,#152314,#152315,#152316,#152317,#152318,
#152319,#152320,#152321,#152322,#152323,#152324,#152325,#152326,#152327,
#152328,#152329,#152330,#152331,#152332,#152333,#152334,#152335,#152336,
#152337,#152338,#152339,#152340,#152341,#152342,#152343,#152344,#152345,
#152346,#152347,#152348,#152349,#152350,#152351,#152352,#152353,#152354,
#152355,#152356,#152357,#152358,#152359,#152360,#152361,#152362,#152363,
#152364,#152365,#152366,#152367,#152368,#152369,#152370,#152371,#152372,
#152373,#152374,#152375,#152376,#152377,#152378,#152379,#152380,#152381,
#152382,#152383,#152384,#152385,#152386,#152387,#152388,#152389,#152390,
#152391,#152392,#152393,#152394,#152395,#152396,#152397,#152398,#152399,
#152400,#152401,#152402,#152403,#152404,#152405,#152406,#152407,#152408,
#152409,#152410,#152411,#152412,#152413,#152414,#152415,#152416,#152417,
#152418,#152419,#152420,#152421,#152422),.UNSPECIFIED.,.F.,.F.,(4,3,3,3,
3,3,3,3,3,3,3,3,3,3,3,3,3,3,3,3,3,3,3,3,3,3,3,3,3,3,3,3,3,3,3,3,3,3,3,3,
3,3,3,3,3,3,3,3,3,3,3,3,3,3,3,3,3,3,3,3,3,3,3,3,3,3,3,3,3,3,3,3,3,3,3,3,
3,3,3,3,3,4),(836.782500948398,836.862408365672,836.942221316432,837.021957377889,
837.101634066293,837.181268850594,837.26089065088,837.340509174496,837.420140195296,
837.499799491666,837.579546446107,837.659342905624,837.739252618905,837.778776983468,
837.858734283599,837.938597080842,838.018382903314,838.098109218509,838.177793446803,
838.257464433024,838.33713188655,838.416811537366,838.49651911976,838.576314348836,
838.656158690544,838.736117117591,838.778512994188,838.858470294319,838.938333091562,
839.018118914034,839.097845229229,839.177529457523,839.257200443744,839.33686789727,
839.416547548087,839.496255130481,839.576050359557,839.655894701264,839.735853128312,
839.778249004908,839.858206305039,839.938069102282,840.017854924754,840.097581239949,
840.177265468243,840.256936454464,840.33660390799,840.416283558806,840.495991141201,
840.575786370276,840.655630711984,840.735589139032,840.777985015628,840.857942315759,
840.937805113002,841.017590935474,841.097317250669,841.177001478963,841.256672465184,
841.33633991871,841.416019569526,841.495727151921,841.575522380996,841.655366722704,
841.735325149751,841.777721026348,841.857678326479,841.937541123722,842.017326946193,
842.097053261388,842.176737489683,842.256408475903,842.336075929429,842.415755580246,
842.49546316264,842.575258391716,842.655102733423,842.735061160471,842.777457037068,
842.876411799539,842.97401212279,843.065686096939),.UNSPECIFIED.);
#1263=B_SPLINE_CURVE_WITH_KNOTS('',3,(#152424,#152425,#152426,#152427,#152428,
#152429,#152430,#152431,#152432,#152433),.UNSPECIFIED.,.F.,.F.,(4,1,1,1,
1,1,1,4),(843.065686255577,843.777193047789,844.776929058509,845.776665069229,
846.776401079949,847.776137090669,848.775873101389,849.348871562757),
 .UNSPECIFIED.);
#1264=B_SPLINE_CURVE_WITH_KNOTS('',3,(#152435,#152436,#152437,#152438,#152439,
#152440,#152441,#152442,#152443,#152444),.UNSPECIFIED.,.F.,.F.,(4,1,1,1,
1,1,1,4),(849.348871562757,849.775609112109,850.77534512283,851.77508113355,
852.77481714427,853.77455315499,854.77428916571,855.632056869936),
 .UNSPECIFIED.);
#1265=B_SPLINE_CURVE_WITH_KNOTS('',3,(#152446,#152447,#152448,#152449,#152450,
#152451,#152452,#152453,#152454,#152455,#152456),.UNSPECIFIED.,.F.,.F.,
(4,1,1,1,1,1,1,1,4),(855.632056869936,855.77402517643,856.77376118715,857.77349719787,
858.773233208591,859.772969219311,860.772705230031,861.772441240751,861.915242177116),
 .UNSPECIFIED.);
#1266=B_SPLINE_CURVE_WITH_KNOTS('',3,(#152458,#152459,#152460,#152461,#152462,
#152463,#152464,#152465,#152466,#152467),.UNSPECIFIED.,.F.,.F.,(4,1,1,1,
1,1,1,4),(861.915242177116,862.772177251471,863.771913262191,864.771649272911,
865.771385283631,866.771121294352,867.770857305072,868.198427484296),
 .UNSPECIFIED.);
#1267=B_SPLINE_CURVE_WITH_KNOTS('',3,(#152469,#152470,#152471,#152472,#152473,
#152474,#152475,#152476,#152477,#152478),.UNSPECIFIED.,.F.,.F.,(4,1,1,1,
1,1,1,4),(868.198427484296,868.770593315792,869.770329326512,870.770065337232,
871.769801347952,872.769537358672,873.769273369393,874.481612791475),
 .UNSPECIFIED.);
#1268=B_SPLINE_CURVE_WITH_KNOTS('',3,(#152480,#152481,#152482,#152483,#152484,
#152485,#152486,#152487,#152488,#152489,#152490,#152491,#152492,#152493,
#152494,#152495,#152496,#152497,#152498,#152499,#152500,#152501,#152502,
#152503,#152504,#152505,#152506,#152507,#152508,#152509,#152510,#152511,
#152512,#152513,#152514,#152515,#152516,#152517,#152518,#152519,#152520,
#152521,#152522,#152523,#152524,#152525,#152526,#152527,#152528,#152529,
#152530,#152531,#152532,#152533,#152534,#152535,#152536,#152537,#152538,
#152539,#152540,#152541,#152542,#152543,#152544,#152545,#152546,#152547,
#152548,#152549,#152550,#152551,#152552,#152553,#152554,#152555,#152556,
#152557,#152558,#152559,#152560,#152561,#152562,#152563,#152564,#152565,
#152566,#152567,#152568,#152569,#152570,#152571,#152572,#152573,#152574,
#152575,#152576,#152577,#152578,#152579,#152580,#152581,#152582,#152583,
#152584,#152585,#152586,#152587,#152588,#152589,#152590,#152591,#152592,
#152593,#152594,#152595,#152596,#152597,#152598,#152599,#152600,#152601,
#152602,#152603,#152604,#152605,#152606,#152607,#152608,#152609,#152610,
#152611,#152612,#152613,#152614,#152615,#152616,#152617,#152618,#152619,
#152620,#152621,#152622,#152623,#152624,#152625,#152626,#152627,#152628,
#152629,#152630,#152631,#152632,#152633,#152634,#152635,#152636,#152637,
#152638,#152639,#152640,#152641,#152642,#152643,#152644,#152645,#152646,
#152647,#152648,#152649,#152650,#152651,#152652,#152653,#152654,#152655,
#152656,#152657,#152658,#152659,#152660,#152661,#152662,#152663,#152664,
#152665,#152666,#152667,#152668,#152669,#152670,#152671,#152672,#152673,
#152674,#152675,#152676,#152677,#152678,#152679,#152680,#152681,#152682,
#152683,#152684,#152685,#152686,#152687,#152688,#152689,#152690,#152691,
#152692,#152693,#152694,#152695,#152696,#152697,#152698,#152699,#152700,
#152701,#152702,#152703,#152704,#152705,#152706,#152707,#152708,#152709,
#152710,#152711,#152712,#152713,#152714,#152715,#152716,#152717,#152718,
#152719,#152720,#152721,#152722,#152723),.UNSPECIFIED.,.F.,.F.,(4,3,3,3,
3,3,3,3,3,3,3,3,3,3,3,3,3,3,3,3,3,3,3,3,3,3,3,3,3,3,3,3,3,3,3,3,3,3,3,3,
3,3,3,3,3,3,3,3,3,3,3,3,3,3,3,3,3,3,3,3,3,3,3,3,3,3,3,3,3,3,3,3,3,3,3,3,
3,3,3,3,3,4),(874.48161294818,874.579018330041,874.677851503058,874.769009380113,
874.848966680244,874.928829477486,875.008615299957,875.088341615152,875.168025843445,
875.247696829666,875.327364283191,875.407043934007,875.486751516401,875.566546745476,
875.646391087183,875.72634951423,875.768745390833,875.848702690964,875.928565488207,
876.008351310679,876.088077625874,876.167761854168,876.247432840389,876.327100293915,
876.406779944732,876.486487527126,876.566282756202,876.646127097909,876.726085524957,
876.768481401553,876.848438701684,876.928301498927,877.008087321399,877.087813636594,
877.167497864888,877.247168851109,877.326836304635,877.406515955452,877.486223537846,
877.566018766922,877.64586310863,877.725821535677,877.768217412273,877.848174712404,
877.928037509647,878.007823332118,878.087549647314,878.167233875608,878.246904861829,
878.326572315354,878.406251966171,878.485959548565,878.565754777641,878.645599119348,
878.725557546396,878.767953422993,878.847910723124,878.927773520367,879.007559342839,
879.087285658034,879.166969886328,879.246640872549,879.326308326075,879.405987976892,
879.485695559286,879.565490788362,879.645335130069,879.725293557117,879.767689433713,
879.847608808449,879.92743369775,880.007181667238,880.086870221649,880.166516818457,
880.246150355548,880.325780545941,880.405423153102,880.485093944973,880.564852380967,
880.644660220934,880.724581505706,880.764798098655),.UNSPECIFIED.);
#1269=B_SPLINE_CURVE_WITH_KNOTS('',3,(#152725,#152726,#152727,#152728,#152729,
#152730,#152731,#152732,#152733,#152734,#152735,#152736,#152737),
 .UNSPECIFIED.,.F.,.F.,(4,3,1,1,1,1,1,1,4),(880.764798098655,880.767425444434,
881.767161455154,882.766897465874,883.766633476594,884.766369487314,885.766105498034,
886.765841508754,887.047978910358),.UNSPECIFIED.);
#1270=B_SPLINE_CURVE_WITH_KNOTS('',3,(#152739,#152740,#152741,#152742,#152743,
#152744,#152745,#152746,#152747,#152748,#152749,#152750,#152751,#152752,
#152753,#152754,#152755,#152756,#152757,#152758,#152759,#152760,#152761,
#152762,#152763,#152764,#152765,#152766,#152767,#152768,#152769,#152770,
#152771,#152772,#152773,#152774,#152775,#152776,#152777,#152778,#152779,
#152780,#152781,#152782,#152783,#152784,#152785,#152786,#152787,#152788,
#152789,#152790,#152791,#152792,#152793,#152794,#152795,#152796,#152797,
#152798,#152799,#152800,#152801,#152802,#152803,#152804,#152805,#152806,
#152807,#152808,#152809,#152810,#152811,#152812,#152813,#152814,#152815,
#152816,#152817,#152818,#152819,#152820,#152821,#152822,#152823,#152824,
#152825,#152826,#152827,#152828,#152829,#152830,#152831,#152832,#152833,
#152834,#152835,#152836,#152837,#152838,#152839,#152840,#152841,#152842,
#152843,#152844,#152845,#152846,#152847,#152848,#152849,#152850,#152851,
#152852,#152853,#152854,#152855,#152856,#152857,#152858,#152859,#152860,
#152861,#152862,#152863,#152864,#152865,#152866,#152867,#152868,#152869,
#152870,#152871,#152872,#152873,#152874,#152875,#152876,#152877,#152878,
#152879,#152880,#152881,#152882,#152883,#152884,#152885,#152886,#152887,
#152888,#152889,#152890,#152891,#152892,#152893,#152894,#152895,#152896,
#152897,#152898,#152899,#152900,#152901,#152902,#152903,#152904,#152905,
#152906,#152907,#152908,#152909,#152910,#152911,#152912,#152913,#152914,
#152915,#152916,#152917,#152918,#152919,#152920,#152921,#152922,#152923,
#152924,#152925,#152926,#152927,#152928,#152929,#152930,#152931,#152932,
#152933,#152934,#152935,#152936,#152937,#152938,#152939,#152940,#152941,
#152942,#152943,#152944,#152945,#152946,#152947,#152948,#152949,#152950,
#152951,#152952,#152953,#152954,#152955,#152956,#152957,#152958,#152959,
#152960,#152961,#152962,#152963,#152964,#152965,#152966,#152967,#152968,
#152969,#152970,#152971,#152972,#152973,#152974,#152975,#152976,#152977,
#152978,#152979,#152980,#152981,#152982),.UNSPECIFIED.,.F.,.F.,(4,3,3,3,
3,3,3,3,3,3,3,3,3,3,3,3,3,3,3,3,3,3,3,3,3,3,3,3,3,3,3,3,3,3,3,3,3,3,3,3,
3,3,3,3,3,3,3,3,3,3,3,3,3,3,3,3,3,3,3,3,3,3,3,3,3,3,3,3,3,3,3,3,3,3,3,3,
3,3,3,3,3,4),(887.047983405834,887.127043212417,887.206860000799,887.28587417662,
887.364889743303,887.443922933897,887.524336580291,887.60349397405,887.684535746762,
887.765577519474,887.845534819605,887.925397616848,888.005183439319,888.084909754515,
888.164593982809,888.24426496903,888.323932422556,888.403612073372,888.483319655766,
888.563114884842,888.642959226549,888.722917653597,888.765313530194,888.845270830325,
888.925133627568,889.00491945004,889.084645765235,889.164329993528,889.244000979749,
889.323668433275,889.403348084091,889.483055666486,889.562850895561,889.642695237269,
889.722653664316,889.765049540914,889.845006841046,889.924869638288,890.00465546076,
890.084381775956,890.16406600425,890.243736990471,890.323404443997,890.403084094814,
890.482791677209,890.562586906284,890.642431247992,890.72238967504,890.764785551635,
890.844742851766,890.924605649009,891.004391471481,891.084117786676,891.16380201497,
891.243473001191,891.323140454717,891.402820105533,891.482527687928,891.562322917003,
891.642167258711,891.722125685758,891.764521562355,891.844478862486,891.924341659729,
892.0041274822,892.083853797395,892.163538025689,892.24320901191,892.322876465436,
892.402556116252,892.482263698646,892.562058927722,892.641903269429,892.721861696477,
892.764257573075,892.846197831132,892.928026862176,893.009757780634,893.091379034572,
893.172936173556,893.254431836687,893.331168713014),.UNSPECIFIED.);
#1271=B_SPLINE_CURVE_WITH_KNOTS('',3,(#152984,#152985,#152986,#152987,#152988,
#152989,#152990,#152991,#152992,#152993),.UNSPECIFIED.,.F.,.F.,(4,1,1,1,
1,1,1,4),(893.331174034399,893.763993583795,894.763729594515,895.763465605235,
896.763201615955,897.762937626676,898.762673637396,899.614354020193),
 .UNSPECIFIED.);
#1272=B_SPLINE_CURVE_WITH_KNOTS('',3,(#152995,#152996,#152997,#152998,#152999,
#153000,#153001,#153002,#153003,#153004,#153005),.UNSPECIFIED.,.F.,.F.,
(4,1,1,1,1,1,1,1,4),(899.614354020193,899.762409648116,900.762145658836,
901.761881669556,902.761617680276,903.761353690997,904.761089701717,905.760825712436,
905.897539327373),.UNSPECIFIED.);
#1273=B_SPLINE_CURVE_WITH_KNOTS('',3,(#153007,#153008,#153009,#153010,#153011,
#153012,#153013,#153014,#153015,#153016),.UNSPECIFIED.,.F.,.F.,(4,1,1,1,
1,1,1,4),(905.897539327373,906.760561723157,907.760297733877,908.760033744597,
909.759769755317,910.759505766037,911.759241776758,912.180724634552),
 .UNSPECIFIED.);
#1274=B_SPLINE_CURVE_WITH_KNOTS('',3,(#153018,#153019,#153020,#153021,#153022,
#153023,#153024,#153025,#153026,#153027),.UNSPECIFIED.,.F.,.F.,(4,1,1,1,
1,1,1,4),(912.180724634552,912.758977787478,913.758713798198,914.758449808918,
915.758185819638,916.757921830358,917.757657841078,918.463909941732),
 .UNSPECIFIED.);
#1275=B_SPLINE_CURVE_WITH_KNOTS('',3,(#153029,#153030,#153031,#153032,#153033,
#153034,#153035,#153036,#153037,#153038,#153039,#153040,#153041,#153042,
#153043,#153044,#153045,#153046,#153047,#153048,#153049,#153050,#153051,
#153052,#153053,#153054,#153055,#153056,#153057,#153058,#153059,#153060,
#153061,#153062,#153063,#153064,#153065,#153066,#153067,#153068,#153069,
#153070,#153071,#153072,#153073,#153074,#153075,#153076,#153077,#153078,
#153079,#153080,#153081,#153082,#153083,#153084,#153085,#153086,#153087,
#153088,#153089,#153090,#153091,#153092,#153093,#153094,#153095,#153096,
#153097,#153098,#153099,#153100,#153101,#153102,#153103,#153104,#153105,
#153106,#153107,#153108,#153109,#153110,#153111,#153112,#153113,#153114,
#153115,#153116,#153117,#153118,#153119,#153120,#153121,#153122,#153123,
#153124,#153125,#153126,#153127,#153128,#153129,#153130,#153131,#153132,
#153133,#153134,#153135,#153136,#153137,#153138,#153139,#153140,#153141,
#153142,#153143,#153144,#153145,#153146,#153147,#153148,#153149,#153150,
#153151,#153152,#153153,#153154,#153155,#153156,#153157,#153158,#153159,
#153160,#153161,#153162,#153163,#153164,#153165,#153166,#153167,#153168,
#153169,#153170,#153171,#153172,#153173,#153174,#153175,#153176,#153177,
#153178,#153179,#153180,#153181,#153182,#153183,#153184,#153185,#153186,
#153187,#153188,#153189,#153190,#153191,#153192,#153193,#153194,#153195,
#153196,#153197,#153198,#153199,#153200,#153201,#153202,#153203,#153204,
#153205,#153206,#153207,#153208,#153209,#153210,#153211,#153212,#153213,
#153214,#153215,#153216,#153217,#153218,#153219,#153220,#153221,#153222,
#153223,#153224,#153225,#153226,#153227,#153228,#153229,#153230,#153231,
#153232,#153233,#153234,#153235,#153236,#153237,#153238,#153239,#153240,
#153241,#153242,#153243,#153244,#153245,#153246,#153247,#153248,#153249,
#153250,#153251,#153252,#153253,#153254,#153255,#153256,#153257,#153258,
#153259,#153260,#153261,#153262,#153263,#153264,#153265,#153266,#153267,
#153268,#153269,#153270,#153271,#153272),.UNSPECIFIED.,.F.,.F.,(4,3,3,3,
3,3,3,3,3,3,3,3,3,3,3,3,3,3,3,3,3,3,3,3,3,3,3,3,3,3,3,3,3,3,3,3,3,3,3,3,
3,3,3,3,3,3,3,3,3,3,3,3,3,3,3,3,3,3,3,3,3,3,3,3,3,3,3,3,3,3,3,3,3,3,3,3,
3,3,3,3,3,4),(918.463910112159,918.560627038663,918.65901044523,918.757393851798,
918.837351151929,918.917213949172,918.996999771644,919.076726086839,919.156410315134,
919.236081301355,919.315748754881,919.395428405697,919.475135988092,919.554931217167,
919.634775558875,919.714733985923,919.757129862518,919.837087162649,919.916949959892,
919.996735782363,920.076462097559,920.156146325852,920.235817312073,920.315484765599,
920.395164416415,920.47487199881,920.554667227885,920.634511569593,920.71446999664,
920.756865873238,920.836823173369,920.916685970612,920.996471793084,921.07619810828,
921.155882336574,921.235553322795,921.315220776321,921.394900427137,921.474608009532,
921.554403238608,921.634247580315,921.714206007363,921.756601883959,921.83655918409,
921.916421981333,921.996207803805,922.075934119001,922.155618347295,922.235289333516,
922.314956787042,922.394636437858,922.474344020253,922.554139249329,922.633983591037,
922.713942018084,922.756337894679,922.83629519481,922.916157992052,922.995943814524,
923.075670129719,923.155354358013,923.235025344234,923.31469279776,923.394372448576,
923.47408003097,923.553875260046,923.633719601753,923.7136780288,923.756073905399,
923.835907939634,923.915647532301,923.995310331492,924.074913923755,924.154475848011,
924.234025104635,924.313571425821,924.393130648538,924.472718614622,924.552394154601,
924.632119742723,924.711957223575,924.747095248912),.UNSPECIFIED.);
#1276=B_SPLINE_CURVE_WITH_KNOTS('',3,(#153274,#153275,#153276,#153277,#153278,
#153279,#153280,#153281,#153282,#153283,#153284,#153285,#153286),
 .UNSPECIFIED.,.F.,.F.,(4,3,1,1,1,1,1,1,4),(924.747095248912,924.755809916119,
925.755545926839,926.755281937559,927.755017948279,928.754753959,929.75448996972,
930.75422598044,931.030276540766),.UNSPECIFIED.);
#1277=B_SPLINE_CURVE_WITH_KNOTS('',3,(#153288,#153289,#153290,#153291,#153292,
#153293,#153294,#153295,#153296,#153297,#153298,#153299,#153300,#153301,
#153302,#153303,#153304,#153305,#153306,#153307,#153308,#153309,#153310,
#153311,#153312,#153313,#153314,#153315,#153316,#153317,#153318,#153319,
#153320,#153321,#153322,#153323,#153324,#153325,#153326,#153327,#153328,
#153329,#153330,#153331,#153332,#153333,#153334,#153335,#153336,#153337,
#153338,#153339,#153340,#153341,#153342,#153343,#153344,#153345,#153346,
#153347,#153348,#153349,#153350,#153351,#153352,#153353,#153354,#153355,
#153356,#153357,#153358,#153359,#153360,#153361,#153362,#153363,#153364,
#153365,#153366,#153367,#153368,#153369,#153370,#153371,#153372,#153373,
#153374,#153375,#153376,#153377,#153378,#153379,#153380,#153381,#153382,
#153383,#153384,#153385,#153386,#153387,#153388,#153389,#153390,#153391,
#153392,#153393,#153394,#153395,#153396,#153397,#153398,#153399,#153400,
#153401,#153402,#153403,#153404,#153405,#153406,#153407,#153408,#153409,
#153410,#153411,#153412,#153413,#153414,#153415,#153416,#153417,#153418,
#153419,#153420,#153421,#153422,#153423,#153424,#153425,#153426,#153427,
#153428,#153429,#153430,#153431,#153432,#153433,#153434,#153435,#153436,
#153437,#153438,#153439,#153440,#153441,#153442,#153443,#153444,#153445,
#153446,#153447,#153448,#153449,#153450,#153451,#153452,#153453,#153454,
#153455,#153456,#153457,#153458,#153459,#153460,#153461,#153462,#153463,
#153464,#153465,#153466,#153467,#153468,#153469,#153470,#153471,#153472,
#153473,#153474,#153475,#153476,#153477,#153478,#153479,#153480,#153481,
#153482,#153483,#153484,#153485,#153486,#153487,#153488,#153489,#153490,
#153491,#153492,#153493,#153494,#153495,#153496,#153497,#153498,#153499,
#153500,#153501,#153502,#153503,#153504,#153505,#153506,#153507,#153508,
#153509,#153510,#153511,#153512,#153513,#153514,#153515,#153516,#153517,
#153518,#153519,#153520,#153521,#153522,#153523,#153524,#153525,#153526,
#153527,#153528,#153529,#153530,#153531),.UNSPECIFIED.,.F.,.F.,(4,3,3,3,
3,3,3,3,3,3,3,3,3,3,3,3,3,3,3,3,3,3,3,3,3,3,3,3,3,3,3,3,3,3,3,3,3,3,3,3,
3,3,3,3,3,3,3,3,3,3,3,3,3,3,3,3,3,3,3,3,3,3,3,3,3,3,3,3,3,3,3,3,3,3,3,3,
3,3,3,3,3,4),(931.030280556091,931.109290663972,931.18987457987,931.268834084094,
931.347793270138,931.426768411011,931.508566806049,931.587664371913,931.670813181537,
931.75396199116,931.833919291291,931.913782088534,931.993567911005,932.0732942262,
932.152978454494,932.232649440715,932.312316894241,932.391996545057,932.471704127452,
932.551499356527,932.631343698235,932.711302125282,932.75369800188,932.833655302011,
932.913518099254,932.993303921726,933.073030236921,933.152714465215,933.232385451436,
933.312052904962,933.391732555778,933.471440138172,933.551235367248,933.631079708955,
933.711038136003,933.7534340126,933.833391312731,933.913254109974,933.993039932446,
934.072766247642,934.152450475936,934.232121462157,934.311788915683,934.3914685665,
934.471176148895,934.55097137797,934.630815719678,934.710774146726,934.753170023321,
934.833127323452,934.912990120695,934.992775943167,935.072502258362,935.152186486656,
935.231857472876,935.311524926402,935.391204577219,935.470912159614,935.550707388689,
935.630551730397,935.710510157445,935.752906034041,935.832863334172,935.912726131415,
935.992511953887,936.072238269082,936.151922497375,936.231593483596,936.311260937122,
936.390940587939,936.470648170334,936.550443399409,936.630287741117,936.710246168164,
936.752642044761,936.83474749776,936.916739891055,936.998632017574,937.080410429156,
937.162122335982,937.243767640152,937.313465863271),.UNSPECIFIED.);
#1278=B_SPLINE_CURVE_WITH_KNOTS('',3,(#153533,#153534,#153535,#153536,#153537,
#153538,#153539,#153540,#153541,#153542),.UNSPECIFIED.,.F.,.F.,(4,1,1,1,
1,1,1,4),(937.3134707844,937.752378055481,938.752114066201,939.751850076921,
940.751586087641,941.751322098361,942.751058109081,943.59665117045),
 .UNSPECIFIED.);
#1279=B_SPLINE_CURVE_WITH_KNOTS('',3,(#153544,#153545,#153546,#153547,#153548,
#153549,#153550,#153551,#153552,#153553,#153554),.UNSPECIFIED.,.F.,.F.,
(4,1,1,1,1,1,1,1,4),(943.59665117045,943.750794119802,944.750530130522,
945.750266141242,946.750002151962,947.749738162682,948.749474173402,949.749210184122,
949.87983647763),.UNSPECIFIED.);
#1280=B_SPLINE_CURVE_WITH_KNOTS('',3,(#153556,#153557,#153558,#153559,#153560,
#153561,#153562,#153563,#153564,#153565,#153566,#153567,#153568,#153569,
#153570,#153571,#153572,#153573,#153574,#153575,#153576,#153577,#153578,
#153579,#153580,#153581,#153582,#153583,#153584,#153585,#153586,#153587,
#153588,#153589,#153590,#153591,#153592,#153593,#153594,#153595,#153596,
#153597,#153598,#153599,#153600,#153601,#153602,#153603,#153604,#153605,
#153606,#153607,#153608,#153609,#153610,#153611,#153612,#153613,#153614,
#153615,#153616,#153617,#153618,#153619,#153620,#153621,#153622,#153623,
#153624,#153625,#153626,#153627,#153628,#153629,#153630,#153631,#153632,
#153633,#153634,#153635,#153636,#153637,#153638,#153639,#153640,#153641,
#153642,#153643,#153644,#153645,#153646,#153647,#153648,#153649,#153650,
#153651,#153652,#153653,#153654,#153655,#153656,#153657,#153658,#153659,
#153660,#153661,#153662,#153663,#153664,#153665,#153666,#153667,#153668,
#153669,#153670,#153671,#153672,#153673,#153674,#153675,#153676,#153677,
#153678,#153679,#153680,#153681,#153682,#153683,#153684,#153685,#153686,
#153687,#153688,#153689,#153690,#153691,#153692,#153693,#153694,#153695,
#153696,#153697,#153698,#153699,#153700,#153701,#153702,#153703,#153704,
#153705,#153706,#153707,#153708,#153709,#153710,#153711,#153712,#153713,
#153714,#153715,#153716,#153717,#153718,#153719,#153720,#153721,#153722,
#153723,#153724,#153725,#153726,#153727,#153728,#153729,#153730,#153731,
#153732,#153733,#153734,#153735,#153736,#153737,#153738,#153739,#153740,
#153741,#153742,#153743,#153744,#153745,#153746,#153747,#153748,#153749,
#153750,#153751,#153752,#153753,#153754,#153755,#153756,#153757,#153758,
#153759,#153760,#153761,#153762,#153763,#153764,#153765,#153766,#153767,
#153768,#153769,#153770,#153771,#153772,#153773,#153774,#153775,#153776,
#153777,#153778,#153779,#153780,#153781,#153782,#153783,#153784,#153785,
#153786,#153787,#153788,#153789,#153790,#153791,#153792,#153793,#153794,
#153795,#153796,#153797,#153798,#153799),.UNSPECIFIED.,.F.,.F.,(4,3,3,3,
3,3,3,3,3,3,3,3,3,3,3,3,3,3,3,3,3,3,3,3,3,3,3,3,3,3,3,3,3,3,3,3,3,3,3,3,
3,3,3,3,3,3,3,3,3,3,3,3,3,3,3,3,3,3,3,3,3,3,3,3,3,3,3,3,3,3,3,3,3,3,3,3,
3,3,3,3,3,4),(949.87983647763,949.958583984239,950.037252173226,950.11585943448,
950.194995279526,950.27354633765,950.352095118929,950.430658160405,950.510230169015,
950.588910166874,950.668928180858,950.748946194843,950.828903494974,950.908766292217,
950.988552114689,951.068278429884,951.147962658178,951.227633644399,951.307301097925,
951.386980748741,951.466688331135,951.546483560211,951.626327901919,951.706286328966,
951.748682205563,951.828639505694,951.908502302937,951.988288125409,952.068014440604,
952.147698668898,952.227369655119,952.307037108645,952.386716759462,952.466424341857,
952.546219570932,952.62606391264,952.706022339687,952.748418216283,952.828375516414,
952.908238313657,952.988024136129,953.067750451324,953.147434679617,953.227105665838,
953.306773119364,953.386452770181,953.466160352575,953.545955581651,953.625799923358,
953.705758350406,953.748154227003,953.828111527134,953.907974324377,953.987760146848,
954.067486462044,954.147170690338,954.22684167656,954.306509130085,954.386188780902,
954.465896363296,954.545691592372,954.62553593408,954.705494361127,954.747890237723,
954.827847537854,954.907710335097,954.987496157569,955.067222472764,955.146906701058,
955.226577687279,955.306245140805,955.385924791622,955.465632374017,955.545427603092,
955.6252719448,955.705230371847,955.747626248443,955.83568619894,955.923413789402,
956.010932353538,956.098105389006,956.163021581478),.UNSPECIFIED.);
#1281=B_SPLINE_CURVE_WITH_KNOTS('',3,(#153801,#153802,#153803,#153804,#153805,
#153806,#153807,#153808,#153809,#153810),.UNSPECIFIED.,.F.,.F.,(4,1,1,1,
1,1,1,4),(956.163021784809,956.747362259163,957.747098269883,958.746834280603,
959.746570291324,960.746306302044,961.746042312764,962.446207091989),
 .UNSPECIFIED.);
#1282=B_SPLINE_CURVE_WITH_KNOTS('',3,(#153812,#153813,#153814,#153815,#153816,
#153817,#153818,#153819,#153820,#153821,#153822,#153823,#153824,#153825,
#153826,#153827,#153828,#153829,#153830,#153831,#153832,#153833,#153834,
#153835,#153836,#153837,#153838,#153839,#153840,#153841,#153842,#153843,
#153844,#153845,#153846,#153847,#153848,#153849,#153850,#153851,#153852,
#153853,#153854,#153855,#153856,#153857,#153858,#153859,#153860,#153861,
#153862,#153863,#153864,#153865,#153866,#153867,#153868,#153869,#153870,
#153871,#153872,#153873,#153874,#153875,#153876,#153877,#153878,#153879,
#153880,#153881,#153882,#153883,#153884,#153885,#153886,#153887,#153888,
#153889,#153890,#153891,#153892,#153893,#153894,#153895,#153896,#153897,
#153898,#153899,#153900,#153901,#153902,#153903,#153904,#153905,#153906,
#153907,#153908,#153909,#153910,#153911,#153912,#153913,#153914,#153915,
#153916,#153917,#153918,#153919,#153920,#153921,#153922,#153923,#153924,
#153925,#153926,#153927,#153928,#153929,#153930,#153931,#153932,#153933,
#153934,#153935,#153936,#153937,#153938,#153939,#153940,#153941,#153942,
#153943,#153944,#153945,#153946,#153947,#153948,#153949,#153950,#153951,
#153952,#153953,#153954,#153955,#153956,#153957,#153958,#153959,#153960,
#153961,#153962,#153963,#153964,#153965,#153966,#153967,#153968,#153969,
#153970,#153971,#153972,#153973,#153974,#153975,#153976,#153977,#153978,
#153979,#153980,#153981,#153982,#153983,#153984,#153985,#153986,#153987,
#153988,#153989,#153990,#153991,#153992,#153993,#153994,#153995,#153996,
#153997,#153998,#153999,#154000,#154001,#154002,#154003,#154004,#154005,
#154006,#154007,#154008,#154009,#154010,#154011,#154012,#154013,#154014,
#154015,#154016,#154017,#154018,#154019,#154020,#154021,#154022,#154023,
#154024,#154025,#154026,#154027,#154028,#154029,#154030,#154031,#154032,
#154033,#154034,#154035,#154036,#154037,#154038,#154039,#154040,#154041,
#154042,#154043,#154044,#154045,#154046,#154047,#154048,#154049,#154050,
#154051,#154052,#154053,#154054,#154055),.UNSPECIFIED.,.F.,.F.,(4,3,3,3,
3,3,3,3,3,3,3,3,3,3,3,3,3,3,3,3,3,3,3,3,3,3,3,3,3,3,3,3,3,3,3,3,3,3,3,3,
3,3,3,3,3,3,3,3,3,3,3,3,3,3,3,3,3,3,3,3,3,3,3,3,3,3,3,3,3,3,3,3,3,3,3,3,
3,3,3,3,3,4),(962.446207275155,962.542264496911,962.644021410198,962.745778323484,
962.825735623615,962.905598420857,962.985384243328,963.065110558523,963.144794786817,
963.224465773037,963.304133226562,963.383812877378,963.463520459772,963.543315688847,
963.623160030554,963.703118457601,963.745514334204,963.825471634335,963.905334431578,
963.985120254049,964.064846569245,964.144530797538,964.224201783759,964.303869237285,
964.383548888101,964.463256470496,964.543051699571,964.622896041279,964.702854468326,
964.745250344924,964.825207645056,964.905070442299,964.984856264771,965.064582579967,
965.144266808261,965.223937794482,965.303605248009,965.383284898825,965.46299248122,
965.542787710296,965.622632052004,965.702590479052,965.744986355645,965.824943655776,
965.904806453018,965.98459227549,966.064318590685,966.144002818979,966.223673805199,
966.303341258725,966.383020909541,966.462728491936,966.542523721011,966.622368062718,
966.702326489765,966.744722366364,966.824679666495,966.904542463738,966.98432828621,
967.064054601406,967.1437388297,967.223409815921,967.303077269447,967.382756920263,
967.462464502658,967.542259731733,967.622104073441,967.702062500489,967.744458377085,
967.824210570906,967.903868370934,967.983449501913,968.062971626318,968.146274222924,
968.22574215201,968.305208295397,968.384688558223,968.464198851361,968.543796861733,
968.623446211697,968.703204821876,968.729392399169),.UNSPECIFIED.);
#1283=B_SPLINE_CURVE_WITH_KNOTS('',3,(#154057,#154058,#154059,#154060,#154061,
#154062,#154063,#154064,#154065,#154066,#154067,#154068),.UNSPECIFIED.,
 .F.,.F.,(4,2,1,1,1,1,1,1,4),(968.729392399169,968.744194387805,969.743930398525,
970.743666409245,971.743402419965,972.743138430685,973.742874441405,974.742610452126,
975.012574196375),.UNSPECIFIED.);
#1284=B_SPLINE_CURVE_WITH_KNOTS('',3,(#154070,#154071,#154072,#154073,#154074,
#154075,#154076,#154077,#154078,#154079,#154080,#154081,#154082,#154083,
#154084,#154085,#154086,#154087,#154088,#154089,#154090,#154091,#154092,
#154093,#154094,#154095,#154096,#154097,#154098,#154099,#154100,#154101,
#154102,#154103,#154104,#154105,#154106,#154107,#154108,#154109,#154110,
#154111,#154112,#154113,#154114,#154115,#154116,#154117,#154118,#154119,
#154120,#154121,#154122,#154123,#154124,#154125,#154126,#154127,#154128,
#154129,#154130,#154131,#154132,#154133,#154134,#154135,#154136,#154137,
#154138,#154139,#154140,#154141,#154142,#154143,#154144,#154145,#154146,
#154147,#154148,#154149,#154150,#154151,#154152,#154153,#154154,#154155,
#154156,#154157,#154158,#154159,#154160,#154161,#154162,#154163,#154164,
#154165,#154166,#154167,#154168,#154169,#154170,#154171,#154172,#154173,
#154174,#154175,#154176,#154177,#154178,#154179,#154180,#154181,#154182,
#154183,#154184,#154185,#154186,#154187,#154188,#154189,#154190,#154191,
#154192,#154193,#154194,#154195,#154196,#154197,#154198,#154199,#154200,
#154201,#154202,#154203,#154204,#154205,#154206,#154207,#154208,#154209,
#154210,#154211,#154212,#154213,#154214,#154215,#154216,#154217,#154218,
#154219,#154220,#154221,#154222,#154223,#154224,#154225,#154226,#154227,
#154228,#154229,#154230,#154231,#154232,#154233,#154234,#154235,#154236,
#154237,#154238,#154239,#154240,#154241,#154242,#154243,#154244,#154245,
#154246,#154247,#154248,#154249,#154250,#154251,#154252,#154253,#154254,
#154255,#154256,#154257,#154258,#154259,#154260,#154261,#154262,#154263,
#154264,#154265,#154266,#154267,#154268,#154269,#154270,#154271,#154272,
#154273,#154274,#154275,#154276,#154277,#154278,#154279,#154280,#154281,
#154282,#154283,#154284,#154285,#154286,#154287,#154288,#154289,#154290,
#154291,#154292,#154293,#154294,#154295,#154296,#154297,#154298,#154299,
#154300,#154301,#154302,#154303,#154304,#154305,#154306,#154307,#154308,
#154309,#154310,#154311,#154312,#154313,#154314,#154315,#154316),
 .UNSPECIFIED.,.F.,.F.,(4,3,3,3,3,3,3,3,3,3,3,3,3,3,3,3,3,3,3,3,3,3,3,3,
3,3,3,3,3,3,3,3,3,3,3,3,3,3,3,3,3,3,3,3,3,3,3,3,3,3,3,3,3,3,3,3,3,3,3,3,
3,3,3,3,3,3,3,3,3,3,3,3,3,3,3,3,3,3,3,3,3,3,4),(975.012577706348,975.091541393563,
975.172892027223,975.251800202913,975.330706392125,975.409626904569,975.488578057374,
975.567616783211,975.646708127336,975.72590644325,975.742346462845,975.822303762976,
975.902166560219,975.981952382691,976.061678697887,976.141362926181,976.221033912402,
976.300701365928,976.380381016745,976.46008859914,976.539883828215,976.619728169923,
976.699686596971,976.742082473566,976.822039773697,976.90190257094,976.981688393412,
977.061414708607,977.141098936901,977.220769923122,977.300437376647,977.380117027464,
977.459824609859,977.539619838934,977.619464180642,977.699422607689,977.741818484286,
977.821775784417,977.90163858166,977.981424404131,978.061150719326,978.14083494762,
978.220505933841,978.300173387367,978.379853038183,978.459560620577,978.539355849653,
978.61920019136,978.699158618407,978.741554495006,978.821511795137,978.90137459238,
978.981160414852,979.060886730047,979.140570958341,979.220241944562,979.299909398088,
979.379589048904,979.459296631298,979.539091860374,979.618936202082,979.69889462913,
979.741290505726,979.821247805857,979.9011106031,979.980896425572,980.060622740767,
980.140306969061,980.219977955282,980.299645408808,980.379325059624,980.459032642019,
980.538827871095,980.618672212802,980.69863063985,980.741026516446,980.823302516335,
980.905463515783,980.987521957406,981.069462465544,981.151333907837,981.233133588715,
981.295763013528),.UNSPECIFIED.);
#1285=B_SPLINE_CURVE_WITH_KNOTS('',3,(#154318,#154319,#154320,#154321,#154322,
#154323,#154324,#154325,#154326,#154327),.UNSPECIFIED.,.F.,.F.,(4,1,1,1,
1,1,1,4),(981.295767365742,981.740762527166,982.740498537887,983.740234548607,
984.739970559327,985.739706570047,986.739442580767,987.578948320707),
 .UNSPECIFIED.);
#1286=B_SPLINE_CURVE_WITH_KNOTS('',3,(#154329,#154330,#154331,#154332,#154333,
#154334,#154335,#154336,#154337,#154338,#154339),.UNSPECIFIED.,.F.,.F.,
(4,1,1,1,1,1,1,1,4),(987.578948320707,987.739178591487,988.738914602207,
989.738650612927,990.738386623648,991.738122634368,992.737858645088,993.737594655808,
993.862133627887),.UNSPECIFIED.);
#1287=B_SPLINE_CURVE_WITH_KNOTS('',3,(#154341,#154342,#154343,#154344,#154345,
#154346,#154347,#154348,#154349,#154350,#154351,#154352,#154353,#154354,
#154355,#154356,#154357,#154358,#154359,#154360,#154361,#154362,#154363,
#154364,#154365,#154366,#154367,#154368,#154369,#154370,#154371,#154372,
#154373,#154374,#154375,#154376,#154377,#154378,#154379,#154380,#154381,
#154382,#154383,#154384,#154385,#154386,#154387,#154388,#154389,#154390,
#154391,#154392,#154393,#154394,#154395,#154396,#154397,#154398,#154399,
#154400,#154401,#154402,#154403,#154404,#154405,#154406,#154407,#154408,
#154409,#154410,#154411,#154412,#154413,#154414,#154415,#154416,#154417,
#154418,#154419,#154420,#154421,#154422,#154423,#154424,#154425,#154426,
#154427,#154428,#154429,#154430,#154431,#154432,#154433,#154434,#154435,
#154436,#154437,#154438,#154439,#154440,#154441,#154442,#154443,#154444,
#154445,#154446,#154447,#154448,#154449,#154450,#154451,#154452,#154453,
#154454,#154455,#154456,#154457,#154458,#154459,#154460,#154461,#154462,
#154463,#154464,#154465,#154466,#154467,#154468,#154469,#154470,#154471,
#154472,#154473,#154474,#154475,#154476,#154477,#154478,#154479,#154480,
#154481,#154482,#154483,#154484,#154485,#154486,#154487,#154488,#154489,
#154490,#154491,#154492,#154493,#154494,#154495,#154496,#154497,#154498,
#154499,#154500,#154501,#154502,#154503,#154504,#154505,#154506,#154507,
#154508,#154509,#154510,#154511,#154512,#154513,#154514,#154515,#154516,
#154517,#154518,#154519,#154520,#154521,#154522,#154523,#154524,#154525,
#154526,#154527,#154528,#154529,#154530,#154531,#154532,#154533,#154534,
#154535,#154536,#154537,#154538,#154539,#154540,#154541,#154542,#154543,
#154544,#154545,#154546,#154547,#154548,#154549,#154550,#154551,#154552,
#154553,#154554,#154555,#154556,#154557,#154558,#154559,#154560,#154561,
#154562,#154563,#154564,#154565,#154566,#154567,#154568,#154569,#154570,
#154571,#154572,#154573,#154574,#154575,#154576,#154577,#154578,#154579,
#154580,#154581,#154582,#154583,#154584),.UNSPECIFIED.,.F.,.F.,(4,3,3,3,
3,3,3,3,3,3,3,3,3,3,3,3,3,3,3,3,3,3,3,3,3,3,3,3,3,3,3,3,3,3,3,3,3,3,3,3,
3,3,3,3,3,3,3,3,3,3,3,3,3,3,3,3,3,3,3,3,3,3,3,3,3,3,3,3,3,3,3,3,3,3,3,3,
3,3,3,3,3,4),(993.862133627887,993.940907294356,994.019600459457,994.098231504359,
994.17811889963,994.256690923096,994.335259715897,994.413841803452,994.494714019221,
994.573412485895,994.655371576211,994.737330666528,994.817287966659,994.897150763902,
994.976936586374,995.056662901569,995.136347129863,995.216018116084,995.29568556961,
995.375365220427,995.455072802822,995.534868031897,995.614712373605,995.694670800652,
995.737066677248,995.817023977379,995.896886774622,995.976672597094,996.056398912289,
996.136083140583,996.215754126804,996.295421580329,996.375101231146,996.45480881354,
996.534604042616,996.614448384323,996.694406811371,996.736802687968,996.816759988099,
996.896622785342,996.976408607813,997.056134923009,997.135819151304,997.215490137525,
997.29515759105,997.374837241867,997.454544824261,997.534340053336,997.614184395044,
997.694142822091,997.736538698688,997.81649599882,997.896358796062,997.976144618534,
998.05587093373,998.135555162024,998.215226148245,998.294893601771,998.374573252588,
998.454280834983,998.534076064059,998.613920405767,998.693878832814,998.736274709409,
998.81623200954,998.896094806782,998.975880629253,999.055606944448,999.135291172742,
999.214962158963,999.294629612488,999.374309263304,999.454016845697,999.533812074773,
999.61365641648,999.693614843527,999.736010720129,999.824431802581,999.912507175443,
1000.00036214251,1000.08785478837,1000.14531872231),.UNSPECIFIED.);
#1288=B_SPLINE_CURVE_WITH_KNOTS('',3,(#154586,#154587,#154588,#154589,#154590,
#154591,#154592,#154593,#154594,#154595),.UNSPECIFIED.,.F.,.F.,(4,1,1,1,
1,1,1,4),(1000.14531893507,1000.73574673085,1001.73548274157,1002.73521875229,
1003.73495476301,1004.73469077373,1005.73442678445,1006.42850424225),
 .UNSPECIFIED.);
#1289=B_SPLINE_CURVE_WITH_KNOTS('',3,(#154597,#154598,#154599,#154600,#154601,
#154602,#154603,#154604,#154605,#154606,#154607,#154608,#154609,#154610,
#154611,#154612,#154613,#154614,#154615,#154616,#154617,#154618,#154619,
#154620,#154621,#154622,#154623,#154624,#154625,#154626,#154627,#154628,
#154629,#154630,#154631,#154632,#154633,#154634,#154635,#154636,#154637,
#154638,#154639,#154640,#154641,#154642,#154643,#154644,#154645,#154646,
#154647,#154648,#154649,#154650,#154651,#154652,#154653,#154654,#154655,
#154656,#154657,#154658,#154659,#154660,#154661,#154662,#154663,#154664,
#154665,#154666,#154667,#154668,#154669,#154670,#154671,#154672,#154673,
#154674,#154675,#154676,#154677,#154678,#154679,#154680,#154681,#154682,
#154683,#154684,#154685,#154686,#154687,#154688,#154689,#154690,#154691,
#154692,#154693,#154694,#154695,#154696,#154697,#154698,#154699,#154700,
#154701,#154702,#154703,#154704,#154705,#154706,#154707,#154708,#154709,
#154710,#154711,#154712,#154713,#154714,#154715,#154716,#154717,#154718,
#154719,#154720,#154721,#154722,#154723,#154724,#154725,#154726,#154727,
#154728,#154729,#154730,#154731,#154732,#154733,#154734,#154735,#154736,
#154737,#154738,#154739,#154740,#154741,#154742,#154743,#154744,#154745,
#154746,#154747,#154748,#154749,#154750,#154751,#154752,#154753,#154754,
#154755,#154756,#154757,#154758,#154759,#154760,#154761,#154762,#154763,
#154764,#154765,#154766,#154767,#154768,#154769,#154770,#154771,#154772,
#154773,#154774,#154775,#154776,#154777,#154778,#154779,#154780,#154781,
#154782,#154783,#154784,#154785,#154786,#154787,#154788,#154789,#154790,
#154791,#154792,#154793,#154794,#154795,#154796,#154797,#154798,#154799,
#154800,#154801,#154802,#154803,#154804,#154805,#154806,#154807,#154808,
#154809,#154810,#154811,#154812,#154813,#154814,#154815,#154816,#154817,
#154818,#154819,#154820,#154821,#154822,#154823,#154824,#154825,#154826,
#154827,#154828,#154829,#154830,#154831,#154832,#154833,#154834,#154835,
#154836,#154837,#154838,#154839,#154840,#154841,#154842,#154843),
 .UNSPECIFIED.,.F.,.F.,(4,3,3,3,3,3,3,3,3,3,3,3,3,3,3,3,3,3,3,3,3,3,3,3,
3,3,3,3,3,3,3,3,3,3,3,3,3,3,3,3,3,3,3,3,3,3,3,3,3,3,3,3,3,3,3,3,3,3,3,3,
3,3,3,3,3,3,3,3,3,3,3,3,3,3,3,3,3,3,3,3,3,3,4),(1006.42850443757,1006.52392891918,
1006.62009994949,1006.71707095298,1006.73416279517,1006.8141200953,1006.89398289255,
1006.97376871502,1007.05349503022,1007.13317925852,1007.21285024474,1007.29251769827,
1007.37219734909,1007.45190493148,1007.53170016056,1007.61154450227,1007.69150292932,
1007.73389880589,1007.81385610602,1007.89371890326,1007.97350472574,1008.05323104093,
1008.13291526922,1008.21258625545,1008.29225370897,1008.37193335979,1008.45164094218,
1008.53143617126,1008.61128051296,1008.69123894001,1008.73363481661,1008.81359211674,
1008.89345491398,1008.97324073645,1009.05296705165,1009.13265127994,1009.21232226616,
1009.29198971969,1009.3716693705,1009.4513769529,1009.53117218197,1009.61101652368,
1009.69097495073,1009.73337082733,1009.81332812746,1009.8931909247,1009.97297674718,
1010.05270306237,1010.13238729067,1010.21205827689,1010.29172573041,1010.37140538123,
1010.45111296362,1010.5309081927,1010.61075253441,1010.69071096146,1010.73310683805,
1010.81306413818,1010.89292693542,1010.97271275789,1011.05243907309,1011.13212330138,
1011.2117942876,1011.29146174113,1011.37114139195,1011.45084897434,1011.53064420341,
1011.61048854512,1011.69044697217,1011.73284284877,1011.81251666311,1011.89209613433,
1011.9715990584,1012.05104316828,1012.13362396592,1012.2130145472,1012.2924035767,
1012.37180702271,1012.45124085961,1012.53076213062,1012.61033519284,1012.69001597921,
1012.71168954943),.UNSPECIFIED.);
#1290=B_SPLINE_CURVE_WITH_KNOTS('',3,(#154845,#154846,#154847,#154848,#154849,
#154850,#154851,#154852,#154853,#154854,#154855,#154856,#154857),
 .UNSPECIFIED.,.F.,.F.,(4,3,1,1,1,1,1,1,4),(1012.71168954943,1012.73257885949,
1013.73231487021,1014.73205088093,1015.73178689165,1016.73152290237,1017.73125891309,
1018.73099492381,1018.99487485661),.UNSPECIFIED.);
#1291=B_SPLINE_CURVE_WITH_KNOTS('',3,(#154859,#154860,#154861,#154862,#154863,
#154864,#154865,#154866,#154867,#154868),.UNSPECIFIED.,.F.,.F.,(4,1,1,1,
1,1,1,4),(1018.99487485661,1019.73073093453,1020.73046694525,1021.73020295597,
1022.72993896669,1023.72967497741,1024.72941098813,1025.27806016378),
 .UNSPECIFIED.);
#1292=B_SPLINE_CURVE_WITH_KNOTS('',3,(#154870,#154871,#154872,#154873,#154874,
#154875,#154876,#154877,#154878,#154879),.UNSPECIFIED.,.F.,.F.,(4,1,1,1,
1,1,1,4),(1025.27806016378,1025.72914699885,1026.72888300957,1027.72861902029,
1028.72835503101,1029.72809104173,1030.72782705245,1031.56124547096),
 .UNSPECIFIED.);
#1293=B_SPLINE_CURVE_WITH_KNOTS('',3,(#154881,#154882,#154883,#154884,#154885,
#154886,#154887,#154888,#154889,#154890,#154891),.UNSPECIFIED.,.F.,.F.,
(4,1,1,1,1,1,1,1,4),(1031.56124547096,1031.72756306317,1032.72729907389,
1033.72703508461,1034.72677109533,1035.72650710605,1036.72624311677,1037.72597912749,
1037.84443077814),.UNSPECIFIED.);
#1294=B_SPLINE_CURVE_WITH_KNOTS('',3,(#154893,#154894,#154895,#154896,#154897,
#154898,#154899,#154900,#154901,#154902,#154903,#154904,#154905,#154906,
#154907,#154908,#154909,#154910,#154911,#154912,#154913,#154914,#154915,
#154916,#154917,#154918,#154919,#154920,#154921,#154922,#154923,#154924,
#154925,#154926,#154927,#154928,#154929,#154930,#154931,#154932,#154933,
#154934,#154935,#154936,#154937,#154938,#154939,#154940,#154941,#154942,
#154943,#154944,#154945,#154946,#154947,#154948,#154949,#154950,#154951,
#154952,#154953,#154954,#154955,#154956,#154957,#154958,#154959,#154960,
#154961,#154962,#154963,#154964,#154965,#154966,#154967,#154968,#154969,
#154970,#154971,#154972,#154973,#154974,#154975,#154976,#154977,#154978,
#154979,#154980,#154981,#154982,#154983,#154984,#154985,#154986,#154987,
#154988,#154989,#154990,#154991,#154992,#154993,#154994,#154995,#154996,
#154997,#154998,#154999,#155000,#155001,#155002,#155003,#155004,#155005,
#155006,#155007,#155008,#155009,#155010,#155011,#155012,#155013,#155014,
#155015,#155016,#155017,#155018,#155019,#155020,#155021,#155022,#155023,
#155024,#155025,#155026,#155027,#155028,#155029,#155030,#155031,#155032,
#155033,#155034,#155035,#155036,#155037,#155038,#155039,#155040,#155041,
#155042,#155043,#155044,#155045,#155046,#155047,#155048,#155049,#155050,
#155051,#155052,#155053,#155054,#155055,#155056,#155057,#155058,#155059,
#155060,#155061,#155062,#155063,#155064,#155065,#155066,#155067,#155068,
#155069,#155070,#155071,#155072,#155073,#155074,#155075,#155076,#155077,
#155078,#155079,#155080,#155081,#155082,#155083,#155084,#155085,#155086,
#155087,#155088,#155089,#155090,#155091,#155092,#155093,#155094,#155095,
#155096,#155097,#155098,#155099,#155100,#155101,#155102,#155103,#155104,
#155105,#155106,#155107,#155108,#155109,#155110,#155111,#155112,#155113,
#155114,#155115,#155116,#155117,#155118,#155119,#155120,#155121,#155122,
#155123,#155124,#155125,#155126,#155127,#155128,#155129,#155130,#155131,
#155132,#155133,#155134,#155135,#155136,#155137,#155138,#155139),
 .UNSPECIFIED.,.F.,.F.,(4,3,3,3,3,3,3,3,3,3,3,3,3,3,3,3,3,3,3,3,3,3,3,3,
3,3,3,3,3,3,3,3,3,3,3,3,3,3,3,3,3,3,3,3,3,3,3,3,3,3,3,3,3,3,3,3,3,3,3,3,
3,3,3,3,3,3,3,3,3,3,3,3,3,3,3,3,3,3,3,3,3,3,4),(1037.84443077814,1037.92323353131,
1038.00195463676,1038.08061246473,1038.16125029891,1038.2398463353,1038.31843821249,
1038.39704244251,1038.47921061644,1038.55793065408,1038.63670281158,1038.71557848102,
1038.72571513821,1038.80567243834,1038.88553523558,1038.96532105806,1039.04504737325,
1039.12473160154,1039.20440258777,1039.28407004129,1039.36374969211,1039.4434572745,
1039.52325250358,1039.60309684529,1039.68305527233,1039.72545114893,1039.80540844906,
1039.8852712463,1039.96505706878,1040.04478338397,1040.12446761226,1040.20413859849,
1040.28380605201,1040.36348570283,1040.44319328522,1040.5229885143,1040.60283285601,
1040.68279128305,1040.72518715965,1040.80514445978,1040.88500725702,1040.9647930795,
1041.04451939469,1041.12420362299,1041.20387460921,1041.28354206273,1041.36322171355,
1041.44292929594,1041.52272452502,1041.60256886673,1041.68252729378,1041.72492317037,
1041.8048804705,1041.88474326774,1041.96452909022,1042.04425540541,1042.12393963371,
1042.20361061993,1042.28327807345,1042.36295772427,1042.44266530666,1042.52246053574,
1042.60230487745,1042.68226330449,1042.72465918109,1042.80461648122,1042.88447927846,
1042.96426510094,1043.04399141613,1043.12367564442,1043.20334663065,1043.28301408417,
1043.36269373499,1043.44240131738,1043.52219654646,1043.60204088816,1043.68199931521,
1043.72439519181,1043.81318968657,1043.90162420445,1043.98982593053,1044.07764761709,
1044.12761586414),.UNSPECIFIED.);
#1295=B_SPLINE_CURVE_WITH_KNOTS('',3,(#155141,#155142,#155143,#155144,#155145,
#155146,#155147,#155148,#155149,#155150),.UNSPECIFIED.,.F.,.F.,(4,1,1,1,
1,1,1,4),(1044.12761608532,1044.72413120253,1045.72386721325,1046.72360322397,
1047.72333923469,1048.72307524541,1049.72281125614,1050.4108013925),
 .UNSPECIFIED.);
#1296=B_SPLINE_CURVE_WITH_KNOTS('',3,(#155152,#155153,#155154,#155155,#155156,
#155157,#155158,#155159,#155160,#155161,#155162,#155163,#155164,#155165,
#155166,#155167,#155168,#155169,#155170,#155171,#155172,#155173,#155174,
#155175,#155176,#155177,#155178,#155179,#155180,#155181,#155182,#155183,
#155184,#155185,#155186,#155187,#155188,#155189,#155190,#155191,#155192,
#155193,#155194,#155195,#155196,#155197,#155198,#155199,#155200,#155201,
#155202,#155203,#155204,#155205,#155206,#155207,#155208,#155209,#155210,
#155211,#155212,#155213,#155214,#155215,#155216,#155217,#155218,#155219,
#155220,#155221,#155222,#155223,#155224,#155225,#155226,#155227,#155228,
#155229,#155230,#155231,#155232,#155233,#155234,#155235,#155236,#155237,
#155238,#155239,#155240,#155241,#155242,#155243,#155244,#155245,#155246,
#155247,#155248,#155249,#155250,#155251,#155252,#155253,#155254,#155255,
#155256,#155257,#155258,#155259,#155260,#155261,#155262,#155263,#155264,
#155265,#155266,#155267,#155268,#155269,#155270,#155271,#155272,#155273,
#155274,#155275,#155276,#155277,#155278,#155279,#155280,#155281,#155282,
#155283,#155284,#155285,#155286,#155287,#155288,#155289,#155290,#155291,
#155292,#155293,#155294,#155295,#155296,#155297,#155298,#155299,#155300,
#155301,#155302,#155303,#155304,#155305,#155306,#155307,#155308,#155309,
#155310,#155311,#155312,#155313,#155314,#155315,#155316,#155317,#155318,
#155319,#155320,#155321,#155322,#155323,#155324,#155325,#155326,#155327,
#155328,#155329,#155330,#155331,#155332,#155333,#155334,#155335,#155336,
#155337,#155338,#155339,#155340,#155341,#155342,#155343,#155344,#155345,
#155346,#155347,#155348,#155349,#155350,#155351,#155352,#155353,#155354,
#155355,#155356,#155357,#155358,#155359,#155360,#155361,#155362,#155363,
#155364,#155365,#155366,#155367,#155368,#155369,#155370,#155371,#155372,
#155373,#155374,#155375,#155376,#155377,#155378,#155379,#155380,#155381,
#155382,#155383,#155384,#155385,#155386,#155387,#155388,#155389,#155390,
#155391,#155392,#155393,#155394,#155395,#155396,#155397,#155398),
 .UNSPECIFIED.,.F.,.F.,(4,3,3,3,3,3,3,3,3,3,3,3,3,3,3,3,3,3,3,3,3,3,3,3,
3,3,3,3,3,3,3,3,3,3,3,3,3,3,3,3,3,3,3,3,3,3,3,3,3,3,3,3,3,3,3,3,3,3,3,3,
3,3,3,3,3,3,3,3,3,3,3,3,3,3,3,3,3,3,3,3,3,3,4),(1050.41080159846,1050.50561867196,
1050.60112629621,1050.69739631959,1050.72254726686,1050.80250456699,1050.88236736423,
1050.9621531867,1051.0418795019,1051.12156373019,1051.20123471641,1051.28090216994,
1051.36058182075,1051.44028940315,1051.52008463222,1051.59992897393,1051.67988740098,
1051.72228327758,1051.80224057771,1051.88210337495,1051.96188919743,1052.04161551262,
1052.12129974091,1052.20097072714,1052.28063818066,1052.36031783148,1052.44002541387,
1052.51982064295,1052.59966498466,1052.6796234117,1052.7220192883,1052.80197658843,
1052.88183938567,1052.96162520815,1053.04135152334,1053.12103575164,1053.20070673786,
1053.28037419138,1053.3600538422,1053.43976142459,1053.51955665367,1053.59940099538,
1053.67935942242,1053.72175529902,1053.80171259915,1053.88157539639,1053.96136121887,
1054.04108753406,1054.12077176236,1054.20044274858,1054.2801102021,1054.35978985292,
1054.43949743531,1054.51929266439,1054.5991370061,1054.67909543314,1054.72149130974,
1054.80144860987,1054.88131140712,1054.96109722959,1055.04082354478,1055.12050777308,
1055.2001787593,1055.27984621283,1055.35952586364,1055.43923344604,1055.51902867512,
1055.59887301682,1055.67883144387,1055.72122732046,1055.80082617924,1055.88033074753,
1055.95975888751,1056.0391283975,1056.12098568527,1056.2003022785,1056.27961752731,
1056.35894745853,1056.43830810537,1056.51775582873,1056.59725575641,1056.67686180204,
1056.69398669968),.UNSPECIFIED.);
#1297=B_SPLINE_CURVE_WITH_KNOTS('',3,(#155400,#155401,#155402,#155403,#155404,
#155405,#155406,#155407,#155408,#155409,#155410,#155411,#155412),
 .UNSPECIFIED.,.F.,.F.,(4,3,1,1,1,1,1,1,4),(1056.69398669968,1056.72096333118,
1057.7206993419,1058.72043535262,1059.72017136334,1060.71990737406,1061.71964338478,
1062.7193793955,1062.97717200686),.UNSPECIFIED.);
#1298=B_SPLINE_CURVE_WITH_KNOTS('',3,(#155414,#155415,#155416,#155417,#155418,
#155419,#155420,#155421,#155422,#155423),.UNSPECIFIED.,.F.,.F.,(4,1,1,1,
1,1,1,4),(1062.97717200686,1063.71911540622,1064.71885141694,1065.71858742766,
1066.71832343838,1067.7180594491,1068.71779545982,1069.26035731404),
 .UNSPECIFIED.);
#1299=B_SPLINE_CURVE_WITH_KNOTS('',3,(#155425,#155426,#155427,#155428,#155429,
#155430,#155431,#155432,#155433,#155434,#155435,#155436,#155437,#155438,
#155439,#155440,#155441,#155442,#155443,#155444,#155445,#155446,#155447,
#155448,#155449,#155450,#155451,#155452,#155453,#155454,#155455,#155456,
#155457,#155458,#155459,#155460,#155461,#155462,#155463,#155464,#155465,
#155466,#155467,#155468,#155469,#155470,#155471,#155472,#155473,#155474,
#155475,#155476,#155477,#155478,#155479,#155480,#155481,#155482,#155483,
#155484,#155485,#155486,#155487,#155488,#155489,#155490,#155491,#155492,
#155493,#155494,#155495,#155496,#155497,#155498,#155499,#155500,#155501,
#155502,#155503,#155504,#155505,#155506,#155507,#155508,#155509,#155510,
#155511,#155512,#155513,#155514,#155515,#155516,#155517,#155518,#155519,
#155520,#155521,#155522,#155523,#155524,#155525,#155526,#155527,#155528,
#155529,#155530,#155531,#155532,#155533,#155534,#155535,#155536,#155537,
#155538,#155539,#155540,#155541,#155542,#155543,#155544,#155545,#155546,
#155547,#155548,#155549,#155550,#155551,#155552,#155553,#155554,#155555,
#155556,#155557,#155558,#155559,#155560,#155561,#155562,#155563,#155564,
#155565,#155566,#155567,#155568,#155569,#155570,#155571,#155572,#155573,
#155574,#155575,#155576,#155577,#155578,#155579,#155580,#155581,#155582,
#155583,#155584,#155585,#155586,#155587,#155588,#155589,#155590,#155591,
#155592,#155593,#155594,#155595,#155596,#155597,#155598,#155599,#155600,
#155601,#155602,#155603,#155604,#155605,#155606,#155607,#155608,#155609,
#155610,#155611,#155612,#155613,#155614,#155615,#155616,#155617,#155618,
#155619,#155620,#155621,#155622,#155623,#155624,#155625,#155626,#155627,
#155628,#155629,#155630,#155631,#155632,#155633,#155634,#155635,#155636,
#155637,#155638,#155639,#155640,#155641,#155642,#155643,#155644,#155645,
#155646,#155647,#155648,#155649,#155650,#155651,#155652,#155653,#155654,
#155655,#155656,#155657,#155658,#155659,#155660,#155661,#155662,#155663,
#155664,#155665,#155666,#155667,#155668,#155669,#155670,#155671),
 .UNSPECIFIED.,.F.,.F.,(4,3,3,3,3,3,3,3,3,3,3,3,3,3,3,3,3,3,3,3,3,3,3,3,
3,3,3,3,3,3,3,3,3,3,3,3,3,3,3,3,3,3,3,3,3,3,3,3,3,3,3,3,3,3,3,3,3,3,3,3,
3,3,3,3,3,3,3,3,3,3,3,3,3,3,3,3,3,3,3,3,3,3,4),(1069.26035754479,1069.34545859664,
1069.43072803692,1069.51625386385,1069.60191842313,1069.6877916665,1069.71753147054,
1069.79748877067,1069.87735156791,1069.95713739038,1070.03686370557,1070.11654793387,
1070.19621892009,1070.27588637361,1070.35556602442,1070.43527360682,1070.51506883589,
1070.5949131776,1070.67487160464,1070.71726748126,1070.79722478139,1070.87708757863,
1070.95687340111,1071.0365997163,1071.11628394459,1071.19595493082,1071.27562238434,
1071.35530203516,1071.43500961755,1071.51480484663,1071.59464918833,1071.67460761538,
1071.71700349198,1071.79696079211,1071.87682358935,1071.95660941183,1072.03633572702,
1072.11601995532,1072.19569094154,1072.27535839506,1072.35503804588,1072.43474562828,
1072.51454085735,1072.59438519906,1072.67434362611,1072.7167395027,1072.79669680283,
1072.87655960007,1072.95634542255,1073.03607173774,1073.11575596603,1073.19542695225,
1073.27509440578,1073.3547740566,1073.43448163899,1073.51427686807,1073.59412120977,
1073.67407963682,1073.71647551342,1073.79643281355,1073.87629561079,1073.95608143327,
1074.03580774846,1074.11549197676,1074.19516296298,1074.27483041651,1074.35451006732,
1074.43421764972,1074.51401287879,1074.5938572205,1074.67381564755,1074.71621152414,
1074.79497519234,1074.87364476551,1074.95223873817,1075.03077190006,1075.10927232987,
1075.18775661242,1075.26624131795,1075.34477454951,1075.42333461854,1075.50197703655,
1075.54354262122),.UNSPECIFIED.);
#1300=B_SPLINE_CURVE_WITH_KNOTS('',3,(#155673,#155674,#155675,#155676,#155677,
#155678,#155679,#155680,#155681,#155682,#155683,#155684),.UNSPECIFIED.,
 .F.,.F.,(4,2,1,1,1,1,1,1,4),(1075.54354262122,1075.71594753486,1076.71568354558,
1077.7154195563,1078.71515556702,1079.71489157774,1080.71462758846,1081.71436359918,
1081.8267279284),.UNSPECIFIED.);
#1301=B_SPLINE_CURVE_WITH_KNOTS('',3,(#155686,#155687,#155688,#155689,#155690,
#155691,#155692,#155693,#155694,#155695),.UNSPECIFIED.,.F.,.F.,(4,1,1,1,
1,1,1,4),(1081.8267279284,1082.7140996099,1083.71383562062,1084.71357163134,
1085.71330764206,1086.71304365278,1087.7127796635,1088.10991323558),
 .UNSPECIFIED.);
#1302=B_SPLINE_CURVE_WITH_KNOTS('',3,(#155697,#155698,#155699,#155700,#155701,
#155702,#155703,#155704,#155705,#155706),.UNSPECIFIED.,.F.,.F.,(4,1,1,1,
1,1,1,4),(1088.10991323558,1088.71251567422,1089.71225168494,1090.71198769566,
1091.71172370638,1092.7114597171,1093.71119572782,1094.39309854276),
 .UNSPECIFIED.);
#1303=B_SPLINE_CURVE_WITH_KNOTS('',3,(#155708,#155709,#155710,#155711,#155712,
#155713,#155714,#155715,#155716,#155717),.UNSPECIFIED.,.F.,.F.,(4,1,1,1,
1,1,1,4),(1094.39309854276,1094.71093173854,1095.71066774926,1096.71040375998,
1097.7101397707,1098.70987578142,1099.70961179214,1100.67627932462),
 .UNSPECIFIED.);
#1304=B_SPLINE_CURVE_WITH_KNOTS('',3,(#155719,#155720,#155721,#155722,#155723,
#155724,#155725,#155726,#155727,#155728,#155729,#155730,#155731,#155732,
#155733,#155734,#155735,#155736,#155737,#155738,#155739,#155740,#155741,
#155742,#155743,#155744,#155745,#155746,#155747,#155748,#155749,#155750,
#155751,#155752,#155753,#155754,#155755,#155756,#155757,#155758,#155759,
#155760,#155761,#155762,#155763,#155764,#155765,#155766,#155767,#155768,
#155769,#155770,#155771,#155772,#155773,#155774,#155775,#155776,#155777,
#155778,#155779,#155780,#155781,#155782,#155783,#155784,#155785,#155786,
#155787,#155788,#155789,#155790,#155791,#155792,#155793,#155794,#155795,
#155796,#155797,#155798,#155799,#155800,#155801,#155802,#155803,#155804,
#155805,#155806,#155807,#155808,#155809,#155810,#155811,#155812,#155813,
#155814,#155815,#155816,#155817,#155818,#155819,#155820,#155821,#155822,
#155823,#155824,#155825,#155826,#155827,#155828,#155829,#155830,#155831,
#155832,#155833,#155834,#155835,#155836,#155837,#155838,#155839,#155840,
#155841,#155842,#155843,#155844,#155845,#155846,#155847,#155848,#155849,
#155850,#155851,#155852,#155853,#155854,#155855,#155856,#155857,#155858,
#155859,#155860,#155861,#155862,#155863,#155864,#155865,#155866,#155867,
#155868,#155869,#155870,#155871,#155872,#155873,#155874,#155875,#155876,
#155877,#155878,#155879,#155880,#155881,#155882,#155883,#155884,#155885,
#155886,#155887,#155888,#155889,#155890,#155891,#155892,#155893,#155894,
#155895,#155896,#155897,#155898,#155899,#155900,#155901,#155902,#155903,
#155904,#155905,#155906,#155907,#155908,#155909,#155910,#155911,#155912,
#155913,#155914,#155915,#155916,#155917,#155918,#155919,#155920,#155921,
#155922,#155923,#155924,#155925,#155926,#155927,#155928,#155929,#155930,
#155931,#155932,#155933,#155934,#155935,#155936,#155937,#155938,#155939,
#155940,#155941,#155942,#155943,#155944,#155945,#155946,#155947,#155948,
#155949,#155950,#155951,#155952,#155953,#155954,#155955,#155956,#155957,
#155958,#155959,#155960,#155961,#155962,#155963,#155964,#155965),
 .UNSPECIFIED.,.F.,.F.,(4,3,3,3,3,3,3,3,3,3,3,3,3,3,3,3,3,3,3,3,3,3,3,3,
3,3,3,3,3,3,3,3,3,3,3,3,3,3,3,3,3,3,3,3,3,3,3,3,3,3,3,3,3,3,3,3,3,3,3,3,
3,3,3,3,3,3,3,3,3,3,3,3,3,3,3,3,3,3,3,3,3,3,4),(1100.67628384994,1100.70934780286,
1100.78930510299,1100.86916790023,1100.94895372271,1101.0286800379,1101.1083642662,
1101.18803525242,1101.26770270594,1101.34738235676,1101.42708993915,1101.50688516823,
1101.58672950994,1101.66668793698,1101.70908381358,1101.78904111371,1101.86890391095,
1101.94868973343,1102.02841604862,1102.10810027692,1102.18777126314,1102.26743871666,
1102.34711836748,1102.42682594987,1102.50662117895,1102.58646552066,1102.6664239477,
1102.7088198243,1102.78877712443,1102.86863992167,1102.94842574415,1103.02815205934,
1103.10783628764,1103.18750727386,1103.26717472738,1103.3468543782,1103.42656196059,
1103.50635718967,1103.58620153138,1103.66615995842,1103.70855583502,1103.78851313515,
1103.86837593239,1103.94816175487,1104.02788807006,1104.10757229835,1104.18724328458,
1104.2669107381,1104.34659038892,1104.42629797131,1104.50609320039,1104.5859375421,
1104.66589596914,1104.70829184574,1104.78824914587,1104.86811194311,1104.94789776559,
1105.02762408078,1105.10730830908,1105.1869792953,1105.26664674882,1105.34632639964,
1105.42603398203,1105.50582921111,1105.58567355282,1105.66563197986,1105.70802785646,
1105.78798515659,1105.86784795383,1105.94763377631,1106.0273600915,1106.10704431979,
1106.18671530602,1106.26638275954,1106.34606241036,1106.42576999275,1106.50556522183,
1106.58540956353,1106.66536799058,1106.70776386718,1106.8123055036,1106.91467660682,
1106.95946909753),.UNSPECIFIED.);
#1305=B_SPLINE_CURVE_WITH_KNOTS('',3,(#155967,#155968,#155969,#155970,#155971,
#155972,#155973,#155974,#155975,#155976),.UNSPECIFIED.,.F.,.F.,(4,1,1,1,
1,1,1,4),(1106.95946915712,1107.7074998779,1108.70723588862,1109.70697189934,
1110.70670791006,1111.70644392078,1112.7061799315,1113.2426544643),
 .UNSPECIFIED.);
#1306=B_SPLINE_CURVE_WITH_KNOTS('',3,(#155978,#155979,#155980,#155981,#155982,
#155983,#155984,#155985,#155986,#155987,#155988,#155989,#155990,#155991,
#155992,#155993,#155994,#155995,#155996,#155997,#155998,#155999,#156000,
#156001,#156002,#156003,#156004,#156005,#156006,#156007,#156008,#156009,
#156010,#156011,#156012,#156013,#156014,#156015,#156016,#156017,#156018,
#156019,#156020,#156021,#156022,#156023,#156024,#156025,#156026,#156027,
#156028,#156029,#156030,#156031,#156032,#156033,#156034,#156035,#156036,
#156037,#156038,#156039,#156040,#156041,#156042,#156043,#156044,#156045,
#156046,#156047,#156048,#156049,#156050,#156051,#156052,#156053,#156054,
#156055,#156056,#156057,#156058,#156059,#156060,#156061,#156062,#156063,
#156064,#156065,#156066,#156067,#156068,#156069,#156070,#156071,#156072,
#156073,#156074,#156075,#156076,#156077,#156078,#156079,#156080,#156081,
#156082,#156083,#156084,#156085,#156086,#156087,#156088,#156089,#156090,
#156091,#156092,#156093,#156094,#156095,#156096,#156097,#156098,#156099,
#156100,#156101,#156102,#156103,#156104,#156105,#156106,#156107,#156108,
#156109,#156110,#156111,#156112,#156113,#156114,#156115,#156116,#156117,
#156118,#156119,#156120,#156121,#156122,#156123,#156124,#156125,#156126,
#156127,#156128,#156129,#156130,#156131,#156132,#156133,#156134,#156135,
#156136,#156137,#156138,#156139,#156140,#156141,#156142,#156143,#156144,
#156145,#156146,#156147,#156148,#156149,#156150,#156151,#156152,#156153,
#156154,#156155,#156156,#156157,#156158,#156159,#156160,#156161,#156162,
#156163,#156164,#156165,#156166,#156167,#156168,#156169,#156170,#156171,
#156172,#156173,#156174,#156175,#156176,#156177,#156178,#156179,#156180,
#156181,#156182,#156183,#156184,#156185,#156186,#156187,#156188,#156189,
#156190,#156191,#156192,#156193,#156194,#156195,#156196,#156197,#156198,
#156199,#156200,#156201,#156202,#156203,#156204,#156205,#156206,#156207,
#156208,#156209,#156210,#156211,#156212,#156213,#156214,#156215,#156216,
#156217,#156218,#156219,#156220,#156221,#156222,#156223,#156224),
 .UNSPECIFIED.,.F.,.F.,(4,3,3,3,3,3,3,3,3,3,3,3,3,3,3,3,3,3,3,3,3,3,3,3,
3,3,3,3,3,3,3,3,3,3,3,3,3,3,3,3,3,3,3,3,3,3,3,3,3,3,3,3,3,3,3,3,3,3,3,3,
3,3,3,3,3,3,3,3,3,3,3,3,3,3,3,3,3,3,3,3,3,3,4),(1113.24265466419,1113.32749967178,
1113.41250237364,1113.49775111346,1113.58313209121,1113.66871953895,1113.70591594222,
1113.78587324235,1113.8657360396,1113.94552186207,1114.02524817726,1114.10493240556,
1114.18460339178,1114.26427084531,1114.34395049612,1114.42365807852,1114.50345330759,
1114.5832976493,1114.66325607635,1114.70565195294,1114.78560925307,1114.86547205031,
1114.94525787279,1115.02498418798,1115.10466841628,1115.1843394025,1115.26400685602,
1115.34368650684,1115.42339408923,1115.50318931831,1115.58303366002,1115.66299208706,
1115.70538796366,1115.78534526379,1115.86520806103,1115.94499388351,1116.0247201987,
1116.10440442699,1116.18407541322,1116.26374286674,1116.34342251756,1116.42313009995,
1116.50292532903,1116.58276967073,1116.66272809778,1116.70512397438,1116.78508127451,
1116.86494407175,1116.94472989423,1117.02445620942,1117.10414043772,1117.18381142394,
1117.26347887746,1117.34315852828,1117.42286611067,1117.50266133975,1117.58250568146,
1117.6624641085,1117.7048599851,1117.78481728523,1117.86468008247,1117.94446590494,
1118.02419222014,1118.10387644843,1118.18354743465,1118.26321488818,1118.342894539,
1118.42260212139,1118.50239735047,1118.58224169217,1118.66220011922,1118.70459599582,
1118.7833633104,1118.86203643875,1118.94063387376,1119.01917018146,1119.09767362819,
1119.17616079713,1119.25464825675,1119.33318293803,1119.41174439006,1119.49038526826,
1119.52583977148),.UNSPECIFIED.);
#1307=B_SPLINE_CURVE_WITH_KNOTS('',3,(#156226,#156227,#156228,#156229,#156230,
#156231,#156232,#156233,#156234,#156235,#156236,#156237),.UNSPECIFIED.,
 .F.,.F.,(4,2,1,1,1,1,1,1,4),(1119.52583977148,1119.70433200654,1120.70406801726,
1121.70380402798,1122.7035400387,1123.70327604942,1124.70301206014,1125.70274807086,
1125.80902507866),.UNSPECIFIED.);
#1308=B_SPLINE_CURVE_WITH_KNOTS('',3,(#156239,#156240,#156241,#156242,#156243,
#156244,#156245,#156246,#156247,#156248),.UNSPECIFIED.,.F.,.F.,(4,1,1,1,
1,1,1,4),(1125.80902507866,1126.70248408158,1127.70222009231,1128.70195610303,
1129.70169211375,1130.70142812447,1131.70116413519,1132.09221038584),
 .UNSPECIFIED.);
#1309=B_SPLINE_CURVE_WITH_KNOTS('',3,(#156250,#156251,#156252,#156253,#156254,
#156255,#156256,#156257,#156258,#156259),.UNSPECIFIED.,.F.,.F.,(4,1,1,1,
1,1,1,4),(1132.09221038584,1132.70090014591,1133.70063615663,1134.70037216735,
1135.70010817807,1136.69984418879,1137.69958019951,1138.37539569302),
 .UNSPECIFIED.);
#1310=B_SPLINE_CURVE_WITH_KNOTS('',3,(#156261,#156262,#156263,#156264,#156265,
#156266,#156267,#156268,#156269,#156270),.UNSPECIFIED.,.F.,.F.,(4,1,1,1,
1,1,1,4),(1138.37539569302,1138.69931621023,1139.69905222095,1140.69878823167,
1141.69852424239,1142.69826025311,1143.69799626383,1144.65857562991),
 .UNSPECIFIED.);
#1311=B_SPLINE_CURVE_WITH_KNOTS('',3,(#156272,#156273,#156274,#156275,#156276,
#156277,#156278,#156279,#156280,#156281,#156282,#156283,#156284,#156285,
#156286,#156287,#156288,#156289,#156290,#156291,#156292,#156293,#156294,
#156295,#156296,#156297,#156298,#156299,#156300,#156301,#156302,#156303,
#156304,#156305,#156306,#156307,#156308,#156309,#156310,#156311,#156312,
#156313,#156314,#156315,#156316,#156317,#156318,#156319,#156320,#156321,
#156322,#156323,#156324,#156325,#156326,#156327,#156328,#156329,#156330,
#156331,#156332,#156333,#156334,#156335,#156336,#156337,#156338,#156339,
#156340,#156341,#156342,#156343,#156344,#156345,#156346,#156347,#156348,
#156349,#156350,#156351,#156352,#156353,#156354,#156355,#156356,#156357,
#156358,#156359,#156360,#156361,#156362,#156363,#156364,#156365,#156366,
#156367,#156368,#156369,#156370,#156371,#156372,#156373,#156374,#156375,
#156376,#156377,#156378,#156379,#156380,#156381,#156382,#156383,#156384,
#156385,#156386,#156387,#156388,#156389,#156390,#156391,#156392,#156393,
#156394,#156395,#156396,#156397,#156398,#156399,#156400,#156401,#156402,
#156403,#156404,#156405,#156406,#156407,#156408,#156409,#156410,#156411,
#156412,#156413,#156414,#156415,#156416,#156417,#156418,#156419,#156420,
#156421,#156422,#156423,#156424,#156425,#156426,#156427,#156428,#156429,
#156430,#156431,#156432,#156433,#156434,#156435,#156436,#156437,#156438,
#156439,#156440,#156441,#156442,#156443,#156444,#156445,#156446,#156447,
#156448,#156449,#156450,#156451,#156452,#156453,#156454,#156455,#156456,
#156457,#156458,#156459,#156460,#156461,#156462,#156463,#156464,#156465,
#156466,#156467,#156468,#156469,#156470,#156471,#156472,#156473,#156474,
#156475,#156476,#156477,#156478,#156479,#156480,#156481,#156482,#156483,
#156484,#156485,#156486,#156487,#156488,#156489,#156490,#156491,#156492,
#156493,#156494,#156495,#156496,#156497,#156498,#156499,#156500,#156501,
#156502,#156503,#156504,#156505,#156506,#156507,#156508,#156509,#156510,
#156511,#156512,#156513,#156514,#156515,#156516,#156517,#156518),
 .UNSPECIFIED.,.F.,.F.,(4,3,3,3,3,3,3,3,3,3,3,3,3,3,3,3,3,3,3,3,3,3,3,3,
3,3,3,3,3,3,3,3,3,3,3,3,3,3,3,3,3,3,3,3,3,3,3,3,3,3,3,3,3,3,3,3,3,3,3,3,
3,3,3,3,3,3,3,3,3,3,3,3,3,3,3,3,3,3,3,3,3,3,4),(1144.6585810002,1144.69773227455,
1144.77768957468,1144.85755237192,1144.93733819439,1145.01706450959,1145.09674873788,
1145.1764197241,1145.25608717763,1145.33576682845,1145.41547441084,1145.49526963992,
1145.57511398162,1145.65507240867,1145.69746828527,1145.7774255854,1145.85728838264,
1145.93707420512,1146.01680052031,1146.09648474861,1146.17615573483,1146.25582318835,
1146.33550283917,1146.41521042156,1146.49500565064,1146.57484999235,1146.65480841939,
1146.69720429599,1146.77716159612,1146.85702439336,1146.93681021584,1147.01653653103,
1147.09622075933,1147.17589174555,1147.25555919907,1147.33523884989,1147.41494643228,
1147.49474166136,1147.57458600307,1147.65454443011,1147.69694030671,1147.77689760684,
1147.85676040408,1147.93654622656,1148.01627254175,1148.09595677005,1148.17562775627,
1148.25529520979,1148.33497486061,1148.414682443,1148.49447767208,1148.57432201379,
1148.65428044083,1148.69667631743,1148.77663361756,1148.8564964148,1148.93628223728,
1149.01600855247,1149.09569278077,1149.17536376699,1149.25503122051,1149.33471087133,
1149.41441845372,1149.4942136828,1149.57405802451,1149.65401645155,1149.69641232815,
1149.77636962828,1149.85623242552,1149.936018248,1150.01574456319,1150.09542879149,
1150.17509977771,1150.25476723123,1150.33444688205,1150.41415446445,1150.49394969352,
1150.57379403523,1150.65375246228,1150.69614833887,1150.80181973241,1150.90511477516,
1150.94176622539),.UNSPECIFIED.);
#1312=B_SPLINE_CURVE_WITH_KNOTS('',3,(#156520,#156521,#156522,#156523,#156524,
#156525,#156526,#156527,#156528,#156529),.UNSPECIFIED.,.F.,.F.,(4,1,1,1,
1,1,1,4),(1150.94176630738,1151.69588434959,1152.69562036031,1153.69535637103,
1154.69509238175,1155.69482839247,1156.69456440319,1157.22495161456),
 .UNSPECIFIED.);
#1313=B_SPLINE_CURVE_WITH_KNOTS('',3,(#156531,#156532,#156533,#156534,#156535,
#156536,#156537,#156538,#156539,#156540),.UNSPECIFIED.,.F.,.F.,(4,1,1,1,
1,1,1,4),(1157.22495161456,1157.69430041391,1158.69403642463,1159.69377243535,
1160.69350844607,1161.69324445679,1162.69298046751,1163.50813218944),
 .UNSPECIFIED.);
#1314=B_SPLINE_CURVE_WITH_KNOTS('',3,(#156542,#156543,#156544,#156545,#156546,
#156547,#156548,#156549,#156550,#156551,#156552,#156553,#156554,#156555,
#156556,#156557,#156558,#156559,#156560,#156561,#156562,#156563,#156564,
#156565,#156566,#156567,#156568,#156569,#156570,#156571,#156572,#156573,
#156574,#156575,#156576,#156577,#156578,#156579,#156580,#156581,#156582,
#156583,#156584,#156585,#156586,#156587,#156588,#156589,#156590,#156591,
#156592,#156593,#156594,#156595,#156596,#156597,#156598,#156599,#156600,
#156601,#156602,#156603,#156604,#156605,#156606,#156607,#156608,#156609,
#156610,#156611,#156612,#156613,#156614,#156615,#156616,#156617,#156618,
#156619,#156620,#156621,#156622,#156623,#156624,#156625,#156626,#156627,
#156628,#156629,#156630,#156631,#156632,#156633,#156634,#156635,#156636,
#156637,#156638,#156639,#156640,#156641,#156642,#156643,#156644,#156645,
#156646,#156647,#156648,#156649,#156650,#156651,#156652,#156653,#156654,
#156655,#156656,#156657,#156658,#156659,#156660,#156661,#156662,#156663,
#156664,#156665,#156666,#156667,#156668,#156669,#156670,#156671,#156672,
#156673,#156674,#156675,#156676,#156677,#156678,#156679,#156680,#156681,
#156682,#156683,#156684,#156685,#156686,#156687,#156688,#156689,#156690,
#156691,#156692,#156693,#156694,#156695,#156696,#156697,#156698,#156699,
#156700,#156701,#156702,#156703,#156704,#156705,#156706,#156707,#156708,
#156709,#156710,#156711,#156712,#156713,#156714,#156715,#156716,#156717,
#156718,#156719,#156720,#156721,#156722,#156723,#156724,#156725,#156726,
#156727,#156728,#156729,#156730,#156731,#156732,#156733,#156734,#156735,
#156736,#156737,#156738,#156739,#156740,#156741,#156742,#156743,#156744,
#156745,#156746,#156747,#156748,#156749,#156750,#156751,#156752,#156753,
#156754,#156755,#156756,#156757,#156758,#156759,#156760,#156761,#156762,
#156763,#156764,#156765,#156766,#156767,#156768,#156769,#156770,#156771,
#156772,#156773,#156774,#156775,#156776,#156777,#156778,#156779,#156780,
#156781,#156782,#156783,#156784,#156785),.UNSPECIFIED.,.F.,.F.,(4,3,3,3,
3,3,3,3,3,3,3,3,3,3,3,3,3,3,3,3,3,3,3,3,3,3,3,3,3,3,3,3,3,3,3,3,3,3,3,3,
3,3,3,3,3,3,3,3,3,3,3,3,3,3,3,3,3,3,3,3,3,3,3,3,3,3,3,3,3,3,3,3,3,3,3,3,
3,3,3,3,3,4),(1163.50813692174,1163.62789494603,1163.69271647823,1163.77267377836,
1163.8525365756,1163.93232239808,1164.01204871327,1164.09173294157,1164.17140392779,
1164.25107138131,1164.33075103213,1164.41045861452,1164.4902538436,1164.57009818531,
1164.65005661236,1164.69245248895,1164.77240978908,1164.85227258632,1164.9320584088,
1165.01178472399,1165.09146895229,1165.17113993851,1165.25080739203,1165.33048704285,
1165.41019462524,1165.48998985432,1165.56983419603,1165.64979262307,1165.69218849967,
1165.7721457998,1165.85200859704,1165.93179441952,1166.01152073471,1166.091204963,
1166.17087594923,1166.25054340275,1166.33022305357,1166.40993063596,1166.48972586504,
1166.56957020674,1166.64952863379,1166.69192451039,1166.77188181052,1166.85174460776,
1166.93153043024,1167.01125674543,1167.09094097373,1167.17061195995,1167.25027941347,
1167.32995906429,1167.40966664668,1167.48946187576,1167.56930621747,1167.64926464451,
1167.69166052111,1167.77161782124,1167.85148061848,1167.93126644096,1168.01099275615,
1168.09067698445,1168.17034797067,1168.25001542419,1168.32969507501,1168.4094026574,
1168.48919788648,1168.56904222819,1168.64900065523,1168.69139653183,1168.77135383196,
1168.8512166292,1168.93100245167,1169.01072876687,1169.09041299516,1169.17008398138,
1169.24975143491,1169.32943108573,1169.40913866812,1169.4889338972,1169.5687782389,
1169.64873666595,1169.69113254255,1169.79132222892),.UNSPECIFIED.);
#1315=B_SPLINE_CURVE_WITH_KNOTS('',3,(#156787,#156788,#156789,#156790,#156791,
#156792,#156793,#156794,#156795,#156796),.UNSPECIFIED.,.F.,.F.,(4,1,1,1,
1,1,1,4),(1169.79133132335,1170.69086855327,1171.69060456399,1172.69034057471,
1173.69007658543,1174.68981259615,1175.68954860687,1176.07450007552),
 .UNSPECIFIED.);
#1316=B_SPLINE_CURVE_WITH_KNOTS('',3,(#156798,#156799,#156800,#156801,#156802,
#156803,#156804,#156805,#156806,#156807,#156808,#156809,#156810,#156811,
#156812,#156813,#156814,#156815,#156816,#156817,#156818,#156819,#156820,
#156821,#156822,#156823,#156824,#156825,#156826,#156827,#156828,#156829,
#156830,#156831,#156832,#156833,#156834,#156835,#156836,#156837,#156838,
#156839,#156840,#156841,#156842,#156843,#156844,#156845,#156846,#156847,
#156848,#156849,#156850,#156851,#156852,#156853,#156854,#156855,#156856,
#156857,#156858,#156859,#156860,#156861,#156862,#156863,#156864,#156865,
#156866,#156867,#156868,#156869,#156870,#156871,#156872,#156873,#156874,
#156875,#156876,#156877,#156878,#156879,#156880,#156881,#156882,#156883,
#156884,#156885,#156886,#156887,#156888,#156889,#156890,#156891,#156892,
#156893,#156894,#156895,#156896,#156897,#156898,#156899,#156900,#156901,
#156902,#156903,#156904,#156905,#156906,#156907,#156908,#156909,#156910,
#156911,#156912,#156913,#156914,#156915,#156916,#156917,#156918,#156919,
#156920,#156921,#156922,#156923,#156924,#156925,#156926,#156927,#156928,
#156929,#156930,#156931,#156932,#156933,#156934,#156935,#156936,#156937,
#156938,#156939,#156940,#156941,#156942,#156943,#156944,#156945,#156946,
#156947,#156948,#156949,#156950,#156951,#156952,#156953,#156954,#156955,
#156956,#156957,#156958,#156959,#156960,#156961,#156962,#156963,#156964,
#156965,#156966,#156967,#156968,#156969,#156970,#156971,#156972,#156973,
#156974,#156975,#156976,#156977,#156978,#156979,#156980,#156981,#156982,
#156983,#156984,#156985,#156986,#156987,#156988,#156989,#156990,#156991,
#156992,#156993,#156994,#156995,#156996,#156997,#156998,#156999,#157000,
#157001,#157002,#157003,#157004,#157005,#157006,#157007,#157008,#157009,
#157010,#157011,#157012,#157013,#157014,#157015,#157016,#157017,#157018,
#157019,#157020,#157021,#157022,#157023,#157024,#157025,#157026,#157027,
#157028,#157029,#157030,#157031,#157032,#157033,#157034,#157035,#157036,
#157037,#157038,#157039,#157040,#157041,#157042,#157043,#157044),
 .UNSPECIFIED.,.F.,.F.,(4,3,3,3,3,3,3,3,3,3,3,3,3,3,3,3,3,3,3,3,3,3,3,3,
3,3,3,3,3,3,3,3,3,3,3,3,3,3,3,3,3,3,3,3,3,3,3,3,3,3,3,3,3,3,3,3,3,3,3,3,
3,3,3,3,3,3,3,3,3,3,3,3,3,3,3,3,3,3,3,3,3,3,4),(1176.0745075361,1176.15495807891,
1176.2354201739,1176.31590851967,1176.39643782787,1176.47707359616,1176.55776784111,
1176.63859250809,1176.68928461759,1176.76924191772,1176.84910471496,1176.92889053744,
1177.00861685263,1177.08830108093,1177.16797206715,1177.24763952067,1177.32731917149,
1177.40702675388,1177.48682198296,1177.56666632467,1177.64662475172,1177.68902062831,
1177.76897792844,1177.84884072568,1177.92862654816,1178.00835286335,1178.08803709165,
1178.16770807787,1178.24737553139,1178.32705518221,1178.4067627646,1178.48655799368,
1178.56640233539,1178.64636076243,1178.68875663903,1178.76871393916,1178.8485767364,
1178.92836255888,1179.00808887407,1179.08777310236,1179.16744408859,1179.24711154211,
1179.32679119293,1179.40649877532,1179.4862940044,1179.56613834611,1179.64609677315,
1179.68849264975,1179.76844994988,1179.84831274712,1179.9280985696,1180.00782488479,
1180.08750911308,1180.16718009931,1180.24684755283,1180.32652720365,1180.40623478604,
1180.48603001512,1180.56587435683,1180.64583278387,1180.68822866047,1180.7681859606,
1180.84804875784,1180.92783458031,1181.00756089551,1181.0872451238,1181.16691611002,
1181.24658356355,1181.32626321437,1181.40597079676,1181.48576602583,1181.56561036754,
1181.64556879459,1181.68796467119,1181.7716806927,1181.85144234334,1181.93112890649,
1182.01075624757,1182.09034019153,1182.16990326689,1182.2494544396,1182.32902377031,
1182.35769284328),.UNSPECIFIED.);
#1317=B_SPLINE_CURVE_WITH_KNOTS('',3,(#157046,#157047,#157048,#157049,#157050,
#157051,#157052,#157053,#157054,#157055),.UNSPECIFIED.,.F.,.F.,(4,1,1,1,
1,1,1,4),(1182.3577001467,1182.68770068191,1183.68743669263,1184.68717270335,
1185.68690871407,1186.68664472479,1187.68638073551,1188.64087815046),
 .UNSPECIFIED.);
#1318=B_SPLINE_CURVE_WITH_KNOTS('',3,(#157057,#157058,#157059,#157060,#157061,
#157062,#157063,#157064,#157065,#157066,#157067,#157068,#157069),
 .UNSPECIFIED.,.F.,.F.,(4,3,1,1,1,1,1,1,4),(1188.64087815046,1188.68611674623,
1189.68585275695,1190.68558876767,1191.68532477839,1192.68506078911,1193.68479679983,
1194.68453281055,1194.92406345764),.UNSPECIFIED.);
#1319=B_SPLINE_CURVE_WITH_KNOTS('',3,(#157071,#157072,#157073,#157074,#157075,
#157076,#157077,#157078,#157079,#157080),.UNSPECIFIED.,.F.,.F.,(4,1,1,1,
1,1,1,4),(1194.92406345764,1195.68426882127,1196.68400483199,1197.68374084271,
1198.68347685343,1199.68321286415,1200.68294887487,1201.20724876482),
 .UNSPECIFIED.);
#1320=B_SPLINE_CURVE_WITH_KNOTS('',3,(#157082,#157083,#157084,#157085,#157086,
#157087,#157088,#157089,#157090,#157091),.UNSPECIFIED.,.F.,.F.,(4,1,1,1,
1,1,1,4),(1201.20724876482,1201.68268488559,1202.68242089631,1203.68215690704,
1204.68189291776,1205.68162892848,1206.6813649392,1207.49042990411),
 .UNSPECIFIED.);
#1321=B_SPLINE_CURVE_WITH_KNOTS('',3,(#157093,#157094,#157095,#157096,#157097,
#157098,#157099,#157100,#157101,#157102,#157103,#157104,#157105,#157106,
#157107,#157108,#157109,#157110,#157111,#157112,#157113,#157114,#157115,
#157116,#157117,#157118,#157119,#157120,#157121,#157122,#157123,#157124,
#157125,#157126,#157127,#157128,#157129,#157130,#157131,#157132,#157133,
#157134,#157135,#157136,#157137,#157138,#157139,#157140,#157141,#157142,
#157143,#157144,#157145,#157146,#157147,#157148,#157149,#157150,#157151,
#157152,#157153,#157154,#157155,#157156,#157157,#157158,#157159,#157160,
#157161,#157162,#157163,#157164,#157165,#157166,#157167,#157168,#157169,
#157170,#157171,#157172,#157173,#157174,#157175,#157176,#157177,#157178,
#157179,#157180,#157181,#157182,#157183,#157184,#157185,#157186,#157187,
#157188,#157189,#157190,#157191,#157192,#157193,#157194,#157195,#157196,
#157197,#157198,#157199,#157200,#157201,#157202,#157203,#157204,#157205,
#157206,#157207,#157208,#157209,#157210,#157211,#157212,#157213,#157214,
#157215,#157216,#157217,#157218,#157219,#157220,#157221,#157222,#157223,
#157224,#157225,#157226,#157227,#157228,#157229,#157230,#157231,#157232,
#157233,#157234,#157235,#157236,#157237,#157238,#157239,#157240,#157241,
#157242,#157243,#157244,#157245,#157246,#157247,#157248,#157249,#157250,
#157251,#157252,#157253,#157254,#157255,#157256,#157257,#157258,#157259,
#157260,#157261,#157262,#157263,#157264,#157265,#157266,#157267,#157268,
#157269,#157270,#157271,#157272,#157273,#157274,#157275,#157276,#157277,
#157278,#157279,#157280,#157281,#157282,#157283,#157284,#157285,#157286,
#157287,#157288,#157289,#157290,#157291,#157292,#157293,#157294,#157295,
#157296,#157297,#157298,#157299,#157300,#157301,#157302,#157303,#157304,
#157305,#157306,#157307,#157308,#157309,#157310,#157311,#157312,#157313,
#157314,#157315,#157316,#157317,#157318,#157319,#157320,#157321,#157322,
#157323,#157324,#157325,#157326,#157327,#157328,#157329,#157330,#157331,
#157332,#157333,#157334,#157335,#157336),.UNSPECIFIED.,.F.,.F.,(4,3,3,3,
3,3,3,3,3,3,3,3,3,3,3,3,3,3,3,3,3,3,3,3,3,3,3,3,3,3,3,3,3,3,3,3,3,3,3,3,
3,3,3,3,3,3,3,3,3,3,3,3,3,3,3,3,3,3,3,3,3,3,3,3,3,3,3,3,3,3,3,3,3,3,3,3,
3,3,3,3,3,4),(1207.490434072,1207.6080995271,1207.68110094992,1207.76105825005,
1207.84092104729,1207.92070686976,1208.00043318496,1208.08011741325,1208.15978839947,
1208.239455853,1208.31913550382,1208.39884308621,1208.47863831529,1208.55848265699,
1208.63844108404,1208.68083696064,1208.76079426077,1208.84065705801,1208.92044288049,
1209.00016919568,1209.07985342397,1209.1595244102,1209.23919186372,1209.31887151454,
1209.39857909693,1209.47837432601,1209.55821866772,1209.63817709476,1209.68057297136,
1209.76053027149,1209.84039306873,1209.92017889121,1209.9999052064,1210.0795894347,
1210.15926042092,1210.23892787444,1210.31860752526,1210.39831510765,1210.47811033673,
1210.55795467844,1210.63791310548,1210.68030898208,1210.76026628221,1210.84012907945,
1210.91991490193,1210.99964121712,1211.07932544542,1211.15899643164,1211.23866388516,
1211.31834353598,1211.39805111837,1211.47784634745,1211.55769068916,1211.6376491162,
1211.6800449928,1211.76000229293,1211.83986509017,1211.91965091265,1211.99937722784,
1212.07906145614,1212.15873244236,1212.23839989588,1212.3180795467,1212.39778712909,
1212.47758235817,1212.55742669988,1212.63738512692,1212.67978100352,1212.75973830365,
1212.83960110089,1212.91938692337,1212.99911323856,1213.07879746686,1213.15846845308,
1213.2381359066,1213.31781555742,1213.39752313982,1213.47731836889,1213.5571627106,
1213.63712113765,1213.67951701424,1213.77361937918),.UNSPECIFIED.);
#1322=B_SPLINE_CURVE_WITH_KNOTS('',3,(#157338,#157339,#157340,#157341,#157342,
#157343,#157344,#157345,#157346,#157347),.UNSPECIFIED.,.F.,.F.,(4,1,1,1,
1,1,1,4),(1213.77362840169,1214.67925302496,1215.67898903568,1216.6787250464,
1217.67846105712,1218.67819706784,1219.67793307856,1220.05679710292),
 .UNSPECIFIED.);
#1323=B_SPLINE_CURVE_WITH_KNOTS('',3,(#157349,#157350,#157351,#157352,#157353,
#157354,#157355,#157356,#157357,#157358,#157359,#157360,#157361,#157362,
#157363,#157364,#157365,#157366,#157367,#157368,#157369,#157370,#157371,
#157372,#157373,#157374,#157375,#157376,#157377,#157378,#157379,#157380,
#157381,#157382,#157383,#157384,#157385,#157386,#157387,#157388,#157389,
#157390,#157391,#157392,#157393,#157394,#157395,#157396,#157397,#157398,
#157399,#157400,#157401,#157402,#157403,#157404,#157405,#157406,#157407,
#157408,#157409,#157410,#157411,#157412,#157413,#157414,#157415,#157416,
#157417,#157418,#157419,#157420,#157421,#157422,#157423,#157424,#157425,
#157426,#157427,#157428,#157429,#157430,#157431,#157432,#157433,#157434,
#157435,#157436,#157437,#157438,#157439,#157440,#157441,#157442,#157443,
#157444,#157445,#157446,#157447,#157448,#157449,#157450,#157451,#157452,
#157453,#157454,#157455,#157456,#157457,#157458,#157459,#157460,#157461,
#157462,#157463,#157464,#157465,#157466,#157467,#157468,#157469,#157470,
#157471,#157472,#157473,#157474,#157475,#157476,#157477,#157478,#157479,
#157480,#157481,#157482,#157483,#157484,#157485,#157486,#157487,#157488,
#157489,#157490,#157491,#157492,#157493,#157494,#157495,#157496,#157497,
#157498,#157499,#157500,#157501,#157502,#157503,#157504,#157505,#157506,
#157507,#157508,#157509,#157510,#157511,#157512,#157513,#157514,#157515,
#157516,#157517,#157518,#157519,#157520,#157521,#157522,#157523,#157524,
#157525,#157526,#157527,#157528,#157529,#157530,#157531,#157532,#157533,
#157534,#157535,#157536,#157537,#157538,#157539,#157540,#157541,#157542,
#157543,#157544,#157545,#157546,#157547,#157548,#157549,#157550,#157551,
#157552,#157553,#157554,#157555,#157556,#157557,#157558,#157559,#157560,
#157561,#157562,#157563,#157564,#157565,#157566,#157567,#157568,#157569,
#157570,#157571,#157572,#157573,#157574,#157575,#157576,#157577,#157578,
#157579,#157580,#157581,#157582,#157583,#157584,#157585,#157586,#157587,
#157588,#157589,#157590,#157591,#157592,#157593,#157594,#157595),
 .UNSPECIFIED.,.F.,.F.,(4,3,3,3,3,3,3,3,3,3,3,3,3,3,3,3,3,3,3,3,3,3,3,3,
3,3,3,3,3,3,3,3,3,3,3,3,3,3,3,3,3,3,3,3,3,3,3,3,3,3,3,3,3,3,3,3,3,3,3,3,
3,3,3,3,3,3,3,3,3,3,3,3,3,3,3,3,3,3,3,3,3,3,4),(1220.05680468636,1220.13714268496,
1220.21748902712,1220.29785857117,1220.37826618643,1220.45877790638,1220.5393458432,
1220.62004504479,1220.67766908928,1220.75762638941,1220.83748918665,1220.91727500912,
1220.99700132432,1221.07668555261,1221.15635653883,1221.23602399236,1221.31570364318,
1221.39541122557,1221.47520645465,1221.55505079635,1221.6350092234,1221.6774051,
1221.75736240013,1221.83722519737,1221.91701101985,1221.99673733504,1222.07642156333,
1222.15609254956,1222.23576000308,1222.3154396539,1222.39514723629,1222.47494246537,
1222.55478680708,1222.63474523412,1222.67714111072,1222.75709841085,1222.83696120809,
1222.91674703057,1222.99647334576,1223.07615757405,1223.15582856028,1223.2354960138,
1223.31517566462,1223.39488324701,1223.47467847609,1223.5545228178,1223.63448124484,
1223.67687712144,1223.75683442157,1223.83669721881,1223.91648304129,1223.99620935648,
1224.07589358478,1224.155564571,1224.23523202452,1224.31491167534,1224.39461925773,
1224.47441448681,1224.55425882852,1224.63421725556,1224.67661313216,1224.75657043229,
1224.83643322953,1224.91621905201,1224.9959453672,1225.0756295955,1225.15530058172,
1225.23496803524,1225.31464768606,1225.39435526845,1225.47415049753,1225.55399483924,
1225.63395326628,1225.67634914288,1225.75930424921,1225.83915601167,1225.9189317184,
1225.9986471538,1226.07831806141,1226.15796572783,1226.23760042992,1226.31725012176,
1226.33998999354),.UNSPECIFIED.);
#1324=B_SPLINE_CURVE_WITH_KNOTS('',3,(#157597,#157598,#157599,#157600,#157601,
#157602,#157603,#157604,#157605,#157606),.UNSPECIFIED.,.F.,.F.,(4,1,1,1,
1,1,1,4),(1226.33999748489,1226.6760851536,1227.67582116432,1228.67555717504,
1229.67529318576,1230.67502919648,1231.6747652072,1232.62317530072),
 .UNSPECIFIED.);
#1325=B_SPLINE_CURVE_WITH_KNOTS('',3,(#157608,#157609,#157610,#157611,#157612,
#157613,#157614,#157615,#157616,#157617,#157618,#157619),.UNSPECIFIED.,
 .F.,.F.,(4,2,1,1,1,1,1,1,4),(1232.62317530072,1232.67450121792,1233.67423722864,
1234.67397323936,1235.67370925008,1236.6734452608,1237.67318127152,1238.67291728224,
1238.9063606079),.UNSPECIFIED.);
#1326=B_SPLINE_CURVE_WITH_KNOTS('',3,(#157621,#157622,#157623,#157624,#157625,
#157626,#157627,#157628,#157629,#157630),.UNSPECIFIED.,.F.,.F.,(4,1,1,1,
1,1,1,4),(1238.9063606079,1239.67265329296,1240.67238930368,1241.6721253144,
1242.67186132512,1243.67159733584,1244.67133334656,1245.18954591508),
 .UNSPECIFIED.);
#1327=B_SPLINE_CURVE_WITH_KNOTS('',3,(#157632,#157633,#157634,#157635,#157636,
#157637,#157638,#157639,#157640,#157641),.UNSPECIFIED.,.F.,.F.,(4,1,1,1,
1,1,1,4),(1245.18954591508,1245.67106935728,1246.670805368,1247.67054137872,
1248.67027738944,1249.67001340016,1250.66974941088,1251.4727276359),
 .UNSPECIFIED.);
#1328=B_SPLINE_CURVE_WITH_KNOTS('',3,(#157643,#157644,#157645,#157646,#157647,
#157648,#157649,#157650,#157651,#157652,#157653,#157654,#157655,#157656,
#157657,#157658,#157659,#157660,#157661,#157662,#157663,#157664,#157665,
#157666,#157667,#157668,#157669,#157670,#157671,#157672,#157673,#157674,
#157675,#157676,#157677,#157678,#157679,#157680,#157681,#157682,#157683,
#157684,#157685,#157686,#157687,#157688,#157689,#157690,#157691,#157692,
#157693,#157694,#157695,#157696,#157697,#157698,#157699,#157700,#157701,
#157702,#157703,#157704,#157705,#157706,#157707,#157708,#157709,#157710,
#157711,#157712,#157713,#157714,#157715,#157716,#157717,#157718,#157719,
#157720,#157721,#157722,#157723,#157724,#157725,#157726,#157727,#157728,
#157729,#157730,#157731,#157732,#157733,#157734,#157735,#157736,#157737,
#157738,#157739,#157740,#157741,#157742,#157743,#157744,#157745,#157746,
#157747,#157748,#157749,#157750,#157751,#157752,#157753,#157754,#157755,
#157756,#157757,#157758,#157759,#157760,#157761,#157762,#157763,#157764,
#157765,#157766,#157767,#157768,#157769,#157770,#157771,#157772,#157773,
#157774,#157775,#157776,#157777,#157778,#157779,#157780,#157781,#157782,
#157783,#157784,#157785,#157786,#157787,#157788,#157789,#157790,#157791,
#157792,#157793,#157794,#157795,#157796,#157797,#157798,#157799,#157800,
#157801,#157802,#157803,#157804,#157805,#157806,#157807,#157808,#157809,
#157810,#157811,#157812,#157813,#157814,#157815,#157816,#157817,#157818,
#157819,#157820,#157821,#157822,#157823,#157824,#157825,#157826,#157827,
#157828,#157829,#157830,#157831,#157832,#157833,#157834,#157835,#157836,
#157837,#157838,#157839,#157840,#157841,#157842,#157843,#157844,#157845,
#157846,#157847,#157848,#157849,#157850,#157851,#157852,#157853,#157854,
#157855,#157856,#157857,#157858,#157859,#157860,#157861,#157862,#157863,
#157864,#157865,#157866,#157867,#157868,#157869,#157870,#157871,#157872,
#157873,#157874,#157875,#157876,#157877,#157878,#157879,#157880,#157881,
#157882,#157883,#157884,#157885,#157886),.UNSPECIFIED.,.F.,.F.,(4,3,3,3,
3,3,3,3,3,3,3,3,3,3,3,3,3,3,3,3,3,3,3,3,3,3,3,3,3,3,3,3,3,3,3,3,3,3,3,3,
3,3,3,3,3,3,3,3,3,3,3,3,3,3,3,3,3,3,3,3,3,3,3,3,3,3,3,3,3,3,3,3,3,3,3,3,
3,3,3,3,3,4),(1251.47273122226,1251.58846939653,1251.6694854216,1251.74944272173,
1251.82930551897,1251.90909134145,1251.98881765664,1252.06850188494,1252.14817287116,
1252.22784032468,1252.3075199755,1252.3872275579,1252.46702278697,1252.54686712868,
1252.62682555573,1252.66922143232,1252.74917873245,1252.82904152969,1252.90882735217,
1252.98855366736,1253.06823789566,1253.14790888188,1253.2275763354,1253.30725598622,
1253.38696356861,1253.46675879769,1253.5466031394,1253.62656156644,1253.66895744304,
1253.74891474317,1253.82877754041,1253.90856336289,1253.98828967808,1254.06797390637,
1254.1476448926,1254.22731234612,1254.30699199694,1254.38669957933,1254.46649480841,
1254.54633915012,1254.62629757716,1254.66869345376,1254.74865075389,1254.82851355113,
1254.90829937361,1254.9880256888,1255.06770991709,1255.14738090332,1255.22704835684,
1255.30672800766,1255.38643559005,1255.46623081913,1255.54607516084,1255.62603358788,
1255.66842946448,1255.74838676461,1255.82824956185,1255.90803538433,1255.98776169952,
1256.06744592781,1256.14711691404,1256.22678436756,1256.30646401838,1256.38617160077,
1256.46596682985,1256.54581117156,1256.6257695986,1256.6681654752,1256.74812277533,
1256.82798557257,1256.90777139504,1256.98749771024,1257.06718193853,1257.14685292475,
1257.22652037828,1257.30620002909,1257.38590761149,1257.46570284056,1257.54554718227,
1257.62550560931,1257.66790148592,1257.75591652944),.UNSPECIFIED.);
#1329=B_SPLINE_CURVE_WITH_KNOTS('',3,(#157888,#157889,#157890,#157891,#157892,
#157893,#157894,#157895,#157896,#157897),.UNSPECIFIED.,.F.,.F.,(4,1,1,1,
1,1,1,4),(1257.75592528103,1258.66763749664,1259.66737350736,1260.66710951808,
1261.6668455288,1262.66658153952,1263.66631755024,1264.03909416751),
 .UNSPECIFIED.);
#1330=B_SPLINE_CURVE_WITH_KNOTS('',3,(#157899,#157900,#157901,#157902,#157903,
#157904,#157905,#157906,#157907,#157908,#157909,#157910,#157911,#157912,
#157913,#157914,#157915,#157916,#157917,#157918,#157919,#157920,#157921,
#157922,#157923,#157924,#157925,#157926,#157927,#157928,#157929,#157930,
#157931,#157932,#157933,#157934,#157935,#157936,#157937,#157938,#157939,
#157940,#157941,#157942,#157943,#157944,#157945,#157946,#157947,#157948,
#157949,#157950,#157951,#157952,#157953,#157954,#157955,#157956,#157957,
#157958,#157959,#157960,#157961,#157962,#157963,#157964,#157965,#157966,
#157967,#157968,#157969,#157970,#157971,#157972,#157973,#157974,#157975,
#157976,#157977,#157978,#157979,#157980,#157981,#157982,#157983,#157984,
#157985,#157986,#157987,#157988,#157989,#157990,#157991,#157992,#157993,
#157994,#157995,#157996,#157997,#157998,#157999,#158000,#158001,#158002,
#158003,#158004,#158005,#158006,#158007,#158008,#158009,#158010,#158011,
#158012,#158013,#158014,#158015,#158016,#158017,#158018,#158019,#158020,
#158021,#158022,#158023,#158024,#158025,#158026,#158027,#158028,#158029,
#158030,#158031,#158032,#158033,#158034,#158035,#158036,#158037,#158038,
#158039,#158040,#158041,#158042,#158043,#158044,#158045,#158046,#158047,
#158048,#158049,#158050,#158051,#158052,#158053,#158054,#158055,#158056,
#158057,#158058,#158059,#158060,#158061,#158062,#158063,#158064,#158065,
#158066,#158067,#158068,#158069,#158070,#158071,#158072,#158073,#158074,
#158075,#158076,#158077,#158078,#158079,#158080,#158081,#158082,#158083,
#158084,#158085,#158086,#158087,#158088,#158089,#158090,#158091,#158092,
#158093,#158094,#158095,#158096,#158097,#158098,#158099,#158100,#158101,
#158102,#158103,#158104,#158105,#158106,#158107,#158108,#158109,#158110,
#158111,#158112,#158113,#158114,#158115,#158116,#158117,#158118,#158119,
#158120,#158121,#158122,#158123,#158124,#158125,#158126,#158127,#158128,
#158129,#158130,#158131,#158132,#158133,#158134,#158135,#158136,#158137,
#158138,#158139,#158140,#158141,#158142,#158143,#158144,#158145),
 .UNSPECIFIED.,.F.,.F.,(4,3,3,3,3,3,3,3,3,3,3,3,3,3,3,3,3,3,3,3,3,3,3,3,
3,3,3,3,3,3,3,3,3,3,3,3,3,3,3,3,3,3,3,3,3,3,3,3,3,3,3,3,3,3,3,3,3,3,3,3,
3,3,3,3,3,3,3,3,3,3,3,3,3,3,3,3,3,3,3,3,3,3,4),(1264.03910183662,1264.11933138465,
1264.1995661766,1264.27982121819,1264.36011152426,1264.44050364496,1264.52094977296,
1264.60152805393,1264.66605356096,1264.74601086109,1264.82587365834,1264.90565948081,
1264.985385796,1265.0650700243,1265.14474101052,1265.22440846405,1265.30408811487,
1265.38379569726,1265.46359092634,1265.54343526805,1265.62339369509,1265.66578957168,
1265.74574687181,1265.82560966905,1265.90539549153,1265.98512180672,1266.06480603502,
1266.14447702124,1266.22414447476,1266.30382412558,1266.38353170798,1266.46332693705,
1266.54317127876,1266.62312970581,1266.6655255824,1266.74548288253,1266.82534567977,
1266.90513150224,1266.98485781744,1267.06454204573,1267.14421303195,1267.22388048548,
1267.3035601363,1267.38326771869,1267.46306294777,1267.54290728947,1267.62286571652,
1267.66526159312,1267.74521889325,1267.82508169049,1267.90486751297,1267.98459382816,
1268.06427805645,1268.14394904268,1268.2236164962,1268.30329614702,1268.38300372941,
1268.46279895849,1268.5426433002,1268.62260172724,1268.66499760384,1268.74495490397,
1268.82481770121,1268.90460352368,1268.98432983888,1269.06401406717,1269.14368505339,
1269.22335250692,1269.30303215773,1269.38273974013,1269.4625349692,1269.54237931091,
1269.62233773796,1269.66473361456,1269.74692780571,1269.82687350363,1269.90674213099,
1269.98654938442,1270.07048382426,1270.15021860611,1270.2299400296,1270.3096734261,
1270.3222871438),.UNSPECIFIED.);
#1331=B_SPLINE_CURVE_WITH_KNOTS('',3,(#158147,#158148,#158149,#158150,#158151,
#158152,#158153,#158154,#158155,#158156,#158157),.UNSPECIFIED.,.F.,.F.,
(4,2,1,1,1,1,1,4),(1270.32229478416,1270.66446962528,1271.664205636,1272.66394164672,
1273.66367765744,1274.66341366816,1275.66314967888,1276.60547245098),
 .UNSPECIFIED.);
#1332=B_SPLINE_CURVE_WITH_KNOTS('',3,(#158159,#158160,#158161,#158162,#158163,
#158164,#158165,#158166,#158167,#158168,#158169,#158170,#158171),
 .UNSPECIFIED.,.F.,.F.,(4,3,1,1,1,1,1,1,4),(1276.60547245098,1276.6628856896,
1277.66262170032,1278.66235771104,1279.66209372177,1280.66182973249,1281.66156574321,
1282.66130175393,1282.88865775816),.UNSPECIFIED.);
#1333=B_SPLINE_CURVE_WITH_KNOTS('',3,(#158173,#158174,#158175,#158176,#158177,
#158178,#158179,#158180,#158181,#158182,#158183,#158184,#158185,#158186,
#158187,#158188,#158189,#158190,#158191,#158192,#158193,#158194,#158195,
#158196,#158197,#158198,#158199,#158200,#158201,#158202,#158203,#158204,
#158205,#158206,#158207,#158208,#158209,#158210,#158211,#158212,#158213,
#158214,#158215,#158216,#158217,#158218,#158219,#158220,#158221,#158222,
#158223,#158224,#158225,#158226,#158227,#158228,#158229,#158230,#158231,
#158232,#158233,#158234,#158235,#158236,#158237,#158238,#158239,#158240,
#158241,#158242,#158243,#158244,#158245,#158246,#158247,#158248,#158249,
#158250,#158251,#158252,#158253,#158254,#158255,#158256,#158257,#158258,
#158259,#158260,#158261,#158262,#158263,#158264,#158265,#158266,#158267,
#158268,#158269,#158270,#158271,#158272,#158273,#158274,#158275,#158276,
#158277,#158278,#158279,#158280,#158281,#158282,#158283,#158284,#158285,
#158286,#158287,#158288,#158289,#158290,#158291,#158292,#158293,#158294,
#158295,#158296,#158297,#158298,#158299,#158300,#158301,#158302,#158303,
#158304,#158305,#158306,#158307,#158308,#158309,#158310,#158311,#158312,
#158313,#158314,#158315,#158316,#158317,#158318,#158319,#158320,#158321,
#158322,#158323,#158324,#158325,#158326,#158327,#158328,#158329,#158330,
#158331,#158332,#158333,#158334,#158335,#158336,#158337,#158338,#158339,
#158340,#158341,#158342,#158343,#158344,#158345,#158346,#158347,#158348,
#158349,#158350,#158351,#158352,#158353,#158354,#158355,#158356,#158357,
#158358,#158359,#158360,#158361,#158362,#158363,#158364,#158365,#158366,
#158367,#158368,#158369,#158370,#158371,#158372,#158373,#158374,#158375,
#158376,#158377,#158378,#158379,#158380,#158381,#158382,#158383,#158384,
#158385,#158386,#158387,#158388,#158389,#158390,#158391,#158392,#158393,
#158394,#158395,#158396,#158397,#158398,#158399,#158400,#158401,#158402,
#158403,#158404,#158405,#158406,#158407,#158408,#158409,#158410,#158411,
#158412,#158413,#158414,#158415,#158416,#158417,#158418,#158419),
 .UNSPECIFIED.,.F.,.F.,(4,3,3,3,3,3,3,3,3,3,3,3,3,3,3,3,3,3,3,3,3,3,3,3,
3,3,3,3,3,3,3,3,3,3,3,3,3,3,3,3,3,3,3,3,3,3,3,3,3,3,3,3,3,3,3,3,3,3,3,3,
3,3,3,3,3,3,3,3,3,3,3,3,3,3,3,3,3,3,3,3,3,3,4),(1282.88865775816,1282.96738598792,
1283.04605850303,1283.12470073832,1283.20332865433,1283.28195874242,1283.36060749377,
1283.43933693173,1283.51810858998,1283.59699808486,1283.66103776465,1283.74099506478,
1283.82085786202,1283.9006436845,1283.98036999969,1284.06005422798,1284.13972521421,
1284.21939266773,1284.29907231855,1284.37877990094,1284.45857513002,1284.53841947172,
1284.61837789877,1284.66077377537,1284.7407310755,1284.82059387274,1284.90037969522,
1284.98010601041,1285.0597902387,1285.13946122493,1285.21912867845,1285.29880832927,
1285.37851591166,1285.45831114074,1285.53815548244,1285.61811390949,1285.66050978609,
1285.74046708622,1285.82032988346,1285.90011570594,1285.97984202113,1286.05952624943,
1286.13919723565,1286.21886468917,1286.29854433999,1286.37825192238,1286.45804715146,
1286.53789149317,1286.61784992022,1286.66024579681,1286.74020309694,1286.82006589418,
1286.89985171666,1286.97957803185,1287.05926226015,1287.13893324637,1287.21860069989,
1287.29828035071,1287.3779879331,1287.45778316218,1287.53762750389,1287.61758593093,
1287.65998180753,1287.73993910766,1287.8198019049,1287.89958772738,1287.97931404257,
1288.05899827086,1288.13866925708,1288.21833671061,1288.29801636143,1288.37772394382,
1288.4575191729,1288.53736351461,1288.61732194165,1288.65971781825,1288.7433496464,
1288.8268491885,1288.91309765771,1288.99631706811,1289.07944368197,1289.16246189708,
1289.17184306534),.UNSPECIFIED.);
#1334=B_SPLINE_CURVE_WITH_KNOTS('',3,(#158421,#158422,#158423,#158424,#158425,
#158426,#158427,#158428,#158429,#158430,#158431,#158432,#158433,#158434,
#158435,#158436,#158437,#158438,#158439,#158440,#158441,#158442,#158443,
#158444,#158445,#158446,#158447,#158448,#158449,#158450,#158451,#158452,
#158453,#158454,#158455,#158456,#158457,#158458,#158459,#158460,#158461,
#158462,#158463,#158464,#158465,#158466,#158467,#158468,#158469,#158470,
#158471,#158472,#158473,#158474,#158475,#158476,#158477,#158478,#158479,
#158480,#158481,#158482,#158483,#158484,#158485,#158486,#158487,#158488,
#158489,#158490,#158491,#158492,#158493,#158494,#158495,#158496,#158497,
#158498,#158499,#158500,#158501,#158502,#158503,#158504,#158505,#158506,
#158507,#158508,#158509,#158510,#158511,#158512,#158513,#158514,#158515,
#158516,#158517,#158518,#158519,#158520,#158521,#158522,#158523,#158524,
#158525,#158526,#158527,#158528,#158529,#158530,#158531,#158532,#158533,
#158534,#158535,#158536,#158537,#158538,#158539,#158540,#158541,#158542,
#158543,#158544,#158545,#158546,#158547,#158548,#158549,#158550,#158551,
#158552,#158553,#158554,#158555,#158556,#158557,#158558,#158559,#158560,
#158561,#158562,#158563,#158564,#158565,#158566,#158567,#158568,#158569,
#158570,#158571,#158572,#158573,#158574,#158575,#158576,#158577,#158578,
#158579,#158580,#158581,#158582,#158583,#158584,#158585,#158586,#158587,
#158588,#158589,#158590,#158591,#158592,#158593,#158594,#158595,#158596,
#158597,#158598,#158599,#158600,#158601,#158602,#158603,#158604,#158605,
#158606,#158607,#158608,#158609,#158610,#158611,#158612,#158613,#158614,
#158615,#158616,#158617,#158618,#158619,#158620,#158621,#158622,#158623,
#158624,#158625,#158626,#158627,#158628,#158629,#158630,#158631,#158632,
#158633,#158634,#158635,#158636,#158637,#158638,#158639,#158640,#158641,
#158642,#158643,#158644,#158645,#158646,#158647,#158648,#158649,#158650,
#158651,#158652,#158653,#158654,#158655,#158656,#158657,#158658,#158659,
#158660,#158661,#158662,#158663,#158664),.UNSPECIFIED.,.F.,.F.,(4,3,3,3,
3,3,3,3,3,3,3,3,3,3,3,3,3,3,3,3,3,3,3,3,3,3,3,3,3,3,3,3,3,3,3,3,3,3,3,3,
3,3,3,3,3,3,3,3,3,3,3,3,3,3,3,3,3,3,3,3,3,3,3,3,3,3,3,3,3,3,3,3,3,3,3,3,
3,3,3,3,3,4),(1289.17184306547,1289.25573730055,1289.33975209835,1289.423976356,
1289.50830956445,1289.59284136574,1289.65945382897,1289.7394111291,1289.81927392634,
1289.89905974882,1289.97878606401,1290.05847029231,1290.13814127853,1290.21780873205,
1290.29748838287,1290.37719596526,1290.45699119434,1290.53683553605,1290.61679396309,
1290.65918983969,1290.73914713982,1290.81900993706,1290.89879575954,1290.97852207473,
1291.05820630303,1291.13787728925,1291.21754474277,1291.29722439359,1291.37693197598,
1291.45672720506,1291.53657154677,1291.61652997381,1291.65892585041,1291.73888315054,
1291.81874594778,1291.89853177026,1291.97825808545,1292.05794231375,1292.13761329997,
1292.21728075349,1292.29696040431,1292.3766679867,1292.45646321578,1292.53630755749,
1292.61626598453,1292.65866186113,1292.73861916126,1292.8184819585,1292.89826778098,
1292.97799409617,1293.05767832447,1293.13734931069,1293.21701676421,1293.29669641503,
1293.37640399742,1293.4561992265,1293.53604356821,1293.61600199525,1293.65839787185,
1293.73835517198,1293.81821796922,1293.8980037917,1293.97773010689,1294.05741433518,
1294.1370853214,1294.21675277493,1294.29643242575,1294.37614000814,1294.45593523722,
1294.53577957892,1294.61573800597,1294.65813388257,1294.73694668814,1294.81566481368,
1294.89558525854,1294.97416387267,1295.05270920096,1295.13123780294,1295.21218544533,
1295.29075645646,1295.37289241449,1295.45502837252),.UNSPECIFIED.);
#1335=B_SPLINE_CURVE_WITH_KNOTS('',3,(#158666,#158667,#158668,#158669,#158670,
#158671,#158672,#158673,#158674,#158675,#158676),.UNSPECIFIED.,.F.,.F.,
(4,1,1,1,1,1,1,1,4),(1295.45502837252,1295.65786989329,1296.65760590401,
1297.65734191473,1298.65707792545,1299.65681393617,1300.65654994689,1301.65628595761,
1301.7382136797),.UNSPECIFIED.);
#1336=B_SPLINE_CURVE_WITH_KNOTS('',3,(#158678,#158679,#158680,#158681,#158682,
#158683,#158684,#158685,#158686,#158687),.UNSPECIFIED.,.F.,.F.,(4,1,1,1,
1,1,1,4),(1301.7382136797,1302.65602196833,1303.65575797905,1304.65549398977,
1305.65523000049,1306.65496601121,1307.65470202193,1308.02139898688),
 .UNSPECIFIED.);
#1337=B_SPLINE_CURVE_WITH_KNOTS('',3,(#158689,#158690,#158691,#158692,#158693,
#158694,#158695,#158696,#158697,#158698),.UNSPECIFIED.,.F.,.F.,(4,1,1,1,
1,1,1,4),(1308.02139898688,1308.65443803265,1309.65417404337,1310.65391005409,
1311.65364606481,1312.65338207553,1313.65311808625,1314.30458429405),
 .UNSPECIFIED.);
#1338=B_SPLINE_CURVE_WITH_KNOTS('',3,(#158700,#158701,#158702,#158703,#158704,
#158705,#158706,#158707,#158708,#158709,#158710,#158711,#158712,#158713,
#158714,#158715,#158716,#158717,#158718,#158719,#158720,#158721,#158722,
#158723,#158724,#158725,#158726,#158727,#158728,#158729,#158730,#158731,
#158732,#158733,#158734,#158735,#158736,#158737,#158738,#158739,#158740,
#158741,#158742,#158743,#158744,#158745,#158746,#158747,#158748,#158749,
#158750,#158751,#158752,#158753,#158754,#158755,#158756,#158757,#158758,
#158759,#158760,#158761,#158762,#158763,#158764,#158765,#158766,#158767,
#158768,#158769,#158770,#158771,#158772,#158773,#158774,#158775,#158776,
#158777,#158778,#158779,#158780,#158781,#158782,#158783,#158784,#158785,
#158786,#158787,#158788,#158789,#158790,#158791,#158792,#158793,#158794,
#158795,#158796,#158797,#158798,#158799,#158800,#158801,#158802,#158803,
#158804,#158805,#158806,#158807,#158808,#158809,#158810,#158811,#158812,
#158813,#158814,#158815,#158816,#158817,#158818,#158819,#158820,#158821,
#158822,#158823,#158824,#158825,#158826,#158827,#158828,#158829,#158830,
#158831,#158832,#158833,#158834,#158835,#158836,#158837,#158838,#158839,
#158840,#158841,#158842,#158843,#158844,#158845,#158846,#158847,#158848,
#158849,#158850,#158851,#158852,#158853,#158854,#158855,#158856,#158857,
#158858,#158859,#158860,#158861,#158862,#158863,#158864,#158865,#158866,
#158867,#158868,#158869,#158870,#158871,#158872,#158873,#158874,#158875,
#158876,#158877,#158878,#158879,#158880,#158881,#158882,#158883,#158884,
#158885,#158886,#158887,#158888,#158889,#158890,#158891,#158892,#158893,
#158894,#158895,#158896,#158897,#158898,#158899,#158900,#158901,#158902,
#158903,#158904,#158905,#158906,#158907,#158908,#158909,#158910,#158911,
#158912,#158913,#158914,#158915,#158916,#158917,#158918,#158919,#158920,
#158921,#158922,#158923,#158924,#158925,#158926,#158927,#158928,#158929,
#158930,#158931,#158932,#158933,#158934,#158935,#158936,#158937,#158938,
#158939,#158940,#158941,#158942,#158943),.UNSPECIFIED.,.F.,.F.,(4,3,3,3,
3,3,3,3,3,3,3,3,3,3,3,3,3,3,3,3,3,3,3,3,3,3,3,3,3,3,3,3,3,3,3,3,3,3,3,3,
3,3,3,3,3,3,3,3,3,3,3,3,3,3,3,3,3,3,3,3,3,3,3,3,3,3,3,3,3,3,3,3,3,3,3,3,
3,3,3,3,3,4),(1314.3045844167,1314.39621327382,1314.48828678864,1314.58094463404,
1314.65285409697,1314.7328113971,1314.81267419434,1314.89246001681,1314.972186332,
1315.05187056029,1315.13154154651,1315.21120900003,1315.29088865084,1315.37059623324,
1315.45039146231,1315.53023580401,1315.61019423106,1315.65259010769,1315.73254740782,
1315.81241020506,1315.89219602754,1315.97192234273,1316.05160657102,1316.13127755725,
1316.21094501077,1316.29062466159,1316.37033224398,1316.45012747306,1316.52997181476,
1316.60993024181,1316.65232611841,1316.73228341854,1316.81214621579,1316.89193203826,
1316.97165835345,1317.05134258175,1317.13101356797,1317.2106810215,1317.29036067231,
1317.37006825471,1317.44986348379,1317.52970782549,1317.60966625254,1317.65206212913,
1317.73201942926,1317.8118822265,1317.89166804897,1317.97139436417,1318.05107859246,
1318.13074957868,1318.21041703221,1318.29009668303,1318.36980426542,1318.44959949449,
1318.5294438362,1318.60940226325,1318.65179813985,1318.73175543998,1318.81161823722,
1318.8914040597,1318.97113037489,1319.05081460319,1319.13048558941,1319.21015304293,
1319.28983269375,1319.36954027615,1319.44933550522,1319.52917984693,1319.60913827398,
1319.65153415057,1319.73075336223,1319.80987859597,1319.88892802244,1319.96791974293,
1320.04687761498,1320.12581889128,1320.20475987108,1320.28371685104,1320.36275030379,
1320.44182335561,1320.52101079753,1320.58776960123),.UNSPECIFIED.);
#1339=B_SPLINE_CURVE_WITH_KNOTS('',3,(#158945,#158946,#158947,#158948,#158949,
#158950,#158951,#158952,#158953,#158954,#158955,#158956,#158957),
 .UNSPECIFIED.,.F.,.F.,(4,3,1,1,1,1,1,1,4),(1320.58776960123,1320.65127016129,
1321.65100617201,1322.65074218273,1323.65047819345,1324.65021420417,1325.64995021489,
1326.64968622561,1326.87095490841),.UNSPECIFIED.);
#1340=B_SPLINE_CURVE_WITH_KNOTS('',3,(#158959,#158960,#158961,#158962,#158963,
#158964,#158965,#158966,#158967,#158968,#158969,#158970,#158971,#158972,
#158973,#158974,#158975,#158976,#158977,#158978,#158979,#158980,#158981,
#158982,#158983,#158984,#158985,#158986,#158987,#158988,#158989,#158990,
#158991,#158992,#158993,#158994,#158995,#158996,#158997,#158998,#158999,
#159000,#159001,#159002,#159003,#159004,#159005,#159006,#159007,#159008,
#159009,#159010,#159011,#159012,#159013,#159014,#159015,#159016,#159017,
#159018,#159019,#159020,#159021,#159022,#159023,#159024,#159025,#159026,
#159027,#159028,#159029,#159030,#159031,#159032,#159033,#159034,#159035,
#159036,#159037,#159038,#159039,#159040,#159041,#159042,#159043,#159044,
#159045,#159046,#159047,#159048,#159049,#159050,#159051,#159052,#159053,
#159054,#159055,#159056,#159057,#159058,#159059,#159060,#159061,#159062,
#159063,#159064,#159065,#159066,#159067,#159068,#159069,#159070,#159071,
#159072,#159073,#159074,#159075,#159076,#159077,#159078,#159079,#159080,
#159081,#159082,#159083,#159084,#159085,#159086,#159087,#159088,#159089,
#159090,#159091,#159092,#159093,#159094,#159095,#159096,#159097,#159098,
#159099,#159100,#159101,#159102,#159103,#159104,#159105,#159106,#159107,
#159108,#159109,#159110,#159111,#159112,#159113,#159114,#159115,#159116,
#159117,#159118,#159119,#159120,#159121,#159122,#159123,#159124,#159125,
#159126,#159127,#159128,#159129,#159130,#159131,#159132,#159133,#159134,
#159135,#159136,#159137,#159138,#159139,#159140,#159141,#159142,#159143,
#159144,#159145,#159146,#159147,#159148,#159149,#159150,#159151,#159152,
#159153,#159154,#159155,#159156,#159157,#159158,#159159,#159160,#159161,
#159162,#159163,#159164,#159165,#159166,#159167,#159168,#159169,#159170,
#159171,#159172,#159173,#159174,#159175,#159176,#159177,#159178,#159179,
#159180,#159181,#159182,#159183,#159184,#159185,#159186,#159187,#159188,
#159189,#159190,#159191,#159192,#159193,#159194,#159195,#159196,#159197,
#159198,#159199,#159200,#159201,#159202),.UNSPECIFIED.,.F.,.F.,(4,3,3,3,
3,3,3,3,3,3,3,3,3,3,3,3,3,3,3,3,3,3,3,3,3,3,3,3,3,3,3,3,3,3,3,3,3,3,3,3,
3,3,3,3,3,3,3,3,3,3,3,3,3,3,3,3,3,3,3,3,3,3,3,3,3,3,3,3,3,3,3,3,3,3,3,3,
3,3,3,3,3,4),(1326.87095490841,1326.94966200019,1327.02831162128,1327.10692865002,
1327.18552980509,1327.26413159478,1327.34275052616,1327.42144926218,1327.50018888353,
1327.579047932,1327.64942223633,1327.72937953646,1327.8092423337,1327.88902815617,
1327.96875447137,1328.04843869966,1328.12810968588,1328.20777713941,1328.28745679023,
1328.36716437262,1328.4469596017,1328.5268039434,1328.60676237045,1328.64915824705,
1328.72911554718,1328.80897834442,1328.88876416689,1328.96849048209,1329.04817471038,
1329.1278456966,1329.20751315013,1329.28719280095,1329.36690038334,1329.44669561241,
1329.52653995412,1329.60649838117,1329.64889425777,1329.7288515579,1329.80871435514,
1329.88850017762,1329.96822649281,1330.04791072111,1330.12758170733,1330.20724916085,
1330.28692881167,1330.36663639406,1330.44643162314,1330.52627596485,1330.60623439189,
1330.64863026849,1330.72858756862,1330.80845036586,1330.88823618834,1330.96796250353,
1331.04764673182,1331.12731771805,1331.20698517157,1331.28666482239,1331.36637240478,
1331.44616763386,1331.52601197557,1331.60597040261,1331.64836627921,1331.72832357934,
1331.80818637658,1331.88797219906,1331.96769851425,1332.04738274255,1332.12705372877,
1332.20672118229,1332.28640083311,1332.36610841551,1332.44590364458,1332.52574798629,
1332.60570641334,1332.64810228993,1332.73195292313,1332.81566815408,1332.90028616946,
1332.98371340598,1333.06892681078,1333.15414021559),.UNSPECIFIED.);
#1341=B_SPLINE_CURVE_WITH_KNOTS('',3,(#159204,#159205,#159206,#159207,#159208,
#159209,#159210,#159211,#159212,#159213,#159214,#159215,#159216,#159217,
#159218,#159219,#159220,#159221,#159222,#159223,#159224,#159225,#159226,
#159227,#159228,#159229,#159230,#159231,#159232,#159233,#159234,#159235,
#159236,#159237,#159238,#159239,#159240,#159241,#159242,#159243,#159244,
#159245,#159246,#159247,#159248,#159249,#159250,#159251,#159252,#159253,
#159254,#159255,#159256,#159257,#159258,#159259,#159260,#159261,#159262,
#159263,#159264,#159265,#159266,#159267,#159268,#159269,#159270,#159271,
#159272,#159273,#159274,#159275,#159276,#159277,#159278,#159279,#159280,
#159281,#159282,#159283,#159284,#159285,#159286,#159287,#159288,#159289,
#159290,#159291,#159292,#159293,#159294,#159295,#159296,#159297,#159298,
#159299,#159300,#159301,#159302,#159303,#159304,#159305,#159306,#159307,
#159308,#159309,#159310,#159311,#159312,#159313,#159314,#159315,#159316,
#159317,#159318,#159319,#159320,#159321,#159322,#159323,#159324,#159325,
#159326,#159327,#159328,#159329,#159330,#159331,#159332,#159333,#159334,
#159335,#159336,#159337,#159338,#159339,#159340,#159341,#159342,#159343,
#159344,#159345,#159346,#159347,#159348,#159349,#159350,#159351,#159352,
#159353,#159354,#159355,#159356,#159357,#159358,#159359,#159360,#159361,
#159362,#159363,#159364,#159365,#159366,#159367,#159368,#159369,#159370,
#159371,#159372,#159373,#159374,#159375,#159376,#159377,#159378,#159379,
#159380,#159381,#159382,#159383,#159384,#159385,#159386,#159387,#159388,
#159389,#159390,#159391,#159392,#159393,#159394,#159395,#159396,#159397,
#159398,#159399,#159400,#159401,#159402,#159403,#159404,#159405,#159406,
#159407,#159408,#159409,#159410,#159411,#159412,#159413,#159414,#159415,
#159416,#159417,#159418,#159419,#159420,#159421,#159422,#159423,#159424,
#159425,#159426,#159427,#159428,#159429,#159430,#159431,#159432,#159433,
#159434,#159435,#159436,#159437,#159438,#159439,#159440,#159441,#159442,
#159443,#159444,#159445,#159446,#159447),.UNSPECIFIED.,.F.,.F.,(4,3,3,3,
3,3,3,3,3,3,3,3,3,3,3,3,3,3,3,3,3,3,3,3,3,3,3,3,3,3,3,3,3,3,3,3,3,3,3,3,
3,3,3,3,3,3,3,3,3,3,3,3,3,3,3,3,3,3,3,3,3,3,3,3,3,3,3,3,3,3,3,3,3,3,3,3,
3,3,3,3,3,4),(1333.15414021572,1333.23781402459,1333.32160032962,1333.40558801224,
1333.48967942233,1333.57396772497,1333.64783830065,1333.72779560078,1333.80765839802,
1333.88744422049,1333.96717053569,1334.04685476398,1334.1265257502,1334.20619320373,
1334.28587285454,1334.36558043693,1334.44537566601,1334.52522000772,1334.60517843476,
1334.64757431137,1334.7275316115,1334.80739440874,1334.88718023122,1334.96690654641,
1335.0465907747,1335.12626176093,1335.20592921445,1335.28560886527,1335.36531644766,
1335.44511167674,1335.52495601845,1335.60491444549,1335.64731032209,1335.72726762222,
1335.80713041946,1335.88691624194,1335.96664255713,1336.04632678543,1336.12599777165,
1336.20566522517,1336.28534487599,1336.36505245839,1336.44484768746,1336.52469202917,
1336.60465045622,1336.64704633281,1336.72700363294,1336.80686643018,1336.88665225266,
1336.96637856785,1337.04606279614,1337.12573378236,1337.20540123589,1337.28508088671,
1337.3647884691,1337.44458369818,1337.52442803988,1337.60438646693,1337.64678234353,
1337.72673964366,1337.8066024409,1337.88638826338,1337.96611457857,1338.04579880687,
1338.12546979309,1338.20513724661,1338.28481689743,1338.36452447983,1338.4443197089,
1338.52416405061,1338.60412247766,1338.64651835425,1338.72535031001,1338.80408742697,
1338.88324218894,1338.9618396062,1339.04040335043,1339.11894997117,1339.19854385907,
1339.27713063129,1339.35722807703,1339.43732552277),.UNSPECIFIED.);
#1342=B_SPLINE_CURVE_WITH_KNOTS('',3,(#159449,#159450,#159451,#159452,#159453,
#159454,#159455,#159456,#159457,#159458,#159459),.UNSPECIFIED.,.F.,.F.,
(4,1,1,1,1,1,1,1,4),(1339.43732552277,1339.64625436497,1340.64599037569,
1341.64572638641,1342.64546239713,1343.64519840785,1344.64493441857,1345.64467042929,
1345.72051082995),.UNSPECIFIED.);
#1343=B_SPLINE_CURVE_WITH_KNOTS('',3,(#159461,#159462,#159463,#159464,#159465,
#159466,#159467,#159468,#159469,#159470),.UNSPECIFIED.,.F.,.F.,(4,1,1,1,
1,1,1,4),(1345.72051082995,1346.64440644001,1347.64414245073,1348.64387846145,
1349.64361447217,1350.64335048289,1351.64308649361,1352.00369613713),
 .UNSPECIFIED.);
#1344=B_SPLINE_CURVE_WITH_KNOTS('',3,(#159472,#159473,#159474,#159475,#159476,
#159477,#159478,#159479,#159480,#159481),.UNSPECIFIED.,.F.,.F.,(4,1,1,1,
1,1,1,4),(1352.00369613713,1352.64282250433,1353.64255851505,1354.64229452577,
1355.64203053649,1356.64176654721,1357.64150255794,1358.28688144431),
 .UNSPECIFIED.);
#1345=B_SPLINE_CURVE_WITH_KNOTS('',3,(#159483,#159484,#159485,#159486,#159487,
#159488,#159489,#159490,#159491,#159492,#159493,#159494,#159495,#159496,
#159497,#159498,#159499,#159500,#159501,#159502,#159503,#159504,#159505,
#159506,#159507,#159508,#159509,#159510,#159511,#159512,#159513,#159514,
#159515,#159516,#159517,#159518,#159519,#159520,#159521,#159522,#159523,
#159524,#159525,#159526,#159527,#159528,#159529,#159530,#159531,#159532,
#159533,#159534,#159535,#159536,#159537,#159538,#159539,#159540,#159541,
#159542,#159543,#159544,#159545,#159546,#159547,#159548,#159549,#159550,
#159551,#159552,#159553,#159554,#159555,#159556,#159557,#159558,#159559,
#159560,#159561,#159562,#159563,#159564,#159565,#159566,#159567,#159568,
#159569,#159570,#159571,#159572,#159573,#159574,#159575,#159576,#159577,
#159578,#159579,#159580,#159581,#159582,#159583,#159584,#159585,#159586,
#159587,#159588,#159589,#159590,#159591,#159592,#159593,#159594,#159595,
#159596,#159597,#159598,#159599,#159600,#159601,#159602,#159603,#159604,
#159605,#159606,#159607,#159608,#159609,#159610,#159611,#159612,#159613,
#159614,#159615,#159616,#159617,#159618,#159619,#159620,#159621,#159622,
#159623,#159624,#159625,#159626,#159627,#159628,#159629,#159630,#159631,
#159632,#159633,#159634,#159635,#159636,#159637,#159638,#159639,#159640,
#159641,#159642,#159643,#159644,#159645,#159646,#159647,#159648,#159649,
#159650,#159651,#159652,#159653,#159654,#159655,#159656,#159657,#159658,
#159659,#159660,#159661,#159662,#159663,#159664,#159665,#159666,#159667,
#159668,#159669,#159670,#159671,#159672,#159673,#159674,#159675,#159676,
#159677,#159678,#159679,#159680,#159681,#159682,#159683,#159684,#159685,
#159686,#159687,#159688,#159689,#159690,#159691,#159692,#159693,#159694,
#159695,#159696,#159697,#159698,#159699,#159700,#159701,#159702,#159703,
#159704,#159705,#159706,#159707,#159708,#159709,#159710,#159711,#159712,
#159713,#159714,#159715,#159716,#159717,#159718,#159719,#159720,#159721,
#159722,#159723,#159724,#159725,#159726),.UNSPECIFIED.,.F.,.F.,(4,3,3,3,
3,3,3,3,3,3,3,3,3,3,3,3,3,3,3,3,3,3,3,3,3,3,3,3,3,3,3,3,3,3,3,3,3,3,3,3,
3,3,3,3,3,3,3,3,3,3,3,3,3,3,3,3,3,3,3,3,3,3,3,3,3,3,3,3,3,3,3,3,3,3,3,3,
3,3,3,3,3,4),(1358.28688169172,1358.37804472668,1358.46962250677,1358.56176130781,
1358.64123856866,1358.72119586879,1358.80105866603,1358.8808444885,1358.9605708037,
1359.04025503199,1359.11992601821,1359.19959347174,1359.27927312255,1359.35898070495,
1359.43877593402,1359.51862027573,1359.59857870278,1359.64097457938,1359.72093187951,
1359.80079467675,1359.88058049923,1359.96030681442,1360.03999104272,1360.11966202894,
1360.19932948246,1360.27900913328,1360.35871671567,1360.43851194475,1360.51835628646,
1360.5983147135,1360.6407105901,1360.72066789023,1360.80053068747,1360.88031650995,
1360.96004282514,1361.03972705343,1361.11939803966,1361.19906549318,1361.278745144,
1361.35845272639,1361.43824795547,1361.51809229718,1361.59805072422,1361.64044660082,
1361.72040390095,1361.80026669819,1361.88005252067,1361.95977883586,1362.03946306416,
1362.11913405038,1362.1988015039,1362.27848115472,1362.35818873711,1362.43798396619,
1362.5178283079,1362.59778673494,1362.64018261154,1362.72013991167,1362.80000270892,
1362.87978853139,1362.95951484658,1363.03919907488,1363.1188700611,1363.19853751463,
1363.27821716544,1363.35792474784,1363.43771997692,1363.51756431862,1363.59752274567,
1363.63991862226,1363.71908597835,1363.79815940171,1363.87715710195,1363.95609721831,
1364.03500353988,1364.11389342232,1364.19278319829,1364.27168919809,1364.35067093608,
1364.429692563,1364.50882608086,1364.57006675149),.UNSPECIFIED.);
#1346=B_SPLINE_CURVE_WITH_KNOTS('',3,(#159728,#159729,#159730,#159731,#159732,
#159733,#159734,#159735,#159736,#159737,#159738,#159739,#159740),
 .UNSPECIFIED.,.F.,.F.,(4,3,1,1,1,1,1,1,4),(1364.57006675149,1364.63965463298,
1365.6393906437,1366.63912665442,1367.63886266514,1368.63859867586,1369.63833468658,
1370.6380706973,1370.85325205867),.UNSPECIFIED.);
#1347=B_SPLINE_CURVE_WITH_KNOTS('',3,(#159742,#159743,#159744,#159745,#159746,
#159747,#159748,#159749,#159750,#159751),.UNSPECIFIED.,.F.,.F.,(4,1,1,1,
1,1,1,4),(1370.85325205867,1371.63780670802,1372.63754271874,1373.63727872946,
1374.63701474018,1375.6367507509,1376.63648676162,1377.13643736585),
 .UNSPECIFIED.);
#1348=B_SPLINE_CURVE_WITH_KNOTS('',3,(#159753,#159754,#159755,#159756,#159757,
#159758,#159759,#159760,#159761,#159762),.UNSPECIFIED.,.F.,.F.,(4,1,1,1,
1,1,1,4),(1377.13643736585,1377.63622277234,1378.63595878306,1379.63569479378,
1380.6354308045,1381.63516681522,1382.63490282594,1383.41962267303),
 .UNSPECIFIED.);
#1349=B_SPLINE_CURVE_WITH_KNOTS('',3,(#159764,#159765,#159766,#159767,#159768,
#159769,#159770,#159771,#159772,#159773,#159774,#159775),.UNSPECIFIED.,
 .F.,.F.,(4,2,1,1,1,1,1,1,4),(1383.41962267303,1383.63463883666,1384.63437484738,
1385.6341108581,1386.63384686882,1387.63358287954,1388.63331889026,1389.63305490098,
1389.70280798021),.UNSPECIFIED.);
#1350=B_SPLINE_CURVE_WITH_KNOTS('',3,(#159777,#159778,#159779,#159780,#159781,
#159782,#159783,#159784,#159785,#159786,#159787,#159788,#159789,#159790,
#159791,#159792,#159793,#159794,#159795,#159796,#159797,#159798,#159799,
#159800,#159801,#159802,#159803,#159804,#159805,#159806,#159807,#159808,
#159809,#159810,#159811,#159812,#159813,#159814,#159815,#159816,#159817,
#159818,#159819,#159820,#159821,#159822,#159823,#159824,#159825,#159826,
#159827,#159828,#159829,#159830,#159831,#159832,#159833,#159834,#159835,
#159836,#159837,#159838,#159839,#159840,#159841,#159842,#159843,#159844,
#159845,#159846,#159847,#159848,#159849,#159850,#159851,#159852,#159853,
#159854,#159855,#159856,#159857,#159858,#159859,#159860,#159861,#159862,
#159863,#159864,#159865,#159866,#159867,#159868,#159869,#159870,#159871,
#159872,#159873,#159874,#159875,#159876,#159877,#159878,#159879,#159880,
#159881,#159882,#159883,#159884,#159885,#159886,#159887,#159888,#159889,
#159890,#159891,#159892,#159893,#159894,#159895,#159896,#159897,#159898,
#159899,#159900,#159901,#159902,#159903,#159904,#159905,#159906,#159907,
#159908,#159909,#159910,#159911,#159912,#159913,#159914,#159915,#159916,
#159917,#159918,#159919,#159920,#159921,#159922,#159923,#159924,#159925,
#159926,#159927,#159928,#159929,#159930,#159931,#159932,#159933,#159934,
#159935,#159936,#159937,#159938,#159939,#159940,#159941,#159942,#159943,
#159944,#159945,#159946,#159947,#159948,#159949,#159950,#159951,#159952,
#159953,#159954,#159955,#159956,#159957,#159958,#159959,#159960,#159961,
#159962,#159963,#159964,#159965,#159966,#159967,#159968,#159969,#159970,
#159971,#159972,#159973,#159974,#159975,#159976,#159977,#159978,#159979,
#159980,#159981,#159982,#159983,#159984,#159985,#159986,#159987,#159988,
#159989,#159990,#159991,#159992,#159993,#159994,#159995,#159996,#159997,
#159998,#159999,#160000,#160001,#160002,#160003,#160004,#160005,#160006,
#160007,#160008,#160009,#160010,#160011,#160012,#160013,#160014,#160015,
#160016,#160017,#160018,#160019,#160020),.UNSPECIFIED.,.F.,.F.,(4,3,3,3,
3,3,3,3,3,3,3,3,3,3,3,3,3,3,3,3,3,3,3,3,3,3,3,3,3,3,3,3,3,3,3,3,3,3,3,3,
3,3,3,3,3,3,3,3,3,3,3,3,3,3,3,3,3,3,3,3,3,3,3,3,3,3,3,3,3,3,3,3,3,3,3,3,
3,3,3,3,3,4),(1389.70280798021,1389.78194901558,1389.86100069503,1389.9399812097,
1390.01890868487,1390.09780924709,1390.17669759541,1390.25559006204,1390.33450297977,
1390.41349813155,1390.49253681273,1390.57169311822,1390.6327909117,1390.71274821183,
1390.79261100907,1390.87239683154,1390.95212314674,1391.03180737503,1391.11147836125,
1391.19114581478,1391.2708254656,1391.35053304799,1391.43032827707,1391.51017261877,
1391.59013104582,1391.63252692242,1391.71248422255,1391.79234701979,1391.87213284226,
1391.95185915746,1392.03154338575,1392.11121437197,1392.1908818255,1392.27056147632,
1392.35026905871,1392.43006428779,1392.50990862949,1392.58986705654,1392.63226293314,
1392.71222023327,1392.79208303051,1392.87186885299,1392.95159516818,1393.03127939647,
1393.1109503827,1393.19061783622,1393.27029748704,1393.35000506943,1393.42980029851,
1393.50964464022,1393.58960306726,1393.63199894386,1393.71195624399,1393.79181904123,
1393.87160486371,1393.9513311789,1394.0310154072,1394.11068639342,1394.19035384694,
1394.27003349776,1394.34974108015,1394.42953630923,1394.50938065094,1394.58933907798,
1394.63173495458,1394.71169225471,1394.79155505195,1394.87134087443,1394.95106718962,
1395.03075141792,1395.11042240414,1395.19008985766,1395.26976950848,1395.34947709088,
1395.42927231995,1395.50911666166,1395.58907508871,1395.6314709653,1395.72358358603,
1395.8153650835,1395.90649484727,1395.98599303994),.UNSPECIFIED.);
#1351=B_SPLINE_CURVE_WITH_KNOTS('',3,(#160022,#160023,#160024,#160025,#160026,
#160027,#160028,#160029,#160030,#160031),.UNSPECIFIED.,.F.,.F.,(4,1,1,1,
1,1,1,4),(1395.98599328739,1396.63120697602,1397.63094298674,1398.63067899746,
1399.63041500818,1400.6301510189,1401.62988702962,1402.26917859457),
 .UNSPECIFIED.);
#1352=B_SPLINE_CURVE_WITH_KNOTS('',3,(#160033,#160034,#160035,#160036,#160037,
#160038,#160039,#160040,#160041,#160042),.UNSPECIFIED.,.F.,.F.,(4,1,1,1,
1,1,1,4),(1402.26917859457,1402.62962304034,1403.62935905106,1404.62909506178,
1405.6288310725,1406.62856708322,1407.62830309394,1408.55236390175),
 .UNSPECIFIED.);
#1353=B_SPLINE_CURVE_WITH_KNOTS('',3,(#160044,#160045,#160046,#160047,#160048,
#160049,#160050,#160051,#160052,#160053,#160054,#160055),.UNSPECIFIED.,
 .F.,.F.,(4,2,1,1,1,1,1,1,4),(1408.55236390175,1408.62803910466,1409.62777511538,
1410.6275111261,1411.62724713682,1412.62698314754,1413.62671915826,1414.62645516898,
1414.83554920893),.UNSPECIFIED.);
#1354=B_SPLINE_CURVE_WITH_KNOTS('',3,(#160057,#160058,#160059,#160060,#160061,
#160062,#160063,#160064,#160065,#160066,#160067,#160068,#160069,#160070,
#160071,#160072,#160073,#160074,#160075,#160076,#160077,#160078,#160079,
#160080,#160081,#160082,#160083,#160084,#160085,#160086,#160087,#160088,
#160089,#160090,#160091,#160092,#160093,#160094,#160095,#160096,#160097,
#160098,#160099,#160100,#160101,#160102,#160103,#160104,#160105,#160106,
#160107,#160108,#160109,#160110,#160111,#160112,#160113,#160114,#160115,
#160116,#160117,#160118,#160119,#160120,#160121,#160122,#160123,#160124,
#160125,#160126,#160127,#160128,#160129,#160130,#160131,#160132,#160133,
#160134,#160135,#160136,#160137,#160138,#160139,#160140,#160141,#160142,
#160143,#160144,#160145,#160146,#160147,#160148,#160149,#160150,#160151,
#160152,#160153,#160154,#160155,#160156,#160157,#160158,#160159,#160160,
#160161,#160162,#160163,#160164,#160165,#160166,#160167,#160168,#160169,
#160170,#160171,#160172,#160173,#160174,#160175,#160176,#160177,#160178,
#160179,#160180,#160181,#160182,#160183,#160184,#160185,#160186,#160187,
#160188,#160189,#160190,#160191,#160192,#160193,#160194,#160195,#160196,
#160197,#160198,#160199,#160200,#160201,#160202,#160203,#160204,#160205,
#160206,#160207,#160208,#160209,#160210,#160211,#160212,#160213,#160214,
#160215,#160216,#160217,#160218,#160219,#160220,#160221,#160222,#160223,
#160224,#160225,#160226,#160227,#160228,#160229,#160230,#160231,#160232,
#160233,#160234,#160235,#160236,#160237,#160238,#160239,#160240,#160241,
#160242,#160243,#160244,#160245,#160246,#160247,#160248,#160249,#160250,
#160251,#160252,#160253,#160254,#160255,#160256,#160257,#160258,#160259,
#160260,#160261,#160262,#160263,#160264,#160265,#160266,#160267,#160268,
#160269,#160270,#160271,#160272,#160273,#160274,#160275,#160276,#160277,
#160278,#160279,#160280,#160281,#160282,#160283,#160284,#160285,#160286,
#160287,#160288,#160289,#160290,#160291,#160292,#160293,#160294,#160295,
#160296,#160297,#160298,#160299,#160300),.UNSPECIFIED.,.F.,.F.,(4,3,3,3,
3,3,3,3,3,3,3,3,3,3,3,3,3,3,3,3,3,3,3,3,3,3,3,3,3,3,3,3,3,3,3,3,3,3,3,3,
3,3,3,3,3,3,3,3,3,3,3,3,3,3,3,3,3,3,3,3,3,3,3,3,3,3,3,3,3,3,3,3,3,3,3,3,
3,3,3,3,3,4),(1414.83554920893,1414.91422319859,1414.99283632039,1415.0720056778,
1415.15056272849,1415.22911755209,1415.3076866817,1415.3873128062,1415.46599905401,
1415.54609511686,1415.6261911797,1415.70614847983,1415.78601127707,1415.86579709955,
1415.94552341474,1416.02520764304,1416.10487862926,1416.18454608278,1416.2642257336,
1416.34393331599,1416.42372854507,1416.50357288678,1416.58353131382,1416.62592719042,
1416.70588449055,1416.78574728779,1416.86553311027,1416.94525942546,1417.02494365375,
1417.10461463998,1417.1842820935,1417.26396174432,1417.34366932671,1417.42346455579,
1417.5033088975,1417.58326732454,1417.62566320114,1417.70562050127,1417.78548329851,
1417.86526912099,1417.94499543618,1418.02467966447,1418.1043506507,1418.18401810422,
1418.26369775504,1418.34340533743,1418.42320056651,1418.50304490822,1418.58300333526,
1418.62539921186,1418.70535651199,1418.78521930923,1418.86500513171,1418.9447314469,
1419.0244156752,1419.10408666142,1419.18375411494,1419.26343376576,1419.34314134815,
1419.42293657723,1419.50278091894,1419.58273934598,1419.62513522258,1419.70509252271,
1419.78495531995,1419.86474114243,1419.94446745762,1420.02415168591,1420.10382267214,
1420.18349012566,1420.26316977648,1420.34287735887,1420.42267258795,1420.50251692965,
1420.5824753567,1420.6248712333,1420.70918020921,1420.79334694167,1420.8773195318,
1420.96117782697,1421.0448782206,1421.11873451598),.UNSPECIFIED.);
#1355=B_SPLINE_CURVE_WITH_KNOTS('',3,(#160302,#160303,#160304,#160305,#160306,
#160307,#160308,#160309,#160310,#160311,#160312,#160313,#160314,#160315,
#160316,#160317,#160318,#160319,#160320,#160321,#160322,#160323,#160324,
#160325,#160326,#160327,#160328,#160329,#160330,#160331,#160332,#160333,
#160334,#160335,#160336,#160337,#160338,#160339,#160340,#160341,#160342,
#160343,#160344,#160345,#160346,#160347,#160348,#160349,#160350,#160351,
#160352,#160353,#160354,#160355,#160356,#160357,#160358,#160359,#160360,
#160361,#160362,#160363,#160364,#160365,#160366,#160367,#160368,#160369,
#160370,#160371,#160372,#160373,#160374,#160375,#160376,#160377,#160378,
#160379,#160380,#160381,#160382,#160383,#160384,#160385,#160386,#160387,
#160388,#160389,#160390,#160391,#160392,#160393,#160394,#160395,#160396,
#160397,#160398,#160399,#160400,#160401,#160402,#160403,#160404,#160405,
#160406,#160407,#160408,#160409,#160410,#160411,#160412,#160413,#160414,
#160415,#160416,#160417,#160418,#160419,#160420,#160421,#160422,#160423,
#160424,#160425,#160426,#160427,#160428,#160429,#160430,#160431,#160432,
#160433,#160434,#160435,#160436,#160437,#160438,#160439,#160440,#160441,
#160442,#160443,#160444,#160445,#160446,#160447,#160448,#160449,#160450,
#160451,#160452,#160453,#160454,#160455,#160456,#160457,#160458,#160459,
#160460,#160461,#160462,#160463,#160464,#160465,#160466,#160467,#160468,
#160469,#160470,#160471,#160472,#160473,#160474,#160475,#160476,#160477,
#160478,#160479,#160480,#160481,#160482,#160483,#160484,#160485,#160486,
#160487,#160488,#160489,#160490,#160491,#160492,#160493,#160494,#160495,
#160496,#160497,#160498,#160499,#160500,#160501,#160502,#160503,#160504,
#160505,#160506,#160507,#160508,#160509,#160510,#160511,#160512,#160513,
#160514,#160515,#160516,#160517,#160518,#160519,#160520,#160521,#160522,
#160523,#160524,#160525,#160526,#160527,#160528,#160529,#160530,#160531,
#160532,#160533,#160534,#160535,#160536,#160537,#160538,#160539,#160540,
#160541,#160542,#160543,#160544,#160545),.UNSPECIFIED.,.F.,.F.,(4,3,3,3,
3,3,3,3,3,3,3,3,3,3,3,3,3,3,3,3,3,3,3,3,3,3,3,3,3,3,3,3,3,3,3,3,3,3,3,3,
3,3,3,3,3,3,3,3,3,3,3,3,3,3,3,3,3,3,3,3,3,3,3,3,3,3,3,3,3,3,3,3,3,3,3,3,
3,3,3,3,3,4),(1421.11873451611,1421.20198682774,1421.28533673185,1421.37015435989,
1421.45378598796,1421.53919661599,1421.62460724402,1421.70456454415,1421.78442734139,
1421.86421316387,1421.94393947906,1422.02362370736,1422.10329469358,1422.1829621471,
1422.26264179792,1422.34234938032,1422.42214460939,1422.5019889511,1422.58194737815,
1422.62434325474,1422.70430055487,1422.78416335211,1422.86394917459,1422.94367548978,
1423.02335971808,1423.1030307043,1423.18269815782,1423.26237780864,1423.34208539104,
1423.42188062011,1423.50172496182,1423.58168338887,1423.62407926546,1423.70403656559,
1423.78389936283,1423.8636851853,1423.9434115005,1424.02309572879,1424.10276671501,
1424.18243416854,1424.26211381936,1424.34182140175,1424.42161663083,1424.50146097253,
1424.58141939958,1424.62381527618,1424.70377257631,1424.78363537355,1424.86342119603,
1424.94314751122,1425.02283173951,1425.10250272574,1425.18217017926,1425.26184983008,
1425.34155741247,1425.42135264155,1425.50119698326,1425.5811554103,1425.6235512869,
1425.70350858703,1425.78337138427,1425.86315720674,1425.94288352194,1426.02256775023,
1426.10223873645,1426.18190618998,1426.2615858408,1426.34129342319,1426.42108865227,
1426.50093299397,1426.58089142102,1426.62328729762,1426.7021669801,1426.78095145909,
1426.85964601321,1426.93828972882,1427.01689915789,1427.09549082411,1427.17410791049,
1427.2527358973,1427.33143433151,1427.40191982329),.UNSPECIFIED.);
#1356=B_SPLINE_CURVE_WITH_KNOTS('',3,(#160547,#160548,#160549,#160550,#160551,
#160552,#160553,#160554,#160555,#160556,#160557),.UNSPECIFIED.,.F.,.F.,
(4,1,1,1,1,1,1,1,4),(1427.40191982329,1427.62302330834,1428.62275931906,
1429.62249532978,1430.6222313405,1431.62196735122,1432.62170336194,1433.62143937266,
1433.68510513047),.UNSPECIFIED.);
#1357=B_SPLINE_CURVE_WITH_KNOTS('',3,(#160559,#160560,#160561,#160562,#160563,
#160564,#160565,#160566,#160567,#160568,#160569,#160570,#160571,#160572,
#160573,#160574,#160575,#160576,#160577,#160578,#160579,#160580,#160581,
#160582,#160583,#160584,#160585,#160586,#160587,#160588,#160589,#160590,
#160591,#160592,#160593,#160594,#160595,#160596,#160597,#160598,#160599,
#160600,#160601,#160602,#160603,#160604,#160605,#160606,#160607,#160608,
#160609,#160610,#160611,#160612,#160613,#160614,#160615,#160616,#160617,
#160618,#160619,#160620,#160621,#160622,#160623,#160624,#160625,#160626,
#160627,#160628,#160629,#160630,#160631,#160632,#160633,#160634,#160635,
#160636,#160637,#160638,#160639,#160640,#160641,#160642,#160643,#160644,
#160645,#160646,#160647,#160648,#160649,#160650,#160651,#160652,#160653,
#160654,#160655,#160656,#160657,#160658,#160659,#160660,#160661,#160662,
#160663,#160664,#160665,#160666,#160667,#160668,#160669,#160670,#160671,
#160672,#160673,#160674,#160675,#160676,#160677,#160678,#160679,#160680,
#160681,#160682,#160683,#160684,#160685,#160686,#160687,#160688,#160689,
#160690,#160691,#160692,#160693,#160694,#160695,#160696,#160697,#160698,
#160699,#160700,#160701,#160702,#160703,#160704,#160705,#160706,#160707,
#160708,#160709,#160710,#160711,#160712,#160713,#160714,#160715,#160716,
#160717,#160718,#160719,#160720,#160721,#160722,#160723,#160724,#160725,
#160726,#160727,#160728,#160729,#160730,#160731,#160732,#160733,#160734,
#160735,#160736,#160737,#160738,#160739,#160740,#160741,#160742,#160743,
#160744,#160745,#160746,#160747,#160748,#160749,#160750,#160751,#160752,
#160753,#160754,#160755,#160756,#160757,#160758,#160759,#160760,#160761,
#160762,#160763,#160764,#160765,#160766,#160767,#160768,#160769,#160770,
#160771,#160772,#160773,#160774,#160775,#160776,#160777,#160778,#160779,
#160780,#160781,#160782,#160783,#160784,#160785,#160786,#160787,#160788,
#160789,#160790,#160791,#160792,#160793,#160794,#160795,#160796,#160797,
#160798,#160799,#160800,#160801,#160802),.UNSPECIFIED.,.F.,.F.,(4,3,3,3,
3,3,3,3,3,3,3,3,3,3,3,3,3,3,3,3,3,3,3,3,3,3,3,3,3,3,3,3,3,3,3,3,3,3,3,3,
3,3,3,3,3,3,3,3,3,3,3,3,3,3,3,3,3,3,3,3,3,3,3,3,3,3,3,3,3,3,3,3,3,3,3,3,
3,3,3,3,3,4),(1433.68510513047,1433.76430171396,1433.84340818076,1433.92244268633,
1434.00142332046,1434.08037593041,1434.1593155102,1434.23825835883,1434.31722077516,
1434.3962651774,1434.47535225123,1434.55455861227,1434.62117538338,1434.70113268351,
1434.78099548076,1434.86078130323,1434.94050761843,1435.02019184673,1435.09986283295,
1435.17953028648,1435.2592099373,1435.33891751969,1435.41871274877,1435.49855709048,
1435.57851551753,1435.62091139411,1435.70086869424,1435.78073149149,1435.86051731396,
1435.94024362915,1436.01992785745,1436.09959884367,1436.1792662972,1436.25894594801,
1436.33865353041,1436.41844875948,1436.49829310119,1436.57825152824,1436.62064740483,
1436.70060470496,1436.7804675022,1436.86025332467,1436.93997963987,1437.01966386816,
1437.09933485438,1437.1790023079,1437.25868195872,1437.33838954111,1437.41818477019,
1437.49802911189,1437.57798753894,1437.62038341555,1437.70034071568,1437.78020351292,
1437.8599893354,1437.93971565059,1438.01939987889,1438.09907086511,1438.17873831863,
1438.25841796945,1438.33812555185,1438.41792078092,1438.49776512263,1438.57772354968,
1438.62011942627,1438.7000767264,1438.77993952365,1438.85972534612,1438.93945166132,
1439.01913588961,1439.09880687583,1439.17847432936,1439.25815398018,1439.33786156257,
1439.41765679165,1439.49750113336,1439.57745956041,1439.61985543699,1439.71247622588,
1439.80474479726,1439.89632503004,1439.96829031496),.UNSPECIFIED.);
#1358=B_SPLINE_CURVE_WITH_KNOTS('',3,(#160804,#160805,#160806,#160807,#160808,
#160809,#160810,#160811,#160812,#160813),.UNSPECIFIED.,.F.,.F.,(4,1,1,1,
1,1,1,4),(1439.96829043765,1440.61959144771,1441.61932745843,1442.61906346915,
1443.61879947987,1444.61853549059,1445.61827150131,1446.25147574483),
 .UNSPECIFIED.);
#1359=B_SPLINE_CURVE_WITH_KNOTS('',3,(#160815,#160816,#160817,#160818,#160819,
#160820,#160821,#160822,#160823,#160824),.UNSPECIFIED.,.F.,.F.,(4,1,1,1,
1,1,1,4),(1446.25147574483,1446.61800751203,1447.61774352275,1448.61747953347,
1449.61721554419,1450.61695155491,1451.61668756563,1452.53466105201),
 .UNSPECIFIED.);
#1360=B_SPLINE_CURVE_WITH_KNOTS('',3,(#160826,#160827,#160828,#160829,#160830,
#160831,#160832,#160833,#160834,#160835,#160836,#160837),.UNSPECIFIED.,
 .F.,.F.,(4,2,1,1,1,1,1,1,4),(1452.53466105201,1452.61642357635,1453.61615958707,
1454.61589559779,1455.61563160851,1456.61536761923,1457.61510362995,1458.61483964067,
1458.81784635919),.UNSPECIFIED.);
#1361=B_SPLINE_CURVE_WITH_KNOTS('',3,(#160839,#160840,#160841,#160842,#160843,
#160844,#160845,#160846,#160847,#160848,#160849,#160850,#160851,#160852,
#160853,#160854,#160855,#160856,#160857,#160858,#160859,#160860,#160861,
#160862,#160863,#160864,#160865,#160866,#160867,#160868,#160869,#160870,
#160871,#160872,#160873,#160874,#160875,#160876,#160877,#160878,#160879,
#160880,#160881,#160882,#160883,#160884,#160885,#160886,#160887,#160888,
#160889,#160890,#160891,#160892,#160893,#160894,#160895,#160896,#160897,
#160898,#160899,#160900,#160901,#160902,#160903,#160904,#160905,#160906,
#160907,#160908,#160909,#160910,#160911,#160912,#160913,#160914,#160915,
#160916,#160917,#160918,#160919,#160920,#160921,#160922,#160923,#160924,
#160925,#160926,#160927,#160928,#160929,#160930,#160931,#160932,#160933,
#160934,#160935,#160936,#160937,#160938,#160939,#160940,#160941,#160942,
#160943,#160944,#160945,#160946,#160947,#160948,#160949,#160950,#160951,
#160952,#160953,#160954,#160955,#160956,#160957,#160958,#160959,#160960,
#160961,#160962,#160963,#160964,#160965,#160966,#160967,#160968,#160969,
#160970,#160971,#160972,#160973,#160974,#160975,#160976,#160977,#160978,
#160979,#160980,#160981,#160982,#160983,#160984,#160985,#160986,#160987,
#160988,#160989,#160990,#160991,#160992,#160993,#160994,#160995,#160996,
#160997,#160998,#160999,#161000,#161001,#161002,#161003,#161004,#161005,
#161006,#161007,#161008,#161009,#161010,#161011,#161012,#161013,#161014,
#161015,#161016,#161017,#161018,#161019,#161020,#161021,#161022,#161023,
#161024,#161025,#161026,#161027,#161028,#161029,#161030,#161031,#161032,
#161033,#161034,#161035,#161036,#161037,#161038,#161039,#161040,#161041,
#161042,#161043,#161044,#161045,#161046,#161047,#161048,#161049,#161050,
#161051,#161052,#161053,#161054,#161055,#161056,#161057,#161058,#161059,
#161060,#161061,#161062,#161063,#161064,#161065,#161066,#161067,#161068,
#161069,#161070,#161071,#161072,#161073,#161074,#161075,#161076,#161077,
#161078,#161079,#161080,#161081,#161082),.UNSPECIFIED.,.F.,.F.,(4,3,3,3,
3,3,3,3,3,3,3,3,3,3,3,3,3,3,3,3,3,3,3,3,3,3,3,3,3,3,3,3,3,3,3,3,3,3,3,3,
3,3,3,3,3,3,3,3,3,3,3,3,3,3,3,3,3,3,3,3,3,3,3,3,3,3,3,3,3,3,3,3,3,3,3,3,
3,3,3,3,3,4),(1458.81784635919,1458.89650835172,1458.97510783377,1459.05504131097,
1459.13358093235,1459.21211704093,1459.29066618012,1459.37164354793,1459.45030870812,
1459.53244217975,1459.61457565139,1459.69453295152,1459.77439574876,1459.85418157123,
1459.93390788643,1460.01359211472,1460.09326310094,1460.17293055447,1460.25261020528,
1460.33231778768,1460.41211301675,1460.49195735846,1460.57191578551,1460.61431166211,
1460.69426896224,1460.77413175948,1460.85391758195,1460.93364389715,1461.01332812544,
1461.09299911166,1461.17266656519,1461.25234621601,1461.3320537984,1461.41184902748,
1461.49169336918,1461.57165179623,1461.61404767283,1461.69400497296,1461.7738677702,
1461.85365359268,1461.93337990787,1462.01306413617,1462.09273512239,1462.17240257591,
1462.25208222673,1462.33178980913,1462.4115850382,1462.49142937991,1462.57138780696,
1462.61378368355,1462.69374098368,1462.77360378092,1462.8533896034,1462.93311591859,
1463.01280014688,1463.09247113311,1463.17213858663,1463.25181823745,1463.33152581984,
1463.41132104892,1463.49116539063,1463.57112381767,1463.61351969427,1463.6934769944,
1463.77333979164,1463.85312561412,1463.93285192931,1464.01253615761,1464.09220714383,
1464.17187459735,1464.25155424817,1464.33126183057,1464.41105705964,1464.49090140135,
1464.5708598284,1464.61325570499,1464.69780465656,1464.7822076085,1464.86640944893,
1464.95049205445,1465.03440868174,1465.10103166624),.UNSPECIFIED.);
#1362=B_SPLINE_CURVE_WITH_KNOTS('',3,(#161084,#161085,#161086,#161087,#161088,
#161089,#161090,#161091,#161092,#161093,#161094,#161095,#161096,#161097,
#161098,#161099,#161100,#161101,#161102,#161103,#161104,#161105,#161106,
#161107,#161108,#161109,#161110,#161111,#161112,#161113,#161114,#161115,
#161116,#161117,#161118,#161119,#161120,#161121,#161122,#161123,#161124,
#161125,#161126,#161127,#161128,#161129,#161130,#161131,#161132,#161133,
#161134,#161135,#161136,#161137,#161138,#161139,#161140,#161141,#161142,
#161143,#161144,#161145,#161146,#161147,#161148,#161149,#161150,#161151,
#161152,#161153,#161154,#161155,#161156,#161157,#161158,#161159,#161160,
#161161,#161162,#161163,#161164,#161165,#161166,#161167,#161168,#161169,
#161170,#161171,#161172,#161173,#161174,#161175,#161176,#161177,#161178,
#161179,#161180,#161181,#161182,#161183,#161184,#161185,#161186,#161187,
#161188,#161189,#161190,#161191,#161192,#161193,#161194,#161195,#161196,
#161197,#161198,#161199,#161200,#161201,#161202,#161203,#161204,#161205,
#161206,#161207,#161208,#161209,#161210,#161211,#161212,#161213,#161214,
#161215,#161216,#161217,#161218,#161219,#161220,#161221,#161222,#161223,
#161224,#161225,#161226,#161227,#161228,#161229,#161230,#161231,#161232,
#161233,#161234,#161235,#161236,#161237,#161238,#161239,#161240,#161241,
#161242,#161243,#161244,#161245,#161246,#161247,#161248,#161249,#161250,
#161251,#161252,#161253,#161254,#161255,#161256,#161257,#161258,#161259,
#161260,#161261,#161262,#161263,#161264,#161265,#161266,#161267,#161268,
#161269,#161270,#161271,#161272,#161273,#161274,#161275,#161276,#161277,
#161278,#161279,#161280,#161281,#161282,#161283,#161284,#161285,#161286,
#161287,#161288,#161289,#161290,#161291,#161292,#161293,#161294,#161295,
#161296,#161297,#161298,#161299,#161300,#161301,#161302,#161303,#161304,
#161305,#161306,#161307,#161308,#161309,#161310,#161311,#161312,#161313,
#161314,#161315,#161316,#161317,#161318,#161319,#161320,#161321,#161322,
#161323,#161324,#161325,#161326,#161327,#161328,#161329,#161330),
 .UNSPECIFIED.,.F.,.F.,(4,3,3,3,3,3,3,3,3,3,3,3,3,3,3,3,3,3,3,3,3,3,3,3,
3,3,3,3,3,3,3,3,3,3,3,3,3,3,3,3,3,3,3,3,3,3,3,3,3,3,3,3,3,3,3,3,3,3,3,3,
3,3,3,3,3,3,3,3,3,3,3,3,3,3,3,3,3,3,3,3,3,3,4),(1465.10103166637,1465.18408255591,
1465.26722414529,1465.3536660379,1465.43707971455,1465.52059140623,1465.60425622782,
1465.61299171571,1465.69294901584,1465.77281181308,1465.85259763555,1465.93232395075,
1466.01200817904,1466.09167916526,1466.17134661879,1466.25102626961,1466.330733852,
1466.41052908107,1466.49037342278,1466.57033184983,1466.61272772643,1466.69268502656,
1466.7725478238,1466.85233364628,1466.93205996147,1467.01174418976,1467.09141517599,
1467.17108262951,1467.25076228033,1467.33046986272,1467.4102650918,1467.49010943351,
1467.57006786055,1467.61246373715,1467.69242103728,1467.77228383452,1467.852069657,
1467.93179597219,1468.01148020049,1468.09115118671,1468.17081864023,1468.25049829105,
1468.33020587345,1468.41000110252,1468.48984544423,1468.56980387128,1468.61219974787,
1468.692157048,1468.77201984524,1468.85180566772,1468.93153198291,1469.01121621121,
1469.09088719743,1469.17055465095,1469.25023430177,1469.32994188416,1469.40973711324,
1469.48958145495,1469.56953988199,1469.61193575859,1469.69189305872,1469.77175585596,
1469.85154167844,1469.93126799363,1470.01095222192,1470.09062320815,1470.17029066167,
1470.24997031249,1470.32967789488,1470.40947312396,1470.48931746567,1470.56927589271,
1470.61167176931,1470.69058006137,1470.76939294258,1470.84811543483,1470.92678681762,
1471.00542362705,1471.08404237083,1471.16268499734,1471.24133829156,1471.32005872964,
1471.38421697355),.UNSPECIFIED.);
#1363=B_SPLINE_CURVE_WITH_KNOTS('',3,(#161332,#161333,#161334,#161335,#161336,
#161337,#161338,#161339,#161340,#161341,#161342),.UNSPECIFIED.,.F.,.F.,
(4,1,1,1,1,1,1,1,4),(1471.38421697355,1471.61140778003,1472.61114379075,
1473.61087980147,1474.61061581219,1475.61035182291,1476.61008783363,1477.60982384435,
1477.66740228073),.UNSPECIFIED.);
#1364=B_SPLINE_CURVE_WITH_KNOTS('',3,(#161344,#161345,#161346,#161347,#161348,
#161349,#161350,#161351,#161352,#161353,#161354,#161355,#161356,#161357,
#161358,#161359,#161360,#161361,#161362,#161363,#161364,#161365,#161366,
#161367,#161368,#161369,#161370,#161371,#161372,#161373,#161374,#161375,
#161376,#161377,#161378,#161379,#161380,#161381,#161382,#161383,#161384,
#161385,#161386,#161387,#161388,#161389,#161390,#161391,#161392,#161393,
#161394,#161395,#161396,#161397,#161398,#161399,#161400,#161401,#161402,
#161403,#161404,#161405,#161406,#161407,#161408,#161409,#161410,#161411,
#161412,#161413,#161414,#161415,#161416,#161417,#161418,#161419,#161420,
#161421,#161422,#161423,#161424,#161425,#161426,#161427,#161428,#161429,
#161430,#161431,#161432,#161433,#161434,#161435,#161436,#161437,#161438,
#161439,#161440,#161441,#161442,#161443,#161444,#161445,#161446,#161447,
#161448,#161449,#161450,#161451,#161452,#161453,#161454,#161455,#161456,
#161457,#161458,#161459,#161460,#161461,#161462,#161463,#161464,#161465,
#161466,#161467,#161468,#161469,#161470,#161471,#161472,#161473,#161474,
#161475,#161476,#161477,#161478,#161479,#161480,#161481,#161482,#161483,
#161484,#161485,#161486,#161487,#161488,#161489,#161490,#161491,#161492,
#161493,#161494,#161495,#161496,#161497,#161498,#161499,#161500,#161501,
#161502,#161503,#161504,#161505,#161506,#161507,#161508,#161509,#161510,
#161511,#161512,#161513,#161514,#161515,#161516,#161517,#161518,#161519,
#161520,#161521,#161522,#161523,#161524,#161525,#161526,#161527,#161528,
#161529,#161530,#161531,#161532,#161533,#161534,#161535,#161536,#161537,
#161538,#161539,#161540,#161541,#161542,#161543,#161544,#161545,#161546,
#161547,#161548,#161549,#161550,#161551,#161552,#161553,#161554,#161555,
#161556,#161557,#161558,#161559,#161560,#161561,#161562,#161563,#161564,
#161565,#161566,#161567,#161568,#161569,#161570,#161571,#161572,#161573,
#161574,#161575,#161576,#161577,#161578,#161579,#161580,#161581,#161582,
#161583,#161584,#161585,#161586,#161587),.UNSPECIFIED.,.F.,.F.,(4,3,3,3,
3,3,3,3,3,3,3,3,3,3,3,3,3,3,3,3,3,3,3,3,3,3,3,3,3,3,3,3,3,3,3,3,3,3,3,3,
3,3,3,3,3,3,3,3,3,3,3,3,3,3,3,3,3,3,3,3,3,3,3,3,3,3,3,3,3,3,3,3,3,3,3,3,
3,3,3,3,3,4),(1477.66740228073,1477.74665738145,1477.82582165558,1477.90491321944,
1477.98395012394,1478.06295794255,1478.14195194843,1478.22094840445,1478.29996357275,
1478.37906049634,1478.45819925348,1478.53745897297,1478.60955985507,1478.6895171552,
1478.76937995244,1478.84916577492,1478.92889209011,1479.00857631841,1479.08824730463,
1479.16791475815,1479.24759440897,1479.32730199136,1479.40709722044,1479.48694156215,
1479.5668999892,1479.60929586579,1479.68925316592,1479.76911596316,1479.84890178564,
1479.92862810083,1480.00831232913,1480.08798331535,1480.16765076887,1480.24733041969,
1480.32703800208,1480.40683323116,1480.48667757287,1480.56663599991,1480.60903187651,
1480.68898917664,1480.76885197388,1480.84863779636,1480.92836411155,1481.00804833985,
1481.08771932607,1481.16738677959,1481.24706643041,1481.3267740128,1481.40656924188,
1481.48641358358,1481.56637201063,1481.60876788723,1481.68872518736,1481.7685879846,
1481.84837380708,1481.92810012227,1482.00778435057,1482.08745533679,1482.16712279031,
1482.24680244113,1482.32651002352,1482.4063052526,1482.48614959431,1482.56610802135,
1482.60850389795,1482.68846119808,1482.76832399532,1482.8481098178,1482.92783613299,
1483.00752036128,1483.0871913475,1483.16685880103,1483.24653845185,1483.32624603424,
1483.40604126332,1483.48588560502,1483.56584403207,1483.60823990867,1483.70138884274,
1483.79416232008,1483.8862079791,1483.9505875878),.UNSPECIFIED.);
#1365=B_SPLINE_CURVE_WITH_KNOTS('',3,(#161589,#161590,#161591,#161592,#161593,
#161594,#161595,#161596,#161597,#161598,#161599,#161600,#161601,#161602,
#161603,#161604,#161605,#161606,#161607,#161608,#161609,#161610,#161611,
#161612,#161613,#161614,#161615,#161616,#161617,#161618,#161619,#161620,
#161621,#161622,#161623,#161624,#161625,#161626,#161627,#161628,#161629,
#161630,#161631,#161632,#161633,#161634,#161635,#161636,#161637,#161638,
#161639,#161640,#161641,#161642,#161643,#161644,#161645,#161646,#161647,
#161648,#161649,#161650,#161651,#161652,#161653,#161654,#161655,#161656,
#161657,#161658,#161659,#161660,#161661,#161662,#161663,#161664,#161665,
#161666,#161667,#161668,#161669,#161670,#161671,#161672,#161673,#161674,
#161675,#161676,#161677,#161678,#161679,#161680,#161681,#161682,#161683,
#161684,#161685,#161686,#161687,#161688,#161689,#161690,#161691,#161692,
#161693,#161694,#161695,#161696,#161697,#161698,#161699,#161700,#161701,
#161702,#161703,#161704,#161705,#161706,#161707,#161708,#161709,#161710,
#161711,#161712,#161713,#161714,#161715,#161716,#161717,#161718,#161719,
#161720,#161721,#161722,#161723,#161724,#161725,#161726,#161727,#161728,
#161729,#161730,#161731,#161732,#161733,#161734,#161735,#161736,#161737,
#161738,#161739,#161740,#161741,#161742,#161743,#161744,#161745,#161746,
#161747,#161748,#161749,#161750,#161751,#161752,#161753,#161754,#161755,
#161756,#161757,#161758,#161759,#161760,#161761,#161762,#161763,#161764,
#161765,#161766,#161767,#161768,#161769,#161770,#161771,#161772,#161773,
#161774,#161775,#161776,#161777,#161778,#161779,#161780,#161781,#161782,
#161783,#161784,#161785,#161786,#161787,#161788,#161789,#161790,#161791,
#161792,#161793,#161794,#161795,#161796,#161797,#161798,#161799,#161800,
#161801,#161802,#161803,#161804,#161805,#161806,#161807,#161808,#161809,
#161810,#161811,#161812,#161813,#161814,#161815,#161816,#161817,#161818,
#161819,#161820,#161821,#161822,#161823,#161824,#161825,#161826,#161827,
#161828,#161829,#161830,#161831,#161832,#161833,#161834,#161835),
 .UNSPECIFIED.,.F.,.F.,(4,3,3,3,3,3,3,3,3,3,3,3,3,3,3,3,3,3,3,3,3,3,3,3,
3,3,3,3,3,3,3,3,3,3,3,3,3,3,3,3,3,3,3,3,3,3,3,3,3,3,3,3,3,3,3,3,3,3,3,3,
3,3,3,3,3,3,3,3,3,3,3,3,3,3,3,3,3,3,3,3,3,3,4),(1483.95058758791,1484.03276112934,
1484.11249874285,1484.19224360271,1484.27201130001,1484.35600245486,1484.43590835349,
1484.5158731071,1484.59594982076,1484.60797591939,1484.68793321952,1484.76779601676,
1484.84758183924,1484.92730815443,1485.00699238273,1485.08666336895,1485.16633082247,
1485.24601047329,1485.32571805569,1485.40551328476,1485.48535762647,1485.56531605352,
1485.60771193011,1485.68766923024,1485.76753202748,1485.84731784996,1485.92704416515,
1486.00672839345,1486.08639937967,1486.16606683319,1486.24574648401,1486.3254540664,
1486.40524929548,1486.48509363719,1486.56505206424,1486.60744794083,1486.68740524096,
1486.7672680382,1486.84705386067,1486.92678017587,1487.00646440416,1487.08613539038,
1487.16580284391,1487.24548249473,1487.32519007712,1487.40498530619,1487.4848296479,
1487.56478807495,1487.60718395155,1487.68714125168,1487.76700404892,1487.8467898714,
1487.92651618659,1488.00620041488,1488.08587140111,1488.16553885463,1488.24521850545,
1488.32492608784,1488.40472131692,1488.48456565863,1488.56452408567,1488.60691996227,
1488.6868772624,1488.76674005964,1488.84652588211,1488.92625219731,1489.0059364256,
1489.08560741182,1489.16527486535,1489.24495451617,1489.32466209856,1489.40445732764,
1489.48430166934,1489.56426009639,1489.60665597299,1489.68722612258,1489.7676985561,
1489.84808846144,1489.92841097225,1490.00867685395,1490.08890876417,1490.16913181602,
1490.23377289509),.UNSPECIFIED.);
#1366=B_SPLINE_CURVE_WITH_KNOTS('',3,(#161837,#161838,#161839,#161840,#161841,
#161842,#161843,#161844,#161845,#161846),.UNSPECIFIED.,.F.,.F.,(4,1,1,1,
1,1,1,4),(1490.233780566,1490.60639198371,1491.60612799443,1492.60586400515,
1493.60560001587,1494.60533602659,1495.60507203731,1496.5169494552),
 .UNSPECIFIED.);
#1367=B_SPLINE_CURVE_WITH_KNOTS('',3,(#161848,#161849,#161850,#161851,#161852,
#161853,#161854,#161855,#161856,#161857,#161858,#161859,#161860,#161861,
#161862,#161863,#161864,#161865,#161866,#161867,#161868,#161869,#161870,
#161871,#161872,#161873,#161874,#161875,#161876,#161877,#161878,#161879,
#161880,#161881,#161882,#161883,#161884,#161885,#161886,#161887,#161888,
#161889,#161890,#161891,#161892,#161893,#161894,#161895,#161896,#161897,
#161898,#161899,#161900,#161901,#161902,#161903,#161904,#161905,#161906,
#161907,#161908,#161909,#161910,#161911,#161912,#161913,#161914,#161915,
#161916,#161917,#161918,#161919,#161920,#161921,#161922,#161923,#161924,
#161925,#161926,#161927,#161928,#161929,#161930,#161931,#161932,#161933,
#161934,#161935,#161936,#161937,#161938,#161939,#161940,#161941,#161942,
#161943,#161944,#161945,#161946,#161947,#161948,#161949,#161950,#161951,
#161952,#161953,#161954,#161955,#161956,#161957,#161958,#161959,#161960,
#161961,#161962,#161963,#161964,#161965,#161966,#161967,#161968,#161969,
#161970,#161971,#161972,#161973,#161974,#161975,#161976,#161977,#161978,
#161979,#161980,#161981,#161982,#161983,#161984,#161985,#161986,#161987,
#161988,#161989,#161990,#161991,#161992,#161993,#161994,#161995,#161996,
#161997,#161998,#161999,#162000,#162001,#162002,#162003,#162004,#162005,
#162006,#162007,#162008,#162009,#162010,#162011,#162012,#162013,#162014,
#162015,#162016,#162017,#162018,#162019,#162020,#162021,#162022,#162023,
#162024,#162025,#162026,#162027,#162028,#162029,#162030,#162031,#162032,
#162033,#162034,#162035,#162036,#162037,#162038,#162039,#162040,#162041,
#162042,#162043,#162044,#162045,#162046,#162047,#162048,#162049,#162050,
#162051,#162052,#162053,#162054,#162055,#162056,#162057,#162058,#162059,
#162060,#162061,#162062,#162063,#162064,#162065,#162066,#162067,#162068,
#162069,#162070,#162071,#162072,#162073,#162074,#162075,#162076,#162077,
#162078,#162079,#162080,#162081,#162082,#162083,#162084,#162085,#162086,
#162087,#162088,#162089,#162090,#162091),.UNSPECIFIED.,.F.,.F.,(4,3,3,3,
3,3,3,3,3,3,3,3,3,3,3,3,3,3,3,3,3,3,3,3,3,3,3,3,3,3,3,3,3,3,3,3,3,3,3,3,
3,3,3,3,3,3,3,3,3,3,3,3,3,3,3,3,3,3,3,3,3,3,3,3,3,3,3,3,3,3,3,3,3,3,3,3,
3,3,3,3,3,4),(1496.51695820227,1496.60480804803,1496.68476534816,1496.7646281454,
1496.84441396788,1496.92414028307,1497.00382451137,1497.08349549759,1497.16316295111,
1497.24284260193,1497.32255018433,1497.4023454134,1497.48218975511,1497.56214818216,
1497.60454405875,1497.68450135888,1497.76436415612,1497.8441499786,1497.92387629379,
1498.00356052209,1498.08323150831,1498.16289896183,1498.24257861265,1498.32228619504,
1498.40208142412,1498.48192576583,1498.56188419287,1498.60428006947,1498.6842373696,
1498.76410016684,1498.84388598932,1498.92361230451,1499.00329653281,1499.08296751903,
1499.16263497255,1499.24231462337,1499.32202220576,1499.40181743484,1499.48166177655,
1499.56162020359,1499.60401608019,1499.68397338032,1499.76383617756,1499.84362200004,
1499.92334831523,1500.00303254352,1500.08270352975,1500.16237098327,1500.24205063409,
1500.32175821648,1500.40155344556,1500.48139778726,1500.56135621431,1500.60375209091,
1500.68370939104,1500.76357218828,1500.84335801076,1500.92308432595,1501.00276855425,
1501.08243954047,1501.16210699399,1501.24178664481,1501.3214942272,1501.40128945628,
1501.48113379799,1501.56109222503,1501.60348810163,1501.68344540176,1501.763308199,
1501.84309402147,1501.92282033667,1502.00250456496,1502.08217555118,1502.16184300471,
1502.24152265552,1502.32123023792,1502.40102546699,1502.4808698087,1502.56082823575,
1502.60322411235,1502.71891210661,1502.80014350945),.UNSPECIFIED.);
#1368=B_SPLINE_CURVE_WITH_KNOTS('',3,(#162093,#162094,#162095,#162096,#162097,
#162098,#162099,#162100,#162101,#162102),.UNSPECIFIED.,.F.,.F.,(4,1,1,1,
1,1,1,4),(1502.80014707982,1503.60296012307,1504.60269613379,1505.60243214451,
1506.60216815523,1507.60190416595,1508.60164017667,1509.08332881663),
 .UNSPECIFIED.);
#1369=B_SPLINE_CURVE_WITH_KNOTS('',3,(#162104,#162105,#162106,#162107,#162108,
#162109,#162110,#162111,#162112,#162113),.UNSPECIFIED.,.F.,.F.,(4,1,1,1,
1,1,1,4),(1509.08332881663,1509.60137618739,1510.60111219811,1511.60084820883,
1512.60058421955,1513.60032023027,1514.60005624099,1515.36651412381),
 .UNSPECIFIED.);
#1370=B_SPLINE_CURVE_WITH_KNOTS('',3,(#162115,#162116,#162117,#162118,#162119,
#162120,#162121,#162122,#162123,#162124,#162125,#162126),.UNSPECIFIED.,
 .F.,.F.,(4,2,1,1,1,1,1,1,4),(1515.36651412381,1515.59979225171,1516.59952826244,
1517.59926427316,1518.59900028388,1519.5987362946,1520.59847230532,1521.59820831604,
1521.64969943099),.UNSPECIFIED.);
#1371=B_SPLINE_CURVE_WITH_KNOTS('',3,(#162128,#162129,#162130,#162131,#162132,
#162133,#162134,#162135,#162136,#162137),.UNSPECIFIED.,.F.,.F.,(4,1,1,1,
1,1,1,4),(1521.64969943099,1522.59794432676,1523.59768033748,1524.5974163482,
1525.59715235892,1526.59688836964,1527.59662438036,1527.93287724226),
 .UNSPECIFIED.);
#1372=B_SPLINE_CURVE_WITH_KNOTS('',3,(#162139,#162140,#162141,#162142,#162143,
#162144,#162145,#162146,#162147,#162148,#162149,#162150,#162151,#162152,
#162153,#162154,#162155,#162156,#162157,#162158,#162159,#162160,#162161,
#162162,#162163,#162164,#162165,#162166,#162167,#162168,#162169,#162170,
#162171,#162172,#162173,#162174,#162175,#162176,#162177,#162178,#162179,
#162180,#162181,#162182,#162183,#162184,#162185,#162186,#162187,#162188,
#162189,#162190,#162191,#162192,#162193,#162194,#162195,#162196,#162197,
#162198,#162199,#162200,#162201,#162202,#162203,#162204,#162205,#162206,
#162207,#162208,#162209,#162210,#162211,#162212,#162213,#162214,#162215,
#162216,#162217,#162218,#162219,#162220,#162221,#162222,#162223,#162224,
#162225,#162226,#162227,#162228,#162229,#162230,#162231,#162232,#162233,
#162234,#162235,#162236,#162237,#162238,#162239,#162240,#162241,#162242,
#162243,#162244,#162245,#162246,#162247,#162248,#162249,#162250,#162251,
#162252,#162253,#162254,#162255,#162256,#162257,#162258,#162259,#162260,
#162261,#162262,#162263,#162264,#162265,#162266,#162267,#162268,#162269,
#162270,#162271,#162272,#162273,#162274,#162275,#162276,#162277,#162278,
#162279,#162280,#162281,#162282,#162283,#162284,#162285,#162286,#162287,
#162288,#162289,#162290,#162291,#162292,#162293,#162294,#162295,#162296,
#162297,#162298,#162299,#162300,#162301,#162302,#162303,#162304,#162305,
#162306,#162307,#162308,#162309,#162310,#162311,#162312,#162313,#162314,
#162315,#162316,#162317,#162318,#162319,#162320,#162321,#162322,#162323,
#162324,#162325,#162326,#162327,#162328,#162329,#162330,#162331,#162332,
#162333,#162334,#162335,#162336,#162337,#162338,#162339,#162340,#162341,
#162342,#162343,#162344,#162345,#162346,#162347,#162348,#162349,#162350,
#162351,#162352,#162353,#162354,#162355,#162356,#162357,#162358,#162359,
#162360,#162361,#162362,#162363,#162364,#162365,#162366,#162367,#162368,
#162369,#162370,#162371,#162372,#162373,#162374,#162375,#162376,#162377,
#162378,#162379,#162380,#162381,#162382,#162383,#162384,#162385),
 .UNSPECIFIED.,.F.,.F.,(4,3,3,3,3,3,3,3,3,3,3,3,3,3,3,3,3,3,3,3,3,3,3,3,
3,3,3,3,3,3,3,3,3,3,3,3,3,3,3,3,3,3,3,3,3,3,3,3,3,3,3,3,3,3,3,3,3,3,3,3,
3,3,3,3,3,3,3,3,3,3,3,3,3,3,3,3,3,3,3,3,3,3,4),(1527.93288473817,1528.01581919478,
1528.09546894363,1528.17512364067,1528.25479896718,1528.33451061385,1528.41431779342,
1528.49418137679,1528.57415894196,1528.59636039108,1528.67631769121,1528.75618048845,
1528.83596631093,1528.91569262612,1528.99537685441,1529.07504784064,1529.15471529416,
1529.23439494498,1529.31410252737,1529.39389775645,1529.47374209815,1529.5537005252,
1529.5960964018,1529.67605370193,1529.75591649917,1529.83570232165,1529.91542863684,
1529.99511286513,1530.07478385136,1530.15445130488,1530.2341309557,1530.31383853809,
1530.39363376717,1530.47347810887,1530.55343653592,1530.59583241252,1530.67578971265,
1530.75565250989,1530.83543833237,1530.91516464756,1530.99484887586,1531.07451986208,
1531.1541873156,1531.23386696642,1531.31357454882,1531.39336977789,1531.4732141196,
1531.55317254665,1531.59556842324,1531.67552572337,1531.75538852061,1531.83517434309,
1531.91490065828,1531.99458488658,1532.0742558728,1532.15392332632,1532.23360297714,
1532.31331055953,1532.39310578861,1532.47295013032,1532.55290855736,1532.59530443396,
1532.67526173409,1532.75512453133,1532.83491035381,1532.914636669,1532.9943208973,
1533.07399188352,1533.15365933704,1533.23333898786,1533.31304657025,1533.39284179933,
1533.47268614104,1533.55264456808,1533.59504044468,1533.67572883148,1533.75631844907,
1533.83682434353,1533.91726150585,1533.99763925535,1534.07798168726,1534.15831132183,
1534.21607004535),.UNSPECIFIED.);
#1373=B_SPLINE_CURVE_WITH_KNOTS('',3,(#162387,#162388,#162389,#162390,#162391,
#162392,#162393,#162394,#162395,#162396),.UNSPECIFIED.,.F.,.F.,(4,1,1,1,
1,1,1,4),(1534.21607763161,1534.5947764554,1535.59451246612,1536.59424847684,
1537.59398448756,1538.59372049828,1539.593456509,1540.49924633286),
 .UNSPECIFIED.);
#1374=B_SPLINE_CURVE_WITH_KNOTS('',3,(#162398,#162399,#162400,#162401,#162402,
#162403,#162404,#162405,#162406,#162407,#162408,#162409,#162410,#162411,
#162412,#162413,#162414,#162415,#162416,#162417,#162418,#162419,#162420,
#162421,#162422,#162423,#162424,#162425,#162426,#162427,#162428,#162429,
#162430,#162431,#162432,#162433,#162434,#162435,#162436,#162437,#162438,
#162439,#162440,#162441,#162442,#162443,#162444,#162445,#162446,#162447,
#162448,#162449,#162450,#162451,#162452,#162453,#162454,#162455,#162456,
#162457,#162458,#162459,#162460,#162461,#162462,#162463,#162464,#162465,
#162466,#162467,#162468,#162469,#162470,#162471,#162472,#162473,#162474,
#162475,#162476,#162477,#162478,#162479,#162480,#162481,#162482,#162483,
#162484,#162485,#162486,#162487,#162488,#162489,#162490,#162491,#162492,
#162493,#162494,#162495,#162496,#162497,#162498,#162499,#162500,#162501,
#162502,#162503,#162504,#162505,#162506,#162507,#162508,#162509,#162510,
#162511,#162512,#162513,#162514,#162515,#162516,#162517,#162518,#162519,
#162520,#162521,#162522,#162523,#162524,#162525,#162526,#162527,#162528,
#162529,#162530,#162531,#162532,#162533,#162534,#162535,#162536,#162537,
#162538,#162539,#162540,#162541,#162542,#162543,#162544,#162545,#162546,
#162547,#162548,#162549,#162550,#162551,#162552,#162553,#162554,#162555,
#162556,#162557,#162558,#162559,#162560,#162561,#162562,#162563,#162564,
#162565,#162566,#162567,#162568,#162569,#162570,#162571,#162572,#162573,
#162574,#162575,#162576,#162577,#162578,#162579,#162580,#162581,#162582,
#162583,#162584,#162585,#162586,#162587,#162588,#162589,#162590,#162591,
#162592,#162593,#162594,#162595,#162596,#162597,#162598,#162599,#162600,
#162601,#162602,#162603,#162604,#162605,#162606,#162607,#162608,#162609,
#162610,#162611,#162612,#162613,#162614,#162615,#162616,#162617,#162618,
#162619,#162620,#162621,#162622,#162623,#162624,#162625,#162626,#162627,
#162628,#162629,#162630,#162631,#162632,#162633,#162634,#162635,#162636,
#162637,#162638,#162639,#162640,#162641),.UNSPECIFIED.,.F.,.F.,(4,3,3,3,
3,3,3,3,3,3,3,3,3,3,3,3,3,3,3,3,3,3,3,3,3,3,3,3,3,3,3,3,3,3,3,3,3,3,3,3,
3,3,3,3,3,3,3,3,3,3,3,3,3,3,3,3,3,3,3,3,3,3,3,3,3,3,3,3,3,3,3,3,3,3,3,3,
3,3,3,3,3,4),(1540.49925535253,1540.59319251972,1540.67314981985,1540.75301261709,
1540.83279843957,1540.91252475476,1540.99220898306,1541.07187996928,1541.1515474228,
1541.23122707362,1541.31093465601,1541.39072988509,1541.4705742268,1541.55053265384,
1541.59292853044,1541.67288583057,1541.75274862781,1541.83253445029,1541.91226076548,
1541.99194499378,1542.07161598,1542.15128343352,1542.23096308434,1542.31067066673,
1542.39046589581,1542.47031023752,1542.55026866456,1542.59266454116,1542.67262184129,
1542.75248463853,1542.83227046101,1542.9119967762,1542.9916810045,1543.07135199072,
1543.15101944424,1543.23069909506,1543.31040667745,1543.39020190653,1543.47004624824,
1543.55000467528,1543.59240055188,1543.67235785201,1543.75222064925,1543.83200647173,
1543.91173278692,1543.99141701522,1544.07108800144,1544.15075545496,1544.23043510578,
1544.31014268817,1544.38993791725,1544.46978225896,1544.549740686,1544.5921365626,
1544.67209386273,1544.75195665997,1544.83174248245,1544.91146879764,1544.99115302593,
1545.07082401216,1545.15049146568,1545.2301711165,1545.30987869889,1545.38967392797,
1545.46951826968,1545.54947669672,1545.59187257332,1545.67182987345,1545.75169267069,
1545.83147849316,1545.91120480836,1545.99088903665,1546.07056002287,1546.1502274764,
1546.22990712722,1546.30961470961,1546.38940993869,1546.46925428039,1546.54921270744,
1546.59160858404,1546.70921964393,1546.78244065971),.UNSPECIFIED.);
#1375=B_SPLINE_CURVE_WITH_KNOTS('',3,(#162643,#162644,#162645,#162646,#162647,
#162648,#162649,#162650,#162651,#162652),.UNSPECIFIED.,.F.,.F.,(4,1,1,1,
1,1,1,4),(1546.78244481203,1547.59134459476,1548.59108060548,1549.5908166162,
1550.59055262692,1551.59028863764,1552.59002464836,1553.06562596689),
 .UNSPECIFIED.);
#1376=B_SPLINE_CURVE_WITH_KNOTS('',3,(#162654,#162655,#162656,#162657,#162658,
#162659,#162660,#162661,#162662,#162663),.UNSPECIFIED.,.F.,.F.,(4,1,1,1,
1,1,1,4),(1553.06562596689,1553.58976065908,1554.5894966698,1555.58923268052,
1556.58896869124,1557.58870470196,1558.58844071268,1559.34881127407),
 .UNSPECIFIED.);
#1377=B_SPLINE_CURVE_WITH_KNOTS('',3,(#162665,#162666,#162667,#162668,#162669,
#162670,#162671,#162672,#162673,#162674,#162675,#162676),.UNSPECIFIED.,
 .F.,.F.,(4,2,1,1,1,1,1,1,4),(1559.34881127407,1559.5881767234,1560.58791273412,
1561.58764874484,1562.58738475556,1563.58712076628,1564.586856777,1565.58659278772,
1565.63199658125),.UNSPECIFIED.);
#1378=B_SPLINE_CURVE_WITH_KNOTS('',3,(#162678,#162679,#162680,#162681,#162682,
#162683,#162684,#162685,#162686,#162687),.UNSPECIFIED.,.F.,.F.,(4,1,1,1,
1,1,1,4),(1565.63199658125,1566.58632879844,1567.58606480916,1568.58580081988,
1569.5855368306,1570.58527284132,1571.58500885204,1571.9151745794),
 .UNSPECIFIED.);
#1379=B_SPLINE_CURVE_WITH_KNOTS('',3,(#162689,#162690,#162691,#162692,#162693,
#162694,#162695,#162696,#162697,#162698,#162699,#162700,#162701,#162702,
#162703,#162704,#162705,#162706,#162707,#162708,#162709,#162710,#162711,
#162712,#162713,#162714,#162715,#162716,#162717,#162718,#162719,#162720,
#162721,#162722,#162723,#162724,#162725,#162726,#162727,#162728,#162729,
#162730,#162731,#162732,#162733,#162734,#162735,#162736,#162737,#162738,
#162739,#162740,#162741,#162742,#162743,#162744,#162745,#162746,#162747,
#162748,#162749,#162750,#162751,#162752,#162753,#162754,#162755,#162756,
#162757,#162758,#162759,#162760,#162761,#162762,#162763,#162764,#162765,
#162766,#162767,#162768,#162769,#162770,#162771,#162772,#162773,#162774,
#162775,#162776,#162777,#162778,#162779,#162780,#162781,#162782,#162783,
#162784,#162785,#162786,#162787,#162788,#162789,#162790,#162791,#162792,
#162793,#162794,#162795,#162796,#162797,#162798,#162799,#162800,#162801,
#162802,#162803,#162804,#162805,#162806,#162807,#162808,#162809,#162810,
#162811,#162812,#162813,#162814,#162815,#162816,#162817,#162818,#162819,
#162820,#162821,#162822,#162823,#162824,#162825,#162826,#162827,#162828,
#162829,#162830,#162831,#162832,#162833,#162834,#162835,#162836,#162837,
#162838,#162839,#162840,#162841,#162842,#162843,#162844,#162845,#162846,
#162847,#162848,#162849,#162850,#162851,#162852,#162853,#162854,#162855,
#162856,#162857,#162858,#162859,#162860,#162861,#162862,#162863,#162864,
#162865,#162866,#162867,#162868,#162869,#162870,#162871,#162872,#162873,
#162874,#162875,#162876,#162877,#162878,#162879,#162880,#162881,#162882,
#162883,#162884,#162885,#162886,#162887,#162888,#162889,#162890,#162891,
#162892,#162893,#162894,#162895,#162896,#162897,#162898,#162899,#162900,
#162901,#162902,#162903,#162904,#162905,#162906,#162907,#162908,#162909,
#162910,#162911,#162912,#162913,#162914,#162915,#162916,#162917,#162918,
#162919,#162920,#162921,#162922,#162923,#162924,#162925,#162926,#162927,
#162928,#162929,#162930,#162931,#162932,#162933,#162934,#162935),
 .UNSPECIFIED.,.F.,.F.,(4,3,3,3,3,3,3,3,3,3,3,3,3,3,3,3,3,3,3,3,3,3,3,3,
3,3,3,3,3,3,3,3,3,3,3,3,3,3,3,3,3,3,3,3,3,3,3,3,3,3,3,3,3,3,3,3,3,3,3,3,
3,3,3,3,3,3,3,3,3,3,3,3,3,3,3,3,3,3,3,3,3,3,4),(1571.91518188843,1571.99887726022,
1572.07844285309,1572.1580111645,1572.23759795907,1572.31721900964,1572.39693410193,
1572.47670391825,1572.55658863134,1572.58474486276,1572.66470216289,1572.74456496014,
1572.82435078261,1572.9040770978,1572.9837613261,1573.06343231232,1573.14309976585,
1573.22277941667,1573.30248699906,1573.38228222814,1573.46212656985,1573.5420849969,
1573.58448087348,1573.66443817361,1573.74430097085,1573.82408679333,1573.90381310852,
1573.98349733682,1574.06316832304,1574.14283577656,1574.22251542738,1574.30222300978,
1574.38201823885,1574.46186258056,1574.54182100761,1574.5842168842,1574.66417418433,
1574.74403698157,1574.82382280404,1574.90354911924,1574.98323334753,1575.06290433375,
1575.14257178728,1575.2222514381,1575.30195902049,1575.38175424957,1575.46159859127,
1575.54155701832,1575.58395289492,1575.66391019505,1575.74377299229,1575.82355881477,
1575.90328512996,1575.98296935825,1576.06264034448,1576.142307798,1576.22198744882,
1576.30169503121,1576.38149026029,1576.461334602,1576.54129302904,1576.58368890564,
1576.66364620577,1576.74350900301,1576.82329482548,1576.90302114068,1576.98270536897,
1577.06237635519,1577.14204380872,1577.22172345953,1577.30143104193,1577.381226271,
1577.46107061271,1577.54102903976,1577.58342491636,1577.66423586784,1577.74494693697,
1577.82557301612,1577.90612894158,1577.98662258522,1578.06707947055,1578.1475196518,
1578.19836719561),.UNSPECIFIED.);
#1380=B_SPLINE_CURVE_WITH_KNOTS('',3,(#162937,#162938,#162939,#162940,#162941,
#162942,#162943,#162944,#162945,#162946),.UNSPECIFIED.,.F.,.F.,(4,1,1,1,
1,1,1,4),(1578.19837466001,1578.58316092708,1579.5828969378,1580.58263294852,
1581.58236895924,1582.58210496996,1583.58184098068,1584.4815434095),
 .UNSPECIFIED.);
#1381=B_SPLINE_CURVE_WITH_KNOTS('',3,(#162948,#162949,#162950,#162951,#162952,
#162953,#162954,#162955,#162956,#162957,#162958,#162959,#162960,#162961,
#162962,#162963,#162964,#162965,#162966,#162967,#162968,#162969,#162970,
#162971,#162972,#162973,#162974,#162975,#162976,#162977,#162978,#162979,
#162980,#162981,#162982,#162983,#162984,#162985,#162986,#162987,#162988,
#162989,#162990,#162991,#162992,#162993,#162994,#162995,#162996,#162997,
#162998,#162999,#163000,#163001,#163002,#163003,#163004,#163005,#163006,
#163007,#163008,#163009,#163010,#163011,#163012,#163013,#163014,#163015,
#163016,#163017,#163018,#163019,#163020,#163021,#163022,#163023,#163024,
#163025,#163026,#163027,#163028,#163029,#163030,#163031,#163032,#163033,
#163034,#163035,#163036,#163037,#163038,#163039,#163040,#163041,#163042,
#163043,#163044,#163045,#163046,#163047,#163048,#163049,#163050,#163051,
#163052,#163053,#163054,#163055,#163056,#163057,#163058,#163059,#163060,
#163061,#163062,#163063,#163064,#163065,#163066,#163067,#163068,#163069,
#163070,#163071,#163072,#163073,#163074,#163075,#163076,#163077,#163078,
#163079,#163080,#163081,#163082,#163083,#163084,#163085,#163086,#163087,
#163088,#163089,#163090,#163091,#163092,#163093,#163094,#163095,#163096,
#163097,#163098,#163099,#163100,#163101,#163102,#163103,#163104,#163105,
#163106,#163107,#163108,#163109,#163110,#163111,#163112,#163113,#163114,
#163115,#163116,#163117,#163118,#163119,#163120,#163121,#163122,#163123,
#163124,#163125,#163126,#163127,#163128,#163129,#163130,#163131,#163132,
#163133,#163134,#163135,#163136,#163137,#163138,#163139,#163140,#163141,
#163142,#163143,#163144,#163145,#163146,#163147,#163148,#163149,#163150,
#163151,#163152,#163153,#163154,#163155,#163156,#163157,#163158,#163159,
#163160,#163161,#163162,#163163,#163164,#163165,#163166,#163167,#163168,
#163169,#163170,#163171,#163172,#163173,#163174,#163175,#163176,#163177,
#163178,#163179,#163180,#163181,#163182,#163183,#163184,#163185,#163186,
#163187,#163188,#163189,#163190,#163191),.UNSPECIFIED.,.F.,.F.,(4,3,3,3,
3,3,3,3,3,3,3,3,3,3,3,3,3,3,3,3,3,3,3,3,3,3,3,3,3,3,3,3,3,3,3,3,3,3,3,3,
3,3,3,3,3,3,3,3,3,3,3,3,3,3,3,3,3,3,3,3,3,3,3,3,3,3,3,3,3,3,3,3,3,3,3,3,
3,3,3,3,3,4),(1584.48155250279,1584.5815769914,1584.66153429153,1584.74139708877,
1584.82118291125,1584.90090922644,1584.98059345474,1585.06026444096,1585.13993189449,
1585.2196115453,1585.2993191277,1585.37911435677,1585.45895869848,1585.53891712553,
1585.58131300212,1585.66127030225,1585.74113309949,1585.82091892197,1585.90064523716,
1585.98032946546,1586.06000045168,1586.1396679052,1586.21934755602,1586.29905513841,
1586.37885036749,1586.4586947092,1586.53865313624,1586.58104901284,1586.66100631297,
1586.74086911021,1586.82065493269,1586.90038124788,1586.98006547618,1587.0597364624,
1587.13940391592,1587.21908356674,1587.29879114913,1587.37858637821,1587.45843071992,
1587.53838914696,1587.58078502356,1587.66074232369,1587.74060512093,1587.82039094341,
1587.9001172586,1587.97980148689,1588.05947247312,1588.13913992664,1588.21881957746,
1588.29852715985,1588.37832238893,1588.45816673064,1588.53812515768,1588.58052103428,
1588.66047833441,1588.74034113165,1588.82012695413,1588.89985326932,1588.97953749762,
1589.05920848384,1589.13887593736,1589.21855558818,1589.29826317057,1589.37805839965,
1589.45790274136,1589.5378611684,1589.580257045,1589.66021434513,1589.74007714237,
1589.81986296484,1589.89958928003,1589.97927350833,1590.05894449455,1590.13861194807,
1590.21829159889,1590.29799918128,1590.37779441035,1590.45763875206,1590.53759717911,
1590.57999305572,1590.69969193202,1590.76473780997),.UNSPECIFIED.);
#1382=B_SPLINE_CURVE_WITH_KNOTS('',3,(#163193,#163194,#163195,#163196,#163197,
#163198,#163199,#163200,#163201,#163202),.UNSPECIFIED.,.F.,.F.,(4,1,1,1,
1,1,1,4),(1590.7647425272,1591.57972906644,1592.57946507717,1593.57920108788,
1594.57893709861,1595.57867310933,1596.57840912005,1597.04792311715),
 .UNSPECIFIED.);
#1383=B_SPLINE_CURVE_WITH_KNOTS('',3,(#163204,#163205,#163206,#163207,#163208,
#163209,#163210,#163211,#163212,#163213),.UNSPECIFIED.,.F.,.F.,(4,1,1,1,
1,1,1,4),(1597.04792311715,1597.57814513077,1598.57788114149,1599.57761715221,
1600.57735316293,1601.57708917365,1602.57682518437,1603.33110842433),
 .UNSPECIFIED.);
#1384=B_SPLINE_CURVE_WITH_KNOTS('',3,(#163215,#163216,#163217,#163218,#163219,
#163220,#163221,#163222,#163223,#163224,#163225,#163226,#163227,#163228,
#163229,#163230,#163231,#163232,#163233,#163234,#163235,#163236,#163237,
#163238,#163239,#163240,#163241,#163242,#163243,#163244,#163245,#163246,
#163247,#163248,#163249,#163250,#163251,#163252,#163253,#163254,#163255,
#163256,#163257,#163258,#163259,#163260,#163261,#163262,#163263,#163264,
#163265,#163266,#163267,#163268,#163269,#163270,#163271,#163272,#163273,
#163274,#163275,#163276,#163277,#163278,#163279,#163280,#163281,#163282,
#163283,#163284,#163285,#163286,#163287,#163288,#163289,#163290,#163291,
#163292,#163293,#163294,#163295,#163296,#163297,#163298,#163299,#163300,
#163301,#163302,#163303,#163304,#163305,#163306,#163307,#163308,#163309,
#163310,#163311,#163312,#163313,#163314,#163315,#163316,#163317,#163318,
#163319,#163320,#163321,#163322,#163323,#163324,#163325,#163326,#163327,
#163328,#163329,#163330,#163331,#163332,#163333,#163334,#163335,#163336,
#163337,#163338,#163339,#163340,#163341,#163342,#163343,#163344,#163345,
#163346,#163347,#163348,#163349,#163350,#163351,#163352,#163353,#163354,
#163355,#163356,#163357,#163358,#163359,#163360,#163361,#163362,#163363,
#163364,#163365,#163366,#163367,#163368,#163369,#163370,#163371,#163372,
#163373,#163374,#163375,#163376,#163377,#163378,#163379,#163380,#163381,
#163382,#163383,#163384,#163385,#163386,#163387,#163388,#163389,#163390,
#163391,#163392,#163393,#163394,#163395,#163396,#163397,#163398,#163399,
#163400,#163401,#163402,#163403,#163404,#163405,#163406,#163407,#163408,
#163409,#163410,#163411,#163412,#163413,#163414,#163415,#163416,#163417,
#163418,#163419,#163420,#163421,#163422,#163423,#163424,#163425,#163426,
#163427,#163428,#163429,#163430,#163431,#163432,#163433,#163434,#163435,
#163436,#163437,#163438,#163439,#163440,#163441,#163442,#163443,#163444,
#163445,#163446,#163447,#163448,#163449,#163450,#163451,#163452,#163453,
#163454,#163455,#163456,#163457,#163458,#163459,#163460,#163461),
 .UNSPECIFIED.,.F.,.F.,(4,3,3,3,3,3,3,3,3,3,3,3,3,3,3,3,3,3,3,3,3,3,3,3,
3,3,3,3,3,3,3,3,3,3,3,3,3,3,3,3,3,3,3,3,3,3,3,3,3,3,3,3,3,3,3,3,3,3,3,3,
3,3,3,3,3,3,3,3,3,3,3,3,3,3,3,3,3,3,3,3,3,3,4),(1603.3311085053,1603.43422233826,
1603.53975581896,1603.57656119509,1603.65651849522,1603.73638129247,1603.81616711494,
1603.89589343014,1603.97557765843,1604.05524864465,1604.13491609818,1604.214595749,
1604.29430333139,1604.37409856047,1604.45394290218,1604.53390132923,1604.57629720581,
1604.65625450594,1604.73611730318,1604.81590312566,1604.89562944085,1604.97531366914,
1605.05498465537,1605.13465210889,1605.21433175971,1605.2940393421,1605.37383457118,
1605.45367891289,1605.53363733993,1605.57603321653,1605.65599051666,1605.7358533139,
1605.81563913638,1605.89536545157,1605.97504967986,1606.05472066609,1606.13438811961,
1606.21406777043,1606.29377535282,1606.3735705819,1606.45341492361,1606.53337335065,
1606.57576922725,1606.65572652738,1606.73558932462,1606.8153751471,1606.89510146229,
1606.97478569059,1607.05445667681,1607.13412413033,1607.21380378115,1607.29351136354,
1607.37330659262,1607.45315093433,1607.53310936137,1607.57550523797,1607.6554625381,
1607.73532533534,1607.81511115782,1607.89483747301,1607.97452170131,1608.05419268753,
1608.13386014105,1608.21353979187,1608.29324737426,1608.37304260334,1608.45288694505,
1608.53284537209,1608.57524124869,1608.65519854882,1608.73506134606,1608.81484716853,
1608.89457348373,1608.97425771202,1609.05392869824,1609.13359615177,1609.21327580259,
1609.29298338498,1609.37277861405,1609.45262295576,1609.53258138281,1609.57497725941,
1609.61429373151),.UNSPECIFIED.);
#1385=B_SPLINE_CURVE_WITH_KNOTS('',3,(#163463,#163464,#163465,#163466,#163467,
#163468,#163469,#163470,#163471,#163472),.UNSPECIFIED.,.F.,.F.,(4,1,1,1,
1,1,1,4),(1609.61429912006,1610.57471327013,1611.57444928085,1612.57418529157,
1613.57392130229,1614.57365731301,1615.57339332373,1615.89747903868),
 .UNSPECIFIED.);
#1386=B_SPLINE_CURVE_WITH_KNOTS('',3,(#163474,#163475,#163476,#163477,#163478,
#163479,#163480,#163481,#163482,#163483),.UNSPECIFIED.,.F.,.F.,(4,1,1,1,
1,1,1,4),(1615.89747903868,1616.57312933445,1617.57286534517,1618.57260135589,
1619.57233736661,1620.57207337733,1621.57180938805,1622.18066434587),
 .UNSPECIFIED.);
#1387=B_SPLINE_CURVE_WITH_KNOTS('',3,(#163485,#163486,#163487,#163488,#163489,
#163490,#163491,#163492,#163493,#163494),.UNSPECIFIED.,.F.,.F.,(4,1,1,1,
1,1,1,4),(1622.18066434587,1622.57154539877,1623.57128140949,1624.57101742021,
1625.57075343093,1626.57048944165,1627.57022545237,1628.46384965304),
 .UNSPECIFIED.);
#1388=B_SPLINE_CURVE_WITH_KNOTS('',3,(#163496,#163497,#163498,#163499,#163500,
#163501,#163502,#163503,#163504,#163505,#163506,#163507,#163508),
 .UNSPECIFIED.,.F.,.F.,(4,3,1,1,1,1,1,1,4),(1628.46384965304,1628.56996146309,
1629.56969747381,1630.56943348453,1631.56916949525,1632.56890550597,1633.56864151669,
1634.56837752741,1634.74703496022),.UNSPECIFIED.);
#1389=B_SPLINE_CURVE_WITH_KNOTS('',3,(#163510,#163511,#163512,#163513,#163514,
#163515,#163516,#163517,#163518,#163519,#163520,#163521,#163522,#163523,
#163524,#163525,#163526,#163527,#163528,#163529,#163530,#163531,#163532,
#163533,#163534,#163535,#163536,#163537,#163538,#163539,#163540,#163541,
#163542,#163543,#163544,#163545,#163546,#163547,#163548,#163549,#163550,
#163551,#163552,#163553,#163554,#163555,#163556,#163557,#163558,#163559,
#163560,#163561,#163562,#163563,#163564,#163565,#163566,#163567,#163568,
#163569,#163570,#163571,#163572,#163573,#163574,#163575,#163576,#163577,
#163578,#163579,#163580,#163581,#163582,#163583,#163584,#163585,#163586,
#163587,#163588,#163589,#163590,#163591,#163592,#163593,#163594,#163595,
#163596,#163597,#163598,#163599,#163600,#163601,#163602,#163603,#163604,
#163605,#163606,#163607,#163608,#163609,#163610,#163611,#163612,#163613,
#163614,#163615,#163616,#163617,#163618,#163619,#163620,#163621,#163622,
#163623,#163624,#163625,#163626,#163627,#163628,#163629,#163630,#163631,
#163632,#163633,#163634,#163635,#163636,#163637,#163638,#163639,#163640,
#163641,#163642,#163643,#163644,#163645,#163646,#163647,#163648,#163649,
#163650,#163651,#163652,#163653,#163654,#163655,#163656,#163657,#163658,
#163659,#163660,#163661,#163662,#163663,#163664,#163665,#163666,#163667,
#163668,#163669,#163670,#163671,#163672,#163673,#163674,#163675,#163676,
#163677,#163678,#163679,#163680,#163681,#163682,#163683,#163684,#163685,
#163686,#163687,#163688,#163689,#163690,#163691,#163692,#163693,#163694,
#163695,#163696,#163697,#163698,#163699,#163700,#163701,#163702,#163703,
#163704,#163705,#163706,#163707,#163708,#163709,#163710,#163711,#163712,
#163713,#163714,#163715,#163716,#163717,#163718,#163719,#163720,#163721,
#163722,#163723,#163724,#163725,#163726,#163727,#163728,#163729,#163730,
#163731,#163732,#163733,#163734,#163735,#163736,#163737,#163738,#163739,
#163740,#163741,#163742,#163743,#163744,#163745,#163746,#163747,#163748,
#163749,#163750,#163751,#163752,#163753,#163754,#163755,#163756),
 .UNSPECIFIED.,.F.,.F.,(4,3,3,3,3,3,3,3,3,3,3,3,3,3,3,3,3,3,3,3,3,3,3,3,
3,3,3,3,3,3,3,3,3,3,3,3,3,3,3,3,3,3,3,3,3,3,3,3,3,3,3,3,3,3,3,3,3,3,3,3,
3,3,3,3,3,3,3,3,3,3,3,3,3,3,3,3,3,3,3,3,3,3,4),(1634.74703496022,1634.82567899522,
1634.90425430968,1634.98277929056,1635.06128097298,1635.13977333159,1635.21827293407,
1635.29679635215,1635.37540216393,1635.45405498737,1635.53281728381,1635.56811353813,
1635.64807083826,1635.7279336355,1635.80771945798,1635.88744577317,1635.96713000146,
1636.04680098768,1636.12646844121,1636.20614809203,1636.28585567442,1636.36565090349,
1636.4454952452,1636.52545367225,1636.56784954885,1636.64780684898,1636.72766964622,
1636.80745546869,1636.88718178389,1636.96686601218,1637.0465369984,1637.12620445193,
1637.20588410275,1637.28559168514,1637.36538691421,1637.44523125592,1637.52518968297,
1637.56758555957,1637.6475428597,1637.72740565694,1637.80719147942,1637.88691779461,
1637.96660202291,1638.04627300913,1638.12594046265,1638.20562011347,1638.28532769587,
1638.36512292494,1638.44496726665,1638.5249256937,1638.56732157029,1638.64727887042,
1638.72714166766,1638.80692749014,1638.88665380533,1638.96633803363,1639.04600901985,
1639.12567647337,1639.20535612419,1639.28506370658,1639.36485893566,1639.44470327737,
1639.52466170441,1639.56705758101,1639.64701488114,1639.72687767838,1639.80666350086,
1639.88638981605,1639.96607404435,1640.04574503057,1640.12541248409,1640.20509213491,
1640.2847997173,1640.36459494638,1640.44443928809,1640.52439771513,1640.56679359173,
1640.65238019264,1640.73780309498,1640.82299284296,1640.90803942774,1640.99288519324,
1641.03022006836),.UNSPECIFIED.);
#1390=B_SPLINE_CURVE_WITH_KNOTS('',3,(#163758,#163759,#163760,#163761,#163762,
#163763,#163764,#163765,#163766,#163767),.UNSPECIFIED.,.F.,.F.,(4,1,1,1,
1,1,1,4),(1641.0302202674,1641.56652960245,1642.56626561317,1643.56600162389,
1644.56573763461,1645.56547364533,1646.56520965605,1647.31340557458),
 .UNSPECIFIED.);
#1391=B_SPLINE_CURVE_WITH_KNOTS('',3,(#163769,#163770,#163771,#163772,#163773,
#163774,#163775,#163776,#163777,#163778,#163779,#163780,#163781,#163782,
#163783,#163784,#163785,#163786,#163787,#163788,#163789,#163790,#163791,
#163792,#163793,#163794,#163795,#163796,#163797,#163798,#163799,#163800,
#163801,#163802,#163803,#163804,#163805,#163806,#163807,#163808,#163809,
#163810,#163811,#163812,#163813,#163814,#163815,#163816,#163817,#163818,
#163819,#163820,#163821,#163822,#163823,#163824,#163825,#163826,#163827,
#163828,#163829,#163830,#163831,#163832,#163833,#163834,#163835,#163836,
#163837,#163838,#163839,#163840,#163841,#163842,#163843,#163844,#163845,
#163846,#163847,#163848,#163849,#163850,#163851,#163852,#163853,#163854,
#163855,#163856,#163857,#163858,#163859,#163860,#163861,#163862,#163863,
#163864,#163865,#163866,#163867,#163868,#163869,#163870,#163871,#163872,
#163873,#163874,#163875,#163876,#163877,#163878,#163879,#163880,#163881,
#163882,#163883,#163884,#163885,#163886,#163887,#163888,#163889,#163890,
#163891,#163892,#163893,#163894,#163895,#163896,#163897,#163898,#163899,
#163900,#163901,#163902,#163903,#163904,#163905,#163906,#163907,#163908,
#163909,#163910,#163911,#163912,#163913,#163914,#163915,#163916,#163917,
#163918,#163919,#163920,#163921,#163922,#163923,#163924,#163925,#163926,
#163927,#163928,#163929,#163930,#163931,#163932,#163933,#163934,#163935,
#163936,#163937,#163938,#163939,#163940,#163941,#163942,#163943,#163944,
#163945,#163946,#163947,#163948,#163949,#163950,#163951,#163952,#163953,
#163954,#163955,#163956,#163957,#163958,#163959,#163960,#163961,#163962,
#163963,#163964,#163965,#163966,#163967,#163968,#163969,#163970,#163971,
#163972,#163973,#163974,#163975,#163976,#163977,#163978,#163979,#163980,
#163981,#163982,#163983,#163984,#163985,#163986,#163987,#163988,#163989,
#163990,#163991,#163992,#163993,#163994,#163995,#163996,#163997,#163998,
#163999,#164000,#164001,#164002,#164003,#164004,#164005,#164006,#164007,
#164008,#164009,#164010,#164011,#164012,#164013,#164014,#164015),
 .UNSPECIFIED.,.F.,.F.,(4,3,3,3,3,3,3,3,3,3,3,3,3,3,3,3,3,3,3,3,3,3,3,3,
3,3,3,3,3,3,3,3,3,3,3,3,3,3,3,3,3,3,3,3,3,3,3,3,3,3,3,3,3,3,3,3,3,3,3,3,
3,3,3,3,3,3,3,3,3,3,3,3,3,3,3,3,3,3,3,3,3,3,4),(1647.31340563367,1647.41556786862,
1647.51995242576,1647.56494566677,1647.6449029669,1647.72476576414,1647.80455158661,
1647.8842779018,1647.9639621301,1648.04363311632,1648.12330056984,1648.20298022065,
1648.28268780305,1648.36248303212,1648.44232737383,1648.52228580087,1648.56468167749,
1648.64463897762,1648.72450177486,1648.80428759734,1648.88401391253,1648.96369814083,
1649.04336912705,1649.12303658057,1649.20271623139,1649.28242381378,1649.36221904286,
1649.44206338457,1649.52202181161,1649.56441768821,1649.64437498834,1649.72423778558,
1649.80402360806,1649.88374992325,1649.96343415155,1650.04310513777,1650.12277259129,
1650.20245224211,1650.28215982451,1650.36195505358,1650.44179939529,1650.52175782234,
1650.56415369893,1650.64411099906,1650.7239737963,1650.80375961878,1650.88348593397,
1650.96317016226,1651.04284114849,1651.12250860201,1651.20218825283,1651.28189583522,
1651.3616910643,1651.44153540601,1651.52149383305,1651.56388970965,1651.64384700978,
1651.72370980702,1651.8034956295,1651.88322194469,1651.96290617298,1652.04257715921,
1652.12224461273,1652.20192426355,1652.28163184594,1652.36142707502,1652.44127141673,
1652.52122984377,1652.56362572037,1652.6435830205,1652.72344581774,1652.80323164022,
1652.88295795541,1652.96264218371,1653.04231316993,1653.12198062346,1653.20166027427,
1653.28136785667,1653.36116308574,1653.44100742745,1653.5209658545,1653.56336173109,
1653.59659088176),.UNSPECIFIED.);
#1392=B_SPLINE_CURVE_WITH_KNOTS('',3,(#164017,#164018,#164019,#164020,#164021,
#164022,#164023,#164024,#164025,#164026),.UNSPECIFIED.,.F.,.F.,(4,1,1,1,
1,1,1,4),(1653.59659542634,1654.56309774181,1655.56283375253,1656.56256976325,
1657.56230577397,1658.56204178469,1659.56177779541,1659.87977618894),
 .UNSPECIFIED.);
#1393=B_SPLINE_CURVE_WITH_KNOTS('',3,(#164028,#164029,#164030,#164031,#164032,
#164033,#164034,#164035,#164036,#164037),.UNSPECIFIED.,.F.,.F.,(4,1,1,1,
1,1,1,4),(1659.87977618894,1660.56151380613,1661.56124981685,1662.56098582757,
1663.56072183829,1664.56045784901,1665.56019385973,1666.16296149612),
 .UNSPECIFIED.);
#1394=B_SPLINE_CURVE_WITH_KNOTS('',3,(#164039,#164040,#164041,#164042,#164043,
#164044,#164045,#164046,#164047,#164048),.UNSPECIFIED.,.F.,.F.,(4,1,1,1,
1,1,1,4),(1666.16296149612,1666.55992987046,1667.55966588118,1668.55940189189,
1669.55913790262,1670.55887391334,1671.55860992406,1672.4461468033),
 .UNSPECIFIED.);
#1395=B_SPLINE_CURVE_WITH_KNOTS('',3,(#164050,#164051,#164052,#164053,#164054,
#164055,#164056,#164057,#164058,#164059,#164060,#164061,#164062),
 .UNSPECIFIED.,.F.,.F.,(4,3,1,1,1,1,1,1,4),(1672.4461468033,1672.55834593478,
1673.5580819455,1674.55781795622,1675.55755396694,1676.55728997766,1677.55702598838,
1678.5567619991,1678.72933211048),.UNSPECIFIED.);
#1396=B_SPLINE_CURVE_WITH_KNOTS('',3,(#164064,#164065,#164066,#164067,#164068,
#164069,#164070,#164071,#164072,#164073),.UNSPECIFIED.,.F.,.F.,(4,1,1,1,
1,1,1,4),(1678.72933211048,1679.55649800982,1680.55623402054,1681.55597003126,
1682.55570604198,1683.5554420527,1684.55517806342,1685.01251361461),
 .UNSPECIFIED.);
#1397=B_SPLINE_CURVE_WITH_KNOTS('',3,(#164075,#164076,#164077,#164078,#164079,
#164080,#164081,#164082,#164083,#164084,#164085,#164086,#164087,#164088,
#164089,#164090,#164091,#164092,#164093,#164094,#164095,#164096,#164097,
#164098,#164099,#164100,#164101,#164102,#164103,#164104,#164105,#164106,
#164107,#164108,#164109,#164110,#164111,#164112,#164113,#164114,#164115,
#164116,#164117,#164118,#164119,#164120,#164121,#164122,#164123,#164124,
#164125,#164126,#164127,#164128,#164129,#164130,#164131,#164132,#164133,
#164134,#164135,#164136,#164137,#164138,#164139,#164140,#164141,#164142,
#164143,#164144,#164145,#164146,#164147,#164148,#164149,#164150,#164151,
#164152,#164153,#164154,#164155,#164156,#164157,#164158,#164159,#164160,
#164161,#164162,#164163,#164164,#164165,#164166,#164167,#164168,#164169,
#164170,#164171),.UNSPECIFIED.,.F.,.F.,(4,3,3,3,3,3,3,3,3,3,3,3,3,3,3,3,
3,3,3,3,3,3,3,3,3,3,3,3,3,3,3,3,4),(1685.01251741766,1685.09464503513,1685.1768300882,
1685.25908398026,1685.34147773866,1685.42394791456,1685.50656741574,1685.55491407414,
1685.63500362071,1685.71500002474,1685.79492066898,1685.87478287743,1685.95460392844,
1686.03441267143,1686.11421844278,1686.19403684709,1686.27388349342,1686.35381754324,
1686.43380077164,1686.5138969839,1686.55465008485,1686.63315643435,1686.71156815778,
1686.78990387943,1686.86818213634,1686.94642830235,1687.02465896155,1687.10289078865,
1687.18114045841,1687.25947107649,1687.3378434626,1687.41633594072,1687.48405392823),
 .UNSPECIFIED.);
#1398=B_SPLINE_CURVE_WITH_KNOTS('',3,(#164175,#164176,#164177,#164178,#164179,
#164180,#164181,#164182,#164183,#164184,#164185,#164186,#164187,#164188,
#164189,#164190,#164191,#164192,#164193,#164194,#164195,#164196,#164197,
#164198,#164199,#164200,#164201,#164202,#164203,#164204,#164205,#164206,
#164207,#164208,#164209,#164210,#164211,#164212,#164213,#164214,#164215,
#164216,#164217,#164218,#164219,#164220,#164221,#164222,#164223,#164224,
#164225,#164226,#164227,#164228,#164229,#164230,#164231,#164232,#164233,
#164234,#164235),.UNSPECIFIED.,.F.,.F.,(4,3,3,3,3,3,3,3,3,3,3,3,3,3,3,3,
3,3,3,3,4),(-1689.55385811702,-1689.46027632283,-1689.36652622404,-1689.27277267436,
-1689.17913803904,-1689.08584706727,-1689.05399011166,-1688.97402951639,
-1688.89407895417,-1688.8141228973,-1688.73411746845,-1688.65408238791,
-1688.57397288094,-1688.5541221063,-1688.47204820899,-1688.39005270228,
-1688.30812304275,-1688.22625402995,-1688.14442248704,-1688.0626097839,
-1687.98620407297),.UNSPECIFIED.);
#1399=B_SPLINE_CURVE_WITH_KNOTS('',3,(#164237,#164238,#164239,#164240,#164241,
#164242,#164243,#164244,#164245,#164246),.UNSPECIFIED.,.F.,.F.,(4,1,1,1,
1,1,1,4),(-1687.98619636525,-1687.55438609558,-1686.55465008486,-1685.55491407414,
-1684.55517806342,-1683.5554420527,-1682.55570604198,-1681.70301876581),
 .UNSPECIFIED.);
#1400=B_SPLINE_CURVE_WITH_KNOTS('',3,(#164248,#164249,#164250,#164251,#164252,
#164253,#164254,#164255,#164256,#164257,#164258),.UNSPECIFIED.,.F.,.F.,
(4,1,1,1,1,1,1,1,4),(-1681.70301876581,-1681.55597003126,-1680.55623402054,
-1679.55649800982,-1678.5567619991,-1677.55702598838,-1676.55728997766,
-1675.55755396694,-1675.41983345863),.UNSPECIFIED.);
#1401=B_SPLINE_CURVE_WITH_KNOTS('',3,(#164260,#164261,#164262,#164263,#164264,
#164265,#164266,#164267,#164268,#164269),.UNSPECIFIED.,.F.,.F.,(4,1,1,1,
1,1,1,4),(-1675.41983345863,-1674.55781795622,-1673.5580819455,-1672.55834593478,
-1671.55860992406,-1670.55887391334,-1669.55913790262,-1669.13664815145),
 .UNSPECIFIED.);
#1402=B_SPLINE_CURVE_WITH_KNOTS('',3,(#164271,#164272,#164273,#164274,#164275,
#164276,#164277,#164278,#164279,#164280),.UNSPECIFIED.,.F.,.F.,(4,1,1,1,
1,1,1,4),(-1669.13664815145,-1668.5594018919,-1667.55966588118,-1666.55992987046,
-1665.56019385974,-1664.56045784902,-1663.5607218383,-1662.85346284427),
 .UNSPECIFIED.);
#1403=B_SPLINE_CURVE_WITH_KNOTS('',3,(#164282,#164283,#164284,#164285,#164286,
#164287,#164288,#164289,#164290,#164291,#164292,#164293,#164294,#164295,
#164296,#164297,#164298,#164299,#164300,#164301,#164302,#164303,#164304,
#164305,#164306,#164307,#164308,#164309,#164310,#164311,#164312,#164313,
#164314,#164315,#164316,#164317,#164318,#164319,#164320,#164321,#164322,
#164323,#164324,#164325,#164326,#164327,#164328,#164329,#164330,#164331,
#164332,#164333,#164334,#164335,#164336,#164337,#164338,#164339,#164340,
#164341,#164342,#164343,#164344,#164345,#164346,#164347,#164348,#164349,
#164350,#164351,#164352,#164353,#164354,#164355,#164356,#164357,#164358,
#164359,#164360,#164361,#164362,#164363,#164364,#164365,#164366,#164367,
#164368,#164369,#164370,#164371,#164372,#164373,#164374,#164375,#164376,
#164377,#164378,#164379,#164380,#164381,#164382,#164383,#164384,#164385,
#164386,#164387,#164388,#164389,#164390,#164391,#164392,#164393,#164394,
#164395,#164396,#164397,#164398,#164399,#164400,#164401,#164402,#164403,
#164404,#164405,#164406,#164407,#164408,#164409,#164410,#164411,#164412,
#164413,#164414,#164415,#164416,#164417,#164418,#164419,#164420,#164421,
#164422,#164423,#164424,#164425,#164426,#164427,#164428,#164429,#164430,
#164431,#164432,#164433,#164434,#164435,#164436,#164437,#164438,#164439,
#164440,#164441,#164442,#164443,#164444,#164445,#164446,#164447,#164448,
#164449,#164450,#164451,#164452,#164453,#164454,#164455,#164456,#164457,
#164458,#164459,#164460,#164461,#164462,#164463,#164464,#164465,#164466,
#164467,#164468,#164469,#164470,#164471,#164472,#164473,#164474,#164475,
#164476,#164477,#164478,#164479,#164480,#164481,#164482,#164483,#164484,
#164485,#164486,#164487,#164488,#164489,#164490,#164491,#164492,#164493,
#164494,#164495,#164496,#164497,#164498,#164499,#164500,#164501,#164502,
#164503,#164504,#164505,#164506,#164507,#164508,#164509,#164510,#164511,
#164512,#164513,#164514,#164515,#164516,#164517,#164518,#164519,#164520,
#164521,#164522,#164523,#164524,#164525),.UNSPECIFIED.,.F.,.F.,(4,3,3,3,
3,3,3,3,3,3,3,3,3,3,3,3,3,3,3,3,3,3,3,3,3,3,3,3,3,3,3,3,3,3,3,3,3,3,3,3,
3,3,3,3,3,3,3,3,3,3,3,3,3,3,3,3,3,3,3,3,3,3,3,3,3,3,3,3,3,3,3,3,3,3,3,3,
3,3,3,3,3,4),(-1662.85346267605,-1662.75663390855,-1662.65845502116,-1662.56098582758,
-1662.48102852737,-1662.40116573004,-1662.32137990749,-1662.24165359221,
-1662.16196936383,-1662.08229837752,-1662.00263092391,-1661.92295127301,
-1661.84324369053,-1661.76344846137,-1661.68360411957,-1661.60364569244,
-1661.56124981686,-1661.48129251675,-1661.40142971953,-1661.32164389708,
-1661.24191758191,-1661.16223335364,-1661.08256236744,-1661.00289491393,
-1660.92321526314,-1660.84350768077,-1660.76371245171,-1660.68386811003,
-1660.603909683,-1660.56151380614,-1660.48155650602,-1660.40169370879,-1660.32190788633,
-1660.24218157114,-1660.16249734286,-1660.08282635665,-1660.00315890313,
-1659.92347925233,-1659.84377166994,-1659.76397644088,-1659.68413209918,
-1659.60417367215,-1659.56177779542,-1659.48182049528,-1659.40195769802,
-1659.32217187554,-1659.24244556033,-1659.16276133202,-1659.08309034579,
-1659.00342289225,-1658.92374324142,-1658.84403565902,-1658.76424042993,
-1658.68439608821,-1658.60443766115,-1658.5620417847,-1658.48208448457,
-1658.40222168733,-1658.32243586487,-1658.24270954968,-1658.16302532139,
-1658.08335433517,-1658.00368688165,-1657.92400723084,-1657.84429964845,
-1657.76450441937,-1657.68466007767,-1657.60470165063,-1657.56230577398,
-1657.48245786639,-1657.40270440793,-1657.32302776372,-1657.24341036034,
-1657.16383467191,-1657.08427171309,-1657.00471175588,-1656.92513897508,
-1656.84553754071,-1656.76584851481,-1656.68610954442,-1656.60625841833,
-1656.57027753709),.UNSPECIFIED.);
#1404=B_SPLINE_CURVE_WITH_KNOTS('',3,(#164527,#164528,#164529,#164530,#164531,
#164532,#164533,#164534,#164535,#164536,#164537,#164538,#164539),
 .UNSPECIFIED.,.F.,.F.,(4,3,1,1,1,1,1,1,4),(-1656.57027753709,-1656.56256976326,
-1655.56283375254,-1654.56309774182,-1653.5633617311,-1652.56362572038,
-1651.56388970966,-1650.56415369894,-1650.28709632645),.UNSPECIFIED.);
#1405=B_SPLINE_CURVE_WITH_KNOTS('',3,(#164541,#164542,#164543,#164544,#164545,
#164546,#164547,#164548,#164549,#164550,#164551,#164552,#164553,#164554,
#164555,#164556,#164557,#164558,#164559,#164560,#164561,#164562,#164563,
#164564,#164565,#164566,#164567,#164568,#164569,#164570,#164571,#164572,
#164573,#164574,#164575,#164576,#164577,#164578,#164579,#164580,#164581,
#164582,#164583,#164584,#164585,#164586,#164587,#164588,#164589,#164590,
#164591,#164592,#164593,#164594,#164595,#164596,#164597,#164598,#164599,
#164600,#164601,#164602,#164603,#164604,#164605,#164606,#164607,#164608,
#164609,#164610,#164611,#164612,#164613,#164614,#164615,#164616,#164617,
#164618,#164619,#164620,#164621,#164622,#164623,#164624,#164625,#164626,
#164627,#164628,#164629,#164630,#164631,#164632,#164633,#164634,#164635,
#164636,#164637,#164638,#164639,#164640,#164641,#164642,#164643,#164644,
#164645,#164646,#164647,#164648,#164649,#164650,#164651,#164652,#164653,
#164654,#164655,#164656,#164657,#164658,#164659,#164660,#164661,#164662,
#164663,#164664,#164665,#164666,#164667,#164668,#164669,#164670,#164671,
#164672,#164673,#164674,#164675,#164676,#164677,#164678,#164679,#164680,
#164681,#164682,#164683,#164684,#164685,#164686,#164687,#164688,#164689,
#164690,#164691,#164692,#164693,#164694,#164695,#164696,#164697,#164698,
#164699,#164700,#164701,#164702,#164703,#164704,#164705,#164706,#164707,
#164708,#164709,#164710,#164711,#164712,#164713,#164714,#164715,#164716,
#164717,#164718,#164719,#164720,#164721,#164722,#164723,#164724,#164725,
#164726,#164727,#164728,#164729,#164730,#164731,#164732,#164733,#164734,
#164735,#164736,#164737,#164738,#164739,#164740,#164741,#164742,#164743,
#164744,#164745,#164746,#164747,#164748,#164749,#164750,#164751,#164752,
#164753,#164754,#164755,#164756,#164757,#164758,#164759,#164760,#164761,
#164762,#164763,#164764,#164765,#164766,#164767,#164768,#164769,#164770,
#164771,#164772,#164773,#164774,#164775,#164776,#164777,#164778,#164779,
#164780,#164781,#164782,#164783,#164784),.UNSPECIFIED.,.F.,.F.,(4,3,3,3,
3,3,3,3,3,3,3,3,3,3,3,3,3,3,3,3,3,3,3,3,3,3,3,3,3,3,3,3,3,3,3,3,3,3,3,3,
3,3,3,3,3,3,3,3,3,3,3,3,3,3,3,3,3,3,3,3,3,3,3,3,3,3,3,3,3,3,3,3,3,3,3,3,
3,3,3,3,3,4),(-1650.28709222991,-1650.20807412853,-1650.1276170735,-1650.04864875777,
-1649.9696804804,-1649.89069597473,-1649.8091264031,-1649.73001917906,-1649.64721843364,
-1649.56441768822,-1649.48446038809,-1649.40459759084,-1649.32481176837,
-1649.24508545318,-1649.16540122488,-1649.08573023866,-1649.00606278513,
-1648.92638313432,-1648.84667555192,-1648.76688032284,-1648.68703598114,
-1648.60707755409,-1648.5646816775,-1648.48472437737,-1648.40486158013,
-1648.32507575765,-1648.24534944246,-1648.16566521416,-1648.08599422794,
-1648.00632677442,-1647.9266471236,-1647.8469395412,-1647.76714431213,-1647.68729997042,
-1647.60734154337,-1647.56494566678,-1647.48498836665,-1647.40512556941,
-1647.32533974694,-1647.24561343174,-1647.16592920345,-1647.08625821723,
-1647.0065907637,-1646.92691111288,-1646.84720353049,-1646.76740830141,
-1646.68756395971,-1646.60760553266,-1646.56520965606,-1646.48525235593,
-1646.40538955869,-1646.32560373621,-1646.24587742102,-1646.16619319272,
-1646.0865222065,-1646.00685475298,-1645.92717510216,-1645.84746751977,
-1645.76767229069,-1645.68782794898,-1645.60786952194,-1645.56547364534,
-1645.48551634521,-1645.40565354797,-1645.3258677255,-1645.2461414103,-1645.16645718201,
-1645.08678619579,-1645.00711874226,-1644.92743909145,-1644.84773150905,
-1644.76793627998,-1644.68809193827,-1644.60813351122,-1644.56573763462,
-1644.48365987216,-1644.40169485898,-1644.31982974707,-1644.23807766884,
-1644.1563916886,-1644.07477146095,-1644.00390692273),.UNSPECIFIED.);
#1406=B_SPLINE_CURVE_WITH_KNOTS('',3,(#164786,#164787,#164788,#164789,#164790,
#164791,#164792,#164793,#164794,#164795),.UNSPECIFIED.,.F.,.F.,(4,1,1,1,
1,1,1,4),(-1644.00390193375,-1643.5660016239,-1642.56626561318,-1641.56652960246,
-1640.56679359174,-1639.56705758102,-1638.56732157029,-1637.72072161555),
 .UNSPECIFIED.);
#1407=B_SPLINE_CURVE_WITH_KNOTS('',3,(#164797,#164798,#164799,#164800,#164801,
#164802,#164803,#164804,#164805,#164806,#164807,#164808),.UNSPECIFIED.,
 .F.,.F.,(4,2,1,1,1,1,1,1,4),(-1637.72072161555,-1637.56758555957,-1636.56784954885,
-1635.56811353813,-1634.56837752741,-1633.56864151669,-1632.56890550597,
-1631.56916949525,-1631.43753630837),.UNSPECIFIED.);
#1408=B_SPLINE_CURVE_WITH_KNOTS('',3,(#164810,#164811,#164812,#164813,#164814,
#164815,#164816,#164817,#164818,#164819),.UNSPECIFIED.,.F.,.F.,(4,1,1,1,
1,1,1,4),(-1631.43753630837,-1630.56943348453,-1629.56969747381,-1628.56996146309,
-1627.57022545237,-1626.57048944165,-1625.57075343093,-1625.15435100119),
 .UNSPECIFIED.);
#1409=B_SPLINE_CURVE_WITH_KNOTS('',3,(#164821,#164822,#164823,#164824,#164825,
#164826,#164827,#164828,#164829,#164830),.UNSPECIFIED.,.F.,.F.,(4,1,1,1,
1,1,1,4),(-1625.15435100119,-1624.57101742021,-1623.57128140949,-1622.57154539877,
-1621.57180938805,-1620.57207337733,-1619.57233736661,-1618.87116569401),
 .UNSPECIFIED.);
#1410=B_SPLINE_CURVE_WITH_KNOTS('',3,(#164832,#164833,#164834,#164835,#164836,
#164837,#164838,#164839,#164840,#164841,#164842,#164843,#164844,#164845,
#164846,#164847,#164848,#164849,#164850,#164851,#164852,#164853,#164854,
#164855,#164856,#164857,#164858,#164859,#164860,#164861,#164862,#164863,
#164864,#164865,#164866,#164867,#164868,#164869,#164870,#164871,#164872,
#164873,#164874,#164875,#164876,#164877,#164878,#164879,#164880,#164881,
#164882,#164883,#164884,#164885,#164886,#164887,#164888,#164889,#164890,
#164891,#164892,#164893,#164894,#164895,#164896,#164897,#164898,#164899,
#164900,#164901,#164902,#164903,#164904,#164905,#164906,#164907,#164908,
#164909,#164910,#164911,#164912,#164913,#164914,#164915,#164916,#164917,
#164918,#164919,#164920,#164921,#164922,#164923,#164924,#164925,#164926,
#164927,#164928,#164929,#164930,#164931,#164932,#164933,#164934,#164935,
#164936,#164937,#164938,#164939,#164940,#164941,#164942,#164943,#164944,
#164945,#164946,#164947,#164948,#164949,#164950,#164951,#164952,#164953,
#164954,#164955,#164956,#164957,#164958,#164959,#164960,#164961,#164962,
#164963,#164964,#164965,#164966,#164967,#164968,#164969,#164970,#164971,
#164972,#164973,#164974,#164975,#164976,#164977,#164978,#164979,#164980,
#164981,#164982,#164983,#164984,#164985,#164986,#164987,#164988,#164989,
#164990,#164991,#164992,#164993,#164994,#164995,#164996,#164997,#164998,
#164999,#165000,#165001,#165002,#165003,#165004,#165005,#165006,#165007,
#165008,#165009,#165010,#165011,#165012,#165013,#165014,#165015,#165016,
#165017,#165018,#165019,#165020,#165021,#165022,#165023,#165024,#165025,
#165026,#165027,#165028,#165029,#165030,#165031,#165032,#165033,#165034,
#165035,#165036,#165037,#165038,#165039,#165040,#165041,#165042,#165043,
#165044,#165045,#165046,#165047,#165048,#165049,#165050,#165051,#165052,
#165053,#165054,#165055,#165056,#165057,#165058,#165059,#165060,#165061,
#165062,#165063,#165064,#165065,#165066,#165067,#165068,#165069,#165070,
#165071,#165072,#165073,#165074,#165075),.UNSPECIFIED.,.F.,.F.,(4,3,3,3,
3,3,3,3,3,3,3,3,3,3,3,3,3,3,3,3,3,3,3,3,3,3,3,3,3,3,3,3,3,3,3,3,3,3,3,3,
3,3,3,3,3,3,3,3,3,3,3,3,3,3,3,3,3,3,3,3,3,3,3,3,3,3,3,3,3,3,3,3,3,3,3,3,
3,3,3,3,3,4),(-1618.87116551288,-1618.77500107763,-1618.67380121676,-1618.57260135589,
-1618.49264405576,-1618.41278125852,-1618.33299543604,-1618.25326912085,
-1618.17358489255,-1618.09391390633,-1618.01424645281,-1617.93456680199,
-1617.8548592196,-1617.77506399052,-1617.69521964881,-1617.61526122176,
-1617.57286534517,-1617.49290804504,-1617.4130452478,-1617.33325942532,
-1617.25353311013,-1617.17384888183,-1617.09417789561,-1617.01451044209,
-1616.93483079127,-1616.85512320888,-1616.7753279798,-1616.69548363809,
-1616.61552521105,-1616.57312933445,-1616.49317203432,-1616.41330923708,
-1616.3335234146,-1616.25379709941,-1616.17411287111,-1616.09444188489,
-1616.01477443137,-1615.93509478055,-1615.85538719816,-1615.77559196908,
-1615.69574762737,-1615.61578920033,-1615.57339332373,-1615.4934360236,
-1615.41357322636,-1615.33378740389,-1615.25406108869,-1615.1743768604,
-1615.09470587418,-1615.01503842065,-1614.93535876983,-1614.85565118744,
-1614.77585595836,-1614.69601161666,-1614.61605318961,-1614.57365731301,
-1614.49370001288,-1614.41383721564,-1614.33405139316,-1614.25432507797,
-1614.17464084968,-1614.09496986345,-1614.01530240993,-1613.93562275911,
-1613.85591517672,-1613.77611994764,-1613.69627560593,-1613.61631717889,
-1613.57392130229,-1613.4941558113,-1613.41448472223,-1613.33489032263,
-1613.2553549622,-1613.17193314028,-1613.09245209091,-1613.01297286857,
-1612.93347957904,-1612.85395632244,-1612.77434530931,-1612.69468303516,
-1612.61491125407,-1612.58798038683),.UNSPECIFIED.);
#1411=B_SPLINE_CURVE_WITH_KNOTS('',3,(#165077,#165078,#165079,#165080,#165081,
#165082,#165083,#165084,#165085,#165086,#165087,#165088,#165089),
 .UNSPECIFIED.,.F.,.F.,(4,3,1,1,1,1,1,1,4),(-1612.58798038683,-1612.57418529157,
-1611.57444928085,-1610.57471327013,-1609.57497725941,-1608.57524124869,
-1607.57550523797,-1606.57576922725,-1606.30479867486),.UNSPECIFIED.);
#1412=B_SPLINE_CURVE_WITH_KNOTS('',3,(#165091,#165092,#165093,#165094,#165095,
#165096,#165097,#165098,#165099,#165100,#165101,#165102,#165103,#165104,
#165105,#165106,#165107,#165108,#165109,#165110,#165111,#165112,#165113,
#165114,#165115,#165116,#165117,#165118,#165119,#165120,#165121,#165122,
#165123,#165124,#165125,#165126,#165127,#165128,#165129,#165130,#165131,
#165132,#165133,#165134,#165135,#165136,#165137,#165138,#165139,#165140,
#165141,#165142,#165143,#165144,#165145,#165146,#165147,#165148,#165149,
#165150,#165151,#165152,#165153,#165154,#165155,#165156,#165157,#165158,
#165159,#165160,#165161,#165162,#165163,#165164,#165165,#165166,#165167,
#165168,#165169,#165170,#165171,#165172,#165173,#165174,#165175,#165176,
#165177,#165178,#165179,#165180,#165181,#165182,#165183,#165184,#165185,
#165186,#165187,#165188,#165189,#165190,#165191,#165192,#165193,#165194,
#165195,#165196,#165197,#165198,#165199,#165200,#165201,#165202,#165203,
#165204,#165205,#165206,#165207,#165208,#165209,#165210,#165211,#165212,
#165213,#165214,#165215,#165216,#165217,#165218,#165219,#165220,#165221,
#165222,#165223,#165224,#165225,#165226,#165227,#165228,#165229,#165230,
#165231,#165232,#165233,#165234,#165235,#165236,#165237,#165238,#165239,
#165240,#165241,#165242,#165243,#165244,#165245,#165246,#165247,#165248,
#165249,#165250,#165251,#165252,#165253,#165254,#165255,#165256,#165257,
#165258,#165259,#165260,#165261,#165262,#165263,#165264,#165265,#165266,
#165267,#165268,#165269,#165270,#165271,#165272,#165273,#165274,#165275,
#165276,#165277,#165278,#165279,#165280,#165281,#165282,#165283,#165284,
#165285,#165286,#165287,#165288,#165289,#165290,#165291,#165292,#165293,
#165294,#165295,#165296,#165297,#165298,#165299,#165300,#165301,#165302,
#165303,#165304,#165305,#165306,#165307,#165308,#165309,#165310,#165311,
#165312,#165313,#165314,#165315,#165316,#165317,#165318,#165319,#165320,
#165321,#165322,#165323,#165324,#165325,#165326,#165327,#165328,#165329,
#165330,#165331,#165332,#165333,#165334,#165335,#165336,#165337),
 .UNSPECIFIED.,.F.,.F.,(4,3,3,3,3,3,3,3,3,3,3,3,3,3,3,3,3,3,3,3,3,3,3,3,
3,3,3,3,3,3,3,3,3,3,3,3,3,3,3,3,3,3,3,3,3,3,3,3,3,3,3,3,3,3,3,3,3,3,3,3,
3,3,3,3,3,3,3,3,3,3,3,3,3,3,3,3,3,3,3,3,3,3,4),(-1606.30479507965,-1606.22582393907,
-1606.14460009875,-1606.06568366228,-1605.98676893908,-1605.90783962531,
-1605.82488802311,-1605.7458377603,-1605.66673391448,-1605.58752429386,
-1605.57603321653,-1605.4960759164,-1605.41621311916,-1605.33642729668,
-1605.25670098149,-1605.17701675319,-1605.09734576697,-1605.01767831345,
-1604.93799866263,-1604.85829108023,-1604.77849585116,-1604.69865150945,
-1604.6186930824,-1604.57629720581,-1604.49633990568,-1604.41647710844,
-1604.33669128596,-1604.25696497077,-1604.17728074247,-1604.09760975625,
-1604.01794230273,-1603.93826265191,-1603.85855506952,-1603.77875984044,
-1603.69891549873,-1603.61895707168,-1603.57656119509,-1603.49660389496,
-1603.41674109772,-1603.33695527524,-1603.25722896005,-1603.17754473176,
-1603.09787374553,-1603.01820629201,-1602.93852664119,-1602.8588190588,
-1602.77902382972,-1602.69917948802,-1602.61922106097,-1602.57682518437,
-1602.49686788424,-1602.417005087,-1602.33721926452,-1602.25749294933,-1602.17780872103,
-1602.09813773481,-1602.01847028129,-1601.93879063047,-1601.85908304808,
-1601.779287819,-1601.69944347729,-1601.61948505025,-1601.57708917365,-1601.49713187352,
-1601.41726907628,-1601.33748325381,-1601.25775693861,-1601.17807271032,
-1601.0984017241,-1601.01873427057,-1600.93905461975,-1600.85934703736,
-1600.77955180829,-1600.69970746658,-1600.61974903953,-1600.57735316293,
-1600.49510574788,-1600.41297300452,-1600.33094243016,-1600.24902907937,
-1600.16718435843,-1600.08541054314,-1600.02160977247),.UNSPECIFIED.);
#1413=B_SPLINE_CURVE_WITH_KNOTS('',3,(#165339,#165340,#165341,#165342,#165343,
#165344,#165345,#165346,#165347,#165348),.UNSPECIFIED.,.F.,.F.,(4,1,1,1,
1,1,1,4),(-1600.02160535103,-1599.57761715221,-1598.57788114149,-1597.57814513077,
-1596.57840912005,-1595.57867310933,-1594.57893709861,-1593.73842446529),
 .UNSPECIFIED.);
#1414=B_SPLINE_CURVE_WITH_KNOTS('',3,(#165350,#165351,#165352,#165353,#165354,
#165355,#165356,#165357,#165358,#165359,#165360,#165361),.UNSPECIFIED.,
 .F.,.F.,(4,2,1,1,1,1,1,1,4),(-1593.73842446529,-1593.57920108789,-1592.57946507717,
-1591.57972906645,-1590.57999305573,-1589.58025704501,-1588.58052103429,
-1587.58078502357,-1587.45523915811),.UNSPECIFIED.);
#1415=B_SPLINE_CURVE_WITH_KNOTS('',3,(#165363,#165364,#165365,#165366,#165367,
#165368,#165369,#165370,#165371,#165372,#165373,#165374,#165375,#165376,
#165377,#165378,#165379,#165380,#165381,#165382,#165383,#165384,#165385,
#165386,#165387,#165388,#165389,#165390,#165391,#165392,#165393,#165394,
#165395,#165396,#165397,#165398,#165399,#165400,#165401,#165402,#165403,
#165404,#165405,#165406,#165407,#165408,#165409,#165410,#165411,#165412,
#165413,#165414,#165415,#165416,#165417,#165418,#165419,#165420,#165421,
#165422,#165423,#165424,#165425,#165426,#165427,#165428,#165429,#165430,
#165431,#165432,#165433,#165434,#165435,#165436,#165437,#165438,#165439,
#165440,#165441,#165442,#165443,#165444,#165445,#165446,#165447,#165448,
#165449,#165450,#165451,#165452,#165453,#165454,#165455,#165456,#165457,
#165458,#165459,#165460,#165461,#165462,#165463,#165464,#165465,#165466,
#165467,#165468,#165469,#165470,#165471,#165472,#165473,#165474,#165475,
#165476,#165477,#165478,#165479,#165480,#165481,#165482,#165483,#165484,
#165485,#165486,#165487,#165488,#165489,#165490,#165491,#165492,#165493,
#165494,#165495,#165496,#165497,#165498,#165499,#165500,#165501,#165502,
#165503,#165504,#165505,#165506,#165507,#165508,#165509,#165510,#165511,
#165512,#165513,#165514,#165515,#165516,#165517,#165518,#165519,#165520,
#165521,#165522,#165523,#165524,#165525,#165526,#165527,#165528,#165529,
#165530,#165531,#165532,#165533,#165534,#165535,#165536,#165537,#165538,
#165539,#165540,#165541,#165542,#165543,#165544,#165545,#165546,#165547,
#165548,#165549,#165550,#165551,#165552,#165553,#165554,#165555,#165556,
#165557,#165558,#165559,#165560,#165561,#165562,#165563,#165564,#165565,
#165566,#165567,#165568,#165569,#165570,#165571,#165572,#165573,#165574,
#165575,#165576,#165577,#165578,#165579,#165580,#165581,#165582,#165583,
#165584,#165585,#165586,#165587,#165588,#165589,#165590,#165591,#165592,
#165593,#165594,#165595,#165596,#165597,#165598,#165599,#165600,#165601,
#165602,#165603,#165604,#165605,#165606),.UNSPECIFIED.,.F.,.F.,(4,3,3,3,
3,3,3,3,3,3,3,3,3,3,3,3,3,3,3,3,3,3,3,3,3,3,3,3,3,3,3,3,3,3,3,3,3,3,3,3,
3,3,3,3,3,3,3,3,3,3,3,3,3,3,3,3,3,3,3,3,3,3,3,3,3,3,3,3,3,3,3,3,3,3,3,3,
3,3,3,3,3,4),(-1587.45523915811,-1587.37647002073,-1587.29778119148,-1587.21915428759,
-1587.13939112825,-1587.06082278289,-1586.98225751216,-1586.9036787886,
-1586.82302134466,-1586.74432614687,-1586.66268757986,-1586.58104901285,
-1586.50109171272,-1586.42122891548,-1586.341443093,-1586.26171677781,-1586.18203254951,
-1586.10236156329,-1586.02269410977,-1585.94301445895,-1585.86330687656,
-1585.78351164748,-1585.70366730577,-1585.62370887872,-1585.58131300213,
-1585.501355702,-1585.42149290476,-1585.34170708228,-1585.26198076709,-1585.18229653879,
-1585.10262555257,-1585.02295809905,-1584.94327844823,-1584.86357086583,
-1584.78377563676,-1584.70393129505,-1584.623972868,-1584.58157699141,-1584.50161969128,
-1584.42175689404,-1584.34197107156,-1584.26224475637,-1584.18256052808,
-1584.10288954185,-1584.02322208833,-1583.94354243751,-1583.86383485512,
-1583.78403962604,-1583.70419528433,-1583.62423685729,-1583.58184098069,
-1583.50188368056,-1583.42202088332,-1583.34223506084,-1583.26250874565,
-1583.18282451735,-1583.10315353113,-1583.02348607761,-1582.94380642679,
-1582.8640988444,-1582.78430361532,-1582.70445927361,-1582.62450084657,
-1582.58210496997,-1582.50214766984,-1582.4222848726,-1582.34249905013,
-1582.26277273493,-1582.18308850664,-1582.10341752042,-1582.02375006689,
-1581.94407041608,-1581.86436283369,-1581.78456760461,-1581.7047232629,
-1581.62476483586,-1581.58236895925,-1581.49400844408,-1581.4059913693,
-1581.31819275127,-1581.23075361509,-1581.1720540622),.UNSPECIFIED.);
#1416=B_SPLINE_CURVE_WITH_KNOTS('',3,(#165608,#165609,#165610,#165611,#165612,
#165613,#165614,#165615,#165616,#165617),.UNSPECIFIED.,.F.,.F.,(4,1,1,1,
1,1,1,4),(-1581.17205385093,-1580.58263294853,-1579.58289693781,-1578.58316092709,
-1577.58342491637,-1576.58368890565,-1575.58395289493,-1574.88886854375),
 .UNSPECIFIED.);
#1417=B_SPLINE_CURVE_WITH_KNOTS('',3,(#165619,#165620,#165621,#165622,#165623,
#165624,#165625,#165626,#165627,#165628,#165629,#165630,#165631,#165632,
#165633,#165634,#165635,#165636,#165637,#165638,#165639,#165640,#165641,
#165642,#165643,#165644,#165645,#165646,#165647,#165648,#165649,#165650,
#165651,#165652,#165653,#165654,#165655,#165656,#165657,#165658,#165659,
#165660,#165661,#165662,#165663,#165664,#165665,#165666,#165667,#165668,
#165669,#165670,#165671,#165672,#165673,#165674,#165675,#165676,#165677,
#165678,#165679,#165680,#165681,#165682,#165683,#165684,#165685,#165686,
#165687,#165688,#165689,#165690,#165691,#165692,#165693,#165694,#165695,
#165696,#165697,#165698,#165699,#165700,#165701,#165702,#165703,#165704,
#165705,#165706,#165707,#165708,#165709,#165710,#165711,#165712,#165713,
#165714,#165715,#165716,#165717,#165718,#165719,#165720,#165721,#165722,
#165723,#165724,#165725,#165726,#165727,#165728,#165729,#165730,#165731,
#165732,#165733,#165734,#165735,#165736,#165737,#165738,#165739,#165740,
#165741,#165742,#165743,#165744,#165745,#165746,#165747,#165748,#165749,
#165750,#165751,#165752,#165753,#165754,#165755,#165756,#165757,#165758,
#165759,#165760,#165761,#165762,#165763,#165764,#165765,#165766,#165767,
#165768,#165769,#165770,#165771,#165772,#165773,#165774,#165775,#165776,
#165777,#165778,#165779,#165780,#165781,#165782,#165783,#165784,#165785,
#165786,#165787,#165788,#165789,#165790,#165791,#165792,#165793,#165794,
#165795,#165796,#165797,#165798,#165799,#165800,#165801,#165802,#165803,
#165804,#165805,#165806,#165807,#165808,#165809,#165810,#165811,#165812,
#165813,#165814,#165815,#165816,#165817,#165818,#165819,#165820,#165821,
#165822,#165823,#165824,#165825,#165826,#165827,#165828,#165829,#165830,
#165831,#165832,#165833,#165834,#165835,#165836,#165837,#165838,#165839,
#165840,#165841,#165842,#165843,#165844,#165845,#165846,#165847,#165848,
#165849,#165850,#165851,#165852,#165853,#165854,#165855,#165856,#165857,
#165858,#165859,#165860,#165861,#165862,#165863,#165864,#165865),
 .UNSPECIFIED.,.F.,.F.,(4,3,3,3,3,3,3,3,3,3,3,3,3,3,3,3,3,3,3,3,3,3,3,3,
3,3,3,3,3,3,3,3,3,3,3,3,3,3,3,3,3,3,3,3,3,3,3,3,3,3,3,3,3,3,3,3,3,3,3,3,
3,3,3,3,3,3,3,3,3,3,3,3,3,3,3,3,3,3,3,3,3,3,4),(-1574.8888683503,-1574.7933409988,
-1574.69705729338,-1574.59996713565,-1574.58421688421,-1574.50425958408,
-1574.42439678684,-1574.34461096436,-1574.26488464917,-1574.18520042087,
-1574.10552943465,-1574.02586198112,-1573.94618233031,-1573.86647474791,
-1573.78667951884,-1573.70683517713,-1573.62687675008,-1573.58448087349,
-1573.50452357336,-1573.42466077612,-1573.34487495364,-1573.26514863845,
-1573.18546441015,-1573.10579342393,-1573.02612597041,-1572.94644631959,
-1572.8667387372,-1572.78694350812,-1572.70709916641,-1572.62714073936,
-1572.58474486277,-1572.50478756264,-1572.4249247654,-1572.34513894292,
-1572.26541262773,-1572.18572839943,-1572.10605741321,-1572.02638995969,
-1571.94671030887,-1571.86700272648,-1571.7872074974,-1571.70736315569,
-1571.62740472865,-1571.58500885205,-1571.50505155192,-1571.42518875468,
-1571.3454029322,-1571.26567661701,-1571.18599238872,-1571.10632140249,
-1571.02665394897,-1570.94697429815,-1570.86726671576,-1570.78747148668,
-1570.70762714498,-1570.62766871793,-1570.58527284133,-1570.5053155412,
-1570.42545274396,-1570.34566692149,-1570.26594060629,-1570.186256378,-1570.10658539178,
-1570.02691793825,-1569.94723828744,-1569.86753070504,-1569.78773547597,
-1569.70789113426,-1569.62793270722,-1569.58553683061,-1569.50585028896,
-1569.42625809896,-1569.34674247608,-1569.26728569865,-1569.18458539089,
-1569.1051822485,-1569.02578069471,-1568.94636477135,-1568.86691851423,
-1568.78738477088,-1568.70779930831,-1568.62810586245,-1568.60568323657),
 .UNSPECIFIED.);
#1418=B_SPLINE_CURVE_WITH_KNOTS('',3,(#165867,#165868,#165869,#165870,#165871,
#165872,#165873,#165874,#165875,#165876,#165877,#165878,#165879),
 .UNSPECIFIED.,.F.,.F.,(4,3,1,1,1,1,1,1,4),(-1568.60568323657,-1568.58580081989,
-1567.58606480917,-1566.58632879845,-1565.58659278773,-1564.58685677701,
-1563.58712076629,-1562.58738475557,-1562.32249792939),.UNSPECIFIED.);
#1419=B_SPLINE_CURVE_WITH_KNOTS('',3,(#165881,#165882,#165883,#165884,#165885,
#165886,#165887,#165888,#165889,#165890),.UNSPECIFIED.,.F.,.F.,(4,1,1,1,
1,1,1,4),(-1562.32249792939,-1561.58764874484,-1560.58791273412,-1559.5881767234,
-1558.58844071268,-1557.58870470196,-1556.58896869124,-1556.03931262221),
 .UNSPECIFIED.);
#1420=B_SPLINE_CURVE_WITH_KNOTS('',3,(#165892,#165893,#165894,#165895,#165896,
#165897,#165898,#165899,#165900,#165901),.UNSPECIFIED.,.F.,.F.,(4,1,1,1,
1,1,1,4),(-1556.03931262221,-1555.58923268052,-1554.5894966698,-1553.58976065908,
-1552.59002464836,-1551.59028863764,-1550.59055262692,-1549.75612731503),
 .UNSPECIFIED.);
#1421=B_SPLINE_CURVE_WITH_KNOTS('',3,(#165903,#165904,#165905,#165906,#165907,
#165908,#165909,#165910,#165911,#165912,#165913,#165914),.UNSPECIFIED.,
 .F.,.F.,(4,2,1,1,1,1,1,1,4),(-1549.75612731503,-1549.5908166162,-1548.59108060548,
-1547.59134459476,-1546.59160858404,-1545.59187257332,-1544.5921365626,
-1543.59240055188,-1543.47294200786),.UNSPECIFIED.);
#1422=B_SPLINE_CURVE_WITH_KNOTS('',3,(#165916,#165917,#165918,#165919,#165920,
#165921,#165922,#165923,#165924,#165925,#165926,#165927,#165928,#165929,
#165930,#165931,#165932,#165933,#165934,#165935,#165936,#165937,#165938,
#165939,#165940,#165941,#165942,#165943,#165944,#165945,#165946,#165947,
#165948,#165949,#165950,#165951,#165952,#165953,#165954,#165955,#165956,
#165957,#165958,#165959,#165960,#165961,#165962,#165963,#165964,#165965,
#165966,#165967,#165968,#165969,#165970,#165971,#165972,#165973,#165974,
#165975,#165976,#165977,#165978,#165979,#165980,#165981,#165982,#165983,
#165984,#165985,#165986,#165987,#165988,#165989,#165990,#165991,#165992,
#165993,#165994,#165995,#165996,#165997,#165998,#165999,#166000,#166001,
#166002,#166003,#166004,#166005,#166006,#166007,#166008,#166009,#166010,
#166011,#166012,#166013,#166014,#166015,#166016,#166017,#166018,#166019,
#166020,#166021,#166022,#166023,#166024,#166025,#166026,#166027,#166028,
#166029,#166030,#166031,#166032,#166033,#166034,#166035,#166036,#166037,
#166038,#166039,#166040,#166041,#166042,#166043,#166044,#166045,#166046,
#166047,#166048,#166049,#166050,#166051,#166052,#166053,#166054,#166055,
#166056,#166057,#166058,#166059,#166060,#166061,#166062,#166063,#166064,
#166065,#166066,#166067,#166068,#166069,#166070,#166071,#166072,#166073,
#166074,#166075,#166076,#166077,#166078,#166079,#166080,#166081,#166082,
#166083,#166084,#166085,#166086,#166087,#166088,#166089,#166090,#166091,
#166092,#166093,#166094,#166095,#166096,#166097,#166098,#166099,#166100,
#166101,#166102,#166103,#166104,#166105,#166106,#166107,#166108,#166109,
#166110,#166111,#166112,#166113,#166114,#166115,#166116,#166117,#166118,
#166119,#166120,#166121,#166122,#166123,#166124,#166125,#166126,#166127,
#166128,#166129,#166130,#166131,#166132,#166133,#166134,#166135,#166136,
#166137,#166138,#166139,#166140,#166141,#166142,#166143,#166144,#166145,
#166146,#166147,#166148,#166149,#166150,#166151,#166152,#166153,#166154,
#166155,#166156,#166157,#166158,#166159,#166160,#166161,#166162),
 .UNSPECIFIED.,.F.,.F.,(4,3,3,3,3,3,3,3,3,3,3,3,3,3,3,3,3,3,3,3,3,3,3,3,
3,3,3,3,3,3,3,3,3,3,3,3,3,3,3,3,3,3,3,3,3,3,3,3,3,3,3,3,3,3,3,3,3,3,3,3,
3,3,3,3,3,3,3,3,3,3,3,3,3,3,3,3,3,3,3,3,3,3,4),(-1543.47294200786,-1543.39414426789,
-1543.31542798864,-1543.2367747979,-1543.15626101581,-1543.07766916188,
-1542.99908131531,-1542.92048096174,-1542.8385268566,-1542.75981060134,
-1542.68104212033,-1542.60217029467,-1542.59266454116,-1542.51270724103,
-1542.43284444379,-1542.35305862132,-1542.27333230612,-1542.19364807783,
-1542.11397709161,-1542.03430963808,-1541.95462998727,-1541.87492240487,
-1541.7951271758,-1541.71528283409,-1541.63532440704,-1541.59292853044,
-1541.51297123031,-1541.43310843307,-1541.3533226106,-1541.2735962954,-1541.19391206711,
-1541.11424108089,-1541.03457362736,-1540.95489397655,-1540.87518639415,
-1540.79539116508,-1540.71554682337,-1540.63558839632,-1540.59319251972,
-1540.51323521959,-1540.43337242235,-1540.35358659987,-1540.27386028468,
-1540.19417605638,-1540.11450507016,-1540.03483761664,-1539.95515796582,
-1539.87545038342,-1539.79565515435,-1539.71581081264,-1539.63585238559,
-1539.593456509,-1539.51349920887,-1539.43363641163,-1539.35385058915,-1539.27412427396,
-1539.19444004567,-1539.11476905944,-1539.03510160592,-1538.9554219551,
-1538.87571437271,-1538.79591914363,-1538.71607480192,-1538.63611637488,
-1538.59372049828,-1538.51376319815,-1538.4339004009,-1538.35411457843,
-1538.27438826324,-1538.19470403494,-1538.11503304872,-1538.03536559519,
-1537.95568594437,-1537.87597836198,-1537.7961831329,-1537.71633879119,
-1537.63638036415,-1537.59398448756,-1537.50525262927,-1537.4168783209,
-1537.32873468176,-1537.24096808399,-1537.18975692054),.UNSPECIFIED.);
#1423=B_SPLINE_CURVE_WITH_KNOTS('',3,(#166164,#166165,#166166,#166167,#166168,
#166169,#166170,#166171,#166172,#166173),.UNSPECIFIED.,.F.,.F.,(4,1,1,1,
1,1,1,4),(-1537.18975670068,-1536.59424847684,-1535.59451246612,-1534.5947764554,
-1533.59504044468,-1532.59530443396,-1531.59556842324,-1530.9065713935),
 .UNSPECIFIED.);
#1424=B_SPLINE_CURVE_WITH_KNOTS('',3,(#166175,#166176,#166177,#166178,#166179,
#166180,#166181,#166182,#166183,#166184,#166185,#166186,#166187,#166188,
#166189,#166190,#166191,#166192,#166193,#166194,#166195,#166196,#166197,
#166198,#166199,#166200,#166201,#166202,#166203,#166204,#166205,#166206,
#166207,#166208,#166209,#166210,#166211,#166212,#166213,#166214,#166215,
#166216,#166217,#166218,#166219,#166220,#166221,#166222,#166223,#166224,
#166225,#166226,#166227,#166228,#166229,#166230,#166231,#166232,#166233,
#166234,#166235,#166236,#166237,#166238,#166239,#166240,#166241,#166242,
#166243,#166244,#166245,#166246,#166247,#166248,#166249,#166250,#166251,
#166252,#166253,#166254,#166255,#166256,#166257,#166258,#166259,#166260,
#166261,#166262,#166263,#166264,#166265,#166266,#166267,#166268,#166269,
#166270,#166271,#166272,#166273,#166274,#166275,#166276,#166277,#166278,
#166279,#166280,#166281,#166282,#166283,#166284,#166285,#166286,#166287,
#166288,#166289,#166290,#166291,#166292,#166293,#166294,#166295,#166296,
#166297,#166298,#166299,#166300,#166301,#166302,#166303,#166304,#166305,
#166306,#166307,#166308,#166309,#166310,#166311,#166312,#166313,#166314,
#166315,#166316,#166317,#166318,#166319,#166320,#166321,#166322,#166323,
#166324,#166325,#166326,#166327,#166328,#166329,#166330,#166331,#166332,
#166333,#166334,#166335,#166336,#166337,#166338,#166339,#166340,#166341,
#166342,#166343,#166344,#166345,#166346,#166347,#166348,#166349,#166350,
#166351,#166352,#166353,#166354,#166355,#166356,#166357,#166358,#166359,
#166360,#166361,#166362,#166363,#166364,#166365,#166366,#166367,#166368,
#166369,#166370,#166371,#166372,#166373,#166374,#166375,#166376,#166377,
#166378,#166379,#166380,#166381,#166382,#166383,#166384,#166385,#166386,
#166387,#166388,#166389,#166390,#166391,#166392,#166393,#166394,#166395,
#166396,#166397,#166398,#166399,#166400,#166401,#166402,#166403,#166404,
#166405,#166406,#166407,#166408,#166409,#166410,#166411,#166412,#166413,
#166414,#166415,#166416,#166417,#166418,#166419,#166420,#166421),
 .UNSPECIFIED.,.F.,.F.,(4,3,3,3,3,3,3,3,3,3,3,3,3,3,3,3,3,3,3,3,3,3,3,3,
3,3,3,3,3,3,3,3,3,3,3,3,3,3,3,3,3,3,3,3,3,3,3,3,3,3,3,3,3,3,3,3,3,3,3,3,
3,3,3,3,3,3,3,3,3,3,3,3,3,3,3,3,3,3,3,3,3,3,4),(-1530.90657118922,-1530.81165532923,
-1530.71604002867,-1530.61965629758,-1530.59583241252,-1530.51587511239,
-1530.43601231515,-1530.35622649269,-1530.27650017749,-1530.1968159492,
-1530.11714496299,-1530.03747750946,-1529.95779785865,-1529.87809027626,
-1529.79829504719,-1529.71845070549,-1529.63849227844,-1529.5960964018,
-1529.51613910167,-1529.43627630443,-1529.35649048195,-1529.27676416676,
-1529.19707993846,-1529.11740895224,-1529.03774149872,-1528.9580618479,
-1528.87835426551,-1528.79855903643,-1528.71871469472,-1528.63875626768,
-1528.59636039108,-1528.51640309095,-1528.4365402937,-1528.35675447123,
-1528.27702815604,-1528.19734392774,-1528.11767294152,-1528.03800548799,
-1527.95832583718,-1527.87861825478,-1527.7988230257,-1527.718978684,-1527.63902025695,
-1527.59662438036,-1527.51666708023,-1527.43680428299,-1527.35701846052,
-1527.27729214532,-1527.19760791703,-1527.11793693081,-1527.03826947728,
-1526.95858982647,-1526.87888224407,-1526.799087015,-1526.71924267329,-1526.63928424624,
-1526.59688836964,-1526.51693106951,-1526.43706827227,-1526.35728244979,
-1526.2775561346,-1526.1978719063,-1526.11820092008,-1526.03853346655,-1525.95885381574,
-1525.87914623334,-1525.79935100427,-1525.71950666256,-1525.63954823551,
-1525.59715235892,-1525.5175413367,-1525.43802461378,-1525.35858433859,
-1525.27920272328,-1525.19722564366,-1525.11789704264,-1525.03856981854,
-1524.95922795393,-1524.87985542501,-1524.8003957555,-1524.72088394743,
-1524.64126575125,-1524.62338608632),.UNSPECIFIED.);
#1425=B_SPLINE_CURVE_WITH_KNOTS('',3,(#166423,#166424,#166425,#166426,#166427,
#166428,#166429,#166430,#166431,#166432,#166433,#166434,#166435),
 .UNSPECIFIED.,.F.,.F.,(4,3,1,1,1,1,1,1,4),(-1524.62338608632,-1524.5974163482,
-1523.59768033748,-1522.59794432676,-1521.59820831604,-1520.59847230532,
-1519.5987362946,-1518.59900028388,-1518.34020077914),.UNSPECIFIED.);
#1426=B_SPLINE_CURVE_WITH_KNOTS('',3,(#166437,#166438,#166439,#166440,#166441,
#166442,#166443,#166444,#166445,#166446),.UNSPECIFIED.,.F.,.F.,(4,1,1,1,
1,1,1,4),(-1518.34020077914,-1517.59926427316,-1516.59952826244,-1515.59979225172,
-1514.600056241,-1513.60032023028,-1512.60058421956,-1512.05701547196),
 .UNSPECIFIED.);
#1427=B_SPLINE_CURVE_WITH_KNOTS('',3,(#166448,#166449,#166450,#166451,#166452,
#166453,#166454,#166455,#166456,#166457),.UNSPECIFIED.,.F.,.F.,(4,1,1,1,
1,1,1,4),(-1512.05701547196,-1511.60084820884,-1510.60111219812,-1509.6013761874,
-1508.60164017668,-1507.60190416596,-1506.60216815524,-1505.77383016478),
 .UNSPECIFIED.);
#1428=B_SPLINE_CURVE_WITH_KNOTS('',3,(#166459,#166460,#166461,#166462,#166463,
#166464,#166465,#166466,#166467,#166468,#166469,#166470),.UNSPECIFIED.,
 .F.,.F.,(4,2,1,1,1,1,1,1,4),(-1505.77383016478,-1505.60243214452,-1504.6026961338,
-1503.60296012308,-1502.60322411236,-1501.60348810164,-1500.60375209092,
-1499.6040160802,-1499.4906448576),.UNSPECIFIED.);
#1429=B_SPLINE_CURVE_WITH_KNOTS('',3,(#166472,#166473,#166474,#166475,#166476,
#166477,#166478,#166479,#166480,#166481),.UNSPECIFIED.,.F.,.F.,(4,1,1,1,
1,1,1,4),(-1499.4906448576,-1498.60428006948,-1497.60454405876,-1496.60480804804,
-1495.60507203732,-1494.6053360266,-1493.60560001588,-1493.20745955042),
 .UNSPECIFIED.);
#1430=B_SPLINE_CURVE_WITH_KNOTS('',3,(#166483,#166484,#166485,#166486,#166487,
#166488,#166489,#166490,#166491,#166492),.UNSPECIFIED.,.F.,.F.,(4,1,1,1,
1,1,1,4),(-1493.20745955042,-1492.60586400516,-1491.60612799444,-1490.60639198372,
-1489.606655973,-1488.60691996228,-1487.60718395156,-1486.92427424324),
 .UNSPECIFIED.);
#1431=B_SPLINE_CURVE_WITH_KNOTS('',3,(#166494,#166495,#166496,#166497,#166498,
#166499,#166500,#166501,#166502,#166503,#166504),.UNSPECIFIED.,.F.,.F.,
(4,2,1,1,1,1,1,4),(-1486.92427424324,-1486.60744794083,-1485.60771193012,
-1484.60797591939,-1483.60823990867,-1482.60850389795,-1481.60876788723,
-1480.64109334394),.UNSPECIFIED.);
#1432=B_SPLINE_CURVE_WITH_KNOTS('',3,(#166506,#166507,#166508,#166509,#166510,
#166511,#166512,#166513,#166514,#166515,#166516,#166517,#166518,#166519,
#166520,#166521,#166522,#166523,#166524,#166525,#166526,#166527,#166528,
#166529,#166530,#166531,#166532,#166533,#166534,#166535,#166536,#166537,
#166538,#166539,#166540,#166541,#166542,#166543,#166544,#166545,#166546,
#166547,#166548,#166549,#166550,#166551,#166552,#166553,#166554,#166555,
#166556,#166557,#166558,#166559,#166560,#166561,#166562,#166563,#166564,
#166565,#166566,#166567,#166568,#166569,#166570,#166571,#166572,#166573,
#166574,#166575,#166576,#166577,#166578,#166579,#166580,#166581,#166582,
#166583,#166584,#166585,#166586,#166587,#166588,#166589,#166590,#166591,
#166592,#166593,#166594,#166595,#166596,#166597,#166598,#166599,#166600,
#166601,#166602,#166603,#166604,#166605,#166606,#166607,#166608,#166609,
#166610,#166611,#166612,#166613,#166614,#166615,#166616,#166617,#166618,
#166619,#166620,#166621,#166622,#166623,#166624,#166625,#166626,#166627,
#166628,#166629,#166630,#166631,#166632,#166633,#166634,#166635,#166636,
#166637,#166638,#166639,#166640,#166641,#166642,#166643,#166644,#166645,
#166646,#166647,#166648,#166649,#166650,#166651,#166652,#166653,#166654,
#166655,#166656,#166657,#166658,#166659,#166660,#166661,#166662,#166663,
#166664,#166665,#166666,#166667,#166668,#166669,#166670,#166671,#166672,
#166673,#166674,#166675,#166676,#166677,#166678,#166679,#166680,#166681,
#166682,#166683,#166684,#166685,#166686,#166687,#166688,#166689,#166690,
#166691,#166692,#166693,#166694,#166695,#166696,#166697,#166698,#166699,
#166700,#166701,#166702,#166703,#166704,#166705,#166706,#166707,#166708,
#166709,#166710,#166711,#166712,#166713,#166714,#166715,#166716,#166717,
#166718,#166719,#166720,#166721,#166722,#166723,#166724,#166725,#166726,
#166727,#166728,#166729,#166730,#166731,#166732,#166733,#166734,#166735,
#166736,#166737,#166738,#166739,#166740,#166741,#166742,#166743,#166744,
#166745,#166746,#166747,#166748,#166749,#166750,#166751,#166752),
 .UNSPECIFIED.,.F.,.F.,(4,3,3,3,3,3,3,3,3,3,3,3,3,3,3,3,3,3,3,3,3,3,3,3,
3,3,3,3,3,3,3,3,3,3,3,3,3,3,3,3,3,3,3,3,3,3,3,3,3,3,3,3,3,3,3,3,3,3,3,3,
3,3,3,3,3,3,3,3,3,3,3,3,3,3,3,3,3,3,3,3,3,3,4),(-1480.64108893606,-1480.60903187651,
-1480.52907457638,-1480.44921177914,-1480.36942595667,-1480.28969964147,
-1480.21001541318,-1480.13034442696,-1480.05067697343,-1479.97099732262,
-1479.89128974022,-1479.81149451115,-1479.73165016944,-1479.6516917424,
-1479.60929586579,-1479.52933856566,-1479.44947576842,-1479.36968994594,
-1479.28996363075,-1479.21027940245,-1479.13060841623,-1479.05094096271,
-1478.97126131189,-1478.8915537295,-1478.81175850042,-1478.73191415871,
-1478.65195573167,-1478.60955985507,-1478.52960255494,-1478.4497397577,
-1478.36995393522,-1478.29022762003,-1478.21054339173,-1478.13087240551,
-1478.05120495199,-1477.97152530117,-1477.89181771878,-1477.8120224897,
-1477.73217814799,-1477.65221972095,-1477.60982384435,-1477.52986654422,
-1477.45000374698,-1477.3702179245,-1477.29049160931,-1477.21080738102,
-1477.13113639479,-1477.05146894127,-1476.97178929045,-1476.89208170806,
-1476.81228647898,-1476.73244213728,-1476.65248371023,-1476.61008783363,
-1476.5301305335,-1476.45026773626,-1476.37048191378,-1476.29075559859,
-1476.21107137029,-1476.13140038407,-1476.05173293055,-1475.97205327973,
-1475.89234569734,-1475.81255046826,-1475.73270612655,-1475.65274769951,
-1475.61035182291,-1475.53039452278,-1475.45053172553,-1475.37074590306,
-1475.29101958787,-1475.21133535957,-1475.13166437335,-1475.05199691982,
-1474.972317269,-1474.89260968661,-1474.81281445753,-1474.73297011582,-1474.65301168878,
-1474.61061581219,-1474.50625453886,-1474.40403233292,-1474.3579036915),
 .UNSPECIFIED.);
#1433=B_SPLINE_CURVE_WITH_KNOTS('',3,(#166754,#166755,#166756,#166757,#166758,
#166759,#166760,#166761,#166762,#166763),.UNSPECIFIED.,.F.,.F.,(4,1,1,1,
1,1,1,4),(-1474.35790362888,-1473.61087980147,-1472.61114379075,-1471.61140778003,
-1470.61167176931,-1469.61193575859,-1468.61219974787,-1468.0747183217),
 .UNSPECIFIED.);
#1434=B_SPLINE_CURVE_WITH_KNOTS('',3,(#166765,#166766,#166767,#166768,#166769,
#166770,#166771,#166772,#166773,#166774,#166775,#166776,#166777,#166778,
#166779,#166780,#166781,#166782,#166783,#166784,#166785,#166786,#166787,
#166788,#166789,#166790,#166791,#166792,#166793,#166794,#166795,#166796,
#166797,#166798,#166799,#166800,#166801,#166802,#166803,#166804,#166805,
#166806,#166807,#166808,#166809,#166810,#166811,#166812,#166813,#166814,
#166815,#166816,#166817,#166818,#166819,#166820,#166821,#166822,#166823,
#166824,#166825,#166826,#166827,#166828,#166829,#166830,#166831,#166832,
#166833,#166834,#166835,#166836,#166837,#166838,#166839,#166840,#166841,
#166842,#166843,#166844,#166845,#166846,#166847,#166848,#166849,#166850,
#166851,#166852,#166853,#166854,#166855,#166856,#166857,#166858,#166859,
#166860,#166861,#166862,#166863,#166864,#166865,#166866,#166867,#166868,
#166869,#166870,#166871,#166872,#166873,#166874,#166875,#166876,#166877,
#166878,#166879,#166880,#166881,#166882,#166883,#166884,#166885,#166886,
#166887,#166888,#166889,#166890,#166891,#166892,#166893,#166894,#166895,
#166896,#166897,#166898,#166899,#166900,#166901,#166902,#166903,#166904,
#166905,#166906,#166907,#166908,#166909,#166910,#166911,#166912,#166913,
#166914,#166915,#166916,#166917,#166918,#166919,#166920,#166921,#166922,
#166923,#166924,#166925,#166926,#166927,#166928,#166929,#166930,#166931,
#166932,#166933,#166934,#166935,#166936,#166937,#166938,#166939,#166940,
#166941,#166942,#166943,#166944,#166945,#166946,#166947,#166948,#166949,
#166950,#166951,#166952,#166953,#166954,#166955,#166956,#166957,#166958,
#166959,#166960,#166961,#166962,#166963,#166964,#166965,#166966,#166967,
#166968,#166969,#166970,#166971,#166972,#166973,#166974,#166975,#166976,
#166977,#166978,#166979,#166980,#166981,#166982,#166983,#166984,#166985,
#166986,#166987,#166988,#166989,#166990,#166991,#166992,#166993,#166994,
#166995,#166996,#166997,#166998,#166999,#167000,#167001,#167002,#167003,
#167004,#167005,#167006,#167007,#167008,#167009,#167010,#167011),
 .UNSPECIFIED.,.F.,.F.,(4,3,3,3,3,3,3,3,3,3,3,3,3,3,3,3,3,3,3,3,3,3,3,3,
3,3,3,3,3,3,3,3,3,3,3,3,3,3,3,3,3,3,3,3,3,3,3,3,3,3,3,3,3,3,3,3,3,3,3,3,
3,3,3,3,3,3,3,3,3,3,3,3,3,3,3,3,3,3,3,3,3,3,4),(-1468.07471811664,-1467.98983128614,
-1467.9047850356,-1467.81949107158,-1467.73406381551,-1467.64842972939,
-1467.61246373715,-1467.53250643702,-1467.45264363978,-1467.37285781731,
-1467.29313150212,-1467.21344727382,-1467.1337762876,-1467.05410883408,
-1466.97442918327,-1466.89472160087,-1466.8149263718,-1466.73508203009,
-1466.65512360305,-1466.61272772643,-1466.5327704263,-1466.45290762906,
-1466.37312180658,-1466.29339549139,-1466.2137112631,-1466.13404027688,
-1466.05437282335,-1465.97469317253,-1465.89498559014,-1465.81519036106,
-1465.73534601936,-1465.65538759231,-1465.61299171571,-1465.53303441558,
-1465.45317161834,-1465.37338579586,-1465.29365948067,-1465.21397525237,
-1465.13430426615,-1465.05463681262,-1464.97495716181,-1464.89524957941,
-1464.81545435034,-1464.73561000863,-1464.65565158158,-1464.61325570499,
-1464.53329840486,-1464.45343560762,-1464.37364978514,-1464.29392346995,
-1464.21423924166,-1464.13456825544,-1464.05490080191,-1463.97522115109,
-1463.8955135687,-1463.81571833962,-1463.73587399792,-1463.65591557087,
-1463.61351969427,-1463.53356239414,-1463.4536995969,-1463.37391377442,
-1463.29418745923,-1463.21450323093,-1463.13483224471,-1463.05516479119,
-1462.97548514037,-1462.89577755797,-1462.8159823289,-1462.73613798719,
-1462.65617956014,-1462.61378368355,-1462.53501718464,-1462.45634485605,
-1462.37774820447,-1462.29921262633,-1462.22070988667,-1462.14222340191,
-1462.06373660319,-1461.98520236571,-1461.90664134508,-1461.82800041734,
-1461.79153301452),.UNSPECIFIED.);
#1435=B_SPLINE_CURVE_WITH_KNOTS('',3,(#167013,#167014,#167015,#167016,#167017,
#167018,#167019,#167020,#167021,#167022,#167023,#167024),.UNSPECIFIED.,
 .F.,.F.,(4,2,1,1,1,1,1,1,4),(-1461.79153301452,-1461.61404767283,-1460.61431166211,
-1459.61457565139,-1458.61483964067,-1457.61510362995,-1456.61536761923,
-1455.61563160851,-1455.50834770734),.UNSPECIFIED.);
#1436=B_SPLINE_CURVE_WITH_KNOTS('',3,(#167026,#167027,#167028,#167029,#167030,
#167031,#167032,#167033,#167034,#167035),.UNSPECIFIED.,.F.,.F.,(4,1,1,1,
1,1,1,4),(-1455.50834770734,-1454.61589559779,-1453.61615958707,-1452.61642357635,
-1451.61668756563,-1450.61695155491,-1449.61721554419,-1449.22516240016),
 .UNSPECIFIED.);
#1437=B_SPLINE_CURVE_WITH_KNOTS('',3,(#167037,#167038,#167039,#167040,#167041,
#167042,#167043,#167044,#167045,#167046),.UNSPECIFIED.,.F.,.F.,(4,1,1,1,
1,1,1,4),(-1449.22516240016,-1448.61747953347,-1447.61774352275,-1446.61800751203,
-1445.61827150131,-1444.61853549059,-1443.61879947987,-1442.94197709298),
 .UNSPECIFIED.);
#1438=B_SPLINE_CURVE_WITH_KNOTS('',3,(#167048,#167049,#167050,#167051,#167052,
#167053,#167054,#167055,#167056,#167057),.UNSPECIFIED.,.F.,.F.,(4,1,1,1,
1,1,1,4),(-1442.94197709298,-1442.61906346915,-1441.61932745843,-1440.61959144771,
-1439.61985543699,-1438.62011942627,-1437.62038341555,-1436.65879704426),
 .UNSPECIFIED.);
#1439=B_SPLINE_CURVE_WITH_KNOTS('',3,(#167059,#167060,#167061,#167062,#167063,
#167064,#167065,#167066,#167067,#167068,#167069,#167070,#167071,#167072,
#167073,#167074,#167075,#167076,#167077,#167078,#167079,#167080,#167081,
#167082,#167083,#167084,#167085,#167086,#167087,#167088,#167089,#167090,
#167091,#167092,#167093,#167094,#167095,#167096,#167097,#167098,#167099,
#167100,#167101,#167102,#167103,#167104,#167105,#167106,#167107,#167108,
#167109,#167110,#167111,#167112,#167113,#167114,#167115,#167116,#167117,
#167118,#167119,#167120,#167121,#167122,#167123,#167124,#167125,#167126,
#167127,#167128,#167129,#167130,#167131,#167132,#167133,#167134,#167135,
#167136,#167137,#167138,#167139,#167140,#167141,#167142,#167143,#167144,
#167145,#167146,#167147,#167148,#167149,#167150,#167151,#167152,#167153,
#167154,#167155,#167156,#167157,#167158,#167159,#167160,#167161,#167162,
#167163,#167164,#167165,#167166,#167167,#167168,#167169,#167170,#167171,
#167172,#167173,#167174,#167175,#167176,#167177,#167178,#167179,#167180,
#167181,#167182,#167183,#167184,#167185,#167186,#167187,#167188,#167189,
#167190,#167191,#167192,#167193,#167194,#167195,#167196,#167197,#167198,
#167199,#167200,#167201,#167202,#167203,#167204,#167205,#167206,#167207,
#167208,#167209,#167210,#167211,#167212,#167213,#167214,#167215,#167216,
#167217,#167218,#167219,#167220,#167221,#167222,#167223,#167224,#167225,
#167226,#167227,#167228,#167229,#167230,#167231,#167232,#167233,#167234,
#167235,#167236,#167237,#167238,#167239,#167240,#167241,#167242,#167243,
#167244,#167245,#167246,#167247,#167248,#167249,#167250,#167251,#167252,
#167253,#167254,#167255,#167256,#167257,#167258,#167259,#167260,#167261,
#167262,#167263,#167264,#167265,#167266,#167267,#167268,#167269,#167270,
#167271,#167272,#167273,#167274,#167275,#167276,#167277,#167278,#167279,
#167280,#167281,#167282,#167283,#167284,#167285,#167286,#167287,#167288,
#167289,#167290,#167291,#167292,#167293,#167294,#167295,#167296,#167297,
#167298,#167299,#167300,#167301,#167302,#167303,#167304,#167305),
 .UNSPECIFIED.,.F.,.F.,(4,3,3,3,3,3,3,3,3,3,3,3,3,3,3,3,3,3,3,3,3,3,3,3,
3,3,3,3,3,3,3,3,3,3,3,3,3,3,3,3,3,3,3,3,3,3,3,3,3,3,3,3,3,3,3,3,3,3,3,3,
3,3,3,3,3,3,3,3,3,3,3,3,3,3,3,3,3,3,3,3,3,3,4),(-1436.6587917858,-1436.62064740483,
-1436.5406901047,-1436.46082730746,-1436.38104148498,-1436.30131516979,
-1436.22163094149,-1436.14195995527,-1436.06229250175,-1435.98261285093,
-1435.90290526854,-1435.82311003946,-1435.74326569775,-1435.66330727071,
-1435.62091139411,-1435.54095409398,-1435.46109129674,-1435.38130547426,
-1435.30157915907,-1435.22189493077,-1435.14222394455,-1435.06255649103,
-1434.98287684021,-1434.90316925782,-1434.82337402874,-1434.74352968703,
-1434.66357125999,-1434.62117538339,-1434.54121808326,-1434.46135528602,
-1434.38156946354,-1434.30184314835,-1434.22215892005,-1434.14248793383,
-1434.06282048031,-1433.98314082949,-1433.9034332471,-1433.82363801802,
-1433.74379367631,-1433.66383524926,-1433.62143937267,-1433.54148207254,
-1433.4616192753,-1433.38183345282,-1433.30210713763,-1433.22242290934,
-1433.14275192312,-1433.06308446959,-1432.98340481877,-1432.90369723638,
-1432.8239020073,-1432.7440576656,-1432.66409923855,-1432.62170336195,-1432.54174606182,
-1432.46188326458,-1432.3820974421,-1432.30237112691,-1432.22268689861,
-1432.14301591239,-1432.06334845887,-1431.98366880805,-1431.90396122566,
-1431.82416599658,-1431.74432165487,-1431.66436322783,-1431.62196735123,
-1431.5420100511,-1431.46214725386,-1431.38236143138,-1431.30263511619,
-1431.2229508879,-1431.14327990167,-1431.06361244815,-1430.98393279733,
-1430.90422521494,-1430.82442998586,-1430.74458564415,-1430.66462721711,
-1430.62223134051,-1430.51675163816,-1430.41361228529,-1430.37560656682),
 .UNSPECIFIED.);
#1440=B_SPLINE_CURVE_WITH_KNOTS('',3,(#167307,#167308,#167309,#167310,#167311,
#167312,#167313,#167314,#167315,#167316),.UNSPECIFIED.,.F.,.F.,(4,1,1,1,
1,1,1,4),(-1430.37560647862,-1429.62249532979,-1428.62275931907,-1427.62302330835,
-1426.62328729763,-1425.62355128691,-1424.62381527619,-1424.09242117144),
 .UNSPECIFIED.);
#1441=B_SPLINE_CURVE_WITH_KNOTS('',3,(#167318,#167319,#167320,#167321,#167322,
#167323,#167324,#167325,#167326,#167327),.UNSPECIFIED.,.F.,.F.,(4,1,1,1,
1,1,1,4),(-1424.09242117144,-1423.62407926547,-1422.62434325475,-1421.62460724403,
-1420.62487123331,-1419.62513522259,-1418.62539921187,-1417.80924068802),
 .UNSPECIFIED.);
#1442=B_SPLINE_CURVE_WITH_KNOTS('',3,(#167329,#167330,#167331,#167332,#167333,
#167334,#167335,#167336,#167337,#167338,#167339,#167340,#167341,#167342,
#167343,#167344,#167345,#167346,#167347,#167348,#167349,#167350,#167351,
#167352,#167353,#167354,#167355,#167356,#167357,#167358,#167359,#167360,
#167361,#167362,#167363,#167364,#167365,#167366,#167367,#167368,#167369,
#167370,#167371,#167372,#167373,#167374,#167375,#167376,#167377,#167378,
#167379,#167380,#167381,#167382,#167383,#167384,#167385,#167386,#167387,
#167388,#167389,#167390,#167391,#167392,#167393,#167394,#167395,#167396,
#167397,#167398,#167399,#167400,#167401,#167402,#167403,#167404,#167405,
#167406,#167407,#167408,#167409,#167410,#167411,#167412,#167413,#167414,
#167415,#167416,#167417,#167418,#167419,#167420,#167421,#167422,#167423,
#167424,#167425,#167426,#167427,#167428,#167429,#167430,#167431,#167432,
#167433,#167434,#167435,#167436,#167437,#167438,#167439,#167440,#167441,
#167442,#167443,#167444,#167445,#167446,#167447,#167448,#167449,#167450,
#167451,#167452,#167453,#167454,#167455,#167456,#167457,#167458,#167459,
#167460,#167461,#167462,#167463,#167464,#167465,#167466,#167467,#167468,
#167469,#167470,#167471,#167472,#167473,#167474,#167475,#167476,#167477,
#167478,#167479,#167480,#167481,#167482,#167483,#167484,#167485,#167486,
#167487,#167488,#167489,#167490,#167491,#167492,#167493,#167494,#167495,
#167496,#167497,#167498,#167499,#167500,#167501,#167502,#167503,#167504,
#167505,#167506,#167507,#167508,#167509,#167510,#167511,#167512,#167513,
#167514,#167515,#167516,#167517,#167518,#167519,#167520,#167521,#167522,
#167523,#167524,#167525,#167526,#167527,#167528,#167529,#167530,#167531,
#167532,#167533,#167534,#167535,#167536,#167537,#167538,#167539,#167540,
#167541,#167542,#167543,#167544,#167545,#167546,#167547,#167548,#167549,
#167550,#167551,#167552,#167553,#167554,#167555,#167556,#167557,#167558,
#167559,#167560,#167561,#167562,#167563,#167564,#167565,#167566,#167567,
#167568,#167569,#167570,#167571,#167572),.UNSPECIFIED.,.F.,.F.,(4,3,3,3,
3,3,3,3,3,3,3,3,3,3,3,3,3,3,3,3,3,3,3,3,3,3,3,3,3,3,3,3,3,3,3,3,3,3,3,3,
3,3,3,3,3,3,3,3,3,3,3,3,3,3,3,3,3,3,3,3,3,3,3,3,3,3,3,3,3,3,3,3,3,3,3,3,
3,3,3,3,3,4),(-1417.80923586426,-1417.689114353,-1417.62566320115,-1417.54570590102,
-1417.46584310378,-1417.3860572813,-1417.30633096611,-1417.22664673781,
-1417.14697575159,-1417.06730829807,-1416.98762864725,-1416.90792106486,
-1416.82812583578,-1416.74828149407,-1416.66832306702,-1416.62592719043,
-1416.5459698903,-1416.46610709306,-1416.38632127058,-1416.30659495539,
-1416.22691072709,-1416.14723974087,-1416.06757228735,-1415.98789263653,
-1415.90818505414,-1415.82838982506,-1415.74854548335,-1415.66858705631,
-1415.62619117971,-1415.54623387958,-1415.46637108234,-1415.38658525986,
-1415.30685894467,-1415.22717471637,-1415.14750373015,-1415.06783627663,
-1414.98815662581,-1414.90844904342,-1414.82865381434,-1414.74880947263,
-1414.66885104559,-1414.62645516899,-1414.54649786886,-1414.46663507162,
-1414.38684924914,-1414.30712293395,-1414.22743870566,-1414.14776771943,
-1414.06810026591,-1413.98842061509,-1413.9087130327,-1413.82891780362,
-1413.74907346191,-1413.66911503487,-1413.62671915827,-1413.54676185814,
-1413.4668990609,-1413.38711323842,-1413.30738692323,-1413.22770269494,
-1413.14803170871,-1413.06836425519,-1412.98868460437,-1412.90897702198,
-1412.8291817929,-1412.74933745119,-1412.66937902415,-1412.62698314755,
-1412.54702584742,-1412.46716305018,-1412.38737722771,-1412.30765091251,
-1412.22796668422,-1412.148295698,-1412.06862824447,-1411.98894859366,-1411.90924101126,
-1411.82944578219,-1411.74960144048,-1411.66964301343,-1411.62724713683,
-1411.52605055708),.UNSPECIFIED.);
#1443=B_SPLINE_CURVE_WITH_KNOTS('',3,(#167574,#167575,#167576,#167577,#167578,
#167579,#167580,#167581,#167582,#167583),.UNSPECIFIED.,.F.,.F.,(4,1,1,1,
1,1,1,4),(-1411.52604145674,-1410.62751112611,-1409.62777511538,-1408.62803910466,
-1407.62830309394,-1406.62856708322,-1405.6288310725,-1405.24287268663),
 .UNSPECIFIED.);
#1444=B_SPLINE_CURVE_WITH_KNOTS('',3,(#167585,#167586,#167587,#167588,#167589,
#167590,#167591,#167592,#167593,#167594,#167595,#167596,#167597,#167598,
#167599,#167600,#167601,#167602,#167603,#167604,#167605,#167606,#167607,
#167608,#167609,#167610,#167611,#167612,#167613,#167614,#167615,#167616,
#167617,#167618,#167619,#167620,#167621,#167622,#167623,#167624,#167625,
#167626,#167627,#167628,#167629,#167630,#167631,#167632,#167633,#167634,
#167635,#167636,#167637,#167638,#167639,#167640,#167641,#167642,#167643,
#167644,#167645,#167646,#167647,#167648,#167649,#167650,#167651,#167652,
#167653,#167654,#167655,#167656,#167657,#167658,#167659,#167660,#167661,
#167662,#167663,#167664,#167665,#167666,#167667,#167668,#167669,#167670,
#167671,#167672,#167673,#167674,#167675,#167676,#167677,#167678,#167679,
#167680,#167681,#167682,#167683,#167684,#167685,#167686,#167687,#167688,
#167689,#167690,#167691,#167692,#167693,#167694,#167695,#167696,#167697,
#167698,#167699,#167700,#167701,#167702,#167703,#167704,#167705,#167706,
#167707,#167708,#167709,#167710,#167711,#167712,#167713,#167714,#167715,
#167716,#167717,#167718,#167719,#167720,#167721,#167722,#167723,#167724,
#167725,#167726,#167727,#167728,#167729,#167730,#167731,#167732,#167733,
#167734,#167735,#167736,#167737,#167738,#167739,#167740,#167741,#167742,
#167743,#167744,#167745,#167746,#167747,#167748,#167749,#167750,#167751,
#167752,#167753,#167754,#167755,#167756,#167757,#167758,#167759,#167760,
#167761,#167762,#167763,#167764,#167765,#167766,#167767,#167768,#167769,
#167770,#167771,#167772,#167773,#167774,#167775,#167776,#167777,#167778,
#167779,#167780,#167781,#167782,#167783,#167784,#167785,#167786,#167787,
#167788,#167789,#167790,#167791,#167792,#167793,#167794,#167795,#167796,
#167797,#167798,#167799,#167800,#167801,#167802,#167803,#167804,#167805,
#167806,#167807,#167808,#167809,#167810,#167811,#167812,#167813,#167814,
#167815,#167816,#167817,#167818,#167819,#167820,#167821,#167822,#167823,
#167824,#167825,#167826,#167827,#167828,#167829,#167830,#167831),
 .UNSPECIFIED.,.F.,.F.,(4,3,3,3,3,3,3,3,3,3,3,3,3,3,3,3,3,3,3,3,3,3,3,3,
3,3,3,3,3,3,3,3,3,3,3,3,3,3,3,3,3,3,3,3,3,3,3,3,3,3,3,3,3,3,3,3,3,3,3,3,
3,3,3,3,3,3,3,3,3,3,3,3,3,3,3,3,3,3,3,3,3,3,4),(-1405.2428652499,-1405.16239569195,
-1405.08191404014,-1405.00140562355,-1404.92085575786,-1404.840199036,-1404.75948345872,
-1404.67863759454,-1404.62909506178,-1404.54913776165,-1404.46927496441,
-1404.38948914194,-1404.30976282674,-1404.23007859845,-1404.15040761223,
-1404.0707401587,-1403.99106050789,-1403.9113529255,-1403.83155769642,-1403.75171335471,
-1403.67175492767,-1403.62935905106,-1403.54940175093,-1403.46953895369,
-1403.38975313121,-1403.31002681602,-1403.23034258773,-1403.1506716015,
-1403.07100414798,-1402.99132449716,-1402.91161691477,-1402.83182168569,
-1402.75197734399,-1402.67201891694,-1402.62962304034,-1402.54966574021,
-1402.46980294297,-1402.39001712049,-1402.3102908053,-1402.230606577,-1402.15093559078,
-1402.07126813726,-1401.99158848644,-1401.91188090405,-1401.83208567497,
-1401.75224133326,-1401.67228290621,-1401.62988702962,-1401.54992972949,
-1401.47006693225,-1401.39028110977,-1401.31055479458,-1401.23087056629,
-1401.15119958006,-1401.07153212654,-1400.99185247572,-1400.91214489333,
-1400.83234966425,-1400.75250532255,-1400.6725468955,-1400.6301510189,-1400.55019371877,
-1400.47033092153,-1400.39054509905,-1400.31081878386,-1400.23113455556,
-1400.15146356934,-1400.07179611582,-1399.992116465,-1399.9124088826,-1399.83261365353,
-1399.75276931182,-1399.67281088477,-1399.63041500818,-1399.546573125,-1399.46682601498,
-1399.38715383661,-1399.30754071169,-1399.22797080243,-1399.14842137439,
-1399.0688836793,-1398.98932729873,-1398.95967994272),.UNSPECIFIED.);
#1445=B_SPLINE_CURVE_WITH_KNOTS('',3,(#167833,#167834,#167835,#167836,#167837,
#167838,#167839,#167840,#167841,#167842),.UNSPECIFIED.,.F.,.F.,(4,1,1,1,
1,1,1,4),(-1398.9596726741,-1398.63067899746,-1397.63094298674,-1396.63120697602,
-1395.6314709653,-1394.63173495458,-1393.63199894386,-1392.67650054561),
 .UNSPECIFIED.);
#1446=B_SPLINE_CURVE_WITH_KNOTS('',3,(#167844,#167845,#167846,#167847,#167848,
#167849,#167850,#167851,#167852,#167853,#167854,#167855,#167856,#167857,
#167858,#167859,#167860,#167861,#167862,#167863,#167864,#167865,#167866,
#167867,#167868,#167869,#167870,#167871,#167872,#167873,#167874,#167875,
#167876,#167877,#167878,#167879,#167880,#167881,#167882,#167883,#167884,
#167885,#167886,#167887,#167888,#167889,#167890,#167891,#167892,#167893,
#167894,#167895,#167896,#167897,#167898,#167899,#167900,#167901,#167902,
#167903,#167904,#167905,#167906,#167907,#167908,#167909,#167910,#167911,
#167912,#167913,#167914,#167915,#167916,#167917,#167918,#167919,#167920,
#167921,#167922,#167923,#167924,#167925,#167926,#167927,#167928,#167929,
#167930,#167931,#167932,#167933,#167934,#167935,#167936,#167937,#167938,
#167939,#167940,#167941,#167942,#167943,#167944,#167945,#167946,#167947,
#167948,#167949,#167950,#167951,#167952,#167953,#167954,#167955,#167956,
#167957,#167958,#167959,#167960,#167961,#167962,#167963,#167964,#167965,
#167966,#167967,#167968,#167969,#167970,#167971,#167972,#167973,#167974,
#167975,#167976,#167977,#167978,#167979,#167980,#167981,#167982,#167983,
#167984,#167985,#167986,#167987,#167988,#167989,#167990,#167991,#167992,
#167993,#167994,#167995,#167996,#167997,#167998,#167999,#168000,#168001,
#168002,#168003,#168004,#168005,#168006,#168007,#168008,#168009,#168010,
#168011,#168012,#168013,#168014,#168015,#168016,#168017,#168018,#168019,
#168020,#168021,#168022,#168023,#168024,#168025,#168026,#168027,#168028,
#168029,#168030,#168031,#168032,#168033,#168034,#168035,#168036,#168037,
#168038,#168039,#168040,#168041,#168042,#168043,#168044,#168045,#168046,
#168047,#168048,#168049,#168050,#168051,#168052,#168053,#168054,#168055,
#168056,#168057,#168058,#168059,#168060,#168061,#168062,#168063,#168064,
#168065,#168066,#168067,#168068,#168069,#168070,#168071,#168072,#168073,
#168074,#168075,#168076,#168077,#168078,#168079,#168080,#168081,#168082,
#168083,#168084,#168085,#168086,#168087,#168088,#168089,#168090),
 .UNSPECIFIED.,.F.,.F.,(4,3,3,3,3,3,3,3,3,3,3,3,3,3,3,3,3,3,3,3,3,3,3,3,
3,3,3,3,3,3,3,3,3,3,3,3,3,3,3,3,3,3,3,3,3,3,3,3,3,3,3,3,3,3,3,3,3,3,3,3,
3,3,3,3,3,3,3,3,3,3,3,3,3,3,3,3,3,3,3,3,3,3,4),(-1392.67649463554,-1392.63226293314,
-1392.55230563301,-1392.47244283577,-1392.3926570133,-1392.3129306981,-1392.23324646981,
-1392.15357548359,-1392.07390803006,-1391.99422837924,-1391.91452079685,
-1391.83472556777,-1391.75488122607,-1391.67492279902,-1391.63252692242,
-1391.55256962229,-1391.47270682505,-1391.39292100257,-1391.31319468738,
-1391.23351045909,-1391.15383947286,-1391.07417201934,-1390.99449236852,
-1390.91478478613,-1390.83498955705,-1390.75514521534,-1390.6751867883,
-1390.6327909117,-1390.55283361157,-1390.47297081433,-1390.39318499185,
-1390.31345867666,-1390.23377444837,-1390.15410346214,-1390.07443600862,
-1389.9947563578,-1389.91504877541,-1389.83525354633,-1389.75540920462,
-1389.67545077758,-1389.63305490098,-1389.55309760085,-1389.47323480361,
-1389.39344898113,-1389.31372266594,-1389.23403843764,-1389.15436745142,
-1389.0746999979,-1388.99502034708,-1388.91531276469,-1388.83551753561,
-1388.7556731939,-1388.67571476686,-1388.63331889026,-1388.55336159013,
-1388.47349879289,-1388.39371297041,-1388.31398665522,-1388.23430242692,
-1388.1546314407,-1388.07496398718,-1387.99528433636,-1387.91557675397,
-1387.83578152489,-1387.75593718318,-1387.67597875614,-1387.63358287954,
-1387.55362557941,-1387.47376278217,-1387.39397695969,-1387.3142506445,
-1387.2345664162,-1387.15489542998,-1387.07522797646,-1386.99554832564,
-1386.91584074324,-1386.83604551417,-1386.75620117246,-1386.67624274541,
-1386.63384686882,-1386.52717722615,-1386.42307878727,-1386.39330937843),
 .UNSPECIFIED.);
#1447=B_SPLINE_CURVE_WITH_KNOTS('',3,(#168092,#168093,#168094,#168095,#168096,
#168097,#168098,#168099,#168100,#168101),.UNSPECIFIED.,.F.,.F.,(4,1,1,1,
1,1,1,4),(-1386.39330932836,-1385.6341108581,-1384.63437484738,-1383.63463883666,
-1382.63490282594,-1381.63516681522,-1380.6354308045,-1380.11012402118),
 .UNSPECIFIED.);
#1448=B_SPLINE_CURVE_WITH_KNOTS('',3,(#168103,#168104,#168105,#168106,#168107,
#168108,#168109,#168110,#168111,#168112),.UNSPECIFIED.,.F.,.F.,(4,1,1,1,
1,1,1,4),(-1380.11012402118,-1379.63569479378,-1378.63595878306,-1377.63622277234,
-1376.63648676162,-1375.6367507509,-1374.63701474018,-1373.82694297653),
 .UNSPECIFIED.);
#1449=B_SPLINE_CURVE_WITH_KNOTS('',3,(#168114,#168115,#168116,#168117,#168118,
#168119,#168120,#168121,#168122,#168123,#168124,#168125,#168126,#168127,
#168128,#168129,#168130,#168131,#168132,#168133,#168134,#168135,#168136,
#168137,#168138,#168139,#168140,#168141,#168142,#168143,#168144,#168145,
#168146,#168147,#168148,#168149,#168150,#168151,#168152,#168153,#168154,
#168155,#168156,#168157,#168158,#168159,#168160,#168161,#168162,#168163,
#168164,#168165,#168166,#168167,#168168,#168169,#168170,#168171,#168172,
#168173,#168174,#168175,#168176,#168177,#168178,#168179,#168180,#168181,
#168182,#168183,#168184,#168185,#168186,#168187,#168188,#168189,#168190,
#168191,#168192,#168193,#168194,#168195,#168196,#168197,#168198,#168199,
#168200,#168201,#168202,#168203,#168204,#168205,#168206,#168207,#168208,
#168209,#168210,#168211,#168212,#168213,#168214,#168215,#168216,#168217,
#168218,#168219,#168220,#168221,#168222,#168223,#168224,#168225,#168226,
#168227,#168228,#168229,#168230,#168231,#168232,#168233,#168234,#168235,
#168236,#168237,#168238,#168239,#168240,#168241,#168242,#168243,#168244,
#168245,#168246,#168247,#168248,#168249,#168250,#168251,#168252,#168253,
#168254,#168255,#168256,#168257,#168258,#168259,#168260,#168261,#168262,
#168263,#168264,#168265,#168266,#168267,#168268,#168269,#168270,#168271,
#168272,#168273,#168274,#168275,#168276,#168277,#168278,#168279,#168280,
#168281,#168282,#168283,#168284,#168285,#168286,#168287,#168288,#168289,
#168290,#168291,#168292,#168293,#168294,#168295,#168296,#168297,#168298,
#168299,#168300,#168301,#168302,#168303,#168304,#168305,#168306,#168307,
#168308,#168309,#168310,#168311,#168312,#168313,#168314,#168315,#168316,
#168317,#168318,#168319,#168320,#168321,#168322,#168323,#168324,#168325,
#168326,#168327,#168328,#168329,#168330,#168331,#168332,#168333,#168334,
#168335,#168336,#168337,#168338,#168339,#168340,#168341,#168342,#168343,
#168344,#168345,#168346,#168347,#168348,#168349,#168350,#168351,#168352,
#168353,#168354,#168355,#168356,#168357),.UNSPECIFIED.,.F.,.F.,(4,3,3,3,
3,3,3,3,3,3,3,3,3,3,3,3,3,3,3,3,3,3,3,3,3,3,3,3,3,3,3,3,3,3,3,3,3,3,3,3,
3,3,3,3,3,3,3,3,3,3,3,3,3,3,3,3,3,3,3,3,3,3,3,3,3,3,3,3,3,3,3,3,3,3,3,3,
3,3,3,3,3,4),(-1373.826938714,-1373.70893907459,-1373.63727872946,-1373.55732142933,
-1373.47745863208,-1373.39767280961,-1373.31794649442,-1373.23826226612,
-1373.1585912799,-1373.07892382637,-1372.99924417556,-1372.91953659316,
-1372.83974136408,-1372.75989702238,-1372.67993859533,-1372.63754271874,
-1372.55758541861,-1372.47772262137,-1372.39793679889,-1372.3182104837,
-1372.23852625541,-1372.15885526918,-1372.07918781566,-1371.99950816484,
-1371.91980058245,-1371.84000535337,-1371.76016101166,-1371.68020258462,
-1371.63780670802,-1371.55784940789,-1371.47798661065,-1371.39820078817,
-1371.31847447298,-1371.23879024469,-1371.15911925846,-1371.07945180494,
-1370.99977215412,-1370.92006457173,-1370.84026934265,-1370.76042500095,
-1370.6804665739,-1370.6380706973,-1370.55811339717,-1370.47825059993,-1370.39846477745,
-1370.31873846226,-1370.23905423396,-1370.15938324774,-1370.07971579422,
-1370.0000361434,-1369.92032856101,-1369.84053333193,-1369.76068899022,
-1369.68073056317,-1369.63833468658,-1369.55837738645,-1369.47851458921,
-1369.39872876673,-1369.31900245154,-1369.23931822325,-1369.15964723702,
-1369.0799797835,-1369.00030013268,-1368.92059255029,-1368.84079732121,
-1368.7609529795,-1368.68099455246,-1368.63859867586,-1368.55864137573,
-1368.47877857849,-1368.39899275602,-1368.31926644082,-1368.23958221253,
-1368.15991122631,-1368.08024377278,-1368.00056412196,-1367.92085653957,
-1367.84106131049,-1367.76121696879,-1367.68125854174,-1367.63886266514,
-1367.54375340682),.UNSPECIFIED.);
#1450=B_SPLINE_CURVE_WITH_KNOTS('',3,(#168359,#168360,#168361,#168362,#168363,
#168364,#168365,#168366,#168367,#168368),.UNSPECIFIED.,.F.,.F.,(4,1,1,1,
1,1,1,4),(-1367.54374436809,-1366.63912665442,-1365.6393906437,-1364.63965463298,
-1363.63991862226,-1362.64018261154,-1361.64044660082,-1361.26057566531),
 .UNSPECIFIED.);
#1451=B_SPLINE_CURVE_WITH_KNOTS('',3,(#168370,#168371,#168372,#168373,#168374,
#168375,#168376,#168377,#168378,#168379,#168380,#168381,#168382,#168383,
#168384,#168385,#168386,#168387,#168388,#168389,#168390,#168391,#168392,
#168393,#168394,#168395,#168396,#168397,#168398,#168399,#168400,#168401,
#168402,#168403,#168404,#168405,#168406,#168407,#168408,#168409,#168410,
#168411,#168412,#168413,#168414,#168415,#168416,#168417,#168418,#168419,
#168420,#168421,#168422,#168423,#168424,#168425,#168426,#168427,#168428,
#168429,#168430,#168431,#168432,#168433,#168434,#168435,#168436,#168437,
#168438,#168439,#168440,#168441,#168442,#168443,#168444,#168445,#168446,
#168447,#168448,#168449,#168450,#168451,#168452,#168453,#168454,#168455,
#168456,#168457,#168458,#168459,#168460,#168461,#168462,#168463,#168464,
#168465,#168466,#168467,#168468,#168469,#168470,#168471,#168472,#168473,
#168474,#168475,#168476,#168477,#168478,#168479,#168480,#168481,#168482,
#168483,#168484,#168485,#168486,#168487,#168488,#168489,#168490,#168491,
#168492,#168493,#168494,#168495,#168496,#168497,#168498,#168499,#168500,
#168501,#168502,#168503,#168504,#168505,#168506,#168507,#168508,#168509,
#168510,#168511,#168512,#168513,#168514,#168515,#168516,#168517,#168518,
#168519,#168520,#168521,#168522,#168523,#168524,#168525,#168526,#168527,
#168528,#168529,#168530,#168531,#168532,#168533,#168534,#168535,#168536,
#168537,#168538,#168539,#168540,#168541,#168542,#168543,#168544,#168545,
#168546,#168547,#168548,#168549,#168550,#168551,#168552,#168553,#168554,
#168555,#168556,#168557,#168558,#168559,#168560,#168561,#168562,#168563,
#168564,#168565,#168566,#168567,#168568,#168569,#168570,#168571,#168572,
#168573,#168574,#168575,#168576,#168577,#168578,#168579,#168580,#168581,
#168582,#168583,#168584,#168585,#168586,#168587,#168588,#168589,#168590,
#168591,#168592,#168593,#168594,#168595,#168596,#168597,#168598,#168599,
#168600,#168601,#168602,#168603,#168604,#168605,#168606,#168607,#168608,
#168609,#168610,#168611,#168612,#168613,#168614,#168615,#168616),
 .UNSPECIFIED.,.F.,.F.,(4,3,3,3,3,3,3,3,3,3,3,3,3,3,3,3,3,3,3,3,3,3,3,3,
3,3,3,3,3,3,3,3,3,3,3,3,3,3,3,3,3,3,3,3,3,3,3,3,3,3,3,3,3,3,3,3,3,3,3,3,
3,3,3,3,3,3,3,3,3,3,3,3,3,3,3,3,3,3,3,3,3,3,4),(-1361.26056809964,-1361.18021176969,
-1361.09984657315,-1361.01945767722,-1360.93903023779,-1360.85849830864,
-1360.77790979235,-1360.69719015379,-1360.6407105901,-1360.56075328997,
-1360.48089049273,-1360.40110467025,-1360.32137835506,-1360.24169412676,
-1360.16202314054,-1360.08235568702,-1360.0026760362,-1359.9229684538,-1359.84317322473,
-1359.76332888302,-1359.68337045597,-1359.64097457938,-1359.56101727925,
-1359.48115448201,-1359.40136865953,-1359.32164234434,-1359.24195811604,
-1359.16228712982,-1359.0826196763,-1359.00294002548,-1358.92323244309,
-1358.84343721401,-1358.7635928723,-1358.68363444525,-1358.64123856866,
-1358.56128126853,-1358.48141847129,-1358.40163264881,-1358.32190633362,
-1358.24222210533,-1358.1625511191,-1358.08288366558,-1358.00320401476,
-1357.92349643237,-1357.84370120329,-1357.76385686159,-1357.68389843454,
-1357.64150255794,-1357.56154525781,-1357.48168246057,-1357.40189663809,
-1357.3221703229,-1357.24248609461,-1357.16281510838,-1357.08314765486,
-1357.00346800404,-1356.92376042165,-1356.84396519257,-1356.76412085086,
-1356.68416242382,-1356.64176654722,-1356.56180924709,-1356.48194644985,
-1356.40216062738,-1356.32243431218,-1356.24275008389,-1356.16307909767,
-1356.08341164414,-1356.00373199333,-1355.92402441093,-1355.84422918186,
-1355.76438484015,-1355.6844264131,-1355.6420305365,-1355.55894956849,-1355.47911297368,
-1355.39935227128,-1355.31965166306,-1355.23999539154,-1355.16036196506,
-1355.08074132298,-1355.00110516955,-1354.97738279246),.UNSPECIFIED.);
#1452=B_SPLINE_CURVE_WITH_KNOTS('',3,(#168618,#168619,#168620,#168621,#168622,
#168623,#168624,#168625,#168626,#168627),.UNSPECIFIED.,.F.,.F.,(4,1,1,1,
1,1,1,4),(-1354.97737532952,-1354.64229452578,-1353.64255851506,-1352.64282250434,
-1351.64308649362,-1350.6433504829,-1349.64361447218,-1348.69419748528),
 .UNSPECIFIED.);
#1453=B_SPLINE_CURVE_WITH_KNOTS('',3,(#168629,#168630,#168631,#168632,#168633,
#168634,#168635,#168636,#168637,#168638,#168639,#168640,#168641),
 .UNSPECIFIED.,.F.,.F.,(4,3,1,1,1,1,1,1,4),(-1348.69419748528,-1348.64387846146,
-1347.64414245074,-1346.64440644002,-1345.6446704293,-1344.64493441858,
-1343.64519840786,-1342.64546239714,-1342.4110121781),.UNSPECIFIED.);
#1454=B_SPLINE_CURVE_WITH_KNOTS('',3,(#168643,#168644,#168645,#168646,#168647,
#168648,#168649,#168650,#168651,#168652),.UNSPECIFIED.,.F.,.F.,(4,1,1,1,
1,1,1,4),(-1342.4110121781,-1341.64572638642,-1340.6459903757,-1339.64625436498,
-1338.64651835426,-1337.64678234354,-1336.64704633282,-1336.12782687092),
 .UNSPECIFIED.);
#1455=B_SPLINE_CURVE_WITH_KNOTS('',3,(#168654,#168655,#168656,#168657,#168658,
#168659,#168660,#168661,#168662,#168663),.UNSPECIFIED.,.F.,.F.,(4,1,1,1,
1,1,1,4),(-1336.12782687092,-1335.6473103221,-1334.64757431137,-1333.64783830065,
-1332.64810228993,-1331.64836627921,-1330.64863026849,-1329.84464524732),
 .UNSPECIFIED.);
#1456=B_SPLINE_CURVE_WITH_KNOTS('',3,(#168665,#168666,#168667,#168668,#168669,
#168670,#168671,#168672,#168673,#168674,#168675,#168676,#168677,#168678,
#168679,#168680,#168681,#168682,#168683,#168684,#168685,#168686,#168687,
#168688,#168689,#168690,#168691,#168692,#168693,#168694,#168695,#168696,
#168697,#168698,#168699,#168700,#168701,#168702,#168703,#168704,#168705,
#168706,#168707,#168708,#168709,#168710,#168711,#168712,#168713,#168714,
#168715,#168716,#168717,#168718,#168719,#168720,#168721,#168722,#168723,
#168724,#168725,#168726,#168727,#168728,#168729,#168730,#168731,#168732,
#168733,#168734,#168735,#168736,#168737,#168738,#168739,#168740,#168741,
#168742,#168743,#168744,#168745,#168746,#168747,#168748,#168749,#168750,
#168751,#168752,#168753,#168754,#168755,#168756,#168757,#168758,#168759,
#168760,#168761,#168762,#168763,#168764,#168765,#168766,#168767,#168768,
#168769,#168770,#168771,#168772,#168773,#168774,#168775,#168776,#168777,
#168778,#168779,#168780,#168781,#168782,#168783,#168784,#168785,#168786,
#168787,#168788,#168789,#168790,#168791,#168792,#168793,#168794,#168795,
#168796,#168797,#168798,#168799,#168800,#168801,#168802,#168803,#168804,
#168805,#168806,#168807,#168808,#168809,#168810,#168811,#168812,#168813,
#168814,#168815,#168816,#168817,#168818,#168819,#168820,#168821,#168822,
#168823,#168824,#168825,#168826,#168827,#168828,#168829,#168830,#168831,
#168832,#168833,#168834,#168835,#168836,#168837,#168838,#168839,#168840,
#168841,#168842,#168843,#168844,#168845,#168846,#168847,#168848,#168849,
#168850,#168851,#168852,#168853,#168854,#168855,#168856,#168857,#168858,
#168859,#168860,#168861,#168862,#168863,#168864,#168865,#168866,#168867,
#168868,#168869,#168870,#168871,#168872,#168873,#168874,#168875,#168876,
#168877,#168878,#168879,#168880,#168881,#168882,#168883,#168884,#168885,
#168886,#168887,#168888,#168889,#168890,#168891,#168892,#168893,#168894,
#168895,#168896,#168897,#168898,#168899,#168900,#168901,#168902,#168903,
#168904,#168905,#168906,#168907,#168908),.UNSPECIFIED.,.F.,.F.,(4,3,3,3,
3,3,3,3,3,3,3,3,3,3,3,3,3,3,3,3,3,3,3,3,3,3,3,3,3,3,3,3,3,3,3,3,3,3,3,3,
3,3,3,3,3,3,3,3,3,3,3,3,3,3,3,3,3,3,3,3,3,3,3,3,3,3,3,3,3,3,3,3,3,3,3,3,
3,3,3,3,3,4),(-1329.84464156374,-1329.72859519301,-1329.64889425777,-1329.56893695764,
-1329.4890741604,-1329.40928833792,-1329.32956202273,-1329.24987779444,
-1329.17020680821,-1329.09053935469,-1329.01085970387,-1328.93115212148,
-1328.8513568924,-1328.7715125507,-1328.69155412365,-1328.64915824705,-1328.56920094692,
-1328.48933814968,-1328.4095523272,-1328.32982601201,-1328.25014178372,
-1328.17047079749,-1328.09080334397,-1328.01112369315,-1327.93141611076,
-1327.85162088168,-1327.77177653997,-1327.69181811293,-1327.64942223633,
-1327.5694649362,-1327.48960213896,-1327.40981631648,-1327.33009000129,
-1327.250405773,-1327.17073478677,-1327.09106733325,-1327.01138768243,-1326.93168010004,
-1326.85188487096,-1326.77204052925,-1326.69208210221,-1326.64968622561,
-1326.56972892548,-1326.48986612824,-1326.41008030576,-1326.33035399057,
-1326.25066976227,-1326.17099877605,-1326.09133132253,-1326.01165167171,
-1325.93194408932,-1325.85214886024,-1325.77230451853,-1325.69234609149,
-1325.64995021489,-1325.56999291476,-1325.49013011752,-1325.41034429504,
-1325.33061797985,-1325.25093375156,-1325.17126276533,-1325.09159531181,
-1325.01191566099,-1324.9322080786,-1324.85241284952,-1324.77256850782,
-1324.69261008077,-1324.65021420417,-1324.57025690404,-1324.4903941068,
-1324.41060828432,-1324.33088196913,-1324.25119774083,-1324.17152675461,
-1324.09185930109,-1324.01217965027,-1323.93247206787,-1323.8526768388,
-1323.77283249709,-1323.69287407004,-1323.65047819345,-1323.56145625656),
 .UNSPECIFIED.);
#1457=B_SPLINE_CURVE_WITH_KNOTS('',3,(#168910,#168911,#168912,#168913,#168914,
#168915,#168916,#168917,#168918,#168919),.UNSPECIFIED.,.F.,.F.,(4,1,1,1,
1,1,1,4),(-1323.56144747861,-1322.65074218273,-1321.65100617201,-1320.65127016129,
-1319.65153415057,-1318.65179813985,-1317.65206212913,-1317.27827860692),
 .UNSPECIFIED.);
#1458=B_SPLINE_CURVE_WITH_KNOTS('',3,(#168921,#168922,#168923,#168924,#168925,
#168926,#168927,#168928,#168929,#168930,#168931,#168932,#168933,#168934,
#168935,#168936,#168937,#168938,#168939,#168940,#168941,#168942,#168943,
#168944,#168945,#168946,#168947,#168948,#168949,#168950,#168951,#168952,
#168953,#168954,#168955,#168956,#168957,#168958,#168959,#168960,#168961,
#168962,#168963,#168964,#168965,#168966,#168967,#168968,#168969,#168970,
#168971,#168972,#168973,#168974,#168975,#168976,#168977,#168978,#168979,
#168980,#168981,#168982,#168983,#168984,#168985,#168986,#168987,#168988,
#168989,#168990,#168991,#168992,#168993,#168994,#168995,#168996,#168997,
#168998,#168999,#169000,#169001,#169002,#169003,#169004,#169005,#169006,
#169007,#169008,#169009,#169010,#169011,#169012,#169013,#169014,#169015,
#169016,#169017,#169018,#169019,#169020,#169021,#169022,#169023,#169024,
#169025,#169026,#169027,#169028,#169029,#169030,#169031,#169032,#169033,
#169034,#169035,#169036,#169037,#169038,#169039,#169040,#169041,#169042,
#169043,#169044,#169045,#169046,#169047,#169048,#169049,#169050,#169051,
#169052,#169053,#169054,#169055,#169056,#169057,#169058,#169059,#169060,
#169061,#169062,#169063,#169064,#169065,#169066,#169067,#169068,#169069,
#169070,#169071,#169072,#169073,#169074,#169075,#169076,#169077,#169078,
#169079,#169080,#169081,#169082,#169083,#169084,#169085,#169086,#169087,
#169088,#169089,#169090,#169091,#169092,#169093,#169094,#169095,#169096,
#169097,#169098,#169099,#169100,#169101,#169102,#169103,#169104,#169105,
#169106,#169107,#169108,#169109,#169110,#169111,#169112,#169113,#169114,
#169115,#169116,#169117,#169118,#169119,#169120,#169121,#169122,#169123,
#169124,#169125,#169126,#169127,#169128,#169129,#169130,#169131,#169132,
#169133,#169134,#169135,#169136,#169137,#169138,#169139,#169140,#169141,
#169142,#169143,#169144,#169145,#169146,#169147,#169148,#169149,#169150,
#169151,#169152,#169153,#169154,#169155,#169156,#169157,#169158,#169159,
#169160,#169161,#169162,#169163,#169164,#169165,#169166,#169167),
 .UNSPECIFIED.,.F.,.F.,(4,3,3,3,3,3,3,3,3,3,3,3,3,3,3,3,3,3,3,3,3,3,3,3,
3,3,3,3,3,3,3,3,3,3,3,3,3,3,3,3,3,3,3,3,3,3,3,3,3,3,3,3,3,3,3,3,3,3,3,3,
3,3,3,3,3,3,3,3,3,3,3,3,3,3,3,3,3,3,3,3,3,3,4),(-1317.27827094938,-1317.19802374242,
-1317.11777078609,-1317.03749709826,-1316.95718768734,-1316.8767760874,
-1316.79631011808,-1316.71571214589,-1316.65232611841,-1316.57236881828,
-1316.49250602104,-1316.41272019856,-1316.33299388337,-1316.25330965508,
-1316.17363866885,-1316.09397121533,-1316.01429156451,-1315.93458398212,
-1315.85478875304,-1315.77494441134,-1315.69498598429,-1315.65259010769,
-1315.57263280756,-1315.49277001032,-1315.41298418785,-1315.33325787265,
-1315.25357364436,-1315.17390265814,-1315.09423520461,-1315.01455555379,
-1314.9348479714,-1314.85505274232,-1314.77520840062,-1314.69524997357,
-1314.65285409697,-1314.57289679684,-1314.4930339996,-1314.41324817712,
-1314.33352186193,-1314.25383763363,-1314.17416664741,-1314.09449919389,
-1314.01481954307,-1313.93511196068,-1313.8553167316,-1313.77547238989,
-1313.69551396285,-1313.65311808625,-1313.57316078612,-1313.49329798888,
-1313.4135121664,-1313.33378585121,-1313.25410162291,-1313.17443063669,
-1313.09476318317,-1313.01508353235,-1312.93537594996,-1312.85558072088,
-1312.77573637917,-1312.69577795213,-1312.65338207553,-1312.5734247754,
-1312.49356197816,-1312.41377615568,-1312.33404984049,-1312.2543656122,
-1312.17469462597,-1312.09502717245,-1312.01534752163,-1311.93563993924,
-1311.85584471016,-1311.77600036845,-1311.69604194141,-1311.65364606481,
-1311.57132601198,-1311.49139611813,-1311.41154312364,-1311.3317513169,
-1311.25200502747,-1311.17228400148,-1311.09257687473,-1311.01285737541,
-1310.9950856422),.UNSPECIFIED.);
#1459=B_SPLINE_CURVE_WITH_KNOTS('',3,(#169169,#169170,#169171,#169172,#169173,
#169174,#169175,#169176,#169177,#169178),.UNSPECIFIED.,.F.,.F.,(4,1,1,1,
1,1,1,4),(-1310.99507802379,-1310.65391005409,-1309.65417404337,-1308.65443803265,
-1307.65470202193,-1306.65496601121,-1305.65523000049,-1304.71190033502),
 .UNSPECIFIED.);
#1460=B_SPLINE_CURVE_WITH_KNOTS('',3,(#169180,#169181,#169182,#169183,#169184,
#169185,#169186,#169187,#169188,#169189,#169190,#169191),.UNSPECIFIED.,
 .F.,.F.,(4,2,1,1,1,1,1,1,4),(-1304.71190033502,-1304.65549398977,-1303.65575797905,
-1302.65602196833,-1301.65628595761,-1300.65654994689,-1299.65681393617,
-1298.65707792545,-1298.42871502784),.UNSPECIFIED.);
#1461=B_SPLINE_CURVE_WITH_KNOTS('',3,(#169193,#169194,#169195,#169196,#169197,
#169198,#169199,#169200,#169201,#169202,#169203,#169204,#169205,#169206,
#169207,#169208,#169209,#169210,#169211,#169212,#169213,#169214,#169215,
#169216,#169217,#169218,#169219,#169220,#169221,#169222,#169223,#169224,
#169225,#169226,#169227,#169228,#169229,#169230,#169231,#169232,#169233,
#169234,#169235,#169236,#169237,#169238,#169239,#169240,#169241,#169242,
#169243,#169244,#169245,#169246,#169247,#169248,#169249,#169250,#169251,
#169252,#169253,#169254,#169255,#169256,#169257,#169258,#169259,#169260,
#169261,#169262,#169263,#169264,#169265,#169266,#169267,#169268,#169269,
#169270,#169271,#169272,#169273,#169274,#169275,#169276,#169277,#169278,
#169279,#169280,#169281,#169282,#169283,#169284,#169285,#169286,#169287,
#169288,#169289,#169290,#169291,#169292,#169293,#169294,#169295,#169296,
#169297,#169298,#169299,#169300,#169301,#169302,#169303,#169304,#169305,
#169306,#169307,#169308,#169309,#169310,#169311,#169312,#169313,#169314,
#169315,#169316,#169317,#169318,#169319,#169320,#169321,#169322,#169323,
#169324,#169325,#169326,#169327,#169328,#169329,#169330,#169331,#169332,
#169333,#169334,#169335,#169336,#169337,#169338,#169339,#169340,#169341,
#169342,#169343,#169344,#169345,#169346,#169347,#169348,#169349,#169350,
#169351,#169352,#169353,#169354,#169355,#169356,#169357,#169358,#169359,
#169360,#169361,#169362,#169363,#169364,#169365,#169366,#169367,#169368,
#169369,#169370,#169371,#169372,#169373,#169374,#169375,#169376,#169377,
#169378,#169379,#169380,#169381,#169382,#169383,#169384,#169385,#169386,
#169387,#169388,#169389,#169390,#169391,#169392,#169393,#169394,#169395,
#169396,#169397,#169398,#169399,#169400,#169401,#169402,#169403,#169404,
#169405,#169406,#169407,#169408,#169409,#169410,#169411,#169412,#169413,
#169414,#169415,#169416,#169417,#169418,#169419,#169420,#169421,#169422,
#169423,#169424,#169425,#169426,#169427,#169428,#169429,#169430,#169431,
#169432,#169433,#169434,#169435,#169436,#169437,#169438,#169439),
 .UNSPECIFIED.,.F.,.F.,(4,3,3,3,3,3,3,3,3,3,3,3,3,3,3,3,3,3,3,3,3,3,3,3,
3,3,3,3,3,3,3,3,3,3,3,3,3,3,3,3,3,3,3,3,3,3,3,3,3,3,3,3,3,3,3,3,3,3,3,3,
3,3,3,3,3,3,3,3,3,3,3,3,3,3,3,3,3,3,3,3,3,3,4),(-1298.42871502784,-1298.34998300514,
-1298.27130640284,-1298.19265969411,-1298.11402704446,-1298.03539196553,
-1297.95673796895,-1297.87800313816,-1297.79922586424,-1297.72033101374,
-1297.65734191473,-1297.5773846146,-1297.49752181736,-1297.41773599488,
-1297.33800967969,-1297.25832545139,-1297.17865446517,-1297.09898701165,
-1297.01930736083,-1296.93959977843,-1296.85980454936,-1296.77996020765,
-1296.7000017806,-1296.65760590401,-1296.57764860388,-1296.49778580664,
-1296.41799998416,-1296.33827366897,-1296.25858944067,-1296.17891845445,
-1296.09925100093,-1296.01957135011,-1295.93986376772,-1295.86006853864,
-1295.78022419693,-1295.70026576988,-1295.65786989329,-1295.57791259316,
-1295.49804979592,-1295.41826397344,-1295.33853765825,-1295.25885342996,
-1295.17918244374,-1295.09951499021,-1295.01983533939,-1294.940127757,-1294.86033252792,
-1294.78048818622,-1294.70052975917,-1294.65813388257,-1294.57817658244,
-1294.4983137852,-1294.41852796272,-1294.33880164753,-1294.25911741924,
-1294.17944643301,-1294.09977897949,-1294.02009932867,-1293.94039174628,
-1293.8605965172,-1293.78075217549,-1293.70079374845,-1293.65839787185,
-1293.57844057172,-1293.49857777448,-1293.41879195201,-1293.33906563681,
-1293.25938140852,-1293.1797104223,-1293.10004296877,-1293.02036331796,
-1292.94065573556,-1292.86086050649,-1292.78101616478,-1292.70105773773,
-1292.65866186113,-1292.57506558009,-1292.49160108778,-1292.405083246,-1292.32189762189,
-1292.23880404213,-1292.15581784198,-1292.14552972066),.UNSPECIFIED.);
#1462=B_SPLINE_CURVE_WITH_KNOTS('',3,(#169441,#169442,#169443,#169444,#169445,
#169446,#169447,#169448,#169449,#169450,#169451,#169452,#169453,#169454,
#169455,#169456,#169457,#169458,#169459,#169460,#169461,#169462,#169463,
#169464,#169465,#169466,#169467,#169468,#169469,#169470,#169471,#169472,
#169473,#169474,#169475,#169476,#169477,#169478,#169479,#169480,#169481,
#169482,#169483,#169484,#169485,#169486,#169487,#169488,#169489,#169490,
#169491,#169492,#169493,#169494,#169495,#169496,#169497,#169498,#169499,
#169500,#169501,#169502,#169503,#169504,#169505,#169506,#169507,#169508,
#169509,#169510,#169511,#169512,#169513,#169514,#169515,#169516,#169517,
#169518,#169519,#169520,#169521,#169522,#169523,#169524,#169525,#169526,
#169527,#169528,#169529,#169530,#169531,#169532,#169533,#169534,#169535,
#169536,#169537,#169538,#169539,#169540,#169541,#169542,#169543,#169544,
#169545,#169546,#169547,#169548,#169549,#169550,#169551,#169552,#169553,
#169554,#169555,#169556,#169557,#169558,#169559,#169560,#169561,#169562,
#169563,#169564,#169565,#169566,#169567,#169568,#169569,#169570,#169571,
#169572,#169573,#169574,#169575,#169576,#169577,#169578,#169579,#169580,
#169581,#169582,#169583,#169584,#169585,#169586,#169587,#169588,#169589,
#169590,#169591,#169592,#169593,#169594,#169595,#169596,#169597,#169598,
#169599,#169600,#169601,#169602,#169603,#169604,#169605,#169606,#169607,
#169608,#169609,#169610,#169611,#169612,#169613,#169614,#169615,#169616,
#169617,#169618,#169619,#169620,#169621,#169622,#169623,#169624,#169625,
#169626,#169627,#169628,#169629,#169630,#169631,#169632,#169633,#169634,
#169635,#169636,#169637,#169638,#169639,#169640,#169641,#169642,#169643,
#169644,#169645,#169646,#169647,#169648,#169649,#169650,#169651,#169652,
#169653,#169654,#169655,#169656,#169657,#169658,#169659,#169660,#169661,
#169662,#169663,#169664,#169665,#169666,#169667,#169668,#169669,#169670,
#169671,#169672,#169673,#169674,#169675,#169676,#169677,#169678,#169679,
#169680,#169681,#169682,#169683,#169684),.UNSPECIFIED.,.F.,.F.,(4,3,3,3,
3,3,3,3,3,3,3,3,3,3,3,3,3,3,3,3,3,3,3,3,3,3,3,3,3,3,3,3,3,3,3,3,3,3,3,3,
3,3,3,3,3,3,3,3,3,3,3,3,3,3,3,3,3,3,3,3,3,3,3,3,3,3,3,3,3,3,3,3,3,3,3,3,
3,3,3,3,3,4),(-1292.14552972052,-1292.06159838444,-1291.9775451088,-1291.89328099867,
-1291.80890705239,-1291.72433422119,-1291.65892585041,-1291.57896855028,
-1291.49910575303,-1291.41931993056,-1291.33959361536,-1291.25990938707,
-1291.18023840085,-1291.10057094732,-1291.0208912965,-1290.94118371411,
-1290.86138848503,-1290.78154414332,-1290.70158571627,-1290.65918983969,
-1290.57923253956,-1290.49936974232,-1290.41958391984,-1290.33985760465,
-1290.26017337635,-1290.18050239013,-1290.10083493661,-1290.02115528579,
-1289.9414477034,-1289.86165247432,-1289.78180813261,-1289.70184970556,
-1289.65945382897,-1289.57949652884,-1289.4996337316,-1289.41984790912,
-1289.34012159393,-1289.26043736564,-1289.18076637942,-1289.10109892589,
-1289.02141927507,-1288.94171169268,-1288.8619164636,-1288.7820721219,-1288.70211369485,
-1288.65971781825,-1288.57976051812,-1288.49989772088,-1288.4201118984,
-1288.34038558321,-1288.26070135491,-1288.18103036869,-1288.10136291517,
-1288.02168326435,-1287.94197568196,-1287.86218045288,-1287.78233611117,
-1287.70237768413,-1287.65998180753,-1287.5800245074,-1287.50016171016,
-1287.42037588769,-1287.34064957249,-1287.2609653442,-1287.18129435798,
-1287.10162690445,-1287.02194725364,-1286.94223967124,-1286.86244444217,
-1286.78260010046,-1286.70264167341,-1286.66024579681,-1286.5814358575,
-1286.5027205734,-1286.42267355341,-1286.34409775286,-1286.2655551761,-1286.18702926213,
-1286.10585804997,-1286.02728935643,-1285.94481688495,-1285.86234441348),
 .UNSPECIFIED.);
#1463=B_SPLINE_CURVE_WITH_KNOTS('',3,(#169686,#169687,#169688,#169689,#169690,
#169691,#169692,#169693,#169694,#169695,#169696,#169697),.UNSPECIFIED.,
 .F.,.F.,(4,2,1,1,1,1,1,1,4),(-1285.86234441348,-1285.66050978609,-1284.66077377537,
-1283.66103776465,-1282.66130175393,-1281.66156574321,-1280.66182973249,
-1279.66209372177,-1279.5791591063),.UNSPECIFIED.);
#1464=B_SPLINE_CURVE_WITH_KNOTS('',3,(#169699,#169700,#169701,#169702,#169703,
#169704,#169705,#169706,#169707,#169708),.UNSPECIFIED.,.F.,.F.,(4,1,1,1,
1,1,1,4),(-1279.5791591063,-1278.66235771105,-1277.66262170033,-1276.66288568961,
-1275.66314967889,-1274.66341366817,-1273.66367765745,-1273.29597379912),
 .UNSPECIFIED.);
#1465=B_SPLINE_CURVE_WITH_KNOTS('',3,(#169710,#169711,#169712,#169713,#169714,
#169715,#169716,#169717,#169718,#169719),.UNSPECIFIED.,.F.,.F.,(4,1,1,1,
1,1,1,4),(-1273.29597379912,-1272.66394164673,-1271.66420563601,-1270.66446962529,
-1269.66473361457,-1268.66499760385,-1267.66526159313,-1267.01278849194),
 .UNSPECIFIED.);
#1466=B_SPLINE_CURVE_WITH_KNOTS('',3,(#169721,#169722,#169723,#169724,#169725,
#169726,#169727,#169728,#169729,#169730,#169731,#169732,#169733,#169734,
#169735,#169736,#169737,#169738,#169739,#169740,#169741,#169742,#169743,
#169744,#169745,#169746,#169747,#169748,#169749,#169750,#169751,#169752,
#169753,#169754,#169755,#169756,#169757,#169758,#169759,#169760,#169761,
#169762,#169763,#169764,#169765,#169766,#169767,#169768,#169769,#169770,
#169771,#169772,#169773,#169774,#169775,#169776,#169777,#169778,#169779,
#169780,#169781,#169782,#169783,#169784,#169785,#169786,#169787,#169788,
#169789,#169790,#169791,#169792,#169793,#169794,#169795,#169796,#169797,
#169798,#169799,#169800,#169801,#169802,#169803,#169804,#169805,#169806,
#169807,#169808,#169809,#169810,#169811,#169812,#169813,#169814,#169815,
#169816,#169817,#169818,#169819,#169820,#169821,#169822,#169823,#169824,
#169825,#169826,#169827,#169828,#169829,#169830,#169831,#169832,#169833,
#169834,#169835,#169836,#169837,#169838,#169839,#169840,#169841,#169842,
#169843,#169844,#169845,#169846,#169847,#169848,#169849,#169850,#169851,
#169852,#169853,#169854,#169855,#169856,#169857,#169858,#169859,#169860,
#169861,#169862,#169863,#169864,#169865,#169866,#169867,#169868,#169869,
#169870,#169871,#169872,#169873,#169874,#169875,#169876,#169877,#169878,
#169879,#169880,#169881,#169882,#169883,#169884,#169885,#169886,#169887,
#169888,#169889,#169890,#169891,#169892,#169893,#169894,#169895,#169896,
#169897,#169898,#169899,#169900,#169901,#169902,#169903,#169904,#169905,
#169906,#169907,#169908,#169909,#169910,#169911,#169912,#169913,#169914,
#169915,#169916,#169917,#169918,#169919,#169920,#169921,#169922,#169923,
#169924,#169925,#169926,#169927,#169928,#169929,#169930,#169931,#169932,
#169933,#169934,#169935,#169936,#169937,#169938,#169939,#169940,#169941,
#169942,#169943,#169944,#169945,#169946,#169947,#169948,#169949,#169950,
#169951,#169952,#169953,#169954,#169955,#169956,#169957,#169958,#169959,
#169960,#169961,#169962,#169963,#169964),.UNSPECIFIED.,.F.,.F.,(4,3,3,3,
3,3,3,3,3,3,3,3,3,3,3,3,3,3,3,3,3,3,3,3,3,3,3,3,3,3,3,3,3,3,3,3,3,3,3,3,
3,3,3,3,3,3,3,3,3,3,3,3,3,3,3,3,3,3,3,3,3,3,3,3,3,3,3,3,3,3,3,3,3,3,3,3,
3,3,3,3,3,4),(-1267.01278836953,-1266.92108083957,-1266.8289234614,-1266.73617774725,
-1266.66552558241,-1266.58556828228,-1266.50570548503,-1266.42591966256,
-1266.34619334737,-1266.26650911907,-1266.18683813285,-1266.10717067932,
-1266.02749102851,-1265.94778344611,-1265.86798821703,-1265.78814387533,
-1265.70818544828,-1265.66578957169,-1265.58583227156,-1265.50596947432,
-1265.42618365184,-1265.34645733665,-1265.26677310836,-1265.18710212213,
-1265.10743466861,-1265.02775501779,-1264.9480474354,-1264.86825220632,
-1264.78840786461,-1264.70844943757,-1264.66605356097,-1264.58609626084,
-1264.5062334636,-1264.42644764112,-1264.34672132593,-1264.26703709764,
-1264.18736611141,-1264.10769865789,-1264.02801900707,-1263.94831142468,
-1263.8685161956,-1263.78867185389,-1263.70871342685,-1263.66631755025,
-1263.58636025012,-1263.50649745288,-1263.4267116304,-1263.34698531521,
-1263.26730108691,-1263.18763010069,-1263.10796264717,-1263.02828299635,
-1262.94857541396,-1262.86878018488,-1262.78893584317,-1262.70897741613,
-1262.66658153953,-1262.5866242394,-1262.50676144216,-1262.42697561969,
-1262.34724930449,-1262.2675650762,-1262.18789408998,-1262.10822663645,
-1262.02854698564,-1261.94883940325,-1261.86904417417,-1261.78919983246,
-1261.70924140542,-1261.66684552881,-1261.58761743001,-1261.50848331692,
-1261.42942502562,-1261.35042446142,-1261.27145775696,-1261.19250767568,
-1261.11355792414,-1261.03459221153,-1260.95554990908,-1260.87646805771,
-1260.79727140574,-1260.72960318476),.UNSPECIFIED.);
#1467=B_SPLINE_CURVE_WITH_KNOTS('',3,(#169966,#169967,#169968,#169969,#169970,
#169971,#169972,#169973,#169974,#169975,#169976,#169977,#169978),
 .UNSPECIFIED.,.F.,.F.,(4,3,1,1,1,1,1,1,4),(-1260.72960318476,-1260.66710951809,
-1259.66737350737,-1258.66763749665,-1257.66790148592,-1256.6681654752,
-1255.66842946448,-1254.66869345376,-1254.44641787758),.UNSPECIFIED.);
#1468=B_SPLINE_CURVE_WITH_KNOTS('',3,(#169980,#169981,#169982,#169983,#169984,
#169985,#169986,#169987,#169988,#169989,#169990,#169991,#169992,#169993,
#169994,#169995,#169996,#169997,#169998,#169999,#170000,#170001,#170002,
#170003,#170004,#170005,#170006,#170007,#170008,#170009,#170010,#170011,
#170012,#170013,#170014,#170015,#170016,#170017,#170018,#170019,#170020,
#170021,#170022,#170023,#170024,#170025,#170026,#170027,#170028,#170029,
#170030,#170031,#170032,#170033,#170034,#170035,#170036,#170037,#170038,
#170039,#170040,#170041,#170042,#170043,#170044,#170045,#170046,#170047,
#170048,#170049,#170050,#170051,#170052,#170053,#170054,#170055,#170056,
#170057,#170058,#170059,#170060,#170061,#170062,#170063,#170064,#170065,
#170066,#170067,#170068,#170069,#170070,#170071,#170072,#170073,#170074,
#170075,#170076,#170077,#170078,#170079,#170080,#170081,#170082,#170083,
#170084,#170085,#170086,#170087,#170088,#170089,#170090,#170091,#170092,
#170093,#170094,#170095,#170096,#170097,#170098,#170099,#170100,#170101,
#170102,#170103,#170104,#170105,#170106,#170107,#170108,#170109,#170110,
#170111,#170112,#170113,#170114,#170115,#170116,#170117,#170118,#170119,
#170120,#170121,#170122,#170123,#170124,#170125,#170126,#170127,#170128,
#170129,#170130,#170131,#170132,#170133,#170134,#170135,#170136,#170137,
#170138,#170139,#170140,#170141,#170142,#170143,#170144,#170145,#170146,
#170147,#170148,#170149,#170150,#170151,#170152,#170153,#170154,#170155,
#170156,#170157,#170158,#170159,#170160,#170161,#170162,#170163,#170164,
#170165,#170166,#170167,#170168,#170169,#170170,#170171,#170172,#170173,
#170174,#170175,#170176,#170177,#170178,#170179,#170180,#170181,#170182,
#170183,#170184,#170185,#170186,#170187,#170188,#170189,#170190,#170191,
#170192,#170193,#170194,#170195,#170196,#170197,#170198,#170199,#170200,
#170201,#170202,#170203,#170204,#170205,#170206,#170207,#170208,#170209,
#170210,#170211,#170212,#170213,#170214,#170215,#170216,#170217,#170218,
#170219,#170220,#170221,#170222,#170223),.UNSPECIFIED.,.F.,.F.,(4,3,3,3,
3,3,3,3,3,3,3,3,3,3,3,3,3,3,3,3,3,3,3,3,3,3,3,3,3,3,3,3,3,3,3,3,3,3,3,3,
3,3,3,3,3,3,3,3,3,3,3,3,3,3,3,3,3,3,3,3,3,3,3,3,3,3,3,3,3,3,3,3,3,3,3,3,
3,3,3,3,3,4),(-1254.44641787758,-1254.36770750134,-1254.28905430803,-1254.21043332721,
-1254.13182796515,-1254.05322171621,-1253.97459807584,-1253.89589448617,
-1253.81714979179,-1253.73828593555,-1253.66895744304,-1253.58900014291,
-1253.50913734567,-1253.42935152319,-1253.349625208,-1253.26994097971,-1253.19026999348,
-1253.11060253996,-1253.03092288914,-1252.95121530675,-1252.87142007767,
-1252.79157573596,-1252.71161730892,-1252.66922143232,-1252.58926413219,
-1252.50940133495,-1252.42961551247,-1252.34988919728,-1252.27020496899,
-1252.19053398276,-1252.11086652924,-1252.03118687842,-1251.95147929603,
-1251.87168406695,-1251.79183972524,-1251.7118812982,-1251.6694854216,-1251.58952812147,
-1251.50966532423,-1251.42987950175,-1251.35015318656,-1251.27046895826,
-1251.19079797204,-1251.11113051852,-1251.0314508677,-1250.95174328531,
-1250.87194805623,-1250.79210371452,-1250.71214528748,-1250.66974941088,
-1250.58979211075,-1250.50992931351,-1250.43014349103,-1250.35041717584,
-1250.27073294755,-1250.19106196132,-1250.1113945078,-1250.03171485698,
-1249.95200727459,-1249.87221204551,-1249.7923677038,-1249.71240927676,
-1249.67001340016,-1249.59005610003,-1249.51019330279,-1249.43040748032,
-1249.35068116512,-1249.27099693683,-1249.19132595061,-1249.11165849708,
-1249.03197884626,-1248.95227126387,-1248.87247603479,-1248.79263169309,
-1248.71267326604,-1248.67027738944,-1248.58646341498,-1248.50278431403,
-1248.41789637812,-1248.3345039439,-1248.24886825715,-1248.1632325704),
 .UNSPECIFIED.);
#1469=B_SPLINE_CURVE_WITH_KNOTS('',3,(#170225,#170226,#170227,#170228,#170229,
#170230,#170231,#170232,#170233,#170234,#170235,#170236,#170237,#170238,
#170239,#170240,#170241,#170242,#170243,#170244,#170245,#170246,#170247,
#170248,#170249,#170250,#170251,#170252,#170253,#170254,#170255,#170256,
#170257,#170258,#170259,#170260,#170261,#170262,#170263,#170264,#170265,
#170266,#170267,#170268,#170269,#170270,#170271,#170272,#170273,#170274,
#170275,#170276,#170277,#170278,#170279,#170280,#170281,#170282,#170283,
#170284,#170285,#170286,#170287,#170288,#170289,#170290,#170291,#170292,
#170293,#170294,#170295,#170296,#170297,#170298,#170299,#170300,#170301,
#170302,#170303,#170304,#170305,#170306,#170307,#170308,#170309,#170310,
#170311,#170312,#170313,#170314,#170315,#170316,#170317,#170318,#170319,
#170320,#170321,#170322,#170323,#170324,#170325,#170326,#170327,#170328,
#170329,#170330,#170331,#170332,#170333,#170334,#170335,#170336,#170337,
#170338,#170339,#170340,#170341,#170342,#170343,#170344,#170345,#170346,
#170347,#170348,#170349,#170350,#170351,#170352,#170353,#170354,#170355,
#170356,#170357,#170358,#170359,#170360,#170361,#170362,#170363,#170364,
#170365,#170366,#170367,#170368,#170369,#170370,#170371,#170372,#170373,
#170374,#170375,#170376,#170377,#170378,#170379,#170380,#170381,#170382,
#170383,#170384,#170385,#170386,#170387,#170388,#170389,#170390,#170391,
#170392,#170393,#170394,#170395,#170396,#170397,#170398,#170399,#170400,
#170401,#170402,#170403,#170404,#170405,#170406,#170407,#170408,#170409,
#170410,#170411,#170412,#170413,#170414,#170415,#170416,#170417,#170418,
#170419,#170420,#170421,#170422,#170423,#170424,#170425,#170426,#170427,
#170428,#170429,#170430,#170431,#170432,#170433,#170434,#170435,#170436,
#170437,#170438,#170439,#170440,#170441,#170442,#170443,#170444,#170445,
#170446,#170447,#170448,#170449,#170450,#170451,#170452,#170453,#170454,
#170455,#170456,#170457,#170458,#170459,#170460,#170461,#170462,#170463,
#170464,#170465,#170466,#170467,#170468),.UNSPECIFIED.,.F.,.F.,(4,3,3,3,
3,3,3,3,3,3,3,3,3,3,3,3,3,3,3,3,3,3,3,3,3,3,3,3,3,3,3,3,3,3,3,3,3,3,3,3,
3,3,3,3,3,3,3,3,3,3,3,3,3,3,3,3,3,3,3,3,3,3,3,3,3,3,3,3,3,3,3,3,3,3,3,3,
3,3,3,3,3,4),(-1248.16323257024,-1248.07952275549,-1247.99569914006,-1247.91167283667,
-1247.82754195684,-1247.74321391104,-1247.67054137872,-1247.59058407859,
-1247.51072128135,-1247.43093545887,-1247.35120914368,-1247.27152491538,
-1247.19185392916,-1247.11218647564,-1247.03250682482,-1246.95279924242,
-1246.87300401335,-1246.79315967164,-1246.71320124459,-1246.670805368,-1246.59084806787,
-1246.51098527063,-1246.43119944815,-1246.35147313296,-1246.27178890466,
-1246.19211791844,-1246.11245046492,-1246.0327708141,-1245.95306323171,
-1245.87326800263,-1245.79342366092,-1245.71346523388,-1245.67106935728,
-1245.59111205715,-1245.51124925991,-1245.43146343743,-1245.35173712224,
-1245.27205289395,-1245.19238190772,-1245.1127144542,-1245.03303480338,
-1244.95332722099,-1244.87353199191,-1244.7936876502,-1244.71372922316,
-1244.67133334656,-1244.59137604643,-1244.51151324919,-1244.43172742671,
-1244.35200111152,-1244.27231688323,-1244.192645897,-1244.11297844348,-1244.03329879266,
-1243.95359121027,-1243.87379598119,-1243.79395163948,-1243.71399321244,
-1243.67159733584,-1243.59164003571,-1243.51177723847,-1243.43199141599,
-1243.3522651008,-1243.27258087251,-1243.19290988628,-1243.11324243276,
-1243.03356278194,-1242.95385519955,-1242.87405997047,-1242.79421562877,
-1242.71425720172,-1242.67186132512,-1242.59303275308,-1242.51429899253,
-1242.43501752637,-1242.35642343201,-1242.27786294518,-1242.19931951457,
-1242.11950145173,-1242.04091749406,-1241.96048237864,-1241.88004726322),
 .UNSPECIFIED.);
#1470=B_SPLINE_CURVE_WITH_KNOTS('',3,(#170470,#170471,#170472,#170473,#170474,
#170475,#170476,#170477,#170478,#170479,#170480,#170481),.UNSPECIFIED.,
 .F.,.F.,(4,2,1,1,1,1,1,1,4),(-1241.88004726322,-1241.6721253144,-1240.67238930368,
-1239.67265329296,-1238.67291728224,-1237.67318127152,-1236.6734452608,
-1235.67370925008,-1235.59686195605),.UNSPECIFIED.);
#1471=B_SPLINE_CURVE_WITH_KNOTS('',3,(#170483,#170484,#170485,#170486,#170487,
#170488,#170489,#170490,#170491,#170492),.UNSPECIFIED.,.F.,.F.,(4,1,1,1,
1,1,1,4),(-1235.59686195605,-1234.67397323936,-1233.67423722864,-1232.67450121792,
-1231.6747652072,-1230.67502919648,-1229.67529318576,-1229.31367664887),
 .UNSPECIFIED.);
#1472=B_SPLINE_CURVE_WITH_KNOTS('',3,(#170494,#170495,#170496,#170497,#170498,
#170499,#170500,#170501,#170502,#170503),.UNSPECIFIED.,.F.,.F.,(4,1,1,1,
1,1,1,4),(-1229.31367664887,-1228.67555717504,-1227.67582116432,-1226.6760851536,
-1225.67634914288,-1224.67661313216,-1223.67687712144,-1223.03049134169),
 .UNSPECIFIED.);
#1473=B_SPLINE_CURVE_WITH_KNOTS('',3,(#170505,#170506,#170507,#170508,#170509,
#170510,#170511,#170512,#170513,#170514,#170515,#170516,#170517,#170518,
#170519,#170520,#170521,#170522,#170523,#170524,#170525,#170526,#170527,
#170528,#170529,#170530,#170531,#170532,#170533,#170534,#170535,#170536,
#170537,#170538,#170539,#170540,#170541,#170542,#170543,#170544,#170545,
#170546,#170547,#170548,#170549,#170550,#170551,#170552,#170553,#170554,
#170555,#170556,#170557,#170558,#170559,#170560,#170561,#170562,#170563,
#170564,#170565,#170566,#170567,#170568,#170569,#170570,#170571,#170572,
#170573,#170574,#170575,#170576,#170577,#170578,#170579,#170580,#170581,
#170582,#170583,#170584,#170585,#170586,#170587,#170588,#170589,#170590,
#170591,#170592,#170593,#170594,#170595,#170596,#170597,#170598,#170599,
#170600,#170601,#170602,#170603,#170604,#170605,#170606,#170607,#170608,
#170609,#170610,#170611,#170612,#170613,#170614,#170615,#170616,#170617,
#170618,#170619,#170620,#170621,#170622,#170623,#170624,#170625,#170626,
#170627,#170628,#170629,#170630,#170631,#170632,#170633,#170634,#170635,
#170636,#170637,#170638,#170639,#170640,#170641,#170642,#170643,#170644,
#170645,#170646,#170647,#170648,#170649,#170650,#170651,#170652,#170653,
#170654,#170655,#170656,#170657,#170658,#170659,#170660,#170661,#170662,
#170663,#170664,#170665,#170666,#170667,#170668,#170669,#170670,#170671,
#170672,#170673,#170674,#170675,#170676,#170677,#170678,#170679,#170680,
#170681,#170682,#170683,#170684,#170685,#170686,#170687,#170688,#170689,
#170690,#170691,#170692,#170693,#170694,#170695,#170696,#170697,#170698,
#170699,#170700,#170701,#170702,#170703,#170704,#170705,#170706,#170707,
#170708,#170709,#170710,#170711,#170712,#170713,#170714,#170715,#170716,
#170717,#170718,#170719,#170720,#170721,#170722,#170723,#170724,#170725,
#170726,#170727,#170728,#170729,#170730,#170731,#170732,#170733,#170734,
#170735,#170736,#170737,#170738,#170739,#170740,#170741,#170742,#170743,
#170744,#170745,#170746,#170747,#170748),.UNSPECIFIED.,.F.,.F.,(4,3,3,3,
3,3,3,3,3,3,3,3,3,3,3,3,3,3,3,3,3,3,3,3,3,3,3,3,3,3,3,3,3,3,3,3,3,3,3,3,
3,3,3,3,3,3,3,3,3,3,3,3,3,3,3,3,3,3,3,3,3,3,3,3,3,3,3,3,3,3,3,3,3,3,3,3,
3,3,3,3,3,4),(-1223.03049109457,-1222.93925215063,-1222.84759368162,-1222.75537044079,
-1222.67714111072,-1222.59718381059,-1222.51732101335,-1222.43753519088,
-1222.35780887569,-1222.2781246474,-1222.19845366118,-1222.11878620766,
-1222.03910655684,-1221.95939897445,-1221.87960374538,-1221.79975940368,
-1221.71980097663,-1221.6774051,-1221.59744779987,-1221.51758500263,-1221.43779918015,
-1221.35807286496,-1221.27838863667,-1221.19871765044,-1221.11905019692,
-1221.0393705461,-1220.95966296371,-1220.87986773463,-1220.80002339292,
-1220.72006496588,-1220.67766908928,-1220.59771178915,-1220.51784899191,
-1220.43806316943,-1220.35833685424,-1220.27865262594,-1220.19898163972,
-1220.11931418619,-1220.03963453538,-1219.95992695298,-1219.88013172391,
-1219.8002873822,-1219.72032895515,-1219.67793307856,-1219.59797577843,
-1219.51811298119,-1219.43832715872,-1219.35860084352,-1219.27891661523,
-1219.19924562901,-1219.11957817548,-1219.03989852466,-1218.96019094227,
-1218.88039571319,-1218.80055137149,-1218.72059294444,-1218.67819706784,
-1218.59823976771,-1218.51837697047,-1218.43859114799,-1218.3588648328,
-1218.2791806045,-1218.19950961828,-1218.11984216476,-1218.04016251394,
-1217.96045493154,-1217.88065970247,-1217.80081536076,-1217.72085693371,
-1217.67846105712,-1217.59928534504,-1217.52020357293,-1217.44119753742,
-1217.36224910532,-1217.28333447517,-1217.20443630897,-1217.12553827937,
-1217.04662406147,-1216.96763398074,-1216.88860405746,-1216.80946182794,
-1216.74730603451),.UNSPECIFIED.);
#1474=B_SPLINE_CURVE_WITH_KNOTS('',3,(#170750,#170751,#170752,#170753,#170754,
#170755,#170756,#170757,#170758,#170759,#170760,#170761,#170762),
 .UNSPECIFIED.,.F.,.F.,(4,3,1,1,1,1,1,1,4),(-1216.74730603451,-1216.6787250464,
-1215.67898903568,-1214.67925302496,-1213.67951701424,-1212.67978100352,
-1211.6800449928,-1210.68030898208,-1210.46412072733),.UNSPECIFIED.);
#1475=B_SPLINE_CURVE_WITH_KNOTS('',3,(#170764,#170765,#170766,#170767,#170768,
#170769,#170770,#170771,#170772,#170773),.UNSPECIFIED.,.F.,.F.,(4,1,1,1,
1,1,1,4),(-1210.46412072733,-1209.68057297136,-1208.68083696064,-1207.68110094992,
-1206.6813649392,-1205.68162892848,-1204.68189291776,-1204.18093542015),
 .UNSPECIFIED.);
#1476=B_SPLINE_CURVE_WITH_KNOTS('',3,(#170775,#170776,#170777,#170778,#170779,
#170780,#170781,#170782,#170783,#170784),.UNSPECIFIED.,.F.,.F.,(4,1,1,1,
1,1,1,4),(-1204.18093542015,-1203.68215690704,-1202.68242089632,-1201.6826848856,
-1200.68294887488,-1199.68321286416,-1198.68347685344,-1197.89775011297),
 .UNSPECIFIED.);
#1477=B_SPLINE_CURVE_WITH_KNOTS('',3,(#170786,#170787,#170788,#170789,#170790,
#170791,#170792,#170793,#170794,#170795,#170796),.UNSPECIFIED.,.F.,.F.,
(4,1,1,1,1,1,1,1,4),(-1197.89775011297,-1197.68374084272,-1196.684004832,
-1195.68426882128,-1194.68453281056,-1193.68479679984,-1192.68506078912,
-1191.6853247784,-1191.61456480579),.UNSPECIFIED.);
#1478=B_SPLINE_CURVE_WITH_KNOTS('',3,(#170798,#170799,#170800,#170801,#170802,
#170803,#170804,#170805,#170806,#170807,#170808,#170809,#170810,#170811,
#170812,#170813,#170814,#170815,#170816,#170817,#170818,#170819,#170820,
#170821,#170822,#170823,#170824,#170825,#170826,#170827,#170828,#170829,
#170830,#170831,#170832,#170833,#170834,#170835,#170836,#170837,#170838,
#170839,#170840,#170841,#170842,#170843,#170844,#170845,#170846,#170847,
#170848,#170849,#170850,#170851,#170852,#170853,#170854,#170855,#170856,
#170857,#170858,#170859,#170860,#170861,#170862,#170863,#170864,#170865,
#170866,#170867,#170868,#170869,#170870,#170871,#170872,#170873,#170874,
#170875,#170876,#170877,#170878,#170879,#170880,#170881,#170882,#170883,
#170884,#170885,#170886,#170887,#170888,#170889,#170890,#170891,#170892,
#170893,#170894,#170895,#170896,#170897,#170898,#170899,#170900,#170901,
#170902,#170903,#170904,#170905,#170906,#170907,#170908,#170909,#170910,
#170911,#170912,#170913,#170914,#170915,#170916,#170917,#170918,#170919,
#170920,#170921,#170922,#170923,#170924,#170925,#170926,#170927,#170928,
#170929,#170930,#170931,#170932,#170933,#170934,#170935,#170936,#170937,
#170938,#170939,#170940,#170941,#170942,#170943,#170944,#170945,#170946,
#170947,#170948,#170949,#170950,#170951,#170952,#170953,#170954,#170955,
#170956,#170957,#170958,#170959,#170960,#170961,#170962,#170963,#170964,
#170965,#170966,#170967,#170968,#170969,#170970,#170971,#170972,#170973,
#170974,#170975,#170976,#170977,#170978,#170979,#170980,#170981,#170982,
#170983,#170984,#170985,#170986,#170987,#170988,#170989,#170990,#170991,
#170992,#170993,#170994,#170995,#170996,#170997,#170998,#170999,#171000,
#171001,#171002,#171003,#171004,#171005,#171006,#171007,#171008,#171009,
#171010,#171011,#171012,#171013,#171014,#171015,#171016,#171017,#171018,
#171019,#171020,#171021,#171022,#171023,#171024,#171025,#171026,#171027,
#171028,#171029,#171030,#171031,#171032,#171033,#171034,#171035,#171036,
#171037,#171038,#171039,#171040,#171041),.UNSPECIFIED.,.F.,.F.,(4,3,3,3,
3,3,3,3,3,3,3,3,3,3,3,3,3,3,3,3,3,3,3,3,3,3,3,3,3,3,3,3,3,3,3,3,3,3,3,3,
3,3,3,3,3,3,3,3,3,3,3,3,3,3,3,3,3,3,3,3,3,3,3,3,3,3,3,3,3,3,3,3,3,3,3,3,
3,3,3,3,3,4),(-1191.61456480579,-1191.53543267293,-1191.45638976538,-1191.37741788645,
-1191.29849890527,-1191.21960664864,-1191.14072646774,-1191.0618420251,
-1190.98293698261,-1190.90394966339,-1190.824918671,-1190.74577032809,-1190.68558876768,
-1190.60563146755,-1190.52576867031,-1190.44598284783,-1190.36625653264,
-1190.28657230435,-1190.20690131812,-1190.1272338646,-1190.04755421378,
-1189.96784663139,-1189.88805140231,-1189.8082070606,-1189.72824863356,
-1189.68585275696,-1189.60589545683,-1189.52603265959,-1189.44624683711,
-1189.36652052192,-1189.28683629362,-1189.2071653074,-1189.12749785388,
-1189.04781820306,-1188.96811062067,-1188.88831539159,-1188.80847104988,
-1188.72851262284,-1188.68611674624,-1188.60615944611,-1188.52629664887,
-1188.44651082639,-1188.3667845112,-1188.2871002829,-1188.20742929668,-1188.12776184316,
-1188.04808219234,-1187.96837460995,-1187.88857938087,-1187.80873503916,
-1187.72877661212,-1187.68638073552,-1187.60642343539,-1187.52656063815,
-1187.44677481567,-1187.36704850048,-1187.28736427218,-1187.20769328596,
-1187.12802583244,-1187.04834618162,-1186.96863859923,-1186.88884337015,
-1186.80899902844,-1186.7290406014,-1186.6866447248,-1186.60668742467,-1186.52682462743,
-1186.44703880496,-1186.36731248976,-1186.28762826147,-1186.20795727525,
-1186.12828982172,-1186.04861017091,-1185.96890258851,-1185.88910735944,
-1185.80926301773,-1185.72930459068,-1185.68690871408,-1185.59487830074,
-1185.50317571114,-1185.41211905715,-1185.3313797463),.UNSPECIFIED.);
#1479=B_SPLINE_CURVE_WITH_KNOTS('',3,(#171043,#171044,#171045,#171046,#171047,
#171048,#171049,#171050,#171051,#171052),.UNSPECIFIED.,.F.,.F.,(4,1,1,1,
1,1,1,4),(-1185.33137949861,-1184.68717270336,-1183.68743669263,-1182.68770068191,
-1181.6879646712,-1180.68822866048,-1179.68849264975,-1179.04819419143),
 .UNSPECIFIED.);
#1480=B_SPLINE_CURVE_WITH_KNOTS('',3,(#171054,#171055,#171056,#171057,#171058,
#171059,#171060,#171061,#171062,#171063),.UNSPECIFIED.,.F.,.F.,(4,1,1,1,
1,1,1,4),(-1179.04819419143,-1178.68875663903,-1177.68902062831,-1176.68928461759,
-1175.68954860687,-1174.68981259615,-1173.69007658543,-1172.76500888425),
 .UNSPECIFIED.);
#1481=B_SPLINE_CURVE_WITH_KNOTS('',3,(#171065,#171066,#171067,#171068,#171069,
#171070,#171071,#171072,#171073,#171074,#171075,#171076,#171077),
 .UNSPECIFIED.,.F.,.F.,(4,3,1,1,1,1,1,1,4),(-1172.76500888425,-1172.69034057471,
-1171.69060456399,-1170.69086855327,-1169.69113254255,-1168.69139653183,
-1167.69166052111,-1166.69192451039,-1166.48182357707),.UNSPECIFIED.);
#1482=B_SPLINE_CURVE_WITH_KNOTS('',3,(#171079,#171080,#171081,#171082,#171083,
#171084,#171085,#171086,#171087,#171088,#171089,#171090,#171091,#171092,
#171093,#171094,#171095,#171096,#171097,#171098,#171099,#171100,#171101,
#171102,#171103,#171104,#171105,#171106,#171107,#171108,#171109,#171110,
#171111,#171112,#171113,#171114,#171115,#171116,#171117,#171118,#171119,
#171120,#171121,#171122,#171123,#171124,#171125,#171126,#171127,#171128,
#171129,#171130,#171131,#171132,#171133,#171134,#171135,#171136,#171137,
#171138,#171139,#171140,#171141,#171142,#171143,#171144,#171145,#171146,
#171147,#171148,#171149,#171150,#171151,#171152,#171153,#171154,#171155,
#171156,#171157,#171158,#171159,#171160,#171161,#171162,#171163,#171164,
#171165,#171166,#171167,#171168,#171169,#171170,#171171,#171172,#171173,
#171174,#171175,#171176,#171177,#171178,#171179,#171180,#171181,#171182,
#171183,#171184,#171185,#171186,#171187,#171188,#171189,#171190,#171191,
#171192,#171193,#171194,#171195,#171196,#171197,#171198,#171199,#171200,
#171201,#171202,#171203,#171204,#171205,#171206,#171207,#171208,#171209,
#171210,#171211,#171212,#171213,#171214,#171215,#171216,#171217,#171218,
#171219,#171220,#171221,#171222,#171223,#171224,#171225,#171226,#171227,
#171228,#171229,#171230,#171231,#171232,#171233,#171234,#171235,#171236,
#171237,#171238,#171239,#171240,#171241,#171242,#171243,#171244,#171245,
#171246,#171247,#171248,#171249,#171250,#171251,#171252,#171253,#171254,
#171255,#171256,#171257,#171258,#171259,#171260,#171261,#171262,#171263,
#171264,#171265,#171266,#171267,#171268,#171269,#171270,#171271,#171272,
#171273,#171274,#171275,#171276,#171277,#171278,#171279,#171280,#171281,
#171282,#171283,#171284,#171285,#171286,#171287,#171288,#171289,#171290,
#171291,#171292,#171293,#171294,#171295,#171296,#171297,#171298,#171299,
#171300,#171301,#171302,#171303,#171304,#171305,#171306,#171307,#171308,
#171309,#171310,#171311,#171312,#171313,#171314,#171315,#171316,#171317,
#171318,#171319,#171320,#171321,#171322),.UNSPECIFIED.,.F.,.F.,(4,3,3,3,
3,3,3,3,3,3,3,3,3,3,3,3,3,3,3,3,3,3,3,3,3,3,3,3,3,3,3,3,3,3,3,3,3,3,3,3,
3,3,3,3,3,3,3,3,3,3,3,3,3,3,3,3,3,3,3,3,3,3,3,3,3,3,3,3,3,3,3,3,3,3,3,3,
3,3,3,3,3,4),(-1166.48182357707,-1166.40314731128,-1166.32453163811,-1166.2454887458,
-1166.16692851299,-1166.08837029189,-1166.00979755129,-1165.93039528838,
-1165.85170524793,-1165.7719468738,-1165.69218849967,-1165.61223119954,
-1165.5323684023,-1165.45258257983,-1165.37285626463,-1165.29317203634,
-1165.21350105012,-1165.13383359659,-1165.05415394577,-1164.97444636338,
-1164.89465113431,-1164.8148067926,-1164.73484836555,-1164.69245248895,
-1164.61249518882,-1164.53263239158,-1164.4528465691,-1164.37312025391,
-1164.29343602562,-1164.2137650394,-1164.13409758587,-1164.05441793505,
-1163.97471035266,-1163.89491512358,-1163.81507078188,-1163.73511235483,
-1163.69271647823,-1163.6127591781,-1163.53289638086,-1163.45311055838,
-1163.37338424319,-1163.29370001489,-1163.21402902867,-1163.13436157515,
-1163.05468192433,-1162.97497434194,-1162.89517911286,-1162.81533477115,
-1162.7353763441,-1162.69298046751,-1162.61302316738,-1162.53316037014,
-1162.45337454766,-1162.37364823247,-1162.29396400417,-1162.21429301795,
-1162.13462556443,-1162.05494591361,-1161.97523833122,-1161.89544310214,
-1161.81559876043,-1161.73564033339,-1161.69324445679,-1161.61328715666,
-1161.53342435941,-1161.45363853694,-1161.37391222175,-1161.29422799345,
-1161.21455700723,-1161.1348895537,-1161.05520990289,-1160.97550232049,
-1160.89570709142,-1160.81586274971,-1160.73590432266,-1160.69350844607,
-1160.60923845646,-1160.52511011155,-1160.44117479101,-1160.35735298291,
-1160.2736877613,-1160.19863827),.UNSPECIFIED.);
#1483=B_SPLINE_CURVE_WITH_KNOTS('',3,(#171324,#171325,#171326,#171327,#171328,
#171329,#171330,#171331,#171332,#171333,#171334,#171335,#171336,#171337,
#171338,#171339,#171340,#171341,#171342,#171343,#171344,#171345,#171346,
#171347,#171348,#171349,#171350,#171351,#171352,#171353,#171354,#171355,
#171356,#171357,#171358,#171359,#171360,#171361,#171362,#171363,#171364,
#171365,#171366,#171367,#171368,#171369,#171370,#171371,#171372,#171373,
#171374,#171375,#171376,#171377,#171378,#171379,#171380,#171381,#171382,
#171383,#171384,#171385,#171386,#171387,#171388,#171389,#171390,#171391,
#171392,#171393,#171394,#171395,#171396,#171397,#171398,#171399,#171400,
#171401,#171402,#171403,#171404,#171405,#171406,#171407,#171408,#171409,
#171410,#171411,#171412,#171413,#171414,#171415,#171416,#171417,#171418,
#171419,#171420,#171421,#171422,#171423,#171424,#171425,#171426,#171427,
#171428,#171429,#171430,#171431,#171432,#171433,#171434,#171435,#171436,
#171437,#171438,#171439,#171440,#171441,#171442,#171443,#171444,#171445,
#171446,#171447,#171448,#171449,#171450,#171451,#171452,#171453,#171454,
#171455,#171456,#171457,#171458,#171459,#171460,#171461,#171462,#171463,
#171464,#171465,#171466,#171467,#171468,#171469,#171470,#171471,#171472,
#171473,#171474,#171475,#171476,#171477,#171478,#171479,#171480,#171481,
#171482,#171483,#171484,#171485,#171486,#171487,#171488,#171489,#171490,
#171491,#171492,#171493,#171494,#171495,#171496,#171497,#171498,#171499,
#171500,#171501,#171502,#171503,#171504,#171505,#171506,#171507,#171508,
#171509,#171510,#171511,#171512,#171513,#171514,#171515,#171516,#171517,
#171518,#171519,#171520,#171521,#171522,#171523,#171524,#171525,#171526,
#171527,#171528,#171529,#171530,#171531,#171532,#171533,#171534,#171535,
#171536,#171537,#171538,#171539,#171540,#171541,#171542,#171543,#171544,
#171545,#171546,#171547,#171548,#171549,#171550,#171551,#171552,#171553,
#171554,#171555,#171556,#171557,#171558,#171559,#171560,#171561,#171562,
#171563,#171564,#171565,#171566,#171567),.UNSPECIFIED.,.F.,.F.,(4,3,3,3,
3,3,3,3,3,3,3,3,3,3,3,3,3,3,3,3,3,3,3,3,3,3,3,3,3,3,3,3,3,3,3,3,3,3,3,3,
3,3,3,3,3,3,3,3,3,3,3,3,3,3,3,3,3,3,3,3,3,3,3,3,3,3,3,3,3,3,3,3,3,3,3,3,
3,3,3,3,3,4),(-1160.19863826989,-1160.11535205206,-1160.03196706726,-1159.94741840929,
-1159.86375007496,-1159.77876125516,-1159.69377243535,-1159.61381513522,
-1159.53395233798,-1159.45416651551,-1159.37444020032,-1159.29475597202,
-1159.2150849858,-1159.13541753228,-1159.05573788146,-1158.97603029907,
-1158.89623507,-1158.81639072829,-1158.73643230125,-1158.69403642463,-1158.6140791245,
-1158.53421632726,-1158.45443050478,-1158.37470418959,-1158.2950199613,
-1158.21534897507,-1158.13568152155,-1158.05600187073,-1157.97629428834,
-1157.89649905926,-1157.81665471755,-1157.73669629051,-1157.69430041391,
-1157.61434311378,-1157.53448031654,-1157.45469449406,-1157.37496817887,
-1157.29528395057,-1157.21561296435,-1157.13594551083,-1157.05626586001,
-1156.97655827761,-1156.89676304854,-1156.81691870683,-1156.73696027978,
-1156.69456440319,-1156.61460710306,-1156.53474430582,-1156.45495848335,
-1156.37523216815,-1156.29554793986,-1156.21587695364,-1156.13620950011,
-1156.05652984929,-1155.9768222669,-1155.89702703782,-1155.81718269612,
-1155.73722426907,-1155.69482839247,-1155.61487109234,-1155.5350082951,
-1155.45522247262,-1155.37549615743,-1155.29581192913,-1155.21614094291,
-1155.13647348939,-1155.05679383857,-1154.97708625617,-1154.8972910271,
-1154.81744668539,-1154.73748825834,-1154.69509238175,-1154.61621712552,
-1154.53743704012,-1154.45874680529,-1154.38010736615,-1154.30150216832,
-1154.22291468565,-1154.1443015305,-1154.06567743878,-1153.98698234884,
-1153.91545296271),.UNSPECIFIED.);
#1484=B_SPLINE_CURVE_WITH_KNOTS('',3,(#171569,#171570,#171571,#171572,#171573,
#171574,#171575,#171576,#171577,#171578,#171579,#171580),.UNSPECIFIED.,
 .F.,.F.,(4,2,1,1,1,1,1,1,4),(-1153.91545296271,-1153.69535637103,-1152.69562036031,
-1151.69588434959,-1150.69614833887,-1149.69641232815,-1148.69667631743,
-1147.69694030671,-1147.63226765553),.UNSPECIFIED.);
#1485=B_SPLINE_CURVE_WITH_KNOTS('',3,(#171582,#171583,#171584,#171585,#171586,
#171587,#171588,#171589,#171590,#171591,#171592,#171593,#171594,#171595,
#171596,#171597,#171598,#171599,#171600,#171601,#171602,#171603,#171604,
#171605,#171606,#171607,#171608,#171609,#171610,#171611,#171612,#171613,
#171614,#171615,#171616,#171617,#171618,#171619,#171620,#171621,#171622,
#171623,#171624,#171625,#171626,#171627,#171628,#171629,#171630,#171631,
#171632,#171633,#171634,#171635,#171636,#171637,#171638,#171639,#171640,
#171641,#171642,#171643,#171644,#171645,#171646,#171647,#171648,#171649,
#171650,#171651,#171652,#171653,#171654,#171655,#171656,#171657,#171658,
#171659,#171660,#171661,#171662,#171663,#171664,#171665,#171666,#171667,
#171668,#171669,#171670,#171671,#171672,#171673,#171674,#171675,#171676,
#171677,#171678,#171679,#171680,#171681,#171682,#171683,#171684,#171685,
#171686,#171687,#171688,#171689,#171690,#171691,#171692,#171693,#171694,
#171695,#171696,#171697,#171698,#171699,#171700,#171701,#171702,#171703,
#171704,#171705,#171706,#171707,#171708,#171709,#171710,#171711,#171712,
#171713,#171714,#171715,#171716,#171717,#171718,#171719,#171720,#171721,
#171722,#171723,#171724,#171725,#171726,#171727,#171728,#171729,#171730,
#171731,#171732,#171733,#171734,#171735,#171736,#171737,#171738,#171739,
#171740,#171741,#171742,#171743,#171744,#171745,#171746,#171747,#171748,
#171749,#171750,#171751,#171752,#171753,#171754,#171755,#171756,#171757,
#171758,#171759,#171760,#171761,#171762,#171763,#171764,#171765,#171766,
#171767,#171768,#171769,#171770,#171771,#171772,#171773,#171774,#171775,
#171776,#171777,#171778,#171779,#171780,#171781,#171782,#171783,#171784,
#171785,#171786,#171787,#171788,#171789,#171790,#171791,#171792,#171793,
#171794,#171795,#171796,#171797,#171798,#171799,#171800,#171801,#171802,
#171803,#171804,#171805,#171806,#171807,#171808,#171809,#171810,#171811,
#171812,#171813,#171814,#171815,#171816,#171817,#171818,#171819,#171820,
#171821,#171822,#171823,#171824,#171825),.UNSPECIFIED.,.F.,.F.,(4,3,3,3,
3,3,3,3,3,3,3,3,3,3,3,3,3,3,3,3,3,3,3,3,3,3,3,3,3,3,3,3,3,3,3,3,3,3,3,3,
3,3,3,3,3,3,3,3,3,3,3,3,3,3,3,3,3,3,3,3,3,3,3,3,3,3,3,3,3,3,3,3,3,3,3,3,
3,3,3,3,3,4),(-1147.63226765553,-1147.55308046487,-1147.47398326853,-1147.3949579049,
-1147.31598627808,-1147.23704249499,-1147.15811160934,-1147.07917731644,
-1147.00022331162,-1146.92118728103,-1146.84210843834,-1146.76291058435,
-1146.69720429599,-1146.61724699586,-1146.53738419862,-1146.45759837614,
-1146.37787206095,-1146.29818783266,-1146.21851684644,-1146.13884939291,
-1146.05916974209,-1145.9794621597,-1145.89966693062,-1145.81982258892,
-1145.73986416187,-1145.69746828527,-1145.61751098514,-1145.5376481879,
-1145.45786236543,-1145.37813605023,-1145.29845182194,-1145.21878083572,
-1145.13911338219,-1145.05943373137,-1144.97972614898,-1144.8999309199,
-1144.8200865782,-1144.74012815115,-1144.69773227455,-1144.61777497442,
-1144.53791217718,-1144.4581263547,-1144.37840003951,-1144.29871581122,
-1144.21904482499,-1144.13937737147,-1144.05969772065,-1143.97999013826,
-1143.90019490918,-1143.82035056747,-1143.74039214043,-1143.69799626383,
-1143.6180389637,-1143.53817616646,-1143.45839034398,-1143.37866402879,
-1143.29897980049,-1143.21930881427,-1143.13964136075,-1143.05996170993,
-1142.98025412754,-1142.90045889846,-1142.82061455675,-1142.74065612971,
-1142.69826025311,-1142.61830295298,-1142.53844015574,-1142.45865433326,
-1142.37892801807,-1142.29924378977,-1142.21957280355,-1142.13990535003,
-1142.06022569921,-1141.98051811681,-1141.90072288774,-1141.82087854603,
-1141.74092011898,-1141.69852424239,-1141.6059888571,-1141.51380205893,
-1141.42229735434,-1141.34908247127),.UNSPECIFIED.);
#1486=B_SPLINE_CURVE_WITH_KNOTS('',3,(#171827,#171828,#171829,#171830,#171831,
#171832,#171833,#171834,#171835,#171836),.UNSPECIFIED.,.F.,.F.,(4,1,1,1,
1,1,1,4),(-1141.34908234835,-1140.69878823167,-1139.69905222095,-1138.69931621023,
-1137.69958019951,-1136.69984418879,-1135.70010817807,-1135.06589704117),
 .UNSPECIFIED.);
#1487=B_SPLINE_CURVE_WITH_KNOTS('',3,(#171838,#171839,#171840,#171841,#171842,
#171843,#171844,#171845,#171846,#171847),.UNSPECIFIED.,.F.,.F.,(4,1,1,1,
1,1,1,4),(-1135.06589704117,-1134.70037216735,-1133.70063615663,-1132.70090014591,
-1131.70116413519,-1130.70142812447,-1129.70169211375,-1128.78271173399),
 .UNSPECIFIED.);
#1488=B_SPLINE_CURVE_WITH_KNOTS('',3,(#171849,#171850,#171851,#171852,#171853,
#171854,#171855,#171856,#171857,#171858,#171859,#171860),.UNSPECIFIED.,
 .F.,.F.,(4,2,1,1,1,1,1,1,4),(-1128.78271173399,-1128.70195610303,-1127.70222009231,
-1126.70248408159,-1125.70274807087,-1124.70301206015,-1123.70327604943,
-1122.70354003871,-1122.49952642681),.UNSPECIFIED.);
#1489=B_SPLINE_CURVE_WITH_KNOTS('',3,(#171862,#171863,#171864,#171865,#171866,
#171867,#171868,#171869,#171870,#171871,#171872,#171873,#171874,#171875,
#171876,#171877,#171878,#171879,#171880,#171881,#171882,#171883,#171884,
#171885,#171886,#171887,#171888,#171889,#171890,#171891,#171892,#171893,
#171894,#171895,#171896,#171897,#171898,#171899,#171900,#171901,#171902,
#171903,#171904,#171905,#171906,#171907,#171908,#171909,#171910,#171911,
#171912,#171913,#171914,#171915,#171916,#171917,#171918,#171919,#171920,
#171921,#171922,#171923,#171924,#171925,#171926,#171927,#171928,#171929,
#171930,#171931,#171932,#171933,#171934,#171935,#171936,#171937,#171938,
#171939,#171940,#171941,#171942,#171943,#171944,#171945,#171946,#171947,
#171948,#171949,#171950,#171951,#171952,#171953,#171954,#171955,#171956,
#171957,#171958,#171959,#171960,#171961,#171962,#171963,#171964,#171965,
#171966,#171967,#171968,#171969,#171970,#171971,#171972,#171973,#171974,
#171975,#171976,#171977,#171978,#171979,#171980,#171981,#171982,#171983,
#171984,#171985,#171986,#171987,#171988,#171989,#171990,#171991,#171992,
#171993,#171994,#171995,#171996,#171997,#171998,#171999,#172000,#172001,
#172002,#172003,#172004,#172005,#172006,#172007,#172008,#172009,#172010,
#172011,#172012,#172013,#172014,#172015,#172016,#172017,#172018,#172019,
#172020,#172021,#172022,#172023,#172024,#172025,#172026,#172027,#172028,
#172029,#172030,#172031,#172032,#172033,#172034,#172035,#172036,#172037,
#172038,#172039,#172040,#172041,#172042,#172043,#172044,#172045,#172046,
#172047,#172048,#172049,#172050,#172051,#172052,#172053,#172054,#172055,
#172056,#172057,#172058,#172059,#172060,#172061,#172062,#172063,#172064,
#172065,#172066,#172067,#172068,#172069,#172070,#172071,#172072,#172073,
#172074,#172075,#172076,#172077,#172078,#172079,#172080,#172081,#172082,
#172083,#172084,#172085,#172086,#172087,#172088,#172089,#172090,#172091,
#172092,#172093,#172094,#172095,#172096,#172097,#172098,#172099,#172100,
#172101,#172102,#172103,#172104,#172105),.UNSPECIFIED.,.F.,.F.,(4,3,3,3,
3,3,3,3,3,3,3,3,3,3,3,3,3,3,3,3,3,3,3,3,3,3,3,3,3,3,3,3,3,3,3,3,3,3,3,3,
3,3,3,3,3,3,3,3,3,3,3,3,3,3,3,3,3,3,3,3,3,3,3,3,3,3,3,3,3,3,3,3,3,3,3,3,
3,3,3,3,3,4),(-1122.49952642681,-1122.42086265841,-1122.34226113132,-1122.26245399341,
-1122.18391170298,-1122.10537271461,-1122.02682048646,-1121.94606637184,
-1121.86739794136,-1121.78560098468,-1121.70380402799,-1121.62384672786,
-1121.54398393062,-1121.46419810814,-1121.38447179295,-1121.30478756465,
-1121.22511657843,-1121.14544912491,-1121.06576947409,-1120.9860618917,
-1120.90626666262,-1120.82642232091,-1120.74646389386,-1120.70406801727,
-1120.62411071714,-1120.5442479199,-1120.46446209742,-1120.38473578223,
-1120.30505155393,-1120.22538056771,-1120.14571311419,-1120.06603346337,
-1119.98632588098,-1119.9065306519,-1119.82668631019,-1119.74672788314,
-1119.70433200655,-1119.62437470642,-1119.54451190918,-1119.4647260867,
-1119.38499977151,-1119.30531554322,-1119.22564455699,-1119.14597710347,
-1119.06629745265,-1118.98658987026,-1118.90679464118,-1118.82695029948,
-1118.74699187243,-1118.70459599583,-1118.6246386957,-1118.54477589846,
-1118.46499007598,-1118.38526376079,-1118.3055795325,-1118.22590854627,
-1118.14624109275,-1118.06656144193,-1117.98685385954,-1117.90705863046,
-1117.82721428875,-1117.74725586171,-1117.70485998511,-1117.62490268498,
-1117.54503988774,-1117.46525406527,-1117.38552775007,-1117.30584352178,
-1117.22617253556,-1117.14650508203,-1117.06682543121,-1116.98711784882,
-1116.90732261974,-1116.82747827804,-1116.74751985099,-1116.70512397439,
-1116.620615229,-1116.53625184539,-1116.45208839494,-1116.36804333682,-1116.28416290556,
-1116.21634111975),.UNSPECIFIED.);
#1490=B_SPLINE_CURVE_WITH_KNOTS('',3,(#172107,#172108,#172109,#172110,#172111,
#172112,#172113,#172114,#172115,#172116,#172117,#172118,#172119,#172120,
#172121,#172122,#172123,#172124,#172125,#172126,#172127,#172128,#172129,
#172130,#172131,#172132,#172133,#172134,#172135,#172136,#172137,#172138,
#172139,#172140,#172141,#172142,#172143,#172144,#172145,#172146,#172147,
#172148,#172149,#172150,#172151,#172152,#172153,#172154,#172155,#172156,
#172157,#172158,#172159,#172160,#172161,#172162,#172163,#172164,#172165,
#172166,#172167,#172168,#172169,#172170,#172171,#172172,#172173,#172174,
#172175,#172176,#172177,#172178,#172179,#172180,#172181,#172182,#172183,
#172184,#172185,#172186,#172187,#172188,#172189,#172190,#172191,#172192,
#172193,#172194,#172195,#172196,#172197,#172198,#172199,#172200,#172201,
#172202,#172203,#172204,#172205,#172206,#172207,#172208,#172209,#172210,
#172211,#172212,#172213,#172214,#172215,#172216,#172217,#172218,#172219,
#172220,#172221,#172222,#172223,#172224,#172225,#172226,#172227,#172228,
#172229,#172230,#172231,#172232,#172233,#172234,#172235,#172236,#172237,
#172238,#172239,#172240,#172241,#172242,#172243,#172244,#172245,#172246,
#172247,#172248,#172249,#172250,#172251,#172252,#172253,#172254,#172255,
#172256,#172257,#172258,#172259,#172260,#172261,#172262,#172263,#172264,
#172265,#172266,#172267,#172268,#172269,#172270,#172271,#172272,#172273,
#172274,#172275,#172276,#172277,#172278,#172279,#172280,#172281,#172282,
#172283,#172284,#172285,#172286,#172287,#172288,#172289,#172290,#172291,
#172292,#172293,#172294,#172295,#172296,#172297,#172298,#172299,#172300,
#172301,#172302,#172303,#172304,#172305,#172306,#172307,#172308,#172309,
#172310,#172311,#172312,#172313,#172314,#172315,#172316,#172317,#172318,
#172319,#172320,#172321,#172322,#172323,#172324,#172325,#172326,#172327,
#172328,#172329,#172330,#172331,#172332,#172333,#172334,#172335,#172336,
#172337,#172338,#172339,#172340,#172341,#172342,#172343,#172344,#172345,
#172346,#172347,#172348,#172349,#172350),.UNSPECIFIED.,.F.,.F.,(4,3,3,3,
3,3,3,3,3,3,3,3,3,3,3,3,3,3,3,3,3,3,3,3,3,3,3,3,3,3,3,3,3,3,3,3,3,3,3,3,
3,3,3,3,3,3,3,3,3,3,3,3,3,3,3,3,3,3,3,3,3,3,3,3,3,3,3,3,3,3,3,3,3,3,3,3,
3,3,3,3,3,4),(-1116.21634111963,-1116.13325733148,-1116.05008172745,-1115.96390828651,
-1115.8804590234,-1115.79292349354,-1115.70538796367,-1115.62543066354,
-1115.54556786629,-1115.46578204382,-1115.38605572863,-1115.30637150033,
-1115.22670051411,-1115.14703306058,-1115.06735340976,-1114.98764582737,
-1114.90785059829,-1114.82800625658,-1114.74804782954,-1114.70565195295,
-1114.62569465282,-1114.54583185558,-1114.4660460331,-1114.38631971791,
-1114.30663548961,-1114.22696450339,-1114.14729704987,-1114.06761739905,
-1113.98790981666,-1113.90811458758,-1113.82827024587,-1113.74831181882,
-1113.70591594223,-1113.6259586421,-1113.54609584486,-1113.46631002239,
-1113.38658370719,-1113.3068994789,-1113.22722849268,-1113.14756103915,
-1113.06788138833,-1112.98817380594,-1112.90837857687,-1112.82853423516,
-1112.74857580811,-1112.70617993151,-1112.62622263138,-1112.54635983414,
-1112.46657401166,-1112.38684769647,-1112.30716346817,-1112.22749248195,
-1112.14782502843,-1112.06814537761,-1111.98843779522,-1111.90864256614,
-1111.82879822443,-1111.74883979739,-1111.70644392079,-1111.62648662066,
-1111.54662382342,-1111.46683800095,-1111.38711168575,-1111.30742745746,
-1111.22775647124,-1111.14808901771,-1111.0684093669,-1110.9887017845,-1110.90890655543,
-1110.82906221372,-1110.74910378667,-1110.70670791007,-1110.62780456985,
-1110.54899660499,-1110.47027895055,-1110.39161235929,-1110.31298029234,
-1110.23436623922,-1110.15572804764,-1110.07707914813,-1109.99836256153,
-1109.93315581245),.UNSPECIFIED.);
#1491=B_SPLINE_CURVE_WITH_KNOTS('',3,(#172352,#172353,#172354,#172355,#172356,
#172357,#172358,#172359,#172360,#172361,#172362,#172363),.UNSPECIFIED.,
 .F.,.F.,(4,2,1,1,1,1,1,1,4),(-1109.93315581245,-1109.70697189935,-1108.70723588863,
-1107.70749987791,-1106.70776386719,-1105.70802785646,-1104.70829184574,
-1103.70855583502,-1103.64997050527),.UNSPECIFIED.);
#1492=B_SPLINE_CURVE_WITH_KNOTS('',3,(#172365,#172366,#172367,#172368,#172369,
#172370,#172371,#172372,#172373,#172374,#172375,#172376,#172377,#172378,
#172379,#172380,#172381,#172382,#172383,#172384,#172385,#172386,#172387,
#172388,#172389,#172390,#172391,#172392,#172393,#172394,#172395,#172396,
#172397,#172398,#172399,#172400,#172401,#172402,#172403,#172404,#172405,
#172406,#172407,#172408,#172409,#172410,#172411,#172412,#172413,#172414,
#172415,#172416,#172417,#172418,#172419,#172420,#172421,#172422,#172423,
#172424,#172425,#172426,#172427,#172428,#172429,#172430,#172431,#172432,
#172433,#172434,#172435,#172436,#172437,#172438,#172439,#172440,#172441,
#172442,#172443,#172444,#172445,#172446,#172447,#172448,#172449,#172450,
#172451,#172452,#172453,#172454,#172455,#172456,#172457,#172458,#172459,
#172460,#172461,#172462,#172463,#172464,#172465,#172466,#172467,#172468,
#172469,#172470,#172471,#172472,#172473,#172474,#172475,#172476,#172477,
#172478,#172479,#172480,#172481,#172482,#172483,#172484,#172485,#172486,
#172487,#172488,#172489,#172490,#172491,#172492,#172493,#172494,#172495,
#172496,#172497,#172498,#172499,#172500,#172501,#172502,#172503,#172504,
#172505,#172506,#172507,#172508,#172509,#172510,#172511,#172512,#172513,
#172514,#172515,#172516,#172517,#172518,#172519,#172520,#172521,#172522,
#172523,#172524,#172525,#172526,#172527,#172528,#172529,#172530,#172531,
#172532,#172533,#172534,#172535,#172536,#172537,#172538,#172539,#172540,
#172541,#172542,#172543,#172544,#172545,#172546,#172547,#172548,#172549,
#172550,#172551,#172552,#172553,#172554,#172555,#172556,#172557,#172558,
#172559,#172560,#172561,#172562,#172563,#172564,#172565,#172566,#172567,
#172568,#172569,#172570,#172571,#172572,#172573,#172574,#172575,#172576,
#172577,#172578,#172579,#172580,#172581,#172582,#172583,#172584,#172585,
#172586,#172587,#172588,#172589,#172590,#172591,#172592,#172593,#172594,
#172595,#172596,#172597,#172598,#172599,#172600,#172601,#172602,#172603,
#172604,#172605,#172606,#172607,#172608),.UNSPECIFIED.,.F.,.F.,(4,3,3,3,
3,3,3,3,3,3,3,3,3,3,3,3,3,3,3,3,3,3,3,3,3,3,3,3,3,3,3,3,3,3,3,3,3,3,3,3,
3,3,3,3,3,3,3,3,3,3,3,3,3,3,3,3,3,3,3,3,3,3,3,3,3,3,3,3,3,3,3,3,3,3,3,3,
3,3,3,3,3,4),(-1103.64997050527,-1103.57072528908,-1103.49157078566,-1103.41248887196,
-1103.33346149041,-1103.25446302266,-1103.17547824058,-1103.0964908751,
-1103.01748465782,-1102.93839664834,-1102.85926666808,-1102.78001600334,
-1102.7088198243,-1102.62886252417,-1102.54899972693,-1102.46921390445,
-1102.38948758926,-1102.30980336097,-1102.23013237475,-1102.15046492122,
-1102.0707852704,-1101.99107768801,-1101.91128245893,-1101.83143811723,
-1101.75147969018,-1101.70908381358,-1101.62912651345,-1101.54926371621,
-1101.46947789373,-1101.38975157854,-1101.31006735025,-1101.23039636403,
-1101.1507289105,-1101.07104925968,-1100.99134167729,-1100.91154644821,
-1100.83170210651,-1100.75174367946,-1100.70934780286,-1100.62939050273,
-1100.54952770549,-1100.46974188301,-1100.39001556782,-1100.31033133952,
-1100.2306603533,-1100.15099289978,-1100.07131324896,-1099.99160566657,
-1099.91181043749,-1099.83196609578,-1099.75200766874,-1099.70961179214,
-1099.62965449201,-1099.54979169477,-1099.47000587229,-1099.3902795571,
-1099.3105953288,-1099.23092434258,-1099.15125688906,-1099.07157723824,
-1098.99186965585,-1098.91207442677,-1098.83223008506,-1098.75227165802,
-1098.70987578142,-1098.62991848129,-1098.55005568404,-1098.47026986157,
-1098.39054354638,-1098.31085931808,-1098.23118833186,-1098.15152087833,
-1098.07184122752,-1097.99213364512,-1097.91233841605,-1097.83249407434,
-1097.75253564729,-1097.7101397707,-1097.61707962411,-1097.52439093108,
-1097.43242331425,-1097.36678531938),.UNSPECIFIED.);
#1493=B_SPLINE_CURVE_WITH_KNOTS('',3,(#172610,#172611,#172612,#172613,#172614,
#172615,#172616,#172617,#172618,#172619),.UNSPECIFIED.,.F.,.F.,(4,1,1,1,
1,1,1,4),(-1097.36678519809,-1096.71040375998,-1095.71066774926,-1094.71093173854,
-1093.71119572782,-1092.7114597171,-1091.71172370638,-1091.08359989091),
 .UNSPECIFIED.);
#1494=B_SPLINE_CURVE_WITH_KNOTS('',3,(#172621,#172622,#172623,#172624,#172625,
#172626,#172627,#172628,#172629,#172630),.UNSPECIFIED.,.F.,.F.,(4,1,1,1,
1,1,1,4),(-1091.08359989091,-1090.71198769566,-1089.71225168494,-1088.71251567422,
-1087.7127796635,-1086.71304365278,-1085.71330764206,-1084.80042330243),
 .UNSPECIFIED.);
#1495=B_SPLINE_CURVE_WITH_KNOTS('',3,(#172632,#172633,#172634,#172635,#172636,
#172637,#172638,#172639,#172640,#172641,#172642,#172643,#172644,#172645,
#172646,#172647,#172648,#172649,#172650,#172651,#172652,#172653,#172654,
#172655,#172656,#172657,#172658,#172659,#172660,#172661,#172662,#172663,
#172664,#172665,#172666,#172667,#172668,#172669,#172670,#172671,#172672,
#172673,#172674,#172675,#172676,#172677,#172678,#172679,#172680,#172681,
#172682,#172683,#172684,#172685,#172686,#172687,#172688,#172689,#172690,
#172691,#172692,#172693,#172694,#172695,#172696,#172697,#172698,#172699,
#172700,#172701,#172702,#172703,#172704,#172705,#172706,#172707,#172708,
#172709,#172710,#172711,#172712,#172713,#172714,#172715,#172716,#172717,
#172718,#172719,#172720,#172721,#172722,#172723,#172724,#172725,#172726,
#172727,#172728,#172729,#172730,#172731,#172732,#172733,#172734,#172735,
#172736,#172737,#172738,#172739,#172740,#172741,#172742,#172743,#172744,
#172745,#172746,#172747,#172748,#172749,#172750,#172751,#172752,#172753,
#172754,#172755,#172756,#172757,#172758,#172759,#172760,#172761,#172762,
#172763,#172764,#172765,#172766,#172767,#172768,#172769,#172770,#172771,
#172772,#172773,#172774,#172775,#172776,#172777,#172778,#172779,#172780,
#172781,#172782,#172783,#172784,#172785,#172786,#172787,#172788,#172789,
#172790,#172791,#172792,#172793,#172794,#172795,#172796,#172797,#172798,
#172799,#172800,#172801,#172802,#172803,#172804,#172805,#172806,#172807,
#172808,#172809,#172810,#172811,#172812,#172813,#172814,#172815,#172816,
#172817,#172818,#172819,#172820,#172821,#172822,#172823,#172824,#172825,
#172826,#172827,#172828,#172829,#172830,#172831,#172832,#172833,#172834,
#172835,#172836,#172837,#172838,#172839,#172840,#172841,#172842,#172843,
#172844,#172845,#172846,#172847,#172848,#172849,#172850,#172851,#172852,
#172853,#172854,#172855,#172856,#172857,#172858,#172859,#172860,#172861,
#172862,#172863,#172864,#172865,#172866,#172867,#172868,#172869,#172870,
#172871,#172872,#172873,#172874,#172875),.UNSPECIFIED.,.F.,.F.,(4,3,3,3,
3,3,3,3,3,3,3,3,3,3,3,3,3,3,3,3,3,3,3,3,3,3,3,3,3,3,3,3,3,3,3,3,3,3,3,3,
3,3,3,3,3,3,3,3,3,3,3,3,3,3,3,3,3,3,3,3,3,3,3,3,3,3,3,3,3,3,3,3,3,3,3,3,
3,3,3,3,3,4),(-1084.80041458373,-1084.71357163134,-1084.63361433121,-1084.55375153397,
-1084.47396571149,-1084.3942393963,-1084.31455516801,-1084.23488418178,
-1084.15521672826,-1084.07553707744,-1083.99582949505,-1083.91603426597,
-1083.83618992427,-1083.75623149722,-1083.71383562062,-1083.63387832049,
-1083.55401552325,-1083.47422970077,-1083.39450338558,-1083.31481915728,
-1083.23514817106,-1083.15548071754,-1083.07580106672,-1082.99609348433,
-1082.91629825525,-1082.83645391354,-1082.7564954865,-1082.7140996099,-1082.63414230977,
-1082.55427951253,-1082.47449369005,-1082.39476737486,-1082.31508314657,
-1082.23541216034,-1082.15574470682,-1082.076065056,-1081.99635747361,-1081.91656224453,
-1081.83671790283,-1081.75675947578,-1081.71436359918,-1081.63440629905,
-1081.55454350181,-1081.47475767933,-1081.39503136414,-1081.31534713584,
-1081.23567614962,-1081.1560086961,-1081.07632904528,-1080.99662146289,
-1080.91682623381,-1080.8369818921,-1080.75702346506,-1080.71462758846,
-1080.63467028833,-1080.55480749109,-1080.47502166861,-1080.39529535342,
-1080.31561112513,-1080.2359401389,-1080.15627268538,-1080.07659303456,
-1079.99688545217,-1079.91709022309,-1079.83724588138,-1079.75728745434,
-1079.71489157774,-1079.63493427761,-1079.55507148037,-1079.47528565789,
-1079.3955593427,-1079.3158751144,-1079.23620412818,-1079.15653667466,-1079.07685702384,
-1078.99714944145,-1078.91735421237,-1078.83750987066,-1078.75755144361,
-1078.71515556702,-1078.59977111222,-1078.51722927655),.UNSPECIFIED.);
#1496=B_SPLINE_CURVE_WITH_KNOTS('',3,(#172877,#172878,#172879,#172880,#172881,
#172882,#172883,#172884,#172885,#172886),.UNSPECIFIED.,.F.,.F.,(4,1,1,1,
1,1,1,4),(-1078.51722580384,-1077.7154195563,-1076.71568354558,-1075.71594753486,
-1074.71621152414,-1073.71647551342,-1072.7167395027,-1072.23404396937),
 .UNSPECIFIED.);
#1497=B_SPLINE_CURVE_WITH_KNOTS('',3,(#172888,#172889,#172890,#172891,#172892,
#172893,#172894,#172895,#172896,#172897),.UNSPECIFIED.,.F.,.F.,(4,1,1,1,
1,1,1,4),(-1072.23404396937,-1071.71700349198,-1070.71726748126,-1069.71753147054,
-1068.71779545982,-1067.7180594491,-1066.71832343838,-1065.95085866219),
 .UNSPECIFIED.);
#1498=B_SPLINE_CURVE_WITH_KNOTS('',3,(#172899,#172900,#172901,#172902,#172903,
#172904,#172905,#172906,#172907,#172908,#172909),.UNSPECIFIED.,.F.,.F.,
(4,1,1,1,1,1,1,1,4),(-1065.95085866219,-1065.71858742766,-1064.71885141694,
-1063.71911540622,-1062.7193793955,-1061.71964338478,-1060.71990737406,
-1059.72017136334,-1059.66767335501),.UNSPECIFIED.);
#1499=B_SPLINE_CURVE_WITH_KNOTS('',3,(#172911,#172912,#172913,#172914,#172915,
#172916,#172917,#172918,#172919,#172920),.UNSPECIFIED.,.F.,.F.,(4,1,1,1,
1,1,1,4),(-1059.66767335501,-1058.72043535262,-1057.7206993419,-1056.72096333118,
-1055.72122732046,-1054.72149130974,-1053.72175529902,-1053.38449557091),
 .UNSPECIFIED.);
#1500=B_SPLINE_CURVE_WITH_KNOTS('',3,(#172922,#172923,#172924,#172925,#172926,
#172927,#172928,#172929,#172930,#172931,#172932,#172933,#172934,#172935,
#172936,#172937,#172938,#172939,#172940,#172941,#172942,#172943,#172944,
#172945,#172946,#172947,#172948,#172949,#172950,#172951,#172952,#172953,
#172954,#172955,#172956,#172957,#172958,#172959,#172960,#172961,#172962,
#172963,#172964,#172965,#172966,#172967,#172968,#172969,#172970,#172971,
#172972,#172973,#172974,#172975,#172976,#172977,#172978,#172979,#172980,
#172981,#172982,#172983,#172984,#172985,#172986,#172987,#172988,#172989,
#172990,#172991,#172992,#172993,#172994,#172995,#172996,#172997,#172998,
#172999,#173000,#173001,#173002,#173003,#173004,#173005,#173006,#173007,
#173008,#173009,#173010,#173011,#173012,#173013,#173014,#173015,#173016,
#173017,#173018,#173019,#173020,#173021,#173022,#173023,#173024,#173025,
#173026,#173027,#173028,#173029,#173030,#173031,#173032,#173033,#173034,
#173035,#173036,#173037,#173038,#173039,#173040,#173041,#173042,#173043,
#173044,#173045,#173046,#173047,#173048,#173049,#173050,#173051,#173052,
#173053,#173054,#173055,#173056,#173057,#173058,#173059,#173060,#173061,
#173062,#173063,#173064,#173065,#173066,#173067,#173068,#173069,#173070,
#173071,#173072,#173073,#173074,#173075,#173076,#173077,#173078,#173079,
#173080,#173081,#173082,#173083,#173084,#173085,#173086,#173087,#173088,
#173089,#173090,#173091,#173092,#173093,#173094,#173095,#173096,#173097,
#173098,#173099,#173100,#173101,#173102,#173103,#173104,#173105,#173106,
#173107,#173108,#173109,#173110,#173111,#173112,#173113,#173114,#173115,
#173116,#173117,#173118,#173119,#173120,#173121,#173122,#173123,#173124,
#173125,#173126,#173127,#173128,#173129,#173130,#173131,#173132,#173133,
#173134,#173135,#173136,#173137,#173138,#173139,#173140,#173141,#173142,
#173143,#173144,#173145,#173146,#173147,#173148,#173149,#173150,#173151,
#173152,#173153,#173154,#173155,#173156,#173157,#173158,#173159,#173160,
#173161,#173162,#173163,#173164,#173165,#173166,#173167,#173168),
 .UNSPECIFIED.,.F.,.F.,(4,3,3,3,3,3,3,3,3,3,3,3,3,3,3,3,3,3,3,3,3,3,3,3,
3,3,3,3,3,3,3,3,3,3,3,3,3,3,3,3,3,3,3,3,3,3,3,3,3,3,3,3,3,3,3,3,3,3,3,3,
3,3,3,3,3,3,3,3,3,3,3,3,3,3,3,3,3,3,3,3,3,3,4),(-1053.38448804783,-1053.30167945289,
-1053.22201542787,-1053.14234607935,-1053.06265574047,-1052.9829287348,
-1052.90310594554,-1052.82322647131,-1052.74323316342,-1052.7220192883,
-1052.64206198817,-1052.56219919093,-1052.48241336845,-1052.40268705326,
-1052.32300282496,-1052.24333183874,-1052.16366438522,-1052.0839847344,
-1052.004277152,-1051.92448192293,-1051.84463758122,-1051.76467915417,-1051.72228327758,
-1051.64232597745,-1051.56246318021,-1051.48267735773,-1051.40295104254,
-1051.32326681424,-1051.24359582802,-1051.1639283745,-1051.08424872368,
-1051.00454114129,-1050.92474591221,-1050.8449015705,-1050.76494314345,
-1050.72254726686,-1050.64258996673,-1050.56272716949,-1050.48294134702,
-1050.40321503182,-1050.32353080353,-1050.24385981731,-1050.16419236378,
-1050.08451271296,-1050.00480513057,-1049.92500990149,-1049.84516555979,
-1049.76520713274,-1049.72281125614,-1049.64285395601,-1049.56299115877,
-1049.48320533629,-1049.4034790211,-1049.32379479281,-1049.24412380658,
-1049.16445635306,-1049.08477670224,-1049.00506911985,-1048.92527389077,
-1048.84542954906,-1048.76547112202,-1048.72307524542,-1048.64311794529,
-1048.56325514805,-1048.48346932558,-1048.40374301038,-1048.32405878209,
-1048.24438779587,-1048.16472034234,-1048.08504069153,-1048.00533310913,
-1047.92553788006,-1047.84569353835,-1047.7657351113,-1047.7233392347,-1047.64267070184,
-1047.56210075995,-1047.48161433869,-1047.40119642267,-1047.32083745328,
-1047.24051357248,-1047.16020183974,-1047.10130274065),.UNSPECIFIED.);
#1501=B_SPLINE_CURVE_WITH_KNOTS('',3,(#173170,#173171,#173172,#173173,#173174,
#173175,#173176,#173177,#173178,#173179),.UNSPECIFIED.,.F.,.F.,(4,1,1,1,
1,1,1,4),(-1047.1012951378,-1046.72360322398,-1045.72386721326,-1044.72413120254,
-1043.72439519182,-1042.7246591811,-1041.72492317038,-1040.8181264349),
 .UNSPECIFIED.);
#1502=B_SPLINE_CURVE_WITH_KNOTS('',3,(#173181,#173182,#173183,#173184,#173185,
#173186,#173187,#173188,#173189,#173190,#173191,#173192,#173193,#173194,
#173195,#173196,#173197,#173198,#173199,#173200,#173201,#173202,#173203,
#173204,#173205,#173206,#173207,#173208,#173209,#173210,#173211,#173212,
#173213,#173214,#173215,#173216,#173217,#173218,#173219,#173220,#173221,
#173222,#173223,#173224,#173225,#173226,#173227,#173228,#173229,#173230,
#173231,#173232,#173233,#173234,#173235,#173236,#173237,#173238,#173239,
#173240,#173241,#173242,#173243,#173244,#173245,#173246,#173247,#173248,
#173249,#173250,#173251,#173252,#173253,#173254,#173255,#173256,#173257,
#173258,#173259,#173260,#173261,#173262,#173263,#173264,#173265,#173266,
#173267,#173268,#173269,#173270,#173271,#173272,#173273,#173274,#173275,
#173276,#173277,#173278,#173279,#173280,#173281,#173282,#173283,#173284,
#173285,#173286,#173287,#173288,#173289,#173290,#173291,#173292,#173293,
#173294,#173295,#173296,#173297,#173298,#173299,#173300,#173301,#173302,
#173303,#173304,#173305,#173306,#173307,#173308,#173309,#173310,#173311,
#173312,#173313,#173314,#173315,#173316,#173317,#173318,#173319,#173320,
#173321,#173322,#173323,#173324,#173325,#173326,#173327,#173328,#173329,
#173330,#173331,#173332,#173333,#173334,#173335,#173336,#173337,#173338,
#173339,#173340,#173341,#173342,#173343,#173344,#173345,#173346,#173347,
#173348,#173349,#173350,#173351,#173352,#173353,#173354,#173355,#173356,
#173357,#173358,#173359,#173360,#173361,#173362,#173363,#173364,#173365,
#173366,#173367,#173368,#173369,#173370,#173371,#173372,#173373,#173374,
#173375,#173376,#173377,#173378,#173379,#173380,#173381,#173382,#173383,
#173384,#173385,#173386,#173387,#173388,#173389,#173390,#173391,#173392,
#173393,#173394,#173395,#173396,#173397,#173398,#173399,#173400,#173401,
#173402,#173403,#173404,#173405,#173406,#173407,#173408,#173409,#173410,
#173411,#173412,#173413,#173414,#173415,#173416,#173417,#173418,#173419,
#173420,#173421,#173422,#173423,#173424),.UNSPECIFIED.,.F.,.F.,(4,3,3,3,
3,3,3,3,3,3,3,3,3,3,3,3,3,3,3,3,3,3,3,3,3,3,3,3,3,3,3,3,3,3,3,3,3,3,3,3,
3,3,3,3,3,3,3,3,3,3,3,3,3,3,3,3,3,3,3,3,3,3,3,3,3,3,3,3,3,3,3,3,3,3,3,3,
3,3,3,3,3,4),(-1040.81811743347,-1040.72518715966,-1040.64522985953,-1040.56536706229,
-1040.48558123981,-1040.40585492462,-1040.32617069632,-1040.2464997101,
-1040.16683225657,-1040.08715260576,-1040.00744502336,-1039.92764979429,
-1039.84780545258,-1039.76784702553,-1039.72545114894,-1039.64549384881,
-1039.56563105157,-1039.48584522909,-1039.4061189139,-1039.3264346856,-1039.24676369938,
-1039.16709624586,-1039.08741659504,-1039.00770901265,-1038.92791378357,
-1038.84806944186,-1038.76811101482,-1038.72571513822,-1038.64575783809,
-1038.56589504085,-1038.48610921837,-1038.40638290318,-1038.32669867489,
-1038.24702768866,-1038.16736023514,-1038.08768058432,-1038.00797300193,
-1037.92817777285,-1037.84833343114,-1037.7683750041,-1037.7259791275,-1037.64602182737,
-1037.56615903013,-1037.48637320765,-1037.40664689246,-1037.32696266416,
-1037.24729167794,-1037.16762422442,-1037.0879445736,-1037.00823699121,
-1036.92844176213,-1036.84859742042,-1036.76863899338,-1036.72624311678,
-1036.64628581665,-1036.56642301941,-1036.48663719693,-1036.40691088174,
-1036.32722665344,-1036.24755566722,-1036.1678882137,-1036.08820856288,
-1036.00850098049,-1035.92870575141,-1035.8488614097,-1035.76890298266,
-1035.72650710606,-1035.64654980593,-1035.56668700869,-1035.48690118622,
-1035.40717487102,-1035.32749064273,-1035.24781965651,-1035.16815220299,
-1035.08847255217,-1035.00876496978,-1034.9289697407,-1034.849125399,-1034.76916697195,
-1034.72677109534,-1034.60948897058,-1034.53493212629),.UNSPECIFIED.);
#1503=B_SPLINE_CURVE_WITH_KNOTS('',3,(#173426,#173427,#173428,#173429,#173430,
#173431,#173432,#173433,#173434,#173435),.UNSPECIFIED.,.F.,.F.,(4,1,1,1,
1,1,1,4),(-1034.53492806915,-1033.72703508462,-1032.7272990739,-1031.72756306318,
-1030.72782705246,-1029.72809104174,-1028.72835503102,-1028.25174681911),
 .UNSPECIFIED.);
#1504=B_SPLINE_CURVE_WITH_KNOTS('',3,(#173437,#173438,#173439,#173440,#173441,
#173442,#173443,#173444,#173445,#173446),.UNSPECIFIED.,.F.,.F.,(4,1,1,1,
1,1,1,4),(-1028.25174681911,-1027.72861902029,-1026.72888300957,-1025.72914699885,
-1024.72941098813,-1023.72967497741,-1022.72993896669,-1021.96856151193),
 .UNSPECIFIED.);
#1505=B_SPLINE_CURVE_WITH_KNOTS('',3,(#173448,#173449,#173450,#173451,#173452,
#173453,#173454,#173455,#173456,#173457,#173458),.UNSPECIFIED.,.F.,.F.,
(4,1,1,1,1,1,1,1,4),(-1021.96856151193,-1021.73020295597,-1020.73046694525,
-1019.73073093453,-1018.73099492381,-1017.73125891309,-1016.73152290237,
-1015.73178689165,-1015.68537620475),.UNSPECIFIED.);
#1506=B_SPLINE_CURVE_WITH_KNOTS('',3,(#173460,#173461,#173462,#173463,#173464,
#173465,#173466,#173467,#173468,#173469),.UNSPECIFIED.,.F.,.F.,(4,1,1,1,
1,1,1,4),(-1015.68537620475,-1014.73205088093,-1013.73231487021,-1012.73257885949,
-1011.73284284877,-1010.73310683805,-1009.73337082733,-1009.40219824018),
 .UNSPECIFIED.);
#1507=B_SPLINE_CURVE_WITH_KNOTS('',3,(#173471,#173472,#173473,#173474,#173475,
#173476,#173477,#173478,#173479,#173480,#173481,#173482,#173483,#173484,
#173485,#173486,#173487,#173488,#173489,#173490,#173491,#173492,#173493,
#173494,#173495,#173496,#173497,#173498,#173499,#173500,#173501,#173502,
#173503,#173504,#173505,#173506,#173507,#173508,#173509,#173510,#173511,
#173512,#173513,#173514,#173515,#173516,#173517,#173518,#173519,#173520,
#173521,#173522,#173523,#173524,#173525,#173526,#173527,#173528,#173529,
#173530,#173531,#173532,#173533,#173534,#173535,#173536,#173537,#173538,
#173539,#173540,#173541,#173542,#173543,#173544,#173545,#173546,#173547,
#173548,#173549,#173550,#173551,#173552,#173553,#173554,#173555,#173556,
#173557,#173558,#173559,#173560,#173561,#173562,#173563,#173564,#173565,
#173566,#173567,#173568,#173569,#173570,#173571,#173572,#173573,#173574,
#173575,#173576,#173577,#173578,#173579,#173580,#173581,#173582,#173583,
#173584,#173585,#173586,#173587,#173588,#173589,#173590,#173591,#173592,
#173593,#173594,#173595,#173596,#173597,#173598,#173599,#173600,#173601,
#173602,#173603,#173604,#173605,#173606,#173607,#173608,#173609,#173610,
#173611,#173612,#173613,#173614,#173615,#173616,#173617,#173618,#173619,
#173620,#173621,#173622,#173623,#173624,#173625,#173626,#173627,#173628,
#173629,#173630,#173631,#173632,#173633,#173634,#173635,#173636,#173637,
#173638,#173639,#173640,#173641,#173642,#173643,#173644,#173645,#173646,
#173647,#173648,#173649,#173650,#173651,#173652,#173653,#173654,#173655,
#173656,#173657,#173658,#173659,#173660,#173661,#173662,#173663,#173664,
#173665,#173666,#173667,#173668,#173669,#173670,#173671,#173672,#173673,
#173674,#173675,#173676,#173677,#173678,#173679,#173680,#173681,#173682,
#173683,#173684,#173685,#173686,#173687,#173688,#173689,#173690,#173691,
#173692,#173693,#173694,#173695,#173696,#173697,#173698,#173699,#173700,
#173701,#173702,#173703,#173704,#173705,#173706,#173707,#173708,#173709,
#173710,#173711,#173712,#173713,#173714,#173715,#173716,#173717),
 .UNSPECIFIED.,.F.,.F.,(4,3,3,3,3,3,3,3,3,3,3,3,3,3,3,3,3,3,3,3,3,3,3,3,
3,3,3,3,3,3,3,3,3,3,3,3,3,3,3,3,3,3,3,3,3,3,3,3,3,3,3,3,3,3,3,3,3,3,3,3,
3,3,3,3,3,3,3,3,3,3,3,3,3,3,3,3,3,3,3,3,3,3,4),(-1009.40219089757,-1009.31862138745,
-1009.23904212832,-1009.15945978643,-1009.0798586105,-1009.00022284082,
-1008.92049278562,-1008.84070773089,-1008.76080793305,-1008.73363481661,
-1008.65367751648,-1008.57381471924,-1008.49402889676,-1008.41430258157,
-1008.33461835327,-1008.25494736705,-1008.17527991353,-1008.09560026271,
-1008.01589268032,-1007.93609745124,-1007.85625310953,-1007.77629468249,
-1007.73389880589,-1007.65394150576,-1007.57407870852,-1007.49429288604,
-1007.41456657085,-1007.33488234256,-1007.25521135633,-1007.17554390281,
-1007.09586425199,-1007.0161566696,-1006.93636144052,-1006.85651709881,
-1006.77655867177,-1006.73416279517,-1006.65420549504,-1006.5743426978,
-1006.49455687532,-1006.41483056013,-1006.33514633183,-1006.25547534561,
-1006.17580789209,-1006.09612824127,-1006.01642065888,-1005.9366254298,
-1005.85678108809,-1005.77682266105,-1005.73442678445,-1005.65446948432,
-1005.57460668708,-1005.4948208646,-1005.41509454941,-1005.33541032112,
-1005.25573933489,-1005.17607188137,-1005.09639223055,-1005.01668464816,
-1004.93688941908,-1004.85704507737,-1004.77708665033,-1004.73469077373,
-1004.6547334736,-1004.57487067636,-1004.49508485389,-1004.41535853869,
-1004.3356743104,-1004.25600332418,-1004.17633587065,-1004.09665621983,
-1004.01694863744,-1003.93715340836,-1003.85730906666,-1003.77735063961,
-1003.73495476301,-1003.65416438689,-1003.57347370472,-1003.49286779783,
-1003.41233180347,-1003.33185761023,-1003.25141993018,-1003.17099831016,
-1003.11900559039),.UNSPECIFIED.);
#1508=B_SPLINE_CURVE_WITH_KNOTS('',3,(#173719,#173720,#173721,#173722,#173723,
#173724,#173725,#173726,#173727,#173728),.UNSPECIFIED.,.F.,.F.,(4,1,1,1,
1,1,1,4),(-1003.1189981033,-1002.73521875229,-1001.73548274157,-1000.73574673085,
-999.736010720131,-998.736274709411,-997.736538698691,-996.835829368632),
 .UNSPECIFIED.);
#1509=B_SPLINE_CURVE_WITH_KNOTS('',3,(#173730,#173731,#173732,#173733,#173734,
#173735,#173736,#173737,#173738,#173739,#173740,#173741,#173742,#173743,
#173744,#173745,#173746,#173747,#173748,#173749,#173750,#173751,#173752,
#173753,#173754,#173755,#173756,#173757,#173758,#173759,#173760,#173761,
#173762,#173763,#173764,#173765,#173766,#173767,#173768,#173769,#173770,
#173771,#173772,#173773,#173774,#173775,#173776,#173777,#173778,#173779,
#173780,#173781,#173782,#173783,#173784,#173785,#173786,#173787,#173788,
#173789,#173790,#173791,#173792,#173793,#173794,#173795,#173796,#173797,
#173798,#173799,#173800,#173801,#173802,#173803,#173804,#173805,#173806,
#173807,#173808,#173809,#173810,#173811,#173812,#173813,#173814,#173815,
#173816,#173817,#173818,#173819,#173820,#173821,#173822,#173823,#173824,
#173825,#173826,#173827,#173828,#173829,#173830,#173831,#173832,#173833,
#173834,#173835,#173836,#173837,#173838,#173839,#173840,#173841,#173842,
#173843,#173844,#173845,#173846,#173847,#173848,#173849,#173850,#173851,
#173852,#173853,#173854,#173855,#173856,#173857,#173858,#173859,#173860,
#173861,#173862,#173863,#173864,#173865,#173866,#173867,#173868,#173869,
#173870,#173871,#173872,#173873,#173874,#173875,#173876,#173877,#173878,
#173879,#173880,#173881,#173882,#173883,#173884,#173885,#173886,#173887,
#173888,#173889,#173890,#173891,#173892,#173893,#173894,#173895,#173896,
#173897,#173898,#173899,#173900,#173901,#173902,#173903,#173904,#173905,
#173906,#173907,#173908,#173909,#173910,#173911,#173912,#173913,#173914,
#173915,#173916,#173917,#173918,#173919,#173920,#173921,#173922,#173923,
#173924,#173925,#173926,#173927,#173928,#173929,#173930,#173931,#173932,
#173933,#173934,#173935,#173936,#173937,#173938,#173939,#173940,#173941,
#173942,#173943,#173944,#173945,#173946,#173947,#173948,#173949,#173950,
#173951,#173952,#173953,#173954,#173955,#173956,#173957,#173958,#173959,
#173960,#173961,#173962,#173963,#173964,#173965,#173966,#173967,#173968,
#173969,#173970,#173971,#173972,#173973),.UNSPECIFIED.,.F.,.F.,(4,3,3,3,
3,3,3,3,3,3,3,3,3,3,3,3,3,3,3,3,3,3,3,3,3,3,3,3,3,3,3,3,3,3,3,3,3,3,3,3,
3,3,3,3,3,3,3,3,3,3,3,3,3,3,3,3,3,3,3,3,3,3,3,3,3,3,3,3,3,3,3,3,3,3,3,3,
3,3,3,3,3,4),(-996.835820283214,-996.736802687971,-996.656845387839,-996.576982590595,
-996.497196768122,-996.417470452926,-996.337786224631,-996.258115238409,
-996.178447784882,-996.098768134065,-996.019060551669,-995.939265322593,
-995.859420980884,-995.779462553835,-995.737066677251,-995.65710937712,
-995.577246579877,-995.497460757405,-995.41773444221,-995.338050213916,
-995.258379227695,-995.178711774169,-995.099032123353,-995.019324540959,
-994.939529311883,-994.859684970175,-994.779726543128,-994.73733066653,
-994.657373366399,-994.577510569156,-994.497724746684,-994.417998431489,
-994.338314203195,-994.258643216974,-994.178975763448,-994.099296112632,
-994.019588530237,-993.939793301162,-993.859948959454,-993.779990532407,
-993.73759465581,-993.657637355679,-993.577774558436,-993.497988735965,
-993.418262420769,-993.338578192475,-993.258907206254,-993.179239752729,
-993.099560101912,-993.019852519518,-992.940057290442,-992.860212948735,
-992.780254521687,-992.73785864509,-992.657901344959,-992.578038547716,
-992.498252725244,-992.418526410049,-992.338842181755,-992.259171195534,
-992.179503742008,-992.099824091192,-992.020116508798,-991.940321279722,
-991.860476938015,-991.780518510967,-991.73812263437,-991.658165334239,
-991.578302536996,-991.498516714524,-991.418790399329,-991.339106171035,
-991.259435184814,-991.179767731288,-991.100088080471,-991.020380498077,
-990.940585269001,-990.860740927293,-990.780782500246,-990.73838662365,
-990.619045316449,-990.552634976034),.UNSPECIFIED.);
#1510=B_SPLINE_CURVE_WITH_KNOTS('',3,(#173975,#173976,#173977,#173978,#173979,
#173980,#173981,#173982,#173983,#173984),.UNSPECIFIED.,.F.,.F.,(4,1,1,1,
1,1,1,4),(-990.552630350918,-989.73865061293,-988.73891460221,-987.739178591489,
-986.739442580769,-985.739706570049,-984.739970559329,-984.269449668855),
 .UNSPECIFIED.);
#1511=B_SPLINE_CURVE_WITH_KNOTS('',3,(#173986,#173987,#173988,#173989,#173990,
#173991,#173992,#173993,#173994,#173995),.UNSPECIFIED.,.F.,.F.,(4,1,1,1,
1,1,1,4),(-984.269449668855,-983.740234548609,-982.740498537889,-981.740762527169,
-980.741026516449,-979.741290505728,-978.741554495008,-977.986264361675),
 .UNSPECIFIED.);
#1512=B_SPLINE_CURVE_WITH_KNOTS('',3,(#173997,#173998,#173999,#174000,#174001,
#174002,#174003,#174004,#174005,#174006,#174007,#174008,#174009,#174010,
#174011,#174012,#174013,#174014,#174015,#174016,#174017,#174018,#174019,
#174020,#174021,#174022,#174023,#174024,#174025,#174026,#174027,#174028,
#174029,#174030,#174031,#174032,#174033,#174034,#174035,#174036,#174037,
#174038,#174039,#174040,#174041,#174042,#174043,#174044,#174045,#174046,
#174047,#174048,#174049,#174050,#174051,#174052,#174053,#174054,#174055,
#174056,#174057,#174058,#174059,#174060,#174061,#174062,#174063,#174064,
#174065,#174066,#174067,#174068,#174069,#174070,#174071,#174072,#174073,
#174074,#174075,#174076,#174077,#174078,#174079,#174080,#174081,#174082,
#174083,#174084,#174085,#174086,#174087,#174088,#174089,#174090,#174091,
#174092,#174093,#174094,#174095,#174096,#174097,#174098,#174099,#174100,
#174101,#174102,#174103,#174104,#174105,#174106,#174107,#174108,#174109,
#174110,#174111,#174112,#174113,#174114,#174115,#174116,#174117,#174118,
#174119,#174120,#174121,#174122,#174123,#174124,#174125,#174126,#174127,
#174128,#174129,#174130,#174131,#174132,#174133,#174134,#174135,#174136,
#174137,#174138,#174139,#174140,#174141,#174142,#174143,#174144,#174145,
#174146,#174147,#174148,#174149,#174150,#174151,#174152,#174153,#174154,
#174155,#174156,#174157,#174158,#174159,#174160,#174161,#174162,#174163,
#174164,#174165,#174166,#174167,#174168,#174169,#174170,#174171,#174172,
#174173,#174174,#174175,#174176,#174177,#174178,#174179,#174180,#174181,
#174182,#174183,#174184,#174185,#174186,#174187,#174188,#174189,#174190,
#174191,#174192,#174193,#174194,#174195,#174196,#174197,#174198,#174199,
#174200,#174201,#174202,#174203,#174204,#174205,#174206,#174207,#174208,
#174209,#174210,#174211,#174212,#174213,#174214,#174215,#174216,#174217,
#174218,#174219,#174220,#174221,#174222,#174223,#174224,#174225,#174226,
#174227,#174228,#174229,#174230,#174231,#174232,#174233,#174234,#174235,
#174236,#174237,#174238,#174239,#174240,#174241,#174242,#174243),
 .UNSPECIFIED.,.F.,.F.,(4,3,3,3,3,3,3,3,3,3,3,3,3,3,3,3,3,3,3,3,3,3,3,3,
3,3,3,3,3,3,3,3,3,3,3,3,3,3,3,3,3,3,3,3,3,3,3,3,3,3,3,3,3,3,3,3,3,3,3,3,
3,3,3,3,3,3,3,3,3,3,3,3,3,3,3,3,3,3,3,3,3,3,4),(-977.986264286946,-977.882988264251,
-977.777257487168,-977.741818484288,-977.661861184157,-977.581998386914,
-977.502212564442,-977.422486249247,-977.342802020953,-977.263131034732,
-977.183463581206,-977.103783930389,-977.024076347995,-976.944281118919,
-976.864436777212,-976.784478350164,-976.742082473568,-976.662125173437,
-976.582262376194,-976.502476553722,-976.422750238527,-976.343066010233,
-976.263395024012,-976.183727570486,-976.10404791967,-976.024340337275,
-975.9445451082,-975.864700766492,-975.784742339445,-975.742346462848,-975.662389162717,
-975.582526365474,-975.502740543002,-975.423014227807,-975.343329999513,
-975.263659013292,-975.183991559766,-975.104311908949,-975.024604326555,
-974.944809097479,-974.864964755772,-974.785006328724,-974.742610452128,
-974.662653151997,-974.582790354754,-974.503004532282,-974.423278217087,
-974.343593988793,-974.263923002572,-974.184255549046,-974.10457589823,
-974.024868315835,-973.94507308676,-973.865228745052,-973.785270318005,
-973.742874441408,-973.662917141277,-973.583054344035,-973.503268521563,
-973.423542206368,-973.343857978074,-973.264186991853,-973.184519538327,
-973.104839887511,-973.025132305117,-972.945337076041,-972.865492734334,
-972.785534307287,-972.743138430688,-972.663181130556,-972.583318333313,
-972.503532510841,-972.423806195645,-972.344121967351,-972.26445098113,
-972.184783527603,-972.105103876787,-972.025396294392,-971.945601065316,
-971.865756723608,-971.78579829656,-971.743402419967,-971.703079054496),
 .UNSPECIFIED.);
#1513=B_SPLINE_CURVE_WITH_KNOTS('',3,(#174245,#174246,#174247,#174248,#174249,
#174250,#174251,#174252,#174253,#174254),.UNSPECIFIED.,.F.,.F.,(4,1,1,1,
1,1,1,4),(-971.703073555962,-970.743666409247,-969.743930398527,-968.744194387807,
-967.744458377087,-966.744722366367,-965.744986355647,-965.419893747316),
 .UNSPECIFIED.);
#1514=B_SPLINE_CURVE_WITH_KNOTS('',3,(#174256,#174257,#174258,#174259,#174260,
#174261,#174262,#174263,#174264,#174265),.UNSPECIFIED.,.F.,.F.,(4,1,1,1,
1,1,1,4),(-965.419893747316,-964.745250344926,-963.745514334207,-962.745778323486,
-961.746042312766,-960.746306302046,-959.746570291326,-959.136708440137),
 .UNSPECIFIED.);
#1515=B_SPLINE_CURVE_WITH_KNOTS('',3,(#174267,#174268,#174269,#174270,#174271,
#174272,#174273,#174274,#174275,#174276),.UNSPECIFIED.,.F.,.F.,(4,1,1,1,
1,1,1,4),(-959.136708440137,-958.746834280606,-957.747098269886,-956.747362259165,
-955.747626248445,-954.747890237725,-953.748154227005,-952.853523132957),
 .UNSPECIFIED.);
#1516=B_SPLINE_CURVE_WITH_KNOTS('',3,(#174278,#174279,#174280,#174281,#174282,
#174283,#174284,#174285,#174286,#174287,#174288),.UNSPECIFIED.,.F.,.F.,
(4,1,1,1,1,1,1,1,4),(-952.853523132957,-952.748418216285,-951.748682205565,
-950.748946194845,-949.749210184125,-948.749474173404,-947.749738162684,
-946.750002151964,-946.570337825777),.UNSPECIFIED.);
#1517=B_SPLINE_CURVE_WITH_KNOTS('',3,(#174290,#174291,#174292,#174293,#174294,
#174295,#174296,#174297,#174298,#174299,#174300,#174301,#174302,#174303,
#174304,#174305,#174306,#174307,#174308,#174309,#174310,#174311,#174312,
#174313,#174314,#174315,#174316,#174317,#174318,#174319,#174320,#174321,
#174322,#174323,#174324,#174325,#174326,#174327,#174328,#174329,#174330,
#174331,#174332,#174333,#174334,#174335,#174336,#174337,#174338,#174339,
#174340,#174341,#174342,#174343,#174344,#174345,#174346,#174347,#174348,
#174349,#174350,#174351,#174352,#174353,#174354,#174355,#174356,#174357,
#174358,#174359,#174360,#174361,#174362,#174363,#174364,#174365,#174366,
#174367,#174368,#174369,#174370,#174371,#174372,#174373,#174374,#174375,
#174376,#174377,#174378,#174379,#174380,#174381,#174382,#174383,#174384,
#174385,#174386,#174387,#174388,#174389,#174390,#174391,#174392,#174393,
#174394,#174395,#174396,#174397,#174398,#174399,#174400,#174401,#174402,
#174403,#174404,#174405,#174406,#174407,#174408,#174409,#174410,#174411,
#174412,#174413,#174414,#174415,#174416,#174417,#174418,#174419,#174420,
#174421,#174422,#174423,#174424,#174425,#174426,#174427,#174428,#174429,
#174430,#174431,#174432,#174433,#174434,#174435,#174436,#174437,#174438,
#174439,#174440,#174441,#174442,#174443,#174444,#174445,#174446,#174447,
#174448,#174449,#174450,#174451,#174452,#174453,#174454,#174455,#174456,
#174457,#174458,#174459,#174460,#174461,#174462,#174463,#174464,#174465,
#174466,#174467,#174468,#174469,#174470,#174471,#174472,#174473,#174474,
#174475,#174476,#174477,#174478,#174479,#174480,#174481,#174482,#174483,
#174484,#174485,#174486,#174487,#174488,#174489,#174490,#174491,#174492,
#174493,#174494,#174495,#174496,#174497,#174498,#174499,#174500,#174501,
#174502,#174503,#174504,#174505,#174506,#174507,#174508,#174509,#174510,
#174511,#174512,#174513,#174514,#174515,#174516,#174517,#174518,#174519,
#174520,#174521,#174522,#174523,#174524,#174525,#174526,#174527,#174528,
#174529,#174530,#174531,#174532,#174533,#174534,#174535,#174536),
 .UNSPECIFIED.,.F.,.F.,(4,3,3,3,3,3,3,3,3,3,3,3,3,3,3,3,3,3,3,3,3,3,3,3,
3,3,3,3,3,3,3,3,3,3,3,3,3,3,3,3,3,3,3,3,3,3,3,3,3,3,3,3,3,3,3,3,3,3,3,3,
3,3,3,3,3,3,3,3,3,3,3,3,3,3,3,3,3,3,3,3,3,3,4),(-946.570337825777,-946.49169399442,
-946.413118638042,-946.334593371033,-946.256091089334,-946.177597911869,
-946.099097271433,-946.020572596639,-945.941965426675,-945.863311049155,
-945.7845474559,-945.750266141244,-945.670308841113,-945.59044604387,-945.510660221398,
-945.430933906203,-945.351249677909,-945.271578691688,-945.191911238163,
-945.112231587346,-945.032524004952,-944.952728775876,-944.872884434168,
-944.792926007121,-944.750530130524,-944.670572830393,-944.59071003315,
-944.510924210678,-944.431197895483,-944.351513667189,-944.271842680968,
-944.192175227442,-944.112495576626,-944.032787994232,-943.952992765156,
-943.873148423448,-943.793189996401,-943.750794119804,-943.670836819673,
-943.59097402243,-943.511188199958,-943.431461884764,-943.351777656469,
-943.272106670248,-943.192439216723,-943.112759565906,-943.033051983512,
-942.953256754436,-942.873412412728,-942.793453985681,-942.751058109084,
-942.671100808953,-942.59123801171,-942.511452189238,-942.431725874042,
-942.352041645748,-942.272370659527,-942.192703206002,-942.113023555185,
-942.033315972791,-941.953520743716,-941.873676402008,-941.793717974961,
-941.751322098364,-941.671364798233,-941.59150200099,-941.511716178518,
-941.431989863322,-941.352305635028,-941.272634648806,-941.19296719528,
-941.113287544464,-941.033579962069,-940.953784732993,-940.873940391285,
-940.793981964238,-940.751586087643,-940.666044999251,-940.580666781501,
-940.495520242455,-940.410515725407,-940.325710494659,-940.287152712433),
 .UNSPECIFIED.);
#1518=B_SPLINE_CURVE_WITH_KNOTS('',3,(#174538,#174539,#174540,#174541,#174542,
#174543,#174544,#174545,#174546,#174547),.UNSPECIFIED.,.F.,.F.,(4,1,1,1,
1,1,1,4),(-940.287152518598,-939.751850076923,-938.752114066203,-937.752378055483,
-936.752642044763,-935.752906034043,-934.753170023323,-934.003967211418),
 .UNSPECIFIED.);
#1519=B_SPLINE_CURVE_WITH_KNOTS('',3,(#174549,#174550,#174551,#174552,#174553,
#174554,#174555,#174556,#174557,#174558,#174559,#174560,#174561,#174562,
#174563,#174564,#174565,#174566,#174567,#174568,#174569,#174570,#174571,
#174572,#174573,#174574,#174575,#174576,#174577,#174578,#174579,#174580,
#174581,#174582,#174583,#174584,#174585,#174586,#174587,#174588,#174589,
#174590,#174591,#174592,#174593,#174594,#174595,#174596,#174597,#174598,
#174599,#174600,#174601,#174602,#174603,#174604,#174605,#174606,#174607,
#174608,#174609,#174610,#174611,#174612,#174613,#174614,#174615,#174616,
#174617,#174618,#174619,#174620,#174621,#174622,#174623,#174624,#174625,
#174626,#174627,#174628,#174629,#174630,#174631,#174632,#174633,#174634,
#174635,#174636,#174637,#174638,#174639,#174640,#174641,#174642,#174643,
#174644,#174645,#174646,#174647,#174648,#174649,#174650,#174651,#174652,
#174653,#174654,#174655,#174656,#174657,#174658,#174659,#174660,#174661,
#174662,#174663,#174664,#174665,#174666,#174667,#174668,#174669,#174670,
#174671,#174672,#174673,#174674,#174675,#174676,#174677,#174678,#174679,
#174680,#174681,#174682,#174683,#174684,#174685,#174686,#174687,#174688,
#174689,#174690,#174691,#174692,#174693,#174694,#174695,#174696,#174697,
#174698,#174699,#174700,#174701,#174702,#174703,#174704,#174705,#174706,
#174707,#174708,#174709,#174710,#174711,#174712,#174713,#174714,#174715,
#174716,#174717,#174718,#174719,#174720,#174721,#174722,#174723,#174724,
#174725,#174726,#174727,#174728,#174729,#174730,#174731,#174732,#174733,
#174734,#174735,#174736,#174737,#174738,#174739,#174740,#174741,#174742,
#174743,#174744,#174745,#174746,#174747,#174748,#174749,#174750,#174751,
#174752,#174753,#174754,#174755,#174756,#174757,#174758,#174759,#174760,
#174761,#174762,#174763,#174764,#174765,#174766,#174767,#174768,#174769,
#174770,#174771,#174772,#174773,#174774,#174775,#174776,#174777,#174778,
#174779,#174780,#174781,#174782,#174783,#174784,#174785,#174786,#174787,
#174788,#174789,#174790,#174791,#174792,#174793,#174794,#174795),
 .UNSPECIFIED.,.F.,.F.,(4,3,3,3,3,3,3,3,3,3,3,3,3,3,3,3,3,3,3,3,3,3,3,3,
3,3,3,3,3,3,3,3,3,3,3,3,3,3,3,3,3,3,3,3,3,3,3,3,3,3,3,3,3,3,3,3,3,3,3,3,
3,3,3,3,3,3,3,3,3,3,3,3,3,3,3,3,3,3,3,3,3,3,4),(-934.003967155371,-933.901650858112,
-933.797081270037,-933.753434012602,-933.673476712471,-933.593613915228,
-933.513828092756,-933.434101777561,-933.354417549267,-933.274746563046,
-933.19507910952,-933.115399458704,-933.035691876309,-932.955896647234,
-932.876052305526,-932.796093878479,-932.753698001882,-932.673740701751,
-932.593877904508,-932.514092082036,-932.434365766841,-932.354681538547,
-932.275010552326,-932.1953430988,-932.115663447983,-932.035955865589,-931.956160636513,
-931.876316294806,-931.796357867758,-931.753961991162,-931.674004691031,
-931.594141893788,-931.514356071316,-931.434629756121,-931.354945527827,
-931.275274541606,-931.19560708808,-931.115927437264,-931.036219854869,
-930.956424625794,-930.876580284086,-930.796621857039,-930.754225980442,
-930.674268680311,-930.594405883068,-930.514620060596,-930.434893745401,
-930.355209517107,-930.275538530886,-930.19587107736,-930.116191426543,
-930.036483844149,-929.956688615073,-929.876844273366,-929.796885846318,
-929.754489969722,-929.674532669591,-929.594669872348,-929.514884049876,
-929.435157734681,-929.355473506387,-929.275802520166,-929.19613506664,
-929.116455415824,-929.036747833429,-928.956952604354,-928.877108262646,
-928.797149835599,-928.754753959002,-928.674796658871,-928.594933861628,
-928.515148039157,-928.435421723961,-928.355737495667,-928.276066509446,
-928.19639905592,-928.116719405104,-928.037011822709,-927.957216593634,
-927.877372251926,-927.797413824879,-927.755017948282,-927.720781904239),
 .UNSPECIFIED.);
#1520=B_SPLINE_CURVE_WITH_KNOTS('',3,(#174797,#174798,#174799,#174800,#174801,
#174802,#174803,#174804,#174805,#174806),.UNSPECIFIED.,.F.,.F.,(4,1,1,1,
1,1,1,4),(-927.720777243923,-926.755281937562,-925.755545926841,-924.755809916121,
-923.756073905401,-922.756337894681,-921.756601883961,-921.437596597059),
 .UNSPECIFIED.);
#1521=B_SPLINE_CURVE_WITH_KNOTS('',3,(#174808,#174809,#174810,#174811,#174812,
#174813,#174814,#174815,#174816,#174817),.UNSPECIFIED.,.F.,.F.,(4,1,1,1,
1,1,1,4),(-921.437596597059,-920.756865873241,-919.757129862521,-918.7573938518,
-917.75765784108,-916.75792183036,-915.75818581964,-915.15441128988),
 .UNSPECIFIED.);
#1522=B_SPLINE_CURVE_WITH_KNOTS('',3,(#174819,#174820,#174821,#174822,#174823,
#174824,#174825,#174826,#174827,#174828),.UNSPECIFIED.,.F.,.F.,(4,1,1,1,
1,1,1,4),(-915.15441128988,-914.75844980892,-913.7587137982,-912.75897778748,
-911.75924177676,-910.75950576604,-909.759769755319,-908.8712259827),
 .UNSPECIFIED.);
#1523=B_SPLINE_CURVE_WITH_KNOTS('',3,(#174830,#174831,#174832,#174833,#174834,
#174835,#174836,#174837,#174838,#174839,#174840),.UNSPECIFIED.,.F.,.F.,
(4,1,1,1,1,1,1,1,4),(-908.8712259827,-908.760033744599,-907.760297733879,
-906.760561723159,-905.760825712439,-904.761089701719,-903.761353690998,
-902.761617680278,-902.588040675521),.UNSPECIFIED.);
#1524=B_SPLINE_CURVE_WITH_KNOTS('',3,(#174842,#174843,#174844,#174845,#174846,
#174847,#174848,#174849,#174850,#174851,#174852,#174853,#174854,#174855,
#174856,#174857,#174858,#174859,#174860,#174861,#174862,#174863,#174864,
#174865,#174866,#174867,#174868,#174869,#174870,#174871,#174872,#174873,
#174874,#174875,#174876,#174877,#174878,#174879,#174880,#174881,#174882,
#174883,#174884,#174885,#174886,#174887,#174888,#174889,#174890,#174891,
#174892,#174893,#174894,#174895,#174896,#174897,#174898,#174899,#174900,
#174901,#174902,#174903,#174904,#174905,#174906,#174907,#174908,#174909,
#174910,#174911,#174912,#174913,#174914,#174915,#174916,#174917,#174918,
#174919,#174920,#174921,#174922,#174923,#174924,#174925,#174926,#174927,
#174928,#174929,#174930,#174931,#174932,#174933,#174934,#174935,#174936,
#174937,#174938,#174939,#174940,#174941,#174942,#174943,#174944,#174945,
#174946,#174947,#174948,#174949,#174950,#174951,#174952,#174953,#174954,
#174955,#174956,#174957,#174958,#174959,#174960,#174961,#174962,#174963,
#174964,#174965,#174966,#174967,#174968,#174969,#174970,#174971,#174972,
#174973,#174974,#174975,#174976,#174977,#174978,#174979,#174980,#174981,
#174982,#174983,#174984,#174985,#174986,#174987,#174988,#174989,#174990,
#174991,#174992,#174993,#174994,#174995,#174996,#174997,#174998,#174999,
#175000,#175001,#175002,#175003,#175004,#175005,#175006,#175007,#175008,
#175009,#175010,#175011,#175012,#175013,#175014,#175015,#175016,#175017,
#175018,#175019,#175020,#175021,#175022,#175023,#175024,#175025,#175026,
#175027,#175028,#175029,#175030,#175031,#175032,#175033,#175034,#175035,
#175036,#175037,#175038,#175039,#175040,#175041,#175042,#175043,#175044,
#175045,#175046,#175047,#175048,#175049,#175050,#175051,#175052,#175053,
#175054,#175055,#175056,#175057,#175058,#175059,#175060,#175061,#175062,
#175063,#175064,#175065,#175066,#175067,#175068,#175069,#175070,#175071,
#175072,#175073,#175074,#175075,#175076,#175077,#175078,#175079,#175080,
#175081,#175082,#175083,#175084,#175085,#175086,#175087,#175088),
 .UNSPECIFIED.,.F.,.F.,(4,3,3,3,3,3,3,3,3,3,3,3,3,3,3,3,3,3,3,3,3,3,3,3,
3,3,3,3,3,3,3,3,3,3,3,3,3,3,3,3,3,3,3,3,3,3,3,3,3,3,3,3,3,3,3,3,3,3,3,3,
3,3,3,3,3,3,3,3,3,3,3,3,3,3,3,3,3,3,3,3,3,3,4),(-902.588040675521,-902.509394374953,
-902.430818019321,-902.352293215628,-902.273793277036,-902.195303758856,
-902.116808091585,-902.03828970253,-901.959689426147,-901.881043118882,
-901.802286029661,-901.761881669558,-901.681924369427,-901.602061572184,
-901.522275749713,-901.442549434517,-901.362865206223,-901.283194220002,
-901.203526766476,-901.12384711566,-901.044139533266,-900.96434430419,-900.884499962482,
-900.804541535435,-900.762145658838,-900.682188358707,-900.602325561464,
-900.522539738992,-900.442813423797,-900.363129195503,-900.283458209282,
-900.203790755757,-900.12411110494,-900.044403522546,-899.96460829347,-899.884763951762,
-899.804805524715,-899.762409648118,-899.682452347987,-899.602589550744,
-899.522803728272,-899.443077413077,-899.363393184783,-899.283722198563,
-899.204054745037,-899.12437509422,-899.044667511825,-898.96487228275,-898.885027941042,
-898.805069513995,-898.762673637398,-898.682716337267,-898.602853540024,
-898.523067717552,-898.443341402357,-898.363657174063,-898.283986187842,
-898.204318734316,-898.1246390835,-898.044931501105,-897.965136272029,-897.885291930322,
-897.805333503274,-897.762937626678,-897.682980326547,-897.603117529304,
-897.523331706833,-897.443605391638,-897.363921163344,-897.284250177123,
-897.204582723597,-897.124903072781,-897.045195490386,-896.965400261311,
-896.885555919603,-896.805597492556,-896.763201615958,-896.677381751715,
-896.591729906743,-896.506318888007,-896.421057019866,-896.336003844487,
-896.30485559323),.UNSPECIFIED.);
#1525=B_SPLINE_CURVE_WITH_KNOTS('',3,(#175090,#175091,#175092,#175093,#175094,
#175095,#175096,#175097,#175098,#175099),.UNSPECIFIED.,.F.,.F.,(4,1,1,1,
1,1,1,4),(-896.304855368341,-895.763465605238,-894.763729594517,-893.763993583797,
-892.764257573077,-891.764521562357,-890.764785551637,-890.021670061161),
 .UNSPECIFIED.);
#1526=B_SPLINE_CURVE_WITH_KNOTS('',3,(#175101,#175102,#175103,#175104,#175105,
#175106,#175107,#175108,#175109,#175110,#175111,#175112,#175113,#175114,
#175115,#175116,#175117,#175118,#175119,#175120,#175121,#175122,#175123,
#175124,#175125,#175126,#175127,#175128,#175129,#175130,#175131,#175132,
#175133,#175134,#175135,#175136,#175137,#175138,#175139,#175140,#175141,
#175142,#175143,#175144,#175145,#175146,#175147,#175148,#175149,#175150,
#175151,#175152,#175153,#175154,#175155,#175156,#175157,#175158,#175159,
#175160,#175161,#175162,#175163,#175164,#175165,#175166,#175167,#175168,
#175169,#175170,#175171,#175172,#175173,#175174,#175175,#175176,#175177,
#175178,#175179,#175180,#175181,#175182,#175183,#175184,#175185,#175186,
#175187,#175188,#175189,#175190,#175191,#175192,#175193,#175194,#175195,
#175196,#175197,#175198,#175199,#175200,#175201,#175202,#175203,#175204,
#175205,#175206,#175207,#175208,#175209,#175210,#175211,#175212,#175213,
#175214,#175215,#175216,#175217,#175218,#175219,#175220,#175221,#175222,
#175223,#175224,#175225,#175226,#175227,#175228,#175229,#175230,#175231,
#175232,#175233,#175234,#175235,#175236,#175237,#175238,#175239,#175240,
#175241,#175242,#175243,#175244,#175245,#175246,#175247,#175248,#175249,
#175250,#175251,#175252,#175253,#175254,#175255,#175256,#175257,#175258,
#175259,#175260,#175261,#175262,#175263,#175264,#175265,#175266,#175267,
#175268,#175269,#175270,#175271,#175272,#175273,#175274,#175275,#175276,
#175277,#175278,#175279,#175280,#175281,#175282,#175283,#175284,#175285,
#175286,#175287,#175288,#175289,#175290,#175291,#175292,#175293,#175294,
#175295,#175296,#175297,#175298,#175299,#175300,#175301,#175302,#175303,
#175304,#175305,#175306,#175307,#175308,#175309,#175310,#175311,#175312,
#175313,#175314,#175315,#175316,#175317,#175318,#175319,#175320,#175321,
#175322,#175323,#175324,#175325,#175326,#175327,#175328,#175329,#175330,
#175331,#175332,#175333,#175334,#175335,#175336,#175337,#175338,#175339,
#175340,#175341,#175342,#175343,#175344,#175345,#175346,#175347),
 .UNSPECIFIED.,.F.,.F.,(4,3,3,3,3,3,3,3,3,3,3,3,3,3,3,3,3,3,3,3,3,3,3,3,
3,3,3,3,3,3,3,3,3,3,3,3,3,3,3,3,3,3,3,3,3,3,3,3,3,3,3,3,3,3,3,3,3,3,3,3,
3,3,3,3,3,3,3,3,3,3,3,3,3,3,3,3,3,3,3,3,3,3,4),(-890.021669986904,-889.920265842706,
-889.816786494554,-889.765049540917,-889.685092240785,-889.605229443542,
-889.52544362107,-889.445717305874,-889.366033077579,-889.286362091358,
-889.206694637831,-889.127014987014,-889.047307404619,-888.967512175543,
-888.887667833835,-888.807709406787,-888.765313530197,-888.685356230066,
-888.605493432823,-888.525707610351,-888.445981295155,-888.366297066861,
-888.28662608064,-888.206958627114,-888.127278976297,-888.047571393903,
-887.967776164827,-887.887931823119,-887.807973396071,-887.765577519476,
-887.685620219345,-887.605757422102,-887.52597159963,-887.446245284435,
-887.366561056141,-887.28689006992,-887.207222616394,-887.127542965578,
-887.047835383184,-886.968040154108,-886.888195812401,-886.808237385353,
-886.765841508756,-886.685884208625,-886.606021411382,-886.526235588911,
-886.446509273715,-886.366825045421,-886.287154059201,-886.207486605675,
-886.127806954858,-886.048099372464,-885.968304143389,-885.888459801681,
-885.808501374634,-885.766105498036,-885.686148197905,-885.606285400662,
-885.52649957819,-885.446773262995,-885.367089034701,-885.28741804848,-885.207750594954,
-885.128070944137,-885.048363361743,-884.968568132667,-884.888723790959,
-884.808765363912,-884.766369487316,-884.686412187185,-884.606549389942,
-884.52676356747,-884.447037252275,-884.367353023981,-884.28768203776,-884.208014584234,
-884.128334933417,-884.048627351023,-883.968832121947,-883.888987780239,
-883.809029353192,-883.766633476596,-883.738484753982),.UNSPECIFIED.);
#1527=B_SPLINE_CURVE_WITH_KNOTS('',3,(#175349,#175350,#175351,#175352,#175353,
#175354,#175355,#175356,#175357,#175358,#175359,#175360,#175361,#175362,
#175363,#175364,#175365,#175366,#175367,#175368,#175369,#175370,#175371,
#175372,#175373,#175374,#175375,#175376,#175377,#175378,#175379,#175380,
#175381,#175382,#175383,#175384,#175385,#175386,#175387,#175388,#175389,
#175390,#175391,#175392,#175393,#175394,#175395,#175396,#175397,#175398,
#175399,#175400,#175401,#175402,#175403,#175404,#175405,#175406,#175407,
#175408,#175409,#175410,#175411,#175412,#175413,#175414,#175415,#175416,
#175417,#175418,#175419,#175420,#175421,#175422,#175423,#175424,#175425,
#175426,#175427,#175428,#175429,#175430,#175431,#175432,#175433,#175434,
#175435,#175436,#175437,#175438,#175439,#175440,#175441,#175442,#175443,
#175444,#175445,#175446,#175447,#175448,#175449,#175450,#175451,#175452,
#175453,#175454,#175455,#175456,#175457,#175458,#175459,#175460,#175461,
#175462,#175463,#175464,#175465,#175466,#175467,#175468,#175469,#175470,
#175471,#175472,#175473,#175474,#175475,#175476,#175477,#175478,#175479,
#175480,#175481,#175482,#175483,#175484,#175485,#175486,#175487,#175488,
#175489,#175490,#175491,#175492,#175493,#175494,#175495,#175496,#175497,
#175498,#175499,#175500,#175501,#175502,#175503,#175504,#175505,#175506,
#175507,#175508,#175509,#175510,#175511,#175512,#175513,#175514,#175515,
#175516,#175517,#175518,#175519,#175520,#175521,#175522,#175523,#175524,
#175525,#175526,#175527,#175528,#175529,#175530,#175531,#175532,#175533,
#175534,#175535,#175536,#175537,#175538,#175539,#175540,#175541,#175542,
#175543,#175544,#175545,#175546,#175547,#175548,#175549,#175550,#175551,
#175552,#175553,#175554,#175555,#175556,#175557,#175558,#175559,#175560,
#175561,#175562,#175563,#175564,#175565,#175566,#175567,#175568,#175569,
#175570,#175571,#175572,#175573,#175574,#175575,#175576,#175577,#175578,
#175579,#175580,#175581,#175582,#175583,#175584,#175585,#175586,#175587,
#175588,#175589,#175590,#175591,#175592,#175593,#175594,#175595),
 .UNSPECIFIED.,.F.,.F.,(4,3,3,3,3,3,3,3,3,3,3,3,3,3,3,3,3,3,3,3,3,3,3,3,
3,3,3,3,3,3,3,3,3,3,3,3,3,3,3,3,3,3,3,3,3,3,3,3,3,3,3,3,3,3,3,3,3,3,3,3,
3,3,3,3,3,3,3,3,3,3,3,3,3,3,3,3,3,3,3,3,3,3,4),(-883.73848475388,-883.658904576264,
-883.579417860576,-883.500006735715,-883.420653393899,-883.338933902896,
-883.259631332509,-883.180329314193,-883.1010118102,-883.021662775846,-882.942225636669,
-882.862735566645,-882.783138781002,-882.766897465876,-882.686940165745,
-882.607077368502,-882.52729154603,-882.447565230835,-882.367881002541,
-882.28821001632,-882.208542562794,-882.128862911978,-882.049155329583,
-881.969360100508,-881.8895157588,-881.809557331752,-881.767161455156,-881.687204155025,
-881.607341357782,-881.527555535311,-881.447829220115,-881.368144991821,
-881.2884740056,-881.208806552074,-881.129126901258,-881.049419318863,-880.969624089788,
-880.889779748081,-880.809821321033,-880.767425444436,-880.687468144304,
-880.607605347062,-880.52781952459,-880.448093209394,-880.368408981099,
-880.288737994878,-880.209070541352,-880.129390890535,-880.04968330814,
-879.969888079065,-879.890043737357,-879.810085310309,-879.767689433715,
-879.687732133584,-879.607869336341,-879.528083513869,-879.448357198674,
-879.36867297038,-879.289001984159,-879.209334530633,-879.129654879816,
-879.049947297422,-878.970152068346,-878.890307726639,-878.810349299592,
-878.767953422995,-878.687996122864,-878.608133325622,-878.52834750315,
-878.448621187955,-878.368936959661,-878.28926597344,-878.209598519914,
-878.129918869098,-878.050211286704,-877.970416057628,-877.890571715921,
-877.810613288874,-877.768217412275,-877.672191336738,-877.576693682037,
-877.482167121906,-877.455299654684),.UNSPECIFIED.);
#1528=B_SPLINE_CURVE_WITH_KNOTS('',3,(#175597,#175598,#175599,#175600,#175601,
#175602,#175603,#175604,#175605,#175606),.UNSPECIFIED.,.F.,.F.,(4,1,1,1,
1,1,1,4),(-877.455299446802,-876.768481401555,-875.768745390835,-874.769009380115,
-873.769273369395,-872.769537358675,-871.769801347954,-871.172114139623),
 .UNSPECIFIED.);
#1529=B_SPLINE_CURVE_WITH_KNOTS('',3,(#175608,#175609,#175610,#175611,#175612,
#175613,#175614,#175615,#175616,#175617,#175618,#175619,#175620,#175621,
#175622,#175623,#175624,#175625,#175626,#175627,#175628,#175629,#175630,
#175631,#175632,#175633,#175634,#175635,#175636,#175637,#175638,#175639,
#175640,#175641,#175642,#175643,#175644,#175645,#175646,#175647,#175648,
#175649,#175650,#175651,#175652,#175653,#175654,#175655,#175656,#175657,
#175658,#175659,#175660,#175661,#175662,#175663,#175664,#175665,#175666,
#175667,#175668,#175669,#175670,#175671,#175672,#175673,#175674,#175675,
#175676,#175677,#175678,#175679,#175680,#175681,#175682,#175683,#175684,
#175685,#175686,#175687,#175688,#175689,#175690,#175691,#175692,#175693,
#175694,#175695,#175696,#175697,#175698,#175699,#175700,#175701,#175702,
#175703,#175704,#175705,#175706,#175707,#175708,#175709,#175710,#175711,
#175712,#175713,#175714,#175715,#175716,#175717,#175718,#175719,#175720,
#175721,#175722,#175723,#175724,#175725,#175726,#175727,#175728,#175729,
#175730,#175731,#175732,#175733,#175734,#175735,#175736,#175737,#175738,
#175739,#175740,#175741,#175742,#175743,#175744,#175745,#175746,#175747,
#175748,#175749,#175750,#175751,#175752,#175753,#175754,#175755,#175756,
#175757,#175758,#175759,#175760,#175761,#175762,#175763,#175764,#175765,
#175766,#175767,#175768,#175769,#175770,#175771,#175772,#175773,#175774,
#175775,#175776,#175777,#175778,#175779,#175780,#175781,#175782,#175783,
#175784,#175785,#175786,#175787,#175788,#175789,#175790,#175791,#175792,
#175793,#175794,#175795,#175796,#175797,#175798,#175799,#175800,#175801,
#175802,#175803,#175804,#175805,#175806,#175807,#175808,#175809,#175810,
#175811,#175812,#175813,#175814,#175815,#175816,#175817,#175818,#175819,
#175820,#175821,#175822,#175823,#175824,#175825,#175826,#175827,#175828,
#175829,#175830,#175831,#175832,#175833,#175834,#175835,#175836,#175837,
#175838,#175839,#175840,#175841,#175842,#175843,#175844,#175845,#175846,
#175847,#175848,#175849,#175850,#175851,#175852,#175853,#175854),
 .UNSPECIFIED.,.F.,.F.,(4,3,3,3,3,3,3,3,3,3,3,3,3,3,3,3,3,3,3,3,3,3,3,3,
3,3,3,3,3,3,3,3,3,3,3,3,3,3,3,3,3,3,3,3,3,3,3,3,3,3,3,3,3,3,3,3,3,3,3,3,
3,3,3,3,3,3,3,3,3,3,3,3,3,3,3,3,3,3,3,3,3,3,4),(-871.172113916944,-871.084302572035,
-870.996038084311,-870.907543334164,-870.818727704578,-870.770065337234,
-870.690108037103,-870.610245239861,-870.530459417389,-870.450733102194,
-870.371048873901,-870.29137788768,-870.211710434154,-870.132030783338,
-870.052323200944,-869.972527971869,-869.892683630162,-869.812725203114,
-869.770329326514,-869.690372026383,-869.61050922914,-869.530723406668,
-869.450997091473,-869.371312863179,-869.291641876958,-869.211974423432,
-869.132294772616,-869.052587190221,-868.972791961146,-868.892947619438,
-868.812989192391,-868.770593315794,-868.690636015663,-868.61077321842,
-868.530987395948,-868.451261080753,-868.371576852459,-868.291905866238,
-868.212238412712,-868.132558761895,-868.052851179501,-867.973055950425,
-867.893211608718,-867.81325318167,-867.770857305074,-867.690900004943,
-867.6110372077,-867.531251385228,-867.451525070033,-867.371840841739,-867.292169855518,
-867.212502401992,-867.132822751176,-867.053115168781,-866.973319939706,
-866.893475597998,-866.813517170951,-866.771121294354,-866.691163994223,
-866.61130119698,-866.531515374508,-866.451789059313,-866.372104831019,
-866.292433844798,-866.212766391272,-866.133086740456,-866.053379158062,
-865.973583928986,-865.893739587279,-865.813781160231,-865.771385283634,
-865.692514875663,-865.613738208896,-865.535036863318,-865.454273359459,
-865.375663826956,-865.29706959623,-865.218474156873,-865.136087825765,
-865.057404123793,-864.978677878304,-864.899860992298,-864.888928832443),
 .UNSPECIFIED.);
#1530=B_SPLINE_CURVE_WITH_KNOTS('',3,(#175856,#175857,#175858,#175859,#175860,
#175861,#175862,#175863,#175864,#175865,#175866),.UNSPECIFIED.,.F.,.F.,
(4,1,1,1,1,1,1,1,4),(-864.888928832443,-864.771649272913,-863.771913262193,
-862.772177251473,-861.772441240753,-860.772705230033,-859.772969219313,
-858.773233208593,-858.605743525264),.UNSPECIFIED.);
#1531=B_SPLINE_CURVE_WITH_KNOTS('',3,(#175868,#175869,#175870,#175871,#175872,
#175873,#175874,#175875,#175876,#175877),.UNSPECIFIED.,.F.,.F.,(4,1,1,1,
1,1,1,4),(-858.605743525264,-857.773497197872,-856.773761187152,-855.774025176432,
-854.774289165712,-853.774553154992,-852.774817144272,-852.322558218084),
 .UNSPECIFIED.);
#1532=B_SPLINE_CURVE_WITH_KNOTS('',3,(#175879,#175880,#175881,#175882,#175883,
#175884,#175885,#175886,#175887,#175888),.UNSPECIFIED.,.F.,.F.,(4,1,1,1,
1,1,1,4),(-852.322558218084,-851.775081133552,-850.775345122832,-849.775609112111,
-848.775873101391,-847.776137090671,-846.776401079951,-846.039372910904),
 .UNSPECIFIED.);
#1533=B_SPLINE_CURVE_WITH_KNOTS('',3,(#175890,#175891,#175892,#175893,#175894,
#175895,#175896,#175897,#175898,#175899,#175900),.UNSPECIFIED.,.F.,.F.,
(4,1,1,1,1,1,1,1,4),(-846.039372910904,-845.776665069231,-844.776929058511,
-843.777193047791,-842.777457037071,-841.77772102635,-840.77798501563,-839.77824900491,
-839.756187603725),.UNSPECIFIED.);
#1534=B_SPLINE_CURVE_WITH_KNOTS('',3,(#175902,#175903,#175904,#175905,#175906,
#175907,#175908,#175909,#175910,#175911,#175912,#175913,#175914,#175915,
#175916,#175917,#175918,#175919,#175920,#175921,#175922,#175923,#175924,
#175925,#175926,#175927,#175928,#175929,#175930,#175931,#175932,#175933,
#175934,#175935,#175936,#175937,#175938,#175939,#175940,#175941,#175942,
#175943,#175944,#175945,#175946,#175947,#175948,#175949,#175950,#175951,
#175952,#175953,#175954,#175955,#175956,#175957,#175958,#175959,#175960,
#175961,#175962,#175963,#175964,#175965,#175966,#175967,#175968,#175969,
#175970,#175971,#175972,#175973,#175974,#175975,#175976,#175977,#175978,
#175979,#175980,#175981,#175982,#175983,#175984,#175985,#175986,#175987,
#175988,#175989,#175990,#175991,#175992,#175993,#175994,#175995,#175996,
#175997,#175998,#175999,#176000,#176001,#176002,#176003,#176004,#176005,
#176006,#176007,#176008,#176009,#176010,#176011,#176012,#176013,#176014,
#176015,#176016,#176017,#176018,#176019,#176020,#176021,#176022,#176023,
#176024,#176025,#176026,#176027,#176028,#176029,#176030,#176031,#176032,
#176033,#176034,#176035,#176036,#176037,#176038,#176039,#176040,#176041,
#176042,#176043,#176044,#176045,#176046,#176047,#176048,#176049,#176050,
#176051,#176052,#176053,#176054,#176055,#176056,#176057,#176058,#176059,
#176060,#176061,#176062,#176063,#176064,#176065,#176066,#176067,#176068,
#176069,#176070,#176071,#176072,#176073,#176074,#176075,#176076,#176077,
#176078,#176079,#176080,#176081,#176082,#176083,#176084,#176085,#176086,
#176087,#176088,#176089,#176090,#176091,#176092,#176093,#176094,#176095,
#176096,#176097,#176098,#176099,#176100,#176101,#176102,#176103,#176104,
#176105,#176106,#176107,#176108,#176109,#176110,#176111,#176112,#176113,
#176114,#176115,#176116,#176117,#176118,#176119,#176120,#176121,#176122,
#176123,#176124,#176125,#176126,#176127,#176128,#176129,#176130,#176131,
#176132,#176133,#176134,#176135,#176136,#176137,#176138,#176139,#176140,
#176141,#176142,#176143,#176144,#176145,#176146,#176147,#176148),
 .UNSPECIFIED.,.F.,.F.,(4,3,3,3,3,3,3,3,3,3,3,3,3,3,3,3,3,3,3,3,3,3,3,3,
3,3,3,3,3,3,3,3,3,3,3,3,3,3,3,3,3,3,3,3,3,3,3,3,3,3,3,3,3,3,3,3,3,3,3,3,
3,3,3,3,3,3,3,3,3,3,3,3,3,3,3,3,3,3,3,3,3,3,4),(-839.756187603725,-839.676531395756,
-839.596969010512,-839.517482640912,-839.438054542635,-839.355611849079,
-839.276235882847,-839.196860955274,-839.117471086351,-839.038050289642,
-838.95854142878,-838.878980288109,-838.79931114942,-838.77851299419,-838.698555694059,
-838.618692896816,-838.538907074344,-838.459180759149,-838.379496530855,
-838.299825544634,-838.220158091108,-838.140478440292,-838.060770857898,
-837.980975628822,-837.901131287115,-837.821172860067,-837.77877698347,
-837.698819683339,-837.618956886096,-837.539171063624,-837.459444748429,
-837.379760520135,-837.300089533914,-837.220422080388,-837.140742429571,
-837.061034847177,-836.981239618101,-836.901395276393,-836.821436849346,
-836.77904097275,-836.699083672619,-836.619220875376,-836.539435052904,
-836.459708737709,-836.380024509415,-836.300353523194,-836.220686069668,
-836.141006418851,-836.061298836457,-835.981503607381,-835.901659265674,
-835.821700838626,-835.77930496203,-835.699347661899,-835.619484864656,
-835.539699042185,-835.459972726989,-835.380288498695,-835.300617512474,
-835.220950058948,-835.141270408132,-835.061562825738,-834.981767596663,
-834.901923254955,-834.821964827908,-834.77956895131,-834.699611651178,
-834.619748853936,-834.539963031464,-834.460236716268,-834.380552487973,
-834.300881501752,-834.221214048226,-834.141534397409,-834.061826815015,
-833.982031585939,-833.902187244231,-833.822228817184,-833.779832940589,
-833.683134355094,-833.587007138293,-833.491915336761,-833.473002493996),
 .UNSPECIFIED.);
#1535=B_SPLINE_CURVE_WITH_KNOTS('',3,(#176150,#176151,#176152,#176153,#176154,
#176155,#176156,#176157,#176158,#176159),.UNSPECIFIED.,.F.,.F.,(4,1,1,1,
1,1,1,4),(-833.473002296545,-832.780096929869,-831.780360919149,-830.780624908429,
-829.780888897709,-828.781152886989,-827.781416876269,-827.189816989366),
 .UNSPECIFIED.);
#1536=B_SPLINE_CURVE_WITH_KNOTS('',3,(#176161,#176162,#176163,#176164,#176165,
#176166,#176167,#176168,#176169,#176170,#176171,#176172,#176173,#176174,
#176175,#176176,#176177,#176178,#176179,#176180,#176181,#176182,#176183,
#176184,#176185,#176186,#176187,#176188,#176189,#176190,#176191,#176192,
#176193,#176194,#176195,#176196,#176197,#176198,#176199,#176200,#176201,
#176202,#176203,#176204,#176205,#176206,#176207,#176208,#176209,#176210,
#176211,#176212,#176213,#176214,#176215,#176216,#176217,#176218,#176219,
#176220,#176221,#176222,#176223,#176224,#176225,#176226,#176227,#176228,
#176229,#176230,#176231,#176232,#176233,#176234,#176235,#176236,#176237,
#176238,#176239,#176240,#176241,#176242,#176243,#176244,#176245,#176246,
#176247,#176248,#176249,#176250,#176251,#176252,#176253,#176254,#176255,
#176256,#176257,#176258,#176259,#176260,#176261,#176262,#176263,#176264,
#176265,#176266,#176267,#176268,#176269,#176270,#176271,#176272,#176273,
#176274,#176275,#176276,#176277,#176278,#176279,#176280,#176281,#176282,
#176283,#176284,#176285,#176286,#176287,#176288,#176289,#176290,#176291,
#176292,#176293,#176294,#176295,#176296,#176297,#176298,#176299,#176300,
#176301,#176302,#176303,#176304,#176305,#176306,#176307,#176308,#176309,
#176310,#176311,#176312,#176313,#176314,#176315,#176316,#176317,#176318,
#176319,#176320,#176321,#176322,#176323,#176324,#176325,#176326,#176327,
#176328,#176329,#176330,#176331,#176332,#176333,#176334,#176335,#176336,
#176337,#176338,#176339,#176340,#176341,#176342,#176343,#176344,#176345,
#176346,#176347,#176348,#176349,#176350,#176351,#176352,#176353,#176354,
#176355,#176356,#176357,#176358,#176359,#176360,#176361,#176362,#176363,
#176364,#176365,#176366,#176367,#176368,#176369,#176370,#176371,#176372,
#176373,#176374,#176375,#176376,#176377,#176378,#176379,#176380,#176381,
#176382,#176383,#176384,#176385,#176386,#176387,#176388,#176389,#176390,
#176391,#176392,#176393,#176394,#176395,#176396,#176397,#176398,#176399,
#176400,#176401,#176402,#176403,#176404),.UNSPECIFIED.,.F.,.F.,(4,3,3,3,
3,3,3,3,3,3,3,3,3,3,3,3,3,3,3,3,3,3,3,3,3,3,3,3,3,3,3,3,3,3,3,3,3,3,3,3,
3,3,3,3,3,3,3,3,3,3,3,3,3,3,3,3,3,3,3,3,3,3,3,3,3,3,3,3,3,3,3,3,3,3,3,3,
3,3,3,3,3,4),(-827.189816774901,-827.102343305138,-827.014439944225,-826.926319122299,
-826.837884784447,-826.781680865548,-826.701723565417,-826.621860768175,
-826.542074945703,-826.462348630508,-826.382664402214,-826.302993415994,
-826.223325962468,-826.143646311652,-826.063938729258,-825.984143500182,
-825.904299158475,-825.824340731428,-825.781944854828,-825.701987554697,
-825.622124757454,-825.542338934982,-825.462612619787,-825.382928391493,
-825.303257405272,-825.223589951747,-825.14391030093,-825.064202718536,
-824.98440748946,-824.904563147753,-824.824604720705,-824.782208844108,
-824.702251543977,-824.622388746734,-824.542602924262,-824.462876609067,
-824.383192380772,-824.303521394551,-824.223853941025,-824.144174290209,
-824.064466707814,-823.984671478739,-823.904827137031,-823.824868709983,
-823.782472833388,-823.702515533257,-823.622652736014,-823.542866913542,
-823.463140598347,-823.383456370053,-823.303785383832,-823.224117930306,
-823.14443827949,-823.064730697095,-822.98493546802,-822.905091126312,-822.825132699265,
-822.782736822668,-822.702779522537,-822.622916725294,-822.543130902822,
-822.463404587627,-822.383720359333,-822.304049373112,-822.224381919586,
-822.14470226877,-822.064994686376,-821.9851994573,-821.905355115593,-821.825396688545,
-821.783000811948,-821.704154560128,-821.625402052782,-821.54672485351,
-821.466713207095,-821.388127723732,-821.30955767386,-821.230986533456,
-821.149897820638,-821.071240210406,-820.988935946296,-820.906631682186),
 .UNSPECIFIED.);
#1537=B_SPLINE_CURVE_WITH_KNOTS('',3,(#176406,#176407,#176408,#176409,#176410,
#176411,#176412,#176413,#176414,#176415,#176416),.UNSPECIFIED.,.F.,.F.,
(4,1,1,1,1,1,1,1,4),(-820.906631682186,-820.783264801228,-819.783528790507,
-818.783792779787,-817.784056769067,-816.784320758347,-815.784584747627,
-814.784848736907,-814.623446375007),.UNSPECIFIED.);
#1538=B_SPLINE_CURVE_WITH_KNOTS('',3,(#176418,#176419,#176420,#176421,#176422,
#176423,#176424,#176425,#176426,#176427),.UNSPECIFIED.,.F.,.F.,(4,1,1,1,
1,1,1,4),(-814.623446375007,-813.785112726187,-812.785376715467,-811.785640704747,
-810.785904694026,-809.786168683306,-808.786432672586,-808.340261067827),
 .UNSPECIFIED.);
#1539=B_SPLINE_CURVE_WITH_KNOTS('',3,(#176429,#176430,#176431,#176432,#176433,
#176434,#176435,#176436,#176437,#176438),.UNSPECIFIED.,.F.,.F.,(4,1,1,1,
1,1,1,4),(-808.340261067827,-807.786696661866,-806.786960651146,-805.787224640426,
-804.787488629706,-803.787752618985,-802.788016608265,-802.057075760647),
 .UNSPECIFIED.);
#1540=B_SPLINE_CURVE_WITH_KNOTS('',3,(#176440,#176441,#176442,#176443,#176444,
#176445,#176446,#176447,#176448,#176449,#176450),.UNSPECIFIED.,.F.,.F.,
(4,1,1,1,1,1,1,1,4),(-802.057075760647,-801.788280597545,-800.788544586825,
-799.788808576105,-798.789072565385,-797.789336554665,-796.789600543945,
-795.789864533224,-795.773890453468),.UNSPECIFIED.);
#1541=B_SPLINE_CURVE_WITH_KNOTS('',3,(#176452,#176453,#176454,#176455,#176456,
#176457,#176458,#176459,#176460,#176461,#176462,#176463,#176464,#176465,
#176466,#176467,#176468,#176469,#176470,#176471,#176472,#176473,#176474,
#176475,#176476,#176477,#176478,#176479,#176480,#176481,#176482,#176483,
#176484,#176485,#176486,#176487,#176488,#176489,#176490,#176491,#176492,
#176493,#176494,#176495,#176496,#176497,#176498,#176499,#176500,#176501,
#176502,#176503,#176504,#176505,#176506,#176507,#176508,#176509,#176510,
#176511,#176512,#176513,#176514,#176515,#176516,#176517,#176518,#176519,
#176520,#176521,#176522,#176523,#176524,#176525,#176526,#176527,#176528,
#176529,#176530,#176531,#176532,#176533,#176534,#176535,#176536,#176537,
#176538,#176539,#176540,#176541,#176542,#176543,#176544,#176545,#176546,
#176547,#176548,#176549,#176550,#176551,#176552,#176553,#176554,#176555,
#176556,#176557,#176558,#176559,#176560,#176561,#176562,#176563,#176564,
#176565,#176566,#176567,#176568,#176569,#176570,#176571,#176572,#176573,
#176574,#176575,#176576,#176577,#176578,#176579,#176580,#176581,#176582,
#176583,#176584,#176585,#176586,#176587,#176588,#176589,#176590,#176591,
#176592,#176593,#176594,#176595,#176596,#176597,#176598,#176599,#176600,
#176601,#176602,#176603,#176604,#176605,#176606,#176607,#176608,#176609,
#176610,#176611,#176612,#176613,#176614,#176615,#176616,#176617,#176618,
#176619,#176620,#176621,#176622,#176623,#176624,#176625,#176626,#176627,
#176628,#176629,#176630,#176631,#176632,#176633,#176634,#176635,#176636,
#176637,#176638,#176639,#176640,#176641,#176642,#176643,#176644,#176645,
#176646,#176647,#176648,#176649,#176650,#176651,#176652,#176653,#176654,
#176655,#176656,#176657,#176658,#176659,#176660,#176661,#176662,#176663,
#176664,#176665,#176666,#176667,#176668,#176669,#176670,#176671,#176672,
#176673,#176674,#176675,#176676,#176677,#176678,#176679,#176680,#176681,
#176682,#176683,#176684,#176685,#176686,#176687,#176688,#176689,#176690,
#176691,#176692,#176693,#176694,#176695,#176696,#176697,#176698),
 .UNSPECIFIED.,.F.,.F.,(4,3,3,3,3,3,3,3,3,3,3,3,3,3,3,3,3,3,3,3,3,3,3,3,
3,3,3,3,3,3,3,3,3,3,3,3,3,3,3,3,3,3,3,3,3,3,3,3,3,3,3,3,3,3,3,3,3,3,3,3,
3,3,3,3,3,3,3,3,3,3,3,3,3,3,3,3,3,3,3,3,3,3,4),(-795.773890453468,-795.694155176644,
-795.614514012216,-795.534949222386,-795.455443131542,-795.372278805412,
-795.292826095086,-795.21337487234,-795.133909219456,-795.054413212759,
-794.974829166046,-794.895193473398,-794.815448498595,-794.790128522504,
-794.710171222373,-794.63030842513,-794.550522602658,-794.470796287463,
-794.391112059169,-794.311441072948,-794.231773619423,-794.152093968606,
-794.072386386212,-793.992591157136,-793.912746815429,-793.832788388382,
-793.790392511784,-793.710435211653,-793.63057241441,-793.550786591939,
-793.471060276743,-793.391376048449,-793.311705062228,-793.232037608702,
-793.152357957886,-793.072650375491,-792.992855146416,-792.913010804708,
-792.833052377661,-792.790656501064,-792.710699200933,-792.63083640369,
-792.551050581218,-792.471324266023,-792.391640037729,-792.311969051508,
-792.232301597982,-792.152621947165,-792.072914364771,-791.993119135695,
-791.913274793988,-791.83331636694,-791.790920490344,-791.710963190213,
-791.63110039297,-791.551314570498,-791.471588255303,-791.391904027008,
-791.312233040788,-791.232565587262,-791.152885936445,-791.07317835405,
-790.993383124975,-790.913538783267,-790.83358035622,-790.791184479624,
-790.711227179493,-790.63136438225,-790.551578559778,-790.471852244583,
-790.392168016289,-790.312497030068,-790.232829576543,-790.153149925726,
-790.073442343332,-789.993647114257,-789.913802772549,-789.833844345502,
-789.791448468904,-789.694046533938,-789.592375932863,-789.496729054174,
-789.490705331789),.UNSPECIFIED.);
#1542=B_SPLINE_CURVE_WITH_KNOTS('',3,(#176700,#176701,#176702,#176703,#176704,
#176705,#176706,#176707,#176708,#176709),.UNSPECIFIED.,.F.,.F.,(4,1,1,1,
1,1,1,4),(-789.490705146288,-788.791712458183,-787.791976447463,-786.792240436743,
-785.792504426023,-784.792768415303,-783.793032404583,-783.207519839109),
 .UNSPECIFIED.);
#1543=B_SPLINE_CURVE_WITH_KNOTS('',3,(#176711,#176712,#176713,#176714,#176715,
#176716,#176717,#176718,#176719,#176720,#176721,#176722,#176723,#176724,
#176725,#176726,#176727,#176728,#176729,#176730,#176731,#176732,#176733,
#176734,#176735,#176736,#176737,#176738,#176739,#176740,#176741,#176742,
#176743,#176744,#176745,#176746,#176747,#176748,#176749,#176750,#176751,
#176752,#176753,#176754,#176755,#176756,#176757,#176758,#176759,#176760,
#176761,#176762,#176763,#176764,#176765,#176766,#176767,#176768,#176769,
#176770,#176771,#176772,#176773,#176774,#176775,#176776,#176777,#176778,
#176779,#176780,#176781,#176782,#176783,#176784,#176785,#176786,#176787,
#176788,#176789,#176790,#176791,#176792,#176793,#176794,#176795,#176796,
#176797,#176798,#176799,#176800,#176801,#176802,#176803,#176804,#176805,
#176806,#176807,#176808,#176809,#176810,#176811,#176812,#176813,#176814,
#176815,#176816,#176817,#176818,#176819,#176820,#176821,#176822,#176823,
#176824,#176825,#176826,#176827,#176828,#176829,#176830,#176831,#176832,
#176833,#176834,#176835,#176836,#176837,#176838,#176839,#176840,#176841,
#176842,#176843,#176844,#176845,#176846,#176847,#176848,#176849,#176850,
#176851,#176852,#176853,#176854,#176855,#176856,#176857,#176858,#176859,
#176860,#176861,#176862,#176863,#176864,#176865,#176866,#176867,#176868,
#176869,#176870,#176871,#176872,#176873,#176874,#176875,#176876,#176877,
#176878,#176879,#176880,#176881,#176882,#176883,#176884,#176885,#176886,
#176887,#176888,#176889,#176890,#176891,#176892,#176893,#176894,#176895,
#176896,#176897,#176898,#176899,#176900,#176901,#176902,#176903,#176904,
#176905,#176906,#176907,#176908,#176909,#176910,#176911,#176912,#176913,
#176914,#176915,#176916,#176917,#176918,#176919,#176920,#176921,#176922,
#176923,#176924,#176925,#176926,#176927,#176928,#176929,#176930,#176931,
#176932,#176933,#176934,#176935,#176936,#176937,#176938,#176939,#176940,
#176941,#176942,#176943,#176944,#176945,#176946,#176947,#176948,#176949,
#176950,#176951,#176952,#176953,#176954),.UNSPECIFIED.,.F.,.F.,(4,3,3,3,
3,3,3,3,3,3,3,3,3,3,3,3,3,3,3,3,3,3,3,3,3,3,3,3,3,3,3,3,3,3,3,3,3,3,3,3,
3,3,3,3,3,3,3,3,3,3,3,3,3,3,3,3,3,3,3,3,3,3,3,3,3,3,3,3,3,3,3,3,3,3,3,3,
3,3,3,3,3,4),(-783.207519633885,-783.120373602226,-783.032819475524,-782.94505992763,
-782.856993893478,-782.793296393863,-782.713339093731,-782.633476296488,
-782.553690474016,-782.47396415882,-782.394279930526,-782.314608944304,
-782.234941490778,-782.155261839961,-782.075554257566,-781.99575902849,
-781.915914686782,-781.835956259734,-781.793560383142,-781.713603083011,
-781.633740285768,-781.553954463296,-781.474228148101,-781.394543919807,
-781.314872933586,-781.23520548006,-781.155525829244,-781.075818246849,
-780.996023017774,-780.916178676066,-780.836220249019,-780.793824372422,
-780.713867072291,-780.634004275048,-780.554218452577,-780.474492137382,
-780.394807909087,-780.315136922867,-780.235469469341,-780.155789818525,
-780.07608223613,-779.996287007055,-779.916442665347,-779.8364842383,-779.794088361702,
-779.714131061571,-779.634268264328,-779.554482441856,-779.474756126661,
-779.395071898367,-779.315400912146,-779.23573345862,-779.156053807803,
-779.076346225409,-778.996550996333,-778.916706654626,-778.836748227578,
-778.794352350982,-778.714395050851,-778.634532253608,-778.554746431136,
-778.475020115941,-778.395335887647,-778.315664901426,-778.2359974479,-778.156317797083,
-778.076610214689,-777.996814985613,-777.916970643906,-777.837012216858,
-777.794616340262,-777.715791165492,-777.63705974625,-777.558403631865,
-777.479144994373,-777.400580530135,-777.322031647876,-777.243481811772,
-777.163694991812,-777.085060525394,-777.004697528662,-776.924334531929),
 .UNSPECIFIED.);
#1544=B_SPLINE_CURVE_WITH_KNOTS('',3,(#176956,#176957,#176958,#176959,#176960,
#176961,#176962,#176963,#176964,#176965,#176966),.UNSPECIFIED.,.F.,.F.,
(4,1,1,1,1,1,1,1,4),(-776.924334531929,-776.794880329542,-775.795144318822,
-774.795408308102,-773.795672297381,-772.795936286661,-771.796200275941,
-770.796464265221,-770.64114922475),.UNSPECIFIED.);
#1545=B_SPLINE_CURVE_WITH_KNOTS('',3,(#176968,#176969,#176970,#176971,#176972,
#176973,#176974,#176975,#176976,#176977),.UNSPECIFIED.,.F.,.F.,(4,1,1,1,
1,1,1,4),(-770.64114922475,-769.796728254501,-768.796992243781,-767.797256233061,
-766.79752022234,-765.79778421162,-764.7980482009,-764.357968758915),
 .UNSPECIFIED.);
#1546=B_SPLINE_CURVE_WITH_KNOTS('',3,(#176979,#176980,#176981,#176982,#176983,
#176984,#176985,#176986,#176987,#176988,#176989,#176990,#176991,#176992,
#176993,#176994,#176995,#176996,#176997,#176998,#176999,#177000,#177001,
#177002,#177003,#177004,#177005,#177006,#177007,#177008,#177009,#177010,
#177011,#177012,#177013,#177014,#177015,#177016,#177017,#177018,#177019,
#177020,#177021,#177022,#177023,#177024,#177025,#177026,#177027,#177028,
#177029,#177030,#177031,#177032,#177033,#177034,#177035,#177036,#177037,
#177038,#177039,#177040,#177041,#177042,#177043,#177044,#177045,#177046,
#177047,#177048,#177049,#177050,#177051,#177052,#177053,#177054,#177055,
#177056,#177057,#177058,#177059,#177060,#177061,#177062,#177063,#177064,
#177065,#177066,#177067,#177068,#177069,#177070,#177071,#177072,#177073,
#177074,#177075,#177076,#177077,#177078,#177079,#177080,#177081,#177082,
#177083,#177084,#177085,#177086,#177087,#177088,#177089,#177090,#177091,
#177092,#177093,#177094,#177095,#177096,#177097,#177098,#177099,#177100,
#177101,#177102,#177103,#177104,#177105,#177106,#177107,#177108,#177109,
#177110,#177111,#177112,#177113,#177114,#177115,#177116,#177117,#177118,
#177119,#177120,#177121,#177122,#177123,#177124,#177125,#177126,#177127,
#177128,#177129,#177130,#177131,#177132,#177133,#177134,#177135,#177136,
#177137,#177138,#177139,#177140,#177141,#177142,#177143,#177144,#177145,
#177146,#177147,#177148,#177149,#177150,#177151,#177152,#177153,#177154,
#177155,#177156,#177157,#177158,#177159,#177160,#177161,#177162,#177163,
#177164,#177165,#177166,#177167,#177168,#177169,#177170,#177171,#177172,
#177173,#177174,#177175,#177176,#177177,#177178,#177179,#177180,#177181,
#177182,#177183,#177184,#177185,#177186,#177187,#177188,#177189,#177190,
#177191,#177192,#177193,#177194,#177195,#177196,#177197,#177198,#177199,
#177200,#177201,#177202,#177203,#177204,#177205,#177206,#177207,#177208,
#177209,#177210,#177211,#177212,#177213,#177214,#177215,#177216,#177217,
#177218,#177219,#177220,#177221,#177222,#177223,#177224,#177225),
 .UNSPECIFIED.,.F.,.F.,(4,3,3,3,3,3,3,3,3,3,3,3,3,3,3,3,3,3,3,3,3,3,3,3,
3,3,3,3,3,3,3,3,3,3,3,3,3,3,3,3,3,3,3,3,3,3,3,3,3,3,3,3,3,3,3,3,3,3,3,3,
3,3,3,3,3,3,3,3,3,3,3,3,3,3,3,3,3,3,3,3,3,3,4),(-764.35796391757,-764.276294881444,
-764.19457900503,-764.112803816722,-764.030895575215,-763.948917289433,
-763.866785413175,-763.79831219018,-763.718354890049,-763.638492092806,
-763.558706270334,-763.478979955139,-763.399295726844,-763.319624740623,
-763.239957287097,-763.160277636281,-763.080570053887,-763.000774824811,
-762.920930483103,-762.840972056056,-762.79857617946,-762.718618879329,
-762.638756082086,-762.558970259614,-762.479243944419,-762.399559716125,
-762.319888729904,-762.240221276378,-762.160541625562,-762.080834043167,
-762.001038814092,-761.921194472384,-761.841236045336,-761.79884016874,
-761.718882868609,-761.639020071366,-761.559234248894,-761.479507933699,
-761.399823705405,-761.320152719184,-761.240485265658,-761.160805614842,
-761.081098032448,-761.001302803372,-760.921458461664,-760.841500034617,
-760.79910415802,-760.719146857889,-760.639284060646,-760.559498238175,
-760.479771922979,-760.400087694685,-760.320416708464,-760.240749254938,
-760.161069604121,-760.081362021726,-760.001566792651,-759.921722450943,
-759.841764023896,-759.7993681473,-759.719410847169,-759.639548049926,-759.559762227454,
-759.480035912258,-759.400351683963,-759.320680697742,-759.241013244216,
-759.161333593399,-759.081626011005,-759.00183078193,-758.921986440222,
-758.842028013175,-758.799632136579,-758.720387508559,-758.639686396288,
-758.560635712157,-758.481638770385,-758.402679241637,-758.320704083825,
-758.24175427393,-758.162795757206,-758.083794480984,-758.07477861039),
 .UNSPECIFIED.);
#1547=B_SPLINE_CURVE_WITH_KNOTS('',3,(#177227,#177228,#177229,#177230,#177231,
#177232,#177233,#177234,#177235,#177236,#177237),.UNSPECIFIED.,.F.,.F.,
(4,1,1,1,1,1,1,1,4),(-758.074774690477,-757.799896125859,-756.800160115139,
-755.800424104419,-754.800688093699,-753.800952082979,-752.801216072259,
-751.801480061539,-751.791593303211),.UNSPECIFIED.);
#1548=B_SPLINE_CURVE_WITH_KNOTS('',3,(#177239,#177240,#177241,#177242,#177243,
#177244,#177245,#177246,#177247,#177248,#177249,#177250,#177251,#177252,
#177253,#177254,#177255,#177256,#177257,#177258,#177259,#177260,#177261,
#177262,#177263,#177264,#177265,#177266,#177267,#177268,#177269,#177270,
#177271,#177272,#177273,#177274,#177275,#177276,#177277,#177278,#177279,
#177280,#177281,#177282,#177283,#177284,#177285,#177286,#177287,#177288,
#177289,#177290,#177291,#177292,#177293,#177294,#177295,#177296,#177297,
#177298,#177299,#177300,#177301,#177302,#177303,#177304,#177305,#177306,
#177307,#177308,#177309,#177310,#177311,#177312,#177313,#177314,#177315,
#177316,#177317,#177318,#177319,#177320,#177321,#177322,#177323,#177324,
#177325,#177326,#177327,#177328,#177329,#177330,#177331,#177332,#177333,
#177334,#177335,#177336,#177337,#177338,#177339,#177340,#177341,#177342,
#177343,#177344,#177345,#177346,#177347,#177348,#177349,#177350,#177351,
#177352,#177353,#177354,#177355,#177356,#177357,#177358,#177359,#177360,
#177361,#177362,#177363,#177364,#177365,#177366,#177367,#177368,#177369,
#177370,#177371,#177372,#177373,#177374,#177375,#177376,#177377,#177378,
#177379,#177380,#177381,#177382,#177383,#177384,#177385,#177386,#177387,
#177388,#177389,#177390,#177391,#177392,#177393,#177394,#177395,#177396,
#177397,#177398,#177399,#177400,#177401,#177402,#177403,#177404,#177405,
#177406,#177407,#177408,#177409,#177410,#177411,#177412,#177413,#177414,
#177415,#177416,#177417,#177418,#177419,#177420,#177421,#177422,#177423,
#177424,#177425,#177426,#177427,#177428,#177429,#177430,#177431,#177432,
#177433,#177434,#177435,#177436,#177437,#177438,#177439,#177440,#177441,
#177442,#177443,#177444,#177445,#177446,#177447,#177448,#177449,#177450,
#177451,#177452,#177453,#177454,#177455,#177456,#177457,#177458,#177459,
#177460,#177461,#177462,#177463,#177464,#177465,#177466,#177467,#177468,
#177469,#177470,#177471,#177472,#177473,#177474,#177475,#177476,#177477,
#177478,#177479,#177480,#177481,#177482),.UNSPECIFIED.,.F.,.F.,(4,3,3,3,
3,3,3,3,3,3,3,3,3,3,3,3,3,3,3,3,3,3,3,3,3,3,3,3,3,3,3,3,3,3,3,3,3,3,3,3,
3,3,3,3,3,3,3,3,3,3,3,3,3,3,3,3,3,3,3,3,3,3,3,3,3,3,3,3,3,3,3,3,3,3,3,3,
3,3,3,3,3,4),(-751.791593303211,-751.71177590738,-751.632052838358,-751.552406433267,
-751.472819090824,-751.393273257364,-751.313739864144,-751.23420923262,
-751.15466551229,-751.075092847645,-750.995432486505,-750.915721873857,
-750.835899552971,-750.801744050818,-750.721786750687,-750.641923953444,
-750.562138130972,-750.482411815777,-750.402727587483,-750.323056601262,
-750.243389147736,-750.16370949692,-750.084001914525,-750.00420668545,-749.924362343742,
-749.844403916695,-749.802008040098,-749.722050739967,-749.642187942724,
-749.562402120252,-749.482675805057,-749.402991576763,-749.323320590542,
-749.243653137016,-749.1639734862,-749.084265903805,-749.00447067473,-748.924626333022,
-748.844667905974,-748.802272029378,-748.722314729247,-748.642451932004,
-748.562666109532,-748.482939794337,-748.403255566043,-748.323584579822,
-748.243917126296,-748.16423747548,-748.084529893086,-748.00473466401,-747.924890322302,
-747.844931895255,-747.802536018658,-747.722578718527,-747.642715921284,
-747.562930098813,-747.483203783617,-747.403519555322,-747.323848569101,
-747.244181115575,-747.164501464759,-747.084793882364,-747.004998653289,
-746.925154311582,-746.845195884534,-746.802800007938,-746.722842707807,
-746.642979910564,-746.563194088092,-746.483467772897,-746.403783544603,
-746.324112558383,-746.244445104857,-746.16476545404,-746.085057871645,
-746.005262642569,-745.925418300862,-745.845459873815,-745.803063997218,
-745.704925577428,-745.606666873208,-745.508408168989),.UNSPECIFIED.);
#1549=B_SPLINE_CURVE_WITH_KNOTS('',3,(#177484,#177485,#177486,#177487,#177488,
#177489,#177490,#177491,#177492,#177493),.UNSPECIFIED.,.F.,.F.,(4,1,1,1,
1,1,1,4),(-745.508407996031,-744.803327986498,-743.803591975778,-742.803855965058,
-741.804119954337,-740.804383943617,-739.804647932897,-739.225222688852),
 .UNSPECIFIED.);
#1550=B_SPLINE_CURVE_WITH_KNOTS('',3,(#177495,#177496,#177497,#177498,#177499,
#177500,#177501,#177502,#177503,#177504),.UNSPECIFIED.,.F.,.F.,(4,1,1,1,
1,1,1,4),(-739.225222688852,-738.804911922177,-737.805175911457,-736.805439900736,
-735.805703890017,-734.805967879296,-733.806231868576,-732.942037381672),
 .UNSPECIFIED.);
#1551=B_SPLINE_CURVE_WITH_KNOTS('',3,(#177506,#177507,#177508,#177509,#177510,
#177511,#177512,#177513,#177514,#177515,#177516),.UNSPECIFIED.,.F.,.F.,
(4,1,1,1,1,1,1,1,4),(-732.942037381672,-732.806495857856,-731.806759847136,
-730.807023836416,-729.807287825696,-728.807551814976,-727.807815804255,
-726.808079793535,-726.658852074493),.UNSPECIFIED.);
#1552=B_SPLINE_CURVE_WITH_KNOTS('',3,(#177518,#177519,#177520,#177521,#177522,
#177523,#177524,#177525,#177526,#177527),.UNSPECIFIED.,.F.,.F.,(4,1,1,1,
1,1,1,4),(-726.658852074493,-725.808343782815,-724.808607772095,-723.808871761375,
-722.809135750655,-721.809399739935,-720.809663729215,-720.37567201352),
 .UNSPECIFIED.);
#1553=B_SPLINE_CURVE_WITH_KNOTS('',3,(#177529,#177530,#177531,#177532,#177533,
#177534,#177535,#177536,#177537,#177538,#177539,#177540,#177541,#177542,
#177543,#177544,#177545,#177546,#177547,#177548,#177549,#177550,#177551,
#177552,#177553,#177554,#177555,#177556,#177557,#177558,#177559,#177560,
#177561,#177562,#177563,#177564,#177565,#177566,#177567,#177568,#177569,
#177570,#177571,#177572,#177573,#177574,#177575,#177576,#177577,#177578,
#177579,#177580,#177581,#177582,#177583,#177584,#177585,#177586,#177587,
#177588,#177589,#177590,#177591,#177592,#177593,#177594,#177595,#177596,
#177597,#177598,#177599,#177600,#177601,#177602,#177603,#177604,#177605,
#177606,#177607,#177608,#177609,#177610,#177611,#177612,#177613,#177614,
#177615,#177616,#177617,#177618,#177619,#177620,#177621,#177622,#177623,
#177624,#177625,#177626,#177627,#177628,#177629,#177630,#177631,#177632,
#177633,#177634,#177635,#177636,#177637,#177638,#177639,#177640,#177641,
#177642,#177643,#177644,#177645,#177646,#177647,#177648,#177649,#177650,
#177651,#177652,#177653,#177654,#177655,#177656,#177657,#177658,#177659,
#177660,#177661,#177662,#177663,#177664,#177665,#177666,#177667,#177668,
#177669,#177670,#177671,#177672,#177673,#177674,#177675,#177676,#177677,
#177678,#177679,#177680,#177681,#177682,#177683,#177684,#177685,#177686,
#177687,#177688,#177689,#177690,#177691,#177692,#177693,#177694,#177695,
#177696,#177697,#177698,#177699,#177700,#177701,#177702,#177703,#177704,
#177705,#177706,#177707,#177708,#177709,#177710,#177711,#177712,#177713,
#177714,#177715,#177716,#177717,#177718,#177719,#177720,#177721,#177722,
#177723,#177724,#177725,#177726,#177727,#177728,#177729,#177730,#177731,
#177732,#177733,#177734,#177735,#177736,#177737,#177738,#177739,#177740,
#177741,#177742,#177743,#177744,#177745,#177746,#177747,#177748,#177749,
#177750,#177751,#177752,#177753,#177754,#177755,#177756,#177757,#177758,
#177759,#177760,#177761,#177762,#177763,#177764,#177765,#177766,#177767,
#177768,#177769,#177770,#177771,#177772),.UNSPECIFIED.,.F.,.F.,(4,3,3,3,
3,3,3,3,3,3,3,3,3,3,3,3,3,3,3,3,3,3,3,3,3,3,3,3,3,3,3,3,3,3,3,3,3,3,3,3,
3,3,3,3,3,3,3,3,3,3,3,3,3,3,3,3,3,3,3,3,3,3,3,3,3,3,3,3,3,3,3,3,3,3,3,3,
3,3,3,3,3,4),(-720.375666767313,-720.294150968666,-720.212592887853,-720.130979718437,
-720.049237393192,-719.967428093136,-719.885465069706,-719.809927718494,
-719.729970418363,-719.65010762112,-719.570321798648,-719.490595483453,
-719.410911255159,-719.331240268938,-719.251572815412,-719.171893164596,
-719.092185582201,-719.012390353126,-718.932546011418,-718.852587584371,
-718.810191707774,-718.730234407643,-718.6503716104,-718.570585787928,-718.490859472733,
-718.411175244439,-718.331504258218,-718.251836804692,-718.172157153875,
-718.092449571481,-718.012654342405,-717.932810000698,-717.85285157365,
-717.810455697054,-717.730498396923,-717.65063559968,-717.570849777208,
-717.491123462013,-717.411439233719,-717.331768247498,-717.252100793972,
-717.172421143155,-717.09271356076,-717.012918331685,-716.933073989977,
-716.85311556293,-716.810719686334,-716.730762386203,-716.65089958896,-716.571113766489,
-716.491387451293,-716.411703222999,-716.332032236778,-716.252364783252,
-716.172685132435,-716.09297755004,-716.013182320965,-715.933337979258,
-715.85337955221,-715.810983675614,-715.731026375483,-715.65116357824,-715.571377755768,
-715.491651440573,-715.411967212279,-715.332296226058,-715.252628772532,
-715.172949121715,-715.09324153932,-715.013446310245,-714.933601968538,
-714.85364354149,-714.811247664894,-714.731945400098,-714.652012407602,
-714.572904570939,-714.493851148949,-714.414835850797,-714.334247253131,
-714.255244345521,-714.173862902827,-714.092481460134),.UNSPECIFIED.);
#1554=B_SPLINE_CURVE_WITH_KNOTS('',3,(#177774,#177775,#177776,#177777,#177778,
#177779,#177780,#177781,#177782,#177783,#177784),.UNSPECIFIED.,.F.,.F.,
(4,1,1,1,1,1,1,1,4),(-714.092477055051,-713.811511654174,-712.811775643453,
-711.812039632733,-710.812303622013,-709.812567611293,-708.812831600573,
-707.813095589853,-707.809296152954),.UNSPECIFIED.);
#1555=B_SPLINE_CURVE_WITH_KNOTS('',3,(#177786,#177787,#177788,#177789,#177790,
#177791,#177792,#177793,#177794,#177795,#177796,#177797,#177798,#177799,
#177800,#177801,#177802,#177803,#177804,#177805,#177806,#177807,#177808,
#177809,#177810,#177811,#177812,#177813,#177814,#177815,#177816,#177817,
#177818,#177819,#177820,#177821,#177822,#177823,#177824,#177825,#177826,
#177827,#177828,#177829,#177830,#177831,#177832,#177833,#177834,#177835,
#177836,#177837,#177838,#177839,#177840,#177841,#177842,#177843,#177844,
#177845,#177846,#177847,#177848,#177849,#177850,#177851,#177852,#177853,
#177854,#177855,#177856,#177857,#177858,#177859,#177860,#177861,#177862,
#177863,#177864,#177865,#177866,#177867,#177868,#177869,#177870,#177871,
#177872,#177873,#177874,#177875,#177876,#177877,#177878,#177879,#177880,
#177881,#177882,#177883,#177884,#177885,#177886,#177887,#177888,#177889,
#177890,#177891,#177892,#177893,#177894,#177895,#177896,#177897,#177898,
#177899,#177900,#177901,#177902,#177903,#177904,#177905,#177906,#177907,
#177908,#177909,#177910,#177911,#177912,#177913,#177914,#177915,#177916,
#177917,#177918,#177919,#177920,#177921,#177922,#177923,#177924,#177925,
#177926,#177927,#177928,#177929,#177930,#177931,#177932,#177933,#177934,
#177935,#177936,#177937,#177938,#177939,#177940,#177941,#177942,#177943,
#177944,#177945,#177946,#177947,#177948,#177949,#177950,#177951,#177952,
#177953,#177954,#177955,#177956,#177957,#177958,#177959,#177960,#177961,
#177962,#177963,#177964,#177965,#177966,#177967,#177968,#177969,#177970,
#177971,#177972,#177973,#177974,#177975,#177976,#177977,#177978,#177979,
#177980,#177981,#177982,#177983,#177984,#177985,#177986,#177987,#177988,
#177989,#177990,#177991,#177992,#177993,#177994,#177995,#177996,#177997,
#177998,#177999,#178000,#178001,#178002,#178003,#178004,#178005,#178006,
#178007,#178008,#178009,#178010,#178011,#178012,#178013,#178014,#178015,
#178016,#178017,#178018,#178019,#178020,#178021,#178022,#178023,#178024,
#178025,#178026,#178027,#178028,#178029),.UNSPECIFIED.,.F.,.F.,(4,3,3,3,
3,3,3,3,3,3,3,3,3,3,3,3,3,3,3,3,3,3,3,3,3,3,3,3,3,3,3,3,3,3,3,3,3,3,3,3,
3,3,3,3,3,3,3,3,3,3,3,3,3,3,3,3,3,3,3,3,3,3,3,3,3,3,3,3,3,3,3,3,3,3,3,3,
3,3,3,3,3,4),(-707.809296152954,-707.729393576193,-707.649585460883,-707.56985422511,
-707.490182347959,-707.410552355825,-707.330935321053,-707.251321537018,
-707.171695225664,-707.092040604376,-707.012298323543,-706.932506498773,
-706.852601501857,-706.813359579133,-706.733402279002,-706.653539481759,
-706.573753659287,-706.494027344092,-706.414343115798,-706.334672129577,
-706.255004676051,-706.175325025235,-706.095617442841,-706.015822213765,
-705.935977872058,-705.85601944501,-705.813623568413,-705.733666268282,
-705.653803471039,-705.574017648568,-705.494291333373,-705.414607105079,
-705.334936118858,-705.255268665332,-705.175589014516,-705.095881432121,
-705.016086203046,-704.936241861339,-704.856283434291,-704.813887557693,
-704.733930257561,-704.654067460319,-704.574281637847,-704.494555322651,
-704.414871094357,-704.335200108136,-704.25553265461,-704.175853003793,
-704.096145421398,-704.016350192322,-703.936505850614,-703.856547423567,
-703.814151546972,-703.734194246841,-703.654331449598,-703.574545627126,
-703.494819311931,-703.415135083637,-703.335464097416,-703.25579664389,
-703.176116993074,-703.09640941068,-703.016614181604,-702.936769839897,
-702.856811412849,-702.814415536252,-702.734458236121,-702.654595438879,
-702.574809616407,-702.495083301212,-702.415399072918,-702.335728086698,
-702.256060633172,-702.176380982356,-702.096673399962,-702.016878170886,
-701.937033829179,-701.857075402131,-701.814679525532,-701.71576893031,
-701.618207500733,-701.526111005195),.UNSPECIFIED.);
#1556=B_SPLINE_CURVE_WITH_KNOTS('',3,(#178031,#178032,#178033,#178034,#178035,
#178036,#178037,#178038,#178039,#178040),.UNSPECIFIED.,.F.,.F.,(4,1,1,1,
1,1,1,4),(-701.526110845774,-700.814943514812,-699.815207504092,-698.815471493372,
-697.815735482651,-696.815999471931,-695.816263461211,-695.242925538595),
 .UNSPECIFIED.);
#1557=B_SPLINE_CURVE_WITH_KNOTS('',3,(#178042,#178043,#178044,#178045,#178046,
#178047,#178048,#178049,#178050,#178051),.UNSPECIFIED.,.F.,.F.,(4,1,1,1,
1,1,1,4),(-695.242925538595,-694.816527450491,-693.816791439771,-692.817055429051,
-691.817319418331,-690.817583407611,-689.81784739689,-688.959740231415),
 .UNSPECIFIED.);
#1558=B_SPLINE_CURVE_WITH_KNOTS('',3,(#178053,#178054,#178055,#178056,#178057,
#178058,#178059,#178060,#178061,#178062,#178063),.UNSPECIFIED.,.F.,.F.,
(4,1,1,1,1,1,1,1,4),(-688.959740231415,-688.81811138617,-687.81837537545,
-686.81863936473,-685.81890335401,-684.81916734329,-683.81943133257,-682.81969532185,
-682.676554924236),.UNSPECIFIED.);
#1559=B_SPLINE_CURVE_WITH_KNOTS('',3,(#178065,#178066,#178067,#178068,#178069,
#178070,#178071,#178072,#178073,#178074),.UNSPECIFIED.,.F.,.F.,(4,1,1,1,
1,1,1,4),(-682.676554924236,-681.819959311129,-680.820223300409,-679.820487289689,
-678.820751278969,-677.821015268249,-676.821279257529,-676.393369617056),
 .UNSPECIFIED.);
#1560=B_SPLINE_CURVE_WITH_KNOTS('',3,(#178076,#178077,#178078,#178079,#178080,
#178081,#178082,#178083,#178084,#178085),.UNSPECIFIED.,.F.,.F.,(4,1,1,1,
1,1,1,4),(-676.393369617056,-675.821543246809,-674.821807236089,-673.822071225368,
-672.822335214648,-671.822599203928,-670.822863193208,-670.110184309877),
 .UNSPECIFIED.);
#1561=B_SPLINE_CURVE_WITH_KNOTS('',3,(#178087,#178088,#178089,#178090,#178091,
#178092,#178093,#178094,#178095,#178096,#178097,#178098,#178099,#178100,
#178101,#178102,#178103,#178104,#178105,#178106,#178107,#178108,#178109,
#178110,#178111,#178112,#178113,#178114,#178115,#178116,#178117,#178118,
#178119,#178120,#178121,#178122,#178123,#178124,#178125,#178126,#178127,
#178128,#178129,#178130,#178131,#178132,#178133,#178134,#178135,#178136,
#178137,#178138,#178139,#178140,#178141,#178142,#178143,#178144,#178145,
#178146,#178147,#178148,#178149,#178150,#178151,#178152,#178153,#178154,
#178155,#178156,#178157,#178158,#178159,#178160,#178161,#178162,#178163,
#178164,#178165,#178166,#178167,#178168,#178169,#178170,#178171,#178172,
#178173,#178174,#178175,#178176,#178177,#178178,#178179,#178180,#178181,
#178182,#178183,#178184,#178185,#178186,#178187,#178188,#178189,#178190,
#178191,#178192,#178193,#178194,#178195,#178196,#178197,#178198,#178199,
#178200,#178201,#178202,#178203,#178204,#178205,#178206,#178207,#178208,
#178209,#178210,#178211,#178212,#178213,#178214,#178215,#178216,#178217,
#178218,#178219,#178220,#178221,#178222,#178223,#178224,#178225,#178226,
#178227,#178228,#178229,#178230,#178231,#178232,#178233,#178234,#178235,
#178236,#178237,#178238,#178239,#178240,#178241,#178242,#178243,#178244,
#178245,#178246,#178247,#178248,#178249,#178250,#178251,#178252,#178253,
#178254,#178255,#178256,#178257,#178258,#178259,#178260,#178261,#178262,
#178263,#178264,#178265,#178266,#178267,#178268,#178269,#178270,#178271,
#178272,#178273,#178274,#178275,#178276,#178277,#178278,#178279,#178280,
#178281,#178282,#178283,#178284,#178285,#178286,#178287,#178288,#178289,
#178290,#178291,#178292,#178293,#178294,#178295,#178296,#178297,#178298,
#178299,#178300,#178301,#178302,#178303,#178304,#178305,#178306,#178307,
#178308,#178309,#178310,#178311,#178312,#178313,#178314,#178315,#178316,
#178317,#178318,#178319,#178320,#178321,#178322,#178323,#178324,#178325,
#178326,#178327,#178328,#178329,#178330),.UNSPECIFIED.,.F.,.F.,(4,3,3,3,
3,3,3,3,3,3,3,3,3,3,3,3,3,3,3,3,3,3,3,3,3,3,3,3,3,3,3,3,3,3,3,3,3,3,3,3,
3,3,3,3,3,3,3,3,3,3,3,3,3,3,3,3,3,3,3,3,3,3,3,3,3,3,3,3,3,3,3,3,3,3,3,3,
3,3,3,3,3,4),(-670.110184153965,-670.012739495242,-669.913861623891,-669.823127182488,
-669.743169882357,-669.663307085115,-669.583521262643,-669.503794947448,
-669.424110719154,-669.344439732933,-669.264772279407,-669.185092628591,
-669.105385046197,-669.025589817122,-668.945745475414,-668.865787048367,
-668.823391171768,-668.743433871637,-668.663571074394,-668.583785251923,
-668.504058936727,-668.424374708433,-668.344703722213,-668.265036268687,
-668.18535661787,-668.105649035476,-668.0258538064,-667.946009464693,-667.866051037646,
-667.823655161048,-667.743697860916,-667.663835063674,-667.584049241201,
-667.504322926006,-667.424638697711,-667.34496771149,-667.265300257964,
-667.185620607147,-667.105913024752,-667.026117795676,-666.946273453968,
-666.866315026921,-666.823919150327,-666.743961850196,-666.664099052953,
-666.584313230481,-666.504586915286,-666.424902686992,-666.345231700771,
-666.265564247245,-666.185884596429,-666.106177014035,-666.026381784959,
-665.946537443251,-665.866579016204,-665.824183139607,-665.744225839476,
-665.664363042233,-665.584577219762,-665.504850904567,-665.425166676273,
-665.345495690052,-665.265828236526,-665.18614858571,-665.106441003315,
-665.02664577424,-664.946801432533,-664.866843005485,-664.824447128887,
-664.744522891255,-664.664693141368,-664.584940318383,-664.505246922308,
-664.425595500394,-664.345957161305,-664.266322192653,-664.186674835235,
-664.106999325398,-664.027236170141,-663.947423648092,-663.867497597443,
-663.826999002697),.UNSPECIFIED.);
#1562=B_SPLINE_CURVE_WITH_KNOTS('',3,(#178332,#178333,#178334,#178335,#178336,
#178337,#178338,#178339,#178340,#178341,#178342,#178343),.UNSPECIFIED.,
 .F.,.F.,(4,2,1,1,1,1,1,1,4),(-663.826999002697,-663.824711118167,-662.824975107447,
-661.825239096727,-660.825503086007,-659.825767075287,-658.826031064566,
-657.826295053846,-657.543818216983),.UNSPECIFIED.);
#1563=B_SPLINE_CURVE_WITH_KNOTS('',3,(#178345,#178346,#178347,#178348,#178349,
#178350,#178351,#178352,#178353,#178354,#178355,#178356,#178357,#178358,
#178359,#178360,#178361,#178362,#178363,#178364,#178365,#178366,#178367,
#178368,#178369,#178370,#178371,#178372,#178373,#178374,#178375,#178376,
#178377,#178378,#178379,#178380,#178381,#178382,#178383,#178384,#178385,
#178386,#178387,#178388,#178389,#178390,#178391,#178392,#178393,#178394,
#178395,#178396,#178397,#178398,#178399,#178400,#178401,#178402,#178403,
#178404,#178405,#178406,#178407,#178408,#178409,#178410,#178411,#178412,
#178413,#178414,#178415,#178416,#178417,#178418,#178419,#178420,#178421,
#178422,#178423,#178424,#178425,#178426,#178427,#178428,#178429,#178430,
#178431,#178432,#178433,#178434,#178435,#178436,#178437,#178438,#178439,
#178440,#178441,#178442,#178443,#178444,#178445,#178446,#178447,#178448,
#178449,#178450,#178451,#178452,#178453,#178454,#178455,#178456,#178457,
#178458,#178459,#178460,#178461,#178462,#178463,#178464,#178465,#178466,
#178467,#178468,#178469,#178470,#178471,#178472,#178473,#178474,#178475,
#178476,#178477,#178478,#178479,#178480,#178481,#178482,#178483,#178484,
#178485,#178486,#178487,#178488,#178489,#178490,#178491,#178492,#178493,
#178494,#178495,#178496,#178497,#178498,#178499,#178500,#178501,#178502,
#178503,#178504,#178505,#178506,#178507,#178508,#178509,#178510,#178511,
#178512,#178513,#178514,#178515,#178516,#178517,#178518,#178519,#178520,
#178521,#178522,#178523,#178524,#178525,#178526,#178527,#178528,#178529,
#178530,#178531,#178532,#178533,#178534,#178535,#178536,#178537,#178538,
#178539,#178540,#178541,#178542,#178543,#178544,#178545,#178546,#178547,
#178548,#178549,#178550,#178551,#178552,#178553,#178554,#178555,#178556,
#178557,#178558,#178559,#178560,#178561,#178562,#178563,#178564,#178565,
#178566,#178567,#178568,#178569,#178570,#178571,#178572,#178573,#178574,
#178575,#178576,#178577,#178578,#178579,#178580,#178581,#178582,#178583,
#178584,#178585,#178586,#178587,#178588),.UNSPECIFIED.,.F.,.F.,(4,3,3,3,
3,3,3,3,3,3,3,3,3,3,3,3,3,3,3,3,3,3,3,3,3,3,3,3,3,3,3,3,3,3,3,3,3,3,3,3,
3,3,3,3,3,3,3,3,3,3,3,3,3,3,3,3,3,3,3,3,3,3,3,3,3,3,3,3,3,3,3,3,3,3,3,3,
3,3,3,3,3,4),(-657.543813695517,-657.464751020353,-657.3849770232,-657.305959699517,
-657.226940888437,-657.147904359238,-657.06756803021,-656.988407198372,
-656.907483120749,-656.826559043126,-656.746601742995,-656.666738945752,
-656.58695312328,-656.507226808085,-656.427542579791,-656.34787159357,-656.268204140044,
-656.188524489227,-656.108816906833,-656.029021677757,-655.94917733605,
-655.869218909002,-655.826823032406,-655.746865732275,-655.667002935032,
-655.58721711256,-655.507490797365,-655.42780656907,-655.348135582849,-655.268468129323,
-655.188788478506,-655.109080896112,-655.029285667036,-654.949441325329,
-654.869482898281,-654.827087021686,-654.747129721555,-654.667266924312,
-654.587481101841,-654.507754786645,-654.428070558352,-654.348399572131,
-654.268732118605,-654.189052467789,-654.109344885395,-654.029549656319,
-653.949705314611,-653.869746887564,-653.827351010966,-653.747393710834,
-653.667530913592,-653.58774509112,-653.508018775925,-653.42833454763,-653.348663561409,
-653.268996107883,-653.189316457066,-653.109608874671,-653.029813645595,
-652.949969303887,-652.870010876839,-652.827615000245,-652.747657700114,
-652.667794902871,-652.5880090804,-652.508282765205,-652.428598536911,-652.34892755069,
-652.269260097164,-652.189580446348,-652.109872863953,-652.030077634878,
-651.95023329317,-651.870274866122,-651.827878989526,-651.745947788662,
-651.664127715656,-651.582405638949,-651.500793005596,-651.419244358718,
-651.337756902616,-651.260628388338),.UNSPECIFIED.);
#1564=B_SPLINE_CURVE_WITH_KNOTS('',3,(#178590,#178591,#178592,#178593,#178594,
#178595,#178596,#178597,#178598,#178599),.UNSPECIFIED.,.F.,.F.,(4,1,1,1,
1,1,1,4),(-651.260623045353,-650.828142978805,-649.828406968085,-648.828670957365,
-647.828934946645,-646.829198935925,-645.829462925205,-644.977443081158),
 .UNSPECIFIED.);
#1565=B_SPLINE_CURVE_WITH_KNOTS('',3,(#178601,#178602,#178603,#178604,#178605,
#178606,#178607,#178608,#178609,#178610,#178611),.UNSPECIFIED.,.F.,.F.,
(4,1,1,1,1,1,1,1,4),(-644.977443081158,-644.829726914485,-643.829990903764,
-642.830254893044,-641.830518882324,-640.830782871604,-639.831046860884,
-638.831310850164,-638.694257773979),.UNSPECIFIED.);
#1566=B_SPLINE_CURVE_WITH_KNOTS('',3,(#178613,#178614,#178615,#178616,#178617,
#178618,#178619,#178620,#178621,#178622),.UNSPECIFIED.,.F.,.F.,(4,1,1,1,
1,1,1,4),(-638.694257773979,-637.831574839444,-636.831838828723,-635.832102818003,
-634.832366807283,-633.832630796563,-632.832894785843,-632.411072466799),
 .UNSPECIFIED.);
#1567=B_SPLINE_CURVE_WITH_KNOTS('',3,(#178624,#178625,#178626,#178627,#178628,
#178629,#178630,#178631,#178632,#178633),.UNSPECIFIED.,.F.,.F.,(4,1,1,1,
1,1,1,4),(-632.411072466799,-631.833158775123,-630.833422764403,-629.833686753683,
-628.833950742962,-627.834214732242,-626.834478721522,-626.12788715962),
 .UNSPECIFIED.);
#1568=B_SPLINE_CURVE_WITH_KNOTS('',3,(#178635,#178636,#178637,#178638,#178639,
#178640,#178641,#178642,#178643,#178644,#178645,#178646,#178647,#178648,
#178649,#178650,#178651,#178652,#178653,#178654,#178655,#178656,#178657,
#178658,#178659,#178660,#178661,#178662,#178663,#178664,#178665,#178666,
#178667,#178668,#178669,#178670,#178671,#178672,#178673,#178674,#178675,
#178676,#178677,#178678,#178679,#178680,#178681,#178682,#178683,#178684,
#178685,#178686,#178687,#178688,#178689,#178690,#178691,#178692,#178693,
#178694,#178695,#178696,#178697,#178698,#178699,#178700,#178701,#178702,
#178703,#178704,#178705,#178706,#178707,#178708,#178709,#178710,#178711,
#178712,#178713,#178714,#178715,#178716,#178717,#178718,#178719,#178720,
#178721,#178722,#178723,#178724,#178725,#178726,#178727,#178728,#178729,
#178730,#178731,#178732,#178733,#178734,#178735,#178736,#178737,#178738,
#178739,#178740,#178741,#178742,#178743,#178744,#178745,#178746,#178747,
#178748,#178749,#178750,#178751,#178752,#178753,#178754,#178755,#178756,
#178757,#178758,#178759,#178760,#178761,#178762,#178763,#178764,#178765,
#178766,#178767,#178768,#178769,#178770,#178771,#178772,#178773,#178774,
#178775,#178776,#178777,#178778,#178779,#178780,#178781,#178782,#178783,
#178784,#178785,#178786,#178787,#178788,#178789,#178790,#178791,#178792,
#178793,#178794,#178795,#178796,#178797,#178798,#178799,#178800,#178801,
#178802,#178803,#178804,#178805,#178806,#178807,#178808,#178809,#178810,
#178811,#178812,#178813,#178814,#178815,#178816,#178817,#178818,#178819,
#178820,#178821,#178822,#178823,#178824,#178825,#178826,#178827,#178828,
#178829,#178830,#178831,#178832,#178833,#178834,#178835,#178836,#178837,
#178838,#178839,#178840,#178841,#178842,#178843,#178844,#178845,#178846,
#178847,#178848,#178849,#178850,#178851,#178852,#178853,#178854,#178855,
#178856,#178857,#178858,#178859,#178860,#178861,#178862,#178863,#178864,
#178865,#178866,#178867,#178868,#178869,#178870,#178871,#178872,#178873,
#178874,#178875,#178876,#178877,#178878),.UNSPECIFIED.,.F.,.F.,(4,3,3,3,
3,3,3,3,3,3,3,3,3,3,3,3,3,3,3,3,3,3,3,3,3,3,3,3,3,3,3,3,3,3,3,3,3,3,3,3,
3,3,3,3,3,3,3,3,3,3,3,3,3,3,3,3,3,3,3,3,3,3,3,3,3,3,3,3,3,3,3,3,3,3,3,3,
3,3,3,3,3,4),(-626.127886989932,-626.031132445784,-625.932937578293,-625.834742710802,
-625.754785410671,-625.674922613429,-625.595136790957,-625.515410475762,
-625.435726247468,-625.356055261248,-625.276387807722,-625.196708156906,
-625.117000574512,-625.037205345437,-624.95736100373,-624.877402576683,
-624.835006700082,-624.755049399951,-624.675186602708,-624.595400780236,
-624.515674465041,-624.435990236747,-624.356319250526,-624.276651797,-624.196972146184,
-624.117264563789,-624.037469334714,-623.957624993006,-623.877666565959,
-623.835270689362,-623.755313389231,-623.675450591988,-623.595664769516,
-623.515938454321,-623.436254226027,-623.356583239806,-623.27691578628,
-623.197236135464,-623.117528553069,-623.037733323994,-622.957888982286,
-622.877930555239,-622.835534678642,-622.755577378511,-622.675714581268,
-622.595928758796,-622.5162024436,-622.436518215306,-622.356847229085,-622.277179775559,
-622.197500124743,-622.117792542348,-622.037997313272,-621.958152971564,
-621.878194544517,-621.835798667921,-621.75584136779,-621.675978570547,
-621.596192748075,-621.51646643288,-621.436782204585,-621.357111218364,
-621.277443764838,-621.197764114022,-621.118056531627,-621.038261302552,
-620.958416960844,-620.878458533796,-620.836062657201,-620.756223956451,
-620.676479699828,-620.596812243681,-620.517204005867,-620.437637451845,
-620.358083586226,-620.278532678271,-620.198968894966,-620.119376398451,
-620.039696321836,-619.959966231899,-619.880124160307,-619.84470185244),
 .UNSPECIFIED.);
#1569=B_SPLINE_CURVE_WITH_KNOTS('',3,(#178880,#178881,#178882,#178883,#178884,
#178885,#178886,#178887,#178888,#178889,#178890,#178891),.UNSPECIFIED.,
 .F.,.F.,(4,2,1,1,1,1,1,1,4),(-619.84470185244,-619.836326646481,-618.836590635761,
-617.836854625041,-616.837118614321,-615.837382603601,-614.837646592881,
-613.83791058216,-613.561520588044),.UNSPECIFIED.);
#1570=B_SPLINE_CURVE_WITH_KNOTS('',3,(#178893,#178894,#178895,#178896,#178897,
#178898,#178899,#178900,#178901,#178902,#178903,#178904,#178905,#178906,
#178907,#178908,#178909,#178910,#178911,#178912,#178913,#178914,#178915,
#178916,#178917,#178918,#178919,#178920,#178921,#178922,#178923,#178924,
#178925,#178926,#178927,#178928,#178929,#178930,#178931,#178932,#178933,
#178934,#178935,#178936,#178937,#178938,#178939,#178940,#178941,#178942,
#178943,#178944,#178945,#178946,#178947,#178948,#178949,#178950,#178951,
#178952,#178953,#178954,#178955,#178956,#178957,#178958,#178959,#178960,
#178961,#178962,#178963,#178964,#178965,#178966,#178967,#178968,#178969,
#178970,#178971,#178972,#178973,#178974,#178975,#178976,#178977,#178978,
#178979,#178980,#178981,#178982,#178983,#178984,#178985,#178986,#178987,
#178988,#178989,#178990,#178991,#178992,#178993,#178994,#178995,#178996,
#178997,#178998,#178999,#179000,#179001,#179002,#179003,#179004,#179005,
#179006,#179007,#179008,#179009,#179010,#179011,#179012,#179013,#179014,
#179015,#179016,#179017,#179018,#179019,#179020,#179021,#179022,#179023,
#179024,#179025,#179026,#179027,#179028,#179029,#179030,#179031,#179032,
#179033,#179034,#179035,#179036,#179037,#179038,#179039,#179040,#179041,
#179042,#179043,#179044,#179045,#179046,#179047,#179048,#179049,#179050,
#179051,#179052,#179053,#179054,#179055,#179056,#179057,#179058,#179059,
#179060,#179061,#179062,#179063,#179064,#179065,#179066,#179067,#179068,
#179069,#179070,#179071,#179072,#179073,#179074,#179075,#179076,#179077,
#179078,#179079,#179080,#179081,#179082,#179083,#179084,#179085,#179086,
#179087,#179088,#179089,#179090,#179091,#179092,#179093,#179094,#179095,
#179096,#179097,#179098,#179099,#179100,#179101,#179102,#179103,#179104,
#179105,#179106,#179107,#179108,#179109,#179110,#179111,#179112,#179113,
#179114,#179115,#179116,#179117,#179118,#179119,#179120,#179121,#179122,
#179123,#179124,#179125,#179126,#179127,#179128,#179129,#179130,#179131,
#179132,#179133,#179134,#179135,#179136),.UNSPECIFIED.,.F.,.F.,(4,3,3,3,
3,3,3,3,3,3,3,3,3,3,3,3,3,3,3,3,3,3,3,3,3,3,3,3,3,3,3,3,3,3,3,3,3,3,3,3,
3,3,3,3,3,3,3,3,3,3,3,3,3,3,3,3,3,3,3,3,3,3,3,3,3,3,3,3,3,3,3,3,3,3,3,3,
3,3,3,3,3,4),(-613.56151654526,-613.482503752502,-613.401962604869,-613.323000140188,
-613.244037899469,-613.165059611842,-613.083338351741,-613.004237540242,
-612.921206055841,-612.83817457144,-612.758217271309,-612.678354474066,
-612.598568651595,-612.518842336399,-612.439158108106,-612.359487121885,
-612.279819668359,-612.200140017542,-612.120432435148,-612.040637206073,
-611.960792864365,-611.880834437318,-611.83843856072,-611.758481260589,
-611.678618463346,-611.598832640874,-611.519106325679,-611.439422097385,
-611.359751111164,-611.280083657638,-611.200404006821,-611.120696424427,
-611.040901195352,-610.961056853644,-610.881098426597,-610.83870255,-610.758745249869,
-610.678882452626,-610.599096630154,-610.519370314959,-610.439686086665,
-610.360015100444,-610.280347646918,-610.200667996101,-610.120960413707,
-610.041165184631,-609.961320842923,-609.881362415876,-609.83896653928,
-609.759009239149,-609.679146441906,-609.599360619435,-609.519634304239,
-609.439950075945,-609.360279089724,-609.280611636198,-609.200931985382,
-609.121224402987,-609.041429173912,-608.961584832204,-608.881626405157,
-608.83923052856,-608.759273228429,-608.679410431186,-608.599624608714,
-608.519898293519,-608.440214065225,-608.360543079004,-608.280875625478,
-608.201195974662,-608.121488392268,-608.041693163193,-607.961848821485,
-607.881890394438,-607.83949451784,-607.757398416682,-607.675415270246,
-607.593532266941,-607.511762748388,-607.430059596932,-607.34842276145,
-607.278331238081),.UNSPECIFIED.);
#1571=B_SPLINE_CURVE_WITH_KNOTS('',3,(#179138,#179139,#179140,#179141,#179142,
#179143,#179144,#179145,#179146,#179147),.UNSPECIFIED.,.F.,.F.,(4,1,1,1,
1,1,1,4),(-607.278326294004,-606.839758507119,-605.840022496399,-604.840286485679,
-603.840550474959,-602.840814464239,-601.841078453519,-600.995145930901),
 .UNSPECIFIED.);
#1572=B_SPLINE_CURVE_WITH_KNOTS('',3,(#179149,#179150,#179151,#179152,#179153,
#179154,#179155,#179156,#179157,#179158,#179159),.UNSPECIFIED.,.F.,.F.,
(4,1,1,1,1,1,1,1,4),(-600.995145930901,-600.841342442799,-599.841606432079,
-598.841870421359,-597.842134410638,-596.842398399918,-595.842662389198,
-594.842926378478,-594.711960623722),.UNSPECIFIED.);
#1573=B_SPLINE_CURVE_WITH_KNOTS('',3,(#179161,#179162,#179163,#179164,#179165,
#179166,#179167,#179168,#179169,#179170,#179171,#179172,#179173,#179174,
#179175,#179176,#179177,#179178,#179179,#179180,#179181,#179182,#179183,
#179184,#179185,#179186,#179187,#179188,#179189,#179190,#179191,#179192,
#179193,#179194,#179195,#179196,#179197,#179198,#179199,#179200,#179201,
#179202,#179203,#179204,#179205,#179206,#179207,#179208,#179209,#179210,
#179211,#179212,#179213,#179214,#179215,#179216,#179217,#179218,#179219,
#179220,#179221,#179222,#179223,#179224,#179225,#179226,#179227,#179228,
#179229,#179230,#179231,#179232,#179233,#179234,#179235,#179236,#179237,
#179238,#179239,#179240,#179241,#179242,#179243,#179244,#179245,#179246,
#179247,#179248,#179249,#179250,#179251,#179252,#179253,#179254,#179255,
#179256,#179257,#179258,#179259,#179260,#179261,#179262,#179263,#179264,
#179265,#179266,#179267,#179268,#179269,#179270,#179271,#179272,#179273,
#179274,#179275,#179276,#179277,#179278,#179279,#179280,#179281,#179282,
#179283,#179284,#179285,#179286,#179287,#179288,#179289,#179290,#179291,
#179292,#179293,#179294,#179295,#179296,#179297,#179298,#179299,#179300,
#179301,#179302,#179303,#179304,#179305,#179306,#179307,#179308,#179309,
#179310,#179311,#179312,#179313,#179314,#179315,#179316,#179317,#179318,
#179319,#179320,#179321,#179322,#179323,#179324,#179325,#179326,#179327,
#179328,#179329,#179330,#179331,#179332,#179333,#179334,#179335,#179336,
#179337,#179338,#179339,#179340,#179341,#179342,#179343,#179344,#179345,
#179346,#179347,#179348,#179349,#179350,#179351,#179352,#179353,#179354,
#179355,#179356,#179357,#179358,#179359,#179360,#179361,#179362,#179363,
#179364,#179365,#179366,#179367,#179368,#179369,#179370,#179371,#179372,
#179373,#179374,#179375,#179376,#179377,#179378,#179379,#179380,#179381,
#179382,#179383,#179384,#179385,#179386,#179387,#179388,#179389,#179390,
#179391,#179392,#179393,#179394,#179395,#179396,#179397,#179398,#179399,
#179400,#179401,#179402,#179403,#179404),.UNSPECIFIED.,.F.,.F.,(4,3,3,3,
3,3,3,3,3,3,3,3,3,3,3,3,3,3,3,3,3,3,3,3,3,3,3,3,3,3,3,3,3,3,3,3,3,3,3,3,
3,3,3,3,3,3,3,3,3,3,3,3,3,3,3,3,3,3,3,3,3,3,3,3,3,3,3,3,3,3,3,3,3,3,3,3,
3,3,3,3,3,4),(-594.711960623722,-594.633214489757,-594.554547606313,-594.475941583082,
-594.396847681166,-594.318297702532,-594.239749946813,-594.161187876371,
-594.081688499218,-594.003009440059,-593.923099903909,-593.843190367758,
-593.763233067627,-593.683370270384,-593.603584447913,-593.523858132717,
-593.444173904423,-593.364502918202,-593.284835464676,-593.20515581386,
-593.125448231465,-593.04565300239,-592.965808660682,-592.885850233635,
-592.843454357038,-592.763497056907,-592.683634259664,-592.603848437192,
-592.524122121997,-592.444437893703,-592.364766907482,-592.285099453956,
-592.20541980314,-592.125712220745,-592.045916991669,-591.966072649962,
-591.886114222915,-591.843718346318,-591.763761046187,-591.683898248944,
-591.604112426473,-591.524386111277,-591.444701882984,-591.365030896763,
-591.285363443237,-591.205683792421,-591.125976210027,-591.046180980951,
-590.966336639243,-590.886378212196,-590.843982335598,-590.764025035466,
-590.684162238224,-590.604376415752,-590.524650100556,-590.444965872261,
-590.36529488604,-590.285627432514,-590.205947781697,-590.126240199303,
-590.046444970227,-589.966600628519,-589.886642201472,-589.844246324877,
-589.764289024746,-589.684426227503,-589.604640405031,-589.524914089836,
-589.445229861541,-589.36555887532,-589.285891421794,-589.206211770978,
-589.126504188583,-589.046708959508,-588.9668646178,-588.886906190753,-588.844510314157,
-588.756470151581,-588.668761629949,-588.581261527724,-588.494106043377,
-588.428775519318),.UNSPECIFIED.);
#1574=B_SPLINE_CURVE_WITH_KNOTS('',3,(#179406,#179407,#179408,#179409,#179410,
#179411,#179412,#179413,#179414,#179415),.UNSPECIFIED.,.F.,.F.,(4,1,1,1,
1,1,1,4),(-588.428775316542,-587.844774303437,-586.845038292717,-585.845302281997,
-584.845566271277,-583.845830260557,-582.846094249836,-582.145590009363),
 .UNSPECIFIED.);
#1575=B_SPLINE_CURVE_WITH_KNOTS('',3,(#179417,#179418,#179419,#179420,#179421,
#179422,#179423,#179424,#179425,#179426,#179427,#179428,#179429,#179430,
#179431,#179432,#179433,#179434,#179435,#179436,#179437,#179438,#179439,
#179440,#179441,#179442,#179443,#179444,#179445,#179446,#179447,#179448,
#179449,#179450,#179451,#179452,#179453,#179454,#179455,#179456,#179457,
#179458,#179459,#179460,#179461,#179462,#179463,#179464,#179465,#179466,
#179467,#179468,#179469,#179470,#179471,#179472,#179473,#179474,#179475,
#179476,#179477,#179478,#179479,#179480,#179481,#179482,#179483,#179484,
#179485,#179486,#179487,#179488,#179489,#179490,#179491,#179492,#179493,
#179494,#179495,#179496,#179497,#179498,#179499,#179500,#179501,#179502,
#179503,#179504,#179505,#179506,#179507,#179508,#179509,#179510,#179511,
#179512,#179513,#179514,#179515,#179516,#179517,#179518,#179519,#179520,
#179521,#179522,#179523,#179524,#179525,#179526,#179527,#179528,#179529,
#179530,#179531,#179532,#179533,#179534,#179535,#179536,#179537,#179538,
#179539,#179540,#179541,#179542,#179543,#179544,#179545,#179546,#179547,
#179548,#179549,#179550,#179551,#179552,#179553,#179554,#179555,#179556,
#179557,#179558,#179559,#179560,#179561,#179562,#179563,#179564,#179565,
#179566,#179567,#179568,#179569,#179570,#179571,#179572,#179573,#179574,
#179575,#179576,#179577,#179578,#179579,#179580,#179581,#179582,#179583,
#179584,#179585,#179586,#179587,#179588,#179589,#179590,#179591,#179592,
#179593,#179594,#179595,#179596,#179597,#179598,#179599,#179600,#179601,
#179602,#179603,#179604,#179605,#179606,#179607,#179608,#179609,#179610,
#179611,#179612,#179613,#179614,#179615,#179616,#179617,#179618,#179619,
#179620,#179621,#179622,#179623,#179624,#179625,#179626,#179627,#179628,
#179629,#179630,#179631,#179632,#179633,#179634,#179635,#179636,#179637,
#179638,#179639,#179640,#179641,#179642,#179643,#179644,#179645,#179646,
#179647,#179648,#179649,#179650,#179651,#179652,#179653,#179654,#179655,
#179656,#179657,#179658,#179659,#179660),.UNSPECIFIED.,.F.,.F.,(4,3,3,3,
3,3,3,3,3,3,3,3,3,3,3,3,3,3,3,3,3,3,3,3,3,3,3,3,3,3,3,3,3,3,3,3,3,3,3,3,
3,3,3,3,3,3,3,3,3,3,3,3,3,3,3,3,3,3,3,3,3,3,3,3,3,3,3,3,3,3,3,3,3,3,3,3,
3,3,3,3,3,4),(-582.145589826881,-582.049496542247,-581.947927390681,-581.846358239116,
-581.766400938985,-581.686538141743,-581.606752319271,-581.527026004076,
-581.447341775783,-581.367670789562,-581.288003336036,-581.20832368522,
-581.128616102826,-581.048820873751,-580.968976532043,-580.889018104996,
-580.846622228396,-580.766664928265,-580.686802131022,-580.60701630855,
-580.527289993355,-580.447605765061,-580.36793477884,-580.288267325314,
-580.208587674498,-580.128880092103,-580.049084863028,-579.96924052132,
-579.889282094273,-579.846886217676,-579.766928917545,-579.687066120302,
-579.60728029783,-579.527553982635,-579.447869754341,-579.36819876812,-579.288531314594,
-579.208851663777,-579.129144081383,-579.049348852307,-578.9695045106,-578.889546083552,
-578.847150206956,-578.767192906825,-578.687330109582,-578.60754428711,
-578.527817971915,-578.448133743621,-578.3684627574,-578.288795303875,-578.209115653058,
-578.129408070664,-578.049612841588,-577.969768499881,-577.889810072833,
-577.847414196236,-577.767456896105,-577.687594098862,-577.60780827639,
-577.528081961195,-577.448397732901,-577.36872674668,-577.289059293154,
-577.209379642337,-577.129672059943,-577.049876830867,-576.97003248916,
-576.890074062112,-576.847678185516,-576.767921519313,-576.688259249651,
-576.608673655916,-576.52914707972,-576.445804282528,-576.366331940496,
-576.286861398012,-576.207376753605,-576.127862100087,-576.048259715846,
-575.968606018376,-575.888842977266,-575.862404702183),.UNSPECIFIED.);
#1576=B_SPLINE_CURVE_WITH_KNOTS('',3,(#179662,#179663,#179664,#179665,#179666,
#179667,#179668,#179669,#179670,#179671,#179672,#179673),.UNSPECIFIED.,
 .F.,.F.,(4,2,1,1,1,1,1,1,4),(-575.862404702183,-575.847942174796,-574.848206164075,
-573.848470153355,-572.848734142635,-571.848998131915,-570.849262121195,
-569.849526110475,-569.579222933784),.UNSPECIFIED.);
#1577=B_SPLINE_CURVE_WITH_KNOTS('',3,(#179675,#179676,#179677,#179678,#179679,
#179680,#179681,#179682,#179683,#179684,#179685,#179686,#179687,#179688,
#179689,#179690,#179691,#179692,#179693,#179694,#179695,#179696,#179697,
#179698,#179699,#179700,#179701,#179702,#179703,#179704,#179705,#179706,
#179707,#179708,#179709,#179710,#179711,#179712,#179713,#179714,#179715,
#179716,#179717,#179718,#179719,#179720,#179721,#179722,#179723,#179724,
#179725,#179726,#179727,#179728,#179729,#179730,#179731,#179732,#179733,
#179734,#179735,#179736,#179737,#179738,#179739,#179740,#179741,#179742,
#179743,#179744,#179745,#179746,#179747,#179748,#179749,#179750,#179751,
#179752,#179753,#179754,#179755,#179756,#179757,#179758,#179759,#179760,
#179761,#179762,#179763,#179764,#179765,#179766,#179767,#179768,#179769,
#179770,#179771,#179772,#179773,#179774,#179775,#179776,#179777,#179778,
#179779,#179780,#179781,#179782,#179783,#179784,#179785,#179786,#179787,
#179788,#179789,#179790,#179791,#179792,#179793,#179794,#179795,#179796,
#179797,#179798,#179799,#179800,#179801,#179802,#179803,#179804,#179805,
#179806,#179807,#179808,#179809,#179810,#179811,#179812,#179813,#179814,
#179815,#179816,#179817,#179818,#179819,#179820,#179821,#179822,#179823,
#179824,#179825,#179826,#179827,#179828,#179829,#179830,#179831,#179832,
#179833,#179834,#179835,#179836,#179837,#179838,#179839,#179840,#179841,
#179842,#179843,#179844,#179845,#179846,#179847,#179848,#179849,#179850,
#179851,#179852,#179853,#179854,#179855,#179856,#179857,#179858,#179859,
#179860,#179861,#179862,#179863,#179864,#179865,#179866,#179867,#179868,
#179869,#179870,#179871,#179872,#179873,#179874,#179875,#179876,#179877,
#179878,#179879,#179880,#179881,#179882,#179883,#179884,#179885,#179886,
#179887,#179888,#179889,#179890,#179891,#179892,#179893,#179894,#179895,
#179896,#179897,#179898,#179899,#179900,#179901,#179902,#179903,#179904,
#179905,#179906,#179907,#179908,#179909,#179910,#179911,#179912,#179913,
#179914,#179915,#179916,#179917,#179918,#179919,#179920,#179921),
 .UNSPECIFIED.,.F.,.F.,(4,3,3,3,3,3,3,3,3,3,3,3,3,3,3,3,3,3,3,3,3,3,3,3,
3,3,3,3,3,3,3,3,3,3,3,3,3,3,3,3,3,3,3,3,3,3,3,3,3,3,3,3,3,3,3,3,3,3,3,3,
3,3,3,3,3,3,3,3,3,3,3,3,3,3,3,3,3,3,3,3,3,3,4),(-569.579219395004,-569.500253204918,
-569.418945316773,-569.340034366194,-569.261125310107,-569.182201840767,
-569.099098905514,-569.020054680491,-568.940956990892,-568.86175344233,
-568.849790099755,-568.769832799623,-568.689970002381,-568.610184179909,
-568.530457864713,-568.450773636419,-568.371102650198,-568.291435196672,
-568.211755545855,-568.13204796346,-568.052252734384,-567.972408392676,
-567.892449965629,-567.850054089034,-567.770096788903,-567.69023399166,
-567.610448169188,-567.530721853993,-567.451037625699,-567.371366639478,
-567.291699185952,-567.212019535136,-567.132311952741,-567.052516723666,
-566.972672381958,-566.892713954911,-566.850318078314,-566.770360778183,
-566.69049798094,-566.610712158469,-566.530985843273,-566.451301614979,
-566.371630628758,-566.291963175232,-566.212283524416,-566.132575942021,
-566.052780712946,-565.972936371238,-565.892977944191,-565.850582067594,
-565.770624767463,-565.69076197022,-565.610976147748,-565.531249832553,
-565.451565604259,-565.371894618038,-565.292227164512,-565.212547513696,
-565.132839931302,-565.053044702226,-564.973200360518,-564.893241933471,
-564.850846056874,-564.770888756743,-564.6910259595,-564.611240137028,-564.531513821833,
-564.451829593539,-564.372158607318,-564.292491153792,-564.212811502976,
-564.133103920581,-564.053308691505,-563.973464349798,-563.89350592275,
-563.851110046154,-563.768843700018,-563.686692243135,-563.604643212547,
-563.522711875554,-563.440849456856,-563.359058510945,-563.296034087824),
 .UNSPECIFIED.);
#1578=B_SPLINE_CURVE_WITH_KNOTS('',3,(#179923,#179924,#179925,#179926,#179927,
#179928,#179929,#179930,#179931,#179932),.UNSPECIFIED.,.F.,.F.,(4,1,1,1,
1,1,1,4),(-563.296029712208,-562.851374035434,-561.851638024714,-560.851902013993,
-559.852166003273,-558.852429992553,-557.852693981833,-557.012848780644),
 .UNSPECIFIED.);
#1579=B_SPLINE_CURVE_WITH_KNOTS('',3,(#179934,#179935,#179936,#179937,#179938,
#179939,#179940,#179941,#179942,#179943,#179944),.UNSPECIFIED.,.F.,.F.,
(4,1,1,1,1,1,1,1,4),(-557.012848780644,-556.852957971113,-555.853221960393,
-554.853485949673,-553.853749938953,-552.854013928232,-551.854277917512,
-550.854541906792,-550.729663473465),.UNSPECIFIED.);
#1580=B_SPLINE_CURVE_WITH_KNOTS('',3,(#179946,#179947,#179948,#179949,#179950,
#179951,#179952,#179953,#179954,#179955,#179956,#179957,#179958,#179959,
#179960,#179961,#179962,#179963,#179964,#179965,#179966,#179967,#179968,
#179969,#179970,#179971,#179972,#179973,#179974,#179975,#179976,#179977,
#179978,#179979,#179980,#179981,#179982,#179983,#179984,#179985,#179986,
#179987,#179988,#179989,#179990,#179991,#179992,#179993,#179994,#179995,
#179996,#179997,#179998,#179999,#180000,#180001,#180002,#180003,#180004,
#180005,#180006,#180007,#180008,#180009,#180010,#180011,#180012,#180013,
#180014,#180015,#180016,#180017,#180018,#180019,#180020,#180021,#180022,
#180023,#180024,#180025,#180026,#180027,#180028,#180029,#180030,#180031,
#180032,#180033,#180034,#180035,#180036,#180037,#180038,#180039,#180040,
#180041,#180042,#180043,#180044,#180045,#180046,#180047,#180048,#180049,
#180050,#180051,#180052,#180053,#180054,#180055,#180056,#180057,#180058,
#180059,#180060,#180061,#180062,#180063,#180064,#180065,#180066,#180067,
#180068,#180069,#180070,#180071,#180072,#180073,#180074,#180075,#180076,
#180077,#180078,#180079,#180080,#180081,#180082,#180083,#180084,#180085,
#180086,#180087,#180088,#180089,#180090,#180091,#180092,#180093,#180094,
#180095,#180096,#180097,#180098,#180099,#180100,#180101,#180102,#180103,
#180104,#180105,#180106,#180107,#180108,#180109,#180110,#180111,#180112,
#180113,#180114,#180115,#180116,#180117,#180118,#180119,#180120,#180121,
#180122,#180123,#180124,#180125,#180126,#180127,#180128,#180129,#180130,
#180131,#180132,#180133,#180134,#180135,#180136,#180137,#180138,#180139,
#180140,#180141,#180142,#180143,#180144,#180145,#180146,#180147,#180148,
#180149,#180150,#180151,#180152,#180153,#180154,#180155,#180156,#180157,
#180158,#180159,#180160,#180161,#180162,#180163,#180164,#180165,#180166,
#180167,#180168,#180169,#180170,#180171,#180172,#180173,#180174,#180175,
#180176,#180177,#180178,#180179,#180180,#180181,#180182,#180183,#180184,
#180185,#180186,#180187,#180188,#180189),.UNSPECIFIED.,.F.,.F.,(4,3,3,3,
3,3,3,3,3,3,3,3,3,3,3,3,3,3,3,3,3,3,3,3,3,3,3,3,3,3,3,3,3,3,3,3,3,3,3,3,
3,3,3,3,3,3,3,3,3,3,3,3,3,3,3,3,3,3,3,3,3,3,3,3,3,3,3,3,3,3,3,3,3,3,3,3,
3,3,3,3,3,4),(-550.729663473465,-550.650891342868,-550.572199648605,-550.493570008962,
-550.413724494851,-550.335153720726,-550.256586124739,-550.178005180778,
-550.097205359601,-550.018508004469,-549.93665695027,-549.854805896072,
-549.774848595941,-549.694985798698,-549.615199976226,-549.535473661031,
-549.455789432737,-549.376118446516,-549.29645099299,-549.216771342174,
-549.13706375978,-549.057268530704,-548.977424188996,-548.897465761949,
-548.855069885352,-548.775112585221,-548.695249787978,-548.615463965506,
-548.535737650311,-548.456053422017,-548.376382435796,-548.29671498227,
-548.217035331454,-548.13732774906,-548.057532519984,-547.977688178277,
-547.897729751229,-547.855333874632,-547.775376574501,-547.695513777258,
-547.615727954786,-547.536001639591,-547.456317411296,-547.376646425075,
-547.296978971549,-547.217299320733,-547.137591738338,-547.057796509262,
-546.977952167554,-546.897993740507,-546.855597863912,-546.775640563781,
-546.695777766538,-546.615991944066,-546.536265628871,-546.456581400576,
-546.376910414356,-546.29724296083,-546.217563310013,-546.137855727619,
-546.058060498543,-545.978216156835,-545.898257729788,-545.855861853192,
-545.775904553061,-545.696041755818,-545.616255933346,-545.536529618151,
-545.456845389857,-545.377174403636,-545.29750695011,-545.217827299294,
-545.1381197169,-545.058324487824,-544.978480146117,-544.89852171907,-544.856125842472,
-544.767725216914,-544.679669533128,-544.591833594987,-544.504359017994,
-544.44647837855),.UNSPECIFIED.);
#1581=B_SPLINE_CURVE_WITH_KNOTS('',3,(#180191,#180192,#180193,#180194,#180195,
#180196,#180197,#180198,#180199,#180200),.UNSPECIFIED.,.F.,.F.,(4,1,1,1,
1,1,1,4),(-544.446478166285,-543.856389831751,-542.856653821031,-541.856917810311,
-540.857181799591,-539.857445788871,-538.857709778151,-538.163292859106),
 .UNSPECIFIED.);
#1582=B_SPLINE_CURVE_WITH_KNOTS('',3,(#180202,#180203,#180204,#180205,#180206,
#180207,#180208,#180209,#180210,#180211,#180212,#180213,#180214,#180215,
#180216,#180217,#180218,#180219,#180220,#180221,#180222,#180223,#180224,
#180225,#180226,#180227,#180228,#180229,#180230,#180231,#180232,#180233,
#180234,#180235,#180236,#180237,#180238,#180239,#180240,#180241,#180242,
#180243,#180244,#180245,#180246,#180247,#180248,#180249,#180250,#180251,
#180252,#180253,#180254,#180255,#180256,#180257,#180258,#180259,#180260,
#180261,#180262,#180263,#180264,#180265,#180266,#180267,#180268,#180269,
#180270,#180271,#180272,#180273,#180274,#180275,#180276,#180277,#180278,
#180279,#180280,#180281,#180282,#180283,#180284,#180285,#180286,#180287,
#180288,#180289,#180290,#180291,#180292,#180293,#180294,#180295,#180296,
#180297,#180298,#180299,#180300,#180301,#180302,#180303,#180304,#180305,
#180306,#180307,#180308,#180309,#180310,#180311,#180312,#180313,#180314,
#180315,#180316,#180317,#180318,#180319,#180320,#180321,#180322,#180323,
#180324,#180325,#180326,#180327,#180328,#180329,#180330,#180331,#180332,
#180333,#180334,#180335,#180336,#180337,#180338,#180339,#180340,#180341,
#180342,#180343,#180344,#180345,#180346,#180347,#180348,#180349,#180350,
#180351,#180352,#180353,#180354,#180355,#180356,#180357,#180358,#180359,
#180360,#180361,#180362,#180363,#180364,#180365,#180366,#180367,#180368,
#180369,#180370,#180371,#180372,#180373,#180374,#180375,#180376,#180377,
#180378,#180379,#180380,#180381,#180382,#180383,#180384,#180385,#180386,
#180387,#180388,#180389,#180390,#180391,#180392,#180393,#180394,#180395,
#180396,#180397,#180398,#180399,#180400,#180401,#180402,#180403,#180404,
#180405,#180406,#180407,#180408,#180409,#180410,#180411,#180412,#180413,
#180414,#180415,#180416,#180417,#180418,#180419,#180420,#180421,#180422,
#180423,#180424,#180425,#180426,#180427,#180428,#180429,#180430,#180431,
#180432,#180433,#180434,#180435,#180436,#180437,#180438,#180439,#180440,
#180441,#180442,#180443,#180444,#180445,#180446,#180447,#180448),
 .UNSPECIFIED.,.F.,.F.,(4,3,3,3,3,3,3,3,3,3,3,3,3,3,3,3,3,3,3,3,3,3,3,3,
3,3,3,3,3,3,3,3,3,3,3,3,3,3,3,3,3,3,3,3,3,3,3,3,3,3,3,3,3,3,3,3,3,3,3,3,
3,3,3,3,3,3,3,3,3,3,3,3,3,3,3,3,3,3,3,3,3,3,4),(-538.163292664416,-538.067833579261,
-537.971624657692,-537.874613587217,-537.85797376743,-537.778016467299,
-537.698153670057,-537.618367847586,-537.538641532391,-537.458957304097,
-537.379286317877,-537.299618864351,-537.219939213535,-537.140231631141,
-537.060436402066,-536.980592060359,-536.900633633312,-536.85823775671,
-536.778280456579,-536.698417659336,-536.618631836864,-536.538905521669,
-536.459221293375,-536.379550307154,-536.299882853628,-536.220203202811,
-536.140495620417,-536.060700391342,-535.980856049634,-535.900897622587,
-535.85850174599,-535.778544445859,-535.698681648616,-535.618895826144,
-535.539169510949,-535.459485282654,-535.379814296433,-535.300146842907,
-535.220467192091,-535.140759609696,-535.060964380621,-534.981120038913,
-534.901161611866,-534.85876573527,-534.778808435139,-534.698945637896,
-534.619159815425,-534.539433500229,-534.459749271935,-534.380078285714,
-534.300410832189,-534.220731181372,-534.141023598978,-534.061228369902,
-533.981384028195,-533.901425601147,-533.85902972455,-533.779072424419,
-533.699209627176,-533.619423804704,-533.539697489509,-533.460013261215,
-533.380342274994,-533.300674821468,-533.220995170652,-533.141287588257,
-533.061492359181,-532.981648017474,-532.901689590426,-532.85929371383,
-532.779615619115,-532.700031870406,-532.62052467556,-532.541076305429,
-532.458455211241,-532.37906040542,-532.299667163717,-532.220259521228,
-532.140821507006,-532.061296040865,-531.981718807671,-531.90203376275,
-531.880107551926),.UNSPECIFIED.);
#1583=B_SPLINE_CURVE_WITH_KNOTS('',3,(#180450,#180451,#180452,#180453,#180454,
#180455,#180456,#180457,#180458,#180459,#180460,#180461),.UNSPECIFIED.,
 .F.,.F.,(4,2,1,1,1,1,1,1,4),(-531.880107551926,-531.85955770311,-530.85982169239,
-529.860085681669,-528.860349670949,-527.860613660229,-526.860877649509,
-525.861141638789,-525.596922244747),.UNSPECIFIED.);
#1584=B_SPLINE_CURVE_WITH_KNOTS('',3,(#180463,#180464,#180465,#180466,#180467,
#180468,#180469,#180470,#180471,#180472),.UNSPECIFIED.,.F.,.F.,(4,1,1,1,
1,1,1,4),(-525.596922244747,-524.861405628069,-523.861669617349,-522.861933606629,
-521.862197595908,-520.862461585188,-519.862725574468,-519.313736937567),
 .UNSPECIFIED.);
#1585=B_SPLINE_CURVE_WITH_KNOTS('',3,(#180474,#180475,#180476,#180477,#180478,
#180479,#180480,#180481,#180482,#180483),.UNSPECIFIED.,.F.,.F.,(4,1,1,1,
1,1,1,4),(-519.313736937567,-518.862989563748,-517.863253553028,-516.863517542308,
-515.863781531588,-514.864045520868,-513.864309510147,-513.030551630387),
 .UNSPECIFIED.);
#1586=B_SPLINE_CURVE_WITH_KNOTS('',3,(#180485,#180486,#180487,#180488,#180489,
#180490,#180491,#180492,#180493,#180494,#180495),.UNSPECIFIED.,.F.,.F.,
(4,1,1,1,1,1,1,1,4),(-513.030551630387,-512.864573499427,-511.864837488707,
-510.865101477987,-509.865365467267,-508.865629456547,-507.865893445827,
-506.866157435107,-506.747366323208),.UNSPECIFIED.);
#1587=B_SPLINE_CURVE_WITH_KNOTS('',3,(#180497,#180498,#180499,#180500,#180501,
#180502,#180503,#180504,#180505,#180506,#180507,#180508,#180509,#180510,
#180511,#180512,#180513,#180514,#180515,#180516,#180517,#180518,#180519,
#180520,#180521,#180522,#180523,#180524,#180525,#180526,#180527,#180528,
#180529,#180530,#180531,#180532,#180533,#180534,#180535,#180536,#180537,
#180538,#180539,#180540,#180541,#180542,#180543,#180544,#180545,#180546,
#180547,#180548,#180549,#180550,#180551,#180552,#180553,#180554,#180555,
#180556,#180557,#180558,#180559,#180560,#180561,#180562,#180563,#180564,
#180565,#180566,#180567,#180568,#180569,#180570,#180571,#180572,#180573,
#180574,#180575,#180576,#180577,#180578,#180579,#180580,#180581,#180582,
#180583,#180584,#180585,#180586,#180587,#180588,#180589,#180590,#180591,
#180592,#180593,#180594,#180595,#180596,#180597,#180598,#180599,#180600,
#180601,#180602,#180603,#180604,#180605,#180606,#180607,#180608,#180609,
#180610,#180611,#180612,#180613,#180614,#180615,#180616,#180617,#180618,
#180619,#180620,#180621,#180622,#180623,#180624,#180625,#180626,#180627,
#180628,#180629,#180630,#180631,#180632,#180633,#180634,#180635,#180636,
#180637,#180638,#180639,#180640,#180641,#180642,#180643,#180644,#180645,
#180646,#180647,#180648,#180649,#180650,#180651,#180652,#180653,#180654,
#180655,#180656,#180657,#180658,#180659,#180660,#180661,#180662,#180663,
#180664,#180665,#180666,#180667,#180668,#180669,#180670,#180671,#180672,
#180673,#180674,#180675,#180676,#180677,#180678,#180679,#180680,#180681,
#180682,#180683,#180684,#180685,#180686,#180687,#180688,#180689,#180690,
#180691,#180692,#180693,#180694,#180695,#180696,#180697,#180698,#180699,
#180700,#180701,#180702,#180703,#180704,#180705,#180706,#180707,#180708,
#180709,#180710,#180711,#180712,#180713,#180714,#180715,#180716,#180717,
#180718,#180719,#180720,#180721,#180722,#180723,#180724,#180725,#180726,
#180727,#180728,#180729,#180730,#180731,#180732,#180733,#180734,#180735,
#180736,#180737,#180738,#180739,#180740,#180741,#180742,#180743),
 .UNSPECIFIED.,.F.,.F.,(4,3,3,3,3,3,3,3,3,3,3,3,3,3,3,3,3,3,3,3,3,3,3,3,
3,3,3,3,3,3,3,3,3,3,3,3,3,3,3,3,3,3,3,3,3,3,3,3,3,3,3,3,3,3,3,3,3,3,3,3,
3,3,3,3,3,3,3,3,3,3,3,3,3,3,3,3,3,3,3,3,3,3,4),(-506.747366323208,-506.668565269127,
-506.589845799829,-506.511189544419,-506.430593529415,-506.351998912421,
-506.273408403512,-506.194805489864,-506.112709473494,-506.033990720535,
-505.955219812063,-505.876345448082,-505.866421424386,-505.786464124255,
-505.706601327012,-505.62681550454,-505.547089189345,-505.467404961051,
-505.38773397483,-505.308066521304,-505.228386870488,-505.148679288093,
-505.068884059018,-504.98903971731,-504.909081290263,-504.866685413666,
-504.786728113535,-504.706865316292,-504.627079493821,-504.547353178625,
-504.467668950331,-504.38799796411,-504.308330510585,-504.228650859768,
-504.148943277374,-504.069148048298,-503.989303706591,-503.909345279544,
-503.866949402946,-503.786992102815,-503.707129305572,-503.6273434831,-503.547617167905,
-503.467932939611,-503.38826195339,-503.308594499864,-503.228914849047,
-503.149207266652,-503.069412037577,-502.989567695869,-502.909609268821,
-502.867213392226,-502.787256092095,-502.707393294852,-502.627607472381,
-502.547881157185,-502.468196928891,-502.38852594267,-502.308858489144,
-502.229178838328,-502.149471255933,-502.069676026858,-501.98983168515,
-501.909873258103,-501.867477381506,-501.787520081375,-501.707657284132,
-501.62787146166,-501.548145146465,-501.468460918171,-501.38878993195,-501.309122478424,
-501.229442827608,-501.149735245214,-501.069940016139,-500.990095674431,
-500.910137247384,-500.867741370786,-500.77896803224,-500.6905538493,-500.602371739187,
-500.51456865474,-500.464181236766),.UNSPECIFIED.);
#1588=B_SPLINE_CURVE_WITH_KNOTS('',3,(#180745,#180746,#180747,#180748,#180749,
#180750,#180751,#180752,#180753,#180754),.UNSPECIFIED.,.F.,.F.,(4,1,1,1,
1,1,1,4),(-500.464181016028,-499.868005360066,-498.868269349345,-497.868533338625,
-496.868797327905,-495.869061317185,-494.869325306465,-494.180995708849),
 .UNSPECIFIED.);
#1589=B_SPLINE_CURVE_WITH_KNOTS('',3,(#180756,#180757,#180758,#180759,#180760,
#180761,#180762,#180763,#180764,#180765,#180766,#180767,#180768,#180769,
#180770,#180771,#180772,#180773,#180774,#180775,#180776,#180777,#180778,
#180779,#180780,#180781,#180782,#180783,#180784,#180785,#180786,#180787,
#180788,#180789,#180790,#180791,#180792,#180793,#180794,#180795,#180796,
#180797,#180798,#180799,#180800,#180801,#180802,#180803,#180804,#180805,
#180806,#180807,#180808,#180809,#180810,#180811,#180812,#180813,#180814,
#180815,#180816,#180817,#180818,#180819,#180820,#180821,#180822,#180823,
#180824,#180825,#180826,#180827,#180828,#180829,#180830,#180831,#180832,
#180833,#180834,#180835,#180836,#180837,#180838,#180839,#180840,#180841,
#180842,#180843,#180844,#180845,#180846,#180847,#180848,#180849,#180850,
#180851,#180852,#180853,#180854,#180855,#180856,#180857,#180858,#180859,
#180860,#180861,#180862,#180863,#180864,#180865,#180866,#180867,#180868,
#180869,#180870,#180871,#180872,#180873,#180874,#180875,#180876,#180877,
#180878,#180879,#180880,#180881,#180882,#180883,#180884,#180885,#180886,
#180887,#180888,#180889,#180890,#180891,#180892,#180893,#180894,#180895,
#180896,#180897,#180898,#180899,#180900,#180901,#180902,#180903,#180904,
#180905,#180906,#180907,#180908,#180909,#180910,#180911,#180912,#180913,
#180914,#180915,#180916,#180917,#180918,#180919,#180920,#180921,#180922,
#180923,#180924,#180925,#180926,#180927,#180928,#180929,#180930,#180931,
#180932,#180933,#180934,#180935,#180936,#180937,#180938,#180939,#180940,
#180941,#180942,#180943,#180944,#180945,#180946,#180947,#180948,#180949,
#180950,#180951,#180952,#180953,#180954,#180955,#180956,#180957,#180958,
#180959,#180960,#180961,#180962,#180963,#180964,#180965,#180966,#180967,
#180968,#180969,#180970,#180971,#180972,#180973,#180974,#180975,#180976,
#180977,#180978,#180979,#180980,#180981,#180982,#180983,#180984,#180985,
#180986,#180987,#180988,#180989,#180990,#180991,#180992,#180993,#180994,
#180995,#180996,#180997,#180998,#180999,#181000,#181001,#181002),
 .UNSPECIFIED.,.F.,.F.,(4,3,3,3,3,3,3,3,3,3,3,3,3,3,3,3,3,3,3,3,3,3,3,3,
3,3,3,3,3,3,3,3,3,3,3,3,3,3,3,3,3,3,3,3,3,3,3,3,3,3,3,3,3,3,3,3,3,3,3,3,
3,3,3,3,3,3,3,3,3,3,3,3,3,3,3,3,3,3,3,3,3,3,4),(-494.180995503453,-494.086145198552,
-493.990601361686,-493.894293100197,-493.869589295745,-493.789631995614,
-493.709769198372,-493.6299833759,-493.550257060705,-493.470572832411,-493.390901846191,
-493.311234392665,-493.231554741849,-493.151847159454,-493.072051930379,
-492.992207588672,-492.912249161625,-492.869853285025,-492.789895984894,
-492.710033187651,-492.63024736518,-492.550521049984,-492.470836821691,
-492.39116583547,-492.311498381944,-492.231818731127,-492.152111148733,
-492.072315919658,-491.99247157795,-491.912513150903,-491.870117274305,
-491.790159974173,-491.710297176931,-491.630511354459,-491.550785039263,
-491.471100810969,-491.391429824747,-491.311762371221,-491.232082720404,
-491.15237513801,-491.072579908934,-490.992735567226,-490.912777140178,
-490.870381263584,-490.790423963453,-490.71056116621,-490.630775343738,
-490.551049028543,-490.471364800249,-490.391693814028,-490.312026360502,
-490.232346709686,-490.152639127291,-490.072843898216,-489.992999556508,
-489.913041129461,-489.870645252864,-489.790687952733,-489.71082515549,
-489.631039333019,-489.551313017823,-489.471628789529,-489.391957803309,
-489.312290349783,-489.232610698966,-489.152903116572,-489.073107887497,
-488.993263545789,-488.913305118742,-488.870909242144,-488.791306292984,
-488.711797637287,-488.632365416433,-488.552991835624,-488.471094156379,
-488.391773525049,-488.312454249021,-488.233120304614,-488.153755661784,
-488.074303920618,-487.994799997186,-487.915189864538,-487.897810401669),
 .UNSPECIFIED.);
#1590=B_SPLINE_CURVE_WITH_KNOTS('',3,(#181004,#181005,#181006,#181007,#181008,
#181009,#181010,#181011,#181012,#181013,#181014,#181015),.UNSPECIFIED.,
 .F.,.F.,(4,2,1,1,1,1,1,1,4),(-487.897810401669,-487.871173231424,-486.871437220704,
-485.871701209984,-484.871965199264,-483.872229188543,-482.872493177823,
-481.872757167103,-481.61462509449),.UNSPECIFIED.);
#1591=B_SPLINE_CURVE_WITH_KNOTS('',3,(#181017,#181018,#181019,#181020,#181021,
#181022,#181023,#181024,#181025,#181026),.UNSPECIFIED.,.F.,.F.,(4,1,1,1,
1,1,1,4),(-481.61462509449,-480.873021156383,-479.873285145663,-478.873549134943,
-477.873813124223,-476.874077113502,-475.874341102782,-475.33143978731),
 .UNSPECIFIED.);
#1592=B_SPLINE_CURVE_WITH_KNOTS('',3,(#181028,#181029,#181030,#181031,#181032,
#181033,#181034,#181035,#181036,#181037,#181038,#181039,#181040,#181041,
#181042,#181043,#181044,#181045,#181046,#181047,#181048,#181049,#181050,
#181051,#181052,#181053,#181054,#181055,#181056,#181057,#181058,#181059,
#181060,#181061,#181062,#181063,#181064,#181065,#181066,#181067,#181068,
#181069,#181070,#181071,#181072,#181073,#181074,#181075,#181076,#181077,
#181078,#181079,#181080,#181081,#181082,#181083,#181084,#181085,#181086,
#181087,#181088,#181089,#181090,#181091,#181092,#181093,#181094,#181095,
#181096,#181097,#181098,#181099,#181100,#181101,#181102,#181103,#181104,
#181105,#181106,#181107,#181108,#181109,#181110,#181111,#181112,#181113,
#181114,#181115,#181116,#181117,#181118,#181119,#181120,#181121,#181122,
#181123,#181124,#181125,#181126,#181127,#181128,#181129,#181130,#181131,
#181132,#181133,#181134,#181135,#181136,#181137,#181138,#181139,#181140,
#181141,#181142,#181143,#181144,#181145,#181146,#181147,#181148,#181149,
#181150,#181151,#181152,#181153,#181154,#181155,#181156,#181157,#181158,
#181159,#181160,#181161,#181162,#181163,#181164,#181165,#181166,#181167,
#181168,#181169,#181170,#181171,#181172,#181173,#181174,#181175,#181176,
#181177,#181178,#181179,#181180,#181181,#181182,#181183,#181184,#181185,
#181186,#181187,#181188,#181189,#181190,#181191,#181192,#181193,#181194,
#181195,#181196,#181197,#181198,#181199,#181200,#181201,#181202,#181203,
#181204,#181205,#181206,#181207,#181208,#181209,#181210,#181211,#181212,
#181213,#181214,#181215,#181216,#181217,#181218,#181219,#181220,#181221,
#181222,#181223,#181224,#181225,#181226,#181227,#181228,#181229,#181230,
#181231,#181232,#181233,#181234,#181235,#181236,#181237,#181238,#181239,
#181240,#181241,#181242,#181243,#181244,#181245,#181246,#181247,#181248,
#181249,#181250,#181251,#181252,#181253,#181254,#181255,#181256,#181257,
#181258,#181259,#181260,#181261,#181262,#181263,#181264,#181265,#181266,
#181267,#181268,#181269,#181270,#181271,#181272,#181273,#181274),
 .UNSPECIFIED.,.F.,.F.,(4,3,3,3,3,3,3,3,3,3,3,3,3,3,3,3,3,3,3,3,3,3,3,3,
3,3,3,3,3,3,3,3,3,3,3,3,3,3,3,3,3,3,3,3,3,3,3,3,3,3,3,3,3,3,3,3,3,3,3,3,
3,3,3,3,3,3,3,3,3,3,3,3,3,3,3,3,3,3,3,3,3,3,4),(-475.331439554867,-475.246323996886,
-475.161039435295,-475.075497894197,-474.989817249859,-474.903927795396,
-474.874605092062,-474.794647791931,-474.714784994688,-474.634999172216,
-474.555272857021,-474.475588628726,-474.395917642505,-474.316250188979,
-474.236570538163,-474.156862955768,-474.077067726693,-473.997223384985,
-473.917264957938,-473.874869081342,-473.794911781211,-473.715048983968,
-473.635263161496,-473.555536846301,-473.475852618007,-473.396181631786,
-473.31651417826,-473.236834527444,-473.157126945049,-473.077331715973,
-472.997487374266,-472.917528947218,-472.875133070622,-472.795175770491,
-472.715312973248,-472.635527150776,-472.555800835581,-472.476116607287,
-472.396445621066,-472.31677816754,-472.237098516724,-472.157390934329,
-472.077595705254,-471.997751363546,-471.917792936499,-471.875397059902,
-471.795439759771,-471.715576962528,-471.635791140056,-471.556064824861,
-471.476380596567,-471.396709610346,-471.31704215682,-471.237362506004,
-471.157654923609,-471.077859694534,-470.998015352826,-470.918056925779,
-470.875661049182,-470.795703749051,-470.715840951808,-470.636055129337,
-470.556328814141,-470.476644585847,-470.396973599626,-470.317306146101,
-470.237626495284,-470.15791891289,-470.078123683814,-469.998279342107,
-469.918320915059,-469.875925038462,-469.797161483017,-469.718492017867,
-469.639898148453,-469.561365072808,-469.482864722549,-469.404380512817,
-469.325895873312,-469.247362635622,-469.168802557328,-469.090159966002,
-469.04825448013),.UNSPECIFIED.);
#1593=B_SPLINE_CURVE_WITH_KNOTS('',3,(#181276,#181277,#181278,#181279,#181280,
#181281,#181282,#181283,#181284,#181285,#181286),.UNSPECIFIED.,.F.,.F.,
(4,1,1,1,1,1,1,1,4),(-469.04825448013,-468.876189027742,-467.876453017021,
-466.876717006301,-465.876980995581,-464.877244984861,-463.877508974141,
-462.877772963421,-462.765069172951),.UNSPECIFIED.);
#1594=B_SPLINE_CURVE_WITH_KNOTS('',3,(#181288,#181289,#181290,#181291,#181292,
#181293,#181294,#181295,#181296,#181297),.UNSPECIFIED.,.F.,.F.,(4,1,1,1,
1,1,1,4),(-462.765069172951,-461.878036952701,-460.87830094198,-459.87856493126,
-458.87882892054,-457.87909290982,-456.8793568991,-456.481883865771),
 .UNSPECIFIED.);
#1595=B_SPLINE_CURVE_WITH_KNOTS('',3,(#181299,#181300,#181301,#181302,#181303,
#181304,#181305,#181306,#181307,#181308),.UNSPECIFIED.,.F.,.F.,(4,1,1,1,
1,1,1,4),(-456.481883865771,-455.87962088838,-454.87988487766,-453.88014886694,
-452.880412856219,-451.880676845499,-450.880940834779,-450.198698558592),
 .UNSPECIFIED.);
#1596=B_SPLINE_CURVE_WITH_KNOTS('',3,(#181310,#181311,#181312,#181313,#181314,
#181315,#181316,#181317,#181318,#181319),.UNSPECIFIED.,.F.,.F.,(4,1,1,1,
1,1,1,4),(-450.198698558592,-449.881204824059,-448.881468813339,-447.881732802619,
-446.881996791899,-445.882260781179,-444.882524770458,-443.915517737304),
 .UNSPECIFIED.);
#1597=B_SPLINE_CURVE_WITH_KNOTS('',3,(#181321,#181322,#181323,#181324,#181325,
#181326,#181327,#181328,#181329,#181330,#181331,#181332,#181333,#181334,
#181335,#181336,#181337,#181338,#181339,#181340,#181341,#181342,#181343,
#181344,#181345,#181346,#181347,#181348,#181349,#181350,#181351,#181352,
#181353,#181354,#181355,#181356,#181357,#181358,#181359,#181360,#181361,
#181362,#181363,#181364,#181365,#181366,#181367,#181368,#181369,#181370,
#181371,#181372,#181373,#181374,#181375,#181376,#181377,#181378,#181379,
#181380,#181381,#181382,#181383,#181384,#181385,#181386,#181387,#181388,
#181389,#181390,#181391,#181392,#181393,#181394,#181395,#181396,#181397,
#181398,#181399,#181400,#181401,#181402,#181403,#181404,#181405,#181406,
#181407,#181408,#181409,#181410,#181411,#181412,#181413,#181414,#181415,
#181416,#181417,#181418,#181419,#181420,#181421,#181422,#181423,#181424,
#181425,#181426,#181427,#181428,#181429,#181430,#181431,#181432,#181433,
#181434,#181435,#181436,#181437,#181438,#181439,#181440,#181441,#181442,
#181443,#181444,#181445,#181446,#181447,#181448,#181449,#181450,#181451,
#181452,#181453,#181454,#181455,#181456,#181457,#181458,#181459,#181460,
#181461,#181462,#181463,#181464,#181465,#181466,#181467,#181468,#181469,
#181470,#181471,#181472,#181473,#181474,#181475,#181476,#181477,#181478,
#181479,#181480,#181481,#181482,#181483,#181484,#181485,#181486,#181487,
#181488,#181489,#181490,#181491,#181492,#181493,#181494,#181495,#181496,
#181497,#181498,#181499,#181500,#181501,#181502,#181503,#181504,#181505,
#181506,#181507,#181508,#181509,#181510,#181511,#181512,#181513,#181514,
#181515,#181516,#181517,#181518,#181519,#181520,#181521,#181522,#181523,
#181524,#181525,#181526,#181527,#181528,#181529,#181530,#181531,#181532,
#181533,#181534,#181535,#181536,#181537,#181538,#181539,#181540,#181541,
#181542,#181543,#181544,#181545,#181546,#181547,#181548,#181549,#181550,
#181551,#181552,#181553,#181554,#181555,#181556,#181557,#181558,#181559,
#181560,#181561,#181562,#181563,#181564,#181565,#181566,#181567),
 .UNSPECIFIED.,.F.,.F.,(4,3,3,3,3,3,3,3,3,3,3,3,3,3,3,3,3,3,3,3,3,3,3,3,
3,3,3,3,3,3,3,3,3,3,3,3,3,3,3,3,3,3,3,3,3,3,3,3,3,3,3,3,3,3,3,3,3,3,3,3,
3,3,3,3,3,3,3,3,3,3,3,3,3,3,3,3,3,3,3,3,3,3,4),(-443.915513251412,-443.882788759738,
-443.802831459607,-443.722968662364,-443.643182839892,-443.563456524697,
-443.483772296403,-443.404101310182,-443.324433856656,-443.244754205839,
-443.165046623445,-443.085251394369,-443.005407052661,-442.925448625614,
-442.883052749018,-442.803095448887,-442.723232651644,-442.643446829172,
-442.563720513977,-442.484036285683,-442.404365299462,-442.324697845936,
-442.24501819512,-442.165310612725,-442.085515383649,-442.005671041942,
-441.925712614894,-441.883316738298,-441.803359438167,-441.723496640924,
-441.643710818452,-441.563984503257,-441.484300274963,-441.404629288742,
-441.324961835216,-441.2452821844,-441.165574602005,-441.08577937293,-441.005935031222,
-440.925976604175,-440.883580727578,-440.803623427447,-440.723760630204,
-440.643974807732,-440.564248492537,-440.484564264243,-440.404893278022,
-440.325225824496,-440.245546173679,-440.165838591285,-440.086043362209,
-440.006199020502,-439.926240593454,-439.883844716858,-439.803887416727,
-439.724024619484,-439.644238797013,-439.564512481817,-439.484828253523,
-439.405157267303,-439.325489813777,-439.24581016296,-439.166102580566,
-439.086307351491,-439.006463009783,-438.926504582736,-438.884108706138,
-438.804151406007,-438.724288608764,-438.644502786292,-438.564776471096,
-438.485092242802,-438.405421256581,-438.325753803055,-438.246074152238,
-438.166366569843,-438.086571340767,-438.00672699906,-437.926768572012,
-437.884372695417,-437.779892065321,-437.677571283294,-437.632328004849),
 .UNSPECIFIED.);
#1598=B_SPLINE_CURVE_WITH_KNOTS('',3,(#181569,#181570,#181571,#181572,#181573,
#181574,#181575,#181576,#181577,#181578),.UNSPECIFIED.,.F.,.F.,(4,1,1,1,
1,1,1,4),(-437.632327944233,-436.884636684697,-435.884900673977,-434.885164663257,
-433.885428652537,-432.885692641817,-431.885956631097,-431.349142637053),
 .UNSPECIFIED.);
#1599=B_SPLINE_CURVE_WITH_KNOTS('',3,(#181580,#181581,#181582,#181583,#181584,
#181585,#181586,#181587,#181588,#181589,#181590,#181591,#181592,#181593,
#181594,#181595,#181596,#181597,#181598,#181599,#181600,#181601,#181602,
#181603,#181604,#181605,#181606,#181607,#181608,#181609,#181610,#181611,
#181612,#181613,#181614,#181615,#181616,#181617,#181618,#181619,#181620,
#181621,#181622,#181623,#181624,#181625,#181626,#181627,#181628,#181629,
#181630,#181631,#181632,#181633,#181634,#181635,#181636,#181637,#181638,
#181639,#181640,#181641,#181642,#181643,#181644,#181645,#181646,#181647,
#181648,#181649,#181650,#181651,#181652,#181653,#181654,#181655,#181656,
#181657,#181658,#181659,#181660,#181661,#181662,#181663,#181664,#181665,
#181666,#181667,#181668,#181669,#181670,#181671,#181672,#181673,#181674,
#181675,#181676,#181677,#181678,#181679,#181680,#181681,#181682,#181683,
#181684,#181685,#181686,#181687,#181688,#181689,#181690,#181691,#181692,
#181693,#181694,#181695,#181696,#181697,#181698,#181699,#181700,#181701,
#181702,#181703,#181704,#181705,#181706,#181707,#181708,#181709,#181710,
#181711,#181712,#181713,#181714,#181715,#181716,#181717,#181718,#181719,
#181720,#181721,#181722,#181723,#181724,#181725,#181726,#181727,#181728,
#181729,#181730,#181731,#181732,#181733,#181734,#181735,#181736,#181737,
#181738,#181739,#181740,#181741,#181742,#181743,#181744,#181745,#181746,
#181747,#181748,#181749,#181750,#181751,#181752,#181753,#181754,#181755,
#181756,#181757,#181758,#181759,#181760,#181761,#181762,#181763,#181764,
#181765,#181766,#181767,#181768,#181769,#181770,#181771,#181772,#181773,
#181774,#181775,#181776,#181777,#181778,#181779,#181780,#181781,#181782,
#181783,#181784,#181785,#181786,#181787,#181788,#181789,#181790,#181791,
#181792,#181793,#181794,#181795,#181796,#181797,#181798,#181799,#181800,
#181801,#181802,#181803,#181804,#181805,#181806,#181807,#181808,#181809,
#181810,#181811,#181812,#181813,#181814,#181815,#181816,#181817,#181818,
#181819,#181820,#181821,#181822,#181823,#181824,#181825,#181826),
 .UNSPECIFIED.,.F.,.F.,(4,3,3,3,3,3,3,3,3,3,3,3,3,3,3,3,3,3,3,3,3,3,3,3,
3,3,3,3,3,3,3,3,3,3,3,3,3,3,3,3,3,3,3,3,3,3,3,3,3,3,3,3,3,3,3,3,3,3,3,3,
3,3,3,3,3,3,3,3,3,3,3,3,3,3,3,3,3,3,3,3,3,3,4),(-431.349142435417,-431.264283350958,
-431.179265992277,-431.094002032319,-431.008605479933,-430.923002336439,
-430.886220620377,-430.806263320245,-430.726400523002,-430.64661470053,
-430.566888385334,-430.48720415704,-430.407533170818,-430.327865717292,
-430.248186066475,-430.16847848408,-430.088683255004,-430.008838913296,
-429.928880486248,-429.886484609656,-429.806527309525,-429.726664512282,
-429.64687868981,-429.567152374615,-429.487468146321,-429.4077971601,-429.328129706574,
-429.248450055757,-429.168742473363,-429.088947244287,-429.00910290258,
-428.929144475532,-428.886748598936,-428.806791298805,-428.726928501562,
-428.647142679091,-428.567416363896,-428.487732135602,-428.408061149381,
-428.328393695855,-428.248714045039,-428.169006462644,-428.089211233569,
-428.009366891862,-427.929408464814,-427.887012588216,-427.807055288085,
-427.727192490842,-427.64740666837,-427.567680353175,-427.487996124881,
-427.40832513866,-427.328657685134,-427.248978034317,-427.169270451923,
-427.089475222847,-427.00963088114,-426.929672454092,-426.887276577496,
-426.807319277365,-426.727456480122,-426.64767065765,-426.567944342455,
-426.488260114161,-426.40858912794,-426.328921674414,-426.249242023598,
-426.169534441203,-426.089739212128,-426.009894870421,-425.929936443373,
-425.887540566776,-425.808773536607,-425.730100687268,-425.651503525719,
-425.572967473253,-425.494464274122,-425.41597734501,-425.337490117298,
-425.25895559468,-425.180394297064,-425.101753411262,-425.065957329874),
 .UNSPECIFIED.);
#1600=B_SPLINE_CURVE_WITH_KNOTS('',3,(#181828,#181829,#181830,#181831,#181832,
#181833,#181834,#181835,#181836,#181837,#181838),.UNSPECIFIED.,.F.,.F.,
(4,1,1,1,1,1,1,1,4),(-425.065957329874,-424.887804556056,-423.888068545336,
-422.888332534616,-421.888596523895,-420.888860513175,-419.889124502455,
-418.889388491735,-418.782772022694),.UNSPECIFIED.);
#1601=B_SPLINE_CURVE_WITH_KNOTS('',3,(#181840,#181841,#181842,#181843,#181844,
#181845,#181846,#181847,#181848,#181849),.UNSPECIFIED.,.F.,.F.,(4,1,1,1,
1,1,1,4),(-418.782772022694,-417.889652481015,-416.889916470295,-415.890180459574,
-414.890444448854,-413.890708438134,-412.890972427414,-412.499586715514),
 .UNSPECIFIED.);
#1602=B_SPLINE_CURVE_WITH_KNOTS('',3,(#181851,#181852,#181853,#181854,#181855,
#181856,#181857,#181858,#181859,#181860),.UNSPECIFIED.,.F.,.F.,(4,1,1,1,
1,1,1,4),(-412.499586715514,-411.891236416694,-410.891500405974,-409.891764395254,
-408.892028384534,-407.892292373813,-406.892556363093,-406.216401408335),
 .UNSPECIFIED.);
#1603=B_SPLINE_CURVE_WITH_KNOTS('',3,(#181862,#181863,#181864,#181865,#181866,
#181867,#181868,#181869,#181870,#181871),.UNSPECIFIED.,.F.,.F.,(4,1,1,1,
1,1,1,4),(-406.216401408335,-405.892820352373,-404.893084341653,-403.893348330933,
-402.893612320213,-401.893876309493,-400.894140298773,-399.933221433922),
 .UNSPECIFIED.);
#1604=B_SPLINE_CURVE_WITH_KNOTS('',3,(#181873,#181874,#181875,#181876,#181877,
#181878,#181879,#181880,#181881,#181882,#181883,#181884,#181885,#181886,
#181887,#181888,#181889,#181890,#181891,#181892,#181893,#181894,#181895,
#181896,#181897,#181898,#181899,#181900,#181901,#181902,#181903,#181904,
#181905,#181906,#181907,#181908,#181909,#181910,#181911,#181912,#181913,
#181914,#181915,#181916,#181917,#181918,#181919,#181920,#181921,#181922,
#181923,#181924,#181925,#181926,#181927,#181928,#181929,#181930,#181931,
#181932,#181933,#181934,#181935,#181936,#181937,#181938,#181939,#181940,
#181941,#181942,#181943,#181944,#181945,#181946,#181947,#181948,#181949,
#181950,#181951,#181952,#181953,#181954,#181955,#181956,#181957,#181958,
#181959,#181960,#181961,#181962,#181963,#181964,#181965,#181966,#181967,
#181968,#181969,#181970,#181971,#181972,#181973,#181974,#181975,#181976,
#181977,#181978,#181979,#181980,#181981,#181982,#181983,#181984,#181985,
#181986,#181987,#181988,#181989,#181990,#181991,#181992,#181993,#181994,
#181995,#181996,#181997,#181998,#181999,#182000,#182001,#182002,#182003,
#182004,#182005,#182006,#182007,#182008,#182009,#182010,#182011,#182012,
#182013,#182014,#182015,#182016,#182017,#182018,#182019,#182020,#182021,
#182022,#182023,#182024,#182025,#182026,#182027,#182028,#182029,#182030,
#182031,#182032,#182033,#182034,#182035,#182036,#182037,#182038,#182039,
#182040,#182041,#182042,#182043,#182044,#182045,#182046,#182047,#182048,
#182049,#182050,#182051,#182052,#182053,#182054,#182055,#182056,#182057,
#182058,#182059,#182060,#182061,#182062,#182063,#182064,#182065,#182066,
#182067,#182068,#182069,#182070,#182071,#182072,#182073,#182074,#182075,
#182076,#182077,#182078,#182079,#182080,#182081,#182082,#182083,#182084,
#182085,#182086,#182087,#182088,#182089,#182090,#182091,#182092,#182093,
#182094,#182095,#182096,#182097,#182098,#182099,#182100,#182101,#182102,
#182103,#182104,#182105,#182106,#182107,#182108,#182109,#182110,#182111,
#182112,#182113,#182114,#182115,#182116,#182117,#182118,#182119),
 .UNSPECIFIED.,.F.,.F.,(4,3,3,3,3,3,3,3,3,3,3,3,3,3,3,3,3,3,3,3,3,3,3,3,
3,3,3,3,3,3,3,3,3,3,3,3,3,3,3,3,3,3,3,3,3,3,3,3,3,3,3,3,3,3,3,3,3,3,3,3,
3,3,3,3,3,3,3,3,3,3,3,3,3,3,3,3,3,3,3,3,3,3,4),(-399.933216101155,-399.894404288052,
-399.814446987921,-399.734584190678,-399.654798368206,-399.575072053011,
-399.495387824717,-399.415716838496,-399.33604938497,-399.256369734153,
-399.176662151759,-399.096866922683,-399.017022580976,-398.937064153929,
-398.894668277332,-398.814710977201,-398.734848179958,-398.655062357486,
-398.575336042291,-398.495651813997,-398.415980827776,-398.33631337425,
-398.256633723433,-398.176926141039,-398.097130911963,-398.017286570256,
-397.937328143208,-397.894932266612,-397.814974966481,-397.735112169238,
-397.655326346766,-397.575600031571,-397.495915803277,-397.416244817056,
-397.33657736353,-397.256897712713,-397.177190130319,-397.097394901243,
-397.017550559535,-396.937592132488,-396.895196255892,-396.815238955761,
-396.735376158518,-396.655590336046,-396.575864020851,-396.496179792557,
-396.416508806336,-396.33684135281,-396.257161701994,-396.177454119599,
-396.097658890524,-396.017814548816,-395.937856121769,-395.895460245172,
-395.815502945041,-395.735640147798,-395.655854325326,-395.576128010131,
-395.496443781837,-395.416772795616,-395.33710534209,-395.257425691274,
-395.177718108879,-395.097922879804,-395.018078538096,-394.938120111049,
-394.895724234452,-394.815766934321,-394.735904137078,-394.656118314606,
-394.576391999411,-394.496707771117,-394.417036784896,-394.33736933137,
-394.257689680554,-394.177982098159,-394.098186869083,-394.018342527376,
-393.938384100329,-393.895988223732,-393.790381676865,-393.68713925179,
-393.650030878059),.UNSPECIFIED.);
#1605=B_SPLINE_CURVE_WITH_KNOTS('',3,(#182121,#182122,#182123,#182124,#182125,
#182126,#182127,#182128,#182129,#182130),.UNSPECIFIED.,.F.,.F.,(4,1,1,1,
1,1,1,4),(-393.650030793976,-392.896252213012,-391.896516202291,-390.896780191571,
-389.897044180851,-388.897308170131,-387.897572159411,-387.366845486796),
 .UNSPECIFIED.);
#1606=B_SPLINE_CURVE_WITH_KNOTS('',3,(#182132,#182133,#182134,#182135,#182136,
#182137,#182138,#182139,#182140,#182141),.UNSPECIFIED.,.F.,.F.,(4,1,1,1,
1,1,1,4),(-387.366845486796,-386.897836148691,-385.898100137971,-384.89836412725,
-383.89862811653,-382.89889210581,-381.89915609509,-381.083664942812),
 .UNSPECIFIED.);
#1607=B_SPLINE_CURVE_WITH_KNOTS('',3,(#182143,#182144,#182145,#182146,#182147,
#182148,#182149,#182150,#182151,#182152,#182153,#182154,#182155,#182156,
#182157,#182158,#182159,#182160,#182161,#182162,#182163,#182164,#182165,
#182166,#182167,#182168,#182169,#182170,#182171,#182172,#182173,#182174,
#182175,#182176,#182177,#182178,#182179,#182180,#182181,#182182,#182183,
#182184,#182185,#182186,#182187,#182188,#182189,#182190,#182191,#182192,
#182193,#182194,#182195,#182196,#182197,#182198,#182199,#182200,#182201,
#182202,#182203,#182204,#182205,#182206,#182207,#182208,#182209,#182210,
#182211,#182212,#182213,#182214,#182215,#182216,#182217,#182218,#182219,
#182220,#182221,#182222,#182223,#182224,#182225,#182226,#182227,#182228,
#182229,#182230,#182231,#182232,#182233,#182234,#182235,#182236,#182237,
#182238,#182239,#182240,#182241,#182242,#182243,#182244,#182245,#182246,
#182247,#182248,#182249,#182250,#182251,#182252,#182253,#182254,#182255,
#182256,#182257,#182258,#182259,#182260,#182261,#182262,#182263,#182264,
#182265,#182266,#182267,#182268,#182269,#182270,#182271,#182272,#182273,
#182274,#182275,#182276,#182277,#182278,#182279,#182280,#182281,#182282,
#182283,#182284,#182285,#182286,#182287,#182288,#182289,#182290,#182291,
#182292,#182293,#182294,#182295,#182296,#182297,#182298,#182299,#182300,
#182301,#182302,#182303,#182304,#182305,#182306,#182307,#182308,#182309,
#182310,#182311,#182312,#182313,#182314,#182315,#182316,#182317,#182318,
#182319,#182320,#182321,#182322,#182323,#182324,#182325,#182326,#182327,
#182328,#182329,#182330,#182331,#182332,#182333,#182334,#182335,#182336,
#182337,#182338,#182339,#182340,#182341,#182342,#182343,#182344,#182345,
#182346,#182347,#182348,#182349,#182350,#182351,#182352,#182353,#182354,
#182355,#182356,#182357,#182358,#182359,#182360,#182361,#182362,#182363,
#182364,#182365,#182366,#182367,#182368,#182369,#182370,#182371,#182372,
#182373,#182374,#182375,#182376,#182377,#182378,#182379,#182380,#182381,
#182382,#182383,#182384,#182385,#182386),.UNSPECIFIED.,.F.,.F.,(4,3,3,3,
3,3,3,3,3,3,3,3,3,3,3,3,3,3,3,3,3,3,3,3,3,3,3,3,3,3,3,3,3,3,3,3,3,3,3,3,
3,3,3,3,3,3,3,3,3,3,3,3,3,3,3,3,3,3,3,3,3,3,3,3,3,3,3,3,3,3,3,3,3,3,3,3,
3,3,3,3,3,4),(-381.083660179617,-380.963780184145,-380.89942008437,-380.819462784239,
-380.739599986997,-380.659814164526,-380.580087849331,-380.500403621037,
-380.420732634817,-380.341065181291,-380.261385530475,-380.181677948081,
-380.101882719006,-380.022038377299,-379.942079950252,-379.89968407365,
-379.819726773519,-379.739863976276,-379.660078153804,-379.580351838609,
-379.500667610315,-379.420996624094,-379.341329170568,-379.261649519751,
-379.181941937356,-379.102146708281,-379.022302366573,-378.942343939526,
-378.89994806293,-378.819990762799,-378.740127965556,-378.660342143084,
-378.580615827889,-378.500931599595,-378.421260613374,-378.341593159848,
-378.261913509032,-378.182205926637,-378.102410697561,-378.022566355854,
-377.942607928807,-377.90021205221,-377.820254752079,-377.740391954836,
-377.660606132364,-377.580879817169,-377.501195588874,-377.421524602653,
-377.341857149127,-377.262177498311,-377.182469915916,-377.10267468684,
-377.022830345133,-376.942871918085,-376.900476041489,-376.820518741358,
-376.740655944115,-376.660870121643,-376.581143806448,-376.501459578154,
-376.421788591933,-376.342121138407,-376.26244148759,-376.182733905196,
-376.10293867612,-376.023094334413,-375.943135907365,-375.900740030769,
-375.820782730638,-375.740919933395,-375.661134110923,-375.581407795728,
-375.501723567434,-375.422052581213,-375.342385127687,-375.262705476871,
-375.182997894476,-375.103202665401,-375.023358323693,-374.943399896646,
-374.901004020049,-374.800474872437),.UNSPECIFIED.);
#1608=B_SPLINE_CURVE_WITH_KNOTS('',3,(#182388,#182389,#182390,#182391,#182392,
#182393,#182394,#182395,#182396,#182397),.UNSPECIFIED.,.F.,.F.,(4,1,1,1,
1,1,1,4),(-374.800465775823,-373.901268009329,-372.901531998609,-371.901795987889,
-370.902059977169,-369.902323966449,-368.902587955728,-368.517297017911),
 .UNSPECIFIED.);
#1609=B_SPLINE_CURVE_WITH_KNOTS('',3,(#182399,#182400,#182401,#182402,#182403,
#182404,#182405,#182406,#182407,#182408,#182409,#182410,#182411,#182412,
#182413,#182414,#182415,#182416,#182417,#182418,#182419,#182420,#182421,
#182422,#182423,#182424,#182425,#182426,#182427,#182428,#182429,#182430,
#182431,#182432,#182433,#182434,#182435,#182436,#182437,#182438,#182439,
#182440,#182441,#182442,#182443,#182444,#182445,#182446,#182447,#182448,
#182449,#182450,#182451,#182452,#182453,#182454,#182455,#182456,#182457,
#182458,#182459,#182460,#182461,#182462,#182463,#182464,#182465,#182466,
#182467,#182468,#182469,#182470,#182471,#182472,#182473,#182474,#182475,
#182476,#182477,#182478,#182479,#182480,#182481,#182482,#182483,#182484,
#182485,#182486,#182487,#182488,#182489,#182490,#182491,#182492,#182493,
#182494,#182495,#182496,#182497,#182498,#182499,#182500,#182501,#182502,
#182503,#182504,#182505,#182506,#182507,#182508,#182509,#182510,#182511,
#182512,#182513,#182514,#182515,#182516,#182517,#182518,#182519,#182520,
#182521,#182522,#182523,#182524,#182525,#182526,#182527,#182528,#182529,
#182530,#182531,#182532,#182533,#182534,#182535,#182536,#182537,#182538,
#182539,#182540,#182541,#182542,#182543,#182544,#182545,#182546,#182547,
#182548,#182549,#182550,#182551,#182552,#182553,#182554,#182555,#182556,
#182557,#182558,#182559,#182560,#182561,#182562,#182563,#182564,#182565,
#182566,#182567,#182568,#182569,#182570,#182571,#182572,#182573,#182574,
#182575,#182576,#182577,#182578,#182579,#182580,#182581,#182582,#182583,
#182584,#182585,#182586,#182587,#182588,#182589,#182590,#182591,#182592,
#182593,#182594,#182595,#182596,#182597,#182598,#182599,#182600,#182601,
#182602,#182603,#182604,#182605,#182606,#182607,#182608,#182609,#182610,
#182611,#182612,#182613,#182614,#182615,#182616,#182617,#182618,#182619,
#182620,#182621,#182622,#182623,#182624,#182625,#182626,#182627,#182628,
#182629,#182630,#182631,#182632,#182633,#182634,#182635,#182636,#182637,
#182638,#182639,#182640,#182641,#182642,#182643,#182644,#182645),
 .UNSPECIFIED.,.F.,.F.,(4,3,3,3,3,3,3,3,3,3,3,3,3,3,3,3,3,3,3,3,3,3,3,3,
3,3,3,3,3,3,3,3,3,3,3,3,3,3,3,3,3,3,3,3,3,3,3,3,3,3,3,3,3,3,3,3,3,3,3,3,
3,3,3,3,3,3,3,3,3,3,3,3,3,3,3,3,3,3,3,3,3,3,4),(-368.517289565257,-368.436832624477,
-368.356363949258,-368.275868850284,-368.195332625071,-368.114689806444,
-368.033988383624,-367.953156584468,-367.902851945008,-367.822894644877,
-367.743031847634,-367.663246025162,-367.583519709966,-367.503835481672,
-367.424164495451,-367.344497041925,-367.264817391109,-367.185109808714,
-367.105314579639,-367.025470237931,-366.945511810883,-366.903115934288,
-366.823158634157,-366.743295836914,-366.663510014442,-366.583783699247,
-366.504099470953,-366.424428484732,-366.344761031206,-366.26508138039,
-366.185373797995,-366.10557856892,-366.025734227212,-365.945775800164,
-365.903379923568,-365.823422623437,-365.743559826194,-365.663774003722,
-365.584047688527,-365.504363460234,-365.424692474013,-365.345025020487,
-365.26534536967,-365.185637787276,-365.1058425582,-365.025998216493,-364.946039789446,
-364.903643912848,-364.823686612717,-364.743823815474,-364.664037993002,
-364.584311677807,-364.504627449513,-364.424956463292,-364.345289009766,
-364.265609358949,-364.185901776555,-364.106106547479,-364.026262205772,
-363.946303778725,-363.903907902128,-363.823950601997,-363.744087804754,
-363.664301982283,-363.584575667088,-363.504891438794,-363.425220452573,
-363.345552999047,-363.265873348231,-363.186165765837,-363.106370536762,
-363.026526195054,-362.946567768006,-362.904171891408,-362.820413437242,
-362.740656700297,-362.660974998161,-362.581352461097,-362.501773259803,
-362.422214796349,-362.342668178147,-362.263103224232,-362.234104258078),
 .UNSPECIFIED.);
#1610=B_SPLINE_CURVE_WITH_KNOTS('',3,(#182647,#182648,#182649,#182650,#182651,
#182652,#182653,#182654,#182655,#182656),.UNSPECIFIED.,.F.,.F.,(4,1,1,1,
1,1,1,4),(-362.23409696627,-361.904435880687,-360.904699869967,-359.904963859247,
-358.905227848527,-357.905491837807,-356.905755827087,-355.950918950898),
 .UNSPECIFIED.);
#1611=B_SPLINE_CURVE_WITH_KNOTS('',3,(#182658,#182659,#182660,#182661,#182662,
#182663,#182664,#182665,#182666,#182667,#182668,#182669),.UNSPECIFIED.,
 .F.,.F.,(4,2,1,1,1,1,1,1,4),(-355.950918950898,-355.906019816367,-354.906283805647,
-353.906547794926,-352.906811784206,-351.907075773486,-350.907339762766,
-349.907603752046,-349.667733643719),.UNSPECIFIED.);
#1612=B_SPLINE_CURVE_WITH_KNOTS('',3,(#182671,#182672,#182673,#182674,#182675,
#182676,#182677,#182678,#182679,#182680),.UNSPECIFIED.,.F.,.F.,(4,1,1,1,
1,1,1,4),(-349.667733643719,-348.907867741326,-347.908131730606,-346.908395719885,
-345.908659709165,-344.908923698445,-343.909187687725,-343.384548336539),
 .UNSPECIFIED.);
#1613=B_SPLINE_CURVE_WITH_KNOTS('',3,(#182682,#182683,#182684,#182685,#182686,
#182687,#182688,#182689,#182690,#182691),.UNSPECIFIED.,.F.,.F.,(4,1,1,1,
1,1,1,4),(-343.384548336539,-342.909451677005,-341.909715666285,-340.909979655565,
-339.910243644845,-338.910507634124,-337.910771623404,-337.10136722921),
 .UNSPECIFIED.);
#1614=B_SPLINE_CURVE_WITH_KNOTS('',3,(#182693,#182694,#182695,#182696,#182697,
#182698,#182699,#182700,#182701,#182702,#182703,#182704,#182705,#182706,
#182707,#182708,#182709,#182710,#182711,#182712,#182713,#182714,#182715,
#182716,#182717,#182718,#182719,#182720,#182721,#182722,#182723,#182724,
#182725,#182726,#182727,#182728,#182729,#182730,#182731,#182732,#182733,
#182734,#182735,#182736,#182737,#182738,#182739,#182740,#182741,#182742,
#182743,#182744,#182745,#182746,#182747,#182748,#182749,#182750,#182751,
#182752,#182753,#182754,#182755,#182756,#182757,#182758,#182759,#182760,
#182761,#182762,#182763,#182764,#182765,#182766,#182767,#182768,#182769,
#182770,#182771,#182772,#182773,#182774,#182775,#182776,#182777,#182778,
#182779,#182780,#182781,#182782,#182783,#182784,#182785,#182786,#182787,
#182788,#182789,#182790,#182791,#182792,#182793,#182794,#182795,#182796,
#182797,#182798,#182799,#182800,#182801,#182802,#182803,#182804,#182805,
#182806,#182807,#182808,#182809,#182810,#182811,#182812,#182813,#182814,
#182815,#182816,#182817,#182818,#182819,#182820,#182821,#182822,#182823,
#182824,#182825,#182826,#182827,#182828,#182829,#182830,#182831,#182832,
#182833,#182834,#182835,#182836,#182837,#182838,#182839,#182840,#182841,
#182842,#182843,#182844,#182845,#182846,#182847,#182848,#182849,#182850,
#182851,#182852,#182853,#182854,#182855,#182856,#182857,#182858,#182859,
#182860,#182861,#182862,#182863,#182864,#182865,#182866,#182867,#182868,
#182869,#182870,#182871,#182872,#182873,#182874,#182875,#182876,#182877,
#182878,#182879,#182880,#182881,#182882,#182883,#182884,#182885,#182886,
#182887,#182888,#182889,#182890,#182891,#182892,#182893,#182894,#182895,
#182896,#182897,#182898,#182899,#182900,#182901,#182902,#182903,#182904,
#182905,#182906,#182907,#182908,#182909,#182910,#182911,#182912,#182913,
#182914,#182915,#182916,#182917,#182918,#182919,#182920,#182921,#182922,
#182923,#182924,#182925,#182926,#182927,#182928,#182929,#182930,#182931,
#182932,#182933,#182934,#182935,#182936),.UNSPECIFIED.,.F.,.F.,(4,3,3,3,
3,3,3,3,3,3,3,3,3,3,3,3,3,3,3,3,3,3,3,3,3,3,3,3,3,3,3,3,3,3,3,3,3,3,3,3,
3,3,3,3,3,3,3,3,3,3,3,3,3,3,3,3,3,3,3,3,3,3,3,3,3,3,3,3,3,3,3,3,3,3,3,3,
3,3,3,3,3,4),(-337.10136302936,-336.983585417605,-336.911035612684,-336.831078312553,
-336.751215515311,-336.67142969284,-336.591703377646,-336.512019149352,
-336.432348163132,-336.352680709607,-336.273001058791,-336.193293476397,
-336.113498247322,-336.033653905615,-335.953695478568,-335.911299601964,
-335.831342301833,-335.75147950459,-335.671693682118,-335.591967366923,
-335.512283138629,-335.432612152408,-335.352944698882,-335.273265048065,
-335.19355746567,-335.113762236595,-335.033917894887,-334.95395946784,-334.911563591244,
-334.831606291113,-334.75174349387,-334.671957671398,-334.592231356202,
-334.512547127908,-334.432876141687,-334.353208688161,-334.273529037344,
-334.19382145495,-334.114026225874,-334.034181884166,-333.954223457119,
-333.911827580524,-333.831870280393,-333.752007483151,-333.672221660679,
-333.592495345484,-333.51281111719,-333.433140130969,-333.353472677443,
-333.273793026627,-333.194085444233,-333.114290215158,-333.03444587345,
-332.954487446403,-332.912091569804,-332.832134269673,-332.75227147243,
-332.672485649958,-332.592759334762,-332.513075106468,-332.433404120247,
-332.35373666672,-332.274057015904,-332.194349433509,-332.114554204433,
-332.034709862725,-331.954751435678,-331.912355559083,-331.832398258952,
-331.752535461709,-331.672749639237,-331.593023324042,-331.513339095748,
-331.433668109527,-331.354000656001,-331.274321005184,-331.19461342279,
-331.114818193714,-331.034973852006,-330.955015424959,-330.912619548363,
-330.81817772218),.UNSPECIFIED.);
#1615=B_SPLINE_CURVE_WITH_KNOTS('',3,(#182938,#182939,#182940,#182941,#182942,
#182943,#182944,#182945,#182946,#182947),.UNSPECIFIED.,.F.,.F.,(4,1,1,1,
1,1,1,4),(-330.81816869401,-329.912883537643,-328.913147526923,-327.913411516203,
-326.913675505483,-325.913939494763,-324.914203484043,-324.534999992564),
 .UNSPECIFIED.);
#1616=B_SPLINE_CURVE_WITH_KNOTS('',3,(#182949,#182950,#182951,#182952,#182953,
#182954,#182955,#182956,#182957,#182958,#182959,#182960,#182961,#182962,
#182963,#182964,#182965,#182966,#182967,#182968,#182969,#182970,#182971,
#182972,#182973,#182974,#182975,#182976,#182977,#182978,#182979,#182980,
#182981,#182982,#182983,#182984,#182985,#182986,#182987,#182988,#182989,
#182990,#182991,#182992,#182993,#182994,#182995,#182996,#182997,#182998,
#182999,#183000,#183001,#183002,#183003,#183004,#183005,#183006,#183007,
#183008,#183009,#183010,#183011,#183012,#183013,#183014,#183015,#183016,
#183017,#183018,#183019,#183020,#183021,#183022,#183023,#183024,#183025,
#183026,#183027,#183028,#183029,#183030,#183031,#183032,#183033,#183034,
#183035,#183036,#183037,#183038,#183039,#183040,#183041,#183042,#183043,
#183044,#183045,#183046,#183047,#183048,#183049,#183050,#183051,#183052,
#183053,#183054,#183055,#183056,#183057,#183058,#183059,#183060,#183061,
#183062,#183063,#183064,#183065,#183066,#183067,#183068,#183069,#183070,
#183071,#183072,#183073,#183074,#183075,#183076,#183077,#183078,#183079,
#183080,#183081,#183082,#183083,#183084,#183085,#183086,#183087,#183088,
#183089,#183090,#183091,#183092,#183093,#183094,#183095,#183096,#183097,
#183098,#183099,#183100,#183101,#183102,#183103,#183104,#183105,#183106,
#183107,#183108,#183109,#183110,#183111,#183112,#183113,#183114,#183115,
#183116,#183117,#183118,#183119,#183120,#183121,#183122,#183123,#183124,
#183125,#183126,#183127,#183128,#183129,#183130,#183131,#183132,#183133,
#183134,#183135,#183136,#183137,#183138,#183139,#183140,#183141,#183142,
#183143,#183144,#183145,#183146,#183147,#183148,#183149,#183150,#183151,
#183152,#183153,#183154,#183155,#183156,#183157,#183158,#183159,#183160,
#183161,#183162,#183163,#183164,#183165,#183166,#183167,#183168,#183169,
#183170,#183171,#183172,#183173,#183174,#183175,#183176,#183177,#183178,
#183179,#183180,#183181,#183182,#183183,#183184,#183185,#183186,#183187,
#183188,#183189,#183190,#183191,#183192,#183193,#183194,#183195),
 .UNSPECIFIED.,.F.,.F.,(4,3,3,3,3,3,3,3,3,3,3,3,3,3,3,3,3,3,3,3,3,3,3,3,
3,3,3,3,3,3,3,3,3,3,3,3,3,3,3,3,3,3,3,3,3,3,3,3,3,3,3,3,3,3,3,3,3,3,3,3,
3,3,3,3,3,3,3,3,3,3,3,3,3,3,3,3,3,3,3,3,3,3,4),(-324.534992415001,-324.454648248748,
-324.374295562936,-324.293919507813,-324.213505222498,-324.132986702897,
-324.052411841748,-323.971705764006,-323.914467473322,-323.834510173191,
-323.754647375949,-323.674861553477,-323.595135238282,-323.515451009989,
-323.435780023768,-323.356112570243,-323.276432919427,-323.196725337033,
-323.116930107957,-323.03708576625,-322.957127339203,-322.914731462602,
-322.834774162471,-322.754911365228,-322.675125542756,-322.595399227561,
-322.515714999267,-322.436044013046,-322.35637655952,-322.276696908704,
-322.19698932631,-322.117194097234,-322.037349755527,-321.95739132848,-321.914995451882,
-321.835038151751,-321.755175354508,-321.675389532036,-321.595663216841,
-321.515978988548,-321.436308002326,-321.3566405488,-321.276960897984,-321.197253315588,
-321.117458086513,-321.037613744805,-320.957655317758,-320.915259441162,
-320.835302141031,-320.755439343788,-320.675653521317,-320.595927206121,
-320.516242977827,-320.436571991607,-320.356904538081,-320.277224887264,
-320.197517304869,-320.117722075794,-320.037877734087,-319.957919307039,
-319.915523430442,-319.835566130311,-319.755703333068,-319.675917510597,
-319.596191195401,-319.516506967108,-319.436835980887,-319.357168527361,
-319.277488876545,-319.197781294151,-319.117986065075,-319.038141723368,
-318.95818329632,-318.915787419722,-318.832789880734,-318.752943243527,
-318.67317260685,-318.593462181619,-318.513796219564,-318.434153364985,
-318.354523413875,-318.274878297269,-318.251807107821),.UNSPECIFIED.);
#1617=B_SPLINE_CURVE_WITH_KNOTS('',3,(#183197,#183198,#183199,#183200,#183201,
#183202,#183203,#183204,#183205,#183206),.UNSPECIFIED.,.F.,.F.,(4,1,1,1,
1,1,1,4),(-318.251799625932,-317.916051409002,-316.916315398281,-315.916579387561,
-314.916843376841,-313.917107366121,-312.917371355401,-311.968621800641),
 .UNSPECIFIED.);
#1618=B_SPLINE_CURVE_WITH_KNOTS('',3,(#183208,#183209,#183210,#183211,#183212,
#183213,#183214,#183215,#183216,#183217,#183218,#183219),.UNSPECIFIED.,
 .F.,.F.,(4,2,1,1,1,1,1,1,4),(-311.968621800641,-311.917635344681,-310.917899333961,
-309.918163323241,-308.918427312521,-307.9186913018,-306.91895529108,-305.91921928036,
-305.685436493462),.UNSPECIFIED.);
#1619=B_SPLINE_CURVE_WITH_KNOTS('',3,(#183221,#183222,#183223,#183224,#183225,
#183226,#183227,#183228,#183229,#183230),.UNSPECIFIED.,.F.,.F.,(4,1,1,1,
1,1,1,4),(-305.685436493462,-304.91948326964,-303.91974725892,-302.9200112482,
-301.92027523748,-300.920539226759,-299.920803216039,-299.402251186282),
 .UNSPECIFIED.);
#1620=B_SPLINE_CURVE_WITH_KNOTS('',3,(#183232,#183233,#183234,#183235,#183236,
#183237,#183238,#183239,#183240,#183241),.UNSPECIFIED.,.F.,.F.,(4,1,1,1,
1,1,1,4),(-299.402251186282,-298.921067205319,-297.921331194599,-296.921595183879,
-295.921859173159,-294.922123162439,-293.922387151719,-293.119069498281),
 .UNSPECIFIED.);
#1621=B_SPLINE_CURVE_WITH_KNOTS('',3,(#183243,#183244,#183245,#183246,#183247,
#183248,#183249,#183250,#183251,#183252,#183253,#183254,#183255,#183256,
#183257,#183258,#183259,#183260,#183261,#183262,#183263,#183264,#183265,
#183266,#183267,#183268,#183269,#183270,#183271,#183272,#183273,#183274,
#183275,#183276,#183277,#183278,#183279,#183280,#183281,#183282,#183283,
#183284,#183285,#183286,#183287,#183288,#183289,#183290,#183291,#183292,
#183293,#183294,#183295,#183296,#183297,#183298,#183299,#183300,#183301,
#183302,#183303,#183304,#183305,#183306,#183307,#183308,#183309,#183310,
#183311,#183312,#183313,#183314,#183315,#183316,#183317,#183318,#183319,
#183320,#183321,#183322,#183323,#183324,#183325,#183326,#183327,#183328,
#183329,#183330,#183331,#183332,#183333,#183334,#183335,#183336,#183337,
#183338,#183339,#183340,#183341,#183342,#183343,#183344,#183345,#183346,
#183347,#183348,#183349,#183350,#183351,#183352,#183353,#183354,#183355,
#183356,#183357,#183358,#183359,#183360,#183361,#183362,#183363,#183364,
#183365,#183366,#183367,#183368,#183369,#183370,#183371,#183372,#183373,
#183374,#183375,#183376,#183377,#183378,#183379,#183380,#183381,#183382,
#183383,#183384,#183385,#183386,#183387,#183388,#183389,#183390,#183391,
#183392,#183393,#183394,#183395,#183396,#183397,#183398,#183399,#183400,
#183401,#183402,#183403,#183404,#183405,#183406,#183407,#183408,#183409,
#183410,#183411,#183412,#183413,#183414,#183415,#183416,#183417,#183418,
#183419,#183420,#183421,#183422,#183423,#183424,#183425,#183426,#183427,
#183428,#183429,#183430,#183431,#183432,#183433,#183434,#183435,#183436,
#183437,#183438,#183439,#183440,#183441,#183442,#183443,#183444,#183445,
#183446,#183447,#183448,#183449,#183450,#183451,#183452,#183453,#183454,
#183455,#183456,#183457,#183458,#183459,#183460,#183461,#183462,#183463,
#183464,#183465,#183466,#183467,#183468,#183469,#183470,#183471,#183472,
#183473,#183474,#183475,#183476,#183477,#183478,#183479,#183480,#183481,
#183482,#183483,#183484,#183485,#183486),.UNSPECIFIED.,.F.,.F.,(4,3,3,3,
3,3,3,3,3,3,3,3,3,3,3,3,3,3,3,3,3,3,3,3,3,3,3,3,3,3,3,3,3,3,3,3,3,3,3,3,
3,3,3,3,3,3,3,3,3,3,3,3,3,3,3,3,3,3,3,3,3,3,3,3,3,3,3,3,3,3,3,3,3,3,3,3,
3,3,3,3,3,4),(-293.119065879103,-293.003224251817,-292.922651140998,-292.842693840867,
-292.762831043625,-292.683045221154,-292.603318905959,-292.523634677665,
-292.443963691445,-292.36429623792,-292.284616587104,-292.204909004709,
-292.125113775634,-292.045269433927,-291.965311006881,-291.922915130278,
-291.842957830147,-291.763095032904,-291.683309210432,-291.603582895237,
-291.523898666943,-291.444227680721,-291.364560227196,-291.284880576379,
-291.205172993984,-291.125377764909,-291.045533423201,-290.965574996154,
-290.923179119558,-290.843221819427,-290.763359022184,-290.683573199712,
-290.603846884517,-290.524162656223,-290.444491670002,-290.364824216476,
-290.285144565659,-290.205436983265,-290.125641754189,-290.045797412481,
-289.965838985434,-289.923443108838,-289.843485808707,-289.763623011464,
-289.683837188992,-289.604110873797,-289.524426645503,-289.444755659282,
-289.365088205756,-289.28540855494,-289.205700972545,-289.12590574347,-289.046061401762,
-288.966102974715,-288.923707098118,-288.843749797987,-288.763887000744,
-288.684101178272,-288.604374863077,-288.524690634783,-288.445019648562,
-288.365352195036,-288.28567254422,-288.205964961825,-288.12616973275,-288.046325391042,
-287.966366963995,-287.923971087398,-287.844013787267,-287.764150990024,
-287.684365167553,-287.604638852357,-287.524954624064,-287.445283637843,
-287.365616184317,-287.2859365335,-287.206228951106,-287.12643372203,-287.046589380323,
-286.966630953275,-286.924235076678,-286.835880571923),.UNSPECIFIED.);
#1622=B_SPLINE_CURVE_WITH_KNOTS('',3,(#183488,#183489,#183490,#183491,#183492,
#183493,#183494,#183495,#183496,#183497),.UNSPECIFIED.,.F.,.F.,(4,1,1,1,
1,1,1,4),(-286.835871811251,-285.924499065957,-284.924763055237,-283.925027044517,
-282.925291033797,-281.925555023077,-280.925819012357,-280.552702930068),
 .UNSPECIFIED.);
#1623=B_SPLINE_CURVE_WITH_KNOTS('',3,(#183499,#183500,#183501,#183502,#183503,
#183504,#183505,#183506,#183507,#183508,#183509,#183510,#183511,#183512,
#183513,#183514,#183515,#183516,#183517,#183518,#183519,#183520,#183521,
#183522,#183523,#183524,#183525,#183526,#183527,#183528,#183529,#183530,
#183531,#183532,#183533,#183534,#183535,#183536,#183537,#183538,#183539,
#183540,#183541,#183542,#183543,#183544,#183545,#183546,#183547,#183548,
#183549,#183550,#183551,#183552,#183553,#183554,#183555,#183556,#183557,
#183558,#183559,#183560,#183561,#183562,#183563,#183564,#183565,#183566,
#183567,#183568,#183569,#183570,#183571,#183572,#183573,#183574,#183575,
#183576,#183577,#183578,#183579,#183580,#183581,#183582,#183583,#183584,
#183585,#183586,#183587,#183588,#183589,#183590,#183591,#183592,#183593,
#183594,#183595,#183596,#183597,#183598,#183599,#183600,#183601,#183602,
#183603,#183604,#183605,#183606,#183607,#183608,#183609,#183610,#183611,
#183612,#183613,#183614,#183615,#183616,#183617,#183618,#183619,#183620,
#183621,#183622,#183623,#183624,#183625,#183626,#183627,#183628,#183629,
#183630,#183631,#183632,#183633,#183634,#183635,#183636,#183637,#183638,
#183639,#183640,#183641,#183642,#183643,#183644,#183645,#183646,#183647,
#183648,#183649,#183650,#183651,#183652,#183653,#183654,#183655,#183656,
#183657,#183658,#183659,#183660,#183661,#183662,#183663,#183664,#183665,
#183666,#183667,#183668,#183669,#183670,#183671,#183672,#183673,#183674,
#183675,#183676,#183677,#183678,#183679,#183680,#183681,#183682,#183683,
#183684,#183685,#183686,#183687,#183688,#183689,#183690,#183691,#183692,
#183693,#183694,#183695,#183696,#183697,#183698,#183699,#183700,#183701,
#183702,#183703,#183704,#183705,#183706,#183707,#183708,#183709,#183710,
#183711,#183712,#183713,#183714,#183715,#183716,#183717,#183718,#183719,
#183720,#183721,#183722,#183723,#183724,#183725,#183726,#183727,#183728,
#183729,#183730,#183731,#183732,#183733,#183734,#183735,#183736,#183737,
#183738,#183739,#183740,#183741,#183742,#183743,#183744,#183745),
 .UNSPECIFIED.,.F.,.F.,(4,3,3,3,3,3,3,3,3,3,3,3,3,3,3,3,3,3,3,3,3,3,3,3,
3,3,3,3,3,3,3,3,3,3,3,3,3,3,3,3,3,3,3,3,3,3,3,3,3,3,3,3,3,3,3,3,3,3,3,3,
3,3,3,3,3,3,3,3,3,3,3,3,3,3,3,3,3,3,3,3,3,3,4),(-280.552695264744,-280.472459775551,
-280.392218872353,-280.311957557339,-280.231660823479,-280.151262148967,
-280.070809345223,-279.990224439258,-279.926083001637,-279.846125701506,
-279.766262904263,-279.686477081792,-279.606750766596,-279.527066538302,
-279.447395552081,-279.367728098555,-279.288048447739,-279.208340865344,
-279.128545636268,-279.048701294561,-278.968742867514,-278.926346990917,
-278.846389690786,-278.766526893543,-278.686741071071,-278.607014755875,
-278.527330527581,-278.44765954136,-278.367992087833,-278.288312437017,
-278.208604854622,-278.128809625546,-278.048965283838,-277.969006856791,
-277.926610980196,-277.846653680065,-277.766790882822,-277.68700506035,
-277.607278745154,-277.52759451686,-277.447923530639,-277.368256077113,
-277.288576426296,-277.208868843902,-277.129073614826,-277.049229273118,
-276.96927084607,-276.926874969476,-276.846917669345,-276.767054872103,
-276.687269049631,-276.607542734435,-276.527858506141,-276.44818751992,
-276.368520066394,-276.288840415578,-276.209132833184,-276.129337604108,
-276.0494932624,-275.969534835353,-275.927138958756,-275.847181658625,-275.767318861382,
-275.68753303891,-275.607806723715,-275.528122495421,-275.4484515092,-275.368784055674,
-275.289104404858,-275.209396822464,-275.129601593388,-275.049757251681,
-274.969798824633,-274.927402948036,-274.845166324227,-274.765225966303,
-274.685362621073,-274.605560586828,-274.525804203116,-274.446073351479,
-274.366356525348,-274.286627668652,-274.269509957564),.UNSPECIFIED.);
#1624=B_SPLINE_CURVE_WITH_KNOTS('',3,(#183747,#183748,#183749,#183750,#183751,
#183752,#183753,#183754,#183755,#183756),.UNSPECIFIED.,.F.,.F.,(4,1,1,1,
1,1,1,4),(-274.269502324484,-273.927666937316,-272.927930926596,-271.928194915876,
-270.928458905156,-269.928722894435,-268.928986883715,-267.986324650384),
 .UNSPECIFIED.);
#1625=B_SPLINE_CURVE_WITH_KNOTS('',3,(#183758,#183759,#183760,#183761,#183762,
#183763,#183764,#183765,#183766,#183767,#183768,#183769),.UNSPECIFIED.,
 .F.,.F.,(4,2,1,1,1,1,1,1,4),(-267.986324650384,-267.929250872995,-266.929514862275,
-265.929778851555,-264.930042840835,-263.930306830115,-262.930570819394,
-261.930834808674,-261.703139343205),.UNSPECIFIED.);
#1626=B_SPLINE_CURVE_WITH_KNOTS('',3,(#183771,#183772,#183773,#183774,#183775,
#183776,#183777,#183778,#183779,#183780,#183781,#183782,#183783,#183784,
#183785,#183786,#183787,#183788,#183789,#183790,#183791,#183792,#183793,
#183794,#183795,#183796,#183797,#183798,#183799,#183800,#183801,#183802,
#183803,#183804,#183805,#183806,#183807,#183808,#183809,#183810,#183811,
#183812,#183813,#183814,#183815,#183816,#183817,#183818,#183819,#183820,
#183821,#183822,#183823,#183824,#183825,#183826,#183827,#183828,#183829,
#183830,#183831,#183832,#183833,#183834,#183835,#183836,#183837,#183838,
#183839,#183840,#183841,#183842,#183843,#183844,#183845,#183846,#183847,
#183848,#183849,#183850,#183851,#183852,#183853,#183854,#183855,#183856,
#183857,#183858,#183859,#183860,#183861,#183862,#183863,#183864,#183865,
#183866,#183867,#183868,#183869,#183870,#183871,#183872,#183873,#183874,
#183875,#183876,#183877,#183878,#183879,#183880,#183881,#183882,#183883,
#183884,#183885,#183886,#183887,#183888,#183889,#183890,#183891,#183892,
#183893,#183894,#183895,#183896,#183897,#183898,#183899,#183900,#183901,
#183902,#183903,#183904,#183905,#183906,#183907,#183908,#183909,#183910,
#183911,#183912,#183913,#183914,#183915,#183916,#183917,#183918,#183919,
#183920,#183921,#183922,#183923,#183924,#183925,#183926,#183927,#183928,
#183929,#183930,#183931,#183932,#183933,#183934,#183935,#183936,#183937,
#183938,#183939,#183940,#183941,#183942,#183943,#183944,#183945,#183946,
#183947,#183948,#183949,#183950,#183951,#183952,#183953,#183954,#183955,
#183956,#183957,#183958,#183959,#183960,#183961,#183962,#183963,#183964,
#183965,#183966,#183967,#183968,#183969,#183970,#183971,#183972,#183973,
#183974,#183975,#183976,#183977,#183978,#183979,#183980,#183981,#183982,
#183983,#183984,#183985,#183986,#183987,#183988,#183989,#183990,#183991,
#183992,#183993,#183994,#183995,#183996,#183997,#183998,#183999,#184000,
#184001,#184002,#184003,#184004,#184005,#184006,#184007,#184008,#184009,
#184010,#184011,#184012,#184013,#184014,#184015,#184016,#184017),
 .UNSPECIFIED.,.F.,.F.,(4,3,3,3,3,3,3,3,3,3,3,3,3,3,3,3,3,3,3,3,3,3,3,3,
3,3,3,3,3,3,3,3,3,3,3,3,3,3,3,3,3,3,3,3,3,3,3,3,3,3,3,3,3,3,3,3,3,3,3,3,
3,3,3,3,3,3,3,3,3,3,3,3,3,3,3,3,3,3,3,3,3,3,4),(-261.703139343205,-261.624409844129,
-261.545735960619,-261.467092226832,-261.388462724706,-261.309830963874,
-261.231180454103,-261.152449208019,-261.073675666579,-260.994784376284,
-260.931098797954,-260.851141497823,-260.77127870058,-260.691492878109,
-260.611766562913,-260.53208233462,-260.452411348399,-260.372743894873,
-260.293064244057,-260.213356661662,-260.133561432586,-260.053717090879,
-259.973758663832,-259.931362787234,-259.851405487103,-259.77154268986,
-259.691756867388,-259.612030552193,-259.532346323899,-259.452675337678,
-259.373007884152,-259.293328233336,-259.213620650942,-259.133825421866,
-259.053981080158,-258.974022653111,-258.931626776514,-258.851669476383,
-258.77180667914,-258.692020856668,-258.612294541473,-258.532610313179,
-258.452939326958,-258.373271873432,-258.293592222615,-258.213884640221,
-258.134089411145,-258.054245069438,-257.97428664239,-257.931890765794,
-257.851933465663,-257.77207066842,-257.692284845948,-257.612558530753,
-257.532874302459,-257.453203316238,-257.373535862713,-257.293856211896,
-257.214148629501,-257.134353400426,-257.054509058718,-256.974550631671,
-256.932154755074,-256.852197454943,-256.7723346577,-256.692548835229,-256.612822520034,
-256.533138291739,-256.453467305518,-256.373799851992,-256.294120201176,
-256.214412618781,-256.134617389706,-256.054773047998,-255.974814620951,
-255.932418744354,-255.848798920709,-255.765311214882,-255.678971920168,
-255.595763918918,-255.512648459724,-255.429641055154,-255.419954036025),
 .UNSPECIFIED.);
#1627=B_SPLINE_CURVE_WITH_KNOTS('',3,(#184019,#184020,#184021,#184022,#184023,
#184024,#184025,#184026,#184027,#184028,#184029,#184030,#184031,#184032,
#184033,#184034,#184035,#184036,#184037,#184038,#184039,#184040,#184041,
#184042,#184043,#184044,#184045,#184046,#184047,#184048,#184049,#184050,
#184051,#184052,#184053,#184054,#184055,#184056,#184057,#184058,#184059,
#184060,#184061,#184062,#184063,#184064,#184065,#184066,#184067,#184068,
#184069,#184070,#184071,#184072,#184073,#184074,#184075,#184076,#184077,
#184078,#184079,#184080,#184081,#184082,#184083,#184084,#184085,#184086,
#184087,#184088,#184089,#184090,#184091,#184092,#184093,#184094,#184095,
#184096,#184097,#184098,#184099,#184100,#184101,#184102,#184103,#184104,
#184105,#184106,#184107,#184108,#184109,#184110,#184111,#184112,#184113,
#184114,#184115,#184116,#184117,#184118,#184119,#184120,#184121,#184122,
#184123,#184124,#184125,#184126,#184127,#184128,#184129,#184130,#184131,
#184132,#184133,#184134,#184135,#184136,#184137,#184138,#184139,#184140,
#184141,#184142,#184143,#184144,#184145,#184146,#184147,#184148,#184149,
#184150,#184151,#184152,#184153,#184154,#184155,#184156,#184157,#184158,
#184159,#184160,#184161,#184162,#184163,#184164,#184165,#184166,#184167,
#184168,#184169,#184170,#184171,#184172,#184173,#184174,#184175,#184176,
#184177,#184178,#184179,#184180,#184181,#184182,#184183,#184184,#184185,
#184186,#184187,#184188,#184189,#184190,#184191,#184192,#184193,#184194,
#184195,#184196,#184197,#184198,#184199,#184200,#184201,#184202,#184203,
#184204,#184205,#184206,#184207,#184208,#184209,#184210,#184211,#184212,
#184213,#184214,#184215,#184216,#184217,#184218,#184219,#184220,#184221,
#184222,#184223,#184224,#184225,#184226,#184227,#184228,#184229,#184230,
#184231,#184232,#184233,#184234,#184235,#184236,#184237,#184238,#184239,
#184240,#184241,#184242,#184243,#184244,#184245,#184246,#184247,#184248,
#184249,#184250,#184251,#184252,#184253,#184254,#184255,#184256,#184257,
#184258,#184259,#184260,#184261,#184262),.UNSPECIFIED.,.F.,.F.,(4,3,3,3,
3,3,3,3,3,3,3,3,3,3,3,3,3,3,3,3,3,3,3,3,3,3,3,3,3,3,3,3,3,3,3,3,3,3,3,3,
3,3,3,3,3,3,3,3,3,3,3,3,3,3,3,3,3,3,3,3,3,3,3,3,3,3,3,3,3,3,3,3,3,3,3,3,
3,3,3,3,3,4),(-255.419954035887,-255.336047313209,-255.252019565011,-255.167781894743,
-255.083434975878,-254.99888936605,-254.932682733633,-254.852725433502,
-254.772862636259,-254.693076813787,-254.613350498592,-254.533666270298,
-254.453995284077,-254.374327830551,-254.294648179734,-254.21494059734,
-254.135145368264,-254.055301026557,-253.975342599509,-253.932946722913,
-253.852989422782,-253.773126625539,-253.693340803067,-253.613614487872,
-253.533930259578,-253.454259273357,-253.374591819831,-253.294912169015,
-253.21520458662,-253.135409357545,-253.055565015837,-252.97560658879,-252.933210712193,
-252.853253412062,-252.773390614819,-252.693604792347,-252.613878477152,
-252.534194248858,-252.454523262637,-252.374855809111,-252.295176158294,
-252.2154685759,-252.135673346824,-252.055829005117,-251.975870578069,-251.933474701473,
-251.853517401342,-251.773654604099,-251.693868781627,-251.614142466432,
-251.534458238138,-251.454787251917,-251.375119798391,-251.295440147575,
-251.21573256518,-251.135937336105,-251.056092994397,-250.97613456735,-250.933738690753,
-250.853781390622,-250.773918593379,-250.694132770907,-250.614406455712,
-250.534722227418,-250.455051241197,-250.375383787671,-250.295704136855,
-250.21599655446,-250.136201325385,-250.056356983677,-249.97639855663,-249.934002680033,
-249.855190850333,-249.776473692243,-249.696510571818,-249.617932915645,
-249.539388524333,-249.460860837844,-249.379837810594,-249.30126758998,
-249.219018159413,-249.136768728846),.UNSPECIFIED.);
#1628=B_SPLINE_CURVE_WITH_KNOTS('',3,(#184264,#184265,#184266,#184267,#184268,
#184269,#184270,#184271,#184272,#184273,#184274),.UNSPECIFIED.,.F.,.F.,
(4,1,1,1,1,1,1,1,4),(-249.136768728846,-248.934266669313,-247.934530658593,
-246.934794647872,-245.935058637152,-244.935322626432,-243.935586615712,
-242.935850604992,-242.853583421666),.UNSPECIFIED.);
#1629=B_SPLINE_CURVE_WITH_KNOTS('',3,(#184276,#184277,#184278,#184279,#184280,
#184281,#184282,#184283,#184284,#184285),.UNSPECIFIED.,.F.,.F.,(4,1,1,1,
1,1,1,4),(-242.853583421666,-241.936114594272,-240.936378583552,-239.936642572831,
-238.936906562111,-237.937170551391,-236.937434540671,-236.570398114487),
 .UNSPECIFIED.);
#1630=B_SPLINE_CURVE_WITH_KNOTS('',3,(#184287,#184288,#184289,#184290,#184291,
#184292,#184293,#184294,#184295,#184296),.UNSPECIFIED.,.F.,.F.,(4,1,1,1,
1,1,1,4),(-236.570398114487,-235.937698529951,-234.937962519231,-233.938226508511,
-232.938490497791,-231.93875448707,-230.93901847635,-230.287212807307),
 .UNSPECIFIED.);
#1631=B_SPLINE_CURVE_WITH_KNOTS('',3,(#184298,#184299,#184300,#184301,#184302,
#184303,#184304,#184305,#184306,#184307,#184308,#184309,#184310,#184311,
#184312,#184313,#184314,#184315,#184316,#184317,#184318,#184319,#184320,
#184321,#184322,#184323,#184324,#184325,#184326,#184327,#184328,#184329,
#184330,#184331,#184332,#184333,#184334,#184335,#184336,#184337,#184338,
#184339,#184340,#184341,#184342,#184343,#184344,#184345,#184346,#184347,
#184348,#184349,#184350,#184351,#184352,#184353,#184354,#184355,#184356,
#184357,#184358,#184359,#184360,#184361,#184362,#184363,#184364,#184365,
#184366,#184367,#184368,#184369,#184370,#184371,#184372,#184373,#184374,
#184375,#184376,#184377,#184378,#184379,#184380,#184381,#184382,#184383,
#184384,#184385,#184386,#184387,#184388,#184389,#184390,#184391,#184392,
#184393,#184394,#184395,#184396,#184397,#184398,#184399,#184400,#184401,
#184402,#184403,#184404,#184405,#184406,#184407,#184408,#184409,#184410,
#184411,#184412,#184413,#184414,#184415,#184416,#184417,#184418,#184419,
#184420,#184421,#184422,#184423,#184424,#184425,#184426,#184427,#184428,
#184429,#184430,#184431,#184432,#184433,#184434,#184435,#184436,#184437,
#184438,#184439,#184440,#184441,#184442,#184443,#184444,#184445,#184446,
#184447,#184448,#184449,#184450,#184451,#184452,#184453,#184454,#184455,
#184456,#184457,#184458,#184459,#184460,#184461,#184462,#184463,#184464,
#184465,#184466,#184467,#184468,#184469,#184470,#184471,#184472,#184473,
#184474,#184475,#184476,#184477,#184478,#184479,#184480,#184481,#184482,
#184483,#184484,#184485,#184486,#184487,#184488,#184489,#184490,#184491,
#184492,#184493,#184494,#184495,#184496,#184497,#184498,#184499,#184500,
#184501,#184502,#184503,#184504,#184505,#184506,#184507,#184508,#184509,
#184510,#184511,#184512,#184513,#184514,#184515,#184516,#184517,#184518,
#184519,#184520,#184521,#184522,#184523,#184524,#184525,#184526,#184527,
#184528,#184529,#184530,#184531,#184532,#184533,#184534,#184535,#184536,
#184537,#184538,#184539,#184540,#184541),.UNSPECIFIED.,.F.,.F.,(4,3,3,3,
3,3,3,3,3,3,3,3,3,3,3,3,3,3,3,3,3,3,3,3,3,3,3,3,3,3,3,3,3,3,3,3,3,3,3,3,
3,3,3,3,3,3,3,3,3,3,3,3,3,3,3,3,3,3,3,3,3,3,3,3,3,3,3,3,3,3,3,3,3,3,3,3,
3,3,3,3,3,4),(-230.287212684737,-230.195557356441,-230.103455628521,-230.010768224531,
-229.93928246563,-229.859325165499,-229.779462368256,-229.699676545784,
-229.619950230589,-229.540266002295,-229.460595016074,-229.380927562548,
-229.301247911732,-229.221540329337,-229.141745100262,-229.061900758554,
-228.981942331507,-228.93954645491,-228.859589154779,-228.779726357536,
-228.699940535064,-228.620214219869,-228.540529991575,-228.460859005354,
-228.381191551828,-228.301511901012,-228.221804318617,-228.142009089542,
-228.062164747834,-227.982206320787,-227.93981044419,-227.859853144059,
-227.779990346816,-227.700204524344,-227.620478209149,-227.540793980855,
-227.461122994634,-227.381455541108,-227.301775890292,-227.222068307897,
-227.142273078822,-227.062428737114,-226.982470310067,-226.94007443347,
-226.860117133339,-226.780254336096,-226.700468513624,-226.620742198429,
-226.541057970135,-226.461386983914,-226.381719530388,-226.302039879572,
-226.222332297177,-226.142537068101,-226.062692726394,-225.982734299346,
-225.94033842275,-225.860381122619,-225.780518325376,-225.700732502905,
-225.621006187709,-225.541321959415,-225.461650973195,-225.381983519669,
-225.302303868853,-225.222596286458,-225.142801057383,-225.062956715675,
-224.982998288628,-224.94060241203,-224.861380214033,-224.782251996577,
-224.703199591262,-224.624204899021,-224.545244058955,-224.466299823835,
-224.387355896365,-224.308395981842,-224.229359554931,-224.150283545781,
-224.071093008039,-224.004027500127),.UNSPECIFIED.);
#1632=B_SPLINE_CURVE_WITH_KNOTS('',3,(#184543,#184544,#184545,#184546,#184547,
#184548,#184549,#184550,#184551,#184552,#184553,#184554),.UNSPECIFIED.,
 .F.,.F.,(4,2,1,1,1,1,1,1,4),(-224.004027500127,-223.940866401309,-222.941130390589,
-221.941394379869,-220.941658369149,-219.941922358429,-218.942186347709,
-217.942450336989,-217.720842192948),.UNSPECIFIED.);
#1633=B_SPLINE_CURVE_WITH_KNOTS('',3,(#184556,#184557,#184558,#184559,#184560,
#184561,#184562,#184563,#184564,#184565,#184566,#184567,#184568,#184569,
#184570,#184571,#184572,#184573,#184574,#184575,#184576,#184577,#184578,
#184579,#184580,#184581,#184582,#184583,#184584,#184585,#184586,#184587,
#184588,#184589,#184590,#184591,#184592,#184593,#184594,#184595,#184596,
#184597,#184598,#184599,#184600,#184601,#184602,#184603,#184604,#184605,
#184606,#184607,#184608,#184609,#184610,#184611,#184612,#184613,#184614,
#184615,#184616,#184617,#184618,#184619,#184620,#184621,#184622,#184623,
#184624,#184625,#184626,#184627,#184628,#184629,#184630,#184631,#184632,
#184633,#184634,#184635,#184636,#184637,#184638,#184639,#184640,#184641,
#184642,#184643,#184644,#184645,#184646,#184647,#184648,#184649,#184650,
#184651,#184652,#184653,#184654,#184655,#184656,#184657,#184658,#184659,
#184660,#184661,#184662,#184663,#184664,#184665,#184666,#184667,#184668,
#184669,#184670,#184671,#184672,#184673,#184674,#184675,#184676,#184677,
#184678,#184679,#184680,#184681,#184682,#184683,#184684,#184685,#184686,
#184687,#184688,#184689,#184690,#184691,#184692,#184693,#184694,#184695,
#184696,#184697,#184698,#184699,#184700,#184701,#184702,#184703,#184704,
#184705,#184706,#184707,#184708,#184709,#184710,#184711,#184712,#184713,
#184714,#184715,#184716,#184717,#184718,#184719,#184720,#184721,#184722,
#184723,#184724,#184725,#184726,#184727,#184728,#184729,#184730,#184731,
#184732,#184733,#184734,#184735,#184736,#184737,#184738,#184739,#184740,
#184741,#184742,#184743,#184744,#184745,#184746,#184747,#184748,#184749,
#184750,#184751,#184752,#184753,#184754,#184755,#184756,#184757,#184758,
#184759,#184760,#184761,#184762,#184763,#184764,#184765,#184766,#184767,
#184768,#184769,#184770,#184771,#184772,#184773,#184774,#184775,#184776,
#184777,#184778,#184779,#184780,#184781,#184782,#184783,#184784,#184785,
#184786,#184787,#184788,#184789,#184790,#184791,#184792,#184793,#184794,
#184795,#184796,#184797,#184798,#184799),.UNSPECIFIED.,.F.,.F.,(4,3,3,3,
3,3,3,3,3,3,3,3,3,3,3,3,3,3,3,3,3,3,3,3,3,3,3,3,3,3,3,3,3,3,3,3,3,3,3,3,
3,3,3,3,3,3,3,3,3,3,3,3,3,3,3,3,3,3,3,3,3,3,3,3,3,3,3,3,3,3,3,3,3,3,3,3,
3,3,3,3,3,4),(-217.720842192948,-217.642134003223,-217.563483187297,-217.484864835763,
-217.406262272064,-217.327658988786,-217.249038479712,-217.170338117275,
-217.091596795613,-217.01273613636,-216.942714326268,-216.862757026137,
-216.782894228894,-216.703108406423,-216.623382091228,-216.543697862933,
-216.464026876712,-216.384359423187,-216.30467977237,-216.224972189976,
-216.145176960901,-216.065332619193,-215.985374192146,-215.942978315548,
-215.863021015417,-215.783158218174,-215.703372395702,-215.623646080507,
-215.543961852213,-215.464290865992,-215.384623412466,-215.30494376165,
-215.225236179255,-215.14544095018,-215.065596608472,-214.985638181425,
-214.943242304828,-214.863285004697,-214.783422207454,-214.703636384983,
-214.623910069787,-214.544225841493,-214.464554855272,-214.384887401746,
-214.305207750929,-214.225500168535,-214.14570493946,-214.065860597752,
-213.985902170705,-213.943506294108,-213.863548993977,-213.783686196734,
-213.703900374262,-213.624174059067,-213.544489830773,-213.464818844552,
-213.385151391026,-213.30547174021,-213.225764157815,-213.14596892874,-213.066124587032,
-212.986166159985,-212.943770283388,-212.863812983257,-212.783950186014,
-212.704164363543,-212.624438048348,-212.544753820053,-212.465082833832,
-212.385415380307,-212.30573572949,-212.226028147096,-212.14623291802,-212.066388576313,
-211.986430149266,-211.944034272668,-211.860196019356,-211.77649298943,
-211.691783963515,-211.608368479178,-211.523012682473,-211.437656885768),
 .UNSPECIFIED.);
#1634=B_SPLINE_CURVE_WITH_KNOTS('',3,(#184801,#184802,#184803,#184804,#184805,
#184806,#184807,#184808,#184809,#184810,#184811,#184812,#184813,#184814,
#184815,#184816,#184817,#184818,#184819,#184820,#184821,#184822,#184823,
#184824,#184825,#184826,#184827,#184828,#184829,#184830,#184831,#184832,
#184833,#184834,#184835,#184836,#184837,#184838,#184839,#184840,#184841,
#184842,#184843,#184844,#184845,#184846,#184847,#184848,#184849,#184850,
#184851,#184852,#184853,#184854,#184855,#184856,#184857,#184858,#184859,
#184860,#184861,#184862,#184863,#184864,#184865,#184866,#184867,#184868,
#184869,#184870,#184871,#184872,#184873,#184874,#184875,#184876,#184877,
#184878,#184879,#184880,#184881,#184882,#184883,#184884,#184885,#184886,
#184887,#184888,#184889,#184890,#184891,#184892,#184893,#184894,#184895,
#184896,#184897,#184898,#184899,#184900,#184901,#184902,#184903,#184904,
#184905,#184906,#184907,#184908,#184909,#184910,#184911,#184912,#184913,
#184914,#184915,#184916,#184917,#184918,#184919,#184920,#184921,#184922,
#184923,#184924,#184925,#184926,#184927,#184928,#184929,#184930,#184931,
#184932,#184933,#184934,#184935,#184936,#184937,#184938,#184939,#184940,
#184941,#184942,#184943,#184944,#184945,#184946,#184947,#184948,#184949,
#184950,#184951,#184952,#184953,#184954,#184955,#184956,#184957,#184958,
#184959,#184960,#184961,#184962,#184963,#184964,#184965,#184966,#184967,
#184968,#184969,#184970,#184971,#184972,#184973,#184974,#184975,#184976,
#184977,#184978,#184979,#184980,#184981,#184982,#184983,#184984,#184985,
#184986,#184987,#184988,#184989,#184990,#184991,#184992,#184993,#184994,
#184995,#184996,#184997,#184998,#184999,#185000,#185001,#185002,#185003,
#185004,#185005,#185006,#185007,#185008,#185009,#185010,#185011,#185012,
#185013,#185014,#185015,#185016,#185017,#185018,#185019,#185020,#185021,
#185022,#185023,#185024,#185025,#185026,#185027,#185028,#185029,#185030,
#185031,#185032,#185033,#185034,#185035,#185036,#185037,#185038,#185039,
#185040,#185041,#185042,#185043,#185044),.UNSPECIFIED.,.F.,.F.,(4,3,3,3,
3,3,3,3,3,3,3,3,3,3,3,3,3,3,3,3,3,3,3,3,3,3,3,3,3,3,3,3,3,3,3,3,3,3,3,3,
3,3,3,3,3,3,3,3,3,3,3,3,3,3,3,3,3,3,3,3,3,3,3,3,3,3,3,3,3,3,3,3,3,3,3,3,
3,3,3,3,3,4),(-211.437656885626,-211.353970957782,-211.27017209527,-211.186171414536,
-211.102066720774,-211.017765042623,-210.944298261948,-210.864340961817,
-210.784478164574,-210.704692342102,-210.624966026906,-210.545281798612,
-210.465610812391,-210.385943358865,-210.306263708048,-210.226556125653,
-210.146760896578,-210.06691655487,-209.986958127822,-209.944562251228,
-209.864604951096,-209.784742153854,-209.704956331381,-209.625230016186,
-209.545545787892,-209.46587480167,-209.386207348144,-209.306527697328,
-209.226820114933,-209.147024885857,-209.067180544149,-208.987222117101,
-208.944826240507,-208.864868940376,-208.785006143133,-208.705220320661,
-208.625494005466,-208.545809777172,-208.466138790951,-208.386471337425,
-208.306791686609,-208.227084104215,-208.147288875139,-208.067444533432,
-207.987486106384,-207.945090229787,-207.865132929656,-207.785270132413,
-207.705484309942,-207.625757994746,-207.546073766452,-207.466402780232,
-207.386735326706,-207.307055675889,-207.227348093495,-207.14755286442,
-207.067708522712,-206.987750095665,-206.945354219067,-206.865396918936,
-206.785534121693,-206.705748299221,-206.626021984026,-206.546337755732,
-206.466666769511,-206.386999315985,-206.307319665169,-206.227612082774,
-206.147816853699,-206.067972511991,-205.988014084944,-205.945618208347,
-205.86678740295,-205.788051427103,-205.708853946039,-205.630257658485,
-205.55169502182,-205.473149485886,-205.393480009062,-205.314894194931,
-205.23468288676,-205.154471578589),.UNSPECIFIED.);
#1635=B_SPLINE_CURVE_WITH_KNOTS('',3,(#185046,#185047,#185048,#185049,#185050,
#185051,#185052,#185053,#185054,#185055,#185056),.UNSPECIFIED.,.F.,.F.,
(4,1,1,1,1,1,1,1,4),(-205.154471578589,-204.945882197627,-203.946146186907,
-202.946410176187,-201.946674165466,-200.946938154746,-199.947202144026,
-198.947466133306,-198.871286271409),.UNSPECIFIED.);
#1636=B_SPLINE_CURVE_WITH_KNOTS('',3,(#185058,#185059,#185060,#185061,#185062,
#185063,#185064,#185065,#185066,#185067),.UNSPECIFIED.,.F.,.F.,(4,1,1,1,
1,1,1,4),(-198.871286271409,-197.947730122586,-196.947994111866,-195.948258101146,
-194.948522090426,-193.948786079705,-192.949050068985,-192.58810096423),
 .UNSPECIFIED.);
#1637=B_SPLINE_CURVE_WITH_KNOTS('',3,(#185069,#185070,#185071,#185072,#185073,
#185074,#185075,#185076,#185077,#185078),.UNSPECIFIED.,.F.,.F.,(4,1,1,1,
1,1,1,4),(-192.58810096423,-191.949314058265,-190.949578047545,-189.949842036825,
-188.950106026105,-187.950370015385,-186.950634004665,-186.30491565705),
 .UNSPECIFIED.);
#1638=B_SPLINE_CURVE_WITH_KNOTS('',3,(#185080,#185081,#185082,#185083,#185084,
#185085,#185086,#185087,#185088,#185089,#185090,#185091,#185092,#185093,
#185094,#185095,#185096,#185097,#185098,#185099,#185100,#185101,#185102,
#185103,#185104,#185105,#185106,#185107,#185108,#185109,#185110,#185111,
#185112,#185113,#185114,#185115,#185116,#185117,#185118,#185119,#185120,
#185121,#185122,#185123,#185124,#185125,#185126,#185127,#185128,#185129,
#185130,#185131,#185132,#185133,#185134,#185135,#185136,#185137,#185138,
#185139,#185140,#185141,#185142,#185143,#185144,#185145,#185146,#185147,
#185148,#185149,#185150,#185151,#185152,#185153,#185154,#185155,#185156,
#185157,#185158,#185159,#185160,#185161,#185162,#185163,#185164,#185165,
#185166,#185167,#185168,#185169,#185170,#185171,#185172,#185173,#185174,
#185175,#185176,#185177,#185178,#185179,#185180,#185181,#185182,#185183,
#185184,#185185,#185186,#185187,#185188,#185189,#185190,#185191,#185192,
#185193,#185194,#185195,#185196,#185197,#185198,#185199,#185200,#185201,
#185202,#185203,#185204,#185205,#185206,#185207,#185208,#185209,#185210,
#185211,#185212,#185213,#185214,#185215,#185216,#185217,#185218,#185219,
#185220,#185221,#185222,#185223,#185224,#185225,#185226,#185227,#185228,
#185229,#185230,#185231,#185232,#185233,#185234,#185235,#185236,#185237,
#185238,#185239,#185240,#185241,#185242,#185243,#185244,#185245,#185246,
#185247,#185248,#185249,#185250,#185251,#185252,#185253,#185254,#185255,
#185256,#185257,#185258,#185259,#185260,#185261,#185262,#185263,#185264,
#185265,#185266,#185267,#185268,#185269,#185270,#185271,#185272,#185273,
#185274,#185275,#185276,#185277,#185278,#185279,#185280,#185281,#185282,
#185283,#185284,#185285,#185286,#185287,#185288,#185289,#185290,#185291,
#185292,#185293,#185294,#185295,#185296,#185297,#185298,#185299,#185300,
#185301,#185302,#185303,#185304,#185305,#185306,#185307,#185308,#185309,
#185310,#185311,#185312,#185313,#185314,#185315,#185316,#185317,#185318,
#185319,#185320,#185321,#185322,#185323),.UNSPECIFIED.,.F.,.F.,(4,3,3,3,
3,3,3,3,3,3,3,3,3,3,3,3,3,3,3,3,3,3,3,3,3,3,3,3,3,3,3,3,3,3,3,3,3,3,3,3,
3,3,3,3,3,3,3,3,3,3,3,3,3,3,3,3,3,3,3,3,3,3,3,3,3,3,3,3,3,3,3,3,3,3,3,3,
3,3,3,3,3,4),(-186.304915409735,-186.213726832839,-186.122121906506,-186.0299546992,
-185.950897993944,-185.870940693813,-185.79107789657,-185.711292074098,
-185.631565758903,-185.551881530609,-185.472210544388,-185.392543090862,
-185.312863440046,-185.233155857651,-185.153360628576,-185.073516286868,
-184.993557859821,-184.951161983224,-184.871204683093,-184.79134188585,
-184.711556063378,-184.631829748183,-184.552145519889,-184.472474533668,
-184.392807080142,-184.313127429326,-184.233419846931,-184.153624617856,
-184.073780276148,-183.993821849101,-183.951425972504,-183.871468672373,
-183.79160587513,-183.711820052658,-183.632093737463,-183.552409509169,
-183.472738522948,-183.393071069422,-183.313391418605,-183.233683836211,
-183.153888607135,-183.074044265427,-182.99408583838,-182.951689961784,
-182.871732661653,-182.79186986441,-182.712084041939,-182.632357726743,
-182.552673498449,-182.473002512228,-182.393335058703,-182.313655407886,
-182.233947825492,-182.154152596416,-182.074308254709,-181.994349827661,
-181.951953951064,-181.871996650933,-181.79213385369,-181.712348031218,
-181.632621716023,-181.552937487729,-181.473266501508,-181.393599047982,
-181.313919397166,-181.234211814771,-181.154416585696,-181.074572243988,
-180.994613816941,-180.952217940344,-180.873047776925,-180.793971548658,
-180.714971048043,-180.636028137857,-180.557119024801,-180.478226359198,
-180.399333810161,-180.320425049214,-180.241440507916,-180.162416093261,
-180.083279647565,-180.021730349871),.UNSPECIFIED.);
#1639=B_SPLINE_CURVE_WITH_KNOTS('',3,(#185325,#185326,#185327,#185328,#185329,
#185330,#185331,#185332,#185333,#185334,#185335,#185336),.UNSPECIFIED.,
 .F.,.F.,(4,2,1,1,1,1,1,1,4),(-180.021730349871,-179.952481929624,-178.952745918903,
-177.953009908183,-176.953273897463,-175.953537886743,-174.953801876023,
-173.954065865303,-173.738545042691),.UNSPECIFIED.);
#1640=B_SPLINE_CURVE_WITH_KNOTS('',3,(#185338,#185339,#185340,#185341,#185342,
#185343,#185344,#185345,#185346,#185347),.UNSPECIFIED.,.F.,.F.,(4,1,1,1,
1,1,1,4),(-173.738545042691,-172.954329854583,-171.954593843863,-170.954857833142,
-169.955121822422,-168.955385811702,-167.955649800982,-167.455359735511),
 .UNSPECIFIED.);
#1641=B_SPLINE_CURVE_WITH_KNOTS('',3,(#185349,#185350,#185351,#185352,#185353,
#185354,#185355,#185356,#185357,#185358),.UNSPECIFIED.,.F.,.F.,(4,1,1,1,
1,1,1,4),(-167.455359735511,-166.955913790262,-165.956177779542,-164.956441768822,
-163.956705758101,-162.956969747381,-161.957233736661,-161.172174428332),
 .UNSPECIFIED.);
#1642=B_SPLINE_CURVE_WITH_KNOTS('',3,(#185360,#185361,#185362,#185363,#185364,
#185365,#185366,#185367,#185368,#185369,#185370),.UNSPECIFIED.,.F.,.F.,
(4,1,1,1,1,1,1,1,4),(-161.172174428332,-160.957497725941,-159.957761715221,
-158.958025704501,-157.958289693781,-156.958553683061,-155.95881767234,
-154.95908166162,-154.888989121152),.UNSPECIFIED.);
#1643=B_SPLINE_CURVE_WITH_KNOTS('',3,(#185372,#185373,#185374,#185375,#185376,
#185377,#185378,#185379,#185380,#185381,#185382,#185383,#185384,#185385,
#185386,#185387,#185388,#185389,#185390,#185391,#185392,#185393,#185394,
#185395,#185396,#185397,#185398,#185399,#185400,#185401,#185402,#185403,
#185404,#185405,#185406,#185407,#185408,#185409,#185410,#185411,#185412,
#185413,#185414,#185415,#185416,#185417,#185418,#185419,#185420,#185421,
#185422,#185423,#185424,#185425,#185426,#185427,#185428,#185429,#185430,
#185431,#185432,#185433,#185434,#185435,#185436,#185437,#185438,#185439,
#185440,#185441,#185442,#185443,#185444,#185445,#185446,#185447,#185448,
#185449,#185450,#185451,#185452,#185453,#185454,#185455,#185456,#185457,
#185458,#185459,#185460,#185461,#185462,#185463,#185464,#185465,#185466,
#185467,#185468,#185469,#185470,#185471,#185472,#185473,#185474,#185475,
#185476,#185477,#185478,#185479,#185480,#185481,#185482,#185483,#185484,
#185485,#185486,#185487,#185488,#185489,#185490,#185491,#185492,#185493,
#185494,#185495,#185496,#185497,#185498,#185499,#185500,#185501,#185502,
#185503,#185504,#185505,#185506,#185507,#185508,#185509,#185510,#185511,
#185512,#185513,#185514,#185515,#185516,#185517,#185518,#185519,#185520,
#185521,#185522,#185523,#185524,#185525,#185526,#185527,#185528,#185529,
#185530,#185531,#185532,#185533,#185534,#185535,#185536,#185537,#185538,
#185539,#185540,#185541,#185542,#185543,#185544,#185545,#185546,#185547,
#185548,#185549,#185550,#185551,#185552,#185553,#185554,#185555,#185556,
#185557,#185558,#185559,#185560,#185561,#185562,#185563,#185564,#185565,
#185566,#185567,#185568,#185569,#185570,#185571,#185572,#185573,#185574,
#185575,#185576,#185577,#185578,#185579,#185580,#185581,#185582,#185583,
#185584,#185585,#185586,#185587,#185588,#185589,#185590,#185591,#185592,
#185593,#185594,#185595,#185596,#185597,#185598,#185599,#185600,#185601,
#185602,#185603,#185604,#185605,#185606,#185607,#185608,#185609,#185610,
#185611,#185612,#185613,#185614,#185615),.UNSPECIFIED.,.F.,.F.,(4,3,3,3,
3,3,3,3,3,3,3,3,3,3,3,3,3,3,3,3,3,3,3,3,3,3,3,3,3,3,3,3,3,3,3,3,3,3,3,3,
3,3,3,3,3,3,3,3,3,3,3,3,3,3,3,3,3,3,3,3,3,3,3,3,3,3,3,3,3,3,3,3,3,3,3,3,
3,3,3,3,3,4),(-154.888989121152,-154.809851096199,-154.730802383284,-154.651824789386,
-154.572900187323,-154.494002434836,-154.415116849767,-154.336227098127,
-154.257316845318,-154.178324344123,-154.099288265117,-154.020134654139,
-153.9593456509,-153.879388350769,-153.799525553526,-153.719739731054,-153.640013415859,
-153.560329187565,-153.480658201344,-153.400990747818,-153.321311097002,
-153.241603514607,-153.161808285532,-153.081963943824,-153.002005516777,
-152.95960964018,-152.879652340049,-152.799789542806,-152.720003720334,
-152.640277405139,-152.560593176846,-152.480922190625,-152.401254737099,
-152.321575086282,-152.241867503888,-152.162072274812,-152.082227933105,
-152.002269506057,-151.95987362946,-151.879916329329,-151.800053532086,
-151.720267709614,-151.640541394419,-151.560857166125,-151.481186179904,
-151.401518726378,-151.321839075561,-151.242131493167,-151.162336264091,
-151.082491922383,-151.002533495336,-150.96013761874,-150.880180318609,
-150.800317521366,-150.720531698895,-150.6408053837,-150.561121155404,-150.481450169184,
-150.401782715658,-150.322103064841,-150.242395482447,-150.162600253372,
-150.082755911664,-150.002797484616,-149.96040160802,-149.880444307889,
-149.800581510646,-149.720795688174,-149.641069372979,-149.561385144685,
-149.481714158464,-149.402046704939,-149.322367054122,-149.242659471728,
-149.162864242652,-149.083019900944,-149.003061473897,-148.9606655973,-148.86858074921,
-148.776825906217,-148.68572083433,-148.605804061509),.UNSPECIFIED.);
#1644=B_SPLINE_CURVE_WITH_KNOTS('',3,(#185617,#185618,#185619,#185620,#185621,
#185622,#185623,#185624,#185625,#185626),.UNSPECIFIED.,.F.,.F.,(4,1,1,1,
1,1,1,4),(-148.605803813973,-147.960929586579,-146.961193575859,-145.961457565139,
-144.961721554419,-143.961985543699,-142.962249532979,-142.322618506793),
 .UNSPECIFIED.);
#1645=B_SPLINE_CURVE_WITH_KNOTS('',3,(#185628,#185629,#185630,#185631,#185632,
#185633,#185634,#185635,#185636,#185637),.UNSPECIFIED.,.F.,.F.,(4,1,1,1,
1,1,1,4),(-142.322618506793,-141.962513522259,-140.962777511538,-139.963041500818,
-138.963305490098,-137.963569479378,-136.963833468658,-136.039433199614),
 .UNSPECIFIED.);
#1646=B_SPLINE_CURVE_WITH_KNOTS('',3,(#185639,#185640,#185641,#185642,#185643,
#185644,#185645,#185646,#185647,#185648,#185649),.UNSPECIFIED.,.F.,.F.,
(4,1,1,1,1,1,1,1,4),(-136.039433199614,-135.964097457938,-134.964361447218,
-133.964625436498,-132.964889425777,-131.965153415057,-130.965417404337,
-129.965681393617,-129.756247892434),.UNSPECIFIED.);
#1647=B_SPLINE_CURVE_WITH_KNOTS('',3,(#185651,#185652,#185653,#185654,#185655,
#185656,#185657,#185658,#185659,#185660,#185661,#185662,#185663,#185664,
#185665,#185666,#185667,#185668,#185669,#185670,#185671,#185672,#185673,
#185674,#185675,#185676,#185677,#185678,#185679,#185680,#185681,#185682,
#185683,#185684,#185685,#185686,#185687,#185688,#185689,#185690,#185691,
#185692,#185693,#185694,#185695,#185696,#185697,#185698,#185699,#185700,
#185701,#185702,#185703,#185704,#185705,#185706,#185707,#185708,#185709,
#185710,#185711,#185712,#185713,#185714,#185715,#185716,#185717,#185718,
#185719,#185720,#185721,#185722,#185723,#185724,#185725,#185726,#185727,
#185728,#185729,#185730,#185731,#185732,#185733,#185734,#185735,#185736,
#185737,#185738,#185739,#185740,#185741,#185742,#185743,#185744,#185745,
#185746,#185747,#185748,#185749,#185750,#185751,#185752,#185753,#185754,
#185755,#185756,#185757,#185758,#185759,#185760,#185761,#185762,#185763,
#185764,#185765,#185766,#185767,#185768,#185769,#185770,#185771,#185772,
#185773,#185774,#185775,#185776,#185777,#185778,#185779,#185780,#185781,
#185782,#185783,#185784,#185785,#185786,#185787,#185788,#185789,#185790,
#185791,#185792,#185793,#185794,#185795,#185796,#185797,#185798,#185799,
#185800,#185801,#185802,#185803,#185804,#185805,#185806,#185807,#185808,
#185809,#185810,#185811,#185812,#185813,#185814,#185815,#185816,#185817,
#185818,#185819,#185820,#185821,#185822,#185823,#185824,#185825,#185826,
#185827,#185828,#185829,#185830,#185831,#185832,#185833,#185834,#185835,
#185836,#185837,#185838,#185839,#185840,#185841,#185842,#185843,#185844,
#185845,#185846,#185847,#185848,#185849,#185850,#185851,#185852,#185853,
#185854,#185855,#185856,#185857,#185858,#185859,#185860,#185861,#185862,
#185863,#185864,#185865,#185866,#185867,#185868,#185869,#185870,#185871,
#185872,#185873,#185874,#185875,#185876,#185877,#185878,#185879,#185880,
#185881,#185882,#185883,#185884,#185885,#185886,#185887,#185888,#185889,
#185890,#185891,#185892,#185893,#185894),.UNSPECIFIED.,.F.,.F.,(4,3,3,3,
3,3,3,3,3,3,3,3,3,3,3,3,3,3,3,3,3,3,3,3,3,3,3,3,3,3,3,3,3,3,3,3,3,3,3,3,
3,3,3,3,3,3,3,3,3,3,3,3,3,3,3,3,3,3,3,3,3,3,3,3,3,3,3,3,3,3,3,3,3,3,3,3,
3,3,3,3,3,4),(-129.756247892434,-129.677573144673,-129.598959172096,-129.519832448446,
-129.441274334452,-129.36271837502,-129.28414803768,-129.204597373984,-129.125909857212,
-129.045927620055,-128.965945382897,-128.885988082766,-128.806125285523,
-128.726339463052,-128.646613147856,-128.566928919562,-128.487257933341,
-128.407590479815,-128.327910828999,-128.248203246604,-128.168408017529,
-128.088563675821,-128.008605248774,-127.966209372177,-127.886252072046,
-127.806389274803,-127.726603452331,-127.646877137136,-127.567192908842,
-127.487521922621,-127.407854469095,-127.328174818279,-127.248467235884,
-127.168672006808,-127.088827665101,-127.008869238054,-126.966473361457,
-126.886516061326,-126.806653264083,-126.726867441612,-126.647141126417,
-126.567456898122,-126.487785911901,-126.408118458375,-126.328438807559,
-126.248731225164,-126.168935996089,-126.089091654381,-126.009133227334,
-125.966737350737,-125.886780050606,-125.806917253363,-125.727131430891,
-125.647405115695,-125.567720887402,-125.48804990118,-125.408382447654,
-125.328702796838,-125.248995214444,-125.169199985368,-125.08935564366,
-125.009397216612,-124.967001340016,-124.887044039885,-124.807181242642,
-124.727395420171,-124.647669104975,-124.567984876682,-124.488313890461,
-124.408646436935,-124.328966786118,-124.249259203724,-124.169463974648,
-124.089619632941,-124.009661205894,-123.967265329296,-123.882969519311,
-123.798815750226,-123.714855745484,-123.631009770825,-123.547321253712,
-123.473062585378),.UNSPECIFIED.);
#1648=B_SPLINE_CURVE_WITH_KNOTS('',3,(#185896,#185897,#185898,#185899,#185900,
#185901,#185902,#185903,#185904,#185905,#185906,#185907,#185908,#185909,
#185910,#185911,#185912,#185913,#185914,#185915,#185916,#185917,#185918,
#185919,#185920,#185921,#185922,#185923,#185924,#185925,#185926,#185927,
#185928,#185929,#185930,#185931,#185932,#185933,#185934,#185935,#185936,
#185937,#185938,#185939,#185940,#185941,#185942,#185943,#185944,#185945,
#185946,#185947,#185948,#185949,#185950,#185951,#185952,#185953,#185954,
#185955,#185956,#185957,#185958,#185959,#185960,#185961,#185962,#185963,
#185964,#185965,#185966,#185967,#185968,#185969,#185970,#185971,#185972,
#185973,#185974,#185975,#185976,#185977,#185978,#185979,#185980,#185981,
#185982,#185983,#185984,#185985,#185986,#185987,#185988,#185989,#185990,
#185991,#185992,#185993,#185994,#185995,#185996,#185997,#185998,#185999,
#186000,#186001,#186002,#186003,#186004,#186005,#186006,#186007,#186008,
#186009,#186010,#186011,#186012,#186013,#186014,#186015,#186016,#186017,
#186018,#186019,#186020,#186021,#186022,#186023,#186024,#186025,#186026,
#186027,#186028,#186029,#186030,#186031,#186032,#186033,#186034,#186035,
#186036,#186037,#186038,#186039,#186040,#186041,#186042,#186043,#186044,
#186045,#186046,#186047,#186048,#186049,#186050,#186051,#186052,#186053,
#186054,#186055,#186056,#186057,#186058,#186059,#186060,#186061,#186062,
#186063,#186064,#186065,#186066,#186067,#186068,#186069,#186070,#186071,
#186072,#186073,#186074,#186075,#186076,#186077,#186078,#186079,#186080,
#186081,#186082,#186083,#186084,#186085,#186086,#186087,#186088,#186089,
#186090,#186091,#186092,#186093,#186094,#186095,#186096,#186097,#186098,
#186099,#186100,#186101,#186102,#186103,#186104,#186105,#186106,#186107,
#186108,#186109,#186110,#186111,#186112,#186113,#186114,#186115,#186116,
#186117,#186118,#186119,#186120,#186121,#186122,#186123,#186124,#186125,
#186126,#186127,#186128,#186129,#186130,#186131,#186132,#186133,#186134,
#186135,#186136,#186137,#186138,#186139),.UNSPECIFIED.,.F.,.F.,(4,3,3,3,
3,3,3,3,3,3,3,3,3,3,3,3,3,3,3,3,3,3,3,3,3,3,3,3,3,3,3,3,3,3,3,3,3,3,3,3,
3,3,3,3,3,3,3,3,3,3,3,3,3,3,3,3,3,3,3,3,3,3,3,3,3,3,3,3,3,3,3,3,3,3,3,3,
3,3,3,3,3,4),(-123.473062585254,-123.389798861451,-123.306437150327,-123.22171019239,
-123.138066210288,-123.052797764432,-122.967529318576,-122.887572018445,
-122.807709221202,-122.727923398731,-122.648197083535,-122.568512855241,
-122.48884186902,-122.409174415494,-122.329494764678,-122.249787182283,
-122.169991953208,-122.0901476115,-122.010189184453,-121.967793307856,-121.887836007725,
-121.807973210482,-121.72818738801,-121.648461072815,-121.568776844521,
-121.4891058583,-121.409438404774,-121.329758753957,-121.250051171563,-121.170255942487,
-121.09041160078,-121.010453173732,-120.968057297136,-120.888099997005,
-120.808237199762,-120.728451377291,-120.648725062095,-120.569040833801,
-120.48936984758,-120.409702394055,-120.330022743238,-120.250315160843,
-120.170519931768,-120.09067559006,-120.010717163013,-119.968321286416,
-119.888363986285,-119.808501189042,-119.728715366571,-119.648989051376,
-119.569304823081,-119.48963383686,-119.409966383334,-119.330286732518,
-119.250579150123,-119.170783921048,-119.09093957934,-119.010981152293,
-118.968585275696,-118.888627975565,-118.808765178322,-118.72897935585,
-118.649253040654,-118.56956881236,-118.489897826139,-118.410230372612,
-118.330550721796,-118.250843139401,-118.171047910325,-118.091203568617,
-118.01124514157,-117.968849264975,-117.889971084437,-117.811188096325,
-117.732495007955,-117.653852743602,-117.575244750464,-117.496654504028,
-117.418038752298,-117.339412087883,-117.260714790506,-117.189877278075),
 .UNSPECIFIED.);
#1649=B_SPLINE_CURVE_WITH_KNOTS('',3,(#186141,#186142,#186143,#186144,#186145,
#186146,#186147,#186148,#186149,#186150,#186151),.UNSPECIFIED.,.F.,.F.,
(4,1,1,1,1,1,1,1,4),(-117.189877278075,-116.969113254255,-115.969377243535,
-114.969641232815,-113.969905222095,-112.970169211375,-111.970433200655,
-110.970697189935,-110.906691970895),.UNSPECIFIED.);
#1650=B_SPLINE_CURVE_WITH_KNOTS('',3,(#186153,#186154,#186155,#186156,#186157,
#186158,#186159,#186160,#186161,#186162,#186163,#186164,#186165,#186166,
#186167,#186168,#186169,#186170,#186171,#186172,#186173,#186174,#186175,
#186176,#186177,#186178,#186179,#186180,#186181,#186182,#186183,#186184,
#186185,#186186,#186187,#186188,#186189,#186190,#186191,#186192,#186193,
#186194,#186195,#186196,#186197,#186198,#186199,#186200,#186201,#186202,
#186203,#186204,#186205,#186206,#186207,#186208,#186209,#186210,#186211,
#186212,#186213,#186214,#186215,#186216,#186217,#186218,#186219,#186220,
#186221,#186222,#186223,#186224,#186225,#186226,#186227,#186228,#186229,
#186230,#186231,#186232,#186233,#186234,#186235,#186236,#186237,#186238,
#186239,#186240,#186241,#186242,#186243,#186244,#186245,#186246,#186247,
#186248,#186249,#186250,#186251,#186252,#186253,#186254,#186255,#186256,
#186257,#186258,#186259,#186260,#186261,#186262,#186263,#186264,#186265,
#186266,#186267,#186268,#186269,#186270,#186271,#186272,#186273,#186274,
#186275,#186276,#186277,#186278,#186279,#186280,#186281,#186282,#186283,
#186284,#186285,#186286,#186287,#186288,#186289,#186290,#186291,#186292,
#186293,#186294,#186295,#186296,#186297,#186298,#186299,#186300,#186301,
#186302,#186303,#186304,#186305,#186306,#186307,#186308,#186309,#186310,
#186311,#186312,#186313,#186314,#186315,#186316,#186317,#186318,#186319,
#186320,#186321,#186322,#186323,#186324,#186325,#186326,#186327,#186328,
#186329,#186330,#186331,#186332,#186333,#186334,#186335,#186336,#186337,
#186338,#186339,#186340,#186341,#186342,#186343,#186344,#186345,#186346,
#186347,#186348,#186349,#186350,#186351,#186352,#186353,#186354,#186355,
#186356,#186357,#186358,#186359,#186360,#186361,#186362,#186363,#186364,
#186365,#186366,#186367,#186368,#186369,#186370,#186371,#186372,#186373,
#186374,#186375,#186376,#186377,#186378,#186379,#186380,#186381,#186382,
#186383,#186384,#186385,#186386,#186387,#186388,#186389,#186390,#186391,
#186392,#186393,#186394,#186395,#186396),.UNSPECIFIED.,.F.,.F.,(4,3,3,3,
3,3,3,3,3,3,3,3,3,3,3,3,3,3,3,3,3,3,3,3,3,3,3,3,3,3,3,3,3,3,3,3,3,3,3,3,
3,3,3,3,3,3,3,3,3,3,3,3,3,3,3,3,3,3,3,3,3,3,3,3,3,3,3,3,3,3,3,3,3,3,3,3,
3,3,3,3,3,4),(-110.906691970895,-110.82749856315,-110.748395230993,-110.669363816888,
-110.590386228964,-110.511436604536,-110.432499965624,-110.35356001131,
-110.27460044075,-110.195558870897,-110.116474582147,-110.037271099244,
-109.970961179214,-109.891003879083,-109.81114108184,-109.731355259369,
-109.651628944173,-109.571944715879,-109.492273729658,-109.412606276133,
-109.332926625316,-109.253219042922,-109.173423813846,-109.093579472138,
-109.013621045091,-108.971225168494,-108.891267868363,-108.81140507112,
-108.731619248648,-108.651892933453,-108.572208705159,-108.492537718938,
-108.412870265412,-108.333190614595,-108.253483032201,-108.173687803125,
-108.093843461418,-108.013885034371,-107.971489157774,-107.891531857643,
-107.8116690604,-107.731883237929,-107.652156922733,-107.572472694439,-107.492801708218,
-107.413134254692,-107.333454603876,-107.253747021481,-107.173951792405,
-107.094107450698,-107.01414902365,-106.971753147054,-106.891795846923,
-106.81193304968,-106.732147227209,-106.652420912013,-106.572736683719,
-106.493065697498,-106.413398243972,-106.333718593156,-106.254011010761,
-106.174215781686,-106.094371439978,-106.014413012931,-105.972017136334,
-105.892059836203,-105.81219703896,-105.732411216489,-105.652684901294,
-105.573000672999,-105.493329686778,-105.413662233252,-105.333982582435,
-105.254275000041,-105.174479770965,-105.094635429257,-105.01467700221,
-104.972281125614,-104.879689190256,-104.787448241979,-104.695893518158,
-104.623506786484),.UNSPECIFIED.);
#1651=B_SPLINE_CURVE_WITH_KNOTS('',3,(#186398,#186399,#186400,#186401,#186402,
#186403,#186404,#186405,#186406,#186407),.UNSPECIFIED.,.F.,.F.,(4,1,1,1,
1,1,1,4),(-104.623506663716,-103.972545114894,-102.972809104174,-101.973073093453,
-100.973337082733,-99.9736010720131,-98.973865061293,-98.340321356536),
 .UNSPECIFIED.);
#1652=B_SPLINE_CURVE_WITH_KNOTS('',3,(#186409,#186410,#186411,#186412,#186413,
#186414,#186415,#186416,#186417,#186418),.UNSPECIFIED.,.F.,.F.,(4,1,1,1,
1,1,1,4),(-98.340321356536,-97.9741290505729,-96.9743930398527,-95.9746570291326,
-94.9749210184124,-93.9751850076923,-92.9754489969722,-92.0571360493564),
 .UNSPECIFIED.);
#1653=B_SPLINE_CURVE_WITH_KNOTS('',3,(#186420,#186421,#186422,#186423,#186424,
#186425,#186426,#186427,#186428,#186429,#186430),.UNSPECIFIED.,.F.,.F.,
(4,1,1,1,1,1,1,1,4),(-92.0571360493564,-91.9757129862521,-90.9759769755319,
-89.9762409648118,-88.9765049540917,-87.9767689433716,-86.9770329326514,
-85.9772969219313,-85.7739507421768),.UNSPECIFIED.);
#1654=B_SPLINE_CURVE_WITH_KNOTS('',3,(#186432,#186433,#186434,#186435,#186436,
#186437,#186438,#186439,#186440,#186441,#186442,#186443,#186444,#186445,
#186446,#186447,#186448,#186449,#186450,#186451,#186452,#186453,#186454,
#186455,#186456,#186457,#186458,#186459,#186460,#186461,#186462,#186463,
#186464,#186465,#186466,#186467,#186468,#186469,#186470,#186471,#186472,
#186473,#186474,#186475,#186476,#186477,#186478,#186479,#186480,#186481,
#186482,#186483,#186484,#186485,#186486,#186487,#186488,#186489,#186490,
#186491,#186492,#186493,#186494,#186495,#186496,#186497,#186498,#186499,
#186500,#186501,#186502,#186503,#186504,#186505,#186506,#186507,#186508,
#186509,#186510,#186511,#186512,#186513,#186514,#186515,#186516,#186517,
#186518,#186519,#186520,#186521,#186522,#186523,#186524,#186525,#186526,
#186527,#186528,#186529,#186530,#186531,#186532,#186533,#186534,#186535,
#186536,#186537,#186538,#186539,#186540,#186541,#186542,#186543,#186544,
#186545,#186546,#186547,#186548,#186549,#186550,#186551,#186552,#186553,
#186554,#186555,#186556,#186557,#186558,#186559,#186560,#186561,#186562,
#186563,#186564,#186565,#186566,#186567,#186568,#186569,#186570,#186571,
#186572,#186573,#186574,#186575,#186576,#186577,#186578,#186579,#186580,
#186581,#186582,#186583,#186584,#186585,#186586,#186587,#186588,#186589,
#186590,#186591,#186592,#186593,#186594,#186595,#186596,#186597,#186598,
#186599,#186600,#186601,#186602,#186603,#186604,#186605,#186606,#186607,
#186608,#186609,#186610,#186611,#186612,#186613,#186614,#186615,#186616,
#186617,#186618,#186619,#186620,#186621,#186622,#186623,#186624,#186625,
#186626,#186627,#186628,#186629,#186630,#186631,#186632,#186633,#186634,
#186635,#186636,#186637,#186638,#186639,#186640,#186641,#186642,#186643,
#186644,#186645,#186646,#186647,#186648,#186649,#186650,#186651,#186652,
#186653,#186654,#186655,#186656,#186657,#186658,#186659,#186660,#186661,
#186662,#186663,#186664,#186665,#186666,#186667,#186668,#186669,#186670,
#186671,#186672,#186673,#186674,#186675),.UNSPECIFIED.,.F.,.F.,(4,3,3,3,
3,3,3,3,3,3,3,3,3,3,3,3,3,3,3,3,3,3,3,3,3,3,3,3,3,3,3,3,3,3,3,3,3,3,3,3,
3,3,3,3,3,3,3,3,3,3,3,3,3,3,3,3,3,3,3,3,3,3,3,3,3,3,3,3,3,3,3,3,3,3,3,3,
3,3,3,3,3,4),(-85.7739507421768,-85.6952881601577,-85.616687997987,-85.53679711214,
-85.4582566003864,-85.379719530466,-85.3011693595009,-85.2202672474284,
-85.1416009943376,-85.0595809527744,-84.9775609112112,-84.89760361108,-84.8177408138373,
-84.7379549913655,-84.6582286761703,-84.5785444478759,-84.498873461655,
-84.419206008129,-84.3395263573124,-84.2598187749181,-84.1800235458425,
-84.1001792041348,-84.0202207770874,-83.977824900491,-83.8978676003597,
-83.8180048031171,-83.7382189806452,-83.6584926654501,-83.5788084371562,
-83.4991374509353,-83.4194699974093,-83.3397903465929,-83.2600827641988,
-83.1802875351232,-83.1004431934156,-83.0204847663682,-82.9780888897709,
-82.8981315896397,-82.8182687923971,-82.7384829699253,-82.65875665473,-82.579072426436,
-82.4994014402152,-82.4197339866892,-82.3400543358726,-82.2603467534779,
-82.1805515244024,-82.1007071826946,-82.0207487556472,-81.9783528790508,
-81.8983955789195,-81.818532781677,-81.7387469592052,-81.65902064401,-81.5793364157154,
-81.4996654294946,-81.4199979759686,-81.3403183251522,-81.2606107427579,
-81.1808155136824,-81.100971171975,-81.0210127449277,-80.9786168683306,
-80.8986595681993,-80.818796770957,-80.7390109484849,-80.6592846332902,
-80.5796004049962,-80.4999294187752,-80.4202619652489,-80.3405823144325,
-80.2608747320383,-80.1810795029628,-80.1012351612554,-80.0212767342081,
-79.9788808576105,-79.894345483959,-79.8099558941397,-79.7257670174106,
-79.6416970903594,-79.5577926852418,-79.4907654351257),.UNSPECIFIED.);
#1655=B_SPLINE_CURVE_WITH_KNOTS('',3,(#186677,#186678,#186679,#186680,#186681,
#186682,#186683,#186684,#186685,#186686,#186687,#186688,#186689,#186690,
#186691,#186692,#186693,#186694,#186695,#186696,#186697,#186698,#186699,
#186700,#186701,#186702,#186703,#186704,#186705,#186706,#186707,#186708,
#186709,#186710,#186711,#186712,#186713,#186714,#186715,#186716,#186717,
#186718,#186719,#186720,#186721,#186722,#186723,#186724,#186725,#186726,
#186727,#186728,#186729,#186730,#186731,#186732,#186733,#186734,#186735,
#186736,#186737,#186738,#186739,#186740,#186741,#186742,#186743,#186744,
#186745,#186746,#186747,#186748,#186749,#186750,#186751,#186752,#186753,
#186754,#186755,#186756,#186757,#186758,#186759,#186760,#186761,#186762,
#186763,#186764,#186765,#186766,#186767,#186768,#186769,#186770,#186771,
#186772,#186773,#186774,#186775,#186776,#186777,#186778,#186779,#186780,
#186781,#186782,#186783,#186784,#186785,#186786,#186787,#186788,#186789,
#186790,#186791,#186792,#186793,#186794,#186795,#186796,#186797,#186798,
#186799,#186800,#186801,#186802,#186803,#186804,#186805,#186806,#186807,
#186808,#186809,#186810,#186811,#186812,#186813,#186814,#186815,#186816,
#186817,#186818,#186819,#186820,#186821,#186822,#186823,#186824,#186825,
#186826,#186827,#186828,#186829,#186830,#186831,#186832,#186833,#186834,
#186835,#186836,#186837,#186838,#186839,#186840,#186841,#186842,#186843,
#186844,#186845,#186846,#186847,#186848,#186849,#186850,#186851,#186852,
#186853,#186854,#186855,#186856,#186857,#186858,#186859,#186860,#186861,
#186862,#186863,#186864,#186865,#186866,#186867,#186868,#186869,#186870,
#186871,#186872,#186873,#186874,#186875,#186876,#186877,#186878,#186879,
#186880,#186881,#186882,#186883,#186884,#186885,#186886,#186887,#186888,
#186889,#186890,#186891,#186892,#186893,#186894,#186895,#186896,#186897,
#186898,#186899,#186900,#186901,#186902,#186903,#186904,#186905,#186906,
#186907,#186908,#186909,#186910,#186911,#186912,#186913,#186914,#186915,
#186916,#186917,#186918,#186919,#186920),.UNSPECIFIED.,.F.,.F.,(4,3,3,3,
3,3,3,3,3,3,3,3,3,3,3,3,3,3,3,3,3,3,3,3,3,3,3,3,3,3,3,3,3,3,3,3,3,3,3,3,
3,3,3,3,3,3,3,3,3,3,3,3,3,3,3,3,3,3,3,3,3,3,3,3,3,3,3,3,3,3,3,3,3,3,3,3,
3,3,3,3,3,4),(-79.4907654349973,-79.4077034724819,-79.3245504349086,-79.2381990379041,
-79.1547733841094,-79.0669591154998,-78.9791448468903,-78.8991875467591,
-78.8193247495167,-78.7395389270448,-78.6598126118496,-78.5801283835557,
-78.5004573973348,-78.4207899438089,-78.3411102929926,-78.2614027105983,
-78.1816074815228,-78.101763139815,-78.0218047127677,-77.9794088361702,
-77.8994515360389,-77.8195887387963,-77.7398029163244,-77.6600766011291,
-77.5803923728351,-77.5007213866142,-77.4210539330884,-77.3413742822718,
-77.2616666998774,-77.1818714708018,-77.1020271290941,-77.0220687020468,
-76.9796728254501,-76.8997155253188,-76.819852728076,-76.7400669056043,
-76.6603405904092,-76.5806563621158,-76.5009853758948,-76.4213179223689,
-76.3416382715525,-76.2619306891576,-76.182135460082,-76.1022911183746,
-76.0223326913272,-75.97993681473,-75.8999795145987,-75.820116717356,-75.7403308948843,
-75.6606045796891,-75.5809203513952,-75.5012493651742,-75.4215819116484,
-75.3419022608322,-75.2621946784377,-75.1823994493621,-75.1025551076547,
-75.0225966806073,-74.9802008040098,-74.9002435038785,-74.8203807066359,
-74.7405948841641,-74.6608685689692,-74.5811843406744,-74.5015133544535,
-74.4218459009276,-74.3421662501111,-74.2624586677158,-74.1826634386403,
-74.1028190969327,-74.0228606698853,-73.9804647932897,-73.9015581804217,
-73.8227469663865,-73.7440261147531,-73.6653563569114,-73.5867211558266,
-73.5081040028306,-73.4294628808362,-73.3508110774882,-73.2720919472877,
-73.2075801278176),.UNSPECIFIED.);
#1656=B_SPLINE_CURVE_WITH_KNOTS('',3,(#186922,#186923,#186924,#186925,#186926,
#186927,#186928,#186929,#186930,#186931,#186932),.UNSPECIFIED.,.F.,.F.,
(4,1,1,1,1,1,1,1,4),(-73.2075801278176,-72.9807287825696,-71.9809927718494,
-70.9812567611293,-69.9815207504092,-68.981784739689,-67.9820487289689,
-66.9823127182488,-66.9243948206381),.UNSPECIFIED.);
#1657=B_SPLINE_CURVE_WITH_KNOTS('',3,(#186934,#186935,#186936,#186937,#186938,
#186939,#186940,#186941,#186942,#186943,#186944,#186945,#186946,#186947,
#186948,#186949,#186950,#186951,#186952,#186953,#186954,#186955,#186956,
#186957,#186958,#186959,#186960,#186961,#186962,#186963,#186964,#186965,
#186966,#186967,#186968,#186969,#186970,#186971,#186972,#186973,#186974,
#186975,#186976,#186977,#186978,#186979,#186980,#186981,#186982,#186983,
#186984,#186985,#186986,#186987,#186988,#186989,#186990,#186991,#186992,
#186993,#186994,#186995,#186996,#186997,#186998,#186999,#187000,#187001,
#187002,#187003,#187004,#187005,#187006,#187007,#187008,#187009,#187010,
#187011,#187012,#187013,#187014,#187015,#187016,#187017,#187018,#187019,
#187020,#187021,#187022,#187023,#187024,#187025,#187026,#187027,#187028,
#187029,#187030,#187031,#187032,#187033,#187034,#187035,#187036,#187037,
#187038,#187039,#187040,#187041,#187042,#187043,#187044,#187045,#187046,
#187047,#187048,#187049,#187050,#187051,#187052,#187053,#187054,#187055,
#187056,#187057,#187058,#187059,#187060,#187061,#187062,#187063,#187064,
#187065,#187066,#187067,#187068,#187069,#187070,#187071,#187072,#187073,
#187074,#187075,#187076,#187077,#187078,#187079,#187080,#187081,#187082,
#187083,#187084,#187085,#187086,#187087,#187088,#187089,#187090,#187091,
#187092,#187093,#187094,#187095,#187096,#187097,#187098,#187099,#187100,
#187101,#187102,#187103,#187104,#187105,#187106,#187107,#187108,#187109,
#187110,#187111,#187112,#187113,#187114,#187115,#187116,#187117,#187118,
#187119,#187120,#187121,#187122,#187123,#187124,#187125,#187126,#187127,
#187128,#187129,#187130,#187131,#187132,#187133,#187134,#187135,#187136,
#187137,#187138,#187139,#187140,#187141,#187142,#187143,#187144,#187145,
#187146,#187147,#187148,#187149,#187150,#187151,#187152,#187153,#187154,
#187155,#187156,#187157,#187158,#187159,#187160,#187161,#187162,#187163,
#187164,#187165,#187166,#187167,#187168,#187169,#187170,#187171,#187172,
#187173,#187174,#187175,#187176,#187177),.UNSPECIFIED.,.F.,.F.,(4,3,3,3,
3,3,3,3,3,3,3,3,3,3,3,3,3,3,3,3,3,3,3,3,3,3,3,3,3,3,3,3,3,3,3,3,3,3,3,3,
3,3,3,3,3,3,3,3,3,3,3,3,3,3,3,3,3,3,3,3,3,3,3,3,3,3,3,3,3,3,3,3,3,3,3,3,
3,3,3,3,3,4),(-66.9243948206381,-66.8451430614651,-66.7659820906656,-66.68689378965,
-66.6078601052444,-66.5288554488661,-66.4498645624908,-66.3708711811437,
-66.2918590405673,-66.2127651323194,-66.1336293443134,-66.054372687672,
-65.9825767075287,-65.9026194073974,-65.8227566101546,-65.7429707876828,
-65.6632444724872,-65.5835602441933,-65.5038892579723,-65.4242218044462,
-65.3445421536298,-65.2648345712352,-65.1850393421596,-65.105195000452,
-65.0252365734045,-64.9828406968085,-64.9028833966772,-64.8230205994346,
-64.7432347769627,-64.6635084617673,-64.5838242334732,-64.5041532472523,
-64.4244857937264,-64.3448061429098,-64.2650985605154,-64.1853033314399,
-64.1054589897322,-64.0255005626848,-63.9831046860884,-63.9031473859572,
-63.8232845887147,-63.7434987662427,-63.6637724510475,-63.5840882227535,
-63.5044172365327,-63.4247497830068,-63.3450701321903,-63.2653625497957,
-63.1855673207202,-63.1057229790125,-63.0257645519651,-62.9833686753683,
-62.903411375237,-62.8235485779942,-62.7437627555225,-62.6640364403274,
-62.5843522120328,-62.5046812258119,-62.425013772286,-62.3453341214695,
-62.2656265390753,-62.1858313099998,-62.1059869682922,-62.0260285412449,
-61.9836326646481,-61.9036753645168,-61.823812567274,-61.7440267448023,
-61.6643004296077,-61.5846162013138,-61.5049452150927,-61.4252777615666,
-61.3455981107502,-61.2658905283563,-61.1860952992806,-61.1062509575726,
-61.0262925305251,-60.983896653928,-60.8907777178953,-60.798032881653,-60.7060135811139,
-60.6412095135729),.UNSPECIFIED.);
#1658=B_SPLINE_CURVE_WITH_KNOTS('',3,(#187179,#187180,#187181,#187182,#187183,
#187184,#187185,#187186,#187187,#187188,#187189,#187190,#187191,#187192,
#187193,#187194,#187195,#187196,#187197,#187198,#187199,#187200,#187201,
#187202,#187203,#187204,#187205,#187206,#187207,#187208,#187209,#187210,
#187211,#187212,#187213,#187214,#187215,#187216,#187217,#187218,#187219,
#187220,#187221,#187222,#187223,#187224,#187225,#187226,#187227,#187228,
#187229,#187230,#187231,#187232,#187233,#187234,#187235,#187236,#187237,
#187238,#187239,#187240,#187241,#187242,#187243,#187244,#187245,#187246,
#187247,#187248,#187249,#187250,#187251,#187252,#187253,#187254,#187255,
#187256,#187257,#187258,#187259,#187260,#187261,#187262,#187263,#187264,
#187265,#187266,#187267,#187268,#187269,#187270,#187271,#187272,#187273,
#187274,#187275,#187276,#187277,#187278,#187279,#187280,#187281,#187282,
#187283,#187284,#187285,#187286,#187287,#187288,#187289,#187290,#187291,
#187292,#187293,#187294,#187295,#187296,#187297,#187298,#187299,#187300,
#187301,#187302,#187303,#187304,#187305,#187306,#187307,#187308,#187309,
#187310,#187311,#187312,#187313,#187314,#187315,#187316,#187317,#187318,
#187319,#187320,#187321,#187322,#187323,#187324,#187325,#187326,#187327,
#187328,#187329,#187330,#187331,#187332,#187333,#187334,#187335,#187336,
#187337,#187338,#187339,#187340,#187341,#187342,#187343,#187344,#187345,
#187346,#187347,#187348,#187349,#187350,#187351,#187352,#187353,#187354,
#187355,#187356,#187357,#187358,#187359,#187360,#187361,#187362,#187363,
#187364,#187365,#187366,#187367,#187368,#187369,#187370,#187371,#187372,
#187373,#187374,#187375,#187376,#187377,#187378,#187379,#187380,#187381,
#187382,#187383,#187384,#187385,#187386,#187387,#187388,#187389,#187390,
#187391,#187392,#187393,#187394,#187395,#187396,#187397,#187398,#187399,
#187400,#187401,#187402,#187403,#187404,#187405,#187406,#187407,#187408,
#187409,#187410,#187411,#187412,#187413,#187414,#187415,#187416,#187417,
#187418,#187419,#187420,#187421,#187422,#187423,#187424,#187425),
 .UNSPECIFIED.,.F.,.F.,(4,3,3,3,3,3,3,3,3,3,3,3,3,3,3,3,3,3,3,3,3,3,3,3,
3,3,3,3,3,3,3,3,3,3,3,3,3,3,3,3,3,3,3,3,3,3,3,3,3,3,3,3,3,3,3,3,3,3,3,3,
3,3,3,3,3,3,3,3,3,3,3,3,3,3,3,3,3,3,3,3,3,3,4),(-60.6412095134584,-60.5590784046771,
-60.4793357811508,-60.3995857810152,-60.3198128184427,-60.235899774634,
-60.1559884534018,-60.0760181955046,-59.995936002992,-59.9841606432079,
-59.9042033430767,-59.8243405458341,-59.7445547233624,-59.664828408167,
-59.5851441798728,-59.5054731936519,-59.4258057401261,-59.3461260893097,
-59.2664185069152,-59.1866232778397,-59.106778936132,-59.0268205090847,
-58.9844246324877,-58.9044673323564,-58.8246045351137,-58.7448187126417,
-58.6650923974462,-58.5854081691519,-58.5057371829309,-58.4260697294049,
-58.3463900785883,-58.2666824961936,-58.186887267118,-58.1070429254103,
-58.0270844983627,-57.9846886217676,-57.9047313216364,-57.8248685243939,
-57.7450827019221,-57.6653563867272,-57.5856721584333,-57.5060011722124,
-57.4263337186865,-57.3466540678699,-57.2669464854756,-57.1871512564001,
-57.1073069146926,-57.0273484876453,-56.9849526110475,-56.9049953109163,
-56.8251325136738,-56.7453466912019,-56.6656203760066,-56.5859361477129,
-56.5062651614919,-56.4265977079658,-56.3469180571494,-56.2672104747552,
-56.1874152456796,-56.1075709039718,-56.0276124769243,-55.9852166003274,
-55.9052593001963,-55.8253965029537,-55.7456106804819,-55.665884365286,
-55.5862001369919,-55.506529150771,-55.426861697245,-55.3471820464283,-55.2674744640334,
-55.1876792349578,-55.1078348932506,-55.0278764662033,-54.9854805896072,
-54.9049169077671,-54.8244508849754,-54.7440673257589,-54.6637510888401,
-54.5834913281942,-54.5032654666035,-54.4230482427655,-54.3580242062788),
 .UNSPECIFIED.);
#1659=B_SPLINE_CURVE_WITH_KNOTS('',3,(#187427,#187428,#187429,#187430,#187431,
#187432,#187433,#187434,#187435,#187436),.UNSPECIFIED.,.F.,.F.,(4,1,1,1,
1,1,1,4),(-54.3580165317574,-53.9857445788871,-52.9860085681669,-51.9862725574468,
-50.9865365467267,-49.9868005360066,-48.9870645252864,-48.0748476368028),
 .UNSPECIFIED.);
#1660=B_SPLINE_CURVE_WITH_KNOTS('',3,(#187438,#187439,#187440,#187441,#187442,
#187443,#187444,#187445,#187446,#187447,#187448,#187449,#187450,#187451,
#187452,#187453,#187454,#187455,#187456,#187457,#187458,#187459,#187460,
#187461,#187462,#187463,#187464,#187465,#187466,#187467,#187468,#187469,
#187470,#187471,#187472,#187473,#187474,#187475,#187476,#187477,#187478,
#187479,#187480,#187481,#187482,#187483,#187484,#187485,#187486,#187487,
#187488,#187489,#187490,#187491,#187492,#187493,#187494,#187495,#187496,
#187497,#187498,#187499,#187500,#187501,#187502,#187503,#187504,#187505,
#187506,#187507,#187508,#187509,#187510,#187511,#187512,#187513,#187514,
#187515,#187516,#187517,#187518,#187519,#187520,#187521,#187522,#187523,
#187524,#187525,#187526,#187527,#187528,#187529,#187530,#187531,#187532,
#187533,#187534,#187535,#187536,#187537,#187538,#187539,#187540,#187541,
#187542,#187543,#187544,#187545,#187546,#187547,#187548,#187549,#187550,
#187551,#187552,#187553,#187554,#187555,#187556,#187557,#187558,#187559,
#187560,#187561,#187562,#187563,#187564,#187565,#187566,#187567,#187568,
#187569,#187570,#187571,#187572,#187573,#187574,#187575,#187576,#187577,
#187578,#187579,#187580,#187581,#187582,#187583,#187584,#187585,#187586,
#187587,#187588,#187589,#187590,#187591,#187592,#187593,#187594,#187595,
#187596,#187597,#187598,#187599,#187600,#187601,#187602,#187603,#187604,
#187605,#187606,#187607,#187608,#187609,#187610,#187611,#187612,#187613,
#187614,#187615,#187616,#187617,#187618,#187619,#187620,#187621,#187622,
#187623,#187624,#187625,#187626,#187627,#187628,#187629,#187630,#187631,
#187632,#187633,#187634,#187635,#187636,#187637,#187638,#187639,#187640,
#187641,#187642,#187643,#187644,#187645,#187646,#187647,#187648,#187649,
#187650,#187651,#187652,#187653,#187654,#187655,#187656,#187657,#187658,
#187659,#187660,#187661,#187662,#187663,#187664,#187665,#187666,#187667,
#187668,#187669,#187670,#187671,#187672,#187673,#187674,#187675,#187676,
#187677,#187678,#187679,#187680,#187681),.UNSPECIFIED.,.F.,.F.,(4,3,3,3,
3,3,3,3,3,3,3,3,3,3,3,3,3,3,3,3,3,3,3,3,3,3,3,3,3,3,3,3,3,3,3,3,3,3,3,3,
3,3,3,3,3,3,3,3,3,3,3,3,3,3,3,3,3,3,3,3,3,3,3,3,3,3,3,3,3,3,3,3,3,3,3,3,
3,3,3,3,3,4),(-48.0748388990992,-47.9873285145663,-47.9073712144349,-47.8275084171922,
-47.7477225947202,-47.6679962795249,-47.5883120512307,-47.5086410650096,
-47.4289736114836,-47.3492939606671,-47.2695863782722,-47.1897911491966,
-47.1099468074887,-47.0299883804412,-46.9875925038462,-46.9076352037149,
-46.8277724064724,-46.7479865840006,-46.6682602688053,-46.5885760405113,
-46.5089050542904,-46.4292376007644,-46.3495579499479,-46.2698503675534,
-46.1900551384779,-46.1102107967703,-46.0302523697229,-45.987856493126,
-45.9078991929947,-45.8280363957522,-45.7482505732803,-45.668524258085,
-45.5888400297908,-45.5091690435699,-45.429501590044,-45.3498219392276,
-45.270114356833,-45.1903191277575,-45.1104747860499,-45.0305163590025,
-44.9881204824059,-44.9081631822747,-44.8283003850321,-44.7485145625602,
-44.668788247365,-44.5891040190709,-44.50943303285,-44.4297655793241,-44.3500859285076,
-44.2703783461131,-44.1905831170376,-44.1107387753299,-44.0307803482826,
-43.9883844716858,-43.9084271715545,-43.8285643743119,-43.74877855184,-43.6690522366447,
-43.5893680083507,-43.5096970221298,-43.4300295686039,-43.3503499177874,
-43.2706423353929,-43.1908471063174,-43.1110027646097,-43.0310443375623,
-42.9886484609656,-42.9086911608343,-42.8288283635917,-42.7490425411198,
-42.6693162259245,-42.5896319976304,-42.5099610114094,-42.4302935578836,
-42.3506139070671,-42.2709063246724,-42.1911110955969,-42.1112667538892,
-42.0313083268418,-41.9889124502455,-41.8733272325874,-41.7916535919196),
 .UNSPECIFIED.);
#1661=B_SPLINE_CURVE_WITH_KNOTS('',3,(#187683,#187684,#187685,#187686,#187687,
#187688,#187689,#187690,#187691,#187692),.UNSPECIFIED.,.F.,.F.,(4,1,1,1,
1,1,1,4),(-41.7916500544357,-40.9891764395254,-39.9894404288052,-38.9897044180851,
-37.989968407365,-36.9902323966448,-35.9904963859247,-35.50846828474),
 .UNSPECIFIED.);
#1662=B_SPLINE_CURVE_WITH_KNOTS('',3,(#187694,#187695,#187696,#187697,#187698,
#187699,#187700,#187701,#187702,#187703),.UNSPECIFIED.,.F.,.F.,(4,1,1,1,
1,1,1,4),(-35.50846828474,-34.9907603752046,-33.9910243644845,-32.9912883537643,
-31.9915523430442,-30.9918163323241,-29.9920803216039,-29.2252829775605),
 .UNSPECIFIED.);
#1663=B_SPLINE_CURVE_WITH_KNOTS('',3,(#187705,#187706,#187707,#187708,#187709,
#187710,#187711,#187712,#187713,#187714,#187715),.UNSPECIFIED.,.F.,.F.,
(4,1,1,1,1,1,1,1,4),(-29.2252829775605,-28.9923443108838,-27.9926083001637,
-26.9928722894435,-25.9931362787234,-24.9934002680033,-23.9936642572832,
-22.993928246563,-22.9420976703809),.UNSPECIFIED.);
#1664=B_SPLINE_CURVE_WITH_KNOTS('',3,(#187717,#187718,#187719,#187720,#187721,
#187722,#187723,#187724,#187725,#187726),.UNSPECIFIED.,.F.,.F.,(4,1,1,1,
1,1,1,4),(-22.9420976703809,-21.9941922358429,-20.9944562251228,-19.9947202144026,
-18.9949842036825,-17.9952481929624,-16.9955121822422,-16.6589198685825),
 .UNSPECIFIED.);
#1665=B_SPLINE_CURVE_WITH_KNOTS('',3,(#187728,#187729,#187730,#187731,#187732,
#187733,#187734,#187735,#187736,#187737,#187738,#187739,#187740,#187741,
#187742,#187743,#187744,#187745,#187746,#187747,#187748,#187749,#187750,
#187751,#187752,#187753,#187754,#187755,#187756,#187757,#187758,#187759,
#187760,#187761,#187762,#187763,#187764,#187765,#187766,#187767,#187768,
#187769,#187770,#187771,#187772,#187773,#187774,#187775,#187776,#187777,
#187778,#187779,#187780,#187781,#187782,#187783,#187784,#187785,#187786,
#187787,#187788,#187789,#187790,#187791,#187792,#187793,#187794,#187795,
#187796,#187797,#187798,#187799,#187800,#187801,#187802,#187803,#187804,
#187805,#187806,#187807,#187808,#187809,#187810,#187811,#187812,#187813,
#187814,#187815,#187816,#187817,#187818,#187819,#187820,#187821,#187822,
#187823,#187824,#187825,#187826,#187827,#187828,#187829,#187830,#187831,
#187832,#187833,#187834,#187835,#187836,#187837,#187838,#187839,#187840,
#187841,#187842,#187843,#187844,#187845,#187846,#187847,#187848,#187849,
#187850,#187851,#187852,#187853,#187854,#187855,#187856,#187857,#187858,
#187859,#187860,#187861,#187862,#187863,#187864,#187865,#187866,#187867,
#187868,#187869,#187870,#187871,#187872,#187873,#187874,#187875,#187876,
#187877,#187878,#187879,#187880,#187881,#187882,#187883,#187884,#187885,
#187886,#187887,#187888,#187889,#187890,#187891,#187892,#187893,#187894,
#187895,#187896,#187897,#187898,#187899,#187900,#187901,#187902,#187903,
#187904,#187905,#187906,#187907,#187908,#187909,#187910,#187911,#187912,
#187913,#187914,#187915,#187916,#187917,#187918,#187919,#187920,#187921,
#187922,#187923,#187924,#187925,#187926,#187927,#187928,#187929,#187930,
#187931,#187932,#187933,#187934,#187935,#187936,#187937,#187938,#187939,
#187940,#187941,#187942,#187943,#187944,#187945,#187946,#187947,#187948,
#187949,#187950,#187951,#187952,#187953,#187954,#187955,#187956,#187957,
#187958,#187959,#187960,#187961,#187962,#187963,#187964,#187965,#187966,
#187967,#187968,#187969,#187970,#187971,#187972,#187973,#187974),
 .UNSPECIFIED.,.F.,.F.,(4,3,3,3,3,3,3,3,3,3,3,3,3,3,3,3,3,3,3,3,3,3,3,3,
3,3,3,3,3,3,3,3,3,3,3,3,3,3,3,3,3,3,3,3,3,3,3,3,3,3,3,3,3,3,3,3,3,3,3,3,
3,3,3,3,3,3,3,3,3,3,3,3,3,3,3,3,3,3,3,3,3,3,4),(-16.6589123632013,-16.5760203392414,
-16.4963658357425,-16.4167062586062,-16.3370259313394,-16.257309167994,
-16.1774967883031,-16.0976279107091,-16.0176451019278,-15.9957761715221,
-15.9158187324329,-15.8359557956803,-15.7561698332831,-15.6764433778821,
-15.5967590092361,-15.5170878828934,-15.4374202894017,-15.3577404988956,
-15.2780327772076,-15.198237410145,-15.118392930983,-15.0384343685027,-14.996040160802,
-14.9160831648467,-14.8362206718143,-14.7564351533039,-14.6767091415404,
-14.5970252158687,-14.5173545301081,-14.4376873756752,-14.3580080223317,
-14.278300735536,-14.1985057977278,-14.1186617452726,-14.0387036018344,
-13.9963041500818,-13.9163467244748,-13.8364838036549,-13.7566978595949,
-13.6769714248916,-13.5972870792623,-13.5176159792993,-13.4379484142671,
-13.3582686542674,-13.2785609651013,-13.1987656334396,-13.1189211913599,
-13.0389626682531,-12.9965681393617,-12.9166100108447,-12.8367463812177,
-12.7569597231879,-12.6772325700763,-12.5975475023185,-12.5178756770059,
-12.4382073847008,-12.3585268961407,-12.2788184777613,-12.199022419603,
-12.1191772514785,-12.0392180093319,-11.9968321286416,-11.9168769666291,
-11.8370163088955,-11.7572326253178,-11.6775084464124,-11.5978263498226,
-11.5181574817392,-11.4384921377459,-11.3588145860714,-11.2791090906347,
-11.1993159195183,-11.1194736224419,-11.0395172015575,-10.9970961179214,
-10.9164104612956,-10.8358235390977,-10.7553203015422,-10.6748857539066,
-10.5945105281505,-10.5141705799335,-10.4338432861696,-10.3757270560217),
 .UNSPECIFIED.);
#1666=B_SPLINE_CURVE_WITH_KNOTS('',3,(#187975,#187976,#187977,#187978,#187979,
#187980,#187981,#187982,#187983,#187984),.UNSPECIFIED.,.F.,.F.,(4,1,1,1,
1,1,1,4),(-10.3757194590647,-9.99736010720131,-8.99762409648118,-7.99788808576105,
-6.99815207504092,-5.99841606432079,-4.99868005360065,-4.09255001849307),
 .UNSPECIFIED.);
#1667=B_SPLINE_CURVE_WITH_KNOTS('',3,(#187987,#187988,#187989,#187990,#187991,
#187992,#187993,#187994,#187995,#187996),.UNSPECIFIED.,.F.,.F.,(4,3,3,4),
(1693.06690371234,1693.1506377533,1693.17139155035,1693.3184402849),
 .UNSPECIFIED.);
#1668=B_SPLINE_CURVE_WITH_KNOTS('',3,(#187998,#187999,#188000,#188001,#188002,
#188003,#188004,#188005,#188006,#188007,#188008,#188009,#188010,#188011,
#188012,#188013,#188014,#188015,#188016,#188017,#188018,#188019,#188020,
#188021,#188022,#188023,#188024,#188025,#188026,#188027,#188028,#188029,
#188030,#188031,#188032,#188033,#188034,#188035,#188036,#188037,#188038,
#188039,#188040,#188041,#188042,#188043,#188044,#188045,#188046,#188047,
#188048,#188049,#188050,#188051,#188052,#188053,#188054,#188055,#188056,
#188057,#188058,#188059,#188060,#188061,#188062,#188063,#188064,#188065,
#188066,#188067,#188068,#188069,#188070,#188071,#188072,#188073,#188074,
#188075,#188076,#188077,#188078,#188079,#188080,#188081,#188082,#188083,
#188084,#188085,#188086,#188087,#188088,#188089,#188090,#188091,#188092,
#188093,#188094,#188095,#188096,#188097,#188098,#188099,#188100,#188101,
#188102,#188103,#188104,#188105,#188106,#188107,#188108,#188109,#188110,
#188111,#188112,#188113,#188114,#188115,#188116,#188117,#188118,#188119,
#188120,#188121,#188122,#188123,#188124,#188125,#188126,#188127,#188128,
#188129,#188130,#188131,#188132,#188133,#188134,#188135,#188136,#188137,
#188138,#188139,#188140,#188141,#188142,#188143,#188144,#188145,#188146,
#188147,#188148,#188149,#188150,#188151,#188152,#188153,#188154,#188155,
#188156,#188157,#188158,#188159,#188160,#188161,#188162,#188163,#188164,
#188165,#188166,#188167,#188168,#188169,#188170,#188171,#188172,#188173,
#188174,#188175,#188176,#188177,#188178,#188179,#188180,#188181,#188182,
#188183,#188184,#188185,#188186,#188187,#188188,#188189,#188190,#188191,
#188192,#188193,#188194,#188195,#188196,#188197,#188198,#188199,#188200,
#188201,#188202,#188203,#188204,#188205,#188206,#188207,#188208,#188209,
#188210,#188211),.UNSPECIFIED.,.F.,.F.,(4,3,3,3,3,3,3,3,3,3,3,3,3,3,3,3,
3,3,3,3,3,3,3,3,3,3,3,3,3,3,3,3,3,3,3,3,3,3,3,3,3,3,3,3,3,3,3,3,3,3,3,3,
3,3,3,3,3,3,3,3,3,3,3,3,3,3,3,3,3,3,3,4),(1693.31844028502,1693.4008614421,
1693.48319961379,1693.5691906072,1693.65143266586,1693.73366105159,1693.81589478312,
1693.89815288144,1693.98049848208,1694.0628955963,1694.14540833862,1694.17112756107,
1694.25489318401,1694.33855582112,1694.42213557425,1694.50565247357,1694.58913402256,
1694.67259819274,1694.75606303016,1694.83954657748,1694.92311870335,1695.00673539827,
1695.09048596028,1695.17086357179,1695.25449860037,1695.33803025765,1695.42147878235,
1695.50486434011,1695.58821483354,1695.67154813761,1695.75488241889,1695.83823584083,
1695.92167925488,1696.00516779981,1696.088792476,1696.17059958251,1696.25445516476,
1696.33820713564,1696.42187551199,1696.50548023893,1696.58904810639,1696.67259766383,
1696.75614687949,1696.83971371749,1696.92336695497,1697.00706370128,1697.09089170662,
1697.17033559323,1697.25421280583,1697.33798830632,1697.42168206028,1697.50531396346,
1697.58891161285,1697.6724925293,1697.75607464121,1697.8396758739,1697.92336565213,
1698.00710016425,1698.09096762072,1698.17007160395,1698.25229074706,1698.33440658285,
1698.4164405015,1698.50181651835,1698.58375783067,1698.665686824,1698.74762265115,
1698.82958446971,1698.91163608436,1698.99374084933,1699.0759627348,1699.09944863636),
 .UNSPECIFIED.);
#1669=B_SPLINE_CURVE_WITH_KNOTS('',3,(#188215,#188216,#188217,#188218,#188219,
#188220,#188221,#188222,#188223,#188224,#188225,#188226,#188227,#188228,
#188229,#188230,#188231,#188232,#188233,#188234,#188235,#188236,#188237,
#188238,#188239,#188240,#188241,#188242,#188243,#188244,#188245,#188246,
#188247,#188248,#188249,#188250,#188251,#188252,#188253,#188254,#188255,
#188256,#188257,#188258,#188259,#188260,#188261,#188262,#188263,#188264,
#188265,#188266,#188267,#188268,#188269,#188270,#188271,#188272,#188273,
#188274,#188275,#188276,#188277,#188278,#188279,#188280,#188281,#188282,
#188283,#188284,#188285,#188286,#188287,#188288,#188289,#188290,#188291,
#188292,#188293,#188294,#188295,#188296,#188297,#188298,#188299,#188300,
#188301,#188302,#188303,#188304,#188305,#188306,#188307,#188308,#188309,
#188310,#188311,#188312,#188313,#188314,#188315,#188316,#188317,#188318,
#188319,#188320,#188321,#188322,#188323,#188324,#188325,#188326,#188327,
#188328,#188329,#188330,#188331,#188332,#188333,#188334,#188335,#188336,
#188337,#188338,#188339,#188340,#188341,#188342,#188343,#188344,#188345,
#188346,#188347,#188348,#188349,#188350,#188351,#188352,#188353,#188354,
#188355,#188356,#188357,#188358,#188359,#188360,#188361,#188362,#188363,
#188364,#188365,#188366,#188367,#188368,#188369,#188370,#188371,#188372,
#188373,#188374,#188375,#188376,#188377),.UNSPECIFIED.,.F.,.F.,(4,3,3,3,
3,3,3,3,3,3,3,3,3,3,3,3,3,3,3,3,3,3,3,3,3,3,3,3,3,3,3,3,3,3,3,3,3,3,3,3,
3,3,3,3,3,3,3,3,3,3,3,3,3,3,4),(1693.3184402849,1693.40445195466,1693.49052691538,
1693.57667826784,1693.66297932812,1693.74936613508,1693.8359058484,1693.86083694135,
1693.94471415395,1694.02848965444,1694.1121834084,1694.19581531157,1694.27941296097,
1694.36299387742,1694.44657598933,1694.53017722202,1694.61386700025,1694.69760151237,
1694.78146896884,1694.86057295207,1694.94357842618,1695.02647983489,1695.10929799024,
1695.19205362182,1695.27558553944,1695.35829320941,1695.44100417102,1695.52373709062,
1695.60788005866,1695.69075989804,1695.77553443042,1695.86030896279,1695.94531027662,
1696.03020068413,1696.11499871164,1696.19972280846,1696.2843898248,1696.36902560792,
1696.45364676064,1696.53826987213,1696.62294846804,1696.70765480488,1696.79245608915,
1696.86004497351,1696.94393615237,1697.02775838711,1697.11153137067,1697.19527348557,
1697.27902402691,1697.35991297887,1697.45761556266,1697.55815691806,1697.65637442568,
1697.75807770495,1697.85978098423),.UNSPECIFIED.);
#1670=B_SPLINE_CURVE_WITH_KNOTS('',3,(#188378,#188379,#188380,#188381,#188382,
#188383,#188384,#188385,#188386,#188387),.UNSPECIFIED.,.F.,.F.,(4,3,3,4),
(1693.06812991347,1693.15787446388,1693.24735628336,1693.3184402848),
 .UNSPECIFIED.);
#1671=B_SPLINE_CURVE_WITH_KNOTS('',3,(#188398,#188399,#188400,#188401,#188402,
#188403,#188404,#188405,#188406,#188407,#188408,#188409,#188410,#188411,
#188412,#188413,#188414,#188415,#188416,#188417,#188418,#188419,#188420,
#188421,#188422,#188423,#188424,#188425,#188426,#188427,#188428,#188429,
#188430,#188431,#188432,#188433,#188434,#188435,#188436,#188437,#188438,
#188439,#188440,#188441,#188442,#188443,#188444,#188445,#188446,#188447,
#188448,#188449,#188450,#188451,#188452,#188453,#188454,#188455,#188456,
#188457,#188458,#188459,#188460,#188461,#188462,#188463,#188464,#188465,
#188466,#188467,#188468,#188469,#188470,#188471,#188472,#188473,#188474,
#188475,#188476,#188477,#188478,#188479,#188480,#188481,#188482,#188483,
#188484,#188485,#188486,#188487,#188488,#188489,#188490,#188491,#188492,
#188493,#188494,#188495,#188496,#188497,#188498,#188499,#188500,#188501,
#188502,#188503),.UNSPECIFIED.,.F.,.F.,(4,3,3,3,3,3,3,3,3,3,3,3,3,3,3,3,
3,3,3,3,3,3,3,3,3,3,3,3,3,3,3,3,3,3,3,4),(0.,0.0349249411505533,0.077348853415627,
0.121065958001284,0.164783062586941,0.189329869490245,0.195424600648578,
0.241029503011481,0.286450338806425,0.332357184633421,0.37784421010019,
0.390926586700649,0.397162835114324,0.444154447221939,0.491251570163209,
0.537752846290075,0.557531973039803,0.592379688295695,0.602095847517636,
0.609874760882364,0.656076546176515,0.703084256260691,0.75095048994342,
0.793453887845117,0.814883791466027,0.821323462530115,0.828310165375817,
0.836313695086938,0.885124880906474,0.93393606672601,0.958011516551483,
0.969491304425174,0.977480420947961,1.02729690957154,1.07695759308116,1.1265396653275),
 .UNSPECIFIED.);
#1672=B_SPLINE_CURVE_WITH_KNOTS('',3,(#188504,#188505,#188506,#188507,#188508,
#188509,#188510,#188511,#188512,#188513,#188514,#188515,#188516,#188517,
#188518,#188519,#188520,#188521,#188522,#188523,#188524,#188525,#188526,
#188527,#188528,#188529,#188530,#188531,#188532,#188533,#188534,#188535,
#188536,#188537,#188538,#188539,#188540,#188541,#188542,#188543,#188544,
#188545,#188546,#188547,#188548,#188549,#188550,#188551,#188552,#188553,
#188554,#188555,#188556,#188557,#188558,#188559,#188560,#188561,#188562,
#188563,#188564,#188565,#188566,#188567,#188568,#188569,#188570,#188571,
#188572,#188573,#188574,#188575,#188576,#188577,#188578,#188579,#188580,
#188581,#188582,#188583,#188584,#188585,#188586,#188587,#188588,#188589,
#188590,#188591,#188592,#188593,#188594,#188595,#188596,#188597,#188598,
#188599,#188600,#188601,#188602,#188603,#188604,#188605,#188606,#188607,
#188608,#188609,#188610,#188611,#188612),.UNSPECIFIED.,.F.,.F.,(4,3,3,3,
3,3,3,3,3,3,3,3,3,3,3,3,3,3,3,3,3,3,3,3,3,3,3,3,3,3,3,3,3,3,3,3,4),(0.,
0.041701088542356,0.0909472972506543,0.141057893902492,0.191015907286953,
0.217221518357794,0.225657279792899,0.231692767572414,0.280603377364562,
0.329547178464156,0.377736289482342,0.425495421787918,0.43983668838786,
0.446522460479898,0.452442110700344,0.499701052287928,0.546385278965876,
0.591957470686799,0.610305684420423,0.652878075156173,0.658871161398199,
0.664713829125931,0.71062307702576,0.756799778329133,0.802540179953837,
0.839581075287956,0.858865496482928,0.865300881974491,0.876732522103725,
0.92192199373265,0.966865006644529,0.987435883002153,0.996596083696916,
1.00397196471875,1.04808827133039,1.09146893286586,1.13094109509354),
 .UNSPECIFIED.);
#1673=B_SPLINE_CURVE_WITH_KNOTS('',3,(#195422,#195423,#195424,#195425,#195426,
#195427,#195428,#195429,#195430,#195431,#195432,#195433,#195434,#195435,
#195436,#195437,#195438,#195439,#195440,#195441,#195442,#195443,#195444,
#195445,#195446,#195447,#195448,#195449,#195450,#195451,#195452,#195453,
#195454,#195455,#195456,#195457,#195458,#195459,#195460,#195461,#195462,
#195463,#195464,#195465,#195466,#195467,#195468,#195469,#195470,#195471,
#195472,#195473,#195474,#195475,#195476,#195477,#195478,#195479,#195480,
#195481,#195482,#195483,#195484,#195485,#195486,#195487,#195488,#195489,
#195490,#195491,#195492,#195493,#195494,#195495,#195496,#195497,#195498,
#195499,#195500,#195501,#195502,#195503,#195504,#195505,#195506,#195507,
#195508,#195509,#195510,#195511,#195512,#195513,#195514,#195515,#195516,
#195517,#195518,#195519,#195520,#195521,#195522,#195523,#195524,#195525,
#195526,#195527,#195528,#195529,#195530,#195531,#195532,#195533),
 .UNSPECIFIED.,.F.,.F.,(4,3,3,3,3,3,3,3,3,3,3,3,3,3,3,3,3,3,3,3,3,3,3,3,
3,3,3,3,3,3,3,3,3,3,3,3,3,4),(8.35256518316599E-5,0.041701088540131,0.0910835065821966,
0.141049325530906,0.19113697887595,0.217221517785501,0.225657277714787,
0.231692761965483,0.280603371493228,0.329547172995227,0.377736284294025,
0.425495416317654,0.439836687990196,0.446522457868978,0.452442110036265,
0.499758065245721,0.546067231244348,0.59195747025222,0.610305684420784,
0.643609039131399,0.652878075055363,0.658871161296266,0.664713829119152,
0.710623077230221,0.756799777861816,0.802540179620603,0.839581075225947,
0.858865496404956,0.865300878338205,0.876732522105704,0.921906064998915,
0.966935138622801,0.987435883182548,0.996596084006623,1.00397196652038,
1.04808827280157,1.09146893461145,1.13094109510077),.UNSPECIFIED.);
#1674=B_SPLINE_CURVE_WITH_KNOTS('',3,(#202314,#202315,#202316,#202317,#202318,
#202319,#202320,#202321,#202322,#202323,#202324,#202325,#202326,#202327,
#202328,#202329,#202330,#202331,#202332,#202333,#202334,#202335,#202336,
#202337,#202338,#202339,#202340,#202341,#202342,#202343,#202344,#202345,
#202346,#202347,#202348,#202349,#202350,#202351,#202352,#202353,#202354,
#202355,#202356,#202357,#202358,#202359,#202360,#202361,#202362,#202363,
#202364,#202365,#202366,#202367,#202368,#202369,#202370,#202371,#202372,
#202373,#202374,#202375,#202376,#202377,#202378,#202379,#202380,#202381,
#202382,#202383,#202384,#202385,#202386,#202387,#202388,#202389,#202390,
#202391,#202392,#202393,#202394,#202395,#202396,#202397,#202398,#202399,
#202400,#202401,#202402,#202403,#202404,#202405,#202406,#202407,#202408,
#202409,#202410,#202411,#202412,#202413,#202414,#202415,#202416,#202417,
#202418,#202419),.UNSPECIFIED.,.F.,.F.,(4,3,3,3,3,3,3,3,3,3,3,3,3,3,3,3,
3,3,3,3,3,3,3,3,3,3,3,3,3,3,3,3,3,3,3,4),(0.,0.0349249411503097,0.0774968629053873,
0.120798554477859,0.164983976463475,0.189329869243756,0.195424599752804,
0.241029502145285,0.286450337938425,0.33235718364418,0.377844209322727,
0.390926586284597,0.397162832866434,0.444107542409823,0.491089657327383,
0.537752844152331,0.557531973038066,0.592379688293954,0.602095847495157,
0.609874759394341,0.65562314585235,0.70310861257605,0.75059407929975,0.793453887192463,
0.814883791138819,0.821323461655805,0.828310165215568,0.836313695085176,
0.885124880977893,0.93393606687061,0.958011516677791,0.969491304629128,
0.977480415130059,1.02729689945038,1.07695758373463,1.12653966532806),
 .UNSPECIFIED.);
#1675=B_SPLINE_CURVE_WITH_KNOTS('',3,(#202538,#202539,#202540,#202541,#202542,
#202543,#202544,#202545,#202546,#202547,#202548,#202549,#202550),
 .UNSPECIFIED.,.F.,.F.,(4,3,3,3,4),(122.271018544109,122.275828089307,122.386363683307,
122.494373601401,122.522113489845),.UNSPECIFIED.);
#1676=B_SPLINE_CURVE_WITH_KNOTS('',3,(#202552,#202553,#202554,#202555,#202556,
#202557,#202558,#202559,#202560,#202561,#202562,#202563,#202564,#202565,
#202566,#202567,#202568,#202569,#202570,#202571,#202572,#202573,#202574,
#202575,#202576,#202577,#202578,#202579,#202580,#202581,#202582,#202583,
#202584,#202585,#202586,#202587,#202588,#202589,#202590,#202591,#202592,
#202593,#202594,#202595,#202596,#202597,#202598,#202599,#202600,#202601,
#202602,#202603,#202604,#202605,#202606,#202607,#202608,#202609,#202610,
#202611,#202612,#202613,#202614,#202615,#202616,#202617,#202618,#202619,
#202620,#202621,#202622,#202623,#202624,#202625,#202626,#202627,#202628,
#202629,#202630,#202631,#202632,#202633,#202634,#202635,#202636,#202637,
#202638,#202639,#202640,#202641,#202642,#202643,#202644,#202645,#202646,
#202647,#202648,#202649,#202650,#202651,#202652,#202653,#202654,#202655,
#202656,#202657,#202658,#202659,#202660,#202661,#202662,#202663,#202664,
#202665,#202666,#202667,#202668,#202669,#202670,#202671,#202672,#202673,
#202674,#202675,#202676,#202677,#202678,#202679,#202680,#202681,#202682,
#202683,#202684,#202685,#202686,#202687),.UNSPECIFIED.,.F.,.F.,(4,3,3,3,
3,3,3,3,3,3,3,3,3,3,3,3,3,3,3,3,3,3,3,3,3,3,3,3,3,3,3,3,3,3,3,3,3,3,3,3,
3,3,3,3,3,4),(122.522113489983,122.604654564358,122.688518256317,122.770981109149,
122.853436233243,122.93590249609,123.020817897075,123.103407097541,123.189485598785,
123.275564100028,123.359302811874,123.442938323242,123.52649076664,123.609980202491,
123.693434153104,123.77687064695,123.860307756706,123.943763551624,124.027308044353,
124.110897127294,124.194620394852,124.275300110748,124.359038822594,124.442674333961,
124.52622677736,124.609716213211,124.693170163825,124.776606657671,124.860043767426,
124.943499562344,125.027044055074,125.110633138015,125.194356405572,125.275036121468,
125.358775798738,125.442412049688,125.52596500778,125.609454734154,125.692907813588,
125.776343116971,125.859778716762,125.943232681716,126.026770899361,126.110353575267,
126.194059974238,126.257648866041),.UNSPECIFIED.);
#1677=B_SPLINE_CURVE_WITH_KNOTS('',3,(#202689,#202690,#202691,#202692,#202693,
#202694),.UNSPECIFIED.,.F.,.F.,(4,2,4),(0.311503179138839,0.373508504209549,
0.467472020546751),.UNSPECIFIED.);
#1678=B_SPLINE_CURVE_WITH_KNOTS('',3,(#202696,#202697,#202698,#202699,#202700,
#202701,#202702,#202703,#202704,#202705,#202706,#202707,#202708,#202709,
#202710,#202711,#202712,#202713,#202714,#202715,#202716,#202717,#202718,
#202719,#202720,#202721,#202722,#202723,#202724,#202725,#202726,#202727,
#202728,#202729,#202730,#202731,#202732,#202733,#202734,#202735,#202736,
#202737,#202738,#202739,#202740,#202741,#202742,#202743,#202744,#202745,
#202746,#202747,#202748,#202749,#202750,#202751,#202752,#202753,#202754,
#202755,#202756,#202757,#202758,#202759,#202760,#202761,#202762,#202763,
#202764,#202765,#202766,#202767,#202768,#202769,#202770,#202771,#202772,
#202773,#202774,#202775,#202776,#202777,#202778,#202779,#202780,#202781,
#202782,#202783,#202784,#202785,#202786,#202787,#202788,#202789,#202790,
#202791,#202792,#202793,#202794,#202795,#202796,#202797,#202798,#202799,
#202800,#202801,#202802,#202803,#202804,#202805,#202806,#202807,#202808,
#202809,#202810,#202811,#202812,#202813,#202814,#202815,#202816,#202817,
#202818,#202819,#202820,#202821,#202822,#202823,#202824,#202825,#202826,
#202827,#202828,#202829,#202830,#202831,#202832,#202833,#202834,#202835,
#202836,#202837,#202838,#202839,#202840,#202841,#202842,#202843),
 .UNSPECIFIED.,.F.,.F.,(4,3,3,3,3,3,3,3,3,3,3,3,3,3,3,3,3,3,3,3,3,3,3,3,
3,3,3,3,3,3,3,3,3,3,3,3,3,3,3,3,3,3,3,3,3,3,3,3,3,4),(122.522113489987,
122.586118709022,122.669857420868,122.753492932236,122.837045375634,122.920534811485,
123.003988762099,123.087425255945,123.170862365701,123.254318160619,123.337862653349,
123.42145173629,123.505175003848,123.585854719742,123.669593431588,123.753228942956,
123.836781386354,123.920270822205,124.003724772819,124.087161266665,124.170598376421,
124.254054171338,124.337598664068,124.421187747009,124.504911014567,124.585590730463,
124.669329442309,124.752964953677,124.836517397075,124.920006832926,125.00346078354,
125.086897277386,125.170334387142,125.253790182059,125.337334674789,125.42092375773,
125.504647025288,125.585326741183,125.669066152481,125.752702199374,125.836255015062,
125.91974466049,126.003197973538,126.086633598068,126.170069606594,126.253524068008,
126.337063985111,126.420648396645,126.504359337024,126.572633808289),
 .UNSPECIFIED.);
#1679=B_SPLINE_CURVE_WITH_KNOTS('',3,(#202844,#202845,#202846,#202847,#202848,
#202849,#202850,#202851,#202852,#202853),.UNSPECIFIED.,.F.,.F.,(4,3,3,4),
(122.27028827519,122.35308028165,122.43759688576,122.52211348987),
 .UNSPECIFIED.);
#1680=B_SPLINE_CURVE_WITH_KNOTS('',3,(#202859,#202860,#202861,#202862,#202863,
#202864,#202865,#202866,#202867,#202868),.UNSPECIFIED.,.F.,.F.,(4,3,3,4),
(115.987147173825,116.070212549419,116.154570366029,116.238928182639),
 .UNSPECIFIED.);
#1681=B_SPLINE_CURVE_WITH_KNOTS('',3,(#202869,#202870,#202871,#202872,#202873,
#202874,#202875,#202876,#202877,#202878,#202879,#202880,#202881,#202882,
#202883,#202884,#202885,#202886,#202887,#202888,#202889,#202890,#202891,
#202892,#202893,#202894,#202895,#202896,#202897,#202898,#202899,#202900,
#202901,#202902,#202903,#202904,#202905,#202906,#202907,#202908,#202909,
#202910,#202911,#202912,#202913,#202914,#202915,#202916,#202917,#202918,
#202919,#202920,#202921,#202922,#202923,#202924,#202925,#202926,#202927,
#202928,#202929,#202930,#202931,#202932,#202933,#202934,#202935,#202936,
#202937,#202938,#202939,#202940,#202941,#202942,#202943,#202944,#202945,
#202946,#202947,#202948,#202949,#202950,#202951,#202952,#202953,#202954,
#202955,#202956,#202957,#202958,#202959,#202960,#202961,#202962,#202963,
#202964,#202965,#202966,#202967,#202968,#202969,#202970,#202971,#202972,
#202973,#202974,#202975,#202976,#202977,#202978,#202979,#202980,#202981,
#202982,#202983,#202984,#202985,#202986,#202987,#202988,#202989,#202990,
#202991,#202992,#202993,#202994,#202995,#202996,#202997,#202998,#202999,
#203000,#203001,#203002,#203003,#203004,#203005,#203006,#203007,#203008,
#203009,#203010,#203011,#203012,#203013,#203014,#203015,#203016,#203017,
#203018,#203019,#203020,#203021,#203022,#203023,#203024,#203025,#203026,
#203027,#203028,#203029,#203030,#203031,#203032,#203033,#203034,#203035,
#203036,#203037,#203038,#203039,#203040,#203041,#203042,#203043,#203044,
#203045,#203046,#203047,#203048,#203049,#203050,#203051,#203052,#203053,
#203054,#203055,#203056,#203057,#203058,#203059,#203060,#203061,#203062,
#203063,#203064,#203065,#203066,#203067,#203068,#203069,#203070,#203071,
#203072,#203073,#203074,#203075,#203076,#203077,#203078,#203079,#203080,
#203081,#203082,#203083,#203084,#203085,#203086,#203087,#203088),
 .UNSPECIFIED.,.F.,.F.,(4,3,3,3,3,3,3,3,3,3,3,3,3,3,3,3,3,3,3,3,3,3,3,3,
3,3,3,3,3,3,3,3,3,3,3,3,3,3,3,3,3,3,3,3,3,3,3,3,3,3,3,3,3,3,3,3,3,3,3,3,
3,3,3,3,3,3,3,3,3,3,3,3,3,4),(116.238928182803,116.277412024987,116.361150736833,
116.4447862482,116.528338691599,116.61182812745,116.695282078063,116.778718571909,
116.862155681664,116.945611476582,117.029155969311,117.112745052252,117.19646831981,
117.277148035707,117.360886747553,117.44452225892,117.528074702319,117.61156413817,
117.695018088784,117.77845458263,117.861891692385,117.945347487303,118.028891980033,
118.112481062974,118.196204330531,118.276884046427,118.360622758273,118.44425826964,
118.527810713039,118.61130014889,118.694754099503,118.77819059335,118.861627703105,
118.945083498023,119.028627990752,119.112217073693,119.195940341251,119.276620057147,
119.360358768993,119.44399428036,119.527546723759,119.61103615961,119.694490110224,
119.77792660407,119.861363713826,119.944819508743,120.028364001473,120.111953084414,
120.195676351972,120.276356067867,120.360094779713,120.44373029108,120.527282734479,
120.61077217033,120.694226120944,120.77766261479,120.861099724545,120.944555519463,
121.028100012192,121.111689095133,121.195412362691,121.276092078587,121.359831060277,
121.443466778056,121.5270193647,121.610508880833,121.693962581455,121.77739873563,
121.860835415973,121.944290691593,122.027833400628,122.111420662809,122.195139108014,
122.271018544109),.UNSPECIFIED.);
#1682=B_SPLINE_CURVE_WITH_KNOTS('',3,(#203090,#203091,#203092,#203093,#203094,
#203095,#203096,#203097,#203098,#203099,#203100,#203101,#203102,#203103,
#203104,#203105,#203106,#203107,#203108,#203109,#203110,#203111,#203112,
#203113,#203114,#203115,#203116,#203117,#203118,#203119,#203120,#203121,
#203122,#203123,#203124,#203125,#203126,#203127,#203128,#203129,#203130,
#203131,#203132,#203133,#203134,#203135,#203136,#203137,#203138,#203139,
#203140,#203141,#203142,#203143,#203144,#203145,#203146,#203147,#203148,
#203149,#203150,#203151,#203152,#203153,#203154,#203155,#203156,#203157,
#203158,#203159,#203160,#203161,#203162,#203163,#203164,#203165,#203166,
#203167,#203168,#203169,#203170,#203171,#203172,#203173,#203174,#203175,
#203176,#203177,#203178,#203179,#203180,#203181,#203182,#203183,#203184,
#203185,#203186,#203187,#203188,#203189,#203190,#203191,#203192,#203193,
#203194,#203195,#203196,#203197,#203198,#203199,#203200,#203201,#203202,
#203203,#203204,#203205,#203206,#203207,#203208,#203209,#203210,#203211,
#203212,#203213,#203214,#203215,#203216,#203217,#203218,#203219,#203220,
#203221,#203222,#203223,#203224,#203225,#203226,#203227,#203228,#203229,
#203230,#203231,#203232,#203233,#203234,#203235,#203236,#203237,#203238,
#203239,#203240,#203241,#203242,#203243,#203244,#203245,#203246,#203247,
#203248,#203249,#203250,#203251,#203252,#203253,#203254,#203255,#203256,
#203257,#203258,#203259,#203260,#203261,#203262,#203263,#203264,#203265,
#203266,#203267,#203268,#203269,#203270,#203271,#203272,#203273,#203274,
#203275,#203276,#203277,#203278,#203279,#203280,#203281,#203282,#203283,
#203284,#203285,#203286,#203287,#203288,#203289,#203290,#203291,#203292,
#203293,#203294,#203295,#203296,#203297,#203298,#203299,#203300,#203301,
#203302,#203303,#203304,#203305,#203306,#203307,#203308,#203309),
 .UNSPECIFIED.,.F.,.F.,(4,3,3,3,3,3,3,3,3,3,3,3,3,3,3,3,3,3,3,3,3,3,3,3,
3,3,3,3,3,3,3,3,3,3,3,3,3,3,3,3,3,3,3,3,3,3,3,3,3,3,3,3,3,3,3,3,3,3,3,3,
3,3,3,3,3,3,3,3,3,3,3,3,3,4),(116.238928183003,116.334849321083,116.431253899856,
116.528269407277,116.587702644701,116.671441356547,116.755076867914,116.838629311313,
116.922118747164,117.005572697778,117.089009191624,117.17244630138,117.255902096297,
117.339446589027,117.423035671968,117.506758939526,117.587438655422,117.671177367268,
117.754812878636,117.838365322034,117.921854757885,118.005308708499,118.088745202345,
118.172182312101,118.255638107018,118.339182599748,118.422771682689,118.506494950247,
118.587174666142,118.670913377988,118.754548889355,118.838101332754,118.921590768605,
119.005044719218,119.088481213064,119.17191832282,119.255374117737,119.338918610467,
119.422507693408,119.506230960966,119.586910676862,119.670649388708,119.754284900075,
119.837837343474,119.921326779325,120.004780729939,120.088217223785,120.17165433354,
120.255110128458,120.338654621188,120.422243704129,120.505966971687,120.586646687582,
120.670385399428,120.754020910795,120.837573354194,120.921062790045,121.004516740659,
121.087953234505,121.17139034426,121.254846139178,121.338390631908,121.421979714849,
121.505702982407,121.586382698302,121.671870895413,121.754714488921,121.837482997203,
121.920195242189,122.002869998466,122.085539448033,122.168206900628,122.250910091201,
122.27028827519),.UNSPECIFIED.);
#1683=B_SPLINE_CURVE_WITH_KNOTS('',3,(#203310,#203311,#203312,#203313,#203314,
#203315,#203316,#203317,#203318,#203319),.UNSPECIFIED.,.F.,.F.,(4,3,3,4),
(115.988071988884,116.071683453257,116.155305818032,116.238928182807),
 .UNSPECIFIED.);
#1684=B_SPLINE_CURVE_WITH_KNOTS('',3,(#203325,#203326,#203327,#203328,#203329,
#203330,#203331,#203332,#203333,#203334),.UNSPECIFIED.,.F.,.F.,(4,3,3,4),
(109.704756567473,109.787983735154,109.871863305389,109.955742875624),
 .UNSPECIFIED.);
#1685=B_SPLINE_CURVE_WITH_KNOTS('',3,(#203335,#203336,#203337,#203338,#203339,
#203340,#203341,#203342,#203343,#203344,#203345,#203346,#203347,#203348,
#203349,#203350,#203351,#203352,#203353,#203354,#203355,#203356,#203357,
#203358,#203359,#203360,#203361,#203362,#203363,#203364,#203365,#203366,
#203367,#203368,#203369,#203370,#203371,#203372,#203373,#203374,#203375,
#203376,#203377,#203378,#203379,#203380,#203381,#203382,#203383,#203384,
#203385,#203386,#203387,#203388,#203389,#203390,#203391,#203392,#203393,
#203394,#203395,#203396,#203397,#203398,#203399,#203400,#203401,#203402,
#203403,#203404,#203405,#203406,#203407,#203408,#203409,#203410,#203411,
#203412,#203413,#203414,#203415,#203416,#203417,#203418,#203419,#203420,
#203421,#203422,#203423,#203424,#203425,#203426,#203427,#203428,#203429,
#203430,#203431,#203432,#203433,#203434,#203435,#203436,#203437,#203438,
#203439,#203440,#203441,#203442,#203443,#203444,#203445,#203446,#203447,
#203448,#203449,#203450,#203451,#203452,#203453,#203454,#203455,#203456,
#203457,#203458,#203459,#203460,#203461,#203462,#203463,#203464,#203465,
#203466,#203467,#203468,#203469,#203470,#203471,#203472,#203473,#203474,
#203475,#203476,#203477,#203478,#203479,#203480,#203481,#203482,#203483,
#203484,#203485,#203486,#203487,#203488,#203489,#203490,#203491,#203492,
#203493,#203494,#203495,#203496,#203497,#203498,#203499,#203500,#203501,
#203502,#203503,#203504,#203505,#203506,#203507,#203508,#203509,#203510,
#203511,#203512,#203513,#203514,#203515,#203516,#203517,#203518,#203519,
#203520,#203521,#203522,#203523,#203524,#203525,#203526,#203527,#203528,
#203529,#203530,#203531,#203532,#203533,#203534,#203535,#203536,#203537,
#203538,#203539,#203540,#203541,#203542,#203543,#203544,#203545,#203546,
#203547,#203548,#203549,#203550,#203551,#203552,#203553,#203554),
 .UNSPECIFIED.,.F.,.F.,(4,3,3,3,3,3,3,3,3,3,3,3,3,3,3,3,3,3,3,3,3,3,3,3,
3,3,3,3,3,3,3,3,3,3,3,3,3,3,3,3,3,3,3,3,3,3,3,3,3,3,3,3,3,3,3,3,3,3,3,3,
3,3,3,3,3,3,3,3,3,3,3,3,3,4),(109.955742875801,110.053908632085,110.152728187028,
110.252279042651,110.278995960666,110.362734672512,110.446370183879,110.529922627278,
110.613412063129,110.696866013743,110.780302507589,110.863739617344,110.947195412262,
111.030739904991,111.114328987932,111.19805225549,111.278731971386,111.362470683232,
111.446106194599,111.529658637998,111.613148073849,111.696602024463,111.780038518309,
111.863475628064,111.946931422982,112.030475915712,112.114064998653,112.19778826621,
112.278467982106,112.362206693952,112.445842205319,112.529394648718,112.612884084569,
112.696338035182,112.779774529029,112.863211638784,112.946667433702,113.030211926431,
113.113801009372,113.19752427693,113.278203992826,113.361942704672,113.445578216039,
113.529130659438,113.612620095289,113.696074045903,113.779510539749,113.862947649505,
113.946403444422,114.029947937152,114.113537020093,114.197260287651,114.277940003546,
114.361678715392,114.44531422676,114.528866670158,114.612356106009,114.695810056623,
114.779246550469,114.862683660225,114.946139455142,115.029683947872,115.113273030813,
115.196996298371,115.277676014266,115.360916343682,115.444025174985,115.527058070878,
115.610033652872,115.692970496751,115.775902763453,115.858831416099,115.94180178495,
115.987147173825),.UNSPECIFIED.);
#1686=B_SPLINE_CURVE_WITH_KNOTS('',3,(#203556,#203557,#203558,#203559,#203560,
#203561,#203562,#203563,#203564,#203565,#203566,#203567,#203568,#203569,
#203570,#203571,#203572,#203573,#203574,#203575,#203576,#203577,#203578,
#203579,#203580,#203581,#203582,#203583,#203584,#203585,#203586,#203587,
#203588,#203589,#203590,#203591,#203592,#203593,#203594,#203595,#203596,
#203597,#203598,#203599,#203600,#203601,#203602,#203603,#203604,#203605,
#203606,#203607,#203608,#203609,#203610,#203611,#203612,#203613,#203614,
#203615,#203616,#203617,#203618,#203619,#203620,#203621,#203622,#203623,
#203624,#203625,#203626,#203627,#203628,#203629,#203630,#203631,#203632,
#203633,#203634,#203635,#203636,#203637,#203638,#203639,#203640,#203641,
#203642,#203643,#203644,#203645,#203646,#203647,#203648,#203649,#203650,
#203651,#203652,#203653,#203654,#203655,#203656,#203657,#203658,#203659,
#203660,#203661,#203662,#203663,#203664,#203665,#203666,#203667,#203668,
#203669,#203670,#203671,#203672,#203673,#203674,#203675,#203676,#203677,
#203678,#203679,#203680,#203681,#203682,#203683,#203684,#203685,#203686,
#203687,#203688,#203689,#203690,#203691,#203692,#203693,#203694,#203695,
#203696,#203697,#203698,#203699,#203700,#203701,#203702,#203703,#203704,
#203705,#203706,#203707,#203708,#203709,#203710,#203711,#203712,#203713,
#203714,#203715,#203716,#203717,#203718,#203719,#203720,#203721,#203722,
#203723,#203724,#203725,#203726,#203727,#203728,#203729,#203730,#203731,
#203732,#203733,#203734,#203735,#203736,#203737,#203738,#203739,#203740,
#203741,#203742,#203743,#203744,#203745,#203746,#203747,#203748,#203749,
#203750,#203751,#203752,#203753,#203754,#203755,#203756,#203757,#203758,
#203759,#203760,#203761,#203762,#203763,#203764,#203765,#203766,#203767,
#203768,#203769,#203770,#203771,#203772,#203773,#203774,#203775),
 .UNSPECIFIED.,.F.,.F.,(4,3,3,3,3,3,3,3,3,3,3,3,3,3,3,3,3,3,3,3,3,3,3,3,
3,3,3,3,3,3,3,3,3,3,3,3,3,3,3,3,3,3,3,3,3,3,3,3,3,3,3,3,3,3,3,3,3,3,3,3,
3,3,3,3,3,3,3,3,3,3,3,3,3,4),(109.955742875628,110.039648469011,110.123556652528,
110.207484832012,110.291450422462,110.375523162037,110.459655763239,110.543923584594,
110.589286580381,110.673025292227,110.756660803595,110.840213246993,110.923702682844,
111.007156633458,111.090593127304,111.17403023706,111.257486031977,111.341030524707,
111.424619607648,111.508342875206,111.589022591101,111.672761302947,111.756396814314,
111.839949257713,111.923438693564,112.006892644178,112.090329138024,112.173766247779,
112.257222042697,112.340766535426,112.424355618367,112.508078885925,112.588758601821,
112.672497313667,112.756132825034,112.839685268433,112.923174704284,113.006628654898,
113.090065148744,113.173502258499,113.256958053417,113.340502546147,113.424091629088,
113.507814896646,113.588494612541,113.672233324387,113.755868835754,113.839421279153,
113.922910715004,114.006364665617,114.089801159464,114.173238269219,114.256694064136,
114.340238556866,114.423827639807,114.507550907365,114.588230623261,114.671969335107,
114.755604846474,114.839157289873,114.922646725724,115.006100676337,115.089537170184,
115.172974279939,115.256430074857,115.339974567586,115.423563650527,115.507286918084,
115.587966633981,115.671933979496,115.755764025857,115.839515095663,115.923193376346,
115.988071988884),.UNSPECIFIED.);
#1687=B_SPLINE_CURVE_WITH_KNOTS('',3,(#203776,#203777,#203778,#203779,#203780,
#203781,#203782,#203783,#203784,#203785),.UNSPECIFIED.,.F.,.F.,(4,3,3,4),
(109.705270710528,109.800372858636,109.894864507288,109.955742875431),
 .UNSPECIFIED.);
#1688=B_SPLINE_CURVE_WITH_KNOTS('',3,(#203791,#203792,#203793,#203794,#203795,
#203796,#203797,#203798,#203799,#203800),.UNSPECIFIED.,.F.,.F.,(4,3,3,4),
(103.422164115585,103.515371370637,103.608104590454,103.672557568256),
 .UNSPECIFIED.);
#1689=B_SPLINE_CURVE_WITH_KNOTS('',3,(#203801,#203802,#203803,#203804,#203805,
#203806,#203807,#203808,#203809,#203810,#203811,#203812,#203813,#203814,
#203815,#203816,#203817,#203818,#203819,#203820,#203821,#203822,#203823,
#203824,#203825,#203826,#203827,#203828,#203829,#203830,#203831,#203832,
#203833,#203834,#203835,#203836,#203837,#203838,#203839,#203840,#203841,
#203842,#203843,#203844,#203845,#203846,#203847,#203848,#203849,#203850,
#203851,#203852,#203853,#203854,#203855,#203856,#203857,#203858,#203859,
#203860,#203861,#203862,#203863,#203864,#203865,#203866,#203867,#203868,
#203869,#203870,#203871,#203872,#203873,#203874,#203875,#203876,#203877,
#203878,#203879,#203880,#203881,#203882,#203883,#203884,#203885,#203886,
#203887,#203888,#203889,#203890,#203891,#203892,#203893,#203894,#203895,
#203896,#203897,#203898,#203899,#203900,#203901,#203902,#203903,#203904,
#203905,#203906,#203907,#203908,#203909,#203910,#203911,#203912,#203913,
#203914,#203915,#203916,#203917,#203918,#203919,#203920,#203921,#203922,
#203923,#203924,#203925,#203926,#203927,#203928,#203929,#203930,#203931,
#203932,#203933,#203934,#203935,#203936,#203937,#203938,#203939,#203940,
#203941,#203942,#203943,#203944,#203945,#203946,#203947,#203948,#203949,
#203950,#203951,#203952,#203953,#203954,#203955,#203956,#203957,#203958,
#203959,#203960,#203961,#203962,#203963,#203964,#203965,#203966,#203967,
#203968,#203969,#203970,#203971,#203972,#203973,#203974,#203975,#203976,
#203977,#203978,#203979,#203980,#203981,#203982,#203983,#203984,#203985,
#203986,#203987,#203988,#203989,#203990,#203991,#203992,#203993,#203994,
#203995,#203996,#203997,#203998,#203999,#204000,#204001,#204002,#204003,
#204004,#204005,#204006,#204007,#204008,#204009,#204010,#204011,#204012,
#204013,#204014,#204015,#204016,#204017,#204018,#204019,#204020),
 .UNSPECIFIED.,.F.,.F.,(4,3,3,3,3,3,3,3,3,3,3,3,3,3,3,3,3,3,3,3,3,3,3,3,
3,3,3,3,3,3,3,3,3,3,3,3,3,3,3,3,3,3,3,3,3,3,3,3,3,3,3,3,3,3,3,3,3,3,3,3,
3,3,3,3,3,3,3,3,3,3,3,3,3,4),(103.672557568444,103.756948747136,103.841357026278,
103.925799068812,104.014494275695,104.099107419003,104.18379133639,104.268605737223,
104.280579896345,104.364318608191,104.447954119558,104.531506562957,104.614995998808,
104.698449949422,104.781886443268,104.865323553023,104.948779347941,105.03232384067,
105.115912923611,105.199636191169,105.280315907065,105.364054618911,105.447690130278,
105.531242573677,105.614732009527,105.698185960141,105.781622453987,105.865059563743,
105.94851535866,106.03205985139,106.115648934331,106.199372201889,106.280051917785,
106.363790629631,106.447426140998,106.530978584397,106.614468020248,106.697921970862,
106.781358464708,106.864795574464,106.948251369382,107.031795862111,107.115384945052,
107.19910821261,107.279787928505,107.363526640351,107.447162151719,107.530714595117,
107.614204030968,107.697657981582,107.781094475428,107.864531585183,107.947987380101,
108.031531872831,108.115120955772,108.198844223329,108.279523939226,108.363262651072,
108.44689816244,108.530450605838,108.613940041689,108.697393992303,108.780830486149,
108.864267595905,108.947723390823,109.031267883552,109.114856966493,109.198580234051,
109.279259949946,109.362821357527,109.448305160013,109.531656885119,109.618206726296,
109.704756567473),.UNSPECIFIED.);
#1690=B_SPLINE_CURVE_WITH_KNOTS('',3,(#204022,#204023,#204024,#204025,#204026,
#204027,#204028,#204029,#204030,#204031,#204032,#204033,#204034,#204035,
#204036,#204037,#204038,#204039,#204040,#204041,#204042,#204043,#204044,
#204045,#204046,#204047,#204048,#204049,#204050,#204051,#204052,#204053,
#204054,#204055,#204056,#204057,#204058,#204059,#204060,#204061,#204062,
#204063,#204064,#204065,#204066,#204067,#204068,#204069,#204070,#204071,
#204072,#204073,#204074,#204075,#204076,#204077,#204078,#204079,#204080,
#204081,#204082,#204083,#204084,#204085,#204086,#204087,#204088,#204089,
#204090,#204091,#204092,#204093,#204094,#204095,#204096,#204097,#204098,
#204099,#204100,#204101,#204102,#204103,#204104,#204105,#204106,#204107,
#204108,#204109,#204110,#204111,#204112,#204113,#204114,#204115,#204116,
#204117,#204118,#204119,#204120,#204121,#204122,#204123,#204124,#204125,
#204126,#204127,#204128,#204129,#204130,#204131,#204132,#204133,#204134,
#204135,#204136,#204137,#204138,#204139,#204140,#204141,#204142,#204143,
#204144,#204145,#204146,#204147,#204148,#204149,#204150,#204151,#204152,
#204153,#204154,#204155,#204156,#204157,#204158,#204159,#204160,#204161,
#204162,#204163,#204164,#204165,#204166,#204167,#204168,#204169,#204170,
#204171,#204172,#204173,#204174,#204175,#204176,#204177,#204178,#204179,
#204180,#204181,#204182,#204183,#204184,#204185,#204186,#204187,#204188,
#204189,#204190,#204191,#204192,#204193,#204194,#204195,#204196,#204197,
#204198,#204199,#204200,#204201,#204202,#204203,#204204,#204205,#204206,
#204207,#204208,#204209,#204210,#204211,#204212,#204213,#204214,#204215,
#204216,#204217,#204218,#204219,#204220,#204221,#204222,#204223,#204224,
#204225,#204226,#204227,#204228,#204229,#204230,#204231,#204232,#204233,
#204234,#204235,#204236,#204237,#204238,#204239,#204240,#204241),
 .UNSPECIFIED.,.F.,.F.,(4,3,3,3,3,3,3,3,3,3,3,3,3,3,3,3,3,3,3,3,3,3,3,3,
3,3,3,3,3,3,3,3,3,3,3,3,3,3,3,3,3,3,3,3,3,3,3,3,3,3,3,3,3,3,3,3,3,3,3,3,
3,3,3,3,3,3,3,3,3,3,3,3,3,4),(103.672557568579,103.755338549975,103.838023743102,
103.920634109801,104.004413660583,104.086946693849,104.169472251958,104.252009159745,
104.336724498823,104.419384236231,104.505127376145,104.59087051606,104.674609227906,
104.758244739273,104.841797182672,104.925286618523,105.008740569137,105.092177062983,
105.175614172739,105.259069967657,105.342614460386,105.426203543327,105.509926810885,
105.59060652678,105.674345238626,105.757980749993,105.841533193392,105.925022629242,
106.008476579856,106.091913073702,106.175350183458,106.258805978375,106.342350471105,
106.425939554046,106.509662821604,106.5903425375,106.674081249346,106.757716760713,
106.841269204112,106.924758639964,107.008212590577,107.091649084424,107.175086194179,
107.258541989097,107.342086481826,107.425675564767,107.509398832325,107.59007854822,
107.673817260066,107.757452771433,107.841005214832,107.924494650683,108.007948601297,
108.091385095143,108.174822204899,108.258277999817,108.341822492546,108.425411575487,
108.509134843045,108.58981455894,108.673553270786,108.757188782154,108.840741225552,
108.924230661404,109.007684612017,109.091121105864,109.174558215619,109.258014010538,
109.341558503267,109.425147586208,109.508870853766,109.589550569661,109.68519153841,
109.705270710528),.UNSPECIFIED.);
#1691=B_SPLINE_CURVE_WITH_KNOTS('',3,(#204242,#204243,#204244,#204245,#204246,
#204247,#204248,#204249,#204250,#204251),.UNSPECIFIED.,.F.,.F.,(4,3,3,4),
(103.420910293148,103.506022399244,103.59113450534,103.672557568448),
 .UNSPECIFIED.);
#1692=B_SPLINE_CURVE_WITH_KNOTS('',3,(#204257,#204258,#204259,#204260,#204261,
#204262,#204263,#204264,#204265,#204266),.UNSPECIFIED.,.F.,.F.,(4,3,3,4),
(97.1377575899893,97.2214880297379,97.2824278213041,97.3893722612645),
 .UNSPECIFIED.);
#1693=B_SPLINE_CURVE_WITH_KNOTS('',3,(#204267,#204268,#204269,#204270,#204271,
#204272,#204273,#204274,#204275,#204276,#204277,#204278,#204279,#204280,
#204281,#204282,#204283,#204284,#204285,#204286,#204287,#204288,#204289,
#204290,#204291,#204292,#204293,#204294,#204295,#204296,#204297,#204298,
#204299,#204300,#204301,#204302,#204303,#204304,#204305,#204306,#204307,
#204308,#204309,#204310,#204311,#204312,#204313,#204314,#204315,#204316,
#204317,#204318,#204319,#204320,#204321,#204322,#204323,#204324,#204325,
#204326,#204327,#204328,#204329,#204330,#204331,#204332,#204333,#204334,
#204335,#204336,#204337,#204338,#204339,#204340,#204341,#204342,#204343,
#204344,#204345,#204346,#204347,#204348,#204349,#204350,#204351,#204352,
#204353,#204354,#204355,#204356,#204357,#204358,#204359,#204360,#204361,
#204362,#204363,#204364,#204365,#204366,#204367,#204368,#204369,#204370,
#204371,#204372,#204373,#204374,#204375,#204376,#204377,#204378,#204379,
#204380,#204381,#204382,#204383,#204384,#204385,#204386,#204387,#204388,
#204389,#204390,#204391,#204392,#204393,#204394,#204395,#204396,#204397,
#204398,#204399,#204400,#204401,#204402,#204403,#204404,#204405,#204406,
#204407,#204408,#204409,#204410,#204411,#204412,#204413,#204414,#204415,
#204416,#204417,#204418,#204419,#204420,#204421,#204422,#204423,#204424,
#204425,#204426,#204427,#204428,#204429,#204430,#204431,#204432,#204433,
#204434,#204435,#204436,#204437,#204438,#204439,#204440,#204441,#204442,
#204443,#204444,#204445,#204446,#204447,#204448,#204449,#204450,#204451,
#204452,#204453,#204454,#204455,#204456,#204457,#204458,#204459,#204460,
#204461,#204462,#204463,#204464,#204465,#204466,#204467,#204468,#204469,
#204470,#204471,#204472,#204473,#204474,#204475,#204476,#204477,#204478,
#204479,#204480,#204481,#204482,#204483,#204484,#204485,#204486),
 .UNSPECIFIED.,.F.,.F.,(4,3,3,3,3,3,3,3,3,3,3,3,3,3,3,3,3,3,3,3,3,3,3,3,
3,3,3,3,3,3,3,3,3,3,3,3,3,3,3,3,3,3,3,3,3,3,3,3,3,3,3,3,3,3,3,3,3,3,3,3,
3,3,3,3,3,3,3,3,3,3,3,3,3,4),(97.3893722614005,97.4719677846863,97.5544719674218,
97.6369058779297,97.7192955269354,97.8016628999257,97.884026934726,97.9664065640542,
98.0488700592945,98.1313770056035,98.2140118307161,98.2821638320243,98.3659025438702,
98.4495380552377,98.5330904986362,98.6165799344873,98.7000338851009,98.7834703789472,
98.8669074887027,98.9503632836207,99.0339077763503,99.1174968592912,99.2012201268488,
99.2818998427444,99.3656385545902,99.449274065958,99.5328265093568,99.6163159452077,
99.6997698958214,99.7832063896676,99.8666434994231,99.9500992943405,100.03364378707,
100.117232870011,100.200956137569,100.281635853465,100.365374565311,100.449010076678,
100.532562520077,100.616051955928,100.699505906542,100.782942400388,100.866379510144,
100.949835305062,101.033379797791,101.116968880732,101.20069214829,101.281371864185,
101.365110576031,101.448746087398,101.532298530797,101.615787966648,101.699241917262,
101.782678411108,101.866115520863,101.949571315781,102.033115808511,102.116704891452,
102.200428159009,102.281107874905,102.364846586751,102.448482098118,102.532034541517,
102.615523977367,102.698977927981,102.782414421827,102.865851531583,102.949307326501,
103.03285181923,103.116440902171,103.200164169729,103.280843885625,103.374544855062,
103.422164115585),.UNSPECIFIED.);
#1694=B_SPLINE_CURVE_WITH_KNOTS('',3,(#204488,#204489,#204490,#204491,#204492,
#204493,#204494,#204495,#204496,#204497,#204498,#204499,#204500,#204501,
#204502,#204503,#204504,#204505,#204506,#204507,#204508,#204509,#204510,
#204511,#204512,#204513,#204514,#204515,#204516,#204517,#204518,#204519,
#204520,#204521,#204522,#204523,#204524,#204525,#204526,#204527,#204528,
#204529,#204530,#204531,#204532,#204533,#204534,#204535,#204536,#204537,
#204538,#204539,#204540,#204541,#204542,#204543,#204544,#204545,#204546,
#204547,#204548,#204549,#204550,#204551,#204552,#204553,#204554,#204555,
#204556,#204557,#204558,#204559,#204560,#204561,#204562,#204563,#204564,
#204565,#204566,#204567,#204568,#204569,#204570,#204571,#204572,#204573,
#204574,#204575,#204576,#204577,#204578,#204579,#204580,#204581,#204582,
#204583,#204584,#204585,#204586,#204587,#204588,#204589,#204590,#204591,
#204592,#204593,#204594,#204595,#204596,#204597,#204598,#204599,#204600,
#204601,#204602,#204603,#204604,#204605,#204606,#204607,#204608,#204609,
#204610,#204611,#204612,#204613,#204614,#204615,#204616,#204617,#204618,
#204619,#204620,#204621,#204622,#204623,#204624,#204625,#204626,#204627,
#204628,#204629,#204630,#204631,#204632,#204633,#204634,#204635,#204636,
#204637,#204638,#204639,#204640,#204641,#204642,#204643,#204644,#204645,
#204646,#204647,#204648,#204649,#204650,#204651,#204652,#204653,#204654,
#204655,#204656,#204657,#204658,#204659,#204660,#204661,#204662,#204663,
#204664,#204665,#204666,#204667,#204668,#204669,#204670,#204671,#204672,
#204673,#204674,#204675,#204676,#204677,#204678,#204679,#204680,#204681,
#204682,#204683,#204684,#204685,#204686,#204687,#204688,#204689,#204690,
#204691,#204692,#204693,#204694,#204695,#204696,#204697,#204698,#204699,
#204700,#204701,#204702,#204703,#204704),.UNSPECIFIED.,.F.,.F.,(4,3,3,3,
3,3,3,3,3,3,3,3,3,3,3,3,3,3,3,3,3,3,3,3,3,3,3,3,3,3,3,3,3,3,3,3,3,3,3,3,
3,3,3,3,3,3,3,3,3,3,3,3,3,3,3,3,3,3,3,3,3,3,3,3,3,3,3,3,3,3,3,3,4),(97.3893722612683,
97.5085709008744,97.592718441019,97.676457152865,97.7600926642325,97.8436451076312,
97.9271345434824,98.0105884940961,98.0940249879424,98.177462097698,98.2609178926158,
98.3444623853455,98.4280514682866,98.5117747358442,98.5924544517391,98.676193163585,
98.7598286749525,98.843381118351,98.926870554202,99.0103245048157,99.0937609986619,
99.1771981084174,99.2606539033351,99.3441983960647,99.4277874790057,99.5115107465633,
99.5921904624593,99.6759291743052,99.7595646856727,99.8431171290711,99.9266065649221,
100.010060515536,100.093497009382,100.176934119137,100.260389914055,100.343934406785,
100.427523489726,100.511246757283,100.591926473179,100.675665185025,100.759300696393,
100.842853139791,100.926342575642,101.009796526256,101.093233020102,101.176670129858,
101.260125924776,101.343670417505,101.427259500446,101.510982768004,101.5916624839,
101.675401195746,101.759036707114,101.842589150512,101.926078586363,102.009532536977,
102.092969030823,102.176406140579,102.259861935497,102.343406428226,102.426995511167,
102.510718778725,102.59139849462,102.675147385514,102.758790830291,102.84233402803,
102.925820381412,103.009268009692,103.09269500225,103.176148517115,103.2596128892,
103.3431540916,103.420910293148),.UNSPECIFIED.);
#1695=B_SPLINE_CURVE_WITH_KNOTS('',3,(#204705,#204706,#204707,#204708,#204709,
#204710,#204711,#204712,#204713,#204714),.UNSPECIFIED.,.F.,.F.,(4,3,3,4),
(97.1377977613825,97.2200836147453,97.3047279379176,97.3893722610898),
 .UNSPECIFIED.);
#1696=B_SPLINE_CURVE_WITH_KNOTS('',3,(#204720,#204721,#204722,#204723,#204724,
#204725,#204726,#204727,#204728,#204729),.UNSPECIFIED.,.F.,.F.,(4,3,3,4),
(90.8545165002977,90.9367707195664,91.0214788367447,91.106186953923),
 .UNSPECIFIED.);
#1697=B_SPLINE_CURVE_WITH_KNOTS('',3,(#204730,#204731,#204732,#204733,#204734,
#204735,#204736,#204737,#204738,#204739,#204740,#204741,#204742,#204743,
#204744,#204745,#204746,#204747,#204748,#204749,#204750,#204751,#204752,
#204753,#204754,#204755,#204756,#204757,#204758,#204759,#204760,#204761,
#204762,#204763,#204764,#204765,#204766,#204767,#204768,#204769,#204770,
#204771,#204772,#204773,#204774,#204775,#204776,#204777,#204778,#204779,
#204780,#204781,#204782,#204783,#204784,#204785,#204786,#204787,#204788,
#204789,#204790,#204791,#204792,#204793,#204794,#204795,#204796,#204797,
#204798,#204799,#204800,#204801,#204802,#204803,#204804,#204805,#204806,
#204807,#204808,#204809,#204810,#204811,#204812,#204813,#204814,#204815,
#204816,#204817,#204818,#204819,#204820,#204821,#204822,#204823,#204824,
#204825,#204826,#204827,#204828,#204829,#204830,#204831,#204832,#204833,
#204834,#204835,#204836,#204837,#204838,#204839,#204840,#204841,#204842,
#204843,#204844,#204845,#204846,#204847,#204848,#204849,#204850,#204851,
#204852,#204853,#204854,#204855,#204856,#204857,#204858,#204859,#204860,
#204861,#204862,#204863,#204864,#204865,#204866,#204867,#204868,#204869,
#204870,#204871,#204872,#204873,#204874,#204875,#204876,#204877,#204878,
#204879,#204880,#204881,#204882,#204883,#204884,#204885,#204886,#204887,
#204888,#204889,#204890,#204891,#204892,#204893,#204894,#204895,#204896,
#204897,#204898,#204899,#204900,#204901,#204902,#204903,#204904,#204905,
#204906,#204907,#204908,#204909,#204910,#204911,#204912,#204913,#204914,
#204915,#204916,#204917,#204918,#204919,#204920,#204921,#204922,#204923,
#204924,#204925,#204926,#204927,#204928,#204929,#204930,#204931,#204932,
#204933,#204934,#204935,#204936,#204937,#204938,#204939,#204940,#204941,
#204942,#204943,#204944,#204945,#204946,#204947,#204948,#204949),
 .UNSPECIFIED.,.F.,.F.,(4,3,3,3,3,3,3,3,3,3,3,3,3,3,3,3,3,3,3,3,3,3,3,3,
3,3,3,3,3,3,3,3,3,3,3,3,3,3,3,3,3,3,3,3,3,3,3,3,3,3,3,3,3,3,3,3,3,3,3,3,
3,3,3,3,3,3,3,3,3,3,3,3,3,4),(91.1061869540849,91.2342698388801,91.2840117569834,
91.3677504688293,91.4513859801969,91.5349384235956,91.6184278594466,91.7018818100603,
91.7853183039066,91.8687554136621,91.95221120858,92.0357557013097,92.1193447842506,
92.2030680518082,92.2837477677035,92.3674864795494,92.4511219909169,92.5346744343155,
92.6181638701666,92.7016178207802,92.7850543146265,92.8684914243819,92.9519472192995,
93.0354917120292,93.1190807949702,93.2028040625277,93.2834837784236,93.3672224902695,
93.450858001637,93.5344104450355,93.6178998808865,93.7013538315002,93.7847903253464,
93.8682274351018,93.9516832300195,94.0352277227491,94.1188168056901,94.2025400732476,
94.2832197891438,94.3669585009898,94.4505940123573,94.5341464557559,94.6176358916069,
94.7010898422206,94.7845263360669,94.8679634458224,94.9514192407401,95.0349637334698,
95.1185528164108,95.2022760839684,95.2829557998639,95.3666945117099,95.4503300230774,
95.5338824664759,95.6173719023269,95.7008258529406,95.7842623467869,95.8676994565424,
95.9511552514601,96.0346997441898,96.1182888271308,96.2020120946884,96.282691810584,
96.3664390909035,96.4500812622947,96.5360408032565,96.6195259372999,96.7029733472777,
96.7864011215343,96.8698273312194,96.9532987109112,97.0367978149355,97.120372459563,
97.1377575899893),.UNSPECIFIED.);
#1698=B_SPLINE_CURVE_WITH_KNOTS('',3,(#204951,#204952,#204953,#204954,#204955,
#204956,#204957,#204958,#204959,#204960,#204961,#204962,#204963,#204964,
#204965,#204966,#204967,#204968,#204969,#204970,#204971,#204972,#204973,
#204974,#204975,#204976,#204977,#204978,#204979,#204980,#204981,#204982,
#204983,#204984,#204985,#204986,#204987,#204988,#204989,#204990,#204991,
#204992,#204993,#204994,#204995,#204996,#204997,#204998,#204999,#205000,
#205001,#205002,#205003,#205004,#205005,#205006,#205007,#205008,#205009,
#205010,#205011,#205012,#205013,#205014,#205015,#205016,#205017,#205018,
#205019,#205020,#205021,#205022,#205023,#205024,#205025,#205026,#205027,
#205028,#205029,#205030,#205031,#205032,#205033,#205034,#205035,#205036,
#205037,#205038,#205039,#205040,#205041,#205042,#205043,#205044,#205045,
#205046,#205047,#205048,#205049,#205050,#205051,#205052,#205053,#205054,
#205055,#205056,#205057,#205058,#205059,#205060,#205061,#205062,#205063,
#205064,#205065,#205066,#205067,#205068,#205069,#205070,#205071,#205072,
#205073,#205074,#205075,#205076,#205077,#205078,#205079,#205080,#205081,
#205082,#205083,#205084,#205085,#205086,#205087,#205088,#205089,#205090,
#205091,#205092,#205093,#205094,#205095,#205096,#205097,#205098,#205099,
#205100,#205101,#205102,#205103,#205104,#205105,#205106,#205107,#205108,
#205109,#205110,#205111,#205112,#205113,#205114,#205115,#205116,#205117,
#205118,#205119,#205120,#205121,#205122,#205123,#205124,#205125,#205126,
#205127,#205128,#205129,#205130,#205131,#205132,#205133,#205134,#205135,
#205136,#205137,#205138,#205139,#205140,#205141,#205142,#205143,#205144,
#205145,#205146,#205147,#205148,#205149,#205150,#205151,#205152,#205153,
#205154,#205155,#205156,#205157,#205158,#205159,#205160,#205161,#205162,
#205163,#205164,#205165,#205166,#205167,#205168,#205169,#205170),
 .UNSPECIFIED.,.F.,.F.,(4,3,3,3,3,3,3,3,3,3,3,3,3,3,3,3,3,3,3,3,3,3,3,3,
3,3,3,3,3,3,3,3,3,3,3,3,3,3,3,3,3,3,3,3,3,3,3,3,3,3,3,3,3,3,3,3,3,3,3,3,
3,3,3,3,3,3,3,3,3,3,3,3,3,4),(91.1061869542033,91.1940293877261,91.2820034417824,
91.3702005362681,91.4585174044926,91.5470388628258,91.5943023766982,91.6780410885441,
91.7616765999115,91.8452290433101,91.9287184791611,92.0121724297747,92.095608923621,
92.1790460333764,92.262501828294,92.3460463210237,92.4296354039646,92.5133586715222,
92.5940383874183,92.6777770992642,92.7614126106318,92.8449650540303,92.9284544898813,
93.011908440495,93.0953449343413,93.1787820440968,93.2622378390145,93.3457823317442,
93.4293714146852,93.5130946822428,93.5937743981385,93.6775131099844,93.7611486213519,
93.8447010647504,93.9281905006014,94.0116444512151,94.0950809450613,94.1785180548168,
94.2619738497344,94.3455183424641,94.429107425405,94.5128306929626,94.5935104088586,
94.6772491207046,94.7608846320721,94.8444370754706,94.9279265113217,95.0113804619354,
95.0948169557816,95.1782540655371,95.2617098604549,95.3452543531846,95.4288434361256,
95.5125667036832,95.5932464195787,95.6769851314246,95.7606206427921,95.8441730861908,
95.927662522042,96.0111164726556,96.0945529665019,96.1779900762574,96.2614458711751,
96.3449903639048,96.4285794468458,96.5123027144034,96.5929824302989,96.6755077426029,
96.7579368247763,96.8402888703964,96.9225805906639,97.0048367170366,97.0870887865323,
97.1377977613825),.UNSPECIFIED.);
#1699=B_SPLINE_CURVE_WITH_KNOTS('',3,(#205171,#205172,#205173,#205174,#205175,
#205176,#205177,#205178,#205179,#205180),.UNSPECIFIED.,.F.,.F.,(4,3,3,4),
(90.8558404966185,90.943003649067,91.0300245809721,91.1061869540887),
 .UNSPECIFIED.);
#1700=B_SPLINE_CURVE_WITH_KNOTS('',3,(#205186,#205187,#205188,#205189,#205190,
#205191,#205192,#205193,#205194,#205195),.UNSPECIFIED.,.F.,.F.,(4,3,3,4),
(84.5725992439732,84.6588962802708,84.7450885344468,84.8230016469053),
 .UNSPECIFIED.);
#1701=B_SPLINE_CURVE_WITH_KNOTS('',3,(#205196,#205197,#205198,#205199,#205200,
#205201,#205202,#205203,#205204,#205205,#205206,#205207,#205208,#205209,
#205210,#205211,#205212,#205213,#205214,#205215,#205216,#205217,#205218,
#205219,#205220,#205221,#205222,#205223,#205224,#205225,#205226,#205227,
#205228,#205229,#205230,#205231,#205232,#205233,#205234,#205235,#205236,
#205237,#205238,#205239,#205240,#205241,#205242,#205243,#205244,#205245,
#205246,#205247,#205248,#205249,#205250,#205251,#205252,#205253,#205254,
#205255,#205256,#205257,#205258,#205259,#205260,#205261,#205262,#205263,
#205264,#205265,#205266,#205267,#205268,#205269,#205270,#205271,#205272,
#205273,#205274,#205275,#205276,#205277,#205278,#205279,#205280,#205281,
#205282,#205283,#205284,#205285,#205286,#205287,#205288,#205289,#205290,
#205291,#205292,#205293,#205294,#205295,#205296,#205297,#205298,#205299,
#205300,#205301,#205302,#205303,#205304,#205305,#205306,#205307,#205308,
#205309,#205310,#205311,#205312,#205313,#205314,#205315,#205316,#205317,
#205318,#205319,#205320,#205321,#205322,#205323,#205324,#205325,#205326,
#205327,#205328,#205329,#205330,#205331,#205332,#205333,#205334,#205335,
#205336,#205337,#205338,#205339,#205340,#205341,#205342,#205343,#205344,
#205345,#205346,#205347,#205348,#205349,#205350,#205351,#205352,#205353,
#205354,#205355,#205356,#205357,#205358,#205359,#205360,#205361,#205362,
#205363,#205364,#205365,#205366,#205367,#205368,#205369,#205370,#205371,
#205372,#205373,#205374,#205375,#205376,#205377,#205378,#205379,#205380,
#205381,#205382,#205383,#205384,#205385,#205386,#205387,#205388,#205389,
#205390,#205391,#205392,#205393,#205394,#205395,#205396,#205397,#205398,
#205399,#205400,#205401,#205402,#205403,#205404,#205405,#205406,#205407,
#205408,#205409,#205410,#205411,#205412,#205413,#205414,#205415),
 .UNSPECIFIED.,.F.,.F.,(4,3,3,3,3,3,3,3,3,3,3,3,3,3,3,3,3,3,3,3,3,3,3,3,
3,3,3,3,3,3,3,3,3,3,3,3,3,3,3,3,3,3,3,3,3,3,3,3,3,3,3,3,3,3,3,3,3,3,3,3,
3,3,3,3,3,3,3,3,3,3,3,3,3,4),(84.8230016470632,84.9118882294179,85.0053150952291,
85.0946470022648,85.1841250841541,85.2738132970661,85.2855956926626,85.3693344045085,
85.452969915876,85.5365223592745,85.6200117951256,85.7034657457393,85.7869022395855,
85.8703393493409,85.9537951442584,86.0373396369881,86.1209287199291,86.2046519874867,
86.2853317033827,86.3690704152286,86.4527059265962,86.5362583699947,86.6197478058457,
86.7032017564594,86.7866382503057,86.8700753600612,86.9535311549789,87.0370756477086,
87.1206647306495,87.2043879982071,87.2850677141029,87.3688064259488,87.4524419373163,
87.5359943807148,87.6194838165659,87.7029377671795,87.7863742610257,87.8698113707812,
87.9532671656989,88.0368116584285,88.1204007413695,88.2041240089271,88.284803724823,
88.368542436669,88.4521779480365,88.535730391435,88.619219827286,88.7026737778997,
88.786110271746,88.8695473815015,88.9530031764193,89.036547669149,89.12013675209,
89.2038600196476,89.2845397355431,89.368278447389,89.4519139587565,89.5354664021551,
89.6189558380062,89.7024097886198,89.7858462824661,89.8692833922215,89.9527391871391,
90.0362836798687,90.1198727628097,90.2035960303673,90.2842757462633,90.3667505459319,
90.4491298248377,90.5314328034189,90.6136786176278,90.69588927706,90.7781041156691,
90.8545165002977),.UNSPECIFIED.);
#1702=B_SPLINE_CURVE_WITH_KNOTS('',3,(#205417,#205418,#205419,#205420,#205421,
#205422,#205423,#205424,#205425,#205426,#205427,#205428,#205429,#205430,
#205431,#205432,#205433,#205434,#205435,#205436,#205437,#205438,#205439,
#205440,#205441,#205442,#205443,#205444,#205445,#205446,#205447,#205448,
#205449,#205450,#205451,#205452,#205453,#205454,#205455,#205456,#205457,
#205458,#205459,#205460,#205461,#205462,#205463,#205464,#205465,#205466,
#205467,#205468,#205469,#205470,#205471,#205472,#205473,#205474,#205475,
#205476,#205477,#205478,#205479,#205480,#205481,#205482,#205483,#205484,
#205485,#205486,#205487,#205488,#205489,#205490,#205491,#205492,#205493,
#205494,#205495,#205496,#205497,#205498,#205499,#205500,#205501,#205502,
#205503,#205504,#205505,#205506,#205507,#205508,#205509,#205510,#205511,
#205512,#205513,#205514,#205515,#205516,#205517,#205518,#205519,#205520,
#205521,#205522,#205523,#205524,#205525,#205526,#205527,#205528,#205529,
#205530,#205531,#205532,#205533,#205534,#205535,#205536,#205537,#205538,
#205539,#205540,#205541,#205542,#205543,#205544,#205545,#205546,#205547,
#205548,#205549,#205550,#205551,#205552,#205553,#205554,#205555,#205556,
#205557,#205558,#205559,#205560,#205561,#205562,#205563,#205564,#205565,
#205566,#205567,#205568,#205569,#205570,#205571,#205572,#205573,#205574,
#205575,#205576,#205577,#205578,#205579,#205580,#205581,#205582,#205583,
#205584,#205585,#205586,#205587,#205588,#205589,#205590,#205591,#205592,
#205593,#205594,#205595,#205596,#205597,#205598,#205599,#205600,#205601,
#205602,#205603,#205604,#205605,#205606,#205607,#205608,#205609,#205610,
#205611,#205612,#205613,#205614,#205615,#205616,#205617,#205618,#205619,
#205620,#205621,#205622,#205623,#205624,#205625,#205626,#205627,#205628,
#205629,#205630,#205631,#205632,#205633,#205634,#205635,#205636),
 .UNSPECIFIED.,.F.,.F.,(4,3,3,3,3,3,3,3,3,3,3,3,3,3,3,3,3,3,3,3,3,3,3,3,
3,3,3,3,3,3,3,3,3,3,3,3,3,3,3,3,3,3,3,3,3,3,3,3,3,3,3,3,3,3,3,3,3,3,3,3,
3,3,3,3,3,3,3,3,3,3,3,3,3,4),(84.8230016470494,84.9054512045182,84.9917555930006,
85.0741114802006,85.1564545594353,85.2388037750452,85.3211780738551,85.4036410329863,
85.4861559906397,85.5687878473739,85.5958863123774,85.6796250242234,85.763260535591,
85.8468129789896,85.9303024148405,86.0137563654542,86.0971928593005,86.180629969056,
86.2640857639739,86.3476302567036,86.4312193396445,86.5149426072021,86.5956223230975,
86.6793610349434,86.762996546311,86.8465489897096,86.9300384255609,87.0134923761746,
87.0969288700208,87.1803659797762,87.2638217746938,87.3473662674234,87.4309553503644,
87.514678617922,87.5953583338177,87.6790970456637,87.7627325570311,87.8462850004296,
87.9297744362802,88.0132283868939,88.0966648807401,88.1801019904954,88.2635577854131,
88.3471022781427,88.4306913610839,88.5144146286414,88.5950943445378,88.6788330563837,
88.7624685677512,88.8460210111494,88.9295104470006,89.0129643976143,89.0964008914605,
89.1798380012159,89.2632937961336,89.3468382888634,89.4304273718043,89.5141506393619,
89.5948303552579,89.6785690671039,89.7622045784714,89.8457570218702,89.929246457721,
90.0127004083347,90.0961369021807,90.1795740119362,90.2630298068536,90.3465742995832,
90.430163382524,90.5138866500815,90.5945663659781,90.6821700263414,90.7695849001495,
90.8558404966185),.UNSPECIFIED.);
#1703=B_SPLINE_CURVE_WITH_KNOTS('',3,(#205637,#205638,#205639,#205640,#205641,
#205642,#205643,#205644,#205645,#205646),.UNSPECIFIED.,.F.,.F.,(4,3,3,4),
(84.571795089726,84.5961503016573,84.7095759742832,84.8230016469091),
 .UNSPECIFIED.);
#1704=B_SPLINE_CURVE_WITH_KNOTS('',3,(#205652,#205653,#205654,#205655,#205656,
#205657,#205658,#205659,#205660,#205661),.UNSPECIFIED.,.F.,.F.,(4,3,3,4),
(78.2887592231474,78.3981054868849,78.5051444124938,78.5398163395285),
 .UNSPECIFIED.);
#1705=B_SPLINE_CURVE_WITH_KNOTS('',3,(#205662,#205663,#205664,#205665,#205666,
#205667,#205668,#205669,#205670,#205671,#205672,#205673,#205674,#205675,
#205676,#205677,#205678,#205679,#205680,#205681,#205682,#205683,#205684,
#205685,#205686,#205687,#205688,#205689,#205690,#205691,#205692,#205693,
#205694,#205695,#205696,#205697,#205698,#205699,#205700,#205701,#205702,
#205703,#205704,#205705,#205706,#205707,#205708,#205709,#205710,#205711,
#205712,#205713,#205714,#205715,#205716,#205717,#205718,#205719,#205720,
#205721,#205722,#205723,#205724,#205725,#205726,#205727,#205728,#205729,
#205730,#205731,#205732,#205733,#205734,#205735,#205736,#205737,#205738,
#205739,#205740,#205741,#205742,#205743,#205744,#205745,#205746,#205747,
#205748,#205749,#205750,#205751,#205752,#205753,#205754,#205755,#205756,
#205757,#205758,#205759,#205760,#205761,#205762,#205763,#205764,#205765,
#205766,#205767,#205768,#205769,#205770,#205771,#205772,#205773,#205774,
#205775,#205776,#205777,#205778,#205779,#205780,#205781,#205782,#205783,
#205784,#205785,#205786,#205787,#205788,#205789,#205790,#205791,#205792,
#205793,#205794,#205795,#205796,#205797,#205798,#205799,#205800,#205801,
#205802,#205803,#205804,#205805,#205806,#205807,#205808,#205809,#205810,
#205811,#205812,#205813,#205814,#205815,#205816,#205817,#205818,#205819,
#205820,#205821,#205822,#205823,#205824,#205825,#205826,#205827,#205828,
#205829,#205830,#205831,#205832,#205833,#205834,#205835,#205836,#205837,
#205838,#205839,#205840,#205841,#205842,#205843,#205844,#205845,#205846,
#205847,#205848,#205849,#205850,#205851,#205852,#205853,#205854,#205855,
#205856,#205857,#205858,#205859,#205860,#205861,#205862,#205863,#205864,
#205865,#205866,#205867,#205868,#205869,#205870,#205871,#205872,#205873,
#205874,#205875,#205876,#205877,#205878,#205879,#205880,#205881),
 .UNSPECIFIED.,.F.,.F.,(4,3,3,3,3,3,3,3,3,3,3,3,3,3,3,3,3,3,3,3,3,3,3,3,
3,3,3,3,3,3,3,3,3,3,3,3,3,3,3,3,3,3,3,3,3,3,3,3,3,3,3,3,3,3,3,3,3,3,3,3,
3,3,3,3,3,3,3,3,3,3,3,3,3,4),(78.5398163397257,78.62239295459,78.705491288809,
78.7879946449525,78.8704919407165,78.9530020139644,79.0365464175588,79.1191811714259,
79.2031803998838,79.2871796283418,79.3709183401877,79.4545538515552,79.5381062949538,
79.6215957308051,79.7050496814187,79.788486175265,79.8719232850204,79.955379079938,
80.0389235726677,80.1225126556086,80.2062359231661,80.286915639062,80.3706543509079,
80.4542898622755,80.5378423056737,80.6213317415248,80.7047856921384,80.7882221859847,
80.8716592957401,80.9551150906578,81.0386595833875,81.1222486663285,81.2059719338861,
81.2866516497821,81.370390361628,81.4540258729957,81.5375783163942,81.6210677522452,
81.7045217028589,81.7879581967051,81.8713953064607,81.9548511013783,82.038395594108,
82.121984677049,82.2057079446065,82.2863876605022,82.3701263723481,82.4537618837154,
82.5373143271138,82.6208037629648,82.7042577135786,82.787694207425,82.8711313171803,
82.9545871120976,83.0381316048273,83.1217206877683,83.2054439553258,83.2861236712224,
83.3698623830682,83.4534978944356,83.5370503378342,83.6205397736848,83.7039937242985,
83.7874302181448,83.8708673279002,83.9543231228179,84.0378676155475,84.1214566984884,
84.2051799660461,84.2858596819425,84.3725698184977,84.4591613046955,84.5456123157065,
84.5725992439732),.UNSPECIFIED.);
#1706=B_SPLINE_CURVE_WITH_KNOTS('',3,(#205883,#205884,#205885,#205886,#205887,
#205888,#205889,#205890,#205891,#205892,#205893,#205894,#205895,#205896,
#205897,#205898,#205899,#205900,#205901,#205902,#205903,#205904,#205905,
#205906,#205907,#205908,#205909,#205910,#205911,#205912,#205913,#205914,
#205915,#205916,#205917,#205918,#205919,#205920,#205921,#205922,#205923,
#205924,#205925,#205926,#205927,#205928,#205929,#205930,#205931,#205932,
#205933,#205934,#205935,#205936,#205937,#205938,#205939,#205940,#205941,
#205942,#205943,#205944,#205945,#205946,#205947,#205948,#205949,#205950,
#205951,#205952,#205953,#205954,#205955,#205956,#205957,#205958,#205959,
#205960,#205961,#205962,#205963,#205964,#205965,#205966,#205967,#205968,
#205969,#205970,#205971,#205972,#205973,#205974,#205975,#205976,#205977,
#205978,#205979,#205980,#205981,#205982,#205983,#205984,#205985,#205986,
#205987,#205988,#205989,#205990,#205991,#205992,#205993,#205994,#205995,
#205996,#205997,#205998,#205999,#206000,#206001,#206002,#206003,#206004,
#206005,#206006,#206007,#206008,#206009,#206010,#206011,#206012,#206013,
#206014,#206015,#206016,#206017,#206018,#206019,#206020,#206021,#206022,
#206023,#206024,#206025,#206026,#206027,#206028,#206029,#206030,#206031,
#206032,#206033,#206034,#206035,#206036,#206037,#206038,#206039,#206040,
#206041,#206042,#206043,#206044,#206045,#206046,#206047,#206048,#206049,
#206050,#206051,#206052,#206053,#206054,#206055,#206056,#206057,#206058,
#206059,#206060,#206061,#206062,#206063,#206064,#206065,#206066,#206067,
#206068,#206069,#206070,#206071,#206072,#206073,#206074,#206075,#206076,
#206077,#206078,#206079,#206080,#206081,#206082,#206083,#206084,#206085,
#206086,#206087,#206088,#206089,#206090,#206091,#206092,#206093,#206094,
#206095,#206096,#206097,#206098,#206099,#206100,#206101,#206102),
 .UNSPECIFIED.,.F.,.F.,(4,3,3,3,3,3,3,3,3,3,3,3,3,3,3,3,3,3,3,3,3,3,3,3,
3,3,3,3,3,3,3,3,3,3,3,3,3,3,3,3,3,3,3,3,3,3,3,3,3,3,3,3,3,3,3,3,3,3,3,3,
3,3,3,3,3,3,3,3,3,3,3,3,3,4),(78.5398163397295,78.5977342373365,78.6814729491824,
78.7651084605499,78.8486609039486,78.9321503397996,79.0156042904133,79.0990407842595,
79.1824778940149,79.2659336889324,79.3494781816621,79.4330672646031,79.5167905321606,
79.5974702480566,79.6812089599025,79.76484447127,79.8483969146685,79.9318863505195,
80.0153403011332,80.0987767949795,80.1822139047349,80.2656696996526,80.3492141923823,
80.4328032753233,80.5165265428808,80.5972062587768,80.6809449706228,80.7645804819903,
80.8481329253889,80.93162236124,81.0150763118536,81.0985128056999,81.1819499154554,
81.2654057103731,81.3489502031028,81.4325392860438,81.5162625536014,81.5969422694969,
81.6806809813428,81.7643164927103,81.8478689361088,81.9313583719598,82.0148123225734,
82.0982488164197,82.1816859261751,82.2651417210928,82.3486862138224,82.4322752967634,
82.5159985643209,82.596678280217,82.680416992063,82.7640525034305,82.8476049468291,
82.9310943826802,83.0145483332938,83.0979848271401,83.1814219368956,83.2648777318133,
83.348422224543,83.432011307484,83.5157345750416,83.5964142909372,83.6801543798819,
83.7637909471208,83.847344126517,83.9308339795196,84.0142867067674,84.0977215231147,
84.1811565009327,84.264609708774,84.3481453391041,84.4317253719729,84.5154248974244,
84.571795089726),.UNSPECIFIED.);
#1707=B_SPLINE_CURVE_WITH_KNOTS('',3,(#206103,#206104,#206105,#206106),
 .UNSPECIFIED.,.F.,.F.,(4,4),(78.2879140477243,78.5398092039209),
 .UNSPECIFIED.);
#1708=B_SPLINE_CURVE_WITH_KNOTS('',3,(#206112,#206113,#206114,#206115,#206116,
#206117,#206118,#206119,#206120,#206121),.UNSPECIFIED.,.F.,.F.,(4,3,3,4),
(72.0048655224089,72.0880045572239,72.172317794814,72.256631032404),
 .UNSPECIFIED.);
#1709=B_SPLINE_CURVE_WITH_KNOTS('',3,(#206122,#206123,#206124,#206125,#206126,
#206127,#206128,#206129,#206130,#206131,#206132,#206133,#206134,#206135,
#206136,#206137,#206138,#206139,#206140,#206141,#206142,#206143,#206144,
#206145,#206146,#206147,#206148,#206149,#206150,#206151,#206152,#206153,
#206154,#206155,#206156,#206157,#206158,#206159,#206160,#206161,#206162,
#206163,#206164,#206165,#206166,#206167,#206168,#206169,#206170,#206171,
#206172,#206173,#206174,#206175,#206176,#206177,#206178,#206179,#206180,
#206181,#206182,#206183,#206184,#206185,#206186,#206187,#206188,#206189,
#206190,#206191,#206192,#206193,#206194,#206195,#206196,#206197,#206198,
#206199,#206200,#206201,#206202,#206203,#206204,#206205,#206206,#206207,
#206208,#206209,#206210,#206211,#206212,#206213,#206214,#206215,#206216,
#206217,#206218,#206219,#206220,#206221,#206222,#206223,#206224,#206225,
#206226,#206227,#206228,#206229,#206230,#206231,#206232,#206233,#206234,
#206235,#206236,#206237,#206238,#206239,#206240,#206241,#206242,#206243,
#206244,#206245,#206246,#206247,#206248,#206249,#206250,#206251,#206252,
#206253,#206254,#206255,#206256,#206257,#206258,#206259,#206260,#206261,
#206262,#206263,#206264,#206265,#206266,#206267,#206268,#206269,#206270,
#206271,#206272,#206273,#206274,#206275,#206276,#206277,#206278,#206279,
#206280,#206281,#206282,#206283,#206284,#206285,#206286,#206287,#206288,
#206289,#206290,#206291,#206292,#206293,#206294,#206295,#206296,#206297,
#206298,#206299,#206300,#206301,#206302,#206303,#206304,#206305,#206306,
#206307,#206308,#206309,#206310,#206311,#206312,#206313,#206314,#206315,
#206316,#206317,#206318,#206319,#206320,#206321,#206322,#206323,#206324,
#206325,#206326,#206327,#206328,#206329,#206330,#206331,#206332,#206333,
#206334,#206335,#206336,#206337,#206338,#206339,#206340,#206341,#206342,
#206343,#206344),.UNSPECIFIED.,.F.,.F.,(4,3,3,3,3,3,3,3,3,3,3,3,3,3,3,3,
3,3,3,3,3,3,3,3,3,3,3,3,3,3,3,3,3,3,3,3,3,3,3,3,3,3,3,3,3,3,3,3,3,3,3,3,
3,3,3,3,3,3,3,3,3,3,3,3,3,3,3,3,3,3,3,3,3,3,4),(72.2566310325461,72.2890275533009,
72.3727662651468,72.4564017765142,72.5399542199127,72.6234436557635,72.7068976063771,
72.7903341002233,72.8737712099786,72.9572270048961,73.0407714976257,73.1243605805666,
73.2080838481241,73.2887635640211,73.372502275867,73.4561377872345,73.539690230633,
73.6231796664841,73.7066336170977,73.790070110944,73.8735072206994,73.956963015617,
74.0405075083467,74.1240965912877,74.2078198588453,74.2884995747412,74.3722382865871,
74.4558737979546,74.5394262413532,74.6229156772043,74.7063696278179,74.7898061216642,
74.8732432314197,74.9566990263373,75.0402435190669,75.1238326020079,75.2075558695655,
75.2882355854613,75.3719742973073,75.4556098086748,75.5391622520734,75.6226516879244,
75.7061056385381,75.7895421323844,75.87297924214,75.9564350370577,76.0399795297874,
76.1235686127284,76.207291880286,76.2879715961814,76.3717103080273,76.4553458193948,
76.5388982627933,76.6223876986444,76.7058416492581,76.7892781431043,76.8727152528598,
76.9561710477774,77.0397155405071,77.1233046234481,77.2070278910057,77.2877076069016,
77.3714463187476,77.4550818301151,77.5386342735135,77.6221237093646,77.7055776599783,
77.7890141538246,77.8724512635801,77.9559070584978,78.0394515512275,78.1230406341685,
78.2067639017261,78.2874436176217,78.2887592231474),.UNSPECIFIED.);
#1710=B_SPLINE_CURVE_WITH_KNOTS('',3,(#206346,#206347,#206348,#206349,#206350,
#206351,#206352,#206353,#206354,#206355),.UNSPECIFIED.,.F.,.F.,(4,1,1,1,
1,1,1,4),(72.2566310325499,72.5993181730157,73.5990541837358,74.598790194456,
75.5985262051761,76.5982622158962,77.5979982266164,78.2879140477243),
 .UNSPECIFIED.);
#1711=B_SPLINE_CURVE_WITH_KNOTS('',3,(#206356,#206357,#206358,#206359),
 .UNSPECIFIED.,.F.,.F.,(4,4),(72.0060503087704,72.2566310325499),
 .UNSPECIFIED.);
#1712=B_SPLINE_CURVE_WITH_KNOTS('',3,(#206365,#206366,#206367,#206368,#206369,
#206370,#206371,#206372,#206373,#206374),.UNSPECIFIED.,.F.,.F.,(4,3,3,4),
(65.7224278061069,65.8055735571319,65.8895096412492,65.9734457253665),
 .UNSPECIFIED.);
#1713=B_SPLINE_CURVE_WITH_KNOTS('',3,(#206375,#206376,#206377,#206378,#206379,
#206380,#206381,#206382,#206383,#206384,#206385,#206386,#206387,#206388,
#206389,#206390,#206391,#206392,#206393,#206394,#206395,#206396,#206397,
#206398,#206399,#206400,#206401,#206402,#206403,#206404,#206405,#206406,
#206407,#206408,#206409,#206410,#206411,#206412,#206413,#206414,#206415,
#206416,#206417,#206418,#206419,#206420,#206421,#206422,#206423,#206424,
#206425,#206426,#206427,#206428,#206429,#206430,#206431,#206432,#206433,
#206434,#206435,#206436,#206437,#206438,#206439,#206440,#206441,#206442,
#206443,#206444,#206445,#206446,#206447,#206448,#206449,#206450,#206451,
#206452,#206453,#206454,#206455,#206456,#206457,#206458,#206459,#206460,
#206461,#206462,#206463,#206464,#206465,#206466,#206467,#206468,#206469,
#206470,#206471,#206472,#206473,#206474,#206475,#206476,#206477,#206478,
#206479,#206480,#206481,#206482,#206483,#206484,#206485,#206486,#206487,
#206488,#206489,#206490,#206491,#206492,#206493,#206494,#206495,#206496,
#206497,#206498,#206499,#206500,#206501,#206502,#206503,#206504,#206505,
#206506,#206507,#206508,#206509,#206510,#206511,#206512,#206513,#206514,
#206515,#206516,#206517,#206518,#206519,#206520,#206521,#206522,#206523,
#206524,#206525,#206526,#206527,#206528,#206529,#206530,#206531,#206532,
#206533,#206534,#206535,#206536,#206537,#206538,#206539,#206540,#206541,
#206542,#206543,#206544,#206545,#206546,#206547,#206548,#206549,#206550,
#206551,#206552,#206553,#206554,#206555,#206556,#206557,#206558,#206559,
#206560,#206561,#206562,#206563,#206564,#206565,#206566,#206567,#206568,
#206569,#206570,#206571,#206572,#206573,#206574,#206575,#206576,#206577,
#206578,#206579,#206580,#206581,#206582,#206583,#206584,#206585,#206586,
#206587,#206588,#206589,#206590,#206591,#206592,#206593,#206594),
 .UNSPECIFIED.,.F.,.F.,(4,3,3,3,3,3,3,3,3,3,3,3,3,3,3,3,3,3,3,3,3,3,3,3,
3,3,3,3,3,3,3,3,3,3,3,3,3,3,3,3,3,3,3,3,3,3,3,3,3,3,3,3,3,3,3,3,3,3,3,3,
3,3,3,3,3,3,3,3,3,3,3,3,3,4),(65.973445725537,66.0722016376632,66.1716623230831,
66.2718883360919,66.2906114889802,66.3743502008262,66.4579857121937,66.5415381555923,
66.6250275914434,66.7084815420572,66.7919180359034,66.875355145659,66.9588109405769,
67.0423554333066,67.1259445162477,67.2096677838053,67.2903474997003,67.3740862115462,
67.4577217229137,67.5412741663122,67.6247636021632,67.7082175527769,67.7916540466231,
67.8750911563786,67.9585469512962,68.0420914440259,68.1256805269669,68.2094037945244,
68.2900835104204,68.3738222222663,68.4574577336338,68.5410101770324,68.6244996128835,
68.7079535634972,68.7913900573434,68.8748271670989,68.9582829620166,69.0418274547463,
69.1254165376873,69.2091398052449,69.2898195211405,69.3735582329864,69.4571937443539,
69.5407461877524,69.6242356236035,69.7076895742171,69.7911260680634,69.8745631778188,
69.9580189727365,70.0415634654662,70.1251525484071,70.2088758159647,70.2895555318607,
70.3732942437067,70.4569297550742,70.5404821984727,70.6239716343238,70.7074255849375,
70.7908620787838,70.8742991885393,70.957754983457,71.0412994761868,71.1248885591278,
71.2086118266854,71.2892915425808,71.3726036548392,71.4557840971122,71.5388885214543,
71.6219354908015,71.7049435228024,71.7879472022301,71.8709469547149,71.9539898147039,
72.0048655224089),.UNSPECIFIED.);
#1714=B_SPLINE_CURVE_WITH_KNOTS('',3,(#206596,#206597,#206598,#206599,#206600,
#206601,#206602,#206603,#206604,#206605),.UNSPECIFIED.,.F.,.F.,(4,1,1,1,
1,1,1,4),(65.9734457253704,66.6009021086949,67.6006381194151,68.6003741301352,
69.6001101408553,70.5998461515754,71.5995821622956,72.0060503087704),
 .UNSPECIFIED.);
#1715=B_SPLINE_CURVE_WITH_KNOTS('',3,(#206606,#206607,#206608,#206609,#206610,
#206611,#206612,#206613,#206614,#206615),.UNSPECIFIED.,.F.,.F.,(4,3,3,4),
(65.7229944280855,65.8176176411345,65.9116665109351,65.9734457253704),
 .UNSPECIFIED.);
#1716=B_SPLINE_CURVE_WITH_KNOTS('',3,(#206621,#206622,#206623,#206624,#206625,
#206626,#206627,#206628,#206629,#206630),.UNSPECIFIED.,.F.,.F.,(4,3,3,4),
(59.4398822683535,59.5326783695403,59.6250277789513,59.6902604180037),
 .UNSPECIFIED.);
#1717=B_SPLINE_CURVE_WITH_KNOTS('',3,(#206631,#206632,#206633,#206634,#206635,
#206636,#206637,#206638,#206639,#206640,#206641,#206642,#206643,#206644,
#206645,#206646,#206647,#206648,#206649,#206650,#206651,#206652,#206653,
#206654,#206655,#206656,#206657,#206658,#206659,#206660,#206661,#206662,
#206663,#206664,#206665,#206666,#206667,#206668,#206669,#206670,#206671,
#206672,#206673,#206674,#206675,#206676,#206677,#206678,#206679,#206680,
#206681,#206682,#206683,#206684,#206685,#206686,#206687,#206688,#206689,
#206690,#206691,#206692,#206693,#206694,#206695,#206696,#206697,#206698,
#206699,#206700,#206701,#206702,#206703,#206704,#206705,#206706,#206707,
#206708,#206709,#206710,#206711,#206712,#206713,#206714,#206715,#206716,
#206717,#206718,#206719,#206720,#206721,#206722,#206723,#206724,#206725,
#206726,#206727,#206728,#206729,#206730,#206731,#206732,#206733,#206734,
#206735,#206736,#206737,#206738,#206739,#206740,#206741,#206742,#206743,
#206744,#206745,#206746,#206747,#206748,#206749,#206750,#206751,#206752,
#206753,#206754,#206755,#206756,#206757,#206758,#206759,#206760,#206761,
#206762,#206763,#206764,#206765,#206766,#206767,#206768,#206769,#206770,
#206771,#206772,#206773,#206774,#206775,#206776,#206777,#206778,#206779,
#206780,#206781,#206782,#206783,#206784,#206785,#206786,#206787,#206788,
#206789,#206790,#206791,#206792,#206793,#206794,#206795,#206796,#206797,
#206798,#206799,#206800,#206801,#206802,#206803,#206804,#206805,#206806,
#206807,#206808,#206809,#206810,#206811,#206812,#206813,#206814,#206815,
#206816,#206817,#206818,#206819,#206820,#206821,#206822,#206823,#206824,
#206825,#206826,#206827,#206828,#206829,#206830,#206831,#206832,#206833,
#206834,#206835,#206836,#206837,#206838,#206839,#206840,#206841,#206842,
#206843,#206844,#206845,#206846,#206847,#206848,#206849,#206850),
 .UNSPECIFIED.,.F.,.F.,(4,3,3,3,3,3,3,3,3,3,3,3,3,3,3,3,3,3,3,3,3,3,3,3,
3,3,3,3,3,3,3,3,3,3,3,3,3,3,3,3,3,3,3,3,3,3,3,3,3,3,3,3,3,3,3,3,3,3,3,3,
3,3,3,3,3,3,3,3,3,3,3,3,3,4),(59.6902604181869,59.7747787530522,59.8593179788568,
59.9438945410883,60.0309697619811,60.1157222054673,60.2039588150634,60.2921954246594,
60.3759341365053,60.4595696478729,60.5431220912715,60.6266115271223,60.710065477736,
60.7935019715823,60.8769390813379,60.9603948762555,61.0439393689852,61.1275284519262,
61.2112517194837,61.2919314353795,61.3756701472254,61.4593056585929,61.5428581019914,
61.6263475378422,61.7098014884559,61.7932379823021,61.8766750920576,61.9601308869752,
62.0436753797049,62.1272644626459,62.2109877302035,62.2916674460996,62.3754061579455,
62.459041669313,62.5425941127115,62.6260835485626,62.7095374991762,62.7929739930223,
62.8764111027777,62.959866897695,63.0434113904248,63.1270004733656,63.2107237409232,
63.2914034568198,63.3751421686657,63.4587776800333,63.5423301234322,63.6258195592835,
63.7092735098971,63.7927100037433,63.8761471134986,63.9596029084161,64.0431474011459,
64.1267364840869,64.2104597516445,64.2911394675399,64.3748781793858,64.4585136907535,
64.5420661341521,64.625555570003,64.7090095206166,64.792446014463,64.8758831242186,
64.9593389191362,65.0428834118659,65.1264724948068,65.2101957623644,65.29087547826,
65.3743504055609,65.4613697556974,65.544635511258,65.6278429630006,65.7110052807257,
65.7224278061069),.UNSPECIFIED.);
#1718=B_SPLINE_CURVE_WITH_KNOTS('',3,(#206852,#206853,#206854,#206855,#206856,
#206857,#206858,#206859,#206860,#206861,#206862,#206863,#206864,#206865,
#206866,#206867,#206868,#206869,#206870,#206871,#206872,#206873,#206874,
#206875,#206876,#206877,#206878,#206879,#206880,#206881,#206882,#206883,
#206884,#206885,#206886,#206887,#206888,#206889,#206890,#206891,#206892,
#206893,#206894,#206895,#206896,#206897,#206898,#206899,#206900,#206901,
#206902,#206903,#206904,#206905,#206906,#206907,#206908,#206909,#206910,
#206911,#206912,#206913,#206914,#206915,#206916,#206917,#206918,#206919,
#206920,#206921,#206922,#206923,#206924,#206925,#206926,#206927,#206928,
#206929,#206930,#206931,#206932,#206933,#206934,#206935,#206936,#206937,
#206938,#206939,#206940,#206941,#206942,#206943,#206944,#206945,#206946,
#206947,#206948,#206949,#206950,#206951,#206952,#206953,#206954,#206955,
#206956,#206957,#206958,#206959,#206960,#206961,#206962,#206963,#206964,
#206965,#206966,#206967,#206968,#206969,#206970,#206971,#206972,#206973,
#206974,#206975,#206976,#206977,#206978,#206979,#206980,#206981,#206982,
#206983,#206984,#206985,#206986,#206987,#206988,#206989,#206990,#206991,
#206992,#206993,#206994,#206995,#206996,#206997,#206998,#206999,#207000,
#207001,#207002,#207003,#207004,#207005,#207006,#207007,#207008,#207009,
#207010,#207011,#207012,#207013,#207014,#207015,#207016,#207017,#207018,
#207019,#207020,#207021,#207022,#207023,#207024,#207025,#207026,#207027,
#207028,#207029,#207030,#207031,#207032,#207033,#207034,#207035,#207036,
#207037,#207038,#207039,#207040,#207041,#207042,#207043,#207044,#207045,
#207046,#207047,#207048,#207049,#207050,#207051,#207052,#207053,#207054,
#207055,#207056,#207057,#207058,#207059,#207060,#207061,#207062,#207063,
#207064,#207065,#207066,#207067,#207068,#207069,#207070,#207071),
 .UNSPECIFIED.,.F.,.F.,(4,3,3,3,3,3,3,3,3,3,3,3,3,3,3,3,3,3,3,3,3,3,3,3,
3,3,3,3,3,3,3,3,3,3,3,3,3,3,3,3,3,3,3,3,3,3,3,3,3,3,3,3,3,3,3,3,3,3,3,3,
3,3,3,3,3,3,3,3,3,3,3,3,3,4),(59.690260418325,59.7729922509435,59.8556292811794,
59.9381925013212,60.0212291942028,60.1037176127869,60.1861993999656,60.2686934103523,
60.3521415688578,60.4347588661806,60.5186224552774,60.6024860443741,60.68622475622,
60.7698602675875,60.8534127109862,60.936902146837,61.0203560974506,61.1037925912969,
61.1872297010523,61.2706854959699,61.3542299886996,61.4378190716406,61.5215423391982,
61.6022220550943,61.6859607669403,61.7695962783077,61.8531487217063,61.9366381575571,
62.0200921081707,62.1035286020169,62.1869657117725,62.2704215066901,62.3539659994198,
62.4375550823607,62.5212783499182,62.6019580658144,62.6856967776603,62.7693322890281,
62.8528847324265,62.9363741682772,63.0198281188909,63.1032646127372,63.1867017224929,
63.2701575174107,63.3537020101404,63.4372910930814,63.521014360639,63.6016940765345,
63.6854327883804,63.7690682997479,63.8526207431468,63.9361101789976,64.0195641296113,
64.1030006234575,64.1864377332125,64.2698935281301,64.3534380208598,64.4370271038007,
64.5207503713583,64.6014300872547,64.6851687991007,64.7688043104682,64.8523567538665,
64.9358461897175,65.0193001403312,65.1027366341774,65.186173743933,65.269629538851,
65.3531740315807,65.4367631145216,65.5204863820792,65.6011660979748,65.6963168570349,
65.7229944280855),.UNSPECIFIED.);
#1719=B_SPLINE_CURVE_WITH_KNOTS('',3,(#207072,#207073,#207074,#207075,#207076,
#207077,#207078,#207079,#207080,#207081),.UNSPECIFIED.,.F.,.F.,(4,3,3,4),
(59.4386194045287,59.5223427634998,59.602750033654,59.6902604181908),
 .UNSPECIFIED.);
#1720=B_SPLINE_CURVE_WITH_KNOTS('',3,(#207087,#207088,#207089,#207090,#207091,
#207092,#207093,#207094,#207095,#207096),.UNSPECIFIED.,.F.,.F.,(4,3,3,4),
(53.1554707439118,53.2392036250967,53.2940433496185,53.4070751110074),
 .UNSPECIFIED.);
#1721=B_SPLINE_CURVE_WITH_KNOTS('',3,(#207097,#207098,#207099,#207100,#207101,
#207102,#207103,#207104,#207105,#207106,#207107,#207108,#207109,#207110,
#207111,#207112,#207113,#207114,#207115,#207116,#207117,#207118,#207119,
#207120,#207121,#207122,#207123,#207124,#207125,#207126,#207127,#207128,
#207129,#207130,#207131,#207132,#207133,#207134,#207135,#207136,#207137,
#207138,#207139,#207140,#207141,#207142,#207143,#207144,#207145,#207146,
#207147,#207148,#207149,#207150,#207151,#207152,#207153,#207154,#207155,
#207156,#207157,#207158,#207159,#207160,#207161,#207162,#207163,#207164,
#207165,#207166,#207167,#207168,#207169,#207170,#207171,#207172,#207173,
#207174,#207175,#207176,#207177,#207178,#207179,#207180,#207181,#207182,
#207183,#207184,#207185,#207186,#207187,#207188,#207189,#207190,#207191,
#207192,#207193,#207194,#207195,#207196,#207197,#207198,#207199,#207200,
#207201,#207202,#207203,#207204,#207205,#207206,#207207,#207208,#207209,
#207210,#207211,#207212,#207213,#207214,#207215,#207216,#207217,#207218,
#207219,#207220,#207221,#207222,#207223,#207224,#207225,#207226,#207227,
#207228,#207229,#207230,#207231,#207232,#207233,#207234,#207235,#207236,
#207237,#207238,#207239,#207240,#207241,#207242,#207243,#207244,#207245,
#207246,#207247,#207248,#207249,#207250,#207251,#207252,#207253,#207254,
#207255,#207256,#207257,#207258,#207259,#207260,#207261,#207262,#207263,
#207264,#207265,#207266,#207267,#207268,#207269,#207270,#207271,#207272,
#207273,#207274,#207275,#207276,#207277,#207278,#207279,#207280,#207281,
#207282,#207283,#207284,#207285,#207286,#207287,#207288,#207289,#207290,
#207291,#207292,#207293,#207294,#207295,#207296,#207297,#207298,#207299,
#207300,#207301,#207302,#207303,#207304,#207305,#207306,#207307,#207308,
#207309,#207310,#207311,#207312,#207313,#207314,#207315,#207316),
 .UNSPECIFIED.,.F.,.F.,(4,3,3,3,3,3,3,3,3,3,3,3,3,3,3,3,3,3,3,3,3,3,3,3,
3,3,3,3,3,3,3,3,3,3,3,3,3,3,3,3,3,3,3,3,3,3,3,3,3,3,3,3,3,3,3,3,3,3,3,3,
3,3,3,3,3,3,3,3,3,3,3,3,3,4),(53.4070751111425,53.4896343762135,53.5721034786018,
53.6545035043015,53.7368608751334,53.819197084156,53.9015310878447,53.9838818385131,
54.066316941824,54.1487965694145,54.2314023405145,54.2937793603386,54.3775180721845,
54.4611535835521,54.5447060269508,54.6281954628017,54.7116494134154,54.7950859072616,
54.8785230170172,54.9619788119348,55.0455233046645,55.1291123876056,55.2128356551632,
55.2935153710587,55.3772540829047,55.4608895942722,55.5444420376709,55.627931473522,
55.7113854241356,55.7948219179819,55.8782590277374,55.961714822655,56.0452593153847,
56.1288483983257,56.2125716658834,56.2932513817789,56.3769900936248,56.4606256049923,
56.5441780483911,56.6276674842419,56.7111214348556,56.7945579287019,56.8779950384574,
56.9614508333752,57.0449953261048,57.1285844090459,57.2123076766035,57.292987392499,
57.376726104345,57.4603616157126,57.5439140591111,57.6274034949616,57.7108574455754,
57.7942939394216,57.8777310491771,57.9611868440946,58.0447313368243,58.1283204197652,
58.2120436873228,58.2927234032191,58.3764621150651,58.4600976264325,58.5436500698315,
58.6271395056821,58.7105934562957,58.7940299501419,58.8774670598972,58.9609228548147,
59.0444673475445,59.1280564304858,59.2117796980434,59.2924594139393,59.3857393267099,
59.4398822683535),.UNSPECIFIED.);
#1722=B_SPLINE_CURVE_WITH_KNOTS('',3,(#207318,#207319,#207320,#207321,#207322,
#207323,#207324,#207325,#207326,#207327,#207328,#207329,#207330,#207331,
#207332,#207333,#207334,#207335,#207336,#207337,#207338,#207339,#207340,
#207341,#207342,#207343,#207344,#207345,#207346,#207347,#207348,#207349,
#207350,#207351,#207352,#207353,#207354,#207355,#207356,#207357,#207358,
#207359,#207360,#207361,#207362,#207363,#207364,#207365,#207366,#207367,
#207368,#207369,#207370,#207371,#207372,#207373,#207374,#207375,#207376,
#207377,#207378,#207379,#207380,#207381,#207382,#207383,#207384,#207385,
#207386,#207387,#207388,#207389,#207390,#207391,#207392,#207393,#207394,
#207395,#207396,#207397,#207398,#207399,#207400,#207401,#207402,#207403,
#207404,#207405,#207406,#207407,#207408,#207409,#207410,#207411,#207412,
#207413,#207414,#207415,#207416,#207417,#207418,#207419,#207420,#207421,
#207422,#207423,#207424,#207425,#207426,#207427,#207428,#207429,#207430,
#207431,#207432,#207433,#207434,#207435,#207436,#207437,#207438,#207439,
#207440,#207441,#207442,#207443,#207444,#207445,#207446,#207447,#207448,
#207449,#207450,#207451,#207452,#207453,#207454,#207455,#207456,#207457,
#207458,#207459,#207460,#207461,#207462,#207463,#207464,#207465,#207466,
#207467,#207468,#207469,#207470,#207471,#207472,#207473,#207474,#207475,
#207476,#207477,#207478,#207479,#207480,#207481,#207482,#207483,#207484,
#207485,#207486,#207487,#207488,#207489,#207490,#207491,#207492,#207493,
#207494,#207495,#207496,#207497,#207498,#207499,#207500,#207501,#207502,
#207503,#207504,#207505,#207506,#207507,#207508,#207509,#207510,#207511,
#207512,#207513,#207514,#207515,#207516,#207517,#207518,#207519,#207520,
#207521,#207522,#207523,#207524,#207525,#207526,#207527,#207528,#207529,
#207530,#207531,#207532,#207533,#207534),.UNSPECIFIED.,.F.,.F.,(4,3,3,3,
3,3,3,3,3,3,3,3,3,3,3,3,3,3,3,3,3,3,3,3,3,3,3,3,3,3,3,3,3,3,3,3,3,3,3,3,
3,3,3,3,3,3,3,3,3,3,3,3,3,3,3,3,3,3,3,3,3,3,3,3,3,3,3,3,3,3,3,3,4),(53.4070751110112,
53.5281266875687,53.6043339693332,53.6880726811791,53.7717081925466,53.8552606359451,
53.9387500717959,54.0222040224095,54.1056405162557,54.1890776260112,54.2725334209287,
54.3560779136583,54.4396669965993,54.5233902641568,54.6040699800534,54.6878086918993,
54.7714442032668,54.8549966466653,54.9384860825163,55.02194003313,55.1053765269762,
55.1888136367316,55.2722694316493,55.3558139243789,55.4394030073199,55.5231262748775,
55.6038059907735,55.6875447026194,55.771180213987,55.8547326573855,55.9382220932365,
56.0216760438502,56.1051125376965,56.188549647452,56.2720054423696,56.3555499350993,
56.4391390180403,56.522862285598,56.6035420014936,56.6872807133395,56.7709162247071,
56.8544686681056,56.9379581039566,57.0214120545703,57.1048485484165,57.188285658172,
57.2717414530897,57.3552859458194,57.4388750287604,57.522598296318,57.6032780122137,
57.6870167240596,57.7706522354271,57.8542046788257,57.9376941146768,58.0211480652904,
58.1045845591367,58.1880216688921,58.2714774638097,58.3550219565394,58.4386110394804,
58.522334307038,58.6030140229339,58.6867625271259,58.7704056656083,58.8539487725955,
58.9374351492175,59.0208829145339,59.1043101578345,59.1878874695081,59.2713533662358,
59.3549863853822,59.4386194045287),.UNSPECIFIED.);
#1723=B_SPLINE_CURVE_WITH_KNOTS('',3,(#207535,#207536,#207537,#207538,#207539,
#207540,#207541,#207542,#207543,#207544),.UNSPECIFIED.,.F.,.F.,(4,3,3,4),
(53.1554762266557,53.2377493943412,53.3224122526225,53.4070751109039),
 .UNSPECIFIED.);
#1724=B_SPLINE_CURVE_WITH_KNOTS('',3,(#207550,#207551,#207552,#207553,#207554,
#207555,#207556,#207557,#207558,#207559),.UNSPECIFIED.,.F.,.F.,(4,3,3,4),
(46.872199078263,46.9544540684318,47.039171936041,47.1238898036503),
 .UNSPECIFIED.);
#1725=B_SPLINE_CURVE_WITH_KNOTS('',3,(#207560,#207561,#207562,#207563,#207564,
#207565,#207566,#207567,#207568,#207569,#207570,#207571,#207572,#207573,
#207574,#207575,#207576,#207577,#207578,#207579,#207580,#207581,#207582,
#207583,#207584,#207585,#207586,#207587,#207588,#207589,#207590,#207591,
#207592,#207593,#207594,#207595,#207596,#207597,#207598,#207599,#207600,
#207601,#207602,#207603,#207604,#207605,#207606,#207607,#207608,#207609,
#207610,#207611,#207612,#207613,#207614,#207615,#207616,#207617,#207618,
#207619,#207620,#207621,#207622,#207623,#207624,#207625,#207626,#207627,
#207628,#207629,#207630,#207631,#207632,#207633,#207634,#207635,#207636,
#207637,#207638,#207639,#207640,#207641,#207642,#207643,#207644,#207645,
#207646,#207647,#207648,#207649,#207650,#207651,#207652,#207653,#207654,
#207655,#207656,#207657,#207658,#207659,#207660,#207661,#207662,#207663,
#207664,#207665,#207666,#207667,#207668,#207669,#207670,#207671,#207672,
#207673,#207674,#207675,#207676,#207677,#207678,#207679,#207680,#207681,
#207682,#207683,#207684,#207685,#207686,#207687,#207688,#207689,#207690,
#207691,#207692,#207693,#207694,#207695,#207696,#207697,#207698,#207699,
#207700,#207701,#207702,#207703,#207704,#207705,#207706,#207707,#207708,
#207709,#207710,#207711,#207712,#207713,#207714,#207715,#207716,#207717,
#207718,#207719,#207720,#207721,#207722,#207723,#207724,#207725,#207726,
#207727,#207728,#207729,#207730,#207731,#207732,#207733,#207734,#207735,
#207736,#207737,#207738,#207739,#207740,#207741,#207742,#207743,#207744,
#207745,#207746,#207747,#207748,#207749,#207750,#207751,#207752,#207753,
#207754,#207755,#207756,#207757,#207758,#207759,#207760,#207761,#207762,
#207763,#207764,#207765,#207766,#207767,#207768,#207769,#207770,#207771,
#207772,#207773,#207774,#207775,#207776,#207777,#207778,#207779),
 .UNSPECIFIED.,.F.,.F.,(4,3,3,3,3,3,3,3,3,3,3,3,3,3,3,3,3,3,3,3,3,3,3,3,
3,3,3,3,3,3,3,3,3,3,3,3,3,3,3,3,3,3,3,3,3,3,3,3,3,3,3,3,3,3,3,3,3,3,3,3,
3,3,3,3,3,3,3,3,3,3,3,3,3,4),(47.1238898038278,47.2546038085429,47.2956272852977,
47.3793659971438,47.4630015085113,47.54655395191,47.6300433877611,47.7134973383749,
47.7969338322212,47.8803709419768,47.9638267368945,48.0473712296243,48.1309603125654,
48.2146835801231,48.2953632960178,48.3791020078637,48.4627375192312,48.5462899626297,
48.6297793984807,48.7132333490943,48.7966698429405,48.880106952696,48.9635627476137,
49.0471072403433,49.1306963232843,49.2144195908419,49.295099306738,49.3788380185839,
49.4624735299514,49.54602597335,49.6295154092011,49.7129693598147,49.796405853661,
49.8798429634164,49.9632987583341,50.0468432510638,50.1304323340048,50.2141556015624,
50.2948353174581,50.3785740293041,50.4622095406716,50.5457619840702,50.6292514199212,
50.7127053705349,50.7961418643812,50.8795789741367,50.9630347690544,51.0465792617841,
51.1301683447251,51.2138916122827,51.2945713281782,51.3783100400241,51.4619455513916,
51.5454979947902,51.6289874306412,51.7124413812548,51.795877875101,51.8793149848565,
51.9627707797741,52.0463152725038,52.1299043554448,52.2136276230024,52.2943073388984,
52.3780542392129,52.4616961110549,52.548417940162,52.6319027033865,52.7153500216485,
52.7987779830063,52.8822046585315,52.9656778285902,53.0491789172906,53.1327580827016,
53.1554707439118),.UNSPECIFIED.);
#1726=B_SPLINE_CURVE_WITH_KNOTS('',3,(#207781,#207782,#207783,#207784,#207785,
#207786,#207787,#207788,#207789,#207790,#207791,#207792,#207793,#207794,
#207795,#207796,#207797,#207798,#207799,#207800,#207801,#207802,#207803,
#207804,#207805,#207806,#207807,#207808,#207809,#207810,#207811,#207812,
#207813,#207814,#207815,#207816,#207817,#207818,#207819,#207820,#207821,
#207822,#207823,#207824,#207825,#207826,#207827,#207828,#207829,#207830,
#207831,#207832,#207833,#207834,#207835,#207836,#207837,#207838,#207839,
#207840,#207841,#207842,#207843,#207844,#207845,#207846,#207847,#207848,
#207849,#207850,#207851,#207852,#207853,#207854,#207855,#207856,#207857,
#207858,#207859,#207860,#207861,#207862,#207863,#207864,#207865,#207866,
#207867,#207868,#207869,#207870,#207871,#207872,#207873,#207874,#207875,
#207876,#207877,#207878,#207879,#207880,#207881,#207882,#207883,#207884,
#207885,#207886,#207887,#207888,#207889,#207890,#207891,#207892,#207893,
#207894,#207895,#207896,#207897,#207898,#207899,#207900,#207901,#207902,
#207903,#207904,#207905,#207906,#207907,#207908,#207909,#207910,#207911,
#207912,#207913,#207914,#207915,#207916,#207917,#207918,#207919,#207920,
#207921,#207922,#207923,#207924,#207925,#207926,#207927,#207928,#207929,
#207930,#207931,#207932,#207933,#207934,#207935,#207936,#207937,#207938,
#207939,#207940,#207941,#207942,#207943,#207944,#207945,#207946,#207947,
#207948,#207949,#207950,#207951,#207952,#207953,#207954,#207955,#207956,
#207957,#207958,#207959,#207960,#207961,#207962,#207963,#207964,#207965,
#207966,#207967,#207968,#207969,#207970,#207971,#207972,#207973,#207974,
#207975,#207976,#207977,#207978,#207979,#207980,#207981,#207982,#207983,
#207984,#207985,#207986,#207987,#207988,#207989,#207990,#207991,#207992,
#207993,#207994,#207995,#207996,#207997,#207998,#207999,#208000),
 .UNSPECIFIED.,.F.,.F.,(4,3,3,3,3,3,3,3,3,3,3,3,3,3,3,3,3,3,3,3,3,3,3,3,
3,3,3,3,3,3,3,3,3,3,3,3,3,3,3,3,3,3,3,3,3,3,3,3,3,3,3,3,3,3,3,3,3,3,3,3,
3,3,3,3,3,3,3,3,3,3,3,3,3,4),(47.123889804,47.2119695169777,47.3001901238871,
47.3886427955167,47.4772210930821,47.5660058086749,47.6059179050124,47.6896566168586,
47.7732921282264,47.8568445716251,47.9403340074762,48.0237879580902,48.1072244519367,
48.1906615616924,48.2741173566102,48.3576618493402,48.4412509322814,48.5249741998393,
48.6056539157326,48.6893926275784,48.7730281389457,48.8565805823441,48.940070018195,
49.0235239688085,49.1069604626546,49.1903975724099,49.2738533673274,49.3573978600569,
49.4409869429977,49.5247102105551,49.6053899264527,49.6891286382987,49.7727641496662,
49.8563165930648,49.9398060289159,50.0232599795296,50.1066964733759,50.1901335831314,
50.2735893780492,50.3571338707789,50.4407229537199,50.5244462212776,50.6051259371728,
50.6888646490187,50.7725001603863,50.8560526037849,50.9395420396359,51.0229959902495,
51.1064324840958,51.1898695938513,51.273325388769,51.3568698814987,51.4404589644397,
51.5241822319973,51.604861947893,51.688600659739,51.7722361711065,51.8557886145051,
51.939278050356,52.0227320009698,52.1061684948161,52.1896056045716,52.2730613994893,
52.356605892219,52.44019497516,52.5239182427177,52.6045979586131,52.6871060320478,
52.7695180670308,52.8518532668798,52.934128908709,53.0163690882775,53.0986070875677,
53.1554762266557),.UNSPECIFIED.);
#1727=B_SPLINE_CURVE_WITH_KNOTS('',3,(#208001,#208002,#208003,#208004,#208005,
#208006,#208007,#208008,#208009,#208010),.UNSPECIFIED.,.F.,.F.,(4,3,3,4),
(46.873531912371,46.960478001365,47.047291421921,47.1238898038316),
 .UNSPECIFIED.);
#1728=B_SPLINE_CURVE_WITH_KNOTS('',3,(#208016,#208017,#208018,#208019,#208020,
#208021,#208022,#208023,#208024,#208025),.UNSPECIFIED.,.F.,.F.,(4,3,3,4),
(40.5902857429648,40.6763925853647,40.7624026469278,40.8407044966482),
 .UNSPECIFIED.);
#1729=B_SPLINE_CURVE_WITH_KNOTS('',3,(#208026,#208027,#208028,#208029,#208030,
#208031,#208032,#208033,#208034,#208035,#208036,#208037,#208038,#208039,
#208040,#208041,#208042,#208043,#208044,#208045,#208046,#208047,#208048,
#208049,#208050,#208051,#208052,#208053,#208054,#208055,#208056,#208057,
#208058,#208059,#208060,#208061,#208062,#208063,#208064,#208065,#208066,
#208067,#208068,#208069,#208070,#208071,#208072,#208073,#208074,#208075,
#208076,#208077,#208078,#208079,#208080,#208081,#208082,#208083,#208084,
#208085,#208086,#208087,#208088,#208089,#208090,#208091,#208092,#208093,
#208094,#208095,#208096,#208097,#208098,#208099,#208100,#208101,#208102,
#208103,#208104,#208105,#208106,#208107,#208108,#208109,#208110,#208111,
#208112,#208113,#208114,#208115,#208116,#208117,#208118,#208119,#208120,
#208121,#208122,#208123,#208124,#208125,#208126,#208127,#208128,#208129,
#208130,#208131,#208132,#208133,#208134,#208135,#208136,#208137,#208138,
#208139,#208140,#208141,#208142,#208143,#208144,#208145,#208146,#208147,
#208148,#208149,#208150,#208151,#208152,#208153,#208154,#208155,#208156,
#208157,#208158,#208159,#208160,#208161,#208162,#208163,#208164,#208165,
#208166,#208167,#208168,#208169,#208170,#208171,#208172,#208173,#208174,
#208175,#208176,#208177,#208178,#208179,#208180,#208181,#208182,#208183,
#208184,#208185,#208186,#208187,#208188,#208189,#208190,#208191,#208192,
#208193,#208194,#208195,#208196,#208197,#208198,#208199,#208200,#208201,
#208202,#208203,#208204,#208205,#208206,#208207,#208208,#208209,#208210,
#208211,#208212,#208213,#208214,#208215,#208216,#208217,#208218,#208219,
#208220,#208221,#208222,#208223,#208224,#208225,#208226,#208227,#208228,
#208229,#208230,#208231,#208232,#208233,#208234,#208235,#208236,#208237,
#208238,#208239,#208240,#208241,#208242),.UNSPECIFIED.,.F.,.F.,(4,3,3,3,
3,3,3,3,3,3,3,3,3,3,3,3,3,3,3,3,3,3,3,3,3,3,3,3,3,3,3,3,3,3,3,3,3,3,3,3,
3,3,3,3,3,3,3,3,3,3,3,3,3,3,3,3,3,3,3,3,3,3,3,3,3,3,3,3,3,3,3,3,4),(40.8407044968307,
40.9298601171088,41.0216978930758,41.1113188688309,41.2042650449039,41.2972112209769,
41.3809499328246,41.4645854441938,41.5481378875942,41.631627323447,41.7150812740625,
41.7985177679105,41.8819548776678,41.9654106725873,42.0489551653189,42.1325442482617,
42.2162675158211,42.2969472316971,42.3806859435423,42.4643214549091,42.547873898307,
42.6313633341573,42.7148172847703,42.7982537786158,42.8816908883705,42.9651466832875,
43.0486911760164,43.1322802589567,43.2160035265135,43.2966832424172,43.380421954263,
43.4640574656304,43.5476099090288,43.6310993448798,43.7145532954933,43.7979897893395,
43.8814268990948,43.9648826940124,44.0484271867419,44.1320162696828,44.2157395372403,
44.2964192531373,44.3801579649835,44.4637934763512,44.54734591975,44.6308353556013,
44.7142893062153,44.7977258000618,44.8811629098175,44.9646187047355,45.0481631974655,
45.1317522804067,45.2154755479646,45.2961552638575,45.3798939757033,45.4635294870707,
45.5470819304692,45.6305713663201,45.7140253169337,45.7974618107799,45.8808989205352,
45.9643547154527,46.0478992081823,46.1314882911231,46.2152115586806,46.2958912745776,
46.3783624320973,46.4607382036819,46.5430378108789,46.625328127725,46.7075361957602,
46.7898676370116,46.872199078263),.UNSPECIFIED.);
#1730=B_SPLINE_CURVE_WITH_KNOTS('',3,(#208244,#208245,#208246,#208247,#208248,
#208249,#208250,#208251,#208252,#208253,#208254,#208255,#208256,#208257,
#208258,#208259,#208260,#208261,#208262,#208263,#208264,#208265,#208266,
#208267,#208268,#208269,#208270,#208271,#208272,#208273,#208274,#208275,
#208276,#208277,#208278,#208279,#208280,#208281,#208282,#208283,#208284,
#208285,#208286,#208287,#208288,#208289,#208290,#208291,#208292,#208293,
#208294,#208295,#208296,#208297,#208298,#208299,#208300,#208301,#208302,
#208303,#208304,#208305,#208306,#208307,#208308,#208309,#208310,#208311,
#208312,#208313,#208314,#208315,#208316,#208317,#208318,#208319,#208320,
#208321,#208322,#208323,#208324,#208325,#208326,#208327,#208328,#208329,
#208330,#208331,#208332,#208333,#208334,#208335,#208336,#208337,#208338,
#208339,#208340,#208341,#208342,#208343,#208344,#208345,#208346,#208347,
#208348,#208349,#208350,#208351,#208352,#208353,#208354,#208355,#208356,
#208357,#208358,#208359,#208360,#208361,#208362,#208363,#208364,#208365,
#208366,#208367,#208368,#208369,#208370,#208371,#208372,#208373,#208374,
#208375,#208376,#208377,#208378,#208379,#208380,#208381,#208382,#208383,
#208384,#208385,#208386,#208387,#208388,#208389,#208390,#208391,#208392,
#208393,#208394,#208395,#208396,#208397,#208398,#208399,#208400,#208401,
#208402,#208403,#208404,#208405,#208406,#208407,#208408,#208409,#208410,
#208411,#208412,#208413,#208414,#208415,#208416,#208417,#208418,#208419,
#208420,#208421,#208422,#208423,#208424,#208425,#208426,#208427,#208428,
#208429,#208430,#208431,#208432,#208433,#208434,#208435,#208436,#208437,
#208438,#208439,#208440,#208441,#208442,#208443,#208444,#208445,#208446,
#208447,#208448,#208449,#208450,#208451,#208452,#208453,#208454,#208455,
#208456,#208457,#208458,#208459,#208460,#208461,#208462,#208463),
 .UNSPECIFIED.,.F.,.F.,(4,3,3,3,3,3,3,3,3,3,3,3,3,3,3,3,3,3,3,3,3,3,3,3,
3,3,3,3,3,3,3,3,3,3,3,3,3,3,3,3,3,3,3,3,3,3,3,3,3,3,3,3,3,3,3,3,3,3,3,3,
3,3,3,3,3,3,3,3,3,3,3,3,3,4),(40.840704496652,40.9231791511788,41.0087194873679,
41.0911052472321,41.1734797508196,41.2558619211434,41.3382706848019,41.4207689799329,
41.5033205891009,41.5859878354084,41.6075018406916,41.6912405525498,41.7748760639297,
41.8584285073409,41.9419179432047,42.0253718938312,42.1088083876904,42.1922454974588,
42.2757012923896,42.3592457851324,42.4428348680864,42.526558135657,42.6072378514118,
42.6909765632536,42.7746120746171,42.8581645180118,42.9416539538587,43.0251079044681,
43.1085443983101,43.1919815080613,43.2754373029746,43.3589817957001,43.4425708786367,
43.5262941461901,43.6069738621319,43.6907125739767,43.774348085343,43.8579005287403,
43.9413899645904,44.0248439152029,44.1082804090481,44.1917175188026,44.2751733137188,
44.3587178064472,44.442306889387,44.5260301569433,44.606709872852,44.6904485846998,
44.7740840960691,44.8576365394695,44.9411259753222,45.0245799259379,45.1080164197859,
45.191453529543,45.2749093244626,45.3584538171943,45.4420429001373,45.5257661676968,
45.6064458835722,45.6901845954174,45.7738201067842,45.8573725501822,45.9408619860327,
46.0243159366455,46.1077524304912,46.1911895402463,46.2746453351632,46.3581898278923,
46.4417789108326,46.5255021783895,46.6061818942923,46.6935617353949,46.7835468238829,
46.873531912371),.UNSPECIFIED.);
#1731=B_SPLINE_CURVE_WITH_KNOTS('',3,(#208464,#208465,#208466,#208467,#208468,
#208469,#208470,#208471,#208472,#208473,#208474,#208475,#208476),
 .UNSPECIFIED.,.F.,.F.,(4,3,3,3,4),(40.5895313989693,40.6077658299715,40.7242351632557,
40.8344463524574,40.8407044965399),.UNSPECIFIED.);
#1732=B_SPLINE_CURVE_WITH_KNOTS('',3,(#208482,#208483,#208484,#208485,#208486,
#208487,#208488,#208489,#208490,#208491),.UNSPECIFIED.,.F.,.F.,(4,3,3,4),
(34.3065000825424,34.4146795617861,34.5207421559751,34.557519189341),
 .UNSPECIFIED.);
#1733=B_SPLINE_CURVE_WITH_KNOTS('',3,(#208492,#208493,#208494,#208495,#208496,
#208497,#208498,#208499,#208500,#208501,#208502,#208503,#208504,#208505,
#208506,#208507,#208508,#208509,#208510,#208511,#208512,#208513,#208514,
#208515,#208516,#208517,#208518,#208519,#208520,#208521,#208522,#208523,
#208524,#208525,#208526,#208527,#208528,#208529,#208530,#208531,#208532,
#208533,#208534,#208535,#208536,#208537,#208538,#208539,#208540,#208541,
#208542,#208543,#208544,#208545,#208546,#208547,#208548,#208549,#208550,
#208551,#208552,#208553,#208554,#208555,#208556,#208557,#208558,#208559,
#208560,#208561,#208562,#208563,#208564,#208565,#208566,#208567,#208568,
#208569,#208570,#208571,#208572,#208573,#208574,#208575,#208576,#208577,
#208578,#208579,#208580,#208581,#208582,#208583,#208584,#208585,#208586,
#208587,#208588,#208589,#208590,#208591,#208592,#208593,#208594,#208595,
#208596,#208597,#208598,#208599,#208600,#208601,#208602,#208603,#208604,
#208605,#208606,#208607,#208608,#208609,#208610,#208611,#208612,#208613,
#208614,#208615,#208616,#208617,#208618,#208619,#208620,#208621,#208622,
#208623,#208624,#208625,#208626,#208627,#208628,#208629,#208630,#208631,
#208632,#208633,#208634,#208635,#208636,#208637,#208638,#208639,#208640,
#208641,#208642,#208643,#208644,#208645,#208646,#208647,#208648,#208649,
#208650,#208651,#208652,#208653,#208654,#208655,#208656,#208657,#208658,
#208659,#208660,#208661,#208662,#208663,#208664,#208665,#208666,#208667,
#208668,#208669,#208670,#208671,#208672,#208673,#208674,#208675,#208676,
#208677,#208678,#208679,#208680,#208681,#208682,#208683,#208684,#208685,
#208686,#208687,#208688,#208689,#208690,#208691,#208692,#208693,#208694,
#208695,#208696,#208697,#208698,#208699,#208700,#208701,#208702,#208703,
#208704,#208705,#208706,#208707,#208708,#208709,#208710,#208711),
 .UNSPECIFIED.,.F.,.F.,(4,3,3,3,3,3,3,3,3,3,3,3,3,3,3,3,3,3,3,3,3,3,3,3,
3,3,3,3,3,3,3,3,3,3,3,3,3,3,3,3,3,3,3,3,3,3,3,3,3,3,3,3,3,3,3,3,3,3,3,3,
3,3,3,3,3,3,3,3,3,3,3,3,3,4),(34.5575191894685,34.6401346660436,34.7227049790521,
34.8052521817043,34.8877950853622,34.9703524953451,35.0529944964819,35.1356787053279,
35.2184958070966,35.2987951566562,35.3825338685851,35.4661693800365,35.5497218235198,
35.6332112594563,35.7166652101566,35.8001017040901,35.8835388139334,35.9669946089394,
36.0505391017574,36.134128184787,36.2178514524327,36.2985311673763,36.3822698791994,
36.465905390544,36.5494578339196,36.6329472697474,36.7164012203379,36.7998377141608,
36.8832748238929,36.9667306187873,37.0502751114939,37.1338641944118,37.2175874619467,
37.2982671780964,37.3820058899321,37.4656414012895,37.5491938446774,37.632683280518,
37.7161372311207,37.7995737249558,37.8830108347001,37.9664666296065,38.0500111223246,
38.1336002052539,38.2173234727998,38.2980031888166,38.3817419006748,38.4653774120547,
38.548929855466,38.6324192913301,38.7158732419566,38.7993097358158,38.8827468455844,
38.9662026405151,39.049747133258,39.133336216212,39.2170594837827,39.2977391995367,
39.3814779113784,39.4651134227418,39.5486658661357,39.6321553019831,39.7156092525924,
39.7990457464345,39.8824828561857,39.9659386510992,40.0494831438246,40.1330722267613,
40.2167954943148,40.2974752102568,40.3839889562121,40.4703860712489,40.5566452121474,
40.5902857429648),.UNSPECIFIED.);
#1734=B_SPLINE_CURVE_WITH_KNOTS('',3,(#208713,#208714,#208715,#208716,#208717,
#208718,#208719,#208720,#208721,#208722,#208723,#208724,#208725,#208726,
#208727,#208728,#208729,#208730,#208731,#208732,#208733,#208734,#208735,
#208736,#208737,#208738,#208739,#208740,#208741,#208742,#208743,#208744,
#208745,#208746,#208747,#208748,#208749,#208750,#208751,#208752,#208753,
#208754,#208755,#208756,#208757,#208758,#208759,#208760,#208761,#208762,
#208763,#208764,#208765,#208766,#208767,#208768,#208769,#208770,#208771,
#208772,#208773,#208774,#208775,#208776,#208777,#208778,#208779,#208780,
#208781,#208782,#208783,#208784,#208785,#208786,#208787,#208788,#208789,
#208790,#208791,#208792,#208793,#208794,#208795,#208796,#208797,#208798,
#208799,#208800,#208801,#208802,#208803,#208804,#208805,#208806,#208807,
#208808,#208809,#208810,#208811,#208812,#208813,#208814,#208815,#208816,
#208817,#208818,#208819,#208820,#208821,#208822,#208823,#208824,#208825,
#208826,#208827,#208828,#208829,#208830,#208831,#208832,#208833,#208834,
#208835,#208836,#208837,#208838,#208839,#208840,#208841,#208842,#208843,
#208844,#208845,#208846,#208847,#208848,#208849,#208850,#208851,#208852,
#208853,#208854,#208855,#208856,#208857,#208858,#208859,#208860,#208861,
#208862,#208863,#208864,#208865,#208866,#208867,#208868,#208869,#208870,
#208871,#208872,#208873,#208874,#208875,#208876,#208877,#208878,#208879,
#208880,#208881,#208882,#208883,#208884,#208885,#208886,#208887,#208888,
#208889,#208890,#208891,#208892,#208893,#208894,#208895,#208896,#208897,
#208898,#208899,#208900,#208901,#208902,#208903,#208904,#208905,#208906,
#208907,#208908,#208909,#208910,#208911,#208912,#208913,#208914,#208915,
#208916,#208917,#208918,#208919,#208920,#208921,#208922,#208923,#208924,
#208925,#208926,#208927,#208928,#208929,#208930,#208931,#208932),
 .UNSPECIFIED.,.F.,.F.,(4,3,3,3,3,3,3,3,3,3,3,3,3,3,3,3,3,3,3,3,3,3,3,3,
3,3,3,3,3,3,3,3,3,3,3,3,3,3,3,3,3,3,3,3,3,3,3,3,3,3,3,3,3,3,3,3,3,3,3,3,
3,3,3,3,3,3,3,3,3,3,3,3,3,4),(34.5575191894724,34.6093497656507,34.6930884767872,
34.7767239874333,34.8602764300995,34.9437658652082,35.0272198150664,35.1106563081493,
35.1940934171344,35.2775492112753,35.3610937032224,35.4446827853765,35.5284060521475,
35.6090857763709,35.6928244887674,35.776460000692,35.8600124446535,35.9435018810726,
36.0269558322605,36.1103923266845,36.1938294370208,36.2772852325218,36.3608297258354,
36.4444188093616,36.5281420775006,36.608821787091,36.6925604988207,36.7761960100715,
36.8597484533532,36.9432378890873,37.0266918395841,37.1101283333137,37.1935654429527,
37.2770212377544,37.3605657303692,37.4441548131959,37.5278780806412,37.6085577978111,
37.6922965095691,37.7759320208472,37.8594844641547,37.9429738999134,38.0264278504329,
38.1098643441839,38.1933014538431,38.2767572486637,38.3603017412953,38.4438908241376,
38.5276140915964,38.6082938085313,38.6920325204602,38.7756680319116,38.859220475395,
38.9427099113317,39.026163862032,39.1096003559656,39.1930374658088,39.2764932608146,
39.3600377536327,39.4436268366622,39.5273501043079,39.6080298192514,39.6917695595991,
39.7754058589717,39.8589588508911,39.9424485965472,40.0259016212374,40.109336849158,
40.1927723527529,40.2762262007468,40.3597640184065,40.4433462857643,40.5270516189311,
40.5895313989693),.UNSPECIFIED.);
#1735=B_SPLINE_CURVE_WITH_KNOTS('',3,(#208933,#208934,#208935,#208936,#208937,
#208938,#208939,#208940,#208941,#208942),.UNSPECIFIED.,.F.,.F.,(4,3,3,4),
(34.3057109399742,34.3886262459297,34.4730727175991,34.5575191892685),
 .UNSPECIFIED.);
#1736=B_SPLINE_CURVE_WITH_KNOTS('',3,(#208948,#208949,#208950,#208951,#208952,
#208953,#208954,#208955,#208956,#208957),.UNSPECIFIED.,.F.,.F.,(4,3,3,4),
(28.0225858316167,28.1058018123903,28.1900678472803,28.2743338821704),
 .UNSPECIFIED.);
#1737=B_SPLINE_CURVE_WITH_KNOTS('',3,(#208958,#208959,#208960,#208961,#208962,
#208963,#208964,#208965,#208966,#208967,#208968,#208969,#208970,#208971,
#208972,#208973,#208974,#208975,#208976,#208977,#208978,#208979,#208980,
#208981,#208982,#208983,#208984,#208985,#208986,#208987,#208988,#208989,
#208990,#208991,#208992,#208993,#208994,#208995,#208996,#208997,#208998,
#208999,#209000,#209001,#209002,#209003,#209004,#209005,#209006,#209007,
#209008,#209009,#209010,#209011,#209012,#209013,#209014,#209015,#209016,
#209017,#209018,#209019,#209020,#209021,#209022,#209023,#209024,#209025,
#209026,#209027,#209028,#209029,#209030,#209031,#209032,#209033,#209034,
#209035,#209036,#209037,#209038,#209039,#209040,#209041,#209042,#209043,
#209044,#209045,#209046,#209047,#209048,#209049,#209050,#209051,#209052,
#209053,#209054,#209055,#209056,#209057,#209058,#209059,#209060,#209061,
#209062,#209063,#209064,#209065,#209066,#209067,#209068,#209069,#209070,
#209071,#209072,#209073,#209074,#209075,#209076,#209077,#209078,#209079,
#209080,#209081,#209082,#209083,#209084,#209085,#209086,#209087,#209088,
#209089,#209090,#209091,#209092,#209093,#209094,#209095,#209096,#209097,
#209098,#209099,#209100,#209101,#209102,#209103,#209104,#209105,#209106,
#209107,#209108,#209109,#209110,#209111,#209112,#209113,#209114,#209115,
#209116,#209117,#209118,#209119,#209120,#209121,#209122,#209123,#209124,
#209125,#209126,#209127,#209128,#209129,#209130,#209131,#209132,#209133,
#209134,#209135,#209136,#209137,#209138,#209139,#209140,#209141,#209142,
#209143,#209144,#209145,#209146,#209147,#209148,#209149,#209150,#209151,
#209152,#209153,#209154,#209155,#209156,#209157,#209158,#209159,#209160,
#209161,#209162,#209163,#209164,#209165,#209166,#209167,#209168,#209169,
#209170,#209171,#209172,#209173,#209174,#209175,#209176,#209177,#209178,
#209179,#209180),.UNSPECIFIED.,.F.,.F.,(4,3,3,3,3,3,3,3,3,3,3,3,3,3,3,3,
3,3,3,3,3,3,3,3,3,3,3,3,3,3,3,3,3,3,3,3,3,3,3,3,3,3,3,3,3,3,3,3,3,3,3,3,
3,3,3,3,3,3,3,3,3,3,3,3,3,3,3,3,3,3,3,3,3,3,4),(28.2743338822889,28.3006430816153,
28.3843817879882,28.468017293797,28.5515697315575,28.6350591616976,28.7185131065089,
28.8019495944981,28.8853866983471,28.9688424873144,29.0523869740573,29.1359760509821,
29.2196993125341,29.3003790923354,29.3841178077619,29.4677533227502,29.5513057698054,
29.6347952093454,29.7182491636837,29.801685661276,29.8851227747951,29.9685785734908,
30.0521230699997,30.1357121567266,30.2194354280432,30.3001151030555,30.3838538143865,
30.4674893252401,30.5510417681263,30.6345312034672,30.7179851535757,30.80142164692,
30.8848587561773,30.9683145506009,31.051859042846,31.1354481253068,31.2191713923966,
31.2998511137757,31.3835898249122,31.4672253355584,31.5507777782246,31.6342672133331,
31.7177211631913,31.8011576562743,31.8845947652594,31.9680505594003,32.0515950513474,
32.1351841335015,32.2189074002725,32.2995871244958,32.3833258368923,32.466961348817,
32.5505137927785,32.6340032291978,32.7174571803857,32.8008936748098,32.884330785146,
32.967786580647,33.0513310739606,33.1349201574868,33.2186434256259,33.2993231352159,
33.3830618469456,33.4666973581966,33.5502498014783,33.6337392372124,33.7171931877092,
33.8006296814388,33.8840667910778,33.9675225858795,34.0510670784944,34.1346561613211,
34.2183794287664,34.299059145936,34.3065000825424),.UNSPECIFIED.);
#1738=B_SPLINE_CURVE_WITH_KNOTS('',3,(#209182,#209183,#209184,#209185,#209186,
#209187,#209188,#209189,#209190,#209191,#209192,#209193,#209194,#209195,
#209196,#209197,#209198,#209199,#209200,#209201,#209202,#209203,#209204,
#209205,#209206,#209207,#209208,#209209,#209210,#209211,#209212,#209213,
#209214,#209215,#209216,#209217,#209218,#209219,#209220,#209221,#209222,
#209223,#209224,#209225,#209226,#209227,#209228,#209229,#209230,#209231,
#209232,#209233,#209234,#209235,#209236,#209237,#209238,#209239,#209240,
#209241,#209242,#209243,#209244,#209245,#209246,#209247,#209248,#209249,
#209250,#209251,#209252,#209253,#209254,#209255,#209256,#209257,#209258,
#209259,#209260,#209261,#209262,#209263,#209264,#209265,#209266,#209267,
#209268,#209269,#209270,#209271,#209272,#209273,#209274,#209275,#209276,
#209277,#209278,#209279,#209280,#209281,#209282,#209283,#209284,#209285,
#209286,#209287,#209288,#209289,#209290,#209291,#209292,#209293,#209294,
#209295,#209296,#209297,#209298,#209299,#209300,#209301,#209302,#209303,
#209304,#209305,#209306,#209307,#209308,#209309,#209310,#209311,#209312,
#209313,#209314,#209315,#209316,#209317,#209318,#209319,#209320,#209321,
#209322,#209323,#209324,#209325,#209326,#209327,#209328,#209329,#209330,
#209331,#209332,#209333,#209334,#209335,#209336,#209337,#209338,#209339,
#209340,#209341,#209342,#209343,#209344,#209345,#209346,#209347,#209348,
#209349,#209350,#209351,#209352,#209353,#209354,#209355,#209356,#209357,
#209358,#209359,#209360,#209361,#209362,#209363,#209364,#209365,#209366,
#209367,#209368,#209369,#209370,#209371,#209372,#209373,#209374,#209375,
#209376,#209377,#209378,#209379,#209380,#209381,#209382,#209383,#209384,
#209385,#209386,#209387,#209388,#209389,#209390,#209391,#209392,#209393,
#209394,#209395,#209396,#209397,#209398,#209399,#209400,#209401),
 .UNSPECIFIED.,.F.,.F.,(4,3,3,3,3,3,3,3,3,3,3,3,3,3,3,3,3,3,3,3,3,3,3,3,
3,3,3,3,3,3,3,3,3,3,3,3,3,3,3,3,3,3,3,3,3,3,3,3,3,3,3,3,3,3,3,3,3,3,3,3,
3,3,3,3,3,3,3,3,3,3,3,3,3,4),(28.2743338824827,28.3712824055307,28.4687879362423,
28.5669577034657,28.6109337013299,28.6946723723872,28.7783078423616,28.8618602438099,
28.9453496371999,29.0288035447238,29.1122399951033,29.1956770610554,29.2791328118729,
29.3626772602797,29.4462662987062,29.5299895218703,29.6106697120501,29.6944084466627,
29.7780439810379,29.8615964476591,29.9450859069223,30.0285398811537,30.1119763987395,
30.1954135323339,30.2788693511678,30.362413867801,30.4460029746765,30.5297262659791,
30.6104057227702,30.694144433022,30.777779942827,30.8613323846962,30.9448218190526,
31.0282757682304,31.1117122606767,31.1951493690697,31.2786051626639,31.3621496541399,
31.4457387358632,31.5294620022777,31.6101417334903,31.6938804398633,31.7775159456722,
31.8610683834328,31.9445578135729,32.0280117583843,32.1114482463736,32.1948853502228,
32.2783411391901,32.3618856259331,32.4454747028581,32.5291979644102,32.6098777442105,
32.693616459637,32.7772519746252,32.8608044216806,32.9442938612206,33.0277478155589,
33.1111843131511,33.1946214266703,33.2780772253658,33.3616217218747,33.4452108086016,
33.5289340799181,33.6096137549306,33.696625903061,33.7795858721787,33.8624709514653,
33.9452998737482,34.0280913257695,34.1108784301918,34.1936633276373,34.2764866832596,
34.3057109399742),.UNSPECIFIED.);
#1739=B_SPLINE_CURVE_WITH_KNOTS('',3,(#209402,#209403,#209404,#209405,#209406,
#209407,#209408,#209409,#209410,#209411),.UNSPECIFIED.,.F.,.F.,(4,3,3,4),
(28.0234162092491,28.1068355155373,28.190584698915,28.2743338822928),
 .UNSPECIFIED.);
#1740=B_SPLINE_CURVE_WITH_KNOTS('',3,(#209417,#209418,#209419,#209420,#209421,
#209422,#209423,#209424,#209425,#209426,#209427,#209428,#209429,#209430,
#209431,#209432,#209433,#209434,#209435,#209436,#209437,#209438,#209439,
#209440,#209441,#209442,#209443,#209444,#209445,#209446,#209447),
 .UNSPECIFIED.,.F.,.F.,(4,3,3,3,3,3,3,3,3,3,4),(20.99221161231,21.0756590159651,
21.1590986605133,21.2425486105237,21.3260269334585,21.4095983367567,21.4932230327364,
21.5769691760559,21.612781626289,21.7074539497444,21.740715980233),
 .UNSPECIFIED.);
#1741=B_SPLINE_CURVE_WITH_KNOTS('',3,(#209449,#209450,#209451,#209452,#209453,
#209454),.UNSPECIFIED.,.F.,.F.,(4,2,4),(0.0691804534626763,0.186754252104775,
0.270033766278533),.UNSPECIFIED.);
#1742=B_SPLINE_CURVE_WITH_KNOTS('',3,(#209455,#209456,#209457,#209458,#209459,
#209460,#209461,#209462,#209463,#209464,#209465,#209466,#209467,#209468,
#209469,#209470,#209471,#209472,#209473,#209474,#209475,#209476,#209477,
#209478,#209479,#209480,#209481,#209482,#209483,#209484,#209485,#209486,
#209487,#209488,#209489,#209490,#209491,#209492,#209493,#209494,#209495,
#209496,#209497,#209498,#209499,#209500),.UNSPECIFIED.,.F.,.F.,(4,3,3,3,
3,3,3,3,3,3,3,3,3,3,3,4),(20.5644249259299,20.6479085815111,20.731360149683,
20.8147965890331,20.8982359703094,20.9816963623492,21.0652465555357,21.1488434281147,
21.2325713349974,21.3024910065744,21.3858830961901,21.4691722628339,21.5523598572504,
21.6354890394005,21.718573857478,21.7400988072349),.UNSPECIFIED.);
#1743=B_SPLINE_CURVE_WITH_KNOTS('',3,(#216282,#216283,#216284,#216285,#216286,
#216287,#216288,#216289,#216290,#216291),.UNSPECIFIED.,.F.,.F.,(4,2,2,2,
4),(0.000592050309002955,0.00995120211491283,0.0520685380789643,0.0963518572333416,
0.180104991815336),.UNSPECIFIED.);
#1744=B_SPLINE_CURVE_WITH_KNOTS('',3,(#216293,#216294,#216295,#216296,#216297,
#216298,#216299,#216300,#216301),.UNSPECIFIED.,.F.,.F.,(4,1,1,1,1,1,4),
(-115.221526233207,-114.969641232815,-113.969905222095,-112.970169211375,
-111.970433200655,-110.970697189935,-110.906691970895),.UNSPECIFIED.);
#1745=B_SPLINE_CURVE_WITH_KNOTS('',3,(#216303,#216304,#216305,#216306,#216307,
#216308,#216309,#216310,#216311,#216312,#216313,#216314,#216315,#216316,
#216317,#216318,#216319,#216320,#216321,#216322,#216323,#216324,#216325,
#216326,#216327,#216328,#216329,#216330,#216331,#216332,#216333,#216334,
#216335,#216336,#216337,#216338,#216339,#216340,#216341,#216342,#216343,
#216344,#216345,#216346,#216347,#216348,#216349,#216350,#216351,#216352,
#216353,#216354,#216355,#216356,#216357,#216358,#216359,#216360,#216361,
#216362,#216363,#216364,#216365,#216366,#216367,#216368,#216369,#216370,
#216371,#216372,#216373,#216374,#216375,#216376,#216377,#216378,#216379,
#216380,#216381,#216382,#216383,#216384,#216385,#216386,#216387,#216388,
#216389,#216390,#216391,#216392,#216393,#216394,#216395,#216396,#216397,
#216398,#216399,#216400,#216401,#216402,#216403,#216404,#216405,#216406,
#216407,#216408,#216409,#216410,#216411,#216412,#216413,#216414,#216415,
#216416,#216417,#216418,#216419,#216420,#216421,#216422,#216423,#216424,
#216425,#216426,#216427,#216428,#216429,#216430,#216431,#216432,#216433,
#216434,#216435,#216436,#216437,#216438,#216439,#216440,#216441,#216442,
#216443,#216444,#216445,#216446,#216447,#216448,#216449,#216450,#216451,
#216452,#216453,#216454,#216455,#216456,#216457,#216458,#216459,#216460,
#216461,#216462,#216463,#216464,#216465,#216466,#216467,#216468,#216469,
#216470,#216471,#216472,#216473,#216474,#216475,#216476,#216477,#216478,
#216479,#216480,#216481,#216482,#216483,#216484,#216485,#216486,#216487,
#216488,#216489,#216490,#216491,#216492,#216493,#216494,#216495,#216496,
#216497,#216498,#216499,#216500,#216501,#216502,#216503,#216504,#216505,
#216506,#216507,#216508,#216509,#216510,#216511,#216512,#216513,#216514,
#216515,#216516,#216517,#216518,#216519,#216520,#216521,#216522,#216523,
#216524,#216525,#216526,#216527,#216528,#216529,#216530,#216531,#216532,
#216533,#216534,#216535,#216536,#216537,#216538,#216539,#216540,#216541,
#216542,#216543,#216544,#216545,#216546),.UNSPECIFIED.,.F.,.F.,(4,3,3,3,
3,3,3,3,3,3,3,3,3,3,3,3,3,3,3,3,3,3,3,3,3,3,3,3,3,3,3,3,3,3,3,3,3,3,3,3,
3,3,3,3,3,3,3,3,3,3,3,3,3,3,3,3,3,3,3,3,3,3,3,3,3,3,3,3,3,3,3,3,3,3,3,3,
3,3,3,3,3,4),(-110.906691970895,-110.82749856315,-110.748395230993,-110.669363816888,
-110.590386228964,-110.511436604536,-110.432499965624,-110.35356001131,
-110.27460044075,-110.195558870897,-110.116474582147,-110.037271099244,
-109.970961179214,-109.891003879083,-109.81114108184,-109.731355259369,
-109.651628944173,-109.571944715879,-109.492273729658,-109.412606276133,
-109.332926625316,-109.253219042922,-109.173423813846,-109.093579472138,
-109.013621045091,-108.971225168494,-108.891267868363,-108.81140507112,
-108.731619248648,-108.651892933453,-108.572208705159,-108.492537718938,
-108.412870265412,-108.333190614595,-108.253483032201,-108.173687803125,
-108.093843461418,-108.013885034371,-107.971489157774,-107.891531857643,
-107.8116690604,-107.731883237929,-107.652156922733,-107.572472694439,-107.492801708218,
-107.413134254692,-107.333454603876,-107.253747021481,-107.173951792405,
-107.094107450698,-107.01414902365,-106.971753147054,-106.891795846923,
-106.81193304968,-106.732147227209,-106.652420912013,-106.572736683719,
-106.493065697498,-106.413398243972,-106.333718593156,-106.254011010761,
-106.174215781686,-106.094371439978,-106.014413012931,-105.972017136334,
-105.892059836203,-105.81219703896,-105.732411216489,-105.652684901294,
-105.573000672999,-105.493329686778,-105.413662233252,-105.333982582435,
-105.254275000041,-105.174479770965,-105.094635429257,-105.01467700221,
-104.972281125614,-104.879689190256,-104.787448241979,-104.695893518158,
-104.623506786484),.UNSPECIFIED.);
#1746=B_SPLINE_CURVE_WITH_KNOTS('',3,(#216548,#216549,#216550,#216551,#216552,
#216553,#216554,#216555,#216556,#216557),.UNSPECIFIED.,.F.,.F.,(4,1,1,1,
1,1,1,4),(-104.623506663716,-103.972545114894,-102.972809104174,-101.973073093453,
-100.973337082733,-99.9736010720131,-98.973865061293,-98.340321356536),
 .UNSPECIFIED.);
#1747=B_SPLINE_CURVE_WITH_KNOTS('',3,(#216559,#216560,#216561,#216562,#216563,
#216564,#216565,#216566,#216567,#216568),.UNSPECIFIED.,.F.,.F.,(4,1,1,1,
1,1,1,4),(-98.340321356536,-97.9741290505729,-96.9743930398527,-95.9746570291326,
-94.9749210184124,-93.9751850076923,-92.9754489969722,-92.0571360493564),
 .UNSPECIFIED.);
#1748=B_SPLINE_CURVE_WITH_KNOTS('',3,(#216570,#216571,#216572,#216573,#216574,
#216575,#216576,#216577,#216578,#216579,#216580),.UNSPECIFIED.,.F.,.F.,
(4,1,1,1,1,1,1,1,4),(-92.0571360493564,-91.9757129862521,-90.9759769755319,
-89.9762409648118,-88.9765049540917,-87.9767689433716,-86.9770329326514,
-85.9772969219313,-85.7739507421768),.UNSPECIFIED.);
#1749=B_SPLINE_CURVE_WITH_KNOTS('',3,(#216582,#216583,#216584,#216585,#216586,
#216587,#216588,#216589,#216590,#216591,#216592,#216593,#216594,#216595,
#216596,#216597,#216598,#216599,#216600,#216601,#216602,#216603,#216604,
#216605,#216606,#216607,#216608,#216609,#216610,#216611,#216612,#216613,
#216614,#216615,#216616,#216617,#216618,#216619,#216620,#216621,#216622,
#216623,#216624,#216625,#216626,#216627,#216628,#216629,#216630,#216631,
#216632,#216633,#216634,#216635,#216636,#216637,#216638,#216639,#216640,
#216641,#216642,#216643,#216644,#216645,#216646,#216647,#216648,#216649,
#216650,#216651,#216652,#216653,#216654,#216655,#216656,#216657,#216658,
#216659,#216660,#216661,#216662,#216663,#216664,#216665,#216666,#216667,
#216668,#216669,#216670,#216671,#216672,#216673,#216674,#216675,#216676,
#216677,#216678,#216679,#216680,#216681,#216682,#216683,#216684,#216685,
#216686,#216687,#216688,#216689,#216690,#216691,#216692,#216693,#216694,
#216695,#216696,#216697,#216698,#216699,#216700,#216701,#216702,#216703,
#216704,#216705,#216706,#216707,#216708,#216709,#216710,#216711,#216712,
#216713,#216714,#216715,#216716,#216717,#216718,#216719,#216720,#216721,
#216722,#216723,#216724,#216725,#216726,#216727,#216728,#216729,#216730,
#216731,#216732,#216733,#216734,#216735,#216736,#216737,#216738,#216739,
#216740,#216741,#216742,#216743,#216744,#216745,#216746,#216747,#216748,
#216749,#216750,#216751,#216752,#216753,#216754,#216755,#216756,#216757,
#216758,#216759,#216760,#216761,#216762,#216763,#216764,#216765,#216766,
#216767,#216768,#216769,#216770,#216771,#216772,#216773,#216774,#216775,
#216776,#216777,#216778,#216779,#216780,#216781,#216782,#216783,#216784,
#216785,#216786,#216787,#216788,#216789,#216790,#216791,#216792,#216793,
#216794,#216795,#216796,#216797,#216798,#216799,#216800,#216801,#216802,
#216803,#216804,#216805,#216806,#216807,#216808,#216809,#216810,#216811,
#216812,#216813,#216814,#216815,#216816,#216817,#216818,#216819,#216820,
#216821,#216822,#216823,#216824,#216825),.UNSPECIFIED.,.F.,.F.,(4,3,3,3,
3,3,3,3,3,3,3,3,3,3,3,3,3,3,3,3,3,3,3,3,3,3,3,3,3,3,3,3,3,3,3,3,3,3,3,3,
3,3,3,3,3,3,3,3,3,3,3,3,3,3,3,3,3,3,3,3,3,3,3,3,3,3,3,3,3,3,3,3,3,3,3,3,
3,3,3,3,3,4),(-85.7739507421768,-85.6952881601577,-85.616687997987,-85.53679711214,
-85.4582566003864,-85.379719530466,-85.3011693595009,-85.2202672474284,
-85.1416009943376,-85.0595809527744,-84.9775609112112,-84.89760361108,-84.8177408138373,
-84.7379549913655,-84.6582286761703,-84.5785444478759,-84.498873461655,
-84.419206008129,-84.3395263573124,-84.2598187749181,-84.1800235458425,
-84.1001792041348,-84.0202207770874,-83.977824900491,-83.8978676003597,
-83.8180048031171,-83.7382189806452,-83.6584926654501,-83.5788084371562,
-83.4991374509353,-83.4194699974093,-83.3397903465929,-83.2600827641988,
-83.1802875351232,-83.1004431934156,-83.0204847663682,-82.9780888897709,
-82.8981315896397,-82.8182687923971,-82.7384829699253,-82.65875665473,-82.579072426436,
-82.4994014402152,-82.4197339866892,-82.3400543358726,-82.2603467534779,
-82.1805515244024,-82.1007071826946,-82.0207487556472,-81.9783528790508,
-81.8983955789195,-81.818532781677,-81.7387469592052,-81.65902064401,-81.5793364157154,
-81.4996654294946,-81.4199979759686,-81.3403183251522,-81.2606107427579,
-81.1808155136824,-81.100971171975,-81.0210127449277,-80.9786168683306,
-80.8986595681993,-80.818796770957,-80.7390109484849,-80.6592846332902,
-80.5796004049962,-80.4999294187752,-80.4202619652489,-80.3405823144325,
-80.2608747320383,-80.1810795029628,-80.1012351612554,-80.0212767342081,
-79.9788808576105,-79.894345483959,-79.8099558941397,-79.7257670174106,
-79.6416970903594,-79.5577926852418,-79.4907654351257),.UNSPECIFIED.);
#1750=B_SPLINE_CURVE_WITH_KNOTS('',3,(#216827,#216828,#216829,#216830,#216831,
#216832,#216833,#216834,#216835,#216836,#216837,#216838,#216839,#216840,
#216841,#216842,#216843,#216844,#216845,#216846,#216847,#216848,#216849,
#216850,#216851,#216852,#216853,#216854,#216855,#216856,#216857,#216858,
#216859,#216860,#216861,#216862,#216863,#216864,#216865,#216866,#216867,
#216868,#216869,#216870,#216871,#216872,#216873,#216874,#216875,#216876,
#216877,#216878,#216879,#216880,#216881,#216882,#216883,#216884,#216885,
#216886,#216887,#216888,#216889,#216890,#216891,#216892,#216893,#216894,
#216895,#216896,#216897,#216898,#216899,#216900,#216901,#216902,#216903,
#216904,#216905,#216906,#216907,#216908,#216909,#216910,#216911,#216912,
#216913,#216914,#216915,#216916,#216917,#216918,#216919,#216920,#216921,
#216922,#216923,#216924,#216925,#216926,#216927,#216928,#216929,#216930,
#216931,#216932,#216933,#216934,#216935,#216936,#216937,#216938,#216939,
#216940,#216941,#216942,#216943,#216944,#216945,#216946,#216947,#216948,
#216949,#216950,#216951,#216952,#216953,#216954,#216955,#216956,#216957,
#216958,#216959,#216960,#216961,#216962,#216963,#216964,#216965,#216966,
#216967,#216968,#216969,#216970,#216971,#216972,#216973,#216974,#216975,
#216976,#216977,#216978,#216979,#216980,#216981,#216982,#216983,#216984,
#216985,#216986,#216987,#216988,#216989,#216990,#216991,#216992,#216993,
#216994,#216995,#216996,#216997,#216998,#216999,#217000,#217001,#217002,
#217003,#217004,#217005,#217006,#217007,#217008,#217009,#217010,#217011,
#217012,#217013,#217014,#217015,#217016,#217017,#217018,#217019,#217020,
#217021,#217022,#217023,#217024,#217025,#217026,#217027,#217028,#217029,
#217030,#217031,#217032,#217033,#217034,#217035,#217036,#217037,#217038,
#217039,#217040,#217041,#217042,#217043,#217044,#217045,#217046,#217047,
#217048,#217049,#217050,#217051,#217052,#217053,#217054,#217055,#217056,
#217057,#217058,#217059,#217060,#217061,#217062,#217063,#217064,#217065,
#217066,#217067,#217068,#217069,#217070),.UNSPECIFIED.,.F.,.F.,(4,3,3,3,
3,3,3,3,3,3,3,3,3,3,3,3,3,3,3,3,3,3,3,3,3,3,3,3,3,3,3,3,3,3,3,3,3,3,3,3,
3,3,3,3,3,3,3,3,3,3,3,3,3,3,3,3,3,3,3,3,3,3,3,3,3,3,3,3,3,3,3,3,3,3,3,3,
3,3,3,3,3,4),(-79.4907654349973,-79.4077034724819,-79.3245504349086,-79.2381990379041,
-79.1547733841094,-79.0669591154998,-78.9791448468903,-78.8991875467591,
-78.8193247495167,-78.7395389270448,-78.6598126118496,-78.5801283835557,
-78.5004573973348,-78.4207899438089,-78.3411102929926,-78.2614027105983,
-78.1816074815228,-78.101763139815,-78.0218047127677,-77.9794088361702,
-77.8994515360389,-77.8195887387963,-77.7398029163244,-77.6600766011291,
-77.5803923728351,-77.5007213866142,-77.4210539330884,-77.3413742822718,
-77.2616666998774,-77.1818714708018,-77.1020271290941,-77.0220687020468,
-76.9796728254501,-76.8997155253188,-76.819852728076,-76.7400669056043,
-76.6603405904092,-76.5806563621158,-76.5009853758948,-76.4213179223689,
-76.3416382715525,-76.2619306891576,-76.182135460082,-76.1022911183746,
-76.0223326913272,-75.97993681473,-75.8999795145987,-75.820116717356,-75.7403308948843,
-75.6606045796891,-75.5809203513952,-75.5012493651742,-75.4215819116484,
-75.3419022608322,-75.2621946784377,-75.1823994493621,-75.1025551076547,
-75.0225966806073,-74.9802008040098,-74.9002435038785,-74.8203807066359,
-74.7405948841641,-74.6608685689692,-74.5811843406744,-74.5015133544535,
-74.4218459009276,-74.3421662501111,-74.2624586677158,-74.1826634386403,
-74.1028190969327,-74.0228606698853,-73.9804647932897,-73.9015581804217,
-73.8227469663865,-73.7440261147531,-73.6653563569114,-73.5867211558266,
-73.5081040028306,-73.4294628808362,-73.3508110774882,-73.2720919472877,
-73.2075801278176),.UNSPECIFIED.);
#1751=B_SPLINE_CURVE_WITH_KNOTS('',3,(#217072,#217073,#217074,#217075,#217076,
#217077,#217078,#217079,#217080,#217081,#217082),.UNSPECIFIED.,.F.,.F.,
(4,1,1,1,1,1,1,1,4),(-73.2075801278176,-72.9807287825696,-71.9809927718494,
-70.9812567611293,-69.9815207504092,-68.981784739689,-67.9820487289689,
-66.9823127182488,-66.9243948206381),.UNSPECIFIED.);
#1752=B_SPLINE_CURVE_WITH_KNOTS('',3,(#217084,#217085,#217086,#217087,#217088,
#217089,#217090,#217091,#217092,#217093,#217094,#217095,#217096,#217097,
#217098,#217099,#217100,#217101,#217102,#217103,#217104,#217105,#217106,
#217107,#217108,#217109,#217110,#217111,#217112,#217113,#217114,#217115,
#217116,#217117,#217118,#217119,#217120,#217121,#217122,#217123,#217124,
#217125,#217126,#217127,#217128,#217129,#217130,#217131,#217132,#217133,
#217134,#217135,#217136,#217137,#217138,#217139,#217140,#217141,#217142,
#217143,#217144,#217145,#217146,#217147,#217148,#217149,#217150,#217151,
#217152,#217153,#217154,#217155,#217156,#217157,#217158,#217159,#217160,
#217161,#217162,#217163,#217164,#217165,#217166,#217167,#217168,#217169,
#217170,#217171,#217172,#217173,#217174,#217175,#217176,#217177,#217178,
#217179,#217180,#217181,#217182,#217183,#217184,#217185,#217186,#217187,
#217188,#217189,#217190,#217191,#217192,#217193,#217194,#217195,#217196,
#217197,#217198,#217199,#217200,#217201,#217202,#217203,#217204,#217205,
#217206,#217207,#217208,#217209,#217210,#217211,#217212,#217213,#217214,
#217215,#217216,#217217,#217218,#217219,#217220,#217221,#217222,#217223,
#217224,#217225,#217226,#217227,#217228,#217229,#217230,#217231,#217232,
#217233,#217234,#217235,#217236,#217237,#217238,#217239,#217240,#217241,
#217242,#217243,#217244,#217245,#217246,#217247,#217248,#217249,#217250,
#217251,#217252,#217253,#217254,#217255,#217256,#217257,#217258,#217259,
#217260,#217261,#217262,#217263,#217264,#217265,#217266,#217267,#217268,
#217269,#217270,#217271,#217272,#217273,#217274,#217275,#217276,#217277,
#217278,#217279,#217280,#217281,#217282,#217283,#217284,#217285,#217286,
#217287,#217288,#217289,#217290,#217291,#217292,#217293,#217294,#217295,
#217296,#217297,#217298,#217299,#217300,#217301,#217302,#217303,#217304,
#217305,#217306,#217307,#217308,#217309,#217310,#217311,#217312,#217313,
#217314,#217315,#217316,#217317,#217318,#217319,#217320,#217321,#217322,
#217323,#217324,#217325,#217326,#217327),.UNSPECIFIED.,.F.,.F.,(4,3,3,3,
3,3,3,3,3,3,3,3,3,3,3,3,3,3,3,3,3,3,3,3,3,3,3,3,3,3,3,3,3,3,3,3,3,3,3,3,
3,3,3,3,3,3,3,3,3,3,3,3,3,3,3,3,3,3,3,3,3,3,3,3,3,3,3,3,3,3,3,3,3,3,3,3,
3,3,3,3,3,4),(-66.9243948206381,-66.8451430614651,-66.7659820906656,-66.68689378965,
-66.6078601052444,-66.5288554488661,-66.4498645624908,-66.3708711811437,
-66.2918590405673,-66.2127651323194,-66.1336293443134,-66.054372687672,
-65.9825767075287,-65.9026194073974,-65.8227566101546,-65.7429707876828,
-65.6632444724872,-65.5835602441933,-65.5038892579723,-65.4242218044462,
-65.3445421536298,-65.2648345712352,-65.1850393421596,-65.105195000452,
-65.0252365734045,-64.9828406968085,-64.9028833966772,-64.8230205994346,
-64.7432347769627,-64.6635084617673,-64.5838242334732,-64.5041532472523,
-64.4244857937264,-64.3448061429098,-64.2650985605154,-64.1853033314399,
-64.1054589897322,-64.0255005626848,-63.9831046860884,-63.9031473859572,
-63.8232845887147,-63.7434987662427,-63.6637724510475,-63.5840882227535,
-63.5044172365327,-63.4247497830068,-63.3450701321903,-63.2653625497957,
-63.1855673207202,-63.1057229790125,-63.0257645519651,-62.9833686753683,
-62.903411375237,-62.8235485779942,-62.7437627555225,-62.6640364403274,
-62.5843522120328,-62.5046812258119,-62.425013772286,-62.3453341214695,
-62.2656265390753,-62.1858313099998,-62.1059869682922,-62.0260285412449,
-61.9836326646481,-61.9036753645168,-61.823812567274,-61.7440267448023,
-61.6643004296077,-61.5846162013138,-61.5049452150927,-61.4252777615666,
-61.3455981107502,-61.2658905283563,-61.1860952992806,-61.1062509575726,
-61.0262925305251,-60.983896653928,-60.8907777178953,-60.798032881653,-60.7060135811139,
-60.6412095135729),.UNSPECIFIED.);
#1753=B_SPLINE_CURVE_WITH_KNOTS('',3,(#217329,#217330,#217331,#217332,#217333,
#217334,#217335,#217336,#217337,#217338,#217339,#217340,#217341,#217342,
#217343,#217344,#217345,#217346,#217347,#217348,#217349,#217350,#217351,
#217352,#217353,#217354,#217355,#217356,#217357,#217358,#217359,#217360,
#217361,#217362,#217363,#217364,#217365,#217366,#217367,#217368,#217369,
#217370,#217371,#217372,#217373,#217374,#217375,#217376,#217377,#217378,
#217379,#217380,#217381,#217382,#217383,#217384,#217385,#217386,#217387,
#217388,#217389,#217390,#217391,#217392,#217393,#217394,#217395,#217396,
#217397,#217398,#217399,#217400,#217401,#217402,#217403,#217404,#217405,
#217406,#217407,#217408,#217409,#217410,#217411,#217412,#217413,#217414,
#217415,#217416,#217417,#217418,#217419,#217420,#217421,#217422,#217423,
#217424,#217425,#217426,#217427,#217428,#217429,#217430,#217431,#217432,
#217433,#217434,#217435,#217436,#217437,#217438,#217439,#217440,#217441,
#217442,#217443,#217444,#217445,#217446,#217447,#217448,#217449,#217450,
#217451,#217452,#217453,#217454,#217455,#217456,#217457,#217458,#217459,
#217460,#217461,#217462,#217463,#217464,#217465,#217466,#217467,#217468,
#217469,#217470,#217471,#217472,#217473,#217474,#217475,#217476,#217477,
#217478,#217479,#217480,#217481,#217482,#217483,#217484,#217485,#217486,
#217487,#217488,#217489,#217490,#217491,#217492,#217493,#217494,#217495,
#217496,#217497,#217498,#217499,#217500,#217501,#217502,#217503,#217504,
#217505,#217506,#217507,#217508,#217509,#217510,#217511,#217512,#217513,
#217514,#217515,#217516,#217517,#217518,#217519,#217520,#217521,#217522,
#217523,#217524,#217525,#217526,#217527,#217528,#217529,#217530,#217531,
#217532,#217533,#217534,#217535,#217536,#217537,#217538,#217539,#217540,
#217541,#217542,#217543,#217544,#217545,#217546,#217547,#217548,#217549,
#217550,#217551,#217552,#217553,#217554,#217555,#217556,#217557,#217558,
#217559,#217560,#217561,#217562,#217563,#217564,#217565,#217566,#217567,
#217568,#217569,#217570,#217571,#217572,#217573,#217574,#217575),
 .UNSPECIFIED.,.F.,.F.,(4,3,3,3,3,3,3,3,3,3,3,3,3,3,3,3,3,3,3,3,3,3,3,3,
3,3,3,3,3,3,3,3,3,3,3,3,3,3,3,3,3,3,3,3,3,3,3,3,3,3,3,3,3,3,3,3,3,3,3,3,
3,3,3,3,3,3,3,3,3,3,3,3,3,3,3,3,3,3,3,3,3,3,4),(-60.6412095134584,-60.5590784046771,
-60.4793357811508,-60.3995857810152,-60.3198128184427,-60.235899774634,
-60.1559884534018,-60.0760181955046,-59.995936002992,-59.9841606432079,
-59.9042033430767,-59.8243405458341,-59.7445547233624,-59.664828408167,
-59.5851441798728,-59.5054731936519,-59.4258057401261,-59.3461260893097,
-59.2664185069152,-59.1866232778397,-59.106778936132,-59.0268205090847,
-58.9844246324877,-58.9044673323564,-58.8246045351137,-58.7448187126417,
-58.6650923974462,-58.5854081691519,-58.5057371829309,-58.4260697294049,
-58.3463900785883,-58.2666824961936,-58.186887267118,-58.1070429254103,
-58.0270844983627,-57.9846886217676,-57.9047313216364,-57.8248685243939,
-57.7450827019221,-57.6653563867272,-57.5856721584333,-57.5060011722124,
-57.4263337186865,-57.3466540678699,-57.2669464854756,-57.1871512564001,
-57.1073069146926,-57.0273484876453,-56.9849526110475,-56.9049953109163,
-56.8251325136738,-56.7453466912019,-56.6656203760066,-56.5859361477129,
-56.5062651614919,-56.4265977079658,-56.3469180571494,-56.2672104747552,
-56.1874152456796,-56.1075709039718,-56.0276124769243,-55.9852166003274,
-55.9052593001963,-55.8253965029537,-55.7456106804819,-55.665884365286,
-55.5862001369919,-55.506529150771,-55.426861697245,-55.3471820464283,-55.2674744640334,
-55.1876792349578,-55.1078348932506,-55.0278764662033,-54.9854805896072,
-54.9049169077671,-54.8244508849754,-54.7440673257589,-54.6637510888401,
-54.5834913281942,-54.5032654666035,-54.4230482427655,-54.3580242062788),
 .UNSPECIFIED.);
#1754=B_SPLINE_CURVE_WITH_KNOTS('',3,(#217577,#217578,#217579,#217580,#217581,
#217582,#217583,#217584,#217585,#217586),.UNSPECIFIED.,.F.,.F.,(4,1,1,1,
1,1,1,4),(-54.3580165317574,-53.9857445788871,-52.9860085681669,-51.9862725574468,
-50.9865365467267,-49.9868005360066,-48.9870645252864,-48.0748476368028),
 .UNSPECIFIED.);
#1755=B_SPLINE_CURVE_WITH_KNOTS('',3,(#217588,#217589,#217590,#217591,#217592,
#217593,#217594,#217595,#217596,#217597,#217598,#217599,#217600,#217601,
#217602,#217603,#217604,#217605,#217606,#217607,#217608,#217609,#217610,
#217611,#217612,#217613,#217614,#217615,#217616,#217617,#217618,#217619,
#217620,#217621,#217622,#217623,#217624,#217625,#217626,#217627,#217628,
#217629,#217630,#217631,#217632,#217633,#217634,#217635,#217636,#217637,
#217638,#217639,#217640,#217641,#217642,#217643,#217644,#217645,#217646,
#217647,#217648,#217649,#217650,#217651,#217652,#217653,#217654,#217655,
#217656,#217657,#217658,#217659,#217660,#217661,#217662,#217663,#217664,
#217665,#217666,#217667,#217668,#217669,#217670,#217671,#217672,#217673,
#217674,#217675,#217676,#217677,#217678,#217679,#217680,#217681,#217682,
#217683,#217684,#217685,#217686,#217687,#217688,#217689,#217690,#217691,
#217692,#217693,#217694,#217695,#217696,#217697,#217698,#217699,#217700,
#217701,#217702,#217703,#217704,#217705,#217706,#217707,#217708,#217709,
#217710,#217711,#217712,#217713,#217714,#217715,#217716,#217717,#217718,
#217719,#217720,#217721,#217722,#217723,#217724,#217725,#217726,#217727,
#217728,#217729,#217730,#217731,#217732,#217733,#217734,#217735,#217736,
#217737,#217738,#217739,#217740,#217741,#217742,#217743,#217744,#217745,
#217746,#217747,#217748,#217749,#217750,#217751,#217752,#217753,#217754,
#217755,#217756,#217757,#217758,#217759,#217760,#217761,#217762,#217763,
#217764,#217765,#217766,#217767,#217768,#217769,#217770,#217771,#217772,
#217773,#217774,#217775,#217776,#217777,#217778,#217779,#217780,#217781,
#217782,#217783,#217784,#217785,#217786,#217787,#217788,#217789,#217790,
#217791,#217792,#217793,#217794,#217795,#217796,#217797,#217798,#217799,
#217800,#217801,#217802,#217803,#217804,#217805,#217806,#217807,#217808,
#217809,#217810,#217811,#217812,#217813,#217814,#217815,#217816,#217817,
#217818,#217819,#217820,#217821,#217822,#217823,#217824,#217825,#217826,
#217827,#217828,#217829,#217830,#217831),.UNSPECIFIED.,.F.,.F.,(4,3,3,3,
3,3,3,3,3,3,3,3,3,3,3,3,3,3,3,3,3,3,3,3,3,3,3,3,3,3,3,3,3,3,3,3,3,3,3,3,
3,3,3,3,3,3,3,3,3,3,3,3,3,3,3,3,3,3,3,3,3,3,3,3,3,3,3,3,3,3,3,3,3,3,3,3,
3,3,3,3,3,4),(-48.0748388990992,-47.9873285145663,-47.9073712144349,-47.8275084171922,
-47.7477225947202,-47.6679962795249,-47.5883120512307,-47.5086410650096,
-47.4289736114836,-47.3492939606671,-47.2695863782722,-47.1897911491966,
-47.1099468074887,-47.0299883804412,-46.9875925038462,-46.9076352037149,
-46.8277724064724,-46.7479865840006,-46.6682602688053,-46.5885760405113,
-46.5089050542904,-46.4292376007644,-46.3495579499479,-46.2698503675534,
-46.1900551384779,-46.1102107967703,-46.0302523697229,-45.987856493126,
-45.9078991929947,-45.8280363957522,-45.7482505732803,-45.668524258085,
-45.5888400297908,-45.5091690435699,-45.429501590044,-45.3498219392276,
-45.270114356833,-45.1903191277575,-45.1104747860499,-45.0305163590025,
-44.9881204824059,-44.9081631822747,-44.8283003850321,-44.7485145625602,
-44.668788247365,-44.5891040190709,-44.50943303285,-44.4297655793241,-44.3500859285076,
-44.2703783461131,-44.1905831170376,-44.1107387753299,-44.0307803482826,
-43.9883844716858,-43.9084271715545,-43.8285643743119,-43.74877855184,-43.6690522366447,
-43.5893680083507,-43.5096970221298,-43.4300295686039,-43.3503499177874,
-43.2706423353929,-43.1908471063174,-43.1110027646097,-43.0310443375623,
-42.9886484609656,-42.9086911608343,-42.8288283635917,-42.7490425411198,
-42.6693162259245,-42.5896319976304,-42.5099610114094,-42.4302935578836,
-42.3506139070671,-42.2709063246724,-42.1911110955969,-42.1112667538892,
-42.0313083268418,-41.9889124502455,-41.8733272325874,-41.7916535919196),
 .UNSPECIFIED.);
#1756=B_SPLINE_CURVE_WITH_KNOTS('',3,(#217833,#217834,#217835,#217836,#217837,
#217838,#217839,#217840,#217841,#217842),.UNSPECIFIED.,.F.,.F.,(4,1,1,1,
1,1,1,4),(-41.7916500544357,-40.9891764395254,-39.9894404288052,-38.9897044180851,
-37.989968407365,-36.9902323966448,-35.9904963859247,-35.50846828474),
 .UNSPECIFIED.);
#1757=B_SPLINE_CURVE_WITH_KNOTS('',3,(#217844,#217845,#217846,#217847,#217848,
#217849,#217850,#217851,#217852,#217853),.UNSPECIFIED.,.F.,.F.,(4,1,1,1,
1,1,1,4),(-35.50846828474,-34.9907603752046,-33.9910243644845,-32.9912883537643,
-31.9915523430442,-30.9918163323241,-29.9920803216039,-29.2252829775605),
 .UNSPECIFIED.);
#1758=B_SPLINE_CURVE_WITH_KNOTS('',3,(#217855,#217856,#217857,#217858,#217859,
#217860,#217861,#217862,#217863,#217864,#217865),.UNSPECIFIED.,.F.,.F.,
(4,1,1,1,1,1,1,1,4),(-29.2252829775605,-28.9923443108838,-27.9926083001637,
-26.9928722894435,-25.9931362787234,-24.9934002680033,-23.9936642572832,
-22.993928246563,-22.9420976703809),.UNSPECIFIED.);
#1759=B_SPLINE_CURVE_WITH_KNOTS('',3,(#217867,#217868,#217869,#217870,#217871,
#217872,#217873,#217874,#217875,#217876),.UNSPECIFIED.,.F.,.F.,(4,1,1,1,
1,1,1,4),(-22.9420976703809,-21.9941922358429,-20.9944562251228,-19.9947202144026,
-18.9949842036825,-17.9952481929624,-16.9955121822422,-16.6589198685825),
 .UNSPECIFIED.);
#1760=B_SPLINE_CURVE_WITH_KNOTS('',3,(#217878,#217879,#217880,#217881,#217882,
#217883,#217884,#217885,#217886,#217887,#217888,#217889,#217890,#217891,
#217892,#217893,#217894,#217895,#217896,#217897,#217898,#217899,#217900,
#217901,#217902,#217903,#217904,#217905,#217906,#217907,#217908,#217909,
#217910,#217911,#217912,#217913,#217914,#217915,#217916,#217917,#217918,
#217919,#217920,#217921,#217922,#217923,#217924,#217925,#217926,#217927,
#217928,#217929,#217930,#217931,#217932,#217933,#217934,#217935,#217936,
#217937,#217938,#217939,#217940,#217941,#217942,#217943,#217944,#217945,
#217946,#217947,#217948,#217949,#217950,#217951,#217952,#217953,#217954,
#217955,#217956,#217957,#217958,#217959,#217960,#217961,#217962,#217963,
#217964,#217965,#217966,#217967,#217968,#217969,#217970,#217971,#217972,
#217973,#217974,#217975,#217976,#217977,#217978,#217979,#217980,#217981,
#217982,#217983,#217984,#217985,#217986,#217987,#217988,#217989,#217990,
#217991,#217992,#217993,#217994,#217995,#217996,#217997,#217998,#217999,
#218000,#218001,#218002,#218003,#218004,#218005,#218006,#218007,#218008,
#218009,#218010,#218011,#218012,#218013,#218014,#218015,#218016,#218017,
#218018,#218019,#218020,#218021,#218022,#218023,#218024,#218025,#218026,
#218027,#218028,#218029,#218030,#218031,#218032,#218033,#218034,#218035,
#218036,#218037,#218038,#218039,#218040,#218041,#218042,#218043),
 .UNSPECIFIED.,.F.,.F.,(4,3,3,3,3,3,3,3,3,3,3,3,3,3,3,3,3,3,3,3,3,3,3,3,
3,3,3,3,3,3,3,3,3,3,3,3,3,3,3,3,3,3,3,3,3,3,3,3,3,3,3,3,3,3,3,4),(-16.6589123632013,
-16.5760203392414,-16.4963658357425,-16.4167062586062,-16.3370259313394,
-16.257309167994,-16.1774967883031,-16.0976279107091,-16.0176451019278,
-15.9957761715221,-15.9158187324329,-15.8359557956803,-15.7561698332831,
-15.6764433778821,-15.5967590092361,-15.5170878828934,-15.4374202894017,
-15.3577404988956,-15.2780327772076,-15.198237410145,-15.118392930983,-15.0384343685027,
-14.996040160802,-14.9160831648467,-14.8362206718143,-14.7564351533039,
-14.6767091415404,-14.5970252158687,-14.5173545301081,-14.4376873756752,
-14.3580080223317,-14.278300735536,-14.1985057977278,-14.1186617452726,
-14.0387036018344,-13.9963041500818,-13.9163467244748,-13.8364838036546,
-13.7566978595943,-13.6769714248905,-13.5972870792609,-13.5176159792981,
-13.4379484142657,-13.3582686542656,-13.2785609651003,-13.1987656334386,
-13.1189211913589,-13.0389626682522,-12.9965681393617,-12.9166104714522,
-12.8367437733771,-12.7569521629902,-12.6772283666737,-12.5975435612502,
-12.5178804549894,-12.4923778478243),.UNSPECIFIED.);
#1761=B_SPLINE_CURVE_WITH_KNOTS('',3,(#218045,#218046,#218047,#218048,#218049,
#218050,#218051,#218052,#218053,#218054,#218055,#218056,#218057,#218058,
#218059,#218060,#218061,#218062,#218063,#218064,#218065,#218066,#218067,
#218068,#218069,#218070,#218071,#218072,#218073,#218074,#218075,#218076,
#218077,#218078,#218079,#218080),.UNSPECIFIED.,.F.,.F.,(4,2,2,2,2,2,2,2,
2,2,2,2,2,2,2,2,2,4),(0.00526237292542417,0.138566189979076,0.366294164048727,
0.418967542934504,0.430275546436095,0.431328859894763,0.431533790643745,
0.431789609184076,0.431892486759413,0.431959062395792,0.43202128231436,
0.432103906517542,0.432281648026571,0.434594111412943,0.465840068485782,
0.538620422200195,0.640014286401001,0.807590978544382),.UNSPECIFIED.);
#1762=B_SPLINE_CURVE_WITH_KNOTS('',3,(#218082,#218083,#218084,#218085,#218086,
#218087,#218088,#218089,#218090,#218091,#218092,#218093,#218094,#218095,
#218096,#218097,#218098,#218099,#218100,#218101,#218102,#218103,#218104,
#218105,#218106,#218107,#218108,#218109),.UNSPECIFIED.,.F.,.F.,(4,3,3,3,
3,3,3,3,3,4),(-11.06261597483,-10.9970961179214,-10.9164104612955,-10.8358235390976,
-10.7553203015422,-10.6748857539058,-10.5945105281497,-10.5141705799321,
-10.4338432861682,-10.3757270560217),.UNSPECIFIED.);
#1763=B_SPLINE_CURVE_WITH_KNOTS('',3,(#218111,#218112,#218113,#218114,#218115),
 .UNSPECIFIED.,.F.,.F.,(4,1,4),(-10.3757194590647,-9.99736010720131,-9.9877456995066),
 .UNSPECIFIED.);
#1764=B_SPLINE_CURVE_WITH_KNOTS('',3,(#218116,#218117,#218118,#218119,#218120,
#218121,#218122,#218123,#218124,#218125),.UNSPECIFIED.,.F.,.F.,(4,2,2,2,
4),(0.00246287485863373,0.0946583498619244,0.18080663761715,0.264674289446545,
0.349802769075605),.UNSPECIFIED.);
#1765=B_SPLINE_CURVE_WITH_KNOTS('',3,(#218127,#218128,#218129,#218130,#218131,
#218132,#218133,#218134,#218135,#218136),.UNSPECIFIED.,.F.,.F.,(4,3,3,4),
(21.740715980233,21.8348722215429,21.9284884766943,21.9911485749198),
 .UNSPECIFIED.);
#1766=B_SPLINE_CURVE_WITH_KNOTS('',3,(#218137,#218138,#218139,#218140,#218141,
#218142,#218143,#218144,#218145,#218146,#218147,#218148,#218149,#218150,
#218151,#218152,#218153,#218154,#218155,#218156,#218157,#218158,#218159,
#218160,#218161,#218162,#218163,#218164,#218165,#218166,#218167,#218168,
#218169,#218170,#218171,#218172,#218173,#218174,#218175,#218176,#218177,
#218178,#218179,#218180,#218181,#218182,#218183,#218184,#218185,#218186,
#218187,#218188,#218189,#218190,#218191,#218192,#218193,#218194,#218195,
#218196,#218197,#218198,#218199,#218200,#218201,#218202,#218203,#218204,
#218205,#218206,#218207,#218208,#218209,#218210,#218211,#218212,#218213,
#218214,#218215,#218216,#218217,#218218,#218219,#218220,#218221,#218222,
#218223,#218224,#218225,#218226,#218227,#218228,#218229,#218230,#218231,
#218232,#218233,#218234,#218235,#218236,#218237,#218238,#218239,#218240,
#218241,#218242,#218243,#218244,#218245,#218246,#218247,#218248,#218249,
#218250,#218251,#218252,#218253,#218254,#218255,#218256,#218257,#218258,
#218259,#218260,#218261,#218262,#218263,#218264,#218265,#218266,#218267,
#218268,#218269,#218270,#218271,#218272,#218273,#218274,#218275,#218276,
#218277,#218278,#218279,#218280,#218281,#218282,#218283,#218284,#218285,
#218286,#218287,#218288,#218289,#218290,#218291,#218292,#218293,#218294,
#218295,#218296,#218297,#218298,#218299,#218300,#218301,#218302,#218303,
#218304,#218305,#218306,#218307,#218308,#218309,#218310,#218311,#218312,
#218313,#218314,#218315,#218316,#218317,#218318,#218319,#218320,#218321,
#218322,#218323,#218324,#218325,#218326,#218327,#218328,#218329,#218330,
#218331,#218332,#218333,#218334,#218335,#218336,#218337,#218338,#218339,
#218340,#218341,#218342,#218343,#218344,#218345,#218346,#218347,#218348,
#218349,#218350,#218351,#218352,#218353,#218354,#218355,#218356),
 .UNSPECIFIED.,.F.,.F.,(4,3,3,3,3,3,3,3,3,3,3,3,3,3,3,3,3,3,3,3,3,3,3,3,
3,3,3,3,3,3,3,3,3,3,3,3,3,3,3,3,3,3,3,3,3,3,3,3,3,3,3,3,3,3,3,3,3,3,3,3,
3,3,3,3,3,3,3,3,3,3,3,3,3,4),(21.9911485751133,22.0752803066499,22.1594213519125,
22.2435887880297,22.327799705763,22.412122635211,22.496510193649,22.5810312627201,
22.6125176370092,22.6962542579476,22.7798876501835,22.8634379486364,22.9469252160963,
23.0303769702507,23.1138112508511,23.1972461326295,23.2806996868859,23.3642419314503,
23.4478287585743,23.531549780005,23.6122536477293,23.6959932091553,23.7796295777105,
23.8631828849443,23.946673190331,24.0301280160616,24.113565388298,24.1970033788866,
24.2804600562506,24.3640054289813,24.4475953919903,24.5313195307922,24.6119896584494,
24.6957284703853,24.7793640854067,24.8629166358964,24.9464061821532,25.0298602478526,
25.11329685962,25.1967340900312,25.2801900082394,25.3637346277638,25.4473238396068,
25.5310472383997,25.6117256691696,25.6954640854281,25.7790992970342,25.8626514368397,
25.9461405656013,26.0295942048811,26.1130303848521,26.196467178482,26.2799226553132,
26.3634668286356,26.4470555909439,26.5307785390076,26.6114616798897,26.6952005328961,
26.7788361868141,26.8623887739932,26.9458783546974,27.0293324512814,27.1127690917577,
27.1962063486646,27.2796622911176,27.3632069311557,27.4467961615158,27.530519575186,
27.6111976906098,27.6949624620804,27.7785925584211,27.8621451536583,27.9456293039383,
28.0234162092491),.UNSPECIFIED.);
#1767=B_SPLINE_CURVE_WITH_KNOTS('',3,(#225139,#225140,#225141,#225142,#225143,
#225144,#225145,#225146,#225147,#225148),.UNSPECIFIED.,.F.,.F.,(4,2,2,2,
4),(0.00207047843994134,0.0654884822806935,0.146439093390922,0.270589396385427,
0.30899941932235),.UNSPECIFIED.);
#1768=B_SPLINE_CURVE_WITH_KNOTS('',3,(#225150,#225151,#225152,#225153,#225154,
#225155,#225156,#225157,#225158,#225159,#225160,#225161,#225162,#225163,
#225164,#225165,#225166,#225167,#225168,#225169,#225170,#225171),
 .UNSPECIFIED.,.F.,.F.,(4,3,3,3,3,3,3,4),(-117.731943690408,-117.653301723801,
-117.574693912514,-117.496103732189,-117.417487955491,-117.338861162405,
-117.260163820455,-117.189877278075),.UNSPECIFIED.);
#1769=B_SPLINE_CURVE_WITH_KNOTS('',3,(#225173,#225174,#225175,#225176,#225177),
 .UNSPECIFIED.,.F.,.F.,(4,1,4),(-117.189877278075,-116.969113254255,-116.302843017259),
 .UNSPECIFIED.);
#1770=B_SPLINE_CURVE_WITH_KNOTS('',3,(#225178,#225179,#225180,#225181,#225182,
#225183,#225184,#225185,#225186,#225187,#225188,#225189,#225190,#225191,
#225192,#225193,#225194,#225195,#225196,#225197,#225198,#225199,#225200,
#225201,#225202,#225203,#225204,#225205,#225206,#225207,#225208,#225209,
#225210,#225211),.UNSPECIFIED.,.F.,.F.,(4,2,2,2,2,2,2,2,2,2,2,2,2,2,2,2,
4),(0.30899941932235,0.382261953082336,0.394186641374844,0.394544069032282,
0.394634720258392,0.394685917699195,0.394729273851375,0.394781112651507,
0.394874741417267,0.39532213142483,0.396149736574269,0.399586578362255,
0.423862460061527,0.495493129981234,0.635502803715609,0.721928150979562,
0.797536521561463),.UNSPECIFIED.);
#1771=B_SPLINE_CURVE_WITH_KNOTS('',3,(#225214,#225215,#225216,#225217,#225218,
#225219),.UNSPECIFIED.,.F.,.F.,(4,2,4),(0.0641900250749046,0.225569656006002,
0.227853963255062),.UNSPECIFIED.);
#1772=B_SPLINE_CURVE_WITH_KNOTS('',3,(#225221,#225222,#225223,#225224,#225225,
#225226,#225227,#225228,#225229,#225230,#225231,#225232,#225233,#225234,
#225235,#225236,#225237,#225238,#225239,#225240,#225241,#225242,#225243,
#225244,#225245,#225246,#225247,#225248,#225249,#225250,#225251,#225252,
#225253,#225254,#225255,#225256,#225257,#225258,#225259,#225260,#225261,
#225262,#225263,#225264,#225265,#225266,#225267,#225268,#225269,#225270,
#225271,#225272,#225273,#225274,#225275,#225276,#225277,#225278,#225279,
#225280,#225281,#225282,#225283,#225284,#225285,#225286,#225287,#225288,
#225289,#225290,#225291,#225292,#225293,#225294,#225295,#225296,#225297,
#225298,#225299,#225300,#225301,#225302,#225303,#225304,#225305,#225306,
#225307,#225308,#225309,#225310,#225311,#225312,#225313,#225314,#225315,
#225316,#225317,#225318,#225319,#225320,#225321,#225322,#225323,#225324,
#225325,#225326,#225327,#225328,#225329,#225330,#225331,#225332,#225333,
#225334,#225335,#225336,#225337,#225338,#225339,#225340,#225341,#225342,
#225343,#225344,#225345,#225346,#225347,#225348,#225349,#225350,#225351,
#225352,#225353,#225354,#225355,#225356,#225357,#225358,#225359,#225360,
#225361,#225362,#225363,#225364,#225365,#225366,#225367,#225368,#225369,
#225370,#225371,#225372,#225373,#225374,#225375,#225376,#225377,#225378,
#225379,#225380,#225381,#225382,#225383,#225384,#225385,#225386,#225387,
#225388,#225389,#225390,#225391,#225392,#225393,#225394,#225395,#225396,
#225397,#225398,#225399,#225400,#225401),.UNSPECIFIED.,.F.,.F.,(4,3,3,3,
3,3,3,3,3,3,3,3,3,3,3,3,3,3,3,3,3,3,3,3,3,3,3,3,3,3,3,3,3,3,3,3,3,3,3,3,
3,3,3,3,3,3,3,3,3,3,3,3,3,3,3,3,3,3,3,3,4),(107.933005315568,107.971489157774,
108.051446457905,108.131309255148,108.21109507762,108.290821392815,108.370505621109,
108.45017660733,108.529844060856,108.609523711672,108.689231294067,108.769026523142,
108.84887086485,108.928829291897,108.971225168494,109.051182468625,109.131045265868,
109.21083108834,109.290557403535,109.370241631829,109.44991261805,109.529580071576,
109.609259722392,109.688967304787,109.768762533862,109.84860687557,109.928565302617,
109.970961179214,110.050918479345,110.130781276588,110.21056709906,110.290293414255,
110.369977642549,110.44964862877,110.529316082296,110.608995733112,110.688703315507,
110.768498544582,110.84834288629,110.928301313337,110.970697189934,111.050654490065,
111.130517287308,111.210303109779,111.290029424975,111.369713653269,111.449384639489,
111.529052093015,111.608731743832,111.688439326226,111.768234555301,111.848078897009,
111.928037324056,111.970433200654,112.05038393002,112.130244727001,112.210031469601,
112.29129664253,112.370980493117,112.453036327217,112.535092161318),
 .UNSPECIFIED.);
#1773=B_SPLINE_CURVE_WITH_KNOTS('',3,(#225403,#225404,#225405,#225406,#225407,
#225408,#225409,#225410,#225411,#225412),.UNSPECIFIED.,.F.,.F.,(4,1,1,1,
1,1,1,4),(101.649820008388,101.973073093453,102.972809104173,103.972545114893,
104.972281125613,105.972017136334,106.971753147054,107.93300001923),
 .UNSPECIFIED.);
#1774=B_SPLINE_CURVE_WITH_KNOTS('',3,(#225414,#225415,#225416,#225417,#225418,
#225419,#225420,#225421,#225422,#225423),.UNSPECIFIED.,.F.,.F.,(4,1,1,1,
1,1,1,4),(95.3666347012089,95.9746570291324,96.9743930398526,97.9741290505727,
98.9738650612928,99.973601072013,100.973337082733,101.649820008388),
 .UNSPECIFIED.);
#1775=B_SPLINE_CURVE_WITH_KNOTS('',3,(#225425,#225426,#225427,#225428,#225429,
#225430,#225431,#225432,#225433,#225434),.UNSPECIFIED.,.F.,.F.,(4,1,1,1,
1,1,1,4),(89.0834493940292,89.9762409648117,90.9759769755319,91.975712986252,
92.9754489969721,93.9751850076922,94.9749210184123,95.3666347012089),
 .UNSPECIFIED.);
#1776=B_SPLINE_CURVE_WITH_KNOTS('',3,(#225436,#225437,#225438,#225439,#225440,
#225441,#225442,#225443,#225444,#225445,#225446),.UNSPECIFIED.,.F.,.F.,
(4,1,1,1,1,1,1,1,4),(82.8002640868496,82.9780888897707,83.9778249004908,
84.977560911211,85.9772969219311,86.9770329326513,87.9767689433714,88.9765049540916,
89.0834493940292),.UNSPECIFIED.);
#1777=B_SPLINE_CURVE_WITH_KNOTS('',3,(#225448,#225449,#225450,#225451,#225452,
#225453,#225454,#225455,#225456,#225457,#225458,#225459,#225460,#225461,
#225462,#225463,#225464,#225465,#225466,#225467,#225468,#225469,#225470,
#225471,#225472,#225473,#225474,#225475,#225476,#225477,#225478,#225479,
#225480,#225481,#225482,#225483,#225484,#225485,#225486,#225487,#225488,
#225489,#225490,#225491,#225492,#225493,#225494,#225495,#225496,#225497,
#225498,#225499,#225500,#225501,#225502,#225503,#225504,#225505,#225506,
#225507,#225508,#225509,#225510,#225511,#225512,#225513,#225514,#225515,
#225516,#225517,#225518,#225519,#225520,#225521,#225522,#225523,#225524,
#225525,#225526,#225527,#225528,#225529,#225530,#225531,#225532,#225533,
#225534,#225535,#225536,#225537,#225538,#225539,#225540,#225541,#225542,
#225543,#225544,#225545,#225546,#225547,#225548,#225549,#225550,#225551,
#225552,#225553,#225554,#225555,#225556,#225557,#225558,#225559,#225560,
#225561,#225562,#225563,#225564,#225565,#225566,#225567,#225568,#225569,
#225570,#225571,#225572,#225573,#225574,#225575,#225576,#225577,#225578,
#225579,#225580,#225581,#225582,#225583,#225584,#225585,#225586,#225587,
#225588,#225589,#225590,#225591,#225592,#225593,#225594,#225595,#225596,
#225597,#225598,#225599,#225600,#225601,#225602,#225603,#225604,#225605,
#225606,#225607,#225608,#225609,#225610,#225611,#225612,#225613,#225614,
#225615,#225616,#225617,#225618,#225619,#225620,#225621,#225622,#225623,
#225624,#225625,#225626,#225627,#225628,#225629,#225630,#225631,#225632,
#225633,#225634,#225635,#225636,#225637,#225638,#225639,#225640,#225641,
#225642,#225643,#225644,#225645,#225646,#225647,#225648,#225649,#225650,
#225651,#225652,#225653,#225654,#225655,#225656,#225657,#225658,#225659,
#225660,#225661,#225662,#225663,#225664,#225665,#225666,#225667,#225668,
#225669,#225670,#225671,#225672,#225673,#225674,#225675,#225676,#225677,
#225678,#225679,#225680,#225681,#225682,#225683,#225684,#225685,#225686,
#225687,#225688,#225689,#225690,#225691,#225692,#225693,#225694),
 .UNSPECIFIED.,.F.,.F.,(4,3,3,3,3,3,3,3,3,3,3,3,3,3,3,3,3,3,3,3,3,3,3,3,
3,3,3,3,3,3,3,3,3,3,3,3,3,3,3,3,3,3,3,3,3,3,3,3,3,3,3,3,3,3,3,3,3,3,3,3,
3,3,3,3,3,3,3,3,3,3,3,3,3,3,3,3,3,3,3,3,3,3,4),(76.5170789829915,76.6019516902264,
76.6869832338072,76.7722619244241,76.8576735508233,76.9432918856119,76.97967282545,
77.0596301255811,77.1394929228235,77.2192787452951,77.2990050604903,77.3786892887841,
77.4583602750048,77.5380277285305,77.6177073793468,77.6974149617411,77.7772101908165,
77.8570545325239,77.9370129595711,77.9794088361701,78.0593661363013,78.1392289335439,
78.2190147560157,78.298741071211,78.3784252995052,78.4580962857261,78.537763739252,
78.6174433900685,78.6971509724629,78.7769462015385,78.8567905432461,78.9367489702935,
78.9791448468902,79.0591021470215,79.1389649442642,79.2187507667361,79.2984770819315,
79.3781613102257,79.4578322964467,79.5374997499727,79.6171794007892,79.6968869831838,
79.7766822122594,79.8565265539671,79.9364849810146,79.9788808576104,80.0588381577416,
80.1387009549841,80.2184867774559,80.2982130926512,80.3778973209452,80.4575683071661,
80.537235760692,80.6169154115085,80.696622993903,80.7764182229785,80.856262564686,
80.9362209917334,80.9786168683304,81.0585741684617,81.1384369657043,81.2182227881762,
81.2979491033716,81.3776333316657,81.4573043178867,81.5369717714127,81.6166514222292,
81.6963590046238,81.7761542336994,81.8559985754071,81.9359570024545,81.9783528790506,
82.0571196435331,82.1357922323713,82.2143891387368,82.2929249535672,82.37142792239,
82.4499146286459,82.5284016410875,82.6069360191478,82.6854971762447,82.764138078185,
82.8002640868496),.UNSPECIFIED.);
#1778=B_SPLINE_CURVE_WITH_KNOTS('',3,(#225696,#225697,#225698,#225699,#225700,
#225701,#225702,#225703,#225704,#225705),.UNSPECIFIED.,.F.,.F.,(4,1,1,1,
1,1,1,4),(70.2338934724905,70.9812567611292,71.9809927718493,72.9807287825695,
73.9804647932896,74.9802008040097,75.9799368147299,76.5170787796701),
 .UNSPECIFIED.);
#1779=B_SPLINE_CURVE_WITH_KNOTS('',3,(#225707,#225708,#225709,#225710,#225711,
#225712,#225713,#225714,#225715,#225716,#225717,#225718,#225719,#225720,
#225721,#225722,#225723,#225724,#225725,#225726,#225727,#225728,#225729,
#225730,#225731,#225732,#225733,#225734,#225735,#225736,#225737,#225738,
#225739,#225740,#225741,#225742,#225743,#225744,#225745,#225746,#225747,
#225748,#225749,#225750,#225751,#225752,#225753,#225754,#225755,#225756,
#225757,#225758,#225759,#225760,#225761,#225762,#225763,#225764,#225765,
#225766,#225767,#225768,#225769,#225770,#225771,#225772,#225773,#225774,
#225775,#225776,#225777,#225778,#225779,#225780,#225781,#225782,#225783,
#225784,#225785,#225786,#225787,#225788,#225789,#225790,#225791,#225792,
#225793,#225794,#225795,#225796,#225797,#225798,#225799,#225800,#225801,
#225802,#225803,#225804,#225805,#225806,#225807,#225808,#225809,#225810,
#225811,#225812,#225813,#225814,#225815,#225816,#225817,#225818,#225819,
#225820,#225821,#225822,#225823,#225824,#225825,#225826,#225827,#225828,
#225829,#225830,#225831,#225832,#225833,#225834,#225835,#225836,#225837,
#225838,#225839,#225840,#225841,#225842,#225843,#225844,#225845,#225846,
#225847,#225848,#225849,#225850,#225851,#225852,#225853,#225854,#225855,
#225856,#225857,#225858,#225859,#225860,#225861,#225862,#225863,#225864,
#225865,#225866,#225867,#225868,#225869,#225870,#225871,#225872,#225873,
#225874,#225875,#225876,#225877,#225878,#225879,#225880,#225881,#225882,
#225883,#225884,#225885,#225886,#225887,#225888,#225889,#225890,#225891,
#225892,#225893,#225894,#225895,#225896,#225897,#225898,#225899,#225900,
#225901,#225902,#225903,#225904,#225905,#225906,#225907,#225908,#225909,
#225910,#225911,#225912,#225913,#225914,#225915,#225916,#225917,#225918,
#225919,#225920,#225921,#225922,#225923,#225924,#225925,#225926,#225927,
#225928,#225929,#225930,#225931,#225932,#225933,#225934,#225935,#225936,
#225937,#225938,#225939,#225940,#225941,#225942,#225943,#225944,#225945,
#225946,#225947,#225948,#225949,#225950,#225951,#225952,#225953),
 .UNSPECIFIED.,.F.,.F.,(4,3,3,3,3,3,3,3,3,3,3,3,3,3,3,3,3,3,3,3,3,3,3,3,
3,3,3,3,3,3,3,3,3,3,3,3,3,3,3,3,3,3,3,3,3,3,3,3,3,3,3,3,3,3,3,3,3,3,3,3,
3,3,3,3,3,3,3,3,3,3,3,3,3,3,3,3,3,3,3,3,3,3,4),(63.9507081653109,63.9831046860883,
64.0630619862195,64.142924783462,64.2227106059338,64.3024369211289,64.382121149423,
64.4617921356438,64.5414595891696,64.621139239986,64.7008468223806,64.7806420514561,
64.8604863931635,64.9404448202108,64.9828406968084,65.0627979969396,65.1426607941822,
65.2224466166541,65.3021729318493,65.3818571601433,65.4615281463642,65.5411955998901,
65.6208752507066,65.7005828331011,65.7803780621766,65.8602224038843,65.9401808309317,
65.9825767075286,66.0625340076599,66.1423968049025,66.2221826273744,66.3019089425698,
66.381593170864,66.461264157085,66.540931610611,66.6206112614275,66.7003188438221,
66.7801140728977,66.8599584146054,66.9399168416528,66.9823127182487,67.0622700183799,
67.1421328156224,67.2219186380942,67.3016449532894,67.3813291815834,67.4610001678043,
67.5406676213301,67.6203472721465,67.700054854541,67.7798500836165,67.8596944253241,
67.9396528523714,67.9820487289688,68.0620060291001,68.1418688263428,68.2216546488147,
68.30138096401,68.381065192304,68.460736178525,68.540403632051,68.6200832828675,
68.6997908652621,68.7795860943376,68.8594304360453,68.9393888630927,68.9817847396889,
69.0617420398201,69.1416048370627,69.2213906595346,69.3011169747299,69.3808012030239,
69.4604721892448,69.5401396427707,69.6198192935872,69.6995268759819,69.7793221050574,
69.8591664467649,69.9391248738123,69.981520750409,70.0859426319418,70.1882149143938,
70.2338934108873),.UNSPECIFIED.);
#1780=B_SPLINE_CURVE_WITH_KNOTS('',3,(#225955,#225956,#225957,#225958,#225959,
#225960,#225961,#225962,#225963,#225964),.UNSPECIFIED.,.F.,.F.,(4,1,1,1,
1,1,1,4),(57.6675228581313,57.9846886217673,58.9844246324875,59.9841606432076,
60.9838966539278,61.983632664648,62.9833686753681,63.9507037176747),
 .UNSPECIFIED.);
#1781=B_SPLINE_CURVE_WITH_KNOTS('',3,(#225966,#225967,#225968,#225969,#225970,
#225971,#225972,#225973,#225974,#225975),.UNSPECIFIED.,.F.,.F.,(4,1,1,1,
1,1,1,4),(51.3843375509517,51.9862725574467,52.9860085681668,53.9857445788869,
54.985480589607,55.9852166003271,56.9849526110472,57.6675228581313),
 .UNSPECIFIED.);
#1782=B_SPLINE_CURVE_WITH_KNOTS('',3,(#225977,#225978,#225979,#225980,#225981,
#225982,#225983,#225984,#225985,#225986),.UNSPECIFIED.,.F.,.F.,(4,1,1,1,
1,1,1,4),(45.1011522437721,45.9878564931259,46.9875925038461,47.9873285145662,
48.9870645252863,49.9868005360065,50.9865365467266,51.3843375509517),
 .UNSPECIFIED.);
#1783=B_SPLINE_CURVE_WITH_KNOTS('',3,(#225988,#225989,#225990,#225991,#225992,
#225993,#225994,#225995,#225996,#225997,#225998),.UNSPECIFIED.,.F.,.F.,
(4,1,1,1,1,1,1,1,4),(38.8179669365925,38.9897044180849,39.9894404288051,
40.9891764395252,41.9889124502454,42.9886484609655,43.9883844716856,44.9881204824058,
45.1011522437721),.UNSPECIFIED.);
#1784=B_SPLINE_CURVE_WITH_KNOTS('',3,(#226000,#226001,#226002,#226003,#226004,
#226005,#226006,#226007,#226008,#226009),.UNSPECIFIED.,.F.,.F.,(4,1,1,1,
1,1,1,4),(32.534781629413,32.9912883537643,33.9910243644844,34.9907603752045,
35.9904963859246,36.9902323966447,37.9899684073648,38.8179669365925),
 .UNSPECIFIED.);
#1785=B_SPLINE_CURVE_WITH_KNOTS('',3,(#226011,#226012,#226013,#226014,#226015,
#226016,#226017,#226018,#226019,#226020),.UNSPECIFIED.,.F.,.F.,(4,1,1,1,
1,1,1,4),(26.2515963222334,26.9928722894435,27.9926083001636,28.9923443108837,
29.9920803216039,30.991816332324,31.9915523430441,32.534781629413),
 .UNSPECIFIED.);
#1786=B_SPLINE_CURVE_WITH_KNOTS('',3,(#226022,#226023,#226024,#226025,#226026,
#226027,#226028,#226029,#226030,#226031,#226032,#226033),.UNSPECIFIED.,
 .F.,.F.,(4,2,1,1,1,1,1,1,4),(19.9684110150538,19.9947202144025,20.9944562251227,
21.9941922358428,22.9939282465629,23.9936642572831,24.9934002680032,25.9931362787233,
26.2515963222334),.UNSPECIFIED.);
#1787=B_SPLINE_CURVE_WITH_KNOTS('',3,(#226035,#226036,#226037,#226038,#226039,
#226040,#226041,#226042,#226043,#226044,#226045,#226046,#226047,#226048,
#226049,#226050,#226051,#226052,#226053,#226054,#226055,#226056,#226057,
#226058,#226059,#226060,#226061,#226062,#226063,#226064,#226065,#226066,
#226067,#226068,#226069,#226070,#226071,#226072,#226073,#226074,#226075,
#226076,#226077,#226078,#226079,#226080,#226081,#226082,#226083,#226084,
#226085,#226086,#226087,#226088,#226089,#226090,#226091,#226092,#226093,
#226094,#226095,#226096,#226097,#226098,#226099,#226100,#226101,#226102,
#226103,#226104,#226105,#226106,#226107,#226108,#226109,#226110,#226111,
#226112,#226113,#226114,#226115,#226116,#226117,#226118,#226119,#226120,
#226121,#226122,#226123,#226124,#226125,#226126,#226127,#226128,#226129,
#226130,#226131,#226132,#226133,#226134,#226135,#226136,#226137,#226138,
#226139,#226140,#226141,#226142,#226143,#226144,#226145,#226146,#226147,
#226148,#226149,#226150,#226151,#226152,#226153,#226154,#226155,#226156,
#226157,#226158,#226159,#226160,#226161,#226162,#226163,#226164,#226165,
#226166,#226167,#226168,#226169,#226170,#226171,#226172,#226173,#226174,
#226175,#226176,#226177,#226178,#226179,#226180,#226181,#226182,#226183,
#226184,#226185,#226186,#226187,#226188,#226189,#226190,#226191,#226192,
#226193,#226194,#226195,#226196,#226197,#226198,#226199,#226200,#226201,
#226202,#226203,#226204,#226205,#226206,#226207,#226208,#226209,#226210,
#226211,#226212,#226213,#226214,#226215,#226216,#226217,#226218,#226219,
#226220,#226221,#226222,#226223,#226224,#226225,#226226,#226227,#226228,
#226229,#226230,#226231,#226232,#226233,#226234,#226235,#226236,#226237,
#226238,#226239,#226240,#226241,#226242,#226243,#226244,#226245,#226246,
#226247,#226248,#226249,#226250,#226251,#226252,#226253,#226254,#226255,
#226256,#226257,#226258,#226259,#226260,#226261,#226262,#226263,#226264,
#226265,#226266,#226267,#226268,#226269,#226270,#226271,#226272,#226273,
#226274,#226275,#226276,#226277,#226278,#226279,#226280,#226281),
 .UNSPECIFIED.,.F.,.F.,(4,3,3,3,3,3,3,3,3,3,3,3,3,3,3,3,3,3,3,3,3,3,3,3,
3,3,3,3,3,3,3,3,3,3,3,3,3,3,3,3,3,3,3,3,3,3,3,3,3,3,3,3,3,3,3,3,3,3,3,3,
3,3,3,3,3,3,3,3,3,3,3,3,3,3,3,3,3,3,3,3,3,3,4),(13.6852259127505,13.7801099435782,
13.8756905427146,13.9720376507108,13.9963041500819,14.0762611679736,14.1561236791645,
14.2359092120701,14.3156352344774,14.3953191670501,14.4749898540935,14.5546570063244,
14.6343363539807,14.7140436316013,14.7938385549703,14.8736825899846,14.9536407114316,
14.996040160802,15.0759975957193,15.1558605290186,15.2356464886784,15.3153729420553,
15.3950573093886,15.4747284354873,15.5543960293979,15.6340758209858,15.7137835444186,
15.7935789142272,15.8734233967061,15.9533819633687,15.9957761715221,16.075733473648,
16.1555962732271,16.2353820983737,16.3151084165785,16.3947926482139,16.4744636382654,
16.5541310959256,16.6338107511781,16.7135183383086,16.7933135725563,16.873157919691,
16.9531163525208,16.9955121822422,17.0754694434268,17.1553322011706,17.2351179836328,
17.314844258348,17.3945284457316,17.4741993905267,17.5538668023107,17.633546411104,
17.713253951229,17.7930491378706,17.8728934369877,17.9528518215654,17.9952481929623,
18.0752055148322,18.1550683340336,18.2348541786619,18.3145805161891,18.3942647669683,
18.4739357758324,18.5536032520972,18.6332829257289,18.7129905309957,18.7927857829151,
18.8726301474848,18.9525885972255,18.9949842036824,19.0745911127166,19.1541037254495,
19.2335398970435,19.3129174188851,19.3948541184062,19.4741786590968,19.5535018339292,
19.6328396635326,19.7122081748832,19.7916638055052,19.8711715970075,19.9507856857916,
19.9684110150538),.UNSPECIFIED.);
#1788=B_SPLINE_CURVE_WITH_KNOTS('',3,(#226283,#226284,#226285,#226286,#226287,
#226288,#226289,#226290),.UNSPECIFIED.,.F.,.F.,(4,1,1,1,1,4),(9.69384021421591,
9.99736010720132,10.9970961179215,11.9968321286416,12.9965681393618,13.6852257078742),
 .UNSPECIFIED.);
#1789=B_SPLINE_CURVE_WITH_KNOTS('',3,(#226291,#226292,#226293,#226294),
 .UNSPECIFIED.,.F.,.F.,(4,4),(2.11499176853536,2.21729342848466),
 .UNSPECIFIED.);
#1790=B_SPLINE_CURVE_WITH_KNOTS('',3,(#226297,#226298,#226299,#226300),
 .UNSPECIFIED.,.F.,.F.,(4,4),(0.680042556218447,0.864704436494292),
 .UNSPECIFIED.);
#1791=B_SPLINE_CURVE_WITH_KNOTS('',3,(#226302,#226303,#226304,#226305,#226306,
#226307),.UNSPECIFIED.,.F.,.F.,(4,2,4),(1.08095347481491,1.12724697765872,
1.29160843392453),.UNSPECIFIED.);
#1792=B_SPLINE_CURVE_WITH_KNOTS('',3,(#226309,#226310,#226311,#226312),
 .UNSPECIFIED.,.F.,.F.,(4,4),(7.40204040069455,7.71374059257392),
 .UNSPECIFIED.);
#1793=B_SPLINE_CURVE_WITH_KNOTS('',3,(#226313,#226314,#226315,#226316),
 .UNSPECIFIED.,.F.,.F.,(4,4),(7.33678677271359,7.40204018020966),
 .UNSPECIFIED.);
#1794=B_SPLINE_CURVE_WITH_KNOTS('',3,(#233097,#233098,#233099,#233100,#233101,
#233102,#233103,#233104,#233105,#233106,#233107,#233108,#233109,#233110,
#233111,#233112,#233113,#233114,#233115,#233116,#233117,#233118,#233119,
#233120,#233121,#233122),.UNSPECIFIED.,.F.,.F.,(4,2,2,2,2,2,2,2,2,2,2,2,
4),(0.00142388210668726,0.102461957337261,0.113522908460601,0.113690938992141,
0.113757861101401,0.113798818001596,0.113835523929253,0.113882073960433,
0.113974496333833,0.114650839173592,0.121077466272109,0.143151309422213,
0.224602262057577),.UNSPECIFIED.);
#1795=B_SPLINE_CURVE_WITH_KNOTS('',3,(#233126,#233127,#233128,#233129,#233130,
#233131,#233132,#233133),.UNSPECIFIED.,.F.,.F.,(4,2,2,4),(2.33046280664109,
2.42727660829376,2.61395533624592,2.74540526220401),.UNSPECIFIED.);
#1796=B_SPLINE_CURVE_WITH_KNOTS('',3,(#233135,#233136,#233137,#233138,#233139,
#233140,#233141,#233142),.UNSPECIFIED.,.F.,.F.,(4,2,2,4),(2.00538747380151,
2.05391915238944,2.2405978803416,2.32226381429565),.UNSPECIFIED.);
#1797=B_SPLINE_CURVE_WITH_KNOTS('',3,(#233143,#233144,#233145,#233146,#233147,
#233148,#233149,#233150,#233151,#233152,#233153,#233154,#233155,#233156,
#233157,#233158,#233159,#233160,#233161,#233162,#233163,#233164,#233165,
#233166,#233167,#233168,#233169,#233170,#233171,#233172,#233173,#233174,
#233175,#233176,#233177,#233178,#233179,#233180,#233181,#233182,#233183,
#233184,#233185,#233186,#233187,#233188,#233189,#233190,#233191,#233192,
#233193,#233194,#233195,#233196,#233197,#233198,#233199,#233200,#233201,
#233202,#233203),.UNSPECIFIED.,.F.,.F.,(4,3,3,3,3,3,3,3,3,3,3,3,3,3,3,3,
3,3,3,3,4),(18.355181505216,18.4388551554013,18.5224381182464,18.6059504780618,
18.6930840414458,18.7765257696782,18.8599620560646,18.9434109684692,19.0268905791748,
19.1104642874994,19.1940933848967,19.277841130172,19.3030189851341,19.3867448283189,
19.4703731737785,19.5539222575379,19.6374102562577,19.7208568886211,19.804280273106,
19.8877082391123,19.907870678554),.UNSPECIFIED.);
#1798=B_SPLINE_CURVE_WITH_KNOTS('',3,(#233206,#233207,#233208,#233209),
 .UNSPECIFIED.,.F.,.F.,(4,4),(2.29240291271631,2.39658298756549),
 .UNSPECIFIED.);
#1799=B_SPLINE_CURVE_WITH_KNOTS('',3,(#233211,#233212,#233213,#233214),
 .UNSPECIFIED.,.F.,.F.,(4,4),(114.216190622748,114.937428679585),
 .UNSPECIFIED.);
#1800=B_SPLINE_CURVE_WITH_KNOTS('',3,(#233216,#233217,#233218,#233219,#233220,
#233221,#233222,#233223,#233224,#233225,#233226,#233227,#233228,#233229,
#233230,#233231,#233232,#233233,#233234,#233235,#233236,#233237,#233238,
#233239,#233240,#233241,#233242,#233243,#233244,#233245,#233246,#233247,
#233248,#233249,#233250,#233251,#233252,#233253,#233254,#233255,#233256,
#233257,#233258,#233259,#233260,#233261,#233262,#233263,#233264),
 .UNSPECIFIED.,.F.,.F.,(4,3,3,3,3,3,3,3,3,3,3,3,3,3,3,3,4),(112.983899304452,
113.06383913655,113.143687478933,113.223461848315,113.303179703167,113.386520393033,
113.466189271689,113.545858040054,113.625542428248,113.705258172749,113.785062875852,
113.864919771647,113.944886163636,113.969905222095,114.075449330658,114.178641043672,
114.216190536642),.UNSPECIFIED.);
#1801=B_SPLINE_CURVE_WITH_KNOTS('',3,(#233265,#233266,#233267,#233268,#233269,
#233270),.UNSPECIFIED.,.F.,.F.,(4,2,4),(3.21716342272831,3.38194136709993,
3.40990698571987),.UNSPECIFIED.);
#1802=B_SPLINE_CURVE_WITH_KNOTS('',3,(#233273,#233274,#233275,#233276,#233277,
#233278,#233279,#233280,#233281,#233282),.UNSPECIFIED.,.F.,.F.,(4,3,3,4),
(21.7400988072349,21.8231667809187,21.907157678014,21.9911485751093),
 .UNSPECIFIED.);
#1803=B_SPLINE_CURVE_WITH_KNOTS('',3,(#233283,#233284,#233285,#233286,#233287,
#233288,#233289,#233290,#233291,#233292,#233293,#233294,#233295,#233296,
#233297,#233298,#233299,#233300,#233301,#233302,#233303,#233304,#233305,
#233306,#233307,#233308,#233309,#233310,#233311,#233312,#233313,#233314,
#233315,#233316,#233317,#233318,#233319,#233320,#233321,#233322,#233323,
#233324,#233325,#233326,#233327,#233328,#233329,#233330,#233331,#233332,
#233333,#233334,#233335,#233336,#233337,#233338,#233339,#233340,#233341,
#233342,#233343,#233344,#233345,#233346,#233347,#233348,#233349,#233350,
#233351,#233352,#233353,#233354,#233355,#233356,#233357,#233358,#233359,
#233360,#233361,#233362,#233363,#233364,#233365,#233366,#233367,#233368,
#233369,#233370,#233371,#233372,#233373,#233374,#233375,#233376,#233377,
#233378,#233379,#233380,#233381,#233382,#233383,#233384,#233385,#233386,
#233387,#233388,#233389,#233390,#233391,#233392,#233393,#233394,#233395,
#233396,#233397,#233398,#233399,#233400,#233401,#233402,#233403,#233404,
#233405,#233406,#233407,#233408,#233409,#233410,#233411,#233412,#233413,
#233414,#233415,#233416,#233417,#233418,#233419,#233420,#233421,#233422,
#233423,#233424,#233425,#233426,#233427,#233428,#233429,#233430,#233431,
#233432,#233433,#233434,#233435,#233436,#233437,#233438,#233439,#233440,
#233441,#233442,#233443,#233444,#233445,#233446,#233447,#233448,#233449,
#233450,#233451,#233452,#233453,#233454,#233455,#233456,#233457,#233458,
#233459,#233460,#233461,#233462,#233463,#233464,#233465,#233466,#233467,
#233468,#233469,#233470,#233471,#233472,#233473,#233474,#233475,#233476,
#233477,#233478,#233479,#233480,#233481,#233482,#233483,#233484,#233485,
#233486,#233487,#233488,#233489,#233490,#233491,#233492,#233493,#233494,
#233495,#233496,#233497,#233498,#233499,#233500,#233501,#233502),
 .UNSPECIFIED.,.F.,.F.,(4,3,3,3,3,3,3,3,3,3,3,3,3,3,3,3,3,3,3,3,3,3,3,3,
3,3,3,3,3,3,3,3,3,3,3,3,3,3,3,3,3,3,3,3,3,3,3,3,3,3,3,3,3,3,3,3,3,3,3,3,
3,3,3,3,3,3,3,3,3,3,3,3,3,4),(21.9911485752722,22.0905199443307,22.1906522436346,
22.2915864234119,22.3022270172945,22.3859654335529,22.4696006451592,22.5531527849645,
22.6366419137261,22.7200955530059,22.8035317329769,22.8869685266068,22.9704240034381,
23.0539681767605,23.1375569390688,23.2212798871326,23.3019630280146,23.385701881021,
23.4693375349391,23.5528901221183,23.6363797028221,23.719833799406,23.8032704398822,
23.8867076967894,23.9701636392423,24.0537082792805,24.1372975096405,24.2210209233106,
24.3016990387348,24.3854377526698,24.4690732665012,24.5526257127343,24.6361151517867,
24.7195691061525,24.803005604086,24.8864427182613,24.9698985179291,25.0534430159093,
25.1370321043811,25.2207553778982,25.3014350494549,25.3851737205122,25.4688091904866,
25.5523615919349,25.6358509853249,25.7193048928488,25.8027413432284,25.8861784091806,
25.9696341599982,26.0531786084049,26.1367676468314,26.2204908699956,26.301171060175,
26.3849097947876,26.4685453291628,26.5520977957841,26.6355872550472,26.7190412292786,
26.8024777468644,26.8859148804588,26.9693706992928,27.052915215926,27.1365043228015,
27.2202276141041,27.3009070708951,27.3842944828408,27.4675500501445,27.550729511587,
27.633851366961,27.7169340711784,27.8000126126222,27.8830868940955,27.9662056561429,
28.0225858316167),.UNSPECIFIED.);
#1804=B_SPLINE_CURVE_WITH_KNOTS('',3,(#240284,#240285,#240286,#240287,#240288,
#240289,#240290,#240291,#240292,#240293,#240294,#240295),.UNSPECIFIED.,
 .F.,.F.,(4,2,2,2,2,4),(6.24097663211903E-6,0.021580083937109,0.110840866786185,
0.217918405967283,0.317351591624377,0.326345639146483),.UNSPECIFIED.);
#1805=B_SPLINE_CURVE_WITH_KNOTS('',3,(#240296,#240297,#240298,#240299,#240300,
#240301,#240302,#240303,#240304,#240305,#240306,#240307,#240308,#240309,
#240310,#240311,#240312,#240313,#240314,#240315,#240316,#240317,#240318,
#240319,#240320,#240321,#240322,#240323,#240324,#240325,#240326,#240327,
#240328,#240329,#240330,#240331,#240332,#240333,#240334,#240335),
 .UNSPECIFIED.,.F.,.F.,(4,2,2,2,2,2,2,2,2,2,2,2,2,2,2,2,2,2,2,4),(0.00239488436222245,
0.102201826640357,0.181209549188827,0.193475035579474,0.193971074266331,
0.194663958026065,0.195057404656709,0.19519989369731,0.195235582116475,
0.195270182708239,0.19528749027832,0.195301045811009,0.195315937093886,
0.195340101780065,0.19542079041973,0.199626232853206,0.219414959447415,
0.256408927732008,0.309909372043629,0.350021811302258),.UNSPECIFIED.);
#1806=B_SPLINE_CURVE_WITH_KNOTS('',3,(#240336,#240337,#240338,#240339,#240340,
#240341,#240342,#240343,#240344,#240345),.UNSPECIFIED.,.F.,.F.,(4,2,2,2,
4),(0.000659999465871507,0.0472322359860498,0.0984434332088515,0.155288380275565,
0.220269663386073),.UNSPECIFIED.);
#1807=B_SPLINE_CURVE_WITH_KNOTS('',3,(#240346,#240347,#240348,#240349,#240350,
#240351,#240352,#240353,#240354,#240355,#240356,#240357,#240358,#240359,
#240360,#240361,#240362,#240363,#240364,#240365,#240366,#240367,#240368,
#240369,#240370,#240371,#240372,#240373,#240374,#240375),.UNSPECIFIED.,
 .F.,.F.,(4,2,2,2,2,2,2,2,2,2,2,2,2,2,4),(0.0120072812196319,0.124651425623479,
0.129299183636369,0.137626079649342,0.137766129259384,0.138318251653115,
0.138447846329851,0.138519129454569,0.138578433547788,0.138648094876172,
0.138770572390779,0.139302371484231,0.149636581332025,0.170304854177609,
0.277058970671051),.UNSPECIFIED.);
#1808=B_SPLINE_CURVE_WITH_KNOTS('',3,(#240376,#240377,#240378,#240379,#240380,
#240381,#240382,#240383,#240384,#240385,#240386,#240387,#240388,#240389,
#240390,#240391,#240392,#240393,#240394,#240395,#240396,#240397,#240398,
#240399,#240400,#240401,#240402,#240403,#240404,#240405,#240406,#240407,
#240408,#240409,#240410,#240411,#240412,#240413,#240414,#240415,#240416,
#240417,#240418,#240419,#240420,#240421,#240422,#240423,#240424,#240425,
#240426,#240427,#240428,#240429,#240430,#240431,#240432,#240433,#240434,
#240435,#240436,#240437,#240438,#240439,#240440,#240441),.UNSPECIFIED.,
 .F.,.F.,(4,2,2,2,2,2,2,2,2,2,2,2,2,2,2,2,2,2,2,2,2,2,2,2,2,2,2,2,2,2,2,
2,4),(0.326345639146483,0.39717698474622,0.401652761356229,0.402004293626876,
0.402088366886084,0.402134901523776,0.402173777520773,0.402219222079272,
0.402299830966666,0.402652644059501,0.421430642133052,0.478736005391261,
0.57626086556828,0.720833256739961,0.847312020492082,0.931615895673563,
1.06112874522252,1.06509356720185,1.0700343312839,1.07436288411271,1.07465542728212,
1.07475922918139,1.07482626368171,1.07488881226853,1.07497172318178,1.07514950344775,
1.07739277037847,1.10748082532148,1.17423178070239,1.27214718241461,1.40528589051194,
1.50493087009919,1.61754120424573),.UNSPECIFIED.);
#1809=B_SPLINE_CURVE_WITH_KNOTS('',3,(#240811,#240812,#240813,#240814,#240815,
#240816,#240817,#240818,#240819,#240820),.UNSPECIFIED.,.F.,.F.,(4,3,3,4),
(1504.57104348731,1504.65363118549,1504.73825612743,1504.82288106937),
 .UNSPECIFIED.);
#1810=B_SPLINE_CURVE_WITH_KNOTS('',3,(#240822,#240823,#240824,#240825,#240826,
#240827,#240828,#240829,#240830,#240831,#240832,#240833,#240834,#240835,
#240836,#240837,#240838,#240839,#240840,#240841,#240842,#240843,#240844,
#240845,#240846,#240847,#240848,#240849,#240850,#240851,#240852,#240853,
#240854,#240855,#240856,#240857,#240858,#240859,#240860,#240861,#240862,
#240863,#240864,#240865,#240866,#240867,#240868,#240869,#240870,#240871,
#240872,#240873,#240874,#240875,#240876,#240877,#240878,#240879,#240880,
#240881,#240882,#240883,#240884,#240885,#240886,#240887,#240888,#240889,
#240890,#240891,#240892,#240893,#240894,#240895,#240896,#240897,#240898,
#240899,#240900,#240901,#240902,#240903,#240904,#240905,#240906,#240907,
#240908,#240909,#240910,#240911,#240912,#240913,#240914,#240915,#240916,
#240917,#240918,#240919,#240920,#240921,#240922,#240923,#240924,#240925,
#240926,#240927,#240928,#240929,#240930,#240931,#240932,#240933,#240934,
#240935,#240936,#240937,#240938,#240939,#240940,#240941,#240942,#240943,
#240944,#240945,#240946,#240947,#240948,#240949,#240950,#240951,#240952,
#240953,#240954,#240955,#240956,#240957,#240958,#240959,#240960,#240961,
#240962,#240963,#240964,#240965,#240966,#240967,#240968,#240969,#240970,
#240971,#240972),.UNSPECIFIED.,.F.,.F.,(4,3,3,3,3,3,3,3,3,3,3,3,3,3,3,3,
3,3,3,3,3,3,3,3,3,3,3,3,3,3,3,3,3,3,3,3,3,3,3,3,3,3,3,3,3,3,3,3,3,3,4),
(1504.8228810695,1504.91073091525,1504.9944696271,1505.07810513846,1505.16165758186,
1505.24514701771,1505.32860096832,1505.41203746217,1505.49547457192,1505.57893036684,
1505.66247485957,1505.74606394251,1505.82978721006,1505.91046692597,1505.99420563782,
1506.07784114918,1506.16139359258,1506.24488302843,1506.32833697905,1506.41177347289,
1506.49521058265,1506.57866637757,1506.6622108703,1506.74579995324,1506.82952322079,
1506.91020293669,1506.99394164854,1507.0775771599,1507.1611296033,1507.24461903915,
1507.32807298977,1507.41150948361,1507.49494659337,1507.57840238829,1507.66194688102,
1507.74553596396,1507.82925923151,1507.90993894741,1507.99367765926,1508.07731317062,
1508.16086561402,1508.24435504987,1508.32780900049,1508.41124549433,1508.49468260409,
1508.57813839901,1508.66168289173,1508.74527197468,1508.82899524223,1508.90967495813,
1508.96603014687),.UNSPECIFIED.);
#1811=B_SPLINE_CURVE_WITH_KNOTS('',3,(#240974,#240975,#240976,#240977,#240978,
#240979),.UNSPECIFIED.,.F.,.F.,(4,2,4),(1.56320921069321,1.68048617233251,
1.7638474477127),.UNSPECIFIED.);
#1812=B_SPLINE_CURVE_WITH_KNOTS('',3,(#240981,#240982,#240983,#240984,#240985,
#240986,#240987,#240988,#240989,#240990,#240991,#240992,#240993,#240994,
#240995,#240996,#240997,#240998,#240999,#241000,#241001,#241002,#241003,
#241004,#241005,#241006,#241007,#241008,#241009,#241010,#241011,#241012,
#241013,#241014,#241015,#241016,#241017,#241018,#241019,#241020,#241021,
#241022,#241023,#241024,#241025,#241026,#241027,#241028,#241029,#241030,
#241031,#241032,#241033,#241034,#241035,#241036,#241037,#241038,#241039,
#241040,#241041,#241042,#241043,#241044,#241045,#241046,#241047,#241048,
#241049,#241050,#241051,#241052,#241053,#241054,#241055,#241056,#241057,
#241058,#241059,#241060,#241061,#241062,#241063,#241064,#241065,#241066,
#241067,#241068,#241069,#241070,#241071,#241072,#241073,#241074,#241075,
#241076,#241077,#241078,#241079,#241080,#241081,#241082,#241083,#241084,
#241085,#241086,#241087,#241088,#241089,#241090,#241091,#241092,#241093,
#241094,#241095,#241096,#241097,#241098,#241099,#241100,#241101,#241102,
#241103,#241104,#241105,#241106,#241107,#241108,#241109,#241110,#241111,
#241112,#241113,#241114,#241115,#241116,#241117,#241118,#241119,#241120,
#241121,#241122,#241123,#241124,#241125,#241126,#241127,#241128,#241129,
#241130,#241131,#241132,#241133,#241134,#241135,#241136,#241137,#241138,
#241139,#241140,#241141,#241142,#241143,#241144,#241145,#241146),
 .UNSPECIFIED.,.F.,.F.,(4,3,3,3,3,3,3,3,3,3,3,3,3,3,3,3,3,3,3,3,3,3,3,3,
3,3,3,3,3,3,3,3,3,3,3,3,3,3,3,3,3,3,3,3,3,3,3,3,3,3,3,3,3,3,3,4),(1504.82288106969,
1504.91507842316,1505.00777905537,1505.1007403094,1505.19403937815,1505.22102153496,
1505.30476024681,1505.38839575818,1505.47194820158,1505.55543763743,1505.63889158805,
1505.7223280819,1505.80576519166,1505.88922098658,1505.97276547931,1506.05635456225,
1506.14007782982,1506.22075754568,1506.30449625753,1506.38813176889,1506.47168421229,
1506.55517364814,1506.63862759876,1506.7220640926,1506.80550120236,1506.88895699728,
1506.97250149001,1507.05609057295,1507.13981384051,1507.2204935564,1507.30423226825,
1507.38786777961,1507.47142022301,1507.55490965886,1507.63836360947,1507.72180010332,
1507.80523721307,1507.88869300799,1507.97223750072,1508.05582658366,1508.13954985122,
1508.22022956712,1508.30396827897,1508.38760379033,1508.47115623373,1508.55464566958,
1508.6380996202,1508.72153611404,1508.8049732238,1508.88842901872,1508.97197351145,
1509.05556259439,1509.13928586195,1509.21996557784,1509.30425789109,1509.38855020433),
 .UNSPECIFIED.);
#1813=B_SPLINE_CURVE_WITH_KNOTS('',3,(#241147,#241148,#241149,#241150,#241151,
#241152,#241153,#241154,#241155,#241156),.UNSPECIFIED.,.F.,.F.,(4,3,3,4),
(1504.57225479568,1504.65682073549,1504.74135303069,1504.82288106951),
 .UNSPECIFIED.);
#1814=B_SPLINE_CURVE_WITH_KNOTS('',3,(#241162,#241163,#241164,#241165),
 .UNSPECIFIED.,.F.,.F.,(4,4),(1498.28924643674,1498.53969576232),
 .UNSPECIFIED.);
#1815=B_SPLINE_CURVE_WITH_KNOTS('',3,(#241166,#241167,#241168,#241169,#241170,
#241171,#241172,#241173,#241174,#241175,#241176,#241177,#241178,#241179,
#241180,#241181,#241182,#241183,#241184,#241185,#241186,#241187,#241188,
#241189,#241190,#241191,#241192,#241193,#241194,#241195,#241196,#241197,
#241198,#241199,#241200,#241201,#241202,#241203,#241204,#241205,#241206,
#241207,#241208,#241209,#241210,#241211,#241212,#241213,#241214,#241215,
#241216,#241217,#241218,#241219,#241220,#241221,#241222,#241223,#241224,
#241225,#241226,#241227,#241228,#241229,#241230,#241231,#241232,#241233,
#241234,#241235,#241236,#241237,#241238,#241239,#241240,#241241,#241242,
#241243,#241244,#241245,#241246,#241247,#241248,#241249,#241250,#241251,
#241252,#241253,#241254,#241255,#241256,#241257,#241258,#241259,#241260,
#241261,#241262,#241263,#241264,#241265,#241266,#241267,#241268,#241269,
#241270,#241271,#241272,#241273,#241274,#241275,#241276,#241277,#241278,
#241279,#241280,#241281,#241282,#241283,#241284,#241285,#241286,#241287,
#241288,#241289,#241290,#241291,#241292,#241293,#241294,#241295,#241296,
#241297,#241298,#241299,#241300,#241301,#241302,#241303,#241304,#241305,
#241306,#241307,#241308,#241309,#241310,#241311,#241312,#241313,#241314,
#241315,#241316,#241317,#241318,#241319,#241320,#241321,#241322,#241323,
#241324,#241325,#241326,#241327,#241328,#241329,#241330,#241331,#241332,
#241333,#241334,#241335,#241336,#241337,#241338,#241339,#241340,#241341,
#241342,#241343,#241344,#241345,#241346,#241347,#241348,#241349,#241350,
#241351,#241352,#241353,#241354,#241355,#241356,#241357,#241358,#241359,
#241360,#241361,#241362,#241363,#241364,#241365,#241366,#241367,#241368,
#241369,#241370,#241371,#241372,#241373,#241374,#241375,#241376,#241377,
#241378,#241379,#241380,#241381,#241382),.UNSPECIFIED.,.F.,.F.,(4,3,3,3,
3,3,3,3,3,3,3,3,3,3,3,3,3,3,3,3,3,3,3,3,3,3,3,3,3,3,3,3,3,3,3,3,3,3,3,3,
3,3,3,3,3,3,3,3,3,3,3,3,3,3,3,3,3,3,3,3,3,3,3,3,3,3,3,3,3,3,3,3,4),(1498.53969576232,
1498.63380533641,1498.72828492247,1498.82328898073,1498.91231485092,1498.99605356277,
1499.07968907413,1499.16324151753,1499.24673095338,1499.33018490399,1499.41362139784,
1499.4970585076,1499.58051430251,1499.66405879524,1499.74764787818,1499.83137114574,
1499.91205086164,1499.99578957349,1500.07942508486,1500.16297752826,1500.24646696411,
1500.32992091473,1500.41335740858,1500.49679451833,1500.58025031325,1500.66379480598,
1500.74738388893,1500.83110715649,1500.91178687237,1500.99552558422,1501.07916109558,
1501.16271353898,1501.24620297483,1501.32965692545,1501.41309341929,1501.49653052905,
1501.57998632397,1501.6635308167,1501.74711989964,1501.8308431672,1501.91152288309,
1501.99526159493,1502.0788971063,1502.1624495497,1502.24593898555,1502.32939293616,
1502.41282943001,1502.49626653976,1502.57972233468,1502.66326682741,1502.74685591035,
1502.8305791779,1502.91125889381,1502.99499760566,1503.07863311703,1503.16218556043,
1503.24567499628,1503.32912894689,1503.41256544074,1503.4960025505,1503.57945834542,
1503.66300283815,1503.74659192109,1503.83031518865,1503.91099490453,1503.99374376682,
1504.0763980856,1504.15897688734,1504.24149913172,1504.32399495184,1504.4064721317,
1504.48898209449,1504.57104348731),.UNSPECIFIED.);
#1816=B_SPLINE_CURVE_WITH_KNOTS('',3,(#241384,#241385,#241386,#241387,#241388,
#241389,#241390,#241391,#241392,#241393,#241394,#241395,#241396,#241397,
#241398,#241399,#241400,#241401,#241402,#241403,#241404,#241405,#241406,
#241407,#241408,#241409,#241410,#241411,#241412,#241413,#241414,#241415,
#241416,#241417,#241418,#241419,#241420,#241421,#241422,#241423,#241424,
#241425,#241426,#241427,#241428,#241429,#241430,#241431,#241432,#241433,
#241434,#241435,#241436,#241437,#241438,#241439,#241440,#241441,#241442,
#241443,#241444,#241445,#241446,#241447,#241448,#241449,#241450,#241451,
#241452,#241453,#241454,#241455,#241456,#241457,#241458,#241459,#241460,
#241461,#241462,#241463,#241464,#241465,#241466,#241467,#241468,#241469,
#241470,#241471,#241472,#241473,#241474,#241475,#241476,#241477,#241478,
#241479,#241480,#241481,#241482,#241483,#241484,#241485,#241486,#241487,
#241488,#241489,#241490,#241491,#241492,#241493,#241494,#241495,#241496,
#241497,#241498,#241499,#241500,#241501,#241502,#241503,#241504,#241505,
#241506,#241507,#241508,#241509,#241510,#241511,#241512,#241513,#241514,
#241515,#241516,#241517,#241518,#241519,#241520,#241521,#241522,#241523,
#241524,#241525,#241526,#241527,#241528,#241529,#241530,#241531,#241532,
#241533,#241534,#241535,#241536,#241537,#241538,#241539,#241540,#241541,
#241542,#241543,#241544,#241545,#241546,#241547,#241548,#241549,#241550,
#241551,#241552,#241553,#241554,#241555,#241556,#241557,#241558,#241559,
#241560,#241561,#241562,#241563,#241564,#241565,#241566,#241567,#241568,
#241569,#241570,#241571,#241572,#241573,#241574,#241575,#241576,#241577,
#241578,#241579,#241580,#241581,#241582,#241583,#241584,#241585,#241586,
#241587,#241588,#241589,#241590,#241591,#241592,#241593,#241594,#241595,
#241596,#241597,#241598,#241599,#241600,#241601,#241602,#241603,#241604,
#241605,#241606),.UNSPECIFIED.,.F.,.F.,(4,3,3,3,3,3,3,3,3,3,3,3,3,3,3,3,
3,3,3,3,3,3,3,3,3,3,3,3,3,3,3,3,3,3,3,3,3,3,3,3,3,3,3,3,3,3,3,3,3,3,3,3,
3,3,3,3,3,3,3,3,3,3,3,3,3,3,3,3,3,3,3,3,3,3,4),(1498.53969576233,1498.62505947587,
1498.70820805334,1498.79135490896,1498.87451833665,1498.96154012015,1499.04483918337,
1499.12819845884,1499.21167592631,1499.22260547064,1499.30634418249,1499.38997969385,
1499.47353213725,1499.55702157311,1499.64047552372,1499.72391201757,1499.80734912732,
1499.89080492224,1499.97434941497,1500.05793849791,1500.14166176547,1500.22234148136,
1500.30608019321,1500.38971570457,1500.47326814797,1500.55675758382,1500.64021153444,
1500.72364802828,1500.80708513804,1500.89054093296,1500.97408542569,1501.05767450863,
1501.14139777619,1501.22207749208,1501.30581620393,1501.38945171529,1501.47300415869,
1501.55649359454,1501.63994754516,1501.723384039,1501.80682114876,1501.89027694367,
1501.9738214364,1502.05741051934,1502.1411337869,1502.2218135028,1502.30555221465,
1502.38918772601,1502.47274016941,1502.55622960526,1502.63968355588,1502.72312004972,
1502.80655715948,1502.8900129544,1502.97355744713,1503.05714653007,1503.14086979762,
1503.22154951352,1503.30528822537,1503.38892373673,1503.47247618013,1503.55596561598,
1503.63941956659,1503.72285606044,1503.80629317019,1503.88974896511,1503.97329345784,
1504.05688254078,1504.14060580834,1504.22128552424,1504.3090278421,1504.39384146299,
1504.47856831567,1504.56320793387,1504.57225479568),.UNSPECIFIED.);
#1817=B_SPLINE_CURVE_WITH_KNOTS('',3,(#241607,#241608,#241609,#241610,#241611,
#241612,#241613,#241614,#241615,#241616),.UNSPECIFIED.,.F.,.F.,(4,3,3,4),
(1498.28900992258,1498.38879043601,1498.48754282435,1498.53969576216),
 .UNSPECIFIED.);
#1818=B_SPLINE_CURVE_WITH_KNOTS('',3,(#241622,#241623,#241624,#241625),
 .UNSPECIFIED.,.F.,.F.,(4,4),(1492.00598701905,1492.25651045514),
 .UNSPECIFIED.);
#1819=B_SPLINE_CURVE_WITH_KNOTS('',3,(#241626,#241627,#241628,#241629,#241630,
#241631,#241632,#241633,#241634,#241635),.UNSPECIFIED.,.F.,.F.,(4,1,1,1,
1,1,1,4),(1492.25651045514,1492.9138987866,1493.91363479732,1494.91337080804,
1495.91310681876,1496.91284282948,1497.9125788402,1498.28924643674),
 .UNSPECIFIED.);
#1820=B_SPLINE_CURVE_WITH_KNOTS('',3,(#241637,#241638,#241639,#241640,#241641,
#241642,#241643,#241644,#241645,#241646,#241647,#241648,#241649,#241650,
#241651,#241652,#241653,#241654,#241655,#241656,#241657,#241658,#241659,
#241660,#241661,#241662,#241663,#241664,#241665,#241666,#241667,#241668,
#241669,#241670,#241671,#241672,#241673,#241674,#241675,#241676,#241677,
#241678,#241679,#241680,#241681,#241682,#241683,#241684,#241685,#241686,
#241687,#241688,#241689,#241690,#241691,#241692,#241693,#241694,#241695,
#241696,#241697,#241698,#241699,#241700,#241701,#241702,#241703,#241704,
#241705,#241706,#241707,#241708,#241709,#241710,#241711,#241712,#241713,
#241714,#241715,#241716,#241717,#241718,#241719,#241720,#241721,#241722,
#241723,#241724,#241725,#241726,#241727,#241728,#241729,#241730,#241731,
#241732,#241733,#241734,#241735,#241736,#241737,#241738,#241739,#241740,
#241741,#241742,#241743,#241744,#241745,#241746,#241747,#241748,#241749,
#241750,#241751,#241752,#241753,#241754,#241755,#241756,#241757,#241758,
#241759,#241760,#241761,#241762,#241763,#241764,#241765,#241766,#241767,
#241768,#241769,#241770,#241771,#241772,#241773,#241774,#241775,#241776,
#241777,#241778,#241779,#241780,#241781,#241782,#241783,#241784,#241785,
#241786,#241787,#241788,#241789,#241790,#241791,#241792,#241793,#241794,
#241795,#241796,#241797,#241798,#241799,#241800,#241801,#241802,#241803,
#241804,#241805,#241806,#241807,#241808,#241809,#241810,#241811,#241812,
#241813,#241814,#241815,#241816,#241817,#241818,#241819,#241820,#241821,
#241822,#241823,#241824,#241825,#241826,#241827,#241828,#241829,#241830,
#241831,#241832,#241833,#241834,#241835,#241836,#241837,#241838,#241839,
#241840,#241841,#241842,#241843,#241844,#241845,#241846,#241847,#241848,
#241849,#241850,#241851,#241852,#241853,#241854,#241855,#241856),
 .UNSPECIFIED.,.F.,.F.,(4,3,3,3,3,3,3,3,3,3,3,3,3,3,3,3,3,3,3,3,3,3,3,3,
3,3,3,3,3,3,3,3,3,3,3,3,3,3,3,3,3,3,3,3,3,3,3,3,3,3,3,3,3,3,3,3,3,3,3,3,
3,3,3,3,3,3,3,3,3,3,3,3,3,4),(1492.25651045529,1492.33980475775,1492.42299730472,
1492.50610866675,1492.58915933873,1492.67217794586,1492.75518199317,1492.83818994494,
1492.92122026463,1493.00433983238,1493.08750804642,1493.1708018184,1493.22418940632,
1493.30792811817,1493.39156362953,1493.47511607293,1493.55860550878,1493.6420594594,
1493.72549595324,1493.808933063,1493.89238885792,1493.97593335065,1494.05952243359,
1494.14324570114,1494.22392541704,1494.30766412889,1494.39129964025,1494.47485208365,
1494.5583415195,1494.64179547012,1494.72523196396,1494.80866907372,1494.89212486864,
1494.97566936137,1495.05925844431,1495.14298171187,1495.22366142776,1495.30740013961,
1495.39103565097,1495.47458809437,1495.55807753022,1495.64153148084,1495.72496797468,
1495.80840508444,1495.89186087936,1495.97540537209,1496.05899445503,1496.14271772258,
1496.22339743848,1496.30713615033,1496.39077166169,1496.47432410509,1496.55781354094,
1496.64126749156,1496.7247039854,1496.80814109516,1496.89159689008,1496.9751413828,
1497.05873046575,1497.1424537333,1497.2231334492,1497.30687216105,1497.39050767241,
1497.47406011581,1497.55754955166,1497.64100350227,1497.72443999612,1497.80787710587,
1497.89133290079,1497.97487739352,1498.05846647646,1498.14218974402,1498.22286945992,
1498.28900992258),.UNSPECIFIED.);
#1821=B_SPLINE_CURVE_WITH_KNOTS('',3,(#241857,#241858,#241859,#241860,#241861,
#241862,#241863,#241864,#241865,#241866,#241867,#241868,#241869),
 .UNSPECIFIED.,.F.,.F.,(4,3,3,3,4),(1492.00484482495,1492.08845275128,1492.17218669413,
1492.2244533956,1492.25651045515),.UNSPECIFIED.);
#1822=B_SPLINE_CURVE_WITH_KNOTS('',3,(#241875,#241876,#241877,#241878,#241879,
#241880,#241881,#241882,#241883,#241884,#241885,#241886,#241887),
 .UNSPECIFIED.,.F.,.F.,(4,3,3,3,4),(1485.72166203219,1485.80528850285,1485.88903401518,
1485.91574671156,1485.97332514797),.UNSPECIFIED.);
#1823=B_SPLINE_CURVE_WITH_KNOTS('',3,(#241888,#241889,#241890,#241891,#241892,
#241893,#241894,#241895,#241896,#241897),.UNSPECIFIED.,.F.,.F.,(4,1,1,1,
1,1,1,4),(1485.97333225685,1486.91548272228,1487.915218733,1488.91495474372,
1489.91469075444,1490.91442676516,1491.91416277588,1492.00598701905),
 .UNSPECIFIED.);
#1824=B_SPLINE_CURVE_WITH_KNOTS('',3,(#241899,#241900,#241901,#241902,#241903,
#241904,#241905,#241906,#241907,#241908,#241909,#241910,#241911,#241912,
#241913,#241914,#241915,#241916,#241917,#241918,#241919,#241920,#241921,
#241922,#241923,#241924,#241925,#241926,#241927,#241928,#241929,#241930,
#241931,#241932,#241933,#241934,#241935,#241936,#241937,#241938,#241939,
#241940,#241941,#241942,#241943,#241944,#241945,#241946,#241947,#241948,
#241949,#241950,#241951,#241952,#241953,#241954,#241955,#241956,#241957,
#241958,#241959,#241960,#241961,#241962,#241963,#241964,#241965,#241966,
#241967,#241968,#241969,#241970,#241971,#241972,#241973,#241974,#241975,
#241976,#241977,#241978,#241979,#241980,#241981,#241982,#241983,#241984,
#241985,#241986,#241987,#241988,#241989,#241990,#241991,#241992,#241993,
#241994,#241995,#241996,#241997,#241998,#241999,#242000,#242001,#242002,
#242003,#242004,#242005,#242006,#242007,#242008,#242009,#242010,#242011,
#242012,#242013,#242014,#242015,#242016,#242017,#242018,#242019,#242020,
#242021,#242022,#242023,#242024,#242025,#242026,#242027,#242028,#242029,
#242030,#242031,#242032,#242033,#242034,#242035,#242036,#242037,#242038,
#242039,#242040,#242041,#242042,#242043,#242044,#242045,#242046,#242047,
#242048,#242049,#242050,#242051,#242052,#242053,#242054,#242055,#242056,
#242057,#242058,#242059,#242060,#242061,#242062,#242063,#242064,#242065,
#242066,#242067,#242068,#242069,#242070,#242071,#242072,#242073,#242074,
#242075,#242076,#242077,#242078,#242079,#242080,#242081,#242082,#242083,
#242084,#242085,#242086,#242087,#242088,#242089,#242090,#242091,#242092,
#242093,#242094,#242095,#242096,#242097,#242098,#242099,#242100,#242101,
#242102,#242103,#242104,#242105,#242106,#242107,#242108,#242109,#242110,
#242111,#242112,#242113,#242114,#242115,#242116,#242117,#242118),
 .UNSPECIFIED.,.F.,.F.,(4,3,3,3,3,3,3,3,3,3,3,3,3,3,3,3,3,3,3,3,3,3,3,3,
3,3,3,3,3,3,3,3,3,3,3,3,3,3,3,3,3,3,3,3,3,3,3,3,3,3,3,3,3,3,3,3,3,3,3,3,
3,3,3,3,3,3,3,3,3,3,3,3,3,4),(1485.97332514817,1486.08013280166,1486.18927155072,
1486.22603733128,1486.30977604313,1486.39341155449,1486.47696399789,1486.56045343374,
1486.64390738436,1486.7273438782,1486.81078098796,1486.89423678288,1486.97778127561,
1487.06137035855,1487.1450936261,1487.225773342,1487.30951205385,1487.39314756521,
1487.47670000861,1487.56018944446,1487.64364339508,1487.72707988892,1487.81051699868,
1487.8939727936,1487.97751728633,1488.06110636927,1488.14482963682,1488.22550935272,
1488.30924806457,1488.39288357593,1488.47643601933,1488.55992545518,1488.6433794058,
1488.72681589964,1488.8102530094,1488.89370880432,1488.97725329705,1489.06084237999,
1489.14456564755,1489.22524536344,1489.30898407529,1489.39261958665,1489.47617203005,
1489.5596614659,1489.64311541652,1489.72655191036,1489.80998902012,1489.89344481504,
1489.97698930776,1490.06057839071,1490.14430165826,1490.22498137416,1490.30872008601,
1490.39235559737,1490.47590804077,1490.55939747662,1490.64285142724,1490.72628792108,
1490.80972503084,1490.89318082576,1490.97672531848,1491.06031440143,1491.14403766898,
1491.22471738488,1491.30846947086,1491.39551639012,1491.47905786342,1491.56254230654,
1491.64598783891,1491.72941254974,1491.81285539563,1491.89630938701,1491.97981837138,
1492.00484482495),.UNSPECIFIED.);
#1825=B_SPLINE_CURVE_WITH_KNOTS('',3,(#242119,#242120,#242121,#242122,#242123,
#242124,#242125,#242126,#242127,#242128),.UNSPECIFIED.,.F.,.F.,(4,3,3,4),
(1485.72197536628,1485.80448560964,1485.8889053788,1485.97332514797),
 .UNSPECIFIED.);
#1826=B_SPLINE_CURVE_WITH_KNOTS('',3,(#242134,#242135,#242136,#242137,#242138,
#242139,#242140,#242141,#242142,#242143),.UNSPECIFIED.,.F.,.F.,(4,3,3,4),
(1479.43866858093,1479.52103553806,1479.60558768936,1479.69013984066),
 .UNSPECIFIED.);
#1827=B_SPLINE_CURVE_WITH_KNOTS('',3,(#242144,#242145,#242146,#242147,#242148,
#242149,#242150,#242151,#242152,#242153,#242154,#242155,#242156,#242157,
#242158,#242159,#242160,#242161,#242162,#242163,#242164,#242165,#242166,
#242167,#242168,#242169,#242170,#242171,#242172,#242173,#242174,#242175,
#242176,#242177,#242178,#242179,#242180,#242181,#242182,#242183,#242184,
#242185,#242186,#242187,#242188,#242189,#242190,#242191,#242192,#242193,
#242194,#242195,#242196,#242197,#242198,#242199,#242200,#242201,#242202,
#242203,#242204,#242205,#242206,#242207,#242208,#242209,#242210,#242211,
#242212,#242213,#242214,#242215,#242216,#242217,#242218,#242219,#242220,
#242221,#242222,#242223,#242224,#242225,#242226,#242227,#242228,#242229,
#242230,#242231,#242232,#242233,#242234,#242235,#242236,#242237,#242238,
#242239,#242240,#242241,#242242,#242243,#242244,#242245,#242246,#242247,
#242248,#242249,#242250,#242251,#242252,#242253,#242254,#242255,#242256,
#242257,#242258,#242259,#242260,#242261,#242262,#242263,#242264,#242265,
#242266,#242267,#242268,#242269,#242270,#242271,#242272,#242273,#242274,
#242275,#242276,#242277,#242278,#242279,#242280,#242281,#242282,#242283,
#242284,#242285,#242286,#242287,#242288,#242289,#242290,#242291,#242292,
#242293,#242294,#242295,#242296,#242297,#242298,#242299,#242300,#242301,
#242302,#242303,#242304,#242305,#242306,#242307,#242308,#242309,#242310,
#242311,#242312,#242313,#242314,#242315,#242316,#242317,#242318,#242319,
#242320,#242321,#242322,#242323,#242324,#242325,#242326,#242327,#242328,
#242329,#242330,#242331,#242332,#242333,#242334,#242335,#242336,#242337,
#242338,#242339,#242340,#242341,#242342,#242343,#242344,#242345,#242346,
#242347,#242348,#242349,#242350,#242351,#242352,#242353,#242354,#242355,
#242356,#242357,#242358,#242359,#242360),.UNSPECIFIED.,.F.,.F.,(4,3,3,3,
3,3,3,3,3,3,3,3,3,3,3,3,3,3,3,3,3,3,3,3,3,3,3,3,3,3,3,3,3,3,3,3,3,3,3,3,
3,3,3,3,3,3,3,3,3,3,3,3,3,3,3,3,3,3,3,3,3,3,3,3,3,3,3,3,3,3,3,3,4),(1479.69013984079,
1479.80373524402,1479.91733064724,1480.00106935909,1480.08470487045,1480.16825731385,
1480.2517467497,1480.33520070032,1480.41863719416,1480.50207430392,1480.58553009884,
1480.66907459157,1480.75266367451,1480.83638694206,1480.91706665796,1481.00080536981,
1481.08444088117,1481.16799332457,1481.25148276042,1481.33493671104,1481.41837320488,
1481.50181031464,1481.58526610956,1481.66881060229,1481.75239968523,1481.83612295279,
1481.91680266868,1482.00054138053,1482.08417689189,1482.16772933529,1482.25121877114,
1482.33467272176,1482.4181092156,1482.50154632536,1482.58500212028,1482.66854661301,
1482.75213569595,1482.8358589635,1482.9165386794,1483.00027739125,1483.08391290261,
1483.16746534601,1483.25095478186,1483.33440873248,1483.41784522632,1483.50128233608,
1483.584738131,1483.66828262373,1483.75187170667,1483.83559497422,1483.91627469012,
1484.00001340197,1484.08364891333,1484.16720135673,1484.25069079258,1484.33414474319,
1484.41758123704,1484.5010183468,1484.58447414171,1484.66801863444,1484.75160771738,
1484.83533098494,1484.91601070084,1484.99976112188,1485.08340578193,1485.16694939894,
1485.25043572519,1485.33388288075,1485.41730895535,1485.50075704418,1485.58421581109,
1485.66774035371,1485.72166203219),.UNSPECIFIED.);
#1828=B_SPLINE_CURVE_WITH_KNOTS('',3,(#242362,#242363,#242364,#242365,#242366,
#242367,#242368,#242369,#242370,#242371,#242372,#242373,#242374,#242375,
#242376,#242377,#242378,#242379,#242380,#242381,#242382,#242383,#242384,
#242385,#242386,#242387,#242388,#242389,#242390,#242391,#242392,#242393,
#242394,#242395,#242396,#242397,#242398,#242399,#242400,#242401,#242402,
#242403,#242404,#242405,#242406,#242407,#242408,#242409,#242410,#242411,
#242412,#242413,#242414,#242415,#242416,#242417,#242418,#242419,#242420,
#242421,#242422,#242423,#242424,#242425,#242426,#242427,#242428,#242429,
#242430,#242431,#242432,#242433,#242434,#242435,#242436,#242437,#242438,
#242439,#242440,#242441,#242442,#242443,#242444,#242445,#242446,#242447,
#242448,#242449,#242450,#242451,#242452,#242453,#242454,#242455,#242456,
#242457,#242458,#242459,#242460,#242461,#242462,#242463,#242464,#242465,
#242466,#242467,#242468,#242469,#242470,#242471,#242472,#242473,#242474,
#242475,#242476,#242477,#242478,#242479,#242480,#242481,#242482,#242483,
#242484,#242485,#242486,#242487,#242488,#242489,#242490,#242491,#242492,
#242493,#242494,#242495,#242496,#242497,#242498,#242499,#242500,#242501,
#242502,#242503,#242504,#242505,#242506,#242507,#242508,#242509,#242510,
#242511,#242512,#242513,#242514,#242515,#242516,#242517,#242518,#242519,
#242520,#242521,#242522,#242523,#242524,#242525,#242526,#242527,#242528,
#242529,#242530,#242531,#242532,#242533,#242534,#242535,#242536,#242537,
#242538,#242539,#242540,#242541,#242542,#242543,#242544,#242545,#242546,
#242547,#242548,#242549,#242550,#242551,#242552,#242553,#242554,#242555,
#242556,#242557,#242558,#242559,#242560,#242561,#242562,#242563,#242564,
#242565,#242566,#242567,#242568,#242569,#242570,#242571,#242572,#242573,
#242574,#242575,#242576,#242577,#242578,#242579,#242580,#242581),
 .UNSPECIFIED.,.F.,.F.,(4,3,3,3,3,3,3,3,3,3,3,3,3,3,3,3,3,3,3,3,3,3,3,3,
3,3,3,3,3,3,3,3,3,3,3,3,3,3,3,3,3,3,3,3,3,3,3,3,3,3,3,3,3,3,3,3,3,3,3,3,
3,3,3,3,3,3,3,3,3,3,3,3,3,4),(1479.69013984079,1479.77630058833,1479.86253318071,
1479.94885023975,1480.03532621794,1480.1218940574,1480.20861921668,1480.22762126696,
1480.31135997881,1480.39499549017,1480.47854793357,1480.56203736942,1480.64549132004,
1480.72892781388,1480.81236492364,1480.89582071856,1480.97936521129,1481.06295429423,
1481.14667756178,1481.22735727768,1481.31109598953,1481.39473150089,1481.47828394429,
1481.56177338014,1481.64522733076,1481.7286638246,1481.81210093436,1481.89555672928,
1481.97910122201,1482.06269030495,1482.1464135725,1482.2270932884,1482.31083200025,
1482.39446751161,1482.47801995501,1482.56150939086,1482.64496334148,1482.72839983532,
1482.81183694508,1482.89529274,1482.97883723273,1483.06242631567,1483.14614958322,
1483.22682929912,1483.31056801097,1483.39420352233,1483.47775596573,1483.56124540158,
1483.6446993522,1483.72813584604,1483.8115729558,1483.89502875072,1483.97857324344,
1484.06216232639,1484.14588559394,1484.22656530984,1484.31030402169,1484.39393953305,
1484.47749197645,1484.5609814123,1484.64443536292,1484.72787185676,1484.81130896652,
1484.89476476144,1484.97830925417,1485.06189833711,1485.14562160467,1485.22630132056,
1485.3090888973,1485.39177806216,1485.47437529998,1485.5569182117,1485.63944678899,
1485.72197536628),.UNSPECIFIED.);
#1829=B_SPLINE_CURVE_WITH_KNOTS('',3,(#242582,#242583,#242584,#242585,#242586,
#242587,#242588,#242589,#242590,#242591),.UNSPECIFIED.,.F.,.F.,(4,3,3,4),
(1479.43983851051,1479.52903735213,1479.61799758571,1479.69013984063),
 .UNSPECIFIED.);
#1830=B_SPLINE_CURVE_WITH_KNOTS('',3,(#242597,#242598,#242599,#242600,#242601,
#242602,#242603,#242604,#242605,#242606),.UNSPECIFIED.,.F.,.F.,(4,3,3,4),
(1473.15664071279,1473.24472264985,1473.3326204829,1473.40695453349),
 .UNSPECIFIED.);
#1831=B_SPLINE_CURVE_WITH_KNOTS('',3,(#242607,#242608,#242609,#242610,#242611,
#242612,#242613,#242614,#242615,#242616,#242617,#242618,#242619,#242620,
#242621,#242622,#242623,#242624,#242625,#242626,#242627,#242628,#242629,
#242630,#242631,#242632,#242633,#242634,#242635,#242636,#242637,#242638,
#242639,#242640,#242641,#242642,#242643,#242644,#242645,#242646,#242647,
#242648,#242649,#242650,#242651,#242652,#242653,#242654,#242655,#242656,
#242657,#242658,#242659,#242660,#242661,#242662,#242663,#242664,#242665,
#242666,#242667,#242668,#242669,#242670,#242671,#242672,#242673,#242674,
#242675,#242676,#242677,#242678,#242679,#242680,#242681,#242682,#242683,
#242684,#242685,#242686,#242687,#242688,#242689,#242690,#242691,#242692,
#242693,#242694,#242695,#242696,#242697,#242698,#242699,#242700,#242701,
#242702,#242703,#242704,#242705,#242706,#242707,#242708,#242709,#242710,
#242711,#242712,#242713,#242714,#242715,#242716,#242717,#242718,#242719,
#242720,#242721,#242722,#242723,#242724,#242725,#242726,#242727,#242728,
#242729,#242730,#242731,#242732,#242733,#242734,#242735,#242736,#242737,
#242738,#242739,#242740,#242741,#242742,#242743,#242744,#242745,#242746,
#242747,#242748,#242749,#242750,#242751,#242752,#242753,#242754,#242755,
#242756,#242757,#242758,#242759,#242760,#242761,#242762,#242763,#242764,
#242765,#242766,#242767,#242768,#242769,#242770,#242771,#242772,#242773,
#242774,#242775,#242776,#242777,#242778,#242779,#242780,#242781,#242782,
#242783,#242784,#242785,#242786,#242787,#242788,#242789,#242790,#242791,
#242792,#242793,#242794,#242795,#242796,#242797,#242798,#242799,#242800,
#242801,#242802,#242803,#242804,#242805,#242806,#242807,#242808,#242809,
#242810,#242811,#242812,#242813,#242814,#242815,#242816,#242817,#242818,
#242819,#242820,#242821,#242822,#242823,#242824,#242825,#242826),
 .UNSPECIFIED.,.F.,.F.,(4,3,3,3,3,3,3,3,3,3,3,3,3,3,3,3,3,3,3,3,3,3,3,3,
3,3,3,3,3,3,3,3,3,3,3,3,3,3,3,3,3,3,3,3,3,3,3,3,3,3,3,3,3,3,3,3,3,3,3,3,
3,3,3,3,3,3,3,3,3,3,3,3,3,4),(1473.40695453361,1473.49393313965,1473.5810114473,
1473.66828127154,1473.75565011186,1473.8432173964,1473.91891458292,1474.00265329477,
1474.08628880613,1474.16984124953,1474.25333068538,1474.336784636,1474.42022112984,
1474.5036582396,1474.58711403452,1474.67065852724,1474.75424761019,1474.83797087774,
1474.91865059364,1475.00238930549,1475.08602481685,1475.16957726025,1475.2530666961,
1475.33652064672,1475.41995714056,1475.50339425032,1475.58685004524,1475.67039453797,
1475.75398362091,1475.83770688847,1475.91838660436,1476.00212531621,1476.08576082757,
1476.16931327097,1476.25280270682,1476.33625665744,1476.41969315128,1476.50313026104,
1476.58658605596,1476.67013054869,1476.75371963163,1476.83744289918,1476.91812261508,
1477.00186132693,1477.08549683829,1477.16904928169,1477.25253871754,1477.33599266816,
1477.419429162,1477.50286627176,1477.58632206667,1477.6698665594,1477.75345564234,
1477.8371789099,1477.9178586258,1478.00159733765,1478.08523284901,1478.16878529241,
1478.25227472826,1478.33572867888,1478.41916517272,1478.50260228248,1478.5860580774,
1478.66960257013,1478.75319165307,1478.83691492063,1478.91759463652,1479.00021914845,
1479.08274652633,1479.16519590404,1479.24758186863,1479.32993154163,1479.41227038175,
1479.43866858093),.UNSPECIFIED.);
#1832=B_SPLINE_CURVE_WITH_KNOTS('',3,(#242828,#242829,#242830,#242831,#242832,
#242833,#242834,#242835,#242836,#242837,#242838,#242839,#242840,#242841,
#242842,#242843,#242844,#242845,#242846,#242847,#242848,#242849,#242850,
#242851,#242852,#242853,#242854,#242855,#242856,#242857,#242858,#242859,
#242860,#242861,#242862,#242863,#242864,#242865,#242866,#242867,#242868,
#242869,#242870,#242871,#242872,#242873,#242874,#242875,#242876,#242877,
#242878,#242879,#242880,#242881,#242882,#242883,#242884,#242885,#242886,
#242887,#242888,#242889,#242890,#242891,#242892,#242893,#242894,#242895,
#242896,#242897,#242898,#242899,#242900,#242901,#242902,#242903,#242904,
#242905,#242906,#242907,#242908,#242909,#242910,#242911,#242912,#242913,
#242914,#242915,#242916,#242917,#242918,#242919,#242920,#242921,#242922,
#242923,#242924,#242925,#242926,#242927,#242928,#242929,#242930,#242931,
#242932,#242933,#242934,#242935,#242936,#242937,#242938,#242939,#242940,
#242941,#242942,#242943,#242944,#242945,#242946,#242947,#242948,#242949,
#242950,#242951,#242952,#242953,#242954,#242955,#242956,#242957,#242958,
#242959,#242960,#242961,#242962,#242963,#242964,#242965,#242966,#242967,
#242968,#242969,#242970,#242971,#242972,#242973,#242974,#242975,#242976,
#242977,#242978,#242979,#242980,#242981,#242982,#242983,#242984,#242985,
#242986,#242987,#242988,#242989,#242990,#242991,#242992,#242993,#242994,
#242995,#242996,#242997,#242998,#242999,#243000,#243001,#243002,#243003,
#243004,#243005,#243006,#243007,#243008,#243009,#243010,#243011,#243012,
#243013,#243014,#243015,#243016,#243017,#243018,#243019,#243020,#243021,
#243022,#243023,#243024,#243025,#243026,#243027,#243028,#243029,#243030,
#243031,#243032,#243033,#243034,#243035,#243036,#243037,#243038,#243039,
#243040,#243041,#243042,#243043,#243044,#243045,#243046,#243047),
 .UNSPECIFIED.,.F.,.F.,(4,3,3,3,3,3,3,3,3,3,3,3,3,3,3,3,3,3,3,3,3,3,3,3,
3,3,3,3,3,3,3,3,3,3,3,3,3,3,3,3,3,3,3,3,3,3,3,3,3,3,3,3,3,3,3,3,3,3,3,3,
3,3,3,3,3,3,3,3,3,3,3,3,3,4),(1473.40695453377,1473.4893182278,1473.57160671137,
1473.65384440038,1473.73605555324,1473.81825920997,1473.90047440225,1473.98277068985,
1474.06510696983,1474.14757432633,1474.22920520264,1474.31294391449,1474.39657942585,
1474.48013186925,1474.5636213051,1474.64707525572,1474.73051174956,1474.81394885932,
1474.89740465424,1474.98094914697,1475.06453822991,1475.14826149746,1475.22894121336,
1475.31267992521,1475.39631543657,1475.47986787997,1475.56335731582,1475.64681126644,
1475.73024776028,1475.81368487004,1475.89714066496,1475.98068515769,1476.06427424063,
1476.14799750818,1476.22867722408,1476.31241593593,1476.39605144729,1476.47960389069,
1476.56309332654,1476.64654727716,1476.729983771,1476.81342088076,1476.89687667568,
1476.98042116841,1477.06401025135,1477.1477335189,1477.2284132348,1477.31215194665,
1477.39578745801,1477.47933990141,1477.56282933726,1477.64628328788,1477.72971978172,
1477.81315689148,1477.8966126864,1477.98015717913,1478.06374626207,1478.14746952962,
1478.22814924552,1478.31188795737,1478.39552346873,1478.47907591213,1478.56256534798,
1478.6460192986,1478.72945579244,1478.8128929022,1478.89634869712,1478.97989318985,
1479.06348227279,1479.14720554034,1479.22788525624,1479.31758500425,1479.40706476103,
1479.43983851051),.UNSPECIFIED.);
#1833=B_SPLINE_CURVE_WITH_KNOTS('',3,(#243048,#243049,#243050,#243051,#243052,
#243053,#243054,#243055,#243056,#243057),.UNSPECIFIED.,.F.,.F.,(4,3,3,4),
(1473.15552466501,1473.22946919192,1473.35769273628,1473.40695453361),
 .UNSPECIFIED.);
#1834=B_SPLINE_CURVE_WITH_KNOTS('',3,(#243063,#243064,#243065,#243066,#243067,
#243068,#243069,#243070,#243071,#243072),.UNSPECIFIED.,.F.,.F.,(4,3,3,4),
(1466.87244437141,1466.92076250788,1467.04006077289,1467.12376922643),
 .UNSPECIFIED.);
#1835=B_SPLINE_CURVE_WITH_KNOTS('',3,(#243073,#243074,#243075,#243076,#243077,
#243078,#243079,#243080,#243081,#243082,#243083,#243084,#243085,#243086,
#243087,#243088,#243089,#243090,#243091,#243092,#243093,#243094,#243095,
#243096,#243097,#243098,#243099,#243100,#243101,#243102,#243103,#243104,
#243105,#243106,#243107,#243108,#243109,#243110,#243111,#243112,#243113,
#243114,#243115,#243116,#243117,#243118,#243119,#243120,#243121,#243122,
#243123,#243124,#243125,#243126,#243127,#243128,#243129,#243130,#243131,
#243132,#243133,#243134,#243135,#243136,#243137,#243138,#243139,#243140,
#243141,#243142,#243143,#243144,#243145,#243146,#243147,#243148,#243149,
#243150,#243151,#243152,#243153,#243154,#243155,#243156,#243157,#243158,
#243159,#243160,#243161,#243162,#243163,#243164,#243165,#243166,#243167,
#243168,#243169,#243170,#243171,#243172,#243173,#243174,#243175,#243176,
#243177,#243178,#243179,#243180,#243181,#243182,#243183,#243184,#243185,
#243186,#243187,#243188,#243189,#243190,#243191,#243192,#243193,#243194,
#243195,#243196,#243197,#243198,#243199,#243200,#243201,#243202,#243203,
#243204,#243205,#243206,#243207,#243208,#243209,#243210,#243211,#243212,
#243213,#243214,#243215,#243216,#243217,#243218,#243219,#243220,#243221,
#243222,#243223,#243224,#243225,#243226,#243227,#243228,#243229,#243230,
#243231,#243232,#243233,#243234,#243235,#243236,#243237,#243238,#243239,
#243240,#243241,#243242,#243243,#243244,#243245,#243246,#243247,#243248,
#243249,#243250,#243251,#243252,#243253,#243254,#243255,#243256,#243257,
#243258,#243259,#243260,#243261,#243262,#243263,#243264,#243265,#243266,
#243267,#243268,#243269,#243270,#243271,#243272,#243273,#243274,#243275,
#243276,#243277,#243278,#243279,#243280,#243281,#243282,#243283,#243284,
#243285,#243286,#243287,#243288,#243289,#243290,#243291,#243292),
 .UNSPECIFIED.,.F.,.F.,(4,3,3,3,3,3,3,3,3,3,3,3,3,3,3,3,3,3,3,3,3,3,3,3,
3,3,3,3,3,3,3,3,3,3,3,3,3,3,3,3,3,3,3,3,3,3,3,3,3,3,3,3,3,3,3,3,3,3,3,3,
3,3,3,3,3,3,3,3,3,3,3,3,3,4),(1467.12376922661,1467.20615137202,1467.28846542945,
1467.37073818782,1467.45299077312,1467.53524219248,1467.61751144987,1467.69986534415,
1467.78226484149,1467.86478835703,1467.9204985186,1468.00423723045,1468.08787274181,
1468.17142518521,1468.25491462106,1468.33836857168,1468.42180506552,1468.50524217528,
1468.5886979702,1468.67224246292,1468.75583154587,1468.83955481342,1468.92023452932,
1469.00397324117,1469.08760875253,1469.17116119593,1469.25465063178,1469.3381045824,
1469.42154107624,1469.504978186,1469.58843398092,1469.67197847365,1469.75556755659,
1469.83929082415,1469.91997054004,1470.00370925189,1470.08734476325,1470.17089720665,
1470.2543866425,1470.33784059312,1470.42127708696,1470.50471419672,1470.58816999164,
1470.67171448437,1470.75530356731,1470.83902683487,1470.91970655076,1471.00344526261,
1471.08708077397,1471.17063321737,1471.25412265322,1471.33757660384,1471.42101309768,
1471.50445020744,1471.58790600235,1471.67145049508,1471.75503957802,1471.83876284558,
1471.91944256148,1472.00318127333,1472.08681678469,1472.17036922809,1472.25385866394,
1472.33731261456,1472.4207491084,1472.50418621816,1472.58764201308,1472.67118650581,
1472.75477558875,1472.83849885631,1472.9191785722,1473.00772889966,1473.09607576719,
1473.15664071279),.UNSPECIFIED.);
#1836=B_SPLINE_CURVE_WITH_KNOTS('',3,(#243294,#243295,#243296,#243297,#243298,
#243299,#243300,#243301,#243302,#243303,#243304,#243305,#243306,#243307,
#243308,#243309,#243310,#243311,#243312,#243313,#243314,#243315,#243316,
#243317,#243318,#243319,#243320,#243321,#243322,#243323,#243324,#243325,
#243326,#243327,#243328,#243329,#243330,#243331,#243332,#243333,#243334,
#243335,#243336,#243337,#243338,#243339,#243340,#243341,#243342,#243343,
#243344,#243345,#243346,#243347,#243348,#243349,#243350,#243351,#243352,
#243353,#243354,#243355,#243356,#243357,#243358,#243359,#243360,#243361,
#243362,#243363,#243364,#243365,#243366,#243367,#243368,#243369,#243370,
#243371,#243372,#243373,#243374,#243375,#243376,#243377,#243378,#243379,
#243380,#243381,#243382,#243383,#243384,#243385,#243386,#243387,#243388,
#243389,#243390,#243391,#243392,#243393,#243394,#243395,#243396,#243397,
#243398,#243399,#243400,#243401,#243402,#243403,#243404,#243405,#243406,
#243407,#243408,#243409,#243410,#243411,#243412,#243413,#243414,#243415,
#243416,#243417,#243418,#243419,#243420,#243421,#243422,#243423,#243424,
#243425,#243426,#243427,#243428,#243429,#243430,#243431,#243432,#243433,
#243434,#243435,#243436,#243437,#243438,#243439,#243440,#243441,#243442,
#243443,#243444,#243445,#243446,#243447,#243448,#243449,#243450,#243451,
#243452,#243453,#243454,#243455,#243456,#243457,#243458,#243459,#243460,
#243461,#243462,#243463,#243464,#243465,#243466,#243467,#243468,#243469,
#243470,#243471,#243472,#243473,#243474,#243475,#243476,#243477,#243478,
#243479,#243480,#243481,#243482,#243483,#243484,#243485,#243486,#243487,
#243488,#243489,#243490,#243491,#243492,#243493,#243494,#243495,#243496,
#243497,#243498,#243499,#243500,#243501,#243502,#243503,#243504,#243505,
#243506,#243507,#243508,#243509,#243510),.UNSPECIFIED.,.F.,.F.,(4,3,3,3,
3,3,3,3,3,3,3,3,3,3,3,3,3,3,3,3,3,3,3,3,3,3,3,3,3,3,3,3,3,3,3,3,3,3,3,3,
3,3,3,3,3,3,3,3,3,3,3,3,3,3,3,3,3,3,3,3,3,3,3,3,3,3,3,3,3,3,3,3,4),(1467.12376922643,
1467.2310531276,1467.31479183945,1467.39842735081,1467.48197979421,1467.56546923006,
1467.64892318068,1467.73235967452,1467.81579678428,1467.8992525792,1467.98279707193,
1468.06638615487,1468.15010942242,1468.23078913832,1468.31452785017,1468.39816336153,
1468.48171580493,1468.56520524078,1468.6486591914,1468.73209568524,1468.815532795,
1468.89898858992,1468.98253308265,1469.06612216559,1469.14984543314,1469.23052514904,
1469.31426386089,1469.39789937225,1469.48145181565,1469.5649412515,1469.64839520212,
1469.73183169596,1469.81526880572,1469.89872460064,1469.98226909337,1470.06585817631,
1470.14958144386,1470.23026115976,1470.31399987161,1470.39763538297,1470.48118782637,
1470.56467726222,1470.64813121284,1470.73156770668,1470.81500481644,1470.89846061136,
1470.98200510409,1471.06559418703,1471.14931745458,1471.22999717048,1471.31373588233,
1471.39737139369,1471.48092383709,1471.56441327294,1471.64786722356,1471.7313037174,
1471.81474082716,1471.89819662208,1471.98174111481,1472.06533019775,1472.1490534653,
1472.2297331812,1472.31347615588,1472.39711495474,1472.48066971443,1472.56502658325,
1472.64847685927,1472.73190848728,1472.81533953906,1472.90038582054,1472.98390578302,
1473.06971522401,1473.15552466501),.UNSPECIFIED.);
#1837=B_SPLINE_CURVE_WITH_KNOTS('',3,(#243511,#243512,#243513,#243514,#243515,
#243516,#243517,#243518,#243519,#243520),.UNSPECIFIED.,.F.,.F.,(4,3,3,4),
(1466.8719408414,1466.9543981102,1467.03908366825,1467.12376922629),
 .UNSPECIFIED.);
#1838=B_SPLINE_CURVE_WITH_KNOTS('',3,(#243526,#243527,#243528,#243529,#243530,
#243531,#243532,#243533,#243534,#243535),.UNSPECIFIED.,.F.,.F.,(4,3,3,4),
(1460.5887469457,1460.67138214754,1460.75598303333,1460.84058391912),
 .UNSPECIFIED.);
#1839=B_SPLINE_CURVE_WITH_KNOTS('',3,(#243536,#243537,#243538,#243539,#243540,
#243541,#243542,#243543,#243544,#243545,#243546,#243547,#243548,#243549,
#243550,#243551,#243552,#243553,#243554,#243555,#243556,#243557,#243558,
#243559,#243560,#243561,#243562,#243563,#243564,#243565,#243566,#243567,
#243568,#243569,#243570,#243571,#243572,#243573,#243574,#243575,#243576,
#243577,#243578,#243579,#243580,#243581,#243582,#243583,#243584,#243585,
#243586,#243587,#243588,#243589,#243590,#243591,#243592,#243593,#243594,
#243595,#243596,#243597,#243598,#243599,#243600,#243601,#243602,#243603,
#243604,#243605,#243606,#243607,#243608,#243609,#243610,#243611,#243612,
#243613,#243614,#243615,#243616,#243617,#243618,#243619,#243620,#243621,
#243622,#243623,#243624,#243625,#243626,#243627,#243628,#243629,#243630,
#243631,#243632,#243633,#243634,#243635,#243636,#243637,#243638,#243639,
#243640,#243641,#243642,#243643,#243644,#243645,#243646,#243647,#243648,
#243649,#243650,#243651,#243652,#243653,#243654,#243655,#243656,#243657,
#243658,#243659,#243660,#243661,#243662,#243663,#243664,#243665,#243666,
#243667,#243668,#243669,#243670,#243671,#243672,#243673,#243674,#243675,
#243676,#243677,#243678,#243679,#243680,#243681,#243682,#243683,#243684,
#243685,#243686,#243687,#243688,#243689,#243690,#243691,#243692,#243693,
#243694,#243695,#243696,#243697,#243698,#243699,#243700,#243701,#243702,
#243703,#243704,#243705,#243706,#243707,#243708,#243709,#243710,#243711,
#243712,#243713,#243714,#243715,#243716,#243717,#243718,#243719,#243720,
#243721,#243722,#243723,#243724,#243725,#243726,#243727,#243728,#243729,
#243730,#243731,#243732,#243733,#243734,#243735,#243736,#243737,#243738,
#243739,#243740,#243741,#243742,#243743,#243744,#243745,#243746,#243747,
#243748,#243749,#243750,#243751,#243752,#243753,#243754,#243755),
 .UNSPECIFIED.,.F.,.F.,(4,3,3,3,3,3,3,3,3,3,3,3,3,3,3,3,3,3,3,3,3,3,3,3,
3,3,3,3,3,3,3,3,3,3,3,3,3,3,3,3,3,3,3,3,3,3,3,3,3,3,3,3,3,3,3,3,3,3,3,3,
3,3,3,3,3,3,3,3,3,3,3,3,3,4),(1460.84058391925,1460.92234644356,1461.00608515541,
1461.08972066677,1461.17327311017,1461.25676254602,1461.34021649664,1461.42365299048,
1461.50709010024,1461.59054589516,1461.67409038789,1461.75767947083,1461.84140273838,
1461.92208245428,1462.00582116613,1462.08945667749,1462.17300912089,1462.25649855674,
1462.33995250736,1462.4233890012,1462.50682611096,1462.59028190588,1462.67382639861,
1462.75741548155,1462.84113874911,1462.921818465,1463.00555717685,1463.08919268821,
1463.17274513161,1463.25623456746,1463.33968851808,1463.42312501192,1463.50656212168,
1463.5900179166,1463.67356240933,1463.75715149227,1463.84087475982,1463.92155447572,
1464.00529318757,1464.08892869893,1464.17248114233,1464.25597057818,1464.3394245288,
1464.42286102264,1464.5062981324,1464.58975392732,1464.67329842005,1464.75688750299,
1464.84061077054,1464.92129048644,1465.00502919829,1465.08866470965,1465.17221715305,
1465.2557065889,1465.33916053952,1465.42259703336,1465.50603414312,1465.58948993803,
1465.67303443076,1465.7566235137,1465.84034678126,1465.92102649716,1466.00476796687,
1466.08840559879,1466.17195952814,1466.25952013355,1466.34297044609,1466.42640328248,
1466.50983671436,1466.59328880972,1466.67681791279,1466.76039202568,1466.84407147563,
1466.87244437141),.UNSPECIFIED.);
#1840=B_SPLINE_CURVE_WITH_KNOTS('',3,(#243757,#243758,#243759,#243760,#243761,
#243762,#243763,#243764,#243765,#243766,#243767,#243768,#243769,#243770,
#243771,#243772,#243773,#243774,#243775,#243776,#243777,#243778,#243779,
#243780,#243781,#243782,#243783,#243784,#243785,#243786,#243787,#243788,
#243789,#243790,#243791,#243792,#243793,#243794,#243795,#243796,#243797,
#243798,#243799,#243800,#243801,#243802,#243803,#243804,#243805,#243806,
#243807,#243808,#243809,#243810,#243811,#243812,#243813,#243814,#243815,
#243816,#243817,#243818,#243819,#243820,#243821,#243822,#243823,#243824,
#243825,#243826,#243827,#243828,#243829,#243830,#243831,#243832,#243833,
#243834,#243835,#243836,#243837,#243838,#243839,#243840,#243841,#243842,
#243843,#243844,#243845,#243846,#243847,#243848,#243849,#243850,#243851,
#243852,#243853,#243854,#243855,#243856,#243857,#243858,#243859,#243860,
#243861,#243862,#243863,#243864,#243865,#243866,#243867,#243868,#243869,
#243870,#243871,#243872,#243873,#243874,#243875,#243876,#243877,#243878,
#243879,#243880,#243881,#243882,#243883,#243884,#243885,#243886,#243887,
#243888,#243889,#243890,#243891,#243892,#243893,#243894,#243895,#243896,
#243897,#243898,#243899,#243900,#243901,#243902,#243903,#243904,#243905,
#243906,#243907,#243908,#243909,#243910,#243911,#243912,#243913,#243914,
#243915,#243916,#243917,#243918,#243919,#243920,#243921,#243922,#243923,
#243924,#243925,#243926,#243927,#243928,#243929,#243930,#243931,#243932,
#243933,#243934,#243935,#243936,#243937,#243938,#243939,#243940,#243941,
#243942,#243943,#243944,#243945,#243946,#243947,#243948,#243949,#243950,
#243951,#243952,#243953,#243954,#243955,#243956,#243957,#243958,#243959,
#243960,#243961,#243962,#243963,#243964,#243965,#243966,#243967,#243968,
#243969,#243970,#243971,#243972,#243973,#243974,#243975,#243976),
 .UNSPECIFIED.,.F.,.F.,(4,3,3,3,3,3,3,3,3,3,3,3,3,3,3,3,3,3,3,3,3,3,3,3,
3,3,3,3,3,3,3,3,3,3,3,3,3,3,3,3,3,3,3,3,3,3,3,3,3,3,3,3,3,3,3,3,3,3,3,3,
3,3,3,3,3,3,3,3,3,3,3,3,3,4),(1460.84058391944,1460.93315405195,1461.02625537987,
1461.11963264212,1461.21335570444,1461.23263706328,1461.31637577513,1461.40001128649,
1461.48356372989,1461.56705316574,1461.65050711636,1461.7339436102,1461.81738071996,
1461.90083651488,1461.98438100761,1462.06797009055,1462.1516933581,1462.232373074,
1462.31611178585,1462.39974729721,1462.48329974061,1462.56678917646,1462.65024312708,
1462.73367962092,1462.81711673068,1462.9005725256,1462.98411701832,1463.06770610127,
1463.15142936882,1463.23210908472,1463.31584779657,1463.39948330793,1463.48303575133,
1463.56652518718,1463.6499791378,1463.73341563164,1463.8168527414,1463.90030853632,
1463.98385302905,1464.06744211199,1464.15116537954,1464.23184509544,1464.31558380729,
1464.39921931865,1464.48277176205,1464.5662611979,1464.64971514852,1464.73315164236,
1464.81658875212,1464.90004454704,1464.98358903977,1465.06717812271,1465.15090139026,
1465.23158110616,1465.31531981801,1465.39895532937,1465.48250777277,1465.56599720862,
1465.64945115924,1465.73288765308,1465.81632476284,1465.89978055776,1465.98332505049,
1466.06691413343,1466.15063740098,1466.23131711688,1466.31394700638,1466.39648229565,
1466.47894209376,1466.56134544058,1466.64372069725,1466.72607768958,1466.80846141686,
1466.8719408414),.UNSPECIFIED.);
#1841=B_SPLINE_CURVE_WITH_KNOTS('',3,(#243977,#243978,#243979,#243980,#243981,
#243982,#243983,#243984,#243985,#243986),.UNSPECIFIED.,.F.,.F.,(4,3,3,4),
(1460.58993146501,1460.67436365968,1460.75876766208,1460.84058391925),
 .UNSPECIFIED.);
#1842=B_SPLINE_CURVE_WITH_KNOTS('',3,(#243992,#243993,#243994,#243995,#243996,
#243997,#243998,#243999,#244000,#244001),.UNSPECIFIED.,.F.,.F.,(4,3,3,4),
(1454.30662927058,1454.3905507352,1454.47446510851,1454.55739861207),
 .UNSPECIFIED.);
#1843=B_SPLINE_CURVE_WITH_KNOTS('',3,(#244002,#244003,#244004,#244005,#244006,
#244007,#244008,#244009,#244010,#244011,#244012,#244013,#244014,#244015,
#244016,#244017,#244018,#244019,#244020,#244021,#244022,#244023,#244024,
#244025,#244026,#244027,#244028,#244029,#244030,#244031,#244032,#244033,
#244034,#244035,#244036,#244037,#244038,#244039,#244040,#244041,#244042,
#244043,#244044,#244045,#244046,#244047,#244048,#244049,#244050,#244051,
#244052,#244053,#244054,#244055,#244056,#244057,#244058,#244059,#244060,
#244061,#244062,#244063,#244064,#244065,#244066,#244067,#244068,#244069,
#244070,#244071,#244072,#244073,#244074,#244075,#244076,#244077,#244078,
#244079,#244080,#244081,#244082,#244083,#244084,#244085,#244086,#244087,
#244088,#244089,#244090,#244091,#244092,#244093,#244094,#244095,#244096,
#244097,#244098,#244099,#244100,#244101,#244102,#244103,#244104,#244105,
#244106,#244107,#244108,#244109,#244110,#244111,#244112,#244113,#244114,
#244115,#244116,#244117,#244118,#244119,#244120,#244121,#244122,#244123,
#244124,#244125,#244126,#244127,#244128,#244129,#244130,#244131,#244132,
#244133,#244134,#244135,#244136,#244137,#244138,#244139,#244140,#244141,
#244142,#244143,#244144,#244145,#244146,#244147,#244148,#244149,#244150,
#244151,#244152,#244153,#244154,#244155,#244156,#244157,#244158,#244159,
#244160,#244161,#244162,#244163,#244164,#244165,#244166,#244167,#244168,
#244169,#244170,#244171,#244172,#244173,#244174,#244175,#244176,#244177,
#244178,#244179,#244180,#244181,#244182,#244183,#244184,#244185,#244186,
#244187,#244188,#244189,#244190,#244191,#244192,#244193,#244194,#244195,
#244196,#244197,#244198,#244199,#244200,#244201,#244202,#244203,#244204,
#244205,#244206,#244207,#244208,#244209,#244210,#244211,#244212,#244213,
#244214,#244215,#244216,#244217,#244218),.UNSPECIFIED.,.F.,.F.,(4,3,3,3,
3,3,3,3,3,3,3,3,3,3,3,3,3,3,3,3,3,3,3,3,3,3,3,3,3,3,3,3,3,3,3,3,3,3,3,3,
3,3,3,3,3,3,3,3,3,3,3,3,3,3,3,3,3,3,3,3,3,3,3,3,3,3,3,3,3,3,3,3,4),(1454.55739861227,
1454.65194746431,1454.74689204477,1454.84238116431,1454.92393037924,1455.00766909109,
1455.09130460245,1455.17485704585,1455.2583464817,1455.34180043232,1455.42523692616,
1455.50867403592,1455.59212983084,1455.67567432356,1455.75926340651,1455.84298667406,
1455.92366638996,1456.00740510181,1456.09104061317,1456.17459305657,1456.25808249242,
1456.34153644304,1456.42497293688,1456.50841004664,1456.59186584156,1456.67541033429,
1456.75899941723,1456.84272268479,1456.92340240068,1457.00714111253,1457.09077662389,
1457.17432906729,1457.25781850314,1457.34127245376,1457.4247089476,1457.50814605736,
1457.59160185228,1457.67514634501,1457.75873542795,1457.8424586955,1457.9231384114,
1458.00687712325,1458.09051263461,1458.17406507801,1458.25755451386,1458.34100846448,
1458.42444495832,1458.50788206808,1458.591337863,1458.67488235572,1458.75847143867,
1458.84219470622,1458.92287442212,1459.00661313397,1459.09024864533,1459.17380108873,
1459.25729052458,1459.3407444752,1459.42418096904,1459.5076180788,1459.59107387372,
1459.67461836645,1459.75820744939,1459.84193071695,1459.92261043284,1460.00587749695,
1460.08857547718,1460.17119802281,1460.25376406267,1460.33750978343,1460.4200311627,
1460.5043890542,1460.5887469457),.UNSPECIFIED.);
#1844=B_SPLINE_CURVE_WITH_KNOTS('',3,(#244220,#244221,#244222,#244223,#244224,
#244225,#244226,#244227,#244228,#244229,#244230,#244231,#244232,#244233,
#244234,#244235,#244236,#244237,#244238,#244239,#244240,#244241,#244242,
#244243,#244244,#244245,#244246,#244247,#244248,#244249,#244250,#244251,
#244252,#244253,#244254,#244255,#244256,#244257,#244258,#244259,#244260,
#244261,#244262,#244263,#244264,#244265,#244266,#244267,#244268,#244269,
#244270,#244271,#244272,#244273,#244274,#244275,#244276,#244277,#244278,
#244279,#244280,#244281,#244282,#244283,#244284,#244285,#244286,#244287,
#244288,#244289,#244290,#244291,#244292,#244293,#244294,#244295,#244296,
#244297,#244298,#244299,#244300,#244301,#244302,#244303,#244304,#244305,
#244306,#244307,#244308,#244309,#244310,#244311,#244312,#244313,#244314,
#244315,#244316,#244317,#244318,#244319,#244320,#244321,#244322,#244323,
#244324,#244325,#244326,#244327,#244328,#244329,#244330,#244331,#244332,
#244333,#244334,#244335,#244336,#244337,#244338,#244339,#244340,#244341,
#244342,#244343,#244344,#244345,#244346,#244347,#244348,#244349,#244350,
#244351,#244352,#244353,#244354,#244355,#244356,#244357,#244358,#244359,
#244360,#244361,#244362,#244363,#244364,#244365,#244366,#244367,#244368,
#244369,#244370,#244371,#244372,#244373,#244374,#244375,#244376,#244377,
#244378,#244379,#244380,#244381,#244382,#244383,#244384,#244385,#244386,
#244387,#244388,#244389,#244390,#244391,#244392,#244393,#244394,#244395,
#244396,#244397,#244398,#244399,#244400,#244401,#244402,#244403,#244404,
#244405,#244406,#244407,#244408,#244409,#244410,#244411,#244412,#244413,
#244414,#244415,#244416,#244417,#244418,#244419,#244420,#244421,#244422,
#244423,#244424,#244425,#244426,#244427,#244428,#244429,#244430,#244431,
#244432,#244433,#244434,#244435,#244436,#244437,#244438,#244439),
 .UNSPECIFIED.,.F.,.F.,(4,3,3,3,3,3,3,3,3,3,3,3,3,3,3,3,3,3,3,3,3,3,3,3,
3,3,3,3,3,3,3,3,3,3,3,3,3,3,3,3,3,3,3,3,3,3,3,3,3,3,3,3,3,3,3,3,3,3,3,3,
3,3,3,3,3,3,3,3,3,3,3,3,3,4),(1454.55739861207,1454.64200141043,1454.72522978866,
1454.80845873658,1454.89170646772,1454.97733510053,1455.06072123565,1455.1474711173,
1455.23422099896,1455.31795971081,1455.40159522217,1455.48514766557,1455.56863710142,
1455.65209105204,1455.73552754588,1455.81896465564,1455.90242045056,1455.98596494329,
1456.06955402623,1456.15327729378,1456.23395700968,1456.31769572153,1456.40133123289,
1456.48488367629,1456.56837311214,1456.65182706276,1456.7352635566,1456.81870066636,
1456.90215646127,1456.985700954,1457.06929003695,1457.1530133045,1457.2336930204,
1457.31743173225,1457.40106724361,1457.48461968701,1457.56810912286,1457.65156307348,
1457.73499956732,1457.81843667708,1457.901892472,1457.98543696473,1458.06902604767,
1458.15274931522,1458.23342903112,1458.31716774297,1458.40080325433,1458.48435569773,
1458.56784513358,1458.6512990842,1458.73473557804,1458.8181726878,1458.90162848272,
1458.98517297545,1459.06876205839,1459.15248532595,1459.23316504184,1459.31690375369,
1459.40053926505,1459.48409170845,1459.5675811443,1459.65103509492,1459.73447158876,
1459.81790869852,1459.90136449344,1459.98490898617,1460.06849806911,1460.15222133666,
1460.23290105256,1460.32215865567,1460.40683272219,1460.49142158211,1460.57592537746,
1460.58993146501),.UNSPECIFIED.);
#1845=B_SPLINE_CURVE_WITH_KNOTS('',3,(#244440,#244441,#244442,#244443,#244444,
#244445,#244446,#244447,#244448,#244449),.UNSPECIFIED.,.F.,.F.,(4,3,3,4),
(1454.30674307549,1454.40585639479,1454.50400867407,1454.55739861189),
 .UNSPECIFIED.);
#1846=B_SPLINE_CURVE_WITH_KNOTS('',3,(#244455,#244456,#244457,#244458,#244459,
#244460,#244461,#244462,#244463,#244464),.UNSPECIFIED.,.F.,.F.,(4,3,3,4),
(1448.0236730871,1448.12028229969,1448.21615954937,1448.27421330469),
 .UNSPECIFIED.);
#1847=B_SPLINE_CURVE_WITH_KNOTS('',3,(#244465,#244466,#244467,#244468,#244469,
#244470,#244471,#244472,#244473,#244474,#244475,#244476,#244477,#244478,
#244479,#244480,#244481,#244482,#244483,#244484,#244485,#244486,#244487,
#244488,#244489,#244490,#244491,#244492,#244493,#244494,#244495,#244496,
#244497,#244498,#244499,#244500,#244501,#244502,#244503,#244504,#244505,
#244506,#244507,#244508,#244509,#244510,#244511,#244512,#244513,#244514,
#244515,#244516,#244517,#244518,#244519,#244520,#244521,#244522,#244523,
#244524,#244525,#244526,#244527,#244528,#244529,#244530,#244531,#244532,
#244533,#244534,#244535,#244536,#244537,#244538,#244539,#244540,#244541,
#244542,#244543,#244544,#244545,#244546,#244547,#244548,#244549,#244550,
#244551,#244552,#244553,#244554,#244555,#244556,#244557,#244558,#244559,
#244560,#244561,#244562,#244563,#244564,#244565,#244566,#244567,#244568,
#244569,#244570,#244571,#244572,#244573,#244574,#244575,#244576,#244577,
#244578,#244579,#244580,#244581,#244582,#244583,#244584,#244585,#244586,
#244587,#244588,#244589,#244590,#244591,#244592,#244593,#244594,#244595,
#244596,#244597,#244598,#244599,#244600,#244601,#244602,#244603,#244604,
#244605,#244606,#244607,#244608,#244609,#244610,#244611,#244612,#244613,
#244614,#244615,#244616,#244617,#244618,#244619,#244620,#244621,#244622,
#244623,#244624,#244625,#244626,#244627,#244628,#244629,#244630,#244631,
#244632,#244633,#244634,#244635,#244636,#244637,#244638,#244639,#244640,
#244641,#244642,#244643,#244644,#244645,#244646,#244647,#244648,#244649,
#244650,#244651,#244652,#244653,#244654,#244655,#244656,#244657,#244658,
#244659,#244660,#244661,#244662,#244663,#244664,#244665,#244666,#244667,
#244668,#244669,#244670,#244671,#244672,#244673,#244674,#244675,#244676,
#244677,#244678,#244679,#244680,#244681,#244682,#244683,#244684),
 .UNSPECIFIED.,.F.,.F.,(4,3,3,3,3,3,3,3,3,3,3,3,3,3,3,3,3,3,3,3,3,3,3,3,
3,3,3,3,3,3,3,3,3,3,3,3,3,3,3,3,3,3,3,3,3,3,3,3,3,3,3,3,3,3,3,3,3,3,3,3,
3,3,3,3,3,3,3,3,3,3,3,3,3,4),(1448.27421330489,1448.35782433656,1448.44142899155,
1448.52504506398,1448.60869035153,1448.69243622458,1448.77623540817,1448.8601726709,
1448.92551431492,1449.00925302677,1449.09288853813,1449.17644098153,1449.25993041738,
1449.343384368,1449.42682086184,1449.5102579716,1449.59371376652,1449.67725825924,
1449.76084734219,1449.84457060974,1449.92525032564,1450.00898903749,1450.09262454885,
1450.17617699225,1450.2596664281,1450.34312037872,1450.42655687256,1450.50999398232,
1450.59344977724,1450.67699426997,1450.76058335291,1450.84430662046,1450.92498633636,
1451.00872504821,1451.09236055957,1451.17591300297,1451.25940243882,1451.34285638944,
1451.42629288328,1451.50972999304,1451.59318578796,1451.67673028069,1451.76031936363,
1451.84404263118,1451.92472234708,1452.00846105893,1452.09209657029,1452.17564901369,
1452.25913844954,1452.34259240016,1452.426028894,1452.50946600376,1452.59292179867,
1452.6764662914,1452.76005537434,1452.8437786419,1452.9244583578,1453.00819706965,
1453.09183258101,1453.17538502441,1453.25887446026,1453.34232841088,1453.42576490472,
1453.50920201448,1453.5926578094,1453.67620230213,1453.75979138507,1453.84351465263,
1453.92419436852,1454.00848723102,1454.09263873748,1454.17670875473,1454.26070005874,
1454.30662927058),.UNSPECIFIED.);
#1848=B_SPLINE_CURVE_WITH_KNOTS('',3,(#244686,#244687,#244688,#244689,#244690,
#244691,#244692,#244693,#244694,#244695,#244696,#244697,#244698,#244699,
#244700,#244701,#244702,#244703,#244704,#244705,#244706,#244707,#244708,
#244709,#244710,#244711,#244712,#244713,#244714,#244715,#244716,#244717,
#244718,#244719,#244720,#244721,#244722,#244723,#244724,#244725,#244726,
#244727,#244728,#244729,#244730,#244731,#244732,#244733,#244734,#244735,
#244736,#244737,#244738,#244739,#244740,#244741,#244742,#244743,#244744,
#244745,#244746,#244747,#244748,#244749,#244750,#244751,#244752,#244753,
#244754,#244755,#244756,#244757,#244758,#244759,#244760,#244761,#244762,
#244763,#244764,#244765,#244766,#244767,#244768,#244769,#244770,#244771,
#244772,#244773,#244774,#244775,#244776,#244777,#244778,#244779,#244780,
#244781,#244782,#244783,#244784,#244785,#244786,#244787,#244788,#244789,
#244790,#244791,#244792,#244793,#244794,#244795,#244796,#244797,#244798,
#244799,#244800,#244801,#244802,#244803,#244804,#244805,#244806,#244807,
#244808,#244809,#244810,#244811,#244812,#244813,#244814,#244815,#244816,
#244817,#244818,#244819,#244820,#244821,#244822,#244823,#244824,#244825,
#244826,#244827,#244828,#244829,#244830,#244831,#244832,#244833,#244834,
#244835,#244836,#244837,#244838,#244839,#244840,#244841,#244842,#244843,
#244844,#244845,#244846,#244847,#244848,#244849,#244850,#244851,#244852,
#244853,#244854,#244855,#244856,#244857,#244858,#244859,#244860,#244861,
#244862,#244863,#244864,#244865,#244866,#244867,#244868,#244869,#244870,
#244871,#244872,#244873,#244874,#244875,#244876,#244877,#244878,#244879,
#244880,#244881,#244882,#244883,#244884,#244885,#244886,#244887,#244888,
#244889,#244890,#244891,#244892,#244893,#244894,#244895,#244896,#244897,
#244898,#244899,#244900,#244901,#244902,#244903,#244904,#244905),
 .UNSPECIFIED.,.F.,.F.,(4,3,3,3,3,3,3,3,3,3,3,3,3,3,3,3,3,3,3,3,3,3,3,3,
3,3,3,3,3,3,3,3,3,3,3,3,3,3,3,3,3,3,3,3,3,3,3,3,3,3,3,3,3,3,3,3,3,3,3,3,
3,3,3,3,3,3,3,3,3,3,3,3,3,4),(1448.27421330505,1448.35743318097,1448.4405518179,
1448.52358985075,1448.60656783825,1448.68951465084,1448.77244760275,1448.85538521634,
1448.93834601377,1449.02139624031,1449.10449595701,1449.18771960852,1449.23580493464,
1449.31954364649,1449.40317915785,1449.48673160125,1449.5702210371,1449.65367498772,
1449.73711148156,1449.82054859132,1449.90400438624,1449.98754887897,1450.07113796191,
1450.15486122947,1450.23554094536,1450.31927965721,1450.40291516857,1450.48646761197,
1450.56995704782,1450.65341099844,1450.73684749228,1450.82028460204,1450.90374039696,
1450.98728488969,1451.07087397263,1451.15459724018,1451.23527695608,1451.31901566793,
1451.40265117929,1451.48620362269,1451.56969305854,1451.65314700916,1451.736583503,
1451.82002061276,1451.90347640768,1451.98702090041,1452.07060998335,1452.1543332509,
1452.2350129668,1452.31875167865,1452.40238719001,1452.48593963341,1452.56942906926,
1452.65288301988,1452.73631951372,1452.81975662348,1452.9032124184,1452.98675691113,
1453.07034599407,1453.15406926163,1453.23474897752,1453.31848768937,1453.40212320073,
1453.48567564413,1453.56916507998,1453.6526190306,1453.73605552444,1453.8194926342,
1453.90294842912,1453.98649292185,1454.07008200479,1454.15380527234,1454.23448498824,
1454.30674307549),.UNSPECIFIED.);
#1849=B_SPLINE_CURVE_WITH_KNOTS('',3,(#244906,#244907,#244908,#244909,#244910,
#244911,#244912,#244913,#244914,#244915,#244916,#244917,#244918),
 .UNSPECIFIED.,.F.,.F.,(4,3,3,3,4),(1448.02254698393,1448.10615919498,1448.18989572745,
1448.23606892392,1448.27421330489),.UNSPECIFIED.);
#1850=B_SPLINE_CURVE_WITH_KNOTS('',3,(#244924,#244925,#244926,#244927,#244928,
#244929,#244930,#244931,#244932,#244933,#244934,#244935,#244936),
 .UNSPECIFIED.,.F.,.F.,(4,3,3,3,4),(1441.73936764326,1441.82299876243,1441.9067473108,
1441.92736223988,1441.99102799771),.UNSPECIFIED.);
#1851=B_SPLINE_CURVE_WITH_KNOTS('',3,(#244937,#244938,#244939,#244940,#244941,
#244942,#244943,#244944,#244945,#244946,#244947,#244948,#244949,#244950,
#244951,#244952,#244953,#244954,#244955,#244956,#244957,#244958,#244959,
#244960,#244961,#244962,#244963,#244964,#244965,#244966,#244967,#244968,
#244969,#244970,#244971,#244972,#244973,#244974,#244975,#244976,#244977,
#244978,#244979,#244980,#244981,#244982,#244983,#244984,#244985,#244986,
#244987,#244988,#244989,#244990,#244991,#244992,#244993,#244994,#244995,
#244996,#244997,#244998,#244999,#245000,#245001,#245002,#245003,#245004,
#245005,#245006,#245007,#245008,#245009,#245010,#245011,#245012,#245013,
#245014,#245015,#245016,#245017,#245018,#245019,#245020,#245021,#245022,
#245023,#245024,#245025,#245026,#245027,#245028,#245029,#245030,#245031,
#245032,#245033,#245034,#245035,#245036,#245037,#245038,#245039,#245040,
#245041,#245042,#245043,#245044,#245045,#245046,#245047,#245048,#245049,
#245050,#245051,#245052,#245053,#245054,#245055,#245056,#245057,#245058,
#245059,#245060,#245061,#245062,#245063,#245064,#245065,#245066,#245067,
#245068,#245069,#245070,#245071,#245072,#245073,#245074,#245075,#245076,
#245077,#245078,#245079,#245080,#245081,#245082,#245083,#245084,#245085,
#245086,#245087,#245088,#245089,#245090,#245091,#245092,#245093,#245094,
#245095,#245096,#245097,#245098,#245099,#245100,#245101,#245102,#245103,
#245104,#245105,#245106,#245107,#245108,#245109,#245110,#245111,#245112,
#245113,#245114,#245115,#245116,#245117,#245118,#245119,#245120,#245121,
#245122,#245123,#245124,#245125,#245126,#245127,#245128,#245129,#245130,
#245131,#245132,#245133,#245134,#245135,#245136,#245137,#245138,#245139,
#245140,#245141,#245142,#245143,#245144,#245145,#245146,#245147,#245148,
#245149,#245150,#245151,#245152,#245153,#245154,#245155,#245156),
 .UNSPECIFIED.,.F.,.F.,(4,3,3,3,3,3,3,3,3,3,3,3,3,3,3,3,3,3,3,3,3,3,3,3,
3,3,3,3,3,3,3,3,3,3,3,3,3,3,3,3,3,3,3,3,3,3,3,3,3,3,3,3,3,3,3,3,3,3,3,3,
3,3,3,3,3,3,3,3,3,3,3,3,3,4),(1441.99102799783,1442.07397001655,1442.15681366223,
1442.23957978767,1442.32551959554,1442.40820144904,1442.49087354865,1442.5735546158,
1442.65626337548,1442.73906287441,1442.82191629707,1442.90488611973,1442.9270982506,
1443.01083696245,1443.09447247381,1443.17802491721,1443.26151435306,1443.34496830368,
1443.42840479752,1443.51184190728,1443.5952977022,1443.67884219493,1443.76243127787,
1443.84615454542,1443.92683426132,1444.01057297317,1444.09420848453,1444.17776092793,
1444.26125036378,1444.3447043144,1444.42814080824,1444.511577918,1444.59503371292,
1444.67857820565,1444.76216728859,1444.84589055615,1444.92657027204,1445.01030898389,
1445.09394449525,1445.17749693865,1445.2609863745,1445.34444032512,1445.42787681896,
1445.51131392872,1445.59476972363,1445.67831421636,1445.7619032993,1445.84562656686,
1445.92630628276,1446.01004499461,1446.09368050597,1446.17723294937,1446.26072238522,
1446.34417633584,1446.42761282968,1446.51104993944,1446.59450573436,1446.67805022709,
1446.76163931003,1446.84536257758,1446.92604229348,1447.00978100533,1447.09341651669,
1447.17696896009,1447.26045839594,1447.34391234655,1447.4273488404,1447.51078595016,
1447.59424174507,1447.6777862378,1447.76137532074,1447.8450985883,1447.9257783042,
1448.0236730871),.UNSPECIFIED.);
#1852=B_SPLINE_CURVE_WITH_KNOTS('',3,(#245158,#245159,#245160,#245161,#245162,
#245163,#245164,#245165,#245166,#245167,#245168,#245169,#245170,#245171,
#245172,#245173,#245174,#245175,#245176,#245177,#245178,#245179,#245180,
#245181,#245182,#245183,#245184,#245185,#245186,#245187,#245188,#245189,
#245190,#245191,#245192,#245193,#245194,#245195,#245196,#245197,#245198,
#245199,#245200,#245201,#245202,#245203,#245204,#245205,#245206,#245207,
#245208,#245209,#245210,#245211,#245212,#245213,#245214,#245215,#245216,
#245217,#245218,#245219,#245220,#245221,#245222,#245223,#245224,#245225,
#245226,#245227,#245228,#245229,#245230,#245231,#245232,#245233,#245234,
#245235,#245236,#245237,#245238,#245239,#245240,#245241,#245242,#245243,
#245244,#245245,#245246,#245247,#245248,#245249,#245250,#245251,#245252,
#245253,#245254,#245255,#245256,#245257,#245258,#245259,#245260,#245261,
#245262,#245263,#245264,#245265,#245266,#245267,#245268,#245269,#245270,
#245271,#245272,#245273,#245274,#245275,#245276,#245277,#245278,#245279,
#245280,#245281,#245282,#245283,#245284,#245285,#245286,#245287,#245288,
#245289,#245290,#245291,#245292,#245293,#245294,#245295,#245296,#245297,
#245298,#245299,#245300,#245301,#245302,#245303,#245304,#245305,#245306,
#245307,#245308,#245309,#245310,#245311,#245312,#245313,#245314,#245315,
#245316,#245317,#245318,#245319,#245320,#245321,#245322,#245323,#245324,
#245325,#245326,#245327,#245328,#245329,#245330,#245331,#245332,#245333,
#245334,#245335,#245336,#245337,#245338,#245339,#245340,#245341,#245342,
#245343,#245344,#245345,#245346,#245347,#245348,#245349,#245350,#245351,
#245352,#245353,#245354,#245355,#245356,#245357,#245358,#245359,#245360,
#245361,#245362,#245363,#245364,#245365,#245366,#245367,#245368,#245369,
#245370,#245371,#245372,#245373,#245374,#245375,#245376,#245377),
 .UNSPECIFIED.,.F.,.F.,(4,3,3,3,3,3,3,3,3,3,3,3,3,3,3,3,3,3,3,3,3,3,3,3,
3,3,3,3,3,3,3,3,3,3,3,3,3,3,3,3,3,3,3,3,3,3,3,3,3,3,3,3,3,3,3,3,3,3,3,3,
3,3,3,3,3,3,3,3,3,3,3,3,3,4),(1441.99102799785,1442.09882248263,1442.20915371554,
1442.2376528596,1442.32139157145,1442.40502708281,1442.48857952621,1442.57206896206,
1442.65552291267,1442.73895940652,1442.82239651628,1442.90585231119,1442.98939680392,
1443.07298588686,1443.15670915442,1443.23738887032,1443.32112758217,1443.40476309353,
1443.48831553693,1443.57180497278,1443.6552589234,1443.73869541724,1443.822132527,
1443.90558832192,1443.98913281465,1444.07272189759,1444.15644516514,1444.23712488104,
1444.32086359289,1444.40449910425,1444.48805154765,1444.5715409835,1444.65499493412,
1444.73843142796,1444.82186853772,1444.90532433264,1444.98886882536,1445.07245790831,
1445.15618117586,1445.23686089176,1445.32059960361,1445.40423511497,1445.48778755837,
1445.57127699422,1445.65473094484,1445.73816743868,1445.82160454844,1445.90506034336,
1445.98860483609,1446.07219391903,1446.15591718658,1446.23659690248,1446.32033561433,
1446.40397112569,1446.48752356909,1446.57101300494,1446.65446695556,1446.7379034494,
1446.82134055916,1446.90479635408,1446.98834084681,1447.07192992975,1447.1556531973,
1447.2363329132,1447.32008459951,1447.40789239756,1447.49143313082,1447.57491711298,
1447.65836246294,1447.74178726958,1447.82523138041,1447.90868683001,1447.99219954226,
1448.02254698393),.UNSPECIFIED.);
#1853=B_SPLINE_CURVE_WITH_KNOTS('',3,(#245378,#245379,#245380,#245381,#245382,
#245383,#245384,#245385,#245386,#245387),.UNSPECIFIED.,.F.,.F.,(4,3,3,4),
(1441.73964840693,1441.82211908339,1441.90657354055,1441.99102799771),
 .UNSPECIFIED.);
#1854=B_SPLINE_CURVE_WITH_KNOTS('',3,(#245393,#245394,#245395,#245396,#245397,
#245398,#245399,#245400,#245401,#245402),.UNSPECIFIED.,.F.,.F.,(4,3,3,4),
(1435.45634400191,1435.53868546224,1435.62326407632,1435.70784269039),
 .UNSPECIFIED.);
#1855=B_SPLINE_CURVE_WITH_KNOTS('',3,(#245403,#245404,#245405,#245406,#245407,
#245408,#245409,#245410,#245411,#245412,#245413,#245414,#245415,#245416,
#245417,#245418,#245419,#245420,#245421,#245422,#245423,#245424,#245425,
#245426,#245427,#245428,#245429,#245430,#245431,#245432,#245433,#245434,
#245435,#245436,#245437,#245438,#245439,#245440,#245441,#245442,#245443,
#245444,#245445,#245446,#245447,#245448,#245449,#245450,#245451,#245452,
#245453,#245454,#245455,#245456,#245457,#245458,#245459,#245460,#245461,
#245462,#245463,#245464,#245465,#245466,#245467,#245468,#245469,#245470,
#245471,#245472,#245473,#245474,#245475,#245476,#245477,#245478,#245479,
#245480,#245481,#245482,#245483,#245484,#245485,#245486,#245487,#245488,
#245489,#245490,#245491,#245492,#245493,#245494,#245495,#245496,#245497,
#245498,#245499,#245500,#245501,#245502,#245503,#245504,#245505,#245506,
#245507,#245508,#245509,#245510,#245511,#245512,#245513,#245514,#245515,
#245516,#245517,#245518,#245519,#245520,#245521,#245522,#245523,#245524,
#245525,#245526,#245527,#245528,#245529,#245530,#245531,#245532,#245533,
#245534,#245535,#245536,#245537,#245538,#245539,#245540,#245541,#245542,
#245543,#245544,#245545,#245546,#245547,#245548,#245549,#245550,#245551,
#245552,#245553,#245554,#245555,#245556,#245557,#245558,#245559,#245560,
#245561,#245562,#245563,#245564,#245565,#245566,#245567,#245568,#245569,
#245570,#245571,#245572,#245573,#245574,#245575,#245576,#245577,#245578,
#245579,#245580,#245581,#245582,#245583,#245584,#245585,#245586,#245587,
#245588,#245589,#245590,#245591,#245592,#245593,#245594,#245595,#245596,
#245597,#245598,#245599,#245600,#245601,#245602,#245603,#245604,#245605,
#245606,#245607,#245608,#245609,#245610,#245611,#245612,#245613,#245614,
#245615,#245616,#245617,#245618,#245619),.UNSPECIFIED.,.F.,.F.,(4,3,3,3,
3,3,3,3,3,3,3,3,3,3,3,3,3,3,3,3,3,3,3,3,3,3,3,3,3,3,3,3,3,3,3,3,3,3,3,3,
3,3,3,3,3,3,3,3,3,3,3,3,3,3,3,3,3,3,3,3,3,3,3,3,3,3,3,3,3,3,3,3,4),(1435.70784269053,
1435.82235604207,1435.92894617556,1436.01268488741,1436.09632039877,1436.17987284217,
1436.26336227802,1436.34681622863,1436.43025272248,1436.51368983223,1436.59714562715,
1436.68069011988,1436.76427920282,1436.84800247038,1436.92868218628,1437.01242089813,
1437.09605640949,1437.17960885289,1437.26309828874,1437.34655223936,1437.4299887332,
1437.51342584296,1437.59688163788,1437.68042613061,1437.76401521355,1437.8477384811,
1437.928418197,1438.01215690885,1438.09579242021,1438.17934486361,1438.26283429946,
1438.34628825008,1438.42972474392,1438.51316185368,1438.5966176486,1438.68016214133,
1438.76375122427,1438.84747449183,1438.92815420772,1439.01189291957,1439.09552843093,
1439.17908087433,1439.26257031018,1439.3460242608,1439.42946075464,1439.5128978644,
1439.59635365932,1439.67989815205,1439.76348723499,1439.84721050254,1439.92789021844,
1440.01162893029,1440.09526444165,1440.17881688505,1440.2623063209,1440.34576027152,
1440.42919676536,1440.51263387512,1440.59608967004,1440.67963416277,1440.76322324571,
1440.84694651326,1440.92762622916,1441.01137625723,1441.09502060469,1441.17856410501,
1441.26205042852,1441.34549769506,1441.42892399429,1441.51237342932,1441.59583358817,
1441.67936222842,1441.73936764326),.UNSPECIFIED.);
#1856=B_SPLINE_CURVE_WITH_KNOTS('',3,(#245621,#245622,#245623,#245624,#245625,
#245626,#245627,#245628,#245629,#245630,#245631,#245632,#245633,#245634,
#245635,#245636,#245637,#245638,#245639,#245640,#245641,#245642,#245643,
#245644,#245645,#245646,#245647,#245648,#245649,#245650,#245651,#245652,
#245653,#245654,#245655,#245656,#245657,#245658,#245659,#245660,#245661,
#245662,#245663,#245664,#245665,#245666,#245667,#245668,#245669,#245670,
#245671,#245672,#245673,#245674,#245675,#245676,#245677,#245678,#245679,
#245680,#245681,#245682,#245683,#245684,#245685,#245686,#245687,#245688,
#245689,#245690,#245691,#245692,#245693,#245694,#245695,#245696,#245697,
#245698,#245699,#245700,#245701,#245702,#245703,#245704,#245705,#245706,
#245707,#245708,#245709,#245710,#245711,#245712,#245713,#245714,#245715,
#245716,#245717,#245718,#245719,#245720,#245721,#245722,#245723,#245724,
#245725,#245726,#245727,#245728,#245729,#245730,#245731,#245732,#245733,
#245734,#245735,#245736,#245737,#245738,#245739,#245740,#245741,#245742,
#245743,#245744,#245745,#245746,#245747,#245748,#245749,#245750,#245751,
#245752,#245753,#245754,#245755,#245756,#245757,#245758,#245759,#245760,
#245761,#245762,#245763,#245764,#245765,#245766,#245767,#245768,#245769,
#245770,#245771,#245772,#245773,#245774,#245775,#245776,#245777,#245778,
#245779,#245780,#245781,#245782,#245783,#245784,#245785,#245786,#245787,
#245788,#245789,#245790,#245791,#245792,#245793,#245794,#245795,#245796,
#245797,#245798,#245799,#245800,#245801,#245802,#245803,#245804,#245805,
#245806,#245807,#245808,#245809,#245810,#245811,#245812,#245813,#245814,
#245815,#245816,#245817,#245818,#245819,#245820,#245821,#245822,#245823,
#245824,#245825,#245826,#245827,#245828,#245829,#245830,#245831,#245832,
#245833,#245834,#245835,#245836,#245837),.UNSPECIFIED.,.F.,.F.,(4,3,3,3,
3,3,3,3,3,3,3,3,3,3,3,3,3,3,3,3,3,3,3,3,3,3,3,3,3,3,3,3,3,3,3,3,3,3,3,3,
3,3,3,3,3,3,3,3,3,3,3,3,3,3,3,3,3,3,3,3,3,3,3,3,3,3,3,3,3,3,3,3,4),(1435.70784269053,
1435.79418909534,1435.8806134886,1435.97026931526,1436.05695086,1436.14809382764,
1436.23923679527,1436.32297550712,1436.40661101849,1436.49016346189,1436.57365289774,
1436.65710684835,1436.7405433422,1436.82398045196,1436.90743624688,1436.99098073961,
1437.07456982255,1437.15829309011,1437.23897280599,1437.32271151783,1437.4063470292,
1437.4898994726,1437.57338890845,1437.65684285906,1437.74027935291,1437.82371646266,
1437.90717225758,1437.99071675031,1438.07430583325,1438.15802910081,1438.23870881671,
1438.32244752856,1438.40608303993,1438.48963548333,1438.57312491918,1438.6565788698,
1438.74001536364,1438.8234524734,1438.90690826832,1438.99045276105,1439.07404184399,
1439.15776511155,1439.23844482744,1439.32218353929,1439.40581905065,1439.48937149405,
1439.57286092991,1439.65631488052,1439.73975137437,1439.82318848412,1439.90664427904,
1439.99018877177,1440.07377785471,1440.15750112227,1440.23818083816,1440.32191955001,
1440.40555506137,1440.48910750477,1440.57259694062,1440.65605089123,1440.73948738508,
1440.82292449483,1440.90638028975,1440.98992478248,1441.07351386542,1441.15723713298,
1441.23791684888,1441.32066010468,1441.40330528578,1441.48739106607,1441.56989035993,
1441.65476938343,1441.73964840693),.UNSPECIFIED.);
#1857=B_SPLINE_CURVE_WITH_KNOTS('',3,(#245838,#245839,#245840,#245841,#245842,
#245843,#245844,#245845,#245846,#245847),.UNSPECIFIED.,.F.,.F.,(4,3,3,4),
(1435.45754054782,1435.54645941689,1435.63515374008,1435.7078426904),
 .UNSPECIFIED.);
#1858=B_SPLINE_CURVE_WITH_KNOTS('',3,(#245853,#245854,#245855,#245856,#245857,
#245858,#245859,#245860,#245861,#245862),.UNSPECIFIED.,.F.,.F.,(4,3,3,4),
(1429.17433711171,1429.26217368456,1429.3498375818,1429.42465738322),
 .UNSPECIFIED.);
#1859=B_SPLINE_CURVE_WITH_KNOTS('',3,(#245863,#245864,#245865,#245866,#245867,
#245868,#245869,#245870,#245871,#245872,#245873,#245874,#245875,#245876,
#245877,#245878,#245879,#245880,#245881,#245882,#245883,#245884,#245885,
#245886,#245887,#245888,#245889,#245890,#245891,#245892,#245893,#245894,
#245895,#245896,#245897,#245898,#245899,#245900,#245901,#245902,#245903,
#245904,#245905,#245906,#245907,#245908,#245909,#245910,#245911,#245912,
#245913,#245914,#245915,#245916,#245917,#245918,#245919,#245920,#245921,
#245922,#245923,#245924,#245925,#245926,#245927,#245928,#245929,#245930,
#245931,#245932,#245933,#245934,#245935,#245936,#245937,#245938,#245939,
#245940,#245941,#245942,#245943,#245944,#245945,#245946,#245947,#245948,
#245949,#245950,#245951,#245952,#245953,#245954,#245955,#245956,#245957,
#245958,#245959,#245960,#245961,#245962,#245963,#245964,#245965,#245966,
#245967,#245968,#245969,#245970,#245971,#245972,#245973,#245974,#245975,
#245976,#245977,#245978,#245979,#245980,#245981,#245982,#245983,#245984,
#245985,#245986,#245987,#245988,#245989,#245990,#245991,#245992,#245993,
#245994,#245995,#245996,#245997,#245998,#245999,#246000,#246001,#246002,
#246003,#246004,#246005,#246006,#246007,#246008,#246009,#246010,#246011,
#246012,#246013,#246014,#246015,#246016,#246017,#246018,#246019,#246020,
#246021,#246022,#246023,#246024,#246025,#246026,#246027,#246028,#246029,
#246030,#246031,#246032,#246033,#246034,#246035,#246036,#246037,#246038,
#246039,#246040,#246041,#246042,#246043,#246044,#246045,#246046,#246047,
#246048,#246049,#246050,#246051,#246052,#246053,#246054,#246055,#246056,
#246057,#246058,#246059,#246060,#246061,#246062,#246063,#246064,#246065,
#246066,#246067,#246068,#246069,#246070,#246071,#246072,#246073,#246074,
#246075,#246076,#246077,#246078,#246079,#246080,#246081,#246082),
 .UNSPECIFIED.,.F.,.F.,(4,3,3,3,3,3,3,3,3,3,3,3,3,3,3,3,3,3,3,3,3,3,3,3,
3,3,3,3,3,3,3,3,3,3,3,3,3,3,3,3,3,3,3,3,3,3,3,3,3,3,3,3,3,3,3,3,3,3,3,3,
3,3,3,3,3,3,3,3,3,3,3,3,3,4),(1429.42465738335,1429.51184693731,1429.59914373417,
1429.6866395601,1429.77423939675,1429.86203908662,1429.93053011124,1430.01426882309,
1430.09790433445,1430.18145677785,1430.2649462137,1430.34840016431,1430.43183665816,
1430.51527376791,1430.59872956283,1430.68227405556,1430.7658631385,1430.84958640606,
1430.93026612196,1431.01400483381,1431.09764034517,1431.18119278857,1431.26468222442,
1431.34813617504,1431.43157266888,1431.51500977864,1431.59846557356,1431.68201006629,
1431.76559914923,1431.84932241678,1431.93000213268,1432.01374084453,1432.09737635589,
1432.18092879929,1432.26441823514,1432.34787218576,1432.4313086796,1432.51474578936,
1432.59820158428,1432.68174607701,1432.76533515995,1432.84905842751,1432.9297381434,
1433.01347685525,1433.09711236661,1433.18066481001,1433.26415424586,1433.34760819648,
1433.43104469032,1433.51448180008,1433.597937595,1433.68148208772,1433.76507117067,
1433.84879443822,1433.92947415412,1434.01321286597,1434.09684837733,1434.18040082073,
1434.26389025658,1434.3473442072,1434.43078070104,1434.5142178108,1434.59767360572,
1434.68121809845,1434.76480718139,1434.84853044895,1434.92921016484,1435.01180452316,
1435.09430200276,1435.17672175617,1435.25907889747,1435.34139995451,1435.42371181849,
1435.45634400191),.UNSPECIFIED.);
#1860=B_SPLINE_CURVE_WITH_KNOTS('',3,(#246084,#246085,#246086,#246087,#246088,
#246089,#246090,#246091,#246092,#246093,#246094,#246095,#246096,#246097,
#246098,#246099,#246100,#246101,#246102,#246103,#246104,#246105,#246106,
#246107,#246108,#246109,#246110,#246111,#246112,#246113,#246114,#246115,
#246116,#246117,#246118,#246119,#246120,#246121,#246122,#246123,#246124,
#246125,#246126,#246127,#246128,#246129,#246130,#246131,#246132,#246133,
#246134,#246135,#246136,#246137,#246138,#246139,#246140,#246141,#246142,
#246143,#246144,#246145,#246146,#246147,#246148,#246149,#246150,#246151,
#246152,#246153,#246154,#246155,#246156,#246157,#246158,#246159,#246160,
#246161,#246162,#246163,#246164,#246165,#246166,#246167,#246168,#246169,
#246170,#246171,#246172,#246173,#246174,#246175,#246176,#246177,#246178,
#246179,#246180,#246181,#246182,#246183,#246184,#246185,#246186,#246187,
#246188,#246189,#246190,#246191,#246192,#246193,#246194,#246195,#246196,
#246197,#246198,#246199,#246200,#246201,#246202,#246203,#246204,#246205,
#246206,#246207,#246208,#246209,#246210,#246211,#246212,#246213,#246214,
#246215,#246216,#246217,#246218,#246219,#246220,#246221,#246222,#246223,
#246224,#246225,#246226,#246227,#246228,#246229,#246230,#246231,#246232,
#246233,#246234,#246235,#246236,#246237,#246238,#246239,#246240,#246241,
#246242,#246243,#246244,#246245,#246246,#246247,#246248,#246249,#246250,
#246251,#246252,#246253,#246254,#246255,#246256,#246257,#246258,#246259,
#246260,#246261,#246262,#246263,#246264,#246265,#246266,#246267,#246268,
#246269,#246270,#246271,#246272,#246273,#246274,#246275,#246276,#246277,
#246278,#246279,#246280,#246281,#246282,#246283,#246284,#246285,#246286,
#246287,#246288,#246289,#246290,#246291,#246292,#246293,#246294,#246295,
#246296,#246297,#246298,#246299,#246300,#246301,#246302,#246303),
 .UNSPECIFIED.,.F.,.F.,(4,3,3,3,3,3,3,3,3,3,3,3,3,3,3,3,3,3,3,3,3,3,3,3,
3,3,3,3,3,3,3,3,3,3,3,3,3,3,3,3,3,3,3,3,3,3,3,3,3,3,3,3,3,3,3,3,3,3,3,3,
3,3,3,3,3,3,3,3,3,3,3,3,3,4),(1429.4246573835,1429.50702048783,1429.58931001852,
1429.67155095664,1429.75376682562,1429.83597666066,1429.91819948982,1430.0005042299,
1430.08285026655,1430.16532564741,1430.24082073095,1430.3245594428,1430.40819495416,
1430.49174739756,1430.57523683341,1430.65869078403,1430.74212727787,1430.82556438763,
1430.90902018255,1430.99256467528,1431.07615375822,1431.15987702578,1431.24055674167,
1431.32429545352,1431.40793096488,1431.49148340828,1431.57497284413,1431.65842679475,
1431.74186328859,1431.82530039835,1431.90875619327,1431.992300686,1432.07588976894,
1432.1596130365,1432.24029275239,1432.32403146424,1432.4076669756,1432.491219419,
1432.57470885485,1432.65816280547,1432.74159929931,1432.82503640907,1432.90849220399,
1432.99203669672,1433.07562577966,1433.15934904721,1433.24002876311,1433.32376747496,
1433.40740298632,1433.49095542972,1433.57444486557,1433.65789881619,1433.74133531003,
1433.82477241979,1433.90822821471,1433.99177270744,1434.07536179038,1434.15908505794,
1434.23976477383,1434.32350348568,1434.40713899704,1434.49069144044,1434.57418087629,
1434.6576348269,1434.74107132075,1434.8245084305,1434.90796422542,1434.99150871815,
1435.07509780109,1435.15882106865,1435.23950078455,1435.32891254343,1435.41810836263,
1435.45754054782),.UNSPECIFIED.);
#1861=B_SPLINE_CURVE_WITH_KNOTS('',3,(#246304,#246305,#246306,#246307,#246308,
#246309,#246310,#246311,#246312,#246313),.UNSPECIFIED.,.F.,.F.,(4,3,3,4),
(1429.17325060202,1429.24108472023,1429.36688712493,1429.42465738335),
 .UNSPECIFIED.);
#1862=B_SPLINE_CURVE_WITH_KNOTS('',3,(#246319,#246320,#246321,#246322,#246323,
#246324,#246325,#246326,#246327,#246328),.UNSPECIFIED.,.F.,.F.,(4,3,3,4),
(1422.89017552255,1422.93237803619,1423.04995135785,1423.14147207617),
 .UNSPECIFIED.);
#1863=B_SPLINE_CURVE_WITH_KNOTS('',3,(#246329,#246330,#246331,#246332,#246333,
#246334,#246335,#246336,#246337,#246338,#246339,#246340,#246341,#246342,
#246343,#246344,#246345,#246346,#246347,#246348,#246349,#246350,#246351,
#246352,#246353,#246354,#246355,#246356,#246357,#246358,#246359,#246360,
#246361,#246362,#246363,#246364,#246365,#246366,#246367,#246368,#246369,
#246370,#246371,#246372,#246373,#246374,#246375,#246376,#246377,#246378,
#246379,#246380,#246381,#246382,#246383,#246384,#246385,#246386,#246387,
#246388,#246389,#246390,#246391,#246392,#246393,#246394,#246395,#246396,
#246397,#246398,#246399,#246400,#246401,#246402,#246403,#246404,#246405,
#246406,#246407,#246408,#246409,#246410,#246411,#246412,#246413,#246414,
#246415,#246416,#246417,#246418,#246419,#246420,#246421,#246422,#246423,
#246424,#246425,#246426,#246427,#246428,#246429,#246430,#246431,#246432,
#246433,#246434,#246435,#246436,#246437,#246438,#246439,#246440,#246441,
#246442,#246443,#246444,#246445,#246446,#246447,#246448,#246449,#246450,
#246451,#246452,#246453,#246454,#246455,#246456,#246457,#246458,#246459,
#246460,#246461,#246462,#246463,#246464,#246465,#246466,#246467,#246468,
#246469,#246470,#246471,#246472,#246473,#246474,#246475,#246476,#246477,
#246478,#246479,#246480,#246481,#246482,#246483,#246484,#246485,#246486,
#246487,#246488,#246489,#246490,#246491,#246492,#246493,#246494,#246495,
#246496,#246497,#246498,#246499,#246500,#246501,#246502,#246503,#246504,
#246505,#246506,#246507,#246508,#246509,#246510,#246511,#246512,#246513,
#246514,#246515,#246516,#246517,#246518,#246519,#246520,#246521,#246522,
#246523,#246524,#246525,#246526,#246527,#246528,#246529,#246530,#246531,
#246532,#246533,#246534,#246535,#246536,#246537,#246538,#246539,#246540,
#246541,#246542,#246543,#246544,#246545,#246546,#246547,#246548),
 .UNSPECIFIED.,.F.,.F.,(4,3,3,3,3,3,3,3,3,3,3,3,3,3,3,3,3,3,3,3,3,3,3,3,
3,3,3,3,3,3,3,3,3,3,3,3,3,3,3,3,3,3,3,3,3,3,3,3,3,3,3,3,3,3,3,3,3,3,3,3,
3,3,3,3,3,3,3,3,3,3,3,3,3,4),(1423.14147207631,1423.22386678623,1423.30619520945,
1423.38848470131,1423.47075562151,1423.55302696428,1423.63531772196,1423.71769400858,
1423.80011729223,1423.88266299128,1423.93211404692,1424.01585275877,1424.09948827013,
1424.18304071353,1424.26653014938,1424.3499841,1424.43342059384,1424.5168577036,
1424.60031349852,1424.68385799124,1424.76744707419,1424.85117034174,1424.93185005764,
1425.01558876949,1425.09922428085,1425.18277672425,1425.2662661601,1425.34972011072,
1425.43315660456,1425.51659371432,1425.60004950923,1425.68359400196,1425.7671830849,
1425.85090635246,1425.93158606836,1426.01532478021,1426.09896029157,1426.18251273497,
1426.26600217082,1426.34945612144,1426.43289261528,1426.51632972504,1426.59978551996,
1426.68333001269,1426.76691909563,1426.85064236319,1426.93132207908,1427.01506079093,
1427.09869630229,1427.18224874569,1427.26573818154,1427.34919213216,1427.432628626,
1427.51606573576,1427.59952153068,1427.68306602341,1427.76665510635,1427.85037837391,
1427.9310580898,1428.01479680165,1428.09843231301,1428.18198475641,1428.26547419226,
1428.34892814288,1428.43236463672,1428.51580174648,1428.5992575414,1428.68280203413,
1428.76639111707,1428.85011438462,1428.93079410052,1429.01909172383,1429.10718968499,
1429.17433711171),.UNSPECIFIED.);
#1864=B_SPLINE_CURVE_WITH_KNOTS('',3,(#246550,#246551,#246552,#246553,#246554,
#246555,#246556,#246557,#246558,#246559,#246560,#246561,#246562,#246563,
#246564,#246565,#246566,#246567,#246568,#246569,#246570,#246571,#246572,
#246573,#246574,#246575,#246576,#246577,#246578,#246579,#246580,#246581,
#246582,#246583,#246584,#246585,#246586,#246587,#246588,#246589,#246590,
#246591,#246592,#246593,#246594,#246595,#246596,#246597,#246598,#246599,
#246600,#246601,#246602,#246603,#246604,#246605,#246606,#246607,#246608,
#246609,#246610,#246611,#246612,#246613,#246614,#246615,#246616,#246617,
#246618,#246619,#246620,#246621,#246622,#246623,#246624,#246625,#246626,
#246627,#246628,#246629,#246630,#246631,#246632,#246633,#246634,#246635,
#246636,#246637,#246638,#246639,#246640,#246641,#246642,#246643,#246644,
#246645,#246646,#246647,#246648,#246649,#246650,#246651,#246652,#246653,
#246654,#246655,#246656,#246657,#246658,#246659,#246660,#246661,#246662,
#246663,#246664,#246665,#246666,#246667,#246668,#246669,#246670,#246671,
#246672,#246673,#246674,#246675,#246676,#246677,#246678,#246679,#246680,
#246681,#246682,#246683,#246684,#246685,#246686,#246687,#246688,#246689,
#246690,#246691,#246692,#246693,#246694,#246695,#246696,#246697,#246698,
#246699,#246700,#246701,#246702,#246703,#246704,#246705,#246706,#246707,
#246708,#246709,#246710,#246711,#246712,#246713,#246714,#246715,#246716,
#246717,#246718,#246719,#246720,#246721,#246722,#246723,#246724,#246725,
#246726,#246727,#246728,#246729,#246730,#246731,#246732,#246733,#246734,
#246735,#246736,#246737,#246738,#246739,#246740,#246741,#246742,#246743,
#246744,#246745,#246746,#246747,#246748,#246749,#246750,#246751,#246752,
#246753,#246754,#246755,#246756,#246757,#246758,#246759,#246760,#246761,
#246762,#246763,#246764,#246765,#246766),.UNSPECIFIED.,.F.,.F.,(4,3,3,3,
3,3,3,3,3,3,3,3,3,3,3,3,3,3,3,3,3,3,3,3,3,3,3,3,3,3,3,3,3,3,3,3,3,3,3,3,
3,3,3,3,3,3,3,3,3,3,3,3,3,3,3,3,3,3,3,3,3,3,3,3,3,3,3,3,3,3,3,3,4),(1423.14147207617,
1423.24266865591,1423.32640736776,1423.41004287912,1423.49359532252,1423.57708475837,
1423.66053870899,1423.74397520283,1423.82741231259,1423.91086810751,1423.99441260024,
1424.07800168318,1424.16172495074,1424.24240466663,1424.32614337848,1424.40977888984,
1424.49333133324,1424.57682076909,1424.66027471971,1424.74371121355,1424.82714832331,
1424.91060411823,1424.99414861096,1425.0777376939,1425.16146096146,1425.24214067735,
1425.3258793892,1425.40951490056,1425.49306734396,1425.57655677981,1425.66001073043,
1425.74344722427,1425.82688433403,1425.91034012894,1425.99388462167,1426.07747370462,
1426.16119697217,1426.24187668807,1426.32561539992,1426.40925091128,1426.49280335468,
1426.57629279053,1426.65974674115,1426.74318323499,1426.82662034475,1426.91007613967,
1426.9936206324,1427.07720971534,1427.1609329829,1427.24161269879,1427.32535141064,
1427.408986922,1427.4925393654,1427.57602880125,1427.65948275187,1427.74291924571,
1427.82635635547,1427.90981215039,1427.99335664312,1428.07694572606,1428.16066899361,
1428.24134870951,1428.32509132268,1428.40872984063,1428.49228439967,1428.57740517497,
1428.66085544328,1428.74428734301,1428.82771894588,1428.91410185992,1428.9976247119,
1429.08543765696,1429.17325060202),.UNSPECIFIED.);
#1865=B_SPLINE_CURVE_WITH_KNOTS('',3,(#246767,#246768,#246769,#246770,#246771,
#246772,#246773,#246774,#246775,#246776),.UNSPECIFIED.,.F.,.F.,(4,3,3,4),
(1422.88963902832,1422.97213368162,1423.05680287883,1423.14147207603),
 .UNSPECIFIED.);
#1866=B_SPLINE_CURVE_WITH_KNOTS('',3,(#246782,#246783,#246784,#246785,#246786,
#246787,#246788,#246789,#246790,#246791),.UNSPECIFIED.,.F.,.F.,(4,3,3,4),
(1416.60645213015,1416.68913802073,1416.7737123948,1416.85828676886),
 .UNSPECIFIED.);
#1867=B_SPLINE_CURVE_WITH_KNOTS('',3,(#246792,#246793,#246794,#246795,#246796,
#246797,#246798,#246799,#246800,#246801,#246802,#246803,#246804,#246805,
#246806,#246807,#246808,#246809,#246810,#246811,#246812,#246813,#246814,
#246815,#246816,#246817,#246818,#246819,#246820,#246821,#246822,#246823,
#246824,#246825,#246826,#246827,#246828,#246829,#246830,#246831,#246832,
#246833,#246834,#246835,#246836,#246837,#246838,#246839,#246840,#246841,
#246842,#246843,#246844,#246845,#246846,#246847,#246848,#246849,#246850,
#246851,#246852,#246853,#246854,#246855,#246856,#246857,#246858,#246859,
#246860,#246861,#246862,#246863,#246864,#246865,#246866,#246867,#246868,
#246869,#246870,#246871,#246872,#246873,#246874,#246875,#246876,#246877,
#246878,#246879,#246880,#246881,#246882,#246883,#246884,#246885,#246886,
#246887,#246888,#246889,#246890,#246891,#246892,#246893,#246894,#246895,
#246896,#246897,#246898,#246899,#246900,#246901,#246902,#246903,#246904,
#246905,#246906,#246907,#246908,#246909,#246910,#246911,#246912,#246913,
#246914,#246915,#246916,#246917,#246918,#246919,#246920,#246921,#246922,
#246923,#246924,#246925,#246926,#246927,#246928,#246929,#246930,#246931,
#246932,#246933,#246934,#246935,#246936,#246937,#246938,#246939,#246940,
#246941,#246942,#246943,#246944,#246945,#246946,#246947,#246948,#246949,
#246950,#246951,#246952,#246953,#246954,#246955,#246956,#246957,#246958,
#246959,#246960,#246961,#246962,#246963,#246964,#246965,#246966,#246967,
#246968,#246969,#246970,#246971,#246972,#246973,#246974,#246975,#246976,
#246977,#246978,#246979,#246980,#246981,#246982,#246983,#246984,#246985,
#246986,#246987,#246988,#246989,#246990,#246991,#246992,#246993,#246994,
#246995,#246996,#246997,#246998,#246999,#247000,#247001,#247002,#247003,
#247004,#247005,#247006,#247007,#247008,#247009,#247010,#247011),
 .UNSPECIFIED.,.F.,.F.,(4,3,3,3,3,3,3,3,3,3,3,3,3,3,3,3,3,3,3,3,3,3,3,3,
3,3,3,3,3,3,3,3,3,3,3,3,3,3,3,3,3,3,3,3,3,3,3,3,3,3,3,3,3,3,3,3,3,3,3,3,
3,3,3,3,3,3,3,3,3,3,3,3,3,4),(1416.85828676899,1416.93396197187,1417.01770068372,
1417.10133619508,1417.18488863848,1417.26837807433,1417.35183202495,1417.43526851879,
1417.51870562855,1417.60216142347,1417.6857059162,1417.76929499914,1417.8530182667,
1417.93369798259,1418.01743669444,1418.1010722058,1418.1846246492,1418.26811408505,
1418.35156803567,1418.43500452951,1418.51844163927,1418.60189743419,1418.68544192692,
1418.76903100986,1418.85275427742,1418.93343399331,1419.01717270516,1419.10080821652,
1419.18436065992,1419.26785009577,1419.35130404639,1419.43474054023,1419.51817764999,
1419.60163344491,1419.68517793764,1419.76876702058,1419.85249028813,1419.93317000403,
1420.01690871588,1420.10054422724,1420.18409667064,1420.26758610649,1420.35104005711,
1420.43447655095,1420.51791366071,1420.60136945563,1420.68491394836,1420.7685030313,
1420.85222629885,1420.93290601475,1421.0166447266,1421.10028023796,1421.18383268136,
1421.26732211721,1421.35077606783,1421.43421256167,1421.51764967143,1421.60110546634,
1421.68464995907,1421.76823904201,1421.85196230957,1421.93264202547,1422.01638314035,
1422.10002049812,1422.18357423364,1422.26706440912,1422.35051630726,1422.4339499617,
1422.51738344462,1422.60083482409,1422.68436422929,1422.76793789954,1422.85162109986,
1422.89017552255),.UNSPECIFIED.);
#1868=B_SPLINE_CURVE_WITH_KNOTS('',3,(#247013,#247014,#247015,#247016,#247017,
#247018,#247019,#247020,#247021,#247022,#247023,#247024,#247025,#247026,
#247027,#247028,#247029,#247030,#247031,#247032,#247033,#247034,#247035,
#247036,#247037,#247038,#247039,#247040,#247041,#247042,#247043,#247044,
#247045,#247046,#247047,#247048,#247049,#247050,#247051,#247052,#247053,
#247054,#247055,#247056,#247057,#247058,#247059,#247060,#247061,#247062,
#247063,#247064,#247065,#247066,#247067,#247068,#247069,#247070,#247071,
#247072,#247073,#247074,#247075,#247076,#247077,#247078,#247079,#247080,
#247081,#247082,#247083,#247084,#247085,#247086,#247087,#247088,#247089,
#247090,#247091,#247092,#247093,#247094,#247095,#247096,#247097,#247098,
#247099,#247100,#247101,#247102,#247103,#247104,#247105,#247106,#247107,
#247108,#247109,#247110,#247111,#247112,#247113,#247114,#247115,#247116,
#247117,#247118,#247119,#247120,#247121,#247122,#247123,#247124,#247125,
#247126,#247127,#247128,#247129,#247130,#247131,#247132,#247133,#247134,
#247135,#247136,#247137,#247138,#247139,#247140,#247141,#247142,#247143,
#247144,#247145,#247146,#247147,#247148,#247149,#247150,#247151,#247152,
#247153,#247154,#247155,#247156,#247157,#247158,#247159,#247160,#247161,
#247162,#247163,#247164,#247165,#247166,#247167,#247168,#247169,#247170,
#247171,#247172,#247173,#247174,#247175,#247176,#247177,#247178,#247179,
#247180,#247181,#247182,#247183,#247184,#247185,#247186,#247187,#247188,
#247189,#247190,#247191,#247192,#247193,#247194,#247195,#247196,#247197,
#247198,#247199,#247200,#247201,#247202,#247203,#247204,#247205,#247206,
#247207,#247208,#247209,#247210,#247211,#247212,#247213,#247214,#247215,
#247216,#247217,#247218,#247219,#247220,#247221,#247222,#247223,#247224,
#247225,#247226,#247227,#247228,#247229),.UNSPECIFIED.,.F.,.F.,(4,3,3,3,
3,3,3,3,3,3,3,3,3,3,3,3,3,3,3,3,3,3,3,3,3,3,3,3,3,3,3,3,3,3,3,3,3,3,3,3,
3,3,3,3,3,3,3,3,3,3,3,3,3,3,3,3,3,3,3,3,3,3,3,3,3,3,3,3,3,3,3,3,4),(1416.85828676918,
1416.95477822478,1417.04830595778,1417.14627927468,1417.24425259159,1417.32799130344,
1417.4116268148,1417.4951792582,1417.57866869405,1417.66212264467,1417.74555913851,
1417.82899624827,1417.91245204319,1417.99599653592,1418.07958561886,1418.16330888641,
1418.24398860231,1418.32772731416,1418.41136282552,1418.49491526892,1418.57840470477,
1418.66185865539,1418.74529514923,1418.82873225899,1418.91218805391,1418.99573254664,
1419.07932162958,1419.16304489713,1419.24372461303,1419.32746332488,1419.41109883624,
1419.49465127964,1419.57814071549,1419.66159466611,1419.74503115995,1419.82846826971,
1419.91192406463,1419.99546855736,1420.0790576403,1420.16278090785,1420.24346062375,
1420.3271993356,1420.41083484696,1420.49438729036,1420.57787672621,1420.66133067683,
1420.74476717067,1420.82820428043,1420.91166007535,1420.99520456808,1421.07879365102,
1421.16251691857,1421.24319663447,1421.32693534632,1421.41057085768,1421.49412330108,
1421.57761273693,1421.66106668755,1421.74450318139,1421.82794029115,1421.91139608607,
1421.9949405788,1422.07852966174,1422.16225292929,1422.24293264519,1422.32559622083,
1422.40816522113,1422.490658732,1422.57309577088,1422.6555052585,1422.73789637857,
1422.82031610301,1422.88963902832),.UNSPECIFIED.);
#1869=B_SPLINE_CURVE_WITH_KNOTS('',3,(#247230,#247231,#247232,#247233,#247234,
#247235,#247236,#247237,#247238,#247239),.UNSPECIFIED.,.F.,.F.,(4,3,3,4),
(1416.60760743314,1416.69191056942,1416.77619079502,1416.85828676899),
 .UNSPECIFIED.);
#1870=B_SPLINE_CURVE_WITH_KNOTS('',3,(#247245,#247246,#247247,#247248,#247249,
#247250,#247251,#247252,#247253,#247254),.UNSPECIFIED.,.F.,.F.,(4,3,3,4),
(1410.32430278068,1410.40811390766,1410.49192260022,1410.57510146181),
 .UNSPECIFIED.);
#1871=B_SPLINE_CURVE_WITH_KNOTS('',3,(#247255,#247256,#247257,#247258,#247259,
#247260,#247261,#247262,#247263,#247264,#247265,#247266,#247267,#247268,
#247269,#247270,#247271,#247272,#247273,#247274,#247275,#247276,#247277,
#247278,#247279,#247280,#247281,#247282,#247283,#247284,#247285,#247286,
#247287,#247288,#247289,#247290,#247291,#247292,#247293,#247294,#247295,
#247296,#247297,#247298,#247299,#247300,#247301,#247302,#247303,#247304,
#247305,#247306,#247307,#247308,#247309,#247310,#247311,#247312,#247313,
#247314,#247315,#247316,#247317,#247318,#247319,#247320,#247321,#247322,
#247323,#247324,#247325,#247326,#247327,#247328,#247329,#247330,#247331,
#247332,#247333,#247334,#247335,#247336,#247337,#247338,#247339,#247340,
#247341,#247342,#247343,#247344,#247345,#247346,#247347,#247348,#247349,
#247350,#247351,#247352,#247353,#247354,#247355,#247356,#247357,#247358,
#247359,#247360,#247361,#247362,#247363,#247364,#247365,#247366,#247367,
#247368,#247369,#247370,#247371,#247372,#247373,#247374,#247375,#247376,
#247377,#247378,#247379,#247380,#247381,#247382,#247383,#247384,#247385,
#247386,#247387,#247388,#247389,#247390,#247391,#247392,#247393,#247394,
#247395,#247396,#247397,#247398,#247399,#247400,#247401,#247402,#247403,
#247404,#247405,#247406,#247407,#247408,#247409,#247410,#247411,#247412,
#247413,#247414,#247415,#247416,#247417,#247418,#247419,#247420,#247421,
#247422,#247423,#247424,#247425,#247426,#247427,#247428,#247429,#247430,
#247431,#247432,#247433,#247434,#247435,#247436,#247437,#247438,#247439,
#247440,#247441,#247442,#247443,#247444,#247445,#247446,#247447,#247448,
#247449,#247450,#247451,#247452,#247453,#247454,#247455,#247456,#247457,
#247458,#247459,#247460,#247461,#247462,#247463,#247464,#247465,#247466,
#247467,#247468,#247469,#247470,#247471),.UNSPECIFIED.,.F.,.F.,(4,3,3,3,
3,3,3,3,3,3,3,3,3,3,3,3,3,3,3,3,3,3,3,3,3,3,3,3,3,3,3,3,3,3,3,3,3,3,3,3,
3,3,3,3,3,3,3,3,3,3,3,3,3,3,3,3,3,3,3,3,3,3,3,3,3,3,3,3,3,3,3,3,4),(1410.57510146201,
1410.67010500045,1410.76553206136,1410.86152504162,1410.93554590755,1411.0192846194,
1411.10292013076,1411.18647257416,1411.26996201001,1411.35341596063,1411.43685245447,
1411.52028956423,1411.60374535915,1411.68728985187,1411.77087893482,1411.85460220237,
1411.93528191827,1412.01902063012,1412.10265614148,1412.18620858488,1412.26969802073,
1412.35315197135,1412.43658846519,1412.52002557495,1412.60348136987,1412.6870258626,
1412.77061494554,1412.8543382131,1412.93501792899,1413.01875664084,1413.1023921522,
1413.1859445956,1413.26943403145,1413.35288798207,1413.43632447591,1413.51976158567,
1413.60321738059,1413.68676187332,1413.77035095626,1413.85407422381,1413.93475393971,
1414.01849265156,1414.10212816292,1414.18568060632,1414.26917004217,1414.35262399279,
1414.43606048663,1414.51949759639,1414.6029533913,1414.68649788403,1414.77008696697,
1414.85381023453,1414.93448995043,1415.01822866228,1415.10186417364,1415.18541661704,
1415.26890605289,1415.35236000351,1415.43579649735,1415.51923360711,1415.60268940203,
1415.68623389476,1415.7698229777,1415.85354624526,1415.93422596115,1416.01825423227,
1416.10099893318,1416.18366832812,1416.26628131214,1416.35132401664,1416.43389281429,
1416.52017247222,1416.60645213015),.UNSPECIFIED.);
#1872=B_SPLINE_CURVE_WITH_KNOTS('',3,(#247473,#247474,#247475,#247476,#247477,
#247478,#247479,#247480,#247481,#247482,#247483,#247484,#247485,#247486,
#247487,#247488,#247489,#247490,#247491,#247492,#247493,#247494,#247495,
#247496,#247497,#247498,#247499,#247500,#247501,#247502,#247503,#247504,
#247505,#247506,#247507,#247508,#247509,#247510,#247511,#247512,#247513,
#247514,#247515,#247516,#247517,#247518,#247519,#247520,#247521,#247522,
#247523,#247524,#247525,#247526,#247527,#247528,#247529,#247530,#247531,
#247532,#247533,#247534,#247535,#247536,#247537,#247538,#247539,#247540,
#247541,#247542,#247543,#247544,#247545,#247546,#247547,#247548,#247549,
#247550,#247551,#247552,#247553,#247554,#247555,#247556,#247557,#247558,
#247559,#247560,#247561,#247562,#247563,#247564,#247565,#247566,#247567,
#247568,#247569,#247570,#247571,#247572,#247573,#247574,#247575,#247576,
#247577,#247578,#247579,#247580,#247581,#247582,#247583,#247584,#247585,
#247586,#247587,#247588,#247589,#247590,#247591,#247592,#247593,#247594,
#247595,#247596,#247597,#247598,#247599,#247600,#247601,#247602,#247603,
#247604,#247605,#247606,#247607,#247608,#247609,#247610,#247611,#247612,
#247613,#247614,#247615,#247616,#247617,#247618,#247619,#247620,#247621,
#247622,#247623,#247624,#247625,#247626,#247627,#247628,#247629,#247630,
#247631,#247632,#247633,#247634,#247635,#247636,#247637,#247638,#247639,
#247640,#247641,#247642,#247643,#247644,#247645,#247646,#247647,#247648,
#247649,#247650,#247651,#247652,#247653,#247654,#247655,#247656,#247657,
#247658,#247659,#247660,#247661,#247662,#247663,#247664,#247665,#247666,
#247667,#247668,#247669,#247670,#247671,#247672,#247673,#247674,#247675,
#247676,#247677,#247678,#247679,#247680,#247681,#247682,#247683,#247684,
#247685,#247686,#247687,#247688,#247689,#247690,#247691,#247692),
 .UNSPECIFIED.,.F.,.F.,(4,3,3,3,3,3,3,3,3,3,3,3,3,3,3,3,3,3,3,3,3,3,3,3,
3,3,3,3,3,3,3,3,3,3,3,3,3,3,3,3,3,3,3,3,3,3,3,3,3,3,3,3,3,3,3,3,3,3,3,3,
3,3,3,3,3,3,3,3,3,3,3,3,3,4),(1410.57510146181,1410.65894334499,1410.74225529584,
1410.82557017512,1410.9089061093,1410.9931387138,1411.07661585494,1411.1612261911,
1411.24583652727,1411.32957523912,1411.41321075048,1411.49676319388,1411.58025262973,
1411.66370658035,1411.74714307419,1411.83058018395,1411.91403597887,1411.9975804716,
1412.08116955454,1412.16489282209,1412.24557253799,1412.32931124984,1412.4129467612,
1412.4964992046,1412.57998864045,1412.66344259107,1412.74687908491,1412.83031619467,
1412.91377198959,1412.99731648232,1413.08090556526,1413.16462883281,1413.24530854871,
1413.32904726056,1413.41268277192,1413.49623521532,1413.57972465117,1413.66317860179,
1413.74661509563,1413.83005220539,1413.91350800031,1413.99705249304,1414.08064157598,
1414.16436484353,1414.24504455943,1414.32878327128,1414.41241878264,1414.49597122604,
1414.57946066189,1414.66291461251,1414.74635110635,1414.82978821611,1414.91324401103,
1414.99678850376,1415.0803775867,1415.16410085425,1415.24478057015,1415.328519282,
1415.41215479336,1415.49570723676,1415.57919667261,1415.66265062323,1415.74608711707,
1415.82952422683,1415.91298002175,1415.99652451447,1416.08011359742,1416.16383686497,
1416.24451658087,1416.32920862088,1416.41375449164,1416.49821554759,1416.5825919458,
1416.60760743314),.UNSPECIFIED.);
#1873=B_SPLINE_CURVE_WITH_KNOTS('',3,(#247693,#247694,#247695,#247696,#247697,
#247698,#247699,#247700,#247701,#247702),.UNSPECIFIED.,.F.,.F.,(4,3,3,4),
(1410.3244751935,1410.42295017058,1410.52052586119,1410.57510146163),
 .UNSPECIFIED.);
#1874=B_SPLINE_CURVE_WITH_KNOTS('',3,(#247708,#247709,#247710,#247711,#247712,
#247713,#247714,#247715,#247716,#247717,#247718,#247719,#247720),
 .UNSPECIFIED.,.F.,.F.,(4,3,3,3,4),(1403.7003517852,1403.78532632359,1403.86877413941,
1403.95451203908,1404.04024993874),.UNSPECIFIED.);
#1875=B_SPLINE_CURVE_WITH_KNOTS('',3,(#247722,#247723,#247724,#247725,#247726,
#247727),.UNSPECIFIED.,.F.,.F.,(4,2,4),(1.8052198339721,1.86724042443728,
1.96119997683881),.UNSPECIFIED.);
#1876=B_SPLINE_CURVE_WITH_KNOTS('',3,(#247728,#247729,#247730,#247731,#247732,
#247733,#247734,#247735,#247736,#247737,#247738,#247739,#247740,#247741,
#247742,#247743,#247744,#247745,#247746,#247747,#247748,#247749,#247750,
#247751,#247752,#247753,#247754,#247755),.UNSPECIFIED.,.F.,.F.,(4,3,3,3,
3,3,3,3,3,4),(1403.37979373757,1403.46322854723,1403.54666922749,1403.63013384884,
1403.71368962522,1403.79729471688,1403.88102697689,1403.93739383251,1404.03402820369,
1404.04140044517),.UNSPECIFIED.);
#1877=B_SPLINE_CURVE_WITH_KNOTS('',3,(#254538,#254539,#254540,#254541,#254542,
#254543,#254544,#254545,#254546,#254547),.UNSPECIFIED.,.F.,.F.,(4,2,2,2,
4),(0.000477622210521881,0.0654985715592456,0.146298798970954,0.27193450855757,
0.311339098434402),.UNSPECIFIED.);
#1878=B_SPLINE_CURVE_WITH_KNOTS('',3,(#254549,#254550,#254551,#254552,#254553,
#254554,#254555,#254556,#254557,#254558,#254559,#254560,#254561,#254562,
#254563,#254564,#254565,#254566,#254567,#254568,#254569,#254570,#254571,
#254572,#254573,#254574,#254575,#254576,#254577,#254578,#254579,#254580,
#254581,#254582,#254583,#254584,#254585,#254586,#254587,#254588,#254589,
#254590,#254591,#254592,#254593,#254594,#254595,#254596,#254597,#254598,
#254599,#254600,#254601,#254602,#254603,#254604,#254605,#254606,#254607,
#254608,#254609),.UNSPECIFIED.,.F.,.F.,(4,3,3,3,3,3,3,3,3,3,3,3,3,3,3,3,
3,3,3,3,4),(1392.30062248289,1392.38353259545,1392.46334657938,1392.54321558283,
1392.62319000748,1392.63226293314,1392.71222023327,1392.79208303051,1392.87186885299,
1392.95159516818,1393.03127939648,1393.1109503827,1393.19061783622,1393.27029748704,
1393.35000506944,1393.42980029851,1393.50964464022,1393.58960306727,1393.63199894386,
1393.71196956209,1393.72842800165),.UNSPECIFIED.);
#1879=B_SPLINE_CURVE_WITH_KNOTS('',3,(#254610,#254611,#254612,#254613,#254614,
#254615,#254616,#254617,#254618,#254619,#254620,#254621,#254622,#254623,
#254624,#254625,#254626,#254627,#254628,#254629,#254630,#254631,#254632,
#254633,#254634,#254635,#254636,#254637,#254638,#254639,#254640,#254641),
 .UNSPECIFIED.,.F.,.F.,(4,2,2,2,2,2,2,2,2,2,2,2,2,2,2,4),(0.311339098434402,
0.384933689166427,0.397094845809577,0.39736868756705,0.397450522008619,
0.397499655154026,0.397543081273146,0.397597345360711,0.397702470611355,
0.398379451119274,0.399871523283459,0.425219733962204,0.476781426924293,
0.631008672365873,0.720388372997854,0.803428429579855),.UNSPECIFIED.);
#1880=B_SPLINE_CURVE_WITH_KNOTS('',3,(#261424,#261425,#261426,#261427,#261428,
#261429,#261430,#261431,#261432,#261433,#261434,#261435,#261436,#261437,
#261438,#261439,#261440,#261441,#261442,#261443,#261444,#261445,#261446,
#261447,#261448,#261449,#261450,#261451,#261452,#261453,#261454,#261455,
#261456,#261457,#261458,#261459,#261460,#261461),.UNSPECIFIED.,.F.,.F.,
(4,2,2,2,2,2,2,2,2,2,2,2,2,2,2,2,2,2,4),(0.00239242256924691,0.134902032668107,
0.296770312006015,0.324000698094346,0.326552911280465,0.326929349600861,
0.327178375312593,0.327616377021976,0.32773031959246,0.327805417519109,
0.327847482964747,0.327882907829789,0.327925026518018,0.328000448551939,
0.328349673398392,0.328987017831634,0.347385760741725,0.39081477612345,
0.517465670307461),.UNSPECIFIED.);
#1881=B_SPLINE_CURVE_WITH_KNOTS('',3,(#261463,#261464,#261465,#261466,#261467,
#261468,#261469,#261470,#261471,#261472,#261473,#261474,#261475,#261476,
#261477,#261478,#261479,#261480,#261481,#261482,#261483,#261484,#261485,
#261486,#261487,#261488,#261489,#261490,#261491,#261492,#261493,#261494,
#261495,#261496,#261497,#261498,#261499,#261500,#261501,#261502,#261503,
#261504,#261505),.UNSPECIFIED.,.F.,.F.,(4,3,3,3,3,3,3,3,3,3,3,3,3,3,4),
(1498.97655487521,1499.05623057304,1499.1358974584,1499.21557126196,1499.2952677155,
1499.3750496428,1499.45487593369,1499.53482369084,1499.60401608019,1499.68397970309,
1499.76385130304,1499.84363027147,1499.92335568368,1500.00304021085,1500.04731086453),
 .UNSPECIFIED.);
#1882=B_SPLINE_CURVE_WITH_KNOTS('',3,(#261506,#261507,#261508,#261509,#261510,
#261511,#261512,#261513,#261514,#261515),.UNSPECIFIED.,.F.,.F.,(4,2,2,2,
4),(6.24789745713582E-5,0.0249353959329077,0.115784953094516,0.19994556386008,
0.348086239184528),.UNSPECIFIED.);
#1883=B_SPLINE_CURVE_WITH_KNOTS('',3,(#261517,#261518,#261519,#261520,#261521,
#261522,#261523,#261524,#261525,#261526,#261527,#261528,#261529,#261530,
#261531,#261532,#261533,#261534,#261535,#261536,#261537,#261538,#261539,
#261540,#261541,#261542,#261543,#261544,#261545,#261546,#261547,#261548,
#261549,#261550,#261551,#261552,#261553,#261554,#261555,#261556,#261557,
#261558,#261559,#261560,#261561,#261562,#261563,#261564,#261565,#261566,
#261567,#261568,#261569,#261570,#261571,#261572,#261573,#261574,#261575,
#261576,#261577,#261578,#261579,#261580,#261581,#261582,#261583,#261584,
#261585,#261586,#261587,#261588,#261589,#261590,#261591,#261592,#261593,
#261594,#261595,#261596,#261597,#261598,#261599,#261600,#261601,#261602,
#261603,#261604,#261605,#261606,#261607,#261608,#261609,#261610,#261611,
#261612,#261613,#261614,#261615,#261616,#261617,#261618,#261619,#261620,
#261621,#261622,#261623,#261624,#261625,#261626,#261627,#261628,#261629,
#261630,#261631,#261632,#261633,#261634,#261635,#261636,#261637,#261638,
#261639,#261640,#261641,#261642,#261643,#261644,#261645,#261646,#261647,
#261648,#261649,#261650,#261651,#261652,#261653,#261654,#261655,#261656,
#261657,#261658,#261659,#261660,#261661,#261662,#261663,#261664,#261665,
#261666,#261667,#261668,#261669,#261670,#261671,#261672,#261673,#261674,
#261675,#261676,#261677,#261678,#261679,#261680,#261681,#261682,#261683,
#261684,#261685,#261686,#261687,#261688,#261689,#261690,#261691,#261692,
#261693,#261694,#261695,#261696,#261697,#261698,#261699,#261700,#261701,
#261702,#261703,#261704,#261705,#261706,#261707,#261708,#261709,#261710,
#261711,#261712,#261713,#261714,#261715,#261716,#261717,#261718,#261719,
#261720,#261721,#261722,#261723,#261724,#261725,#261726,#261727,#261728,
#261729,#261730,#261731,#261732,#261733,#261734,#261735,#261736),
 .UNSPECIFIED.,.F.,.F.,(4,3,3,3,3,3,3,3,3,3,3,3,3,3,3,3,3,3,3,3,3,3,3,3,
3,3,3,3,3,3,3,3,3,3,3,3,3,3,3,3,3,3,3,3,3,3,3,3,3,3,3,3,3,3,3,3,3,3,3,3,
3,3,3,3,3,3,3,3,3,3,3,3,3,4),(1404.29191615463,1404.37562428831,1404.4593290263,
1404.54304803957,1404.62679900449,1404.7106527483,1404.79456200366,1404.87860831265,
1404.93712984323,1405.02086855508,1405.10450406644,1405.18805650984,1405.27154594569,
1405.35499989631,1405.43843639015,1405.52187349991,1405.60532929482,1405.68887378755,
1405.7724628705,1405.85618613805,1405.93686585395,1406.0206045658,1406.10424007716,
1406.18779252056,1406.27128195641,1406.35473590703,1406.43817240087,1406.52160951063,
1406.60506530555,1406.68860979828,1406.77219888122,1406.85592214878,1406.93660186467,
1407.02034057652,1407.10397608788,1407.18752853128,1407.27101796713,1407.35447191775,
1407.43790841159,1407.52134552135,1407.60480131627,1407.688345809,1407.77193489194,
1407.85565815949,1407.93633787539,1408.02007658724,1408.1037120986,1408.187264542,
1408.27075397785,1408.35420792847,1408.43764442231,1408.52108153207,1408.60453732698,
1408.68808181971,1408.77167090265,1408.85539417021,1408.93607388611,1409.01981259796,
1409.10344810932,1409.18700055272,1409.27048998857,1409.35394393919,1409.43738043303,
1409.52081754279,1409.60427333771,1409.68781783044,1409.77140691338,1409.85513018094,
1409.93580989683,1410.01998705489,1410.10402428112,1410.18798093152,1410.2718608454,
1410.32430278068),.UNSPECIFIED.);
#1884=B_SPLINE_CURVE_WITH_KNOTS('',3,(#261737,#261738,#261739,#261740,#261741,
#261742,#261743,#261744,#261745,#261746),.UNSPECIFIED.,.F.,.F.,(4,3,3,4),
(1404.04140044517,1404.13747352714,1404.23285921852,1404.29191615443),
 .UNSPECIFIED.);
#1885=B_SPLINE_CURVE_WITH_KNOTS('',3,(#261748,#261749,#261750,#261751,#261752,
#261753,#261754,#261755,#261756,#261757),.UNSPECIFIED.,.F.,.F.,(4,2,2,2,
4),(0.0014226223468972,0.0413177149723191,0.0846967743397222,0.130628866228341,
0.178453317484416),.UNSPECIFIED.);
#1886=B_SPLINE_CURVE_WITH_KNOTS('',3,(#261759,#261760,#261761,#261762,#261763,
#261764,#261765,#261766,#261767,#261768,#261769,#261770,#261771,#261772,
#261773,#261774,#261775,#261776,#261777,#261778,#261779,#261780,#261781,
#261782,#261783,#261784,#261785,#261786,#261787,#261788,#261789,#261790,
#261791,#261792,#261793,#261794,#261795,#261796,#261797,#261798,#261799,
#261800,#261801,#261802,#261803,#261804),.UNSPECIFIED.,.F.,.F.,(4,3,3,3,
3,3,3,3,3,3,3,3,3,3,3,4),(1394.81425368482,1394.89402080788,1394.97373338235,
1395.05595058022,1395.13561874826,1395.21528835869,1395.29497514184,1395.37469483532,
1395.45450405754,1395.53436687025,1395.61433714781,1395.6314709653,1395.72358358603,
1395.8153650835,1395.90649484727,1395.98599303994),.UNSPECIFIED.);
#1887=B_SPLINE_CURVE_WITH_KNOTS('',3,(#261806,#261807,#261808,#261809,#261810,
#261811,#261812,#261813,#261814,#261815),.UNSPECIFIED.,.F.,.F.,(4,1,1,1,
1,1,1,4),(1395.98599328739,1396.63120697602,1397.63094298674,1398.63067899746,
1399.63041500818,1400.6301510189,1401.62988702962,1402.26917859457),
 .UNSPECIFIED.);
#1888=B_SPLINE_CURVE_WITH_KNOTS('',3,(#261817,#261818,#261819,#261820,#261821,
#261822,#261823,#261824,#261825,#261826),.UNSPECIFIED.,.F.,.F.,(4,1,1,1,
1,1,1,4),(1402.26917859457,1402.62962304034,1403.62935905106,1404.62909506178,
1405.6288310725,1406.62856708322,1407.62830309394,1408.55236390175),
 .UNSPECIFIED.);
#1889=B_SPLINE_CURVE_WITH_KNOTS('',3,(#261828,#261829,#261830,#261831,#261832,
#261833,#261834,#261835,#261836,#261837,#261838,#261839),.UNSPECIFIED.,
 .F.,.F.,(4,2,1,1,1,1,1,1,4),(1408.55236390175,1408.62803910466,1409.62777511538,
1410.6275111261,1411.62724713682,1412.62698314754,1413.62671915826,1414.62645516898,
1414.83554920893),.UNSPECIFIED.);
#1890=B_SPLINE_CURVE_WITH_KNOTS('',3,(#261841,#261842,#261843,#261844,#261845,
#261846,#261847,#261848,#261849,#261850,#261851,#261852,#261853,#261854,
#261855,#261856,#261857,#261858,#261859,#261860,#261861,#261862,#261863,
#261864,#261865,#261866,#261867,#261868,#261869,#261870,#261871,#261872,
#261873,#261874,#261875,#261876,#261877,#261878,#261879,#261880,#261881,
#261882,#261883,#261884,#261885,#261886,#261887,#261888,#261889,#261890,
#261891,#261892,#261893,#261894,#261895,#261896,#261897,#261898,#261899,
#261900,#261901,#261902,#261903,#261904,#261905,#261906,#261907,#261908,
#261909,#261910,#261911,#261912,#261913,#261914,#261915,#261916,#261917,
#261918,#261919,#261920,#261921,#261922,#261923,#261924,#261925,#261926,
#261927,#261928,#261929,#261930,#261931,#261932,#261933,#261934,#261935,
#261936,#261937,#261938,#261939,#261940,#261941,#261942,#261943,#261944,
#261945,#261946,#261947,#261948,#261949,#261950,#261951,#261952,#261953,
#261954,#261955,#261956,#261957,#261958,#261959,#261960,#261961,#261962,
#261963,#261964,#261965,#261966,#261967,#261968,#261969,#261970,#261971,
#261972,#261973,#261974,#261975,#261976,#261977,#261978,#261979,#261980,
#261981,#261982,#261983,#261984,#261985,#261986,#261987,#261988,#261989,
#261990,#261991,#261992,#261993,#261994,#261995,#261996,#261997,#261998,
#261999,#262000,#262001,#262002,#262003,#262004,#262005,#262006,#262007,
#262008,#262009,#262010,#262011,#262012,#262013,#262014,#262015,#262016,
#262017,#262018,#262019,#262020,#262021,#262022,#262023,#262024,#262025,
#262026,#262027,#262028,#262029,#262030,#262031,#262032,#262033,#262034,
#262035,#262036,#262037,#262038,#262039,#262040,#262041,#262042,#262043,
#262044,#262045,#262046,#262047,#262048,#262049,#262050,#262051,#262052,
#262053,#262054,#262055,#262056,#262057,#262058,#262059,#262060,#262061,
#262062,#262063,#262064,#262065,#262066,#262067,#262068,#262069,#262070,
#262071,#262072,#262073,#262074,#262075,#262076,#262077,#262078,#262079,
#262080,#262081,#262082,#262083,#262084),.UNSPECIFIED.,.F.,.F.,(4,3,3,3,
3,3,3,3,3,3,3,3,3,3,3,3,3,3,3,3,3,3,3,3,3,3,3,3,3,3,3,3,3,3,3,3,3,3,3,3,
3,3,3,3,3,3,3,3,3,3,3,3,3,3,3,3,3,3,3,3,3,3,3,3,3,3,3,3,3,3,3,3,3,3,3,3,
3,3,3,3,3,4),(1414.83554920893,1414.91422319859,1414.99283632039,1415.0720056778,
1415.15056272849,1415.22911755209,1415.3076866817,1415.3873128062,1415.46599905401,
1415.54609511686,1415.6261911797,1415.70614847983,1415.78601127707,1415.86579709955,
1415.94552341474,1416.02520764304,1416.10487862926,1416.18454608278,1416.2642257336,
1416.34393331599,1416.42372854507,1416.50357288678,1416.58353131382,1416.62592719042,
1416.70588449055,1416.78574728779,1416.86553311027,1416.94525942546,1417.02494365375,
1417.10461463998,1417.1842820935,1417.26396174432,1417.34366932671,1417.42346455579,
1417.5033088975,1417.58326732454,1417.62566320114,1417.70562050127,1417.78548329851,
1417.86526912099,1417.94499543618,1418.02467966447,1418.1043506507,1418.18401810422,
1418.26369775504,1418.34340533743,1418.42320056651,1418.50304490822,1418.58300333526,
1418.62539921186,1418.70535651199,1418.78521930923,1418.86500513171,1418.9447314469,
1419.0244156752,1419.10408666142,1419.18375411494,1419.26343376576,1419.34314134815,
1419.42293657723,1419.50278091894,1419.58273934598,1419.62513522258,1419.70509252271,
1419.78495531995,1419.86474114243,1419.94446745762,1420.02415168591,1420.10382267214,
1420.18349012566,1420.26316977648,1420.34287735887,1420.42267258795,1420.50251692965,
1420.5824753567,1420.6248712333,1420.70918020921,1420.79334694167,1420.8773195318,
1420.96117782697,1421.0448782206,1421.11873451598),.UNSPECIFIED.);
#1891=B_SPLINE_CURVE_WITH_KNOTS('',3,(#262086,#262087,#262088,#262089,#262090,
#262091,#262092,#262093,#262094,#262095,#262096,#262097,#262098,#262099,
#262100,#262101,#262102,#262103,#262104,#262105,#262106,#262107,#262108,
#262109,#262110,#262111,#262112,#262113,#262114,#262115,#262116,#262117,
#262118,#262119,#262120,#262121,#262122,#262123,#262124,#262125,#262126,
#262127,#262128,#262129,#262130,#262131,#262132,#262133,#262134,#262135,
#262136,#262137,#262138,#262139,#262140,#262141,#262142,#262143,#262144,
#262145,#262146,#262147,#262148,#262149,#262150,#262151,#262152,#262153,
#262154,#262155,#262156,#262157,#262158,#262159,#262160,#262161,#262162,
#262163,#262164,#262165,#262166,#262167,#262168,#262169,#262170,#262171,
#262172,#262173,#262174,#262175,#262176,#262177,#262178,#262179,#262180,
#262181,#262182,#262183,#262184,#262185,#262186,#262187,#262188,#262189,
#262190,#262191,#262192,#262193,#262194,#262195,#262196,#262197,#262198,
#262199,#262200,#262201,#262202,#262203,#262204,#262205,#262206,#262207,
#262208,#262209,#262210,#262211,#262212,#262213,#262214,#262215,#262216,
#262217,#262218,#262219,#262220,#262221,#262222,#262223,#262224,#262225,
#262226,#262227,#262228,#262229,#262230,#262231,#262232,#262233,#262234,
#262235,#262236,#262237,#262238,#262239,#262240,#262241,#262242,#262243,
#262244,#262245,#262246,#262247,#262248,#262249,#262250,#262251,#262252,
#262253,#262254,#262255,#262256,#262257,#262258,#262259,#262260,#262261,
#262262,#262263,#262264,#262265,#262266,#262267,#262268,#262269,#262270,
#262271,#262272,#262273,#262274,#262275,#262276,#262277,#262278,#262279,
#262280,#262281,#262282,#262283,#262284,#262285,#262286,#262287,#262288,
#262289,#262290,#262291,#262292,#262293,#262294,#262295,#262296,#262297,
#262298,#262299,#262300,#262301,#262302,#262303,#262304,#262305,#262306,
#262307,#262308,#262309,#262310,#262311,#262312,#262313,#262314,#262315,
#262316,#262317,#262318,#262319,#262320,#262321,#262322,#262323,#262324,
#262325,#262326,#262327,#262328,#262329),.UNSPECIFIED.,.F.,.F.,(4,3,3,3,
3,3,3,3,3,3,3,3,3,3,3,3,3,3,3,3,3,3,3,3,3,3,3,3,3,3,3,3,3,3,3,3,3,3,3,3,
3,3,3,3,3,3,3,3,3,3,3,3,3,3,3,3,3,3,3,3,3,3,3,3,3,3,3,3,3,3,3,3,3,3,3,3,
3,3,3,3,3,4),(1421.11873451611,1421.20198682774,1421.28533673185,1421.37015435989,
1421.45378598796,1421.53919661599,1421.62460724402,1421.70456454415,1421.78442734139,
1421.86421316387,1421.94393947906,1422.02362370736,1422.10329469358,1422.1829621471,
1422.26264179792,1422.34234938032,1422.42214460939,1422.5019889511,1422.58194737815,
1422.62434325474,1422.70430055487,1422.78416335211,1422.86394917459,1422.94367548978,
1423.02335971808,1423.1030307043,1423.18269815782,1423.26237780864,1423.34208539104,
1423.42188062011,1423.50172496182,1423.58168338887,1423.62407926546,1423.70403656559,
1423.78389936283,1423.8636851853,1423.9434115005,1424.02309572879,1424.10276671501,
1424.18243416854,1424.26211381936,1424.34182140175,1424.42161663083,1424.50146097253,
1424.58141939958,1424.62381527618,1424.70377257631,1424.78363537355,1424.86342119603,
1424.94314751122,1425.02283173951,1425.10250272574,1425.18217017926,1425.26184983008,
1425.34155741247,1425.42135264155,1425.50119698326,1425.5811554103,1425.6235512869,
1425.70350858703,1425.78337138427,1425.86315720674,1425.94288352194,1426.02256775023,
1426.10223873645,1426.18190618998,1426.2615858408,1426.34129342319,1426.42108865227,
1426.50093299397,1426.58089142102,1426.62328729762,1426.7021669801,1426.78095145909,
1426.85964601321,1426.93828972882,1427.01689915789,1427.09549082411,1427.17410791049,
1427.2527358973,1427.33143433151,1427.40191982329),.UNSPECIFIED.);
#1892=B_SPLINE_CURVE_WITH_KNOTS('',3,(#262331,#262332,#262333,#262334,#262335,
#262336,#262337,#262338,#262339,#262340,#262341),.UNSPECIFIED.,.F.,.F.,
(4,1,1,1,1,1,1,1,4),(1427.40191982329,1427.62302330834,1428.62275931906,
1429.62249532978,1430.6222313405,1431.62196735122,1432.62170336194,1433.62143937266,
1433.68510513047),.UNSPECIFIED.);
#1893=B_SPLINE_CURVE_WITH_KNOTS('',3,(#262343,#262344,#262345,#262346,#262347,
#262348,#262349,#262350,#262351,#262352,#262353,#262354,#262355,#262356,
#262357,#262358,#262359,#262360,#262361,#262362,#262363,#262364,#262365,
#262366,#262367,#262368,#262369,#262370,#262371,#262372,#262373,#262374,
#262375,#262376,#262377,#262378,#262379,#262380,#262381,#262382,#262383,
#262384,#262385,#262386,#262387,#262388,#262389,#262390,#262391,#262392,
#262393,#262394,#262395,#262396,#262397,#262398,#262399,#262400,#262401,
#262402,#262403,#262404,#262405,#262406,#262407,#262408,#262409,#262410,
#262411,#262412,#262413,#262414,#262415,#262416,#262417,#262418,#262419,
#262420,#262421,#262422,#262423,#262424,#262425,#262426,#262427,#262428,
#262429,#262430,#262431,#262432,#262433,#262434,#262435,#262436,#262437,
#262438,#262439,#262440,#262441,#262442,#262443,#262444,#262445,#262446,
#262447,#262448,#262449,#262450,#262451,#262452,#262453,#262454,#262455,
#262456,#262457,#262458,#262459,#262460,#262461,#262462,#262463,#262464,
#262465,#262466,#262467,#262468,#262469,#262470,#262471,#262472,#262473,
#262474,#262475,#262476,#262477,#262478,#262479,#262480,#262481,#262482,
#262483,#262484,#262485,#262486,#262487,#262488,#262489,#262490,#262491,
#262492,#262493,#262494,#262495,#262496,#262497,#262498,#262499,#262500,
#262501,#262502,#262503,#262504,#262505,#262506,#262507,#262508,#262509,
#262510,#262511,#262512,#262513,#262514,#262515,#262516,#262517,#262518,
#262519,#262520,#262521,#262522,#262523,#262524,#262525,#262526,#262527,
#262528,#262529,#262530,#262531,#262532,#262533,#262534,#262535,#262536,
#262537,#262538,#262539,#262540,#262541,#262542,#262543,#262544,#262545,
#262546,#262547,#262548,#262549,#262550,#262551,#262552,#262553,#262554,
#262555,#262556,#262557,#262558,#262559,#262560,#262561,#262562,#262563,
#262564,#262565,#262566,#262567,#262568,#262569,#262570,#262571,#262572,
#262573,#262574,#262575,#262576,#262577,#262578,#262579,#262580,#262581,
#262582,#262583,#262584,#262585,#262586),.UNSPECIFIED.,.F.,.F.,(4,3,3,3,
3,3,3,3,3,3,3,3,3,3,3,3,3,3,3,3,3,3,3,3,3,3,3,3,3,3,3,3,3,3,3,3,3,3,3,3,
3,3,3,3,3,3,3,3,3,3,3,3,3,3,3,3,3,3,3,3,3,3,3,3,3,3,3,3,3,3,3,3,3,3,3,3,
3,3,3,3,3,4),(1433.68510513047,1433.76430171396,1433.84340818076,1433.92244268633,
1434.00142332046,1434.08037593041,1434.1593155102,1434.23825835883,1434.31722077516,
1434.3962651774,1434.47535225123,1434.55455861227,1434.62117538338,1434.70113268351,
1434.78099548076,1434.86078130323,1434.94050761843,1435.02019184673,1435.09986283295,
1435.17953028648,1435.2592099373,1435.33891751969,1435.41871274877,1435.49855709048,
1435.57851551753,1435.62091139411,1435.70086869424,1435.78073149149,1435.86051731396,
1435.94024362915,1436.01992785745,1436.09959884367,1436.1792662972,1436.25894594801,
1436.33865353041,1436.41844875948,1436.49829310119,1436.57825152824,1436.62064740483,
1436.70060470496,1436.7804675022,1436.86025332467,1436.93997963987,1437.01966386816,
1437.09933485438,1437.1790023079,1437.25868195872,1437.33838954111,1437.41818477019,
1437.49802911189,1437.57798753894,1437.62038341555,1437.70034071568,1437.78020351292,
1437.8599893354,1437.93971565059,1438.01939987889,1438.09907086511,1438.17873831863,
1438.25841796945,1438.33812555185,1438.41792078092,1438.49776512263,1438.57772354968,
1438.62011942627,1438.7000767264,1438.77993952365,1438.85972534612,1438.93945166132,
1439.01913588961,1439.09880687583,1439.17847432936,1439.25815398018,1439.33786156257,
1439.41765679165,1439.49750113336,1439.57745956041,1439.61985543699,1439.71247622588,
1439.80474479726,1439.89632503004,1439.96829031496),.UNSPECIFIED.);
#1894=B_SPLINE_CURVE_WITH_KNOTS('',3,(#262588,#262589,#262590,#262591,#262592,
#262593,#262594,#262595,#262596,#262597),.UNSPECIFIED.,.F.,.F.,(4,1,1,1,
1,1,1,4),(1439.96829043765,1440.61959144771,1441.61932745843,1442.61906346915,
1443.61879947987,1444.61853549059,1445.61827150131,1446.25147574483),
 .UNSPECIFIED.);
#1895=B_SPLINE_CURVE_WITH_KNOTS('',3,(#262599,#262600,#262601,#262602,#262603,
#262604,#262605,#262606,#262607,#262608),.UNSPECIFIED.,.F.,.F.,(4,1,1,1,
1,1,1,4),(1446.25147574483,1446.61800751203,1447.61774352275,1448.61747953347,
1449.61721554419,1450.61695155491,1451.61668756563,1452.53466105201),
 .UNSPECIFIED.);
#1896=B_SPLINE_CURVE_WITH_KNOTS('',3,(#262610,#262611,#262612,#262613,#262614,
#262615,#262616,#262617,#262618,#262619,#262620,#262621),.UNSPECIFIED.,
 .F.,.F.,(4,2,1,1,1,1,1,1,4),(1452.53466105201,1452.61642357635,1453.61615958707,
1454.61589559779,1455.61563160851,1456.61536761923,1457.61510362995,1458.61483964067,
1458.81784635919),.UNSPECIFIED.);
#1897=B_SPLINE_CURVE_WITH_KNOTS('',3,(#262623,#262624,#262625,#262626,#262627,
#262628,#262629,#262630,#262631,#262632,#262633,#262634,#262635,#262636,
#262637,#262638,#262639,#262640,#262641,#262642,#262643,#262644,#262645,
#262646,#262647,#262648,#262649,#262650,#262651,#262652,#262653,#262654,
#262655,#262656,#262657,#262658,#262659,#262660,#262661,#262662,#262663,
#262664,#262665,#262666,#262667,#262668,#262669,#262670,#262671,#262672,
#262673,#262674,#262675,#262676,#262677,#262678,#262679,#262680,#262681,
#262682,#262683,#262684,#262685,#262686,#262687,#262688,#262689,#262690,
#262691,#262692,#262693,#262694,#262695,#262696,#262697,#262698,#262699,
#262700,#262701,#262702,#262703,#262704,#262705,#262706,#262707,#262708,
#262709,#262710,#262711,#262712,#262713,#262714,#262715,#262716,#262717,
#262718,#262719,#262720,#262721,#262722,#262723,#262724,#262725,#262726,
#262727,#262728,#262729,#262730,#262731,#262732,#262733,#262734,#262735,
#262736,#262737,#262738,#262739,#262740,#262741,#262742,#262743,#262744,
#262745,#262746,#262747,#262748,#262749,#262750,#262751,#262752,#262753,
#262754,#262755,#262756,#262757,#262758,#262759,#262760,#262761,#262762,
#262763,#262764,#262765,#262766,#262767,#262768,#262769,#262770,#262771,
#262772,#262773,#262774,#262775,#262776,#262777,#262778,#262779,#262780,
#262781,#262782,#262783,#262784,#262785,#262786,#262787,#262788,#262789,
#262790,#262791,#262792,#262793,#262794,#262795,#262796,#262797,#262798,
#262799,#262800,#262801,#262802,#262803,#262804,#262805,#262806,#262807,
#262808,#262809,#262810,#262811,#262812,#262813,#262814,#262815,#262816,
#262817,#262818,#262819,#262820,#262821,#262822,#262823,#262824,#262825,
#262826,#262827,#262828,#262829,#262830,#262831,#262832,#262833,#262834,
#262835,#262836,#262837,#262838,#262839,#262840,#262841,#262842,#262843,
#262844,#262845,#262846,#262847,#262848,#262849,#262850,#262851,#262852,
#262853,#262854,#262855,#262856,#262857,#262858,#262859,#262860,#262861,
#262862,#262863,#262864,#262865,#262866),.UNSPECIFIED.,.F.,.F.,(4,3,3,3,
3,3,3,3,3,3,3,3,3,3,3,3,3,3,3,3,3,3,3,3,3,3,3,3,3,3,3,3,3,3,3,3,3,3,3,3,
3,3,3,3,3,3,3,3,3,3,3,3,3,3,3,3,3,3,3,3,3,3,3,3,3,3,3,3,3,3,3,3,3,3,3,3,
3,3,3,3,3,4),(1458.81784635919,1458.89650835172,1458.97510783377,1459.05504131097,
1459.13358093235,1459.21211704093,1459.29066618012,1459.37164354793,1459.45030870812,
1459.53244217975,1459.61457565139,1459.69453295152,1459.77439574876,1459.85418157123,
1459.93390788643,1460.01359211472,1460.09326310094,1460.17293055447,1460.25261020528,
1460.33231778768,1460.41211301675,1460.49195735846,1460.57191578551,1460.61431166211,
1460.69426896224,1460.77413175948,1460.85391758195,1460.93364389715,1461.01332812544,
1461.09299911166,1461.17266656519,1461.25234621601,1461.3320537984,1461.41184902748,
1461.49169336918,1461.57165179623,1461.61404767283,1461.69400497296,1461.7738677702,
1461.85365359268,1461.93337990787,1462.01306413617,1462.09273512239,1462.17240257591,
1462.25208222673,1462.33178980913,1462.4115850382,1462.49142937991,1462.57138780696,
1462.61378368355,1462.69374098368,1462.77360378092,1462.8533896034,1462.93311591859,
1463.01280014688,1463.09247113311,1463.17213858663,1463.25181823745,1463.33152581984,
1463.41132104892,1463.49116539063,1463.57112381767,1463.61351969427,1463.6934769944,
1463.77333979164,1463.85312561412,1463.93285192931,1464.01253615761,1464.09220714383,
1464.17187459735,1464.25155424817,1464.33126183057,1464.41105705964,1464.49090140135,
1464.5708598284,1464.61325570499,1464.69780465656,1464.7822076085,1464.86640944893,
1464.95049205445,1465.03440868174,1465.10103166624),.UNSPECIFIED.);
#1898=B_SPLINE_CURVE_WITH_KNOTS('',3,(#262868,#262869,#262870,#262871,#262872,
#262873,#262874,#262875,#262876,#262877,#262878,#262879,#262880,#262881,
#262882,#262883,#262884,#262885,#262886,#262887,#262888,#262889,#262890,
#262891,#262892,#262893,#262894,#262895,#262896,#262897,#262898,#262899,
#262900,#262901,#262902,#262903,#262904,#262905,#262906,#262907,#262908,
#262909,#262910,#262911,#262912,#262913,#262914,#262915,#262916,#262917,
#262918,#262919,#262920,#262921,#262922,#262923,#262924,#262925,#262926,
#262927,#262928,#262929,#262930,#262931,#262932,#262933,#262934,#262935,
#262936,#262937,#262938,#262939,#262940,#262941,#262942,#262943,#262944,
#262945,#262946,#262947,#262948,#262949,#262950,#262951,#262952,#262953,
#262954,#262955,#262956,#262957,#262958,#262959,#262960,#262961,#262962,
#262963,#262964,#262965,#262966,#262967,#262968,#262969,#262970,#262971,
#262972,#262973,#262974,#262975,#262976,#262977,#262978,#262979,#262980,
#262981,#262982,#262983,#262984,#262985,#262986,#262987,#262988,#262989,
#262990,#262991,#262992,#262993,#262994,#262995,#262996,#262997,#262998,
#262999,#263000,#263001,#263002,#263003,#263004,#263005,#263006,#263007,
#263008,#263009,#263010,#263011,#263012,#263013,#263014,#263015,#263016,
#263017,#263018,#263019,#263020,#263021,#263022,#263023,#263024,#263025,
#263026,#263027,#263028,#263029,#263030,#263031,#263032,#263033,#263034,
#263035,#263036,#263037,#263038,#263039,#263040,#263041,#263042,#263043,
#263044,#263045,#263046,#263047,#263048,#263049,#263050,#263051,#263052,
#263053,#263054,#263055,#263056,#263057,#263058,#263059,#263060,#263061,
#263062,#263063,#263064,#263065,#263066,#263067,#263068,#263069,#263070,
#263071,#263072,#263073,#263074,#263075,#263076,#263077,#263078,#263079,
#263080,#263081,#263082,#263083,#263084,#263085,#263086,#263087,#263088,
#263089,#263090,#263091,#263092,#263093,#263094,#263095,#263096,#263097,
#263098,#263099,#263100,#263101,#263102,#263103,#263104,#263105,#263106,
#263107,#263108,#263109,#263110,#263111,#263112,#263113,#263114),
 .UNSPECIFIED.,.F.,.F.,(4,3,3,3,3,3,3,3,3,3,3,3,3,3,3,3,3,3,3,3,3,3,3,3,
3,3,3,3,3,3,3,3,3,3,3,3,3,3,3,3,3,3,3,3,3,3,3,3,3,3,3,3,3,3,3,3,3,3,3,3,
3,3,3,3,3,3,3,3,3,3,3,3,3,3,3,3,3,3,3,3,3,3,4),(1465.10103166637,1465.18408255591,
1465.26722414529,1465.3536660379,1465.43707971455,1465.52059140623,1465.60425622782,
1465.61299171571,1465.69294901584,1465.77281181308,1465.85259763555,1465.93232395075,
1466.01200817904,1466.09167916526,1466.17134661879,1466.25102626961,1466.330733852,
1466.41052908107,1466.49037342278,1466.57033184983,1466.61272772643,1466.69268502656,
1466.7725478238,1466.85233364628,1466.93205996147,1467.01174418976,1467.09141517599,
1467.17108262951,1467.25076228033,1467.33046986272,1467.4102650918,1467.49010943351,
1467.57006786055,1467.61246373715,1467.69242103728,1467.77228383452,1467.852069657,
1467.93179597219,1468.01148020049,1468.09115118671,1468.17081864023,1468.25049829105,
1468.33020587345,1468.41000110252,1468.48984544423,1468.56980387128,1468.61219974787,
1468.692157048,1468.77201984524,1468.85180566772,1468.93153198291,1469.01121621121,
1469.09088719743,1469.17055465095,1469.25023430177,1469.32994188416,1469.40973711324,
1469.48958145495,1469.56953988199,1469.61193575859,1469.69189305872,1469.77175585596,
1469.85154167844,1469.93126799363,1470.01095222192,1470.09062320815,1470.17029066167,
1470.24997031249,1470.32967789488,1470.40947312396,1470.48931746567,1470.56927589271,
1470.61167176931,1470.69058006137,1470.76939294258,1470.84811543483,1470.92678681762,
1471.00542362705,1471.08404237083,1471.16268499734,1471.24133829156,1471.32005872964,
1471.38421697355),.UNSPECIFIED.);
#1899=B_SPLINE_CURVE_WITH_KNOTS('',3,(#263116,#263117,#263118,#263119,#263120,
#263121,#263122,#263123,#263124,#263125,#263126),.UNSPECIFIED.,.F.,.F.,
(4,1,1,1,1,1,1,1,4),(1471.38421697355,1471.61140778003,1472.61114379075,
1473.61087980147,1474.61061581219,1475.61035182291,1476.61008783363,1477.60982384435,
1477.66740228073),.UNSPECIFIED.);
#1900=B_SPLINE_CURVE_WITH_KNOTS('',3,(#263128,#263129,#263130,#263131,#263132,
#263133,#263134,#263135,#263136,#263137,#263138,#263139,#263140,#263141,
#263142,#263143,#263144,#263145,#263146,#263147,#263148,#263149,#263150,
#263151,#263152,#263153,#263154,#263155,#263156,#263157,#263158,#263159,
#263160,#263161,#263162,#263163,#263164,#263165,#263166,#263167,#263168,
#263169,#263170,#263171,#263172,#263173,#263174,#263175,#263176,#263177,
#263178,#263179,#263180,#263181,#263182,#263183,#263184,#263185,#263186,
#263187,#263188,#263189,#263190,#263191,#263192,#263193,#263194,#263195,
#263196,#263197,#263198,#263199,#263200,#263201,#263202,#263203,#263204,
#263205,#263206,#263207,#263208,#263209,#263210,#263211,#263212,#263213,
#263214,#263215,#263216,#263217,#263218,#263219,#263220,#263221,#263222,
#263223,#263224,#263225,#263226,#263227,#263228,#263229,#263230,#263231,
#263232,#263233,#263234,#263235,#263236,#263237,#263238,#263239,#263240,
#263241,#263242,#263243,#263244,#263245,#263246,#263247,#263248,#263249,
#263250,#263251,#263252,#263253,#263254,#263255,#263256,#263257,#263258,
#263259,#263260,#263261,#263262,#263263,#263264,#263265,#263266,#263267,
#263268,#263269,#263270,#263271,#263272,#263273,#263274,#263275,#263276,
#263277,#263278,#263279,#263280,#263281,#263282,#263283,#263284,#263285,
#263286,#263287,#263288,#263289,#263290,#263291,#263292,#263293,#263294,
#263295,#263296,#263297,#263298,#263299,#263300,#263301,#263302,#263303,
#263304,#263305,#263306,#263307,#263308,#263309,#263310,#263311,#263312,
#263313,#263314,#263315,#263316,#263317,#263318,#263319,#263320,#263321,
#263322,#263323,#263324,#263325,#263326,#263327,#263328,#263329,#263330,
#263331,#263332,#263333,#263334,#263335,#263336,#263337,#263338,#263339,
#263340,#263341,#263342,#263343,#263344,#263345,#263346,#263347,#263348,
#263349,#263350,#263351,#263352,#263353,#263354,#263355,#263356,#263357,
#263358,#263359,#263360,#263361,#263362,#263363,#263364,#263365,#263366,
#263367,#263368,#263369,#263370,#263371),.UNSPECIFIED.,.F.,.F.,(4,3,3,3,
3,3,3,3,3,3,3,3,3,3,3,3,3,3,3,3,3,3,3,3,3,3,3,3,3,3,3,3,3,3,3,3,3,3,3,3,
3,3,3,3,3,3,3,3,3,3,3,3,3,3,3,3,3,3,3,3,3,3,3,3,3,3,3,3,3,3,3,3,3,3,3,3,
3,3,3,3,3,4),(1477.66740228073,1477.74665738145,1477.82582165558,1477.90491321944,
1477.98395012394,1478.06295794255,1478.14195194843,1478.22094840445,1478.29996357275,
1478.37906049634,1478.45819925348,1478.53745897297,1478.60955985507,1478.6895171552,
1478.76937995244,1478.84916577492,1478.92889209011,1479.00857631841,1479.08824730463,
1479.16791475815,1479.24759440897,1479.32730199136,1479.40709722044,1479.48694156215,
1479.5668999892,1479.60929586579,1479.68925316592,1479.76911596316,1479.84890178564,
1479.92862810083,1480.00831232913,1480.08798331535,1480.16765076887,1480.24733041969,
1480.32703800208,1480.40683323116,1480.48667757287,1480.56663599991,1480.60903187651,
1480.68898917664,1480.76885197388,1480.84863779636,1480.92836411155,1481.00804833985,
1481.08771932607,1481.16738677959,1481.24706643041,1481.3267740128,1481.40656924188,
1481.48641358358,1481.56637201063,1481.60876788723,1481.68872518736,1481.7685879846,
1481.84837380708,1481.92810012227,1482.00778435057,1482.08745533679,1482.16712279031,
1482.24680244113,1482.32651002352,1482.4063052526,1482.48614959431,1482.56610802135,
1482.60850389795,1482.68846119808,1482.76832399532,1482.8481098178,1482.92783613299,
1483.00752036128,1483.0871913475,1483.16685880103,1483.24653845185,1483.32624603424,
1483.40604126332,1483.48588560502,1483.56584403207,1483.60823990867,1483.70138884274,
1483.79416232008,1483.8862079791,1483.9505875878),.UNSPECIFIED.);
#1901=B_SPLINE_CURVE_WITH_KNOTS('',3,(#263373,#263374,#263375,#263376,#263377,
#263378,#263379,#263380,#263381,#263382,#263383,#263384,#263385,#263386,
#263387,#263388,#263389,#263390,#263391,#263392,#263393,#263394,#263395,
#263396,#263397,#263398,#263399,#263400,#263401,#263402,#263403,#263404,
#263405,#263406,#263407,#263408,#263409,#263410,#263411,#263412,#263413,
#263414,#263415,#263416,#263417,#263418,#263419,#263420,#263421,#263422,
#263423,#263424,#263425,#263426,#263427,#263428,#263429,#263430,#263431,
#263432,#263433,#263434,#263435,#263436,#263437,#263438,#263439,#263440,
#263441,#263442,#263443,#263444,#263445,#263446,#263447,#263448,#263449,
#263450,#263451,#263452,#263453,#263454,#263455,#263456,#263457,#263458,
#263459,#263460,#263461,#263462,#263463,#263464,#263465,#263466,#263467,
#263468,#263469,#263470,#263471,#263472,#263473,#263474,#263475,#263476,
#263477,#263478,#263479,#263480,#263481,#263482,#263483,#263484,#263485,
#263486,#263487,#263488,#263489,#263490,#263491,#263492,#263493,#263494,
#263495,#263496,#263497,#263498,#263499,#263500,#263501,#263502,#263503,
#263504,#263505,#263506,#263507,#263508,#263509,#263510,#263511,#263512,
#263513,#263514,#263515,#263516,#263517,#263518,#263519,#263520,#263521,
#263522,#263523,#263524,#263525,#263526,#263527,#263528,#263529,#263530,
#263531,#263532,#263533,#263534,#263535,#263536,#263537,#263538,#263539,
#263540,#263541,#263542,#263543,#263544,#263545,#263546,#263547,#263548,
#263549,#263550,#263551,#263552,#263553,#263554,#263555,#263556,#263557,
#263558,#263559,#263560,#263561,#263562,#263563,#263564,#263565,#263566,
#263567,#263568,#263569,#263570,#263571,#263572,#263573,#263574,#263575,
#263576,#263577,#263578,#263579,#263580,#263581,#263582,#263583,#263584,
#263585,#263586,#263587,#263588,#263589,#263590,#263591,#263592,#263593,
#263594,#263595,#263596,#263597,#263598,#263599,#263600,#263601,#263602,
#263603,#263604,#263605,#263606,#263607,#263608,#263609,#263610,#263611,
#263612,#263613,#263614,#263615,#263616,#263617,#263618,#263619),
 .UNSPECIFIED.,.F.,.F.,(4,3,3,3,3,3,3,3,3,3,3,3,3,3,3,3,3,3,3,3,3,3,3,3,
3,3,3,3,3,3,3,3,3,3,3,3,3,3,3,3,3,3,3,3,3,3,3,3,3,3,3,3,3,3,3,3,3,3,3,3,
3,3,3,3,3,3,3,3,3,3,3,3,3,3,3,3,3,3,3,3,3,3,4),(1483.95058758791,1484.03276112934,
1484.11249874285,1484.19224360271,1484.27201130001,1484.35600245486,1484.43590835349,
1484.5158731071,1484.59594982076,1484.60797591939,1484.68793321952,1484.76779601676,
1484.84758183924,1484.92730815443,1485.00699238273,1485.08666336895,1485.16633082247,
1485.24601047329,1485.32571805569,1485.40551328476,1485.48535762647,1485.56531605352,
1485.60771193011,1485.68766923024,1485.76753202748,1485.84731784996,1485.92704416515,
1486.00672839345,1486.08639937967,1486.16606683319,1486.24574648401,1486.3254540664,
1486.40524929548,1486.48509363719,1486.56505206424,1486.60744794083,1486.68740524096,
1486.7672680382,1486.84705386067,1486.92678017587,1487.00646440416,1487.08613539038,
1487.16580284391,1487.24548249473,1487.32519007712,1487.40498530619,1487.4848296479,
1487.56478807495,1487.60718395155,1487.68714125168,1487.76700404892,1487.8467898714,
1487.92651618659,1488.00620041488,1488.08587140111,1488.16553885463,1488.24521850545,
1488.32492608784,1488.40472131692,1488.48456565863,1488.56452408567,1488.60691996227,
1488.6868772624,1488.76674005964,1488.84652588211,1488.92625219731,1489.0059364256,
1489.08560741182,1489.16527486535,1489.24495451617,1489.32466209856,1489.40445732764,
1489.48430166934,1489.56426009639,1489.60665597299,1489.68722612258,1489.7676985561,
1489.84808846144,1489.92841097225,1490.00867685395,1490.08890876417,1490.16913181602,
1490.23377289509),.UNSPECIFIED.);
#1902=B_SPLINE_CURVE_WITH_KNOTS('',3,(#263621,#263622,#263623,#263624,#263625,
#263626,#263627,#263628,#263629,#263630),.UNSPECIFIED.,.F.,.F.,(4,1,1,1,
1,1,1,4),(1490.233780566,1490.60639198371,1491.60612799443,1492.60586400515,
1493.60560001587,1494.60533602659,1495.60507203731,1496.5169494552),
 .UNSPECIFIED.);
#1903=B_SPLINE_CURVE_WITH_KNOTS('',3,(#263631,#263632,#263633,#263634,#263635,
#263636,#263637,#263638,#263639,#263640,#263641,#263642,#263643,#263644,
#263645,#263646,#263647,#263648,#263649,#263650,#263651,#263652,#263653,
#263654,#263655,#263656,#263657,#263658,#263659,#263660,#263661,#263662,
#263663,#263664,#263665,#263666,#263667,#263668,#263669,#263670),
 .UNSPECIFIED.,.F.,.F.,(4,3,3,3,3,3,3,3,3,3,3,3,3,4),(1496.51695820227,
1496.60480804803,1496.68476866345,1496.76463404788,1496.84442173243,1496.92414918687,
1497.00383691716,1497.08350435156,1497.16316722471,1497.24284126536,1497.32258142435,
1497.40235613046,1497.48223246019,1497.54400219811),.UNSPECIFIED.);
#1904=B_SPLINE_CURVE_WITH_KNOTS('',3,(#263673,#263674,#263675,#263676,#263677,
#263678),.UNSPECIFIED.,.F.,.F.,(4,2,4),(1.41357350471954,1.57818585554697,
1.60627031745981),.UNSPECIFIED.);
#1905=B_SPLINE_CURVE_WITH_KNOTS('',3,(#263680,#263681,#263682,#263683),
 .UNSPECIFIED.,.F.,.F.,(4,4),(0.488654425026599,0.592941394652162),
 .UNSPECIFIED.);
#1906=B_SPLINE_CURVE_WITH_KNOTS('',3,(#263684,#263685,#263686,#263687,#263688,
#263689),.UNSPECIFIED.,.F.,.F.,(4,1,1,4),(-1397.04440853625,-1396.63120697602,
-1395.6314709653,-1395.09571822406),.UNSPECIFIED.);
#1907=B_SPLINE_CURVE_WITH_KNOTS('',3,(#263692,#263693,#263694,#263695),
 .UNSPECIFIED.,.F.,.F.,(4,4),(0.311200159847851,0.413415476057656),
 .UNSPECIFIED.);
#1908=B_SPLINE_CURVE_WITH_KNOTS('',3,(#263697,#263698,#263699,#263700,#263701,
#263702),.UNSPECIFIED.,.F.,.F.,(4,2,4),(1.8681568300393,2.02932516755897,
2.03144978473733),.UNSPECIFIED.);
#1909=B_SPLINE_CURVE_WITH_KNOTS('',3,(#263704,#263705,#263706,#263707,#263708,
#263709),.UNSPECIFIED.,.F.,.F.,(4,1,1,4),(-1398.9596726741,-1398.63067899746,
-1397.63094298674,-1397.50325618979),.UNSPECIFIED.);
#1910=B_SPLINE_CURVE_WITH_KNOTS('',3,(#263711,#263712,#263713,#263714,#263715,
#263716,#263717,#263718,#263719,#263720,#263721,#263722,#263723,#263724,
#263725,#263726,#263727,#263728,#263729,#263730,#263731,#263732,#263733,
#263734,#263735,#263736,#263737,#263738,#263739,#263740,#263741,#263742,
#263743,#263744,#263745,#263746,#263747,#263748,#263749,#263750,#263751,
#263752,#263753,#263754,#263755,#263756,#263757,#263758,#263759,#263760,
#263761,#263762,#263763,#263764,#263765,#263766,#263767,#263768,#263769,
#263770,#263771,#263772,#263773,#263774,#263775,#263776,#263777,#263778,
#263779,#263780,#263781,#263782,#263783,#263784,#263785,#263786,#263787,
#263788,#263789,#263790,#263791,#263792,#263793,#263794,#263795,#263796,
#263797,#263798,#263799,#263800,#263801,#263802,#263803,#263804,#263805,
#263806,#263807,#263808,#263809,#263810,#263811,#263812,#263813,#263814,
#263815,#263816,#263817,#263818,#263819,#263820,#263821,#263822,#263823,
#263824,#263825,#263826,#263827,#263828,#263829,#263830,#263831,#263832,
#263833,#263834,#263835,#263836,#263837,#263838,#263839,#263840,#263841,
#263842,#263843,#263844,#263845,#263846,#263847,#263848,#263849,#263850,
#263851,#263852,#263853,#263854,#263855,#263856,#263857,#263858,#263859,
#263860,#263861,#263862,#263863,#263864,#263865,#263866,#263867,#263868,
#263869,#263870,#263871,#263872,#263873,#263874,#263875,#263876,#263877,
#263878,#263879,#263880,#263881,#263882,#263883,#263884,#263885,#263886,
#263887,#263888,#263889,#263890,#263891,#263892,#263893,#263894,#263895,
#263896,#263897,#263898,#263899,#263900,#263901,#263902,#263903,#263904,
#263905,#263906,#263907,#263908,#263909,#263910,#263911,#263912,#263913,
#263914,#263915,#263916,#263917,#263918,#263919,#263920,#263921,#263922,
#263923,#263924,#263925,#263926,#263927,#263928,#263929,#263930,#263931,
#263932,#263933,#263934,#263935,#263936,#263937,#263938,#263939,#263940,
#263941,#263942,#263943,#263944,#263945,#263946,#263947,#263948,#263949,
#263950,#263951,#263952,#263953,#263954,#263955,#263956,#263957),
 .UNSPECIFIED.,.F.,.F.,(4,3,3,3,3,3,3,3,3,3,3,3,3,3,3,3,3,3,3,3,3,3,3,3,
3,3,3,3,3,3,3,3,3,3,3,3,3,3,3,3,3,3,3,3,3,3,3,3,3,3,3,3,3,3,3,3,3,3,3,3,
3,3,3,3,3,3,3,3,3,3,3,3,3,3,3,3,3,3,3,3,3,3,4),(-1405.2428652499,-1405.16239569195,
-1405.08191404014,-1405.00140562355,-1404.92085575786,-1404.840199036,-1404.75948345872,
-1404.67863759454,-1404.62909506178,-1404.54913776165,-1404.46927496441,
-1404.38948914194,-1404.30976282674,-1404.23007859845,-1404.15040761223,
-1404.0707401587,-1403.99106050789,-1403.9113529255,-1403.83155769642,-1403.75171335471,
-1403.67175492767,-1403.62935905106,-1403.54940175093,-1403.46953895369,
-1403.38975313121,-1403.31002681602,-1403.23034258773,-1403.1506716015,
-1403.07100414798,-1402.99132449716,-1402.91161691477,-1402.83182168569,
-1402.75197734399,-1402.67201891694,-1402.62962304034,-1402.54966574021,
-1402.46980294297,-1402.39001712049,-1402.3102908053,-1402.230606577,-1402.15093559078,
-1402.07126813726,-1401.99158848644,-1401.91188090405,-1401.83208567497,
-1401.75224133326,-1401.67228290621,-1401.62988702962,-1401.54992972949,
-1401.47006693225,-1401.39028110977,-1401.31055479458,-1401.23087056629,
-1401.15119958006,-1401.07153212654,-1400.99185247572,-1400.91214489333,
-1400.83234966425,-1400.75250532255,-1400.6725468955,-1400.6301510189,-1400.55019371877,
-1400.47033092153,-1400.39054509905,-1400.31081878386,-1400.23113455556,
-1400.15146356934,-1400.07179611582,-1399.992116465,-1399.9124088826,-1399.83261365353,
-1399.75276931182,-1399.67281088477,-1399.63041500818,-1399.546573125,-1399.46682601498,
-1399.38715383661,-1399.30754071169,-1399.22797080243,-1399.14842137439,
-1399.0688836793,-1398.98932729873,-1398.95967994272),.UNSPECIFIED.);
#1911=B_SPLINE_CURVE_WITH_KNOTS('',3,(#263959,#263960,#263961,#263962,#263963,
#263964,#263965,#263966,#263967,#263968),.UNSPECIFIED.,.F.,.F.,(4,1,1,1,
1,1,1,4),(-1411.52604145674,-1410.62751112611,-1409.62777511538,-1408.62803910466,
-1407.62830309394,-1406.62856708322,-1405.6288310725,-1405.24287268663),
 .UNSPECIFIED.);
#1912=B_SPLINE_CURVE_WITH_KNOTS('',3,(#263970,#263971,#263972,#263973,#263974,
#263975,#263976,#263977,#263978,#263979,#263980,#263981,#263982,#263983,
#263984,#263985,#263986,#263987,#263988,#263989,#263990,#263991,#263992,
#263993,#263994,#263995,#263996,#263997,#263998,#263999,#264000,#264001,
#264002,#264003,#264004,#264005,#264006,#264007,#264008,#264009,#264010,
#264011,#264012,#264013,#264014,#264015,#264016,#264017,#264018,#264019,
#264020,#264021,#264022,#264023,#264024,#264025,#264026,#264027,#264028,
#264029,#264030,#264031,#264032,#264033,#264034,#264035,#264036,#264037,
#264038,#264039,#264040,#264041,#264042,#264043,#264044,#264045,#264046,
#264047,#264048,#264049,#264050,#264051,#264052,#264053,#264054,#264055,
#264056,#264057,#264058,#264059,#264060,#264061,#264062,#264063,#264064,
#264065,#264066,#264067,#264068,#264069,#264070,#264071,#264072,#264073,
#264074,#264075,#264076,#264077,#264078,#264079,#264080,#264081,#264082,
#264083,#264084,#264085,#264086,#264087,#264088,#264089,#264090,#264091,
#264092,#264093,#264094,#264095,#264096,#264097,#264098,#264099,#264100,
#264101,#264102,#264103,#264104,#264105,#264106,#264107,#264108,#264109,
#264110,#264111,#264112,#264113,#264114,#264115,#264116,#264117,#264118,
#264119,#264120,#264121,#264122,#264123,#264124,#264125,#264126,#264127,
#264128,#264129,#264130,#264131,#264132,#264133,#264134,#264135,#264136,
#264137,#264138,#264139,#264140,#264141,#264142,#264143,#264144,#264145,
#264146,#264147,#264148,#264149,#264150,#264151,#264152,#264153,#264154,
#264155,#264156,#264157,#264158,#264159,#264160,#264161,#264162,#264163,
#264164,#264165,#264166,#264167,#264168,#264169,#264170,#264171,#264172,
#264173,#264174,#264175,#264176,#264177,#264178,#264179,#264180,#264181,
#264182,#264183,#264184,#264185,#264186,#264187,#264188,#264189,#264190,
#264191,#264192,#264193,#264194,#264195,#264196,#264197,#264198,#264199,
#264200,#264201,#264202,#264203,#264204,#264205,#264206,#264207,#264208,
#264209,#264210,#264211,#264212,#264213),.UNSPECIFIED.,.F.,.F.,(4,3,3,3,
3,3,3,3,3,3,3,3,3,3,3,3,3,3,3,3,3,3,3,3,3,3,3,3,3,3,3,3,3,3,3,3,3,3,3,3,
3,3,3,3,3,3,3,3,3,3,3,3,3,3,3,3,3,3,3,3,3,3,3,3,3,3,3,3,3,3,3,3,3,3,3,3,
3,3,3,3,3,4),(-1417.80923586426,-1417.689114353,-1417.62566320115,-1417.54570590102,
-1417.46584310378,-1417.3860572813,-1417.30633096611,-1417.22664673781,
-1417.14697575159,-1417.06730829807,-1416.98762864725,-1416.90792106486,
-1416.82812583578,-1416.74828149407,-1416.66832306702,-1416.62592719043,
-1416.5459698903,-1416.46610709306,-1416.38632127058,-1416.30659495539,
-1416.22691072709,-1416.14723974087,-1416.06757228735,-1415.98789263653,
-1415.90818505414,-1415.82838982506,-1415.74854548335,-1415.66858705631,
-1415.62619117971,-1415.54623387958,-1415.46637108234,-1415.38658525986,
-1415.30685894467,-1415.22717471637,-1415.14750373015,-1415.06783627663,
-1414.98815662581,-1414.90844904342,-1414.82865381434,-1414.74880947263,
-1414.66885104559,-1414.62645516899,-1414.54649786886,-1414.46663507162,
-1414.38684924914,-1414.30712293395,-1414.22743870566,-1414.14776771943,
-1414.06810026591,-1413.98842061509,-1413.9087130327,-1413.82891780362,
-1413.74907346191,-1413.66911503487,-1413.62671915827,-1413.54676185814,
-1413.4668990609,-1413.38711323842,-1413.30738692323,-1413.22770269494,
-1413.14803170871,-1413.06836425519,-1412.98868460437,-1412.90897702198,
-1412.8291817929,-1412.74933745119,-1412.66937902415,-1412.62698314755,
-1412.54702584742,-1412.46716305018,-1412.38737722771,-1412.30765091251,
-1412.22796668422,-1412.148295698,-1412.06862824447,-1411.98894859366,-1411.90924101126,
-1411.82944578219,-1411.74960144048,-1411.66964301343,-1411.62724713683,
-1411.52605055708),.UNSPECIFIED.);
#1913=B_SPLINE_CURVE_WITH_KNOTS('',3,(#264215,#264216,#264217,#264218,#264219,
#264220,#264221,#264222,#264223,#264224),.UNSPECIFIED.,.F.,.F.,(4,1,1,1,
1,1,1,4),(-1424.09242117144,-1423.62407926547,-1422.62434325475,-1421.62460724403,
-1420.62487123331,-1419.62513522259,-1418.62539921187,-1417.80924068802),
 .UNSPECIFIED.);
#1914=B_SPLINE_CURVE_WITH_KNOTS('',3,(#264226,#264227,#264228,#264229,#264230,
#264231,#264232,#264233,#264234,#264235),.UNSPECIFIED.,.F.,.F.,(4,1,1,1,
1,1,1,4),(-1430.37560647862,-1429.62249532979,-1428.62275931907,-1427.62302330835,
-1426.62328729763,-1425.62355128691,-1424.62381527619,-1424.09242117144),
 .UNSPECIFIED.);
#1915=B_SPLINE_CURVE_WITH_KNOTS('',3,(#264237,#264238,#264239,#264240,#264241,
#264242,#264243,#264244,#264245,#264246,#264247,#264248,#264249,#264250,
#264251,#264252,#264253,#264254,#264255,#264256,#264257,#264258,#264259,
#264260,#264261,#264262,#264263,#264264,#264265,#264266,#264267,#264268,
#264269,#264270,#264271,#264272,#264273,#264274,#264275,#264276,#264277,
#264278,#264279,#264280,#264281,#264282,#264283,#264284,#264285,#264286,
#264287,#264288,#264289,#264290,#264291,#264292,#264293,#264294,#264295,
#264296,#264297,#264298,#264299,#264300,#264301,#264302,#264303,#264304,
#264305,#264306,#264307,#264308,#264309,#264310,#264311,#264312,#264313,
#264314,#264315,#264316,#264317,#264318,#264319,#264320,#264321,#264322,
#264323,#264324,#264325,#264326,#264327,#264328,#264329,#264330,#264331,
#264332,#264333,#264334,#264335,#264336,#264337,#264338,#264339,#264340,
#264341,#264342,#264343,#264344,#264345,#264346,#264347,#264348,#264349,
#264350,#264351,#264352,#264353,#264354,#264355,#264356,#264357,#264358,
#264359,#264360,#264361,#264362,#264363,#264364,#264365,#264366,#264367,
#264368,#264369,#264370,#264371,#264372,#264373,#264374,#264375,#264376,
#264377,#264378,#264379,#264380,#264381,#264382,#264383,#264384,#264385,
#264386,#264387,#264388,#264389,#264390,#264391,#264392,#264393,#264394,
#264395,#264396,#264397,#264398,#264399,#264400,#264401,#264402,#264403,
#264404,#264405,#264406,#264407,#264408,#264409,#264410,#264411,#264412,
#264413,#264414,#264415,#264416,#264417,#264418,#264419,#264420,#264421,
#264422,#264423,#264424,#264425,#264426,#264427,#264428,#264429,#264430,
#264431,#264432,#264433,#264434,#264435,#264436,#264437,#264438,#264439,
#264440,#264441,#264442,#264443,#264444,#264445,#264446,#264447,#264448,
#264449,#264450,#264451,#264452,#264453,#264454,#264455,#264456,#264457,
#264458,#264459,#264460,#264461,#264462,#264463,#264464,#264465,#264466,
#264467,#264468,#264469,#264470,#264471,#264472,#264473,#264474,#264475,
#264476,#264477,#264478,#264479,#264480,#264481,#264482,#264483),
 .UNSPECIFIED.,.F.,.F.,(4,3,3,3,3,3,3,3,3,3,3,3,3,3,3,3,3,3,3,3,3,3,3,3,
3,3,3,3,3,3,3,3,3,3,3,3,3,3,3,3,3,3,3,3,3,3,3,3,3,3,3,3,3,3,3,3,3,3,3,3,
3,3,3,3,3,3,3,3,3,3,3,3,3,3,3,3,3,3,3,3,3,3,4),(-1436.6587917858,-1436.62064740483,
-1436.5406901047,-1436.46082730746,-1436.38104148498,-1436.30131516979,
-1436.22163094149,-1436.14195995527,-1436.06229250175,-1435.98261285093,
-1435.90290526854,-1435.82311003946,-1435.74326569775,-1435.66330727071,
-1435.62091139411,-1435.54095409398,-1435.46109129674,-1435.38130547426,
-1435.30157915907,-1435.22189493077,-1435.14222394455,-1435.06255649103,
-1434.98287684021,-1434.90316925782,-1434.82337402874,-1434.74352968703,
-1434.66357125999,-1434.62117538339,-1434.54121808326,-1434.46135528602,
-1434.38156946354,-1434.30184314835,-1434.22215892005,-1434.14248793383,
-1434.06282048031,-1433.98314082949,-1433.9034332471,-1433.82363801802,
-1433.74379367631,-1433.66383524926,-1433.62143937267,-1433.54148207254,
-1433.4616192753,-1433.38183345282,-1433.30210713763,-1433.22242290934,
-1433.14275192312,-1433.06308446959,-1432.98340481877,-1432.90369723638,
-1432.8239020073,-1432.7440576656,-1432.66409923855,-1432.62170336195,-1432.54174606182,
-1432.46188326458,-1432.3820974421,-1432.30237112691,-1432.22268689861,
-1432.14301591239,-1432.06334845887,-1431.98366880805,-1431.90396122566,
-1431.82416599658,-1431.74432165487,-1431.66436322783,-1431.62196735123,
-1431.5420100511,-1431.46214725386,-1431.38236143138,-1431.30263511619,
-1431.2229508879,-1431.14327990167,-1431.06361244815,-1430.98393279733,
-1430.90422521494,-1430.82442998586,-1430.74458564415,-1430.66462721711,
-1430.62223134051,-1430.51675163816,-1430.41361228529,-1430.37560656682),
 .UNSPECIFIED.);
#1916=B_SPLINE_CURVE_WITH_KNOTS('',3,(#264485,#264486,#264487,#264488,#264489,
#264490,#264491,#264492,#264493,#264494),.UNSPECIFIED.,.F.,.F.,(4,1,1,1,
1,1,1,4),(-1442.94197709298,-1442.61906346915,-1441.61932745843,-1440.61959144771,
-1439.61985543699,-1438.62011942627,-1437.62038341555,-1436.65879704426),
 .UNSPECIFIED.);
#1917=B_SPLINE_CURVE_WITH_KNOTS('',3,(#264496,#264497,#264498,#264499,#264500,
#264501,#264502,#264503,#264504,#264505),.UNSPECIFIED.,.F.,.F.,(4,1,1,1,
1,1,1,4),(-1449.22516240016,-1448.61747953347,-1447.61774352275,-1446.61800751203,
-1445.61827150131,-1444.61853549059,-1443.61879947987,-1442.94197709298),
 .UNSPECIFIED.);
#1918=B_SPLINE_CURVE_WITH_KNOTS('',3,(#264507,#264508,#264509,#264510,#264511,
#264512,#264513,#264514,#264515,#264516),.UNSPECIFIED.,.F.,.F.,(4,1,1,1,
1,1,1,4),(-1455.50834770734,-1454.61589559779,-1453.61615958707,-1452.61642357635,
-1451.61668756563,-1450.61695155491,-1449.61721554419,-1449.22516240016),
 .UNSPECIFIED.);
#1919=B_SPLINE_CURVE_WITH_KNOTS('',3,(#264518,#264519,#264520,#264521,#264522,
#264523,#264524,#264525,#264526,#264527,#264528,#264529),.UNSPECIFIED.,
 .F.,.F.,(4,2,1,1,1,1,1,1,4),(-1461.79153301452,-1461.61404767283,-1460.61431166211,
-1459.61457565139,-1458.61483964067,-1457.61510362995,-1456.61536761923,
-1455.61563160851,-1455.50834770734),.UNSPECIFIED.);
#1920=B_SPLINE_CURVE_WITH_KNOTS('',3,(#264531,#264532,#264533,#264534,#264535,
#264536,#264537,#264538,#264539,#264540,#264541,#264542,#264543,#264544,
#264545,#264546,#264547,#264548,#264549,#264550,#264551,#264552,#264553,
#264554,#264555,#264556,#264557,#264558,#264559,#264560,#264561,#264562,
#264563,#264564,#264565,#264566,#264567,#264568,#264569,#264570,#264571,
#264572,#264573,#264574,#264575,#264576,#264577,#264578,#264579,#264580,
#264581,#264582,#264583,#264584,#264585,#264586,#264587,#264588,#264589,
#264590,#264591,#264592,#264593,#264594,#264595,#264596,#264597,#264598,
#264599,#264600,#264601,#264602,#264603,#264604,#264605,#264606,#264607,
#264608,#264609,#264610,#264611,#264612,#264613,#264614,#264615,#264616,
#264617,#264618,#264619,#264620,#264621,#264622,#264623,#264624,#264625,
#264626,#264627,#264628,#264629,#264630,#264631,#264632,#264633,#264634,
#264635,#264636,#264637,#264638,#264639,#264640,#264641,#264642,#264643,
#264644,#264645,#264646,#264647,#264648,#264649,#264650,#264651,#264652,
#264653,#264654,#264655,#264656,#264657,#264658,#264659,#264660,#264661,
#264662,#264663,#264664,#264665,#264666,#264667,#264668,#264669,#264670,
#264671,#264672,#264673,#264674,#264675,#264676,#264677,#264678,#264679,
#264680,#264681,#264682,#264683,#264684,#264685,#264686,#264687,#264688,
#264689,#264690,#264691,#264692,#264693,#264694,#264695,#264696,#264697,
#264698,#264699,#264700,#264701,#264702,#264703,#264704,#264705,#264706,
#264707,#264708,#264709,#264710,#264711,#264712,#264713,#264714,#264715,
#264716,#264717,#264718,#264719,#264720,#264721,#264722,#264723,#264724,
#264725,#264726,#264727,#264728,#264729,#264730,#264731,#264732,#264733,
#264734,#264735,#264736,#264737,#264738,#264739,#264740,#264741,#264742,
#264743,#264744,#264745,#264746,#264747,#264748,#264749,#264750,#264751,
#264752,#264753,#264754,#264755,#264756,#264757,#264758,#264759,#264760,
#264761,#264762,#264763,#264764,#264765,#264766,#264767,#264768,#264769,
#264770,#264771,#264772,#264773,#264774,#264775,#264776,#264777),
 .UNSPECIFIED.,.F.,.F.,(4,3,3,3,3,3,3,3,3,3,3,3,3,3,3,3,3,3,3,3,3,3,3,3,
3,3,3,3,3,3,3,3,3,3,3,3,3,3,3,3,3,3,3,3,3,3,3,3,3,3,3,3,3,3,3,3,3,3,3,3,
3,3,3,3,3,3,3,3,3,3,3,3,3,3,3,3,3,3,3,3,3,3,4),(-1468.07471811664,-1467.98983128614,
-1467.9047850356,-1467.81949107158,-1467.73406381551,-1467.64842972939,
-1467.61246373715,-1467.53250643702,-1467.45264363978,-1467.37285781731,
-1467.29313150212,-1467.21344727382,-1467.1337762876,-1467.05410883408,
-1466.97442918327,-1466.89472160087,-1466.8149263718,-1466.73508203009,
-1466.65512360305,-1466.61272772643,-1466.5327704263,-1466.45290762906,
-1466.37312180658,-1466.29339549139,-1466.2137112631,-1466.13404027688,
-1466.05437282335,-1465.97469317253,-1465.89498559014,-1465.81519036106,
-1465.73534601936,-1465.65538759231,-1465.61299171571,-1465.53303441558,
-1465.45317161834,-1465.37338579586,-1465.29365948067,-1465.21397525237,
-1465.13430426615,-1465.05463681262,-1464.97495716181,-1464.89524957941,
-1464.81545435034,-1464.73561000863,-1464.65565158158,-1464.61325570499,
-1464.53329840486,-1464.45343560762,-1464.37364978514,-1464.29392346995,
-1464.21423924166,-1464.13456825544,-1464.05490080191,-1463.97522115109,
-1463.8955135687,-1463.81571833962,-1463.73587399792,-1463.65591557087,
-1463.61351969427,-1463.53356239414,-1463.4536995969,-1463.37391377442,
-1463.29418745923,-1463.21450323093,-1463.13483224471,-1463.05516479119,
-1462.97548514037,-1462.89577755797,-1462.8159823289,-1462.73613798719,
-1462.65617956014,-1462.61378368355,-1462.53501718464,-1462.45634485605,
-1462.37774820447,-1462.29921262633,-1462.22070988667,-1462.14222340191,
-1462.06373660319,-1461.98520236571,-1461.90664134508,-1461.82800041734,
-1461.79153301452),.UNSPECIFIED.);
#1921=B_SPLINE_CURVE_WITH_KNOTS('',3,(#264779,#264780,#264781,#264782,#264783,
#264784,#264785,#264786,#264787,#264788),.UNSPECIFIED.,.F.,.F.,(4,1,1,1,
1,1,1,4),(-1474.35790362888,-1473.61087980147,-1472.61114379075,-1471.61140778003,
-1470.61167176931,-1469.61193575859,-1468.61219974787,-1468.0747183217),
 .UNSPECIFIED.);
#1922=B_SPLINE_CURVE_WITH_KNOTS('',3,(#264790,#264791,#264792,#264793,#264794,
#264795,#264796,#264797,#264798,#264799,#264800,#264801,#264802,#264803,
#264804,#264805,#264806,#264807,#264808,#264809,#264810,#264811,#264812,
#264813,#264814,#264815,#264816,#264817,#264818,#264819,#264820,#264821,
#264822,#264823,#264824,#264825,#264826,#264827,#264828,#264829,#264830,
#264831,#264832,#264833,#264834,#264835,#264836,#264837,#264838,#264839,
#264840,#264841,#264842,#264843,#264844,#264845,#264846,#264847,#264848,
#264849,#264850,#264851,#264852,#264853,#264854,#264855,#264856,#264857,
#264858,#264859,#264860,#264861,#264862,#264863,#264864,#264865,#264866,
#264867,#264868,#264869,#264870,#264871,#264872,#264873,#264874,#264875,
#264876,#264877,#264878,#264879,#264880,#264881,#264882,#264883,#264884,
#264885,#264886,#264887,#264888,#264889,#264890,#264891,#264892,#264893,
#264894,#264895,#264896,#264897,#264898,#264899,#264900,#264901,#264902,
#264903,#264904,#264905,#264906,#264907,#264908,#264909,#264910,#264911,
#264912,#264913,#264914,#264915,#264916,#264917,#264918,#264919,#264920,
#264921,#264922,#264923,#264924,#264925,#264926,#264927,#264928,#264929,
#264930,#264931,#264932,#264933,#264934,#264935,#264936,#264937,#264938,
#264939,#264940,#264941,#264942,#264943,#264944,#264945,#264946,#264947,
#264948,#264949,#264950,#264951,#264952,#264953,#264954,#264955,#264956,
#264957,#264958,#264959,#264960,#264961,#264962,#264963,#264964,#264965,
#264966,#264967,#264968,#264969,#264970,#264971,#264972,#264973,#264974,
#264975,#264976,#264977,#264978,#264979,#264980,#264981,#264982,#264983,
#264984,#264985,#264986,#264987,#264988,#264989,#264990,#264991,#264992,
#264993,#264994,#264995,#264996,#264997,#264998,#264999,#265000,#265001,
#265002,#265003,#265004,#265005,#265006,#265007,#265008,#265009,#265010,
#265011,#265012,#265013,#265014,#265015,#265016,#265017,#265018,#265019,
#265020,#265021,#265022,#265023,#265024,#265025,#265026,#265027,#265028,
#265029,#265030,#265031,#265032,#265033,#265034,#265035,#265036),
 .UNSPECIFIED.,.F.,.F.,(4,3,3,3,3,3,3,3,3,3,3,3,3,3,3,3,3,3,3,3,3,3,3,3,
3,3,3,3,3,3,3,3,3,3,3,3,3,3,3,3,3,3,3,3,3,3,3,3,3,3,3,3,3,3,3,3,3,3,3,3,
3,3,3,3,3,3,3,3,3,3,3,3,3,3,3,3,3,3,3,3,3,3,4),(-1480.64108893606,-1480.60903187651,
-1480.52907457638,-1480.44921177914,-1480.36942595667,-1480.28969964147,
-1480.21001541318,-1480.13034442696,-1480.05067697343,-1479.97099732262,
-1479.89128974022,-1479.81149451115,-1479.73165016944,-1479.6516917424,
-1479.60929586579,-1479.52933856566,-1479.44947576842,-1479.36968994594,
-1479.28996363075,-1479.21027940245,-1479.13060841623,-1479.05094096271,
-1478.97126131189,-1478.8915537295,-1478.81175850042,-1478.73191415871,
-1478.65195573167,-1478.60955985507,-1478.52960255494,-1478.4497397577,
-1478.36995393522,-1478.29022762003,-1478.21054339173,-1478.13087240551,
-1478.05120495199,-1477.97152530117,-1477.89181771878,-1477.8120224897,
-1477.73217814799,-1477.65221972095,-1477.60982384435,-1477.52986654422,
-1477.45000374698,-1477.3702179245,-1477.29049160931,-1477.21080738102,
-1477.13113639479,-1477.05146894127,-1476.97178929045,-1476.89208170806,
-1476.81228647898,-1476.73244213728,-1476.65248371023,-1476.61008783363,
-1476.5301305335,-1476.45026773626,-1476.37048191378,-1476.29075559859,
-1476.21107137029,-1476.13140038407,-1476.05173293055,-1475.97205327973,
-1475.89234569734,-1475.81255046826,-1475.73270612655,-1475.65274769951,
-1475.61035182291,-1475.53039452278,-1475.45053172553,-1475.37074590306,
-1475.29101958787,-1475.21133535957,-1475.13166437335,-1475.05199691982,
-1474.972317269,-1474.89260968661,-1474.81281445753,-1474.73297011582,-1474.65301168878,
-1474.61061581219,-1474.50625453886,-1474.40403233292,-1474.3579036915),
 .UNSPECIFIED.);
#1923=B_SPLINE_CURVE_WITH_KNOTS('',3,(#265038,#265039,#265040,#265041,#265042,
#265043,#265044,#265045,#265046,#265047,#265048),.UNSPECIFIED.,.F.,.F.,
(4,2,1,1,1,1,1,4),(-1486.92427424324,-1486.60744794083,-1485.60771193012,
-1484.60797591939,-1483.60823990867,-1482.60850389795,-1481.60876788723,
-1480.64109334394),.UNSPECIFIED.);
#1924=B_SPLINE_CURVE_WITH_KNOTS('',3,(#265050,#265051,#265052,#265053,#265054,
#265055,#265056,#265057,#265058,#265059),.UNSPECIFIED.,.F.,.F.,(4,1,1,1,
1,1,1,4),(-1493.20745955042,-1492.60586400516,-1491.60612799444,-1490.60639198372,
-1489.606655973,-1488.60691996228,-1487.60718395156,-1486.92427424324),
 .UNSPECIFIED.);
#1925=B_SPLINE_CURVE_WITH_KNOTS('',3,(#265061,#265062,#265063,#265064,#265065,
#265066,#265067,#265068,#265069,#265070),.UNSPECIFIED.,.F.,.F.,(4,1,1,1,
1,1,1,4),(-1499.4906448576,-1498.60428006948,-1497.60454405876,-1496.60480804804,
-1495.60507203732,-1494.6053360266,-1493.60560001588,-1493.20745955042),
 .UNSPECIFIED.);
#1926=B_SPLINE_CURVE_WITH_KNOTS('',3,(#265071,#265072,#265073,#265074,#265075),
 .UNSPECIFIED.,.F.,.F.,(4,1,4),(-1500.33866773228,-1499.6040160802,-1499.4906448576),
 .UNSPECIFIED.);
#1927=B_SPLINE_CURVE_WITH_KNOTS('',3,(#265078,#265079,#265080,#265081,#265082,
#265083,#265084,#265085,#265086,#265087,#265088,#265089,#265090,#265091,
#265092,#265093,#265094,#265095,#265096,#265097,#265098,#265099,#265100,
#265101,#265102,#265103,#265104,#265105,#265106,#265107,#265108,#265109,
#265110,#265111,#265112,#265113,#265114,#265115,#265116,#265117,#265118,
#265119,#265120,#265121,#265122,#265123,#265124,#265125,#265126,#265127,
#265128,#265129,#265130,#265131,#265132,#265133,#265134,#265135,#265136,
#265137,#265138,#265139,#265140,#265141,#265142,#265143,#265144,#265145,
#265146,#265147,#265148,#265149,#265150,#265151,#265152,#265153,#265154,
#265155,#265156,#265157,#265158,#265159,#265160,#265161,#265162,#265163,
#265164,#265165,#265166,#265167,#265168,#265169,#265170,#265171,#265172,
#265173,#265174,#265175,#265176,#265177,#265178,#265179,#265180,#265181,
#265182,#265183,#265184,#265185,#265186,#265187,#265188,#265189,#265190,
#265191,#265192,#265193,#265194,#265195,#265196,#265197,#265198,#265199,
#265200,#265201,#265202,#265203,#265204,#265205,#265206,#265207,#265208,
#265209,#265210,#265211,#265212,#265213,#265214,#265215,#265216,#265217,
#265218,#265219,#265220,#265221,#265222,#265223,#265224,#265225,#265226,
#265227,#265228,#265229,#265230,#265231,#265232,#265233,#265234,#265235,
#265236,#265237,#265238,#265239,#265240,#265241,#265242,#265243,#265244,
#265245,#265246,#265247,#265248,#265249,#265250,#265251,#265252,#265253,
#265254,#265255,#265256,#265257,#265258,#265259,#265260,#265261,#265262,
#265263,#265264,#265265,#265266,#265267,#265268,#265269,#265270,#265271,
#265272,#265273,#265274,#265275,#265276,#265277,#265278,#265279,#265280,
#265281,#265282,#265283,#265284,#265285,#265286,#265287,#265288,#265289,
#265290,#265291,#265292,#265293,#265294,#265295,#265296,#265297),
 .UNSPECIFIED.,.F.,.F.,(4,3,3,3,3,3,3,3,3,3,3,3,3,3,3,3,3,3,3,3,3,3,3,3,
3,3,3,3,3,3,3,3,3,3,3,3,3,3,3,3,3,3,3,3,3,3,3,3,3,3,3,3,3,3,3,3,3,3,3,3,
3,3,3,3,3,3,3,3,3,3,3,3,3,4),(1404.29191615481,1404.37506475554,1404.45811270144,
1404.54108068674,1404.62398932894,1404.70686775223,1404.78973305654,1404.87260381792,
1404.95549861295,1405.03848303953,1405.1215178224,1405.20467492572,1405.24742046295,
1405.3311591748,1405.41479468616,1405.49834712956,1405.58183656541,1405.66529051603,
1405.74872700987,1405.83216411963,1405.91561991455,1405.99916440728,1406.08275349022,
1406.16647675777,1406.24715647367,1406.33089518552,1406.41453069688,1406.49808314028,
1406.58157257613,1406.66502652675,1406.74846302059,1406.83190013035,1406.91535592527,
1406.998900418,1407.08248950094,1407.16621276849,1407.24689248439,1407.33063119624,
1407.4142667076,1407.497819151,1407.58130858685,1407.66476253747,1407.74819903131,
1407.83163614107,1407.91509193599,1407.99863642872,1408.08222551166,1408.16594877921,
1408.24662849511,1408.33036720696,1408.41400271832,1408.49755516172,1408.58104459757,
1408.66449854819,1408.74793504203,1408.83137215179,1408.91482794671,1408.99837243944,
1409.08196152238,1409.16568478993,1409.24636450583,1409.33010321768,1409.41373872904,
1409.49729117244,1409.58078060829,1409.66423455891,1409.74767105275,1409.83110816251,
1409.91456395743,1409.99810845016,1410.0816975331,1410.16542080065,1410.24610051655,
1410.3244751935),.UNSPECIFIED.);
#1928=B_SPLINE_CURVE_WITH_KNOTS('',3,(#265298,#265299,#265300,#265301,#265302,
#265303,#265304,#265305,#265306,#265307,#265308,#265309,#265310),
 .UNSPECIFIED.,.F.,.F.,(4,3,3,3,4),(1404.04024993874,1404.12386652121,1404.20760574971,
1404.24768445223,1404.29191615463),.UNSPECIFIED.);
#1929=B_SPLINE_CURVE_WITH_KNOTS('',3,(#265314,#265315,#265316,#265317,#265318,
#265319,#265320,#265321),.UNSPECIFIED.,.F.,.F.,(4,2,2,4),(0.511738111681904,
0.560187232161708,0.746865960113868,0.833421149073491),.UNSPECIFIED.);
#1930=B_SPLINE_CURVE_WITH_KNOTS('',3,(#265323,#265324,#265325,#265326,#265327,
#265328,#265329,#265330,#265331,#265332,#265333,#265334,#265335,#265336,
#265337,#265338,#265339,#265340,#265341),.UNSPECIFIED.,.F.,.F.,(4,3,3,3,
3,3,4),(1511.10606637669,1511.21943759928,1511.30319040684,1511.38681542686,
1511.47036680961,1511.55385319882,1511.60403841566),.UNSPECIFIED.);
#1931=B_SPLINE_CURVE_WITH_KNOTS('',3,(#265343,#265344,#265345,#265346,#265347,
#265348,#265349,#265350,#265351,#265352,#265353,#265354,#265355,#265356,
#265357,#265358,#265359,#265360,#265361,#265362,#265363,#265364,#265365,
#265366,#265367,#265368,#265369,#265370,#265371,#265372,#265373,#265374,
#265375,#265376,#265377,#265378,#265379,#265380,#265381,#265382),
 .UNSPECIFIED.,.F.,.F.,(4,3,3,3,3,3,3,3,3,3,3,3,3,4),(1510.04626900307,
1510.13298529582,1510.21970158856,1510.30231995216,1510.38483597174,1510.46727079007,
1510.54964461587,1510.63198603367,1510.71431401009,1510.79664749822,1510.8790479625,
1510.96148328965,1511.04402920436,1511.10606637655),.UNSPECIFIED.);
#1932=B_SPLINE_CURVE_WITH_KNOTS('',3,(#265383,#265384,#265385,#265386,#265387,
#265388,#265389,#265390),.UNSPECIFIED.,.F.,.F.,(4,2,2,4),(0.833421149073491,
0.933544688066027,1.12022341601819,1.25194814216481),.UNSPECIFIED.);
#1933=B_SPLINE_CURVE_WITH_KNOTS('',3,(#272171,#272172,#272173,#272174,#272175,
#272176,#272177,#272178,#272179,#272180),.UNSPECIFIED.,.F.,.F.,(4,2,2,2,
4),(0.000658062556380468,0.0111047509489515,0.0590298249892507,0.111505910077716,
0.21897564774011),.UNSPECIFIED.);
#1934=B_SPLINE_CURVE_WITH_KNOTS('',3,(#272181,#272182,#272183,#272184,#272185,
#272186,#272187,#272188,#272189,#272190,#272191,#272192,#272193,#272194,
#272195,#272196,#272197,#272198,#272199,#272200,#272201,#272202,#272203,
#272204,#272205,#272206,#272207,#272208,#272209,#272210),.UNSPECIFIED.,
 .F.,.F.,(4,2,2,2,2,2,2,2,2,2,2,2,2,2,4),(0.00421488007861112,0.126209593249118,
0.138553986655518,0.139238723759837,0.139494495774474,0.139701646022053,
0.139825836912464,0.139896118986021,0.139956803150512,0.140030152514862,
0.140167078926622,0.140893495700786,0.142281953339915,0.175403086699887,
0.271081612417309),.UNSPECIFIED.);
#1935=B_SPLINE_CURVE_WITH_KNOTS('',3,(#272212,#272213,#272214,#272215,#272216,
#272217,#272218,#272219,#272220,#272221,#272222,#272223,#272224,#272225,
#272226,#272227,#272228,#272229,#272230,#272231,#272232,#272233,#272234,
#272235,#272236,#272237,#272238,#272239,#272240,#272241,#272242,#272243,
#272244,#272245,#272246,#272247,#272248,#272249,#272250,#272251,#272252,
#272253,#272254,#272255,#272256,#272257,#272258,#272259,#272260,#272261,
#272262,#272263,#272264,#272265,#272266,#272267,#272268,#272269,#272270,
#272271,#272272,#272273,#272274,#272275,#272276,#272277),.UNSPECIFIED.,
 .F.,.F.,(4,2,2,2,2,2,2,2,2,2,2,2,2,2,2,2,2,2,2,2,2,2,2,2,2,2,2,2,2,2,2,
2,4),(0.327283840054511,0.396783892533185,0.398753154793215,0.39883104940972,
0.398913914893828,0.398957630479319,0.398993023019997,0.399033143424731,
0.399101184070818,0.399358824404068,0.425945100779195,0.48786691587727,
0.590116051707203,0.728147561875147,0.915995373334799,1.00257399236972,
1.01107722098825,1.01145699741804,1.01152254445187,1.01160528707227,1.01187936515956,
1.01198328823823,1.01205251272225,1.01211868643199,1.01220807494068,1.01240984189626,
1.01682708804678,1.04338539683548,1.10926355513005,1.20121102692353,1.32043543719856,
1.40835082600552,1.50774934918788),.UNSPECIFIED.);
#1936=B_SPLINE_CURVE_WITH_KNOTS('',3,(#272278,#272279,#272280,#272281,#272282,
#272283,#272284,#272285,#272286,#272287),.UNSPECIFIED.,.F.,.F.,(4,2,2,2,
4),(0.0020693068779551,0.0883072267821443,0.189117057255197,0.276553971900186,
0.327283840054511),.UNSPECIFIED.);
#1937=B_SPLINE_CURVE_WITH_KNOTS('',3,(#272288,#272289,#272290,#272291,#272292,
#272293,#272294,#272295,#272296,#272297,#272298,#272299,#272300,#272301,
#272302,#272303,#272304,#272305,#272306,#272307,#272308,#272309,#272310,
#272311,#272312,#272313,#272314,#272315,#272316,#272317,#272318,#272319,
#272320,#272321,#272322,#272323,#272324,#272325,#272326,#272327,#272328,
#272329,#272330,#272331,#272332,#272333),.UNSPECIFIED.,.F.,.F.,(4,2,2,2,
2,2,2,2,2,2,2,2,2,2,2,2,2,2,2,2,2,2,4),(0.000477110384091791,0.110358824121838,
0.172331397524916,0.183780301788713,0.187764976788729,0.191717661689663,
0.192789629652419,0.194532929434185,0.195126939526276,0.195487384399954,
0.195561053638385,0.195617377487698,0.195648423799949,0.195666662922991,
0.195682536300503,0.195701880767454,0.195738461322392,0.195943378897047,
0.196314700337278,0.212692416929255,0.248840090507569,0.30101993643223,
0.351147893655916),.UNSPECIFIED.);
#1938=B_SPLINE_CURVE_WITH_KNOTS('',3,(#272336,#272337,#272338,#272339,#272340,
#272341),.UNSPECIFIED.,.F.,.F.,(4,2,4),(2.88515402066428,2.93100248921169,
3.09523639416926),.UNSPECIFIED.);
#1939=B_SPLINE_CURVE_WITH_KNOTS('',3,(#272343,#272344,#272345,#272346,#272347),
 .UNSPECIFIED.,.F.,.F.,(4,1,4),(-1502.69543409617,-1502.60322411236,-1502.3180309781),
 .UNSPECIFIED.);
#1940=B_SPLINE_CURVE_WITH_KNOTS('',3,(#272348,#272349,#272350,#272351),
 .UNSPECIFIED.,.F.,.F.,(4,4),(2.48381435072133,2.66889972571145),
 .UNSPECIFIED.);
#1941=B_SPLINE_CURVE_WITH_KNOTS('',3,(#279132,#279133,#279134,#279135,#279136,
#279137,#279138,#279139,#279140,#279141,#279142,#279143,#279144,#279145,
#279146,#279147,#279148,#279149,#279150,#279151,#279152,#279153,#279154,
#279155),.UNSPECIFIED.,.F.,.F.,(4,2,2,2,2,2,2,2,2,2,2,4),(0.00293506500743818,
0.102989889801783,0.114060948170188,0.114147673612461,0.114232131538629,
0.11427719251539,0.11431393964835,0.114355889157666,0.114427166018751,0.114704271772878,
0.148089581915078,0.224846674886138),.UNSPECIFIED.);
#1942=SHAPE_REPRESENTATION_RELATIONSHIP('SRR','None',#279301,#1951);
#1943=SHAPE_REPRESENTATION_RELATIONSHIP('SRR','None',#279302,#1952);
#1944=SHAPE_REPRESENTATION_RELATIONSHIP('SRR','None',#279303,#1953);
#1945=SHAPE_REPRESENTATION_RELATIONSHIP('SRR','None',#279304,#1954);
#1946=SHAPE_REPRESENTATION_RELATIONSHIP('SRR','None',#279305,#1955);
#1947=SHAPE_REPRESENTATION_RELATIONSHIP('SRR','None',#279306,#1956);
#1948=SHAPE_REPRESENTATION_RELATIONSHIP('SRR','None',#279307,#1957);
#1949=SHAPE_REPRESENTATION_RELATIONSHIP('SRR','None',#279308,#1958);
#1950=SHAPE_REPRESENTATION_RELATIONSHIP('SRR','None',#279309,#1959);
#1951=ADVANCED_BREP_SHAPE_REPRESENTATION('',(#1969),#279257);
#1952=ADVANCED_BREP_SHAPE_REPRESENTATION('',(#1970),#279258);
#1953=ADVANCED_BREP_SHAPE_REPRESENTATION('',(#1971),#279259);
#1954=ADVANCED_BREP_SHAPE_REPRESENTATION('',(#1972),#279260);
#1955=ADVANCED_BREP_SHAPE_REPRESENTATION('',(#1973),#279261);
#1956=ADVANCED_BREP_SHAPE_REPRESENTATION('',(#1974),#279262);
#1957=ADVANCED_BREP_SHAPE_REPRESENTATION('',(#1975),#279263);
#1958=ADVANCED_BREP_SHAPE_REPRESENTATION('',(#1976),#279264);
#1959=ADVANCED_BREP_SHAPE_REPRESENTATION('',(#1977),#279265);
#1960=STYLED_ITEM('',(#279355),#1969);
#1961=STYLED_ITEM('',(#279355),#1970);
#1962=STYLED_ITEM('',(#279355),#1971);
#1963=STYLED_ITEM('',(#279355),#1972);
#1964=STYLED_ITEM('',(#279355),#1973);
#1965=STYLED_ITEM('',(#279355),#1974);
#1966=STYLED_ITEM('',(#279355),#1975);
#1967=STYLED_ITEM('',(#279355),#1976);
#1968=STYLED_ITEM('',(#279355),#1977);
#1969=MANIFOLD_SOLID_BREP('Body1',#14938);
#1970=MANIFOLD_SOLID_BREP('Body1',#14939);
#1971=MANIFOLD_SOLID_BREP('Body1',#14940);
#1972=MANIFOLD_SOLID_BREP('Body1',#14941);
#1973=MANIFOLD_SOLID_BREP('Body1',#14942);
#1974=MANIFOLD_SOLID_BREP('Body1',#14943);
#1975=MANIFOLD_SOLID_BREP('Body1',#14944);
#1976=MANIFOLD_SOLID_BREP('Body1',#14945);
#1977=MANIFOLD_SOLID_BREP('Body1',#14946);
#1978=FACE_BOUND('',#2587,.T.);
#1979=FACE_BOUND('',#2588,.T.);
#1980=FACE_BOUND('',#2591,.T.);
#1981=FACE_BOUND('',#2592,.T.);
#1982=FACE_BOUND('',#2604,.T.);
#1983=FACE_BOUND('',#2609,.T.);
#1984=FACE_BOUND('',#2610,.T.);
#1985=FACE_BOUND('',#2613,.T.);
#1986=FACE_BOUND('',#2614,.T.);
#1987=FACE_BOUND('',#2891,.T.);
#1988=FACE_BOUND('',#2894,.T.);
#1989=FACE_BOUND('',#2908,.T.);
#1990=FACE_BOUND('',#2909,.T.);
#1991=FACE_BOUND('',#2911,.T.);
#1992=FACE_BOUND('',#2921,.T.);
#1993=FACE_BOUND('',#2928,.T.);
#1994=FACE_BOUND('',#2929,.T.);
#1995=FACE_BOUND('',#2957,.T.);
#1996=FACE_BOUND('',#2965,.T.);
#1997=FACE_BOUND('',#2967,.T.);
#1998=FACE_BOUND('',#2968,.T.);
#1999=FACE_BOUND('',#2976,.T.);
#2000=FACE_BOUND('',#2978,.T.);
#2001=FACE_BOUND('',#2979,.T.);
#2002=FACE_BOUND('',#2985,.T.);
#2003=FACE_BOUND('',#2992,.T.);
#2004=FACE_BOUND('',#2993,.T.);
#2005=FACE_BOUND('',#2996,.T.);
#2006=FACE_BOUND('',#2997,.T.);
#2007=FACE_BOUND('',#2999,.T.);
#2008=FACE_BOUND('',#3013,.T.);
#2009=FACE_BOUND('',#3014,.T.);
#2010=FACE_BOUND('',#3017,.T.);
#2011=FACE_BOUND('',#3018,.T.);
#2012=FACE_BOUND('',#3030,.T.);
#2013=FACE_BOUND('',#3035,.T.);
#2014=FACE_BOUND('',#3036,.T.);
#2015=FACE_BOUND('',#3039,.T.);
#2016=FACE_BOUND('',#3040,.T.);
#2017=FACE_BOUND('',#3073,.T.);
#2018=FACE_BOUND('',#3081,.T.);
#2019=FACE_BOUND('',#3083,.T.);
#2020=FACE_BOUND('',#3084,.T.);
#2021=FACE_BOUND('',#3092,.T.);
#2022=FACE_BOUND('',#3094,.T.);
#2023=FACE_BOUND('',#3095,.T.);
#2024=PLANE('',#15055);
#2025=PLANE('',#15059);
#2026=PLANE('',#15063);
#2027=PLANE('',#15068);
#2028=PLANE('',#15071);
#2029=PLANE('',#15072);
#2030=PLANE('',#15076);
#2031=PLANE('',#15077);
#2032=PLANE('',#15083);
#2033=PLANE('',#15087);
#2034=PLANE('',#15088);
#2035=PLANE('',#15089);
#2036=PLANE('',#15090);
#2037=PLANE('',#15093);
#2038=PLANE('',#15097);
#2039=PLANE('',#15099);
#2040=PLANE('',#15101);
#2041=PLANE('',#15102);
#2042=PLANE('',#15103);
#2043=PLANE('',#15379);
#2044=PLANE('',#15384);
#2045=PLANE('',#15385);
#2046=PLANE('',#15386);
#2047=PLANE('',#15388);
#2048=PLANE('',#15389);
#2049=PLANE('',#15395);
#2050=PLANE('',#15396);
#2051=PLANE('',#15415);
#2052=PLANE('',#15419);
#2053=PLANE('',#15424);
#2054=PLANE('',#15426);
#2055=PLANE('',#15428);
#2056=PLANE('',#15432);
#2057=PLANE('',#15433);
#2058=PLANE('',#15437);
#2059=PLANE('',#15440);
#2060=PLANE('',#15445);
#2061=PLANE('',#15472);
#2062=PLANE('',#15473);
#2063=PLANE('',#15478);
#2064=PLANE('',#15482);
#2065=PLANE('',#15483);
#2066=PLANE('',#15485);
#2067=PLANE('',#15493);
#2068=PLANE('',#15497);
#2069=PLANE('',#15501);
#2070=PLANE('',#15502);
#2071=PLANE('',#15521);
#2072=PLANE('',#15522);
#2073=PLANE('',#15526);
#2074=PLANE('',#15529);
#2075=PLANE('',#15534);
#2076=PLANE('',#15538);
#2077=PLANE('',#15542);
#2078=PLANE('',#15547);
#2079=PLANE('',#15549);
#2080=PLANE('',#15551);
#2081=PLANE('',#15559);
#2082=PLANE('',#15563);
#2083=PLANE('',#15567);
#2084=PLANE('',#15572);
#2085=PLANE('',#15575);
#2086=PLANE('',#15576);
#2087=PLANE('',#15580);
#2088=PLANE('',#15581);
#2089=PLANE('',#15587);
#2090=PLANE('',#15591);
#2091=PLANE('',#15592);
#2092=PLANE('',#15593);
#2093=PLANE('',#15594);
#2094=PLANE('',#15597);
#2095=PLANE('',#15601);
#2096=PLANE('',#15603);
#2097=PLANE('',#15605);
#2098=PLANE('',#15606);
#2099=PLANE('',#15607);
#2100=PLANE('',#15634);
#2101=PLANE('',#15635);
#2102=PLANE('',#15640);
#2103=PLANE('',#15644);
#2104=PLANE('',#15645);
#2105=PLANE('',#15647);
#2106=PLANE('',#15655);
#2107=PLANE('',#15659);
#2108=PLANE('',#15663);
#2109=PLANE('',#15664);
#2110=FACE_OUTER_BOUND('',#2580,.T.);
#2111=FACE_OUTER_BOUND('',#2581,.T.);
#2112=FACE_OUTER_BOUND('',#2582,.T.);
#2113=FACE_OUTER_BOUND('',#2583,.T.);
#2114=FACE_OUTER_BOUND('',#2584,.T.);
#2115=FACE_OUTER_BOUND('',#2585,.T.);
#2116=FACE_OUTER_BOUND('',#2586,.T.);
#2117=FACE_OUTER_BOUND('',#2589,.T.);
#2118=FACE_OUTER_BOUND('',#2590,.T.);
#2119=FACE_OUTER_BOUND('',#2593,.T.);
#2120=FACE_OUTER_BOUND('',#2594,.T.);
#2121=FACE_OUTER_BOUND('',#2595,.T.);
#2122=FACE_OUTER_BOUND('',#2596,.T.);
#2123=FACE_OUTER_BOUND('',#2597,.T.);
#2124=FACE_OUTER_BOUND('',#2598,.T.);
#2125=FACE_OUTER_BOUND('',#2599,.T.);
#2126=FACE_OUTER_BOUND('',#2600,.T.);
#2127=FACE_OUTER_BOUND('',#2601,.T.);
#2128=FACE_OUTER_BOUND('',#2602,.T.);
#2129=FACE_OUTER_BOUND('',#2603,.T.);
#2130=FACE_OUTER_BOUND('',#2605,.T.);
#2131=FACE_OUTER_BOUND('',#2606,.T.);
#2132=FACE_OUTER_BOUND('',#2607,.T.);
#2133=FACE_OUTER_BOUND('',#2608,.T.);
#2134=FACE_OUTER_BOUND('',#2611,.T.);
#2135=FACE_OUTER_BOUND('',#2612,.T.);
#2136=FACE_OUTER_BOUND('',#2615,.T.);
#2137=FACE_OUTER_BOUND('',#2616,.T.);
#2138=FACE_OUTER_BOUND('',#2617,.T.);
#2139=FACE_OUTER_BOUND('',#2618,.T.);
#2140=FACE_OUTER_BOUND('',#2619,.T.);
#2141=FACE_OUTER_BOUND('',#2620,.T.);
#2142=FACE_OUTER_BOUND('',#2621,.T.);
#2143=FACE_OUTER_BOUND('',#2622,.T.);
#2144=FACE_OUTER_BOUND('',#2623,.T.);
#2145=FACE_OUTER_BOUND('',#2624,.T.);
#2146=FACE_OUTER_BOUND('',#2625,.T.);
#2147=FACE_OUTER_BOUND('',#2626,.T.);
#2148=FACE_OUTER_BOUND('',#2627,.T.);
#2149=FACE_OUTER_BOUND('',#2628,.T.);
#2150=FACE_OUTER_BOUND('',#2629,.T.);
#2151=FACE_OUTER_BOUND('',#2630,.T.);
#2152=FACE_OUTER_BOUND('',#2631,.T.);
#2153=FACE_OUTER_BOUND('',#2632,.T.);
#2154=FACE_OUTER_BOUND('',#2633,.T.);
#2155=FACE_OUTER_BOUND('',#2634,.T.);
#2156=FACE_OUTER_BOUND('',#2635,.T.);
#2157=FACE_OUTER_BOUND('',#2636,.T.);
#2158=FACE_OUTER_BOUND('',#2637,.T.);
#2159=FACE_OUTER_BOUND('',#2638,.T.);
#2160=FACE_OUTER_BOUND('',#2639,.T.);
#2161=FACE_OUTER_BOUND('',#2640,.T.);
#2162=FACE_OUTER_BOUND('',#2641,.T.);
#2163=FACE_OUTER_BOUND('',#2642,.T.);
#2164=FACE_OUTER_BOUND('',#2643,.T.);
#2165=FACE_OUTER_BOUND('',#2644,.T.);
#2166=FACE_OUTER_BOUND('',#2645,.T.);
#2167=FACE_OUTER_BOUND('',#2646,.T.);
#2168=FACE_OUTER_BOUND('',#2647,.T.);
#2169=FACE_OUTER_BOUND('',#2648,.T.);
#2170=FACE_OUTER_BOUND('',#2649,.T.);
#2171=FACE_OUTER_BOUND('',#2650,.T.);
#2172=FACE_OUTER_BOUND('',#2651,.T.);
#2173=FACE_OUTER_BOUND('',#2652,.T.);
#2174=FACE_OUTER_BOUND('',#2653,.T.);
#2175=FACE_OUTER_BOUND('',#2654,.T.);
#2176=FACE_OUTER_BOUND('',#2655,.T.);
#2177=FACE_OUTER_BOUND('',#2656,.T.);
#2178=FACE_OUTER_BOUND('',#2657,.T.);
#2179=FACE_OUTER_BOUND('',#2658,.T.);
#2180=FACE_OUTER_BOUND('',#2659,.T.);
#2181=FACE_OUTER_BOUND('',#2660,.T.);
#2182=FACE_OUTER_BOUND('',#2661,.T.);
#2183=FACE_OUTER_BOUND('',#2662,.T.);
#2184=FACE_OUTER_BOUND('',#2663,.T.);
#2185=FACE_OUTER_BOUND('',#2664,.T.);
#2186=FACE_OUTER_BOUND('',#2665,.T.);
#2187=FACE_OUTER_BOUND('',#2666,.T.);
#2188=FACE_OUTER_BOUND('',#2667,.T.);
#2189=FACE_OUTER_BOUND('',#2668,.T.);
#2190=FACE_OUTER_BOUND('',#2669,.T.);
#2191=FACE_OUTER_BOUND('',#2670,.T.);
#2192=FACE_OUTER_BOUND('',#2671,.T.);
#2193=FACE_OUTER_BOUND('',#2672,.T.);
#2194=FACE_OUTER_BOUND('',#2673,.T.);
#2195=FACE_OUTER_BOUND('',#2674,.T.);
#2196=FACE_OUTER_BOUND('',#2675,.T.);
#2197=FACE_OUTER_BOUND('',#2676,.T.);
#2198=FACE_OUTER_BOUND('',#2677,.T.);
#2199=FACE_OUTER_BOUND('',#2678,.T.);
#2200=FACE_OUTER_BOUND('',#2679,.T.);
#2201=FACE_OUTER_BOUND('',#2680,.T.);
#2202=FACE_OUTER_BOUND('',#2681,.T.);
#2203=FACE_OUTER_BOUND('',#2682,.T.);
#2204=FACE_OUTER_BOUND('',#2683,.T.);
#2205=FACE_OUTER_BOUND('',#2684,.T.);
#2206=FACE_OUTER_BOUND('',#2685,.T.);
#2207=FACE_OUTER_BOUND('',#2686,.T.);
#2208=FACE_OUTER_BOUND('',#2687,.T.);
#2209=FACE_OUTER_BOUND('',#2688,.T.);
#2210=FACE_OUTER_BOUND('',#2689,.T.);
#2211=FACE_OUTER_BOUND('',#2690,.T.);
#2212=FACE_OUTER_BOUND('',#2691,.T.);
#2213=FACE_OUTER_BOUND('',#2692,.T.);
#2214=FACE_OUTER_BOUND('',#2693,.T.);
#2215=FACE_OUTER_BOUND('',#2694,.T.);
#2216=FACE_OUTER_BOUND('',#2695,.T.);
#2217=FACE_OUTER_BOUND('',#2696,.T.);
#2218=FACE_OUTER_BOUND('',#2697,.T.);
#2219=FACE_OUTER_BOUND('',#2698,.T.);
#2220=FACE_OUTER_BOUND('',#2699,.T.);
#2221=FACE_OUTER_BOUND('',#2700,.T.);
#2222=FACE_OUTER_BOUND('',#2701,.T.);
#2223=FACE_OUTER_BOUND('',#2702,.T.);
#2224=FACE_OUTER_BOUND('',#2703,.T.);
#2225=FACE_OUTER_BOUND('',#2704,.T.);
#2226=FACE_OUTER_BOUND('',#2705,.T.);
#2227=FACE_OUTER_BOUND('',#2706,.T.);
#2228=FACE_OUTER_BOUND('',#2707,.T.);
#2229=FACE_OUTER_BOUND('',#2708,.T.);
#2230=FACE_OUTER_BOUND('',#2709,.T.);
#2231=FACE_OUTER_BOUND('',#2710,.T.);
#2232=FACE_OUTER_BOUND('',#2711,.T.);
#2233=FACE_OUTER_BOUND('',#2712,.T.);
#2234=FACE_OUTER_BOUND('',#2713,.T.);
#2235=FACE_OUTER_BOUND('',#2714,.T.);
#2236=FACE_OUTER_BOUND('',#2715,.T.);
#2237=FACE_OUTER_BOUND('',#2716,.T.);
#2238=FACE_OUTER_BOUND('',#2717,.T.);
#2239=FACE_OUTER_BOUND('',#2718,.T.);
#2240=FACE_OUTER_BOUND('',#2719,.T.);
#2241=FACE_OUTER_BOUND('',#2720,.T.);
#2242=FACE_OUTER_BOUND('',#2721,.T.);
#2243=FACE_OUTER_BOUND('',#2722,.T.);
#2244=FACE_OUTER_BOUND('',#2723,.T.);
#2245=FACE_OUTER_BOUND('',#2724,.T.);
#2246=FACE_OUTER_BOUND('',#2725,.T.);
#2247=FACE_OUTER_BOUND('',#2726,.T.);
#2248=FACE_OUTER_BOUND('',#2727,.T.);
#2249=FACE_OUTER_BOUND('',#2728,.T.);
#2250=FACE_OUTER_BOUND('',#2729,.T.);
#2251=FACE_OUTER_BOUND('',#2730,.T.);
#2252=FACE_OUTER_BOUND('',#2731,.T.);
#2253=FACE_OUTER_BOUND('',#2732,.T.);
#2254=FACE_OUTER_BOUND('',#2733,.T.);
#2255=FACE_OUTER_BOUND('',#2734,.T.);
#2256=FACE_OUTER_BOUND('',#2735,.T.);
#2257=FACE_OUTER_BOUND('',#2736,.T.);
#2258=FACE_OUTER_BOUND('',#2737,.T.);
#2259=FACE_OUTER_BOUND('',#2738,.T.);
#2260=FACE_OUTER_BOUND('',#2739,.T.);
#2261=FACE_OUTER_BOUND('',#2740,.T.);
#2262=FACE_OUTER_BOUND('',#2741,.T.);
#2263=FACE_OUTER_BOUND('',#2742,.T.);
#2264=FACE_OUTER_BOUND('',#2743,.T.);
#2265=FACE_OUTER_BOUND('',#2744,.T.);
#2266=FACE_OUTER_BOUND('',#2745,.T.);
#2267=FACE_OUTER_BOUND('',#2746,.T.);
#2268=FACE_OUTER_BOUND('',#2747,.T.);
#2269=FACE_OUTER_BOUND('',#2748,.T.);
#2270=FACE_OUTER_BOUND('',#2749,.T.);
#2271=FACE_OUTER_BOUND('',#2750,.T.);
#2272=FACE_OUTER_BOUND('',#2751,.T.);
#2273=FACE_OUTER_BOUND('',#2752,.T.);
#2274=FACE_OUTER_BOUND('',#2753,.T.);
#2275=FACE_OUTER_BOUND('',#2754,.T.);
#2276=FACE_OUTER_BOUND('',#2755,.T.);
#2277=FACE_OUTER_BOUND('',#2756,.T.);
#2278=FACE_OUTER_BOUND('',#2757,.T.);
#2279=FACE_OUTER_BOUND('',#2758,.T.);
#2280=FACE_OUTER_BOUND('',#2759,.T.);
#2281=FACE_OUTER_BOUND('',#2760,.T.);
#2282=FACE_OUTER_BOUND('',#2761,.T.);
#2283=FACE_OUTER_BOUND('',#2762,.T.);
#2284=FACE_OUTER_BOUND('',#2763,.T.);
#2285=FACE_OUTER_BOUND('',#2764,.T.);
#2286=FACE_OUTER_BOUND('',#2765,.T.);
#2287=FACE_OUTER_BOUND('',#2766,.T.);
#2288=FACE_OUTER_BOUND('',#2767,.T.);
#2289=FACE_OUTER_BOUND('',#2768,.T.);
#2290=FACE_OUTER_BOUND('',#2769,.T.);
#2291=FACE_OUTER_BOUND('',#2770,.T.);
#2292=FACE_OUTER_BOUND('',#2771,.T.);
#2293=FACE_OUTER_BOUND('',#2772,.T.);
#2294=FACE_OUTER_BOUND('',#2773,.T.);
#2295=FACE_OUTER_BOUND('',#2774,.T.);
#2296=FACE_OUTER_BOUND('',#2775,.T.);
#2297=FACE_OUTER_BOUND('',#2776,.T.);
#2298=FACE_OUTER_BOUND('',#2777,.T.);
#2299=FACE_OUTER_BOUND('',#2778,.T.);
#2300=FACE_OUTER_BOUND('',#2779,.T.);
#2301=FACE_OUTER_BOUND('',#2780,.T.);
#2302=FACE_OUTER_BOUND('',#2781,.T.);
#2303=FACE_OUTER_BOUND('',#2782,.T.);
#2304=FACE_OUTER_BOUND('',#2783,.T.);
#2305=FACE_OUTER_BOUND('',#2784,.T.);
#2306=FACE_OUTER_BOUND('',#2785,.T.);
#2307=FACE_OUTER_BOUND('',#2786,.T.);
#2308=FACE_OUTER_BOUND('',#2787,.T.);
#2309=FACE_OUTER_BOUND('',#2788,.T.);
#2310=FACE_OUTER_BOUND('',#2789,.T.);
#2311=FACE_OUTER_BOUND('',#2790,.T.);
#2312=FACE_OUTER_BOUND('',#2791,.T.);
#2313=FACE_OUTER_BOUND('',#2792,.T.);
#2314=FACE_OUTER_BOUND('',#2793,.T.);
#2315=FACE_OUTER_BOUND('',#2794,.T.);
#2316=FACE_OUTER_BOUND('',#2795,.T.);
#2317=FACE_OUTER_BOUND('',#2796,.T.);
#2318=FACE_OUTER_BOUND('',#2797,.T.);
#2319=FACE_OUTER_BOUND('',#2798,.T.);
#2320=FACE_OUTER_BOUND('',#2799,.T.);
#2321=FACE_OUTER_BOUND('',#2800,.T.);
#2322=FACE_OUTER_BOUND('',#2801,.T.);
#2323=FACE_OUTER_BOUND('',#2802,.T.);
#2324=FACE_OUTER_BOUND('',#2803,.T.);
#2325=FACE_OUTER_BOUND('',#2804,.T.);
#2326=FACE_OUTER_BOUND('',#2805,.T.);
#2327=FACE_OUTER_BOUND('',#2806,.T.);
#2328=FACE_OUTER_BOUND('',#2807,.T.);
#2329=FACE_OUTER_BOUND('',#2808,.T.);
#2330=FACE_OUTER_BOUND('',#2809,.T.);
#2331=FACE_OUTER_BOUND('',#2810,.T.);
#2332=FACE_OUTER_BOUND('',#2811,.T.);
#2333=FACE_OUTER_BOUND('',#2812,.T.);
#2334=FACE_OUTER_BOUND('',#2813,.T.);
#2335=FACE_OUTER_BOUND('',#2814,.T.);
#2336=FACE_OUTER_BOUND('',#2815,.T.);
#2337=FACE_OUTER_BOUND('',#2816,.T.);
#2338=FACE_OUTER_BOUND('',#2817,.T.);
#2339=FACE_OUTER_BOUND('',#2818,.T.);
#2340=FACE_OUTER_BOUND('',#2819,.T.);
#2341=FACE_OUTER_BOUND('',#2820,.T.);
#2342=FACE_OUTER_BOUND('',#2821,.T.);
#2343=FACE_OUTER_BOUND('',#2822,.T.);
#2344=FACE_OUTER_BOUND('',#2823,.T.);
#2345=FACE_OUTER_BOUND('',#2824,.T.);
#2346=FACE_OUTER_BOUND('',#2825,.T.);
#2347=FACE_OUTER_BOUND('',#2826,.T.);
#2348=FACE_OUTER_BOUND('',#2827,.T.);
#2349=FACE_OUTER_BOUND('',#2828,.T.);
#2350=FACE_OUTER_BOUND('',#2829,.T.);
#2351=FACE_OUTER_BOUND('',#2830,.T.);
#2352=FACE_OUTER_BOUND('',#2831,.T.);
#2353=FACE_OUTER_BOUND('',#2832,.T.);
#2354=FACE_OUTER_BOUND('',#2833,.T.);
#2355=FACE_OUTER_BOUND('',#2834,.T.);
#2356=FACE_OUTER_BOUND('',#2835,.T.);
#2357=FACE_OUTER_BOUND('',#2836,.T.);
#2358=FACE_OUTER_BOUND('',#2837,.T.);
#2359=FACE_OUTER_BOUND('',#2838,.T.);
#2360=FACE_OUTER_BOUND('',#2839,.T.);
#2361=FACE_OUTER_BOUND('',#2840,.T.);
#2362=FACE_OUTER_BOUND('',#2841,.T.);
#2363=FACE_OUTER_BOUND('',#2842,.T.);
#2364=FACE_OUTER_BOUND('',#2843,.T.);
#2365=FACE_OUTER_BOUND('',#2844,.T.);
#2366=FACE_OUTER_BOUND('',#2845,.T.);
#2367=FACE_OUTER_BOUND('',#2846,.T.);
#2368=FACE_OUTER_BOUND('',#2847,.T.);
#2369=FACE_OUTER_BOUND('',#2848,.T.);
#2370=FACE_OUTER_BOUND('',#2849,.T.);
#2371=FACE_OUTER_BOUND('',#2850,.T.);
#2372=FACE_OUTER_BOUND('',#2851,.T.);
#2373=FACE_OUTER_BOUND('',#2852,.T.);
#2374=FACE_OUTER_BOUND('',#2853,.T.);
#2375=FACE_OUTER_BOUND('',#2854,.T.);
#2376=FACE_OUTER_BOUND('',#2855,.T.);
#2377=FACE_OUTER_BOUND('',#2856,.T.);
#2378=FACE_OUTER_BOUND('',#2857,.T.);
#2379=FACE_OUTER_BOUND('',#2858,.T.);
#2380=FACE_OUTER_BOUND('',#2859,.T.);
#2381=FACE_OUTER_BOUND('',#2860,.T.);
#2382=FACE_OUTER_BOUND('',#2861,.T.);
#2383=FACE_OUTER_BOUND('',#2862,.T.);
#2384=FACE_OUTER_BOUND('',#2863,.T.);
#2385=FACE_OUTER_BOUND('',#2864,.T.);
#2386=FACE_OUTER_BOUND('',#2865,.T.);
#2387=FACE_OUTER_BOUND('',#2866,.T.);
#2388=FACE_OUTER_BOUND('',#2867,.T.);
#2389=FACE_OUTER_BOUND('',#2868,.T.);
#2390=FACE_OUTER_BOUND('',#2869,.T.);
#2391=FACE_OUTER_BOUND('',#2870,.T.);
#2392=FACE_OUTER_BOUND('',#2871,.T.);
#2393=FACE_OUTER_BOUND('',#2872,.T.);
#2394=FACE_OUTER_BOUND('',#2873,.T.);
#2395=FACE_OUTER_BOUND('',#2874,.T.);
#2396=FACE_OUTER_BOUND('',#2875,.T.);
#2397=FACE_OUTER_BOUND('',#2876,.T.);
#2398=FACE_OUTER_BOUND('',#2877,.T.);
#2399=FACE_OUTER_BOUND('',#2878,.T.);
#2400=FACE_OUTER_BOUND('',#2879,.T.);
#2401=FACE_OUTER_BOUND('',#2880,.T.);
#2402=FACE_OUTER_BOUND('',#2881,.T.);
#2403=FACE_OUTER_BOUND('',#2882,.T.);
#2404=FACE_OUTER_BOUND('',#2883,.T.);
#2405=FACE_OUTER_BOUND('',#2884,.T.);
#2406=FACE_OUTER_BOUND('',#2885,.T.);
#2407=FACE_OUTER_BOUND('',#2886,.T.);
#2408=FACE_OUTER_BOUND('',#2887,.T.);
#2409=FACE_OUTER_BOUND('',#2888,.T.);
#2410=FACE_OUTER_BOUND('',#2889,.T.);
#2411=FACE_OUTER_BOUND('',#2890,.T.);
#2412=FACE_OUTER_BOUND('',#2892,.T.);
#2413=FACE_OUTER_BOUND('',#2893,.T.);
#2414=FACE_OUTER_BOUND('',#2895,.T.);
#2415=FACE_OUTER_BOUND('',#2896,.T.);
#2416=FACE_OUTER_BOUND('',#2897,.T.);
#2417=FACE_OUTER_BOUND('',#2898,.T.);
#2418=FACE_OUTER_BOUND('',#2899,.T.);
#2419=FACE_OUTER_BOUND('',#2900,.T.);
#2420=FACE_OUTER_BOUND('',#2901,.T.);
#2421=FACE_OUTER_BOUND('',#2902,.T.);
#2422=FACE_OUTER_BOUND('',#2903,.T.);
#2423=FACE_OUTER_BOUND('',#2904,.T.);
#2424=FACE_OUTER_BOUND('',#2905,.T.);
#2425=FACE_OUTER_BOUND('',#2906,.T.);
#2426=FACE_OUTER_BOUND('',#2907,.T.);
#2427=FACE_OUTER_BOUND('',#2910,.T.);
#2428=FACE_OUTER_BOUND('',#2912,.T.);
#2429=FACE_OUTER_BOUND('',#2913,.T.);
#2430=FACE_OUTER_BOUND('',#2914,.T.);
#2431=FACE_OUTER_BOUND('',#2915,.T.);
#2432=FACE_OUTER_BOUND('',#2916,.T.);
#2433=FACE_OUTER_BOUND('',#2917,.T.);
#2434=FACE_OUTER_BOUND('',#2918,.T.);
#2435=FACE_OUTER_BOUND('',#2919,.T.);
#2436=FACE_OUTER_BOUND('',#2920,.T.);
#2437=FACE_OUTER_BOUND('',#2922,.T.);
#2438=FACE_OUTER_BOUND('',#2923,.T.);
#2439=FACE_OUTER_BOUND('',#2924,.T.);
#2440=FACE_OUTER_BOUND('',#2925,.T.);
#2441=FACE_OUTER_BOUND('',#2926,.T.);
#2442=FACE_OUTER_BOUND('',#2927,.T.);
#2443=FACE_OUTER_BOUND('',#2930,.T.);
#2444=FACE_OUTER_BOUND('',#2931,.T.);
#2445=FACE_OUTER_BOUND('',#2932,.T.);
#2446=FACE_OUTER_BOUND('',#2933,.T.);
#2447=FACE_OUTER_BOUND('',#2934,.T.);
#2448=FACE_OUTER_BOUND('',#2935,.T.);
#2449=FACE_OUTER_BOUND('',#2936,.T.);
#2450=FACE_OUTER_BOUND('',#2937,.T.);
#2451=FACE_OUTER_BOUND('',#2938,.T.);
#2452=FACE_OUTER_BOUND('',#2939,.T.);
#2453=FACE_OUTER_BOUND('',#2940,.T.);
#2454=FACE_OUTER_BOUND('',#2941,.T.);
#2455=FACE_OUTER_BOUND('',#2942,.T.);
#2456=FACE_OUTER_BOUND('',#2943,.T.);
#2457=FACE_OUTER_BOUND('',#2944,.T.);
#2458=FACE_OUTER_BOUND('',#2945,.T.);
#2459=FACE_OUTER_BOUND('',#2946,.T.);
#2460=FACE_OUTER_BOUND('',#2947,.T.);
#2461=FACE_OUTER_BOUND('',#2948,.T.);
#2462=FACE_OUTER_BOUND('',#2949,.T.);
#2463=FACE_OUTER_BOUND('',#2950,.T.);
#2464=FACE_OUTER_BOUND('',#2951,.T.);
#2465=FACE_OUTER_BOUND('',#2952,.T.);
#2466=FACE_OUTER_BOUND('',#2953,.T.);
#2467=FACE_OUTER_BOUND('',#2954,.T.);
#2468=FACE_OUTER_BOUND('',#2955,.T.);
#2469=FACE_OUTER_BOUND('',#2956,.T.);
#2470=FACE_OUTER_BOUND('',#2958,.T.);
#2471=FACE_OUTER_BOUND('',#2959,.T.);
#2472=FACE_OUTER_BOUND('',#2960,.T.);
#2473=FACE_OUTER_BOUND('',#2961,.T.);
#2474=FACE_OUTER_BOUND('',#2962,.T.);
#2475=FACE_OUTER_BOUND('',#2963,.T.);
#2476=FACE_OUTER_BOUND('',#2964,.T.);
#2477=FACE_OUTER_BOUND('',#2966,.T.);
#2478=FACE_OUTER_BOUND('',#2969,.T.);
#2479=FACE_OUTER_BOUND('',#2970,.T.);
#2480=FACE_OUTER_BOUND('',#2971,.T.);
#2481=FACE_OUTER_BOUND('',#2972,.T.);
#2482=FACE_OUTER_BOUND('',#2973,.T.);
#2483=FACE_OUTER_BOUND('',#2974,.T.);
#2484=FACE_OUTER_BOUND('',#2975,.T.);
#2485=FACE_OUTER_BOUND('',#2977,.T.);
#2486=FACE_OUTER_BOUND('',#2980,.T.);
#2487=FACE_OUTER_BOUND('',#2981,.T.);
#2488=FACE_OUTER_BOUND('',#2982,.T.);
#2489=FACE_OUTER_BOUND('',#2983,.T.);
#2490=FACE_OUTER_BOUND('',#2984,.T.);
#2491=FACE_OUTER_BOUND('',#2986,.T.);
#2492=FACE_OUTER_BOUND('',#2987,.T.);
#2493=FACE_OUTER_BOUND('',#2988,.T.);
#2494=FACE_OUTER_BOUND('',#2989,.T.);
#2495=FACE_OUTER_BOUND('',#2990,.T.);
#2496=FACE_OUTER_BOUND('',#2991,.T.);
#2497=FACE_OUTER_BOUND('',#2994,.T.);
#2498=FACE_OUTER_BOUND('',#2995,.T.);
#2499=FACE_OUTER_BOUND('',#2998,.T.);
#2500=FACE_OUTER_BOUND('',#3000,.T.);
#2501=FACE_OUTER_BOUND('',#3001,.T.);
#2502=FACE_OUTER_BOUND('',#3002,.T.);
#2503=FACE_OUTER_BOUND('',#3003,.T.);
#2504=FACE_OUTER_BOUND('',#3004,.T.);
#2505=FACE_OUTER_BOUND('',#3005,.T.);
#2506=FACE_OUTER_BOUND('',#3006,.T.);
#2507=FACE_OUTER_BOUND('',#3007,.T.);
#2508=FACE_OUTER_BOUND('',#3008,.T.);
#2509=FACE_OUTER_BOUND('',#3009,.T.);
#2510=FACE_OUTER_BOUND('',#3010,.T.);
#2511=FACE_OUTER_BOUND('',#3011,.T.);
#2512=FACE_OUTER_BOUND('',#3012,.T.);
#2513=FACE_OUTER_BOUND('',#3015,.T.);
#2514=FACE_OUTER_BOUND('',#3016,.T.);
#2515=FACE_OUTER_BOUND('',#3019,.T.);
#2516=FACE_OUTER_BOUND('',#3020,.T.);
#2517=FACE_OUTER_BOUND('',#3021,.T.);
#2518=FACE_OUTER_BOUND('',#3022,.T.);
#2519=FACE_OUTER_BOUND('',#3023,.T.);
#2520=FACE_OUTER_BOUND('',#3024,.T.);
#2521=FACE_OUTER_BOUND('',#3025,.T.);
#2522=FACE_OUTER_BOUND('',#3026,.T.);
#2523=FACE_OUTER_BOUND('',#3027,.T.);
#2524=FACE_OUTER_BOUND('',#3028,.T.);
#2525=FACE_OUTER_BOUND('',#3029,.T.);
#2526=FACE_OUTER_BOUND('',#3031,.T.);
#2527=FACE_OUTER_BOUND('',#3032,.T.);
#2528=FACE_OUTER_BOUND('',#3033,.T.);
#2529=FACE_OUTER_BOUND('',#3034,.T.);
#2530=FACE_OUTER_BOUND('',#3037,.T.);
#2531=FACE_OUTER_BOUND('',#3038,.T.);
#2532=FACE_OUTER_BOUND('',#3041,.T.);
#2533=FACE_OUTER_BOUND('',#3042,.T.);
#2534=FACE_OUTER_BOUND('',#3043,.T.);
#2535=FACE_OUTER_BOUND('',#3044,.T.);
#2536=FACE_OUTER_BOUND('',#3045,.T.);
#2537=FACE_OUTER_BOUND('',#3046,.T.);
#2538=FACE_OUTER_BOUND('',#3047,.T.);
#2539=FACE_OUTER_BOUND('',#3048,.T.);
#2540=FACE_OUTER_BOUND('',#3049,.T.);
#2541=FACE_OUTER_BOUND('',#3050,.T.);
#2542=FACE_OUTER_BOUND('',#3051,.T.);
#2543=FACE_OUTER_BOUND('',#3052,.T.);
#2544=FACE_OUTER_BOUND('',#3053,.T.);
#2545=FACE_OUTER_BOUND('',#3054,.T.);
#2546=FACE_OUTER_BOUND('',#3055,.T.);
#2547=FACE_OUTER_BOUND('',#3056,.T.);
#2548=FACE_OUTER_BOUND('',#3057,.T.);
#2549=FACE_OUTER_BOUND('',#3058,.T.);
#2550=FACE_OUTER_BOUND('',#3059,.T.);
#2551=FACE_OUTER_BOUND('',#3060,.T.);
#2552=FACE_OUTER_BOUND('',#3061,.T.);
#2553=FACE_OUTER_BOUND('',#3062,.T.);
#2554=FACE_OUTER_BOUND('',#3063,.T.);
#2555=FACE_OUTER_BOUND('',#3064,.T.);
#2556=FACE_OUTER_BOUND('',#3065,.T.);
#2557=FACE_OUTER_BOUND('',#3066,.T.);
#2558=FACE_OUTER_BOUND('',#3067,.T.);
#2559=FACE_OUTER_BOUND('',#3068,.T.);
#2560=FACE_OUTER_BOUND('',#3069,.T.);
#2561=FACE_OUTER_BOUND('',#3070,.T.);
#2562=FACE_OUTER_BOUND('',#3071,.T.);
#2563=FACE_OUTER_BOUND('',#3072,.T.);
#2564=FACE_OUTER_BOUND('',#3074,.T.);
#2565=FACE_OUTER_BOUND('',#3075,.T.);
#2566=FACE_OUTER_BOUND('',#3076,.T.);
#2567=FACE_OUTER_BOUND('',#3077,.T.);
#2568=FACE_OUTER_BOUND('',#3078,.T.);
#2569=FACE_OUTER_BOUND('',#3079,.T.);
#2570=FACE_OUTER_BOUND('',#3080,.T.);
#2571=FACE_OUTER_BOUND('',#3082,.T.);
#2572=FACE_OUTER_BOUND('',#3085,.T.);
#2573=FACE_OUTER_BOUND('',#3086,.T.);
#2574=FACE_OUTER_BOUND('',#3087,.T.);
#2575=FACE_OUTER_BOUND('',#3088,.T.);
#2576=FACE_OUTER_BOUND('',#3089,.T.);
#2577=FACE_OUTER_BOUND('',#3090,.T.);
#2578=FACE_OUTER_BOUND('',#3091,.T.);
#2579=FACE_OUTER_BOUND('',#3093,.T.);
#2580=EDGE_LOOP('',(#8972,#8973,#8974,#8975));
#2581=EDGE_LOOP('',(#8976,#8977,#8978,#8979));
#2582=EDGE_LOOP('',(#8980,#8981,#8982,#8983));
#2583=EDGE_LOOP('',(#8984,#8985,#8986,#8987));
#2584=EDGE_LOOP('',(#8988,#8989,#8990,#8991));
#2585=EDGE_LOOP('',(#8992,#8993,#8994,#8995));
#2586=EDGE_LOOP('',(#8996,#8997,#8998,#8999,#9000,#9001));
#2587=EDGE_LOOP('',(#9002));
#2588=EDGE_LOOP('',(#9003));
#2589=EDGE_LOOP('',(#9004,#9005,#9006,#9007));
#2590=EDGE_LOOP('',(#9008,#9009,#9010,#9011,#9012,#9013));
#2591=EDGE_LOOP('',(#9014));
#2592=EDGE_LOOP('',(#9015));
#2593=EDGE_LOOP('',(#9016,#9017,#9018,#9019));
#2594=EDGE_LOOP('',(#9020,#9021,#9022,#9023));
#2595=EDGE_LOOP('',(#9024,#9025,#9026,#9027));
#2596=EDGE_LOOP('',(#9028,#9029,#9030,#9031));
#2597=EDGE_LOOP('',(#9032,#9033,#9034,#9035));
#2598=EDGE_LOOP('',(#9036,#9037,#9038,#9039,#9040,#9041,#9042,#9043,#9044,
#9045,#9046,#9047));
#2599=EDGE_LOOP('',(#9048,#9049,#9050,#9051));
#2600=EDGE_LOOP('',(#9052,#9053,#9054,#9055));
#2601=EDGE_LOOP('',(#9056,#9057,#9058,#9059));
#2602=EDGE_LOOP('',(#9060,#9061,#9062,#9063));
#2603=EDGE_LOOP('',(#9064,#9065,#9066,#9067,#9068,#9069,#9070,#9071));
#2604=EDGE_LOOP('',(#9072,#9073,#9074,#9075));
#2605=EDGE_LOOP('',(#9076,#9077,#9078,#9079));
#2606=EDGE_LOOP('',(#9080,#9081,#9082,#9083,#9084,#9085,#9086,#9087));
#2607=EDGE_LOOP('',(#9088,#9089,#9090,#9091));
#2608=EDGE_LOOP('',(#9092,#9093,#9094,#9095,#9096,#9097));
#2609=EDGE_LOOP('',(#9098));
#2610=EDGE_LOOP('',(#9099));
#2611=EDGE_LOOP('',(#9100,#9101,#9102,#9103));
#2612=EDGE_LOOP('',(#9104,#9105,#9106,#9107,#9108,#9109));
#2613=EDGE_LOOP('',(#9110));
#2614=EDGE_LOOP('',(#9111));
#2615=EDGE_LOOP('',(#9112,#9113,#9114,#9115,#9116,#9117,#9118,#9119,#9120,
#9121,#9122,#9123));
#2616=EDGE_LOOP('',(#9124,#9125,#9126,#9127));
#2617=EDGE_LOOP('',(#9128,#9129,#9130,#9131));
#2618=EDGE_LOOP('',(#9132,#9133,#9134,#9135));
#2619=EDGE_LOOP('',(#9136,#9137,#9138,#9139));
#2620=EDGE_LOOP('',(#9140,#9141,#9142,#9143));
#2621=EDGE_LOOP('',(#9144,#9145,#9146,#9147,#9148,#9149));
#2622=EDGE_LOOP('',(#9150,#9151,#9152,#9153,#9154,#9155));
#2623=EDGE_LOOP('',(#9156,#9157,#9158,#9159,#9160,#9161));
#2624=EDGE_LOOP('',(#9162,#9163,#9164,#9165,#9166,#9167));
#2625=EDGE_LOOP('',(#9168,#9169,#9170,#9171,#9172,#9173));
#2626=EDGE_LOOP('',(#9174,#9175,#9176,#9177,#9178,#9179));
#2627=EDGE_LOOP('',(#9180,#9181,#9182,#9183,#9184,#9185));
#2628=EDGE_LOOP('',(#9186,#9187,#9188,#9189,#9190,#9191));
#2629=EDGE_LOOP('',(#9192,#9193,#9194,#9195,#9196,#9197));
#2630=EDGE_LOOP('',(#9198,#9199,#9200,#9201,#9202,#9203));
#2631=EDGE_LOOP('',(#9204,#9205,#9206,#9207,#9208,#9209));
#2632=EDGE_LOOP('',(#9210,#9211,#9212,#9213,#9214,#9215));
#2633=EDGE_LOOP('',(#9216,#9217,#9218,#9219,#9220,#9221));
#2634=EDGE_LOOP('',(#9222,#9223,#9224,#9225,#9226,#9227));
#2635=EDGE_LOOP('',(#9228,#9229,#9230,#9231,#9232,#9233));
#2636=EDGE_LOOP('',(#9234,#9235,#9236,#9237,#9238,#9239));
#2637=EDGE_LOOP('',(#9240,#9241,#9242,#9243,#9244,#9245));
#2638=EDGE_LOOP('',(#9246,#9247,#9248,#9249,#9250,#9251));
#2639=EDGE_LOOP('',(#9252,#9253,#9254,#9255,#9256,#9257));
#2640=EDGE_LOOP('',(#9258,#9259,#9260,#9261,#9262,#9263));
#2641=EDGE_LOOP('',(#9264,#9265,#9266,#9267,#9268,#9269));
#2642=EDGE_LOOP('',(#9270,#9271,#9272,#9273,#9274,#9275));
#2643=EDGE_LOOP('',(#9276,#9277,#9278,#9279,#9280,#9281));
#2644=EDGE_LOOP('',(#9282,#9283,#9284,#9285,#9286,#9287));
#2645=EDGE_LOOP('',(#9288,#9289,#9290,#9291,#9292,#9293));
#2646=EDGE_LOOP('',(#9294,#9295,#9296,#9297,#9298,#9299));
#2647=EDGE_LOOP('',(#9300,#9301,#9302,#9303,#9304,#9305));
#2648=EDGE_LOOP('',(#9306,#9307,#9308,#9309,#9310,#9311));
#2649=EDGE_LOOP('',(#9312,#9313,#9314,#9315,#9316,#9317));
#2650=EDGE_LOOP('',(#9318,#9319,#9320,#9321,#9322,#9323));
#2651=EDGE_LOOP('',(#9324,#9325,#9326,#9327,#9328,#9329));
#2652=EDGE_LOOP('',(#9330,#9331,#9332,#9333,#9334,#9335));
#2653=EDGE_LOOP('',(#9336,#9337,#9338,#9339,#9340,#9341));
#2654=EDGE_LOOP('',(#9342,#9343,#9344,#9345,#9346,#9347));
#2655=EDGE_LOOP('',(#9348,#9349,#9350,#9351,#9352,#9353));
#2656=EDGE_LOOP('',(#9354,#9355,#9356,#9357,#9358,#9359));
#2657=EDGE_LOOP('',(#9360,#9361,#9362,#9363,#9364,#9365));
#2658=EDGE_LOOP('',(#9366,#9367,#9368,#9369,#9370,#9371));
#2659=EDGE_LOOP('',(#9372,#9373,#9374,#9375,#9376,#9377));
#2660=EDGE_LOOP('',(#9378,#9379,#9380,#9381,#9382,#9383));
#2661=EDGE_LOOP('',(#9384,#9385,#9386,#9387,#9388,#9389));
#2662=EDGE_LOOP('',(#9390,#9391,#9392,#9393,#9394,#9395));
#2663=EDGE_LOOP('',(#9396,#9397,#9398,#9399,#9400,#9401));
#2664=EDGE_LOOP('',(#9402,#9403,#9404,#9405,#9406,#9407));
#2665=EDGE_LOOP('',(#9408,#9409,#9410,#9411,#9412,#9413));
#2666=EDGE_LOOP('',(#9414,#9415,#9416,#9417,#9418,#9419));
#2667=EDGE_LOOP('',(#9420,#9421,#9422,#9423,#9424,#9425));
#2668=EDGE_LOOP('',(#9426,#9427,#9428,#9429,#9430,#9431));
#2669=EDGE_LOOP('',(#9432,#9433,#9434,#9435,#9436,#9437));
#2670=EDGE_LOOP('',(#9438,#9439,#9440,#9441,#9442,#9443));
#2671=EDGE_LOOP('',(#9444,#9445,#9446,#9447,#9448,#9449));
#2672=EDGE_LOOP('',(#9450,#9451,#9452,#9453,#9454,#9455));
#2673=EDGE_LOOP('',(#9456,#9457,#9458,#9459,#9460,#9461));
#2674=EDGE_LOOP('',(#9462,#9463,#9464,#9465,#9466,#9467));
#2675=EDGE_LOOP('',(#9468,#9469,#9470,#9471,#9472,#9473));
#2676=EDGE_LOOP('',(#9474,#9475,#9476,#9477,#9478,#9479));
#2677=EDGE_LOOP('',(#9480,#9481,#9482,#9483,#9484,#9485));
#2678=EDGE_LOOP('',(#9486,#9487,#9488,#9489,#9490,#9491));
#2679=EDGE_LOOP('',(#9492,#9493,#9494,#9495,#9496,#9497));
#2680=EDGE_LOOP('',(#9498,#9499,#9500,#9501,#9502,#9503));
#2681=EDGE_LOOP('',(#9504,#9505,#9506,#9507,#9508,#9509));
#2682=EDGE_LOOP('',(#9510,#9511,#9512,#9513,#9514,#9515));
#2683=EDGE_LOOP('',(#9516,#9517,#9518,#9519,#9520,#9521));
#2684=EDGE_LOOP('',(#9522,#9523,#9524,#9525,#9526,#9527));
#2685=EDGE_LOOP('',(#9528,#9529,#9530,#9531,#9532,#9533));
#2686=EDGE_LOOP('',(#9534,#9535,#9536,#9537,#9538,#9539));
#2687=EDGE_LOOP('',(#9540,#9541,#9542,#9543,#9544,#9545));
#2688=EDGE_LOOP('',(#9546,#9547,#9548,#9549,#9550,#9551));
#2689=EDGE_LOOP('',(#9552,#9553,#9554,#9555,#9556,#9557));
#2690=EDGE_LOOP('',(#9558,#9559,#9560,#9561,#9562,#9563));
#2691=EDGE_LOOP('',(#9564,#9565,#9566,#9567,#9568,#9569));
#2692=EDGE_LOOP('',(#9570,#9571,#9572,#9573,#9574,#9575));
#2693=EDGE_LOOP('',(#9576,#9577,#9578,#9579,#9580,#9581));
#2694=EDGE_LOOP('',(#9582,#9583,#9584,#9585,#9586,#9587));
#2695=EDGE_LOOP('',(#9588,#9589,#9590,#9591,#9592,#9593));
#2696=EDGE_LOOP('',(#9594,#9595,#9596,#9597,#9598,#9599));
#2697=EDGE_LOOP('',(#9600,#9601,#9602,#9603,#9604,#9605));
#2698=EDGE_LOOP('',(#9606,#9607,#9608,#9609,#9610,#9611));
#2699=EDGE_LOOP('',(#9612,#9613,#9614,#9615,#9616,#9617));
#2700=EDGE_LOOP('',(#9618,#9619,#9620,#9621,#9622,#9623));
#2701=EDGE_LOOP('',(#9624,#9625,#9626,#9627,#9628,#9629));
#2702=EDGE_LOOP('',(#9630,#9631,#9632,#9633,#9634,#9635));
#2703=EDGE_LOOP('',(#9636,#9637,#9638,#9639,#9640,#9641));
#2704=EDGE_LOOP('',(#9642,#9643,#9644,#9645,#9646,#9647));
#2705=EDGE_LOOP('',(#9648,#9649,#9650,#9651,#9652,#9653));
#2706=EDGE_LOOP('',(#9654,#9655,#9656,#9657,#9658,#9659));
#2707=EDGE_LOOP('',(#9660,#9661,#9662,#9663,#9664,#9665));
#2708=EDGE_LOOP('',(#9666,#9667,#9668,#9669,#9670,#9671));
#2709=EDGE_LOOP('',(#9672,#9673,#9674,#9675,#9676,#9677));
#2710=EDGE_LOOP('',(#9678,#9679,#9680,#9681,#9682,#9683));
#2711=EDGE_LOOP('',(#9684,#9685,#9686,#9687,#9688,#9689));
#2712=EDGE_LOOP('',(#9690,#9691,#9692,#9693,#9694,#9695));
#2713=EDGE_LOOP('',(#9696,#9697,#9698,#9699,#9700,#9701));
#2714=EDGE_LOOP('',(#9702,#9703,#9704,#9705,#9706,#9707));
#2715=EDGE_LOOP('',(#9708,#9709,#9710,#9711,#9712,#9713));
#2716=EDGE_LOOP('',(#9714,#9715,#9716,#9717,#9718,#9719));
#2717=EDGE_LOOP('',(#9720,#9721,#9722,#9723,#9724,#9725));
#2718=EDGE_LOOP('',(#9726,#9727,#9728,#9729,#9730,#9731));
#2719=EDGE_LOOP('',(#9732,#9733,#9734,#9735,#9736,#9737));
#2720=EDGE_LOOP('',(#9738,#9739,#9740,#9741,#9742,#9743));
#2721=EDGE_LOOP('',(#9744,#9745,#9746,#9747,#9748,#9749));
#2722=EDGE_LOOP('',(#9750,#9751,#9752,#9753,#9754,#9755));
#2723=EDGE_LOOP('',(#9756,#9757,#9758,#9759,#9760,#9761));
#2724=EDGE_LOOP('',(#9762,#9763,#9764,#9765,#9766,#9767));
#2725=EDGE_LOOP('',(#9768,#9769,#9770,#9771,#9772,#9773));
#2726=EDGE_LOOP('',(#9774,#9775,#9776,#9777,#9778,#9779));
#2727=EDGE_LOOP('',(#9780,#9781,#9782,#9783,#9784,#9785));
#2728=EDGE_LOOP('',(#9786,#9787,#9788,#9789,#9790,#9791));
#2729=EDGE_LOOP('',(#9792,#9793,#9794,#9795,#9796,#9797));
#2730=EDGE_LOOP('',(#9798,#9799,#9800,#9801,#9802,#9803));
#2731=EDGE_LOOP('',(#9804,#9805,#9806,#9807,#9808,#9809));
#2732=EDGE_LOOP('',(#9810,#9811,#9812,#9813,#9814,#9815));
#2733=EDGE_LOOP('',(#9816,#9817,#9818,#9819,#9820,#9821));
#2734=EDGE_LOOP('',(#9822,#9823,#9824,#9825,#9826,#9827));
#2735=EDGE_LOOP('',(#9828,#9829,#9830,#9831,#9832,#9833));
#2736=EDGE_LOOP('',(#9834,#9835,#9836,#9837,#9838,#9839));
#2737=EDGE_LOOP('',(#9840,#9841,#9842,#9843,#9844,#9845));
#2738=EDGE_LOOP('',(#9846,#9847,#9848,#9849,#9850,#9851));
#2739=EDGE_LOOP('',(#9852,#9853,#9854,#9855,#9856,#9857));
#2740=EDGE_LOOP('',(#9858,#9859,#9860,#9861,#9862,#9863));
#2741=EDGE_LOOP('',(#9864,#9865,#9866,#9867,#9868,#9869));
#2742=EDGE_LOOP('',(#9870,#9871,#9872,#9873,#9874,#9875));
#2743=EDGE_LOOP('',(#9876,#9877,#9878,#9879,#9880,#9881));
#2744=EDGE_LOOP('',(#9882,#9883,#9884,#9885,#9886,#9887));
#2745=EDGE_LOOP('',(#9888,#9889,#9890,#9891,#9892,#9893));
#2746=EDGE_LOOP('',(#9894,#9895,#9896,#9897,#9898,#9899));
#2747=EDGE_LOOP('',(#9900,#9901,#9902,#9903,#9904,#9905));
#2748=EDGE_LOOP('',(#9906,#9907,#9908,#9909,#9910,#9911));
#2749=EDGE_LOOP('',(#9912,#9913,#9914,#9915,#9916,#9917));
#2750=EDGE_LOOP('',(#9918,#9919,#9920,#9921,#9922,#9923));
#2751=EDGE_LOOP('',(#9924,#9925,#9926,#9927,#9928,#9929));
#2752=EDGE_LOOP('',(#9930,#9931,#9932,#9933,#9934,#9935));
#2753=EDGE_LOOP('',(#9936,#9937,#9938,#9939,#9940,#9941));
#2754=EDGE_LOOP('',(#9942,#9943,#9944,#9945,#9946,#9947));
#2755=EDGE_LOOP('',(#9948,#9949,#9950,#9951,#9952,#9953));
#2756=EDGE_LOOP('',(#9954,#9955,#9956,#9957,#9958,#9959));
#2757=EDGE_LOOP('',(#9960,#9961,#9962,#9963,#9964,#9965));
#2758=EDGE_LOOP('',(#9966,#9967,#9968,#9969,#9970,#9971));
#2759=EDGE_LOOP('',(#9972,#9973,#9974,#9975,#9976,#9977));
#2760=EDGE_LOOP('',(#9978,#9979,#9980,#9981,#9982,#9983));
#2761=EDGE_LOOP('',(#9984,#9985,#9986,#9987,#9988,#9989));
#2762=EDGE_LOOP('',(#9990,#9991,#9992,#9993,#9994,#9995));
#2763=EDGE_LOOP('',(#9996,#9997,#9998,#9999,#10000,#10001));
#2764=EDGE_LOOP('',(#10002,#10003,#10004,#10005,#10006,#10007));
#2765=EDGE_LOOP('',(#10008,#10009,#10010,#10011,#10012,#10013));
#2766=EDGE_LOOP('',(#10014,#10015,#10016,#10017,#10018,#10019));
#2767=EDGE_LOOP('',(#10020,#10021,#10022,#10023,#10024,#10025));
#2768=EDGE_LOOP('',(#10026,#10027,#10028,#10029,#10030,#10031));
#2769=EDGE_LOOP('',(#10032,#10033,#10034,#10035,#10036,#10037));
#2770=EDGE_LOOP('',(#10038,#10039,#10040,#10041,#10042,#10043));
#2771=EDGE_LOOP('',(#10044,#10045,#10046,#10047,#10048,#10049));
#2772=EDGE_LOOP('',(#10050,#10051,#10052,#10053,#10054,#10055));
#2773=EDGE_LOOP('',(#10056,#10057,#10058,#10059,#10060,#10061));
#2774=EDGE_LOOP('',(#10062,#10063,#10064,#10065,#10066,#10067));
#2775=EDGE_LOOP('',(#10068,#10069,#10070,#10071,#10072,#10073));
#2776=EDGE_LOOP('',(#10074,#10075,#10076,#10077,#10078,#10079));
#2777=EDGE_LOOP('',(#10080,#10081,#10082,#10083,#10084,#10085));
#2778=EDGE_LOOP('',(#10086,#10087,#10088,#10089,#10090,#10091));
#2779=EDGE_LOOP('',(#10092,#10093,#10094,#10095,#10096,#10097));
#2780=EDGE_LOOP('',(#10098,#10099,#10100,#10101,#10102,#10103));
#2781=EDGE_LOOP('',(#10104,#10105,#10106,#10107,#10108,#10109));
#2782=EDGE_LOOP('',(#10110,#10111,#10112,#10113,#10114,#10115));
#2783=EDGE_LOOP('',(#10116,#10117,#10118,#10119,#10120,#10121));
#2784=EDGE_LOOP('',(#10122,#10123,#10124,#10125,#10126,#10127));
#2785=EDGE_LOOP('',(#10128,#10129,#10130,#10131,#10132,#10133));
#2786=EDGE_LOOP('',(#10134,#10135,#10136,#10137,#10138,#10139));
#2787=EDGE_LOOP('',(#10140,#10141,#10142,#10143,#10144,#10145));
#2788=EDGE_LOOP('',(#10146,#10147,#10148,#10149,#10150,#10151));
#2789=EDGE_LOOP('',(#10152,#10153,#10154,#10155,#10156,#10157));
#2790=EDGE_LOOP('',(#10158,#10159,#10160,#10161,#10162,#10163));
#2791=EDGE_LOOP('',(#10164,#10165,#10166,#10167,#10168,#10169));
#2792=EDGE_LOOP('',(#10170,#10171,#10172,#10173,#10174,#10175));
#2793=EDGE_LOOP('',(#10176,#10177,#10178,#10179,#10180,#10181));
#2794=EDGE_LOOP('',(#10182,#10183,#10184,#10185,#10186,#10187));
#2795=EDGE_LOOP('',(#10188,#10189,#10190,#10191,#10192,#10193));
#2796=EDGE_LOOP('',(#10194,#10195,#10196,#10197,#10198,#10199));
#2797=EDGE_LOOP('',(#10200,#10201,#10202,#10203,#10204,#10205));
#2798=EDGE_LOOP('',(#10206,#10207,#10208,#10209,#10210,#10211));
#2799=EDGE_LOOP('',(#10212,#10213,#10214,#10215,#10216,#10217));
#2800=EDGE_LOOP('',(#10218,#10219,#10220,#10221,#10222,#10223));
#2801=EDGE_LOOP('',(#10224,#10225,#10226,#10227,#10228,#10229));
#2802=EDGE_LOOP('',(#10230,#10231,#10232,#10233,#10234,#10235));
#2803=EDGE_LOOP('',(#10236,#10237,#10238,#10239,#10240,#10241));
#2804=EDGE_LOOP('',(#10242,#10243,#10244,#10245,#10246,#10247));
#2805=EDGE_LOOP('',(#10248,#10249,#10250,#10251,#10252,#10253));
#2806=EDGE_LOOP('',(#10254,#10255,#10256,#10257,#10258,#10259));
#2807=EDGE_LOOP('',(#10260,#10261,#10262,#10263,#10264,#10265));
#2808=EDGE_LOOP('',(#10266,#10267,#10268,#10269,#10270,#10271));
#2809=EDGE_LOOP('',(#10272,#10273,#10274,#10275,#10276,#10277));
#2810=EDGE_LOOP('',(#10278,#10279,#10280,#10281,#10282,#10283));
#2811=EDGE_LOOP('',(#10284,#10285,#10286,#10287,#10288,#10289));
#2812=EDGE_LOOP('',(#10290,#10291,#10292,#10293,#10294,#10295));
#2813=EDGE_LOOP('',(#10296,#10297,#10298,#10299,#10300,#10301));
#2814=EDGE_LOOP('',(#10302,#10303,#10304,#10305,#10306,#10307));
#2815=EDGE_LOOP('',(#10308,#10309,#10310,#10311,#10312,#10313));
#2816=EDGE_LOOP('',(#10314,#10315,#10316,#10317,#10318,#10319));
#2817=EDGE_LOOP('',(#10320,#10321,#10322,#10323,#10324,#10325));
#2818=EDGE_LOOP('',(#10326,#10327,#10328,#10329,#10330,#10331));
#2819=EDGE_LOOP('',(#10332,#10333,#10334,#10335,#10336,#10337));
#2820=EDGE_LOOP('',(#10338,#10339,#10340,#10341,#10342,#10343));
#2821=EDGE_LOOP('',(#10344,#10345,#10346,#10347,#10348,#10349));
#2822=EDGE_LOOP('',(#10350,#10351,#10352,#10353,#10354,#10355));
#2823=EDGE_LOOP('',(#10356,#10357,#10358,#10359,#10360,#10361));
#2824=EDGE_LOOP('',(#10362,#10363,#10364,#10365,#10366,#10367));
#2825=EDGE_LOOP('',(#10368,#10369,#10370,#10371,#10372,#10373));
#2826=EDGE_LOOP('',(#10374,#10375,#10376,#10377,#10378,#10379));
#2827=EDGE_LOOP('',(#10380,#10381,#10382,#10383,#10384,#10385));
#2828=EDGE_LOOP('',(#10386,#10387,#10388,#10389,#10390,#10391));
#2829=EDGE_LOOP('',(#10392,#10393,#10394,#10395,#10396,#10397));
#2830=EDGE_LOOP('',(#10398,#10399,#10400,#10401,#10402,#10403));
#2831=EDGE_LOOP('',(#10404,#10405,#10406,#10407,#10408,#10409));
#2832=EDGE_LOOP('',(#10410,#10411,#10412,#10413,#10414,#10415));
#2833=EDGE_LOOP('',(#10416,#10417,#10418,#10419,#10420,#10421));
#2834=EDGE_LOOP('',(#10422,#10423,#10424,#10425,#10426,#10427));
#2835=EDGE_LOOP('',(#10428,#10429,#10430,#10431,#10432,#10433));
#2836=EDGE_LOOP('',(#10434,#10435,#10436,#10437,#10438,#10439));
#2837=EDGE_LOOP('',(#10440,#10441,#10442,#10443,#10444,#10445));
#2838=EDGE_LOOP('',(#10446,#10447,#10448,#10449,#10450,#10451));
#2839=EDGE_LOOP('',(#10452,#10453,#10454,#10455,#10456,#10457));
#2840=EDGE_LOOP('',(#10458,#10459,#10460,#10461,#10462,#10463));
#2841=EDGE_LOOP('',(#10464,#10465,#10466,#10467,#10468,#10469));
#2842=EDGE_LOOP('',(#10470,#10471,#10472,#10473,#10474,#10475));
#2843=EDGE_LOOP('',(#10476,#10477,#10478,#10479,#10480,#10481));
#2844=EDGE_LOOP('',(#10482,#10483,#10484,#10485,#10486,#10487));
#2845=EDGE_LOOP('',(#10488,#10489,#10490,#10491,#10492,#10493));
#2846=EDGE_LOOP('',(#10494,#10495,#10496,#10497,#10498,#10499));
#2847=EDGE_LOOP('',(#10500,#10501,#10502,#10503,#10504,#10505));
#2848=EDGE_LOOP('',(#10506,#10507,#10508,#10509,#10510,#10511));
#2849=EDGE_LOOP('',(#10512,#10513,#10514,#10515,#10516,#10517));
#2850=EDGE_LOOP('',(#10518,#10519,#10520,#10521,#10522,#10523));
#2851=EDGE_LOOP('',(#10524,#10525,#10526,#10527,#10528,#10529));
#2852=EDGE_LOOP('',(#10530,#10531,#10532,#10533,#10534,#10535));
#2853=EDGE_LOOP('',(#10536,#10537,#10538,#10539,#10540,#10541));
#2854=EDGE_LOOP('',(#10542,#10543,#10544,#10545,#10546,#10547));
#2855=EDGE_LOOP('',(#10548,#10549,#10550,#10551,#10552,#10553));
#2856=EDGE_LOOP('',(#10554,#10555,#10556,#10557,#10558,#10559));
#2857=EDGE_LOOP('',(#10560,#10561,#10562,#10563,#10564,#10565));
#2858=EDGE_LOOP('',(#10566,#10567,#10568,#10569,#10570,#10571));
#2859=EDGE_LOOP('',(#10572,#10573,#10574,#10575,#10576,#10577));
#2860=EDGE_LOOP('',(#10578,#10579,#10580,#10581,#10582,#10583));
#2861=EDGE_LOOP('',(#10584,#10585,#10586,#10587,#10588,#10589));
#2862=EDGE_LOOP('',(#10590,#10591,#10592,#10593,#10594,#10595));
#2863=EDGE_LOOP('',(#10596,#10597,#10598,#10599,#10600,#10601));
#2864=EDGE_LOOP('',(#10602,#10603,#10604,#10605,#10606,#10607));
#2865=EDGE_LOOP('',(#10608,#10609,#10610,#10611,#10612,#10613));
#2866=EDGE_LOOP('',(#10614,#10615,#10616,#10617,#10618,#10619));
#2867=EDGE_LOOP('',(#10620,#10621,#10622,#10623,#10624,#10625));
#2868=EDGE_LOOP('',(#10626,#10627,#10628,#10629,#10630,#10631));
#2869=EDGE_LOOP('',(#10632,#10633,#10634,#10635,#10636,#10637));
#2870=EDGE_LOOP('',(#10638,#10639,#10640,#10641,#10642,#10643));
#2871=EDGE_LOOP('',(#10644,#10645,#10646,#10647,#10648,#10649));
#2872=EDGE_LOOP('',(#10650,#10651,#10652,#10653,#10654,#10655));
#2873=EDGE_LOOP('',(#10656,#10657,#10658,#10659,#10660,#10661));
#2874=EDGE_LOOP('',(#10662,#10663,#10664,#10665,#10666,#10667));
#2875=EDGE_LOOP('',(#10668,#10669,#10670,#10671,#10672,#10673));
#2876=EDGE_LOOP('',(#10674,#10675,#10676,#10677,#10678,#10679));
#2877=EDGE_LOOP('',(#10680,#10681,#10682,#10683,#10684,#10685));
#2878=EDGE_LOOP('',(#10686,#10687,#10688,#10689,#10690,#10691));
#2879=EDGE_LOOP('',(#10692,#10693,#10694,#10695,#10696,#10697));
#2880=EDGE_LOOP('',(#10698,#10699,#10700,#10701,#10702,#10703));
#2881=EDGE_LOOP('',(#10704,#10705,#10706,#10707,#10708,#10709));
#2882=EDGE_LOOP('',(#10710,#10711,#10712,#10713,#10714,#10715));
#2883=EDGE_LOOP('',(#10716,#10717,#10718,#10719,#10720,#10721));
#2884=EDGE_LOOP('',(#10722,#10723,#10724,#10725,#10726,#10727));
#2885=EDGE_LOOP('',(#10728,#10729,#10730,#10731,#10732,#10733));
#2886=EDGE_LOOP('',(#10734,#10735,#10736,#10737,#10738,#10739));
#2887=EDGE_LOOP('',(#10740,#10741,#10742,#10743,#10744,#10745));
#2888=EDGE_LOOP('',(#10746,#10747,#10748,#10749,#10750,#10751,#10752,#10753,
#10754,#10755,#10756,#10757,#10758,#10759,#10760,#10761,#10762,#10763,#10764,
#10765,#10766,#10767,#10768,#10769,#10770,#10771,#10772,#10773,#10774,#10775,
#10776,#10777,#10778,#10779,#10780,#10781,#10782,#10783,#10784,#10785,#10786,
#10787,#10788,#10789,#10790,#10791,#10792,#10793,#10794,#10795,#10796,#10797,
#10798,#10799,#10800,#10801,#10802,#10803,#10804,#10805,#10806,#10807,#10808,
#10809,#10810,#10811,#10812,#10813,#10814,#10815,#10816,#10817,#10818,#10819,
#10820,#10821,#10822,#10823,#10824,#10825,#10826,#10827,#10828,#10829,#10830,
#10831,#10832,#10833,#10834,#10835,#10836,#10837,#10838,#10839,#10840,#10841,
#10842,#10843,#10844,#10845,#10846,#10847,#10848,#10849,#10850,#10851,#10852,
#10853,#10854,#10855,#10856,#10857,#10858,#10859,#10860,#10861,#10862,#10863,
#10864,#10865,#10866,#10867,#10868,#10869,#10870,#10871,#10872,#10873,#10874,
#10875,#10876,#10877,#10878,#10879,#10880,#10881,#10882,#10883,#10884,#10885,
#10886,#10887,#10888,#10889,#10890,#10891,#10892,#10893,#10894,#10895,#10896,
#10897,#10898,#10899,#10900,#10901,#10902,#10903,#10904,#10905,#10906,#10907,
#10908,#10909,#10910,#10911,#10912,#10913,#10914,#10915,#10916,#10917,#10918,
#10919,#10920,#10921,#10922,#10923,#10924,#10925,#10926,#10927,#10928,#10929,
#10930,#10931,#10932,#10933,#10934,#10935,#10936,#10937,#10938,#10939,#10940,
#10941,#10942,#10943,#10944,#10945,#10946,#10947,#10948,#10949,#10950,#10951,
#10952,#10953,#10954,#10955,#10956,#10957,#10958,#10959,#10960,#10961,#10962,
#10963,#10964,#10965,#10966,#10967,#10968,#10969,#10970,#10971,#10972,#10973,
#10974,#10975,#10976,#10977,#10978,#10979,#10980,#10981,#10982,#10983,#10984,
#10985,#10986,#10987,#10988,#10989,#10990,#10991,#10992,#10993,#10994,#10995,
#10996,#10997,#10998,#10999,#11000,#11001,#11002,#11003,#11004,#11005,#11006,
#11007,#11008,#11009,#11010,#11011,#11012,#11013,#11014,#11015,#11016,#11017,
#11018,#11019,#11020,#11021,#11022,#11023,#11024,#11025,#11026,#11027,#11028,
#11029,#11030,#11031,#11032,#11033,#11034,#11035,#11036,#11037,#11038,#11039,
#11040,#11041,#11042,#11043,#11044,#11045,#11046,#11047,#11048,#11049,#11050,
#11051,#11052,#11053,#11054,#11055,#11056,#11057,#11058,#11059,#11060,#11061,
#11062,#11063,#11064,#11065,#11066,#11067,#11068,#11069,#11070,#11071,#11072,
#11073,#11074,#11075,#11076,#11077,#11078,#11079,#11080,#11081,#11082,#11083,
#11084,#11085,#11086,#11087,#11088,#11089,#11090,#11091,#11092,#11093,#11094,
#11095,#11096,#11097,#11098,#11099,#11100,#11101,#11102,#11103,#11104,#11105,
#11106,#11107,#11108,#11109,#11110,#11111,#11112,#11113,#11114,#11115,#11116,
#11117,#11118,#11119,#11120,#11121,#11122,#11123,#11124,#11125,#11126,#11127,
#11128,#11129,#11130,#11131,#11132,#11133,#11134,#11135,#11136,#11137,#11138,
#11139,#11140,#11141,#11142,#11143,#11144,#11145,#11146,#11147,#11148,#11149,
#11150,#11151,#11152,#11153,#11154,#11155,#11156,#11157,#11158,#11159,#11160,
#11161,#11162,#11163,#11164,#11165,#11166,#11167,#11168,#11169,#11170,#11171,
#11172,#11173,#11174,#11175,#11176,#11177,#11178,#11179,#11180,#11181,#11182,
#11183,#11184,#11185,#11186,#11187,#11188,#11189,#11190,#11191,#11192,#11193,
#11194,#11195,#11196,#11197,#11198,#11199,#11200,#11201,#11202,#11203,#11204,
#11205,#11206,#11207,#11208,#11209,#11210,#11211,#11212,#11213,#11214,#11215,
#11216,#11217,#11218,#11219,#11220,#11221,#11222,#11223,#11224,#11225,#11226,
#11227,#11228,#11229,#11230,#11231,#11232,#11233,#11234,#11235,#11236,#11237,
#11238,#11239,#11240,#11241,#11242,#11243,#11244,#11245,#11246,#11247,#11248,
#11249,#11250,#11251,#11252,#11253,#11254,#11255,#11256,#11257,#11258,#11259,
#11260,#11261,#11262,#11263,#11264,#11265,#11266,#11267,#11268,#11269,#11270,
#11271,#11272,#11273,#11274,#11275,#11276,#11277,#11278,#11279,#11280,#11281,
#11282,#11283,#11284,#11285,#11286,#11287));
#2889=EDGE_LOOP('',(#11288,#11289,#11290,#11291,#11292,#11293));
#2890=EDGE_LOOP('',(#11294));
#2891=EDGE_LOOP('',(#11295));
#2892=EDGE_LOOP('',(#11296,#11297,#11298,#11299));
#2893=EDGE_LOOP('',(#11300));
#2894=EDGE_LOOP('',(#11301,#11302,#11303,#11304));
#2895=EDGE_LOOP('',(#11305,#11306,#11307,#11308));
#2896=EDGE_LOOP('',(#11309,#11310));
#2897=EDGE_LOOP('',(#11311,#11312,#11313,#11314));
#2898=EDGE_LOOP('',(#11315,#11316,#11317));
#2899=EDGE_LOOP('',(#11318,#11319,#11320,#11321,#11322,#11323,#11324,#11325,
#11326,#11327,#11328,#11329));
#2900=EDGE_LOOP('',(#11330,#11331,#11332,#11333));
#2901=EDGE_LOOP('',(#11334,#11335,#11336,#11337,#11338,#11339,#11340,#11341,
#11342,#11343,#11344,#11345,#11346,#11347,#11348,#11349,#11350,#11351,#11352,
#11353,#11354,#11355,#11356,#11357,#11358,#11359,#11360,#11361,#11362,#11363,
#11364,#11365,#11366,#11367,#11368,#11369,#11370,#11371,#11372,#11373,#11374,
#11375,#11376,#11377,#11378,#11379,#11380,#11381,#11382,#11383,#11384,#11385,
#11386,#11387,#11388,#11389,#11390,#11391,#11392,#11393,#11394,#11395,#11396,
#11397,#11398,#11399,#11400,#11401,#11402,#11403,#11404,#11405,#11406,#11407,
#11408,#11409,#11410,#11411,#11412,#11413,#11414,#11415,#11416,#11417,#11418,
#11419,#11420,#11421,#11422,#11423,#11424,#11425,#11426,#11427,#11428,#11429,
#11430,#11431,#11432,#11433,#11434,#11435,#11436,#11437,#11438,#11439,#11440,
#11441,#11442,#11443,#11444,#11445,#11446,#11447,#11448,#11449,#11450,#11451,
#11452,#11453,#11454,#11455,#11456,#11457,#11458,#11459,#11460,#11461,#11462,
#11463,#11464,#11465,#11466,#11467,#11468,#11469,#11470,#11471,#11472,#11473,
#11474,#11475,#11476,#11477,#11478,#11479,#11480,#11481,#11482,#11483,#11484,
#11485,#11486,#11487,#11488,#11489,#11490,#11491,#11492,#11493,#11494,#11495,
#11496,#11497,#11498,#11499,#11500,#11501,#11502,#11503,#11504,#11505,#11506,
#11507,#11508,#11509,#11510,#11511,#11512,#11513,#11514,#11515,#11516,#11517,
#11518,#11519,#11520,#11521,#11522,#11523,#11524,#11525,#11526,#11527,#11528,
#11529,#11530,#11531,#11532,#11533,#11534,#11535,#11536,#11537,#11538,#11539,
#11540,#11541,#11542,#11543,#11544,#11545,#11546,#11547,#11548,#11549,#11550,
#11551,#11552,#11553,#11554,#11555,#11556,#11557,#11558,#11559,#11560,#11561,
#11562,#11563,#11564,#11565,#11566,#11567,#11568,#11569,#11570,#11571,#11572,
#11573,#11574,#11575,#11576,#11577,#11578,#11579,#11580,#11581,#11582,#11583,
#11584,#11585,#11586,#11587,#11588,#11589,#11590,#11591,#11592,#11593,#11594,
#11595,#11596,#11597,#11598,#11599,#11600,#11601,#11602,#11603,#11604,#11605,
#11606,#11607,#11608,#11609,#11610,#11611,#11612,#11613,#11614,#11615,#11616,
#11617,#11618,#11619,#11620,#11621,#11622,#11623,#11624,#11625,#11626,#11627,
#11628,#11629,#11630,#11631,#11632,#11633,#11634,#11635,#11636,#11637,#11638,
#11639,#11640,#11641,#11642,#11643,#11644,#11645,#11646,#11647,#11648,#11649,
#11650,#11651,#11652,#11653,#11654,#11655,#11656,#11657,#11658,#11659,#11660,
#11661,#11662,#11663,#11664,#11665,#11666,#11667,#11668,#11669,#11670,#11671,
#11672,#11673,#11674,#11675,#11676,#11677,#11678,#11679,#11680,#11681,#11682,
#11683,#11684,#11685,#11686,#11687,#11688,#11689,#11690,#11691,#11692,#11693,
#11694,#11695,#11696,#11697,#11698,#11699,#11700,#11701,#11702,#11703,#11704,
#11705,#11706,#11707,#11708,#11709,#11710,#11711,#11712,#11713,#11714,#11715,
#11716,#11717,#11718,#11719,#11720,#11721,#11722,#11723,#11724,#11725,#11726,
#11727,#11728,#11729,#11730,#11731,#11732,#11733,#11734,#11735,#11736,#11737,
#11738,#11739,#11740,#11741,#11742,#11743,#11744,#11745,#11746,#11747,#11748,
#11749,#11750,#11751,#11752,#11753,#11754,#11755,#11756,#11757,#11758,#11759,
#11760,#11761,#11762,#11763,#11764,#11765,#11766,#11767,#11768,#11769,#11770,
#11771,#11772,#11773,#11774,#11775,#11776,#11777,#11778,#11779,#11780,#11781,
#11782,#11783,#11784,#11785,#11786,#11787,#11788,#11789,#11790,#11791,#11792,
#11793,#11794,#11795,#11796,#11797,#11798,#11799,#11800,#11801,#11802,#11803,
#11804,#11805,#11806,#11807,#11808,#11809,#11810,#11811,#11812,#11813,#11814,
#11815,#11816,#11817,#11818,#11819,#11820,#11821,#11822,#11823,#11824,#11825,
#11826,#11827,#11828,#11829,#11830,#11831,#11832,#11833,#11834,#11835,#11836,
#11837,#11838,#11839,#11840,#11841,#11842,#11843,#11844,#11845,#11846,#11847,
#11848,#11849,#11850,#11851,#11852,#11853,#11854,#11855,#11856,#11857,#11858,
#11859,#11860,#11861,#11862,#11863,#11864,#11865,#11866,#11867,#11868,#11869,
#11870,#11871,#11872,#11873,#11874,#11875,#11876,#11877,#11878,#11879,#11880,
#11881,#11882,#11883,#11884,#11885,#11886,#11887,#11888,#11889,#11890,#11891,
#11892,#11893,#11894,#11895,#11896,#11897,#11898,#11899,#11900,#11901,#11902,
#11903,#11904,#11905,#11906,#11907,#11908,#11909,#11910,#11911,#11912,#11913,
#11914,#11915,#11916,#11917,#11918,#11919,#11920,#11921,#11922,#11923,#11924,
#11925,#11926,#11927,#11928,#11929,#11930,#11931,#11932,#11933,#11934,#11935,
#11936,#11937,#11938,#11939,#11940,#11941,#11942,#11943,#11944,#11945,#11946,
#11947,#11948,#11949,#11950,#11951,#11952,#11953,#11954,#11955,#11956,#11957,
#11958,#11959,#11960,#11961,#11962,#11963,#11964,#11965,#11966,#11967,#11968,
#11969,#11970,#11971,#11972,#11973,#11974,#11975,#11976,#11977,#11978,#11979,
#11980,#11981,#11982,#11983,#11984,#11985,#11986,#11987,#11988,#11989,#11990,
#11991,#11992,#11993,#11994,#11995,#11996,#11997,#11998,#11999,#12000,#12001,
#12002,#12003,#12004,#12005,#12006,#12007,#12008,#12009,#12010,#12011,#12012,
#12013,#12014,#12015,#12016,#12017,#12018,#12019,#12020,#12021,#12022,#12023,
#12024,#12025,#12026,#12027,#12028,#12029,#12030,#12031,#12032,#12033,#12034,
#12035,#12036,#12037,#12038,#12039,#12040,#12041,#12042,#12043,#12044,#12045,
#12046,#12047,#12048,#12049,#12050,#12051,#12052,#12053,#12054,#12055,#12056,
#12057,#12058,#12059,#12060,#12061,#12062,#12063,#12064,#12065,#12066,#12067,
#12068,#12069,#12070,#12071,#12072,#12073,#12074,#12075,#12076,#12077,#12078,
#12079,#12080,#12081,#12082,#12083,#12084,#12085,#12086,#12087,#12088,#12089,
#12090,#12091,#12092,#12093,#12094,#12095,#12096,#12097,#12098,#12099,#12100,
#12101,#12102,#12103,#12104,#12105,#12106,#12107,#12108,#12109,#12110,#12111,
#12112,#12113,#12114,#12115,#12116,#12117,#12118,#12119,#12120,#12121,#12122,
#12123,#12124,#12125,#12126,#12127,#12128,#12129,#12130,#12131,#12132,#12133,
#12134,#12135,#12136,#12137,#12138,#12139,#12140,#12141,#12142));
#2902=EDGE_LOOP('',(#12143,#12144,#12145,#12146,#12147,#12148,#12149,#12150,
#12151,#12152,#12153,#12154,#12155,#12156,#12157,#12158,#12159,#12160,#12161,
#12162,#12163,#12164,#12165,#12166,#12167,#12168,#12169,#12170,#12171,#12172,
#12173,#12174,#12175,#12176,#12177,#12178,#12179,#12180,#12181,#12182,#12183,
#12184,#12185,#12186,#12187,#12188,#12189,#12190,#12191,#12192,#12193,#12194,
#12195,#12196,#12197,#12198,#12199,#12200,#12201,#12202,#12203,#12204,#12205,
#12206,#12207,#12208,#12209,#12210,#12211,#12212,#12213,#12214,#12215,#12216,
#12217,#12218,#12219,#12220,#12221,#12222,#12223,#12224,#12225,#12226,#12227,
#12228,#12229,#12230,#12231,#12232,#12233,#12234,#12235,#12236,#12237,#12238,
#12239,#12240,#12241,#12242,#12243,#12244,#12245,#12246,#12247,#12248,#12249,
#12250,#12251,#12252,#12253,#12254,#12255,#12256,#12257,#12258,#12259,#12260,
#12261,#12262,#12263,#12264,#12265,#12266,#12267,#12268,#12269,#12270,#12271,
#12272,#12273,#12274,#12275,#12276,#12277,#12278,#12279,#12280,#12281,#12282,
#12283,#12284,#12285,#12286,#12287,#12288,#12289,#12290,#12291,#12292,#12293,
#12294,#12295,#12296,#12297,#12298,#12299,#12300,#12301,#12302,#12303,#12304,
#12305,#12306,#12307,#12308,#12309,#12310,#12311,#12312,#12313,#12314,#12315,
#12316,#12317,#12318,#12319,#12320,#12321,#12322,#12323,#12324,#12325,#12326,
#12327,#12328,#12329,#12330,#12331,#12332,#12333,#12334,#12335,#12336,#12337,
#12338,#12339,#12340,#12341,#12342,#12343,#12344,#12345,#12346,#12347,#12348,
#12349,#12350,#12351,#12352,#12353,#12354,#12355,#12356,#12357,#12358,#12359,
#12360,#12361,#12362,#12363,#12364,#12365,#12366,#12367,#12368,#12369,#12370,
#12371,#12372,#12373,#12374,#12375,#12376,#12377,#12378,#12379,#12380,#12381,
#12382,#12383,#12384,#12385,#12386,#12387,#12388,#12389,#12390,#12391,#12392,
#12393,#12394,#12395,#12396,#12397,#12398,#12399,#12400,#12401,#12402,#12403,
#12404,#12405,#12406,#12407,#12408,#12409,#12410,#12411,#12412,#12413,#12414,
#12415,#12416,#12417,#12418,#12419,#12420,#12421,#12422,#12423,#12424,#12425,
#12426,#12427,#12428,#12429,#12430,#12431,#12432,#12433,#12434,#12435,#12436,
#12437,#12438,#12439,#12440,#12441,#12442,#12443,#12444,#12445,#12446,#12447,
#12448,#12449,#12450,#12451,#12452,#12453,#12454,#12455,#12456,#12457,#12458,
#12459,#12460,#12461,#12462,#12463,#12464,#12465,#12466,#12467,#12468,#12469,
#12470,#12471,#12472,#12473,#12474,#12475,#12476,#12477,#12478,#12479,#12480,
#12481,#12482,#12483,#12484,#12485,#12486,#12487,#12488,#12489,#12490,#12491,
#12492,#12493,#12494,#12495,#12496,#12497,#12498,#12499,#12500,#12501,#12502,
#12503,#12504,#12505,#12506,#12507,#12508,#12509,#12510,#12511,#12512,#12513,
#12514,#12515,#12516,#12517,#12518,#12519,#12520,#12521,#12522,#12523,#12524,
#12525,#12526,#12527,#12528,#12529,#12530,#12531,#12532,#12533,#12534,#12535,
#12536,#12537,#12538,#12539,#12540,#12541,#12542,#12543,#12544,#12545,#12546,
#12547,#12548,#12549,#12550,#12551,#12552,#12553,#12554,#12555,#12556,#12557,
#12558,#12559,#12560,#12561,#12562,#12563,#12564,#12565,#12566,#12567,#12568,
#12569,#12570,#12571,#12572,#12573,#12574,#12575,#12576,#12577,#12578,#12579,
#12580,#12581,#12582,#12583,#12584,#12585,#12586,#12587,#12588,#12589,#12590,
#12591,#12592,#12593,#12594,#12595,#12596,#12597,#12598,#12599,#12600,#12601,
#12602,#12603,#12604,#12605,#12606,#12607,#12608,#12609,#12610,#12611,#12612,
#12613,#12614,#12615,#12616,#12617,#12618,#12619,#12620,#12621,#12622,#12623,
#12624,#12625,#12626,#12627,#12628,#12629,#12630,#12631,#12632,#12633,#12634,
#12635,#12636,#12637,#12638,#12639,#12640,#12641,#12642,#12643,#12644,#12645,
#12646,#12647,#12648,#12649,#12650,#12651,#12652,#12653,#12654,#12655,#12656,
#12657,#12658,#12659,#12660,#12661,#12662,#12663,#12664,#12665,#12666,#12667,
#12668,#12669,#12670,#12671,#12672,#12673,#12674,#12675,#12676,#12677,#12678,
#12679,#12680,#12681,#12682,#12683,#12684,#12685,#12686,#12687,#12688,#12689,
#12690,#12691,#12692,#12693,#12694,#12695,#12696,#12697,#12698,#12699,#12700,
#12701,#12702,#12703,#12704,#12705,#12706,#12707,#12708,#12709,#12710,#12711,
#12712,#12713,#12714,#12715,#12716,#12717,#12718,#12719,#12720,#12721,#12722,
#12723,#12724,#12725,#12726,#12727,#12728,#12729,#12730,#12731,#12732,#12733,
#12734,#12735,#12736,#12737,#12738,#12739,#12740,#12741,#12742,#12743,#12744,
#12745,#12746,#12747,#12748,#12749,#12750,#12751,#12752,#12753,#12754,#12755,
#12756,#12757,#12758,#12759,#12760,#12761,#12762,#12763,#12764,#12765,#12766,
#12767,#12768,#12769,#12770,#12771,#12772,#12773,#12774,#12775,#12776,#12777,
#12778,#12779,#12780,#12781,#12782,#12783,#12784,#12785,#12786,#12787,#12788,
#12789,#12790,#12791,#12792,#12793,#12794,#12795,#12796,#12797,#12798,#12799,
#12800,#12801,#12802,#12803,#12804,#12805,#12806,#12807,#12808,#12809,#12810,
#12811,#12812,#12813,#12814,#12815,#12816,#12817,#12818,#12819,#12820,#12821,
#12822,#12823,#12824,#12825,#12826,#12827,#12828,#12829,#12830,#12831,#12832,
#12833,#12834,#12835,#12836,#12837,#12838,#12839,#12840,#12841,#12842,#12843,
#12844,#12845,#12846,#12847,#12848,#12849,#12850,#12851,#12852,#12853,#12854,
#12855,#12856,#12857,#12858,#12859,#12860,#12861,#12862,#12863,#12864,#12865,
#12866,#12867,#12868,#12869,#12870,#12871,#12872,#12873,#12874,#12875,#12876,
#12877,#12878,#12879,#12880,#12881,#12882,#12883,#12884,#12885,#12886,#12887,
#12888,#12889,#12890,#12891,#12892,#12893,#12894,#12895,#12896,#12897,#12898,
#12899,#12900,#12901,#12902,#12903,#12904,#12905,#12906,#12907,#12908,#12909,
#12910,#12911,#12912,#12913,#12914,#12915,#12916,#12917,#12918,#12919,#12920,
#12921,#12922,#12923,#12924,#12925,#12926,#12927,#12928,#12929,#12930,#12931,
#12932,#12933,#12934,#12935,#12936,#12937,#12938,#12939,#12940,#12941,#12942,
#12943,#12944,#12945,#12946,#12947,#12948,#12949,#12950,#12951));
#2903=EDGE_LOOP('',(#12952,#12953,#12954,#12955));
#2904=EDGE_LOOP('',(#12956,#12957,#12958,#12959,#12960,#12961,#12962,#12963,
#12964,#12965,#12966,#12967));
#2905=EDGE_LOOP('',(#12968,#12969,#12970,#12971,#12972,#12973,#12974,#12975,
#12976,#12977,#12978,#12979));
#2906=EDGE_LOOP('',(#12980,#12981,#12982,#12983));
#2907=EDGE_LOOP('',(#12984,#12985,#12986,#12987,#12988));
#2908=EDGE_LOOP('',(#12989));
#2909=EDGE_LOOP('',(#12990,#12991,#12992));
#2910=EDGE_LOOP('',(#12993,#12994,#12995,#12996,#12997,#12998));
#2911=EDGE_LOOP('',(#12999));
#2912=EDGE_LOOP('',(#13000,#13001,#13002,#13003));
#2913=EDGE_LOOP('',(#13004,#13005,#13006,#13007));
#2914=EDGE_LOOP('',(#13008,#13009,#13010,#13011));
#2915=EDGE_LOOP('',(#13012,#13013,#13014,#13015));
#2916=EDGE_LOOP('',(#13016,#13017,#13018,#13019));
#2917=EDGE_LOOP('',(#13020,#13021));
#2918=EDGE_LOOP('',(#13022,#13023,#13024,#13025));
#2919=EDGE_LOOP('',(#13026,#13027,#13028,#13029));
#2920=EDGE_LOOP('',(#13030,#13031,#13032,#13033,#13034,#13035));
#2921=EDGE_LOOP('',(#13036));
#2922=EDGE_LOOP('',(#13037,#13038));
#2923=EDGE_LOOP('',(#13039,#13040,#13041,#13042));
#2924=EDGE_LOOP('',(#13043,#13044,#13045,#13046));
#2925=EDGE_LOOP('',(#13047,#13048,#13049,#13050));
#2926=EDGE_LOOP('',(#13051,#13052,#13053,#13054));
#2927=EDGE_LOOP('',(#13055,#13056,#13057,#13058,#13059));
#2928=EDGE_LOOP('',(#13060));
#2929=EDGE_LOOP('',(#13061,#13062,#13063));
#2930=EDGE_LOOP('',(#13064,#13065,#13066,#13067,#13068,#13069));
#2931=EDGE_LOOP('',(#13070,#13071,#13072,#13073,#13074,#13075));
#2932=EDGE_LOOP('',(#13076,#13077,#13078,#13079,#13080,#13081));
#2933=EDGE_LOOP('',(#13082,#13083,#13084,#13085,#13086,#13087));
#2934=EDGE_LOOP('',(#13088,#13089,#13090,#13091,#13092,#13093));
#2935=EDGE_LOOP('',(#13094,#13095,#13096,#13097,#13098,#13099));
#2936=EDGE_LOOP('',(#13100,#13101,#13102,#13103,#13104,#13105));
#2937=EDGE_LOOP('',(#13106,#13107,#13108,#13109,#13110,#13111));
#2938=EDGE_LOOP('',(#13112,#13113,#13114,#13115,#13116,#13117));
#2939=EDGE_LOOP('',(#13118,#13119,#13120,#13121,#13122,#13123));
#2940=EDGE_LOOP('',(#13124,#13125,#13126,#13127,#13128,#13129));
#2941=EDGE_LOOP('',(#13130,#13131,#13132,#13133,#13134,#13135));
#2942=EDGE_LOOP('',(#13136,#13137,#13138,#13139,#13140,#13141));
#2943=EDGE_LOOP('',(#13142,#13143,#13144,#13145,#13146,#13147));
#2944=EDGE_LOOP('',(#13148,#13149,#13150,#13151,#13152,#13153));
#2945=EDGE_LOOP('',(#13154,#13155,#13156,#13157,#13158,#13159));
#2946=EDGE_LOOP('',(#13160,#13161,#13162,#13163));
#2947=EDGE_LOOP('',(#13164,#13165,#13166,#13167,#13168,#13169,#13170,#13171,
#13172,#13173,#13174,#13175,#13176,#13177,#13178,#13179,#13180,#13181,#13182,
#13183,#13184,#13185,#13186,#13187,#13188,#13189,#13190,#13191,#13192,#13193,
#13194,#13195,#13196,#13197,#13198,#13199,#13200,#13201,#13202,#13203,#13204,
#13205,#13206,#13207,#13208,#13209,#13210,#13211,#13212,#13213,#13214,#13215,
#13216,#13217,#13218,#13219,#13220));
#2948=EDGE_LOOP('',(#13221,#13222,#13223,#13224));
#2949=EDGE_LOOP('',(#13225,#13226,#13227,#13228,#13229,#13230,#13231,#13232,
#13233,#13234,#13235,#13236,#13237,#13238,#13239,#13240,#13241,#13242,#13243,
#13244,#13245,#13246,#13247,#13248,#13249,#13250,#13251,#13252,#13253,#13254,
#13255,#13256,#13257,#13258,#13259,#13260));
#2950=EDGE_LOOP('',(#13261,#13262,#13263,#13264,#13265,#13266));
#2951=EDGE_LOOP('',(#13267,#13268,#13269));
#2952=EDGE_LOOP('',(#13270,#13271,#13272));
#2953=EDGE_LOOP('',(#13273,#13274,#13275,#13276,#13277,#13278));
#2954=EDGE_LOOP('',(#13279,#13280,#13281,#13282,#13283,#13284));
#2955=EDGE_LOOP('',(#13285,#13286,#13287,#13288,#13289,#13290,#13291,#13292,
#13293,#13294,#13295,#13296,#13297,#13298,#13299,#13300,#13301,#13302,#13303,
#13304,#13305,#13306,#13307,#13308,#13309,#13310,#13311,#13312,#13313,#13314,
#13315,#13316,#13317,#13318,#13319,#13320,#13321,#13322,#13323,#13324,#13325,
#13326,#13327,#13328,#13329,#13330,#13331,#13332,#13333,#13334,#13335,#13336,
#13337,#13338,#13339,#13340,#13341,#13342,#13343,#13344));
#2956=EDGE_LOOP('',(#13345,#13346,#13347,#13348,#13349,#13350,#13351,#13352,
#13353,#13354,#13355,#13356,#13357,#13358,#13359,#13360));
#2957=EDGE_LOOP('',(#13361,#13362,#13363,#13364,#13365,#13366,#13367,#13368,
#13369,#13370,#13371));
#2958=EDGE_LOOP('',(#13372));
#2959=EDGE_LOOP('',(#13373));
#2960=EDGE_LOOP('',(#13374,#13375,#13376,#13377));
#2961=EDGE_LOOP('',(#13378,#13379,#13380,#13381));
#2962=EDGE_LOOP('',(#13382,#13383,#13384,#13385));
#2963=EDGE_LOOP('',(#13386,#13387,#13388,#13389));
#2964=EDGE_LOOP('',(#13390,#13391,#13392,#13393));
#2965=EDGE_LOOP('',(#13394));
#2966=EDGE_LOOP('',(#13395,#13396,#13397,#13398));
#2967=EDGE_LOOP('',(#13399));
#2968=EDGE_LOOP('',(#13400));
#2969=EDGE_LOOP('',(#13401,#13402,#13403,#13404));
#2970=EDGE_LOOP('',(#13405,#13406,#13407,#13408));
#2971=EDGE_LOOP('',(#13409,#13410,#13411,#13412));
#2972=EDGE_LOOP('',(#13413,#13414,#13415,#13416));
#2973=EDGE_LOOP('',(#13417,#13418,#13419,#13420));
#2974=EDGE_LOOP('',(#13421,#13422,#13423,#13424,#13425,#13426,#13427,#13428,
#13429,#13430));
#2975=EDGE_LOOP('',(#13431,#13432,#13433,#13434));
#2976=EDGE_LOOP('',(#13435));
#2977=EDGE_LOOP('',(#13436,#13437,#13438,#13439));
#2978=EDGE_LOOP('',(#13440));
#2979=EDGE_LOOP('',(#13441));
#2980=EDGE_LOOP('',(#13442,#13443,#13444,#13445,#13446,#13447,#13448,#13449,
#13450,#13451,#13452,#13453));
#2981=EDGE_LOOP('',(#13454,#13455,#13456,#13457,#13458,#13459,#13460,#13461,
#13462,#13463,#13464,#13465));
#2982=EDGE_LOOP('',(#13466,#13467,#13468,#13469));
#2983=EDGE_LOOP('',(#13470,#13471,#13472,#13473));
#2984=EDGE_LOOP('',(#13474,#13475,#13476,#13477,#13478,#13479));
#2985=EDGE_LOOP('',(#13480));
#2986=EDGE_LOOP('',(#13481,#13482));
#2987=EDGE_LOOP('',(#13483,#13484,#13485,#13486));
#2988=EDGE_LOOP('',(#13487,#13488,#13489,#13490));
#2989=EDGE_LOOP('',(#13491,#13492,#13493,#13494));
#2990=EDGE_LOOP('',(#13495,#13496,#13497,#13498));
#2991=EDGE_LOOP('',(#13499,#13500,#13501,#13502,#13503));
#2992=EDGE_LOOP('',(#13504));
#2993=EDGE_LOOP('',(#13505,#13506,#13507));
#2994=EDGE_LOOP('',(#13508,#13509,#13510,#13511));
#2995=EDGE_LOOP('',(#13512,#13513,#13514,#13515,#13516));
#2996=EDGE_LOOP('',(#13517));
#2997=EDGE_LOOP('',(#13518,#13519,#13520));
#2998=EDGE_LOOP('',(#13521,#13522,#13523,#13524,#13525,#13526));
#2999=EDGE_LOOP('',(#13527));
#3000=EDGE_LOOP('',(#13528,#13529,#13530,#13531));
#3001=EDGE_LOOP('',(#13532,#13533,#13534,#13535));
#3002=EDGE_LOOP('',(#13536,#13537,#13538,#13539));
#3003=EDGE_LOOP('',(#13540,#13541,#13542,#13543));
#3004=EDGE_LOOP('',(#13544,#13545,#13546,#13547));
#3005=EDGE_LOOP('',(#13548,#13549));
#3006=EDGE_LOOP('',(#13550,#13551,#13552,#13553));
#3007=EDGE_LOOP('',(#13554,#13555,#13556,#13557));
#3008=EDGE_LOOP('',(#13558,#13559,#13560,#13561));
#3009=EDGE_LOOP('',(#13562,#13563,#13564,#13565));
#3010=EDGE_LOOP('',(#13566,#13567,#13568,#13569));
#3011=EDGE_LOOP('',(#13570,#13571,#13572,#13573));
#3012=EDGE_LOOP('',(#13574,#13575,#13576,#13577,#13578,#13579));
#3013=EDGE_LOOP('',(#13580));
#3014=EDGE_LOOP('',(#13581));
#3015=EDGE_LOOP('',(#13582,#13583,#13584,#13585));
#3016=EDGE_LOOP('',(#13586,#13587,#13588,#13589,#13590,#13591));
#3017=EDGE_LOOP('',(#13592));
#3018=EDGE_LOOP('',(#13593));
#3019=EDGE_LOOP('',(#13594,#13595,#13596,#13597));
#3020=EDGE_LOOP('',(#13598,#13599,#13600,#13601));
#3021=EDGE_LOOP('',(#13602,#13603,#13604,#13605));
#3022=EDGE_LOOP('',(#13606,#13607,#13608,#13609));
#3023=EDGE_LOOP('',(#13610,#13611,#13612,#13613));
#3024=EDGE_LOOP('',(#13614,#13615,#13616,#13617,#13618,#13619,#13620,#13621,
#13622,#13623,#13624,#13625));
#3025=EDGE_LOOP('',(#13626,#13627,#13628,#13629));
#3026=EDGE_LOOP('',(#13630,#13631,#13632,#13633));
#3027=EDGE_LOOP('',(#13634,#13635,#13636,#13637));
#3028=EDGE_LOOP('',(#13638,#13639,#13640,#13641));
#3029=EDGE_LOOP('',(#13642,#13643,#13644,#13645,#13646,#13647,#13648,#13649));
#3030=EDGE_LOOP('',(#13650,#13651,#13652,#13653));
#3031=EDGE_LOOP('',(#13654,#13655,#13656,#13657));
#3032=EDGE_LOOP('',(#13658,#13659,#13660,#13661,#13662,#13663,#13664,#13665));
#3033=EDGE_LOOP('',(#13666,#13667,#13668,#13669));
#3034=EDGE_LOOP('',(#13670,#13671,#13672,#13673,#13674,#13675));
#3035=EDGE_LOOP('',(#13676));
#3036=EDGE_LOOP('',(#13677));
#3037=EDGE_LOOP('',(#13678,#13679,#13680,#13681));
#3038=EDGE_LOOP('',(#13682,#13683,#13684,#13685,#13686,#13687));
#3039=EDGE_LOOP('',(#13688));
#3040=EDGE_LOOP('',(#13689));
#3041=EDGE_LOOP('',(#13690,#13691,#13692,#13693,#13694,#13695,#13696,#13697,
#13698,#13699,#13700,#13701));
#3042=EDGE_LOOP('',(#13702,#13703,#13704,#13705));
#3043=EDGE_LOOP('',(#13706,#13707,#13708,#13709));
#3044=EDGE_LOOP('',(#13710,#13711,#13712,#13713));
#3045=EDGE_LOOP('',(#13714,#13715,#13716,#13717));
#3046=EDGE_LOOP('',(#13718,#13719,#13720,#13721,#13722,#13723));
#3047=EDGE_LOOP('',(#13724,#13725,#13726,#13727,#13728,#13729));
#3048=EDGE_LOOP('',(#13730,#13731,#13732,#13733,#13734,#13735));
#3049=EDGE_LOOP('',(#13736,#13737,#13738,#13739,#13740,#13741));
#3050=EDGE_LOOP('',(#13742,#13743,#13744,#13745,#13746,#13747));
#3051=EDGE_LOOP('',(#13748,#13749,#13750,#13751,#13752,#13753));
#3052=EDGE_LOOP('',(#13754,#13755,#13756,#13757,#13758,#13759));
#3053=EDGE_LOOP('',(#13760,#13761,#13762,#13763,#13764,#13765));
#3054=EDGE_LOOP('',(#13766,#13767,#13768,#13769,#13770,#13771));
#3055=EDGE_LOOP('',(#13772,#13773,#13774,#13775,#13776,#13777));
#3056=EDGE_LOOP('',(#13778,#13779,#13780,#13781,#13782,#13783));
#3057=EDGE_LOOP('',(#13784,#13785,#13786,#13787,#13788,#13789));
#3058=EDGE_LOOP('',(#13790,#13791,#13792,#13793,#13794,#13795));
#3059=EDGE_LOOP('',(#13796,#13797,#13798,#13799,#13800,#13801));
#3060=EDGE_LOOP('',(#13802,#13803,#13804,#13805,#13806,#13807));
#3061=EDGE_LOOP('',(#13808,#13809,#13810,#13811,#13812,#13813));
#3062=EDGE_LOOP('',(#13814,#13815,#13816,#13817));
#3063=EDGE_LOOP('',(#13818,#13819,#13820));
#3064=EDGE_LOOP('',(#13821,#13822,#13823,#13824,#13825,#13826,#13827,#13828,
#13829,#13830,#13831,#13832,#13833,#13834,#13835,#13836,#13837,#13838,#13839,
#13840,#13841,#13842,#13843,#13844,#13845,#13846,#13847,#13848,#13849,#13850,
#13851,#13852,#13853,#13854,#13855,#13856,#13857,#13858,#13859,#13860,#13861,
#13862,#13863,#13864,#13865,#13866,#13867,#13868,#13869,#13870,#13871,#13872,
#13873,#13874,#13875,#13876,#13877));
#3065=EDGE_LOOP('',(#13878,#13879,#13880,#13881));
#3066=EDGE_LOOP('',(#13882,#13883,#13884,#13885,#13886,#13887,#13888,#13889,
#13890,#13891,#13892,#13893,#13894,#13895,#13896,#13897,#13898,#13899,#13900,
#13901,#13902,#13903,#13904,#13905,#13906,#13907,#13908,#13909,#13910,#13911,
#13912,#13913,#13914,#13915,#13916,#13917,#13918,#13919));
#3067=EDGE_LOOP('',(#13920,#13921,#13922,#13923,#13924,#13925));
#3068=EDGE_LOOP('',(#13926,#13927,#13928,#13929));
#3069=EDGE_LOOP('',(#13930,#13931,#13932,#13933,#13934,#13935,#13936,#13937,
#13938,#13939,#13940,#13941,#13942,#13943,#13944,#13945,#13946,#13947,#13948,
#13949,#13950,#13951,#13952,#13953,#13954,#13955,#13956,#13957,#13958,#13959,
#13960,#13961,#13962,#13963,#13964,#13965,#13966,#13967,#13968,#13969,#13970,
#13971,#13972,#13973,#13974,#13975,#13976,#13977,#13978,#13979,#13980,#13981,
#13982,#13983,#13984,#13985,#13986,#13987,#13988,#13989,#13990));
#3070=EDGE_LOOP('',(#13991,#13992,#13993,#13994));
#3071=EDGE_LOOP('',(#13995,#13996));
#3072=EDGE_LOOP('',(#13997,#13998,#13999,#14000,#14001,#14002,#14003,#14004,
#14005,#14006,#14007,#14008,#14009,#14010,#14011,#14012));
#3073=EDGE_LOOP('',(#14013,#14014,#14015,#14016,#14017,#14018,#14019,#14020,
#14021,#14022,#14023));
#3074=EDGE_LOOP('',(#14024));
#3075=EDGE_LOOP('',(#14025));
#3076=EDGE_LOOP('',(#14026,#14027,#14028,#14029));
#3077=EDGE_LOOP('',(#14030,#14031,#14032,#14033));
#3078=EDGE_LOOP('',(#14034,#14035,#14036,#14037));
#3079=EDGE_LOOP('',(#14038,#14039,#14040,#14041));
#3080=EDGE_LOOP('',(#14042,#14043,#14044,#14045));
#3081=EDGE_LOOP('',(#14046));
#3082=EDGE_LOOP('',(#14047,#14048,#14049,#14050));
#3083=EDGE_LOOP('',(#14051));
#3084=EDGE_LOOP('',(#14052));
#3085=EDGE_LOOP('',(#14053,#14054,#14055,#14056));
#3086=EDGE_LOOP('',(#14057,#14058,#14059,#14060));
#3087=EDGE_LOOP('',(#14061,#14062,#14063,#14064));
#3088=EDGE_LOOP('',(#14065,#14066,#14067,#14068));
#3089=EDGE_LOOP('',(#14069,#14070,#14071,#14072));
#3090=EDGE_LOOP('',(#14073,#14074,#14075,#14076,#14077,#14078,#14079,#14080,
#14081,#14082));
#3091=EDGE_LOOP('',(#14083,#14084,#14085,#14086));
#3092=EDGE_LOOP('',(#14087));
#3093=EDGE_LOOP('',(#14088,#14089,#14090,#14091));
#3094=EDGE_LOOP('',(#14092));
#3095=EDGE_LOOP('',(#14093));
#3096=LINE('',#17463,#3624);
#3097=LINE('',#17466,#3625);
#3098=LINE('',#17471,#3626);
#3099=LINE('',#17476,#3627);
#3100=LINE('',#17478,#3628);
#3101=LINE('',#17480,#3629);
#3102=LINE('',#17481,#3630);
#3103=LINE('',#17487,#3631);
#3104=LINE('',#17490,#3632);
#3105=LINE('',#17492,#3633);
#3106=LINE('',#17493,#3634);
#3107=LINE('',#17497,#3635);
#3108=LINE('',#17501,#3636);
#3109=LINE('',#17505,#3637);
#3110=LINE('',#17507,#3638);
#3111=LINE('',#17508,#3639);
#3112=LINE('',#17509,#3640);
#3113=LINE('',#17517,#3641);
#3114=LINE('',#17520,#3642);
#3115=LINE('',#17522,#3643);
#3116=LINE('',#17524,#3644);
#3117=LINE('',#17526,#3645);
#3118=LINE('',#17527,#3646);
#3119=LINE('',#17531,#3647);
#3120=LINE('',#17533,#3648);
#3121=LINE('',#17535,#3649);
#3122=LINE('',#17541,#3650);
#3123=LINE('',#17544,#3651);
#3124=LINE('',#17546,#3652);
#3125=LINE('',#17547,#3653);
#3126=LINE('',#17553,#3654);
#3127=LINE('',#17555,#3655);
#3128=LINE('',#17557,#3656);
#3129=LINE('',#17560,#3657);
#3130=LINE('',#17561,#3658);
#3131=LINE('',#17566,#3659);
#3132=LINE('',#17570,#3660);
#3133=LINE('',#17572,#3661);
#3134=LINE('',#17573,#3662);
#3135=LINE('',#17579,#3663);
#3136=LINE('',#17582,#3664);
#3137=LINE('',#17584,#3665);
#3138=LINE('',#17585,#3666);
#3139=LINE('',#17587,#3667);
#3140=LINE('',#17589,#3668);
#3141=LINE('',#17590,#3669);
#3142=LINE('',#17592,#3670);
#3143=LINE('',#17596,#3671);
#3144=LINE('',#17599,#3672);
#3145=LINE('',#17602,#3673);
#3146=LINE('',#17604,#3674);
#3147=LINE('',#17605,#3675);
#3148=LINE('',#17611,#3676);
#3149=LINE('',#17614,#3677);
#3150=LINE('',#17616,#3678);
#3151=LINE('',#17617,#3679);
#3152=LINE('',#17621,#3680);
#3153=LINE('',#17622,#3681);
#3154=LINE('',#17624,#3682);
#3155=LINE('',#17626,#3683);
#3156=LINE('',#17633,#3684);
#3157=LINE('',#17963,#3685);
#3158=LINE('',#18429,#3686);
#3159=LINE('',#18895,#3687);
#3160=LINE('',#19364,#3688);
#3161=LINE('',#19830,#3689);
#3162=LINE('',#20296,#3690);
#3163=LINE('',#20762,#3691);
#3164=LINE('',#21225,#3692);
#3165=LINE('',#21691,#3693);
#3166=LINE('',#21947,#3694);
#3167=LINE('',#22200,#3695);
#3168=LINE('',#22660,#3696);
#3169=LINE('',#23126,#3697);
#3170=LINE('',#23592,#3698);
#3171=LINE('',#24055,#3699);
#3172=LINE('',#24521,#3700);
#3173=LINE('',#24987,#3701);
#3174=LINE('',#25453,#3702);
#3175=LINE('',#25922,#3703);
#3176=LINE('',#26388,#3704);
#3177=LINE('',#26854,#3705);
#3178=LINE('',#27317,#3706);
#3179=LINE('',#27789,#3707);
#3180=LINE('',#28255,#3708);
#3181=LINE('',#28721,#3709);
#3182=LINE('',#29193,#3710);
#3183=LINE('',#29659,#3711);
#3184=LINE('',#30122,#3712);
#3185=LINE('',#30585,#3713);
#3186=LINE('',#31057,#3714);
#3187=LINE('',#31523,#3715);
#3188=LINE('',#31986,#3716);
#3189=LINE('',#32455,#3717);
#3190=LINE('',#32921,#3718);
#3191=LINE('',#33384,#3719);
#3192=LINE('',#33847,#3720);
#3193=LINE('',#34316,#3721);
#3194=LINE('',#34782,#3722);
#3195=LINE('',#35245,#3723);
#3196=LINE('',#35711,#3724);
#3197=LINE('',#36177,#3725);
#3198=LINE('',#36640,#3726);
#3199=LINE('',#37103,#3727);
#3200=LINE('',#37572,#3728);
#3201=LINE('',#38038,#3729);
#3202=LINE('',#38501,#3730);
#3203=LINE('',#38967,#3731);
#3204=LINE('',#39433,#3732);
#3205=LINE('',#39896,#3733);
#3206=LINE('',#40365,#3734);
#3207=LINE('',#40834,#3735);
#3208=LINE('',#41300,#3736);
#3209=LINE('',#41763,#3737);
#3210=LINE('',#42229,#3738);
#3211=LINE('',#42695,#3739);
#3212=LINE('',#43158,#3740);
#3213=LINE('',#43630,#3741);
#3214=LINE('',#44099,#3742);
#3215=LINE('',#44562,#3743);
#3216=LINE('',#45025,#3744);
#3217=LINE('',#45491,#3745);
#3218=LINE('',#45957,#3746);
#3219=LINE('',#46417,#3747);
#3220=LINE('',#46886,#3748);
#3221=LINE('',#47355,#3749);
#3222=LINE('',#47818,#3750);
#3223=LINE('',#48284,#3751);
#3224=LINE('',#48747,#3752);
#3225=LINE('',#49213,#3753);
#3226=LINE('',#49676,#3754);
#3227=LINE('',#49935,#3755);
#3228=LINE('',#50188,#3756);
#3229=LINE('',#50648,#3757);
#3230=LINE('',#51114,#3758);
#3231=LINE('',#51577,#3759);
#3232=LINE('',#52043,#3760);
#3233=LINE('',#52509,#3761);
#3234=LINE('',#52978,#3762);
#3235=LINE('',#53447,#3763);
#3236=LINE('',#53910,#3764);
#3237=LINE('',#54376,#3765);
#3238=LINE('',#54839,#3766);
#3239=LINE('',#55305,#3767);
#3240=LINE('',#55771,#3768);
#3241=LINE('',#56240,#3769);
#3242=LINE('',#56709,#3770);
#3243=LINE('',#57172,#3771);
#3244=LINE('',#57638,#3772);
#3245=LINE('',#58101,#3773);
#3246=LINE('',#58570,#3774);
#3247=LINE('',#59036,#3775);
#3248=LINE('',#59502,#3776);
#3249=LINE('',#59971,#3777);
#3250=LINE('',#60437,#3778);
#3251=LINE('',#60900,#3779);
#3252=LINE('',#61363,#3780);
#3253=LINE('',#61832,#3781);
#3254=LINE('',#62298,#3782);
#3255=LINE('',#62764,#3783);
#3256=LINE('',#63236,#3784);
#3257=LINE('',#63702,#3785);
#3258=LINE('',#64165,#3786);
#3259=LINE('',#64628,#3787);
#3260=LINE('',#65094,#3788);
#3261=LINE('',#65560,#3789);
#3262=LINE('',#66026,#3790);
#3263=LINE('',#66495,#3791);
#3264=LINE('',#66961,#3792);
#3265=LINE('',#67424,#3793);
#3266=LINE('',#67887,#3794);
#3267=LINE('',#68353,#3795);
#3268=LINE('',#68819,#3796);
#3269=LINE('',#69285,#3797);
#3270=LINE('',#69754,#3798);
#3271=LINE('',#70220,#3799);
#3272=LINE('',#70683,#3800);
#3273=LINE('',#71152,#3801);
#3274=LINE('',#71618,#3802);
#3275=LINE('',#72081,#3803);
#3276=LINE('',#72547,#3804);
#3277=LINE('',#73016,#3805);
#3278=LINE('',#73482,#3806);
#3279=LINE('',#73945,#3807);
#3280=LINE('',#74414,#3808);
#3281=LINE('',#74880,#3809);
#3282=LINE('',#75343,#3810);
#3283=LINE('',#75809,#3811);
#3284=LINE('',#76278,#3812);
#3285=LINE('',#76744,#3813);
#3286=LINE('',#77204,#3814);
#3287=LINE('',#77670,#3815);
#3288=LINE('',#78136,#3816);
#3289=LINE('',#78599,#3817);
#3290=LINE('',#79065,#3818);
#3291=LINE('',#79534,#3819);
#3292=LINE('',#80000,#3820);
#3293=LINE('',#80460,#3821);
#3294=LINE('',#80926,#3822);
#3295=LINE('',#81392,#3823);
#3296=LINE('',#81855,#3824);
#3297=LINE('',#82114,#3825);
#3298=LINE('',#82365,#3826);
#3299=LINE('',#82825,#3827);
#3300=LINE('',#83285,#3828);
#3301=LINE('',#83751,#3829);
#3302=LINE('',#84217,#3830);
#3303=LINE('',#84680,#3831);
#3304=LINE('',#85149,#3832);
#3305=LINE('',#85615,#3833);
#3306=LINE('',#86084,#3834);
#3307=LINE('',#86550,#3835);
#3308=LINE('',#87016,#3836);
#3309=LINE('',#87482,#3837);
#3310=LINE('',#87945,#3838);
#3311=LINE('',#88414,#3839);
#3312=LINE('',#88880,#3840);
#3313=LINE('',#89349,#3841);
#3314=LINE('',#89815,#3842);
#3315=LINE('',#90278,#3843);
#3316=LINE('',#90744,#3844);
#3317=LINE('',#91207,#3845);
#3318=LINE('',#91676,#3846);
#3319=LINE('',#92142,#3847);
#3320=LINE('',#92611,#3848);
#3321=LINE('',#93077,#3849);
#3322=LINE('',#93540,#3850);
#3323=LINE('',#94006,#3851);
#3324=LINE('',#94472,#3852);
#3325=LINE('',#94941,#3853);
#3326=LINE('',#95407,#3854);
#3327=LINE('',#95870,#3855);
#3328=LINE('',#96336,#3856);
#3329=LINE('',#96799,#3857);
#3330=LINE('',#97265,#3858);
#3331=LINE('',#97731,#3859);
#3332=LINE('',#97990,#3860);
#3333=LINE('',#98450,#3861);
#3334=LINE('',#98916,#3862);
#3335=LINE('',#99382,#3863);
#3336=LINE('',#99845,#3864);
#3337=LINE('',#100311,#3865);
#3338=LINE('',#100777,#3866);
#3339=LINE('',#101243,#3867);
#3340=LINE('',#101712,#3868);
#3341=LINE('',#102178,#3869);
#3342=LINE('',#102641,#3870);
#3343=LINE('',#103104,#3871);
#3344=LINE('',#103576,#3872);
#3345=LINE('',#104042,#3873);
#3346=LINE('',#104508,#3874);
#3347=LINE('',#104980,#3875);
#3348=LINE('',#105446,#3876);
#3349=LINE('',#105909,#3877);
#3350=LINE('',#106372,#3878);
#3351=LINE('',#106844,#3879);
#3352=LINE('',#107310,#3880);
#3353=LINE('',#107773,#3881);
#3354=LINE('',#108242,#3882);
#3355=LINE('',#108708,#3883);
#3356=LINE('',#109171,#3884);
#3357=LINE('',#109634,#3885);
#3358=LINE('',#109893,#3886);
#3359=LINE('',#110353,#3887);
#3360=LINE('',#110816,#3888);
#3361=LINE('',#111282,#3889);
#3362=LINE('',#111748,#3890);
#3363=LINE('',#112211,#3891);
#3364=LINE('',#112674,#3892);
#3365=LINE('',#113143,#3893);
#3366=LINE('',#113609,#3894);
#3367=LINE('',#114072,#3895);
#3368=LINE('',#114538,#3896);
#3369=LINE('',#115004,#3897);
#3370=LINE('',#115467,#3898);
#3371=LINE('',#115936,#3899);
#3372=LINE('',#116405,#3900);
#3373=LINE('',#116871,#3901);
#3374=LINE('',#117334,#3902);
#3375=LINE('',#117800,#3903);
#3376=LINE('',#118266,#3904);
#3377=LINE('',#118729,#3905);
#3378=LINE('',#119201,#3906);
#3379=LINE('',#119670,#3907);
#3380=LINE('',#120133,#3908);
#3381=LINE('',#120596,#3909);
#3382=LINE('',#121059,#3910);
#3383=LINE('',#121525,#3911);
#3384=LINE('',#121985,#3912);
#3385=LINE('',#122454,#3913);
#3386=LINE('',#122923,#3914);
#3387=LINE('',#123386,#3915);
#3388=LINE('',#123852,#3916);
#3389=LINE('',#124315,#3917);
#3390=LINE('',#124781,#3918);
#3391=LINE('',#125244,#3919);
#3392=LINE('',#125503,#3920);
#3393=LINE('',#125756,#3921);
#3394=LINE('',#126216,#3922);
#3395=LINE('',#126682,#3923);
#3396=LINE('',#127145,#3924);
#3397=LINE('',#127611,#3925);
#3398=LINE('',#128077,#3926);
#3399=LINE('',#128546,#3927);
#3400=LINE('',#129015,#3928);
#3401=LINE('',#129478,#3929);
#3402=LINE('',#129944,#3930);
#3403=LINE('',#130407,#3931);
#3404=LINE('',#130873,#3932);
#3405=LINE('',#131339,#3933);
#3406=LINE('',#131808,#3934);
#3407=LINE('',#132277,#3935);
#3408=LINE('',#132740,#3936);
#3409=LINE('',#133206,#3937);
#3410=LINE('',#133669,#3938);
#3411=LINE('',#134138,#3939);
#3412=LINE('',#134604,#3940);
#3413=LINE('',#135070,#3941);
#3414=LINE('',#135539,#3942);
#3415=LINE('',#136005,#3943);
#3416=LINE('',#136468,#3944);
#3417=LINE('',#136931,#3945);
#3418=LINE('',#137400,#3946);
#3419=LINE('',#137866,#3947);
#3420=LINE('',#138332,#3948);
#3421=LINE('',#138804,#3949);
#3422=LINE('',#139270,#3950);
#3423=LINE('',#139733,#3951);
#3424=LINE('',#188395,#3952);
#3425=LINE('',#188616,#3953);
#3426=LINE('',#188618,#3954);
#3427=LINE('',#188620,#3955);
#3428=LINE('',#188621,#3956);
#3429=LINE('',#188627,#3957);
#3430=LINE('',#188629,#3958);
#3431=LINE('',#188631,#3959);
#3432=LINE('',#188632,#3960);
#3433=LINE('',#188638,#3961);
#3434=LINE('',#202427,#3962);
#3435=LINE('',#202431,#3963);
#3436=LINE('',#202435,#3964);
#3437=LINE('',#202440,#3965);
#3438=LINE('',#202443,#3966);
#3439=LINE('',#202449,#3967);
#3440=LINE('',#202453,#3968);
#3441=LINE('',#202456,#3969);
#3442=LINE('',#202460,#3970);
#3443=LINE('',#202464,#3971);
#3444=LINE('',#202473,#3972);
#3445=LINE('',#202476,#3973);
#3446=LINE('',#202481,#3974);
#3447=LINE('',#202485,#3975);
#3448=LINE('',#202490,#3976);
#3449=LINE('',#202492,#3977);
#3450=LINE('',#202493,#3978);
#3451=LINE('',#202495,#3979);
#3452=LINE('',#202504,#3980);
#3453=LINE('',#202506,#3981);
#3454=LINE('',#202507,#3982);
#3455=LINE('',#202512,#3983);
#3456=LINE('',#202519,#3984);
#3457=LINE('',#202524,#3985);
#3458=LINE('',#202525,#3986);
#3459=LINE('',#202526,#3987);
#3460=LINE('',#202536,#3988);
#3461=LINE('',#202857,#3989);
#3462=LINE('',#203323,#3990);
#3463=LINE('',#203789,#3991);
#3464=LINE('',#204255,#3992);
#3465=LINE('',#204718,#3993);
#3466=LINE('',#205184,#3994);
#3467=LINE('',#205650,#3995);
#3468=LINE('',#206110,#3996);
#3469=LINE('',#206363,#3997);
#3470=LINE('',#206619,#3998);
#3471=LINE('',#207085,#3999);
#3472=LINE('',#207548,#4000);
#3473=LINE('',#208014,#4001);
#3474=LINE('',#208480,#4002);
#3475=LINE('',#208946,#4003);
#3476=LINE('',#209415,#4004);
#3477=LINE('',#240445,#4005);
#3478=LINE('',#240447,#4006);
#3479=LINE('',#240456,#4007);
#3480=LINE('',#240461,#4008);
#3481=LINE('',#240463,#4009);
#3482=LINE('',#240465,#4010);
#3483=LINE('',#240466,#4011);
#3484=LINE('',#240471,#4012);
#3485=LINE('',#240475,#4013);
#3486=LINE('',#240477,#4014);
#3487=LINE('',#240478,#4015);
#3488=LINE('',#240488,#4016);
#3489=LINE('',#240493,#4017);
#3490=LINE('',#240498,#4018);
#3491=LINE('',#240500,#4019);
#3492=LINE('',#240502,#4020);
#3493=LINE('',#240503,#4021);
#3494=LINE('',#240509,#4022);
#3495=LINE('',#240512,#4023);
#3496=LINE('',#240514,#4024);
#3497=LINE('',#240515,#4025);
#3498=LINE('',#240517,#4026);
#3499=LINE('',#240528,#4027);
#3500=LINE('',#240532,#4028);
#3501=LINE('',#240536,#4029);
#3502=LINE('',#240541,#4030);
#3503=LINE('',#240544,#4031);
#3504=LINE('',#240550,#4032);
#3505=LINE('',#240554,#4033);
#3506=LINE('',#240557,#4034);
#3507=LINE('',#240561,#4035);
#3508=LINE('',#240565,#4036);
#3509=LINE('',#240572,#4037);
#3510=LINE('',#240574,#4038);
#3511=LINE('',#240575,#4039);
#3512=LINE('',#240580,#4040);
#3513=LINE('',#240587,#4041);
#3514=LINE('',#240592,#4042);
#3515=LINE('',#240593,#4043);
#3516=LINE('',#240594,#4044);
#3517=LINE('',#240607,#4045);
#3518=LINE('',#240610,#4046);
#3519=LINE('',#240615,#4047);
#3520=LINE('',#240619,#4048);
#3521=LINE('',#240624,#4049);
#3522=LINE('',#240626,#4050);
#3523=LINE('',#240627,#4051);
#3524=LINE('',#240629,#4052);
#3525=LINE('',#240639,#4053);
#3526=LINE('',#240642,#4054);
#3527=LINE('',#240647,#4055);
#3528=LINE('',#240652,#4056);
#3529=LINE('',#240654,#4057);
#3530=LINE('',#240656,#4058);
#3531=LINE('',#240657,#4059);
#3532=LINE('',#240663,#4060);
#3533=LINE('',#240666,#4061);
#3534=LINE('',#240668,#4062);
#3535=LINE('',#240669,#4063);
#3536=LINE('',#240673,#4064);
#3537=LINE('',#240677,#4065);
#3538=LINE('',#240680,#4066);
#3539=LINE('',#240682,#4067);
#3540=LINE('',#240684,#4068);
#3541=LINE('',#240685,#4069);
#3542=LINE('',#240693,#4070);
#3543=LINE('',#240696,#4071);
#3544=LINE('',#240699,#4072);
#3545=LINE('',#240701,#4073);
#3546=LINE('',#240702,#4074);
#3547=LINE('',#240703,#4075);
#3548=LINE('',#240707,#4076);
#3549=LINE('',#240709,#4077);
#3550=LINE('',#240711,#4078);
#3551=LINE('',#240717,#4079);
#3552=LINE('',#240720,#4080);
#3553=LINE('',#240722,#4081);
#3554=LINE('',#240723,#4082);
#3555=LINE('',#240728,#4083);
#3556=LINE('',#240730,#4084);
#3557=LINE('',#240734,#4085);
#3558=LINE('',#240736,#4086);
#3559=LINE('',#240737,#4087);
#3560=LINE('',#240742,#4088);
#3561=LINE('',#240746,#4089);
#3562=LINE('',#240748,#4090);
#3563=LINE('',#240749,#4091);
#3564=LINE('',#240755,#4092);
#3565=LINE('',#240758,#4093);
#3566=LINE('',#240760,#4094);
#3567=LINE('',#240761,#4095);
#3568=LINE('',#240763,#4096);
#3569=LINE('',#240765,#4097);
#3570=LINE('',#240766,#4098);
#3571=LINE('',#240768,#4099);
#3572=LINE('',#240772,#4100);
#3573=LINE('',#240774,#4101);
#3574=LINE('',#240778,#4102);
#3575=LINE('',#240780,#4103);
#3576=LINE('',#240781,#4104);
#3577=LINE('',#240787,#4105);
#3578=LINE('',#240790,#4106);
#3579=LINE('',#240792,#4107);
#3580=LINE('',#240793,#4108);
#3581=LINE('',#240797,#4109);
#3582=LINE('',#240798,#4110);
#3583=LINE('',#240800,#4111);
#3584=LINE('',#240802,#4112);
#3585=LINE('',#240809,#4113);
#3586=LINE('',#241160,#4114);
#3587=LINE('',#241620,#4115);
#3588=LINE('',#241873,#4116);
#3589=LINE('',#242132,#4117);
#3590=LINE('',#242595,#4118);
#3591=LINE('',#243061,#4119);
#3592=LINE('',#243524,#4120);
#3593=LINE('',#243990,#4121);
#3594=LINE('',#244453,#4122);
#3595=LINE('',#244922,#4123);
#3596=LINE('',#245391,#4124);
#3597=LINE('',#245851,#4125);
#3598=LINE('',#246317,#4126);
#3599=LINE('',#246780,#4127);
#3600=LINE('',#247243,#4128);
#3601=LINE('',#247706,#4129);
#3602=LINE('',#279159,#4130);
#3603=LINE('',#279161,#4131);
#3604=LINE('',#279170,#4132);
#3605=LINE('',#279175,#4133);
#3606=LINE('',#279177,#4134);
#3607=LINE('',#279179,#4135);
#3608=LINE('',#279180,#4136);
#3609=LINE('',#279186,#4137);
#3610=LINE('',#279189,#4138);
#3611=LINE('',#279191,#4139);
#3612=LINE('',#279192,#4140);
#3613=LINE('',#279201,#4141);
#3614=LINE('',#279207,#4142);
#3615=LINE('',#279212,#4143);
#3616=LINE('',#279214,#4144);
#3617=LINE('',#279216,#4145);
#3618=LINE('',#279217,#4146);
#3619=LINE('',#279222,#4147);
#3620=LINE('',#279226,#4148);
#3621=LINE('',#279228,#4149);
#3622=LINE('',#279229,#4150);
#3623=LINE('',#279233,#4151);
#3624=VECTOR('',#15682,10.);
#3625=VECTOR('',#15685,10.);
#3626=VECTOR('',#15690,7.55784864301595);
#3627=VECTOR('',#15695,10.);
#3628=VECTOR('',#15696,10.);
#3629=VECTOR('',#15697,9.99999999999999);
#3630=VECTOR('',#15698,10.);
#3631=VECTOR('',#15703,10.);
#3632=VECTOR('',#15706,10.);
#3633=VECTOR('',#15709,10.);
#3634=VECTOR('',#15710,10.);
#3635=VECTOR('',#15713,10.);
#3636=VECTOR('',#15716,10.);
#3637=VECTOR('',#15721,10.);
#3638=VECTOR('',#15722,10.);
#3639=VECTOR('',#15723,10.);
#3640=VECTOR('',#15724,10.);
#3641=VECTOR('',#15731,10.);
#3642=VECTOR('',#15734,10.);
#3643=VECTOR('',#15737,10.);
#3644=VECTOR('',#15738,10.);
#3645=VECTOR('',#15739,9.99999999999999);
#3646=VECTOR('',#15740,10.);
#3647=VECTOR('',#15745,7.55784864301595);
#3648=VECTOR('',#15748,10.);
#3649=VECTOR('',#15751,10.);
#3650=VECTOR('',#15756,10.);
#3651=VECTOR('',#15759,10.);
#3652=VECTOR('',#15762,10.);
#3653=VECTOR('',#15763,10.);
#3654=VECTOR('',#15768,10.);
#3655=VECTOR('',#15769,10.);
#3656=VECTOR('',#15770,10.);
#3657=VECTOR('',#15773,10.);
#3658=VECTOR('',#15774,10.);
#3659=VECTOR('',#15779,7.55784864301595);
#3660=VECTOR('',#15784,10.);
#3661=VECTOR('',#15785,9.99999999999999);
#3662=VECTOR('',#15786,10.);
#3663=VECTOR('',#15791,10.);
#3664=VECTOR('',#15794,10.);
#3665=VECTOR('',#15797,10.);
#3666=VECTOR('',#15798,10.);
#3667=VECTOR('',#15801,10.);
#3668=VECTOR('',#15802,10.);
#3669=VECTOR('',#15803,10.);
#3670=VECTOR('',#15806,10.);
#3671=VECTOR('',#15811,10.);
#3672=VECTOR('',#15814,10.);
#3673=VECTOR('',#15817,10.);
#3674=VECTOR('',#15818,10.);
#3675=VECTOR('',#15819,10.);
#3676=VECTOR('',#15826,10.);
#3677=VECTOR('',#15829,10.);
#3678=VECTOR('',#15830,9.99999999999999);
#3679=VECTOR('',#15831,10.);
#3680=VECTOR('',#15836,10.);
#3681=VECTOR('',#15837,10.);
#3682=VECTOR('',#15840,7.55784864301595);
#3683=VECTOR('',#15843,10.);
#3684=VECTOR('',#15852,4.91825);
#3685=VECTOR('',#15857,4.91825);
#3686=VECTOR('',#15860,4.91825);
#3687=VECTOR('',#15863,4.91825);
#3688=VECTOR('',#15866,4.91825);
#3689=VECTOR('',#15869,4.91825);
#3690=VECTOR('',#15872,4.91825);
#3691=VECTOR('',#15875,4.91825);
#3692=VECTOR('',#15878,4.91825);
#3693=VECTOR('',#15881,4.91825);
#3694=VECTOR('',#15884,4.91825);
#3695=VECTOR('',#15887,4.91825);
#3696=VECTOR('',#15890,4.91825);
#3697=VECTOR('',#15893,4.91825);
#3698=VECTOR('',#15896,4.91825);
#3699=VECTOR('',#15899,4.91825);
#3700=VECTOR('',#15902,4.91825);
#3701=VECTOR('',#15905,4.91825);
#3702=VECTOR('',#15908,4.91825);
#3703=VECTOR('',#15911,4.91825);
#3704=VECTOR('',#15914,4.91825);
#3705=VECTOR('',#15917,4.91825);
#3706=VECTOR('',#15920,4.91825);
#3707=VECTOR('',#15923,4.91825);
#3708=VECTOR('',#15926,4.91825);
#3709=VECTOR('',#15929,4.91825);
#3710=VECTOR('',#15932,4.91825);
#3711=VECTOR('',#15935,4.91825);
#3712=VECTOR('',#15938,4.91825);
#3713=VECTOR('',#15941,4.91825);
#3714=VECTOR('',#15944,4.91825);
#3715=VECTOR('',#15947,4.91825);
#3716=VECTOR('',#15950,4.91825);
#3717=VECTOR('',#15953,4.91825);
#3718=VECTOR('',#15956,4.91825);
#3719=VECTOR('',#15959,4.91825);
#3720=VECTOR('',#15962,4.91825);
#3721=VECTOR('',#15965,4.91825);
#3722=VECTOR('',#15968,4.91825);
#3723=VECTOR('',#15971,4.91825);
#3724=VECTOR('',#15974,4.91825);
#3725=VECTOR('',#15977,4.91825);
#3726=VECTOR('',#15980,4.91825);
#3727=VECTOR('',#15983,4.91825);
#3728=VECTOR('',#15986,4.91825);
#3729=VECTOR('',#15989,4.91825);
#3730=VECTOR('',#15992,4.91825);
#3731=VECTOR('',#15995,4.91825);
#3732=VECTOR('',#15998,4.91825);
#3733=VECTOR('',#16001,4.91825);
#3734=VECTOR('',#16004,4.91825);
#3735=VECTOR('',#16007,4.91825);
#3736=VECTOR('',#16010,4.91825);
#3737=VECTOR('',#16013,4.91825);
#3738=VECTOR('',#16016,4.91825);
#3739=VECTOR('',#16019,4.91825);
#3740=VECTOR('',#16022,4.91825);
#3741=VECTOR('',#16025,4.91825);
#3742=VECTOR('',#16028,4.91825);
#3743=VECTOR('',#16031,4.91825);
#3744=VECTOR('',#16034,4.91825);
#3745=VECTOR('',#16037,4.91825);
#3746=VECTOR('',#16040,4.91825);
#3747=VECTOR('',#16043,4.91825);
#3748=VECTOR('',#16046,4.91825);
#3749=VECTOR('',#16049,4.91825);
#3750=VECTOR('',#16052,4.91825);
#3751=VECTOR('',#16055,4.91825);
#3752=VECTOR('',#16058,4.91825);
#3753=VECTOR('',#16061,4.91825);
#3754=VECTOR('',#16064,4.91825);
#3755=VECTOR('',#16067,4.91825);
#3756=VECTOR('',#16070,4.91825);
#3757=VECTOR('',#16073,4.91825);
#3758=VECTOR('',#16076,4.91825);
#3759=VECTOR('',#16079,4.91825);
#3760=VECTOR('',#16082,4.91825);
#3761=VECTOR('',#16085,4.91825);
#3762=VECTOR('',#16088,4.91825);
#3763=VECTOR('',#16091,4.91825);
#3764=VECTOR('',#16094,4.91825);
#3765=VECTOR('',#16097,4.91825);
#3766=VECTOR('',#16100,4.91825);
#3767=VECTOR('',#16103,4.91825);
#3768=VECTOR('',#16106,4.91825);
#3769=VECTOR('',#16109,4.91825);
#3770=VECTOR('',#16112,4.91825);
#3771=VECTOR('',#16115,4.91825);
#3772=VECTOR('',#16118,4.91825);
#3773=VECTOR('',#16121,4.91825);
#3774=VECTOR('',#16124,4.91825);
#3775=VECTOR('',#16127,4.91825);
#3776=VECTOR('',#16130,4.91825);
#3777=VECTOR('',#16133,4.91825);
#3778=VECTOR('',#16136,4.91825);
#3779=VECTOR('',#16139,4.91825);
#3780=VECTOR('',#16142,4.91825);
#3781=VECTOR('',#16145,4.91825);
#3782=VECTOR('',#16148,4.91825);
#3783=VECTOR('',#16151,4.91825);
#3784=VECTOR('',#16154,4.91825);
#3785=VECTOR('',#16157,4.91825);
#3786=VECTOR('',#16160,4.91825);
#3787=VECTOR('',#16163,4.91825);
#3788=VECTOR('',#16166,4.91825);
#3789=VECTOR('',#16169,4.91825);
#3790=VECTOR('',#16172,4.91825);
#3791=VECTOR('',#16175,4.91825);
#3792=VECTOR('',#16178,4.91825);
#3793=VECTOR('',#16181,4.91825);
#3794=VECTOR('',#16184,4.91825);
#3795=VECTOR('',#16187,4.91825);
#3796=VECTOR('',#16190,4.91825);
#3797=VECTOR('',#16193,4.91825);
#3798=VECTOR('',#16196,4.91825);
#3799=VECTOR('',#16199,4.91825);
#3800=VECTOR('',#16202,4.91825);
#3801=VECTOR('',#16205,4.91825);
#3802=VECTOR('',#16208,4.91825);
#3803=VECTOR('',#16211,4.91825);
#3804=VECTOR('',#16214,4.91825);
#3805=VECTOR('',#16217,4.91825);
#3806=VECTOR('',#16220,4.91825);
#3807=VECTOR('',#16223,4.91825);
#3808=VECTOR('',#16226,4.91825);
#3809=VECTOR('',#16229,4.91825);
#3810=VECTOR('',#16232,4.91825);
#3811=VECTOR('',#16235,4.91825);
#3812=VECTOR('',#16238,4.91825);
#3813=VECTOR('',#16241,4.91825);
#3814=VECTOR('',#16244,4.91825);
#3815=VECTOR('',#16247,4.91825);
#3816=VECTOR('',#16250,4.91825);
#3817=VECTOR('',#16253,4.91825);
#3818=VECTOR('',#16256,4.91825);
#3819=VECTOR('',#16259,4.91825);
#3820=VECTOR('',#16262,4.91825);
#3821=VECTOR('',#16265,4.91825);
#3822=VECTOR('',#16268,4.91825);
#3823=VECTOR('',#16271,4.91825);
#3824=VECTOR('',#16274,4.91825);
#3825=VECTOR('',#16277,4.91825);
#3826=VECTOR('',#16280,4.91825);
#3827=VECTOR('',#16283,4.91825);
#3828=VECTOR('',#16286,4.91825);
#3829=VECTOR('',#16289,4.91825);
#3830=VECTOR('',#16292,4.91825);
#3831=VECTOR('',#16295,4.91825);
#3832=VECTOR('',#16298,4.91825);
#3833=VECTOR('',#16301,4.91825);
#3834=VECTOR('',#16304,4.91825);
#3835=VECTOR('',#16307,4.91825);
#3836=VECTOR('',#16310,4.91825);
#3837=VECTOR('',#16313,4.91825);
#3838=VECTOR('',#16316,4.91825);
#3839=VECTOR('',#16319,4.91825);
#3840=VECTOR('',#16322,4.91825);
#3841=VECTOR('',#16325,4.91825);
#3842=VECTOR('',#16328,4.91825);
#3843=VECTOR('',#16331,4.91825);
#3844=VECTOR('',#16334,4.91825);
#3845=VECTOR('',#16337,4.91825);
#3846=VECTOR('',#16340,4.91825);
#3847=VECTOR('',#16343,4.91825);
#3848=VECTOR('',#16346,4.91825);
#3849=VECTOR('',#16349,4.91825);
#3850=VECTOR('',#16352,4.91825);
#3851=VECTOR('',#16355,4.91825);
#3852=VECTOR('',#16358,4.91825);
#3853=VECTOR('',#16361,4.91825);
#3854=VECTOR('',#16364,4.91825);
#3855=VECTOR('',#16367,4.91825);
#3856=VECTOR('',#16370,4.91825);
#3857=VECTOR('',#16373,4.91825);
#3858=VECTOR('',#16376,4.91825);
#3859=VECTOR('',#16379,4.91825);
#3860=VECTOR('',#16382,4.91825);
#3861=VECTOR('',#16385,4.91825);
#3862=VECTOR('',#16388,4.91825);
#3863=VECTOR('',#16391,4.91825);
#3864=VECTOR('',#16394,4.91825);
#3865=VECTOR('',#16397,4.91825);
#3866=VECTOR('',#16400,4.91825);
#3867=VECTOR('',#16403,4.91825);
#3868=VECTOR('',#16406,4.91825);
#3869=VECTOR('',#16409,4.91825);
#3870=VECTOR('',#16412,4.91825);
#3871=VECTOR('',#16415,4.91825);
#3872=VECTOR('',#16418,4.91825);
#3873=VECTOR('',#16421,4.91825);
#3874=VECTOR('',#16424,4.91825);
#3875=VECTOR('',#16427,4.91825);
#3876=VECTOR('',#16430,4.91825);
#3877=VECTOR('',#16433,4.91825);
#3878=VECTOR('',#16436,4.91825);
#3879=VECTOR('',#16439,4.91825);
#3880=VECTOR('',#16442,4.91825);
#3881=VECTOR('',#16445,4.91825);
#3882=VECTOR('',#16448,4.91825);
#3883=VECTOR('',#16451,4.91825);
#3884=VECTOR('',#16454,4.91825);
#3885=VECTOR('',#16457,4.91825);
#3886=VECTOR('',#16460,4.91825);
#3887=VECTOR('',#16463,4.91825);
#3888=VECTOR('',#16466,4.91825);
#3889=VECTOR('',#16469,4.91825);
#3890=VECTOR('',#16472,4.91825);
#3891=VECTOR('',#16475,4.91825);
#3892=VECTOR('',#16478,4.91825);
#3893=VECTOR('',#16481,4.91825);
#3894=VECTOR('',#16484,4.91825);
#3895=VECTOR('',#16487,4.91825);
#3896=VECTOR('',#16490,4.91825);
#3897=VECTOR('',#16493,4.91825);
#3898=VECTOR('',#16496,4.91825);
#3899=VECTOR('',#16499,4.91825);
#3900=VECTOR('',#16502,4.91825);
#3901=VECTOR('',#16505,4.91825);
#3902=VECTOR('',#16508,4.91825);
#3903=VECTOR('',#16511,4.91825);
#3904=VECTOR('',#16514,4.91825);
#3905=VECTOR('',#16517,4.91825);
#3906=VECTOR('',#16520,4.91825);
#3907=VECTOR('',#16523,4.91825);
#3908=VECTOR('',#16526,4.91825);
#3909=VECTOR('',#16529,4.91825);
#3910=VECTOR('',#16532,4.91825);
#3911=VECTOR('',#16535,4.91825);
#3912=VECTOR('',#16538,4.91825);
#3913=VECTOR('',#16541,4.91825);
#3914=VECTOR('',#16544,4.91825);
#3915=VECTOR('',#16547,4.91825);
#3916=VECTOR('',#16550,4.91825);
#3917=VECTOR('',#16553,4.91825);
#3918=VECTOR('',#16556,4.91825);
#3919=VECTOR('',#16559,4.91825);
#3920=VECTOR('',#16562,4.91825);
#3921=VECTOR('',#16565,4.91825);
#3922=VECTOR('',#16568,4.91825);
#3923=VECTOR('',#16571,4.91825);
#3924=VECTOR('',#16574,4.91825);
#3925=VECTOR('',#16577,4.91825);
#3926=VECTOR('',#16580,4.91825);
#3927=VECTOR('',#16583,4.91825);
#3928=VECTOR('',#16586,4.91825);
#3929=VECTOR('',#16589,4.91825);
#3930=VECTOR('',#16592,4.91825);
#3931=VECTOR('',#16595,4.91825);
#3932=VECTOR('',#16598,4.91825);
#3933=VECTOR('',#16601,4.91825);
#3934=VECTOR('',#16604,4.91825);
#3935=VECTOR('',#16607,4.91825);
#3936=VECTOR('',#16610,4.91825);
#3937=VECTOR('',#16613,4.91825);
#3938=VECTOR('',#16616,4.91825);
#3939=VECTOR('',#16619,4.91825);
#3940=VECTOR('',#16622,4.91825);
#3941=VECTOR('',#16625,4.91825);
#3942=VECTOR('',#16628,4.91825);
#3943=VECTOR('',#16631,4.91825);
#3944=VECTOR('',#16634,4.91825);
#3945=VECTOR('',#16637,4.91825);
#3946=VECTOR('',#16640,4.91825);
#3947=VECTOR('',#16643,4.91825);
#3948=VECTOR('',#16646,4.91825);
#3949=VECTOR('',#16649,4.91825);
#3950=VECTOR('',#16652,4.91825);
#3951=VECTOR('',#16655,4.91825);
#3952=VECTOR('',#16674,9.);
#3953=VECTOR('',#16681,10.);
#3954=VECTOR('',#16682,10.);
#3955=VECTOR('',#16683,10.);
#3956=VECTOR('',#16684,10.);
#3957=VECTOR('',#16691,10.);
#3958=VECTOR('',#16692,10.);
#3959=VECTOR('',#16693,10.);
#3960=VECTOR('',#16694,10.);
#3961=VECTOR('',#16703,7.);
#3962=VECTOR('',#16718,7.55784864301595);
#3963=VECTOR('',#16721,10.);
#3964=VECTOR('',#16724,10.);
#3965=VECTOR('',#16729,10.);
#3966=VECTOR('',#16732,10.);
#3967=VECTOR('',#16737,10.);
#3968=VECTOR('',#16740,10.);
#3969=VECTOR('',#16743,15.2420394990918);
#3970=VECTOR('',#16746,10.);
#3971=VECTOR('',#16749,10.);
#3972=VECTOR('',#16762,10.);
#3973=VECTOR('',#16765,10.);
#3974=VECTOR('',#16770,10.);
#3975=VECTOR('',#16773,10.);
#3976=VECTOR('',#16780,6.50110764916953);
#3977=VECTOR('',#16783,10.);
#3978=VECTOR('',#16784,10.);
#3979=VECTOR('',#16787,10.);
#3980=VECTOR('',#16802,10.);
#3981=VECTOR('',#16803,10.);
#3982=VECTOR('',#16804,10.);
#3983=VECTOR('',#16809,10.);
#3984=VECTOR('',#16818,6.50110764916953);
#3985=VECTOR('',#16823,10.);
#3986=VECTOR('',#16824,10.);
#3987=VECTOR('',#16825,10.);
#3988=VECTOR('',#16840,4.91825);
#3989=VECTOR('',#16843,4.91825);
#3990=VECTOR('',#16846,4.91825);
#3991=VECTOR('',#16849,4.91825);
#3992=VECTOR('',#16852,4.91825);
#3993=VECTOR('',#16855,4.91825);
#3994=VECTOR('',#16858,4.91825);
#3995=VECTOR('',#16861,4.91825);
#3996=VECTOR('',#16864,4.91825);
#3997=VECTOR('',#16867,4.91825);
#3998=VECTOR('',#16870,4.91825);
#3999=VECTOR('',#16873,4.91825);
#4000=VECTOR('',#16876,4.91825);
#4001=VECTOR('',#16879,4.91825);
#4002=VECTOR('',#16882,4.91825);
#4003=VECTOR('',#16885,4.91825);
#4004=VECTOR('',#16888,4.91825);
#4005=VECTOR('',#16903,15.2420394990918);
#4006=VECTOR('',#16904,15.2420394990918);
#4007=VECTOR('',#16917,6.50110764916953);
#4008=VECTOR('',#16922,10.);
#4009=VECTOR('',#16923,10.);
#4010=VECTOR('',#16924,10.);
#4011=VECTOR('',#16925,10.);
#4012=VECTOR('',#16930,10.);
#4013=VECTOR('',#16935,10.);
#4014=VECTOR('',#16936,10.);
#4015=VECTOR('',#16937,10.);
#4016=VECTOR('',#16952,7.55784864301595);
#4017=VECTOR('',#16957,6.50110764916953);
#4018=VECTOR('',#16962,10.);
#4019=VECTOR('',#16963,10.);
#4020=VECTOR('',#16964,10.);
#4021=VECTOR('',#16965,10.);
#4022=VECTOR('',#16972,10.);
#4023=VECTOR('',#16975,10.);
#4024=VECTOR('',#16976,10.);
#4025=VECTOR('',#16977,10.);
#4026=VECTOR('',#16980,15.2420394990918);
#4027=VECTOR('',#16995,7.55784864301595);
#4028=VECTOR('',#16998,10.);
#4029=VECTOR('',#17001,10.);
#4030=VECTOR('',#17006,10.);
#4031=VECTOR('',#17009,10.);
#4032=VECTOR('',#17014,10.);
#4033=VECTOR('',#17017,10.);
#4034=VECTOR('',#17020,15.2420394990918);
#4035=VECTOR('',#17023,10.);
#4036=VECTOR('',#17026,10.);
#4037=VECTOR('',#17037,10.);
#4038=VECTOR('',#17038,10.);
#4039=VECTOR('',#17039,10.);
#4040=VECTOR('',#17044,10.);
#4041=VECTOR('',#17053,6.50110764916953);
#4042=VECTOR('',#17058,10.);
#4043=VECTOR('',#17059,10.);
#4044=VECTOR('',#17060,10.);
#4045=VECTOR('',#17081,10.);
#4046=VECTOR('',#17084,10.);
#4047=VECTOR('',#17089,10.);
#4048=VECTOR('',#17092,10.);
#4049=VECTOR('',#17099,6.50110764916953);
#4050=VECTOR('',#17102,10.);
#4051=VECTOR('',#17103,10.);
#4052=VECTOR('',#17106,10.);
#4053=VECTOR('',#17119,10.);
#4054=VECTOR('',#17122,10.);
#4055=VECTOR('',#17127,7.55784864301595);
#4056=VECTOR('',#17132,10.);
#4057=VECTOR('',#17133,10.);
#4058=VECTOR('',#17134,9.99999999999999);
#4059=VECTOR('',#17135,10.);
#4060=VECTOR('',#17140,10.);
#4061=VECTOR('',#17143,10.);
#4062=VECTOR('',#17146,10.);
#4063=VECTOR('',#17147,10.);
#4064=VECTOR('',#17150,10.);
#4065=VECTOR('',#17153,10.);
#4066=VECTOR('',#17158,10.);
#4067=VECTOR('',#17159,10.);
#4068=VECTOR('',#17160,10.);
#4069=VECTOR('',#17161,10.);
#4070=VECTOR('',#17168,10.);
#4071=VECTOR('',#17171,10.);
#4072=VECTOR('',#17174,10.);
#4073=VECTOR('',#17175,9.99999999999999);
#4074=VECTOR('',#17176,10.);
#4075=VECTOR('',#17177,10.);
#4076=VECTOR('',#17182,7.55784864301595);
#4077=VECTOR('',#17185,10.);
#4078=VECTOR('',#17188,10.);
#4079=VECTOR('',#17193,10.);
#4080=VECTOR('',#17196,10.);
#4081=VECTOR('',#17199,10.);
#4082=VECTOR('',#17200,10.);
#4083=VECTOR('',#17205,10.);
#4084=VECTOR('',#17206,10.);
#4085=VECTOR('',#17209,10.);
#4086=VECTOR('',#17210,10.);
#4087=VECTOR('',#17211,10.);
#4088=VECTOR('',#17216,7.55784864301595);
#4089=VECTOR('',#17221,10.);
#4090=VECTOR('',#17222,10.);
#4091=VECTOR('',#17223,9.99999999999999);
#4092=VECTOR('',#17228,10.);
#4093=VECTOR('',#17231,10.);
#4094=VECTOR('',#17234,10.);
#4095=VECTOR('',#17235,10.);
#4096=VECTOR('',#17238,10.);
#4097=VECTOR('',#17239,10.);
#4098=VECTOR('',#17240,10.);
#4099=VECTOR('',#17243,10.);
#4100=VECTOR('',#17248,10.);
#4101=VECTOR('',#17249,10.);
#4102=VECTOR('',#17254,10.);
#4103=VECTOR('',#17255,10.);
#4104=VECTOR('',#17256,10.);
#4105=VECTOR('',#17263,10.);
#4106=VECTOR('',#17266,10.);
#4107=VECTOR('',#17267,9.99999999999999);
#4108=VECTOR('',#17268,10.);
#4109=VECTOR('',#17273,10.);
#4110=VECTOR('',#17274,10.);
#4111=VECTOR('',#17277,7.55784864301595);
#4112=VECTOR('',#17280,10.);
#4113=VECTOR('',#17289,4.91825);
#4114=VECTOR('',#17292,4.91825);
#4115=VECTOR('',#17295,4.91825);
#4116=VECTOR('',#17298,4.91825);
#4117=VECTOR('',#17301,4.91825);
#4118=VECTOR('',#17304,4.91825);
#4119=VECTOR('',#17307,4.91825);
#4120=VECTOR('',#17310,4.91825);
#4121=VECTOR('',#17313,4.91825);
#4122=VECTOR('',#17316,4.91825);
#4123=VECTOR('',#17319,4.91825);
#4124=VECTOR('',#17322,4.91825);
#4125=VECTOR('',#17325,4.91825);
#4126=VECTOR('',#17328,4.91825);
#4127=VECTOR('',#17331,4.91825);
#4128=VECTOR('',#17334,4.91825);
#4129=VECTOR('',#17337,4.91825);
#4130=VECTOR('',#17352,15.2420394990918);
#4131=VECTOR('',#17353,15.2420394990918);
#4132=VECTOR('',#17366,6.50110764916953);
#4133=VECTOR('',#17371,10.);
#4134=VECTOR('',#17372,10.);
#4135=VECTOR('',#17373,10.);
#4136=VECTOR('',#17374,10.);
#4137=VECTOR('',#17381,10.);
#4138=VECTOR('',#17384,10.);
#4139=VECTOR('',#17385,10.);
#4140=VECTOR('',#17386,10.);
#4141=VECTOR('',#17399,7.55784864301595);
#4142=VECTOR('',#17406,6.50110764916953);
#4143=VECTOR('',#17411,10.);
#4144=VECTOR('',#17412,10.);
#4145=VECTOR('',#17413,10.);
#4146=VECTOR('',#17414,10.);
#4147=VECTOR('',#17419,10.);
#4148=VECTOR('',#17424,10.);
#4149=VECTOR('',#17425,10.);
#4150=VECTOR('',#17426,10.);
#4151=VECTOR('',#17433,15.2420394990918);
#4152=CIRCLE('',#15050,10.);
#4153=CIRCLE('',#15051,10.);
#4154=CIRCLE('',#15053,7.55784864301595);
#4155=CIRCLE('',#15054,7.55784864301595);
#4156=CIRCLE('',#15057,10.);
#4157=CIRCLE('',#15058,10.);
#4158=CIRCLE('',#15061,3.);
#4159=CIRCLE('',#15062,3.);
#4160=CIRCLE('',#15064,7.55784864301595);
#4161=CIRCLE('',#15066,5.5);
#4162=CIRCLE('',#15067,5.5);
#4163=CIRCLE('',#15069,7.55784864301595);
#4164=CIRCLE('',#15074,10.);
#4165=CIRCLE('',#15075,10.);
#4166=CIRCLE('',#15078,5.5);
#4167=CIRCLE('',#15079,3.);
#4168=CIRCLE('',#15081,7.55784864301595);
#4169=CIRCLE('',#15082,7.55784864301595);
#4170=CIRCLE('',#15085,10.);
#4171=CIRCLE('',#15086,10.);
#4172=CIRCLE('',#15092,3.);
#4173=CIRCLE('',#15094,7.55784864301595);
#4174=CIRCLE('',#15096,5.5);
#4175=CIRCLE('',#15098,7.55784864301595);
#4176=CIRCLE('',#15106,4.91825);
#4177=CIRCLE('',#15375,5.91675);
#4178=CIRCLE('',#15376,5.91675);
#4179=CIRCLE('',#15378,4.91825);
#4180=CIRCLE('',#15380,9.);
#4181=CIRCLE('',#15381,7.);
#4182=CIRCLE('',#15383,9.);
#4183=CIRCLE('',#15387,7.);
#4184=CIRCLE('',#15390,7.);
#4185=CIRCLE('',#15391,7.);
#4186=CIRCLE('',#15393,7.);
#4187=CIRCLE('',#15394,7.);
#4188=CIRCLE('',#15399,7.55784864301595);
#4189=CIRCLE('',#15400,7.55784864301595);
#4190=CIRCLE('',#15401,7.55784864301595);
#4191=CIRCLE('',#15402,7.55784864301595);
#4192=CIRCLE('',#15403,7.55784864301595);
#4193=CIRCLE('',#15404,7.55784864301595);
#4194=CIRCLE('',#15406,15.2420394990918);
#4195=CIRCLE('',#15407,15.2420394990918);
#4196=CIRCLE('',#15408,15.2420394990918);
#4197=CIRCLE('',#15409,15.2420394990918);
#4198=CIRCLE('',#15410,15.2420394990918);
#4199=CIRCLE('',#15411,15.2420394990918);
#4200=CIRCLE('',#15413,7.55784864301595);
#4201=CIRCLE('',#15414,7.55784864301595);
#4202=CIRCLE('',#15416,15.2420394990918);
#4203=CIRCLE('',#15417,15.2420394990918);
#4204=CIRCLE('',#15418,6.50110764916953);
#4205=CIRCLE('',#15420,15.2420394990918);
#4206=CIRCLE('',#15421,15.2420394990918);
#4207=CIRCLE('',#15422,6.50110764916953);
#4208=CIRCLE('',#15430,7.55784864301595);
#4209=CIRCLE('',#15431,7.55784864301595);
#4210=CIRCLE('',#15434,15.2420394990918);
#4211=CIRCLE('',#15435,15.2420394990918);
#4212=CIRCLE('',#15436,6.50110764916953);
#4213=CIRCLE('',#15439,6.50110764916953);
#4214=CIRCLE('',#15442,15.2420394990918);
#4215=CIRCLE('',#15444,15.2420394990918);
#4216=CIRCLE('',#15470,15.2420394990918);
#4217=CIRCLE('',#15471,15.2420394990918);
#4218=CIRCLE('',#15476,6.50110764916953);
#4219=CIRCLE('',#15477,6.50110764916953);
#4220=CIRCLE('',#15480,15.2420394990918);
#4221=CIRCLE('',#15481,15.2420394990918);
#4222=CIRCLE('',#15484,15.2420394990918);
#4223=CIRCLE('',#15486,15.2420394990918);
#4224=CIRCLE('',#15487,7.55784864301595);
#4225=CIRCLE('',#15489,7.55784864301595);
#4226=CIRCLE('',#15491,6.50110764916953);
#4227=CIRCLE('',#15492,6.50110764916953);
#4228=CIRCLE('',#15495,15.2420394990918);
#4229=CIRCLE('',#15496,15.2420394990918);
#4230=CIRCLE('',#15499,15.2420394990918);
#4231=CIRCLE('',#15500,15.2420394990918);
#4232=CIRCLE('',#15505,7.55784864301595);
#4233=CIRCLE('',#15506,7.55784864301595);
#4234=CIRCLE('',#15507,7.55784864301595);
#4235=CIRCLE('',#15508,7.55784864301595);
#4236=CIRCLE('',#15509,7.55784864301595);
#4237=CIRCLE('',#15510,7.55784864301595);
#4238=CIRCLE('',#15512,15.2420394990918);
#4239=CIRCLE('',#15513,15.2420394990918);
#4240=CIRCLE('',#15514,15.2420394990918);
#4241=CIRCLE('',#15515,15.2420394990918);
#4242=CIRCLE('',#15516,15.2420394990918);
#4243=CIRCLE('',#15517,15.2420394990918);
#4244=CIRCLE('',#15519,7.55784864301595);
#4245=CIRCLE('',#15520,7.55784864301595);
#4246=CIRCLE('',#15523,15.2420394990918);
#4247=CIRCLE('',#15524,15.2420394990918);
#4248=CIRCLE('',#15525,6.50110764916953);
#4249=CIRCLE('',#15528,6.50110764916953);
#4250=CIRCLE('',#15531,15.2420394990918);
#4251=CIRCLE('',#15533,15.2420394990918);
#4252=CIRCLE('',#15536,7.55784864301595);
#4253=CIRCLE('',#15537,7.55784864301595);
#4254=CIRCLE('',#15539,15.2420394990918);
#4255=CIRCLE('',#15540,15.2420394990918);
#4256=CIRCLE('',#15541,6.50110764916953);
#4257=CIRCLE('',#15543,15.2420394990918);
#4258=CIRCLE('',#15544,15.2420394990918);
#4259=CIRCLE('',#15545,6.50110764916953);
#4260=CIRCLE('',#15554,10.);
#4261=CIRCLE('',#15555,10.);
#4262=CIRCLE('',#15557,7.55784864301595);
#4263=CIRCLE('',#15558,7.55784864301595);
#4264=CIRCLE('',#15561,10.);
#4265=CIRCLE('',#15562,10.);
#4266=CIRCLE('',#15565,3.);
#4267=CIRCLE('',#15566,3.);
#4268=CIRCLE('',#15568,7.55784864301595);
#4269=CIRCLE('',#15570,5.5);
#4270=CIRCLE('',#15571,5.5);
#4271=CIRCLE('',#15573,7.55784864301595);
#4272=CIRCLE('',#15578,10.);
#4273=CIRCLE('',#15579,10.);
#4274=CIRCLE('',#15582,5.5);
#4275=CIRCLE('',#15583,3.);
#4276=CIRCLE('',#15585,7.55784864301595);
#4277=CIRCLE('',#15586,7.55784864301595);
#4278=CIRCLE('',#15589,10.);
#4279=CIRCLE('',#15590,10.);
#4280=CIRCLE('',#15596,3.);
#4281=CIRCLE('',#15598,7.55784864301595);
#4282=CIRCLE('',#15600,5.5);
#4283=CIRCLE('',#15602,7.55784864301595);
#4284=CIRCLE('',#15632,15.2420394990918);
#4285=CIRCLE('',#15633,15.2420394990918);
#4286=CIRCLE('',#15638,6.50110764916953);
#4287=CIRCLE('',#15639,6.50110764916953);
#4288=CIRCLE('',#15642,15.2420394990918);
#4289=CIRCLE('',#15643,15.2420394990918);
#4290=CIRCLE('',#15646,15.2420394990918);
#4291=CIRCLE('',#15648,15.2420394990918);
#4292=CIRCLE('',#15649,7.55784864301595);
#4293=CIRCLE('',#15651,7.55784864301595);
#4294=CIRCLE('',#15653,6.50110764916953);
#4295=CIRCLE('',#15654,6.50110764916953);
#4296=CIRCLE('',#15657,15.2420394990918);
#4297=CIRCLE('',#15658,15.2420394990918);
#4298=CIRCLE('',#15661,15.2420394990918);
#4299=CIRCLE('',#15662,15.2420394990918);
#4300=VERTEX_POINT('',#17459);
#4301=VERTEX_POINT('',#17460);
#4302=VERTEX_POINT('',#17462);
#4303=VERTEX_POINT('',#17464);
#4304=VERTEX_POINT('',#17468);
#4305=VERTEX_POINT('',#17470);
#4306=VERTEX_POINT('',#17474);
#4307=VERTEX_POINT('',#17475);
#4308=VERTEX_POINT('',#17477);
#4309=VERTEX_POINT('',#17479);
#4310=VERTEX_POINT('',#17483);
#4311=VERTEX_POINT('',#17484);
#4312=VERTEX_POINT('',#17486);
#4313=VERTEX_POINT('',#17488);
#4314=VERTEX_POINT('',#17495);
#4315=VERTEX_POINT('',#17496);
#4316=VERTEX_POINT('',#17498);
#4317=VERTEX_POINT('',#17500);
#4318=VERTEX_POINT('',#17504);
#4319=VERTEX_POINT('',#17506);
#4320=VERTEX_POINT('',#17510);
#4321=VERTEX_POINT('',#17513);
#4322=VERTEX_POINT('',#17514);
#4323=VERTEX_POINT('',#17516);
#4324=VERTEX_POINT('',#17518);
#4325=VERTEX_POINT('',#17523);
#4326=VERTEX_POINT('',#17525);
#4327=VERTEX_POINT('',#17528);
#4328=VERTEX_POINT('',#17537);
#4329=VERTEX_POINT('',#17538);
#4330=VERTEX_POINT('',#17540);
#4331=VERTEX_POINT('',#17542);
#4332=VERTEX_POINT('',#17549);
#4333=VERTEX_POINT('',#17550);
#4334=VERTEX_POINT('',#17552);
#4335=VERTEX_POINT('',#17554);
#4336=VERTEX_POINT('',#17556);
#4337=VERTEX_POINT('',#17558);
#4338=VERTEX_POINT('',#17563);
#4339=VERTEX_POINT('',#17565);
#4340=VERTEX_POINT('',#17569);
#4341=VERTEX_POINT('',#17571);
#4342=VERTEX_POINT('',#17575);
#4343=VERTEX_POINT('',#17576);
#4344=VERTEX_POINT('',#17578);
#4345=VERTEX_POINT('',#17580);
#4346=VERTEX_POINT('',#17588);
#4347=VERTEX_POINT('',#17595);
#4348=VERTEX_POINT('',#17597);
#4349=VERTEX_POINT('',#17601);
#4350=VERTEX_POINT('',#17603);
#4351=VERTEX_POINT('',#17606);
#4352=VERTEX_POINT('',#17609);
#4353=VERTEX_POINT('',#17613);
#4354=VERTEX_POINT('',#17615);
#4355=VERTEX_POINT('',#17618);
#4356=VERTEX_POINT('',#17631);
#4357=VERTEX_POINT('',#17632);
#4358=VERTEX_POINT('',#17634);
#4359=VERTEX_POINT('',#17822);
#4360=VERTEX_POINT('',#17961);
#4361=VERTEX_POINT('',#17962);
#4362=VERTEX_POINT('',#17964);
#4363=VERTEX_POINT('',#18195);
#4364=VERTEX_POINT('',#18427);
#4365=VERTEX_POINT('',#18428);
#4366=VERTEX_POINT('',#18430);
#4367=VERTEX_POINT('',#18661);
#4368=VERTEX_POINT('',#18893);
#4369=VERTEX_POINT('',#18894);
#4370=VERTEX_POINT('',#18896);
#4371=VERTEX_POINT('',#19130);
#4372=VERTEX_POINT('',#19362);
#4373=VERTEX_POINT('',#19363);
#4374=VERTEX_POINT('',#19365);
#4375=VERTEX_POINT('',#19596);
#4376=VERTEX_POINT('',#19828);
#4377=VERTEX_POINT('',#19829);
#4378=VERTEX_POINT('',#19831);
#4379=VERTEX_POINT('',#20059);
#4380=VERTEX_POINT('',#20294);
#4381=VERTEX_POINT('',#20295);
#4382=VERTEX_POINT('',#20297);
#4383=VERTEX_POINT('',#20528);
#4384=VERTEX_POINT('',#20760);
#4385=VERTEX_POINT('',#20761);
#4386=VERTEX_POINT('',#20763);
#4387=VERTEX_POINT('',#20994);
#4388=VERTEX_POINT('',#21223);
#4389=VERTEX_POINT('',#21224);
#4390=VERTEX_POINT('',#21226);
#4391=VERTEX_POINT('',#21457);
#4392=VERTEX_POINT('',#21689);
#4393=VERTEX_POINT('',#21690);
#4394=VERTEX_POINT('',#21692);
#4395=VERTEX_POINT('',#21923);
#4396=VERTEX_POINT('',#21945);
#4397=VERTEX_POINT('',#21946);
#4398=VERTEX_POINT('',#21948);
#4399=VERTEX_POINT('',#22182);
#4400=VERTEX_POINT('',#22198);
#4401=VERTEX_POINT('',#22199);
#4402=VERTEX_POINT('',#22201);
#4403=VERTEX_POINT('',#22432);
#4404=VERTEX_POINT('',#22658);
#4405=VERTEX_POINT('',#22659);
#4406=VERTEX_POINT('',#22661);
#4407=VERTEX_POINT('',#22892);
#4408=VERTEX_POINT('',#23124);
#4409=VERTEX_POINT('',#23125);
#4410=VERTEX_POINT('',#23127);
#4411=VERTEX_POINT('',#23358);
#4412=VERTEX_POINT('',#23590);
#4413=VERTEX_POINT('',#23591);
#4414=VERTEX_POINT('',#23593);
#4415=VERTEX_POINT('',#23824);
#4416=VERTEX_POINT('',#24053);
#4417=VERTEX_POINT('',#24054);
#4418=VERTEX_POINT('',#24056);
#4419=VERTEX_POINT('',#24287);
#4420=VERTEX_POINT('',#24519);
#4421=VERTEX_POINT('',#24520);
#4422=VERTEX_POINT('',#24522);
#4423=VERTEX_POINT('',#24753);
#4424=VERTEX_POINT('',#24985);
#4425=VERTEX_POINT('',#24986);
#4426=VERTEX_POINT('',#24988);
#4427=VERTEX_POINT('',#25219);
#4428=VERTEX_POINT('',#25451);
#4429=VERTEX_POINT('',#25452);
#4430=VERTEX_POINT('',#25454);
#4431=VERTEX_POINT('',#25688);
#4432=VERTEX_POINT('',#25920);
#4433=VERTEX_POINT('',#25921);
#4434=VERTEX_POINT('',#25923);
#4435=VERTEX_POINT('',#26154);
#4436=VERTEX_POINT('',#26386);
#4437=VERTEX_POINT('',#26387);
#4438=VERTEX_POINT('',#26389);
#4439=VERTEX_POINT('',#26620);
#4440=VERTEX_POINT('',#26852);
#4441=VERTEX_POINT('',#26853);
#4442=VERTEX_POINT('',#26855);
#4443=VERTEX_POINT('',#27086);
#4444=VERTEX_POINT('',#27315);
#4445=VERTEX_POINT('',#27316);
#4446=VERTEX_POINT('',#27318);
#4447=VERTEX_POINT('',#27549);
#4448=VERTEX_POINT('',#27787);
#4449=VERTEX_POINT('',#27788);
#4450=VERTEX_POINT('',#27790);
#4451=VERTEX_POINT('',#28021);
#4452=VERTEX_POINT('',#28253);
#4453=VERTEX_POINT('',#28254);
#4454=VERTEX_POINT('',#28256);
#4455=VERTEX_POINT('',#28487);
#4456=VERTEX_POINT('',#28719);
#4457=VERTEX_POINT('',#28720);
#4458=VERTEX_POINT('',#28722);
#4459=VERTEX_POINT('',#28959);
#4460=VERTEX_POINT('',#29191);
#4461=VERTEX_POINT('',#29192);
#4462=VERTEX_POINT('',#29194);
#4463=VERTEX_POINT('',#29425);
#4464=VERTEX_POINT('',#29657);
#4465=VERTEX_POINT('',#29658);
#4466=VERTEX_POINT('',#29660);
#4467=VERTEX_POINT('',#29888);
#4468=VERTEX_POINT('',#30120);
#4469=VERTEX_POINT('',#30121);
#4470=VERTEX_POINT('',#30123);
#4471=VERTEX_POINT('',#30354);
#4472=VERTEX_POINT('',#30583);
#4473=VERTEX_POINT('',#30584);
#4474=VERTEX_POINT('',#30586);
#4475=VERTEX_POINT('',#30817);
#4476=VERTEX_POINT('',#31055);
#4477=VERTEX_POINT('',#31056);
#4478=VERTEX_POINT('',#31058);
#4479=VERTEX_POINT('',#31289);
#4480=VERTEX_POINT('',#31521);
#4481=VERTEX_POINT('',#31522);
#4482=VERTEX_POINT('',#31524);
#4483=VERTEX_POINT('',#31755);
#4484=VERTEX_POINT('',#31984);
#4485=VERTEX_POINT('',#31985);
#4486=VERTEX_POINT('',#31987);
#4487=VERTEX_POINT('',#32221);
#4488=VERTEX_POINT('',#32453);
#4489=VERTEX_POINT('',#32454);
#4490=VERTEX_POINT('',#32456);
#4491=VERTEX_POINT('',#32687);
#4492=VERTEX_POINT('',#32919);
#4493=VERTEX_POINT('',#32920);
#4494=VERTEX_POINT('',#32922);
#4495=VERTEX_POINT('',#33150);
#4496=VERTEX_POINT('',#33382);
#4497=VERTEX_POINT('',#33383);
#4498=VERTEX_POINT('',#33385);
#4499=VERTEX_POINT('',#33616);
#4500=VERTEX_POINT('',#33845);
#4501=VERTEX_POINT('',#33846);
#4502=VERTEX_POINT('',#33848);
#4503=VERTEX_POINT('',#34079);
#4504=VERTEX_POINT('',#34314);
#4505=VERTEX_POINT('',#34315);
#4506=VERTEX_POINT('',#34317);
#4507=VERTEX_POINT('',#34548);
#4508=VERTEX_POINT('',#34780);
#4509=VERTEX_POINT('',#34781);
#4510=VERTEX_POINT('',#34783);
#4511=VERTEX_POINT('',#35014);
#4512=VERTEX_POINT('',#35243);
#4513=VERTEX_POINT('',#35244);
#4514=VERTEX_POINT('',#35246);
#4515=VERTEX_POINT('',#35477);
#4516=VERTEX_POINT('',#35709);
#4517=VERTEX_POINT('',#35710);
#4518=VERTEX_POINT('',#35712);
#4519=VERTEX_POINT('',#35943);
#4520=VERTEX_POINT('',#36175);
#4521=VERTEX_POINT('',#36176);
#4522=VERTEX_POINT('',#36178);
#4523=VERTEX_POINT('',#36406);
#4524=VERTEX_POINT('',#36638);
#4525=VERTEX_POINT('',#36639);
#4526=VERTEX_POINT('',#36641);
#4527=VERTEX_POINT('',#36872);
#4528=VERTEX_POINT('',#37101);
#4529=VERTEX_POINT('',#37102);
#4530=VERTEX_POINT('',#37104);
#4531=VERTEX_POINT('',#37335);
#4532=VERTEX_POINT('',#37570);
#4533=VERTEX_POINT('',#37571);
#4534=VERTEX_POINT('',#37573);
#4535=VERTEX_POINT('',#37804);
#4536=VERTEX_POINT('',#38036);
#4537=VERTEX_POINT('',#38037);
#4538=VERTEX_POINT('',#38039);
#4539=VERTEX_POINT('',#38270);
#4540=VERTEX_POINT('',#38499);
#4541=VERTEX_POINT('',#38500);
#4542=VERTEX_POINT('',#38502);
#4543=VERTEX_POINT('',#38733);
#4544=VERTEX_POINT('',#38965);
#4545=VERTEX_POINT('',#38966);
#4546=VERTEX_POINT('',#38968);
#4547=VERTEX_POINT('',#39199);
#4548=VERTEX_POINT('',#39431);
#4549=VERTEX_POINT('',#39432);
#4550=VERTEX_POINT('',#39434);
#4551=VERTEX_POINT('',#39662);
#4552=VERTEX_POINT('',#39894);
#4553=VERTEX_POINT('',#39895);
#4554=VERTEX_POINT('',#39897);
#4555=VERTEX_POINT('',#40131);
#4556=VERTEX_POINT('',#40363);
#4557=VERTEX_POINT('',#40364);
#4558=VERTEX_POINT('',#40366);
#4559=VERTEX_POINT('',#40597);
#4560=VERTEX_POINT('',#40832);
#4561=VERTEX_POINT('',#40833);
#4562=VERTEX_POINT('',#40835);
#4563=VERTEX_POINT('',#41066);
#4564=VERTEX_POINT('',#41298);
#4565=VERTEX_POINT('',#41299);
#4566=VERTEX_POINT('',#41301);
#4567=VERTEX_POINT('',#41532);
#4568=VERTEX_POINT('',#41761);
#4569=VERTEX_POINT('',#41762);
#4570=VERTEX_POINT('',#41764);
#4571=VERTEX_POINT('',#41995);
#4572=VERTEX_POINT('',#42227);
#4573=VERTEX_POINT('',#42228);
#4574=VERTEX_POINT('',#42230);
#4575=VERTEX_POINT('',#42461);
#4576=VERTEX_POINT('',#42693);
#4577=VERTEX_POINT('',#42694);
#4578=VERTEX_POINT('',#42696);
#4579=VERTEX_POINT('',#42924);
#4580=VERTEX_POINT('',#43156);
#4581=VERTEX_POINT('',#43157);
#4582=VERTEX_POINT('',#43159);
#4583=VERTEX_POINT('',#43396);
#4584=VERTEX_POINT('',#43628);
#4585=VERTEX_POINT('',#43629);
#4586=VERTEX_POINT('',#43631);
#4587=VERTEX_POINT('',#43862);
#4588=VERTEX_POINT('',#44097);
#4589=VERTEX_POINT('',#44098);
#4590=VERTEX_POINT('',#44100);
#4591=VERTEX_POINT('',#44328);
#4592=VERTEX_POINT('',#44560);
#4593=VERTEX_POINT('',#44561);
#4594=VERTEX_POINT('',#44563);
#4595=VERTEX_POINT('',#44794);
#4596=VERTEX_POINT('',#45023);
#4597=VERTEX_POINT('',#45024);
#4598=VERTEX_POINT('',#45026);
#4599=VERTEX_POINT('',#45257);
#4600=VERTEX_POINT('',#45489);
#4601=VERTEX_POINT('',#45490);
#4602=VERTEX_POINT('',#45492);
#4603=VERTEX_POINT('',#45723);
#4604=VERTEX_POINT('',#45955);
#4605=VERTEX_POINT('',#45956);
#4606=VERTEX_POINT('',#45958);
#4607=VERTEX_POINT('',#46186);
#4608=VERTEX_POINT('',#46415);
#4609=VERTEX_POINT('',#46416);
#4610=VERTEX_POINT('',#46418);
#4611=VERTEX_POINT('',#46652);
#4612=VERTEX_POINT('',#46884);
#4613=VERTEX_POINT('',#46885);
#4614=VERTEX_POINT('',#46887);
#4615=VERTEX_POINT('',#47118);
#4616=VERTEX_POINT('',#47353);
#4617=VERTEX_POINT('',#47354);
#4618=VERTEX_POINT('',#47356);
#4619=VERTEX_POINT('',#47584);
#4620=VERTEX_POINT('',#47816);
#4621=VERTEX_POINT('',#47817);
#4622=VERTEX_POINT('',#47819);
#4623=VERTEX_POINT('',#48050);
#4624=VERTEX_POINT('',#48282);
#4625=VERTEX_POINT('',#48283);
#4626=VERTEX_POINT('',#48285);
#4627=VERTEX_POINT('',#48516);
#4628=VERTEX_POINT('',#48745);
#4629=VERTEX_POINT('',#48746);
#4630=VERTEX_POINT('',#48748);
#4631=VERTEX_POINT('',#48979);
#4632=VERTEX_POINT('',#49211);
#4633=VERTEX_POINT('',#49212);
#4634=VERTEX_POINT('',#49214);
#4635=VERTEX_POINT('',#49442);
#4636=VERTEX_POINT('',#49674);
#4637=VERTEX_POINT('',#49675);
#4638=VERTEX_POINT('',#49677);
#4639=VERTEX_POINT('',#49701);
#4640=VERTEX_POINT('',#49933);
#4641=VERTEX_POINT('',#49934);
#4642=VERTEX_POINT('',#49936);
#4643=VERTEX_POINT('',#49951);
#4644=VERTEX_POINT('',#50186);
#4645=VERTEX_POINT('',#50187);
#4646=VERTEX_POINT('',#50189);
#4647=VERTEX_POINT('',#50411);
#4648=VERTEX_POINT('',#50646);
#4649=VERTEX_POINT('',#50647);
#4650=VERTEX_POINT('',#50649);
#4651=VERTEX_POINT('',#50880);
#4652=VERTEX_POINT('',#51112);
#4653=VERTEX_POINT('',#51113);
#4654=VERTEX_POINT('',#51115);
#4655=VERTEX_POINT('',#51346);
#4656=VERTEX_POINT('',#51575);
#4657=VERTEX_POINT('',#51576);
#4658=VERTEX_POINT('',#51578);
#4659=VERTEX_POINT('',#51809);
#4660=VERTEX_POINT('',#52041);
#4661=VERTEX_POINT('',#52042);
#4662=VERTEX_POINT('',#52044);
#4663=VERTEX_POINT('',#52275);
#4664=VERTEX_POINT('',#52507);
#4665=VERTEX_POINT('',#52508);
#4666=VERTEX_POINT('',#52510);
#4667=VERTEX_POINT('',#52744);
#4668=VERTEX_POINT('',#52976);
#4669=VERTEX_POINT('',#52977);
#4670=VERTEX_POINT('',#52979);
#4671=VERTEX_POINT('',#53210);
#4672=VERTEX_POINT('',#53445);
#4673=VERTEX_POINT('',#53446);
#4674=VERTEX_POINT('',#53448);
#4675=VERTEX_POINT('',#53676);
#4676=VERTEX_POINT('',#53908);
#4677=VERTEX_POINT('',#53909);
#4678=VERTEX_POINT('',#53911);
#4679=VERTEX_POINT('',#54142);
#4680=VERTEX_POINT('',#54374);
#4681=VERTEX_POINT('',#54375);
#4682=VERTEX_POINT('',#54377);
#4683=VERTEX_POINT('',#54608);
#4684=VERTEX_POINT('',#54837);
#4685=VERTEX_POINT('',#54838);
#4686=VERTEX_POINT('',#54840);
#4687=VERTEX_POINT('',#55071);
#4688=VERTEX_POINT('',#55303);
#4689=VERTEX_POINT('',#55304);
#4690=VERTEX_POINT('',#55306);
#4691=VERTEX_POINT('',#55537);
#4692=VERTEX_POINT('',#55769);
#4693=VERTEX_POINT('',#55770);
#4694=VERTEX_POINT('',#55772);
#4695=VERTEX_POINT('',#56006);
#4696=VERTEX_POINT('',#56238);
#4697=VERTEX_POINT('',#56239);
#4698=VERTEX_POINT('',#56241);
#4699=VERTEX_POINT('',#56472);
#4700=VERTEX_POINT('',#56707);
#4701=VERTEX_POINT('',#56708);
#4702=VERTEX_POINT('',#56710);
#4703=VERTEX_POINT('',#56938);
#4704=VERTEX_POINT('',#57170);
#4705=VERTEX_POINT('',#57171);
#4706=VERTEX_POINT('',#57173);
#4707=VERTEX_POINT('',#57404);
#4708=VERTEX_POINT('',#57636);
#4709=VERTEX_POINT('',#57637);
#4710=VERTEX_POINT('',#57639);
#4711=VERTEX_POINT('',#57870);
#4712=VERTEX_POINT('',#58099);
#4713=VERTEX_POINT('',#58100);
#4714=VERTEX_POINT('',#58102);
#4715=VERTEX_POINT('',#58330);
#4716=VERTEX_POINT('',#58568);
#4717=VERTEX_POINT('',#58569);
#4718=VERTEX_POINT('',#58571);
#4719=VERTEX_POINT('',#58802);
#4720=VERTEX_POINT('',#59034);
#4721=VERTEX_POINT('',#59035);
#4722=VERTEX_POINT('',#59037);
#4723=VERTEX_POINT('',#59271);
#4724=VERTEX_POINT('',#59500);
#4725=VERTEX_POINT('',#59501);
#4726=VERTEX_POINT('',#59503);
#4727=VERTEX_POINT('',#59734);
#4728=VERTEX_POINT('',#59969);
#4729=VERTEX_POINT('',#59970);
#4730=VERTEX_POINT('',#59972);
#4731=VERTEX_POINT('',#60203);
#4732=VERTEX_POINT('',#60435);
#4733=VERTEX_POINT('',#60436);
#4734=VERTEX_POINT('',#60438);
#4735=VERTEX_POINT('',#60666);
#4736=VERTEX_POINT('',#60898);
#4737=VERTEX_POINT('',#60899);
#4738=VERTEX_POINT('',#60901);
#4739=VERTEX_POINT('',#61132);
#4740=VERTEX_POINT('',#61361);
#4741=VERTEX_POINT('',#61362);
#4742=VERTEX_POINT('',#61364);
#4743=VERTEX_POINT('',#61595);
#4744=VERTEX_POINT('',#61830);
#4745=VERTEX_POINT('',#61831);
#4746=VERTEX_POINT('',#61833);
#4747=VERTEX_POINT('',#62064);
#4748=VERTEX_POINT('',#62296);
#4749=VERTEX_POINT('',#62297);
#4750=VERTEX_POINT('',#62299);
#4751=VERTEX_POINT('',#62533);
#4752=VERTEX_POINT('',#62762);
#4753=VERTEX_POINT('',#62763);
#4754=VERTEX_POINT('',#62765);
#4755=VERTEX_POINT('',#62999);
#4756=VERTEX_POINT('',#63234);
#4757=VERTEX_POINT('',#63235);
#4758=VERTEX_POINT('',#63237);
#4759=VERTEX_POINT('',#63468);
#4760=VERTEX_POINT('',#63700);
#4761=VERTEX_POINT('',#63701);
#4762=VERTEX_POINT('',#63703);
#4763=VERTEX_POINT('',#63931);
#4764=VERTEX_POINT('',#64163);
#4765=VERTEX_POINT('',#64164);
#4766=VERTEX_POINT('',#64166);
#4767=VERTEX_POINT('',#64397);
#4768=VERTEX_POINT('',#64626);
#4769=VERTEX_POINT('',#64627);
#4770=VERTEX_POINT('',#64629);
#4771=VERTEX_POINT('',#64860);
#4772=VERTEX_POINT('',#65092);
#4773=VERTEX_POINT('',#65093);
#4774=VERTEX_POINT('',#65095);
#4775=VERTEX_POINT('',#65326);
#4776=VERTEX_POINT('',#65558);
#4777=VERTEX_POINT('',#65559);
#4778=VERTEX_POINT('',#65561);
#4779=VERTEX_POINT('',#65795);
#4780=VERTEX_POINT('',#66024);
#4781=VERTEX_POINT('',#66025);
#4782=VERTEX_POINT('',#66027);
#4783=VERTEX_POINT('',#66258);
#4784=VERTEX_POINT('',#66493);
#4785=VERTEX_POINT('',#66494);
#4786=VERTEX_POINT('',#66496);
#4787=VERTEX_POINT('',#66727);
#4788=VERTEX_POINT('',#66959);
#4789=VERTEX_POINT('',#66960);
#4790=VERTEX_POINT('',#66962);
#4791=VERTEX_POINT('',#67190);
#4792=VERTEX_POINT('',#67422);
#4793=VERTEX_POINT('',#67423);
#4794=VERTEX_POINT('',#67425);
#4795=VERTEX_POINT('',#67656);
#4796=VERTEX_POINT('',#67885);
#4797=VERTEX_POINT('',#67886);
#4798=VERTEX_POINT('',#67888);
#4799=VERTEX_POINT('',#68119);
#4800=VERTEX_POINT('',#68351);
#4801=VERTEX_POINT('',#68352);
#4802=VERTEX_POINT('',#68354);
#4803=VERTEX_POINT('',#68585);
#4804=VERTEX_POINT('',#68817);
#4805=VERTEX_POINT('',#68818);
#4806=VERTEX_POINT('',#68820);
#4807=VERTEX_POINT('',#69054);
#4808=VERTEX_POINT('',#69283);
#4809=VERTEX_POINT('',#69284);
#4810=VERTEX_POINT('',#69286);
#4811=VERTEX_POINT('',#69517);
#4812=VERTEX_POINT('',#69752);
#4813=VERTEX_POINT('',#69753);
#4814=VERTEX_POINT('',#69755);
#4815=VERTEX_POINT('',#69986);
#4816=VERTEX_POINT('',#70218);
#4817=VERTEX_POINT('',#70219);
#4818=VERTEX_POINT('',#70221);
#4819=VERTEX_POINT('',#70449);
#4820=VERTEX_POINT('',#70681);
#4821=VERTEX_POINT('',#70682);
#4822=VERTEX_POINT('',#70684);
#4823=VERTEX_POINT('',#70921);
#4824=VERTEX_POINT('',#71150);
#4825=VERTEX_POINT('',#71151);
#4826=VERTEX_POINT('',#71153);
#4827=VERTEX_POINT('',#71384);
#4828=VERTEX_POINT('',#71616);
#4829=VERTEX_POINT('',#71617);
#4830=VERTEX_POINT('',#71619);
#4831=VERTEX_POINT('',#71847);
#4832=VERTEX_POINT('',#72079);
#4833=VERTEX_POINT('',#72080);
#4834=VERTEX_POINT('',#72082);
#4835=VERTEX_POINT('',#72316);
#4836=VERTEX_POINT('',#72545);
#4837=VERTEX_POINT('',#72546);
#4838=VERTEX_POINT('',#72548);
#4839=VERTEX_POINT('',#72779);
#4840=VERTEX_POINT('',#73014);
#4841=VERTEX_POINT('',#73015);
#4842=VERTEX_POINT('',#73017);
#4843=VERTEX_POINT('',#73248);
#4844=VERTEX_POINT('',#73480);
#4845=VERTEX_POINT('',#73481);
#4846=VERTEX_POINT('',#73483);
#4847=VERTEX_POINT('',#73711);
#4848=VERTEX_POINT('',#73943);
#4849=VERTEX_POINT('',#73944);
#4850=VERTEX_POINT('',#73946);
#4851=VERTEX_POINT('',#74180);
#4852=VERTEX_POINT('',#74412);
#4853=VERTEX_POINT('',#74413);
#4854=VERTEX_POINT('',#74415);
#4855=VERTEX_POINT('',#74646);
#4856=VERTEX_POINT('',#74878);
#4857=VERTEX_POINT('',#74879);
#4858=VERTEX_POINT('',#74881);
#4859=VERTEX_POINT('',#75109);
#4860=VERTEX_POINT('',#75341);
#4861=VERTEX_POINT('',#75342);
#4862=VERTEX_POINT('',#75344);
#4863=VERTEX_POINT('',#75578);
#4864=VERTEX_POINT('',#75807);
#4865=VERTEX_POINT('',#75808);
#4866=VERTEX_POINT('',#75810);
#4867=VERTEX_POINT('',#76041);
#4868=VERTEX_POINT('',#76276);
#4869=VERTEX_POINT('',#76277);
#4870=VERTEX_POINT('',#76279);
#4871=VERTEX_POINT('',#76510);
#4872=VERTEX_POINT('',#76742);
#4873=VERTEX_POINT('',#76743);
#4874=VERTEX_POINT('',#76745);
#4875=VERTEX_POINT('',#76973);
#4876=VERTEX_POINT('',#77202);
#4877=VERTEX_POINT('',#77203);
#4878=VERTEX_POINT('',#77205);
#4879=VERTEX_POINT('',#77436);
#4880=VERTEX_POINT('',#77668);
#4881=VERTEX_POINT('',#77669);
#4882=VERTEX_POINT('',#77671);
#4883=VERTEX_POINT('',#77902);
#4884=VERTEX_POINT('',#78134);
#4885=VERTEX_POINT('',#78135);
#4886=VERTEX_POINT('',#78137);
#4887=VERTEX_POINT('',#78365);
#4888=VERTEX_POINT('',#78597);
#4889=VERTEX_POINT('',#78598);
#4890=VERTEX_POINT('',#78600);
#4891=VERTEX_POINT('',#78834);
#4892=VERTEX_POINT('',#79063);
#4893=VERTEX_POINT('',#79064);
#4894=VERTEX_POINT('',#79066);
#4895=VERTEX_POINT('',#79297);
#4896=VERTEX_POINT('',#79532);
#4897=VERTEX_POINT('',#79533);
#4898=VERTEX_POINT('',#79535);
#4899=VERTEX_POINT('',#79766);
#4900=VERTEX_POINT('',#79998);
#4901=VERTEX_POINT('',#79999);
#4902=VERTEX_POINT('',#80001);
#4903=VERTEX_POINT('',#80229);
#4904=VERTEX_POINT('',#80458);
#4905=VERTEX_POINT('',#80459);
#4906=VERTEX_POINT('',#80461);
#4907=VERTEX_POINT('',#80692);
#4908=VERTEX_POINT('',#80924);
#4909=VERTEX_POINT('',#80925);
#4910=VERTEX_POINT('',#80927);
#4911=VERTEX_POINT('',#81158);
#4912=VERTEX_POINT('',#81390);
#4913=VERTEX_POINT('',#81391);
#4914=VERTEX_POINT('',#81393);
#4915=VERTEX_POINT('',#81621);
#4916=VERTEX_POINT('',#81853);
#4917=VERTEX_POINT('',#81854);
#4918=VERTEX_POINT('',#81856);
#4919=VERTEX_POINT('',#82090);
#4920=VERTEX_POINT('',#82112);
#4921=VERTEX_POINT('',#82113);
#4922=VERTEX_POINT('',#82115);
#4923=VERTEX_POINT('',#82346);
#4924=VERTEX_POINT('',#82363);
#4925=VERTEX_POINT('',#82364);
#4926=VERTEX_POINT('',#82366);
#4927=VERTEX_POINT('',#82597);
#4928=VERTEX_POINT('',#82823);
#4929=VERTEX_POINT('',#82824);
#4930=VERTEX_POINT('',#82826);
#4931=VERTEX_POINT('',#83054);
#4932=VERTEX_POINT('',#83283);
#4933=VERTEX_POINT('',#83284);
#4934=VERTEX_POINT('',#83286);
#4935=VERTEX_POINT('',#83517);
#4936=VERTEX_POINT('',#83749);
#4937=VERTEX_POINT('',#83750);
#4938=VERTEX_POINT('',#83752);
#4939=VERTEX_POINT('',#83983);
#4940=VERTEX_POINT('',#84215);
#4941=VERTEX_POINT('',#84216);
#4942=VERTEX_POINT('',#84218);
#4943=VERTEX_POINT('',#84446);
#4944=VERTEX_POINT('',#84678);
#4945=VERTEX_POINT('',#84679);
#4946=VERTEX_POINT('',#84681);
#4947=VERTEX_POINT('',#84915);
#4948=VERTEX_POINT('',#85147);
#4949=VERTEX_POINT('',#85148);
#4950=VERTEX_POINT('',#85150);
#4951=VERTEX_POINT('',#85381);
#4952=VERTEX_POINT('',#85613);
#4953=VERTEX_POINT('',#85614);
#4954=VERTEX_POINT('',#85616);
#4955=VERTEX_POINT('',#85847);
#4956=VERTEX_POINT('',#86082);
#4957=VERTEX_POINT('',#86083);
#4958=VERTEX_POINT('',#86085);
#4959=VERTEX_POINT('',#86316);
#4960=VERTEX_POINT('',#86548);
#4961=VERTEX_POINT('',#86549);
#4962=VERTEX_POINT('',#86551);
#4963=VERTEX_POINT('',#86782);
#4964=VERTEX_POINT('',#87014);
#4965=VERTEX_POINT('',#87015);
#4966=VERTEX_POINT('',#87017);
#4967=VERTEX_POINT('',#87248);
#4968=VERTEX_POINT('',#87480);
#4969=VERTEX_POINT('',#87481);
#4970=VERTEX_POINT('',#87483);
#4971=VERTEX_POINT('',#87711);
#4972=VERTEX_POINT('',#87943);
#4973=VERTEX_POINT('',#87944);
#4974=VERTEX_POINT('',#87946);
#4975=VERTEX_POINT('',#88180);
#4976=VERTEX_POINT('',#88412);
#4977=VERTEX_POINT('',#88413);
#4978=VERTEX_POINT('',#88415);
#4979=VERTEX_POINT('',#88646);
#4980=VERTEX_POINT('',#88878);
#4981=VERTEX_POINT('',#88879);
#4982=VERTEX_POINT('',#88881);
#4983=VERTEX_POINT('',#89112);
#4984=VERTEX_POINT('',#89347);
#4985=VERTEX_POINT('',#89348);
#4986=VERTEX_POINT('',#89350);
#4987=VERTEX_POINT('',#89581);
#4988=VERTEX_POINT('',#89813);
#4989=VERTEX_POINT('',#89814);
#4990=VERTEX_POINT('',#89816);
#4991=VERTEX_POINT('',#90047);
#4992=VERTEX_POINT('',#90276);
#4993=VERTEX_POINT('',#90277);
#4994=VERTEX_POINT('',#90279);
#4995=VERTEX_POINT('',#90510);
#4996=VERTEX_POINT('',#90742);
#4997=VERTEX_POINT('',#90743);
#4998=VERTEX_POINT('',#90745);
#4999=VERTEX_POINT('',#90973);
#5000=VERTEX_POINT('',#91205);
#5001=VERTEX_POINT('',#91206);
#5002=VERTEX_POINT('',#91208);
#5003=VERTEX_POINT('',#91442);
#5004=VERTEX_POINT('',#91674);
#5005=VERTEX_POINT('',#91675);
#5006=VERTEX_POINT('',#91677);
#5007=VERTEX_POINT('',#91908);
#5008=VERTEX_POINT('',#92140);
#5009=VERTEX_POINT('',#92141);
#5010=VERTEX_POINT('',#92143);
#5011=VERTEX_POINT('',#92371);
#5012=VERTEX_POINT('',#92609);
#5013=VERTEX_POINT('',#92610);
#5014=VERTEX_POINT('',#92612);
#5015=VERTEX_POINT('',#92843);
#5016=VERTEX_POINT('',#93075);
#5017=VERTEX_POINT('',#93076);
#5018=VERTEX_POINT('',#93078);
#5019=VERTEX_POINT('',#93309);
#5020=VERTEX_POINT('',#93538);
#5021=VERTEX_POINT('',#93539);
#5022=VERTEX_POINT('',#93541);
#5023=VERTEX_POINT('',#93772);
#5024=VERTEX_POINT('',#94004);
#5025=VERTEX_POINT('',#94005);
#5026=VERTEX_POINT('',#94007);
#5027=VERTEX_POINT('',#94238);
#5028=VERTEX_POINT('',#94470);
#5029=VERTEX_POINT('',#94471);
#5030=VERTEX_POINT('',#94473);
#5031=VERTEX_POINT('',#94707);
#5032=VERTEX_POINT('',#94939);
#5033=VERTEX_POINT('',#94940);
#5034=VERTEX_POINT('',#94942);
#5035=VERTEX_POINT('',#95173);
#5036=VERTEX_POINT('',#95405);
#5037=VERTEX_POINT('',#95406);
#5038=VERTEX_POINT('',#95408);
#5039=VERTEX_POINT('',#95636);
#5040=VERTEX_POINT('',#95868);
#5041=VERTEX_POINT('',#95869);
#5042=VERTEX_POINT('',#95871);
#5043=VERTEX_POINT('',#96102);
#5044=VERTEX_POINT('',#96334);
#5045=VERTEX_POINT('',#96335);
#5046=VERTEX_POINT('',#96337);
#5047=VERTEX_POINT('',#96568);
#5048=VERTEX_POINT('',#96797);
#5049=VERTEX_POINT('',#96798);
#5050=VERTEX_POINT('',#96800);
#5051=VERTEX_POINT('',#97031);
#5052=VERTEX_POINT('',#97263);
#5053=VERTEX_POINT('',#97264);
#5054=VERTEX_POINT('',#97266);
#5055=VERTEX_POINT('',#97497);
#5056=VERTEX_POINT('',#97729);
#5057=VERTEX_POINT('',#97730);
#5058=VERTEX_POINT('',#97732);
#5059=VERTEX_POINT('',#97966);
#5060=VERTEX_POINT('',#97988);
#5061=VERTEX_POINT('',#97989);
#5062=VERTEX_POINT('',#97991);
#5063=VERTEX_POINT('',#98222);
#5064=VERTEX_POINT('',#98448);
#5065=VERTEX_POINT('',#98449);
#5066=VERTEX_POINT('',#98451);
#5067=VERTEX_POINT('',#98682);
#5068=VERTEX_POINT('',#98914);
#5069=VERTEX_POINT('',#98915);
#5070=VERTEX_POINT('',#98917);
#5071=VERTEX_POINT('',#99148);
#5072=VERTEX_POINT('',#99380);
#5073=VERTEX_POINT('',#99381);
#5074=VERTEX_POINT('',#99383);
#5075=VERTEX_POINT('',#99614);
#5076=VERTEX_POINT('',#99843);
#5077=VERTEX_POINT('',#99844);
#5078=VERTEX_POINT('',#99846);
#5079=VERTEX_POINT('',#100077);
#5080=VERTEX_POINT('',#100309);
#5081=VERTEX_POINT('',#100310);
#5082=VERTEX_POINT('',#100312);
#5083=VERTEX_POINT('',#100543);
#5084=VERTEX_POINT('',#100775);
#5085=VERTEX_POINT('',#100776);
#5086=VERTEX_POINT('',#100778);
#5087=VERTEX_POINT('',#101009);
#5088=VERTEX_POINT('',#101241);
#5089=VERTEX_POINT('',#101242);
#5090=VERTEX_POINT('',#101244);
#5091=VERTEX_POINT('',#101478);
#5092=VERTEX_POINT('',#101710);
#5093=VERTEX_POINT('',#101711);
#5094=VERTEX_POINT('',#101713);
#5095=VERTEX_POINT('',#101944);
#5096=VERTEX_POINT('',#102176);
#5097=VERTEX_POINT('',#102177);
#5098=VERTEX_POINT('',#102179);
#5099=VERTEX_POINT('',#102407);
#5100=VERTEX_POINT('',#102639);
#5101=VERTEX_POINT('',#102640);
#5102=VERTEX_POINT('',#102642);
#5103=VERTEX_POINT('',#102873);
#5104=VERTEX_POINT('',#103102);
#5105=VERTEX_POINT('',#103103);
#5106=VERTEX_POINT('',#103105);
#5107=VERTEX_POINT('',#103336);
#5108=VERTEX_POINT('',#103574);
#5109=VERTEX_POINT('',#103575);
#5110=VERTEX_POINT('',#103577);
#5111=VERTEX_POINT('',#103808);
#5112=VERTEX_POINT('',#104040);
#5113=VERTEX_POINT('',#104041);
#5114=VERTEX_POINT('',#104043);
#5115=VERTEX_POINT('',#104274);
#5116=VERTEX_POINT('',#104506);
#5117=VERTEX_POINT('',#104507);
#5118=VERTEX_POINT('',#104509);
#5119=VERTEX_POINT('',#104746);
#5120=VERTEX_POINT('',#104978);
#5121=VERTEX_POINT('',#104979);
#5122=VERTEX_POINT('',#104981);
#5123=VERTEX_POINT('',#105212);
#5124=VERTEX_POINT('',#105444);
#5125=VERTEX_POINT('',#105445);
#5126=VERTEX_POINT('',#105447);
#5127=VERTEX_POINT('',#105675);
#5128=VERTEX_POINT('',#105907);
#5129=VERTEX_POINT('',#105908);
#5130=VERTEX_POINT('',#105910);
#5131=VERTEX_POINT('',#106141);
#5132=VERTEX_POINT('',#106370);
#5133=VERTEX_POINT('',#106371);
#5134=VERTEX_POINT('',#106373);
#5135=VERTEX_POINT('',#106604);
#5136=VERTEX_POINT('',#106842);
#5137=VERTEX_POINT('',#106843);
#5138=VERTEX_POINT('',#106845);
#5139=VERTEX_POINT('',#107076);
#5140=VERTEX_POINT('',#107308);
#5141=VERTEX_POINT('',#107309);
#5142=VERTEX_POINT('',#107311);
#5143=VERTEX_POINT('',#107542);
#5144=VERTEX_POINT('',#107771);
#5145=VERTEX_POINT('',#107772);
#5146=VERTEX_POINT('',#107774);
#5147=VERTEX_POINT('',#108008);
#5148=VERTEX_POINT('',#108240);
#5149=VERTEX_POINT('',#108241);
#5150=VERTEX_POINT('',#108243);
#5151=VERTEX_POINT('',#108474);
#5152=VERTEX_POINT('',#108706);
#5153=VERTEX_POINT('',#108707);
#5154=VERTEX_POINT('',#108709);
#5155=VERTEX_POINT('',#108937);
#5156=VERTEX_POINT('',#109169);
#5157=VERTEX_POINT('',#109170);
#5158=VERTEX_POINT('',#109172);
#5159=VERTEX_POINT('',#109403);
#5160=VERTEX_POINT('',#109632);
#5161=VERTEX_POINT('',#109633);
#5162=VERTEX_POINT('',#109635);
#5163=VERTEX_POINT('',#109656);
#5164=VERTEX_POINT('',#109891);
#5165=VERTEX_POINT('',#109892);
#5166=VERTEX_POINT('',#109894);
#5167=VERTEX_POINT('',#110119);
#5168=VERTEX_POINT('',#110351);
#5169=VERTEX_POINT('',#110352);
#5170=VERTEX_POINT('',#110354);
#5171=VERTEX_POINT('',#110585);
#5172=VERTEX_POINT('',#110814);
#5173=VERTEX_POINT('',#110815);
#5174=VERTEX_POINT('',#110817);
#5175=VERTEX_POINT('',#111048);
#5176=VERTEX_POINT('',#111280);
#5177=VERTEX_POINT('',#111281);
#5178=VERTEX_POINT('',#111283);
#5179=VERTEX_POINT('',#111514);
#5180=VERTEX_POINT('',#111746);
#5181=VERTEX_POINT('',#111747);
#5182=VERTEX_POINT('',#111749);
#5183=VERTEX_POINT('',#111977);
#5184=VERTEX_POINT('',#112209);
#5185=VERTEX_POINT('',#112210);
#5186=VERTEX_POINT('',#112212);
#5187=VERTEX_POINT('',#112443);
#5188=VERTEX_POINT('',#112672);
#5189=VERTEX_POINT('',#112673);
#5190=VERTEX_POINT('',#112675);
#5191=VERTEX_POINT('',#112906);
#5192=VERTEX_POINT('',#113141);
#5193=VERTEX_POINT('',#113142);
#5194=VERTEX_POINT('',#113144);
#5195=VERTEX_POINT('',#113375);
#5196=VERTEX_POINT('',#113607);
#5197=VERTEX_POINT('',#113608);
#5198=VERTEX_POINT('',#113610);
#5199=VERTEX_POINT('',#113841);
#5200=VERTEX_POINT('',#114070);
#5201=VERTEX_POINT('',#114071);
#5202=VERTEX_POINT('',#114073);
#5203=VERTEX_POINT('',#114304);
#5204=VERTEX_POINT('',#114536);
#5205=VERTEX_POINT('',#114537);
#5206=VERTEX_POINT('',#114539);
#5207=VERTEX_POINT('',#114770);
#5208=VERTEX_POINT('',#115002);
#5209=VERTEX_POINT('',#115003);
#5210=VERTEX_POINT('',#115005);
#5211=VERTEX_POINT('',#115233);
#5212=VERTEX_POINT('',#115465);
#5213=VERTEX_POINT('',#115466);
#5214=VERTEX_POINT('',#115468);
#5215=VERTEX_POINT('',#115702);
#5216=VERTEX_POINT('',#115934);
#5217=VERTEX_POINT('',#115935);
#5218=VERTEX_POINT('',#115937);
#5219=VERTEX_POINT('',#116168);
#5220=VERTEX_POINT('',#116403);
#5221=VERTEX_POINT('',#116404);
#5222=VERTEX_POINT('',#116406);
#5223=VERTEX_POINT('',#116637);
#5224=VERTEX_POINT('',#116869);
#5225=VERTEX_POINT('',#116870);
#5226=VERTEX_POINT('',#116872);
#5227=VERTEX_POINT('',#117103);
#5228=VERTEX_POINT('',#117332);
#5229=VERTEX_POINT('',#117333);
#5230=VERTEX_POINT('',#117335);
#5231=VERTEX_POINT('',#117566);
#5232=VERTEX_POINT('',#117798);
#5233=VERTEX_POINT('',#117799);
#5234=VERTEX_POINT('',#117801);
#5235=VERTEX_POINT('',#118032);
#5236=VERTEX_POINT('',#118264);
#5237=VERTEX_POINT('',#118265);
#5238=VERTEX_POINT('',#118267);
#5239=VERTEX_POINT('',#118495);
#5240=VERTEX_POINT('',#118727);
#5241=VERTEX_POINT('',#118728);
#5242=VERTEX_POINT('',#118730);
#5243=VERTEX_POINT('',#118967);
#5244=VERTEX_POINT('',#119199);
#5245=VERTEX_POINT('',#119200);
#5246=VERTEX_POINT('',#119202);
#5247=VERTEX_POINT('',#119433);
#5248=VERTEX_POINT('',#119668);
#5249=VERTEX_POINT('',#119669);
#5250=VERTEX_POINT('',#119671);
#5251=VERTEX_POINT('',#119899);
#5252=VERTEX_POINT('',#120131);
#5253=VERTEX_POINT('',#120132);
#5254=VERTEX_POINT('',#120134);
#5255=VERTEX_POINT('',#120365);
#5256=VERTEX_POINT('',#120594);
#5257=VERTEX_POINT('',#120595);
#5258=VERTEX_POINT('',#120597);
#5259=VERTEX_POINT('',#120828);
#5260=VERTEX_POINT('',#121057);
#5261=VERTEX_POINT('',#121058);
#5262=VERTEX_POINT('',#121060);
#5263=VERTEX_POINT('',#121291);
#5264=VERTEX_POINT('',#121523);
#5265=VERTEX_POINT('',#121524);
#5266=VERTEX_POINT('',#121526);
#5267=VERTEX_POINT('',#121754);
#5268=VERTEX_POINT('',#121983);
#5269=VERTEX_POINT('',#121984);
#5270=VERTEX_POINT('',#121986);
#5271=VERTEX_POINT('',#122220);
#5272=VERTEX_POINT('',#122452);
#5273=VERTEX_POINT('',#122453);
#5274=VERTEX_POINT('',#122455);
#5275=VERTEX_POINT('',#122686);
#5276=VERTEX_POINT('',#122921);
#5277=VERTEX_POINT('',#122922);
#5278=VERTEX_POINT('',#122924);
#5279=VERTEX_POINT('',#123152);
#5280=VERTEX_POINT('',#123384);
#5281=VERTEX_POINT('',#123385);
#5282=VERTEX_POINT('',#123387);
#5283=VERTEX_POINT('',#123618);
#5284=VERTEX_POINT('',#123850);
#5285=VERTEX_POINT('',#123851);
#5286=VERTEX_POINT('',#123853);
#5287=VERTEX_POINT('',#124084);
#5288=VERTEX_POINT('',#124313);
#5289=VERTEX_POINT('',#124314);
#5290=VERTEX_POINT('',#124316);
#5291=VERTEX_POINT('',#124547);
#5292=VERTEX_POINT('',#124779);
#5293=VERTEX_POINT('',#124780);
#5294=VERTEX_POINT('',#124782);
#5295=VERTEX_POINT('',#125010);
#5296=VERTEX_POINT('',#125242);
#5297=VERTEX_POINT('',#125243);
#5298=VERTEX_POINT('',#125245);
#5299=VERTEX_POINT('',#125269);
#5300=VERTEX_POINT('',#125501);
#5301=VERTEX_POINT('',#125502);
#5302=VERTEX_POINT('',#125504);
#5303=VERTEX_POINT('',#125519);
#5304=VERTEX_POINT('',#125754);
#5305=VERTEX_POINT('',#125755);
#5306=VERTEX_POINT('',#125757);
#5307=VERTEX_POINT('',#125979);
#5308=VERTEX_POINT('',#126214);
#5309=VERTEX_POINT('',#126215);
#5310=VERTEX_POINT('',#126217);
#5311=VERTEX_POINT('',#126448);
#5312=VERTEX_POINT('',#126680);
#5313=VERTEX_POINT('',#126681);
#5314=VERTEX_POINT('',#126683);
#5315=VERTEX_POINT('',#126914);
#5316=VERTEX_POINT('',#127143);
#5317=VERTEX_POINT('',#127144);
#5318=VERTEX_POINT('',#127146);
#5319=VERTEX_POINT('',#127377);
#5320=VERTEX_POINT('',#127609);
#5321=VERTEX_POINT('',#127610);
#5322=VERTEX_POINT('',#127612);
#5323=VERTEX_POINT('',#127843);
#5324=VERTEX_POINT('',#128075);
#5325=VERTEX_POINT('',#128076);
#5326=VERTEX_POINT('',#128078);
#5327=VERTEX_POINT('',#128312);
#5328=VERTEX_POINT('',#128544);
#5329=VERTEX_POINT('',#128545);
#5330=VERTEX_POINT('',#128547);
#5331=VERTEX_POINT('',#128778);
#5332=VERTEX_POINT('',#129013);
#5333=VERTEX_POINT('',#129014);
#5334=VERTEX_POINT('',#129016);
#5335=VERTEX_POINT('',#129244);
#5336=VERTEX_POINT('',#129476);
#5337=VERTEX_POINT('',#129477);
#5338=VERTEX_POINT('',#129479);
#5339=VERTEX_POINT('',#129710);
#5340=VERTEX_POINT('',#129942);
#5341=VERTEX_POINT('',#129943);
#5342=VERTEX_POINT('',#129945);
#5343=VERTEX_POINT('',#130176);
#5344=VERTEX_POINT('',#130405);
#5345=VERTEX_POINT('',#130406);
#5346=VERTEX_POINT('',#130408);
#5347=VERTEX_POINT('',#130639);
#5348=VERTEX_POINT('',#130871);
#5349=VERTEX_POINT('',#130872);
#5350=VERTEX_POINT('',#130874);
#5351=VERTEX_POINT('',#131105);
#5352=VERTEX_POINT('',#131337);
#5353=VERTEX_POINT('',#131338);
#5354=VERTEX_POINT('',#131340);
#5355=VERTEX_POINT('',#131574);
#5356=VERTEX_POINT('',#131806);
#5357=VERTEX_POINT('',#131807);
#5358=VERTEX_POINT('',#131809);
#5359=VERTEX_POINT('',#132040);
#5360=VERTEX_POINT('',#132275);
#5361=VERTEX_POINT('',#132276);
#5362=VERTEX_POINT('',#132278);
#5363=VERTEX_POINT('',#132506);
#5364=VERTEX_POINT('',#132738);
#5365=VERTEX_POINT('',#132739);
#5366=VERTEX_POINT('',#132741);
#5367=VERTEX_POINT('',#132972);
#5368=VERTEX_POINT('',#133204);
#5369=VERTEX_POINT('',#133205);
#5370=VERTEX_POINT('',#133207);
#5371=VERTEX_POINT('',#133438);
#5372=VERTEX_POINT('',#133667);
#5373=VERTEX_POINT('',#133668);
#5374=VERTEX_POINT('',#133670);
#5375=VERTEX_POINT('',#133898);
#5376=VERTEX_POINT('',#134136);
#5377=VERTEX_POINT('',#134137);
#5378=VERTEX_POINT('',#134139);
#5379=VERTEX_POINT('',#134370);
#5380=VERTEX_POINT('',#134602);
#5381=VERTEX_POINT('',#134603);
#5382=VERTEX_POINT('',#134605);
#5383=VERTEX_POINT('',#134839);
#5384=VERTEX_POINT('',#135068);
#5385=VERTEX_POINT('',#135069);
#5386=VERTEX_POINT('',#135071);
#5387=VERTEX_POINT('',#135302);
#5388=VERTEX_POINT('',#135537);
#5389=VERTEX_POINT('',#135538);
#5390=VERTEX_POINT('',#135540);
#5391=VERTEX_POINT('',#135771);
#5392=VERTEX_POINT('',#136003);
#5393=VERTEX_POINT('',#136004);
#5394=VERTEX_POINT('',#136006);
#5395=VERTEX_POINT('',#136234);
#5396=VERTEX_POINT('',#136466);
#5397=VERTEX_POINT('',#136467);
#5398=VERTEX_POINT('',#136469);
#5399=VERTEX_POINT('',#136700);
#5400=VERTEX_POINT('',#136929);
#5401=VERTEX_POINT('',#136930);
#5402=VERTEX_POINT('',#136932);
#5403=VERTEX_POINT('',#137163);
#5404=VERTEX_POINT('',#137398);
#5405=VERTEX_POINT('',#137399);
#5406=VERTEX_POINT('',#137401);
#5407=VERTEX_POINT('',#137632);
#5408=VERTEX_POINT('',#137864);
#5409=VERTEX_POINT('',#137865);
#5410=VERTEX_POINT('',#137867);
#5411=VERTEX_POINT('',#138101);
#5412=VERTEX_POINT('',#138330);
#5413=VERTEX_POINT('',#138331);
#5414=VERTEX_POINT('',#138333);
#5415=VERTEX_POINT('',#138567);
#5416=VERTEX_POINT('',#138802);
#5417=VERTEX_POINT('',#138803);
#5418=VERTEX_POINT('',#138805);
#5419=VERTEX_POINT('',#139036);
#5420=VERTEX_POINT('',#139268);
#5421=VERTEX_POINT('',#139269);
#5422=VERTEX_POINT('',#139271);
#5423=VERTEX_POINT('',#139499);
#5424=VERTEX_POINT('',#139731);
#5425=VERTEX_POINT('',#139732);
#5426=VERTEX_POINT('',#139734);
#5427=VERTEX_POINT('',#139965);
#5428=VERTEX_POINT('',#140194);
#5429=VERTEX_POINT('',#140195);
#5430=VERTEX_POINT('',#140275);
#5431=VERTEX_POINT('',#140277);
#5432=VERTEX_POINT('',#140321);
#5433=VERTEX_POINT('',#140566);
#5434=VERTEX_POINT('',#140577);
#5435=VERTEX_POINT('',#140825);
#5436=VERTEX_POINT('',#140838);
#5437=VERTEX_POINT('',#140849);
#5438=VERTEX_POINT('',#140860);
#5439=VERTEX_POINT('',#140872);
#5440=VERTEX_POINT('',#140883);
#5441=VERTEX_POINT('',#140894);
#5442=VERTEX_POINT('',#140905);
#5443=VERTEX_POINT('',#141153);
#5444=VERTEX_POINT('',#141164);
#5445=VERTEX_POINT('',#141412);
#5446=VERTEX_POINT('',#141424);
#5447=VERTEX_POINT('',#141435);
#5448=VERTEX_POINT('',#141446);
#5449=VERTEX_POINT('',#141457);
#5450=VERTEX_POINT('',#141705);
#5451=VERTEX_POINT('',#141716);
#5452=VERTEX_POINT('',#141727);
#5453=VERTEX_POINT('',#141972);
#5454=VERTEX_POINT('',#141983);
#5455=VERTEX_POINT('',#142231);
#5456=VERTEX_POINT('',#142242);
#5457=VERTEX_POINT('',#142490);
#5458=VERTEX_POINT('',#142501);
#5459=VERTEX_POINT('',#142512);
#5460=VERTEX_POINT('',#142757);
#5461=VERTEX_POINT('',#142768);
#5462=VERTEX_POINT('',#143016);
#5463=VERTEX_POINT('',#143027);
#5464=VERTEX_POINT('',#143040);
#5465=VERTEX_POINT('',#143051);
#5466=VERTEX_POINT('',#143062);
#5467=VERTEX_POINT('',#143307);
#5468=VERTEX_POINT('',#143318);
#5469=VERTEX_POINT('',#143566);
#5470=VERTEX_POINT('',#143577);
#5471=VERTEX_POINT('',#143590);
#5472=VERTEX_POINT('',#143838);
#5473=VERTEX_POINT('',#144083);
#5474=VERTEX_POINT('',#144095);
#5475=VERTEX_POINT('',#144106);
#5476=VERTEX_POINT('',#144117);
#5477=VERTEX_POINT('',#144362);
#5478=VERTEX_POINT('',#144375);
#5479=VERTEX_POINT('',#144620);
#5480=VERTEX_POINT('',#144865);
#5481=VERTEX_POINT('',#144877);
#5482=VERTEX_POINT('',#144888);
#5483=VERTEX_POINT('',#144899);
#5484=VERTEX_POINT('',#145144);
#5485=VERTEX_POINT('',#145157);
#5486=VERTEX_POINT('',#145168);
#5487=VERTEX_POINT('',#145179);
#5488=VERTEX_POINT('',#145191);
#5489=VERTEX_POINT('',#145436);
#5490=VERTEX_POINT('',#145447);
#5491=VERTEX_POINT('',#145458);
#5492=VERTEX_POINT('',#145471);
#5493=VERTEX_POINT('',#145716);
#5494=VERTEX_POINT('',#145961);
#5495=VERTEX_POINT('',#145973);
#5496=VERTEX_POINT('',#146218);
#5497=VERTEX_POINT('',#146229);
#5498=VERTEX_POINT('',#146240);
#5499=VERTEX_POINT('',#146252);
#5500=VERTEX_POINT('',#146497);
#5501=VERTEX_POINT('',#146742);
#5502=VERTEX_POINT('',#146754);
#5503=VERTEX_POINT('',#146999);
#5504=VERTEX_POINT('',#147247);
#5505=VERTEX_POINT('',#147258);
#5506=VERTEX_POINT('',#147503);
#5507=VERTEX_POINT('',#147514);
#5508=VERTEX_POINT('',#147525);
#5509=VERTEX_POINT('',#147537);
#5510=VERTEX_POINT('',#147548);
#5511=VERTEX_POINT('',#147796);
#5512=VERTEX_POINT('',#147807);
#5513=VERTEX_POINT('',#148052);
#5514=VERTEX_POINT('',#148063);
#5515=VERTEX_POINT('',#148074);
#5516=VERTEX_POINT('',#148086);
#5517=VERTEX_POINT('',#148097);
#5518=VERTEX_POINT('',#148345);
#5519=VERTEX_POINT('',#148356);
#5520=VERTEX_POINT('',#148601);
#5521=VERTEX_POINT('',#148612);
#5522=VERTEX_POINT('',#148623);
#5523=VERTEX_POINT('',#148871);
#5524=VERTEX_POINT('',#148882);
#5525=VERTEX_POINT('',#148893);
#5526=VERTEX_POINT('',#148904);
#5527=VERTEX_POINT('',#148917);
#5528=VERTEX_POINT('',#149165);
#5529=VERTEX_POINT('',#149176);
#5530=VERTEX_POINT('',#149424);
#5531=VERTEX_POINT('',#149435);
#5532=VERTEX_POINT('',#149446);
#5533=VERTEX_POINT('',#149457);
#5534=VERTEX_POINT('',#149469);
#5535=VERTEX_POINT('',#149717);
#5536=VERTEX_POINT('',#149728);
#5537=VERTEX_POINT('',#149740);
#5538=VERTEX_POINT('',#149988);
#5539=VERTEX_POINT('',#149999);
#5540=VERTEX_POINT('',#150247);
#5541=VERTEX_POINT('',#150260);
#5542=VERTEX_POINT('',#150271);
#5543=VERTEX_POINT('',#150282);
#5544=VERTEX_POINT('',#150294);
#5545=VERTEX_POINT('',#150542);
#5546=VERTEX_POINT('',#150553);
#5547=VERTEX_POINT('',#150798);
#5548=VERTEX_POINT('',#150810);
#5549=VERTEX_POINT('',#150821);
#5550=VERTEX_POINT('',#150832);
#5551=VERTEX_POINT('',#150844);
#5552=VERTEX_POINT('',#151092);
#5553=VERTEX_POINT('',#151103);
#5554=VERTEX_POINT('',#151348);
#5555=VERTEX_POINT('',#151360);
#5556=VERTEX_POINT('',#151371);
#5557=VERTEX_POINT('',#151619);
#5558=VERTEX_POINT('',#151631);
#5559=VERTEX_POINT('',#151876);
#5560=VERTEX_POINT('',#151887);
#5561=VERTEX_POINT('',#151898);
#5562=VERTEX_POINT('',#151910);
#5563=VERTEX_POINT('',#151921);
#5564=VERTEX_POINT('',#152166);
#5565=VERTEX_POINT('',#152178);
#5566=VERTEX_POINT('',#152423);
#5567=VERTEX_POINT('',#152434);
#5568=VERTEX_POINT('',#152445);
#5569=VERTEX_POINT('',#152457);
#5570=VERTEX_POINT('',#152468);
#5571=VERTEX_POINT('',#152479);
#5572=VERTEX_POINT('',#152724);
#5573=VERTEX_POINT('',#152738);
#5574=VERTEX_POINT('',#152983);
#5575=VERTEX_POINT('',#152994);
#5576=VERTEX_POINT('',#153006);
#5577=VERTEX_POINT('',#153017);
#5578=VERTEX_POINT('',#153028);
#5579=VERTEX_POINT('',#153273);
#5580=VERTEX_POINT('',#153287);
#5581=VERTEX_POINT('',#153532);
#5582=VERTEX_POINT('',#153543);
#5583=VERTEX_POINT('',#153555);
#5584=VERTEX_POINT('',#153800);
#5585=VERTEX_POINT('',#153811);
#5586=VERTEX_POINT('',#154056);
#5587=VERTEX_POINT('',#154069);
#5588=VERTEX_POINT('',#154317);
#5589=VERTEX_POINT('',#154328);
#5590=VERTEX_POINT('',#154340);
#5591=VERTEX_POINT('',#154585);
#5592=VERTEX_POINT('',#154596);
#5593=VERTEX_POINT('',#154844);
#5594=VERTEX_POINT('',#154858);
#5595=VERTEX_POINT('',#154869);
#5596=VERTEX_POINT('',#154880);
#5597=VERTEX_POINT('',#154892);
#5598=VERTEX_POINT('',#155140);
#5599=VERTEX_POINT('',#155151);
#5600=VERTEX_POINT('',#155399);
#5601=VERTEX_POINT('',#155413);
#5602=VERTEX_POINT('',#155424);
#5603=VERTEX_POINT('',#155672);
#5604=VERTEX_POINT('',#155685);
#5605=VERTEX_POINT('',#155696);
#5606=VERTEX_POINT('',#155707);
#5607=VERTEX_POINT('',#155718);
#5608=VERTEX_POINT('',#155966);
#5609=VERTEX_POINT('',#155977);
#5610=VERTEX_POINT('',#156225);
#5611=VERTEX_POINT('',#156238);
#5612=VERTEX_POINT('',#156249);
#5613=VERTEX_POINT('',#156260);
#5614=VERTEX_POINT('',#156271);
#5615=VERTEX_POINT('',#156519);
#5616=VERTEX_POINT('',#156530);
#5617=VERTEX_POINT('',#156541);
#5618=VERTEX_POINT('',#156786);
#5619=VERTEX_POINT('',#156797);
#5620=VERTEX_POINT('',#157045);
#5621=VERTEX_POINT('',#157056);
#5622=VERTEX_POINT('',#157070);
#5623=VERTEX_POINT('',#157081);
#5624=VERTEX_POINT('',#157092);
#5625=VERTEX_POINT('',#157337);
#5626=VERTEX_POINT('',#157348);
#5627=VERTEX_POINT('',#157596);
#5628=VERTEX_POINT('',#157607);
#5629=VERTEX_POINT('',#157620);
#5630=VERTEX_POINT('',#157631);
#5631=VERTEX_POINT('',#157642);
#5632=VERTEX_POINT('',#157887);
#5633=VERTEX_POINT('',#157898);
#5634=VERTEX_POINT('',#158146);
#5635=VERTEX_POINT('',#158158);
#5636=VERTEX_POINT('',#158172);
#5637=VERTEX_POINT('',#158420);
#5638=VERTEX_POINT('',#158665);
#5639=VERTEX_POINT('',#158677);
#5640=VERTEX_POINT('',#158688);
#5641=VERTEX_POINT('',#158699);
#5642=VERTEX_POINT('',#158944);
#5643=VERTEX_POINT('',#158958);
#5644=VERTEX_POINT('',#159203);
#5645=VERTEX_POINT('',#159448);
#5646=VERTEX_POINT('',#159460);
#5647=VERTEX_POINT('',#159471);
#5648=VERTEX_POINT('',#159482);
#5649=VERTEX_POINT('',#159727);
#5650=VERTEX_POINT('',#159741);
#5651=VERTEX_POINT('',#159752);
#5652=VERTEX_POINT('',#159763);
#5653=VERTEX_POINT('',#159776);
#5654=VERTEX_POINT('',#160021);
#5655=VERTEX_POINT('',#160032);
#5656=VERTEX_POINT('',#160043);
#5657=VERTEX_POINT('',#160056);
#5658=VERTEX_POINT('',#160301);
#5659=VERTEX_POINT('',#160546);
#5660=VERTEX_POINT('',#160558);
#5661=VERTEX_POINT('',#160803);
#5662=VERTEX_POINT('',#160814);
#5663=VERTEX_POINT('',#160825);
#5664=VERTEX_POINT('',#160838);
#5665=VERTEX_POINT('',#161083);
#5666=VERTEX_POINT('',#161331);
#5667=VERTEX_POINT('',#161343);
#5668=VERTEX_POINT('',#161588);
#5669=VERTEX_POINT('',#161836);
#5670=VERTEX_POINT('',#161847);
#5671=VERTEX_POINT('',#162092);
#5672=VERTEX_POINT('',#162103);
#5673=VERTEX_POINT('',#162114);
#5674=VERTEX_POINT('',#162127);
#5675=VERTEX_POINT('',#162138);
#5676=VERTEX_POINT('',#162386);
#5677=VERTEX_POINT('',#162397);
#5678=VERTEX_POINT('',#162642);
#5679=VERTEX_POINT('',#162653);
#5680=VERTEX_POINT('',#162664);
#5681=VERTEX_POINT('',#162677);
#5682=VERTEX_POINT('',#162688);
#5683=VERTEX_POINT('',#162936);
#5684=VERTEX_POINT('',#162947);
#5685=VERTEX_POINT('',#163192);
#5686=VERTEX_POINT('',#163203);
#5687=VERTEX_POINT('',#163214);
#5688=VERTEX_POINT('',#163462);
#5689=VERTEX_POINT('',#163473);
#5690=VERTEX_POINT('',#163484);
#5691=VERTEX_POINT('',#163495);
#5692=VERTEX_POINT('',#163509);
#5693=VERTEX_POINT('',#163757);
#5694=VERTEX_POINT('',#163768);
#5695=VERTEX_POINT('',#164016);
#5696=VERTEX_POINT('',#164027);
#5697=VERTEX_POINT('',#164038);
#5698=VERTEX_POINT('',#164049);
#5699=VERTEX_POINT('',#164063);
#5700=VERTEX_POINT('',#164074);
#5701=VERTEX_POINT('',#164172);
#5702=VERTEX_POINT('',#164174);
#5703=VERTEX_POINT('',#164236);
#5704=VERTEX_POINT('',#164247);
#5705=VERTEX_POINT('',#164259);
#5706=VERTEX_POINT('',#164270);
#5707=VERTEX_POINT('',#164281);
#5708=VERTEX_POINT('',#164526);
#5709=VERTEX_POINT('',#164540);
#5710=VERTEX_POINT('',#164785);
#5711=VERTEX_POINT('',#164796);
#5712=VERTEX_POINT('',#164809);
#5713=VERTEX_POINT('',#164820);
#5714=VERTEX_POINT('',#164831);
#5715=VERTEX_POINT('',#165076);
#5716=VERTEX_POINT('',#165090);
#5717=VERTEX_POINT('',#165338);
#5718=VERTEX_POINT('',#165349);
#5719=VERTEX_POINT('',#165362);
#5720=VERTEX_POINT('',#165607);
#5721=VERTEX_POINT('',#165618);
#5722=VERTEX_POINT('',#165866);
#5723=VERTEX_POINT('',#165880);
#5724=VERTEX_POINT('',#165891);
#5725=VERTEX_POINT('',#165902);
#5726=VERTEX_POINT('',#165915);
#5727=VERTEX_POINT('',#166163);
#5728=VERTEX_POINT('',#166174);
#5729=VERTEX_POINT('',#166422);
#5730=VERTEX_POINT('',#166436);
#5731=VERTEX_POINT('',#166447);
#5732=VERTEX_POINT('',#166458);
#5733=VERTEX_POINT('',#166471);
#5734=VERTEX_POINT('',#166482);
#5735=VERTEX_POINT('',#166493);
#5736=VERTEX_POINT('',#166505);
#5737=VERTEX_POINT('',#166753);
#5738=VERTEX_POINT('',#166764);
#5739=VERTEX_POINT('',#167012);
#5740=VERTEX_POINT('',#167025);
#5741=VERTEX_POINT('',#167036);
#5742=VERTEX_POINT('',#167047);
#5743=VERTEX_POINT('',#167058);
#5744=VERTEX_POINT('',#167306);
#5745=VERTEX_POINT('',#167317);
#5746=VERTEX_POINT('',#167328);
#5747=VERTEX_POINT('',#167573);
#5748=VERTEX_POINT('',#167584);
#5749=VERTEX_POINT('',#167832);
#5750=VERTEX_POINT('',#167843);
#5751=VERTEX_POINT('',#168091);
#5752=VERTEX_POINT('',#168102);
#5753=VERTEX_POINT('',#168113);
#5754=VERTEX_POINT('',#168358);
#5755=VERTEX_POINT('',#168369);
#5756=VERTEX_POINT('',#168617);
#5757=VERTEX_POINT('',#168628);
#5758=VERTEX_POINT('',#168642);
#5759=VERTEX_POINT('',#168653);
#5760=VERTEX_POINT('',#168664);
#5761=VERTEX_POINT('',#168909);
#5762=VERTEX_POINT('',#168920);
#5763=VERTEX_POINT('',#169168);
#5764=VERTEX_POINT('',#169179);
#5765=VERTEX_POINT('',#169192);
#5766=VERTEX_POINT('',#169440);
#5767=VERTEX_POINT('',#169685);
#5768=VERTEX_POINT('',#169698);
#5769=VERTEX_POINT('',#169709);
#5770=VERTEX_POINT('',#169720);
#5771=VERTEX_POINT('',#169965);
#5772=VERTEX_POINT('',#169979);
#5773=VERTEX_POINT('',#170224);
#5774=VERTEX_POINT('',#170469);
#5775=VERTEX_POINT('',#170482);
#5776=VERTEX_POINT('',#170493);
#5777=VERTEX_POINT('',#170504);
#5778=VERTEX_POINT('',#170749);
#5779=VERTEX_POINT('',#170763);
#5780=VERTEX_POINT('',#170774);
#5781=VERTEX_POINT('',#170785);
#5782=VERTEX_POINT('',#170797);
#5783=VERTEX_POINT('',#171042);
#5784=VERTEX_POINT('',#171053);
#5785=VERTEX_POINT('',#171064);
#5786=VERTEX_POINT('',#171078);
#5787=VERTEX_POINT('',#171323);
#5788=VERTEX_POINT('',#171568);
#5789=VERTEX_POINT('',#171581);
#5790=VERTEX_POINT('',#171826);
#5791=VERTEX_POINT('',#171837);
#5792=VERTEX_POINT('',#171848);
#5793=VERTEX_POINT('',#171861);
#5794=VERTEX_POINT('',#172106);
#5795=VERTEX_POINT('',#172351);
#5796=VERTEX_POINT('',#172364);
#5797=VERTEX_POINT('',#172609);
#5798=VERTEX_POINT('',#172620);
#5799=VERTEX_POINT('',#172631);
#5800=VERTEX_POINT('',#172876);
#5801=VERTEX_POINT('',#172887);
#5802=VERTEX_POINT('',#172898);
#5803=VERTEX_POINT('',#172910);
#5804=VERTEX_POINT('',#172921);
#5805=VERTEX_POINT('',#173169);
#5806=VERTEX_POINT('',#173180);
#5807=VERTEX_POINT('',#173425);
#5808=VERTEX_POINT('',#173436);
#5809=VERTEX_POINT('',#173447);
#5810=VERTEX_POINT('',#173459);
#5811=VERTEX_POINT('',#173470);
#5812=VERTEX_POINT('',#173718);
#5813=VERTEX_POINT('',#173729);
#5814=VERTEX_POINT('',#173974);
#5815=VERTEX_POINT('',#173985);
#5816=VERTEX_POINT('',#173996);
#5817=VERTEX_POINT('',#174244);
#5818=VERTEX_POINT('',#174255);
#5819=VERTEX_POINT('',#174266);
#5820=VERTEX_POINT('',#174277);
#5821=VERTEX_POINT('',#174289);
#5822=VERTEX_POINT('',#174537);
#5823=VERTEX_POINT('',#174548);
#5824=VERTEX_POINT('',#174796);
#5825=VERTEX_POINT('',#174807);
#5826=VERTEX_POINT('',#174818);
#5827=VERTEX_POINT('',#174829);
#5828=VERTEX_POINT('',#174841);
#5829=VERTEX_POINT('',#175089);
#5830=VERTEX_POINT('',#175100);
#5831=VERTEX_POINT('',#175348);
#5832=VERTEX_POINT('',#175596);
#5833=VERTEX_POINT('',#175607);
#5834=VERTEX_POINT('',#175855);
#5835=VERTEX_POINT('',#175867);
#5836=VERTEX_POINT('',#175878);
#5837=VERTEX_POINT('',#175889);
#5838=VERTEX_POINT('',#175901);
#5839=VERTEX_POINT('',#176149);
#5840=VERTEX_POINT('',#176160);
#5841=VERTEX_POINT('',#176405);
#5842=VERTEX_POINT('',#176417);
#5843=VERTEX_POINT('',#176428);
#5844=VERTEX_POINT('',#176439);
#5845=VERTEX_POINT('',#176451);
#5846=VERTEX_POINT('',#176699);
#5847=VERTEX_POINT('',#176710);
#5848=VERTEX_POINT('',#176955);
#5849=VERTEX_POINT('',#176967);
#5850=VERTEX_POINT('',#176978);
#5851=VERTEX_POINT('',#177226);
#5852=VERTEX_POINT('',#177238);
#5853=VERTEX_POINT('',#177483);
#5854=VERTEX_POINT('',#177494);
#5855=VERTEX_POINT('',#177505);
#5856=VERTEX_POINT('',#177517);
#5857=VERTEX_POINT('',#177528);
#5858=VERTEX_POINT('',#177773);
#5859=VERTEX_POINT('',#177785);
#5860=VERTEX_POINT('',#178030);
#5861=VERTEX_POINT('',#178041);
#5862=VERTEX_POINT('',#178052);
#5863=VERTEX_POINT('',#178064);
#5864=VERTEX_POINT('',#178075);
#5865=VERTEX_POINT('',#178086);
#5866=VERTEX_POINT('',#178331);
#5867=VERTEX_POINT('',#178344);
#5868=VERTEX_POINT('',#178589);
#5869=VERTEX_POINT('',#178600);
#5870=VERTEX_POINT('',#178612);
#5871=VERTEX_POINT('',#178623);
#5872=VERTEX_POINT('',#178634);
#5873=VERTEX_POINT('',#178879);
#5874=VERTEX_POINT('',#178892);
#5875=VERTEX_POINT('',#179137);
#5876=VERTEX_POINT('',#179148);
#5877=VERTEX_POINT('',#179160);
#5878=VERTEX_POINT('',#179405);
#5879=VERTEX_POINT('',#179416);
#5880=VERTEX_POINT('',#179661);
#5881=VERTEX_POINT('',#179674);
#5882=VERTEX_POINT('',#179922);
#5883=VERTEX_POINT('',#179933);
#5884=VERTEX_POINT('',#179945);
#5885=VERTEX_POINT('',#180190);
#5886=VERTEX_POINT('',#180201);
#5887=VERTEX_POINT('',#180449);
#5888=VERTEX_POINT('',#180462);
#5889=VERTEX_POINT('',#180473);
#5890=VERTEX_POINT('',#180484);
#5891=VERTEX_POINT('',#180496);
#5892=VERTEX_POINT('',#180744);
#5893=VERTEX_POINT('',#180755);
#5894=VERTEX_POINT('',#181003);
#5895=VERTEX_POINT('',#181016);
#5896=VERTEX_POINT('',#181027);
#5897=VERTEX_POINT('',#181275);
#5898=VERTEX_POINT('',#181287);
#5899=VERTEX_POINT('',#181298);
#5900=VERTEX_POINT('',#181309);
#5901=VERTEX_POINT('',#181320);
#5902=VERTEX_POINT('',#181568);
#5903=VERTEX_POINT('',#181579);
#5904=VERTEX_POINT('',#181827);
#5905=VERTEX_POINT('',#181839);
#5906=VERTEX_POINT('',#181850);
#5907=VERTEX_POINT('',#181861);
#5908=VERTEX_POINT('',#181872);
#5909=VERTEX_POINT('',#182120);
#5910=VERTEX_POINT('',#182131);
#5911=VERTEX_POINT('',#182142);
#5912=VERTEX_POINT('',#182387);
#5913=VERTEX_POINT('',#182398);
#5914=VERTEX_POINT('',#182646);
#5915=VERTEX_POINT('',#182657);
#5916=VERTEX_POINT('',#182670);
#5917=VERTEX_POINT('',#182681);
#5918=VERTEX_POINT('',#182692);
#5919=VERTEX_POINT('',#182937);
#5920=VERTEX_POINT('',#182948);
#5921=VERTEX_POINT('',#183196);
#5922=VERTEX_POINT('',#183207);
#5923=VERTEX_POINT('',#183220);
#5924=VERTEX_POINT('',#183231);
#5925=VERTEX_POINT('',#183242);
#5926=VERTEX_POINT('',#183487);
#5927=VERTEX_POINT('',#183498);
#5928=VERTEX_POINT('',#183746);
#5929=VERTEX_POINT('',#183757);
#5930=VERTEX_POINT('',#183770);
#5931=VERTEX_POINT('',#184018);
#5932=VERTEX_POINT('',#184263);
#5933=VERTEX_POINT('',#184275);
#5934=VERTEX_POINT('',#184286);
#5935=VERTEX_POINT('',#184297);
#5936=VERTEX_POINT('',#184542);
#5937=VERTEX_POINT('',#184555);
#5938=VERTEX_POINT('',#184800);
#5939=VERTEX_POINT('',#185045);
#5940=VERTEX_POINT('',#185057);
#5941=VERTEX_POINT('',#185068);
#5942=VERTEX_POINT('',#185079);
#5943=VERTEX_POINT('',#185324);
#5944=VERTEX_POINT('',#185337);
#5945=VERTEX_POINT('',#185348);
#5946=VERTEX_POINT('',#185359);
#5947=VERTEX_POINT('',#185371);
#5948=VERTEX_POINT('',#185616);
#5949=VERTEX_POINT('',#185627);
#5950=VERTEX_POINT('',#185638);
#5951=VERTEX_POINT('',#185650);
#5952=VERTEX_POINT('',#185895);
#5953=VERTEX_POINT('',#186140);
#5954=VERTEX_POINT('',#186152);
#5955=VERTEX_POINT('',#186397);
#5956=VERTEX_POINT('',#186408);
#5957=VERTEX_POINT('',#186419);
#5958=VERTEX_POINT('',#186431);
#5959=VERTEX_POINT('',#186676);
#5960=VERTEX_POINT('',#186921);
#5961=VERTEX_POINT('',#186933);
#5962=VERTEX_POINT('',#187178);
#5963=VERTEX_POINT('',#187426);
#5964=VERTEX_POINT('',#187437);
#5965=VERTEX_POINT('',#187682);
#5966=VERTEX_POINT('',#187693);
#5967=VERTEX_POINT('',#187704);
#5968=VERTEX_POINT('',#187716);
#5969=VERTEX_POINT('',#187727);
#5970=VERTEX_POINT('',#187986);
#5971=VERTEX_POINT('',#187997);
#5972=VERTEX_POINT('',#188212);
#5973=VERTEX_POINT('',#188214);
#5974=VERTEX_POINT('',#188389);
#5975=VERTEX_POINT('',#188391);
#5976=VERTEX_POINT('',#188394);
#5977=VERTEX_POINT('',#188614);
#5978=VERTEX_POINT('',#188615);
#5979=VERTEX_POINT('',#188617);
#5980=VERTEX_POINT('',#188619);
#5981=VERTEX_POINT('',#188625);
#5982=VERTEX_POINT('',#188626);
#5983=VERTEX_POINT('',#188628);
#5984=VERTEX_POINT('',#188630);
#5985=VERTEX_POINT('',#188634);
#5986=VERTEX_POINT('',#202423);
#5987=VERTEX_POINT('',#202424);
#5988=VERTEX_POINT('',#202426);
#5989=VERTEX_POINT('',#202428);
#5990=VERTEX_POINT('',#202430);
#5991=VERTEX_POINT('',#202432);
#5992=VERTEX_POINT('',#202434);
#5993=VERTEX_POINT('',#202437);
#5994=VERTEX_POINT('',#202439);
#5995=VERTEX_POINT('',#202441);
#5996=VERTEX_POINT('',#202445);
#5997=VERTEX_POINT('',#202446);
#5998=VERTEX_POINT('',#202448);
#5999=VERTEX_POINT('',#202450);
#6000=VERTEX_POINT('',#202452);
#6001=VERTEX_POINT('',#202455);
#6002=VERTEX_POINT('',#202457);
#6003=VERTEX_POINT('',#202459);
#6004=VERTEX_POINT('',#202461);
#6005=VERTEX_POINT('',#202463);
#6006=VERTEX_POINT('',#202470);
#6007=VERTEX_POINT('',#202472);
#6008=VERTEX_POINT('',#202474);
#6009=VERTEX_POINT('',#202477);
#6010=VERTEX_POINT('',#202480);
#6011=VERTEX_POINT('',#202482);
#6012=VERTEX_POINT('',#202484);
#6013=VERTEX_POINT('',#202487);
#6014=VERTEX_POINT('',#202503);
#6015=VERTEX_POINT('',#202505);
#6016=VERTEX_POINT('',#202509);
#6017=VERTEX_POINT('',#202511);
#6018=VERTEX_POINT('',#202514);
#6019=VERTEX_POINT('',#202518);
#6020=VERTEX_POINT('',#202522);
#6021=VERTEX_POINT('',#202523);
#6022=VERTEX_POINT('',#202534);
#6023=VERTEX_POINT('',#202535);
#6024=VERTEX_POINT('',#202537);
#6025=VERTEX_POINT('',#202551);
#6026=VERTEX_POINT('',#202688);
#6027=VERTEX_POINT('',#202695);
#6028=VERTEX_POINT('',#202855);
#6029=VERTEX_POINT('',#202856);
#6030=VERTEX_POINT('',#202858);
#6031=VERTEX_POINT('',#203089);
#6032=VERTEX_POINT('',#203321);
#6033=VERTEX_POINT('',#203322);
#6034=VERTEX_POINT('',#203324);
#6035=VERTEX_POINT('',#203555);
#6036=VERTEX_POINT('',#203787);
#6037=VERTEX_POINT('',#203788);
#6038=VERTEX_POINT('',#203790);
#6039=VERTEX_POINT('',#204021);
#6040=VERTEX_POINT('',#204253);
#6041=VERTEX_POINT('',#204254);
#6042=VERTEX_POINT('',#204256);
#6043=VERTEX_POINT('',#204487);
#6044=VERTEX_POINT('',#204716);
#6045=VERTEX_POINT('',#204717);
#6046=VERTEX_POINT('',#204719);
#6047=VERTEX_POINT('',#204950);
#6048=VERTEX_POINT('',#205182);
#6049=VERTEX_POINT('',#205183);
#6050=VERTEX_POINT('',#205185);
#6051=VERTEX_POINT('',#205416);
#6052=VERTEX_POINT('',#205648);
#6053=VERTEX_POINT('',#205649);
#6054=VERTEX_POINT('',#205651);
#6055=VERTEX_POINT('',#205882);
#6056=VERTEX_POINT('',#206108);
#6057=VERTEX_POINT('',#206109);
#6058=VERTEX_POINT('',#206111);
#6059=VERTEX_POINT('',#206345);
#6060=VERTEX_POINT('',#206361);
#6061=VERTEX_POINT('',#206362);
#6062=VERTEX_POINT('',#206364);
#6063=VERTEX_POINT('',#206595);
#6064=VERTEX_POINT('',#206617);
#6065=VERTEX_POINT('',#206618);
#6066=VERTEX_POINT('',#206620);
#6067=VERTEX_POINT('',#206851);
#6068=VERTEX_POINT('',#207083);
#6069=VERTEX_POINT('',#207084);
#6070=VERTEX_POINT('',#207086);
#6071=VERTEX_POINT('',#207317);
#6072=VERTEX_POINT('',#207546);
#6073=VERTEX_POINT('',#207547);
#6074=VERTEX_POINT('',#207549);
#6075=VERTEX_POINT('',#207780);
#6076=VERTEX_POINT('',#208012);
#6077=VERTEX_POINT('',#208013);
#6078=VERTEX_POINT('',#208015);
#6079=VERTEX_POINT('',#208243);
#6080=VERTEX_POINT('',#208478);
#6081=VERTEX_POINT('',#208479);
#6082=VERTEX_POINT('',#208481);
#6083=VERTEX_POINT('',#208712);
#6084=VERTEX_POINT('',#208944);
#6085=VERTEX_POINT('',#208945);
#6086=VERTEX_POINT('',#208947);
#6087=VERTEX_POINT('',#209181);
#6088=VERTEX_POINT('',#209413);
#6089=VERTEX_POINT('',#209414);
#6090=VERTEX_POINT('',#209416);
#6091=VERTEX_POINT('',#209448);
#6092=VERTEX_POINT('',#216281);
#6093=VERTEX_POINT('',#216292);
#6094=VERTEX_POINT('',#216302);
#6095=VERTEX_POINT('',#216547);
#6096=VERTEX_POINT('',#216558);
#6097=VERTEX_POINT('',#216569);
#6098=VERTEX_POINT('',#216581);
#6099=VERTEX_POINT('',#216826);
#6100=VERTEX_POINT('',#217071);
#6101=VERTEX_POINT('',#217083);
#6102=VERTEX_POINT('',#217328);
#6103=VERTEX_POINT('',#217576);
#6104=VERTEX_POINT('',#217587);
#6105=VERTEX_POINT('',#217832);
#6106=VERTEX_POINT('',#217843);
#6107=VERTEX_POINT('',#217854);
#6108=VERTEX_POINT('',#217866);
#6109=VERTEX_POINT('',#217877);
#6110=VERTEX_POINT('',#218044);
#6111=VERTEX_POINT('',#218081);
#6112=VERTEX_POINT('',#218110);
#6113=VERTEX_POINT('',#218126);
#6114=VERTEX_POINT('',#225137);
#6115=VERTEX_POINT('',#225138);
#6116=VERTEX_POINT('',#225149);
#6117=VERTEX_POINT('',#225172);
#6118=VERTEX_POINT('',#225213);
#6119=VERTEX_POINT('',#225220);
#6120=VERTEX_POINT('',#225402);
#6121=VERTEX_POINT('',#225413);
#6122=VERTEX_POINT('',#225424);
#6123=VERTEX_POINT('',#225435);
#6124=VERTEX_POINT('',#225447);
#6125=VERTEX_POINT('',#225695);
#6126=VERTEX_POINT('',#225706);
#6127=VERTEX_POINT('',#225954);
#6128=VERTEX_POINT('',#225965);
#6129=VERTEX_POINT('',#225976);
#6130=VERTEX_POINT('',#225987);
#6131=VERTEX_POINT('',#225999);
#6132=VERTEX_POINT('',#226010);
#6133=VERTEX_POINT('',#226021);
#6134=VERTEX_POINT('',#226034);
#6135=VERTEX_POINT('',#226282);
#6136=VERTEX_POINT('',#226296);
#6137=VERTEX_POINT('',#226301);
#6138=VERTEX_POINT('',#226308);
#6139=VERTEX_POINT('',#233124);
#6140=VERTEX_POINT('',#233125);
#6141=VERTEX_POINT('',#233134);
#6142=VERTEX_POINT('',#233205);
#6143=VERTEX_POINT('',#233210);
#6144=VERTEX_POINT('',#233215);
#6145=VERTEX_POINT('',#233272);
#6146=VERTEX_POINT('',#240283);
#6147=VERTEX_POINT('',#240443);
#6148=VERTEX_POINT('',#240446);
#6149=VERTEX_POINT('',#240453);
#6150=VERTEX_POINT('',#240455);
#6151=VERTEX_POINT('',#240459);
#6152=VERTEX_POINT('',#240460);
#6153=VERTEX_POINT('',#240462);
#6154=VERTEX_POINT('',#240464);
#6155=VERTEX_POINT('',#240468);
#6156=VERTEX_POINT('',#240470);
#6157=VERTEX_POINT('',#240474);
#6158=VERTEX_POINT('',#240476);
#6159=VERTEX_POINT('',#240483);
#6160=VERTEX_POINT('',#240486);
#6161=VERTEX_POINT('',#240490);
#6162=VERTEX_POINT('',#240492);
#6163=VERTEX_POINT('',#240496);
#6164=VERTEX_POINT('',#240497);
#6165=VERTEX_POINT('',#240499);
#6166=VERTEX_POINT('',#240501);
#6167=VERTEX_POINT('',#240505);
#6168=VERTEX_POINT('',#240507);
#6169=VERTEX_POINT('',#240511);
#6170=VERTEX_POINT('',#240513);
#6171=VERTEX_POINT('',#240524);
#6172=VERTEX_POINT('',#240525);
#6173=VERTEX_POINT('',#240527);
#6174=VERTEX_POINT('',#240529);
#6175=VERTEX_POINT('',#240531);
#6176=VERTEX_POINT('',#240533);
#6177=VERTEX_POINT('',#240535);
#6178=VERTEX_POINT('',#240538);
#6179=VERTEX_POINT('',#240540);
#6180=VERTEX_POINT('',#240542);
#6181=VERTEX_POINT('',#240546);
#6182=VERTEX_POINT('',#240547);
#6183=VERTEX_POINT('',#240549);
#6184=VERTEX_POINT('',#240551);
#6185=VERTEX_POINT('',#240553);
#6186=VERTEX_POINT('',#240556);
#6187=VERTEX_POINT('',#240558);
#6188=VERTEX_POINT('',#240560);
#6189=VERTEX_POINT('',#240562);
#6190=VERTEX_POINT('',#240564);
#6191=VERTEX_POINT('',#240571);
#6192=VERTEX_POINT('',#240573);
#6193=VERTEX_POINT('',#240577);
#6194=VERTEX_POINT('',#240579);
#6195=VERTEX_POINT('',#240582);
#6196=VERTEX_POINT('',#240586);
#6197=VERTEX_POINT('',#240590);
#6198=VERTEX_POINT('',#240591);
#6199=VERTEX_POINT('',#240604);
#6200=VERTEX_POINT('',#240606);
#6201=VERTEX_POINT('',#240608);
#6202=VERTEX_POINT('',#240611);
#6203=VERTEX_POINT('',#240614);
#6204=VERTEX_POINT('',#240616);
#6205=VERTEX_POINT('',#240618);
#6206=VERTEX_POINT('',#240621);
#6207=VERTEX_POINT('',#240635);
#6208=VERTEX_POINT('',#240636);
#6209=VERTEX_POINT('',#240638);
#6210=VERTEX_POINT('',#240640);
#6211=VERTEX_POINT('',#240644);
#6212=VERTEX_POINT('',#240646);
#6213=VERTEX_POINT('',#240650);
#6214=VERTEX_POINT('',#240651);
#6215=VERTEX_POINT('',#240653);
#6216=VERTEX_POINT('',#240655);
#6217=VERTEX_POINT('',#240659);
#6218=VERTEX_POINT('',#240660);
#6219=VERTEX_POINT('',#240662);
#6220=VERTEX_POINT('',#240664);
#6221=VERTEX_POINT('',#240671);
#6222=VERTEX_POINT('',#240672);
#6223=VERTEX_POINT('',#240674);
#6224=VERTEX_POINT('',#240676);
#6225=VERTEX_POINT('',#240681);
#6226=VERTEX_POINT('',#240683);
#6227=VERTEX_POINT('',#240686);
#6228=VERTEX_POINT('',#240689);
#6229=VERTEX_POINT('',#240690);
#6230=VERTEX_POINT('',#240692);
#6231=VERTEX_POINT('',#240694);
#6232=VERTEX_POINT('',#240698);
#6233=VERTEX_POINT('',#240700);
#6234=VERTEX_POINT('',#240704);
#6235=VERTEX_POINT('',#240713);
#6236=VERTEX_POINT('',#240714);
#6237=VERTEX_POINT('',#240716);
#6238=VERTEX_POINT('',#240718);
#6239=VERTEX_POINT('',#240725);
#6240=VERTEX_POINT('',#240726);
#6241=VERTEX_POINT('',#240729);
#6242=VERTEX_POINT('',#240731);
#6243=VERTEX_POINT('',#240733);
#6244=VERTEX_POINT('',#240735);
#6245=VERTEX_POINT('',#240739);
#6246=VERTEX_POINT('',#240741);
#6247=VERTEX_POINT('',#240745);
#6248=VERTEX_POINT('',#240747);
#6249=VERTEX_POINT('',#240751);
#6250=VERTEX_POINT('',#240752);
#6251=VERTEX_POINT('',#240754);
#6252=VERTEX_POINT('',#240756);
#6253=VERTEX_POINT('',#240764);
#6254=VERTEX_POINT('',#240771);
#6255=VERTEX_POINT('',#240773);
#6256=VERTEX_POINT('',#240777);
#6257=VERTEX_POINT('',#240779);
#6258=VERTEX_POINT('',#240782);
#6259=VERTEX_POINT('',#240785);
#6260=VERTEX_POINT('',#240789);
#6261=VERTEX_POINT('',#240791);
#6262=VERTEX_POINT('',#240794);
#6263=VERTEX_POINT('',#240807);
#6264=VERTEX_POINT('',#240808);
#6265=VERTEX_POINT('',#240810);
#6266=VERTEX_POINT('',#240821);
#6267=VERTEX_POINT('',#240973);
#6268=VERTEX_POINT('',#240980);
#6269=VERTEX_POINT('',#241158);
#6270=VERTEX_POINT('',#241159);
#6271=VERTEX_POINT('',#241161);
#6272=VERTEX_POINT('',#241383);
#6273=VERTEX_POINT('',#241618);
#6274=VERTEX_POINT('',#241619);
#6275=VERTEX_POINT('',#241621);
#6276=VERTEX_POINT('',#241636);
#6277=VERTEX_POINT('',#241871);
#6278=VERTEX_POINT('',#241872);
#6279=VERTEX_POINT('',#241874);
#6280=VERTEX_POINT('',#241898);
#6281=VERTEX_POINT('',#242130);
#6282=VERTEX_POINT('',#242131);
#6283=VERTEX_POINT('',#242133);
#6284=VERTEX_POINT('',#242361);
#6285=VERTEX_POINT('',#242593);
#6286=VERTEX_POINT('',#242594);
#6287=VERTEX_POINT('',#242596);
#6288=VERTEX_POINT('',#242827);
#6289=VERTEX_POINT('',#243059);
#6290=VERTEX_POINT('',#243060);
#6291=VERTEX_POINT('',#243062);
#6292=VERTEX_POINT('',#243293);
#6293=VERTEX_POINT('',#243522);
#6294=VERTEX_POINT('',#243523);
#6295=VERTEX_POINT('',#243525);
#6296=VERTEX_POINT('',#243756);
#6297=VERTEX_POINT('',#243988);
#6298=VERTEX_POINT('',#243989);
#6299=VERTEX_POINT('',#243991);
#6300=VERTEX_POINT('',#244219);
#6301=VERTEX_POINT('',#244451);
#6302=VERTEX_POINT('',#244452);
#6303=VERTEX_POINT('',#244454);
#6304=VERTEX_POINT('',#244685);
#6305=VERTEX_POINT('',#244920);
#6306=VERTEX_POINT('',#244921);
#6307=VERTEX_POINT('',#244923);
#6308=VERTEX_POINT('',#245157);
#6309=VERTEX_POINT('',#245389);
#6310=VERTEX_POINT('',#245390);
#6311=VERTEX_POINT('',#245392);
#6312=VERTEX_POINT('',#245620);
#6313=VERTEX_POINT('',#245849);
#6314=VERTEX_POINT('',#245850);
#6315=VERTEX_POINT('',#245852);
#6316=VERTEX_POINT('',#246083);
#6317=VERTEX_POINT('',#246315);
#6318=VERTEX_POINT('',#246316);
#6319=VERTEX_POINT('',#246318);
#6320=VERTEX_POINT('',#246549);
#6321=VERTEX_POINT('',#246778);
#6322=VERTEX_POINT('',#246779);
#6323=VERTEX_POINT('',#246781);
#6324=VERTEX_POINT('',#247012);
#6325=VERTEX_POINT('',#247241);
#6326=VERTEX_POINT('',#247242);
#6327=VERTEX_POINT('',#247244);
#6328=VERTEX_POINT('',#247472);
#6329=VERTEX_POINT('',#247704);
#6330=VERTEX_POINT('',#247705);
#6331=VERTEX_POINT('',#247707);
#6332=VERTEX_POINT('',#247721);
#6333=VERTEX_POINT('',#254536);
#6334=VERTEX_POINT('',#254537);
#6335=VERTEX_POINT('',#254548);
#6336=VERTEX_POINT('',#261422);
#6337=VERTEX_POINT('',#261423);
#6338=VERTEX_POINT('',#261462);
#6339=VERTEX_POINT('',#261516);
#6340=VERTEX_POINT('',#261747);
#6341=VERTEX_POINT('',#261758);
#6342=VERTEX_POINT('',#261805);
#6343=VERTEX_POINT('',#261816);
#6344=VERTEX_POINT('',#261827);
#6345=VERTEX_POINT('',#261840);
#6346=VERTEX_POINT('',#262085);
#6347=VERTEX_POINT('',#262330);
#6348=VERTEX_POINT('',#262342);
#6349=VERTEX_POINT('',#262587);
#6350=VERTEX_POINT('',#262598);
#6351=VERTEX_POINT('',#262609);
#6352=VERTEX_POINT('',#262622);
#6353=VERTEX_POINT('',#262867);
#6354=VERTEX_POINT('',#263115);
#6355=VERTEX_POINT('',#263127);
#6356=VERTEX_POINT('',#263372);
#6357=VERTEX_POINT('',#263620);
#6358=VERTEX_POINT('',#263672);
#6359=VERTEX_POINT('',#263679);
#6360=VERTEX_POINT('',#263691);
#6361=VERTEX_POINT('',#263696);
#6362=VERTEX_POINT('',#263703);
#6363=VERTEX_POINT('',#263710);
#6364=VERTEX_POINT('',#263958);
#6365=VERTEX_POINT('',#263969);
#6366=VERTEX_POINT('',#264214);
#6367=VERTEX_POINT('',#264225);
#6368=VERTEX_POINT('',#264236);
#6369=VERTEX_POINT('',#264484);
#6370=VERTEX_POINT('',#264495);
#6371=VERTEX_POINT('',#264506);
#6372=VERTEX_POINT('',#264517);
#6373=VERTEX_POINT('',#264530);
#6374=VERTEX_POINT('',#264778);
#6375=VERTEX_POINT('',#264789);
#6376=VERTEX_POINT('',#265037);
#6377=VERTEX_POINT('',#265049);
#6378=VERTEX_POINT('',#265060);
#6379=VERTEX_POINT('',#265077);
#6380=VERTEX_POINT('',#265312);
#6381=VERTEX_POINT('',#265313);
#6382=VERTEX_POINT('',#265322);
#6383=VERTEX_POINT('',#265342);
#6384=VERTEX_POINT('',#272211);
#6385=VERTEX_POINT('',#272335);
#6386=VERTEX_POINT('',#272342);
#6387=VERTEX_POINT('',#279157);
#6388=VERTEX_POINT('',#279160);
#6389=VERTEX_POINT('',#279167);
#6390=VERTEX_POINT('',#279169);
#6391=VERTEX_POINT('',#279173);
#6392=VERTEX_POINT('',#279174);
#6393=VERTEX_POINT('',#279176);
#6394=VERTEX_POINT('',#279178);
#6395=VERTEX_POINT('',#279182);
#6396=VERTEX_POINT('',#279184);
#6397=VERTEX_POINT('',#279188);
#6398=VERTEX_POINT('',#279190);
#6399=VERTEX_POINT('',#279197);
#6400=VERTEX_POINT('',#279200);
#6401=VERTEX_POINT('',#279204);
#6402=VERTEX_POINT('',#279206);
#6403=VERTEX_POINT('',#279210);
#6404=VERTEX_POINT('',#279211);
#6405=VERTEX_POINT('',#279213);
#6406=VERTEX_POINT('',#279215);
#6407=VERTEX_POINT('',#279219);
#6408=VERTEX_POINT('',#279221);
#6409=VERTEX_POINT('',#279225);
#6410=VERTEX_POINT('',#279227);
#6411=EDGE_CURVE('',#4300,#4301,#4152,.T.);
#6412=EDGE_CURVE('',#4301,#4302,#3096,.T.);
#6413=EDGE_CURVE('',#4302,#4303,#4153,.T.);
#6414=EDGE_CURVE('',#4303,#4300,#3097,.T.);
#6415=EDGE_CURVE('',#4304,#4304,#4154,.T.);
#6416=EDGE_CURVE('',#4304,#4305,#3098,.T.);
#6417=EDGE_CURVE('',#4305,#4305,#4155,.T.);
#6418=EDGE_CURVE('',#4306,#4307,#3099,.T.);
#6419=EDGE_CURVE('',#4307,#4308,#3100,.T.);
#6420=EDGE_CURVE('',#4309,#4308,#3101,.T.);
#6421=EDGE_CURVE('',#4306,#4309,#3102,.T.);
#6422=EDGE_CURVE('',#4310,#4311,#4156,.T.);
#6423=EDGE_CURVE('',#4312,#4310,#3103,.T.);
#6424=EDGE_CURVE('',#4313,#4312,#4157,.T.);
#6425=EDGE_CURVE('',#4311,#4313,#3104,.T.);
#6426=EDGE_CURVE('',#4313,#4302,#3105,.T.);
#6427=EDGE_CURVE('',#4311,#4301,#3106,.T.);
#6428=EDGE_CURVE('',#4314,#4315,#3107,.T.);
#6429=EDGE_CURVE('',#4314,#4316,#4158,.T.);
#6430=EDGE_CURVE('',#4317,#4316,#3108,.T.);
#6431=EDGE_CURVE('',#4315,#4317,#4159,.T.);
#6432=EDGE_CURVE('',#4315,#4318,#3109,.T.);
#6433=EDGE_CURVE('',#4318,#4319,#3110,.T.);
#6434=EDGE_CURVE('',#4307,#4319,#3111,.T.);
#6435=EDGE_CURVE('',#4314,#4306,#3112,.T.);
#6436=EDGE_CURVE('',#4320,#4320,#4160,.T.);
#6437=EDGE_CURVE('',#4321,#4322,#4161,.T.);
#6438=EDGE_CURVE('',#4323,#4321,#3113,.T.);
#6439=EDGE_CURVE('',#4323,#4324,#4162,.T.);
#6440=EDGE_CURVE('',#4322,#4324,#3114,.T.);
#6441=EDGE_CURVE('',#4324,#4309,#3115,.T.);
#6442=EDGE_CURVE('',#4325,#4308,#3116,.T.);
#6443=EDGE_CURVE('',#4326,#4325,#3117,.T.);
#6444=EDGE_CURVE('',#4322,#4326,#3118,.T.);
#6445=EDGE_CURVE('',#4327,#4327,#4163,.T.);
#6446=EDGE_CURVE('',#4327,#4320,#3119,.T.);
#6447=EDGE_CURVE('',#4319,#4325,#3120,.T.);
#6448=EDGE_CURVE('',#4318,#4326,#3121,.T.);
#6449=EDGE_CURVE('',#4328,#4329,#4164,.T.);
#6450=EDGE_CURVE('',#4330,#4328,#3122,.T.);
#6451=EDGE_CURVE('',#4331,#4330,#4165,.T.);
#6452=EDGE_CURVE('',#4329,#4331,#3123,.T.);
#6453=EDGE_CURVE('',#4300,#4328,#3124,.T.);
#6454=EDGE_CURVE('',#4303,#4330,#3125,.T.);
#6455=EDGE_CURVE('',#4332,#4333,#4166,.T.);
#6456=EDGE_CURVE('',#4333,#4334,#3126,.T.);
#6457=EDGE_CURVE('',#4335,#4334,#3127,.T.);
#6458=EDGE_CURVE('',#4336,#4335,#3128,.T.);
#6459=EDGE_CURVE('',#4336,#4337,#4167,.T.);
#6460=EDGE_CURVE('',#4337,#4316,#3129,.T.);
#6461=EDGE_CURVE('',#4323,#4332,#3130,.T.);
#6462=EDGE_CURVE('',#4338,#4338,#4168,.T.);
#6463=EDGE_CURVE('',#4338,#4339,#3131,.T.);
#6464=EDGE_CURVE('',#4339,#4339,#4169,.T.);
#6465=EDGE_CURVE('',#4335,#4340,#3132,.T.);
#6466=EDGE_CURVE('',#4334,#4341,#3133,.T.);
#6467=EDGE_CURVE('',#4340,#4341,#3134,.T.);
#6468=EDGE_CURVE('',#4342,#4343,#4170,.T.);
#6469=EDGE_CURVE('',#4343,#4344,#3135,.T.);
#6470=EDGE_CURVE('',#4344,#4345,#4171,.T.);
#6471=EDGE_CURVE('',#4345,#4342,#3136,.T.);
#6472=EDGE_CURVE('',#4343,#4329,#3137,.T.);
#6473=EDGE_CURVE('',#4344,#4331,#3138,.T.);
#6474=EDGE_CURVE('',#4342,#4310,#3139,.T.);
#6475=EDGE_CURVE('',#4346,#4321,#3140,.T.);
#6476=EDGE_CURVE('',#4332,#4346,#3141,.T.);
#6477=EDGE_CURVE('',#4345,#4312,#3142,.T.);
#6478=EDGE_CURVE('',#4336,#4347,#3143,.T.);
#6479=EDGE_CURVE('',#4347,#4348,#4172,.T.);
#6480=EDGE_CURVE('',#4348,#4337,#3144,.T.);
#6481=EDGE_CURVE('',#4340,#4349,#3145,.T.);
#6482=EDGE_CURVE('',#4350,#4349,#3146,.T.);
#6483=EDGE_CURVE('',#4347,#4350,#3147,.T.);
#6484=EDGE_CURVE('',#4351,#4351,#4173,.T.);
#6485=EDGE_CURVE('',#4346,#4352,#4174,.T.);
#6486=EDGE_CURVE('',#4352,#4333,#3148,.T.);
#6487=EDGE_CURVE('',#4352,#4353,#3149,.T.);
#6488=EDGE_CURVE('',#4353,#4354,#3150,.T.);
#6489=EDGE_CURVE('',#4354,#4341,#3151,.T.);
#6490=EDGE_CURVE('',#4355,#4355,#4175,.T.);
#6491=EDGE_CURVE('',#4348,#4317,#3152,.T.);
#6492=EDGE_CURVE('',#4350,#4353,#3153,.T.);
#6493=EDGE_CURVE('',#4351,#4355,#3154,.T.);
#6494=EDGE_CURVE('',#4349,#4354,#3155,.T.);
#6495=EDGE_CURVE('',#4356,#4357,#3156,.T.);
#6496=EDGE_CURVE('',#4358,#4356,#57,.T.);
#6497=EDGE_CURVE('',#4359,#4358,#4176,.T.);
#6498=EDGE_CURVE('',#4359,#4357,#58,.T.);
#6499=EDGE_CURVE('',#4360,#4361,#3157,.T.);
#6500=EDGE_CURVE('',#4362,#4360,#59,.T.);
#6501=EDGE_CURVE('',#4356,#4362,#60,.T.);
#6502=EDGE_CURVE('',#4357,#4363,#61,.T.);
#6503=EDGE_CURVE('',#4363,#4361,#62,.T.);
#6504=EDGE_CURVE('',#4364,#4365,#3158,.T.);
#6505=EDGE_CURVE('',#4366,#4364,#63,.T.);
#6506=EDGE_CURVE('',#4360,#4366,#64,.T.);
#6507=EDGE_CURVE('',#4361,#4367,#65,.T.);
#6508=EDGE_CURVE('',#4367,#4365,#66,.T.);
#6509=EDGE_CURVE('',#4368,#4369,#3159,.T.);
#6510=EDGE_CURVE('',#4370,#4368,#67,.T.);
#6511=EDGE_CURVE('',#4364,#4370,#68,.T.);
#6512=EDGE_CURVE('',#4365,#4371,#69,.T.);
#6513=EDGE_CURVE('',#4371,#4369,#70,.T.);
#6514=EDGE_CURVE('',#4372,#4373,#3160,.T.);
#6515=EDGE_CURVE('',#4374,#4372,#71,.T.);
#6516=EDGE_CURVE('',#4368,#4374,#72,.T.);
#6517=EDGE_CURVE('',#4369,#4375,#73,.T.);
#6518=EDGE_CURVE('',#4375,#4373,#74,.T.);
#6519=EDGE_CURVE('',#4376,#4377,#3161,.T.);
#6520=EDGE_CURVE('',#4378,#4376,#75,.T.);
#6521=EDGE_CURVE('',#4372,#4378,#76,.T.);
#6522=EDGE_CURVE('',#4373,#4379,#77,.T.);
#6523=EDGE_CURVE('',#4379,#4377,#78,.T.);
#6524=EDGE_CURVE('',#4380,#4381,#3162,.T.);
#6525=EDGE_CURVE('',#4382,#4380,#79,.T.);
#6526=EDGE_CURVE('',#4376,#4382,#80,.T.);
#6527=EDGE_CURVE('',#4377,#4383,#81,.T.);
#6528=EDGE_CURVE('',#4383,#4381,#82,.T.);
#6529=EDGE_CURVE('',#4384,#4385,#3163,.T.);
#6530=EDGE_CURVE('',#4386,#4384,#83,.T.);
#6531=EDGE_CURVE('',#4380,#4386,#84,.T.);
#6532=EDGE_CURVE('',#4381,#4387,#85,.T.);
#6533=EDGE_CURVE('',#4387,#4385,#86,.T.);
#6534=EDGE_CURVE('',#4388,#4389,#3164,.T.);
#6535=EDGE_CURVE('',#4390,#4388,#87,.T.);
#6536=EDGE_CURVE('',#4384,#4390,#88,.T.);
#6537=EDGE_CURVE('',#4385,#4391,#89,.T.);
#6538=EDGE_CURVE('',#4391,#4389,#90,.T.);
#6539=EDGE_CURVE('',#4392,#4393,#3165,.T.);
#6540=EDGE_CURVE('',#4394,#4392,#91,.T.);
#6541=EDGE_CURVE('',#4388,#4394,#92,.T.);
#6542=EDGE_CURVE('',#4389,#4395,#93,.T.);
#6543=EDGE_CURVE('',#4395,#4393,#94,.T.);
#6544=EDGE_CURVE('',#4396,#4397,#3166,.T.);
#6545=EDGE_CURVE('',#4398,#4396,#95,.T.);
#6546=EDGE_CURVE('',#4392,#4398,#96,.T.);
#6547=EDGE_CURVE('',#4393,#4399,#97,.T.);
#6548=EDGE_CURVE('',#4399,#4397,#98,.T.);
#6549=EDGE_CURVE('',#4400,#4401,#3167,.T.);
#6550=EDGE_CURVE('',#4402,#4400,#99,.T.);
#6551=EDGE_CURVE('',#4396,#4402,#100,.T.);
#6552=EDGE_CURVE('',#4397,#4403,#101,.T.);
#6553=EDGE_CURVE('',#4403,#4401,#102,.T.);
#6554=EDGE_CURVE('',#4404,#4405,#3168,.T.);
#6555=EDGE_CURVE('',#4406,#4404,#103,.T.);
#6556=EDGE_CURVE('',#4400,#4406,#104,.T.);
#6557=EDGE_CURVE('',#4401,#4407,#105,.T.);
#6558=EDGE_CURVE('',#4407,#4405,#106,.T.);
#6559=EDGE_CURVE('',#4408,#4409,#3169,.T.);
#6560=EDGE_CURVE('',#4410,#4408,#107,.T.);
#6561=EDGE_CURVE('',#4404,#4410,#108,.T.);
#6562=EDGE_CURVE('',#4405,#4411,#109,.T.);
#6563=EDGE_CURVE('',#4411,#4409,#110,.T.);
#6564=EDGE_CURVE('',#4412,#4413,#3170,.T.);
#6565=EDGE_CURVE('',#4414,#4412,#111,.T.);
#6566=EDGE_CURVE('',#4408,#4414,#112,.T.);
#6567=EDGE_CURVE('',#4409,#4415,#113,.T.);
#6568=EDGE_CURVE('',#4415,#4413,#114,.T.);
#6569=EDGE_CURVE('',#4416,#4417,#3171,.T.);
#6570=EDGE_CURVE('',#4418,#4416,#115,.T.);
#6571=EDGE_CURVE('',#4412,#4418,#116,.T.);
#6572=EDGE_CURVE('',#4413,#4419,#117,.T.);
#6573=EDGE_CURVE('',#4419,#4417,#118,.T.);
#6574=EDGE_CURVE('',#4420,#4421,#3172,.T.);
#6575=EDGE_CURVE('',#4422,#4420,#119,.T.);
#6576=EDGE_CURVE('',#4416,#4422,#120,.T.);
#6577=EDGE_CURVE('',#4417,#4423,#121,.T.);
#6578=EDGE_CURVE('',#4423,#4421,#122,.T.);
#6579=EDGE_CURVE('',#4424,#4425,#3173,.T.);
#6580=EDGE_CURVE('',#4426,#4424,#123,.T.);
#6581=EDGE_CURVE('',#4420,#4426,#124,.T.);
#6582=EDGE_CURVE('',#4421,#4427,#125,.T.);
#6583=EDGE_CURVE('',#4427,#4425,#126,.T.);
#6584=EDGE_CURVE('',#4428,#4429,#3174,.T.);
#6585=EDGE_CURVE('',#4430,#4428,#127,.T.);
#6586=EDGE_CURVE('',#4424,#4430,#128,.T.);
#6587=EDGE_CURVE('',#4425,#4431,#129,.T.);
#6588=EDGE_CURVE('',#4431,#4429,#130,.T.);
#6589=EDGE_CURVE('',#4432,#4433,#3175,.T.);
#6590=EDGE_CURVE('',#4434,#4432,#131,.T.);
#6591=EDGE_CURVE('',#4428,#4434,#132,.T.);
#6592=EDGE_CURVE('',#4429,#4435,#133,.T.);
#6593=EDGE_CURVE('',#4435,#4433,#134,.T.);
#6594=EDGE_CURVE('',#4436,#4437,#3176,.T.);
#6595=EDGE_CURVE('',#4438,#4436,#135,.T.);
#6596=EDGE_CURVE('',#4432,#4438,#136,.T.);
#6597=EDGE_CURVE('',#4433,#4439,#137,.T.);
#6598=EDGE_CURVE('',#4439,#4437,#138,.T.);
#6599=EDGE_CURVE('',#4440,#4441,#3177,.T.);
#6600=EDGE_CURVE('',#4442,#4440,#139,.T.);
#6601=EDGE_CURVE('',#4436,#4442,#140,.T.);
#6602=EDGE_CURVE('',#4437,#4443,#141,.T.);
#6603=EDGE_CURVE('',#4443,#4441,#142,.T.);
#6604=EDGE_CURVE('',#4444,#4445,#3178,.T.);
#6605=EDGE_CURVE('',#4446,#4444,#143,.T.);
#6606=EDGE_CURVE('',#4440,#4446,#144,.T.);
#6607=EDGE_CURVE('',#4441,#4447,#145,.T.);
#6608=EDGE_CURVE('',#4447,#4445,#146,.T.);
#6609=EDGE_CURVE('',#4448,#4449,#3179,.T.);
#6610=EDGE_CURVE('',#4450,#4448,#147,.T.);
#6611=EDGE_CURVE('',#4444,#4450,#148,.T.);
#6612=EDGE_CURVE('',#4445,#4451,#149,.T.);
#6613=EDGE_CURVE('',#4451,#4449,#150,.T.);
#6614=EDGE_CURVE('',#4452,#4453,#3180,.T.);
#6615=EDGE_CURVE('',#4454,#4452,#151,.T.);
#6616=EDGE_CURVE('',#4448,#4454,#152,.T.);
#6617=EDGE_CURVE('',#4449,#4455,#153,.T.);
#6618=EDGE_CURVE('',#4455,#4453,#154,.T.);
#6619=EDGE_CURVE('',#4456,#4457,#3181,.T.);
#6620=EDGE_CURVE('',#4458,#4456,#155,.T.);
#6621=EDGE_CURVE('',#4452,#4458,#156,.T.);
#6622=EDGE_CURVE('',#4453,#4459,#157,.T.);
#6623=EDGE_CURVE('',#4459,#4457,#158,.T.);
#6624=EDGE_CURVE('',#4460,#4461,#3182,.T.);
#6625=EDGE_CURVE('',#4462,#4460,#159,.T.);
#6626=EDGE_CURVE('',#4456,#4462,#160,.T.);
#6627=EDGE_CURVE('',#4457,#4463,#161,.T.);
#6628=EDGE_CURVE('',#4463,#4461,#162,.T.);
#6629=EDGE_CURVE('',#4464,#4465,#3183,.T.);
#6630=EDGE_CURVE('',#4466,#4464,#163,.T.);
#6631=EDGE_CURVE('',#4460,#4466,#164,.T.);
#6632=EDGE_CURVE('',#4461,#4467,#165,.T.);
#6633=EDGE_CURVE('',#4467,#4465,#166,.T.);
#6634=EDGE_CURVE('',#4468,#4469,#3184,.T.);
#6635=EDGE_CURVE('',#4470,#4468,#167,.T.);
#6636=EDGE_CURVE('',#4464,#4470,#168,.T.);
#6637=EDGE_CURVE('',#4465,#4471,#169,.T.);
#6638=EDGE_CURVE('',#4471,#4469,#170,.T.);
#6639=EDGE_CURVE('',#4472,#4473,#3185,.T.);
#6640=EDGE_CURVE('',#4474,#4472,#171,.T.);
#6641=EDGE_CURVE('',#4468,#4474,#172,.T.);
#6642=EDGE_CURVE('',#4469,#4475,#173,.T.);
#6643=EDGE_CURVE('',#4475,#4473,#174,.T.);
#6644=EDGE_CURVE('',#4476,#4477,#3186,.T.);
#6645=EDGE_CURVE('',#4478,#4476,#175,.T.);
#6646=EDGE_CURVE('',#4472,#4478,#176,.T.);
#6647=EDGE_CURVE('',#4473,#4479,#177,.T.);
#6648=EDGE_CURVE('',#4479,#4477,#178,.T.);
#6649=EDGE_CURVE('',#4480,#4481,#3187,.T.);
#6650=EDGE_CURVE('',#4482,#4480,#179,.T.);
#6651=EDGE_CURVE('',#4476,#4482,#180,.T.);
#6652=EDGE_CURVE('',#4477,#4483,#181,.T.);
#6653=EDGE_CURVE('',#4483,#4481,#182,.T.);
#6654=EDGE_CURVE('',#4484,#4485,#3188,.T.);
#6655=EDGE_CURVE('',#4486,#4484,#183,.T.);
#6656=EDGE_CURVE('',#4480,#4486,#184,.T.);
#6657=EDGE_CURVE('',#4481,#4487,#185,.T.);
#6658=EDGE_CURVE('',#4487,#4485,#186,.T.);
#6659=EDGE_CURVE('',#4488,#4489,#3189,.T.);
#6660=EDGE_CURVE('',#4490,#4488,#187,.T.);
#6661=EDGE_CURVE('',#4484,#4490,#188,.T.);
#6662=EDGE_CURVE('',#4485,#4491,#189,.T.);
#6663=EDGE_CURVE('',#4491,#4489,#190,.T.);
#6664=EDGE_CURVE('',#4492,#4493,#3190,.T.);
#6665=EDGE_CURVE('',#4494,#4492,#191,.T.);
#6666=EDGE_CURVE('',#4488,#4494,#192,.T.);
#6667=EDGE_CURVE('',#4489,#4495,#193,.T.);
#6668=EDGE_CURVE('',#4495,#4493,#194,.T.);
#6669=EDGE_CURVE('',#4496,#4497,#3191,.T.);
#6670=EDGE_CURVE('',#4498,#4496,#195,.T.);
#6671=EDGE_CURVE('',#4492,#4498,#196,.T.);
#6672=EDGE_CURVE('',#4493,#4499,#197,.T.);
#6673=EDGE_CURVE('',#4499,#4497,#198,.T.);
#6674=EDGE_CURVE('',#4500,#4501,#3192,.T.);
#6675=EDGE_CURVE('',#4502,#4500,#199,.T.);
#6676=EDGE_CURVE('',#4496,#4502,#200,.T.);
#6677=EDGE_CURVE('',#4497,#4503,#201,.T.);
#6678=EDGE_CURVE('',#4503,#4501,#202,.T.);
#6679=EDGE_CURVE('',#4504,#4505,#3193,.T.);
#6680=EDGE_CURVE('',#4506,#4504,#203,.T.);
#6681=EDGE_CURVE('',#4500,#4506,#204,.T.);
#6682=EDGE_CURVE('',#4501,#4507,#205,.T.);
#6683=EDGE_CURVE('',#4507,#4505,#206,.T.);
#6684=EDGE_CURVE('',#4508,#4509,#3194,.T.);
#6685=EDGE_CURVE('',#4510,#4508,#207,.T.);
#6686=EDGE_CURVE('',#4504,#4510,#208,.T.);
#6687=EDGE_CURVE('',#4505,#4511,#209,.T.);
#6688=EDGE_CURVE('',#4511,#4509,#210,.T.);
#6689=EDGE_CURVE('',#4512,#4513,#3195,.T.);
#6690=EDGE_CURVE('',#4514,#4512,#211,.T.);
#6691=EDGE_CURVE('',#4508,#4514,#212,.T.);
#6692=EDGE_CURVE('',#4509,#4515,#213,.T.);
#6693=EDGE_CURVE('',#4515,#4513,#214,.T.);
#6694=EDGE_CURVE('',#4516,#4517,#3196,.T.);
#6695=EDGE_CURVE('',#4518,#4516,#215,.T.);
#6696=EDGE_CURVE('',#4512,#4518,#216,.T.);
#6697=EDGE_CURVE('',#4513,#4519,#217,.T.);
#6698=EDGE_CURVE('',#4519,#4517,#218,.T.);
#6699=EDGE_CURVE('',#4520,#4521,#3197,.T.);
#6700=EDGE_CURVE('',#4522,#4520,#219,.T.);
#6701=EDGE_CURVE('',#4516,#4522,#220,.T.);
#6702=EDGE_CURVE('',#4517,#4523,#221,.T.);
#6703=EDGE_CURVE('',#4523,#4521,#222,.T.);
#6704=EDGE_CURVE('',#4524,#4525,#3198,.T.);
#6705=EDGE_CURVE('',#4526,#4524,#223,.T.);
#6706=EDGE_CURVE('',#4520,#4526,#224,.T.);
#6707=EDGE_CURVE('',#4521,#4527,#225,.T.);
#6708=EDGE_CURVE('',#4527,#4525,#226,.T.);
#6709=EDGE_CURVE('',#4528,#4529,#3199,.T.);
#6710=EDGE_CURVE('',#4530,#4528,#227,.T.);
#6711=EDGE_CURVE('',#4524,#4530,#228,.T.);
#6712=EDGE_CURVE('',#4525,#4531,#229,.T.);
#6713=EDGE_CURVE('',#4531,#4529,#230,.T.);
#6714=EDGE_CURVE('',#4532,#4533,#3200,.T.);
#6715=EDGE_CURVE('',#4534,#4532,#231,.T.);
#6716=EDGE_CURVE('',#4528,#4534,#232,.T.);
#6717=EDGE_CURVE('',#4529,#4535,#233,.T.);
#6718=EDGE_CURVE('',#4535,#4533,#234,.T.);
#6719=EDGE_CURVE('',#4536,#4537,#3201,.T.);
#6720=EDGE_CURVE('',#4538,#4536,#235,.T.);
#6721=EDGE_CURVE('',#4532,#4538,#236,.T.);
#6722=EDGE_CURVE('',#4533,#4539,#237,.T.);
#6723=EDGE_CURVE('',#4539,#4537,#238,.T.);
#6724=EDGE_CURVE('',#4540,#4541,#3202,.T.);
#6725=EDGE_CURVE('',#4542,#4540,#239,.T.);
#6726=EDGE_CURVE('',#4536,#4542,#240,.T.);
#6727=EDGE_CURVE('',#4537,#4543,#241,.T.);
#6728=EDGE_CURVE('',#4543,#4541,#242,.T.);
#6729=EDGE_CURVE('',#4544,#4545,#3203,.T.);
#6730=EDGE_CURVE('',#4546,#4544,#243,.T.);
#6731=EDGE_CURVE('',#4540,#4546,#244,.T.);
#6732=EDGE_CURVE('',#4541,#4547,#245,.T.);
#6733=EDGE_CURVE('',#4547,#4545,#246,.T.);
#6734=EDGE_CURVE('',#4548,#4549,#3204,.T.);
#6735=EDGE_CURVE('',#4550,#4548,#247,.T.);
#6736=EDGE_CURVE('',#4544,#4550,#248,.T.);
#6737=EDGE_CURVE('',#4545,#4551,#249,.T.);
#6738=EDGE_CURVE('',#4551,#4549,#250,.T.);
#6739=EDGE_CURVE('',#4552,#4553,#3205,.T.);
#6740=EDGE_CURVE('',#4554,#4552,#251,.T.);
#6741=EDGE_CURVE('',#4548,#4554,#252,.T.);
#6742=EDGE_CURVE('',#4549,#4555,#253,.T.);
#6743=EDGE_CURVE('',#4555,#4553,#254,.T.);
#6744=EDGE_CURVE('',#4556,#4557,#3206,.T.);
#6745=EDGE_CURVE('',#4558,#4556,#255,.T.);
#6746=EDGE_CURVE('',#4552,#4558,#256,.T.);
#6747=EDGE_CURVE('',#4553,#4559,#257,.T.);
#6748=EDGE_CURVE('',#4559,#4557,#258,.T.);
#6749=EDGE_CURVE('',#4560,#4561,#3207,.T.);
#6750=EDGE_CURVE('',#4562,#4560,#259,.T.);
#6751=EDGE_CURVE('',#4556,#4562,#260,.T.);
#6752=EDGE_CURVE('',#4557,#4563,#261,.T.);
#6753=EDGE_CURVE('',#4563,#4561,#262,.T.);
#6754=EDGE_CURVE('',#4564,#4565,#3208,.T.);
#6755=EDGE_CURVE('',#4566,#4564,#263,.T.);
#6756=EDGE_CURVE('',#4560,#4566,#264,.T.);
#6757=EDGE_CURVE('',#4561,#4567,#265,.T.);
#6758=EDGE_CURVE('',#4567,#4565,#266,.T.);
#6759=EDGE_CURVE('',#4568,#4569,#3209,.T.);
#6760=EDGE_CURVE('',#4570,#4568,#267,.T.);
#6761=EDGE_CURVE('',#4564,#4570,#268,.T.);
#6762=EDGE_CURVE('',#4565,#4571,#269,.T.);
#6763=EDGE_CURVE('',#4571,#4569,#270,.T.);
#6764=EDGE_CURVE('',#4572,#4573,#3210,.T.);
#6765=EDGE_CURVE('',#4574,#4572,#271,.T.);
#6766=EDGE_CURVE('',#4568,#4574,#272,.T.);
#6767=EDGE_CURVE('',#4569,#4575,#273,.T.);
#6768=EDGE_CURVE('',#4575,#4573,#274,.T.);
#6769=EDGE_CURVE('',#4576,#4577,#3211,.T.);
#6770=EDGE_CURVE('',#4578,#4576,#275,.T.);
#6771=EDGE_CURVE('',#4572,#4578,#276,.T.);
#6772=EDGE_CURVE('',#4573,#4579,#277,.T.);
#6773=EDGE_CURVE('',#4579,#4577,#278,.T.);
#6774=EDGE_CURVE('',#4580,#4581,#3212,.T.);
#6775=EDGE_CURVE('',#4582,#4580,#279,.T.);
#6776=EDGE_CURVE('',#4576,#4582,#280,.T.);
#6777=EDGE_CURVE('',#4577,#4583,#281,.T.);
#6778=EDGE_CURVE('',#4583,#4581,#282,.T.);
#6779=EDGE_CURVE('',#4584,#4585,#3213,.T.);
#6780=EDGE_CURVE('',#4586,#4584,#283,.T.);
#6781=EDGE_CURVE('',#4580,#4586,#284,.T.);
#6782=EDGE_CURVE('',#4581,#4587,#285,.T.);
#6783=EDGE_CURVE('',#4587,#4585,#286,.T.);
#6784=EDGE_CURVE('',#4588,#4589,#3214,.T.);
#6785=EDGE_CURVE('',#4590,#4588,#287,.T.);
#6786=EDGE_CURVE('',#4584,#4590,#288,.T.);
#6787=EDGE_CURVE('',#4585,#4591,#289,.T.);
#6788=EDGE_CURVE('',#4591,#4589,#290,.T.);
#6789=EDGE_CURVE('',#4592,#4593,#3215,.T.);
#6790=EDGE_CURVE('',#4594,#4592,#291,.T.);
#6791=EDGE_CURVE('',#4588,#4594,#292,.T.);
#6792=EDGE_CURVE('',#4589,#4595,#293,.T.);
#6793=EDGE_CURVE('',#4595,#4593,#294,.T.);
#6794=EDGE_CURVE('',#4596,#4597,#3216,.T.);
#6795=EDGE_CURVE('',#4598,#4596,#295,.T.);
#6796=EDGE_CURVE('',#4592,#4598,#296,.T.);
#6797=EDGE_CURVE('',#4593,#4599,#297,.T.);
#6798=EDGE_CURVE('',#4599,#4597,#298,.T.);
#6799=EDGE_CURVE('',#4600,#4601,#3217,.T.);
#6800=EDGE_CURVE('',#4602,#4600,#299,.T.);
#6801=EDGE_CURVE('',#4596,#4602,#300,.T.);
#6802=EDGE_CURVE('',#4597,#4603,#301,.T.);
#6803=EDGE_CURVE('',#4603,#4601,#302,.T.);
#6804=EDGE_CURVE('',#4604,#4605,#3218,.T.);
#6805=EDGE_CURVE('',#4606,#4604,#303,.T.);
#6806=EDGE_CURVE('',#4600,#4606,#304,.T.);
#6807=EDGE_CURVE('',#4601,#4607,#305,.T.);
#6808=EDGE_CURVE('',#4607,#4605,#306,.T.);
#6809=EDGE_CURVE('',#4608,#4609,#3219,.T.);
#6810=EDGE_CURVE('',#4610,#4608,#307,.T.);
#6811=EDGE_CURVE('',#4604,#4610,#308,.T.);
#6812=EDGE_CURVE('',#4605,#4611,#309,.T.);
#6813=EDGE_CURVE('',#4611,#4609,#310,.T.);
#6814=EDGE_CURVE('',#4612,#4613,#3220,.T.);
#6815=EDGE_CURVE('',#4614,#4612,#311,.T.);
#6816=EDGE_CURVE('',#4608,#4614,#312,.T.);
#6817=EDGE_CURVE('',#4609,#4615,#313,.T.);
#6818=EDGE_CURVE('',#4615,#4613,#314,.T.);
#6819=EDGE_CURVE('',#4616,#4617,#3221,.T.);
#6820=EDGE_CURVE('',#4618,#4616,#315,.T.);
#6821=EDGE_CURVE('',#4612,#4618,#316,.T.);
#6822=EDGE_CURVE('',#4613,#4619,#317,.T.);
#6823=EDGE_CURVE('',#4619,#4617,#318,.T.);
#6824=EDGE_CURVE('',#4620,#4621,#3222,.T.);
#6825=EDGE_CURVE('',#4622,#4620,#319,.T.);
#6826=EDGE_CURVE('',#4616,#4622,#320,.T.);
#6827=EDGE_CURVE('',#4617,#4623,#321,.T.);
#6828=EDGE_CURVE('',#4623,#4621,#322,.T.);
#6829=EDGE_CURVE('',#4624,#4625,#3223,.T.);
#6830=EDGE_CURVE('',#4626,#4624,#323,.T.);
#6831=EDGE_CURVE('',#4620,#4626,#324,.T.);
#6832=EDGE_CURVE('',#4621,#4627,#325,.T.);
#6833=EDGE_CURVE('',#4627,#4625,#326,.T.);
#6834=EDGE_CURVE('',#4628,#4629,#3224,.T.);
#6835=EDGE_CURVE('',#4630,#4628,#327,.T.);
#6836=EDGE_CURVE('',#4624,#4630,#328,.T.);
#6837=EDGE_CURVE('',#4625,#4631,#329,.T.);
#6838=EDGE_CURVE('',#4631,#4629,#330,.T.);
#6839=EDGE_CURVE('',#4632,#4633,#3225,.T.);
#6840=EDGE_CURVE('',#4634,#4632,#331,.T.);
#6841=EDGE_CURVE('',#4628,#4634,#332,.T.);
#6842=EDGE_CURVE('',#4629,#4635,#333,.T.);
#6843=EDGE_CURVE('',#4635,#4633,#334,.T.);
#6844=EDGE_CURVE('',#4636,#4637,#3226,.T.);
#6845=EDGE_CURVE('',#4638,#4636,#335,.T.);
#6846=EDGE_CURVE('',#4632,#4638,#336,.T.);
#6847=EDGE_CURVE('',#4633,#4639,#337,.T.);
#6848=EDGE_CURVE('',#4639,#4637,#338,.T.);
#6849=EDGE_CURVE('',#4640,#4641,#3227,.T.);
#6850=EDGE_CURVE('',#4642,#4640,#339,.T.);
#6851=EDGE_CURVE('',#4636,#4642,#340,.T.);
#6852=EDGE_CURVE('',#4637,#4643,#341,.T.);
#6853=EDGE_CURVE('',#4643,#4641,#342,.T.);
#6854=EDGE_CURVE('',#4644,#4645,#3228,.T.);
#6855=EDGE_CURVE('',#4646,#4644,#343,.T.);
#6856=EDGE_CURVE('',#4640,#4646,#344,.T.);
#6857=EDGE_CURVE('',#4641,#4647,#345,.T.);
#6858=EDGE_CURVE('',#4647,#4645,#346,.T.);
#6859=EDGE_CURVE('',#4648,#4649,#3229,.T.);
#6860=EDGE_CURVE('',#4650,#4648,#347,.T.);
#6861=EDGE_CURVE('',#4644,#4650,#348,.T.);
#6862=EDGE_CURVE('',#4645,#4651,#349,.T.);
#6863=EDGE_CURVE('',#4651,#4649,#350,.T.);
#6864=EDGE_CURVE('',#4652,#4653,#3230,.T.);
#6865=EDGE_CURVE('',#4654,#4652,#351,.T.);
#6866=EDGE_CURVE('',#4648,#4654,#352,.T.);
#6867=EDGE_CURVE('',#4649,#4655,#353,.T.);
#6868=EDGE_CURVE('',#4655,#4653,#354,.T.);
#6869=EDGE_CURVE('',#4656,#4657,#3231,.T.);
#6870=EDGE_CURVE('',#4658,#4656,#355,.T.);
#6871=EDGE_CURVE('',#4652,#4658,#356,.T.);
#6872=EDGE_CURVE('',#4653,#4659,#357,.T.);
#6873=EDGE_CURVE('',#4659,#4657,#358,.T.);
#6874=EDGE_CURVE('',#4660,#4661,#3232,.T.);
#6875=EDGE_CURVE('',#4662,#4660,#359,.T.);
#6876=EDGE_CURVE('',#4656,#4662,#360,.T.);
#6877=EDGE_CURVE('',#4657,#4663,#361,.T.);
#6878=EDGE_CURVE('',#4663,#4661,#362,.T.);
#6879=EDGE_CURVE('',#4664,#4665,#3233,.T.);
#6880=EDGE_CURVE('',#4666,#4664,#363,.T.);
#6881=EDGE_CURVE('',#4660,#4666,#364,.T.);
#6882=EDGE_CURVE('',#4661,#4667,#365,.T.);
#6883=EDGE_CURVE('',#4667,#4665,#366,.T.);
#6884=EDGE_CURVE('',#4668,#4669,#3234,.T.);
#6885=EDGE_CURVE('',#4670,#4668,#367,.T.);
#6886=EDGE_CURVE('',#4664,#4670,#368,.T.);
#6887=EDGE_CURVE('',#4665,#4671,#369,.T.);
#6888=EDGE_CURVE('',#4671,#4669,#370,.T.);
#6889=EDGE_CURVE('',#4672,#4673,#3235,.T.);
#6890=EDGE_CURVE('',#4674,#4672,#371,.T.);
#6891=EDGE_CURVE('',#4668,#4674,#372,.T.);
#6892=EDGE_CURVE('',#4669,#4675,#373,.T.);
#6893=EDGE_CURVE('',#4675,#4673,#374,.T.);
#6894=EDGE_CURVE('',#4676,#4677,#3236,.T.);
#6895=EDGE_CURVE('',#4678,#4676,#375,.T.);
#6896=EDGE_CURVE('',#4672,#4678,#376,.T.);
#6897=EDGE_CURVE('',#4673,#4679,#377,.T.);
#6898=EDGE_CURVE('',#4679,#4677,#378,.T.);
#6899=EDGE_CURVE('',#4680,#4681,#3237,.T.);
#6900=EDGE_CURVE('',#4682,#4680,#379,.T.);
#6901=EDGE_CURVE('',#4676,#4682,#380,.T.);
#6902=EDGE_CURVE('',#4677,#4683,#381,.T.);
#6903=EDGE_CURVE('',#4683,#4681,#382,.T.);
#6904=EDGE_CURVE('',#4684,#4685,#3238,.T.);
#6905=EDGE_CURVE('',#4686,#4684,#383,.T.);
#6906=EDGE_CURVE('',#4680,#4686,#384,.T.);
#6907=EDGE_CURVE('',#4681,#4687,#385,.T.);
#6908=EDGE_CURVE('',#4687,#4685,#386,.T.);
#6909=EDGE_CURVE('',#4688,#4689,#3239,.T.);
#6910=EDGE_CURVE('',#4690,#4688,#387,.T.);
#6911=EDGE_CURVE('',#4684,#4690,#388,.T.);
#6912=EDGE_CURVE('',#4685,#4691,#389,.T.);
#6913=EDGE_CURVE('',#4691,#4689,#390,.T.);
#6914=EDGE_CURVE('',#4692,#4693,#3240,.T.);
#6915=EDGE_CURVE('',#4694,#4692,#391,.T.);
#6916=EDGE_CURVE('',#4688,#4694,#392,.T.);
#6917=EDGE_CURVE('',#4689,#4695,#393,.T.);
#6918=EDGE_CURVE('',#4695,#4693,#394,.T.);
#6919=EDGE_CURVE('',#4696,#4697,#3241,.T.);
#6920=EDGE_CURVE('',#4698,#4696,#395,.T.);
#6921=EDGE_CURVE('',#4692,#4698,#396,.T.);
#6922=EDGE_CURVE('',#4693,#4699,#397,.T.);
#6923=EDGE_CURVE('',#4699,#4697,#398,.T.);
#6924=EDGE_CURVE('',#4700,#4701,#3242,.T.);
#6925=EDGE_CURVE('',#4702,#4700,#399,.T.);
#6926=EDGE_CURVE('',#4696,#4702,#400,.T.);
#6927=EDGE_CURVE('',#4697,#4703,#401,.T.);
#6928=EDGE_CURVE('',#4703,#4701,#402,.T.);
#6929=EDGE_CURVE('',#4704,#4705,#3243,.T.);
#6930=EDGE_CURVE('',#4706,#4704,#403,.T.);
#6931=EDGE_CURVE('',#4700,#4706,#404,.T.);
#6932=EDGE_CURVE('',#4701,#4707,#405,.T.);
#6933=EDGE_CURVE('',#4707,#4705,#406,.T.);
#6934=EDGE_CURVE('',#4708,#4709,#3244,.T.);
#6935=EDGE_CURVE('',#4710,#4708,#407,.T.);
#6936=EDGE_CURVE('',#4704,#4710,#408,.T.);
#6937=EDGE_CURVE('',#4705,#4711,#409,.T.);
#6938=EDGE_CURVE('',#4711,#4709,#410,.T.);
#6939=EDGE_CURVE('',#4712,#4713,#3245,.T.);
#6940=EDGE_CURVE('',#4714,#4712,#411,.T.);
#6941=EDGE_CURVE('',#4708,#4714,#412,.T.);
#6942=EDGE_CURVE('',#4709,#4715,#413,.T.);
#6943=EDGE_CURVE('',#4715,#4713,#414,.T.);
#6944=EDGE_CURVE('',#4716,#4717,#3246,.T.);
#6945=EDGE_CURVE('',#4718,#4716,#415,.T.);
#6946=EDGE_CURVE('',#4712,#4718,#416,.T.);
#6947=EDGE_CURVE('',#4713,#4719,#417,.T.);
#6948=EDGE_CURVE('',#4719,#4717,#418,.T.);
#6949=EDGE_CURVE('',#4720,#4721,#3247,.T.);
#6950=EDGE_CURVE('',#4722,#4720,#419,.T.);
#6951=EDGE_CURVE('',#4716,#4722,#420,.T.);
#6952=EDGE_CURVE('',#4717,#4723,#421,.T.);
#6953=EDGE_CURVE('',#4723,#4721,#422,.T.);
#6954=EDGE_CURVE('',#4724,#4725,#3248,.T.);
#6955=EDGE_CURVE('',#4726,#4724,#423,.T.);
#6956=EDGE_CURVE('',#4720,#4726,#424,.T.);
#6957=EDGE_CURVE('',#4721,#4727,#425,.T.);
#6958=EDGE_CURVE('',#4727,#4725,#426,.T.);
#6959=EDGE_CURVE('',#4728,#4729,#3249,.T.);
#6960=EDGE_CURVE('',#4730,#4728,#427,.T.);
#6961=EDGE_CURVE('',#4724,#4730,#428,.T.);
#6962=EDGE_CURVE('',#4725,#4731,#429,.T.);
#6963=EDGE_CURVE('',#4731,#4729,#430,.T.);
#6964=EDGE_CURVE('',#4732,#4733,#3250,.T.);
#6965=EDGE_CURVE('',#4734,#4732,#431,.T.);
#6966=EDGE_CURVE('',#4728,#4734,#432,.T.);
#6967=EDGE_CURVE('',#4729,#4735,#433,.T.);
#6968=EDGE_CURVE('',#4735,#4733,#434,.T.);
#6969=EDGE_CURVE('',#4736,#4737,#3251,.T.);
#6970=EDGE_CURVE('',#4738,#4736,#435,.T.);
#6971=EDGE_CURVE('',#4732,#4738,#436,.T.);
#6972=EDGE_CURVE('',#4733,#4739,#437,.T.);
#6973=EDGE_CURVE('',#4739,#4737,#438,.T.);
#6974=EDGE_CURVE('',#4740,#4741,#3252,.T.);
#6975=EDGE_CURVE('',#4742,#4740,#439,.T.);
#6976=EDGE_CURVE('',#4736,#4742,#440,.T.);
#6977=EDGE_CURVE('',#4737,#4743,#441,.T.);
#6978=EDGE_CURVE('',#4743,#4741,#442,.T.);
#6979=EDGE_CURVE('',#4744,#4745,#3253,.T.);
#6980=EDGE_CURVE('',#4746,#4744,#443,.T.);
#6981=EDGE_CURVE('',#4740,#4746,#444,.T.);
#6982=EDGE_CURVE('',#4741,#4747,#445,.T.);
#6983=EDGE_CURVE('',#4747,#4745,#446,.T.);
#6984=EDGE_CURVE('',#4748,#4749,#3254,.T.);
#6985=EDGE_CURVE('',#4750,#4748,#447,.T.);
#6986=EDGE_CURVE('',#4744,#4750,#448,.T.);
#6987=EDGE_CURVE('',#4745,#4751,#449,.T.);
#6988=EDGE_CURVE('',#4751,#4749,#450,.T.);
#6989=EDGE_CURVE('',#4752,#4753,#3255,.T.);
#6990=EDGE_CURVE('',#4754,#4752,#451,.T.);
#6991=EDGE_CURVE('',#4748,#4754,#452,.T.);
#6992=EDGE_CURVE('',#4749,#4755,#453,.T.);
#6993=EDGE_CURVE('',#4755,#4753,#454,.T.);
#6994=EDGE_CURVE('',#4756,#4757,#3256,.T.);
#6995=EDGE_CURVE('',#4758,#4756,#455,.T.);
#6996=EDGE_CURVE('',#4752,#4758,#456,.T.);
#6997=EDGE_CURVE('',#4753,#4759,#457,.T.);
#6998=EDGE_CURVE('',#4759,#4757,#458,.T.);
#6999=EDGE_CURVE('',#4760,#4761,#3257,.T.);
#7000=EDGE_CURVE('',#4762,#4760,#459,.T.);
#7001=EDGE_CURVE('',#4756,#4762,#460,.T.);
#7002=EDGE_CURVE('',#4757,#4763,#461,.T.);
#7003=EDGE_CURVE('',#4763,#4761,#462,.T.);
#7004=EDGE_CURVE('',#4764,#4765,#3258,.T.);
#7005=EDGE_CURVE('',#4766,#4764,#463,.T.);
#7006=EDGE_CURVE('',#4760,#4766,#464,.T.);
#7007=EDGE_CURVE('',#4761,#4767,#465,.T.);
#7008=EDGE_CURVE('',#4767,#4765,#466,.T.);
#7009=EDGE_CURVE('',#4768,#4769,#3259,.T.);
#7010=EDGE_CURVE('',#4770,#4768,#467,.T.);
#7011=EDGE_CURVE('',#4764,#4770,#468,.T.);
#7012=EDGE_CURVE('',#4765,#4771,#469,.T.);
#7013=EDGE_CURVE('',#4771,#4769,#470,.T.);
#7014=EDGE_CURVE('',#4772,#4773,#3260,.T.);
#7015=EDGE_CURVE('',#4774,#4772,#471,.T.);
#7016=EDGE_CURVE('',#4768,#4774,#472,.T.);
#7017=EDGE_CURVE('',#4769,#4775,#473,.T.);
#7018=EDGE_CURVE('',#4775,#4773,#474,.T.);
#7019=EDGE_CURVE('',#4776,#4777,#3261,.T.);
#7020=EDGE_CURVE('',#4778,#4776,#475,.T.);
#7021=EDGE_CURVE('',#4772,#4778,#476,.T.);
#7022=EDGE_CURVE('',#4773,#4779,#477,.T.);
#7023=EDGE_CURVE('',#4779,#4777,#478,.T.);
#7024=EDGE_CURVE('',#4780,#4781,#3262,.T.);
#7025=EDGE_CURVE('',#4782,#4780,#479,.T.);
#7026=EDGE_CURVE('',#4776,#4782,#480,.T.);
#7027=EDGE_CURVE('',#4777,#4783,#481,.T.);
#7028=EDGE_CURVE('',#4783,#4781,#482,.T.);
#7029=EDGE_CURVE('',#4784,#4785,#3263,.T.);
#7030=EDGE_CURVE('',#4786,#4784,#483,.T.);
#7031=EDGE_CURVE('',#4780,#4786,#484,.T.);
#7032=EDGE_CURVE('',#4781,#4787,#485,.T.);
#7033=EDGE_CURVE('',#4787,#4785,#486,.T.);
#7034=EDGE_CURVE('',#4788,#4789,#3264,.T.);
#7035=EDGE_CURVE('',#4790,#4788,#487,.T.);
#7036=EDGE_CURVE('',#4784,#4790,#488,.T.);
#7037=EDGE_CURVE('',#4785,#4791,#489,.T.);
#7038=EDGE_CURVE('',#4791,#4789,#490,.T.);
#7039=EDGE_CURVE('',#4792,#4793,#3265,.T.);
#7040=EDGE_CURVE('',#4794,#4792,#491,.T.);
#7041=EDGE_CURVE('',#4788,#4794,#492,.T.);
#7042=EDGE_CURVE('',#4789,#4795,#493,.T.);
#7043=EDGE_CURVE('',#4795,#4793,#494,.T.);
#7044=EDGE_CURVE('',#4796,#4797,#3266,.T.);
#7045=EDGE_CURVE('',#4798,#4796,#495,.T.);
#7046=EDGE_CURVE('',#4792,#4798,#496,.T.);
#7047=EDGE_CURVE('',#4793,#4799,#497,.T.);
#7048=EDGE_CURVE('',#4799,#4797,#498,.T.);
#7049=EDGE_CURVE('',#4800,#4801,#3267,.T.);
#7050=EDGE_CURVE('',#4802,#4800,#499,.T.);
#7051=EDGE_CURVE('',#4796,#4802,#500,.T.);
#7052=EDGE_CURVE('',#4797,#4803,#501,.T.);
#7053=EDGE_CURVE('',#4803,#4801,#502,.T.);
#7054=EDGE_CURVE('',#4804,#4805,#3268,.T.);
#7055=EDGE_CURVE('',#4806,#4804,#503,.T.);
#7056=EDGE_CURVE('',#4800,#4806,#504,.T.);
#7057=EDGE_CURVE('',#4801,#4807,#505,.T.);
#7058=EDGE_CURVE('',#4807,#4805,#506,.T.);
#7059=EDGE_CURVE('',#4808,#4809,#3269,.T.);
#7060=EDGE_CURVE('',#4810,#4808,#507,.T.);
#7061=EDGE_CURVE('',#4804,#4810,#508,.T.);
#7062=EDGE_CURVE('',#4805,#4811,#509,.T.);
#7063=EDGE_CURVE('',#4811,#4809,#510,.T.);
#7064=EDGE_CURVE('',#4812,#4813,#3270,.T.);
#7065=EDGE_CURVE('',#4814,#4812,#511,.T.);
#7066=EDGE_CURVE('',#4808,#4814,#512,.T.);
#7067=EDGE_CURVE('',#4809,#4815,#513,.T.);
#7068=EDGE_CURVE('',#4815,#4813,#514,.T.);
#7069=EDGE_CURVE('',#4816,#4817,#3271,.T.);
#7070=EDGE_CURVE('',#4818,#4816,#515,.T.);
#7071=EDGE_CURVE('',#4812,#4818,#516,.T.);
#7072=EDGE_CURVE('',#4813,#4819,#517,.T.);
#7073=EDGE_CURVE('',#4819,#4817,#518,.T.);
#7074=EDGE_CURVE('',#4820,#4821,#3272,.T.);
#7075=EDGE_CURVE('',#4822,#4820,#519,.T.);
#7076=EDGE_CURVE('',#4816,#4822,#520,.T.);
#7077=EDGE_CURVE('',#4817,#4823,#521,.T.);
#7078=EDGE_CURVE('',#4823,#4821,#522,.T.);
#7079=EDGE_CURVE('',#4824,#4825,#3273,.T.);
#7080=EDGE_CURVE('',#4826,#4824,#523,.T.);
#7081=EDGE_CURVE('',#4820,#4826,#524,.T.);
#7082=EDGE_CURVE('',#4821,#4827,#525,.T.);
#7083=EDGE_CURVE('',#4827,#4825,#526,.T.);
#7084=EDGE_CURVE('',#4828,#4829,#3274,.T.);
#7085=EDGE_CURVE('',#4830,#4828,#527,.T.);
#7086=EDGE_CURVE('',#4824,#4830,#528,.T.);
#7087=EDGE_CURVE('',#4825,#4831,#529,.T.);
#7088=EDGE_CURVE('',#4831,#4829,#530,.T.);
#7089=EDGE_CURVE('',#4832,#4833,#3275,.T.);
#7090=EDGE_CURVE('',#4834,#4832,#531,.T.);
#7091=EDGE_CURVE('',#4828,#4834,#532,.T.);
#7092=EDGE_CURVE('',#4829,#4835,#533,.T.);
#7093=EDGE_CURVE('',#4835,#4833,#534,.T.);
#7094=EDGE_CURVE('',#4836,#4837,#3276,.T.);
#7095=EDGE_CURVE('',#4838,#4836,#535,.T.);
#7096=EDGE_CURVE('',#4832,#4838,#536,.T.);
#7097=EDGE_CURVE('',#4833,#4839,#537,.T.);
#7098=EDGE_CURVE('',#4839,#4837,#538,.T.);
#7099=EDGE_CURVE('',#4840,#4841,#3277,.T.);
#7100=EDGE_CURVE('',#4842,#4840,#539,.T.);
#7101=EDGE_CURVE('',#4836,#4842,#540,.T.);
#7102=EDGE_CURVE('',#4837,#4843,#541,.T.);
#7103=EDGE_CURVE('',#4843,#4841,#542,.T.);
#7104=EDGE_CURVE('',#4844,#4845,#3278,.T.);
#7105=EDGE_CURVE('',#4846,#4844,#543,.T.);
#7106=EDGE_CURVE('',#4840,#4846,#544,.T.);
#7107=EDGE_CURVE('',#4841,#4847,#545,.T.);
#7108=EDGE_CURVE('',#4847,#4845,#546,.T.);
#7109=EDGE_CURVE('',#4848,#4849,#3279,.T.);
#7110=EDGE_CURVE('',#4850,#4848,#547,.T.);
#7111=EDGE_CURVE('',#4844,#4850,#548,.T.);
#7112=EDGE_CURVE('',#4845,#4851,#549,.T.);
#7113=EDGE_CURVE('',#4851,#4849,#550,.T.);
#7114=EDGE_CURVE('',#4852,#4853,#3280,.T.);
#7115=EDGE_CURVE('',#4854,#4852,#551,.T.);
#7116=EDGE_CURVE('',#4848,#4854,#552,.T.);
#7117=EDGE_CURVE('',#4849,#4855,#553,.T.);
#7118=EDGE_CURVE('',#4855,#4853,#554,.T.);
#7119=EDGE_CURVE('',#4856,#4857,#3281,.T.);
#7120=EDGE_CURVE('',#4858,#4856,#555,.T.);
#7121=EDGE_CURVE('',#4852,#4858,#556,.T.);
#7122=EDGE_CURVE('',#4853,#4859,#557,.T.);
#7123=EDGE_CURVE('',#4859,#4857,#558,.T.);
#7124=EDGE_CURVE('',#4860,#4861,#3282,.T.);
#7125=EDGE_CURVE('',#4862,#4860,#559,.T.);
#7126=EDGE_CURVE('',#4856,#4862,#560,.T.);
#7127=EDGE_CURVE('',#4857,#4863,#561,.T.);
#7128=EDGE_CURVE('',#4863,#4861,#562,.T.);
#7129=EDGE_CURVE('',#4864,#4865,#3283,.T.);
#7130=EDGE_CURVE('',#4866,#4864,#563,.T.);
#7131=EDGE_CURVE('',#4860,#4866,#564,.T.);
#7132=EDGE_CURVE('',#4861,#4867,#565,.T.);
#7133=EDGE_CURVE('',#4867,#4865,#566,.T.);
#7134=EDGE_CURVE('',#4868,#4869,#3284,.T.);
#7135=EDGE_CURVE('',#4870,#4868,#567,.T.);
#7136=EDGE_CURVE('',#4864,#4870,#568,.T.);
#7137=EDGE_CURVE('',#4865,#4871,#569,.T.);
#7138=EDGE_CURVE('',#4871,#4869,#570,.T.);
#7139=EDGE_CURVE('',#4872,#4873,#3285,.T.);
#7140=EDGE_CURVE('',#4874,#4872,#571,.T.);
#7141=EDGE_CURVE('',#4868,#4874,#572,.T.);
#7142=EDGE_CURVE('',#4869,#4875,#573,.T.);
#7143=EDGE_CURVE('',#4875,#4873,#574,.T.);
#7144=EDGE_CURVE('',#4876,#4877,#3286,.T.);
#7145=EDGE_CURVE('',#4878,#4876,#575,.T.);
#7146=EDGE_CURVE('',#4872,#4878,#576,.T.);
#7147=EDGE_CURVE('',#4873,#4879,#577,.T.);
#7148=EDGE_CURVE('',#4879,#4877,#578,.T.);
#7149=EDGE_CURVE('',#4880,#4881,#3287,.T.);
#7150=EDGE_CURVE('',#4882,#4880,#579,.T.);
#7151=EDGE_CURVE('',#4876,#4882,#580,.T.);
#7152=EDGE_CURVE('',#4877,#4883,#581,.T.);
#7153=EDGE_CURVE('',#4883,#4881,#582,.T.);
#7154=EDGE_CURVE('',#4884,#4885,#3288,.T.);
#7155=EDGE_CURVE('',#4886,#4884,#583,.T.);
#7156=EDGE_CURVE('',#4880,#4886,#584,.T.);
#7157=EDGE_CURVE('',#4881,#4887,#585,.T.);
#7158=EDGE_CURVE('',#4887,#4885,#586,.T.);
#7159=EDGE_CURVE('',#4888,#4889,#3289,.T.);
#7160=EDGE_CURVE('',#4890,#4888,#587,.T.);
#7161=EDGE_CURVE('',#4884,#4890,#588,.T.);
#7162=EDGE_CURVE('',#4885,#4891,#589,.T.);
#7163=EDGE_CURVE('',#4891,#4889,#590,.T.);
#7164=EDGE_CURVE('',#4892,#4893,#3290,.T.);
#7165=EDGE_CURVE('',#4894,#4892,#591,.T.);
#7166=EDGE_CURVE('',#4888,#4894,#592,.T.);
#7167=EDGE_CURVE('',#4889,#4895,#593,.T.);
#7168=EDGE_CURVE('',#4895,#4893,#594,.T.);
#7169=EDGE_CURVE('',#4896,#4897,#3291,.T.);
#7170=EDGE_CURVE('',#4898,#4896,#595,.T.);
#7171=EDGE_CURVE('',#4892,#4898,#596,.T.);
#7172=EDGE_CURVE('',#4893,#4899,#597,.T.);
#7173=EDGE_CURVE('',#4899,#4897,#598,.T.);
#7174=EDGE_CURVE('',#4900,#4901,#3292,.T.);
#7175=EDGE_CURVE('',#4902,#4900,#599,.T.);
#7176=EDGE_CURVE('',#4896,#4902,#600,.T.);
#7177=EDGE_CURVE('',#4897,#4903,#601,.T.);
#7178=EDGE_CURVE('',#4903,#4901,#602,.T.);
#7179=EDGE_CURVE('',#4904,#4905,#3293,.T.);
#7180=EDGE_CURVE('',#4906,#4904,#603,.T.);
#7181=EDGE_CURVE('',#4900,#4906,#604,.T.);
#7182=EDGE_CURVE('',#4901,#4907,#605,.T.);
#7183=EDGE_CURVE('',#4907,#4905,#606,.T.);
#7184=EDGE_CURVE('',#4908,#4909,#3294,.T.);
#7185=EDGE_CURVE('',#4910,#4908,#607,.T.);
#7186=EDGE_CURVE('',#4904,#4910,#608,.T.);
#7187=EDGE_CURVE('',#4905,#4911,#609,.T.);
#7188=EDGE_CURVE('',#4911,#4909,#610,.T.);
#7189=EDGE_CURVE('',#4912,#4913,#3295,.T.);
#7190=EDGE_CURVE('',#4914,#4912,#611,.T.);
#7191=EDGE_CURVE('',#4908,#4914,#612,.T.);
#7192=EDGE_CURVE('',#4909,#4915,#613,.T.);
#7193=EDGE_CURVE('',#4915,#4913,#614,.T.);
#7194=EDGE_CURVE('',#4916,#4917,#3296,.T.);
#7195=EDGE_CURVE('',#4918,#4916,#615,.T.);
#7196=EDGE_CURVE('',#4912,#4918,#616,.T.);
#7197=EDGE_CURVE('',#4913,#4919,#617,.T.);
#7198=EDGE_CURVE('',#4919,#4917,#618,.T.);
#7199=EDGE_CURVE('',#4920,#4921,#3297,.T.);
#7200=EDGE_CURVE('',#4922,#4920,#619,.T.);
#7201=EDGE_CURVE('',#4916,#4922,#620,.T.);
#7202=EDGE_CURVE('',#4917,#4923,#621,.T.);
#7203=EDGE_CURVE('',#4923,#4921,#622,.T.);
#7204=EDGE_CURVE('',#4924,#4925,#3298,.T.);
#7205=EDGE_CURVE('',#4926,#4924,#623,.T.);
#7206=EDGE_CURVE('',#4920,#4926,#624,.T.);
#7207=EDGE_CURVE('',#4921,#4927,#625,.T.);
#7208=EDGE_CURVE('',#4927,#4925,#626,.T.);
#7209=EDGE_CURVE('',#4928,#4929,#3299,.T.);
#7210=EDGE_CURVE('',#4930,#4928,#627,.T.);
#7211=EDGE_CURVE('',#4924,#4930,#628,.T.);
#7212=EDGE_CURVE('',#4925,#4931,#629,.T.);
#7213=EDGE_CURVE('',#4931,#4929,#630,.T.);
#7214=EDGE_CURVE('',#4932,#4933,#3300,.T.);
#7215=EDGE_CURVE('',#4934,#4932,#631,.T.);
#7216=EDGE_CURVE('',#4928,#4934,#632,.T.);
#7217=EDGE_CURVE('',#4929,#4935,#633,.T.);
#7218=EDGE_CURVE('',#4935,#4933,#634,.T.);
#7219=EDGE_CURVE('',#4936,#4937,#3301,.T.);
#7220=EDGE_CURVE('',#4938,#4936,#635,.T.);
#7221=EDGE_CURVE('',#4932,#4938,#636,.T.);
#7222=EDGE_CURVE('',#4933,#4939,#637,.T.);
#7223=EDGE_CURVE('',#4939,#4937,#638,.T.);
#7224=EDGE_CURVE('',#4940,#4941,#3302,.T.);
#7225=EDGE_CURVE('',#4942,#4940,#639,.T.);
#7226=EDGE_CURVE('',#4936,#4942,#640,.T.);
#7227=EDGE_CURVE('',#4937,#4943,#641,.T.);
#7228=EDGE_CURVE('',#4943,#4941,#642,.T.);
#7229=EDGE_CURVE('',#4944,#4945,#3303,.T.);
#7230=EDGE_CURVE('',#4946,#4944,#643,.T.);
#7231=EDGE_CURVE('',#4940,#4946,#644,.T.);
#7232=EDGE_CURVE('',#4941,#4947,#645,.T.);
#7233=EDGE_CURVE('',#4947,#4945,#646,.T.);
#7234=EDGE_CURVE('',#4948,#4949,#3304,.T.);
#7235=EDGE_CURVE('',#4950,#4948,#647,.T.);
#7236=EDGE_CURVE('',#4944,#4950,#648,.T.);
#7237=EDGE_CURVE('',#4945,#4951,#649,.T.);
#7238=EDGE_CURVE('',#4951,#4949,#650,.T.);
#7239=EDGE_CURVE('',#4952,#4953,#3305,.T.);
#7240=EDGE_CURVE('',#4954,#4952,#651,.T.);
#7241=EDGE_CURVE('',#4948,#4954,#652,.T.);
#7242=EDGE_CURVE('',#4949,#4955,#653,.T.);
#7243=EDGE_CURVE('',#4955,#4953,#654,.T.);
#7244=EDGE_CURVE('',#4956,#4957,#3306,.T.);
#7245=EDGE_CURVE('',#4958,#4956,#655,.T.);
#7246=EDGE_CURVE('',#4952,#4958,#656,.T.);
#7247=EDGE_CURVE('',#4953,#4959,#657,.T.);
#7248=EDGE_CURVE('',#4959,#4957,#658,.T.);
#7249=EDGE_CURVE('',#4960,#4961,#3307,.T.);
#7250=EDGE_CURVE('',#4962,#4960,#659,.T.);
#7251=EDGE_CURVE('',#4956,#4962,#660,.T.);
#7252=EDGE_CURVE('',#4957,#4963,#661,.T.);
#7253=EDGE_CURVE('',#4963,#4961,#662,.T.);
#7254=EDGE_CURVE('',#4964,#4965,#3308,.T.);
#7255=EDGE_CURVE('',#4966,#4964,#663,.T.);
#7256=EDGE_CURVE('',#4960,#4966,#664,.T.);
#7257=EDGE_CURVE('',#4961,#4967,#665,.T.);
#7258=EDGE_CURVE('',#4967,#4965,#666,.T.);
#7259=EDGE_CURVE('',#4968,#4969,#3309,.T.);
#7260=EDGE_CURVE('',#4970,#4968,#667,.T.);
#7261=EDGE_CURVE('',#4964,#4970,#668,.T.);
#7262=EDGE_CURVE('',#4965,#4971,#669,.T.);
#7263=EDGE_CURVE('',#4971,#4969,#670,.T.);
#7264=EDGE_CURVE('',#4972,#4973,#3310,.T.);
#7265=EDGE_CURVE('',#4974,#4972,#671,.T.);
#7266=EDGE_CURVE('',#4968,#4974,#672,.T.);
#7267=EDGE_CURVE('',#4969,#4975,#673,.T.);
#7268=EDGE_CURVE('',#4975,#4973,#674,.T.);
#7269=EDGE_CURVE('',#4976,#4977,#3311,.T.);
#7270=EDGE_CURVE('',#4978,#4976,#675,.T.);
#7271=EDGE_CURVE('',#4972,#4978,#676,.T.);
#7272=EDGE_CURVE('',#4973,#4979,#677,.T.);
#7273=EDGE_CURVE('',#4979,#4977,#678,.T.);
#7274=EDGE_CURVE('',#4980,#4981,#3312,.T.);
#7275=EDGE_CURVE('',#4982,#4980,#679,.T.);
#7276=EDGE_CURVE('',#4976,#4982,#680,.T.);
#7277=EDGE_CURVE('',#4977,#4983,#681,.T.);
#7278=EDGE_CURVE('',#4983,#4981,#682,.T.);
#7279=EDGE_CURVE('',#4984,#4985,#3313,.T.);
#7280=EDGE_CURVE('',#4986,#4984,#683,.T.);
#7281=EDGE_CURVE('',#4980,#4986,#684,.T.);
#7282=EDGE_CURVE('',#4981,#4987,#685,.T.);
#7283=EDGE_CURVE('',#4987,#4985,#686,.T.);
#7284=EDGE_CURVE('',#4988,#4989,#3314,.T.);
#7285=EDGE_CURVE('',#4990,#4988,#687,.T.);
#7286=EDGE_CURVE('',#4984,#4990,#688,.T.);
#7287=EDGE_CURVE('',#4985,#4991,#689,.T.);
#7288=EDGE_CURVE('',#4991,#4989,#690,.T.);
#7289=EDGE_CURVE('',#4992,#4993,#3315,.T.);
#7290=EDGE_CURVE('',#4994,#4992,#691,.T.);
#7291=EDGE_CURVE('',#4988,#4994,#692,.T.);
#7292=EDGE_CURVE('',#4989,#4995,#693,.T.);
#7293=EDGE_CURVE('',#4995,#4993,#694,.T.);
#7294=EDGE_CURVE('',#4996,#4997,#3316,.T.);
#7295=EDGE_CURVE('',#4998,#4996,#695,.T.);
#7296=EDGE_CURVE('',#4992,#4998,#696,.T.);
#7297=EDGE_CURVE('',#4993,#4999,#697,.T.);
#7298=EDGE_CURVE('',#4999,#4997,#698,.T.);
#7299=EDGE_CURVE('',#5000,#5001,#3317,.T.);
#7300=EDGE_CURVE('',#5002,#5000,#699,.T.);
#7301=EDGE_CURVE('',#4996,#5002,#700,.T.);
#7302=EDGE_CURVE('',#4997,#5003,#701,.T.);
#7303=EDGE_CURVE('',#5003,#5001,#702,.T.);
#7304=EDGE_CURVE('',#5004,#5005,#3318,.T.);
#7305=EDGE_CURVE('',#5006,#5004,#703,.T.);
#7306=EDGE_CURVE('',#5000,#5006,#704,.T.);
#7307=EDGE_CURVE('',#5001,#5007,#705,.T.);
#7308=EDGE_CURVE('',#5007,#5005,#706,.T.);
#7309=EDGE_CURVE('',#5008,#5009,#3319,.T.);
#7310=EDGE_CURVE('',#5010,#5008,#707,.T.);
#7311=EDGE_CURVE('',#5004,#5010,#708,.T.);
#7312=EDGE_CURVE('',#5005,#5011,#709,.T.);
#7313=EDGE_CURVE('',#5011,#5009,#710,.T.);
#7314=EDGE_CURVE('',#5012,#5013,#3320,.T.);
#7315=EDGE_CURVE('',#5014,#5012,#711,.T.);
#7316=EDGE_CURVE('',#5008,#5014,#712,.T.);
#7317=EDGE_CURVE('',#5009,#5015,#713,.T.);
#7318=EDGE_CURVE('',#5015,#5013,#714,.T.);
#7319=EDGE_CURVE('',#5016,#5017,#3321,.T.);
#7320=EDGE_CURVE('',#5018,#5016,#715,.T.);
#7321=EDGE_CURVE('',#5012,#5018,#716,.T.);
#7322=EDGE_CURVE('',#5013,#5019,#717,.T.);
#7323=EDGE_CURVE('',#5019,#5017,#718,.T.);
#7324=EDGE_CURVE('',#5020,#5021,#3322,.T.);
#7325=EDGE_CURVE('',#5022,#5020,#719,.T.);
#7326=EDGE_CURVE('',#5016,#5022,#720,.T.);
#7327=EDGE_CURVE('',#5017,#5023,#721,.T.);
#7328=EDGE_CURVE('',#5023,#5021,#722,.T.);
#7329=EDGE_CURVE('',#5024,#5025,#3323,.T.);
#7330=EDGE_CURVE('',#5026,#5024,#723,.T.);
#7331=EDGE_CURVE('',#5020,#5026,#724,.T.);
#7332=EDGE_CURVE('',#5021,#5027,#725,.T.);
#7333=EDGE_CURVE('',#5027,#5025,#726,.T.);
#7334=EDGE_CURVE('',#5028,#5029,#3324,.T.);
#7335=EDGE_CURVE('',#5030,#5028,#727,.T.);
#7336=EDGE_CURVE('',#5024,#5030,#728,.T.);
#7337=EDGE_CURVE('',#5025,#5031,#729,.T.);
#7338=EDGE_CURVE('',#5031,#5029,#730,.T.);
#7339=EDGE_CURVE('',#5032,#5033,#3325,.T.);
#7340=EDGE_CURVE('',#5034,#5032,#731,.T.);
#7341=EDGE_CURVE('',#5028,#5034,#732,.T.);
#7342=EDGE_CURVE('',#5029,#5035,#733,.T.);
#7343=EDGE_CURVE('',#5035,#5033,#734,.T.);
#7344=EDGE_CURVE('',#5036,#5037,#3326,.T.);
#7345=EDGE_CURVE('',#5038,#5036,#735,.T.);
#7346=EDGE_CURVE('',#5032,#5038,#736,.T.);
#7347=EDGE_CURVE('',#5033,#5039,#737,.T.);
#7348=EDGE_CURVE('',#5039,#5037,#738,.T.);
#7349=EDGE_CURVE('',#5040,#5041,#3327,.T.);
#7350=EDGE_CURVE('',#5042,#5040,#739,.T.);
#7351=EDGE_CURVE('',#5036,#5042,#740,.T.);
#7352=EDGE_CURVE('',#5037,#5043,#741,.T.);
#7353=EDGE_CURVE('',#5043,#5041,#742,.T.);
#7354=EDGE_CURVE('',#5044,#5045,#3328,.T.);
#7355=EDGE_CURVE('',#5046,#5044,#743,.T.);
#7356=EDGE_CURVE('',#5040,#5046,#744,.T.);
#7357=EDGE_CURVE('',#5041,#5047,#745,.T.);
#7358=EDGE_CURVE('',#5047,#5045,#746,.T.);
#7359=EDGE_CURVE('',#5048,#5049,#3329,.T.);
#7360=EDGE_CURVE('',#5050,#5048,#747,.T.);
#7361=EDGE_CURVE('',#5044,#5050,#748,.T.);
#7362=EDGE_CURVE('',#5045,#5051,#749,.T.);
#7363=EDGE_CURVE('',#5051,#5049,#750,.T.);
#7364=EDGE_CURVE('',#5052,#5053,#3330,.T.);
#7365=EDGE_CURVE('',#5054,#5052,#751,.T.);
#7366=EDGE_CURVE('',#5048,#5054,#752,.T.);
#7367=EDGE_CURVE('',#5049,#5055,#753,.T.);
#7368=EDGE_CURVE('',#5055,#5053,#754,.T.);
#7369=EDGE_CURVE('',#5056,#5057,#3331,.T.);
#7370=EDGE_CURVE('',#5058,#5056,#755,.T.);
#7371=EDGE_CURVE('',#5052,#5058,#756,.T.);
#7372=EDGE_CURVE('',#5053,#5059,#757,.T.);
#7373=EDGE_CURVE('',#5059,#5057,#758,.T.);
#7374=EDGE_CURVE('',#5060,#5061,#3332,.T.);
#7375=EDGE_CURVE('',#5062,#5060,#759,.T.);
#7376=EDGE_CURVE('',#5056,#5062,#760,.T.);
#7377=EDGE_CURVE('',#5057,#5063,#761,.T.);
#7378=EDGE_CURVE('',#5063,#5061,#762,.T.);
#7379=EDGE_CURVE('',#5064,#5065,#3333,.T.);
#7380=EDGE_CURVE('',#5066,#5064,#763,.T.);
#7381=EDGE_CURVE('',#5060,#5066,#764,.T.);
#7382=EDGE_CURVE('',#5061,#5067,#765,.T.);
#7383=EDGE_CURVE('',#5067,#5065,#766,.T.);
#7384=EDGE_CURVE('',#5068,#5069,#3334,.T.);
#7385=EDGE_CURVE('',#5070,#5068,#767,.T.);
#7386=EDGE_CURVE('',#5064,#5070,#768,.T.);
#7387=EDGE_CURVE('',#5065,#5071,#769,.T.);
#7388=EDGE_CURVE('',#5071,#5069,#770,.T.);
#7389=EDGE_CURVE('',#5072,#5073,#3335,.T.);
#7390=EDGE_CURVE('',#5074,#5072,#771,.T.);
#7391=EDGE_CURVE('',#5068,#5074,#772,.T.);
#7392=EDGE_CURVE('',#5069,#5075,#773,.T.);
#7393=EDGE_CURVE('',#5075,#5073,#774,.T.);
#7394=EDGE_CURVE('',#5076,#5077,#3336,.T.);
#7395=EDGE_CURVE('',#5078,#5076,#775,.T.);
#7396=EDGE_CURVE('',#5072,#5078,#776,.T.);
#7397=EDGE_CURVE('',#5073,#5079,#777,.T.);
#7398=EDGE_CURVE('',#5079,#5077,#778,.T.);
#7399=EDGE_CURVE('',#5080,#5081,#3337,.T.);
#7400=EDGE_CURVE('',#5082,#5080,#779,.T.);
#7401=EDGE_CURVE('',#5076,#5082,#780,.T.);
#7402=EDGE_CURVE('',#5077,#5083,#781,.T.);
#7403=EDGE_CURVE('',#5083,#5081,#782,.T.);
#7404=EDGE_CURVE('',#5084,#5085,#3338,.T.);
#7405=EDGE_CURVE('',#5086,#5084,#783,.T.);
#7406=EDGE_CURVE('',#5080,#5086,#784,.T.);
#7407=EDGE_CURVE('',#5081,#5087,#785,.T.);
#7408=EDGE_CURVE('',#5087,#5085,#786,.T.);
#7409=EDGE_CURVE('',#5088,#5089,#3339,.T.);
#7410=EDGE_CURVE('',#5090,#5088,#787,.T.);
#7411=EDGE_CURVE('',#5084,#5090,#788,.T.);
#7412=EDGE_CURVE('',#5085,#5091,#789,.T.);
#7413=EDGE_CURVE('',#5091,#5089,#790,.T.);
#7414=EDGE_CURVE('',#5092,#5093,#3340,.T.);
#7415=EDGE_CURVE('',#5094,#5092,#791,.T.);
#7416=EDGE_CURVE('',#5088,#5094,#792,.T.);
#7417=EDGE_CURVE('',#5089,#5095,#793,.T.);
#7418=EDGE_CURVE('',#5095,#5093,#794,.T.);
#7419=EDGE_CURVE('',#5096,#5097,#3341,.T.);
#7420=EDGE_CURVE('',#5098,#5096,#795,.T.);
#7421=EDGE_CURVE('',#5092,#5098,#796,.T.);
#7422=EDGE_CURVE('',#5093,#5099,#797,.T.);
#7423=EDGE_CURVE('',#5099,#5097,#798,.T.);
#7424=EDGE_CURVE('',#5100,#5101,#3342,.T.);
#7425=EDGE_CURVE('',#5102,#5100,#799,.T.);
#7426=EDGE_CURVE('',#5096,#5102,#800,.T.);
#7427=EDGE_CURVE('',#5097,#5103,#801,.T.);
#7428=EDGE_CURVE('',#5103,#5101,#802,.T.);
#7429=EDGE_CURVE('',#5104,#5105,#3343,.T.);
#7430=EDGE_CURVE('',#5106,#5104,#803,.T.);
#7431=EDGE_CURVE('',#5100,#5106,#804,.T.);
#7432=EDGE_CURVE('',#5101,#5107,#805,.T.);
#7433=EDGE_CURVE('',#5107,#5105,#806,.T.);
#7434=EDGE_CURVE('',#5108,#5109,#3344,.T.);
#7435=EDGE_CURVE('',#5110,#5108,#807,.T.);
#7436=EDGE_CURVE('',#5104,#5110,#808,.T.);
#7437=EDGE_CURVE('',#5105,#5111,#809,.T.);
#7438=EDGE_CURVE('',#5111,#5109,#810,.T.);
#7439=EDGE_CURVE('',#5112,#5113,#3345,.T.);
#7440=EDGE_CURVE('',#5114,#5112,#811,.T.);
#7441=EDGE_CURVE('',#5108,#5114,#812,.T.);
#7442=EDGE_CURVE('',#5109,#5115,#813,.T.);
#7443=EDGE_CURVE('',#5115,#5113,#814,.T.);
#7444=EDGE_CURVE('',#5116,#5117,#3346,.T.);
#7445=EDGE_CURVE('',#5118,#5116,#815,.T.);
#7446=EDGE_CURVE('',#5112,#5118,#816,.T.);
#7447=EDGE_CURVE('',#5113,#5119,#817,.T.);
#7448=EDGE_CURVE('',#5119,#5117,#818,.T.);
#7449=EDGE_CURVE('',#5120,#5121,#3347,.T.);
#7450=EDGE_CURVE('',#5122,#5120,#819,.T.);
#7451=EDGE_CURVE('',#5116,#5122,#820,.T.);
#7452=EDGE_CURVE('',#5117,#5123,#821,.T.);
#7453=EDGE_CURVE('',#5123,#5121,#822,.T.);
#7454=EDGE_CURVE('',#5124,#5125,#3348,.T.);
#7455=EDGE_CURVE('',#5126,#5124,#823,.T.);
#7456=EDGE_CURVE('',#5120,#5126,#824,.T.);
#7457=EDGE_CURVE('',#5121,#5127,#825,.T.);
#7458=EDGE_CURVE('',#5127,#5125,#826,.T.);
#7459=EDGE_CURVE('',#5128,#5129,#3349,.T.);
#7460=EDGE_CURVE('',#5130,#5128,#827,.T.);
#7461=EDGE_CURVE('',#5124,#5130,#828,.T.);
#7462=EDGE_CURVE('',#5125,#5131,#829,.T.);
#7463=EDGE_CURVE('',#5131,#5129,#830,.T.);
#7464=EDGE_CURVE('',#5132,#5133,#3350,.T.);
#7465=EDGE_CURVE('',#5134,#5132,#831,.T.);
#7466=EDGE_CURVE('',#5128,#5134,#832,.T.);
#7467=EDGE_CURVE('',#5129,#5135,#833,.T.);
#7468=EDGE_CURVE('',#5135,#5133,#834,.T.);
#7469=EDGE_CURVE('',#5136,#5137,#3351,.T.);
#7470=EDGE_CURVE('',#5138,#5136,#835,.T.);
#7471=EDGE_CURVE('',#5132,#5138,#836,.T.);
#7472=EDGE_CURVE('',#5133,#5139,#837,.T.);
#7473=EDGE_CURVE('',#5139,#5137,#838,.T.);
#7474=EDGE_CURVE('',#5140,#5141,#3352,.T.);
#7475=EDGE_CURVE('',#5142,#5140,#839,.T.);
#7476=EDGE_CURVE('',#5136,#5142,#840,.T.);
#7477=EDGE_CURVE('',#5137,#5143,#841,.T.);
#7478=EDGE_CURVE('',#5143,#5141,#842,.T.);
#7479=EDGE_CURVE('',#5144,#5145,#3353,.T.);
#7480=EDGE_CURVE('',#5146,#5144,#843,.T.);
#7481=EDGE_CURVE('',#5140,#5146,#844,.T.);
#7482=EDGE_CURVE('',#5141,#5147,#845,.T.);
#7483=EDGE_CURVE('',#5147,#5145,#846,.T.);
#7484=EDGE_CURVE('',#5148,#5149,#3354,.T.);
#7485=EDGE_CURVE('',#5150,#5148,#847,.T.);
#7486=EDGE_CURVE('',#5144,#5150,#848,.T.);
#7487=EDGE_CURVE('',#5145,#5151,#849,.T.);
#7488=EDGE_CURVE('',#5151,#5149,#850,.T.);
#7489=EDGE_CURVE('',#5152,#5153,#3355,.T.);
#7490=EDGE_CURVE('',#5154,#5152,#851,.T.);
#7491=EDGE_CURVE('',#5148,#5154,#852,.T.);
#7492=EDGE_CURVE('',#5149,#5155,#853,.T.);
#7493=EDGE_CURVE('',#5155,#5153,#854,.T.);
#7494=EDGE_CURVE('',#5156,#5157,#3356,.T.);
#7495=EDGE_CURVE('',#5158,#5156,#855,.T.);
#7496=EDGE_CURVE('',#5152,#5158,#856,.T.);
#7497=EDGE_CURVE('',#5153,#5159,#857,.T.);
#7498=EDGE_CURVE('',#5159,#5157,#858,.T.);
#7499=EDGE_CURVE('',#5160,#5161,#3357,.T.);
#7500=EDGE_CURVE('',#5162,#5160,#859,.T.);
#7501=EDGE_CURVE('',#5156,#5162,#860,.T.);
#7502=EDGE_CURVE('',#5157,#5163,#861,.T.);
#7503=EDGE_CURVE('',#5163,#5161,#862,.T.);
#7504=EDGE_CURVE('',#5164,#5165,#3358,.T.);
#7505=EDGE_CURVE('',#5166,#5164,#863,.T.);
#7506=EDGE_CURVE('',#5160,#5166,#864,.T.);
#7507=EDGE_CURVE('',#5161,#5167,#865,.T.);
#7508=EDGE_CURVE('',#5167,#5165,#866,.T.);
#7509=EDGE_CURVE('',#5168,#5169,#3359,.T.);
#7510=EDGE_CURVE('',#5170,#5168,#867,.T.);
#7511=EDGE_CURVE('',#5164,#5170,#868,.T.);
#7512=EDGE_CURVE('',#5165,#5171,#869,.T.);
#7513=EDGE_CURVE('',#5171,#5169,#870,.T.);
#7514=EDGE_CURVE('',#5172,#5173,#3360,.T.);
#7515=EDGE_CURVE('',#5174,#5172,#871,.T.);
#7516=EDGE_CURVE('',#5168,#5174,#872,.T.);
#7517=EDGE_CURVE('',#5169,#5175,#873,.T.);
#7518=EDGE_CURVE('',#5175,#5173,#874,.T.);
#7519=EDGE_CURVE('',#5176,#5177,#3361,.T.);
#7520=EDGE_CURVE('',#5178,#5176,#875,.T.);
#7521=EDGE_CURVE('',#5172,#5178,#876,.T.);
#7522=EDGE_CURVE('',#5173,#5179,#877,.T.);
#7523=EDGE_CURVE('',#5179,#5177,#878,.T.);
#7524=EDGE_CURVE('',#5180,#5181,#3362,.T.);
#7525=EDGE_CURVE('',#5182,#5180,#879,.T.);
#7526=EDGE_CURVE('',#5176,#5182,#880,.T.);
#7527=EDGE_CURVE('',#5177,#5183,#881,.T.);
#7528=EDGE_CURVE('',#5183,#5181,#882,.T.);
#7529=EDGE_CURVE('',#5184,#5185,#3363,.T.);
#7530=EDGE_CURVE('',#5186,#5184,#883,.T.);
#7531=EDGE_CURVE('',#5180,#5186,#884,.T.);
#7532=EDGE_CURVE('',#5181,#5187,#885,.T.);
#7533=EDGE_CURVE('',#5187,#5185,#886,.T.);
#7534=EDGE_CURVE('',#5188,#5189,#3364,.T.);
#7535=EDGE_CURVE('',#5190,#5188,#887,.T.);
#7536=EDGE_CURVE('',#5184,#5190,#888,.T.);
#7537=EDGE_CURVE('',#5185,#5191,#889,.T.);
#7538=EDGE_CURVE('',#5191,#5189,#890,.T.);
#7539=EDGE_CURVE('',#5192,#5193,#3365,.T.);
#7540=EDGE_CURVE('',#5194,#5192,#891,.T.);
#7541=EDGE_CURVE('',#5188,#5194,#892,.T.);
#7542=EDGE_CURVE('',#5189,#5195,#893,.T.);
#7543=EDGE_CURVE('',#5195,#5193,#894,.T.);
#7544=EDGE_CURVE('',#5196,#5197,#3366,.T.);
#7545=EDGE_CURVE('',#5198,#5196,#895,.T.);
#7546=EDGE_CURVE('',#5192,#5198,#896,.T.);
#7547=EDGE_CURVE('',#5193,#5199,#897,.T.);
#7548=EDGE_CURVE('',#5199,#5197,#898,.T.);
#7549=EDGE_CURVE('',#5200,#5201,#3367,.T.);
#7550=EDGE_CURVE('',#5202,#5200,#899,.T.);
#7551=EDGE_CURVE('',#5196,#5202,#900,.T.);
#7552=EDGE_CURVE('',#5197,#5203,#901,.T.);
#7553=EDGE_CURVE('',#5203,#5201,#902,.T.);
#7554=EDGE_CURVE('',#5204,#5205,#3368,.T.);
#7555=EDGE_CURVE('',#5206,#5204,#903,.T.);
#7556=EDGE_CURVE('',#5200,#5206,#904,.T.);
#7557=EDGE_CURVE('',#5201,#5207,#905,.T.);
#7558=EDGE_CURVE('',#5207,#5205,#906,.T.);
#7559=EDGE_CURVE('',#5208,#5209,#3369,.T.);
#7560=EDGE_CURVE('',#5210,#5208,#907,.T.);
#7561=EDGE_CURVE('',#5204,#5210,#908,.T.);
#7562=EDGE_CURVE('',#5205,#5211,#909,.T.);
#7563=EDGE_CURVE('',#5211,#5209,#910,.T.);
#7564=EDGE_CURVE('',#5212,#5213,#3370,.T.);
#7565=EDGE_CURVE('',#5214,#5212,#911,.T.);
#7566=EDGE_CURVE('',#5208,#5214,#912,.T.);
#7567=EDGE_CURVE('',#5209,#5215,#913,.T.);
#7568=EDGE_CURVE('',#5215,#5213,#914,.T.);
#7569=EDGE_CURVE('',#5216,#5217,#3371,.T.);
#7570=EDGE_CURVE('',#5218,#5216,#915,.T.);
#7571=EDGE_CURVE('',#5212,#5218,#916,.T.);
#7572=EDGE_CURVE('',#5213,#5219,#917,.T.);
#7573=EDGE_CURVE('',#5219,#5217,#918,.T.);
#7574=EDGE_CURVE('',#5220,#5221,#3372,.T.);
#7575=EDGE_CURVE('',#5222,#5220,#919,.T.);
#7576=EDGE_CURVE('',#5216,#5222,#920,.T.);
#7577=EDGE_CURVE('',#5217,#5223,#921,.T.);
#7578=EDGE_CURVE('',#5223,#5221,#922,.T.);
#7579=EDGE_CURVE('',#5224,#5225,#3373,.T.);
#7580=EDGE_CURVE('',#5226,#5224,#923,.T.);
#7581=EDGE_CURVE('',#5220,#5226,#924,.T.);
#7582=EDGE_CURVE('',#5221,#5227,#925,.T.);
#7583=EDGE_CURVE('',#5227,#5225,#926,.T.);
#7584=EDGE_CURVE('',#5228,#5229,#3374,.T.);
#7585=EDGE_CURVE('',#5230,#5228,#927,.T.);
#7586=EDGE_CURVE('',#5224,#5230,#928,.T.);
#7587=EDGE_CURVE('',#5225,#5231,#929,.T.);
#7588=EDGE_CURVE('',#5231,#5229,#930,.T.);
#7589=EDGE_CURVE('',#5232,#5233,#3375,.T.);
#7590=EDGE_CURVE('',#5234,#5232,#931,.T.);
#7591=EDGE_CURVE('',#5228,#5234,#932,.T.);
#7592=EDGE_CURVE('',#5229,#5235,#933,.T.);
#7593=EDGE_CURVE('',#5235,#5233,#934,.T.);
#7594=EDGE_CURVE('',#5236,#5237,#3376,.T.);
#7595=EDGE_CURVE('',#5238,#5236,#935,.T.);
#7596=EDGE_CURVE('',#5232,#5238,#936,.T.);
#7597=EDGE_CURVE('',#5233,#5239,#937,.T.);
#7598=EDGE_CURVE('',#5239,#5237,#938,.T.);
#7599=EDGE_CURVE('',#5240,#5241,#3377,.T.);
#7600=EDGE_CURVE('',#5242,#5240,#939,.T.);
#7601=EDGE_CURVE('',#5236,#5242,#940,.T.);
#7602=EDGE_CURVE('',#5237,#5243,#941,.T.);
#7603=EDGE_CURVE('',#5243,#5241,#942,.T.);
#7604=EDGE_CURVE('',#5244,#5245,#3378,.T.);
#7605=EDGE_CURVE('',#5246,#5244,#943,.T.);
#7606=EDGE_CURVE('',#5240,#5246,#944,.T.);
#7607=EDGE_CURVE('',#5241,#5247,#945,.T.);
#7608=EDGE_CURVE('',#5247,#5245,#946,.T.);
#7609=EDGE_CURVE('',#5248,#5249,#3379,.T.);
#7610=EDGE_CURVE('',#5250,#5248,#947,.T.);
#7611=EDGE_CURVE('',#5244,#5250,#948,.T.);
#7612=EDGE_CURVE('',#5245,#5251,#949,.T.);
#7613=EDGE_CURVE('',#5251,#5249,#950,.T.);
#7614=EDGE_CURVE('',#5252,#5253,#3380,.T.);
#7615=EDGE_CURVE('',#5254,#5252,#951,.T.);
#7616=EDGE_CURVE('',#5248,#5254,#952,.T.);
#7617=EDGE_CURVE('',#5249,#5255,#953,.T.);
#7618=EDGE_CURVE('',#5255,#5253,#954,.T.);
#7619=EDGE_CURVE('',#5256,#5257,#3381,.T.);
#7620=EDGE_CURVE('',#5258,#5256,#955,.T.);
#7621=EDGE_CURVE('',#5252,#5258,#956,.T.);
#7622=EDGE_CURVE('',#5253,#5259,#957,.T.);
#7623=EDGE_CURVE('',#5259,#5257,#958,.T.);
#7624=EDGE_CURVE('',#5260,#5261,#3382,.T.);
#7625=EDGE_CURVE('',#5262,#5260,#959,.T.);
#7626=EDGE_CURVE('',#5256,#5262,#960,.T.);
#7627=EDGE_CURVE('',#5257,#5263,#961,.T.);
#7628=EDGE_CURVE('',#5263,#5261,#962,.T.);
#7629=EDGE_CURVE('',#5264,#5265,#3383,.T.);
#7630=EDGE_CURVE('',#5266,#5264,#963,.T.);
#7631=EDGE_CURVE('',#5260,#5266,#964,.T.);
#7632=EDGE_CURVE('',#5261,#5267,#965,.T.);
#7633=EDGE_CURVE('',#5267,#5265,#966,.T.);
#7634=EDGE_CURVE('',#5268,#5269,#3384,.T.);
#7635=EDGE_CURVE('',#5270,#5268,#967,.T.);
#7636=EDGE_CURVE('',#5264,#5270,#968,.T.);
#7637=EDGE_CURVE('',#5265,#5271,#969,.T.);
#7638=EDGE_CURVE('',#5271,#5269,#970,.T.);
#7639=EDGE_CURVE('',#5272,#5273,#3385,.T.);
#7640=EDGE_CURVE('',#5274,#5272,#971,.T.);
#7641=EDGE_CURVE('',#5268,#5274,#972,.T.);
#7642=EDGE_CURVE('',#5269,#5275,#973,.T.);
#7643=EDGE_CURVE('',#5275,#5273,#974,.T.);
#7644=EDGE_CURVE('',#5276,#5277,#3386,.T.);
#7645=EDGE_CURVE('',#5278,#5276,#975,.T.);
#7646=EDGE_CURVE('',#5272,#5278,#976,.T.);
#7647=EDGE_CURVE('',#5273,#5279,#977,.T.);
#7648=EDGE_CURVE('',#5279,#5277,#978,.T.);
#7649=EDGE_CURVE('',#5280,#5281,#3387,.T.);
#7650=EDGE_CURVE('',#5282,#5280,#979,.T.);
#7651=EDGE_CURVE('',#5276,#5282,#980,.T.);
#7652=EDGE_CURVE('',#5277,#5283,#981,.T.);
#7653=EDGE_CURVE('',#5283,#5281,#982,.T.);
#7654=EDGE_CURVE('',#5284,#5285,#3388,.T.);
#7655=EDGE_CURVE('',#5286,#5284,#983,.T.);
#7656=EDGE_CURVE('',#5280,#5286,#984,.T.);
#7657=EDGE_CURVE('',#5281,#5287,#985,.T.);
#7658=EDGE_CURVE('',#5287,#5285,#986,.T.);
#7659=EDGE_CURVE('',#5288,#5289,#3389,.T.);
#7660=EDGE_CURVE('',#5290,#5288,#987,.T.);
#7661=EDGE_CURVE('',#5284,#5290,#988,.T.);
#7662=EDGE_CURVE('',#5285,#5291,#989,.T.);
#7663=EDGE_CURVE('',#5291,#5289,#990,.T.);
#7664=EDGE_CURVE('',#5292,#5293,#3390,.T.);
#7665=EDGE_CURVE('',#5294,#5292,#991,.T.);
#7666=EDGE_CURVE('',#5288,#5294,#992,.T.);
#7667=EDGE_CURVE('',#5289,#5295,#993,.T.);
#7668=EDGE_CURVE('',#5295,#5293,#994,.T.);
#7669=EDGE_CURVE('',#5296,#5297,#3391,.T.);
#7670=EDGE_CURVE('',#5298,#5296,#995,.T.);
#7671=EDGE_CURVE('',#5292,#5298,#996,.T.);
#7672=EDGE_CURVE('',#5293,#5299,#997,.T.);
#7673=EDGE_CURVE('',#5299,#5297,#998,.T.);
#7674=EDGE_CURVE('',#5300,#5301,#3392,.T.);
#7675=EDGE_CURVE('',#5302,#5300,#999,.T.);
#7676=EDGE_CURVE('',#5296,#5302,#1000,.T.);
#7677=EDGE_CURVE('',#5297,#5303,#1001,.T.);
#7678=EDGE_CURVE('',#5303,#5301,#1002,.T.);
#7679=EDGE_CURVE('',#5304,#5305,#3393,.T.);
#7680=EDGE_CURVE('',#5306,#5304,#1003,.T.);
#7681=EDGE_CURVE('',#5300,#5306,#1004,.T.);
#7682=EDGE_CURVE('',#5301,#5307,#1005,.T.);
#7683=EDGE_CURVE('',#5307,#5305,#1006,.T.);
#7684=EDGE_CURVE('',#5308,#5309,#3394,.T.);
#7685=EDGE_CURVE('',#5310,#5308,#1007,.T.);
#7686=EDGE_CURVE('',#5304,#5310,#1008,.T.);
#7687=EDGE_CURVE('',#5305,#5311,#1009,.T.);
#7688=EDGE_CURVE('',#5311,#5309,#1010,.T.);
#7689=EDGE_CURVE('',#5312,#5313,#3395,.T.);
#7690=EDGE_CURVE('',#5314,#5312,#1011,.T.);
#7691=EDGE_CURVE('',#5308,#5314,#1012,.T.);
#7692=EDGE_CURVE('',#5309,#5315,#1013,.T.);
#7693=EDGE_CURVE('',#5315,#5313,#1014,.T.);
#7694=EDGE_CURVE('',#5316,#5317,#3396,.T.);
#7695=EDGE_CURVE('',#5318,#5316,#1015,.T.);
#7696=EDGE_CURVE('',#5312,#5318,#1016,.T.);
#7697=EDGE_CURVE('',#5313,#5319,#1017,.T.);
#7698=EDGE_CURVE('',#5319,#5317,#1018,.T.);
#7699=EDGE_CURVE('',#5320,#5321,#3397,.T.);
#7700=EDGE_CURVE('',#5322,#5320,#1019,.T.);
#7701=EDGE_CURVE('',#5316,#5322,#1020,.T.);
#7702=EDGE_CURVE('',#5317,#5323,#1021,.T.);
#7703=EDGE_CURVE('',#5323,#5321,#1022,.T.);
#7704=EDGE_CURVE('',#5324,#5325,#3398,.T.);
#7705=EDGE_CURVE('',#5326,#5324,#1023,.T.);
#7706=EDGE_CURVE('',#5320,#5326,#1024,.T.);
#7707=EDGE_CURVE('',#5321,#5327,#1025,.T.);
#7708=EDGE_CURVE('',#5327,#5325,#1026,.T.);
#7709=EDGE_CURVE('',#5328,#5329,#3399,.T.);
#7710=EDGE_CURVE('',#5330,#5328,#1027,.T.);
#7711=EDGE_CURVE('',#5324,#5330,#1028,.T.);
#7712=EDGE_CURVE('',#5325,#5331,#1029,.T.);
#7713=EDGE_CURVE('',#5331,#5329,#1030,.T.);
#7714=EDGE_CURVE('',#5332,#5333,#3400,.T.);
#7715=EDGE_CURVE('',#5334,#5332,#1031,.T.);
#7716=EDGE_CURVE('',#5328,#5334,#1032,.T.);
#7717=EDGE_CURVE('',#5329,#5335,#1033,.T.);
#7718=EDGE_CURVE('',#5335,#5333,#1034,.T.);
#7719=EDGE_CURVE('',#5336,#5337,#3401,.T.);
#7720=EDGE_CURVE('',#5338,#5336,#1035,.T.);
#7721=EDGE_CURVE('',#5332,#5338,#1036,.T.);
#7722=EDGE_CURVE('',#5333,#5339,#1037,.T.);
#7723=EDGE_CURVE('',#5339,#5337,#1038,.T.);
#7724=EDGE_CURVE('',#5340,#5341,#3402,.T.);
#7725=EDGE_CURVE('',#5342,#5340,#1039,.T.);
#7726=EDGE_CURVE('',#5336,#5342,#1040,.T.);
#7727=EDGE_CURVE('',#5337,#5343,#1041,.T.);
#7728=EDGE_CURVE('',#5343,#5341,#1042,.T.);
#7729=EDGE_CURVE('',#5344,#5345,#3403,.T.);
#7730=EDGE_CURVE('',#5346,#5344,#1043,.T.);
#7731=EDGE_CURVE('',#5340,#5346,#1044,.T.);
#7732=EDGE_CURVE('',#5341,#5347,#1045,.T.);
#7733=EDGE_CURVE('',#5347,#5345,#1046,.T.);
#7734=EDGE_CURVE('',#5348,#5349,#3404,.T.);
#7735=EDGE_CURVE('',#5350,#5348,#1047,.T.);
#7736=EDGE_CURVE('',#5344,#5350,#1048,.T.);
#7737=EDGE_CURVE('',#5345,#5351,#1049,.T.);
#7738=EDGE_CURVE('',#5351,#5349,#1050,.T.);
#7739=EDGE_CURVE('',#5352,#5353,#3405,.T.);
#7740=EDGE_CURVE('',#5354,#5352,#1051,.T.);
#7741=EDGE_CURVE('',#5348,#5354,#1052,.T.);
#7742=EDGE_CURVE('',#5349,#5355,#1053,.T.);
#7743=EDGE_CURVE('',#5355,#5353,#1054,.T.);
#7744=EDGE_CURVE('',#5356,#5357,#3406,.T.);
#7745=EDGE_CURVE('',#5358,#5356,#1055,.T.);
#7746=EDGE_CURVE('',#5352,#5358,#1056,.T.);
#7747=EDGE_CURVE('',#5353,#5359,#1057,.T.);
#7748=EDGE_CURVE('',#5359,#5357,#1058,.T.);
#7749=EDGE_CURVE('',#5360,#5361,#3407,.T.);
#7750=EDGE_CURVE('',#5362,#5360,#1059,.T.);
#7751=EDGE_CURVE('',#5356,#5362,#1060,.T.);
#7752=EDGE_CURVE('',#5357,#5363,#1061,.T.);
#7753=EDGE_CURVE('',#5363,#5361,#1062,.T.);
#7754=EDGE_CURVE('',#5364,#5365,#3408,.T.);
#7755=EDGE_CURVE('',#5366,#5364,#1063,.T.);
#7756=EDGE_CURVE('',#5360,#5366,#1064,.T.);
#7757=EDGE_CURVE('',#5361,#5367,#1065,.T.);
#7758=EDGE_CURVE('',#5367,#5365,#1066,.T.);
#7759=EDGE_CURVE('',#5368,#5369,#3409,.T.);
#7760=EDGE_CURVE('',#5370,#5368,#1067,.T.);
#7761=EDGE_CURVE('',#5364,#5370,#1068,.T.);
#7762=EDGE_CURVE('',#5365,#5371,#1069,.T.);
#7763=EDGE_CURVE('',#5371,#5369,#1070,.T.);
#7764=EDGE_CURVE('',#5372,#5373,#3410,.T.);
#7765=EDGE_CURVE('',#5374,#5372,#1071,.T.);
#7766=EDGE_CURVE('',#5368,#5374,#1072,.T.);
#7767=EDGE_CURVE('',#5369,#5375,#1073,.T.);
#7768=EDGE_CURVE('',#5375,#5373,#1074,.T.);
#7769=EDGE_CURVE('',#5376,#5377,#3411,.T.);
#7770=EDGE_CURVE('',#5378,#5376,#1075,.T.);
#7771=EDGE_CURVE('',#5372,#5378,#1076,.T.);
#7772=EDGE_CURVE('',#5373,#5379,#1077,.T.);
#7773=EDGE_CURVE('',#5379,#5377,#1078,.T.);
#7774=EDGE_CURVE('',#5380,#5381,#3412,.T.);
#7775=EDGE_CURVE('',#5382,#5380,#1079,.T.);
#7776=EDGE_CURVE('',#5376,#5382,#1080,.T.);
#7777=EDGE_CURVE('',#5377,#5383,#1081,.T.);
#7778=EDGE_CURVE('',#5383,#5381,#1082,.T.);
#7779=EDGE_CURVE('',#5384,#5385,#3413,.T.);
#7780=EDGE_CURVE('',#5386,#5384,#1083,.T.);
#7781=EDGE_CURVE('',#5380,#5386,#1084,.T.);
#7782=EDGE_CURVE('',#5381,#5387,#1085,.T.);
#7783=EDGE_CURVE('',#5387,#5385,#1086,.T.);
#7784=EDGE_CURVE('',#5388,#5389,#3414,.T.);
#7785=EDGE_CURVE('',#5390,#5388,#1087,.T.);
#7786=EDGE_CURVE('',#5384,#5390,#1088,.T.);
#7787=EDGE_CURVE('',#5385,#5391,#1089,.T.);
#7788=EDGE_CURVE('',#5391,#5389,#1090,.T.);
#7789=EDGE_CURVE('',#5392,#5393,#3415,.T.);
#7790=EDGE_CURVE('',#5394,#5392,#1091,.T.);
#7791=EDGE_CURVE('',#5388,#5394,#1092,.T.);
#7792=EDGE_CURVE('',#5389,#5395,#1093,.T.);
#7793=EDGE_CURVE('',#5395,#5393,#1094,.T.);
#7794=EDGE_CURVE('',#5396,#5397,#3416,.T.);
#7795=EDGE_CURVE('',#5398,#5396,#1095,.T.);
#7796=EDGE_CURVE('',#5392,#5398,#1096,.T.);
#7797=EDGE_CURVE('',#5393,#5399,#1097,.T.);
#7798=EDGE_CURVE('',#5399,#5397,#1098,.T.);
#7799=EDGE_CURVE('',#5400,#5401,#3417,.T.);
#7800=EDGE_CURVE('',#5402,#5400,#1099,.T.);
#7801=EDGE_CURVE('',#5396,#5402,#1100,.T.);
#7802=EDGE_CURVE('',#5397,#5403,#1101,.T.);
#7803=EDGE_CURVE('',#5403,#5401,#1102,.T.);
#7804=EDGE_CURVE('',#5404,#5405,#3418,.T.);
#7805=EDGE_CURVE('',#5406,#5404,#1103,.T.);
#7806=EDGE_CURVE('',#5400,#5406,#1104,.T.);
#7807=EDGE_CURVE('',#5401,#5407,#1105,.T.);
#7808=EDGE_CURVE('',#5407,#5405,#1106,.T.);
#7809=EDGE_CURVE('',#5408,#5409,#3419,.T.);
#7810=EDGE_CURVE('',#5410,#5408,#1107,.T.);
#7811=EDGE_CURVE('',#5404,#5410,#1108,.T.);
#7812=EDGE_CURVE('',#5405,#5411,#1109,.T.);
#7813=EDGE_CURVE('',#5411,#5409,#1110,.T.);
#7814=EDGE_CURVE('',#5412,#5413,#3420,.T.);
#7815=EDGE_CURVE('',#5414,#5412,#1111,.T.);
#7816=EDGE_CURVE('',#5408,#5414,#1112,.T.);
#7817=EDGE_CURVE('',#5409,#5415,#1113,.T.);
#7818=EDGE_CURVE('',#5415,#5413,#1114,.T.);
#7819=EDGE_CURVE('',#5416,#5417,#3421,.T.);
#7820=EDGE_CURVE('',#5418,#5416,#1115,.T.);
#7821=EDGE_CURVE('',#5412,#5418,#1116,.T.);
#7822=EDGE_CURVE('',#5413,#5419,#1117,.T.);
#7823=EDGE_CURVE('',#5419,#5417,#1118,.T.);
#7824=EDGE_CURVE('',#5420,#5421,#3422,.T.);
#7825=EDGE_CURVE('',#5422,#5420,#1119,.T.);
#7826=EDGE_CURVE('',#5416,#5422,#1120,.T.);
#7827=EDGE_CURVE('',#5417,#5423,#1121,.T.);
#7828=EDGE_CURVE('',#5423,#5421,#1122,.T.);
#7829=EDGE_CURVE('',#5424,#5425,#3423,.T.);
#7830=EDGE_CURVE('',#5426,#5424,#1123,.T.);
#7831=EDGE_CURVE('',#5420,#5426,#1124,.T.);
#7832=EDGE_CURVE('',#5421,#5427,#1125,.T.);
#7833=EDGE_CURVE('',#5427,#5425,#1126,.T.);
#7834=EDGE_CURVE('',#5428,#5429,#1127,.T.);
#7835=EDGE_CURVE('',#5430,#5429,#4177,.F.);
#7836=EDGE_CURVE('',#5430,#5431,#1128,.T.);
#7837=EDGE_CURVE('',#5431,#5432,#1129,.T.);
#7838=EDGE_CURVE('',#5432,#5433,#1130,.T.);
#7839=EDGE_CURVE('',#5433,#5434,#1131,.T.);
#7840=EDGE_CURVE('',#5434,#5435,#1132,.T.);
#7841=EDGE_CURVE('',#5435,#5436,#1133,.T.);
#7842=EDGE_CURVE('',#5436,#5437,#1134,.T.);
#7843=EDGE_CURVE('',#5437,#5438,#1135,.T.);
#7844=EDGE_CURVE('',#5438,#5439,#1136,.T.);
#7845=EDGE_CURVE('',#5439,#5440,#1137,.T.);
#7846=EDGE_CURVE('',#5440,#5441,#1138,.T.);
#7847=EDGE_CURVE('',#5441,#5442,#1139,.T.);
#7848=EDGE_CURVE('',#5442,#5443,#1140,.T.);
#7849=EDGE_CURVE('',#5443,#5444,#1141,.T.);
#7850=EDGE_CURVE('',#5444,#5445,#1142,.T.);
#7851=EDGE_CURVE('',#5445,#5446,#1143,.T.);
#7852=EDGE_CURVE('',#5446,#5447,#1144,.T.);
#7853=EDGE_CURVE('',#5447,#5448,#1145,.T.);
#7854=EDGE_CURVE('',#5448,#5449,#1146,.T.);
#7855=EDGE_CURVE('',#5449,#5450,#1147,.T.);
#7856=EDGE_CURVE('',#5450,#5451,#1148,.T.);
#7857=EDGE_CURVE('',#5451,#5452,#1149,.T.);
#7858=EDGE_CURVE('',#5452,#5453,#1150,.T.);
#7859=EDGE_CURVE('',#5453,#5454,#1151,.T.);
#7860=EDGE_CURVE('',#5454,#5455,#1152,.T.);
#7861=EDGE_CURVE('',#5455,#5456,#1153,.T.);
#7862=EDGE_CURVE('',#5456,#5457,#1154,.T.);
#7863=EDGE_CURVE('',#5457,#5458,#1155,.T.);
#7864=EDGE_CURVE('',#5458,#5459,#1156,.T.);
#7865=EDGE_CURVE('',#5459,#5460,#1157,.T.);
#7866=EDGE_CURVE('',#5460,#5461,#1158,.T.);
#7867=EDGE_CURVE('',#5461,#5462,#1159,.T.);
#7868=EDGE_CURVE('',#5462,#5463,#1160,.T.);
#7869=EDGE_CURVE('',#5463,#5464,#1161,.T.);
#7870=EDGE_CURVE('',#5464,#5465,#1162,.T.);
#7871=EDGE_CURVE('',#5465,#5466,#1163,.T.);
#7872=EDGE_CURVE('',#5466,#5467,#1164,.T.);
#7873=EDGE_CURVE('',#5467,#5468,#1165,.T.);
#7874=EDGE_CURVE('',#5468,#5469,#1166,.T.);
#7875=EDGE_CURVE('',#5469,#5470,#1167,.T.);
#7876=EDGE_CURVE('',#5470,#5471,#1168,.T.);
#7877=EDGE_CURVE('',#5471,#5472,#1169,.T.);
#7878=EDGE_CURVE('',#5472,#5473,#1170,.T.);
#7879=EDGE_CURVE('',#5473,#5474,#1171,.T.);
#7880=EDGE_CURVE('',#5474,#5475,#1172,.T.);
#7881=EDGE_CURVE('',#5475,#5476,#1173,.T.);
#7882=EDGE_CURVE('',#5476,#5477,#1174,.T.);
#7883=EDGE_CURVE('',#5477,#5478,#1175,.T.);
#7884=EDGE_CURVE('',#5478,#5479,#1176,.T.);
#7885=EDGE_CURVE('',#5479,#5480,#1177,.T.);
#7886=EDGE_CURVE('',#5480,#5481,#1178,.T.);
#7887=EDGE_CURVE('',#5481,#5482,#1179,.T.);
#7888=EDGE_CURVE('',#5482,#5483,#1180,.T.);
#7889=EDGE_CURVE('',#5483,#5484,#1181,.T.);
#7890=EDGE_CURVE('',#5484,#5485,#1182,.T.);
#7891=EDGE_CURVE('',#5485,#5486,#1183,.T.);
#7892=EDGE_CURVE('',#5486,#5487,#1184,.T.);
#7893=EDGE_CURVE('',#5487,#5488,#1185,.T.);
#7894=EDGE_CURVE('',#5488,#5489,#1186,.T.);
#7895=EDGE_CURVE('',#5489,#5490,#1187,.T.);
#7896=EDGE_CURVE('',#5490,#5491,#1188,.T.);
#7897=EDGE_CURVE('',#5491,#5492,#1189,.T.);
#7898=EDGE_CURVE('',#5492,#5493,#1190,.T.);
#7899=EDGE_CURVE('',#5493,#5494,#1191,.T.);
#7900=EDGE_CURVE('',#5494,#5495,#1192,.T.);
#7901=EDGE_CURVE('',#5495,#5496,#1193,.T.);
#7902=EDGE_CURVE('',#5496,#5497,#1194,.T.);
#7903=EDGE_CURVE('',#5497,#5498,#1195,.T.);
#7904=EDGE_CURVE('',#5498,#5499,#1196,.T.);
#7905=EDGE_CURVE('',#5499,#5500,#1197,.T.);
#7906=EDGE_CURVE('',#5500,#5501,#1198,.T.);
#7907=EDGE_CURVE('',#5501,#5502,#1199,.T.);
#7908=EDGE_CURVE('',#5502,#5503,#1200,.T.);
#7909=EDGE_CURVE('',#5503,#5504,#1201,.T.);
#7910=EDGE_CURVE('',#5504,#5505,#1202,.T.);
#7911=EDGE_CURVE('',#5505,#5506,#1203,.T.);
#7912=EDGE_CURVE('',#5506,#5507,#1204,.T.);
#7913=EDGE_CURVE('',#5507,#5508,#1205,.T.);
#7914=EDGE_CURVE('',#5508,#5509,#1206,.T.);
#7915=EDGE_CURVE('',#5509,#5510,#1207,.T.);
#7916=EDGE_CURVE('',#5510,#5511,#1208,.T.);
#7917=EDGE_CURVE('',#5511,#5512,#1209,.T.);
#7918=EDGE_CURVE('',#5512,#5513,#1210,.T.);
#7919=EDGE_CURVE('',#5513,#5514,#1211,.T.);
#7920=EDGE_CURVE('',#5514,#5515,#1212,.T.);
#7921=EDGE_CURVE('',#5515,#5516,#1213,.T.);
#7922=EDGE_CURVE('',#5516,#5517,#1214,.T.);
#7923=EDGE_CURVE('',#5517,#5518,#1215,.T.);
#7924=EDGE_CURVE('',#5518,#5519,#1216,.T.);
#7925=EDGE_CURVE('',#5519,#5520,#1217,.T.);
#7926=EDGE_CURVE('',#5520,#5521,#1218,.T.);
#7927=EDGE_CURVE('',#5521,#5522,#1219,.T.);
#7928=EDGE_CURVE('',#5522,#5523,#1220,.T.);
#7929=EDGE_CURVE('',#5523,#5524,#1221,.T.);
#7930=EDGE_CURVE('',#5524,#5525,#1222,.T.);
#7931=EDGE_CURVE('',#5525,#5526,#1223,.T.);
#7932=EDGE_CURVE('',#5526,#5527,#1224,.T.);
#7933=EDGE_CURVE('',#5527,#5528,#1225,.T.);
#7934=EDGE_CURVE('',#5528,#5529,#1226,.T.);
#7935=EDGE_CURVE('',#5529,#5530,#1227,.T.);
#7936=EDGE_CURVE('',#5530,#5531,#1228,.T.);
#7937=EDGE_CURVE('',#5531,#5532,#1229,.T.);
#7938=EDGE_CURVE('',#5532,#5533,#1230,.T.);
#7939=EDGE_CURVE('',#5533,#5534,#1231,.T.);
#7940=EDGE_CURVE('',#5534,#5535,#1232,.T.);
#7941=EDGE_CURVE('',#5535,#5536,#1233,.T.);
#7942=EDGE_CURVE('',#5536,#5537,#1234,.T.);
#7943=EDGE_CURVE('',#5537,#5538,#1235,.T.);
#7944=EDGE_CURVE('',#5538,#5539,#1236,.T.);
#7945=EDGE_CURVE('',#5539,#5540,#1237,.T.);
#7946=EDGE_CURVE('',#5540,#5541,#1238,.T.);
#7947=EDGE_CURVE('',#5541,#5542,#1239,.T.);
#7948=EDGE_CURVE('',#5542,#5543,#1240,.T.);
#7949=EDGE_CURVE('',#5543,#5544,#1241,.T.);
#7950=EDGE_CURVE('',#5544,#5545,#1242,.T.);
#7951=EDGE_CURVE('',#5545,#5546,#1243,.T.);
#7952=EDGE_CURVE('',#5546,#5547,#1244,.T.);
#7953=EDGE_CURVE('',#5547,#5548,#1245,.T.);
#7954=EDGE_CURVE('',#5548,#5549,#1246,.T.);
#7955=EDGE_CURVE('',#5549,#5550,#1247,.T.);
#7956=EDGE_CURVE('',#5550,#5551,#1248,.T.);
#7957=EDGE_CURVE('',#5551,#5552,#1249,.T.);
#7958=EDGE_CURVE('',#5552,#5553,#1250,.T.);
#7959=EDGE_CURVE('',#5553,#5554,#1251,.T.);
#7960=EDGE_CURVE('',#5554,#5555,#1252,.T.);
#7961=EDGE_CURVE('',#5555,#5556,#1253,.T.);
#7962=EDGE_CURVE('',#5556,#5557,#1254,.T.);
#7963=EDGE_CURVE('',#5557,#5558,#1255,.T.);
#7964=EDGE_CURVE('',#5558,#5559,#1256,.T.);
#7965=EDGE_CURVE('',#5559,#5560,#1257,.T.);
#7966=EDGE_CURVE('',#5560,#5561,#1258,.T.);
#7967=EDGE_CURVE('',#5561,#5562,#1259,.T.);
#7968=EDGE_CURVE('',#5562,#5563,#1260,.T.);
#7969=EDGE_CURVE('',#5563,#5564,#1261,.T.);
#7970=EDGE_CURVE('',#5564,#5565,#1262,.T.);
#7971=EDGE_CURVE('',#5565,#5566,#1263,.T.);
#7972=EDGE_CURVE('',#5566,#5567,#1264,.T.);
#7973=EDGE_CURVE('',#5567,#5568,#1265,.T.);
#7974=EDGE_CURVE('',#5568,#5569,#1266,.T.);
#7975=EDGE_CURVE('',#5569,#5570,#1267,.T.);
#7976=EDGE_CURVE('',#5570,#5571,#1268,.T.);
#7977=EDGE_CURVE('',#5571,#5572,#1269,.T.);
#7978=EDGE_CURVE('',#5572,#5573,#1270,.T.);
#7979=EDGE_CURVE('',#5573,#5574,#1271,.T.);
#7980=EDGE_CURVE('',#5574,#5575,#1272,.T.);
#7981=EDGE_CURVE('',#5575,#5576,#1273,.T.);
#7982=EDGE_CURVE('',#5576,#5577,#1274,.T.);
#7983=EDGE_CURVE('',#5577,#5578,#1275,.T.);
#7984=EDGE_CURVE('',#5578,#5579,#1276,.T.);
#7985=EDGE_CURVE('',#5579,#5580,#1277,.T.);
#7986=EDGE_CURVE('',#5580,#5581,#1278,.T.);
#7987=EDGE_CURVE('',#5581,#5582,#1279,.T.);
#7988=EDGE_CURVE('',#5582,#5583,#1280,.T.);
#7989=EDGE_CURVE('',#5583,#5584,#1281,.T.);
#7990=EDGE_CURVE('',#5584,#5585,#1282,.T.);
#7991=EDGE_CURVE('',#5585,#5586,#1283,.T.);
#7992=EDGE_CURVE('',#5586,#5587,#1284,.T.);
#7993=EDGE_CURVE('',#5587,#5588,#1285,.T.);
#7994=EDGE_CURVE('',#5588,#5589,#1286,.T.);
#7995=EDGE_CURVE('',#5589,#5590,#1287,.T.);
#7996=EDGE_CURVE('',#5590,#5591,#1288,.T.);
#7997=EDGE_CURVE('',#5591,#5592,#1289,.T.);
#7998=EDGE_CURVE('',#5592,#5593,#1290,.T.);
#7999=EDGE_CURVE('',#5593,#5594,#1291,.T.);
#8000=EDGE_CURVE('',#5594,#5595,#1292,.T.);
#8001=EDGE_CURVE('',#5595,#5596,#1293,.T.);
#8002=EDGE_CURVE('',#5596,#5597,#1294,.T.);
#8003=EDGE_CURVE('',#5597,#5598,#1295,.T.);
#8004=EDGE_CURVE('',#5598,#5599,#1296,.T.);
#8005=EDGE_CURVE('',#5599,#5600,#1297,.T.);
#8006=EDGE_CURVE('',#5600,#5601,#1298,.T.);
#8007=EDGE_CURVE('',#5601,#5602,#1299,.T.);
#8008=EDGE_CURVE('',#5602,#5603,#1300,.T.);
#8009=EDGE_CURVE('',#5603,#5604,#1301,.T.);
#8010=EDGE_CURVE('',#5604,#5605,#1302,.T.);
#8011=EDGE_CURVE('',#5605,#5606,#1303,.T.);
#8012=EDGE_CURVE('',#5606,#5607,#1304,.T.);
#8013=EDGE_CURVE('',#5607,#5608,#1305,.T.);
#8014=EDGE_CURVE('',#5608,#5609,#1306,.T.);
#8015=EDGE_CURVE('',#5609,#5610,#1307,.T.);
#8016=EDGE_CURVE('',#5610,#5611,#1308,.T.);
#8017=EDGE_CURVE('',#5611,#5612,#1309,.T.);
#8018=EDGE_CURVE('',#5612,#5613,#1310,.T.);
#8019=EDGE_CURVE('',#5613,#5614,#1311,.T.);
#8020=EDGE_CURVE('',#5614,#5615,#1312,.T.);
#8021=EDGE_CURVE('',#5615,#5616,#1313,.T.);
#8022=EDGE_CURVE('',#5616,#5617,#1314,.T.);
#8023=EDGE_CURVE('',#5617,#5618,#1315,.T.);
#8024=EDGE_CURVE('',#5618,#5619,#1316,.T.);
#8025=EDGE_CURVE('',#5619,#5620,#1317,.T.);
#8026=EDGE_CURVE('',#5620,#5621,#1318,.T.);
#8027=EDGE_CURVE('',#5621,#5622,#1319,.T.);
#8028=EDGE_CURVE('',#5622,#5623,#1320,.T.);
#8029=EDGE_CURVE('',#5623,#5624,#1321,.T.);
#8030=EDGE_CURVE('',#5624,#5625,#1322,.T.);
#8031=EDGE_CURVE('',#5625,#5626,#1323,.T.);
#8032=EDGE_CURVE('',#5626,#5627,#1324,.T.);
#8033=EDGE_CURVE('',#5627,#5628,#1325,.T.);
#8034=EDGE_CURVE('',#5628,#5629,#1326,.T.);
#8035=EDGE_CURVE('',#5629,#5630,#1327,.T.);
#8036=EDGE_CURVE('',#5630,#5631,#1328,.T.);
#8037=EDGE_CURVE('',#5631,#5632,#1329,.T.);
#8038=EDGE_CURVE('',#5632,#5633,#1330,.T.);
#8039=EDGE_CURVE('',#5633,#5634,#1331,.T.);
#8040=EDGE_CURVE('',#5634,#5635,#1332,.T.);
#8041=EDGE_CURVE('',#5635,#5636,#1333,.T.);
#8042=EDGE_CURVE('',#5636,#5637,#1334,.T.);
#8043=EDGE_CURVE('',#5637,#5638,#1335,.T.);
#8044=EDGE_CURVE('',#5638,#5639,#1336,.T.);
#8045=EDGE_CURVE('',#5639,#5640,#1337,.T.);
#8046=EDGE_CURVE('',#5640,#5641,#1338,.T.);
#8047=EDGE_CURVE('',#5641,#5642,#1339,.T.);
#8048=EDGE_CURVE('',#5642,#5643,#1340,.T.);
#8049=EDGE_CURVE('',#5643,#5644,#1341,.T.);
#8050=EDGE_CURVE('',#5644,#5645,#1342,.T.);
#8051=EDGE_CURVE('',#5645,#5646,#1343,.T.);
#8052=EDGE_CURVE('',#5646,#5647,#1344,.T.);
#8053=EDGE_CURVE('',#5647,#5648,#1345,.T.);
#8054=EDGE_CURVE('',#5648,#5649,#1346,.T.);
#8055=EDGE_CURVE('',#5649,#5650,#1347,.T.);
#8056=EDGE_CURVE('',#5650,#5651,#1348,.T.);
#8057=EDGE_CURVE('',#5651,#5652,#1349,.T.);
#8058=EDGE_CURVE('',#5652,#5653,#1350,.T.);
#8059=EDGE_CURVE('',#5653,#5654,#1351,.T.);
#8060=EDGE_CURVE('',#5654,#5655,#1352,.T.);
#8061=EDGE_CURVE('',#5655,#5656,#1353,.T.);
#8062=EDGE_CURVE('',#5656,#5657,#1354,.T.);
#8063=EDGE_CURVE('',#5657,#5658,#1355,.T.);
#8064=EDGE_CURVE('',#5658,#5659,#1356,.T.);
#8065=EDGE_CURVE('',#5659,#5660,#1357,.T.);
#8066=EDGE_CURVE('',#5660,#5661,#1358,.T.);
#8067=EDGE_CURVE('',#5661,#5662,#1359,.T.);
#8068=EDGE_CURVE('',#5662,#5663,#1360,.T.);
#8069=EDGE_CURVE('',#5663,#5664,#1361,.T.);
#8070=EDGE_CURVE('',#5664,#5665,#1362,.T.);
#8071=EDGE_CURVE('',#5665,#5666,#1363,.T.);
#8072=EDGE_CURVE('',#5666,#5667,#1364,.T.);
#8073=EDGE_CURVE('',#5667,#5668,#1365,.T.);
#8074=EDGE_CURVE('',#5668,#5669,#1366,.T.);
#8075=EDGE_CURVE('',#5669,#5670,#1367,.T.);
#8076=EDGE_CURVE('',#5670,#5671,#1368,.T.);
#8077=EDGE_CURVE('',#5671,#5672,#1369,.T.);
#8078=EDGE_CURVE('',#5672,#5673,#1370,.T.);
#8079=EDGE_CURVE('',#5673,#5674,#1371,.T.);
#8080=EDGE_CURVE('',#5674,#5675,#1372,.T.);
#8081=EDGE_CURVE('',#5675,#5676,#1373,.T.);
#8082=EDGE_CURVE('',#5676,#5677,#1374,.T.);
#8083=EDGE_CURVE('',#5677,#5678,#1375,.T.);
#8084=EDGE_CURVE('',#5678,#5679,#1376,.T.);
#8085=EDGE_CURVE('',#5679,#5680,#1377,.T.);
#8086=EDGE_CURVE('',#5680,#5681,#1378,.T.);
#8087=EDGE_CURVE('',#5681,#5682,#1379,.T.);
#8088=EDGE_CURVE('',#5682,#5683,#1380,.T.);
#8089=EDGE_CURVE('',#5683,#5684,#1381,.T.);
#8090=EDGE_CURVE('',#5684,#5685,#1382,.T.);
#8091=EDGE_CURVE('',#5685,#5686,#1383,.T.);
#8092=EDGE_CURVE('',#5686,#5687,#1384,.T.);
#8093=EDGE_CURVE('',#5687,#5688,#1385,.T.);
#8094=EDGE_CURVE('',#5688,#5689,#1386,.T.);
#8095=EDGE_CURVE('',#5689,#5690,#1387,.T.);
#8096=EDGE_CURVE('',#5690,#5691,#1388,.T.);
#8097=EDGE_CURVE('',#5691,#5692,#1389,.T.);
#8098=EDGE_CURVE('',#5692,#5693,#1390,.T.);
#8099=EDGE_CURVE('',#5693,#5694,#1391,.T.);
#8100=EDGE_CURVE('',#5694,#5695,#1392,.T.);
#8101=EDGE_CURVE('',#5695,#5696,#1393,.T.);
#8102=EDGE_CURVE('',#5696,#5697,#1394,.T.);
#8103=EDGE_CURVE('',#5697,#5698,#1395,.T.);
#8104=EDGE_CURVE('',#5698,#5699,#1396,.T.);
#8105=EDGE_CURVE('',#5699,#5700,#1397,.T.);
#8106=EDGE_CURVE('',#5701,#5700,#4178,.T.);
#8107=EDGE_CURVE('',#5701,#5702,#1398,.T.);
#8108=EDGE_CURVE('',#5702,#5703,#1399,.T.);
#8109=EDGE_CURVE('',#5703,#5704,#1400,.T.);
#8110=EDGE_CURVE('',#5704,#5705,#1401,.T.);
#8111=EDGE_CURVE('',#5705,#5706,#1402,.T.);
#8112=EDGE_CURVE('',#5706,#5707,#1403,.T.);
#8113=EDGE_CURVE('',#5707,#5708,#1404,.T.);
#8114=EDGE_CURVE('',#5708,#5709,#1405,.T.);
#8115=EDGE_CURVE('',#5709,#5710,#1406,.T.);
#8116=EDGE_CURVE('',#5710,#5711,#1407,.T.);
#8117=EDGE_CURVE('',#5711,#5712,#1408,.T.);
#8118=EDGE_CURVE('',#5712,#5713,#1409,.T.);
#8119=EDGE_CURVE('',#5713,#5714,#1410,.T.);
#8120=EDGE_CURVE('',#5714,#5715,#1411,.T.);
#8121=EDGE_CURVE('',#5715,#5716,#1412,.T.);
#8122=EDGE_CURVE('',#5716,#5717,#1413,.T.);
#8123=EDGE_CURVE('',#5717,#5718,#1414,.T.);
#8124=EDGE_CURVE('',#5718,#5719,#1415,.T.);
#8125=EDGE_CURVE('',#5719,#5720,#1416,.T.);
#8126=EDGE_CURVE('',#5720,#5721,#1417,.T.);
#8127=EDGE_CURVE('',#5721,#5722,#1418,.T.);
#8128=EDGE_CURVE('',#5722,#5723,#1419,.T.);
#8129=EDGE_CURVE('',#5723,#5724,#1420,.T.);
#8130=EDGE_CURVE('',#5724,#5725,#1421,.T.);
#8131=EDGE_CURVE('',#5725,#5726,#1422,.T.);
#8132=EDGE_CURVE('',#5726,#5727,#1423,.T.);
#8133=EDGE_CURVE('',#5727,#5728,#1424,.T.);
#8134=EDGE_CURVE('',#5728,#5729,#1425,.T.);
#8135=EDGE_CURVE('',#5729,#5730,#1426,.T.);
#8136=EDGE_CURVE('',#5730,#5731,#1427,.T.);
#8137=EDGE_CURVE('',#5731,#5732,#1428,.T.);
#8138=EDGE_CURVE('',#5732,#5733,#1429,.T.);
#8139=EDGE_CURVE('',#5733,#5734,#1430,.T.);
#8140=EDGE_CURVE('',#5734,#5735,#1431,.T.);
#8141=EDGE_CURVE('',#5735,#5736,#1432,.T.);
#8142=EDGE_CURVE('',#5736,#5737,#1433,.T.);
#8143=EDGE_CURVE('',#5737,#5738,#1434,.T.);
#8144=EDGE_CURVE('',#5738,#5739,#1435,.T.);
#8145=EDGE_CURVE('',#5739,#5740,#1436,.T.);
#8146=EDGE_CURVE('',#5740,#5741,#1437,.T.);
#8147=EDGE_CURVE('',#5741,#5742,#1438,.T.);
#8148=EDGE_CURVE('',#5742,#5743,#1439,.T.);
#8149=EDGE_CURVE('',#5743,#5744,#1440,.T.);
#8150=EDGE_CURVE('',#5744,#5745,#1441,.T.);
#8151=EDGE_CURVE('',#5745,#5746,#1442,.T.);
#8152=EDGE_CURVE('',#5746,#5747,#1443,.T.);
#8153=EDGE_CURVE('',#5747,#5748,#1444,.T.);
#8154=EDGE_CURVE('',#5748,#5749,#1445,.T.);
#8155=EDGE_CURVE('',#5749,#5750,#1446,.T.);
#8156=EDGE_CURVE('',#5750,#5751,#1447,.T.);
#8157=EDGE_CURVE('',#5751,#5752,#1448,.T.);
#8158=EDGE_CURVE('',#5752,#5753,#1449,.T.);
#8159=EDGE_CURVE('',#5753,#5754,#1450,.T.);
#8160=EDGE_CURVE('',#5754,#5755,#1451,.T.);
#8161=EDGE_CURVE('',#5755,#5756,#1452,.T.);
#8162=EDGE_CURVE('',#5756,#5757,#1453,.T.);
#8163=EDGE_CURVE('',#5757,#5758,#1454,.T.);
#8164=EDGE_CURVE('',#5758,#5759,#1455,.T.);
#8165=EDGE_CURVE('',#5759,#5760,#1456,.T.);
#8166=EDGE_CURVE('',#5760,#5761,#1457,.T.);
#8167=EDGE_CURVE('',#5761,#5762,#1458,.T.);
#8168=EDGE_CURVE('',#5762,#5763,#1459,.T.);
#8169=EDGE_CURVE('',#5763,#5764,#1460,.T.);
#8170=EDGE_CURVE('',#5764,#5765,#1461,.T.);
#8171=EDGE_CURVE('',#5765,#5766,#1462,.T.);
#8172=EDGE_CURVE('',#5766,#5767,#1463,.T.);
#8173=EDGE_CURVE('',#5767,#5768,#1464,.T.);
#8174=EDGE_CURVE('',#5768,#5769,#1465,.T.);
#8175=EDGE_CURVE('',#5769,#5770,#1466,.T.);
#8176=EDGE_CURVE('',#5770,#5771,#1467,.T.);
#8177=EDGE_CURVE('',#5771,#5772,#1468,.T.);
#8178=EDGE_CURVE('',#5772,#5773,#1469,.T.);
#8179=EDGE_CURVE('',#5773,#5774,#1470,.T.);
#8180=EDGE_CURVE('',#5774,#5775,#1471,.T.);
#8181=EDGE_CURVE('',#5775,#5776,#1472,.T.);
#8182=EDGE_CURVE('',#5776,#5777,#1473,.T.);
#8183=EDGE_CURVE('',#5777,#5778,#1474,.T.);
#8184=EDGE_CURVE('',#5778,#5779,#1475,.T.);
#8185=EDGE_CURVE('',#5779,#5780,#1476,.T.);
#8186=EDGE_CURVE('',#5780,#5781,#1477,.T.);
#8187=EDGE_CURVE('',#5781,#5782,#1478,.T.);
#8188=EDGE_CURVE('',#5782,#5783,#1479,.T.);
#8189=EDGE_CURVE('',#5783,#5784,#1480,.T.);
#8190=EDGE_CURVE('',#5784,#5785,#1481,.T.);
#8191=EDGE_CURVE('',#5785,#5786,#1482,.T.);
#8192=EDGE_CURVE('',#5786,#5787,#1483,.T.);
#8193=EDGE_CURVE('',#5787,#5788,#1484,.T.);
#8194=EDGE_CURVE('',#5788,#5789,#1485,.T.);
#8195=EDGE_CURVE('',#5789,#5790,#1486,.T.);
#8196=EDGE_CURVE('',#5790,#5791,#1487,.T.);
#8197=EDGE_CURVE('',#5791,#5792,#1488,.T.);
#8198=EDGE_CURVE('',#5792,#5793,#1489,.T.);
#8199=EDGE_CURVE('',#5793,#5794,#1490,.T.);
#8200=EDGE_CURVE('',#5794,#5795,#1491,.T.);
#8201=EDGE_CURVE('',#5795,#5796,#1492,.T.);
#8202=EDGE_CURVE('',#5796,#5797,#1493,.T.);
#8203=EDGE_CURVE('',#5797,#5798,#1494,.T.);
#8204=EDGE_CURVE('',#5798,#5799,#1495,.T.);
#8205=EDGE_CURVE('',#5799,#5800,#1496,.T.);
#8206=EDGE_CURVE('',#5800,#5801,#1497,.T.);
#8207=EDGE_CURVE('',#5801,#5802,#1498,.T.);
#8208=EDGE_CURVE('',#5802,#5803,#1499,.T.);
#8209=EDGE_CURVE('',#5803,#5804,#1500,.T.);
#8210=EDGE_CURVE('',#5804,#5805,#1501,.T.);
#8211=EDGE_CURVE('',#5805,#5806,#1502,.T.);
#8212=EDGE_CURVE('',#5806,#5807,#1503,.T.);
#8213=EDGE_CURVE('',#5807,#5808,#1504,.T.);
#8214=EDGE_CURVE('',#5808,#5809,#1505,.T.);
#8215=EDGE_CURVE('',#5809,#5810,#1506,.T.);
#8216=EDGE_CURVE('',#5810,#5811,#1507,.T.);
#8217=EDGE_CURVE('',#5811,#5812,#1508,.T.);
#8218=EDGE_CURVE('',#5812,#5813,#1509,.T.);
#8219=EDGE_CURVE('',#5813,#5814,#1510,.T.);
#8220=EDGE_CURVE('',#5814,#5815,#1511,.T.);
#8221=EDGE_CURVE('',#5815,#5816,#1512,.T.);
#8222=EDGE_CURVE('',#5816,#5817,#1513,.T.);
#8223=EDGE_CURVE('',#5817,#5818,#1514,.T.);
#8224=EDGE_CURVE('',#5818,#5819,#1515,.T.);
#8225=EDGE_CURVE('',#5819,#5820,#1516,.T.);
#8226=EDGE_CURVE('',#5820,#5821,#1517,.T.);
#8227=EDGE_CURVE('',#5821,#5822,#1518,.T.);
#8228=EDGE_CURVE('',#5822,#5823,#1519,.T.);
#8229=EDGE_CURVE('',#5823,#5824,#1520,.T.);
#8230=EDGE_CURVE('',#5824,#5825,#1521,.T.);
#8231=EDGE_CURVE('',#5825,#5826,#1522,.T.);
#8232=EDGE_CURVE('',#5826,#5827,#1523,.T.);
#8233=EDGE_CURVE('',#5827,#5828,#1524,.T.);
#8234=EDGE_CURVE('',#5828,#5829,#1525,.T.);
#8235=EDGE_CURVE('',#5829,#5830,#1526,.T.);
#8236=EDGE_CURVE('',#5830,#5831,#1527,.T.);
#8237=EDGE_CURVE('',#5831,#5832,#1528,.T.);
#8238=EDGE_CURVE('',#5832,#5833,#1529,.T.);
#8239=EDGE_CURVE('',#5833,#5834,#1530,.T.);
#8240=EDGE_CURVE('',#5834,#5835,#1531,.T.);
#8241=EDGE_CURVE('',#5835,#5836,#1532,.T.);
#8242=EDGE_CURVE('',#5836,#5837,#1533,.T.);
#8243=EDGE_CURVE('',#5837,#5838,#1534,.T.);
#8244=EDGE_CURVE('',#5838,#5839,#1535,.T.);
#8245=EDGE_CURVE('',#5839,#5840,#1536,.T.);
#8246=EDGE_CURVE('',#5840,#5841,#1537,.T.);
#8247=EDGE_CURVE('',#5841,#5842,#1538,.T.);
#8248=EDGE_CURVE('',#5842,#5843,#1539,.T.);
#8249=EDGE_CURVE('',#5843,#5844,#1540,.T.);
#8250=EDGE_CURVE('',#5844,#5845,#1541,.T.);
#8251=EDGE_CURVE('',#5845,#5846,#1542,.T.);
#8252=EDGE_CURVE('',#5846,#5847,#1543,.T.);
#8253=EDGE_CURVE('',#5847,#5848,#1544,.T.);
#8254=EDGE_CURVE('',#5848,#5849,#1545,.T.);
#8255=EDGE_CURVE('',#5849,#5850,#1546,.T.);
#8256=EDGE_CURVE('',#5850,#5851,#1547,.T.);
#8257=EDGE_CURVE('',#5851,#5852,#1548,.T.);
#8258=EDGE_CURVE('',#5852,#5853,#1549,.T.);
#8259=EDGE_CURVE('',#5853,#5854,#1550,.T.);
#8260=EDGE_CURVE('',#5854,#5855,#1551,.T.);
#8261=EDGE_CURVE('',#5855,#5856,#1552,.T.);
#8262=EDGE_CURVE('',#5856,#5857,#1553,.T.);
#8263=EDGE_CURVE('',#5857,#5858,#1554,.T.);
#8264=EDGE_CURVE('',#5858,#5859,#1555,.T.);
#8265=EDGE_CURVE('',#5859,#5860,#1556,.T.);
#8266=EDGE_CURVE('',#5860,#5861,#1557,.T.);
#8267=EDGE_CURVE('',#5861,#5862,#1558,.T.);
#8268=EDGE_CURVE('',#5862,#5863,#1559,.T.);
#8269=EDGE_CURVE('',#5863,#5864,#1560,.T.);
#8270=EDGE_CURVE('',#5864,#5865,#1561,.T.);
#8271=EDGE_CURVE('',#5865,#5866,#1562,.T.);
#8272=EDGE_CURVE('',#5866,#5867,#1563,.T.);
#8273=EDGE_CURVE('',#5867,#5868,#1564,.T.);
#8274=EDGE_CURVE('',#5868,#5869,#1565,.T.);
#8275=EDGE_CURVE('',#5869,#5870,#1566,.T.);
#8276=EDGE_CURVE('',#5870,#5871,#1567,.T.);
#8277=EDGE_CURVE('',#5871,#5872,#1568,.T.);
#8278=EDGE_CURVE('',#5872,#5873,#1569,.T.);
#8279=EDGE_CURVE('',#5873,#5874,#1570,.T.);
#8280=EDGE_CURVE('',#5874,#5875,#1571,.T.);
#8281=EDGE_CURVE('',#5875,#5876,#1572,.T.);
#8282=EDGE_CURVE('',#5876,#5877,#1573,.T.);
#8283=EDGE_CURVE('',#5877,#5878,#1574,.T.);
#8284=EDGE_CURVE('',#5878,#5879,#1575,.T.);
#8285=EDGE_CURVE('',#5879,#5880,#1576,.T.);
#8286=EDGE_CURVE('',#5880,#5881,#1577,.T.);
#8287=EDGE_CURVE('',#5881,#5882,#1578,.T.);
#8288=EDGE_CURVE('',#5882,#5883,#1579,.T.);
#8289=EDGE_CURVE('',#5883,#5884,#1580,.T.);
#8290=EDGE_CURVE('',#5884,#5885,#1581,.T.);
#8291=EDGE_CURVE('',#5885,#5886,#1582,.T.);
#8292=EDGE_CURVE('',#5886,#5887,#1583,.T.);
#8293=EDGE_CURVE('',#5887,#5888,#1584,.T.);
#8294=EDGE_CURVE('',#5888,#5889,#1585,.T.);
#8295=EDGE_CURVE('',#5889,#5890,#1586,.T.);
#8296=EDGE_CURVE('',#5890,#5891,#1587,.T.);
#8297=EDGE_CURVE('',#5891,#5892,#1588,.T.);
#8298=EDGE_CURVE('',#5892,#5893,#1589,.T.);
#8299=EDGE_CURVE('',#5893,#5894,#1590,.T.);
#8300=EDGE_CURVE('',#5894,#5895,#1591,.T.);
#8301=EDGE_CURVE('',#5895,#5896,#1592,.T.);
#8302=EDGE_CURVE('',#5896,#5897,#1593,.T.);
#8303=EDGE_CURVE('',#5897,#5898,#1594,.T.);
#8304=EDGE_CURVE('',#5898,#5899,#1595,.T.);
#8305=EDGE_CURVE('',#5899,#5900,#1596,.T.);
#8306=EDGE_CURVE('',#5900,#5901,#1597,.T.);
#8307=EDGE_CURVE('',#5901,#5902,#1598,.T.);
#8308=EDGE_CURVE('',#5902,#5903,#1599,.T.);
#8309=EDGE_CURVE('',#5903,#5904,#1600,.T.);
#8310=EDGE_CURVE('',#5904,#5905,#1601,.T.);
#8311=EDGE_CURVE('',#5905,#5906,#1602,.T.);
#8312=EDGE_CURVE('',#5906,#5907,#1603,.T.);
#8313=EDGE_CURVE('',#5907,#5908,#1604,.T.);
#8314=EDGE_CURVE('',#5908,#5909,#1605,.T.);
#8315=EDGE_CURVE('',#5909,#5910,#1606,.T.);
#8316=EDGE_CURVE('',#5910,#5911,#1607,.T.);
#8317=EDGE_CURVE('',#5911,#5912,#1608,.T.);
#8318=EDGE_CURVE('',#5912,#5913,#1609,.T.);
#8319=EDGE_CURVE('',#5913,#5914,#1610,.T.);
#8320=EDGE_CURVE('',#5914,#5915,#1611,.T.);
#8321=EDGE_CURVE('',#5915,#5916,#1612,.T.);
#8322=EDGE_CURVE('',#5916,#5917,#1613,.T.);
#8323=EDGE_CURVE('',#5917,#5918,#1614,.T.);
#8324=EDGE_CURVE('',#5918,#5919,#1615,.T.);
#8325=EDGE_CURVE('',#5919,#5920,#1616,.T.);
#8326=EDGE_CURVE('',#5920,#5921,#1617,.T.);
#8327=EDGE_CURVE('',#5921,#5922,#1618,.T.);
#8328=EDGE_CURVE('',#5922,#5923,#1619,.T.);
#8329=EDGE_CURVE('',#5923,#5924,#1620,.T.);
#8330=EDGE_CURVE('',#5924,#5925,#1621,.T.);
#8331=EDGE_CURVE('',#5925,#5926,#1622,.T.);
#8332=EDGE_CURVE('',#5926,#5927,#1623,.T.);
#8333=EDGE_CURVE('',#5927,#5928,#1624,.T.);
#8334=EDGE_CURVE('',#5928,#5929,#1625,.T.);
#8335=EDGE_CURVE('',#5929,#5930,#1626,.T.);
#8336=EDGE_CURVE('',#5930,#5931,#1627,.T.);
#8337=EDGE_CURVE('',#5931,#5932,#1628,.T.);
#8338=EDGE_CURVE('',#5932,#5933,#1629,.T.);
#8339=EDGE_CURVE('',#5933,#5934,#1630,.T.);
#8340=EDGE_CURVE('',#5934,#5935,#1631,.T.);
#8341=EDGE_CURVE('',#5935,#5936,#1632,.T.);
#8342=EDGE_CURVE('',#5936,#5937,#1633,.T.);
#8343=EDGE_CURVE('',#5937,#5938,#1634,.T.);
#8344=EDGE_CURVE('',#5938,#5939,#1635,.T.);
#8345=EDGE_CURVE('',#5939,#5940,#1636,.T.);
#8346=EDGE_CURVE('',#5940,#5941,#1637,.T.);
#8347=EDGE_CURVE('',#5941,#5942,#1638,.T.);
#8348=EDGE_CURVE('',#5942,#5943,#1639,.T.);
#8349=EDGE_CURVE('',#5943,#5944,#1640,.T.);
#8350=EDGE_CURVE('',#5944,#5945,#1641,.T.);
#8351=EDGE_CURVE('',#5945,#5946,#1642,.T.);
#8352=EDGE_CURVE('',#5946,#5947,#1643,.T.);
#8353=EDGE_CURVE('',#5947,#5948,#1644,.T.);
#8354=EDGE_CURVE('',#5948,#5949,#1645,.T.);
#8355=EDGE_CURVE('',#5949,#5950,#1646,.T.);
#8356=EDGE_CURVE('',#5950,#5951,#1647,.T.);
#8357=EDGE_CURVE('',#5951,#5952,#1648,.T.);
#8358=EDGE_CURVE('',#5952,#5953,#1649,.T.);
#8359=EDGE_CURVE('',#5953,#5954,#1650,.T.);
#8360=EDGE_CURVE('',#5954,#5955,#1651,.T.);
#8361=EDGE_CURVE('',#5955,#5956,#1652,.T.);
#8362=EDGE_CURVE('',#5956,#5957,#1653,.T.);
#8363=EDGE_CURVE('',#5957,#5958,#1654,.T.);
#8364=EDGE_CURVE('',#5958,#5959,#1655,.T.);
#8365=EDGE_CURVE('',#5959,#5960,#1656,.T.);
#8366=EDGE_CURVE('',#5960,#5961,#1657,.T.);
#8367=EDGE_CURVE('',#5961,#5962,#1658,.T.);
#8368=EDGE_CURVE('',#5962,#5963,#1659,.T.);
#8369=EDGE_CURVE('',#5963,#5964,#1660,.T.);
#8370=EDGE_CURVE('',#5964,#5965,#1661,.T.);
#8371=EDGE_CURVE('',#5965,#5966,#1662,.T.);
#8372=EDGE_CURVE('',#5966,#5967,#1663,.T.);
#8373=EDGE_CURVE('',#5967,#5968,#1664,.T.);
#8374=EDGE_CURVE('',#5968,#5969,#1665,.T.);
#8375=EDGE_CURVE('',#5969,#5428,#1666,.T.);
#8376=EDGE_CURVE('',#5425,#5970,#1667,.T.);
#8377=EDGE_CURVE('',#5970,#5971,#1668,.T.);
#8378=EDGE_CURVE('',#5972,#5971,#4179,.T.);
#8379=EDGE_CURVE('',#5973,#5972,#1669,.T.);
#8380=EDGE_CURVE('',#5424,#5973,#1670,.T.);
#8381=EDGE_CURVE('',#5974,#5974,#4180,.T.);
#8382=EDGE_CURVE('',#5975,#5975,#4181,.T.);
#8383=EDGE_CURVE('',#5974,#5976,#3424,.T.);
#8384=EDGE_CURVE('',#5976,#5976,#4182,.T.);
#8385=EDGE_CURVE('',#4358,#5430,#1671,.T.);
#8386=EDGE_CURVE('',#5429,#4359,#1672,.T.);
#8387=EDGE_CURVE('',#5977,#5978,#3425,.T.);
#8388=EDGE_CURVE('',#5979,#5977,#3426,.T.);
#8389=EDGE_CURVE('',#5979,#5980,#3427,.T.);
#8390=EDGE_CURVE('',#5978,#5980,#3428,.T.);
#8391=EDGE_CURVE('',#5980,#5979,#4183,.T.);
#8392=EDGE_CURVE('',#5981,#5982,#3429,.T.);
#8393=EDGE_CURVE('',#5983,#5981,#3430,.T.);
#8394=EDGE_CURVE('',#5983,#5984,#3431,.T.);
#8395=EDGE_CURVE('',#5982,#5984,#3432,.T.);
#8396=EDGE_CURVE('',#5984,#5985,#4184,.T.);
#8397=EDGE_CURVE('',#5985,#5983,#4185,.T.);
#8398=EDGE_CURVE('',#5985,#5975,#3433,.T.);
#8399=EDGE_CURVE('',#5978,#5981,#4186,.T.);
#8400=EDGE_CURVE('',#5982,#5977,#4187,.T.);
#8401=EDGE_CURVE('',#5700,#5972,#1673,.T.);
#8402=EDGE_CURVE('',#5971,#5701,#1674,.T.);
#8403=EDGE_CURVE('',#5986,#5987,#4188,.T.);
#8404=EDGE_CURVE('',#5987,#5988,#3434,.T.);
#8405=EDGE_CURVE('',#5989,#5988,#4189,.T.);
#8406=EDGE_CURVE('',#5990,#5989,#3435,.T.);
#8407=EDGE_CURVE('',#5991,#5990,#4190,.T.);
#8408=EDGE_CURVE('',#5992,#5991,#3436,.T.);
#8409=EDGE_CURVE('',#5988,#5992,#4191,.T.);
#8410=EDGE_CURVE('',#5987,#5993,#4192,.T.);
#8411=EDGE_CURVE('',#5994,#5993,#3437,.T.);
#8412=EDGE_CURVE('',#5995,#5994,#4193,.T.);
#8413=EDGE_CURVE('',#5986,#5995,#3438,.T.);
#8414=EDGE_CURVE('',#5996,#5997,#4194,.T.);
#8415=EDGE_CURVE('',#5998,#5996,#3439,.T.);
#8416=EDGE_CURVE('',#5999,#5998,#4195,.T.);
#8417=EDGE_CURVE('',#6000,#5999,#3440,.T.);
#8418=EDGE_CURVE('',#5997,#6000,#4196,.T.);
#8419=EDGE_CURVE('',#5997,#6001,#3441,.T.);
#8420=EDGE_CURVE('',#6002,#6001,#4197,.T.);
#8421=EDGE_CURVE('',#6003,#6002,#3442,.T.);
#8422=EDGE_CURVE('',#6003,#6004,#4198,.T.);
#8423=EDGE_CURVE('',#6005,#6004,#3443,.T.);
#8424=EDGE_CURVE('',#6001,#6005,#4199,.T.);
#8425=EDGE_CURVE('',#5993,#5986,#4200,.T.);
#8426=EDGE_CURVE('',#5994,#5995,#4201,.T.);
#8427=EDGE_CURVE('',#6006,#6003,#4202,.T.);
#8428=EDGE_CURVE('',#6007,#6006,#3444,.T.);
#8429=EDGE_CURVE('',#6008,#6007,#4203,.T.);
#8430=EDGE_CURVE('',#6004,#6008,#3445,.T.);
#8431=EDGE_CURVE('',#6009,#6009,#4204,.T.);
#8432=EDGE_CURVE('',#6005,#6010,#3446,.T.);
#8433=EDGE_CURVE('',#6010,#6011,#4205,.T.);
#8434=EDGE_CURVE('',#6011,#6012,#3447,.T.);
#8435=EDGE_CURVE('',#6012,#6002,#4206,.T.);
#8436=EDGE_CURVE('',#6013,#6013,#4207,.T.);
#8437=EDGE_CURVE('',#6009,#6013,#3448,.T.);
#8438=EDGE_CURVE('',#6006,#6012,#3449,.T.);
#8439=EDGE_CURVE('',#6007,#6011,#3450,.T.);
#8440=EDGE_CURVE('',#6008,#6010,#3451,.T.);
#8441=EDGE_CURVE('',#5991,#5990,#4208,.T.);
#8442=EDGE_CURVE('',#5992,#5989,#4209,.T.);
#8443=EDGE_CURVE('',#5996,#6014,#3452,.T.);
#8444=EDGE_CURVE('',#6015,#6014,#3453,.T.);
#8445=EDGE_CURVE('',#5998,#6015,#3454,.T.);
#8446=EDGE_CURVE('',#6016,#6000,#4210,.T.);
#8447=EDGE_CURVE('',#6017,#6016,#3455,.T.);
#8448=EDGE_CURVE('',#6014,#6017,#4211,.T.);
#8449=EDGE_CURVE('',#6018,#6018,#4212,.T.);
#8450=EDGE_CURVE('',#6018,#6019,#3456,.T.);
#8451=EDGE_CURVE('',#6019,#6019,#4213,.T.);
#8452=EDGE_CURVE('',#6020,#6021,#3457,.T.);
#8453=EDGE_CURVE('',#6020,#6017,#3458,.T.);
#8454=EDGE_CURVE('',#6021,#6016,#3459,.T.);
#8455=EDGE_CURVE('',#6015,#6020,#4214,.T.);
#8456=EDGE_CURVE('',#6021,#5999,#4215,.T.);
#8457=EDGE_CURVE('',#6022,#6023,#3460,.T.);
#8458=EDGE_CURVE('',#6023,#6024,#1675,.T.);
#8459=EDGE_CURVE('',#6024,#6025,#1676,.T.);
#8460=EDGE_CURVE('',#6026,#6025,#1677,.T.);
#8461=EDGE_CURVE('',#6027,#6026,#1678,.T.);
#8462=EDGE_CURVE('',#6022,#6027,#1679,.T.);
#8463=EDGE_CURVE('',#6028,#6029,#3461,.T.);
#8464=EDGE_CURVE('',#6029,#6030,#1680,.T.);
#8465=EDGE_CURVE('',#6030,#6023,#1681,.T.);
#8466=EDGE_CURVE('',#6031,#6022,#1682,.T.);
#8467=EDGE_CURVE('',#6028,#6031,#1683,.T.);
#8468=EDGE_CURVE('',#6032,#6033,#3462,.T.);
#8469=EDGE_CURVE('',#6033,#6034,#1684,.T.);
#8470=EDGE_CURVE('',#6034,#6029,#1685,.T.);
#8471=EDGE_CURVE('',#6035,#6028,#1686,.T.);
#8472=EDGE_CURVE('',#6032,#6035,#1687,.T.);
#8473=EDGE_CURVE('',#6036,#6037,#3463,.T.);
#8474=EDGE_CURVE('',#6037,#6038,#1688,.T.);
#8475=EDGE_CURVE('',#6038,#6033,#1689,.T.);
#8476=EDGE_CURVE('',#6039,#6032,#1690,.T.);
#8477=EDGE_CURVE('',#6036,#6039,#1691,.T.);
#8478=EDGE_CURVE('',#6040,#6041,#3464,.T.);
#8479=EDGE_CURVE('',#6041,#6042,#1692,.T.);
#8480=EDGE_CURVE('',#6042,#6037,#1693,.T.);
#8481=EDGE_CURVE('',#6043,#6036,#1694,.T.);
#8482=EDGE_CURVE('',#6040,#6043,#1695,.T.);
#8483=EDGE_CURVE('',#6044,#6045,#3465,.T.);
#8484=EDGE_CURVE('',#6045,#6046,#1696,.T.);
#8485=EDGE_CURVE('',#6046,#6041,#1697,.T.);
#8486=EDGE_CURVE('',#6047,#6040,#1698,.T.);
#8487=EDGE_CURVE('',#6044,#6047,#1699,.T.);
#8488=EDGE_CURVE('',#6048,#6049,#3466,.T.);
#8489=EDGE_CURVE('',#6049,#6050,#1700,.T.);
#8490=EDGE_CURVE('',#6050,#6045,#1701,.T.);
#8491=EDGE_CURVE('',#6051,#6044,#1702,.T.);
#8492=EDGE_CURVE('',#6048,#6051,#1703,.T.);
#8493=EDGE_CURVE('',#6052,#6053,#3467,.T.);
#8494=EDGE_CURVE('',#6053,#6054,#1704,.T.);
#8495=EDGE_CURVE('',#6054,#6049,#1705,.T.);
#8496=EDGE_CURVE('',#6055,#6048,#1706,.T.);
#8497=EDGE_CURVE('',#6052,#6055,#1707,.T.);
#8498=EDGE_CURVE('',#6056,#6057,#3468,.T.);
#8499=EDGE_CURVE('',#6057,#6058,#1708,.T.);
#8500=EDGE_CURVE('',#6058,#6053,#1709,.T.);
#8501=EDGE_CURVE('',#6059,#6052,#1710,.T.);
#8502=EDGE_CURVE('',#6056,#6059,#1711,.T.);
#8503=EDGE_CURVE('',#6060,#6061,#3469,.T.);
#8504=EDGE_CURVE('',#6061,#6062,#1712,.T.);
#8505=EDGE_CURVE('',#6062,#6057,#1713,.T.);
#8506=EDGE_CURVE('',#6063,#6056,#1714,.T.);
#8507=EDGE_CURVE('',#6060,#6063,#1715,.T.);
#8508=EDGE_CURVE('',#6064,#6065,#3470,.T.);
#8509=EDGE_CURVE('',#6065,#6066,#1716,.T.);
#8510=EDGE_CURVE('',#6066,#6061,#1717,.T.);
#8511=EDGE_CURVE('',#6067,#6060,#1718,.T.);
#8512=EDGE_CURVE('',#6064,#6067,#1719,.T.);
#8513=EDGE_CURVE('',#6068,#6069,#3471,.T.);
#8514=EDGE_CURVE('',#6069,#6070,#1720,.T.);
#8515=EDGE_CURVE('',#6070,#6065,#1721,.T.);
#8516=EDGE_CURVE('',#6071,#6064,#1722,.T.);
#8517=EDGE_CURVE('',#6068,#6071,#1723,.T.);
#8518=EDGE_CURVE('',#6072,#6073,#3472,.T.);
#8519=EDGE_CURVE('',#6073,#6074,#1724,.T.);
#8520=EDGE_CURVE('',#6074,#6069,#1725,.T.);
#8521=EDGE_CURVE('',#6075,#6068,#1726,.T.);
#8522=EDGE_CURVE('',#6072,#6075,#1727,.T.);
#8523=EDGE_CURVE('',#6076,#6077,#3473,.T.);
#8524=EDGE_CURVE('',#6077,#6078,#1728,.T.);
#8525=EDGE_CURVE('',#6078,#6073,#1729,.T.);
#8526=EDGE_CURVE('',#6079,#6072,#1730,.T.);
#8527=EDGE_CURVE('',#6076,#6079,#1731,.T.);
#8528=EDGE_CURVE('',#6080,#6081,#3474,.T.);
#8529=EDGE_CURVE('',#6081,#6082,#1732,.T.);
#8530=EDGE_CURVE('',#6082,#6077,#1733,.T.);
#8531=EDGE_CURVE('',#6083,#6076,#1734,.T.);
#8532=EDGE_CURVE('',#6080,#6083,#1735,.T.);
#8533=EDGE_CURVE('',#6084,#6085,#3475,.T.);
#8534=EDGE_CURVE('',#6085,#6086,#1736,.T.);
#8535=EDGE_CURVE('',#6086,#6081,#1737,.T.);
#8536=EDGE_CURVE('',#6087,#6080,#1738,.T.);
#8537=EDGE_CURVE('',#6084,#6087,#1739,.T.);
#8538=EDGE_CURVE('',#6088,#6089,#3476,.T.);
#8539=EDGE_CURVE('',#6090,#6088,#1740,.T.);
#8540=EDGE_CURVE('',#6091,#6090,#1741,.T.);
#8541=EDGE_CURVE('',#6091,#6089,#1742,.T.);
#8542=EDGE_CURVE('',#6092,#6026,#1743,.T.);
#8543=EDGE_CURVE('',#6092,#6093,#1744,.T.);
#8544=EDGE_CURVE('',#6093,#6094,#1745,.T.);
#8545=EDGE_CURVE('',#6094,#6095,#1746,.T.);
#8546=EDGE_CURVE('',#6095,#6096,#1747,.T.);
#8547=EDGE_CURVE('',#6096,#6097,#1748,.T.);
#8548=EDGE_CURVE('',#6097,#6098,#1749,.T.);
#8549=EDGE_CURVE('',#6098,#6099,#1750,.T.);
#8550=EDGE_CURVE('',#6099,#6100,#1751,.T.);
#8551=EDGE_CURVE('',#6100,#6101,#1752,.T.);
#8552=EDGE_CURVE('',#6101,#6102,#1753,.T.);
#8553=EDGE_CURVE('',#6102,#6103,#1754,.T.);
#8554=EDGE_CURVE('',#6103,#6104,#1755,.T.);
#8555=EDGE_CURVE('',#6104,#6105,#1756,.T.);
#8556=EDGE_CURVE('',#6105,#6106,#1757,.T.);
#8557=EDGE_CURVE('',#6106,#6107,#1758,.T.);
#8558=EDGE_CURVE('',#6107,#6108,#1759,.T.);
#8559=EDGE_CURVE('',#6108,#6109,#1760,.T.);
#8560=EDGE_CURVE('',#6110,#6109,#1761,.T.);
#8561=EDGE_CURVE('',#6110,#6111,#1762,.T.);
#8562=EDGE_CURVE('',#6111,#6112,#1763,.T.);
#8563=EDGE_CURVE('',#6090,#6112,#1764,.T.);
#8564=EDGE_CURVE('',#6088,#6113,#1765,.T.);
#8565=EDGE_CURVE('',#6113,#6084,#1766,.T.);
#8566=EDGE_CURVE('',#6114,#6115,#1767,.T.);
#8567=EDGE_CURVE('',#6114,#6116,#1768,.T.);
#8568=EDGE_CURVE('',#6116,#6117,#1769,.T.);
#8569=EDGE_CURVE('',#6115,#6117,#1770,.T.);
#8570=EDGE_CURVE('',#6118,#6092,#1771,.T.);
#8571=EDGE_CURVE('',#6119,#6118,#1772,.T.);
#8572=EDGE_CURVE('',#6120,#6119,#1773,.T.);
#8573=EDGE_CURVE('',#6121,#6120,#1774,.T.);
#8574=EDGE_CURVE('',#6122,#6121,#1775,.T.);
#8575=EDGE_CURVE('',#6123,#6122,#1776,.T.);
#8576=EDGE_CURVE('',#6124,#6123,#1777,.T.);
#8577=EDGE_CURVE('',#6125,#6124,#1778,.T.);
#8578=EDGE_CURVE('',#6126,#6125,#1779,.T.);
#8579=EDGE_CURVE('',#6127,#6126,#1780,.T.);
#8580=EDGE_CURVE('',#6128,#6127,#1781,.T.);
#8581=EDGE_CURVE('',#6129,#6128,#1782,.T.);
#8582=EDGE_CURVE('',#6130,#6129,#1783,.T.);
#8583=EDGE_CURVE('',#6131,#6130,#1784,.T.);
#8584=EDGE_CURVE('',#6132,#6131,#1785,.T.);
#8585=EDGE_CURVE('',#6133,#6132,#1786,.T.);
#8586=EDGE_CURVE('',#6134,#6133,#1787,.T.);
#8587=EDGE_CURVE('',#6135,#6134,#1788,.T.);
#8588=EDGE_CURVE('',#6109,#6135,#1789,.T.);
#8589=EDGE_CURVE('',#6112,#6136,#1790,.T.);
#8590=EDGE_CURVE('',#6137,#6110,#1791,.T.);
#8591=EDGE_CURVE('',#6138,#6137,#1792,.T.);
#8592=EDGE_CURVE('',#6136,#6138,#1793,.T.);
#8593=EDGE_CURVE('',#6136,#6137,#1794,.T.);
#8594=EDGE_CURVE('',#6139,#6140,#1795,.T.);
#8595=EDGE_CURVE('',#6141,#6139,#1796,.T.);
#8596=EDGE_CURVE('',#6141,#6140,#1797,.T.);
#8597=EDGE_CURVE('',#6142,#6114,#1798,.T.);
#8598=EDGE_CURVE('',#6143,#6142,#1799,.T.);
#8599=EDGE_CURVE('',#6144,#6143,#1800,.T.);
#8600=EDGE_CURVE('',#6117,#6144,#1801,.T.);
#8601=EDGE_CURVE('',#6089,#6145,#1802,.T.);
#8602=EDGE_CURVE('',#6145,#6085,#1803,.T.);
#8603=EDGE_CURVE('',#6025,#6146,#1804,.T.);
#8604=EDGE_CURVE('',#6140,#6091,#1805,.T.);
#8605=EDGE_CURVE('',#6135,#6141,#1806,.T.);
#8606=EDGE_CURVE('',#6144,#6118,#1807,.T.);
#8607=EDGE_CURVE('',#6146,#6142,#1808,.T.);
#8608=EDGE_CURVE('',#6147,#6147,#4216,.T.);
#8609=EDGE_CURVE('',#6147,#6115,#3477,.T.);
#8610=EDGE_CURVE('',#6146,#6148,#3478,.T.);
#8611=EDGE_CURVE('',#6148,#6148,#4217,.T.);
#8612=EDGE_CURVE('',#6149,#6149,#4218,.T.);
#8613=EDGE_CURVE('',#6149,#6150,#3479,.T.);
#8614=EDGE_CURVE('',#6150,#6150,#4219,.T.);
#8615=EDGE_CURVE('',#6151,#6152,#3480,.T.);
#8616=EDGE_CURVE('',#6151,#6153,#3481,.T.);
#8617=EDGE_CURVE('',#6153,#6154,#3482,.T.);
#8618=EDGE_CURVE('',#6152,#6154,#3483,.T.);
#8619=EDGE_CURVE('',#6155,#6151,#4220,.T.);
#8620=EDGE_CURVE('',#6155,#6156,#3484,.T.);
#8621=EDGE_CURVE('',#6156,#6153,#4221,.T.);
#8622=EDGE_CURVE('',#6157,#6155,#3485,.T.);
#8623=EDGE_CURVE('',#6157,#6158,#3486,.T.);
#8624=EDGE_CURVE('',#6158,#6156,#3487,.T.);
#8625=EDGE_CURVE('',#6158,#6154,#4222,.T.);
#8626=EDGE_CURVE('',#6152,#6157,#4223,.T.);
#8627=EDGE_CURVE('',#6159,#6159,#4224,.T.);
#8628=EDGE_CURVE('',#6160,#6160,#4225,.T.);
#8629=EDGE_CURVE('',#6160,#6159,#3488,.T.);
#8630=EDGE_CURVE('',#6161,#6161,#4226,.T.);
#8631=EDGE_CURVE('',#6161,#6162,#3489,.T.);
#8632=EDGE_CURVE('',#6162,#6162,#4227,.T.);
#8633=EDGE_CURVE('',#6163,#6164,#3490,.T.);
#8634=EDGE_CURVE('',#6164,#6165,#3491,.T.);
#8635=EDGE_CURVE('',#6166,#6165,#3492,.T.);
#8636=EDGE_CURVE('',#6163,#6166,#3493,.T.);
#8637=EDGE_CURVE('',#6167,#6163,#4228,.T.);
#8638=EDGE_CURVE('',#6168,#6166,#4229,.T.);
#8639=EDGE_CURVE('',#6167,#6168,#3494,.T.);
#8640=EDGE_CURVE('',#6169,#6167,#3495,.T.);
#8641=EDGE_CURVE('',#6170,#6168,#3496,.T.);
#8642=EDGE_CURVE('',#6169,#6170,#3497,.T.);
#8643=EDGE_CURVE('',#6158,#6170,#3498,.T.);
#8644=EDGE_CURVE('',#6165,#6170,#4230,.T.);
#8645=EDGE_CURVE('',#6164,#6169,#4231,.T.);
#8646=EDGE_CURVE('',#6171,#6172,#4232,.T.);
#8647=EDGE_CURVE('',#6172,#6173,#3499,.T.);
#8648=EDGE_CURVE('',#6174,#6173,#4233,.T.);
#8649=EDGE_CURVE('',#6175,#6174,#3500,.T.);
#8650=EDGE_CURVE('',#6176,#6175,#4234,.T.);
#8651=EDGE_CURVE('',#6177,#6176,#3501,.T.);
#8652=EDGE_CURVE('',#6173,#6177,#4235,.T.);
#8653=EDGE_CURVE('',#6172,#6178,#4236,.T.);
#8654=EDGE_CURVE('',#6179,#6178,#3502,.T.);
#8655=EDGE_CURVE('',#6180,#6179,#4237,.T.);
#8656=EDGE_CURVE('',#6171,#6180,#3503,.T.);
#8657=EDGE_CURVE('',#6181,#6182,#4238,.T.);
#8658=EDGE_CURVE('',#6183,#6181,#3504,.T.);
#8659=EDGE_CURVE('',#6184,#6183,#4239,.T.);
#8660=EDGE_CURVE('',#6185,#6184,#3505,.T.);
#8661=EDGE_CURVE('',#6182,#6185,#4240,.T.);
#8662=EDGE_CURVE('',#6182,#6186,#3506,.T.);
#8663=EDGE_CURVE('',#6187,#6186,#4241,.T.);
#8664=EDGE_CURVE('',#6188,#6187,#3507,.T.);
#8665=EDGE_CURVE('',#6188,#6189,#4242,.T.);
#8666=EDGE_CURVE('',#6190,#6189,#3508,.T.);
#8667=EDGE_CURVE('',#6186,#6190,#4243,.T.);
#8668=EDGE_CURVE('',#6176,#6175,#4244,.T.);
#8669=EDGE_CURVE('',#6177,#6174,#4245,.T.);
#8670=EDGE_CURVE('',#6181,#6191,#3509,.T.);
#8671=EDGE_CURVE('',#6192,#6191,#3510,.T.);
#8672=EDGE_CURVE('',#6183,#6192,#3511,.T.);
#8673=EDGE_CURVE('',#6193,#6185,#4246,.T.);
#8674=EDGE_CURVE('',#6194,#6193,#3512,.T.);
#8675=EDGE_CURVE('',#6191,#6194,#4247,.T.);
#8676=EDGE_CURVE('',#6195,#6195,#4248,.T.);
#8677=EDGE_CURVE('',#6195,#6196,#3513,.T.);
#8678=EDGE_CURVE('',#6196,#6196,#4249,.T.);
#8679=EDGE_CURVE('',#6197,#6198,#3514,.T.);
#8680=EDGE_CURVE('',#6197,#6194,#3515,.T.);
#8681=EDGE_CURVE('',#6198,#6193,#3516,.T.);
#8682=EDGE_CURVE('',#6192,#6197,#4250,.T.);
#8683=EDGE_CURVE('',#6198,#6184,#4251,.T.);
#8684=EDGE_CURVE('',#6178,#6171,#4252,.T.);
#8685=EDGE_CURVE('',#6179,#6180,#4253,.T.);
#8686=EDGE_CURVE('',#6199,#6188,#4254,.T.);
#8687=EDGE_CURVE('',#6200,#6199,#3517,.T.);
#8688=EDGE_CURVE('',#6201,#6200,#4255,.T.);
#8689=EDGE_CURVE('',#6189,#6201,#3518,.T.);
#8690=EDGE_CURVE('',#6202,#6202,#4256,.T.);
#8691=EDGE_CURVE('',#6190,#6203,#3519,.T.);
#8692=EDGE_CURVE('',#6203,#6204,#4257,.T.);
#8693=EDGE_CURVE('',#6204,#6205,#3520,.T.);
#8694=EDGE_CURVE('',#6205,#6187,#4258,.T.);
#8695=EDGE_CURVE('',#6206,#6206,#4259,.T.);
#8696=EDGE_CURVE('',#6202,#6206,#3521,.T.);
#8697=EDGE_CURVE('',#6199,#6205,#3522,.T.);
#8698=EDGE_CURVE('',#6200,#6204,#3523,.T.);
#8699=EDGE_CURVE('',#6201,#6203,#3524,.T.);
#8700=EDGE_CURVE('',#6207,#6208,#4260,.T.);
#8701=EDGE_CURVE('',#6209,#6207,#3525,.T.);
#8702=EDGE_CURVE('',#6210,#6209,#4261,.T.);
#8703=EDGE_CURVE('',#6208,#6210,#3526,.T.);
#8704=EDGE_CURVE('',#6211,#6211,#4262,.T.);
#8705=EDGE_CURVE('',#6211,#6212,#3527,.T.);
#8706=EDGE_CURVE('',#6212,#6212,#4263,.T.);
#8707=EDGE_CURVE('',#6213,#6214,#3528,.T.);
#8708=EDGE_CURVE('',#6213,#6215,#3529,.T.);
#8709=EDGE_CURVE('',#6215,#6216,#3530,.T.);
#8710=EDGE_CURVE('',#6214,#6216,#3531,.T.);
#8711=EDGE_CURVE('',#6217,#6218,#4264,.T.);
#8712=EDGE_CURVE('',#6218,#6219,#3532,.T.);
#8713=EDGE_CURVE('',#6219,#6220,#4265,.T.);
#8714=EDGE_CURVE('',#6220,#6217,#3533,.T.);
#8715=EDGE_CURVE('',#6218,#6208,#3534,.T.);
#8716=EDGE_CURVE('',#6219,#6210,#3535,.T.);
#8717=EDGE_CURVE('',#6221,#6222,#3536,.T.);
#8718=EDGE_CURVE('',#6222,#6223,#4266,.T.);
#8719=EDGE_CURVE('',#6223,#6224,#3537,.T.);
#8720=EDGE_CURVE('',#6221,#6224,#4267,.T.);
#8721=EDGE_CURVE('',#6221,#6213,#3538,.T.);
#8722=EDGE_CURVE('',#6214,#6225,#3539,.T.);
#8723=EDGE_CURVE('',#6226,#6225,#3540,.T.);
#8724=EDGE_CURVE('',#6222,#6226,#3541,.T.);
#8725=EDGE_CURVE('',#6227,#6227,#4268,.T.);
#8726=EDGE_CURVE('',#6228,#6229,#4269,.T.);
#8727=EDGE_CURVE('',#6229,#6230,#3542,.T.);
#8728=EDGE_CURVE('',#6231,#6230,#4270,.T.);
#8729=EDGE_CURVE('',#6231,#6228,#3543,.T.);
#8730=EDGE_CURVE('',#6229,#6232,#3544,.T.);
#8731=EDGE_CURVE('',#6232,#6233,#3545,.T.);
#8732=EDGE_CURVE('',#6233,#6216,#3546,.T.);
#8733=EDGE_CURVE('',#6230,#6215,#3547,.T.);
#8734=EDGE_CURVE('',#6234,#6234,#4271,.T.);
#8735=EDGE_CURVE('',#6227,#6234,#3548,.T.);
#8736=EDGE_CURVE('',#6225,#6233,#3549,.T.);
#8737=EDGE_CURVE('',#6226,#6232,#3550,.T.);
#8738=EDGE_CURVE('',#6235,#6236,#4272,.T.);
#8739=EDGE_CURVE('',#6236,#6237,#3551,.T.);
#8740=EDGE_CURVE('',#6237,#6238,#4273,.T.);
#8741=EDGE_CURVE('',#6238,#6235,#3552,.T.);
#8742=EDGE_CURVE('',#6209,#6238,#3553,.T.);
#8743=EDGE_CURVE('',#6207,#6235,#3554,.T.);
#8744=EDGE_CURVE('',#6239,#6240,#4274,.T.);
#8745=EDGE_CURVE('',#6231,#6239,#3555,.T.);
#8746=EDGE_CURVE('',#6241,#6224,#3556,.T.);
#8747=EDGE_CURVE('',#6242,#6241,#4275,.T.);
#8748=EDGE_CURVE('',#6242,#6243,#3557,.T.);
#8749=EDGE_CURVE('',#6243,#6244,#3558,.T.);
#8750=EDGE_CURVE('',#6240,#6244,#3559,.T.);
#8751=EDGE_CURVE('',#6245,#6245,#4276,.T.);
#8752=EDGE_CURVE('',#6245,#6246,#3560,.T.);
#8753=EDGE_CURVE('',#6246,#6246,#4277,.T.);
#8754=EDGE_CURVE('',#6243,#6247,#3561,.T.);
#8755=EDGE_CURVE('',#6247,#6248,#3562,.T.);
#8756=EDGE_CURVE('',#6244,#6248,#3563,.T.);
#8757=EDGE_CURVE('',#6249,#6250,#4278,.T.);
#8758=EDGE_CURVE('',#6251,#6249,#3564,.T.);
#8759=EDGE_CURVE('',#6252,#6251,#4279,.T.);
#8760=EDGE_CURVE('',#6250,#6252,#3565,.T.);
#8761=EDGE_CURVE('',#6252,#6237,#3566,.T.);
#8762=EDGE_CURVE('',#6250,#6236,#3567,.T.);
#8763=EDGE_CURVE('',#6249,#6217,#3568,.T.);
#8764=EDGE_CURVE('',#6239,#6253,#3569,.T.);
#8765=EDGE_CURVE('',#6253,#6228,#3570,.T.);
#8766=EDGE_CURVE('',#6251,#6220,#3571,.T.);
#8767=EDGE_CURVE('',#6242,#6254,#3572,.T.);
#8768=EDGE_CURVE('',#6255,#6241,#3573,.T.);
#8769=EDGE_CURVE('',#6254,#6255,#4280,.T.);
#8770=EDGE_CURVE('',#6254,#6256,#3574,.T.);
#8771=EDGE_CURVE('',#6256,#6257,#3575,.T.);
#8772=EDGE_CURVE('',#6247,#6257,#3576,.T.);
#8773=EDGE_CURVE('',#6258,#6258,#4281,.T.);
#8774=EDGE_CURVE('',#6253,#6259,#4282,.T.);
#8775=EDGE_CURVE('',#6259,#6240,#3577,.T.);
#8776=EDGE_CURVE('',#6260,#6248,#3578,.T.);
#8777=EDGE_CURVE('',#6261,#6260,#3579,.T.);
#8778=EDGE_CURVE('',#6259,#6261,#3580,.T.);
#8779=EDGE_CURVE('',#6262,#6262,#4283,.T.);
#8780=EDGE_CURVE('',#6256,#6261,#3581,.T.);
#8781=EDGE_CURVE('',#6255,#6223,#3582,.T.);
#8782=EDGE_CURVE('',#6262,#6258,#3583,.T.);
#8783=EDGE_CURVE('',#6257,#6260,#3584,.T.);
#8784=EDGE_CURVE('',#6263,#6264,#3585,.T.);
#8785=EDGE_CURVE('',#6264,#6265,#1809,.T.);
#8786=EDGE_CURVE('',#6265,#6266,#1810,.T.);
#8787=EDGE_CURVE('',#6267,#6266,#1811,.T.);
#8788=EDGE_CURVE('',#6268,#6267,#1812,.T.);
#8789=EDGE_CURVE('',#6263,#6268,#1813,.T.);
#8790=EDGE_CURVE('',#6269,#6270,#3586,.T.);
#8791=EDGE_CURVE('',#6270,#6271,#1814,.T.);
#8792=EDGE_CURVE('',#6271,#6264,#1815,.T.);
#8793=EDGE_CURVE('',#6272,#6263,#1816,.T.);
#8794=EDGE_CURVE('',#6269,#6272,#1817,.T.);
#8795=EDGE_CURVE('',#6273,#6274,#3587,.T.);
#8796=EDGE_CURVE('',#6274,#6275,#1818,.T.);
#8797=EDGE_CURVE('',#6275,#6270,#1819,.T.);
#8798=EDGE_CURVE('',#6276,#6269,#1820,.T.);
#8799=EDGE_CURVE('',#6273,#6276,#1821,.T.);
#8800=EDGE_CURVE('',#6277,#6278,#3588,.T.);
#8801=EDGE_CURVE('',#6278,#6279,#1822,.T.);
#8802=EDGE_CURVE('',#6279,#6274,#1823,.T.);
#8803=EDGE_CURVE('',#6280,#6273,#1824,.T.);
#8804=EDGE_CURVE('',#6277,#6280,#1825,.T.);
#8805=EDGE_CURVE('',#6281,#6282,#3589,.T.);
#8806=EDGE_CURVE('',#6282,#6283,#1826,.T.);
#8807=EDGE_CURVE('',#6283,#6278,#1827,.T.);
#8808=EDGE_CURVE('',#6284,#6277,#1828,.T.);
#8809=EDGE_CURVE('',#6281,#6284,#1829,.T.);
#8810=EDGE_CURVE('',#6285,#6286,#3590,.T.);
#8811=EDGE_CURVE('',#6286,#6287,#1830,.T.);
#8812=EDGE_CURVE('',#6287,#6282,#1831,.T.);
#8813=EDGE_CURVE('',#6288,#6281,#1832,.T.);
#8814=EDGE_CURVE('',#6285,#6288,#1833,.T.);
#8815=EDGE_CURVE('',#6289,#6290,#3591,.T.);
#8816=EDGE_CURVE('',#6290,#6291,#1834,.T.);
#8817=EDGE_CURVE('',#6291,#6286,#1835,.T.);
#8818=EDGE_CURVE('',#6292,#6285,#1836,.T.);
#8819=EDGE_CURVE('',#6289,#6292,#1837,.T.);
#8820=EDGE_CURVE('',#6293,#6294,#3592,.T.);
#8821=EDGE_CURVE('',#6294,#6295,#1838,.T.);
#8822=EDGE_CURVE('',#6295,#6290,#1839,.T.);
#8823=EDGE_CURVE('',#6296,#6289,#1840,.T.);
#8824=EDGE_CURVE('',#6293,#6296,#1841,.T.);
#8825=EDGE_CURVE('',#6297,#6298,#3593,.T.);
#8826=EDGE_CURVE('',#6298,#6299,#1842,.T.);
#8827=EDGE_CURVE('',#6299,#6294,#1843,.T.);
#8828=EDGE_CURVE('',#6300,#6293,#1844,.T.);
#8829=EDGE_CURVE('',#6297,#6300,#1845,.T.);
#8830=EDGE_CURVE('',#6301,#6302,#3594,.T.);
#8831=EDGE_CURVE('',#6302,#6303,#1846,.T.);
#8832=EDGE_CURVE('',#6303,#6298,#1847,.T.);
#8833=EDGE_CURVE('',#6304,#6297,#1848,.T.);
#8834=EDGE_CURVE('',#6301,#6304,#1849,.T.);
#8835=EDGE_CURVE('',#6305,#6306,#3595,.T.);
#8836=EDGE_CURVE('',#6306,#6307,#1850,.T.);
#8837=EDGE_CURVE('',#6307,#6302,#1851,.T.);
#8838=EDGE_CURVE('',#6308,#6301,#1852,.T.);
#8839=EDGE_CURVE('',#6305,#6308,#1853,.T.);
#8840=EDGE_CURVE('',#6309,#6310,#3596,.T.);
#8841=EDGE_CURVE('',#6310,#6311,#1854,.T.);
#8842=EDGE_CURVE('',#6311,#6306,#1855,.T.);
#8843=EDGE_CURVE('',#6312,#6305,#1856,.T.);
#8844=EDGE_CURVE('',#6309,#6312,#1857,.T.);
#8845=EDGE_CURVE('',#6313,#6314,#3597,.T.);
#8846=EDGE_CURVE('',#6314,#6315,#1858,.T.);
#8847=EDGE_CURVE('',#6315,#6310,#1859,.T.);
#8848=EDGE_CURVE('',#6316,#6309,#1860,.T.);
#8849=EDGE_CURVE('',#6313,#6316,#1861,.T.);
#8850=EDGE_CURVE('',#6317,#6318,#3598,.T.);
#8851=EDGE_CURVE('',#6318,#6319,#1862,.T.);
#8852=EDGE_CURVE('',#6319,#6314,#1863,.T.);
#8853=EDGE_CURVE('',#6320,#6313,#1864,.T.);
#8854=EDGE_CURVE('',#6317,#6320,#1865,.T.);
#8855=EDGE_CURVE('',#6321,#6322,#3599,.T.);
#8856=EDGE_CURVE('',#6322,#6323,#1866,.T.);
#8857=EDGE_CURVE('',#6323,#6318,#1867,.T.);
#8858=EDGE_CURVE('',#6324,#6317,#1868,.T.);
#8859=EDGE_CURVE('',#6321,#6324,#1869,.T.);
#8860=EDGE_CURVE('',#6325,#6326,#3600,.T.);
#8861=EDGE_CURVE('',#6326,#6327,#1870,.T.);
#8862=EDGE_CURVE('',#6327,#6322,#1871,.T.);
#8863=EDGE_CURVE('',#6328,#6321,#1872,.T.);
#8864=EDGE_CURVE('',#6325,#6328,#1873,.T.);
#8865=EDGE_CURVE('',#6329,#6330,#3601,.T.);
#8866=EDGE_CURVE('',#6331,#6329,#1874,.T.);
#8867=EDGE_CURVE('',#6332,#6331,#1875,.T.);
#8868=EDGE_CURVE('',#6332,#6330,#1876,.T.);
#8869=EDGE_CURVE('',#6333,#6334,#1877,.T.);
#8870=EDGE_CURVE('',#6333,#6335,#1878,.T.);
#8871=EDGE_CURVE('',#6334,#6335,#1879,.T.);
#8872=EDGE_CURVE('',#6336,#6337,#1880,.T.);
#8873=EDGE_CURVE('',#6336,#6338,#1881,.T.);
#8874=EDGE_CURVE('',#6266,#6338,#1882,.T.);
#8875=EDGE_CURVE('',#6339,#6326,#1883,.T.);
#8876=EDGE_CURVE('',#6330,#6339,#1884,.T.);
#8877=EDGE_CURVE('',#6340,#6332,#1885,.T.);
#8878=EDGE_CURVE('',#6340,#6341,#1886,.T.);
#8879=EDGE_CURVE('',#6341,#6342,#1887,.T.);
#8880=EDGE_CURVE('',#6342,#6343,#1888,.T.);
#8881=EDGE_CURVE('',#6343,#6344,#1889,.T.);
#8882=EDGE_CURVE('',#6344,#6345,#1890,.T.);
#8883=EDGE_CURVE('',#6345,#6346,#1891,.T.);
#8884=EDGE_CURVE('',#6346,#6347,#1892,.T.);
#8885=EDGE_CURVE('',#6347,#6348,#1893,.T.);
#8886=EDGE_CURVE('',#6348,#6349,#1894,.T.);
#8887=EDGE_CURVE('',#6349,#6350,#1895,.T.);
#8888=EDGE_CURVE('',#6350,#6351,#1896,.T.);
#8889=EDGE_CURVE('',#6351,#6352,#1897,.T.);
#8890=EDGE_CURVE('',#6352,#6353,#1898,.T.);
#8891=EDGE_CURVE('',#6353,#6354,#1899,.T.);
#8892=EDGE_CURVE('',#6354,#6355,#1900,.T.);
#8893=EDGE_CURVE('',#6355,#6356,#1901,.T.);
#8894=EDGE_CURVE('',#6356,#6357,#1902,.T.);
#8895=EDGE_CURVE('',#6357,#6337,#1903,.T.);
#8896=EDGE_CURVE('',#6335,#6358,#1904,.T.);
#8897=EDGE_CURVE('',#6359,#6333,#1905,.T.);
#8898=EDGE_CURVE('',#6358,#6359,#1906,.T.);
#8899=EDGE_CURVE('',#6337,#6360,#1907,.T.);
#8900=EDGE_CURVE('',#6361,#6340,#1908,.T.);
#8901=EDGE_CURVE('',#6362,#6361,#1909,.T.);
#8902=EDGE_CURVE('',#6363,#6362,#1910,.T.);
#8903=EDGE_CURVE('',#6364,#6363,#1911,.T.);
#8904=EDGE_CURVE('',#6365,#6364,#1912,.T.);
#8905=EDGE_CURVE('',#6366,#6365,#1913,.T.);
#8906=EDGE_CURVE('',#6367,#6366,#1914,.T.);
#8907=EDGE_CURVE('',#6368,#6367,#1915,.T.);
#8908=EDGE_CURVE('',#6369,#6368,#1916,.T.);
#8909=EDGE_CURVE('',#6370,#6369,#1917,.T.);
#8910=EDGE_CURVE('',#6371,#6370,#1918,.T.);
#8911=EDGE_CURVE('',#6372,#6371,#1919,.T.);
#8912=EDGE_CURVE('',#6373,#6372,#1920,.T.);
#8913=EDGE_CURVE('',#6374,#6373,#1921,.T.);
#8914=EDGE_CURVE('',#6375,#6374,#1922,.T.);
#8915=EDGE_CURVE('',#6376,#6375,#1923,.T.);
#8916=EDGE_CURVE('',#6377,#6376,#1924,.T.);
#8917=EDGE_CURVE('',#6378,#6377,#1925,.T.);
#8918=EDGE_CURVE('',#6360,#6378,#1926,.T.);
#8919=EDGE_CURVE('',#6379,#6325,#1927,.T.);
#8920=EDGE_CURVE('',#6329,#6379,#1928,.T.);
#8921=EDGE_CURVE('',#6380,#6381,#1929,.T.);
#8922=EDGE_CURVE('',#6382,#6380,#1930,.T.);
#8923=EDGE_CURVE('',#6383,#6382,#1931,.T.);
#8924=EDGE_CURVE('',#6381,#6383,#1932,.T.);
#8925=EDGE_CURVE('',#6360,#6380,#1933,.T.);
#8926=EDGE_CURVE('',#6358,#6361,#1934,.T.);
#8927=EDGE_CURVE('',#6384,#6359,#1935,.T.);
#8928=EDGE_CURVE('',#6331,#6384,#1936,.T.);
#8929=EDGE_CURVE('',#6383,#6267,#1937,.T.);
#8930=EDGE_CURVE('',#6385,#6336,#1938,.T.);
#8931=EDGE_CURVE('',#6386,#6385,#1939,.T.);
#8932=EDGE_CURVE('',#6338,#6386,#1940,.T.);
#8933=EDGE_CURVE('',#6386,#6385,#1941,.T.);
#8934=EDGE_CURVE('',#6387,#6387,#4284,.T.);
#8935=EDGE_CURVE('',#6387,#6334,#3602,.T.);
#8936=EDGE_CURVE('',#6384,#6388,#3603,.T.);
#8937=EDGE_CURVE('',#6388,#6388,#4285,.T.);
#8938=EDGE_CURVE('',#6389,#6389,#4286,.T.);
#8939=EDGE_CURVE('',#6389,#6390,#3604,.T.);
#8940=EDGE_CURVE('',#6390,#6390,#4287,.T.);
#8941=EDGE_CURVE('',#6391,#6392,#3605,.T.);
#8942=EDGE_CURVE('',#6392,#6393,#3606,.T.);
#8943=EDGE_CURVE('',#6394,#6393,#3607,.T.);
#8944=EDGE_CURVE('',#6391,#6394,#3608,.T.);
#8945=EDGE_CURVE('',#6395,#6391,#4288,.T.);
#8946=EDGE_CURVE('',#6396,#6394,#4289,.T.);
#8947=EDGE_CURVE('',#6395,#6396,#3609,.T.);
#8948=EDGE_CURVE('',#6397,#6395,#3610,.T.);
#8949=EDGE_CURVE('',#6398,#6396,#3611,.T.);
#8950=EDGE_CURVE('',#6397,#6398,#3612,.T.);
#8951=EDGE_CURVE('',#6393,#6398,#4290,.T.);
#8952=EDGE_CURVE('',#6392,#6397,#4291,.T.);
#8953=EDGE_CURVE('',#6399,#6399,#4292,.T.);
#8954=EDGE_CURVE('',#6399,#6400,#3613,.T.);
#8955=EDGE_CURVE('',#6400,#6400,#4293,.T.);
#8956=EDGE_CURVE('',#6401,#6401,#4294,.T.);
#8957=EDGE_CURVE('',#6401,#6402,#3614,.T.);
#8958=EDGE_CURVE('',#6402,#6402,#4295,.T.);
#8959=EDGE_CURVE('',#6403,#6404,#3615,.T.);
#8960=EDGE_CURVE('',#6403,#6405,#3616,.T.);
#8961=EDGE_CURVE('',#6405,#6406,#3617,.T.);
#8962=EDGE_CURVE('',#6404,#6406,#3618,.T.);
#8963=EDGE_CURVE('',#6407,#6403,#4296,.T.);
#8964=EDGE_CURVE('',#6407,#6408,#3619,.T.);
#8965=EDGE_CURVE('',#6408,#6405,#4297,.T.);
#8966=EDGE_CURVE('',#6409,#6407,#3620,.T.);
#8967=EDGE_CURVE('',#6409,#6410,#3621,.T.);
#8968=EDGE_CURVE('',#6410,#6408,#3622,.T.);
#8969=EDGE_CURVE('',#6404,#6409,#4298,.T.);
#8970=EDGE_CURVE('',#6410,#6406,#4299,.T.);
#8971=EDGE_CURVE('',#6410,#6398,#3623,.T.);
#8972=ORIENTED_EDGE('',*,*,#6411,.T.);
#8973=ORIENTED_EDGE('',*,*,#6412,.T.);
#8974=ORIENTED_EDGE('',*,*,#6413,.T.);
#8975=ORIENTED_EDGE('',*,*,#6414,.T.);
#8976=ORIENTED_EDGE('',*,*,#6415,.T.);
#8977=ORIENTED_EDGE('',*,*,#6416,.T.);
#8978=ORIENTED_EDGE('',*,*,#6417,.F.);
#8979=ORIENTED_EDGE('',*,*,#6416,.F.);
#8980=ORIENTED_EDGE('',*,*,#6418,.T.);
#8981=ORIENTED_EDGE('',*,*,#6419,.T.);
#8982=ORIENTED_EDGE('',*,*,#6420,.F.);
#8983=ORIENTED_EDGE('',*,*,#6421,.F.);
#8984=ORIENTED_EDGE('',*,*,#6422,.F.);
#8985=ORIENTED_EDGE('',*,*,#6423,.F.);
#8986=ORIENTED_EDGE('',*,*,#6424,.F.);
#8987=ORIENTED_EDGE('',*,*,#6425,.F.);
#8988=ORIENTED_EDGE('',*,*,#6425,.T.);
#8989=ORIENTED_EDGE('',*,*,#6426,.T.);
#8990=ORIENTED_EDGE('',*,*,#6412,.F.);
#8991=ORIENTED_EDGE('',*,*,#6427,.F.);
#8992=ORIENTED_EDGE('',*,*,#6428,.F.);
#8993=ORIENTED_EDGE('',*,*,#6429,.T.);
#8994=ORIENTED_EDGE('',*,*,#6430,.F.);
#8995=ORIENTED_EDGE('',*,*,#6431,.F.);
#8996=ORIENTED_EDGE('',*,*,#6428,.T.);
#8997=ORIENTED_EDGE('',*,*,#6432,.T.);
#8998=ORIENTED_EDGE('',*,*,#6433,.T.);
#8999=ORIENTED_EDGE('',*,*,#6434,.F.);
#9000=ORIENTED_EDGE('',*,*,#6418,.F.);
#9001=ORIENTED_EDGE('',*,*,#6435,.F.);
#9002=ORIENTED_EDGE('',*,*,#6415,.F.);
#9003=ORIENTED_EDGE('',*,*,#6436,.T.);
#9004=ORIENTED_EDGE('',*,*,#6437,.F.);
#9005=ORIENTED_EDGE('',*,*,#6438,.F.);
#9006=ORIENTED_EDGE('',*,*,#6439,.T.);
#9007=ORIENTED_EDGE('',*,*,#6440,.F.);
#9008=ORIENTED_EDGE('',*,*,#6440,.T.);
#9009=ORIENTED_EDGE('',*,*,#6441,.T.);
#9010=ORIENTED_EDGE('',*,*,#6420,.T.);
#9011=ORIENTED_EDGE('',*,*,#6442,.F.);
#9012=ORIENTED_EDGE('',*,*,#6443,.F.);
#9013=ORIENTED_EDGE('',*,*,#6444,.F.);
#9014=ORIENTED_EDGE('',*,*,#6417,.T.);
#9015=ORIENTED_EDGE('',*,*,#6445,.F.);
#9016=ORIENTED_EDGE('',*,*,#6445,.T.);
#9017=ORIENTED_EDGE('',*,*,#6446,.T.);
#9018=ORIENTED_EDGE('',*,*,#6436,.F.);
#9019=ORIENTED_EDGE('',*,*,#6446,.F.);
#9020=ORIENTED_EDGE('',*,*,#6434,.T.);
#9021=ORIENTED_EDGE('',*,*,#6447,.T.);
#9022=ORIENTED_EDGE('',*,*,#6442,.T.);
#9023=ORIENTED_EDGE('',*,*,#6419,.F.);
#9024=ORIENTED_EDGE('',*,*,#6433,.F.);
#9025=ORIENTED_EDGE('',*,*,#6448,.T.);
#9026=ORIENTED_EDGE('',*,*,#6443,.T.);
#9027=ORIENTED_EDGE('',*,*,#6447,.F.);
#9028=ORIENTED_EDGE('',*,*,#6449,.F.);
#9029=ORIENTED_EDGE('',*,*,#6450,.F.);
#9030=ORIENTED_EDGE('',*,*,#6451,.F.);
#9031=ORIENTED_EDGE('',*,*,#6452,.F.);
#9032=ORIENTED_EDGE('',*,*,#6450,.T.);
#9033=ORIENTED_EDGE('',*,*,#6453,.F.);
#9034=ORIENTED_EDGE('',*,*,#6414,.F.);
#9035=ORIENTED_EDGE('',*,*,#6454,.T.);
#9036=ORIENTED_EDGE('',*,*,#6455,.T.);
#9037=ORIENTED_EDGE('',*,*,#6456,.T.);
#9038=ORIENTED_EDGE('',*,*,#6457,.F.);
#9039=ORIENTED_EDGE('',*,*,#6458,.F.);
#9040=ORIENTED_EDGE('',*,*,#6459,.T.);
#9041=ORIENTED_EDGE('',*,*,#6460,.T.);
#9042=ORIENTED_EDGE('',*,*,#6429,.F.);
#9043=ORIENTED_EDGE('',*,*,#6435,.T.);
#9044=ORIENTED_EDGE('',*,*,#6421,.T.);
#9045=ORIENTED_EDGE('',*,*,#6441,.F.);
#9046=ORIENTED_EDGE('',*,*,#6439,.F.);
#9047=ORIENTED_EDGE('',*,*,#6461,.T.);
#9048=ORIENTED_EDGE('',*,*,#6462,.T.);
#9049=ORIENTED_EDGE('',*,*,#6463,.T.);
#9050=ORIENTED_EDGE('',*,*,#6464,.F.);
#9051=ORIENTED_EDGE('',*,*,#6463,.F.);
#9052=ORIENTED_EDGE('',*,*,#6465,.F.);
#9053=ORIENTED_EDGE('',*,*,#6457,.T.);
#9054=ORIENTED_EDGE('',*,*,#6466,.T.);
#9055=ORIENTED_EDGE('',*,*,#6467,.F.);
#9056=ORIENTED_EDGE('',*,*,#6468,.T.);
#9057=ORIENTED_EDGE('',*,*,#6469,.T.);
#9058=ORIENTED_EDGE('',*,*,#6470,.T.);
#9059=ORIENTED_EDGE('',*,*,#6471,.T.);
#9060=ORIENTED_EDGE('',*,*,#6469,.F.);
#9061=ORIENTED_EDGE('',*,*,#6472,.T.);
#9062=ORIENTED_EDGE('',*,*,#6452,.T.);
#9063=ORIENTED_EDGE('',*,*,#6473,.F.);
#9064=ORIENTED_EDGE('',*,*,#6453,.T.);
#9065=ORIENTED_EDGE('',*,*,#6449,.T.);
#9066=ORIENTED_EDGE('',*,*,#6472,.F.);
#9067=ORIENTED_EDGE('',*,*,#6468,.F.);
#9068=ORIENTED_EDGE('',*,*,#6474,.T.);
#9069=ORIENTED_EDGE('',*,*,#6422,.T.);
#9070=ORIENTED_EDGE('',*,*,#6427,.T.);
#9071=ORIENTED_EDGE('',*,*,#6411,.F.);
#9072=ORIENTED_EDGE('',*,*,#6461,.F.);
#9073=ORIENTED_EDGE('',*,*,#6438,.T.);
#9074=ORIENTED_EDGE('',*,*,#6475,.F.);
#9075=ORIENTED_EDGE('',*,*,#6476,.F.);
#9076=ORIENTED_EDGE('',*,*,#6471,.F.);
#9077=ORIENTED_EDGE('',*,*,#6477,.T.);
#9078=ORIENTED_EDGE('',*,*,#6423,.T.);
#9079=ORIENTED_EDGE('',*,*,#6474,.F.);
#9080=ORIENTED_EDGE('',*,*,#6470,.F.);
#9081=ORIENTED_EDGE('',*,*,#6473,.T.);
#9082=ORIENTED_EDGE('',*,*,#6451,.T.);
#9083=ORIENTED_EDGE('',*,*,#6454,.F.);
#9084=ORIENTED_EDGE('',*,*,#6413,.F.);
#9085=ORIENTED_EDGE('',*,*,#6426,.F.);
#9086=ORIENTED_EDGE('',*,*,#6424,.T.);
#9087=ORIENTED_EDGE('',*,*,#6477,.F.);
#9088=ORIENTED_EDGE('',*,*,#6478,.T.);
#9089=ORIENTED_EDGE('',*,*,#6479,.T.);
#9090=ORIENTED_EDGE('',*,*,#6480,.T.);
#9091=ORIENTED_EDGE('',*,*,#6459,.F.);
#9092=ORIENTED_EDGE('',*,*,#6478,.F.);
#9093=ORIENTED_EDGE('',*,*,#6458,.T.);
#9094=ORIENTED_EDGE('',*,*,#6465,.T.);
#9095=ORIENTED_EDGE('',*,*,#6481,.T.);
#9096=ORIENTED_EDGE('',*,*,#6482,.F.);
#9097=ORIENTED_EDGE('',*,*,#6483,.F.);
#9098=ORIENTED_EDGE('',*,*,#6464,.T.);
#9099=ORIENTED_EDGE('',*,*,#6484,.F.);
#9100=ORIENTED_EDGE('',*,*,#6485,.T.);
#9101=ORIENTED_EDGE('',*,*,#6486,.T.);
#9102=ORIENTED_EDGE('',*,*,#6455,.F.);
#9103=ORIENTED_EDGE('',*,*,#6476,.T.);
#9104=ORIENTED_EDGE('',*,*,#6486,.F.);
#9105=ORIENTED_EDGE('',*,*,#6487,.T.);
#9106=ORIENTED_EDGE('',*,*,#6488,.T.);
#9107=ORIENTED_EDGE('',*,*,#6489,.T.);
#9108=ORIENTED_EDGE('',*,*,#6466,.F.);
#9109=ORIENTED_EDGE('',*,*,#6456,.F.);
#9110=ORIENTED_EDGE('',*,*,#6462,.F.);
#9111=ORIENTED_EDGE('',*,*,#6490,.T.);
#9112=ORIENTED_EDGE('',*,*,#6485,.F.);
#9113=ORIENTED_EDGE('',*,*,#6475,.T.);
#9114=ORIENTED_EDGE('',*,*,#6437,.T.);
#9115=ORIENTED_EDGE('',*,*,#6444,.T.);
#9116=ORIENTED_EDGE('',*,*,#6448,.F.);
#9117=ORIENTED_EDGE('',*,*,#6432,.F.);
#9118=ORIENTED_EDGE('',*,*,#6431,.T.);
#9119=ORIENTED_EDGE('',*,*,#6491,.F.);
#9120=ORIENTED_EDGE('',*,*,#6479,.F.);
#9121=ORIENTED_EDGE('',*,*,#6483,.T.);
#9122=ORIENTED_EDGE('',*,*,#6492,.T.);
#9123=ORIENTED_EDGE('',*,*,#6487,.F.);
#9124=ORIENTED_EDGE('',*,*,#6484,.T.);
#9125=ORIENTED_EDGE('',*,*,#6493,.T.);
#9126=ORIENTED_EDGE('',*,*,#6490,.F.);
#9127=ORIENTED_EDGE('',*,*,#6493,.F.);
#9128=ORIENTED_EDGE('',*,*,#6481,.F.);
#9129=ORIENTED_EDGE('',*,*,#6467,.T.);
#9130=ORIENTED_EDGE('',*,*,#6489,.F.);
#9131=ORIENTED_EDGE('',*,*,#6494,.F.);
#9132=ORIENTED_EDGE('',*,*,#6482,.T.);
#9133=ORIENTED_EDGE('',*,*,#6494,.T.);
#9134=ORIENTED_EDGE('',*,*,#6488,.F.);
#9135=ORIENTED_EDGE('',*,*,#6492,.F.);
#9136=ORIENTED_EDGE('',*,*,#6480,.F.);
#9137=ORIENTED_EDGE('',*,*,#6491,.T.);
#9138=ORIENTED_EDGE('',*,*,#6430,.T.);
#9139=ORIENTED_EDGE('',*,*,#6460,.F.);
#9140=ORIENTED_EDGE('',*,*,#6495,.F.);
#9141=ORIENTED_EDGE('',*,*,#6496,.F.);
#9142=ORIENTED_EDGE('',*,*,#6497,.F.);
#9143=ORIENTED_EDGE('',*,*,#6498,.T.);
#9144=ORIENTED_EDGE('',*,*,#6499,.F.);
#9145=ORIENTED_EDGE('',*,*,#6500,.F.);
#9146=ORIENTED_EDGE('',*,*,#6501,.F.);
#9147=ORIENTED_EDGE('',*,*,#6495,.T.);
#9148=ORIENTED_EDGE('',*,*,#6502,.T.);
#9149=ORIENTED_EDGE('',*,*,#6503,.T.);
#9150=ORIENTED_EDGE('',*,*,#6504,.F.);
#9151=ORIENTED_EDGE('',*,*,#6505,.F.);
#9152=ORIENTED_EDGE('',*,*,#6506,.F.);
#9153=ORIENTED_EDGE('',*,*,#6499,.T.);
#9154=ORIENTED_EDGE('',*,*,#6507,.T.);
#9155=ORIENTED_EDGE('',*,*,#6508,.T.);
#9156=ORIENTED_EDGE('',*,*,#6509,.F.);
#9157=ORIENTED_EDGE('',*,*,#6510,.F.);
#9158=ORIENTED_EDGE('',*,*,#6511,.F.);
#9159=ORIENTED_EDGE('',*,*,#6504,.T.);
#9160=ORIENTED_EDGE('',*,*,#6512,.T.);
#9161=ORIENTED_EDGE('',*,*,#6513,.T.);
#9162=ORIENTED_EDGE('',*,*,#6514,.F.);
#9163=ORIENTED_EDGE('',*,*,#6515,.F.);
#9164=ORIENTED_EDGE('',*,*,#6516,.F.);
#9165=ORIENTED_EDGE('',*,*,#6509,.T.);
#9166=ORIENTED_EDGE('',*,*,#6517,.T.);
#9167=ORIENTED_EDGE('',*,*,#6518,.T.);
#9168=ORIENTED_EDGE('',*,*,#6519,.F.);
#9169=ORIENTED_EDGE('',*,*,#6520,.F.);
#9170=ORIENTED_EDGE('',*,*,#6521,.F.);
#9171=ORIENTED_EDGE('',*,*,#6514,.T.);
#9172=ORIENTED_EDGE('',*,*,#6522,.T.);
#9173=ORIENTED_EDGE('',*,*,#6523,.T.);
#9174=ORIENTED_EDGE('',*,*,#6524,.F.);
#9175=ORIENTED_EDGE('',*,*,#6525,.F.);
#9176=ORIENTED_EDGE('',*,*,#6526,.F.);
#9177=ORIENTED_EDGE('',*,*,#6519,.T.);
#9178=ORIENTED_EDGE('',*,*,#6527,.T.);
#9179=ORIENTED_EDGE('',*,*,#6528,.T.);
#9180=ORIENTED_EDGE('',*,*,#6529,.F.);
#9181=ORIENTED_EDGE('',*,*,#6530,.F.);
#9182=ORIENTED_EDGE('',*,*,#6531,.F.);
#9183=ORIENTED_EDGE('',*,*,#6524,.T.);
#9184=ORIENTED_EDGE('',*,*,#6532,.T.);
#9185=ORIENTED_EDGE('',*,*,#6533,.T.);
#9186=ORIENTED_EDGE('',*,*,#6534,.F.);
#9187=ORIENTED_EDGE('',*,*,#6535,.F.);
#9188=ORIENTED_EDGE('',*,*,#6536,.F.);
#9189=ORIENTED_EDGE('',*,*,#6529,.T.);
#9190=ORIENTED_EDGE('',*,*,#6537,.T.);
#9191=ORIENTED_EDGE('',*,*,#6538,.T.);
#9192=ORIENTED_EDGE('',*,*,#6539,.F.);
#9193=ORIENTED_EDGE('',*,*,#6540,.F.);
#9194=ORIENTED_EDGE('',*,*,#6541,.F.);
#9195=ORIENTED_EDGE('',*,*,#6534,.T.);
#9196=ORIENTED_EDGE('',*,*,#6542,.T.);
#9197=ORIENTED_EDGE('',*,*,#6543,.T.);
#9198=ORIENTED_EDGE('',*,*,#6544,.F.);
#9199=ORIENTED_EDGE('',*,*,#6545,.F.);
#9200=ORIENTED_EDGE('',*,*,#6546,.F.);
#9201=ORIENTED_EDGE('',*,*,#6539,.T.);
#9202=ORIENTED_EDGE('',*,*,#6547,.T.);
#9203=ORIENTED_EDGE('',*,*,#6548,.T.);
#9204=ORIENTED_EDGE('',*,*,#6549,.F.);
#9205=ORIENTED_EDGE('',*,*,#6550,.F.);
#9206=ORIENTED_EDGE('',*,*,#6551,.F.);
#9207=ORIENTED_EDGE('',*,*,#6544,.T.);
#9208=ORIENTED_EDGE('',*,*,#6552,.T.);
#9209=ORIENTED_EDGE('',*,*,#6553,.T.);
#9210=ORIENTED_EDGE('',*,*,#6554,.F.);
#9211=ORIENTED_EDGE('',*,*,#6555,.F.);
#9212=ORIENTED_EDGE('',*,*,#6556,.F.);
#9213=ORIENTED_EDGE('',*,*,#6549,.T.);
#9214=ORIENTED_EDGE('',*,*,#6557,.T.);
#9215=ORIENTED_EDGE('',*,*,#6558,.T.);
#9216=ORIENTED_EDGE('',*,*,#6559,.F.);
#9217=ORIENTED_EDGE('',*,*,#6560,.F.);
#9218=ORIENTED_EDGE('',*,*,#6561,.F.);
#9219=ORIENTED_EDGE('',*,*,#6554,.T.);
#9220=ORIENTED_EDGE('',*,*,#6562,.T.);
#9221=ORIENTED_EDGE('',*,*,#6563,.T.);
#9222=ORIENTED_EDGE('',*,*,#6564,.F.);
#9223=ORIENTED_EDGE('',*,*,#6565,.F.);
#9224=ORIENTED_EDGE('',*,*,#6566,.F.);
#9225=ORIENTED_EDGE('',*,*,#6559,.T.);
#9226=ORIENTED_EDGE('',*,*,#6567,.T.);
#9227=ORIENTED_EDGE('',*,*,#6568,.T.);
#9228=ORIENTED_EDGE('',*,*,#6569,.F.);
#9229=ORIENTED_EDGE('',*,*,#6570,.F.);
#9230=ORIENTED_EDGE('',*,*,#6571,.F.);
#9231=ORIENTED_EDGE('',*,*,#6564,.T.);
#9232=ORIENTED_EDGE('',*,*,#6572,.T.);
#9233=ORIENTED_EDGE('',*,*,#6573,.T.);
#9234=ORIENTED_EDGE('',*,*,#6574,.F.);
#9235=ORIENTED_EDGE('',*,*,#6575,.F.);
#9236=ORIENTED_EDGE('',*,*,#6576,.F.);
#9237=ORIENTED_EDGE('',*,*,#6569,.T.);
#9238=ORIENTED_EDGE('',*,*,#6577,.T.);
#9239=ORIENTED_EDGE('',*,*,#6578,.T.);
#9240=ORIENTED_EDGE('',*,*,#6579,.F.);
#9241=ORIENTED_EDGE('',*,*,#6580,.F.);
#9242=ORIENTED_EDGE('',*,*,#6581,.F.);
#9243=ORIENTED_EDGE('',*,*,#6574,.T.);
#9244=ORIENTED_EDGE('',*,*,#6582,.T.);
#9245=ORIENTED_EDGE('',*,*,#6583,.T.);
#9246=ORIENTED_EDGE('',*,*,#6584,.F.);
#9247=ORIENTED_EDGE('',*,*,#6585,.F.);
#9248=ORIENTED_EDGE('',*,*,#6586,.F.);
#9249=ORIENTED_EDGE('',*,*,#6579,.T.);
#9250=ORIENTED_EDGE('',*,*,#6587,.T.);
#9251=ORIENTED_EDGE('',*,*,#6588,.T.);
#9252=ORIENTED_EDGE('',*,*,#6589,.F.);
#9253=ORIENTED_EDGE('',*,*,#6590,.F.);
#9254=ORIENTED_EDGE('',*,*,#6591,.F.);
#9255=ORIENTED_EDGE('',*,*,#6584,.T.);
#9256=ORIENTED_EDGE('',*,*,#6592,.T.);
#9257=ORIENTED_EDGE('',*,*,#6593,.T.);
#9258=ORIENTED_EDGE('',*,*,#6594,.F.);
#9259=ORIENTED_EDGE('',*,*,#6595,.F.);
#9260=ORIENTED_EDGE('',*,*,#6596,.F.);
#9261=ORIENTED_EDGE('',*,*,#6589,.T.);
#9262=ORIENTED_EDGE('',*,*,#6597,.T.);
#9263=ORIENTED_EDGE('',*,*,#6598,.T.);
#9264=ORIENTED_EDGE('',*,*,#6599,.F.);
#9265=ORIENTED_EDGE('',*,*,#6600,.F.);
#9266=ORIENTED_EDGE('',*,*,#6601,.F.);
#9267=ORIENTED_EDGE('',*,*,#6594,.T.);
#9268=ORIENTED_EDGE('',*,*,#6602,.T.);
#9269=ORIENTED_EDGE('',*,*,#6603,.T.);
#9270=ORIENTED_EDGE('',*,*,#6604,.F.);
#9271=ORIENTED_EDGE('',*,*,#6605,.F.);
#9272=ORIENTED_EDGE('',*,*,#6606,.F.);
#9273=ORIENTED_EDGE('',*,*,#6599,.T.);
#9274=ORIENTED_EDGE('',*,*,#6607,.T.);
#9275=ORIENTED_EDGE('',*,*,#6608,.T.);
#9276=ORIENTED_EDGE('',*,*,#6609,.F.);
#9277=ORIENTED_EDGE('',*,*,#6610,.F.);
#9278=ORIENTED_EDGE('',*,*,#6611,.F.);
#9279=ORIENTED_EDGE('',*,*,#6604,.T.);
#9280=ORIENTED_EDGE('',*,*,#6612,.T.);
#9281=ORIENTED_EDGE('',*,*,#6613,.T.);
#9282=ORIENTED_EDGE('',*,*,#6614,.F.);
#9283=ORIENTED_EDGE('',*,*,#6615,.F.);
#9284=ORIENTED_EDGE('',*,*,#6616,.F.);
#9285=ORIENTED_EDGE('',*,*,#6609,.T.);
#9286=ORIENTED_EDGE('',*,*,#6617,.T.);
#9287=ORIENTED_EDGE('',*,*,#6618,.T.);
#9288=ORIENTED_EDGE('',*,*,#6619,.F.);
#9289=ORIENTED_EDGE('',*,*,#6620,.F.);
#9290=ORIENTED_EDGE('',*,*,#6621,.F.);
#9291=ORIENTED_EDGE('',*,*,#6614,.T.);
#9292=ORIENTED_EDGE('',*,*,#6622,.T.);
#9293=ORIENTED_EDGE('',*,*,#6623,.T.);
#9294=ORIENTED_EDGE('',*,*,#6624,.F.);
#9295=ORIENTED_EDGE('',*,*,#6625,.F.);
#9296=ORIENTED_EDGE('',*,*,#6626,.F.);
#9297=ORIENTED_EDGE('',*,*,#6619,.T.);
#9298=ORIENTED_EDGE('',*,*,#6627,.T.);
#9299=ORIENTED_EDGE('',*,*,#6628,.T.);
#9300=ORIENTED_EDGE('',*,*,#6629,.F.);
#9301=ORIENTED_EDGE('',*,*,#6630,.F.);
#9302=ORIENTED_EDGE('',*,*,#6631,.F.);
#9303=ORIENTED_EDGE('',*,*,#6624,.T.);
#9304=ORIENTED_EDGE('',*,*,#6632,.T.);
#9305=ORIENTED_EDGE('',*,*,#6633,.T.);
#9306=ORIENTED_EDGE('',*,*,#6634,.F.);
#9307=ORIENTED_EDGE('',*,*,#6635,.F.);
#9308=ORIENTED_EDGE('',*,*,#6636,.F.);
#9309=ORIENTED_EDGE('',*,*,#6629,.T.);
#9310=ORIENTED_EDGE('',*,*,#6637,.T.);
#9311=ORIENTED_EDGE('',*,*,#6638,.T.);
#9312=ORIENTED_EDGE('',*,*,#6639,.F.);
#9313=ORIENTED_EDGE('',*,*,#6640,.F.);
#9314=ORIENTED_EDGE('',*,*,#6641,.F.);
#9315=ORIENTED_EDGE('',*,*,#6634,.T.);
#9316=ORIENTED_EDGE('',*,*,#6642,.T.);
#9317=ORIENTED_EDGE('',*,*,#6643,.T.);
#9318=ORIENTED_EDGE('',*,*,#6644,.F.);
#9319=ORIENTED_EDGE('',*,*,#6645,.F.);
#9320=ORIENTED_EDGE('',*,*,#6646,.F.);
#9321=ORIENTED_EDGE('',*,*,#6639,.T.);
#9322=ORIENTED_EDGE('',*,*,#6647,.T.);
#9323=ORIENTED_EDGE('',*,*,#6648,.T.);
#9324=ORIENTED_EDGE('',*,*,#6649,.F.);
#9325=ORIENTED_EDGE('',*,*,#6650,.F.);
#9326=ORIENTED_EDGE('',*,*,#6651,.F.);
#9327=ORIENTED_EDGE('',*,*,#6644,.T.);
#9328=ORIENTED_EDGE('',*,*,#6652,.T.);
#9329=ORIENTED_EDGE('',*,*,#6653,.T.);
#9330=ORIENTED_EDGE('',*,*,#6654,.F.);
#9331=ORIENTED_EDGE('',*,*,#6655,.F.);
#9332=ORIENTED_EDGE('',*,*,#6656,.F.);
#9333=ORIENTED_EDGE('',*,*,#6649,.T.);
#9334=ORIENTED_EDGE('',*,*,#6657,.T.);
#9335=ORIENTED_EDGE('',*,*,#6658,.T.);
#9336=ORIENTED_EDGE('',*,*,#6659,.F.);
#9337=ORIENTED_EDGE('',*,*,#6660,.F.);
#9338=ORIENTED_EDGE('',*,*,#6661,.F.);
#9339=ORIENTED_EDGE('',*,*,#6654,.T.);
#9340=ORIENTED_EDGE('',*,*,#6662,.T.);
#9341=ORIENTED_EDGE('',*,*,#6663,.T.);
#9342=ORIENTED_EDGE('',*,*,#6664,.F.);
#9343=ORIENTED_EDGE('',*,*,#6665,.F.);
#9344=ORIENTED_EDGE('',*,*,#6666,.F.);
#9345=ORIENTED_EDGE('',*,*,#6659,.T.);
#9346=ORIENTED_EDGE('',*,*,#6667,.T.);
#9347=ORIENTED_EDGE('',*,*,#6668,.T.);
#9348=ORIENTED_EDGE('',*,*,#6669,.F.);
#9349=ORIENTED_EDGE('',*,*,#6670,.F.);
#9350=ORIENTED_EDGE('',*,*,#6671,.F.);
#9351=ORIENTED_EDGE('',*,*,#6664,.T.);
#9352=ORIENTED_EDGE('',*,*,#6672,.T.);
#9353=ORIENTED_EDGE('',*,*,#6673,.T.);
#9354=ORIENTED_EDGE('',*,*,#6674,.F.);
#9355=ORIENTED_EDGE('',*,*,#6675,.F.);
#9356=ORIENTED_EDGE('',*,*,#6676,.F.);
#9357=ORIENTED_EDGE('',*,*,#6669,.T.);
#9358=ORIENTED_EDGE('',*,*,#6677,.T.);
#9359=ORIENTED_EDGE('',*,*,#6678,.T.);
#9360=ORIENTED_EDGE('',*,*,#6679,.F.);
#9361=ORIENTED_EDGE('',*,*,#6680,.F.);
#9362=ORIENTED_EDGE('',*,*,#6681,.F.);
#9363=ORIENTED_EDGE('',*,*,#6674,.T.);
#9364=ORIENTED_EDGE('',*,*,#6682,.T.);
#9365=ORIENTED_EDGE('',*,*,#6683,.T.);
#9366=ORIENTED_EDGE('',*,*,#6684,.F.);
#9367=ORIENTED_EDGE('',*,*,#6685,.F.);
#9368=ORIENTED_EDGE('',*,*,#6686,.F.);
#9369=ORIENTED_EDGE('',*,*,#6679,.T.);
#9370=ORIENTED_EDGE('',*,*,#6687,.T.);
#9371=ORIENTED_EDGE('',*,*,#6688,.T.);
#9372=ORIENTED_EDGE('',*,*,#6689,.F.);
#9373=ORIENTED_EDGE('',*,*,#6690,.F.);
#9374=ORIENTED_EDGE('',*,*,#6691,.F.);
#9375=ORIENTED_EDGE('',*,*,#6684,.T.);
#9376=ORIENTED_EDGE('',*,*,#6692,.T.);
#9377=ORIENTED_EDGE('',*,*,#6693,.T.);
#9378=ORIENTED_EDGE('',*,*,#6694,.F.);
#9379=ORIENTED_EDGE('',*,*,#6695,.F.);
#9380=ORIENTED_EDGE('',*,*,#6696,.F.);
#9381=ORIENTED_EDGE('',*,*,#6689,.T.);
#9382=ORIENTED_EDGE('',*,*,#6697,.T.);
#9383=ORIENTED_EDGE('',*,*,#6698,.T.);
#9384=ORIENTED_EDGE('',*,*,#6699,.F.);
#9385=ORIENTED_EDGE('',*,*,#6700,.F.);
#9386=ORIENTED_EDGE('',*,*,#6701,.F.);
#9387=ORIENTED_EDGE('',*,*,#6694,.T.);
#9388=ORIENTED_EDGE('',*,*,#6702,.T.);
#9389=ORIENTED_EDGE('',*,*,#6703,.T.);
#9390=ORIENTED_EDGE('',*,*,#6704,.F.);
#9391=ORIENTED_EDGE('',*,*,#6705,.F.);
#9392=ORIENTED_EDGE('',*,*,#6706,.F.);
#9393=ORIENTED_EDGE('',*,*,#6699,.T.);
#9394=ORIENTED_EDGE('',*,*,#6707,.T.);
#9395=ORIENTED_EDGE('',*,*,#6708,.T.);
#9396=ORIENTED_EDGE('',*,*,#6709,.F.);
#9397=ORIENTED_EDGE('',*,*,#6710,.F.);
#9398=ORIENTED_EDGE('',*,*,#6711,.F.);
#9399=ORIENTED_EDGE('',*,*,#6704,.T.);
#9400=ORIENTED_EDGE('',*,*,#6712,.T.);
#9401=ORIENTED_EDGE('',*,*,#6713,.T.);
#9402=ORIENTED_EDGE('',*,*,#6714,.F.);
#9403=ORIENTED_EDGE('',*,*,#6715,.F.);
#9404=ORIENTED_EDGE('',*,*,#6716,.F.);
#9405=ORIENTED_EDGE('',*,*,#6709,.T.);
#9406=ORIENTED_EDGE('',*,*,#6717,.T.);
#9407=ORIENTED_EDGE('',*,*,#6718,.T.);
#9408=ORIENTED_EDGE('',*,*,#6719,.F.);
#9409=ORIENTED_EDGE('',*,*,#6720,.F.);
#9410=ORIENTED_EDGE('',*,*,#6721,.F.);
#9411=ORIENTED_EDGE('',*,*,#6714,.T.);
#9412=ORIENTED_EDGE('',*,*,#6722,.T.);
#9413=ORIENTED_EDGE('',*,*,#6723,.T.);
#9414=ORIENTED_EDGE('',*,*,#6724,.F.);
#9415=ORIENTED_EDGE('',*,*,#6725,.F.);
#9416=ORIENTED_EDGE('',*,*,#6726,.F.);
#9417=ORIENTED_EDGE('',*,*,#6719,.T.);
#9418=ORIENTED_EDGE('',*,*,#6727,.T.);
#9419=ORIENTED_EDGE('',*,*,#6728,.T.);
#9420=ORIENTED_EDGE('',*,*,#6729,.F.);
#9421=ORIENTED_EDGE('',*,*,#6730,.F.);
#9422=ORIENTED_EDGE('',*,*,#6731,.F.);
#9423=ORIENTED_EDGE('',*,*,#6724,.T.);
#9424=ORIENTED_EDGE('',*,*,#6732,.T.);
#9425=ORIENTED_EDGE('',*,*,#6733,.T.);
#9426=ORIENTED_EDGE('',*,*,#6734,.F.);
#9427=ORIENTED_EDGE('',*,*,#6735,.F.);
#9428=ORIENTED_EDGE('',*,*,#6736,.F.);
#9429=ORIENTED_EDGE('',*,*,#6729,.T.);
#9430=ORIENTED_EDGE('',*,*,#6737,.T.);
#9431=ORIENTED_EDGE('',*,*,#6738,.T.);
#9432=ORIENTED_EDGE('',*,*,#6739,.F.);
#9433=ORIENTED_EDGE('',*,*,#6740,.F.);
#9434=ORIENTED_EDGE('',*,*,#6741,.F.);
#9435=ORIENTED_EDGE('',*,*,#6734,.T.);
#9436=ORIENTED_EDGE('',*,*,#6742,.T.);
#9437=ORIENTED_EDGE('',*,*,#6743,.T.);
#9438=ORIENTED_EDGE('',*,*,#6744,.F.);
#9439=ORIENTED_EDGE('',*,*,#6745,.F.);
#9440=ORIENTED_EDGE('',*,*,#6746,.F.);
#9441=ORIENTED_EDGE('',*,*,#6739,.T.);
#9442=ORIENTED_EDGE('',*,*,#6747,.T.);
#9443=ORIENTED_EDGE('',*,*,#6748,.T.);
#9444=ORIENTED_EDGE('',*,*,#6749,.F.);
#9445=ORIENTED_EDGE('',*,*,#6750,.F.);
#9446=ORIENTED_EDGE('',*,*,#6751,.F.);
#9447=ORIENTED_EDGE('',*,*,#6744,.T.);
#9448=ORIENTED_EDGE('',*,*,#6752,.T.);
#9449=ORIENTED_EDGE('',*,*,#6753,.T.);
#9450=ORIENTED_EDGE('',*,*,#6754,.F.);
#9451=ORIENTED_EDGE('',*,*,#6755,.F.);
#9452=ORIENTED_EDGE('',*,*,#6756,.F.);
#9453=ORIENTED_EDGE('',*,*,#6749,.T.);
#9454=ORIENTED_EDGE('',*,*,#6757,.T.);
#9455=ORIENTED_EDGE('',*,*,#6758,.T.);
#9456=ORIENTED_EDGE('',*,*,#6759,.F.);
#9457=ORIENTED_EDGE('',*,*,#6760,.F.);
#9458=ORIENTED_EDGE('',*,*,#6761,.F.);
#9459=ORIENTED_EDGE('',*,*,#6754,.T.);
#9460=ORIENTED_EDGE('',*,*,#6762,.T.);
#9461=ORIENTED_EDGE('',*,*,#6763,.T.);
#9462=ORIENTED_EDGE('',*,*,#6764,.F.);
#9463=ORIENTED_EDGE('',*,*,#6765,.F.);
#9464=ORIENTED_EDGE('',*,*,#6766,.F.);
#9465=ORIENTED_EDGE('',*,*,#6759,.T.);
#9466=ORIENTED_EDGE('',*,*,#6767,.T.);
#9467=ORIENTED_EDGE('',*,*,#6768,.T.);
#9468=ORIENTED_EDGE('',*,*,#6769,.F.);
#9469=ORIENTED_EDGE('',*,*,#6770,.F.);
#9470=ORIENTED_EDGE('',*,*,#6771,.F.);
#9471=ORIENTED_EDGE('',*,*,#6764,.T.);
#9472=ORIENTED_EDGE('',*,*,#6772,.T.);
#9473=ORIENTED_EDGE('',*,*,#6773,.T.);
#9474=ORIENTED_EDGE('',*,*,#6774,.F.);
#9475=ORIENTED_EDGE('',*,*,#6775,.F.);
#9476=ORIENTED_EDGE('',*,*,#6776,.F.);
#9477=ORIENTED_EDGE('',*,*,#6769,.T.);
#9478=ORIENTED_EDGE('',*,*,#6777,.T.);
#9479=ORIENTED_EDGE('',*,*,#6778,.T.);
#9480=ORIENTED_EDGE('',*,*,#6779,.F.);
#9481=ORIENTED_EDGE('',*,*,#6780,.F.);
#9482=ORIENTED_EDGE('',*,*,#6781,.F.);
#9483=ORIENTED_EDGE('',*,*,#6774,.T.);
#9484=ORIENTED_EDGE('',*,*,#6782,.T.);
#9485=ORIENTED_EDGE('',*,*,#6783,.T.);
#9486=ORIENTED_EDGE('',*,*,#6784,.F.);
#9487=ORIENTED_EDGE('',*,*,#6785,.F.);
#9488=ORIENTED_EDGE('',*,*,#6786,.F.);
#9489=ORIENTED_EDGE('',*,*,#6779,.T.);
#9490=ORIENTED_EDGE('',*,*,#6787,.T.);
#9491=ORIENTED_EDGE('',*,*,#6788,.T.);
#9492=ORIENTED_EDGE('',*,*,#6789,.F.);
#9493=ORIENTED_EDGE('',*,*,#6790,.F.);
#9494=ORIENTED_EDGE('',*,*,#6791,.F.);
#9495=ORIENTED_EDGE('',*,*,#6784,.T.);
#9496=ORIENTED_EDGE('',*,*,#6792,.T.);
#9497=ORIENTED_EDGE('',*,*,#6793,.T.);
#9498=ORIENTED_EDGE('',*,*,#6794,.F.);
#9499=ORIENTED_EDGE('',*,*,#6795,.F.);
#9500=ORIENTED_EDGE('',*,*,#6796,.F.);
#9501=ORIENTED_EDGE('',*,*,#6789,.T.);
#9502=ORIENTED_EDGE('',*,*,#6797,.T.);
#9503=ORIENTED_EDGE('',*,*,#6798,.T.);
#9504=ORIENTED_EDGE('',*,*,#6799,.F.);
#9505=ORIENTED_EDGE('',*,*,#6800,.F.);
#9506=ORIENTED_EDGE('',*,*,#6801,.F.);
#9507=ORIENTED_EDGE('',*,*,#6794,.T.);
#9508=ORIENTED_EDGE('',*,*,#6802,.T.);
#9509=ORIENTED_EDGE('',*,*,#6803,.T.);
#9510=ORIENTED_EDGE('',*,*,#6804,.F.);
#9511=ORIENTED_EDGE('',*,*,#6805,.F.);
#9512=ORIENTED_EDGE('',*,*,#6806,.F.);
#9513=ORIENTED_EDGE('',*,*,#6799,.T.);
#9514=ORIENTED_EDGE('',*,*,#6807,.T.);
#9515=ORIENTED_EDGE('',*,*,#6808,.T.);
#9516=ORIENTED_EDGE('',*,*,#6809,.F.);
#9517=ORIENTED_EDGE('',*,*,#6810,.F.);
#9518=ORIENTED_EDGE('',*,*,#6811,.F.);
#9519=ORIENTED_EDGE('',*,*,#6804,.T.);
#9520=ORIENTED_EDGE('',*,*,#6812,.T.);
#9521=ORIENTED_EDGE('',*,*,#6813,.T.);
#9522=ORIENTED_EDGE('',*,*,#6814,.F.);
#9523=ORIENTED_EDGE('',*,*,#6815,.F.);
#9524=ORIENTED_EDGE('',*,*,#6816,.F.);
#9525=ORIENTED_EDGE('',*,*,#6809,.T.);
#9526=ORIENTED_EDGE('',*,*,#6817,.T.);
#9527=ORIENTED_EDGE('',*,*,#6818,.T.);
#9528=ORIENTED_EDGE('',*,*,#6819,.F.);
#9529=ORIENTED_EDGE('',*,*,#6820,.F.);
#9530=ORIENTED_EDGE('',*,*,#6821,.F.);
#9531=ORIENTED_EDGE('',*,*,#6814,.T.);
#9532=ORIENTED_EDGE('',*,*,#6822,.T.);
#9533=ORIENTED_EDGE('',*,*,#6823,.T.);
#9534=ORIENTED_EDGE('',*,*,#6824,.F.);
#9535=ORIENTED_EDGE('',*,*,#6825,.F.);
#9536=ORIENTED_EDGE('',*,*,#6826,.F.);
#9537=ORIENTED_EDGE('',*,*,#6819,.T.);
#9538=ORIENTED_EDGE('',*,*,#6827,.T.);
#9539=ORIENTED_EDGE('',*,*,#6828,.T.);
#9540=ORIENTED_EDGE('',*,*,#6829,.F.);
#9541=ORIENTED_EDGE('',*,*,#6830,.F.);
#9542=ORIENTED_EDGE('',*,*,#6831,.F.);
#9543=ORIENTED_EDGE('',*,*,#6824,.T.);
#9544=ORIENTED_EDGE('',*,*,#6832,.T.);
#9545=ORIENTED_EDGE('',*,*,#6833,.T.);
#9546=ORIENTED_EDGE('',*,*,#6834,.F.);
#9547=ORIENTED_EDGE('',*,*,#6835,.F.);
#9548=ORIENTED_EDGE('',*,*,#6836,.F.);
#9549=ORIENTED_EDGE('',*,*,#6829,.T.);
#9550=ORIENTED_EDGE('',*,*,#6837,.T.);
#9551=ORIENTED_EDGE('',*,*,#6838,.T.);
#9552=ORIENTED_EDGE('',*,*,#6839,.F.);
#9553=ORIENTED_EDGE('',*,*,#6840,.F.);
#9554=ORIENTED_EDGE('',*,*,#6841,.F.);
#9555=ORIENTED_EDGE('',*,*,#6834,.T.);
#9556=ORIENTED_EDGE('',*,*,#6842,.T.);
#9557=ORIENTED_EDGE('',*,*,#6843,.T.);
#9558=ORIENTED_EDGE('',*,*,#6844,.F.);
#9559=ORIENTED_EDGE('',*,*,#6845,.F.);
#9560=ORIENTED_EDGE('',*,*,#6846,.F.);
#9561=ORIENTED_EDGE('',*,*,#6839,.T.);
#9562=ORIENTED_EDGE('',*,*,#6847,.T.);
#9563=ORIENTED_EDGE('',*,*,#6848,.T.);
#9564=ORIENTED_EDGE('',*,*,#6849,.F.);
#9565=ORIENTED_EDGE('',*,*,#6850,.F.);
#9566=ORIENTED_EDGE('',*,*,#6851,.F.);
#9567=ORIENTED_EDGE('',*,*,#6844,.T.);
#9568=ORIENTED_EDGE('',*,*,#6852,.T.);
#9569=ORIENTED_EDGE('',*,*,#6853,.T.);
#9570=ORIENTED_EDGE('',*,*,#6854,.F.);
#9571=ORIENTED_EDGE('',*,*,#6855,.F.);
#9572=ORIENTED_EDGE('',*,*,#6856,.F.);
#9573=ORIENTED_EDGE('',*,*,#6849,.T.);
#9574=ORIENTED_EDGE('',*,*,#6857,.T.);
#9575=ORIENTED_EDGE('',*,*,#6858,.T.);
#9576=ORIENTED_EDGE('',*,*,#6859,.F.);
#9577=ORIENTED_EDGE('',*,*,#6860,.F.);
#9578=ORIENTED_EDGE('',*,*,#6861,.F.);
#9579=ORIENTED_EDGE('',*,*,#6854,.T.);
#9580=ORIENTED_EDGE('',*,*,#6862,.T.);
#9581=ORIENTED_EDGE('',*,*,#6863,.T.);
#9582=ORIENTED_EDGE('',*,*,#6864,.F.);
#9583=ORIENTED_EDGE('',*,*,#6865,.F.);
#9584=ORIENTED_EDGE('',*,*,#6866,.F.);
#9585=ORIENTED_EDGE('',*,*,#6859,.T.);
#9586=ORIENTED_EDGE('',*,*,#6867,.T.);
#9587=ORIENTED_EDGE('',*,*,#6868,.T.);
#9588=ORIENTED_EDGE('',*,*,#6869,.F.);
#9589=ORIENTED_EDGE('',*,*,#6870,.F.);
#9590=ORIENTED_EDGE('',*,*,#6871,.F.);
#9591=ORIENTED_EDGE('',*,*,#6864,.T.);
#9592=ORIENTED_EDGE('',*,*,#6872,.T.);
#9593=ORIENTED_EDGE('',*,*,#6873,.T.);
#9594=ORIENTED_EDGE('',*,*,#6874,.F.);
#9595=ORIENTED_EDGE('',*,*,#6875,.F.);
#9596=ORIENTED_EDGE('',*,*,#6876,.F.);
#9597=ORIENTED_EDGE('',*,*,#6869,.T.);
#9598=ORIENTED_EDGE('',*,*,#6877,.T.);
#9599=ORIENTED_EDGE('',*,*,#6878,.T.);
#9600=ORIENTED_EDGE('',*,*,#6879,.F.);
#9601=ORIENTED_EDGE('',*,*,#6880,.F.);
#9602=ORIENTED_EDGE('',*,*,#6881,.F.);
#9603=ORIENTED_EDGE('',*,*,#6874,.T.);
#9604=ORIENTED_EDGE('',*,*,#6882,.T.);
#9605=ORIENTED_EDGE('',*,*,#6883,.T.);
#9606=ORIENTED_EDGE('',*,*,#6884,.F.);
#9607=ORIENTED_EDGE('',*,*,#6885,.F.);
#9608=ORIENTED_EDGE('',*,*,#6886,.F.);
#9609=ORIENTED_EDGE('',*,*,#6879,.T.);
#9610=ORIENTED_EDGE('',*,*,#6887,.T.);
#9611=ORIENTED_EDGE('',*,*,#6888,.T.);
#9612=ORIENTED_EDGE('',*,*,#6889,.F.);
#9613=ORIENTED_EDGE('',*,*,#6890,.F.);
#9614=ORIENTED_EDGE('',*,*,#6891,.F.);
#9615=ORIENTED_EDGE('',*,*,#6884,.T.);
#9616=ORIENTED_EDGE('',*,*,#6892,.T.);
#9617=ORIENTED_EDGE('',*,*,#6893,.T.);
#9618=ORIENTED_EDGE('',*,*,#6894,.F.);
#9619=ORIENTED_EDGE('',*,*,#6895,.F.);
#9620=ORIENTED_EDGE('',*,*,#6896,.F.);
#9621=ORIENTED_EDGE('',*,*,#6889,.T.);
#9622=ORIENTED_EDGE('',*,*,#6897,.T.);
#9623=ORIENTED_EDGE('',*,*,#6898,.T.);
#9624=ORIENTED_EDGE('',*,*,#6899,.F.);
#9625=ORIENTED_EDGE('',*,*,#6900,.F.);
#9626=ORIENTED_EDGE('',*,*,#6901,.F.);
#9627=ORIENTED_EDGE('',*,*,#6894,.T.);
#9628=ORIENTED_EDGE('',*,*,#6902,.T.);
#9629=ORIENTED_EDGE('',*,*,#6903,.T.);
#9630=ORIENTED_EDGE('',*,*,#6904,.F.);
#9631=ORIENTED_EDGE('',*,*,#6905,.F.);
#9632=ORIENTED_EDGE('',*,*,#6906,.F.);
#9633=ORIENTED_EDGE('',*,*,#6899,.T.);
#9634=ORIENTED_EDGE('',*,*,#6907,.T.);
#9635=ORIENTED_EDGE('',*,*,#6908,.T.);
#9636=ORIENTED_EDGE('',*,*,#6909,.F.);
#9637=ORIENTED_EDGE('',*,*,#6910,.F.);
#9638=ORIENTED_EDGE('',*,*,#6911,.F.);
#9639=ORIENTED_EDGE('',*,*,#6904,.T.);
#9640=ORIENTED_EDGE('',*,*,#6912,.T.);
#9641=ORIENTED_EDGE('',*,*,#6913,.T.);
#9642=ORIENTED_EDGE('',*,*,#6914,.F.);
#9643=ORIENTED_EDGE('',*,*,#6915,.F.);
#9644=ORIENTED_EDGE('',*,*,#6916,.F.);
#9645=ORIENTED_EDGE('',*,*,#6909,.T.);
#9646=ORIENTED_EDGE('',*,*,#6917,.T.);
#9647=ORIENTED_EDGE('',*,*,#6918,.T.);
#9648=ORIENTED_EDGE('',*,*,#6919,.F.);
#9649=ORIENTED_EDGE('',*,*,#6920,.F.);
#9650=ORIENTED_EDGE('',*,*,#6921,.F.);
#9651=ORIENTED_EDGE('',*,*,#6914,.T.);
#9652=ORIENTED_EDGE('',*,*,#6922,.T.);
#9653=ORIENTED_EDGE('',*,*,#6923,.T.);
#9654=ORIENTED_EDGE('',*,*,#6924,.F.);
#9655=ORIENTED_EDGE('',*,*,#6925,.F.);
#9656=ORIENTED_EDGE('',*,*,#6926,.F.);
#9657=ORIENTED_EDGE('',*,*,#6919,.T.);
#9658=ORIENTED_EDGE('',*,*,#6927,.T.);
#9659=ORIENTED_EDGE('',*,*,#6928,.T.);
#9660=ORIENTED_EDGE('',*,*,#6929,.F.);
#9661=ORIENTED_EDGE('',*,*,#6930,.F.);
#9662=ORIENTED_EDGE('',*,*,#6931,.F.);
#9663=ORIENTED_EDGE('',*,*,#6924,.T.);
#9664=ORIENTED_EDGE('',*,*,#6932,.T.);
#9665=ORIENTED_EDGE('',*,*,#6933,.T.);
#9666=ORIENTED_EDGE('',*,*,#6934,.F.);
#9667=ORIENTED_EDGE('',*,*,#6935,.F.);
#9668=ORIENTED_EDGE('',*,*,#6936,.F.);
#9669=ORIENTED_EDGE('',*,*,#6929,.T.);
#9670=ORIENTED_EDGE('',*,*,#6937,.T.);
#9671=ORIENTED_EDGE('',*,*,#6938,.T.);
#9672=ORIENTED_EDGE('',*,*,#6939,.F.);
#9673=ORIENTED_EDGE('',*,*,#6940,.F.);
#9674=ORIENTED_EDGE('',*,*,#6941,.F.);
#9675=ORIENTED_EDGE('',*,*,#6934,.T.);
#9676=ORIENTED_EDGE('',*,*,#6942,.T.);
#9677=ORIENTED_EDGE('',*,*,#6943,.T.);
#9678=ORIENTED_EDGE('',*,*,#6944,.F.);
#9679=ORIENTED_EDGE('',*,*,#6945,.F.);
#9680=ORIENTED_EDGE('',*,*,#6946,.F.);
#9681=ORIENTED_EDGE('',*,*,#6939,.T.);
#9682=ORIENTED_EDGE('',*,*,#6947,.T.);
#9683=ORIENTED_EDGE('',*,*,#6948,.T.);
#9684=ORIENTED_EDGE('',*,*,#6949,.F.);
#9685=ORIENTED_EDGE('',*,*,#6950,.F.);
#9686=ORIENTED_EDGE('',*,*,#6951,.F.);
#9687=ORIENTED_EDGE('',*,*,#6944,.T.);
#9688=ORIENTED_EDGE('',*,*,#6952,.T.);
#9689=ORIENTED_EDGE('',*,*,#6953,.T.);
#9690=ORIENTED_EDGE('',*,*,#6954,.F.);
#9691=ORIENTED_EDGE('',*,*,#6955,.F.);
#9692=ORIENTED_EDGE('',*,*,#6956,.F.);
#9693=ORIENTED_EDGE('',*,*,#6949,.T.);
#9694=ORIENTED_EDGE('',*,*,#6957,.T.);
#9695=ORIENTED_EDGE('',*,*,#6958,.T.);
#9696=ORIENTED_EDGE('',*,*,#6959,.F.);
#9697=ORIENTED_EDGE('',*,*,#6960,.F.);
#9698=ORIENTED_EDGE('',*,*,#6961,.F.);
#9699=ORIENTED_EDGE('',*,*,#6954,.T.);
#9700=ORIENTED_EDGE('',*,*,#6962,.T.);
#9701=ORIENTED_EDGE('',*,*,#6963,.T.);
#9702=ORIENTED_EDGE('',*,*,#6964,.F.);
#9703=ORIENTED_EDGE('',*,*,#6965,.F.);
#9704=ORIENTED_EDGE('',*,*,#6966,.F.);
#9705=ORIENTED_EDGE('',*,*,#6959,.T.);
#9706=ORIENTED_EDGE('',*,*,#6967,.T.);
#9707=ORIENTED_EDGE('',*,*,#6968,.T.);
#9708=ORIENTED_EDGE('',*,*,#6969,.F.);
#9709=ORIENTED_EDGE('',*,*,#6970,.F.);
#9710=ORIENTED_EDGE('',*,*,#6971,.F.);
#9711=ORIENTED_EDGE('',*,*,#6964,.T.);
#9712=ORIENTED_EDGE('',*,*,#6972,.T.);
#9713=ORIENTED_EDGE('',*,*,#6973,.T.);
#9714=ORIENTED_EDGE('',*,*,#6974,.F.);
#9715=ORIENTED_EDGE('',*,*,#6975,.F.);
#9716=ORIENTED_EDGE('',*,*,#6976,.F.);
#9717=ORIENTED_EDGE('',*,*,#6969,.T.);
#9718=ORIENTED_EDGE('',*,*,#6977,.T.);
#9719=ORIENTED_EDGE('',*,*,#6978,.T.);
#9720=ORIENTED_EDGE('',*,*,#6979,.F.);
#9721=ORIENTED_EDGE('',*,*,#6980,.F.);
#9722=ORIENTED_EDGE('',*,*,#6981,.F.);
#9723=ORIENTED_EDGE('',*,*,#6974,.T.);
#9724=ORIENTED_EDGE('',*,*,#6982,.T.);
#9725=ORIENTED_EDGE('',*,*,#6983,.T.);
#9726=ORIENTED_EDGE('',*,*,#6984,.F.);
#9727=ORIENTED_EDGE('',*,*,#6985,.F.);
#9728=ORIENTED_EDGE('',*,*,#6986,.F.);
#9729=ORIENTED_EDGE('',*,*,#6979,.T.);
#9730=ORIENTED_EDGE('',*,*,#6987,.T.);
#9731=ORIENTED_EDGE('',*,*,#6988,.T.);
#9732=ORIENTED_EDGE('',*,*,#6989,.F.);
#9733=ORIENTED_EDGE('',*,*,#6990,.F.);
#9734=ORIENTED_EDGE('',*,*,#6991,.F.);
#9735=ORIENTED_EDGE('',*,*,#6984,.T.);
#9736=ORIENTED_EDGE('',*,*,#6992,.T.);
#9737=ORIENTED_EDGE('',*,*,#6993,.T.);
#9738=ORIENTED_EDGE('',*,*,#6994,.F.);
#9739=ORIENTED_EDGE('',*,*,#6995,.F.);
#9740=ORIENTED_EDGE('',*,*,#6996,.F.);
#9741=ORIENTED_EDGE('',*,*,#6989,.T.);
#9742=ORIENTED_EDGE('',*,*,#6997,.T.);
#9743=ORIENTED_EDGE('',*,*,#6998,.T.);
#9744=ORIENTED_EDGE('',*,*,#6999,.F.);
#9745=ORIENTED_EDGE('',*,*,#7000,.F.);
#9746=ORIENTED_EDGE('',*,*,#7001,.F.);
#9747=ORIENTED_EDGE('',*,*,#6994,.T.);
#9748=ORIENTED_EDGE('',*,*,#7002,.T.);
#9749=ORIENTED_EDGE('',*,*,#7003,.T.);
#9750=ORIENTED_EDGE('',*,*,#7004,.F.);
#9751=ORIENTED_EDGE('',*,*,#7005,.F.);
#9752=ORIENTED_EDGE('',*,*,#7006,.F.);
#9753=ORIENTED_EDGE('',*,*,#6999,.T.);
#9754=ORIENTED_EDGE('',*,*,#7007,.T.);
#9755=ORIENTED_EDGE('',*,*,#7008,.T.);
#9756=ORIENTED_EDGE('',*,*,#7009,.F.);
#9757=ORIENTED_EDGE('',*,*,#7010,.F.);
#9758=ORIENTED_EDGE('',*,*,#7011,.F.);
#9759=ORIENTED_EDGE('',*,*,#7004,.T.);
#9760=ORIENTED_EDGE('',*,*,#7012,.T.);
#9761=ORIENTED_EDGE('',*,*,#7013,.T.);
#9762=ORIENTED_EDGE('',*,*,#7014,.F.);
#9763=ORIENTED_EDGE('',*,*,#7015,.F.);
#9764=ORIENTED_EDGE('',*,*,#7016,.F.);
#9765=ORIENTED_EDGE('',*,*,#7009,.T.);
#9766=ORIENTED_EDGE('',*,*,#7017,.T.);
#9767=ORIENTED_EDGE('',*,*,#7018,.T.);
#9768=ORIENTED_EDGE('',*,*,#7019,.F.);
#9769=ORIENTED_EDGE('',*,*,#7020,.F.);
#9770=ORIENTED_EDGE('',*,*,#7021,.F.);
#9771=ORIENTED_EDGE('',*,*,#7014,.T.);
#9772=ORIENTED_EDGE('',*,*,#7022,.T.);
#9773=ORIENTED_EDGE('',*,*,#7023,.T.);
#9774=ORIENTED_EDGE('',*,*,#7024,.F.);
#9775=ORIENTED_EDGE('',*,*,#7025,.F.);
#9776=ORIENTED_EDGE('',*,*,#7026,.F.);
#9777=ORIENTED_EDGE('',*,*,#7019,.T.);
#9778=ORIENTED_EDGE('',*,*,#7027,.T.);
#9779=ORIENTED_EDGE('',*,*,#7028,.T.);
#9780=ORIENTED_EDGE('',*,*,#7029,.F.);
#9781=ORIENTED_EDGE('',*,*,#7030,.F.);
#9782=ORIENTED_EDGE('',*,*,#7031,.F.);
#9783=ORIENTED_EDGE('',*,*,#7024,.T.);
#9784=ORIENTED_EDGE('',*,*,#7032,.T.);
#9785=ORIENTED_EDGE('',*,*,#7033,.T.);
#9786=ORIENTED_EDGE('',*,*,#7034,.F.);
#9787=ORIENTED_EDGE('',*,*,#7035,.F.);
#9788=ORIENTED_EDGE('',*,*,#7036,.F.);
#9789=ORIENTED_EDGE('',*,*,#7029,.T.);
#9790=ORIENTED_EDGE('',*,*,#7037,.T.);
#9791=ORIENTED_EDGE('',*,*,#7038,.T.);
#9792=ORIENTED_EDGE('',*,*,#7039,.F.);
#9793=ORIENTED_EDGE('',*,*,#7040,.F.);
#9794=ORIENTED_EDGE('',*,*,#7041,.F.);
#9795=ORIENTED_EDGE('',*,*,#7034,.T.);
#9796=ORIENTED_EDGE('',*,*,#7042,.T.);
#9797=ORIENTED_EDGE('',*,*,#7043,.T.);
#9798=ORIENTED_EDGE('',*,*,#7044,.F.);
#9799=ORIENTED_EDGE('',*,*,#7045,.F.);
#9800=ORIENTED_EDGE('',*,*,#7046,.F.);
#9801=ORIENTED_EDGE('',*,*,#7039,.T.);
#9802=ORIENTED_EDGE('',*,*,#7047,.T.);
#9803=ORIENTED_EDGE('',*,*,#7048,.T.);
#9804=ORIENTED_EDGE('',*,*,#7049,.F.);
#9805=ORIENTED_EDGE('',*,*,#7050,.F.);
#9806=ORIENTED_EDGE('',*,*,#7051,.F.);
#9807=ORIENTED_EDGE('',*,*,#7044,.T.);
#9808=ORIENTED_EDGE('',*,*,#7052,.T.);
#9809=ORIENTED_EDGE('',*,*,#7053,.T.);
#9810=ORIENTED_EDGE('',*,*,#7054,.F.);
#9811=ORIENTED_EDGE('',*,*,#7055,.F.);
#9812=ORIENTED_EDGE('',*,*,#7056,.F.);
#9813=ORIENTED_EDGE('',*,*,#7049,.T.);
#9814=ORIENTED_EDGE('',*,*,#7057,.T.);
#9815=ORIENTED_EDGE('',*,*,#7058,.T.);
#9816=ORIENTED_EDGE('',*,*,#7059,.F.);
#9817=ORIENTED_EDGE('',*,*,#7060,.F.);
#9818=ORIENTED_EDGE('',*,*,#7061,.F.);
#9819=ORIENTED_EDGE('',*,*,#7054,.T.);
#9820=ORIENTED_EDGE('',*,*,#7062,.T.);
#9821=ORIENTED_EDGE('',*,*,#7063,.T.);
#9822=ORIENTED_EDGE('',*,*,#7064,.F.);
#9823=ORIENTED_EDGE('',*,*,#7065,.F.);
#9824=ORIENTED_EDGE('',*,*,#7066,.F.);
#9825=ORIENTED_EDGE('',*,*,#7059,.T.);
#9826=ORIENTED_EDGE('',*,*,#7067,.T.);
#9827=ORIENTED_EDGE('',*,*,#7068,.T.);
#9828=ORIENTED_EDGE('',*,*,#7069,.F.);
#9829=ORIENTED_EDGE('',*,*,#7070,.F.);
#9830=ORIENTED_EDGE('',*,*,#7071,.F.);
#9831=ORIENTED_EDGE('',*,*,#7064,.T.);
#9832=ORIENTED_EDGE('',*,*,#7072,.T.);
#9833=ORIENTED_EDGE('',*,*,#7073,.T.);
#9834=ORIENTED_EDGE('',*,*,#7074,.F.);
#9835=ORIENTED_EDGE('',*,*,#7075,.F.);
#9836=ORIENTED_EDGE('',*,*,#7076,.F.);
#9837=ORIENTED_EDGE('',*,*,#7069,.T.);
#9838=ORIENTED_EDGE('',*,*,#7077,.T.);
#9839=ORIENTED_EDGE('',*,*,#7078,.T.);
#9840=ORIENTED_EDGE('',*,*,#7079,.F.);
#9841=ORIENTED_EDGE('',*,*,#7080,.F.);
#9842=ORIENTED_EDGE('',*,*,#7081,.F.);
#9843=ORIENTED_EDGE('',*,*,#7074,.T.);
#9844=ORIENTED_EDGE('',*,*,#7082,.T.);
#9845=ORIENTED_EDGE('',*,*,#7083,.T.);
#9846=ORIENTED_EDGE('',*,*,#7084,.F.);
#9847=ORIENTED_EDGE('',*,*,#7085,.F.);
#9848=ORIENTED_EDGE('',*,*,#7086,.F.);
#9849=ORIENTED_EDGE('',*,*,#7079,.T.);
#9850=ORIENTED_EDGE('',*,*,#7087,.T.);
#9851=ORIENTED_EDGE('',*,*,#7088,.T.);
#9852=ORIENTED_EDGE('',*,*,#7089,.F.);
#9853=ORIENTED_EDGE('',*,*,#7090,.F.);
#9854=ORIENTED_EDGE('',*,*,#7091,.F.);
#9855=ORIENTED_EDGE('',*,*,#7084,.T.);
#9856=ORIENTED_EDGE('',*,*,#7092,.T.);
#9857=ORIENTED_EDGE('',*,*,#7093,.T.);
#9858=ORIENTED_EDGE('',*,*,#7094,.F.);
#9859=ORIENTED_EDGE('',*,*,#7095,.F.);
#9860=ORIENTED_EDGE('',*,*,#7096,.F.);
#9861=ORIENTED_EDGE('',*,*,#7089,.T.);
#9862=ORIENTED_EDGE('',*,*,#7097,.T.);
#9863=ORIENTED_EDGE('',*,*,#7098,.T.);
#9864=ORIENTED_EDGE('',*,*,#7099,.F.);
#9865=ORIENTED_EDGE('',*,*,#7100,.F.);
#9866=ORIENTED_EDGE('',*,*,#7101,.F.);
#9867=ORIENTED_EDGE('',*,*,#7094,.T.);
#9868=ORIENTED_EDGE('',*,*,#7102,.T.);
#9869=ORIENTED_EDGE('',*,*,#7103,.T.);
#9870=ORIENTED_EDGE('',*,*,#7104,.F.);
#9871=ORIENTED_EDGE('',*,*,#7105,.F.);
#9872=ORIENTED_EDGE('',*,*,#7106,.F.);
#9873=ORIENTED_EDGE('',*,*,#7099,.T.);
#9874=ORIENTED_EDGE('',*,*,#7107,.T.);
#9875=ORIENTED_EDGE('',*,*,#7108,.T.);
#9876=ORIENTED_EDGE('',*,*,#7109,.F.);
#9877=ORIENTED_EDGE('',*,*,#7110,.F.);
#9878=ORIENTED_EDGE('',*,*,#7111,.F.);
#9879=ORIENTED_EDGE('',*,*,#7104,.T.);
#9880=ORIENTED_EDGE('',*,*,#7112,.T.);
#9881=ORIENTED_EDGE('',*,*,#7113,.T.);
#9882=ORIENTED_EDGE('',*,*,#7114,.F.);
#9883=ORIENTED_EDGE('',*,*,#7115,.F.);
#9884=ORIENTED_EDGE('',*,*,#7116,.F.);
#9885=ORIENTED_EDGE('',*,*,#7109,.T.);
#9886=ORIENTED_EDGE('',*,*,#7117,.T.);
#9887=ORIENTED_EDGE('',*,*,#7118,.T.);
#9888=ORIENTED_EDGE('',*,*,#7119,.F.);
#9889=ORIENTED_EDGE('',*,*,#7120,.F.);
#9890=ORIENTED_EDGE('',*,*,#7121,.F.);
#9891=ORIENTED_EDGE('',*,*,#7114,.T.);
#9892=ORIENTED_EDGE('',*,*,#7122,.T.);
#9893=ORIENTED_EDGE('',*,*,#7123,.T.);
#9894=ORIENTED_EDGE('',*,*,#7124,.F.);
#9895=ORIENTED_EDGE('',*,*,#7125,.F.);
#9896=ORIENTED_EDGE('',*,*,#7126,.F.);
#9897=ORIENTED_EDGE('',*,*,#7119,.T.);
#9898=ORIENTED_EDGE('',*,*,#7127,.T.);
#9899=ORIENTED_EDGE('',*,*,#7128,.T.);
#9900=ORIENTED_EDGE('',*,*,#7129,.F.);
#9901=ORIENTED_EDGE('',*,*,#7130,.F.);
#9902=ORIENTED_EDGE('',*,*,#7131,.F.);
#9903=ORIENTED_EDGE('',*,*,#7124,.T.);
#9904=ORIENTED_EDGE('',*,*,#7132,.T.);
#9905=ORIENTED_EDGE('',*,*,#7133,.T.);
#9906=ORIENTED_EDGE('',*,*,#7134,.F.);
#9907=ORIENTED_EDGE('',*,*,#7135,.F.);
#9908=ORIENTED_EDGE('',*,*,#7136,.F.);
#9909=ORIENTED_EDGE('',*,*,#7129,.T.);
#9910=ORIENTED_EDGE('',*,*,#7137,.T.);
#9911=ORIENTED_EDGE('',*,*,#7138,.T.);
#9912=ORIENTED_EDGE('',*,*,#7139,.F.);
#9913=ORIENTED_EDGE('',*,*,#7140,.F.);
#9914=ORIENTED_EDGE('',*,*,#7141,.F.);
#9915=ORIENTED_EDGE('',*,*,#7134,.T.);
#9916=ORIENTED_EDGE('',*,*,#7142,.T.);
#9917=ORIENTED_EDGE('',*,*,#7143,.T.);
#9918=ORIENTED_EDGE('',*,*,#7144,.F.);
#9919=ORIENTED_EDGE('',*,*,#7145,.F.);
#9920=ORIENTED_EDGE('',*,*,#7146,.F.);
#9921=ORIENTED_EDGE('',*,*,#7139,.T.);
#9922=ORIENTED_EDGE('',*,*,#7147,.T.);
#9923=ORIENTED_EDGE('',*,*,#7148,.T.);
#9924=ORIENTED_EDGE('',*,*,#7149,.F.);
#9925=ORIENTED_EDGE('',*,*,#7150,.F.);
#9926=ORIENTED_EDGE('',*,*,#7151,.F.);
#9927=ORIENTED_EDGE('',*,*,#7144,.T.);
#9928=ORIENTED_EDGE('',*,*,#7152,.T.);
#9929=ORIENTED_EDGE('',*,*,#7153,.T.);
#9930=ORIENTED_EDGE('',*,*,#7154,.F.);
#9931=ORIENTED_EDGE('',*,*,#7155,.F.);
#9932=ORIENTED_EDGE('',*,*,#7156,.F.);
#9933=ORIENTED_EDGE('',*,*,#7149,.T.);
#9934=ORIENTED_EDGE('',*,*,#7157,.T.);
#9935=ORIENTED_EDGE('',*,*,#7158,.T.);
#9936=ORIENTED_EDGE('',*,*,#7159,.F.);
#9937=ORIENTED_EDGE('',*,*,#7160,.F.);
#9938=ORIENTED_EDGE('',*,*,#7161,.F.);
#9939=ORIENTED_EDGE('',*,*,#7154,.T.);
#9940=ORIENTED_EDGE('',*,*,#7162,.T.);
#9941=ORIENTED_EDGE('',*,*,#7163,.T.);
#9942=ORIENTED_EDGE('',*,*,#7164,.F.);
#9943=ORIENTED_EDGE('',*,*,#7165,.F.);
#9944=ORIENTED_EDGE('',*,*,#7166,.F.);
#9945=ORIENTED_EDGE('',*,*,#7159,.T.);
#9946=ORIENTED_EDGE('',*,*,#7167,.T.);
#9947=ORIENTED_EDGE('',*,*,#7168,.T.);
#9948=ORIENTED_EDGE('',*,*,#7169,.F.);
#9949=ORIENTED_EDGE('',*,*,#7170,.F.);
#9950=ORIENTED_EDGE('',*,*,#7171,.F.);
#9951=ORIENTED_EDGE('',*,*,#7164,.T.);
#9952=ORIENTED_EDGE('',*,*,#7172,.T.);
#9953=ORIENTED_EDGE('',*,*,#7173,.T.);
#9954=ORIENTED_EDGE('',*,*,#7174,.F.);
#9955=ORIENTED_EDGE('',*,*,#7175,.F.);
#9956=ORIENTED_EDGE('',*,*,#7176,.F.);
#9957=ORIENTED_EDGE('',*,*,#7169,.T.);
#9958=ORIENTED_EDGE('',*,*,#7177,.T.);
#9959=ORIENTED_EDGE('',*,*,#7178,.T.);
#9960=ORIENTED_EDGE('',*,*,#7179,.F.);
#9961=ORIENTED_EDGE('',*,*,#7180,.F.);
#9962=ORIENTED_EDGE('',*,*,#7181,.F.);
#9963=ORIENTED_EDGE('',*,*,#7174,.T.);
#9964=ORIENTED_EDGE('',*,*,#7182,.T.);
#9965=ORIENTED_EDGE('',*,*,#7183,.T.);
#9966=ORIENTED_EDGE('',*,*,#7184,.F.);
#9967=ORIENTED_EDGE('',*,*,#7185,.F.);
#9968=ORIENTED_EDGE('',*,*,#7186,.F.);
#9969=ORIENTED_EDGE('',*,*,#7179,.T.);
#9970=ORIENTED_EDGE('',*,*,#7187,.T.);
#9971=ORIENTED_EDGE('',*,*,#7188,.T.);
#9972=ORIENTED_EDGE('',*,*,#7189,.F.);
#9973=ORIENTED_EDGE('',*,*,#7190,.F.);
#9974=ORIENTED_EDGE('',*,*,#7191,.F.);
#9975=ORIENTED_EDGE('',*,*,#7184,.T.);
#9976=ORIENTED_EDGE('',*,*,#7192,.T.);
#9977=ORIENTED_EDGE('',*,*,#7193,.T.);
#9978=ORIENTED_EDGE('',*,*,#7194,.F.);
#9979=ORIENTED_EDGE('',*,*,#7195,.F.);
#9980=ORIENTED_EDGE('',*,*,#7196,.F.);
#9981=ORIENTED_EDGE('',*,*,#7189,.T.);
#9982=ORIENTED_EDGE('',*,*,#7197,.T.);
#9983=ORIENTED_EDGE('',*,*,#7198,.T.);
#9984=ORIENTED_EDGE('',*,*,#7199,.F.);
#9985=ORIENTED_EDGE('',*,*,#7200,.F.);
#9986=ORIENTED_EDGE('',*,*,#7201,.F.);
#9987=ORIENTED_EDGE('',*,*,#7194,.T.);
#9988=ORIENTED_EDGE('',*,*,#7202,.T.);
#9989=ORIENTED_EDGE('',*,*,#7203,.T.);
#9990=ORIENTED_EDGE('',*,*,#7204,.F.);
#9991=ORIENTED_EDGE('',*,*,#7205,.F.);
#9992=ORIENTED_EDGE('',*,*,#7206,.F.);
#9993=ORIENTED_EDGE('',*,*,#7199,.T.);
#9994=ORIENTED_EDGE('',*,*,#7207,.T.);
#9995=ORIENTED_EDGE('',*,*,#7208,.T.);
#9996=ORIENTED_EDGE('',*,*,#7209,.F.);
#9997=ORIENTED_EDGE('',*,*,#7210,.F.);
#9998=ORIENTED_EDGE('',*,*,#7211,.F.);
#9999=ORIENTED_EDGE('',*,*,#7204,.T.);
#10000=ORIENTED_EDGE('',*,*,#7212,.T.);
#10001=ORIENTED_EDGE('',*,*,#7213,.T.);
#10002=ORIENTED_EDGE('',*,*,#7214,.F.);
#10003=ORIENTED_EDGE('',*,*,#7215,.F.);
#10004=ORIENTED_EDGE('',*,*,#7216,.F.);
#10005=ORIENTED_EDGE('',*,*,#7209,.T.);
#10006=ORIENTED_EDGE('',*,*,#7217,.T.);
#10007=ORIENTED_EDGE('',*,*,#7218,.T.);
#10008=ORIENTED_EDGE('',*,*,#7219,.F.);
#10009=ORIENTED_EDGE('',*,*,#7220,.F.);
#10010=ORIENTED_EDGE('',*,*,#7221,.F.);
#10011=ORIENTED_EDGE('',*,*,#7214,.T.);
#10012=ORIENTED_EDGE('',*,*,#7222,.T.);
#10013=ORIENTED_EDGE('',*,*,#7223,.T.);
#10014=ORIENTED_EDGE('',*,*,#7224,.F.);
#10015=ORIENTED_EDGE('',*,*,#7225,.F.);
#10016=ORIENTED_EDGE('',*,*,#7226,.F.);
#10017=ORIENTED_EDGE('',*,*,#7219,.T.);
#10018=ORIENTED_EDGE('',*,*,#7227,.T.);
#10019=ORIENTED_EDGE('',*,*,#7228,.T.);
#10020=ORIENTED_EDGE('',*,*,#7229,.F.);
#10021=ORIENTED_EDGE('',*,*,#7230,.F.);
#10022=ORIENTED_EDGE('',*,*,#7231,.F.);
#10023=ORIENTED_EDGE('',*,*,#7224,.T.);
#10024=ORIENTED_EDGE('',*,*,#7232,.T.);
#10025=ORIENTED_EDGE('',*,*,#7233,.T.);
#10026=ORIENTED_EDGE('',*,*,#7234,.F.);
#10027=ORIENTED_EDGE('',*,*,#7235,.F.);
#10028=ORIENTED_EDGE('',*,*,#7236,.F.);
#10029=ORIENTED_EDGE('',*,*,#7229,.T.);
#10030=ORIENTED_EDGE('',*,*,#7237,.T.);
#10031=ORIENTED_EDGE('',*,*,#7238,.T.);
#10032=ORIENTED_EDGE('',*,*,#7239,.F.);
#10033=ORIENTED_EDGE('',*,*,#7240,.F.);
#10034=ORIENTED_EDGE('',*,*,#7241,.F.);
#10035=ORIENTED_EDGE('',*,*,#7234,.T.);
#10036=ORIENTED_EDGE('',*,*,#7242,.T.);
#10037=ORIENTED_EDGE('',*,*,#7243,.T.);
#10038=ORIENTED_EDGE('',*,*,#7244,.F.);
#10039=ORIENTED_EDGE('',*,*,#7245,.F.);
#10040=ORIENTED_EDGE('',*,*,#7246,.F.);
#10041=ORIENTED_EDGE('',*,*,#7239,.T.);
#10042=ORIENTED_EDGE('',*,*,#7247,.T.);
#10043=ORIENTED_EDGE('',*,*,#7248,.T.);
#10044=ORIENTED_EDGE('',*,*,#7249,.F.);
#10045=ORIENTED_EDGE('',*,*,#7250,.F.);
#10046=ORIENTED_EDGE('',*,*,#7251,.F.);
#10047=ORIENTED_EDGE('',*,*,#7244,.T.);
#10048=ORIENTED_EDGE('',*,*,#7252,.T.);
#10049=ORIENTED_EDGE('',*,*,#7253,.T.);
#10050=ORIENTED_EDGE('',*,*,#7254,.F.);
#10051=ORIENTED_EDGE('',*,*,#7255,.F.);
#10052=ORIENTED_EDGE('',*,*,#7256,.F.);
#10053=ORIENTED_EDGE('',*,*,#7249,.T.);
#10054=ORIENTED_EDGE('',*,*,#7257,.T.);
#10055=ORIENTED_EDGE('',*,*,#7258,.T.);
#10056=ORIENTED_EDGE('',*,*,#7259,.F.);
#10057=ORIENTED_EDGE('',*,*,#7260,.F.);
#10058=ORIENTED_EDGE('',*,*,#7261,.F.);
#10059=ORIENTED_EDGE('',*,*,#7254,.T.);
#10060=ORIENTED_EDGE('',*,*,#7262,.T.);
#10061=ORIENTED_EDGE('',*,*,#7263,.T.);
#10062=ORIENTED_EDGE('',*,*,#7264,.F.);
#10063=ORIENTED_EDGE('',*,*,#7265,.F.);
#10064=ORIENTED_EDGE('',*,*,#7266,.F.);
#10065=ORIENTED_EDGE('',*,*,#7259,.T.);
#10066=ORIENTED_EDGE('',*,*,#7267,.T.);
#10067=ORIENTED_EDGE('',*,*,#7268,.T.);
#10068=ORIENTED_EDGE('',*,*,#7269,.F.);
#10069=ORIENTED_EDGE('',*,*,#7270,.F.);
#10070=ORIENTED_EDGE('',*,*,#7271,.F.);
#10071=ORIENTED_EDGE('',*,*,#7264,.T.);
#10072=ORIENTED_EDGE('',*,*,#7272,.T.);
#10073=ORIENTED_EDGE('',*,*,#7273,.T.);
#10074=ORIENTED_EDGE('',*,*,#7274,.F.);
#10075=ORIENTED_EDGE('',*,*,#7275,.F.);
#10076=ORIENTED_EDGE('',*,*,#7276,.F.);
#10077=ORIENTED_EDGE('',*,*,#7269,.T.);
#10078=ORIENTED_EDGE('',*,*,#7277,.T.);
#10079=ORIENTED_EDGE('',*,*,#7278,.T.);
#10080=ORIENTED_EDGE('',*,*,#7279,.F.);
#10081=ORIENTED_EDGE('',*,*,#7280,.F.);
#10082=ORIENTED_EDGE('',*,*,#7281,.F.);
#10083=ORIENTED_EDGE('',*,*,#7274,.T.);
#10084=ORIENTED_EDGE('',*,*,#7282,.T.);
#10085=ORIENTED_EDGE('',*,*,#7283,.T.);
#10086=ORIENTED_EDGE('',*,*,#7284,.F.);
#10087=ORIENTED_EDGE('',*,*,#7285,.F.);
#10088=ORIENTED_EDGE('',*,*,#7286,.F.);
#10089=ORIENTED_EDGE('',*,*,#7279,.T.);
#10090=ORIENTED_EDGE('',*,*,#7287,.T.);
#10091=ORIENTED_EDGE('',*,*,#7288,.T.);
#10092=ORIENTED_EDGE('',*,*,#7289,.F.);
#10093=ORIENTED_EDGE('',*,*,#7290,.F.);
#10094=ORIENTED_EDGE('',*,*,#7291,.F.);
#10095=ORIENTED_EDGE('',*,*,#7284,.T.);
#10096=ORIENTED_EDGE('',*,*,#7292,.T.);
#10097=ORIENTED_EDGE('',*,*,#7293,.T.);
#10098=ORIENTED_EDGE('',*,*,#7294,.F.);
#10099=ORIENTED_EDGE('',*,*,#7295,.F.);
#10100=ORIENTED_EDGE('',*,*,#7296,.F.);
#10101=ORIENTED_EDGE('',*,*,#7289,.T.);
#10102=ORIENTED_EDGE('',*,*,#7297,.T.);
#10103=ORIENTED_EDGE('',*,*,#7298,.T.);
#10104=ORIENTED_EDGE('',*,*,#7299,.F.);
#10105=ORIENTED_EDGE('',*,*,#7300,.F.);
#10106=ORIENTED_EDGE('',*,*,#7301,.F.);
#10107=ORIENTED_EDGE('',*,*,#7294,.T.);
#10108=ORIENTED_EDGE('',*,*,#7302,.T.);
#10109=ORIENTED_EDGE('',*,*,#7303,.T.);
#10110=ORIENTED_EDGE('',*,*,#7304,.F.);
#10111=ORIENTED_EDGE('',*,*,#7305,.F.);
#10112=ORIENTED_EDGE('',*,*,#7306,.F.);
#10113=ORIENTED_EDGE('',*,*,#7299,.T.);
#10114=ORIENTED_EDGE('',*,*,#7307,.T.);
#10115=ORIENTED_EDGE('',*,*,#7308,.T.);
#10116=ORIENTED_EDGE('',*,*,#7309,.F.);
#10117=ORIENTED_EDGE('',*,*,#7310,.F.);
#10118=ORIENTED_EDGE('',*,*,#7311,.F.);
#10119=ORIENTED_EDGE('',*,*,#7304,.T.);
#10120=ORIENTED_EDGE('',*,*,#7312,.T.);
#10121=ORIENTED_EDGE('',*,*,#7313,.T.);
#10122=ORIENTED_EDGE('',*,*,#7314,.F.);
#10123=ORIENTED_EDGE('',*,*,#7315,.F.);
#10124=ORIENTED_EDGE('',*,*,#7316,.F.);
#10125=ORIENTED_EDGE('',*,*,#7309,.T.);
#10126=ORIENTED_EDGE('',*,*,#7317,.T.);
#10127=ORIENTED_EDGE('',*,*,#7318,.T.);
#10128=ORIENTED_EDGE('',*,*,#7319,.F.);
#10129=ORIENTED_EDGE('',*,*,#7320,.F.);
#10130=ORIENTED_EDGE('',*,*,#7321,.F.);
#10131=ORIENTED_EDGE('',*,*,#7314,.T.);
#10132=ORIENTED_EDGE('',*,*,#7322,.T.);
#10133=ORIENTED_EDGE('',*,*,#7323,.T.);
#10134=ORIENTED_EDGE('',*,*,#7324,.F.);
#10135=ORIENTED_EDGE('',*,*,#7325,.F.);
#10136=ORIENTED_EDGE('',*,*,#7326,.F.);
#10137=ORIENTED_EDGE('',*,*,#7319,.T.);
#10138=ORIENTED_EDGE('',*,*,#7327,.T.);
#10139=ORIENTED_EDGE('',*,*,#7328,.T.);
#10140=ORIENTED_EDGE('',*,*,#7329,.F.);
#10141=ORIENTED_EDGE('',*,*,#7330,.F.);
#10142=ORIENTED_EDGE('',*,*,#7331,.F.);
#10143=ORIENTED_EDGE('',*,*,#7324,.T.);
#10144=ORIENTED_EDGE('',*,*,#7332,.T.);
#10145=ORIENTED_EDGE('',*,*,#7333,.T.);
#10146=ORIENTED_EDGE('',*,*,#7334,.F.);
#10147=ORIENTED_EDGE('',*,*,#7335,.F.);
#10148=ORIENTED_EDGE('',*,*,#7336,.F.);
#10149=ORIENTED_EDGE('',*,*,#7329,.T.);
#10150=ORIENTED_EDGE('',*,*,#7337,.T.);
#10151=ORIENTED_EDGE('',*,*,#7338,.T.);
#10152=ORIENTED_EDGE('',*,*,#7339,.F.);
#10153=ORIENTED_EDGE('',*,*,#7340,.F.);
#10154=ORIENTED_EDGE('',*,*,#7341,.F.);
#10155=ORIENTED_EDGE('',*,*,#7334,.T.);
#10156=ORIENTED_EDGE('',*,*,#7342,.T.);
#10157=ORIENTED_EDGE('',*,*,#7343,.T.);
#10158=ORIENTED_EDGE('',*,*,#7344,.F.);
#10159=ORIENTED_EDGE('',*,*,#7345,.F.);
#10160=ORIENTED_EDGE('',*,*,#7346,.F.);
#10161=ORIENTED_EDGE('',*,*,#7339,.T.);
#10162=ORIENTED_EDGE('',*,*,#7347,.T.);
#10163=ORIENTED_EDGE('',*,*,#7348,.T.);
#10164=ORIENTED_EDGE('',*,*,#7349,.F.);
#10165=ORIENTED_EDGE('',*,*,#7350,.F.);
#10166=ORIENTED_EDGE('',*,*,#7351,.F.);
#10167=ORIENTED_EDGE('',*,*,#7344,.T.);
#10168=ORIENTED_EDGE('',*,*,#7352,.T.);
#10169=ORIENTED_EDGE('',*,*,#7353,.T.);
#10170=ORIENTED_EDGE('',*,*,#7354,.F.);
#10171=ORIENTED_EDGE('',*,*,#7355,.F.);
#10172=ORIENTED_EDGE('',*,*,#7356,.F.);
#10173=ORIENTED_EDGE('',*,*,#7349,.T.);
#10174=ORIENTED_EDGE('',*,*,#7357,.T.);
#10175=ORIENTED_EDGE('',*,*,#7358,.T.);
#10176=ORIENTED_EDGE('',*,*,#7359,.F.);
#10177=ORIENTED_EDGE('',*,*,#7360,.F.);
#10178=ORIENTED_EDGE('',*,*,#7361,.F.);
#10179=ORIENTED_EDGE('',*,*,#7354,.T.);
#10180=ORIENTED_EDGE('',*,*,#7362,.T.);
#10181=ORIENTED_EDGE('',*,*,#7363,.T.);
#10182=ORIENTED_EDGE('',*,*,#7364,.F.);
#10183=ORIENTED_EDGE('',*,*,#7365,.F.);
#10184=ORIENTED_EDGE('',*,*,#7366,.F.);
#10185=ORIENTED_EDGE('',*,*,#7359,.T.);
#10186=ORIENTED_EDGE('',*,*,#7367,.T.);
#10187=ORIENTED_EDGE('',*,*,#7368,.T.);
#10188=ORIENTED_EDGE('',*,*,#7369,.F.);
#10189=ORIENTED_EDGE('',*,*,#7370,.F.);
#10190=ORIENTED_EDGE('',*,*,#7371,.F.);
#10191=ORIENTED_EDGE('',*,*,#7364,.T.);
#10192=ORIENTED_EDGE('',*,*,#7372,.T.);
#10193=ORIENTED_EDGE('',*,*,#7373,.T.);
#10194=ORIENTED_EDGE('',*,*,#7374,.F.);
#10195=ORIENTED_EDGE('',*,*,#7375,.F.);
#10196=ORIENTED_EDGE('',*,*,#7376,.F.);
#10197=ORIENTED_EDGE('',*,*,#7369,.T.);
#10198=ORIENTED_EDGE('',*,*,#7377,.T.);
#10199=ORIENTED_EDGE('',*,*,#7378,.T.);
#10200=ORIENTED_EDGE('',*,*,#7379,.F.);
#10201=ORIENTED_EDGE('',*,*,#7380,.F.);
#10202=ORIENTED_EDGE('',*,*,#7381,.F.);
#10203=ORIENTED_EDGE('',*,*,#7374,.T.);
#10204=ORIENTED_EDGE('',*,*,#7382,.T.);
#10205=ORIENTED_EDGE('',*,*,#7383,.T.);
#10206=ORIENTED_EDGE('',*,*,#7384,.F.);
#10207=ORIENTED_EDGE('',*,*,#7385,.F.);
#10208=ORIENTED_EDGE('',*,*,#7386,.F.);
#10209=ORIENTED_EDGE('',*,*,#7379,.T.);
#10210=ORIENTED_EDGE('',*,*,#7387,.T.);
#10211=ORIENTED_EDGE('',*,*,#7388,.T.);
#10212=ORIENTED_EDGE('',*,*,#7389,.F.);
#10213=ORIENTED_EDGE('',*,*,#7390,.F.);
#10214=ORIENTED_EDGE('',*,*,#7391,.F.);
#10215=ORIENTED_EDGE('',*,*,#7384,.T.);
#10216=ORIENTED_EDGE('',*,*,#7392,.T.);
#10217=ORIENTED_EDGE('',*,*,#7393,.T.);
#10218=ORIENTED_EDGE('',*,*,#7394,.F.);
#10219=ORIENTED_EDGE('',*,*,#7395,.F.);
#10220=ORIENTED_EDGE('',*,*,#7396,.F.);
#10221=ORIENTED_EDGE('',*,*,#7389,.T.);
#10222=ORIENTED_EDGE('',*,*,#7397,.T.);
#10223=ORIENTED_EDGE('',*,*,#7398,.T.);
#10224=ORIENTED_EDGE('',*,*,#7399,.F.);
#10225=ORIENTED_EDGE('',*,*,#7400,.F.);
#10226=ORIENTED_EDGE('',*,*,#7401,.F.);
#10227=ORIENTED_EDGE('',*,*,#7394,.T.);
#10228=ORIENTED_EDGE('',*,*,#7402,.T.);
#10229=ORIENTED_EDGE('',*,*,#7403,.T.);
#10230=ORIENTED_EDGE('',*,*,#7404,.F.);
#10231=ORIENTED_EDGE('',*,*,#7405,.F.);
#10232=ORIENTED_EDGE('',*,*,#7406,.F.);
#10233=ORIENTED_EDGE('',*,*,#7399,.T.);
#10234=ORIENTED_EDGE('',*,*,#7407,.T.);
#10235=ORIENTED_EDGE('',*,*,#7408,.T.);
#10236=ORIENTED_EDGE('',*,*,#7409,.F.);
#10237=ORIENTED_EDGE('',*,*,#7410,.F.);
#10238=ORIENTED_EDGE('',*,*,#7411,.F.);
#10239=ORIENTED_EDGE('',*,*,#7404,.T.);
#10240=ORIENTED_EDGE('',*,*,#7412,.T.);
#10241=ORIENTED_EDGE('',*,*,#7413,.T.);
#10242=ORIENTED_EDGE('',*,*,#7414,.F.);
#10243=ORIENTED_EDGE('',*,*,#7415,.F.);
#10244=ORIENTED_EDGE('',*,*,#7416,.F.);
#10245=ORIENTED_EDGE('',*,*,#7409,.T.);
#10246=ORIENTED_EDGE('',*,*,#7417,.T.);
#10247=ORIENTED_EDGE('',*,*,#7418,.T.);
#10248=ORIENTED_EDGE('',*,*,#7419,.F.);
#10249=ORIENTED_EDGE('',*,*,#7420,.F.);
#10250=ORIENTED_EDGE('',*,*,#7421,.F.);
#10251=ORIENTED_EDGE('',*,*,#7414,.T.);
#10252=ORIENTED_EDGE('',*,*,#7422,.T.);
#10253=ORIENTED_EDGE('',*,*,#7423,.T.);
#10254=ORIENTED_EDGE('',*,*,#7424,.F.);
#10255=ORIENTED_EDGE('',*,*,#7425,.F.);
#10256=ORIENTED_EDGE('',*,*,#7426,.F.);
#10257=ORIENTED_EDGE('',*,*,#7419,.T.);
#10258=ORIENTED_EDGE('',*,*,#7427,.T.);
#10259=ORIENTED_EDGE('',*,*,#7428,.T.);
#10260=ORIENTED_EDGE('',*,*,#7429,.F.);
#10261=ORIENTED_EDGE('',*,*,#7430,.F.);
#10262=ORIENTED_EDGE('',*,*,#7431,.F.);
#10263=ORIENTED_EDGE('',*,*,#7424,.T.);
#10264=ORIENTED_EDGE('',*,*,#7432,.T.);
#10265=ORIENTED_EDGE('',*,*,#7433,.T.);
#10266=ORIENTED_EDGE('',*,*,#7434,.F.);
#10267=ORIENTED_EDGE('',*,*,#7435,.F.);
#10268=ORIENTED_EDGE('',*,*,#7436,.F.);
#10269=ORIENTED_EDGE('',*,*,#7429,.T.);
#10270=ORIENTED_EDGE('',*,*,#7437,.T.);
#10271=ORIENTED_EDGE('',*,*,#7438,.T.);
#10272=ORIENTED_EDGE('',*,*,#7439,.F.);
#10273=ORIENTED_EDGE('',*,*,#7440,.F.);
#10274=ORIENTED_EDGE('',*,*,#7441,.F.);
#10275=ORIENTED_EDGE('',*,*,#7434,.T.);
#10276=ORIENTED_EDGE('',*,*,#7442,.T.);
#10277=ORIENTED_EDGE('',*,*,#7443,.T.);
#10278=ORIENTED_EDGE('',*,*,#7444,.F.);
#10279=ORIENTED_EDGE('',*,*,#7445,.F.);
#10280=ORIENTED_EDGE('',*,*,#7446,.F.);
#10281=ORIENTED_EDGE('',*,*,#7439,.T.);
#10282=ORIENTED_EDGE('',*,*,#7447,.T.);
#10283=ORIENTED_EDGE('',*,*,#7448,.T.);
#10284=ORIENTED_EDGE('',*,*,#7449,.F.);
#10285=ORIENTED_EDGE('',*,*,#7450,.F.);
#10286=ORIENTED_EDGE('',*,*,#7451,.F.);
#10287=ORIENTED_EDGE('',*,*,#7444,.T.);
#10288=ORIENTED_EDGE('',*,*,#7452,.T.);
#10289=ORIENTED_EDGE('',*,*,#7453,.T.);
#10290=ORIENTED_EDGE('',*,*,#7454,.F.);
#10291=ORIENTED_EDGE('',*,*,#7455,.F.);
#10292=ORIENTED_EDGE('',*,*,#7456,.F.);
#10293=ORIENTED_EDGE('',*,*,#7449,.T.);
#10294=ORIENTED_EDGE('',*,*,#7457,.T.);
#10295=ORIENTED_EDGE('',*,*,#7458,.T.);
#10296=ORIENTED_EDGE('',*,*,#7459,.F.);
#10297=ORIENTED_EDGE('',*,*,#7460,.F.);
#10298=ORIENTED_EDGE('',*,*,#7461,.F.);
#10299=ORIENTED_EDGE('',*,*,#7454,.T.);
#10300=ORIENTED_EDGE('',*,*,#7462,.T.);
#10301=ORIENTED_EDGE('',*,*,#7463,.T.);
#10302=ORIENTED_EDGE('',*,*,#7464,.F.);
#10303=ORIENTED_EDGE('',*,*,#7465,.F.);
#10304=ORIENTED_EDGE('',*,*,#7466,.F.);
#10305=ORIENTED_EDGE('',*,*,#7459,.T.);
#10306=ORIENTED_EDGE('',*,*,#7467,.T.);
#10307=ORIENTED_EDGE('',*,*,#7468,.T.);
#10308=ORIENTED_EDGE('',*,*,#7469,.F.);
#10309=ORIENTED_EDGE('',*,*,#7470,.F.);
#10310=ORIENTED_EDGE('',*,*,#7471,.F.);
#10311=ORIENTED_EDGE('',*,*,#7464,.T.);
#10312=ORIENTED_EDGE('',*,*,#7472,.T.);
#10313=ORIENTED_EDGE('',*,*,#7473,.T.);
#10314=ORIENTED_EDGE('',*,*,#7474,.F.);
#10315=ORIENTED_EDGE('',*,*,#7475,.F.);
#10316=ORIENTED_EDGE('',*,*,#7476,.F.);
#10317=ORIENTED_EDGE('',*,*,#7469,.T.);
#10318=ORIENTED_EDGE('',*,*,#7477,.T.);
#10319=ORIENTED_EDGE('',*,*,#7478,.T.);
#10320=ORIENTED_EDGE('',*,*,#7479,.F.);
#10321=ORIENTED_EDGE('',*,*,#7480,.F.);
#10322=ORIENTED_EDGE('',*,*,#7481,.F.);
#10323=ORIENTED_EDGE('',*,*,#7474,.T.);
#10324=ORIENTED_EDGE('',*,*,#7482,.T.);
#10325=ORIENTED_EDGE('',*,*,#7483,.T.);
#10326=ORIENTED_EDGE('',*,*,#7484,.F.);
#10327=ORIENTED_EDGE('',*,*,#7485,.F.);
#10328=ORIENTED_EDGE('',*,*,#7486,.F.);
#10329=ORIENTED_EDGE('',*,*,#7479,.T.);
#10330=ORIENTED_EDGE('',*,*,#7487,.T.);
#10331=ORIENTED_EDGE('',*,*,#7488,.T.);
#10332=ORIENTED_EDGE('',*,*,#7489,.F.);
#10333=ORIENTED_EDGE('',*,*,#7490,.F.);
#10334=ORIENTED_EDGE('',*,*,#7491,.F.);
#10335=ORIENTED_EDGE('',*,*,#7484,.T.);
#10336=ORIENTED_EDGE('',*,*,#7492,.T.);
#10337=ORIENTED_EDGE('',*,*,#7493,.T.);
#10338=ORIENTED_EDGE('',*,*,#7494,.F.);
#10339=ORIENTED_EDGE('',*,*,#7495,.F.);
#10340=ORIENTED_EDGE('',*,*,#7496,.F.);
#10341=ORIENTED_EDGE('',*,*,#7489,.T.);
#10342=ORIENTED_EDGE('',*,*,#7497,.T.);
#10343=ORIENTED_EDGE('',*,*,#7498,.T.);
#10344=ORIENTED_EDGE('',*,*,#7499,.F.);
#10345=ORIENTED_EDGE('',*,*,#7500,.F.);
#10346=ORIENTED_EDGE('',*,*,#7501,.F.);
#10347=ORIENTED_EDGE('',*,*,#7494,.T.);
#10348=ORIENTED_EDGE('',*,*,#7502,.T.);
#10349=ORIENTED_EDGE('',*,*,#7503,.T.);
#10350=ORIENTED_EDGE('',*,*,#7504,.F.);
#10351=ORIENTED_EDGE('',*,*,#7505,.F.);
#10352=ORIENTED_EDGE('',*,*,#7506,.F.);
#10353=ORIENTED_EDGE('',*,*,#7499,.T.);
#10354=ORIENTED_EDGE('',*,*,#7507,.T.);
#10355=ORIENTED_EDGE('',*,*,#7508,.T.);
#10356=ORIENTED_EDGE('',*,*,#7509,.F.);
#10357=ORIENTED_EDGE('',*,*,#7510,.F.);
#10358=ORIENTED_EDGE('',*,*,#7511,.F.);
#10359=ORIENTED_EDGE('',*,*,#7504,.T.);
#10360=ORIENTED_EDGE('',*,*,#7512,.T.);
#10361=ORIENTED_EDGE('',*,*,#7513,.T.);
#10362=ORIENTED_EDGE('',*,*,#7514,.F.);
#10363=ORIENTED_EDGE('',*,*,#7515,.F.);
#10364=ORIENTED_EDGE('',*,*,#7516,.F.);
#10365=ORIENTED_EDGE('',*,*,#7509,.T.);
#10366=ORIENTED_EDGE('',*,*,#7517,.T.);
#10367=ORIENTED_EDGE('',*,*,#7518,.T.);
#10368=ORIENTED_EDGE('',*,*,#7519,.F.);
#10369=ORIENTED_EDGE('',*,*,#7520,.F.);
#10370=ORIENTED_EDGE('',*,*,#7521,.F.);
#10371=ORIENTED_EDGE('',*,*,#7514,.T.);
#10372=ORIENTED_EDGE('',*,*,#7522,.T.);
#10373=ORIENTED_EDGE('',*,*,#7523,.T.);
#10374=ORIENTED_EDGE('',*,*,#7524,.F.);
#10375=ORIENTED_EDGE('',*,*,#7525,.F.);
#10376=ORIENTED_EDGE('',*,*,#7526,.F.);
#10377=ORIENTED_EDGE('',*,*,#7519,.T.);
#10378=ORIENTED_EDGE('',*,*,#7527,.T.);
#10379=ORIENTED_EDGE('',*,*,#7528,.T.);
#10380=ORIENTED_EDGE('',*,*,#7529,.F.);
#10381=ORIENTED_EDGE('',*,*,#7530,.F.);
#10382=ORIENTED_EDGE('',*,*,#7531,.F.);
#10383=ORIENTED_EDGE('',*,*,#7524,.T.);
#10384=ORIENTED_EDGE('',*,*,#7532,.T.);
#10385=ORIENTED_EDGE('',*,*,#7533,.T.);
#10386=ORIENTED_EDGE('',*,*,#7534,.F.);
#10387=ORIENTED_EDGE('',*,*,#7535,.F.);
#10388=ORIENTED_EDGE('',*,*,#7536,.F.);
#10389=ORIENTED_EDGE('',*,*,#7529,.T.);
#10390=ORIENTED_EDGE('',*,*,#7537,.T.);
#10391=ORIENTED_EDGE('',*,*,#7538,.T.);
#10392=ORIENTED_EDGE('',*,*,#7539,.F.);
#10393=ORIENTED_EDGE('',*,*,#7540,.F.);
#10394=ORIENTED_EDGE('',*,*,#7541,.F.);
#10395=ORIENTED_EDGE('',*,*,#7534,.T.);
#10396=ORIENTED_EDGE('',*,*,#7542,.T.);
#10397=ORIENTED_EDGE('',*,*,#7543,.T.);
#10398=ORIENTED_EDGE('',*,*,#7544,.F.);
#10399=ORIENTED_EDGE('',*,*,#7545,.F.);
#10400=ORIENTED_EDGE('',*,*,#7546,.F.);
#10401=ORIENTED_EDGE('',*,*,#7539,.T.);
#10402=ORIENTED_EDGE('',*,*,#7547,.T.);
#10403=ORIENTED_EDGE('',*,*,#7548,.T.);
#10404=ORIENTED_EDGE('',*,*,#7549,.F.);
#10405=ORIENTED_EDGE('',*,*,#7550,.F.);
#10406=ORIENTED_EDGE('',*,*,#7551,.F.);
#10407=ORIENTED_EDGE('',*,*,#7544,.T.);
#10408=ORIENTED_EDGE('',*,*,#7552,.T.);
#10409=ORIENTED_EDGE('',*,*,#7553,.T.);
#10410=ORIENTED_EDGE('',*,*,#7554,.F.);
#10411=ORIENTED_EDGE('',*,*,#7555,.F.);
#10412=ORIENTED_EDGE('',*,*,#7556,.F.);
#10413=ORIENTED_EDGE('',*,*,#7549,.T.);
#10414=ORIENTED_EDGE('',*,*,#7557,.T.);
#10415=ORIENTED_EDGE('',*,*,#7558,.T.);
#10416=ORIENTED_EDGE('',*,*,#7559,.F.);
#10417=ORIENTED_EDGE('',*,*,#7560,.F.);
#10418=ORIENTED_EDGE('',*,*,#7561,.F.);
#10419=ORIENTED_EDGE('',*,*,#7554,.T.);
#10420=ORIENTED_EDGE('',*,*,#7562,.T.);
#10421=ORIENTED_EDGE('',*,*,#7563,.T.);
#10422=ORIENTED_EDGE('',*,*,#7564,.F.);
#10423=ORIENTED_EDGE('',*,*,#7565,.F.);
#10424=ORIENTED_EDGE('',*,*,#7566,.F.);
#10425=ORIENTED_EDGE('',*,*,#7559,.T.);
#10426=ORIENTED_EDGE('',*,*,#7567,.T.);
#10427=ORIENTED_EDGE('',*,*,#7568,.T.);
#10428=ORIENTED_EDGE('',*,*,#7569,.F.);
#10429=ORIENTED_EDGE('',*,*,#7570,.F.);
#10430=ORIENTED_EDGE('',*,*,#7571,.F.);
#10431=ORIENTED_EDGE('',*,*,#7564,.T.);
#10432=ORIENTED_EDGE('',*,*,#7572,.T.);
#10433=ORIENTED_EDGE('',*,*,#7573,.T.);
#10434=ORIENTED_EDGE('',*,*,#7574,.F.);
#10435=ORIENTED_EDGE('',*,*,#7575,.F.);
#10436=ORIENTED_EDGE('',*,*,#7576,.F.);
#10437=ORIENTED_EDGE('',*,*,#7569,.T.);
#10438=ORIENTED_EDGE('',*,*,#7577,.T.);
#10439=ORIENTED_EDGE('',*,*,#7578,.T.);
#10440=ORIENTED_EDGE('',*,*,#7579,.F.);
#10441=ORIENTED_EDGE('',*,*,#7580,.F.);
#10442=ORIENTED_EDGE('',*,*,#7581,.F.);
#10443=ORIENTED_EDGE('',*,*,#7574,.T.);
#10444=ORIENTED_EDGE('',*,*,#7582,.T.);
#10445=ORIENTED_EDGE('',*,*,#7583,.T.);
#10446=ORIENTED_EDGE('',*,*,#7584,.F.);
#10447=ORIENTED_EDGE('',*,*,#7585,.F.);
#10448=ORIENTED_EDGE('',*,*,#7586,.F.);
#10449=ORIENTED_EDGE('',*,*,#7579,.T.);
#10450=ORIENTED_EDGE('',*,*,#7587,.T.);
#10451=ORIENTED_EDGE('',*,*,#7588,.T.);
#10452=ORIENTED_EDGE('',*,*,#7589,.F.);
#10453=ORIENTED_EDGE('',*,*,#7590,.F.);
#10454=ORIENTED_EDGE('',*,*,#7591,.F.);
#10455=ORIENTED_EDGE('',*,*,#7584,.T.);
#10456=ORIENTED_EDGE('',*,*,#7592,.T.);
#10457=ORIENTED_EDGE('',*,*,#7593,.T.);
#10458=ORIENTED_EDGE('',*,*,#7594,.F.);
#10459=ORIENTED_EDGE('',*,*,#7595,.F.);
#10460=ORIENTED_EDGE('',*,*,#7596,.F.);
#10461=ORIENTED_EDGE('',*,*,#7589,.T.);
#10462=ORIENTED_EDGE('',*,*,#7597,.T.);
#10463=ORIENTED_EDGE('',*,*,#7598,.T.);
#10464=ORIENTED_EDGE('',*,*,#7599,.F.);
#10465=ORIENTED_EDGE('',*,*,#7600,.F.);
#10466=ORIENTED_EDGE('',*,*,#7601,.F.);
#10467=ORIENTED_EDGE('',*,*,#7594,.T.);
#10468=ORIENTED_EDGE('',*,*,#7602,.T.);
#10469=ORIENTED_EDGE('',*,*,#7603,.T.);
#10470=ORIENTED_EDGE('',*,*,#7604,.F.);
#10471=ORIENTED_EDGE('',*,*,#7605,.F.);
#10472=ORIENTED_EDGE('',*,*,#7606,.F.);
#10473=ORIENTED_EDGE('',*,*,#7599,.T.);
#10474=ORIENTED_EDGE('',*,*,#7607,.T.);
#10475=ORIENTED_EDGE('',*,*,#7608,.T.);
#10476=ORIENTED_EDGE('',*,*,#7609,.F.);
#10477=ORIENTED_EDGE('',*,*,#7610,.F.);
#10478=ORIENTED_EDGE('',*,*,#7611,.F.);
#10479=ORIENTED_EDGE('',*,*,#7604,.T.);
#10480=ORIENTED_EDGE('',*,*,#7612,.T.);
#10481=ORIENTED_EDGE('',*,*,#7613,.T.);
#10482=ORIENTED_EDGE('',*,*,#7614,.F.);
#10483=ORIENTED_EDGE('',*,*,#7615,.F.);
#10484=ORIENTED_EDGE('',*,*,#7616,.F.);
#10485=ORIENTED_EDGE('',*,*,#7609,.T.);
#10486=ORIENTED_EDGE('',*,*,#7617,.T.);
#10487=ORIENTED_EDGE('',*,*,#7618,.T.);
#10488=ORIENTED_EDGE('',*,*,#7619,.F.);
#10489=ORIENTED_EDGE('',*,*,#7620,.F.);
#10490=ORIENTED_EDGE('',*,*,#7621,.F.);
#10491=ORIENTED_EDGE('',*,*,#7614,.T.);
#10492=ORIENTED_EDGE('',*,*,#7622,.T.);
#10493=ORIENTED_EDGE('',*,*,#7623,.T.);
#10494=ORIENTED_EDGE('',*,*,#7624,.F.);
#10495=ORIENTED_EDGE('',*,*,#7625,.F.);
#10496=ORIENTED_EDGE('',*,*,#7626,.F.);
#10497=ORIENTED_EDGE('',*,*,#7619,.T.);
#10498=ORIENTED_EDGE('',*,*,#7627,.T.);
#10499=ORIENTED_EDGE('',*,*,#7628,.T.);
#10500=ORIENTED_EDGE('',*,*,#7629,.F.);
#10501=ORIENTED_EDGE('',*,*,#7630,.F.);
#10502=ORIENTED_EDGE('',*,*,#7631,.F.);
#10503=ORIENTED_EDGE('',*,*,#7624,.T.);
#10504=ORIENTED_EDGE('',*,*,#7632,.T.);
#10505=ORIENTED_EDGE('',*,*,#7633,.T.);
#10506=ORIENTED_EDGE('',*,*,#7634,.F.);
#10507=ORIENTED_EDGE('',*,*,#7635,.F.);
#10508=ORIENTED_EDGE('',*,*,#7636,.F.);
#10509=ORIENTED_EDGE('',*,*,#7629,.T.);
#10510=ORIENTED_EDGE('',*,*,#7637,.T.);
#10511=ORIENTED_EDGE('',*,*,#7638,.T.);
#10512=ORIENTED_EDGE('',*,*,#7639,.F.);
#10513=ORIENTED_EDGE('',*,*,#7640,.F.);
#10514=ORIENTED_EDGE('',*,*,#7641,.F.);
#10515=ORIENTED_EDGE('',*,*,#7634,.T.);
#10516=ORIENTED_EDGE('',*,*,#7642,.T.);
#10517=ORIENTED_EDGE('',*,*,#7643,.T.);
#10518=ORIENTED_EDGE('',*,*,#7644,.F.);
#10519=ORIENTED_EDGE('',*,*,#7645,.F.);
#10520=ORIENTED_EDGE('',*,*,#7646,.F.);
#10521=ORIENTED_EDGE('',*,*,#7639,.T.);
#10522=ORIENTED_EDGE('',*,*,#7647,.T.);
#10523=ORIENTED_EDGE('',*,*,#7648,.T.);
#10524=ORIENTED_EDGE('',*,*,#7649,.F.);
#10525=ORIENTED_EDGE('',*,*,#7650,.F.);
#10526=ORIENTED_EDGE('',*,*,#7651,.F.);
#10527=ORIENTED_EDGE('',*,*,#7644,.T.);
#10528=ORIENTED_EDGE('',*,*,#7652,.T.);
#10529=ORIENTED_EDGE('',*,*,#7653,.T.);
#10530=ORIENTED_EDGE('',*,*,#7654,.F.);
#10531=ORIENTED_EDGE('',*,*,#7655,.F.);
#10532=ORIENTED_EDGE('',*,*,#7656,.F.);
#10533=ORIENTED_EDGE('',*,*,#7649,.T.);
#10534=ORIENTED_EDGE('',*,*,#7657,.T.);
#10535=ORIENTED_EDGE('',*,*,#7658,.T.);
#10536=ORIENTED_EDGE('',*,*,#7659,.F.);
#10537=ORIENTED_EDGE('',*,*,#7660,.F.);
#10538=ORIENTED_EDGE('',*,*,#7661,.F.);
#10539=ORIENTED_EDGE('',*,*,#7654,.T.);
#10540=ORIENTED_EDGE('',*,*,#7662,.T.);
#10541=ORIENTED_EDGE('',*,*,#7663,.T.);
#10542=ORIENTED_EDGE('',*,*,#7664,.F.);
#10543=ORIENTED_EDGE('',*,*,#7665,.F.);
#10544=ORIENTED_EDGE('',*,*,#7666,.F.);
#10545=ORIENTED_EDGE('',*,*,#7659,.T.);
#10546=ORIENTED_EDGE('',*,*,#7667,.T.);
#10547=ORIENTED_EDGE('',*,*,#7668,.T.);
#10548=ORIENTED_EDGE('',*,*,#7669,.F.);
#10549=ORIENTED_EDGE('',*,*,#7670,.F.);
#10550=ORIENTED_EDGE('',*,*,#7671,.F.);
#10551=ORIENTED_EDGE('',*,*,#7664,.T.);
#10552=ORIENTED_EDGE('',*,*,#7672,.T.);
#10553=ORIENTED_EDGE('',*,*,#7673,.T.);
#10554=ORIENTED_EDGE('',*,*,#7674,.F.);
#10555=ORIENTED_EDGE('',*,*,#7675,.F.);
#10556=ORIENTED_EDGE('',*,*,#7676,.F.);
#10557=ORIENTED_EDGE('',*,*,#7669,.T.);
#10558=ORIENTED_EDGE('',*,*,#7677,.T.);
#10559=ORIENTED_EDGE('',*,*,#7678,.T.);
#10560=ORIENTED_EDGE('',*,*,#7679,.F.);
#10561=ORIENTED_EDGE('',*,*,#7680,.F.);
#10562=ORIENTED_EDGE('',*,*,#7681,.F.);
#10563=ORIENTED_EDGE('',*,*,#7674,.T.);
#10564=ORIENTED_EDGE('',*,*,#7682,.T.);
#10565=ORIENTED_EDGE('',*,*,#7683,.T.);
#10566=ORIENTED_EDGE('',*,*,#7684,.F.);
#10567=ORIENTED_EDGE('',*,*,#7685,.F.);
#10568=ORIENTED_EDGE('',*,*,#7686,.F.);
#10569=ORIENTED_EDGE('',*,*,#7679,.T.);
#10570=ORIENTED_EDGE('',*,*,#7687,.T.);
#10571=ORIENTED_EDGE('',*,*,#7688,.T.);
#10572=ORIENTED_EDGE('',*,*,#7689,.F.);
#10573=ORIENTED_EDGE('',*,*,#7690,.F.);
#10574=ORIENTED_EDGE('',*,*,#7691,.F.);
#10575=ORIENTED_EDGE('',*,*,#7684,.T.);
#10576=ORIENTED_EDGE('',*,*,#7692,.T.);
#10577=ORIENTED_EDGE('',*,*,#7693,.T.);
#10578=ORIENTED_EDGE('',*,*,#7694,.F.);
#10579=ORIENTED_EDGE('',*,*,#7695,.F.);
#10580=ORIENTED_EDGE('',*,*,#7696,.F.);
#10581=ORIENTED_EDGE('',*,*,#7689,.T.);
#10582=ORIENTED_EDGE('',*,*,#7697,.T.);
#10583=ORIENTED_EDGE('',*,*,#7698,.T.);
#10584=ORIENTED_EDGE('',*,*,#7699,.F.);
#10585=ORIENTED_EDGE('',*,*,#7700,.F.);
#10586=ORIENTED_EDGE('',*,*,#7701,.F.);
#10587=ORIENTED_EDGE('',*,*,#7694,.T.);
#10588=ORIENTED_EDGE('',*,*,#7702,.T.);
#10589=ORIENTED_EDGE('',*,*,#7703,.T.);
#10590=ORIENTED_EDGE('',*,*,#7704,.F.);
#10591=ORIENTED_EDGE('',*,*,#7705,.F.);
#10592=ORIENTED_EDGE('',*,*,#7706,.F.);
#10593=ORIENTED_EDGE('',*,*,#7699,.T.);
#10594=ORIENTED_EDGE('',*,*,#7707,.T.);
#10595=ORIENTED_EDGE('',*,*,#7708,.T.);
#10596=ORIENTED_EDGE('',*,*,#7709,.F.);
#10597=ORIENTED_EDGE('',*,*,#7710,.F.);
#10598=ORIENTED_EDGE('',*,*,#7711,.F.);
#10599=ORIENTED_EDGE('',*,*,#7704,.T.);
#10600=ORIENTED_EDGE('',*,*,#7712,.T.);
#10601=ORIENTED_EDGE('',*,*,#7713,.T.);
#10602=ORIENTED_EDGE('',*,*,#7714,.F.);
#10603=ORIENTED_EDGE('',*,*,#7715,.F.);
#10604=ORIENTED_EDGE('',*,*,#7716,.F.);
#10605=ORIENTED_EDGE('',*,*,#7709,.T.);
#10606=ORIENTED_EDGE('',*,*,#7717,.T.);
#10607=ORIENTED_EDGE('',*,*,#7718,.T.);
#10608=ORIENTED_EDGE('',*,*,#7719,.F.);
#10609=ORIENTED_EDGE('',*,*,#7720,.F.);
#10610=ORIENTED_EDGE('',*,*,#7721,.F.);
#10611=ORIENTED_EDGE('',*,*,#7714,.T.);
#10612=ORIENTED_EDGE('',*,*,#7722,.T.);
#10613=ORIENTED_EDGE('',*,*,#7723,.T.);
#10614=ORIENTED_EDGE('',*,*,#7724,.F.);
#10615=ORIENTED_EDGE('',*,*,#7725,.F.);
#10616=ORIENTED_EDGE('',*,*,#7726,.F.);
#10617=ORIENTED_EDGE('',*,*,#7719,.T.);
#10618=ORIENTED_EDGE('',*,*,#7727,.T.);
#10619=ORIENTED_EDGE('',*,*,#7728,.T.);
#10620=ORIENTED_EDGE('',*,*,#7729,.F.);
#10621=ORIENTED_EDGE('',*,*,#7730,.F.);
#10622=ORIENTED_EDGE('',*,*,#7731,.F.);
#10623=ORIENTED_EDGE('',*,*,#7724,.T.);
#10624=ORIENTED_EDGE('',*,*,#7732,.T.);
#10625=ORIENTED_EDGE('',*,*,#7733,.T.);
#10626=ORIENTED_EDGE('',*,*,#7734,.F.);
#10627=ORIENTED_EDGE('',*,*,#7735,.F.);
#10628=ORIENTED_EDGE('',*,*,#7736,.F.);
#10629=ORIENTED_EDGE('',*,*,#7729,.T.);
#10630=ORIENTED_EDGE('',*,*,#7737,.T.);
#10631=ORIENTED_EDGE('',*,*,#7738,.T.);
#10632=ORIENTED_EDGE('',*,*,#7739,.F.);
#10633=ORIENTED_EDGE('',*,*,#7740,.F.);
#10634=ORIENTED_EDGE('',*,*,#7741,.F.);
#10635=ORIENTED_EDGE('',*,*,#7734,.T.);
#10636=ORIENTED_EDGE('',*,*,#7742,.T.);
#10637=ORIENTED_EDGE('',*,*,#7743,.T.);
#10638=ORIENTED_EDGE('',*,*,#7744,.F.);
#10639=ORIENTED_EDGE('',*,*,#7745,.F.);
#10640=ORIENTED_EDGE('',*,*,#7746,.F.);
#10641=ORIENTED_EDGE('',*,*,#7739,.T.);
#10642=ORIENTED_EDGE('',*,*,#7747,.T.);
#10643=ORIENTED_EDGE('',*,*,#7748,.T.);
#10644=ORIENTED_EDGE('',*,*,#7749,.F.);
#10645=ORIENTED_EDGE('',*,*,#7750,.F.);
#10646=ORIENTED_EDGE('',*,*,#7751,.F.);
#10647=ORIENTED_EDGE('',*,*,#7744,.T.);
#10648=ORIENTED_EDGE('',*,*,#7752,.T.);
#10649=ORIENTED_EDGE('',*,*,#7753,.T.);
#10650=ORIENTED_EDGE('',*,*,#7754,.F.);
#10651=ORIENTED_EDGE('',*,*,#7755,.F.);
#10652=ORIENTED_EDGE('',*,*,#7756,.F.);
#10653=ORIENTED_EDGE('',*,*,#7749,.T.);
#10654=ORIENTED_EDGE('',*,*,#7757,.T.);
#10655=ORIENTED_EDGE('',*,*,#7758,.T.);
#10656=ORIENTED_EDGE('',*,*,#7759,.F.);
#10657=ORIENTED_EDGE('',*,*,#7760,.F.);
#10658=ORIENTED_EDGE('',*,*,#7761,.F.);
#10659=ORIENTED_EDGE('',*,*,#7754,.T.);
#10660=ORIENTED_EDGE('',*,*,#7762,.T.);
#10661=ORIENTED_EDGE('',*,*,#7763,.T.);
#10662=ORIENTED_EDGE('',*,*,#7764,.F.);
#10663=ORIENTED_EDGE('',*,*,#7765,.F.);
#10664=ORIENTED_EDGE('',*,*,#7766,.F.);
#10665=ORIENTED_EDGE('',*,*,#7759,.T.);
#10666=ORIENTED_EDGE('',*,*,#7767,.T.);
#10667=ORIENTED_EDGE('',*,*,#7768,.T.);
#10668=ORIENTED_EDGE('',*,*,#7769,.F.);
#10669=ORIENTED_EDGE('',*,*,#7770,.F.);
#10670=ORIENTED_EDGE('',*,*,#7771,.F.);
#10671=ORIENTED_EDGE('',*,*,#7764,.T.);
#10672=ORIENTED_EDGE('',*,*,#7772,.T.);
#10673=ORIENTED_EDGE('',*,*,#7773,.T.);
#10674=ORIENTED_EDGE('',*,*,#7774,.F.);
#10675=ORIENTED_EDGE('',*,*,#7775,.F.);
#10676=ORIENTED_EDGE('',*,*,#7776,.F.);
#10677=ORIENTED_EDGE('',*,*,#7769,.T.);
#10678=ORIENTED_EDGE('',*,*,#7777,.T.);
#10679=ORIENTED_EDGE('',*,*,#7778,.T.);
#10680=ORIENTED_EDGE('',*,*,#7779,.F.);
#10681=ORIENTED_EDGE('',*,*,#7780,.F.);
#10682=ORIENTED_EDGE('',*,*,#7781,.F.);
#10683=ORIENTED_EDGE('',*,*,#7774,.T.);
#10684=ORIENTED_EDGE('',*,*,#7782,.T.);
#10685=ORIENTED_EDGE('',*,*,#7783,.T.);
#10686=ORIENTED_EDGE('',*,*,#7784,.F.);
#10687=ORIENTED_EDGE('',*,*,#7785,.F.);
#10688=ORIENTED_EDGE('',*,*,#7786,.F.);
#10689=ORIENTED_EDGE('',*,*,#7779,.T.);
#10690=ORIENTED_EDGE('',*,*,#7787,.T.);
#10691=ORIENTED_EDGE('',*,*,#7788,.T.);
#10692=ORIENTED_EDGE('',*,*,#7789,.F.);
#10693=ORIENTED_EDGE('',*,*,#7790,.F.);
#10694=ORIENTED_EDGE('',*,*,#7791,.F.);
#10695=ORIENTED_EDGE('',*,*,#7784,.T.);
#10696=ORIENTED_EDGE('',*,*,#7792,.T.);
#10697=ORIENTED_EDGE('',*,*,#7793,.T.);
#10698=ORIENTED_EDGE('',*,*,#7794,.F.);
#10699=ORIENTED_EDGE('',*,*,#7795,.F.);
#10700=ORIENTED_EDGE('',*,*,#7796,.F.);
#10701=ORIENTED_EDGE('',*,*,#7789,.T.);
#10702=ORIENTED_EDGE('',*,*,#7797,.T.);
#10703=ORIENTED_EDGE('',*,*,#7798,.T.);
#10704=ORIENTED_EDGE('',*,*,#7799,.F.);
#10705=ORIENTED_EDGE('',*,*,#7800,.F.);
#10706=ORIENTED_EDGE('',*,*,#7801,.F.);
#10707=ORIENTED_EDGE('',*,*,#7794,.T.);
#10708=ORIENTED_EDGE('',*,*,#7802,.T.);
#10709=ORIENTED_EDGE('',*,*,#7803,.T.);
#10710=ORIENTED_EDGE('',*,*,#7804,.F.);
#10711=ORIENTED_EDGE('',*,*,#7805,.F.);
#10712=ORIENTED_EDGE('',*,*,#7806,.F.);
#10713=ORIENTED_EDGE('',*,*,#7799,.T.);
#10714=ORIENTED_EDGE('',*,*,#7807,.T.);
#10715=ORIENTED_EDGE('',*,*,#7808,.T.);
#10716=ORIENTED_EDGE('',*,*,#7809,.F.);
#10717=ORIENTED_EDGE('',*,*,#7810,.F.);
#10718=ORIENTED_EDGE('',*,*,#7811,.F.);
#10719=ORIENTED_EDGE('',*,*,#7804,.T.);
#10720=ORIENTED_EDGE('',*,*,#7812,.T.);
#10721=ORIENTED_EDGE('',*,*,#7813,.T.);
#10722=ORIENTED_EDGE('',*,*,#7814,.F.);
#10723=ORIENTED_EDGE('',*,*,#7815,.F.);
#10724=ORIENTED_EDGE('',*,*,#7816,.F.);
#10725=ORIENTED_EDGE('',*,*,#7809,.T.);
#10726=ORIENTED_EDGE('',*,*,#7817,.T.);
#10727=ORIENTED_EDGE('',*,*,#7818,.T.);
#10728=ORIENTED_EDGE('',*,*,#7819,.F.);
#10729=ORIENTED_EDGE('',*,*,#7820,.F.);
#10730=ORIENTED_EDGE('',*,*,#7821,.F.);
#10731=ORIENTED_EDGE('',*,*,#7814,.T.);
#10732=ORIENTED_EDGE('',*,*,#7822,.T.);
#10733=ORIENTED_EDGE('',*,*,#7823,.T.);
#10734=ORIENTED_EDGE('',*,*,#7824,.F.);
#10735=ORIENTED_EDGE('',*,*,#7825,.F.);
#10736=ORIENTED_EDGE('',*,*,#7826,.F.);
#10737=ORIENTED_EDGE('',*,*,#7819,.T.);
#10738=ORIENTED_EDGE('',*,*,#7827,.T.);
#10739=ORIENTED_EDGE('',*,*,#7828,.T.);
#10740=ORIENTED_EDGE('',*,*,#7829,.F.);
#10741=ORIENTED_EDGE('',*,*,#7830,.F.);
#10742=ORIENTED_EDGE('',*,*,#7831,.F.);
#10743=ORIENTED_EDGE('',*,*,#7824,.T.);
#10744=ORIENTED_EDGE('',*,*,#7832,.T.);
#10745=ORIENTED_EDGE('',*,*,#7833,.T.);
#10746=ORIENTED_EDGE('',*,*,#7834,.T.);
#10747=ORIENTED_EDGE('',*,*,#7835,.F.);
#10748=ORIENTED_EDGE('',*,*,#7836,.T.);
#10749=ORIENTED_EDGE('',*,*,#7837,.T.);
#10750=ORIENTED_EDGE('',*,*,#7838,.T.);
#10751=ORIENTED_EDGE('',*,*,#7839,.T.);
#10752=ORIENTED_EDGE('',*,*,#7840,.T.);
#10753=ORIENTED_EDGE('',*,*,#7841,.T.);
#10754=ORIENTED_EDGE('',*,*,#7842,.T.);
#10755=ORIENTED_EDGE('',*,*,#7843,.T.);
#10756=ORIENTED_EDGE('',*,*,#7844,.T.);
#10757=ORIENTED_EDGE('',*,*,#7845,.T.);
#10758=ORIENTED_EDGE('',*,*,#7846,.T.);
#10759=ORIENTED_EDGE('',*,*,#7847,.T.);
#10760=ORIENTED_EDGE('',*,*,#7848,.T.);
#10761=ORIENTED_EDGE('',*,*,#7849,.T.);
#10762=ORIENTED_EDGE('',*,*,#7850,.T.);
#10763=ORIENTED_EDGE('',*,*,#7851,.T.);
#10764=ORIENTED_EDGE('',*,*,#7852,.T.);
#10765=ORIENTED_EDGE('',*,*,#7853,.T.);
#10766=ORIENTED_EDGE('',*,*,#7854,.T.);
#10767=ORIENTED_EDGE('',*,*,#7855,.T.);
#10768=ORIENTED_EDGE('',*,*,#7856,.T.);
#10769=ORIENTED_EDGE('',*,*,#7857,.T.);
#10770=ORIENTED_EDGE('',*,*,#7858,.T.);
#10771=ORIENTED_EDGE('',*,*,#7859,.T.);
#10772=ORIENTED_EDGE('',*,*,#7860,.T.);
#10773=ORIENTED_EDGE('',*,*,#7861,.T.);
#10774=ORIENTED_EDGE('',*,*,#7862,.T.);
#10775=ORIENTED_EDGE('',*,*,#7863,.T.);
#10776=ORIENTED_EDGE('',*,*,#7864,.T.);
#10777=ORIENTED_EDGE('',*,*,#7865,.T.);
#10778=ORIENTED_EDGE('',*,*,#7866,.T.);
#10779=ORIENTED_EDGE('',*,*,#7867,.T.);
#10780=ORIENTED_EDGE('',*,*,#7868,.T.);
#10781=ORIENTED_EDGE('',*,*,#7869,.T.);
#10782=ORIENTED_EDGE('',*,*,#7870,.T.);
#10783=ORIENTED_EDGE('',*,*,#7871,.T.);
#10784=ORIENTED_EDGE('',*,*,#7872,.T.);
#10785=ORIENTED_EDGE('',*,*,#7873,.T.);
#10786=ORIENTED_EDGE('',*,*,#7874,.T.);
#10787=ORIENTED_EDGE('',*,*,#7875,.T.);
#10788=ORIENTED_EDGE('',*,*,#7876,.T.);
#10789=ORIENTED_EDGE('',*,*,#7877,.T.);
#10790=ORIENTED_EDGE('',*,*,#7878,.T.);
#10791=ORIENTED_EDGE('',*,*,#7879,.T.);
#10792=ORIENTED_EDGE('',*,*,#7880,.T.);
#10793=ORIENTED_EDGE('',*,*,#7881,.T.);
#10794=ORIENTED_EDGE('',*,*,#7882,.T.);
#10795=ORIENTED_EDGE('',*,*,#7883,.T.);
#10796=ORIENTED_EDGE('',*,*,#7884,.T.);
#10797=ORIENTED_EDGE('',*,*,#7885,.T.);
#10798=ORIENTED_EDGE('',*,*,#7886,.T.);
#10799=ORIENTED_EDGE('',*,*,#7887,.T.);
#10800=ORIENTED_EDGE('',*,*,#7888,.T.);
#10801=ORIENTED_EDGE('',*,*,#7889,.T.);
#10802=ORIENTED_EDGE('',*,*,#7890,.T.);
#10803=ORIENTED_EDGE('',*,*,#7891,.T.);
#10804=ORIENTED_EDGE('',*,*,#7892,.T.);
#10805=ORIENTED_EDGE('',*,*,#7893,.T.);
#10806=ORIENTED_EDGE('',*,*,#7894,.T.);
#10807=ORIENTED_EDGE('',*,*,#7895,.T.);
#10808=ORIENTED_EDGE('',*,*,#7896,.T.);
#10809=ORIENTED_EDGE('',*,*,#7897,.T.);
#10810=ORIENTED_EDGE('',*,*,#7898,.T.);
#10811=ORIENTED_EDGE('',*,*,#7899,.T.);
#10812=ORIENTED_EDGE('',*,*,#7900,.T.);
#10813=ORIENTED_EDGE('',*,*,#7901,.T.);
#10814=ORIENTED_EDGE('',*,*,#7902,.T.);
#10815=ORIENTED_EDGE('',*,*,#7903,.T.);
#10816=ORIENTED_EDGE('',*,*,#7904,.T.);
#10817=ORIENTED_EDGE('',*,*,#7905,.T.);
#10818=ORIENTED_EDGE('',*,*,#7906,.T.);
#10819=ORIENTED_EDGE('',*,*,#7907,.T.);
#10820=ORIENTED_EDGE('',*,*,#7908,.T.);
#10821=ORIENTED_EDGE('',*,*,#7909,.T.);
#10822=ORIENTED_EDGE('',*,*,#7910,.T.);
#10823=ORIENTED_EDGE('',*,*,#7911,.T.);
#10824=ORIENTED_EDGE('',*,*,#7912,.T.);
#10825=ORIENTED_EDGE('',*,*,#7913,.T.);
#10826=ORIENTED_EDGE('',*,*,#7914,.T.);
#10827=ORIENTED_EDGE('',*,*,#7915,.T.);
#10828=ORIENTED_EDGE('',*,*,#7916,.T.);
#10829=ORIENTED_EDGE('',*,*,#7917,.T.);
#10830=ORIENTED_EDGE('',*,*,#7918,.T.);
#10831=ORIENTED_EDGE('',*,*,#7919,.T.);
#10832=ORIENTED_EDGE('',*,*,#7920,.T.);
#10833=ORIENTED_EDGE('',*,*,#7921,.T.);
#10834=ORIENTED_EDGE('',*,*,#7922,.T.);
#10835=ORIENTED_EDGE('',*,*,#7923,.T.);
#10836=ORIENTED_EDGE('',*,*,#7924,.T.);
#10837=ORIENTED_EDGE('',*,*,#7925,.T.);
#10838=ORIENTED_EDGE('',*,*,#7926,.T.);
#10839=ORIENTED_EDGE('',*,*,#7927,.T.);
#10840=ORIENTED_EDGE('',*,*,#7928,.T.);
#10841=ORIENTED_EDGE('',*,*,#7929,.T.);
#10842=ORIENTED_EDGE('',*,*,#7930,.T.);
#10843=ORIENTED_EDGE('',*,*,#7931,.T.);
#10844=ORIENTED_EDGE('',*,*,#7932,.T.);
#10845=ORIENTED_EDGE('',*,*,#7933,.T.);
#10846=ORIENTED_EDGE('',*,*,#7934,.T.);
#10847=ORIENTED_EDGE('',*,*,#7935,.T.);
#10848=ORIENTED_EDGE('',*,*,#7936,.T.);
#10849=ORIENTED_EDGE('',*,*,#7937,.T.);
#10850=ORIENTED_EDGE('',*,*,#7938,.T.);
#10851=ORIENTED_EDGE('',*,*,#7939,.T.);
#10852=ORIENTED_EDGE('',*,*,#7940,.T.);
#10853=ORIENTED_EDGE('',*,*,#7941,.T.);
#10854=ORIENTED_EDGE('',*,*,#7942,.T.);
#10855=ORIENTED_EDGE('',*,*,#7943,.T.);
#10856=ORIENTED_EDGE('',*,*,#7944,.T.);
#10857=ORIENTED_EDGE('',*,*,#7945,.T.);
#10858=ORIENTED_EDGE('',*,*,#7946,.T.);
#10859=ORIENTED_EDGE('',*,*,#7947,.T.);
#10860=ORIENTED_EDGE('',*,*,#7948,.T.);
#10861=ORIENTED_EDGE('',*,*,#7949,.T.);
#10862=ORIENTED_EDGE('',*,*,#7950,.T.);
#10863=ORIENTED_EDGE('',*,*,#7951,.T.);
#10864=ORIENTED_EDGE('',*,*,#7952,.T.);
#10865=ORIENTED_EDGE('',*,*,#7953,.T.);
#10866=ORIENTED_EDGE('',*,*,#7954,.T.);
#10867=ORIENTED_EDGE('',*,*,#7955,.T.);
#10868=ORIENTED_EDGE('',*,*,#7956,.T.);
#10869=ORIENTED_EDGE('',*,*,#7957,.T.);
#10870=ORIENTED_EDGE('',*,*,#7958,.T.);
#10871=ORIENTED_EDGE('',*,*,#7959,.T.);
#10872=ORIENTED_EDGE('',*,*,#7960,.T.);
#10873=ORIENTED_EDGE('',*,*,#7961,.T.);
#10874=ORIENTED_EDGE('',*,*,#7962,.T.);
#10875=ORIENTED_EDGE('',*,*,#7963,.T.);
#10876=ORIENTED_EDGE('',*,*,#7964,.T.);
#10877=ORIENTED_EDGE('',*,*,#7965,.T.);
#10878=ORIENTED_EDGE('',*,*,#7966,.T.);
#10879=ORIENTED_EDGE('',*,*,#7967,.T.);
#10880=ORIENTED_EDGE('',*,*,#7968,.T.);
#10881=ORIENTED_EDGE('',*,*,#7969,.T.);
#10882=ORIENTED_EDGE('',*,*,#7970,.T.);
#10883=ORIENTED_EDGE('',*,*,#7971,.T.);
#10884=ORIENTED_EDGE('',*,*,#7972,.T.);
#10885=ORIENTED_EDGE('',*,*,#7973,.T.);
#10886=ORIENTED_EDGE('',*,*,#7974,.T.);
#10887=ORIENTED_EDGE('',*,*,#7975,.T.);
#10888=ORIENTED_EDGE('',*,*,#7976,.T.);
#10889=ORIENTED_EDGE('',*,*,#7977,.T.);
#10890=ORIENTED_EDGE('',*,*,#7978,.T.);
#10891=ORIENTED_EDGE('',*,*,#7979,.T.);
#10892=ORIENTED_EDGE('',*,*,#7980,.T.);
#10893=ORIENTED_EDGE('',*,*,#7981,.T.);
#10894=ORIENTED_EDGE('',*,*,#7982,.T.);
#10895=ORIENTED_EDGE('',*,*,#7983,.T.);
#10896=ORIENTED_EDGE('',*,*,#7984,.T.);
#10897=ORIENTED_EDGE('',*,*,#7985,.T.);
#10898=ORIENTED_EDGE('',*,*,#7986,.T.);
#10899=ORIENTED_EDGE('',*,*,#7987,.T.);
#10900=ORIENTED_EDGE('',*,*,#7988,.T.);
#10901=ORIENTED_EDGE('',*,*,#7989,.T.);
#10902=ORIENTED_EDGE('',*,*,#7990,.T.);
#10903=ORIENTED_EDGE('',*,*,#7991,.T.);
#10904=ORIENTED_EDGE('',*,*,#7992,.T.);
#10905=ORIENTED_EDGE('',*,*,#7993,.T.);
#10906=ORIENTED_EDGE('',*,*,#7994,.T.);
#10907=ORIENTED_EDGE('',*,*,#7995,.T.);
#10908=ORIENTED_EDGE('',*,*,#7996,.T.);
#10909=ORIENTED_EDGE('',*,*,#7997,.T.);
#10910=ORIENTED_EDGE('',*,*,#7998,.T.);
#10911=ORIENTED_EDGE('',*,*,#7999,.T.);
#10912=ORIENTED_EDGE('',*,*,#8000,.T.);
#10913=ORIENTED_EDGE('',*,*,#8001,.T.);
#10914=ORIENTED_EDGE('',*,*,#8002,.T.);
#10915=ORIENTED_EDGE('',*,*,#8003,.T.);
#10916=ORIENTED_EDGE('',*,*,#8004,.T.);
#10917=ORIENTED_EDGE('',*,*,#8005,.T.);
#10918=ORIENTED_EDGE('',*,*,#8006,.T.);
#10919=ORIENTED_EDGE('',*,*,#8007,.T.);
#10920=ORIENTED_EDGE('',*,*,#8008,.T.);
#10921=ORIENTED_EDGE('',*,*,#8009,.T.);
#10922=ORIENTED_EDGE('',*,*,#8010,.T.);
#10923=ORIENTED_EDGE('',*,*,#8011,.T.);
#10924=ORIENTED_EDGE('',*,*,#8012,.T.);
#10925=ORIENTED_EDGE('',*,*,#8013,.T.);
#10926=ORIENTED_EDGE('',*,*,#8014,.T.);
#10927=ORIENTED_EDGE('',*,*,#8015,.T.);
#10928=ORIENTED_EDGE('',*,*,#8016,.T.);
#10929=ORIENTED_EDGE('',*,*,#8017,.T.);
#10930=ORIENTED_EDGE('',*,*,#8018,.T.);
#10931=ORIENTED_EDGE('',*,*,#8019,.T.);
#10932=ORIENTED_EDGE('',*,*,#8020,.T.);
#10933=ORIENTED_EDGE('',*,*,#8021,.T.);
#10934=ORIENTED_EDGE('',*,*,#8022,.T.);
#10935=ORIENTED_EDGE('',*,*,#8023,.T.);
#10936=ORIENTED_EDGE('',*,*,#8024,.T.);
#10937=ORIENTED_EDGE('',*,*,#8025,.T.);
#10938=ORIENTED_EDGE('',*,*,#8026,.T.);
#10939=ORIENTED_EDGE('',*,*,#8027,.T.);
#10940=ORIENTED_EDGE('',*,*,#8028,.T.);
#10941=ORIENTED_EDGE('',*,*,#8029,.T.);
#10942=ORIENTED_EDGE('',*,*,#8030,.T.);
#10943=ORIENTED_EDGE('',*,*,#8031,.T.);
#10944=ORIENTED_EDGE('',*,*,#8032,.T.);
#10945=ORIENTED_EDGE('',*,*,#8033,.T.);
#10946=ORIENTED_EDGE('',*,*,#8034,.T.);
#10947=ORIENTED_EDGE('',*,*,#8035,.T.);
#10948=ORIENTED_EDGE('',*,*,#8036,.T.);
#10949=ORIENTED_EDGE('',*,*,#8037,.T.);
#10950=ORIENTED_EDGE('',*,*,#8038,.T.);
#10951=ORIENTED_EDGE('',*,*,#8039,.T.);
#10952=ORIENTED_EDGE('',*,*,#8040,.T.);
#10953=ORIENTED_EDGE('',*,*,#8041,.T.);
#10954=ORIENTED_EDGE('',*,*,#8042,.T.);
#10955=ORIENTED_EDGE('',*,*,#8043,.T.);
#10956=ORIENTED_EDGE('',*,*,#8044,.T.);
#10957=ORIENTED_EDGE('',*,*,#8045,.T.);
#10958=ORIENTED_EDGE('',*,*,#8046,.T.);
#10959=ORIENTED_EDGE('',*,*,#8047,.T.);
#10960=ORIENTED_EDGE('',*,*,#8048,.T.);
#10961=ORIENTED_EDGE('',*,*,#8049,.T.);
#10962=ORIENTED_EDGE('',*,*,#8050,.T.);
#10963=ORIENTED_EDGE('',*,*,#8051,.T.);
#10964=ORIENTED_EDGE('',*,*,#8052,.T.);
#10965=ORIENTED_EDGE('',*,*,#8053,.T.);
#10966=ORIENTED_EDGE('',*,*,#8054,.T.);
#10967=ORIENTED_EDGE('',*,*,#8055,.T.);
#10968=ORIENTED_EDGE('',*,*,#8056,.T.);
#10969=ORIENTED_EDGE('',*,*,#8057,.T.);
#10970=ORIENTED_EDGE('',*,*,#8058,.T.);
#10971=ORIENTED_EDGE('',*,*,#8059,.T.);
#10972=ORIENTED_EDGE('',*,*,#8060,.T.);
#10973=ORIENTED_EDGE('',*,*,#8061,.T.);
#10974=ORIENTED_EDGE('',*,*,#8062,.T.);
#10975=ORIENTED_EDGE('',*,*,#8063,.T.);
#10976=ORIENTED_EDGE('',*,*,#8064,.T.);
#10977=ORIENTED_EDGE('',*,*,#8065,.T.);
#10978=ORIENTED_EDGE('',*,*,#8066,.T.);
#10979=ORIENTED_EDGE('',*,*,#8067,.T.);
#10980=ORIENTED_EDGE('',*,*,#8068,.T.);
#10981=ORIENTED_EDGE('',*,*,#8069,.T.);
#10982=ORIENTED_EDGE('',*,*,#8070,.T.);
#10983=ORIENTED_EDGE('',*,*,#8071,.T.);
#10984=ORIENTED_EDGE('',*,*,#8072,.T.);
#10985=ORIENTED_EDGE('',*,*,#8073,.T.);
#10986=ORIENTED_EDGE('',*,*,#8074,.T.);
#10987=ORIENTED_EDGE('',*,*,#8075,.T.);
#10988=ORIENTED_EDGE('',*,*,#8076,.T.);
#10989=ORIENTED_EDGE('',*,*,#8077,.T.);
#10990=ORIENTED_EDGE('',*,*,#8078,.T.);
#10991=ORIENTED_EDGE('',*,*,#8079,.T.);
#10992=ORIENTED_EDGE('',*,*,#8080,.T.);
#10993=ORIENTED_EDGE('',*,*,#8081,.T.);
#10994=ORIENTED_EDGE('',*,*,#8082,.T.);
#10995=ORIENTED_EDGE('',*,*,#8083,.T.);
#10996=ORIENTED_EDGE('',*,*,#8084,.T.);
#10997=ORIENTED_EDGE('',*,*,#8085,.T.);
#10998=ORIENTED_EDGE('',*,*,#8086,.T.);
#10999=ORIENTED_EDGE('',*,*,#8087,.T.);
#11000=ORIENTED_EDGE('',*,*,#8088,.T.);
#11001=ORIENTED_EDGE('',*,*,#8089,.T.);
#11002=ORIENTED_EDGE('',*,*,#8090,.T.);
#11003=ORIENTED_EDGE('',*,*,#8091,.T.);
#11004=ORIENTED_EDGE('',*,*,#8092,.T.);
#11005=ORIENTED_EDGE('',*,*,#8093,.T.);
#11006=ORIENTED_EDGE('',*,*,#8094,.T.);
#11007=ORIENTED_EDGE('',*,*,#8095,.T.);
#11008=ORIENTED_EDGE('',*,*,#8096,.T.);
#11009=ORIENTED_EDGE('',*,*,#8097,.T.);
#11010=ORIENTED_EDGE('',*,*,#8098,.T.);
#11011=ORIENTED_EDGE('',*,*,#8099,.T.);
#11012=ORIENTED_EDGE('',*,*,#8100,.T.);
#11013=ORIENTED_EDGE('',*,*,#8101,.T.);
#11014=ORIENTED_EDGE('',*,*,#8102,.T.);
#11015=ORIENTED_EDGE('',*,*,#8103,.T.);
#11016=ORIENTED_EDGE('',*,*,#8104,.T.);
#11017=ORIENTED_EDGE('',*,*,#8105,.T.);
#11018=ORIENTED_EDGE('',*,*,#8106,.F.);
#11019=ORIENTED_EDGE('',*,*,#8107,.T.);
#11020=ORIENTED_EDGE('',*,*,#8108,.T.);
#11021=ORIENTED_EDGE('',*,*,#8109,.T.);
#11022=ORIENTED_EDGE('',*,*,#8110,.T.);
#11023=ORIENTED_EDGE('',*,*,#8111,.T.);
#11024=ORIENTED_EDGE('',*,*,#8112,.T.);
#11025=ORIENTED_EDGE('',*,*,#8113,.T.);
#11026=ORIENTED_EDGE('',*,*,#8114,.T.);
#11027=ORIENTED_EDGE('',*,*,#8115,.T.);
#11028=ORIENTED_EDGE('',*,*,#8116,.T.);
#11029=ORIENTED_EDGE('',*,*,#8117,.T.);
#11030=ORIENTED_EDGE('',*,*,#8118,.T.);
#11031=ORIENTED_EDGE('',*,*,#8119,.T.);
#11032=ORIENTED_EDGE('',*,*,#8120,.T.);
#11033=ORIENTED_EDGE('',*,*,#8121,.T.);
#11034=ORIENTED_EDGE('',*,*,#8122,.T.);
#11035=ORIENTED_EDGE('',*,*,#8123,.T.);
#11036=ORIENTED_EDGE('',*,*,#8124,.T.);
#11037=ORIENTED_EDGE('',*,*,#8125,.T.);
#11038=ORIENTED_EDGE('',*,*,#8126,.T.);
#11039=ORIENTED_EDGE('',*,*,#8127,.T.);
#11040=ORIENTED_EDGE('',*,*,#8128,.T.);
#11041=ORIENTED_EDGE('',*,*,#8129,.T.);
#11042=ORIENTED_EDGE('',*,*,#8130,.T.);
#11043=ORIENTED_EDGE('',*,*,#8131,.T.);
#11044=ORIENTED_EDGE('',*,*,#8132,.T.);
#11045=ORIENTED_EDGE('',*,*,#8133,.T.);
#11046=ORIENTED_EDGE('',*,*,#8134,.T.);
#11047=ORIENTED_EDGE('',*,*,#8135,.T.);
#11048=ORIENTED_EDGE('',*,*,#8136,.T.);
#11049=ORIENTED_EDGE('',*,*,#8137,.T.);
#11050=ORIENTED_EDGE('',*,*,#8138,.T.);
#11051=ORIENTED_EDGE('',*,*,#8139,.T.);
#11052=ORIENTED_EDGE('',*,*,#8140,.T.);
#11053=ORIENTED_EDGE('',*,*,#8141,.T.);
#11054=ORIENTED_EDGE('',*,*,#8142,.T.);
#11055=ORIENTED_EDGE('',*,*,#8143,.T.);
#11056=ORIENTED_EDGE('',*,*,#8144,.T.);
#11057=ORIENTED_EDGE('',*,*,#8145,.T.);
#11058=ORIENTED_EDGE('',*,*,#8146,.T.);
#11059=ORIENTED_EDGE('',*,*,#8147,.T.);
#11060=ORIENTED_EDGE('',*,*,#8148,.T.);
#11061=ORIENTED_EDGE('',*,*,#8149,.T.);
#11062=ORIENTED_EDGE('',*,*,#8150,.T.);
#11063=ORIENTED_EDGE('',*,*,#8151,.T.);
#11064=ORIENTED_EDGE('',*,*,#8152,.T.);
#11065=ORIENTED_EDGE('',*,*,#8153,.T.);
#11066=ORIENTED_EDGE('',*,*,#8154,.T.);
#11067=ORIENTED_EDGE('',*,*,#8155,.T.);
#11068=ORIENTED_EDGE('',*,*,#8156,.T.);
#11069=ORIENTED_EDGE('',*,*,#8157,.T.);
#11070=ORIENTED_EDGE('',*,*,#8158,.T.);
#11071=ORIENTED_EDGE('',*,*,#8159,.T.);
#11072=ORIENTED_EDGE('',*,*,#8160,.T.);
#11073=ORIENTED_EDGE('',*,*,#8161,.T.);
#11074=ORIENTED_EDGE('',*,*,#8162,.T.);
#11075=ORIENTED_EDGE('',*,*,#8163,.T.);
#11076=ORIENTED_EDGE('',*,*,#8164,.T.);
#11077=ORIENTED_EDGE('',*,*,#8165,.T.);
#11078=ORIENTED_EDGE('',*,*,#8166,.T.);
#11079=ORIENTED_EDGE('',*,*,#8167,.T.);
#11080=ORIENTED_EDGE('',*,*,#8168,.T.);
#11081=ORIENTED_EDGE('',*,*,#8169,.T.);
#11082=ORIENTED_EDGE('',*,*,#8170,.T.);
#11083=ORIENTED_EDGE('',*,*,#8171,.T.);
#11084=ORIENTED_EDGE('',*,*,#8172,.T.);
#11085=ORIENTED_EDGE('',*,*,#8173,.T.);
#11086=ORIENTED_EDGE('',*,*,#8174,.T.);
#11087=ORIENTED_EDGE('',*,*,#8175,.T.);
#11088=ORIENTED_EDGE('',*,*,#8176,.T.);
#11089=ORIENTED_EDGE('',*,*,#8177,.T.);
#11090=ORIENTED_EDGE('',*,*,#8178,.T.);
#11091=ORIENTED_EDGE('',*,*,#8179,.T.);
#11092=ORIENTED_EDGE('',*,*,#8180,.T.);
#11093=ORIENTED_EDGE('',*,*,#8181,.T.);
#11094=ORIENTED_EDGE('',*,*,#8182,.T.);
#11095=ORIENTED_EDGE('',*,*,#8183,.T.);
#11096=ORIENTED_EDGE('',*,*,#8184,.T.);
#11097=ORIENTED_EDGE('',*,*,#8185,.T.);
#11098=ORIENTED_EDGE('',*,*,#8186,.T.);
#11099=ORIENTED_EDGE('',*,*,#8187,.T.);
#11100=ORIENTED_EDGE('',*,*,#8188,.T.);
#11101=ORIENTED_EDGE('',*,*,#8189,.T.);
#11102=ORIENTED_EDGE('',*,*,#8190,.T.);
#11103=ORIENTED_EDGE('',*,*,#8191,.T.);
#11104=ORIENTED_EDGE('',*,*,#8192,.T.);
#11105=ORIENTED_EDGE('',*,*,#8193,.T.);
#11106=ORIENTED_EDGE('',*,*,#8194,.T.);
#11107=ORIENTED_EDGE('',*,*,#8195,.T.);
#11108=ORIENTED_EDGE('',*,*,#8196,.T.);
#11109=ORIENTED_EDGE('',*,*,#8197,.T.);
#11110=ORIENTED_EDGE('',*,*,#8198,.T.);
#11111=ORIENTED_EDGE('',*,*,#8199,.T.);
#11112=ORIENTED_EDGE('',*,*,#8200,.T.);
#11113=ORIENTED_EDGE('',*,*,#8201,.T.);
#11114=ORIENTED_EDGE('',*,*,#8202,.T.);
#11115=ORIENTED_EDGE('',*,*,#8203,.T.);
#11116=ORIENTED_EDGE('',*,*,#8204,.T.);
#11117=ORIENTED_EDGE('',*,*,#8205,.T.);
#11118=ORIENTED_EDGE('',*,*,#8206,.T.);
#11119=ORIENTED_EDGE('',*,*,#8207,.T.);
#11120=ORIENTED_EDGE('',*,*,#8208,.T.);
#11121=ORIENTED_EDGE('',*,*,#8209,.T.);
#11122=ORIENTED_EDGE('',*,*,#8210,.T.);
#11123=ORIENTED_EDGE('',*,*,#8211,.T.);
#11124=ORIENTED_EDGE('',*,*,#8212,.T.);
#11125=ORIENTED_EDGE('',*,*,#8213,.T.);
#11126=ORIENTED_EDGE('',*,*,#8214,.T.);
#11127=ORIENTED_EDGE('',*,*,#8215,.T.);
#11128=ORIENTED_EDGE('',*,*,#8216,.T.);
#11129=ORIENTED_EDGE('',*,*,#8217,.T.);
#11130=ORIENTED_EDGE('',*,*,#8218,.T.);
#11131=ORIENTED_EDGE('',*,*,#8219,.T.);
#11132=ORIENTED_EDGE('',*,*,#8220,.T.);
#11133=ORIENTED_EDGE('',*,*,#8221,.T.);
#11134=ORIENTED_EDGE('',*,*,#8222,.T.);
#11135=ORIENTED_EDGE('',*,*,#8223,.T.);
#11136=ORIENTED_EDGE('',*,*,#8224,.T.);
#11137=ORIENTED_EDGE('',*,*,#8225,.T.);
#11138=ORIENTED_EDGE('',*,*,#8226,.T.);
#11139=ORIENTED_EDGE('',*,*,#8227,.T.);
#11140=ORIENTED_EDGE('',*,*,#8228,.T.);
#11141=ORIENTED_EDGE('',*,*,#8229,.T.);
#11142=ORIENTED_EDGE('',*,*,#8230,.T.);
#11143=ORIENTED_EDGE('',*,*,#8231,.T.);
#11144=ORIENTED_EDGE('',*,*,#8232,.T.);
#11145=ORIENTED_EDGE('',*,*,#8233,.T.);
#11146=ORIENTED_EDGE('',*,*,#8234,.T.);
#11147=ORIENTED_EDGE('',*,*,#8235,.T.);
#11148=ORIENTED_EDGE('',*,*,#8236,.T.);
#11149=ORIENTED_EDGE('',*,*,#8237,.T.);
#11150=ORIENTED_EDGE('',*,*,#8238,.T.);
#11151=ORIENTED_EDGE('',*,*,#8239,.T.);
#11152=ORIENTED_EDGE('',*,*,#8240,.T.);
#11153=ORIENTED_EDGE('',*,*,#8241,.T.);
#11154=ORIENTED_EDGE('',*,*,#8242,.T.);
#11155=ORIENTED_EDGE('',*,*,#8243,.T.);
#11156=ORIENTED_EDGE('',*,*,#8244,.T.);
#11157=ORIENTED_EDGE('',*,*,#8245,.T.);
#11158=ORIENTED_EDGE('',*,*,#8246,.T.);
#11159=ORIENTED_EDGE('',*,*,#8247,.T.);
#11160=ORIENTED_EDGE('',*,*,#8248,.T.);
#11161=ORIENTED_EDGE('',*,*,#8249,.T.);
#11162=ORIENTED_EDGE('',*,*,#8250,.T.);
#11163=ORIENTED_EDGE('',*,*,#8251,.T.);
#11164=ORIENTED_EDGE('',*,*,#8252,.T.);
#11165=ORIENTED_EDGE('',*,*,#8253,.T.);
#11166=ORIENTED_EDGE('',*,*,#8254,.T.);
#11167=ORIENTED_EDGE('',*,*,#8255,.T.);
#11168=ORIENTED_EDGE('',*,*,#8256,.T.);
#11169=ORIENTED_EDGE('',*,*,#8257,.T.);
#11170=ORIENTED_EDGE('',*,*,#8258,.T.);
#11171=ORIENTED_EDGE('',*,*,#8259,.T.);
#11172=ORIENTED_EDGE('',*,*,#8260,.T.);
#11173=ORIENTED_EDGE('',*,*,#8261,.T.);
#11174=ORIENTED_EDGE('',*,*,#8262,.T.);
#11175=ORIENTED_EDGE('',*,*,#8263,.T.);
#11176=ORIENTED_EDGE('',*,*,#8264,.T.);
#11177=ORIENTED_EDGE('',*,*,#8265,.T.);
#11178=ORIENTED_EDGE('',*,*,#8266,.T.);
#11179=ORIENTED_EDGE('',*,*,#8267,.T.);
#11180=ORIENTED_EDGE('',*,*,#8268,.T.);
#11181=ORIENTED_EDGE('',*,*,#8269,.T.);
#11182=ORIENTED_EDGE('',*,*,#8270,.T.);
#11183=ORIENTED_EDGE('',*,*,#8271,.T.);
#11184=ORIENTED_EDGE('',*,*,#8272,.T.);
#11185=ORIENTED_EDGE('',*,*,#8273,.T.);
#11186=ORIENTED_EDGE('',*,*,#8274,.T.);
#11187=ORIENTED_EDGE('',*,*,#8275,.T.);
#11188=ORIENTED_EDGE('',*,*,#8276,.T.);
#11189=ORIENTED_EDGE('',*,*,#8277,.T.);
#11190=ORIENTED_EDGE('',*,*,#8278,.T.);
#11191=ORIENTED_EDGE('',*,*,#8279,.T.);
#11192=ORIENTED_EDGE('',*,*,#8280,.T.);
#11193=ORIENTED_EDGE('',*,*,#8281,.T.);
#11194=ORIENTED_EDGE('',*,*,#8282,.T.);
#11195=ORIENTED_EDGE('',*,*,#8283,.T.);
#11196=ORIENTED_EDGE('',*,*,#8284,.T.);
#11197=ORIENTED_EDGE('',*,*,#8285,.T.);
#11198=ORIENTED_EDGE('',*,*,#8286,.T.);
#11199=ORIENTED_EDGE('',*,*,#8287,.T.);
#11200=ORIENTED_EDGE('',*,*,#8288,.T.);
#11201=ORIENTED_EDGE('',*,*,#8289,.T.);
#11202=ORIENTED_EDGE('',*,*,#8290,.T.);
#11203=ORIENTED_EDGE('',*,*,#8291,.T.);
#11204=ORIENTED_EDGE('',*,*,#8292,.T.);
#11205=ORIENTED_EDGE('',*,*,#8293,.T.);
#11206=ORIENTED_EDGE('',*,*,#8294,.T.);
#11207=ORIENTED_EDGE('',*,*,#8295,.T.);
#11208=ORIENTED_EDGE('',*,*,#8296,.T.);
#11209=ORIENTED_EDGE('',*,*,#8297,.T.);
#11210=ORIENTED_EDGE('',*,*,#8298,.T.);
#11211=ORIENTED_EDGE('',*,*,#8299,.T.);
#11212=ORIENTED_EDGE('',*,*,#8300,.T.);
#11213=ORIENTED_EDGE('',*,*,#8301,.T.);
#11214=ORIENTED_EDGE('',*,*,#8302,.T.);
#11215=ORIENTED_EDGE('',*,*,#8303,.T.);
#11216=ORIENTED_EDGE('',*,*,#8304,.T.);
#11217=ORIENTED_EDGE('',*,*,#8305,.T.);
#11218=ORIENTED_EDGE('',*,*,#8306,.T.);
#11219=ORIENTED_EDGE('',*,*,#8307,.T.);
#11220=ORIENTED_EDGE('',*,*,#8308,.T.);
#11221=ORIENTED_EDGE('',*,*,#8309,.T.);
#11222=ORIENTED_EDGE('',*,*,#8310,.T.);
#11223=ORIENTED_EDGE('',*,*,#8311,.T.);
#11224=ORIENTED_EDGE('',*,*,#8312,.T.);
#11225=ORIENTED_EDGE('',*,*,#8313,.T.);
#11226=ORIENTED_EDGE('',*,*,#8314,.T.);
#11227=ORIENTED_EDGE('',*,*,#8315,.T.);
#11228=ORIENTED_EDGE('',*,*,#8316,.T.);
#11229=ORIENTED_EDGE('',*,*,#8317,.T.);
#11230=ORIENTED_EDGE('',*,*,#8318,.T.);
#11231=ORIENTED_EDGE('',*,*,#8319,.T.);
#11232=ORIENTED_EDGE('',*,*,#8320,.T.);
#11233=ORIENTED_EDGE('',*,*,#8321,.T.);
#11234=ORIENTED_EDGE('',*,*,#8322,.T.);
#11235=ORIENTED_EDGE('',*,*,#8323,.T.);
#11236=ORIENTED_EDGE('',*,*,#8324,.T.);
#11237=ORIENTED_EDGE('',*,*,#8325,.T.);
#11238=ORIENTED_EDGE('',*,*,#8326,.T.);
#11239=ORIENTED_EDGE('',*,*,#8327,.T.);
#11240=ORIENTED_EDGE('',*,*,#8328,.T.);
#11241=ORIENTED_EDGE('',*,*,#8329,.T.);
#11242=ORIENTED_EDGE('',*,*,#8330,.T.);
#11243=ORIENTED_EDGE('',*,*,#8331,.T.);
#11244=ORIENTED_EDGE('',*,*,#8332,.T.);
#11245=ORIENTED_EDGE('',*,*,#8333,.T.);
#11246=ORIENTED_EDGE('',*,*,#8334,.T.);
#11247=ORIENTED_EDGE('',*,*,#8335,.T.);
#11248=ORIENTED_EDGE('',*,*,#8336,.T.);
#11249=ORIENTED_EDGE('',*,*,#8337,.T.);
#11250=ORIENTED_EDGE('',*,*,#8338,.T.);
#11251=ORIENTED_EDGE('',*,*,#8339,.T.);
#11252=ORIENTED_EDGE('',*,*,#8340,.T.);
#11253=ORIENTED_EDGE('',*,*,#8341,.T.);
#11254=ORIENTED_EDGE('',*,*,#8342,.T.);
#11255=ORIENTED_EDGE('',*,*,#8343,.T.);
#11256=ORIENTED_EDGE('',*,*,#8344,.T.);
#11257=ORIENTED_EDGE('',*,*,#8345,.T.);
#11258=ORIENTED_EDGE('',*,*,#8346,.T.);
#11259=ORIENTED_EDGE('',*,*,#8347,.T.);
#11260=ORIENTED_EDGE('',*,*,#8348,.T.);
#11261=ORIENTED_EDGE('',*,*,#8349,.T.);
#11262=ORIENTED_EDGE('',*,*,#8350,.T.);
#11263=ORIENTED_EDGE('',*,*,#8351,.T.);
#11264=ORIENTED_EDGE('',*,*,#8352,.T.);
#11265=ORIENTED_EDGE('',*,*,#8353,.T.);
#11266=ORIENTED_EDGE('',*,*,#8354,.T.);
#11267=ORIENTED_EDGE('',*,*,#8355,.T.);
#11268=ORIENTED_EDGE('',*,*,#8356,.T.);
#11269=ORIENTED_EDGE('',*,*,#8357,.T.);
#11270=ORIENTED_EDGE('',*,*,#8358,.T.);
#11271=ORIENTED_EDGE('',*,*,#8359,.T.);
#11272=ORIENTED_EDGE('',*,*,#8360,.T.);
#11273=ORIENTED_EDGE('',*,*,#8361,.T.);
#11274=ORIENTED_EDGE('',*,*,#8362,.T.);
#11275=ORIENTED_EDGE('',*,*,#8363,.T.);
#11276=ORIENTED_EDGE('',*,*,#8364,.T.);
#11277=ORIENTED_EDGE('',*,*,#8365,.T.);
#11278=ORIENTED_EDGE('',*,*,#8366,.T.);
#11279=ORIENTED_EDGE('',*,*,#8367,.T.);
#11280=ORIENTED_EDGE('',*,*,#8368,.T.);
#11281=ORIENTED_EDGE('',*,*,#8369,.T.);
#11282=ORIENTED_EDGE('',*,*,#8370,.T.);
#11283=ORIENTED_EDGE('',*,*,#8371,.T.);
#11284=ORIENTED_EDGE('',*,*,#8372,.T.);
#11285=ORIENTED_EDGE('',*,*,#8373,.T.);
#11286=ORIENTED_EDGE('',*,*,#8374,.T.);
#11287=ORIENTED_EDGE('',*,*,#8375,.T.);
#11288=ORIENTED_EDGE('',*,*,#7829,.T.);
#11289=ORIENTED_EDGE('',*,*,#8376,.T.);
#11290=ORIENTED_EDGE('',*,*,#8377,.T.);
#11291=ORIENTED_EDGE('',*,*,#8378,.F.);
#11292=ORIENTED_EDGE('',*,*,#8379,.F.);
#11293=ORIENTED_EDGE('',*,*,#8380,.F.);
#11294=ORIENTED_EDGE('',*,*,#8381,.T.);
#11295=ORIENTED_EDGE('',*,*,#8382,.F.);
#11296=ORIENTED_EDGE('',*,*,#8381,.F.);
#11297=ORIENTED_EDGE('',*,*,#8383,.T.);
#11298=ORIENTED_EDGE('',*,*,#8384,.T.);
#11299=ORIENTED_EDGE('',*,*,#8383,.F.);
#11300=ORIENTED_EDGE('',*,*,#8384,.F.);
#11301=ORIENTED_EDGE('',*,*,#8385,.T.);
#11302=ORIENTED_EDGE('',*,*,#7835,.T.);
#11303=ORIENTED_EDGE('',*,*,#8386,.T.);
#11304=ORIENTED_EDGE('',*,*,#6497,.T.);
#11305=ORIENTED_EDGE('',*,*,#8387,.F.);
#11306=ORIENTED_EDGE('',*,*,#8388,.F.);
#11307=ORIENTED_EDGE('',*,*,#8389,.T.);
#11308=ORIENTED_EDGE('',*,*,#8390,.F.);
#11309=ORIENTED_EDGE('',*,*,#8391,.F.);
#11310=ORIENTED_EDGE('',*,*,#8389,.F.);
#11311=ORIENTED_EDGE('',*,*,#8392,.F.);
#11312=ORIENTED_EDGE('',*,*,#8393,.F.);
#11313=ORIENTED_EDGE('',*,*,#8394,.T.);
#11314=ORIENTED_EDGE('',*,*,#8395,.F.);
#11315=ORIENTED_EDGE('',*,*,#8396,.F.);
#11316=ORIENTED_EDGE('',*,*,#8394,.F.);
#11317=ORIENTED_EDGE('',*,*,#8397,.F.);
#11318=ORIENTED_EDGE('',*,*,#8396,.T.);
#11319=ORIENTED_EDGE('',*,*,#8398,.T.);
#11320=ORIENTED_EDGE('',*,*,#8382,.T.);
#11321=ORIENTED_EDGE('',*,*,#8398,.F.);
#11322=ORIENTED_EDGE('',*,*,#8397,.T.);
#11323=ORIENTED_EDGE('',*,*,#8393,.T.);
#11324=ORIENTED_EDGE('',*,*,#8399,.F.);
#11325=ORIENTED_EDGE('',*,*,#8390,.T.);
#11326=ORIENTED_EDGE('',*,*,#8391,.T.);
#11327=ORIENTED_EDGE('',*,*,#8388,.T.);
#11328=ORIENTED_EDGE('',*,*,#8400,.F.);
#11329=ORIENTED_EDGE('',*,*,#8395,.T.);
#11330=ORIENTED_EDGE('',*,*,#8387,.T.);
#11331=ORIENTED_EDGE('',*,*,#8399,.T.);
#11332=ORIENTED_EDGE('',*,*,#8392,.T.);
#11333=ORIENTED_EDGE('',*,*,#8400,.T.);
#11334=ORIENTED_EDGE('',*,*,#8401,.F.);
#11335=ORIENTED_EDGE('',*,*,#8105,.F.);
#11336=ORIENTED_EDGE('',*,*,#8104,.F.);
#11337=ORIENTED_EDGE('',*,*,#8103,.F.);
#11338=ORIENTED_EDGE('',*,*,#8102,.F.);
#11339=ORIENTED_EDGE('',*,*,#8101,.F.);
#11340=ORIENTED_EDGE('',*,*,#8100,.F.);
#11341=ORIENTED_EDGE('',*,*,#8099,.F.);
#11342=ORIENTED_EDGE('',*,*,#8098,.F.);
#11343=ORIENTED_EDGE('',*,*,#8097,.F.);
#11344=ORIENTED_EDGE('',*,*,#8096,.F.);
#11345=ORIENTED_EDGE('',*,*,#8095,.F.);
#11346=ORIENTED_EDGE('',*,*,#8094,.F.);
#11347=ORIENTED_EDGE('',*,*,#8093,.F.);
#11348=ORIENTED_EDGE('',*,*,#8092,.F.);
#11349=ORIENTED_EDGE('',*,*,#8091,.F.);
#11350=ORIENTED_EDGE('',*,*,#8090,.F.);
#11351=ORIENTED_EDGE('',*,*,#8089,.F.);
#11352=ORIENTED_EDGE('',*,*,#8088,.F.);
#11353=ORIENTED_EDGE('',*,*,#8087,.F.);
#11354=ORIENTED_EDGE('',*,*,#8086,.F.);
#11355=ORIENTED_EDGE('',*,*,#8085,.F.);
#11356=ORIENTED_EDGE('',*,*,#8084,.F.);
#11357=ORIENTED_EDGE('',*,*,#8083,.F.);
#11358=ORIENTED_EDGE('',*,*,#8082,.F.);
#11359=ORIENTED_EDGE('',*,*,#8081,.F.);
#11360=ORIENTED_EDGE('',*,*,#8080,.F.);
#11361=ORIENTED_EDGE('',*,*,#8079,.F.);
#11362=ORIENTED_EDGE('',*,*,#8078,.F.);
#11363=ORIENTED_EDGE('',*,*,#8077,.F.);
#11364=ORIENTED_EDGE('',*,*,#8076,.F.);
#11365=ORIENTED_EDGE('',*,*,#8075,.F.);
#11366=ORIENTED_EDGE('',*,*,#8074,.F.);
#11367=ORIENTED_EDGE('',*,*,#8073,.F.);
#11368=ORIENTED_EDGE('',*,*,#8072,.F.);
#11369=ORIENTED_EDGE('',*,*,#8071,.F.);
#11370=ORIENTED_EDGE('',*,*,#8070,.F.);
#11371=ORIENTED_EDGE('',*,*,#8069,.F.);
#11372=ORIENTED_EDGE('',*,*,#8068,.F.);
#11373=ORIENTED_EDGE('',*,*,#8067,.F.);
#11374=ORIENTED_EDGE('',*,*,#8066,.F.);
#11375=ORIENTED_EDGE('',*,*,#8065,.F.);
#11376=ORIENTED_EDGE('',*,*,#8064,.F.);
#11377=ORIENTED_EDGE('',*,*,#8063,.F.);
#11378=ORIENTED_EDGE('',*,*,#8062,.F.);
#11379=ORIENTED_EDGE('',*,*,#8061,.F.);
#11380=ORIENTED_EDGE('',*,*,#8060,.F.);
#11381=ORIENTED_EDGE('',*,*,#8059,.F.);
#11382=ORIENTED_EDGE('',*,*,#8058,.F.);
#11383=ORIENTED_EDGE('',*,*,#8057,.F.);
#11384=ORIENTED_EDGE('',*,*,#8056,.F.);
#11385=ORIENTED_EDGE('',*,*,#8055,.F.);
#11386=ORIENTED_EDGE('',*,*,#8054,.F.);
#11387=ORIENTED_EDGE('',*,*,#8053,.F.);
#11388=ORIENTED_EDGE('',*,*,#8052,.F.);
#11389=ORIENTED_EDGE('',*,*,#8051,.F.);
#11390=ORIENTED_EDGE('',*,*,#8050,.F.);
#11391=ORIENTED_EDGE('',*,*,#8049,.F.);
#11392=ORIENTED_EDGE('',*,*,#8048,.F.);
#11393=ORIENTED_EDGE('',*,*,#8047,.F.);
#11394=ORIENTED_EDGE('',*,*,#8046,.F.);
#11395=ORIENTED_EDGE('',*,*,#8045,.F.);
#11396=ORIENTED_EDGE('',*,*,#8044,.F.);
#11397=ORIENTED_EDGE('',*,*,#8043,.F.);
#11398=ORIENTED_EDGE('',*,*,#8042,.F.);
#11399=ORIENTED_EDGE('',*,*,#8041,.F.);
#11400=ORIENTED_EDGE('',*,*,#8040,.F.);
#11401=ORIENTED_EDGE('',*,*,#8039,.F.);
#11402=ORIENTED_EDGE('',*,*,#8038,.F.);
#11403=ORIENTED_EDGE('',*,*,#8037,.F.);
#11404=ORIENTED_EDGE('',*,*,#8036,.F.);
#11405=ORIENTED_EDGE('',*,*,#8035,.F.);
#11406=ORIENTED_EDGE('',*,*,#8034,.F.);
#11407=ORIENTED_EDGE('',*,*,#8033,.F.);
#11408=ORIENTED_EDGE('',*,*,#8032,.F.);
#11409=ORIENTED_EDGE('',*,*,#8031,.F.);
#11410=ORIENTED_EDGE('',*,*,#8030,.F.);
#11411=ORIENTED_EDGE('',*,*,#8029,.F.);
#11412=ORIENTED_EDGE('',*,*,#8028,.F.);
#11413=ORIENTED_EDGE('',*,*,#8027,.F.);
#11414=ORIENTED_EDGE('',*,*,#8026,.F.);
#11415=ORIENTED_EDGE('',*,*,#8025,.F.);
#11416=ORIENTED_EDGE('',*,*,#8024,.F.);
#11417=ORIENTED_EDGE('',*,*,#8023,.F.);
#11418=ORIENTED_EDGE('',*,*,#8022,.F.);
#11419=ORIENTED_EDGE('',*,*,#8021,.F.);
#11420=ORIENTED_EDGE('',*,*,#8020,.F.);
#11421=ORIENTED_EDGE('',*,*,#8019,.F.);
#11422=ORIENTED_EDGE('',*,*,#8018,.F.);
#11423=ORIENTED_EDGE('',*,*,#8017,.F.);
#11424=ORIENTED_EDGE('',*,*,#8016,.F.);
#11425=ORIENTED_EDGE('',*,*,#8015,.F.);
#11426=ORIENTED_EDGE('',*,*,#8014,.F.);
#11427=ORIENTED_EDGE('',*,*,#8013,.F.);
#11428=ORIENTED_EDGE('',*,*,#8012,.F.);
#11429=ORIENTED_EDGE('',*,*,#8011,.F.);
#11430=ORIENTED_EDGE('',*,*,#8010,.F.);
#11431=ORIENTED_EDGE('',*,*,#8009,.F.);
#11432=ORIENTED_EDGE('',*,*,#8008,.F.);
#11433=ORIENTED_EDGE('',*,*,#8007,.F.);
#11434=ORIENTED_EDGE('',*,*,#8006,.F.);
#11435=ORIENTED_EDGE('',*,*,#8005,.F.);
#11436=ORIENTED_EDGE('',*,*,#8004,.F.);
#11437=ORIENTED_EDGE('',*,*,#8003,.F.);
#11438=ORIENTED_EDGE('',*,*,#8002,.F.);
#11439=ORIENTED_EDGE('',*,*,#8001,.F.);
#11440=ORIENTED_EDGE('',*,*,#8000,.F.);
#11441=ORIENTED_EDGE('',*,*,#7999,.F.);
#11442=ORIENTED_EDGE('',*,*,#7998,.F.);
#11443=ORIENTED_EDGE('',*,*,#7997,.F.);
#11444=ORIENTED_EDGE('',*,*,#7996,.F.);
#11445=ORIENTED_EDGE('',*,*,#7995,.F.);
#11446=ORIENTED_EDGE('',*,*,#7994,.F.);
#11447=ORIENTED_EDGE('',*,*,#7993,.F.);
#11448=ORIENTED_EDGE('',*,*,#7992,.F.);
#11449=ORIENTED_EDGE('',*,*,#7991,.F.);
#11450=ORIENTED_EDGE('',*,*,#7990,.F.);
#11451=ORIENTED_EDGE('',*,*,#7989,.F.);
#11452=ORIENTED_EDGE('',*,*,#7988,.F.);
#11453=ORIENTED_EDGE('',*,*,#7987,.F.);
#11454=ORIENTED_EDGE('',*,*,#7986,.F.);
#11455=ORIENTED_EDGE('',*,*,#7985,.F.);
#11456=ORIENTED_EDGE('',*,*,#7984,.F.);
#11457=ORIENTED_EDGE('',*,*,#7983,.F.);
#11458=ORIENTED_EDGE('',*,*,#7982,.F.);
#11459=ORIENTED_EDGE('',*,*,#7981,.F.);
#11460=ORIENTED_EDGE('',*,*,#7980,.F.);
#11461=ORIENTED_EDGE('',*,*,#7979,.F.);
#11462=ORIENTED_EDGE('',*,*,#7978,.F.);
#11463=ORIENTED_EDGE('',*,*,#7977,.F.);
#11464=ORIENTED_EDGE('',*,*,#7976,.F.);
#11465=ORIENTED_EDGE('',*,*,#7975,.F.);
#11466=ORIENTED_EDGE('',*,*,#7974,.F.);
#11467=ORIENTED_EDGE('',*,*,#7973,.F.);
#11468=ORIENTED_EDGE('',*,*,#7972,.F.);
#11469=ORIENTED_EDGE('',*,*,#7971,.F.);
#11470=ORIENTED_EDGE('',*,*,#7970,.F.);
#11471=ORIENTED_EDGE('',*,*,#7969,.F.);
#11472=ORIENTED_EDGE('',*,*,#7968,.F.);
#11473=ORIENTED_EDGE('',*,*,#7967,.F.);
#11474=ORIENTED_EDGE('',*,*,#7966,.F.);
#11475=ORIENTED_EDGE('',*,*,#7965,.F.);
#11476=ORIENTED_EDGE('',*,*,#7964,.F.);
#11477=ORIENTED_EDGE('',*,*,#7963,.F.);
#11478=ORIENTED_EDGE('',*,*,#7962,.F.);
#11479=ORIENTED_EDGE('',*,*,#7961,.F.);
#11480=ORIENTED_EDGE('',*,*,#7960,.F.);
#11481=ORIENTED_EDGE('',*,*,#7959,.F.);
#11482=ORIENTED_EDGE('',*,*,#7958,.F.);
#11483=ORIENTED_EDGE('',*,*,#7957,.F.);
#11484=ORIENTED_EDGE('',*,*,#7956,.F.);
#11485=ORIENTED_EDGE('',*,*,#7955,.F.);
#11486=ORIENTED_EDGE('',*,*,#7954,.F.);
#11487=ORIENTED_EDGE('',*,*,#7953,.F.);
#11488=ORIENTED_EDGE('',*,*,#7952,.F.);
#11489=ORIENTED_EDGE('',*,*,#7951,.F.);
#11490=ORIENTED_EDGE('',*,*,#7950,.F.);
#11491=ORIENTED_EDGE('',*,*,#7949,.F.);
#11492=ORIENTED_EDGE('',*,*,#7948,.F.);
#11493=ORIENTED_EDGE('',*,*,#7947,.F.);
#11494=ORIENTED_EDGE('',*,*,#7946,.F.);
#11495=ORIENTED_EDGE('',*,*,#7945,.F.);
#11496=ORIENTED_EDGE('',*,*,#7944,.F.);
#11497=ORIENTED_EDGE('',*,*,#7943,.F.);
#11498=ORIENTED_EDGE('',*,*,#7942,.F.);
#11499=ORIENTED_EDGE('',*,*,#7941,.F.);
#11500=ORIENTED_EDGE('',*,*,#7940,.F.);
#11501=ORIENTED_EDGE('',*,*,#7939,.F.);
#11502=ORIENTED_EDGE('',*,*,#7938,.F.);
#11503=ORIENTED_EDGE('',*,*,#7937,.F.);
#11504=ORIENTED_EDGE('',*,*,#7936,.F.);
#11505=ORIENTED_EDGE('',*,*,#7935,.F.);
#11506=ORIENTED_EDGE('',*,*,#7934,.F.);
#11507=ORIENTED_EDGE('',*,*,#7933,.F.);
#11508=ORIENTED_EDGE('',*,*,#7932,.F.);
#11509=ORIENTED_EDGE('',*,*,#7931,.F.);
#11510=ORIENTED_EDGE('',*,*,#7930,.F.);
#11511=ORIENTED_EDGE('',*,*,#7929,.F.);
#11512=ORIENTED_EDGE('',*,*,#7928,.F.);
#11513=ORIENTED_EDGE('',*,*,#7927,.F.);
#11514=ORIENTED_EDGE('',*,*,#7926,.F.);
#11515=ORIENTED_EDGE('',*,*,#7925,.F.);
#11516=ORIENTED_EDGE('',*,*,#7924,.F.);
#11517=ORIENTED_EDGE('',*,*,#7923,.F.);
#11518=ORIENTED_EDGE('',*,*,#7922,.F.);
#11519=ORIENTED_EDGE('',*,*,#7921,.F.);
#11520=ORIENTED_EDGE('',*,*,#7920,.F.);
#11521=ORIENTED_EDGE('',*,*,#7919,.F.);
#11522=ORIENTED_EDGE('',*,*,#7918,.F.);
#11523=ORIENTED_EDGE('',*,*,#7917,.F.);
#11524=ORIENTED_EDGE('',*,*,#7916,.F.);
#11525=ORIENTED_EDGE('',*,*,#7915,.F.);
#11526=ORIENTED_EDGE('',*,*,#7914,.F.);
#11527=ORIENTED_EDGE('',*,*,#7913,.F.);
#11528=ORIENTED_EDGE('',*,*,#7912,.F.);
#11529=ORIENTED_EDGE('',*,*,#7911,.F.);
#11530=ORIENTED_EDGE('',*,*,#7910,.F.);
#11531=ORIENTED_EDGE('',*,*,#7909,.F.);
#11532=ORIENTED_EDGE('',*,*,#7908,.F.);
#11533=ORIENTED_EDGE('',*,*,#7907,.F.);
#11534=ORIENTED_EDGE('',*,*,#7906,.F.);
#11535=ORIENTED_EDGE('',*,*,#7905,.F.);
#11536=ORIENTED_EDGE('',*,*,#7904,.F.);
#11537=ORIENTED_EDGE('',*,*,#7903,.F.);
#11538=ORIENTED_EDGE('',*,*,#7902,.F.);
#11539=ORIENTED_EDGE('',*,*,#7901,.F.);
#11540=ORIENTED_EDGE('',*,*,#7900,.F.);
#11541=ORIENTED_EDGE('',*,*,#7899,.F.);
#11542=ORIENTED_EDGE('',*,*,#7898,.F.);
#11543=ORIENTED_EDGE('',*,*,#7897,.F.);
#11544=ORIENTED_EDGE('',*,*,#7896,.F.);
#11545=ORIENTED_EDGE('',*,*,#7895,.F.);
#11546=ORIENTED_EDGE('',*,*,#7894,.F.);
#11547=ORIENTED_EDGE('',*,*,#7893,.F.);
#11548=ORIENTED_EDGE('',*,*,#7892,.F.);
#11549=ORIENTED_EDGE('',*,*,#7891,.F.);
#11550=ORIENTED_EDGE('',*,*,#7890,.F.);
#11551=ORIENTED_EDGE('',*,*,#7889,.F.);
#11552=ORIENTED_EDGE('',*,*,#7888,.F.);
#11553=ORIENTED_EDGE('',*,*,#7887,.F.);
#11554=ORIENTED_EDGE('',*,*,#7886,.F.);
#11555=ORIENTED_EDGE('',*,*,#7885,.F.);
#11556=ORIENTED_EDGE('',*,*,#7884,.F.);
#11557=ORIENTED_EDGE('',*,*,#7883,.F.);
#11558=ORIENTED_EDGE('',*,*,#7882,.F.);
#11559=ORIENTED_EDGE('',*,*,#7881,.F.);
#11560=ORIENTED_EDGE('',*,*,#7880,.F.);
#11561=ORIENTED_EDGE('',*,*,#7879,.F.);
#11562=ORIENTED_EDGE('',*,*,#7878,.F.);
#11563=ORIENTED_EDGE('',*,*,#7877,.F.);
#11564=ORIENTED_EDGE('',*,*,#7876,.F.);
#11565=ORIENTED_EDGE('',*,*,#7875,.F.);
#11566=ORIENTED_EDGE('',*,*,#7874,.F.);
#11567=ORIENTED_EDGE('',*,*,#7873,.F.);
#11568=ORIENTED_EDGE('',*,*,#7872,.F.);
#11569=ORIENTED_EDGE('',*,*,#7871,.F.);
#11570=ORIENTED_EDGE('',*,*,#7870,.F.);
#11571=ORIENTED_EDGE('',*,*,#7869,.F.);
#11572=ORIENTED_EDGE('',*,*,#7868,.F.);
#11573=ORIENTED_EDGE('',*,*,#7867,.F.);
#11574=ORIENTED_EDGE('',*,*,#7866,.F.);
#11575=ORIENTED_EDGE('',*,*,#7865,.F.);
#11576=ORIENTED_EDGE('',*,*,#7864,.F.);
#11577=ORIENTED_EDGE('',*,*,#7863,.F.);
#11578=ORIENTED_EDGE('',*,*,#7862,.F.);
#11579=ORIENTED_EDGE('',*,*,#7861,.F.);
#11580=ORIENTED_EDGE('',*,*,#7860,.F.);
#11581=ORIENTED_EDGE('',*,*,#7859,.F.);
#11582=ORIENTED_EDGE('',*,*,#7858,.F.);
#11583=ORIENTED_EDGE('',*,*,#7857,.F.);
#11584=ORIENTED_EDGE('',*,*,#7856,.F.);
#11585=ORIENTED_EDGE('',*,*,#7855,.F.);
#11586=ORIENTED_EDGE('',*,*,#7854,.F.);
#11587=ORIENTED_EDGE('',*,*,#7853,.F.);
#11588=ORIENTED_EDGE('',*,*,#7852,.F.);
#11589=ORIENTED_EDGE('',*,*,#7851,.F.);
#11590=ORIENTED_EDGE('',*,*,#7850,.F.);
#11591=ORIENTED_EDGE('',*,*,#7849,.F.);
#11592=ORIENTED_EDGE('',*,*,#7848,.F.);
#11593=ORIENTED_EDGE('',*,*,#7847,.F.);
#11594=ORIENTED_EDGE('',*,*,#7846,.F.);
#11595=ORIENTED_EDGE('',*,*,#7845,.F.);
#11596=ORIENTED_EDGE('',*,*,#7844,.F.);
#11597=ORIENTED_EDGE('',*,*,#7843,.F.);
#11598=ORIENTED_EDGE('',*,*,#7842,.F.);
#11599=ORIENTED_EDGE('',*,*,#7841,.F.);
#11600=ORIENTED_EDGE('',*,*,#7840,.F.);
#11601=ORIENTED_EDGE('',*,*,#7839,.F.);
#11602=ORIENTED_EDGE('',*,*,#7838,.F.);
#11603=ORIENTED_EDGE('',*,*,#7837,.F.);
#11604=ORIENTED_EDGE('',*,*,#7836,.F.);
#11605=ORIENTED_EDGE('',*,*,#8385,.F.);
#11606=ORIENTED_EDGE('',*,*,#6496,.T.);
#11607=ORIENTED_EDGE('',*,*,#6501,.T.);
#11608=ORIENTED_EDGE('',*,*,#6500,.T.);
#11609=ORIENTED_EDGE('',*,*,#6506,.T.);
#11610=ORIENTED_EDGE('',*,*,#6505,.T.);
#11611=ORIENTED_EDGE('',*,*,#6511,.T.);
#11612=ORIENTED_EDGE('',*,*,#6510,.T.);
#11613=ORIENTED_EDGE('',*,*,#6516,.T.);
#11614=ORIENTED_EDGE('',*,*,#6515,.T.);
#11615=ORIENTED_EDGE('',*,*,#6521,.T.);
#11616=ORIENTED_EDGE('',*,*,#6520,.T.);
#11617=ORIENTED_EDGE('',*,*,#6526,.T.);
#11618=ORIENTED_EDGE('',*,*,#6525,.T.);
#11619=ORIENTED_EDGE('',*,*,#6531,.T.);
#11620=ORIENTED_EDGE('',*,*,#6530,.T.);
#11621=ORIENTED_EDGE('',*,*,#6536,.T.);
#11622=ORIENTED_EDGE('',*,*,#6535,.T.);
#11623=ORIENTED_EDGE('',*,*,#6541,.T.);
#11624=ORIENTED_EDGE('',*,*,#6540,.T.);
#11625=ORIENTED_EDGE('',*,*,#6546,.T.);
#11626=ORIENTED_EDGE('',*,*,#6545,.T.);
#11627=ORIENTED_EDGE('',*,*,#6551,.T.);
#11628=ORIENTED_EDGE('',*,*,#6550,.T.);
#11629=ORIENTED_EDGE('',*,*,#6556,.T.);
#11630=ORIENTED_EDGE('',*,*,#6555,.T.);
#11631=ORIENTED_EDGE('',*,*,#6561,.T.);
#11632=ORIENTED_EDGE('',*,*,#6560,.T.);
#11633=ORIENTED_EDGE('',*,*,#6566,.T.);
#11634=ORIENTED_EDGE('',*,*,#6565,.T.);
#11635=ORIENTED_EDGE('',*,*,#6571,.T.);
#11636=ORIENTED_EDGE('',*,*,#6570,.T.);
#11637=ORIENTED_EDGE('',*,*,#6576,.T.);
#11638=ORIENTED_EDGE('',*,*,#6575,.T.);
#11639=ORIENTED_EDGE('',*,*,#6581,.T.);
#11640=ORIENTED_EDGE('',*,*,#6580,.T.);
#11641=ORIENTED_EDGE('',*,*,#6586,.T.);
#11642=ORIENTED_EDGE('',*,*,#6585,.T.);
#11643=ORIENTED_EDGE('',*,*,#6591,.T.);
#11644=ORIENTED_EDGE('',*,*,#6590,.T.);
#11645=ORIENTED_EDGE('',*,*,#6596,.T.);
#11646=ORIENTED_EDGE('',*,*,#6595,.T.);
#11647=ORIENTED_EDGE('',*,*,#6601,.T.);
#11648=ORIENTED_EDGE('',*,*,#6600,.T.);
#11649=ORIENTED_EDGE('',*,*,#6606,.T.);
#11650=ORIENTED_EDGE('',*,*,#6605,.T.);
#11651=ORIENTED_EDGE('',*,*,#6611,.T.);
#11652=ORIENTED_EDGE('',*,*,#6610,.T.);
#11653=ORIENTED_EDGE('',*,*,#6616,.T.);
#11654=ORIENTED_EDGE('',*,*,#6615,.T.);
#11655=ORIENTED_EDGE('',*,*,#6621,.T.);
#11656=ORIENTED_EDGE('',*,*,#6620,.T.);
#11657=ORIENTED_EDGE('',*,*,#6626,.T.);
#11658=ORIENTED_EDGE('',*,*,#6625,.T.);
#11659=ORIENTED_EDGE('',*,*,#6631,.T.);
#11660=ORIENTED_EDGE('',*,*,#6630,.T.);
#11661=ORIENTED_EDGE('',*,*,#6636,.T.);
#11662=ORIENTED_EDGE('',*,*,#6635,.T.);
#11663=ORIENTED_EDGE('',*,*,#6641,.T.);
#11664=ORIENTED_EDGE('',*,*,#6640,.T.);
#11665=ORIENTED_EDGE('',*,*,#6646,.T.);
#11666=ORIENTED_EDGE('',*,*,#6645,.T.);
#11667=ORIENTED_EDGE('',*,*,#6651,.T.);
#11668=ORIENTED_EDGE('',*,*,#6650,.T.);
#11669=ORIENTED_EDGE('',*,*,#6656,.T.);
#11670=ORIENTED_EDGE('',*,*,#6655,.T.);
#11671=ORIENTED_EDGE('',*,*,#6661,.T.);
#11672=ORIENTED_EDGE('',*,*,#6660,.T.);
#11673=ORIENTED_EDGE('',*,*,#6666,.T.);
#11674=ORIENTED_EDGE('',*,*,#6665,.T.);
#11675=ORIENTED_EDGE('',*,*,#6671,.T.);
#11676=ORIENTED_EDGE('',*,*,#6670,.T.);
#11677=ORIENTED_EDGE('',*,*,#6676,.T.);
#11678=ORIENTED_EDGE('',*,*,#6675,.T.);
#11679=ORIENTED_EDGE('',*,*,#6681,.T.);
#11680=ORIENTED_EDGE('',*,*,#6680,.T.);
#11681=ORIENTED_EDGE('',*,*,#6686,.T.);
#11682=ORIENTED_EDGE('',*,*,#6685,.T.);
#11683=ORIENTED_EDGE('',*,*,#6691,.T.);
#11684=ORIENTED_EDGE('',*,*,#6690,.T.);
#11685=ORIENTED_EDGE('',*,*,#6696,.T.);
#11686=ORIENTED_EDGE('',*,*,#6695,.T.);
#11687=ORIENTED_EDGE('',*,*,#6701,.T.);
#11688=ORIENTED_EDGE('',*,*,#6700,.T.);
#11689=ORIENTED_EDGE('',*,*,#6706,.T.);
#11690=ORIENTED_EDGE('',*,*,#6705,.T.);
#11691=ORIENTED_EDGE('',*,*,#6711,.T.);
#11692=ORIENTED_EDGE('',*,*,#6710,.T.);
#11693=ORIENTED_EDGE('',*,*,#6716,.T.);
#11694=ORIENTED_EDGE('',*,*,#6715,.T.);
#11695=ORIENTED_EDGE('',*,*,#6721,.T.);
#11696=ORIENTED_EDGE('',*,*,#6720,.T.);
#11697=ORIENTED_EDGE('',*,*,#6726,.T.);
#11698=ORIENTED_EDGE('',*,*,#6725,.T.);
#11699=ORIENTED_EDGE('',*,*,#6731,.T.);
#11700=ORIENTED_EDGE('',*,*,#6730,.T.);
#11701=ORIENTED_EDGE('',*,*,#6736,.T.);
#11702=ORIENTED_EDGE('',*,*,#6735,.T.);
#11703=ORIENTED_EDGE('',*,*,#6741,.T.);
#11704=ORIENTED_EDGE('',*,*,#6740,.T.);
#11705=ORIENTED_EDGE('',*,*,#6746,.T.);
#11706=ORIENTED_EDGE('',*,*,#6745,.T.);
#11707=ORIENTED_EDGE('',*,*,#6751,.T.);
#11708=ORIENTED_EDGE('',*,*,#6750,.T.);
#11709=ORIENTED_EDGE('',*,*,#6756,.T.);
#11710=ORIENTED_EDGE('',*,*,#6755,.T.);
#11711=ORIENTED_EDGE('',*,*,#6761,.T.);
#11712=ORIENTED_EDGE('',*,*,#6760,.T.);
#11713=ORIENTED_EDGE('',*,*,#6766,.T.);
#11714=ORIENTED_EDGE('',*,*,#6765,.T.);
#11715=ORIENTED_EDGE('',*,*,#6771,.T.);
#11716=ORIENTED_EDGE('',*,*,#6770,.T.);
#11717=ORIENTED_EDGE('',*,*,#6776,.T.);
#11718=ORIENTED_EDGE('',*,*,#6775,.T.);
#11719=ORIENTED_EDGE('',*,*,#6781,.T.);
#11720=ORIENTED_EDGE('',*,*,#6780,.T.);
#11721=ORIENTED_EDGE('',*,*,#6786,.T.);
#11722=ORIENTED_EDGE('',*,*,#6785,.T.);
#11723=ORIENTED_EDGE('',*,*,#6791,.T.);
#11724=ORIENTED_EDGE('',*,*,#6790,.T.);
#11725=ORIENTED_EDGE('',*,*,#6796,.T.);
#11726=ORIENTED_EDGE('',*,*,#6795,.T.);
#11727=ORIENTED_EDGE('',*,*,#6801,.T.);
#11728=ORIENTED_EDGE('',*,*,#6800,.T.);
#11729=ORIENTED_EDGE('',*,*,#6806,.T.);
#11730=ORIENTED_EDGE('',*,*,#6805,.T.);
#11731=ORIENTED_EDGE('',*,*,#6811,.T.);
#11732=ORIENTED_EDGE('',*,*,#6810,.T.);
#11733=ORIENTED_EDGE('',*,*,#6816,.T.);
#11734=ORIENTED_EDGE('',*,*,#6815,.T.);
#11735=ORIENTED_EDGE('',*,*,#6821,.T.);
#11736=ORIENTED_EDGE('',*,*,#6820,.T.);
#11737=ORIENTED_EDGE('',*,*,#6826,.T.);
#11738=ORIENTED_EDGE('',*,*,#6825,.T.);
#11739=ORIENTED_EDGE('',*,*,#6831,.T.);
#11740=ORIENTED_EDGE('',*,*,#6830,.T.);
#11741=ORIENTED_EDGE('',*,*,#6836,.T.);
#11742=ORIENTED_EDGE('',*,*,#6835,.T.);
#11743=ORIENTED_EDGE('',*,*,#6841,.T.);
#11744=ORIENTED_EDGE('',*,*,#6840,.T.);
#11745=ORIENTED_EDGE('',*,*,#6846,.T.);
#11746=ORIENTED_EDGE('',*,*,#6845,.T.);
#11747=ORIENTED_EDGE('',*,*,#6851,.T.);
#11748=ORIENTED_EDGE('',*,*,#6850,.T.);
#11749=ORIENTED_EDGE('',*,*,#6856,.T.);
#11750=ORIENTED_EDGE('',*,*,#6855,.T.);
#11751=ORIENTED_EDGE('',*,*,#6861,.T.);
#11752=ORIENTED_EDGE('',*,*,#6860,.T.);
#11753=ORIENTED_EDGE('',*,*,#6866,.T.);
#11754=ORIENTED_EDGE('',*,*,#6865,.T.);
#11755=ORIENTED_EDGE('',*,*,#6871,.T.);
#11756=ORIENTED_EDGE('',*,*,#6870,.T.);
#11757=ORIENTED_EDGE('',*,*,#6876,.T.);
#11758=ORIENTED_EDGE('',*,*,#6875,.T.);
#11759=ORIENTED_EDGE('',*,*,#6881,.T.);
#11760=ORIENTED_EDGE('',*,*,#6880,.T.);
#11761=ORIENTED_EDGE('',*,*,#6886,.T.);
#11762=ORIENTED_EDGE('',*,*,#6885,.T.);
#11763=ORIENTED_EDGE('',*,*,#6891,.T.);
#11764=ORIENTED_EDGE('',*,*,#6890,.T.);
#11765=ORIENTED_EDGE('',*,*,#6896,.T.);
#11766=ORIENTED_EDGE('',*,*,#6895,.T.);
#11767=ORIENTED_EDGE('',*,*,#6901,.T.);
#11768=ORIENTED_EDGE('',*,*,#6900,.T.);
#11769=ORIENTED_EDGE('',*,*,#6906,.T.);
#11770=ORIENTED_EDGE('',*,*,#6905,.T.);
#11771=ORIENTED_EDGE('',*,*,#6911,.T.);
#11772=ORIENTED_EDGE('',*,*,#6910,.T.);
#11773=ORIENTED_EDGE('',*,*,#6916,.T.);
#11774=ORIENTED_EDGE('',*,*,#6915,.T.);
#11775=ORIENTED_EDGE('',*,*,#6921,.T.);
#11776=ORIENTED_EDGE('',*,*,#6920,.T.);
#11777=ORIENTED_EDGE('',*,*,#6926,.T.);
#11778=ORIENTED_EDGE('',*,*,#6925,.T.);
#11779=ORIENTED_EDGE('',*,*,#6931,.T.);
#11780=ORIENTED_EDGE('',*,*,#6930,.T.);
#11781=ORIENTED_EDGE('',*,*,#6936,.T.);
#11782=ORIENTED_EDGE('',*,*,#6935,.T.);
#11783=ORIENTED_EDGE('',*,*,#6941,.T.);
#11784=ORIENTED_EDGE('',*,*,#6940,.T.);
#11785=ORIENTED_EDGE('',*,*,#6946,.T.);
#11786=ORIENTED_EDGE('',*,*,#6945,.T.);
#11787=ORIENTED_EDGE('',*,*,#6951,.T.);
#11788=ORIENTED_EDGE('',*,*,#6950,.T.);
#11789=ORIENTED_EDGE('',*,*,#6956,.T.);
#11790=ORIENTED_EDGE('',*,*,#6955,.T.);
#11791=ORIENTED_EDGE('',*,*,#6961,.T.);
#11792=ORIENTED_EDGE('',*,*,#6960,.T.);
#11793=ORIENTED_EDGE('',*,*,#6966,.T.);
#11794=ORIENTED_EDGE('',*,*,#6965,.T.);
#11795=ORIENTED_EDGE('',*,*,#6971,.T.);
#11796=ORIENTED_EDGE('',*,*,#6970,.T.);
#11797=ORIENTED_EDGE('',*,*,#6976,.T.);
#11798=ORIENTED_EDGE('',*,*,#6975,.T.);
#11799=ORIENTED_EDGE('',*,*,#6981,.T.);
#11800=ORIENTED_EDGE('',*,*,#6980,.T.);
#11801=ORIENTED_EDGE('',*,*,#6986,.T.);
#11802=ORIENTED_EDGE('',*,*,#6985,.T.);
#11803=ORIENTED_EDGE('',*,*,#6991,.T.);
#11804=ORIENTED_EDGE('',*,*,#6990,.T.);
#11805=ORIENTED_EDGE('',*,*,#6996,.T.);
#11806=ORIENTED_EDGE('',*,*,#6995,.T.);
#11807=ORIENTED_EDGE('',*,*,#7001,.T.);
#11808=ORIENTED_EDGE('',*,*,#7000,.T.);
#11809=ORIENTED_EDGE('',*,*,#7006,.T.);
#11810=ORIENTED_EDGE('',*,*,#7005,.T.);
#11811=ORIENTED_EDGE('',*,*,#7011,.T.);
#11812=ORIENTED_EDGE('',*,*,#7010,.T.);
#11813=ORIENTED_EDGE('',*,*,#7016,.T.);
#11814=ORIENTED_EDGE('',*,*,#7015,.T.);
#11815=ORIENTED_EDGE('',*,*,#7021,.T.);
#11816=ORIENTED_EDGE('',*,*,#7020,.T.);
#11817=ORIENTED_EDGE('',*,*,#7026,.T.);
#11818=ORIENTED_EDGE('',*,*,#7025,.T.);
#11819=ORIENTED_EDGE('',*,*,#7031,.T.);
#11820=ORIENTED_EDGE('',*,*,#7030,.T.);
#11821=ORIENTED_EDGE('',*,*,#7036,.T.);
#11822=ORIENTED_EDGE('',*,*,#7035,.T.);
#11823=ORIENTED_EDGE('',*,*,#7041,.T.);
#11824=ORIENTED_EDGE('',*,*,#7040,.T.);
#11825=ORIENTED_EDGE('',*,*,#7046,.T.);
#11826=ORIENTED_EDGE('',*,*,#7045,.T.);
#11827=ORIENTED_EDGE('',*,*,#7051,.T.);
#11828=ORIENTED_EDGE('',*,*,#7050,.T.);
#11829=ORIENTED_EDGE('',*,*,#7056,.T.);
#11830=ORIENTED_EDGE('',*,*,#7055,.T.);
#11831=ORIENTED_EDGE('',*,*,#7061,.T.);
#11832=ORIENTED_EDGE('',*,*,#7060,.T.);
#11833=ORIENTED_EDGE('',*,*,#7066,.T.);
#11834=ORIENTED_EDGE('',*,*,#7065,.T.);
#11835=ORIENTED_EDGE('',*,*,#7071,.T.);
#11836=ORIENTED_EDGE('',*,*,#7070,.T.);
#11837=ORIENTED_EDGE('',*,*,#7076,.T.);
#11838=ORIENTED_EDGE('',*,*,#7075,.T.);
#11839=ORIENTED_EDGE('',*,*,#7081,.T.);
#11840=ORIENTED_EDGE('',*,*,#7080,.T.);
#11841=ORIENTED_EDGE('',*,*,#7086,.T.);
#11842=ORIENTED_EDGE('',*,*,#7085,.T.);
#11843=ORIENTED_EDGE('',*,*,#7091,.T.);
#11844=ORIENTED_EDGE('',*,*,#7090,.T.);
#11845=ORIENTED_EDGE('',*,*,#7096,.T.);
#11846=ORIENTED_EDGE('',*,*,#7095,.T.);
#11847=ORIENTED_EDGE('',*,*,#7101,.T.);
#11848=ORIENTED_EDGE('',*,*,#7100,.T.);
#11849=ORIENTED_EDGE('',*,*,#7106,.T.);
#11850=ORIENTED_EDGE('',*,*,#7105,.T.);
#11851=ORIENTED_EDGE('',*,*,#7111,.T.);
#11852=ORIENTED_EDGE('',*,*,#7110,.T.);
#11853=ORIENTED_EDGE('',*,*,#7116,.T.);
#11854=ORIENTED_EDGE('',*,*,#7115,.T.);
#11855=ORIENTED_EDGE('',*,*,#7121,.T.);
#11856=ORIENTED_EDGE('',*,*,#7120,.T.);
#11857=ORIENTED_EDGE('',*,*,#7126,.T.);
#11858=ORIENTED_EDGE('',*,*,#7125,.T.);
#11859=ORIENTED_EDGE('',*,*,#7131,.T.);
#11860=ORIENTED_EDGE('',*,*,#7130,.T.);
#11861=ORIENTED_EDGE('',*,*,#7136,.T.);
#11862=ORIENTED_EDGE('',*,*,#7135,.T.);
#11863=ORIENTED_EDGE('',*,*,#7141,.T.);
#11864=ORIENTED_EDGE('',*,*,#7140,.T.);
#11865=ORIENTED_EDGE('',*,*,#7146,.T.);
#11866=ORIENTED_EDGE('',*,*,#7145,.T.);
#11867=ORIENTED_EDGE('',*,*,#7151,.T.);
#11868=ORIENTED_EDGE('',*,*,#7150,.T.);
#11869=ORIENTED_EDGE('',*,*,#7156,.T.);
#11870=ORIENTED_EDGE('',*,*,#7155,.T.);
#11871=ORIENTED_EDGE('',*,*,#7161,.T.);
#11872=ORIENTED_EDGE('',*,*,#7160,.T.);
#11873=ORIENTED_EDGE('',*,*,#7166,.T.);
#11874=ORIENTED_EDGE('',*,*,#7165,.T.);
#11875=ORIENTED_EDGE('',*,*,#7171,.T.);
#11876=ORIENTED_EDGE('',*,*,#7170,.T.);
#11877=ORIENTED_EDGE('',*,*,#7176,.T.);
#11878=ORIENTED_EDGE('',*,*,#7175,.T.);
#11879=ORIENTED_EDGE('',*,*,#7181,.T.);
#11880=ORIENTED_EDGE('',*,*,#7180,.T.);
#11881=ORIENTED_EDGE('',*,*,#7186,.T.);
#11882=ORIENTED_EDGE('',*,*,#7185,.T.);
#11883=ORIENTED_EDGE('',*,*,#7191,.T.);
#11884=ORIENTED_EDGE('',*,*,#7190,.T.);
#11885=ORIENTED_EDGE('',*,*,#7196,.T.);
#11886=ORIENTED_EDGE('',*,*,#7195,.T.);
#11887=ORIENTED_EDGE('',*,*,#7201,.T.);
#11888=ORIENTED_EDGE('',*,*,#7200,.T.);
#11889=ORIENTED_EDGE('',*,*,#7206,.T.);
#11890=ORIENTED_EDGE('',*,*,#7205,.T.);
#11891=ORIENTED_EDGE('',*,*,#7211,.T.);
#11892=ORIENTED_EDGE('',*,*,#7210,.T.);
#11893=ORIENTED_EDGE('',*,*,#7216,.T.);
#11894=ORIENTED_EDGE('',*,*,#7215,.T.);
#11895=ORIENTED_EDGE('',*,*,#7221,.T.);
#11896=ORIENTED_EDGE('',*,*,#7220,.T.);
#11897=ORIENTED_EDGE('',*,*,#7226,.T.);
#11898=ORIENTED_EDGE('',*,*,#7225,.T.);
#11899=ORIENTED_EDGE('',*,*,#7231,.T.);
#11900=ORIENTED_EDGE('',*,*,#7230,.T.);
#11901=ORIENTED_EDGE('',*,*,#7236,.T.);
#11902=ORIENTED_EDGE('',*,*,#7235,.T.);
#11903=ORIENTED_EDGE('',*,*,#7241,.T.);
#11904=ORIENTED_EDGE('',*,*,#7240,.T.);
#11905=ORIENTED_EDGE('',*,*,#7246,.T.);
#11906=ORIENTED_EDGE('',*,*,#7245,.T.);
#11907=ORIENTED_EDGE('',*,*,#7251,.T.);
#11908=ORIENTED_EDGE('',*,*,#7250,.T.);
#11909=ORIENTED_EDGE('',*,*,#7256,.T.);
#11910=ORIENTED_EDGE('',*,*,#7255,.T.);
#11911=ORIENTED_EDGE('',*,*,#7261,.T.);
#11912=ORIENTED_EDGE('',*,*,#7260,.T.);
#11913=ORIENTED_EDGE('',*,*,#7266,.T.);
#11914=ORIENTED_EDGE('',*,*,#7265,.T.);
#11915=ORIENTED_EDGE('',*,*,#7271,.T.);
#11916=ORIENTED_EDGE('',*,*,#7270,.T.);
#11917=ORIENTED_EDGE('',*,*,#7276,.T.);
#11918=ORIENTED_EDGE('',*,*,#7275,.T.);
#11919=ORIENTED_EDGE('',*,*,#7281,.T.);
#11920=ORIENTED_EDGE('',*,*,#7280,.T.);
#11921=ORIENTED_EDGE('',*,*,#7286,.T.);
#11922=ORIENTED_EDGE('',*,*,#7285,.T.);
#11923=ORIENTED_EDGE('',*,*,#7291,.T.);
#11924=ORIENTED_EDGE('',*,*,#7290,.T.);
#11925=ORIENTED_EDGE('',*,*,#7296,.T.);
#11926=ORIENTED_EDGE('',*,*,#7295,.T.);
#11927=ORIENTED_EDGE('',*,*,#7301,.T.);
#11928=ORIENTED_EDGE('',*,*,#7300,.T.);
#11929=ORIENTED_EDGE('',*,*,#7306,.T.);
#11930=ORIENTED_EDGE('',*,*,#7305,.T.);
#11931=ORIENTED_EDGE('',*,*,#7311,.T.);
#11932=ORIENTED_EDGE('',*,*,#7310,.T.);
#11933=ORIENTED_EDGE('',*,*,#7316,.T.);
#11934=ORIENTED_EDGE('',*,*,#7315,.T.);
#11935=ORIENTED_EDGE('',*,*,#7321,.T.);
#11936=ORIENTED_EDGE('',*,*,#7320,.T.);
#11937=ORIENTED_EDGE('',*,*,#7326,.T.);
#11938=ORIENTED_EDGE('',*,*,#7325,.T.);
#11939=ORIENTED_EDGE('',*,*,#7331,.T.);
#11940=ORIENTED_EDGE('',*,*,#7330,.T.);
#11941=ORIENTED_EDGE('',*,*,#7336,.T.);
#11942=ORIENTED_EDGE('',*,*,#7335,.T.);
#11943=ORIENTED_EDGE('',*,*,#7341,.T.);
#11944=ORIENTED_EDGE('',*,*,#7340,.T.);
#11945=ORIENTED_EDGE('',*,*,#7346,.T.);
#11946=ORIENTED_EDGE('',*,*,#7345,.T.);
#11947=ORIENTED_EDGE('',*,*,#7351,.T.);
#11948=ORIENTED_EDGE('',*,*,#7350,.T.);
#11949=ORIENTED_EDGE('',*,*,#7356,.T.);
#11950=ORIENTED_EDGE('',*,*,#7355,.T.);
#11951=ORIENTED_EDGE('',*,*,#7361,.T.);
#11952=ORIENTED_EDGE('',*,*,#7360,.T.);
#11953=ORIENTED_EDGE('',*,*,#7366,.T.);
#11954=ORIENTED_EDGE('',*,*,#7365,.T.);
#11955=ORIENTED_EDGE('',*,*,#7371,.T.);
#11956=ORIENTED_EDGE('',*,*,#7370,.T.);
#11957=ORIENTED_EDGE('',*,*,#7376,.T.);
#11958=ORIENTED_EDGE('',*,*,#7375,.T.);
#11959=ORIENTED_EDGE('',*,*,#7381,.T.);
#11960=ORIENTED_EDGE('',*,*,#7380,.T.);
#11961=ORIENTED_EDGE('',*,*,#7386,.T.);
#11962=ORIENTED_EDGE('',*,*,#7385,.T.);
#11963=ORIENTED_EDGE('',*,*,#7391,.T.);
#11964=ORIENTED_EDGE('',*,*,#7390,.T.);
#11965=ORIENTED_EDGE('',*,*,#7396,.T.);
#11966=ORIENTED_EDGE('',*,*,#7395,.T.);
#11967=ORIENTED_EDGE('',*,*,#7401,.T.);
#11968=ORIENTED_EDGE('',*,*,#7400,.T.);
#11969=ORIENTED_EDGE('',*,*,#7406,.T.);
#11970=ORIENTED_EDGE('',*,*,#7405,.T.);
#11971=ORIENTED_EDGE('',*,*,#7411,.T.);
#11972=ORIENTED_EDGE('',*,*,#7410,.T.);
#11973=ORIENTED_EDGE('',*,*,#7416,.T.);
#11974=ORIENTED_EDGE('',*,*,#7415,.T.);
#11975=ORIENTED_EDGE('',*,*,#7421,.T.);
#11976=ORIENTED_EDGE('',*,*,#7420,.T.);
#11977=ORIENTED_EDGE('',*,*,#7426,.T.);
#11978=ORIENTED_EDGE('',*,*,#7425,.T.);
#11979=ORIENTED_EDGE('',*,*,#7431,.T.);
#11980=ORIENTED_EDGE('',*,*,#7430,.T.);
#11981=ORIENTED_EDGE('',*,*,#7436,.T.);
#11982=ORIENTED_EDGE('',*,*,#7435,.T.);
#11983=ORIENTED_EDGE('',*,*,#7441,.T.);
#11984=ORIENTED_EDGE('',*,*,#7440,.T.);
#11985=ORIENTED_EDGE('',*,*,#7446,.T.);
#11986=ORIENTED_EDGE('',*,*,#7445,.T.);
#11987=ORIENTED_EDGE('',*,*,#7451,.T.);
#11988=ORIENTED_EDGE('',*,*,#7450,.T.);
#11989=ORIENTED_EDGE('',*,*,#7456,.T.);
#11990=ORIENTED_EDGE('',*,*,#7455,.T.);
#11991=ORIENTED_EDGE('',*,*,#7461,.T.);
#11992=ORIENTED_EDGE('',*,*,#7460,.T.);
#11993=ORIENTED_EDGE('',*,*,#7466,.T.);
#11994=ORIENTED_EDGE('',*,*,#7465,.T.);
#11995=ORIENTED_EDGE('',*,*,#7471,.T.);
#11996=ORIENTED_EDGE('',*,*,#7470,.T.);
#11997=ORIENTED_EDGE('',*,*,#7476,.T.);
#11998=ORIENTED_EDGE('',*,*,#7475,.T.);
#11999=ORIENTED_EDGE('',*,*,#7481,.T.);
#12000=ORIENTED_EDGE('',*,*,#7480,.T.);
#12001=ORIENTED_EDGE('',*,*,#7486,.T.);
#12002=ORIENTED_EDGE('',*,*,#7485,.T.);
#12003=ORIENTED_EDGE('',*,*,#7491,.T.);
#12004=ORIENTED_EDGE('',*,*,#7490,.T.);
#12005=ORIENTED_EDGE('',*,*,#7496,.T.);
#12006=ORIENTED_EDGE('',*,*,#7495,.T.);
#12007=ORIENTED_EDGE('',*,*,#7501,.T.);
#12008=ORIENTED_EDGE('',*,*,#7500,.T.);
#12009=ORIENTED_EDGE('',*,*,#7506,.T.);
#12010=ORIENTED_EDGE('',*,*,#7505,.T.);
#12011=ORIENTED_EDGE('',*,*,#7511,.T.);
#12012=ORIENTED_EDGE('',*,*,#7510,.T.);
#12013=ORIENTED_EDGE('',*,*,#7516,.T.);
#12014=ORIENTED_EDGE('',*,*,#7515,.T.);
#12015=ORIENTED_EDGE('',*,*,#7521,.T.);
#12016=ORIENTED_EDGE('',*,*,#7520,.T.);
#12017=ORIENTED_EDGE('',*,*,#7526,.T.);
#12018=ORIENTED_EDGE('',*,*,#7525,.T.);
#12019=ORIENTED_EDGE('',*,*,#7531,.T.);
#12020=ORIENTED_EDGE('',*,*,#7530,.T.);
#12021=ORIENTED_EDGE('',*,*,#7536,.T.);
#12022=ORIENTED_EDGE('',*,*,#7535,.T.);
#12023=ORIENTED_EDGE('',*,*,#7541,.T.);
#12024=ORIENTED_EDGE('',*,*,#7540,.T.);
#12025=ORIENTED_EDGE('',*,*,#7546,.T.);
#12026=ORIENTED_EDGE('',*,*,#7545,.T.);
#12027=ORIENTED_EDGE('',*,*,#7551,.T.);
#12028=ORIENTED_EDGE('',*,*,#7550,.T.);
#12029=ORIENTED_EDGE('',*,*,#7556,.T.);
#12030=ORIENTED_EDGE('',*,*,#7555,.T.);
#12031=ORIENTED_EDGE('',*,*,#7561,.T.);
#12032=ORIENTED_EDGE('',*,*,#7560,.T.);
#12033=ORIENTED_EDGE('',*,*,#7566,.T.);
#12034=ORIENTED_EDGE('',*,*,#7565,.T.);
#12035=ORIENTED_EDGE('',*,*,#7571,.T.);
#12036=ORIENTED_EDGE('',*,*,#7570,.T.);
#12037=ORIENTED_EDGE('',*,*,#7576,.T.);
#12038=ORIENTED_EDGE('',*,*,#7575,.T.);
#12039=ORIENTED_EDGE('',*,*,#7581,.T.);
#12040=ORIENTED_EDGE('',*,*,#7580,.T.);
#12041=ORIENTED_EDGE('',*,*,#7586,.T.);
#12042=ORIENTED_EDGE('',*,*,#7585,.T.);
#12043=ORIENTED_EDGE('',*,*,#7591,.T.);
#12044=ORIENTED_EDGE('',*,*,#7590,.T.);
#12045=ORIENTED_EDGE('',*,*,#7596,.T.);
#12046=ORIENTED_EDGE('',*,*,#7595,.T.);
#12047=ORIENTED_EDGE('',*,*,#7601,.T.);
#12048=ORIENTED_EDGE('',*,*,#7600,.T.);
#12049=ORIENTED_EDGE('',*,*,#7606,.T.);
#12050=ORIENTED_EDGE('',*,*,#7605,.T.);
#12051=ORIENTED_EDGE('',*,*,#7611,.T.);
#12052=ORIENTED_EDGE('',*,*,#7610,.T.);
#12053=ORIENTED_EDGE('',*,*,#7616,.T.);
#12054=ORIENTED_EDGE('',*,*,#7615,.T.);
#12055=ORIENTED_EDGE('',*,*,#7621,.T.);
#12056=ORIENTED_EDGE('',*,*,#7620,.T.);
#12057=ORIENTED_EDGE('',*,*,#7626,.T.);
#12058=ORIENTED_EDGE('',*,*,#7625,.T.);
#12059=ORIENTED_EDGE('',*,*,#7631,.T.);
#12060=ORIENTED_EDGE('',*,*,#7630,.T.);
#12061=ORIENTED_EDGE('',*,*,#7636,.T.);
#12062=ORIENTED_EDGE('',*,*,#7635,.T.);
#12063=ORIENTED_EDGE('',*,*,#7641,.T.);
#12064=ORIENTED_EDGE('',*,*,#7640,.T.);
#12065=ORIENTED_EDGE('',*,*,#7646,.T.);
#12066=ORIENTED_EDGE('',*,*,#7645,.T.);
#12067=ORIENTED_EDGE('',*,*,#7651,.T.);
#12068=ORIENTED_EDGE('',*,*,#7650,.T.);
#12069=ORIENTED_EDGE('',*,*,#7656,.T.);
#12070=ORIENTED_EDGE('',*,*,#7655,.T.);
#12071=ORIENTED_EDGE('',*,*,#7661,.T.);
#12072=ORIENTED_EDGE('',*,*,#7660,.T.);
#12073=ORIENTED_EDGE('',*,*,#7666,.T.);
#12074=ORIENTED_EDGE('',*,*,#7665,.T.);
#12075=ORIENTED_EDGE('',*,*,#7671,.T.);
#12076=ORIENTED_EDGE('',*,*,#7670,.T.);
#12077=ORIENTED_EDGE('',*,*,#7676,.T.);
#12078=ORIENTED_EDGE('',*,*,#7675,.T.);
#12079=ORIENTED_EDGE('',*,*,#7681,.T.);
#12080=ORIENTED_EDGE('',*,*,#7680,.T.);
#12081=ORIENTED_EDGE('',*,*,#7686,.T.);
#12082=ORIENTED_EDGE('',*,*,#7685,.T.);
#12083=ORIENTED_EDGE('',*,*,#7691,.T.);
#12084=ORIENTED_EDGE('',*,*,#7690,.T.);
#12085=ORIENTED_EDGE('',*,*,#7696,.T.);
#12086=ORIENTED_EDGE('',*,*,#7695,.T.);
#12087=ORIENTED_EDGE('',*,*,#7701,.T.);
#12088=ORIENTED_EDGE('',*,*,#7700,.T.);
#12089=ORIENTED_EDGE('',*,*,#7706,.T.);
#12090=ORIENTED_EDGE('',*,*,#7705,.T.);
#12091=ORIENTED_EDGE('',*,*,#7711,.T.);
#12092=ORIENTED_EDGE('',*,*,#7710,.T.);
#12093=ORIENTED_EDGE('',*,*,#7716,.T.);
#12094=ORIENTED_EDGE('',*,*,#7715,.T.);
#12095=ORIENTED_EDGE('',*,*,#7721,.T.);
#12096=ORIENTED_EDGE('',*,*,#7720,.T.);
#12097=ORIENTED_EDGE('',*,*,#7726,.T.);
#12098=ORIENTED_EDGE('',*,*,#7725,.T.);
#12099=ORIENTED_EDGE('',*,*,#7731,.T.);
#12100=ORIENTED_EDGE('',*,*,#7730,.T.);
#12101=ORIENTED_EDGE('',*,*,#7736,.T.);
#12102=ORIENTED_EDGE('',*,*,#7735,.T.);
#12103=ORIENTED_EDGE('',*,*,#7741,.T.);
#12104=ORIENTED_EDGE('',*,*,#7740,.T.);
#12105=ORIENTED_EDGE('',*,*,#7746,.T.);
#12106=ORIENTED_EDGE('',*,*,#7745,.T.);
#12107=ORIENTED_EDGE('',*,*,#7751,.T.);
#12108=ORIENTED_EDGE('',*,*,#7750,.T.);
#12109=ORIENTED_EDGE('',*,*,#7756,.T.);
#12110=ORIENTED_EDGE('',*,*,#7755,.T.);
#12111=ORIENTED_EDGE('',*,*,#7761,.T.);
#12112=ORIENTED_EDGE('',*,*,#7760,.T.);
#12113=ORIENTED_EDGE('',*,*,#7766,.T.);
#12114=ORIENTED_EDGE('',*,*,#7765,.T.);
#12115=ORIENTED_EDGE('',*,*,#7771,.T.);
#12116=ORIENTED_EDGE('',*,*,#7770,.T.);
#12117=ORIENTED_EDGE('',*,*,#7776,.T.);
#12118=ORIENTED_EDGE('',*,*,#7775,.T.);
#12119=ORIENTED_EDGE('',*,*,#7781,.T.);
#12120=ORIENTED_EDGE('',*,*,#7780,.T.);
#12121=ORIENTED_EDGE('',*,*,#7786,.T.);
#12122=ORIENTED_EDGE('',*,*,#7785,.T.);
#12123=ORIENTED_EDGE('',*,*,#7791,.T.);
#12124=ORIENTED_EDGE('',*,*,#7790,.T.);
#12125=ORIENTED_EDGE('',*,*,#7796,.T.);
#12126=ORIENTED_EDGE('',*,*,#7795,.T.);
#12127=ORIENTED_EDGE('',*,*,#7801,.T.);
#12128=ORIENTED_EDGE('',*,*,#7800,.T.);
#12129=ORIENTED_EDGE('',*,*,#7806,.T.);
#12130=ORIENTED_EDGE('',*,*,#7805,.T.);
#12131=ORIENTED_EDGE('',*,*,#7811,.T.);
#12132=ORIENTED_EDGE('',*,*,#7810,.T.);
#12133=ORIENTED_EDGE('',*,*,#7816,.T.);
#12134=ORIENTED_EDGE('',*,*,#7815,.T.);
#12135=ORIENTED_EDGE('',*,*,#7821,.T.);
#12136=ORIENTED_EDGE('',*,*,#7820,.T.);
#12137=ORIENTED_EDGE('',*,*,#7826,.T.);
#12138=ORIENTED_EDGE('',*,*,#7825,.T.);
#12139=ORIENTED_EDGE('',*,*,#7831,.T.);
#12140=ORIENTED_EDGE('',*,*,#7830,.T.);
#12141=ORIENTED_EDGE('',*,*,#8380,.T.);
#12142=ORIENTED_EDGE('',*,*,#8379,.T.);
#12143=ORIENTED_EDGE('',*,*,#8402,.F.);
#12144=ORIENTED_EDGE('',*,*,#8377,.F.);
#12145=ORIENTED_EDGE('',*,*,#8376,.F.);
#12146=ORIENTED_EDGE('',*,*,#7833,.F.);
#12147=ORIENTED_EDGE('',*,*,#7832,.F.);
#12148=ORIENTED_EDGE('',*,*,#7828,.F.);
#12149=ORIENTED_EDGE('',*,*,#7827,.F.);
#12150=ORIENTED_EDGE('',*,*,#7823,.F.);
#12151=ORIENTED_EDGE('',*,*,#7822,.F.);
#12152=ORIENTED_EDGE('',*,*,#7818,.F.);
#12153=ORIENTED_EDGE('',*,*,#7817,.F.);
#12154=ORIENTED_EDGE('',*,*,#7813,.F.);
#12155=ORIENTED_EDGE('',*,*,#7812,.F.);
#12156=ORIENTED_EDGE('',*,*,#7808,.F.);
#12157=ORIENTED_EDGE('',*,*,#7807,.F.);
#12158=ORIENTED_EDGE('',*,*,#7803,.F.);
#12159=ORIENTED_EDGE('',*,*,#7802,.F.);
#12160=ORIENTED_EDGE('',*,*,#7798,.F.);
#12161=ORIENTED_EDGE('',*,*,#7797,.F.);
#12162=ORIENTED_EDGE('',*,*,#7793,.F.);
#12163=ORIENTED_EDGE('',*,*,#7792,.F.);
#12164=ORIENTED_EDGE('',*,*,#7788,.F.);
#12165=ORIENTED_EDGE('',*,*,#7787,.F.);
#12166=ORIENTED_EDGE('',*,*,#7783,.F.);
#12167=ORIENTED_EDGE('',*,*,#7782,.F.);
#12168=ORIENTED_EDGE('',*,*,#7778,.F.);
#12169=ORIENTED_EDGE('',*,*,#7777,.F.);
#12170=ORIENTED_EDGE('',*,*,#7773,.F.);
#12171=ORIENTED_EDGE('',*,*,#7772,.F.);
#12172=ORIENTED_EDGE('',*,*,#7768,.F.);
#12173=ORIENTED_EDGE('',*,*,#7767,.F.);
#12174=ORIENTED_EDGE('',*,*,#7763,.F.);
#12175=ORIENTED_EDGE('',*,*,#7762,.F.);
#12176=ORIENTED_EDGE('',*,*,#7758,.F.);
#12177=ORIENTED_EDGE('',*,*,#7757,.F.);
#12178=ORIENTED_EDGE('',*,*,#7753,.F.);
#12179=ORIENTED_EDGE('',*,*,#7752,.F.);
#12180=ORIENTED_EDGE('',*,*,#7748,.F.);
#12181=ORIENTED_EDGE('',*,*,#7747,.F.);
#12182=ORIENTED_EDGE('',*,*,#7743,.F.);
#12183=ORIENTED_EDGE('',*,*,#7742,.F.);
#12184=ORIENTED_EDGE('',*,*,#7738,.F.);
#12185=ORIENTED_EDGE('',*,*,#7737,.F.);
#12186=ORIENTED_EDGE('',*,*,#7733,.F.);
#12187=ORIENTED_EDGE('',*,*,#7732,.F.);
#12188=ORIENTED_EDGE('',*,*,#7728,.F.);
#12189=ORIENTED_EDGE('',*,*,#7727,.F.);
#12190=ORIENTED_EDGE('',*,*,#7723,.F.);
#12191=ORIENTED_EDGE('',*,*,#7722,.F.);
#12192=ORIENTED_EDGE('',*,*,#7718,.F.);
#12193=ORIENTED_EDGE('',*,*,#7717,.F.);
#12194=ORIENTED_EDGE('',*,*,#7713,.F.);
#12195=ORIENTED_EDGE('',*,*,#7712,.F.);
#12196=ORIENTED_EDGE('',*,*,#7708,.F.);
#12197=ORIENTED_EDGE('',*,*,#7707,.F.);
#12198=ORIENTED_EDGE('',*,*,#7703,.F.);
#12199=ORIENTED_EDGE('',*,*,#7702,.F.);
#12200=ORIENTED_EDGE('',*,*,#7698,.F.);
#12201=ORIENTED_EDGE('',*,*,#7697,.F.);
#12202=ORIENTED_EDGE('',*,*,#7693,.F.);
#12203=ORIENTED_EDGE('',*,*,#7692,.F.);
#12204=ORIENTED_EDGE('',*,*,#7688,.F.);
#12205=ORIENTED_EDGE('',*,*,#7687,.F.);
#12206=ORIENTED_EDGE('',*,*,#7683,.F.);
#12207=ORIENTED_EDGE('',*,*,#7682,.F.);
#12208=ORIENTED_EDGE('',*,*,#7678,.F.);
#12209=ORIENTED_EDGE('',*,*,#7677,.F.);
#12210=ORIENTED_EDGE('',*,*,#7673,.F.);
#12211=ORIENTED_EDGE('',*,*,#7672,.F.);
#12212=ORIENTED_EDGE('',*,*,#7668,.F.);
#12213=ORIENTED_EDGE('',*,*,#7667,.F.);
#12214=ORIENTED_EDGE('',*,*,#7663,.F.);
#12215=ORIENTED_EDGE('',*,*,#7662,.F.);
#12216=ORIENTED_EDGE('',*,*,#7658,.F.);
#12217=ORIENTED_EDGE('',*,*,#7657,.F.);
#12218=ORIENTED_EDGE('',*,*,#7653,.F.);
#12219=ORIENTED_EDGE('',*,*,#7652,.F.);
#12220=ORIENTED_EDGE('',*,*,#7648,.F.);
#12221=ORIENTED_EDGE('',*,*,#7647,.F.);
#12222=ORIENTED_EDGE('',*,*,#7643,.F.);
#12223=ORIENTED_EDGE('',*,*,#7642,.F.);
#12224=ORIENTED_EDGE('',*,*,#7638,.F.);
#12225=ORIENTED_EDGE('',*,*,#7637,.F.);
#12226=ORIENTED_EDGE('',*,*,#7633,.F.);
#12227=ORIENTED_EDGE('',*,*,#7632,.F.);
#12228=ORIENTED_EDGE('',*,*,#7628,.F.);
#12229=ORIENTED_EDGE('',*,*,#7627,.F.);
#12230=ORIENTED_EDGE('',*,*,#7623,.F.);
#12231=ORIENTED_EDGE('',*,*,#7622,.F.);
#12232=ORIENTED_EDGE('',*,*,#7618,.F.);
#12233=ORIENTED_EDGE('',*,*,#7617,.F.);
#12234=ORIENTED_EDGE('',*,*,#7613,.F.);
#12235=ORIENTED_EDGE('',*,*,#7612,.F.);
#12236=ORIENTED_EDGE('',*,*,#7608,.F.);
#12237=ORIENTED_EDGE('',*,*,#7607,.F.);
#12238=ORIENTED_EDGE('',*,*,#7603,.F.);
#12239=ORIENTED_EDGE('',*,*,#7602,.F.);
#12240=ORIENTED_EDGE('',*,*,#7598,.F.);
#12241=ORIENTED_EDGE('',*,*,#7597,.F.);
#12242=ORIENTED_EDGE('',*,*,#7593,.F.);
#12243=ORIENTED_EDGE('',*,*,#7592,.F.);
#12244=ORIENTED_EDGE('',*,*,#7588,.F.);
#12245=ORIENTED_EDGE('',*,*,#7587,.F.);
#12246=ORIENTED_EDGE('',*,*,#7583,.F.);
#12247=ORIENTED_EDGE('',*,*,#7582,.F.);
#12248=ORIENTED_EDGE('',*,*,#7578,.F.);
#12249=ORIENTED_EDGE('',*,*,#7577,.F.);
#12250=ORIENTED_EDGE('',*,*,#7573,.F.);
#12251=ORIENTED_EDGE('',*,*,#7572,.F.);
#12252=ORIENTED_EDGE('',*,*,#7568,.F.);
#12253=ORIENTED_EDGE('',*,*,#7567,.F.);
#12254=ORIENTED_EDGE('',*,*,#7563,.F.);
#12255=ORIENTED_EDGE('',*,*,#7562,.F.);
#12256=ORIENTED_EDGE('',*,*,#7558,.F.);
#12257=ORIENTED_EDGE('',*,*,#7557,.F.);
#12258=ORIENTED_EDGE('',*,*,#7553,.F.);
#12259=ORIENTED_EDGE('',*,*,#7552,.F.);
#12260=ORIENTED_EDGE('',*,*,#7548,.F.);
#12261=ORIENTED_EDGE('',*,*,#7547,.F.);
#12262=ORIENTED_EDGE('',*,*,#7543,.F.);
#12263=ORIENTED_EDGE('',*,*,#7542,.F.);
#12264=ORIENTED_EDGE('',*,*,#7538,.F.);
#12265=ORIENTED_EDGE('',*,*,#7537,.F.);
#12266=ORIENTED_EDGE('',*,*,#7533,.F.);
#12267=ORIENTED_EDGE('',*,*,#7532,.F.);
#12268=ORIENTED_EDGE('',*,*,#7528,.F.);
#12269=ORIENTED_EDGE('',*,*,#7527,.F.);
#12270=ORIENTED_EDGE('',*,*,#7523,.F.);
#12271=ORIENTED_EDGE('',*,*,#7522,.F.);
#12272=ORIENTED_EDGE('',*,*,#7518,.F.);
#12273=ORIENTED_EDGE('',*,*,#7517,.F.);
#12274=ORIENTED_EDGE('',*,*,#7513,.F.);
#12275=ORIENTED_EDGE('',*,*,#7512,.F.);
#12276=ORIENTED_EDGE('',*,*,#7508,.F.);
#12277=ORIENTED_EDGE('',*,*,#7507,.F.);
#12278=ORIENTED_EDGE('',*,*,#7503,.F.);
#12279=ORIENTED_EDGE('',*,*,#7502,.F.);
#12280=ORIENTED_EDGE('',*,*,#7498,.F.);
#12281=ORIENTED_EDGE('',*,*,#7497,.F.);
#12282=ORIENTED_EDGE('',*,*,#7493,.F.);
#12283=ORIENTED_EDGE('',*,*,#7492,.F.);
#12284=ORIENTED_EDGE('',*,*,#7488,.F.);
#12285=ORIENTED_EDGE('',*,*,#7487,.F.);
#12286=ORIENTED_EDGE('',*,*,#7483,.F.);
#12287=ORIENTED_EDGE('',*,*,#7482,.F.);
#12288=ORIENTED_EDGE('',*,*,#7478,.F.);
#12289=ORIENTED_EDGE('',*,*,#7477,.F.);
#12290=ORIENTED_EDGE('',*,*,#7473,.F.);
#12291=ORIENTED_EDGE('',*,*,#7472,.F.);
#12292=ORIENTED_EDGE('',*,*,#7468,.F.);
#12293=ORIENTED_EDGE('',*,*,#7467,.F.);
#12294=ORIENTED_EDGE('',*,*,#7463,.F.);
#12295=ORIENTED_EDGE('',*,*,#7462,.F.);
#12296=ORIENTED_EDGE('',*,*,#7458,.F.);
#12297=ORIENTED_EDGE('',*,*,#7457,.F.);
#12298=ORIENTED_EDGE('',*,*,#7453,.F.);
#12299=ORIENTED_EDGE('',*,*,#7452,.F.);
#12300=ORIENTED_EDGE('',*,*,#7448,.F.);
#12301=ORIENTED_EDGE('',*,*,#7447,.F.);
#12302=ORIENTED_EDGE('',*,*,#7443,.F.);
#12303=ORIENTED_EDGE('',*,*,#7442,.F.);
#12304=ORIENTED_EDGE('',*,*,#7438,.F.);
#12305=ORIENTED_EDGE('',*,*,#7437,.F.);
#12306=ORIENTED_EDGE('',*,*,#7433,.F.);
#12307=ORIENTED_EDGE('',*,*,#7432,.F.);
#12308=ORIENTED_EDGE('',*,*,#7428,.F.);
#12309=ORIENTED_EDGE('',*,*,#7427,.F.);
#12310=ORIENTED_EDGE('',*,*,#7423,.F.);
#12311=ORIENTED_EDGE('',*,*,#7422,.F.);
#12312=ORIENTED_EDGE('',*,*,#7418,.F.);
#12313=ORIENTED_EDGE('',*,*,#7417,.F.);
#12314=ORIENTED_EDGE('',*,*,#7413,.F.);
#12315=ORIENTED_EDGE('',*,*,#7412,.F.);
#12316=ORIENTED_EDGE('',*,*,#7408,.F.);
#12317=ORIENTED_EDGE('',*,*,#7407,.F.);
#12318=ORIENTED_EDGE('',*,*,#7403,.F.);
#12319=ORIENTED_EDGE('',*,*,#7402,.F.);
#12320=ORIENTED_EDGE('',*,*,#7398,.F.);
#12321=ORIENTED_EDGE('',*,*,#7397,.F.);
#12322=ORIENTED_EDGE('',*,*,#7393,.F.);
#12323=ORIENTED_EDGE('',*,*,#7392,.F.);
#12324=ORIENTED_EDGE('',*,*,#7388,.F.);
#12325=ORIENTED_EDGE('',*,*,#7387,.F.);
#12326=ORIENTED_EDGE('',*,*,#7383,.F.);
#12327=ORIENTED_EDGE('',*,*,#7382,.F.);
#12328=ORIENTED_EDGE('',*,*,#7378,.F.);
#12329=ORIENTED_EDGE('',*,*,#7377,.F.);
#12330=ORIENTED_EDGE('',*,*,#7373,.F.);
#12331=ORIENTED_EDGE('',*,*,#7372,.F.);
#12332=ORIENTED_EDGE('',*,*,#7368,.F.);
#12333=ORIENTED_EDGE('',*,*,#7367,.F.);
#12334=ORIENTED_EDGE('',*,*,#7363,.F.);
#12335=ORIENTED_EDGE('',*,*,#7362,.F.);
#12336=ORIENTED_EDGE('',*,*,#7358,.F.);
#12337=ORIENTED_EDGE('',*,*,#7357,.F.);
#12338=ORIENTED_EDGE('',*,*,#7353,.F.);
#12339=ORIENTED_EDGE('',*,*,#7352,.F.);
#12340=ORIENTED_EDGE('',*,*,#7348,.F.);
#12341=ORIENTED_EDGE('',*,*,#7347,.F.);
#12342=ORIENTED_EDGE('',*,*,#7343,.F.);
#12343=ORIENTED_EDGE('',*,*,#7342,.F.);
#12344=ORIENTED_EDGE('',*,*,#7338,.F.);
#12345=ORIENTED_EDGE('',*,*,#7337,.F.);
#12346=ORIENTED_EDGE('',*,*,#7333,.F.);
#12347=ORIENTED_EDGE('',*,*,#7332,.F.);
#12348=ORIENTED_EDGE('',*,*,#7328,.F.);
#12349=ORIENTED_EDGE('',*,*,#7327,.F.);
#12350=ORIENTED_EDGE('',*,*,#7323,.F.);
#12351=ORIENTED_EDGE('',*,*,#7322,.F.);
#12352=ORIENTED_EDGE('',*,*,#7318,.F.);
#12353=ORIENTED_EDGE('',*,*,#7317,.F.);
#12354=ORIENTED_EDGE('',*,*,#7313,.F.);
#12355=ORIENTED_EDGE('',*,*,#7312,.F.);
#12356=ORIENTED_EDGE('',*,*,#7308,.F.);
#12357=ORIENTED_EDGE('',*,*,#7307,.F.);
#12358=ORIENTED_EDGE('',*,*,#7303,.F.);
#12359=ORIENTED_EDGE('',*,*,#7302,.F.);
#12360=ORIENTED_EDGE('',*,*,#7298,.F.);
#12361=ORIENTED_EDGE('',*,*,#7297,.F.);
#12362=ORIENTED_EDGE('',*,*,#7293,.F.);
#12363=ORIENTED_EDGE('',*,*,#7292,.F.);
#12364=ORIENTED_EDGE('',*,*,#7288,.F.);
#12365=ORIENTED_EDGE('',*,*,#7287,.F.);
#12366=ORIENTED_EDGE('',*,*,#7283,.F.);
#12367=ORIENTED_EDGE('',*,*,#7282,.F.);
#12368=ORIENTED_EDGE('',*,*,#7278,.F.);
#12369=ORIENTED_EDGE('',*,*,#7277,.F.);
#12370=ORIENTED_EDGE('',*,*,#7273,.F.);
#12371=ORIENTED_EDGE('',*,*,#7272,.F.);
#12372=ORIENTED_EDGE('',*,*,#7268,.F.);
#12373=ORIENTED_EDGE('',*,*,#7267,.F.);
#12374=ORIENTED_EDGE('',*,*,#7263,.F.);
#12375=ORIENTED_EDGE('',*,*,#7262,.F.);
#12376=ORIENTED_EDGE('',*,*,#7258,.F.);
#12377=ORIENTED_EDGE('',*,*,#7257,.F.);
#12378=ORIENTED_EDGE('',*,*,#7253,.F.);
#12379=ORIENTED_EDGE('',*,*,#7252,.F.);
#12380=ORIENTED_EDGE('',*,*,#7248,.F.);
#12381=ORIENTED_EDGE('',*,*,#7247,.F.);
#12382=ORIENTED_EDGE('',*,*,#7243,.F.);
#12383=ORIENTED_EDGE('',*,*,#7242,.F.);
#12384=ORIENTED_EDGE('',*,*,#7238,.F.);
#12385=ORIENTED_EDGE('',*,*,#7237,.F.);
#12386=ORIENTED_EDGE('',*,*,#7233,.F.);
#12387=ORIENTED_EDGE('',*,*,#7232,.F.);
#12388=ORIENTED_EDGE('',*,*,#7228,.F.);
#12389=ORIENTED_EDGE('',*,*,#7227,.F.);
#12390=ORIENTED_EDGE('',*,*,#7223,.F.);
#12391=ORIENTED_EDGE('',*,*,#7222,.F.);
#12392=ORIENTED_EDGE('',*,*,#7218,.F.);
#12393=ORIENTED_EDGE('',*,*,#7217,.F.);
#12394=ORIENTED_EDGE('',*,*,#7213,.F.);
#12395=ORIENTED_EDGE('',*,*,#7212,.F.);
#12396=ORIENTED_EDGE('',*,*,#7208,.F.);
#12397=ORIENTED_EDGE('',*,*,#7207,.F.);
#12398=ORIENTED_EDGE('',*,*,#7203,.F.);
#12399=ORIENTED_EDGE('',*,*,#7202,.F.);
#12400=ORIENTED_EDGE('',*,*,#7198,.F.);
#12401=ORIENTED_EDGE('',*,*,#7197,.F.);
#12402=ORIENTED_EDGE('',*,*,#7193,.F.);
#12403=ORIENTED_EDGE('',*,*,#7192,.F.);
#12404=ORIENTED_EDGE('',*,*,#7188,.F.);
#12405=ORIENTED_EDGE('',*,*,#7187,.F.);
#12406=ORIENTED_EDGE('',*,*,#7183,.F.);
#12407=ORIENTED_EDGE('',*,*,#7182,.F.);
#12408=ORIENTED_EDGE('',*,*,#7178,.F.);
#12409=ORIENTED_EDGE('',*,*,#7177,.F.);
#12410=ORIENTED_EDGE('',*,*,#7173,.F.);
#12411=ORIENTED_EDGE('',*,*,#7172,.F.);
#12412=ORIENTED_EDGE('',*,*,#7168,.F.);
#12413=ORIENTED_EDGE('',*,*,#7167,.F.);
#12414=ORIENTED_EDGE('',*,*,#7163,.F.);
#12415=ORIENTED_EDGE('',*,*,#7162,.F.);
#12416=ORIENTED_EDGE('',*,*,#7158,.F.);
#12417=ORIENTED_EDGE('',*,*,#7157,.F.);
#12418=ORIENTED_EDGE('',*,*,#7153,.F.);
#12419=ORIENTED_EDGE('',*,*,#7152,.F.);
#12420=ORIENTED_EDGE('',*,*,#7148,.F.);
#12421=ORIENTED_EDGE('',*,*,#7147,.F.);
#12422=ORIENTED_EDGE('',*,*,#7143,.F.);
#12423=ORIENTED_EDGE('',*,*,#7142,.F.);
#12424=ORIENTED_EDGE('',*,*,#7138,.F.);
#12425=ORIENTED_EDGE('',*,*,#7137,.F.);
#12426=ORIENTED_EDGE('',*,*,#7133,.F.);
#12427=ORIENTED_EDGE('',*,*,#7132,.F.);
#12428=ORIENTED_EDGE('',*,*,#7128,.F.);
#12429=ORIENTED_EDGE('',*,*,#7127,.F.);
#12430=ORIENTED_EDGE('',*,*,#7123,.F.);
#12431=ORIENTED_EDGE('',*,*,#7122,.F.);
#12432=ORIENTED_EDGE('',*,*,#7118,.F.);
#12433=ORIENTED_EDGE('',*,*,#7117,.F.);
#12434=ORIENTED_EDGE('',*,*,#7113,.F.);
#12435=ORIENTED_EDGE('',*,*,#7112,.F.);
#12436=ORIENTED_EDGE('',*,*,#7108,.F.);
#12437=ORIENTED_EDGE('',*,*,#7107,.F.);
#12438=ORIENTED_EDGE('',*,*,#7103,.F.);
#12439=ORIENTED_EDGE('',*,*,#7102,.F.);
#12440=ORIENTED_EDGE('',*,*,#7098,.F.);
#12441=ORIENTED_EDGE('',*,*,#7097,.F.);
#12442=ORIENTED_EDGE('',*,*,#7093,.F.);
#12443=ORIENTED_EDGE('',*,*,#7092,.F.);
#12444=ORIENTED_EDGE('',*,*,#7088,.F.);
#12445=ORIENTED_EDGE('',*,*,#7087,.F.);
#12446=ORIENTED_EDGE('',*,*,#7083,.F.);
#12447=ORIENTED_EDGE('',*,*,#7082,.F.);
#12448=ORIENTED_EDGE('',*,*,#7078,.F.);
#12449=ORIENTED_EDGE('',*,*,#7077,.F.);
#12450=ORIENTED_EDGE('',*,*,#7073,.F.);
#12451=ORIENTED_EDGE('',*,*,#7072,.F.);
#12452=ORIENTED_EDGE('',*,*,#7068,.F.);
#12453=ORIENTED_EDGE('',*,*,#7067,.F.);
#12454=ORIENTED_EDGE('',*,*,#7063,.F.);
#12455=ORIENTED_EDGE('',*,*,#7062,.F.);
#12456=ORIENTED_EDGE('',*,*,#7058,.F.);
#12457=ORIENTED_EDGE('',*,*,#7057,.F.);
#12458=ORIENTED_EDGE('',*,*,#7053,.F.);
#12459=ORIENTED_EDGE('',*,*,#7052,.F.);
#12460=ORIENTED_EDGE('',*,*,#7048,.F.);
#12461=ORIENTED_EDGE('',*,*,#7047,.F.);
#12462=ORIENTED_EDGE('',*,*,#7043,.F.);
#12463=ORIENTED_EDGE('',*,*,#7042,.F.);
#12464=ORIENTED_EDGE('',*,*,#7038,.F.);
#12465=ORIENTED_EDGE('',*,*,#7037,.F.);
#12466=ORIENTED_EDGE('',*,*,#7033,.F.);
#12467=ORIENTED_EDGE('',*,*,#7032,.F.);
#12468=ORIENTED_EDGE('',*,*,#7028,.F.);
#12469=ORIENTED_EDGE('',*,*,#7027,.F.);
#12470=ORIENTED_EDGE('',*,*,#7023,.F.);
#12471=ORIENTED_EDGE('',*,*,#7022,.F.);
#12472=ORIENTED_EDGE('',*,*,#7018,.F.);
#12473=ORIENTED_EDGE('',*,*,#7017,.F.);
#12474=ORIENTED_EDGE('',*,*,#7013,.F.);
#12475=ORIENTED_EDGE('',*,*,#7012,.F.);
#12476=ORIENTED_EDGE('',*,*,#7008,.F.);
#12477=ORIENTED_EDGE('',*,*,#7007,.F.);
#12478=ORIENTED_EDGE('',*,*,#7003,.F.);
#12479=ORIENTED_EDGE('',*,*,#7002,.F.);
#12480=ORIENTED_EDGE('',*,*,#6998,.F.);
#12481=ORIENTED_EDGE('',*,*,#6997,.F.);
#12482=ORIENTED_EDGE('',*,*,#6993,.F.);
#12483=ORIENTED_EDGE('',*,*,#6992,.F.);
#12484=ORIENTED_EDGE('',*,*,#6988,.F.);
#12485=ORIENTED_EDGE('',*,*,#6987,.F.);
#12486=ORIENTED_EDGE('',*,*,#6983,.F.);
#12487=ORIENTED_EDGE('',*,*,#6982,.F.);
#12488=ORIENTED_EDGE('',*,*,#6978,.F.);
#12489=ORIENTED_EDGE('',*,*,#6977,.F.);
#12490=ORIENTED_EDGE('',*,*,#6973,.F.);
#12491=ORIENTED_EDGE('',*,*,#6972,.F.);
#12492=ORIENTED_EDGE('',*,*,#6968,.F.);
#12493=ORIENTED_EDGE('',*,*,#6967,.F.);
#12494=ORIENTED_EDGE('',*,*,#6963,.F.);
#12495=ORIENTED_EDGE('',*,*,#6962,.F.);
#12496=ORIENTED_EDGE('',*,*,#6958,.F.);
#12497=ORIENTED_EDGE('',*,*,#6957,.F.);
#12498=ORIENTED_EDGE('',*,*,#6953,.F.);
#12499=ORIENTED_EDGE('',*,*,#6952,.F.);
#12500=ORIENTED_EDGE('',*,*,#6948,.F.);
#12501=ORIENTED_EDGE('',*,*,#6947,.F.);
#12502=ORIENTED_EDGE('',*,*,#6943,.F.);
#12503=ORIENTED_EDGE('',*,*,#6942,.F.);
#12504=ORIENTED_EDGE('',*,*,#6938,.F.);
#12505=ORIENTED_EDGE('',*,*,#6937,.F.);
#12506=ORIENTED_EDGE('',*,*,#6933,.F.);
#12507=ORIENTED_EDGE('',*,*,#6932,.F.);
#12508=ORIENTED_EDGE('',*,*,#6928,.F.);
#12509=ORIENTED_EDGE('',*,*,#6927,.F.);
#12510=ORIENTED_EDGE('',*,*,#6923,.F.);
#12511=ORIENTED_EDGE('',*,*,#6922,.F.);
#12512=ORIENTED_EDGE('',*,*,#6918,.F.);
#12513=ORIENTED_EDGE('',*,*,#6917,.F.);
#12514=ORIENTED_EDGE('',*,*,#6913,.F.);
#12515=ORIENTED_EDGE('',*,*,#6912,.F.);
#12516=ORIENTED_EDGE('',*,*,#6908,.F.);
#12517=ORIENTED_EDGE('',*,*,#6907,.F.);
#12518=ORIENTED_EDGE('',*,*,#6903,.F.);
#12519=ORIENTED_EDGE('',*,*,#6902,.F.);
#12520=ORIENTED_EDGE('',*,*,#6898,.F.);
#12521=ORIENTED_EDGE('',*,*,#6897,.F.);
#12522=ORIENTED_EDGE('',*,*,#6893,.F.);
#12523=ORIENTED_EDGE('',*,*,#6892,.F.);
#12524=ORIENTED_EDGE('',*,*,#6888,.F.);
#12525=ORIENTED_EDGE('',*,*,#6887,.F.);
#12526=ORIENTED_EDGE('',*,*,#6883,.F.);
#12527=ORIENTED_EDGE('',*,*,#6882,.F.);
#12528=ORIENTED_EDGE('',*,*,#6878,.F.);
#12529=ORIENTED_EDGE('',*,*,#6877,.F.);
#12530=ORIENTED_EDGE('',*,*,#6873,.F.);
#12531=ORIENTED_EDGE('',*,*,#6872,.F.);
#12532=ORIENTED_EDGE('',*,*,#6868,.F.);
#12533=ORIENTED_EDGE('',*,*,#6867,.F.);
#12534=ORIENTED_EDGE('',*,*,#6863,.F.);
#12535=ORIENTED_EDGE('',*,*,#6862,.F.);
#12536=ORIENTED_EDGE('',*,*,#6858,.F.);
#12537=ORIENTED_EDGE('',*,*,#6857,.F.);
#12538=ORIENTED_EDGE('',*,*,#6853,.F.);
#12539=ORIENTED_EDGE('',*,*,#6852,.F.);
#12540=ORIENTED_EDGE('',*,*,#6848,.F.);
#12541=ORIENTED_EDGE('',*,*,#6847,.F.);
#12542=ORIENTED_EDGE('',*,*,#6843,.F.);
#12543=ORIENTED_EDGE('',*,*,#6842,.F.);
#12544=ORIENTED_EDGE('',*,*,#6838,.F.);
#12545=ORIENTED_EDGE('',*,*,#6837,.F.);
#12546=ORIENTED_EDGE('',*,*,#6833,.F.);
#12547=ORIENTED_EDGE('',*,*,#6832,.F.);
#12548=ORIENTED_EDGE('',*,*,#6828,.F.);
#12549=ORIENTED_EDGE('',*,*,#6827,.F.);
#12550=ORIENTED_EDGE('',*,*,#6823,.F.);
#12551=ORIENTED_EDGE('',*,*,#6822,.F.);
#12552=ORIENTED_EDGE('',*,*,#6818,.F.);
#12553=ORIENTED_EDGE('',*,*,#6817,.F.);
#12554=ORIENTED_EDGE('',*,*,#6813,.F.);
#12555=ORIENTED_EDGE('',*,*,#6812,.F.);
#12556=ORIENTED_EDGE('',*,*,#6808,.F.);
#12557=ORIENTED_EDGE('',*,*,#6807,.F.);
#12558=ORIENTED_EDGE('',*,*,#6803,.F.);
#12559=ORIENTED_EDGE('',*,*,#6802,.F.);
#12560=ORIENTED_EDGE('',*,*,#6798,.F.);
#12561=ORIENTED_EDGE('',*,*,#6797,.F.);
#12562=ORIENTED_EDGE('',*,*,#6793,.F.);
#12563=ORIENTED_EDGE('',*,*,#6792,.F.);
#12564=ORIENTED_EDGE('',*,*,#6788,.F.);
#12565=ORIENTED_EDGE('',*,*,#6787,.F.);
#12566=ORIENTED_EDGE('',*,*,#6783,.F.);
#12567=ORIENTED_EDGE('',*,*,#6782,.F.);
#12568=ORIENTED_EDGE('',*,*,#6778,.F.);
#12569=ORIENTED_EDGE('',*,*,#6777,.F.);
#12570=ORIENTED_EDGE('',*,*,#6773,.F.);
#12571=ORIENTED_EDGE('',*,*,#6772,.F.);
#12572=ORIENTED_EDGE('',*,*,#6768,.F.);
#12573=ORIENTED_EDGE('',*,*,#6767,.F.);
#12574=ORIENTED_EDGE('',*,*,#6763,.F.);
#12575=ORIENTED_EDGE('',*,*,#6762,.F.);
#12576=ORIENTED_EDGE('',*,*,#6758,.F.);
#12577=ORIENTED_EDGE('',*,*,#6757,.F.);
#12578=ORIENTED_EDGE('',*,*,#6753,.F.);
#12579=ORIENTED_EDGE('',*,*,#6752,.F.);
#12580=ORIENTED_EDGE('',*,*,#6748,.F.);
#12581=ORIENTED_EDGE('',*,*,#6747,.F.);
#12582=ORIENTED_EDGE('',*,*,#6743,.F.);
#12583=ORIENTED_EDGE('',*,*,#6742,.F.);
#12584=ORIENTED_EDGE('',*,*,#6738,.F.);
#12585=ORIENTED_EDGE('',*,*,#6737,.F.);
#12586=ORIENTED_EDGE('',*,*,#6733,.F.);
#12587=ORIENTED_EDGE('',*,*,#6732,.F.);
#12588=ORIENTED_EDGE('',*,*,#6728,.F.);
#12589=ORIENTED_EDGE('',*,*,#6727,.F.);
#12590=ORIENTED_EDGE('',*,*,#6723,.F.);
#12591=ORIENTED_EDGE('',*,*,#6722,.F.);
#12592=ORIENTED_EDGE('',*,*,#6718,.F.);
#12593=ORIENTED_EDGE('',*,*,#6717,.F.);
#12594=ORIENTED_EDGE('',*,*,#6713,.F.);
#12595=ORIENTED_EDGE('',*,*,#6712,.F.);
#12596=ORIENTED_EDGE('',*,*,#6708,.F.);
#12597=ORIENTED_EDGE('',*,*,#6707,.F.);
#12598=ORIENTED_EDGE('',*,*,#6703,.F.);
#12599=ORIENTED_EDGE('',*,*,#6702,.F.);
#12600=ORIENTED_EDGE('',*,*,#6698,.F.);
#12601=ORIENTED_EDGE('',*,*,#6697,.F.);
#12602=ORIENTED_EDGE('',*,*,#6693,.F.);
#12603=ORIENTED_EDGE('',*,*,#6692,.F.);
#12604=ORIENTED_EDGE('',*,*,#6688,.F.);
#12605=ORIENTED_EDGE('',*,*,#6687,.F.);
#12606=ORIENTED_EDGE('',*,*,#6683,.F.);
#12607=ORIENTED_EDGE('',*,*,#6682,.F.);
#12608=ORIENTED_EDGE('',*,*,#6678,.F.);
#12609=ORIENTED_EDGE('',*,*,#6677,.F.);
#12610=ORIENTED_EDGE('',*,*,#6673,.F.);
#12611=ORIENTED_EDGE('',*,*,#6672,.F.);
#12612=ORIENTED_EDGE('',*,*,#6668,.F.);
#12613=ORIENTED_EDGE('',*,*,#6667,.F.);
#12614=ORIENTED_EDGE('',*,*,#6663,.F.);
#12615=ORIENTED_EDGE('',*,*,#6662,.F.);
#12616=ORIENTED_EDGE('',*,*,#6658,.F.);
#12617=ORIENTED_EDGE('',*,*,#6657,.F.);
#12618=ORIENTED_EDGE('',*,*,#6653,.F.);
#12619=ORIENTED_EDGE('',*,*,#6652,.F.);
#12620=ORIENTED_EDGE('',*,*,#6648,.F.);
#12621=ORIENTED_EDGE('',*,*,#6647,.F.);
#12622=ORIENTED_EDGE('',*,*,#6643,.F.);
#12623=ORIENTED_EDGE('',*,*,#6642,.F.);
#12624=ORIENTED_EDGE('',*,*,#6638,.F.);
#12625=ORIENTED_EDGE('',*,*,#6637,.F.);
#12626=ORIENTED_EDGE('',*,*,#6633,.F.);
#12627=ORIENTED_EDGE('',*,*,#6632,.F.);
#12628=ORIENTED_EDGE('',*,*,#6628,.F.);
#12629=ORIENTED_EDGE('',*,*,#6627,.F.);
#12630=ORIENTED_EDGE('',*,*,#6623,.F.);
#12631=ORIENTED_EDGE('',*,*,#6622,.F.);
#12632=ORIENTED_EDGE('',*,*,#6618,.F.);
#12633=ORIENTED_EDGE('',*,*,#6617,.F.);
#12634=ORIENTED_EDGE('',*,*,#6613,.F.);
#12635=ORIENTED_EDGE('',*,*,#6612,.F.);
#12636=ORIENTED_EDGE('',*,*,#6608,.F.);
#12637=ORIENTED_EDGE('',*,*,#6607,.F.);
#12638=ORIENTED_EDGE('',*,*,#6603,.F.);
#12639=ORIENTED_EDGE('',*,*,#6602,.F.);
#12640=ORIENTED_EDGE('',*,*,#6598,.F.);
#12641=ORIENTED_EDGE('',*,*,#6597,.F.);
#12642=ORIENTED_EDGE('',*,*,#6593,.F.);
#12643=ORIENTED_EDGE('',*,*,#6592,.F.);
#12644=ORIENTED_EDGE('',*,*,#6588,.F.);
#12645=ORIENTED_EDGE('',*,*,#6587,.F.);
#12646=ORIENTED_EDGE('',*,*,#6583,.F.);
#12647=ORIENTED_EDGE('',*,*,#6582,.F.);
#12648=ORIENTED_EDGE('',*,*,#6578,.F.);
#12649=ORIENTED_EDGE('',*,*,#6577,.F.);
#12650=ORIENTED_EDGE('',*,*,#6573,.F.);
#12651=ORIENTED_EDGE('',*,*,#6572,.F.);
#12652=ORIENTED_EDGE('',*,*,#6568,.F.);
#12653=ORIENTED_EDGE('',*,*,#6567,.F.);
#12654=ORIENTED_EDGE('',*,*,#6563,.F.);
#12655=ORIENTED_EDGE('',*,*,#6562,.F.);
#12656=ORIENTED_EDGE('',*,*,#6558,.F.);
#12657=ORIENTED_EDGE('',*,*,#6557,.F.);
#12658=ORIENTED_EDGE('',*,*,#6553,.F.);
#12659=ORIENTED_EDGE('',*,*,#6552,.F.);
#12660=ORIENTED_EDGE('',*,*,#6548,.F.);
#12661=ORIENTED_EDGE('',*,*,#6547,.F.);
#12662=ORIENTED_EDGE('',*,*,#6543,.F.);
#12663=ORIENTED_EDGE('',*,*,#6542,.F.);
#12664=ORIENTED_EDGE('',*,*,#6538,.F.);
#12665=ORIENTED_EDGE('',*,*,#6537,.F.);
#12666=ORIENTED_EDGE('',*,*,#6533,.F.);
#12667=ORIENTED_EDGE('',*,*,#6532,.F.);
#12668=ORIENTED_EDGE('',*,*,#6528,.F.);
#12669=ORIENTED_EDGE('',*,*,#6527,.F.);
#12670=ORIENTED_EDGE('',*,*,#6523,.F.);
#12671=ORIENTED_EDGE('',*,*,#6522,.F.);
#12672=ORIENTED_EDGE('',*,*,#6518,.F.);
#12673=ORIENTED_EDGE('',*,*,#6517,.F.);
#12674=ORIENTED_EDGE('',*,*,#6513,.F.);
#12675=ORIENTED_EDGE('',*,*,#6512,.F.);
#12676=ORIENTED_EDGE('',*,*,#6508,.F.);
#12677=ORIENTED_EDGE('',*,*,#6507,.F.);
#12678=ORIENTED_EDGE('',*,*,#6503,.F.);
#12679=ORIENTED_EDGE('',*,*,#6502,.F.);
#12680=ORIENTED_EDGE('',*,*,#6498,.F.);
#12681=ORIENTED_EDGE('',*,*,#8386,.F.);
#12682=ORIENTED_EDGE('',*,*,#7834,.F.);
#12683=ORIENTED_EDGE('',*,*,#8375,.F.);
#12684=ORIENTED_EDGE('',*,*,#8374,.F.);
#12685=ORIENTED_EDGE('',*,*,#8373,.F.);
#12686=ORIENTED_EDGE('',*,*,#8372,.F.);
#12687=ORIENTED_EDGE('',*,*,#8371,.F.);
#12688=ORIENTED_EDGE('',*,*,#8370,.F.);
#12689=ORIENTED_EDGE('',*,*,#8369,.F.);
#12690=ORIENTED_EDGE('',*,*,#8368,.F.);
#12691=ORIENTED_EDGE('',*,*,#8367,.F.);
#12692=ORIENTED_EDGE('',*,*,#8366,.F.);
#12693=ORIENTED_EDGE('',*,*,#8365,.F.);
#12694=ORIENTED_EDGE('',*,*,#8364,.F.);
#12695=ORIENTED_EDGE('',*,*,#8363,.F.);
#12696=ORIENTED_EDGE('',*,*,#8362,.F.);
#12697=ORIENTED_EDGE('',*,*,#8361,.F.);
#12698=ORIENTED_EDGE('',*,*,#8360,.F.);
#12699=ORIENTED_EDGE('',*,*,#8359,.F.);
#12700=ORIENTED_EDGE('',*,*,#8358,.F.);
#12701=ORIENTED_EDGE('',*,*,#8357,.F.);
#12702=ORIENTED_EDGE('',*,*,#8356,.F.);
#12703=ORIENTED_EDGE('',*,*,#8355,.F.);
#12704=ORIENTED_EDGE('',*,*,#8354,.F.);
#12705=ORIENTED_EDGE('',*,*,#8353,.F.);
#12706=ORIENTED_EDGE('',*,*,#8352,.F.);
#12707=ORIENTED_EDGE('',*,*,#8351,.F.);
#12708=ORIENTED_EDGE('',*,*,#8350,.F.);
#12709=ORIENTED_EDGE('',*,*,#8349,.F.);
#12710=ORIENTED_EDGE('',*,*,#8348,.F.);
#12711=ORIENTED_EDGE('',*,*,#8347,.F.);
#12712=ORIENTED_EDGE('',*,*,#8346,.F.);
#12713=ORIENTED_EDGE('',*,*,#8345,.F.);
#12714=ORIENTED_EDGE('',*,*,#8344,.F.);
#12715=ORIENTED_EDGE('',*,*,#8343,.F.);
#12716=ORIENTED_EDGE('',*,*,#8342,.F.);
#12717=ORIENTED_EDGE('',*,*,#8341,.F.);
#12718=ORIENTED_EDGE('',*,*,#8340,.F.);
#12719=ORIENTED_EDGE('',*,*,#8339,.F.);
#12720=ORIENTED_EDGE('',*,*,#8338,.F.);
#12721=ORIENTED_EDGE('',*,*,#8337,.F.);
#12722=ORIENTED_EDGE('',*,*,#8336,.F.);
#12723=ORIENTED_EDGE('',*,*,#8335,.F.);
#12724=ORIENTED_EDGE('',*,*,#8334,.F.);
#12725=ORIENTED_EDGE('',*,*,#8333,.F.);
#12726=ORIENTED_EDGE('',*,*,#8332,.F.);
#12727=ORIENTED_EDGE('',*,*,#8331,.F.);
#12728=ORIENTED_EDGE('',*,*,#8330,.F.);
#12729=ORIENTED_EDGE('',*,*,#8329,.F.);
#12730=ORIENTED_EDGE('',*,*,#8328,.F.);
#12731=ORIENTED_EDGE('',*,*,#8327,.F.);
#12732=ORIENTED_EDGE('',*,*,#8326,.F.);
#12733=ORIENTED_EDGE('',*,*,#8325,.F.);
#12734=ORIENTED_EDGE('',*,*,#8324,.F.);
#12735=ORIENTED_EDGE('',*,*,#8323,.F.);
#12736=ORIENTED_EDGE('',*,*,#8322,.F.);
#12737=ORIENTED_EDGE('',*,*,#8321,.F.);
#12738=ORIENTED_EDGE('',*,*,#8320,.F.);
#12739=ORIENTED_EDGE('',*,*,#8319,.F.);
#12740=ORIENTED_EDGE('',*,*,#8318,.F.);
#12741=ORIENTED_EDGE('',*,*,#8317,.F.);
#12742=ORIENTED_EDGE('',*,*,#8316,.F.);
#12743=ORIENTED_EDGE('',*,*,#8315,.F.);
#12744=ORIENTED_EDGE('',*,*,#8314,.F.);
#12745=ORIENTED_EDGE('',*,*,#8313,.F.);
#12746=ORIENTED_EDGE('',*,*,#8312,.F.);
#12747=ORIENTED_EDGE('',*,*,#8311,.F.);
#12748=ORIENTED_EDGE('',*,*,#8310,.F.);
#12749=ORIENTED_EDGE('',*,*,#8309,.F.);
#12750=ORIENTED_EDGE('',*,*,#8308,.F.);
#12751=ORIENTED_EDGE('',*,*,#8307,.F.);
#12752=ORIENTED_EDGE('',*,*,#8306,.F.);
#12753=ORIENTED_EDGE('',*,*,#8305,.F.);
#12754=ORIENTED_EDGE('',*,*,#8304,.F.);
#12755=ORIENTED_EDGE('',*,*,#8303,.F.);
#12756=ORIENTED_EDGE('',*,*,#8302,.F.);
#12757=ORIENTED_EDGE('',*,*,#8301,.F.);
#12758=ORIENTED_EDGE('',*,*,#8300,.F.);
#12759=ORIENTED_EDGE('',*,*,#8299,.F.);
#12760=ORIENTED_EDGE('',*,*,#8298,.F.);
#12761=ORIENTED_EDGE('',*,*,#8297,.F.);
#12762=ORIENTED_EDGE('',*,*,#8296,.F.);
#12763=ORIENTED_EDGE('',*,*,#8295,.F.);
#12764=ORIENTED_EDGE('',*,*,#8294,.F.);
#12765=ORIENTED_EDGE('',*,*,#8293,.F.);
#12766=ORIENTED_EDGE('',*,*,#8292,.F.);
#12767=ORIENTED_EDGE('',*,*,#8291,.F.);
#12768=ORIENTED_EDGE('',*,*,#8290,.F.);
#12769=ORIENTED_EDGE('',*,*,#8289,.F.);
#12770=ORIENTED_EDGE('',*,*,#8288,.F.);
#12771=ORIENTED_EDGE('',*,*,#8287,.F.);
#12772=ORIENTED_EDGE('',*,*,#8286,.F.);
#12773=ORIENTED_EDGE('',*,*,#8285,.F.);
#12774=ORIENTED_EDGE('',*,*,#8284,.F.);
#12775=ORIENTED_EDGE('',*,*,#8283,.F.);
#12776=ORIENTED_EDGE('',*,*,#8282,.F.);
#12777=ORIENTED_EDGE('',*,*,#8281,.F.);
#12778=ORIENTED_EDGE('',*,*,#8280,.F.);
#12779=ORIENTED_EDGE('',*,*,#8279,.F.);
#12780=ORIENTED_EDGE('',*,*,#8278,.F.);
#12781=ORIENTED_EDGE('',*,*,#8277,.F.);
#12782=ORIENTED_EDGE('',*,*,#8276,.F.);
#12783=ORIENTED_EDGE('',*,*,#8275,.F.);
#12784=ORIENTED_EDGE('',*,*,#8274,.F.);
#12785=ORIENTED_EDGE('',*,*,#8273,.F.);
#12786=ORIENTED_EDGE('',*,*,#8272,.F.);
#12787=ORIENTED_EDGE('',*,*,#8271,.F.);
#12788=ORIENTED_EDGE('',*,*,#8270,.F.);
#12789=ORIENTED_EDGE('',*,*,#8269,.F.);
#12790=ORIENTED_EDGE('',*,*,#8268,.F.);
#12791=ORIENTED_EDGE('',*,*,#8267,.F.);
#12792=ORIENTED_EDGE('',*,*,#8266,.F.);
#12793=ORIENTED_EDGE('',*,*,#8265,.F.);
#12794=ORIENTED_EDGE('',*,*,#8264,.F.);
#12795=ORIENTED_EDGE('',*,*,#8263,.F.);
#12796=ORIENTED_EDGE('',*,*,#8262,.F.);
#12797=ORIENTED_EDGE('',*,*,#8261,.F.);
#12798=ORIENTED_EDGE('',*,*,#8260,.F.);
#12799=ORIENTED_EDGE('',*,*,#8259,.F.);
#12800=ORIENTED_EDGE('',*,*,#8258,.F.);
#12801=ORIENTED_EDGE('',*,*,#8257,.F.);
#12802=ORIENTED_EDGE('',*,*,#8256,.F.);
#12803=ORIENTED_EDGE('',*,*,#8255,.F.);
#12804=ORIENTED_EDGE('',*,*,#8254,.F.);
#12805=ORIENTED_EDGE('',*,*,#8253,.F.);
#12806=ORIENTED_EDGE('',*,*,#8252,.F.);
#12807=ORIENTED_EDGE('',*,*,#8251,.F.);
#12808=ORIENTED_EDGE('',*,*,#8250,.F.);
#12809=ORIENTED_EDGE('',*,*,#8249,.F.);
#12810=ORIENTED_EDGE('',*,*,#8248,.F.);
#12811=ORIENTED_EDGE('',*,*,#8247,.F.);
#12812=ORIENTED_EDGE('',*,*,#8246,.F.);
#12813=ORIENTED_EDGE('',*,*,#8245,.F.);
#12814=ORIENTED_EDGE('',*,*,#8244,.F.);
#12815=ORIENTED_EDGE('',*,*,#8243,.F.);
#12816=ORIENTED_EDGE('',*,*,#8242,.F.);
#12817=ORIENTED_EDGE('',*,*,#8241,.F.);
#12818=ORIENTED_EDGE('',*,*,#8240,.F.);
#12819=ORIENTED_EDGE('',*,*,#8239,.F.);
#12820=ORIENTED_EDGE('',*,*,#8238,.F.);
#12821=ORIENTED_EDGE('',*,*,#8237,.F.);
#12822=ORIENTED_EDGE('',*,*,#8236,.F.);
#12823=ORIENTED_EDGE('',*,*,#8235,.F.);
#12824=ORIENTED_EDGE('',*,*,#8234,.F.);
#12825=ORIENTED_EDGE('',*,*,#8233,.F.);
#12826=ORIENTED_EDGE('',*,*,#8232,.F.);
#12827=ORIENTED_EDGE('',*,*,#8231,.F.);
#12828=ORIENTED_EDGE('',*,*,#8230,.F.);
#12829=ORIENTED_EDGE('',*,*,#8229,.F.);
#12830=ORIENTED_EDGE('',*,*,#8228,.F.);
#12831=ORIENTED_EDGE('',*,*,#8227,.F.);
#12832=ORIENTED_EDGE('',*,*,#8226,.F.);
#12833=ORIENTED_EDGE('',*,*,#8225,.F.);
#12834=ORIENTED_EDGE('',*,*,#8224,.F.);
#12835=ORIENTED_EDGE('',*,*,#8223,.F.);
#12836=ORIENTED_EDGE('',*,*,#8222,.F.);
#12837=ORIENTED_EDGE('',*,*,#8221,.F.);
#12838=ORIENTED_EDGE('',*,*,#8220,.F.);
#12839=ORIENTED_EDGE('',*,*,#8219,.F.);
#12840=ORIENTED_EDGE('',*,*,#8218,.F.);
#12841=ORIENTED_EDGE('',*,*,#8217,.F.);
#12842=ORIENTED_EDGE('',*,*,#8216,.F.);
#12843=ORIENTED_EDGE('',*,*,#8215,.F.);
#12844=ORIENTED_EDGE('',*,*,#8214,.F.);
#12845=ORIENTED_EDGE('',*,*,#8213,.F.);
#12846=ORIENTED_EDGE('',*,*,#8212,.F.);
#12847=ORIENTED_EDGE('',*,*,#8211,.F.);
#12848=ORIENTED_EDGE('',*,*,#8210,.F.);
#12849=ORIENTED_EDGE('',*,*,#8209,.F.);
#12850=ORIENTED_EDGE('',*,*,#8208,.F.);
#12851=ORIENTED_EDGE('',*,*,#8207,.F.);
#12852=ORIENTED_EDGE('',*,*,#8206,.F.);
#12853=ORIENTED_EDGE('',*,*,#8205,.F.);
#12854=ORIENTED_EDGE('',*,*,#8204,.F.);
#12855=ORIENTED_EDGE('',*,*,#8203,.F.);
#12856=ORIENTED_EDGE('',*,*,#8202,.F.);
#12857=ORIENTED_EDGE('',*,*,#8201,.F.);
#12858=ORIENTED_EDGE('',*,*,#8200,.F.);
#12859=ORIENTED_EDGE('',*,*,#8199,.F.);
#12860=ORIENTED_EDGE('',*,*,#8198,.F.);
#12861=ORIENTED_EDGE('',*,*,#8197,.F.);
#12862=ORIENTED_EDGE('',*,*,#8196,.F.);
#12863=ORIENTED_EDGE('',*,*,#8195,.F.);
#12864=ORIENTED_EDGE('',*,*,#8194,.F.);
#12865=ORIENTED_EDGE('',*,*,#8193,.F.);
#12866=ORIENTED_EDGE('',*,*,#8192,.F.);
#12867=ORIENTED_EDGE('',*,*,#8191,.F.);
#12868=ORIENTED_EDGE('',*,*,#8190,.F.);
#12869=ORIENTED_EDGE('',*,*,#8189,.F.);
#12870=ORIENTED_EDGE('',*,*,#8188,.F.);
#12871=ORIENTED_EDGE('',*,*,#8187,.F.);
#12872=ORIENTED_EDGE('',*,*,#8186,.F.);
#12873=ORIENTED_EDGE('',*,*,#8185,.F.);
#12874=ORIENTED_EDGE('',*,*,#8184,.F.);
#12875=ORIENTED_EDGE('',*,*,#8183,.F.);
#12876=ORIENTED_EDGE('',*,*,#8182,.F.);
#12877=ORIENTED_EDGE('',*,*,#8181,.F.);
#12878=ORIENTED_EDGE('',*,*,#8180,.F.);
#12879=ORIENTED_EDGE('',*,*,#8179,.F.);
#12880=ORIENTED_EDGE('',*,*,#8178,.F.);
#12881=ORIENTED_EDGE('',*,*,#8177,.F.);
#12882=ORIENTED_EDGE('',*,*,#8176,.F.);
#12883=ORIENTED_EDGE('',*,*,#8175,.F.);
#12884=ORIENTED_EDGE('',*,*,#8174,.F.);
#12885=ORIENTED_EDGE('',*,*,#8173,.F.);
#12886=ORIENTED_EDGE('',*,*,#8172,.F.);
#12887=ORIENTED_EDGE('',*,*,#8171,.F.);
#12888=ORIENTED_EDGE('',*,*,#8170,.F.);
#12889=ORIENTED_EDGE('',*,*,#8169,.F.);
#12890=ORIENTED_EDGE('',*,*,#8168,.F.);
#12891=ORIENTED_EDGE('',*,*,#8167,.F.);
#12892=ORIENTED_EDGE('',*,*,#8166,.F.);
#12893=ORIENTED_EDGE('',*,*,#8165,.F.);
#12894=ORIENTED_EDGE('',*,*,#8164,.F.);
#12895=ORIENTED_EDGE('',*,*,#8163,.F.);
#12896=ORIENTED_EDGE('',*,*,#8162,.F.);
#12897=ORIENTED_EDGE('',*,*,#8161,.F.);
#12898=ORIENTED_EDGE('',*,*,#8160,.F.);
#12899=ORIENTED_EDGE('',*,*,#8159,.F.);
#12900=ORIENTED_EDGE('',*,*,#8158,.F.);
#12901=ORIENTED_EDGE('',*,*,#8157,.F.);
#12902=ORIENTED_EDGE('',*,*,#8156,.F.);
#12903=ORIENTED_EDGE('',*,*,#8155,.F.);
#12904=ORIENTED_EDGE('',*,*,#8154,.F.);
#12905=ORIENTED_EDGE('',*,*,#8153,.F.);
#12906=ORIENTED_EDGE('',*,*,#8152,.F.);
#12907=ORIENTED_EDGE('',*,*,#8151,.F.);
#12908=ORIENTED_EDGE('',*,*,#8150,.F.);
#12909=ORIENTED_EDGE('',*,*,#8149,.F.);
#12910=ORIENTED_EDGE('',*,*,#8148,.F.);
#12911=ORIENTED_EDGE('',*,*,#8147,.F.);
#12912=ORIENTED_EDGE('',*,*,#8146,.F.);
#12913=ORIENTED_EDGE('',*,*,#8145,.F.);
#12914=ORIENTED_EDGE('',*,*,#8144,.F.);
#12915=ORIENTED_EDGE('',*,*,#8143,.F.);
#12916=ORIENTED_EDGE('',*,*,#8142,.F.);
#12917=ORIENTED_EDGE('',*,*,#8141,.F.);
#12918=ORIENTED_EDGE('',*,*,#8140,.F.);
#12919=ORIENTED_EDGE('',*,*,#8139,.F.);
#12920=ORIENTED_EDGE('',*,*,#8138,.F.);
#12921=ORIENTED_EDGE('',*,*,#8137,.F.);
#12922=ORIENTED_EDGE('',*,*,#8136,.F.);
#12923=ORIENTED_EDGE('',*,*,#8135,.F.);
#12924=ORIENTED_EDGE('',*,*,#8134,.F.);
#12925=ORIENTED_EDGE('',*,*,#8133,.F.);
#12926=ORIENTED_EDGE('',*,*,#8132,.F.);
#12927=ORIENTED_EDGE('',*,*,#8131,.F.);
#12928=ORIENTED_EDGE('',*,*,#8130,.F.);
#12929=ORIENTED_EDGE('',*,*,#8129,.F.);
#12930=ORIENTED_EDGE('',*,*,#8128,.F.);
#12931=ORIENTED_EDGE('',*,*,#8127,.F.);
#12932=ORIENTED_EDGE('',*,*,#8126,.F.);
#12933=ORIENTED_EDGE('',*,*,#8125,.F.);
#12934=ORIENTED_EDGE('',*,*,#8124,.F.);
#12935=ORIENTED_EDGE('',*,*,#8123,.F.);
#12936=ORIENTED_EDGE('',*,*,#8122,.F.);
#12937=ORIENTED_EDGE('',*,*,#8121,.F.);
#12938=ORIENTED_EDGE('',*,*,#8120,.F.);
#12939=ORIENTED_EDGE('',*,*,#8119,.F.);
#12940=ORIENTED_EDGE('',*,*,#8118,.F.);
#12941=ORIENTED_EDGE('',*,*,#8117,.F.);
#12942=ORIENTED_EDGE('',*,*,#8116,.F.);
#12943=ORIENTED_EDGE('',*,*,#8115,.F.);
#12944=ORIENTED_EDGE('',*,*,#8114,.F.);
#12945=ORIENTED_EDGE('',*,*,#8113,.F.);
#12946=ORIENTED_EDGE('',*,*,#8112,.F.);
#12947=ORIENTED_EDGE('',*,*,#8111,.F.);
#12948=ORIENTED_EDGE('',*,*,#8110,.F.);
#12949=ORIENTED_EDGE('',*,*,#8109,.F.);
#12950=ORIENTED_EDGE('',*,*,#8108,.F.);
#12951=ORIENTED_EDGE('',*,*,#8107,.F.);
#12952=ORIENTED_EDGE('',*,*,#8401,.T.);
#12953=ORIENTED_EDGE('',*,*,#8378,.T.);
#12954=ORIENTED_EDGE('',*,*,#8402,.T.);
#12955=ORIENTED_EDGE('',*,*,#8106,.T.);
#12956=ORIENTED_EDGE('',*,*,#8403,.T.);
#12957=ORIENTED_EDGE('',*,*,#8404,.T.);
#12958=ORIENTED_EDGE('',*,*,#8405,.F.);
#12959=ORIENTED_EDGE('',*,*,#8406,.F.);
#12960=ORIENTED_EDGE('',*,*,#8407,.F.);
#12961=ORIENTED_EDGE('',*,*,#8408,.F.);
#12962=ORIENTED_EDGE('',*,*,#8409,.F.);
#12963=ORIENTED_EDGE('',*,*,#8404,.F.);
#12964=ORIENTED_EDGE('',*,*,#8410,.T.);
#12965=ORIENTED_EDGE('',*,*,#8411,.F.);
#12966=ORIENTED_EDGE('',*,*,#8412,.F.);
#12967=ORIENTED_EDGE('',*,*,#8413,.F.);
#12968=ORIENTED_EDGE('',*,*,#8414,.F.);
#12969=ORIENTED_EDGE('',*,*,#8415,.F.);
#12970=ORIENTED_EDGE('',*,*,#8416,.F.);
#12971=ORIENTED_EDGE('',*,*,#8417,.F.);
#12972=ORIENTED_EDGE('',*,*,#8418,.F.);
#12973=ORIENTED_EDGE('',*,*,#8419,.T.);
#12974=ORIENTED_EDGE('',*,*,#8420,.F.);
#12975=ORIENTED_EDGE('',*,*,#8421,.F.);
#12976=ORIENTED_EDGE('',*,*,#8422,.T.);
#12977=ORIENTED_EDGE('',*,*,#8423,.F.);
#12978=ORIENTED_EDGE('',*,*,#8424,.F.);
#12979=ORIENTED_EDGE('',*,*,#8419,.F.);
#12980=ORIENTED_EDGE('',*,*,#8411,.T.);
#12981=ORIENTED_EDGE('',*,*,#8425,.T.);
#12982=ORIENTED_EDGE('',*,*,#8413,.T.);
#12983=ORIENTED_EDGE('',*,*,#8426,.F.);
#12984=ORIENTED_EDGE('',*,*,#8422,.F.);
#12985=ORIENTED_EDGE('',*,*,#8427,.F.);
#12986=ORIENTED_EDGE('',*,*,#8428,.F.);
#12987=ORIENTED_EDGE('',*,*,#8429,.F.);
#12988=ORIENTED_EDGE('',*,*,#8430,.F.);
#12989=ORIENTED_EDGE('',*,*,#8431,.F.);
#12990=ORIENTED_EDGE('',*,*,#8425,.F.);
#12991=ORIENTED_EDGE('',*,*,#8410,.F.);
#12992=ORIENTED_EDGE('',*,*,#8403,.F.);
#12993=ORIENTED_EDGE('',*,*,#8420,.T.);
#12994=ORIENTED_EDGE('',*,*,#8424,.T.);
#12995=ORIENTED_EDGE('',*,*,#8432,.T.);
#12996=ORIENTED_EDGE('',*,*,#8433,.T.);
#12997=ORIENTED_EDGE('',*,*,#8434,.T.);
#12998=ORIENTED_EDGE('',*,*,#8435,.T.);
#12999=ORIENTED_EDGE('',*,*,#8436,.T.);
#13000=ORIENTED_EDGE('',*,*,#8431,.T.);
#13001=ORIENTED_EDGE('',*,*,#8437,.T.);
#13002=ORIENTED_EDGE('',*,*,#8436,.F.);
#13003=ORIENTED_EDGE('',*,*,#8437,.F.);
#13004=ORIENTED_EDGE('',*,*,#8428,.T.);
#13005=ORIENTED_EDGE('',*,*,#8438,.T.);
#13006=ORIENTED_EDGE('',*,*,#8434,.F.);
#13007=ORIENTED_EDGE('',*,*,#8439,.F.);
#13008=ORIENTED_EDGE('',*,*,#8429,.T.);
#13009=ORIENTED_EDGE('',*,*,#8439,.T.);
#13010=ORIENTED_EDGE('',*,*,#8433,.F.);
#13011=ORIENTED_EDGE('',*,*,#8440,.F.);
#13012=ORIENTED_EDGE('',*,*,#8423,.T.);
#13013=ORIENTED_EDGE('',*,*,#8430,.T.);
#13014=ORIENTED_EDGE('',*,*,#8440,.T.);
#13015=ORIENTED_EDGE('',*,*,#8432,.F.);
#13016=ORIENTED_EDGE('',*,*,#8421,.T.);
#13017=ORIENTED_EDGE('',*,*,#8435,.F.);
#13018=ORIENTED_EDGE('',*,*,#8438,.F.);
#13019=ORIENTED_EDGE('',*,*,#8427,.T.);
#13020=ORIENTED_EDGE('',*,*,#8412,.T.);
#13021=ORIENTED_EDGE('',*,*,#8426,.T.);
#13022=ORIENTED_EDGE('',*,*,#8408,.T.);
#13023=ORIENTED_EDGE('',*,*,#8441,.T.);
#13024=ORIENTED_EDGE('',*,*,#8406,.T.);
#13025=ORIENTED_EDGE('',*,*,#8442,.F.);
#13026=ORIENTED_EDGE('',*,*,#8415,.T.);
#13027=ORIENTED_EDGE('',*,*,#8443,.T.);
#13028=ORIENTED_EDGE('',*,*,#8444,.F.);
#13029=ORIENTED_EDGE('',*,*,#8445,.F.);
#13030=ORIENTED_EDGE('',*,*,#8414,.T.);
#13031=ORIENTED_EDGE('',*,*,#8418,.T.);
#13032=ORIENTED_EDGE('',*,*,#8446,.F.);
#13033=ORIENTED_EDGE('',*,*,#8447,.F.);
#13034=ORIENTED_EDGE('',*,*,#8448,.F.);
#13035=ORIENTED_EDGE('',*,*,#8443,.F.);
#13036=ORIENTED_EDGE('',*,*,#8449,.F.);
#13037=ORIENTED_EDGE('',*,*,#8407,.T.);
#13038=ORIENTED_EDGE('',*,*,#8441,.F.);
#13039=ORIENTED_EDGE('',*,*,#8449,.T.);
#13040=ORIENTED_EDGE('',*,*,#8450,.T.);
#13041=ORIENTED_EDGE('',*,*,#8451,.F.);
#13042=ORIENTED_EDGE('',*,*,#8450,.F.);
#13043=ORIENTED_EDGE('',*,*,#8452,.F.);
#13044=ORIENTED_EDGE('',*,*,#8453,.T.);
#13045=ORIENTED_EDGE('',*,*,#8447,.T.);
#13046=ORIENTED_EDGE('',*,*,#8454,.F.);
#13047=ORIENTED_EDGE('',*,*,#8455,.F.);
#13048=ORIENTED_EDGE('',*,*,#8444,.T.);
#13049=ORIENTED_EDGE('',*,*,#8448,.T.);
#13050=ORIENTED_EDGE('',*,*,#8453,.F.);
#13051=ORIENTED_EDGE('',*,*,#8417,.T.);
#13052=ORIENTED_EDGE('',*,*,#8456,.F.);
#13053=ORIENTED_EDGE('',*,*,#8454,.T.);
#13054=ORIENTED_EDGE('',*,*,#8446,.T.);
#13055=ORIENTED_EDGE('',*,*,#8445,.T.);
#13056=ORIENTED_EDGE('',*,*,#8455,.T.);
#13057=ORIENTED_EDGE('',*,*,#8452,.T.);
#13058=ORIENTED_EDGE('',*,*,#8456,.T.);
#13059=ORIENTED_EDGE('',*,*,#8416,.T.);
#13060=ORIENTED_EDGE('',*,*,#8451,.T.);
#13061=ORIENTED_EDGE('',*,*,#8442,.T.);
#13062=ORIENTED_EDGE('',*,*,#8405,.T.);
#13063=ORIENTED_EDGE('',*,*,#8409,.T.);
#13064=ORIENTED_EDGE('',*,*,#8457,.T.);
#13065=ORIENTED_EDGE('',*,*,#8458,.T.);
#13066=ORIENTED_EDGE('',*,*,#8459,.T.);
#13067=ORIENTED_EDGE('',*,*,#8460,.F.);
#13068=ORIENTED_EDGE('',*,*,#8461,.F.);
#13069=ORIENTED_EDGE('',*,*,#8462,.F.);
#13070=ORIENTED_EDGE('',*,*,#8463,.T.);
#13071=ORIENTED_EDGE('',*,*,#8464,.T.);
#13072=ORIENTED_EDGE('',*,*,#8465,.T.);
#13073=ORIENTED_EDGE('',*,*,#8457,.F.);
#13074=ORIENTED_EDGE('',*,*,#8466,.F.);
#13075=ORIENTED_EDGE('',*,*,#8467,.F.);
#13076=ORIENTED_EDGE('',*,*,#8468,.T.);
#13077=ORIENTED_EDGE('',*,*,#8469,.T.);
#13078=ORIENTED_EDGE('',*,*,#8470,.T.);
#13079=ORIENTED_EDGE('',*,*,#8463,.F.);
#13080=ORIENTED_EDGE('',*,*,#8471,.F.);
#13081=ORIENTED_EDGE('',*,*,#8472,.F.);
#13082=ORIENTED_EDGE('',*,*,#8473,.T.);
#13083=ORIENTED_EDGE('',*,*,#8474,.T.);
#13084=ORIENTED_EDGE('',*,*,#8475,.T.);
#13085=ORIENTED_EDGE('',*,*,#8468,.F.);
#13086=ORIENTED_EDGE('',*,*,#8476,.F.);
#13087=ORIENTED_EDGE('',*,*,#8477,.F.);
#13088=ORIENTED_EDGE('',*,*,#8478,.T.);
#13089=ORIENTED_EDGE('',*,*,#8479,.T.);
#13090=ORIENTED_EDGE('',*,*,#8480,.T.);
#13091=ORIENTED_EDGE('',*,*,#8473,.F.);
#13092=ORIENTED_EDGE('',*,*,#8481,.F.);
#13093=ORIENTED_EDGE('',*,*,#8482,.F.);
#13094=ORIENTED_EDGE('',*,*,#8483,.T.);
#13095=ORIENTED_EDGE('',*,*,#8484,.T.);
#13096=ORIENTED_EDGE('',*,*,#8485,.T.);
#13097=ORIENTED_EDGE('',*,*,#8478,.F.);
#13098=ORIENTED_EDGE('',*,*,#8486,.F.);
#13099=ORIENTED_EDGE('',*,*,#8487,.F.);
#13100=ORIENTED_EDGE('',*,*,#8488,.T.);
#13101=ORIENTED_EDGE('',*,*,#8489,.T.);
#13102=ORIENTED_EDGE('',*,*,#8490,.T.);
#13103=ORIENTED_EDGE('',*,*,#8483,.F.);
#13104=ORIENTED_EDGE('',*,*,#8491,.F.);
#13105=ORIENTED_EDGE('',*,*,#8492,.F.);
#13106=ORIENTED_EDGE('',*,*,#8493,.T.);
#13107=ORIENTED_EDGE('',*,*,#8494,.T.);
#13108=ORIENTED_EDGE('',*,*,#8495,.T.);
#13109=ORIENTED_EDGE('',*,*,#8488,.F.);
#13110=ORIENTED_EDGE('',*,*,#8496,.F.);
#13111=ORIENTED_EDGE('',*,*,#8497,.F.);
#13112=ORIENTED_EDGE('',*,*,#8498,.T.);
#13113=ORIENTED_EDGE('',*,*,#8499,.T.);
#13114=ORIENTED_EDGE('',*,*,#8500,.T.);
#13115=ORIENTED_EDGE('',*,*,#8493,.F.);
#13116=ORIENTED_EDGE('',*,*,#8501,.F.);
#13117=ORIENTED_EDGE('',*,*,#8502,.F.);
#13118=ORIENTED_EDGE('',*,*,#8503,.T.);
#13119=ORIENTED_EDGE('',*,*,#8504,.T.);
#13120=ORIENTED_EDGE('',*,*,#8505,.T.);
#13121=ORIENTED_EDGE('',*,*,#8498,.F.);
#13122=ORIENTED_EDGE('',*,*,#8506,.F.);
#13123=ORIENTED_EDGE('',*,*,#8507,.F.);
#13124=ORIENTED_EDGE('',*,*,#8508,.T.);
#13125=ORIENTED_EDGE('',*,*,#8509,.T.);
#13126=ORIENTED_EDGE('',*,*,#8510,.T.);
#13127=ORIENTED_EDGE('',*,*,#8503,.F.);
#13128=ORIENTED_EDGE('',*,*,#8511,.F.);
#13129=ORIENTED_EDGE('',*,*,#8512,.F.);
#13130=ORIENTED_EDGE('',*,*,#8513,.T.);
#13131=ORIENTED_EDGE('',*,*,#8514,.T.);
#13132=ORIENTED_EDGE('',*,*,#8515,.T.);
#13133=ORIENTED_EDGE('',*,*,#8508,.F.);
#13134=ORIENTED_EDGE('',*,*,#8516,.F.);
#13135=ORIENTED_EDGE('',*,*,#8517,.F.);
#13136=ORIENTED_EDGE('',*,*,#8518,.T.);
#13137=ORIENTED_EDGE('',*,*,#8519,.T.);
#13138=ORIENTED_EDGE('',*,*,#8520,.T.);
#13139=ORIENTED_EDGE('',*,*,#8513,.F.);
#13140=ORIENTED_EDGE('',*,*,#8521,.F.);
#13141=ORIENTED_EDGE('',*,*,#8522,.F.);
#13142=ORIENTED_EDGE('',*,*,#8523,.T.);
#13143=ORIENTED_EDGE('',*,*,#8524,.T.);
#13144=ORIENTED_EDGE('',*,*,#8525,.T.);
#13145=ORIENTED_EDGE('',*,*,#8518,.F.);
#13146=ORIENTED_EDGE('',*,*,#8526,.F.);
#13147=ORIENTED_EDGE('',*,*,#8527,.F.);
#13148=ORIENTED_EDGE('',*,*,#8528,.T.);
#13149=ORIENTED_EDGE('',*,*,#8529,.T.);
#13150=ORIENTED_EDGE('',*,*,#8530,.T.);
#13151=ORIENTED_EDGE('',*,*,#8523,.F.);
#13152=ORIENTED_EDGE('',*,*,#8531,.F.);
#13153=ORIENTED_EDGE('',*,*,#8532,.F.);
#13154=ORIENTED_EDGE('',*,*,#8533,.T.);
#13155=ORIENTED_EDGE('',*,*,#8534,.T.);
#13156=ORIENTED_EDGE('',*,*,#8535,.T.);
#13157=ORIENTED_EDGE('',*,*,#8528,.F.);
#13158=ORIENTED_EDGE('',*,*,#8536,.F.);
#13159=ORIENTED_EDGE('',*,*,#8537,.F.);
#13160=ORIENTED_EDGE('',*,*,#8538,.F.);
#13161=ORIENTED_EDGE('',*,*,#8539,.F.);
#13162=ORIENTED_EDGE('',*,*,#8540,.F.);
#13163=ORIENTED_EDGE('',*,*,#8541,.T.);
#13164=ORIENTED_EDGE('',*,*,#8542,.F.);
#13165=ORIENTED_EDGE('',*,*,#8543,.T.);
#13166=ORIENTED_EDGE('',*,*,#8544,.T.);
#13167=ORIENTED_EDGE('',*,*,#8545,.T.);
#13168=ORIENTED_EDGE('',*,*,#8546,.T.);
#13169=ORIENTED_EDGE('',*,*,#8547,.T.);
#13170=ORIENTED_EDGE('',*,*,#8548,.T.);
#13171=ORIENTED_EDGE('',*,*,#8549,.T.);
#13172=ORIENTED_EDGE('',*,*,#8550,.T.);
#13173=ORIENTED_EDGE('',*,*,#8551,.T.);
#13174=ORIENTED_EDGE('',*,*,#8552,.T.);
#13175=ORIENTED_EDGE('',*,*,#8553,.T.);
#13176=ORIENTED_EDGE('',*,*,#8554,.T.);
#13177=ORIENTED_EDGE('',*,*,#8555,.T.);
#13178=ORIENTED_EDGE('',*,*,#8556,.T.);
#13179=ORIENTED_EDGE('',*,*,#8557,.T.);
#13180=ORIENTED_EDGE('',*,*,#8558,.T.);
#13181=ORIENTED_EDGE('',*,*,#8559,.T.);
#13182=ORIENTED_EDGE('',*,*,#8560,.F.);
#13183=ORIENTED_EDGE('',*,*,#8561,.T.);
#13184=ORIENTED_EDGE('',*,*,#8562,.T.);
#13185=ORIENTED_EDGE('',*,*,#8563,.F.);
#13186=ORIENTED_EDGE('',*,*,#8539,.T.);
#13187=ORIENTED_EDGE('',*,*,#8564,.T.);
#13188=ORIENTED_EDGE('',*,*,#8565,.T.);
#13189=ORIENTED_EDGE('',*,*,#8537,.T.);
#13190=ORIENTED_EDGE('',*,*,#8536,.T.);
#13191=ORIENTED_EDGE('',*,*,#8532,.T.);
#13192=ORIENTED_EDGE('',*,*,#8531,.T.);
#13193=ORIENTED_EDGE('',*,*,#8527,.T.);
#13194=ORIENTED_EDGE('',*,*,#8526,.T.);
#13195=ORIENTED_EDGE('',*,*,#8522,.T.);
#13196=ORIENTED_EDGE('',*,*,#8521,.T.);
#13197=ORIENTED_EDGE('',*,*,#8517,.T.);
#13198=ORIENTED_EDGE('',*,*,#8516,.T.);
#13199=ORIENTED_EDGE('',*,*,#8512,.T.);
#13200=ORIENTED_EDGE('',*,*,#8511,.T.);
#13201=ORIENTED_EDGE('',*,*,#8507,.T.);
#13202=ORIENTED_EDGE('',*,*,#8506,.T.);
#13203=ORIENTED_EDGE('',*,*,#8502,.T.);
#13204=ORIENTED_EDGE('',*,*,#8501,.T.);
#13205=ORIENTED_EDGE('',*,*,#8497,.T.);
#13206=ORIENTED_EDGE('',*,*,#8496,.T.);
#13207=ORIENTED_EDGE('',*,*,#8492,.T.);
#13208=ORIENTED_EDGE('',*,*,#8491,.T.);
#13209=ORIENTED_EDGE('',*,*,#8487,.T.);
#13210=ORIENTED_EDGE('',*,*,#8486,.T.);
#13211=ORIENTED_EDGE('',*,*,#8482,.T.);
#13212=ORIENTED_EDGE('',*,*,#8481,.T.);
#13213=ORIENTED_EDGE('',*,*,#8477,.T.);
#13214=ORIENTED_EDGE('',*,*,#8476,.T.);
#13215=ORIENTED_EDGE('',*,*,#8472,.T.);
#13216=ORIENTED_EDGE('',*,*,#8471,.T.);
#13217=ORIENTED_EDGE('',*,*,#8467,.T.);
#13218=ORIENTED_EDGE('',*,*,#8466,.T.);
#13219=ORIENTED_EDGE('',*,*,#8462,.T.);
#13220=ORIENTED_EDGE('',*,*,#8461,.T.);
#13221=ORIENTED_EDGE('',*,*,#8566,.F.);
#13222=ORIENTED_EDGE('',*,*,#8567,.T.);
#13223=ORIENTED_EDGE('',*,*,#8568,.T.);
#13224=ORIENTED_EDGE('',*,*,#8569,.F.);
#13225=ORIENTED_EDGE('',*,*,#8570,.F.);
#13226=ORIENTED_EDGE('',*,*,#8571,.F.);
#13227=ORIENTED_EDGE('',*,*,#8572,.F.);
#13228=ORIENTED_EDGE('',*,*,#8573,.F.);
#13229=ORIENTED_EDGE('',*,*,#8574,.F.);
#13230=ORIENTED_EDGE('',*,*,#8575,.F.);
#13231=ORIENTED_EDGE('',*,*,#8576,.F.);
#13232=ORIENTED_EDGE('',*,*,#8577,.F.);
#13233=ORIENTED_EDGE('',*,*,#8578,.F.);
#13234=ORIENTED_EDGE('',*,*,#8579,.F.);
#13235=ORIENTED_EDGE('',*,*,#8580,.F.);
#13236=ORIENTED_EDGE('',*,*,#8581,.F.);
#13237=ORIENTED_EDGE('',*,*,#8582,.F.);
#13238=ORIENTED_EDGE('',*,*,#8583,.F.);
#13239=ORIENTED_EDGE('',*,*,#8584,.F.);
#13240=ORIENTED_EDGE('',*,*,#8585,.F.);
#13241=ORIENTED_EDGE('',*,*,#8586,.F.);
#13242=ORIENTED_EDGE('',*,*,#8587,.F.);
#13243=ORIENTED_EDGE('',*,*,#8588,.F.);
#13244=ORIENTED_EDGE('',*,*,#8559,.F.);
#13245=ORIENTED_EDGE('',*,*,#8558,.F.);
#13246=ORIENTED_EDGE('',*,*,#8557,.F.);
#13247=ORIENTED_EDGE('',*,*,#8556,.F.);
#13248=ORIENTED_EDGE('',*,*,#8555,.F.);
#13249=ORIENTED_EDGE('',*,*,#8554,.F.);
#13250=ORIENTED_EDGE('',*,*,#8553,.F.);
#13251=ORIENTED_EDGE('',*,*,#8552,.F.);
#13252=ORIENTED_EDGE('',*,*,#8551,.F.);
#13253=ORIENTED_EDGE('',*,*,#8550,.F.);
#13254=ORIENTED_EDGE('',*,*,#8549,.F.);
#13255=ORIENTED_EDGE('',*,*,#8548,.F.);
#13256=ORIENTED_EDGE('',*,*,#8547,.F.);
#13257=ORIENTED_EDGE('',*,*,#8546,.F.);
#13258=ORIENTED_EDGE('',*,*,#8545,.F.);
#13259=ORIENTED_EDGE('',*,*,#8544,.F.);
#13260=ORIENTED_EDGE('',*,*,#8543,.F.);
#13261=ORIENTED_EDGE('',*,*,#8589,.F.);
#13262=ORIENTED_EDGE('',*,*,#8562,.F.);
#13263=ORIENTED_EDGE('',*,*,#8561,.F.);
#13264=ORIENTED_EDGE('',*,*,#8590,.F.);
#13265=ORIENTED_EDGE('',*,*,#8591,.F.);
#13266=ORIENTED_EDGE('',*,*,#8592,.F.);
#13267=ORIENTED_EDGE('',*,*,#8593,.F.);
#13268=ORIENTED_EDGE('',*,*,#8592,.T.);
#13269=ORIENTED_EDGE('',*,*,#8591,.T.);
#13270=ORIENTED_EDGE('',*,*,#8594,.F.);
#13271=ORIENTED_EDGE('',*,*,#8595,.F.);
#13272=ORIENTED_EDGE('',*,*,#8596,.T.);
#13273=ORIENTED_EDGE('',*,*,#8597,.F.);
#13274=ORIENTED_EDGE('',*,*,#8598,.F.);
#13275=ORIENTED_EDGE('',*,*,#8599,.F.);
#13276=ORIENTED_EDGE('',*,*,#8600,.F.);
#13277=ORIENTED_EDGE('',*,*,#8568,.F.);
#13278=ORIENTED_EDGE('',*,*,#8567,.F.);
#13279=ORIENTED_EDGE('',*,*,#8538,.T.);
#13280=ORIENTED_EDGE('',*,*,#8601,.T.);
#13281=ORIENTED_EDGE('',*,*,#8602,.T.);
#13282=ORIENTED_EDGE('',*,*,#8533,.F.);
#13283=ORIENTED_EDGE('',*,*,#8565,.F.);
#13284=ORIENTED_EDGE('',*,*,#8564,.F.);
#13285=ORIENTED_EDGE('',*,*,#8603,.F.);
#13286=ORIENTED_EDGE('',*,*,#8459,.F.);
#13287=ORIENTED_EDGE('',*,*,#8458,.F.);
#13288=ORIENTED_EDGE('',*,*,#8465,.F.);
#13289=ORIENTED_EDGE('',*,*,#8464,.F.);
#13290=ORIENTED_EDGE('',*,*,#8470,.F.);
#13291=ORIENTED_EDGE('',*,*,#8469,.F.);
#13292=ORIENTED_EDGE('',*,*,#8475,.F.);
#13293=ORIENTED_EDGE('',*,*,#8474,.F.);
#13294=ORIENTED_EDGE('',*,*,#8480,.F.);
#13295=ORIENTED_EDGE('',*,*,#8479,.F.);
#13296=ORIENTED_EDGE('',*,*,#8485,.F.);
#13297=ORIENTED_EDGE('',*,*,#8484,.F.);
#13298=ORIENTED_EDGE('',*,*,#8490,.F.);
#13299=ORIENTED_EDGE('',*,*,#8489,.F.);
#13300=ORIENTED_EDGE('',*,*,#8495,.F.);
#13301=ORIENTED_EDGE('',*,*,#8494,.F.);
#13302=ORIENTED_EDGE('',*,*,#8500,.F.);
#13303=ORIENTED_EDGE('',*,*,#8499,.F.);
#13304=ORIENTED_EDGE('',*,*,#8505,.F.);
#13305=ORIENTED_EDGE('',*,*,#8504,.F.);
#13306=ORIENTED_EDGE('',*,*,#8510,.F.);
#13307=ORIENTED_EDGE('',*,*,#8509,.F.);
#13308=ORIENTED_EDGE('',*,*,#8515,.F.);
#13309=ORIENTED_EDGE('',*,*,#8514,.F.);
#13310=ORIENTED_EDGE('',*,*,#8520,.F.);
#13311=ORIENTED_EDGE('',*,*,#8519,.F.);
#13312=ORIENTED_EDGE('',*,*,#8525,.F.);
#13313=ORIENTED_EDGE('',*,*,#8524,.F.);
#13314=ORIENTED_EDGE('',*,*,#8530,.F.);
#13315=ORIENTED_EDGE('',*,*,#8529,.F.);
#13316=ORIENTED_EDGE('',*,*,#8535,.F.);
#13317=ORIENTED_EDGE('',*,*,#8534,.F.);
#13318=ORIENTED_EDGE('',*,*,#8602,.F.);
#13319=ORIENTED_EDGE('',*,*,#8601,.F.);
#13320=ORIENTED_EDGE('',*,*,#8541,.F.);
#13321=ORIENTED_EDGE('',*,*,#8604,.F.);
#13322=ORIENTED_EDGE('',*,*,#8596,.F.);
#13323=ORIENTED_EDGE('',*,*,#8605,.F.);
#13324=ORIENTED_EDGE('',*,*,#8587,.T.);
#13325=ORIENTED_EDGE('',*,*,#8586,.T.);
#13326=ORIENTED_EDGE('',*,*,#8585,.T.);
#13327=ORIENTED_EDGE('',*,*,#8584,.T.);
#13328=ORIENTED_EDGE('',*,*,#8583,.T.);
#13329=ORIENTED_EDGE('',*,*,#8582,.T.);
#13330=ORIENTED_EDGE('',*,*,#8581,.T.);
#13331=ORIENTED_EDGE('',*,*,#8580,.T.);
#13332=ORIENTED_EDGE('',*,*,#8579,.T.);
#13333=ORIENTED_EDGE('',*,*,#8578,.T.);
#13334=ORIENTED_EDGE('',*,*,#8577,.T.);
#13335=ORIENTED_EDGE('',*,*,#8576,.T.);
#13336=ORIENTED_EDGE('',*,*,#8575,.T.);
#13337=ORIENTED_EDGE('',*,*,#8574,.T.);
#13338=ORIENTED_EDGE('',*,*,#8573,.T.);
#13339=ORIENTED_EDGE('',*,*,#8572,.T.);
#13340=ORIENTED_EDGE('',*,*,#8571,.T.);
#13341=ORIENTED_EDGE('',*,*,#8606,.F.);
#13342=ORIENTED_EDGE('',*,*,#8599,.T.);
#13343=ORIENTED_EDGE('',*,*,#8598,.T.);
#13344=ORIENTED_EDGE('',*,*,#8607,.F.);
#13345=ORIENTED_EDGE('',*,*,#8608,.F.);
#13346=ORIENTED_EDGE('',*,*,#8609,.T.);
#13347=ORIENTED_EDGE('',*,*,#8569,.T.);
#13348=ORIENTED_EDGE('',*,*,#8600,.T.);
#13349=ORIENTED_EDGE('',*,*,#8606,.T.);
#13350=ORIENTED_EDGE('',*,*,#8570,.T.);
#13351=ORIENTED_EDGE('',*,*,#8542,.T.);
#13352=ORIENTED_EDGE('',*,*,#8460,.T.);
#13353=ORIENTED_EDGE('',*,*,#8603,.T.);
#13354=ORIENTED_EDGE('',*,*,#8610,.T.);
#13355=ORIENTED_EDGE('',*,*,#8611,.T.);
#13356=ORIENTED_EDGE('',*,*,#8610,.F.);
#13357=ORIENTED_EDGE('',*,*,#8607,.T.);
#13358=ORIENTED_EDGE('',*,*,#8597,.T.);
#13359=ORIENTED_EDGE('',*,*,#8566,.T.);
#13360=ORIENTED_EDGE('',*,*,#8609,.F.);
#13361=ORIENTED_EDGE('',*,*,#8595,.T.);
#13362=ORIENTED_EDGE('',*,*,#8594,.T.);
#13363=ORIENTED_EDGE('',*,*,#8604,.T.);
#13364=ORIENTED_EDGE('',*,*,#8540,.T.);
#13365=ORIENTED_EDGE('',*,*,#8563,.T.);
#13366=ORIENTED_EDGE('',*,*,#8589,.T.);
#13367=ORIENTED_EDGE('',*,*,#8593,.T.);
#13368=ORIENTED_EDGE('',*,*,#8590,.T.);
#13369=ORIENTED_EDGE('',*,*,#8560,.T.);
#13370=ORIENTED_EDGE('',*,*,#8588,.T.);
#13371=ORIENTED_EDGE('',*,*,#8605,.T.);
#13372=ORIENTED_EDGE('',*,*,#8608,.T.);
#13373=ORIENTED_EDGE('',*,*,#8611,.F.);
#13374=ORIENTED_EDGE('',*,*,#8612,.T.);
#13375=ORIENTED_EDGE('',*,*,#8613,.T.);
#13376=ORIENTED_EDGE('',*,*,#8614,.F.);
#13377=ORIENTED_EDGE('',*,*,#8613,.F.);
#13378=ORIENTED_EDGE('',*,*,#8615,.F.);
#13379=ORIENTED_EDGE('',*,*,#8616,.T.);
#13380=ORIENTED_EDGE('',*,*,#8617,.T.);
#13381=ORIENTED_EDGE('',*,*,#8618,.F.);
#13382=ORIENTED_EDGE('',*,*,#8619,.F.);
#13383=ORIENTED_EDGE('',*,*,#8620,.T.);
#13384=ORIENTED_EDGE('',*,*,#8621,.T.);
#13385=ORIENTED_EDGE('',*,*,#8616,.F.);
#13386=ORIENTED_EDGE('',*,*,#8622,.F.);
#13387=ORIENTED_EDGE('',*,*,#8623,.T.);
#13388=ORIENTED_EDGE('',*,*,#8624,.T.);
#13389=ORIENTED_EDGE('',*,*,#8620,.F.);
#13390=ORIENTED_EDGE('',*,*,#8625,.T.);
#13391=ORIENTED_EDGE('',*,*,#8617,.F.);
#13392=ORIENTED_EDGE('',*,*,#8621,.F.);
#13393=ORIENTED_EDGE('',*,*,#8624,.F.);
#13394=ORIENTED_EDGE('',*,*,#8612,.F.);
#13395=ORIENTED_EDGE('',*,*,#8626,.T.);
#13396=ORIENTED_EDGE('',*,*,#8622,.T.);
#13397=ORIENTED_EDGE('',*,*,#8619,.T.);
#13398=ORIENTED_EDGE('',*,*,#8615,.T.);
#13399=ORIENTED_EDGE('',*,*,#8614,.T.);
#13400=ORIENTED_EDGE('',*,*,#8627,.T.);
#13401=ORIENTED_EDGE('',*,*,#8628,.T.);
#13402=ORIENTED_EDGE('',*,*,#8629,.T.);
#13403=ORIENTED_EDGE('',*,*,#8627,.F.);
#13404=ORIENTED_EDGE('',*,*,#8629,.F.);
#13405=ORIENTED_EDGE('',*,*,#8630,.T.);
#13406=ORIENTED_EDGE('',*,*,#8631,.T.);
#13407=ORIENTED_EDGE('',*,*,#8632,.F.);
#13408=ORIENTED_EDGE('',*,*,#8631,.F.);
#13409=ORIENTED_EDGE('',*,*,#8633,.T.);
#13410=ORIENTED_EDGE('',*,*,#8634,.T.);
#13411=ORIENTED_EDGE('',*,*,#8635,.F.);
#13412=ORIENTED_EDGE('',*,*,#8636,.F.);
#13413=ORIENTED_EDGE('',*,*,#8637,.T.);
#13414=ORIENTED_EDGE('',*,*,#8636,.T.);
#13415=ORIENTED_EDGE('',*,*,#8638,.F.);
#13416=ORIENTED_EDGE('',*,*,#8639,.F.);
#13417=ORIENTED_EDGE('',*,*,#8640,.T.);
#13418=ORIENTED_EDGE('',*,*,#8639,.T.);
#13419=ORIENTED_EDGE('',*,*,#8641,.F.);
#13420=ORIENTED_EDGE('',*,*,#8642,.F.);
#13421=ORIENTED_EDGE('',*,*,#8623,.F.);
#13422=ORIENTED_EDGE('',*,*,#8626,.F.);
#13423=ORIENTED_EDGE('',*,*,#8618,.T.);
#13424=ORIENTED_EDGE('',*,*,#8625,.F.);
#13425=ORIENTED_EDGE('',*,*,#8643,.T.);
#13426=ORIENTED_EDGE('',*,*,#8644,.F.);
#13427=ORIENTED_EDGE('',*,*,#8634,.F.);
#13428=ORIENTED_EDGE('',*,*,#8645,.T.);
#13429=ORIENTED_EDGE('',*,*,#8642,.T.);
#13430=ORIENTED_EDGE('',*,*,#8643,.F.);
#13431=ORIENTED_EDGE('',*,*,#8644,.T.);
#13432=ORIENTED_EDGE('',*,*,#8641,.T.);
#13433=ORIENTED_EDGE('',*,*,#8638,.T.);
#13434=ORIENTED_EDGE('',*,*,#8635,.T.);
#13435=ORIENTED_EDGE('',*,*,#8632,.T.);
#13436=ORIENTED_EDGE('',*,*,#8645,.F.);
#13437=ORIENTED_EDGE('',*,*,#8633,.F.);
#13438=ORIENTED_EDGE('',*,*,#8637,.F.);
#13439=ORIENTED_EDGE('',*,*,#8640,.F.);
#13440=ORIENTED_EDGE('',*,*,#8630,.F.);
#13441=ORIENTED_EDGE('',*,*,#8628,.F.);
#13442=ORIENTED_EDGE('',*,*,#8646,.T.);
#13443=ORIENTED_EDGE('',*,*,#8647,.T.);
#13444=ORIENTED_EDGE('',*,*,#8648,.F.);
#13445=ORIENTED_EDGE('',*,*,#8649,.F.);
#13446=ORIENTED_EDGE('',*,*,#8650,.F.);
#13447=ORIENTED_EDGE('',*,*,#8651,.F.);
#13448=ORIENTED_EDGE('',*,*,#8652,.F.);
#13449=ORIENTED_EDGE('',*,*,#8647,.F.);
#13450=ORIENTED_EDGE('',*,*,#8653,.T.);
#13451=ORIENTED_EDGE('',*,*,#8654,.F.);
#13452=ORIENTED_EDGE('',*,*,#8655,.F.);
#13453=ORIENTED_EDGE('',*,*,#8656,.F.);
#13454=ORIENTED_EDGE('',*,*,#8657,.F.);
#13455=ORIENTED_EDGE('',*,*,#8658,.F.);
#13456=ORIENTED_EDGE('',*,*,#8659,.F.);
#13457=ORIENTED_EDGE('',*,*,#8660,.F.);
#13458=ORIENTED_EDGE('',*,*,#8661,.F.);
#13459=ORIENTED_EDGE('',*,*,#8662,.T.);
#13460=ORIENTED_EDGE('',*,*,#8663,.F.);
#13461=ORIENTED_EDGE('',*,*,#8664,.F.);
#13462=ORIENTED_EDGE('',*,*,#8665,.T.);
#13463=ORIENTED_EDGE('',*,*,#8666,.F.);
#13464=ORIENTED_EDGE('',*,*,#8667,.F.);
#13465=ORIENTED_EDGE('',*,*,#8662,.F.);
#13466=ORIENTED_EDGE('',*,*,#8651,.T.);
#13467=ORIENTED_EDGE('',*,*,#8668,.T.);
#13468=ORIENTED_EDGE('',*,*,#8649,.T.);
#13469=ORIENTED_EDGE('',*,*,#8669,.F.);
#13470=ORIENTED_EDGE('',*,*,#8658,.T.);
#13471=ORIENTED_EDGE('',*,*,#8670,.T.);
#13472=ORIENTED_EDGE('',*,*,#8671,.F.);
#13473=ORIENTED_EDGE('',*,*,#8672,.F.);
#13474=ORIENTED_EDGE('',*,*,#8657,.T.);
#13475=ORIENTED_EDGE('',*,*,#8661,.T.);
#13476=ORIENTED_EDGE('',*,*,#8673,.F.);
#13477=ORIENTED_EDGE('',*,*,#8674,.F.);
#13478=ORIENTED_EDGE('',*,*,#8675,.F.);
#13479=ORIENTED_EDGE('',*,*,#8670,.F.);
#13480=ORIENTED_EDGE('',*,*,#8676,.F.);
#13481=ORIENTED_EDGE('',*,*,#8650,.T.);
#13482=ORIENTED_EDGE('',*,*,#8668,.F.);
#13483=ORIENTED_EDGE('',*,*,#8676,.T.);
#13484=ORIENTED_EDGE('',*,*,#8677,.T.);
#13485=ORIENTED_EDGE('',*,*,#8678,.F.);
#13486=ORIENTED_EDGE('',*,*,#8677,.F.);
#13487=ORIENTED_EDGE('',*,*,#8679,.F.);
#13488=ORIENTED_EDGE('',*,*,#8680,.T.);
#13489=ORIENTED_EDGE('',*,*,#8674,.T.);
#13490=ORIENTED_EDGE('',*,*,#8681,.F.);
#13491=ORIENTED_EDGE('',*,*,#8682,.F.);
#13492=ORIENTED_EDGE('',*,*,#8671,.T.);
#13493=ORIENTED_EDGE('',*,*,#8675,.T.);
#13494=ORIENTED_EDGE('',*,*,#8680,.F.);
#13495=ORIENTED_EDGE('',*,*,#8660,.T.);
#13496=ORIENTED_EDGE('',*,*,#8683,.F.);
#13497=ORIENTED_EDGE('',*,*,#8681,.T.);
#13498=ORIENTED_EDGE('',*,*,#8673,.T.);
#13499=ORIENTED_EDGE('',*,*,#8672,.T.);
#13500=ORIENTED_EDGE('',*,*,#8682,.T.);
#13501=ORIENTED_EDGE('',*,*,#8679,.T.);
#13502=ORIENTED_EDGE('',*,*,#8683,.T.);
#13503=ORIENTED_EDGE('',*,*,#8659,.T.);
#13504=ORIENTED_EDGE('',*,*,#8678,.T.);
#13505=ORIENTED_EDGE('',*,*,#8669,.T.);
#13506=ORIENTED_EDGE('',*,*,#8648,.T.);
#13507=ORIENTED_EDGE('',*,*,#8652,.T.);
#13508=ORIENTED_EDGE('',*,*,#8654,.T.);
#13509=ORIENTED_EDGE('',*,*,#8684,.T.);
#13510=ORIENTED_EDGE('',*,*,#8656,.T.);
#13511=ORIENTED_EDGE('',*,*,#8685,.F.);
#13512=ORIENTED_EDGE('',*,*,#8665,.F.);
#13513=ORIENTED_EDGE('',*,*,#8686,.F.);
#13514=ORIENTED_EDGE('',*,*,#8687,.F.);
#13515=ORIENTED_EDGE('',*,*,#8688,.F.);
#13516=ORIENTED_EDGE('',*,*,#8689,.F.);
#13517=ORIENTED_EDGE('',*,*,#8690,.F.);
#13518=ORIENTED_EDGE('',*,*,#8684,.F.);
#13519=ORIENTED_EDGE('',*,*,#8653,.F.);
#13520=ORIENTED_EDGE('',*,*,#8646,.F.);
#13521=ORIENTED_EDGE('',*,*,#8663,.T.);
#13522=ORIENTED_EDGE('',*,*,#8667,.T.);
#13523=ORIENTED_EDGE('',*,*,#8691,.T.);
#13524=ORIENTED_EDGE('',*,*,#8692,.T.);
#13525=ORIENTED_EDGE('',*,*,#8693,.T.);
#13526=ORIENTED_EDGE('',*,*,#8694,.T.);
#13527=ORIENTED_EDGE('',*,*,#8695,.T.);
#13528=ORIENTED_EDGE('',*,*,#8690,.T.);
#13529=ORIENTED_EDGE('',*,*,#8696,.T.);
#13530=ORIENTED_EDGE('',*,*,#8695,.F.);
#13531=ORIENTED_EDGE('',*,*,#8696,.F.);
#13532=ORIENTED_EDGE('',*,*,#8687,.T.);
#13533=ORIENTED_EDGE('',*,*,#8697,.T.);
#13534=ORIENTED_EDGE('',*,*,#8693,.F.);
#13535=ORIENTED_EDGE('',*,*,#8698,.F.);
#13536=ORIENTED_EDGE('',*,*,#8688,.T.);
#13537=ORIENTED_EDGE('',*,*,#8698,.T.);
#13538=ORIENTED_EDGE('',*,*,#8692,.F.);
#13539=ORIENTED_EDGE('',*,*,#8699,.F.);
#13540=ORIENTED_EDGE('',*,*,#8666,.T.);
#13541=ORIENTED_EDGE('',*,*,#8689,.T.);
#13542=ORIENTED_EDGE('',*,*,#8699,.T.);
#13543=ORIENTED_EDGE('',*,*,#8691,.F.);
#13544=ORIENTED_EDGE('',*,*,#8664,.T.);
#13545=ORIENTED_EDGE('',*,*,#8694,.F.);
#13546=ORIENTED_EDGE('',*,*,#8697,.F.);
#13547=ORIENTED_EDGE('',*,*,#8686,.T.);
#13548=ORIENTED_EDGE('',*,*,#8655,.T.);
#13549=ORIENTED_EDGE('',*,*,#8685,.T.);
#13550=ORIENTED_EDGE('',*,*,#8700,.F.);
#13551=ORIENTED_EDGE('',*,*,#8701,.F.);
#13552=ORIENTED_EDGE('',*,*,#8702,.F.);
#13553=ORIENTED_EDGE('',*,*,#8703,.F.);
#13554=ORIENTED_EDGE('',*,*,#8704,.T.);
#13555=ORIENTED_EDGE('',*,*,#8705,.T.);
#13556=ORIENTED_EDGE('',*,*,#8706,.F.);
#13557=ORIENTED_EDGE('',*,*,#8705,.F.);
#13558=ORIENTED_EDGE('',*,*,#8707,.F.);
#13559=ORIENTED_EDGE('',*,*,#8708,.T.);
#13560=ORIENTED_EDGE('',*,*,#8709,.T.);
#13561=ORIENTED_EDGE('',*,*,#8710,.F.);
#13562=ORIENTED_EDGE('',*,*,#8711,.T.);
#13563=ORIENTED_EDGE('',*,*,#8712,.T.);
#13564=ORIENTED_EDGE('',*,*,#8713,.T.);
#13565=ORIENTED_EDGE('',*,*,#8714,.T.);
#13566=ORIENTED_EDGE('',*,*,#8712,.F.);
#13567=ORIENTED_EDGE('',*,*,#8715,.T.);
#13568=ORIENTED_EDGE('',*,*,#8703,.T.);
#13569=ORIENTED_EDGE('',*,*,#8716,.F.);
#13570=ORIENTED_EDGE('',*,*,#8717,.T.);
#13571=ORIENTED_EDGE('',*,*,#8718,.T.);
#13572=ORIENTED_EDGE('',*,*,#8719,.T.);
#13573=ORIENTED_EDGE('',*,*,#8720,.F.);
#13574=ORIENTED_EDGE('',*,*,#8717,.F.);
#13575=ORIENTED_EDGE('',*,*,#8721,.T.);
#13576=ORIENTED_EDGE('',*,*,#8707,.T.);
#13577=ORIENTED_EDGE('',*,*,#8722,.T.);
#13578=ORIENTED_EDGE('',*,*,#8723,.F.);
#13579=ORIENTED_EDGE('',*,*,#8724,.F.);
#13580=ORIENTED_EDGE('',*,*,#8706,.T.);
#13581=ORIENTED_EDGE('',*,*,#8725,.F.);
#13582=ORIENTED_EDGE('',*,*,#8726,.T.);
#13583=ORIENTED_EDGE('',*,*,#8727,.T.);
#13584=ORIENTED_EDGE('',*,*,#8728,.F.);
#13585=ORIENTED_EDGE('',*,*,#8729,.T.);
#13586=ORIENTED_EDGE('',*,*,#8727,.F.);
#13587=ORIENTED_EDGE('',*,*,#8730,.T.);
#13588=ORIENTED_EDGE('',*,*,#8731,.T.);
#13589=ORIENTED_EDGE('',*,*,#8732,.T.);
#13590=ORIENTED_EDGE('',*,*,#8709,.F.);
#13591=ORIENTED_EDGE('',*,*,#8733,.F.);
#13592=ORIENTED_EDGE('',*,*,#8704,.F.);
#13593=ORIENTED_EDGE('',*,*,#8734,.T.);
#13594=ORIENTED_EDGE('',*,*,#8725,.T.);
#13595=ORIENTED_EDGE('',*,*,#8735,.T.);
#13596=ORIENTED_EDGE('',*,*,#8734,.F.);
#13597=ORIENTED_EDGE('',*,*,#8735,.F.);
#13598=ORIENTED_EDGE('',*,*,#8722,.F.);
#13599=ORIENTED_EDGE('',*,*,#8710,.T.);
#13600=ORIENTED_EDGE('',*,*,#8732,.F.);
#13601=ORIENTED_EDGE('',*,*,#8736,.F.);
#13602=ORIENTED_EDGE('',*,*,#8723,.T.);
#13603=ORIENTED_EDGE('',*,*,#8736,.T.);
#13604=ORIENTED_EDGE('',*,*,#8731,.F.);
#13605=ORIENTED_EDGE('',*,*,#8737,.F.);
#13606=ORIENTED_EDGE('',*,*,#8738,.T.);
#13607=ORIENTED_EDGE('',*,*,#8739,.T.);
#13608=ORIENTED_EDGE('',*,*,#8740,.T.);
#13609=ORIENTED_EDGE('',*,*,#8741,.T.);
#13610=ORIENTED_EDGE('',*,*,#8741,.F.);
#13611=ORIENTED_EDGE('',*,*,#8742,.F.);
#13612=ORIENTED_EDGE('',*,*,#8701,.T.);
#13613=ORIENTED_EDGE('',*,*,#8743,.T.);
#13614=ORIENTED_EDGE('',*,*,#8744,.F.);
#13615=ORIENTED_EDGE('',*,*,#8745,.F.);
#13616=ORIENTED_EDGE('',*,*,#8728,.T.);
#13617=ORIENTED_EDGE('',*,*,#8733,.T.);
#13618=ORIENTED_EDGE('',*,*,#8708,.F.);
#13619=ORIENTED_EDGE('',*,*,#8721,.F.);
#13620=ORIENTED_EDGE('',*,*,#8720,.T.);
#13621=ORIENTED_EDGE('',*,*,#8746,.F.);
#13622=ORIENTED_EDGE('',*,*,#8747,.F.);
#13623=ORIENTED_EDGE('',*,*,#8748,.T.);
#13624=ORIENTED_EDGE('',*,*,#8749,.T.);
#13625=ORIENTED_EDGE('',*,*,#8750,.F.);
#13626=ORIENTED_EDGE('',*,*,#8751,.T.);
#13627=ORIENTED_EDGE('',*,*,#8752,.T.);
#13628=ORIENTED_EDGE('',*,*,#8753,.F.);
#13629=ORIENTED_EDGE('',*,*,#8752,.F.);
#13630=ORIENTED_EDGE('',*,*,#8754,.T.);
#13631=ORIENTED_EDGE('',*,*,#8755,.T.);
#13632=ORIENTED_EDGE('',*,*,#8756,.F.);
#13633=ORIENTED_EDGE('',*,*,#8749,.F.);
#13634=ORIENTED_EDGE('',*,*,#8757,.F.);
#13635=ORIENTED_EDGE('',*,*,#8758,.F.);
#13636=ORIENTED_EDGE('',*,*,#8759,.F.);
#13637=ORIENTED_EDGE('',*,*,#8760,.F.);
#13638=ORIENTED_EDGE('',*,*,#8760,.T.);
#13639=ORIENTED_EDGE('',*,*,#8761,.T.);
#13640=ORIENTED_EDGE('',*,*,#8739,.F.);
#13641=ORIENTED_EDGE('',*,*,#8762,.F.);
#13642=ORIENTED_EDGE('',*,*,#8743,.F.);
#13643=ORIENTED_EDGE('',*,*,#8700,.T.);
#13644=ORIENTED_EDGE('',*,*,#8715,.F.);
#13645=ORIENTED_EDGE('',*,*,#8711,.F.);
#13646=ORIENTED_EDGE('',*,*,#8763,.F.);
#13647=ORIENTED_EDGE('',*,*,#8757,.T.);
#13648=ORIENTED_EDGE('',*,*,#8762,.T.);
#13649=ORIENTED_EDGE('',*,*,#8738,.F.);
#13650=ORIENTED_EDGE('',*,*,#8745,.T.);
#13651=ORIENTED_EDGE('',*,*,#8764,.T.);
#13652=ORIENTED_EDGE('',*,*,#8765,.T.);
#13653=ORIENTED_EDGE('',*,*,#8729,.F.);
#13654=ORIENTED_EDGE('',*,*,#8758,.T.);
#13655=ORIENTED_EDGE('',*,*,#8763,.T.);
#13656=ORIENTED_EDGE('',*,*,#8714,.F.);
#13657=ORIENTED_EDGE('',*,*,#8766,.F.);
#13658=ORIENTED_EDGE('',*,*,#8759,.T.);
#13659=ORIENTED_EDGE('',*,*,#8766,.T.);
#13660=ORIENTED_EDGE('',*,*,#8713,.F.);
#13661=ORIENTED_EDGE('',*,*,#8716,.T.);
#13662=ORIENTED_EDGE('',*,*,#8702,.T.);
#13663=ORIENTED_EDGE('',*,*,#8742,.T.);
#13664=ORIENTED_EDGE('',*,*,#8740,.F.);
#13665=ORIENTED_EDGE('',*,*,#8761,.F.);
#13666=ORIENTED_EDGE('',*,*,#8767,.F.);
#13667=ORIENTED_EDGE('',*,*,#8747,.T.);
#13668=ORIENTED_EDGE('',*,*,#8768,.F.);
#13669=ORIENTED_EDGE('',*,*,#8769,.F.);
#13670=ORIENTED_EDGE('',*,*,#8767,.T.);
#13671=ORIENTED_EDGE('',*,*,#8770,.T.);
#13672=ORIENTED_EDGE('',*,*,#8771,.T.);
#13673=ORIENTED_EDGE('',*,*,#8772,.F.);
#13674=ORIENTED_EDGE('',*,*,#8754,.F.);
#13675=ORIENTED_EDGE('',*,*,#8748,.F.);
#13676=ORIENTED_EDGE('',*,*,#8751,.F.);
#13677=ORIENTED_EDGE('',*,*,#8773,.T.);
#13678=ORIENTED_EDGE('',*,*,#8774,.F.);
#13679=ORIENTED_EDGE('',*,*,#8764,.F.);
#13680=ORIENTED_EDGE('',*,*,#8744,.T.);
#13681=ORIENTED_EDGE('',*,*,#8775,.F.);
#13682=ORIENTED_EDGE('',*,*,#8775,.T.);
#13683=ORIENTED_EDGE('',*,*,#8750,.T.);
#13684=ORIENTED_EDGE('',*,*,#8756,.T.);
#13685=ORIENTED_EDGE('',*,*,#8776,.F.);
#13686=ORIENTED_EDGE('',*,*,#8777,.F.);
#13687=ORIENTED_EDGE('',*,*,#8778,.F.);
#13688=ORIENTED_EDGE('',*,*,#8753,.T.);
#13689=ORIENTED_EDGE('',*,*,#8779,.F.);
#13690=ORIENTED_EDGE('',*,*,#8774,.T.);
#13691=ORIENTED_EDGE('',*,*,#8778,.T.);
#13692=ORIENTED_EDGE('',*,*,#8780,.F.);
#13693=ORIENTED_EDGE('',*,*,#8770,.F.);
#13694=ORIENTED_EDGE('',*,*,#8769,.T.);
#13695=ORIENTED_EDGE('',*,*,#8781,.T.);
#13696=ORIENTED_EDGE('',*,*,#8718,.F.);
#13697=ORIENTED_EDGE('',*,*,#8724,.T.);
#13698=ORIENTED_EDGE('',*,*,#8737,.T.);
#13699=ORIENTED_EDGE('',*,*,#8730,.F.);
#13700=ORIENTED_EDGE('',*,*,#8726,.F.);
#13701=ORIENTED_EDGE('',*,*,#8765,.F.);
#13702=ORIENTED_EDGE('',*,*,#8779,.T.);
#13703=ORIENTED_EDGE('',*,*,#8782,.T.);
#13704=ORIENTED_EDGE('',*,*,#8773,.F.);
#13705=ORIENTED_EDGE('',*,*,#8782,.F.);
#13706=ORIENTED_EDGE('',*,*,#8772,.T.);
#13707=ORIENTED_EDGE('',*,*,#8783,.T.);
#13708=ORIENTED_EDGE('',*,*,#8776,.T.);
#13709=ORIENTED_EDGE('',*,*,#8755,.F.);
#13710=ORIENTED_EDGE('',*,*,#8771,.F.);
#13711=ORIENTED_EDGE('',*,*,#8780,.T.);
#13712=ORIENTED_EDGE('',*,*,#8777,.T.);
#13713=ORIENTED_EDGE('',*,*,#8783,.F.);
#13714=ORIENTED_EDGE('',*,*,#8768,.T.);
#13715=ORIENTED_EDGE('',*,*,#8746,.T.);
#13716=ORIENTED_EDGE('',*,*,#8719,.F.);
#13717=ORIENTED_EDGE('',*,*,#8781,.F.);
#13718=ORIENTED_EDGE('',*,*,#8784,.T.);
#13719=ORIENTED_EDGE('',*,*,#8785,.T.);
#13720=ORIENTED_EDGE('',*,*,#8786,.T.);
#13721=ORIENTED_EDGE('',*,*,#8787,.F.);
#13722=ORIENTED_EDGE('',*,*,#8788,.F.);
#13723=ORIENTED_EDGE('',*,*,#8789,.F.);
#13724=ORIENTED_EDGE('',*,*,#8790,.T.);
#13725=ORIENTED_EDGE('',*,*,#8791,.T.);
#13726=ORIENTED_EDGE('',*,*,#8792,.T.);
#13727=ORIENTED_EDGE('',*,*,#8784,.F.);
#13728=ORIENTED_EDGE('',*,*,#8793,.F.);
#13729=ORIENTED_EDGE('',*,*,#8794,.F.);
#13730=ORIENTED_EDGE('',*,*,#8795,.T.);
#13731=ORIENTED_EDGE('',*,*,#8796,.T.);
#13732=ORIENTED_EDGE('',*,*,#8797,.T.);
#13733=ORIENTED_EDGE('',*,*,#8790,.F.);
#13734=ORIENTED_EDGE('',*,*,#8798,.F.);
#13735=ORIENTED_EDGE('',*,*,#8799,.F.);
#13736=ORIENTED_EDGE('',*,*,#8800,.T.);
#13737=ORIENTED_EDGE('',*,*,#8801,.T.);
#13738=ORIENTED_EDGE('',*,*,#8802,.T.);
#13739=ORIENTED_EDGE('',*,*,#8795,.F.);
#13740=ORIENTED_EDGE('',*,*,#8803,.F.);
#13741=ORIENTED_EDGE('',*,*,#8804,.F.);
#13742=ORIENTED_EDGE('',*,*,#8805,.T.);
#13743=ORIENTED_EDGE('',*,*,#8806,.T.);
#13744=ORIENTED_EDGE('',*,*,#8807,.T.);
#13745=ORIENTED_EDGE('',*,*,#8800,.F.);
#13746=ORIENTED_EDGE('',*,*,#8808,.F.);
#13747=ORIENTED_EDGE('',*,*,#8809,.F.);
#13748=ORIENTED_EDGE('',*,*,#8810,.T.);
#13749=ORIENTED_EDGE('',*,*,#8811,.T.);
#13750=ORIENTED_EDGE('',*,*,#8812,.T.);
#13751=ORIENTED_EDGE('',*,*,#8805,.F.);
#13752=ORIENTED_EDGE('',*,*,#8813,.F.);
#13753=ORIENTED_EDGE('',*,*,#8814,.F.);
#13754=ORIENTED_EDGE('',*,*,#8815,.T.);
#13755=ORIENTED_EDGE('',*,*,#8816,.T.);
#13756=ORIENTED_EDGE('',*,*,#8817,.T.);
#13757=ORIENTED_EDGE('',*,*,#8810,.F.);
#13758=ORIENTED_EDGE('',*,*,#8818,.F.);
#13759=ORIENTED_EDGE('',*,*,#8819,.F.);
#13760=ORIENTED_EDGE('',*,*,#8820,.T.);
#13761=ORIENTED_EDGE('',*,*,#8821,.T.);
#13762=ORIENTED_EDGE('',*,*,#8822,.T.);
#13763=ORIENTED_EDGE('',*,*,#8815,.F.);
#13764=ORIENTED_EDGE('',*,*,#8823,.F.);
#13765=ORIENTED_EDGE('',*,*,#8824,.F.);
#13766=ORIENTED_EDGE('',*,*,#8825,.T.);
#13767=ORIENTED_EDGE('',*,*,#8826,.T.);
#13768=ORIENTED_EDGE('',*,*,#8827,.T.);
#13769=ORIENTED_EDGE('',*,*,#8820,.F.);
#13770=ORIENTED_EDGE('',*,*,#8828,.F.);
#13771=ORIENTED_EDGE('',*,*,#8829,.F.);
#13772=ORIENTED_EDGE('',*,*,#8830,.T.);
#13773=ORIENTED_EDGE('',*,*,#8831,.T.);
#13774=ORIENTED_EDGE('',*,*,#8832,.T.);
#13775=ORIENTED_EDGE('',*,*,#8825,.F.);
#13776=ORIENTED_EDGE('',*,*,#8833,.F.);
#13777=ORIENTED_EDGE('',*,*,#8834,.F.);
#13778=ORIENTED_EDGE('',*,*,#8835,.T.);
#13779=ORIENTED_EDGE('',*,*,#8836,.T.);
#13780=ORIENTED_EDGE('',*,*,#8837,.T.);
#13781=ORIENTED_EDGE('',*,*,#8830,.F.);
#13782=ORIENTED_EDGE('',*,*,#8838,.F.);
#13783=ORIENTED_EDGE('',*,*,#8839,.F.);
#13784=ORIENTED_EDGE('',*,*,#8840,.T.);
#13785=ORIENTED_EDGE('',*,*,#8841,.T.);
#13786=ORIENTED_EDGE('',*,*,#8842,.T.);
#13787=ORIENTED_EDGE('',*,*,#8835,.F.);
#13788=ORIENTED_EDGE('',*,*,#8843,.F.);
#13789=ORIENTED_EDGE('',*,*,#8844,.F.);
#13790=ORIENTED_EDGE('',*,*,#8845,.T.);
#13791=ORIENTED_EDGE('',*,*,#8846,.T.);
#13792=ORIENTED_EDGE('',*,*,#8847,.T.);
#13793=ORIENTED_EDGE('',*,*,#8840,.F.);
#13794=ORIENTED_EDGE('',*,*,#8848,.F.);
#13795=ORIENTED_EDGE('',*,*,#8849,.F.);
#13796=ORIENTED_EDGE('',*,*,#8850,.T.);
#13797=ORIENTED_EDGE('',*,*,#8851,.T.);
#13798=ORIENTED_EDGE('',*,*,#8852,.T.);
#13799=ORIENTED_EDGE('',*,*,#8845,.F.);
#13800=ORIENTED_EDGE('',*,*,#8853,.F.);
#13801=ORIENTED_EDGE('',*,*,#8854,.F.);
#13802=ORIENTED_EDGE('',*,*,#8855,.T.);
#13803=ORIENTED_EDGE('',*,*,#8856,.T.);
#13804=ORIENTED_EDGE('',*,*,#8857,.T.);
#13805=ORIENTED_EDGE('',*,*,#8850,.F.);
#13806=ORIENTED_EDGE('',*,*,#8858,.F.);
#13807=ORIENTED_EDGE('',*,*,#8859,.F.);
#13808=ORIENTED_EDGE('',*,*,#8860,.T.);
#13809=ORIENTED_EDGE('',*,*,#8861,.T.);
#13810=ORIENTED_EDGE('',*,*,#8862,.T.);
#13811=ORIENTED_EDGE('',*,*,#8855,.F.);
#13812=ORIENTED_EDGE('',*,*,#8863,.F.);
#13813=ORIENTED_EDGE('',*,*,#8864,.F.);
#13814=ORIENTED_EDGE('',*,*,#8865,.F.);
#13815=ORIENTED_EDGE('',*,*,#8866,.F.);
#13816=ORIENTED_EDGE('',*,*,#8867,.F.);
#13817=ORIENTED_EDGE('',*,*,#8868,.T.);
#13818=ORIENTED_EDGE('',*,*,#8869,.F.);
#13819=ORIENTED_EDGE('',*,*,#8870,.T.);
#13820=ORIENTED_EDGE('',*,*,#8871,.F.);
#13821=ORIENTED_EDGE('',*,*,#8872,.F.);
#13822=ORIENTED_EDGE('',*,*,#8873,.T.);
#13823=ORIENTED_EDGE('',*,*,#8874,.F.);
#13824=ORIENTED_EDGE('',*,*,#8786,.F.);
#13825=ORIENTED_EDGE('',*,*,#8785,.F.);
#13826=ORIENTED_EDGE('',*,*,#8792,.F.);
#13827=ORIENTED_EDGE('',*,*,#8791,.F.);
#13828=ORIENTED_EDGE('',*,*,#8797,.F.);
#13829=ORIENTED_EDGE('',*,*,#8796,.F.);
#13830=ORIENTED_EDGE('',*,*,#8802,.F.);
#13831=ORIENTED_EDGE('',*,*,#8801,.F.);
#13832=ORIENTED_EDGE('',*,*,#8807,.F.);
#13833=ORIENTED_EDGE('',*,*,#8806,.F.);
#13834=ORIENTED_EDGE('',*,*,#8812,.F.);
#13835=ORIENTED_EDGE('',*,*,#8811,.F.);
#13836=ORIENTED_EDGE('',*,*,#8817,.F.);
#13837=ORIENTED_EDGE('',*,*,#8816,.F.);
#13838=ORIENTED_EDGE('',*,*,#8822,.F.);
#13839=ORIENTED_EDGE('',*,*,#8821,.F.);
#13840=ORIENTED_EDGE('',*,*,#8827,.F.);
#13841=ORIENTED_EDGE('',*,*,#8826,.F.);
#13842=ORIENTED_EDGE('',*,*,#8832,.F.);
#13843=ORIENTED_EDGE('',*,*,#8831,.F.);
#13844=ORIENTED_EDGE('',*,*,#8837,.F.);
#13845=ORIENTED_EDGE('',*,*,#8836,.F.);
#13846=ORIENTED_EDGE('',*,*,#8842,.F.);
#13847=ORIENTED_EDGE('',*,*,#8841,.F.);
#13848=ORIENTED_EDGE('',*,*,#8847,.F.);
#13849=ORIENTED_EDGE('',*,*,#8846,.F.);
#13850=ORIENTED_EDGE('',*,*,#8852,.F.);
#13851=ORIENTED_EDGE('',*,*,#8851,.F.);
#13852=ORIENTED_EDGE('',*,*,#8857,.F.);
#13853=ORIENTED_EDGE('',*,*,#8856,.F.);
#13854=ORIENTED_EDGE('',*,*,#8862,.F.);
#13855=ORIENTED_EDGE('',*,*,#8861,.F.);
#13856=ORIENTED_EDGE('',*,*,#8875,.F.);
#13857=ORIENTED_EDGE('',*,*,#8876,.F.);
#13858=ORIENTED_EDGE('',*,*,#8868,.F.);
#13859=ORIENTED_EDGE('',*,*,#8877,.F.);
#13860=ORIENTED_EDGE('',*,*,#8878,.T.);
#13861=ORIENTED_EDGE('',*,*,#8879,.T.);
#13862=ORIENTED_EDGE('',*,*,#8880,.T.);
#13863=ORIENTED_EDGE('',*,*,#8881,.T.);
#13864=ORIENTED_EDGE('',*,*,#8882,.T.);
#13865=ORIENTED_EDGE('',*,*,#8883,.T.);
#13866=ORIENTED_EDGE('',*,*,#8884,.T.);
#13867=ORIENTED_EDGE('',*,*,#8885,.T.);
#13868=ORIENTED_EDGE('',*,*,#8886,.T.);
#13869=ORIENTED_EDGE('',*,*,#8887,.T.);
#13870=ORIENTED_EDGE('',*,*,#8888,.T.);
#13871=ORIENTED_EDGE('',*,*,#8889,.T.);
#13872=ORIENTED_EDGE('',*,*,#8890,.T.);
#13873=ORIENTED_EDGE('',*,*,#8891,.T.);
#13874=ORIENTED_EDGE('',*,*,#8892,.T.);
#13875=ORIENTED_EDGE('',*,*,#8893,.T.);
#13876=ORIENTED_EDGE('',*,*,#8894,.T.);
#13877=ORIENTED_EDGE('',*,*,#8895,.T.);
#13878=ORIENTED_EDGE('',*,*,#8896,.F.);
#13879=ORIENTED_EDGE('',*,*,#8870,.F.);
#13880=ORIENTED_EDGE('',*,*,#8897,.F.);
#13881=ORIENTED_EDGE('',*,*,#8898,.F.);
#13882=ORIENTED_EDGE('',*,*,#8899,.F.);
#13883=ORIENTED_EDGE('',*,*,#8895,.F.);
#13884=ORIENTED_EDGE('',*,*,#8894,.F.);
#13885=ORIENTED_EDGE('',*,*,#8893,.F.);
#13886=ORIENTED_EDGE('',*,*,#8892,.F.);
#13887=ORIENTED_EDGE('',*,*,#8891,.F.);
#13888=ORIENTED_EDGE('',*,*,#8890,.F.);
#13889=ORIENTED_EDGE('',*,*,#8889,.F.);
#13890=ORIENTED_EDGE('',*,*,#8888,.F.);
#13891=ORIENTED_EDGE('',*,*,#8887,.F.);
#13892=ORIENTED_EDGE('',*,*,#8886,.F.);
#13893=ORIENTED_EDGE('',*,*,#8885,.F.);
#13894=ORIENTED_EDGE('',*,*,#8884,.F.);
#13895=ORIENTED_EDGE('',*,*,#8883,.F.);
#13896=ORIENTED_EDGE('',*,*,#8882,.F.);
#13897=ORIENTED_EDGE('',*,*,#8881,.F.);
#13898=ORIENTED_EDGE('',*,*,#8880,.F.);
#13899=ORIENTED_EDGE('',*,*,#8879,.F.);
#13900=ORIENTED_EDGE('',*,*,#8878,.F.);
#13901=ORIENTED_EDGE('',*,*,#8900,.F.);
#13902=ORIENTED_EDGE('',*,*,#8901,.F.);
#13903=ORIENTED_EDGE('',*,*,#8902,.F.);
#13904=ORIENTED_EDGE('',*,*,#8903,.F.);
#13905=ORIENTED_EDGE('',*,*,#8904,.F.);
#13906=ORIENTED_EDGE('',*,*,#8905,.F.);
#13907=ORIENTED_EDGE('',*,*,#8906,.F.);
#13908=ORIENTED_EDGE('',*,*,#8907,.F.);
#13909=ORIENTED_EDGE('',*,*,#8908,.F.);
#13910=ORIENTED_EDGE('',*,*,#8909,.F.);
#13911=ORIENTED_EDGE('',*,*,#8910,.F.);
#13912=ORIENTED_EDGE('',*,*,#8911,.F.);
#13913=ORIENTED_EDGE('',*,*,#8912,.F.);
#13914=ORIENTED_EDGE('',*,*,#8913,.F.);
#13915=ORIENTED_EDGE('',*,*,#8914,.F.);
#13916=ORIENTED_EDGE('',*,*,#8915,.F.);
#13917=ORIENTED_EDGE('',*,*,#8916,.F.);
#13918=ORIENTED_EDGE('',*,*,#8917,.F.);
#13919=ORIENTED_EDGE('',*,*,#8918,.F.);
#13920=ORIENTED_EDGE('',*,*,#8865,.T.);
#13921=ORIENTED_EDGE('',*,*,#8876,.T.);
#13922=ORIENTED_EDGE('',*,*,#8875,.T.);
#13923=ORIENTED_EDGE('',*,*,#8860,.F.);
#13924=ORIENTED_EDGE('',*,*,#8919,.F.);
#13925=ORIENTED_EDGE('',*,*,#8920,.F.);
#13926=ORIENTED_EDGE('',*,*,#8921,.F.);
#13927=ORIENTED_EDGE('',*,*,#8922,.F.);
#13928=ORIENTED_EDGE('',*,*,#8923,.F.);
#13929=ORIENTED_EDGE('',*,*,#8924,.F.);
#13930=ORIENTED_EDGE('',*,*,#8925,.F.);
#13931=ORIENTED_EDGE('',*,*,#8918,.T.);
#13932=ORIENTED_EDGE('',*,*,#8917,.T.);
#13933=ORIENTED_EDGE('',*,*,#8916,.T.);
#13934=ORIENTED_EDGE('',*,*,#8915,.T.);
#13935=ORIENTED_EDGE('',*,*,#8914,.T.);
#13936=ORIENTED_EDGE('',*,*,#8913,.T.);
#13937=ORIENTED_EDGE('',*,*,#8912,.T.);
#13938=ORIENTED_EDGE('',*,*,#8911,.T.);
#13939=ORIENTED_EDGE('',*,*,#8910,.T.);
#13940=ORIENTED_EDGE('',*,*,#8909,.T.);
#13941=ORIENTED_EDGE('',*,*,#8908,.T.);
#13942=ORIENTED_EDGE('',*,*,#8907,.T.);
#13943=ORIENTED_EDGE('',*,*,#8906,.T.);
#13944=ORIENTED_EDGE('',*,*,#8905,.T.);
#13945=ORIENTED_EDGE('',*,*,#8904,.T.);
#13946=ORIENTED_EDGE('',*,*,#8903,.T.);
#13947=ORIENTED_EDGE('',*,*,#8902,.T.);
#13948=ORIENTED_EDGE('',*,*,#8901,.T.);
#13949=ORIENTED_EDGE('',*,*,#8926,.F.);
#13950=ORIENTED_EDGE('',*,*,#8898,.T.);
#13951=ORIENTED_EDGE('',*,*,#8927,.F.);
#13952=ORIENTED_EDGE('',*,*,#8928,.F.);
#13953=ORIENTED_EDGE('',*,*,#8866,.T.);
#13954=ORIENTED_EDGE('',*,*,#8920,.T.);
#13955=ORIENTED_EDGE('',*,*,#8919,.T.);
#13956=ORIENTED_EDGE('',*,*,#8864,.T.);
#13957=ORIENTED_EDGE('',*,*,#8863,.T.);
#13958=ORIENTED_EDGE('',*,*,#8859,.T.);
#13959=ORIENTED_EDGE('',*,*,#8858,.T.);
#13960=ORIENTED_EDGE('',*,*,#8854,.T.);
#13961=ORIENTED_EDGE('',*,*,#8853,.T.);
#13962=ORIENTED_EDGE('',*,*,#8849,.T.);
#13963=ORIENTED_EDGE('',*,*,#8848,.T.);
#13964=ORIENTED_EDGE('',*,*,#8844,.T.);
#13965=ORIENTED_EDGE('',*,*,#8843,.T.);
#13966=ORIENTED_EDGE('',*,*,#8839,.T.);
#13967=ORIENTED_EDGE('',*,*,#8838,.T.);
#13968=ORIENTED_EDGE('',*,*,#8834,.T.);
#13969=ORIENTED_EDGE('',*,*,#8833,.T.);
#13970=ORIENTED_EDGE('',*,*,#8829,.T.);
#13971=ORIENTED_EDGE('',*,*,#8828,.T.);
#13972=ORIENTED_EDGE('',*,*,#8824,.T.);
#13973=ORIENTED_EDGE('',*,*,#8823,.T.);
#13974=ORIENTED_EDGE('',*,*,#8819,.T.);
#13975=ORIENTED_EDGE('',*,*,#8818,.T.);
#13976=ORIENTED_EDGE('',*,*,#8814,.T.);
#13977=ORIENTED_EDGE('',*,*,#8813,.T.);
#13978=ORIENTED_EDGE('',*,*,#8809,.T.);
#13979=ORIENTED_EDGE('',*,*,#8808,.T.);
#13980=ORIENTED_EDGE('',*,*,#8804,.T.);
#13981=ORIENTED_EDGE('',*,*,#8803,.T.);
#13982=ORIENTED_EDGE('',*,*,#8799,.T.);
#13983=ORIENTED_EDGE('',*,*,#8798,.T.);
#13984=ORIENTED_EDGE('',*,*,#8794,.T.);
#13985=ORIENTED_EDGE('',*,*,#8793,.T.);
#13986=ORIENTED_EDGE('',*,*,#8789,.T.);
#13987=ORIENTED_EDGE('',*,*,#8788,.T.);
#13988=ORIENTED_EDGE('',*,*,#8929,.F.);
#13989=ORIENTED_EDGE('',*,*,#8923,.T.);
#13990=ORIENTED_EDGE('',*,*,#8922,.T.);
#13991=ORIENTED_EDGE('',*,*,#8930,.F.);
#13992=ORIENTED_EDGE('',*,*,#8931,.F.);
#13993=ORIENTED_EDGE('',*,*,#8932,.F.);
#13994=ORIENTED_EDGE('',*,*,#8873,.F.);
#13995=ORIENTED_EDGE('',*,*,#8933,.F.);
#13996=ORIENTED_EDGE('',*,*,#8931,.T.);
#13997=ORIENTED_EDGE('',*,*,#8934,.F.);
#13998=ORIENTED_EDGE('',*,*,#8935,.T.);
#13999=ORIENTED_EDGE('',*,*,#8871,.T.);
#14000=ORIENTED_EDGE('',*,*,#8896,.T.);
#14001=ORIENTED_EDGE('',*,*,#8926,.T.);
#14002=ORIENTED_EDGE('',*,*,#8900,.T.);
#14003=ORIENTED_EDGE('',*,*,#8877,.T.);
#14004=ORIENTED_EDGE('',*,*,#8867,.T.);
#14005=ORIENTED_EDGE('',*,*,#8928,.T.);
#14006=ORIENTED_EDGE('',*,*,#8936,.T.);
#14007=ORIENTED_EDGE('',*,*,#8937,.T.);
#14008=ORIENTED_EDGE('',*,*,#8936,.F.);
#14009=ORIENTED_EDGE('',*,*,#8927,.T.);
#14010=ORIENTED_EDGE('',*,*,#8897,.T.);
#14011=ORIENTED_EDGE('',*,*,#8869,.T.);
#14012=ORIENTED_EDGE('',*,*,#8935,.F.);
#14013=ORIENTED_EDGE('',*,*,#8929,.T.);
#14014=ORIENTED_EDGE('',*,*,#8787,.T.);
#14015=ORIENTED_EDGE('',*,*,#8874,.T.);
#14016=ORIENTED_EDGE('',*,*,#8932,.T.);
#14017=ORIENTED_EDGE('',*,*,#8933,.T.);
#14018=ORIENTED_EDGE('',*,*,#8930,.T.);
#14019=ORIENTED_EDGE('',*,*,#8872,.T.);
#14020=ORIENTED_EDGE('',*,*,#8899,.T.);
#14021=ORIENTED_EDGE('',*,*,#8925,.T.);
#14022=ORIENTED_EDGE('',*,*,#8921,.T.);
#14023=ORIENTED_EDGE('',*,*,#8924,.T.);
#14024=ORIENTED_EDGE('',*,*,#8937,.F.);
#14025=ORIENTED_EDGE('',*,*,#8934,.T.);
#14026=ORIENTED_EDGE('',*,*,#8938,.T.);
#14027=ORIENTED_EDGE('',*,*,#8939,.T.);
#14028=ORIENTED_EDGE('',*,*,#8940,.F.);
#14029=ORIENTED_EDGE('',*,*,#8939,.F.);
#14030=ORIENTED_EDGE('',*,*,#8941,.T.);
#14031=ORIENTED_EDGE('',*,*,#8942,.T.);
#14032=ORIENTED_EDGE('',*,*,#8943,.F.);
#14033=ORIENTED_EDGE('',*,*,#8944,.F.);
#14034=ORIENTED_EDGE('',*,*,#8945,.T.);
#14035=ORIENTED_EDGE('',*,*,#8944,.T.);
#14036=ORIENTED_EDGE('',*,*,#8946,.F.);
#14037=ORIENTED_EDGE('',*,*,#8947,.F.);
#14038=ORIENTED_EDGE('',*,*,#8948,.T.);
#14039=ORIENTED_EDGE('',*,*,#8947,.T.);
#14040=ORIENTED_EDGE('',*,*,#8949,.F.);
#14041=ORIENTED_EDGE('',*,*,#8950,.F.);
#14042=ORIENTED_EDGE('',*,*,#8951,.T.);
#14043=ORIENTED_EDGE('',*,*,#8949,.T.);
#14044=ORIENTED_EDGE('',*,*,#8946,.T.);
#14045=ORIENTED_EDGE('',*,*,#8943,.T.);
#14046=ORIENTED_EDGE('',*,*,#8940,.T.);
#14047=ORIENTED_EDGE('',*,*,#8952,.F.);
#14048=ORIENTED_EDGE('',*,*,#8941,.F.);
#14049=ORIENTED_EDGE('',*,*,#8945,.F.);
#14050=ORIENTED_EDGE('',*,*,#8948,.F.);
#14051=ORIENTED_EDGE('',*,*,#8938,.F.);
#14052=ORIENTED_EDGE('',*,*,#8953,.F.);
#14053=ORIENTED_EDGE('',*,*,#8953,.T.);
#14054=ORIENTED_EDGE('',*,*,#8954,.T.);
#14055=ORIENTED_EDGE('',*,*,#8955,.F.);
#14056=ORIENTED_EDGE('',*,*,#8954,.F.);
#14057=ORIENTED_EDGE('',*,*,#8956,.T.);
#14058=ORIENTED_EDGE('',*,*,#8957,.T.);
#14059=ORIENTED_EDGE('',*,*,#8958,.F.);
#14060=ORIENTED_EDGE('',*,*,#8957,.F.);
#14061=ORIENTED_EDGE('',*,*,#8959,.F.);
#14062=ORIENTED_EDGE('',*,*,#8960,.T.);
#14063=ORIENTED_EDGE('',*,*,#8961,.T.);
#14064=ORIENTED_EDGE('',*,*,#8962,.F.);
#14065=ORIENTED_EDGE('',*,*,#8963,.F.);
#14066=ORIENTED_EDGE('',*,*,#8964,.T.);
#14067=ORIENTED_EDGE('',*,*,#8965,.T.);
#14068=ORIENTED_EDGE('',*,*,#8960,.F.);
#14069=ORIENTED_EDGE('',*,*,#8966,.F.);
#14070=ORIENTED_EDGE('',*,*,#8967,.T.);
#14071=ORIENTED_EDGE('',*,*,#8968,.T.);
#14072=ORIENTED_EDGE('',*,*,#8964,.F.);
#14073=ORIENTED_EDGE('',*,*,#8967,.F.);
#14074=ORIENTED_EDGE('',*,*,#8969,.F.);
#14075=ORIENTED_EDGE('',*,*,#8962,.T.);
#14076=ORIENTED_EDGE('',*,*,#8970,.F.);
#14077=ORIENTED_EDGE('',*,*,#8971,.T.);
#14078=ORIENTED_EDGE('',*,*,#8951,.F.);
#14079=ORIENTED_EDGE('',*,*,#8942,.F.);
#14080=ORIENTED_EDGE('',*,*,#8952,.T.);
#14081=ORIENTED_EDGE('',*,*,#8950,.T.);
#14082=ORIENTED_EDGE('',*,*,#8971,.F.);
#14083=ORIENTED_EDGE('',*,*,#8970,.T.);
#14084=ORIENTED_EDGE('',*,*,#8961,.F.);
#14085=ORIENTED_EDGE('',*,*,#8965,.F.);
#14086=ORIENTED_EDGE('',*,*,#8968,.F.);
#14087=ORIENTED_EDGE('',*,*,#8956,.F.);
#14088=ORIENTED_EDGE('',*,*,#8969,.T.);
#14089=ORIENTED_EDGE('',*,*,#8966,.T.);
#14090=ORIENTED_EDGE('',*,*,#8963,.T.);
#14091=ORIENTED_EDGE('',*,*,#8959,.T.);
#14092=ORIENTED_EDGE('',*,*,#8958,.T.);
#14093=ORIENTED_EDGE('',*,*,#8955,.T.);
#14094=CYLINDRICAL_SURFACE('',#15049,10.);
#14095=CYLINDRICAL_SURFACE('',#15052,7.55784864301595);
#14096=CYLINDRICAL_SURFACE('',#15056,10.);
#14097=CYLINDRICAL_SURFACE('',#15060,3.);
#14098=CYLINDRICAL_SURFACE('',#15065,5.5);
#14099=CYLINDRICAL_SURFACE('',#15070,7.55784864301595);
#14100=CYLINDRICAL_SURFACE('',#15073,10.);
#14101=CYLINDRICAL_SURFACE('',#15080,7.55784864301595);
#14102=CYLINDRICAL_SURFACE('',#15084,10.);
#14103=CYLINDRICAL_SURFACE('',#15091,3.);
#14104=CYLINDRICAL_SURFACE('',#15095,5.5);
#14105=CYLINDRICAL_SURFACE('',#15100,7.55784864301595);
#14106=CYLINDRICAL_SURFACE('',#15105,4.91825);
#14107=CYLINDRICAL_SURFACE('',#15107,4.91825);
#14108=CYLINDRICAL_SURFACE('',#15108,4.91825);
#14109=CYLINDRICAL_SURFACE('',#15109,4.91825);
#14110=CYLINDRICAL_SURFACE('',#15110,4.91825);
#14111=CYLINDRICAL_SURFACE('',#15111,4.91825);
#14112=CYLINDRICAL_SURFACE('',#15112,4.91825);
#14113=CYLINDRICAL_SURFACE('',#15113,4.91825);
#14114=CYLINDRICAL_SURFACE('',#15114,4.91825);
#14115=CYLINDRICAL_SURFACE('',#15115,4.91825);
#14116=CYLINDRICAL_SURFACE('',#15116,4.91825);
#14117=CYLINDRICAL_SURFACE('',#15117,4.91825);
#14118=CYLINDRICAL_SURFACE('',#15118,4.91825);
#14119=CYLINDRICAL_SURFACE('',#15119,4.91825);
#14120=CYLINDRICAL_SURFACE('',#15120,4.91825);
#14121=CYLINDRICAL_SURFACE('',#15121,4.91825);
#14122=CYLINDRICAL_SURFACE('',#15122,4.91825);
#14123=CYLINDRICAL_SURFACE('',#15123,4.91825);
#14124=CYLINDRICAL_SURFACE('',#15124,4.91825);
#14125=CYLINDRICAL_SURFACE('',#15125,4.91825);
#14126=CYLINDRICAL_SURFACE('',#15126,4.91825);
#14127=CYLINDRICAL_SURFACE('',#15127,4.91825);
#14128=CYLINDRICAL_SURFACE('',#15128,4.91825);
#14129=CYLINDRICAL_SURFACE('',#15129,4.91825);
#14130=CYLINDRICAL_SURFACE('',#15130,4.91825);
#14131=CYLINDRICAL_SURFACE('',#15131,4.91825);
#14132=CYLINDRICAL_SURFACE('',#15132,4.91825);
#14133=CYLINDRICAL_SURFACE('',#15133,4.91825);
#14134=CYLINDRICAL_SURFACE('',#15134,4.91825);
#14135=CYLINDRICAL_SURFACE('',#15135,4.91825);
#14136=CYLINDRICAL_SURFACE('',#15136,4.91825);
#14137=CYLINDRICAL_SURFACE('',#15137,4.91825);
#14138=CYLINDRICAL_SURFACE('',#15138,4.91825);
#14139=CYLINDRICAL_SURFACE('',#15139,4.91825);
#14140=CYLINDRICAL_SURFACE('',#15140,4.91825);
#14141=CYLINDRICAL_SURFACE('',#15141,4.91825);
#14142=CYLINDRICAL_SURFACE('',#15142,4.91825);
#14143=CYLINDRICAL_SURFACE('',#15143,4.91825);
#14144=CYLINDRICAL_SURFACE('',#15144,4.91825);
#14145=CYLINDRICAL_SURFACE('',#15145,4.91825);
#14146=CYLINDRICAL_SURFACE('',#15146,4.91825);
#14147=CYLINDRICAL_SURFACE('',#15147,4.91825);
#14148=CYLINDRICAL_SURFACE('',#15148,4.91825);
#14149=CYLINDRICAL_SURFACE('',#15149,4.91825);
#14150=CYLINDRICAL_SURFACE('',#15150,4.91825);
#14151=CYLINDRICAL_SURFACE('',#15151,4.91825);
#14152=CYLINDRICAL_SURFACE('',#15152,4.91825);
#14153=CYLINDRICAL_SURFACE('',#15153,4.91825);
#14154=CYLINDRICAL_SURFACE('',#15154,4.91825);
#14155=CYLINDRICAL_SURFACE('',#15155,4.91825);
#14156=CYLINDRICAL_SURFACE('',#15156,4.91825);
#14157=CYLINDRICAL_SURFACE('',#15157,4.91825);
#14158=CYLINDRICAL_SURFACE('',#15158,4.91825);
#14159=CYLINDRICAL_SURFACE('',#15159,4.91825);
#14160=CYLINDRICAL_SURFACE('',#15160,4.91825);
#14161=CYLINDRICAL_SURFACE('',#15161,4.91825);
#14162=CYLINDRICAL_SURFACE('',#15162,4.91825);
#14163=CYLINDRICAL_SURFACE('',#15163,4.91825);
#14164=CYLINDRICAL_SURFACE('',#15164,4.91825);
#14165=CYLINDRICAL_SURFACE('',#15165,4.91825);
#14166=CYLINDRICAL_SURFACE('',#15166,4.91825);
#14167=CYLINDRICAL_SURFACE('',#15167,4.91825);
#14168=CYLINDRICAL_SURFACE('',#15168,4.91825);
#14169=CYLINDRICAL_SURFACE('',#15169,4.91825);
#14170=CYLINDRICAL_SURFACE('',#15170,4.91825);
#14171=CYLINDRICAL_SURFACE('',#15171,4.91825);
#14172=CYLINDRICAL_SURFACE('',#15172,4.91825);
#14173=CYLINDRICAL_SURFACE('',#15173,4.91825);
#14174=CYLINDRICAL_SURFACE('',#15174,4.91825);
#14175=CYLINDRICAL_SURFACE('',#15175,4.91825);
#14176=CYLINDRICAL_SURFACE('',#15176,4.91825);
#14177=CYLINDRICAL_SURFACE('',#15177,4.91825);
#14178=CYLINDRICAL_SURFACE('',#15178,4.91825);
#14179=CYLINDRICAL_SURFACE('',#15179,4.91825);
#14180=CYLINDRICAL_SURFACE('',#15180,4.91825);
#14181=CYLINDRICAL_SURFACE('',#15181,4.91825);
#14182=CYLINDRICAL_SURFACE('',#15182,4.91825);
#14183=CYLINDRICAL_SURFACE('',#15183,4.91825);
#14184=CYLINDRICAL_SURFACE('',#15184,4.91825);
#14185=CYLINDRICAL_SURFACE('',#15185,4.91825);
#14186=CYLINDRICAL_SURFACE('',#15186,4.91825);
#14187=CYLINDRICAL_SURFACE('',#15187,4.91825);
#14188=CYLINDRICAL_SURFACE('',#15188,4.91825);
#14189=CYLINDRICAL_SURFACE('',#15189,4.91825);
#14190=CYLINDRICAL_SURFACE('',#15190,4.91825);
#14191=CYLINDRICAL_SURFACE('',#15191,4.91825);
#14192=CYLINDRICAL_SURFACE('',#15192,4.91825);
#14193=CYLINDRICAL_SURFACE('',#15193,4.91825);
#14194=CYLINDRICAL_SURFACE('',#15194,4.91825);
#14195=CYLINDRICAL_SURFACE('',#15195,4.91825);
#14196=CYLINDRICAL_SURFACE('',#15196,4.91825);
#14197=CYLINDRICAL_SURFACE('',#15197,4.91825);
#14198=CYLINDRICAL_SURFACE('',#15198,4.91825);
#14199=CYLINDRICAL_SURFACE('',#15199,4.91825);
#14200=CYLINDRICAL_SURFACE('',#15200,4.91825);
#14201=CYLINDRICAL_SURFACE('',#15201,4.91825);
#14202=CYLINDRICAL_SURFACE('',#15202,4.91825);
#14203=CYLINDRICAL_SURFACE('',#15203,4.91825);
#14204=CYLINDRICAL_SURFACE('',#15204,4.91825);
#14205=CYLINDRICAL_SURFACE('',#15205,4.91825);
#14206=CYLINDRICAL_SURFACE('',#15206,4.91825);
#14207=CYLINDRICAL_SURFACE('',#15207,4.91825);
#14208=CYLINDRICAL_SURFACE('',#15208,4.91825);
#14209=CYLINDRICAL_SURFACE('',#15209,4.91825);
#14210=CYLINDRICAL_SURFACE('',#15210,4.91825);
#14211=CYLINDRICAL_SURFACE('',#15211,4.91825);
#14212=CYLINDRICAL_SURFACE('',#15212,4.91825);
#14213=CYLINDRICAL_SURFACE('',#15213,4.91825);
#14214=CYLINDRICAL_SURFACE('',#15214,4.91825);
#14215=CYLINDRICAL_SURFACE('',#15215,4.91825);
#14216=CYLINDRICAL_SURFACE('',#15216,4.91825);
#14217=CYLINDRICAL_SURFACE('',#15217,4.91825);
#14218=CYLINDRICAL_SURFACE('',#15218,4.91825);
#14219=CYLINDRICAL_SURFACE('',#15219,4.91825);
#14220=CYLINDRICAL_SURFACE('',#15220,4.91825);
#14221=CYLINDRICAL_SURFACE('',#15221,4.91825);
#14222=CYLINDRICAL_SURFACE('',#15222,4.91825);
#14223=CYLINDRICAL_SURFACE('',#15223,4.91825);
#14224=CYLINDRICAL_SURFACE('',#15224,4.91825);
#14225=CYLINDRICAL_SURFACE('',#15225,4.91825);
#14226=CYLINDRICAL_SURFACE('',#15226,4.91825);
#14227=CYLINDRICAL_SURFACE('',#15227,4.91825);
#14228=CYLINDRICAL_SURFACE('',#15228,4.91825);
#14229=CYLINDRICAL_SURFACE('',#15229,4.91825);
#14230=CYLINDRICAL_SURFACE('',#15230,4.91825);
#14231=CYLINDRICAL_SURFACE('',#15231,4.91825);
#14232=CYLINDRICAL_SURFACE('',#15232,4.91825);
#14233=CYLINDRICAL_SURFACE('',#15233,4.91825);
#14234=CYLINDRICAL_SURFACE('',#15234,4.91825);
#14235=CYLINDRICAL_SURFACE('',#15235,4.91825);
#14236=CYLINDRICAL_SURFACE('',#15236,4.91825);
#14237=CYLINDRICAL_SURFACE('',#15237,4.91825);
#14238=CYLINDRICAL_SURFACE('',#15238,4.91825);
#14239=CYLINDRICAL_SURFACE('',#15239,4.91825);
#14240=CYLINDRICAL_SURFACE('',#15240,4.91825);
#14241=CYLINDRICAL_SURFACE('',#15241,4.91825);
#14242=CYLINDRICAL_SURFACE('',#15242,4.91825);
#14243=CYLINDRICAL_SURFACE('',#15243,4.91825);
#14244=CYLINDRICAL_SURFACE('',#15244,4.91825);
#14245=CYLINDRICAL_SURFACE('',#15245,4.91825);
#14246=CYLINDRICAL_SURFACE('',#15246,4.91825);
#14247=CYLINDRICAL_SURFACE('',#15247,4.91825);
#14248=CYLINDRICAL_SURFACE('',#15248,4.91825);
#14249=CYLINDRICAL_SURFACE('',#15249,4.91825);
#14250=CYLINDRICAL_SURFACE('',#15250,4.91825);
#14251=CYLINDRICAL_SURFACE('',#15251,4.91825);
#14252=CYLINDRICAL_SURFACE('',#15252,4.91825);
#14253=CYLINDRICAL_SURFACE('',#15253,4.91825);
#14254=CYLINDRICAL_SURFACE('',#15254,4.91825);
#14255=CYLINDRICAL_SURFACE('',#15255,4.91825);
#14256=CYLINDRICAL_SURFACE('',#15256,4.91825);
#14257=CYLINDRICAL_SURFACE('',#15257,4.91825);
#14258=CYLINDRICAL_SURFACE('',#15258,4.91825);
#14259=CYLINDRICAL_SURFACE('',#15259,4.91825);
#14260=CYLINDRICAL_SURFACE('',#15260,4.91825);
#14261=CYLINDRICAL_SURFACE('',#15261,4.91825);
#14262=CYLINDRICAL_SURFACE('',#15262,4.91825);
#14263=CYLINDRICAL_SURFACE('',#15263,4.91825);
#14264=CYLINDRICAL_SURFACE('',#15264,4.91825);
#14265=CYLINDRICAL_SURFACE('',#15265,4.91825);
#14266=CYLINDRICAL_SURFACE('',#15266,4.91825);
#14267=CYLINDRICAL_SURFACE('',#15267,4.91825);
#14268=CYLINDRICAL_SURFACE('',#15268,4.91825);
#14269=CYLINDRICAL_SURFACE('',#15269,4.91825);
#14270=CYLINDRICAL_SURFACE('',#15270,4.91825);
#14271=CYLINDRICAL_SURFACE('',#15271,4.91825);
#14272=CYLINDRICAL_SURFACE('',#15272,4.91825);
#14273=CYLINDRICAL_SURFACE('',#15273,4.91825);
#14274=CYLINDRICAL_SURFACE('',#15274,4.91825);
#14275=CYLINDRICAL_SURFACE('',#15275,4.91825);
#14276=CYLINDRICAL_SURFACE('',#15276,4.91825);
#14277=CYLINDRICAL_SURFACE('',#15277,4.91825);
#14278=CYLINDRICAL_SURFACE('',#15278,4.91825);
#14279=CYLINDRICAL_SURFACE('',#15279,4.91825);
#14280=CYLINDRICAL_SURFACE('',#15280,4.91825);
#14281=CYLINDRICAL_SURFACE('',#15281,4.91825);
#14282=CYLINDRICAL_SURFACE('',#15282,4.91825);
#14283=CYLINDRICAL_SURFACE('',#15283,4.91825);
#14284=CYLINDRICAL_SURFACE('',#15284,4.91825);
#14285=CYLINDRICAL_SURFACE('',#15285,4.91825);
#14286=CYLINDRICAL_SURFACE('',#15286,4.91825);
#14287=CYLINDRICAL_SURFACE('',#15287,4.91825);
#14288=CYLINDRICAL_SURFACE('',#15288,4.91825);
#14289=CYLINDRICAL_SURFACE('',#15289,4.91825);
#14290=CYLINDRICAL_SURFACE('',#15290,4.91825);
#14291=CYLINDRICAL_SURFACE('',#15291,4.91825);
#14292=CYLINDRICAL_SURFACE('',#15292,4.91825);
#14293=CYLINDRICAL_SURFACE('',#15293,4.91825);
#14294=CYLINDRICAL_SURFACE('',#15294,4.91825);
#14295=CYLINDRICAL_SURFACE('',#15295,4.91825);
#14296=CYLINDRICAL_SURFACE('',#15296,4.91825);
#14297=CYLINDRICAL_SURFACE('',#15297,4.91825);
#14298=CYLINDRICAL_SURFACE('',#15298,4.91825);
#14299=CYLINDRICAL_SURFACE('',#15299,4.91825);
#14300=CYLINDRICAL_SURFACE('',#15300,4.91825);
#14301=CYLINDRICAL_SURFACE('',#15301,4.91825);
#14302=CYLINDRICAL_SURFACE('',#15302,4.91825);
#14303=CYLINDRICAL_SURFACE('',#15303,4.91825);
#14304=CYLINDRICAL_SURFACE('',#15304,4.91825);
#14305=CYLINDRICAL_SURFACE('',#15305,4.91825);
#14306=CYLINDRICAL_SURFACE('',#15306,4.91825);
#14307=CYLINDRICAL_SURFACE('',#15307,4.91825);
#14308=CYLINDRICAL_SURFACE('',#15308,4.91825);
#14309=CYLINDRICAL_SURFACE('',#15309,4.91825);
#14310=CYLINDRICAL_SURFACE('',#15310,4.91825);
#14311=CYLINDRICAL_SURFACE('',#15311,4.91825);
#14312=CYLINDRICAL_SURFACE('',#15312,4.91825);
#14313=CYLINDRICAL_SURFACE('',#15313,4.91825);
#14314=CYLINDRICAL_SURFACE('',#15314,4.91825);
#14315=CYLINDRICAL_SURFACE('',#15315,4.91825);
#14316=CYLINDRICAL_SURFACE('',#15316,4.91825);
#14317=CYLINDRICAL_SURFACE('',#15317,4.91825);
#14318=CYLINDRICAL_SURFACE('',#15318,4.91825);
#14319=CYLINDRICAL_SURFACE('',#15319,4.91825);
#14320=CYLINDRICAL_SURFACE('',#15320,4.91825);
#14321=CYLINDRICAL_SURFACE('',#15321,4.91825);
#14322=CYLINDRICAL_SURFACE('',#15322,4.91825);
#14323=CYLINDRICAL_SURFACE('',#15323,4.91825);
#14324=CYLINDRICAL_SURFACE('',#15324,4.91825);
#14325=CYLINDRICAL_SURFACE('',#15325,4.91825);
#14326=CYLINDRICAL_SURFACE('',#15326,4.91825);
#14327=CYLINDRICAL_SURFACE('',#15327,4.91825);
#14328=CYLINDRICAL_SURFACE('',#15328,4.91825);
#14329=CYLINDRICAL_SURFACE('',#15329,4.91825);
#14330=CYLINDRICAL_SURFACE('',#15330,4.91825);
#14331=CYLINDRICAL_SURFACE('',#15331,4.91825);
#14332=CYLINDRICAL_SURFACE('',#15332,4.91825);
#14333=CYLINDRICAL_SURFACE('',#15333,4.91825);
#14334=CYLINDRICAL_SURFACE('',#15334,4.91825);
#14335=CYLINDRICAL_SURFACE('',#15335,4.91825);
#14336=CYLINDRICAL_SURFACE('',#15336,4.91825);
#14337=CYLINDRICAL_SURFACE('',#15337,4.91825);
#14338=CYLINDRICAL_SURFACE('',#15338,4.91825);
#14339=CYLINDRICAL_SURFACE('',#15339,4.91825);
#14340=CYLINDRICAL_SURFACE('',#15340,4.91825);
#14341=CYLINDRICAL_SURFACE('',#15341,4.91825);
#14342=CYLINDRICAL_SURFACE('',#15342,4.91825);
#14343=CYLINDRICAL_SURFACE('',#15343,4.91825);
#14344=CYLINDRICAL_SURFACE('',#15344,4.91825);
#14345=CYLINDRICAL_SURFACE('',#15345,4.91825);
#14346=CYLINDRICAL_SURFACE('',#15346,4.91825);
#14347=CYLINDRICAL_SURFACE('',#15347,4.91825);
#14348=CYLINDRICAL_SURFACE('',#15348,4.91825);
#14349=CYLINDRICAL_SURFACE('',#15349,4.91825);
#14350=CYLINDRICAL_SURFACE('',#15350,4.91825);
#14351=CYLINDRICAL_SURFACE('',#15351,4.91825);
#14352=CYLINDRICAL_SURFACE('',#15352,4.91825);
#14353=CYLINDRICAL_SURFACE('',#15353,4.91825);
#14354=CYLINDRICAL_SURFACE('',#15354,4.91825);
#14355=CYLINDRICAL_SURFACE('',#15355,4.91825);
#14356=CYLINDRICAL_SURFACE('',#15356,4.91825);
#14357=CYLINDRICAL_SURFACE('',#15357,4.91825);
#14358=CYLINDRICAL_SURFACE('',#15358,4.91825);
#14359=CYLINDRICAL_SURFACE('',#15359,4.91825);
#14360=CYLINDRICAL_SURFACE('',#15360,4.91825);
#14361=CYLINDRICAL_SURFACE('',#15361,4.91825);
#14362=CYLINDRICAL_SURFACE('',#15362,4.91825);
#14363=CYLINDRICAL_SURFACE('',#15363,4.91825);
#14364=CYLINDRICAL_SURFACE('',#15364,4.91825);
#14365=CYLINDRICAL_SURFACE('',#15365,4.91825);
#14366=CYLINDRICAL_SURFACE('',#15366,4.91825);
#14367=CYLINDRICAL_SURFACE('',#15367,4.91825);
#14368=CYLINDRICAL_SURFACE('',#15368,4.91825);
#14369=CYLINDRICAL_SURFACE('',#15369,4.91825);
#14370=CYLINDRICAL_SURFACE('',#15370,4.91825);
#14371=CYLINDRICAL_SURFACE('',#15371,4.91825);
#14372=CYLINDRICAL_SURFACE('',#15372,4.91825);
#14373=CYLINDRICAL_SURFACE('',#15373,4.91825);
#14374=CYLINDRICAL_SURFACE('',#15374,5.91675);
#14375=CYLINDRICAL_SURFACE('',#15377,4.91825);
#14376=CYLINDRICAL_SURFACE('',#15382,9.);
#14377=CYLINDRICAL_SURFACE('',#15392,7.);
#14378=CYLINDRICAL_SURFACE('',#15398,7.55784864301595);
#14379=CYLINDRICAL_SURFACE('',#15405,15.2420394990918);
#14380=CYLINDRICAL_SURFACE('',#15412,7.55784864301595);
#14381=CYLINDRICAL_SURFACE('',#15423,6.50110764916953);
#14382=CYLINDRICAL_SURFACE('',#15425,15.2420394990918);
#14383=CYLINDRICAL_SURFACE('',#15427,15.2420394990918);
#14384=CYLINDRICAL_SURFACE('',#15429,7.55784864301595);
#14385=CYLINDRICAL_SURFACE('',#15438,6.50110764916953);
#14386=CYLINDRICAL_SURFACE('',#15441,15.2420394990918);
#14387=CYLINDRICAL_SURFACE('',#15443,15.2420394990918);
#14388=CYLINDRICAL_SURFACE('',#15447,4.91825);
#14389=CYLINDRICAL_SURFACE('',#15448,4.91825);
#14390=CYLINDRICAL_SURFACE('',#15449,4.91825);
#14391=CYLINDRICAL_SURFACE('',#15450,4.91825);
#14392=CYLINDRICAL_SURFACE('',#15451,4.91825);
#14393=CYLINDRICAL_SURFACE('',#15452,4.91825);
#14394=CYLINDRICAL_SURFACE('',#15453,4.91825);
#14395=CYLINDRICAL_SURFACE('',#15454,4.91825);
#14396=CYLINDRICAL_SURFACE('',#15455,4.91825);
#14397=CYLINDRICAL_SURFACE('',#15456,4.91825);
#14398=CYLINDRICAL_SURFACE('',#15457,4.91825);
#14399=CYLINDRICAL_SURFACE('',#15458,4.91825);
#14400=CYLINDRICAL_SURFACE('',#15459,4.91825);
#14401=CYLINDRICAL_SURFACE('',#15460,4.91825);
#14402=CYLINDRICAL_SURFACE('',#15461,4.91825);
#14403=CYLINDRICAL_SURFACE('',#15462,4.91825);
#14404=CYLINDRICAL_SURFACE('',#15463,4.91825);
#14405=CYLINDRICAL_SURFACE('',#15464,5.91675);
#14406=CYLINDRICAL_SURFACE('',#15465,5.91675);
#14407=CYLINDRICAL_SURFACE('',#15466,4.91825);
#14408=CYLINDRICAL_SURFACE('',#15467,5.91675);
#14409=CYLINDRICAL_SURFACE('',#15468,4.91825);
#14410=CYLINDRICAL_SURFACE('',#15469,15.2420394990918);
#14411=CYLINDRICAL_SURFACE('',#15475,6.50110764916953);
#14412=CYLINDRICAL_SURFACE('',#15479,15.2420394990918);
#14413=CYLINDRICAL_SURFACE('',#15488,7.55784864301595);
#14414=CYLINDRICAL_SURFACE('',#15490,6.50110764916953);
#14415=CYLINDRICAL_SURFACE('',#15494,15.2420394990918);
#14416=CYLINDRICAL_SURFACE('',#15498,15.2420394990918);
#14417=CYLINDRICAL_SURFACE('',#15504,7.55784864301595);
#14418=CYLINDRICAL_SURFACE('',#15511,15.2420394990918);
#14419=CYLINDRICAL_SURFACE('',#15518,7.55784864301595);
#14420=CYLINDRICAL_SURFACE('',#15527,6.50110764916953);
#14421=CYLINDRICAL_SURFACE('',#15530,15.2420394990918);
#14422=CYLINDRICAL_SURFACE('',#15532,15.2420394990918);
#14423=CYLINDRICAL_SURFACE('',#15535,7.55784864301595);
#14424=CYLINDRICAL_SURFACE('',#15546,6.50110764916953);
#14425=CYLINDRICAL_SURFACE('',#15548,15.2420394990918);
#14426=CYLINDRICAL_SURFACE('',#15550,15.2420394990918);
#14427=CYLINDRICAL_SURFACE('',#15553,10.);
#14428=CYLINDRICAL_SURFACE('',#15556,7.55784864301595);
#14429=CYLINDRICAL_SURFACE('',#15560,10.);
#14430=CYLINDRICAL_SURFACE('',#15564,3.);
#14431=CYLINDRICAL_SURFACE('',#15569,5.5);
#14432=CYLINDRICAL_SURFACE('',#15574,7.55784864301595);
#14433=CYLINDRICAL_SURFACE('',#15577,10.);
#14434=CYLINDRICAL_SURFACE('',#15584,7.55784864301595);
#14435=CYLINDRICAL_SURFACE('',#15588,10.);
#14436=CYLINDRICAL_SURFACE('',#15595,3.);
#14437=CYLINDRICAL_SURFACE('',#15599,5.5);
#14438=CYLINDRICAL_SURFACE('',#15604,7.55784864301595);
#14439=CYLINDRICAL_SURFACE('',#15609,4.91825);
#14440=CYLINDRICAL_SURFACE('',#15610,4.91825);
#14441=CYLINDRICAL_SURFACE('',#15611,4.91825);
#14442=CYLINDRICAL_SURFACE('',#15612,4.91825);
#14443=CYLINDRICAL_SURFACE('',#15613,4.91825);
#14444=CYLINDRICAL_SURFACE('',#15614,4.91825);
#14445=CYLINDRICAL_SURFACE('',#15615,4.91825);
#14446=CYLINDRICAL_SURFACE('',#15616,4.91825);
#14447=CYLINDRICAL_SURFACE('',#15617,4.91825);
#14448=CYLINDRICAL_SURFACE('',#15618,4.91825);
#14449=CYLINDRICAL_SURFACE('',#15619,4.91825);
#14450=CYLINDRICAL_SURFACE('',#15620,4.91825);
#14451=CYLINDRICAL_SURFACE('',#15621,4.91825);
#14452=CYLINDRICAL_SURFACE('',#15622,4.91825);
#14453=CYLINDRICAL_SURFACE('',#15623,4.91825);
#14454=CYLINDRICAL_SURFACE('',#15624,4.91825);
#14455=CYLINDRICAL_SURFACE('',#15625,4.91825);
#14456=CYLINDRICAL_SURFACE('',#15626,5.91675);
#14457=CYLINDRICAL_SURFACE('',#15627,5.91675);
#14458=CYLINDRICAL_SURFACE('',#15628,4.91825);
#14459=CYLINDRICAL_SURFACE('',#15629,4.91825);
#14460=CYLINDRICAL_SURFACE('',#15630,5.91675);
#14461=CYLINDRICAL_SURFACE('',#15631,15.2420394990918);
#14462=CYLINDRICAL_SURFACE('',#15637,6.50110764916953);
#14463=CYLINDRICAL_SURFACE('',#15641,15.2420394990918);
#14464=CYLINDRICAL_SURFACE('',#15650,7.55784864301595);
#14465=CYLINDRICAL_SURFACE('',#15652,6.50110764916953);
#14466=CYLINDRICAL_SURFACE('',#15656,15.2420394990918);
#14467=CYLINDRICAL_SURFACE('',#15660,15.2420394990918);
#14468=ADVANCED_FACE('',(#2110),#14094,.T.);
#14469=ADVANCED_FACE('',(#2111),#14095,.F.);
#14470=ADVANCED_FACE('',(#2112),#2024,.T.);
#14471=ADVANCED_FACE('',(#2113),#14096,.T.);
#14472=ADVANCED_FACE('',(#2114),#2025,.F.);
#14473=ADVANCED_FACE('',(#2115),#14097,.F.);
#14474=ADVANCED_FACE('',(#2116,#1978,#1979),#2026,.F.);
#14475=ADVANCED_FACE('',(#2117),#14098,.T.);
#14476=ADVANCED_FACE('',(#2118,#1980,#1981),#2027,.F.);
#14477=ADVANCED_FACE('',(#2119),#14099,.F.);
#14478=ADVANCED_FACE('',(#2120),#2028,.F.);
#14479=ADVANCED_FACE('',(#2121),#2029,.F.);
#14480=ADVANCED_FACE('',(#2122),#14100,.T.);
#14481=ADVANCED_FACE('',(#2123),#2030,.F.);
#14482=ADVANCED_FACE('',(#2124),#2031,.F.);
#14483=ADVANCED_FACE('',(#2125),#14101,.F.);
#14484=ADVANCED_FACE('',(#2126),#2032,.F.);
#14485=ADVANCED_FACE('',(#2127),#14102,.T.);
#14486=ADVANCED_FACE('',(#2128),#2033,.T.);
#14487=ADVANCED_FACE('',(#2129,#1982),#2034,.T.);
#14488=ADVANCED_FACE('',(#2130),#2035,.T.);
#14489=ADVANCED_FACE('',(#2131),#2036,.T.);
#14490=ADVANCED_FACE('',(#2132),#14103,.F.);
#14491=ADVANCED_FACE('',(#2133,#1983,#1984),#2037,.T.);
#14492=ADVANCED_FACE('',(#2134),#14104,.T.);
#14493=ADVANCED_FACE('',(#2135,#1985,#1986),#2038,.T.);
#14494=ADVANCED_FACE('',(#2136),#2039,.T.);
#14495=ADVANCED_FACE('',(#2137),#14105,.F.);
#14496=ADVANCED_FACE('',(#2138),#2040,.T.);
#14497=ADVANCED_FACE('',(#2139),#2041,.T.);
#14498=ADVANCED_FACE('',(#2140),#2042,.T.);
#14499=ADVANCED_FACE('',(#2141),#14106,.T.);
#14500=ADVANCED_FACE('',(#2142),#14107,.T.);
#14501=ADVANCED_FACE('',(#2143),#14108,.T.);
#14502=ADVANCED_FACE('',(#2144),#14109,.T.);
#14503=ADVANCED_FACE('',(#2145),#14110,.T.);
#14504=ADVANCED_FACE('',(#2146),#14111,.T.);
#14505=ADVANCED_FACE('',(#2147),#14112,.T.);
#14506=ADVANCED_FACE('',(#2148),#14113,.T.);
#14507=ADVANCED_FACE('',(#2149),#14114,.T.);
#14508=ADVANCED_FACE('',(#2150),#14115,.T.);
#14509=ADVANCED_FACE('',(#2151),#14116,.T.);
#14510=ADVANCED_FACE('',(#2152),#14117,.T.);
#14511=ADVANCED_FACE('',(#2153),#14118,.T.);
#14512=ADVANCED_FACE('',(#2154),#14119,.T.);
#14513=ADVANCED_FACE('',(#2155),#14120,.T.);
#14514=ADVANCED_FACE('',(#2156),#14121,.T.);
#14515=ADVANCED_FACE('',(#2157),#14122,.T.);
#14516=ADVANCED_FACE('',(#2158),#14123,.T.);
#14517=ADVANCED_FACE('',(#2159),#14124,.T.);
#14518=ADVANCED_FACE('',(#2160),#14125,.T.);
#14519=ADVANCED_FACE('',(#2161),#14126,.T.);
#14520=ADVANCED_FACE('',(#2162),#14127,.T.);
#14521=ADVANCED_FACE('',(#2163),#14128,.T.);
#14522=ADVANCED_FACE('',(#2164),#14129,.T.);
#14523=ADVANCED_FACE('',(#2165),#14130,.T.);
#14524=ADVANCED_FACE('',(#2166),#14131,.T.);
#14525=ADVANCED_FACE('',(#2167),#14132,.T.);
#14526=ADVANCED_FACE('',(#2168),#14133,.T.);
#14527=ADVANCED_FACE('',(#2169),#14134,.T.);
#14528=ADVANCED_FACE('',(#2170),#14135,.T.);
#14529=ADVANCED_FACE('',(#2171),#14136,.T.);
#14530=ADVANCED_FACE('',(#2172),#14137,.T.);
#14531=ADVANCED_FACE('',(#2173),#14138,.T.);
#14532=ADVANCED_FACE('',(#2174),#14139,.T.);
#14533=ADVANCED_FACE('',(#2175),#14140,.T.);
#14534=ADVANCED_FACE('',(#2176),#14141,.T.);
#14535=ADVANCED_FACE('',(#2177),#14142,.T.);
#14536=ADVANCED_FACE('',(#2178),#14143,.T.);
#14537=ADVANCED_FACE('',(#2179),#14144,.T.);
#14538=ADVANCED_FACE('',(#2180),#14145,.T.);
#14539=ADVANCED_FACE('',(#2181),#14146,.T.);
#14540=ADVANCED_FACE('',(#2182),#14147,.T.);
#14541=ADVANCED_FACE('',(#2183),#14148,.T.);
#14542=ADVANCED_FACE('',(#2184),#14149,.T.);
#14543=ADVANCED_FACE('',(#2185),#14150,.T.);
#14544=ADVANCED_FACE('',(#2186),#14151,.T.);
#14545=ADVANCED_FACE('',(#2187),#14152,.T.);
#14546=ADVANCED_FACE('',(#2188),#14153,.T.);
#14547=ADVANCED_FACE('',(#2189),#14154,.T.);
#14548=ADVANCED_FACE('',(#2190),#14155,.T.);
#14549=ADVANCED_FACE('',(#2191),#14156,.T.);
#14550=ADVANCED_FACE('',(#2192),#14157,.T.);
#14551=ADVANCED_FACE('',(#2193),#14158,.T.);
#14552=ADVANCED_FACE('',(#2194),#14159,.T.);
#14553=ADVANCED_FACE('',(#2195),#14160,.T.);
#14554=ADVANCED_FACE('',(#2196),#14161,.T.);
#14555=ADVANCED_FACE('',(#2197),#14162,.T.);
#14556=ADVANCED_FACE('',(#2198),#14163,.T.);
#14557=ADVANCED_FACE('',(#2199),#14164,.T.);
#14558=ADVANCED_FACE('',(#2200),#14165,.T.);
#14559=ADVANCED_FACE('',(#2201),#14166,.T.);
#14560=ADVANCED_FACE('',(#2202),#14167,.T.);
#14561=ADVANCED_FACE('',(#2203),#14168,.T.);
#14562=ADVANCED_FACE('',(#2204),#14169,.T.);
#14563=ADVANCED_FACE('',(#2205),#14170,.T.);
#14564=ADVANCED_FACE('',(#2206),#14171,.T.);
#14565=ADVANCED_FACE('',(#2207),#14172,.T.);
#14566=ADVANCED_FACE('',(#2208),#14173,.T.);
#14567=ADVANCED_FACE('',(#2209),#14174,.T.);
#14568=ADVANCED_FACE('',(#2210),#14175,.T.);
#14569=ADVANCED_FACE('',(#2211),#14176,.T.);
#14570=ADVANCED_FACE('',(#2212),#14177,.T.);
#14571=ADVANCED_FACE('',(#2213),#14178,.T.);
#14572=ADVANCED_FACE('',(#2214),#14179,.T.);
#14573=ADVANCED_FACE('',(#2215),#14180,.T.);
#14574=ADVANCED_FACE('',(#2216),#14181,.T.);
#14575=ADVANCED_FACE('',(#2217),#14182,.T.);
#14576=ADVANCED_FACE('',(#2218),#14183,.T.);
#14577=ADVANCED_FACE('',(#2219),#14184,.T.);
#14578=ADVANCED_FACE('',(#2220),#14185,.T.);
#14579=ADVANCED_FACE('',(#2221),#14186,.T.);
#14580=ADVANCED_FACE('',(#2222),#14187,.T.);
#14581=ADVANCED_FACE('',(#2223),#14188,.T.);
#14582=ADVANCED_FACE('',(#2224),#14189,.T.);
#14583=ADVANCED_FACE('',(#2225),#14190,.T.);
#14584=ADVANCED_FACE('',(#2226),#14191,.T.);
#14585=ADVANCED_FACE('',(#2227),#14192,.T.);
#14586=ADVANCED_FACE('',(#2228),#14193,.T.);
#14587=ADVANCED_FACE('',(#2229),#14194,.T.);
#14588=ADVANCED_FACE('',(#2230),#14195,.T.);
#14589=ADVANCED_FACE('',(#2231),#14196,.T.);
#14590=ADVANCED_FACE('',(#2232),#14197,.T.);
#14591=ADVANCED_FACE('',(#2233),#14198,.T.);
#14592=ADVANCED_FACE('',(#2234),#14199,.T.);
#14593=ADVANCED_FACE('',(#2235),#14200,.T.);
#14594=ADVANCED_FACE('',(#2236),#14201,.T.);
#14595=ADVANCED_FACE('',(#2237),#14202,.T.);
#14596=ADVANCED_FACE('',(#2238),#14203,.T.);
#14597=ADVANCED_FACE('',(#2239),#14204,.T.);
#14598=ADVANCED_FACE('',(#2240),#14205,.T.);
#14599=ADVANCED_FACE('',(#2241),#14206,.T.);
#14600=ADVANCED_FACE('',(#2242),#14207,.T.);
#14601=ADVANCED_FACE('',(#2243),#14208,.T.);
#14602=ADVANCED_FACE('',(#2244),#14209,.T.);
#14603=ADVANCED_FACE('',(#2245),#14210,.T.);
#14604=ADVANCED_FACE('',(#2246),#14211,.T.);
#14605=ADVANCED_FACE('',(#2247),#14212,.T.);
#14606=ADVANCED_FACE('',(#2248),#14213,.T.);
#14607=ADVANCED_FACE('',(#2249),#14214,.T.);
#14608=ADVANCED_FACE('',(#2250),#14215,.T.);
#14609=ADVANCED_FACE('',(#2251),#14216,.T.);
#14610=ADVANCED_FACE('',(#2252),#14217,.T.);
#14611=ADVANCED_FACE('',(#2253),#14218,.T.);
#14612=ADVANCED_FACE('',(#2254),#14219,.T.);
#14613=ADVANCED_FACE('',(#2255),#14220,.T.);
#14614=ADVANCED_FACE('',(#2256),#14221,.T.);
#14615=ADVANCED_FACE('',(#2257),#14222,.T.);
#14616=ADVANCED_FACE('',(#2258),#14223,.T.);
#14617=ADVANCED_FACE('',(#2259),#14224,.T.);
#14618=ADVANCED_FACE('',(#2260),#14225,.T.);
#14619=ADVANCED_FACE('',(#2261),#14226,.T.);
#14620=ADVANCED_FACE('',(#2262),#14227,.T.);
#14621=ADVANCED_FACE('',(#2263),#14228,.T.);
#14622=ADVANCED_FACE('',(#2264),#14229,.T.);
#14623=ADVANCED_FACE('',(#2265),#14230,.T.);
#14624=ADVANCED_FACE('',(#2266),#14231,.T.);
#14625=ADVANCED_FACE('',(#2267),#14232,.T.);
#14626=ADVANCED_FACE('',(#2268),#14233,.T.);
#14627=ADVANCED_FACE('',(#2269),#14234,.T.);
#14628=ADVANCED_FACE('',(#2270),#14235,.T.);
#14629=ADVANCED_FACE('',(#2271),#14236,.T.);
#14630=ADVANCED_FACE('',(#2272),#14237,.T.);
#14631=ADVANCED_FACE('',(#2273),#14238,.T.);
#14632=ADVANCED_FACE('',(#2274),#14239,.T.);
#14633=ADVANCED_FACE('',(#2275),#14240,.T.);
#14634=ADVANCED_FACE('',(#2276),#14241,.T.);
#14635=ADVANCED_FACE('',(#2277),#14242,.T.);
#14636=ADVANCED_FACE('',(#2278),#14243,.T.);
#14637=ADVANCED_FACE('',(#2279),#14244,.T.);
#14638=ADVANCED_FACE('',(#2280),#14245,.T.);
#14639=ADVANCED_FACE('',(#2281),#14246,.T.);
#14640=ADVANCED_FACE('',(#2282),#14247,.T.);
#14641=ADVANCED_FACE('',(#2283),#14248,.T.);
#14642=ADVANCED_FACE('',(#2284),#14249,.T.);
#14643=ADVANCED_FACE('',(#2285),#14250,.T.);
#14644=ADVANCED_FACE('',(#2286),#14251,.T.);
#14645=ADVANCED_FACE('',(#2287),#14252,.T.);
#14646=ADVANCED_FACE('',(#2288),#14253,.T.);
#14647=ADVANCED_FACE('',(#2289),#14254,.T.);
#14648=ADVANCED_FACE('',(#2290),#14255,.T.);
#14649=ADVANCED_FACE('',(#2291),#14256,.T.);
#14650=ADVANCED_FACE('',(#2292),#14257,.T.);
#14651=ADVANCED_FACE('',(#2293),#14258,.T.);
#14652=ADVANCED_FACE('',(#2294),#14259,.T.);
#14653=ADVANCED_FACE('',(#2295),#14260,.T.);
#14654=ADVANCED_FACE('',(#2296),#14261,.T.);
#14655=ADVANCED_FACE('',(#2297),#14262,.T.);
#14656=ADVANCED_FACE('',(#2298),#14263,.T.);
#14657=ADVANCED_FACE('',(#2299),#14264,.T.);
#14658=ADVANCED_FACE('',(#2300),#14265,.T.);
#14659=ADVANCED_FACE('',(#2301),#14266,.T.);
#14660=ADVANCED_FACE('',(#2302),#14267,.T.);
#14661=ADVANCED_FACE('',(#2303),#14268,.T.);
#14662=ADVANCED_FACE('',(#2304),#14269,.T.);
#14663=ADVANCED_FACE('',(#2305),#14270,.T.);
#14664=ADVANCED_FACE('',(#2306),#14271,.T.);
#14665=ADVANCED_FACE('',(#2307),#14272,.T.);
#14666=ADVANCED_FACE('',(#2308),#14273,.T.);
#14667=ADVANCED_FACE('',(#2309),#14274,.T.);
#14668=ADVANCED_FACE('',(#2310),#14275,.T.);
#14669=ADVANCED_FACE('',(#2311),#14276,.T.);
#14670=ADVANCED_FACE('',(#2312),#14277,.T.);
#14671=ADVANCED_FACE('',(#2313),#14278,.T.);
#14672=ADVANCED_FACE('',(#2314),#14279,.T.);
#14673=ADVANCED_FACE('',(#2315),#14280,.T.);
#14674=ADVANCED_FACE('',(#2316),#14281,.T.);
#14675=ADVANCED_FACE('',(#2317),#14282,.T.);
#14676=ADVANCED_FACE('',(#2318),#14283,.T.);
#14677=ADVANCED_FACE('',(#2319),#14284,.T.);
#14678=ADVANCED_FACE('',(#2320),#14285,.T.);
#14679=ADVANCED_FACE('',(#2321),#14286,.T.);
#14680=ADVANCED_FACE('',(#2322),#14287,.T.);
#14681=ADVANCED_FACE('',(#2323),#14288,.T.);
#14682=ADVANCED_FACE('',(#2324),#14289,.T.);
#14683=ADVANCED_FACE('',(#2325),#14290,.T.);
#14684=ADVANCED_FACE('',(#2326),#14291,.T.);
#14685=ADVANCED_FACE('',(#2327),#14292,.T.);
#14686=ADVANCED_FACE('',(#2328),#14293,.T.);
#14687=ADVANCED_FACE('',(#2329),#14294,.T.);
#14688=ADVANCED_FACE('',(#2330),#14295,.T.);
#14689=ADVANCED_FACE('',(#2331),#14296,.T.);
#14690=ADVANCED_FACE('',(#2332),#14297,.T.);
#14691=ADVANCED_FACE('',(#2333),#14298,.T.);
#14692=ADVANCED_FACE('',(#2334),#14299,.T.);
#14693=ADVANCED_FACE('',(#2335),#14300,.T.);
#14694=ADVANCED_FACE('',(#2336),#14301,.T.);
#14695=ADVANCED_FACE('',(#2337),#14302,.T.);
#14696=ADVANCED_FACE('',(#2338),#14303,.T.);
#14697=ADVANCED_FACE('',(#2339),#14304,.T.);
#14698=ADVANCED_FACE('',(#2340),#14305,.T.);
#14699=ADVANCED_FACE('',(#2341),#14306,.T.);
#14700=ADVANCED_FACE('',(#2342),#14307,.T.);
#14701=ADVANCED_FACE('',(#2343),#14308,.T.);
#14702=ADVANCED_FACE('',(#2344),#14309,.T.);
#14703=ADVANCED_FACE('',(#2345),#14310,.T.);
#14704=ADVANCED_FACE('',(#2346),#14311,.T.);
#14705=ADVANCED_FACE('',(#2347),#14312,.T.);
#14706=ADVANCED_FACE('',(#2348),#14313,.T.);
#14707=ADVANCED_FACE('',(#2349),#14314,.T.);
#14708=ADVANCED_FACE('',(#2350),#14315,.T.);
#14709=ADVANCED_FACE('',(#2351),#14316,.T.);
#14710=ADVANCED_FACE('',(#2352),#14317,.T.);
#14711=ADVANCED_FACE('',(#2353),#14318,.T.);
#14712=ADVANCED_FACE('',(#2354),#14319,.T.);
#14713=ADVANCED_FACE('',(#2355),#14320,.T.);
#14714=ADVANCED_FACE('',(#2356),#14321,.T.);
#14715=ADVANCED_FACE('',(#2357),#14322,.T.);
#14716=ADVANCED_FACE('',(#2358),#14323,.T.);
#14717=ADVANCED_FACE('',(#2359),#14324,.T.);
#14718=ADVANCED_FACE('',(#2360),#14325,.T.);
#14719=ADVANCED_FACE('',(#2361),#14326,.T.);
#14720=ADVANCED_FACE('',(#2362),#14327,.T.);
#14721=ADVANCED_FACE('',(#2363),#14328,.T.);
#14722=ADVANCED_FACE('',(#2364),#14329,.T.);
#14723=ADVANCED_FACE('',(#2365),#14330,.T.);
#14724=ADVANCED_FACE('',(#2366),#14331,.T.);
#14725=ADVANCED_FACE('',(#2367),#14332,.T.);
#14726=ADVANCED_FACE('',(#2368),#14333,.T.);
#14727=ADVANCED_FACE('',(#2369),#14334,.T.);
#14728=ADVANCED_FACE('',(#2370),#14335,.T.);
#14729=ADVANCED_FACE('',(#2371),#14336,.T.);
#14730=ADVANCED_FACE('',(#2372),#14337,.T.);
#14731=ADVANCED_FACE('',(#2373),#14338,.T.);
#14732=ADVANCED_FACE('',(#2374),#14339,.T.);
#14733=ADVANCED_FACE('',(#2375),#14340,.T.);
#14734=ADVANCED_FACE('',(#2376),#14341,.T.);
#14735=ADVANCED_FACE('',(#2377),#14342,.T.);
#14736=ADVANCED_FACE('',(#2378),#14343,.T.);
#14737=ADVANCED_FACE('',(#2379),#14344,.T.);
#14738=ADVANCED_FACE('',(#2380),#14345,.T.);
#14739=ADVANCED_FACE('',(#2381),#14346,.T.);
#14740=ADVANCED_FACE('',(#2382),#14347,.T.);
#14741=ADVANCED_FACE('',(#2383),#14348,.T.);
#14742=ADVANCED_FACE('',(#2384),#14349,.T.);
#14743=ADVANCED_FACE('',(#2385),#14350,.T.);
#14744=ADVANCED_FACE('',(#2386),#14351,.T.);
#14745=ADVANCED_FACE('',(#2387),#14352,.T.);
#14746=ADVANCED_FACE('',(#2388),#14353,.T.);
#14747=ADVANCED_FACE('',(#2389),#14354,.T.);
#14748=ADVANCED_FACE('',(#2390),#14355,.T.);
#14749=ADVANCED_FACE('',(#2391),#14356,.T.);
#14750=ADVANCED_FACE('',(#2392),#14357,.T.);
#14751=ADVANCED_FACE('',(#2393),#14358,.T.);
#14752=ADVANCED_FACE('',(#2394),#14359,.T.);
#14753=ADVANCED_FACE('',(#2395),#14360,.T.);
#14754=ADVANCED_FACE('',(#2396),#14361,.T.);
#14755=ADVANCED_FACE('',(#2397),#14362,.T.);
#14756=ADVANCED_FACE('',(#2398),#14363,.T.);
#14757=ADVANCED_FACE('',(#2399),#14364,.T.);
#14758=ADVANCED_FACE('',(#2400),#14365,.T.);
#14759=ADVANCED_FACE('',(#2401),#14366,.T.);
#14760=ADVANCED_FACE('',(#2402),#14367,.T.);
#14761=ADVANCED_FACE('',(#2403),#14368,.T.);
#14762=ADVANCED_FACE('',(#2404),#14369,.T.);
#14763=ADVANCED_FACE('',(#2405),#14370,.T.);
#14764=ADVANCED_FACE('',(#2406),#14371,.T.);
#14765=ADVANCED_FACE('',(#2407),#14372,.T.);
#14766=ADVANCED_FACE('',(#2408),#14373,.T.);
#14767=ADVANCED_FACE('',(#2409),#14374,.T.);
#14768=ADVANCED_FACE('',(#2410),#14375,.T.);
#14769=ADVANCED_FACE('',(#2411,#1987),#2043,.T.);
#14770=ADVANCED_FACE('',(#2412),#14376,.T.);
#14771=ADVANCED_FACE('',(#2413,#1988),#2044,.F.);
#14772=ADVANCED_FACE('',(#2414),#2045,.F.);
#14773=ADVANCED_FACE('',(#2415),#2046,.T.);
#14774=ADVANCED_FACE('',(#2416),#2047,.F.);
#14775=ADVANCED_FACE('',(#2417),#2048,.T.);
#14776=ADVANCED_FACE('',(#2418),#14377,.T.);
#14777=ADVANCED_FACE('',(#2419),#2049,.T.);
#14778=ADVANCED_FACE('',(#2420),#47,.F.);
#14779=ADVANCED_FACE('',(#2421),#48,.F.);
#14780=ADVANCED_FACE('',(#2422),#2050,.F.);
#14781=ADVANCED_FACE('',(#2423),#14378,.F.);
#14782=ADVANCED_FACE('',(#2424),#14379,.T.);
#14783=ADVANCED_FACE('',(#2425),#14380,.F.);
#14784=ADVANCED_FACE('',(#2426,#1989,#1990),#2051,.F.);
#14785=ADVANCED_FACE('',(#2427,#1991),#2052,.T.);
#14786=ADVANCED_FACE('',(#2428),#14381,.F.);
#14787=ADVANCED_FACE('',(#2429),#2053,.T.);
#14788=ADVANCED_FACE('',(#2430),#14382,.T.);
#14789=ADVANCED_FACE('',(#2431),#2054,.T.);
#14790=ADVANCED_FACE('',(#2432),#14383,.T.);
#14791=ADVANCED_FACE('',(#2433),#2055,.T.);
#14792=ADVANCED_FACE('',(#2434),#14384,.F.);
#14793=ADVANCED_FACE('',(#2435),#2056,.F.);
#14794=ADVANCED_FACE('',(#2436,#1992),#2057,.F.);
#14795=ADVANCED_FACE('',(#2437),#2058,.F.);
#14796=ADVANCED_FACE('',(#2438),#14385,.F.);
#14797=ADVANCED_FACE('',(#2439),#2059,.F.);
#14798=ADVANCED_FACE('',(#2440),#14386,.T.);
#14799=ADVANCED_FACE('',(#2441),#14387,.T.);
#14800=ADVANCED_FACE('',(#2442,#1993,#1994),#2060,.T.);
#14801=ADVANCED_FACE('',(#2443),#14388,.F.);
#14802=ADVANCED_FACE('',(#2444),#14389,.F.);
#14803=ADVANCED_FACE('',(#2445),#14390,.F.);
#14804=ADVANCED_FACE('',(#2446),#14391,.F.);
#14805=ADVANCED_FACE('',(#2447),#14392,.F.);
#14806=ADVANCED_FACE('',(#2448),#14393,.F.);
#14807=ADVANCED_FACE('',(#2449),#14394,.F.);
#14808=ADVANCED_FACE('',(#2450),#14395,.F.);
#14809=ADVANCED_FACE('',(#2451),#14396,.F.);
#14810=ADVANCED_FACE('',(#2452),#14397,.F.);
#14811=ADVANCED_FACE('',(#2453),#14398,.F.);
#14812=ADVANCED_FACE('',(#2454),#14399,.F.);
#14813=ADVANCED_FACE('',(#2455),#14400,.F.);
#14814=ADVANCED_FACE('',(#2456),#14401,.F.);
#14815=ADVANCED_FACE('',(#2457),#14402,.F.);
#14816=ADVANCED_FACE('',(#2458),#14403,.F.);
#14817=ADVANCED_FACE('',(#2459),#14404,.F.);
#14818=ADVANCED_FACE('',(#2460),#49,.T.);
#14819=ADVANCED_FACE('',(#2461),#50,.T.);
#14820=ADVANCED_FACE('',(#2462),#14405,.F.);
#14821=ADVANCED_FACE('',(#2463),#14406,.F.);
#14822=ADVANCED_FACE('',(#2464),#51,.T.);
#14823=ADVANCED_FACE('',(#2465),#14407,.F.);
#14824=ADVANCED_FACE('',(#2466),#14408,.F.);
#14825=ADVANCED_FACE('',(#2467),#14409,.F.);
#14826=ADVANCED_FACE('',(#2468),#52,.T.);
#14827=ADVANCED_FACE('',(#2469,#1995),#14410,.T.);
#14828=ADVANCED_FACE('',(#2470),#2061,.T.);
#14829=ADVANCED_FACE('',(#2471),#2062,.F.);
#14830=ADVANCED_FACE('',(#2472),#14411,.F.);
#14831=ADVANCED_FACE('',(#2473),#2063,.F.);
#14832=ADVANCED_FACE('',(#2474),#14412,.T.);
#14833=ADVANCED_FACE('',(#2475),#2064,.F.);
#14834=ADVANCED_FACE('',(#2476,#1996),#2065,.F.);
#14835=ADVANCED_FACE('',(#2477,#1997,#1998),#2066,.T.);
#14836=ADVANCED_FACE('',(#2478),#14413,.F.);
#14837=ADVANCED_FACE('',(#2479),#14414,.F.);
#14838=ADVANCED_FACE('',(#2480),#2067,.T.);
#14839=ADVANCED_FACE('',(#2481),#14415,.T.);
#14840=ADVANCED_FACE('',(#2482),#2068,.T.);
#14841=ADVANCED_FACE('',(#2483),#14416,.T.);
#14842=ADVANCED_FACE('',(#2484,#1999),#2069,.T.);
#14843=ADVANCED_FACE('',(#2485,#2000,#2001),#2070,.F.);
#14844=ADVANCED_FACE('',(#2486),#14417,.F.);
#14845=ADVANCED_FACE('',(#2487),#14418,.T.);
#14846=ADVANCED_FACE('',(#2488),#14419,.F.);
#14847=ADVANCED_FACE('',(#2489),#2071,.F.);
#14848=ADVANCED_FACE('',(#2490,#2002),#2072,.F.);
#14849=ADVANCED_FACE('',(#2491),#2073,.F.);
#14850=ADVANCED_FACE('',(#2492),#14420,.F.);
#14851=ADVANCED_FACE('',(#2493),#2074,.F.);
#14852=ADVANCED_FACE('',(#2494),#14421,.T.);
#14853=ADVANCED_FACE('',(#2495),#14422,.T.);
#14854=ADVANCED_FACE('',(#2496,#2003,#2004),#2075,.T.);
#14855=ADVANCED_FACE('',(#2497),#14423,.F.);
#14856=ADVANCED_FACE('',(#2498,#2005,#2006),#2076,.F.);
#14857=ADVANCED_FACE('',(#2499,#2007),#2077,.T.);
#14858=ADVANCED_FACE('',(#2500),#14424,.F.);
#14859=ADVANCED_FACE('',(#2501),#2078,.T.);
#14860=ADVANCED_FACE('',(#2502),#14425,.T.);
#14861=ADVANCED_FACE('',(#2503),#2079,.T.);
#14862=ADVANCED_FACE('',(#2504),#14426,.T.);
#14863=ADVANCED_FACE('',(#2505),#2080,.T.);
#14864=ADVANCED_FACE('',(#2506),#14427,.T.);
#14865=ADVANCED_FACE('',(#2507),#14428,.F.);
#14866=ADVANCED_FACE('',(#2508),#2081,.F.);
#14867=ADVANCED_FACE('',(#2509),#14429,.T.);
#14868=ADVANCED_FACE('',(#2510),#2082,.T.);
#14869=ADVANCED_FACE('',(#2511),#14430,.F.);
#14870=ADVANCED_FACE('',(#2512,#2008,#2009),#2083,.T.);
#14871=ADVANCED_FACE('',(#2513),#14431,.T.);
#14872=ADVANCED_FACE('',(#2514,#2010,#2011),#2084,.T.);
#14873=ADVANCED_FACE('',(#2515),#14432,.F.);
#14874=ADVANCED_FACE('',(#2516),#2085,.T.);
#14875=ADVANCED_FACE('',(#2517),#2086,.T.);
#14876=ADVANCED_FACE('',(#2518),#14433,.T.);
#14877=ADVANCED_FACE('',(#2519),#2087,.T.);
#14878=ADVANCED_FACE('',(#2520),#2088,.T.);
#14879=ADVANCED_FACE('',(#2521),#14434,.F.);
#14880=ADVANCED_FACE('',(#2522),#2089,.T.);
#14881=ADVANCED_FACE('',(#2523),#14435,.T.);
#14882=ADVANCED_FACE('',(#2524),#2090,.F.);
#14883=ADVANCED_FACE('',(#2525,#2012),#2091,.F.);
#14884=ADVANCED_FACE('',(#2526),#2092,.F.);
#14885=ADVANCED_FACE('',(#2527),#2093,.F.);
#14886=ADVANCED_FACE('',(#2528),#14436,.F.);
#14887=ADVANCED_FACE('',(#2529,#2013,#2014),#2094,.F.);
#14888=ADVANCED_FACE('',(#2530),#14437,.T.);
#14889=ADVANCED_FACE('',(#2531,#2015,#2016),#2095,.F.);
#14890=ADVANCED_FACE('',(#2532),#2096,.F.);
#14891=ADVANCED_FACE('',(#2533),#14438,.F.);
#14892=ADVANCED_FACE('',(#2534),#2097,.F.);
#14893=ADVANCED_FACE('',(#2535),#2098,.F.);
#14894=ADVANCED_FACE('',(#2536),#2099,.F.);
#14895=ADVANCED_FACE('',(#2537),#14439,.F.);
#14896=ADVANCED_FACE('',(#2538),#14440,.F.);
#14897=ADVANCED_FACE('',(#2539),#14441,.F.);
#14898=ADVANCED_FACE('',(#2540),#14442,.F.);
#14899=ADVANCED_FACE('',(#2541),#14443,.F.);
#14900=ADVANCED_FACE('',(#2542),#14444,.F.);
#14901=ADVANCED_FACE('',(#2543),#14445,.F.);
#14902=ADVANCED_FACE('',(#2544),#14446,.F.);
#14903=ADVANCED_FACE('',(#2545),#14447,.F.);
#14904=ADVANCED_FACE('',(#2546),#14448,.F.);
#14905=ADVANCED_FACE('',(#2547),#14449,.F.);
#14906=ADVANCED_FACE('',(#2548),#14450,.F.);
#14907=ADVANCED_FACE('',(#2549),#14451,.F.);
#14908=ADVANCED_FACE('',(#2550),#14452,.F.);
#14909=ADVANCED_FACE('',(#2551),#14453,.F.);
#14910=ADVANCED_FACE('',(#2552),#14454,.F.);
#14911=ADVANCED_FACE('',(#2553),#14455,.F.);
#14912=ADVANCED_FACE('',(#2554),#53,.T.);
#14913=ADVANCED_FACE('',(#2555),#54,.T.);
#14914=ADVANCED_FACE('',(#2556),#14456,.F.);
#14915=ADVANCED_FACE('',(#2557),#14457,.F.);
#14916=ADVANCED_FACE('',(#2558),#14458,.F.);
#14917=ADVANCED_FACE('',(#2559),#14459,.F.);
#14918=ADVANCED_FACE('',(#2560),#55,.T.);
#14919=ADVANCED_FACE('',(#2561),#14460,.F.);
#14920=ADVANCED_FACE('',(#2562),#56,.T.);
#14921=ADVANCED_FACE('',(#2563,#2017),#14461,.T.);
#14922=ADVANCED_FACE('',(#2564),#2100,.F.);
#14923=ADVANCED_FACE('',(#2565),#2101,.T.);
#14924=ADVANCED_FACE('',(#2566),#14462,.F.);
#14925=ADVANCED_FACE('',(#2567),#2102,.T.);
#14926=ADVANCED_FACE('',(#2568),#14463,.T.);
#14927=ADVANCED_FACE('',(#2569),#2103,.T.);
#14928=ADVANCED_FACE('',(#2570,#2018),#2104,.T.);
#14929=ADVANCED_FACE('',(#2571,#2019,#2020),#2105,.F.);
#14930=ADVANCED_FACE('',(#2572),#14464,.F.);
#14931=ADVANCED_FACE('',(#2573),#14465,.F.);
#14932=ADVANCED_FACE('',(#2574),#2106,.F.);
#14933=ADVANCED_FACE('',(#2575),#14466,.T.);
#14934=ADVANCED_FACE('',(#2576),#2107,.F.);
#14935=ADVANCED_FACE('',(#2577),#14467,.T.);
#14936=ADVANCED_FACE('',(#2578,#2021),#2108,.F.);
#14937=ADVANCED_FACE('',(#2579,#2022,#2023),#2109,.T.);
#14938=CLOSED_SHELL('',(#14468,#14469,#14470,#14471,#14472,#14473,#14474,
#14475,#14476,#14477,#14478,#14479,#14480,#14481,#14482,#14483,#14484,#14485,
#14486,#14487,#14488,#14489,#14490,#14491,#14492,#14493,#14494,#14495,#14496,
#14497,#14498));
#14939=CLOSED_SHELL('',(#14499,#14500,#14501,#14502,#14503,#14504,#14505,
#14506,#14507,#14508,#14509,#14510,#14511,#14512,#14513,#14514,#14515,#14516,
#14517,#14518,#14519,#14520,#14521,#14522,#14523,#14524,#14525,#14526,#14527,
#14528,#14529,#14530,#14531,#14532,#14533,#14534,#14535,#14536,#14537,#14538,
#14539,#14540,#14541,#14542,#14543,#14544,#14545,#14546,#14547,#14548,#14549,
#14550,#14551,#14552,#14553,#14554,#14555,#14556,#14557,#14558,#14559,#14560,
#14561,#14562,#14563,#14564,#14565,#14566,#14567,#14568,#14569,#14570,#14571,
#14572,#14573,#14574,#14575,#14576,#14577,#14578,#14579,#14580,#14581,#14582,
#14583,#14584,#14585,#14586,#14587,#14588,#14589,#14590,#14591,#14592,#14593,
#14594,#14595,#14596,#14597,#14598,#14599,#14600,#14601,#14602,#14603,#14604,
#14605,#14606,#14607,#14608,#14609,#14610,#14611,#14612,#14613,#14614,#14615,
#14616,#14617,#14618,#14619,#14620,#14621,#14622,#14623,#14624,#14625,#14626,
#14627,#14628,#14629,#14630,#14631,#14632,#14633,#14634,#14635,#14636,#14637,
#14638,#14639,#14640,#14641,#14642,#14643,#14644,#14645,#14646,#14647,#14648,
#14649,#14650,#14651,#14652,#14653,#14654,#14655,#14656,#14657,#14658,#14659,
#14660,#14661,#14662,#14663,#14664,#14665,#14666,#14667,#14668,#14669,#14670,
#14671,#14672,#14673,#14674,#14675,#14676,#14677,#14678,#14679,#14680,#14681,
#14682,#14683,#14684,#14685,#14686,#14687,#14688,#14689,#14690,#14691,#14692,
#14693,#14694,#14695,#14696,#14697,#14698,#14699,#14700,#14701,#14702,#14703,
#14704,#14705,#14706,#14707,#14708,#14709,#14710,#14711,#14712,#14713,#14714,
#14715,#14716,#14717,#14718,#14719,#14720,#14721,#14722,#14723,#14724,#14725,
#14726,#14727,#14728,#14729,#14730,#14731,#14732,#14733,#14734,#14735,#14736,
#14737,#14738,#14739,#14740,#14741,#14742,#14743,#14744,#14745,#14746,#14747,
#14748,#14749,#14750,#14751,#14752,#14753,#14754,#14755,#14756,#14757,#14758,
#14759,#14760,#14761,#14762,#14763,#14764,#14765,#14766,#14767,#14768,#14769,
#14770,#14771,#14772,#14773,#14774,#14775,#14776,#14777,#14778,#14779,#14780));
#14940=CLOSED_SHELL('',(#14781,#14782,#14783,#14784,#14785,#14786,#14787,
#14788,#14789,#14790,#14791,#14792,#14793,#14794,#14795,#14796,#14797,#14798,
#14799,#14800));
#14941=CLOSED_SHELL('',(#14801,#14802,#14803,#14804,#14805,#14806,#14807,
#14808,#14809,#14810,#14811,#14812,#14813,#14814,#14815,#14816,#14817,#14818,
#14819,#14820,#14821,#14822,#14823,#14824,#14825,#14826,#14827,#14828,#14829));
#14942=CLOSED_SHELL('',(#14830,#14831,#14832,#14833,#14834,#14835,#14836,
#14837,#14838,#14839,#14840,#14841,#14842,#14843));
#14943=CLOSED_SHELL('',(#14844,#14845,#14846,#14847,#14848,#14849,#14850,
#14851,#14852,#14853,#14854,#14855,#14856,#14857,#14858,#14859,#14860,#14861,
#14862,#14863));
#14944=CLOSED_SHELL('',(#14864,#14865,#14866,#14867,#14868,#14869,#14870,
#14871,#14872,#14873,#14874,#14875,#14876,#14877,#14878,#14879,#14880,#14881,
#14882,#14883,#14884,#14885,#14886,#14887,#14888,#14889,#14890,#14891,#14892,
#14893,#14894));
#14945=CLOSED_SHELL('',(#14895,#14896,#14897,#14898,#14899,#14900,#14901,
#14902,#14903,#14904,#14905,#14906,#14907,#14908,#14909,#14910,#14911,#14912,
#14913,#14914,#14915,#14916,#14917,#14918,#14919,#14920,#14921,#14922,#14923));
#14946=CLOSED_SHELL('',(#14924,#14925,#14926,#14927,#14928,#14929,#14930,
#14931,#14932,#14933,#14934,#14935,#14936,#14937));
#14947=DERIVED_UNIT_ELEMENT(#14965,1.);
#14948=DERIVED_UNIT_ELEMENT(#279268,-3.);
#14949=DERIVED_UNIT_ELEMENT(#14965,1.);
#14950=DERIVED_UNIT_ELEMENT(#279268,-3.);
#14951=DERIVED_UNIT_ELEMENT(#14965,1.);
#14952=DERIVED_UNIT_ELEMENT(#279268,-3.);
#14953=DERIVED_UNIT_ELEMENT(#14965,1.);
#14954=DERIVED_UNIT_ELEMENT(#279268,-3.);
#14955=DERIVED_UNIT_ELEMENT(#14965,1.);
#14956=DERIVED_UNIT_ELEMENT(#279268,-3.);
#14957=DERIVED_UNIT_ELEMENT(#14965,1.);
#14958=DERIVED_UNIT_ELEMENT(#279268,-3.);
#14959=DERIVED_UNIT_ELEMENT(#14965,1.);
#14960=DERIVED_UNIT_ELEMENT(#279268,-3.);
#14961=DERIVED_UNIT_ELEMENT(#14965,1.);
#14962=DERIVED_UNIT_ELEMENT(#279268,-3.);
#14963=DERIVED_UNIT_ELEMENT(#14965,1.);
#14964=DERIVED_UNIT_ELEMENT(#279268,-3.);
#14965=(
MASS_UNIT()
NAMED_UNIT(*)
SI_UNIT(.KILO.,.GRAM.)
);
#14966=DERIVED_UNIT((#14947,#14948));
#14967=DERIVED_UNIT((#14949,#14950));
#14968=DERIVED_UNIT((#14951,#14952));
#14969=DERIVED_UNIT((#14953,#14954));
#14970=DERIVED_UNIT((#14955,#14956));
#14971=DERIVED_UNIT((#14957,#14958));
#14972=DERIVED_UNIT((#14959,#14960));
#14973=DERIVED_UNIT((#14961,#14962));
#14974=DERIVED_UNIT((#14963,#14964));
#14975=MEASURE_REPRESENTATION_ITEM('density measure',
POSITIVE_RATIO_MEASURE(7850.),#14966);
#14976=MEASURE_REPRESENTATION_ITEM('density measure',
POSITIVE_RATIO_MEASURE(7850.),#14967);
#14977=MEASURE_REPRESENTATION_ITEM('density measure',
POSITIVE_RATIO_MEASURE(7850.),#14968);
#14978=MEASURE_REPRESENTATION_ITEM('density measure',
POSITIVE_RATIO_MEASURE(7850.),#14969);
#14979=MEASURE_REPRESENTATION_ITEM('density measure',
POSITIVE_RATIO_MEASURE(7850.),#14970);
#14980=MEASURE_REPRESENTATION_ITEM('density measure',
POSITIVE_RATIO_MEASURE(7850.),#14971);
#14981=MEASURE_REPRESENTATION_ITEM('density measure',
POSITIVE_RATIO_MEASURE(7850.),#14972);
#14982=MEASURE_REPRESENTATION_ITEM('density measure',
POSITIVE_RATIO_MEASURE(7850.),#14973);
#14983=MEASURE_REPRESENTATION_ITEM('density measure',
POSITIVE_RATIO_MEASURE(7850.),#14974);
#14984=PROPERTY_DEFINITION_REPRESENTATION(#15029,#15002);
#14985=PROPERTY_DEFINITION_REPRESENTATION(#15030,#15003);
#14986=PROPERTY_DEFINITION_REPRESENTATION(#15031,#15004);
#14987=PROPERTY_DEFINITION_REPRESENTATION(#15032,#15005);
#14988=PROPERTY_DEFINITION_REPRESENTATION(#15033,#15006);
#14989=PROPERTY_DEFINITION_REPRESENTATION(#15034,#15007);
#14990=PROPERTY_DEFINITION_REPRESENTATION(#15035,#15008);
#14991=PROPERTY_DEFINITION_REPRESENTATION(#15036,#15009);
#14992=PROPERTY_DEFINITION_REPRESENTATION(#15037,#15010);
#14993=PROPERTY_DEFINITION_REPRESENTATION(#15038,#15011);
#14994=PROPERTY_DEFINITION_REPRESENTATION(#15039,#15012);
#14995=PROPERTY_DEFINITION_REPRESENTATION(#15040,#15013);
#14996=PROPERTY_DEFINITION_REPRESENTATION(#15041,#15014);
#14997=PROPERTY_DEFINITION_REPRESENTATION(#15042,#15015);
#14998=PROPERTY_DEFINITION_REPRESENTATION(#15043,#15016);
#14999=PROPERTY_DEFINITION_REPRESENTATION(#15044,#15017);
#15000=PROPERTY_DEFINITION_REPRESENTATION(#15045,#15018);
#15001=PROPERTY_DEFINITION_REPRESENTATION(#15046,#15019);
#15002=REPRESENTATION('material name',(#15020),#279257);
#15003=REPRESENTATION('density',(#14975),#279257);
#15004=REPRESENTATION('material name',(#15021),#279258);
#15005=REPRESENTATION('density',(#14976),#279258);
#15006=REPRESENTATION('material name',(#15022),#279259);
#15007=REPRESENTATION('density',(#14977),#279259);
#15008=REPRESENTATION('material name',(#15023),#279260);
#15009=REPRESENTATION('density',(#14978),#279260);
#15010=REPRESENTATION('material name',(#15024),#279261);
#15011=REPRESENTATION('density',(#14979),#279261);
#15012=REPRESENTATION('material name',(#15025),#279262);
#15013=REPRESENTATION('density',(#14980),#279262);
#15014=REPRESENTATION('material name',(#15026),#279263);
#15015=REPRESENTATION('density',(#14981),#279263);
#15016=REPRESENTATION('material name',(#15027),#279264);
#15017=REPRESENTATION('density',(#14982),#279264);
#15018=REPRESENTATION('material name',(#15028),#279265);
#15019=REPRESENTATION('density',(#14983),#279265);
#15020=DESCRIPTIVE_REPRESENTATION_ITEM('Steel','Steel');
#15021=DESCRIPTIVE_REPRESENTATION_ITEM('Steel','Steel');
#15022=DESCRIPTIVE_REPRESENTATION_ITEM('Steel','Steel');
#15023=DESCRIPTIVE_REPRESENTATION_ITEM('Steel','Steel');
#15024=DESCRIPTIVE_REPRESENTATION_ITEM('Steel','Steel');
#15025=DESCRIPTIVE_REPRESENTATION_ITEM('Steel','Steel');
#15026=DESCRIPTIVE_REPRESENTATION_ITEM('Steel','Steel');
#15027=DESCRIPTIVE_REPRESENTATION_ITEM('Steel','Steel');
#15028=DESCRIPTIVE_REPRESENTATION_ITEM('Steel','Steel');
#15029=PROPERTY_DEFINITION('material property','material name',#279312);
#15030=PROPERTY_DEFINITION('material property','density of part',#279312);
#15031=PROPERTY_DEFINITION('material property','material name',#279313);
#15032=PROPERTY_DEFINITION('material property','density of part',#279313);
#15033=PROPERTY_DEFINITION('material property','material name',#279314);
#15034=PROPERTY_DEFINITION('material property','density of part',#279314);
#15035=PROPERTY_DEFINITION('material property','material name',#279315);
#15036=PROPERTY_DEFINITION('material property','density of part',#279315);
#15037=PROPERTY_DEFINITION('material property','material name',#279316);
#15038=PROPERTY_DEFINITION('material property','density of part',#279316);
#15039=PROPERTY_DEFINITION('material property','material name',#279317);
#15040=PROPERTY_DEFINITION('material property','density of part',#279317);
#15041=PROPERTY_DEFINITION('material property','material name',#279318);
#15042=PROPERTY_DEFINITION('material property','density of part',#279318);
#15043=PROPERTY_DEFINITION('material property','material name',#279319);
#15044=PROPERTY_DEFINITION('material property','density of part',#279319);
#15045=PROPERTY_DEFINITION('material property','material name',#279320);
#15046=PROPERTY_DEFINITION('material property','density of part',#279320);
#15047=AXIS2_PLACEMENT_3D('',#17456,#15674,#15675);
#15048=AXIS2_PLACEMENT_3D('',#17457,#15676,#15677);
#15049=AXIS2_PLACEMENT_3D('',#17458,#15678,#15679);
#15050=AXIS2_PLACEMENT_3D('',#17461,#15680,#15681);
#15051=AXIS2_PLACEMENT_3D('',#17465,#15683,#15684);
#15052=AXIS2_PLACEMENT_3D('',#17467,#15686,#15687);
#15053=AXIS2_PLACEMENT_3D('',#17469,#15688,#15689);
#15054=AXIS2_PLACEMENT_3D('',#17472,#15691,#15692);
#15055=AXIS2_PLACEMENT_3D('',#17473,#15693,#15694);
#15056=AXIS2_PLACEMENT_3D('',#17482,#15699,#15700);
#15057=AXIS2_PLACEMENT_3D('',#17485,#15701,#15702);
#15058=AXIS2_PLACEMENT_3D('',#17489,#15704,#15705);
#15059=AXIS2_PLACEMENT_3D('',#17491,#15707,#15708);
#15060=AXIS2_PLACEMENT_3D('',#17494,#15711,#15712);
#15061=AXIS2_PLACEMENT_3D('',#17499,#15714,#15715);
#15062=AXIS2_PLACEMENT_3D('',#17502,#15717,#15718);
#15063=AXIS2_PLACEMENT_3D('',#17503,#15719,#15720);
#15064=AXIS2_PLACEMENT_3D('',#17511,#15725,#15726);
#15065=AXIS2_PLACEMENT_3D('',#17512,#15727,#15728);
#15066=AXIS2_PLACEMENT_3D('',#17515,#15729,#15730);
#15067=AXIS2_PLACEMENT_3D('',#17519,#15732,#15733);
#15068=AXIS2_PLACEMENT_3D('',#17521,#15735,#15736);
#15069=AXIS2_PLACEMENT_3D('',#17529,#15741,#15742);
#15070=AXIS2_PLACEMENT_3D('',#17530,#15743,#15744);
#15071=AXIS2_PLACEMENT_3D('',#17532,#15746,#15747);
#15072=AXIS2_PLACEMENT_3D('',#17534,#15749,#15750);
#15073=AXIS2_PLACEMENT_3D('',#17536,#15752,#15753);
#15074=AXIS2_PLACEMENT_3D('',#17539,#15754,#15755);
#15075=AXIS2_PLACEMENT_3D('',#17543,#15757,#15758);
#15076=AXIS2_PLACEMENT_3D('',#17545,#15760,#15761);
#15077=AXIS2_PLACEMENT_3D('',#17548,#15764,#15765);
#15078=AXIS2_PLACEMENT_3D('',#17551,#15766,#15767);
#15079=AXIS2_PLACEMENT_3D('',#17559,#15771,#15772);
#15080=AXIS2_PLACEMENT_3D('',#17562,#15775,#15776);
#15081=AXIS2_PLACEMENT_3D('',#17564,#15777,#15778);
#15082=AXIS2_PLACEMENT_3D('',#17567,#15780,#15781);
#15083=AXIS2_PLACEMENT_3D('',#17568,#15782,#15783);
#15084=AXIS2_PLACEMENT_3D('',#17574,#15787,#15788);
#15085=AXIS2_PLACEMENT_3D('',#17577,#15789,#15790);
#15086=AXIS2_PLACEMENT_3D('',#17581,#15792,#15793);
#15087=AXIS2_PLACEMENT_3D('',#17583,#15795,#15796);
#15088=AXIS2_PLACEMENT_3D('',#17586,#15799,#15800);
#15089=AXIS2_PLACEMENT_3D('',#17591,#15804,#15805);
#15090=AXIS2_PLACEMENT_3D('',#17593,#15807,#15808);
#15091=AXIS2_PLACEMENT_3D('',#17594,#15809,#15810);
#15092=AXIS2_PLACEMENT_3D('',#17598,#15812,#15813);
#15093=AXIS2_PLACEMENT_3D('',#17600,#15815,#15816);
#15094=AXIS2_PLACEMENT_3D('',#17607,#15820,#15821);
#15095=AXIS2_PLACEMENT_3D('',#17608,#15822,#15823);
#15096=AXIS2_PLACEMENT_3D('',#17610,#15824,#15825);
#15097=AXIS2_PLACEMENT_3D('',#17612,#15827,#15828);
#15098=AXIS2_PLACEMENT_3D('',#17619,#15832,#15833);
#15099=AXIS2_PLACEMENT_3D('',#17620,#15834,#15835);
#15100=AXIS2_PLACEMENT_3D('',#17623,#15838,#15839);
#15101=AXIS2_PLACEMENT_3D('',#17625,#15841,#15842);
#15102=AXIS2_PLACEMENT_3D('',#17627,#15844,#15845);
#15103=AXIS2_PLACEMENT_3D('',#17628,#15846,#15847);
#15104=AXIS2_PLACEMENT_3D('',#17629,#15848,#15849);
#15105=AXIS2_PLACEMENT_3D('',#17630,#15850,#15851);
#15106=AXIS2_PLACEMENT_3D('',#17823,#15853,#15854);
#15107=AXIS2_PLACEMENT_3D('',#17960,#15855,#15856);
#15108=AXIS2_PLACEMENT_3D('',#18426,#15858,#15859);
#15109=AXIS2_PLACEMENT_3D('',#18892,#15861,#15862);
#15110=AXIS2_PLACEMENT_3D('',#19361,#15864,#15865);
#15111=AXIS2_PLACEMENT_3D('',#19827,#15867,#15868);
#15112=AXIS2_PLACEMENT_3D('',#20293,#15870,#15871);
#15113=AXIS2_PLACEMENT_3D('',#20759,#15873,#15874);
#15114=AXIS2_PLACEMENT_3D('',#21222,#15876,#15877);
#15115=AXIS2_PLACEMENT_3D('',#21688,#15879,#15880);
#15116=AXIS2_PLACEMENT_3D('',#21944,#15882,#15883);
#15117=AXIS2_PLACEMENT_3D('',#22197,#15885,#15886);
#15118=AXIS2_PLACEMENT_3D('',#22657,#15888,#15889);
#15119=AXIS2_PLACEMENT_3D('',#23123,#15891,#15892);
#15120=AXIS2_PLACEMENT_3D('',#23589,#15894,#15895);
#15121=AXIS2_PLACEMENT_3D('',#24052,#15897,#15898);
#15122=AXIS2_PLACEMENT_3D('',#24518,#15900,#15901);
#15123=AXIS2_PLACEMENT_3D('',#24984,#15903,#15904);
#15124=AXIS2_PLACEMENT_3D('',#25450,#15906,#15907);
#15125=AXIS2_PLACEMENT_3D('',#25919,#15909,#15910);
#15126=AXIS2_PLACEMENT_3D('',#26385,#15912,#15913);
#15127=AXIS2_PLACEMENT_3D('',#26851,#15915,#15916);
#15128=AXIS2_PLACEMENT_3D('',#27314,#15918,#15919);
#15129=AXIS2_PLACEMENT_3D('',#27786,#15921,#15922);
#15130=AXIS2_PLACEMENT_3D('',#28252,#15924,#15925);
#15131=AXIS2_PLACEMENT_3D('',#28718,#15927,#15928);
#15132=AXIS2_PLACEMENT_3D('',#29190,#15930,#15931);
#15133=AXIS2_PLACEMENT_3D('',#29656,#15933,#15934);
#15134=AXIS2_PLACEMENT_3D('',#30119,#15936,#15937);
#15135=AXIS2_PLACEMENT_3D('',#30582,#15939,#15940);
#15136=AXIS2_PLACEMENT_3D('',#31054,#15942,#15943);
#15137=AXIS2_PLACEMENT_3D('',#31520,#15945,#15946);
#15138=AXIS2_PLACEMENT_3D('',#31983,#15948,#15949);
#15139=AXIS2_PLACEMENT_3D('',#32452,#15951,#15952);
#15140=AXIS2_PLACEMENT_3D('',#32918,#15954,#15955);
#15141=AXIS2_PLACEMENT_3D('',#33381,#15957,#15958);
#15142=AXIS2_PLACEMENT_3D('',#33844,#15960,#15961);
#15143=AXIS2_PLACEMENT_3D('',#34313,#15963,#15964);
#15144=AXIS2_PLACEMENT_3D('',#34779,#15966,#15967);
#15145=AXIS2_PLACEMENT_3D('',#35242,#15969,#15970);
#15146=AXIS2_PLACEMENT_3D('',#35708,#15972,#15973);
#15147=AXIS2_PLACEMENT_3D('',#36174,#15975,#15976);
#15148=AXIS2_PLACEMENT_3D('',#36637,#15978,#15979);
#15149=AXIS2_PLACEMENT_3D('',#37100,#15981,#15982);
#15150=AXIS2_PLACEMENT_3D('',#37569,#15984,#15985);
#15151=AXIS2_PLACEMENT_3D('',#38035,#15987,#15988);
#15152=AXIS2_PLACEMENT_3D('',#38498,#15990,#15991);
#15153=AXIS2_PLACEMENT_3D('',#38964,#15993,#15994);
#15154=AXIS2_PLACEMENT_3D('',#39430,#15996,#15997);
#15155=AXIS2_PLACEMENT_3D('',#39893,#15999,#16000);
#15156=AXIS2_PLACEMENT_3D('',#40362,#16002,#16003);
#15157=AXIS2_PLACEMENT_3D('',#40831,#16005,#16006);
#15158=AXIS2_PLACEMENT_3D('',#41297,#16008,#16009);
#15159=AXIS2_PLACEMENT_3D('',#41760,#16011,#16012);
#15160=AXIS2_PLACEMENT_3D('',#42226,#16014,#16015);
#15161=AXIS2_PLACEMENT_3D('',#42692,#16017,#16018);
#15162=AXIS2_PLACEMENT_3D('',#43155,#16020,#16021);
#15163=AXIS2_PLACEMENT_3D('',#43627,#16023,#16024);
#15164=AXIS2_PLACEMENT_3D('',#44096,#16026,#16027);
#15165=AXIS2_PLACEMENT_3D('',#44559,#16029,#16030);
#15166=AXIS2_PLACEMENT_3D('',#45022,#16032,#16033);
#15167=AXIS2_PLACEMENT_3D('',#45488,#16035,#16036);
#15168=AXIS2_PLACEMENT_3D('',#45954,#16038,#16039);
#15169=AXIS2_PLACEMENT_3D('',#46414,#16041,#16042);
#15170=AXIS2_PLACEMENT_3D('',#46883,#16044,#16045);
#15171=AXIS2_PLACEMENT_3D('',#47352,#16047,#16048);
#15172=AXIS2_PLACEMENT_3D('',#47815,#16050,#16051);
#15173=AXIS2_PLACEMENT_3D('',#48281,#16053,#16054);
#15174=AXIS2_PLACEMENT_3D('',#48744,#16056,#16057);
#15175=AXIS2_PLACEMENT_3D('',#49210,#16059,#16060);
#15176=AXIS2_PLACEMENT_3D('',#49673,#16062,#16063);
#15177=AXIS2_PLACEMENT_3D('',#49932,#16065,#16066);
#15178=AXIS2_PLACEMENT_3D('',#50185,#16068,#16069);
#15179=AXIS2_PLACEMENT_3D('',#50645,#16071,#16072);
#15180=AXIS2_PLACEMENT_3D('',#51111,#16074,#16075);
#15181=AXIS2_PLACEMENT_3D('',#51574,#16077,#16078);
#15182=AXIS2_PLACEMENT_3D('',#52040,#16080,#16081);
#15183=AXIS2_PLACEMENT_3D('',#52506,#16083,#16084);
#15184=AXIS2_PLACEMENT_3D('',#52975,#16086,#16087);
#15185=AXIS2_PLACEMENT_3D('',#53444,#16089,#16090);
#15186=AXIS2_PLACEMENT_3D('',#53907,#16092,#16093);
#15187=AXIS2_PLACEMENT_3D('',#54373,#16095,#16096);
#15188=AXIS2_PLACEMENT_3D('',#54836,#16098,#16099);
#15189=AXIS2_PLACEMENT_3D('',#55302,#16101,#16102);
#15190=AXIS2_PLACEMENT_3D('',#55768,#16104,#16105);
#15191=AXIS2_PLACEMENT_3D('',#56237,#16107,#16108);
#15192=AXIS2_PLACEMENT_3D('',#56706,#16110,#16111);
#15193=AXIS2_PLACEMENT_3D('',#57169,#16113,#16114);
#15194=AXIS2_PLACEMENT_3D('',#57635,#16116,#16117);
#15195=AXIS2_PLACEMENT_3D('',#58098,#16119,#16120);
#15196=AXIS2_PLACEMENT_3D('',#58567,#16122,#16123);
#15197=AXIS2_PLACEMENT_3D('',#59033,#16125,#16126);
#15198=AXIS2_PLACEMENT_3D('',#59499,#16128,#16129);
#15199=AXIS2_PLACEMENT_3D('',#59968,#16131,#16132);
#15200=AXIS2_PLACEMENT_3D('',#60434,#16134,#16135);
#15201=AXIS2_PLACEMENT_3D('',#60897,#16137,#16138);
#15202=AXIS2_PLACEMENT_3D('',#61360,#16140,#16141);
#15203=AXIS2_PLACEMENT_3D('',#61829,#16143,#16144);
#15204=AXIS2_PLACEMENT_3D('',#62295,#16146,#16147);
#15205=AXIS2_PLACEMENT_3D('',#62761,#16149,#16150);
#15206=AXIS2_PLACEMENT_3D('',#63233,#16152,#16153);
#15207=AXIS2_PLACEMENT_3D('',#63699,#16155,#16156);
#15208=AXIS2_PLACEMENT_3D('',#64162,#16158,#16159);
#15209=AXIS2_PLACEMENT_3D('',#64625,#16161,#16162);
#15210=AXIS2_PLACEMENT_3D('',#65091,#16164,#16165);
#15211=AXIS2_PLACEMENT_3D('',#65557,#16167,#16168);
#15212=AXIS2_PLACEMENT_3D('',#66023,#16170,#16171);
#15213=AXIS2_PLACEMENT_3D('',#66492,#16173,#16174);
#15214=AXIS2_PLACEMENT_3D('',#66958,#16176,#16177);
#15215=AXIS2_PLACEMENT_3D('',#67421,#16179,#16180);
#15216=AXIS2_PLACEMENT_3D('',#67884,#16182,#16183);
#15217=AXIS2_PLACEMENT_3D('',#68350,#16185,#16186);
#15218=AXIS2_PLACEMENT_3D('',#68816,#16188,#16189);
#15219=AXIS2_PLACEMENT_3D('',#69282,#16191,#16192);
#15220=AXIS2_PLACEMENT_3D('',#69751,#16194,#16195);
#15221=AXIS2_PLACEMENT_3D('',#70217,#16197,#16198);
#15222=AXIS2_PLACEMENT_3D('',#70680,#16200,#16201);
#15223=AXIS2_PLACEMENT_3D('',#71149,#16203,#16204);
#15224=AXIS2_PLACEMENT_3D('',#71615,#16206,#16207);
#15225=AXIS2_PLACEMENT_3D('',#72078,#16209,#16210);
#15226=AXIS2_PLACEMENT_3D('',#72544,#16212,#16213);
#15227=AXIS2_PLACEMENT_3D('',#73013,#16215,#16216);
#15228=AXIS2_PLACEMENT_3D('',#73479,#16218,#16219);
#15229=AXIS2_PLACEMENT_3D('',#73942,#16221,#16222);
#15230=AXIS2_PLACEMENT_3D('',#74411,#16224,#16225);
#15231=AXIS2_PLACEMENT_3D('',#74877,#16227,#16228);
#15232=AXIS2_PLACEMENT_3D('',#75340,#16230,#16231);
#15233=AXIS2_PLACEMENT_3D('',#75806,#16233,#16234);
#15234=AXIS2_PLACEMENT_3D('',#76275,#16236,#16237);
#15235=AXIS2_PLACEMENT_3D('',#76741,#16239,#16240);
#15236=AXIS2_PLACEMENT_3D('',#77201,#16242,#16243);
#15237=AXIS2_PLACEMENT_3D('',#77667,#16245,#16246);
#15238=AXIS2_PLACEMENT_3D('',#78133,#16248,#16249);
#15239=AXIS2_PLACEMENT_3D('',#78596,#16251,#16252);
#15240=AXIS2_PLACEMENT_3D('',#79062,#16254,#16255);
#15241=AXIS2_PLACEMENT_3D('',#79531,#16257,#16258);
#15242=AXIS2_PLACEMENT_3D('',#79997,#16260,#16261);
#15243=AXIS2_PLACEMENT_3D('',#80457,#16263,#16264);
#15244=AXIS2_PLACEMENT_3D('',#80923,#16266,#16267);
#15245=AXIS2_PLACEMENT_3D('',#81389,#16269,#16270);
#15246=AXIS2_PLACEMENT_3D('',#81852,#16272,#16273);
#15247=AXIS2_PLACEMENT_3D('',#82111,#16275,#16276);
#15248=AXIS2_PLACEMENT_3D('',#82362,#16278,#16279);
#15249=AXIS2_PLACEMENT_3D('',#82822,#16281,#16282);
#15250=AXIS2_PLACEMENT_3D('',#83282,#16284,#16285);
#15251=AXIS2_PLACEMENT_3D('',#83748,#16287,#16288);
#15252=AXIS2_PLACEMENT_3D('',#84214,#16290,#16291);
#15253=AXIS2_PLACEMENT_3D('',#84677,#16293,#16294);
#15254=AXIS2_PLACEMENT_3D('',#85146,#16296,#16297);
#15255=AXIS2_PLACEMENT_3D('',#85612,#16299,#16300);
#15256=AXIS2_PLACEMENT_3D('',#86081,#16302,#16303);
#15257=AXIS2_PLACEMENT_3D('',#86547,#16305,#16306);
#15258=AXIS2_PLACEMENT_3D('',#87013,#16308,#16309);
#15259=AXIS2_PLACEMENT_3D('',#87479,#16311,#16312);
#15260=AXIS2_PLACEMENT_3D('',#87942,#16314,#16315);
#15261=AXIS2_PLACEMENT_3D('',#88411,#16317,#16318);
#15262=AXIS2_PLACEMENT_3D('',#88877,#16320,#16321);
#15263=AXIS2_PLACEMENT_3D('',#89346,#16323,#16324);
#15264=AXIS2_PLACEMENT_3D('',#89812,#16326,#16327);
#15265=AXIS2_PLACEMENT_3D('',#90275,#16329,#16330);
#15266=AXIS2_PLACEMENT_3D('',#90741,#16332,#16333);
#15267=AXIS2_PLACEMENT_3D('',#91204,#16335,#16336);
#15268=AXIS2_PLACEMENT_3D('',#91673,#16338,#16339);
#15269=AXIS2_PLACEMENT_3D('',#92139,#16341,#16342);
#15270=AXIS2_PLACEMENT_3D('',#92608,#16344,#16345);
#15271=AXIS2_PLACEMENT_3D('',#93074,#16347,#16348);
#15272=AXIS2_PLACEMENT_3D('',#93537,#16350,#16351);
#15273=AXIS2_PLACEMENT_3D('',#94003,#16353,#16354);
#15274=AXIS2_PLACEMENT_3D('',#94469,#16356,#16357);
#15275=AXIS2_PLACEMENT_3D('',#94938,#16359,#16360);
#15276=AXIS2_PLACEMENT_3D('',#95404,#16362,#16363);
#15277=AXIS2_PLACEMENT_3D('',#95867,#16365,#16366);
#15278=AXIS2_PLACEMENT_3D('',#96333,#16368,#16369);
#15279=AXIS2_PLACEMENT_3D('',#96796,#16371,#16372);
#15280=AXIS2_PLACEMENT_3D('',#97262,#16374,#16375);
#15281=AXIS2_PLACEMENT_3D('',#97728,#16377,#16378);
#15282=AXIS2_PLACEMENT_3D('',#97987,#16380,#16381);
#15283=AXIS2_PLACEMENT_3D('',#98447,#16383,#16384);
#15284=AXIS2_PLACEMENT_3D('',#98913,#16386,#16387);
#15285=AXIS2_PLACEMENT_3D('',#99379,#16389,#16390);
#15286=AXIS2_PLACEMENT_3D('',#99842,#16392,#16393);
#15287=AXIS2_PLACEMENT_3D('',#100308,#16395,#16396);
#15288=AXIS2_PLACEMENT_3D('',#100774,#16398,#16399);
#15289=AXIS2_PLACEMENT_3D('',#101240,#16401,#16402);
#15290=AXIS2_PLACEMENT_3D('',#101709,#16404,#16405);
#15291=AXIS2_PLACEMENT_3D('',#102175,#16407,#16408);
#15292=AXIS2_PLACEMENT_3D('',#102638,#16410,#16411);
#15293=AXIS2_PLACEMENT_3D('',#103101,#16413,#16414);
#15294=AXIS2_PLACEMENT_3D('',#103573,#16416,#16417);
#15295=AXIS2_PLACEMENT_3D('',#104039,#16419,#16420);
#15296=AXIS2_PLACEMENT_3D('',#104505,#16422,#16423);
#15297=AXIS2_PLACEMENT_3D('',#104977,#16425,#16426);
#15298=AXIS2_PLACEMENT_3D('',#105443,#16428,#16429);
#15299=AXIS2_PLACEMENT_3D('',#105906,#16431,#16432);
#15300=AXIS2_PLACEMENT_3D('',#106369,#16434,#16435);
#15301=AXIS2_PLACEMENT_3D('',#106841,#16437,#16438);
#15302=AXIS2_PLACEMENT_3D('',#107307,#16440,#16441);
#15303=AXIS2_PLACEMENT_3D('',#107770,#16443,#16444);
#15304=AXIS2_PLACEMENT_3D('',#108239,#16446,#16447);
#15305=AXIS2_PLACEMENT_3D('',#108705,#16449,#16450);
#15306=AXIS2_PLACEMENT_3D('',#109168,#16452,#16453);
#15307=AXIS2_PLACEMENT_3D('',#109631,#16455,#16456);
#15308=AXIS2_PLACEMENT_3D('',#109890,#16458,#16459);
#15309=AXIS2_PLACEMENT_3D('',#110350,#16461,#16462);
#15310=AXIS2_PLACEMENT_3D('',#110813,#16464,#16465);
#15311=AXIS2_PLACEMENT_3D('',#111279,#16467,#16468);
#15312=AXIS2_PLACEMENT_3D('',#111745,#16470,#16471);
#15313=AXIS2_PLACEMENT_3D('',#112208,#16473,#16474);
#15314=AXIS2_PLACEMENT_3D('',#112671,#16476,#16477);
#15315=AXIS2_PLACEMENT_3D('',#113140,#16479,#16480);
#15316=AXIS2_PLACEMENT_3D('',#113606,#16482,#16483);
#15317=AXIS2_PLACEMENT_3D('',#114069,#16485,#16486);
#15318=AXIS2_PLACEMENT_3D('',#114535,#16488,#16489);
#15319=AXIS2_PLACEMENT_3D('',#115001,#16491,#16492);
#15320=AXIS2_PLACEMENT_3D('',#115464,#16494,#16495);
#15321=AXIS2_PLACEMENT_3D('',#115933,#16497,#16498);
#15322=AXIS2_PLACEMENT_3D('',#116402,#16500,#16501);
#15323=AXIS2_PLACEMENT_3D('',#116868,#16503,#16504);
#15324=AXIS2_PLACEMENT_3D('',#117331,#16506,#16507);
#15325=AXIS2_PLACEMENT_3D('',#117797,#16509,#16510);
#15326=AXIS2_PLACEMENT_3D('',#118263,#16512,#16513);
#15327=AXIS2_PLACEMENT_3D('',#118726,#16515,#16516);
#15328=AXIS2_PLACEMENT_3D('',#119198,#16518,#16519);
#15329=AXIS2_PLACEMENT_3D('',#119667,#16521,#16522);
#15330=AXIS2_PLACEMENT_3D('',#120130,#16524,#16525);
#15331=AXIS2_PLACEMENT_3D('',#120593,#16527,#16528);
#15332=AXIS2_PLACEMENT_3D('',#121056,#16530,#16531);
#15333=AXIS2_PLACEMENT_3D('',#121522,#16533,#16534);
#15334=AXIS2_PLACEMENT_3D('',#121982,#16536,#16537);
#15335=AXIS2_PLACEMENT_3D('',#122451,#16539,#16540);
#15336=AXIS2_PLACEMENT_3D('',#122920,#16542,#16543);
#15337=AXIS2_PLACEMENT_3D('',#123383,#16545,#16546);
#15338=AXIS2_PLACEMENT_3D('',#123849,#16548,#16549);
#15339=AXIS2_PLACEMENT_3D('',#124312,#16551,#16552);
#15340=AXIS2_PLACEMENT_3D('',#124778,#16554,#16555);
#15341=AXIS2_PLACEMENT_3D('',#125241,#16557,#16558);
#15342=AXIS2_PLACEMENT_3D('',#125500,#16560,#16561);
#15343=AXIS2_PLACEMENT_3D('',#125753,#16563,#16564);
#15344=AXIS2_PLACEMENT_3D('',#126213,#16566,#16567);
#15345=AXIS2_PLACEMENT_3D('',#126679,#16569,#16570);
#15346=AXIS2_PLACEMENT_3D('',#127142,#16572,#16573);
#15347=AXIS2_PLACEMENT_3D('',#127608,#16575,#16576);
#15348=AXIS2_PLACEMENT_3D('',#128074,#16578,#16579);
#15349=AXIS2_PLACEMENT_3D('',#128543,#16581,#16582);
#15350=AXIS2_PLACEMENT_3D('',#129012,#16584,#16585);
#15351=AXIS2_PLACEMENT_3D('',#129475,#16587,#16588);
#15352=AXIS2_PLACEMENT_3D('',#129941,#16590,#16591);
#15353=AXIS2_PLACEMENT_3D('',#130404,#16593,#16594);
#15354=AXIS2_PLACEMENT_3D('',#130870,#16596,#16597);
#15355=AXIS2_PLACEMENT_3D('',#131336,#16599,#16600);
#15356=AXIS2_PLACEMENT_3D('',#131805,#16602,#16603);
#15357=AXIS2_PLACEMENT_3D('',#132274,#16605,#16606);
#15358=AXIS2_PLACEMENT_3D('',#132737,#16608,#16609);
#15359=AXIS2_PLACEMENT_3D('',#133203,#16611,#16612);
#15360=AXIS2_PLACEMENT_3D('',#133666,#16614,#16615);
#15361=AXIS2_PLACEMENT_3D('',#134135,#16617,#16618);
#15362=AXIS2_PLACEMENT_3D('',#134601,#16620,#16621);
#15363=AXIS2_PLACEMENT_3D('',#135067,#16623,#16624);
#15364=AXIS2_PLACEMENT_3D('',#135536,#16626,#16627);
#15365=AXIS2_PLACEMENT_3D('',#136002,#16629,#16630);
#15366=AXIS2_PLACEMENT_3D('',#136465,#16632,#16633);
#15367=AXIS2_PLACEMENT_3D('',#136928,#16635,#16636);
#15368=AXIS2_PLACEMENT_3D('',#137397,#16638,#16639);
#15369=AXIS2_PLACEMENT_3D('',#137863,#16641,#16642);
#15370=AXIS2_PLACEMENT_3D('',#138329,#16644,#16645);
#15371=AXIS2_PLACEMENT_3D('',#138801,#16647,#16648);
#15372=AXIS2_PLACEMENT_3D('',#139267,#16650,#16651);
#15373=AXIS2_PLACEMENT_3D('',#139730,#16653,#16654);
#15374=AXIS2_PLACEMENT_3D('',#140193,#16656,#16657);
#15375=AXIS2_PLACEMENT_3D('',#140276,#16658,#16659);
#15376=AXIS2_PLACEMENT_3D('',#164173,#16660,#16661);
#15377=AXIS2_PLACEMENT_3D('',#187985,#16662,#16663);
#15378=AXIS2_PLACEMENT_3D('',#188213,#16664,#16665);
#15379=AXIS2_PLACEMENT_3D('',#188388,#16666,#16667);
#15380=AXIS2_PLACEMENT_3D('',#188390,#16668,#16669);
#15381=AXIS2_PLACEMENT_3D('',#188392,#16670,#16671);
#15382=AXIS2_PLACEMENT_3D('',#188393,#16672,#16673);
#15383=AXIS2_PLACEMENT_3D('',#188396,#16675,#16676);
#15384=AXIS2_PLACEMENT_3D('',#188397,#16677,#16678);
#15385=AXIS2_PLACEMENT_3D('',#188613,#16679,#16680);
#15386=AXIS2_PLACEMENT_3D('',#188622,#16685,#16686);
#15387=AXIS2_PLACEMENT_3D('',#188623,#16687,#16688);
#15388=AXIS2_PLACEMENT_3D('',#188624,#16689,#16690);
#15389=AXIS2_PLACEMENT_3D('',#188633,#16695,#16696);
#15390=AXIS2_PLACEMENT_3D('',#188635,#16697,#16698);
#15391=AXIS2_PLACEMENT_3D('',#188636,#16699,#16700);
#15392=AXIS2_PLACEMENT_3D('',#188637,#16701,#16702);
#15393=AXIS2_PLACEMENT_3D('',#188639,#16704,#16705);
#15394=AXIS2_PLACEMENT_3D('',#188640,#16706,#16707);
#15395=AXIS2_PLACEMENT_3D('',#188641,#16708,#16709);
#15396=AXIS2_PLACEMENT_3D('',#202420,#16710,#16711);
#15397=AXIS2_PLACEMENT_3D('',#202421,#16712,#16713);
#15398=AXIS2_PLACEMENT_3D('',#202422,#16714,#16715);
#15399=AXIS2_PLACEMENT_3D('',#202425,#16716,#16717);
#15400=AXIS2_PLACEMENT_3D('',#202429,#16719,#16720);
#15401=AXIS2_PLACEMENT_3D('',#202433,#16722,#16723);
#15402=AXIS2_PLACEMENT_3D('',#202436,#16725,#16726);
#15403=AXIS2_PLACEMENT_3D('',#202438,#16727,#16728);
#15404=AXIS2_PLACEMENT_3D('',#202442,#16730,#16731);
#15405=AXIS2_PLACEMENT_3D('',#202444,#16733,#16734);
#15406=AXIS2_PLACEMENT_3D('',#202447,#16735,#16736);
#15407=AXIS2_PLACEMENT_3D('',#202451,#16738,#16739);
#15408=AXIS2_PLACEMENT_3D('',#202454,#16741,#16742);
#15409=AXIS2_PLACEMENT_3D('',#202458,#16744,#16745);
#15410=AXIS2_PLACEMENT_3D('',#202462,#16747,#16748);
#15411=AXIS2_PLACEMENT_3D('',#202465,#16750,#16751);
#15412=AXIS2_PLACEMENT_3D('',#202466,#16752,#16753);
#15413=AXIS2_PLACEMENT_3D('',#202467,#16754,#16755);
#15414=AXIS2_PLACEMENT_3D('',#202468,#16756,#16757);
#15415=AXIS2_PLACEMENT_3D('',#202469,#16758,#16759);
#15416=AXIS2_PLACEMENT_3D('',#202471,#16760,#16761);
#15417=AXIS2_PLACEMENT_3D('',#202475,#16763,#16764);
#15418=AXIS2_PLACEMENT_3D('',#202478,#16766,#16767);
#15419=AXIS2_PLACEMENT_3D('',#202479,#16768,#16769);
#15420=AXIS2_PLACEMENT_3D('',#202483,#16771,#16772);
#15421=AXIS2_PLACEMENT_3D('',#202486,#16774,#16775);
#15422=AXIS2_PLACEMENT_3D('',#202488,#16776,#16777);
#15423=AXIS2_PLACEMENT_3D('',#202489,#16778,#16779);
#15424=AXIS2_PLACEMENT_3D('',#202491,#16781,#16782);
#15425=AXIS2_PLACEMENT_3D('',#202494,#16785,#16786);
#15426=AXIS2_PLACEMENT_3D('',#202496,#16788,#16789);
#15427=AXIS2_PLACEMENT_3D('',#202497,#16790,#16791);
#15428=AXIS2_PLACEMENT_3D('',#202498,#16792,#16793);
#15429=AXIS2_PLACEMENT_3D('',#202499,#16794,#16795);
#15430=AXIS2_PLACEMENT_3D('',#202500,#16796,#16797);
#15431=AXIS2_PLACEMENT_3D('',#202501,#16798,#16799);
#15432=AXIS2_PLACEMENT_3D('',#202502,#16800,#16801);
#15433=AXIS2_PLACEMENT_3D('',#202508,#16805,#16806);
#15434=AXIS2_PLACEMENT_3D('',#202510,#16807,#16808);
#15435=AXIS2_PLACEMENT_3D('',#202513,#16810,#16811);
#15436=AXIS2_PLACEMENT_3D('',#202515,#16812,#16813);
#15437=AXIS2_PLACEMENT_3D('',#202516,#16814,#16815);
#15438=AXIS2_PLACEMENT_3D('',#202517,#16816,#16817);
#15439=AXIS2_PLACEMENT_3D('',#202520,#16819,#16820);
#15440=AXIS2_PLACEMENT_3D('',#202521,#16821,#16822);
#15441=AXIS2_PLACEMENT_3D('',#202527,#16826,#16827);
#15442=AXIS2_PLACEMENT_3D('',#202528,#16828,#16829);
#15443=AXIS2_PLACEMENT_3D('',#202529,#16830,#16831);
#15444=AXIS2_PLACEMENT_3D('',#202530,#16832,#16833);
#15445=AXIS2_PLACEMENT_3D('',#202531,#16834,#16835);
#15446=AXIS2_PLACEMENT_3D('',#202532,#16836,#16837);
#15447=AXIS2_PLACEMENT_3D('',#202533,#16838,#16839);
#15448=AXIS2_PLACEMENT_3D('',#202854,#16841,#16842);
#15449=AXIS2_PLACEMENT_3D('',#203320,#16844,#16845);
#15450=AXIS2_PLACEMENT_3D('',#203786,#16847,#16848);
#15451=AXIS2_PLACEMENT_3D('',#204252,#16850,#16851);
#15452=AXIS2_PLACEMENT_3D('',#204715,#16853,#16854);
#15453=AXIS2_PLACEMENT_3D('',#205181,#16856,#16857);
#15454=AXIS2_PLACEMENT_3D('',#205647,#16859,#16860);
#15455=AXIS2_PLACEMENT_3D('',#206107,#16862,#16863);
#15456=AXIS2_PLACEMENT_3D('',#206360,#16865,#16866);
#15457=AXIS2_PLACEMENT_3D('',#206616,#16868,#16869);
#15458=AXIS2_PLACEMENT_3D('',#207082,#16871,#16872);
#15459=AXIS2_PLACEMENT_3D('',#207545,#16874,#16875);
#15460=AXIS2_PLACEMENT_3D('',#208011,#16877,#16878);
#15461=AXIS2_PLACEMENT_3D('',#208477,#16880,#16881);
#15462=AXIS2_PLACEMENT_3D('',#208943,#16883,#16884);
#15463=AXIS2_PLACEMENT_3D('',#209412,#16886,#16887);
#15464=AXIS2_PLACEMENT_3D('',#225212,#16889,#16890);
#15465=AXIS2_PLACEMENT_3D('',#226295,#16891,#16892);
#15466=AXIS2_PLACEMENT_3D('',#233123,#16893,#16894);
#15467=AXIS2_PLACEMENT_3D('',#233204,#16895,#16896);
#15468=AXIS2_PLACEMENT_3D('',#233271,#16897,#16898);
#15469=AXIS2_PLACEMENT_3D('',#240442,#16899,#16900);
#15470=AXIS2_PLACEMENT_3D('',#240444,#16901,#16902);
#15471=AXIS2_PLACEMENT_3D('',#240448,#16905,#16906);
#15472=AXIS2_PLACEMENT_3D('',#240449,#16907,#16908);
#15473=AXIS2_PLACEMENT_3D('',#240450,#16909,#16910);
#15474=AXIS2_PLACEMENT_3D('',#240451,#16911,#16912);
#15475=AXIS2_PLACEMENT_3D('',#240452,#16913,#16914);
#15476=AXIS2_PLACEMENT_3D('',#240454,#16915,#16916);
#15477=AXIS2_PLACEMENT_3D('',#240457,#16918,#16919);
#15478=AXIS2_PLACEMENT_3D('',#240458,#16920,#16921);
#15479=AXIS2_PLACEMENT_3D('',#240467,#16926,#16927);
#15480=AXIS2_PLACEMENT_3D('',#240469,#16928,#16929);
#15481=AXIS2_PLACEMENT_3D('',#240472,#16931,#16932);
#15482=AXIS2_PLACEMENT_3D('',#240473,#16933,#16934);
#15483=AXIS2_PLACEMENT_3D('',#240479,#16938,#16939);
#15484=AXIS2_PLACEMENT_3D('',#240480,#16940,#16941);
#15485=AXIS2_PLACEMENT_3D('',#240481,#16942,#16943);
#15486=AXIS2_PLACEMENT_3D('',#240482,#16944,#16945);
#15487=AXIS2_PLACEMENT_3D('',#240484,#16946,#16947);
#15488=AXIS2_PLACEMENT_3D('',#240485,#16948,#16949);
#15489=AXIS2_PLACEMENT_3D('',#240487,#16950,#16951);
#15490=AXIS2_PLACEMENT_3D('',#240489,#16953,#16954);
#15491=AXIS2_PLACEMENT_3D('',#240491,#16955,#16956);
#15492=AXIS2_PLACEMENT_3D('',#240494,#16958,#16959);
#15493=AXIS2_PLACEMENT_3D('',#240495,#16960,#16961);
#15494=AXIS2_PLACEMENT_3D('',#240504,#16966,#16967);
#15495=AXIS2_PLACEMENT_3D('',#240506,#16968,#16969);
#15496=AXIS2_PLACEMENT_3D('',#240508,#16970,#16971);
#15497=AXIS2_PLACEMENT_3D('',#240510,#16973,#16974);
#15498=AXIS2_PLACEMENT_3D('',#240516,#16978,#16979);
#15499=AXIS2_PLACEMENT_3D('',#240518,#16981,#16982);
#15500=AXIS2_PLACEMENT_3D('',#240519,#16983,#16984);
#15501=AXIS2_PLACEMENT_3D('',#240520,#16985,#16986);
#15502=AXIS2_PLACEMENT_3D('',#240521,#16987,#16988);
#15503=AXIS2_PLACEMENT_3D('',#240522,#16989,#16990);
#15504=AXIS2_PLACEMENT_3D('',#240523,#16991,#16992);
#15505=AXIS2_PLACEMENT_3D('',#240526,#16993,#16994);
#15506=AXIS2_PLACEMENT_3D('',#240530,#16996,#16997);
#15507=AXIS2_PLACEMENT_3D('',#240534,#16999,#17000);
#15508=AXIS2_PLACEMENT_3D('',#240537,#17002,#17003);
#15509=AXIS2_PLACEMENT_3D('',#240539,#17004,#17005);
#15510=AXIS2_PLACEMENT_3D('',#240543,#17007,#17008);
#15511=AXIS2_PLACEMENT_3D('',#240545,#17010,#17011);
#15512=AXIS2_PLACEMENT_3D('',#240548,#17012,#17013);
#15513=AXIS2_PLACEMENT_3D('',#240552,#17015,#17016);
#15514=AXIS2_PLACEMENT_3D('',#240555,#17018,#17019);
#15515=AXIS2_PLACEMENT_3D('',#240559,#17021,#17022);
#15516=AXIS2_PLACEMENT_3D('',#240563,#17024,#17025);
#15517=AXIS2_PLACEMENT_3D('',#240566,#17027,#17028);
#15518=AXIS2_PLACEMENT_3D('',#240567,#17029,#17030);
#15519=AXIS2_PLACEMENT_3D('',#240568,#17031,#17032);
#15520=AXIS2_PLACEMENT_3D('',#240569,#17033,#17034);
#15521=AXIS2_PLACEMENT_3D('',#240570,#17035,#17036);
#15522=AXIS2_PLACEMENT_3D('',#240576,#17040,#17041);
#15523=AXIS2_PLACEMENT_3D('',#240578,#17042,#17043);
#15524=AXIS2_PLACEMENT_3D('',#240581,#17045,#17046);
#15525=AXIS2_PLACEMENT_3D('',#240583,#17047,#17048);
#15526=AXIS2_PLACEMENT_3D('',#240584,#17049,#17050);
#15527=AXIS2_PLACEMENT_3D('',#240585,#17051,#17052);
#15528=AXIS2_PLACEMENT_3D('',#240588,#17054,#17055);
#15529=AXIS2_PLACEMENT_3D('',#240589,#17056,#17057);
#15530=AXIS2_PLACEMENT_3D('',#240595,#17061,#17062);
#15531=AXIS2_PLACEMENT_3D('',#240596,#17063,#17064);
#15532=AXIS2_PLACEMENT_3D('',#240597,#17065,#17066);
#15533=AXIS2_PLACEMENT_3D('',#240598,#17067,#17068);
#15534=AXIS2_PLACEMENT_3D('',#240599,#17069,#17070);
#15535=AXIS2_PLACEMENT_3D('',#240600,#17071,#17072);
#15536=AXIS2_PLACEMENT_3D('',#240601,#17073,#17074);
#15537=AXIS2_PLACEMENT_3D('',#240602,#17075,#17076);
#15538=AXIS2_PLACEMENT_3D('',#240603,#17077,#17078);
#15539=AXIS2_PLACEMENT_3D('',#240605,#17079,#17080);
#15540=AXIS2_PLACEMENT_3D('',#240609,#17082,#17083);
#15541=AXIS2_PLACEMENT_3D('',#240612,#17085,#17086);
#15542=AXIS2_PLACEMENT_3D('',#240613,#17087,#17088);
#15543=AXIS2_PLACEMENT_3D('',#240617,#17090,#17091);
#15544=AXIS2_PLACEMENT_3D('',#240620,#17093,#17094);
#15545=AXIS2_PLACEMENT_3D('',#240622,#17095,#17096);
#15546=AXIS2_PLACEMENT_3D('',#240623,#17097,#17098);
#15547=AXIS2_PLACEMENT_3D('',#240625,#17100,#17101);
#15548=AXIS2_PLACEMENT_3D('',#240628,#17104,#17105);
#15549=AXIS2_PLACEMENT_3D('',#240630,#17107,#17108);
#15550=AXIS2_PLACEMENT_3D('',#240631,#17109,#17110);
#15551=AXIS2_PLACEMENT_3D('',#240632,#17111,#17112);
#15552=AXIS2_PLACEMENT_3D('',#240633,#17113,#17114);
#15553=AXIS2_PLACEMENT_3D('',#240634,#17115,#17116);
#15554=AXIS2_PLACEMENT_3D('',#240637,#17117,#17118);
#15555=AXIS2_PLACEMENT_3D('',#240641,#17120,#17121);
#15556=AXIS2_PLACEMENT_3D('',#240643,#17123,#17124);
#15557=AXIS2_PLACEMENT_3D('',#240645,#17125,#17126);
#15558=AXIS2_PLACEMENT_3D('',#240648,#17128,#17129);
#15559=AXIS2_PLACEMENT_3D('',#240649,#17130,#17131);
#15560=AXIS2_PLACEMENT_3D('',#240658,#17136,#17137);
#15561=AXIS2_PLACEMENT_3D('',#240661,#17138,#17139);
#15562=AXIS2_PLACEMENT_3D('',#240665,#17141,#17142);
#15563=AXIS2_PLACEMENT_3D('',#240667,#17144,#17145);
#15564=AXIS2_PLACEMENT_3D('',#240670,#17148,#17149);
#15565=AXIS2_PLACEMENT_3D('',#240675,#17151,#17152);
#15566=AXIS2_PLACEMENT_3D('',#240678,#17154,#17155);
#15567=AXIS2_PLACEMENT_3D('',#240679,#17156,#17157);
#15568=AXIS2_PLACEMENT_3D('',#240687,#17162,#17163);
#15569=AXIS2_PLACEMENT_3D('',#240688,#17164,#17165);
#15570=AXIS2_PLACEMENT_3D('',#240691,#17166,#17167);
#15571=AXIS2_PLACEMENT_3D('',#240695,#17169,#17170);
#15572=AXIS2_PLACEMENT_3D('',#240697,#17172,#17173);
#15573=AXIS2_PLACEMENT_3D('',#240705,#17178,#17179);
#15574=AXIS2_PLACEMENT_3D('',#240706,#17180,#17181);
#15575=AXIS2_PLACEMENT_3D('',#240708,#17183,#17184);
#15576=AXIS2_PLACEMENT_3D('',#240710,#17186,#17187);
#15577=AXIS2_PLACEMENT_3D('',#240712,#17189,#17190);
#15578=AXIS2_PLACEMENT_3D('',#240715,#17191,#17192);
#15579=AXIS2_PLACEMENT_3D('',#240719,#17194,#17195);
#15580=AXIS2_PLACEMENT_3D('',#240721,#17197,#17198);
#15581=AXIS2_PLACEMENT_3D('',#240724,#17201,#17202);
#15582=AXIS2_PLACEMENT_3D('',#240727,#17203,#17204);
#15583=AXIS2_PLACEMENT_3D('',#240732,#17207,#17208);
#15584=AXIS2_PLACEMENT_3D('',#240738,#17212,#17213);
#15585=AXIS2_PLACEMENT_3D('',#240740,#17214,#17215);
#15586=AXIS2_PLACEMENT_3D('',#240743,#17217,#17218);
#15587=AXIS2_PLACEMENT_3D('',#240744,#17219,#17220);
#15588=AXIS2_PLACEMENT_3D('',#240750,#17224,#17225);
#15589=AXIS2_PLACEMENT_3D('',#240753,#17226,#17227);
#15590=AXIS2_PLACEMENT_3D('',#240757,#17229,#17230);
#15591=AXIS2_PLACEMENT_3D('',#240759,#17232,#17233);
#15592=AXIS2_PLACEMENT_3D('',#240762,#17236,#17237);
#15593=AXIS2_PLACEMENT_3D('',#240767,#17241,#17242);
#15594=AXIS2_PLACEMENT_3D('',#240769,#17244,#17245);
#15595=AXIS2_PLACEMENT_3D('',#240770,#17246,#17247);
#15596=AXIS2_PLACEMENT_3D('',#240775,#17250,#17251);
#15597=AXIS2_PLACEMENT_3D('',#240776,#17252,#17253);
#15598=AXIS2_PLACEMENT_3D('',#240783,#17257,#17258);
#15599=AXIS2_PLACEMENT_3D('',#240784,#17259,#17260);
#15600=AXIS2_PLACEMENT_3D('',#240786,#17261,#17262);
#15601=AXIS2_PLACEMENT_3D('',#240788,#17264,#17265);
#15602=AXIS2_PLACEMENT_3D('',#240795,#17269,#17270);
#15603=AXIS2_PLACEMENT_3D('',#240796,#17271,#17272);
#15604=AXIS2_PLACEMENT_3D('',#240799,#17275,#17276);
#15605=AXIS2_PLACEMENT_3D('',#240801,#17278,#17279);
#15606=AXIS2_PLACEMENT_3D('',#240803,#17281,#17282);
#15607=AXIS2_PLACEMENT_3D('',#240804,#17283,#17284);
#15608=AXIS2_PLACEMENT_3D('',#240805,#17285,#17286);
#15609=AXIS2_PLACEMENT_3D('',#240806,#17287,#17288);
#15610=AXIS2_PLACEMENT_3D('',#241157,#17290,#17291);
#15611=AXIS2_PLACEMENT_3D('',#241617,#17293,#17294);
#15612=AXIS2_PLACEMENT_3D('',#241870,#17296,#17297);
#15613=AXIS2_PLACEMENT_3D('',#242129,#17299,#17300);
#15614=AXIS2_PLACEMENT_3D('',#242592,#17302,#17303);
#15615=AXIS2_PLACEMENT_3D('',#243058,#17305,#17306);
#15616=AXIS2_PLACEMENT_3D('',#243521,#17308,#17309);
#15617=AXIS2_PLACEMENT_3D('',#243987,#17311,#17312);
#15618=AXIS2_PLACEMENT_3D('',#244450,#17314,#17315);
#15619=AXIS2_PLACEMENT_3D('',#244919,#17317,#17318);
#15620=AXIS2_PLACEMENT_3D('',#245388,#17320,#17321);
#15621=AXIS2_PLACEMENT_3D('',#245848,#17323,#17324);
#15622=AXIS2_PLACEMENT_3D('',#246314,#17326,#17327);
#15623=AXIS2_PLACEMENT_3D('',#246777,#17329,#17330);
#15624=AXIS2_PLACEMENT_3D('',#247240,#17332,#17333);
#15625=AXIS2_PLACEMENT_3D('',#247703,#17335,#17336);
#15626=AXIS2_PLACEMENT_3D('',#263671,#17338,#17339);
#15627=AXIS2_PLACEMENT_3D('',#263690,#17340,#17341);
#15628=AXIS2_PLACEMENT_3D('',#265076,#17342,#17343);
#15629=AXIS2_PLACEMENT_3D('',#265311,#17344,#17345);
#15630=AXIS2_PLACEMENT_3D('',#272334,#17346,#17347);
#15631=AXIS2_PLACEMENT_3D('',#279156,#17348,#17349);
#15632=AXIS2_PLACEMENT_3D('',#279158,#17350,#17351);
#15633=AXIS2_PLACEMENT_3D('',#279162,#17354,#17355);
#15634=AXIS2_PLACEMENT_3D('',#279163,#17356,#17357);
#15635=AXIS2_PLACEMENT_3D('',#279164,#17358,#17359);
#15636=AXIS2_PLACEMENT_3D('',#279165,#17360,#17361);
#15637=AXIS2_PLACEMENT_3D('',#279166,#17362,#17363);
#15638=AXIS2_PLACEMENT_3D('',#279168,#17364,#17365);
#15639=AXIS2_PLACEMENT_3D('',#279171,#17367,#17368);
#15640=AXIS2_PLACEMENT_3D('',#279172,#17369,#17370);
#15641=AXIS2_PLACEMENT_3D('',#279181,#17375,#17376);
#15642=AXIS2_PLACEMENT_3D('',#279183,#17377,#17378);
#15643=AXIS2_PLACEMENT_3D('',#279185,#17379,#17380);
#15644=AXIS2_PLACEMENT_3D('',#279187,#17382,#17383);
#15645=AXIS2_PLACEMENT_3D('',#279193,#17387,#17388);
#15646=AXIS2_PLACEMENT_3D('',#279194,#17389,#17390);
#15647=AXIS2_PLACEMENT_3D('',#279195,#17391,#17392);
#15648=AXIS2_PLACEMENT_3D('',#279196,#17393,#17394);
#15649=AXIS2_PLACEMENT_3D('',#279198,#17395,#17396);
#15650=AXIS2_PLACEMENT_3D('',#279199,#17397,#17398);
#15651=AXIS2_PLACEMENT_3D('',#279202,#17400,#17401);
#15652=AXIS2_PLACEMENT_3D('',#279203,#17402,#17403);
#15653=AXIS2_PLACEMENT_3D('',#279205,#17404,#17405);
#15654=AXIS2_PLACEMENT_3D('',#279208,#17407,#17408);
#15655=AXIS2_PLACEMENT_3D('',#279209,#17409,#17410);
#15656=AXIS2_PLACEMENT_3D('',#279218,#17415,#17416);
#15657=AXIS2_PLACEMENT_3D('',#279220,#17417,#17418);
#15658=AXIS2_PLACEMENT_3D('',#279223,#17420,#17421);
#15659=AXIS2_PLACEMENT_3D('',#279224,#17422,#17423);
#15660=AXIS2_PLACEMENT_3D('',#279230,#17427,#17428);
#15661=AXIS2_PLACEMENT_3D('',#279231,#17429,#17430);
#15662=AXIS2_PLACEMENT_3D('',#279232,#17431,#17432);
#15663=AXIS2_PLACEMENT_3D('',#279234,#17434,#17435);
#15664=AXIS2_PLACEMENT_3D('',#279235,#17436,#17437);
#15665=AXIS2_PLACEMENT_3D('',#279236,#17438,#17439);
#15666=AXIS2_PLACEMENT_3D('',#279237,#17440,#17441);
#15667=AXIS2_PLACEMENT_3D('',#279238,#17442,#17443);
#15668=AXIS2_PLACEMENT_3D('',#279239,#17444,#17445);
#15669=AXIS2_PLACEMENT_3D('',#279240,#17446,#17447);
#15670=AXIS2_PLACEMENT_3D('',#279241,#17448,#17449);
#15671=AXIS2_PLACEMENT_3D('',#279242,#17450,#17451);
#15672=AXIS2_PLACEMENT_3D('',#279243,#17452,#17453);
#15673=AXIS2_PLACEMENT_3D('',#279244,#17454,#17455);
#15674=DIRECTION('axis',(0.,0.,1.));
#15675=DIRECTION('refdir',(1.,0.,0.));
#15676=DIRECTION('axis',(0.,0.,1.));
#15677=DIRECTION('refdir',(1.,0.,0.));
#15678=DIRECTION('center_axis',(0.,0.,1.));
#15679=DIRECTION('ref_axis',(-0.707106781186548,0.707106781186548,0.));
#15680=DIRECTION('center_axis',(0.,0.,-1.));
#15681=DIRECTION('ref_axis',(-0.707106781186548,0.707106781186548,0.));
#15682=DIRECTION('',(0.,0.,-1.));
#15683=DIRECTION('center_axis',(0.,0.,1.));
#15684=DIRECTION('ref_axis',(-0.707106781186548,0.707106781186548,0.));
#15685=DIRECTION('',(0.,0.,1.));
#15686=DIRECTION('center_axis',(0.,1.,0.));
#15687=DIRECTION('ref_axis',(-1.,0.,0.));
#15688=DIRECTION('center_axis',(0.,-1.,0.));
#15689=DIRECTION('ref_axis',(-1.,0.,0.));
#15690=DIRECTION('',(0.,1.,0.));
#15691=DIRECTION('center_axis',(0.,-1.,0.));
#15692=DIRECTION('ref_axis',(-1.,0.,0.));
#15693=DIRECTION('center_axis',(-0.707106781186548,0.,0.707106781186548));
#15694=DIRECTION('ref_axis',(0.707106781186548,0.,0.707106781186548));
#15695=DIRECTION('',(0.707106781186547,0.,0.707106781186547));
#15696=DIRECTION('',(0.,1.,0.));
#15697=DIRECTION('',(0.707106781186547,0.,0.707106781186547));
#15698=DIRECTION('',(0.,1.,0.));
#15699=DIRECTION('center_axis',(0.,0.,-1.));
#15700=DIRECTION('ref_axis',(0.707106781186548,0.707106781186548,0.));
#15701=DIRECTION('center_axis',(0.,0.,1.));
#15702=DIRECTION('ref_axis',(0.707106781186548,0.707106781186548,0.));
#15703=DIRECTION('',(0.,0.,1.));
#15704=DIRECTION('center_axis',(0.,0.,-1.));
#15705=DIRECTION('ref_axis',(0.707106781186548,0.707106781186548,0.));
#15706=DIRECTION('',(0.,0.,-1.));
#15707=DIRECTION('center_axis',(0.,-1.,0.));
#15708=DIRECTION('ref_axis',(0.,0.,-1.));
#15709=DIRECTION('',(-1.,0.,0.));
#15710=DIRECTION('',(-1.,0.,0.));
#15711=DIRECTION('center_axis',(-1.,0.,0.));
#15712=DIRECTION('ref_axis',(0.,0.707106781186548,-0.707106781186547));
#15713=DIRECTION('',(1.,0.,0.));
#15714=DIRECTION('center_axis',(-1.,0.,0.));
#15715=DIRECTION('ref_axis',(0.,0.707106781186548,-0.707106781186547));
#15716=DIRECTION('',(-1.,0.,0.));
#15717=DIRECTION('center_axis',(-1.,0.,0.));
#15718=DIRECTION('ref_axis',(0.,0.707106781186548,-0.707106781186547));
#15719=DIRECTION('center_axis',(0.,1.,0.));
#15720=DIRECTION('ref_axis',(1.,0.,0.));
#15721=DIRECTION('',(0.,0.,1.));
#15722=DIRECTION('',(-0.707106781186547,0.,0.707106781186547));
#15723=DIRECTION('',(1.,0.,0.));
#15724=DIRECTION('',(0.,0.,1.));
#15725=DIRECTION('center_axis',(0.,1.,0.));
#15726=DIRECTION('ref_axis',(1.,0.,0.));
#15727=DIRECTION('center_axis',(-1.,0.,0.));
#15728=DIRECTION('ref_axis',(0.,0.707106781186548,-0.707106781186547));
#15729=DIRECTION('center_axis',(1.,0.,0.));
#15730=DIRECTION('ref_axis',(0.,0.707106781186548,-0.707106781186547));
#15731=DIRECTION('',(1.,0.,0.));
#15732=DIRECTION('center_axis',(1.,0.,0.));
#15733=DIRECTION('ref_axis',(0.,0.707106781186548,-0.707106781186547));
#15734=DIRECTION('',(-1.,0.,0.));
#15735=DIRECTION('center_axis',(0.,-1.,0.));
#15736=DIRECTION('ref_axis',(0.,0.,-1.));
#15737=DIRECTION('',(0.,0.,1.));
#15738=DIRECTION('',(-1.,0.,0.));
#15739=DIRECTION('',(-0.707106781186547,0.,0.707106781186547));
#15740=DIRECTION('',(0.,0.,1.));
#15741=DIRECTION('center_axis',(0.,1.,0.));
#15742=DIRECTION('ref_axis',(1.,0.,0.));
#15743=DIRECTION('center_axis',(0.,-1.,0.));
#15744=DIRECTION('ref_axis',(1.,0.,0.));
#15745=DIRECTION('',(0.,-1.,0.));
#15746=DIRECTION('center_axis',(0.,0.,-1.));
#15747=DIRECTION('ref_axis',(-1.,0.,0.));
#15748=DIRECTION('',(0.,1.,0.));
#15749=DIRECTION('center_axis',(-0.707106781186548,0.,-0.707106781186548));
#15750=DIRECTION('ref_axis',(-0.707106781186548,0.,0.707106781186548));
#15751=DIRECTION('',(0.,1.,0.));
#15752=DIRECTION('center_axis',(0.,0.,-1.));
#15753=DIRECTION('ref_axis',(-0.707106781186548,-0.707106781186548,0.));
#15754=DIRECTION('center_axis',(0.,0.,1.));
#15755=DIRECTION('ref_axis',(-0.707106781186548,-0.707106781186548,0.));
#15756=DIRECTION('',(0.,0.,1.));
#15757=DIRECTION('center_axis',(0.,0.,-1.));
#15758=DIRECTION('ref_axis',(-0.707106781186548,-0.707106781186548,0.));
#15759=DIRECTION('',(0.,0.,-1.));
#15760=DIRECTION('center_axis',(1.,0.,0.));
#15761=DIRECTION('ref_axis',(0.,0.,1.));
#15762=DIRECTION('',(0.,-1.,0.));
#15763=DIRECTION('',(0.,-1.,0.));
#15764=DIRECTION('center_axis',(1.,0.,0.));
#15765=DIRECTION('ref_axis',(0.,0.,1.));
#15766=DIRECTION('center_axis',(-1.,0.,0.));
#15767=DIRECTION('ref_axis',(0.,-0.707106781186548,-0.707106781186547));
#15768=DIRECTION('',(0.,0.,1.));
#15769=DIRECTION('',(0.,-1.,0.));
#15770=DIRECTION('',(0.,0.,1.));
#15771=DIRECTION('center_axis',(1.,0.,0.));
#15772=DIRECTION('ref_axis',(0.,-0.707106781186548,-0.707106781186547));
#15773=DIRECTION('',(0.,1.,0.));
#15774=DIRECTION('',(0.,-1.,0.));
#15775=DIRECTION('center_axis',(0.,1.,0.));
#15776=DIRECTION('ref_axis',(-1.,0.,0.));
#15777=DIRECTION('center_axis',(0.,-1.,0.));
#15778=DIRECTION('ref_axis',(-1.,0.,0.));
#15779=DIRECTION('',(0.,1.,0.));
#15780=DIRECTION('center_axis',(0.,-1.,0.));
#15781=DIRECTION('ref_axis',(-1.,0.,0.));
#15782=DIRECTION('center_axis',(0.707106781186548,0.,-0.707106781186548));
#15783=DIRECTION('ref_axis',(0.707106781186548,0.,0.707106781186548));
#15784=DIRECTION('',(0.707106781186547,0.,0.707106781186547));
#15785=DIRECTION('',(0.707106781186547,0.,0.707106781186547));
#15786=DIRECTION('',(0.,-1.,0.));
#15787=DIRECTION('center_axis',(0.,0.,1.));
#15788=DIRECTION('ref_axis',(0.707106781186548,-0.707106781186548,0.));
#15789=DIRECTION('center_axis',(0.,0.,-1.));
#15790=DIRECTION('ref_axis',(0.707106781186548,-0.707106781186548,0.));
#15791=DIRECTION('',(0.,0.,-1.));
#15792=DIRECTION('center_axis',(0.,0.,1.));
#15793=DIRECTION('ref_axis',(0.707106781186548,-0.707106781186548,0.));
#15794=DIRECTION('',(0.,0.,1.));
#15795=DIRECTION('center_axis',(0.,-1.,0.));
#15796=DIRECTION('ref_axis',(0.,0.,-1.));
#15797=DIRECTION('',(-1.,0.,0.));
#15798=DIRECTION('',(-1.,0.,0.));
#15799=DIRECTION('center_axis',(0.,0.,1.));
#15800=DIRECTION('ref_axis',(-1.,0.,0.));
#15801=DIRECTION('',(0.,1.,0.));
#15802=DIRECTION('',(0.,1.,0.));
#15803=DIRECTION('',(1.,0.,0.));
#15804=DIRECTION('center_axis',(1.,0.,0.));
#15805=DIRECTION('ref_axis',(0.,0.,1.));
#15806=DIRECTION('',(0.,1.,0.));
#15807=DIRECTION('center_axis',(0.,0.,-1.));
#15808=DIRECTION('ref_axis',(1.,0.,0.));
#15809=DIRECTION('center_axis',(1.,0.,0.));
#15810=DIRECTION('ref_axis',(0.,-0.707106781186548,-0.707106781186547));
#15811=DIRECTION('',(1.,0.,0.));
#15812=DIRECTION('center_axis',(1.,0.,0.));
#15813=DIRECTION('ref_axis',(0.,-0.707106781186548,-0.707106781186547));
#15814=DIRECTION('',(-1.,0.,0.));
#15815=DIRECTION('center_axis',(0.,1.,0.));
#15816=DIRECTION('ref_axis',(1.,0.,0.));
#15817=DIRECTION('',(1.,0.,0.));
#15818=DIRECTION('',(-0.707106781186547,0.,0.707106781186547));
#15819=DIRECTION('',(0.,0.,1.));
#15820=DIRECTION('center_axis',(0.,1.,0.));
#15821=DIRECTION('ref_axis',(1.,0.,0.));
#15822=DIRECTION('center_axis',(1.,0.,0.));
#15823=DIRECTION('ref_axis',(0.,-0.707106781186548,-0.707106781186547));
#15824=DIRECTION('center_axis',(-1.,0.,0.));
#15825=DIRECTION('ref_axis',(0.,-0.707106781186548,-0.707106781186547));
#15826=DIRECTION('',(-1.,0.,0.));
#15827=DIRECTION('center_axis',(0.,-1.,0.));
#15828=DIRECTION('ref_axis',(0.,0.,-1.));
#15829=DIRECTION('',(0.,0.,1.));
#15830=DIRECTION('',(-0.707106781186547,0.,0.707106781186547));
#15831=DIRECTION('',(-1.,0.,0.));
#15832=DIRECTION('center_axis',(0.,1.,0.));
#15833=DIRECTION('ref_axis',(1.,0.,0.));
#15834=DIRECTION('center_axis',(1.,0.,0.));
#15835=DIRECTION('ref_axis',(0.,0.,1.));
#15836=DIRECTION('',(0.,1.,0.));
#15837=DIRECTION('',(0.,-1.,0.));
#15838=DIRECTION('center_axis',(0.,-1.,0.));
#15839=DIRECTION('ref_axis',(1.,0.,0.));
#15840=DIRECTION('',(0.,-1.,0.));
#15841=DIRECTION('center_axis',(0.,0.,1.));
#15842=DIRECTION('ref_axis',(-1.,0.,0.));
#15843=DIRECTION('',(0.,-1.,0.));
#15844=DIRECTION('center_axis',(0.707106781186548,0.,0.707106781186548));
#15845=DIRECTION('ref_axis',(-0.707106781186548,0.,0.707106781186548));
#15846=DIRECTION('center_axis',(0.,0.,1.));
#15847=DIRECTION('ref_axis',(-1.,0.,0.));
#15848=DIRECTION('axis',(0.,0.,1.));
#15849=DIRECTION('refdir',(1.,0.,0.));
#15850=DIRECTION('center_axis',(-1.,0.,0.));
#15851=DIRECTION('ref_axis',(0.,0.968648305440766,0.248436028721142));
#15852=DIRECTION('',(1.,0.,0.));
#15853=DIRECTION('center_axis',(1.,0.,0.));
#15854=DIRECTION('ref_axis',(0.,1.,-2.30250085928462E-11));
#15855=DIRECTION('center_axis',(-1.,0.,0.));
#15856=DIRECTION('ref_axis',(0.,0.968648305440766,0.248436028721142));
#15857=DIRECTION('',(1.,0.,0.));
#15858=DIRECTION('center_axis',(-1.,0.,0.));
#15859=DIRECTION('ref_axis',(0.,0.968648305440766,0.248436028721142));
#15860=DIRECTION('',(1.,0.,0.));
#15861=DIRECTION('center_axis',(-1.,0.,0.));
#15862=DIRECTION('ref_axis',(0.,0.968648305440766,0.248436028721142));
#15863=DIRECTION('',(1.,0.,0.));
#15864=DIRECTION('center_axis',(-1.,0.,0.));
#15865=DIRECTION('ref_axis',(0.,0.968648305440766,0.248436028721142));
#15866=DIRECTION('',(1.,0.,0.));
#15867=DIRECTION('center_axis',(-1.,0.,0.));
#15868=DIRECTION('ref_axis',(0.,0.968648305440766,0.248436028721142));
#15869=DIRECTION('',(1.,0.,0.));
#15870=DIRECTION('center_axis',(-1.,0.,0.));
#15871=DIRECTION('ref_axis',(0.,0.968648305440766,0.248436028721142));
#15872=DIRECTION('',(1.,0.,0.));
#15873=DIRECTION('center_axis',(-1.,0.,0.));
#15874=DIRECTION('ref_axis',(0.,0.968648305440766,0.248436028721142));
#15875=DIRECTION('',(1.,0.,0.));
#15876=DIRECTION('center_axis',(-1.,0.,0.));
#15877=DIRECTION('ref_axis',(0.,0.968648305440766,0.248436028721142));
#15878=DIRECTION('',(1.,0.,0.));
#15879=DIRECTION('center_axis',(-1.,0.,0.));
#15880=DIRECTION('ref_axis',(0.,0.968648305440766,0.248436028721142));
#15881=DIRECTION('',(1.,0.,0.));
#15882=DIRECTION('center_axis',(-1.,0.,0.));
#15883=DIRECTION('ref_axis',(0.,0.968648305440766,0.248436028721142));
#15884=DIRECTION('',(1.,0.,0.));
#15885=DIRECTION('center_axis',(-1.,0.,0.));
#15886=DIRECTION('ref_axis',(0.,0.968648305440766,0.248436028721142));
#15887=DIRECTION('',(1.,0.,0.));
#15888=DIRECTION('center_axis',(-1.,0.,0.));
#15889=DIRECTION('ref_axis',(0.,0.968648305440766,0.248436028721142));
#15890=DIRECTION('',(1.,0.,0.));
#15891=DIRECTION('center_axis',(-1.,0.,0.));
#15892=DIRECTION('ref_axis',(0.,0.968648305440766,0.248436028721142));
#15893=DIRECTION('',(1.,0.,0.));
#15894=DIRECTION('center_axis',(-1.,0.,0.));
#15895=DIRECTION('ref_axis',(0.,0.968648305440766,0.248436028721142));
#15896=DIRECTION('',(1.,0.,0.));
#15897=DIRECTION('center_axis',(-1.,0.,0.));
#15898=DIRECTION('ref_axis',(0.,0.968648305440766,0.248436028721142));
#15899=DIRECTION('',(1.,0.,0.));
#15900=DIRECTION('center_axis',(-1.,0.,0.));
#15901=DIRECTION('ref_axis',(0.,0.968648305440766,0.248436028721142));
#15902=DIRECTION('',(1.,0.,0.));
#15903=DIRECTION('center_axis',(-1.,0.,0.));
#15904=DIRECTION('ref_axis',(0.,0.968648305440766,0.248436028721142));
#15905=DIRECTION('',(1.,0.,0.));
#15906=DIRECTION('center_axis',(-1.,0.,0.));
#15907=DIRECTION('ref_axis',(0.,0.968648305440766,0.248436028721142));
#15908=DIRECTION('',(1.,0.,0.));
#15909=DIRECTION('center_axis',(-1.,0.,0.));
#15910=DIRECTION('ref_axis',(0.,0.968648305440766,0.248436028721142));
#15911=DIRECTION('',(1.,0.,0.));
#15912=DIRECTION('center_axis',(-1.,0.,0.));
#15913=DIRECTION('ref_axis',(0.,0.968648305440766,0.248436028721142));
#15914=DIRECTION('',(1.,0.,0.));
#15915=DIRECTION('center_axis',(-1.,0.,0.));
#15916=DIRECTION('ref_axis',(0.,0.968648305440766,0.248436028721142));
#15917=DIRECTION('',(1.,0.,0.));
#15918=DIRECTION('center_axis',(-1.,0.,0.));
#15919=DIRECTION('ref_axis',(0.,0.968648305440766,0.248436028721142));
#15920=DIRECTION('',(1.,0.,0.));
#15921=DIRECTION('center_axis',(-1.,0.,0.));
#15922=DIRECTION('ref_axis',(0.,0.968648305440766,0.248436028721142));
#15923=DIRECTION('',(1.,0.,0.));
#15924=DIRECTION('center_axis',(-1.,0.,0.));
#15925=DIRECTION('ref_axis',(0.,0.968648305440766,0.248436028721142));
#15926=DIRECTION('',(1.,0.,0.));
#15927=DIRECTION('center_axis',(-1.,0.,0.));
#15928=DIRECTION('ref_axis',(0.,0.968648305440766,0.248436028721142));
#15929=DIRECTION('',(1.,0.,0.));
#15930=DIRECTION('center_axis',(-1.,0.,0.));
#15931=DIRECTION('ref_axis',(0.,0.968648305440766,0.248436028721142));
#15932=DIRECTION('',(1.,0.,0.));
#15933=DIRECTION('center_axis',(-1.,0.,0.));
#15934=DIRECTION('ref_axis',(0.,0.968648305440766,0.248436028721142));
#15935=DIRECTION('',(1.,0.,0.));
#15936=DIRECTION('center_axis',(-1.,0.,0.));
#15937=DIRECTION('ref_axis',(0.,0.968648305440766,0.248436028721142));
#15938=DIRECTION('',(1.,0.,0.));
#15939=DIRECTION('center_axis',(-1.,0.,0.));
#15940=DIRECTION('ref_axis',(0.,0.968648305440766,0.248436028721142));
#15941=DIRECTION('',(1.,0.,0.));
#15942=DIRECTION('center_axis',(-1.,0.,0.));
#15943=DIRECTION('ref_axis',(0.,0.968648305440766,0.248436028721142));
#15944=DIRECTION('',(1.,0.,0.));
#15945=DIRECTION('center_axis',(-1.,0.,0.));
#15946=DIRECTION('ref_axis',(0.,0.968648305440766,0.248436028721142));
#15947=DIRECTION('',(1.,0.,0.));
#15948=DIRECTION('center_axis',(-1.,0.,0.));
#15949=DIRECTION('ref_axis',(0.,0.968648305440766,0.248436028721142));
#15950=DIRECTION('',(1.,0.,0.));
#15951=DIRECTION('center_axis',(-1.,0.,0.));
#15952=DIRECTION('ref_axis',(0.,0.968648305440766,0.248436028721142));
#15953=DIRECTION('',(1.,0.,0.));
#15954=DIRECTION('center_axis',(-1.,0.,0.));
#15955=DIRECTION('ref_axis',(0.,0.968648305440766,0.248436028721142));
#15956=DIRECTION('',(1.,0.,0.));
#15957=DIRECTION('center_axis',(-1.,0.,0.));
#15958=DIRECTION('ref_axis',(0.,0.968648305440766,0.248436028721142));
#15959=DIRECTION('',(1.,0.,0.));
#15960=DIRECTION('center_axis',(-1.,0.,0.));
#15961=DIRECTION('ref_axis',(0.,0.968648305440766,0.248436028721142));
#15962=DIRECTION('',(1.,0.,0.));
#15963=DIRECTION('center_axis',(-1.,0.,0.));
#15964=DIRECTION('ref_axis',(0.,0.968648305440766,0.248436028721142));
#15965=DIRECTION('',(1.,0.,0.));
#15966=DIRECTION('center_axis',(-1.,0.,0.));
#15967=DIRECTION('ref_axis',(0.,0.968648305440766,0.248436028721142));
#15968=DIRECTION('',(1.,0.,0.));
#15969=DIRECTION('center_axis',(-1.,0.,0.));
#15970=DIRECTION('ref_axis',(0.,0.968648305440766,0.248436028721142));
#15971=DIRECTION('',(1.,0.,0.));
#15972=DIRECTION('center_axis',(-1.,0.,0.));
#15973=DIRECTION('ref_axis',(0.,0.968648305440766,0.248436028721142));
#15974=DIRECTION('',(1.,0.,0.));
#15975=DIRECTION('center_axis',(-1.,0.,0.));
#15976=DIRECTION('ref_axis',(0.,0.968648305440766,0.248436028721142));
#15977=DIRECTION('',(1.,0.,0.));
#15978=DIRECTION('center_axis',(-1.,0.,0.));
#15979=DIRECTION('ref_axis',(0.,0.968648305440766,0.248436028721142));
#15980=DIRECTION('',(1.,0.,0.));
#15981=DIRECTION('center_axis',(-1.,0.,0.));
#15982=DIRECTION('ref_axis',(0.,0.968648305440766,0.248436028721142));
#15983=DIRECTION('',(1.,0.,0.));
#15984=DIRECTION('center_axis',(-1.,0.,0.));
#15985=DIRECTION('ref_axis',(0.,0.968648305440766,0.248436028721142));
#15986=DIRECTION('',(1.,0.,0.));
#15987=DIRECTION('center_axis',(-1.,0.,0.));
#15988=DIRECTION('ref_axis',(0.,0.968648305440766,0.248436028721142));
#15989=DIRECTION('',(1.,0.,0.));
#15990=DIRECTION('center_axis',(-1.,0.,0.));
#15991=DIRECTION('ref_axis',(0.,0.968648305440766,0.248436028721142));
#15992=DIRECTION('',(1.,0.,0.));
#15993=DIRECTION('center_axis',(-1.,0.,0.));
#15994=DIRECTION('ref_axis',(0.,0.968648305440766,0.248436028721142));
#15995=DIRECTION('',(1.,0.,0.));
#15996=DIRECTION('center_axis',(-1.,0.,0.));
#15997=DIRECTION('ref_axis',(0.,0.968648305440766,0.248436028721142));
#15998=DIRECTION('',(1.,0.,0.));
#15999=DIRECTION('center_axis',(-1.,0.,0.));
#16000=DIRECTION('ref_axis',(0.,0.968648305440766,0.248436028721142));
#16001=DIRECTION('',(1.,0.,0.));
#16002=DIRECTION('center_axis',(-1.,0.,0.));
#16003=DIRECTION('ref_axis',(0.,0.968648305440766,0.248436028721142));
#16004=DIRECTION('',(1.,0.,0.));
#16005=DIRECTION('center_axis',(-1.,0.,0.));
#16006=DIRECTION('ref_axis',(0.,0.968648305440766,0.248436028721142));
#16007=DIRECTION('',(1.,0.,0.));
#16008=DIRECTION('center_axis',(-1.,0.,0.));
#16009=DIRECTION('ref_axis',(0.,0.968648305440766,0.248436028721142));
#16010=DIRECTION('',(1.,0.,0.));
#16011=DIRECTION('center_axis',(-1.,0.,0.));
#16012=DIRECTION('ref_axis',(0.,0.968648305440766,0.248436028721142));
#16013=DIRECTION('',(1.,0.,0.));
#16014=DIRECTION('center_axis',(-1.,0.,0.));
#16015=DIRECTION('ref_axis',(0.,0.968648305440766,0.248436028721142));
#16016=DIRECTION('',(1.,0.,0.));
#16017=DIRECTION('center_axis',(-1.,0.,0.));
#16018=DIRECTION('ref_axis',(0.,0.968648305440766,0.248436028721142));
#16019=DIRECTION('',(1.,0.,0.));
#16020=DIRECTION('center_axis',(-1.,0.,0.));
#16021=DIRECTION('ref_axis',(0.,0.968648305440766,0.248436028721142));
#16022=DIRECTION('',(1.,0.,0.));
#16023=DIRECTION('center_axis',(-1.,0.,0.));
#16024=DIRECTION('ref_axis',(0.,0.968648305440766,0.248436028721142));
#16025=DIRECTION('',(1.,0.,0.));
#16026=DIRECTION('center_axis',(-1.,0.,0.));
#16027=DIRECTION('ref_axis',(0.,0.968648305440766,0.248436028721142));
#16028=DIRECTION('',(1.,0.,0.));
#16029=DIRECTION('center_axis',(-1.,0.,0.));
#16030=DIRECTION('ref_axis',(0.,0.968648305440766,0.248436028721142));
#16031=DIRECTION('',(1.,0.,0.));
#16032=DIRECTION('center_axis',(-1.,0.,0.));
#16033=DIRECTION('ref_axis',(0.,0.968648305440766,0.248436028721142));
#16034=DIRECTION('',(1.,0.,0.));
#16035=DIRECTION('center_axis',(-1.,0.,0.));
#16036=DIRECTION('ref_axis',(0.,0.968648305440766,0.248436028721142));
#16037=DIRECTION('',(1.,0.,0.));
#16038=DIRECTION('center_axis',(-1.,0.,0.));
#16039=DIRECTION('ref_axis',(0.,0.968648305440766,0.248436028721142));
#16040=DIRECTION('',(1.,0.,0.));
#16041=DIRECTION('center_axis',(-1.,0.,0.));
#16042=DIRECTION('ref_axis',(0.,0.968648305440766,0.248436028721142));
#16043=DIRECTION('',(1.,0.,0.));
#16044=DIRECTION('center_axis',(-1.,0.,0.));
#16045=DIRECTION('ref_axis',(0.,0.968648305440766,0.248436028721142));
#16046=DIRECTION('',(1.,0.,0.));
#16047=DIRECTION('center_axis',(-1.,0.,0.));
#16048=DIRECTION('ref_axis',(0.,0.968648305440766,0.248436028721142));
#16049=DIRECTION('',(1.,0.,0.));
#16050=DIRECTION('center_axis',(-1.,0.,0.));
#16051=DIRECTION('ref_axis',(0.,0.968648305440766,0.248436028721142));
#16052=DIRECTION('',(1.,0.,0.));
#16053=DIRECTION('center_axis',(-1.,0.,0.));
#16054=DIRECTION('ref_axis',(0.,0.968648305440766,0.248436028721142));
#16055=DIRECTION('',(1.,0.,0.));
#16056=DIRECTION('center_axis',(-1.,0.,0.));
#16057=DIRECTION('ref_axis',(0.,0.968648305440766,0.248436028721142));
#16058=DIRECTION('',(1.,0.,0.));
#16059=DIRECTION('center_axis',(-1.,0.,0.));
#16060=DIRECTION('ref_axis',(0.,0.968648305440766,0.248436028721142));
#16061=DIRECTION('',(1.,0.,0.));
#16062=DIRECTION('center_axis',(-1.,0.,0.));
#16063=DIRECTION('ref_axis',(0.,0.968648305440766,0.248436028721142));
#16064=DIRECTION('',(1.,0.,0.));
#16065=DIRECTION('center_axis',(-1.,0.,0.));
#16066=DIRECTION('ref_axis',(0.,0.968648305440766,0.248436028721142));
#16067=DIRECTION('',(1.,0.,0.));
#16068=DIRECTION('center_axis',(-1.,0.,0.));
#16069=DIRECTION('ref_axis',(0.,0.968648305440766,0.248436028721142));
#16070=DIRECTION('',(1.,0.,0.));
#16071=DIRECTION('center_axis',(-1.,0.,0.));
#16072=DIRECTION('ref_axis',(0.,0.968648305440766,0.248436028721142));
#16073=DIRECTION('',(1.,0.,0.));
#16074=DIRECTION('center_axis',(-1.,0.,0.));
#16075=DIRECTION('ref_axis',(0.,0.968648305440766,0.248436028721142));
#16076=DIRECTION('',(1.,0.,0.));
#16077=DIRECTION('center_axis',(-1.,0.,0.));
#16078=DIRECTION('ref_axis',(0.,0.968648305440766,0.248436028721142));
#16079=DIRECTION('',(1.,0.,0.));
#16080=DIRECTION('center_axis',(-1.,0.,0.));
#16081=DIRECTION('ref_axis',(0.,0.968648305440766,0.248436028721142));
#16082=DIRECTION('',(1.,0.,0.));
#16083=DIRECTION('center_axis',(-1.,0.,0.));
#16084=DIRECTION('ref_axis',(0.,0.968648305440766,0.248436028721142));
#16085=DIRECTION('',(1.,0.,0.));
#16086=DIRECTION('center_axis',(-1.,0.,0.));
#16087=DIRECTION('ref_axis',(0.,0.968648305440766,0.248436028721142));
#16088=DIRECTION('',(1.,0.,0.));
#16089=DIRECTION('center_axis',(-1.,0.,0.));
#16090=DIRECTION('ref_axis',(0.,0.968648305440766,0.248436028721142));
#16091=DIRECTION('',(1.,0.,0.));
#16092=DIRECTION('center_axis',(-1.,0.,0.));
#16093=DIRECTION('ref_axis',(0.,0.968648305440766,0.248436028721142));
#16094=DIRECTION('',(1.,0.,0.));
#16095=DIRECTION('center_axis',(-1.,0.,0.));
#16096=DIRECTION('ref_axis',(0.,0.968648305440766,0.248436028721142));
#16097=DIRECTION('',(1.,0.,0.));
#16098=DIRECTION('center_axis',(-1.,0.,0.));
#16099=DIRECTION('ref_axis',(0.,0.968648305440766,0.248436028721142));
#16100=DIRECTION('',(1.,0.,0.));
#16101=DIRECTION('center_axis',(-1.,0.,0.));
#16102=DIRECTION('ref_axis',(0.,0.968648305440766,0.248436028721142));
#16103=DIRECTION('',(1.,0.,0.));
#16104=DIRECTION('center_axis',(-1.,0.,0.));
#16105=DIRECTION('ref_axis',(0.,0.968648305440766,0.248436028721142));
#16106=DIRECTION('',(1.,0.,0.));
#16107=DIRECTION('center_axis',(-1.,0.,0.));
#16108=DIRECTION('ref_axis',(0.,0.968648305440766,0.248436028721142));
#16109=DIRECTION('',(1.,0.,0.));
#16110=DIRECTION('center_axis',(-1.,0.,0.));
#16111=DIRECTION('ref_axis',(0.,0.968648305440766,0.248436028721142));
#16112=DIRECTION('',(1.,0.,0.));
#16113=DIRECTION('center_axis',(-1.,0.,0.));
#16114=DIRECTION('ref_axis',(0.,0.968648305440766,0.248436028721142));
#16115=DIRECTION('',(1.,0.,0.));
#16116=DIRECTION('center_axis',(-1.,0.,0.));
#16117=DIRECTION('ref_axis',(0.,0.968648305440766,0.248436028721142));
#16118=DIRECTION('',(1.,0.,0.));
#16119=DIRECTION('center_axis',(-1.,0.,0.));
#16120=DIRECTION('ref_axis',(0.,0.968648305440766,0.248436028721142));
#16121=DIRECTION('',(1.,0.,0.));
#16122=DIRECTION('center_axis',(-1.,0.,0.));
#16123=DIRECTION('ref_axis',(0.,0.968648305440766,0.248436028721142));
#16124=DIRECTION('',(1.,0.,0.));
#16125=DIRECTION('center_axis',(-1.,0.,0.));
#16126=DIRECTION('ref_axis',(0.,0.968648305440766,0.248436028721142));
#16127=DIRECTION('',(1.,0.,0.));
#16128=DIRECTION('center_axis',(-1.,0.,0.));
#16129=DIRECTION('ref_axis',(0.,0.968648305440766,0.248436028721142));
#16130=DIRECTION('',(1.,0.,0.));
#16131=DIRECTION('center_axis',(-1.,0.,0.));
#16132=DIRECTION('ref_axis',(0.,0.968648305440766,0.248436028721142));
#16133=DIRECTION('',(1.,0.,0.));
#16134=DIRECTION('center_axis',(-1.,0.,0.));
#16135=DIRECTION('ref_axis',(0.,0.968648305440766,0.248436028721142));
#16136=DIRECTION('',(1.,0.,0.));
#16137=DIRECTION('center_axis',(-1.,0.,0.));
#16138=DIRECTION('ref_axis',(0.,0.968648305440766,0.248436028721142));
#16139=DIRECTION('',(1.,0.,0.));
#16140=DIRECTION('center_axis',(-1.,0.,0.));
#16141=DIRECTION('ref_axis',(0.,0.968648305440766,0.248436028721142));
#16142=DIRECTION('',(1.,0.,0.));
#16143=DIRECTION('center_axis',(-1.,0.,0.));
#16144=DIRECTION('ref_axis',(0.,0.968648305440766,0.248436028721142));
#16145=DIRECTION('',(1.,0.,0.));
#16146=DIRECTION('center_axis',(-1.,0.,0.));
#16147=DIRECTION('ref_axis',(0.,0.968648305440766,0.248436028721142));
#16148=DIRECTION('',(1.,0.,0.));
#16149=DIRECTION('center_axis',(-1.,0.,0.));
#16150=DIRECTION('ref_axis',(0.,0.968648305440766,0.248436028721142));
#16151=DIRECTION('',(1.,0.,0.));
#16152=DIRECTION('center_axis',(-1.,0.,0.));
#16153=DIRECTION('ref_axis',(0.,0.968648305440766,0.248436028721142));
#16154=DIRECTION('',(1.,0.,0.));
#16155=DIRECTION('center_axis',(-1.,0.,0.));
#16156=DIRECTION('ref_axis',(0.,0.968648305440766,0.248436028721142));
#16157=DIRECTION('',(1.,0.,0.));
#16158=DIRECTION('center_axis',(-1.,0.,0.));
#16159=DIRECTION('ref_axis',(0.,0.968648305440766,0.248436028721142));
#16160=DIRECTION('',(1.,0.,0.));
#16161=DIRECTION('center_axis',(-1.,0.,0.));
#16162=DIRECTION('ref_axis',(0.,0.968648305440766,0.248436028721142));
#16163=DIRECTION('',(1.,0.,0.));
#16164=DIRECTION('center_axis',(-1.,0.,0.));
#16165=DIRECTION('ref_axis',(0.,0.968648305440766,0.248436028721142));
#16166=DIRECTION('',(1.,0.,0.));
#16167=DIRECTION('center_axis',(-1.,0.,0.));
#16168=DIRECTION('ref_axis',(0.,0.968648305440766,0.248436028721142));
#16169=DIRECTION('',(1.,0.,0.));
#16170=DIRECTION('center_axis',(-1.,0.,0.));
#16171=DIRECTION('ref_axis',(0.,0.968648305440766,0.248436028721142));
#16172=DIRECTION('',(1.,0.,0.));
#16173=DIRECTION('center_axis',(-1.,0.,0.));
#16174=DIRECTION('ref_axis',(0.,0.968648305440766,0.248436028721142));
#16175=DIRECTION('',(1.,0.,0.));
#16176=DIRECTION('center_axis',(-1.,0.,0.));
#16177=DIRECTION('ref_axis',(0.,0.968648305440766,0.248436028721142));
#16178=DIRECTION('',(1.,0.,0.));
#16179=DIRECTION('center_axis',(-1.,0.,0.));
#16180=DIRECTION('ref_axis',(0.,0.968648305440766,0.248436028721142));
#16181=DIRECTION('',(1.,0.,0.));
#16182=DIRECTION('center_axis',(-1.,0.,0.));
#16183=DIRECTION('ref_axis',(0.,0.968648305440766,0.248436028721142));
#16184=DIRECTION('',(1.,0.,0.));
#16185=DIRECTION('center_axis',(-1.,0.,0.));
#16186=DIRECTION('ref_axis',(0.,0.968648305440766,0.248436028721142));
#16187=DIRECTION('',(1.,0.,0.));
#16188=DIRECTION('center_axis',(-1.,0.,0.));
#16189=DIRECTION('ref_axis',(0.,0.968648305440766,0.248436028721142));
#16190=DIRECTION('',(1.,0.,0.));
#16191=DIRECTION('center_axis',(-1.,0.,0.));
#16192=DIRECTION('ref_axis',(0.,0.968648305440766,0.248436028721142));
#16193=DIRECTION('',(1.,0.,0.));
#16194=DIRECTION('center_axis',(-1.,0.,0.));
#16195=DIRECTION('ref_axis',(0.,0.968648305440766,0.248436028721142));
#16196=DIRECTION('',(1.,0.,0.));
#16197=DIRECTION('center_axis',(-1.,0.,0.));
#16198=DIRECTION('ref_axis',(0.,0.968648305440766,0.248436028721142));
#16199=DIRECTION('',(1.,0.,0.));
#16200=DIRECTION('center_axis',(-1.,0.,0.));
#16201=DIRECTION('ref_axis',(0.,0.968648305440766,0.248436028721142));
#16202=DIRECTION('',(1.,0.,0.));
#16203=DIRECTION('center_axis',(-1.,0.,0.));
#16204=DIRECTION('ref_axis',(0.,0.968648305440766,0.248436028721142));
#16205=DIRECTION('',(1.,0.,0.));
#16206=DIRECTION('center_axis',(-1.,0.,0.));
#16207=DIRECTION('ref_axis',(0.,0.968648305440766,0.248436028721142));
#16208=DIRECTION('',(1.,0.,0.));
#16209=DIRECTION('center_axis',(-1.,0.,0.));
#16210=DIRECTION('ref_axis',(0.,0.968648305440766,0.248436028721142));
#16211=DIRECTION('',(1.,0.,0.));
#16212=DIRECTION('center_axis',(-1.,0.,0.));
#16213=DIRECTION('ref_axis',(0.,0.968648305440766,0.248436028721142));
#16214=DIRECTION('',(1.,0.,0.));
#16215=DIRECTION('center_axis',(-1.,0.,0.));
#16216=DIRECTION('ref_axis',(0.,0.968648305440766,0.248436028721142));
#16217=DIRECTION('',(1.,0.,0.));
#16218=DIRECTION('center_axis',(-1.,0.,0.));
#16219=DIRECTION('ref_axis',(0.,0.968648305440766,0.248436028721142));
#16220=DIRECTION('',(1.,0.,0.));
#16221=DIRECTION('center_axis',(-1.,0.,0.));
#16222=DIRECTION('ref_axis',(0.,0.968648305440766,0.248436028721142));
#16223=DIRECTION('',(1.,0.,0.));
#16224=DIRECTION('center_axis',(-1.,0.,0.));
#16225=DIRECTION('ref_axis',(0.,0.968648305440766,0.248436028721142));
#16226=DIRECTION('',(1.,0.,0.));
#16227=DIRECTION('center_axis',(-1.,0.,0.));
#16228=DIRECTION('ref_axis',(0.,0.968648305440766,0.248436028721142));
#16229=DIRECTION('',(1.,0.,0.));
#16230=DIRECTION('center_axis',(-1.,0.,0.));
#16231=DIRECTION('ref_axis',(0.,0.968648305440766,0.248436028721142));
#16232=DIRECTION('',(1.,0.,0.));
#16233=DIRECTION('center_axis',(-1.,0.,0.));
#16234=DIRECTION('ref_axis',(0.,0.968648305440766,0.248436028721142));
#16235=DIRECTION('',(1.,0.,0.));
#16236=DIRECTION('center_axis',(-1.,0.,0.));
#16237=DIRECTION('ref_axis',(0.,0.968648305440766,0.248436028721142));
#16238=DIRECTION('',(1.,0.,0.));
#16239=DIRECTION('center_axis',(-1.,0.,0.));
#16240=DIRECTION('ref_axis',(0.,0.968648305440766,0.248436028721142));
#16241=DIRECTION('',(1.,0.,0.));
#16242=DIRECTION('center_axis',(-1.,0.,0.));
#16243=DIRECTION('ref_axis',(0.,0.968648305440766,0.248436028721142));
#16244=DIRECTION('',(1.,0.,0.));
#16245=DIRECTION('center_axis',(-1.,0.,0.));
#16246=DIRECTION('ref_axis',(0.,0.968648305440766,0.248436028721142));
#16247=DIRECTION('',(1.,0.,0.));
#16248=DIRECTION('center_axis',(-1.,0.,0.));
#16249=DIRECTION('ref_axis',(0.,0.968648305440766,0.248436028721142));
#16250=DIRECTION('',(1.,0.,0.));
#16251=DIRECTION('center_axis',(-1.,0.,0.));
#16252=DIRECTION('ref_axis',(0.,0.968648305440766,0.248436028721142));
#16253=DIRECTION('',(1.,0.,0.));
#16254=DIRECTION('center_axis',(-1.,0.,0.));
#16255=DIRECTION('ref_axis',(0.,0.968648305440766,0.248436028721142));
#16256=DIRECTION('',(1.,0.,0.));
#16257=DIRECTION('center_axis',(-1.,0.,0.));
#16258=DIRECTION('ref_axis',(0.,0.968648305440766,0.248436028721142));
#16259=DIRECTION('',(1.,0.,0.));
#16260=DIRECTION('center_axis',(-1.,0.,0.));
#16261=DIRECTION('ref_axis',(0.,0.968648305440766,0.248436028721142));
#16262=DIRECTION('',(1.,0.,0.));
#16263=DIRECTION('center_axis',(-1.,0.,0.));
#16264=DIRECTION('ref_axis',(0.,0.968648305440766,0.248436028721142));
#16265=DIRECTION('',(1.,0.,0.));
#16266=DIRECTION('center_axis',(-1.,0.,0.));
#16267=DIRECTION('ref_axis',(0.,0.968648305440766,0.248436028721142));
#16268=DIRECTION('',(1.,0.,0.));
#16269=DIRECTION('center_axis',(-1.,0.,0.));
#16270=DIRECTION('ref_axis',(0.,0.968648305440766,0.248436028721142));
#16271=DIRECTION('',(1.,0.,0.));
#16272=DIRECTION('center_axis',(-1.,0.,0.));
#16273=DIRECTION('ref_axis',(0.,0.968648305440766,0.248436028721142));
#16274=DIRECTION('',(1.,0.,0.));
#16275=DIRECTION('center_axis',(-1.,0.,0.));
#16276=DIRECTION('ref_axis',(0.,0.968648305440766,0.248436028721142));
#16277=DIRECTION('',(1.,0.,0.));
#16278=DIRECTION('center_axis',(-1.,0.,0.));
#16279=DIRECTION('ref_axis',(0.,0.968648305440766,0.248436028721142));
#16280=DIRECTION('',(1.,0.,0.));
#16281=DIRECTION('center_axis',(-1.,0.,0.));
#16282=DIRECTION('ref_axis',(0.,0.968648305440766,0.248436028721142));
#16283=DIRECTION('',(1.,0.,0.));
#16284=DIRECTION('center_axis',(-1.,0.,0.));
#16285=DIRECTION('ref_axis',(0.,0.968648305440766,0.248436028721142));
#16286=DIRECTION('',(1.,0.,0.));
#16287=DIRECTION('center_axis',(-1.,0.,0.));
#16288=DIRECTION('ref_axis',(0.,0.968648305440766,0.248436028721142));
#16289=DIRECTION('',(1.,0.,0.));
#16290=DIRECTION('center_axis',(-1.,0.,0.));
#16291=DIRECTION('ref_axis',(0.,0.968648305440766,0.248436028721142));
#16292=DIRECTION('',(1.,0.,0.));
#16293=DIRECTION('center_axis',(-1.,0.,0.));
#16294=DIRECTION('ref_axis',(0.,0.968648305440766,0.248436028721142));
#16295=DIRECTION('',(1.,0.,0.));
#16296=DIRECTION('center_axis',(-1.,0.,0.));
#16297=DIRECTION('ref_axis',(0.,0.968648305440766,0.248436028721142));
#16298=DIRECTION('',(1.,0.,0.));
#16299=DIRECTION('center_axis',(-1.,0.,0.));
#16300=DIRECTION('ref_axis',(0.,0.968648305440766,0.248436028721142));
#16301=DIRECTION('',(1.,0.,0.));
#16302=DIRECTION('center_axis',(-1.,0.,0.));
#16303=DIRECTION('ref_axis',(0.,0.968648305440766,0.248436028721142));
#16304=DIRECTION('',(1.,0.,0.));
#16305=DIRECTION('center_axis',(-1.,0.,0.));
#16306=DIRECTION('ref_axis',(0.,0.968648305440766,0.248436028721142));
#16307=DIRECTION('',(1.,0.,0.));
#16308=DIRECTION('center_axis',(-1.,0.,0.));
#16309=DIRECTION('ref_axis',(0.,0.968648305440766,0.248436028721142));
#16310=DIRECTION('',(1.,0.,0.));
#16311=DIRECTION('center_axis',(-1.,0.,0.));
#16312=DIRECTION('ref_axis',(0.,0.968648305440766,0.248436028721142));
#16313=DIRECTION('',(1.,0.,0.));
#16314=DIRECTION('center_axis',(-1.,0.,0.));
#16315=DIRECTION('ref_axis',(0.,0.968648305440766,0.248436028721142));
#16316=DIRECTION('',(1.,0.,0.));
#16317=DIRECTION('center_axis',(-1.,0.,0.));
#16318=DIRECTION('ref_axis',(0.,0.968648305440766,0.248436028721142));
#16319=DIRECTION('',(1.,0.,0.));
#16320=DIRECTION('center_axis',(-1.,0.,0.));
#16321=DIRECTION('ref_axis',(0.,0.968648305440766,0.248436028721142));
#16322=DIRECTION('',(1.,0.,0.));
#16323=DIRECTION('center_axis',(-1.,0.,0.));
#16324=DIRECTION('ref_axis',(0.,0.968648305440766,0.248436028721142));
#16325=DIRECTION('',(1.,0.,0.));
#16326=DIRECTION('center_axis',(-1.,0.,0.));
#16327=DIRECTION('ref_axis',(0.,0.968648305440766,0.248436028721142));
#16328=DIRECTION('',(1.,0.,0.));
#16329=DIRECTION('center_axis',(-1.,0.,0.));
#16330=DIRECTION('ref_axis',(0.,0.968648305440766,0.248436028721142));
#16331=DIRECTION('',(1.,0.,0.));
#16332=DIRECTION('center_axis',(-1.,0.,0.));
#16333=DIRECTION('ref_axis',(0.,0.968648305440766,0.248436028721142));
#16334=DIRECTION('',(1.,0.,0.));
#16335=DIRECTION('center_axis',(-1.,0.,0.));
#16336=DIRECTION('ref_axis',(0.,0.968648305440766,0.248436028721142));
#16337=DIRECTION('',(1.,0.,0.));
#16338=DIRECTION('center_axis',(-1.,0.,0.));
#16339=DIRECTION('ref_axis',(0.,0.968648305440766,0.248436028721142));
#16340=DIRECTION('',(1.,0.,0.));
#16341=DIRECTION('center_axis',(-1.,0.,0.));
#16342=DIRECTION('ref_axis',(0.,0.968648305440766,0.248436028721142));
#16343=DIRECTION('',(1.,0.,0.));
#16344=DIRECTION('center_axis',(-1.,0.,0.));
#16345=DIRECTION('ref_axis',(0.,0.968648305440766,0.248436028721142));
#16346=DIRECTION('',(1.,0.,0.));
#16347=DIRECTION('center_axis',(-1.,0.,0.));
#16348=DIRECTION('ref_axis',(0.,0.968648305440766,0.248436028721142));
#16349=DIRECTION('',(1.,0.,0.));
#16350=DIRECTION('center_axis',(-1.,0.,0.));
#16351=DIRECTION('ref_axis',(0.,0.968648305440766,0.248436028721142));
#16352=DIRECTION('',(1.,0.,0.));
#16353=DIRECTION('center_axis',(-1.,0.,0.));
#16354=DIRECTION('ref_axis',(0.,0.968648305440766,0.248436028721142));
#16355=DIRECTION('',(1.,0.,0.));
#16356=DIRECTION('center_axis',(-1.,0.,0.));
#16357=DIRECTION('ref_axis',(0.,0.968648305440766,0.248436028721142));
#16358=DIRECTION('',(1.,0.,0.));
#16359=DIRECTION('center_axis',(-1.,0.,0.));
#16360=DIRECTION('ref_axis',(0.,0.968648305440766,0.248436028721142));
#16361=DIRECTION('',(1.,0.,0.));
#16362=DIRECTION('center_axis',(-1.,0.,0.));
#16363=DIRECTION('ref_axis',(0.,0.968648305440766,0.248436028721142));
#16364=DIRECTION('',(1.,0.,0.));
#16365=DIRECTION('center_axis',(-1.,0.,0.));
#16366=DIRECTION('ref_axis',(0.,0.968648305440766,0.248436028721142));
#16367=DIRECTION('',(1.,0.,0.));
#16368=DIRECTION('center_axis',(-1.,0.,0.));
#16369=DIRECTION('ref_axis',(0.,0.968648305440766,0.248436028721142));
#16370=DIRECTION('',(1.,0.,0.));
#16371=DIRECTION('center_axis',(-1.,0.,0.));
#16372=DIRECTION('ref_axis',(0.,0.968648305440766,0.248436028721142));
#16373=DIRECTION('',(1.,0.,0.));
#16374=DIRECTION('center_axis',(-1.,0.,0.));
#16375=DIRECTION('ref_axis',(0.,0.968648305440766,0.248436028721142));
#16376=DIRECTION('',(1.,0.,0.));
#16377=DIRECTION('center_axis',(-1.,0.,0.));
#16378=DIRECTION('ref_axis',(0.,0.968648305440766,0.248436028721142));
#16379=DIRECTION('',(1.,0.,0.));
#16380=DIRECTION('center_axis',(-1.,0.,0.));
#16381=DIRECTION('ref_axis',(0.,0.968648305440766,0.248436028721142));
#16382=DIRECTION('',(1.,0.,0.));
#16383=DIRECTION('center_axis',(-1.,0.,0.));
#16384=DIRECTION('ref_axis',(0.,0.968648305440766,0.248436028721142));
#16385=DIRECTION('',(1.,0.,0.));
#16386=DIRECTION('center_axis',(-1.,0.,0.));
#16387=DIRECTION('ref_axis',(0.,0.968648305440766,0.248436028721142));
#16388=DIRECTION('',(1.,0.,0.));
#16389=DIRECTION('center_axis',(-1.,0.,0.));
#16390=DIRECTION('ref_axis',(0.,0.968648305440766,0.248436028721142));
#16391=DIRECTION('',(1.,0.,0.));
#16392=DIRECTION('center_axis',(-1.,0.,0.));
#16393=DIRECTION('ref_axis',(0.,0.968648305440766,0.248436028721142));
#16394=DIRECTION('',(1.,0.,0.));
#16395=DIRECTION('center_axis',(-1.,0.,0.));
#16396=DIRECTION('ref_axis',(0.,0.968648305440766,0.248436028721142));
#16397=DIRECTION('',(1.,0.,0.));
#16398=DIRECTION('center_axis',(-1.,0.,0.));
#16399=DIRECTION('ref_axis',(0.,0.968648305440766,0.248436028721142));
#16400=DIRECTION('',(1.,0.,0.));
#16401=DIRECTION('center_axis',(-1.,0.,0.));
#16402=DIRECTION('ref_axis',(0.,0.968648305440766,0.248436028721142));
#16403=DIRECTION('',(1.,0.,0.));
#16404=DIRECTION('center_axis',(-1.,0.,0.));
#16405=DIRECTION('ref_axis',(0.,0.968648305440766,0.248436028721142));
#16406=DIRECTION('',(1.,0.,0.));
#16407=DIRECTION('center_axis',(-1.,0.,0.));
#16408=DIRECTION('ref_axis',(0.,0.968648305440766,0.248436028721142));
#16409=DIRECTION('',(1.,0.,0.));
#16410=DIRECTION('center_axis',(-1.,0.,0.));
#16411=DIRECTION('ref_axis',(0.,0.968648305440766,0.248436028721142));
#16412=DIRECTION('',(1.,0.,0.));
#16413=DIRECTION('center_axis',(-1.,0.,0.));
#16414=DIRECTION('ref_axis',(0.,0.968648305440766,0.248436028721142));
#16415=DIRECTION('',(1.,0.,0.));
#16416=DIRECTION('center_axis',(-1.,0.,0.));
#16417=DIRECTION('ref_axis',(0.,0.968648305440766,0.248436028721142));
#16418=DIRECTION('',(1.,0.,0.));
#16419=DIRECTION('center_axis',(-1.,0.,0.));
#16420=DIRECTION('ref_axis',(0.,0.968648305440766,0.248436028721142));
#16421=DIRECTION('',(1.,0.,0.));
#16422=DIRECTION('center_axis',(-1.,0.,0.));
#16423=DIRECTION('ref_axis',(0.,0.968648305440766,0.248436028721142));
#16424=DIRECTION('',(1.,0.,0.));
#16425=DIRECTION('center_axis',(-1.,0.,0.));
#16426=DIRECTION('ref_axis',(0.,0.968648305440766,0.248436028721142));
#16427=DIRECTION('',(1.,0.,0.));
#16428=DIRECTION('center_axis',(-1.,0.,0.));
#16429=DIRECTION('ref_axis',(0.,0.968648305440766,0.248436028721142));
#16430=DIRECTION('',(1.,0.,0.));
#16431=DIRECTION('center_axis',(-1.,0.,0.));
#16432=DIRECTION('ref_axis',(0.,0.968648305440766,0.248436028721142));
#16433=DIRECTION('',(1.,0.,0.));
#16434=DIRECTION('center_axis',(-1.,0.,0.));
#16435=DIRECTION('ref_axis',(0.,0.968648305440766,0.248436028721142));
#16436=DIRECTION('',(1.,0.,0.));
#16437=DIRECTION('center_axis',(-1.,0.,0.));
#16438=DIRECTION('ref_axis',(0.,0.968648305440766,0.248436028721142));
#16439=DIRECTION('',(1.,0.,0.));
#16440=DIRECTION('center_axis',(-1.,0.,0.));
#16441=DIRECTION('ref_axis',(0.,0.968648305440766,0.248436028721142));
#16442=DIRECTION('',(1.,0.,0.));
#16443=DIRECTION('center_axis',(-1.,0.,0.));
#16444=DIRECTION('ref_axis',(0.,0.968648305440766,0.248436028721142));
#16445=DIRECTION('',(1.,0.,0.));
#16446=DIRECTION('center_axis',(-1.,0.,0.));
#16447=DIRECTION('ref_axis',(0.,0.968648305440766,0.248436028721142));
#16448=DIRECTION('',(1.,0.,0.));
#16449=DIRECTION('center_axis',(-1.,0.,0.));
#16450=DIRECTION('ref_axis',(0.,0.968648305440766,0.248436028721142));
#16451=DIRECTION('',(1.,0.,0.));
#16452=DIRECTION('center_axis',(-1.,0.,0.));
#16453=DIRECTION('ref_axis',(0.,0.968648305440766,0.248436028721142));
#16454=DIRECTION('',(1.,0.,0.));
#16455=DIRECTION('center_axis',(-1.,0.,0.));
#16456=DIRECTION('ref_axis',(0.,0.968648305440766,0.248436028721142));
#16457=DIRECTION('',(1.,0.,0.));
#16458=DIRECTION('center_axis',(-1.,0.,0.));
#16459=DIRECTION('ref_axis',(0.,0.968648305440766,0.248436028721142));
#16460=DIRECTION('',(1.,0.,0.));
#16461=DIRECTION('center_axis',(-1.,0.,0.));
#16462=DIRECTION('ref_axis',(0.,0.968648305440766,0.248436028721142));
#16463=DIRECTION('',(1.,0.,0.));
#16464=DIRECTION('center_axis',(-1.,0.,0.));
#16465=DIRECTION('ref_axis',(0.,0.968648305440766,0.248436028721142));
#16466=DIRECTION('',(1.,0.,0.));
#16467=DIRECTION('center_axis',(-1.,0.,0.));
#16468=DIRECTION('ref_axis',(0.,0.968648305440766,0.248436028721142));
#16469=DIRECTION('',(1.,0.,0.));
#16470=DIRECTION('center_axis',(-1.,0.,0.));
#16471=DIRECTION('ref_axis',(0.,0.968648305440766,0.248436028721142));
#16472=DIRECTION('',(1.,0.,0.));
#16473=DIRECTION('center_axis',(-1.,0.,0.));
#16474=DIRECTION('ref_axis',(0.,0.968648305440766,0.248436028721142));
#16475=DIRECTION('',(1.,0.,0.));
#16476=DIRECTION('center_axis',(-1.,0.,0.));
#16477=DIRECTION('ref_axis',(0.,0.968648305440766,0.248436028721142));
#16478=DIRECTION('',(1.,0.,0.));
#16479=DIRECTION('center_axis',(-1.,0.,0.));
#16480=DIRECTION('ref_axis',(0.,0.968648305440766,0.248436028721142));
#16481=DIRECTION('',(1.,0.,0.));
#16482=DIRECTION('center_axis',(-1.,0.,0.));
#16483=DIRECTION('ref_axis',(0.,0.968648305440766,0.248436028721142));
#16484=DIRECTION('',(1.,0.,0.));
#16485=DIRECTION('center_axis',(-1.,0.,0.));
#16486=DIRECTION('ref_axis',(0.,0.968648305440766,0.248436028721142));
#16487=DIRECTION('',(1.,0.,0.));
#16488=DIRECTION('center_axis',(-1.,0.,0.));
#16489=DIRECTION('ref_axis',(0.,0.968648305440766,0.248436028721142));
#16490=DIRECTION('',(1.,0.,0.));
#16491=DIRECTION('center_axis',(-1.,0.,0.));
#16492=DIRECTION('ref_axis',(0.,0.968648305440766,0.248436028721142));
#16493=DIRECTION('',(1.,0.,0.));
#16494=DIRECTION('center_axis',(-1.,0.,0.));
#16495=DIRECTION('ref_axis',(0.,0.968648305440766,0.248436028721142));
#16496=DIRECTION('',(1.,0.,0.));
#16497=DIRECTION('center_axis',(-1.,0.,0.));
#16498=DIRECTION('ref_axis',(0.,0.968648305440766,0.248436028721142));
#16499=DIRECTION('',(1.,0.,0.));
#16500=DIRECTION('center_axis',(-1.,0.,0.));
#16501=DIRECTION('ref_axis',(0.,0.968648305440766,0.248436028721142));
#16502=DIRECTION('',(1.,0.,0.));
#16503=DIRECTION('center_axis',(-1.,0.,0.));
#16504=DIRECTION('ref_axis',(0.,0.968648305440766,0.248436028721142));
#16505=DIRECTION('',(1.,0.,0.));
#16506=DIRECTION('center_axis',(-1.,0.,0.));
#16507=DIRECTION('ref_axis',(0.,0.968648305440766,0.248436028721142));
#16508=DIRECTION('',(1.,0.,0.));
#16509=DIRECTION('center_axis',(-1.,0.,0.));
#16510=DIRECTION('ref_axis',(0.,0.968648305440766,0.248436028721142));
#16511=DIRECTION('',(1.,0.,0.));
#16512=DIRECTION('center_axis',(-1.,0.,0.));
#16513=DIRECTION('ref_axis',(0.,0.968648305440766,0.248436028721142));
#16514=DIRECTION('',(1.,0.,0.));
#16515=DIRECTION('center_axis',(-1.,0.,0.));
#16516=DIRECTION('ref_axis',(0.,0.968648305440766,0.248436028721142));
#16517=DIRECTION('',(1.,0.,0.));
#16518=DIRECTION('center_axis',(-1.,0.,0.));
#16519=DIRECTION('ref_axis',(0.,0.968648305440766,0.248436028721142));
#16520=DIRECTION('',(1.,0.,0.));
#16521=DIRECTION('center_axis',(-1.,0.,0.));
#16522=DIRECTION('ref_axis',(0.,0.968648305440766,0.248436028721142));
#16523=DIRECTION('',(1.,0.,0.));
#16524=DIRECTION('center_axis',(-1.,0.,0.));
#16525=DIRECTION('ref_axis',(0.,0.968648305440766,0.248436028721142));
#16526=DIRECTION('',(1.,0.,0.));
#16527=DIRECTION('center_axis',(-1.,0.,0.));
#16528=DIRECTION('ref_axis',(0.,0.968648305440766,0.248436028721142));
#16529=DIRECTION('',(1.,0.,0.));
#16530=DIRECTION('center_axis',(-1.,0.,0.));
#16531=DIRECTION('ref_axis',(0.,0.968648305440766,0.248436028721142));
#16532=DIRECTION('',(1.,0.,0.));
#16533=DIRECTION('center_axis',(-1.,0.,0.));
#16534=DIRECTION('ref_axis',(0.,0.968648305440766,0.248436028721142));
#16535=DIRECTION('',(1.,0.,0.));
#16536=DIRECTION('center_axis',(-1.,0.,0.));
#16537=DIRECTION('ref_axis',(0.,0.968648305440766,0.248436028721142));
#16538=DIRECTION('',(1.,0.,0.));
#16539=DIRECTION('center_axis',(-1.,0.,0.));
#16540=DIRECTION('ref_axis',(0.,0.968648305440766,0.248436028721142));
#16541=DIRECTION('',(1.,0.,0.));
#16542=DIRECTION('center_axis',(-1.,0.,0.));
#16543=DIRECTION('ref_axis',(0.,0.968648305440766,0.248436028721142));
#16544=DIRECTION('',(1.,0.,0.));
#16545=DIRECTION('center_axis',(-1.,0.,0.));
#16546=DIRECTION('ref_axis',(0.,0.968648305440766,0.248436028721142));
#16547=DIRECTION('',(1.,0.,0.));
#16548=DIRECTION('center_axis',(-1.,0.,0.));
#16549=DIRECTION('ref_axis',(0.,0.968648305440766,0.248436028721142));
#16550=DIRECTION('',(1.,0.,0.));
#16551=DIRECTION('center_axis',(-1.,0.,0.));
#16552=DIRECTION('ref_axis',(0.,0.968648305440766,0.248436028721142));
#16553=DIRECTION('',(1.,0.,0.));
#16554=DIRECTION('center_axis',(-1.,0.,0.));
#16555=DIRECTION('ref_axis',(0.,0.968648305440766,0.248436028721142));
#16556=DIRECTION('',(1.,0.,0.));
#16557=DIRECTION('center_axis',(-1.,0.,0.));
#16558=DIRECTION('ref_axis',(0.,0.968648305440766,0.248436028721142));
#16559=DIRECTION('',(1.,0.,0.));
#16560=DIRECTION('center_axis',(-1.,0.,0.));
#16561=DIRECTION('ref_axis',(0.,0.968648305440766,0.248436028721142));
#16562=DIRECTION('',(1.,0.,0.));
#16563=DIRECTION('center_axis',(-1.,0.,0.));
#16564=DIRECTION('ref_axis',(0.,0.968648305440766,0.248436028721142));
#16565=DIRECTION('',(1.,0.,0.));
#16566=DIRECTION('center_axis',(-1.,0.,0.));
#16567=DIRECTION('ref_axis',(0.,0.968648305440766,0.248436028721142));
#16568=DIRECTION('',(1.,0.,0.));
#16569=DIRECTION('center_axis',(-1.,0.,0.));
#16570=DIRECTION('ref_axis',(0.,0.968648305440766,0.248436028721142));
#16571=DIRECTION('',(1.,0.,0.));
#16572=DIRECTION('center_axis',(-1.,0.,0.));
#16573=DIRECTION('ref_axis',(0.,0.968648305440766,0.248436028721142));
#16574=DIRECTION('',(1.,0.,0.));
#16575=DIRECTION('center_axis',(-1.,0.,0.));
#16576=DIRECTION('ref_axis',(0.,0.968648305440766,0.248436028721142));
#16577=DIRECTION('',(1.,0.,0.));
#16578=DIRECTION('center_axis',(-1.,0.,0.));
#16579=DIRECTION('ref_axis',(0.,0.968648305440766,0.248436028721142));
#16580=DIRECTION('',(1.,0.,0.));
#16581=DIRECTION('center_axis',(-1.,0.,0.));
#16582=DIRECTION('ref_axis',(0.,0.968648305440766,0.248436028721142));
#16583=DIRECTION('',(1.,0.,0.));
#16584=DIRECTION('center_axis',(-1.,0.,0.));
#16585=DIRECTION('ref_axis',(0.,0.968648305440766,0.248436028721142));
#16586=DIRECTION('',(1.,0.,0.));
#16587=DIRECTION('center_axis',(-1.,0.,0.));
#16588=DIRECTION('ref_axis',(0.,0.968648305440766,0.248436028721142));
#16589=DIRECTION('',(1.,0.,0.));
#16590=DIRECTION('center_axis',(-1.,0.,0.));
#16591=DIRECTION('ref_axis',(0.,0.968648305440766,0.248436028721142));
#16592=DIRECTION('',(1.,0.,0.));
#16593=DIRECTION('center_axis',(-1.,0.,0.));
#16594=DIRECTION('ref_axis',(0.,0.968648305440766,0.248436028721142));
#16595=DIRECTION('',(1.,0.,0.));
#16596=DIRECTION('center_axis',(-1.,0.,0.));
#16597=DIRECTION('ref_axis',(0.,0.968648305440766,0.248436028721142));
#16598=DIRECTION('',(1.,0.,0.));
#16599=DIRECTION('center_axis',(-1.,0.,0.));
#16600=DIRECTION('ref_axis',(0.,0.968648305440766,0.248436028721142));
#16601=DIRECTION('',(1.,0.,0.));
#16602=DIRECTION('center_axis',(-1.,0.,0.));
#16603=DIRECTION('ref_axis',(0.,0.968648305440766,0.248436028721142));
#16604=DIRECTION('',(1.,0.,0.));
#16605=DIRECTION('center_axis',(-1.,0.,0.));
#16606=DIRECTION('ref_axis',(0.,0.968648305440766,0.248436028721142));
#16607=DIRECTION('',(1.,0.,0.));
#16608=DIRECTION('center_axis',(-1.,0.,0.));
#16609=DIRECTION('ref_axis',(0.,0.968648305440766,0.248436028721142));
#16610=DIRECTION('',(1.,0.,0.));
#16611=DIRECTION('center_axis',(-1.,0.,0.));
#16612=DIRECTION('ref_axis',(0.,0.968648305440766,0.248436028721142));
#16613=DIRECTION('',(1.,0.,0.));
#16614=DIRECTION('center_axis',(-1.,0.,0.));
#16615=DIRECTION('ref_axis',(0.,0.968648305440766,0.248436028721142));
#16616=DIRECTION('',(1.,0.,0.));
#16617=DIRECTION('center_axis',(-1.,0.,0.));
#16618=DIRECTION('ref_axis',(0.,0.968648305440766,0.248436028721142));
#16619=DIRECTION('',(1.,0.,0.));
#16620=DIRECTION('center_axis',(-1.,0.,0.));
#16621=DIRECTION('ref_axis',(0.,0.968648305440766,0.248436028721142));
#16622=DIRECTION('',(1.,0.,0.));
#16623=DIRECTION('center_axis',(-1.,0.,0.));
#16624=DIRECTION('ref_axis',(0.,0.968648305440766,0.248436028721142));
#16625=DIRECTION('',(1.,0.,0.));
#16626=DIRECTION('center_axis',(-1.,0.,0.));
#16627=DIRECTION('ref_axis',(0.,0.968648305440766,0.248436028721142));
#16628=DIRECTION('',(1.,0.,0.));
#16629=DIRECTION('center_axis',(-1.,0.,0.));
#16630=DIRECTION('ref_axis',(0.,0.968648305440766,0.248436028721142));
#16631=DIRECTION('',(1.,0.,0.));
#16632=DIRECTION('center_axis',(-1.,0.,0.));
#16633=DIRECTION('ref_axis',(0.,0.968648305440766,0.248436028721142));
#16634=DIRECTION('',(1.,0.,0.));
#16635=DIRECTION('center_axis',(-1.,0.,0.));
#16636=DIRECTION('ref_axis',(0.,0.968648305440766,0.248436028721142));
#16637=DIRECTION('',(1.,0.,0.));
#16638=DIRECTION('center_axis',(-1.,0.,0.));
#16639=DIRECTION('ref_axis',(0.,0.968648305440766,0.248436028721142));
#16640=DIRECTION('',(1.,0.,0.));
#16641=DIRECTION('center_axis',(-1.,0.,0.));
#16642=DIRECTION('ref_axis',(0.,0.968648305440766,0.248436028721142));
#16643=DIRECTION('',(1.,0.,0.));
#16644=DIRECTION('center_axis',(-1.,0.,0.));
#16645=DIRECTION('ref_axis',(0.,0.968648305440766,0.248436028721142));
#16646=DIRECTION('',(1.,0.,0.));
#16647=DIRECTION('center_axis',(-1.,0.,0.));
#16648=DIRECTION('ref_axis',(0.,0.968648305440766,0.248436028721142));
#16649=DIRECTION('',(1.,0.,0.));
#16650=DIRECTION('center_axis',(-1.,0.,0.));
#16651=DIRECTION('ref_axis',(0.,0.968648305440766,0.248436028721142));
#16652=DIRECTION('',(1.,0.,0.));
#16653=DIRECTION('center_axis',(-1.,0.,0.));
#16654=DIRECTION('ref_axis',(0.,0.968648305440766,0.248436028721142));
#16655=DIRECTION('',(1.,0.,0.));
#16656=DIRECTION('center_axis',(-1.,0.,0.));
#16657=DIRECTION('ref_axis',(0.,1.,0.));
#16658=DIRECTION('center_axis',(-1.,0.,0.));
#16659=DIRECTION('ref_axis',(0.,1.,0.));
#16660=DIRECTION('center_axis',(-1.,0.,0.));
#16661=DIRECTION('ref_axis',(0.,1.,0.));
#16662=DIRECTION('center_axis',(-1.,0.,0.));
#16663=DIRECTION('ref_axis',(0.,0.968648305440766,0.248436028721142));
#16664=DIRECTION('center_axis',(-1.,0.,0.));
#16665=DIRECTION('ref_axis',(0.,1.,-2.30250085928462E-11));
#16666=DIRECTION('center_axis',(1.,0.,0.));
#16667=DIRECTION('ref_axis',(0.,1.,0.));
#16668=DIRECTION('center_axis',(1.,0.,0.));
#16669=DIRECTION('ref_axis',(0.,1.,0.));
#16670=DIRECTION('center_axis',(1.,0.,0.));
#16671=DIRECTION('ref_axis',(0.,1.,0.));
#16672=DIRECTION('center_axis',(1.,0.,0.));
#16673=DIRECTION('ref_axis',(0.,1.,0.));
#16674=DIRECTION('',(-1.,0.,0.));
#16675=DIRECTION('center_axis',(1.,0.,0.));
#16676=DIRECTION('ref_axis',(0.,1.,0.));
#16677=DIRECTION('center_axis',(1.,0.,0.));
#16678=DIRECTION('ref_axis',(0.,1.,0.));
#16679=DIRECTION('center_axis',(0.,-1.,0.));
#16680=DIRECTION('ref_axis',(0.,0.,1.));
#16681=DIRECTION('',(0.,0.,1.));
#16682=DIRECTION('',(1.,0.,0.));
#16683=DIRECTION('',(0.,0.,1.));
#16684=DIRECTION('',(-1.,0.,0.));
#16685=DIRECTION('center_axis',(1.,0.,0.));
#16686=DIRECTION('ref_axis',(0.,1.,0.));
#16687=DIRECTION('center_axis',(-1.,0.,0.));
#16688=DIRECTION('ref_axis',(0.,1.,0.));
#16689=DIRECTION('center_axis',(0.,1.,0.));
#16690=DIRECTION('ref_axis',(0.,0.,-1.));
#16691=DIRECTION('',(0.,0.,-1.));
#16692=DIRECTION('',(1.,0.,0.));
#16693=DIRECTION('',(0.,0.,-1.));
#16694=DIRECTION('',(-1.,0.,0.));
#16695=DIRECTION('center_axis',(1.,0.,0.));
#16696=DIRECTION('ref_axis',(0.,1.,0.));
#16697=DIRECTION('center_axis',(-1.,0.,0.));
#16698=DIRECTION('ref_axis',(0.,1.,0.));
#16699=DIRECTION('center_axis',(-1.,0.,0.));
#16700=DIRECTION('ref_axis',(0.,1.,0.));
#16701=DIRECTION('center_axis',(1.,0.,0.));
#16702=DIRECTION('ref_axis',(0.,1.,0.));
#16703=DIRECTION('',(-1.,0.,0.));
#16704=DIRECTION('center_axis',(1.,0.,0.));
#16705=DIRECTION('ref_axis',(0.,1.,0.));
#16706=DIRECTION('center_axis',(1.,0.,0.));
#16707=DIRECTION('ref_axis',(0.,1.,0.));
#16708=DIRECTION('center_axis',(1.,0.,0.));
#16709=DIRECTION('ref_axis',(0.,1.,0.));
#16710=DIRECTION('center_axis',(1.,0.,0.));
#16711=DIRECTION('ref_axis',(0.,1.,0.));
#16712=DIRECTION('axis',(0.,0.,1.));
#16713=DIRECTION('refdir',(1.,0.,0.));
#16714=DIRECTION('center_axis',(0.,-1.,0.));
#16715=DIRECTION('ref_axis',(-1.,0.,0.));
#16716=DIRECTION('center_axis',(0.,1.,0.));
#16717=DIRECTION('ref_axis',(-1.,0.,0.));
#16718=DIRECTION('',(0.,-1.,0.));
#16719=DIRECTION('center_axis',(0.,1.,0.));
#16720=DIRECTION('ref_axis',(-1.,0.,0.));
#16721=DIRECTION('',(0.,-1.,0.));
#16722=DIRECTION('center_axis',(0.,1.,0.));
#16723=DIRECTION('ref_axis',(-1.,0.,0.));
#16724=DIRECTION('',(0.,1.,0.));
#16725=DIRECTION('center_axis',(0.,1.,0.));
#16726=DIRECTION('ref_axis',(-1.,0.,0.));
#16727=DIRECTION('center_axis',(0.,1.,0.));
#16728=DIRECTION('ref_axis',(-1.,0.,0.));
#16729=DIRECTION('',(0.,1.,0.));
#16730=DIRECTION('center_axis',(0.,-1.,0.));
#16731=DIRECTION('ref_axis',(-1.,0.,0.));
#16732=DIRECTION('',(0.,-1.,0.));
#16733=DIRECTION('center_axis',(0.,-1.,0.));
#16734=DIRECTION('ref_axis',(-1.,0.,0.));
#16735=DIRECTION('center_axis',(0.,-1.,0.));
#16736=DIRECTION('ref_axis',(-1.,0.,0.));
#16737=DIRECTION('',(0.,1.,0.));
#16738=DIRECTION('center_axis',(0.,-1.,0.));
#16739=DIRECTION('ref_axis',(-1.,0.,0.));
#16740=DIRECTION('',(0.,-1.,0.));
#16741=DIRECTION('center_axis',(0.,-1.,0.));
#16742=DIRECTION('ref_axis',(-1.,0.,0.));
#16743=DIRECTION('',(0.,1.,0.));
#16744=DIRECTION('center_axis',(0.,1.,0.));
#16745=DIRECTION('ref_axis',(-1.,0.,0.));
#16746=DIRECTION('',(0.,-1.,0.));
#16747=DIRECTION('center_axis',(0.,-1.,0.));
#16748=DIRECTION('ref_axis',(-1.,0.,0.));
#16749=DIRECTION('',(0.,1.,0.));
#16750=DIRECTION('center_axis',(0.,1.,0.));
#16751=DIRECTION('ref_axis',(-1.,0.,0.));
#16752=DIRECTION('center_axis',(0.,-1.,0.));
#16753=DIRECTION('ref_axis',(-0.503773977045354,0.,0.863835505204496));
#16754=DIRECTION('center_axis',(-1.19937668507924E-53,1.,-2.1198911140988E-53));
#16755=DIRECTION('ref_axis',(-0.492423560103467,-2.43566064310008E-53,-0.8703556959399));
#16756=DIRECTION('center_axis',(-1.19937668507924E-53,1.,-2.1198911140988E-53));
#16757=DIRECTION('ref_axis',(-0.492423560103467,-2.43566064310008E-53,-0.8703556959399));
#16758=DIRECTION('center_axis',(0.,-1.,0.));
#16759=DIRECTION('ref_axis',(-0.492423560103467,0.,-0.8703556959399));
#16760=DIRECTION('center_axis',(0.,-1.,0.));
#16761=DIRECTION('ref_axis',(0.503443599526488,0.,-0.864028091033974));
#16762=DIRECTION('',(0.864028091033974,0.,0.503443599526487));
#16763=DIRECTION('center_axis',(0.,-1.,0.));
#16764=DIRECTION('ref_axis',(-0.503443599526489,0.,0.864028091033974));
#16765=DIRECTION('',(-0.864028091033974,0.,-0.503443599526487));
#16766=DIRECTION('center_axis',(0.,1.,0.));
#16767=DIRECTION('ref_axis',(-0.492423560103467,0.,-0.8703556959399));
#16768=DIRECTION('center_axis',(0.,-1.,0.));
#16769=DIRECTION('ref_axis',(-0.492423560103467,0.,-0.8703556959399));
#16770=DIRECTION('',(-0.864028091033974,0.,-0.503443599526487));
#16771=DIRECTION('center_axis',(0.,-1.,0.));
#16772=DIRECTION('ref_axis',(-0.503443599526489,0.,0.864028091033974));
#16773=DIRECTION('',(0.864028091033974,0.,0.503443599526487));
#16774=DIRECTION('center_axis',(0.,-1.,0.));
#16775=DIRECTION('ref_axis',(0.503443599526488,0.,-0.864028091033974));
#16776=DIRECTION('center_axis',(0.,1.,0.));
#16777=DIRECTION('ref_axis',(-0.492423560103467,0.,-0.8703556959399));
#16778=DIRECTION('center_axis',(0.,-1.,0.));
#16779=DIRECTION('ref_axis',(-0.492423560103467,0.,-0.8703556959399));
#16780=DIRECTION('',(0.,-1.,0.));
#16781=DIRECTION('center_axis',(0.503443599526487,0.,-0.864028091033974));
#16782=DIRECTION('ref_axis',(0.864028091033974,0.,0.503443599526487));
#16783=DIRECTION('',(0.,-1.,0.));
#16784=DIRECTION('',(0.,-1.,0.));
#16785=DIRECTION('center_axis',(0.,-1.,0.));
#16786=DIRECTION('ref_axis',(-0.503443599526489,0.,0.864028091033974));
#16787=DIRECTION('',(0.,-1.,0.));
#16788=DIRECTION('center_axis',(-0.503443599526487,0.,0.864028091033974));
#16789=DIRECTION('ref_axis',(-0.864028091033974,0.,-0.503443599526487));
#16790=DIRECTION('center_axis',(0.,-1.,0.));
#16791=DIRECTION('ref_axis',(0.503443599526488,0.,-0.864028091033974));
#16792=DIRECTION('center_axis',(0.,-1.,0.));
#16793=DIRECTION('ref_axis',(-0.492423560103467,0.,-0.8703556959399));
#16794=DIRECTION('center_axis',(0.,-1.,0.));
#16795=DIRECTION('ref_axis',(-0.503773977045354,0.,0.863835505204496));
#16796=DIRECTION('center_axis',(1.19937668507924E-53,1.,2.1198911140988E-53));
#16797=DIRECTION('ref_axis',(-0.492423560103467,2.43566064310008E-53,-0.8703556959399));
#16798=DIRECTION('center_axis',(1.19937668507924E-53,1.,2.1198911140988E-53));
#16799=DIRECTION('ref_axis',(-0.492423560103467,2.43566064310008E-53,-0.8703556959399));
#16800=DIRECTION('center_axis',(0.503443599526487,0.,-0.864028091033974));
#16801=DIRECTION('ref_axis',(-0.864028091033974,0.,-0.503443599526487));
#16802=DIRECTION('',(-0.864028091033974,0.,-0.503443599526487));
#16803=DIRECTION('',(0.,1.,0.));
#16804=DIRECTION('',(-0.864028091033974,0.,-0.503443599526487));
#16805=DIRECTION('center_axis',(0.,-1.,0.));
#16806=DIRECTION('ref_axis',(-0.492423560103467,0.,-0.8703556959399));
#16807=DIRECTION('center_axis',(0.,-1.,0.));
#16808=DIRECTION('ref_axis',(0.503443599526488,0.,-0.864028091033974));
#16809=DIRECTION('',(0.864028091033974,0.,0.503443599526487));
#16810=DIRECTION('center_axis',(0.,-1.,0.));
#16811=DIRECTION('ref_axis',(-0.503443599526489,0.,0.864028091033974));
#16812=DIRECTION('center_axis',(0.,1.,0.));
#16813=DIRECTION('ref_axis',(-0.492423560103467,0.,-0.8703556959399));
#16814=DIRECTION('center_axis',(0.,-1.,0.));
#16815=DIRECTION('ref_axis',(-0.492423560103467,0.,-0.8703556959399));
#16816=DIRECTION('center_axis',(0.,-1.,0.));
#16817=DIRECTION('ref_axis',(-0.492423560103467,0.,-0.8703556959399));
#16818=DIRECTION('',(0.,-1.,0.));
#16819=DIRECTION('center_axis',(0.,1.,0.));
#16820=DIRECTION('ref_axis',(-0.492423560103467,0.,-0.8703556959399));
#16821=DIRECTION('center_axis',(-0.503443599526487,0.,0.864028091033974));
#16822=DIRECTION('ref_axis',(0.864028091033974,0.,0.503443599526487));
#16823=DIRECTION('',(0.864028091033974,0.,0.503443599526487));
#16824=DIRECTION('',(0.,1.,0.));
#16825=DIRECTION('',(0.,1.,0.));
#16826=DIRECTION('center_axis',(0.,-1.,0.));
#16827=DIRECTION('ref_axis',(-0.503443599526489,0.,0.864028091033974));
#16828=DIRECTION('center_axis',(0.,-1.,0.));
#16829=DIRECTION('ref_axis',(-0.503443599526489,0.,0.864028091033974));
#16830=DIRECTION('center_axis',(0.,-1.,0.));
#16831=DIRECTION('ref_axis',(0.503443599526488,0.,-0.864028091033974));
#16832=DIRECTION('center_axis',(0.,-1.,0.));
#16833=DIRECTION('ref_axis',(0.503443599526488,0.,-0.864028091033974));
#16834=DIRECTION('center_axis',(0.,-1.,0.));
#16835=DIRECTION('ref_axis',(-0.492423560103467,0.,-0.8703556959399));
#16836=DIRECTION('axis',(0.,0.,1.));
#16837=DIRECTION('refdir',(1.,0.,0.));
#16838=DIRECTION('center_axis',(-1.,0.,0.));
#16839=DIRECTION('ref_axis',(0.,0.968648305440766,0.248436028721142));
#16840=DIRECTION('',(-1.,0.,0.));
#16841=DIRECTION('center_axis',(-1.,0.,0.));
#16842=DIRECTION('ref_axis',(0.,0.968648305440766,0.248436028721142));
#16843=DIRECTION('',(-1.,0.,0.));
#16844=DIRECTION('center_axis',(-1.,0.,0.));
#16845=DIRECTION('ref_axis',(0.,0.968648305440766,0.248436028721142));
#16846=DIRECTION('',(-1.,0.,0.));
#16847=DIRECTION('center_axis',(-1.,0.,0.));
#16848=DIRECTION('ref_axis',(0.,0.968648305440766,0.248436028721142));
#16849=DIRECTION('',(-1.,0.,0.));
#16850=DIRECTION('center_axis',(-1.,0.,0.));
#16851=DIRECTION('ref_axis',(0.,0.968648305440766,0.248436028721142));
#16852=DIRECTION('',(-1.,0.,0.));
#16853=DIRECTION('center_axis',(-1.,0.,0.));
#16854=DIRECTION('ref_axis',(0.,0.968648305440766,0.248436028721142));
#16855=DIRECTION('',(-1.,0.,0.));
#16856=DIRECTION('center_axis',(-1.,0.,0.));
#16857=DIRECTION('ref_axis',(0.,0.968648305440766,0.248436028721142));
#16858=DIRECTION('',(-1.,0.,0.));
#16859=DIRECTION('center_axis',(-1.,0.,0.));
#16860=DIRECTION('ref_axis',(0.,0.968648305440766,0.248436028721142));
#16861=DIRECTION('',(-1.,0.,0.));
#16862=DIRECTION('center_axis',(-1.,0.,0.));
#16863=DIRECTION('ref_axis',(0.,0.968648305440766,0.248436028721142));
#16864=DIRECTION('',(-1.,0.,0.));
#16865=DIRECTION('center_axis',(-1.,0.,0.));
#16866=DIRECTION('ref_axis',(0.,0.968648305440766,0.248436028721142));
#16867=DIRECTION('',(-1.,0.,0.));
#16868=DIRECTION('center_axis',(-1.,0.,0.));
#16869=DIRECTION('ref_axis',(0.,0.968648305440766,0.248436028721142));
#16870=DIRECTION('',(-1.,0.,0.));
#16871=DIRECTION('center_axis',(-1.,0.,0.));
#16872=DIRECTION('ref_axis',(0.,0.968648305440766,0.248436028721142));
#16873=DIRECTION('',(-1.,0.,0.));
#16874=DIRECTION('center_axis',(-1.,0.,0.));
#16875=DIRECTION('ref_axis',(0.,0.968648305440766,0.248436028721142));
#16876=DIRECTION('',(-1.,0.,0.));
#16877=DIRECTION('center_axis',(-1.,0.,0.));
#16878=DIRECTION('ref_axis',(0.,0.968648305440766,0.248436028721142));
#16879=DIRECTION('',(-1.,0.,0.));
#16880=DIRECTION('center_axis',(-1.,0.,0.));
#16881=DIRECTION('ref_axis',(0.,0.968648305440766,0.248436028721142));
#16882=DIRECTION('',(-1.,0.,0.));
#16883=DIRECTION('center_axis',(-1.,0.,0.));
#16884=DIRECTION('ref_axis',(0.,0.968648305440766,0.248436028721142));
#16885=DIRECTION('',(-1.,0.,0.));
#16886=DIRECTION('center_axis',(-1.,0.,0.));
#16887=DIRECTION('ref_axis',(0.,0.968648305440766,0.248436028721142));
#16888=DIRECTION('',(-1.,0.,0.));
#16889=DIRECTION('center_axis',(-1.,0.,0.));
#16890=DIRECTION('ref_axis',(0.,1.,0.));
#16891=DIRECTION('center_axis',(-1.,0.,0.));
#16892=DIRECTION('ref_axis',(0.,-0.988910129220642,0.148515172035763));
#16893=DIRECTION('center_axis',(-1.,0.,0.));
#16894=DIRECTION('ref_axis',(0.,0.968648305440766,0.248436028721142));
#16895=DIRECTION('center_axis',(-1.,0.,0.));
#16896=DIRECTION('ref_axis',(0.,-0.967688737574893,-0.252147788351813));
#16897=DIRECTION('center_axis',(-1.,0.,0.));
#16898=DIRECTION('ref_axis',(0.,0.968648305440766,0.248436028721142));
#16899=DIRECTION('center_axis',(0.,-1.,0.));
#16900=DIRECTION('ref_axis',(1.,0.,0.));
#16901=DIRECTION('center_axis',(0.,-1.,0.));
#16902=DIRECTION('ref_axis',(1.,0.,0.));
#16903=DIRECTION('',(0.,1.,0.));
#16904=DIRECTION('',(0.,1.,0.));
#16905=DIRECTION('center_axis',(0.,-1.,0.));
#16906=DIRECTION('ref_axis',(1.,0.,0.));
#16907=DIRECTION('center_axis',(0.,-1.,0.));
#16908=DIRECTION('ref_axis',(1.,0.,0.));
#16909=DIRECTION('center_axis',(0.,-1.,0.));
#16910=DIRECTION('ref_axis',(1.,0.,0.));
#16911=DIRECTION('axis',(0.,0.,1.));
#16912=DIRECTION('refdir',(1.,0.,0.));
#16913=DIRECTION('center_axis',(0.,1.,0.));
#16914=DIRECTION('ref_axis',(1.,0.,0.));
#16915=DIRECTION('center_axis',(0.,-1.,0.));
#16916=DIRECTION('ref_axis',(1.,0.,0.));
#16917=DIRECTION('',(0.,1.,0.));
#16918=DIRECTION('center_axis',(0.,-1.,0.));
#16919=DIRECTION('ref_axis',(1.,0.,0.));
#16920=DIRECTION('center_axis',(-0.504104280893361,0.,0.863642793048716));
#16921=DIRECTION('ref_axis',(-0.863642793048716,0.,-0.504104280893361));
#16922=DIRECTION('',(-0.863642793048716,0.,-0.504104280893361));
#16923=DIRECTION('',(0.,-1.,0.));
#16924=DIRECTION('',(-0.863642793048716,0.,-0.504104280893361));
#16925=DIRECTION('',(0.,-1.,0.));
#16926=DIRECTION('center_axis',(0.,1.,0.));
#16927=DIRECTION('ref_axis',(-0.504104280893359,0.,0.863642793048717));
#16928=DIRECTION('center_axis',(0.,1.,0.));
#16929=DIRECTION('ref_axis',(-0.504104280893359,0.,0.863642793048717));
#16930=DIRECTION('',(0.,-1.,0.));
#16931=DIRECTION('center_axis',(0.,1.,0.));
#16932=DIRECTION('ref_axis',(-0.504104280893359,0.,0.863642793048717));
#16933=DIRECTION('center_axis',(0.504104280893361,0.,-0.863642793048716));
#16934=DIRECTION('ref_axis',(0.863642793048716,0.,0.504104280893361));
#16935=DIRECTION('',(0.863642793048716,0.,0.504104280893361));
#16936=DIRECTION('',(0.,-1.,0.));
#16937=DIRECTION('',(0.863642793048716,0.,0.504104280893361));
#16938=DIRECTION('center_axis',(0.,1.,0.));
#16939=DIRECTION('ref_axis',(1.,0.,0.));
#16940=DIRECTION('center_axis',(0.,1.,0.));
#16941=DIRECTION('ref_axis',(1.,0.,0.));
#16942=DIRECTION('center_axis',(0.,1.,0.));
#16943=DIRECTION('ref_axis',(1.,0.,0.));
#16944=DIRECTION('center_axis',(0.,1.,0.));
#16945=DIRECTION('ref_axis',(0.50410428089336,0.,-0.863642793048716));
#16946=DIRECTION('center_axis',(-2.43566064310008E-53,-1.,1.62748695315959E-104));
#16947=DIRECTION('ref_axis',(1.,-2.43566064310008E-53,0.));
#16948=DIRECTION('center_axis',(0.,1.,0.));
#16949=DIRECTION('ref_axis',(1.,0.,0.));
#16950=DIRECTION('center_axis',(2.43566064310008E-53,-1.,-1.62748695315959E-104));
#16951=DIRECTION('ref_axis',(1.,2.43566064310008E-53,0.));
#16952=DIRECTION('',(0.,1.,0.));
#16953=DIRECTION('center_axis',(0.,1.,0.));
#16954=DIRECTION('ref_axis',(1.,0.,0.));
#16955=DIRECTION('center_axis',(0.,-1.,0.));
#16956=DIRECTION('ref_axis',(1.,0.,0.));
#16957=DIRECTION('',(0.,1.,0.));
#16958=DIRECTION('center_axis',(0.,-1.,0.));
#16959=DIRECTION('ref_axis',(1.,0.,0.));
#16960=DIRECTION('center_axis',(0.504104280893361,0.,-0.863642793048716));
#16961=DIRECTION('ref_axis',(-0.863642793048716,0.,-0.504104280893361));
#16962=DIRECTION('',(-0.863642793048716,0.,-0.504104280893361));
#16963=DIRECTION('',(0.,1.,0.));
#16964=DIRECTION('',(-0.863642793048716,0.,-0.504104280893361));
#16965=DIRECTION('',(0.,1.,0.));
#16966=DIRECTION('center_axis',(0.,1.,0.));
#16967=DIRECTION('ref_axis',(-0.504104280893359,0.,0.863642793048717));
#16968=DIRECTION('center_axis',(0.,1.,0.));
#16969=DIRECTION('ref_axis',(-0.504104280893359,0.,0.863642793048717));
#16970=DIRECTION('center_axis',(0.,1.,0.));
#16971=DIRECTION('ref_axis',(-0.504104280893359,0.,0.863642793048717));
#16972=DIRECTION('',(0.,1.,0.));
#16973=DIRECTION('center_axis',(-0.504104280893361,0.,0.863642793048716));
#16974=DIRECTION('ref_axis',(0.863642793048716,0.,0.504104280893361));
#16975=DIRECTION('',(0.863642793048716,0.,0.504104280893361));
#16976=DIRECTION('',(0.863642793048716,0.,0.504104280893361));
#16977=DIRECTION('',(0.,1.,0.));
#16978=DIRECTION('center_axis',(0.,1.,0.));
#16979=DIRECTION('ref_axis',(0.50410428089336,0.,-0.863642793048716));
#16980=DIRECTION('',(0.,-1.,0.));
#16981=DIRECTION('center_axis',(0.,-1.,0.));
#16982=DIRECTION('ref_axis',(1.,0.,0.));
#16983=DIRECTION('center_axis',(0.,1.,0.));
#16984=DIRECTION('ref_axis',(0.50410428089336,0.,-0.863642793048716));
#16985=DIRECTION('center_axis',(0.,1.,0.));
#16986=DIRECTION('ref_axis',(1.,0.,0.));
#16987=DIRECTION('center_axis',(0.,1.,0.));
#16988=DIRECTION('ref_axis',(1.,0.,0.));
#16989=DIRECTION('axis',(0.,0.,1.));
#16990=DIRECTION('refdir',(1.,0.,0.));
#16991=DIRECTION('center_axis',(0.,1.,0.));
#16992=DIRECTION('ref_axis',(1.,0.,0.));
#16993=DIRECTION('center_axis',(0.,-1.,0.));
#16994=DIRECTION('ref_axis',(1.,0.,0.));
#16995=DIRECTION('',(0.,1.,0.));
#16996=DIRECTION('center_axis',(0.,-1.,0.));
#16997=DIRECTION('ref_axis',(1.,0.,0.));
#16998=DIRECTION('',(0.,1.,0.));
#16999=DIRECTION('center_axis',(0.,-1.,0.));
#17000=DIRECTION('ref_axis',(1.,0.,0.));
#17001=DIRECTION('',(0.,-1.,0.));
#17002=DIRECTION('center_axis',(0.,-1.,0.));
#17003=DIRECTION('ref_axis',(1.,0.,0.));
#17004=DIRECTION('center_axis',(0.,-1.,0.));
#17005=DIRECTION('ref_axis',(1.,0.,0.));
#17006=DIRECTION('',(0.,-1.,0.));
#17007=DIRECTION('center_axis',(0.,1.,0.));
#17008=DIRECTION('ref_axis',(1.,0.,0.));
#17009=DIRECTION('',(0.,1.,0.));
#17010=DIRECTION('center_axis',(0.,1.,0.));
#17011=DIRECTION('ref_axis',(1.,0.,0.));
#17012=DIRECTION('center_axis',(0.,1.,0.));
#17013=DIRECTION('ref_axis',(1.,0.,0.));
#17014=DIRECTION('',(0.,-1.,0.));
#17015=DIRECTION('center_axis',(0.,1.,0.));
#17016=DIRECTION('ref_axis',(1.,0.,0.));
#17017=DIRECTION('',(0.,1.,0.));
#17018=DIRECTION('center_axis',(0.,1.,0.));
#17019=DIRECTION('ref_axis',(1.,0.,0.));
#17020=DIRECTION('',(0.,-1.,0.));
#17021=DIRECTION('center_axis',(0.,-1.,0.));
#17022=DIRECTION('ref_axis',(1.,0.,0.));
#17023=DIRECTION('',(0.,1.,0.));
#17024=DIRECTION('center_axis',(0.,1.,0.));
#17025=DIRECTION('ref_axis',(1.,0.,0.));
#17026=DIRECTION('',(0.,-1.,0.));
#17027=DIRECTION('center_axis',(0.,-1.,0.));
#17028=DIRECTION('ref_axis',(1.,0.,0.));
#17029=DIRECTION('center_axis',(0.,1.,0.));
#17030=DIRECTION('ref_axis',(0.503773977045354,0.,0.863835505204496));
#17031=DIRECTION('center_axis',(-1.19937668507924E-53,-1.,2.1198911140988E-53));
#17032=DIRECTION('ref_axis',(0.492423560103467,-2.43566064310008E-53,-0.8703556959399));
#17033=DIRECTION('center_axis',(-1.19937668507924E-53,-1.,2.1198911140988E-53));
#17034=DIRECTION('ref_axis',(0.492423560103467,-2.43566064310008E-53,-0.8703556959399));
#17035=DIRECTION('center_axis',(-0.503443599526487,0.,-0.864028091033974));
#17036=DIRECTION('ref_axis',(0.864028091033974,0.,-0.503443599526487));
#17037=DIRECTION('',(0.864028091033974,0.,-0.503443599526487));
#17038=DIRECTION('',(0.,-1.,0.));
#17039=DIRECTION('',(0.864028091033974,0.,-0.503443599526487));
#17040=DIRECTION('center_axis',(0.,1.,0.));
#17041=DIRECTION('ref_axis',(0.492423560103467,0.,-0.8703556959399));
#17042=DIRECTION('center_axis',(0.,1.,0.));
#17043=DIRECTION('ref_axis',(-0.503443599526488,0.,-0.864028091033974));
#17044=DIRECTION('',(-0.864028091033974,0.,0.503443599526487));
#17045=DIRECTION('center_axis',(0.,1.,0.));
#17046=DIRECTION('ref_axis',(0.503443599526489,0.,0.864028091033974));
#17047=DIRECTION('center_axis',(0.,-1.,0.));
#17048=DIRECTION('ref_axis',(0.492423560103467,0.,-0.8703556959399));
#17049=DIRECTION('center_axis',(0.,1.,0.));
#17050=DIRECTION('ref_axis',(0.492423560103467,0.,-0.8703556959399));
#17051=DIRECTION('center_axis',(0.,1.,0.));
#17052=DIRECTION('ref_axis',(0.492423560103467,0.,-0.8703556959399));
#17053=DIRECTION('',(0.,1.,0.));
#17054=DIRECTION('center_axis',(0.,-1.,0.));
#17055=DIRECTION('ref_axis',(0.492423560103467,0.,-0.8703556959399));
#17056=DIRECTION('center_axis',(0.503443599526487,0.,0.864028091033974));
#17057=DIRECTION('ref_axis',(-0.864028091033974,0.,0.503443599526487));
#17058=DIRECTION('',(-0.864028091033974,0.,0.503443599526487));
#17059=DIRECTION('',(0.,-1.,0.));
#17060=DIRECTION('',(0.,-1.,0.));
#17061=DIRECTION('center_axis',(0.,1.,0.));
#17062=DIRECTION('ref_axis',(0.503443599526489,0.,0.864028091033974));
#17063=DIRECTION('center_axis',(0.,1.,0.));
#17064=DIRECTION('ref_axis',(0.503443599526489,0.,0.864028091033974));
#17065=DIRECTION('center_axis',(0.,1.,0.));
#17066=DIRECTION('ref_axis',(-0.503443599526488,0.,-0.864028091033974));
#17067=DIRECTION('center_axis',(0.,1.,0.));
#17068=DIRECTION('ref_axis',(-0.503443599526488,0.,-0.864028091033974));
#17069=DIRECTION('center_axis',(0.,1.,0.));
#17070=DIRECTION('ref_axis',(0.492423560103467,0.,-0.8703556959399));
#17071=DIRECTION('center_axis',(0.,1.,0.));
#17072=DIRECTION('ref_axis',(0.503773977045354,0.,0.863835505204496));
#17073=DIRECTION('center_axis',(1.19937668507924E-53,-1.,-2.1198911140988E-53));
#17074=DIRECTION('ref_axis',(0.492423560103467,2.43566064310008E-53,-0.8703556959399));
#17075=DIRECTION('center_axis',(1.19937668507924E-53,-1.,-2.1198911140988E-53));
#17076=DIRECTION('ref_axis',(0.492423560103467,2.43566064310008E-53,-0.8703556959399));
#17077=DIRECTION('center_axis',(0.,1.,0.));
#17078=DIRECTION('ref_axis',(0.492423560103467,0.,-0.8703556959399));
#17079=DIRECTION('center_axis',(0.,1.,0.));
#17080=DIRECTION('ref_axis',(-0.503443599526488,0.,-0.864028091033974));
#17081=DIRECTION('',(-0.864028091033974,0.,0.503443599526487));
#17082=DIRECTION('center_axis',(0.,1.,0.));
#17083=DIRECTION('ref_axis',(0.503443599526489,0.,0.864028091033974));
#17084=DIRECTION('',(0.864028091033974,0.,-0.503443599526487));
#17085=DIRECTION('center_axis',(0.,-1.,0.));
#17086=DIRECTION('ref_axis',(0.492423560103467,0.,-0.8703556959399));
#17087=DIRECTION('center_axis',(0.,1.,0.));
#17088=DIRECTION('ref_axis',(0.492423560103467,0.,-0.8703556959399));
#17089=DIRECTION('',(0.864028091033974,0.,-0.503443599526487));
#17090=DIRECTION('center_axis',(0.,1.,0.));
#17091=DIRECTION('ref_axis',(0.503443599526489,0.,0.864028091033974));
#17092=DIRECTION('',(-0.864028091033974,0.,0.503443599526487));
#17093=DIRECTION('center_axis',(0.,1.,0.));
#17094=DIRECTION('ref_axis',(-0.503443599526488,0.,-0.864028091033974));
#17095=DIRECTION('center_axis',(0.,-1.,0.));
#17096=DIRECTION('ref_axis',(0.492423560103467,0.,-0.8703556959399));
#17097=DIRECTION('center_axis',(0.,1.,0.));
#17098=DIRECTION('ref_axis',(0.492423560103467,0.,-0.8703556959399));
#17099=DIRECTION('',(0.,1.,0.));
#17100=DIRECTION('center_axis',(-0.503443599526487,0.,-0.864028091033974));
#17101=DIRECTION('ref_axis',(-0.864028091033974,0.,0.503443599526487));
#17102=DIRECTION('',(0.,1.,0.));
#17103=DIRECTION('',(0.,1.,0.));
#17104=DIRECTION('center_axis',(0.,1.,0.));
#17105=DIRECTION('ref_axis',(0.503443599526489,0.,0.864028091033974));
#17106=DIRECTION('',(0.,1.,0.));
#17107=DIRECTION('center_axis',(0.503443599526487,0.,0.864028091033974));
#17108=DIRECTION('ref_axis',(0.864028091033974,0.,-0.503443599526487));
#17109=DIRECTION('center_axis',(0.,1.,0.));
#17110=DIRECTION('ref_axis',(-0.503443599526488,0.,-0.864028091033974));
#17111=DIRECTION('center_axis',(0.,1.,0.));
#17112=DIRECTION('ref_axis',(0.492423560103467,0.,-0.8703556959399));
#17113=DIRECTION('axis',(0.,0.,1.));
#17114=DIRECTION('refdir',(1.,0.,0.));
#17115=DIRECTION('center_axis',(0.,0.,1.));
#17116=DIRECTION('ref_axis',(-0.707106781186548,0.707106781186548,0.));
#17117=DIRECTION('center_axis',(0.,0.,-1.));
#17118=DIRECTION('ref_axis',(-0.707106781186548,0.707106781186548,0.));
#17119=DIRECTION('',(0.,0.,-1.));
#17120=DIRECTION('center_axis',(0.,0.,1.));
#17121=DIRECTION('ref_axis',(-0.707106781186548,0.707106781186548,0.));
#17122=DIRECTION('',(0.,0.,1.));
#17123=DIRECTION('center_axis',(0.,-1.,0.));
#17124=DIRECTION('ref_axis',(-1.,0.,0.));
#17125=DIRECTION('center_axis',(0.,1.,0.));
#17126=DIRECTION('ref_axis',(-1.,0.,0.));
#17127=DIRECTION('',(0.,-1.,0.));
#17128=DIRECTION('center_axis',(0.,1.,0.));
#17129=DIRECTION('ref_axis',(-1.,0.,0.));
#17130=DIRECTION('center_axis',(0.707106781186548,0.,0.707106781186548));
#17131=DIRECTION('ref_axis',(0.707106781186548,0.,-0.707106781186548));
#17132=DIRECTION('',(0.707106781186547,0.,-0.707106781186547));
#17133=DIRECTION('',(0.,1.,0.));
#17134=DIRECTION('',(0.707106781186547,0.,-0.707106781186547));
#17135=DIRECTION('',(0.,1.,0.));
#17136=DIRECTION('center_axis',(0.,0.,-1.));
#17137=DIRECTION('ref_axis',(0.707106781186548,0.707106781186548,0.));
#17138=DIRECTION('center_axis',(0.,0.,1.));
#17139=DIRECTION('ref_axis',(0.707106781186548,0.707106781186548,0.));
#17140=DIRECTION('',(0.,0.,1.));
#17141=DIRECTION('center_axis',(0.,0.,-1.));
#17142=DIRECTION('ref_axis',(0.707106781186548,0.707106781186548,0.));
#17143=DIRECTION('',(0.,0.,-1.));
#17144=DIRECTION('center_axis',(0.,1.,0.));
#17145=DIRECTION('ref_axis',(0.,0.,1.));
#17146=DIRECTION('',(-1.,0.,0.));
#17147=DIRECTION('',(-1.,0.,0.));
#17148=DIRECTION('center_axis',(1.,0.,0.));
#17149=DIRECTION('ref_axis',(0.,0.707106781186548,0.707106781186547));
#17150=DIRECTION('',(1.,0.,0.));
#17151=DIRECTION('center_axis',(1.,0.,0.));
#17152=DIRECTION('ref_axis',(0.,0.707106781186548,0.707106781186547));
#17153=DIRECTION('',(-1.,0.,0.));
#17154=DIRECTION('center_axis',(1.,0.,0.));
#17155=DIRECTION('ref_axis',(0.,0.707106781186548,0.707106781186547));
#17156=DIRECTION('center_axis',(0.,-1.,0.));
#17157=DIRECTION('ref_axis',(1.,0.,0.));
#17158=DIRECTION('',(0.,0.,-1.));
#17159=DIRECTION('',(1.,0.,0.));
#17160=DIRECTION('',(-0.707106781186547,0.,-0.707106781186547));
#17161=DIRECTION('',(0.,0.,-1.));
#17162=DIRECTION('center_axis',(0.,-1.,0.));
#17163=DIRECTION('ref_axis',(1.,0.,0.));
#17164=DIRECTION('center_axis',(1.,0.,0.));
#17165=DIRECTION('ref_axis',(0.,0.707106781186548,0.707106781186547));
#17166=DIRECTION('center_axis',(-1.,0.,0.));
#17167=DIRECTION('ref_axis',(0.,0.707106781186548,0.707106781186547));
#17168=DIRECTION('',(-1.,0.,0.));
#17169=DIRECTION('center_axis',(-1.,0.,0.));
#17170=DIRECTION('ref_axis',(0.,0.707106781186548,0.707106781186547));
#17171=DIRECTION('',(1.,0.,0.));
#17172=DIRECTION('center_axis',(0.,1.,0.));
#17173=DIRECTION('ref_axis',(0.,0.,1.));
#17174=DIRECTION('',(0.,0.,-1.));
#17175=DIRECTION('',(-0.707106781186547,0.,-0.707106781186547));
#17176=DIRECTION('',(-1.,0.,0.));
#17177=DIRECTION('',(0.,0.,-1.));
#17178=DIRECTION('center_axis',(0.,-1.,0.));
#17179=DIRECTION('ref_axis',(1.,0.,0.));
#17180=DIRECTION('center_axis',(0.,1.,0.));
#17181=DIRECTION('ref_axis',(1.,0.,0.));
#17182=DIRECTION('',(0.,1.,0.));
#17183=DIRECTION('center_axis',(0.,0.,-1.));
#17184=DIRECTION('ref_axis',(-1.,0.,0.));
#17185=DIRECTION('',(0.,1.,0.));
#17186=DIRECTION('center_axis',(0.707106781186548,0.,-0.707106781186548));
#17187=DIRECTION('ref_axis',(-0.707106781186548,0.,-0.707106781186548));
#17188=DIRECTION('',(0.,1.,0.));
#17189=DIRECTION('center_axis',(0.,0.,-1.));
#17190=DIRECTION('ref_axis',(-0.707106781186548,-0.707106781186548,0.));
#17191=DIRECTION('center_axis',(0.,0.,1.));
#17192=DIRECTION('ref_axis',(-0.707106781186548,-0.707106781186548,0.));
#17193=DIRECTION('',(0.,0.,1.));
#17194=DIRECTION('center_axis',(0.,0.,-1.));
#17195=DIRECTION('ref_axis',(-0.707106781186548,-0.707106781186548,0.));
#17196=DIRECTION('',(0.,0.,-1.));
#17197=DIRECTION('center_axis',(-1.,0.,0.));
#17198=DIRECTION('ref_axis',(0.,0.,-1.));
#17199=DIRECTION('',(0.,-1.,0.));
#17200=DIRECTION('',(0.,-1.,0.));
#17201=DIRECTION('center_axis',(-1.,0.,0.));
#17202=DIRECTION('ref_axis',(0.,0.,-1.));
#17203=DIRECTION('center_axis',(1.,0.,0.));
#17204=DIRECTION('ref_axis',(0.,-0.707106781186548,0.707106781186547));
#17205=DIRECTION('',(0.,-1.,0.));
#17206=DIRECTION('',(0.,1.,0.));
#17207=DIRECTION('center_axis',(-1.,0.,0.));
#17208=DIRECTION('ref_axis',(0.,-0.707106781186548,0.707106781186547));
#17209=DIRECTION('',(0.,0.,-1.));
#17210=DIRECTION('',(0.,-1.,0.));
#17211=DIRECTION('',(0.,0.,-1.));
#17212=DIRECTION('center_axis',(0.,-1.,0.));
#17213=DIRECTION('ref_axis',(-1.,0.,0.));
#17214=DIRECTION('center_axis',(0.,1.,0.));
#17215=DIRECTION('ref_axis',(-1.,0.,0.));
#17216=DIRECTION('',(0.,-1.,0.));
#17217=DIRECTION('center_axis',(0.,1.,0.));
#17218=DIRECTION('ref_axis',(-1.,0.,0.));
#17219=DIRECTION('center_axis',(-0.707106781186548,0.,-0.707106781186548));
#17220=DIRECTION('ref_axis',(0.707106781186548,0.,-0.707106781186548));
#17221=DIRECTION('',(0.707106781186547,0.,-0.707106781186547));
#17222=DIRECTION('',(0.,-1.,0.));
#17223=DIRECTION('',(0.707106781186547,0.,-0.707106781186547));
#17224=DIRECTION('center_axis',(0.,0.,1.));
#17225=DIRECTION('ref_axis',(0.707106781186548,-0.707106781186548,0.));
#17226=DIRECTION('center_axis',(0.,0.,-1.));
#17227=DIRECTION('ref_axis',(0.707106781186548,-0.707106781186548,0.));
#17228=DIRECTION('',(0.,0.,-1.));
#17229=DIRECTION('center_axis',(0.,0.,1.));
#17230=DIRECTION('ref_axis',(0.707106781186548,-0.707106781186548,0.));
#17231=DIRECTION('',(0.,0.,1.));
#17232=DIRECTION('center_axis',(0.,1.,0.));
#17233=DIRECTION('ref_axis',(0.,0.,1.));
#17234=DIRECTION('',(-1.,0.,0.));
#17235=DIRECTION('',(-1.,0.,0.));
#17236=DIRECTION('center_axis',(0.,0.,1.));
#17237=DIRECTION('ref_axis',(-1.,0.,0.));
#17238=DIRECTION('',(0.,1.,0.));
#17239=DIRECTION('',(1.,0.,0.));
#17240=DIRECTION('',(0.,1.,0.));
#17241=DIRECTION('center_axis',(-1.,0.,0.));
#17242=DIRECTION('ref_axis',(0.,0.,-1.));
#17243=DIRECTION('',(0.,1.,0.));
#17244=DIRECTION('center_axis',(0.,0.,-1.));
#17245=DIRECTION('ref_axis',(1.,0.,0.));
#17246=DIRECTION('center_axis',(-1.,0.,0.));
#17247=DIRECTION('ref_axis',(0.,-0.707106781186548,0.707106781186547));
#17248=DIRECTION('',(1.,0.,0.));
#17249=DIRECTION('',(-1.,0.,0.));
#17250=DIRECTION('center_axis',(-1.,0.,0.));
#17251=DIRECTION('ref_axis',(0.,-0.707106781186548,0.707106781186547));
#17252=DIRECTION('center_axis',(0.,-1.,0.));
#17253=DIRECTION('ref_axis',(1.,0.,0.));
#17254=DIRECTION('',(0.,0.,-1.));
#17255=DIRECTION('',(-0.707106781186547,0.,-0.707106781186547));
#17256=DIRECTION('',(1.,0.,0.));
#17257=DIRECTION('center_axis',(0.,-1.,0.));
#17258=DIRECTION('ref_axis',(1.,0.,0.));
#17259=DIRECTION('center_axis',(-1.,0.,0.));
#17260=DIRECTION('ref_axis',(0.,-0.707106781186548,0.707106781186547));
#17261=DIRECTION('center_axis',(1.,0.,0.));
#17262=DIRECTION('ref_axis',(0.,-0.707106781186548,0.707106781186547));
#17263=DIRECTION('',(-1.,0.,0.));
#17264=DIRECTION('center_axis',(0.,1.,0.));
#17265=DIRECTION('ref_axis',(0.,0.,1.));
#17266=DIRECTION('',(-1.,0.,0.));
#17267=DIRECTION('',(-0.707106781186547,0.,-0.707106781186547));
#17268=DIRECTION('',(0.,0.,-1.));
#17269=DIRECTION('center_axis',(0.,-1.,0.));
#17270=DIRECTION('ref_axis',(1.,0.,0.));
#17271=DIRECTION('center_axis',(-1.,0.,0.));
#17272=DIRECTION('ref_axis',(0.,0.,-1.));
#17273=DIRECTION('',(0.,-1.,0.));
#17274=DIRECTION('',(0.,1.,0.));
#17275=DIRECTION('center_axis',(0.,1.,0.));
#17276=DIRECTION('ref_axis',(1.,0.,0.));
#17277=DIRECTION('',(0.,1.,0.));
#17278=DIRECTION('center_axis',(0.,0.,1.));
#17279=DIRECTION('ref_axis',(-1.,0.,0.));
#17280=DIRECTION('',(0.,-1.,0.));
#17281=DIRECTION('center_axis',(-0.707106781186548,0.,0.707106781186548));
#17282=DIRECTION('ref_axis',(-0.707106781186548,0.,-0.707106781186548));
#17283=DIRECTION('center_axis',(0.,0.,1.));
#17284=DIRECTION('ref_axis',(-1.,0.,0.));
#17285=DIRECTION('axis',(0.,0.,1.));
#17286=DIRECTION('refdir',(1.,0.,0.));
#17287=DIRECTION('center_axis',(-1.,0.,0.));
#17288=DIRECTION('ref_axis',(0.,0.968648305440766,0.248436028721142));
#17289=DIRECTION('',(-1.,0.,0.));
#17290=DIRECTION('center_axis',(-1.,0.,0.));
#17291=DIRECTION('ref_axis',(0.,0.968648305440766,0.248436028721142));
#17292=DIRECTION('',(-1.,0.,0.));
#17293=DIRECTION('center_axis',(-1.,0.,0.));
#17294=DIRECTION('ref_axis',(0.,0.968648305440766,0.248436028721142));
#17295=DIRECTION('',(-1.,0.,0.));
#17296=DIRECTION('center_axis',(-1.,0.,0.));
#17297=DIRECTION('ref_axis',(0.,0.968648305440766,0.248436028721142));
#17298=DIRECTION('',(-1.,0.,0.));
#17299=DIRECTION('center_axis',(-1.,0.,0.));
#17300=DIRECTION('ref_axis',(0.,0.968648305440766,0.248436028721142));
#17301=DIRECTION('',(-1.,0.,0.));
#17302=DIRECTION('center_axis',(-1.,0.,0.));
#17303=DIRECTION('ref_axis',(0.,0.968648305440766,0.248436028721142));
#17304=DIRECTION('',(-1.,0.,0.));
#17305=DIRECTION('center_axis',(-1.,0.,0.));
#17306=DIRECTION('ref_axis',(0.,0.968648305440766,0.248436028721142));
#17307=DIRECTION('',(-1.,0.,0.));
#17308=DIRECTION('center_axis',(-1.,0.,0.));
#17309=DIRECTION('ref_axis',(0.,0.968648305440766,0.248436028721142));
#17310=DIRECTION('',(-1.,0.,0.));
#17311=DIRECTION('center_axis',(-1.,0.,0.));
#17312=DIRECTION('ref_axis',(0.,0.968648305440766,0.248436028721142));
#17313=DIRECTION('',(-1.,0.,0.));
#17314=DIRECTION('center_axis',(-1.,0.,0.));
#17315=DIRECTION('ref_axis',(0.,0.968648305440766,0.248436028721142));
#17316=DIRECTION('',(-1.,0.,0.));
#17317=DIRECTION('center_axis',(-1.,0.,0.));
#17318=DIRECTION('ref_axis',(0.,0.968648305440766,0.248436028721142));
#17319=DIRECTION('',(-1.,0.,0.));
#17320=DIRECTION('center_axis',(-1.,0.,0.));
#17321=DIRECTION('ref_axis',(0.,0.968648305440766,0.248436028721142));
#17322=DIRECTION('',(-1.,0.,0.));
#17323=DIRECTION('center_axis',(-1.,0.,0.));
#17324=DIRECTION('ref_axis',(0.,0.968648305440766,0.248436028721142));
#17325=DIRECTION('',(-1.,0.,0.));
#17326=DIRECTION('center_axis',(-1.,0.,0.));
#17327=DIRECTION('ref_axis',(0.,0.968648305440766,0.248436028721142));
#17328=DIRECTION('',(-1.,0.,0.));
#17329=DIRECTION('center_axis',(-1.,0.,0.));
#17330=DIRECTION('ref_axis',(0.,0.968648305440766,0.248436028721142));
#17331=DIRECTION('',(-1.,0.,0.));
#17332=DIRECTION('center_axis',(-1.,0.,0.));
#17333=DIRECTION('ref_axis',(0.,0.968648305440766,0.248436028721142));
#17334=DIRECTION('',(-1.,0.,0.));
#17335=DIRECTION('center_axis',(-1.,0.,0.));
#17336=DIRECTION('ref_axis',(0.,0.968648305440766,0.248436028721142));
#17337=DIRECTION('',(-1.,0.,0.));
#17338=DIRECTION('center_axis',(-1.,0.,0.));
#17339=DIRECTION('ref_axis',(0.,1.,0.));
#17340=DIRECTION('center_axis',(-1.,0.,0.));
#17341=DIRECTION('ref_axis',(0.,1.,0.));
#17342=DIRECTION('center_axis',(-1.,0.,0.));
#17343=DIRECTION('ref_axis',(0.,0.968648305440766,0.248436028721142));
#17344=DIRECTION('center_axis',(-1.,0.,0.));
#17345=DIRECTION('ref_axis',(0.,-0.960836623023769,-0.277115470257942));
#17346=DIRECTION('center_axis',(-1.,0.,0.));
#17347=DIRECTION('ref_axis',(0.,1.,0.));
#17348=DIRECTION('center_axis',(0.,1.,0.));
#17349=DIRECTION('ref_axis',(-1.,0.,0.));
#17350=DIRECTION('center_axis',(0.,1.,0.));
#17351=DIRECTION('ref_axis',(-1.,0.,0.));
#17352=DIRECTION('',(0.,-1.,0.));
#17353=DIRECTION('',(0.,-1.,0.));
#17354=DIRECTION('center_axis',(0.,1.,0.));
#17355=DIRECTION('ref_axis',(-1.,0.,0.));
#17356=DIRECTION('center_axis',(0.,1.,0.));
#17357=DIRECTION('ref_axis',(-1.,0.,0.));
#17358=DIRECTION('center_axis',(0.,1.,0.));
#17359=DIRECTION('ref_axis',(-1.,0.,0.));
#17360=DIRECTION('axis',(0.,0.,1.));
#17361=DIRECTION('refdir',(1.,0.,0.));
#17362=DIRECTION('center_axis',(0.,-1.,0.));
#17363=DIRECTION('ref_axis',(-1.,0.,0.));
#17364=DIRECTION('center_axis',(0.,1.,0.));
#17365=DIRECTION('ref_axis',(-1.,0.,0.));
#17366=DIRECTION('',(0.,-1.,0.));
#17367=DIRECTION('center_axis',(0.,1.,0.));
#17368=DIRECTION('ref_axis',(-1.,0.,0.));
#17369=DIRECTION('center_axis',(-0.504104280893361,0.,-0.863642793048716));
#17370=DIRECTION('ref_axis',(0.863642793048716,0.,-0.504104280893361));
#17371=DIRECTION('',(0.863642793048716,0.,-0.504104280893361));
#17372=DIRECTION('',(0.,-1.,0.));
#17373=DIRECTION('',(0.863642793048716,0.,-0.504104280893361));
#17374=DIRECTION('',(0.,-1.,0.));
#17375=DIRECTION('center_axis',(0.,-1.,0.));
#17376=DIRECTION('ref_axis',(0.504104280893359,0.,0.863642793048717));
#17377=DIRECTION('center_axis',(0.,-1.,0.));
#17378=DIRECTION('ref_axis',(0.504104280893359,0.,0.863642793048717));
#17379=DIRECTION('center_axis',(0.,-1.,0.));
#17380=DIRECTION('ref_axis',(0.504104280893359,0.,0.863642793048717));
#17381=DIRECTION('',(0.,-1.,0.));
#17382=DIRECTION('center_axis',(0.504104280893361,0.,0.863642793048716));
#17383=DIRECTION('ref_axis',(-0.863642793048716,0.,0.504104280893361));
#17384=DIRECTION('',(-0.863642793048716,0.,0.504104280893361));
#17385=DIRECTION('',(-0.863642793048716,0.,0.504104280893361));
#17386=DIRECTION('',(0.,-1.,0.));
#17387=DIRECTION('center_axis',(0.,-1.,0.));
#17388=DIRECTION('ref_axis',(-1.,0.,0.));
#17389=DIRECTION('center_axis',(0.,1.,0.));
#17390=DIRECTION('ref_axis',(-1.,0.,0.));
#17391=DIRECTION('center_axis',(0.,-1.,0.));
#17392=DIRECTION('ref_axis',(-1.,0.,0.));
#17393=DIRECTION('center_axis',(0.,-1.,0.));
#17394=DIRECTION('ref_axis',(-0.50410428089336,0.,-0.863642793048716));
#17395=DIRECTION('center_axis',(-2.43566064310008E-53,1.,-1.62748695315959E-104));
#17396=DIRECTION('ref_axis',(-1.,-2.43566064310008E-53,0.));
#17397=DIRECTION('center_axis',(0.,-1.,0.));
#17398=DIRECTION('ref_axis',(-1.,0.,0.));
#17399=DIRECTION('',(0.,-1.,0.));
#17400=DIRECTION('center_axis',(2.43566064310008E-53,1.,1.62748695315959E-104));
#17401=DIRECTION('ref_axis',(-1.,2.43566064310008E-53,0.));
#17402=DIRECTION('center_axis',(0.,-1.,0.));
#17403=DIRECTION('ref_axis',(-1.,0.,0.));
#17404=DIRECTION('center_axis',(0.,1.,0.));
#17405=DIRECTION('ref_axis',(-1.,0.,0.));
#17406=DIRECTION('',(0.,-1.,0.));
#17407=DIRECTION('center_axis',(0.,1.,0.));
#17408=DIRECTION('ref_axis',(-1.,0.,0.));
#17409=DIRECTION('center_axis',(0.504104280893361,0.,0.863642793048716));
#17410=DIRECTION('ref_axis',(0.863642793048716,0.,-0.504104280893361));
#17411=DIRECTION('',(0.863642793048716,0.,-0.504104280893361));
#17412=DIRECTION('',(0.,1.,0.));
#17413=DIRECTION('',(0.863642793048716,0.,-0.504104280893361));
#17414=DIRECTION('',(0.,1.,0.));
#17415=DIRECTION('center_axis',(0.,-1.,0.));
#17416=DIRECTION('ref_axis',(0.504104280893359,0.,0.863642793048717));
#17417=DIRECTION('center_axis',(0.,-1.,0.));
#17418=DIRECTION('ref_axis',(0.504104280893359,0.,0.863642793048717));
#17419=DIRECTION('',(0.,1.,0.));
#17420=DIRECTION('center_axis',(0.,-1.,0.));
#17421=DIRECTION('ref_axis',(0.504104280893359,0.,0.863642793048717));
#17422=DIRECTION('center_axis',(-0.504104280893361,0.,-0.863642793048716));
#17423=DIRECTION('ref_axis',(-0.863642793048716,0.,0.504104280893361));
#17424=DIRECTION('',(-0.863642793048716,0.,0.504104280893361));
#17425=DIRECTION('',(0.,1.,0.));
#17426=DIRECTION('',(-0.863642793048716,0.,0.504104280893361));
#17427=DIRECTION('center_axis',(0.,-1.,0.));
#17428=DIRECTION('ref_axis',(-0.50410428089336,0.,-0.863642793048716));
#17429=DIRECTION('center_axis',(0.,-1.,0.));
#17430=DIRECTION('ref_axis',(-0.50410428089336,0.,-0.863642793048716));
#17431=DIRECTION('center_axis',(0.,-1.,0.));
#17432=DIRECTION('ref_axis',(-1.,0.,0.));
#17433=DIRECTION('',(0.,1.,0.));
#17434=DIRECTION('center_axis',(0.,-1.,0.));
#17435=DIRECTION('ref_axis',(-1.,0.,0.));
#17436=DIRECTION('center_axis',(0.,-1.,0.));
#17437=DIRECTION('ref_axis',(-1.,0.,0.));
#17438=DIRECTION('',(0.,0.,1.));
#17439=DIRECTION('',(1.,0.,0.));
#17440=DIRECTION('',(0.,0.,1.));
#17441=DIRECTION('',(1.,0.,0.));
#17442=DIRECTION('',(0.,0.,1.));
#17443=DIRECTION('',(1.,0.,0.));
#17444=DIRECTION('',(0.,0.,1.));
#17445=DIRECTION('',(1.,0.,0.));
#17446=DIRECTION('',(0.,0.,1.));
#17447=DIRECTION('',(1.,0.,0.));
#17448=DIRECTION('',(0.,0.,1.));
#17449=DIRECTION('',(1.,0.,0.));
#17450=DIRECTION('',(0.,0.,1.));
#17451=DIRECTION('',(1.,0.,0.));
#17452=DIRECTION('',(0.,0.,1.));
#17453=DIRECTION('',(1.,0.,0.));
#17454=DIRECTION('',(0.,0.,1.));
#17455=DIRECTION('',(1.,0.,0.));
#17456=CARTESIAN_POINT('',(0.,0.,0.));
#17457=CARTESIAN_POINT('',(0.,0.,0.));
#17458=CARTESIAN_POINT('Origin',(-39.9751670169646,25.,1.25));
#17459=CARTESIAN_POINT('',(-49.9751670169646,25.,5.));
#17460=CARTESIAN_POINT('',(-39.9751670169646,35.,5.));
#17461=CARTESIAN_POINT('Origin',(-39.9751670169646,25.,5.));
#17462=CARTESIAN_POINT('',(-39.9751670169646,35.,0.));
#17463=CARTESIAN_POINT('',(-39.9751670169646,35.,1.25));
#17464=CARTESIAN_POINT('',(-49.9751670169646,25.,0.));
#17465=CARTESIAN_POINT('Origin',(-39.9751670169646,25.,0.));
#17466=CARTESIAN_POINT('',(-49.9751670169646,25.,1.25));
#17467=CARTESIAN_POINT('Origin',(-19.9792411332937,0.,29.9773129029999));
#17468=CARTESIAN_POINT('',(-12.4213924902778,22.,29.9773129029999));
#17469=CARTESIAN_POINT('Origin',(-19.9792411332937,22.,29.9773129029999));
#17470=CARTESIAN_POINT('',(-12.4213924902778,25.,29.9773129029999));
#17471=CARTESIAN_POINT('',(-12.4213924902778,0.,29.9773129029999));
#17472=CARTESIAN_POINT('Origin',(-19.9792411332937,25.,29.9773129029999));
#17473=CARTESIAN_POINT('Origin',(-35.0075079285187,0.,37.0308437753216));
#17474=CARTESIAN_POINT('',(-35.0075079285187,22.,37.0308437753216));
#17475=CARTESIAN_POINT('',(-27.0075079285187,22.,45.0308437753216));
#17476=CARTESIAN_POINT('',(-33.010424909369,22.,39.0279267944712));
#17477=CARTESIAN_POINT('',(-27.0075079285187,25.,45.0308437753216));
#17478=CARTESIAN_POINT('',(-27.0075079285187,0.,45.0308437753216));
#17479=CARTESIAN_POINT('',(-35.0075079285187,25.,37.0308437753216));
#17480=CARTESIAN_POINT('',(-35.0075079285187,25.,37.0308437753216));
#17481=CARTESIAN_POINT('',(-35.0075079285187,0.,37.0308437753216));
#17482=CARTESIAN_POINT('Origin',(39.9751670169646,25.,1.25));
#17483=CARTESIAN_POINT('',(49.9751670169646,25.,5.));
#17484=CARTESIAN_POINT('',(39.9751670169646,35.,5.));
#17485=CARTESIAN_POINT('Origin',(39.9751670169646,25.,5.));
#17486=CARTESIAN_POINT('',(49.9751670169646,25.,0.));
#17487=CARTESIAN_POINT('',(49.9751670169646,25.,1.25));
#17488=CARTESIAN_POINT('',(39.9751670169646,35.,0.));
#17489=CARTESIAN_POINT('Origin',(39.9751670169646,25.,0.));
#17490=CARTESIAN_POINT('',(39.9751670169646,35.,1.25));
#17491=CARTESIAN_POINT('Origin',(24.9875835084823,35.,2.5));
#17492=CARTESIAN_POINT('',(0.,35.,0.));
#17493=CARTESIAN_POINT('',(0.,35.,5.));
#17494=CARTESIAN_POINT('Origin',(26.255630946389,19.,13.));
#17495=CARTESIAN_POINT('',(-35.0075079285187,22.,13.));
#17496=CARTESIAN_POINT('',(35.0075079285187,22.,13.));
#17497=CARTESIAN_POINT('',(26.255630946389,22.,13.));
#17498=CARTESIAN_POINT('',(-35.0075079285187,19.,10.));
#17499=CARTESIAN_POINT('Origin',(-35.0075079285187,19.,13.));
#17500=CARTESIAN_POINT('',(35.0075079285187,19.,10.));
#17501=CARTESIAN_POINT('',(26.255630946389,19.,10.));
#17502=CARTESIAN_POINT('Origin',(35.0075079285187,19.,13.));
#17503=CARTESIAN_POINT('Origin',(17.5037539642593,22.,27.5154218876608));
#17504=CARTESIAN_POINT('',(35.0075079285187,22.,37.0308437753216));
#17505=CARTESIAN_POINT('',(35.0075079285187,22.,18.7577109438304));
#17506=CARTESIAN_POINT('',(27.0075079285187,22.,45.0308437753216));
#17507=CARTESIAN_POINT('',(33.010424909369,22.,39.0279267944712));
#17508=CARTESIAN_POINT('',(-22.255630946389,22.,45.0308437753216));
#17509=CARTESIAN_POINT('',(-35.0075079285187,22.,18.7577109438304));
#17510=CARTESIAN_POINT('',(12.4213924902778,22.,29.9773129029999));
#17511=CARTESIAN_POINT('Origin',(19.9792411332937,22.,29.9773129029999));
#17512=CARTESIAN_POINT('Origin',(8.75187698212967,19.5,10.5));
#17513=CARTESIAN_POINT('',(35.0075079285187,19.5,5.));
#17514=CARTESIAN_POINT('',(35.0075079285187,25.,10.5));
#17515=CARTESIAN_POINT('Origin',(35.0075079285187,19.5,10.5));
#17516=CARTESIAN_POINT('',(-35.0075079285187,19.5,5.));
#17517=CARTESIAN_POINT('',(8.75187698212967,19.5,5.));
#17518=CARTESIAN_POINT('',(-35.0075079285187,25.,10.5));
#17519=CARTESIAN_POINT('Origin',(-35.0075079285187,19.5,10.5));
#17520=CARTESIAN_POINT('',(8.75187698212967,25.,10.5));
#17521=CARTESIAN_POINT('Origin',(17.5037539642593,25.,7.5));
#17522=CARTESIAN_POINT('',(-35.0075079285187,25.,5.));
#17523=CARTESIAN_POINT('',(27.0075079285187,25.,45.0308437753216));
#17524=CARTESIAN_POINT('',(27.0075079285187,25.,45.0308437753216));
#17525=CARTESIAN_POINT('',(35.0075079285187,25.,37.0308437753216));
#17526=CARTESIAN_POINT('',(35.0075079285187,25.,37.0308437753216));
#17527=CARTESIAN_POINT('',(35.0075079285187,25.,5.));
#17528=CARTESIAN_POINT('',(12.4213924902778,25.,29.9773129029999));
#17529=CARTESIAN_POINT('Origin',(19.9792411332937,25.,29.9773129029999));
#17530=CARTESIAN_POINT('Origin',(19.9792411332937,0.,29.9773129029999));
#17531=CARTESIAN_POINT('',(12.4213924902778,0.,29.9773129029999));
#17532=CARTESIAN_POINT('Origin',(27.0075079285187,0.,45.0308437753216));
#17533=CARTESIAN_POINT('',(27.0075079285187,0.,45.0308437753216));
#17534=CARTESIAN_POINT('Origin',(35.0075079285187,0.,37.0308437753216));
#17535=CARTESIAN_POINT('',(35.0075079285187,0.,37.0308437753216));
#17536=CARTESIAN_POINT('Origin',(-39.9751670169646,-25.,1.25));
#17537=CARTESIAN_POINT('',(-49.9751670169646,-25.,5.));
#17538=CARTESIAN_POINT('',(-39.9751670169646,-35.,5.));
#17539=CARTESIAN_POINT('Origin',(-39.9751670169646,-25.,5.));
#17540=CARTESIAN_POINT('',(-49.9751670169646,-25.,0.));
#17541=CARTESIAN_POINT('',(-49.9751670169646,-25.,1.25));
#17542=CARTESIAN_POINT('',(-39.9751670169646,-35.,0.));
#17543=CARTESIAN_POINT('Origin',(-39.9751670169646,-25.,0.));
#17544=CARTESIAN_POINT('',(-39.9751670169646,-35.,1.25));
#17545=CARTESIAN_POINT('Origin',(-49.9751670169646,0.,0.));
#17546=CARTESIAN_POINT('',(-49.9751670169646,0.,5.));
#17547=CARTESIAN_POINT('',(-49.9751670169646,0.,0.));
#17548=CARTESIAN_POINT('Origin',(-35.0075079285187,0.,5.));
#17549=CARTESIAN_POINT('',(-35.0075079285187,-19.5,5.));
#17550=CARTESIAN_POINT('',(-35.0075079285187,-25.,10.5));
#17551=CARTESIAN_POINT('Origin',(-35.0075079285187,-19.5,10.5));
#17552=CARTESIAN_POINT('',(-35.0075079285187,-25.,37.0308437753216));
#17553=CARTESIAN_POINT('',(-35.0075079285187,-25.,5.));
#17554=CARTESIAN_POINT('',(-35.0075079285187,-22.,37.0308437753216));
#17555=CARTESIAN_POINT('',(-35.0075079285187,0.,37.0308437753216));
#17556=CARTESIAN_POINT('',(-35.0075079285187,-22.,13.));
#17557=CARTESIAN_POINT('',(-35.0075079285187,-22.,18.7577109438304));
#17558=CARTESIAN_POINT('',(-35.0075079285187,-19.,10.));
#17559=CARTESIAN_POINT('Origin',(-35.0075079285187,-19.,13.));
#17560=CARTESIAN_POINT('',(-35.0075079285187,0.,10.));
#17561=CARTESIAN_POINT('',(-35.0075079285187,0.,5.));
#17562=CARTESIAN_POINT('Origin',(-19.9792411332937,0.,29.9773129029999));
#17563=CARTESIAN_POINT('',(-12.4213924902778,-25.,29.9773129029999));
#17564=CARTESIAN_POINT('Origin',(-19.9792411332937,-25.,29.9773129029999));
#17565=CARTESIAN_POINT('',(-12.4213924902778,-22.,29.9773129029999));
#17566=CARTESIAN_POINT('',(-12.4213924902778,0.,29.9773129029999));
#17567=CARTESIAN_POINT('Origin',(-19.9792411332937,-22.,29.9773129029999));
#17568=CARTESIAN_POINT('Origin',(-35.0075079285187,0.,37.0308437753216));
#17569=CARTESIAN_POINT('',(-27.0075079285187,-22.,45.0308437753216));
#17570=CARTESIAN_POINT('',(-33.010424909369,-22.,39.0279267944712));
#17571=CARTESIAN_POINT('',(-27.0075079285187,-25.,45.0308437753216));
#17572=CARTESIAN_POINT('',(-35.0075079285187,-25.,37.0308437753216));
#17573=CARTESIAN_POINT('',(-27.0075079285187,0.,45.0308437753216));
#17574=CARTESIAN_POINT('Origin',(39.9751670169646,-25.,1.25));
#17575=CARTESIAN_POINT('',(49.9751670169646,-25.,5.));
#17576=CARTESIAN_POINT('',(39.9751670169646,-35.,5.));
#17577=CARTESIAN_POINT('Origin',(39.9751670169646,-25.,5.));
#17578=CARTESIAN_POINT('',(39.9751670169646,-35.,0.));
#17579=CARTESIAN_POINT('',(39.9751670169646,-35.,1.25));
#17580=CARTESIAN_POINT('',(49.9751670169646,-25.,0.));
#17581=CARTESIAN_POINT('Origin',(39.9751670169646,-25.,0.));
#17582=CARTESIAN_POINT('',(49.9751670169646,-25.,1.25));
#17583=CARTESIAN_POINT('Origin',(24.9875835084823,-35.,2.5));
#17584=CARTESIAN_POINT('',(0.,-35.,5.));
#17585=CARTESIAN_POINT('',(0.,-35.,0.));
#17586=CARTESIAN_POINT('Origin',(49.9751670169646,0.,5.));
#17587=CARTESIAN_POINT('',(49.9751670169646,0.,5.));
#17588=CARTESIAN_POINT('',(35.0075079285187,-19.5,5.));
#17589=CARTESIAN_POINT('',(35.0075079285187,0.,5.));
#17590=CARTESIAN_POINT('',(8.75187698212967,-19.5,5.));
#17591=CARTESIAN_POINT('Origin',(49.9751670169646,0.,0.));
#17592=CARTESIAN_POINT('',(49.9751670169646,0.,0.));
#17593=CARTESIAN_POINT('Origin',(0.,0.,0.));
#17594=CARTESIAN_POINT('Origin',(26.255630946389,-19.,13.));
#17595=CARTESIAN_POINT('',(35.0075079285187,-22.,13.));
#17596=CARTESIAN_POINT('',(26.255630946389,-22.,13.));
#17597=CARTESIAN_POINT('',(35.0075079285187,-19.,10.));
#17598=CARTESIAN_POINT('Origin',(35.0075079285187,-19.,13.));
#17599=CARTESIAN_POINT('',(26.255630946389,-19.,10.));
#17600=CARTESIAN_POINT('Origin',(17.5037539642593,-22.,27.5154218876608));
#17601=CARTESIAN_POINT('',(27.0075079285187,-22.,45.0308437753216));
#17602=CARTESIAN_POINT('',(-22.255630946389,-22.,45.0308437753216));
#17603=CARTESIAN_POINT('',(35.0075079285187,-22.,37.0308437753216));
#17604=CARTESIAN_POINT('',(33.010424909369,-22.,39.0279267944712));
#17605=CARTESIAN_POINT('',(35.0075079285187,-22.,18.7577109438304));
#17606=CARTESIAN_POINT('',(12.4213924902778,-22.,29.9773129029999));
#17607=CARTESIAN_POINT('Origin',(19.9792411332937,-22.,29.9773129029999));
#17608=CARTESIAN_POINT('Origin',(8.75187698212967,-19.5,10.5));
#17609=CARTESIAN_POINT('',(35.0075079285187,-25.,10.5));
#17610=CARTESIAN_POINT('Origin',(35.0075079285187,-19.5,10.5));
#17611=CARTESIAN_POINT('',(8.75187698212967,-25.,10.5));
#17612=CARTESIAN_POINT('Origin',(17.5037539642593,-25.,7.5));
#17613=CARTESIAN_POINT('',(35.0075079285187,-25.,37.0308437753216));
#17614=CARTESIAN_POINT('',(35.0075079285187,-25.,5.));
#17615=CARTESIAN_POINT('',(27.0075079285187,-25.,45.0308437753216));
#17616=CARTESIAN_POINT('',(35.0075079285187,-25.,37.0308437753216));
#17617=CARTESIAN_POINT('',(27.0075079285187,-25.,45.0308437753216));
#17618=CARTESIAN_POINT('',(12.4213924902778,-25.,29.9773129029999));
#17619=CARTESIAN_POINT('Origin',(19.9792411332937,-25.,29.9773129029999));
#17620=CARTESIAN_POINT('Origin',(35.0075079285187,0.,5.));
#17621=CARTESIAN_POINT('',(35.0075079285187,0.,10.));
#17622=CARTESIAN_POINT('',(35.0075079285187,0.,37.0308437753216));
#17623=CARTESIAN_POINT('Origin',(19.9792411332937,0.,29.9773129029999));
#17624=CARTESIAN_POINT('',(12.4213924902778,0.,29.9773129029999));
#17625=CARTESIAN_POINT('Origin',(27.0075079285187,0.,45.0308437753216));
#17626=CARTESIAN_POINT('',(27.0075079285187,0.,45.0308437753216));
#17627=CARTESIAN_POINT('Origin',(35.0075079285187,0.,37.0308437753216));
#17628=CARTESIAN_POINT('Origin',(35.0075079285187,0.,10.));
#17629=CARTESIAN_POINT('',(0.,0.,0.));
#17630=CARTESIAN_POINT('Origin',(213.235140564004,0.,130.804360617566));
#17631=CARTESIAN_POINT('',(208.584593534951,-4.76405452823405,129.582490119308));
#17632=CARTESIAN_POINT('',(208.930233502018,-4.76405452823405,129.582490119308));
#17633=CARTESIAN_POINT('',(213.235140564004,-4.76405452823405,129.582490119308));
#17634=CARTESIAN_POINT('',(209.999775289582,-2.85698121911692,134.807714383612));
#17635=CARTESIAN_POINT('Ctrl Pts',(209.999775289582,-2.85698121911692,134.807714383612));
#17636=CARTESIAN_POINT('Ctrl Pts',(209.992142339133,-2.74793414685712,134.885535494523));
#17637=CARTESIAN_POINT('Ctrl Pts',(209.984509388684,-2.6354991820663,134.95904446143));
#17638=CARTESIAN_POINT('Ctrl Pts',(209.976876438235,-2.52005924303919,135.027923624563));
#17639=CARTESIAN_POINT('Ctrl Pts',(209.969253020602,-2.40476347730548,135.096716764298));
#17640=CARTESIAN_POINT('Ctrl Pts',(209.961629602968,-2.28647054353313,135.160891390807));
#17641=CARTESIAN_POINT('Ctrl Pts',(209.954006185334,-2.16559535772989,135.220170827378));
#17642=CARTESIAN_POINT('Ctrl Pts',(209.946390314966,-2.04483983966827,135.279391576665));
#17643=CARTESIAN_POINT('Ctrl Pts',(209.938774444599,-1.92150751515212,135.333726595951));
#17644=CARTESIAN_POINT('Ctrl Pts',(209.931158574231,-1.79604065581658,135.38294347967));
#17645=CARTESIAN_POINT('Ctrl Pts',(209.923241190819,-1.66560655139177,135.434108864574));
#17646=CARTESIAN_POINT('Ctrl Pts',(209.915323807407,-1.53286579519913,135.47974227831));
#17647=CARTESIAN_POINT('Ctrl Pts',(209.907406423995,-1.39834203382079,135.519636072823));
#17648=CARTESIAN_POINT('Ctrl Pts',(209.899799007078,-1.26908489356805,135.557968020575));
#17649=CARTESIAN_POINT('Ctrl Pts',(209.892191590161,-1.13818215001209,135.591001152623));
#17650=CARTESIAN_POINT('Ctrl Pts',(209.884584173243,-1.00611629719668,135.618601269945));
#17651=CARTESIAN_POINT('Ctrl Pts',(209.876977848994,-0.874069413258891,
135.646197423007));
#17652=CARTESIAN_POINT('Ctrl Pts',(209.869371524745,-0.740860149380113,
135.668362029476));
#17653=CARTESIAN_POINT('Ctrl Pts',(209.861765200496,-0.606982515147129,
135.685011730769));
#17654=CARTESIAN_POINT('Ctrl Pts',(209.854158190768,-0.473092815912997,
135.701662932526));
#17655=CARTESIAN_POINT('Ctrl Pts',(209.84655118104,-0.338535029477726,135.712798191257));
#17656=CARTESIAN_POINT('Ctrl Pts',(209.838944171311,-0.203809027959443,
135.718385947438));
#17657=CARTESIAN_POINT('Ctrl Pts',(209.831334697465,-0.069039385009203,
135.723975513646));
#17658=CARTESIAN_POINT('Ctrl Pts',(209.823725223619,0.0658981760508359,
135.724013988275));
#17659=CARTESIAN_POINT('Ctrl Pts',(209.816115749772,0.200503645000317,135.718521924528));
#17660=CARTESIAN_POINT('Ctrl Pts',(209.808497878904,0.335257650513392,135.713023800312));
#17661=CARTESIAN_POINT('Ctrl Pts',(209.800880008035,0.469678427016586,135.70198297531));
#17662=CARTESIAN_POINT('Ctrl Pts',(209.793262137167,0.603270740406474,135.68547191278));
#17663=CARTESIAN_POINT('Ctrl Pts',(209.785639287196,0.736950370812096,135.668950058486));
#17664=CARTESIAN_POINT('Ctrl Pts',(209.778016437226,0.86980006175104,135.646950918129));
#17665=CARTESIAN_POINT('Ctrl Pts',(209.770393587255,1.0013360320228,135.619597809385));
#17666=CARTESIAN_POINT('Ctrl Pts',(209.762759835517,1.13306011758494,135.592205581774));
#17667=CARTESIAN_POINT('Ctrl Pts',(209.755126083778,1.26346634291021,135.55944420817));
#17668=CARTESIAN_POINT('Ctrl Pts',(209.74749233204,1.3920871137774,135.521486493579));
#17669=CARTESIAN_POINT('Ctrl Pts',(209.745375345476,1.42775613382599,135.510960087357));
#17670=CARTESIAN_POINT('Ctrl Pts',(209.743258358912,1.4632879682488,135.500034332974));
#17671=CARTESIAN_POINT('Ctrl Pts',(209.741141372347,1.49867295217247,135.488713555265));
#17672=CARTESIAN_POINT('Ctrl Pts',(209.733353704104,1.62884218435411,135.44706829282));
#17673=CARTESIAN_POINT('Ctrl Pts',(209.72556603586,1.75747564403554,135.399928764541));
#17674=CARTESIAN_POINT('Ctrl Pts',(209.717778367616,1.88407583976038,135.347425804478));
#17675=CARTESIAN_POINT('Ctrl Pts',(209.710000228288,2.01052112871054,135.294987086528));
#17676=CARTESIAN_POINT('Ctrl Pts',(209.70222208896,2.13493774786161,135.237198143303));
#17677=CARTESIAN_POINT('Ctrl Pts',(209.694443949632,2.25684297289465,135.174239661452));
#17678=CARTESIAN_POINT('Ctrl Pts',(209.686673485267,2.37862790975512,135.111343302949));
#17679=CARTESIAN_POINT('Ctrl Pts',(209.678903020903,2.49790604053664,135.043287735315));
#17680=CARTESIAN_POINT('Ctrl Pts',(209.671132556538,2.61421457479356,134.970301714058));
#17681=CARTESIAN_POINT('Ctrl Pts',(209.663367919743,2.73043588183068,134.897370429692));
#17682=CARTESIAN_POINT('Ctrl Pts',(209.655603282947,2.84369169700696,134.819516258395));
#17683=CARTESIAN_POINT('Ctrl Pts',(209.647838646152,2.95354411037853,134.737013697937));
#17684=CARTESIAN_POINT('Ctrl Pts',(209.640077319747,3.06334968905691,134.654546311782));
#17685=CARTESIAN_POINT('Ctrl Pts',(209.632315993341,3.16975444150301,134.567434711988));
#17686=CARTESIAN_POINT('Ctrl Pts',(209.624554666936,3.27234990255257,134.475996380787));
#17687=CARTESIAN_POINT('Ctrl Pts',(209.616794973343,3.37492377977697,134.384577286197));
#17688=CARTESIAN_POINT('Ctrl Pts',(209.60903527975,3.47368966925553,134.288833529858));
#17689=CARTESIAN_POINT('Ctrl Pts',(209.601275586157,3.56827293312915,134.189122254254));
#17690=CARTESIAN_POINT('Ctrl Pts',(209.593515860863,3.662856583417,134.089410571287));
#17691=CARTESIAN_POINT('Ctrl Pts',(209.585756135568,3.75325730596229,133.985731619193));
#17692=CARTESIAN_POINT('Ctrl Pts',(209.577996410273,3.83913828939138,133.878478419055));
#17693=CARTESIAN_POINT('Ctrl Pts',(209.570234989105,3.92503804195145,133.771201778926));
#17694=CARTESIAN_POINT('Ctrl Pts',(209.562473567936,4.00641584635018,133.660349640188));
#17695=CARTESIAN_POINT('Ctrl Pts',(209.554712146768,4.08297628367845,133.546346709693));
#17696=CARTESIAN_POINT('Ctrl Pts',(209.546942629375,4.15961658401883,133.432224858542));
#17697=CARTESIAN_POINT('Ctrl Pts',(209.539173111982,4.2314292613647,133.314945973776));
#17698=CARTESIAN_POINT('Ctrl Pts',(209.53140359459,4.29816293429022,133.194962728498));
#17699=CARTESIAN_POINT('Ctrl Pts',(209.523629992291,4.36493169314774,133.074916400764));
#17700=CARTESIAN_POINT('Ctrl Pts',(209.515856389993,4.42661595131892,132.95216322687));
#17701=CARTESIAN_POINT('Ctrl Pts',(209.508082787694,4.48301157575842,132.827178027545));
#17702=CARTESIAN_POINT('Ctrl Pts',(209.50029695563,4.539495924226,132.701996196116));
#17703=CARTESIAN_POINT('Ctrl Pts',(209.492511123565,4.59067486682162,132.574575683597));
#17704=CARTESIAN_POINT('Ctrl Pts',(209.4847252915,4.63639315079776,132.445409554599));
#17705=CARTESIAN_POINT('Ctrl Pts',(209.477381443845,4.67951610924217,132.323575900122));
#17706=CARTESIAN_POINT('Ctrl Pts',(209.470037596189,4.71778115993259,132.200189593167));
#17707=CARTESIAN_POINT('Ctrl Pts',(209.462693748534,4.75109968643114,132.075672865636));
#17708=CARTESIAN_POINT('Ctrl Pts',(209.454909765657,4.78641507584487,131.943693538115));
#17709=CARTESIAN_POINT('Ctrl Pts',(209.447125782781,4.81628128369982,131.810038662946));
#17710=CARTESIAN_POINT('Ctrl Pts',(209.439341799904,4.84053990021811,131.675197305411));
#17711=CARTESIAN_POINT('Ctrl Pts',(209.431567219374,4.86476921452188,131.540518824038));
#17712=CARTESIAN_POINT('Ctrl Pts',(209.423792638845,4.88340434715897,131.404657092206));
#17713=CARTESIAN_POINT('Ctrl Pts',(209.416018058316,4.89633682733635,131.268115656104));
#17714=CARTESIAN_POINT('Ctrl Pts',(209.408251022624,4.90925675719497,131.13170672657));
#17715=CARTESIAN_POINT('Ctrl Pts',(209.400483986932,4.91648501195897,130.994619791219));
#17716=CARTESIAN_POINT('Ctrl Pts',(209.39271695124,4.91796434783536,130.857367559755));
#17717=CARTESIAN_POINT('Ctrl Pts',(209.384955609346,4.91944259925179,130.720215944083));
#17718=CARTESIAN_POINT('Ctrl Pts',(209.377194267452,4.91518031659135,130.582899661805));
#17719=CARTESIAN_POINT('Ctrl Pts',(209.369432925558,4.90517219417271,130.44593516086));
#17720=CARTESIAN_POINT('Ctrl Pts',(209.361674676742,4.89516806022735,130.309025243505));
#17721=CARTESIAN_POINT('Ctrl Pts',(209.353916427926,4.8794226688716,130.172467216696));
#17722=CARTESIAN_POINT('Ctrl Pts',(209.34615817911,4.85798279483743,130.036775946299));
#17723=CARTESIAN_POINT('Ctrl Pts',(209.33840142992,4.83654706500869,129.901110904251));
#17724=CARTESIAN_POINT('Ctrl Pts',(209.330644680729,4.80941910276508,129.766312670191));
#17725=CARTESIAN_POINT('Ctrl Pts',(209.322887931538,4.77669732786597,129.632889021471));
#17726=CARTESIAN_POINT('Ctrl Pts',(209.315131013878,4.74397484227869,129.499462474906));
#17727=CARTESIAN_POINT('Ctrl Pts',(209.307374096217,4.70565839487186,129.367410951764));
#17728=CARTESIAN_POINT('Ctrl Pts',(209.299617178557,4.66189702139654,129.237229728204));
#17729=CARTESIAN_POINT('Ctrl Pts',(209.291858424581,4.61812528817876,129.107017686507));
#17730=CARTESIAN_POINT('Ctrl Pts',(209.284099670606,4.56890618792866,128.978677194934));
#17731=CARTESIAN_POINT('Ctrl Pts',(209.27634091663,4.51443776230667,128.852685759205));
#17732=CARTESIAN_POINT('Ctrl Pts',(209.268573827102,4.45991081898621,128.726558965628));
#17733=CARTESIAN_POINT('Ctrl Pts',(209.260806737574,4.40012343960792,128.602786627605));
#17734=CARTESIAN_POINT('Ctrl Pts',(209.253039648046,4.33532097135991,128.481824258801));
#17735=CARTESIAN_POINT('Ctrl Pts',(209.245268346918,4.27048336484057,128.36079629977));
#17736=CARTESIAN_POINT('Ctrl Pts',(209.237497045789,4.20062544887419,128.242581681554));
#17737=CARTESIAN_POINT('Ctrl Pts',(209.229725744661,4.12603669423767,128.127608058904));
#17738=CARTESIAN_POINT('Ctrl Pts',(209.221941972209,4.05132824014885,128.01244992748));
#17739=CARTESIAN_POINT('Ctrl Pts',(209.214158199757,3.97187400192915,127.900543503149));
#17740=CARTESIAN_POINT('Ctrl Pts',(209.206374427305,3.88800517419154,127.792285115863));
#17741=CARTESIAN_POINT('Ctrl Pts',(209.198998326444,3.80852893868575,127.68969671305));
#17742=CARTESIAN_POINT('Ctrl Pts',(209.191622225582,3.72508894865644,127.590384153448));
#17743=CARTESIAN_POINT('Ctrl Pts',(209.184246124721,3.63799708228773,127.494653637822));
#17744=CARTESIAN_POINT('Ctrl Pts',(209.176480887067,3.54631055945193,127.393872721383));
#17745=CARTESIAN_POINT('Ctrl Pts',(209.168715649414,3.4502845118794,127.296741308387));
#17746=CARTESIAN_POINT('Ctrl Pts',(209.16095041176,3.35024118689397,127.203656929099));
#17747=CARTESIAN_POINT('Ctrl Pts',(209.153194866534,3.25032273416257,127.110688736036));
#17748=CARTESIAN_POINT('Ctrl Pts',(209.145439321308,3.14639726453247,127.021757790806));
#17749=CARTESIAN_POINT('Ctrl Pts',(209.137683776083,3.03882640608876,126.93722768267));
#17750=CARTESIAN_POINT('Ctrl Pts',(209.129936043924,2.9313639163431,126.852782731591));
#17751=CARTESIAN_POINT('Ctrl Pts',(209.122188311766,2.82026365182958,126.772730035885));
#17752=CARTESIAN_POINT('Ctrl Pts',(209.114440579607,2.70592284873513,126.697395241623));
#17753=CARTESIAN_POINT('Ctrl Pts',(209.106698788025,2.59166971649979,126.622118210347));
#17754=CARTESIAN_POINT('Ctrl Pts',(209.098956996444,2.47418131699825,126.551552095381));
#17755=CARTESIAN_POINT('Ctrl Pts',(209.091215204862,2.35388631216353,126.485981026573));
#17756=CARTESIAN_POINT('Ctrl Pts',(209.083476813463,2.23364414070448,126.420438756474));
#17757=CARTESIAN_POINT('Ctrl Pts',(209.075738422064,2.11059815902803,126.359887356409));
#17758=CARTESIAN_POINT('Ctrl Pts',(209.068000030665,1.98520403181973,126.304566398433));
#17759=CARTESIAN_POINT('Ctrl Pts',(209.060263323162,1.85983719073276,126.249257478455));
#17760=CARTESIAN_POINT('Ctrl Pts',(209.052526615659,1.73212357881766,126.19917689495));
#17761=CARTESIAN_POINT('Ctrl Pts',(209.044789908156,1.60254099859459,126.154517027689));
#17762=CARTESIAN_POINT('Ctrl Pts',(209.037053197922,1.47295837263404,126.109857144664));
#17763=CARTESIAN_POINT('Ctrl Pts',(209.029316487689,1.34150714759864,126.070618109647));
#17764=CARTESIAN_POINT('Ctrl Pts',(209.021579777455,1.20868213452804,126.036943018889));
#17765=CARTESIAN_POINT('Ctrl Pts',(209.013841378212,1.07582812427986,126.003260576484));
#17766=CARTESIAN_POINT('Ctrl Pts',(209.006102978968,0.941600109169617,125.975144591564));
#17767=CARTESIAN_POINT('Ctrl Pts',(208.998364579724,0.806504581770787,125.952687357537));
#17768=CARTESIAN_POINT('Ctrl Pts',(208.990617964067,0.67126561374634,125.930206279051));
#17769=CARTESIAN_POINT('Ctrl Pts',(208.982871348409,0.535157680777325,125.913396018048));
#17770=CARTESIAN_POINT('Ctrl Pts',(208.975124732751,0.398694459805113,125.902297195881));
#17771=CARTESIAN_POINT('Ctrl Pts',(208.96737400283,0.262158762602129,125.89119247908));
#17772=CARTESIAN_POINT('Ctrl Pts',(208.95962327291,0.125267792947886,125.885805260436));
#17773=CARTESIAN_POINT('Ctrl Pts',(208.95187254299,-0.0114642699424184,
125.886123978992));
#17774=CARTESIAN_POINT('Ctrl Pts',(208.944109300736,-0.148417065233437,
125.886443212069));
#17775=CARTESIAN_POINT('Ctrl Pts',(208.936346058481,-0.285210049268953,
125.892486772142));
#17776=CARTESIAN_POINT('Ctrl Pts',(208.928582816227,-0.421332761867055,
125.904191052512));
#17777=CARTESIAN_POINT('Ctrl Pts',(208.920988044454,-0.554501469148627,
125.91564133775));
#17778=CARTESIAN_POINT('Ctrl Pts',(208.913393272681,-0.687028371328897,
125.932509047985));
#17779=CARTESIAN_POINT('Ctrl Pts',(208.905798500908,-0.818446588343237,
125.954687613689));
#17780=CARTESIAN_POINT('Ctrl Pts',(208.898021644216,-0.953015561718216,
125.977397911284));
#17781=CARTESIAN_POINT('Ctrl Pts',(208.890244787523,-1.08685066963772,126.005749285875));
#17782=CARTESIAN_POINT('Ctrl Pts',(208.88246793083,-1.21944203414923,126.03968390368));
#17783=CARTESIAN_POINT('Ctrl Pts',(208.874700639736,-1.35187031017909,126.073576781623));
#17784=CARTESIAN_POINT('Ctrl Pts',(208.866933348642,-1.48305751185494,126.113039142483));
#17785=CARTESIAN_POINT('Ctrl Pts',(208.859166057548,-1.61250119783885,126.157961694801));
#17786=CARTESIAN_POINT('Ctrl Pts',(208.851406465771,-1.74181657293481,126.202839717698));
#17787=CARTESIAN_POINT('Ctrl Pts',(208.843646873995,-1.86939150499281,126.253167033694));
#17788=CARTESIAN_POINT('Ctrl Pts',(208.835887282218,-1.99473637499177,126.308783918545));
#17789=CARTESIAN_POINT('Ctrl Pts',(208.828133530137,-2.11998691323083,126.364358947365));
#17790=CARTESIAN_POINT('Ctrl Pts',(208.820379778057,-2.24301037434021,126.425215463548));
#17791=CARTESIAN_POINT('Ctrl Pts',(208.812626025976,-2.36333520675677,126.491144907333));
#17792=CARTESIAN_POINT('Ctrl Pts',(208.804875562439,-2.48360900666527,126.557046388935));
#17793=CARTESIAN_POINT('Ctrl Pts',(208.797125098901,-2.60118611244184,126.62801633147));
#17794=CARTESIAN_POINT('Ctrl Pts',(208.789374635364,-2.71561796378144,126.703799419719));
#17795=CARTESIAN_POINT('Ctrl Pts',(208.7816257893,-2.83002593389613,126.779566692503));
#17796=CARTESIAN_POINT('Ctrl Pts',(208.773876943237,-2.94128962968789,126.860144897434));
#17797=CARTESIAN_POINT('Ctrl Pts',(208.766128097174,-3.04898831266746,126.94523463728));
#17798=CARTESIAN_POINT('Ctrl Pts',(208.758379193181,-3.15668780079374,127.03032501325));
#17799=CARTESIAN_POINT('Ctrl Pts',(208.750630289188,-3.26082191638816,127.119926749237));
#17800=CARTESIAN_POINT('Ctrl Pts',(208.742881385195,-3.36100225403236,127.213699548781));
#17801=CARTESIAN_POINT('Ctrl Pts',(208.735130748187,-3.46120499665153,127.307493320276));
#17802=CARTESIAN_POINT('Ctrl Pts',(208.72738011118,-3.55745191658161,127.405459744678));
#17803=CARTESIAN_POINT('Ctrl Pts',(208.719629474172,-3.64939108013971,127.507221280702));
#17804=CARTESIAN_POINT('Ctrl Pts',(208.711870619809,-3.74142771913452,127.609090706006));
#17805=CARTESIAN_POINT('Ctrl Pts',(208.704111765447,-3.82914721603231,127.714762990261));
#17806=CARTESIAN_POINT('Ctrl Pts',(208.696352911084,-3.91223725814708,127.823826655594));
#17807=CARTESIAN_POINT('Ctrl Pts',(208.68858992237,-3.9953715752872,127.932948436153));
#17808=CARTESIAN_POINT('Ctrl Pts',(208.680826933656,-4.07387129874455,128.045464878446));
#17809=CARTESIAN_POINT('Ctrl Pts',(208.673063944941,-4.14746775971367,128.160935898639));
#17810=CARTESIAN_POINT('Ctrl Pts',(208.665288533692,-4.2211819916358,128.276591698534));
#17811=CARTESIAN_POINT('Ctrl Pts',(208.657513122443,-4.28997708545372,128.39521118624));
#17812=CARTESIAN_POINT('Ctrl Pts',(208.649737711194,-4.35363018030978,128.516329298813));
#17813=CARTESIAN_POINT('Ctrl Pts',(208.642275433161,-4.41471982254941,128.632569713871));
#17814=CARTESIAN_POINT('Ctrl Pts',(208.634813155129,-4.47107348551401,128.751111125156));
#17815=CARTESIAN_POINT('Ctrl Pts',(208.627350877096,-4.52253673740703,128.871527329022));
#17816=CARTESIAN_POINT('Ctrl Pts',(208.618730890364,-4.58198407326541,129.010625078401));
#17817=CARTESIAN_POINT('Ctrl Pts',(208.610110903632,-4.63506623355969,129.152598212464));
#17818=CARTESIAN_POINT('Ctrl Pts',(208.601490916901,-4.68152517477817,129.296877582697));
#17819=CARTESIAN_POINT('Ctrl Pts',(208.595858456251,-4.7118823164303,129.391152423336));
#17820=CARTESIAN_POINT('Ctrl Pts',(208.590225995601,-4.73941254095081,129.486411384885));
#17821=CARTESIAN_POINT('Ctrl Pts',(208.584593534951,-4.76405452823405,129.582490119308));
#17822=CARTESIAN_POINT('',(210.,2.85706463458491,134.807654853105));
#17823=CARTESIAN_POINT('Origin',(210.,0.,130.804360617566));
#17824=CARTESIAN_POINT('Ctrl Pts',(210.000000000001,2.8570646345852,134.807654853105));
#17825=CARTESIAN_POINT('Ctrl Pts',(209.9909009417,2.98784898468668,134.714316887059));
#17826=CARTESIAN_POINT('Ctrl Pts',(209.981801883399,3.11395234888589,134.614641121174));
#17827=CARTESIAN_POINT('Ctrl Pts',(209.972702825097,3.23483545810878,134.509090381187));
#17828=CARTESIAN_POINT('Ctrl Pts',(209.963375605347,3.35874974533411,134.400892926674));
#17829=CARTESIAN_POINT('Ctrl Pts',(209.954048385597,3.47717847121068,134.286522118141));
#17830=CARTESIAN_POINT('Ctrl Pts',(209.944721165847,3.5895811378025,134.166516223369));
#17831=CARTESIAN_POINT('Ctrl Pts',(209.935606290089,3.69942483916691,134.049242389331));
#17832=CARTESIAN_POINT('Ctrl Pts',(209.926491414332,3.80351381339523,133.926587349353));
#17833=CARTESIAN_POINT('Ctrl Pts',(209.917376538574,3.90138231724316,133.799089165732));
#17834=CARTESIAN_POINT('Ctrl Pts',(209.907943146828,4.00267080004885,133.667135604866));
#17835=CARTESIAN_POINT('Ctrl Pts',(209.898509755081,4.09729611895824,133.529994361329));
#17836=CARTESIAN_POINT('Ctrl Pts',(209.889076363335,4.18478649255116,133.388300453216));
#17837=CARTESIAN_POINT('Ctrl Pts',(209.879642971588,4.27227686614407,133.246606545104));
#17838=CARTESIAN_POINT('Ctrl Pts',(209.870209579841,4.35263215794215,133.100360040818));
#17839=CARTESIAN_POINT('Ctrl Pts',(209.860776188095,4.42542767858449,132.95023408171));
#17840=CARTESIAN_POINT('Ctrl Pts',(209.853001533586,4.48542306921053,132.826505787987));
#17841=CARTESIAN_POINT('Ctrl Pts',(209.845226879078,4.54024783943048,132.700213797986));
#17842=CARTESIAN_POINT('Ctrl Pts',(209.837452224569,4.58968782858598,132.571830192588));
#17843=CARTESIAN_POINT('Ctrl Pts',(209.829678554328,4.63912155866696,132.443462840482));
#17844=CARTESIAN_POINT('Ctrl Pts',(209.821904884086,4.68317172608175,132.313004762609));
#17845=CARTESIAN_POINT('Ctrl Pts',(209.814131213844,4.72167262205471,132.180947234034));
#17846=CARTESIAN_POINT('Ctrl Pts',(209.806353640484,4.76019284912417,132.048823400072));
#17847=CARTESIAN_POINT('Ctrl Pts',(209.798576067123,4.79315812506151,131.915098882938));
#17848=CARTESIAN_POINT('Ctrl Pts',(209.790798493763,4.82045280424895,131.780279581675));
#17849=CARTESIAN_POINT('Ctrl Pts',(209.783019152641,4.8477536872307,131.6454296374));
#17850=CARTESIAN_POINT('Ctrl Pts',(209.77523981152,4.86938133801002,131.509484795897));
#17851=CARTESIAN_POINT('Ctrl Pts',(209.767460470399,4.88527157757875,131.372959488301));
#17852=CARTESIAN_POINT('Ctrl Pts',(209.759672670713,4.90117909478188,131.236285735218));
#17853=CARTESIAN_POINT('Ctrl Pts',(209.751884871028,4.91133669930707,131.099030642188));
#17854=CARTESIAN_POINT('Ctrl Pts',(209.744097071342,4.91573223244676,130.961712711241));
#17855=CARTESIAN_POINT('Ctrl Pts',(209.736582172957,4.9199737366231,130.82920669682));
#17856=CARTESIAN_POINT('Ctrl Pts',(209.729067274573,4.91885023632,130.696642495085));
#17857=CARTESIAN_POINT('Ctrl Pts',(209.721552376188,4.91239674626941,130.564483003476));
#17858=CARTESIAN_POINT('Ctrl Pts',(209.713678765481,4.9056352086199,130.426015078175));
#17859=CARTESIAN_POINT('Ctrl Pts',(209.705805154774,4.89300771239889,130.287688864539));
#17860=CARTESIAN_POINT('Ctrl Pts',(209.697931544067,4.87452930506278,130.150031100744));
#17861=CARTESIAN_POINT('Ctrl Pts',(209.690064949113,4.85606736284523,130.012495996406));
#17862=CARTESIAN_POINT('Ctrl Pts',(209.682198354159,4.83176494040784,129.875628528245));
#17863=CARTESIAN_POINT('Ctrl Pts',(209.674331759204,4.80168901966641,129.739952039568));
#17864=CARTESIAN_POINT('Ctrl Pts',(209.666470472472,4.77163339355775,129.604367102686));
#17865=CARTESIAN_POINT('Ctrl Pts',(209.658609185739,4.7358121091933,129.469971912218));
#17866=CARTESIAN_POINT('Ctrl Pts',(209.650747899006,4.69434349581246,129.337281135798));
#17867=CARTESIAN_POINT('Ctrl Pts',(209.642890217533,4.65289390032517,129.204651212609));
#17868=CARTESIAN_POINT('Ctrl Pts',(209.63503253606,4.60580224712704,129.073724506109));
#17869=CARTESIAN_POINT('Ctrl Pts',(209.627174854587,4.5532370807101,128.945001816972));
#17870=CARTESIAN_POINT('Ctrl Pts',(209.619317529717,4.50067429984411,128.816284969622));
#17871=CARTESIAN_POINT('Ctrl Pts',(209.611460204847,4.44263863419322,128.689772293342));
#17872=CARTESIAN_POINT('Ctrl Pts',(209.603602879977,4.37934731209041,128.565945959245));
#17873=CARTESIAN_POINT('Ctrl Pts',(209.595745424998,4.31605494195501,128.442117574724));
#17874=CARTESIAN_POINT('Ctrl Pts',(209.58788797002,4.24750691313248,128.320975957634));
#17875=CARTESIAN_POINT('Ctrl Pts',(209.580030515041,4.17396689693851,128.202979560173));
#17876=CARTESIAN_POINT('Ctrl Pts',(209.572171389685,4.10041124723336,128.084958078438));
#17877=CARTESIAN_POINT('Ctrl Pts',(209.564312264329,4.02186169619298,127.970083468555));
#17878=CARTESIAN_POINT('Ctrl Pts',(209.556453138973,3.93862568001678,127.858785832365));
#17879=CARTESIAN_POINT('Ctrl Pts',(209.548590802169,3.85535565139079,127.747442717001));
#17880=CARTESIAN_POINT('Ctrl Pts',(209.540728465365,3.76739556974505,127.639679788538));
#17881=CARTESIAN_POINT('Ctrl Pts',(209.532866128561,3.67509348629992,127.535894474334));
#17882=CARTESIAN_POINT('Ctrl Pts',(209.524993952985,3.58267589786456,127.431979285253));
#17883=CARTESIAN_POINT('Ctrl Pts',(209.51712177741,3.4859057045839,127.332051936366));
#17884=CARTESIAN_POINT('Ctrl Pts',(209.509249601834,3.38516874447327,127.236473899361));
#17885=CARTESIAN_POINT('Ctrl Pts',(209.501372245105,3.28436548329557,127.140832956688));
#17886=CARTESIAN_POINT('Ctrl Pts',(209.493494888376,3.17959053527948,127.049547279982));
#17887=CARTESIAN_POINT('Ctrl Pts',(209.485617531647,3.07126268549045,126.962937889043));
#17888=CARTESIAN_POINT('Ctrl Pts',(209.477727176986,2.96275609071294,126.876185589382));
#17889=CARTESIAN_POINT('Ctrl Pts',(209.469836822325,2.8506851836161,126.794125217976));
#17890=CARTESIAN_POINT('Ctrl Pts',(209.461946467663,2.73549839812863,126.717034893289));
#17891=CARTESIAN_POINT('Ctrl Pts',(209.455665895901,2.64381191463777,126.655672465717));
#17892=CARTESIAN_POINT('Ctrl Pts',(209.449385324138,2.55015185656929,126.59745814901));
#17893=CARTESIAN_POINT('Ctrl Pts',(209.443104752375,2.45475470409811,126.542510971555));
#17894=CARTESIAN_POINT('Ctrl Pts',(209.435394730144,2.33764527615028,126.47505788357));
#17895=CARTESIAN_POINT('Ctrl Pts',(209.427684707913,2.21753700128125,126.412310841026));
#17896=CARTESIAN_POINT('Ctrl Pts',(209.419974685682,2.09484840718725,126.354552395473));
#17897=CARTESIAN_POINT('Ctrl Pts',(209.412274998352,1.97232427104564,126.296871372241));
#17898=CARTESIAN_POINT('Ctrl Pts',(209.404575311022,1.84722705072554,126.244165814112));
#17899=CARTESIAN_POINT('Ctrl Pts',(209.396875623692,1.72000313242919,126.196674399199));
#17900=CARTESIAN_POINT('Ctrl Pts',(209.389184335902,1.59291800189124,126.149234792365));
#17901=CARTESIAN_POINT('Ctrl Pts',(209.381493048111,1.46371115844236,126.106998152058));
#17902=CARTESIAN_POINT('Ctrl Pts',(209.373801760321,1.33285200466186,126.070156503233));
#17903=CARTESIAN_POINT('Ctrl Pts',(209.366116945084,1.2021029745474,126.033345858257));
#17904=CARTESIAN_POINT('Ctrl Pts',(209.358432129846,1.0697047820666,126.001921279021));
#17905=CARTESIAN_POINT('Ctrl Pts',(209.350747314609,0.936144727381679,125.976025903413));
#17906=CARTESIAN_POINT('Ctrl Pts',(209.342993556857,0.801386470042141,125.949898213526));
#17907=CARTESIAN_POINT('Ctrl Pts',(209.335239799105,0.665445784867029,125.929399571767));
#17908=CARTESIAN_POINT('Ctrl Pts',(209.327486041353,0.528837072948192,125.914624999685));
#17909=CARTESIAN_POINT('Ctrl Pts',(209.319807329801,0.393550554092795,125.899993426072));
#17910=CARTESIAN_POINT('Ctrl Pts',(209.312128618249,0.257609288411705,125.890975634284));
#17911=CARTESIAN_POINT('Ctrl Pts',(209.304449906697,0.121520480433024,125.887612115219));
#17912=CARTESIAN_POINT('Ctrl Pts',(209.29677151016,-0.0145627445721506,
125.88424873414));
#17913=CARTESIAN_POINT('Ctrl Pts',(209.289093113624,-0.150793101684035,
125.886539174479));
#17914=CARTESIAN_POINT('Ctrl Pts',(209.281414717087,-0.286661848309734,
125.894471815646));
#17915=CARTESIAN_POINT('Ctrl Pts',(209.273734902769,-0.422555682476961,
125.902405921538));
#17916=CARTESIAN_POINT('Ctrl Pts',(209.266055088452,-0.558087375780228,
125.915984277149));
#17917=CARTESIAN_POINT('Ctrl Pts',(209.258375274134,-0.692752271574411,
125.935143293116));
#17918=CARTESIAN_POINT('Ctrl Pts',(209.25056542867,-0.82969725255273,125.954626700886));
#17919=CARTESIAN_POINT('Ctrl Pts',(209.242755583206,-0.965745392709727,
125.979881406748));
#17920=CARTESIAN_POINT('Ctrl Pts',(209.234945737741,-1.10037688251651,126.010786400041));
#17921=CARTESIAN_POINT('Ctrl Pts',(209.22725380964,-1.23297563168889,126.041224772666));
#17922=CARTESIAN_POINT('Ctrl Pts',(209.219561881538,-1.36419984247571,126.077143833343));
#17923=CARTESIAN_POINT('Ctrl Pts',(209.211869953437,-1.49356918075577,126.118377885545));
#17924=CARTESIAN_POINT('Ctrl Pts',(209.204001149291,-1.62591336961785,126.160560115622));
#17925=CARTESIAN_POINT('Ctrl Pts',(209.196132345145,-1.75631592647879,126.208304581786));
#17926=CARTESIAN_POINT('Ctrl Pts',(209.188263540999,-1.88428613385585,126.261382648408));
#17927=CARTESIAN_POINT('Ctrl Pts',(209.180394736854,-2.0122563412329,126.314460715029));
#17928=CARTESIAN_POINT('Ctrl Pts',(209.172525932708,-2.1377938314257,126.372872133719));
#17929=CARTESIAN_POINT('Ctrl Pts',(209.164657128562,-2.26043738552501,126.436339797032));
#17930=CARTESIAN_POINT('Ctrl Pts',(209.156868592286,-2.38182988080303,126.499160041239));
#17931=CARTESIAN_POINT('Ctrl Pts',(209.14908005601,-2.500789467108,126.567141780581));
#17932=CARTESIAN_POINT('Ctrl Pts',(209.141291519734,-2.61684735835623,126.64007280744));
#17933=CARTESIAN_POINT('Ctrl Pts',(209.133512703956,-2.73276040333477,126.712912812594));
#17934=CARTESIAN_POINT('Ctrl Pts',(209.125733888177,-2.84577863326455,126.790689607508));
#17935=CARTESIAN_POINT('Ctrl Pts',(209.117955072399,-2.95545619587902,126.873144299842));
#17936=CARTESIAN_POINT('Ctrl Pts',(209.1101333403,-3.06573885798239,126.956053901011));
#17937=CARTESIAN_POINT('Ctrl Pts',(209.1023116082,-3.17264351427431,127.043693011678));
#17938=CARTESIAN_POINT('Ctrl Pts',(209.094489876101,-3.27574388721603,127.135752564385));
#17939=CARTESIAN_POINT('Ctrl Pts',(209.086725556799,-3.37808748650062,127.227136384867));
#17940=CARTESIAN_POINT('Ctrl Pts',(209.078961237497,-3.47668216349184,127.322875713582));
#17941=CARTESIAN_POINT('Ctrl Pts',(209.071196918195,-3.57114231524718,127.422626502241));
#17942=CARTESIAN_POINT('Ctrl Pts',(209.063436157677,-3.66555917109043,127.522331570019));
#17943=CARTESIAN_POINT('Ctrl Pts',(209.055675397159,-3.75584500575455,127.62604415669));
#17944=CARTESIAN_POINT('Ctrl Pts',(209.047914636642,-3.84165048643871,127.733382824982));
#17945=CARTESIAN_POINT('Ctrl Pts',(209.040155768875,-3.92743504024807,127.840695314726));
#17946=CARTESIAN_POINT('Ctrl Pts',(209.032396901109,-4.0087411727101,127.951631821533));
#17947=CARTESIAN_POINT('Ctrl Pts',(209.024638033343,-4.08525957467433,128.065777540493));
#17948=CARTESIAN_POINT('Ctrl Pts',(209.016770989066,-4.16284481963531,128.181514714027));
#17949=CARTESIAN_POINT('Ctrl Pts',(209.008903944789,-4.23550756808287,128.300550941316));
#17950=CARTESIAN_POINT('Ctrl Pts',(209.001036900512,-4.30297085348242,128.422423402486));
#17951=CARTESIAN_POINT('Ctrl Pts',(208.993274395468,-4.36953767002672,128.54267639219));
#17952=CARTESIAN_POINT('Ctrl Pts',(208.985511890425,-4.43104221440763,128.665690330152));
#17953=CARTESIAN_POINT('Ctrl Pts',(208.977749385382,-4.48726508102552,128.79099647884));
#17954=CARTESIAN_POINT('Ctrl Pts',(208.969830071488,-4.54462369481051,128.918833912607));
#17955=CARTESIAN_POINT('Ctrl Pts',(208.961910757594,-4.59648477390531,129.049056774179));
#17956=CARTESIAN_POINT('Ctrl Pts',(208.9539914437,-4.64266756080343,129.181147451539));
#17957=CARTESIAN_POINT('Ctrl Pts',(208.946072129806,-4.68885034770155,129.313238128898));
#17958=CARTESIAN_POINT('Ctrl Pts',(208.938152815912,-4.72935474820577,129.447196203621));
#17959=CARTESIAN_POINT('Ctrl Pts',(208.930233502018,-4.76405452823405,129.582490119308));
#17960=CARTESIAN_POINT('Origin',(213.235140564004,0.,130.804360617566));
#17961=CARTESIAN_POINT('',(206.834782106149,-4.76405452823405,129.582490119308));
#17962=CARTESIAN_POINT('',(207.179891338435,-4.76405452823405,129.582490119308));
#17963=CARTESIAN_POINT('',(213.235140564004,-4.76405452823405,129.582490119308));
#17964=CARTESIAN_POINT('',(208.51485943604,-4.91824939693558,130.801925039035));
#17965=CARTESIAN_POINT('Ctrl Pts',(208.514859435991,-4.91824939693602,130.801925039913));
#17966=CARTESIAN_POINT('Ctrl Pts',(208.5069976833,-4.91831846622271,130.941399130231));
#17967=CARTESIAN_POINT('Ctrl Pts',(208.49913593061,-4.91245027592863,131.080863938173));
#17968=CARTESIAN_POINT('Ctrl Pts',(208.491274177919,-4.90067369759928,131.219788556153));
#17969=CARTESIAN_POINT('Ctrl Pts',(208.483410074226,-4.88889359756652,131.358754718568));
#17970=CARTESIAN_POINT('Ctrl Pts',(208.475545970533,-4.87120162119958,131.497179995886));
#17971=CARTESIAN_POINT('Ctrl Pts',(208.46768186684,-4.84767848973048,131.634539106028));
#17972=CARTESIAN_POINT('Ctrl Pts',(208.459813911939,-4.82414383851507,131.771965483663));
#17973=CARTESIAN_POINT('Ctrl Pts',(208.451945957038,-4.79477240682799,131.908324285026));
#17974=CARTESIAN_POINT('Ctrl Pts',(208.444078002137,-4.75969590309668,132.043101095852));
#17975=CARTESIAN_POINT('Ctrl Pts',(208.436146773066,-4.72433731378016,132.178961783106));
#17976=CARTESIAN_POINT('Ctrl Pts',(208.428215543994,-4.68318159239801,132.313214549761));
#17977=CARTESIAN_POINT('Ctrl Pts',(208.420284314923,-4.6364142414082,132.445349966882));
#17978=CARTESIAN_POINT('Ctrl Pts',(208.41239950935,-4.58992063160245,132.576711961844));
#17979=CARTESIAN_POINT('Ctrl Pts',(208.404514703777,-4.53788111459692,132.705981006347));
#17980=CARTESIAN_POINT('Ctrl Pts',(208.396629898205,-4.48052538922162,132.832678960194));
#17981=CARTESIAN_POINT('Ctrl Pts',(208.388675457384,-4.422663122488,132.960495856452));
#17982=CARTESIAN_POINT('Ctrl Pts',(208.380721016564,-4.35939048241694,133.085695687326));
#17983=CARTESIAN_POINT('Ctrl Pts',(208.372766575744,-4.29098908859084,133.207815569109));
#17984=CARTESIAN_POINT('Ctrl Pts',(208.364812134923,-4.22258769476473,133.329935450891));
#17985=CARTESIAN_POINT('Ctrl Pts',(208.356857694103,-4.14905780241504,133.448975089334));
#17986=CARTESIAN_POINT('Ctrl Pts',(208.348903253283,-4.07072345201489,133.564504389132));
#17987=CARTESIAN_POINT('Ctrl Pts',(208.341130262337,-3.99417599755729,133.677398333739));
#17988=CARTESIAN_POINT('Ctrl Pts',(208.333357271391,-3.91280696466297,133.787284943416));
#17989=CARTESIAN_POINT('Ctrl Pts',(208.325584280444,-3.82688028292267,133.893724688484));
#17990=CARTESIAN_POINT('Ctrl Pts',(208.317820888004,-3.74105970805478,134.000032996049));
#17991=CARTESIAN_POINT('Ctrl Pts',(208.310057495564,-3.65069292565359,134.10290260645));
#17992=CARTESIAN_POINT('Ctrl Pts',(208.302294103124,-3.55608760223375,134.201922100121));
#17993=CARTESIAN_POINT('Ctrl Pts',(208.294538438539,-3.46157645107868,134.300843027563));
#17994=CARTESIAN_POINT('Ctrl Pts',(208.286782773954,-3.36283542354201,134.395921184087));
#17995=CARTESIAN_POINT('Ctrl Pts',(208.279027109369,-3.26021275313167,134.486777740438));
#17996=CARTESIAN_POINT('Ctrl Pts',(208.271277308707,-3.15766767394118,134.577565601723));
#17997=CARTESIAN_POINT('Ctrl Pts',(208.263527508046,-3.05124708510556,134.664137957811));
#17998=CARTESIAN_POINT('Ctrl Pts',(208.255777707384,-2.94133615365521,134.746152683835));
#17999=CARTESIAN_POINT('Ctrl Pts',(208.248031218034,-2.83147218461794,134.828132366852));
#18000=CARTESIAN_POINT('Ctrl Pts',(208.240284728684,-2.71812115194593,134.905558059566));
#18001=CARTESIAN_POINT('Ctrl Pts',(208.232538239334,-2.60170121537788,134.978127962352));
#18002=CARTESIAN_POINT('Ctrl Pts',(208.224793380744,-2.48530578706252,135.050682588017));
#18003=CARTESIAN_POINT('Ctrl Pts',(208.217048522153,-2.3658430715812,135.118383250226));
#18004=CARTESIAN_POINT('Ctrl Pts',(208.209303663563,-2.24375977991022,135.18097176234));
#18005=CARTESIAN_POINT('Ctrl Pts',(208.201558756542,-2.12167572482072,135.243560665835));
#18006=CARTESIAN_POINT('Ctrl Pts',(208.193813849521,-1.99697140887362,135.30103717698));
#18007=CARTESIAN_POINT('Ctrl Pts',(208.186068942499,-1.87011732041024,135.353189507555));
#18008=CARTESIAN_POINT('Ctrl Pts',(208.17832230818,-1.74323494047574,135.405353469337));
#18009=CARTESIAN_POINT('Ctrl Pts',(208.170575673861,-1.61420219565832,135.452190739054));
#18010=CARTESIAN_POINT('Ctrl Pts',(208.162829039542,-1.48350830287314,135.49353817635));
#18011=CARTESIAN_POINT('Ctrl Pts',(208.155074174212,-1.35267554425398,135.534929546429));
#18012=CARTESIAN_POINT('Ctrl Pts',(208.147319308882,-1.22017848536061,135.570819313687));
#18013=CARTESIAN_POINT('Ctrl Pts',(208.139564443553,-1.08652075107271,135.601094477182));
#18014=CARTESIAN_POINT('Ctrl Pts',(208.131805442764,-0.952791740747417,
135.6313857856));
#18015=CARTESIAN_POINT('Ctrl Pts',(208.124046441975,-0.817901206265174,
135.656056453942));
#18016=CARTESIAN_POINT('Ctrl Pts',(208.116287441186,-0.682360651451801,
135.675045066784));
#18017=CARTESIAN_POINT('Ctrl Pts',(208.108515975456,-0.5466023488804,135.694064185092));
#18018=CARTESIAN_POINT('Ctrl Pts',(208.100744509727,-0.410192328696788,
135.707382968629));
#18019=CARTESIAN_POINT('Ctrl Pts',(208.092973043997,-0.273645776384339,
135.714992048611));
#18020=CARTESIAN_POINT('Ctrl Pts',(208.085467239154,-0.141766950797409,
135.722341018723));
#18021=CARTESIAN_POINT('Ctrl Pts',(208.077961434312,-0.00976108821497224,
135.724364294266));
#18022=CARTESIAN_POINT('Ctrl Pts',(208.07045562947,0.121911747919636,135.721099433918));
#18023=CARTESIAN_POINT('Ctrl Pts',(208.062680838016,0.258303362492575,135.717717570297));
#18024=CARTESIAN_POINT('Ctrl Pts',(208.054906046562,0.394769977134225,135.708650746295));
#18025=CARTESIAN_POINT('Ctrl Pts',(208.047131255108,0.530798916088052,135.693883659048));
#18026=CARTESIAN_POINT('Ctrl Pts',(208.03936604126,0.66666028378857,135.679134763071));
#18027=CARTESIAN_POINT('Ctrl Pts',(208.031600827411,0.802084663675805,135.658699617433));
#18028=CARTESIAN_POINT('Ctrl Pts',(208.023835613563,0.936559415699432,135.632614911135));
#18029=CARTESIAN_POINT('Ctrl Pts',(208.016078108725,1.0709006662788,135.606556100746));
#18030=CARTESIAN_POINT('Ctrl Pts',(208.008320603888,1.20429378384447,135.574858965191));
#18031=CARTESIAN_POINT('Ctrl Pts',(208.00056309905,1.33623164391999,135.537611937355));
#18032=CARTESIAN_POINT('Ctrl Pts',(207.992811441313,1.46807005784367,135.500392983899));
#18033=CARTESIAN_POINT('Ctrl Pts',(207.985059783576,1.59845502286451,135.45763257026));
#18034=CARTESIAN_POINT('Ctrl Pts',(207.977308125839,1.72689035222872,135.409470037968));
#18035=CARTESIAN_POINT('Ctrl Pts',(207.969559760361,1.85527113296102,135.36132796111));
#18036=CARTESIAN_POINT('Ctrl Pts',(207.961811394883,1.98170355969654,135.307788465907));
#18037=CARTESIAN_POINT('Ctrl Pts',(207.954063029405,2.10570755579637,135.249040443151));
#18038=CARTESIAN_POINT('Ctrl Pts',(207.946316283345,2.22968563490169,135.190304698807));
#18039=CARTESIAN_POINT('Ctrl Pts',(207.938569537285,2.35123593986109,135.126362759441));
#18040=CARTESIAN_POINT('Ctrl Pts',(207.930822791226,2.46989966875899,135.057451104349));
#18041=CARTESIAN_POINT('Ctrl Pts',(207.923075987157,2.58856428623285,134.988538933234));
#18042=CARTESIAN_POINT('Ctrl Pts',(207.915329183088,2.70434194647162,134.914657168452));
#18043=CARTESIAN_POINT('Ctrl Pts',(207.907582379019,2.8168000428877,134.836087366849));
#18044=CARTESIAN_POINT('Ctrl Pts',(207.899833839831,2.92928332751887,134.757499967287));
#18045=CARTESIAN_POINT('Ctrl Pts',(207.892085300644,3.03844524843345,134.674222665321));
#18046=CARTESIAN_POINT('Ctrl Pts',(207.884336761456,3.14388401280121,134.586579064001));
#18047=CARTESIAN_POINT('Ctrl Pts',(207.876579989602,3.24943480372359,134.498842343127));
#18048=CARTESIAN_POINT('Ctrl Pts',(207.868823217748,3.35125423490542,134.406730306064));
#18049=CARTESIAN_POINT('Ctrl Pts',(207.861066445894,3.44897491534359,134.310605773831));
#18050=CARTESIAN_POINT('Ctrl Pts',(207.853305534651,3.54674774427149,134.21442994489));
#18051=CARTESIAN_POINT('Ctrl Pts',(207.845544623408,3.64041719724162,134.114237639535));
#18052=CARTESIAN_POINT('Ctrl Pts',(207.837783712165,3.72965502772357,134.010426187182));
#18053=CARTESIAN_POINT('Ctrl Pts',(207.830010348593,3.81903603968545,133.906448170074));
#18054=CARTESIAN_POINT('Ctrl Pts',(207.822236985022,3.90397097776096,133.798839708958));
#18055=CARTESIAN_POINT('Ctrl Pts',(207.81446362145,3.98417339609271,133.688029359354));
#18056=CARTESIAN_POINT('Ctrl Pts',(207.806978416186,4.06140271367255,133.581326745409));
#18057=CARTESIAN_POINT('Ctrl Pts',(207.799493210921,4.13424399164836,133.471655678562));
#18058=CARTESIAN_POINT('Ctrl Pts',(207.792008005657,4.20248194836357,133.359420017302));
#18059=CARTESIAN_POINT('Ctrl Pts',(207.784233556478,4.27335676178718,133.242847336433));
#18060=CARTESIAN_POINT('Ctrl Pts',(207.776459107299,4.33948969755912,133.123138859218));
#18061=CARTESIAN_POINT('Ctrl Pts',(207.76868465812,4.40059076633519,133.000717594413));
#18062=CARTESIAN_POINT('Ctrl Pts',(207.76091978728,4.46161655688566,132.87844715603));
#18063=CARTESIAN_POINT('Ctrl Pts',(207.75315491644,4.51762264249707,132.753470926551));
#18064=CARTESIAN_POINT('Ctrl Pts',(207.7453900456,4.56836279360575,132.626239990219));
#18065=CARTESIAN_POINT('Ctrl Pts',(207.737632884128,4.61905256725022,132.499135375386));
#18066=CARTESIAN_POINT('Ctrl Pts',(207.729875722656,4.66448666705683,132.36978086939));
#18067=CARTESIAN_POINT('Ctrl Pts',(207.722118561184,4.70446537714295,132.238650887269));
#18068=CARTESIAN_POINT('Ctrl Pts',(207.714367246798,4.74441395262572,132.107619746505));
#18069=CARTESIAN_POINT('Ctrl Pts',(207.706615932413,4.7789152097074,131.974816165857));
#18070=CARTESIAN_POINT('Ctrl Pts',(207.698864618028,4.80781817473379,131.840732877519));
#18071=CARTESIAN_POINT('Ctrl Pts',(207.691116594631,4.83670886837882,131.706706517151));
#18072=CARTESIAN_POINT('Ctrl Pts',(207.683368571235,4.86000591517799,131.571401911102));
#18073=CARTESIAN_POINT('Ctrl Pts',(207.675620547838,4.87760873613739,131.435325021995));
#18074=CARTESIAN_POINT('Ctrl Pts',(207.667874143036,4.89520787979476,131.299276559912));
#18075=CARTESIAN_POINT('Ctrl Pts',(207.660127738233,4.90711511356422,131.162456523146));
#18076=CARTESIAN_POINT('Ctrl Pts',(207.652381333431,4.91328139537258,131.025378699147));
#18077=CARTESIAN_POINT('Ctrl Pts',(207.644634869463,4.91944772427759,130.888299828178));
#18078=CARTESIAN_POINT('Ctrl Pts',(207.636888405496,4.91987299616475,130.750963556604));
#18079=CARTESIAN_POINT('Ctrl Pts',(207.629141941528,4.9145602531883,130.613885999095));
#18080=CARTESIAN_POINT('Ctrl Pts',(207.621393740952,4.90924631919717,130.476777711437));
#18081=CARTESIAN_POINT('Ctrl Pts',(207.613645540377,4.89819182578494,130.339928643839));
#18082=CARTESIAN_POINT('Ctrl Pts',(207.605897339801,4.88145184537105,130.203851713532));
#18083=CARTESIAN_POINT('Ctrl Pts',(207.598140902255,4.86469406898943,130.067630122324));
#18084=CARTESIAN_POINT('Ctrl Pts',(207.590384464708,4.84223877960226,129.932182696777));
#18085=CARTESIAN_POINT('Ctrl Pts',(207.582628027162,4.81419263987389,129.798014609135));
#18086=CARTESIAN_POINT('Ctrl Pts',(207.574867448415,4.78613152617349,129.663774888491));
#18087=CARTESIAN_POINT('Ctrl Pts',(207.567106869669,4.75247371019375,129.530816245587));
#18088=CARTESIAN_POINT('Ctrl Pts',(207.559346290922,4.71337604578668,129.399629570887));
#18089=CARTESIAN_POINT('Ctrl Pts',(207.55157325334,4.67421561397873,129.268232289064));
#18090=CARTESIAN_POINT('Ctrl Pts',(207.543800215759,4.62959800947895,129.138613029973));
#18091=CARTESIAN_POINT('Ctrl Pts',(207.536027178177,4.57972895160504,129.011244393689));
#18092=CARTESIAN_POINT('Ctrl Pts',(207.528538246066,4.53168261387283,128.888531096581));
#18093=CARTESIAN_POINT('Ctrl Pts',(207.521049313955,4.47876212574444,128.767907055659));
#18094=CARTESIAN_POINT('Ctrl Pts',(207.513560381844,4.42119126588728,128.649772291936));
#18095=CARTESIAN_POINT('Ctrl Pts',(207.505786241846,4.36142788203951,128.527138493384));
#18096=CARTESIAN_POINT('Ctrl Pts',(207.498012101847,4.29646354793691,128.406798788378));
#18097=CARTESIAN_POINT('Ctrl Pts',(207.490237961849,4.22649734688889,128.289225782365));
#18098=CARTESIAN_POINT('Ctrl Pts',(207.482473405643,4.15661739866639,128.171797717822));
#18099=CARTESIAN_POINT('Ctrl Pts',(207.474708849436,4.08174805039643,128.057129898718));
#18100=CARTESIAN_POINT('Ctrl Pts',(207.46694429323,4.00213566156389,127.945673294871));
#18101=CARTESIAN_POINT('Ctrl Pts',(207.459187451483,3.92260237145483,127.834327428501));
#18102=CARTESIAN_POINT('Ctrl Pts',(207.451430609736,3.83833564452231,127.726186744262));
#18103=CARTESIAN_POINT('Ctrl Pts',(207.443673767988,3.74962661345412,127.621675694081));
#18104=CARTESIAN_POINT('Ctrl Pts',(207.435922778062,3.66098450516628,127.517243487847));
#18105=CARTESIAN_POINT('Ctrl Pts',(207.428171788136,3.56790701530164,127.416435762287));
#18106=CARTESIAN_POINT('Ctrl Pts',(207.42042079821,3.47072703641595,127.319645865798));
#18107=CARTESIAN_POINT('Ctrl Pts',(207.412673105353,3.37358839535843,127.222897141206));
#18108=CARTESIAN_POINT('Ctrl Pts',(207.404925412496,3.27235101258055,127.130163121791));
#18109=CARTESIAN_POINT('Ctrl Pts',(207.39717771964,3.16738615389837,127.041801911766));
#18110=CARTESIAN_POINT('Ctrl Pts',(207.389431649034,3.06244327329369,126.953459203261));
#18111=CARTESIAN_POINT('Ctrl Pts',(207.381685578428,2.95377476812009,126.869487734607));
#18112=CARTESIAN_POINT('Ctrl Pts',(207.373939507823,2.84178634723068,126.790206482609));
#18113=CARTESIAN_POINT('Ctrl Pts',(207.366193381404,2.72979711941912,126.710924659357));
#18114=CARTESIAN_POINT('Ctrl Pts',(207.358447254985,2.61448824726982,126.636333346117));
#18115=CARTESIAN_POINT('Ctrl Pts',(207.350701128566,2.49629555308794,126.566708959615));
#18116=CARTESIAN_POINT('Ctrl Pts',(207.342953268587,2.37807640773334,126.497068991383));
#18117=CARTESIAN_POINT('Ctrl Pts',(207.335205408607,2.2569724929127,126.432398360219));
#18118=CARTESIAN_POINT('Ctrl Pts',(207.327457548628,2.13344506692891,126.372927981398));
#18119=CARTESIAN_POINT('Ctrl Pts',(207.319701454607,2.009786362109,126.3133944004));
#18120=CARTESIAN_POINT('Ctrl Pts',(207.311945360586,1.88369935396116,126.259072281538));
#18121=CARTESIAN_POINT('Ctrl Pts',(207.304189266564,1.75566667258516,126.210144950309));
#18122=CARTESIAN_POINT('Ctrl Pts',(207.296429033481,1.62756566619945,126.161191508867));
#18123=CARTESIAN_POINT('Ctrl Pts',(207.288668800398,1.49751728822706,126.117638715693));
#18124=CARTESIAN_POINT('Ctrl Pts',(207.280908567314,1.36601928450809,126.079619949884));
#18125=CARTESIAN_POINT('Ctrl Pts',(207.27313587558,1.23431016757891,126.041540146922));
#18126=CARTESIAN_POINT('Ctrl Pts',(207.265363183846,1.10114715425798,126.009012218405));
#18127=CARTESIAN_POINT('Ctrl Pts',(207.257590492112,0.967039016842553,125.982118545417));
#18128=CARTESIAN_POINT('Ctrl Pts',(207.250097914085,0.837763893371229,125.956194071607));
#18129=CARTESIAN_POINT('Ctrl Pts',(207.242605336058,0.707610899911634,125.935504790949));
#18130=CARTESIAN_POINT('Ctrl Pts',(207.235112758031,0.577038241873283,125.920078691846));
#18131=CARTESIAN_POINT('Ctrl Pts',(207.227338345037,0.441554064636067,125.904072336639));
#18132=CARTESIAN_POINT('Ctrl Pts',(207.219563932042,0.305188826807901,125.893682160164));
#18133=CARTESIAN_POINT('Ctrl Pts',(207.211789519048,0.16844779316213,125.888996093598));
#18134=CARTESIAN_POINT('Ctrl Pts',(207.204024686519,0.0318752664866379,
125.884315801707));
#18135=CARTESIAN_POINT('Ctrl Pts',(207.19625985399,-0.105071747606433,125.885325646935));
#18136=CARTESIAN_POINT('Ctrl Pts',(207.188495021462,-0.241880637176841,
125.892062090414));
#18137=CARTESIAN_POINT('Ctrl Pts',(207.180737900378,-0.378553658495936,
125.898791843767));
#18138=CARTESIAN_POINT('Ctrl Pts',(207.172980779294,-0.515088440319783,
125.911236858428));
#18139=CARTESIAN_POINT('Ctrl Pts',(207.16522365821,-0.650970483668557,125.929381592802));
#18140=CARTESIAN_POINT('Ctrl Pts',(207.157472386242,-0.786750067641371,
125.947512645469));
#18141=CARTESIAN_POINT('Ctrl Pts',(207.149721114274,-0.921877506856219,
125.971334811858));
#18142=CARTESIAN_POINT('Ctrl Pts',(207.141969842306,-1.05584190167843,126.00078060458));
#18143=CARTESIAN_POINT('Ctrl Pts',(207.134221864282,-1.18974936760714,126.030213884153));
#18144=CARTESIAN_POINT('Ctrl Pts',(207.126473886259,-1.32249439111151,126.065265953194));
#18145=CARTESIAN_POINT('Ctrl Pts',(207.118725908236,-1.45357498549394,126.105817989894));
#18146=CARTESIAN_POINT('Ctrl Pts',(207.110979550602,-1.58462816607085,126.146361545663));
#18147=CARTESIAN_POINT('Ctrl Pts',(207.103233192967,-1.71401723664896,126.192402665714));
#18148=CARTESIAN_POINT('Ctrl Pts',(207.095486835333,-1.84125451462641,126.243772401681));
#18149=CARTESIAN_POINT('Ctrl Pts',(207.087740420291,-1.96849273555578,126.295142518348));
#18150=CARTESIAN_POINT('Ctrl Pts',(207.079994005249,-2.09357876953884,126.351841183367));
#18151=CARTESIAN_POINT('Ctrl Pts',(207.072247590207,-2.21604446583207,126.413651109075));
#18152=CARTESIAN_POINT('Ctrl Pts',(207.064499440277,-2.33853758954754,126.475474877736));
#18153=CARTESIAN_POINT('Ctrl Pts',(207.056751290347,-2.45840885885262,126.542412008823));
#18154=CARTESIAN_POINT('Ctrl Pts',(207.049003140418,-2.5752146573241,126.61419922077));
#18155=CARTESIAN_POINT('Ctrl Pts',(207.041246755976,-2.69214459365274,126.686062726109));
#18156=CARTESIAN_POINT('Ctrl Pts',(207.033490371535,-2.80600221754134,126.762786404001));
#18157=CARTESIAN_POINT('Ctrl Pts',(207.025733987093,-2.91637240029103,126.844063269472));
#18158=CARTESIAN_POINT('Ctrl Pts',(207.017973462873,-3.0268014903987,126.925383514462));
#18159=CARTESIAN_POINT('Ctrl Pts',(207.010212938653,-3.13373912581693,127.011261544638));
#18160=CARTESIAN_POINT('Ctrl Pts',(207.002452414433,-3.23680402931943,127.10135066102));
#18161=CARTESIAN_POINT('Ctrl Pts',(206.994679433281,-3.34003436913308,127.191584385416));
#18162=CARTESIAN_POINT('Ctrl Pts',(206.986906452129,-3.43937927123302,127.286042434095));
#18163=CARTESIAN_POINT('Ctrl Pts',(206.979133470977,-3.53449440489227,127.384341266117));
#18164=CARTESIAN_POINT('Ctrl Pts',(206.971644025391,-3.62614001730631,127.47905444491));
#18165=CARTESIAN_POINT('Ctrl Pts',(206.964154579804,-3.71385885862058,127.577332858762));
#18166=CARTESIAN_POINT('Ctrl Pts',(206.956665134218,-3.79738005623955,127.678806623316));
#18167=CARTESIAN_POINT('Ctrl Pts',(206.94892298064,-3.88371941628567,127.783704303698));
#18168=CARTESIAN_POINT('Ctrl Pts',(206.941180827061,-3.96585449861154,127.892359049907));
#18169=CARTESIAN_POINT('Ctrl Pts',(206.933438673483,-4.04343822436208,128.004398048483));
#18170=CARTESIAN_POINT('Ctrl Pts',(206.925706075313,-4.12092619585451,128.116298767914));
#18171=CARTESIAN_POINT('Ctrl Pts',(206.917973477143,-4.19387376171797,128.231575110578));
#18172=CARTESIAN_POINT('Ctrl Pts',(206.910240878973,-4.26197290981049,128.349819931706));
#18173=CARTESIAN_POINT('Ctrl Pts',(206.902517710807,-4.32998901010207,128.46792055173));
#18174=CARTESIAN_POINT('Ctrl Pts',(206.894794542642,-4.39316827069876,128.588982102231));
#18175=CARTESIAN_POINT('Ctrl Pts',(206.887071374476,-4.45124539391763,128.712567724943));
#18176=CARTESIAN_POINT('Ctrl Pts',(206.879353629328,-4.50928173682022,128.836066568895));
#18177=CARTESIAN_POINT('Ctrl Pts',(206.871635884179,-4.56222290117181,128.962085604511));
#18178=CARTESIAN_POINT('Ctrl Pts',(206.863918139031,-4.60984903856988,129.090162582304));
#18179=CARTESIAN_POINT('Ctrl Pts',(206.85620451266,-4.65744975902835,129.218171208453));
#18180=CARTESIAN_POINT('Ctrl Pts',(206.848490886289,-4.69974096176733,129.348235221746));
#18181=CARTESIAN_POINT('Ctrl Pts',(206.840777259918,-4.73655075729518,129.479872042279));
#18182=CARTESIAN_POINT('Ctrl Pts',(206.838778875329,-4.74608714453948,129.513975456281));
#18183=CARTESIAN_POINT('Ctrl Pts',(206.836780490739,-4.75525588437582,129.548184340443));
#18184=CARTESIAN_POINT('Ctrl Pts',(206.834782106149,-4.76405452823405,129.582490119308));
#18185=CARTESIAN_POINT('Ctrl Pts',(208.584593534951,-4.76405452823405,129.582490119308));
#18186=CARTESIAN_POINT('Ctrl Pts',(208.576017307781,-4.80157547937709,129.728783738355));
#18187=CARTESIAN_POINT('Ctrl Pts',(208.567441080611,-4.83239790014226,129.876978832491));
#18188=CARTESIAN_POINT('Ctrl Pts',(208.558864853441,-4.85634444651292,130.026477799062));
#18189=CARTESIAN_POINT('Ctrl Pts',(208.550327451534,-4.88018258496171,130.175299971911));
#18190=CARTESIAN_POINT('Ctrl Pts',(208.541790049627,-4.89720686488144,130.325414009242));
#18191=CARTESIAN_POINT('Ctrl Pts',(208.53325264772,-4.90729068591846,130.476212501012));
#18192=CARTESIAN_POINT('Ctrl Pts',(208.52712157716,-4.91453230567176,130.584507296483));
#18193=CARTESIAN_POINT('Ctrl Pts',(208.5209905066,-4.91819553250619,130.693154702108));
#18194=CARTESIAN_POINT('Ctrl Pts',(208.51485943604,-4.91824939693558,130.801925039035));
#18195=CARTESIAN_POINT('',(208.860140563973,-4.91824943730512,130.802007970582));
#18196=CARTESIAN_POINT('Ctrl Pts',(208.930233502018,-4.76405452823405,129.582490119308));
#18197=CARTESIAN_POINT('Ctrl Pts',(208.922447515776,-4.79817011116022,129.715506259361));
#18198=CARTESIAN_POINT('Ctrl Pts',(208.914661529535,-4.82667498858406,129.849813218037));
#18199=CARTESIAN_POINT('Ctrl Pts',(208.906875543294,-4.84950153322439,129.984898634461));
#18200=CARTESIAN_POINT('Ctrl Pts',(208.899986863779,-4.86969740123493,130.104415945698));
#18201=CARTESIAN_POINT('Ctrl Pts',(208.893098184264,-4.88544907649643,130.224542348731));
#18202=CARTESIAN_POINT('Ctrl Pts',(208.88620950475,-4.89674374081455,130.344922047904));
#18203=CARTESIAN_POINT('Ctrl Pts',(208.877519857836,-4.91099126745915,130.496773658817));
#18204=CARTESIAN_POINT('Ctrl Pts',(208.868830210922,-4.9181763870815,130.64929524746));
#18205=CARTESIAN_POINT('Ctrl Pts',(208.860140564008,-4.91824943730483,130.802007969968));
#18206=CARTESIAN_POINT('Ctrl Pts',(208.860140563973,-4.91824943730512,130.802007970582));
#18207=CARTESIAN_POINT('Ctrl Pts',(208.852452334247,-4.91831406901657,130.93712168745));
#18208=CARTESIAN_POINT('Ctrl Pts',(208.84476410452,-4.91280674963555,131.072453879537));
#18209=CARTESIAN_POINT('Ctrl Pts',(208.837075874794,-4.90169979502435,131.207501017375));
#18210=CARTESIAN_POINT('Ctrl Pts',(208.829396198239,-4.89060519692236,131.342397915002));
#18211=CARTESIAN_POINT('Ctrl Pts',(208.821716521683,-4.87392338696553,131.477009993859));
#18212=CARTESIAN_POINT('Ctrl Pts',(208.814036845128,-4.85167868744603,131.610832549056));
#18213=CARTESIAN_POINT('Ctrl Pts',(208.806363779643,-4.82945313733591,131.744539902748));
#18214=CARTESIAN_POINT('Ctrl Pts',(208.798690714157,-4.80167428999412,131.877458692401));
#18215=CARTESIAN_POINT('Ctrl Pts',(208.791017648672,-4.76841833750263,132.009088645408));
#18216=CARTESIAN_POINT('Ctrl Pts',(208.783348819167,-4.73518074423976,132.140645930992));
#18217=CARTESIAN_POINT('Ctrl Pts',(208.775679989662,-4.69647215728822,132.270915408287));
#18218=CARTESIAN_POINT('Ctrl Pts',(208.768011160158,-4.65241990971906,132.399406712872));
#18219=CARTESIAN_POINT('Ctrl Pts',(208.760344500522,-4.60838012658386,132.527861661278));
#18220=CARTESIAN_POINT('Ctrl Pts',(208.752677840887,-4.55899981853378,132.654539059235));
#18221=CARTESIAN_POINT('Ctrl Pts',(208.745011181251,-4.50445613078236,132.778963876035));
#18222=CARTESIAN_POINT('Ctrl Pts',(208.737344945431,-4.44991545822423,132.90338181459));
#18223=CARTESIAN_POINT('Ctrl Pts',(208.729678709611,-4.39021213419317,133.025547053232));
#18224=CARTESIAN_POINT('Ctrl Pts',(208.722012473791,-4.32557117553024,133.145005201419));
#18225=CARTESIAN_POINT('Ctrl Pts',(208.714344916315,-4.2609190727916,133.264483944144));
#18226=CARTESIAN_POINT('Ctrl Pts',(208.706677358839,-4.19132783308178,133.381254316553));
#18227=CARTESIAN_POINT('Ctrl Pts',(208.699009801363,-4.11706782546444,133.494887625984));
#18228=CARTESIAN_POINT('Ctrl Pts',(208.691334452229,-4.04273235593582,133.608636407888));
#18229=CARTESIAN_POINT('Ctrl Pts',(208.683659103096,-3.96371886154607,133.71924142412));
#18230=CARTESIAN_POINT('Ctrl Pts',(208.675983753962,-3.88034058749315,133.826303699021));
#18231=CARTESIAN_POINT('Ctrl Pts',(208.668304507765,-3.79691997915443,133.933420333466));
#18232=CARTESIAN_POINT('Ctrl Pts',(208.660625261568,-3.70913043605773,134.036990339263));
#18233=CARTESIAN_POINT('Ctrl Pts',(208.652946015371,-3.61732387877702,134.136649773466));
#18234=CARTESIAN_POINT('Ctrl Pts',(208.64525452406,-3.52537092928688,134.236468121861));
#18235=CARTESIAN_POINT('Ctrl Pts',(208.637563032748,-3.42938845130611,134.332363157705));
#18236=CARTESIAN_POINT('Ctrl Pts',(208.629871541437,-3.32976397282271,134.424009073948));
#18237=CARTESIAN_POINT('Ctrl Pts',(208.622501654603,-3.23430509462818,134.511822997684));
#18238=CARTESIAN_POINT('Ctrl Pts',(208.61513176777,-3.13550289223388,134.595735802233));
#18239=CARTESIAN_POINT('Ctrl Pts',(208.607761880937,-3.03372331873832,134.675498161989));
#18240=CARTESIAN_POINT('Ctrl Pts',(208.599996643283,-2.92648387336159,134.759539300387));
#18241=CARTESIAN_POINT('Ctrl Pts',(208.592231405629,-2.81557582884422,134.839257045366));
#18242=CARTESIAN_POINT('Ctrl Pts',(208.584466167976,-2.70138333523345,134.914313310557));
#18243=CARTESIAN_POINT('Ctrl Pts',(208.57671062275,-2.5873333746107,134.989275891887));
#18244=CARTESIAN_POINT('Ctrl Pts',(208.568955077524,-2.4700074457162,135.059588356404));
#18245=CARTESIAN_POINT('Ctrl Pts',(208.561199532298,-2.34982285338321,135.12495266267));
#18246=CARTESIAN_POINT('Ctrl Pts',(208.55345180014,-2.22975933703701,135.190251119831));
#18247=CARTESIAN_POINT('Ctrl Pts',(208.545704067981,-2.10684323005938,135.250611152222));
#18248=CARTESIAN_POINT('Ctrl Pts',(208.537956335823,-1.98152060362814,135.305778078755));
#18249=CARTESIAN_POINT('Ctrl Pts',(208.530214544241,-1.85629406837336,135.360902706024));
#18250=CARTESIAN_POINT('Ctrl Pts',(208.522472752659,-1.7286650435057,135.410841995268));
#18251=CARTESIAN_POINT('Ctrl Pts',(208.514730961078,-1.59910364588964,135.455387449589));
#18252=CARTESIAN_POINT('Ctrl Pts',(208.506992569679,-1.4695991514346,135.499913339618));
#18253=CARTESIAN_POINT('Ctrl Pts',(208.49925417828,-1.33816434213286,135.539049979232));
#18254=CARTESIAN_POINT('Ctrl Pts',(208.491515786881,-1.20528851144165,135.572637315356));
#18255=CARTESIAN_POINT('Ctrl Pts',(208.483779079378,-1.07244159491196,135.606217342779));
#18256=CARTESIAN_POINT('Ctrl Pts',(208.476042371875,-0.938154660477446,
135.634250372453));
#18257=CARTESIAN_POINT('Ctrl Pts',(208.468305664372,-0.802930941415024,
135.656626579549));
#18258=CARTESIAN_POINT('Ctrl Pts',(208.460568954138,-0.667707174624105,
135.679002794542));
#18259=CARTESIAN_POINT('Ctrl Pts',(208.452832243905,-0.531547009266178,
135.695722118751));
#18260=CARTESIAN_POINT('Ctrl Pts',(208.445095533671,-0.394962211773451,
135.706726160217));
#18261=CARTESIAN_POINT('Ctrl Pts',(208.437357134427,-0.258347596300371,
135.717732603987));
#18262=CARTESIAN_POINT('Ctrl Pts',(208.429618735184,-0.121308554920572,
135.723021250898));
#18263=CARTESIAN_POINT('Ctrl Pts',(208.42188033594,0.0156401187563764,135.722585749581));
#18264=CARTESIAN_POINT('Ctrl Pts',(208.414133720282,0.152734200677577,135.722149785862));
#18265=CARTESIAN_POINT('Ctrl Pts',(208.406387104625,0.289737330576747,135.715977534255));
#18266=CARTESIAN_POINT('Ctrl Pts',(208.398640488967,0.426136266850155,135.704114789417));
#18267=CARTESIAN_POINT('Ctrl Pts',(208.390889759046,0.562607645212518,135.692245744223));
#18268=CARTESIAN_POINT('Ctrl Pts',(208.383139029126,0.698473801993175,135.674680234289));
#18269=CARTESIAN_POINT('Ctrl Pts',(208.375388299206,0.833229720990087,135.651515586675));
#18270=CARTESIAN_POINT('Ctrl Pts',(208.367625056951,0.968203182214324,135.628313543383));
#18271=CARTESIAN_POINT('Ctrl Pts',(208.359861814697,1.10206244061413,135.59949438239));
#18272=CARTESIAN_POINT('Ctrl Pts',(208.352098572443,1.23431484450832,135.565206123054));
#18273=CARTESIAN_POINT('Ctrl Pts',(208.34450380067,1.36369723283556,135.531661954829));
#18274=CARTESIAN_POINT('Ctrl Pts',(208.336909028897,1.4915414917313,135.492883804827));
#18275=CARTESIAN_POINT('Ctrl Pts',(208.329314257124,1.61740511662782,135.449054768014));
#18276=CARTESIAN_POINT('Ctrl Pts',(208.321537400431,1.7462863263438,135.404174928507));
#18277=CARTESIAN_POINT('Ctrl Pts',(208.313760543739,1.87350126461924,135.353855985428));
#18278=CARTESIAN_POINT('Ctrl Pts',(208.305983687046,1.99855688905477,135.298240169102));
#18279=CARTESIAN_POINT('Ctrl Pts',(208.298216395952,2.12345869403154,135.242692760692));
#18280=CARTESIAN_POINT('Ctrl Pts',(208.290449104858,2.24620611628277,135.181861599773));
#18281=CARTESIAN_POINT('Ctrl Pts',(208.282681813764,2.36632204495425,135.115938407896));
#18282=CARTESIAN_POINT('Ctrl Pts',(208.274922221987,2.48631890886508,135.050080562298));
#18283=CARTESIAN_POINT('Ctrl Pts',(208.26716263021,2.60368912995268,134.97914091734));
#18284=CARTESIAN_POINT('Ctrl Pts',(208.259403038434,2.71797666759268,134.903358775277));
#18285=CARTESIAN_POINT('Ctrl Pts',(208.251649286353,2.8321781949754,134.827633665168));
#18286=CARTESIAN_POINT('Ctrl Pts',(208.243895534272,2.94330133242635,134.747073526959));
#18287=CARTESIAN_POINT('Ctrl Pts',(208.236141782192,3.05091601399587,134.661962792239));
#18288=CARTESIAN_POINT('Ctrl Pts',(208.228391318654,3.1584850537225,134.576888154925));
#18289=CARTESIAN_POINT('Ctrl Pts',(208.220640855117,3.26254829138391,134.487267001654));
#18290=CARTESIAN_POINT('Ctrl Pts',(208.212890391579,3.36270614264577,134.393426019688));
#18291=CARTESIAN_POINT('Ctrl Pts',(208.205141545516,3.46284309157885,134.29960462176));
#18292=CARTESIAN_POINT('Ctrl Pts',(208.197392699453,3.55907599036995,134.201565413779));
#18293=CARTESIAN_POINT('Ctrl Pts',(208.18964385339,3.65104005214414,134.099673895562));
#18294=CARTESIAN_POINT('Ctrl Pts',(208.181894949397,3.74300480143419,133.997781615613));
#18295=CARTESIAN_POINT('Ctrl Pts',(208.174146045404,3.8307003882748,133.89203725798));
#18296=CARTESIAN_POINT('Ctrl Pts',(208.166397141411,3.91380073916163,133.782841243093));
#18297=CARTESIAN_POINT('Ctrl Pts',(208.158646504403,3.99691967514536,133.673620806907));
#18298=CARTESIAN_POINT('Ctrl Pts',(208.150895867395,4.0754410935826,133.560947488181));
#18299=CARTESIAN_POINT('Ctrl Pts',(208.143145230388,4.14908110408418,133.4452523333));
#18300=CARTESIAN_POINT('Ctrl Pts',(208.135386376025,4.22279918895488,133.329434516483));
#18301=CARTESIAN_POINT('Ctrl Pts',(208.127627521662,4.2916253174381,133.210588793658));
#18302=CARTESIAN_POINT('Ctrl Pts',(208.1198686673,4.3553203343671,133.089173049156));
#18303=CARTESIAN_POINT('Ctrl Pts',(208.112105678585,4.41904929156633,132.967692607549));
#18304=CARTESIAN_POINT('Ctrl Pts',(208.104342689871,4.47764152232339,132.84363976855));
#18305=CARTESIAN_POINT('Ctrl Pts',(208.096579701157,4.53090568215799,132.717493326473));
#18306=CARTESIAN_POINT('Ctrl Pts',(208.088804289908,4.58425507667346,132.591145021609));
#18307=CARTESIAN_POINT('Ctrl Pts',(208.081028878659,4.63225922547976,132.462696784975));
#18308=CARTESIAN_POINT('Ctrl Pts',(208.07325346741,4.67477612230475,132.332644383373));
#18309=CARTESIAN_POINT('Ctrl Pts',(208.065791189377,4.71558076852147,132.207829483103));
#18310=CARTESIAN_POINT('Ctrl Pts',(208.058328911344,4.7513314998731,132.081537413966));
#18311=CARTESIAN_POINT('Ctrl Pts',(208.050866633311,4.78194728272723,131.954214194209));
#18312=CARTESIAN_POINT('Ctrl Pts',(208.043091186579,4.81384791517326,131.821547613227));
#18313=CARTESIAN_POINT('Ctrl Pts',(208.035315739847,4.84027381515582,131.687343110404));
#18314=CARTESIAN_POINT('Ctrl Pts',(208.027540293115,4.861078124341,131.552092208147));
#18315=CARTESIAN_POINT('Ctrl Pts',(208.019774404755,4.88185685874992,131.417007570078));
#18316=CARTESIAN_POINT('Ctrl Pts',(208.012008516394,4.89702769371413,131.280879474633));
#18317=CARTESIAN_POINT('Ctrl Pts',(208.004242628033,4.90649401890281,131.144212798626));
#18318=CARTESIAN_POINT('Ctrl Pts',(207.996484430259,4.91595096955634,131.007681464108));
#18319=CARTESIAN_POINT('Ctrl Pts',(207.988726232485,4.91971462584261,130.870612997836));
#18320=CARTESIAN_POINT('Ctrl Pts',(207.980968034711,4.91773979670522,130.733520273117));
#18321=CARTESIAN_POINT('Ctrl Pts',(207.973215666403,4.91576645144328,130.596530559095));
#18322=CARTESIAN_POINT('Ctrl Pts',(207.965463298095,4.90806320893691,130.45951701213));
#18323=CARTESIAN_POINT('Ctrl Pts',(207.957710929787,4.89463688659452,130.322995048701));
#18324=CARTESIAN_POINT('Ctrl Pts',(207.949961829292,4.88121622377604,130.186530632626));
#18325=CARTESIAN_POINT('Ctrl Pts',(207.942212728797,4.86207731735958,130.050557776108));
#18326=CARTESIAN_POINT('Ctrl Pts',(207.934463628302,4.83727901203156,129.915589093349));
#18327=CARTESIAN_POINT('Ctrl Pts',(207.926716132436,4.81248584176035,129.780648358946));
#18328=CARTESIAN_POINT('Ctrl Pts',(207.91896863657,4.78203567415954,129.646711768862));
#18329=CARTESIAN_POINT('Ctrl Pts',(207.911221140703,4.74603881690609,129.514283638886));
#18330=CARTESIAN_POINT('Ctrl Pts',(207.903473572699,4.71004162447949,129.381854275848));
#18331=CARTESIAN_POINT('Ctrl Pts',(207.895726004694,4.66849774191739,129.25093377808));
#18332=CARTESIAN_POINT('Ctrl Pts',(207.88797843669,4.6215677813401,129.122012762639));
#18333=CARTESIAN_POINT('Ctrl Pts',(207.880229120088,4.57462722884883,128.993062650213));
#18334=CARTESIAN_POINT('Ctrl Pts',(207.872479803487,4.52229831304401,128.866113285295));
#18335=CARTESIAN_POINT('Ctrl Pts',(207.864730486886,4.46479021150502,128.74163634376));
#18336=CARTESIAN_POINT('Ctrl Pts',(207.856972920531,4.40722088809477,128.617026886786));
#18337=CARTESIAN_POINT('Ctrl Pts',(207.849215354176,4.34446152902774,128.494895466436));
#18338=CARTESIAN_POINT('Ctrl Pts',(207.841457787822,4.27676806979314,128.375690623578));
#18339=CARTESIAN_POINT('Ctrl Pts',(207.833696071523,4.20903839765145,128.256422011576));
#18340=CARTESIAN_POINT('Ctrl Pts',(207.825934355225,4.13636957280799,128.140083427958));
#18341=CARTESIAN_POINT('Ctrl Pts',(207.818172638927,4.05906096002361,128.027094482441));
#18342=CARTESIAN_POINT('Ctrl Pts',(207.810398460242,3.98162821878381,127.913924119321));
#18343=CARTESIAN_POINT('Ctrl Pts',(207.802624281556,3.8995410367762,127.804114454981));
#18344=CARTESIAN_POINT('Ctrl Pts',(207.794850102871,3.8131397215582,127.698052756717));
#18345=CARTESIAN_POINT('Ctrl Pts',(207.787373071747,3.73004086967696,127.596044988292));
#18346=CARTESIAN_POINT('Ctrl Pts',(207.779896040622,3.64295184134694,127.49750414666));
#18347=CARTESIAN_POINT('Ctrl Pts',(207.772419009498,3.55220619704574,127.402741268466));
#18348=CARTESIAN_POINT('Ctrl Pts',(207.764646018552,3.45786861039906,127.304227435639));
#18349=CARTESIAN_POINT('Ctrl Pts',(207.756873027606,3.35927983207107,127.209484418543));
#18350=CARTESIAN_POINT('Ctrl Pts',(207.74910003666,3.25677353337066,127.11890145827));
#18351=CARTESIAN_POINT('Ctrl Pts',(207.741336644219,3.15439381494258,127.028430354693));
#18352=CARTESIAN_POINT('Ctrl Pts',(207.733573251779,3.04810649162547,126.942109343302));
#18353=CARTESIAN_POINT('Ctrl Pts',(207.725809859339,2.93828365886333,126.860292641154));
#18354=CARTESIAN_POINT('Ctrl Pts',(207.718054194754,2.82857014621654,126.778557381191));
#18355=CARTESIAN_POINT('Ctrl Pts',(207.710298530169,2.71532843929129,126.701317739946));
#18356=CARTESIAN_POINT('Ctrl Pts',(207.702542865584,2.59896518359309,126.628889023007));
#18357=CARTESIAN_POINT('Ctrl Pts',(207.694793064922,2.48268990813262,126.556515068163));
#18358=CARTESIAN_POINT('Ctrl Pts',(207.687043264261,2.36329811229435,126.488945003391));
#18359=CARTESIAN_POINT('Ctrl Pts',(207.679293463599,2.24122672173557,126.426451773805));
#18360=CARTESIAN_POINT('Ctrl Pts',(207.671546974249,2.11920748947454,126.363985246139));
#18361=CARTESIAN_POINT('Ctrl Pts',(207.663800484899,1.99451128709021,126.306591417108));
#18362=CARTESIAN_POINT('Ctrl Pts',(207.656053995549,1.86760082988694,126.254497960001));
#18363=CARTESIAN_POINT('Ctrl Pts',(207.648309136959,1.74071708935821,126.202415469397));
#18364=CARTESIAN_POINT('Ctrl Pts',(207.640564278368,1.61162038276766,126.155631279747));
#18365=CARTESIAN_POINT('Ctrl Pts',(207.632819419778,1.48079428661614,126.114325293261));
#18366=CARTESIAN_POINT('Ctrl Pts',(207.625074512757,1.34996737237454,126.073019048479));
#18367=CARTESIAN_POINT('Ctrl Pts',(207.617329605736,1.2174114199546,126.037191193011));
#18368=CARTESIAN_POINT('Ctrl Pts',(207.609584698714,1.083625694819,126.006971909526));
#18369=CARTESIAN_POINT('Ctrl Pts',(207.601838064395,0.949810132293465,125.976745886424));
#18370=CARTESIAN_POINT('Ctrl Pts',(207.594091430076,0.814764632732653,125.952131010475));
#18371=CARTESIAN_POINT('Ctrl Pts',(207.586344795757,0.67899879684924,125.933206370739));
#18372=CARTESIAN_POINT('Ctrl Pts',(207.578589930427,0.543088706053562,125.914261623057));
#18373=CARTESIAN_POINT('Ctrl Pts',(207.570835065097,0.40645713800771,125.901019243266));
#18374=CARTESIAN_POINT('Ctrl Pts',(207.563080199768,0.269619519560986,125.893506478297));
#18375=CARTESIAN_POINT('Ctrl Pts',(207.555321198979,0.13270892933102,125.885989706975));
#18376=CARTESIAN_POINT('Ctrl Pts',(207.54756219819,-0.00440753934836094,
125.884208643743));
#18377=CARTESIAN_POINT('Ctrl Pts',(207.539803197401,-0.141215312361107,
125.888138358752));
#18378=CARTESIAN_POINT('Ctrl Pts',(207.532031731671,-0.278242868935376,
125.892074386903));
#18379=CARTESIAN_POINT('Ctrl Pts',(207.524260265942,-0.414960348456821,
125.901739499148));
#18380=CARTESIAN_POINT('Ctrl Pts',(207.516488800212,-0.550858244866477,
125.917056835667));
#18381=CARTESIAN_POINT('Ctrl Pts',(207.508982995369,-0.68211058829548,125.93185056218));
#18382=CARTESIAN_POINT('Ctrl Pts',(207.501477190527,-0.812598161887337,
125.951916317537));
#18383=CARTESIAN_POINT('Ctrl Pts',(207.493971385685,-0.941873648865784,
125.977140186296));
#18384=CARTESIAN_POINT('Ctrl Pts',(207.486196594231,-1.07578200013542,126.003268006481));
#18385=CARTESIAN_POINT('Ctrl Pts',(207.478421802777,-1.20881423660003,126.035013372608));
#18386=CARTESIAN_POINT('Ctrl Pts',(207.470647011323,-1.34046233494028,126.072305694902));
#18387=CARTESIAN_POINT('Ctrl Pts',(207.462881797475,-1.4719482586946,126.109552077552));
#18388=CARTESIAN_POINT('Ctrl Pts',(207.455116583626,-1.60205306444991,126.152331714816));
#18389=CARTESIAN_POINT('Ctrl Pts',(207.447351369778,-1.730277452876,126.200522762193));
#18390=CARTESIAN_POINT('Ctrl Pts',(207.43959386494,-1.85837454498173,126.248665967321));
#18391=CARTESIAN_POINT('Ctrl Pts',(207.431836360103,-1.9845945712413,126.302209754889));
#18392=CARTESIAN_POINT('Ctrl Pts',(207.424078855265,-2.1084523176746,126.360982185945));
#18393=CARTESIAN_POINT('Ctrl Pts',(207.416327197528,-2.23221670822011,126.419710318178));
#18394=CARTESIAN_POINT('Ctrl Pts',(207.408575539791,-2.35362201124919,126.483659082629));
#18395=CARTESIAN_POINT('Ctrl Pts',(207.400823882054,-2.47220230444564,126.552608175526));
#18396=CARTESIAN_POINT('Ctrl Pts',(207.393075516576,-2.59073223460783,126.62152798459));
#18397=CARTESIAN_POINT('Ctrl Pts',(207.385327151098,-2.70643920407983,126.695443702083));
#18398=CARTESIAN_POINT('Ctrl Pts',(207.37757878562,-2.81888145468325,126.774088864081));
#18399=CARTESIAN_POINT('Ctrl Pts',(207.36983203956,-2.93130020471219,126.852717589139));
#18400=CARTESIAN_POINT('Ctrl Pts',(207.3620852935,-3.04045527293811,126.936073568687));
#18401=CARTESIAN_POINT('Ctrl Pts',(207.354338547441,-3.14593382962058,127.023846974931));
#18402=CARTESIAN_POINT('Ctrl Pts',(207.346591743372,-3.25141317614579,127.111621038439));
#18403=CARTESIAN_POINT('Ctrl Pts',(207.338844939303,-3.35321565571256,127.2038123446));
#18404=CARTESIAN_POINT('Ctrl Pts',(207.331098135234,-3.45096179879728,127.30007099972));
#18405=CARTESIAN_POINT('Ctrl Pts',(207.323349596046,-3.54872983493361,127.396351214726));
#18406=CARTESIAN_POINT('Ctrl Pts',(207.315601056858,-3.64243944823346,127.496700317242));
#18407=CARTESIAN_POINT('Ctrl Pts',(207.307852517671,-3.73174857627695,127.600732108211));
#18408=CARTESIAN_POINT('Ctrl Pts',(207.300095745817,-3.82115259346241,127.704874430852));
#18409=CARTESIAN_POINT('Ctrl Pts',(207.292338973963,-3.9061465306836,127.812706961073));
#18410=CARTESIAN_POINT('Ctrl Pts',(207.284582202109,-3.98642879758559,127.923810582541));
#18411=CARTESIAN_POINT('Ctrl Pts',(207.276821290866,-4.06675390699494,128.034973494286));
#18412=CARTESIAN_POINT('Ctrl Pts',(207.269060379623,-4.14236212057786,128.149410649576));
#18413=CARTESIAN_POINT('Ctrl Pts',(207.26129946838,-4.21299620893864,128.266675450732));
#18414=CARTESIAN_POINT('Ctrl Pts',(207.253526104808,-4.28374362920411,128.384128402448));
#18415=CARTESIAN_POINT('Ctrl Pts',(207.245752741237,-4.34950078814551,128.504417723078));
#18416=CARTESIAN_POINT('Ctrl Pts',(207.237979377665,-4.41005688764098,128.627073013626));
#18417=CARTESIAN_POINT('Ctrl Pts',(207.230494172401,-4.46836817471339,128.74518147698));
#18418=CARTESIAN_POINT('Ctrl Pts',(207.223008967137,-4.52185704933858,128.865483326389));
#18419=CARTESIAN_POINT('Ctrl Pts',(207.215523761872,-4.57037874948208,128.987544405402));
#18420=CARTESIAN_POINT('Ctrl Pts',(207.206734347059,-4.6273547888774,129.130873201093));
#18421=CARTESIAN_POINT('Ctrl Pts',(207.197944932245,-4.67763395894565,129.2770080242));
#18422=CARTESIAN_POINT('Ctrl Pts',(207.189155517432,-4.72096468861576,129.425348118949));
#18423=CARTESIAN_POINT('Ctrl Pts',(207.186067457766,-4.73618844143788,129.47746570278));
#18424=CARTESIAN_POINT('Ctrl Pts',(207.1829793981,-4.75055490266602,129.529855284104));
#18425=CARTESIAN_POINT('Ctrl Pts',(207.179891338435,-4.76405452823404,129.582490119308));
#18426=CARTESIAN_POINT('Origin',(213.235140564004,0.,130.804360617566));
#18427=CARTESIAN_POINT('',(205.084976592678,-4.76405452823405,129.582490119308));
#18428=CARTESIAN_POINT('',(205.430026442963,-4.76405452823405,129.582490119308));
#18429=CARTESIAN_POINT('',(213.235140564004,-4.76405452823405,129.582490119308));
#18430=CARTESIAN_POINT('',(206.764859435946,-4.91824826123457,130.808496238813));
#18431=CARTESIAN_POINT('Ctrl Pts',(206.764859435946,-4.91824826123457,130.808496238813));
#18432=CARTESIAN_POINT('Ctrl Pts',(206.755633759936,-4.91811095036783,130.971791882044));
#18433=CARTESIAN_POINT('Ctrl Pts',(206.746408083927,-4.9098372427412,131.134736331661));
#18434=CARTESIAN_POINT('Ctrl Pts',(206.737182407917,-4.89355472835045,131.296605661359));
#18435=CARTESIAN_POINT('Ctrl Pts',(206.727886086852,-4.87714753159103,131.459714495655));
#18436=CARTESIAN_POINT('Ctrl Pts',(206.718589765787,-4.85260850573713,131.621731650502));
#18437=CARTESIAN_POINT('Ctrl Pts',(206.709293444722,-4.82011683649341,131.781937594102));
#18438=CARTESIAN_POINT('Ctrl Pts',(206.699922676766,-4.7873649671415,131.94342650053));
#18439=CARTESIAN_POINT('Ctrl Pts',(206.69055190881,-4.74653262850223,132.103075044456));
#18440=CARTESIAN_POINT('Ctrl Pts',(206.681181140855,-4.69785138332069,132.260168105777));
#18441=CARTESIAN_POINT('Ctrl Pts',(206.680193264038,-4.69271935212153,132.27672903163));
#18442=CARTESIAN_POINT('Ctrl Pts',(206.679205387222,-4.68750013448521,132.293261576894));
#18443=CARTESIAN_POINT('Ctrl Pts',(206.678217510405,-4.68219403218519,132.309764917902));
#18444=CARTESIAN_POINT('Ctrl Pts',(206.670443203729,-4.64043653180415,132.439641469363));
#18445=CARTESIAN_POINT('Ctrl Pts',(206.662668897052,-4.59320493957362,132.567985005214));
#18446=CARTESIAN_POINT('Ctrl Pts',(206.654894590376,-4.54062928664211,132.694299437684));
#18447=CARTESIAN_POINT('Ctrl Pts',(206.647129865258,-4.48811843135327,132.820458192059));
#18448=CARTESIAN_POINT('Ctrl Pts',(206.639365140141,-4.43027676906317,132.944592461411));
#18449=CARTESIAN_POINT('Ctrl Pts',(206.631600415024,-4.36728419816986,133.066220868536));
#18450=CARTESIAN_POINT('Ctrl Pts',(206.623843402325,-4.30435419549641,133.187728466606));
#18451=CARTESIAN_POINT('Ctrl Pts',(206.616086389625,-4.23628364434482,133.306734810711));
#18452=CARTESIAN_POINT('Ctrl Pts',(206.608329376926,-4.16330052534937,133.422778421914));
#18453=CARTESIAN_POINT('Ctrl Pts',(206.600578214196,-4.09037244674563,133.538734518553));
#18454=CARTESIAN_POINT('Ctrl Pts',(206.592827051467,-4.01253938183014,133.651732000017));
#18455=CARTESIAN_POINT('Ctrl Pts',(206.585075888737,-3.93007506123518,133.761334252139));
#18456=CARTESIAN_POINT('Ctrl Pts',(206.577328020864,-3.84764579449751,133.870889914636));
#18457=CARTESIAN_POINT('Ctrl Pts',(206.569580152991,-3.76058942214285,133.977052906525));
#18458=CARTESIAN_POINT('Ctrl Pts',(206.561832285118,-3.66922266005811,134.079416057313));
#18459=CARTESIAN_POINT('Ctrl Pts',(206.554086038175,-3.577875012784,134.181757792739));
#18460=CARTESIAN_POINT('Ctrl Pts',(206.546339791231,-3.48221902964024,134.280300976796));
#18461=CARTESIAN_POINT('Ctrl Pts',(206.538593544287,-3.38261107228556,134.374672284095));
#18462=CARTESIAN_POINT('Ctrl Pts',(206.530847240371,-3.28300238233128,134.469044285479));
#18463=CARTESIAN_POINT('Ctrl Pts',(206.523100936455,-3.17944194398242,134.559244079983));
#18464=CARTESIAN_POINT('Ctrl Pts',(206.515354632539,-3.07232196606475,134.644936199342));
#18465=CARTESIAN_POINT('Ctrl Pts',(206.507606594067,-2.96517800179731,134.730647506916));
#18466=CARTESIAN_POINT('Ctrl Pts',(206.499858555595,-2.85447321715903,134.811848886652));
#18467=CARTESIAN_POINT('Ctrl Pts',(206.492110517123,-2.74063145552457,134.888246302485));
#18468=CARTESIAN_POINT('Ctrl Pts',(206.484354244035,-2.62666870285167,134.964724913502));
#18469=CARTESIAN_POINT('Ctrl Pts',(206.476597970948,-2.50956263835897,135.036389143314));
#18470=CARTESIAN_POINT('Ctrl Pts',(206.46884169786,-2.38976501336611,135.102989031769));
#18471=CARTESIAN_POINT('Ctrl Pts',(206.461081285113,-2.26990345028647,135.169624465748));
#18472=CARTESIAN_POINT('Ctrl Pts',(206.453320872367,-2.14734781348686,135.231189997141));
#18473=CARTESIAN_POINT('Ctrl Pts',(206.44556045962,-2.02257190409865,135.28748296201));
#18474=CARTESIAN_POINT('Ctrl Pts',(206.437787589017,-1.8975956908752,135.343866294457));
#18475=CARTESIAN_POINT('Ctrl Pts',(206.430014718413,-1.77039244561536,135.394960000609));
#18476=CARTESIAN_POINT('Ctrl Pts',(206.422241847809,-1.64145412060007,135.440610333928));
#18477=CARTESIAN_POINT('Ctrl Pts',(206.41475119407,-1.5171972796397,135.484603198007));
#18478=CARTESIAN_POINT('Ctrl Pts',(206.407260540331,-1.39132946298595,135.523541019782));
#18479=CARTESIAN_POINT('Ctrl Pts',(206.399769886592,-1.26429990602564,135.557331142419));
#18480=CARTESIAN_POINT('Ctrl Pts',(206.391995539368,-1.13245935939483,135.592400998174));
#18481=CARTESIAN_POINT('Ctrl Pts',(206.384221192143,-0.998949706372701,
135.622036643276));
#18482=CARTESIAN_POINT('Ctrl Pts',(206.376446844919,-0.864258611065781,
135.646079332619));
#18483=CARTESIAN_POINT('Ctrl Pts',(206.368682078737,-0.72973350798047,135.670092391946));
#18484=CARTESIAN_POINT('Ctrl Pts',(206.360917312556,-0.594030240801939,
135.688526141918));
#18485=CARTESIAN_POINT('Ctrl Pts',(206.353152546374,-0.457651051086741,
135.70127174377));
#18486=CARTESIAN_POINT('Ctrl Pts',(206.345395492141,-0.321407312868765,
135.71400468672));
#18487=CARTESIAN_POINT('Ctrl Pts',(206.337638437907,-0.184489374829276,
135.721060688077));
#18488=CARTESIAN_POINT('Ctrl Pts',(206.329881383673,-0.0474087266159011,
135.722382117635));
#18489=CARTESIAN_POINT('Ctrl Pts',(206.322130178985,0.0895685499512351,
135.723702550711));
#18490=CARTESIAN_POINT('Ctrl Pts',(206.314378974297,0.226707903104169,135.719297015699));
#18491=CARTESIAN_POINT('Ctrl Pts',(206.306627769608,0.363494034138324,135.709159813216));
#18492=CARTESIAN_POINT('Ctrl Pts',(206.298879859279,0.500222029349606,135.699026919171));
#18493=CARTESIAN_POINT('Ctrl Pts',(206.29113194895,0.636596711948773,135.68316723157));
#18494=CARTESIAN_POINT('Ctrl Pts',(206.283384038621,0.772104320862591,135.661627130761));
#18495=CARTESIAN_POINT('Ctrl Pts',(206.275637748924,0.907583585626675,135.640091535498));
#18496=CARTESIAN_POINT('Ctrl Pts',(206.267891459227,1.04219575158091,135.612877951706));
#18497=CARTESIAN_POINT('Ctrl Pts',(206.26014516953,1.17543410337159,135.580084408902));
#18498=CARTESIAN_POINT('Ctrl Pts',(206.252398822603,1.30867343952879,135.547290623819));
#18499=CARTESIAN_POINT('Ctrl Pts',(206.244652475676,1.44053856163545,135.508916890901));
#18500=CARTESIAN_POINT('Ctrl Pts',(206.236906128749,1.57053522864704,135.465111861526));
#18501=CARTESIAN_POINT('Ctrl Pts',(206.229158047049,1.70056100805719,135.421297022135));
#18502=CARTESIAN_POINT('Ctrl Pts',(206.221409965348,1.8287171293106,135.372048590765));
#18503=CARTESIAN_POINT('Ctrl Pts',(206.213661883648,1.95452711044093,135.317564228866));
#18504=CARTESIAN_POINT('Ctrl Pts',(206.20590556723,2.08047080333817,135.263021960589));
#18505=CARTESIAN_POINT('Ctrl Pts',(206.198149250812,2.2040630157501,135.203232801142));
#18506=CARTESIAN_POINT('Ctrl Pts',(206.190392934394,2.32484926327892,135.138441715738));
#18507=CARTESIAN_POINT('Ctrl Pts',(206.182632478194,2.44569997811104,135.073616049356));
#18508=CARTESIAN_POINT('Ctrl Pts',(206.174872021993,2.5637414075819,135.003783336419));
#18509=CARTESIAN_POINT('Ctrl Pts',(206.167111565792,2.67854694058481,134.929232657955));
#18510=CARTESIAN_POINT('Ctrl Pts',(206.159338651962,2.79353676750179,134.8545623055));
#18511=CARTESIAN_POINT('Ctrl Pts',(206.151565738131,2.90527999882711,134.775159079624));
#18512=CARTESIAN_POINT('Ctrl Pts',(206.143792824301,3.01338136800174,134.691353773397));
#18513=CARTESIAN_POINT('Ctrl Pts',(206.136302637127,3.1175507318328,134.61059674412));
#18514=CARTESIAN_POINT('Ctrl Pts',(206.128812449953,3.21833832869957,134.525752506211));
#18515=CARTESIAN_POINT('Ctrl Pts',(206.12132226278,3.31542344251232,134.43714886619));
#18516=CARTESIAN_POINT('Ctrl Pts',(206.113547928467,3.41619156940981,134.345183965593));
#18517=CARTESIAN_POINT('Ctrl Pts',(206.105773594154,3.51328995165438,134.248877485937));
#18518=CARTESIAN_POINT('Ctrl Pts',(206.097999259841,3.60632143845033,134.148553905203));
#18519=CARTESIAN_POINT('Ctrl Pts',(206.090234506665,3.69923827267255,134.048353963863));
#18520=CARTESIAN_POINT('Ctrl Pts',(206.082469753489,3.78809792067824,133.944147055788));
#18521=CARTESIAN_POINT('Ctrl Pts',(206.074705000313,3.87253733969881,133.836296899076));
#18522=CARTESIAN_POINT('Ctrl Pts',(206.066947959165,3.95689289267469,133.72855386018));
#18523=CARTESIAN_POINT('Ctrl Pts',(206.059190918017,4.03683671393217,133.617175079492));
#18524=CARTESIAN_POINT('Ctrl Pts',(206.051433876869,4.11204384499684,133.502559735371));
#18525=CARTESIAN_POINT('Ctrl Pts',(206.043682685331,4.18719426211104,133.388030823066));
#18526=CARTESIAN_POINT('Ctrl Pts',(206.035931493794,4.2576148851709,133.270270530956));
#18527=CARTESIAN_POINT('Ctrl Pts',(206.028180302257,4.32302238761605,133.14970931204));
#18528=CARTESIAN_POINT('Ctrl Pts',(206.020432405131,4.38840209056044,133.029199334061));
#18529=CARTESIAN_POINT('Ctrl Pts',(206.012684508006,4.44877272459587,132.90589113992));
#18530=CARTESIAN_POINT('Ctrl Pts',(206.00493661088,4.50389561038913,132.780242039417));
#18531=CARTESIAN_POINT('Ctrl Pts',(205.997190334417,4.55900696588485,132.654619221492));
#18532=CARTESIAN_POINT('Ctrl Pts',(205.989444057953,4.60887259954457,132.52665682896));
#18533=CARTESIAN_POINT('Ctrl Pts',(205.98169778149,4.65330109429353,132.396834161568));
#18534=CARTESIAN_POINT('Ctrl Pts',(205.973951447814,4.69772991718062,132.267010535338));
#18535=CARTESIAN_POINT('Ctrl Pts',(205.966205114138,4.73672139443581,132.135326976735));
#18536=CARTESIAN_POINT('Ctrl Pts',(205.958458780463,4.77013344123859,132.002279652926));
#18537=CARTESIAN_POINT('Ctrl Pts',(205.950710712019,4.80355297056946,131.869202533566));
#18538=CARTESIAN_POINT('Ctrl Pts',(205.942962643575,4.83139048788632,131.734761420386));
#18539=CARTESIAN_POINT('Ctrl Pts',(205.935214575131,4.85355474113685,131.599464030518));
#18540=CARTESIAN_POINT('Ctrl Pts',(205.927458271901,4.87574255095105,131.464022844171));
#18541=CARTESIAN_POINT('Ctrl Pts',(205.919701968672,4.89224498852538,131.327723949617));
#18542=CARTESIAN_POINT('Ctrl Pts',(205.911945665443,4.90302249002199,131.191082125681));
#18543=CARTESIAN_POINT('Ctrl Pts',(205.904185222415,4.91380574383149,131.054367371435));
#18544=CARTESIAN_POINT('Ctrl Pts',(205.896424779388,4.91885795864703,130.917309713606));
#18545=CARTESIAN_POINT('Ctrl Pts',(205.88866433636,4.91819175271269,130.780424326105));
#18546=CARTESIAN_POINT('Ctrl Pts',(205.880891435541,4.91752447732209,130.643319197341));
#18547=CARTESIAN_POINT('Ctrl Pts',(205.873118534722,4.91112045540052,130.506387282292));
#18548=CARTESIAN_POINT('Ctrl Pts',(205.865345633904,4.89904434121163,130.370139930193));
#18549=CARTESIAN_POINT('Ctrl Pts',(205.857855302258,4.8874072314151,130.238845594031));
#18550=CARTESIAN_POINT('Ctrl Pts',(205.850364970613,4.87050330540731,130.108187218426));
#18551=CARTESIAN_POINT('Ctrl Pts',(205.842874638967,4.84843500802732,129.978611844975));
#18552=CARTESIAN_POINT('Ctrl Pts',(205.835100308635,4.82552998301369,129.844123573455));
#18553=CARTESIAN_POINT('Ctrl Pts',(205.827325978302,4.79698868437903,129.710376028441));
#18554=CARTESIAN_POINT('Ctrl Pts',(205.81955164797,4.76286943415894,129.577878731987));
#18555=CARTESIAN_POINT('Ctrl Pts',(205.811786898866,4.72879223313221,129.445544727644));
#18556=CARTESIAN_POINT('Ctrl Pts',(205.804022149762,4.68915085502848,129.31445828105));
#18557=CARTESIAN_POINT('Ctrl Pts',(205.796257400658,4.64405507193892,129.185121428534));
#18558=CARTESIAN_POINT('Ctrl Pts',(205.788500363668,4.59900407893947,129.055913036128));
#18559=CARTESIAN_POINT('Ctrl Pts',(205.780743326677,4.54850958977095,128.928451146412));
#18560=CARTESIAN_POINT('Ctrl Pts',(205.772986289687,4.49273179575291,128.803224921535));
#18561=CARTESIAN_POINT('Ctrl Pts',(205.765235102389,4.43699606456529,128.67809313154));
#18562=CARTESIAN_POINT('Ctrl Pts',(205.757483915091,4.37598511729972,128.555194006304));
#18563=CARTESIAN_POINT('Ctrl Pts',(205.749732727793,4.30990796060895,128.434998586643));
#18564=CARTESIAN_POINT('Ctrl Pts',(205.741984835016,4.24385888898434,128.314854254173));
#18565=CARTESIAN_POINT('Ctrl Pts',(205.73423694224,4.17274807866374,128.197411683559));
#18566=CARTESIAN_POINT('Ctrl Pts',(205.726489049463,4.09683126462683,128.083118869452));
#18567=CARTESIAN_POINT('Ctrl Pts',(205.718742777414,4.0209303311019,127.968849963467));
#18568=CARTESIAN_POINT('Ctrl Pts',(205.710996505366,3.94022560970842,127.85772982891));
#18569=CARTESIAN_POINT('Ctrl Pts',(205.703250233317,3.85501688262898,127.750178583511));
#18570=CARTESIAN_POINT('Ctrl Pts',(205.695503904118,3.76980752690164,127.642626544626));
#18571=CARTESIAN_POINT('Ctrl Pts',(205.68775757492,3.68009434196701,127.538643753886));
#18572=CARTESIAN_POINT('Ctrl Pts',(205.680011245721,3.58621796636794,127.438617941692));
#18573=CARTESIAN_POINT('Ctrl Pts',(205.672263181812,3.49232056812825,127.338569729755));
#18574=CARTESIAN_POINT('Ctrl Pts',(205.664515117904,3.39425839154965,127.242480544672));
#18575=CARTESIAN_POINT('Ctrl Pts',(205.656767053995,3.29240926887433,127.150701592872));
#18576=CARTESIAN_POINT('Ctrl Pts',(205.649010755368,3.19045189995416,127.058825097503));
#18577=CARTESIAN_POINT('Ctrl Pts',(205.641254456741,3.0846998358618,126.971268248513));
#18578=CARTESIAN_POINT('Ctrl Pts',(205.633498158114,2.97556478881364,126.888342582614));
#18579=CARTESIAN_POINT('Ctrl Pts',(205.625737719733,2.86637149332416,126.805372656956));
#18580=CARTESIAN_POINT('Ctrl Pts',(205.617977281351,2.75379193784736,126.727039062836));
#18581=CARTESIAN_POINT('Ctrl Pts',(205.61021684297,2.63826637271815,126.653609648273));
#18582=CARTESIAN_POINT('Ctrl Pts',(205.602443946826,2.52255535542982,126.580062358127));
#18583=CARTESIAN_POINT('Ctrl Pts',(205.594671050682,2.40388921667307,126.511435175415));
#18584=CARTESIAN_POINT('Ctrl Pts',(205.586898154538,2.2827331157452,126.447950101467));
#18585=CARTESIAN_POINT('Ctrl Pts',(205.579407774743,2.16598059601619,126.386772477791));
#18586=CARTESIAN_POINT('Ctrl Pts',(205.571917394949,2.04691625263489,126.330369789491));
#18587=CARTESIAN_POINT('Ctrl Pts',(205.564427015154,1.92597157701165,126.278897486897));
#18588=CARTESIAN_POINT('Ctrl Pts',(205.556652678921,1.80044195106122,126.225473895836));
#18589=CARTESIAN_POINT('Ctrl Pts',(205.548878342688,1.67248897498338,126.177192652376));
#18590=CARTESIAN_POINT('Ctrl Pts',(205.541104006456,1.54257284960153,126.134280097257));
#18591=CARTESIAN_POINT('Ctrl Pts',(205.533339251373,1.412816833816,126.091420427889));
#18592=CARTESIAN_POINT('Ctrl Pts',(205.525574496289,1.28110285028441,126.053916403621));
#18593=CARTESIAN_POINT('Ctrl Pts',(205.517809741206,1.14791261180821,126.021947032549));
#18594=CARTESIAN_POINT('Ctrl Pts',(205.510052698165,1.01485465937561,125.990009413817));
#18595=CARTESIAN_POINT('Ctrl Pts',(205.502295655124,0.88032374757524,125.963595599504));
#18596=CARTESIAN_POINT('Ctrl Pts',(205.494538612083,0.744818010538801,125.942835219743));
#18597=CARTESIAN_POINT('Ctrl Pts',(205.48678741867,0.609414459097139,125.922090495495));
#18598=CARTESIAN_POINT('Ctrl Pts',(205.479036225256,0.473037930525041,125.906990778956));
#18599=CARTESIAN_POINT('Ctrl Pts',(205.471285031842,0.33619769877146,125.897614835498));
#18600=CARTESIAN_POINT('Ctrl Pts',(205.463537132872,0.199415627413407,125.888242877042));
#18601=CARTESIAN_POINT('Ctrl Pts',(205.455789233902,0.0621706340948198,
125.884589879799));
#18602=CARTESIAN_POINT('Ctrl Pts',(205.448041334933,-0.0750221388880692,
125.88668283825));
#18603=CARTESIAN_POINT('Ctrl Pts',(205.440295056645,-0.212186214308715,
125.888775358903));
#18604=CARTESIAN_POINT('Ctrl Pts',(205.432548778357,-0.349297700448874,
125.896611438603));
#18605=CARTESIAN_POINT('Ctrl Pts',(205.424802500068,-0.485841100123671,
125.910165945515));
#18606=CARTESIAN_POINT('Ctrl Pts',(205.41705616459,-0.622385507893228,125.9237205525));
#18607=CARTESIAN_POINT('Ctrl Pts',(205.409309829111,-0.758361431775545,
125.942993632321));
#18608=CARTESIAN_POINT('Ctrl Pts',(205.401563493633,-0.89325853914859,125.967908173394));
#18609=CARTESIAN_POINT('Ctrl Pts',(205.393815423409,-1.02818585590989,125.992828293927));
#18610=CARTESIAN_POINT('Ctrl Pts',(205.386067353186,-1.16203349102794,126.02339231868));
#18611=CARTESIAN_POINT('Ctrl Pts',(205.378319282963,-1.29430173647038,126.059472201863));
#18612=CARTESIAN_POINT('Ctrl Pts',(205.370562978002,-1.42671055811762,126.095590431159));
#18613=CARTESIAN_POINT('Ctrl Pts',(205.36280667304,-1.55753625913267,126.137236126444));
#18614=CARTESIAN_POINT('Ctrl Pts',(205.355050368079,-1.68629419381508,126.184231295306));
#18615=CARTESIAN_POINT('Ctrl Pts',(205.347289923343,-1.81512085051228,126.231251546915));
#18616=CARTESIAN_POINT('Ctrl Pts',(205.339529478607,-1.94187718064387,126.283626812052));
#18617=CARTESIAN_POINT('Ctrl Pts',(205.331769033871,-2.06609986951013,126.341131473582));
#18618=CARTESIAN_POINT('Ctrl Pts',(205.323996131401,-2.19052197132574,126.398728446543));
#18619=CARTESIAN_POINT('Ctrl Pts',(205.316223228931,-2.31240195646745,126.461471091301));
#18620=CARTESIAN_POINT('Ctrl Pts',(205.308450326461,-2.43130161847012,126.52908805286));
#18621=CARTESIAN_POINT('Ctrl Pts',(205.300960014754,-2.54587857780558,126.594246739811));
#18622=CARTESIAN_POINT('Ctrl Pts',(205.293469703048,-2.65768789450607,126.663931314284));
#18623=CARTESIAN_POINT('Ctrl Pts',(205.285979391341,-2.7663655623862,126.737862783097));
#18624=CARTESIAN_POINT('Ctrl Pts',(205.278237672039,-2.87869092774278,126.814275715097));
#18625=CARTESIAN_POINT('Ctrl Pts',(205.270495952738,-2.98803353029666,126.895472526408));
#18626=CARTESIAN_POINT('Ctrl Pts',(205.262754233436,-3.09395614481765,126.981191979323));
#18627=CARTESIAN_POINT('Ctrl Pts',(205.255024754641,-3.19971128407027,127.066775900384));
#18628=CARTESIAN_POINT('Ctrl Pts',(205.247295275847,-3.30205689954337,127.156867976875));
#18629=CARTESIAN_POINT('Ctrl Pts',(205.239565797052,-3.40058421415425,127.251163456565));
#18630=CARTESIAN_POINT('Ctrl Pts',(205.231843383955,-3.4990214626426,127.345372738552));
#18631=CARTESIAN_POINT('Ctrl Pts',(205.224120970858,-3.59364706915702,127.443777510556));
#18632=CARTESIAN_POINT('Ctrl Pts',(205.216398557761,-3.68408468413249,127.546032349475));
#18633=CARTESIAN_POINT('Ctrl Pts',(205.208681492833,-3.77445966639361,127.648216371643));
#18634=CARTESIAN_POINT('Ctrl Pts',(205.200964427906,-3.86065216668493,127.75424486186));
#18635=CARTESIAN_POINT('Ctrl Pts',(205.193247362978,-3.94232245691661,127.863735393538));
#18636=CARTESIAN_POINT('Ctrl Pts',(205.185533932859,-4.02395427969229,127.97317435417));
#18637=CARTESIAN_POINT('Ctrl Pts',(205.177820502739,-4.1010678957911,128.086071795385));
#18638=CARTESIAN_POINT('Ctrl Pts',(205.17010707262,-4.17336396541682,128.202012394391));
#18639=CARTESIAN_POINT('Ctrl Pts',(205.162394028974,-4.24565641272213,128.317947184313));
#18640=CARTESIAN_POINT('Ctrl Pts',(205.154680985329,-4.31313157631286,128.436924499339));
#18641=CARTESIAN_POINT('Ctrl Pts',(205.146967941683,-4.37553364940197,128.558500349105));
#18642=CARTESIAN_POINT('Ctrl Pts',(205.139255293534,-4.43793252273594,128.680069964896));
#18643=CARTESIAN_POINT('Ctrl Pts',(205.131542645386,-4.49525864776658,128.804237496571));
#18644=CARTESIAN_POINT('Ctrl Pts',(205.123829997237,-4.54730272990832,128.930535400245));
#18645=CARTESIAN_POINT('Ctrl Pts',(205.116113219495,-4.59937467808288,129.056900927775));
#18646=CARTESIAN_POINT('Ctrl Pts',(205.108396441753,-4.64615878721881,129.185398739042));
#18647=CARTESIAN_POINT('Ctrl Pts',(205.100679664011,-4.68749433319855,129.315542314773));
#18648=CARTESIAN_POINT('Ctrl Pts',(205.0954453069,-4.71553259168844,129.403819828246));
#18649=CARTESIAN_POINT('Ctrl Pts',(205.090210949789,-4.74106497151865,129.49285418659));
#18650=CARTESIAN_POINT('Ctrl Pts',(205.084976592678,-4.76405452823405,129.582490119308));
#18651=CARTESIAN_POINT('Ctrl Pts',(206.834782106149,-4.76405452823405,129.582490119308));
#18652=CARTESIAN_POINT('Ctrl Pts',(206.827070043619,-4.79800979989384,129.714881208167));
#18653=CARTESIAN_POINT('Ctrl Pts',(206.819357981088,-4.82644926951694,129.84871625431));
#18654=CARTESIAN_POINT('Ctrl Pts',(206.811645918557,-4.84926402357277,129.983494311653));
#18655=CARTESIAN_POINT('Ctrl Pts',(206.803848171462,-4.8723322600444,130.119769815232));
#18656=CARTESIAN_POINT('Ctrl Pts',(206.796050424368,-4.8896499380063,130.257009012014));
#18657=CARTESIAN_POINT('Ctrl Pts',(206.788252677274,-4.90115795633873,130.394685441948));
#18658=CARTESIAN_POINT('Ctrl Pts',(206.78045493018,-4.91266597467115,130.532361871882));
#18659=CARTESIAN_POINT('Ctrl Pts',(206.772657183085,-4.9183643194193,130.67047511888));
#18660=CARTESIAN_POINT('Ctrl Pts',(206.764859435991,-4.91824826123525,130.80849623801));
#18661=CARTESIAN_POINT('',(207.110140564062,-4.91824906508338,130.801328076312));
#18662=CARTESIAN_POINT('Ctrl Pts',(207.179891338435,-4.76405452823404,129.582490119308));
#18663=CARTESIAN_POINT('Ctrl Pts',(207.171149836886,-4.80226849123941,129.731485781088));
#18664=CARTESIAN_POINT('Ctrl Pts',(207.162408335336,-4.83353292882372,129.882448181632));
#18665=CARTESIAN_POINT('Ctrl Pts',(207.153666833787,-4.85766325863286,130.034756350278));
#18666=CARTESIAN_POINT('Ctrl Pts',(207.14497546476,-4.88165520097116,130.186191031391));
#18667=CARTESIAN_POINT('Ctrl Pts',(207.136284095732,-4.89859453685566,130.338955897152));
#18668=CARTESIAN_POINT('Ctrl Pts',(207.127592726705,-4.90834771356455,130.492421865171));
#18669=CARTESIAN_POINT('Ctrl Pts',(207.121775339157,-4.91487580005554,130.595141127065));
#18670=CARTESIAN_POINT('Ctrl Pts',(207.11595795161,-4.91818546141412,130.698174100575));
#18671=CARTESIAN_POINT('Ctrl Pts',(207.110140564062,-4.91824906508338,130.801328076312));
#18672=CARTESIAN_POINT('Ctrl Pts',(207.110140564008,-4.91824906508397,130.801328077268));
#18673=CARTESIAN_POINT('Ctrl Pts',(207.10232974179,-4.91833446369157,130.939829657053));
#18674=CARTESIAN_POINT('Ctrl Pts',(207.094518919572,-4.91256506400957,131.078351340995));
#18675=CARTESIAN_POINT('Ctrl Pts',(207.086708097354,-4.90096241100966,131.216368515998));
#18676=CARTESIAN_POINT('Ctrl Pts',(207.078896410447,-4.88935847354873,131.354400970065));
#18677=CARTESIAN_POINT('Ctrl Pts',(207.071084723539,-4.87192002824314,131.491928423436));
#18678=CARTESIAN_POINT('Ctrl Pts',(207.063273036631,-4.84872054892325,131.62843106416));
#18679=CARTESIAN_POINT('Ctrl Pts',(207.055458899586,-4.82551379308231,131.764976518963));
#18680=CARTESIAN_POINT('Ctrl Pts',(207.047644762541,-4.79654246897585,131.90049614474));
#18681=CARTESIAN_POINT('Ctrl Pts',(207.039830625497,-4.76193119291241,132.034480276976));
#18682=CARTESIAN_POINT('Ctrl Pts',(207.032012451602,-4.72730203636823,132.168533626559));
#18683=CARTESIAN_POINT('Ctrl Pts',(207.024194277707,-4.68702722138493,132.301049533832));
#18684=CARTESIAN_POINT('Ctrl Pts',(207.016376103812,-4.64128115697165,132.431533713595));
#18685=CARTESIAN_POINT('Ctrl Pts',(207.008547530707,-4.59547424421175,132.562191454661));
#18686=CARTESIAN_POINT('Ctrl Pts',(207.000718957602,-4.54418167570927,132.690811711221));
#18687=CARTESIAN_POINT('Ctrl Pts',(206.992890384497,-4.48762617673331,132.816919774559));
#18688=CARTESIAN_POINT('Ctrl Pts',(206.985055811211,-4.43102733100928,132.943124492946));
#18689=CARTESIAN_POINT('Ctrl Pts',(206.977221237926,-4.36915768710697,133.066812840935));
#18690=CARTESIAN_POINT('Ctrl Pts',(206.96938666464,-4.30228542176686,133.187535645161));
#18691=CARTESIAN_POINT('Ctrl Pts',(206.961539696176,-4.23530735696238,133.308449446476));
#18692=CARTESIAN_POINT('Ctrl Pts',(206.953692727712,-4.16331106348637,133.426388009929));
#18693=CARTESIAN_POINT('Ctrl Pts',(206.945845759248,-4.08660777588555,133.540931455051));
#18694=CARTESIAN_POINT('Ctrl Pts',(206.942922552185,-4.05803373571842,133.583601972889));
#18695=CARTESIAN_POINT('Ctrl Pts',(206.939999345122,-4.02880687363292,133.625801664281));
#18696=CARTESIAN_POINT('Ctrl Pts',(206.937076138059,-3.99894465188146,133.667510060695));
#18697=CARTESIAN_POINT('Ctrl Pts',(206.929301998061,-3.91952739284056,133.77843169773));
#18698=CARTESIAN_POINT('Ctrl Pts',(206.921527858062,-3.83536570986394,133.886222330092));
#18699=CARTESIAN_POINT('Ctrl Pts',(206.913753718064,-3.74673486748187,133.990449269078));
#18700=CARTESIAN_POINT('Ctrl Pts',(206.905989161858,-3.658213287293,134.09454771934));
#18701=CARTESIAN_POINT('Ctrl Pts',(206.898224605652,-3.56523376076694,134.195090922469));
#18702=CARTESIAN_POINT('Ctrl Pts',(206.890460049446,-3.46811454805166,134.291675421838));
#18703=CARTESIAN_POINT('Ctrl Pts',(206.882703207698,-3.37109182792838,134.388163959878));
#18704=CARTESIAN_POINT('Ctrl Pts',(206.874946365951,-3.26993788205166,134.480701347399));
#18705=CARTESIAN_POINT('Ctrl Pts',(206.867189524203,-3.16501068250007,134.568917755153));
#18706=CARTESIAN_POINT('Ctrl Pts',(206.859438534277,-3.0601626408413,134.657067611766));
#18707=CARTESIAN_POINT('Ctrl Pts',(206.851687544352,-2.9515473094897,134.74090272641));
#18708=CARTESIAN_POINT('Ctrl Pts',(206.843936554426,-2.83955863515276,134.820090914788));
#18709=CARTESIAN_POINT('Ctrl Pts',(206.836188861569,-2.72761759787636,134.899245418577));
#18710=CARTESIAN_POINT('Ctrl Pts',(206.828441168712,-2.61230639015696,134.973756702305));
#18711=CARTESIAN_POINT('Ctrl Pts',(206.820693475855,-2.49405090237109,135.043333743086));
#18712=CARTESIAN_POINT('Ctrl Pts',(206.812947405249,-2.37582017552251,135.112896215471));
#18713=CARTESIAN_POINT('Ctrl Pts',(206.805201334644,-2.25464673160865,135.177526301768));
#18714=CARTESIAN_POINT('Ctrl Pts',(206.797455264038,-2.13098388076607,135.236977312298));
#18715=CARTESIAN_POINT('Ctrl Pts',(206.789709137619,-2.00732013888212,135.296428751197));
#18716=CARTESIAN_POINT('Ctrl Pts',(206.7819630112,-1.88116730665591,135.350700870453));
#18717=CARTESIAN_POINT('Ctrl Pts',(206.774216884781,-1.75300127162441,135.399593974446));
#18718=CARTESIAN_POINT('Ctrl Pts',(206.766469024802,-1.62480655341618,135.44849802057));
#18719=CARTESIAN_POINT('Ctrl Pts',(206.758721164823,-1.49459810110302,135.492020516664));
#18720=CARTESIAN_POINT('Ctrl Pts',(206.750973304844,-1.36286927639058,135.530010879485));
#18721=CARTESIAN_POINT('Ctrl Pts',(206.743217210822,-1.23100045680149,135.568041616583));
#18722=CARTESIAN_POINT('Ctrl Pts',(206.735461116801,-1.09760841340135,135.600528367403));
#18723=CARTESIAN_POINT('Ctrl Pts',(206.72770502278,-0.963199626022195,135.627371040832));
#18724=CARTESIAN_POINT('Ctrl Pts',(206.719944789696,-0.828719111006118,
135.654228038931));
#18725=CARTESIAN_POINT('Ctrl Pts',(206.712184556613,-0.693221156955318,
135.675434897598));
#18726=CARTESIAN_POINT('Ctrl Pts',(206.70442432353,-0.557218799917317,135.690943295831));
#18727=CARTESIAN_POINT('Ctrl Pts',(206.696651631796,-0.420998098163723,
135.706476591992));
#18728=CARTESIAN_POINT('Ctrl Pts',(206.688878940061,-0.284271765407574,
135.716293117923));
#18729=CARTESIAN_POINT('Ctrl Pts',(206.681106248327,-0.147555186392696,
135.720396676167));
#18730=CARTESIAN_POINT('Ctrl Pts',(206.6736136703,-0.015765624822631,135.724352349619));
#18731=CARTESIAN_POINT('Ctrl Pts',(206.666121092273,0.11601456527462,135.722999745079));
#18732=CARTESIAN_POINT('Ctrl Pts',(206.658628514246,0.247328944919121,135.716387842196));
#18733=CARTESIAN_POINT('Ctrl Pts',(206.650854101252,0.383582743781857,135.709527231134));
#18734=CARTESIAN_POINT('Ctrl Pts',(206.643079688257,0.519766647294013,135.696982181141));
#18735=CARTESIAN_POINT('Ctrl Pts',(206.635305275263,0.655367801387527,135.678750436549));
#18736=CARTESIAN_POINT('Ctrl Pts',(206.627540442734,0.790801853192383,135.660541159068));
#18737=CARTESIAN_POINT('Ctrl Pts',(206.619775610205,0.925654200685813,135.636659181934));
#18738=CARTESIAN_POINT('Ctrl Pts',(206.612010777677,1.05941334753652,135.607154223538));
#18739=CARTESIAN_POINT('Ctrl Pts',(206.604253656593,1.19303965490963,135.577678567237));
#18740=CARTESIAN_POINT('Ctrl Pts',(206.596496535509,1.32557454289324,135.542591126398));
#18741=CARTESIAN_POINT('Ctrl Pts',(206.588739414425,1.45651334525474,135.501993206179));
#18742=CARTESIAN_POINT('Ctrl Pts',(206.580988142457,1.5873534156012,135.461425898081));
#18743=CARTESIAN_POINT('Ctrl Pts',(206.573236870489,1.71659942391051,135.415356496345));
#18744=CARTESIAN_POINT('Ctrl Pts',(206.565485598521,1.84375893376221,135.363936919885));
#18745=CARTESIAN_POINT('Ctrl Pts',(206.557737620497,1.97086440649336,135.312539194452));
#18746=CARTESIAN_POINT('Ctrl Pts',(206.549989642474,2.09588478259786,135.255795962539));
#18747=CARTESIAN_POINT('Ctrl Pts',(206.542241664451,2.21834499216241,135.193908266043));
#18748=CARTESIAN_POINT('Ctrl Pts',(206.534495306817,2.34077959076295,135.132033512555));
#18749=CARTESIAN_POINT('Ctrl Pts',(206.526748949182,2.46065473910694,135.065016610731));
#18750=CARTESIAN_POINT('Ctrl Pts',(206.519002591548,2.57751784727511,134.993105633615));
#18751=CARTESIAN_POINT('Ctrl Pts',(206.511256176506,2.69438182151258,134.92119412357));
#18752=CARTESIAN_POINT('Ctrl Pts',(206.503509761464,2.80823337806547,134.844388670749));
#18753=CARTESIAN_POINT('Ctrl Pts',(206.495763346422,2.9186472625684,134.762981743565));
#18754=CARTESIAN_POINT('Ctrl Pts',(206.488015196492,3.0290858753689,134.681556584482));
#18755=CARTESIAN_POINT('Ctrl Pts',(206.480267046562,3.13608496949048,134.595528132329));
#18756=CARTESIAN_POINT('Ctrl Pts',(206.472518896633,3.23925116627507,134.505230102469));
#18757=CARTESIAN_POINT('Ctrl Pts',(206.464762512191,3.34252700513922,134.414836106449));
#18758=CARTESIAN_POINT('Ctrl Pts',(206.45700612775,3.44196151476943,134.320163726309));
#18759=CARTESIAN_POINT('Ctrl Pts',(206.449249743308,3.53719670723884,134.221585005399));
#18760=CARTESIAN_POINT('Ctrl Pts',(206.441489219088,3.63248272913906,134.122953670532));
#18761=CARTESIAN_POINT('Ctrl Pts',(206.433728694868,3.7235647084274,134.020412132682));
#18762=CARTESIAN_POINT('Ctrl Pts',(206.425968170648,3.81012466952417,133.914365933507));
#18763=CARTESIAN_POINT('Ctrl Pts',(206.418195189496,3.89682357375458,133.808149512546));
#18764=CARTESIAN_POINT('Ctrl Pts',(206.410422208344,3.9789857203556,133.698417501723));
#18765=CARTESIAN_POINT('Ctrl Pts',(206.402649227192,4.05633571762412,133.58560559211));
#18766=CARTESIAN_POINT('Ctrl Pts',(206.395159781606,4.13086421374525,133.47690873025));
#18767=CARTESIAN_POINT('Ctrl Pts',(206.387670336019,4.20092534590809,133.365353006456));
#18768=CARTESIAN_POINT('Ctrl Pts',(206.380180890433,4.266313865227,133.251348371085));
#18769=CARTESIAN_POINT('Ctrl Pts',(206.372406547022,4.33418975784089,133.133007009811));
#18770=CARTESIAN_POINT('Ctrl Pts',(206.36463220361,4.39724549814214,133.011651903751));
#18771=CARTESIAN_POINT('Ctrl Pts',(206.356857860199,4.45520197698344,132.887713301771));
#18772=CARTESIAN_POINT('Ctrl Pts',(206.349093097628,4.51308703219629,132.763927437583));
#18773=CARTESIAN_POINT('Ctrl Pts',(206.341328335058,4.56588516553323,132.637564763071));
#18774=CARTESIAN_POINT('Ctrl Pts',(206.333563572488,4.61336172857185,132.509082478706));
#18775=CARTESIAN_POINT('Ctrl Pts',(206.32580652166,4.66079113922843,132.380727799318));
#18776=CARTESIAN_POINT('Ctrl Pts',(206.318049470833,4.70290936280457,132.250258063749));
#18777=CARTESIAN_POINT('Ctrl Pts',(206.310292420006,4.73952884382674,132.118152610628));
#18778=CARTESIAN_POINT('Ctrl Pts',(206.302541218515,4.7761207113015,131.986146773889));
#18779=CARTESIAN_POINT('Ctrl Pts',(206.294790017025,4.80722198540851,131.852508049919));
#18780=CARTESIAN_POINT('Ctrl Pts',(206.287038815535,4.83269430378063,131.717732846565));
#18781=CARTESIAN_POINT('Ctrl Pts',(206.279290908073,4.85815579718011,131.583014918637));
#18782=CARTESIAN_POINT('Ctrl Pts',(206.271543000612,4.87799302016867,131.447161855274));
#18783=CARTESIAN_POINT('Ctrl Pts',(206.26379509315,4.89211832584772,131.310682006019));
#18784=CARTESIAN_POINT('Ctrl Pts',(206.256048806118,4.90624067730134,131.17423070073));
#18785=CARTESIAN_POINT('Ctrl Pts',(206.248302519086,4.9146534473754,131.037153258931));
#18786=CARTESIAN_POINT('Ctrl Pts',(206.240556232054,4.91732070875142,130.899964538952));
#18787=CARTESIAN_POINT('Ctrl Pts',(206.232809887587,4.91998798990394,130.762774801783));
#18788=CARTESIAN_POINT('Ctrl Pts',(206.22506354312,4.91690966975381,130.625474175676));
#18789=CARTESIAN_POINT('Ctrl Pts',(206.217317198653,4.90810194759419,130.488578517817));
#18790=CARTESIAN_POINT('Ctrl Pts',(206.209569119204,4.89929225273097,130.351652198845));
#18791=CARTESIAN_POINT('Ctrl Pts',(206.201821039754,4.88475062745858,130.21513141869));
#18792=CARTESIAN_POINT('Ctrl Pts',(206.194072960305,4.86454520291237,130.079527511726));
#18793=CARTESIAN_POINT('Ctrl Pts',(206.186316645792,4.84431830298384,129.943779477834));
#18794=CARTESIAN_POINT('Ctrl Pts',(206.178560331278,4.81841563632905,129.808950651116));
#18795=CARTESIAN_POINT('Ctrl Pts',(206.170804016765,4.78695671008173,129.675543308032));
#18796=CARTESIAN_POINT('Ctrl Pts',(206.163043562283,4.75548099249017,129.542064758175));
#18797=CARTESIAN_POINT('Ctrl Pts',(206.155283107802,4.71844321146889,129.410009580029));
#18798=CARTESIAN_POINT('Ctrl Pts',(206.14752265332,4.6760126848635,129.279864493105));
#18799=CARTESIAN_POINT('Ctrl Pts',(206.139749740871,4.63351404393066,129.149510482424));
#18800=CARTESIAN_POINT('Ctrl Pts',(206.131976828422,4.5856054945835,129.021073056925));
#18801=CARTESIAN_POINT('Ctrl Pts',(206.124203915972,4.53250473784456,128.895019405546));
#18802=CARTESIAN_POINT('Ctrl Pts',(206.116713699522,4.48133522265336,128.773550247191));
#18803=CARTESIAN_POINT('Ctrl Pts',(206.109223483071,4.42534474547032,128.654294760804));
#18804=CARTESIAN_POINT('Ctrl Pts',(206.101733266621,4.36476734543776,128.537647339999));
#18805=CARTESIAN_POINT('Ctrl Pts',(206.093958959944,4.30189235529015,128.416575695624));
#18806=CARTESIAN_POINT('Ctrl Pts',(206.086184653268,4.23387645089009,128.297930328045));
#18807=CARTESIAN_POINT('Ctrl Pts',(206.078410346591,4.16093074001882,128.18217861792));
#18808=CARTESIAN_POINT('Ctrl Pts',(206.070645621474,4.08807493217016,128.066569567707));
#18809=CARTESIAN_POINT('Ctrl Pts',(206.062880896357,4.01030161335004,127.953847406604));
#18810=CARTESIAN_POINT('Ctrl Pts',(206.05511617124,3.92786859889688,127.844456677858));
#18811=CARTESIAN_POINT('Ctrl Pts',(206.04735915854,3.84551746214591,127.735174602927));
#18812=CARTESIAN_POINT('Ctrl Pts',(206.039602145841,3.7585160740671,127.629217685533));
#18813=CARTESIAN_POINT('Ctrl Pts',(206.031845133142,3.66716633068647,127.52700281507));
#18814=CARTESIAN_POINT('Ctrl Pts',(206.024093970412,3.57588547893075,127.424865030194));
#18815=CARTESIAN_POINT('Ctrl Pts',(206.016342807682,3.48026305863852,127.326463965419));
#18816=CARTESIAN_POINT('Ctrl Pts',(206.008591644952,3.38064191709146,127.232184349392));
#18817=CARTESIAN_POINT('Ctrl Pts',(206.000843777079,3.28106312240745,127.137944809658));
#18818=CARTESIAN_POINT('Ctrl Pts',(205.993095909207,3.17748927055705,127.04782350237));
#18819=CARTESIAN_POINT('Ctrl Pts',(205.985348041334,3.070300668997,126.962168942954));
#18820=CARTESIAN_POINT('Ctrl Pts',(205.97760179439,2.96313449232946,126.876532303301));
#18821=CARTESIAN_POINT('Ctrl Pts',(205.969855547446,2.85235537539139,126.79536079669));
#18822=CARTESIAN_POINT('Ctrl Pts',(205.962109300503,2.73837705773569,126.718962943879));
#18823=CARTESIAN_POINT('Ctrl Pts',(205.954362996587,2.62439790178891,126.642564529175));
#18824=CARTESIAN_POINT('Ctrl Pts',(205.94661669267,2.5072198229346,126.570940056014));
#18825=CARTESIAN_POINT('Ctrl Pts',(205.938870388754,2.38728557715688,126.50435472971));
#18826=CARTESIAN_POINT('Ctrl Pts',(205.931122350283,2.26732447565317,126.437754493592));
#18827=CARTESIAN_POINT('Ctrl Pts',(205.923374311811,2.14460632090196,126.376195839389));
#18828=CARTESIAN_POINT('Ctrl Pts',(205.915626273339,2.01959813448211,126.319897836173));
#18829=CARTESIAN_POINT('Ctrl Pts',(205.907870000251,1.8944570893462,126.263539999433));
#18830=CARTESIAN_POINT('Ctrl Pts',(205.900113727163,1.76702150772587,126.212454143145));
#18831=CARTESIAN_POINT('Ctrl Pts',(205.892357454075,1.63777856078686,126.166811216392));
#18832=CARTESIAN_POINT('Ctrl Pts',(205.884597041329,1.5084666346276,126.121143929212));
#18833=CARTESIAN_POINT('Ctrl Pts',(205.876836628582,1.3773457946557,126.08092547459));
#18834=CARTESIAN_POINT('Ctrl Pts',(205.869076215836,1.24491704770284,126.046276485603));
#18835=CARTESIAN_POINT('Ctrl Pts',(205.861303345232,1.11227571174918,126.011571874297));
#18836=CARTESIAN_POINT('Ctrl Pts',(205.853530474629,0.97832265542302,125.982454678108));
#18837=CARTESIAN_POINT('Ctrl Pts',(205.845757604025,0.843568606457823,125.958994267258));
#18838=CARTESIAN_POINT('Ctrl Pts',(205.838266950286,0.713707198462261,125.93638565543));
#18839=CARTESIAN_POINT('Ctrl Pts',(205.830776296547,0.583102259513571,125.919030219509));
#18840=CARTESIAN_POINT('Ctrl Pts',(205.823285642808,0.452212191984598,125.90694423789));
#18841=CARTESIAN_POINT('Ctrl Pts',(205.815511295583,0.316364925691163,125.894400523959));
#18842=CARTESIAN_POINT('Ctrl Pts',(205.807736948359,0.179780181164248,125.887493536688));
#18843=CARTESIAN_POINT('Ctrl Pts',(205.799962601134,0.0429652936190226,
125.886298291198));
#18844=CARTESIAN_POINT('Ctrl Pts',(205.792197834953,-0.0936809843600888,
125.885104518719));
#18845=CARTESIAN_POINT('Ctrl Pts',(205.784433068771,-0.23055645382959,125.889608485683));
#18846=CARTESIAN_POINT('Ctrl Pts',(205.77666830259,-0.367147747384615,125.899833566556));
#18847=CARTESIAN_POINT('Ctrl Pts',(205.768911248356,-0.503603378781414,
125.910048491902));
#18848=CARTESIAN_POINT('Ctrl Pts',(205.761154194123,-0.639775008589745,
125.925973194331));
#18849=CARTESIAN_POINT('Ctrl Pts',(205.753397139889,-0.775148709250783,
125.94757901438));
#18850=CARTESIAN_POINT('Ctrl Pts',(205.745645935201,-0.910420325464687,
125.969168541617));
#18851=CARTESIAN_POINT('Ctrl Pts',(205.737894730512,-1.04489482568991,125.996430597873));
#18852=CARTESIAN_POINT('Ctrl Pts',(205.730143525824,-1.17806320546229,126.029284686606));
#18853=CARTESIAN_POINT('Ctrl Pts',(205.722395615495,-1.31117498700093,126.062124811938));
#18854=CARTESIAN_POINT('Ctrl Pts',(205.714647705166,-1.44298137338557,126.100552149252));
#18855=CARTESIAN_POINT('Ctrl Pts',(205.706899794837,-1.57298357962825,126.144435111646));
#18856=CARTESIAN_POINT('Ctrl Pts',(205.699153505139,-1.70295859328728,126.188308895034));
#18857=CARTESIAN_POINT('Ctrl Pts',(205.691407215442,-1.83112980724108,126.237635908722));
#18858=CARTESIAN_POINT('Ctrl Pts',(205.683660925745,-1.9570140146508,126.292234820454));
#18859=CARTESIAN_POINT('Ctrl Pts',(205.675914578818,-2.08289915209403,126.346834135564));
#18860=CARTESIAN_POINT('Ctrl Pts',(205.668168231891,-2.2064968905978,126.406705270871));
#18861=CARTESIAN_POINT('Ctrl Pts',(205.660421884964,-2.32734478203693,126.471619068844));
#18862=CARTESIAN_POINT('Ctrl Pts',(205.652673803264,-2.44821973703175,126.536547404084));
#18863=CARTESIAN_POINT('Ctrl Pts',(205.644925721563,-2.56634327519558,126.606520464177));
#18864=CARTESIAN_POINT('Ctrl Pts',(205.637177639863,-2.6812786482065,126.68126373862));
#18865=CARTESIAN_POINT('Ctrl Pts',(205.629421323445,-2.79633617537112,126.756086450761));
#18866=CARTESIAN_POINT('Ctrl Pts',(205.621665007027,-2.90819844040077,126.835689291279));
#18867=CARTESIAN_POINT('Ctrl Pts',(205.613908690609,-3.01645828850523,126.919754787342));
#18868=CARTESIAN_POINT('Ctrl Pts',(205.606148234409,-3.12477591819194,127.003865151724));
#18869=CARTESIAN_POINT('Ctrl Pts',(205.598387778208,-3.22948700142695,127.092442665323));
#18870=CARTESIAN_POINT('Ctrl Pts',(205.590627322007,-3.3302192372797,127.185131018031));
#18871=CARTESIAN_POINT('Ctrl Pts',(205.582854408177,-3.43111317560035,127.277968160599));
#18872=CARTESIAN_POINT('Ctrl Pts',(205.575081494346,-3.52801522649826,127.374929052501));
#18873=CARTESIAN_POINT('Ctrl Pts',(205.567308580516,-3.62059096362825,127.475621496428));
#18874=CARTESIAN_POINT('Ctrl Pts',(205.559818393342,-3.70979941414655,127.572651422196));
#18875=CARTESIAN_POINT('Ctrl Pts',(205.552328206168,-3.79499060911529,127.673145922983));
#18876=CARTESIAN_POINT('Ctrl Pts',(205.544838018995,-3.87590312513928,127.776728204766));
#18877=CARTESIAN_POINT('Ctrl Pts',(205.53706126549,-3.95991126511941,127.884273430835));
#18878=CARTESIAN_POINT('Ctrl Pts',(205.529284511985,-4.03957765797006,127.995494127098));
#18879=CARTESIAN_POINT('Ctrl Pts',(205.521507758481,-4.11456321009359,128.110004914871));
#18880=CARTESIAN_POINT('Ctrl Pts',(205.513743508267,-4.18942820212018,128.224331594755));
#18881=CARTESIAN_POINT('Ctrl Pts',(205.505979258053,-4.25962712878069,128.341937508539));
#18882=CARTESIAN_POINT('Ctrl Pts',(205.498215007839,-4.32486122114154,128.462404494927));
#18883=CARTESIAN_POINT('Ctrl Pts',(205.490457952857,-4.39003486021618,128.582759842984));
#18884=CARTESIAN_POINT('Ctrl Pts',(205.482700897876,-4.45025263063646,128.705970650087));
#18885=CARTESIAN_POINT('Ctrl Pts',(205.474943842894,-4.50525896992651,128.831589805638));
#18886=CARTESIAN_POINT('Ctrl Pts',(205.467193142368,-4.5602202488983,128.957106055974));
#18887=CARTESIAN_POINT('Ctrl Pts',(205.459442441842,-4.60997843839768,129.085026371888));
#18888=CARTESIAN_POINT('Ctrl Pts',(205.451691741317,-4.65432411968393,129.214879554002));
#18889=CARTESIAN_POINT('Ctrl Pts',(205.444469975199,-4.69564349946542,129.335871109256));
#18890=CARTESIAN_POINT('Ctrl Pts',(205.437248209081,-4.73226423551571,129.458540250484));
#18891=CARTESIAN_POINT('Ctrl Pts',(205.430026442963,-4.76405452823405,129.582490119308));
#18892=CARTESIAN_POINT('Origin',(213.235140564004,0.,130.804360617566));
#18893=CARTESIAN_POINT('',(203.334773566427,-4.76405452823405,129.582490119308));
#18894=CARTESIAN_POINT('',(203.680274487341,-4.76405452823405,129.582490119308));
#18895=CARTESIAN_POINT('',(213.235140564004,-4.76405452823405,129.582490119308));
#18896=CARTESIAN_POINT('',(205.014859436024,-4.91824993440617,130.805163869501));
#18897=CARTESIAN_POINT('Ctrl Pts',(205.014859435991,-4.91824993440608,130.80516387008));
#18898=CARTESIAN_POINT('Ctrl Pts',(205.012416879836,-4.91824293327168,130.848031247661));
#18899=CARTESIAN_POINT('Ctrl Pts',(205.009974323682,-4.91767549764493,130.890893474637));
#18900=CARTESIAN_POINT('Ctrl Pts',(205.007531767528,-4.91654795620673,130.933740897437));
#18901=CARTESIAN_POINT('Ctrl Pts',(204.999757433917,-4.91295914074164,131.070118584653));
#18902=CARTESIAN_POINT('Ctrl Pts',(204.991983100306,-4.9036859709115,131.206562848942));
#18903=CARTESIAN_POINT('Ctrl Pts',(204.984208766695,-4.88871387579036,131.342561047847));
#18904=CARTESIAN_POINT('Ctrl Pts',(204.976444014264,-4.87376023245488,131.478391640977));
#18905=CARTESIAN_POINT('Ctrl Pts',(204.968679261833,-4.85312168071783,131.613776877648));
#18906=CARTESIAN_POINT('Ctrl Pts',(204.960914509402,-4.82683564131106,131.748204224457));
#18907=CARTESIAN_POINT('Ctrl Pts',(204.95315746904,-4.80057570959591,131.882498055994));
#18908=CARTESIAN_POINT('Ctrl Pts',(204.945400428679,-4.76867952725585,132.015835509765));
#18909=CARTESIAN_POINT('Ctrl Pts',(204.937643388317,-4.73123625092355,132.147709641627));
#18910=CARTESIAN_POINT('Ctrl Pts',(204.929892197607,-4.69382121089179,132.27948432606));
#18911=CARTESIAN_POINT('Ctrl Pts',(204.922141006897,-4.65086750945265,132.409797510464));
#18912=CARTESIAN_POINT('Ctrl Pts',(204.914389816187,-4.60251519606229,132.538153261603));
#18913=CARTESIAN_POINT('Ctrl Pts',(204.906641919949,-4.55418343374924,132.666454457979));
#18914=CARTESIAN_POINT('Ctrl Pts',(204.898894023711,-4.50045776072558,132.792799510701));
#18915=CARTESIAN_POINT('Ctrl Pts',(204.891146127472,-4.44152775223612,132.916708668579));
#18916=CARTESIAN_POINT('Ctrl Pts',(204.883399851932,-4.38261007067356,133.040591907248));
#18917=CARTESIAN_POINT('Ctrl Pts',(204.875653576392,-4.31849038681639,133.162039911728));
#18918=CARTESIAN_POINT('Ctrl Pts',(204.867907300851,-4.2494058332061,133.280594275203));
#18919=CARTESIAN_POINT('Ctrl Pts',(204.860160968134,-4.18032076967024,133.399149513749));
#18920=CARTESIAN_POINT('Ctrl Pts',(204.852414635417,-4.10627096009826,133.514810730874));
#18921=CARTESIAN_POINT('Ctrl Pts',(204.8446683027,-4.02753857581953,133.627145781688));
#18922=CARTESIAN_POINT('Ctrl Pts',(204.83692023525,-3.94878856000942,133.7395059891));
#18923=CARTESIAN_POINT('Ctrl Pts',(204.829172167799,-3.86535410719281,133.848538227898));
#18924=CARTESIAN_POINT('Ctrl Pts',(204.821424100349,-3.77755938889782,133.953841229643));
#18925=CARTESIAN_POINT('Ctrl Pts',(204.813667798163,-3.68967136136312,134.059256148634));
#18926=CARTESIAN_POINT('Ctrl Pts',(204.805911495977,-3.5974140619154,134.160933612335));
#18927=CARTESIAN_POINT('Ctrl Pts',(204.798155193791,-3.50115082848458,134.258506812894));
#18928=CARTESIAN_POINT('Ctrl Pts',(204.790394751835,-3.40483621649768,134.356132091179));
#18929=CARTESIAN_POINT('Ctrl Pts',(204.782634309879,-3.30451169605726,134.449648474981));
#18930=CARTESIAN_POINT('Ctrl Pts',(204.774873867924,-3.20057505400699,134.538728353364));
#18931=CARTESIAN_POINT('Ctrl Pts',(204.767100968216,-3.09647156360682,134.627951230698));
#18932=CARTESIAN_POINT('Ctrl Pts',(204.759328068508,-2.98874467176853,134.712723128926));
#18933=CARTESIAN_POINT('Ctrl Pts',(204.7515551688,-2.87782332804817,134.792758285182));
#18934=CARTESIAN_POINT('Ctrl Pts',(204.744064827105,-2.77093416223283,134.869884028534));
#18935=CARTESIAN_POINT('Ctrl Pts',(204.73657448541,-2.66107901674024,134.942611258251));
#18936=CARTESIAN_POINT('Ctrl Pts',(204.729084143715,-2.54866295096712,135.010724870085));
#18937=CARTESIAN_POINT('Ctrl Pts',(204.721309809264,-2.43198468332284,135.08142097724));
#18938=CARTESIAN_POINT('Ctrl Pts',(204.713535474812,-2.31217786981156,135.147370661178));
#18939=CARTESIAN_POINT('Ctrl Pts',(204.70576114036,-2.18966593526101,135.208284567234));
#18940=CARTESIAN_POINT('Ctrl Pts',(204.697996387077,-2.0673049856553,135.269123402377));
#18941=CARTESIAN_POINT('Ctrl Pts',(204.690231633794,-1.94224589503469,135.324938635623));
#18942=CARTESIAN_POINT('Ctrl Pts',(204.682466880511,-1.8149400992257,135.375484713313));
#18943=CARTESIAN_POINT('Ctrl Pts',(204.674709839286,-1.68776074526766,135.425980587951));
#18944=CARTESIAN_POINT('Ctrl Pts',(204.666952798062,-1.55833948784361,135.471217578389));
#18945=CARTESIAN_POINT('Ctrl Pts',(204.659195756837,-1.42715102488418,135.510996678987));
#18946=CARTESIAN_POINT('Ctrl Pts',(204.651444565255,-1.29606149211033,135.550745781873));
#18947=CARTESIAN_POINT('Ctrl Pts',(204.643693373672,-1.16320777901492,135.585045074249));
#18948=CARTESIAN_POINT('Ctrl Pts',(204.635942182089,-1.02908282854748,135.613744319714));
#18949=CARTESIAN_POINT('Ctrl Pts',(204.628194284967,-0.895014884701764,
135.642431367248));
#18950=CARTESIAN_POINT('Ctrl Pts',(204.620446387844,-0.759677159628549,
135.665523020208));
#18951=CARTESIAN_POINT('Ctrl Pts',(204.612698490721,-0.623575751751765,
135.682919456437));
#18952=CARTESIAN_POINT('Ctrl Pts',(204.604952214289,-0.487502813319543,
135.700312253712));
#18953=CARTESIAN_POINT('Ctrl Pts',(204.597205937857,-0.350666897391173,
135.712012154308));
#18954=CARTESIAN_POINT('Ctrl Pts',(204.589459661425,-0.213581850635355,
135.717970884526));
#18955=CARTESIAN_POINT('Ctrl Pts',(204.58171332781,-0.0764957919198511,
135.723929658732));
#18956=CARTESIAN_POINT('Ctrl Pts',(204.573966994196,0.0608390106965075,
135.724147161014));
#18957=CARTESIAN_POINT('Ctrl Pts',(204.566220660581,0.197906460888714,135.718627205292));
#18958=CARTESIAN_POINT('Ctrl Pts',(204.558472592227,0.335004606408075,135.713106013413));
#18959=CARTESIAN_POINT('Ctrl Pts',(204.550724523873,0.471834889791658,135.701844822528));
#18960=CARTESIAN_POINT('Ctrl Pts',(204.54297645552,0.607884489820787,135.684899471989));
#18961=CARTESIAN_POINT('Ctrl Pts',(204.535220152427,0.744078684979407,135.667936111731));
#18962=CARTESIAN_POINT('Ctrl Pts',(204.527463849334,0.879490150743396,135.645276572288));
#18963=CARTESIAN_POINT('Ctrl Pts',(204.519707546241,1.01361388816882,135.617028271603));
#18964=CARTESIAN_POINT('Ctrl Pts',(204.511947103376,1.14780921147885,135.588764893948));
#18965=CARTESIAN_POINT('Ctrl Pts',(204.50418666051,1.28071505826876,135.554906907859));
#18966=CARTESIAN_POINT('Ctrl Pts',(204.496426217644,1.41184078659271,135.515611901016));
#18967=CARTESIAN_POINT('Ctrl Pts',(204.48865331703,1.54317700952478,135.476253814356));
#18968=CARTESIAN_POINT('Ctrl Pts',(204.480880416416,1.67272703389122,135.431441393526));
#18969=CARTESIAN_POINT('Ctrl Pts',(204.473107515801,1.80001858150718,135.381381064181));
#18970=CARTESIAN_POINT('Ctrl Pts',(204.465617183835,1.9226826930735,135.333140580513));
#18971=CARTESIAN_POINT('Ctrl Pts',(204.458126851868,2.04324940016541,135.280027243014));
#18972=CARTESIAN_POINT('Ctrl Pts',(204.450636519902,2.16131878660124,135.222265569598));
#18973=CARTESIAN_POINT('Ctrl Pts',(204.442862185831,2.28386487105517,135.162313814766));
#18974=CARTESIAN_POINT('Ctrl Pts',(204.435087851759,2.40410871112534,135.097164368467));
#18975=CARTESIAN_POINT('Ctrl Pts',(204.427313517688,2.52157799309945,135.027017066677));
#18976=CARTESIAN_POINT('Ctrl Pts',(204.419548764789,2.63890250468257,134.956956215167));
#18977=CARTESIAN_POINT('Ctrl Pts',(204.411784011889,2.75345892929808,134.881909962079));
#18978=CARTESIAN_POINT('Ctrl Pts',(204.40401925899,2.86479666362884,134.802125385353));
#18979=CARTESIAN_POINT('Ctrl Pts',(204.396262218153,2.9760238157537,134.722420051793));
#18980=CARTESIAN_POINT('Ctrl Pts',(204.388505177315,3.08403832372975,134.637985986342));
#18981=CARTESIAN_POINT('Ctrl Pts',(204.380748136478,3.18841617266462,134.549114998349));
#18982=CARTESIAN_POINT('Ctrl Pts',(204.372996945285,3.29271530945384,134.460311028657));
#18983=CARTESIAN_POINT('Ctrl Pts',(204.365245754092,3.39338294937173,134.3670770487));
#18984=CARTESIAN_POINT('Ctrl Pts',(204.357494562899,3.49002624658722,134.269746578845));
#18985=CARTESIAN_POINT('Ctrl Pts',(204.349746666169,3.58662846782897,134.172457477031));
#18986=CARTESIAN_POINT('Ctrl Pts',(204.341998769439,3.67920947343216,134.07107562512));
#18987=CARTESIAN_POINT('Ctrl Pts',(204.334250872709,3.76741172163867,133.965972861684));
#18988=CARTESIAN_POINT('Ctrl Pts',(204.326504596671,3.85559551983956,133.860892083477));
#18989=CARTESIAN_POINT('Ctrl Pts',(204.318758320634,3.9394021313356,133.752092241188));
#18990=CARTESIAN_POINT('Ctrl Pts',(204.311012044596,4.01851319542896,133.639979555411));
#18991=CARTESIAN_POINT('Ctrl Pts',(204.303265711377,4.09762484350567,133.527866042038));
#18992=CARTESIAN_POINT('Ctrl Pts',(204.295519378158,4.17204064960371,133.412439955821));
#18993=CARTESIAN_POINT('Ctrl Pts',(204.287773044939,4.24148485981986,133.294137564688));
#18994=CARTESIAN_POINT('Ctrl Pts',(204.280024976982,4.31094462158894,133.175808680548));
#18995=CARTESIAN_POINT('Ctrl Pts',(204.272276909025,4.37543037414788,133.054602546852));
#18996=CARTESIAN_POINT('Ctrl Pts',(204.264528841068,4.43471190433788,132.930980797105));
#18997=CARTESIAN_POINT('Ctrl Pts',(204.256772538371,4.49405643965077,132.807227660677));
#18998=CARTESIAN_POINT('Ctrl Pts',(204.249016235674,4.54818553428607,132.681054132738));
#18999=CARTESIAN_POINT('Ctrl Pts',(204.241259932977,4.59691659774419,132.552943145182));
#19000=CARTESIAN_POINT('Ctrl Pts',(204.233499490508,4.64567367044088,132.424763780927));
#19001=CARTESIAN_POINT('Ctrl Pts',(204.225739048038,4.68902684761736,132.2946452673));
#19002=CARTESIAN_POINT('Ctrl Pts',(204.217978605568,4.72684350830149,132.163085575211));
#19003=CARTESIAN_POINT('Ctrl Pts',(204.210205705346,4.76472087565255,132.031314691805));
#19004=CARTESIAN_POINT('Ctrl Pts',(204.202432805124,4.79704387379708,131.898098386972));
#19005=CARTESIAN_POINT('Ctrl Pts',(204.194659904902,4.82373089659542,131.763945579792));
#19006=CARTESIAN_POINT('Ctrl Pts',(204.187169568631,4.849447780786,131.634669555555));
#19007=CARTESIAN_POINT('Ctrl Pts',(204.17967923236,4.86993129066992,131.504524239439));
#19008=CARTESIAN_POINT('Ctrl Pts',(204.172188896089,4.88515415502804,131.373967450489));
#19009=CARTESIAN_POINT('Ctrl Pts',(204.164414562036,4.90095419770749,131.238460571561));
#19010=CARTESIAN_POINT('Ctrl Pts',(204.156640227983,4.91113685606931,131.102081156815));
#19011=CARTESIAN_POINT('Ctrl Pts',(204.14886589393,4.915614960675,130.965334593376));
#19012=CARTESIAN_POINT('Ctrl Pts',(204.141101141049,4.9200875464163,130.828756557876));
#19013=CARTESIAN_POINT('Ctrl Pts',(204.133336388169,4.91886955403614,130.691812660983));
#19014=CARTESIAN_POINT('Ctrl Pts',(204.125571635289,4.9119252950968,130.555015559688));
#19015=CARTESIAN_POINT('Ctrl Pts',(204.117814594472,4.90498793329431,130.418354327222));
#19016=CARTESIAN_POINT('Ctrl Pts',(204.110057553655,4.892335642827,130.281839988143));
#19017=CARTESIAN_POINT('Ctrl Pts',(204.102300512838,4.87398474075138,130.145987008266));
#19018=CARTESIAN_POINT('Ctrl Pts',(204.094549321667,4.85564767723613,130.010236476196));
#19019=CARTESIAN_POINT('Ctrl Pts',(204.086798130496,4.83162060788727,129.875146696503));
#19020=CARTESIAN_POINT('Ctrl Pts',(204.079046939325,4.80197179006196,129.741228457414));
#19021=CARTESIAN_POINT('Ctrl Pts',(204.071299042618,4.77233557377983,129.607367137171));
#19022=CARTESIAN_POINT('Ctrl Pts',(204.063551145911,4.73708244567803,129.474676748098));
#19023=CARTESIAN_POINT('Ctrl Pts',(204.055803249204,4.69633198401899,129.343659088033));
#19024=CARTESIAN_POINT('Ctrl Pts',(204.048056973191,4.65559004648194,129.21266883405));
#19025=CARTESIAN_POINT('Ctrl Pts',(204.040310697177,4.60935317869152,129.083350986195));
#19026=CARTESIAN_POINT('Ctrl Pts',(204.032564421164,4.55779106379823,128.956192962492));
#19027=CARTESIAN_POINT('Ctrl Pts',(204.02481808797,4.50622856828952,128.829034000148));
#19028=CARTESIAN_POINT('Ctrl Pts',(204.017071754777,4.44934089415499,128.704035256081));
#19029=CARTESIAN_POINT('Ctrl Pts',(204.009325421583,4.3873460342304,128.58166454333));
#19030=CARTESIAN_POINT('Ctrl Pts',(204.001577353652,4.3253372909914,128.459266426516));
#19031=CARTESIAN_POINT('Ctrl Pts',(203.993829285721,4.25821926274942,128.339497860818));
#19032=CARTESIAN_POINT('Ctrl Pts',(203.98608121779,4.18625589900541,128.222802055274));
#19033=CARTESIAN_POINT('Ctrl Pts',(203.978324915121,4.1142160517463,128.105982224046));
#19034=CARTESIAN_POINT('Ctrl Pts',(203.970568612452,4.03732078748716,127.992242009999));
#19035=CARTESIAN_POINT('Ctrl Pts',(203.962812309783,3.95587771587694,127.881996068177));
#19036=CARTESIAN_POINT('Ctrl Pts',(203.955051867342,3.87439117565101,127.771691284781));
#19037=CARTESIAN_POINT('Ctrl Pts',(203.9472914249,3.78835223661492,127.664884794093));
#19038=CARTESIAN_POINT('Ctrl Pts',(203.939530982459,3.6981081709207,127.561957339337));
#19039=CARTESIAN_POINT('Ctrl Pts',(203.931758082267,3.60771923743896,127.458864656291));
#19040=CARTESIAN_POINT('Ctrl Pts',(203.923985182075,3.51311195774471,127.359663735743));
#19041=CARTESIAN_POINT('Ctrl Pts',(203.916212281882,3.41467038975604,127.264698318444));
#19042=CARTESIAN_POINT('Ctrl Pts',(203.908721945347,3.3198074100404,127.173185122963));
#19043=CARTESIAN_POINT('Ctrl Pts',(203.901231608812,3.22138430351891,127.085605040283));
#19044=CARTESIAN_POINT('Ctrl Pts',(203.893741272277,3.11977150560056,127.002228476866));
#19045=CARTESIAN_POINT('Ctrl Pts',(203.885966938106,3.01430603775704,126.915690674068));
#19046=CARTESIAN_POINT('Ctrl Pts',(203.878192603936,2.90507014731187,126.83340730906));
#19047=CARTESIAN_POINT('Ctrl Pts',(203.870418269766,2.79244191357776,126.755724894042));
#19048=CARTESIAN_POINT('Ctrl Pts',(203.862653516767,2.67995248406615,126.678138215651));
#19049=CARTESIAN_POINT('Ctrl Pts',(203.854888763768,2.56407934847872,126.605141424973));
#19050=CARTESIAN_POINT('Ctrl Pts',(203.84712401077,2.44523452920922,126.537041651322));
#19051=CARTESIAN_POINT('Ctrl Pts',(203.839366969832,2.32650774828062,126.469009515322));
#19052=CARTESIAN_POINT('Ctrl Pts',(203.831609928895,2.20481549434958,126.405864910317));
#19053=CARTESIAN_POINT('Ctrl Pts',(203.823852887958,2.08059942186419,126.34787218964));
#19054=CARTESIAN_POINT('Ctrl Pts',(203.816101696665,1.95647702167689,126.289923201721));
#19055=CARTESIAN_POINT('Ctrl Pts',(203.808350505372,1.82983494402628,126.237118529847));
#19056=CARTESIAN_POINT('Ctrl Pts',(203.800599314079,1.70113982430083,126.189676840678));
#19057=CARTESIAN_POINT('Ctrl Pts',(203.792851417249,1.57249940342463,126.142255315488));
#19058=CARTESIAN_POINT('Ctrl Pts',(203.785103520418,1.44180804206936,126.100192374375));
#19059=CARTESIAN_POINT('Ctrl Pts',(203.777355623588,1.30955255195562,126.063658646743));
#19060=CARTESIAN_POINT('Ctrl Pts',(203.76960934745,1.17732472683343,126.027132561177));
#19061=CARTESIAN_POINT('Ctrl Pts',(203.761863071312,1.04353380034826,125.996133492601));
#19062=CARTESIAN_POINT('Ctrl Pts',(203.754116795175,0.908681568991501,125.970782143115));
#19063=CARTESIAN_POINT('Ctrl Pts',(203.746370461855,0.77382834218146,125.945430606491));
#19064=CARTESIAN_POINT('Ctrl Pts',(203.738624128536,0.637914179101389,125.925726944381));
#19065=CARTESIAN_POINT('Ctrl Pts',(203.730877795217,0.501450494577304,125.911740617608));
#19066=CARTESIAN_POINT('Ctrl Pts',(203.72312972716,0.364956249953434,125.897751158694));
#19067=CARTESIAN_POINT('Ctrl Pts',(203.715381659102,0.227912627860709,125.889481622733));
#19068=CARTESIAN_POINT('Ctrl Pts',(203.707633591045,0.0908351837803655,
125.88694950684));
#19069=CARTESIAN_POINT('Ctrl Pts',(203.699877288249,-0.0463879478389493,
125.884414699785));
#19070=CARTESIAN_POINT('Ctrl Pts',(203.692120985453,-0.183644581730893,
125.887629501038));
#19071=CARTESIAN_POINT('Ctrl Pts',(203.684364682657,-0.320419586321026,
125.896559241063));
#19072=CARTESIAN_POINT('Ctrl Pts',(203.676604240088,-0.457267591850978,
125.90549374716));
#19073=CARTESIAN_POINT('Ctrl Pts',(203.66884379752,-0.593633067328671,125.920149228124));
#19074=CARTESIAN_POINT('Ctrl Pts',(203.661083354951,-0.729007973603942,
125.940439315065));
#19075=CARTESIAN_POINT('Ctrl Pts',(203.653310454632,-0.864600195689189,
125.960761973454));
#19076=CARTESIAN_POINT('Ctrl Pts',(203.645537554313,-0.999198286843428,
125.986737238823));
#19077=CARTESIAN_POINT('Ctrl Pts',(203.637764653993,-1.13230545553917,126.018227792638));
#19078=CARTESIAN_POINT('Ctrl Pts',(203.630274318817,-1.26057383246008,126.048573582918));
#19079=CARTESIAN_POINT('Ctrl Pts',(203.62278398364,-1.38745750614367,126.084040550359));
#19080=CARTESIAN_POINT('Ctrl Pts',(203.615293648463,-1.51252874683208,126.124463198551));
#19081=CARTESIAN_POINT('Ctrl Pts',(203.607519314355,-1.64234211159146,126.166418486956));
#19082=CARTESIAN_POINT('Ctrl Pts',(203.599744980247,-1.77061410292081,126.213845566141));
#19083=CARTESIAN_POINT('Ctrl Pts',(203.591970646139,-1.89684882919352,126.266613645589));
#19084=CARTESIAN_POINT('Ctrl Pts',(203.584205893202,-2.02292798244727,126.319316693095));
#19085=CARTESIAN_POINT('Ctrl Pts',(203.576441140266,-2.14697450902767,126.377347494701));
#19086=CARTESIAN_POINT('Ctrl Pts',(203.56867638733,-2.2685073041796,126.440525415203));
#19087=CARTESIAN_POINT('Ctrl Pts',(203.560919346456,-2.38991939124546,126.503640586503));
#19088=CARTESIAN_POINT('Ctrl Pts',(203.553162305581,-2.50882237072727,126.571892524047));
#19089=CARTESIAN_POINT('Ctrl Pts',(203.545405264707,-2.62475510966509,126.64505254088));
#19090=CARTESIAN_POINT('Ctrl Pts',(203.537654073478,-2.74060042282238,126.718157387175));
#19091=CARTESIAN_POINT('Ctrl Pts',(203.529902882249,-2.853479624487,126.7961627379));
#19092=CARTESIAN_POINT('Ctrl Pts',(203.52215169102,-2.96295651638203,126.878794194166));
#19093=CARTESIAN_POINT('Ctrl Pts',(203.514403794253,-3.07238687767773,126.961390529858));
#19094=CARTESIAN_POINT('Ctrl Pts',(203.506655897487,-3.17841749393087,127.048608825393));
#19095=CARTESIAN_POINT('Ctrl Pts',(203.498908000721,-3.28064167616848,127.140131741651));
#19096=CARTESIAN_POINT('Ctrl Pts',(203.491161724648,-3.38284447531104,127.231635513289));
#19097=CARTESIAN_POINT('Ctrl Pts',(203.483415448574,-3.48124213307604,127.327441854015));
#19098=CARTESIAN_POINT('Ctrl Pts',(203.475669172501,-3.57546186610856,127.427193830671));
#19099=CARTESIAN_POINT('Ctrl Pts',(203.467922839247,-3.66968229464993,127.526946543675));
#19100=CARTESIAN_POINT('Ctrl Pts',(203.460176505992,-3.75972446845858,127.630644666505));
#19101=CARTESIAN_POINT('Ctrl Pts',(203.452430172738,-3.8452535159746,127.737895476661));
#19102=CARTESIAN_POINT('Ctrl Pts',(203.444682104745,-3.93080171712827,127.845170304894));
#19103=CARTESIAN_POINT('Ctrl Pts',(203.436934036753,-4.01183453713135,127.955999097993));
#19104=CARTESIAN_POINT('Ctrl Pts',(203.429185968761,-4.08805858483793,128.069957562156));
#19105=CARTESIAN_POINT('Ctrl Pts',(203.42142966603,-4.16436364437073,128.184037142734));
#19106=CARTESIAN_POINT('Ctrl Pts',(203.413673363299,-4.23584950448076,128.301252713431));
#19107=CARTESIAN_POINT('Ctrl Pts',(203.405917060567,-4.30226689243356,128.421152139742));
#19108=CARTESIAN_POINT('Ctrl Pts',(203.398156618064,-4.3687197293466,128.541115559989));
#19109=CARTESIAN_POINT('Ctrl Pts',(203.39039617556,-4.4300985288876,128.663765340678));
#19110=CARTESIAN_POINT('Ctrl Pts',(203.382635733057,-4.48620134808193,128.788627369597));
#19111=CARTESIAN_POINT('Ctrl Pts',(203.374862832802,-4.54239422850365,128.913689838133));
#19112=CARTESIAN_POINT('Ctrl Pts',(203.367089932547,-4.59329405862153,129.040971288298));
#19113=CARTESIAN_POINT('Ctrl Pts',(203.359317032292,-4.63874784045621,129.169979531294));
#19114=CARTESIAN_POINT('Ctrl Pts',(203.351826696411,-4.68254926358041,129.294298001835));
#19115=CARTESIAN_POINT('Ctrl Pts',(203.344336360531,-4.72129362844921,129.420219603998));
#19116=CARTESIAN_POINT('Ctrl Pts',(203.336846024651,-4.75488897347145,129.54729502164));
#19117=CARTESIAN_POINT('Ctrl Pts',(203.336155205243,-4.75798740813817,129.55901494531));
#19118=CARTESIAN_POINT('Ctrl Pts',(203.335464385835,-4.76104262034663,129.570746736167));
#19119=CARTESIAN_POINT('Ctrl Pts',(203.334773566427,-4.76405452823405,129.582490119308));
#19120=CARTESIAN_POINT('Ctrl Pts',(205.084976592678,-4.76405452823405,129.582490119308));
#19121=CARTESIAN_POINT('Ctrl Pts',(205.077250789112,-4.79798664166829,129.714790914597));
#19122=CARTESIAN_POINT('Ctrl Pts',(205.069524985546,-4.82637681902747,129.848402380795));
#19123=CARTESIAN_POINT('Ctrl Pts',(205.06179918198,-4.84914957344003,129.982818484193));
#19124=CARTESIAN_POINT('Ctrl Pts',(205.053975890988,-4.87220968401055,130.118930706311));
#19125=CARTESIAN_POINT('Ctrl Pts',(205.046152599995,-4.88950959216643,130.255867593678));
#19126=CARTESIAN_POINT('Ctrl Pts',(205.038329309002,-4.90102524937068,130.393100885121));
#19127=CARTESIAN_POINT('Ctrl Pts',(205.030506018009,-4.91254090657492,130.530334176563));
#19128=CARTESIAN_POINT('Ctrl Pts',(205.022682727017,-4.9182723584033,130.667863456436));
#19129=CARTESIAN_POINT('Ctrl Pts',(205.014859436024,-4.91824993440617,130.805163869501));
#19130=CARTESIAN_POINT('',(205.360140563955,-4.91824853905311,130.808151475242));
#19131=CARTESIAN_POINT('Ctrl Pts',(205.430026442963,-4.76405452823405,129.582490119308));
#19132=CARTESIAN_POINT('Ctrl Pts',(205.422281762578,-4.79814669522109,129.71541496097));
#19133=CARTESIAN_POINT('Ctrl Pts',(205.414537082193,-4.82668292020064,129.849812538585));
#19134=CARTESIAN_POINT('Ctrl Pts',(205.406792401809,-4.8495489326977,129.985179189633));
#19135=CARTESIAN_POINT('Ctrl Pts',(205.399017095509,-4.87250536759203,130.121081140708));
#19136=CARTESIAN_POINT('Ctrl Pts',(205.391241789208,-4.88974655166597,130.257959461279));
#19137=CARTESIAN_POINT('Ctrl Pts',(205.383466482908,-4.90120888938085,130.395295237518));
#19138=CARTESIAN_POINT('Ctrl Pts',(205.375691176608,-4.91267122709574,130.532631013756));
#19139=CARTESIAN_POINT('Ctrl Pts',(205.367915870308,-4.91835469588896,130.670423848268));
#19140=CARTESIAN_POINT('Ctrl Pts',(205.360140564008,-4.91824853905384,130.808151474305));
#19141=CARTESIAN_POINT('Ctrl Pts',(205.360140563955,-4.91824853905311,130.808151475242));
#19142=CARTESIAN_POINT('Ctrl Pts',(205.351139825899,-4.91812565127672,130.967585745387));
#19143=CARTESIAN_POINT('Ctrl Pts',(205.342139087842,-4.91024632687204,131.126698725876));
#19144=CARTESIAN_POINT('Ctrl Pts',(205.333138349785,-4.89472759256679,131.284802973177));
#19145=CARTESIAN_POINT('Ctrl Pts',(205.324085898924,-4.87911969698644,131.443815592));
#19146=CARTESIAN_POINT('Ctrl Pts',(205.315033448062,-4.85578446545969,131.601807746443));
#19147=CARTESIAN_POINT('Ctrl Pts',(205.3059809972,-4.82489013514455,131.758099704678));
#19148=CARTESIAN_POINT('Ctrl Pts',(205.296866878366,-4.79378534351451,131.915456369954));
#19149=CARTESIAN_POINT('Ctrl Pts',(205.287752759532,-4.75501819248919,132.071089491341));
#19150=CARTESIAN_POINT('Ctrl Pts',(205.278638640698,-4.70880867544122,132.224326786385));
#19151=CARTESIAN_POINT('Ctrl Pts',(205.274555892192,-4.68810872187624,132.292970760494));
#19152=CARTESIAN_POINT('Ctrl Pts',(205.270473143687,-4.6659159667685,132.361134266192));
#19153=CARTESIAN_POINT('Ctrl Pts',(205.266390395182,-4.64225323707004,132.42875833531));
#19154=CARTESIAN_POINT('Ctrl Pts',(205.25861606485,-4.59719489536611,132.557527435603));
#19155=CARTESIAN_POINT('Ctrl Pts',(205.250841734518,-4.54670333252088,132.684624302624));
#19156=CARTESIAN_POINT('Ctrl Pts',(205.243067404185,-4.49092120076951,132.809556326463));
#19157=CARTESIAN_POINT('Ctrl Pts',(205.235302655081,-4.43520781594627,132.934334381772));
#19158=CARTESIAN_POINT('Ctrl Pts',(205.227537905977,-4.3742169933291,133.05695254884));
#19159=CARTESIAN_POINT('Ctrl Pts',(205.219773156873,-4.30814086066012,133.176934196448));
#19160=CARTESIAN_POINT('Ctrl Pts',(205.212016119882,-4.24213035621027,133.296796675734));
#19161=CARTESIAN_POINT('Ctrl Pts',(205.204259082892,-4.17104478048607,133.414027506535));
#19162=CARTESIAN_POINT('Ctrl Pts',(205.196502045902,-4.0951238198962,133.528171176731));
#19163=CARTESIAN_POINT('Ctrl Pts',(205.188750858604,-4.0192601123862,133.642228769556));
#19164=CARTESIAN_POINT('Ctrl Pts',(205.180999671306,-3.93856849366088,133.753203511446));
#19165=CARTESIAN_POINT('Ctrl Pts',(205.173248484008,-3.85333375056227,133.860665914698));
#19166=CARTESIAN_POINT('Ctrl Pts',(205.165500591231,-3.76813523516348,133.96808264273));
#19167=CARTESIAN_POINT('Ctrl Pts',(205.157752698454,-3.67839767841762,134.071989695647));
#19168=CARTESIAN_POINT('Ctrl Pts',(205.150004805678,-3.58444808691414,134.171988116966));
#19169=CARTESIAN_POINT('Ctrl Pts',(205.142258533629,-3.49051814807432,134.271965620309));
#19170=CARTESIAN_POINT('Ctrl Pts',(205.134512261581,-3.39237819453857,134.368035833586));
#19171=CARTESIAN_POINT('Ctrl Pts',(205.126765989532,-3.29039400191811,134.459834646285));
#19172=CARTESIAN_POINT('Ctrl Pts',(205.119019660333,-3.18840905688475,134.551634136252));
#19173=CARTESIAN_POINT('Ctrl Pts',(205.111273331135,-3.0825801067567,134.639161901196));
#19174=CARTESIAN_POINT('Ctrl Pts',(205.103527001936,-2.97330779642674,134.722092590303));
#19175=CARTESIAN_POINT('Ctrl Pts',(205.095778938027,-2.86401101569629,134.805041850878));
#19176=CARTESIAN_POINT('Ctrl Pts',(205.088030874119,-2.75126965172672,134.883391750785));
#19177=CARTESIAN_POINT('Ctrl Pts',(205.08028281021,-2.63551491623087,134.956859165287));
#19178=CARTESIAN_POINT('Ctrl Pts',(205.072526511583,-2.51963715546859,135.030404661676));
#19179=CARTESIAN_POINT('Ctrl Pts',(205.064770212956,-2.40073995618037,135.09905709693));
#19180=CARTESIAN_POINT('Ctrl Pts',(205.057013914329,-2.27928130406476,135.162578120105));
#19181=CARTESIAN_POINT('Ctrl Pts',(205.049253475948,-2.15775782605347,135.226133046236));
#19182=CARTESIAN_POINT('Ctrl Pts',(205.041493037566,-2.03367052466753,135.284550936595));
#19183=CARTESIAN_POINT('Ctrl Pts',(205.033732599185,-1.90749822121525,135.337641283768));
#19184=CARTESIAN_POINT('Ctrl Pts',(205.025959703041,-1.78112337448988,135.390816856402));
#19185=CARTESIAN_POINT('Ctrl Pts',(205.018186806897,-1.65265720386027,135.438647659219));
#19186=CARTESIAN_POINT('Ctrl Pts',(205.010413910753,-1.52259542748432,135.480992549491));
#19187=CARTESIAN_POINT('Ctrl Pts',(205.002923530958,-1.39726092104092,135.521798357858));
#19188=CARTESIAN_POINT('Ctrl Pts',(204.995433151164,-1.27044508084342,135.557510033643));
#19189=CARTESIAN_POINT('Ctrl Pts',(204.987942771369,-1.14259930875746,135.588046422688));
#19190=CARTESIAN_POINT('Ctrl Pts',(204.980168435136,-1.00990696933439,135.619740430505));
#19191=CARTESIAN_POINT('Ctrl Pts',(204.972394098903,-0.875684739349071,
135.645959422382));
#19192=CARTESIAN_POINT('Ctrl Pts',(204.964619762671,-0.740424173411585,
135.666557148552));
#19193=CARTESIAN_POINT('Ctrl Pts',(204.956855007588,-0.605330303598526,
135.687129489931));
#19194=CARTESIAN_POINT('Ctrl Pts',(204.949090252504,-0.469201026759951,
135.702094291348));
#19195=CARTESIAN_POINT('Ctrl Pts',(204.941325497421,-0.332541196813679,
135.711355565079));
#19196=CARTESIAN_POINT('Ctrl Pts',(204.93356845438,-0.196017098948459,135.720607640409));
#19197=CARTESIAN_POINT('Ctrl Pts',(204.925811411339,-0.0589638841786129,
135.724167435013));
#19198=CARTESIAN_POINT('Ctrl Pts',(204.918054368298,0.0781056551375337,
135.721990389025));
#19199=CARTESIAN_POINT('Ctrl Pts',(204.910303174885,0.215071829587541,135.719814984758));
#19200=CARTESIAN_POINT('Ctrl Pts',(204.902551981471,0.35205391474676,135.711911357085));
#19201=CARTESIAN_POINT('Ctrl Pts',(204.894800788057,0.488536635525835,135.69828695725));
#19202=CARTESIAN_POINT('Ctrl Pts',(204.887052889087,0.624961347859993,135.684668348112));
#19203=CARTESIAN_POINT('Ctrl Pts',(204.879304990118,0.760886729730015,135.665333841567));
#19204=CARTESIAN_POINT('Ctrl Pts',(204.871557091148,0.895800372082467,135.640342912393));
#19205=CARTESIAN_POINT('Ctrl Pts',(204.86381081286,1.03068579361427,135.615357210744));
#19206=CARTESIAN_POINT('Ctrl Pts',(204.856064534572,1.16455951239554,135.584717511067));
#19207=CARTESIAN_POINT('Ctrl Pts',(204.848318256284,1.29691748072938,135.548534740707));
#19208=CARTESIAN_POINT('Ctrl Pts',(204.840571920805,1.42927642625718,135.512351703211));
#19209=CARTESIAN_POINT('Ctrl Pts',(204.832825585326,1.56011922188006,135.470625616466));
#19210=CARTESIAN_POINT('Ctrl Pts',(204.825079249848,1.68895558188255,135.423517694883));
#19211=CARTESIAN_POINT('Ctrl Pts',(204.817331179624,1.81782079400553,135.376399223767));
#19212=CARTESIAN_POINT('Ctrl Pts',(204.809583109401,1.9446783092763,135.323896653782));
#19213=CARTESIAN_POINT('Ctrl Pts',(204.801835039178,2.06905684589674,135.26621974028));
#19214=CARTESIAN_POINT('Ctrl Pts',(204.794078734217,2.19356757344921,135.208481527095));
#19215=CARTESIAN_POINT('Ctrl Pts',(204.786322429256,2.31559370402974,135.145558149584));
#19216=CARTESIAN_POINT('Ctrl Pts',(204.778566124295,2.43468715333658,135.077706090129));
#19217=CARTESIAN_POINT('Ctrl Pts',(204.770805679558,2.55384416642928,135.009817815973));
#19218=CARTESIAN_POINT('Ctrl Pts',(204.763045234822,2.67006504819365,134.936995825692));
#19219=CARTESIAN_POINT('Ctrl Pts',(204.755284790086,2.78293070430418,134.85953999184));
#19220=CARTESIAN_POINT('Ctrl Pts',(204.747511887616,2.89597754207783,134.78195981922));
#19221=CARTESIAN_POINT('Ctrl Pts',(204.739738985146,3.00565807806422,134.699731172902));
#19222=CARTESIAN_POINT('Ctrl Pts',(204.731966082676,3.11158561669959,134.613194824045));
#19223=CARTESIAN_POINT('Ctrl Pts',(204.724475770969,3.21366206571824,134.529804580902));
#19224=CARTESIAN_POINT('Ctrl Pts',(204.716985459263,3.31225343579821,134.442414621717));
#19225=CARTESIAN_POINT('Ctrl Pts',(204.709495147556,3.40704746464756,134.351360848203));
#19226=CARTESIAN_POINT('Ctrl Pts',(204.701720813585,3.50543595201642,134.256854441481));
#19227=CARTESIAN_POINT('Ctrl Pts',(204.693946479614,3.60004509988113,134.158101516487));
#19228=CARTESIAN_POINT('Ctrl Pts',(204.686172145643,3.69048616693734,134.055436580097));
#19229=CARTESIAN_POINT('Ctrl Pts',(204.678407392841,3.78081577349329,133.952898169028));
#19230=CARTESIAN_POINT('Ctrl Pts',(204.670642640039,3.86698726395705,133.846457629871));
#19231=CARTESIAN_POINT('Ctrl Pts',(204.662877887237,3.94864699528088,133.736487826464));
#19232=CARTESIAN_POINT('Ctrl Pts',(204.655120846494,4.03022562103922,133.626627246574));
#19233=CARTESIAN_POINT('Ctrl Pts',(204.647363805751,4.107301173756,133.513244690025));
#19234=CARTESIAN_POINT('Ctrl Pts',(204.639606765008,4.17955898715758,133.396747497522));
#19235=CARTESIAN_POINT('Ctrl Pts',(204.631855573906,4.25176231040909,133.280338156412));
#19236=CARTESIAN_POINT('Ctrl Pts',(204.624104382805,4.31915492055407,133.160819185333));
#19237=CARTESIAN_POINT('Ctrl Pts',(204.616353191703,4.38146456774871,133.038628127078));
#19238=CARTESIAN_POINT('Ctrl Pts',(204.60860529506,4.44374773172442,132.916489003198));
#19239=CARTESIAN_POINT('Ctrl Pts',(204.600857398416,4.50095205236715,132.79168039854));
#19240=CARTESIAN_POINT('Ctrl Pts',(204.593109501772,4.55285059786026,132.664665564628));
#19241=CARTESIAN_POINT('Ctrl Pts',(204.585363225818,4.60473828731866,132.537677299427));
#19242=CARTESIAN_POINT('Ctrl Pts',(204.577616949864,4.65132226139587,132.4084840846));
#19243=CARTESIAN_POINT('Ctrl Pts',(204.56987067391,4.6924233962874,132.277569948406));
#19244=CARTESIAN_POINT('Ctrl Pts',(204.562124340771,4.73352483459662,132.146654845776));
#19245=CARTESIAN_POINT('Ctrl Pts',(204.554378007632,4.7691432358447,132.014019169442));
#19246=CARTESIAN_POINT('Ctrl Pts',(204.546631674493,4.7991492228434,131.880162550722));
#19247=CARTESIAN_POINT('Ctrl Pts',(204.538883606613,4.82916192948898,131.746275955676));
#19248=CARTESIAN_POINT('Ctrl Pts',(204.531135538733,4.85355963536943,131.611168255589));
#19249=CARTESIAN_POINT('Ctrl Pts',(204.523387470853,4.87226407424628,131.475349330816));
#19250=CARTESIAN_POINT('Ctrl Pts',(204.515631168227,4.89098839243932,131.339386055957));
#19251=CARTESIAN_POINT('Ctrl Pts',(204.507874865602,4.90400730292682,131.202710434351));
#19252=CARTESIAN_POINT('Ctrl Pts',(204.500118562976,4.91129439105524,131.065838086747));
#19253=CARTESIAN_POINT('Ctrl Pts',(204.492358120575,4.91858536852522,130.92889268619));
#19254=CARTESIAN_POINT('Ctrl Pts',(204.484597678174,4.92013842339908,130.791750741167));
#19255=CARTESIAN_POINT('Ctrl Pts',(204.476837235773,4.91597931619433,130.654926935789));
#19256=CARTESIAN_POINT('Ctrl Pts',(204.469064335614,4.91181353241767,130.517883488567));
#19257=CARTESIAN_POINT('Ctrl Pts',(204.461291435454,4.90191729087102,130.381159591714));
#19258=CARTESIAN_POINT('Ctrl Pts',(204.453518535295,4.88636827354715,130.245264778043));
#19259=CARTESIAN_POINT('Ctrl Pts',(204.446028198111,4.87138449911938,130.114310056498));
#19260=CARTESIAN_POINT('Ctrl Pts',(204.438537860927,4.85115184404818,129.984125490812));
#19261=CARTESIAN_POINT('Ctrl Pts',(204.431047523743,4.8257841278719,129.855155363851));
#19262=CARTESIAN_POINT('Ctrl Pts',(204.423273190132,4.79945459374589,129.721295329489));
#19263=CARTESIAN_POINT('Ctrl Pts',(204.415498856521,4.7675095188085,129.588319613196));
#19264=CARTESIAN_POINT('Ctrl Pts',(204.40772452291,4.73002020891244,129.456736083143));
#19265=CARTESIAN_POINT('Ctrl Pts',(204.399959770479,4.69257710128169,129.325314718175));
#19266=CARTESIAN_POINT('Ctrl Pts',(204.392195018048,4.64960345998627,129.195282498014));
#19267=CARTESIAN_POINT('Ctrl Pts',(204.384430265617,4.60122183314642,129.067138494556));
#19268=CARTESIAN_POINT('Ctrl Pts',(204.376673225255,4.55288825966949,128.939121765658));
#19269=CARTESIAN_POINT('Ctrl Pts',(204.368916184894,4.49915752696644,128.812989884719));
#19270=CARTESIAN_POINT('Ctrl Pts',(204.361159144532,4.44020225742291,128.689227766969));
#19271=CARTESIAN_POINT('Ctrl Pts',(204.353407953822,4.38129144656131,128.565558979308));
#19272=CARTESIAN_POINT('Ctrl Pts',(204.345656763112,4.31716410838634,128.444256749339));
#19273=CARTESIAN_POINT('Ctrl Pts',(204.337905572402,4.24804120227294,128.325786631119));
#19274=CARTESIAN_POINT('Ctrl Pts',(204.330157676164,4.17894767531605,128.207366865993));
#19275=CARTESIAN_POINT('Ctrl Pts',(204.322409779926,4.10486300002969,128.091777155478));
#19276=CARTESIAN_POINT('Ctrl Pts',(204.314661883687,4.02605426077588,127.979458822496));
#19277=CARTESIAN_POINT('Ctrl Pts',(204.306915608147,3.94726200666425,127.867163984164));
#19278=CARTESIAN_POINT('Ctrl Pts',(204.299169332607,3.86374787853738,127.758139482086));
#19279=CARTESIAN_POINT('Ctrl Pts',(204.291423057066,3.77582228221695,127.65279764729));
#19280=CARTESIAN_POINT('Ctrl Pts',(204.283676724349,3.68789603690174,127.547455034947));
#19281=CARTESIAN_POINT('Ctrl Pts',(204.275930391632,3.59555850894457,127.445795444277));
#19282=CARTESIAN_POINT('Ctrl Pts',(204.268184058915,3.49916012072415,127.348197786906));
#19283=CARTESIAN_POINT('Ctrl Pts',(204.260435991465,3.40274014480243,127.250578273267));
#19284=CARTESIAN_POINT('Ctrl Pts',(204.252687924014,3.30225777370524,127.15702278111));
#19285=CARTESIAN_POINT('Ctrl Pts',(204.244939856564,3.19809967933992,127.067872760834));
#19286=CARTESIAN_POINT('Ctrl Pts',(204.237183554378,3.09383088454986,126.978627990887));
#19287=CARTESIAN_POINT('Ctrl Pts',(204.229427252191,2.9858788601325,126.893798300623));
#19288=CARTESIAN_POINT('Ctrl Pts',(204.221670950005,2.87466313460505,126.813684619061));
#19289=CARTESIAN_POINT('Ctrl Pts',(204.21391050805,2.76338804993092,126.73352817844));
#19290=CARTESIAN_POINT('Ctrl Pts',(204.206150066094,2.64884611955096,126.658092976936));
#19291=CARTESIAN_POINT('Ctrl Pts',(204.198389624139,2.53148428592039,126.587635540846));
#19292=CARTESIAN_POINT('Ctrl Pts',(204.190616724431,2.41393405262733,126.517065000208));
#19293=CARTESIAN_POINT('Ctrl Pts',(204.182843824723,2.29355521370091,126.451488380188));
#19294=CARTESIAN_POINT('Ctrl Pts',(204.175070925015,2.17081844249119,126.391115739674));
#19295=CARTESIAN_POINT('Ctrl Pts',(204.16758058332,2.05254335990331,126.332937746457));
#19296=CARTESIAN_POINT('Ctrl Pts',(204.160090241625,1.932079080105,126.279592079101));
#19297=CARTESIAN_POINT('Ctrl Pts',(204.15259989993,1.80986091391834,126.231223124032));
#19298=CARTESIAN_POINT('Ctrl Pts',(204.144825565478,1.68300890386598,126.181020282947));
#19299=CARTESIAN_POINT('Ctrl Pts',(204.137051231027,1.55386555861245,126.136019952371));
#19300=CARTESIAN_POINT('Ctrl Pts',(204.129276896576,1.42289670472903,126.096436655757));
#19301=CARTESIAN_POINT('Ctrl Pts',(204.121512143292,1.2920892581833,126.056902141999));
#19302=CARTESIAN_POINT('Ctrl Pts',(204.113747390009,1.15946115004296,126.022771490962));
#19303=CARTESIAN_POINT('Ctrl Pts',(204.105982636726,1.02549850401181,125.994211359927));
#19304=CARTESIAN_POINT('Ctrl Pts',(204.098225595501,0.891668911505565,125.965679595202));
#19305=CARTESIAN_POINT('Ctrl Pts',(204.090468554277,0.756507798773581,125.942707421116));
#19306=CARTESIAN_POINT('Ctrl Pts',(204.082711513052,0.620516445466882,125.925411714021));
#19307=CARTESIAN_POINT('Ctrl Pts',(204.07496032147,0.484627644240924,125.908129049746));
#19308=CARTESIAN_POINT('Ctrl Pts',(204.067209129887,0.347910234907202,125.896514381183));
#19309=CARTESIAN_POINT('Ctrl Pts',(204.059457938304,0.210875335327797,125.890633452221));
#19310=CARTESIAN_POINT('Ctrl Pts',(204.051710041182,0.0738986791749443,
125.884755022807));
#19311=CARTESIAN_POINT('Ctrl Pts',(204.043962144059,-0.0633948090470082,
125.884605502735));
#19312=CARTESIAN_POINT('Ctrl Pts',(204.036214246936,-0.200489466144424,
125.89019873211));
#19313=CARTESIAN_POINT('Ctrl Pts',(204.028467970504,-0.337555446031198,
125.895790791504));
#19314=CARTESIAN_POINT('Ctrl Pts',(204.020721694072,-0.474422287127775,
125.907123195051));
#19315=CARTESIAN_POINT('Ctrl Pts',(204.01297541764,-0.61057530164394,125.924157664458));
#19316=CARTESIAN_POINT('Ctrl Pts',(204.005229084025,-0.746729321239624,
125.941192259614));
#19317=CARTESIAN_POINT('Ctrl Pts',(203.997482750411,-0.882169115799372,
125.963928956088));
#19318=CARTESIAN_POINT('Ctrl Pts',(203.989736416796,-1.0163864843013,125.992277744523));
#19319=CARTESIAN_POINT('Ctrl Pts',(203.981988348442,-1.15063390987372,126.020632881478));
#19320=CARTESIAN_POINT('Ctrl Pts',(203.974240280088,-1.28365798219704,126.054602530483));
#19321=CARTESIAN_POINT('Ctrl Pts',(203.966492211735,-1.41496242369231,126.094045935717));
#19322=CARTESIAN_POINT('Ctrl Pts',(203.958735908642,-1.54640641710633,126.133531261871));
#19323=CARTESIAN_POINT('Ctrl Pts',(203.950979605549,-1.67612675374356,126.178501852826));
#19324=CARTESIAN_POINT('Ctrl Pts',(203.943223302457,-1.80364348801349,126.228767406774));
#19325=CARTESIAN_POINT('Ctrl Pts',(203.935462859591,-1.93122828181124,126.279059788964));
#19326=CARTESIAN_POINT('Ctrl Pts',(203.927702416725,-2.05660677247295,126.334652606956));
#19327=CARTESIAN_POINT('Ctrl Pts',(203.91994197386,-2.17932155377599,126.395308494065));
#19328=CARTESIAN_POINT('Ctrl Pts',(203.912169073245,-2.30223332769157,126.456061751365));
#19329=CARTESIAN_POINT('Ctrl Pts',(203.904396172631,-2.42247250426769,126.521894131622));
#19330=CARTESIAN_POINT('Ctrl Pts',(203.896623272017,-2.53960794450345,126.592523185908));
#19331=CARTESIAN_POINT('Ctrl Pts',(203.88913294005,-2.65248515417354,126.660584658622));
#19332=CARTESIAN_POINT('Ctrl Pts',(203.881642608084,-2.76248011304978,126.733099943225));
#19333=CARTESIAN_POINT('Ctrl Pts',(203.874152276117,-2.86923605004317,126.809780845971));
#19334=CARTESIAN_POINT('Ctrl Pts',(203.866074034918,-2.98437116185463,126.892480361897));
#19335=CARTESIAN_POINT('Ctrl Pts',(203.857995793719,-3.09613368668095,126.980309741443));
#19336=CARTESIAN_POINT('Ctrl Pts',(203.84991755252,-3.20403203740082,127.07295849962));
#19337=CARTESIAN_POINT('Ctrl Pts',(203.842215517175,-3.30690553306662,127.161292580348));
#19338=CARTESIAN_POINT('Ctrl Pts',(203.834513481829,-3.40626624325742,127.25400703648));
#19339=CARTESIAN_POINT('Ctrl Pts',(203.826811446484,-3.50171630356533,127.350787686261));
#19340=CARTESIAN_POINT('Ctrl Pts',(203.819116363939,-3.59708019895571,127.447480969971));
#19341=CARTESIAN_POINT('Ctrl Pts',(203.811421281394,-3.68854018756952,127.548232866472));
#19342=CARTESIAN_POINT('Ctrl Pts',(203.803726198849,-3.77573196917681,127.65268944826));
#19343=CARTESIAN_POINT('Ctrl Pts',(203.796036329942,-3.8628646758669,127.757075257736));
#19344=CARTESIAN_POINT('Ctrl Pts',(203.788346461035,-3.94573467410029,127.86516045547));
#19345=CARTESIAN_POINT('Ctrl Pts',(203.780656592127,-4.02401534417658,127.976555183606));
#19346=CARTESIAN_POINT('Ctrl Pts',(203.772970201974,-4.10226060153588,128.087899518843));
#19347=CARTESIAN_POINT('Ctrl Pts',(203.76528381182,-4.17592043400376,128.202550080349));
#19348=CARTESIAN_POINT('Ctrl Pts',(203.757597421666,-4.24470957225871,128.320085328941));
#19349=CARTESIAN_POINT('Ctrl Pts',(203.749911435145,-4.31349509821327,128.437614405444));
#19350=CARTESIAN_POINT('Ctrl Pts',(203.742225448624,-4.37741023070302,128.558027528844));
#19351=CARTESIAN_POINT('Ctrl Pts',(203.734539462103,-4.4362141058302,128.680875870803));
#19352=CARTESIAN_POINT('Ctrl Pts',(203.726853680479,-4.49501641333659,128.803720937816));
#19353=CARTESIAN_POINT('Ctrl Pts',(203.719167898855,-4.54870756838372,128.929000732856));
#19354=CARTESIAN_POINT('Ctrl Pts',(203.71148211723,-4.59709392678213,129.056244348308));
#19355=CARTESIAN_POINT('Ctrl Pts',(203.703792765134,-4.64550276332794,129.183547075479));
#19356=CARTESIAN_POINT('Ctrl Pts',(203.696103413038,-4.68860174757454,129.312815070517));
#19357=CARTESIAN_POINT('Ctrl Pts',(203.688414060942,-4.72624641962959,129.443560175386));
#19358=CARTESIAN_POINT('Ctrl Pts',(203.685700869741,-4.73952935838289,129.489693641968));
#19359=CARTESIAN_POINT('Ctrl Pts',(203.682987678541,-4.752133674154,129.536010890174));
#19360=CARTESIAN_POINT('Ctrl Pts',(203.680274487341,-4.76405452823405,129.582490119308));
#19361=CARTESIAN_POINT('Origin',(213.235140564004,0.,130.804360617566));
#19362=CARTESIAN_POINT('',(201.584606355351,-4.76405452823405,129.582490119308));
#19363=CARTESIAN_POINT('',(201.930097584127,-4.76405452823404,129.582490119308));
#19364=CARTESIAN_POINT('',(213.235140564004,-4.76405452823405,129.582490119308));
#19365=CARTESIAN_POINT('',(203.264859436027,-4.91824791911963,130.799836396593));
#19366=CARTESIAN_POINT('Ctrl Pts',(203.264859435991,-4.91824791912021,130.799836397221));
#19367=CARTESIAN_POINT('Ctrl Pts',(203.257189383465,-4.91837258488303,130.935359665711));
#19368=CARTESIAN_POINT('Ctrl Pts',(203.249519330939,-4.91289148263668,131.071020543707));
#19369=CARTESIAN_POINT('Ctrl Pts',(203.241849278414,-4.90179734488421,131.206313167236));
#19370=CARTESIAN_POINT('Ctrl Pts',(203.234183418891,-4.89070927198605,131.341531830077));
#19371=CARTESIAN_POINT('Ctrl Pts',(203.226517559368,-4.8740142988451,131.476382241115));
#19372=CARTESIAN_POINT('Ctrl Pts',(203.218851699845,-4.85175723294996,131.610359882465));
#19373=CARTESIAN_POINT('Ctrl Pts',(203.211187985896,-4.82950639651798,131.744300025216));
#19374=CARTESIAN_POINT('Ctrl Pts',(203.203524271947,-4.80169662793145,131.877367489554));
#19375=CARTESIAN_POINT('Ctrl Pts',(203.195860557999,-4.76842439234139,132.009064679576));
#19376=CARTESIAN_POINT('Ctrl Pts',(203.18819724317,-4.73515388954357,132.140755010911));
#19377=CARTESIAN_POINT('Ctrl Pts',(203.180533928342,-4.69642158345535,132.271074821851));
#19378=CARTESIAN_POINT('Ctrl Pts',(203.172870613514,-4.6523745561182,132.399538993825));
#19379=CARTESIAN_POINT('Ctrl Pts',(203.165205951912,-4.60831978783102,132.528025742458));
#19380=CARTESIAN_POINT('Ctrl Pts',(203.157541290311,-4.55894857073882,132.654655825109));
#19381=CARTESIAN_POINT('Ctrl Pts',(203.14987662871,-4.50445695066178,132.778962005729));
#19382=CARTESIAN_POINT('Ctrl Pts',(203.142204113634,-4.44990949660173,132.903395554725));
#19383=CARTESIAN_POINT('Ctrl Pts',(203.134531598558,-4.39023132120439,133.025500078541));
#19384=CARTESIAN_POINT('Ctrl Pts',(203.126859083481,-4.32566565593964,133.144830590782));
#19385=CARTESIAN_POINT('Ctrl Pts',(203.119182649825,-4.26106701508398,133.264222048637));
#19386=CARTESIAN_POINT('Ctrl Pts',(203.111506216169,-4.19157611789148,133.380836329876));
#19387=CARTESIAN_POINT('Ctrl Pts',(203.103829782513,-4.11748010840755,133.494256641461));
#19388=CARTESIAN_POINT('Ctrl Pts',(203.096141011026,-4.04326500925227,133.607859246098));
#19389=CARTESIAN_POINT('Ctrl Pts',(203.08845223954,-3.9644302428689,133.718257299233));
#19390=CARTESIAN_POINT('Ctrl Pts',(203.080763468054,-3.88130435803297,133.825065757565));
#19391=CARTESIAN_POINT('Ctrl Pts',(203.073308445649,-3.80070561283009,133.928627093911));
#19392=CARTESIAN_POINT('Ctrl Pts',(203.065853423243,-3.71607313595503,134.028813718384));
#19393=CARTESIAN_POINT('Ctrl Pts',(203.058398400838,-3.62773852230693,134.125308716569));
#19394=CARTESIAN_POINT('Ctrl Pts',(203.050624066711,-3.53562038179653,134.225936765238));
#19395=CARTESIAN_POINT('Ctrl Pts',(203.042849732584,-3.43916625203493,134.322888467361));
#19396=CARTESIAN_POINT('Ctrl Pts',(203.035075398457,-3.33870121485528,134.415767166326));
#19397=CARTESIAN_POINT('Ctrl Pts',(203.027310645502,-3.23835999185389,134.508531400596));
#19398=CARTESIAN_POINT('Ctrl Pts',(203.019545892547,-3.13401798102474,134.597232356386));
#19399=CARTESIAN_POINT('Ctrl Pts',(203.011781139593,-3.026039452382,134.68150754477));
#19400=CARTESIAN_POINT('Ctrl Pts',(203.0040240987,-2.91816816953492,134.76569902985));
#19401=CARTESIAN_POINT('Ctrl Pts',(202.996267057807,-2.80666786281095,134.845473256243));
#19402=CARTESIAN_POINT('Ctrl Pts',(202.988510016914,-2.69193820449843,134.920505873222));
#19403=CARTESIAN_POINT('Ctrl Pts',(202.980758825666,-2.57729506471272,134.995481907523));
#19404=CARTESIAN_POINT('Ctrl Pts',(202.973007634418,-2.45942774649362,135.065723236469));
#19405=CARTESIAN_POINT('Ctrl Pts',(202.96525644317,-2.33876713339567,135.130947188784));
#19406=CARTESIAN_POINT('Ctrl Pts',(202.957508546385,-2.21815780427522,135.196143419181));
#19407=CARTESIAN_POINT('Ctrl Pts',(202.949760649599,-2.09475788478772,135.256326328838));
#19408=CARTESIAN_POINT('Ctrl Pts',(202.942012752814,-1.96902504732344,135.311257934514));
#19409=CARTESIAN_POINT('Ctrl Pts',(202.934266476722,-1.84331851045724,135.366178049683));
#19410=CARTESIAN_POINT('Ctrl Pts',(202.92652020063,-1.71528038430399,135.415848889344));
#19411=CARTESIAN_POINT('Ctrl Pts',(202.918773924538,-1.58539025926972,135.460079765916));
#19412=CARTESIAN_POINT('Ctrl Pts',(202.911027591264,-1.45549917541524,135.504310968991));
#19413=CARTESIAN_POINT('Ctrl Pts',(202.903281257991,-1.32375643549607,135.54310200282));
#19414=CARTESIAN_POINT('Ctrl Pts',(202.895534924717,-1.19065842226258,135.576311537682));
#19415=CARTESIAN_POINT('Ctrl Pts',(202.887786856706,-1.05753060265117,135.609528509589));
#19416=CARTESIAN_POINT('Ctrl Pts',(202.880038788695,-0.923047285050385,
135.637161400668));
#19417=CARTESIAN_POINT('Ctrl Pts',(202.872290720684,-0.787716324822747,
135.659119731478));
#19418=CARTESIAN_POINT('Ctrl Pts',(202.864534417934,-0.65224153324019,135.681101399863));
#19419=CARTESIAN_POINT('Ctrl Pts',(202.856778115184,-0.515917685950118,
135.697396397709));
#19420=CARTESIAN_POINT('Ctrl Pts',(202.849021812434,-0.379259621354758,
135.707965944477));
#19421=CARTESIAN_POINT('Ctrl Pts',(202.841261369911,-0.242528618235135,
135.71854113253));
#19422=CARTESIAN_POINT('Ctrl Pts',(202.833500927389,-0.105463432899442,
135.723384766673));
#19423=CARTESIAN_POINT('Ctrl Pts',(202.825740484867,0.0314207805563875,
135.722510248987));
#19424=CARTESIAN_POINT('Ctrl Pts',(202.817967584593,0.168524732702548,135.721634327448));
#19425=CARTESIAN_POINT('Ctrl Pts',(202.810194684319,0.305446741698207,135.715021929815));
#19426=CARTESIAN_POINT('Ctrl Pts',(202.802421784046,0.441675557289912,135.70273848831));
#19427=CARTESIAN_POINT('Ctrl Pts',(202.794931448372,0.572952110607848,135.690901580996));
#19428=CARTESIAN_POINT('Ctrl Pts',(202.787441112698,0.703584688784279,135.673798825022));
#19429=CARTESIAN_POINT('Ctrl Pts',(202.779950777025,0.833126405809881,135.651533345502));
#19430=CARTESIAN_POINT('Ctrl Pts',(202.772176442908,0.96757973795983,135.628423663291));
#19431=CARTESIAN_POINT('Ctrl Pts',(202.764402108791,1.10128376375181,135.599678835429));
#19432=CARTESIAN_POINT('Ctrl Pts',(202.756627774674,1.23372905007338,135.565357959878));
#19433=CARTESIAN_POINT('Ctrl Pts',(202.748863021729,1.36601110941638,135.53107938174));
#19434=CARTESIAN_POINT('Ctrl Pts',(202.741098268784,1.49703714105001,135.491238526238));
#19435=CARTESIAN_POINT('Ctrl Pts',(202.733333515839,1.62630527593573,135.445945929931));
#19436=CARTESIAN_POINT('Ctrl Pts',(202.725576474956,1.75544501988741,135.40069831887));
#19437=CARTESIAN_POINT('Ctrl Pts',(202.717819434073,1.88282997506119,135.350009871036));
#19438=CARTESIAN_POINT('Ctrl Pts',(202.710062393191,2.00797122337188,135.294041522554));
#19439=CARTESIAN_POINT('Ctrl Pts',(202.702311201953,2.13301810169324,135.238115380238));
#19440=CARTESIAN_POINT('Ctrl Pts',(202.694560010715,2.25582428551557,135.17691742141));
#19441=CARTESIAN_POINT('Ctrl Pts',(202.686808819477,2.37591905240151,135.110657369874));
#19442=CARTESIAN_POINT('Ctrl Pts',(202.679060922702,2.49596277580801,135.044425480627));
#19443=CARTESIAN_POINT('Ctrl Pts',(202.671313025927,2.61329703275995,134.973135966364));
#19444=CARTESIAN_POINT('Ctrl Pts',(202.663565129152,2.72747421811156,134.897045244072));
#19445=CARTESIAN_POINT('Ctrl Pts',(202.65581885307,2.84162752005722,134.820970438319));
#19446=CARTESIAN_POINT('Ctrl Pts',(202.648072576988,2.95262473882447,134.740096638841));
#19447=CARTESIAN_POINT('Ctrl Pts',(202.640326300906,3.06004621322242,134.654724267332));
#19448=CARTESIAN_POINT('Ctrl Pts',(202.632579967643,3.1674684805811,134.569351265625));
#19449=CARTESIAN_POINT('Ctrl Pts',(202.62483363438,3.27131464482454,134.479479868875));
#19450=CARTESIAN_POINT('Ctrl Pts',(202.617087301116,3.37119749425472,134.385451305782));
#19451=CARTESIAN_POINT('Ctrl Pts',(202.609339233116,3.47110271175664,134.291401685645));
#19452=CARTESIAN_POINT('Ctrl Pts',(202.601591165115,3.56704256369362,134.193193314579));
#19453=CARTESIAN_POINT('Ctrl Pts',(202.593843097114,3.65866641892285,134.091204559335));
#19454=CARTESIAN_POINT('Ctrl Pts',(202.586086794374,3.75038765307602,133.989107409229));
#19455=CARTESIAN_POINT('Ctrl Pts',(202.578330491635,3.83778346561284,133.883222140185));
#19456=CARTESIAN_POINT('Ctrl Pts',(202.570574188895,3.92054294663494,133.7739609385));
#19457=CARTESIAN_POINT('Ctrl Pts',(202.562813746383,4.00334659888406,133.664641420822));
#19458=CARTESIAN_POINT('Ctrl Pts',(202.555053303871,4.08150876616667,133.551942701296));
#19459=CARTESIAN_POINT('Ctrl Pts',(202.547292861359,4.15476227066247,133.436305437804));
#19460=CARTESIAN_POINT('Ctrl Pts',(202.539519961095,4.22813336818707,133.320482543111));
#19461=CARTESIAN_POINT('Ctrl Pts',(202.531747060832,4.29657986120505,133.201712016897));
#19462=CARTESIAN_POINT('Ctrl Pts',(202.523974160569,4.35988045644892,133.080459356192));
#19463=CARTESIAN_POINT('Ctrl Pts',(202.516483824783,4.42087991581972,132.963614534721));
#19464=CARTESIAN_POINT('Ctrl Pts',(202.508993488998,4.47710098314102,132.844465187877));
#19465=CARTESIAN_POINT('Ctrl Pts',(202.501503153212,4.52838886767896,132.723443035176));
#19466=CARTESIAN_POINT('Ctrl Pts',(202.493728819094,4.58162134777368,132.597832291183));
#19467=CARTESIAN_POINT('Ctrl Pts',(202.485954484976,4.62970780184522,132.46980602598));
#19468=CARTESIAN_POINT('Ctrl Pts',(202.478180150858,4.67242258964327,132.339824783964));
#19469=CARTESIAN_POINT('Ctrl Pts',(202.470415397911,4.7150847352829,132.210003732212));
#19470=CARTESIAN_POINT('Ctrl Pts',(202.462650644965,4.75238826578558,132.078232865362));
#19471=CARTESIAN_POINT('Ctrl Pts',(202.454885892019,4.78415490621555,131.944994167762));
#19472=CARTESIAN_POINT('Ctrl Pts',(202.447128851135,4.81588999557021,131.811887804716));
#19473=CARTESIAN_POINT('Ctrl Pts',(202.439371810251,4.8420990486564,131.677316889991));
#19474=CARTESIAN_POINT('Ctrl Pts',(202.431614769367,4.86265319342588,131.541779754126));
#19475=CARTESIAN_POINT('Ctrl Pts',(202.423863578128,4.88319183815493,131.406344827869));
#19476=CARTESIAN_POINT('Ctrl Pts',(202.416112386889,4.89808400423516,131.269945515757));
#19477=CARTESIAN_POINT('Ctrl Pts',(202.40836119565,4.90725170126882,131.133091210749));
#19478=CARTESIAN_POINT('Ctrl Pts',(202.400613298874,4.91641550178662,130.996295072471));
#19479=CARTESIAN_POINT('Ctrl Pts',(202.392865402097,4.91985964633597,130.859044715197));
#19480=CARTESIAN_POINT('Ctrl Pts',(202.385117505321,4.91755792427646,130.721855321458));
#19481=CARTESIAN_POINT('Ctrl Pts',(202.377371229238,4.91525668368759,130.584694624784));
#19482=CARTESIAN_POINT('Ctrl Pts',(202.369624953155,4.907211973712,130.447595256941));
#19483=CARTESIAN_POINT('Ctrl Pts',(202.361878677072,4.89344971050554,130.311072676042));
#19484=CARTESIAN_POINT('Ctrl Pts',(202.354132343808,4.8796873457092,130.174549087364));
#19485=CARTESIAN_POINT('Ctrl Pts',(202.346386010544,4.86020738267642,130.038602683118));
#19486=CARTESIAN_POINT('Ctrl Pts',(202.338639677279,4.83508760939448,129.903743677918));
#19487=CARTESIAN_POINT('Ctrl Pts',(202.330891609277,4.80996221071351,129.76885447198));
#19488=CARTESIAN_POINT('Ctrl Pts',(202.323143541275,4.77919456014558,129.635053533938));
#19489=CARTESIAN_POINT('Ctrl Pts',(202.315395473273,4.74291346365742,129.502840376172));
#19490=CARTESIAN_POINT('Ctrl Pts',(202.307639170533,4.70659380718827,129.37048670069));
#19491=CARTESIAN_POINT('Ctrl Pts',(202.299882867792,4.66474910293164,129.239724554101));
#19492=CARTESIAN_POINT('Ctrl Pts',(202.292126565051,4.6175580804997,129.111038310469));
#19493=CARTESIAN_POINT('Ctrl Pts',(202.284366122538,4.57034187079823,128.982283383115));
#19494=CARTESIAN_POINT('Ctrl Pts',(202.276605680025,4.51777380687754,128.855606927377));
#19495=CARTESIAN_POINT('Ctrl Pts',(202.268845237512,4.46008021055639,128.731471913872));
#19496=CARTESIAN_POINT('Ctrl Pts',(202.261072337248,4.40229399935262,128.607137627823));
#19497=CARTESIAN_POINT('Ctrl Pts',(202.253299436983,4.33936599324112,128.485353284181));
#19498=CARTESIAN_POINT('Ctrl Pts',(202.245526536719,4.27156821364134,128.366556675755));
#19499=CARTESIAN_POINT('Ctrl Pts',(202.238036200946,4.20623505399508,128.252078623088));
#19500=CARTESIAN_POINT('Ctrl Pts',(202.230545865172,4.13638019427766,128.140375114719));
#19501=CARTESIAN_POINT('Ctrl Pts',(202.223055529399,4.06228318417237,128.03180973542));
#19502=CARTESIAN_POINT('Ctrl Pts',(202.215281195279,3.98537676351187,127.919128066919));
#19503=CARTESIAN_POINT('Ctrl Pts',(202.207506861159,3.90365654367928,127.80947024764));
#19504=CARTESIAN_POINT('Ctrl Pts',(202.199732527038,3.81738802965387,127.703275050614));
#19505=CARTESIAN_POINT('Ctrl Pts',(202.19196777409,3.73122583386185,127.597210729678));
#19506=CARTESIAN_POINT('Ctrl Pts',(202.184203021142,3.64052674103213,127.494600840736));
#19507=CARTESIAN_POINT('Ctrl Pts',(202.176438268194,3.54559989628898,127.395855895854));
#19508=CARTESIAN_POINT('Ctrl Pts',(202.168681227307,3.45076733422572,127.297209025842));
#19509=CARTESIAN_POINT('Ctrl Pts',(202.160924186421,3.35171564577153,127.202419740696));
#19510=CARTESIAN_POINT('Ctrl Pts',(202.153167145535,3.24879443203218,127.111865823948));
#19511=CARTESIAN_POINT('Ctrl Pts',(202.145415954294,3.14595083198053,127.021380194613));
#19512=CARTESIAN_POINT('Ctrl Pts',(202.137664763052,3.03924380716249,126.935123833573));
#19513=CARTESIAN_POINT('Ctrl Pts',(202.129913571811,2.92905976858584,126.853437695697));
#19514=CARTESIAN_POINT('Ctrl Pts',(202.122165675033,2.818922561165,126.771786276608));
#19515=CARTESIAN_POINT('Ctrl Pts',(202.114417778254,2.70531159267622,126.694701449615));
#19516=CARTESIAN_POINT('Ctrl Pts',(202.106669881476,2.58864613328299,126.622483735215));
#19517=CARTESIAN_POINT('Ctrl Pts',(202.098923605391,2.47200507778859,126.550281127204));
#19518=CARTESIAN_POINT('Ctrl Pts',(202.091177329306,2.35231113448206,126.482943812387));
#19519=CARTESIAN_POINT('Ctrl Pts',(202.08343105322,2.23001198118519,126.420728604467));
#19520=CARTESIAN_POINT('Ctrl Pts',(202.075684719954,2.10771192510372,126.358512937288));
#19521=CARTESIAN_POINT('Ctrl Pts',(202.067938386687,1.98280696912467,126.301419629723));
#19522=CARTESIAN_POINT('Ctrl Pts',(202.060192053421,1.85576841756085,126.249659019999));
#19523=CARTESIAN_POINT('Ctrl Pts',(202.052443985416,1.7287014165942,126.197886818844));
#19524=CARTESIAN_POINT('Ctrl Pts',(202.044695917412,1.5995002312647,126.151449839382));
#19525=CARTESIAN_POINT('Ctrl Pts',(202.036947849408,1.46865473825808,126.110509712148));
#19526=CARTESIAN_POINT('Ctrl Pts',(202.029191546665,1.33767018110433,126.06952607326));
#19527=CARTESIAN_POINT('Ctrl Pts',(202.021435243922,1.20503819899675,126.034051073798));
#19528=CARTESIAN_POINT('Ctrl Pts',(202.013678941179,1.07126291727623,126.004196159491));
#19529=CARTESIAN_POINT('Ctrl Pts',(202.005918498663,0.937416235660115,125.974325310717));
#19530=CARTESIAN_POINT('Ctrl Pts',(201.998158056148,0.802425423148925,125.950080593152));
#19531=CARTESIAN_POINT('Ctrl Pts',(201.990397613633,0.666802322505834,125.931521842765));
#19532=CARTESIAN_POINT('Ctrl Pts',(201.982624713366,0.530961507621308,125.912933300225));
#19533=CARTESIAN_POINT('Ctrl Pts',(201.974851813099,0.394486765759838,125.900049001524));
#19534=CARTESIAN_POINT('Ctrl Pts',(201.967078912833,0.257893458632686,125.892876725045));
#19535=CARTESIAN_POINT('Ctrl Pts',(201.959588577084,0.126265662529295,125.885965178895));
#19536=CARTESIAN_POINT('Ctrl Pts',(201.952098241335,-0.00547192021256673,
125.884357576005));
#19537=CARTESIAN_POINT('Ctrl Pts',(201.944607905586,-0.136862291999976,
125.888015249762));
#19538=CARTESIAN_POINT('Ctrl Pts',(201.936833571467,-0.273234369901628,
125.891811605337));
#19539=CARTESIAN_POINT('Ctrl Pts',(201.929059237349,-0.409664373849437,
125.901292410854));
#19540=CARTESIAN_POINT('Ctrl Pts',(201.92128490323,-0.545639639740232,125.916471456993));
#19541=CARTESIAN_POINT('Ctrl Pts',(201.913520150283,-0.681447328268266,
125.931631796315));
#19542=CARTESIAN_POINT('Ctrl Pts',(201.905755397337,-0.816801008994345,
125.952476360477));
#19543=CARTESIAN_POINT('Ctrl Pts',(201.89799064439,-0.951188206001152,125.978966948728));
#19544=CARTESIAN_POINT('Ctrl Pts',(201.890233603505,-1.08544192774853,126.005431226153));
#19545=CARTESIAN_POINT('Ctrl Pts',(201.882476562621,-1.21873069496959,126.037530292947));
#19546=CARTESIAN_POINT('Ctrl Pts',(201.874719521736,-1.35054769974211,126.075174221026));
#19547=CARTESIAN_POINT('Ctrl Pts',(201.866968330497,-1.48226530028765,126.112789761526));
#19548=CARTESIAN_POINT('Ctrl Pts',(201.859217139257,-1.6125129730937,126.155941733518));
#19549=CARTESIAN_POINT('Ctrl Pts',(201.851465948017,-1.74079499858619,126.204489332911));
#19550=CARTESIAN_POINT('Ctrl Pts',(201.84371805124,-1.86902250079471,126.253016298278));
#19551=CARTESIAN_POINT('Ctrl Pts',(201.835970154464,-1.99528565245025,126.306934191786));
#19552=CARTESIAN_POINT('Ctrl Pts',(201.828222257687,-2.11910499138351,126.366052708239));
#19553=CARTESIAN_POINT('Ctrl Pts',(201.820475981603,-2.24289842998043,126.425158858373));
#19554=CARTESIAN_POINT('Ctrl Pts',(201.81272970552,-2.36424872005608,126.489463299298));
#19555=CARTESIAN_POINT('Ctrl Pts',(201.804983429436,-2.48269781617095,126.558728201061));
#19556=CARTESIAN_POINT('Ctrl Pts',(201.797237096171,-2.60114778665004,126.627993614122));
#19557=CARTESIAN_POINT('Ctrl Pts',(201.789490762906,-2.71669618293738,126.702219363732));
#19558=CARTESIAN_POINT('Ctrl Pts',(201.781744429641,-2.82891129003388,126.781122621173));
#19559=CARTESIAN_POINT('Ctrl Pts',(201.773996361638,-2.94115152692565,126.860043548452));
#19560=CARTESIAN_POINT('Ctrl Pts',(201.766248293636,-3.05005666948663,126.943643843122));
#19561=CARTESIAN_POINT('Ctrl Pts',(201.758500225633,-3.15522594305475,127.031598723307));
#19562=CARTESIAN_POINT('Ctrl Pts',(201.750743922892,-3.26050699177834,127.119647082985));
#19563=CARTESIAN_POINT('Ctrl Pts',(201.74298762015,-3.36204393957021,127.212059022098));
#19564=CARTESIAN_POINT('Ctrl Pts',(201.735231317409,-3.45947053192138,127.30847064486));
#19565=CARTESIAN_POINT('Ctrl Pts',(201.727470874895,-3.55694912377835,127.404933725407));
#19566=CARTESIAN_POINT('Ctrl Pts',(201.719710432381,-3.65031272280732,127.505400457023));
#19567=CARTESIAN_POINT('Ctrl Pts',(201.711949989868,-3.73923432379541,127.609472554699));
#19568=CARTESIAN_POINT('Ctrl Pts',(201.704177089603,-3.82829866963167,127.713711718145));
#19569=CARTESIAN_POINT('Ctrl Pts',(201.696404189338,-3.9129065265913,127.821567505439));
#19570=CARTESIAN_POINT('Ctrl Pts',(201.688631289073,-3.99277278490735,127.932610532582));
#19571=CARTESIAN_POINT('Ctrl Pts',(201.681140953306,-4.06973570361064,128.039616866056));
#19572=CARTESIAN_POINT('Ctrl Pts',(201.67365061754,-4.14229560697238,128.14958247704));
#19573=CARTESIAN_POINT('Ctrl Pts',(201.666160281774,-4.21023800794793,128.262101980265));
#19574=CARTESIAN_POINT('Ctrl Pts',(201.658128312424,-4.28309339110042,128.382757879996));
#19575=CARTESIAN_POINT('Ctrl Pts',(201.650096343074,-4.35085732043947,128.506711456361));
#19576=CARTESIAN_POINT('Ctrl Pts',(201.642064373724,-4.41322893384724,128.633509761345));
#19577=CARTESIAN_POINT('Ctrl Pts',(201.634043232433,-4.47551646283025,128.760137126988));
#19578=CARTESIAN_POINT('Ctrl Pts',(201.626022091142,-4.53242599296163,128.889601270105));
#19579=CARTESIAN_POINT('Ctrl Pts',(201.618000949852,-4.58370062266684,129.021421565253));
#19580=CARTESIAN_POINT('Ctrl Pts',(201.609992618133,-4.63489336800769,129.153031346524));
#19581=CARTESIAN_POINT('Ctrl Pts',(201.601984286414,-4.68046901878164,129.286989451782));
#19582=CARTESIAN_POINT('Ctrl Pts',(201.593975954695,-4.72021745497381,129.422792580783));
#19583=CARTESIAN_POINT('Ctrl Pts',(201.590852754914,-4.73571909895888,129.475754960174));
#19584=CARTESIAN_POINT('Ctrl Pts',(201.587729555133,-4.75033495592387,129.528997715094));
#19585=CARTESIAN_POINT('Ctrl Pts',(201.584606355351,-4.76405452823405,129.582490119308));
#19586=CARTESIAN_POINT('Ctrl Pts',(203.334773566427,-4.76405452823405,129.582490119308));
#19587=CARTESIAN_POINT('Ctrl Pts',(203.32473014209,-4.80784291725373,129.753220383514));
#19588=CARTESIAN_POINT('Ctrl Pts',(203.314686717754,-4.84247434312161,129.926402595191));
#19589=CARTESIAN_POINT('Ctrl Pts',(203.304643293417,-4.86772242676584,130.101181096774));
#19590=CARTESIAN_POINT('Ctrl Pts',(203.294796401501,-4.89247644913987,130.272539485777));
#19591=CARTESIAN_POINT('Ctrl Pts',(203.284949509584,-4.90821079695266,130.445432509572));
#19592=CARTESIAN_POINT('Ctrl Pts',(203.275102617668,-4.91475699054651,130.619031757498));
#19593=CARTESIAN_POINT('Ctrl Pts',(203.271688223788,-4.9170268726106,130.679227016553));
#19594=CARTESIAN_POINT('Ctrl Pts',(203.268273829907,-4.91819242300989,130.739506976807));
#19595=CARTESIAN_POINT('Ctrl Pts',(203.264859436027,-4.91824791911963,130.799836396593));
#19596=CARTESIAN_POINT('',(203.610140564065,-4.91824975435206,130.805915067923));
#19597=CARTESIAN_POINT('Ctrl Pts',(203.680274487341,-4.76405452823405,129.582490119308));
#19598=CARTESIAN_POINT('Ctrl Pts',(203.672576598541,-4.7978764752882,129.714361377553));
#19599=CARTESIAN_POINT('Ctrl Pts',(203.664878709741,-4.82619293906168,129.847536976704));
#19600=CARTESIAN_POINT('Ctrl Pts',(203.65718082094,-4.84892836211919,129.981513850825));
#19601=CARTESIAN_POINT('Ctrl Pts',(203.649340778128,-4.87208363166798,130.1179648254));
#19602=CARTESIAN_POINT('Ctrl Pts',(203.641500735315,-4.88944965601479,130.255246526921));
#19603=CARTESIAN_POINT('Ctrl Pts',(203.633660692502,-4.90100205051574,130.392824515455));
#19604=CARTESIAN_POINT('Ctrl Pts',(203.62582064969,-4.9125544450167,130.530402503989));
#19605=CARTESIAN_POINT('Ctrl Pts',(203.617980606877,-4.91829325611943,130.668276348449));
#19606=CARTESIAN_POINT('Ctrl Pts',(203.610140564065,-4.91824975435206,130.805915067923));
#19607=CARTESIAN_POINT('Ctrl Pts',(203.610140564008,-4.91824975435174,130.80591506892));
#19608=CARTESIAN_POINT('Ctrl Pts',(203.60532859344,-4.91822305432427,130.890393366163));
#19609=CARTESIAN_POINT('Ctrl Pts',(203.600516622872,-4.91601993127815,130.974834611061));
#19610=CARTESIAN_POINT('Ctrl Pts',(203.595704652304,-4.91164526425146,131.059162227954));
#19611=CARTESIAN_POINT('Ctrl Pts',(203.587930318251,-4.90457744819619,131.195403930679));
#19612=CARTESIAN_POINT('Ctrl Pts',(203.580155984198,-4.89182542922343,131.331567131691));
#19613=CARTESIAN_POINT('Ctrl Pts',(203.572381650145,-4.87338772313762,131.467138983592));
#19614=CARTESIAN_POINT('Ctrl Pts',(203.564616897265,-4.85497273987956,131.60254375528));
#19615=CARTESIAN_POINT('Ctrl Pts',(203.556852144384,-4.83088606373339,131.737358244241));
#19616=CARTESIAN_POINT('Ctrl Pts',(203.549087391504,-4.80117818244719,131.871071038858));
#19617=CARTESIAN_POINT('Ctrl Pts',(203.541330350687,-4.77149980745165,132.004651028024));
#19618=CARTESIAN_POINT('Ctrl Pts',(203.53357330987,-4.73621142210639,132.1371311212));
#19619=CARTESIAN_POINT('Ctrl Pts',(203.525816269053,-4.69541509058143,132.268006814446));
#19620=CARTESIAN_POINT('Ctrl Pts',(203.518065077882,-4.65464952389258,132.398783813296));
#19621=CARTESIAN_POINT('Ctrl Pts',(203.510313886711,-4.60838439436307,132.527958448688));
#19622=CARTESIAN_POINT('Ctrl Pts',(203.50256269554,-4.55677236142872,132.655038522718));
#19623=CARTESIAN_POINT('Ctrl Pts',(203.494814798833,-4.50518226499348,132.782064584306));
#19624=CARTESIAN_POINT('Ctrl Pts',(203.487066902126,-4.44824993194415,132.906997493689));
#19625=CARTESIAN_POINT('Ctrl Pts',(203.479319005419,-4.38617711843204,133.029362493575));
#19626=CARTESIAN_POINT('Ctrl Pts',(203.471572729406,-4.32411728922029,133.151701897329));
#19627=CARTESIAN_POINT('Ctrl Pts',(203.463826453393,-4.25691929509247,133.271474111561));
#19628=CARTESIAN_POINT('Ctrl Pts',(203.456080177379,-4.18483188932866,133.388226930005));
#19629=CARTESIAN_POINT('Ctrl Pts',(203.448333844186,-4.11274395143813,133.504980610282));
#19630=CARTESIAN_POINT('Ctrl Pts',(203.440587510992,-4.03576673529106,133.618714517632));
#19631=CARTESIAN_POINT('Ctrl Pts',(203.432841177798,-3.95419334811849,133.729003848491));
#19632=CARTESIAN_POINT('Ctrl Pts',(203.425093109867,-3.87260169315755,133.839317877873));
#19633=CARTESIAN_POINT('Ctrl Pts',(203.417345041936,-3.78641205146594,133.946185481521));
#19634=CARTESIAN_POINT('Ctrl Pts',(203.409596974005,-3.69595872886982,134.049213794058));
#19635=CARTESIAN_POINT('Ctrl Pts',(203.401840671336,-3.60540927141139,134.152351606306));
#19636=CARTESIAN_POINT('Ctrl Pts',(203.394084368667,-3.51058733926155,134.251641682045));
#19637=CARTESIAN_POINT('Ctrl Pts',(203.386328065998,-3.41186551250551,134.346726604738));
#19638=CARTESIAN_POINT('Ctrl Pts',(203.378567623557,-3.3130909949427,134.441862277113));
#19639=CARTESIAN_POINT('Ctrl Pts',(203.370807181116,-3.21041272778059,134.532788065183));
#19640=CARTESIAN_POINT('Ctrl Pts',(203.363046738675,-3.10423672854745,134.619186615647));
#19641=CARTESIAN_POINT('Ctrl Pts',(203.355273838482,-2.99789028617232,134.705723860737));
#19642=CARTESIAN_POINT('Ctrl Pts',(203.34750093829,-2.8880352049204,134.787719111404));
#19643=CARTESIAN_POINT('Ctrl Pts',(203.339728038097,-2.77510758697802,134.864897644019));
#19644=CARTESIAN_POINT('Ctrl Pts',(203.332237701562,-2.66628516014054,134.939270550948));
#19645=CARTESIAN_POINT('Ctrl Pts',(203.324747365027,-2.55460996759745,135.009170695082));
#19646=CARTESIAN_POINT('Ctrl Pts',(203.317257028492,-2.44049242510876,135.074393379207));
#19647=CARTESIAN_POINT('Ctrl Pts',(203.309482694322,-2.32204809275828,135.142088994682));
#19648=CARTESIAN_POINT('Ctrl Pts',(203.301708360151,-2.20059735556435,135.204959896962));
#19649=CARTESIAN_POINT('Ctrl Pts',(203.293934025981,-2.0765708843453,135.262727630811));
#19650=CARTESIAN_POINT('Ctrl Pts',(203.286169272982,-1.95269726465683,135.320424171095));
#19651=CARTESIAN_POINT('Ctrl Pts',(203.278404519984,-1.82625457798257,135.373029893092));
#19652=CARTESIAN_POINT('Ctrl Pts',(203.270639766985,-1.69770037928056,135.420310843109));
#19653=CARTESIAN_POINT('Ctrl Pts',(203.262882726048,-1.56927386241116,135.467544833023));
#19654=CARTESIAN_POINT('Ctrl Pts',(203.25512568511,-1.43874037156367,135.509464441505));
#19655=CARTESIAN_POINT('Ctrl Pts',(203.247368644173,-1.30657952838765,135.545882841335));
#19656=CARTESIAN_POINT('Ctrl Pts',(203.23961745288,-1.1745183487227,135.582273777769));
#19657=CARTESIAN_POINT('Ctrl Pts',(203.231866261587,-1.04083263478582,135.613171659453));
#19658=CARTESIAN_POINT('Ctrl Pts',(203.224115070294,-0.906019002783906,
135.638438878113));
#19659=CARTESIAN_POINT('Ctrl Pts',(203.216367173464,-0.771262670161606,
135.663695357533));
#19660=CARTESIAN_POINT('Ctrl Pts',(203.208619276634,-0.635379756424377,
135.683325861913));
#19661=CARTESIAN_POINT('Ctrl Pts',(203.200871379803,-0.498878742470774,
135.697243516513));
#19662=CARTESIAN_POINT('Ctrl Pts',(203.193125103666,-0.362406281580614,
135.711158259841));
#19663=CARTESIAN_POINT('Ctrl Pts',(203.185378827528,-0.22531636634765,135.719362490687));
#19664=CARTESIAN_POINT('Ctrl Pts',(203.17763255139,-0.0881239079495214,
135.721821063706));
#19665=CARTESIAN_POINT('Ctrl Pts',(203.169886218071,0.0490695631770811,
135.724279654873));
#19666=CARTESIAN_POINT('Ctrl Pts',(203.162139884752,0.186365188076857,135.720992496577));
#19667=CARTESIAN_POINT('Ctrl Pts',(203.154393551432,0.323247135849997,135.711976571536));
#19668=CARTESIAN_POINT('Ctrl Pts',(203.146645483375,0.4601597373901,135.702958627442));
#19669=CARTESIAN_POINT('Ctrl Pts',(203.138897415318,0.596658087415218,135.688209389437));
#19670=CARTESIAN_POINT('Ctrl Pts',(203.131149347261,0.73223095668038,135.667797765158));
#19671=CARTESIAN_POINT('Ctrl Pts',(203.123393044465,0.867947914404447,135.647364447162));
#19672=CARTESIAN_POINT('Ctrl Pts',(203.115636741669,1.00273703927327,135.621256779485));
#19673=CARTESIAN_POINT('Ctrl Pts',(203.107880438873,1.13609623798184,135.589595031944));
#19674=CARTESIAN_POINT('Ctrl Pts',(203.100119996304,1.26952661451173,135.557916385574));
#19675=CARTESIAN_POINT('Ctrl Pts',(203.092359553736,1.40152516805726,135.520677858664));
#19676=CARTESIAN_POINT('Ctrl Pts',(203.084599111167,1.53160543789726,135.478049508057));
#19677=CARTESIAN_POINT('Ctrl Pts',(203.076826210848,1.66189452412713,135.435352726641));
#19678=CARTESIAN_POINT('Ctrl Pts',(203.069053310528,1.79025880671704,135.387248968902));
#19679=CARTESIAN_POINT('Ctrl Pts',(203.061280410209,1.9162314290031,135.333956645139));
#19680=CARTESIAN_POINT('Ctrl Pts',(203.053790075032,2.03762461883292,135.282601635949));
#19681=CARTESIAN_POINT('Ctrl Pts',(203.046299739856,2.15679673695984,135.226428878422));
#19682=CARTESIAN_POINT('Ctrl Pts',(203.038809404679,2.27335372629928,135.16567302298));
#19683=CARTESIAN_POINT('Ctrl Pts',(203.031035070571,2.39433001860291,135.102613585972));
#19684=CARTESIAN_POINT('Ctrl Pts',(203.023260736462,2.51287217837938,135.034416900165));
#19685=CARTESIAN_POINT('Ctrl Pts',(203.015486402354,2.62851314525934,134.961294789248));
#19686=CARTESIAN_POINT('Ctrl Pts',(203.007721649418,2.74401159498189,134.888262794799));
#19687=CARTESIAN_POINT('Ctrl Pts',(202.999956896482,2.85661563863572,134.810317659964));
#19688=CARTESIAN_POINT('Ctrl Pts',(202.992192143545,2.96588112472585,134.727717880994));
#19689=CARTESIAN_POINT('Ctrl Pts',(202.984435102671,3.07503808679438,134.64520014129));
#19690=CARTESIAN_POINT('Ctrl Pts',(202.976678061797,3.18086278023441,134.558037191785));
#19691=CARTESIAN_POINT('Ctrl Pts',(202.968921020923,3.28293877480054,134.466531567073));
#19692=CARTESIAN_POINT('Ctrl Pts',(202.961169829694,3.38493779306489,134.375094947464));
#19693=CARTESIAN_POINT('Ctrl Pts',(202.953418638464,3.483193449336,134.279322430943));
#19694=CARTESIAN_POINT('Ctrl Pts',(202.945667447235,3.57732153668663,134.179557454146));
#19695=CARTESIAN_POINT('Ctrl Pts',(202.937919550469,3.67140961708933,134.079834880125));
#19696=CARTESIAN_POINT('Ctrl Pts',(202.930171653703,3.76137335005203,133.976123504614));
#19697=CARTESIAN_POINT('Ctrl Pts',(202.922423756936,3.84686479905085,133.868804169065));
#19698=CARTESIAN_POINT('Ctrl Pts',(202.914677480863,3.93233836508166,133.761507282408));
#19699=CARTESIAN_POINT('Ctrl Pts',(202.90693120479,4.01334126447339,133.650604242471));
#19700=CARTESIAN_POINT('Ctrl Pts',(202.899184928717,4.08956560638427,133.536509261688));
#19701=CARTESIAN_POINT('Ctrl Pts',(202.891438595462,4.16579051096613,133.422413438681));
#19702=CARTESIAN_POINT('Ctrl Pts',(202.883692262207,4.23723657049395,133.305125952902));
#19703=CARTESIAN_POINT('Ctrl Pts',(202.875945928953,4.30363925381155,133.185089967062));
#19704=CARTESIAN_POINT('Ctrl Pts',(202.868197860961,4.37005680754998,133.065027099995));
#19705=CARTESIAN_POINT('Ctrl Pts',(202.860449792968,4.43142854843043,132.942214850122));
#19706=CARTESIAN_POINT('Ctrl Pts',(202.852701724976,4.48753611850486,132.817120575339));
#19707=CARTESIAN_POINT('Ctrl Pts',(202.844945422245,4.54370332037339,132.69189334887));
#19708=CARTESIAN_POINT('Ctrl Pts',(202.837189119514,4.59459501491842,132.564379609861));
#19709=CARTESIAN_POINT('Ctrl Pts',(202.829432816783,4.64004099484783,132.435066792397));
#19710=CARTESIAN_POINT('Ctrl Pts',(202.821672374279,4.68551123066541,132.305684956788));
#19711=CARTESIAN_POINT('Ctrl Pts',(202.813911931776,4.72552984631434,132.174502503168));
#19712=CARTESIAN_POINT('Ctrl Pts',(202.806151489272,4.75997697153195,132.04202062459));
#19713=CARTESIAN_POINT('Ctrl Pts',(202.798378589017,4.79447939433392,131.909326074335));
#19714=CARTESIAN_POINT('Ctrl Pts',(202.790605688762,4.82339237153089,131.775328313116));
#19715=CARTESIAN_POINT('Ctrl Pts',(202.782832788507,4.84664731046149,131.640538176758));
#19716=CARTESIAN_POINT('Ctrl Pts',(202.775342452627,4.86905687417027,131.510647999147));
#19717=CARTESIAN_POINT('Ctrl Pts',(202.767852116746,4.8862125852588,131.380022361244));
#19718=CARTESIAN_POINT('Ctrl Pts',(202.760361780866,4.89809886429187,131.249119628855));
#19719=CARTESIAN_POINT('Ctrl Pts',(202.752587446755,4.91043581499945,131.113253681868));
#19720=CARTESIAN_POINT('Ctrl Pts',(202.744813112644,4.91713494470752,130.976658831053));
#19721=CARTESIAN_POINT('Ctrl Pts',(202.737038778533,4.91812200914719,130.839842523405));
#19722=CARTESIAN_POINT('Ctrl Pts',(202.729274025594,4.91910785711814,130.703194829631));
#19723=CARTESIAN_POINT('Ctrl Pts',(202.721509272656,4.91439564375304,130.566326609267));
#19724=CARTESIAN_POINT('Ctrl Pts',(202.713744519717,4.90396277453586,130.429751263082));
#19725=CARTESIAN_POINT('Ctrl Pts',(202.70598747884,4.89354026739166,130.293311565459));
#19726=CARTESIAN_POINT('Ctrl Pts',(202.698230437964,4.87740844109174,130.157164550445));
#19727=CARTESIAN_POINT('Ctrl Pts',(202.690473397087,4.8555967358373,130.021824099935));
#19728=CARTESIAN_POINT('Ctrl Pts',(202.682722205856,4.83380147895985,129.886585710714));
#19729=CARTESIAN_POINT('Ctrl Pts',(202.674971014624,4.80633493061361,129.752153059763));
#19730=CARTESIAN_POINT('Ctrl Pts',(202.667219823393,4.77327836053893,129.619035027143));
#19731=CARTESIAN_POINT('Ctrl Pts',(202.659471926624,4.74023584038906,129.485973573241));
#19732=CARTESIAN_POINT('Ctrl Pts',(202.651724029856,4.70160811803909,129.35422600501));
#19733=CARTESIAN_POINT('Ctrl Pts',(202.643976133088,4.6575275379995,129.224290905409));
#19734=CARTESIAN_POINT('Ctrl Pts',(202.636229857012,4.61345617866757,129.094382985432));
#19735=CARTESIAN_POINT('Ctrl Pts',(202.628483580937,4.56393435592693,128.966287149981));
#19736=CARTESIAN_POINT('Ctrl Pts',(202.620737304862,4.50914413590637,128.840486328279));
#19737=CARTESIAN_POINT('Ctrl Pts',(202.612990971605,4.45435351143753,128.714684577946));
#19738=CARTESIAN_POINT('Ctrl Pts',(202.605244638349,4.39429456820026,128.591178233612));
#19739=CARTESIAN_POINT('Ctrl Pts',(202.597498305092,4.3291971659843,128.470429393101));
#19740=CARTESIAN_POINT('Ctrl Pts',(202.589750237099,4.26408518565718,128.349653511726));
#19741=CARTESIAN_POINT('Ctrl Pts',(202.582002169105,4.19393268660458,128.231636707049));
#19742=CARTESIAN_POINT('Ctrl Pts',(202.574254101111,4.11901484245543,128.116815308156));
#19743=CARTESIAN_POINT('Ctrl Pts',(202.566497798378,4.04401737473066,128.001871875715));
#19744=CARTESIAN_POINT('Ctrl Pts',(202.558741495645,3.9642446586756,127.890130961117));
#19745=CARTESIAN_POINT('Ctrl Pts',(202.550985192912,3.88001478519079,127.781999234607));
#19746=CARTESIAN_POINT('Ctrl Pts',(202.543224750407,3.79573995568691,127.67380979494));
#19747=CARTESIAN_POINT('Ctrl Pts',(202.535464307902,3.70700348138614,127.569233679702));
#19748=CARTESIAN_POINT('Ctrl Pts',(202.527703865397,3.61416223739328,127.468642646229));
#19749=CARTESIAN_POINT('Ctrl Pts',(202.519930965141,3.52117195639349,127.367890135099));
#19750=CARTESIAN_POINT('Ctrl Pts',(202.512158064885,3.42406401521649,127.2711357655));
#19751=CARTESIAN_POINT('Ctrl Pts',(202.504385164629,3.32323111850202,127.178713365623));
#19752=CARTESIAN_POINT('Ctrl Pts',(202.49689482877,3.22606375019959,127.089650751528));
#19753=CARTESIAN_POINT('Ctrl Pts',(202.489404492912,3.12543778266822,127.004610818164));
#19754=CARTESIAN_POINT('Ctrl Pts',(202.481914157053,3.02173043097238,126.923854430864));
#19755=CARTESIAN_POINT('Ctrl Pts',(202.474139822926,2.91409098479571,126.84003614159));
#19756=CARTESIAN_POINT('Ctrl Pts',(202.466365488799,2.80279091121412,126.760567120498));
#19757=CARTESIAN_POINT('Ctrl Pts',(202.458591154673,2.68821700891863,126.685784118888));
#19758=CARTESIAN_POINT('Ctrl Pts',(202.450826401718,2.57378430871652,126.611093280644));
#19759=CARTESIAN_POINT('Ctrl Pts',(202.443061648763,2.45608613190742,126.541077182797));
#19760=CARTESIAN_POINT('Ctrl Pts',(202.435296895808,2.33554220421387,126.476032340409));
#19761=CARTESIAN_POINT('Ctrl Pts',(202.427539854915,2.21511800244725,126.411052101475));
#19762=CARTESIAN_POINT('Ctrl Pts',(202.419782814022,2.09185401638329,126.351033476568));
#19763=CARTESIAN_POINT('Ctrl Pts',(202.412025773129,1.96619850256614,126.29622946253));
#19764=CARTESIAN_POINT('Ctrl Pts',(202.404274581881,1.8406377465481,126.241466776625));
#19765=CARTESIAN_POINT('Ctrl Pts',(202.396523390633,1.71268940938756,126.191911030093));
#19766=CARTESIAN_POINT('Ctrl Pts',(202.388772199385,1.58282555457417,126.147768910503));
#19767=CARTESIAN_POINT('Ctrl Pts',(202.3810243026,1.45301689536158,126.103645552491));
#19768=CARTESIAN_POINT('Ctrl Pts',(202.373276405815,1.3212947071609,126.064931370595));
#19769=CARTESIAN_POINT('Ctrl Pts',(202.36552850903,1.18814999737997,126.031784515897));
#19770=CARTESIAN_POINT('Ctrl Pts',(202.357782232937,1.05503313860108,125.998644594806));
#19771=CARTESIAN_POINT('Ctrl Pts',(202.350035956845,0.92049472925159,125.97106977892));
#19772=CARTESIAN_POINT('Ctrl Pts',(202.342289680753,0.785039482555496,125.949167925887));
#19773=CARTESIAN_POINT('Ctrl Pts',(202.33454334748,0.649583235958816,125.927265911181));
#19774=CARTESIAN_POINT('Ctrl Pts',(202.326797014206,0.513210524463309,125.911037005295));
#19775=CARTESIAN_POINT('Ctrl Pts',(202.319050680933,0.376434368889621,125.900537595839));
#19776=CARTESIAN_POINT('Ctrl Pts',(202.311302612921,0.239627583243728,125.890035835114));
#19777=CARTESIAN_POINT('Ctrl Pts',(202.30355454491,0.102417563480344,125.885266153919));
#19778=CARTESIAN_POINT('Ctrl Pts',(202.295806476899,-0.0346798563142518,
125.886232887416));
#19779=CARTESIAN_POINT('Ctrl Pts',(202.288050174149,-0.17192298487841,125.887200648369));
#19780=CARTESIAN_POINT('Ctrl Pts',(202.280293871399,-0.309052882836018,
125.893917000127));
#19781=CARTESIAN_POINT('Ctrl Pts',(202.272537568649,-0.445555471089543,
125.906334139005));
#19782=CARTESIAN_POINT('Ctrl Pts',(202.264777126127,-0.58213091488482,125.918757905285));
#19783=CARTESIAN_POINT('Ctrl Pts',(202.257016683604,-0.718077994486212,
125.936888469828));
#19784=CARTESIAN_POINT('Ctrl Pts',(202.249256241082,-0.852891040206172,
125.960626527421));
#19785=CARTESIAN_POINT('Ctrl Pts',(202.241483340808,-0.987920499794184,
125.984402691451));
#19786=CARTESIAN_POINT('Ctrl Pts',(202.233710440535,-1.12181190557149,126.013804252784));
#19787=CARTESIAN_POINT('Ctrl Pts',(202.225937540261,-1.25407213197427,126.048681260176));
#19788=CARTESIAN_POINT('Ctrl Pts',(202.218447204587,-1.38152436436558,126.082290400067));
#19789=CARTESIAN_POINT('Ctrl Pts',(202.210956868914,-1.50746165896199,126.120983714381));
#19790=CARTESIAN_POINT('Ctrl Pts',(202.20346653324,-1.63146064844767,126.164584845498));
#19791=CARTESIAN_POINT('Ctrl Pts',(202.195692103635,-1.76016267956143,126.209839683114));
#19792=CARTESIAN_POINT('Ctrl Pts',(202.187917674029,-1.88718416540828,126.260525329425));
#19793=CARTESIAN_POINT('Ctrl Pts',(202.180143244423,-2.01203269537097,126.316498376447));
#19794=CARTESIAN_POINT('Ctrl Pts',(202.172378418318,-2.1367270040091,126.372402281787));
#19795=CARTESIAN_POINT('Ctrl Pts',(202.164613592212,-2.2592533441934,126.433580433836));
#19796=CARTESIAN_POINT('Ctrl Pts',(202.156848766106,-2.37913536422814,126.499839972804));
#19797=CARTESIAN_POINT('Ctrl Pts',(202.149091674296,-2.49889797360211,126.566033512757));
#19798=CARTESIAN_POINT('Ctrl Pts',(202.141334582486,-2.61602116454483,126.637298179153));
#19799=CARTESIAN_POINT('Ctrl Pts',(202.133577490676,-2.73004978163739,126.713393586132));
#19800=CARTESIAN_POINT('Ctrl Pts',(202.125826270674,-2.84399208364077,126.78943139194));
#19801=CARTESIAN_POINT('Ctrl Pts',(202.118075050671,-2.95484415052419,126.870292443658));
#19802=CARTESIAN_POINT('Ctrl Pts',(202.110323830669,-3.06217692439492,126.955691296073));
#19803=CARTESIAN_POINT('Ctrl Pts',(202.102576019855,-3.16946249051467,127.041052587846));
#19804=CARTESIAN_POINT('Ctrl Pts',(202.094828209041,-3.27323153754679,127.130947467042));
#19805=CARTESIAN_POINT('Ctrl Pts',(202.087080398227,-3.37308562112851,127.225048329565));
#19806=CARTESIAN_POINT('Ctrl Pts',(202.079334239672,-3.47291841033375,127.319129124614));
#19807=CARTESIAN_POINT('Ctrl Pts',(202.071588081117,-3.568837612584,127.417413850761));
#19808=CARTESIAN_POINT('Ctrl Pts',(202.063841922562,-3.66047969139515,127.519536194346));
#19809=CARTESIAN_POINT('Ctrl Pts',(202.056095738413,-3.75212207299657,127.621658875349));
#19810=CARTESIAN_POINT('Ctrl Pts',(202.048349554264,-3.83948704196994,127.727618908041));
#19811=CARTESIAN_POINT('Ctrl Pts',(202.040603370115,-3.92224987613099,127.837015175645));
#19812=CARTESIAN_POINT('Ctrl Pts',(202.032855482865,-4.0050309067957,127.946435495465));
#19813=CARTESIAN_POINT('Ctrl Pts',(202.025107595616,-4.08320755361812,128.059293241692));
#19814=CARTESIAN_POINT('Ctrl Pts',(202.017359708366,-4.1564973670384,128.175156802663));
#19815=CARTESIAN_POINT('Ctrl Pts',(202.00960402534,-4.22986092326722,128.291136943332));
#19816=CARTESIAN_POINT('Ctrl Pts',(202.001848342314,-4.29832761616902,128.410128608468));
#19817=CARTESIAN_POINT('Ctrl Pts',(201.994092659288,-4.36165984536912,128.531673561283));
#19818=CARTESIAN_POINT('Ctrl Pts',(201.986332849536,-4.42502577306113,128.653283187041));
#19819=CARTESIAN_POINT('Ctrl Pts',(201.978573039783,-4.48325162754233,128.777448453866));
#19820=CARTESIAN_POINT('Ctrl Pts',(201.97081323003,-4.5361476689452,128.903690370516));
#19821=CARTESIAN_POINT('Ctrl Pts',(201.9630419948,-4.58912159402284,129.030118164673));
#19822=CARTESIAN_POINT('Ctrl Pts',(201.955270759571,-4.63674989270561,129.158628350682));
#19823=CARTESIAN_POINT('Ctrl Pts',(201.947499524341,-4.67889225145815,129.28872531785));
#19824=CARTESIAN_POINT('Ctrl Pts',(201.941698877603,-4.71034837504711,129.385832988111));
#19825=CARTESIAN_POINT('Ctrl Pts',(201.935898230865,-4.73874903929908,129.483824402015));
#19826=CARTESIAN_POINT('Ctrl Pts',(201.930097584127,-4.76405452823404,129.582490119308));
#19827=CARTESIAN_POINT('Origin',(213.235140564004,0.,130.804360617566));
#19828=CARTESIAN_POINT('',(199.834960626423,-4.76405452823405,129.582490119308));
#19829=CARTESIAN_POINT('',(200.179870531952,-4.76405452823405,129.582490119308));
#19830=CARTESIAN_POINT('',(213.235140564004,-4.76405452823405,129.582490119308));
#19831=CARTESIAN_POINT('',(201.51485943594,-4.91824986053202,130.805531888988));
#19832=CARTESIAN_POINT('Ctrl Pts',(201.51485943594,-4.91824986053202,130.805531888988));
#19833=CARTESIAN_POINT('Ctrl Pts',(201.506582193965,-4.9182148650919,130.952480167015));
#19834=CARTESIAN_POINT('Ctrl Pts',(201.49830495199,-4.91158982122124,131.099253060515));
#19835=CARTESIAN_POINT('Ctrl Pts',(201.490027710014,-4.89844708438231,131.245267891272));
#19836=CARTESIAN_POINT('Ctrl Pts',(201.481501455677,-4.88490896174189,131.395675428935));
#19837=CARTESIAN_POINT('Ctrl Pts',(201.472975201339,-4.86445493793769,131.545278220582));
#19838=CARTESIAN_POINT('Ctrl Pts',(201.464448947001,-4.83721994611014,131.693453557283));
#19839=CARTESIAN_POINT('Ctrl Pts',(201.456128501245,-4.81064235843921,131.838052205476));
#19840=CARTESIAN_POINT('Ctrl Pts',(201.447808055489,-4.77760755788874,131.981291262248));
#19841=CARTESIAN_POINT('Ctrl Pts',(201.439487609733,-4.73829111258486,132.122609605769));
#19842=CARTESIAN_POINT('Ctrl Pts',(201.430858451104,-4.69751591217013,132.269171273154));
#19843=CARTESIAN_POINT('Ctrl Pts',(201.422229292475,-4.6499841405859,132.413666610456));
#19844=CARTESIAN_POINT('Ctrl Pts',(201.413600133847,-4.59594544262833,132.555494122152));
#19845=CARTESIAN_POINT('Ctrl Pts',(201.404970975218,-4.54190674467076,132.697321633848));
#19846=CARTESIAN_POINT('Ctrl Pts',(201.396341816589,-4.48136133127772,132.836481025787));
#19847=CARTESIAN_POINT('Ctrl Pts',(201.38771265796,-4.41461067614117,132.972400202214));
#19848=CARTESIAN_POINT('Ctrl Pts',(201.379938323841,-4.3544724960429,133.094854909123));
#19849=CARTESIAN_POINT('Ctrl Pts',(201.372163989722,-4.28914013406402,133.21499946427));
#19850=CARTESIAN_POINT('Ctrl Pts',(201.364389655603,-4.21881414473507,133.332361858603));
#19851=CARTESIAN_POINT('Ctrl Pts',(201.356624902656,-4.14857482590277,133.449579614273));
#19852=CARTESIAN_POINT('Ctrl Pts',(201.348860149708,-4.07335432377154,133.564021699203));
#19853=CARTESIAN_POINT('Ctrl Pts',(201.341095396761,-3.9934004017413,133.675237886603));
#19854=CARTESIAN_POINT('Ctrl Pts',(201.333338355876,-3.91352589107348,133.786343612518));
#19855=CARTESIAN_POINT('Ctrl Pts',(201.325581314991,-3.8289275430417,133.89422950163));
#19856=CARTESIAN_POINT('Ctrl Pts',(201.317824274106,-3.73989781193985,133.998471983619));
#19857=CARTESIAN_POINT('Ctrl Pts',(201.310073082865,-3.65093521885079,134.102635855541));
#19858=CARTESIAN_POINT('Ctrl Pts',(201.302321891625,-3.55754814710466,134.203161493023));
#19859=CARTESIAN_POINT('Ctrl Pts',(201.294570700385,-3.46007071453197,134.299656558247));
#19860=CARTESIAN_POINT('Ctrl Pts',(201.286822803607,-3.36263471246837,134.396110610494));
#19861=CARTESIAN_POINT('Ctrl Pts',(201.27907490683,-3.26111208461592,134.488537223235));
#19862=CARTESIAN_POINT('Ctrl Pts',(201.271327010053,-3.15587521323921,134.576579420998));
#19863=CARTESIAN_POINT('Ctrl Pts',(201.263580733969,-3.05066035514734,134.664603202231));
#19864=CARTESIAN_POINT('Ctrl Pts',(201.255834457884,-2.94173309858087,134.748244141987));
#19865=CARTESIAN_POINT('Ctrl Pts',(201.2480881818,-2.82950014815832,134.827184498134));
#19866=CARTESIAN_POINT('Ctrl Pts',(201.240341848535,-2.71726636925778,134.906125437001));
#19867=CARTESIAN_POINT('Ctrl Pts',(201.232595515269,-2.60172716759431,134.980365498095));
#19868=CARTESIAN_POINT('Ctrl Pts',(201.224849182004,-2.48331923024386,135.049629591754));
#19869=CARTESIAN_POINT('Ctrl Pts',(201.217101114,-2.36488477625662,135.118909196626));
#19870=CARTESIAN_POINT('Ctrl Pts',(201.209353045997,-2.24358064561767,135.183210419302));
#19871=CARTESIAN_POINT('Ctrl Pts',(201.201604977994,-2.11986882164754,135.242303749413));
#19872=CARTESIAN_POINT('Ctrl Pts',(201.193848675252,-1.99602551527869,135.301459884618));
#19873=CARTESIAN_POINT('Ctrl Pts',(201.18609237251,-1.8697697571969,135.355396901697));
#19874=CARTESIAN_POINT('Ctrl Pts',(201.178336069768,-1.74158475661268,135.403932945298));
#19875=CARTESIAN_POINT('Ctrl Pts',(201.170575627254,-1.61333133983404,135.452494894046));
#19876=CARTESIAN_POINT('Ctrl Pts',(201.162815184739,-1.4831469997239,135.49565000241));
#19877=CARTESIAN_POINT('Ctrl Pts',(201.155054742225,-1.35152990844939,135.533266407394));
#19878=CARTESIAN_POINT('Ctrl Pts',(201.147281841959,-1.21970153373557,135.57094319757));
#19879=CARTESIAN_POINT('Ctrl Pts',(201.139508941694,-1.08643619206553,135.603063425218));
#19880=CARTESIAN_POINT('Ctrl Pts',(201.131736041428,-0.952242926124562,
135.629546258777));
#19881=CARTESIAN_POINT('Ctrl Pts',(201.124245705668,-0.822927923447469,
135.655066374622));
#19882=CARTESIAN_POINT('Ctrl Pts',(201.116755369908,-0.692751594327094,
135.675351800014));
#19883=CARTESIAN_POINT('Ctrl Pts',(201.109265034147,-0.562171798684125,
135.690375960488));
#19884=CARTESIAN_POINT('Ctrl Pts',(201.101490700028,-0.426641030368497,
135.705969766576));
#19885=CARTESIAN_POINT('Ctrl Pts',(201.093716365909,-0.290246275975597,
135.715944866885));
#19886=CARTESIAN_POINT('Ctrl Pts',(201.08594203179,-0.153493054712102,135.7202148612));
#19887=CARTESIAN_POINT('Ctrl Pts',(201.078177278843,-0.0169083695718419,
135.724479593129));
#19888=CARTESIAN_POINT('Ctrl Pts',(201.070412525896,0.12003351640835,135.723053196639));
#19889=CARTESIAN_POINT('Ctrl Pts',(201.062647772949,0.256819892510846,135.715900763519));
#19890=CARTESIAN_POINT('Ctrl Pts',(201.054890732064,0.39347041045627,135.708755434297));
#19891=CARTESIAN_POINT('Ctrl Pts',(201.047133691179,0.52996533799027,135.695895406474));
#19892=CARTESIAN_POINT('Ctrl Pts',(201.039376650294,0.665790234716704,135.677337780026));
#19893=CARTESIAN_POINT('Ctrl Pts',(201.031625459054,0.801512704831837,135.658794148028));
#19894=CARTESIAN_POINT('Ctrl Pts',(201.023874267814,0.936565764060569,135.634561522245));
#19895=CARTESIAN_POINT('Ctrl Pts',(201.016123076574,1.07043872863637,135.604708937296));
#19896=CARTESIAN_POINT('Ctrl Pts',(201.008375179797,1.20425479363109,135.574869040492));
#19897=CARTESIAN_POINT('Ctrl Pts',(201.00062728302,1.33689138076679,135.539414020244));
#19898=CARTESIAN_POINT('Ctrl Pts',(200.992879386243,1.46784687475884,135.498464218336));
#19899=CARTESIAN_POINT('Ctrl Pts',(200.985133110159,1.59877497568463,135.457522982243));
#19900=CARTESIAN_POINT('Ctrl Pts',(200.977386834075,1.72802231000401,135.411089367299));
#19901=CARTESIAN_POINT('Ctrl Pts',(200.969640557991,1.85510171848053,135.359333798232));
#19902=CARTESIAN_POINT('Ctrl Pts',(200.961894224726,1.98218206502826,135.307577847118));
#19903=CARTESIAN_POINT('Ctrl Pts',(200.954147891461,2.10709409171268,135.250500010957));
#19904=CARTESIAN_POINT('Ctrl Pts',(200.946401558195,2.22937031777955,135.188318994273));
#19905=CARTESIAN_POINT('Ctrl Pts',(200.938653490193,2.35167392675948,135.126124052582));
#19906=CARTESIAN_POINT('Ctrl Pts',(200.93090542219,2.47134021212813,135.058823833469));
#19907=CARTESIAN_POINT('Ctrl Pts',(200.923157354187,2.58792636704384,134.986682960626));
#19908=CARTESIAN_POINT('Ctrl Pts',(200.915401051445,2.70463643111238,134.914465415605));
#19909=CARTESIAN_POINT('Ctrl Pts',(200.907644748703,2.81825949236634,134.837397145802));
#19910=CARTESIAN_POINT('Ctrl Pts',(200.899888445961,2.92838136436711,134.755786391553));
#19911=CARTESIAN_POINT('Ctrl Pts',(200.892128003447,3.03856201172679,134.674132079186));
#19912=CARTESIAN_POINT('Ctrl Pts',(200.884367560933,3.14523744236723,134.587930697037));
#19913=CARTESIAN_POINT('Ctrl Pts',(200.876607118419,3.24802744199153,134.497530096289));
#19914=CARTESIAN_POINT('Ctrl Pts',(200.868834218154,3.35098244924848,134.406984376471));
#19915=CARTESIAN_POINT('Ctrl Pts',(200.861061317888,3.45003927881987,134.312226237882));
#19916=CARTESIAN_POINT('Ctrl Pts',(200.853288417623,3.54485477481942,134.213640261118));
#19917=CARTESIAN_POINT('Ctrl Pts',(200.84579808186,3.63622348872338,134.118638132923));
#19918=CARTESIAN_POINT('Ctrl Pts',(200.838307746098,3.723653677273,134.020081868339));
#19919=CARTESIAN_POINT('Ctrl Pts',(200.830817410335,3.80687549814816,133.918342313739));
#19920=CARTESIAN_POINT('Ctrl Pts',(200.823043076216,3.8932526996479,133.812745273014));
#19921=CARTESIAN_POINT('Ctrl Pts',(200.815268742097,3.97536973042481,133.703384288615));
#19922=CARTESIAN_POINT('Ctrl Pts',(200.807494407978,4.052880654051,133.59063796674));
#19923=CARTESIAN_POINT('Ctrl Pts',(200.799729655031,4.13029605239111,133.47803059463));
#19924=CARTESIAN_POINT('Ctrl Pts',(200.791964902084,4.20311641899065,133.362046505414));
#19925=CARTESIAN_POINT('Ctrl Pts',(200.784200149136,4.27103525191642,133.243098188398));
#19926=CARTESIAN_POINT('Ctrl Pts',(200.776443108251,4.33888662689985,133.124268012527));
#19927=CARTESIAN_POINT('Ctrl Pts',(200.768686067366,4.40184596368367,133.002479805092));
#19928=CARTESIAN_POINT('Ctrl Pts',(200.760929026481,4.45964958136172,132.878175622324));
#19929=CARTESIAN_POINT('Ctrl Pts',(200.753177835241,4.51740960888204,132.753965178307));
#19930=CARTESIAN_POINT('Ctrl Pts',(200.745426644001,4.57002149187464,132.627242888525));
#19931=CARTESIAN_POINT('Ctrl Pts',(200.737675452761,4.61726727407009,132.498475720592));
#19932=CARTESIAN_POINT('Ctrl Pts',(200.729927555984,4.66449297554781,132.369763282141));
#19933=CARTESIAN_POINT('Ctrl Pts',(200.722179659207,4.70635697805043,132.239008060438));
#19934=CARTESIAN_POINT('Ctrl Pts',(200.71443176243,4.74268939321458,132.106697126303));
#19935=CARTESIAN_POINT('Ctrl Pts',(200.706685486346,4.77901420842072,131.974413868764));
#19936=CARTESIAN_POINT('Ctrl Pts',(200.698939210262,4.80980963434076,131.840575922843));
#19937=CARTESIAN_POINT('Ctrl Pts',(200.691192934178,4.83495573265951,131.705685268135));
#19938=CARTESIAN_POINT('Ctrl Pts',(200.683446600912,4.86010201660105,131.570793617694));
#19939=CARTESIAN_POINT('Ctrl Pts',(200.675700267647,4.8795988180791,131.434849627302));
#19940=CARTESIAN_POINT('Ctrl Pts',(200.667953934382,4.89337745463654,131.298364816895));
#19941=CARTESIAN_POINT('Ctrl Pts',(200.660205866379,4.90715917682409,131.161849441661));
#19942=CARTESIAN_POINT('Ctrl Pts',(200.652457798376,4.91522014669572,131.024793394324));
#19943=CARTESIAN_POINT('Ctrl Pts',(200.644709730373,4.91754365174374,130.887712256391));
#19944=CARTESIAN_POINT('Ctrl Pts',(200.636953427631,4.91986962624059,130.750485426993));
#19945=CARTESIAN_POINT('Ctrl Pts',(200.629197124889,4.91644594817341,130.613233845261));
#19946=CARTESIAN_POINT('Ctrl Pts',(200.621440822147,4.90730807097843,130.476472589407));
#19947=CARTESIAN_POINT('Ctrl Pts',(200.613680379633,4.89816531662325,130.339638339953));
#19948=CARTESIAN_POINT('Ctrl Pts',(200.605919937119,4.88330232842366,130.203295326312));
#19949=CARTESIAN_POINT('Ctrl Pts',(200.598159494605,4.86280624831729,130.067951455601));
#19950=CARTESIAN_POINT('Ctrl Pts',(200.590386594339,4.84227726608359,129.932390318894));
#19951=CARTESIAN_POINT('Ctrl Pts',(200.582613694074,4.81609719637891,129.797831914236));
#19952=CARTESIAN_POINT('Ctrl Pts',(200.574840793809,4.78440411361137,129.664772823599));
#19953=CARTESIAN_POINT('Ctrl Pts',(200.567350458046,4.75386315423193,129.53655076606));
#19954=CARTESIAN_POINT('Ctrl Pts',(200.559860122284,4.71820313009367,129.409721203914));
#19955=CARTESIAN_POINT('Ctrl Pts',(200.552369786522,4.67759018838714,129.284711614669));
#19956=CARTESIAN_POINT('Ctrl Pts',(200.544595452403,4.63543739465235,129.154962248855));
#19957=CARTESIAN_POINT('Ctrl Pts',(200.536821118284,4.58781516216797,129.026762581828));
#19958=CARTESIAN_POINT('Ctrl Pts',(200.529046784165,4.53485503596222,128.900608305602));
#19959=CARTESIAN_POINT('Ctrl Pts',(200.521282031218,4.48196017837884,128.774609503247));
#19960=CARTESIAN_POINT('Ctrl Pts',(200.51351727827,4.42374066616417,128.650651433156));
#19961=CARTESIAN_POINT('Ctrl Pts',(200.505752525323,4.36037786647262,128.529214924632));
#19962=CARTESIAN_POINT('Ctrl Pts',(200.497995484438,4.29707799960699,128.407899028561));
#19963=CARTESIAN_POINT('Ctrl Pts',(200.490238443553,4.22864519086966,128.289100054462));
#19964=CARTESIAN_POINT('Ctrl Pts',(200.482481402668,4.15530882871568,128.173278786741));
#19965=CARTESIAN_POINT('Ctrl Pts',(200.474730211428,4.08202777008282,128.057544860739));
#19966=CARTESIAN_POINT('Ctrl Pts',(200.466979020188,4.00385072660107,127.944784500539));
#19967=CARTESIAN_POINT('Ctrl Pts',(200.459227828948,3.92105276066194,127.835433486327));
#19968=CARTESIAN_POINT('Ctrl Pts',(200.451479932171,3.83828998606706,127.726128949213));
#19969=CARTESIAN_POINT('Ctrl Pts',(200.443732035394,3.75091043080558,127.620231187053));
#19970=CARTESIAN_POINT('Ctrl Pts',(200.435984138616,3.65923205254183,127.518146405414));
#19971=CARTESIAN_POINT('Ctrl Pts',(200.428237862532,3.56757285141844,127.41608297771));
#19972=CARTESIAN_POINT('Ctrl Pts',(200.420491586448,3.47161687695752,127.317831234768));
#19973=CARTESIAN_POINT('Ctrl Pts',(200.412745310364,3.37172162921752,127.223763416321));
#19974=CARTESIAN_POINT('Ctrl Pts',(200.404998977099,3.27182564407353,127.129694903486));
#19975=CARTESIAN_POINT('Ctrl Pts',(200.397252643833,3.16799061225729,127.039810644801));
#19976=CARTESIAN_POINT('Ctrl Pts',(200.389506310568,3.06060976543159,126.954444913782));
#19977=CARTESIAN_POINT('Ctrl Pts',(200.381758242565,2.95320487140979,126.869060065699));
#19978=CARTESIAN_POINT('Ctrl Pts',(200.374010174562,2.84225288827149,126.788196002082));
#19979=CARTESIAN_POINT('Ctrl Pts',(200.366262106559,2.72817855582115,126.712145468034));
#19980=CARTESIAN_POINT('Ctrl Pts',(200.358505803817,2.61398298381271,126.636014106574));
#19981=CARTESIAN_POINT('Ctrl Pts',(200.350749501075,2.49665875931106,126.564706711413));
#19982=CARTESIAN_POINT('Ctrl Pts',(200.342993198333,2.37665839565136,126.498471866927));
#19983=CARTESIAN_POINT('Ctrl Pts',(200.335232755819,2.25659398418439,126.43220167091));
#19984=CARTESIAN_POINT('Ctrl Pts',(200.327472313305,2.13385093720195,126.371009594588));
#19985=CARTESIAN_POINT('Ctrl Pts',(200.319711870791,2.00890367369267,126.315096859184));
#19986=CARTESIAN_POINT('Ctrl Pts',(200.311938970525,1.8837558337437,126.259094367693));
#19987=CARTESIAN_POINT('Ctrl Pts',(200.30416607026,1.75639706985327,126.208388297305));
#19988=CARTESIAN_POINT('Ctrl Pts',(200.296393169994,1.62731980308813,126.163130896794));
#19989=CARTESIAN_POINT('Ctrl Pts',(200.288902834233,1.50293482010056,126.11951871679));
#19990=CARTESIAN_POINT('Ctrl Pts',(200.281412498471,1.37695440338238,126.08096602872));
#19991=CARTESIAN_POINT('Ctrl Pts',(200.273922162709,1.24982800848328,126.047564110282));
#19992=CARTESIAN_POINT('Ctrl Pts',(200.26614782859,1.11788157767805,126.012895747953));
#19993=CARTESIAN_POINT('Ctrl Pts',(200.258373494471,0.984282587110447,125.983666629395));
#19994=CARTESIAN_POINT('Ctrl Pts',(200.250599160352,0.849519179810192,125.960034015691));
#19995=CARTESIAN_POINT('Ctrl Pts',(200.242834407405,0.714921856365283,125.936430527071));
#19996=CARTESIAN_POINT('Ctrl Pts',(200.235069654458,0.579163352880725,125.918409886831));
#19997=CARTESIAN_POINT('Ctrl Pts',(200.227304901511,0.442746238043899,125.906079405631));
#19998=CARTESIAN_POINT('Ctrl Pts',(200.219547860626,0.306464614608663,125.893761171238));
#19999=CARTESIAN_POINT('Ctrl Pts',(200.211790819741,0.1695260684516,125.88712188402));
#20000=CARTESIAN_POINT('Ctrl Pts',(200.204033778856,0.0324422606050424,
125.886217618199));
#20001=CARTESIAN_POINT('Ctrl Pts',(200.196282587615,-0.104538171275545,
125.885314034291));
#20002=CARTESIAN_POINT('Ctrl Pts',(200.188531396375,-0.241663257432193,
125.890136866048));
#20003=CARTESIAN_POINT('Ctrl Pts',(200.180780205135,-0.378417685712695,
125.900690245524));
#20004=CARTESIAN_POINT('Ctrl Pts',(200.173032308358,-0.515113989713261,
125.911239139532));
#20005=CARTESIAN_POINT('Ctrl Pts',(200.165284411581,-0.651439560181567,
125.927513706947));
#20006=CARTESIAN_POINT('Ctrl Pts',(200.157536514804,-0.78688078098602,125.949466005011));
#20007=CARTESIAN_POINT('Ctrl Pts',(200.14979023872,-0.922293670406798,125.971413711128));
#20008=CARTESIAN_POINT('Ctrl Pts',(200.142043962636,-1.05682219242837,125.999036723063));
#20009=CARTESIAN_POINT('Ctrl Pts',(200.134297686552,-1.18995993370752,126.032235470562));
#20010=CARTESIAN_POINT('Ctrl Pts',(200.126551353286,-1.3230986577791,126.065434463126));
#20011=CARTESIAN_POINT('Ctrl Pts',(200.118805020021,-1.454846201273,126.104209178789));
#20012=CARTESIAN_POINT('Ctrl Pts',(200.111058686756,-1.58470877909421,126.148409463617));
#20013=CARTESIAN_POINT('Ctrl Pts',(200.103310618753,-1.71460043873933,126.192619646792));
#20014=CARTESIAN_POINT('Ctrl Pts',(200.09556255075,-1.84260592268838,126.242257690929));
#20015=CARTESIAN_POINT('Ctrl Pts',(200.087814482747,-1.96824935395539,126.297124486282));
#20016=CARTESIAN_POINT('Ctrl Pts',(200.080058180005,-2.09402632055645,126.352049594717));
#20017=CARTESIAN_POINT('Ctrl Pts',(200.072301877263,-2.21743586078181,126.41221439872));
#20018=CARTESIAN_POINT('Ctrl Pts',(200.064545574521,-2.33802423904589,126.477372551933));
#20019=CARTESIAN_POINT('Ctrl Pts',(200.056785132007,-2.45867697895829,126.542565482013));
#20020=CARTESIAN_POINT('Ctrl Pts',(200.049024689493,-2.57650522087711,126.612756871751));
#20021=CARTESIAN_POINT('Ctrl Pts',(200.041264246979,-2.69108323663666,126.687656344));
#20022=CARTESIAN_POINT('Ctrl Pts',(200.033491346713,-2.80584518319893,126.762676051532));
#20023=CARTESIAN_POINT('Ctrl Pts',(200.025718446448,-2.91734615908058,126.842418716971));
#20024=CARTESIAN_POINT('Ctrl Pts',(200.017945546182,-3.02519190746045,126.926552346708));
#20025=CARTESIAN_POINT('Ctrl Pts',(200.01045521042,-3.12911719124147,127.007627507086));
#20026=CARTESIAN_POINT('Ctrl Pts',(200.002964874658,-3.22964815206794,127.092779730022));
#20027=CARTESIAN_POINT('Ctrl Pts',(199.995474538896,-3.32646505372397,127.181680213659));
#20028=CARTESIAN_POINT('Ctrl Pts',(199.987817885007,-3.42543171291799,127.272554675822));
#20029=CARTESIAN_POINT('Ctrl Pts',(199.980161231117,-3.52085100355156,127.367652463917));
#20030=CARTESIAN_POINT('Ctrl Pts',(199.972504577228,-3.61233263415092,127.466661409616));
#20031=CARTESIAN_POINT('Ctrl Pts',(199.964856779005,-3.7037084573244,127.565555841815));
#20032=CARTESIAN_POINT('Ctrl Pts',(199.957208980783,-3.79115540274886,127.668352146295));
#20033=CARTESIAN_POINT('Ctrl Pts',(199.94956118256,-3.87431677020004,127.774698486792));
#20034=CARTESIAN_POINT('Ctrl Pts',(199.941920455469,-3.95740124690412,127.880946499786));
#20035=CARTESIAN_POINT('Ctrl Pts',(199.934279728377,-4.03620777736056,127.990737706671));
#20036=CARTESIAN_POINT('Ctrl Pts',(199.926639001285,-4.11041742727574,128.10368447333));
#20037=CARTESIAN_POINT('Ctrl Pts',(199.918999136713,-4.18461870007081,128.216618490047));
#20038=CARTESIAN_POINT('Ctrl Pts',(199.911359272141,-4.2542238720399,128.332707043142));
#20039=CARTESIAN_POINT('Ctrl Pts',(199.90371940757,-4.31895501961334,128.451530279217));
#20040=CARTESIAN_POINT('Ctrl Pts',(199.896087179009,-4.38362146868872,128.570234751988));
#20041=CARTESIAN_POINT('Ctrl Pts',(199.888454950448,-4.44342342148269,128.69166809915));
#20042=CARTESIAN_POINT('Ctrl Pts',(199.880822721887,-4.49812811338532,128.815384363793));
#20043=CARTESIAN_POINT('Ctrl Pts',(199.87317903931,-4.55291490299365,128.939286294805));
#20044=CARTESIAN_POINT('Ctrl Pts',(199.865535356733,-4.60258893508908,129.065477639417));
#20045=CARTESIAN_POINT('Ctrl Pts',(199.857891674155,-4.64696388063631,129.19348825932));
#20046=CARTESIAN_POINT('Ctrl Pts',(199.850247991578,-4.69133882618354,129.321498879223));
#20047=CARTESIAN_POINT('Ctrl Pts',(199.842604309,-4.73041455848543,129.451328387816));
#20048=CARTESIAN_POINT('Ctrl Pts',(199.834960626423,-4.76405452823405,129.582490119308));
#20049=CARTESIAN_POINT('Ctrl Pts',(201.584606355351,-4.76405452823405,129.582490119308));
#20050=CARTESIAN_POINT('Ctrl Pts',(201.576612163084,-4.79917136563237,129.719410135352));
#20051=CARTESIAN_POINT('Ctrl Pts',(201.568617970816,-4.82841256673479,129.857966876512));
#20052=CARTESIAN_POINT('Ctrl Pts',(201.560623778548,-4.85163618075089,129.997633010422));
#20053=CARTESIAN_POINT('Ctrl Pts',(201.55263857145,-4.87483369230245,130.137142164875));
#20054=CARTESIAN_POINT('Ctrl Pts',(201.544653364352,-4.89202704125614,130.277757877198));
#20055=CARTESIAN_POINT('Ctrl Pts',(201.536668157254,-4.90312503397178,130.418941412363));
#20056=CARTESIAN_POINT('Ctrl Pts',(201.5293985835,-4.91322842585438,130.547472095315));
#20057=CARTESIAN_POINT('Ctrl Pts',(201.522129009746,-4.9182805956174,130.676473036305));
#20058=CARTESIAN_POINT('Ctrl Pts',(201.514859435991,-4.91824986053224,130.805531888085));
#20059=CARTESIAN_POINT('',(201.860140564039,-4.91824790150174,130.799817284683));
#20060=CARTESIAN_POINT('Ctrl Pts',(201.930097584127,-4.76405452823404,129.582490119308));
#20061=CARTESIAN_POINT('Ctrl Pts',(201.928404692561,-4.77143981658942,129.611285246518));
#20062=CARTESIAN_POINT('Ctrl Pts',(201.926711800994,-4.77856158153426,129.640137793894));
#20063=CARTESIAN_POINT('Ctrl Pts',(201.925018909427,-4.78541909345683,129.669042528888));
#20064=CARTESIAN_POINT('Ctrl Pts',(201.914205851863,-4.82922028700719,129.853666617963));
#20065=CARTESIAN_POINT('Ctrl Pts',(201.903392794298,-4.86235268751459,130.040911499407));
#20066=CARTESIAN_POINT('Ctrl Pts',(201.892579736733,-4.88456555156559,130.22972818291));
#20067=CARTESIAN_POINT('Ctrl Pts',(201.882347687665,-4.90558487136082,130.408399345895));
#20068=CARTESIAN_POINT('Ctrl Pts',(201.872115638597,-4.91682686629452,130.58847825068));
#20069=CARTESIAN_POINT('Ctrl Pts',(201.861883589529,-4.91812325643309,130.769052020427));
#20070=CARTESIAN_POINT('Ctrl Pts',(201.861302581032,-4.91819686961459,130.779305577046));
#20071=CARTESIAN_POINT('Ctrl Pts',(201.860721572536,-4.91823842679033,130.789560721775));
#20072=CARTESIAN_POINT('Ctrl Pts',(201.860140564039,-4.91824790150174,130.799817284683));
#20073=CARTESIAN_POINT('Ctrl Pts',(201.860140564008,-4.91824790150225,130.799817285234));
#20074=CARTESIAN_POINT('Ctrl Pts',(201.852483585455,-4.91837276654937,130.934986190149));
#20075=CARTESIAN_POINT('Ctrl Pts',(201.844826606902,-4.91292114291673,131.07031288466));
#20076=CARTESIAN_POINT('Ctrl Pts',(201.83716962835,-4.90188083750575,131.205293676061));
#20077=CARTESIAN_POINT('Ctrl Pts',(201.829228030736,-4.89043015072319,131.345291865101));
#20078=CARTESIAN_POINT('Ctrl Pts',(201.821286433122,-4.8729672167622,131.484917501621));
#20079=CARTESIAN_POINT('Ctrl Pts',(201.813344835508,-4.84953772420023,131.62360839697));
#20080=CARTESIAN_POINT('Ctrl Pts',(201.80569610997,-4.82697226989009,131.757184617366));
#20081=CARTESIAN_POINT('Ctrl Pts',(201.798047384431,-4.79887259272399,131.889893384014));
#20082=CARTESIAN_POINT('Ctrl Pts',(201.790398658893,-4.76533224076631,132.021238465837));
#20083=CARTESIAN_POINT('Ctrl Pts',(201.782750978392,-4.73179647139039,132.152565602125));
#20084=CARTESIAN_POINT('Ctrl Pts',(201.775103297891,-4.69282160461944,132.282529034708));
#20085=CARTESIAN_POINT('Ctrl Pts',(201.767455617389,-4.64855188812975,132.410644654051));
#20086=CARTESIAN_POINT('Ctrl Pts',(201.759807225106,-4.60427805138161,132.538772197334));
#20087=CARTESIAN_POINT('Ctrl Pts',(201.752158832822,-4.5547085165048,132.665051205577));
#20088=CARTESIAN_POINT('Ctrl Pts',(201.744510440538,-4.50003661315956,132.789015132267));
#20089=CARTESIAN_POINT('Ctrl Pts',(201.736859579318,-4.44534706147838,132.913019075069));
#20090=CARTESIAN_POINT('Ctrl Pts',(201.729208718099,-4.38555202834284,133.034706082836));
#20091=CARTESIAN_POINT('Ctrl Pts',(201.72155785688,-4.32089170944105,133.153632397881));
#20092=CARTESIAN_POINT('Ctrl Pts',(201.713898683524,-4.25616114153522,133.272687918215));
#20093=CARTESIAN_POINT('Ctrl Pts',(201.706239510168,-4.18655493051007,133.388976406699));
#20094=CARTESIAN_POINT('Ctrl Pts',(201.698580336813,-4.11235781880762,133.502081179928));
#20095=CARTESIAN_POINT('Ctrl Pts',(201.690916213761,-4.03811275765906,133.615259046451));
#20096=CARTESIAN_POINT('Ctrl Pts',(201.68325209071,-3.95927112365503,133.725248776863));
#20097=CARTESIAN_POINT('Ctrl Pts',(201.675587967659,-3.87615836955861,133.831666244126));
#20098=CARTESIAN_POINT('Ctrl Pts',(201.667913108811,-3.79292919227884,133.938232779488));
#20099=CARTESIAN_POINT('Ctrl Pts',(201.660238249964,-3.70541721587963,134.041216762563));
#20100=CARTESIAN_POINT('Ctrl Pts',(201.652563391116,-3.61398532778852,134.140270255585));
#20101=CARTESIAN_POINT('Ctrl Pts',(201.650566022616,-3.59019033991468,134.166048752722));
#20102=CARTESIAN_POINT('Ctrl Pts',(201.648568654115,-3.56613003589684,134.191561251679));
#20103=CARTESIAN_POINT('Ctrl Pts',(201.646571285615,-3.54181117222063,134.216802072424));
#20104=CARTESIAN_POINT('Ctrl Pts',(201.638796951494,-3.44715514275093,134.315046624639));
#20105=CARTESIAN_POINT('Ctrl Pts',(201.631022617374,-3.34825835130227,134.409505379128));
#20106=CARTESIAN_POINT('Ctrl Pts',(201.623248283254,-3.24545589596689,134.499790104085));
#20107=CARTESIAN_POINT('Ctrl Pts',(201.615483530306,-3.14278013546986,134.589963561187));
#20108=CARTESIAN_POINT('Ctrl Pts',(201.607718777357,-3.03620857922076,134.675972968507));
#20109=CARTESIAN_POINT('Ctrl Pts',(201.599954024409,-2.92611462881938,134.757465250827));
#20110=CARTESIAN_POINT('Ctrl Pts',(201.592196983523,-2.8161300252812,134.838876593864));
#20111=CARTESIAN_POINT('Ctrl Pts',(201.584439942637,-2.70263030195642,134.915779509083));
#20112=CARTESIAN_POINT('Ctrl Pts',(201.576682901751,-2.58602327795652,134.987859950465));
#20113=CARTESIAN_POINT('Ctrl Pts',(201.568931710509,-2.46950418822028,135.059886035426));
#20114=CARTESIAN_POINT('Ctrl Pts',(201.561180519268,-2.3498827930975,135.127096680372));
#20115=CARTESIAN_POINT('Ctrl Pts',(201.553429328027,-2.22759704920044,135.189220301626));
#20116=CARTESIAN_POINT('Ctrl Pts',(201.545681431248,-2.10536328000659,135.251317518684));
#20117=CARTESIAN_POINT('Ctrl Pts',(201.53793353447,-1.98046776216892,135.308331835635));
#20118=CARTESIAN_POINT('Ctrl Pts',(201.530185637692,-1.85337409203519,135.360037025902));
#20119=CARTESIAN_POINT('Ctrl Pts',(201.522439361606,-1.72630700715721,135.411731400558));
#20120=CARTESIAN_POINT('Ctrl Pts',(201.514693085521,-1.59704304647646,135.458118710247));
#20121=CARTESIAN_POINT('Ctrl Pts',(201.506946809436,-1.46606651029953,135.499020567965));
#20122=CARTESIAN_POINT('Ctrl Pts',(201.499200476169,-1.33508900728361,135.539922727611));
#20123=CARTESIAN_POINT('Ctrl Pts',(201.491454142903,-1.20239927673706,135.575339237944));
#20124=CARTESIAN_POINT('Ctrl Pts',(201.483707809636,-1.0684971462986,135.605141482264));
#20125=CARTESIAN_POINT('Ctrl Pts',(201.475959741632,-0.934565029406161,
135.63495040059));
#20126=CARTESIAN_POINT('Ctrl Pts',(201.468211673628,-0.799420353905459,
135.659142466148));
#20127=CARTESIAN_POINT('Ctrl Pts',(201.460463605623,-0.663573118682993,
135.677640188724));
#20128=CARTESIAN_POINT('Ctrl Pts',(201.45270730288,-0.527581503402445,135.696157570899));
#20129=CARTESIAN_POINT('Ctrl Pts',(201.444951000137,-0.390886224816852,
135.708968467706));
#20130=CARTESIAN_POINT('Ctrl Pts',(201.437194697394,-0.254002943294543,
135.716047249192));
#20131=CARTESIAN_POINT('Ctrl Pts',(201.429434254879,-0.117046603043397,
135.723129808838));
#20132=CARTESIAN_POINT('Ctrl Pts',(201.421673812363,0.0200975493309183,
135.724474153213));
#20133=CARTESIAN_POINT('Ctrl Pts',(201.413913369848,0.156914869496959,135.720106826051));
#20134=CARTESIAN_POINT('Ctrl Pts',(201.406140469581,0.293951820971461,135.715732488067));
#20135=CARTESIAN_POINT('Ctrl Pts',(201.398367569315,0.430660501673616,135.705628185033));
#20136=CARTESIAN_POINT('Ctrl Pts',(201.390594669048,0.566531497579824,135.689872374255));
#20137=CARTESIAN_POINT('Ctrl Pts',(201.383104333299,0.697463240297336,135.674689326915));
#20138=CARTESIAN_POINT('Ctrl Pts',(201.37561399755,0.827616840453072,135.654258578995));
#20139=CARTESIAN_POINT('Ctrl Pts',(201.368123661801,0.956548189162586,135.628694625935));
#20140=CARTESIAN_POINT('Ctrl Pts',(201.360349327683,1.09036800937337,135.60216140778));
#20141=CARTESIAN_POINT('Ctrl Pts',(201.352574993564,1.22329496617451,135.570014000326));
#20142=CARTESIAN_POINT('Ctrl Pts',(201.344800659445,1.35482130044931,135.532324482313));
#20143=CARTESIAN_POINT('Ctrl Pts',(201.337035906498,1.48618554027203,135.494681413262));
#20144=CARTESIAN_POINT('Ctrl Pts',(201.329271153552,1.61615221984584,135.451509930292));
#20145=CARTESIAN_POINT('Ctrl Pts',(201.321506400605,1.74422245430599,135.402933340966));
#20146=CARTESIAN_POINT('Ctrl Pts',(201.31374935972,1.87216548760419,135.354404998592));
#20147=CARTESIAN_POINT('Ctrl Pts',(201.305992318836,1.99821546100229,135.300482371031));
#20148=CARTESIAN_POINT('Ctrl Pts',(201.298235277951,2.12188772249806,135.241338818505));
#20149=CARTESIAN_POINT('Ctrl Pts',(201.290484086711,2.24546672177877,135.182239866593));
#20150=CARTESIAN_POINT('Ctrl Pts',(201.282732895472,2.36667122683608,135.117927994348));
#20151=CARTESIAN_POINT('Ctrl Pts',(201.274981704232,2.48503602038379,135.048624869459));
#20152=CARTESIAN_POINT('Ctrl Pts',(201.267233807455,2.60335050573666,134.979351200247));
#20153=CARTESIAN_POINT('Ctrl Pts',(201.259485910679,2.71882734343585,134.905090694853));
#20154=CARTESIAN_POINT('Ctrl Pts',(201.251738013902,2.83102561750346,134.826111109024));
#20155=CARTESIAN_POINT('Ctrl Pts',(201.243991737818,2.94320042211094,134.747148044021));
#20156=CARTESIAN_POINT('Ctrl Pts',(201.236245461735,3.0520977076928,134.663468086941));
#20157=CARTESIAN_POINT('Ctrl Pts',(201.228499185651,3.15730561606483,134.575382270814));
#20158=CARTESIAN_POINT('Ctrl Pts',(201.220752852386,3.26251430105758,134.487295804458));
#20159=CARTESIAN_POINT('Ctrl Pts',(201.213006519121,3.36403325472788,134.394803665141));
#20160=CARTESIAN_POINT('Ctrl Pts',(201.205260185856,3.46148409915498,134.298256851543));
#20161=CARTESIAN_POINT('Ctrl Pts',(201.197512117854,3.55895676702291,134.201688416955));
#20162=CARTESIAN_POINT('Ctrl Pts',(201.189764049851,3.6523592351274,134.101063776349));
#20163=CARTESIAN_POINT('Ctrl Pts',(201.182015981848,3.74135064190172,133.996770120879));
#20164=CARTESIAN_POINT('Ctrl Pts',(201.174259679107,3.8304366298024,133.89236562087));
#20165=CARTESIAN_POINT('Ctrl Pts',(201.166503376366,3.91510193715322,133.784284614265));
#20166=CARTESIAN_POINT('Ctrl Pts',(201.158747073624,3.99504627372427,133.672947087119));
#20167=CARTESIAN_POINT('Ctrl Pts',(201.15098663111,4.07503327899471,133.561550135783));
#20168=CARTESIAN_POINT('Ctrl Pts',(201.143226188597,4.1502940782862,133.446893527272));
#20169=CARTESIAN_POINT('Ctrl Pts',(201.135465746083,4.22057282576062,133.329424593974));
#20170=CARTESIAN_POINT('Ctrl Pts',(201.127692845818,4.2909643909197,133.211767089115));
#20171=CARTESIAN_POINT('Ctrl Pts',(201.119919945553,4.35635773583158,133.091288581682));
#20172=CARTESIAN_POINT('Ctrl Pts',(201.112147045288,4.41654351812895,132.968460064212));
#20173=CARTESIAN_POINT('Ctrl Pts',(201.104656709521,4.47454139567703,132.850096672665));
#20174=CARTESIAN_POINT('Ctrl Pts',(201.097166373755,4.5277036290204,132.729551444137));
#20175=CARTESIAN_POINT('Ctrl Pts',(201.089676037989,4.57588649471474,132.607259907595));
#20176=CARTESIAN_POINT('Ctrl Pts',(201.08190170387,4.62589622837748,132.48033165035));
#20177=CARTESIAN_POINT('Ctrl Pts',(201.074127369751,4.67069997109745,132.351119977928));
#20178=CARTESIAN_POINT('Ctrl Pts',(201.066353035632,4.71008390855603,132.220091042775));
#20179=CARTESIAN_POINT('Ctrl Pts',(201.058588282685,4.74941930883149,132.089223589074));
#20180=CARTESIAN_POINT('Ctrl Pts',(201.050823529738,4.78334808245175,131.956543699629));
#20181=CARTESIAN_POINT('Ctrl Pts',(201.043058776791,4.81170431210567,131.822537751155));
#20182=CARTESIAN_POINT('Ctrl Pts',(201.035301735906,4.84003237795253,131.688664899279));
#20183=CARTESIAN_POINT('Ctrl Pts',(201.027544695021,4.86279883378002,131.553468989404));
#20184=CARTESIAN_POINT('Ctrl Pts',(201.019787654136,4.87988756620843,131.417451478421));
#20185=CARTESIAN_POINT('Ctrl Pts',(201.012036462896,4.89696341189084,131.281536539302));
#20186=CARTESIAN_POINT('Ctrl Pts',(201.004285271656,4.90837000793079,131.144801618648));
#20187=CARTESIAN_POINT('Ctrl Pts',(200.996534080416,4.91404238832683,131.007757933741));
#20188=CARTESIAN_POINT('Ctrl Pts',(200.988786183639,4.91971235780988,130.870772496056));
#20189=CARTESIAN_POINT('Ctrl Pts',(200.981038286862,4.91965294290856,130.733478944942));
#20190=CARTESIAN_POINT('Ctrl Pts',(200.973290390085,4.91385108825839,130.596392964019));
#20191=CARTESIAN_POINT('Ctrl Pts',(200.965544114001,4.90805044723114,130.459335658529));
#20192=CARTESIAN_POINT('Ctrl Pts',(200.957797837917,4.89650977221841,130.322486227234));
#20193=CARTESIAN_POINT('Ctrl Pts',(200.950051561833,4.87926812470907,130.186359299041));
#20194=CARTESIAN_POINT('Ctrl Pts',(200.942305228568,4.86202634992579,130.050231365991));
#20195=CARTESIAN_POINT('Ctrl Pts',(200.934558895303,4.83908356779839,129.91482633455));
#20196=CARTESIAN_POINT('Ctrl Pts',(200.926812562038,4.81053056094829,129.780652268141));
#20197=CARTESIAN_POINT('Ctrl Pts',(200.919064494035,4.78197115985042,129.646448154381));
#20198=CARTESIAN_POINT('Ctrl Pts',(200.911316426032,4.74779911535903,129.513475936524));
#20199=CARTESIAN_POINT('Ctrl Pts',(200.903568358029,4.70815593835484,129.382231677338));
#20200=CARTESIAN_POINT('Ctrl Pts',(200.895812055287,4.66847062811032,129.250847930191));
#20201=CARTESIAN_POINT('Ctrl Pts',(200.888055752546,4.62330268292331,129.121196185172));
#20202=CARTESIAN_POINT('Ctrl Pts',(200.880299449804,4.57284313475343,128.993756097678));
#20203=CARTESIAN_POINT('Ctrl Pts',(200.87253900729,4.52235665480324,128.866247991572));
#20204=CARTESIAN_POINT('Ctrl Pts',(200.864778564776,4.46657310317764,128.740954252085));
#20205=CARTESIAN_POINT('Ctrl Pts',(200.857018122262,4.40573054235811,128.618331923648));
#20206=CARTESIAN_POINT('Ctrl Pts',(200.849245221996,4.34479031165874,128.495512750964));
#20207=CARTESIAN_POINT('Ctrl Pts',(200.841472321731,4.27877503146672,128.375373901733));
#20208=CARTESIAN_POINT('Ctrl Pts',(200.833699421466,4.20796780647951,128.258346084589));
#20209=CARTESIAN_POINT('Ctrl Pts',(200.826209085702,4.13973460246116,128.145572523353));
#20210=CARTESIAN_POINT('Ctrl Pts',(200.818718749939,4.06705197339164,128.035687990354));
#20211=CARTESIAN_POINT('Ctrl Pts',(200.811228414176,3.99020865609362,127.929048818241));
#20212=CARTESIAN_POINT('Ctrl Pts',(200.803454080057,3.91045180107535,127.818366389521));
#20213=CARTESIAN_POINT('Ctrl Pts',(200.795679745938,3.82595987893068,127.710829666744));
#20214=CARTESIAN_POINT('Ctrl Pts',(200.787905411818,3.73700950505258,127.606870504736));
#20215=CARTESIAN_POINT('Ctrl Pts',(200.780140658871,3.64816875456051,127.503039463103));
#20216=CARTESIAN_POINT('Ctrl Pts',(200.772375905924,3.55488073677464,127.402777503809));
#20217=CARTESIAN_POINT('Ctrl Pts',(200.764611152976,3.45746497184096,127.306487116281));
#20218=CARTESIAN_POINT('Ctrl Pts',(200.756854112091,3.36014596161846,127.210292365723));
#20219=CARTESIAN_POINT('Ctrl Pts',(200.749097071206,3.25870763916541,127.118061610023));
#20220=CARTESIAN_POINT('Ctrl Pts',(200.741340030321,3.15350913224816,127.030163588352));
#20221=CARTESIAN_POINT('Ctrl Pts',(200.733588839081,3.04838995634344,126.942331851264));
#20222=CARTESIAN_POINT('Ctrl Pts',(200.72583764784,2.93951653884054,126.858826594413));
#20223=CARTESIAN_POINT('Ctrl Pts',(200.7180864566,2.82728386560443,126.779978800964));
#20224=CARTESIAN_POINT('Ctrl Pts',(200.710338559823,2.71509889424786,126.701164519931));
#20225=CARTESIAN_POINT('Ctrl Pts',(200.702590663046,2.59955782612968,126.627003989411));
#20226=CARTESIAN_POINT('Ctrl Pts',(200.694842766268,2.48108746374105,126.557786932845));
#20227=CARTESIAN_POINT('Ctrl Pts',(200.687096490184,2.36264188279868,126.488584354995));
#20228=CARTESIAN_POINT('Ctrl Pts',(200.6793502141,2.24126856372764,126.424323391385));
#20229=CARTESIAN_POINT('Ctrl Pts',(200.671603938015,2.11742159208994,126.36524934797));
#20230=CARTESIAN_POINT('Ctrl Pts',(200.66385760475,1.99357370624226,126.306174868485));
#20231=CARTESIAN_POINT('Ctrl Pts',(200.656111271484,1.86725248426869,126.252287553918));
#20232=CARTESIAN_POINT('Ctrl Pts',(200.648364938219,1.7389344445388,126.203785646968));
#20233=CARTESIAN_POINT('Ctrl Pts',(200.640616870216,1.61058766887319,126.155272878351));
#20234=CARTESIAN_POINT('Ctrl Pts',(200.632868802213,1.48024355127012,126.112148055408));
#20235=CARTESIAN_POINT('Ctrl Pts',(200.625120734209,1.34839593347158,126.074560255067));
#20236=CARTESIAN_POINT('Ctrl Pts',(200.617364431467,1.21640818645573,126.036932505965));
#20237=CARTESIAN_POINT('Ctrl Pts',(200.609608128725,1.08291412377568,126.004853642373));
#20238=CARTESIAN_POINT('Ctrl Pts',(200.601851825983,0.948420550542189,125.978422209152));
#20239=CARTESIAN_POINT('Ctrl Pts',(200.594091383469,0.813855194038882,125.951976668679));
#20240=CARTESIAN_POINT('Ctrl Pts',(200.586330940955,0.678289650257551,125.931184623874));
#20241=CARTESIAN_POINT('Ctrl Pts',(200.57857049844,0.54223712220886,125.916092829709));
#20242=CARTESIAN_POINT('Ctrl Pts',(200.570797598175,0.405966190564276,125.900976808856));
#20243=CARTESIAN_POINT('Ctrl Pts',(200.563024697909,0.269207102735885,125.891579351172));
#20244=CARTESIAN_POINT('Ctrl Pts',(200.555251797643,0.132475251099434,125.887895081193));
#20245=CARTESIAN_POINT('Ctrl Pts',(200.547761461883,0.000713946712914748,
125.884344743708));
#20246=CARTESIAN_POINT('Ctrl Pts',(200.540271126123,-0.131021759319523,
125.88609942386));
#20247=CARTESIAN_POINT('Ctrl Pts',(200.532780790363,-0.262276004943429,
125.893108805682));
#20248=CARTESIAN_POINT('Ctrl Pts',(200.525006456244,-0.398506795217166,
125.900383950348));
#20249=CARTESIAN_POINT('Ctrl Pts',(200.517232122125,-0.534650433432306,
125.913343171992));
#20250=CARTESIAN_POINT('Ctrl Pts',(200.509457788006,-0.670194070517084,
125.931987174331));
#20251=CARTESIAN_POINT('Ctrl Pts',(200.501693035059,-0.805570662182922,
125.950608199603));
#20252=CARTESIAN_POINT('Ctrl Pts',(200.493928282112,-0.940348340398937,
125.974900012985));
#20253=CARTESIAN_POINT('Ctrl Pts',(200.486163529165,-1.07401577096679,126.004811348498));
#20254=CARTESIAN_POINT('Ctrl Pts',(200.47840648828,-1.20755044115865,126.03469297565));
#20255=CARTESIAN_POINT('Ctrl Pts',(200.470649447395,-1.33997667909172,126.070182932893));
#20256=CARTESIAN_POINT('Ctrl Pts',(200.46289240651,-1.47079013672649,126.111178388395));
#20257=CARTESIAN_POINT('Ctrl Pts',(200.45514121527,-1.60150494691511,126.152142928905));
#20258=CARTESIAN_POINT('Ctrl Pts',(200.44739002403,-1.73060902603362,126.198604587446));
#20259=CARTESIAN_POINT('Ctrl Pts',(200.43963883279,-1.85761040906449,126.250409955708));
#20260=CARTESIAN_POINT('Ctrl Pts',(200.431890936013,-1.9845578131194,126.302193305306));
#20261=CARTESIAN_POINT('Ctrl Pts',(200.424143039236,-2.10940393734354,126.359315699986));
#20262=CARTESIAN_POINT('Ctrl Pts',(200.416395142459,-2.23167433202904,126.421574661321));
#20263=CARTESIAN_POINT('Ctrl Pts',(200.408648866375,-2.35391915038416,126.483820599422));
#20264=CARTESIAN_POINT('Ctrl Pts',(200.400902590291,-2.47358896269875,126.551200789732));
#20265=CARTESIAN_POINT('Ctrl Pts',(200.393156314207,-2.59023194178586,126.623465791066));
#20266=CARTESIAN_POINT('Ctrl Pts',(200.385409980941,-2.70687578190523,126.695731325845));
#20267=CARTESIAN_POINT('Ctrl Pts',(200.377663647676,-2.82049241186166,126.772881537696));
#20268=CARTESIAN_POINT('Ctrl Pts',(200.369917314411,-2.93065747463995,126.854622673241));
#20269=CARTESIAN_POINT('Ctrl Pts',(200.362169246408,-3.04084720811968,126.936382114147));
#20270=CARTESIAN_POINT('Ctrl Pts',(200.354421178405,-3.14758352241582,127.022734291636));
#20271=CARTESIAN_POINT('Ctrl Pts',(200.346673110402,-3.25047406136048,127.113344302386));
#20272=CARTESIAN_POINT('Ctrl Pts',(200.33891680766,-3.3534739535945,127.204050614535));
#20273=CARTESIAN_POINT('Ctrl Pts',(200.331160504918,-3.45261961170661,127.29902354087));
#20274=CARTESIAN_POINT('Ctrl Pts',(200.323404202176,-3.54755418657293,127.397889957803));
#20275=CARTESIAN_POINT('Ctrl Pts',(200.315643759662,-3.64253943088031,127.496809142719));
#20276=CARTESIAN_POINT('Ctrl Pts',(200.307883317148,-3.73330885482172,127.599625666022));
#20277=CARTESIAN_POINT('Ctrl Pts',(200.300122874634,-3.8195457233528,127.705933027688));
#20278=CARTESIAN_POINT('Ctrl Pts',(200.292349974369,-3.90592102696098,127.812411043368));
#20279=CARTESIAN_POINT('Ctrl Pts',(200.284577074103,-3.98774900175901,127.922390781748));
#20280=CARTESIAN_POINT('Ctrl Pts',(200.276804173838,-4.06475558810789,128.035435723054));
#20281=CARTESIAN_POINT('Ctrl Pts',(200.269313838075,-4.13896279108229,128.144371196012));
#20282=CARTESIAN_POINT('Ctrl Pts',(200.261823502312,-4.20869289593499,128.256152623966));
#20283=CARTESIAN_POINT('Ctrl Pts',(200.25433316655,-4.27374183033709,128.37036928025));
#20284=CARTESIAN_POINT('Ctrl Pts',(200.246220788594,-4.34419281654029,128.494071169452));
#20285=CARTESIAN_POINT('Ctrl Pts',(200.238108410639,-4.40935986504164,128.620992964794));
#20286=CARTESIAN_POINT('Ctrl Pts',(200.229996032683,-4.46895007272139,128.750664362025));
#20287=CARTESIAN_POINT('Ctrl Pts',(200.221641782561,-4.53031697432501,128.88420193782));
#20288=CARTESIAN_POINT('Ctrl Pts',(200.213287532439,-4.58576906133034,129.02065536604));
#20289=CARTESIAN_POINT('Ctrl Pts',(200.204933282317,-4.6350349423211,129.159479422475));
#20290=CARTESIAN_POINT('Ctrl Pts',(200.196579032196,-4.68430082331187,129.298303478911));
#20291=CARTESIAN_POINT('Ctrl Pts',(200.188224782074,-4.7273802889641,129.439497817004));
#20292=CARTESIAN_POINT('Ctrl Pts',(200.179870531952,-4.76405452823405,129.582490119308));
#20293=CARTESIAN_POINT('Origin',(213.235140564004,0.,130.804360617566));
#20294=CARTESIAN_POINT('',(198.084936573762,-4.76405452823404,129.582490119308));
#20295=CARTESIAN_POINT('',(198.430216174721,-4.76405452823404,129.582490119308));
#20296=CARTESIAN_POINT('',(213.235140564004,-4.76405452823405,129.582490119308));
#20297=CARTESIAN_POINT('',(199.76485943604,-4.91824827604694,130.808478585671));
#20298=CARTESIAN_POINT('Ctrl Pts',(199.764859435991,-4.91824827604621,130.808478586542));
#20299=CARTESIAN_POINT('Ctrl Pts',(199.752723897668,-4.91806930075772,131.022235637443));
#20300=CARTESIAN_POINT('Ctrl Pts',(199.740588359346,-4.90395198746022,131.235429274479));
#20301=CARTESIAN_POINT('Ctrl Pts',(199.728452821023,-4.87613221702235,131.446635998237));
#20302=CARTESIAN_POINT('Ctrl Pts',(199.72464418571,-4.86740121908247,131.512921429102));
#20303=CARTESIAN_POINT('Ctrl Pts',(199.720835550396,-4.85732086664738,131.57901143828));
#20304=CARTESIAN_POINT('Ctrl Pts',(199.717026915083,-4.84589923841166,131.64486263045));
#20305=CARTESIAN_POINT('Ctrl Pts',(199.709252580964,-4.82258496786947,131.779280637941));
#20306=CARTESIAN_POINT('Ctrl Pts',(199.701478246845,-4.79363669851475,131.912940764209));
#20307=CARTESIAN_POINT('Ctrl Pts',(199.693703912726,-4.75911430351347,132.045333666666));
#20308=CARTESIAN_POINT('Ctrl Pts',(199.685939159779,-4.7246344542787,132.177563406704));
#20309=CARTESIAN_POINT('Ctrl Pts',(199.678174406832,-4.68459424557846,132.308528655646));
#20310=CARTESIAN_POINT('Ctrl Pts',(199.670409653885,-4.63910497760412,132.437727713252));
#20311=CARTESIAN_POINT('Ctrl Pts',(199.662652613,-4.59366089021201,132.566798448532));
#20312=CARTESIAN_POINT('Ctrl Pts',(199.654895572115,-4.54277864283484,132.694106117038));
#20313=CARTESIAN_POINT('Ctrl Pts',(199.64713853123,-4.48661991546082,132.819162046166));
#20314=CARTESIAN_POINT('Ctrl Pts',(199.63938733999,-4.43050353782002,132.944123669646));
#20315=CARTESIAN_POINT('Ctrl Pts',(199.631636148749,-4.36911875972351,133.066836578412));
#20316=CARTESIAN_POINT('Ctrl Pts',(199.623884957509,-4.30267602109411,133.186830369735));
#20317=CARTESIAN_POINT('Ctrl Pts',(199.616137060732,-4.23626152240097,133.306773160497));
#20318=CARTESIAN_POINT('Ctrl Pts',(199.608389163955,-4.16479352789244,133.423998791095));
#20319=CARTESIAN_POINT('Ctrl Pts',(199.600641267178,-4.08852913543883,133.538060047124));
#20320=CARTESIAN_POINT('Ctrl Pts',(199.592894991094,-4.01228069585204,133.652097443998));
#20321=CARTESIAN_POINT('Ctrl Pts',(199.58514871501,-3.93123807111655,133.762971458094));
#20322=CARTESIAN_POINT('Ctrl Pts',(199.577402438926,-3.84570232123248,133.870262885899));
#20323=CARTESIAN_POINT('Ctrl Pts',(199.56965610566,-3.76016593994299,133.977555105704));
#20324=CARTESIAN_POINT('Ctrl Pts',(199.561909772395,-3.67013661103911,134.081264380741));
#20325=CARTESIAN_POINT('Ctrl Pts',(199.554163439129,-3.57595615209479,134.181004019051));
#20326=CARTESIAN_POINT('Ctrl Pts',(199.546415371126,-3.48175460208978,134.280765993363));
#20327=CARTESIAN_POINT('Ctrl Pts',(199.538667303124,-3.38340034058184,134.376556277787));
#20328=CARTESIAN_POINT('Ctrl Pts',(199.530919235121,-3.28127226748557,134.468024817398));
#20329=CARTESIAN_POINT('Ctrl Pts',(199.523162932379,-3.17903565145775,134.559590570861));
#20330=CARTESIAN_POINT('Ctrl Pts',(199.515406629637,-3.07301750343207,134.646825142842));
#20331=CARTESIAN_POINT('Ctrl Pts',(199.507650326895,-2.96363048238186,134.729418251079));
#20332=CARTESIAN_POINT('Ctrl Pts',(199.499889884381,-2.85418507818486,134.812055441745));
#20333=CARTESIAN_POINT('Ctrl Pts',(199.492129441867,-2.7413675396017,134.890046010246));
#20334=CARTESIAN_POINT('Ctrl Pts',(199.484368999352,-2.62561893060417,134.963123449678));
#20335=CARTESIAN_POINT('Ctrl Pts',(199.476596099087,-2.50968451166382,135.036318199503));
#20336=CARTESIAN_POINT('Ctrl Pts',(199.468823198821,-2.3908099590241,135.104583864727));
#20337=CARTESIAN_POINT('Ctrl Pts',(199.461050298556,-2.26946110594807,135.167699860748));
#20338=CARTESIAN_POINT('Ctrl Pts',(199.453559962794,-2.15252358934225,135.228521431332));
#20339=CARTESIAN_POINT('Ctrl Pts',(199.446069627032,-2.03328882194573,135.284561108335));
#20340=CARTESIAN_POINT('Ctrl Pts',(199.43857929127,-1.91218875833745,135.335664758207));
#20341=CARTESIAN_POINT('Ctrl Pts',(199.430804957151,-1.78649714900839,135.388706018497));
#20342=CARTESIAN_POINT('Ctrl Pts',(199.423030623032,-1.65839785264128,135.436597582708));
#20343=CARTESIAN_POINT('Ctrl Pts',(199.415256288913,-1.52835175648752,135.479114511724));
#20344=CARTESIAN_POINT('Ctrl Pts',(199.407491535966,-1.39846593052474,135.521579042424));
#20345=CARTESIAN_POINT('Ctrl Pts',(199.399726783019,-1.26663844662274,135.558681996903));
#20346=CARTESIAN_POINT('Ctrl Pts',(199.391962030072,-1.13335155987423,135.590245833932));
#20347=CARTESIAN_POINT('Ctrl Pts',(199.384204989187,-1.00019705554075,135.621778321313));
#20348=CARTESIAN_POINT('Ctrl Pts',(199.376447948302,-0.865586410911478,
135.647782550024));
#20349=CARTESIAN_POINT('Ctrl Pts',(199.368690907417,-0.730018152069129,
135.668130406541));
#20350=CARTESIAN_POINT('Ctrl Pts',(199.360939716176,-0.594552126305398,
135.688462918582));
#20351=CARTESIAN_POINT('Ctrl Pts',(199.353188524936,-0.458130308783093,
135.703147490879));
#20352=CARTESIAN_POINT('Ctrl Pts',(199.345437333696,-0.321262210558749,
135.712106908336));
#20353=CARTESIAN_POINT('Ctrl Pts',(199.337689436919,-0.184452284927075,
135.721062517801));
#20354=CARTESIAN_POINT('Ctrl Pts',(199.329941540142,-0.0471968451682756,
135.724297786676));
#20355=CARTESIAN_POINT('Ctrl Pts',(199.322193643365,0.0899888868944208,
135.72178728837));
#20356=CARTESIAN_POINT('Ctrl Pts',(199.314447367281,0.227145922659364,135.719277315206));
#20357=CARTESIAN_POINT('Ctrl Pts',(199.306701091197,0.3642328890792,135.711023972638));
#20358=CARTESIAN_POINT('Ctrl Pts',(199.298954815113,0.500734368080969,135.697053961229));
#20359=CARTESIAN_POINT('Ctrl Pts',(199.291208481847,0.637236854705554,135.683083846697));
#20360=CARTESIAN_POINT('Ctrl Pts',(199.283462148582,0.773153456354327,135.663397018924));
#20361=CARTESIAN_POINT('Ctrl Pts',(199.275715815317,0.907974077383442,135.638072042269));
#20362=CARTESIAN_POINT('Ctrl Pts',(199.267967747314,1.04282489055591,135.61274139426));
#20363=CARTESIAN_POINT('Ctrl Pts',(199.260219679311,1.17657885054553,135.581770157055));
#20364=CARTESIAN_POINT('Ctrl Pts',(199.252471611308,1.30873664156906,135.545287896645));
#20365=CARTESIAN_POINT('Ctrl Pts',(199.244715308566,1.4410348914656,135.508766862454));
#20366=CARTESIAN_POINT('Ctrl Pts',(199.236959005824,1.57173320612938,135.466723208909));
#20367=CARTESIAN_POINT('Ctrl Pts',(199.229202703082,1.70034748405164,135.419336402549));
#20368=CARTESIAN_POINT('Ctrl Pts',(199.221442260568,1.82903040728659,135.371924304424));
#20369=CARTESIAN_POINT('Ctrl Pts',(199.213681818054,1.95562671669996,135.319163521356));
#20370=CARTESIAN_POINT('Ctrl Pts',(199.20592137554,2.0796737866346,135.261281079464));
#20371=CARTESIAN_POINT('Ctrl Pts',(199.198148475274,2.2039199879383,135.203305719538));
#20372=CARTESIAN_POINT('Ctrl Pts',(199.190375575009,2.32560842485003,135.140192451236));
#20373=CARTESIAN_POINT('Ctrl Pts',(199.182602674743,2.44430171903778,135.072213961908));
#20374=CARTESIAN_POINT('Ctrl Pts',(199.175112338981,2.55868021301209,135.006706661894));
#20375=CARTESIAN_POINT('Ctrl Pts',(199.167622003219,2.67027728465172,134.936681889443));
#20376=CARTESIAN_POINT('Ctrl Pts',(199.160131667457,2.7787297750351,134.862419747228));
#20377=CARTESIAN_POINT('Ctrl Pts',(199.152357333338,2.89129427455412,134.78534193332));
#20378=CARTESIAN_POINT('Ctrl Pts',(199.144582999219,3.00082760257082,134.703454927598));
#20379=CARTESIAN_POINT('Ctrl Pts',(199.1368086651,3.10689139061681,134.617024902474));
#20380=CARTESIAN_POINT('Ctrl Pts',(199.129043912153,3.21282446452324,134.530701394631));
#20381=CARTESIAN_POINT('Ctrl Pts',(199.121279159206,3.31529620605177,134.439846252062));
#20382=CARTESIAN_POINT('Ctrl Pts',(199.113514406258,3.41389657407908,134.344769244263));
#20383=CARTESIAN_POINT('Ctrl Pts',(199.105757365373,3.51239901083084,134.249786668289));
#20384=CARTESIAN_POINT('Ctrl Pts',(199.098000324488,3.60703744639372,134.150590841398));
#20385=CARTESIAN_POINT('Ctrl Pts',(199.090243283603,3.69743462970616,134.047531939212));
#20386=CARTESIAN_POINT('Ctrl Pts',(199.082492092363,3.78776364379947,133.944550754547));
#20387=CARTESIAN_POINT('Ctrl Pts',(199.074740901123,3.87385751502113,133.837712585816));
#20388=CARTESIAN_POINT('Ctrl Pts',(199.066989709883,3.95537587695083,133.727404362455));
#20389=CARTESIAN_POINT('Ctrl Pts',(199.059241813106,4.03685959140212,133.617143023032));
#20390=CARTESIAN_POINT('Ctrl Pts',(199.051493916329,4.11377143257403,133.503414876139));
#20391=CARTESIAN_POINT('Ctrl Pts',(199.043746019552,4.18581151837598,133.386639648796));
#20392=CARTESIAN_POINT('Ctrl Pts',(199.035999743468,4.25783653494499,133.269888848313));
#20393=CARTESIAN_POINT('Ctrl Pts',(199.028253467384,4.32499161798016,133.150092567702));
#20394=CARTESIAN_POINT('Ctrl Pts',(199.020507191299,4.38702063536518,133.027698875092));
#20395=CARTESIAN_POINT('Ctrl Pts',(199.012760858034,4.44905011063427,132.905304279));
#20396=CARTESIAN_POINT('Ctrl Pts',(199.005014524769,4.50595326800805,132.780312581386));
#20397=CARTESIAN_POINT('Ctrl Pts',(198.997268191503,4.55752048674992,132.653195406117));
#20398=CARTESIAN_POINT('Ctrl Pts',(198.9895201235,4.60909925361287,132.526049763837));
#20399=CARTESIAN_POINT('Ctrl Pts',(198.981772055497,4.65533955709796,132.396778058965));
#20400=CARTESIAN_POINT('Ctrl Pts',(198.974023987494,4.6960805123652,132.265870413593));
#20401=CARTESIAN_POINT('Ctrl Pts',(198.966267684753,4.73686476760453,132.134823638018));
#20402=CARTESIAN_POINT('Ctrl Pts',(198.958511382011,4.77213788269821,132.002137822608));
#20403=CARTESIAN_POINT('Ctrl Pts',(198.950755079269,4.80178917923892,131.868317261722));
#20404=CARTESIAN_POINT('Ctrl Pts',(198.942994636755,4.8314563015694,131.734425276773));
#20405=CARTESIAN_POINT('Ctrl Pts',(198.935234194241,4.85549555803585,131.599397724268));
#20406=CARTESIAN_POINT('Ctrl Pts',(198.927473751726,4.87384789167415,131.463746537436));
#20407=CARTESIAN_POINT('Ctrl Pts',(198.919700851461,4.89222968610765,131.327877591277));
#20408=CARTESIAN_POINT('Ctrl Pts',(198.911927951196,4.90490627858033,131.191383399763));
#20409=CARTESIAN_POINT('Ctrl Pts',(198.90415505093,4.91187067501122,131.054779335846));
#20410=CARTESIAN_POINT('Ctrl Pts',(198.896664715168,4.91858189808959,130.923141173736));
#20411=CARTESIAN_POINT('Ctrl Pts',(198.889174379406,4.91998901695341,130.791401296814));
#20412=CARTESIAN_POINT('Ctrl Pts',(198.881684043644,4.91613139364612,130.660016643299));
#20413=CARTESIAN_POINT('Ctrl Pts',(198.873909709525,4.91212750737863,130.523650500714));
#20414=CARTESIAN_POINT('Ctrl Pts',(198.866135375406,4.90243908959812,130.387235082915));
#20415=CARTESIAN_POINT('Ctrl Pts',(198.858361041287,4.88705312982617,130.251283074398));
#20416=CARTESIAN_POINT('Ctrl Pts',(198.85059628834,4.87168613187456,130.115498614582));
#20417=CARTESIAN_POINT('Ctrl Pts',(198.842831535393,4.85063560658772,129.980176812465));
#20418=CARTESIAN_POINT('Ctrl Pts',(198.835066782445,4.82394053457245,129.845830085236));
#20419=CARTESIAN_POINT('Ctrl Pts',(198.82730974156,4.79727197647905,129.71161679307));
#20420=CARTESIAN_POINT('Ctrl Pts',(198.819552700675,4.7649701040377,129.578377029504));
#20421=CARTESIAN_POINT('Ctrl Pts',(198.81179565979,4.72712561650387,129.446617465017));
#20422=CARTESIAN_POINT('Ctrl Pts',(198.80404446855,4.68930966779249,129.314957261443));
#20423=CARTESIAN_POINT('Ctrl Pts',(198.79629327731,4.64595953098006,129.184775409413));
#20424=CARTESIAN_POINT('Ctrl Pts',(198.78854208607,4.59721676439492,129.056567413647));
#20425=CARTESIAN_POINT('Ctrl Pts',(198.780794189293,4.54849471478581,128.928413909699));
#20426=CARTESIAN_POINT('Ctrl Pts',(198.773046292516,4.49438473268614,128.802232958104));
#20427=CARTESIAN_POINT('Ctrl Pts',(198.765298395739,4.43507785272916,128.678503730866));
#20428=CARTESIAN_POINT('Ctrl Pts',(198.757552119655,4.37578337849294,128.554800385114));
#20429=CARTESIAN_POINT('Ctrl Pts',(198.749805843571,4.31129433754229,128.433548095968));
#20430=CARTESIAN_POINT('Ctrl Pts',(198.742059567486,4.24184925661964,128.315204546401));
#20431=CARTESIAN_POINT('Ctrl Pts',(198.734313234221,4.1724036630692,128.196860123249));
#20432=CARTESIAN_POINT('Ctrl Pts',(198.726566900956,4.0980021544152,128.081424819717));
#20433=CARTESIAN_POINT('Ctrl Pts',(198.71882056769,4.01892821604465,127.969329919887));
#20434=CARTESIAN_POINT('Ctrl Pts',(198.711072499687,3.93983656961388,127.857209917182));
#20435=CARTESIAN_POINT('Ctrl Pts',(198.703324431684,3.85607063665606,127.748432126146));
#20436=CARTESIAN_POINT('Ctrl Pts',(198.695576363682,3.76795580858273,127.643396826716));
#20437=CARTESIAN_POINT('Ctrl Pts',(198.68782006094,3.67974733102151,127.538249894519));
#20438=CARTESIAN_POINT('Ctrl Pts',(198.680063758198,3.58718097696145,127.436853699544));
#20439=CARTESIAN_POINT('Ctrl Pts',(198.672307455456,3.49062119914604,127.339573942088));
#20440=CARTESIAN_POINT('Ctrl Pts',(198.664547012942,3.39400988446978,127.242242263496));
#20441=CARTESIAN_POINT('Ctrl Pts',(198.656786570428,3.29340118567955,127.149031665843));
#20442=CARTESIAN_POINT('Ctrl Pts',(198.649026127913,3.1891938849692,127.060268547841));
#20443=CARTESIAN_POINT('Ctrl Pts',(198.641253227648,3.08481930144869,126.971362939403));
#20444=CARTESIAN_POINT('Ctrl Pts',(198.633480327383,2.97683488028589,126.886919318566));
#20445=CARTESIAN_POINT('Ctrl Pts',(198.625707427117,2.86567043886961,126.80722214132));
#20446=CARTESIAN_POINT('Ctrl Pts',(198.618217091355,2.7585471049054,126.730422157211));
#20447=CARTESIAN_POINT('Ctrl Pts',(198.610726755593,2.64847119750003,126.658029686858));
#20448=CARTESIAN_POINT('Ctrl Pts',(198.603236419831,2.53584842786697,126.590258600127));
#20449=CARTESIAN_POINT('Ctrl Pts',(198.595462085712,2.4189555316921,126.519917952044));
#20450=CARTESIAN_POINT('Ctrl Pts',(198.587687751593,2.29894855074917,126.454333226861));
#20451=CARTESIAN_POINT('Ctrl Pts',(198.579913417474,2.1762517885438,126.393792489154));
#20452=CARTESIAN_POINT('Ctrl Pts',(198.572148664527,2.05370623913212,126.333326362497));
#20453=CARTESIAN_POINT('Ctrl Pts',(198.56438391158,1.92847785139323,126.277892026139));
#20454=CARTESIAN_POINT('Ctrl Pts',(198.556619158633,1.80101880639067,126.227733658601));
#20455=CARTESIAN_POINT('Ctrl Pts',(198.548862117748,1.6736863555085,126.17762510906));
#20456=CARTESIAN_POINT('Ctrl Pts',(198.541105076863,1.54412801780239,126.132782242412));
#20457=CARTESIAN_POINT('Ctrl Pts',(198.533348035978,1.41281909465994,126.093402618574));
#20458=CARTESIAN_POINT('Ctrl Pts',(198.525596844738,1.2816091925979,126.054052691217));
#20459=CARTESIAN_POINT('Ctrl Pts',(198.517845653498,1.14865170571014,126.020157918166));
#20460=CARTESIAN_POINT('Ctrl Pts',(198.510094462257,1.01444003188544,125.991867034795));
#20461=CARTESIAN_POINT('Ctrl Pts',(198.50234656548,0.880285401602321,125.963588175804));
#20462=CARTESIAN_POINT('Ctrl Pts',(198.494598668703,0.744878026361152,125.940908549741));
#20463=CARTESIAN_POINT('Ctrl Pts',(198.486850771926,0.608724306023622,125.92392643793));
#20464=CARTESIAN_POINT('Ctrl Pts',(198.479104495842,0.472599066109263,125.906947878411));
#20465=CARTESIAN_POINT('Ctrl Pts',(198.471358219758,0.335728179341729,125.895664510952));
#20466=CARTESIAN_POINT('Ctrl Pts',(198.463611943674,0.198625636898631,125.890123045077));
#20467=CARTESIAN_POINT('Ctrl Pts',(198.455865610409,0.061522082395698,125.884581538295));
#20468=CARTESIAN_POINT('Ctrl Pts',(198.448119277143,-0.0758127405487922,
125.884782033463));
#20469=CARTESIAN_POINT('Ctrl Pts',(198.440372943878,-0.212862749645825,
125.890719145876));
#20470=CARTESIAN_POINT('Ctrl Pts',(198.432624875875,-0.349943450142099,
125.896657587864));
#20471=CARTESIAN_POINT('Ctrl Pts',(198.424876807872,-0.486738819347844,
125.908335186536));
#20472=CARTESIAN_POINT('Ctrl Pts',(198.417128739869,-0.622736208410933,
125.925694541964));
#20473=CARTESIAN_POINT('Ctrl Pts',(198.409372437127,-0.75887813711759,125.943072347121));
#20474=CARTESIAN_POINT('Ctrl Pts',(198.401616134385,-0.894220003067948,
125.966143922283));
#20475=CARTESIAN_POINT('Ctrl Pts',(198.393859831644,-1.02825713663446,125.994800312979));
#20476=CARTESIAN_POINT('Ctrl Pts',(198.386099389129,-1.16236580985501,126.023471998453));
#20477=CARTESIAN_POINT('Ctrl Pts',(198.378338946615,-1.2951679847218,126.057734341305));
#20478=CARTESIAN_POINT('Ctrl Pts',(198.370578504101,-1.42617350123758,126.097428261257));
#20479=CARTESIAN_POINT('Ctrl Pts',(198.362805603836,-1.55738931943859,126.137185901413));
#20480=CARTESIAN_POINT('Ctrl Pts',(198.35503270357,-1.68680234652046,126.182392413503));
#20481=CARTESIAN_POINT('Ctrl Pts',(198.347259803305,-1.81394093480719,126.232839935394));
#20482=CARTESIAN_POINT('Ctrl Pts',(198.339769467543,-1.93645771516747,126.281453562794));
#20483=CARTESIAN_POINT('Ctrl Pts',(198.332279131781,-2.05686226744433,126.334933642695));
#20484=CARTESIAN_POINT('Ctrl Pts',(198.324788796019,-2.17475536003933,126.393054440652));
#20485=CARTESIAN_POINT('Ctrl Pts',(198.317013701679,-2.29713037045767,126.453384805213));
#20486=CARTESIAN_POINT('Ctrl Pts',(198.309238607339,-2.41718687346733,126.518906845975));
#20487=CARTESIAN_POINT('Ctrl Pts',(198.301463513,-2.53445302826001,126.589419228882));
#20488=CARTESIAN_POINT('Ctrl Pts',(198.293698169544,-2.65157211748876,126.659843180958));
#20489=CARTESIAN_POINT('Ctrl Pts',(198.285932826088,-2.76590748987507,126.735244822049));
#20490=CARTESIAN_POINT('Ctrl Pts',(198.278167482632,-2.87700919668973,126.815375640825));
#20491=CARTESIAN_POINT('Ctrl Pts',(198.270116194762,-2.99220201841537,126.89845712883));
#20492=CARTESIAN_POINT('Ctrl Pts',(198.262064906893,-3.10391807437486,126.986622596305));
#20493=CARTESIAN_POINT('Ctrl Pts',(198.254013619023,-3.21168484940525,127.079543374989));
#20494=CARTESIAN_POINT('Ctrl Pts',(198.246262861591,-3.31542901381586,127.168995699587));
#20495=CARTESIAN_POINT('Ctrl Pts',(198.23851210416,-3.4155130831933,127.262854447875));
#20496=CARTESIAN_POINT('Ctrl Pts',(198.230761346728,-3.51154654453313,127.360783418188));
#20497=CARTESIAN_POINT('Ctrl Pts',(198.223014065701,-3.60753693251182,127.458668464957));
#20498=CARTESIAN_POINT('Ctrl Pts',(198.215266784674,-3.69948005432967,127.560619822749));
#20499=CARTESIAN_POINT('Ctrl Pts',(198.207519503647,-3.78702100058199,127.666263263491));
#20500=CARTESIAN_POINT('Ctrl Pts',(198.199774019722,-3.8745416403494,127.771882198593));
#20501=CARTESIAN_POINT('Ctrl Pts',(198.192028535798,-3.95766188812499,127.881191211036));
#20502=CARTESIAN_POINT('Ctrl Pts',(198.184283051873,-4.036066276408,127.993782016114));
#20503=CARTESIAN_POINT('Ctrl Pts',(198.176537687326,-4.1144694562842,128.106371085887));
#20504=CARTESIAN_POINT('Ctrl Pts',(198.168792322778,-4.18815669953273,128.222241525939));
#20505=CARTESIAN_POINT('Ctrl Pts',(198.161046958231,-4.25685536445191,128.340955358857));
#20506=CARTESIAN_POINT('Ctrl Pts',(198.153297277113,-4.32559231583465,128.459735352199));
#20507=CARTESIAN_POINT('Ctrl Pts',(198.145547595995,-4.38933494059853,128.581361564616));
#20508=CARTESIAN_POINT('Ctrl Pts',(198.137797914878,-4.44785607756905,128.705370532851));
#20509=CARTESIAN_POINT('Ctrl Pts',(198.130045641782,-4.50639678766299,128.82942097743));
#20510=CARTESIAN_POINT('Ctrl Pts',(198.122293368687,-4.55971237526599,128.955855407105));
#20511=CARTESIAN_POINT('Ctrl Pts',(198.114541095592,-4.60762386482984,129.084190456579));
#20512=CARTESIAN_POINT('Ctrl Pts',(198.106781573825,-4.65558015346834,129.212645504231));
#20513=CARTESIAN_POINT('Ctrl Pts',(198.099022052058,-4.69812213230576,129.343004349367));
#20514=CARTESIAN_POINT('Ctrl Pts',(198.091262530291,-4.73512064756484,129.474768381012));
#20515=CARTESIAN_POINT('Ctrl Pts',(198.089153878115,-4.74517500427239,129.510575292887));
#20516=CARTESIAN_POINT('Ctrl Pts',(198.087045225939,-4.75482027712228,129.546485914373));
#20517=CARTESIAN_POINT('Ctrl Pts',(198.084936573762,-4.76405452823404,129.582490119308));
#20518=CARTESIAN_POINT('Ctrl Pts',(199.834960626423,-4.76405452823405,129.582490119308));
#20519=CARTESIAN_POINT('Ctrl Pts',(199.827324041593,-4.79766326068053,129.713530057033));
#20520=CARTESIAN_POINT('Ctrl Pts',(199.819687456764,-4.82584625215587,129.845899345302));
#20521=CARTESIAN_POINT('Ctrl Pts',(199.812050871934,-4.84851847510395,129.979102076819));
#20522=CARTESIAN_POINT('Ctrl Pts',(199.804185632618,-4.87186954934494,130.116293162135));
#20523=CARTESIAN_POINT('Ctrl Pts',(199.796320393303,-4.88937460082088,130.254367925497));
#20524=CARTESIAN_POINT('Ctrl Pts',(199.788455153987,-4.90099827408403,130.392779544234));
#20525=CARTESIAN_POINT('Ctrl Pts',(199.780589914672,-4.91262194734719,130.53119116297));
#20526=CARTESIAN_POINT('Ctrl Pts',(199.772724675356,-4.91836427281118,130.669939172252));
#20527=CARTESIAN_POINT('Ctrl Pts',(199.76485943604,-4.91824827604694,130.808478585671));
#20528=CARTESIAN_POINT('',(200.110140563961,-4.91824997595732,130.804846925942));
#20529=CARTESIAN_POINT('Ctrl Pts',(200.179870531952,-4.76405452823405,129.582490119308));
#20530=CARTESIAN_POINT('Ctrl Pts',(200.171798423708,-4.79949019568666,129.720653248895));
#20531=CARTESIAN_POINT('Ctrl Pts',(200.163726315465,-4.8289461026174,129.860494510444));
#20532=CARTESIAN_POINT('Ctrl Pts',(200.155654207222,-4.85227401211597,130.001478326166));
#20533=CARTESIAN_POINT('Ctrl Pts',(200.147594415967,-4.87556632625476,130.142247018897));
#20534=CARTESIAN_POINT('Ctrl Pts',(200.139534624712,-4.89274923115088,130.284154452949));
#20535=CARTESIAN_POINT('Ctrl Pts',(200.131474833457,-4.90372514985256,130.426653433092));
#20536=CARTESIAN_POINT('Ctrl Pts',(200.124363410307,-4.91340956969396,130.552385045013));
#20537=CARTESIAN_POINT('Ctrl Pts',(200.117251987158,-4.91826246131281,130.678576831645));
#20538=CARTESIAN_POINT('Ctrl Pts',(200.110140564008,-4.9182499759574,130.804846925109));
#20539=CARTESIAN_POINT('Ctrl Pts',(200.110140563961,-4.91824997595732,130.804846925942));
#20540=CARTESIAN_POINT('Ctrl Pts',(200.101963209632,-4.91823561914748,130.95004364306));
#20541=CARTESIAN_POINT('Ctrl Pts',(200.093785855304,-4.91178722962492,131.095096221673));
#20542=CARTESIAN_POINT('Ctrl Pts',(200.085608500975,-4.8989686251045,131.239434717854));
#20543=CARTESIAN_POINT('Ctrl Pts',(200.077418065999,-4.88612951570811,131.384004100554));
#20544=CARTESIAN_POINT('Ctrl Pts',(200.069227631024,-4.86689987818642,131.527856800843));
#20545=CARTESIAN_POINT('Ctrl Pts',(200.061037196048,-4.84139484664338,131.670431631626));
#20546=CARTESIAN_POINT('Ctrl Pts',(200.052825216095,-4.81582272399528,131.81338150617));
#20547=CARTESIAN_POINT('Ctrl Pts',(200.044613236142,-4.78394225338721,131.955046471638));
#20548=CARTESIAN_POINT('Ctrl Pts',(200.036401256189,-4.74591932059585,132.094877128462));
#20549=CARTESIAN_POINT('Ctrl Pts',(200.028177613076,-4.70784238529188,132.234906381402));
#20550=CARTESIAN_POINT('Ctrl Pts',(200.019953969963,-4.66360567060591,132.373095819458));
#20551=CARTESIAN_POINT('Ctrl Pts',(200.01173032685,-4.61342381118858,132.508914459737));
#20552=CARTESIAN_POINT('Ctrl Pts',(200.003487519808,-4.56312501070649,132.645049604358));
#20553=CARTESIAN_POINT('Ctrl Pts',(199.995244712766,-4.50685348823889,132.778802607651));
#20554=CARTESIAN_POINT('Ctrl Pts',(199.987001905724,-4.4448713186341,132.90966392666));
#20555=CARTESIAN_POINT('Ctrl Pts',(199.983296451395,-4.41700798305935,132.96849105176));
#20556=CARTESIAN_POINT('Ctrl Pts',(199.979590997066,-4.38799121645204,133.026734176052));
#20557=CARTESIAN_POINT('Ctrl Pts',(199.975885542737,-4.35784769754507,133.084348886725));
#20558=CARTESIAN_POINT('Ctrl Pts',(199.968111208618,-4.29460422813576,133.205229073381));
#20559=CARTESIAN_POINT('Ctrl Pts',(199.960336874499,-4.22622722019875,133.3236673123));
#20560=CARTESIAN_POINT('Ctrl Pts',(199.95256254038,-4.15292920796671,133.43919686601));
#20561=CARTESIAN_POINT('Ctrl Pts',(199.944797787433,-4.07972152898389,133.554584039872));
#20562=CARTESIAN_POINT('Ctrl Pts',(199.937033034486,-4.00160512008709,133.667069334041));
#20563=CARTESIAN_POINT('Ctrl Pts',(199.929268281538,-3.91883915315159,133.776208990923));
#20564=CARTESIAN_POINT('Ctrl Pts',(199.921511240653,-3.83615539054131,133.88524024876));
#20565=CARTESIAN_POINT('Ctrl Pts',(199.913754199768,-3.74883149464554,133.990932172596));
#20566=CARTESIAN_POINT('Ctrl Pts',(199.905997158883,-3.65717063344393,134.092868793073));
#20567=CARTESIAN_POINT('Ctrl Pts',(199.898245967643,-3.56557889441098,134.194728542351));
#20568=CARTESIAN_POINT('Ctrl Pts',(199.890494776403,-3.46965696023711,134.292838335461));
#20569=CARTESIAN_POINT('Ctrl Pts',(199.882743585163,-3.36974885186079,134.386814488572));
#20570=CARTESIAN_POINT('Ctrl Pts',(199.874995688386,-3.26988320709536,134.48075069931));
#20571=CARTESIAN_POINT('Ctrl Pts',(199.867247791609,-3.16603504200538,134.570556497095));
#20572=CARTESIAN_POINT('Ctrl Pts',(199.859499894832,-3.05858572710474,134.655884525378));
#20573=CARTESIAN_POINT('Ctrl Pts',(199.851753618747,-2.95115888828444,134.741194704878));
#20574=CARTESIAN_POINT('Ctrl Pts',(199.844007342663,-2.84013270394872,134.822028734951));
#20575=CARTESIAN_POINT('Ctrl Pts',(199.836261066579,-2.72592185460808,134.89807935547));
#20576=CARTESIAN_POINT('Ctrl Pts',(199.828514733314,-2.61171016218902,134.974130537379));
#20577=CARTESIAN_POINT('Ctrl Pts',(199.820768400049,-2.49431408327654,135.045398022584));
#20578=CARTESIAN_POINT('Ctrl Pts',(199.813022066783,-2.37417718264307,135.111617954656));
#20579=CARTESIAN_POINT('Ctrl Pts',(199.80527399878,-2.25401337818375,135.177852716222));
#20580=CARTESIAN_POINT('Ctrl Pts',(199.797525930777,-2.13110787296654,135.239037486666));
#20581=CARTESIAN_POINT('Ctrl Pts',(199.789777862774,-2.00592835665058,135.294954619531));
#20582=CARTESIAN_POINT('Ctrl Pts',(199.782021560032,-1.88061579805486,135.35093118179));
#20583=CARTESIAN_POINT('Ctrl Pts',(199.77426525729,-1.75302475798892,135.401628763137));
#20584=CARTESIAN_POINT('Ctrl Pts',(199.766508954549,-1.623642929,135.446877898267));
#20585=CARTESIAN_POINT('Ctrl Pts',(199.758748512034,-1.49419204503319,135.492151184223));
#20586=CARTESIAN_POINT('Ctrl Pts',(199.75098806952,-1.362948841577,135.531970116074));
#20587=CARTESIAN_POINT('Ctrl Pts',(199.743227627006,-1.23041469352731,135.566215586426));
#20588=CARTESIAN_POINT('Ctrl Pts',(199.73545472674,-1.09766778989741,135.600516030646));
#20589=CARTESIAN_POINT('Ctrl Pts',(199.727681826475,-0.96362618299564,135.629225052453));
#20590=CARTESIAN_POINT('Ctrl Pts',(199.71990892621,-0.828800812444949,135.65227483667));
#20591=CARTESIAN_POINT('Ctrl Pts',(199.712418590448,-0.698876683722678,
135.674486703171));
#20592=CARTESIAN_POINT('Ctrl Pts',(199.704928254686,-0.568225091055471,
135.691443604055));
#20593=CARTESIAN_POINT('Ctrl Pts',(199.697437918924,-0.437304423404299,
135.703130657461));
#20594=CARTESIAN_POINT('Ctrl Pts',(199.689663584805,-0.301419858842875,
135.715260829049));
#20595=CARTESIAN_POINT('Ctrl Pts',(199.681889250686,-0.164814971104963,
135.721752076884));
#20596=CARTESIAN_POINT('Ctrl Pts',(199.674114916567,-0.0279973195866715,
135.722530929033));
#20597=CARTESIAN_POINT('Ctrl Pts',(199.66635016362,0.10865171640381,135.723308821316));
#20598=CARTESIAN_POINT('Ctrl Pts',(199.658585410673,0.245512607244556,135.718388323244));
#20599=CARTESIAN_POINT('Ctrl Pts',(199.650820657726,0.382071918374638,135.707747621637));
#20600=CARTESIAN_POINT('Ctrl Pts',(199.643063616841,0.518495596871722,135.697117488524));
#20601=CARTESIAN_POINT('Ctrl Pts',(199.635306575956,0.654617904481336,135.680778488268));
#20602=CARTESIAN_POINT('Ctrl Pts',(199.627549535071,0.789925004703764,135.658760843077));
#20603=CARTESIAN_POINT('Ctrl Pts',(199.619798343831,0.925130068789412,135.636759801564));
#20604=CARTESIAN_POINT('Ctrl Pts',(199.612047152591,1.05952076479068,135.609088701334));
#20605=CARTESIAN_POINT('Ctrl Pts',(199.604295961351,1.19258833691385,135.575829586464));
#20606=CARTESIAN_POINT('Ctrl Pts',(199.596548064574,1.32559935176917,135.542584607605));
#20607=CARTESIAN_POINT('Ctrl Pts',(199.588800167797,1.45728798274033,135.503756432513));
#20608=CARTESIAN_POINT('Ctrl Pts',(199.581052271019,1.58715584884965,135.459478164306));
#20609=CARTESIAN_POINT('Ctrl Pts',(199.573305994935,1.71699654940101,135.415209158157));
#20610=CARTESIAN_POINT('Ctrl Pts',(199.565559718851,1.84501687283777,135.365492452586));
#20611=CARTESIAN_POINT('Ctrl Pts',(199.557813442767,1.97073416756975,135.310510848447));
#20612=CARTESIAN_POINT('Ctrl Pts',(199.550067109502,2.09645239031821,135.255528838447));
#20613=CARTESIAN_POINT('Ctrl Pts',(199.542320776237,2.21986719223249,135.195282008988));
#20614=CARTESIAN_POINT('Ctrl Pts',(199.534574442971,2.34051682582934,135.130000922828));
#20615=CARTESIAN_POINT('Ctrl Pts',(199.526826374968,2.46119347807506,135.064705217422));
#20616=CARTESIAN_POINT('Ctrl Pts',(199.519078306965,2.57910338599568,134.994373197965));
#20617=CARTESIAN_POINT('Ctrl Pts',(199.511330238962,2.6938106397786,134.919280701786));
#20618=CARTESIAN_POINT('Ctrl Pts',(199.503573936221,2.80863980579594,134.844108396408));
#20619=CARTESIAN_POINT('Ctrl Pts',(199.495817633479,2.92025919055272,134.764165721911));
#20620=CARTESIAN_POINT('Ctrl Pts',(199.488061330737,3.02826260835506,134.679771387709));
#20621=CARTESIAN_POINT('Ctrl Pts',(199.480300888223,3.13632367083349,134.595332009709));
#20622=CARTESIAN_POINT('Ctrl Pts',(199.472540445709,3.24076462319159,134.506436490939));
#20623=CARTESIAN_POINT('Ctrl Pts',(199.464780003195,3.34121425162771,134.41344227184));
#20624=CARTESIAN_POINT('Ctrl Pts',(199.457007102929,3.44182513072487,134.320298770166));
#20625=CARTESIAN_POINT('Ctrl Pts',(199.449234202664,3.53843160653162,134.223043697568));
#20626=CARTESIAN_POINT('Ctrl Pts',(199.441461302398,3.63070044887218,134.122070266263));
#20627=CARTESIAN_POINT('Ctrl Pts',(199.433970966636,3.71961508638472,134.024767473521));
#20628=CARTESIAN_POINT('Ctrl Pts',(199.426480630874,3.8045017845271,133.924012207482));
#20629=CARTESIAN_POINT('Ctrl Pts',(199.418990295112,3.88510025233675,133.820182079754));
#20630=CARTESIAN_POINT('Ctrl Pts',(199.411215960993,3.96875463554883,133.712415201177));
#20631=CARTESIAN_POINT('Ctrl Pts',(199.403441626874,4.04805418477677,133.600994318284));
#20632=CARTESIAN_POINT('Ctrl Pts',(199.395667292754,4.12266273775037,133.486306741795));
#20633=CARTESIAN_POINT('Ctrl Pts',(199.387902539807,4.19717934235037,133.371760507494));
#20634=CARTESIAN_POINT('Ctrl Pts',(199.38013778686,4.26701624247923,133.253955914529));
#20635=CARTESIAN_POINT('Ctrl Pts',(199.372373033913,4.33187756216918,133.133313139382));
#20636=CARTESIAN_POINT('Ctrl Pts',(199.364615993028,4.39667446068206,133.01279018834));
#20637=CARTESIAN_POINT('Ctrl Pts',(199.356858952143,4.45650542925731,132.889435007023));
#20638=CARTESIAN_POINT('Ctrl Pts',(199.349101911258,4.51111815351607,132.763696236473));
#20639=CARTESIAN_POINT('Ctrl Pts',(199.341350720018,4.56568969389464,132.638052286508));
#20640=CARTESIAN_POINT('Ctrl Pts',(199.333599528778,4.61505066744896,132.510028682241));
#20641=CARTESIAN_POINT('Ctrl Pts',(199.325848337538,4.65899510525039,132.380097801158));
#20642=CARTESIAN_POINT('Ctrl Pts',(199.318100440761,4.7029208654935,132.250222144165));
#20643=CARTESIAN_POINT('Ctrl Pts',(199.310352543983,4.74143454383123,132.118441192244));
#20644=CARTESIAN_POINT('Ctrl Pts',(199.302604647206,4.77437873659335,131.985246192914));
#20645=CARTESIAN_POINT('Ctrl Pts',(199.294858371122,4.80731603814052,131.852079055106));
#20646=CARTESIAN_POINT('Ctrl Pts',(199.287112095038,4.83468607758103,131.717498837516));
#20647=CARTESIAN_POINT('Ctrl Pts',(199.279365818954,4.85638176547755,131.582010416921));
#20648=CARTESIAN_POINT('Ctrl Pts',(199.271619485689,4.8780776135267,131.446520996182));
#20649=CARTESIAN_POINT('Ctrl Pts',(199.263873152423,4.89409896463232,131.310123745109));
#20650=CARTESIAN_POINT('Ctrl Pts',(199.256126819158,4.9043902119798,131.17333176974));
#20651=CARTESIAN_POINT('Ctrl Pts',(199.248378751155,4.91468376398078,131.036509160757));
#20652=CARTESIAN_POINT('Ctrl Pts',(199.240630683152,4.91924462944542,130.899292041369));
#20653=CARTESIAN_POINT('Ctrl Pts',(199.232882615149,4.91806925823009,130.762196251662));
#20654=CARTESIAN_POINT('Ctrl Pts',(199.225126312407,4.91689263781624,130.624954754918));
#20655=CARTESIAN_POINT('Ctrl Pts',(199.217370009665,4.90996760558296,130.487835237022));
#20656=CARTESIAN_POINT('Ctrl Pts',(199.209613706923,4.8973427474991,130.351351703727));
#20657=CARTESIAN_POINT('Ctrl Pts',(199.201853264409,4.88471115114836,130.21479532506));
#20658=CARTESIAN_POINT('Ctrl Pts',(199.194092821895,4.86637371941593,130.07887599463));
#20659=CARTESIAN_POINT('Ctrl Pts',(199.186332379381,4.8424305269433,129.944099230412));
#20660=CARTESIAN_POINT('Ctrl Pts',(199.178559479115,4.81844889873255,129.809106110568));
#20661=CARTESIAN_POINT('Ctrl Pts',(199.17078657885,4.788843611667,129.675259604108));
#20662=CARTESIAN_POINT('Ctrl Pts',(199.163013678584,4.75376536727037,129.543052607823));
#20663=CARTESIAN_POINT('Ctrl Pts',(199.155523342822,4.71996230541452,129.415651668864));
#20664=CARTESIAN_POINT('Ctrl Pts',(199.14803300706,4.68107738037903,129.289773403227));
#20665=CARTESIAN_POINT('Ctrl Pts',(199.140542671298,4.63728759387846,129.165840909366));
#20666=CARTESIAN_POINT('Ctrl Pts',(199.132768337179,4.59183750431285,129.037209477331));
#20667=CARTESIAN_POINT('Ctrl Pts',(199.12499400306,4.54095930328843,128.910266811875));
#20668=CARTESIAN_POINT('Ctrl Pts',(199.117219668941,4.48479714236479,128.785505086742));
#20669=CARTESIAN_POINT('Ctrl Pts',(199.109454915994,4.42870419628514,128.660897119286));
#20670=CARTESIAN_POINT('Ctrl Pts',(199.101690163047,4.36734040620565,128.538465097289));
#20671=CARTESIAN_POINT('Ctrl Pts',(199.0939254101,4.30089935031177,128.418685065235));
#20672=CARTESIAN_POINT('Ctrl Pts',(199.086168369215,4.23452428461125,128.299024000398));
#20673=CARTESIAN_POINT('Ctrl Pts',(199.07841132833,4.16308217693648,128.182010023415));
#20674=CARTESIAN_POINT('Ctrl Pts',(199.070654287445,4.08681409961739,128.068097914961));
#20675=CARTESIAN_POINT('Ctrl Pts',(199.062903096205,4.01060353664873,127.954271708514));
#20676=CARTESIAN_POINT('Ctrl Pts',(199.055151904965,3.92957446447712,127.84354303823));
#20677=CARTESIAN_POINT('Ctrl Pts',(199.047400713724,3.84401297642226,127.736340523173));
#20678=CARTESIAN_POINT('Ctrl Pts',(199.039652816947,3.75848785428223,127.629183572045));
#20679=CARTESIAN_POINT('Ctrl Pts',(199.03190492017,3.66843439109177,127.525550100254));
#20680=CARTESIAN_POINT('Ctrl Pts',(199.024157023393,3.57418080677142,127.425838067248));
#20681=CARTESIAN_POINT('Ctrl Pts',(199.016410747309,3.47994693826904,127.32614689185));
#20682=CARTESIAN_POINT('Ctrl Pts',(199.008664471225,3.38151496456809,127.230375807597));
#20683=CARTESIAN_POINT('Ctrl Pts',(199.000918195141,3.27925176834539,127.138887810096));
#20684=CARTESIAN_POINT('Ctrl Pts',(198.993171861876,3.17698781723904,127.047399137251));
#20685=CARTESIAN_POINT('Ctrl Pts',(198.98542552861,3.07089287855635,126.960193874925));
#20686=CARTESIAN_POINT('Ctrl Pts',(198.977679195345,2.96136858609743,126.877596153051));
#20687=CARTESIAN_POINT('Ctrl Pts',(198.969931127342,2.85181976643257,126.794979933991));
#20688=CARTESIAN_POINT('Ctrl Pts',(198.962183059339,2.73884037688976,126.716973543961));
#20689=CARTESIAN_POINT('Ctrl Pts',(198.954434991336,2.62286248940288,126.643858793965));
#20690=CARTESIAN_POINT('Ctrl Pts',(198.946678688594,2.50676133923701,126.570666336743));
#20691=CARTESIAN_POINT('Ctrl Pts',(198.938922385852,2.38765565632938,126.502376113735));
#20692=CARTESIAN_POINT('Ctrl Pts',(198.931166083111,2.26600415017978,126.439225080854));
#20693=CARTESIAN_POINT('Ctrl Pts',(198.923405640596,2.14428771495838,126.376040342365));
#20694=CARTESIAN_POINT('Ctrl Pts',(198.915645198082,2.02002310306419,126.318000424913));
#20695=CARTESIAN_POINT('Ctrl Pts',(198.907884755568,1.8936897138752,126.265294377681));
#20696=CARTESIAN_POINT('Ctrl Pts',(198.900111855303,1.76715352311459,126.212503722024));
#20697=CARTESIAN_POINT('Ctrl Pts',(198.892338955037,1.63854228569136,126.165064182373));
#20698=CARTESIAN_POINT('Ctrl Pts',(198.884566054772,1.50835214749063,126.123115392024));
#20699=CARTESIAN_POINT('Ctrl Pts',(198.87707571901,1.38289474874265,126.082691545867));
#20700=CARTESIAN_POINT('Ctrl Pts',(198.869585383248,1.25597154700458,126.047366257253));
#20701=CARTESIAN_POINT('Ctrl Pts',(198.862095047486,1.12803418073941,126.017219304675));
#20702=CARTESIAN_POINT('Ctrl Pts',(198.854320713367,0.995246030346574,125.985929321228));
#20703=CARTESIAN_POINT('Ctrl Pts',(198.846546379248,0.860944660272916,125.96011898127));
#20704=CARTESIAN_POINT('Ctrl Pts',(198.838772045129,0.72562206766675,125.939933037941));
#20705=CARTESIAN_POINT('Ctrl Pts',(198.831007292181,0.590466248061855,125.919771971984));
#20706=CARTESIAN_POINT('Ctrl Pts',(198.823242539234,0.454292093069238,125.905221568033));
#20707=CARTESIAN_POINT('Ctrl Pts',(198.815477786287,0.317604746131932,125.89637627695));
#20708=CARTESIAN_POINT('Ctrl Pts',(198.807720745402,0.181053158994685,125.887539771135));
#20709=CARTESIAN_POINT('Ctrl Pts',(198.799963704517,0.0439897818821281,
125.884397126882));
#20710=CARTESIAN_POINT('Ctrl Pts',(198.792206663632,-0.0930724598611862,
125.886991343278));
#20711=CARTESIAN_POINT('Ctrl Pts',(198.784455472392,-0.230031341901755,
125.889583603354));
#20712=CARTESIAN_POINT('Ctrl Pts',(198.776704281152,-0.366988700963738,
125.897904105649));
#20713=CARTESIAN_POINT('Ctrl Pts',(198.768953089912,-0.503429287263447,
125.911943830821));
#20714=CARTESIAN_POINT('Ctrl Pts',(198.761205193135,-0.639811882674504,
125.925977588736));
#20715=CARTESIAN_POINT('Ctrl Pts',(198.753457296358,-0.775677754077462,
125.945725694873));
#20716=CARTESIAN_POINT('Ctrl Pts',(198.745709399581,-0.910514676033535,
125.971127115321));
#20717=CARTESIAN_POINT('Ctrl Pts',(198.737963123496,-1.04532339301227,125.996523222339));
#20718=CARTESIAN_POINT('Ctrl Pts',(198.730216847412,-1.17910320469284,126.027570219174));
#20719=CARTESIAN_POINT('Ctrl Pts',(198.722470571328,-1.31135040354105,126.064155645032));
#20720=CARTESIAN_POINT('Ctrl Pts',(198.714724238063,-1.44359857860805,126.100741340956));
#20721=CARTESIAN_POINT('Ctrl Pts',(198.706977904797,-1.57431374145571,126.14286544324));
#20722=CARTESIAN_POINT('Ctrl Pts',(198.699231571532,-1.70300609951057,126.190365246141));
#20723=CARTESIAN_POINT('Ctrl Pts',(198.691483503529,-1.83172727732661,126.237875686293));
#20724=CARTESIAN_POINT('Ctrl Pts',(198.683735435526,-1.95842438223704,126.290764087235));
#20725=CARTESIAN_POINT('Ctrl Pts',(198.675987367523,-2.08262677322981,126.348819260343));
#20726=CARTESIAN_POINT('Ctrl Pts',(198.668231064781,-2.20696116800184,126.406936135179));
#20727=CARTESIAN_POINT('Ctrl Pts',(198.660474762039,-2.32879519762787,126.47023058584));
#20728=CARTESIAN_POINT('Ctrl Pts',(198.652718459298,-2.44768156069828,126.538444767491));
#20729=CARTESIAN_POINT('Ctrl Pts',(198.644958016783,-2.56663137700036,126.606695357105));
#20730=CARTESIAN_POINT('Ctrl Pts',(198.637197574269,-2.68263006138942,126.679870701362));
#20731=CARTESIAN_POINT('Ctrl Pts',(198.629437131755,-2.79525943435933,126.757669653689));
#20732=CARTESIAN_POINT('Ctrl Pts',(198.62166423149,-2.90806960999747,126.835593495801));
#20733=CARTESIAN_POINT('Ctrl Pts',(198.613891331224,-3.01749935359477,126.918155542348));
#20734=CARTESIAN_POINT('Ctrl Pts',(198.606118430959,-3.12316300873507,127.005013846953));
#20735=CARTESIAN_POINT('Ctrl Pts',(198.598628095197,-3.22498552385993,127.088714633402));
#20736=CARTESIAN_POINT('Ctrl Pts',(198.591137759435,-3.32331078044587,127.176404536312));
#20737=CARTESIAN_POINT('Ctrl Pts',(198.583647423673,-3.41782753696518,127.267746701677));
#20738=CARTESIAN_POINT('Ctrl Pts',(198.575987342496,-3.51448622497807,127.361158856193));
#20739=CARTESIAN_POINT('Ctrl Pts',(198.568327261318,-3.60748705227816,127.458705550652));
#20740=CARTESIAN_POINT('Ctrl Pts',(198.560667180141,-3.69644762254403,127.560064386287));
#20741=CARTESIAN_POINT('Ctrl Pts',(198.553016015211,-3.78530464372584,127.6613052414));
#20742=CARTESIAN_POINT('Ctrl Pts',(198.545364850281,-3.87013049362145,127.766349116946));
#20743=CARTESIAN_POINT('Ctrl Pts',(198.53771368535,-3.95057739062617,127.874834829461));
#20744=CARTESIAN_POINT('Ctrl Pts',(198.530069653823,-4.03094928465215,127.983219397595));
#20745=CARTESIAN_POINT('Ctrl Pts',(198.522425622296,-4.10695010528644,128.095039100229));
#20746=CARTESIAN_POINT('Ctrl Pts',(198.514781590769,-4.17827075473654,128.209897944369));
#20747=CARTESIAN_POINT('Ctrl Pts',(198.507143088631,-4.24953981365601,128.324673704173));
#20748=CARTESIAN_POINT('Ctrl Pts',(198.499504586494,-4.31613522474468,128.442483890537));
#20749=CARTESIAN_POINT('Ctrl Pts',(198.491866084356,-4.37779019060595,128.562902139357));
#20750=CARTESIAN_POINT('Ctrl Pts',(198.484230874548,-4.43941858208351,128.683268485777));
#20751=CARTESIAN_POINT('Ctrl Pts',(198.47659566474,-4.49611058101027,128.806240300078));
#20752=CARTESIAN_POINT('Ctrl Pts',(198.468960454932,-4.54764472612785,128.931365554192));
#20753=CARTESIAN_POINT('Ctrl Pts',(198.461325447542,-4.5991775050181,129.056487491098));
#20754=CARTESIAN_POINT('Ctrl Pts',(198.453690440153,-4.64555254017037,129.183762384902));
#20755=CARTESIAN_POINT('Ctrl Pts',(198.446055432763,-4.68659615849717,129.312717392911));
#20756=CARTESIAN_POINT('Ctrl Pts',(198.440775680082,-4.71497860042732,129.401892231183));
#20757=CARTESIAN_POINT('Ctrl Pts',(198.435495927401,-4.74081256549775,129.491870059345));
#20758=CARTESIAN_POINT('Ctrl Pts',(198.430216174721,-4.76405452823404,129.582490119308));
#20759=CARTESIAN_POINT('Origin',(213.235140564004,0.,130.804360617566));
#20760=CARTESIAN_POINT('',(196.33459504632,-4.76405452823405,129.582490119308));
#20761=CARTESIAN_POINT('',(196.680227908624,-4.76405452823405,129.582490119308));
#20762=CARTESIAN_POINT('',(213.235140564004,-4.76405452823405,129.582490119308));
#20763=CARTESIAN_POINT('',(198.014859435953,-4.91824901604543,130.801249561772));
#20764=CARTESIAN_POINT('Ctrl Pts',(198.014859435953,-4.91824901604543,130.801249561772));
#20765=CARTESIAN_POINT('Ctrl Pts',(198.007194602125,-4.91833425441149,130.936002371663));
#20766=CARTESIAN_POINT('Ctrl Pts',(197.999529768297,-4.9128772797748,131.070975950461));
#20767=CARTESIAN_POINT('Ctrl Pts',(197.991864934469,-4.90185011753594,131.205669087091));
#20768=CARTESIAN_POINT('Ctrl Pts',(197.984208471378,-4.89083499802213,131.340215125821));
#20769=CARTESIAN_POINT('Ctrl Pts',(197.976552008288,-4.87426182187178,131.47448093386));
#20770=CARTESIAN_POINT('Ctrl Pts',(197.968895545198,-4.85215462495801,131.607964100634));
#20771=CARTESIAN_POINT('Ctrl Pts',(197.961245495214,-4.83006594518477,131.741335460987));
#20772=CARTESIAN_POINT('Ctrl Pts',(197.95359544523,-4.80245253092967,131.873925089211));
#20773=CARTESIAN_POINT('Ctrl Pts',(197.945945395246,-4.76939029060855,132.005235014974));
#20774=CARTESIAN_POINT('Ctrl Pts',(197.938299305357,-4.73634516515454,132.136476967365));
#20775=CARTESIAN_POINT('Ctrl Pts',(197.930653215467,-4.69785692034788,132.266440145392));
#20776=CARTESIAN_POINT('Ctrl Pts',(197.923007125577,-4.65405260327977,132.394636514511));
#20777=CARTESIAN_POINT('Ctrl Pts',(197.915363000358,-4.61025954177498,132.522799943444));
#20778=CARTESIAN_POINT('Ctrl Pts',(197.907718875139,-4.56115325357192,132.649197085549));
#20779=CARTESIAN_POINT('Ctrl Pts',(197.90007474992,-4.50691057686776,132.773355314008));
#20780=CARTESIAN_POINT('Ctrl Pts',(197.892430829445,-4.45266935302643,132.897510216952));
#20781=CARTESIAN_POINT('Ctrl Pts',(197.88478690897,-4.3932921754651,133.019425956816));
#20782=CARTESIAN_POINT('Ctrl Pts',(197.877142988494,-4.32900370978916,133.138650647346));
#20783=CARTESIAN_POINT('Ctrl Pts',(197.869497513223,-4.26470216764921,133.257899588531));
#20784=CARTESIAN_POINT('Ctrl Pts',(197.861852037952,-4.19548754221391,133.374456038018));
#20785=CARTESIAN_POINT('Ctrl Pts',(197.854206562681,-4.12162977785966,133.487893929593));
#20786=CARTESIAN_POINT('Ctrl Pts',(197.846553256078,-4.04769636030815,133.60144801666));
#20787=CARTESIAN_POINT('Ctrl Pts',(197.838899949475,-3.9691105266443,133.711876829538));
#20788=CARTESIAN_POINT('Ctrl Pts',(197.831246642873,-3.8861849641364,133.818784192152));
#20789=CARTESIAN_POINT('Ctrl Pts',(197.823589202619,-3.80321461244542,133.925749296834));
#20790=CARTESIAN_POINT('Ctrl Pts',(197.815931762365,-3.71590012432521,134.029188857436));
#20791=CARTESIAN_POINT('Ctrl Pts',(197.808274322111,-3.62459270805556,134.128741877772));
#20792=CARTESIAN_POINT('Ctrl Pts',(197.800605170645,-3.53314564714557,134.228447153492));
#20793=CARTESIAN_POINT('Ctrl Pts',(197.792936019179,-3.43769374582733,134.324253733522));
#20794=CARTESIAN_POINT('Ctrl Pts',(197.785266867713,-3.33862350365245,134.415839007832));
#20795=CARTESIAN_POINT('Ctrl Pts',(197.779475761273,-3.26381388226844,134.484996602939));
#20796=CARTESIAN_POINT('Ctrl Pts',(197.773684654833,-3.18694180385115,134.55174800559));
#20797=CARTESIAN_POINT('Ctrl Pts',(197.767893548393,-3.10818467377065,134.615970657462));
#20798=CARTESIAN_POINT('Ctrl Pts',(197.760119214274,-3.00245630392844,134.702187058218));
#20799=CARTESIAN_POINT('Ctrl Pts',(197.752344880155,-2.89297047802538,134.784137565104));
#20800=CARTESIAN_POINT('Ctrl Pts',(197.744570546035,-2.78010632827789,134.861476818264));
#20801=CARTESIAN_POINT('Ctrl Pts',(197.736805793088,-2.66738127350782,134.938720757708));
#20802=CARTESIAN_POINT('Ctrl Pts',(197.729041040141,-2.55128649839717,135.011364531943));
#20803=CARTESIAN_POINT('Ctrl Pts',(197.721276287194,-2.43223495821874,135.07910226713));
#20804=CARTESIAN_POINT('Ctrl Pts',(197.713519246309,-2.31330166170844,135.146772724244));
#20805=CARTESIAN_POINT('Ctrl Pts',(197.705762205424,-2.19141778190944,135.209546647202));
#20806=CARTESIAN_POINT('Ctrl Pts',(197.698005164539,-2.06702577581684,135.267161028139));
#20807=CARTESIAN_POINT('Ctrl Pts',(197.690253973299,-1.94272757470384,135.324731961623));
#20808=CARTESIAN_POINT('Ctrl Pts',(197.682502782059,-1.8159253653342,135.377150933938));
#20809=CARTESIAN_POINT('Ctrl Pts',(197.674751590819,-1.68708644647367,135.424200699714));
#20810=CARTESIAN_POINT('Ctrl Pts',(197.667003694042,-1.55830228759047,135.471230468085));
#20811=CARTESIAN_POINT('Ctrl Pts',(197.659255797265,-1.42748350741483,135.512895434921));
#20812=CARTESIAN_POINT('Ctrl Pts',(197.651507900488,-1.29511743474276,135.549026453294));
#20813=CARTESIAN_POINT('Ctrl Pts',(197.643761624403,-1.16277905019961,135.585149913837));
#20814=CARTESIAN_POINT('Ctrl Pts',(197.636015348319,-1.02889439386554,135.615741625526));
#20815=CARTESIAN_POINT('Ctrl Pts',(197.628269072235,-0.89396562727687,135.640682414112));
#20816=CARTESIAN_POINT('Ctrl Pts',(197.62052273897,-0.759035864674597,135.665623386805));
#20817=CARTESIAN_POINT('Ctrl Pts',(197.612776405705,-0.623062360890706,
135.684913282095));
#20818=CARTESIAN_POINT('Ctrl Pts',(197.605030072439,-0.486556739791109,
135.698484196049));
#20819=CARTESIAN_POINT('Ctrl Pts',(197.597282004436,-0.350020549204351,
135.712058149115));
#20820=CARTESIAN_POINT('Ctrl Pts',(197.589533936433,-0.212952393152231,
135.71991053368));
#20821=CARTESIAN_POINT('Ctrl Pts',(197.58178586843,-0.0758678779773515,
135.72202542188));
#20822=CARTESIAN_POINT('Ctrl Pts',(197.574029565689,0.061362332251699,135.724142557809));
#20823=CARTESIAN_POINT('Ctrl Pts',(197.566273262947,0.198608544793241,135.720510010164));
#20824=CARTESIAN_POINT('Ctrl Pts',(197.558516960205,0.335355735986595,135.711164016199));
#20825=CARTESIAN_POINT('Ctrl Pts',(197.550756517691,0.472175913273558,135.701813033997));
#20826=CARTESIAN_POINT('Ctrl Pts',(197.542996075176,0.608496150094301,135.686742572151));
#20827=CARTESIAN_POINT('Ctrl Pts',(197.535235632662,0.743808672534506,135.666040545447));
#20828=CARTESIAN_POINT('Ctrl Pts',(197.527462732397,0.879338410648007,135.645305286012));
#20829=CARTESIAN_POINT('Ctrl Pts',(197.519689832131,1.01385681788001,135.618920471637));
#20830=CARTESIAN_POINT('Ctrl Pts',(197.511916931866,1.14686752295984,135.587024932284));
#20831=CARTESIAN_POINT('Ctrl Pts',(197.504426596104,1.27504295387604,135.556288876127));
#20832=CARTESIAN_POINT('Ctrl Pts',(197.496936260342,1.40181810066686,135.52043588028));
#20833=CARTESIAN_POINT('Ctrl Pts',(197.48944592458,1.52676573916633,135.479632742289));
#20834=CARTESIAN_POINT('Ctrl Pts',(197.481671590461,1.65645080535675,135.437282540919));
#20835=CARTESIAN_POINT('Ctrl Pts',(197.473897256342,1.78457785099881,135.38946526551));
#20836=CARTESIAN_POINT('Ctrl Pts',(197.466122922223,1.91065138484321,135.336313215299));
#20837=CARTESIAN_POINT('Ctrl Pts',(197.458358169276,2.03656954432468,135.283226670239));
#20838=CARTESIAN_POINT('Ctrl Pts',(197.450593416329,2.16043887068706,135.22481858236));
#20839=CARTESIAN_POINT('Ctrl Pts',(197.442828663381,2.28177881119425,135.161271050348));
#20840=CARTESIAN_POINT('Ctrl Pts',(197.435071622496,2.40299823516199,135.097786634641));
#20841=CARTESIAN_POINT('Ctrl Pts',(197.427314581611,2.52169292860744,135.029173113332));
#20842=CARTESIAN_POINT('Ctrl Pts',(197.419557540726,2.63740245675027,134.955660575847));
#20843=CARTESIAN_POINT('Ctrl Pts',(197.411806349486,2.7530247274378,134.882203474739));
#20844=CARTESIAN_POINT('Ctrl Pts',(197.404055158246,2.86566598491015,134.803854919712));
#20845=CARTESIAN_POINT('Ctrl Pts',(197.396303967006,2.97489086808598,134.720890636023));
#20846=CARTESIAN_POINT('Ctrl Pts',(197.388556070229,3.08406932777271,134.637961614368));
#20847=CARTESIAN_POINT('Ctrl Pts',(197.380808173452,3.18983399049617,134.550421001924));
#20848=CARTESIAN_POINT('Ctrl Pts',(197.373060276675,3.2917791350376,134.458587374163));
#20849=CARTESIAN_POINT('Ctrl Pts',(197.365314000591,3.39370295485246,134.366772956017));
#20850=CARTESIAN_POINT('Ctrl Pts',(197.357567724507,3.49180855536177,134.270667570245));
#20851=CARTESIAN_POINT('Ctrl Pts',(197.349821448422,3.58572424131846,134.170629282976));
#20852=CARTESIAN_POINT('Ctrl Pts',(197.342075115157,3.67964062053938,134.070590257247));
#20853=CARTESIAN_POINT('Ctrl Pts',(197.334328781892,3.76936675589715,133.96661855713));
#20854=CARTESIAN_POINT('Ctrl Pts',(197.326582448626,3.85456897269458,133.859107922539));
#20855=CARTESIAN_POINT('Ctrl Pts',(197.318834380623,3.93979026993763,133.751573211687));
#20856=CARTESIAN_POINT('Ctrl Pts',(197.31108631262,4.02048538988445,133.640498295691));
#20857=CARTESIAN_POINT('Ctrl Pts',(197.303338244617,4.09636223415192,133.52630835937));
#20858=CARTESIAN_POINT('Ctrl Pts',(197.295581941876,4.17231972123249,133.411997060627));
#20859=CARTESIAN_POINT('Ctrl Pts',(197.287825639134,4.24344848632279,133.294564454268));
#20860=CARTESIAN_POINT('Ctrl Pts',(197.280069336392,4.3095006339843,133.17446343141));
#20861=CARTESIAN_POINT('Ctrl Pts',(197.272308893878,4.37558803566593,133.054298307018));
#20862=CARTESIAN_POINT('Ctrl Pts',(197.264548451364,4.43659324710592,132.931462278247));
#20863=CARTESIAN_POINT('Ctrl Pts',(197.256788008849,4.49231576929894,132.80643006976));
#20864=CARTESIAN_POINT('Ctrl Pts',(197.249015108584,4.54812774223136,132.681197148472));
#20865=CARTESIAN_POINT('Ctrl Pts',(197.241242208318,4.59863993554477,132.553761366054));
#20866=CARTESIAN_POINT('Ctrl Pts',(197.233469308053,4.64370085002127,132.424615374699));
#20867=CARTESIAN_POINT('Ctrl Pts',(197.225978972291,4.68712368675483,132.300164165429));
#20868=CARTESIAN_POINT('Ctrl Pts',(197.218488636529,4.72548460943441,132.174125223962));
#20869=CARTESIAN_POINT('Ctrl Pts',(197.210998300767,4.75869302446231,132.046948144235));
#20870=CARTESIAN_POINT('Ctrl Pts',(197.203223966648,4.79316054663953,131.914949106876));
#20871=CARTESIAN_POINT('Ctrl Pts',(197.195449632529,4.82218631642961,131.781305789271));
#20872=CARTESIAN_POINT('Ctrl Pts',(197.18767529841,4.84561381580234,131.646506573209));
#20873=CARTESIAN_POINT('Ctrl Pts',(197.179910545463,4.86901244287585,131.511873485134));
#20874=CARTESIAN_POINT('Ctrl Pts',(197.172145792516,4.88682646091603,131.376087714508));
#20875=CARTESIAN_POINT('Ctrl Pts',(197.164381039568,4.8989493242116,131.239651992747));
#20876=CARTESIAN_POINT('Ctrl Pts',(197.156623998683,4.91106014690847,131.103351780867));
#20877=CARTESIAN_POINT('Ctrl Pts',(197.148866957798,4.91749102928209,130.966403289417));
#20878=CARTESIAN_POINT('Ctrl Pts',(197.141109916913,4.91818667583652,130.829318264172));
#20879=CARTESIAN_POINT('Ctrl Pts',(197.133358725673,4.91888179779847,130.692336615812));
#20880=CARTESIAN_POINT('Ctrl Pts',(197.125607534433,4.91385029058759,130.555219027973));
#20881=CARTESIAN_POINT('Ctrl Pts',(197.117856343193,4.90308880637215,130.418480818499));
#20882=CARTESIAN_POINT('Ctrl Pts',(197.110108446416,4.89233189607456,130.281800726411));
#20883=CARTESIAN_POINT('Ctrl Pts',(197.102360549639,4.87584988319397,130.145500080927));
#20884=CARTESIAN_POINT('Ctrl Pts',(197.094612652862,4.85369149206835,130.010092424621));
#20885=CARTESIAN_POINT('Ctrl Pts',(197.086866376778,4.83153773600045,129.874713092679));
#20886=CARTESIAN_POINT('Ctrl Pts',(197.079120100694,4.80371002654195,129.740226763961));
#20887=CARTESIAN_POINT('Ctrl Pts',(197.071373824609,4.77030870450874,129.607139699695));
#20888=CARTESIAN_POINT('Ctrl Pts',(197.063627491344,4.7369071359146,129.474051653011));
#20889=CARTESIAN_POINT('Ctrl Pts',(197.055881158079,4.69793196781799,129.342363270595));
#20890=CARTESIAN_POINT('Ctrl Pts',(197.048134824813,4.65353410543624,129.212568108461));
#20891=CARTESIAN_POINT('Ctrl Pts',(197.04038675681,4.60912630046099,129.082743879601));
#20892=CARTESIAN_POINT('Ctrl Pts',(197.032638688807,4.55929351124709,128.954814084533));
#20893=CARTESIAN_POINT('Ctrl Pts',(197.024890620804,4.50423557151517,128.829254296682));
#20894=CARTESIAN_POINT('Ctrl Pts',(197.017134318063,4.44911911554975,128.703561062393));
#20895=CARTESIAN_POINT('Ctrl Pts',(197.009378015321,4.3887665729042,128.580243225664));
#20896=CARTESIAN_POINT('Ctrl Pts',(197.001621712579,4.32342498015975,128.459754146657));
#20897=CARTESIAN_POINT('Ctrl Pts',(196.993861270065,4.25804851263973,128.339200759));
#20898=CARTESIAN_POINT('Ctrl Pts',(196.986100827551,4.18767788965592,128.22147947287));
#20899=CARTESIAN_POINT('Ctrl Pts',(196.978340385036,4.11260413590295,128.107015574036));
#20900=CARTESIAN_POINT('Ctrl Pts',(196.970567484771,4.03740986709589,127.992367927591));
#20901=CARTESIAN_POINT('Ctrl Pts',(196.962794584506,3.95749760849355,127.880988435588));
#20902=CARTESIAN_POINT('Ctrl Pts',(196.95502168424,3.87319995331092,127.773270849154));
#20903=CARTESIAN_POINT('Ctrl Pts',(196.947531348478,3.79196673022726,127.669469068311));
#20904=CARTESIAN_POINT('Ctrl Pts',(196.940041012716,3.70666161488837,127.569067811088));
#20905=CARTESIAN_POINT('Ctrl Pts',(196.932550676954,3.61761389535537,127.472386312948));
#20906=CARTESIAN_POINT('Ctrl Pts',(196.924776342835,3.52518990447059,127.372039106421));
#20907=CARTESIAN_POINT('Ctrl Pts',(196.917002008716,3.42844113395928,127.275381426659));
#20908=CARTESIAN_POINT('Ctrl Pts',(196.909227674597,3.32769387143375,127.182808939));
#20909=CARTESIAN_POINT('Ctrl Pts',(196.90146292165,3.22707077090526,127.090350538659));
#20910=CARTESIAN_POINT('Ctrl Pts',(196.893698168703,3.12245926830746,127.001967574988));
#20911=CARTESIAN_POINT('Ctrl Pts',(196.885933415755,3.01422473525758,126.91802142652));
#20912=CARTESIAN_POINT('Ctrl Pts',(196.87817637487,2.90609770227194,126.83415865455));
#20913=CARTESIAN_POINT('Ctrl Pts',(196.870419333985,2.79435510683866,126.754724166296));
#20914=CARTESIAN_POINT('Ctrl Pts',(196.8626622931,2.67939760660565,126.680041094515));
#20915=CARTESIAN_POINT('Ctrl Pts',(196.85491110186,2.56452679671837,126.605414341821));
#20916=CARTESIAN_POINT('Ctrl Pts',(196.84715991062,2.44644623414905,126.535532085827));
#20917=CARTESIAN_POINT('Ctrl Pts',(196.83940871938,2.32558766080939,126.470675685041));
#20918=CARTESIAN_POINT('Ctrl Pts',(196.831660822603,2.20478045558657,126.405846849956));
#20919=CARTESIAN_POINT('Ctrl Pts',(196.823912925826,2.08119793174799,126.346039805974));
#20920=CARTESIAN_POINT('Ctrl Pts',(196.816165029049,1.95529848390204,126.291491142238));
#20921=CARTESIAN_POINT('Ctrl Pts',(196.808418752965,1.82942537150677,126.236953888906));
#20922=CARTESIAN_POINT('Ctrl Pts',(196.800672476881,1.70123665761377,126.187672983311));
#20923=CARTESIAN_POINT('Ctrl Pts',(196.792926200797,1.57121251079405,126.143837652445));
#20924=CARTESIAN_POINT('Ctrl Pts',(196.785179867531,1.44118740416556,126.100001997995));
#20925=CARTESIAN_POINT('Ctrl Pts',(196.777433534266,1.30932720805258,126.061612123386));
#20926=CARTESIAN_POINT('Ctrl Pts',(196.769687201001,1.17612873306436,126.028807846864));
#20927=CARTESIAN_POINT('Ctrl Pts',(196.761939132998,1.04290042920136,125.995996224052));
#20928=CARTESIAN_POINT('Ctrl Pts',(196.754191064995,0.908333629647398,125.968772781862));
#20929=CARTESIAN_POINT('Ctrl Pts',(196.746442996992,0.772936462800047,125.947226453579));
#20930=CARTESIAN_POINT('Ctrl Pts',(196.73868669425,0.63739539423235,125.925657225601));
#20931=CARTESIAN_POINT('Ctrl Pts',(196.730930391508,0.501022582156627,125.909777226043));
#20932=CARTESIAN_POINT('Ctrl Pts',(196.723174088766,0.364332980624142,125.899623668276));
#20933=CARTESIAN_POINT('Ctrl Pts',(196.715413646252,0.227570423735663,125.88946469125));
#20934=CARTESIAN_POINT('Ctrl Pts',(196.707653203738,0.0904911310544043,
125.88503825871));
#20935=CARTESIAN_POINT('Ctrl Pts',(196.699892761224,-0.0463897865020519,
125.886329400686));
#20936=CARTESIAN_POINT('Ctrl Pts',(196.692119860958,-0.183490437459122,
125.887622615317));
#20937=CARTESIAN_POINT('Ctrl Pts',(196.684346960693,-0.320391686252509,
125.894651725689));
#20938=CARTESIAN_POINT('Ctrl Pts',(196.676574060427,-0.456582484150821,
125.907349743812));
#20939=CARTESIAN_POINT('Ctrl Pts',(196.669083724665,-0.587822403502649,
125.919586156992));
#20940=CARTESIAN_POINT('Ctrl Pts',(196.661593388903,-0.718402323251377,
125.937086434526));
#20941=CARTESIAN_POINT('Ctrl Pts',(196.654103053141,-0.847875673318612,
125.959746091611));
#20942=CARTESIAN_POINT('Ctrl Pts',(196.646328719022,-0.982258044805317,
125.983264896481));
#20943=CARTESIAN_POINT('Ctrl Pts',(196.638554384903,-1.11587396195838,126.012416540273));
#20944=CARTESIAN_POINT('Ctrl Pts',(196.630780050784,-1.24821417389864,126.047140374758));
#20945=CARTESIAN_POINT('Ctrl Pts',(196.623015297837,-1.38039128835494,126.081821415221));
#20946=CARTESIAN_POINT('Ctrl Pts',(196.61525054489,-1.51129545125909,126.12206088437));
#20947=CARTESIAN_POINT('Ctrl Pts',(196.607485791943,-1.64042513233221,126.16774671864));
#20948=CARTESIAN_POINT('Ctrl Pts',(196.599728751058,-1.76942655998645,126.213387177096));
#20949=CARTESIAN_POINT('Ctrl Pts',(196.591971710173,-1.89665664695338,126.264463106153));
#20950=CARTESIAN_POINT('Ctrl Pts',(196.584214669288,-2.02162696724649,126.320812082332));
#20951=CARTESIAN_POINT('Ctrl Pts',(196.576463478048,-2.14650304644767,126.377118565309));
#20952=CARTESIAN_POINT('Ctrl Pts',(196.568712286808,-2.26912239593048,126.43869002048));
#20953=CARTESIAN_POINT('Ctrl Pts',(196.560961095568,-2.38901493376489,126.505315292293));
#20954=CARTESIAN_POINT('Ctrl Pts',(196.55321319879,-2.50885651407307,126.571912246589));
#20955=CARTESIAN_POINT('Ctrl Pts',(196.545465302013,-2.62597324680375,126.643558555793));
#20956=CARTESIAN_POINT('Ctrl Pts',(196.537717405236,-2.73991830932937,126.719996441748));
#20957=CARTESIAN_POINT('Ctrl Pts',(196.529971129152,-2.85383953700426,126.796418338546));
#20958=CARTESIAN_POINT('Ctrl Pts',(196.522224853068,-2.96459008963101,126.87762960081));
#20959=CARTESIAN_POINT('Ctrl Pts',(196.514478576984,-3.07175122234275,126.963328530934));
#20960=CARTESIAN_POINT('Ctrl Pts',(196.506732243719,-3.17891314609344,127.049028093668));
#20961=CARTESIAN_POINT('Ctrl Pts',(196.498985910453,-3.28248529172354,127.139215146181));
#20962=CARTESIAN_POINT('Ctrl Pts',(196.491239577188,-3.38208148791119,127.233547282816));
#20963=CARTESIAN_POINT('Ctrl Pts',(196.483491509185,-3.48169998797647,127.327900544479));
#20964=CARTESIAN_POINT('Ctrl Pts',(196.475743441182,-3.57734048303421,127.426400468601));
#20965=CARTESIAN_POINT('Ctrl Pts',(196.467995373179,-3.6686534951838,127.528667622981));
#20966=CARTESIAN_POINT('Ctrl Pts',(196.460239070437,-3.76006355588962,127.631043468109));
#20967=CARTESIAN_POINT('Ctrl Pts',(196.452482767696,-3.8471366852804,127.737194249536));
#20968=CARTESIAN_POINT('Ctrl Pts',(196.444726464954,-3.92956322945105,127.846706836569));
#20969=CARTESIAN_POINT('Ctrl Pts',(196.43696602244,-4.01203376715042,127.956277873767));
#20970=CARTESIAN_POINT('Ctrl Pts',(196.429205579925,-4.08985255625137,128.069213970078));
#20971=CARTESIAN_POINT('Ctrl Pts',(196.421445137411,-4.16275376138207,128.185073656464));
#20972=CARTESIAN_POINT('Ctrl Pts',(196.413672237146,-4.23577199399886,128.301119331103));
#20973=CARTESIAN_POINT('Ctrl Pts',(196.40589933688,-4.30385667334007,128.42009763481));
#20974=CARTESIAN_POINT('Ctrl Pts',(196.398126436615,-4.36678792397595,128.541542399167));
#20975=CARTESIAN_POINT('Ctrl Pts',(196.390636100853,-4.42743146513705,128.65857234044));
#20976=CARTESIAN_POINT('Ctrl Pts',(196.383145765091,-4.48328962222919,128.777892252615));
#20977=CARTESIAN_POINT('Ctrl Pts',(196.375655429329,-4.53420891924256,128.899069947048));
#20978=CARTESIAN_POINT('Ctrl Pts',(196.366995286457,-4.59308056412885,129.03917263136));
#20979=CARTESIAN_POINT('Ctrl Pts',(196.358335143585,-4.64550922581911,129.182135375472));
#20980=CARTESIAN_POINT('Ctrl Pts',(196.349675000714,-4.69123825435021,129.327381706606));
#20981=CARTESIAN_POINT('Ctrl Pts',(196.344648349249,-4.71778099061184,129.411687784913));
#20982=CARTESIAN_POINT('Ctrl Pts',(196.339621697785,-4.74206742463025,129.496762736058));
#20983=CARTESIAN_POINT('Ctrl Pts',(196.33459504632,-4.76405452823405,129.582490119308));
#20984=CARTESIAN_POINT('Ctrl Pts',(198.084936573762,-4.76405452823404,129.582490119308));
#20985=CARTESIAN_POINT('Ctrl Pts',(198.077162780964,-4.79809767465422,129.715223830524));
#20986=CARTESIAN_POINT('Ctrl Pts',(198.069388988166,-4.82655054116148,129.849229756449));
#20987=CARTESIAN_POINT('Ctrl Pts',(198.061615195367,-4.84934911569474,129.983997151406));
#20988=CARTESIAN_POINT('Ctrl Pts',(198.056523854313,-4.8642807354981,130.072261244428));
#20989=CARTESIAN_POINT('Ctrl Pts',(198.051432513259,-4.87678805849738,130.160851841391));
#20990=CARTESIAN_POINT('Ctrl Pts',(198.046341172205,-4.88686521477497,130.249625153473));
#20991=CARTESIAN_POINT('Ctrl Pts',(198.035847260134,-4.90763553654045,130.43259842543));
#20992=CARTESIAN_POINT('Ctrl Pts',(198.025353348062,-4.91813231630581,130.616759698695));
#20993=CARTESIAN_POINT('Ctrl Pts',(198.014859435991,-4.91824901604501,130.80124956111));
#20994=CARTESIAN_POINT('',(198.360140564038,-4.91824805313947,130.80873672198));
#20995=CARTESIAN_POINT('Ctrl Pts',(198.430216174721,-4.76405452823404,129.582490119308));
#20996=CARTESIAN_POINT('Ctrl Pts',(198.422577902284,-4.7976789144689,129.713591090917));
#20997=CARTESIAN_POINT('Ctrl Pts',(198.414939629846,-4.82587604532326,129.846036456349));
#20998=CARTESIAN_POINT('Ctrl Pts',(198.407301357409,-4.84855734705283,129.97933048791));
#20999=CARTESIAN_POINT('Ctrl Pts',(198.399441225181,-4.87189744550764,130.116496152261));
#21000=CARTESIAN_POINT('Ctrl Pts',(198.391581092952,-4.88939633379473,130.254560081246));
#21001=CARTESIAN_POINT('Ctrl Pts',(198.383720960724,-4.90101480488931,130.392976436106));
#21002=CARTESIAN_POINT('Ctrl Pts',(198.375860828495,-4.91263327598389,130.531392790965));
#21003=CARTESIAN_POINT('Ctrl Pts',(198.368000696266,-4.91837135341764,130.670161108681));
#21004=CARTESIAN_POINT('Ctrl Pts',(198.360140564038,-4.91824805313947,130.80873672198));
#21005=CARTESIAN_POINT('Ctrl Pts',(198.360140564008,-4.918248053139,130.808736722507));
#21006=CARTESIAN_POINT('Ctrl Pts',(198.348902089221,-4.91807175747449,131.006873152139));
#21007=CARTESIAN_POINT('Ctrl Pts',(198.337663614434,-4.90591901972274,131.20449843287));
#21008=CARTESIAN_POINT('Ctrl Pts',(198.326425139647,-4.8819937463978,131.400447962368));
#21009=CARTESIAN_POINT('Ctrl Pts',(198.319350026384,-4.86693173648915,131.523806793625));
#21010=CARTESIAN_POINT('Ctrl Pts',(198.312274913122,-4.84720485499847,131.646502289585));
#21011=CARTESIAN_POINT('Ctrl Pts',(198.30519979986,-4.82287271835716,131.768249514185));
#21012=CARTESIAN_POINT('Ctrl Pts',(198.297425465741,-4.79613587993932,131.902028800401));
#21013=CARTESIAN_POINT('Ctrl Pts',(198.289651131622,-4.76378621750837,132.0349066804));
#21014=CARTESIAN_POINT('Ctrl Pts',(198.281876797503,-4.7258965824454,132.166375505345));
#21015=CARTESIAN_POINT('Ctrl Pts',(198.274112044556,-4.68805364297136,132.297682306713));
#21016=CARTESIAN_POINT('Ctrl Pts',(198.266347291608,-4.64468442282832,132.427583136145));
#21017=CARTESIAN_POINT('Ctrl Pts',(198.258582538661,-4.59591298865343,132.555579297008));
#21018=CARTESIAN_POINT('Ctrl Pts',(198.250825497776,-4.54718999495454,132.683448330279));
#21019=CARTESIAN_POINT('Ctrl Pts',(198.243068456891,-4.49307560322901,132.809416096658));
#21020=CARTESIAN_POINT('Ctrl Pts',(198.235311416006,-4.43374391105737,132.932998208529));
#21021=CARTESIAN_POINT('Ctrl Pts',(198.227560224766,-4.37445696137642,133.056487126168));
#21022=CARTESIAN_POINT('Ctrl Pts',(198.219809033526,-4.30996071097418,133.177593619155));
#21023=CARTESIAN_POINT('Ctrl Pts',(198.212057842286,-4.24047753526522,133.295852808084));
#21024=CARTESIAN_POINT('Ctrl Pts',(198.204309945509,-4.17102389175934,133.414061733703));
#21025=CARTESIAN_POINT('Ctrl Pts',(198.196562048732,-4.09658773626326,133.529425425838));
#21026=CARTESIAN_POINT('Ctrl Pts',(198.188814151955,-4.01743749521107,133.6415033765));
#21027=CARTESIAN_POINT('Ctrl Pts',(198.181067875871,-3.93830381068304,133.753557882871));
#21028=CARTESIAN_POINT('Ctrl Pts',(198.173321599787,-3.85445822736556,133.862327695705));
#21029=CARTESIAN_POINT('Ctrl Pts',(198.165575323702,-3.76621240470724,133.967401430633));
#21030=CARTESIAN_POINT('Ctrl Pts',(198.157828990437,-3.67796593063832,134.072475941192));
#21031=CARTESIAN_POINT('Ctrl Pts',(198.150082657172,-3.58531940385276,134.173854020016));
#21032=CARTESIAN_POINT('Ctrl Pts',(198.142336323906,-3.48862439845058,134.271157823783));
#21033=CARTESIAN_POINT('Ctrl Pts',(198.134588255903,-3.3919077388725,134.368483418062));
#21034=CARTESIAN_POINT('Ctrl Pts',(198.126840187901,-3.29114107212411,134.461732644436));
#21035=CARTESIAN_POINT('Ctrl Pts',(198.119092119898,-3.18671210764418,134.550565230971));
#21036=CARTESIAN_POINT('Ctrl Pts',(198.111335817156,-3.08217215481793,134.639492229836));
#21037=CARTESIAN_POINT('Ctrl Pts',(198.103579514414,-2.97396242717541,134.723992958252));
#21038=CARTESIAN_POINT('Ctrl Pts',(198.095823211672,-2.86250336727734,134.803767765485));
#21039=CARTESIAN_POINT('Ctrl Pts',(198.088062769158,-2.75098481832297,134.883585150935));
#21040=CARTESIAN_POINT('Ctrl Pts',(198.080302326644,-2.63621380844923,134.958671375235));
#21041=CARTESIAN_POINT('Ctrl Pts',(198.07254188413,-2.51863805887903,135.028771273606));
#21042=CARTESIAN_POINT('Ctrl Pts',(198.064768983864,-2.40087356627779,135.098983702558));
#21043=CARTESIAN_POINT('Ctrl Pts',(198.056996083599,-2.2802956808095,135.164193623964));
#21044=CARTESIAN_POINT('Ctrl Pts',(198.049223183333,-2.15737571304909,135.22419241247));
#21045=CARTESIAN_POINT('Ctrl Pts',(198.041732847571,-2.03892419573207,135.282010093887));
#21046=CARTESIAN_POINT('Ctrl Pts',(198.034242511809,-1.91829820299034,135.33498881632));
#21047=CARTESIAN_POINT('Ctrl Pts',(198.026752176047,-1.79593348200914,135.382985519291));
#21048=CARTESIAN_POINT('Ctrl Pts',(198.018977841928,-1.66892926544145,135.432802031844));
#21049=CARTESIAN_POINT('Ctrl Pts',(198.011203507809,-1.53964955897284,135.477409084513));
#21050=CARTESIAN_POINT('Ctrl Pts',(198.00342917369,-1.40856083989839,135.516593572631));
#21051=CARTESIAN_POINT('Ctrl Pts',(197.995664420743,-1.27763367595456,135.555729769371));
#21052=CARTESIAN_POINT('Ctrl Pts',(197.987899667796,-1.14490230633097,135.589456587496));
#21053=CARTESIAN_POINT('Ctrl Pts',(197.980134914848,-1.01085335967749,135.617608850073));
#21054=CARTESIAN_POINT('Ctrl Pts',(197.972377873963,-0.876937552327542,
135.645733151425));
#21055=CARTESIAN_POINT('Ctrl Pts',(197.964620833078,-0.741707152334974,
135.668293835729));
#21056=CARTESIAN_POINT('Ctrl Pts',(197.956863792193,-0.605663792714778,
135.685175552871));
#21057=CARTESIAN_POINT('Ctrl Pts',(197.949112600953,-0.469723024450324,
135.702044539379));
#21058=CARTESIAN_POINT('Ctrl Pts',(197.941361409713,-0.332970903234851,
135.713243034937));
#21059=CARTESIAN_POINT('Ctrl Pts',(197.933610218473,-0.195918744622959,
135.718706851604));
#21060=CARTESIAN_POINT('Ctrl Pts',(197.925862321696,-0.0589248368344638,
135.724168346004));
#21061=CARTESIAN_POINT('Ctrl Pts',(197.918114424919,0.0783684648781298,
135.723899993757));
#21062=CARTESIAN_POINT('Ctrl Pts',(197.910366528142,0.215445457623812,135.717889524298));
#21063=CARTESIAN_POINT('Ctrl Pts',(197.902620252058,0.352493776817673,135.711880312099));
#21064=CARTESIAN_POINT('Ctrl Pts',(197.894873975974,0.489325486701273,135.700131388911));
#21065=CARTESIAN_POINT('Ctrl Pts',(197.88712769989,0.625426018410143,135.682682599354));
#21066=CARTESIAN_POINT('Ctrl Pts',(197.879381366624,0.761527554782069,135.665233680994));
#21067=CARTESIAN_POINT('Ctrl Pts',(197.871635033359,0.896897514417944,135.642084862025));
#21068=CARTESIAN_POINT('Ctrl Pts',(197.863888700093,1.03102797264083,135.613327698149));
#21069=CARTESIAN_POINT('Ctrl Pts',(197.856140632091,1.16518846844996,135.584564094306));
#21070=CARTESIAN_POINT('Ctrl Pts',(197.848392564088,1.29810852829368,135.550189728304));
#21071=CARTESIAN_POINT('Ctrl Pts',(197.840644496085,1.42929230533578,135.510346865783));
#21072=CARTESIAN_POINT('Ctrl Pts',(197.832888193343,1.56061550605723,135.470461657794));
#21073=CARTESIAN_POINT('Ctrl Pts',(197.825131890601,1.69019836301931,135.425096457024));
#21074=CARTESIAN_POINT('Ctrl Pts',(197.817375587859,1.81756151209824,135.374443025164));
#21075=CARTESIAN_POINT('Ctrl Pts',(197.809615145345,1.94499263872476,135.323762558043));
#21076=CARTESIAN_POINT('Ctrl Pts',(197.801854702831,2.0702013400551,135.267788395269));
#21077=CARTESIAN_POINT('Ctrl Pts',(197.794094260316,2.19273093447755,135.206759294593));
#21078=CARTESIAN_POINT('Ctrl Pts',(197.786321360051,2.3154572242826,135.145632224586));
#21079=CARTESIAN_POINT('Ctrl Pts',(197.778548459786,2.43549547037675,135.079434189959));
#21080=CARTESIAN_POINT('Ctrl Pts',(197.77077555952,2.55241539546258,135.008448950547));
#21081=CARTESIAN_POINT('Ctrl Pts',(197.763285223758,2.66508498676848,134.940044203388));
#21082=CARTESIAN_POINT('Ctrl Pts',(197.755794887996,2.77485878191613,134.867194432942));
#21083=CARTESIAN_POINT('Ctrl Pts',(197.748304552234,2.88138088807747,134.790188917973));
#21084=CARTESIAN_POINT('Ctrl Pts',(197.740530218115,2.99194181227019,134.710263715498));
#21085=CARTESIAN_POINT('Ctrl Pts',(197.732755883996,3.09934982819655,134.62560823861));
#21086=CARTESIAN_POINT('Ctrl Pts',(197.724981549877,3.20317350249298,134.53649975959));
#21087=CARTESIAN_POINT('Ctrl Pts',(197.71721679693,3.3068692233898,134.447501098806));
#21088=CARTESIAN_POINT('Ctrl Pts',(197.709452043983,3.40698909809778,134.354060607414));
#21089=CARTESIAN_POINT('Ctrl Pts',(197.701687291035,3.50313112391044,134.256498417711));
#21090=CARTESIAN_POINT('Ctrl Pts',(197.69393025015,3.5991776601077,134.15903312815));
#21091=CARTESIAN_POINT('Ctrl Pts',(197.686173209265,3.6912539371464,134.057454563654));
#21092=CARTESIAN_POINT('Ctrl Pts',(197.67841616838,3.77899176281173,133.952122412731));
#21093=CARTESIAN_POINT('Ctrl Pts',(197.67066497714,3.86666342470019,133.846869693603));
#21094=CARTESIAN_POINT('Ctrl Pts',(197.6629137859,3.95000289804419,133.737869321391));
#21095=CARTESIAN_POINT('Ctrl Pts',(197.65516259466,4.02867980116461,133.625516785202));
#21096=CARTESIAN_POINT('Ctrl Pts',(197.647414697883,4.10732326450247,133.513212001837));
#21097=CARTESIAN_POINT('Ctrl Pts',(197.639666801106,4.18130787530829,133.397558207814));
#21098=CARTESIAN_POINT('Ctrl Pts',(197.631918904329,4.25034455999749,133.278982646038));
#21099=CARTESIAN_POINT('Ctrl Pts',(197.624172628245,4.31936680370051,133.160431887714));
#21100=CARTESIAN_POINT('Ctrl Pts',(197.616426352161,4.38344298336774,133.038960914946));
#21101=CARTESIAN_POINT('Ctrl Pts',(197.608680076076,4.4423284843672,132.915024186087));
#21102=CARTESIAN_POINT('Ctrl Pts',(197.600933742811,4.50121442004603,132.791086542354));
#21103=CARTESIAN_POINT('Ctrl Pts',(197.593187409546,4.55490943281703,132.664683459342));
#21104=CARTESIAN_POINT('Ctrl Pts',(197.58544107628,4.60321600539095,132.536291756559));
#21105=CARTESIAN_POINT('Ctrl Pts',(197.577693008277,4.65153339588684,132.407871301344));
#21106=CARTESIAN_POINT('Ctrl Pts',(197.569944940274,4.69445980733516,132.277461706041));
#21107=CARTESIAN_POINT('Ctrl Pts',(197.562196872271,4.73184691452124,132.14555703869));
#21108=CARTESIAN_POINT('Ctrl Pts',(197.55444056953,4.76927375716978,132.013512181488));
#21109=CARTESIAN_POINT('Ctrl Pts',(197.546684266788,4.80114942837765,131.879969454826));
#21110=CARTESIAN_POINT('Ctrl Pts',(197.538927964046,4.82737615466953,131.745435813195));
#21111=CARTESIAN_POINT('Ctrl Pts',(197.531167521532,4.85361687895492,131.610830366909));
#21112=CARTESIAN_POINT('Ctrl Pts',(197.523407079018,4.87420259200423,131.475233338161));
#21113=CARTESIAN_POINT('Ctrl Pts',(197.515646636503,4.88908731990802,131.33915800052));
#21114=CARTESIAN_POINT('Ctrl Pts',(197.507873736238,4.90399594209845,131.202864222668));
#21115=CARTESIAN_POINT('Ctrl Pts',(197.500100835973,4.91318526485212,131.066090991876));
#21116=CARTESIAN_POINT('Ctrl Pts',(197.492327935707,4.91666144796523,130.929353691744));
#21117=CARTESIAN_POINT('Ctrl Pts',(197.484837599945,4.9200112630662,130.797587136892));
#21118=CARTESIAN_POINT('Ctrl Pts',(197.477347264183,4.91805610562799,130.665854253699));
#21119=CARTESIAN_POINT('Ctrl Pts',(197.469856928421,4.91084698530234,130.534610827118));
#21120=CARTESIAN_POINT('Ctrl Pts',(197.462082594302,4.90336452898838,130.398391266127));
#21121=CARTESIAN_POINT('Ctrl Pts',(197.454308260183,4.89019813490943,130.262267507292));
#21122=CARTESIAN_POINT('Ctrl Pts',(197.446533926064,4.87134787981786,130.126752400162));
#21123=CARTESIAN_POINT('Ctrl Pts',(197.438769173117,4.852520855981,129.991404303289));
#21124=CARTESIAN_POINT('Ctrl Pts',(197.43100442017,4.82802396204446,129.856663749147));
#21125=CARTESIAN_POINT('Ctrl Pts',(197.423239667222,4.79790924209346,129.723041993323));
#21126=CARTESIAN_POINT('Ctrl Pts',(197.415482626337,4.76782443250686,129.589552952511));
#21127=CARTESIAN_POINT('Ctrl Pts',(197.407725585452,4.73213298616931,129.457180877599));
#21128=CARTESIAN_POINT('Ctrl Pts',(197.399968544567,4.69093850232438,129.326429959548));
#21129=CARTESIAN_POINT('Ctrl Pts',(197.392217353327,4.64977508356018,129.195777641781));
#21130=CARTESIAN_POINT('Ctrl Pts',(197.384466162087,4.60311700438922,129.066744418897));
#21131=CARTESIAN_POINT('Ctrl Pts',(197.376714970847,4.55111842163095,128.939822021883));
#21132=CARTESIAN_POINT('Ctrl Pts',(197.36896707407,4.49914193965744,128.812953570273));
#21133=CARTESIAN_POINT('Ctrl Pts',(197.361219177293,4.44182961657508,128.688194521179));
#21134=CARTESIAN_POINT('Ctrl Pts',(197.353471280516,4.37938465260795,128.56601901562));
#21135=CARTESIAN_POINT('Ctrl Pts',(197.345725004432,4.3169527507811,128.443869066543));
#21136=CARTESIAN_POINT('Ctrl Pts',(197.337978728348,4.24939052141315,128.324301933984));
#21137=CARTESIAN_POINT('Ctrl Pts',(197.330232452263,4.17694809300133,128.207769064997));
#21138=CARTESIAN_POINT('Ctrl Pts',(197.322486118998,4.10450512983598,128.091235335791));
#21139=CARTESIAN_POINT('Ctrl Pts',(197.314739785733,4.02718210215263,127.97773624689));
#21140=CARTESIAN_POINT('Ctrl Pts',(197.306993452467,3.9452734087893,127.867695707775));
#21141=CARTESIAN_POINT('Ctrl Pts',(197.299245384464,3.86334637254203,127.757630525843));
#21142=CARTESIAN_POINT('Ctrl Pts',(197.291497316461,3.77683186054576,127.65102574846));
#21143=CARTESIAN_POINT('Ctrl Pts',(197.283749248458,3.68606537283357,127.548273221672));
#21144=CARTESIAN_POINT('Ctrl Pts',(197.275992945717,3.59520241741809,127.445411488276));
#21145=CARTESIAN_POINT('Ctrl Pts',(197.268236642975,3.50007871824481,127.3464104776));
#21146=CARTESIAN_POINT('Ctrl Pts',(197.260480340233,3.4010679415342,127.251626470523));
#21147=CARTESIAN_POINT('Ctrl Pts',(197.252719897719,3.30200431979083,127.156791874367));
#21148=CARTESIAN_POINT('Ctrl Pts',(197.244959455205,3.19904977993481,127.066179024781));
#21149=CARTESIAN_POINT('Ctrl Pts',(197.23719901269,3.09261130353576,126.980104037818));
#21150=CARTESIAN_POINT('Ctrl Pts',(197.229426112425,2.98600196264525,126.893890875646));
#21151=CARTESIAN_POINT('Ctrl Pts',(197.22165321216,2.87589782337121,126.812230366043));
#21152=CARTESIAN_POINT('Ctrl Pts',(197.213880311894,2.76273582205164,126.735395904024));
#21153=CARTESIAN_POINT('Ctrl Pts',(197.206389976132,2.65368754451797,126.661354568233));
#21154=CARTESIAN_POINT('Ctrl Pts',(197.19889964037,2.54180012866534,126.591794656438));
#21155=CARTESIAN_POINT('Ctrl Pts',(197.191409304608,2.4274846112473,126.526919615675));
#21156=CARTESIAN_POINT('Ctrl Pts',(197.183634970489,2.30883478624092,126.459584818023));
#21157=CARTESIAN_POINT('Ctrl Pts',(197.17586063637,2.18719325510115,126.397083861596));
#21158=CARTESIAN_POINT('Ctrl Pts',(197.168086302251,2.06299153416462,126.339693889526));
#21159=CARTESIAN_POINT('Ctrl Pts',(197.160321549304,1.93894288074894,126.282374645468));
#21160=CARTESIAN_POINT('Ctrl Pts',(197.152556796357,1.81234066695579,126.230154015391));
#21161=CARTESIAN_POINT('Ctrl Pts',(197.144792043409,1.68364315769026,126.183264559263));
#21162=CARTESIAN_POINT('Ctrl Pts',(197.137035002524,1.55507347260519,126.136421674404));
#21163=CARTESIAN_POINT('Ctrl Pts',(197.129277961639,1.42441299845145,126.094899559184));
#21164=CARTESIAN_POINT('Ctrl Pts',(197.121520920754,1.29214192328729,126.058883580156));
#21165=CARTESIAN_POINT('Ctrl Pts',(197.113769729514,1.15997059476984,126.022894761058));
#21166=CARTESIAN_POINT('Ctrl Pts',(197.106018538274,1.02619145846807,125.99240391571));
#21167=CARTESIAN_POINT('Ctrl Pts',(197.098267347034,0.891301547113867,125.967547140222));
#21168=CARTESIAN_POINT('Ctrl Pts',(197.090519450257,0.756468967570347,125.942700929528));
#21169=CARTESIAN_POINT('Ctrl Pts',(197.08277155348,0.620526935649892,125.923484096662));
#21170=CARTESIAN_POINT('Ctrl Pts',(197.075023656703,0.483984194306158,125.909981968323));
#21171=CARTESIAN_POINT('Ctrl Pts',(197.067277380619,0.347470014760427,125.896482664339));
#21172=CARTESIAN_POINT('Ctrl Pts',(197.059531104535,0.210355764548132,125.88869572563));
#21173=CARTESIAN_POINT('Ctrl Pts',(197.051784828451,0.0731564594262019,
125.886654730168));
#21174=CARTESIAN_POINT('Ctrl Pts',(197.044038495185,-0.0640438584697734,
125.884613719641));
#21175=CARTESIAN_POINT('Ctrl Pts',(197.03629216192,-0.201328841606274,125.888318742812));
#21176=CARTESIAN_POINT('Ctrl Pts',(197.028545828654,-0.338182713167988,
125.897751247032));
#21177=CARTESIAN_POINT('Ctrl Pts',(197.020797760651,-0.475067232205337,
125.907185863595));
#21178=CARTESIAN_POINT('Ctrl Pts',(197.013049692649,-0.611520057590418,
125.922350486614));
#21179=CARTESIAN_POINT('Ctrl Pts',(197.005301624646,-0.747030172182732,
125.943174652768));
#21180=CARTESIAN_POINT('Ctrl Pts',(196.997545321904,-0.882684308537553,
125.964020951094));
#21181=CARTESIAN_POINT('Ctrl Pts',(196.989789019162,-1.01739334560279,125.990538748746));
#21182=CARTESIAN_POINT('Ctrl Pts',(196.98203271642,-1.15065555846418,126.022606248271));
#21183=CARTESIAN_POINT('Ctrl Pts',(196.974272273906,-1.28398889738112,126.054690863185));
#21184=CARTESIAN_POINT('Ctrl Pts',(196.966511831392,-1.41587349762368,126.092330974847));
#21185=CARTESIAN_POINT('Ctrl Pts',(196.958751388877,-1.5458234183235,126.135355046584));
#21186=CARTESIAN_POINT('Ctrl Pts',(196.950978488612,-1.67598194617242,126.17844818438));
#21187=CARTESIAN_POINT('Ctrl Pts',(196.943205588347,-1.80419922236758,126.226942414954));
#21188=CARTESIAN_POINT('Ctrl Pts',(196.935432688081,-1.93000905717825,126.280617908071));
#21189=CARTESIAN_POINT('Ctrl Pts',(196.927942352319,-2.05124538759802,126.332342161813));
#21190=CARTESIAN_POINT('Ctrl Pts',(196.920452016557,-2.17024599270099,126.388877382166));
#21191=CARTESIAN_POINT('Ctrl Pts',(196.912961680795,-2.28661753132807,126.44998772036));
#21192=CARTESIAN_POINT('Ctrl Pts',(196.905186437551,-2.40741545658494,126.513422492751));
#21193=CARTESIAN_POINT('Ctrl Pts',(196.897411194306,-2.52576305120591,126.581988282265));
#21194=CARTESIAN_POINT('Ctrl Pts',(196.889635951062,-2.6411937391818,126.655471766969));
#21195=CARTESIAN_POINT('Ctrl Pts',(196.881870490011,-2.75647920144334,126.728862800595));
#21196=CARTESIAN_POINT('Ctrl Pts',(196.874105028959,-2.86885473277439,126.807159009799));
#21197=CARTESIAN_POINT('Ctrl Pts',(196.866339567908,-2.97787685313513,126.890100469075));
#21198=CARTESIAN_POINT('Ctrl Pts',(196.858583393819,-3.08676859046736,126.972942736017));
#21199=CARTESIAN_POINT('Ctrl Pts',(196.85082721973,-3.19231459493436,127.060418953556));
#21200=CARTESIAN_POINT('Ctrl Pts',(196.843071045641,-3.294099502712,127.152225416244));
#21201=CARTESIAN_POINT('Ctrl Pts',(196.835320138421,-3.39581529293819,127.243969537295));
#21202=CARTESIAN_POINT('Ctrl Pts',(196.827569231201,-3.49377477829833,127.340037793094));
#21203=CARTESIAN_POINT('Ctrl Pts',(196.819818323981,-3.58759484370538,127.440085613955));
#21204=CARTESIAN_POINT('Ctrl Pts',(196.812071001449,-3.6813715186174,127.54008716407));
#21205=CARTESIAN_POINT('Ctrl Pts',(196.804323678917,-3.77101231623895,127.644064332384));
#21206=CARTESIAN_POINT('Ctrl Pts',(196.796576356385,-3.85617053877141,127.751635304274));
#21207=CARTESIAN_POINT('Ctrl Pts',(196.788830939126,-3.94130781864133,127.859179821613));
#21208=CARTESIAN_POINT('Ctrl Pts',(196.781085521866,-4.02196447570508,127.970316076795));
#21209=CARTESIAN_POINT('Ctrl Pts',(196.773340104606,-4.09783398032599,128.084629062396));
#21210=CARTESIAN_POINT('Ctrl Pts',(196.765580754941,-4.17383995850953,128.19914767344));
#21211=CARTESIAN_POINT('Ctrl Pts',(196.757821405275,-4.24504131628586,128.316854134644));
#21212=CARTESIAN_POINT('Ctrl Pts',(196.75006205561,-4.31117357625514,128.437302219913));
#21213=CARTESIAN_POINT('Ctrl Pts',(196.742313049751,-4.37721767686617,128.557589738676));
#21214=CARTESIAN_POINT('Ctrl Pts',(196.734564043892,-4.43820602078034,128.680611220613));
#21215=CARTESIAN_POINT('Ctrl Pts',(196.726815038034,-4.49392167184312,128.805898441332));
#21216=CARTESIAN_POINT('Ctrl Pts',(196.719050516465,-4.54974888145534,128.931436522632));
#21217=CARTESIAN_POINT('Ctrl Pts',(196.711285994897,-4.60028211429378,129.059249060427));
#21218=CARTESIAN_POINT('Ctrl Pts',(196.703521473329,-4.64535222085451,129.188846517751));
#21219=CARTESIAN_POINT('Ctrl Pts',(196.69575695176,-4.69042232741525,129.318443975074));
#21220=CARTESIAN_POINT('Ctrl Pts',(196.687992430192,-4.73002922227267,129.449825967771));
#21221=CARTESIAN_POINT('Ctrl Pts',(196.680227908624,-4.76405452823405,129.582490119308));
#21222=CARTESIAN_POINT('Origin',(213.235140564004,0.,130.804360617566));
#21223=CARTESIAN_POINT('',(194.584773235637,-4.76405452823404,129.582490119308));
#21224=CARTESIAN_POINT('',(194.92989654745,-4.76405452823404,129.582490119308));
#21225=CARTESIAN_POINT('',(213.235140564004,-4.76405452823405,129.582490119308));
#21226=CARTESIAN_POINT('',(196.264859436042,-4.91824930178245,130.801739927489));
#21227=CARTESIAN_POINT('Ctrl Pts',(196.264859435991,-4.91824930178293,130.801739928394));
#21228=CARTESIAN_POINT('Ctrl Pts',(196.257012721372,-4.9183234709409,130.940933241881));
#21229=CARTESIAN_POINT('Ctrl Pts',(196.249166006753,-4.91248424618416,131.080125087051));
#21230=CARTESIAN_POINT('Ctrl Pts',(196.241319292134,-4.90075854751751,131.218786390696));
#21231=CARTESIAN_POINT('Ctrl Pts',(196.233470637992,-4.88902995053467,131.357481968145));
#21232=CARTESIAN_POINT('Ctrl Pts',(196.22562198385,-4.87141201293207,131.495646367384));
#21233=CARTESIAN_POINT('Ctrl Pts',(196.217773329708,-4.84798352666506,131.632755926392));
#21234=CARTESIAN_POINT('Ctrl Pts',(196.209921209237,-4.82454469329633,131.769926039314));
#21235=CARTESIAN_POINT('Ctrl Pts',(196.202069088767,-4.79529026322915,131.906040012911));
#21236=CARTESIAN_POINT('Ctrl Pts',(196.194216968297,-4.76035005680923,132.040584868718));
#21237=CARTESIAN_POINT('Ctrl Pts',(196.186132871399,-4.72437760638351,132.179104604331));
#21238=CARTESIAN_POINT('Ctrl Pts',(196.1780487745,-4.68237835041523,132.315960659695));
#21239=CARTESIAN_POINT('Ctrl Pts',(196.169964677602,-4.63454850944733,132.450611866944));
#21240=CARTESIAN_POINT('Ctrl Pts',(196.162096228248,-4.58799455469389,132.581671182278));
#21241=CARTESIAN_POINT('Ctrl Pts',(196.154227778895,-4.53591733384053,132.710641463661));
#21242=CARTESIAN_POINT('Ctrl Pts',(196.146359329542,-4.47854577483177,132.837046231535));
#21243=CARTESIAN_POINT('Ctrl Pts',(196.138167408871,-4.41881567566367,132.968647489212));
#21244=CARTESIAN_POINT('Ctrl Pts',(196.1299754882,-4.35334689846171,133.097467395895));
#21245=CARTESIAN_POINT('Ctrl Pts',(196.121783567529,-4.2824489092148,133.222999574183));
#21246=CARTESIAN_POINT('Ctrl Pts',(196.113591646858,-4.21155091996789,133.348531752471));
#21247=CARTESIAN_POINT('Ctrl Pts',(196.105399726187,-4.13522401973526,133.470775856601));
#21248=CARTESIAN_POINT('Ctrl Pts',(196.097207805515,-4.05382567680301,133.589262850068));
#21249=CARTESIAN_POINT('Ctrl Pts',(196.089433471396,-3.97657664814305,133.701709919927));
#21250=CARTESIAN_POINT('Ctrl Pts',(196.081659137277,-3.89452304616624,133.811118503023));
#21251=CARTESIAN_POINT('Ctrl Pts',(196.073884803158,-3.80793171009603,133.917050636464));
#21252=CARTESIAN_POINT('Ctrl Pts',(196.066120050211,-3.72144709010858,134.022852218017));
#21253=CARTESIAN_POINT('Ctrl Pts',(196.058355297264,-3.63043610820173,134.125185574825));
#21254=CARTESIAN_POINT('Ctrl Pts',(196.050590544317,-3.53520915752512,134.223641137654));
#21255=CARTESIAN_POINT('Ctrl Pts',(196.042833503432,-3.44007678759841,134.32199891303));
#21256=CARTESIAN_POINT('Ctrl Pts',(196.035076462547,-3.34073705198568,134.41648627984));
#21257=CARTESIAN_POINT('Ctrl Pts',(196.027319421662,-3.2375407000163,134.506726520369));
#21258=CARTESIAN_POINT('Ctrl Pts',(196.019568230422,-3.13442216921906,134.59689871003));
#21259=CARTESIAN_POINT('Ctrl Pts',(196.011817039182,-3.02745310398911,134.68282989205));
#21260=CARTESIAN_POINT('Ctrl Pts',(196.004065847942,-2.91702095129357,134.764180289245));
#21261=CARTESIAN_POINT('Ctrl Pts',(195.996317951164,-2.8066357352085,134.845496110351));
#21262=CARTESIAN_POINT('Ctrl Pts',(195.988570054387,-2.69279067328169,134.92223478758));
#21263=CARTESIAN_POINT('Ctrl Pts',(195.98082215761,-2.57590594841546,134.994097077944));
#21264=CARTESIAN_POINT('Ctrl Pts',(195.973075881526,-2.45904567331386,135.065944336265));
#21265=CARTESIAN_POINT('Ctrl Pts',(195.965329605442,-2.3391473328201,135.13291703199));
#21266=CARTESIAN_POINT('Ctrl Pts',(195.957583329358,-2.2166593843348,135.194759715181));
#21267=CARTESIAN_POINT('Ctrl Pts',(195.949836996093,-2.09417053167117,135.256602854881));
#21268=CARTESIAN_POINT('Ctrl Pts',(195.942090662827,-1.96909238187651,135.313315730276));
#21269=CARTESIAN_POINT('Ctrl Pts',(195.934344329562,-1.84189687727761,135.364689438602));
#21270=CARTESIAN_POINT('Ctrl Pts',(195.926596261559,-1.7146728881277,135.416074651714));
#21271=CARTESIAN_POINT('Ctrl Pts',(195.918848193556,-1.58533096307996,135.462118172125));
#21272=CARTESIAN_POINT('Ctrl Pts',(195.911100125553,-1.45436146849866,135.502659861063));
#21273=CARTESIAN_POINT('Ctrl Pts',(195.903343822811,-1.32325277797986,135.543244638191));
#21274=CARTESIAN_POINT('Ctrl Pts',(195.895587520069,-1.19051343654138,135.578315787215));
#21275=CARTESIAN_POINT('Ctrl Pts',(195.887831217328,-1.0566479063914,135.607763397306));
#21276=CARTESIAN_POINT('Ctrl Pts',(195.880070774813,-0.922710928177224,
135.637226724474));
#21277=CARTESIAN_POINT('Ctrl Pts',(195.872310332299,-0.787646948375374,
135.661060464155));
#21278=CARTESIAN_POINT('Ctrl Pts',(195.864549889785,-0.651967989498143,
135.679206338527));
#21279=CARTESIAN_POINT('Ctrl Pts',(195.85677698952,-0.516071226711214,135.697381342267));
#21280=CARTESIAN_POINT('Ctrl Pts',(195.849004089254,-0.379557901639337,
135.709850199137));
#21281=CARTESIAN_POINT('Ctrl Pts',(195.841231188989,-0.242943397281255,
135.716606699372));
#21282=CARTESIAN_POINT('Ctrl Pts',(195.833740853227,-0.111295174267542,
135.723117583805));
#21283=CARTESIAN_POINT('Ctrl Pts',(195.826250517465,0.0204466914981448,
135.724324215373));
#21284=CARTESIAN_POINT('Ctrl Pts',(195.818760181703,0.151825322225019,135.720266651456));
#21285=CARTESIAN_POINT('Ctrl Pts',(195.810985847584,0.288185213667395,135.716055243769));
#21286=CARTESIAN_POINT('Ctrl Pts',(195.803211513465,0.424585729377166,135.706159236164));
#21287=CARTESIAN_POINT('Ctrl Pts',(195.795437179345,0.560514165651644,135.690566398395));
#21288=CARTESIAN_POINT('Ctrl Pts',(195.787672426398,0.69627508227663,135.674992777405));
#21289=CARTESIAN_POINT('Ctrl Pts',(195.779907673451,0.831564692377237,135.653736339747));
#21290=CARTESIAN_POINT('Ctrl Pts',(195.772142920504,0.96587063867978,135.626836845795));
#21291=CARTESIAN_POINT('Ctrl Pts',(195.764385879619,1.10004319042296,135.5999640688));
#21292=CARTESIAN_POINT('Ctrl Pts',(195.756628838734,1.23323364174855,135.567459465525));
#21293=CARTESIAN_POINT('Ctrl Pts',(195.748871797849,1.36493546079199,135.529414506187));
#21294=CARTESIAN_POINT('Ctrl Pts',(195.741120606609,1.496537962469,135.491398236849));
#21295=CARTESIAN_POINT('Ctrl Pts',(195.733369415369,1.62665369222182,135.447850035617));
#21296=CARTESIAN_POINT('Ctrl Pts',(195.725618224129,1.75478736133172,135.398912214731));
#21297=CARTESIAN_POINT('Ctrl Pts',(195.717870327352,1.88286657021454,135.349995193724));
#21298=CARTESIAN_POINT('Ctrl Pts',(195.710122430575,2.00896502951187,135.295693248354));
#21299=CARTESIAN_POINT('Ctrl Pts',(195.702374533797,2.13260385849881,135.236198142252));
#21300=CARTESIAN_POINT('Ctrl Pts',(195.694628257713,2.25621682490795,135.176715481244));
#21301=CARTESIAN_POINT('Ctrl Pts',(195.686881981629,2.37737083230292,135.112041989627));
#21302=CARTESIAN_POINT('Ctrl Pts',(195.679135705545,2.49560856123834,135.042416890384));
#21303=CARTESIAN_POINT('Ctrl Pts',(195.67138937228,2.61384716297782,134.972791277185));
#21304=CARTESIAN_POINT('Ctrl Pts',(195.663643039014,2.72916910640684,134.898214181805));
#21305=CARTESIAN_POINT('Ctrl Pts',(195.655896705749,2.84114353935931,134.818969745645));
#21306=CARTESIAN_POINT('Ctrl Pts',(195.648148637746,2.95314304820954,134.739707563244));
#21307=CARTESIAN_POINT('Ctrl Pts',(195.640400569743,3.06179323579177,134.655776186005));
#21308=CARTESIAN_POINT('Ctrl Pts',(195.63265250174,3.16669431782458,134.567501614122));
#21309=CARTESIAN_POINT('Ctrl Pts',(195.624896198998,3.27170688997588,134.479133222973));
#21310=CARTESIAN_POINT('Ctrl Pts',(195.617139896256,3.37296209730263,134.386412668355));
#21311=CARTESIAN_POINT('Ctrl Pts',(195.609383593514,3.47009479456587,134.289704959123));
#21312=CARTESIAN_POINT('Ctrl Pts',(195.601623151,3.56727933447434,134.192945634076));
#21313=CARTESIAN_POINT('Ctrl Pts',(195.593862708486,3.660336714878,134.092195201126));
#21314=CARTESIAN_POINT('Ctrl Pts',(195.586102265972,3.74894114432121,133.987852938731));
#21315=CARTESIAN_POINT('Ctrl Pts',(195.578329365706,3.83768780946045,133.883343176873));
#21316=CARTESIAN_POINT('Ctrl Pts',(195.570556465441,3.92196699860579,133.775230371938));
#21317=CARTESIAN_POINT('Ctrl Pts',(195.562783565176,4.00149491020802,133.663944773712));
#21318=CARTESIAN_POINT('Ctrl Pts',(195.555293229414,4.07813178190516,133.556704687292));
#21319=CARTESIAN_POINT('Ctrl Pts',(195.547802893651,4.15035665163739,133.446518738335));
#21320=CARTESIAN_POINT('Ctrl Pts',(195.540312557889,4.21795626720724,133.333792963059));
#21321=CARTESIAN_POINT('Ctrl Pts',(195.53253822377,4.28811894274751,133.216793155752));
#21322=CARTESIAN_POINT('Ctrl Pts',(195.524763889651,4.35352096178859,133.096686504988));
#21323=CARTESIAN_POINT('Ctrl Pts',(195.516989555532,4.41387490580435,132.973897752167));
#21324=CARTESIAN_POINT('Ctrl Pts',(195.509224802585,4.47415446897807,132.851260325509));
#21325=CARTESIAN_POINT('Ctrl Pts',(195.501460049638,4.52939816485493,132.725947721159));
#21326=CARTESIAN_POINT('Ctrl Pts',(195.493695296691,4.57936250334169,132.598412491255));
#21327=CARTESIAN_POINT('Ctrl Pts',(195.485938255806,4.62927721654309,132.47100393114));
#21328=CARTESIAN_POINT('Ctrl Pts',(195.478181214921,4.67392286552881,132.341377500251));
#21329=CARTESIAN_POINT('Ctrl Pts',(195.470424174036,4.71310261393714,132.210008800078));
#21330=CARTESIAN_POINT('Ctrl Pts',(195.462672982796,4.75225281659245,132.078739166064));
#21331=CARTESIAN_POINT('Ctrl Pts',(195.454921791556,4.78594521173213,131.945730251064));
#21332=CARTESIAN_POINT('Ctrl Pts',(195.447170600316,4.81403181502214,131.811475678746));
#21333=CARTESIAN_POINT('Ctrl Pts',(195.439422703538,4.84210648075651,131.677278168202));
#21334=CARTESIAN_POINT('Ctrl Pts',(195.431674806761,4.86458001358226,131.54183643523));
#21335=CARTESIAN_POINT('Ctrl Pts',(195.423926909984,4.88135490294342,131.405657028673));
#21336=CARTESIAN_POINT('Ctrl Pts',(195.4161806339,4.89812628335934,131.269506107912));
#21337=CARTESIAN_POINT('Ctrl Pts',(195.408434357816,4.90920134356196,131.132618208275));
#21338=CARTESIAN_POINT('Ctrl Pts',(195.400688081732,4.91453415629017,130.995507391426));
#21339=CARTESIAN_POINT('Ctrl Pts',(195.392941748467,4.919867008384,130.858395562457));
#21340=CARTESIAN_POINT('Ctrl Pts',(195.385195415201,4.91945751322652,130.721061203664));
#21341=CARTESIAN_POINT('Ctrl Pts',(195.377449081936,4.91331184090468,130.584020388543));
#21342=CARTESIAN_POINT('Ctrl Pts',(195.369701013933,4.90716479230216,130.446948884082));
#21343=CARTESIAN_POINT('Ctrl Pts',(195.36195294593,4.8952790278877,130.310171444601));
#21344=CARTESIAN_POINT('Ctrl Pts',(195.354204877927,4.8777127276868,130.174200631005));
#21345=CARTESIAN_POINT('Ctrl Pts',(195.346448575185,4.86012775781292,130.03808530601));
#21346=CARTESIAN_POINT('Ctrl Pts',(195.338692272444,4.83685024208653,129.902778707793));
#21347=CARTESIAN_POINT('Ctrl Pts',(195.330935969702,4.80798990287418,129.768785339588));
#21348=CARTESIAN_POINT('Ctrl Pts',(195.323175527188,4.77911416002987,129.634720455087));
#21349=CARTESIAN_POINT('Ctrl Pts',(195.315415084674,4.74464975455025,129.501970575457));
#21350=CARTESIAN_POINT('Ctrl Pts',(195.307654642159,4.70475651246827,129.371025618033));
#21351=CARTESIAN_POINT('Ctrl Pts',(195.299881741894,4.66479923021246,129.239870456138));
#21352=CARTESIAN_POINT('Ctrl Pts',(195.292108841629,4.61939582587396,129.11052637553));
#21353=CARTESIAN_POINT('Ctrl Pts',(195.284335941363,4.56875487911233,128.983464707008));
#21354=CARTESIAN_POINT('Ctrl Pts',(195.276845605601,4.5199548583218,128.861022050185));
#21355=CARTESIAN_POINT('Ctrl Pts',(195.269355269839,4.46629160511688,128.740699024911));
#21356=CARTESIAN_POINT('Ctrl Pts',(195.261864934077,4.40799146124495,128.622894518794));
#21357=CARTESIAN_POINT('Ctrl Pts',(195.254090599958,4.3474808496989,128.500623419023));
#21358=CARTESIAN_POINT('Ctrl Pts',(195.246316265839,4.28178311163883,128.380678269616));
#21359=CARTESIAN_POINT('Ctrl Pts',(195.23854193172,4.21110023729952,128.263530467021));
#21360=CARTESIAN_POINT('Ctrl Pts',(195.230777178773,4.14050447328558,128.146527038623));
#21361=CARTESIAN_POINT('Ctrl Pts',(195.223012425825,4.06493599723231,128.032314429117));
#21362=CARTESIAN_POINT('Ctrl Pts',(195.215247672878,3.98464394172745,127.9213421091));
#21363=CARTESIAN_POINT('Ctrl Pts',(195.207490631993,3.90443163342391,127.810480008356));
#21364=CARTESIAN_POINT('Ctrl Pts',(195.199733591108,3.81950530971266,127.702852107236));
#21365=CARTESIAN_POINT('Ctrl Pts',(195.191976550223,3.73015871273531,127.59888108397));
#21366=CARTESIAN_POINT('Ctrl Pts',(195.184225358983,3.64087949272173,127.49498846606));
#21367=CARTESIAN_POINT('Ctrl Pts',(195.176474167743,3.5471868880792,127.39474753233));
#21368=CARTESIAN_POINT('Ctrl Pts',(195.168722976503,3.44941620923195,127.29854960184));
#21369=CARTESIAN_POINT('Ctrl Pts',(195.160975079726,3.35168708553179,127.202392558036));
#21370=CARTESIAN_POINT('Ctrl Pts',(195.153227182949,3.24988361311233,127.110275373367));
#21371=CARTESIAN_POINT('Ctrl Pts',(195.145479286172,3.14437925902386,127.022553888247));
#21372=CARTESIAN_POINT('Ctrl Pts',(195.137733010088,3.03889697417174,126.934850752571));
#21373=CARTESIAN_POINT('Ctrl Pts',(195.129986734003,2.92971564790252,126.851541737333));
#21374=CARTESIAN_POINT('Ctrl Pts',(195.122240457919,2.8172429500486,126.772943345328));
#21375=CARTESIAN_POINT('Ctrl Pts',(195.114494124654,2.70476942194696,126.694344373127));
#21376=CARTESIAN_POINT('Ctrl Pts',(195.106747791389,2.58900479424786,126.620456317494));
#21377=CARTESIAN_POINT('Ctrl Pts',(195.099001458123,2.47038658928282,126.551552937692));
#21378=CARTESIAN_POINT('Ctrl Pts',(195.09125339012,2.35174182059327,126.482634127456));
#21379=CARTESIAN_POINT('Ctrl Pts',(195.083505322117,2.23024254102713,126.418702410666));
#21380=CARTESIAN_POINT('Ctrl Pts',(195.075757254114,2.10635143031566,126.359985890509));
#21381=CARTESIAN_POINT('Ctrl Pts',(195.068000951373,1.98232864665704,126.301206965734));
#21382=CARTESIAN_POINT('Ctrl Pts',(195.060244648631,1.8559093076601,126.247654477585));
#21383=CARTESIAN_POINT('Ctrl Pts',(195.052488345889,1.72757717380225,126.199508809847));
#21384=CARTESIAN_POINT('Ctrl Pts',(195.044727903375,1.59917654522038,126.151337445316));
#21385=CARTESIAN_POINT('Ctrl Pts',(195.036967460861,1.46886145881318,126.108578773192));
#21386=CARTESIAN_POINT('Ctrl Pts',(195.029207018346,1.33713048578585,126.071363139595));
#21387=CARTESIAN_POINT('Ctrl Pts',(195.021434118081,1.2051880465063,126.034087764159));
#21388=CARTESIAN_POINT('Ctrl Pts',(195.013661217816,1.0718255591914,126.002373299147));
#21389=CARTESIAN_POINT('Ctrl Pts',(195.00588831755,0.937552310192054,125.976299026394));
#21390=CARTESIAN_POINT('Ctrl Pts',(194.998397981788,0.808160232008243,125.951172619133));
#21391=CARTESIAN_POINT('Ctrl Pts',(194.990907646026,0.677922763967373,125.931283499663));
#21392=CARTESIAN_POINT('Ctrl Pts',(194.983417310264,0.547297844753216,125.916656848757));
#21393=CARTESIAN_POINT('Ctrl Pts',(194.975642976145,0.411720242024034,125.901475623937));
#21394=CARTESIAN_POINT('Ctrl Pts',(194.967868642026,0.27529575862716,125.891915708546));
#21395=CARTESIAN_POINT('Ctrl Pts',(194.960094307907,0.138530174400293,125.888061963774));
#21396=CARTESIAN_POINT('Ctrl Pts',(194.95232955496,0.00193314153252316,
125.884212968398));
#21397=CARTESIAN_POINT('Ctrl Pts',(194.944564802013,-0.135003768683377,
125.886056162276));
#21398=CARTESIAN_POINT('Ctrl Pts',(194.936800049066,-0.271767741656031,
125.893624892942));
#21399=CARTESIAN_POINT('Ctrl Pts',(194.929043008181,-0.408395878722369,
125.901186106239));
#21400=CARTESIAN_POINT('Ctrl Pts',(194.921285967296,-0.544851032521165,
125.914461518103));
#21401=CARTESIAN_POINT('Ctrl Pts',(194.913528926411,-0.680618817085562,
125.933432462858));
#21402=CARTESIAN_POINT('Ctrl Pts',(194.90577773517,-0.816284218107408,125.952389101476));
#21403=CARTESIAN_POINT('Ctrl Pts',(194.89802654393,-0.951262896003321,125.977032670072));
#21404=CARTESIAN_POINT('Ctrl Pts',(194.89027535269,-1.08504437948985,126.00729258));
#21405=CARTESIAN_POINT('Ctrl Pts',(194.882527455913,-1.21876900227714,126.037539628659));
#21406=CARTESIAN_POINT('Ctrl Pts',(194.874779559136,-1.35129706216439,126.073398184829));
#21407=CARTESIAN_POINT('Ctrl Pts',(194.867031662359,-1.48212731246938,126.114746380538));
#21408=CARTESIAN_POINT('Ctrl Pts',(194.859285386275,-1.61293019590674,126.156085927097));
#21409=CARTESIAN_POINT('Ctrl Pts',(194.851539110191,-1.74203560361091,126.202912711391));
#21410=CARTESIAN_POINT('Ctrl Pts',(194.843792834107,-1.86895689731614,126.255054826737));
#21411=CARTESIAN_POINT('Ctrl Pts',(194.836046500841,-1.9958791279254,126.307197326983));
#21412=CARTESIAN_POINT('Ctrl Pts',(194.828300167576,-2.12061685072737,126.364655088006));
#21413=CARTESIAN_POINT('Ctrl Pts',(194.820553834311,-2.24270325279445,126.427207983444));
#21414=CARTESIAN_POINT('Ctrl Pts',(194.812805766308,-2.3648169952645,126.489774887168));
#21415=CARTESIAN_POINT('Ctrl Pts',(194.805057698305,-2.48427788763078,126.557439017562));
#21416=CARTESIAN_POINT('Ctrl Pts',(194.797309630302,-2.60064393052617,126.629934404406));
#21417=CARTESIAN_POINT('Ctrl Pts',(194.78955332756,-2.71713364863695,126.70250684021));
#21418=CARTESIAN_POINT('Ctrl Pts',(194.781797024818,-2.83052161429419,126.779920582553));
#21419=CARTESIAN_POINT('Ctrl Pts',(194.774040722076,-2.94039458115534,126.861866131887));
#21420=CARTESIAN_POINT('Ctrl Pts',(194.766280279562,-3.050326190527,126.943855418027));
#21421=CARTESIAN_POINT('Ctrl Pts',(194.758519837048,-3.15673875969899,127.030381084215));
#21422=CARTESIAN_POINT('Ctrl Pts',(194.750759394534,-3.25925313487488,127.121094123636));
#21423=CARTESIAN_POINT('Ctrl Pts',(194.742986494268,-3.36193207522668,127.211952783681));
#21424=CARTESIAN_POINT('Ctrl Pts',(194.735213594003,-3.46070003479519,127.307011978273));
#21425=CARTESIAN_POINT('Ctrl Pts',(194.727440693737,-3.55521502981467,127.40588608415));
#21426=CARTESIAN_POINT('Ctrl Pts',(194.719950357975,-3.6462941666962,127.501165867229));
#21427=CARTESIAN_POINT('Ctrl Pts',(194.712460022213,-3.73342397889856,127.599987782716));
#21428=CARTESIAN_POINT('Ctrl Pts',(194.704969686451,-3.81633575408038,127.701980164651));
#21429=CARTESIAN_POINT('Ctrl Pts',(194.697219842191,-3.90212007209462,127.807506151856));
#21430=CARTESIAN_POINT('Ctrl Pts',(194.68946999793,-3.98366789287206,127.916769679002));
#21431=CARTESIAN_POINT('Ctrl Pts',(194.681720153669,-4.06063403806943,128.029394983297));
#21432=CARTESIAN_POINT('Ctrl Pts',(194.673641243833,-4.14086823717748,128.146802462472));
#21433=CARTESIAN_POINT('Ctrl Pts',(194.665562333997,-4.21612278806056,128.26786322798));
#21434=CARTESIAN_POINT('Ctrl Pts',(194.657483424161,-4.28605088173785,128.39211044363));
#21435=CARTESIAN_POINT('Ctrl Pts',(194.649752999485,-4.35296261511464,128.510998234348));
#21436=CARTESIAN_POINT('Ctrl Pts',(194.642022574809,-4.41499755592588,128.632802943297));
#21437=CARTESIAN_POINT('Ctrl Pts',(194.634292150133,-4.47189467077365,128.757084105708));
#21438=CARTESIAN_POINT('Ctrl Pts',(194.626567138405,-4.52875194548538,128.881278244753));
#21439=CARTESIAN_POINT('Ctrl Pts',(194.618842126678,-4.58047838715712,129.007945031798));
#21440=CARTESIAN_POINT('Ctrl Pts',(194.61111711495,-4.62685868724639,129.136619105595));
#21441=CARTESIAN_POINT('Ctrl Pts',(194.603396293483,-4.67321382938121,129.265223383023));
#21442=CARTESIAN_POINT('Ctrl Pts',(194.595675472015,-4.71422847016418,129.395832410166));
#21443=CARTESIAN_POINT('Ctrl Pts',(194.587954650547,-4.74973548014277,129.527961020585));
#21444=CARTESIAN_POINT('Ctrl Pts',(194.58689417891,-4.75461244526093,129.546109172866));
#21445=CARTESIAN_POINT('Ctrl Pts',(194.585833707274,-4.75938558135185,129.564285966276));
#21446=CARTESIAN_POINT('Ctrl Pts',(194.584773235637,-4.76405452823405,129.582490119308));
#21447=CARTESIAN_POINT('Ctrl Pts',(196.33459504632,-4.76405452823405,129.582490119308));
#21448=CARTESIAN_POINT('Ctrl Pts',(196.325979820702,-4.80173843363128,129.729419094519));
#21449=CARTESIAN_POINT('Ctrl Pts',(196.317364595083,-4.83266542359164,129.878265641535));
#21450=CARTESIAN_POINT('Ctrl Pts',(196.308749369464,-4.85665623691895,130.028426819555));
#21451=CARTESIAN_POINT('Ctrl Pts',(196.300175614881,-4.88053156587922,130.177865168033));
#21452=CARTESIAN_POINT('Ctrl Pts',(196.291601860298,-4.89753723731489,130.328605301003));
#21453=CARTESIAN_POINT('Ctrl Pts',(196.283028105715,-4.90754478717536,130.48003481784));
#21454=CARTESIAN_POINT('Ctrl Pts',(196.276971882491,-4.91461379705869,130.586999735934));
#21455=CARTESIAN_POINT('Ctrl Pts',(196.270915659266,-4.91819205678833,130.694308241907));
#21456=CARTESIAN_POINT('Ctrl Pts',(196.264859436042,-4.91824930178245,130.801739927489));
#21457=CARTESIAN_POINT('',(196.610140563971,-4.91824935727201,130.801846220335));
#21458=CARTESIAN_POINT('Ctrl Pts',(196.680227908624,-4.76405452823405,129.582490119308));
#21459=CARTESIAN_POINT('Ctrl Pts',(196.672454999871,-4.79811658810201,129.71529757377));
#21460=CARTESIAN_POINT('Ctrl Pts',(196.664682091119,-4.82658494688575,129.849389568182));
#21461=CARTESIAN_POINT('Ctrl Pts',(196.656909182367,-4.84939273648973,129.984255045228));
#21462=CARTESIAN_POINT('Ctrl Pts',(196.649444140572,-4.87129716224193,130.113778812316));
#21463=CARTESIAN_POINT('Ctrl Pts',(196.641979098777,-4.88798086211456,130.244015655847));
#21464=CARTESIAN_POINT('Ctrl Pts',(196.634514056982,-4.89942987008945,130.374511794635));
#21465=CARTESIAN_POINT('Ctrl Pts',(196.626389559324,-4.91189027433556,130.516535858678));
#21466=CARTESIAN_POINT('Ctrl Pts',(196.618265061666,-4.91817638477932,130.659109497139));
#21467=CARTESIAN_POINT('Ctrl Pts',(196.610140564008,-4.91824935727168,130.801846219679));
#21468=CARTESIAN_POINT('Ctrl Pts',(196.610140563971,-4.91824935727201,130.801846220335));
#21469=CARTESIAN_POINT('Ctrl Pts',(196.602459708905,-4.91831834504391,130.936788726876));
#21470=CARTESIAN_POINT('Ctrl Pts',(196.59477885384,-4.91282949710972,131.071957218089));
#21471=CARTESIAN_POINT('Ctrl Pts',(196.587097998774,-4.90175335462761,131.206849266967));
#21472=CARTESIAN_POINT('Ctrl Pts',(196.579425945198,-4.89068990429389,131.341586743087));
#21473=CARTESIAN_POINT('Ctrl Pts',(196.571753891622,-4.87405192579336,131.476048011019));
#21474=CARTESIAN_POINT('Ctrl Pts',(196.564081838046,-4.85186195546942,131.60972924594));
#21475=CARTESIAN_POINT('Ctrl Pts',(196.556416637028,-4.82969180487755,131.743291078887));
#21476=CARTESIAN_POINT('Ctrl Pts',(196.548751436009,-4.80197959258732,131.8760738716));
#21477=CARTESIAN_POINT('Ctrl Pts',(196.541086234991,-4.76879973819775,132.007578020808));
#21478=CARTESIAN_POINT('Ctrl Pts',(196.533377076582,-4.73542960832549,132.139836302786));
#21479=CARTESIAN_POINT('Ctrl Pts',(196.525667918172,-4.69652895673484,132.270800820309));
#21480=CARTESIAN_POINT('Ctrl Pts',(196.517958759763,-4.65222593936672,132.399972372218));
#21481=CARTESIAN_POINT('Ctrl Pts',(196.51030050335,-4.60821544575988,132.528291030792));
#21482=CARTESIAN_POINT('Ctrl Pts',(196.502642246937,-4.55887385694772,132.654839949545));
#21483=CARTESIAN_POINT('Ctrl Pts',(196.494983990524,-4.50437694002413,132.779144515788));
#21484=CARTESIAN_POINT('Ctrl Pts',(196.487326349773,-4.44988440421434,132.903439088945));
#21485=CARTESIAN_POINT('Ctrl Pts',(196.479668709022,-4.39023752537237,133.025489301258));
#21486=CARTESIAN_POINT('Ctrl Pts',(196.472011068271,-4.32565999840557,133.144841047028));
#21487=CARTESIAN_POINT('Ctrl Pts',(196.464352292712,-4.26107290151344,133.264210479868));
#21488=CARTESIAN_POINT('Ctrl Pts',(196.456693517154,-4.19155389441899,133.380880298477));
#21489=CARTESIAN_POINT('Ctrl Pts',(196.449034741596,-4.11737209033022,133.494421979742));
#21490=CARTESIAN_POINT('Ctrl Pts',(196.44128738256,-4.04233227935724,133.609276914914));
#21491=CARTESIAN_POINT('Ctrl Pts',(196.433540023525,-3.96252135406451,133.720930539313));
#21492=CARTESIAN_POINT('Ctrl Pts',(196.425792664489,-3.87826158539609,133.82897135909));
#21493=CARTESIAN_POINT('Ctrl Pts',(196.418122442924,-3.79484075880011,133.935936458026));
#21494=CARTESIAN_POINT('Ctrl Pts',(196.41045222136,-3.70705958893727,134.03936010492));
#21495=CARTESIAN_POINT('Ctrl Pts',(196.402781999795,-3.61526928634412,134.138878731135));
#21496=CARTESIAN_POINT('Ctrl Pts',(196.394996072024,-3.52209431609966,134.239898607683));
#21497=CARTESIAN_POINT('Ctrl Pts',(196.387210144253,-3.4247885873534,134.336894393959));
#21498=CARTESIAN_POINT('Ctrl Pts',(196.379424216482,-3.32375503379505,134.429527584455));
#21499=CARTESIAN_POINT('Ctrl Pts',(196.371638288711,-3.2227214802367,134.52216077495));
#21500=CARTESIAN_POINT('Ctrl Pts',(196.36385236094,-3.1179604696731,134.610431147627));
#21501=CARTESIAN_POINT('Ctrl Pts',(196.356066433169,-3.00990550869428,134.694045937901));
#21502=CARTESIAN_POINT('Ctrl Pts',(196.34829209905,-2.90201144717865,134.777536221399));
#21503=CARTESIAN_POINT('Ctrl Pts',(196.340517764931,-2.79047001289452,134.856666115183));
#21504=CARTESIAN_POINT('Ctrl Pts',(196.332743430812,-2.67566902769502,134.931100046793));
#21505=CARTESIAN_POINT('Ctrl Pts',(196.324978677865,-2.56100952444973,135.005442245234));
#21506=CARTESIAN_POINT('Ctrl Pts',(196.317213924918,-2.44309878802772,135.075099785956));
#21507=CARTESIAN_POINT('Ctrl Pts',(196.309449171971,-2.32235744469594,135.139777432771));
#21508=CARTESIAN_POINT('Ctrl Pts',(196.301692131086,-2.20173602336822,135.204390840836));
#21509=CARTESIAN_POINT('Ctrl Pts',(196.293935090201,-2.07828993234506,135.264034014541));
#21510=CARTESIAN_POINT('Ctrl Pts',(196.286178049316,-1.95246819612849,135.318455322555));
#21511=CARTESIAN_POINT('Ctrl Pts',(196.278426858075,-1.82674134306254,135.372835591037));
#21512=CARTESIAN_POINT('Ctrl Pts',(196.270675666835,-1.69864276804628,135.4220016773));
#21513=CARTESIAN_POINT('Ctrl Pts',(196.262924475595,-1.56864516146753,135.465748331531));
#21514=CARTESIAN_POINT('Ctrl Pts',(196.255176578818,-1.43870280733915,135.509476392268));
#21515=CARTESIAN_POINT('Ctrl Pts',(196.247428682041,-1.30686339675709,135.547789477832));
#21516=CARTESIAN_POINT('Ctrl Pts',(196.239680785264,-1.17361841621132,135.58053093233));
#21517=CARTESIAN_POINT('Ctrl Pts',(196.23193450918,-1.04040130764291,135.613265538021));
#21518=CARTESIAN_POINT('Ctrl Pts',(196.224188233096,-0.90577959335298,135.640430737586));
#21519=CARTESIAN_POINT('Ctrl Pts',(196.216441957012,-0.770258312508345,
135.661920210048));
#21520=CARTESIAN_POINT('Ctrl Pts',(196.208695623746,-0.634736031276551,
135.68340984114));
#21521=CARTESIAN_POINT('Ctrl Pts',(196.200949290481,-0.49831455638039,135.699223600296));
#21522=CARTESIAN_POINT('Ctrl Pts',(196.193202957216,-0.361507077887804,
135.709306661626));
#21523=CARTESIAN_POINT('Ctrl Pts',(196.185454889213,-0.224668962309024,
135.719391980987));
#21524=CARTESIAN_POINT('Ctrl Pts',(196.17770682121,-0.0874450609556074,
135.723744020074));
#21525=CARTESIAN_POINT('Ctrl Pts',(196.169958753207,0.0496487812816021,
135.722360013765));
#21526=CARTESIAN_POINT('Ctrl Pts',(196.162202450465,0.186888328485989,135.720974536519));
#21527=CARTESIAN_POINT('Ctrl Pts',(196.154446147723,0.323997148879435,135.71384083974));
#21528=CARTESIAN_POINT('Ctrl Pts',(196.146689844981,0.460461311244389,135.701008291572));
#21529=CARTESIAN_POINT('Ctrl Pts',(196.138929402467,0.596998308641748,135.688168894286));
#21530=CARTESIAN_POINT('Ctrl Pts',(196.131168959953,0.732889575229854,135.669624637705));
#21531=CARTESIAN_POINT('Ctrl Pts',(196.123408517439,0.8676297459151,135.645476365666));
#21532=CARTESIAN_POINT('Ctrl Pts',(196.115635617173,1.00258621348393,135.621289328677));
#21533=CARTESIAN_POINT('Ctrl Pts',(196.107862716908,1.13638751074486,135.591480384296));
#21534=CARTESIAN_POINT('Ctrl Pts',(196.100089816642,1.268540970819,135.556200983977));
#21535=CARTESIAN_POINT('Ctrl Pts',(196.09259948088,1.39589031974556,135.522204078723));
#21536=CARTESIAN_POINT('Ctrl Pts',(196.085109145118,1.52170926338293,135.483127633423));
#21537=CARTESIAN_POINT('Ctrl Pts',(196.077618809356,1.64557497313272,135.439149293471));
#21538=CARTESIAN_POINT('Ctrl Pts',(196.069844475237,1.77413708891525,135.393503501393));
#21539=CARTESIAN_POINT('Ctrl Pts',(196.062070141118,1.90100217941226,135.342432174158));
#21540=CARTESIAN_POINT('Ctrl Pts',(196.054295806999,2.02567829082461,135.286080212162));
#21541=CARTESIAN_POINT('Ctrl Pts',(196.046531054052,2.15020075007207,135.229797698922));
#21542=CARTESIAN_POINT('Ctrl Pts',(196.038766301105,2.27253924505167,135.168247659205));
#21543=CARTESIAN_POINT('Ctrl Pts',(196.031001548158,2.3922180264252,135.101624395431));
#21544=CARTESIAN_POINT('Ctrl Pts',(196.023244507273,2.51177794114601,135.03506730282));
#21545=CARTESIAN_POINT('Ctrl Pts',(196.015487466388,2.62868305990259,134.963447202521));
#21546=CARTESIAN_POINT('Ctrl Pts',(196.007730425503,2.7424789694179,134.887005858681));
#21547=CARTESIAN_POINT('Ctrl Pts',(195.999979234263,2.85618906455235,134.810622159854));
#21548=CARTESIAN_POINT('Ctrl Pts',(195.992228043023,2.96679429415914,134.729424671326));
#21549=CARTESIAN_POINT('Ctrl Pts',(195.984476851783,3.0738664750577,134.643700138371));
#21550=CARTESIAN_POINT('Ctrl Pts',(195.976728955005,3.18089314742335,134.55801204063));
#21551=CARTESIAN_POINT('Ctrl Pts',(195.968981058228,3.28438945316746,134.467800969217));
#21552=CARTESIAN_POINT('Ctrl Pts',(195.961233161451,3.38395793279755,134.373395749301));
#21553=CARTESIAN_POINT('Ctrl Pts',(195.953486885367,3.4835055848481,134.279010276921));
#21554=CARTESIAN_POINT('Ctrl Pts',(195.945740609283,3.57912676149234,134.180432669916));
#21555=CARTESIAN_POINT('Ctrl Pts',(195.937994333199,3.67045902587537,134.078030362954));
#21556=CARTESIAN_POINT('Ctrl Pts',(195.930247999934,3.76179196445257,133.975627300082));
#21557=CARTESIAN_POINT('Ctrl Pts',(195.922501666668,3.84883566736076,133.869399772691));
#21558=CARTESIAN_POINT('Ctrl Pts',(195.914755333403,3.93126661625871,133.759749907387));
#21559=CARTESIAN_POINT('Ctrl Pts',(195.9070072654,4.01371602499605,133.650075486756));
#21560=CARTESIAN_POINT('Ctrl Pts',(195.899259197397,4.09155038929708,133.536977515595));
#21561=CARTESIAN_POINT('Ctrl Pts',(195.891511129394,4.16448855602539,133.420888494206));
#21562=CARTESIAN_POINT('Ctrl Pts',(195.883754826652,4.23750424230527,133.304676092023));
#21563=CARTESIAN_POINT('Ctrl Pts',(195.875998523911,4.3056131276605,133.185466620943));
#21564=CARTESIAN_POINT('Ctrl Pts',(195.868242221169,4.36857895453045,133.063719150542));
#21565=CARTESIAN_POINT('Ctrl Pts',(195.860481778655,4.43157838815802,132.941906699851));
#21566=CARTESIAN_POINT('Ctrl Pts',(195.85272133614,4.48942912881509,132.817553904979));
#21567=CARTESIAN_POINT('Ctrl Pts',(195.844960893626,4.5419428571012,132.691140452451));
#21568=CARTESIAN_POINT('Ctrl Pts',(195.837187993361,4.59454088508596,132.564524069826));
#21569=CARTESIAN_POINT('Ctrl Pts',(195.829415093095,4.64178464539287,132.435840786428));
#21570=CARTESIAN_POINT('Ctrl Pts',(195.82164219283,4.68353525993757,132.305586960068));
#21571=CARTESIAN_POINT('Ctrl Pts',(195.814151857068,4.72376813448038,132.180068188384));
#21572=CARTESIAN_POINT('Ctrl Pts',(195.806661521306,4.75890022668183,132.053091374545));
#21573=CARTESIAN_POINT('Ctrl Pts',(195.799171185544,4.78885244545705,131.925108277898));
#21574=CARTESIAN_POINT('Ctrl Pts',(195.791396851425,4.81994031171073,131.792272663244));
#21575=CARTESIAN_POINT('Ctrl Pts',(195.783622517306,4.84554623795796,131.657932169745));
#21576=CARTESIAN_POINT('Ctrl Pts',(195.775848183187,4.86552621996172,131.522579014271));
#21577=CARTESIAN_POINT('Ctrl Pts',(195.76808343024,4.88548157842337,131.387392669463));
#21578=CARTESIAN_POINT('Ctrl Pts',(195.760318677292,4.89982473164211,131.25119652892));
#21579=CARTESIAN_POINT('Ctrl Pts',(195.752553924345,4.90846199760866,131.114495879237));
#21580=CARTESIAN_POINT('Ctrl Pts',(195.74479688346,4.91709068492086,130.977931002566));
#21581=CARTESIAN_POINT('Ctrl Pts',(195.737039842575,4.92002473840631,130.840863001602));
#21582=CARTESIAN_POINT('Ctrl Pts',(195.72928280169,4.91722193961525,130.70380486653));
#21583=CARTESIAN_POINT('Ctrl Pts',(195.72153161045,4.91442125443657,130.566850088065));
#21584=CARTESIAN_POINT('Ctrl Pts',(195.71378041921,4.90589233599108,130.429905549986));
#21585=CARTESIAN_POINT('Ctrl Pts',(195.70602922797,4.89164498773053,130.293486487754));
#21586=CARTESIAN_POINT('Ctrl Pts',(195.698281331193,4.87740369497295,130.157125407263));
#21587=CARTESIAN_POINT('Ctrl Pts',(195.690533434416,4.85744884697578,130.021289746446));
#21588=CARTESIAN_POINT('Ctrl Pts',(195.682785537639,4.83184225710067,129.886491637266));
#21589=CARTESIAN_POINT('Ctrl Pts',(195.675039261555,4.80624102357217,129.751721724946));
#21590=CARTESIAN_POINT('Ctrl Pts',(195.667292985471,4.77499047258891,129.617989316424));
#21591=CARTESIAN_POINT('Ctrl Pts',(195.659546709387,4.73820383137157,129.485797947506));
#21592=CARTESIAN_POINT('Ctrl Pts',(195.651800376121,4.70141691860354,129.353605602781));
#21593=CARTESIAN_POINT('Ctrl Pts',(195.644054042856,4.65909393887212,129.222954697012));
#21594=CARTESIAN_POINT('Ctrl Pts',(195.63630770959,4.61139834311363,129.094334774595));
#21595=CARTESIAN_POINT('Ctrl Pts',(195.628559641587,4.5636920662572,128.965686048638));
#21596=CARTESIAN_POINT('Ctrl Pts',(195.620811573584,4.51061091513302,128.839069577583));
#21597=CARTESIAN_POINT('Ctrl Pts',(195.613063505581,4.45236679435636,128.714955680505));
#21598=CARTESIAN_POINT('Ctrl Pts',(195.60530720284,4.3940607710351,128.590709873701));
#21599=CARTESIAN_POINT('Ctrl Pts',(195.597550900098,4.33058098301466,128.468972308536));
#21600=CARTESIAN_POINT('Ctrl Pts',(195.589794597356,4.26218595554776,128.350189893506));
#21601=CARTESIAN_POINT('Ctrl Pts',(195.582034154842,4.19375442359537,128.231344080725));
#21602=CARTESIAN_POINT('Ctrl Pts',(195.574273712328,4.12040263382347,128.115456891078));
#21603=CARTESIAN_POINT('Ctrl Pts',(195.566513269813,4.04243236885387,128.002946045293));
#21604=CARTESIAN_POINT('Ctrl Pts',(195.558740369548,3.96433693909305,127.89025458711));
#21605=CARTESIAN_POINT('Ctrl Pts',(195.550967469282,3.88160845470985,127.780950615611));
#21606=CARTESIAN_POINT('Ctrl Pts',(195.543194569017,3.79458944858941,127.675419266381));
#21607=CARTESIAN_POINT('Ctrl Pts',(195.535704233255,3.71073380252928,127.573724247514));
#21608=CARTESIAN_POINT('Ctrl Pts',(195.528213897493,3.62289436686037,127.475532553891));
#21609=CARTESIAN_POINT('Ctrl Pts',(195.520723561731,3.53140846885445,127.381154914047));
#21610=CARTESIAN_POINT('Ctrl Pts',(195.512949227612,3.43645385521897,127.283198917303));
#21611=CARTESIAN_POINT('Ctrl Pts',(195.505174893493,3.33727002191439,127.189041608169));
#21612=CARTESIAN_POINT('Ctrl Pts',(195.497400559374,3.23419324712464,127.099070196728));
#21613=CARTESIAN_POINT('Ctrl Pts',(195.489635806427,3.1312435052475,127.009209667011));
#21614=CARTESIAN_POINT('Ctrl Pts',(195.48187105348,3.02441065959921,126.92352502525));
#21615=CARTESIAN_POINT('Ctrl Pts',(195.474106300532,2.91406918468932,126.842368208519));
#21616=CARTESIAN_POINT('Ctrl Pts',(195.466349259647,2.80383730248746,126.761291997883));
#21617=CARTESIAN_POINT('Ctrl Pts',(195.458592218762,2.69010403888476,126.684734892995));
#21618=CARTESIAN_POINT('Ctrl Pts',(195.450835177877,2.57327816695157,126.61300969716));
#21619=CARTESIAN_POINT('Ctrl Pts',(195.443083986637,2.45654039431791,126.541338589853));
#21620=CARTESIAN_POINT('Ctrl Pts',(195.435332795397,2.33671498721072,126.474492342605));
#21621=CARTESIAN_POINT('Ctrl Pts',(195.427581604157,2.2142407268208,126.412741204845));
#21622=CARTESIAN_POINT('Ctrl Pts',(195.41983370738,2.09181852125829,126.351016312966));
#21623=CARTESIAN_POINT('Ctrl Pts',(195.412085810603,1.96675004998067,126.294382399095));
#21624=CARTESIAN_POINT('Ctrl Pts',(195.404337913826,1.83949959574408,126.243064277735));
#21625=CARTESIAN_POINT('Ctrl Pts',(195.396591637742,1.71227575955951,126.19175689102));
#21626=CARTESIAN_POINT('Ctrl Pts',(195.388845361658,1.5828712106282,126.145763231222));
#21627=CARTESIAN_POINT('Ctrl Pts',(195.381099085574,1.45177078996202,126.105260210476));
#21628=CARTESIAN_POINT('Ctrl Pts',(195.373352752308,1.32066940154283,126.064756890746));
#21629=CARTESIAN_POINT('Ctrl Pts',(195.365606419043,1.18787248995334,126.02974440635));
#21630=CARTESIAN_POINT('Ctrl Pts',(195.357860085778,1.05388027198198,126.000349852088));
#21631=CARTESIAN_POINT('Ctrl Pts',(195.350112017775,0.919858047382009,125.97094871512));
#21632=CARTESIAN_POINT('Ctrl Pts',(195.342363949772,0.784640365557708,125.947168095513));
#21633=CARTESIAN_POINT('Ctrl Pts',(195.334615881769,0.648737458886747,125.92908393086));
#21634=CARTESIAN_POINT('Ctrl Pts',(195.326859579027,0.512690112989033,125.910980546142));
#21635=CARTESIAN_POINT('Ctrl Pts',(195.319103276285,0.375956475623729,125.898585762068));
#21636=CARTESIAN_POINT('Ctrl Pts',(195.311346973543,0.239052282779265,125.891923638978));
#21637=CARTESIAN_POINT('Ctrl Pts',(195.303586531029,0.102075020045067,125.885257960113));
#21638=CARTESIAN_POINT('Ctrl Pts',(195.295826088515,-0.0350725887894774,
125.884331041572));
#21639=CARTESIAN_POINT('Ctrl Pts',(195.288065646001,-0.17187598256682,125.889114773347));
#21640=CARTESIAN_POINT('Ctrl Pts',(195.280292745735,-0.308898985296921,
125.893906184392));
#21641=CARTESIAN_POINT('Ctrl Pts',(195.27251984547,-0.445576278733256,125.904426534803));
#21642=CARTESIAN_POINT('Ctrl Pts',(195.264746945204,-0.58139869000898,125.920595817153));
#21643=CARTESIAN_POINT('Ctrl Pts',(195.257256609442,-0.712283614519818,
125.936177305362));
#21644=CARTESIAN_POINT('Ctrl Pts',(195.24976627368,-0.842374427875423,125.957004101464));
#21645=CARTESIAN_POINT('Ctrl Pts',(195.242275937918,-0.971227371730748,
125.982960358834));
#21646=CARTESIAN_POINT('Ctrl Pts',(195.234501603799,-1.10496581411534,126.009900755591));
#21647=CARTESIAN_POINT('Ctrl Pts',(195.22672726968,-1.23779430956464,126.042452598076));
#21648=CARTESIAN_POINT('Ctrl Pts',(195.218952935561,-1.36920532069673,126.080542262435));
#21649=CARTESIAN_POINT('Ctrl Pts',(195.211188182614,-1.50045437950196,126.118584984687));
#21650=CARTESIAN_POINT('Ctrl Pts',(195.203423429667,-1.63028905794107,126.162151841558));
#21651=CARTESIAN_POINT('Ctrl Pts',(195.19565867672,-1.7582108487659,126.211118007625));
#21652=CARTESIAN_POINT('Ctrl Pts',(195.187901635835,-1.88600558586439,126.260035539804));
#21653=CARTESIAN_POINT('Ctrl Pts',(195.18014459495,-2.01189085348242,126.314341570363));
#21654=CARTESIAN_POINT('Ctrl Pts',(195.172387554065,-2.13538252951149,126.373861264766));
#21655=CARTESIAN_POINT('Ctrl Pts',(195.164636362824,-2.25878107950726,126.433336074905));
#21656=CARTESIAN_POINT('Ctrl Pts',(195.156885171584,-2.37978927994142,126.498016554088));
#21657=CARTESIAN_POINT('Ctrl Pts',(195.149133980344,-2.49794259036277,126.567679619691));
#21658=CARTESIAN_POINT('Ctrl Pts',(195.141386083567,-2.61604568247549,126.637313076633));
#21659=CARTESIAN_POINT('Ctrl Pts',(195.13363818679,-2.73129596186393,126.711924709835));
#21660=CARTESIAN_POINT('Ctrl Pts',(195.125890290013,-2.84325332954889,126.791245422794));
#21661=CARTESIAN_POINT('Ctrl Pts',(195.118144013929,-2.95518727816587,126.87054954357));
#21662=CARTESIAN_POINT('Ctrl Pts',(195.110397737845,-3.06382936634111,126.954560558935));
#21663=CARTESIAN_POINT('Ctrl Pts',(195.102651461761,-3.16876868447561,127.042966183744));
#21664=CARTESIAN_POINT('Ctrl Pts',(195.094905128495,-3.27370877724855,127.131372461143));
#21665=CARTESIAN_POINT('Ctrl Pts',(195.08715879523,-3.37494574643612,127.224173160824));
#21666=CARTESIAN_POINT('Ctrl Pts',(195.079412461965,-3.47210228418942,127.321016134081));
#21667=CARTESIAN_POINT('Ctrl Pts',(195.071664393962,-3.56928057947593,127.41788079465));
#21668=CARTESIAN_POINT('Ctrl Pts',(195.063916325959,-3.6623763481555,127.518789254161));
#21669=CARTESIAN_POINT('Ctrl Pts',(195.056168257956,-3.75104990871693,127.62335328579));
#21670=CARTESIAN_POINT('Ctrl Pts',(195.048411955214,-3.83981771259343,127.728028449315));
#21671=CARTESIAN_POINT('Ctrl Pts',(195.040655652472,-3.92415366637445,127.836366647376));
#21672=CARTESIAN_POINT('Ctrl Pts',(195.03289934973,-4.00375875951405,127.947946981883));
#21673=CARTESIAN_POINT('Ctrl Pts',(195.025138907216,-4.08340634028877,128.059586870174));
#21674=CARTESIAN_POINT('Ctrl Pts',(195.017378464702,-4.15831781570031,128.174472015597));
#21675=CARTESIAN_POINT('Ctrl Pts',(195.009618022188,-4.22823870262148,128.292154309128));
#21676=CARTESIAN_POINT('Ctrl Pts',(195.001845121922,-4.29827183275764,128.410025516725));
#21677=CARTESIAN_POINT('Ctrl Pts',(194.994072221657,-4.36329817963602,128.530702500966));
#21678=CARTESIAN_POINT('Ctrl Pts',(194.986299321391,-4.42310983539823,128.65371363433));
#21679=CARTESIAN_POINT('Ctrl Pts',(194.978808985629,-4.48074718681689,128.772253003149));
#21680=CARTESIAN_POINT('Ctrl Pts',(194.971318649867,-4.53354227567348,128.892959480803));
#21681=CARTESIAN_POINT('Ctrl Pts',(194.963828314105,-4.58135270478999,129.015397102898));
#21682=CARTESIAN_POINT('Ctrl Pts',(194.954994481147,-4.63773860762726,129.159795636662));
#21683=CARTESIAN_POINT('Ctrl Pts',(194.946160648188,-4.68734145347547,129.306984074171));
#21684=CARTESIAN_POINT('Ctrl Pts',(194.937326815229,-4.72991114124837,129.456353325896));
#21685=CARTESIAN_POINT('Ctrl Pts',(194.934850059303,-4.74184647294076,129.498232222765));
#21686=CARTESIAN_POINT('Ctrl Pts',(194.932373303377,-4.75322921960265,129.540282405251));
#21687=CARTESIAN_POINT('Ctrl Pts',(194.92989654745,-4.76405452823406,129.582490119308));
#21688=CARTESIAN_POINT('Origin',(213.235140564004,0.,130.804360617566));
#21689=CARTESIAN_POINT('',(192.834981455508,-4.76405452823404,129.582490119308));
#21690=CARTESIAN_POINT('',(193.179932595466,-4.75726252818781,129.584191622251));
#21691=CARTESIAN_POINT('',(213.235140564004,-4.76405452823405,129.582490119308));
#21692=CARTESIAN_POINT('',(194.514859435944,-4.91824832267119,130.808422518846));
#21693=CARTESIAN_POINT('Ctrl Pts',(194.514859435944,-4.91824832267119,130.808422518846));
#21694=CARTESIAN_POINT('Ctrl Pts',(194.505690899192,-4.91811426966856,130.970737137015));
#21695=CARTESIAN_POINT('Ctrl Pts',(194.49652236244,-4.90994121534633,131.132707678005));
#21696=CARTESIAN_POINT('Ctrl Pts',(194.487353825688,-4.89385416878415,131.293619687154));
#21697=CARTESIAN_POINT('Ctrl Pts',(194.478119857513,-4.87765231673291,131.45568004767));
#21698=CARTESIAN_POINT('Ctrl Pts',(194.468885889339,-4.85342321642564,131.616666662758));
#21699=CARTESIAN_POINT('Ctrl Pts',(194.459651921164,-4.82134334935995,131.775870458012));
#21700=CARTESIAN_POINT('Ctrl Pts',(194.450346899683,-4.78901663493732,131.936299290638));
#21701=CARTESIAN_POINT('Ctrl Pts',(194.441041878201,-4.74871793267665,132.094917714119));
#21702=CARTESIAN_POINT('Ctrl Pts',(194.43173685672,-4.70067592055807,132.251021929825));
#21703=CARTESIAN_POINT('Ctrl Pts',(194.429998592026,-4.69170122515761,132.280183651511));
#21704=CARTESIAN_POINT('Ctrl Pts',(194.428260327332,-4.68245643851761,132.309257694875));
#21705=CARTESIAN_POINT('Ctrl Pts',(194.426522062638,-4.67294323328106,132.338239557063));
#21706=CARTESIAN_POINT('Ctrl Pts',(194.418747728519,-4.63039572235757,132.467860023283));
#21707=CARTESIAN_POINT('Ctrl Pts',(194.4109733944,-4.58238351476863,132.595914150803));
#21708=CARTESIAN_POINT('Ctrl Pts',(194.403199060281,-4.5290396636491,132.721906650284));
#21709=CARTESIAN_POINT('Ctrl Pts',(194.395434307334,-4.47576155405861,132.84774387527));
#21710=CARTESIAN_POINT('Ctrl Pts',(194.387669554386,-4.41716502578731,132.971524171027));
#21711=CARTESIAN_POINT('Ctrl Pts',(194.379904801439,-4.35343290862853,133.092767262498));
#21712=CARTESIAN_POINT('Ctrl Pts',(194.372147760554,-4.28976409110701,133.213889933622));
#21713=CARTESIAN_POINT('Ctrl Pts',(194.364390719669,-4.22097001613394,133.332480071522));
#21714=CARTESIAN_POINT('Ctrl Pts',(194.356633678784,-4.14728147357108,133.448077592107));
#21715=CARTESIAN_POINT('Ctrl Pts',(194.348882487544,-4.07364850011134,133.563587939702));
#21716=CARTESIAN_POINT('Ctrl Pts',(194.341131296304,-3.99512861499202,133.676109833574));
#21717=CARTESIAN_POINT('Ctrl Pts',(194.333380105064,-3.91199820569556,133.785208332753));
#21718=CARTESIAN_POINT('Ctrl Pts',(194.325632208287,-3.82890312904064,133.894260462159));
#21719=CARTESIAN_POINT('Ctrl Pts',(194.31788431151,-3.74120166215483,133.999891780499));
#21720=CARTESIAN_POINT('Ctrl Pts',(194.310136414733,-3.64921299757971,134.101697051841));
#21721=CARTESIAN_POINT('Ctrl Pts',(194.302390138649,-3.55724357505019,134.203481027715));
#21722=CARTESIAN_POINT('Ctrl Pts',(194.294643862565,-3.46098900054278,134.301440258582));
#21723=CARTESIAN_POINT('Ctrl Pts',(194.286897586481,-3.3608079054297,134.395203594542));
#21724=CARTESIAN_POINT('Ctrl Pts',(194.279151253215,-3.26062607080245,134.488967622642));
#21725=CARTESIAN_POINT('Ctrl Pts',(194.27140491995,-3.15651794317866,134.578535426871));
#21726=CARTESIAN_POINT('Ctrl Pts',(194.263658586685,-3.04887776981329,134.663573932121));
#21727=CARTESIAN_POINT('Ctrl Pts',(194.255910518682,-2.94121349117735,134.748631481155));
#21728=CARTESIAN_POINT('Ctrl Pts',(194.248162450679,-2.83001589956761,134.829157470545));
#21729=CARTESIAN_POINT('Ctrl Pts',(194.240414382676,-2.71571062383656,134.904860449304));
#21730=CARTESIAN_POINT('Ctrl Pts',(194.232658079934,-2.60128386309834,134.980643886089));
#21731=CARTESIAN_POINT('Ctrl Pts',(194.224901777192,-2.48374314685267,135.051593856377));
#21732=CARTESIAN_POINT('Ctrl Pts',(194.21714547445,-2.36354174294401,135.11746315424));
#21733=CARTESIAN_POINT('Ctrl Pts',(194.209385031936,-2.24327618392683,135.18336760853));
#21734=CARTESIAN_POINT('Ctrl Pts',(194.201624589422,-2.12034745785099,135.244185813801));
#21735=CARTESIAN_POINT('Ctrl Pts',(194.193864146908,-1.99523059395582,135.299717993731));
#21736=CARTESIAN_POINT('Ctrl Pts',(194.186091246642,-1.86991288136339,135.355339318846));
#21737=CARTESIAN_POINT('Ctrl Pts',(194.178318346377,-1.74240037555429,135.4056575181));
#21738=CARTESIAN_POINT('Ctrl Pts',(194.170545446111,-1.61318595870733,135.450521842182));
#21739=CARTESIAN_POINT('Ctrl Pts',(194.16305511035,-1.48866881138538,135.493755235078));
#21740=CARTESIAN_POINT('Ctrl Pts',(194.155564774588,-1.36257163707573,135.531924303522));
#21741=CARTESIAN_POINT('Ctrl Pts',(194.148074438826,-1.23534416706417,135.564939138229));
#21742=CARTESIAN_POINT('Ctrl Pts',(194.140300104707,-1.10329282885606,135.599205740429));
#21743=CARTESIAN_POINT('Ctrl Pts',(194.132525770587,-0.969605493727146,
135.628028094229));
#21744=CARTESIAN_POINT('Ctrl Pts',(194.124751436468,-0.834770781094737,
135.651250425013));
#21745=CARTESIAN_POINT('Ctrl Pts',(194.116986683521,-0.700102240195215,
135.67444413635));
#21746=CARTESIAN_POINT('Ctrl Pts',(194.109221930574,-0.564289516904608,
135.692051490933));
#21747=CARTESIAN_POINT('Ctrl Pts',(194.101457177627,-0.427835504199164,
135.703966708248));
#21748=CARTESIAN_POINT('Ctrl Pts',(194.093700136742,-0.29151701954285,135.715870091201));
#21749=CARTESIAN_POINT('Ctrl Pts',(194.085943095857,-0.154558899969262,
135.722092553836));
#21750=CARTESIAN_POINT('Ctrl Pts',(194.078186054972,-0.0174729748113956,
135.722579579513));
#21751=CARTESIAN_POINT('Ctrl Pts',(194.070434863732,0.119509572784076,135.723066237919));
#21752=CARTESIAN_POINT('Ctrl Pts',(194.062683672492,0.256619344746097,135.717826066908));
#21753=CARTESIAN_POINT('Ctrl Pts',(194.054932481252,0.393341018732792,135.706856502876));
#21754=CARTESIAN_POINT('Ctrl Pts',(194.047184584475,0.530004582360826,135.695891601202));
#21755=CARTESIAN_POINT('Ctrl Pts',(194.039436687697,0.666279987193505,135.679202181027));
#21756=CARTESIAN_POINT('Ctrl Pts',(194.03168879092,0.801653765399529,135.656837748158));
#21757=CARTESIAN_POINT('Ctrl Pts',(194.023942514836,0.936999226329496,135.634477993447));
#21758=CARTESIAN_POINT('Ctrl Pts',(194.016196238752,1.07144305027789,135.606445650913));
#21759=CARTESIAN_POINT('Ctrl Pts',(194.008449962668,1.20447912930477,135.572841831702));
#21760=CARTESIAN_POINT('Ctrl Pts',(194.000703629403,1.33751619037367,135.539237764435));
#21761=CARTESIAN_POINT('Ctrl Pts',(193.992957296137,1.46914510672559,135.50006223417));
#21762=CARTESIAN_POINT('Ctrl Pts',(193.985210962872,1.59887255256962,135.455466897059));
#21763=CARTESIAN_POINT('Ctrl Pts',(193.977462894869,1.72862904997563,135.410861573131));
#21764=CARTESIAN_POINT('Ctrl Pts',(193.969714826866,1.85648285988052,135.360834154252));
#21765=CARTESIAN_POINT('Ctrl Pts',(193.961966758863,1.98195871352415,135.305585197654));
#21766=CARTESIAN_POINT('Ctrl Pts',(193.954210456121,2.10756792439832,135.250277521806));
#21767=CARTESIAN_POINT('Ctrl Pts',(193.946454153379,2.2307937720316,135.189737380293));
#21768=CARTESIAN_POINT('Ctrl Pts',(193.938697850637,2.35118327273367,135.124212499346));
#21769=CARTESIAN_POINT('Ctrl Pts',(193.930937408123,2.47163702893723,135.058652645797));
#21770=CARTESIAN_POINT('Ctrl Pts',(193.923176965609,2.58925108663829,134.988102952543));
#21771=CARTESIAN_POINT('Ctrl Pts',(193.915416523095,2.70360060345122,134.912855091156));
#21772=CARTESIAN_POINT('Ctrl Pts',(193.907643622829,2.81813368425998,134.837486435221));
#21773=CARTESIAN_POINT('Ctrl Pts',(193.899870722564,2.92939143443346,134.757404768529));
#21774=CARTESIAN_POINT('Ctrl Pts',(193.892097822299,3.03698060945102,134.672943283132));
#21775=CARTESIAN_POINT('Ctrl Pts',(193.884607486536,3.14065864695626,134.591552185475));
#21776=CARTESIAN_POINT('Ctrl Pts',(193.877117150774,3.24092996805332,134.506094375295));
#21777=CARTESIAN_POINT('Ctrl Pts',(193.869626815012,3.33747583876709,134.416899626095));
#21778=CARTESIAN_POINT('Ctrl Pts',(193.861852480893,3.43768227551313,134.32432303087));
#21779=CARTESIAN_POINT('Ctrl Pts',(193.854078146774,3.53419260818798,134.227427275858));
#21780=CARTESIAN_POINT('Ctrl Pts',(193.846303812655,3.62661166846604,134.126539250428));
#21781=CARTESIAN_POINT('Ctrl Pts',(193.838539059708,3.71891683051201,134.025775560474));
#21782=CARTESIAN_POINT('Ctrl Pts',(193.830774306761,3.80714049093836,133.921029675189));
#21783=CARTESIAN_POINT('Ctrl Pts',(193.823009553814,3.8909218276634,133.812667515725));
#21784=CARTESIAN_POINT('Ctrl Pts',(193.815252512929,3.97461995158371,133.704412983086));
#21785=CARTESIAN_POINT('Ctrl Pts',(193.807495472044,4.05388429464595,133.59254963128));
#21786=CARTESIAN_POINT('Ctrl Pts',(193.799738431159,4.12839233419866,133.477478609243));
#21787=CARTESIAN_POINT('Ctrl Pts',(193.791987239919,4.20284418665918,133.36249436316));
#21788=CARTESIAN_POINT('Ctrl Pts',(193.784236048679,4.27254666321562,133.244307588428));
#21789=CARTESIAN_POINT('Ctrl Pts',(193.776484857438,4.33721906272395,133.123350454638));
#21790=CARTESIAN_POINT('Ctrl Pts',(193.768736960661,4.40186397473727,133.002444730857));
#21791=CARTESIAN_POINT('Ctrl Pts',(193.760989063884,4.46148287789932,132.878771333985));
#21792=CARTESIAN_POINT('Ctrl Pts',(193.753241167107,4.51583988094174,132.752789018148));
#21793=CARTESIAN_POINT('Ctrl Pts',(193.745494891023,4.57018551367091,132.626833055096));
#21794=CARTESIAN_POINT('Ctrl Pts',(193.737748614939,4.61927128079769,132.498569492494));
#21795=CARTESIAN_POINT('Ctrl Pts',(193.730002338855,4.66290868628648,132.368478786329));
#21796=CARTESIAN_POINT('Ctrl Pts',(193.72225600559,4.70654641389667,132.238387119863));
#21797=CARTESIAN_POINT('Ctrl Pts',(193.714509672324,4.74473557527959,132.106468653588));
#21798=CARTESIAN_POINT('Ctrl Pts',(193.706763339059,4.77733710840989,131.973220410317));
#21799=CARTESIAN_POINT('Ctrl Pts',(193.699015271056,4.80994594242749,131.839942327026));
#21800=CARTESIAN_POINT('Ctrl Pts',(193.691267203053,4.83696456533113,131.705334253853));
#21801=CARTESIAN_POINT('Ctrl Pts',(193.68351913505,4.85830481722543,131.569904453949));
#21802=CARTESIAN_POINT('Ctrl Pts',(193.675762832308,4.87966774979339,131.434330717642));
#21803=CARTESIAN_POINT('Ctrl Pts',(193.668006529566,4.89534019475674,131.297933896828));
#21804=CARTESIAN_POINT('Ctrl Pts',(193.660250226825,4.9052857224612,131.161229001593));
#21805=CARTESIAN_POINT('Ctrl Pts',(193.65248978431,4.91523655839326,131.02445114284));
#21806=CARTESIAN_POINT('Ctrl Pts',(193.644729341796,4.91945437445847,130.887365272617));
#21807=CARTESIAN_POINT('Ctrl Pts',(193.636968899282,4.9179549245226,130.750486478465));
#21808=CARTESIAN_POINT('Ctrl Pts',(193.629195999017,4.91645306753658,130.613387954321));
#21809=CARTESIAN_POINT('Ctrl Pts',(193.621423098751,4.90921562490836,130.476497561166));
#21810=CARTESIAN_POINT('Ctrl Pts',(193.613650198486,4.89631036227887,130.340326245196));
#21811=CARTESIAN_POINT('Ctrl Pts',(193.606159862724,4.88387423845236,130.209105099557));
#21812=CARTESIAN_POINT('Ctrl Pts',(193.598669526962,4.86617526077355,130.078551963462));
#21813=CARTESIAN_POINT('Ctrl Pts',(193.5911791912,4.84331859353017,129.949113247465));
#21814=CARTESIAN_POINT('Ctrl Pts',(193.583404857081,4.81959530880109,129.814766823208));
#21815=CARTESIAN_POINT('Ctrl Pts',(193.575630522962,4.79024035808555,129.68119542462));
#21816=CARTESIAN_POINT('Ctrl Pts',(193.567856188842,4.75531516453582,129.548908209692));
#21817=CARTESIAN_POINT('Ctrl Pts',(193.560091435895,4.7204330131658,129.416784026935));
#21818=CARTESIAN_POINT('Ctrl Pts',(193.552326682948,4.67999437676145,129.285941253237));
#21819=CARTESIAN_POINT('Ctrl Pts',(193.544561930001,4.63411208200157,129.156881247757));
#21820=CARTESIAN_POINT('Ctrl Pts',(193.536804889116,4.5882753581837,129.027949426493));
#21821=CARTESIAN_POINT('Ctrl Pts',(193.529047848231,4.53700586573875,128.900797215727));
#21822=CARTESIAN_POINT('Ctrl Pts',(193.521290807346,4.48046677125739,128.775912793697));
#21823=CARTESIAN_POINT('Ctrl Pts',(193.513539616106,4.42397031334695,128.651122547982));
#21824=CARTESIAN_POINT('Ctrl Pts',(193.505788424866,4.36221232369776,128.528597041763));
#21825=CARTESIAN_POINT('Ctrl Pts',(193.498037233626,4.29540467300197,128.408806035084));
#21826=CARTESIAN_POINT('Ctrl Pts',(193.490289336849,4.22862541733986,128.289065942777));
#21827=CARTESIAN_POINT('Ctrl Pts',(193.482541440072,4.1568009593707,128.172058379152));
#21828=CARTESIAN_POINT('Ctrl Pts',(193.474793543294,4.08018975694076,128.058229774023));
#21829=CARTESIAN_POINT('Ctrl Pts',(193.46704726721,4.00359457992282,127.944424979385));
#21830=CARTESIAN_POINT('Ctrl Pts',(193.459300991126,3.92221486821154,127.833798144722));
#21831=CARTESIAN_POINT('Ctrl Pts',(193.451554715042,3.83635295632385,127.726767555284));
#21832=CARTESIAN_POINT('Ctrl Pts',(193.443808381777,3.75049041062306,127.619736175771));
#21833=CARTESIAN_POINT('Ctrl Pts',(193.436062048511,3.66014584337031,127.516301399417));
#21834=CARTESIAN_POINT('Ctrl Pts',(193.428315715246,3.56566224751357,127.416848876013));
#21835=CARTESIAN_POINT('Ctrl Pts',(193.420567647243,3.47115749271066,127.317374080907));
#21836=CARTESIAN_POINT('Ctrl Pts',(193.41281957924,3.3725121340977,127.221883596716));
#21837=CARTESIAN_POINT('Ctrl Pts',(193.405071511237,3.27010613528105,127.130726323506));
#21838=CARTESIAN_POINT('Ctrl Pts',(193.397315208495,3.16759129815017,127.03947216726));
#21839=CARTESIAN_POINT('Ctrl Pts',(193.389558905753,3.06130812916382,126.952560682118));
#21840=CARTESIAN_POINT('Ctrl Pts',(193.381802603011,2.95167022977636,126.870300892911));
#21841=CARTESIAN_POINT('Ctrl Pts',(193.374042160497,2.8419738133408,126.787997199178));
#21842=CARTESIAN_POINT('Ctrl Pts',(193.366281717983,2.72891942085808,126.710350369704));
#21843=CARTESIAN_POINT('Ctrl Pts',(193.358521275469,2.61294892541234,126.637625567711));
#21844=CARTESIAN_POINT('Ctrl Pts',(193.350748375203,2.49679226383197,126.564784021411));
#21845=CARTESIAN_POINT('Ctrl Pts',(193.342975474938,2.37771048460871,126.496880485635));
#21846=CARTESIAN_POINT('Ctrl Pts',(193.335202574673,2.25617009023159,126.434134126131));
#21847=CARTESIAN_POINT('Ctrl Pts',(193.32771223891,2.13904799533144,126.373668754842));
#21848=CARTESIAN_POINT('Ctrl Pts',(193.320221903148,2.01964321472039,126.317992247027));
#21849=CARTESIAN_POINT('Ctrl Pts',(193.312731567386,1.89838817010611,126.2672574208));
#21850=CARTESIAN_POINT('Ctrl Pts',(193.304957233267,1.77253570362098,126.214598968217));
#21851=CARTESIAN_POINT('Ctrl Pts',(193.297182899148,1.64429123515347,126.167097516029));
#21852=CARTESIAN_POINT('Ctrl Pts',(193.289408565029,1.51411633445749,126.124976599532));
#21853=CARTESIAN_POINT('Ctrl Pts',(193.281643812082,1.38410186269265,126.082907593301));
#21854=CARTESIAN_POINT('Ctrl Pts',(193.273879059135,1.25216206077593,126.046206048193));
#21855=CARTESIAN_POINT('Ctrl Pts',(193.266114306188,1.11877972194069,126.015048036801));
#21856=CARTESIAN_POINT('Ctrl Pts',(193.258357265303,0.985529860324888,125.983920971985));
#21857=CARTESIAN_POINT('Ctrl Pts',(193.250600224418,0.850840691275775,125.958326572221));
#21858=CARTESIAN_POINT('Ctrl Pts',(193.242843183533,0.715211128500449,125.9383914331));
#21859=CARTESIAN_POINT('Ctrl Pts',(193.235091992293,0.579683845033364,125.918471327223));
#21860=CARTESIAN_POINT('Ctrl Pts',(193.227340801053,0.443217964620638,125.904202044029));
#21861=CARTESIAN_POINT('Ctrl Pts',(193.219589609812,0.306323230974984,125.895659247482));
#21862=CARTESIAN_POINT('Ctrl Pts',(193.211841713035,0.169486681242845,125.887120081852));
#21863=CARTESIAN_POINT('Ctrl Pts',(193.204093816258,0.0322220301962203,
125.884302586307));
#21864=CARTESIAN_POINT('Ctrl Pts',(193.196345919481,-0.10495542533834,125.887230619163));
#21865=CARTESIAN_POINT('Ctrl Pts',(193.188599643397,-0.24210418630643,125.890158039538));
#21866=CARTESIAN_POINT('Ctrl Pts',(193.180853367313,-0.379165397413132,
125.898828589448));
#21867=CARTESIAN_POINT('Ctrl Pts',(193.173107091229,-0.515623724240199,
125.913213999696));
#21868=CARTESIAN_POINT('Ctrl Pts',(193.165360757964,-0.65208305837159,125.927599516134));
#21869=CARTESIAN_POINT('Ctrl Pts',(193.157614424698,-0.787939110532302,
125.947699936101));
#21870=CARTESIAN_POINT('Ctrl Pts',(193.149868091433,-0.922682026564098,
125.973435143047));
#21871=CARTESIAN_POINT('Ctrl Pts',(193.14212002343,-1.05745511733767,125.999176113215));
#21872=CARTESIAN_POINT('Ctrl Pts',(193.134371955427,-1.19111419199571,126.030554308008));
#21873=CARTESIAN_POINT('Ctrl Pts',(193.126623887424,-1.32316033142207,126.06743864229));
#21874=CARTESIAN_POINT('Ctrl Pts',(193.118867584682,-1.45534681105682,126.104362177682));
#21875=CARTESIAN_POINT('Ctrl Pts',(193.11111128194,-1.58591655391597,126.146803437196));
#21876=CARTESIAN_POINT('Ctrl Pts',(193.103354979199,-1.71438600696752,126.194581481684));
#21877=CARTESIAN_POINT('Ctrl Pts',(193.095594536684,-1.84292402803436,126.242385026753));
#21878=CARTESIAN_POINT('Ctrl Pts',(193.08783409417,-1.96935916538758,126.295530881055));
#21879=CARTESIAN_POINT('Ctrl Pts',(193.080073651656,-2.09322948650229,126.35379061145));
#21880=CARTESIAN_POINT('Ctrl Pts',(193.072300751391,-2.21729865525309,126.412143865536));
#21881=CARTESIAN_POINT('Ctrl Pts',(193.064527851125,-2.33879443343359,126.475627219245));
#21882=CARTESIAN_POINT('Ctrl Pts',(193.05675495086,-2.45728027470416,126.54396665526));
#21883=CARTESIAN_POINT('Ctrl Pts',(193.049264615098,-2.57145885719628,126.609821780639));
#21884=CARTESIAN_POINT('Ctrl Pts',(193.041774279336,-2.68284228060499,126.680185891838));
#21885=CARTESIAN_POINT('Ctrl Pts',(193.034283943574,-2.791068240227,126.75477778215));
#21886=CARTESIAN_POINT('Ctrl Pts',(193.026549215124,-2.90282536774334,126.831803436867));
#21887=CARTESIAN_POINT('Ctrl Pts',(193.018814486674,-3.01157783489076,126.913587324279));
#21888=CARTESIAN_POINT('Ctrl Pts',(193.011079758224,-3.11689046048007,126.99986631216));
#21889=CARTESIAN_POINT('Ctrl Pts',(193.003357254067,-3.22203664554232,127.086008941079));
#21890=CARTESIAN_POINT('Ctrl Pts',(192.995634749909,-3.32375351182408,127.176632275114));
#21891=CARTESIAN_POINT('Ctrl Pts',(192.987912245751,-3.42163455168092,127.271429814784));
#21892=CARTESIAN_POINT('Ctrl Pts',(192.980196799127,-3.51942613885007,127.366140719753));
#21893=CARTESIAN_POINT('Ctrl Pts',(192.972481352503,-3.613388589409,127.465017970231));
#21894=CARTESIAN_POINT('Ctrl Pts',(192.964765905879,-3.70314804461637,127.567714572328));
#21895=CARTESIAN_POINT('Ctrl Pts',(192.957055793399,-3.79284544381304,127.670340174201));
#21896=CARTESIAN_POINT('Ctrl Pts',(192.949345680918,-3.87834536897914,127.776779578253));
#21897=CARTESIAN_POINT('Ctrl Pts',(192.941635568438,-3.95931079161108,127.886648994062));
#21898=CARTESIAN_POINT('Ctrl Pts',(192.933929070916,-4.04023825284938,127.99646689657));
#21899=CARTESIAN_POINT('Ctrl Pts',(192.926222573394,-4.11663520834471,128.109711292731));
#21900=CARTESIAN_POINT('Ctrl Pts',(192.918516075872,-4.18820520986374,128.225965732648));
#21901=CARTESIAN_POINT('Ctrl Pts',(192.910809982444,-4.25977145856918,128.342214076698));
#21902=CARTESIAN_POINT('Ctrl Pts',(192.903103889017,-4.32651104118669,128.461471819057));
#21903=CARTESIAN_POINT('Ctrl Pts',(192.895397795589,-4.3881712193687,128.583294114283));
#21904=CARTESIAN_POINT('Ctrl Pts',(192.887692066741,-4.44982848037876,128.705110646039));
#21905=CARTESIAN_POINT('Ctrl Pts',(192.879986337892,-4.50640664147058,128.829491133795));
#21906=CARTESIAN_POINT('Ctrl Pts',(192.872280609043,-4.55769962141508,128.955967471222));
#21907=CARTESIAN_POINT('Ctrl Pts',(192.864570878078,-4.60901924134692,129.082509496546));
#21908=CARTESIAN_POINT('Ctrl Pts',(192.856861147112,-4.65504805292081,129.211149177261));
#21909=CARTESIAN_POINT('Ctrl Pts',(192.849151416146,-4.69562867427047,129.341399778764));
#21910=CARTESIAN_POINT('Ctrl Pts',(192.844428095933,-4.72049014737659,129.421197024804));
#21911=CARTESIAN_POINT('Ctrl Pts',(192.839704775721,-4.74330770610149,129.50159857469));
#21912=CARTESIAN_POINT('Ctrl Pts',(192.834981455508,-4.76405452823404,129.582490119308));
#21913=CARTESIAN_POINT('Ctrl Pts',(194.584773235637,-4.76405452823405,129.582490119308));
#21914=CARTESIAN_POINT('Ctrl Pts',(194.577053952228,-4.79804027850044,129.715000043791));
#21915=CARTESIAN_POINT('Ctrl Pts',(194.569334668819,-4.82650137584579,129.848960603857));
#21916=CARTESIAN_POINT('Ctrl Pts',(194.56161538541,-4.84932764823365,129.983870262609));
#21917=CARTESIAN_POINT('Ctrl Pts',(194.553822727173,-4.87237089332568,130.120062290773));
#21918=CARTESIAN_POINT('Ctrl Pts',(194.546030068937,-4.88967153265256,130.257221158943));
#21919=CARTESIAN_POINT('Ctrl Pts',(194.5382374107,-4.90116937806975,130.394822109033));
#21920=CARTESIAN_POINT('Ctrl Pts',(194.530444752464,-4.91266722348695,130.532423059123));
#21921=CARTESIAN_POINT('Ctrl Pts',(194.522652094227,-4.91836225895716,130.670465679262));
#21922=CARTESIAN_POINT('Ctrl Pts',(194.514859435991,-4.91824832267189,130.808422518005));
#21923=CARTESIAN_POINT('',(194.860140564008,-4.91266024513891,130.801203006911));
#21924=CARTESIAN_POINT('Ctrl Pts',(194.92989654745,-4.76405452823406,129.582490119308));
#21925=CARTESIAN_POINT('Ctrl Pts',(194.921111692065,-4.80245103303602,129.732197508783));
#21926=CARTESIAN_POINT('Ctrl Pts',(194.912326836681,-4.83383095715299,129.883888334153));
#21927=CARTESIAN_POINT('Ctrl Pts',(194.903541981296,-4.85800796205853,130.036935244597));
#21928=CARTESIAN_POINT('Ctrl Pts',(194.894810448159,-4.88203821756628,130.189053192086));
#21929=CARTESIAN_POINT('Ctrl Pts',(194.886078915021,-4.89895263873311,130.342510630792));
#21930=CARTESIAN_POINT('Ctrl Pts',(194.877347381884,-4.90861601348531,130.496672634935));
#21931=CARTESIAN_POINT('Ctrl Pts',(194.871611775925,-4.9149637314563,130.597939216148));
#21932=CARTESIAN_POINT('Ctrl Pts',(194.865876169967,-4.91818362286876,130.699509432803));
#21933=CARTESIAN_POINT('Ctrl Pts',(194.860140564008,-4.9182489840691,130.801199414751));
#21934=CARTESIAN_POINT('Ctrl Pts',(194.860140564008,-4.91221266644762,130.801203294592));
#21935=CARTESIAN_POINT('Ctrl Pts',(194.80188727277,-4.90617542648731,131.832747380102));
#21936=CARTESIAN_POINT('Ctrl Pts',(194.650818106927,-4.08404315233992,134.516670434198));
#21937=CARTESIAN_POINT('Ctrl Pts',(194.406933066479,0.327902356760881,136.612472175972));
#21938=CARTESIAN_POINT('Ctrl Pts',(194.128485442666,5.06376798164403,133.667913246476));
#21939=CARTESIAN_POINT('Ctrl Pts',(193.850037818853,5.14627821021483,128.091889343334));
#21940=CARTESIAN_POINT('Ctrl Pts',(193.57159019504,0.499610173265479,125.008494029623));
#21941=CARTESIAN_POINT('Ctrl Pts',(193.348221787245,-3.59620912304385,126.807588037525));
#21942=CARTESIAN_POINT('Ctrl Pts',(193.217669254053,-4.59434972149962,128.935771315469));
#21943=CARTESIAN_POINT('Ctrl Pts',(193.179932595466,-4.75726252818781,129.584191622251));
#21944=CARTESIAN_POINT('Origin',(213.235140564004,0.,130.804360617566));
#21945=CARTESIAN_POINT('',(191.084784152919,-4.76405452823405,129.582490119308));
#21946=CARTESIAN_POINT('',(191.430300680169,-4.76051597898721,129.583432241588));
#21947=CARTESIAN_POINT('',(213.235140564004,-4.76405452823405,129.582490119308));
#21948=CARTESIAN_POINT('',(192.764859436031,-4.9182499011834,130.805346522958));
#21949=CARTESIAN_POINT('Ctrl Pts',(192.764859435991,-4.91824990118326,130.805346523653));
#21950=CARTESIAN_POINT('Ctrl Pts',(192.761851730581,-4.91823931916517,130.85813553689));
#21951=CARTESIAN_POINT('Ctrl Pts',(192.758844025171,-4.91737886410589,130.910915070119));
#21952=CARTESIAN_POINT('Ctrl Pts',(192.755836319761,-4.91566928905583,130.963666936127));
#21953=CARTESIAN_POINT('Ctrl Pts',(192.748061985642,-4.91125036970399,131.100020260621));
#21954=CARTESIAN_POINT('Ctrl Pts',(192.740287651523,-4.90114679519269,131.236405558342));
#21955=CARTESIAN_POINT('Ctrl Pts',(192.732513317404,-4.88534711553905,131.372310107569));
#21956=CARTESIAN_POINT('Ctrl Pts',(192.724748564456,-4.86956690757853,131.508047166585));
#21957=CARTESIAN_POINT('Ctrl Pts',(192.716983811509,-4.84810460677939,131.643304271342));
#21958=CARTESIAN_POINT('Ctrl Pts',(192.709219058562,-4.82100075318953,131.77756912567));
#21959=CARTESIAN_POINT('Ctrl Pts',(192.701462017677,-4.79392381952918,131.911700626251));
#21960=CARTESIAN_POINT('Ctrl Pts',(192.693704976792,-4.76121656070021,132.044841456872));
#21961=CARTESIAN_POINT('Ctrl Pts',(192.685947935907,-4.72297121766863,132.176485225455));
#21962=CARTESIAN_POINT('Ctrl Pts',(192.678196744667,-4.68475471574775,132.308029720448));
#21963=CARTESIAN_POINT('Ctrl Pts',(192.670445553427,-4.6410085509534,132.43807902658));
#21964=CARTESIAN_POINT('Ctrl Pts',(192.662694362187,-4.59187578910414,132.56613807228));
#21965=CARTESIAN_POINT('Ctrl Pts',(192.65494646541,-4.54276390998926,132.69414268947));
#21966=CARTESIAN_POINT('Ctrl Pts',(192.647198568633,-4.48827012711119,132.820158364431));
#21967=CARTESIAN_POINT('Ctrl Pts',(192.639450671856,-4.42858693265309,132.943706508822));
#21968=CARTESIAN_POINT('Ctrl Pts',(192.631704395771,-4.36891622263265,133.067228809605));
#21969=CARTESIAN_POINT('Ctrl Pts',(192.623958119687,-4.30405843013184,133.188284254661));
#21970=CARTESIAN_POINT('Ctrl Pts',(192.616211843603,-4.23425347381781,133.30641588913));
#21971=CARTESIAN_POINT('Ctrl Pts',(192.608465510338,-4.16444800221951,133.42454839562));
#21972=CARTESIAN_POINT('Ctrl Pts',(192.600719177073,-4.08969549283255,133.539756711864));
#21973=CARTESIAN_POINT('Ctrl Pts',(192.592972843807,-4.01028074241126,133.65161041861));
#21974=CARTESIAN_POINT('Ctrl Pts',(192.585224775804,-3.93084820760729,133.763489174218));
#21975=CARTESIAN_POINT('Ctrl Pts',(192.577476707801,-3.84675158046991,133.872011506716));
#21976=CARTESIAN_POINT('Ctrl Pts',(192.569728639798,-3.7583174692179,133.976778128404));
#21977=CARTESIAN_POINT('Ctrl Pts',(192.561972337057,-3.66978936913993,134.081656097304));
#21978=CARTESIAN_POINT('Ctrl Pts',(192.554216034315,-3.57691482870239,134.182770082479));
#21979=CARTESIAN_POINT('Ctrl Pts',(192.546459731573,-3.4800594120266,134.279755494593));
#21980=CARTESIAN_POINT('Ctrl Pts',(192.538699289059,-3.38315230069857,134.376792670742));
#21981=CARTESIAN_POINT('Ctrl Pts',(192.530938846545,-3.28226036692496,134.469696618379));
#21982=CARTESIAN_POINT('Ctrl Pts',(192.523178404031,-3.17778338449789,134.558142154058));
#21983=CARTESIAN_POINT('Ctrl Pts',(192.515405503765,-3.07313868634362,134.646729670363));
#21984=CARTESIAN_POINT('Ctrl Pts',(192.5076326035,-2.96489774802298,134.73084423263));
#21985=CARTESIAN_POINT('Ctrl Pts',(192.499859703234,-2.85349125072007,134.810202694404));
#21986=CARTESIAN_POINT('Ctrl Pts',(192.492369367472,-2.74613466020842,134.886676276202));
#21987=CARTESIAN_POINT('Ctrl Pts',(192.48487903171,-2.63583892488735,134.958733378042));
#21988=CARTESIAN_POINT('Ctrl Pts',(192.477388695948,-2.52301040503746,135.026161365893));
#21989=CARTESIAN_POINT('Ctrl Pts',(192.469614361829,-2.40590395756583,135.096145906396));
#21990=CARTESIAN_POINT('Ctrl Pts',(192.46184002771,-2.28569791514371,135.161365067826));
#21991=CARTESIAN_POINT('Ctrl Pts',(192.454065693591,-2.16281745608086,135.221532078373));
#21992=CARTESIAN_POINT('Ctrl Pts',(192.446300940644,-2.04008843620172,135.281624938458));
#21993=CARTESIAN_POINT('Ctrl Pts',(192.438536187696,-1.91469190546091,135.336677865911));
#21994=CARTESIAN_POINT('Ctrl Pts',(192.430771434749,-1.78708078602292,135.386448059631));
#21995=CARTESIAN_POINT('Ctrl Pts',(192.423014393864,-1.65959641174775,135.436168820892));
#21996=CARTESIAN_POINT('Ctrl Pts',(192.415257352979,-1.52990218788621,135.480617148817));
#21997=CARTESIAN_POINT('Ctrl Pts',(192.407500312094,-1.39847401492876,135.519596931058));
#21998=CARTESIAN_POINT('Ctrl Pts',(192.399749120854,-1.26714495297885,135.558547318341));
#21999=CARTESIAN_POINT('Ctrl Pts',(192.391997929614,-1.13408491791114,135.592037257539));
#22000=CARTESIAN_POINT('Ctrl Pts',(192.384246738374,-0.999787758028332,
135.6199195157));
#22001=CARTESIAN_POINT('Ctrl Pts',(192.376498841597,-0.865547678020963,
135.647789923158));
#22002=CARTESIAN_POINT('Ctrl Pts',(192.36875094482,-0.730071900997154,135.670057310698));
#22003=CARTESIAN_POINT('Ctrl Pts',(192.361003048043,-0.593867123607528,
135.686624938759));
#22004=CARTESIAN_POINT('Ctrl Pts',(192.353256771959,-0.457690837321097,
135.70318910123));
#22005=CARTESIAN_POINT('Ctrl Pts',(192.345510495875,-0.320786241840849,
135.714055828527));
#22006=CARTESIAN_POINT('Ctrl Pts',(192.337764219791,-0.18366746813134,135.719179975757));
#22007=CARTESIAN_POINT('Ctrl Pts',(192.330017886525,-0.0465476822422854,
135.724304160812));
#22008=CARTESIAN_POINT('Ctrl Pts',(192.32227155326,0.0907858943383346,135.723685666614));
#22009=CARTESIAN_POINT('Ctrl Pts',(192.314525219994,0.227817198101151,135.717331448616));
#22010=CARTESIAN_POINT('Ctrl Pts',(192.306777151991,0.364879189074196,135.710975807636));
#22011=CARTESIAN_POINT('Ctrl Pts',(192.299029083989,0.501638382059588,135.698881905005));
#22012=CARTESIAN_POINT('Ctrl Pts',(192.291281015986,0.637582305285388,135.681108700714));
#22013=CARTESIAN_POINT('Ctrl Pts',(192.283524713244,0.773670711330755,135.663316606849));
#22014=CARTESIAN_POINT('Ctrl Pts',(192.275768410502,0.908941728448333,135.639833204469));
#22015=CARTESIAN_POINT('Ctrl Pts',(192.26801210776,1.04289102096811,135.610768983579));
#22016=CARTESIAN_POINT('Ctrl Pts',(192.260251665246,1.17691180625858,135.58168925024));
#22017=CARTESIAN_POINT('Ctrl Pts',(192.252491222732,1.30960908320894,135.547022861951));
#22018=CARTESIAN_POINT('Ctrl Pts',(192.244730780217,1.44049317827798,135.50693039013));
#22019=CARTESIAN_POINT('Ctrl Pts',(192.236957879952,1.5715873801157,135.466773558314));
#22020=CARTESIAN_POINT('Ctrl Pts',(192.229184979687,1.70086221469286,135.42117336688));
#22021=CARTESIAN_POINT('Ctrl Pts',(192.221412079421,1.82784666917891,135.37033911253));
#22022=CARTESIAN_POINT('Ctrl Pts',(192.213921743659,1.95021491889024,135.321352811369));
#22023=CARTESIAN_POINT('Ctrl Pts',(192.206431407897,2.07045613849443,135.267506509144));
#22024=CARTESIAN_POINT('Ctrl Pts',(192.198941072135,2.18817178530026,135.209027154379));
#22025=CARTESIAN_POINT('Ctrl Pts',(192.191166738016,2.31035065663324,135.148330537103));
#22026=CARTESIAN_POINT('Ctrl Pts',(192.183392403897,2.43019568637188,135.082450339021));
#22027=CARTESIAN_POINT('Ctrl Pts',(192.175618069778,2.5472357860093,135.011589267518));
#22028=CARTESIAN_POINT('Ctrl Pts',(192.167853316831,2.66413164418405,134.940815525952));
#22029=CARTESIAN_POINT('Ctrl Pts',(192.160088563884,2.7782291190768,134.865073325257));
#22030=CARTESIAN_POINT('Ctrl Pts',(192.152323810936,2.88907911974915,134.784612481749));
#22031=CARTESIAN_POINT('Ctrl Pts',(192.144566770051,2.99981902263817,134.704231553085));
#22032=CARTESIAN_POINT('Ctrl Pts',(192.136809729166,3.10731755571858,134.619141536373));
#22033=CARTESIAN_POINT('Ctrl Pts',(192.129052688281,3.21115248827715,134.529636816659));
#22034=CARTESIAN_POINT('Ctrl Pts',(192.121301497041,3.3149091181053,134.440199593151));
#22035=CARTESIAN_POINT('Ctrl Pts',(192.113550305801,3.41500735156303,134.346354547366));
#22036=CARTESIAN_POINT('Ctrl Pts',(192.105799114561,3.51105638032787,134.248437584862));
#22037=CARTESIAN_POINT('Ctrl Pts',(192.098051217784,3.60706458569329,134.150562239679));
#22038=CARTESIAN_POINT('Ctrl Pts',(192.090303321007,3.69902673613745,134.048618698472));
#22039=CARTESIAN_POINT('Ctrl Pts',(192.08255542423,3.78658756001065,133.942980969388));
#22040=CARTESIAN_POINT('Ctrl Pts',(192.074809148146,3.87413006804709,133.83736533744));
#22041=CARTESIAN_POINT('Ctrl Pts',(192.067062872062,3.95727283142153,133.728057355462));
#22042=CARTESIAN_POINT('Ctrl Pts',(192.059316595977,4.03569996811177,133.615465174476));
#22043=CARTESIAN_POINT('Ctrl Pts',(192.051570262712,4.1141276837333,133.502872162361));
#22044=CARTESIAN_POINT('Ctrl Pts',(192.043823929447,4.18783947974799,133.386995223673));
#22045=CARTESIAN_POINT('Ctrl Pts',(192.036077596181,4.25656226304545,133.268272296851));
#22046=CARTESIAN_POINT('Ctrl Pts',(192.028329528178,4.32530043633368,133.149522782853));
#22047=CARTESIAN_POINT('Ctrl Pts',(192.020581460175,4.38904717787134,133.027926350791));
#22048=CARTESIAN_POINT('Ctrl Pts',(192.012833392173,4.4475750888561,132.903946026995));
#22049=CARTESIAN_POINT('Ctrl Pts',(192.005077089431,4.50616520400119,132.779833935435));
#22050=CARTESIAN_POINT('Ctrl Pts',(191.997320786689,4.55952524142413,132.653333245059));
#22051=CARTESIAN_POINT('Ctrl Pts',(191.989564483947,4.60747555374874,132.524927990297));
#22052=CARTESIAN_POINT('Ctrl Pts',(191.981804041433,4.65545145859881,132.396454201785));
#22053=CARTESIAN_POINT('Ctrl Pts',(191.974043598919,4.69801176383069,132.266074194861));
#22054=CARTESIAN_POINT('Ctrl Pts',(191.966283156404,4.73502688221655,132.134286738517));
#22055=CARTESIAN_POINT('Ctrl Pts',(191.958510256139,4.77210142055647,132.002287725248));
#22056=CARTESIAN_POINT('Ctrl Pts',(191.950737355874,4.80361289384034,131.868877128348));
#22057=CARTESIAN_POINT('Ctrl Pts',(191.942964455608,4.82948279537217,131.73456435423));
#22058=CARTESIAN_POINT('Ctrl Pts',(191.935474119846,4.85441226082101,131.605134187765));
#22059=CARTESIAN_POINT('Ctrl Pts',(191.927983784084,4.87410315800352,131.474866602682));
#22060=CARTESIAN_POINT('Ctrl Pts',(191.920493448322,4.88853100308117,131.344219575456));
#22061=CARTESIAN_POINT('Ctrl Pts',(191.912719114203,4.90350588429017,131.208619026484));
#22062=CARTESIAN_POINT('Ctrl Pts',(191.904944780084,4.91285817377069,131.0721801525));
#22063=CARTESIAN_POINT('Ctrl Pts',(191.897170445965,4.9165037801426,130.935408861902));
#22064=CARTESIAN_POINT('Ctrl Pts',(191.889405693018,4.92014489363048,130.798806129696));
#22065=CARTESIAN_POINT('Ctrl Pts',(191.881640940071,4.91809330722021,130.661872183078));
#22066=CARTESIAN_POINT('Ctrl Pts',(191.873876187123,4.91031645383257,130.525119886796));
#22067=CARTESIAN_POINT('Ctrl Pts',(191.866119146238,4.90254732452534,130.388503414822));
#22068=CARTESIAN_POINT('Ctrl Pts',(191.858362105353,4.88906426651891,130.252068621953));
#22069=CARTESIAN_POINT('Ctrl Pts',(191.850605064468,4.86988672827563,130.116329865154));
#22070=CARTESIAN_POINT('Ctrl Pts',(191.842853873228,4.85072365196311,129.980693470007));
#22071=CARTESIAN_POINT('Ctrl Pts',(191.835102681988,4.82587469733376,129.84575245173));
#22072=CARTESIAN_POINT('Ctrl Pts',(191.827351490748,4.79541122980165,129.712017173592));
#22073=CARTESIAN_POINT('Ctrl Pts',(191.819603593971,4.76496071005587,129.578338736515));
#22074=CARTESIAN_POINT('Ctrl Pts',(191.811855697194,4.72890051026299,129.445865400711));
#22075=CARTESIAN_POINT('Ctrl Pts',(191.804107800417,4.68735326106434,129.31509822682));
#22076=CARTESIAN_POINT('Ctrl Pts',(191.796361524333,4.64581470265456,129.184358406603));
#22077=CARTESIAN_POINT('Ctrl Pts',(191.788615248249,4.59879149613188,129.055324410796));
#22078=CARTESIAN_POINT('Ctrl Pts',(191.780868972164,4.54645628856314,128.928482615487));
#22079=CARTESIAN_POINT('Ctrl Pts',(191.773122638899,4.49412069466779,128.801639883861));
#22080=CARTESIAN_POINT('Ctrl Pts',(191.765376305634,4.43647317060039,128.676989746434));
#22081=CARTESIAN_POINT('Ctrl Pts',(191.757629972368,4.37373455287664,128.5549986806));
#22082=CARTESIAN_POINT('Ctrl Pts',(191.749881904365,4.31098188527447,128.432980295712));
#22083=CARTESIAN_POINT('Ctrl Pts',(191.742133836362,4.24313603409257,128.313622514967));
#22084=CARTESIAN_POINT('Ctrl Pts',(191.734385768359,4.17046364188854,128.197366932459));
#22085=CARTESIAN_POINT('Ctrl Pts',(191.726629465618,4.09771401260122,128.080987792135));
#22086=CARTESIAN_POINT('Ctrl Pts',(191.718873162876,4.02012780272054,127.967717768317));
#22087=CARTESIAN_POINT('Ctrl Pts',(191.711116860134,3.93801514032661,127.857969635863));
#22088=CARTESIAN_POINT('Ctrl Pts',(191.70335641762,3.85585865193233,127.748162927527));
#22089=CARTESIAN_POINT('Ctrl Pts',(191.695595975106,3.76917114412413,127.641882158914));
#22090=CARTESIAN_POINT('Ctrl Pts',(191.687835532591,3.67830220031926,127.539505952251));
#22091=CARTESIAN_POINT('Ctrl Pts',(191.680062632326,3.58728738561886,127.436965402214));
#22092=CARTESIAN_POINT('Ctrl Pts',(191.67228973206,3.49207799308258,127.338342220929));
#22093=CARTESIAN_POINT('Ctrl Pts',(191.664516831795,3.39306016596735,127.243977804914));
#22094=CARTESIAN_POINT('Ctrl Pts',(191.657026496033,3.29764188627902,127.153043773112));
#22095=CARTESIAN_POINT('Ctrl Pts',(191.649536160271,3.19868748848367,127.066064451937));
#22096=CARTESIAN_POINT('Ctrl Pts',(191.642045824509,3.09656904704697,126.983307987809));
#22097=CARTESIAN_POINT('Ctrl Pts',(191.63427149039,2.99057875386455,126.89741378719));
#22098=CARTESIAN_POINT('Ctrl Pts',(191.626497156271,2.88084400593911,126.815796897087));
#22099=CARTESIAN_POINT('Ctrl Pts',(191.618722822152,2.76774498488753,126.738801521804));
#22100=CARTESIAN_POINT('Ctrl Pts',(191.610958069205,2.65478534827152,126.661901036441));
#22101=CARTESIAN_POINT('Ctrl Pts',(191.603193316258,2.53847000824377,126.589610951247));
#22102=CARTESIAN_POINT('Ctrl Pts',(191.59542856331,2.41921284913904,126.522235881753));
#22103=CARTESIAN_POINT('Ctrl Pts',(191.587671522425,2.30007413792603,126.454927730128));
#22104=CARTESIAN_POINT('Ctrl Pts',(191.57991448154,2.17799976045686,126.392525070538));
#22105=CARTESIAN_POINT('Ctrl Pts',(191.572157440656,2.05343297218267,126.335289562945));
#22106=CARTESIAN_POINT('Ctrl Pts',(191.564406249415,1.92896012069234,126.278097217093));
#22107=CARTESIAN_POINT('Ctrl Pts',(191.556655058175,1.80199895334133,126.226064429886));
#22108=CARTESIAN_POINT('Ctrl Pts',(191.548903866935,1.67301742795112,126.179407023391));
#22109=CARTESIAN_POINT('Ctrl Pts',(191.541155970158,1.54409072314994,126.132769447539));
#22110=CARTESIAN_POINT('Ctrl Pts',(191.533408073381,1.41314573509101,126.09150284106));
#22111=CARTESIAN_POINT('Ctrl Pts',(191.525660176604,1.28067030513812,126.055774866836));
#22112=CARTESIAN_POINT('Ctrl Pts',(191.51791390052,1.14822258618934,126.020054366134));
#22113=CARTESIAN_POINT('Ctrl Pts',(191.510167624436,1.01424543935255,125.989870294983));
#22114=CARTESIAN_POINT('Ctrl Pts',(191.502421348352,0.879241386563487,125.965340298674));
#22115=CARTESIAN_POINT('Ctrl Pts',(191.494675015086,0.744236337205225,125.940810121289));
#22116=CARTESIAN_POINT('Ctrl Pts',(191.486928681821,0.608204751435609,125.921934171922));
#22117=CARTESIAN_POINT('Ctrl Pts',(191.479182348555,0.471658457426965,125.908778796981));
#22118=CARTESIAN_POINT('Ctrl Pts',(191.471434280553,0.335081584822615,125.895620475986));
#22119=CARTESIAN_POINT('Ctrl Pts',(191.46368621255,0.197990163703318,125.888185316112));
#22120=CARTESIAN_POINT('Ctrl Pts',(191.455938144547,0.0608998465023526,
125.886487675816));
#22121=CARTESIAN_POINT('Ctrl Pts',(191.448181841805,-0.0763361719192702,
125.884788231248));
#22122=CARTESIAN_POINT('Ctrl Pts',(191.440425539063,-0.21357069252026,125.888838492329));
#22123=CARTESIAN_POINT('Ctrl Pts',(191.432669236321,-0.350288804319249,
125.898600654414));
#22124=CARTESIAN_POINT('Ctrl Pts',(191.424908793807,-0.487079886691054,
125.908368026859));
#22125=CARTESIAN_POINT('Ctrl Pts',(191.417148351293,-0.623353622783719,
125.923853330808));
#22126=CARTESIAN_POINT('Ctrl Pts',(191.409387908778,-0.758602508617255,
125.944967106394));
#22127=CARTESIAN_POINT('Ctrl Pts',(191.401615008513,-0.894068507969185,
125.966114775688));
#22128=CARTESIAN_POINT('Ctrl Pts',(191.393842108248,-1.02850598582216,125.992908895609));
#22129=CARTESIAN_POINT('Ctrl Pts',(191.386069207982,-1.16141899575531,126.025209126056));
#22130=CARTESIAN_POINT('Ctrl Pts',(191.37857887222,-1.28950028298996,126.056335161768));
#22131=CARTESIAN_POINT('Ctrl Pts',(191.371088536458,-1.41616571838099,126.092573851485));
#22132=CARTESIAN_POINT('Ctrl Pts',(191.363598200696,-1.54098858741563,126.13375709811));
#22133=CARTESIAN_POINT('Ctrl Pts',(191.355823866577,-1.67054415346853,126.176501820048));
#22134=CARTESIAN_POINT('Ctrl Pts',(191.348049532458,-1.79852506629693,126.224708848623));
#22135=CARTESIAN_POINT('Ctrl Pts',(191.340275198339,-1.92443623961998,126.278244377108));
#22136=CARTESIAN_POINT('Ctrl Pts',(191.332510445392,-2.05019223867488,126.331713927838));
#22137=CARTESIAN_POINT('Ctrl Pts',(191.324745692445,-2.17388321715495,126.390498760795));
#22138=CARTESIAN_POINT('Ctrl Pts',(191.316980939498,-2.29502917879571,126.454415315499));
#22139=CARTESIAN_POINT('Ctrl Pts',(191.309223898613,-2.41605481655935,126.51826838738));
#22140=CARTESIAN_POINT('Ctrl Pts',(191.301466857728,-2.53454012426197,126.587242856692));
#22141=CARTESIAN_POINT('Ctrl Pts',(191.293709816843,-2.65002536956902,126.661107233673));
#22142=CARTESIAN_POINT('Ctrl Pts',(191.285958625602,-2.76542352655441,126.734915908953));
#22143=CARTESIAN_POINT('Ctrl Pts',(191.278207434362,-2.87782579622934,126.813606942315));
#22144=CARTESIAN_POINT('Ctrl Pts',(191.270456243122,-2.98679765874186,126.896903284692));
#22145=CARTESIAN_POINT('Ctrl Pts',(191.262708346345,-3.09572320530585,126.980164223901));
#22146=CARTESIAN_POINT('Ctrl Pts',(191.254960449568,-3.20122093462301,127.068026342114));
#22147=CARTESIAN_POINT('Ctrl Pts',(191.247212552791,-3.302886096988,127.160169830461));
#22148=CARTESIAN_POINT('Ctrl Pts',(191.239466276707,-3.40452999319271,127.252294044376));
#22149=CARTESIAN_POINT('Ctrl Pts',(191.231720000623,-3.50234262754816,127.348697584696));
#22150=CARTESIAN_POINT('Ctrl Pts',(191.223973724539,-3.59595339635909,127.449021255636));
#22151=CARTESIAN_POINT('Ctrl Pts',(191.216227391273,-3.68956485618348,127.549345667144));
#22152=CARTESIAN_POINT('Ctrl Pts',(191.208481058008,-3.77897412184559,127.653589981163));
#22153=CARTESIAN_POINT('Ctrl Pts',(191.200734724743,-3.86384871860262,127.761359444012));
#22154=CARTESIAN_POINT('Ctrl Pts',(191.19298665674,-3.94874232243708,127.869153041084));
#22155=CARTESIAN_POINT('Ctrl Pts',(191.185238588737,-4.02909899477355,127.980473050777));
#22156=CARTESIAN_POINT('Ctrl Pts',(191.177490520734,-4.10462793269824,128.094893401191));
#22157=CARTESIAN_POINT('Ctrl Pts',(191.169734217992,-4.18023714367694,128.209435358914));
#22158=CARTESIAN_POINT('Ctrl Pts',(191.16197791525,-4.251008154845,128.327083912827));
#22159=CARTESIAN_POINT('Ctrl Pts',(191.154221612508,-4.31669445035687,128.447385419402));
#22160=CARTESIAN_POINT('Ctrl Pts',(191.146461169994,-4.38241580462248,128.567751134514));
#22161=CARTESIAN_POINT('Ctrl Pts',(191.13870072748,-4.44304686287264,128.690772273196));
#22162=CARTESIAN_POINT('Ctrl Pts',(191.130940284966,-4.49838857192929,128.815973502732));
#22163=CARTESIAN_POINT('Ctrl Pts',(191.1231673847,-4.5538191204103,128.941375716397));
#22164=CARTESIAN_POINT('Ctrl Pts',(191.115394484435,-4.603943209069,129.068964650282));
#22165=CARTESIAN_POINT('Ctrl Pts',(191.107621584169,-4.64861083885302,129.198247193365));
#22166=CARTESIAN_POINT('Ctrl Pts',(191.100131248407,-4.69165468778338,129.322829990364));
#22167=CARTESIAN_POINT('Ctrl Pts',(191.092640912645,-4.72963181359555,129.44898510548));
#22168=CARTESIAN_POINT('Ctrl Pts',(191.085150576883,-4.76245299152071,129.576262671124));
#22169=CARTESIAN_POINT('Ctrl Pts',(191.085028435562,-4.76298819076576,129.578338125491));
#22170=CARTESIAN_POINT('Ctrl Pts',(191.08490629424,-4.76352203648398,129.580413942056));
#22171=CARTESIAN_POINT('Ctrl Pts',(191.084784152919,-4.76405452823405,129.582490119308));
#22172=CARTESIAN_POINT('Ctrl Pts',(192.834981455508,-4.76405452823404,129.582490119308));
#22173=CARTESIAN_POINT('Ctrl Pts',(192.827262795634,-4.79795815032377,129.714679827277));
#22174=CARTESIAN_POINT('Ctrl Pts',(192.819544135761,-4.82632919785479,129.848178265195));
#22175=CARTESIAN_POINT('Ctrl Pts',(192.811825475887,-4.84909224210237,129.982480157838));
#22176=CARTESIAN_POINT('Ctrl Pts',(192.803997802578,-4.87217677708874,130.118678844873));
#22177=CARTESIAN_POINT('Ctrl Pts',(192.796170129268,-4.88949364919261,130.255703433094));
#22178=CARTESIAN_POINT('Ctrl Pts',(192.788342455959,-4.90101880375934,130.393024079319));
#22179=CARTESIAN_POINT('Ctrl Pts',(192.78051478265,-4.91254395832607,130.530344725543));
#22180=CARTESIAN_POINT('Ctrl Pts',(192.77268710934,-4.91827744128822,130.667961010208));
#22181=CARTESIAN_POINT('Ctrl Pts',(192.764859436031,-4.9182499011834,130.805346522958));
#22182=CARTESIAN_POINT('',(193.110140564008,-4.91324924050575,130.80805185308));
#22183=CARTESIAN_POINT('Ctrl Pts',(193.179932595466,-4.75726252818781,129.584191622251));
#22184=CARTESIAN_POINT('Ctrl Pts',(193.15666858498,-4.85769551258501,129.983931752434));
#22185=CARTESIAN_POINT('Ctrl Pts',(193.133404574494,-4.9103928439719,130.396313003733));
#22186=CARTESIAN_POINT('Ctrl Pts',(193.110140564008,-4.91324924050575,130.80805185308));
#22187=CARTESIAN_POINT('Ctrl Pts',(193.110140564008,-4.91324924050575,130.80805185308));
#22188=CARTESIAN_POINT('Ctrl Pts',(193.078325358477,-4.91715556795767,131.371134307201));
#22189=CARTESIAN_POINT('Ctrl Pts',(192.953694278342,-4.56730227853154,133.572215041493));
#22190=CARTESIAN_POINT('Ctrl Pts',(192.736247323602,-1.31701101669081,136.470678805982));
#22191=CARTESIAN_POINT('Ctrl Pts',(192.457799699789,4.05535734608101,134.975182673953));
#22192=CARTESIAN_POINT('Ctrl Pts',(192.179352075976,5.70105042302464,129.646904828089));
#22193=CARTESIAN_POINT('Ctrl Pts',(191.900904452163,2.10775667300519,125.382272307895));
#22194=CARTESIAN_POINT('Ctrl Pts',(191.651220653561,-2.85118716275981,126.026104000732));
#22195=CARTESIAN_POINT('Ctrl Pts',(191.494352729563,-4.4694424636812,128.488577529337));
#22196=CARTESIAN_POINT('Ctrl Pts',(191.430300680169,-4.76051597898714,129.583432241587));
#22197=CARTESIAN_POINT('Origin',(213.235140564004,0.,130.804360617566));
#22198=CARTESIAN_POINT('',(189.334601801321,-4.76405452823404,129.582490119308));
#22199=CARTESIAN_POINT('',(189.680106903305,-4.76405452823404,129.582490119308));
#22200=CARTESIAN_POINT('',(213.235140564004,-4.76405452823405,129.582490119308));
#22201=CARTESIAN_POINT('',(191.014859436046,-4.91824790535574,130.799821458629));
#22202=CARTESIAN_POINT('Ctrl Pts',(191.014859435991,-4.91824790535664,130.799821459599));
#22203=CARTESIAN_POINT('Ctrl Pts',(191.007192991401,-4.9183728969955,130.93525183469));
#22204=CARTESIAN_POINT('Ctrl Pts',(190.999526546812,-4.91289980315623,131.070824814365));
#22205=CARTESIAN_POINT('Ctrl Pts',(190.991860102222,-4.90182013838234,131.206035104495));
#22206=CARTESIAN_POINT('Ctrl Pts',(190.984145221007,-4.8906704722459,131.342099653731));
#22207=CARTESIAN_POINT('Ctrl Pts',(190.976430339793,-4.87384310420628,131.477796505531));
#22208=CARTESIAN_POINT('Ctrl Pts',(190.968715458578,-4.85138271638349,131.612611074835));
#22209=CARTESIAN_POINT('Ctrl Pts',(190.961055815356,-4.82908314331645,131.746460381553));
#22210=CARTESIAN_POINT('Ctrl Pts',(190.953396172134,-4.80123103213926,131.879439600074));
#22211=CARTESIAN_POINT('Ctrl Pts',(190.945736528912,-4.76792200125562,132.011051486199));
#22212=CARTESIAN_POINT('Ctrl Pts',(190.938077448338,-4.7346154171254,132.142653704621));
#22213=CARTESIAN_POINT('Ctrl Pts',(190.930418367764,-4.69585280864405,132.27288840198));
#22214=CARTESIAN_POINT('Ctrl Pts',(190.92275928719,-4.65178043486449,132.401270711564));
#22215=CARTESIAN_POINT('Ctrl Pts',(190.91509902035,-4.60770123499393,132.529672905471));
#22216=CARTESIAN_POINT('Ctrl Pts',(190.907438753509,-4.55831076464351,132.65622176218));
#22217=CARTESIAN_POINT('Ctrl Pts',(190.899778486669,-4.50380428023245,132.780450207605));
#22218=CARTESIAN_POINT('Ctrl Pts',(190.892022192202,-4.44861451305745,132.906235956834));
#22219=CARTESIAN_POINT('Ctrl Pts',(190.884265897736,-4.38817975595761,133.029642333155));
#22220=CARTESIAN_POINT('Ctrl Pts',(190.876509603269,-4.32275123572271,133.150209039045));
#22221=CARTESIAN_POINT('Ctrl Pts',(190.868837761032,-4.25803511551729,133.269462988289));
#22222=CARTESIAN_POINT('Ctrl Pts',(190.861165918795,-4.18843370140229,133.385938486624));
#22223=CARTESIAN_POINT('Ctrl Pts',(190.853494076558,-4.11423393107197,133.499219096766));
#22224=CARTESIAN_POINT('Ctrl Pts',(190.845695555977,-4.03880896557229,133.614370209414));
#22225=CARTESIAN_POINT('Ctrl Pts',(190.837897035395,-3.95863270394605,133.726219643716));
#22226=CARTESIAN_POINT('Ctrl Pts',(190.830098514814,-3.87404868695243,133.834365540602));
#22227=CARTESIAN_POINT('Ctrl Pts',(190.822299994233,-3.78946466995879,133.942511437488));
#22228=CARTESIAN_POINT('Ctrl Pts',(190.814501473652,-3.70047322628425,134.046953515992));
#22229=CARTESIAN_POINT('Ctrl Pts',(190.80670295307,-3.60745575518182,134.147330260998));
#22230=CARTESIAN_POINT('Ctrl Pts',(190.798928618951,-3.51472677001999,134.247395695888));
#22231=CARTESIAN_POINT('Ctrl Pts',(190.791154284832,-3.41768425491403,134.343758457961));
#22232=CARTESIAN_POINT('Ctrl Pts',(190.783379950713,-3.31665570023412,134.436023876818));
#22233=CARTESIAN_POINT('Ctrl Pts',(190.775615197766,-3.21575165421878,134.528175586793));
#22234=CARTESIAN_POINT('Ctrl Pts',(190.767850444819,-3.11087162883549,134.616239739652));
#22235=CARTESIAN_POINT('Ctrl Pts',(190.760085691872,-3.00238209392103,134.699856070599));
#22236=CARTESIAN_POINT('Ctrl Pts',(190.752328650987,-2.89400031234197,134.783389352628));
#22237=CARTESIAN_POINT('Ctrl Pts',(190.744571610102,-2.78201646323467,134.862483366925));
#22238=CARTESIAN_POINT('Ctrl Pts',(190.736814569217,-2.66683218589617,134.936816201691));
#22239=CARTESIAN_POINT('Ctrl Pts',(190.729063377977,-2.55173476991692,135.011092981489));
#22240=CARTESIAN_POINT('Ctrl Pts',(190.721312186737,-2.43344205673886,135.080615517179));
#22241=CARTESIAN_POINT('Ctrl Pts',(190.713560995496,-2.3123866426324,135.145103765631));
#22242=CARTESIAN_POINT('Ctrl Pts',(190.705813098719,-2.19138268030653,135.209564604857));
#22243=CARTESIAN_POINT('Ctrl Pts',(190.698065201942,-2.06761869682469,135.268995229124));
#22244=CARTESIAN_POINT('Ctrl Pts',(190.690317305165,-1.94155380476799,135.323160445584));
#22245=CARTESIAN_POINT('Ctrl Pts',(190.682571029081,-1.81551528276903,135.377314331847));
#22246=CARTESIAN_POINT('Ctrl Pts',(190.674824752997,-1.68717716851246,135.426204846825));
#22247=CARTESIAN_POINT('Ctrl Pts',(190.667078476913,-1.55702020428703,135.469644225873));
#22248=CARTESIAN_POINT('Ctrl Pts',(190.659332143647,-1.42686227927271,135.513083925581));
#22249=CARTESIAN_POINT('Ctrl Pts',(190.651585810382,-1.29488584835446,135.551072285292));
#22250=CARTESIAN_POINT('Ctrl Pts',(190.643839477117,-1.16158814539901,135.583470999527));
#22251=CARTESIAN_POINT('Ctrl Pts',(190.636091409114,-1.02826059134723,135.615876969229));
#22252=CARTESIAN_POINT('Ctrl Pts',(190.628343341111,-0.893611556303883,
135.642690710273));
#22253=CARTESIAN_POINT('Ctrl Pts',(190.620595273108,-0.758149436995237,
135.663824836354));
#22254=CARTESIAN_POINT('Ctrl Pts',(190.612838970366,-0.622543346934008,
135.684981424036));
#22255=CARTESIAN_POINT('Ctrl Pts',(190.605082667624,-0.486122833271634,
135.700446278109));
#22256=CARTESIAN_POINT('Ctrl Pts',(190.597326364882,-0.349402960938852,
135.710183752717));
#22257=CARTESIAN_POINT('Ctrl Pts',(190.589565922368,-0.21261011709358,135.719926424509));
#22258=CARTESIAN_POINT('Ctrl Pts',(190.581805479854,-0.0755179868161497,
135.723935614332));
#22259=CARTESIAN_POINT('Ctrl Pts',(190.57404503734,0.0613583669252786,135.722227859909));
#22260=CARTESIAN_POINT('Ctrl Pts',(190.566272137074,0.198454446740975,135.720517364047));
#22261=CARTESIAN_POINT('Ctrl Pts',(190.558499236809,0.335333667223026,135.713071605924));
#22262=CARTESIAN_POINT('Ctrl Pts',(190.550726336543,0.471485185895587,135.699959128676));
#22263=CARTESIAN_POINT('Ctrl Pts',(190.543236000781,0.602687253919808,135.687323323004));
#22264=CARTESIAN_POINT('Ctrl Pts',(190.535745665019,0.7332133040056,135.669425686172));
#22265=CARTESIAN_POINT('Ctrl Pts',(190.528255329257,0.862617086158864,135.646372061704));
#22266=CARTESIAN_POINT('Ctrl Pts',(190.520480995138,0.996927252043568,135.622444352059));
#22267=CARTESIAN_POINT('Ctrl Pts',(190.512706661019,1.13045382272073,135.592886162405));
#22268=CARTESIAN_POINT('Ctrl Pts',(190.5049323269,1.26268773426236,135.557759690676));
#22269=CARTESIAN_POINT('Ctrl Pts',(190.497167573953,1.3947586793262,135.522676509184));
#22270=CARTESIAN_POINT('Ctrl Pts',(190.489402821006,1.5255397607892,135.482038799179));
#22271=CARTESIAN_POINT('Ctrl Pts',(190.481638068059,1.65452979177848,135.435960150192));
#22272=CARTESIAN_POINT('Ctrl Pts',(190.473881027174,1.78339170804989,135.389927267168));
#22273=CARTESIAN_POINT('Ctrl Pts',(190.466123986289,1.91046574813598,135.338464330073));
#22274=CARTESIAN_POINT('Ctrl Pts',(190.458366945404,2.03526398267376,135.281735248232));
#22275=CARTESIAN_POINT('Ctrl Pts',(190.450615754164,2.15996810589255,135.225048946233));
#22276=CARTESIAN_POINT('Ctrl Pts',(190.442864562924,2.28239948508168,135.163104565135));
#22277=CARTESIAN_POINT('Ctrl Pts',(190.435113371684,2.40208868317336,135.096114690282));
#22278=CARTESIAN_POINT('Ctrl Pts',(190.427365474906,2.52172701016312,135.029153287912));
#22279=CARTESIAN_POINT('Ctrl Pts',(190.419617578129,2.63862513369723,134.95715084752));
#22280=CARTESIAN_POINT('Ctrl Pts',(190.411869681352,2.75233701780585,134.880366506045));
#22281=CARTESIAN_POINT('Ctrl Pts',(190.404123405268,2.86602511583959,134.803598226199));
#22282=CARTESIAN_POINT('Ctrl Pts',(190.396377129184,2.97652797633052,134.722050253513));
#22283=CARTESIAN_POINT('Ctrl Pts',(190.3886308531,3.08342777461511,134.636025558715));
#22284=CARTESIAN_POINT('Ctrl Pts',(190.380884519835,3.1903283620097,134.550000228902));
#22285=CARTESIAN_POINT('Ctrl Pts',(190.373138186569,3.29362552953602,134.459498356145));
#22286=CARTESIAN_POINT('Ctrl Pts',(190.365391853304,3.39293414982598,134.364863519888));
#22287=CARTESIAN_POINT('Ctrl Pts',(190.357643785301,3.49226500959297,134.270207490816));
#22288=CARTESIAN_POINT('Ctrl Pts',(190.349895717298,3.58760526176411,134.171416926171));
#22289=CARTESIAN_POINT('Ctrl Pts',(190.342147649295,3.67860658491866,134.068872320086));
#22290=CARTESIAN_POINT('Ctrl Pts',(190.334391346553,3.76970462536241,133.966218728374));
#22291=CARTESIAN_POINT('Ctrl Pts',(190.326635043811,3.85645426497193,133.859803417977));
#22292=CARTESIAN_POINT('Ctrl Pts',(190.31887874107,3.93854710870415,133.750040460152));
#22293=CARTESIAN_POINT('Ctrl Pts',(190.311118298555,4.02068376785884,133.640218918532));
#22294=CARTESIAN_POINT('Ctrl Pts',(190.303357856041,4.09815845787932,133.527046491708));
#22295=CARTESIAN_POINT('Ctrl Pts',(190.295597413527,4.17070668830499,133.410965455785));
#22296=CARTESIAN_POINT('Ctrl Pts',(190.287824513262,4.24337137959067,133.294698076279));
#22297=CARTESIAN_POINT('Ctrl Pts',(190.280051612996,4.31109361453856,133.175513097328));
#22298=CARTESIAN_POINT('Ctrl Pts',(190.272278712731,4.37365493759366,133.053877354415));
#22299=CARTESIAN_POINT('Ctrl Pts',(190.264788376969,4.43394199897344,132.936663377138));
#22300=CARTESIAN_POINT('Ctrl Pts',(190.257298041207,4.4894367285661,132.817174004629));
#22301=CARTESIAN_POINT('Ctrl Pts',(190.249807705445,4.53998696650629,132.695841890657));
#22302=CARTESIAN_POINT('Ctrl Pts',(190.242033371326,4.59245383208216,132.569909432706));
#22303=CARTESIAN_POINT('Ctrl Pts',(190.234259037206,4.63976006301382,132.44159282362));
#22304=CARTESIAN_POINT('Ctrl Pts',(190.226484703087,4.68168282669612,132.3113539728));
#22305=CARTESIAN_POINT('Ctrl Pts',(190.21871995014,4.72355392431904,132.181275629723));
#22306=CARTESIAN_POINT('Ctrl Pts',(190.210955197193,4.76005463700814,132.049280127086));
#22307=CARTESIAN_POINT('Ctrl Pts',(190.203190444246,4.79100962710627,131.915850525516));
#22308=CARTESIAN_POINT('Ctrl Pts',(190.195433403361,4.82193387227178,131.782553448108));
#22309=CARTESIAN_POINT('Ctrl Pts',(190.187676362476,4.84732326841009,131.647825484707));
#22310=CARTESIAN_POINT('Ctrl Pts',(190.179919321591,4.8670519793402,131.5121657411));
#22311=CARTESIAN_POINT('Ctrl Pts',(190.172168130351,4.8867658126959,131.376608299561));
#22312=CARTESIAN_POINT('Ctrl Pts',(190.164416939111,4.90082740152704,131.240120861754));
#22313=CARTESIAN_POINT('Ctrl Pts',(190.156665747871,4.90916185770046,131.103213285948));
#22314=CARTESIAN_POINT('Ctrl Pts',(190.148917851094,4.91749277150769,130.966363899514));
#22315=CARTESIAN_POINT('Ctrl Pts',(190.141169954316,4.92010137035702,130.829095119669));
#22316=CARTESIAN_POINT('Ctrl Pts',(190.133422057539,4.91696458015609,130.691922278951));
#22317=CARTESIAN_POINT('Ctrl Pts',(190.125675781455,4.91382844610404,130.554778131835));
#22318=CARTESIAN_POINT('Ctrl Pts',(190.117929505371,4.90494932240312,130.417730274544));
#22319=CARTESIAN_POINT('Ctrl Pts',(190.110183229287,4.8903562624689,130.281293997879));
#22320=CARTESIAN_POINT('Ctrl Pts',(190.102436896022,4.87576309481204,130.144856714072));
#22321=CARTESIAN_POINT('Ctrl Pts',(190.094690562756,4.85545594833678,130.009031408648));
#22322=CARTESIAN_POINT('Ctrl Pts',(190.086944229491,4.82951571541046,129.87432781325));
#22323=CARTESIAN_POINT('Ctrl Pts',(190.079196161488,4.80356967334887,129.739594051917));
#22324=CARTESIAN_POINT('Ctrl Pts',(190.071448093485,4.77198810853258,129.605982884305));
#22325=CARTESIAN_POINT('Ctrl Pts',(190.063700025482,4.73490286521561,129.473993029464));
#22326=CARTESIAN_POINT('Ctrl Pts',(190.05594372274,4.69777820726065,129.341862894234));
#22327=CARTESIAN_POINT('Ctrl Pts',(190.048187419998,4.65513829197155,129.211357890945));
#22328=CARTESIAN_POINT('Ctrl Pts',(190.040431117256,4.60716479417153,129.082961296709));
#22329=CARTESIAN_POINT('Ctrl Pts',(190.032670674742,4.55916569147128,128.954496173345));
#22330=CARTESIAN_POINT('Ctrl Pts',(190.024910232228,4.50582748595494,128.828142061345));
#22331=CARTESIAN_POINT('Ctrl Pts',(190.017149789714,4.44737931348167,128.704360545062));
#22332=CARTESIAN_POINT('Ctrl Pts',(190.009376889448,4.38883731481318,128.580380323701));
#22333=CARTESIAN_POINT('Ctrl Pts',(190.001603989183,4.32516913872479,128.458981297068));
#22334=CARTESIAN_POINT('Ctrl Pts',(189.993831088917,4.25664946656522,128.34059959399));
#22335=CARTESIAN_POINT('Ctrl Pts',(189.986340753155,4.19062065707926,128.226521364005));
#22336=CARTESIAN_POINT('Ctrl Pts',(189.978850417393,4.12008712075145,128.115245151775));
#22337=CARTESIAN_POINT('Ctrl Pts',(189.971360081631,4.04533061532805,128.007132833636));
#22338=CARTESIAN_POINT('Ctrl Pts',(189.963585747512,3.96773969427981,127.894921404095));
#22339=CARTESIAN_POINT('Ctrl Pts',(189.955811413393,3.88535347027769,127.785763070711));
#22340=CARTESIAN_POINT('Ctrl Pts',(189.948037079274,3.79844011431754,127.680094982182));
#22341=CARTESIAN_POINT('Ctrl Pts',(189.940272326327,3.71163387130119,127.574557120128));
#22342=CARTESIAN_POINT('Ctrl Pts',(189.93250757338,3.62031184341438,127.472501243445));
#22343=CARTESIAN_POINT('Ctrl Pts',(189.924742820433,3.52478566895689,127.374335974737));
#22344=CARTESIAN_POINT('Ctrl Pts',(189.916985779548,3.42935437244241,127.276268205157));
#22345=CARTESIAN_POINT('Ctrl Pts',(189.909228738663,3.32972750992248,127.18208363199));
#22346=CARTESIAN_POINT('Ctrl Pts',(189.901471697778,3.22625697570096,127.092157903645));
#22347=CARTESIAN_POINT('Ctrl Pts',(189.893720506538,3.12286446941407,127.002299988992));
#22348=CARTESIAN_POINT('Ctrl Pts',(189.885969315298,3.01563435469827,126.916694782037));
#22349=CARTESIAN_POINT('Ctrl Pts',(189.878218124058,2.90495511089095,126.835680879138));
#22350=CARTESIAN_POINT('Ctrl Pts',(189.87047022728,2.79432290871461,126.754701409308));
#22351=CARTESIAN_POINT('Ctrl Pts',(189.862722330503,2.68024480797378,126.678309592735));
#22352=CARTESIAN_POINT('Ctrl Pts',(189.854974433726,2.56314190041725,126.606803392128));
#22353=CARTESIAN_POINT('Ctrl Pts',(189.847228157642,2.44606348826436,126.535312149077));
#22354=CARTESIAN_POINT('Ctrl Pts',(189.839481881558,2.32596186128318,126.468704692871));
#22355=CARTESIAN_POINT('Ctrl Pts',(189.831735605474,2.20328625229884,126.407235107311));
#22356=CARTESIAN_POINT('Ctrl Pts',(189.823989272209,2.0806097377515,126.345765067998));
#22357=CARTESIAN_POINT('Ctrl Pts',(189.816242938943,1.9553595528264,126.289433150157));
#22358=CARTESIAN_POINT('Ctrl Pts',(189.808496605678,1.82800827349247,126.238446819152));
#22359=CARTESIAN_POINT('Ctrl Pts',(189.800748537675,1.70062847472297,126.187449070113));
#22360=CARTESIAN_POINT('Ctrl Pts',(189.793000469672,1.57114700814089,126.141799435301));
#22361=CARTESIAN_POINT('Ctrl Pts',(189.785252401669,1.44005472524652,126.10165656024));
#22362=CARTESIAN_POINT('Ctrl Pts',(189.777496098927,1.30882311591319,126.061471020852));
#22363=CARTESIAN_POINT('Ctrl Pts',(189.769739796186,1.17597764480057,126.02680404717));
#22364=CARTESIAN_POINT('Ctrl Pts',(189.761983493444,1.04202310631098,125.997764014104));
#22365=CARTESIAN_POINT('Ctrl Pts',(189.75422305093,0.907997072250902,125.968708481497));
#22366=CARTESIAN_POINT('Ctrl Pts',(189.746462608415,0.772861176351149,125.945285940508));
#22367=CARTESIAN_POINT('Ctrl Pts',(189.738702165901,0.637127616130016,125.927553110265));
#22368=CARTESIAN_POINT('Ctrl Pts',(189.730929265636,0.501176164348156,125.909791813709));
#22369=CARTESIAN_POINT('Ctrl Pts',(189.723156365371,0.36462552068547,125.897738514198));
#22370=CARTESIAN_POINT('Ctrl Pts',(189.715383465105,0.227991084653854,125.891397852816));
#22371=CARTESIAN_POINT('Ctrl Pts',(189.707893129343,0.0963236545319259,
125.885287690447));
#22372=CARTESIAN_POINT('Ctrl Pts',(189.700402793581,-0.035421273587108,
125.88448204139));
#22373=CARTESIAN_POINT('Ctrl Pts',(189.692912457819,-0.166786945949541,
125.888939457873));
#22374=CARTESIAN_POINT('Ctrl Pts',(189.6851381237,-0.303133387705632,125.893565878656));
#22375=CARTESIAN_POINT('Ctrl Pts',(189.677363789581,-0.439503151574217,
125.903876996674));
#22376=CARTESIAN_POINT('Ctrl Pts',(189.669589455462,-0.575383499002755,
125.91988348162));
#22377=CARTESIAN_POINT('Ctrl Pts',(189.661824702515,-0.711096386047016,
125.935870240005));
#22378=CARTESIAN_POINT('Ctrl Pts',(189.654059949567,-0.846320672210825,
125.95753835424));
#22379=CARTESIAN_POINT('Ctrl Pts',(189.64629519662,-0.980544123610611,125.984846504696));
#22380=CARTESIAN_POINT('Ctrl Pts',(189.638538155735,-1.11463426238657,126.012127532312));
#22381=CARTESIAN_POINT('Ctrl Pts',(189.63078111485,-1.24772516395203,126.045037370947));
#22382=CARTESIAN_POINT('Ctrl Pts',(189.623024073965,-1.37931057719251,126.083483009097));
#22383=CARTESIAN_POINT('Ctrl Pts',(189.615272882725,-1.51079676084857,126.121899655092));
#22384=CARTESIAN_POINT('Ctrl Pts',(189.607521691485,-1.64077934216929,126.165843682135));
#22385=CARTESIAN_POINT('Ctrl Pts',(189.599770500245,-1.76876346787959,126.215171271157));
#22386=CARTESIAN_POINT('Ctrl Pts',(189.592022603468,-1.89669319692298,126.264477894638));
#22387=CARTESIAN_POINT('Ctrl Pts',(189.584274706691,-2.02262579569819,126.319163388819));
#22388=CARTESIAN_POINT('Ctrl Pts',(189.576526809914,-2.14608296936092,126.379034533409));
#22389=CARTESIAN_POINT('Ctrl Pts',(189.56878053383,-2.26951431844442,126.438893154247));
#22390=CARTESIAN_POINT('Ctrl Pts',(189.561034257746,-2.39047092080065,126.503935097423));
#22391=CARTESIAN_POINT('Ctrl Pts',(189.553287981662,-2.50849618721501,126.573919749143));
#22392=CARTESIAN_POINT('Ctrl Pts',(189.545541648396,-2.62652232486488,126.643904917472));
#22393=CARTESIAN_POINT('Ctrl Pts',(189.537795315131,-2.74161674710555,126.718832667743));
#22394=CARTESIAN_POINT('Ctrl Pts',(189.530048981866,-2.85334946859526,126.798417548504));
#22395=CARTESIAN_POINT('Ctrl Pts',(189.522300913863,-2.96510721185335,126.878020251747));
#22396=CARTESIAN_POINT('Ctrl Pts',(189.51455284586,-3.0735014379343,126.962281934019));
#22397=CARTESIAN_POINT('Ctrl Pts',(189.506804777857,-3.17813335664093,127.050875379829));
#22398=CARTESIAN_POINT('Ctrl Pts',(189.499048475115,-3.28287647939589,127.139562983809));
#22399=CARTESIAN_POINT('Ctrl Pts',(189.491292172373,-3.38384900824164,127.232591294972));
#22400=CARTESIAN_POINT('Ctrl Pts',(189.483535869631,-3.48068691059195,127.329594194778));
#22401=CARTESIAN_POINT('Ctrl Pts',(189.475775427117,-3.5775764982465,127.426648867953));
#22402=CARTESIAN_POINT('Ctrl Pts',(189.468014984603,-3.67032679795341,127.527682068888));
#22403=CARTESIAN_POINT('Ctrl Pts',(189.460254542089,-3.75861323503234,127.632293529382));
#22404=CARTESIAN_POINT('Ctrl Pts',(189.452481641823,-3.84704139733793,127.737072921479));
#22405=CARTESIAN_POINT('Ctrl Pts',(189.444708741558,-3.93099113791891,127.845441742504));
#22406=CARTESIAN_POINT('Ctrl Pts',(189.436935841292,-4.01017996607299,127.95696888087));
#22407=CARTESIAN_POINT('Ctrl Pts',(189.42944550553,-4.08649008085959,128.064441726837));
#22408=CARTESIAN_POINT('Ctrl Pts',(189.421955169768,-4.15837924792512,128.174846993079));
#22409=CARTESIAN_POINT('Ctrl Pts',(189.414464834006,-4.22563545189443,128.287777996194));
#22410=CARTESIAN_POINT('Ctrl Pts',(189.406414631678,-4.29791873357895,128.409150048544));
#22411=CARTESIAN_POINT('Ctrl Pts',(189.398364429349,-4.36506593948658,128.533801166826));
#22412=CARTESIAN_POINT('Ctrl Pts',(189.39031422702,-4.42677811181953,128.661274382433));
#22413=CARTESIAN_POINT('Ctrl Pts',(189.382275040237,-4.48840583991566,128.788573169269));
#22414=CARTESIAN_POINT('Ctrl Pts',(189.374235853453,-4.54461318938345,128.918686050171));
#22415=CARTESIAN_POINT('Ctrl Pts',(189.366196666669,-4.59514535868655,129.051128689086));
#22416=CARTESIAN_POINT('Ctrl Pts',(189.358170521655,-4.64559555092435,129.183356469644));
#22417=CARTESIAN_POINT('Ctrl Pts',(189.350144376642,-4.69038878678416,129.317906148175));
#22418=CARTESIAN_POINT('Ctrl Pts',(189.342118231628,-4.72931719504994,129.454271016427));
#22419=CARTESIAN_POINT('Ctrl Pts',(189.339612754859,-4.74146925838755,129.496839274155));
#22420=CARTESIAN_POINT('Ctrl Pts',(189.33710727809,-4.7530501596044,129.539584253036));
#22421=CARTESIAN_POINT('Ctrl Pts',(189.334601801321,-4.76405452823404,129.582490119308));
#22422=CARTESIAN_POINT('Ctrl Pts',(191.084784152919,-4.76405452823405,129.582490119308));
#22423=CARTESIAN_POINT('Ctrl Pts',(191.074632403862,-4.8083124628535,129.755051134682));
#22424=CARTESIAN_POINT('Ctrl Pts',(191.064480654806,-4.84321315731302,129.930105519379));
#22425=CARTESIAN_POINT('Ctrl Pts',(191.054328905749,-4.86852710622365,130.106774150907));
#22426=CARTESIAN_POINT('Ctrl Pts',(191.04439137085,-4.89330690026231,130.279714861098));
#22427=CARTESIAN_POINT('Ctrl Pts',(191.03445383595,-4.90890030782398,130.45420266127));
#22428=CARTESIAN_POINT('Ctrl Pts',(191.02451630105,-4.91513668305779,130.629390764849));
#22429=CARTESIAN_POINT('Ctrl Pts',(191.021297346049,-4.91715676263013,130.686137496098));
#22430=CARTESIAN_POINT('Ctrl Pts',(191.018078391047,-4.91819542437289,130.74295751366));
#22431=CARTESIAN_POINT('Ctrl Pts',(191.014859436046,-4.91824790535574,130.799821458629));
#22432=CARTESIAN_POINT('',(191.360141518956,-4.92180512007539,130.806071931916));
#22433=CARTESIAN_POINT('Ctrl Pts',(191.430300680169,-4.76051597898714,129.583432241587));
#22434=CARTESIAN_POINT('Ctrl Pts',(191.406914637273,-4.86678982625872,129.983174630901));
#22435=CARTESIAN_POINT('Ctrl Pts',(191.383528594377,-4.92378206388031,130.394832064542));
#22436=CARTESIAN_POINT('Ctrl Pts',(191.360142551482,-4.9256493795537,130.806055125649));
#22437=CARTESIAN_POINT('Ctrl Pts',(191.360140564008,-4.9182496968395,130.806087475454));
#22438=CARTESIAN_POINT('Ctrl Pts',(191.354763444185,-4.91821654842555,130.90049719961));
#22439=CARTESIAN_POINT('Ctrl Pts',(191.349386324361,-4.91546519350092,130.994855987655));
#22440=CARTESIAN_POINT('Ctrl Pts',(191.344009204538,-4.91000321302235,131.089056087516));
#22441=CARTESIAN_POINT('Ctrl Pts',(191.336234870419,-4.90210618588047,131.225252243524));
#22442=CARTESIAN_POINT('Ctrl Pts',(191.3284605363,-4.88852553889003,131.361335297868));
#22443=CARTESIAN_POINT('Ctrl Pts',(191.32068620218,-4.86926290974064,131.49679240361));
#22444=CARTESIAN_POINT('Ctrl Pts',(191.312921449233,-4.85002402006014,131.632082570575));
#22445=CARTESIAN_POINT('Ctrl Pts',(191.305156696286,-4.82511713569348,131.76674794049));
#22446=CARTESIAN_POINT('Ctrl Pts',(191.297391943339,-4.79459585657098,131.900277418538));
#22447=CARTESIAN_POINT('Ctrl Pts',(191.289634902454,-4.76410489161315,132.033674273226));
#22448=CARTESIAN_POINT('Ctrl Pts',(191.281877861569,-4.72801071553388,132.165937102515));
#22449=CARTESIAN_POINT('Ctrl Pts',(191.274120820684,-4.68641846168075,132.296562033099));
#22450=CARTESIAN_POINT('Ctrl Pts',(191.266369629444,-4.64485757286983,132.427088458406));
#22451=CARTESIAN_POINT('Ctrl Pts',(191.258618438204,-4.59780697707092,132.555979072473));
#22452=CARTESIAN_POINT('Ctrl Pts',(191.250867246964,-4.5454223270494,132.682742615792));
#22453=CARTESIAN_POINT('Ctrl Pts',(191.243119350187,-4.49305994190156,132.809452281224));
#22454=CARTESIAN_POINT('Ctrl Pts',(191.235371453409,-4.4353681606558,132.934036313446));
#22455=CARTESIAN_POINT('Ctrl Pts',(191.227623556632,-4.37255162571712,133.056021192106));
#22456=CARTESIAN_POINT('Ctrl Pts',(191.219877280548,-4.3097482306434,133.177980554159));
#22457=CARTESIAN_POINT('Ctrl Pts',(191.212131004464,-4.24182239299693,133.297341496706));
#22458=CARTESIAN_POINT('Ctrl Pts',(191.20438472838,-4.16902561416592,133.413653336087));
#22459=CARTESIAN_POINT('Ctrl Pts',(191.196638395115,-4.09622829796563,133.529966034056));
#22460=CARTESIAN_POINT('Ctrl Pts',(191.188892061849,-4.01856017625269,133.643229252539));
#22461=CARTESIAN_POINT('Ctrl Pts',(191.181145728584,-3.93631693673612,133.753019980067));
#22462=CARTESIAN_POINT('Ctrl Pts',(191.173397660581,-3.85405527941647,133.862835294467));
#22463=CARTESIAN_POINT('Ctrl Pts',(191.165649592578,-3.76721669987783,133.969176257649));
#22464=CARTESIAN_POINT('Ctrl Pts',(191.157901524575,-3.67613788924386,134.071652046528));
#22465=CARTESIAN_POINT('Ctrl Pts',(191.150145221833,-3.58496227896587,134.174236747894));
#22466=CARTESIAN_POINT('Ctrl Pts',(191.142388919091,-3.48953769537748,134.272947776186));
#22467=CARTESIAN_POINT('Ctrl Pts',(191.134632616349,-3.3902388873648,134.367429989484));
#22468=CARTESIAN_POINT('Ctrl Pts',(191.126872173835,-3.29088708058837,134.461962630784));
#22469=CARTESIAN_POINT('Ctrl Pts',(191.119111731321,-3.18765722326609,134.552261702453));
#22470=CARTESIAN_POINT('Ctrl Pts',(191.111351288807,-3.08095725723101,134.638012328613));
#22471=CARTESIAN_POINT('Ctrl Pts',(191.103578388541,-2.97408600693812,134.723900609291));
#22472=CARTESIAN_POINT('Ctrl Pts',(191.095805488276,-2.86373383115774,134.805225621522));
#22473=CARTESIAN_POINT('Ctrl Pts',(191.088032588011,-2.7503384963244,134.881715301443));
#22474=CARTESIAN_POINT('Ctrl Pts',(191.080542252248,-2.64106536753748,134.955424388834));
#22475=CARTESIAN_POINT('Ctrl Pts',(191.073051916486,-2.52896675349539,135.024643431626));
#22476=CARTESIAN_POINT('Ctrl Pts',(191.065561580724,-2.41445430827056,135.08917023478));
#22477=CARTESIAN_POINT('Ctrl Pts',(191.057787246605,-2.29560008888017,135.156143591289));
#22478=CARTESIAN_POINT('Ctrl Pts',(191.050012912486,-2.17376888976368,135.218274023238));
#22479=CARTESIAN_POINT('Ctrl Pts',(191.042238578367,-2.04939306878735,135.275285702166));
#22480=CARTESIAN_POINT('Ctrl Pts',(191.03447382542,-1.92517052989461,135.332227119295));
#22481=CARTESIAN_POINT('Ctrl Pts',(191.026709072473,-1.79840996087941,135.384062173901));
#22482=CARTESIAN_POINT('Ctrl Pts',(191.018944319526,-1.66957033235678,135.430559701891));
#22483=CARTESIAN_POINT('Ctrl Pts',(191.011187278641,-1.54085866916962,135.477011047882));
#22484=CARTESIAN_POINT('Ctrl Pts',(191.003430237756,-1.41007242119069,135.518135285236));
#22485=CARTESIAN_POINT('Ctrl Pts',(190.995673196871,-1.27769233844608,135.553748509787));
#22486=CARTESIAN_POINT('Ctrl Pts',(190.987922005631,-1.14541208455148,135.589334878129));
#22487=CARTESIAN_POINT('Ctrl Pts',(190.980170814391,-1.01154076426068,135.619418404572));
#22488=CARTESIAN_POINT('Ctrl Pts',(190.972419623151,-0.876575822233106,
135.643864506435));
#22489=CARTESIAN_POINT('Ctrl Pts',(190.964671726373,-0.741668243906204,
135.668300218052));
#22490=CARTESIAN_POINT('Ctrl Pts',(190.956923829596,-0.605668352230964,
135.687103201124));
#22491=CARTESIAN_POINT('Ctrl Pts',(190.949175932819,-0.469085147509697,
135.700189677785));
#22492=CARTESIAN_POINT('Ctrl Pts',(190.941429656735,-0.332530513050464,
135.713273417038));
#22493=CARTESIAN_POINT('Ctrl Pts',(190.933683380651,-0.195393197179081,
135.720642991066));
#22494=CARTESIAN_POINT('Ctrl Pts',(190.925937104567,-0.0581883154667574,
135.722266389584));
#22495=CARTESIAN_POINT('Ctrl Pts',(190.918190771302,0.0790175790607411,
135.723889800085));
#22496=CARTESIAN_POINT('Ctrl Pts',(190.910444438036,0.216290649486569,135.71976694581));
#22497=CARTESIAN_POINT('Ctrl Pts',(190.902698104771,0.353115177852348,135.709917949172));
#22498=CARTESIAN_POINT('Ctrl Pts',(190.894950036768,0.489970347122603,135.700066746919));
#22499=CARTESIAN_POINT('Ctrl Pts',(190.887201968765,0.626376384571554,135.684486878679));
#22500=CARTESIAN_POINT('Ctrl Pts',(190.879453900762,0.7618224898918,135.663250362806));
#22501=CARTESIAN_POINT('Ctrl Pts',(190.87169759802,0.897412548944634,135.641991276511));
#22502=CARTESIAN_POINT('Ctrl Pts',(190.863941295278,1.03204025099248,135.615063593716));
#22503=CARTESIAN_POINT('Ctrl Pts',(190.856184992537,1.16520424415458,135.58259063839));
#22504=CARTESIAN_POINT('Ctrl Pts',(190.848424550022,1.29843931094942,135.550100351271));
#22505=CARTESIAN_POINT('Ctrl Pts',(190.840664107508,1.43020873675926,135.512059002598));
#22506=CARTESIAN_POINT('Ctrl Pts',(190.832903664994,1.56002710506518,135.468639607288));
#22507=CARTESIAN_POINT('Ctrl Pts',(190.825130764729,1.69005386934062,135.42515051131));
#22508=CARTESIAN_POINT('Ctrl Pts',(190.817357864463,1.81812295188554,135.376266256074));
#22509=CARTESIAN_POINT('Ctrl Pts',(190.809584964198,1.94376883421616,135.322208089718));
#22510=CARTESIAN_POINT('Ctrl Pts',(190.802094628436,2.06484717224159,135.270115073873));
#22511=CARTESIAN_POINT('Ctrl Pts',(190.794604292674,2.1836751523785,135.21321791848));
#22512=CARTESIAN_POINT('Ctrl Pts',(190.787113956912,2.29986015313222,135.151753668411));
#22513=CARTESIAN_POINT('Ctrl Pts',(190.779339622793,2.42045034350282,135.087958982619));
#22514=CARTESIAN_POINT('Ctrl Pts',(190.771565288673,2.5385751745423,135.019041960452));
#22515=CARTESIAN_POINT('Ctrl Pts',(190.763790954554,2.65376888396502,134.945217264807));
#22516=CARTESIAN_POINT('Ctrl Pts',(190.756026201607,2.768820627436,134.871483551501));
#22517=CARTESIAN_POINT('Ctrl Pts',(190.74826144866,2.88094811077286,134.792854407899));
#22518=CARTESIAN_POINT('Ctrl Pts',(190.740496695713,2.98970876424912,134.709591029139));
#22519=CARTESIAN_POINT('Ctrl Pts',(190.732739654828,3.09836139511106,134.62641034874));
#22520=CARTESIAN_POINT('Ctrl Pts',(190.724982613943,3.20365354236057,134.538604829062));
#22521=CARTESIAN_POINT('Ctrl Pts',(190.717225573058,3.3051706250811,134.446479534021));
#22522=CARTESIAN_POINT('Ctrl Pts',(190.709474381818,3.40661115297993,134.354423711382));
#22523=CARTESIAN_POINT('Ctrl Pts',(190.701723190578,3.50428199439297,134.258054859062));
#22524=CARTESIAN_POINT('Ctrl Pts',(190.693971999338,3.59780104010722,134.157718746115));
#22525=CARTESIAN_POINT('Ctrl Pts',(190.68622410256,3.69128033773231,134.057425278691));
#22526=CARTESIAN_POINT('Ctrl Pts',(190.678476205783,3.78061108335151,133.953168189747));
#22527=CARTESIAN_POINT('Ctrl Pts',(190.670728309006,3.86544766517695,133.845330431668));
#22528=CARTESIAN_POINT('Ctrl Pts',(190.662982032922,3.95026650101836,133.737515230923));
#22529=CARTESIAN_POINT('Ctrl Pts',(190.655235756838,4.03059280135912,133.626121157924));
#22530=CARTESIAN_POINT('Ctrl Pts',(190.647489480754,4.10612120249017,133.511564291648));
#22531=CARTESIAN_POINT('Ctrl Pts',(190.639743147489,4.18165016115467,133.397006579739));
#22532=CARTESIAN_POINT('Ctrl Pts',(190.631996814223,4.25238093473435,133.279286354372));
#22533=CARTESIAN_POINT('Ctrl Pts',(190.624250480958,4.31805169463097,133.158848380328));
#22534=CARTESIAN_POINT('Ctrl Pts',(190.616502412955,4.38373716103891,133.038383435034));
#22535=CARTESIAN_POINT('Ctrl Pts',(190.608754344952,4.44436017178771,132.915199873166));
#22536=CARTESIAN_POINT('Ctrl Pts',(190.601006276949,4.49970521791473,132.789766373166));
#22537=CARTESIAN_POINT('Ctrl Pts',(190.593249974207,4.55510908541542,132.664199560951));
#22538=CARTESIAN_POINT('Ctrl Pts',(190.585493671465,4.60522362466958,132.536378392067));
#22539=CARTESIAN_POINT('Ctrl Pts',(190.577737368723,4.64988159868781,132.40679132767));
#22540=CARTESIAN_POINT('Ctrl Pts',(190.569976926209,4.69456340801143,132.277135098755));
#22541=CARTESIAN_POINT('Ctrl Pts',(190.562216483695,4.73378273728387,132.145711470748));
#22542=CARTESIAN_POINT('Ctrl Pts',(190.554456041181,4.76742276936732,132.013022357102));
#22543=CARTESIAN_POINT('Ctrl Pts',(190.546683140915,4.80111680341668,131.880120239111));
#22544=CARTESIAN_POINT('Ctrl Pts',(190.53891024065,4.82921356238978,131.745948958842));
#22545=CARTESIAN_POINT('Ctrl Pts',(190.531137340384,4.85164756449836,131.611019760201));
#22546=CARTESIAN_POINT('Ctrl Pts',(190.523647004622,4.8732660341224,131.480995577798));
#22547=CARTESIAN_POINT('Ctrl Pts',(190.51615666886,4.88962627167772,131.350267930446));
#22548=CARTESIAN_POINT('Ctrl Pts',(190.508666333098,4.90071548822044,131.219295270272));
#22549=CARTESIAN_POINT('Ctrl Pts',(190.500891998979,4.91222515577889,131.083356741879));
#22550=CARTESIAN_POINT('Ctrl Pts',(190.49311766486,4.91809266973481,130.946723642184));
#22551=CARTESIAN_POINT('Ctrl Pts',(190.485343330741,4.91824687616993,130.809903860727));
#22552=CARTESIAN_POINT('Ctrl Pts',(190.477578577794,4.91840089255939,130.673252697422));
#22553=CARTESIAN_POINT('Ctrl Pts',(190.469813824847,4.91285561076338,130.536415697335));
#22554=CARTESIAN_POINT('Ctrl Pts',(190.4620490719,4.90159156190185,130.399906389262));
#22555=CARTESIAN_POINT('Ctrl Pts',(190.454292031015,4.89033870065244,130.26353266416));
#22556=CARTESIAN_POINT('Ctrl Pts',(190.44653499013,4.8733784076575,130.127486370495));
#22557=CARTESIAN_POINT('Ctrl Pts',(190.438777949245,4.85074325071888,129.992281201434));
#22558=CARTESIAN_POINT('Ctrl Pts',(190.431026758005,4.82812516312819,129.857177991643));
#22559=CARTESIAN_POINT('Ctrl Pts',(190.423275566765,4.79984079389075,129.722915027962));
#22560=CARTESIAN_POINT('Ctrl Pts',(190.415524375525,4.76597450893968,129.590000686311));
#22561=CARTESIAN_POINT('Ctrl Pts',(190.407776478747,4.73212261806311,129.457142836802));
#22562=CARTESIAN_POINT('Ctrl Pts',(190.40002858197,4.6926936264518,129.325632847339));
#22563=CARTESIAN_POINT('Ctrl Pts',(190.392280685193,4.64782291118133,129.195968486027));
#22564=CARTESIAN_POINT('Ctrl Pts',(190.384534409109,4.60296158189719,129.066331247704));
#22565=CARTESIAN_POINT('Ctrl Pts',(190.376788133025,4.55266092085215,128.938539238861));
#22566=CARTESIAN_POINT('Ctrl Pts',(190.369041856941,4.49710593053007,128.813074271484));
#22567=CARTESIAN_POINT('Ctrl Pts',(190.361295523676,4.44155053011368,128.687608377954));
#22568=CARTESIAN_POINT('Ctrl Pts',(190.35354919041,4.38074088131789,128.564469917655));
#22569=CARTESIAN_POINT('Ctrl Pts',(190.345802857145,4.31490965259537,128.444119580629));
#22570=CARTESIAN_POINT('Ctrl Pts',(190.338054789142,4.24906368142562,128.32374229198));
#22571=CARTESIAN_POINT('Ctrl Pts',(190.330306721139,4.17819408019494,128.206154711989));
#22572=CARTESIAN_POINT('Ctrl Pts',(190.322558653136,4.10257867349393,128.091791486596));
#22573=CARTESIAN_POINT('Ctrl Pts',(190.314802350394,4.02688290183881,127.977306714606));
#22574=CARTESIAN_POINT('Ctrl Pts',(190.307046047653,3.94643146495612,127.866053469427));
#22575=CARTESIAN_POINT('Ctrl Pts',(190.299289744911,3.86154492337111,127.758436477459));
#22576=CARTESIAN_POINT('Ctrl Pts',(190.291529302397,3.77661307528294,127.650762047062));
#22577=CARTESIAN_POINT('Ctrl Pts',(190.283768859882,3.68724166038745,127.546728033458));
#22578=CARTESIAN_POINT('Ctrl Pts',(190.276008417368,3.59378981017076,127.446704014694));
#22579=CARTESIAN_POINT('Ctrl Pts',(190.268235517103,3.50018794274785,127.346519428494));
#22580=CARTESIAN_POINT('Ctrl Pts',(190.260462616837,3.40249282925593,127.250357975128));
#22581=CARTESIAN_POINT('Ctrl Pts',(190.252689716572,3.30109919916671,127.158551086096));
#22582=CARTESIAN_POINT('Ctrl Pts',(190.24519938081,3.2033914829259,127.070081608727));
#22583=CARTESIAN_POINT('Ctrl Pts',(190.237709045048,3.10224971882835,126.985655790931));
#22584=CARTESIAN_POINT('Ctrl Pts',(190.230218709286,2.99805270289559,126.905532196981));
#22585=CARTESIAN_POINT('Ctrl Pts',(190.222444375167,2.88990502543422,126.822370692614));
#22586=CARTESIAN_POINT('Ctrl Pts',(190.214670041048,2.7781232636251,126.743580659112));
#22587=CARTESIAN_POINT('Ctrl Pts',(190.206895706929,2.66309625889214,126.669496486984));
#22588=CARTESIAN_POINT('Ctrl Pts',(190.199130953982,2.54821101466232,126.595503616977));
#22589=CARTESIAN_POINT('Ctrl Pts',(190.191366201034,2.43008881080192,126.526205278626));
#22590=CARTESIAN_POINT('Ctrl Pts',(190.183601448087,2.30915117022697,126.461895426509));
#22591=CARTESIAN_POINT('Ctrl Pts',(190.175844407202,2.18833364662157,126.397649447844));
#22592=CARTESIAN_POINT('Ctrl Pts',(190.168087366317,2.06470659408811,126.33838227784));
#22593=CARTESIAN_POINT('Ctrl Pts',(190.160330325432,1.938719800928,126.284344179986));
#22594=CARTESIAN_POINT('Ctrl Pts',(190.152579134192,1.81282801538859,126.230346832682));
#22595=CARTESIAN_POINT('Ctrl Pts',(190.144827942952,1.68458038906157,126.181570862152));
#22596=CARTESIAN_POINT('Ctrl Pts',(190.137076751712,1.55445023485514,126.138220078549));
#22597=CARTESIAN_POINT('Ctrl Pts',(190.129328854935,1.42437538943564,126.094887720185));
#22598=CARTESIAN_POINT('Ctrl Pts',(190.121580958158,1.29241997767127,126.0569760859));
#22599=CARTESIAN_POINT('Ctrl Pts',(190.113833061381,1.1590759605821,126.024640334945));
#22600=CARTESIAN_POINT('Ctrl Pts',(190.106086785297,1.02575983618676,125.992311347931));
#22601=CARTESIAN_POINT('Ctrl Pts',(190.098340509213,0.891056063932395,125.965556016384));
#22602=CARTESIAN_POINT('Ctrl Pts',(190.090594233128,0.755470004251004,125.944479123622));
#22603=CARTESIAN_POINT('Ctrl Pts',(190.082847899863,0.619882943704145,125.923402075275));
#22604=CARTESIAN_POINT('Ctrl Pts',(190.075101566598,0.483413969059678,125.90800360941));
#22605=CARTESIAN_POINT('Ctrl Pts',(190.067355233332,0.346576434879642,125.898336989689));
#22606=CARTESIAN_POINT('Ctrl Pts',(190.059607165329,0.20970825688259,125.888668205195));
#22607=CARTESIAN_POINT('Ctrl Pts',(190.051859097326,0.0724717450308378,
125.884733848621));
#22608=CARTESIAN_POINT('Ctrl Pts',(190.044111029323,-0.0646172497580651,
125.886535115016));
#22609=CARTESIAN_POINT('Ctrl Pts',(190.036354726582,-0.201851944362056,
125.888338295818));
#22610=CARTESIAN_POINT('Ctrl Pts',(190.02859842384,-0.33893841715767,125.89588927164));
#22611=CARTESIAN_POINT('Ctrl Pts',(190.020842121098,-0.475362889567487,
125.909137110338));
#22612=CARTESIAN_POINT('Ctrl Pts',(190.013081678584,-0.611860175825985,
125.922392019806));
#22613=CARTESIAN_POINT('Ctrl Pts',(190.00532123607,-0.747694370636893,125.941349796762));
#22614=CARTESIAN_POINT('Ctrl Pts',(189.997560793555,-0.882360418181386,
125.965908059679));
#22615=CARTESIAN_POINT('Ctrl Pts',(189.98978789329,-1.01724264362044,125.990505745699));
#22616=CARTESIAN_POINT('Ctrl Pts',(189.982014993024,-1.15095259295001,126.02072179713));
#22617=CARTESIAN_POINT('Ctrl Pts',(189.974242092759,-1.28299806253933,126.056403263712));
#22618=CARTESIAN_POINT('Ctrl Pts',(189.966751756997,-1.4102433467065,126.090787619106));
#22619=CARTESIAN_POINT('Ctrl Pts',(189.959261421235,-1.53594277230061,126.130246832991));
#22620=CARTESIAN_POINT('Ctrl Pts',(189.951771085473,-1.65967405337326,126.17460197385));
#22621=CARTESIAN_POINT('Ctrl Pts',(189.943996623503,-1.78809875550871,126.220639610442));
#22622=CARTESIAN_POINT('Ctrl Pts',(189.936222161534,-1.91480987036354,126.272097770317));
#22623=CARTESIAN_POINT('Ctrl Pts',(189.928447699565,-2.03931586329617,126.328830048772));
#22624=CARTESIAN_POINT('Ctrl Pts',(189.92068284859,-2.16366793863765,126.385492193289));
#22625=CARTESIAN_POINT('Ctrl Pts',(189.912917997615,-2.28581996373698,126.447415322767));
#22626=CARTESIAN_POINT('Ctrl Pts',(189.905153146641,-2.40529676525213,126.514403679138));
#22627=CARTESIAN_POINT('Ctrl Pts',(189.897396037425,-2.5246544452745,126.581325246367));
#22628=CARTESIAN_POINT('Ctrl Pts',(189.88963892821,-2.6413418709589,126.653301800276));
#22629=CARTESIAN_POINT('Ctrl Pts',(189.881881818995,-2.75490535575686,126.730090186762));
#22630=CARTESIAN_POINT('Ctrl Pts',(189.874130589026,-2.86838276883409,126.806820374008));
#22631=CARTESIAN_POINT('Ctrl Pts',(189.866379359057,-2.97874063130287,126.888354916463));
#22632=CARTESIAN_POINT('Ctrl Pts',(189.858628129089,-3.08555162944487,126.974405760844));
#22633=CARTESIAN_POINT('Ctrl Pts',(189.850880345889,-3.19231513152848,127.060418340663));
#22634=CARTESIAN_POINT('Ctrl Pts',(189.84313256269,-3.29553460322023,127.150942982288));
#22635=CARTESIAN_POINT('Ctrl Pts',(189.835384779491,-3.39481360629566,127.245649665408));
#22636=CARTESIAN_POINT('Ctrl Pts',(189.827638659146,-3.49407130178288,127.340336022266));
#22637=CARTESIAN_POINT('Ctrl Pts',(189.819892538802,-3.58938992840192,127.439202365372));
#22638=CARTESIAN_POINT('Ctrl Pts',(189.812146418457,-3.68040819178631,127.541880180179));
#22639=CARTESIAN_POINT('Ctrl Pts',(189.804400283122,-3.77142663131764,127.644558193698));
#22640=CARTESIAN_POINT('Ctrl Pts',(189.796654147786,-3.85814443183768,127.751047400979));
#22641=CARTESIAN_POINT('Ctrl Pts',(189.788908012451,-3.94023932495192,127.860944723642));
#22642=CARTESIAN_POINT('Ctrl Pts',(189.781160184633,-4.02235215528922,127.970866058186));
#22643=CARTESIAN_POINT('Ctrl Pts',(189.773412356815,-4.0998398346877,128.084196676547));
#22644=CARTESIAN_POINT('Ctrl Pts',(189.765664528998,-4.17242255225989,128.200503265887));
#22645=CARTESIAN_POINT('Ctrl Pts',(189.757909049044,-4.24507695609062,128.31692472533));
#22646=CARTESIAN_POINT('Ctrl Pts',(189.750153569091,-4.31281651589305,128.436327693783));
#22647=CARTESIAN_POINT('Ctrl Pts',(189.742398089138,-4.37540644239081,128.55825253326));
#22648=CARTESIAN_POINT('Ctrl Pts',(189.734638486836,-4.43802963794533,128.68024218068));
#22649=CARTESIAN_POINT('Ctrl Pts',(189.726878884534,-4.49549758245539,128.804756015469));
#22650=CARTESIAN_POINT('Ctrl Pts',(189.719119282232,-4.54762346778534,128.931313939624));
#22651=CARTESIAN_POINT('Ctrl Pts',(189.711348586192,-4.59982387637704,129.058052800933));
#22652=CARTESIAN_POINT('Ctrl Pts',(189.703577890153,-4.64666683607839,129.186841222174));
#22653=CARTESIAN_POINT('Ctrl Pts',(189.695807194114,-4.68801507639694,129.317182852141));
#22654=CARTESIAN_POINT('Ctrl Pts',(189.690573763844,-4.71586240582347,129.404965700449));
#22655=CARTESIAN_POINT('Ctrl Pts',(189.685340333575,-4.74121849260404,129.493452762972));
#22656=CARTESIAN_POINT('Ctrl Pts',(189.680106903305,-4.76405452823404,129.582490119308));
#22657=CARTESIAN_POINT('Origin',(213.235140564004,0.,130.804360617566));
#22658=CARTESIAN_POINT('',(187.584954980304,-4.76405452823404,129.582490119308));
#22659=CARTESIAN_POINT('',(187.929867347344,-4.76405452823404,129.582490119308));
#22660=CARTESIAN_POINT('',(213.235140564004,-4.76405452823405,129.582490119308));
#22661=CARTESIAN_POINT('',(189.264859435947,-4.91824989634823,130.805370355446));
#22662=CARTESIAN_POINT('Ctrl Pts',(189.264859435947,-4.91824989634823,130.805370355446));
#22663=CARTESIAN_POINT('Ctrl Pts',(189.256607171556,-4.91821981685867,130.951882088204));
#22664=CARTESIAN_POINT('Ctrl Pts',(189.248354907165,-4.91163874752937,131.098225889341));
#22665=CARTESIAN_POINT('Ctrl Pts',(189.240102642774,-4.89857698727829,131.243822290761));
#22666=CARTESIAN_POINT('Ctrl Pts',(189.231428856725,-4.88484803865739,131.396855685653));
#22667=CARTESIAN_POINT('Ctrl Pts',(189.222755070677,-4.86395906746465,131.549062909309));
#22668=CARTESIAN_POINT('Ctrl Pts',(189.214081284629,-4.83605175230801,131.699785941922));
#22669=CARTESIAN_POINT('Ctrl Pts',(189.205787676123,-4.80936763247221,131.843902688434));
#22670=CARTESIAN_POINT('Ctrl Pts',(189.197494067618,-4.77626745182874,131.986662328151));
#22671=CARTESIAN_POINT('Ctrl Pts',(189.189200459113,-4.73692581437122,132.127507204926));
#22672=CARTESIAN_POINT('Ctrl Pts',(189.180893279678,-4.69751980172804,132.268582547836));
#22673=CARTESIAN_POINT('Ctrl Pts',(189.172586100243,-4.65185203318383,132.407736580464));
#22674=CARTESIAN_POINT('Ctrl Pts',(189.164278920808,-4.60014566525104,132.544430421043));
#22675=CARTESIAN_POINT('Ctrl Pts',(189.155952232729,-4.54831786968213,132.681445274498));
#22676=CARTESIAN_POINT('Ctrl Pts',(189.147625544649,-4.49042324122083,132.815988102357));
#22677=CARTESIAN_POINT('Ctrl Pts',(189.139298856569,-4.42673210121107,132.947541890022));
#22678=CARTESIAN_POINT('Ctrl Pts',(189.138204974444,-4.41836495704328,132.964824191878));
#22679=CARTESIAN_POINT('Ctrl Pts',(189.137111092319,-4.40989783749088,132.982054947649));
#22680=CARTESIAN_POINT('Ctrl Pts',(189.136017210193,-4.40133141131699,132.99923302166));
#22681=CARTESIAN_POINT('Ctrl Pts',(189.128242876074,-4.34044892888366,133.121319381593));
#22682=CARTESIAN_POINT('Ctrl Pts',(189.120468541955,-4.27438642335554,133.241064014106));
#22683=CARTESIAN_POINT('Ctrl Pts',(189.112694207836,-4.20334731880043,133.357996139725));
#22684=CARTESIAN_POINT('Ctrl Pts',(189.104929454889,-4.13239576359281,133.47478415695));
#22685=CARTESIAN_POINT('Ctrl Pts',(189.097164701942,-4.05648001367186,133.588766232983));
#22686=CARTESIAN_POINT('Ctrl Pts',(189.089399948995,-3.97585056850522,133.699493657586));
#22687=CARTESIAN_POINT('Ctrl Pts',(189.08164290811,-3.8953012056402,133.81011110615));
#22688=CARTESIAN_POINT('Ctrl Pts',(189.073885867225,-3.81004769299365,133.917480022228));
#22689=CARTESIAN_POINT('Ctrl Pts',(189.06612882634,-3.7203850578337,134.0211786236));
#22690=CARTESIAN_POINT('Ctrl Pts',(189.0583776351,-3.63079003796426,134.124799025051));
#22691=CARTESIAN_POINT('Ctrl Pts',(189.050626443859,-3.53679276837891,134.224754326412));
#22692=CARTESIAN_POINT('Ctrl Pts',(189.042875252619,-3.43872974898933,134.320654231006));
#22693=CARTESIAN_POINT('Ctrl Pts',(189.035127355842,-3.34070840899898,134.416513375581));
#22694=CARTESIAN_POINT('Ctrl Pts',(189.027379459065,-3.23862503510299,134.508320278819));
#22695=CARTESIAN_POINT('Ctrl Pts',(189.019631562288,-3.13285417567755,134.595720238657));
#22696=CARTESIAN_POINT('Ctrl Pts',(189.011885286204,-3.02710544123581,134.683101916308));
#22697=CARTESIAN_POINT('Ctrl Pts',(189.00413901012,-2.91767105670176,134.766078235263));
#22698=CARTESIAN_POINT('Ctrl Pts',(188.996392734036,-2.80495965334516,134.844333935003));
#22699=CARTESIAN_POINT('Ctrl Pts',(188.98864640077,-2.69224741797864,134.922590212409));
#22700=CARTESIAN_POINT('Ctrl Pts',(188.980900067505,-2.57625843666835,134.996125578092));
#22701=CARTESIAN_POINT('Ctrl Pts',(188.97315373424,-2.45743106294825,135.064667605725));
#22702=CARTESIAN_POINT('Ctrl Pts',(188.965405666237,-2.33857707866192,135.13322498287));
#22703=CARTESIAN_POINT('Ctrl Pts',(188.957657598234,-2.21688377571787,135.19678660152));
#22704=CARTESIAN_POINT('Ctrl Pts',(188.949909530231,-2.09281452597186,135.255125767782));
#22705=CARTESIAN_POINT('Ctrl Pts',(188.942153227489,-1.96861341395046,135.313526937605));
#22706=CARTESIAN_POINT('Ctrl Pts',(188.934396924747,-1.84203166516669,135.366694400722));
#22707=CARTESIAN_POINT('Ctrl Pts',(188.926640622005,-1.71355358688341,135.414449246582));
#22708=CARTESIAN_POINT('Ctrl Pts',(188.918880179491,-1.5850069359812,135.46222958064));
#22709=CARTESIAN_POINT('Ctrl Pts',(188.911119736977,-1.45456231049509,135.504591420412));
#22710=CARTESIAN_POINT('Ctrl Pts',(188.903359294463,-1.3227186760497,135.541405937861));
#22711=CARTESIAN_POINT('Ctrl Pts',(188.895586394197,-1.19066339449785,135.578279553241));
#22712=CARTESIAN_POINT('Ctrl Pts',(188.887813493932,-1.05720499698669,135.609587961818));
#22713=CARTESIAN_POINT('Ctrl Pts',(188.880040593666,-0.922853008814749,
135.635253432214));
#22714=CARTESIAN_POINT('Ctrl Pts',(188.872550257904,-0.793385053824595,
135.659985898115));
#22715=CARTESIAN_POINT('Ctrl Pts',(188.865059922142,-0.663087653395633,
135.679478527407));
#22716=CARTESIAN_POINT('Ctrl Pts',(188.85756958638,-0.532418820732127,135.693707533242));
#22717=CARTESIAN_POINT('Ctrl Pts',(188.849795252261,-0.396795639562776,
135.708476036158));
#22718=CARTESIAN_POINT('Ctrl Pts',(188.842020918142,-0.260342690980689,
135.717620678069));
#22719=CARTESIAN_POINT('Ctrl Pts',(188.834246584023,-0.123566010769087,
135.721058137597));
#22720=CARTESIAN_POINT('Ctrl Pts',(188.826481831076,0.0130421044082147,
135.724491360764));
#22721=CARTESIAN_POINT('Ctrl Pts',(188.818717078129,0.149972770293301,135.722231386573));
#22722=CARTESIAN_POINT('Ctrl Pts',(188.810952325181,0.28671307317168,135.714246428476));
#22723=CARTESIAN_POINT('Ctrl Pts',(188.803195284296,0.423317563653494,135.706269401151));
#22724=CARTESIAN_POINT('Ctrl Pts',(188.795438243411,0.559731679614168,135.692578728228));
#22725=CARTESIAN_POINT('Ctrl Pts',(188.787681202526,0.695441094281352,135.673194640911));
#22726=CARTESIAN_POINT('Ctrl Pts',(188.779930011286,0.8310481694232,135.653825171285));
#22727=CARTESIAN_POINT('Ctrl Pts',(188.772178820046,0.965951215561337,135.628770888172));
#22728=CARTESIAN_POINT('Ctrl Pts',(188.764427628806,1.09963997862434,135.598103933589));
#22729=CARTESIAN_POINT('Ctrl Pts',(188.756679732029,1.23327192039691,135.567450013279));
#22730=CARTESIAN_POINT('Ctrl Pts',(188.748931835252,1.36569022531323,135.531188253377));
#22731=CARTESIAN_POINT('Ctrl Pts',(188.741183938475,1.49639401993704,135.489442046911));
#22732=CARTESIAN_POINT('Ctrl Pts',(188.733437662391,1.62707047414466,135.447704572852));
#22733=CARTESIAN_POINT('Ctrl Pts',(188.725691386307,1.75603275921754,135.400485053005));
#22734=CARTESIAN_POINT('Ctrl Pts',(188.717945110223,1.88279476236884,135.34795687442));
#22735=CARTESIAN_POINT('Ctrl Pts',(188.710198776957,2.00955770124844,135.295428308083));
#22736=CARTESIAN_POINT('Ctrl Pts',(188.702452443692,2.13411996461381,135.237591154481));
#22737=CARTESIAN_POINT('Ctrl Pts',(188.694706110426,2.25601541168853,135.174666959772));
#22738=CARTESIAN_POINT('Ctrl Pts',(188.686958042423,2.3779381564034,135.111728673626));
#22739=CARTESIAN_POINT('Ctrl Pts',(188.679209974421,2.4971925490977,135.043701258784));
#22740=CARTESIAN_POINT('Ctrl Pts',(188.671461906418,2.61333740197348,134.970852029527));
#22741=CARTESIAN_POINT('Ctrl Pts',(188.663705603676,2.72960569498105,134.897925375242));
#22742=CARTESIAN_POINT('Ctrl Pts',(188.655949300934,2.84275751463042,134.820166877511));
#22743=CARTESIAN_POINT('Ctrl Pts',(188.648192998192,2.95238055850332,134.737887292227));
#22744=CARTESIAN_POINT('Ctrl Pts',(188.640432555678,3.06206211149548,134.655563791851));
#22745=CARTESIAN_POINT('Ctrl Pts',(188.632672113164,3.1682108334075,134.568714643188));
#22746=CARTESIAN_POINT('Ctrl Pts',(188.62491167065,3.27044863445584,134.477690005449));
#22747=CARTESIAN_POINT('Ctrl Pts',(188.617138770384,3.37285055669868,134.386519246881));
#22748=CARTESIAN_POINT('Ctrl Pts',(188.609365870119,3.47132873129138,134.291159876902));
#22749=CARTESIAN_POINT('Ctrl Pts',(188.601592969853,3.5655423497568,134.191998557871));
#22750=CARTESIAN_POINT('Ctrl Pts',(188.594102634091,3.65633106588129,134.096442002558));
#22751=CARTESIAN_POINT('Ctrl Pts',(188.586612298329,3.74315969458697,133.997355351629));
#22752=CARTESIAN_POINT('Ctrl Pts',(188.579121962567,3.82576065600049,133.895111087193));
#22753=CARTESIAN_POINT('Ctrl Pts',(188.571347628448,3.91149345797192,133.788990200394));
#22754=CARTESIAN_POINT('Ctrl Pts',(188.563573294329,3.99294325595813,133.679131372527));
#22755=CARTESIAN_POINT('Ctrl Pts',(188.55579896021,4.06976642462402,133.565915308588));
#22756=CARTESIAN_POINT('Ctrl Pts',(188.548034207263,4.14649491560041,133.452838773329));
#22757=CARTESIAN_POINT('Ctrl Pts',(188.540269454316,4.21860790493604,133.336413554789));
#22758=CARTESIAN_POINT('Ctrl Pts',(188.532504701369,4.28580140731598,133.217054000395));
#22759=CARTESIAN_POINT('Ctrl Pts',(188.524747660484,4.35292817216208,133.097812995594));
#22760=CARTESIAN_POINT('Ctrl Pts',(188.516990619599,4.41514498306898,132.97564379326));
#22761=CARTESIAN_POINT('Ctrl Pts',(188.509233578714,4.47219085493765,132.850990046533));
#22762=CARTESIAN_POINT('Ctrl Pts',(188.501482387474,4.52919370807062,132.726430302165));
#22763=CARTESIAN_POINT('Ctrl Pts',(188.493731196234,4.58103322174094,132.599390096789));
#22764=CARTESIAN_POINT('Ctrl Pts',(188.485980004993,4.6274942862818,132.470337716127));
#22765=CARTESIAN_POINT('Ctrl Pts',(188.478232108216,4.67393560363083,132.341340186169));
#22766=CARTESIAN_POINT('Ctrl Pts',(188.470484211439,4.71500288634316,132.210332548992));
#22767=CARTESIAN_POINT('Ctrl Pts',(188.462736314662,4.75052921414137,132.077802900549));
#22768=CARTESIAN_POINT('Ctrl Pts',(188.454990038578,4.78604811059766,131.945300974451));
#22769=CARTESIAN_POINT('Ctrl Pts',(188.447243762494,4.81602825638518,131.81127804774));
#22770=CARTESIAN_POINT('Ctrl Pts',(188.43949748641,4.84035277110316,131.676236820805));
#22771=CARTESIAN_POINT('Ctrl Pts',(188.431751153145,4.86467746537918,131.541194597026));
#22772=CARTESIAN_POINT('Ctrl Pts',(188.424004819879,4.88334637597157,131.405134442797));
#22773=CARTESIAN_POINT('Ctrl Pts',(188.416258486614,4.89629393546274,131.268568286666));
#22774=CARTESIAN_POINT('Ctrl Pts',(188.408510418611,4.90924439447009,131.13197154749));
#22775=CARTESIAN_POINT('Ctrl Pts',(188.400762350608,4.91647091592922,130.994868970073));
#22776=CARTESIAN_POINT('Ctrl Pts',(188.393014282605,4.91795992613311,130.857776228101));
#22777=CARTESIAN_POINT('Ctrl Pts',(188.385257979863,4.91945051887476,130.720537782331));
#22778=CARTESIAN_POINT('Ctrl Pts',(188.377501677121,4.91519141490565,130.583309584453));
#22779=CARTESIAN_POINT('Ctrl Pts',(188.36974537438,4.90522120243238,130.44660648732));
#22780=CARTESIAN_POINT('Ctrl Pts',(188.361984931865,4.89524566855652,130.309830427629));
#22781=CARTESIAN_POINT('Ctrl Pts',(188.354224489351,4.87955299711073,130.173580415335));
#22782=CARTESIAN_POINT('Ctrl Pts',(188.346464046837,4.85823342019293,130.03836381769));
#22783=CARTESIAN_POINT('Ctrl Pts',(188.338691146572,4.8368796191976,129.902930158358));
#22784=CARTESIAN_POINT('Ctrl Pts',(188.330918246306,4.80988093934744,129.768533612271));
#22785=CARTESIAN_POINT('Ctrl Pts',(188.323145346041,4.77737847532777,129.635669911701));
#22786=CARTESIAN_POINT('Ctrl Pts',(188.315655010279,4.74605755774389,129.50763614131));
#22787=CARTESIAN_POINT('Ctrl Pts',(188.308164674517,4.70962614676043,129.381026001712));
#22788=CARTESIAN_POINT('Ctrl Pts',(188.300674338755,4.66825298866656,129.256265951111));
#22789=CARTESIAN_POINT('Ctrl Pts',(188.292900004636,4.62531115470858,129.126775585272));
#22790=CARTESIAN_POINT('Ctrl Pts',(188.285125670517,4.57690941679345,128.998868183534));
#22791=CARTESIAN_POINT('Ctrl Pts',(188.277351336398,4.52318233493014,128.873038627975));
#22792=CARTESIAN_POINT('Ctrl Pts',(188.269586583451,4.46952146689349,128.747364146098));
#22793=CARTESIAN_POINT('Ctrl Pts',(188.261821830503,4.41054846539562,128.623762771359));
#22794=CARTESIAN_POINT('Ctrl Pts',(188.254057077556,4.34644762117504,128.502714220119));
#22795=CARTESIAN_POINT('Ctrl Pts',(188.246300036671,4.28241044281667,128.381785896006));
#22796=CARTESIAN_POINT('Ctrl Pts',(188.238542995786,4.21325573890659,128.263405692909));
#22797=CARTESIAN_POINT('Ctrl Pts',(188.230785954901,4.13921569857526,128.148032990339));
#22798=CARTESIAN_POINT('Ctrl Pts',(188.223034763661,4.06523149241429,128.032747291222));
#22799=CARTESIAN_POINT('Ctrl Pts',(188.215283572421,3.98636949305475,127.920464906065));
#22800=CARTESIAN_POINT('Ctrl Pts',(188.207532381181,3.90290741050956,127.811619932594));
#22801=CARTESIAN_POINT('Ctrl Pts',(188.199784484404,3.81948080157582,127.702821221139));
#22802=CARTESIAN_POINT('Ctrl Pts',(188.192036587627,3.73145823551986,127.597457325174));
#22803=CARTESIAN_POINT('Ctrl Pts',(188.18428869085,3.63916013680356,127.495932507239));
#22804=CARTESIAN_POINT('Ctrl Pts',(188.176542414766,3.54688134485975,127.394428926108));
#22805=CARTESIAN_POINT('Ctrl Pts',(188.168796138682,3.45032906199472,127.296763114795));
#22806=CARTESIAN_POINT('Ctrl Pts',(188.161049862597,3.34986304757216,127.203305129933));
#22807=CARTESIAN_POINT('Ctrl Pts',(188.153303529332,3.24939629153235,127.109846455185));
#22808=CARTESIAN_POINT('Ctrl Pts',(188.145557196067,3.14501603254435,127.020595935158));
#22809=CARTESIAN_POINT('Ctrl Pts',(188.137810862801,3.03711752980305,126.935885443461));
#22810=CARTESIAN_POINT('Ctrl Pts',(188.130062794798,2.92919486394014,126.851155981437));
#22811=CARTESIAN_POINT('Ctrl Pts',(188.122314726795,2.81775269397828,126.770968812257));
#22812=CARTESIAN_POINT('Ctrl Pts',(188.114566658792,2.703217533875,126.695614090089));
#22813=CARTESIAN_POINT('Ctrl Pts',(188.106810356051,2.58856064444062,126.620179280026));
#22814=CARTESIAN_POINT('Ctrl Pts',(188.099054053309,2.47080452533179,126.549587391881));
#22815=CARTESIAN_POINT('Ctrl Pts',(188.091297750567,2.35040319470329,126.484084250847));
#22816=CARTESIAN_POINT('Ctrl Pts',(188.083537308053,2.22993760225931,126.418546148814));
#22817=CARTESIAN_POINT('Ctrl Pts',(188.075776865539,2.10682433588469,126.358102378005));
#22818=CARTESIAN_POINT('Ctrl Pts',(188.068016423024,1.98153903066888,126.302951267992));
#22819=CARTESIAN_POINT('Ctrl Pts',(188.060243522759,1.85605260635887,126.24771162452));
#22820=CARTESIAN_POINT('Ctrl Pts',(188.052470622493,1.72838753988925,126.197781762542));
#22821=CARTESIAN_POINT('Ctrl Pts',(188.044697722228,1.59903716998487,126.153310930505));
#22822=CARTESIAN_POINT('Ctrl Pts',(188.037207386466,1.47438901184074,126.110456725228));
#22823=CARTESIAN_POINT('Ctrl Pts',(188.029717050704,1.34817624808902,126.072671630003));
#22824=CARTESIAN_POINT('Ctrl Pts',(188.022226714942,1.22084888158536,126.040044184873));
#22825=CARTESIAN_POINT('Ctrl Pts',(188.014452380823,1.08869385928014,126.006179660243));
#22826=CARTESIAN_POINT('Ctrl Pts',(188.006678046704,0.954919418051348,125.977764338209));
#22827=CARTESIAN_POINT('Ctrl Pts',(187.998903712585,0.820014649177363,125.954952505473));
#22828=CARTESIAN_POINT('Ctrl Pts',(187.991138959638,0.685276138374253,125.932168786282));
#22829=CARTESIAN_POINT('Ctrl Pts',(187.98337420669,0.54941045342816,125.914974880467));
#22830=CARTESIAN_POINT('Ctrl Pts',(187.975609453743,0.412920806945482,125.903475037419));
#22831=CARTESIAN_POINT('Ctrl Pts',(187.967852412858,0.276566723903787,125.891986616178));
#22832=CARTESIAN_POINT('Ctrl Pts',(187.960095371973,0.139590299674858,125.886181035769));
#22833=CARTESIAN_POINT('Ctrl Pts',(187.952338331088,0.00250352715083474,
125.886111254749));
#22834=CARTESIAN_POINT('Ctrl Pts',(187.944587139848,-0.134479867171555,
125.886041526351));
#22835=CARTESIAN_POINT('Ctrl Pts',(187.936835948608,-0.271573054772387,
125.891698988073));
#22836=CARTESIAN_POINT('Ctrl Pts',(187.929084757368,-0.408260707894014,
125.90308463504));
#22837=CARTESIAN_POINT('Ctrl Pts',(187.921336860591,-0.544890265116803,
125.914465442803));
#22838=CARTESIAN_POINT('Ctrl Pts',(187.913588963814,-0.681114241876996,
125.931569561129));
#22839=CARTESIAN_POINT('Ctrl Pts',(187.905841067037,-0.816419323400283,
125.954345921621));
#22840=CARTESIAN_POINT('Ctrl Pts',(187.898094790952,-0.951696102017355,
125.977117517791));
#22841=CARTESIAN_POINT('Ctrl Pts',(187.890348514868,-1.08605398242313,126.005558931233));
#22842=CARTESIAN_POINT('Ctrl Pts',(187.882602238784,-1.21898716676947,126.039567510856));
#22843=CARTESIAN_POINT('Ctrl Pts',(187.874855905519,-1.35192133239828,126.073576341522));
#22844=CARTESIAN_POINT('Ctrl Pts',(187.867109572253,-1.48343040221569,126.113152323472));
#22845=CARTESIAN_POINT('Ctrl Pts',(187.859363238988,-1.61302151430496,126.158142299741));
#22846=CARTESIAN_POINT('Ctrl Pts',(187.851615170985,-1.74264164742518,126.203142351204));
#22847=CARTESIAN_POINT('Ctrl Pts',(187.843867102982,-1.87034259886549,126.253558681377));
#22848=CARTESIAN_POINT('Ctrl Pts',(187.836119034979,-1.99564971249439,126.309189287403));
#22849=CARTESIAN_POINT('Ctrl Pts',(187.828362732237,-2.12109000401499,126.364879018299));
#22850=CARTESIAN_POINT('Ctrl Pts',(187.820606429495,-2.24413101750869,126.425793936487));
#22851=CARTESIAN_POINT('Ctrl Pts',(187.812850126754,-2.36432052537678,126.491684938155));
#22852=CARTESIAN_POINT('Ctrl Pts',(187.805089684239,-2.48457418200409,126.557611107835));
#22853=CARTESIAN_POINT('Ctrl Pts',(187.797329241725,-2.60197296592657,126.628518451041));
#22854=CARTESIAN_POINT('Ctrl Pts',(187.789568799211,-2.71609292447437,126.70411400448));
#22855=CARTESIAN_POINT('Ctrl Pts',(187.781795898946,-2.83039607851072,126.779830910613));
#22856=CARTESIAN_POINT('Ctrl Pts',(187.77402299868,-2.94140957229936,126.860250836692));
#22857=CARTESIAN_POINT('Ctrl Pts',(187.766250098415,-3.04874117726313,126.945039395309));
#22858=CARTESIAN_POINT('Ctrl Pts',(187.758759762653,-3.15217100803496,127.026745676251));
#22859=CARTESIAN_POINT('Ctrl Pts',(187.751269426891,-3.25218176050425,127.112508282006));
#22860=CARTESIAN_POINT('Ctrl Pts',(187.743779091128,-3.34845570588935,127.201996470482));
#22861=CARTESIAN_POINT('Ctrl Pts',(187.736122099101,-3.44687169893981,127.293475726888));
#22862=CARTESIAN_POINT('Ctrl Pts',(187.728465107073,-3.54171430929935,127.389156956171));
#22863=CARTESIAN_POINT('Ctrl Pts',(187.720808115045,-3.63259513007057,127.488725582842));
#22864=CARTESIAN_POINT('Ctrl Pts',(187.713159991201,-3.72337069438334,127.588178891002));
#22865=CARTESIAN_POINT('Ctrl Pts',(187.705511867358,-3.81019332122524,127.691510351903));
#22866=CARTESIAN_POINT('Ctrl Pts',(187.697863743514,-3.8927084393723,127.798365928858));
#22867=CARTESIAN_POINT('Ctrl Pts',(187.690222703422,-3.97514713137943,127.905122535353));
#22868=CARTESIAN_POINT('Ctrl Pts',(187.68258166333,-4.05328600255709,128.015396450587));
#22869=CARTESIAN_POINT('Ctrl Pts',(187.674940623237,-4.12680846773921,128.1287980724));
#22870=CARTESIAN_POINT('Ctrl Pts',(187.667304890307,-4.2002798671441,128.242120929961));
#22871=CARTESIAN_POINT('Ctrl Pts',(187.659669157377,-4.26914101941565,128.358566835824));
#22872=CARTESIAN_POINT('Ctrl Pts',(187.652033424447,-4.33311701410075,128.47771496242));
#22873=CARTESIAN_POINT('Ctrl Pts',(187.6444009553,-4.39706566317769,128.596812160883));
#22874=CARTESIAN_POINT('Ctrl Pts',(187.636768486153,-4.45613311784616,128.718608927462));
#22875=CARTESIAN_POINT('Ctrl Pts',(187.629136017006,-4.5100892971886,128.842657889351));
#22876=CARTESIAN_POINT('Ctrl Pts',(187.621503159863,-4.56404821939219,128.966713157266));
#22877=CARTESIAN_POINT('Ctrl Pts',(187.613870302719,-4.61289517533641,129.093020483825));
#22878=CARTESIAN_POINT('Ctrl Pts',(187.606237445576,-4.65644742360532,129.221110651926));
#22879=CARTESIAN_POINT('Ctrl Pts',(187.599143290485,-4.69692589686468,129.340160635574));
#22880=CARTESIAN_POINT('Ctrl Pts',(187.592049135395,-4.73283104437265,129.460750229615));
#22881=CARTESIAN_POINT('Ctrl Pts',(187.584954980304,-4.76405452823404,129.582490119308));
#22882=CARTESIAN_POINT('Ctrl Pts',(189.334601801321,-4.76405452823404,129.582490119308));
#22883=CARTESIAN_POINT('Ctrl Pts',(189.326589951379,-4.79924357938049,129.71969169566));
#22884=CARTESIAN_POINT('Ctrl Pts',(189.318578101437,-4.82853357011572,129.858539643826));
#22885=CARTESIAN_POINT('Ctrl Pts',(189.310566251495,-4.85178106031378,129.99850479592));
#22886=CARTESIAN_POINT('Ctrl Pts',(189.302564129565,-4.8750003233392,130.138300001905));
#22887=CARTESIAN_POINT('Ctrl Pts',(189.294562007635,-4.89219165463957,130.279209361064));
#22888=CARTESIAN_POINT('Ctrl Pts',(189.286559885705,-4.90326234654455,130.420692240633));
#22889=CARTESIAN_POINT('Ctrl Pts',(189.279326402467,-4.91326965023596,130.548585072909));
#22890=CARTESIAN_POINT('Ctrl Pts',(189.272092919229,-4.91827626236202,130.676946189752));
#22891=CARTESIAN_POINT('Ctrl Pts',(189.264859435991,-4.91824989634839,130.805370354665));
#22892=CARTESIAN_POINT('',(189.610140563969,-4.91824791299378,130.799829742121));
#22893=CARTESIAN_POINT('Ctrl Pts',(189.680106903305,-4.76405452823404,129.582490119308));
#22894=CARTESIAN_POINT('Ctrl Pts',(189.67784575609,-4.77392102796961,129.620959452032));
#22895=CARTESIAN_POINT('Ctrl Pts',(189.675584608875,-4.78331723303707,129.659531493429));
#22896=CARTESIAN_POINT('Ctrl Pts',(189.67332346166,-4.79224143417708,129.69819376801));
#22897=CARTESIAN_POINT('Ctrl Pts',(189.662792978718,-4.83380270327263,129.87824945843));
#22898=CARTESIAN_POINT('Ctrl Pts',(189.652262495776,-4.86523011335524,130.060725185327));
#22899=CARTESIAN_POINT('Ctrl Pts',(189.641732012834,-4.88629864809003,130.244656602775));
#22900=CARTESIAN_POINT('Ctrl Pts',(189.631201529892,-4.90736718282481,130.428588020222));
#22901=CARTESIAN_POINT('Ctrl Pts',(189.62067104695,-4.91807669726267,130.613975751142));
#22902=CARTESIAN_POINT('Ctrl Pts',(189.610140564008,-4.91824791299315,130.799829741432));
#22903=CARTESIAN_POINT('Ctrl Pts',(189.610140563969,-4.91824791299378,130.799829742121));
#22904=CARTESIAN_POINT('Ctrl Pts',(189.602485915437,-4.91837237034752,130.934927722133));
#22905=CARTESIAN_POINT('Ctrl Pts',(189.594831266904,-4.91292619023357,131.070187999666));
#22906=CARTESIAN_POINT('Ctrl Pts',(189.587176618372,-4.90189607666226,131.205107315747));
#22907=CARTESIAN_POINT('Ctrl Pts',(189.57916408585,-4.89035026324752,131.346334624011));
#22908=CARTESIAN_POINT('Ctrl Pts',(189.571151553328,-4.87268569848204,131.487187873076));
#22909=CARTESIAN_POINT('Ctrl Pts',(189.563139020806,-4.84894837207892,131.627089459538));
#22910=CARTESIAN_POINT('Ctrl Pts',(189.555493068658,-4.82629704912697,131.760590426017));
#22911=CARTESIAN_POINT('Ctrl Pts',(189.547847116509,-4.79811638583712,131.893224434576));
#22912=CARTESIAN_POINT('Ctrl Pts',(189.54020116436,-4.76449933419752,132.02449551049));
#22913=CARTESIAN_POINT('Ctrl Pts',(189.532556401308,-4.73088751067271,132.155746171162));
#22914=CARTESIAN_POINT('Ctrl Pts',(189.524911638256,-4.69184107950793,132.285633931062));
#22915=CARTESIAN_POINT('Ctrl Pts',(189.517266875204,-4.64750370934258,132.413674861009));
#22916=CARTESIAN_POINT('Ctrl Pts',(189.509621542448,-4.60316303506545,132.541725332827));
#22917=CARTESIAN_POINT('Ctrl Pts',(189.501976209692,-4.55353076963928,132.667928320977));
#22918=CARTESIAN_POINT('Ctrl Pts',(189.494330876936,-4.49879968865441,132.791817390395));
#22919=CARTESIAN_POINT('Ctrl Pts',(189.486683215447,-4.44405193682891,132.915744195865));
#22920=CARTESIAN_POINT('Ctrl Pts',(189.479035553957,-4.38420244384357,133.037355313473));
#22921=CARTESIAN_POINT('Ctrl Pts',(189.471387892468,-4.31949088284538,133.156207035918));
#22922=CARTESIAN_POINT('Ctrl Pts',(189.46373199972,-4.25470967211568,133.275186679718));
#22923=CARTESIAN_POINT('Ctrl Pts',(189.456076106972,-4.18505614095032,133.39140064717));
#22924=CARTESIAN_POINT('Ctrl Pts',(189.448420214224,-4.11081455193053,133.504432242937));
#22925=CARTESIAN_POINT('Ctrl Pts',(189.440759493914,-4.0365261485234,133.617535112838));
#22926=CARTESIAN_POINT('Ctrl Pts',(189.433098773603,-3.95764416228724,133.727451290957));
#22927=CARTESIAN_POINT('Ctrl Pts',(189.425438053292,-3.87449360985302,133.833796593075));
#22928=CARTESIAN_POINT('Ctrl Pts',(189.417766480026,-3.79122525788974,133.940292554763));
#22929=CARTESIAN_POINT('Ctrl Pts',(189.41009490676,-3.70367653135893,134.043207240323));
#22930=CARTESIAN_POINT('Ctrl Pts',(189.402423333494,-3.61220996172295,134.142192586813));
#22931=CARTESIAN_POINT('Ctrl Pts',(189.399907501612,-3.58221422237703,134.174654049665));
#22932=CARTESIAN_POINT('Ctrl Pts',(189.397391669729,-3.55179740394281,134.206693246693));
#22933=CARTESIAN_POINT('Ctrl Pts',(189.394875837847,-3.52097305098158,134.238298857657));
#22934=CARTESIAN_POINT('Ctrl Pts',(189.387101503728,-3.42572073281059,134.335965391495));
#22935=CARTESIAN_POINT('Ctrl Pts',(189.379327169609,-3.32625077645834,134.429820383029));
#22936=CARTESIAN_POINT('Ctrl Pts',(189.37155283549,-3.22290063708545,134.519477647482));
#22937=CARTESIAN_POINT('Ctrl Pts',(189.363788082543,-3.11967786752259,134.609024417371));
#22938=CARTESIAN_POINT('Ctrl Pts',(189.356023329596,-3.01258472214135,134.694383499813));
#22939=CARTESIAN_POINT('Ctrl Pts',(189.348258576648,-2.90199674489212,134.775204099137));
#22940=CARTESIAN_POINT('Ctrl Pts',(189.340501535763,-2.79151860518099,134.855944426302));
#22941=CARTESIAN_POINT('Ctrl Pts',(189.332744494878,-2.67755285489058,134.932155011651));
#22942=CARTESIAN_POINT('Ctrl Pts',(189.324987453993,-2.56050921726351,135.003524297492));
#22943=CARTESIAN_POINT('Ctrl Pts',(189.317236262753,-2.44355384315431,135.074839763199));
#22944=CARTESIAN_POINT('Ctrl Pts',(189.309485071513,-2.32352553408762,135.141320993499));
#22945=CARTESIAN_POINT('Ctrl Pts',(189.301733880273,-2.20086389176815,135.202699075713));
#22946=CARTESIAN_POINT('Ctrl Pts',(189.293985983496,-2.07825438391844,135.264051070604));
#22947=CARTESIAN_POINT('Ctrl Pts',(189.286238086719,-1.95301411779677,135.320304056746));
#22948=CARTESIAN_POINT('Ctrl Pts',(189.278490189942,-1.82560805826677,135.371234633793));
#22949=CARTESIAN_POINT('Ctrl Pts',(189.270743913858,-1.69822864933794,135.422154557262));
#22950=CARTESIAN_POINT('Ctrl Pts',(189.262997637774,-1.56868471092015,135.467754141087));
#22951=CARTESIAN_POINT('Ctrl Pts',(189.255251361689,-1.43746162023923,135.507857949641));
#22952=CARTESIAN_POINT('Ctrl Pts',(189.247505028424,-1.3062375608992,135.547962054233));
#22953=CARTESIAN_POINT('Ctrl Pts',(189.239758695159,-1.1733346984564,135.582570188336));
#22954=CARTESIAN_POINT('Ctrl Pts',(189.232012361893,-1.03925363421513,135.611556780224));
#22955=CARTESIAN_POINT('Ctrl Pts',(189.22426429389,-0.905142543449059,135.640549863458));
#22956=CARTESIAN_POINT('Ctrl Pts',(189.216516225887,-0.76985310791742,135.663918816804));
#22957=CARTESIAN_POINT('Ctrl Pts',(189.208768157884,-0.633895788762408,
135.681589255993));
#22958=CARTESIAN_POINT('Ctrl Pts',(189.201011855143,-0.497793972550918,
135.699278475534));
#22959=CARTESIAN_POINT('Ctrl Pts',(189.193255552401,-0.361023243067375,
135.711257032039));
#22960=CARTESIAN_POINT('Ctrl Pts',(189.185499249659,-0.224099407142775,
135.717502435));
#22961=CARTESIAN_POINT('Ctrl Pts',(189.177738807145,-0.0871024908441983,
135.723751171321));
#22962=CARTESIAN_POINT('Ctrl Pts',(189.16997836463,0.0500473039532961,135.724260655423));
#22963=CARTESIAN_POINT('Ctrl Pts',(189.162217922116,0.186835504032796,135.719060563334));
#22964=CARTESIAN_POINT('Ctrl Pts',(189.154445021851,0.323843288674548,135.713852123596));
#22965=CARTESIAN_POINT('Ctrl Pts',(189.146672121585,0.46048792870308,135.702915823248));
#22966=CARTESIAN_POINT('Ctrl Pts',(189.13889922132,0.596260497125072,135.686333219094));
#22967=CARTESIAN_POINT('Ctrl Pts',(189.131408885558,0.727097390693978,135.67035343437));
#22968=CARTESIAN_POINT('Ctrl Pts',(189.123918549796,0.857124211873021,135.649130783049));
#22969=CARTESIAN_POINT('Ctrl Pts',(189.116428214034,0.985897556969896,135.622782461869));
#22970=CARTESIAN_POINT('Ctrl Pts',(189.108653879915,1.11955338258629,135.595435136084));
#22971=CARTESIAN_POINT('Ctrl Pts',(189.100879545796,1.25228218617169,135.562479160128));
#22972=CARTESIAN_POINT('Ctrl Pts',(189.093105211677,1.38357665678069,135.523989702284));
#22973=CARTESIAN_POINT('Ctrl Pts',(189.08534045873,1.51470931868909,135.485547679256));
#22974=CARTESIAN_POINT('Ctrl Pts',(189.077575705783,1.64441079321712,135.441585852083));
#22975=CARTESIAN_POINT('Ctrl Pts',(189.069810952835,1.7721829553513,135.392230562896));
#22976=CARTESIAN_POINT('Ctrl Pts',(189.06205391195,1.89982821237275,135.342924294078));
#22977=CARTESIAN_POINT('Ctrl Pts',(189.054296871065,2.02554760802274,135.288235363609));
#22978=CARTESIAN_POINT('Ctrl Pts',(189.04653983018,2.14885755457138,135.228340078714));
#22979=CARTESIAN_POINT('Ctrl Pts',(189.03878863894,2.2720745121302,135.16848996132));
#22980=CARTESIAN_POINT('Ctrl Pts',(189.0310374477,2.39288528693343,135.103441474395));
#22981=CARTESIAN_POINT('Ctrl Pts',(189.02328625646,2.51082601966835,135.033419113432));
#22982=CARTESIAN_POINT('Ctrl Pts',(189.015538359683,2.62871662444556,134.963426513841));
#22983=CARTESIAN_POINT('Ctrl Pts',(189.007790462906,2.7437392778564,134.888464444029));
#22984=CARTESIAN_POINT('Ctrl Pts',(189.000042566129,2.85545470199736,134.808803338762));
#22985=CARTESIAN_POINT('Ctrl Pts',(188.992296290045,2.96714675767976,134.729158896881));
#22986=CARTESIAN_POINT('Ctrl Pts',(188.984550013961,3.07553264200004,134.644817601504));
#22987=CARTESIAN_POINT('Ctrl Pts',(188.976803737876,3.18020239775109,134.556092986997));
#22988=CARTESIAN_POINT('Ctrl Pts',(188.969057404611,3.28487292615045,134.467367717545));
#22989=CARTESIAN_POINT('Ctrl Pts',(188.961311071346,3.38582697300727,134.374259317201));
#22990=CARTESIAN_POINT('Ctrl Pts',(188.95356473808,3.48268830403982,134.277121081434));
#22991=CARTESIAN_POINT('Ctrl Pts',(188.945816670077,3.57957132649582,134.179961092233));
#22992=CARTESIAN_POINT('Ctrl Pts',(188.938068602074,3.67235953332192,134.078769748627));
#22993=CARTESIAN_POINT('Ctrl Pts',(188.930320534071,3.76071442620922,133.973936309516));
#22994=CARTESIAN_POINT('Ctrl Pts',(188.92256423133,3.8491632237282,133.868991452179));
#22995=CARTESIAN_POINT('Ctrl Pts',(188.914807928588,3.93316904266262,133.7603970663));
#22996=CARTESIAN_POINT('Ctrl Pts',(188.907051625846,4.01243415492057,133.648574958105));
#22997=CARTESIAN_POINT('Ctrl Pts',(188.899291183332,4.09174157335567,133.536693167084));
#22998=CARTESIAN_POINT('Ctrl Pts',(188.891530740818,4.16630303091852,133.421580549039));
#22999=CARTESIAN_POINT('Ctrl Pts',(188.883770298303,4.23586540955038,133.303685985475));
#23000=CARTESIAN_POINT('Ctrl Pts',(188.875997398038,4.30553945588784,133.185602167092));
#23001=CARTESIAN_POINT('Ctrl Pts',(188.868224497773,4.37019820233963,133.064727823987));
#23002=CARTESIAN_POINT('Ctrl Pts',(188.860451597507,4.42963517748233,132.941535214297));
#23003=CARTESIAN_POINT('Ctrl Pts',(188.852961261745,4.48691146886592,132.822820966272));
#23004=CARTESIAN_POINT('Ctrl Pts',(188.845470925983,4.53933892418261,132.701954357632));
#23005=CARTESIAN_POINT('Ctrl Pts',(188.837980590221,4.58677647383961,132.579371784159));
#23006=CARTESIAN_POINT('Ctrl Pts',(188.830206256102,4.63601263261018,132.452141455156));
#23007=CARTESIAN_POINT('Ctrl Pts',(188.822431921983,4.68002899709644,132.322659443626));
#23008=CARTESIAN_POINT('Ctrl Pts',(188.814657587864,4.7186145945435,132.191393194927));
#23009=CARTESIAN_POINT('Ctrl Pts',(188.806892834917,4.75715263869014,132.060288720149));
#23010=CARTESIAN_POINT('Ctrl Pts',(188.79912808197,4.79027312354286,131.927404754878));
#23011=CARTESIAN_POINT('Ctrl Pts',(188.791363329022,4.8178130955777,131.793228676803));
#23012=CARTESIAN_POINT('Ctrl Pts',(188.783606288137,4.84532571452407,131.659185864302));
#23013=CARTESIAN_POINT('Ctrl Pts',(188.775849247252,4.86726877266508,131.523853873413));
#23014=CARTESIAN_POINT('Ctrl Pts',(188.768092206367,4.88352921128275,131.387734858554));
#23015=CARTESIAN_POINT('Ctrl Pts',(188.760341015127,4.89977738777712,131.251718492103));
#23016=CARTESIAN_POINT('Ctrl Pts',(188.752589823887,4.91035142820668,131.114916669642));
#23017=CARTESIAN_POINT('Ctrl Pts',(188.744838632647,4.91518947969835,130.977840994447));
#23018=CARTESIAN_POINT('Ctrl Pts',(188.73709073587,4.9200254748891,130.840823580069));
#23019=CARTESIAN_POINT('Ctrl Pts',(188.729342839093,4.91913031627366,130.70353293436));
#23020=CARTESIAN_POINT('Ctrl Pts',(188.721594942316,4.91249408784202,130.566484810858));
#23021=CARTESIAN_POINT('Ctrl Pts',(188.713848666232,4.90585924756631,130.429465354868));
#23022=CARTESIAN_POINT('Ctrl Pts',(188.706102390148,4.89348574504375,130.29268871044));
#23023=CARTESIAN_POINT('Ctrl Pts',(188.698356114064,4.87541577373173,130.156669259165));
#23024=CARTESIAN_POINT('Ctrl Pts',(188.690609780798,4.85734566903134,130.020648803825));
#23025=CARTESIAN_POINT('Ctrl Pts',(188.682863447533,4.8335790631205,129.885385940352));
#23026=CARTESIAN_POINT('Ctrl Pts',(188.675117114268,4.8042098296649,129.751388170134));
#23027=CARTESIAN_POINT('Ctrl Pts',(188.667369046265,4.77483401917306,129.617360392044));
#23028=CARTESIAN_POINT('Ctrl Pts',(188.659620978262,4.73985316817686,129.484598652787));
#23029=CARTESIAN_POINT('Ctrl Pts',(188.651872910259,4.69941180461004,129.353598144522));
#23030=CARTESIAN_POINT('Ctrl Pts',(188.644116607517,4.65892745948071,129.222458407358));
#23031=CARTESIAN_POINT('Ctrl Pts',(188.636360304775,4.61297112417784,129.093084014587));
#23032=CARTESIAN_POINT('Ctrl Pts',(188.628604002033,4.56173674692024,128.965953449853));
#23033=CARTESIAN_POINT('Ctrl Pts',(188.620843559519,4.51047502433273,128.838755031709));
#23034=CARTESIAN_POINT('Ctrl Pts',(188.613083117005,4.4539298076903,128.713803183936));
#23035=CARTESIAN_POINT('Ctrl Pts',(188.605322674491,4.39234193722288,128.591553493343));
#23036=CARTESIAN_POINT('Ctrl Pts',(188.597549774225,4.33065520043842,128.469107556694));
#23037=CARTESIAN_POINT('Ctrl Pts',(188.58977687396,4.26390982407976,128.349372787105));
#23038=CARTESIAN_POINT('Ctrl Pts',(188.582003973694,4.1923915294448,128.23277816189));
#23039=CARTESIAN_POINT('Ctrl Pts',(188.574513637932,4.12347310496294,128.120422044985));
#23040=CARTESIAN_POINT('Ctrl Pts',(188.56702330217,4.05012292420374,128.010981987703));
#23041=CARTESIAN_POINT('Ctrl Pts',(188.559532966408,3.9726318877381,127.904812558467));
#23042=CARTESIAN_POINT('Ctrl Pts',(188.551758632289,3.89220275507264,127.794617683053));
#23043=CARTESIAN_POINT('Ctrl Pts',(188.54398429817,3.80705779181573,127.687597278996));
#23044=CARTESIAN_POINT('Ctrl Pts',(188.536209964051,3.71747623705813,127.584181509285));
#23045=CARTESIAN_POINT('Ctrl Pts',(188.528445211104,3.62800508356063,127.480893190268));
#23046=CARTESIAN_POINT('Ctrl Pts',(188.520680458157,3.53410847118426,127.38120095924));
#23047=CARTESIAN_POINT('Ctrl Pts',(188.512915705209,3.4361083642224,127.285505353162));
#23048=CARTESIAN_POINT('Ctrl Pts',(188.505158664324,3.33820559234877,127.18990479331));
#23049=CARTESIAN_POINT('Ctrl Pts',(188.49740162344,3.23620771452785,127.098293230294));
#23050=CARTESIAN_POINT('Ctrl Pts',(188.489644582555,3.13047609649216,127.011037210342));
#23051=CARTESIAN_POINT('Ctrl Pts',(188.481893391314,3.02482421149156,126.923846990833));
#23052=CARTESIAN_POINT('Ctrl Pts',(188.474142200074,2.91544449096346,126.841006024537));
#23053=CARTESIAN_POINT('Ctrl Pts',(188.466391008834,2.80273392824307,126.762842884093));
#23054=CARTESIAN_POINT('Ctrl Pts',(188.458643112057,2.69007127051854,126.684712965069));
#23055=CARTESIAN_POINT('Ctrl Pts',(188.45089521528,2.57408090691345,126.611257139848));
#23056=CARTESIAN_POINT('Ctrl Pts',(188.443147318503,2.45519139564007,126.542762528436));
#23057=CARTESIAN_POINT('Ctrl Pts',(188.435401042419,2.33632675348964,126.47428224462));
#23058=CARTESIAN_POINT('Ctrl Pts',(188.427654766335,2.21456450846326,126.410761305459));
#23059=CARTESIAN_POINT('Ctrl Pts',(188.419908490251,2.09036023095675,126.352442248218));
#23060=CARTESIAN_POINT('Ctrl Pts',(188.412162156985,1.96615503660239,126.294122760479));
#23061=CARTESIAN_POINT('Ctrl Pts',(188.40441582372,1.83950812769249,126.241005397451));
#23062=CARTESIAN_POINT('Ctrl Pts',(188.396669490455,1.71089722052739,126.193285497457));
#23063=CARTESIAN_POINT('Ctrl Pts',(188.388921422452,1.58225751184136,126.145554910922));
#23064=CARTESIAN_POINT('Ctrl Pts',(188.381173354449,1.45165329617858,126.10322432862));
#23065=CARTESIAN_POINT('Ctrl Pts',(188.373425286446,1.31957931360486,126.066439818565));
#23066=CARTESIAN_POINT('Ctrl Pts',(188.365668983704,1.18736496123061,126.029616213495));
#23067=CARTESIAN_POINT('Ctrl Pts',(188.357912680962,1.05367809874174,125.998350560498));
#23068=CARTESIAN_POINT('Ctrl Pts',(188.35015637822,0.919026121729599,125.972738317543));
#23069=CARTESIAN_POINT('Ctrl Pts',(188.342395935706,0.78430227690315,125.947112404563));
#23070=CARTESIAN_POINT('Ctrl Pts',(188.334635493192,0.648612677762575,125.927145970928));
#23071=CARTESIAN_POINT('Ctrl Pts',(188.326875050678,0.512470802420838,125.912882646731));
#23072=CARTESIAN_POINT('Ctrl Pts',(188.319102150412,0.376110380054625,125.89859642578));
#23073=CARTESIAN_POINT('Ctrl Pts',(188.311329250147,0.239296621066078,125.89003163359));
#23074=CARTESIAN_POINT('Ctrl Pts',(188.303556349881,0.102544875559919,125.88717975746));
#23075=CARTESIAN_POINT('Ctrl Pts',(188.296066014119,-0.0292355995406955,
125.88443155421));
#23076=CARTESIAN_POINT('Ctrl Pts',(188.288575678357,-0.160958183613458,
125.886988114484));
#23077=CARTESIAN_POINT('Ctrl Pts',(188.281085342595,-0.292167329337183,
125.894796348288));
#23078=CARTESIAN_POINT('Ctrl Pts',(188.273311008476,-0.428351309700771,
125.90290063365));
#23079=CARTESIAN_POINT('Ctrl Pts',(188.265536674357,-0.564413539030559,
125.916688360158));
#23080=CARTESIAN_POINT('Ctrl Pts',(188.257762340238,-0.699841173472941,
125.936157109658));
#23081=CARTESIAN_POINT('Ctrl Pts',(188.249997587291,-0.835101905459319,
125.955601865663));
#23082=CARTESIAN_POINT('Ctrl Pts',(188.242232834344,-0.9697292153955,125.980713658957));
#23083=CARTESIAN_POINT('Ctrl Pts',(188.234468081397,-1.10321209062758,126.011438111871));
#23084=CARTESIAN_POINT('Ctrl Pts',(188.226711040512,-1.23656238878648,126.042132048826));
#23085=CARTESIAN_POINT('Ctrl Pts',(188.218953999627,-1.36877013572612,126.07842746462));
#23086=CARTESIAN_POINT('Ctrl Pts',(188.211196958742,-1.49933161871793,126.120218459218));
#23087=CARTESIAN_POINT('Ctrl Pts',(188.203445767502,-1.62979464427913,126.161977938902));
#23088=CARTESIAN_POINT('Ctrl Pts',(188.195694576262,-1.75861350609556,126.20922462979));
#23089=CARTESIAN_POINT('Ctrl Pts',(188.187943385022,-1.88529718210462,126.261802131685));
#23090=CARTESIAN_POINT('Ctrl Pts',(188.180195488244,-2.01192701417225,126.314357286739));
#23091=CARTESIAN_POINT('Ctrl Pts',(188.172447591467,-2.13642310505805,126.372238596868));
#23092=CARTESIAN_POINT('Ctrl Pts',(188.16469969469,-2.25831224638831,126.435240699286));
#23093=CARTESIAN_POINT('Ctrl Pts',(188.156953418606,-2.38017589113758,126.498229623022));
#23094=CARTESIAN_POINT('Ctrl Pts',(188.149207142522,-2.49943332390471,126.566337029047));
#23095=CARTESIAN_POINT('Ctrl Pts',(188.141460866438,-2.61563424429333,126.6393107304));
#23096=CARTESIAN_POINT('Ctrl Pts',(188.133714533173,-2.73183602245093,126.712284970429));
#23097=CARTESIAN_POINT('Ctrl Pts',(188.125968199908,-2.84498091211698,126.790125369541));
#23098=CARTESIAN_POINT('Ctrl Pts',(188.118221866642,-2.95464635229878,126.872535596619));
#23099=CARTESIAN_POINT('Ctrl Pts',(188.110473798639,-3.06433635129529,126.954964278895));
#23100=CARTESIAN_POINT('Ctrl Pts',(188.102725730636,-3.17054503780084,127.04196459072));
#23101=CARTESIAN_POINT('Ctrl Pts',(188.094977662633,-3.27288210156859,127.133199246592));
#23102=CARTESIAN_POINT('Ctrl Pts',(188.087221359892,-3.37532793038579,127.224530867742));
#23103=CARTESIAN_POINT('Ctrl Pts',(188.07946505715,-3.47389362439947,127.320105562212));
#23104=CARTESIAN_POINT('Ctrl Pts',(188.071708754408,-3.56822461240654,127.419548041083));
#23105=CARTESIAN_POINT('Ctrl Pts',(188.063948311894,-3.66260594770211,127.519043595399));
#23106=CARTESIAN_POINT('Ctrl Pts',(188.05618786938,-3.75274781653608,127.622410752998));
#23107=CARTESIAN_POINT('Ctrl Pts',(188.048427426866,-3.83833596421348,127.729241093332));
#23108=CARTESIAN_POINT('Ctrl Pts',(188.0406545266,-3.92406150558378,127.836242927212));
#23109=CARTESIAN_POINT('Ctrl Pts',(188.032881626335,-4.00521848641537,127.946718738031));
#23110=CARTESIAN_POINT('Ctrl Pts',(188.025108726069,-4.08153550936666,128.060230345826));
#23111=CARTESIAN_POINT('Ctrl Pts',(188.017618390307,-4.15507821630353,128.169615520761));
#23112=CARTESIAN_POINT('Ctrl Pts',(188.010128054545,-4.22412658393381,128.281819344595));
#23113=CARTESIAN_POINT('Ctrl Pts',(188.002637718783,-4.28847904391944,128.396429856027));
#23114=CARTESIAN_POINT('Ctrl Pts',(187.994504561361,-4.35835424099316,128.52087625753));
#23115=CARTESIAN_POINT('Ctrl Pts',(187.98637140394,-4.42289737344505,128.648524117943));
#23116=CARTESIAN_POINT('Ctrl Pts',(187.978238246518,-4.48181742515692,128.778898786264));
#23117=CARTESIAN_POINT('Ctrl Pts',(187.970122616113,-4.54061050370865,128.908992496183));
#23118=CARTESIAN_POINT('Ctrl Pts',(187.962006985708,-4.59380452073732,129.041800991969));
#23119=CARTESIAN_POINT('Ctrl Pts',(187.953891355302,-4.6411539136234,129.176824623322));
#23120=CARTESIAN_POINT('Ctrl Pts',(187.94588335265,-4.68787536899956,129.310057600188));
#23121=CARTESIAN_POINT('Ctrl Pts',(187.937875349997,-4.72890612235297,129.445447018229));
#23122=CARTESIAN_POINT('Ctrl Pts',(187.929867347344,-4.76405452823405,129.582490119308));
#23123=CARTESIAN_POINT('Origin',(213.235140564004,0.,130.804360617566));
#23124=CARTESIAN_POINT('',(185.834939443695,-4.76405452823405,129.582490119308));
#23125=CARTESIAN_POINT('',(186.18020938313,-4.76405452823405,129.582490119308));
#23126=CARTESIAN_POINT('',(213.235140564004,-4.76405452823405,129.582490119308));
#23127=CARTESIAN_POINT('',(187.514859436036,-4.91824821531416,130.808550493347));
#23128=CARTESIAN_POINT('Ctrl Pts',(187.514859435991,-4.91824821531348,130.808550494141));
#23129=CARTESIAN_POINT('Ctrl Pts',(187.50296817185,-4.91806974195455,131.018049810722));
#23130=CARTESIAN_POINT('Ctrl Pts',(187.49107690771,-4.90450242768287,131.226999653672));
#23131=CARTESIAN_POINT('Ctrl Pts',(187.47918564357,-4.87777335736303,131.434051126228));
#23132=CARTESIAN_POINT('Ctrl Pts',(187.474567584818,-4.86739292886978,131.514461068646));
#23133=CARTESIAN_POINT('Ctrl Pts',(187.469949526067,-4.85502785952663,131.594585104556));
#23134=CARTESIAN_POINT('Ctrl Pts',(187.465331467316,-4.84069308080701,131.674345421989));
#23135=CARTESIAN_POINT('Ctrl Pts',(187.457557133197,-4.8165610016603,131.808619018444));
#23136=CARTESIAN_POINT('Ctrl Pts',(187.449782799078,-4.78679964152417,131.942100451967));
#23137=CARTESIAN_POINT('Ctrl Pts',(187.442008464958,-4.75147197296815,132.074280753873));
#23138=CARTESIAN_POINT('Ctrl Pts',(187.434243712011,-4.71618784260629,132.206298155371));
#23139=CARTESIAN_POINT('Ctrl Pts',(187.426478959064,-4.67535115311574,132.337017241715));
#23140=CARTESIAN_POINT('Ctrl Pts',(187.418714206117,-4.62907625661752,132.465936999476));
#23141=CARTESIAN_POINT('Ctrl Pts',(187.410957165232,-4.58284732099878,132.594728712316));
#23142=CARTESIAN_POINT('Ctrl Pts',(187.403200124347,-4.53119105843935,132.721724287424));
#23143=CARTESIAN_POINT('Ctrl Pts',(187.395443083462,-4.47427212062073,132.846436045442));
#23144=CARTESIAN_POINT('Ctrl Pts',(187.387691892222,-4.41739610581604,132.971053757354));
#23145=CARTESIAN_POINT('Ctrl Pts',(187.379940700982,-4.35526547673165,133.093390725966));
#23146=CARTESIAN_POINT('Ctrl Pts',(187.372189509742,-4.28809353286631,133.212977838274));
#23147=CARTESIAN_POINT('Ctrl Pts',(187.364441612965,-4.22095013886891,133.332514122869));
#23148=CARTESIAN_POINT('Ctrl Pts',(187.356693716188,-4.14876988281084,133.44930253558));
#23149=CARTESIAN_POINT('Ctrl Pts',(187.348945819411,-4.07181258012,133.562897435315));
#23150=CARTESIAN_POINT('Ctrl Pts',(187.341199543326,-3.99487137523789,133.676468573446));
#23151=CARTESIAN_POINT('Ctrl Pts',(187.333453267242,-3.91315533044107,133.786847203844));
#23152=CARTESIAN_POINT('Ctrl Pts',(187.325706991158,-3.82696805196249,133.893615963399));
#23153=CARTESIAN_POINT('Ctrl Pts',(187.317960657893,-3.74078013726901,134.000385511097));
#23154=CARTESIAN_POINT('Ctrl Pts',(187.310214324628,-3.65012116860682,134.103544830563));
#23155=CARTESIAN_POINT('Ctrl Pts',(187.302467991362,-3.55533531112048,134.202709317744));
#23156=CARTESIAN_POINT('Ctrl Pts',(187.294719923359,-3.46052822699846,134.301896012124));
#23157=CARTESIAN_POINT('Ctrl Pts',(187.286971855356,-3.36159268511726,134.397085811471));
#23158=CARTESIAN_POINT('Ctrl Pts',(187.279223787353,-3.25890970925504,134.487930973813));
#23159=CARTESIAN_POINT('Ctrl Pts',(187.271467484611,-3.15611760070424,134.578872687475));
#23160=CARTESIAN_POINT('Ctrl Pts',(187.263711181869,-3.04957039534964,134.665460280642));
#23161=CARTESIAN_POINT('Ctrl Pts',(187.255954879128,-2.93968263329513,134.747385988776));
#23162=CARTESIAN_POINT('Ctrl Pts',(187.248194436613,-2.82973622083337,134.829355423126));
#23163=CARTESIAN_POINT('Ctrl Pts',(187.240433994099,-2.71644602177129,134.906657794264));
#23164=CARTESIAN_POINT('Ctrl Pts',(187.232673551585,-2.60025471421194,134.979029285103));
#23165=CARTESIAN_POINT('Ctrl Pts',(187.22490065132,-2.48387688605068,135.051516953085));
#23166=CARTESIAN_POINT('Ctrl Pts',(187.217127751054,-2.36458898340092,135.119057730363));
#23167=CARTESIAN_POINT('Ctrl Pts',(187.209354850789,-2.24285817365602,135.181433872078));
#23168=CARTESIAN_POINT('Ctrl Pts',(187.201864515027,-2.12555258546736,135.241542483926));
#23169=CARTESIAN_POINT('Ctrl Pts',(187.194374179265,-2.0059788977942,135.296855306772));
#23170=CARTESIAN_POINT('Ctrl Pts',(187.186883843503,-1.88456999546703,135.347220839352));
#23171=CARTESIAN_POINT('Ctrl Pts',(187.179109509384,-1.75855783770604,135.399495996409));
#23172=CARTESIAN_POINT('Ctrl Pts',(187.171335175265,-1.63016938517756,135.446606896525));
#23173=CARTESIAN_POINT('Ctrl Pts',(187.163560841146,-1.49986688586205,135.488331410301));
#23174=CARTESIAN_POINT('Ctrl Pts',(187.155796088199,-1.36972497273157,135.530004502343));
#23175=CARTESIAN_POINT('Ctrl Pts',(187.148031335251,-1.23767407507255,135.566304298079));
#23176=CARTESIAN_POINT('Ctrl Pts',(187.140266582304,-1.10419751978648,135.597056195192));
#23177=CARTESIAN_POINT('Ctrl Pts',(187.132509541419,-0.970853535296745,
135.627777549087));
#23178=CARTESIAN_POINT('Ctrl Pts',(187.124752500534,-0.836087089569735,
135.6529618828));
#23179=CARTESIAN_POINT('Ctrl Pts',(187.116995459649,-0.700397479315045,
135.672484119848));
#23180=CARTESIAN_POINT('Ctrl Pts',(187.109244268409,-0.564810193650936,
135.691991635025));
#23181=CARTESIAN_POINT('Ctrl Pts',(187.101493077169,-0.42830151454915,135.705845496927));
#23182=CARTESIAN_POINT('Ctrl Pts',(187.093741885929,-0.291381413656383,
135.713971593425));
#23183=CARTESIAN_POINT('Ctrl Pts',(187.085993989152,-0.154519507459005,
135.722094236115));
#23184=CARTESIAN_POINT('Ctrl Pts',(187.078246092375,-0.017246916725652,
135.724493932228));
#23185=CARTESIAN_POINT('Ctrl Pts',(187.070498195598,0.119920991487449,135.721148391947));
#23186=CARTESIAN_POINT('Ctrl Pts',(187.062751919514,0.257060207131151,135.717803551481));
#23187=CARTESIAN_POINT('Ctrl Pts',(187.05500564343,0.394094393208233,135.708715874552));
#23188=CARTESIAN_POINT('Ctrl Pts',(187.047259367345,0.53050830372916,135.693915198729));
#23189=CARTESIAN_POINT('Ctrl Pts',(187.03951303408,0.66692322122647,135.679114413651));
#23190=CARTESIAN_POINT('Ctrl Pts',(187.031766700815,0.802717465346965,135.658600587698));
#23191=CARTESIAN_POINT('Ctrl Pts',(187.024020367549,0.937381428141232,135.632455388868));
#23192=CARTESIAN_POINT('Ctrl Pts',(187.016272299546,1.07207554799625,135.606304335003));
#23193=CARTESIAN_POINT('Ctrl Pts',(187.008524231543,1.20563849912314,135.574519473305));
#23194=CARTESIAN_POINT('Ctrl Pts',(187.000776163541,1.33757176369478,135.537233406842));
#23195=CARTESIAN_POINT('Ctrl Pts',(186.993019860799,1.46964524851015,135.499907712303));
#23196=CARTESIAN_POINT('Ctrl Pts',(186.985263558057,1.60008520998432,135.457069239991));
#23197=CARTESIAN_POINT('Ctrl Pts',(186.977507255315,1.7284086480416,135.408900399985));
#23198=CARTESIAN_POINT('Ctrl Pts',(186.969746812801,1.85680057618161,135.360705850817));
#23199=CARTESIAN_POINT('Ctrl Pts',(186.961986370287,1.98307337019677,135.307175417617));
#23200=CARTESIAN_POINT('Ctrl Pts',(186.954225927772,2.10676579497374,135.248538938429));
#23201=CARTESIAN_POINT('Ctrl Pts',(186.946453027507,2.23065678181183,135.189808330759));
#23202=CARTESIAN_POINT('Ctrl Pts',(186.938680127242,2.3519587757408,135.125955479745));
#23203=CARTESIAN_POINT('Ctrl Pts',(186.930907226976,2.47023606645755,135.05725573013));
#23204=CARTESIAN_POINT('Ctrl Pts',(186.923416891214,2.58421367973449,134.991053389458));
#23205=CARTESIAN_POINT('Ctrl Pts',(186.915926555452,2.69538242307315,134.920350591354));
#23206=CARTESIAN_POINT('Ctrl Pts',(186.90843621969,2.80338084934492,134.845429643953));
#23207=CARTESIAN_POINT('Ctrl Pts',(186.900661885571,2.91547406877391,134.76766804606));
#23208=CARTESIAN_POINT('Ctrl Pts',(186.892887551452,3.02450689794558,134.685115797058));
#23209=CARTESIAN_POINT('Ctrl Pts',(186.885113217333,3.13004259678052,134.5980417329));
#23210=CARTESIAN_POINT('Ctrl Pts',(186.877348464386,3.23544823229863,134.511074979743));
#23211=CARTESIAN_POINT('Ctrl Pts',(186.869583711439,3.3373650142225,134.419597745934));
#23212=CARTESIAN_POINT('Ctrl Pts',(186.861818958491,3.43538479468078,134.323922291266));
#23213=CARTESIAN_POINT('Ctrl Pts',(186.854061917606,3.53330722051126,134.228341862808));
#23214=CARTESIAN_POINT('Ctrl Pts',(186.846304876721,3.62734006948965,134.128571782767));
#23215=CARTESIAN_POINT('Ctrl Pts',(186.838547835836,3.7171082291624,134.024964516712));
#23216=CARTESIAN_POINT('Ctrl Pts',(186.830796644596,3.8068086939677,133.921435381702));
#23217=CARTESIAN_POINT('Ctrl Pts',(186.823045453356,3.89225061581199,133.814075114605));
#23218=CARTESIAN_POINT('Ctrl Pts',(186.815294262116,3.97309598993045,133.703272709593));
#23219=CARTESIAN_POINT('Ctrl Pts',(186.807546365339,4.05390700260826,133.592517398559));
#23220=CARTESIAN_POINT('Ctrl Pts',(186.799798468562,4.13012512327185,133.478323174578));
#23221=CARTESIAN_POINT('Ctrl Pts',(186.792050571785,4.20145303038427,133.36111158236));
#23222=CARTESIAN_POINT('Ctrl Pts',(186.784304295701,4.27276601723617,133.24392450828));
#23223=CARTESIAN_POINT('Ctrl Pts',(186.776558019617,4.33919062208088,133.123721655165));
#23224=CARTESIAN_POINT('Ctrl Pts',(186.768811743533,4.40047344506548,133.000952641992));
#23225=CARTESIAN_POINT('Ctrl Pts',(186.761065410267,4.46175672042594,132.878182722566));
#23226=CARTESIAN_POINT('Ctrl Pts',(186.753319077002,4.51789796357578,132.752846955089));
#23227=CARTESIAN_POINT('Ctrl Pts',(186.745572743736,4.56869042857052,132.62541823071));
#23228=CARTESIAN_POINT('Ctrl Pts',(186.737824675734,4.61949426818561,132.497960969551));
#23229=CARTESIAN_POINT('Ctrl Pts',(186.730076607731,4.66494680138576,132.368410181932));
#23230=CARTESIAN_POINT('Ctrl Pts',(186.722328539728,4.70489012982407,132.237256960218));
#23231=CARTESIAN_POINT('Ctrl Pts',(186.714572236986,4.74487591050721,132.105964347298));
#23232=CARTESIAN_POINT('Ctrl Pts',(186.706815934244,4.77934067585266,131.973066272786));
#23233=CARTESIAN_POINT('Ctrl Pts',(186.699059631502,4.80817681928663,131.839067695427));
#23234=CARTESIAN_POINT('Ctrl Pts',(186.691299188988,4.83702835343861,131.704997598992));
#23235=CARTESIAN_POINT('Ctrl Pts',(186.683538746474,4.86024521347585,131.569826214457));
#23236=CARTESIAN_POINT('Ctrl Pts',(186.675778303959,4.8777714598113,131.434065825064));
#23237=CARTESIAN_POINT('Ctrl Pts',(186.668005403694,4.89532584083327,131.298087501042));
#23238=CARTESIAN_POINT('Ctrl Pts',(186.660232503429,4.90717131955267,131.161518672433));
#23239=CARTESIAN_POINT('Ctrl Pts',(186.652459603163,4.91330403923953,131.024874745214));
#23240=CARTESIAN_POINT('Ctrl Pts',(186.644969267401,4.91921381911843,130.893198168935));
#23241=CARTESIAN_POINT('Ctrl Pts',(186.637478931639,4.91981897388855,130.761452167314));
#23242=CARTESIAN_POINT('Ctrl Pts',(186.629988595877,4.91516164637668,130.630093430501));
#23243=CARTESIAN_POINT('Ctrl Pts',(186.622214261758,4.91032773487667,130.493754187256));
#23244=CARTESIAN_POINT('Ctrl Pts',(186.614439927639,4.89980909723262,130.357400273068));
#23245=CARTESIAN_POINT('Ctrl Pts',(186.60666559352,4.88359584406322,130.221544442131));
#23246=CARTESIAN_POINT('Ctrl Pts',(186.598900840573,4.86740257227934,130.085856041365));
#23247=CARTESIAN_POINT('Ctrl Pts',(186.591136087626,4.84552869479156,129.95066488697));
#23248=CARTESIAN_POINT('Ctrl Pts',(186.583371334678,4.81801631071333,129.816483149354));
#23249=CARTESIAN_POINT('Ctrl Pts',(186.575614293793,4.79053125232284,129.682434682933));
#23250=CARTESIAN_POINT('Ctrl Pts',(186.567857252908,4.75741891010157,129.549394018657));
#23251=CARTESIAN_POINT('Ctrl Pts',(186.560100212023,4.71877306587156,129.417867265507));
#23252=CARTESIAN_POINT('Ctrl Pts',(186.552349020783,4.68015636477332,129.286439697704));
#23253=CARTESIAN_POINT('Ctrl Pts',(186.544597829543,4.63601457725516,129.156524142229));
#23254=CARTESIAN_POINT('Ctrl Pts',(186.536846638303,4.58649227530057,129.028615232915));
#23255=CARTESIAN_POINT('Ctrl Pts',(186.529098741526,4.53699102164532,128.9007606883));
#23256=CARTESIAN_POINT('Ctrl Pts',(186.521350844749,4.48211394281148,128.774911457366));
#23257=CARTESIAN_POINT('Ctrl Pts',(186.513602947972,4.42205498674884,128.651545540354));
#23258=CARTESIAN_POINT('Ctrl Pts',(186.505856671888,4.3620085937251,128.528205428834));
#23259=CARTESIAN_POINT('Ctrl Pts',(186.498110395804,4.29678265050747,128.407347949309));
#23260=CARTESIAN_POINT('Ctrl Pts',(186.490364119719,4.2266184654652,128.289429324292));
#23261=CARTESIAN_POINT('Ctrl Pts',(186.482617786454,4.15645376248687,128.171509828827));
#23262=CARTESIAN_POINT('Ctrl Pts',(186.474871453189,4.08135094486343,128.056529567145));
#23263=CARTESIAN_POINT('Ctrl Pts',(186.467125119923,4.00159611807821,127.94491808968));
#23264=CARTESIAN_POINT('Ctrl Pts',(186.45937705192,3.92182343075255,127.833281617599));
#23265=CARTESIAN_POINT('Ctrl Pts',(186.451628983917,3.83739688849461,127.725015748974));
#23266=CARTESIAN_POINT('Ctrl Pts',(186.443880915914,3.74864431330477,127.620518775573));
#23267=CARTESIAN_POINT('Ctrl Pts',(186.436124613173,3.65979741082176,127.515910741544));
#23268=CARTESIAN_POINT('Ctrl Pts',(186.428368310431,3.56661554438332,127.415079902877));
#23269=CARTESIAN_POINT('Ctrl Pts',(186.420612007689,3.46946538610199,127.318389734564));
#23270=CARTESIAN_POINT('Ctrl Pts',(186.412851565175,3.37226337585601,127.221647959797));
#23271=CARTESIAN_POINT('Ctrl Pts',(186.405091122661,3.2710891417477,127.129051522826));
#23272=CARTESIAN_POINT('Ctrl Pts',(186.397330680146,3.166343445464,127.040924388816));
#23273=CARTESIAN_POINT('Ctrl Pts',(186.389557779881,3.06142960208977,126.952655785307));
#23274=CARTESIAN_POINT('Ctrl Pts',(186.381784879615,2.95293314934019,126.868871060837));
#23275=CARTESIAN_POINT('Ctrl Pts',(186.37401197935,2.84128562820487,126.789852049702));
#23276=CARTESIAN_POINT('Ctrl Pts',(186.366521643588,2.73369677568628,126.713705578658));
#23277=CARTESIAN_POINT('Ctrl Pts',(186.359031307826,2.6231822342181,126.641984512861));
#23278=CARTESIAN_POINT('Ctrl Pts',(186.351540972064,2.51014900938351,126.574900248537));
#23279=CARTESIAN_POINT('Ctrl Pts',(186.343766637945,2.39283009547328,126.50527246394));
#23280=CARTESIAN_POINT('Ctrl Pts',(186.335992303826,2.27242610514435,126.440419470445));
#23281=CARTESIAN_POINT('Ctrl Pts',(186.328217969707,2.14936308757183,126.380626744435));
#23282=CARTESIAN_POINT('Ctrl Pts',(186.32045321676,2.02645173417003,126.320907707617));
#23283=CARTESIAN_POINT('Ctrl Pts',(186.312688463813,1.90088822208354,126.266236699069));
#23284=CARTESIAN_POINT('Ctrl Pts',(186.304923710865,1.773126210382,126.216855140233));
#23285=CARTESIAN_POINT('Ctrl Pts',(186.29716666998,1.64549109371175,126.167522627858));
#23286=CARTESIAN_POINT('Ctrl Pts',(186.289409629095,1.51566218516442,126.123469250419));
#23287=CARTESIAN_POINT('Ctrl Pts',(186.28165258821,1.38411597992469,126.08488967088));
#23288=CARTESIAN_POINT('Ctrl Pts',(186.27390139697,1.25266897470157,126.046339184501));
#23289=CARTESIAN_POINT('Ctrl Pts',(186.26615020573,1.11950762410406,126.013254389403));
#23290=CARTESIAN_POINT('Ctrl Pts',(186.25839901449,0.985126222273834,125.985781014749));
#23291=CARTESIAN_POINT('Ctrl Pts',(186.250651117713,0.850801936124037,125.958319317012));
#23292=CARTESIAN_POINT('Ctrl Pts',(186.242903220936,0.715259012346737,125.936464374276));
#23293=CARTESIAN_POINT('Ctrl Pts',(186.235155324159,0.579004439687522,125.920311383445));
#23294=CARTESIAN_POINT('Ctrl Pts',(186.227409048075,0.442778368547621,125.904161771471));
#23295=CARTESIAN_POINT('Ctrl Pts',(186.219662771991,0.305841332620214,125.893711785003));
#23296=CARTESIAN_POINT('Ctrl Pts',(186.211916495907,0.168707597893969,125.889005003888));
#23297=CARTESIAN_POINT('Ctrl Pts',(186.204170162641,0.0315728508776698,
125.884298188029));
#23298=CARTESIAN_POINT('Ctrl Pts',(186.196423829376,-0.10575820709968,125.885334675529));
#23299=CARTESIAN_POINT('Ctrl Pts',(186.18867749611,-0.242769536089092,125.892105940247));
#23300=CARTESIAN_POINT('Ctrl Pts',(186.180929428107,-0.379811547815777,
125.898878721341));
#23301=CARTESIAN_POINT('Ctrl Pts',(186.173181360104,-0.516533297662758,
125.911388815894));
#23302=CARTESIAN_POINT('Ctrl Pts',(186.165433292102,-0.652422495685759,
125.929575704401));
#23303=CARTESIAN_POINT('Ctrl Pts',(186.15767698936,-0.788456118365381,125.947781922149));
#23304=CARTESIAN_POINT('Ctrl Pts',(186.149920686618,-0.923655033517907,
125.971676934201));
#23305=CARTESIAN_POINT('Ctrl Pts',(186.142164383876,-1.05751524410295,126.001148716037));
#23306=CARTESIAN_POINT('Ctrl Pts',(186.134403941362,-1.19144689991294,126.03063622785));
#23307=CARTESIAN_POINT('Ctrl Pts',(186.126643498848,-1.3240380496573,126.065706340432));
#23308=CARTESIAN_POINT('Ctrl Pts',(186.118883056333,-1.45479951078708,126.106196992711));
#23309=CARTESIAN_POINT('Ctrl Pts',(186.111110156068,-1.5857708818227,126.146752644179));
#23310=CARTESIAN_POINT('Ctrl Pts',(186.103337255803,-1.7149063263107,126.192746092524));
#23311=CARTESIAN_POINT('Ctrl Pts',(186.095564355537,-1.8417354706294,126.243966608412));
#23312=CARTESIAN_POINT('Ctrl Pts',(186.088074019775,-1.96395405608863,126.293325129531));
#23313=CARTESIAN_POINT('Ctrl Pts',(186.080583684013,-2.08403082912152,126.347537155255));
#23314=CARTESIAN_POINT('Ctrl Pts',(186.073093348251,-2.20156793963613,126.406374525084));
#23315=CARTESIAN_POINT('Ctrl Pts',(186.065318218632,-2.32357398828093,126.467448980412));
#23316=CARTESIAN_POINT('Ctrl Pts',(186.057543089012,-2.44322994792608,126.533700949362));
#23317=CARTESIAN_POINT('Ctrl Pts',(186.049767959393,-2.56006520571822,126.604926226488));
#23318=CARTESIAN_POINT('Ctrl Pts',(186.042002588127,-2.67675382676365,126.67606211071));
#23319=CARTESIAN_POINT('Ctrl Pts',(186.03423721686,-2.79062845967751,126.75215868097));
#23320=CARTESIAN_POINT('Ctrl Pts',(186.026471845594,-2.90124067215559,126.832964688585));
#23321=CARTESIAN_POINT('Ctrl Pts',(186.018491328848,-3.01491747957512,126.916009487709));
#23322=CARTESIAN_POINT('Ctrl Pts',(186.010510812103,-3.12514807592882,127.004028321582));
#23323=CARTESIAN_POINT('Ctrl Pts',(186.002530295357,-3.2314741111118,127.096698533218));
#23324=CARTESIAN_POINT('Ctrl Pts',(185.994779503498,-3.33473947526146,127.186701166476));
#23325=CARTESIAN_POINT('Ctrl Pts',(185.987028711639,-3.43432165183175,127.28109080366));
#23326=CARTESIAN_POINT('Ctrl Pts',(185.979277919781,-3.52983187439647,127.37952923471));
#23327=CARTESIAN_POINT('Ctrl Pts',(185.971530630239,-3.62529893917089,127.477923184813));
#23328=CARTESIAN_POINT('Ctrl Pts',(185.963783340697,-3.71669743948121,127.580362008493));
#23329=CARTESIAN_POINT('Ctrl Pts',(185.956036051155,-3.80367440789667,127.686469653916));
#23330=CARTESIAN_POINT('Ctrl Pts',(185.948290584601,-3.89063091006273,127.792552331516));
#23331=CARTESIAN_POINT('Ctrl Pts',(185.940545118047,-3.97316770391064,127.902301810235));
#23332=CARTESIAN_POINT('Ctrl Pts',(185.932799651493,-4.05097143863642,128.015308186031));
#23333=CARTESIAN_POINT('Ctrl Pts',(185.925054330194,-4.12877371426179,128.12831244255));
#23334=CARTESIAN_POINT('Ctrl Pts',(185.917309008896,-4.20184288741614,128.244573151684));
#23335=CARTESIAN_POINT('Ctrl Pts',(185.909563687597,-4.26990858509716,128.363650938515));
#23336=CARTESIAN_POINT('Ctrl Pts',(185.901814172698,-4.33801113604076,128.482793198423));
#23337=CARTESIAN_POINT('Ctrl Pts',(185.894064657798,-4.40110460739271,128.604755242451));
#23338=CARTESIAN_POINT('Ctrl Pts',(185.886315142899,-4.45896424491958,128.729072462868));
#23339=CARTESIAN_POINT('Ctrl Pts',(185.878563054062,-4.51684310004943,128.853430974228));
#23340=CARTESIAN_POINT('Ctrl Pts',(185.870810965225,-4.56948450454414,128.980145861196));
#23341=CARTESIAN_POINT('Ctrl Pts',(185.863058876388,-4.61671198790392,129.108732862649));
#23342=CARTESIAN_POINT('Ctrl Pts',(185.855299774332,-4.66398219738179,129.237436195167));
#23343=CARTESIAN_POINT('Ctrl Pts',(185.847540672277,-4.70582858667214,129.368014652284));
#23344=CARTESIAN_POINT('Ctrl Pts',(185.839781570221,-4.74212459112503,129.49996902577));
#23345=CARTESIAN_POINT('Ctrl Pts',(185.838167528046,-4.74967485680883,129.527418068522));
#23346=CARTESIAN_POINT('Ctrl Pts',(185.83655348587,-4.75698512267265,129.554926614318));
#23347=CARTESIAN_POINT('Ctrl Pts',(185.834939443695,-4.76405452823405,129.582490119308));
#23348=CARTESIAN_POINT('Ctrl Pts',(187.584954980304,-4.76405452823404,129.582490119308));
#23349=CARTESIAN_POINT('Ctrl Pts',(187.577318467045,-4.79766509150003,129.713537195371));
#23350=CARTESIAN_POINT('Ctrl Pts',(187.569681953786,-4.82585013568644,129.845916938469));
#23351=CARTESIAN_POINT('Ctrl Pts',(187.562045440527,-4.84852382797168,129.979133526341));
#23352=CARTESIAN_POINT('Ctrl Pts',(187.554181106445,-4.87187394666516,130.116324377291));
#23353=CARTESIAN_POINT('Ctrl Pts',(187.546316772363,-4.88937865955207,130.254402327779));
#23354=CARTESIAN_POINT('Ctrl Pts',(187.538452438282,-4.90100172800805,130.392820674715));
#23355=CARTESIAN_POINT('Ctrl Pts',(187.5305881042,-4.91262479646404,130.53123902165));
#23356=CARTESIAN_POINT('Ctrl Pts',(187.522723770118,-4.91836624934627,130.669997300341));
#23357=CARTESIAN_POINT('Ctrl Pts',(187.514859436036,-4.91824821531416,130.808550493347));
#23358=CARTESIAN_POINT('',(187.860140563976,-4.91824998954374,130.80468132454));
#23359=CARTESIAN_POINT('Ctrl Pts',(187.929867347344,-4.76405452823405,129.582490119308));
#23360=CARTESIAN_POINT('Ctrl Pts',(187.921775086847,-4.79957275528882,129.72097514753));
#23361=CARTESIAN_POINT('Ctrl Pts',(187.913682826349,-4.82908397265096,129.861148571076));
#23362=CARTESIAN_POINT('Ctrl Pts',(187.905590565851,-4.85243842824599,130.00247261879));
#23363=CARTESIAN_POINT('Ctrl Pts',(187.897511509163,-4.87575477733303,130.143566073847));
#23364=CARTESIAN_POINT('Ctrl Pts',(187.889432452475,-4.8929343404035,130.285806076163));
#23365=CARTESIAN_POINT('Ctrl Pts',(187.881353395787,-4.90387800511191,130.428643205833));
#23366=CARTESIAN_POINT('Ctrl Pts',(187.87428245186,-4.91345610840887,130.553656975815));
#23367=CARTESIAN_POINT('Ctrl Pts',(187.867211507934,-4.91825817656564,130.679127798048));
#23368=CARTESIAN_POINT('Ctrl Pts',(187.860140564008,-4.91824998954378,130.804681323973));
#23369=CARTESIAN_POINT('Ctrl Pts',(187.860140563976,-4.91824998954374,130.80468132454));
#23370=CARTESIAN_POINT('Ctrl Pts',(187.851985238763,-4.91824054696515,130.949489407629));
#23371=CARTESIAN_POINT('Ctrl Pts',(187.84382991355,-4.91183143561811,131.094160796668));
#23372=CARTESIAN_POINT('Ctrl Pts',(187.835674588336,-4.89908446976143,131.238128321115));
#23373=CARTESIAN_POINT('Ctrl Pts',(187.827507043422,-4.8863184042239,131.382311562291));
#23374=CARTESIAN_POINT('Ctrl Pts',(187.819339498508,-4.86719555824919,131.525788509872));
#23375=CARTESIAN_POINT('Ctrl Pts',(187.811171953594,-4.84182909625093,131.668000626596));
#23376=CARTESIAN_POINT('Ctrl Pts',(187.802983701521,-4.81639832271632,131.810573293393));
#23377=CARTESIAN_POINT('Ctrl Pts',(187.794795449448,-4.78469233773483,131.951874395443));
#23378=CARTESIAN_POINT('Ctrl Pts',(187.786607197375,-4.74687508460216,132.091357118604));
#23379=CARTESIAN_POINT('Ctrl Pts',(187.778407825462,-4.70900647474592,132.2310292626));
#23380=CARTESIAN_POINT('Ctrl Pts',(187.770208453549,-4.66501012991102,132.368877788919));
#23381=CARTESIAN_POINT('Ctrl Pts',(187.762009081637,-4.61509878206581,132.504374233475));
#23382=CARTESIAN_POINT('Ctrl Pts',(187.7537907155,-4.56507181227561,132.640184561809));
#23383=CARTESIAN_POINT('Ctrl Pts',(187.745572349363,-4.5091025670614,132.773631612781));
#23384=CARTESIAN_POINT('Ctrl Pts',(187.737353983226,-4.44745127249184,132.904208288544));
#23385=CARTESIAN_POINT('Ctrl Pts',(187.732966020474,-4.4145343179928,132.973925989116));
#23386=CARTESIAN_POINT('Ctrl Pts',(187.728578057722,-4.37999833546582,133.042825876845));
#23387=CARTESIAN_POINT('Ctrl Pts',(187.724190094969,-4.34388802098799,133.110834099663));
#23388=CARTESIAN_POINT('Ctrl Pts',(187.71641576085,-4.27990989132784,133.23132706574));
#23389=CARTESIAN_POINT('Ctrl Pts',(187.708641426731,-4.21081318308159,133.349346880017));
#23390=CARTESIAN_POINT('Ctrl Pts',(187.700867092612,-4.13681326770758,133.464428107428));
#23391=CARTESIAN_POINT('Ctrl Pts',(187.693102339665,-4.06290455061579,133.57936750751));
#23392=CARTESIAN_POINT('Ctrl Pts',(187.685337586718,-3.98410485912279,133.691375200834));
#23393=CARTESIAN_POINT('Ctrl Pts',(187.677572833771,-3.90067606158043,133.800009015678));
#23394=CARTESIAN_POINT('Ctrl Pts',(187.669815792886,-3.81733012669587,133.908534933887));
#23395=CARTESIAN_POINT('Ctrl Pts',(187.662058752001,-3.72936447197065,134.013693334156));
#23396=CARTESIAN_POINT('Ctrl Pts',(187.654301711116,-3.63708479189096,134.115070100305));
#23397=CARTESIAN_POINT('Ctrl Pts',(187.646550519876,-3.54487470063586,134.216370417446));
#23398=CARTESIAN_POINT('Ctrl Pts',(187.638799328636,-3.44835732151588,134.313894488769));
#23399=CARTESIAN_POINT('Ctrl Pts',(187.631048137396,-3.34787900468798,134.407260731706));
#23400=CARTESIAN_POINT('Ctrl Pts',(187.623300240619,-3.24744339382506,134.500587291499));
#23401=CARTESIAN_POINT('Ctrl Pts',(187.615552343842,-3.14305047942049,134.589759272133));
#23402=CARTESIAN_POINT('Ctrl Pts',(187.607804447065,-3.03508373938013,134.674431645009));
#23403=CARTESIAN_POINT('Ctrl Pts',(187.60005817098,-2.92713958365424,134.759086306249));
#23404=CARTESIAN_POINT('Ctrl Pts',(187.592311894896,-2.81562339669253,134.839242990757));
#23405=CARTESIAN_POINT('Ctrl Pts',(187.584565618812,-2.70095172170201,134.914596968378));
#23406=CARTESIAN_POINT('Ctrl Pts',(187.576819285547,-2.58627920023135,134.989951502245));
#23407=CARTESIAN_POINT('Ctrl Pts',(187.569072952282,-2.4684514709862,135.060503043776));
#23408=CARTESIAN_POINT('Ctrl Pts',(187.561326619016,-2.34791369668973,135.125990441533));
#23409=CARTESIAN_POINT('Ctrl Pts',(187.553578551013,-2.22734892879446,135.191492504738));
#23410=CARTESIAN_POINT('Ctrl Pts',(187.54583048301,-2.10407325166797,135.251927980875));
#23411=CARTESIAN_POINT('Ctrl Pts',(187.538082415007,-1.97855567117998,135.307082074479));
#23412=CARTESIAN_POINT('Ctrl Pts',(187.530326112265,-1.8529046891137,135.36229478651));
#23413=CARTESIAN_POINT('Ctrl Pts',(187.522569809524,-1.72500740244735,135.412214745672));
#23414=CARTESIAN_POINT('Ctrl Pts',(187.514813506782,-1.59535252627577,135.456675458525));
#23415=CARTESIAN_POINT('Ctrl Pts',(187.507053064268,-1.46562844939287,135.501159901399));
#23416=CARTESIAN_POINT('Ctrl Pts',(187.499292621754,-1.33414528842969,135.540179180866));
#23417=CARTESIAN_POINT('Ctrl Pts',(187.491532179239,-1.20140513403331,135.573617243752));
#23418=CARTESIAN_POINT('Ctrl Pts',(187.483759278974,-1.06845189335697,135.607108984385));
#23419=CARTESIAN_POINT('Ctrl Pts',(187.475986378709,-0.934238009971892,
135.635001524974));
#23420=CARTESIAN_POINT('Ctrl Pts',(187.468213478443,-0.799274826844706,
135.657230161833));
#23421=CARTESIAN_POINT('Ctrl Pts',(187.460723142681,-0.669217895375251,
135.678650731752));
#23422=CARTESIAN_POINT('Ctrl Pts',(187.453232806919,-0.538465501906267,
135.694812005137));
#23423=CARTESIAN_POINT('Ctrl Pts',(187.445742471157,-0.40747611749601,135.705701890745));
#23424=CARTESIAN_POINT('Ctrl Pts',(187.437968137038,-0.271520230763168,
135.717004669676));
#23425=CARTESIAN_POINT('Ctrl Pts',(187.430193802919,-0.134878359929164,
135.722664244519));
#23426=CARTESIAN_POINT('Ctrl Pts',(187.4224194688,0.0019414977692763,135.722610234359));
#23427=CARTESIAN_POINT('Ctrl Pts',(187.414654715853,0.138592737221022,135.722556290762));
#23428=CARTESIAN_POINT('Ctrl Pts',(187.406889962905,0.275421139878357,135.716802772767));
#23429=CARTESIAN_POINT('Ctrl Pts',(187.399125209958,0.411913147910088,135.70533099302));
#23430=CARTESIAN_POINT('Ctrl Pts',(187.391368169073,0.548269590155265,135.693870607207));
#23431=CARTESIAN_POINT('Ctrl Pts',(187.383611128188,0.684289915601994,135.676703294552));
#23432=CARTESIAN_POINT('Ctrl Pts',(187.375854087303,0.819460481241922,135.653862404573));
#23433=CARTESIAN_POINT('Ctrl Pts',(187.368102896063,0.954529113706643,135.631038739087));
#23434=CARTESIAN_POINT('Ctrl Pts',(187.360351704823,1.08874887791857,135.602550077227));
#23435=CARTESIAN_POINT('Ctrl Pts',(187.352600513583,1.22161152693562,135.568481558491));
#23436=CARTESIAN_POINT('Ctrl Pts',(187.344852616806,1.35441770578278,135.534427519784));
#23437=CARTESIAN_POINT('Ctrl Pts',(187.337104720029,1.4858675387463,135.494798438013));
#23438=CARTESIAN_POINT('Ctrl Pts',(187.329356823252,1.6154634643188,135.449730447617));
#23439=CARTESIAN_POINT('Ctrl Pts',(187.321610547168,1.74503228121749,135.404671884473));
#23440=CARTESIAN_POINT('Ctrl Pts',(187.313864271084,1.87274759303631,135.354176803992));
#23441=CARTESIAN_POINT('Ctrl Pts',(187.306117994999,1.99812786988819,135.298430941679));
#23442=CARTESIAN_POINT('Ctrl Pts',(187.298371661734,2.12350907226879,135.242684667863));
#23443=CARTESIAN_POINT('Ctrl Pts',(187.290625328469,2.24655484804188,135.181687693709));
#23444=CARTESIAN_POINT('Ctrl Pts',(187.282878995203,2.36680486178025,135.115673388492));
#23445=CARTESIAN_POINT('Ctrl Pts',(187.2751309272,2.48708180467538,135.04964429983));
#23446=CARTESIAN_POINT('Ctrl Pts',(187.267382859197,2.60456139703364,134.978595832385));
#23447=CARTESIAN_POINT('Ctrl Pts',(187.259634791194,2.71880941621897,134.902806471884));
#23448=CARTESIAN_POINT('Ctrl Pts',(187.251878488453,2.83317885955863,134.826936561549));
#23449=CARTESIAN_POINT('Ctrl Pts',(187.244122185711,2.9443095425167,134.746315909328));
#23450=CARTESIAN_POINT('Ctrl Pts',(187.236365882969,3.05179722699965,134.661265691298));
#23451=CARTESIAN_POINT('Ctrl Pts',(187.228605440455,3.15934228089629,134.576170079406));
#23452=CARTESIAN_POINT('Ctrl Pts',(187.220844997941,3.26324016595116,134.486640445942));
#23453=CARTESIAN_POINT('Ctrl Pts',(187.213084555426,3.36312185108178,134.393036484411));
#23454=CARTESIAN_POINT('Ctrl Pts',(187.205311655161,3.46316387516043,134.299282261492));
#23455=CARTESIAN_POINT('Ctrl Pts',(187.197538754896,3.55917654184175,134.201440919767));
#23456=CARTESIAN_POINT('Ctrl Pts',(187.18976585463,3.65082902071832,134.099907692633));
#23457=CARTESIAN_POINT('Ctrl Pts',(187.182275518868,3.73914970112908,134.002065454052));
#23458=CARTESIAN_POINT('Ctrl Pts',(187.174785183106,3.82342150061338,133.900795325352));
#23459=CARTESIAN_POINT('Ctrl Pts',(187.167294847344,3.90338643166027,133.796476495608));
#23460=CARTESIAN_POINT('Ctrl Pts',(187.159520513225,3.98638325737254,133.688202385727));
#23461=CARTESIAN_POINT('Ctrl Pts',(187.151746179106,4.06500308682427,133.576300848341));
#23462=CARTESIAN_POINT('Ctrl Pts',(187.143971844987,4.13891212164383,133.461161233309));
#23463=CARTESIAN_POINT('Ctrl Pts',(187.13620709204,4.2127300701834,133.346163517562));
#23464=CARTESIAN_POINT('Ctrl Pts',(187.128442339093,4.28184856640189,133.227935990211));
#23465=CARTESIAN_POINT('Ctrl Pts',(187.120677586145,4.34597429754696,133.106900621032));
#23466=CARTESIAN_POINT('Ctrl Pts',(187.11292054526,4.41003633811182,132.985985465888));
#23467=CARTESIAN_POINT('Ctrl Pts',(187.105163504375,4.46911530015668,132.862268361969));
#23468=CARTESIAN_POINT('Ctrl Pts',(187.09740646349,4.52296160498285,132.736199477914));
#23469=CARTESIAN_POINT('Ctrl Pts',(187.08965527225,4.5767673038917,132.610225663385));
#23470=CARTESIAN_POINT('Ctrl Pts',(187.08190408101,4.62534804688488,132.481903956843));
#23471=CARTESIAN_POINT('Ctrl Pts',(187.07415288977,4.6685007443457,132.351707980812));
#23472=CARTESIAN_POINT('Ctrl Pts',(187.066404992993,4.71163510075898,132.221567341544));
#23473=CARTESIAN_POINT('Ctrl Pts',(187.058657096216,4.74934587746924,132.089554387528));
#23474=CARTESIAN_POINT('Ctrl Pts',(187.050909199439,4.7814786640856,131.956161315341));
#23475=CARTESIAN_POINT('Ctrl Pts',(187.043162923355,4.8136047292157,131.822796146108));
#23476=CARTESIAN_POINT('Ctrl Pts',(187.035416647271,4.84015503356989,131.688051812779));
#23477=CARTESIAN_POINT('Ctrl Pts',(187.027670371187,4.86102556302323,131.552433834661));
#23478=CARTESIAN_POINT('Ctrl Pts',(187.019924037921,4.88189624653807,131.416814855442));
#23479=CARTESIAN_POINT('Ctrl Pts',(187.012177704656,4.89708701202375,131.280322604983));
#23480=CARTESIAN_POINT('Ctrl Pts',(187.00443137139,4.90654537711804,131.143470518309));
#23481=CARTESIAN_POINT('Ctrl Pts',(186.996683303387,4.9160058603476,131.006587784559));
#23482=CARTESIAN_POINT('Ctrl Pts',(186.988935235385,4.91973136175744,130.869345444204));
#23483=CARTESIAN_POINT('Ctrl Pts',(186.981187167382,4.9177214713347,130.732259349382));
#23484=CARTESIAN_POINT('Ctrl Pts',(186.97343086464,4.91570944477649,130.595027557828));
#23485=CARTESIAN_POINT('Ctrl Pts',(186.965674561898,4.90794985542348,130.457952735076));
#23486=CARTESIAN_POINT('Ctrl Pts',(186.957918259156,4.89449441724326,130.321548581599));
#23487=CARTESIAN_POINT('Ctrl Pts',(186.950157816642,4.88103179749054,130.185071625118));
#23488=CARTESIAN_POINT('Ctrl Pts',(186.942397374128,4.8618673259655,130.04926643811));
#23489=CARTESIAN_POINT('Ctrl Pts',(186.934636931613,4.83710415268687,129.914637920003));
#23490=CARTESIAN_POINT('Ctrl Pts',(186.926864031348,4.81230122736411,129.779793284246));
#23491=CARTESIAN_POINT('Ctrl Pts',(186.919091131083,4.78188172714106,129.646129473437));
#23492=CARTESIAN_POINT('Ctrl Pts',(186.911318230817,4.74599935115195,129.514138457872));
#23493=CARTESIAN_POINT('Ctrl Pts',(186.903827895055,4.71142138991215,129.386945648188));
#23494=CARTESIAN_POINT('Ctrl Pts',(186.896337559293,4.67177092859245,129.261306418357));
#23495=CARTESIAN_POINT('Ctrl Pts',(186.888847223531,4.62722754114839,129.137642781537));
#23496=CARTESIAN_POINT('Ctrl Pts',(186.881072889412,4.58099527763089,129.00929040034));
#23497=CARTESIAN_POINT('Ctrl Pts',(186.873298555293,4.52934528322642,128.882659796889));
#23498=CARTESIAN_POINT('Ctrl Pts',(186.865524221174,4.47242470282503,128.758242258316));
#23499=CARTESIAN_POINT('Ctrl Pts',(186.857759468227,4.41557427195186,128.63397805324));
#23500=CARTESIAN_POINT('Ctrl Pts',(186.84999471528,4.35346634033301,128.511921838433));
#23501=CARTESIAN_POINT('Ctrl Pts',(186.842229962332,4.28629738038526,128.392548471191));
#23502=CARTESIAN_POINT('Ctrl Pts',(186.834472921447,4.21919513359548,128.27329366726));
#23503=CARTESIAN_POINT('Ctrl Pts',(186.826715880562,4.14704205228711,128.156716746663));
#23504=CARTESIAN_POINT('Ctrl Pts',(186.818958839677,4.07008197270261,128.04327101417));
#23505=CARTESIAN_POINT('Ctrl Pts',(186.811207648437,3.99317992931273,127.929910831987));
#23506=CARTESIAN_POINT('Ctrl Pts',(186.803456457197,3.91147832157752,127.81967746021));
#23507=CARTESIAN_POINT('Ctrl Pts',(186.795705265957,3.82526584664194,127.712997768431));
#23508=CARTESIAN_POINT('Ctrl Pts',(186.78795736918,3.739090014308,127.606363418365));
#23509=CARTESIAN_POINT('Ctrl Pts',(186.780209472403,3.64840737324212,127.503280047653));
#23510=CARTESIAN_POINT('Ctrl Pts',(186.772461575626,3.55354855977579,127.404143610401));
#23511=CARTESIAN_POINT('Ctrl Pts',(186.764715299542,3.45870958872832,127.305027910354));
#23512=CARTESIAN_POINT('Ctrl Pts',(186.756969023458,3.35969645297088,127.209857783879));
#23513=CARTESIAN_POINT('Ctrl Pts',(186.749222747373,3.25687823804013,127.11899398654));
#23514=CARTESIAN_POINT('Ctrl Pts',(186.741476414108,3.15405926412871,127.028129518465));
#23515=CARTESIAN_POINT('Ctrl Pts',(186.733730080843,3.04743544795587,126.941571701855));
#23516=CARTESIAN_POINT('Ctrl Pts',(186.725983747577,2.9374103889513,126.859642215781));
#23517=CARTESIAN_POINT('Ctrl Pts',(186.718235679574,2.82736069059759,126.777694382167));
#23518=CARTESIAN_POINT('Ctrl Pts',(186.710487611571,2.71390854726417,126.700377175026));
#23519=CARTESIAN_POINT('Ctrl Pts',(186.702739543568,2.5974877383432,126.627969769997));
#23520=CARTESIAN_POINT('Ctrl Pts',(186.694983240827,2.48094319600109,126.555485409516));
#23521=CARTESIAN_POINT('Ctrl Pts',(186.687226938085,2.36142401787533,126.487921481866));
#23522=CARTESIAN_POINT('Ctrl Pts',(186.679470635343,2.23939034738478,126.425512146274));
#23523=CARTESIAN_POINT('Ctrl Pts',(186.671710192829,2.11729154384987,126.36306950094));
#23524=CARTESIAN_POINT('Ctrl Pts',(186.663949750315,1.99267592883989,126.305787092796));
#23525=CARTESIAN_POINT('Ctrl Pts',(186.6561893078,1.86602404364675,126.253851049283));
#23526=CARTESIAN_POINT('Ctrl Pts',(186.648416407535,1.73916884560389,126.201831633423));
#23527=CARTESIAN_POINT('Ctrl Pts',(186.64064350727,1.6102712131062,126.155175865823));
#23528=CARTESIAN_POINT('Ctrl Pts',(186.632870607004,1.47982813283383,126.114020357012));
#23529=CARTESIAN_POINT('Ctrl Pts',(186.625380271242,1.35412698709598,126.074360954611));
#23530=CARTESIAN_POINT('Ctrl Pts',(186.61788993548,1.22699110189288,126.039808938046));
#23531=CARTESIAN_POINT('Ctrl Pts',(186.610399599718,1.09887259295406,126.010441335084));
#23532=CARTESIAN_POINT('Ctrl Pts',(186.602625265599,0.965896431807742,125.979960250529));
#23533=CARTESIAN_POINT('Ctrl Pts',(186.59485093148,0.831440435162286,125.954967919335));
#23534=CARTESIAN_POINT('Ctrl Pts',(186.587076597361,0.695997472203889,125.935606097036));
#23535=CARTESIAN_POINT('Ctrl Pts',(186.579311844414,0.560721430592498,125.916268136452));
#23536=CARTESIAN_POINT('Ctrl Pts',(186.571547091467,0.424461226152909,125.902546932818));
#23537=CARTESIAN_POINT('Ctrl Pts',(186.56378233852,0.287722567918223,125.894533860295));
#23538=CARTESIAN_POINT('Ctrl Pts',(186.556025297635,0.151119720446433,125.886528746469));
#23539=CARTESIAN_POINT('Ctrl Pts',(186.54826825675,0.014039752633058,125.884220504122));
#23540=CARTESIAN_POINT('Ctrl Pts',(186.540511215865,-0.123004157933034,
125.887649009221));
#23541=CARTESIAN_POINT('Ctrl Pts',(186.532760024625,-0.259944722620193,
125.891074928858));
#23542=CARTESIAN_POINT('Ctrl Pts',(186.525008833384,-0.396848894920734,
125.90022897531));
#23543=CARTESIAN_POINT('Ctrl Pts',(186.517257642144,-0.533201489500632,
125.915098992935));
#23544=CARTESIAN_POINT('Ctrl Pts',(186.509509745367,-0.669496130590324,
125.929962690404));
#23545=CARTESIAN_POINT('Ctrl Pts',(186.50176184859,-0.805239272386058,125.950537484778));
#23546=CARTESIAN_POINT('Ctrl Pts',(186.494013951813,-0.939919070470149,
125.976759225211));
#23547=CARTESIAN_POINT('Ctrl Pts',(186.486267675729,-1.07457069644382,126.002975480622));
#23548=CARTESIAN_POINT('Ctrl Pts',(186.478521399645,-1.20815903761232,126.034836257913));
#23549=CARTESIAN_POINT('Ctrl Pts',(186.470775123561,-1.34018108035477,126.072226032164));
#23550=CARTESIAN_POINT('Ctrl Pts',(186.463028790295,-1.47220409765393,126.109616082418));
#23551=CARTESIAN_POINT('Ctrl Pts',(186.45528245703,-1.60266041728542,126.152535104537));
#23552=CARTESIAN_POINT('Ctrl Pts',(186.447536123765,-1.73106124618654,126.200817414288));
#23553=CARTESIAN_POINT('Ctrl Pts',(186.439788055762,-1.85949082956307,126.249110536526));
#23554=CARTESIAN_POINT('Ctrl Pts',(186.432039987759,-1.98586364036161,126.302769198807));
#23555=CARTESIAN_POINT('Ctrl Pts',(186.424291919756,-2.10971033185508,126.361579351494));
#23556=CARTESIAN_POINT('Ctrl Pts',(186.416535617014,-2.23368864908604,126.42045200831));
#23557=CARTESIAN_POINT('Ctrl Pts',(186.408779314272,-2.35513513012335,126.484486924591));
#23558=CARTESIAN_POINT('Ctrl Pts',(186.40102301153,-2.47360405141956,126.553423537427));
#23559=CARTESIAN_POINT('Ctrl Pts',(186.393262569016,-2.59213620314615,126.622396943809));
#23560=CARTESIAN_POINT('Ctrl Pts',(186.385502126502,-2.70768729925805,126.696277049213));
#23561=CARTESIAN_POINT('Ctrl Pts',(186.377741683988,-2.81984100116167,126.774760167066));
#23562=CARTESIAN_POINT('Ctrl Pts',(186.369968783722,-2.93217474214415,126.853369272988));
#23563=CARTESIAN_POINT('Ctrl Pts',(186.362195883457,-3.04109987965048,126.936595919761));
#23564=CARTESIAN_POINT('Ctrl Pts',(186.354422983192,-3.14623284593448,127.024095819743));
#23565=CARTESIAN_POINT('Ctrl Pts',(186.346932647429,-3.24754396407987,127.108414877961));
#23566=CARTESIAN_POINT('Ctrl Pts',(186.339442311667,-3.34533360559828,127.196701689925));
#23567=CARTESIAN_POINT('Ctrl Pts',(186.331951975905,-3.43929258525454,127.288617513255));
#23568=CARTESIAN_POINT('Ctrl Pts',(186.324290294265,-3.53540093236302,127.382635965623));
#23569=CARTESIAN_POINT('Ctrl Pts',(186.316628612625,-3.62782449528663,127.480768053431));
#23570=CARTESIAN_POINT('Ctrl Pts',(186.308966930984,-3.7161827594279,127.582688883663));
#23571=CARTESIAN_POINT('Ctrl Pts',(186.301314183386,-3.80443799181967,127.68449086727));
#23572=CARTESIAN_POINT('Ctrl Pts',(186.293661435788,-3.88863708801042,127.790072509402));
#23573=CARTESIAN_POINT('Ctrl Pts',(186.28600868819,-3.96843439155349,127.899070349377));
#23574=CARTESIAN_POINT('Ctrl Pts',(186.278363092695,-4.04815711815039,128.007966322175));
#23575=CARTESIAN_POINT('Ctrl Pts',(186.2707174972,-4.12348599584845,128.120271821147));
#23576=CARTESIAN_POINT('Ctrl Pts',(186.263071901705,-4.19411426884116,128.235588817191));
#23577=CARTESIAN_POINT('Ctrl Pts',(186.255431906839,-4.26469080449765,128.350821340064));
#23578=CARTESIAN_POINT('Ctrl Pts',(186.247791911973,-4.33057337660585,128.469060628456));
#23579=CARTESIAN_POINT('Ctrl Pts',(186.240151917107,-4.39149772261774,128.589878552896));
#23580=CARTESIAN_POINT('Ctrl Pts',(186.232515226792,-4.45239571683195,128.710644219582));
#23581=CARTESIAN_POINT('Ctrl Pts',(186.224878536477,-4.50833957015994,128.833985944203));
#23582=CARTESIAN_POINT('Ctrl Pts',(186.217241846161,-4.5591105114303,128.959450211322));
#23583=CARTESIAN_POINT('Ctrl Pts',(186.209605532488,-4.60987894867488,129.084908290537));
#23584=CARTESIAN_POINT('Ctrl Pts',(186.201969218815,-4.65547482316395,129.212488333294));
#23585=CARTESIAN_POINT('Ctrl Pts',(186.194332905142,-4.695727286753,129.341716330344));
#23586=CARTESIAN_POINT('Ctrl Pts',(186.189625064471,-4.72054321146236,129.421386292359));
#23587=CARTESIAN_POINT('Ctrl Pts',(186.184917223801,-4.74332916114695,129.501682227587));
#23588=CARTESIAN_POINT('Ctrl Pts',(186.18020938313,-4.76405452823405,129.582490119308));
#23589=CARTESIAN_POINT('Origin',(213.235140564004,0.,130.804360617566));
#23590=CARTESIAN_POINT('',(184.084599308536,-4.76405452823405,129.582490119308));
#23591=CARTESIAN_POINT('',(184.430229652623,-4.76405452823406,129.582490119308));
#23592=CARTESIAN_POINT('',(213.235140564004,-4.76405452823405,129.582490119308));
#23593=CARTESIAN_POINT('',(185.764859435953,-4.91824909926408,130.801384027568));
#23594=CARTESIAN_POINT('Ctrl Pts',(185.764859435953,-4.91824909926409,130.801384027568));
#23595=CARTESIAN_POINT('Ctrl Pts',(185.757191235898,-4.9183306751947,130.936172744721));
#23596=CARTESIAN_POINT('Ctrl Pts',(185.749523035843,-4.91286708241096,131.071183771682));
#23597=CARTESIAN_POINT('Ctrl Pts',(185.741854835789,-4.901829924088,131.205915667111));
#23598=CARTESIAN_POINT('Ctrl Pts',(185.734195115826,-4.89080497151269,131.340498565537));
#23599=CARTESIAN_POINT('Ctrl Pts',(185.726535395862,-4.87421874451201,131.474802549089));
#23600=CARTESIAN_POINT('Ctrl Pts',(185.718875675899,-4.85209485286721,131.608324921052));
#23601=CARTESIAN_POINT('Ctrl Pts',(185.711222480037,-4.82998980505673,131.741733566484));
#23602=CARTESIAN_POINT('Ctrl Pts',(185.703569284174,-4.80235654064527,131.874361530089));
#23603=CARTESIAN_POINT('Ctrl Pts',(185.695916088312,-4.76927054522506,132.00571049539));
#23604=CARTESIAN_POINT('Ctrl Pts',(185.688267001704,-4.73620231477376,132.136988935073));
#23605=CARTESIAN_POINT('Ctrl Pts',(185.680617915096,-4.69768727340913,132.266989353296));
#23606=CARTESIAN_POINT('Ctrl Pts',(185.672968828489,-4.65385205465889,132.395223313039));
#23607=CARTESIAN_POINT('Ctrl Pts',(185.665321809995,-4.61002868781017,132.523422601658));
#23608=CARTESIAN_POINT('Ctrl Pts',(185.657674791501,-4.56088813315632,132.649856001177));
#23609=CARTESIAN_POINT('Ctrl Pts',(185.650027773007,-4.50660683515309,132.774050414425));
#23610=CARTESIAN_POINT('Ctrl Pts',(185.642381064432,-4.4523277370657,132.898239794315));
#23611=CARTESIAN_POINT('Ctrl Pts',(185.634734355857,-4.39290847102935,133.020189999991));
#23612=CARTESIAN_POINT('Ctrl Pts',(185.627087647282,-4.3285733387234,133.139448606014));
#23613=CARTESIAN_POINT('Ctrl Pts',(185.619439490905,-4.26422602542105,133.258729792058));
#23614=CARTESIAN_POINT('Ctrl Pts',(185.611791334528,-4.19496118620005,133.37531801141));
#23615=CARTESIAN_POINT('Ctrl Pts',(185.604143178151,-4.12104844176228,133.488786590311));
#23616=CARTESIAN_POINT('Ctrl Pts',(185.596487235631,-4.04706045105567,133.602370684977));
#23617=CARTESIAN_POINT('Ctrl Pts',(185.58883129311,-3.96841532550673,133.71282845947));
#23618=CARTESIAN_POINT('Ctrl Pts',(185.58117535059,-3.88542548694373,133.819763053048));
#23619=CARTESIAN_POINT('Ctrl Pts',(185.573515374056,-3.80239191997511,133.926753991828));
#23620=CARTESIAN_POINT('Ctrl Pts',(185.565855397521,-3.71500934088863,134.03021774658));
#23621=CARTESIAN_POINT('Ctrl Pts',(185.558195420987,-3.62362875719401,134.129792573348));
#23622=CARTESIAN_POINT('Ctrl Pts',(185.550523572136,-3.5321065413066,134.229521732694));
#23623=CARTESIAN_POINT('Ctrl Pts',(185.542851723284,-3.43657422762343,134.325349640552));
#23624=CARTESIAN_POINT('Ctrl Pts',(185.535179874433,-3.33741822988249,134.416952847717));
#23625=CARTESIAN_POINT('Ctrl Pts',(185.528852616497,-3.25564060551483,134.492501405919));
#23626=CARTESIAN_POINT('Ctrl Pts',(185.522525358561,-3.17139888835135,134.56517703643));
#23627=CARTESIAN_POINT('Ctrl Pts',(185.516198100626,-3.08492473413098,134.634820439473));
#23628=CARTESIAN_POINT('Ctrl Pts',(185.508423766507,-2.97867349948799,134.720391644243));
#23629=CARTESIAN_POINT('Ctrl Pts',(185.500649432388,-2.86869084610792,134.801674161477));
#23630=CARTESIAN_POINT('Ctrl Pts',(185.492875098269,-2.75535800148616,134.878324945606));
#23631=CARTESIAN_POINT('Ctrl Pts',(185.485110345321,-2.64216482946666,134.954881264495));
#23632=CARTESIAN_POINT('Ctrl Pts',(185.477345592374,-2.52563000205102,135.026816990961));
#23633=CARTESIAN_POINT('Ctrl Pts',(185.469580839427,-2.4061683288018,135.093828770609));
#23634=CARTESIAN_POINT('Ctrl Pts',(185.461823798542,-2.28682530657056,135.160773993213));
#23635=CARTESIAN_POINT('Ctrl Pts',(185.454066757657,-2.16456156231129,135.222804811345));
#23636=CARTESIAN_POINT('Ctrl Pts',(185.446309716772,-2.03982114582494,135.279660915372));
#23637=CARTESIAN_POINT('Ctrl Pts',(185.438558525532,-1.91517479705691,135.33647414377));
#23638=CARTESIAN_POINT('Ctrl Pts',(185.430807334292,-1.78805584787562,135.388120263844));
#23639=CARTESIAN_POINT('Ctrl Pts',(185.423056143052,-1.65893291082312,135.434384878829));
#23640=CARTESIAN_POINT('Ctrl Pts',(185.415308246275,-1.52986485446345,135.480629830119));
#23641=CARTESIAN_POINT('Ctrl Pts',(185.407560349498,-1.39879487157781,135.521497693954));
#23642=CARTESIAN_POINT('Ctrl Pts',(185.399812452721,-1.2662113115785,135.556822293049));
#23643=CARTESIAN_POINT('Ctrl Pts',(185.392066176637,-1.13365548520171,135.592139502999));
#23644=CARTESIAN_POINT('Ctrl Pts',(185.384319900553,-0.999587089008202,
135.62191565399));
#23645=CARTESIAN_POINT('Ctrl Pts',(185.376573624468,-0.864509000677892,
135.646034630782));
#23646=CARTESIAN_POINT('Ctrl Pts',(185.368827291203,-0.729429915231751,
135.670153785614));
#23647=CARTESIAN_POINT('Ctrl Pts',(185.361080957938,-0.593341507654216,
135.688615614195));
#23648=CARTESIAN_POINT('Ctrl Pts',(185.353334624672,-0.456755805682509,
135.701355328251));
#23649=CARTESIAN_POINT('Ctrl Pts',(185.345586556669,-0.320139516289562,
135.714097895278));
#23650=CARTESIAN_POINT('Ctrl Pts',(185.337838488666,-0.183026100098795,
135.721115761585));
#23651=CARTESIAN_POINT('Ctrl Pts',(185.330090420663,-0.0459312508572161,
135.722396138248));
#23652=CARTESIAN_POINT('Ctrl Pts',(185.322334117922,0.0913093044211189,
135.723677875712));
#23653=CARTESIAN_POINT('Ctrl Pts',(185.31457781518,0.228530861759579,135.719209938718));
#23654=CARTESIAN_POINT('Ctrl Pts',(185.306821512438,0.365218627626155,135.709031698947));
#23655=CARTESIAN_POINT('Ctrl Pts',(185.299061069924,0.501979347869056,135.698848026743));
#23656=CARTESIAN_POINT('Ctrl Pts',(185.29130062741,0.638205320812515,135.682948024144));
#23657=CARTESIAN_POINT('Ctrl Pts',(185.283540184895,0.773389317112324,135.661422695271));
#23658=CARTESIAN_POINT('Ctrl Pts',(185.27576728463,0.908790322764111,135.639862812028));
#23659=CARTESIAN_POINT('Ctrl Pts',(185.267994384365,1.04314562582757,135.612659634777));
#23660=CARTESIAN_POINT('Ctrl Pts',(185.260221484099,1.175959709326,135.57995501246));
#23661=CARTESIAN_POINT('Ctrl Pts',(185.252731148337,1.30394566635063,135.548439285542));
#23662=CARTESIAN_POINT('Ctrl Pts',(185.245240812575,1.43050021692963,135.511815237666));
#23663=CARTESIAN_POINT('Ctrl Pts',(185.237750476813,1.55519716015653,135.470252263923));
#23664=CARTESIAN_POINT('Ctrl Pts',(185.229976142694,1.68462202588672,135.427113417397));
#23665=CARTESIAN_POINT('Ctrl Pts',(185.222201808575,1.81245562030366,135.378517082239));
#23666=CARTESIAN_POINT('Ctrl Pts',(185.214427474456,1.93820326668134,135.324598571427));
#23667=CARTESIAN_POINT('Ctrl Pts',(185.206662721509,2.06379594032369,135.270746510361));
#23668=CARTESIAN_POINT('Ctrl Pts',(185.198897968562,2.18730742506553,135.211585476901));
#23669=CARTESIAN_POINT('Ctrl Pts',(185.191133215614,2.30825828556062,135.147300491619));
#23670=CARTESIAN_POINT('Ctrl Pts',(185.183376174729,2.42908901595603,135.083079355091));
#23671=CARTESIAN_POINT('Ctrl Pts',(185.175619133844,2.54736384028493,135.013744576743));
#23672=CARTESIAN_POINT('Ctrl Pts',(185.167862092959,2.66262373291742,134.939529044535));
#23673=CARTESIAN_POINT('Ctrl Pts',(185.160110901719,2.77779670716764,134.865369478838));
#23674=CARTESIAN_POINT('Ctrl Pts',(185.152359710479,2.8899589477656,134.786336696123));
#23675=CARTESIAN_POINT('Ctrl Pts',(185.144608519239,2.99867678011411,134.702709066705));
#23676=CARTESIAN_POINT('Ctrl Pts',(185.136860622462,3.107348404484,134.61911698126));
#23677=CARTESIAN_POINT('Ctrl Pts',(185.129112725685,3.21257822307831,134.530934171219));
#23678=CARTESIAN_POINT('Ctrl Pts',(185.121364828908,3.31396246145469,134.438481675892));
#23679=CARTESIAN_POINT('Ctrl Pts',(185.113618552824,3.41532549243393,134.346048519634));
#23680=CARTESIAN_POINT('Ctrl Pts',(185.10587227674,3.51284425451252,134.249347717836));
#23681=CARTESIAN_POINT('Ctrl Pts',(185.098126000655,3.60614923898019,134.148739592608));
#23682=CARTESIAN_POINT('Ctrl Pts',(185.09037966739,3.69945491220408,134.048130724714));
#23683=CARTESIAN_POINT('Ctrl Pts',(185.082633334125,3.78854647989511,133.943614762498));
#23684=CARTESIAN_POINT('Ctrl Pts',(185.074887000859,3.87309267034491,133.835587469753));
#23685=CARTESIAN_POINT('Ctrl Pts',(185.067138932856,3.95765779432756,133.727535985046));
#23686=CARTESIAN_POINT('Ctrl Pts',(185.059390864854,4.03767527464004,133.615971912911));
#23687=CARTESIAN_POINT('Ctrl Pts',(185.051642796851,4.11285560653182,133.501322208379));
#23688=CARTESIAN_POINT('Ctrl Pts',(185.043886494109,4.18811584097532,133.386550652776));
#23689=CARTESIAN_POINT('Ctrl Pts',(185.036130191367,4.2585284426082,133.268687241189));
#23690=CARTESIAN_POINT('Ctrl Pts',(185.028373888625,4.32384827746161,133.148186365354));
#23691=CARTESIAN_POINT('Ctrl Pts',(185.020613446111,4.38920297547765,133.027621174572));
#23692=CARTESIAN_POINT('Ctrl Pts',(185.012853003597,4.44945931886022,132.904416065631));
#23693=CARTESIAN_POINT('Ctrl Pts',(185.005092561082,4.50441970210254,132.779046974892));
#23694=CARTESIAN_POINT('Ctrl Pts',(184.997319660817,4.55946831263118,132.65347663056));
#23695=CARTESIAN_POINT('Ctrl Pts',(184.989546760552,4.6092038322925,132.525735727174));
#23696=CARTESIAN_POINT('Ctrl Pts',(184.981773860286,4.65347776358927,132.396317830019));
#23697=CARTESIAN_POINT('Ctrl Pts',(184.974283524524,4.69614222596426,132.271604599409));
#23698=CARTESIAN_POINT('Ctrl Pts',(184.966793188762,4.7337352030942,132.145334479326));
#23699=CARTESIAN_POINT('Ctrl Pts',(184.959302853,4.7661688398658,132.017957606847));
#23700=CARTESIAN_POINT('Ctrl Pts',(184.951528518881,4.79983220783342,131.885751201534));
#23701=CARTESIAN_POINT('Ctrl Pts',(184.943754184762,4.8280439150364,131.751933671931));
#23702=CARTESIAN_POINT('Ctrl Pts',(184.935979850643,4.85065041926304,131.616994343548));
#23703=CARTESIAN_POINT('Ctrl Pts',(184.928215097696,4.87322906299363,131.482221315828));
#23704=CARTESIAN_POINT('Ctrl Pts',(184.920450344748,4.8902161844549,131.346329622014));
#23705=CARTESIAN_POINT('Ctrl Pts',(184.912685591801,4.90150830017843,131.209822632781));
#23706=CARTESIAN_POINT('Ctrl Pts',(184.904928550916,4.91278920041345,131.073451224213));
#23707=CARTESIAN_POINT('Ctrl Pts',(184.897171510031,4.91838631929962,130.936466123495));
#23708=CARTESIAN_POINT('Ctrl Pts',(184.889414469146,4.91824747750727,130.799379403521));
#23709=CARTESIAN_POINT('Ctrl Pts',(184.881663277906,4.9181087404166,130.662396061707));
#23710=CARTESIAN_POINT('Ctrl Pts',(184.873912086666,4.91224265275202,130.525311642551));
#23711=CARTESIAN_POINT('Ctrl Pts',(184.866160895426,4.9006490036298,130.388641474728));
#23712=CARTESIAN_POINT('Ctrl Pts',(184.858412998649,4.88906028211778,130.252029395372));
#23713=CARTESIAN_POINT('Ctrl Pts',(184.850665101872,4.87174887389483,130.115831605913));
#23714=CARTESIAN_POINT('Ctrl Pts',(184.842917205095,4.84876662847558,129.980561342814));
#23715=CARTESIAN_POINT('Ctrl Pts',(184.835170929011,4.82578919044663,129.845319375338));
#23716=CARTESIAN_POINT('Ctrl Pts',(184.827424652926,4.7971433401164,129.711004933506));
#23717=CARTESIAN_POINT('Ctrl Pts',(184.819678376842,4.76293249819749,129.578123658363));
#23718=CARTESIAN_POINT('Ctrl Pts',(184.811932043577,4.72872140374189,129.445241402321));
#23719=CARTESIAN_POINT('Ctrl Pts',(184.804185710312,4.68894533320337,129.313792712696));
#23720=CARTESIAN_POINT('Ctrl Pts',(184.796439377046,4.64375819341888,129.184270217756));
#23721=CARTESIAN_POINT('Ctrl Pts',(184.788691309043,4.59856093428778,129.054718717152));
#23722=CARTESIAN_POINT('Ctrl Pts',(184.78094324104,4.54795032338664,128.927094638659));
#23723=CARTESIAN_POINT('Ctrl Pts',(184.773195173037,4.49212908568403,128.801872330446));
#23724=CARTESIAN_POINT('Ctrl Pts',(184.765438870295,4.43624852050568,128.676516934474));
#23725=CARTESIAN_POINT('Ctrl Pts',(184.757682567554,4.37514642537891,128.553568765596));
#23726=CARTESIAN_POINT('Ctrl Pts',(184.749926264812,4.30907259203993,128.433479671793));
#23727=CARTESIAN_POINT('Ctrl Pts',(184.742165822298,4.24296349310673,128.313326482825));
#23728=CARTESIAN_POINT('Ctrl Pts',(184.734405379783,4.17187757104574,128.196035743754));
#23729=CARTESIAN_POINT('Ctrl Pts',(184.726644937269,4.09610843399477,128.08203096092));
#23730=CARTESIAN_POINT('Ctrl Pts',(184.718872037004,4.02021766559842,127.967843167486));
#23731=CARTESIAN_POINT('Ctrl Pts',(184.711099136738,3.93962888900392,127.856952187687));
#23732=CARTESIAN_POINT('Ctrl Pts',(184.703326236473,3.85467708813893,127.749749740764));
#23733=CARTESIAN_POINT('Ctrl Pts',(184.695835900711,3.77281349921669,127.646444372814));
#23734=CARTESIAN_POINT('Ctrl Pts',(184.688345564949,3.68689879343445,127.546564252244));
#23735=CARTESIAN_POINT('Ctrl Pts',(184.680855229187,3.59726419602927,127.450426604133));
#23736=CARTESIAN_POINT('Ctrl Pts',(184.673080895068,3.50423107561896,127.350643867872));
#23737=CARTESIAN_POINT('Ctrl Pts',(184.665306560949,3.4068957149069,127.25457691618));
#23738=CARTESIAN_POINT('Ctrl Pts',(184.65753222683,3.30558680398728,127.162619420857));
#23739=CARTESIAN_POINT('Ctrl Pts',(184.649767473883,3.20440274724626,127.070775254929));
#23740=CARTESIAN_POINT('Ctrl Pts',(184.642002720936,3.09925517067157,126.983030728698));
#23741=CARTESIAN_POINT('Ctrl Pts',(184.634237967988,2.99051163892463,126.899744989882));
#23742=CARTESIAN_POINT('Ctrl Pts',(184.626480927103,2.88187611278586,126.816541971634));
#23743=CARTESIAN_POINT('Ctrl Pts',(184.618723886218,2.7696520474073,126.737789164012));
#23744=CARTESIAN_POINT('Ctrl Pts',(184.610966845333,2.65424206001439,126.663807254868));
#23745=CARTESIAN_POINT('Ctrl Pts',(184.603215654093,2.53891910419166,126.589881136058));
#23746=CARTESIAN_POINT('Ctrl Pts',(184.595464462853,2.42041533625422,126.52071896472));
#23747=CARTESIAN_POINT('Ctrl Pts',(184.587713271613,2.29916420282371,126.456599466013));
#23748=CARTESIAN_POINT('Ctrl Pts',(184.579965374836,2.17796460435902,126.392507219803));
#23749=CARTESIAN_POINT('Ctrl Pts',(184.572217478059,2.0540203077666,126.333453565807));
#23750=CARTESIAN_POINT('Ctrl Pts',(184.564469581282,1.92779113934713,126.279672298405));
#23751=CARTESIAN_POINT('Ctrl Pts',(184.556723305198,1.80158837534844,126.225902280884));
#23752=CARTESIAN_POINT('Ctrl Pts',(184.548977029114,1.67310204963539,126.177402609436));
#23753=CARTESIAN_POINT('Ctrl Pts',(184.54123075303,1.54281347376092,126.134359584624));
#23754=CARTESIAN_POINT('Ctrl Pts',(184.533484419764,1.41252393612583,126.091316242077));
#23755=CARTESIAN_POINT('Ctrl Pts',(184.525738086499,1.28043249301377,126.053729749183));
#23756=CARTESIAN_POINT('Ctrl Pts',(184.517991753233,1.14703679694263,126.021736897372));
#23757=CARTESIAN_POINT('Ctrl Pts',(184.51024368523,1.01361122783021,125.989736880984));
#23758=CARTESIAN_POINT('Ctrl Pts',(184.502495617228,0.878881204667642,125.963333089485));
#23759=CARTESIAN_POINT('Ctrl Pts',(184.494747549225,0.743355387800147,125.94261136139));
#23760=CARTESIAN_POINT('Ctrl Pts',(184.486991246483,0.607685532481822,125.921867609995));
#23761=CARTESIAN_POINT('Ctrl Pts',(184.479234943741,0.471218581013933,125.906818044672));
#23762=CARTESIAN_POINT('Ctrl Pts',(184.471478640999,0.334469704435209,125.897496743429));
#23763=CARTESIAN_POINT('Ctrl Pts',(184.463718198485,0.197647840863254,125.888170467126));
#23764=CARTESIAN_POINT('Ctrl Pts',(184.455957755971,0.0605441429922865,
125.88457855716));
#23765=CARTESIAN_POINT('Ctrl Pts',(184.448197313456,-0.0763263789303934,
125.886702908211));
#23766=CARTESIAN_POINT('Ctrl Pts',(184.440424413191,-0.213416617565448,
125.888830669458));
#23767=CARTESIAN_POINT('Ctrl Pts',(184.432651512926,-0.350272541705855,
125.896693006356));
#23768=CARTESIAN_POINT('Ctrl Pts',(184.42487861266,-0.486383519863692,125.910219821256));
#23769=CARTESIAN_POINT('Ctrl Pts',(184.417388276898,-0.617546521122763,
125.923254902363));
#23770=CARTESIAN_POINT('Ctrl Pts',(184.409897941136,-0.748017492370623,
125.941549732693));
#23771=CARTESIAN_POINT('Ctrl Pts',(184.402407605374,-0.877350507831442,
125.964997110977));
#23772=CARTESIAN_POINT('Ctrl Pts',(184.394633271255,-1.01158722388324,125.989333503735));
#23773=CARTESIAN_POINT('Ctrl Pts',(184.386858937136,-1.14502321111271,126.019297965427));
#23774=CARTESIAN_POINT('Ctrl Pts',(184.379084603017,-1.27714959725893,126.054826748993));
#23775=CARTESIAN_POINT('Ctrl Pts',(184.37131985007,-1.40911314944234,126.090311746508));
#23776=CARTESIAN_POINT('Ctrl Pts',(184.363555097123,-1.53976993792535,126.131347320907));
#23777=CARTESIAN_POINT('Ctrl Pts',(184.355790344176,-1.66861912388403,126.177818357745));
#23778=CARTESIAN_POINT('Ctrl Pts',(184.348033303291,-1.79734033501496,126.224243238894));
#23779=CARTESIAN_POINT('Ctrl Pts',(184.340276262406,-1.92425715102514,126.276092707283));
#23780=CARTESIAN_POINT('Ctrl Pts',(184.332519221521,-2.04888214369525,126.333201369256));
#23781=CARTESIAN_POINT('Ctrl Pts',(184.32476803028,-2.17341315568864,126.390266965143));
#23782=CARTESIAN_POINT('Ctrl Pts',(184.31701683904,-2.29565543039551,126.452583698322));
#23783=CARTESIAN_POINT('Ctrl Pts',(184.3092656478,-2.41514017995914,126.51993755563));
#23784=CARTESIAN_POINT('Ctrl Pts',(184.301517751023,-2.5345741453172,126.587262785753));
#23785=CARTESIAN_POINT('Ctrl Pts',(184.293769854246,-2.65125257672636,126.659620690311));
#23786=CARTESIAN_POINT('Ctrl Pts',(184.286021957469,-2.76473022900649,126.736750775986));
#23787=CARTESIAN_POINT('Ctrl Pts',(184.278275681385,-2.87818414420808,126.81386472771));
#23788=CARTESIAN_POINT('Ctrl Pts',(184.270529405301,-2.98843828887982,126.895748655367));
#23789=CARTESIAN_POINT('Ctrl Pts',(184.262783129217,-3.09507576243218,126.982098317919));
#23790=CARTESIAN_POINT('Ctrl Pts',(184.255036795951,-3.20171402315806,127.068448617884));
#23791=CARTESIAN_POINT('Ctrl Pts',(184.247290462686,-3.30473525564962,127.159264472488));
#23792=CARTESIAN_POINT('Ctrl Pts',(184.239544129421,-3.40375538006029,127.254201131682));
#23793=CARTESIAN_POINT('Ctrl Pts',(184.231796061418,-3.50279767934135,127.349159051283));
#23794=CARTESIAN_POINT('Ctrl Pts',(184.224047993415,-3.59783680540671,127.448239341269));
#23795=CARTESIAN_POINT('Ctrl Pts',(184.216299925412,-3.6885255965423,127.551060449098));
#23796=CARTESIAN_POINT('Ctrl Pts',(184.20854362267,-3.77931077280425,127.653990836424));
#23797=CARTESIAN_POINT('Ctrl Pts',(184.200787319928,-3.86573611899577,127.760669689976));
#23798=CARTESIAN_POINT('Ctrl Pts',(184.193031017186,-3.94749450179272,127.870682001764));
#23799=CARTESIAN_POINT('Ctrl Pts',(184.185270574672,-4.02929652150032,127.980753030435));
#23800=CARTESIAN_POINT('Ctrl Pts',(184.177510132158,-4.10642639472572,128.094160739358));
#23801=CARTESIAN_POINT('Ctrl Pts',(184.169749689644,-4.17862097836977,128.210462049459));
#23802=CARTESIAN_POINT('Ctrl Pts',(184.161976789378,-4.25093145516856,128.326950056747));
#23803=CARTESIAN_POINT('Ctrl Pts',(184.154203889113,-4.31829061835359,128.446340606829));
#23804=CARTESIAN_POINT('Ctrl Pts',(184.146430988847,-4.38048143426836,128.568166201481));
#23805=CARTESIAN_POINT('Ctrl Pts',(184.138940653085,-4.44041145737599,128.685563128908));
#23806=CARTESIAN_POINT('Ctrl Pts',(184.131450317323,-4.49554224537381,128.805220854819));
#23807=CARTESIAN_POINT('Ctrl Pts',(184.123959981561,-4.54572295595053,128.926706264325));
#23808=CARTESIAN_POINT('Ctrl Pts',(184.115260747627,-4.60400255170544,129.067798737404));
#23809=CARTESIAN_POINT('Ctrl Pts',(184.106561513693,-4.65576212734771,129.211734291794));
#23810=CARTESIAN_POINT('Ctrl Pts',(184.097862279759,-4.70074664434197,129.357929130005));
#23811=CARTESIAN_POINT('Ctrl Pts',(184.093441289351,-4.72360798128571,129.432226014336));
#23812=CARTESIAN_POINT('Ctrl Pts',(184.089020298944,-4.74472023587179,129.507106006827));
#23813=CARTESIAN_POINT('Ctrl Pts',(184.084599308536,-4.76405452823405,129.582490119308));
#23814=CARTESIAN_POINT('Ctrl Pts',(185.834939443695,-4.76405452823405,129.582490119308));
#23815=CARTESIAN_POINT('Ctrl Pts',(185.82716587756,-4.79810227029313,129.71524174885));
#23816=CARTESIAN_POINT('Ctrl Pts',(185.819392311426,-4.82655888961819,129.849268541578));
#23817=CARTESIAN_POINT('Ctrl Pts',(185.811618745292,-4.84935969226982,129.984059674321));
#23818=CARTESIAN_POINT('Ctrl Pts',(185.805961071674,-4.8659543281669,130.082161912396));
#23819=CARTESIAN_POINT('Ctrl Pts',(185.800303398056,-4.87955412703471,130.180668865511));
#23820=CARTESIAN_POINT('Ctrl Pts',(185.794645724439,-4.8901515047038,130.279383167057));
#23821=CARTESIAN_POINT('Ctrl Pts',(185.784716961623,-4.90874905140923,130.45261883826));
#23822=CARTESIAN_POINT('Ctrl Pts',(185.774788198807,-4.91814347496568,130.626859993452));
#23823=CARTESIAN_POINT('Ctrl Pts',(185.764859435991,-4.91824909926368,130.801384026903));
#23824=CARTESIAN_POINT('',(186.110140564058,-4.91824801325411,130.808781321355));
#23825=CARTESIAN_POINT('Ctrl Pts',(186.18020938313,-4.76405452823405,129.582490119308));
#23826=CARTESIAN_POINT('Ctrl Pts',(186.17256993295,-4.79768574483935,129.713617722427));
#23827=CARTESIAN_POINT('Ctrl Pts',(186.164930482769,-4.82588839263014,129.846093738758));
#23828=CARTESIAN_POINT('Ctrl Pts',(186.157291032589,-4.84857298836732,129.979422414441));
#23829=CARTESIAN_POINT('Ctrl Pts',(186.149432621167,-4.87190776796963,130.116572544767));
#23830=CARTESIAN_POINT('Ctrl Pts',(186.141574209745,-4.88940334476083,130.254624496003));
#23831=CARTESIAN_POINT('Ctrl Pts',(186.133715798323,-4.90101953991361,130.393032850591));
#23832=CARTESIAN_POINT('Ctrl Pts',(186.125857386902,-4.9126357350664,130.531441205178));
#23833=CARTESIAN_POINT('Ctrl Pts',(186.11799897548,-4.91837257034282,130.67020550101));
#23834=CARTESIAN_POINT('Ctrl Pts',(186.110140564058,-4.91824801325411,130.808781321355));
#23835=CARTESIAN_POINT('Ctrl Pts',(186.110140564008,-4.91824801325332,130.808781322232));
#23836=CARTESIAN_POINT('Ctrl Pts',(186.099074116598,-4.91807260824191,131.003927891408));
#23837=CARTESIAN_POINT('Ctrl Pts',(186.088007669188,-4.90627932088814,131.198573828951));
#23838=CARTESIAN_POINT('Ctrl Pts',(186.076941221778,-4.88306599966,131.391599500359));
#23839=CARTESIAN_POINT('Ctrl Pts',(186.069128931883,-4.86667869954997,131.527864775596));
#23840=CARTESIAN_POINT('Ctrl Pts',(186.061316641987,-4.84460109965971,131.663323468629));
#23841=CARTESIAN_POINT('Ctrl Pts',(186.053504352092,-4.81691589639799,131.797589850688));
#23842=CARTESIAN_POINT('Ctrl Pts',(186.045730017973,-4.78936520086549,131.931203903559));
#23843=CARTESIAN_POINT('Ctrl Pts',(186.037955683854,-4.75620727242799,132.063882400062));
#23844=CARTESIAN_POINT('Ctrl Pts',(186.030181349735,-4.71751805131938,132.195118144231));
#23845=CARTESIAN_POINT('Ctrl Pts',(186.022416596788,-4.67887651121803,132.326192152075));
#23846=CARTESIAN_POINT('Ctrl Pts',(186.014651843841,-4.63471735138709,132.455826573993));
#23847=CARTESIAN_POINT('Ctrl Pts',(186.006887090894,-4.58516767187299,132.583523477821));
#23848=CARTESIAN_POINT('Ctrl Pts',(185.999130050009,-4.53566720579912,132.711093551284));
#23849=CARTESIAN_POINT('Ctrl Pts',(185.991373009124,-4.48078701513992,132.83672957411));
#23850=CARTESIAN_POINT('Ctrl Pts',(185.983615968239,-4.42070414285521,132.95994822744));
#23851=CARTESIAN_POINT('Ctrl Pts',(185.975864776998,-4.36066657953178,133.083073960625));
#23852=CARTESIAN_POINT('Ctrl Pts',(185.968113585758,-4.29543431449837,133.203785602808));
#23853=CARTESIAN_POINT('Ctrl Pts',(185.960362394518,-4.22523254890233,133.321619636856));
#23854=CARTESIAN_POINT('Ctrl Pts',(185.952614497741,-4.15506062092945,133.439403588296));
#23855=CARTESIAN_POINT('Ctrl Pts',(185.944866600964,-4.07992359302457,133.554312029003));
#23856=CARTESIAN_POINT('Ctrl Pts',(185.937118704187,-4.0000925681456,133.665906093138));
#23857=CARTESIAN_POINT('Ctrl Pts',(185.929372428103,-3.92027824219608,133.7774768142));
#23858=CARTESIAN_POINT('Ctrl Pts',(185.921626152019,-3.83577209961954,133.885734219918));
#23859=CARTESIAN_POINT('Ctrl Pts',(185.913879875934,-3.74688829830369,133.990268830703));
#23860=CARTESIAN_POINT('Ctrl Pts',(185.906133542669,-3.65800384086778,134.09480421314));
#23861=CARTESIAN_POINT('Ctrl Pts',(185.898387209404,-3.56474191346714,134.195616447958));
#23862=CARTESIAN_POINT('Ctrl Pts',(185.890640876138,-3.4674563837275,134.292329838968));
#23863=CARTESIAN_POINT('Ctrl Pts',(185.882892808135,-3.37014906756808,134.389064888271));
#23864=CARTESIAN_POINT('Ctrl Pts',(185.875144740132,-3.26881663328405,134.481698991651));
#23865=CARTESIAN_POINT('Ctrl Pts',(185.867396672129,-3.16384885446265,134.569894243576));
#23866=CARTESIAN_POINT('Ctrl Pts',(185.859640369388,-3.05876951463674,134.658183230465));
#23867=CARTESIAN_POINT('Ctrl Pts',(185.851884066646,-2.95004741195152,134.742023689953));
#23868=CARTESIAN_POINT('Ctrl Pts',(185.844127763904,-2.83810480523698,134.82111853621));
#23869=CARTESIAN_POINT('Ctrl Pts',(185.83636732139,-2.72610245138265,134.900255597768));
#23870=CARTESIAN_POINT('Ctrl Pts',(185.828606878875,-2.6108764967903,134.974641787181));
#23871=CARTESIAN_POINT('Ctrl Pts',(185.820846436361,-2.49287620764804,135.044024669804));
#23872=CARTESIAN_POINT('Ctrl Pts',(185.813073536096,-2.3746864939661,135.11351893199));
#23873=CARTESIAN_POINT('Ctrl Pts',(185.80530063583,-2.25371389122609,135.177993653395));
#23874=CARTESIAN_POINT('Ctrl Pts',(185.797527735565,-2.13043097123238,135.237243081529));
#23875=CARTESIAN_POINT('Ctrl Pts',(185.790037399803,-2.01162969591266,135.294338643711));
#23876=CARTESIAN_POINT('Ctrl Pts',(185.782547064041,-1.89068344157314,135.346582099913));
#23877=CARTESIAN_POINT('Ctrl Pts',(185.775056728279,-1.76802881817535,135.393833044828));
#23878=CARTESIAN_POINT('Ctrl Pts',(185.76728239416,-1.64072370745012,135.442875523682));
#23879=CARTESIAN_POINT('Ctrl Pts',(185.759508060041,-1.51117486044447,135.486694787618));
#23880=CARTESIAN_POINT('Ctrl Pts',(185.751733725922,-1.37985004303931,135.525080575499));
#23881=CARTESIAN_POINT('Ctrl Pts',(185.743968972975,-1.24868707173481,135.563419056326));
#23882=CARTESIAN_POINT('Ctrl Pts',(185.736204220028,-1.11575285660129,135.596337276052));
#23883=CARTESIAN_POINT('Ctrl Pts',(185.728439467081,-0.981535022751411,
135.623673023046));
#23884=CARTESIAN_POINT('Ctrl Pts',(185.720682426196,-0.847450495946294,
135.650981619791));
#23885=CARTESIAN_POINT('Ctrl Pts',(185.712925385311,-0.712085268171024,
135.672718700269));
#23886=CARTESIAN_POINT('Ctrl Pts',(185.705168344426,-0.575941665315386,
135.688771970089));
#23887=CARTESIAN_POINT('Ctrl Pts',(185.697417153186,-0.439900729409612,
135.704813134013));
#23888=CARTESIAN_POINT('Ctrl Pts',(185.689665961946,-0.303082973473198,
135.715178973112));
#23889=CARTESIAN_POINT('Ctrl Pts',(185.681914770705,-0.166000094317469,
135.719808413158));
#23890=CARTESIAN_POINT('Ctrl Pts',(185.674166873928,-0.0289754790421877,
135.724435885568));
#23891=CARTESIAN_POINT('Ctrl Pts',(185.666418977151,0.108313645407252,135.723331794998));
#23892=CARTESIAN_POINT('Ctrl Pts',(185.658671080374,0.245351511000205,135.716487010336));
#23893=CARTESIAN_POINT('Ctrl Pts',(185.65092480429,0.382360711225824,135.709643657456));
#23894=CARTESIAN_POINT('Ctrl Pts',(185.643178528206,0.519118366904536,135.697062018493));
#23895=CARTESIAN_POINT('Ctrl Pts',(185.635432252122,0.655110161251152,135.678785069655));
#23896=CARTESIAN_POINT('Ctrl Pts',(185.627685918857,0.791102959458301,135.660507985901));
#23897=CARTESIAN_POINT('Ctrl Pts',(185.619939585591,0.926329497570983,135.636535560459));
#23898=CARTESIAN_POINT('Ctrl Pts',(185.612193252326,1.06028241764848,135.606962439217));
#23899=CARTESIAN_POINT('Ctrl Pts',(185.604445184323,1.19426533555364,135.577382695279));
#23900=CARTESIAN_POINT('Ctrl Pts',(185.59669711632,1.32697368617402,135.542199844023));
#23901=CARTESIAN_POINT('Ctrl Pts',(185.588949048317,1.45791249787162,135.501559166813));
#23902=CARTESIAN_POINT('Ctrl Pts',(185.581192745575,1.58899047289653,135.460875296208));
#23903=CARTESIAN_POINT('Ctrl Pts',(185.573436442833,1.71829477813514,135.414722128319));
#23904=CARTESIAN_POINT('Ctrl Pts',(185.565680140092,1.84534722565303,135.363294339312));
#23905=CARTESIAN_POINT('Ctrl Pts',(185.557919697577,1.97246748488773,135.311839101746));
#23906=CARTESIAN_POINT('Ctrl Pts',(185.550159255063,2.09733313577467,135.25510379514));
#23907=CARTESIAN_POINT('Ctrl Pts',(185.542398812549,2.21948895854959,135.193329952772));
#23908=CARTESIAN_POINT('Ctrl Pts',(185.534625912284,2.34184087669565,135.131456945548));
#23909=CARTESIAN_POINT('Ctrl Pts',(185.526853012018,2.46147393253308,135.064529430542));
#23910=CARTESIAN_POINT('Ctrl Pts',(185.519080111753,2.57795958406316,134.992833781553));
#23911=CARTESIAN_POINT('Ctrl Pts',(185.511589775991,2.69021068875094,134.923744449994));
#23912=CARTESIAN_POINT('Ctrl Pts',(185.504099440229,2.79953899281448,134.850227805036));
#23913=CARTESIAN_POINT('Ctrl Pts',(185.496609104467,2.90559037094153,134.772575286506));
#23914=CARTESIAN_POINT('Ctrl Pts',(185.488834770348,3.01566271930338,134.691978549134));
#23915=CARTESIAN_POINT('Ctrl Pts',(185.481060436228,3.12255342329199,134.606670817637));
#23916=CARTESIAN_POINT('Ctrl Pts',(185.473286102109,3.22583274537233,134.516931985417));
#23917=CARTESIAN_POINT('Ctrl Pts',(185.465521349162,3.32898478491854,134.427303748286));
#23918=CARTESIAN_POINT('Ctrl Pts',(185.457756596215,3.42853400584439,134.333255530036));
#23919=CARTESIAN_POINT('Ctrl Pts',(185.449991843268,3.52408036162776,134.235109904134));
#23920=CARTESIAN_POINT('Ctrl Pts',(185.442234802383,3.61953181942352,134.137061757852));
#23921=CARTESIAN_POINT('Ctrl Pts',(185.434477761498,3.71098805294843,134.034924580939));
#23922=CARTESIAN_POINT('Ctrl Pts',(185.426720720613,3.79808306633545,133.92906029653));
#23923=CARTESIAN_POINT('Ctrl Pts',(185.418969529373,3.88511240069542,133.823275845201));
#23924=CARTESIAN_POINT('Ctrl Pts',(185.411218338133,3.96778681374832,133.713770181484));
#23925=CARTESIAN_POINT('Ctrl Pts',(185.403467146893,4.0457783373907,133.600940798287));
#23926=CARTESIAN_POINT('Ctrl Pts',(185.395719250116,4.12373671255506,133.488159370587));
#23927=CARTESIAN_POINT('Ctrl Pts',(185.387971353338,4.19701593512668,133.372057354035));
#23928=CARTESIAN_POINT('Ctrl Pts',(185.380223456561,4.2653295376257,133.253063743296));
#23929=CARTESIAN_POINT('Ctrl Pts',(185.372477180477,4.33362885039174,133.134095023454));
#23930=CARTESIAN_POINT('Ctrl Pts',(185.364730904393,4.39696441458693,133.01223625137));
#23931=CARTESIAN_POINT('Ctrl Pts',(185.356984628309,4.45509438652842,132.887943366012));
#23932=CARTESIAN_POINT('Ctrl Pts',(185.349238295044,4.51322478757213,132.763649563153));
#23933=CARTESIAN_POINT('Ctrl Pts',(185.341491961778,4.56614935405513,132.636921965314));
#23934=CARTESIAN_POINT('Ctrl Pts',(185.333745628513,4.61367347488339,132.508238585514));
#23935=CARTESIAN_POINT('Ctrl Pts',(185.32599756051,4.661208238409,132.379526387963));
#23936=CARTESIAN_POINT('Ctrl Pts',(185.318249492507,4.70334001430907,132.248857903597));
#23937=CARTESIAN_POINT('Ctrl Pts',(185.310501424504,4.73992348764949,132.116728094201));
#23938=CARTESIAN_POINT('Ctrl Pts',(185.302745121762,4.77654584234074,131.98445785567));
#23939=CARTESIAN_POINT('Ctrl Pts',(185.29498881902,4.80760801048513,131.850723566987));
#23940=CARTESIAN_POINT('Ctrl Pts',(185.287232516278,4.83301530639473,131.716032768426));
#23941=CARTESIAN_POINT('Ctrl Pts',(185.279472073764,4.85843616294317,131.581270081331));
#23942=CARTESIAN_POINT('Ctrl Pts',(185.27171163125,4.87819607698591,131.445550253803));
#23943=CARTESIAN_POINT('Ctrl Pts',(185.263951188736,4.8922521999072,131.30938682976));
#23944=CARTESIAN_POINT('Ctrl Pts',(185.25617828847,4.90633088696485,131.173004824101));
#23945=CARTESIAN_POINT('Ctrl Pts',(185.248405388205,4.91468746198499,131.036178189385));
#23946=CARTESIAN_POINT('Ctrl Pts',(185.24063248794,4.91733122193595,130.899422262165));
#23947=CARTESIAN_POINT('Ctrl Pts',(185.233142152178,4.91987887455347,130.767637757367));
#23948=CARTESIAN_POINT('Ctrl Pts',(185.225651816415,4.91712185788959,130.635919216476));
#23949=CARTESIAN_POINT('Ctrl Pts',(185.218161480653,4.90911395514333,130.504722105494));
#23950=CARTESIAN_POINT('Ctrl Pts',(185.210387146534,4.90080243033051,130.368550616171));
#23951=CARTESIAN_POINT('Ctrl Pts',(185.202612812415,4.8868076562378,130.232509526972));
#23952=CARTESIAN_POINT('Ctrl Pts',(185.194838478296,4.86713283147692,130.097111677475));
#23953=CARTESIAN_POINT('Ctrl Pts',(185.187073725349,4.84748225417918,129.961880693727));
#23954=CARTESIAN_POINT('Ctrl Pts',(185.179308972402,4.82216561011635,129.827291755562));
#23955=CARTESIAN_POINT('Ctrl Pts',(185.171544219455,4.79123805456728,129.693855792288));
#23956=CARTESIAN_POINT('Ctrl Pts',(185.16378717857,4.76034121670238,129.560552359494));
#23957=CARTESIAN_POINT('Ctrl Pts',(185.156030137685,4.72384464525298,129.428400001093));
#23958=CARTESIAN_POINT('Ctrl Pts',(185.1482730968,4.68185500669668,129.297902268069));
#23959=CARTESIAN_POINT('Ctrl Pts',(185.14052190556,4.63989703285347,129.167502944401));
#23960=CARTESIAN_POINT('Ctrl Pts',(185.13277071432,4.59245435629693,129.038756133175));
#23961=CARTESIAN_POINT('Ctrl Pts',(185.12501952308,4.53968412429643,128.912152617871));
#23962=CARTESIAN_POINT('Ctrl Pts',(185.117271626302,4.48693632105218,128.785602912438));
#23963=CARTESIAN_POINT('Ctrl Pts',(185.109523729525,4.42886561609171,128.661195051217));
#23964=CARTESIAN_POINT('Ctrl Pts',(185.101775832748,4.36567809210519,128.539401929507));
#23965=CARTESIAN_POINT('Ctrl Pts',(185.094029556664,4.30250378558652,128.417634284293));
#23966=CARTESIAN_POINT('Ctrl Pts',(185.08628328058,4.23421496891706,128.298480637502));
#23967=CARTESIAN_POINT('Ctrl Pts',(185.078537004496,4.16106451404611,128.182390905223));
#23968=CARTESIAN_POINT('Ctrl Pts',(185.070790671231,4.08791351919513,128.066300315995));
#23969=CARTESIAN_POINT('Ctrl Pts',(185.063044337965,4.00990102295931,127.953274017186));
#23970=CARTESIAN_POINT('Ctrl Pts',(185.0552980047,3.92732399917947,127.843734118332));
#23971=CARTESIAN_POINT('Ctrl Pts',(185.047549936697,3.84472848284773,127.734169688777));
#23972=CARTESIAN_POINT('Ctrl Pts',(185.039801868694,3.75756664022695,127.628093524923));
#23973=CARTESIAN_POINT('Ctrl Pts',(185.032053800691,3.66617635041229,127.525895423275));
#23974=CARTESIAN_POINT('Ctrl Pts',(185.024297497949,3.57468892991002,127.423588704268));
#23975=CARTESIAN_POINT('Ctrl Pts',(185.016541195207,3.47896434590667,127.325168572807));
#23976=CARTESIAN_POINT('Ctrl Pts',(185.008784892466,3.37937842648236,127.230989028559));
#23977=CARTESIAN_POINT('Ctrl Pts',(185.001024449951,3.27973935505435,127.136759217851));
#23978=CARTESIAN_POINT('Ctrl Pts',(184.993264007437,3.17623513657302,127.046774760618));
#23979=CARTESIAN_POINT('Ctrl Pts',(184.985503564923,3.06927466935573,126.961349289642));
#23980=CARTESIAN_POINT('Ctrl Pts',(184.977730664658,2.96214249970095,126.875786686117));
#23981=CARTESIAN_POINT('Ctrl Pts',(184.969957764392,2.85154330970152,126.794797924641));
#23982=CARTESIAN_POINT('Ctrl Pts',(184.962184864127,2.73791569183312,126.718653735408));
#23983=CARTESIAN_POINT('Ctrl Pts',(184.954694528365,2.62841872408481,126.645277579249));
#23984=CARTESIAN_POINT('Ctrl Pts',(184.947204192603,2.51610995032003,126.576400046695));
#23985=CARTESIAN_POINT('Ctrl Pts',(184.939713856841,2.40140163811663,126.512222078918));
#23986=CARTESIAN_POINT('Ctrl Pts',(184.931939522722,2.28234412539138,126.445610783985));
#23987=CARTESIAN_POINT('Ctrl Pts',(184.924165188603,2.16032438692566,126.383851452082));
#23988=CARTESIAN_POINT('Ctrl Pts',(184.916390854484,2.03577561811003,126.327218594444));
#23989=CARTESIAN_POINT('Ctrl Pts',(184.908626101536,1.91138034452076,126.270655531741));
#23990=CARTESIAN_POINT('Ctrl Pts',(184.900861348589,1.78446259457604,126.2192065328));
#23991=CARTESIAN_POINT('Ctrl Pts',(184.893096595642,1.65548204034892,126.173101363693));
#23992=CARTESIAN_POINT('Ctrl Pts',(184.885339554757,1.5266295914267,126.12704198689));
#23993=CARTESIAN_POINT('Ctrl Pts',(184.877582513872,1.3957187812083,126.086316008371));
#23994=CARTESIAN_POINT('Ctrl Pts',(184.869825472987,1.26323091723401,126.051105868213));
#23995=CARTESIAN_POINT('Ctrl Pts',(184.862074281747,1.13084296338832,126.015922280296));
#23996=CARTESIAN_POINT('Ctrl Pts',(184.854323090507,0.996880699273993,125.986246351446));
#23997=CARTESIAN_POINT('Ctrl Pts',(184.846571899267,0.861841976869711,125.962211149674));
#23998=CARTESIAN_POINT('Ctrl Pts',(184.83882400249,0.726860649524842,125.938186163504));
#23999=CARTESIAN_POINT('Ctrl Pts',(184.831076105713,0.590804157979271,125.919797204415));
#24000=CARTESIAN_POINT('Ctrl Pts',(184.823328208936,0.454181755168668,125.907126500662));
#24001=CARTESIAN_POINT('Ctrl Pts',(184.815581932852,0.317587930819519,125.894458447347));
#24002=CARTESIAN_POINT('Ctrl Pts',(184.807835656767,0.180428819710515,125.88750630627));
#24003=CARTESIAN_POINT('Ctrl Pts',(184.800089380683,0.0432196324551924,
125.886300519736));
#24004=CARTESIAN_POINT('Ctrl Pts',(184.792343047418,-0.0939905676472747,
125.8850947243));
#24005=CARTESIAN_POINT('Ctrl Pts',(184.784596714153,-0.231250453683563,
125.889635371485));
#24006=CARTESIAN_POINT('Ctrl Pts',(184.776850380887,-0.368044371329767,
125.899900769302));
#24007=CARTESIAN_POINT('Ctrl Pts',(184.769102312884,-0.504868923025204,
125.910168465984));
#24008=CARTESIAN_POINT('Ctrl Pts',(184.761354244881,-0.641226908890993,
125.926163435116));
#24009=CARTESIAN_POINT('Ctrl Pts',(184.753606176878,-0.77660775018482,125.947812103976));
#24010=CARTESIAN_POINT('Ctrl Pts',(184.745849874136,-0.912132475847942,
125.969483781299));
#24011=CARTESIAN_POINT('Ctrl Pts',(184.738093571395,-1.04667759570581,125.996821099783));
#24012=CARTESIAN_POINT('Ctrl Pts',(184.730337268653,-1.17974213555564,126.029699210084));
#24013=CARTESIAN_POINT('Ctrl Pts',(184.722576826139,-1.312877695957,126.062594868424));
#24014=CARTESIAN_POINT('Ctrl Pts',(184.714816383624,-1.44453072664021,126.101037101697));
#24015=CARTESIAN_POINT('Ctrl Pts',(184.70705594111,-1.57421633993268,126.144851418349));
#24016=CARTESIAN_POINT('Ctrl Pts',(184.699283040845,-1.70411013608448,126.188736069632));
#24017=CARTESIAN_POINT('Ctrl Pts',(184.691510140579,-1.83202983856468,126.238009896672));
#24018=CARTESIAN_POINT('Ctrl Pts',(184.683737240314,-1.95751060444897,126.292450235481));
#24019=CARTESIAN_POINT('Ctrl Pts',(184.676246904552,-2.07842982842536,126.344911530846));
#24020=CARTESIAN_POINT('Ctrl Pts',(184.66875656879,-2.19708408278854,126.402170094191));
#24021=CARTESIAN_POINT('Ctrl Pts',(184.661266233028,-2.31308146934551,126.463987686737));
#24022=CARTESIAN_POINT('Ctrl Pts',(184.653490953882,-2.43349156701393,126.528156911382));
#24023=CARTESIAN_POINT('Ctrl Pts',(184.645715674736,-2.55142012255629,126.597442189508));
#24024=CARTESIAN_POINT('Ctrl Pts',(184.63794039559,-2.66640186075916,126.671627359849));
#24025=CARTESIAN_POINT('Ctrl Pts',(184.630174906103,-2.78123882835338,126.745719125512));
#24026=CARTESIAN_POINT('Ctrl Pts',(184.622409416615,-2.89313603609128,126.824698297011));
#24027=CARTESIAN_POINT('Ctrl Pts',(184.614643927127,-3.00165158969343,126.908302250884));
#24028=CARTESIAN_POINT('Ctrl Pts',(184.606887744613,-3.11003708692624,126.99180600505));
#24029=CARTESIAN_POINT('Ctrl Pts',(184.599131562098,-3.21504869422354,127.079923265202));
#24030=CARTESIAN_POINT('Ctrl Pts',(184.591375379584,-3.31627290310998,127.172347801702));
#24031=CARTESIAN_POINT('Ctrl Pts',(184.583624474521,-3.41742823714848,127.264709450816));
#24032=CARTESIAN_POINT('Ctrl Pts',(184.575873569458,-3.51480101205282,127.361372283403));
#24033=CARTESIAN_POINT('Ctrl Pts',(184.568122664396,-3.60801021796009,127.461989403952));
#24034=CARTESIAN_POINT('Ctrl Pts',(184.560375354587,-3.70117618882434,127.562559853301));
#24035=CARTESIAN_POINT('Ctrl Pts',(184.552628044778,-3.79018216867158,127.66708065461));
#24036=CARTESIAN_POINT('Ctrl Pts',(184.544880734968,-3.87468379235378,127.77516789148));
#24037=CARTESIAN_POINT('Ctrl Pts',(184.537135340988,-3.9591645196716,127.883228399511));
#24038=CARTESIAN_POINT('Ctrl Pts',(184.529389947007,-4.03914286792834,127.994853279576));
#24039=CARTESIAN_POINT('Ctrl Pts',(184.521644553026,-4.11431484242556,128.10962566958));
#24040=CARTESIAN_POINT('Ctrl Pts',(184.513896696704,-4.18951071487447,128.22443454692));
#24041=CARTESIAN_POINT('Ctrl Pts',(184.506148840382,-4.25989694066962,128.342392609911));
#24042=CARTESIAN_POINT('Ctrl Pts',(184.49840098406,-4.32521289149947,128.463054036679));
#24043=CARTESIAN_POINT('Ctrl Pts',(184.49065211975,-4.39053733987044,128.583731161379));
#24044=CARTESIAN_POINT('Ctrl Pts',(184.482903255439,-4.45079002018339,128.707112002701));
#24045=CARTESIAN_POINT('Ctrl Pts',(184.475154391129,-4.50575679107406,128.832727081082));
#24046=CARTESIAN_POINT('Ctrl Pts',(184.467398393862,-4.56077415977317,128.958457790189));
#24047=CARTESIAN_POINT('Ctrl Pts',(184.459642396596,-4.61049574662458,129.086426484169));
#24048=CARTESIAN_POINT('Ctrl Pts',(184.451886399329,-4.65475582965104,129.216144250433));
#24049=CARTESIAN_POINT('Ctrl Pts',(184.44466748376,-4.6959510224118,129.336879414498));
#24050=CARTESIAN_POINT('Ctrl Pts',(184.437448568192,-4.73241533402233,129.459129381269));
#24051=CARTESIAN_POINT('Ctrl Pts',(184.430229652623,-4.76405452823406,129.582490119308));
#24052=CARTESIAN_POINT('Origin',(213.235140564004,0.,130.804360617566));
#24053=CARTESIAN_POINT('',(182.334764431275,-4.76405452823405,129.582490119308));
#24054=CARTESIAN_POINT('',(182.679902359578,-4.76405452823405,129.582490119308));
#24055=CARTESIAN_POINT('',(213.235140564004,-4.76405452823405,129.582490119308));
#24056=CARTESIAN_POINT('',(184.014859436043,-4.9182492280365,130.801605001777));
#24057=CARTESIAN_POINT('Ctrl Pts',(184.014859435991,-4.91824922803702,130.801605002707));
#24058=CARTESIAN_POINT('Ctrl Pts',(184.0070245266,-4.91832708928895,130.94057255142));
#24059=CARTESIAN_POINT('Ctrl Pts',(183.999189617208,-4.91251071226177,131.079545490942));
#24060=CARTESIAN_POINT('Ctrl Pts',(183.991354707817,-4.90082530395939,131.217996209085));
#24061=CARTESIAN_POINT('Ctrl Pts',(183.983518210813,-4.88913752780615,131.356474981931));
#24062=CARTESIAN_POINT('Ctrl Pts',(183.97568171381,-4.87157838318562,131.494430945472));
#24063=CARTESIAN_POINT('Ctrl Pts',(183.967845216806,-4.84822496807564,131.631341706484));
#24064=CARTESIAN_POINT('Ctrl Pts',(183.960005585196,-4.82486221157711,131.768307231932));
#24065=CARTESIAN_POINT('Ctrl Pts',(183.952165953587,-4.79570063209204,131.904226349297));
#24066=CARTESIAN_POINT('Ctrl Pts',(183.944326321977,-4.76086839271114,132.038587180959));
#24067=CARTESIAN_POINT('Ctrl Pts',(183.936091824958,-4.72428172823233,132.179715479181));
#24068=CARTESIAN_POINT('Ctrl Pts',(183.927857327939,-4.68143846664776,132.319123983606));
#24069=CARTESIAN_POINT('Ctrl Pts',(183.91962283092,-4.63254572439523,132.456239297702));
#24070=CARTESIAN_POINT('Ctrl Pts',(183.911767314248,-4.58590319711227,132.58704408557));
#24071=CARTESIAN_POINT('Ctrl Pts',(183.903911797577,-4.53375578798978,132.71576172528));
#24072=CARTESIAN_POINT('Ctrl Pts',(183.896056280906,-4.47633184758892,132.84191705918));
#24073=CARTESIAN_POINT('Ctrl Pts',(183.888194193542,-4.41885987532938,132.968177914837));
#24074=CARTESIAN_POINT('Ctrl Pts',(183.880332106178,-4.35610274681267,133.09187185747));
#24075=CARTESIAN_POINT('Ctrl Pts',(183.872470018814,-4.28833398097888,133.212549715225));
#24076=CARTESIAN_POINT('Ctrl Pts',(183.864595817316,-4.2204607950577,133.333413516936));
#24077=CARTESIAN_POINT('Ctrl Pts',(183.856721615819,-4.14756075301982,133.451251635519));
#24078=CARTESIAN_POINT('Ctrl Pts',(183.848847414322,-4.06995003088787,133.565644704468));
#24079=CARTESIAN_POINT('Ctrl Pts',(183.847735728798,-4.05899289239229,133.58179480158));
#24080=CARTESIAN_POINT('Ctrl Pts',(183.846624043273,-4.04794192437879,133.597876287981));
#24081=CARTESIAN_POINT('Ctrl Pts',(183.845512357748,-4.03679807846351,133.613888039787));
#24082=CARTESIAN_POINT('Ctrl Pts',(183.837738023629,-3.95886598381865,133.7258627895));
#24083=CARTESIAN_POINT('Ctrl Pts',(183.82996368951,-3.87614790100592,133.834769861943));
#24084=CARTESIAN_POINT('Ctrl Pts',(183.822189355391,-3.78891333030926,133.940172926666));
#24085=CARTESIAN_POINT('Ctrl Pts',(183.814424602444,-3.70178626842471,134.045446091532));
#24086=CARTESIAN_POINT('Ctrl Pts',(183.806659849497,-3.61015404055219,134.147223542661));
#24087=CARTESIAN_POINT('Ctrl Pts',(183.79889509655,-3.51432952725466,134.245097607858));
#24088=CARTESIAN_POINT('Ctrl Pts',(183.791138055665,-3.41860018821441,134.342874463155));
#24089=CARTESIAN_POINT('Ctrl Pts',(183.78338101478,-3.31868712171636,134.436755370167));
#24090=CARTESIAN_POINT('Ctrl Pts',(183.775623973895,-3.21494336377899,134.526365753268));
#24091=CARTESIAN_POINT('Ctrl Pts',(183.767872782655,-3.11127783981671,134.615908560482));
#24092=CARTESIAN_POINT('Ctrl Pts',(183.760121591415,-3.00378766898042,134.701186999335));
#24093=CARTESIAN_POINT('Ctrl Pts',(183.752370400174,-2.89286235937896,134.781863657438));
#24094=CARTESIAN_POINT('Ctrl Pts',(183.744622503397,-2.7819841959931,134.862506025808));
#24095=CARTESIAN_POINT('Ctrl Pts',(183.73687460662,-2.66767411324236,134.938550274043));
#24096=CARTESIAN_POINT('Ctrl Pts',(183.729126709843,-2.55035410782106,135.009699722468));
#24097=CARTESIAN_POINT('Ctrl Pts',(183.721380433759,-2.43305864321574,135.080834287963));
#24098=CARTESIAN_POINT('Ctrl Pts',(183.713634157675,-2.31275484235268,135.147075887609));
#24099=CARTESIAN_POINT('Ctrl Pts',(183.705887881591,-2.18989270931988,135.20817180609));
#24100=CARTESIAN_POINT('Ctrl Pts',(183.698141548325,-2.06702966934689,135.269268175567));
#24101=CARTESIAN_POINT('Ctrl Pts',(183.69039521506,-1.94160860959151,135.325218614004));
#24102=CARTESIAN_POINT('Ctrl Pts',(183.682648881795,-1.81410273528698,135.375817095356));
#24103=CARTESIAN_POINT('Ctrl Pts',(183.674900813792,-1.68656830692579,135.426426907886));
#24104=CARTESIAN_POINT('Ctrl Pts',(183.667152745789,-1.55694849830684,135.471682234208));
#24105=CARTESIAN_POINT('Ctrl Pts',(183.659404677786,-1.4257346415192,135.511425923515));
#24106=CARTESIAN_POINT('Ctrl Pts',(183.651648375044,-1.29438132908304,135.551211852889));
#24107=CARTESIAN_POINT('Ctrl Pts',(183.643892072302,-1.1614309589586,135.585474330078));
#24108=CARTESIAN_POINT('Ctrl Pts',(183.63613576956,-1.02738865306596,135.614106517097));
#24109=CARTESIAN_POINT('Ctrl Pts',(183.628375327046,-0.893274804758753,
135.642753985975));
#24110=CARTESIAN_POINT('Ctrl Pts',(183.620614884532,-0.758068244641496,
135.665765111291));
#24111=CARTESIAN_POINT('Ctrl Pts',(183.612854442018,-0.622281340493539,
135.683084733129));
#24112=CARTESIAN_POINT('Ctrl Pts',(183.605081541752,-0.486276459152402,
135.700432157962));
#24113=CARTESIAN_POINT('Ctrl Pts',(183.597308641487,-0.349689761885385,
135.712069788455));
#24114=CARTESIAN_POINT('Ctrl Pts',(183.589535741221,-0.213036659942975,
135.717994552244));
#24115=CARTESIAN_POINT('Ctrl Pts',(183.582045405459,-0.0813512424637309,
135.723703935946));
#24116=CARTESIAN_POINT('Ctrl Pts',(183.574555069697,0.0503955275397817,
135.724108595028));
#24117=CARTESIAN_POINT('Ctrl Pts',(183.567064733935,0.181747024582314,135.719251367273));
#24118=CARTESIAN_POINT('Ctrl Pts',(183.559290399816,0.318078753557754,135.714209976251));
#24119=CARTESIAN_POINT('Ctrl Pts',(183.551516065697,0.45441650227473,135.703483843342));
#24120=CARTESIAN_POINT('Ctrl Pts',(183.543741731578,0.590247502080792,135.687063859499));
#24121=CARTESIAN_POINT('Ctrl Pts',(183.535976978631,0.725911102318697,135.67066411182));
#24122=CARTESIAN_POINT('Ctrl Pts',(183.528212225684,0.861068811846414,135.648584521738));
#24123=CARTESIAN_POINT('Ctrl Pts',(183.520447472737,0.995208524915738,135.620867967756));
#24124=CARTESIAN_POINT('Ctrl Pts',(183.512690431852,1.12921500853146,135.593178942246));
#24125=CARTESIAN_POINT('Ctrl Pts',(183.504933390967,1.26220512740057,135.559864173125));
#24126=CARTESIAN_POINT('Ctrl Pts',(183.497176350082,1.39367291584853,135.521018212318));
#24127=CARTESIAN_POINT('Ctrl Pts',(183.489425158842,1.52504156341419,135.482201545552));
#24128=CARTESIAN_POINT('Ctrl Pts',(183.481673967602,1.65488979216254,135.43786209979));
#24129=CARTESIAN_POINT('Ctrl Pts',(183.473922776362,1.78272318884635,135.388145199595));
#24130=CARTESIAN_POINT('Ctrl Pts',(183.466174879585,1.91050225292687,135.33844943041));
#24131=CARTESIAN_POINT('Ctrl Pts',(183.458426982807,2.0362678245576,135.283380894017));
#24132=CARTESIAN_POINT('Ctrl Pts',(183.45067908603,2.15954219920582,135.223134265576));
#24133=CARTESIAN_POINT('Ctrl Pts',(183.442932809946,2.28279078751236,135.162900239432));
#24134=CARTESIAN_POINT('Ctrl Pts',(183.435186533862,2.40354886430429,135.097490447235));
#24135=CARTESIAN_POINT('Ctrl Pts',(183.427440257778,2.52136057482751,135.027146891367));
#24136=CARTESIAN_POINT('Ctrl Pts',(183.419693924513,2.63917315501009,134.95680281624));
#24137=CARTESIAN_POINT('Ctrl Pts',(183.411947591247,2.7540389898437,134.881525105199));
#24138=CARTESIAN_POINT('Ctrl Pts',(183.404201257982,2.86552896479428,134.8016005171));
#24139=CARTESIAN_POINT('Ctrl Pts',(183.396453189979,2.97704390715139,134.721658030443));
#24140=CARTESIAN_POINT('Ctrl Pts',(183.388705121976,3.08518116758142,134.637066823728));
#24141=CARTESIAN_POINT('Ctrl Pts',(183.380957053973,3.18954295366573,134.548155324708));
#24142=CARTESIAN_POINT('Ctrl Pts',(183.373200751231,3.29401565669837,134.459149329488));
#24143=CARTESIAN_POINT('Ctrl Pts',(183.36544444849,3.3947045716674,134.36581412358));
#24144=CARTESIAN_POINT('Ctrl Pts',(183.357688145748,3.49124678201167,134.268516931821));
#24145=CARTESIAN_POINT('Ctrl Pts',(183.349927703234,3.58784051984049,134.171167809621));
#24146=CARTESIAN_POINT('Ctrl Pts',(183.342167260719,3.68028287962462,134.069852776656));
#24147=CARTESIAN_POINT('Ctrl Pts',(183.334406818205,3.76825050646584,133.964973087171));
#24148=CARTESIAN_POINT('Ctrl Pts',(183.32663391794,3.85635934675105,133.859925035496));
#24149=CARTESIAN_POINT('Ctrl Pts',(183.318861017674,3.93997886106847,133.751301202296));
#24150=CARTESIAN_POINT('Ctrl Pts',(183.311088117409,4.01882787217965,133.639533556964));
#24151=CARTESIAN_POINT('Ctrl Pts',(183.303597781647,4.094810523129,133.531828947063));
#24152=CARTESIAN_POINT('Ctrl Pts',(183.296107445885,4.16636332155617,133.421205386315));
#24153=CARTESIAN_POINT('Ctrl Pts',(183.288617110123,4.23327549087247,133.308070201539));
#24154=CARTESIAN_POINT('Ctrl Pts',(183.280842776004,4.3027246554253,133.190645461847));
#24155=CARTESIAN_POINT('Ctrl Pts',(183.273068441885,4.36739433944492,133.070142915728));
#24156=CARTESIAN_POINT('Ctrl Pts',(183.265294107765,4.42699971525186,132.94698904631));
#24157=CARTESIAN_POINT('Ctrl Pts',(183.257529354818,4.48653163276008,132.823986953029));
#24158=CARTESIAN_POINT('Ctrl Pts',(183.249764601871,4.5410114917085,132.698340386375));
#24159=CARTESIAN_POINT('Ctrl Pts',(183.241999848924,4.59019856132849,132.570503372294));
#24160=CARTESIAN_POINT('Ctrl Pts',(183.234242808039,4.63933677765773,132.442793327737));
#24161=CARTESIAN_POINT('Ctrl Pts',(183.226485767154,4.6831925265859,132.312897527787));
#24162=CARTESIAN_POINT('Ctrl Pts',(183.218728726269,4.72157187051949,132.181292763323));
#24163=CARTESIAN_POINT('Ctrl Pts',(183.210977535029,4.75992227229126,132.049787243035));
#24164=CARTESIAN_POINT('Ctrl Pts',(183.203226343789,4.79280438017088,131.91657569721));
#24165=CARTESIAN_POINT('Ctrl Pts',(183.195475152549,4.82007321739351,131.782152641192));
#24166=CARTESIAN_POINT('Ctrl Pts',(183.187727255772,4.84733046463286,131.647786718558));
#24167=CARTESIAN_POINT('Ctrl Pts',(183.179979358994,4.86897910880454,131.512210692235));
#24168=CARTESIAN_POINT('Ctrl Pts',(183.172231462217,4.88492472466578,131.375931695254));
#24169=CARTESIAN_POINT('Ctrl Pts',(183.164485186133,4.90086700504792,131.239681204901));
#24170=CARTESIAN_POINT('Ctrl Pts',(183.156738910049,4.91110858455677,131.102728424444));
#24171=CARTESIAN_POINT('Ctrl Pts',(183.148992633965,4.91560666602142,130.965587685597));
#24172=CARTESIAN_POINT('Ctrl Pts',(183.1412463007,4.92010478068989,130.828445934408));
#24173=CARTESIAN_POINT('Ctrl Pts',(183.133499967434,4.91885929989721,130.691116612814));
#24174=CARTESIAN_POINT('Ctrl Pts',(183.125753634169,4.91187953510186,130.554115747194));
#24175=CARTESIAN_POINT('Ctrl Pts',(183.118005566166,4.90489820723658,130.417084201179));
#24176=CARTESIAN_POINT('Ctrl Pts',(183.110257498163,4.89218005994142,130.280381647888));
#24177=CARTESIAN_POINT('Ctrl Pts',(183.10250943016,4.87378639226766,130.144520284571));
#24178=CARTESIAN_POINT('Ctrl Pts',(183.094753127418,4.85537317558499,130.00851452618));
#24179=CARTESIAN_POINT('Ctrl Pts',(183.086996824676,4.83127244146896,129.873352131727));
#24180=CARTESIAN_POINT('Ctrl Pts',(183.079240521934,4.80159698130756,129.739536927184));
#24181=CARTESIAN_POINT('Ctrl Pts',(183.07148007942,4.77190568245958,129.605650301438));
#24182=CARTESIAN_POINT('Ctrl Pts',(183.063719636906,4.73663382932912,129.473112675974));
#24183=CARTESIAN_POINT('Ctrl Pts',(183.055959194392,4.69594422725383,129.342412986144));
#24184=CARTESIAN_POINT('Ctrl Pts',(183.048186294126,4.65518930661703,129.211503485568));
#24185=CARTESIAN_POINT('Ctrl Pts',(183.040413393861,4.6089993893674,129.082438184816));
#24186=CARTESIAN_POINT('Ctrl Pts',(183.032640493595,4.55758592042437,128.955687136269));
#24187=CARTESIAN_POINT('Ctrl Pts',(183.025150157833,4.50804146058063,128.833543807605));
#24188=CARTESIAN_POINT('Ctrl Pts',(183.017659822071,4.453646761226,128.713549675095));
#24189=CARTESIAN_POINT('Ctrl Pts',(183.010169486309,4.39463058805635,128.596102241148));
#24190=CARTESIAN_POINT('Ctrl Pts',(183.00239515219,4.33337679874275,128.474201752045));
#24191=CARTESIAN_POINT('Ctrl Pts',(182.994620818071,4.26695013774061,128.354658745723));
#24192=CARTESIAN_POINT('Ctrl Pts',(182.986846483952,4.19555546106626,128.237943380323));
#24193=CARTESIAN_POINT('Ctrl Pts',(182.979081731005,4.1242487719503,128.121371856181));
#24194=CARTESIAN_POINT('Ctrl Pts',(182.971316978058,4.0479864514346,128.007621369533));
#24195=CARTESIAN_POINT('Ctrl Pts',(182.963552225111,3.96702036354612,127.897139866108));
#24196=CARTESIAN_POINT('Ctrl Pts',(182.955795184226,3.88613469231738,127.786768094469));
#24197=CARTESIAN_POINT('Ctrl Pts',(182.948038143341,3.80055478051184,127.679659158082));
#24198=CARTESIAN_POINT('Ctrl Pts',(182.940281102456,3.71057693779105,127.576233939253));
#24199=CARTESIAN_POINT('Ctrl Pts',(182.932529911216,3.62066694806208,127.472886714187));
#24200=CARTESIAN_POINT('Ctrl Pts',(182.924778719976,3.52636588431209,127.373217971168));
#24201=CARTESIAN_POINT('Ctrl Pts',(182.917027528736,3.42801143282299,127.277616980876));
#24202=CARTESIAN_POINT('Ctrl Pts',(182.909279631959,3.3296987845988,127.182056623554));
#24203=CARTESIAN_POINT('Ctrl Pts',(182.901531735182,3.22733645491275,127.090560852235));
#24204=CARTESIAN_POINT('Ctrl Pts',(182.893783838404,3.12130006999723,127.003483227339));
#24205=CARTESIAN_POINT('Ctrl Pts',(182.88603756232,3.01528586560767,126.916423817206));
#24206=CARTESIAN_POINT('Ctrl Pts',(182.878291286236,2.90559943659399,126.833780963214));
#24207=CARTESIAN_POINT('Ctrl Pts',(182.870545010152,2.79265037187774,126.75586868069));
#24208=CARTESIAN_POINT('Ctrl Pts',(182.862798676887,2.67970047339745,126.677955823035));
#24209=CARTESIAN_POINT('Ctrl Pts',(182.855052343622,2.5634882129824,126.604773828524));
#24210=CARTESIAN_POINT('Ctrl Pts',(182.847306010356,2.4444527713082,126.536593788023));
#24211=CARTESIAN_POINT('Ctrl Pts',(182.839557942353,2.32539067247181,126.468398479076));
#24212=CARTESIAN_POINT('Ctrl Pts',(182.83180987435,2.2035044734996,126.405207547392));
#24213=CARTESIAN_POINT('Ctrl Pts',(182.824061806347,2.07925823407926,126.34724627547));
#24214=CARTESIAN_POINT('Ctrl Pts',(182.816305503605,1.9548799442771,126.289223401619));
#24215=CARTESIAN_POINT('Ctrl Pts',(182.808549200864,1.82813695834241,126.236441456072));
#24216=CARTESIAN_POINT('Ctrl Pts',(182.800792898122,1.69951412583694,126.189077874485));
#24217=CARTESIAN_POINT('Ctrl Pts',(182.793032455608,1.57082264345299,126.141689013529));
#24218=CARTESIAN_POINT('Ctrl Pts',(182.785272013093,1.44024968730915,126.099724398543));
#24219=CARTESIAN_POINT('Ctrl Pts',(182.777511570579,1.3082946128271,126.063311338287));
#24220=CARTESIAN_POINT('Ctrl Pts',(182.769738670314,1.17612771234498,126.026839824555));
#24221=CARTESIAN_POINT('Ctrl Pts',(182.761965770048,1.04257464097785,125.995937762452));
#24222=CARTESIAN_POINT('Ctrl Pts',(182.754192869783,0.908145158251714,125.970681332172));
#24223=CARTESIAN_POINT('Ctrl Pts',(182.746702534021,0.778602525828482,125.94634303675));
#24224=CARTESIAN_POINT('Ctrl Pts',(182.739212198259,0.64824640006857,125.927247078214));
#24225=CARTESIAN_POINT('Ctrl Pts',(182.731721862497,0.517534864453755,125.913415849265));
#24226=CARTESIAN_POINT('Ctrl Pts',(182.723947528378,0.381867361238935,125.899060205066));
#24227=CARTESIAN_POINT('Ctrl Pts',(182.716173194259,0.245387211553195,125.890330921351));
#24228=CARTESIAN_POINT('Ctrl Pts',(182.708398860139,0.108600702437423,125.88730977891));
#24229=CARTESIAN_POINT('Ctrl Pts',(182.700634107192,-0.0280172295310573,
125.884292359757));
#24230=CARTESIAN_POINT('Ctrl Pts',(182.692869354245,-0.164940382578901,
125.886969093325));
#24231=CARTESIAN_POINT('Ctrl Pts',(182.685104601298,-0.301655748620083,
125.895370204882));
#24232=CARTESIAN_POINT('Ctrl Pts',(182.677347560413,-0.438235327031179,
125.903762972337));
#24233=CARTESIAN_POINT('Ctrl Pts',(182.669590519528,-0.57460714143116,125.91786877949));
#24234=CARTESIAN_POINT('Ctrl Pts',(182.661833478643,-0.710256929006805,
125.937665829797));
#24235=CARTESIAN_POINT('Ctrl Pts',(182.654082287403,-0.845804422024122,
125.957447950995));
#24236=CARTESIAN_POINT('Ctrl Pts',(182.646331096163,-0.980630586681961,
125.982912716527));
#24237=CARTESIAN_POINT('Ctrl Pts',(182.638579904923,-1.11422539084784,126.013986431671));
#24238=CARTESIAN_POINT('Ctrl Pts',(182.630832008146,-1.24776341365743,126.045046939657));
#24239=CARTESIAN_POINT('Ctrl Pts',(182.623084111369,-1.38007073689753,126.081711567367));
#24240=CARTESIAN_POINT('Ctrl Pts',(182.615336214591,-1.51064686501784,126.123855397858));
#24241=CARTESIAN_POINT('Ctrl Pts',(182.607589938507,-1.64119567942685,126.165990412768));
#24242=CARTESIAN_POINT('Ctrl Pts',(182.599843662423,-1.7700136471794,126.213602230732));
#24243=CARTESIAN_POINT('Ctrl Pts',(182.592097386339,-1.89661518547082,126.266515985944));
#24244=CARTESIAN_POINT('Ctrl Pts',(182.584351053074,-2.02321765830595,126.319430131753));
#24245=CARTESIAN_POINT('Ctrl Pts',(182.576604719809,-2.14760330830669,126.37764614214));
#24246=CARTESIAN_POINT('Ctrl Pts',(182.568858386543,-2.26930667116602,126.440941053199));
#24247=CARTESIAN_POINT('Ctrl Pts',(182.56111031854,-2.39103728865015,126.504250138715));
#24248=CARTESIAN_POINT('Ctrl Pts',(182.553362250537,-2.51008407691616,126.572640207808));
#24249=CARTESIAN_POINT('Ctrl Pts',(182.545614182534,-2.62600666382235,126.645842604612));
#24250=CARTESIAN_POINT('Ctrl Pts',(182.537857879792,-2.74205245463323,126.719122801795));
#24251=CARTESIAN_POINT('Ctrl Pts',(182.53010157705,-2.85496708005182,126.797225334571));
#24252=CARTESIAN_POINT('Ctrl Pts',(182.522345274309,-2.96433918540366,126.879838193579));
#24253=CARTESIAN_POINT('Ctrl Pts',(182.514584831794,-3.07376966594129,126.962495145556));
#24254=CARTESIAN_POINT('Ctrl Pts',(182.50682438928,-3.17965355724597,127.049666972136));
#24255=CARTESIAN_POINT('Ctrl Pts',(182.499063946766,-3.28161383704965,127.141002364953));
#24256=CARTESIAN_POINT('Ctrl Pts',(182.491291046501,-3.38373779254603,127.232484377452));
#24257=CARTESIAN_POINT('Ctrl Pts',(182.483518146235,-3.4819252698745,127.328143039421));
#24258=CARTESIAN_POINT('Ctrl Pts',(182.47574524597,-3.57583663900372,127.427590652991));
#24259=CARTESIAN_POINT('Ctrl Pts',(182.468254910208,-3.66633409331571,127.523423095313));
#24260=CARTESIAN_POINT('Ctrl Pts',(182.460764574446,-3.75286073415508,127.622773563756));
#24261=CARTESIAN_POINT('Ctrl Pts',(182.453274238684,-3.83515011659531,127.725268763516));
#24262=CARTESIAN_POINT('Ctrl Pts',(182.445516365561,-3.92037868426403,127.831424853274));
#24263=CARTESIAN_POINT('Ctrl Pts',(182.437758492438,-4.00133819468862,127.941298988973));
#24264=CARTESIAN_POINT('Ctrl Pts',(182.430000619315,-4.07768537362654,128.054512429718));
#24265=CARTESIAN_POINT('Ctrl Pts',(182.422064270311,-4.15578897855251,128.170330433359));
#24266=CARTESIAN_POINT('Ctrl Pts',(182.414127921308,-4.22906513008165,128.289642999518));
#24267=CARTESIAN_POINT('Ctrl Pts',(182.406191572305,-4.29718794017761,128.4120063651));
#24268=CARTESIAN_POINT('Ctrl Pts',(182.398453166183,-4.36361167865667,128.53131782896));
#24269=CARTESIAN_POINT('Ctrl Pts',(182.390714760061,-4.42513586114829,128.653529356966));
#24270=CARTESIAN_POINT('Ctrl Pts',(182.382976353939,-4.48150092218885,128.778198593709));
#24271=CARTESIAN_POINT('Ctrl Pts',(182.374941033495,-4.54002865001674,128.907651255019));
#24272=CARTESIAN_POINT('Ctrl Pts',(182.366905713051,-4.5929932099943,129.039753638606));
#24273=CARTESIAN_POINT('Ctrl Pts',(182.358870392607,-4.64015582391395,129.173981216231));
#24274=CARTESIAN_POINT('Ctrl Pts',(182.350835072163,-4.68731843783359,129.308208793856));
#24275=CARTESIAN_POINT('Ctrl Pts',(182.342799751719,-4.72867891245574,129.444561130289));
#24276=CARTESIAN_POINT('Ctrl Pts',(182.334764431275,-4.76405452823405,129.582490119308));
#24277=CARTESIAN_POINT('Ctrl Pts',(184.084599308536,-4.76405452823405,129.582490119308));
#24278=CARTESIAN_POINT('Ctrl Pts',(184.075945911235,-4.8018983817438,129.730042729782));
#24279=CARTESIAN_POINT('Ctrl Pts',(184.067292513934,-4.83292755031847,129.879527941908));
#24280=CARTESIAN_POINT('Ctrl Pts',(184.058639116632,-4.85696110866322,130.030337458072));
#24281=CARTESIAN_POINT('Ctrl Pts',(184.050029728944,-4.88087243667851,130.180379984322));
#24282=CARTESIAN_POINT('Ctrl Pts',(184.041420341256,-4.89785903432467,130.331733166547));
#24283=CARTESIAN_POINT('Ctrl Pts',(184.032810953568,-4.90779083573385,130.483779621269));
#24284=CARTESIAN_POINT('Ctrl Pts',(184.026827114393,-4.91469380078797,130.589457465631));
#24285=CARTESIAN_POINT('Ctrl Pts',(184.020843275218,-4.91818976220946,130.69546982899));
#24286=CARTESIAN_POINT('Ctrl Pts',(184.014859436043,-4.9182492280365,130.801605001777));
#24287=CARTESIAN_POINT('',(184.360140563971,-4.91824943376093,130.802000573005));
#24288=CARTESIAN_POINT('Ctrl Pts',(184.430229652623,-4.76405452823406,129.582490119308));
#24289=CARTESIAN_POINT('Ctrl Pts',(184.422327812055,-4.7986868585295,129.717521049511));
#24290=CARTESIAN_POINT('Ctrl Pts',(184.414425971487,-4.82753715525285,129.853882584735));
#24291=CARTESIAN_POINT('Ctrl Pts',(184.406524130919,-4.85053490297993,129.991037669732));
#24292=CARTESIAN_POINT('Ctrl Pts',(184.398622290351,-4.873532650707,130.128192754729));
#24293=CARTESIAN_POINT('Ctrl Pts',(184.390720449783,-4.89067785997628,130.266140963835));
#24294=CARTESIAN_POINT('Ctrl Pts',(184.382818609216,-4.90195570679255,130.404343978982));
#24295=CARTESIAN_POINT('Ctrl Pts',(184.375259260813,-4.91274473405513,130.536556813798));
#24296=CARTESIAN_POINT('Ctrl Pts',(184.367699912411,-4.91818571452675,130.669211977639));
#24297=CARTESIAN_POINT('Ctrl Pts',(184.360140564008,-4.91824943376062,130.802000572364));
#24298=CARTESIAN_POINT('Ctrl Pts',(184.360140563971,-4.91824943376093,130.802000573005));
#24299=CARTESIAN_POINT('Ctrl Pts',(184.352455145915,-4.9183142156431,130.937003725306));
#24300=CARTESIAN_POINT('Ctrl Pts',(184.344769727858,-4.9128161630471,131.072233610613));
#24301=CARTESIAN_POINT('Ctrl Pts',(184.337084309801,-4.90172557734377,131.207187412745));
#24302=CARTESIAN_POINT('Ctrl Pts',(184.329407784764,-4.89064782487823,131.341985055925));
#24303=CARTESIAN_POINT('Ctrl Pts',(184.321731259727,-4.87399044269163,131.476506855924));
#24304=CARTESIAN_POINT('Ctrl Pts',(184.314054734689,-4.85177572413915,131.610248565828));
#24305=CARTESIAN_POINT('Ctrl Pts',(184.306385156566,-4.82958110892026,131.743869245425));
#24306=CARTESIAN_POINT('Ctrl Pts',(184.298715578444,-4.80183922716559,131.876710846574));
#24307=CARTESIAN_POINT('Ctrl Pts',(184.291046000321,-4.76862425691908,132.008273304941));
#24308=CARTESIAN_POINT('Ctrl Pts',(184.283267874699,-4.73493919537421,132.141697766086));
#24309=CARTESIAN_POINT('Ctrl Pts',(184.275489749077,-4.69562496363401,132.273806182506));
#24310=CARTESIAN_POINT('Ctrl Pts',(184.267711623456,-4.65081294627124,132.404086219441));
#24311=CARTESIAN_POINT('Ctrl Pts',(184.260049224998,-4.606667666365,132.532427879451));
#24312=CARTESIAN_POINT('Ctrl Pts',(184.252386826541,-4.55718721851533,132.658994805512));
#24313=CARTESIAN_POINT('Ctrl Pts',(184.244724428084,-4.50254756195381,132.783311985044));
#24314=CARTESIAN_POINT('Ctrl Pts',(184.237062723623,-4.44791285419833,132.90761790496));
#24315=CARTESIAN_POINT('Ctrl Pts',(184.229401019162,-4.38812002801154,133.029674116977));
#24316=CARTESIAN_POINT('Ctrl Pts',(184.221739314701,-4.32339297491415,133.149026104787));
#24317=CARTESIAN_POINT('Ctrl Pts',(184.214076556531,-4.25865701995485,133.268394506983));
#24318=CARTESIAN_POINT('Ctrl Pts',(184.206413798362,-4.18898567966582,133.385057593469));
#24319=CARTESIAN_POINT('Ctrl Pts',(184.198751040193,-4.11464827331411,133.498586415344));
#24320=CARTESIAN_POINT('Ctrl Pts',(184.190886035627,-4.0383488485568,133.615111651125));
#24321=CARTESIAN_POINT('Ctrl Pts',(184.183021031061,-3.95713386805491,133.728334497134));
#24322=CARTESIAN_POINT('Ctrl Pts',(184.175156026495,-3.87134055205237,133.837824873583));
#24323=CARTESIAN_POINT('Ctrl Pts',(184.167481864777,-3.78762899462731,133.944658486767));
#24324=CARTESIAN_POINT('Ctrl Pts',(184.159807703058,-3.69955904336469,134.047938419428));
#24325=CARTESIAN_POINT('Ctrl Pts',(184.15213354134,-3.60748270613891,134.147301177523));
#24326=CARTESIAN_POINT('Ctrl Pts',(184.14417311535,-3.51197170509786,134.25037040006));
#24327=CARTESIAN_POINT('Ctrl Pts',(184.136212689361,-3.41214997576047,134.34922420526));
#24328=CARTESIAN_POINT('Ctrl Pts',(184.128252263371,-3.30844873692504,134.443502002239));
#24329=CARTESIAN_POINT('Ctrl Pts',(184.120291837381,-3.2047474980896,134.537779799218));
#24330=CARTESIAN_POINT('Ctrl Pts',(184.112331411392,-3.09716715988707,134.627481342045));
#24331=CARTESIAN_POINT('Ctrl Pts',(184.104370985402,-2.98617212354664,134.712296020186));
#24332=CARTESIAN_POINT('Ctrl Pts',(184.096596651283,-2.87777183200501,134.795127975026));
#24333=CARTESIAN_POINT('Ctrl Pts',(184.088822317164,-2.76575077820207,134.873577418346));
#24334=CARTESIAN_POINT('Ctrl Pts',(184.081047983045,-2.65049881953031,134.947311144687));
#24335=CARTESIAN_POINT('Ctrl Pts',(184.073283230098,-2.53538889859732,135.020954000799));
#24336=CARTESIAN_POINT('Ctrl Pts',(184.065518477151,-2.41705632156664,135.089892494809));
#24337=CARTESIAN_POINT('Ctrl Pts',(184.057753724204,-2.29592350409848,135.153833956469));
#24338=CARTESIAN_POINT('Ctrl Pts',(184.049996683319,-2.17491099745172,135.217711910569));
#24339=CARTESIAN_POINT('Ctrl Pts',(184.042239642434,-2.05110412867136,135.27660252783));
#24340=CARTESIAN_POINT('Ctrl Pts',(184.034482601549,-1.92495344569139,135.330256914922));
#24341=CARTESIAN_POINT('Ctrl Pts',(184.026731410308,-1.79889789392326,135.383870840824));
#24342=CARTESIAN_POINT('Ctrl Pts',(184.018980219068,-1.67050240435444,135.432256243768));
#24343=CARTESIAN_POINT('Ctrl Pts',(184.011229027828,-1.54024090802878,135.475210755146));
#24344=CARTESIAN_POINT('Ctrl Pts',(184.003481131051,-1.41003477631391,135.518147009712));
#24345=CARTESIAN_POINT('Ctrl Pts',(183.995733234274,-1.27796458578426,135.55565684151));
#24346=CARTESIAN_POINT('Ctrl Pts',(183.987985337497,-1.14452276743259,135.587586589369));
#24347=CARTESIAN_POINT('Ctrl Pts',(183.980239061413,-1.01110886223263,135.619509658213));
#24348=CARTESIAN_POINT('Ctrl Pts',(183.972492785329,-0.876324279891128,
135.645854873884));
#24349=CARTESIAN_POINT('Ctrl Pts',(183.964746509245,-0.740674697423658,
135.666518991693));
#24350=CARTESIAN_POINT('Ctrl Pts',(183.957000175979,-0.605024113621508,
135.68718326204));
#24351=CARTESIAN_POINT('Ctrl Pts',(183.949253842714,-0.468508903458449,
135.702166291965));
#24352=CARTESIAN_POINT('Ctrl Pts',(183.941507509448,-0.331642581234947,
135.711416380527));
#24353=CARTESIAN_POINT('Ctrl Pts',(183.933759441445,-0.194745608747665,
135.720668540583));
#24354=CARTESIAN_POINT('Ctrl Pts',(183.926011373442,-0.0574977577378105,
135.724185178199));
#24355=CARTESIAN_POINT('Ctrl Pts',(183.918263305439,0.0795851196291304,
135.721966668403));
#24356=CARTESIAN_POINT('Ctrl Pts',(183.910507002698,0.216813690309234,135.719745800749));
#24357=CARTESIAN_POINT('Ctrl Pts',(183.902750699956,0.353876545556638,135.711777615836));
#24358=CARTESIAN_POINT('Ctrl Pts',(183.894994397214,0.490260064193617,135.698114609335));
#24359=CARTESIAN_POINT('Ctrl Pts',(183.8872339547,0.626716374821129,135.684444310477));
#24360=CARTESIAN_POINT('Ctrl Pts',(183.879473512186,0.762492239505508,135.665073188767));
#24361=CARTESIAN_POINT('Ctrl Pts',(183.871713069671,0.89708291638147,135.640105162477));
#24362=CARTESIAN_POINT('Ctrl Pts',(183.863940169406,1.03188965016026,135.615097055295));
#24363=CARTESIAN_POINT('Ctrl Pts',(183.856167269141,1.16550701288779,135.58447417673));
#24364=CARTESIAN_POINT('Ctrl Pts',(183.848394368875,1.29744326874112,135.548390974435));
#24365=CARTESIAN_POINT('Ctrl Pts',(183.840904033113,1.42458330936598,135.513619487432));
#24366=CARTESIAN_POINT('Ctrl Pts',(183.833413697351,1.55016205245454,135.473777870507));
#24367=CARTESIAN_POINT('Ctrl Pts',(183.825923361589,1.67375775862039,135.42904633964));
#24368=CARTESIAN_POINT('Ctrl Pts',(183.81814902747,1.80203963355247,135.382618799184));
#24369=CARTESIAN_POINT('Ctrl Pts',(183.810374693351,1.92859148786851,135.330776154368));
#24370=CARTESIAN_POINT('Ctrl Pts',(183.802600359232,2.05292225893399,135.273666297565));
#24371=CARTESIAN_POINT('Ctrl Pts',(183.794835606285,2.17709980343563,135.216626823557));
#24372=CARTESIAN_POINT('Ctrl Pts',(183.787070853338,2.29906135920444,135.154333215077));
#24373=CARTESIAN_POINT('Ctrl Pts',(183.779306100391,2.41833236849072,135.086982666966));
#24374=CARTESIAN_POINT('Ctrl Pts',(183.771549059506,2.53748491612928,135.019699012369));
#24375=CARTESIAN_POINT('Ctrl Pts',(183.763792018621,2.65395189702597,134.947368604385));
#24376=CARTESIAN_POINT('Ctrl Pts',(183.756034977736,2.76728037800997,134.870235968826));
#24377=CARTESIAN_POINT('Ctrl Pts',(183.748283786496,2.88052339710438,134.793161499588));
#24378=CARTESIAN_POINT('Ctrl Pts',(183.740532595256,2.99063230529288,134.711292230035));
#24379=CARTESIAN_POINT('Ctrl Pts',(183.732781404016,3.09718067282804,134.624917506602));
#24380=CARTESIAN_POINT('Ctrl Pts',(183.725033507239,3.20368375446525,134.53857949473));
#24381=CARTESIAN_POINT('Ctrl Pts',(183.717285610461,3.30662900226592,134.447740083331));
#24382=CARTESIAN_POINT('Ctrl Pts',(183.709537713684,3.4056209657537,134.352730510928));
#24383=CARTESIAN_POINT('Ctrl Pts',(183.7017914376,3.50459222225675,134.25774081248));
#24384=CARTESIAN_POINT('Ctrl Pts',(183.694045161516,3.59961155738863,134.158582958646));
#24385=CARTESIAN_POINT('Ctrl Pts',(183.686298885432,3.6903187776887,134.055626583546));
#24386=CARTESIAN_POINT('Ctrl Pts',(183.678552552167,3.78102666756886,133.952669448445));
#24387=CARTESIAN_POINT('Ctrl Pts',(183.670806218901,3.86742212064859,133.845914029478));
#24388=CARTESIAN_POINT('Ctrl Pts',(183.663059885636,3.94918407243948,133.73576441515));
#24389=CARTESIAN_POINT('Ctrl Pts',(183.655311817633,4.03096433425261,133.625590133579));
#24390=CARTESIAN_POINT('Ctrl Pts',(183.64756374963,4.10810879701171,133.512020457994));
#24391=CARTESIAN_POINT('Ctrl Pts',(183.639815681627,4.18033894554159,133.395489592142));
#24392=CARTESIAN_POINT('Ctrl Pts',(183.632059378885,4.25264586113286,133.278834875899));
#24393=CARTESIAN_POINT('Ctrl Pts',(183.624303076144,4.32002782270208,133.159213015378));
#24394=CARTESIAN_POINT('Ctrl Pts',(183.616546773402,4.38225137155276,133.037084509816));
#24395=CARTESIAN_POINT('Ctrl Pts',(183.608786330888,4.444508130985,132.914890820593));
#24396=CARTESIAN_POINT('Ctrl Pts',(183.601025888373,4.50160082904401,132.790188175812));
#24397=CARTESIAN_POINT('Ctrl Pts',(183.593265445859,4.55334406980649,132.663457399463));
#24398=CARTESIAN_POINT('Ctrl Pts',(183.585492545594,4.60517037341259,132.53652318362));
#24399=CARTESIAN_POINT('Ctrl Pts',(183.577719645328,4.65162992673136,132.407554698248));
#24400=CARTESIAN_POINT('Ctrl Pts',(183.569946745063,4.69258687572239,132.277049137348));
#24401=CARTESIAN_POINT('Ctrl Pts',(183.562456409301,4.73205493645361,132.15128778231));
#24402=CARTESIAN_POINT('Ctrl Pts',(183.554966073539,4.7664134338327,132.024099462039));
#24403=CARTESIAN_POINT('Ctrl Pts',(183.547475737777,4.79558602822751,131.895936408965));
#24404=CARTESIAN_POINT('Ctrl Pts',(183.539701403658,4.82586471040535,131.762914014781));
#24405=CARTESIAN_POINT('Ctrl Pts',(183.531927069538,4.85065239351974,131.62842013976));
#24406=CARTESIAN_POINT('Ctrl Pts',(183.524152735419,4.86980807226552,131.492947868245));
#24407=CARTESIAN_POINT('Ctrl Pts',(183.516387982472,4.88894014334924,131.357642554197));
#24408=CARTESIAN_POINT('Ctrl Pts',(183.508623229525,4.90245396625799,131.221361626208));
#24409=CARTESIAN_POINT('Ctrl Pts',(183.500858476578,4.91025893654111,131.084610931782));
#24410=CARTESIAN_POINT('Ctrl Pts',(183.493101435693,4.91805615481771,130.947996060074));
#24411=CARTESIAN_POINT('Ctrl Pts',(183.485344394808,4.92015578211555,130.810912738245));
#24412=CARTESIAN_POINT('Ctrl Pts',(183.477587353923,4.91651872348393,130.673874203975));
#24413=CARTESIAN_POINT('Ctrl Pts',(183.469836162683,4.9128844075865,130.536939011528));
#24414=CARTESIAN_POINT('Ctrl Pts',(183.462084971443,4.90352202688916,130.40004892866));
#24415=CARTESIAN_POINT('Ctrl Pts',(183.454333780202,4.88844452104653,130.263719121609));
#24416=CARTESIAN_POINT('Ctrl Pts',(183.446585883425,4.87337342354616,130.127447258364));
#24417=CARTESIAN_POINT('Ctrl Pts',(183.438837986648,4.85259207504386,129.991735585091));
#24418=CARTESIAN_POINT('Ctrl Pts',(183.431090089871,4.82616540524861,129.857095847989));
#24419=CARTESIAN_POINT('Ctrl Pts',(183.423343813787,4.79974426334297,129.722484274618));
#24420=CARTESIAN_POINT('Ctrl Pts',(183.415597537703,4.76768022423145,129.588944574821));
#24421=CARTESIAN_POINT('Ctrl Pts',(183.407851261619,4.73008957820223,129.45697958583));
#24422=CARTESIAN_POINT('Ctrl Pts',(183.400104928353,4.69249865468751,129.325013622703));
#24423=CARTESIAN_POINT('Ctrl Pts',(183.392358595088,4.64938114995637,129.194622769583));
#24424=CARTESIAN_POINT('Ctrl Pts',(183.384612261823,4.60090349191246,129.066295566825));
#24425=CARTESIAN_POINT('Ctrl Pts',(183.37686419382,4.55241497763291,128.937939626078));
#24426=CARTESIAN_POINT('Ctrl Pts',(183.369116125817,4.49856405958199,128.811648620967));
#24427=CARTESIAN_POINT('Ctrl Pts',(183.361368057814,4.43956550141456,128.687891571927));
#24428=CARTESIAN_POINT('Ctrl Pts',(183.353611755072,4.38050423887763,128.564002992422));
#24429=CARTESIAN_POINT('Ctrl Pts',(183.34585545233,4.31628457587822,128.44265410226));
#24430=CARTESIAN_POINT('Ctrl Pts',(183.338099149588,4.24716775333799,128.324290227939));
#24431=CARTESIAN_POINT('Ctrl Pts',(183.330338707074,4.17801404106853,128.205863179254));
#24432=CARTESIAN_POINT('Ctrl Pts',(183.32257826456,4.10395817211934,128.090424649892));
#24433=CARTESIAN_POINT('Ctrl Pts',(183.314817822046,4.02530446630552,127.978390515806));
#24434=CARTESIAN_POINT('Ctrl Pts',(183.30704492178,3.94652449858048,127.866176534582));
#24435=CARTESIAN_POINT('Ctrl Pts',(183.299272021515,3.86313218266577,127.757378179998));
#24436=CARTESIAN_POINT('Ctrl Pts',(183.291499121249,3.77547238952982,127.652378495409));
#24437=CARTESIAN_POINT('Ctrl Pts',(183.284008785487,3.69099925067666,127.551195813834));
#24438=CARTESIAN_POINT('Ctrl Pts',(183.276518449725,3.60256372176028,127.453540643053));
#24439=CARTESIAN_POINT('Ctrl Pts',(183.269028113963,3.51050501529534,127.359721652437));
#24440=CARTESIAN_POINT('Ctrl Pts',(183.261253779844,3.41495587499346,127.262345486275));
#24441=CARTESIAN_POINT('Ctrl Pts',(183.253479445725,3.31520071706981,127.168793681802));
#24442=CARTESIAN_POINT('Ctrl Pts',(183.245705111606,3.21157817053554,127.079451394908));
#24443=CARTESIAN_POINT('Ctrl Pts',(183.237940358659,3.10808332952903,126.990219214398));
#24444=CARTESIAN_POINT('Ctrl Pts',(183.230175605712,3.00073087651156,126.905186482029));
#24445=CARTESIAN_POINT('Ctrl Pts',(183.222410852765,2.88989742139538,126.824702848824));
#24446=CARTESIAN_POINT('Ctrl Pts',(183.21465381188,2.77917404762878,126.744299153096));
#24447=CARTESIAN_POINT('Ctrl Pts',(183.206896770995,2.66497686641319,126.668435793291));
#24448=CARTESIAN_POINT('Ctrl Pts',(183.19913973011,2.54771654736785,126.597423078599));
#24449=CARTESIAN_POINT('Ctrl Pts',(183.19138853887,2.43054465524129,126.526463915148));
#24450=CARTESIAN_POINT('Ctrl Pts',(183.18363734763,2.31031455614051,126.460348317669));
#24451=CARTESIAN_POINT('Ctrl Pts',(183.175886156389,2.18746666821171,126.3993438596));
#24452=CARTESIAN_POINT('Ctrl Pts',(183.168138259612,2.0646709939127,126.338365330053));
#24453=CARTESIAN_POINT('Ctrl Pts',(183.160390362835,1.93926009315588,126.282493792761));
#24454=CARTESIAN_POINT('Ctrl Pts',(183.152642466058,1.811699608605,126.231951231839));
#24455=CARTESIAN_POINT('Ctrl Pts',(183.144896189974,1.68416580695755,126.181419243332));
#24456=CARTESIAN_POINT('Ctrl Pts',(183.13714991389,1.55448367913088,126.136214157909));
#24457=CARTESIAN_POINT('Ctrl Pts',(183.129403637806,1.42313913406825,126.096509933062));
#24458=CARTESIAN_POINT('Ctrl Pts',(183.121657304541,1.29179361945,126.056805415127));
#24459=CARTESIAN_POINT('Ctrl Pts',(183.113910971275,1.15878603734873,126.022601951924));
#24460=CARTESIAN_POINT('Ctrl Pts',(183.10616463801,1.02461736894711,125.994023590938));
#24461=CARTESIAN_POINT('Ctrl Pts',(183.098416570007,0.890418654402585,125.965438830026));
#24462=CARTESIAN_POINT('Ctrl Pts',(183.090668502004,0.755058718467256,125.942481759427));
#24463=CARTESIAN_POINT('Ctrl Pts',(183.082920434001,0.619048246319054,125.925225209399));
#24464=CARTESIAN_POINT('Ctrl Pts',(183.075164131259,0.482893220622485,125.907950318904));
#24465=CARTESIAN_POINT('Ctrl Pts',(183.067407828517,0.346086666046123,125.896388100937));
#24466=CARTESIAN_POINT('Ctrl Pts',(183.059651525776,0.209144455485154,125.890559475961));
#24467=CARTESIAN_POINT('Ctrl Pts',(183.051891083261,0.0721291547430187,
125.884727740072));
#24468=CARTESIAN_POINT('Ctrl Pts',(183.044130640747,-0.065021555480375,
125.884635695128));
#24469=CARTESIAN_POINT('Ctrl Pts',(183.036370198233,-0.201793294674736,
125.890252099358));
#24470=CARTESIAN_POINT('Ctrl Pts',(183.028597297968,-0.338784592006899,
125.895877519539));
#24471=CARTESIAN_POINT('Ctrl Pts',(183.020824397702,-0.475395312770501,
125.907229668511));
#24472=CARTESIAN_POINT('Ctrl Pts',(183.013051497437,-0.611116780560397,
125.92422544085));
#24473=CARTESIAN_POINT('Ctrl Pts',(183.005561161675,-0.74190443113344,125.940603374055));
#24474=CARTESIAN_POINT('Ctrl Pts',(182.998070825913,-0.87186605558637,125.96222168399));
#24475=CARTESIAN_POINT('Ctrl Pts',(182.990580490151,-1.00055860898726,125.988961824892));
#24476=CARTESIAN_POINT('Ctrl Pts',(182.982806156032,-1.13413057966649,126.016715826365));
#24477=CARTESIAN_POINT('Ctrl Pts',(182.975031821913,-1.26675846180681,126.050075630492));
#24478=CARTESIAN_POINT('Ctrl Pts',(182.967257487794,-1.39793517559902,126.088964525261));
#24479=CARTESIAN_POINT('Ctrl Pts',(182.959492734846,-1.52895022581513,126.127805492943));
#24480=CARTESIAN_POINT('Ctrl Pts',(182.951727981899,-1.65851729489495,126.172161883161));
#24481=CARTESIAN_POINT('Ctrl Pts',(182.943963228952,-1.78613864467428,126.221905838247));
#24482=CARTESIAN_POINT('Ctrl Pts',(182.936206188067,-1.91363323913031,126.271600386936));
#24483=CARTESIAN_POINT('Ctrl Pts',(182.928449147182,-2.03918559816484,126.326671710685));
#24484=CARTESIAN_POINT('Ctrl Pts',(182.920692106297,-2.16231267290643,126.386942031209));
#24485=CARTESIAN_POINT('Ctrl Pts',(182.912940915057,-2.28534689656263,126.447166901416));
#24486=CARTESIAN_POINT('Ctrl Pts',(182.905189723817,-2.40595912655983,126.512582793482));
#24487=CARTESIAN_POINT('Ctrl Pts',(182.897438532577,-2.52368618902095,126.582963801127));
#24488=CARTESIAN_POINT('Ctrl Pts',(182.8896906358,-2.64136321434017,126.653314894965));
#24489=CARTESIAN_POINT('Ctrl Pts',(182.881942739023,-2.75615717621927,126.728626706948));
#24490=CARTESIAN_POINT('Ctrl Pts',(182.874194842245,-2.86762962189981,126.808627466553));
#24491=CARTESIAN_POINT('Ctrl Pts',(182.866448566161,-2.97907874994782,126.888611491724));
#24492=CARTESIAN_POINT('Ctrl Pts',(182.858702290077,-3.08720742634127,126.973282285786));
#24493=CARTESIAN_POINT('Ctrl Pts',(182.850956013993,-3.1916066500627,127.062325068059));
#24494=CARTESIAN_POINT('Ctrl Pts',(182.843209680728,-3.29600664443559,127.151368507625));
#24495=CARTESIAN_POINT('Ctrl Pts',(182.835463347462,-3.39667683373769,127.24478374609));
#24496=CARTESIAN_POINT('Ctrl Pts',(182.827717014197,-3.49324206073987,127.342216344492));
#24497=CARTESIAN_POINT('Ctrl Pts',(182.819968946194,-3.58982891285543,127.43967076225));
#24498=CARTESIAN_POINT('Ctrl Pts',(182.812220878191,-3.68230869825185,127.541144052529));
#24499=CARTESIAN_POINT('Ctrl Pts',(182.804472810188,-3.77034410495834,127.64624592796));
#24500=CARTESIAN_POINT('Ctrl Pts',(182.796716507446,-3.85847307674226,127.751459506914));
#24501=CARTESIAN_POINT('Ctrl Pts',(182.788960204704,-3.94214798261169,127.860309074608));
#24502=CARTESIAN_POINT('Ctrl Pts',(182.781203901962,-4.02107237968682,127.972371920586));
#24503=CARTESIAN_POINT('Ctrl Pts',(182.773443459448,-4.10003890108901,128.08449457788));
#24504=CARTESIAN_POINT('Ctrl Pts',(182.765683016934,-4.17424965007582,128.19983360216));
#24505=CARTESIAN_POINT('Ctrl Pts',(182.75792257442,-4.24345287600184,128.317939343596));
#24506=CARTESIAN_POINT('Ctrl Pts',(182.750149674154,-4.31276719308979,128.436234678853));
#24507=CARTESIAN_POINT('Ctrl Pts',(182.742376773889,-4.37705774012523,128.557305261059));
#24508=CARTESIAN_POINT('Ctrl Pts',(182.734603873624,-4.43611948403242,128.680678205837));
#24509=CARTESIAN_POINT('Ctrl Pts',(182.727113537862,-4.49303418478051,128.799566233313));
#24510=CARTESIAN_POINT('Ctrl Pts',(182.7196232021,-4.54509352087592,128.920591853246));
#24511=CARTESIAN_POINT('Ctrl Pts',(182.712132866338,-4.59215775161795,129.043318242507));
#24512=CARTESIAN_POINT('Ctrl Pts',(182.703253522123,-4.64794957700628,129.188803023033));
#24513=CARTESIAN_POINT('Ctrl Pts',(182.694374177909,-4.69687000701748,129.337061417581));
#24514=CARTESIAN_POINT('Ctrl Pts',(182.685494833695,-4.73867041310273,129.487475740865));
#24515=CARTESIAN_POINT('Ctrl Pts',(182.683630675656,-4.74744612459306,129.519054206932));
#24516=CARTESIAN_POINT('Ctrl Pts',(182.681766517617,-4.75590817585868,129.550727615035));
#24517=CARTESIAN_POINT('Ctrl Pts',(182.679902359578,-4.76405452823405,129.582490119308));
#24518=CARTESIAN_POINT('Origin',(213.235140564004,0.,130.804360617566));
#24519=CARTESIAN_POINT('',(180.584985772263,-4.76405452823404,129.582490119308));
#24520=CARTESIAN_POINT('',(180.930009319727,-4.76405452823406,129.582490119308));
#24521=CARTESIAN_POINT('',(213.235140564004,-4.76405452823405,129.582490119308));
#24522=CARTESIAN_POINT('',(182.264859435942,-4.91824838731473,130.808343477848));
#24523=CARTESIAN_POINT('Ctrl Pts',(182.264859435942,-4.91824838731473,130.808343477848));
#24524=CARTESIAN_POINT('Ctrl Pts',(182.255745689485,-4.91811770455124,130.969717526973));
#24525=CARTESIAN_POINT('Ctrl Pts',(182.246631943028,-4.91004084791699,131.130754613443));
#24526=CARTESIAN_POINT('Ctrl Pts',(182.237518196571,-4.89414028983605,131.290749233699));
#24527=CARTESIAN_POINT('Ctrl Pts',(182.228343751195,-4.87813383165355,131.451809442121));
#24528=CARTESIAN_POINT('Ctrl Pts',(182.21916930582,-4.85419921674639,131.611813182237));
#24529=CARTESIAN_POINT('Ctrl Pts',(182.209994860445,-4.82251028849471,131.770061181852));
#24530=CARTESIAN_POINT('Ctrl Pts',(182.200752520834,-4.79058685063821,131.929480274271));
#24531=CARTESIAN_POINT('Ctrl Pts',(182.191510181223,-4.75079397460461,132.087117477438));
#24532=CARTESIAN_POINT('Ctrl Pts',(182.182267841612,-4.70335754186608,132.242279563777));
#24533=CARTESIAN_POINT('Ctrl Pts',(182.179787432699,-4.69062680965446,132.28392112189));
#24534=CARTESIAN_POINT('Ctrl Pts',(182.177307023785,-4.67734581439877,132.325384532998));
#24535=CARTESIAN_POINT('Ctrl Pts',(182.174826614871,-4.66351949799474,132.366656669639));
#24536=CARTESIAN_POINT('Ctrl Pts',(182.167052280752,-4.62018373880961,132.496015735516));
#24537=CARTESIAN_POINT('Ctrl Pts',(182.159277946633,-4.57139291895546,132.623775226555));
#24538=CARTESIAN_POINT('Ctrl Pts',(182.151503612514,-4.51728310406877,132.749440672524));
#24539=CARTESIAN_POINT('Ctrl Pts',(182.143738859567,-4.46323997469291,132.874951247062));
#24540=CARTESIAN_POINT('Ctrl Pts',(182.13597410662,-4.40389104628627,132.998372555757));
#24541=CARTESIAN_POINT('Ctrl Pts',(182.128209353673,-4.33942206882534,133.119225445389));
#24542=CARTESIAN_POINT('Ctrl Pts',(182.120452312788,-4.27501712286173,133.239958302227));
#24543=CARTESIAN_POINT('Ctrl Pts',(182.112695271903,-4.20550243065429,133.358127473865));
#24544=CARTESIAN_POINT('Ctrl Pts',(182.104938231018,-4.13111157845121,133.473274289622));
#24545=CARTESIAN_POINT('Ctrl Pts',(182.097187039777,-4.05677682496856,133.588334272269));
#24546=CARTESIAN_POINT('Ctrl Pts',(182.089435848537,-3.97757344193555,133.700376108544));
#24547=CARTESIAN_POINT('Ctrl Pts',(182.081684657297,-3.89378045932293,133.808966547983));
#24548=CARTESIAN_POINT('Ctrl Pts',(182.07393676052,-3.81002309096304,133.917510833588));
#24549=CARTESIAN_POINT('Ctrl Pts',(182.066188863743,-3.72168024116592,134.022606331103));
#24550=CARTESIAN_POINT('Ctrl Pts',(182.058440966966,-3.62907356334536,134.123849755118));
#24551=CARTESIAN_POINT('Ctrl Pts',(182.050694690882,-3.53648625684542,134.225072001192));
#24552=CARTESIAN_POINT('Ctrl Pts',(182.042948414798,-3.43963716006998,134.322443488187));
#24553=CARTESIAN_POINT('Ctrl Pts',(182.035202138714,-3.33888715704143,134.415595256169));
#24554=CARTESIAN_POINT('Ctrl Pts',(182.027455805448,-3.23813641029925,134.508747711776));
#24555=CARTESIAN_POINT('Ctrl Pts',(182.019709472183,-3.1334849869114,134.597680120798));
#24556=CARTESIAN_POINT('Ctrl Pts',(182.011963138918,-3.02532915435104,134.682061814194));
#24557=CARTESIAN_POINT('Ctrl Pts',(182.004215070915,-2.91714910104202,134.766462404286));
#24558=CARTESIAN_POINT('Ctrl Pts',(181.996467002912,-2.8054633851131,134.846310010414));
#24559=CARTESIAN_POINT('Ctrl Pts',(181.988718934909,-2.69069940167571,134.921315777915));
#24560=CARTESIAN_POINT('Ctrl Pts',(181.980962632167,-2.5758134457109,134.996401262438));
#24561=CARTESIAN_POINT('Ctrl Pts',(181.973206329425,-2.45784301461549,135.066634414486));
#24562=CARTESIAN_POINT('Ctrl Pts',(181.965450026683,-2.33724287264859,135.13177079188));
#24563=CARTESIAN_POINT('Ctrl Pts',(181.957689584169,-2.21657836275474,135.196941934519));
#24564=CARTESIAN_POINT('Ctrl Pts',(181.949929141655,-2.09328169658598,135.257010710924));
#24565=CARTESIAN_POINT('Ctrl Pts',(181.942168699141,-1.96782911067562,135.311780240108));
#24566=CARTESIAN_POINT('Ctrl Pts',(181.934395798875,-1.8421751371371,135.366637690203));
#24567=CARTESIAN_POINT('Ctrl Pts',(181.92662289861,-1.71435869267866,135.416178752362));
#24568=CARTESIAN_POINT('Ctrl Pts',(181.918849998344,-1.58487356800099,135.460255680382));
#24569=CARTESIAN_POINT('Ctrl Pts',(181.911359662582,-1.46009555375806,135.502730301045));
#24570=CARTESIAN_POINT('Ctrl Pts',(181.90386932682,-1.33376836978196,135.540131073015));
#24571=CARTESIAN_POINT('Ctrl Pts',(181.896378991058,-1.20634228632941,135.572370826313));
#24572=CARTESIAN_POINT('Ctrl Pts',(181.888604656939,-1.07408480419308,135.605832959655));
#24573=CARTESIAN_POINT('Ctrl Pts',(181.88083032282,-0.940224496132468,135.63384098669));
#24574=CARTESIAN_POINT('Ctrl Pts',(181.873055988701,-0.805250920756176,
135.656242110051));
#24575=CARTESIAN_POINT('Ctrl Pts',(181.865291235754,-0.670443688248645,
135.67861562603));
#24576=CARTESIAN_POINT('Ctrl Pts',(181.857526482807,-0.534526300288229,
135.695395923796));
#24577=CARTESIAN_POINT('Ctrl Pts',(181.849761729859,-0.398002284449767,
135.706480286043));
#24578=CARTESIAN_POINT('Ctrl Pts',(181.842004688974,-0.261613866188487,
135.717553639146));
#24579=CARTESIAN_POINT('Ctrl Pts',(181.834247648089,-0.124620406235299,
135.722942283547));
#24580=CARTESIAN_POINT('Ctrl Pts',(181.826490607204,0.0124659437015487,
135.722594819264));
#24581=CARTESIAN_POINT('Ctrl Pts',(181.818739415964,0.149448915755369,135.722247617006));
#24582=CARTESIAN_POINT('Ctrl Pts',(181.810988224724,0.286524248982427,135.716172916984));
#24583=CARTESIAN_POINT('Ctrl Pts',(181.803237033484,0.423176614983207,135.704371292558));
#24584=CARTESIAN_POINT('Ctrl Pts',(181.795489136707,0.559770900083301,135.692574684136));
#24585=CARTESIAN_POINT('Ctrl Pts',(181.78774123993,0.695942186810799,135.675056026109));
#24586=CARTESIAN_POINT('Ctrl Pts',(181.779993343153,0.831177318203662,135.651867948989));
#24587=CARTESIAN_POINT('Ctrl Pts',(181.772247067069,0.966384161322348,135.628684722316));
#24588=CARTESIAN_POINT('Ctrl Pts',(181.764500790985,1.10065485351256,135.599834501441));
#24589=CARTESIAN_POINT('Ctrl Pts',(181.756754514901,1.2334839117036,135.565421476457));
#24590=CARTESIAN_POINT('Ctrl Pts',(181.749008181635,1.36631395040857,135.531008197445));
#24591=CARTESIAN_POINT('Ctrl Pts',(181.74126184837,1.49770195540958,135.491032130437));
#24592=CARTESIAN_POINT('Ctrl Pts',(181.733515515104,1.62715553322994,135.44564793179));
#24593=CARTESIAN_POINT('Ctrl Pts',(181.725767447101,1.75663810128136,135.400253569667));
#24594=CARTESIAN_POINT('Ctrl Pts',(181.718019379098,1.88418501125313,135.34944879525));
#24595=CARTESIAN_POINT('Ctrl Pts',(181.710271311096,2.00932222403949,135.293437055151));
#24596=CARTESIAN_POINT('Ctrl Pts',(181.702515008354,2.13459243414487,135.237365785108));
#24597=CARTESIAN_POINT('Ctrl Pts',(181.694758705612,2.2574474736639,135.176076654553));
#24598=CARTESIAN_POINT('Ctrl Pts',(181.68700240287,2.37743587527888,135.109820142569));
#24599=CARTESIAN_POINT('Ctrl Pts',(181.679241960356,2.49748831831668,135.043528267489));
#24600=CARTESIAN_POINT('Ctrl Pts',(181.671481517842,2.61467074089446,134.972263931206));
#24601=CARTESIAN_POINT('Ctrl Pts',(181.663721075327,2.72856008398556,134.896321386022));
#24602=CARTESIAN_POINT('Ctrl Pts',(181.655948175062,2.84263225236077,134.820256931122));
#24603=CARTESIAN_POINT('Ctrl Pts',(181.648175274797,2.9534004613508,134.739499490654));
#24604=CARTESIAN_POINT('Ctrl Pts',(181.640402374531,3.06047350195551,134.654384644287));
#24605=CARTESIAN_POINT('Ctrl Pts',(181.632912038769,3.16365416783352,134.572363936976));
#24606=CARTESIAN_POINT('Ctrl Pts',(181.625421703007,3.26340342518855,134.486297330141));
#24607=CARTESIAN_POINT('Ctrl Pts',(181.617931367245,3.35940455337579,134.396516531395));
#24608=CARTESIAN_POINT('Ctrl Pts',(181.610157033126,3.45904559351708,134.303331666377));
#24609=CARTESIAN_POINT('Ctrl Pts',(181.602382699007,3.5549643061159,134.205850220831));
#24610=CARTESIAN_POINT('Ctrl Pts',(181.594608364888,3.64676752003656,134.104401483572));
#24611=CARTESIAN_POINT('Ctrl Pts',(181.586843611941,3.73845759470076,134.003077772814));
#24612=CARTESIAN_POINT('Ctrl Pts',(181.579078858994,3.82604200261285,133.897796785766));
#24613=CARTESIAN_POINT('Ctrl Pts',(181.571314106046,3.90916215584225,133.788926633226));
#24614=CARTESIAN_POINT('Ctrl Pts',(181.563557065161,3.99219975296364,133.680164612056));
#24615=CARTESIAN_POINT('Ctrl Pts',(181.555800024276,4.07078168346808,133.567820828264));
#24616=CARTESIAN_POINT('Ctrl Pts',(181.548042983391,4.14458787258715,133.452298386643));
#24617=CARTESIAN_POINT('Ctrl Pts',(181.540291792151,4.21833840388486,133.336863061394));
#24618=CARTESIAN_POINT('Ctrl Pts',(181.532540600911,4.28732015257257,133.21825417763));
#24619=CARTESIAN_POINT('Ctrl Pts',(181.524789409671,4.35125505344596,133.096905605644));
#24620=CARTESIAN_POINT('Ctrl Pts',(181.517041512894,4.41516278028099,132.975608610038));
#24621=CARTESIAN_POINT('Ctrl Pts',(181.509293616117,4.47402774377339,132.851574587362));
#24622=CARTESIAN_POINT('Ctrl Pts',(181.50154571934,4.52761684959189,132.72526371918));
#24623=CARTESIAN_POINT('Ctrl Pts',(181.493799443256,4.5811947457247,132.598979272509));
#24624=CARTESIAN_POINT('Ctrl Pts',(181.486053167172,4.62949882669481,132.470419287337));
#24625=CARTESIAN_POINT('Ctrl Pts',(181.478306891088,4.67234352463098,132.340065358178));
#24626=CARTESIAN_POINT('Ctrl Pts',(181.470560557822,4.71518853883696,132.209710466776));
#24627=CARTESIAN_POINT('Ctrl Pts',(181.462814224557,4.75257396751604,132.07756197638));
#24628=CARTESIAN_POINT('Ctrl Pts',(181.455067891292,4.78436377673831,131.944117747105));
#24629=CARTESIAN_POINT('Ctrl Pts',(181.447319823289,4.81616070506794,131.810643633919));
#24630=CARTESIAN_POINT('Ctrl Pts',(181.439571755286,4.84235942983139,131.675873584696));
#24631=CARTESIAN_POINT('Ctrl Pts',(181.431823687283,4.86287488670871,131.540316389823));
#24632=CARTESIAN_POINT('Ctrl Pts',(181.424067384541,4.88341214765773,131.404615123149));
#24633=CARTESIAN_POINT('Ctrl Pts',(181.416311081799,4.89825401608467,131.268125426831));
#24634=CARTESIAN_POINT('Ctrl Pts',(181.408554779057,4.90736719802281,131.131362523172));
#24635=CARTESIAN_POINT('Ctrl Pts',(181.400794336543,4.91648524394055,130.994526625032));
#24636=CARTESIAN_POINT('Ctrl Pts',(181.393033894029,4.91986850125779,130.85741761965));
#24637=CARTESIAN_POINT('Ctrl Pts',(181.385273451515,4.91753585903247,130.720550489122));
#24638=CARTESIAN_POINT('Ctrl Pts',(181.377500551249,4.91519947224276,130.583463647326));
#24639=CARTESIAN_POINT('Ctrl Pts',(181.369727650984,4.90712887303039,130.4466198468));
#24640=CARTESIAN_POINT('Ctrl Pts',(181.361954750718,4.89339493605524,130.310529611767));
#24641=CARTESIAN_POINT('Ctrl Pts',(181.354464414956,4.88016026228275,130.179386599566));
#24642=CARTESIAN_POINT('Ctrl Pts',(181.346974079194,4.86166689853009,130.048943621018));
#24643=CARTESIAN_POINT('Ctrl Pts',(181.339483743432,4.83802272456425,129.91964643824));
#24644=CARTESIAN_POINT('Ctrl Pts',(181.331709409313,4.81348207455615,129.785446913479));
#24645=CARTESIAN_POINT('Ctrl Pts',(181.323935075194,4.78331458070452,129.652056681576));
#24646=CARTESIAN_POINT('Ctrl Pts',(181.316160741075,4.74758476441283,129.519984517191));
#24647=CARTESIAN_POINT('Ctrl Pts',(181.308395988128,4.71189898192648,129.388075119944));
#24648=CARTESIAN_POINT('Ctrl Pts',(181.300631235181,4.67066461765525,129.257480931918));
#24649=CARTESIAN_POINT('Ctrl Pts',(181.292866482234,4.62399754810301,129.128702616172));
#24650=CARTESIAN_POINT('Ctrl Pts',(181.285109441349,4.57737682894217,129.000052204864));
#24651=CARTESIAN_POINT('Ctrl Pts',(181.277352400464,4.52533427480508,128.873214441886));
#24652=CARTESIAN_POINT('Ctrl Pts',(181.269595359579,4.46803602093881,128.748676503191));
#24653=CARTESIAN_POINT('Ctrl Pts',(181.261844168339,4.41078097613147,128.624232479525));
#24654=CARTESIAN_POINT('Ctrl Pts',(181.254092977099,4.3482782831815,128.502085181832));
#24655=CARTESIAN_POINT('Ctrl Pts',(181.246341785858,4.28074266841829,128.382703071734));
#24656=CARTESIAN_POINT('Ctrl Pts',(181.238593889081,4.2132357580929,128.263371702218));
#24657=CARTESIAN_POINT('Ctrl Pts',(181.230845992304,4.14070037261404,128.146803522334));
#24658=CARTESIAN_POINT('Ctrl Pts',(181.223098095527,4.06339768258434,128.03344338032));
#24659=CARTESIAN_POINT('Ctrl Pts',(181.215351819443,3.98611116261093,127.920106950803));
#24660=CARTESIAN_POINT('Ctrl Pts',(181.207605543359,3.90405954173491,127.809977547203));
#24661=CARTESIAN_POINT('Ctrl Pts',(181.199859267275,3.81754769509268,127.703471606622));
#24662=CARTESIAN_POINT('Ctrl Pts',(181.19211293401,3.7310352098397,127.596964879839));
#24663=CARTESIAN_POINT('Ctrl Pts',(181.184366600744,3.64006267962051,127.494081972915));
#24664=CARTESIAN_POINT('Ctrl Pts',(181.176620267479,3.54497543858795,127.395206440602));
#24665=CARTESIAN_POINT('Ctrl Pts',(181.168872199476,3.44986690342704,127.2963087658));
#24666=CARTESIAN_POINT('Ctrl Pts',(181.161124131473,3.35064209480331,127.201420533123));
#24667=CARTESIAN_POINT('Ctrl Pts',(181.15337606347,3.24768309313699,127.110888323227));
#24668=CARTESIAN_POINT('Ctrl Pts',(181.145619760728,3.14461466541844,127.02025989462));
#24669=CARTESIAN_POINT('Ctrl Pts',(181.137863457986,3.03780441073446,126.933996995563));
#24670=CARTESIAN_POINT('Ctrl Pts',(181.130107155245,2.92766780399824,126.852406127452));
#24671=CARTESIAN_POINT('Ctrl Pts',(181.12234671273,2.81747241403878,126.770771711838));
#24672=CARTESIAN_POINT('Ctrl Pts',(181.114586270216,2.7039474579022,126.693814515155));
#24673=CARTESIAN_POINT('Ctrl Pts',(181.106825827702,2.58753641460957,126.621797005908));
#24674=CARTESIAN_POINT('Ctrl Pts',(181.099052927437,2.4709384979758,126.54966388776));
#24675=CARTESIAN_POINT('Ctrl Pts',(181.091280027171,2.35144557696644,126.48248649467));
#24676=CARTESIAN_POINT('Ctrl Pts',(181.083507126906,2.22952547955141,126.420481148588));
#24677=CARTESIAN_POINT('Ctrl Pts',(181.076016791144,2.11203748477606,126.360729853018));
#24678=CARTESIAN_POINT('Ctrl Pts',(181.068526455382,1.99229599775392,126.305781227551));
#24679=CARTESIAN_POINT('Ctrl Pts',(181.06103611962,1.87073436242814,126.255785455196));
#24680=CARTESIAN_POINT('Ctrl Pts',(181.053261785501,1.74456368075061,126.203894077936));
#24681=CARTESIAN_POINT('Ctrl Pts',(181.045487451382,1.61603243353411,126.15717416632));
#24682=CARTESIAN_POINT('Ctrl Pts',(181.037713117262,1.48560354270351,126.115846441795));
#24683=CARTESIAN_POINT('Ctrl Pts',(181.029948364315,1.35533539382416,126.074569649997));
#24684=CARTESIAN_POINT('Ctrl Pts',(181.022183611368,1.22317462372418,126.038671939907));
#24685=CARTESIAN_POINT('Ctrl Pts',(181.014418858421,1.08960508849571,126.008326441955));
#24686=CARTESIAN_POINT('Ctrl Pts',(181.006661817536,0.956168216412676,125.97801108358));
#24687=CARTESIAN_POINT('Ctrl Pts',(180.998904776651,0.821325742465903,125.953237049223));
#24688=CARTESIAN_POINT('Ctrl Pts',(180.991147735766,0.685577341742052,125.934127895099));
#24689=CARTESIAN_POINT('Ctrl Pts',(180.983396544526,0.549931309943087,125.915033151336));
#24690=CARTESIAN_POINT('Ctrl Pts',(180.975645353286,0.413381096750075,125.901594839067));
#24691=CARTESIAN_POINT('Ctrl Pts',(180.967894162046,0.276436897019386,125.893885517897));
#24692=CARTESIAN_POINT('Ctrl Pts',(180.960146265269,0.139550902226688,125.886179473395));
#24693=CARTESIAN_POINT('Ctrl Pts',(180.952398368492,0.00227164348105247,
125.884197598944));
#24694=CARTESIAN_POINT('Ctrl Pts',(180.944650471714,-0.134885446705906,
125.887960615657));
#24695=CARTESIAN_POINT('Ctrl Pts',(180.93690419563,-0.272013846586339,125.891722845229));
#24696=CARTESIAN_POINT('Ctrl Pts',(180.929157919546,-0.409019738167906,
125.901227564989));
#24697=CARTESIAN_POINT('Ctrl Pts',(180.921411643462,-0.545387968662936,
125.916443369275));
#24698=CARTESIAN_POINT('Ctrl Pts',(180.913665310197,-0.681757205797242,
125.931659285882));
#24699=CARTESIAN_POINT('Ctrl Pts',(180.905918976931,-0.817488383898427,
125.952586327784));
#24700=CARTESIAN_POINT('Ctrl Pts',(180.898172643666,-0.95207214594684,125.979141276291));
#24701=CARTESIAN_POINT('Ctrl Pts',(180.890424575663,-1.08668604709579,126.005702171595));
#24702=CARTESIAN_POINT('Ctrl Pts',(180.88267650766,-1.22015163738299,126.037893405747));
#24703=CARTESIAN_POINT('Ctrl Pts',(180.874928439657,-1.35197080488857,126.075580858978));
#24704=CARTESIAN_POINT('Ctrl Pts',(180.867172136915,-1.48393007137391,126.113308366883));
#24705=CARTESIAN_POINT('Ctrl Pts',(180.859415834173,-1.61423904308519,126.156543655144));
#24706=CARTESIAN_POINT('Ctrl Pts',(180.851659531431,-1.74241527737747,126.20510284444));
#24707=CARTESIAN_POINT('Ctrl Pts',(180.843899088917,-1.87065992318532,126.253687951238));
#24708=CARTESIAN_POINT('Ctrl Pts',(180.836138646403,-1.99676920408849,126.307602467438));
#24709=CARTESIAN_POINT('Ctrl Pts',(180.828378203889,-2.12028258665798,126.366615152218));
#24710=CARTESIAN_POINT('Ctrl Pts',(180.820605303623,-2.24399424387421,126.425722569399));
#24711=CARTESIAN_POINT('Ctrl Pts',(180.812832403358,-2.3651013298266,126.489944326195));
#24712=CARTESIAN_POINT('Ctrl Pts',(180.805059503092,-2.48316897428491,126.559003752985));
#24713=CARTESIAN_POINT('Ctrl Pts',(180.79756916733,-2.59694456247199,126.62555269566));
#24714=CARTESIAN_POINT('Ctrl Pts',(180.790078831568,-2.707897595887,126.696593525687));
#24715=CARTESIAN_POINT('Ctrl Pts',(180.782588495806,-2.81566748832438,126.771842836118));
#24716=CARTESIAN_POINT('Ctrl Pts',(180.774860431703,-2.92685778253992,126.849480409815));
#24717=CARTESIAN_POINT('Ctrl Pts',(180.7671323676,-3.03502137085671,126.931850825884));
#24718=CARTESIAN_POINT('Ctrl Pts',(180.759404303497,-3.13972510257354,127.018689033452));
#24719=CARTESIAN_POINT('Ctrl Pts',(180.751688447729,-3.24426342957341,127.105390059193));
#24720=CARTESIAN_POINT('Ctrl Pts',(180.743972591961,-3.3453524815515,127.196544571404));
#24721=CARTESIAN_POINT('Ctrl Pts',(180.736256736193,-3.44258800822052,127.291844301852));
#24722=CARTESIAN_POINT('Ctrl Pts',(180.728547930298,-3.53973469210992,127.387056958232));
#24723=CARTESIAN_POINT('Ctrl Pts',(180.720839124402,-3.63303457198762,127.486407025166));
#24724=CARTESIAN_POINT('Ctrl Pts',(180.713130318507,-3.72211626851405,127.589545918993));
#24725=CARTESIAN_POINT('Ctrl Pts',(180.705426833656,-3.81113647592418,127.692613620647));
#24726=CARTESIAN_POINT('Ctrl Pts',(180.697723348805,-3.89594403403888,127.799464648121));
#24727=CARTESIAN_POINT('Ctrl Pts',(180.690019863954,-3.97620460244335,127.909713830476));
#24728=CARTESIAN_POINT('Ctrl Pts',(180.682319975564,-4.05642770026874,128.01991154172));
#24729=CARTESIAN_POINT('Ctrl Pts',(180.674620087175,-4.13210780008793,128.133503931074));
#24730=CARTESIAN_POINT('Ctrl Pts',(180.666920198785,-4.20295133298381,128.250073406803));
#24731=CARTESIAN_POINT('Ctrl Pts',(180.659220735343,-4.27379095611665,128.366636449212));
#24732=CARTESIAN_POINT('Ctrl Pts',(180.6515212719,-4.33979432957215,128.486175917609));
#24733=CARTESIAN_POINT('Ctrl Pts',(180.643821808457,-4.40071176989382,128.608246098508));
#24734=CARTESIAN_POINT('Ctrl Pts',(180.636122680545,-4.46162655553023,128.730310959782));
#24735=CARTESIAN_POINT('Ctrl Pts',(180.628423552633,-4.51745567719539,128.854905956993));
#24736=CARTESIAN_POINT('Ctrl Pts',(180.620724424721,-4.56799625155725,128.981562409245));
#24737=CARTESIAN_POINT('Ctrl Pts',(180.61302142386,-4.61856224971331,129.108282574417));
#24738=CARTESIAN_POINT('Ctrl Pts',(180.605318422999,-4.66383424513525,129.237065895624));
#24739=CARTESIAN_POINT('Ctrl Pts',(180.597615422138,-4.70365818002023,129.367425410944));
#24740=CARTESIAN_POINT('Ctrl Pts',(180.593405538846,-4.72542295989178,129.438670157685));
#24741=CARTESIAN_POINT('Ctrl Pts',(180.589195655555,-4.74556133082426,129.510385423281));
#24742=CARTESIAN_POINT('Ctrl Pts',(180.584985772263,-4.76405452823404,129.582490119308));
#24743=CARTESIAN_POINT('Ctrl Pts',(182.334764431275,-4.76405452823405,129.582490119308));
#24744=CARTESIAN_POINT('Ctrl Pts',(182.327037589112,-4.79807206386625,129.71512397445));
#24745=CARTESIAN_POINT('Ctrl Pts',(182.319310746949,-4.82655566072364,129.849215252561));
#24746=CARTESIAN_POINT('Ctrl Pts',(182.311583904787,-4.84939387740225,129.984261791623));
#24747=CARTESIAN_POINT('Ctrl Pts',(182.303796493321,-4.87241111868681,130.120366935819));
#24748=CARTESIAN_POINT('Ctrl Pts',(182.296009081855,-4.88969399094239,130.257441989725));
#24749=CARTESIAN_POINT('Ctrl Pts',(182.288221670389,-4.90118122870282,130.394963956721));
#24750=CARTESIAN_POINT('Ctrl Pts',(182.280434258923,-4.91266846646326,130.532485923717));
#24751=CARTESIAN_POINT('Ctrl Pts',(182.272646847457,-4.91836005162741,130.670454396298));
#24752=CARTESIAN_POINT('Ctrl Pts',(182.264859435991,-4.91824838731544,130.808343476974));
#24753=CARTESIAN_POINT('',(182.610140564063,-4.91824890646276,130.801080895348));
#24754=CARTESIAN_POINT('Ctrl Pts',(182.679902359578,-4.76405452823405,129.582490119308));
#24755=CARTESIAN_POINT('Ctrl Pts',(182.671073039678,-4.80263856972609,129.732928711491));
#24756=CARTESIAN_POINT('Ctrl Pts',(182.662243719779,-4.83413672793406,129.885367666505));
#24757=CARTESIAN_POINT('Ctrl Pts',(182.65341439988,-4.85836093134102,130.039172978278));
#24758=CARTESIAN_POINT('Ctrl Pts',(182.644641758985,-4.88242962971196,130.19199095106));
#24759=CARTESIAN_POINT('Ctrl Pts',(182.635869118089,-4.89931737459966,130.346157623678));
#24760=CARTESIAN_POINT('Ctrl Pts',(182.627096477193,-4.90888732968651,130.501032005425));
#24761=CARTESIAN_POINT('Ctrl Pts',(182.62144450615,-4.91505298831555,130.600813306337));
#24762=CARTESIAN_POINT('Ctrl Pts',(182.615792535106,-4.91818209306794,130.700887987475));
#24763=CARTESIAN_POINT('Ctrl Pts',(182.610140564063,-4.91824890646276,130.801080895348));
#24764=CARTESIAN_POINT('Ctrl Pts',(182.610140564008,-4.91824890646341,130.80108089632));
#24765=CARTESIAN_POINT('Ctrl Pts',(182.602350736543,-4.91834099197833,130.939171742779));
#24766=CARTESIAN_POINT('Ctrl Pts',(182.594560909078,-4.91261293631802,131.077296116385));
#24767=CARTESIAN_POINT('Ctrl Pts',(182.586771081613,-4.90108295938559,131.214932033668));
#24768=CARTESIAN_POINT('Ctrl Pts',(182.578981013679,-4.88955262652708,131.352572199721));
#24769=CARTESIAN_POINT('Ctrl Pts',(182.571190945745,-4.87222004712722,131.48972349604));
#24770=CARTESIAN_POINT('Ctrl Pts',(182.563400877811,-4.84915540080159,131.625868354217));
#24771=CARTESIAN_POINT('Ctrl Pts',(182.555608953444,-4.82608525799307,131.762045656762));
#24772=CARTESIAN_POINT('Ctrl Pts',(182.547817029077,-4.79728039275426,131.897215664416));
#24773=CARTESIAN_POINT('Ctrl Pts',(182.54002510471,-4.76286219548405,132.030870613175));
#24774=CARTESIAN_POINT('Ctrl Pts',(182.532229707094,-4.72842865631017,132.164585138597));
#24775=CARTESIAN_POINT('Ctrl Pts',(182.524434309478,-4.68837689938111,132.296782888428));
#24776=CARTESIAN_POINT('Ctrl Pts',(182.516638911862,-4.64287820456094,132.42697118086));
#24777=CARTESIAN_POINT('Ctrl Pts',(182.508833566481,-4.59732144851264,132.557325607555));
#24778=CARTESIAN_POINT('Ctrl Pts',(182.501028221099,-4.54630400030386,132.685665092519));
#24779=CARTESIAN_POINT('Ctrl Pts',(182.493222875718,-4.49004557517999,132.811516265568));
#24780=CARTESIAN_POINT('Ctrl Pts',(182.48541197276,-4.43374709282834,132.937457047402));
#24781=CARTESIAN_POINT('Ctrl Pts',(182.477601069802,-4.37220036926214,133.060905643736));
#24782=CARTESIAN_POINT('Ctrl Pts',(182.469790166844,-4.30567070775944,133.181414007552));
#24783=CARTESIAN_POINT('Ctrl Pts',(182.461966709995,-4.23903411801708,133.302116055611));
#24784=CARTESIAN_POINT('Ctrl Pts',(182.454143253146,-4.16739879386563,133.419868104856));
#24785=CARTESIAN_POINT('Ctrl Pts',(182.446319796298,-4.09107330250262,133.534251145783));
#24786=CARTESIAN_POINT('Ctrl Pts',(182.442108278373,-4.04998581634815,133.595825745913));
#24787=CARTESIAN_POINT('Ctrl Pts',(182.437896760449,-4.00753987680767,133.656424612155));
#24788=CARTESIAN_POINT('Ctrl Pts',(182.433685242525,-3.96378825988816,133.715986571097));
#24789=CARTESIAN_POINT('Ctrl Pts',(182.425910908406,-3.88302410446949,133.825936137482));
#24790=CARTESIAN_POINT('Ctrl Pts',(182.418136574287,-3.7975538023016,133.932696893848));
#24791=CARTESIAN_POINT('Ctrl Pts',(182.410362240168,-3.70765790045001,134.035839529106));
#24792=CARTESIAN_POINT('Ctrl Pts',(182.402597487221,-3.61787278726326,134.138855050285));
#24793=CARTESIAN_POINT('Ctrl Pts',(182.394832734273,-3.52367318095091,134.238261030556));
#24794=CARTESIAN_POINT('Ctrl Pts',(182.387067981326,-3.42538226341174,134.333657914763));
#24795=CARTESIAN_POINT('Ctrl Pts',(182.379310940441,-3.32718896979766,134.42896004944));
#24796=CARTESIAN_POINT('Ctrl Pts',(182.371553899556,-3.22491273033872,134.520260741664));
#24797=CARTESIAN_POINT('Ctrl Pts',(182.363796858671,-3.11891602473428,134.607194546777));
#24798=CARTESIAN_POINT('Ctrl Pts',(182.356045667431,-3.01299925206974,134.694062794431));
#24799=CARTESIAN_POINT('Ctrl Pts',(182.348294476191,-2.90336789877549,134.77657046277));
#24800=CARTESIAN_POINT('Ctrl Pts',(182.340543284951,-2.79041995640996,134.854390188985));
#24801=CARTESIAN_POINT('Ctrl Pts',(182.332795388174,-2.67752001993321,134.932176839741));
#24802=CARTESIAN_POINT('Ctrl Pts',(182.325047491397,-2.56130661932331,135.005279289951));
#24803=CARTESIAN_POINT('Ctrl Pts',(182.31729959462,-2.44220918470204,135.073411725325));
#24804=CARTESIAN_POINT('Ctrl Pts',(182.309553318536,-2.32313666269663,135.141529908862));
#24805=CARTESIAN_POINT('Ctrl Pts',(182.301807042451,-2.20118164577595,135.204679951408));
#24806=CARTESIAN_POINT('Ctrl Pts',(182.294060766367,-2.07680044042566,135.262620703423));
#24807=CARTESIAN_POINT('Ctrl Pts',(182.286314433102,-1.95241831692144,135.320561883144));
#24808=CARTESIAN_POINT('Ctrl Pts',(182.278568099837,-1.82561032364971,135.37329353051));
#24809=CARTESIAN_POINT('Ctrl Pts',(182.270821766571,-1.6968547692407,135.420621762108));
#24810=CARTESIAN_POINT('Ctrl Pts',(182.263073698568,-1.56807038091839,135.467960592535));
#24811=CARTESIAN_POINT('Ctrl Pts',(182.255325630565,-1.43733793047416,135.509893464457));
#24812=CARTESIAN_POINT('Ctrl Pts',(182.247577562562,-1.30515260026303,135.546275816357));
#24813=CARTESIAN_POINT('Ctrl Pts',(182.239821259821,-1.17282678190962,135.582696835854));
#24814=CARTESIAN_POINT('Ctrl Pts',(182.232064957079,-1.03904537675643,135.613555447207));
#24815=CARTESIAN_POINT('Ctrl Pts',(182.224308654337,-0.904316068585796,
135.638757737228));
#24816=CARTESIAN_POINT('Ctrl Pts',(182.216548211823,-0.769514851326632,
135.663973478471));
#24817=CARTESIAN_POINT('Ctrl Pts',(182.208787769308,-0.633765109735002,
135.683526827158));
#24818=CARTESIAN_POINT('Ctrl Pts',(182.201027326794,-0.497580452340472,
135.69737571625));
#24819=CARTESIAN_POINT('Ctrl Pts',(182.193254426529,-0.361177179244034,
135.711246836808));
#24820=CARTESIAN_POINT('Ctrl Pts',(182.185481526263,-0.224337985686155,
135.719395175306));
#24821=CARTESIAN_POINT('Ctrl Pts',(182.177708625998,-0.0875781934747493,
135.721830812954));
#24822=CARTESIAN_POINT('Ctrl Pts',(182.170218290236,0.0442100358122264,
135.724177909039));
#24823=CARTESIAN_POINT('Ctrl Pts',(182.162727954474,0.175924228464083,135.72122044237));
#24824=CARTESIAN_POINT('Ctrl Pts',(182.155237618712,0.307109000857396,135.713012889228));
#24825=CARTESIAN_POINT('Ctrl Pts',(182.147463284593,0.443267683768998,135.704494144214));
#24826=CARTESIAN_POINT('Ctrl Pts',(182.139688950474,0.579287317770908,135.690292354947));
#24827=CARTESIAN_POINT('Ctrl Pts',(182.131914616355,0.714655068745021,135.670411500491));
#24828=CARTESIAN_POINT('Ctrl Pts',(182.124149863408,0.849855991064199,135.650555147412));
#24829=CARTESIAN_POINT('Ctrl Pts',(182.116385110461,0.984406245755034,135.625033711212));
#24830=CARTESIAN_POINT('Ctrl Pts',(182.108620357513,1.11779498803749,135.593903124656));
#24831=CARTESIAN_POINT('Ctrl Pts',(182.100863316628,1.25105124674114,135.562803457436));
#24832=CARTESIAN_POINT('Ctrl Pts',(182.093106275743,1.38314791054298,135.526105814856));
#24833=CARTESIAN_POINT('Ctrl Pts',(182.085349234858,1.5135815913709,135.483917629588));
#24834=CARTESIAN_POINT('Ctrl Pts',(182.077598043618,1.64391691114509,135.441761258759));
#24835=CARTESIAN_POINT('Ctrl Pts',(182.069846852378,1.77259137360677,135.39412270641));
#24836=CARTESIAN_POINT('Ctrl Pts',(182.062095661138,1.8991144349961,135.341159866518));
#24837=CARTESIAN_POINT('Ctrl Pts',(182.054347764361,2.02558372070912,135.288219537246));
#24838=CARTESIAN_POINT('Ctrl Pts',(182.046599867584,2.14990306413975,135.229959571943));
#24839=CARTESIAN_POINT('Ctrl Pts',(182.038851970807,2.27159988415978,135.166586772729));
#24840=CARTESIAN_POINT('Ctrl Pts',(182.031105694723,2.39327124782866,135.103227229737));
#24841=CARTESIAN_POINT('Ctrl Pts',(182.023359418639,2.51232083268777,135.034757160578));
#24842=CARTESIAN_POINT('Ctrl Pts',(182.015613142554,2.62829910799688,134.961430121604));
#24843=CARTESIAN_POINT('Ctrl Pts',(182.007866809289,2.74427823943102,134.888102541346));
#24844=CARTESIAN_POINT('Ctrl Pts',(182.000120476024,2.85718568561855,134.809918128662));
#24845=CARTESIAN_POINT('Ctrl Pts',(181.992374142758,2.96659978945404,134.727174499426));
#24846=CARTESIAN_POINT('Ctrl Pts',(181.984626074756,3.07603839581934,134.644412340328));
#24847=CARTESIAN_POINT('Ctrl Pts',(181.976878006753,3.18198179135113,134.557089168775));
#24848=CARTESIAN_POINT('Ctrl Pts',(181.96912993875,3.28404069419147,134.465543456676));
#24849=CARTESIAN_POINT('Ctrl Pts',(181.961373636008,3.3862080664486,134.373900448704));
#24850=CARTESIAN_POINT('Ctrl Pts',(181.953617333266,3.48448240741909,134.278026196862));
#24851=CARTESIAN_POINT('Ctrl Pts',(181.945861030524,3.57851028979258,134.178297067523));
#24852=CARTESIAN_POINT('Ctrl Pts',(181.93810058801,3.67258835767799,134.078514709744));
#24853=CARTESIAN_POINT('Ctrl Pts',(181.930340145496,3.76241519491009,133.974873670094));
#24854=CARTESIAN_POINT('Ctrl Pts',(181.922579702982,3.84767779134117,133.86778332371));
#24855=CARTESIAN_POINT('Ctrl Pts',(181.914806802716,3.93307725886131,133.760521066396));
#24856=CARTESIAN_POINT('Ctrl Pts',(181.907033902451,4.01389761341318,133.64979875336));
#24857=CARTESIAN_POINT('Ctrl Pts',(181.899261002185,4.08986879258137,133.536055388577));
#24858=CARTESIAN_POINT('Ctrl Pts',(181.891770666423,4.16307822802756,133.426446881605));
#24859=CARTESIAN_POINT('Ctrl Pts',(181.884280330661,4.23178476598698,133.314033418012));
#24860=CARTESIAN_POINT('Ctrl Pts',(181.876789994899,4.29578809292371,133.199227570696));
#24861=CARTESIAN_POINT('Ctrl Pts',(181.86901566078,4.36221812545415,133.080068824786));
#24862=CARTESIAN_POINT('Ctrl Pts',(181.861241326661,4.42379169257108,132.957955240427));
#24863=CARTESIAN_POINT('Ctrl Pts',(181.853466992542,4.480234942605,132.833320430268));
#24864=CARTESIAN_POINT('Ctrl Pts',(181.845702239595,4.53660863137767,132.708839221374));
#24865=CARTESIAN_POINT('Ctrl Pts',(181.837937486648,4.5878644235316,132.58184332178));
#24866=CARTESIAN_POINT('Ctrl Pts',(181.8301727337,4.63377325280224,132.452792752692));
#24867=CARTESIAN_POINT('Ctrl Pts',(181.822415692815,4.67963648477647,132.323870358447));
#24868=CARTESIAN_POINT('Ctrl Pts',(181.81465865193,4.72016319216763,132.192897721815));
#24869=CARTESIAN_POINT('Ctrl Pts',(181.806901611045,4.75517166757724,132.06035642742));
#24870=CARTESIAN_POINT('Ctrl Pts',(181.799150419805,4.7901537428232,131.927915083446));
#24871=CARTESIAN_POINT('Ctrl Pts',(181.791399228565,4.81962576954726,131.793907812746));
#24872=CARTESIAN_POINT('Ctrl Pts',(181.783648037325,4.84345543753907,131.658832669229));
#24873=CARTESIAN_POINT('Ctrl Pts',(181.775900140548,4.86727497728632,131.523814936251));
#24874=CARTESIAN_POINT('Ctrl Pts',(181.768152243771,4.88545686026262,131.387730617391));
#24875=CARTESIAN_POINT('Ctrl Pts',(181.760404346994,4.8979196333033,131.251089090133));
#24876=CARTESIAN_POINT('Ctrl Pts',(181.75265807091,4.91037979940052,131.114476145337));
#24877=CARTESIAN_POINT('Ctrl Pts',(181.744911794826,4.91712319960808,130.97730661308));
#24878=CARTESIAN_POINT('Ctrl Pts',(181.737165518741,4.91812017572067,130.840095749709));
#24879=CARTESIAN_POINT('Ctrl Pts',(181.729419185476,4.91911715919271,130.702883873479));
#24880=CARTESIAN_POINT('Ctrl Pts',(181.721672852211,4.91436763108547,130.565631056479));
#24881=CARTESIAN_POINT('Ctrl Pts',(181.713926518945,4.90389406809912,130.428852919426));
#24882=CARTESIAN_POINT('Ctrl Pts',(181.706178450942,4.89341815963096,130.292044151858));
#24883=CARTESIAN_POINT('Ctrl Pts',(181.698430382939,4.87721569537927,130.155710665513));
#24884=CARTESIAN_POINT('Ctrl Pts',(181.690682314937,4.85536102499316,130.020362926576));
#24885=CARTESIAN_POINT('Ctrl Pts',(181.682926012195,4.83348312720327,129.884871338452));
#24886=CARTESIAN_POINT('Ctrl Pts',(181.675169709453,4.80594108560759,129.75036797714));
#24887=CARTESIAN_POINT('Ctrl Pts',(181.667413406711,4.77286051180006,129.617353626264));
#24888=CARTESIAN_POINT('Ctrl Pts',(181.659652964197,4.73976228189421,129.484268281624));
#24889=CARTESIAN_POINT('Ctrl Pts',(181.651892521683,4.70111973963549,129.352673905927));
#24890=CARTESIAN_POINT('Ctrl Pts',(181.644132079168,4.65710811429238,129.22305512074));
#24891=CARTESIAN_POINT('Ctrl Pts',(181.636359178903,4.61302583758112,129.093228259972));
#24892=CARTESIAN_POINT('Ctrl Pts',(181.628586278637,4.5635573955876,128.965383691997));
#24893=CARTESIAN_POINT('Ctrl Pts',(181.620813378372,4.5089261594554,128.839985920346));
#24894=CARTESIAN_POINT('Ctrl Pts',(181.61332304261,4.45628090636462,128.719146673552));
#24895=CARTESIAN_POINT('Ctrl Pts',(181.605832706848,4.39884183774708,128.600579694375));
#24896=CARTESIAN_POINT('Ctrl Pts',(181.598342371086,4.33684778850805,128.484676517993));
#24897=CARTESIAN_POINT('Ctrl Pts',(181.590568036967,4.27250321604925,128.36437883745));
#24898=CARTESIAN_POINT('Ctrl Pts',(181.582793702848,4.20304761613661,128.246569876445));
#24899=CARTESIAN_POINT('Ctrl Pts',(181.575019368729,4.12869777585513,128.13171441237));
#24900=CARTESIAN_POINT('Ctrl Pts',(181.567254615782,4.05443956510713,128.01700049739));
#24901=CARTESIAN_POINT('Ctrl Pts',(181.559489862835,3.97529932571951,127.905233162034));
#24902=CARTESIAN_POINT('Ctrl Pts',(181.551725109888,3.89154027064978,127.796853778935));
#24903=CARTESIAN_POINT('Ctrl Pts',(181.543968069003,3.80786440625398,127.688582039767));
#24904=CARTESIAN_POINT('Ctrl Pts',(181.536211028118,3.71957909298195,127.583691863779));
#24905=CARTESIAN_POINT('Ctrl Pts',(181.528453987233,3.62699128433114,127.482596434803));
#24906=CARTESIAN_POINT('Ctrl Pts',(181.520702795992,3.5344732968673,127.381577242677));
#24907=CARTESIAN_POINT('Ctrl Pts',(181.512951604752,3.43765953508295,127.28434738878));
#24908=CARTESIAN_POINT('Ctrl Pts',(181.505200413512,3.33689750893684,127.191287399743));
#24909=CARTESIAN_POINT('Ctrl Pts',(181.497452516735,3.23617830933978,127.098266963683));
#24910=CARTESIAN_POINT('Ctrl Pts',(181.489704619958,3.13151446964089,127.00941313221));
#24911=CARTESIAN_POINT('Ctrl Pts',(181.481956723181,3.02329051611814,126.925069765149));
#24912=CARTESIAN_POINT('Ctrl Pts',(181.474210447097,2.91508920071343,126.840744040902));
#24913=CARTESIAN_POINT('Ctrl Pts',(181.466464171013,2.80332956091226,126.760927144587));
#24914=CARTESIAN_POINT('Ctrl Pts',(181.458717894929,2.688429065486,126.685922537134));
#24915=CARTESIAN_POINT('Ctrl Pts',(181.450971561663,2.57352772189059,126.610917376014));
#24916=CARTESIAN_POINT('Ctrl Pts',(181.443225228398,2.45548580379192,126.54072478835));
#24917=CARTESIAN_POINT('Ctrl Pts',(181.435478895133,2.33474926670635,126.475604569448));
#24918=CARTESIAN_POINT('Ctrl Pts',(181.42773082713,2.21398569151045,126.410469767325));
#24919=CARTESIAN_POINT('Ctrl Pts',(181.419982759127,2.0905266405883,126.350409779878));
#24920=CARTESIAN_POINT('Ctrl Pts',(181.412234691124,1.96484177140072,126.295637974083));
#24921=CARTESIAN_POINT('Ctrl Pts',(181.404478388382,1.83902332283823,126.240807956161));
#24922=CARTESIAN_POINT('Ctrl Pts',(181.39672208564,1.71097468939951,126.19127750357));
#24923=CARTESIAN_POINT('Ctrl Pts',(181.388965782898,1.58118509066446,126.1472116215));
#24924=CARTESIAN_POINT('Ctrl Pts',(181.381205340384,1.45132621931234,126.103122220142));
#24925=CARTESIAN_POINT('Ctrl Pts',(181.37344489787,1.31972490610537,126.064503310922));
#24926=CARTESIAN_POINT('Ctrl Pts',(181.365684455356,1.18688359259093,126.031469418289));
#24927=CARTESIAN_POINT('Ctrl Pts',(181.35791155509,1.05382903040709,125.998382496718));
#24928=CARTESIAN_POINT('Ctrl Pts',(181.350138654825,0.919530873392618,125.970898586219));
#24929=CARTESIAN_POINT('Ctrl Pts',(181.342365754559,0.784500659081397,125.949080833825));
#24930=CARTESIAN_POINT('Ctrl Pts',(181.334875418797,0.65437913317976,125.928056211687));
#24931=CARTESIAN_POINT('Ctrl Pts',(181.327385083035,0.523578155989451,125.912292978468));
#24932=CARTESIAN_POINT('Ctrl Pts',(181.319894747273,0.39255623324671,125.901801829929));
#24933=CARTESIAN_POINT('Ctrl Pts',(181.312120413154,0.256566574481517,125.890912906304));
#24934=CARTESIAN_POINT('Ctrl Pts',(181.304346079035,0.119908110764656,125.885669248528));
#24935=CARTESIAN_POINT('Ctrl Pts',(181.296571744916,-0.0169109488048534,
125.88613969102));
#24936=CARTESIAN_POINT('Ctrl Pts',(181.288806991969,-0.153561391111778,
125.886609553735));
#24937=CARTESIAN_POINT('Ctrl Pts',(181.281042239022,-0.290371648259795,
125.892779503671));
#24938=CARTESIAN_POINT('Ctrl Pts',(181.273277486075,-0.426828107918584,
125.904666665002));
#24939=CARTESIAN_POINT('Ctrl Pts',(181.26552044519,-0.563149037097825,125.916542019838));
#24940=CARTESIAN_POINT('Ctrl Pts',(181.257763404305,-0.699116481113278,
125.934123252056));
#24941=CARTESIAN_POINT('Ctrl Pts',(181.25000636342,-0.834216900840216,125.957375448943));
#24942=CARTESIAN_POINT('Ctrl Pts',(181.242255172179,-0.969215440289043,
125.980610111167));
#24943=CARTESIAN_POINT('Ctrl Pts',(181.234503980939,-1.1033478731167,126.009507159861));
#24944=CARTESIAN_POINT('Ctrl Pts',(181.226752789699,-1.23610621387061,126.043979908995));
#24945=CARTESIAN_POINT('Ctrl Pts',(181.219004892922,-1.36880812878891,126.078438006292));
#24946=CARTESIAN_POINT('Ctrl Pts',(181.211256996145,-1.50013673559273,126.118466992577));
#24947=CARTESIAN_POINT('Ctrl Pts',(181.203509099368,-1.62959488942576,126.16392921964));
#24948=CARTESIAN_POINT('Ctrl Pts',(181.195762823284,-1.75902596340384,126.209381936985));
#24949=CARTESIAN_POINT('Ctrl Pts',(181.1880165472,-1.88658699399867,126.260265505053));
#24950=CARTESIAN_POINT('Ctrl Pts',(181.180270271116,-2.01179701886858,126.316392723589));
#24951=CARTESIAN_POINT('Ctrl Pts',(181.17252393785,-2.13700796800998,126.372520356442));
#24952=CARTESIAN_POINT('Ctrl Pts',(181.164777604585,-2.25986752003577,126.433891557078));
#24953=CARTESIAN_POINT('Ctrl Pts',(181.15703127132,-2.37991605194676,126.500271556198));
#24954=CARTESIAN_POINT('Ctrl Pts',(181.149283203317,-2.49999146789432,126.566666420659));
#24955=CARTESIAN_POINT('Ctrl Pts',(181.141535135314,-2.61725426899975,126.63807212648));
#24956=CARTESIAN_POINT('Ctrl Pts',(181.133787067311,-2.73127108225299,126.7142088676));
#24957=CARTESIAN_POINT('Ctrl Pts',(181.126030764569,-2.8454090739322,126.790426527755));
#24958=CARTESIAN_POINT('Ctrl Pts',(181.118274461827,-2.95629386060742,126.871385050119));
#24959=CARTESIAN_POINT('Ctrl Pts',(181.110518159085,-3.06352218360704,126.956762029739));
#24960=CARTESIAN_POINT('Ctrl Pts',(181.102757716571,-3.17080773759117,127.042184577624));
#24961=CARTESIAN_POINT('Ctrl Pts',(181.094997274057,-3.27443264399057,127.132030025815));
#24962=CARTESIAN_POINT('Ctrl Pts',(181.087236831543,-3.37402896821536,127.22593755927));
#24963=CARTESIAN_POINT('Ctrl Pts',(181.079463931278,-3.4737851733016,127.319995841434));
#24964=CARTESIAN_POINT('Ctrl Pts',(181.071691031012,-3.56949959987051,127.418128959495));
#24965=CARTESIAN_POINT('Ctrl Pts',(181.063918130747,-3.66084262200152,127.519940674953));
#24966=CARTESIAN_POINT('Ctrl Pts',(181.056427794985,-3.7488650952,127.618051278106));
#24967=CARTESIAN_POINT('Ctrl Pts',(181.048937459222,-3.83282827290767,127.7195774321));
#24968=CARTESIAN_POINT('Ctrl Pts',(181.04144712346,-3.9124753229297,127.824139164391));
#24969=CARTESIAN_POINT('Ctrl Pts',(181.033651562904,-3.99536792231622,127.932961698101));
#24970=CARTESIAN_POINT('Ctrl Pts',(181.025856002347,-4.07385081342254,128.045421065337));
#24971=CARTESIAN_POINT('Ctrl Pts',(181.018060441791,-4.14758872176929,128.161125694682));
#24972=CARTESIAN_POINT('Ctrl Pts',(181.01027762814,-4.22120605762,128.276641129674));
#24973=CARTESIAN_POINT('Ctrl Pts',(181.00249481449,-4.29009365664689,128.395390934063));
#24974=CARTESIAN_POINT('Ctrl Pts',(180.994712000839,-4.35395702277294,128.516951317431));
#24975=CARTESIAN_POINT('Ctrl Pts',(180.986936519403,-4.41776022301778,128.638397178372));
#24976=CARTESIAN_POINT('Ctrl Pts',(180.979161037966,-4.47654842553653,128.762648010892));
#24977=CARTESIAN_POINT('Ctrl Pts',(180.971385556529,-4.53007071000093,128.889251632445));
#24978=CARTESIAN_POINT('Ctrl Pts',(180.963616832862,-4.58354647756522,129.015745221175));
#24979=CARTESIAN_POINT('Ctrl Pts',(180.955848109195,-4.63176528846851,129.144587172));
#24980=CARTESIAN_POINT('Ctrl Pts',(180.948079385529,-4.67452267920003,129.275301827282));
#24981=CARTESIAN_POINT('Ctrl Pts',(180.942056030262,-4.70767393617805,129.376649338295));
#24982=CARTESIAN_POINT('Ctrl Pts',(180.936032674994,-4.73754299834085,129.479122066623));
#24983=CARTESIAN_POINT('Ctrl Pts',(180.930009319727,-4.76405452823405,129.582490119308));
#24984=CARTESIAN_POINT('Origin',(213.235140564004,0.,130.804360617566));
#24985=CARTESIAN_POINT('',(178.834794689177,-4.76405452823405,129.582490119308));
#24986=CARTESIAN_POINT('',(179.180279212536,-4.76405452823405,129.582490119308));
#24987=CARTESIAN_POINT('',(213.235140564004,-4.76405452823405,129.582490119308));
#24988=CARTESIAN_POINT('',(180.514859436037,-4.91824986164052,130.805527225028));
#24989=CARTESIAN_POINT('Ctrl Pts',(180.514859435991,-4.91824986164033,130.805527225829));
#24990=CARTESIAN_POINT('Ctrl Pts',(180.511286581325,-4.91823498623681,130.86823975205));
#24991=CARTESIAN_POINT('Ctrl Pts',(180.507713726659,-4.91702069103772,130.930936615505));
#24992=CARTESIAN_POINT('Ctrl Pts',(180.504140871993,-4.9146084703115,130.993587058748));
#24993=CARTESIAN_POINT('Ctrl Pts',(180.496366537874,-4.90935961144405,131.129910957714));
#24994=CARTESIAN_POINT('Ctrl Pts',(180.488592203755,-4.89842600811054,131.266232225206));
#24995=CARTESIAN_POINT('Ctrl Pts',(180.480817869636,-4.88179933162287,131.402038079301));
#24996=CARTESIAN_POINT('Ctrl Pts',(180.473053116689,-4.86519314602801,131.537676564819));
#24997=CARTESIAN_POINT('Ctrl Pts',(180.465288363742,-4.84290789448837,131.672800516459));
#24998=CARTESIAN_POINT('Ctrl Pts',(180.457523610795,-4.81498723479294,131.80689789432));
#24999=CARTESIAN_POINT('Ctrl Pts',(180.44976656991,-4.78709430629035,131.940862084775));
#25000=CARTESIAN_POINT('Ctrl Pts',(180.442009529025,-4.75357718742527,132.073801350235));
#25001=CARTESIAN_POINT('Ctrl Pts',(180.43425248814,-4.714531200007,132.205209869506));
#25002=CARTESIAN_POINT('Ctrl Pts',(180.4265012969,-4.67551465747153,132.33651929259));
#25003=CARTESIAN_POINT('Ctrl Pts',(180.41875010566,-4.63097765615341,132.466299893888));
#25004=CARTESIAN_POINT('Ctrl Pts',(180.41099891442,-4.58106627286169,132.594057481884));
#25005=CARTESIAN_POINT('Ctrl Pts',(180.403251017643,-4.53117610323931,132.721760769497));
#25006=CARTESIAN_POINT('Ctrl Pts',(180.395503120866,-4.47591623682387,132.847442390555));
#25007=CARTESIAN_POINT('Ctrl Pts',(180.387755224089,-4.41548207553511,132.970624937341));
#25008=CARTESIAN_POINT('Ctrl Pts',(180.380008948005,-4.35506055577006,133.093781716993));
#25009=CARTESIAN_POINT('Ctrl Pts',(180.37226267192,-4.28946706608026,133.21444011138));
#25010=CARTESIAN_POINT('Ctrl Pts',(180.364516395836,-4.21894430230164,133.332144634561));
#25011=CARTESIAN_POINT('Ctrl Pts',(180.356770062571,-4.14842101794008,133.449850026611));
#25012=CARTESIAN_POINT('Ctrl Pts',(180.349023729306,-4.07296858782303,133.56460116857));
#25013=CARTESIAN_POINT('Ctrl Pts',(180.34127739604,-3.99287442351235,133.675969382799));
#25014=CARTESIAN_POINT('Ctrl Pts',(180.333529328037,-3.91276232266898,133.787362537167));
#25015=CARTESIAN_POINT('Ctrl Pts',(180.325781260035,-3.82800664740718,133.895370938959));
#25016=CARTESIAN_POINT('Ctrl Pts',(180.318033192032,-3.73893643047199,133.999597296028));
#25017=CARTESIAN_POINT('Ctrl Pts',(180.31027688929,-3.64977154865013,134.10393442611));
#25018=CARTESIAN_POINT('Ctrl Pts',(180.302520586548,-3.55628321943548,134.204481184188));
#25019=CARTESIAN_POINT('Ctrl Pts',(180.294764283806,-3.45883921953503,134.300875212975));
#25020=CARTESIAN_POINT('Ctrl Pts',(180.287003841292,-3.36134321083779,134.397320690157));
#25021=CARTESIAN_POINT('Ctrl Pts',(180.279243398778,-3.25988761365962,134.489608758661));
#25022=CARTESIAN_POINT('Ctrl Pts',(180.271482956264,-3.15487417386967,134.577416674604));
#25023=CARTESIAN_POINT('Ctrl Pts',(180.263710055998,-3.04969215718354,134.665365547608));
#25024=CARTESIAN_POINT('Ctrl Pts',(180.255937155733,-2.94094119510187,134.748819658113));
#25025=CARTESIAN_POINT('Ctrl Pts',(180.248164255467,-2.82905368442206,134.827498486588));
#25026=CARTESIAN_POINT('Ctrl Pts',(180.240673919705,-2.72123356658074,134.90331714147));
#25027=CARTESIAN_POINT('Ctrl Pts',(180.233183583943,-2.61050124275258,134.974701506813));
#25028=CARTESIAN_POINT('Ctrl Pts',(180.225693248181,-2.49726436005296,135.041441426155));
#25029=CARTESIAN_POINT('Ctrl Pts',(180.217918914062,-2.37973406653057,135.110711809822));
#25030=CARTESIAN_POINT('Ctrl Pts',(180.210144579943,-2.259133243701,135.175198034593));
#25031=CARTESIAN_POINT('Ctrl Pts',(180.202370245824,-2.13588880765785,135.234615922153));
#25032=CARTESIAN_POINT('Ctrl Pts',(180.194605492877,-2.01279625936746,135.293960582477));
#25033=CARTESIAN_POINT('Ctrl Pts',(180.186840739929,-1.88706692913862,135.348249165653));
#25034=CARTESIAN_POINT('Ctrl Pts',(180.179075986982,-1.75915520874346,135.397241632142));
#25035=CARTESIAN_POINT('Ctrl Pts',(180.171318946097,-1.63137053207232,135.446185438622));
#25036=CARTESIAN_POINT('Ctrl Pts',(180.163561905212,-1.5014081415564,135.48984345747));
#25037=CARTESIAN_POINT('Ctrl Pts',(180.155804864327,-1.36974512266039,135.528022476913));
#25038=CARTESIAN_POINT('Ctrl Pts',(180.148053673087,-1.23818139187112,135.56617270526));
#25039=CARTESIAN_POINT('Ctrl Pts',(180.140302481847,-1.10491995933232,135.598852049766));
#25040=CARTESIAN_POINT('Ctrl Pts',(180.132551290607,-0.970455560445589,
135.625916286404));
#25041=CARTESIAN_POINT('Ctrl Pts',(180.12480339383,-0.836048312515253,135.652969020018));
#25042=CARTESIAN_POINT('Ctrl Pts',(180.117055497053,-0.700439497635642,
135.674411315488));
#25043=CARTESIAN_POINT('Ctrl Pts',(180.109307600276,-0.564136391950636,
135.69014951945));
#25044=CARTESIAN_POINT('Ctrl Pts',(180.101561324192,-0.427861797936961,
135.705884431319));
#25045=CARTESIAN_POINT('Ctrl Pts',(180.093815048108,-0.290893590128375,
135.71591758015));
#25046=CARTESIAN_POINT('Ctrl Pts',(180.086068772024,-0.153746164773559,
135.720206951547));
#25047=CARTESIAN_POINT('Ctrl Pts',(180.078322438758,-0.0165977270276053,
135.724496354607));
#25048=CARTESIAN_POINT('Ctrl Pts',(180.070576105493,0.120729540130282,135.723041883407));
#25049=CARTESIAN_POINT('Ctrl Pts',(180.062829772227,0.257719625092028,135.715853634699));
#25050=CARTESIAN_POINT('Ctrl Pts',(180.055081704225,0.394740388033409,135.708663776232));
#25051=CARTESIAN_POINT('Ctrl Pts',(180.047333636222,0.531423428169907,135.695737605649));
#25052=CARTESIAN_POINT('Ctrl Pts',(180.039585568219,0.667256642130682,135.677137201407));
#25053=CARTESIAN_POINT('Ctrl Pts',(180.031829265477,0.803234221247715,135.658517028435));
#25054=CARTESIAN_POINT('Ctrl Pts',(180.024072962735,0.93835978197096,135.634210628072));
#25055=CARTESIAN_POINT('Ctrl Pts',(180.016316659993,1.07212967055861,135.604331558312));
#25056=CARTESIAN_POINT('Ctrl Pts',(180.008556217479,1.20597095616365,135.574436541194));
#25057=CARTESIAN_POINT('Ctrl Pts',(180.000795774965,1.33845475039577,135.538963029203));
#25058=CARTESIAN_POINT('Ctrl Pts',(179.99303533245,1.46909236623006,135.498074571567));
#25059=CARTESIAN_POINT('Ctrl Pts',(179.985262432185,1.59993969316269,135.457120476149));
#25060=CARTESIAN_POINT('Ctrl Pts',(179.97748953192,1.72893455126841,135.41073419697));
#25061=CARTESIAN_POINT('Ctrl Pts',(179.969716631654,1.85560721049188,135.359127894044));
#25062=CARTESIAN_POINT('Ctrl Pts',(179.962226295892,1.97767499948376,135.309397610217));
#25063=CARTESIAN_POINT('Ctrl Pts',(179.95473596013,2.09758621357152,135.254820363207));
#25064=CARTESIAN_POINT('Ctrl Pts',(179.947245624368,2.21494369894812,135.195625523375));
#25065=CARTESIAN_POINT('Ctrl Pts',(179.939471290249,2.33675082905244,135.134186293199));
#25066=CARTESIAN_POINT('Ctrl Pts',(179.93169695613,2.45619260687545,135.067577785012));
#25067=CARTESIAN_POINT('Ctrl Pts',(179.923922622011,2.57279918657586,134.996005570094));
#25068=CARTESIAN_POINT('Ctrl Pts',(179.916157869064,2.68926205908817,134.924521561534));
#25069=CARTESIAN_POINT('Ctrl Pts',(179.908393116117,2.8028963557451,134.848086220452));
#25070=CARTESIAN_POINT('Ctrl Pts',(179.900628363169,2.9132545146317,134.76695209228));
#25071=CARTESIAN_POINT('Ctrl Pts',(179.892871322284,3.02350306423898,134.685898547668));
#25072=CARTESIAN_POINT('Ctrl Pts',(179.8851142814,3.1304816385372,134.600155733395));
#25073=CARTESIAN_POINT('Ctrl Pts',(179.877357240515,3.2337698066414,134.51002059929));
#25074=CARTESIAN_POINT('Ctrl Pts',(179.869606049274,3.33698008433468,134.419953436792));
#25075=CARTESIAN_POINT('Ctrl Pts',(179.861854858034,3.43650520177386,134.32550080338));
#25076=CARTESIAN_POINT('Ctrl Pts',(179.854103666794,3.53195640262972,134.22700097735));
#25077=CARTESIAN_POINT('Ctrl Pts',(179.846355770017,3.627367034179,134.128543016374));
#25078=CARTESIAN_POINT('Ctrl Pts',(179.83860787324,3.71870692150715,134.026041564233));
#25079=CARTESIAN_POINT('Ctrl Pts',(179.830859976463,3.8056230762406,133.919872784784));
#25080=CARTESIAN_POINT('Ctrl Pts',(179.823113700379,3.89252104998818,133.813726213555));
#25081=CARTESIAN_POINT('Ctrl Pts',(179.815367424295,3.97499688420821,133.703914143201));
#25082=CARTESIAN_POINT('Ctrl Pts',(179.807621148211,4.05273718726214,133.590846640047));
#25083=CARTESIAN_POINT('Ctrl Pts',(179.799874814945,4.13047806417734,133.477778302254));
#25084=CARTESIAN_POINT('Ctrl Pts',(179.79212848168,4.20348311866762,133.361454805873));
#25085=CARTESIAN_POINT('Ctrl Pts',(179.784382148415,4.27148192853796,133.242315743624));
#25086=CARTESIAN_POINT('Ctrl Pts',(179.776634080412,4.33949596627027,133.123150001009));
#25087=CARTESIAN_POINT('Ctrl Pts',(179.768886012409,4.40250133473337,133.001167777338));
#25088=CARTESIAN_POINT('Ctrl Pts',(179.761137944406,4.4602734579108,132.876833474603));
#25089=CARTESIAN_POINT('Ctrl Pts',(179.753381641664,4.51810698198826,132.752367027892));
#25090=CARTESIAN_POINT('Ctrl Pts',(179.745625338922,4.57069598516582,132.625543863588));
#25091=CARTESIAN_POINT('Ctrl Pts',(179.73786903618,4.61786376985074,132.496849100717));
#25092=CARTESIAN_POINT('Ctrl Pts',(179.730108593666,4.66505672940257,132.368085649577));
#25093=CARTESIAN_POINT('Ctrl Pts',(179.722348151152,4.7068225859822,132.237448981634));
#25094=CARTESIAN_POINT('Ctrl Pts',(179.714587708638,4.74303479091117,132.105438645474));
#25095=CARTESIAN_POINT('Ctrl Pts',(179.706814808372,4.77930512688626,131.973216394604));
#25096=CARTESIAN_POINT('Ctrl Pts',(179.699041908107,4.81000390816578,131.839616450211));
#25097=CARTESIAN_POINT('Ctrl Pts',(179.691269007841,4.83505573040974,131.705148687165));
#25098=CARTESIAN_POINT('Ctrl Pts',(179.683778672079,4.85919685581355,131.575569166008));
#25099=CARTESIAN_POINT('Ctrl Pts',(179.676288336317,4.8780944124047,131.445184130401));
#25100=CARTESIAN_POINT('Ctrl Pts',(179.668798000555,4.89172670463108,131.314451697373));
#25101=CARTESIAN_POINT('Ctrl Pts',(179.661023666436,4.90587586936059,131.178762504413));
#25102=CARTESIAN_POINT('Ctrl Pts',(179.653249332317,4.91439744341293,131.042269228285));
#25103=CARTESIAN_POINT('Ctrl Pts',(179.645474998198,4.917210416574,130.905478279901));
#25104=CARTESIAN_POINT('Ctrl Pts',(179.637710245251,4.92001992299706,130.768855914136));
#25105=CARTESIAN_POINT('Ctrl Pts',(179.629945492304,4.91713481879837,130.631936993176));
#25106=CARTESIAN_POINT('Ctrl Pts',(179.622180739356,4.9085256594554,130.495234570511));
#25107=CARTESIAN_POINT('Ctrl Pts',(179.614423698471,4.89992505085085,130.358667922619));
#25108=CARTESIAN_POINT('Ctrl Pts',(179.606666657586,4.88561172534523,130.222317732772));
#25109=CARTESIAN_POINT('Ctrl Pts',(179.598909616701,4.86560826207741,130.086698230016));
#25110=CARTESIAN_POINT('Ctrl Pts',(179.591158425461,4.84561988357684,129.951180998982));
#25111=CARTESIAN_POINT('Ctrl Pts',(179.583407234221,4.81994996506197,129.81639374349));
#25112=CARTESIAN_POINT('Ctrl Pts',(179.575656042981,4.78867297735071,129.68284638293));
#25113=CARTESIAN_POINT('Ctrl Pts',(179.567908146204,4.75740928319356,129.549355783561));
#25114=CARTESIAN_POINT('Ctrl Pts',(179.560160249427,4.7205433487172,129.417104410853));
#25115=CARTESIAN_POINT('Ctrl Pts',(179.55241235265,4.67820085238921,129.286592569673));
#25116=CARTESIAN_POINT('Ctrl Pts',(179.544666076566,4.63586721319865,129.156108028757));
#25117=CARTESIAN_POINT('Ctrl Pts',(179.536919800482,4.58805941135035,129.027362667255));
#25118=CARTESIAN_POINT('Ctrl Pts',(179.529173524397,4.53495305142171,128.900841801294));
#25119=CARTESIAN_POINT('Ctrl Pts',(179.521427191132,4.48184629947401,128.774320001385));
#25120=CARTESIAN_POINT('Ctrl Pts',(179.513680857867,4.42344106271525,128.650023090278));
#25121=CARTESIAN_POINT('Ctrl Pts',(179.505934524601,4.35996101314982,128.528416192429));
#25122=CARTESIAN_POINT('Ctrl Pts',(179.498186456598,4.29646674766747,128.406782061558));
#25123=CARTESIAN_POINT('Ctrl Pts',(179.490438388595,4.22789558882288,128.28783948919));
#25124=CARTESIAN_POINT('Ctrl Pts',(179.482690320592,4.15451686234194,128.172028438107));
#25125=CARTESIAN_POINT('Ctrl Pts',(179.474934017851,4.08106014807724,128.056094301661));
#25126=CARTESIAN_POINT('Ctrl Pts',(179.467177715109,4.00278586890444,127.943298665755));
#25127=CARTESIAN_POINT('Ctrl Pts',(179.459421412367,3.92000665983544,127.834052409762));
#25128=CARTESIAN_POINT('Ctrl Pts',(179.451660969853,3.83718326901008,127.724747845754));
#25129=CARTESIAN_POINT('Ctrl Pts',(179.443900527339,3.74985040611597,127.618996737741));
#25130=CARTESIAN_POINT('Ctrl Pts',(179.436140084824,3.65835995287435,127.517175572926));
#25131=CARTESIAN_POINT('Ctrl Pts',(179.428367184559,3.56672263103505,127.415190955737));
#25132=CARTESIAN_POINT('Ctrl Pts',(179.420594284294,3.47091465521116,127.317149168308));
#25133=CARTESIAN_POINT('Ctrl Pts',(179.412821384028,3.37132423968277,127.223389250265));
#25134=CARTESIAN_POINT('Ctrl Pts',(179.405331048266,3.27535418661257,127.133037741411));
#25135=CARTESIAN_POINT('Ctrl Pts',(179.397840712504,3.17587215439751,127.046662395268));
#25136=CARTESIAN_POINT('Ctrl Pts',(179.390350376742,3.07325184289293,126.964529088364));
#25137=CARTESIAN_POINT('Ctrl Pts',(179.382576042623,2.96674065108638,126.879281672164));
#25138=CARTESIAN_POINT('Ctrl Pts',(179.374801708504,2.85651111111605,126.798334280789));
#25139=CARTESIAN_POINT('Ctrl Pts',(179.367027374385,2.74294549282422,126.722028797895));
#25140=CARTESIAN_POINT('Ctrl Pts',(179.359262621438,2.62951983400729,126.645817354689));
#25141=CARTESIAN_POINT('Ctrl Pts',(179.351497868491,2.51276659876644,126.574236653353));
#25142=CARTESIAN_POINT('Ctrl Pts',(179.343733115544,2.39310151804933,126.507588784339));
#25143=CARTESIAN_POINT('Ctrl Pts',(179.335976074659,2.27355529037732,126.441007110929));
#25144=CARTESIAN_POINT('Ctrl Pts',(179.328219033774,2.15110331196261,126.3793487089));
#25145=CARTESIAN_POINT('Ctrl Pts',(179.320461992889,2.0261904228423,126.322872535145));
#25146=CARTESIAN_POINT('Ctrl Pts',(179.312710801649,1.90137173150333,126.266438950512));
#25147=CARTESIAN_POINT('Ctrl Pts',(179.304959610409,1.77409617810434,126.215179976013));
#25148=CARTESIAN_POINT('Ctrl Pts',(179.297208419168,1.64483302556683,126.169308581126));
#25149=CARTESIAN_POINT('Ctrl Pts',(179.289460522391,1.51562481331742,126.123456682806));
#25150=CARTESIAN_POINT('Ctrl Pts',(179.281712625614,1.3844310498194,126.08298794021));
#25151=CARTESIAN_POINT('Ctrl Pts',(179.273964728837,1.25174058800957,126.048067043487));
#25152=CARTESIAN_POINT('Ctrl Pts',(179.266218452753,1.11907788218387,126.013153451461));
#25153=CARTESIAN_POINT('Ctrl Pts',(179.258472176669,0.984919478625015,125.983785496472));
#25154=CARTESIAN_POINT('Ctrl Pts',(179.250725900585,0.849768606098465,125.960077762634));
#25155=CARTESIAN_POINT('Ctrl Pts',(179.24297956732,0.714616735918967,125.936369853791));
#25156=CARTESIAN_POINT('Ctrl Pts',(179.235233234054,0.578472767238265,125.918322317024));
#25157=CARTESIAN_POINT('Ctrl Pts',(179.227486900789,0.441848922615117,125.905998381871));
#25158=CARTESIAN_POINT('Ctrl Pts',(179.219738832786,0.305194482029227,125.893671686858));
#25159=CARTESIAN_POINT('Ctrl Pts',(179.211990764783,0.168060340967948,125.887071179131));
#25160=CARTESIAN_POINT('Ctrl Pts',(179.20424269678,0.0309622297147287,125.88620807796));
#25161=CARTESIAN_POINT('Ctrl Pts',(179.196486394038,-0.10628159104269,125.885344059475));
#25162=CARTESIAN_POINT('Ctrl Pts',(179.188730091296,-0.243488913916986,
125.890229630992));
#25163=CARTESIAN_POINT('Ctrl Pts',(179.180973788555,-0.38014506759449,125.900823854159));
#25164=CARTESIAN_POINT('Ctrl Pts',(179.17321334604,-0.51687415877599,125.911423731781));
#25165=CARTESIAN_POINT('Ctrl Pts',(179.165452903526,-0.653051106591565,
125.927738285734));
#25166=CARTESIAN_POINT('Ctrl Pts',(179.157692461012,-0.788168961031706,
125.949674968488));
#25167=CARTESIAN_POINT('Ctrl Pts',(179.149919560747,-0.923503718646903,
125.971646865952));
#25168=CARTESIAN_POINT('Ctrl Pts',(179.142146660481,-1.05777560227164,125.999258848526));
#25169=CARTESIAN_POINT('Ctrl Pts',(179.134373760216,-1.19048952896382,126.032367559741));
#25170=CARTESIAN_POINT('Ctrl Pts',(179.126883424454,-1.3183789701352,126.064272685909));
#25171=CARTESIAN_POINT('Ctrl Pts',(179.119393088692,-1.44482146351932,126.101281752664));
#25172=CARTESIAN_POINT('Ctrl Pts',(179.11190275293,-1.56939132576419,126.143224068492));
#25173=CARTESIAN_POINT('Ctrl Pts',(179.104128393758,-1.69868470883825,126.186756780254));
#25174=CARTESIAN_POINT('Ctrl Pts',(179.096354034586,-1.82637020688291,126.235742147257));
#25175=CARTESIAN_POINT('Ctrl Pts',(179.088579675415,-1.95195355254964,126.290043350117));
#25176=CARTESIAN_POINT('Ctrl Pts',(179.080814903304,-2.07738203333556,126.34427759068));
#25177=CARTESIAN_POINT('Ctrl Pts',(179.073050131194,-2.2007131642445,126.403814470295));
#25178=CARTESIAN_POINT('Ctrl Pts',(179.065285359084,-2.32146807181828,126.46846750841));
#25179=CARTESIAN_POINT('Ctrl Pts',(179.0575283049,-2.44210295301114,126.533056283545));
#25180=CARTESIAN_POINT('Ctrl Pts',(179.049771250716,-2.56016636431176,126.602750913835));
#25181=CARTESIAN_POINT('Ctrl Pts',(179.042014196532,-2.6751999888338,126.677317113768));
#25182=CARTESIAN_POINT('Ctrl Pts',(179.034262997838,-2.79014677906578,126.751827026654));
#25183=CARTESIAN_POINT('Ctrl Pts',(179.026511799144,-2.9020680080604,126.831200977799));
#25184=CARTESIAN_POINT('Ctrl Pts',(179.018760600451,-3.01053084945795,126.915159277064));
#25185=CARTESIAN_POINT('Ctrl Pts',(179.011012726883,-3.11894716223425,126.999081559718));
#25186=CARTESIAN_POINT('Ctrl Pts',(179.003264853315,-3.22390772980016,127.087584040042));
#25187=CARTESIAN_POINT('Ctrl Pts',(178.995516979748,-3.32500976055551,127.180344453873));
#25188=CARTESIAN_POINT('Ctrl Pts',(178.987770735199,-3.42609053423857,127.273085364487));
#25189=CARTESIAN_POINT('Ctrl Pts',(178.98002449065,-3.5233140969294,127.370082163717));
#25190=CARTESIAN_POINT('Ctrl Pts',(178.972278246101,-3.61631204294623,127.470973410753));
#25191=CARTESIAN_POINT('Ctrl Pts',(178.964531952702,-3.70931057542868,127.571865294032));
#25192=CARTESIAN_POINT('Ctrl Pts',(178.956785659304,-3.79808317311763,127.676651386634));
#25193=CARTESIAN_POINT('Ctrl Pts',(178.949039365905,-3.8822997754526,127.784934924488));
#25194=CARTESIAN_POINT('Ctrl Pts',(178.941291346114,-3.96653514688435,127.893242595163));
#25195=CARTESIAN_POINT('Ctrl Pts',(178.933543326323,-4.04621226256158,128.005048953545));
#25196=CARTESIAN_POINT('Ctrl Pts',(178.925795306531,-4.12104292365446,128.11992617361));
#25197=CARTESIAN_POINT('Ctrl Pts',(178.918039169389,-4.19595198242991,128.234923746853));
#25198=CARTESIAN_POINT('Ctrl Pts',(178.910283032246,-4.26600423054555,128.352998280208));
#25199=CARTESIAN_POINT('Ctrl Pts',(178.902526895103,-4.33095593282109,128.473694667572));
#25200=CARTESIAN_POINT('Ctrl Pts',(178.894766621628,-4.39594227369947,128.594455422059));
#25201=CARTESIAN_POINT('Ctrl Pts',(178.887006348154,-4.4558224781109,128.717840465114));
#25202=CARTESIAN_POINT('Ctrl Pts',(178.87924607468,-4.51040040079451,128.843373293024));
#25203=CARTESIAN_POINT('Ctrl Pts',(178.871473622124,-4.56506397883664,128.969103133919));
#25204=CARTESIAN_POINT('Ctrl Pts',(178.863701169567,-4.61440850661788,129.096987130188));
#25205=CARTESIAN_POINT('Ctrl Pts',(178.855928717011,-4.658287010806,129.226531353211));
#25206=CARTESIAN_POINT('Ctrl Pts',(178.848884041066,-4.69805693422395,129.343945652631));
#25207=CARTESIAN_POINT('Ctrl Pts',(178.841839365122,-4.73333712484633,129.462723429701));
#25208=CARTESIAN_POINT('Ctrl Pts',(178.834794689177,-4.76405452823405,129.582490119308));
#25209=CARTESIAN_POINT('Ctrl Pts',(180.584985772263,-4.76405452823404,129.582490119308));
#25210=CARTESIAN_POINT('Ctrl Pts',(180.57727395094,-4.79793105739994,129.714574192378));
#25211=CARTESIAN_POINT('Ctrl Pts',(180.569562129616,-4.82628395215226,129.847965328554));
#25212=CARTESIAN_POINT('Ctrl Pts',(180.561850308293,-4.84903779404517,129.982158979024));
#25213=CARTESIAN_POINT('Ctrl Pts',(180.55401849625,-4.8721456703155,130.118440591857));
#25214=CARTESIAN_POINT('Ctrl Pts',(180.546186684208,-4.889478756331,130.255549475578));
#25215=CARTESIAN_POINT('Ctrl Pts',(180.538354872165,-4.90101294444811,130.392954272389));
#25216=CARTESIAN_POINT('Ctrl Pts',(180.530523060122,-4.91254713256523,130.5303590692));
#25217=CARTESIAN_POINT('Ctrl Pts',(180.522691248079,-4.91828246897984,130.668059355764));
#25218=CARTESIAN_POINT('Ctrl Pts',(180.514859436037,-4.91824986164052,130.805527225028));
#25219=CARTESIAN_POINT('',(180.860140563953,-4.91824868670176,130.80795481517));
#25220=CARTESIAN_POINT('Ctrl Pts',(180.930009319727,-4.76405452823405,129.582490119308));
#25221=CARTESIAN_POINT('Ctrl Pts',(180.922246799312,-4.79822091605315,129.715704346868));
#25222=CARTESIAN_POINT('Ctrl Pts',(180.914484278898,-4.82680923366528,129.850405798733));
#25223=CARTESIAN_POINT('Ctrl Pts',(180.906721758483,-4.84970257641179,129.986089279412));
#25224=CARTESIAN_POINT('Ctrl Pts',(180.89895822607,-4.87259890375656,130.121790449105));
#25225=CARTESIAN_POINT('Ctrl Pts',(180.891194693658,-4.88979869697442,130.258473522519));
#25226=CARTESIAN_POINT('Ctrl Pts',(180.883431161245,-4.9012362819718,130.395623574));
#25227=CARTESIAN_POINT('Ctrl Pts',(180.875667628833,-4.91267386696918,130.532773625481));
#25228=CARTESIAN_POINT('Ctrl Pts',(180.86790409642,-4.9183492172088,130.670390267495));
#25229=CARTESIAN_POINT('Ctrl Pts',(180.860140564008,-4.91824868670247,130.8079548142));
#25230=CARTESIAN_POINT('Ctrl Pts',(180.860140563953,-4.91824868670176,130.80795481517));
#25231=CARTESIAN_POINT('Ctrl Pts',(180.851235208711,-4.91813337062327,130.96575169062));
#25232=CARTESIAN_POINT('Ctrl Pts',(180.842329853469,-4.91041999025756,131.123241678084));
#25233=CARTESIAN_POINT('Ctrl Pts',(180.833424498227,-4.89522072462637,131.279752161126));
#25234=CARTESIAN_POINT('Ctrl Pts',(180.824474260165,-4.87994485498848,131.437051453996));
#25235=CARTESIAN_POINT('Ctrl Pts',(180.815524022103,-4.85710756303225,131.593361207987));
#25236=CARTESIAN_POINT('Ctrl Pts',(180.806573784042,-4.82687215032326,131.74801749744));
#25237=CARTESIAN_POINT('Ctrl Pts',(180.79756682713,-4.79644513177894,131.903653864388));
#25238=CARTESIAN_POINT('Ctrl Pts',(180.788559870219,-4.75852601683665,132.057615609648));
#25239=CARTESIAN_POINT('Ctrl Pts',(180.779552913307,-4.71332967202739,132.209247255443));
#25240=CARTESIAN_POINT('Ctrl Pts',(180.774035108754,-4.68564167489048,132.302139204833));
#25241=CARTESIAN_POINT('Ctrl Pts',(180.768517304201,-4.65522348627133,132.394157094063));
#25242=CARTESIAN_POINT('Ctrl Pts',(180.762999499647,-4.6221331923805,132.485154422408));
#25243=CARTESIAN_POINT('Ctrl Pts',(180.755225165528,-4.57551048251068,132.613365493978));
#25244=CARTESIAN_POINT('Ctrl Pts',(180.747450831409,-4.52347530734763,132.739838306069));
#25245=CARTESIAN_POINT('Ctrl Pts',(180.73967649729,-4.46617630640889,132.864082021682));
#25246=CARTESIAN_POINT('Ctrl Pts',(180.731911744343,-4.4089479213679,132.988172618018));
#25247=CARTESIAN_POINT('Ctrl Pts',(180.724146991396,-4.34646878029648,133.11003923229));
#25248=CARTESIAN_POINT('Ctrl Pts',(180.716382238449,-4.27893680000363,133.229207607393));
#25249=CARTESIAN_POINT('Ctrl Pts',(180.708625197564,-4.21147189342562,133.348257622787));
#25250=CARTESIAN_POINT('Ctrl Pts',(180.700868156679,-4.13896432627984,133.464614394248));
#25251=CARTESIAN_POINT('Ctrl Pts',(180.693111115794,-4.06165931338313,133.577825361259));
#25252=CARTESIAN_POINT('Ctrl Pts',(180.685359924554,-3.9844125967981,133.690950954998));
#25253=CARTESIAN_POINT('Ctrl Pts',(180.677608733314,-3.90237585503431,133.800935144591));
#25254=CARTESIAN_POINT('Ctrl Pts',(180.669857542074,-3.81583908314369,133.90735194112));
#25255=CARTESIAN_POINT('Ctrl Pts',(180.662109645297,-3.72933909168942,134.013723507672));
#25256=CARTESIAN_POINT('Ctrl Pts',(180.65436174852,-3.6383431203381,134.116530394143));
#25257=CARTESIAN_POINT('Ctrl Pts',(180.646613851742,-3.54318300903784,134.215377654604));
#25258=CARTESIAN_POINT('Ctrl Pts',(180.638867575658,-3.44804280318141,134.314204238349));
#25259=CARTESIAN_POINT('Ctrl Pts',(180.631121299574,-3.34874046091821,134.409072562077));
#25260=CARTESIAN_POINT('Ctrl Pts',(180.62337502349,-3.24564616409112,134.499622995263));
#25261=CARTESIAN_POINT('Ctrl Pts',(180.615628690225,-3.14255110624534,134.590174096871));
#25262=CARTESIAN_POINT('Ctrl Pts',(180.60788235696,-3.03566433172752,134.676406986332));
#25263=CARTESIAN_POINT('Ctrl Pts',(180.600136023694,-2.92539041717838,134.758001214482));
#25264=CARTESIAN_POINT('Ctrl Pts',(180.592387955691,-2.81509180755061,134.839613715093));
#25265=CARTESIAN_POINT('Ctrl Pts',(180.584639887688,-2.70140486273715,134.916585254807));
#25266=CARTESIAN_POINT('Ctrl Pts',(180.576891819685,-2.58476420983551,134.988637979555));
#25267=CARTESIAN_POINT('Ctrl Pts',(180.569135516943,-2.46799958986003,135.060767282796));
#25268=CARTESIAN_POINT('Ctrl Pts',(180.561379214202,-2.34827532398418,135.12796712223));
#25269=CARTESIAN_POINT('Ctrl Pts',(180.55362291146,-2.22605226619562,135.190004740231));
#25270=CARTESIAN_POINT('Ctrl Pts',(180.545862468946,-2.10376397428102,135.252075469577));
#25271=CARTESIAN_POINT('Ctrl Pts',(180.538102026431,-1.97897458853601,135.308978325326));
#25272=CARTESIAN_POINT('Ctrl Pts',(180.530341583917,-1.85216521453456,135.360528643503));
#25273=CARTESIAN_POINT('Ctrl Pts',(180.522568683652,-1.72515227486836,135.412161714826));
#25274=CARTESIAN_POINT('Ctrl Pts',(180.514795783386,-1.59611323530802,135.458424946265));
#25275=CARTESIAN_POINT('Ctrl Pts',(180.507022883121,-1.46554549602716,135.499183240581));
#25276=CARTESIAN_POINT('Ctrl Pts',(180.499532547359,-1.33972422294845,135.538459868235));
#25277=CARTESIAN_POINT('Ctrl Pts',(180.492042211597,-1.21248376217569,135.572624766855));
#25278=CARTESIAN_POINT('Ctrl Pts',(180.484551875835,-1.08427646179028,135.601602285119));
#25279=CARTESIAN_POINT('Ctrl Pts',(180.476777541716,-0.951208142644003,
135.631678494795));
#25280=CARTESIAN_POINT('Ctrl Pts',(180.469003207597,-0.81667670073027,135.656261472423));
#25281=CARTESIAN_POINT('Ctrl Pts',(180.461228873478,-0.68117543440742,135.675210963251));
#25282=CARTESIAN_POINT('Ctrl Pts',(180.45346412053,-0.545841161285354,135.694137100525));
#25283=CARTESIAN_POINT('Ctrl Pts',(180.445699367583,-0.409539825369746,
135.707443511412));
#25284=CARTESIAN_POINT('Ctrl Pts',(180.437934614636,-0.272777411462797,
135.715040361379));
#25285=CARTESIAN_POINT('Ctrl Pts',(180.430177573751,-0.13615083191333,135.722629666048));
#25286=CARTESIAN_POINT('Ctrl Pts',(180.422420532866,0.000935526450582369,
135.724520673434));
#25287=CARTESIAN_POINT('Ctrl Pts',(180.414663491981,0.137968367048358,135.720675069693));
#25288=CARTESIAN_POINT('Ctrl Pts',(180.406912300741,0.274897870115078,135.716832365952));
#25289=CARTESIAN_POINT('Ctrl Pts',(180.399161109501,0.411773546516112,135.707261672693));
#25290=CARTESIAN_POINT('Ctrl Pts',(180.391409918261,0.548080250301332,135.691976713551));
#25291=CARTESIAN_POINT('Ctrl Pts',(180.383662021484,0.684329020101435,135.676698250924));
#25292=CARTESIAN_POINT('Ctrl Pts',(180.375914124707,0.820008910547644,135.655710396422));
#25293=CARTESIAN_POINT('Ctrl Pts',(180.36816622793,0.9546082748462,135.629078858468));
#25294=CARTESIAN_POINT('Ctrl Pts',(180.360419951846,1.08917948385937,135.602452891258));
#25295=CARTESIAN_POINT('Ctrl Pts',(180.352673675761,1.22267023300946,135.570185664586));
#25296=CARTESIAN_POINT('Ctrl Pts',(180.344927399677,1.35457786262363,135.532394233837));
#25297=CARTESIAN_POINT('Ctrl Pts',(180.337181066412,1.4864864659498,135.494602524121));
#25298=CARTESIAN_POINT('Ctrl Pts',(180.329434733147,1.61681155057666,135.451286636637));
#25299=CARTESIAN_POINT('Ctrl Pts',(180.321688399881,1.74506482999139,135.402613742572));
#25300=CARTESIAN_POINT('Ctrl Pts',(180.313940331878,1.87334683083893,135.35392994855));
#25301=CARTESIAN_POINT('Ctrl Pts',(180.306192263875,1.99955573777708,135.299886899446));
#25302=CARTESIAN_POINT('Ctrl Pts',(180.298444195872,2.12322285774621,135.240700072437));
#25303=CARTESIAN_POINT('Ctrl Pts',(180.29068789313,2.24702141260209,135.181450340963));
#25304=CARTESIAN_POINT('Ctrl Pts',(180.282931590389,2.36827243084956,135.117046079976));
#25305=CARTESIAN_POINT('Ctrl Pts',(180.275175287647,2.48653098406956,135.047749207804));
#25306=CARTESIAN_POINT('Ctrl Pts',(180.267414845133,2.60485265544017,134.978415349805));
#25307=CARTESIAN_POINT('Ctrl Pts',(180.259654402618,2.72017835070013,134.904183888821));
#25308=CARTESIAN_POINT('Ctrl Pts',(180.251893960104,2.83209265750178,134.825359777206));
#25309=CARTESIAN_POINT('Ctrl Pts',(180.244121059839,2.94418661908395,134.746409130129));
#25310=CARTESIAN_POINT('Ctrl Pts',(180.236348159573,3.05285793877241,134.662851338207));
#25311=CARTESIAN_POINT('Ctrl Pts',(180.228575259308,3.15772409849079,134.575031854934));
#25312=CARTESIAN_POINT('Ctrl Pts',(180.221084923546,3.25877810916079,134.490404831082));
#25313=CARTESIAN_POINT('Ctrl Pts',(180.213594587784,3.35629858303754,134.401820790026));
#25314=CARTESIAN_POINT('Ctrl Pts',(180.206104252022,3.44997736733326,134.309619413631));
#25315=CARTESIAN_POINT('Ctrl Pts',(180.198329917903,3.54720801120912,134.213922194025));
#25316=CARTESIAN_POINT('Ctrl Pts',(180.190555583784,3.6406078969809,134.114024781695));
#25317=CARTESIAN_POINT('Ctrl Pts',(180.182781249665,3.72979238454181,134.010266391402));
#25318=CARTESIAN_POINT('Ctrl Pts',(180.175016496718,3.81886696019247,133.906635874052));
#25319=CARTESIAN_POINT('Ctrl Pts',(180.167251743771,3.90373622193616,133.799154140003));
#25320=CARTESIAN_POINT('Ctrl Pts',(180.159486990823,3.98405109229198,133.688198330841));
#25321=CARTESIAN_POINT('Ctrl Pts',(180.151729949938,4.06428619278623,133.577352724553));
#25322=CARTESIAN_POINT('Ctrl Pts',(180.143972909054,4.1399756760726,133.463040224457));
#25323=CARTESIAN_POINT('Ctrl Pts',(180.136215868169,4.21080985828836,133.345671971934));
#25324=CARTESIAN_POINT('Ctrl Pts',(180.128464676928,4.28159062389636,133.228392227724));
#25325=CARTESIAN_POINT('Ctrl Pts',(180.120713485688,4.3475231750704,133.108061651164));
#25326=CARTESIAN_POINT('Ctrl Pts',(180.112962294448,4.40834060892407,132.985121067091));
#25327=CARTESIAN_POINT('Ctrl Pts',(180.105214397671,4.46913219374597,132.862232736046));
#25328=CARTESIAN_POINT('Ctrl Pts',(180.097466500894,4.52481281229799,132.736736953544));
#25329=CARTESIAN_POINT('Ctrl Pts',(180.089718604117,4.57516118934884,132.609099699532));
#25330=CARTESIAN_POINT('Ctrl Pts',(180.081972328033,4.62549903460459,132.481489144482));
#25331=CARTESIAN_POINT('Ctrl Pts',(180.074226051949,4.6705067135582,132.351738372381));
#25332=CARTESIAN_POINT('Ctrl Pts',(180.066479775865,4.71001100838992,132.220333556342));
#25333=CARTESIAN_POINT('Ctrl Pts',(180.058733442599,4.74951559483336,132.088927770302));
#25334=CARTESIAN_POINT('Ctrl Pts',(180.050987109334,4.78351660353165,131.955868290373));
#25335=CARTESIAN_POINT('Ctrl Pts',(180.043240776069,4.811890749551,131.821656285937));
#25336=CARTESIAN_POINT('Ctrl Pts',(180.035492708066,4.84027124976361,131.687414225652));
#25337=CARTESIAN_POINT('Ctrl Pts',(180.027744640063,4.86302229899824,131.552019509708));
#25338=CARTESIAN_POINT('Ctrl Pts',(180.01999657206,4.880071844258,131.415982933526));
#25339=CARTESIAN_POINT('Ctrl Pts',(180.012240269318,4.89713950997736,131.279801776052));
#25340=CARTESIAN_POINT('Ctrl Pts',(180.004483966576,4.90849351826859,131.142977784168));
#25341=CARTESIAN_POINT('Ctrl Pts',(179.996727663834,4.9141137337624,131.006026862009));
#25342=CARTESIAN_POINT('Ctrl Pts',(179.98896722132,4.91973694893445,130.869002845019));
#25343=CARTESIAN_POINT('Ctrl Pts',(179.981206778806,4.91962027373891,130.731852153537));
#25344=CARTESIAN_POINT('Ctrl Pts',(179.973446336292,4.91379573270794,130.595089119934));
#25345=CARTESIAN_POINT('Ctrl Pts',(179.965673436026,4.90796184160662,130.458106542167));
#25346=CARTESIAN_POINT('Ctrl Pts',(179.957900535761,4.89640180751873,130.321513255635));
#25347=CARTESIAN_POINT('Ctrl Pts',(179.950127635495,4.87919950989027,130.185817809681));
#25348=CARTESIAN_POINT('Ctrl Pts',(179.942637299733,4.8626225591104,130.055055234982));
#25349=CARTESIAN_POINT('Ctrl Pts',(179.935146963971,4.84080649473996,129.925126660408));
#25350=CARTESIAN_POINT('Ctrl Pts',(179.927656628209,4.81387053664267,129.796474949971));
#25351=CARTESIAN_POINT('Ctrl Pts',(179.91988229409,4.7859132935074,129.662945370831));
#25352=CARTESIAN_POINT('Ctrl Pts',(179.912107959971,4.75235169095122,129.530368410215));
#25353=CARTESIAN_POINT('Ctrl Pts',(179.904333625852,4.71326321258631,129.399251030601));
#25354=CARTESIAN_POINT('Ctrl Pts',(179.896568872905,4.67422290727756,129.268295241439));
#25355=CARTESIAN_POINT('Ctrl Pts',(179.888804119958,4.62966938940084,129.138795825271));
#25356=CARTESIAN_POINT('Ctrl Pts',(179.88103936701,4.57973127394808,129.011250325107));
#25357=CARTESIAN_POINT('Ctrl Pts',(179.873282326125,4.52984275773558,128.883831504932));
#25358=CARTESIAN_POINT('Ctrl Pts',(179.86552528524,4.47458042844114,128.758363100465));
#25359=CARTESIAN_POINT('Ctrl Pts',(179.857768244355,4.41412279926086,128.635327889471));
#25360=CARTESIAN_POINT('Ctrl Pts',(179.850017053115,4.35371076164904,128.512385460287));
#25361=CARTESIAN_POINT('Ctrl Pts',(179.842265861875,4.28811139405136,128.391872921809));
#25362=CARTESIAN_POINT('Ctrl Pts',(179.834514670635,4.21755130735877,128.274253103586));
#25363=CARTESIAN_POINT('Ctrl Pts',(179.826766773858,4.14702121058527,128.156683276924));
#25364=CARTESIAN_POINT('Ctrl Pts',(179.819018877081,4.07153478894331,128.042004059732));
#25365=CARTESIAN_POINT('Ctrl Pts',(179.811270980304,3.99136447989174,127.930653490672));
#25366=CARTESIAN_POINT('Ctrl Pts',(179.80352470422,3.91121094074054,127.819326213751));
#25367=CARTESIAN_POINT('Ctrl Pts',(179.795778428136,3.82637569128667,127.711326517104));
#25368=CARTESIAN_POINT('Ctrl Pts',(179.788032152051,3.7371741342777,127.607062922232));
#25369=CARTESIAN_POINT('Ctrl Pts',(179.780285818786,3.64797191880316,127.50279855771));
#25370=CARTESIAN_POINT('Ctrl Pts',(179.772539485521,3.5544035856207,127.402270647074));
#25371=CARTESIAN_POINT('Ctrl Pts',(179.764793152255,3.4568241442069,127.305853807722));
#25372=CARTESIAN_POINT('Ctrl Pts',(179.757045084252,3.35922285055371,127.209415376487));
#25373=CARTESIAN_POINT('Ctrl Pts',(179.749297016249,3.25760893928871,127.117090123255));
#25374=CARTESIAN_POINT('Ctrl Pts',(179.741548948246,3.15237321066194,127.029214765655));
#25375=CARTESIAN_POINT('Ctrl Pts',(179.733792645505,3.04702563625045,126.94124601308));
#25376=CARTESIAN_POINT('Ctrl Pts',(179.726036342763,2.93804885563987,126.857736854617));
#25377=CARTESIAN_POINT('Ctrl Pts',(179.718280040021,2.82586602993138,126.77898308951));
#25378=CARTESIAN_POINT('Ctrl Pts',(179.710519597507,2.71362332887097,126.700187291147));
#25379=CARTESIAN_POINT('Ctrl Pts',(179.702759154993,2.59817150202462,126.626152154456));
#25380=CARTESIAN_POINT('Ctrl Pts',(179.694998712478,2.4799605818237,126.557128745499));
#25381=CARTESIAN_POINT('Ctrl Pts',(179.687225812213,2.36155989895946,126.487994534039));
#25382=CARTESIAN_POINT('Ctrl Pts',(179.679452911947,2.2403916176828,126.423888310267));
#25383=CARTESIAN_POINT('Ctrl Pts',(179.671680011682,2.11692893384896,126.365014387373));
#25384=CARTESIAN_POINT('Ctrl Pts',(179.66418967592,1.99795442955653,126.30828067987));
#25385=CARTESIAN_POINT('Ctrl Pts',(179.656699340158,1.87684972432121,126.256405584449));
#25386=CARTESIAN_POINT('Ctrl Pts',(179.649209004396,1.75405185342764,126.209528176879));
#25387=CARTESIAN_POINT('Ctrl Pts',(179.641434670277,1.6265980639352,126.160873398153));
#25388=CARTESIAN_POINT('Ctrl Pts',(179.633660336158,1.49691644622467,126.117448639312));
#25389=CARTESIAN_POINT('Ctrl Pts',(179.625886002039,1.36547540397288,126.079462736802));
#25390=CARTESIAN_POINT('Ctrl Pts',(179.618121249092,1.23419635105852,126.041523648523));
#25391=CARTESIAN_POINT('Ctrl Pts',(179.610356496145,1.10116255992973,126.009010187295));
#25392=CARTESIAN_POINT('Ctrl Pts',(179.602591743197,0.966862147156906,125.982083079836));
#25393=CARTESIAN_POINT('Ctrl Pts',(179.594834702312,0.832695123447448,125.955182716759));
#25394=CARTESIAN_POINT('Ctrl Pts',(179.587077661427,0.697264362478954,125.933857742155));
#25395=CARTESIAN_POINT('Ctrl Pts',(179.579320620542,0.561072529599974,125.918218920989));
#25396=CARTESIAN_POINT('Ctrl Pts',(179.571569429302,0.424983400041494,125.90259189318));
#25397=CARTESIAN_POINT('Ctrl Pts',(179.563818238062,0.288134727787094,125.89264252828));
#25398=CARTESIAN_POINT('Ctrl Pts',(179.556067046822,0.151038393166892,125.888430342807));
#25399=CARTESIAN_POINT('Ctrl Pts',(179.548319150045,0.0140003281460682,
125.884219947625));
#25400=CARTESIAN_POINT('Ctrl Pts',(179.540571253268,-0.123284799917584,
125.885741893951));
#25401=CARTESIAN_POINT('Ctrl Pts',(179.532823356491,-0.260301197590463,
125.893003743032));
#25402=CARTESIAN_POINT('Ctrl Pts',(179.525077080407,-0.39728893438668,125.90026407309));
#25403=CARTESIAN_POINT('Ctrl Pts',(179.517330804322,-0.534007662432173,
125.913261897038));
#25404=CARTESIAN_POINT('Ctrl Pts',(179.509584528238,-0.669943198128833,
125.931952673461));
#25405=CARTESIAN_POINT('Ctrl Pts',(179.501838194973,-0.805879737270736,
125.950643587855));
#25406=CARTESIAN_POINT('Ctrl Pts',(179.494091861708,-0.941032685206453,
125.975027485324));
#25407=CARTESIAN_POINT('Ctrl Pts',(179.486345528442,-1.07489497441483,126.005008176197));
#25408=CARTESIAN_POINT('Ctrl Pts',(179.478597460439,-1.20878724115488,126.034995581037));
#25409=CARTESIAN_POINT('Ctrl Pts',(179.470849392436,-1.34138789258256,126.070582187898));
#25410=CARTESIAN_POINT('Ctrl Pts',(179.463101324433,-1.47220240153905,126.111621209565));
#25411=CARTESIAN_POINT('Ctrl Pts',(179.455345021691,-1.60315594171228,126.152703847993));
#25412=CARTESIAN_POINT('Ctrl Pts',(179.44758871895,-1.73231917365516,126.199250359929));
#25413=CARTESIAN_POINT('Ctrl Pts',(179.439832416208,-1.85921450417547,126.251064614673));
#25414=CARTESIAN_POINT('Ctrl Pts',(179.432071973694,-1.98617756255448,126.302906524244));
#25415=CARTESIAN_POINT('Ctrl Pts',(179.424311531179,-2.11086995231502,126.360021616145));
#25416=CARTESIAN_POINT('Ctrl Pts',(179.416551088665,-2.23283719094561,126.422166972686));
#25417=CARTESIAN_POINT('Ctrl Pts',(179.4087781884,-2.35500022221536,126.48441209047));
#25418=CARTESIAN_POINT('Ctrl Pts',(179.401005288134,-2.47442901958706,126.551703417341));
#25419=CARTESIAN_POINT('Ctrl Pts',(179.393232387869,-2.59069591467029,126.623753276496));
#25420=CARTESIAN_POINT('Ctrl Pts',(179.385742052107,-2.70273621525825,126.693183941787));
#25421=CARTESIAN_POINT('Ctrl Pts',(179.378251716345,-2.81184025354116,126.76703300397));
#25422=CARTESIAN_POINT('Ctrl Pts',(179.370761380583,-2.91765479288965,126.845007946734));
#25423=CARTESIAN_POINT('Ctrl Pts',(179.362824623581,-3.02977583963157,126.927630167234));
#25424=CARTESIAN_POINT('Ctrl Pts',(179.354887866579,-3.13858421238573,127.015166053473));
#25425=CARTESIAN_POINT('Ctrl Pts',(179.346951109577,-3.24361582879236,127.107315930562));
#25426=CARTESIAN_POINT('Ctrl Pts',(179.339259878588,-3.34539825992441,127.196615122934));
#25427=CARTESIAN_POINT('Ctrl Pts',(179.331568647598,-3.44363378017725,127.290246806879));
#25428=CARTESIAN_POINT('Ctrl Pts',(179.323877416609,-3.53792844756241,127.387893822406));
#25429=CARTESIAN_POINT('Ctrl Pts',(179.316193156561,-3.63213765104985,127.485452335638));
#25430=CARTESIAN_POINT('Ctrl Pts',(179.308508896513,-3.72241282922045,127.587018658588));
#25431=CARTESIAN_POINT('Ctrl Pts',(179.300824636464,-3.80839397804645,127.692236203202));
#25432=CARTESIAN_POINT('Ctrl Pts',(179.293145599922,-3.89431667973043,127.797382224409));
#25433=CARTESIAN_POINT('Ctrl Pts',(179.28546656338,-3.97595090671817,127.906174222729));
#25434=CARTESIAN_POINT('Ctrl Pts',(179.277787526838,-4.05297468425983,128.018220048383));
#25435=CARTESIAN_POINT('Ctrl Pts',(179.270111970762,-4.12996355134694,128.130215090099));
#25436=CARTESIAN_POINT('Ctrl Pts',(179.262436414686,-4.20234590173357,128.245460696354));
#25437=CARTESIAN_POINT('Ctrl Pts',(179.25476085861,-4.26984142786074,128.363533453791));
#25438=CARTESIAN_POINT('Ctrl Pts',(179.247085795211,-4.33733262159974,128.481598632399));
#25439=CARTESIAN_POINT('Ctrl Pts',(179.239410731811,-4.39993741066976,128.60249025877));
#25440=CARTESIAN_POINT('Ctrl Pts',(179.231735668412,-4.45742018209201,128.725758110404));
#25441=CARTESIAN_POINT('Ctrl Pts',(179.224060790413,-4.51490156495416,128.849022984367));
#25442=CARTESIAN_POINT('Ctrl Pts',(179.216385912414,-4.56726101346593,128.974663605236));
#25443=CARTESIAN_POINT('Ctrl Pts',(179.208711034414,-4.61431036413111,129.102208178455));
#25444=CARTESIAN_POINT('Ctrl Pts',(179.201032838487,-4.66138005470733,129.229807890485));
#25445=CARTESIAN_POINT('Ctrl Pts',(179.19335464256,-4.70313493368093,129.359312821299));
#25446=CARTESIAN_POINT('Ctrl Pts',(179.185676446633,-4.73943621873225,129.490234523514));
#25447=CARTESIAN_POINT('Ctrl Pts',(179.183877368601,-4.74794197257219,129.520910786621));
#25448=CARTESIAN_POINT('Ctrl Pts',(179.182078290568,-4.75614853636364,129.551664776996));
#25449=CARTESIAN_POINT('Ctrl Pts',(179.180279212536,-4.76405452823405,129.582490119308));
#25450=CARTESIAN_POINT('Origin',(213.235140564004,0.,130.804360617566));
#25451=CARTESIAN_POINT('',(177.084597561451,-4.76405452823403,129.582490119308));
#25452=CARTESIAN_POINT('',(177.430115848357,-4.76405452823405,129.582490119308));
#25453=CARTESIAN_POINT('',(213.235140564004,-4.76405452823405,129.582490119308));
#25454=CARTESIAN_POINT('',(178.764859436029,-4.91824789753406,130.799812991619));
#25455=CARTESIAN_POINT('Ctrl Pts',(178.764859435991,-4.91824789753469,130.799812992297));
#25456=CARTESIAN_POINT('Ctrl Pts',(178.757196290994,-4.9183730412926,130.935155723463));
#25457=CARTESIAN_POINT('Ctrl Pts',(178.749533145997,-4.91290734326878,131.070645942394));
#25458=CARTESIAN_POINT('Ctrl Pts',(178.741870001,-4.90184112669081,131.205778892166));
#25459=CARTESIAN_POINT('Ctrl Pts',(178.734084063679,-4.89059758781915,131.343077178612));
#25460=CARTESIAN_POINT('Ctrl Pts',(178.726298126358,-4.87357245610437,131.480006229492));
#25461=CARTESIAN_POINT('Ctrl Pts',(178.718512189038,-4.85081073812513,131.61603681248));
#25462=CARTESIAN_POINT('Ctrl Pts',(178.710856306159,-4.82842922645917,131.749795173024));
#25463=CARTESIAN_POINT('Ctrl Pts',(178.70320042328,-4.80050136400255,131.882684439534));
#25464=CARTESIAN_POINT('Ctrl Pts',(178.695544540401,-4.76712209381898,132.01420771746));
#25465=CARTESIAN_POINT('Ctrl Pts',(178.687889375061,-4.73374595206982,132.145718668516));
#25466=CARTESIAN_POINT('Ctrl Pts',(178.680234209721,-4.69491951717209,132.27586349683));
#25467=CARTESIAN_POINT('Ctrl Pts',(178.672579044381,-4.65078839204757,132.404157603091));
#25468=CARTESIAN_POINT('Ctrl Pts',(178.664922844915,-4.60665130530803,132.532469040433));
#25469=CARTESIAN_POINT('Ctrl Pts',(178.657266645449,-4.55720823398827,132.65892887934));
#25470=CARTESIAN_POINT('Ctrl Pts',(178.649610445982,-4.50265380566106,132.783070239735));
#25471=CARTESIAN_POINT('Ctrl Pts',(178.641726867593,-4.44647918349511,132.910898433141));
#25472=CARTESIAN_POINT('Ctrl Pts',(178.633843289203,-4.3848850536798,133.036267873534));
#25473=CARTESIAN_POINT('Ctrl Pts',(178.625959710813,-4.31813542196403,133.158694820707));
#25474=CARTESIAN_POINT('Ctrl Pts',(178.618292097771,-4.25321435168799,133.277767963686));
#25475=CARTESIAN_POINT('Ctrl Pts',(178.610624484729,-4.18341682154212,133.394057413434));
#25476=CARTESIAN_POINT('Ctrl Pts',(178.602956871687,-4.10902994539855,133.507147322121));
#25477=CARTESIAN_POINT('Ctrl Pts',(178.594965310623,-4.03150030744991,133.625015152183));
#25478=CARTESIAN_POINT('Ctrl Pts',(178.586973749559,-3.94898534362607,133.739406770363));
#25479=CARTESIAN_POINT('Ctrl Pts',(178.578982188495,-3.861856090724,133.849890226195));
#25480=CARTESIAN_POINT('Ctrl Pts',(178.570990627431,-3.77472683782194,133.960373682027));
#25481=CARTESIAN_POINT('Ctrl Pts',(178.562999066367,-3.68298366963375,134.066948657916));
#25482=CARTESIAN_POINT('Ctrl Pts',(178.555007505303,-3.58703931231371,134.169227930614));
#25483=CARTESIAN_POINT('Ctrl Pts',(178.547233171184,-3.493702918501,134.268727043871));
#25484=CARTESIAN_POINT('Ctrl Pts',(178.539458837065,-3.39607561388428,134.364497295231));
#25485=CARTESIAN_POINT('Ctrl Pts',(178.531684502946,-3.2944872852368,134.456146015137));
#25486=CARTESIAN_POINT('Ctrl Pts',(178.523919749999,-3.19302415512523,134.547681786186));
#25487=CARTESIAN_POINT('Ctrl Pts',(178.516154997052,-3.08761000143176,134.635105872937));
#25488=CARTESIAN_POINT('Ctrl Pts',(178.508390244105,-2.97861348023738,134.718060248075));
#25489=CARTESIAN_POINT('Ctrl Pts',(178.50063320322,-2.86972521592481,134.800932231759));
#25490=CARTESIAN_POINT('Ctrl Pts',(178.492876162335,-2.75726197390471,134.879343103152));
#25491=CARTESIAN_POINT('Ctrl Pts',(178.48511912145,-2.64162734560113,134.952973401313));
#25492=CARTESIAN_POINT('Ctrl Pts',(178.47736793021,-2.52607991827016,135.026548174295));
#25493=CARTESIAN_POINT('Ctrl Pts',(178.46961673897,-2.40736619337517,135.095349340572));
#25494=CARTESIAN_POINT('Ctrl Pts',(178.46186554773,-2.28592046387358,135.159099495541));
#25495=CARTESIAN_POINT('Ctrl Pts',(178.454117650953,-2.16452635204637,135.222822554993));
#25496=CARTESIAN_POINT('Ctrl Pts',(178.446369754175,-2.04040289054619,135.281498691652));
#25497=CARTESIAN_POINT('Ctrl Pts',(178.438621857398,-1.91401061513348,135.334895511776));
#25498=CARTESIAN_POINT('Ctrl Pts',(178.430875581314,-1.78764477826022,135.388281162436));
#25499=CARTESIAN_POINT('Ctrl Pts',(178.42312930523,-1.6590114313704,135.436389541058));
#25500=CARTESIAN_POINT('Ctrl Pts',(178.415383029146,-1.52859245082243,135.479035812891));
#25501=CARTESIAN_POINT('Ctrl Pts',(178.407636695881,-1.39817250755127,135.521682399529));
#25502=CARTESIAN_POINT('Ctrl Pts',(178.399890362615,-1.26596727592271,135.55886667741));
#25503=CARTESIAN_POINT('Ctrl Pts',(178.39214402935,-1.1324748224956,135.590453370419));
#25504=CARTESIAN_POINT('Ctrl Pts',(178.384395961347,-0.998952474358899,
135.62204713705));
#25505=CARTESIAN_POINT('Ctrl Pts',(178.376647893344,-0.864142711197707,
135.648040734402));
#25506=CARTESIAN_POINT('Ctrl Pts',(178.368899825341,-0.728554452264122,
135.668349872549));
#25507=CARTESIAN_POINT('Ctrl Pts',(178.361143522599,-0.592822088515468,
135.688680595488));
#25508=CARTESIAN_POINT('Ctrl Pts',(178.353387219857,-0.456309963453038,
135.703314732646));
#25509=CARTESIAN_POINT('Ctrl Pts',(178.345630917115,-0.319533349451039,
135.712219774173));
#25510=CARTESIAN_POINT('Ctrl Pts',(178.337870474601,-0.182683733651767,
135.721129568589));
#25511=CARTESIAN_POINT('Ctrl Pts',(178.330110032087,-0.045569738297517,
135.724304165422));
#25512=CARTESIAN_POINT('Ctrl Pts',(178.322349589573,0.0912936838562829,
135.721763237424));
#25513=CARTESIAN_POINT('Ctrl Pts',(178.314576689307,0.228376811325325,135.719218230503));
#25514=CARTESIAN_POINT('Ctrl Pts',(178.306803789042,0.365208171309374,135.710939387667));
#25515=CARTESIAN_POINT('Ctrl Pts',(178.299030888776,0.501277348038855,135.696998360424));
#25516=CARTESIAN_POINT('Ctrl Pts',(178.291540553014,0.632400067457702,135.683564124637));
#25517=CARTESIAN_POINT('Ctrl Pts',(178.284050217252,0.762814751203412,135.664872270292));
#25518=CARTESIAN_POINT('Ctrl Pts',(178.27655988149,0.89207580184942,135.641031355404));
#25519=CARTESIAN_POINT('Ctrl Pts',(178.268785547371,1.02623782451768,135.616286504981));
#25520=CARTESIAN_POINT('Ctrl Pts',(178.261011213252,1.15958199216667,135.585916048837));
#25521=CARTESIAN_POINT('Ctrl Pts',(178.253236879133,1.29159962891666,135.549985282569));
#25522=CARTESIAN_POINT('Ctrl Pts',(178.245472126186,1.4234545657279,135.514098797758));
#25523=CARTESIAN_POINT('Ctrl Pts',(178.237707373239,1.55398585084488,135.472665739113));
#25524=CARTESIAN_POINT('Ctrl Pts',(178.229942620292,1.68269299813225,135.425802744926));
#25525=CARTESIAN_POINT('Ctrl Pts',(178.222185579407,1.8112723116667,135.378986295725));
#25526=CARTESIAN_POINT('Ctrl Pts',(178.214428538522,1.93803072786065,135.326750776369));
#25527=CARTESIAN_POINT('Ctrl Pts',(178.206671497637,2.0624813241539,135.269263063311));
#25528=CARTESIAN_POINT('Ctrl Pts',(178.198920306396,2.18683807128475,135.211818702184));
#25529=CARTESIAN_POINT('Ctrl Pts',(178.191169115156,2.30889010907471,135.149130194217));
#25530=CARTESIAN_POINT('Ctrl Pts',(178.183417923916,2.4281693032209,135.081412978409));
#25531=CARTESIAN_POINT('Ctrl Pts',(178.175670027139,2.54739780052733,135.013724544225));
#25532=CARTESIAN_POINT('Ctrl Pts',(178.167922130362,2.66385545891849,134.941011845815));
#25533=CARTESIAN_POINT('Ctrl Pts',(178.160174233585,2.77709782812862,134.863536730462));
#25534=CARTESIAN_POINT('Ctrl Pts',(178.152427957501,2.89031650947648,134.786077821232));
#25535=CARTESIAN_POINT('Ctrl Pts',(178.144681681417,3.00032091694965,134.703858697166));
#25536=CARTESIAN_POINT('Ctrl Pts',(178.136935405333,3.10669507789473,134.617184866792));
#25537=CARTESIAN_POINT('Ctrl Pts',(178.129189072067,3.21307002406978,134.530510396611));
#25538=CARTESIAN_POINT('Ctrl Pts',(178.121442738802,3.31581436715207,134.439381401466));
#25539=CARTESIAN_POINT('Ctrl Pts',(178.113696405536,3.41454507837464,134.344143798814));
#25540=CARTESIAN_POINT('Ctrl Pts',(178.105948337533,3.51329789965507,134.248884868362));
#25541=CARTESIAN_POINT('Ctrl Pts',(178.098200269531,3.60803501918481,134.149515770902));
#25542=CARTESIAN_POINT('Ctrl Pts',(178.090452201528,3.69841043817253,134.046419113848));
#25543=CARTESIAN_POINT('Ctrl Pts',(178.082695898786,3.78888190923118,133.943212884441));
#25544=CARTESIAN_POINT('Ctrl Pts',(178.074939596044,3.87498216137205,133.836271475994));
#25545=CARTESIAN_POINT('Ctrl Pts',(178.067183293302,3.95640532583519,133.726010829382));
#25546=CARTESIAN_POINT('Ctrl Pts',(178.059422850788,4.03787194829286,133.615691333343));
#25547=CARTESIAN_POINT('Ctrl Pts',(178.051662408274,4.11465629020247,133.502049392914));
#25548=CARTESIAN_POINT('Ctrl Pts',(178.04390196576,4.18649655826401,133.385528886034));
#25549=CARTESIAN_POINT('Ctrl Pts',(178.036129065494,4.25845215070156,133.268821330092));
#25550=CARTESIAN_POINT('Ctrl Pts',(178.028356165229,4.32544761811766,133.149226314896));
#25551=CARTESIAN_POINT('Ctrl Pts',(178.020583264963,4.38726735076485,133.027211997081));
#25552=CARTESIAN_POINT('Ctrl Pts',(178.013092929201,4.44683978041567,132.909633207054));
#25553=CARTESIAN_POINT('Ctrl Pts',(178.005602593439,4.50160611609361,132.789808236237));
#25554=CARTESIAN_POINT('Ctrl Pts',(177.998112257677,4.5514168344388,132.668170656622));
#25555=CARTESIAN_POINT('Ctrl Pts',(177.990337923558,4.60311614130971,132.541921151206));
#25556=CARTESIAN_POINT('Ctrl Pts',(177.982563589439,4.64964039614636,132.413318953074));
#25557=CARTESIAN_POINT('Ctrl Pts',(177.97478925532,4.69076958224579,132.282827319517));
#25558=CARTESIAN_POINT('Ctrl Pts',(177.967024502373,4.73184808029915,132.152496505236));
#25559=CARTESIAN_POINT('Ctrl Pts',(177.959259749426,4.76754462262512,132.020281257972));
#25560=CARTESIAN_POINT('Ctrl Pts',(177.951494996479,4.79768681534231,131.886665696733));
#25561=CARTESIAN_POINT('Ctrl Pts',(177.943737955594,4.82779907040887,131.753182844352));
#25562=CARTESIAN_POINT('Ctrl Pts',(177.935980914709,4.85236786878697,131.618302824688));
#25563=CARTESIAN_POINT('Ctrl Pts',(177.928223873824,4.87127041482564,131.482525500279));
#25564=CARTESIAN_POINT('Ctrl Pts',(177.920472682584,4.89015870630732,131.346850566606));
#25565=CARTESIAN_POINT('Ctrl Pts',(177.912721491344,4.90338919683614,131.210280060711));
#25566=CARTESIAN_POINT('Ctrl Pts',(177.904970300103,4.91089010331847,131.073324287285));
#25567=CARTESIAN_POINT('Ctrl Pts',(177.897222403326,4.91838782171541,130.936426723716));
#25568=CARTESIAN_POINT('Ctrl Pts',(177.889474506549,4.92016077820899,130.799144607863));
#25569=CARTESIAN_POINT('Ctrl Pts',(177.881726609772,4.91618903610976,130.661993403172));
#25570=CARTESIAN_POINT('Ctrl Pts',(177.873980333688,4.91221812481335,130.524870887557));
#25571=CARTESIAN_POINT('Ctrl Pts',(177.866234057604,4.90250491641586,130.387879619192));
#25572=CARTESIAN_POINT('Ctrl Pts',(177.85848778152,4.88708160051593,130.251534702473));
#25573=CARTESIAN_POINT('Ctrl Pts',(177.850741448255,4.87165817076464,130.115188779287));
#25574=CARTESIAN_POINT('Ctrl Pts',(177.842995114989,4.85052459334789,129.979489605756));
#25575=CARTESIAN_POINT('Ctrl Pts',(177.835248781724,4.82376486201545,129.844946411665));
#25576=CARTESIAN_POINT('Ctrl Pts',(177.827500713721,4.79699913802668,129.710373087558));
#25577=CARTESIAN_POINT('Ctrl Pts',(177.819752645718,4.76460482924301,129.5769566414));
#25578=CARTESIAN_POINT('Ctrl Pts',(177.812004577715,4.72671681332008,129.445194980428));
#25579=CARTESIAN_POINT('Ctrl Pts',(177.804248274973,4.68878852956294,129.313293281594));
#25580=CARTESIAN_POINT('Ctrl Pts',(177.796491972232,4.64535498329599,129.183050257527));
#25581=CARTESIAN_POINT('Ctrl Pts',(177.78873566949,4.59660078782142,129.054948070481));
#25582=CARTESIAN_POINT('Ctrl Pts',(177.780975226976,4.54782057076469,128.92677751144));
#25583=CARTESIAN_POINT('Ctrl Pts',(177.773214784461,4.49371420013841,128.800750425285));
#25584=CARTESIAN_POINT('Ctrl Pts',(177.765454341947,4.43451361735137,128.677326993002));
#25585=CARTESIAN_POINT('Ctrl Pts',(177.757681441682,4.37521800053336,128.553705430469));
#25586=CARTESIAN_POINT('Ctrl Pts',(177.749908541416,4.31081201373659,128.432696219338));
#25587=CARTESIAN_POINT('Ctrl Pts',(177.742135641151,4.24157298806052,128.314733808292));
#25588=CARTESIAN_POINT('Ctrl Pts',(177.734645305389,4.17485097537009,128.201059628016));
#25589=CARTESIAN_POINT('Ctrl Pts',(177.727154969627,4.10364137597732,128.090214835132));
#25590=CARTESIAN_POINT('Ctrl Pts',(177.719664633865,4.02822814525213,127.98255958413));
#25591=CARTESIAN_POINT('Ctrl Pts',(177.711890299746,3.94995559896276,127.870822551566));
#25592=CARTESIAN_POINT('Ctrl Pts',(177.704115965627,3.86690642362824,127.762167748963));
#25593=CARTESIAN_POINT('Ctrl Pts',(177.696341631508,3.77935144632403,127.657030684485));
#25594=CARTESIAN_POINT('Ctrl Pts',(177.68857687856,3.69190437270419,127.552023192042));
#25595=CARTESIAN_POINT('Ctrl Pts',(177.680812125613,3.59996279371412,127.450525109322));
#25596=CARTESIAN_POINT('Ctrl Pts',(177.673047372666,3.50384082928145,127.352943154326));
#25597=CARTESIAN_POINT('Ctrl Pts',(177.665290331781,3.40781433453969,127.255458119104));
#25598=CARTESIAN_POINT('Ctrl Pts',(177.657533290896,3.30761598964536,127.161881747948));
#25599=CARTESIAN_POINT('Ctrl Pts',(177.649776250011,3.20359996906105,127.07258754023));
#25600=CARTESIAN_POINT('Ctrl Pts',(177.642025058771,3.09966238776662,126.983360669968));
#25601=CARTESIAN_POINT('Ctrl Pts',(177.634273867531,2.99191315658411,126.898409789223));
#25602=CARTESIAN_POINT('Ctrl Pts',(177.626522676291,2.88074280878541,126.818071123296));
#25603=CARTESIAN_POINT('Ctrl Pts',(177.618774779514,2.76961971135003,126.737766603444));
#25604=CARTESIAN_POINT('Ctrl Pts',(177.611026882737,2.6550787055422,126.662070628012));
#25605=CARTESIAN_POINT('Ctrl Pts',(177.60327898596,2.53754268909244,126.591278590886));
#25606=CARTESIAN_POINT('Ctrl Pts',(177.595532709876,2.42003125864345,126.520501361928));
#25607=CARTESIAN_POINT('Ctrl Pts',(177.587786433792,2.29952639837607,126.454626232496));
#25608=CARTESIAN_POINT('Ctrl Pts',(177.580040157707,2.17647887947239,126.393904547077));
#25609=CARTESIAN_POINT('Ctrl Pts',(177.572293824442,2.05343045225994,126.333182413425));
#25610=CARTESIAN_POINT('Ctrl Pts',(177.564547491177,1.92783967955764,126.277613972709));
#25611=CARTESIAN_POINT('Ctrl Pts',(177.556801157911,1.80018039147927,126.227403809748));
#25612=CARTESIAN_POINT('Ctrl Pts',(177.549053089908,1.67249251498833,126.177182402568));
#25613=CARTESIAN_POINT('Ctrl Pts',(177.541305021905,1.54273556511313,126.132321803976));
#25614=CARTESIAN_POINT('Ctrl Pts',(177.533556953902,1.41140134997992,126.092977668603));
#25615=CARTESIAN_POINT('Ctrl Pts',(177.525800651161,1.27992755128002,126.053591717815));
#25616=CARTESIAN_POINT('Ctrl Pts',(177.518044348419,1.14687351377778,126.019734054521));
#25617=CARTESIAN_POINT('Ctrl Pts',(177.510288045677,1.01274468223166,125.991509978796));
#25618=CARTESIAN_POINT('Ctrl Pts',(177.502527603163,0.878544262089551,125.963270839032));
#25619=CARTESIAN_POINT('Ctrl Pts',(177.494767160649,0.743268290289755,125.940671342562));
#25620=CARTESIAN_POINT('Ctrl Pts',(177.487006718134,0.607429300126163,125.923765089575));
#25621=CARTESIAN_POINT('Ctrl Pts',(177.479233817869,0.471372249156296,125.906831697169));
#25622=CARTESIAN_POINT('Ctrl Pts',(177.471460917604,0.334750763605367,125.895609843503));
#25623=CARTESIAN_POINT('Ctrl Pts',(177.463688017338,0.198080261687735,125.890101032193));
#25624=CARTESIAN_POINT('Ctrl Pts',(177.456197681576,0.0663780767674675,
125.88479248005));
#25625=CARTESIAN_POINT('Ctrl Pts',(177.448707345814,-0.065369314635894,
125.884788814691));
#25626=CARTESIAN_POINT('Ctrl Pts',(177.441217010052,-0.196705419535636,
125.890045808722));
#25627=CARTESIAN_POINT('Ctrl Pts',(177.433442675933,-0.333021172771505,
125.895502123279));
#25628=CARTESIAN_POINT('Ctrl Pts',(177.425668341814,-0.469325643322197,
125.906643171715));
#25629=CARTESIAN_POINT('Ctrl Pts',(177.417894007695,-0.605106037185557,
125.92347650234));
#25630=CARTESIAN_POINT('Ctrl Pts',(177.410129254748,-0.740719093848522,
125.940289087391));
#25631=CARTESIAN_POINT('Ctrl Pts',(177.402364501801,-0.875808974658048,
125.962779948777));
#25632=CARTESIAN_POINT('Ctrl Pts',(177.394599748854,-1.0098637067454,125.990904649522));
#25633=CARTESIAN_POINT('Ctrl Pts',(177.386842707969,-1.14378529378262,126.019001416418));
#25634=CARTESIAN_POINT('Ctrl Pts',(177.379085667084,-1.27667339795259,126.052720807403));
#25635=CARTESIAN_POINT('Ctrl Pts',(177.371328626199,-1.40802234370792,126.091966731003));
#25636=CARTESIAN_POINT('Ctrl Pts',(177.363577434959,-1.53927223820197,126.131183058947));
#25637=CARTESIAN_POINT('Ctrl Pts',(177.355826243718,-1.66898491148166,126.175917512674));
#25638=CARTESIAN_POINT('Ctrl Pts',(177.348075052478,-1.79666639490785,126.22602326347));
#25639=CARTESIAN_POINT('Ctrl Pts',(177.340327155701,-1.92429361029779,126.276107717985));
#25640=CARTESIAN_POINT('Ctrl Pts',(177.332579258924,-2.04989098970907,126.331558786443));
#25641=CARTESIAN_POINT('Ctrl Pts',(177.324831362147,-2.17298142334587,126.392180340617));
#25642=CARTESIAN_POINT('Ctrl Pts',(177.317085086063,-2.29604610911759,126.452789214069));
#25643=CARTESIAN_POINT('Ctrl Pts',(177.309338809979,-2.41660454165909,126.51856624934));
#25644=CARTESIAN_POINT('Ctrl Pts',(177.301592533895,-2.53420160489976,126.589268057702));
#25645=CARTESIAN_POINT('Ctrl Pts',(177.293846200629,-2.65179953621539,126.659970387969));
#25646=CARTESIAN_POINT('Ctrl Pts',(177.286099867364,-2.76643571954052,126.735597362417));
#25647=CARTESIAN_POINT('Ctrl Pts',(177.278353534098,-2.87768191512406,126.815860917445));
#25648=CARTESIAN_POINT('Ctrl Pts',(177.270605466096,-2.98895302352125,126.896142446938));
#25649=CARTESIAN_POINT('Ctrl Pts',(177.262857398093,-3.09683231653177,126.981062394456));
#25650=CARTESIAN_POINT('Ctrl Pts',(177.25510933009,-3.20092300320065,127.070291123022));
#25651=CARTESIAN_POINT('Ctrl Pts',(177.247353027348,-3.30512431869023,127.159614684944));
#25652=CARTESIAN_POINT('Ctrl Pts',(177.239596724606,-3.40552868701428,127.25325592095));
#25653=CARTESIAN_POINT('Ctrl Pts',(177.231840421864,-3.50177431099875,127.350846503315));
#25654=CARTESIAN_POINT('Ctrl Pts',(177.22407997935,-3.5980713041704,127.448489172712));
#25655=CARTESIAN_POINT('Ctrl Pts',(177.216319536836,-3.69020486765812,127.550085099136));
#25656=CARTESIAN_POINT('Ctrl Pts',(177.208559094322,-3.77785286934135,127.655232046023));
#25657=CARTESIAN_POINT('Ctrl Pts',(177.200786194056,-3.86564157137814,127.760547784123));
#25658=CARTESIAN_POINT('Ctrl Pts',(177.193013293791,-3.94893008479244,127.869425623223));
#25659=CARTESIAN_POINT('Ctrl Pts',(177.185240393525,-4.02743854841442,127.981432740123));
#25660=CARTESIAN_POINT('Ctrl Pts',(177.177750057763,-4.10309303163337,128.089368116195));
#25661=CARTESIAN_POINT('Ctrl Pts',(177.170259722001,-4.17430879856663,128.200208946648));
#25662=CARTESIAN_POINT('Ctrl Pts',(177.162769386239,-4.24087631336455,128.313547265016));
#25663=CARTESIAN_POINT('Ctrl Pts',(177.154700370286,-4.31258662861912,128.435641751572));
#25664=CARTESIAN_POINT('Ctrl Pts',(177.146631354333,-4.37911546164311,128.560996731004));
#25665=CARTESIAN_POINT('Ctrl Pts',(177.13856233838,-4.44016575555388,128.689151141957));
#25666=CARTESIAN_POINT('Ctrl Pts',(177.130504536925,-4.50113120040202,128.817127441046));
#25667=CARTESIAN_POINT('Ctrl Pts',(177.122446735471,-4.55663311807126,128.947895111476));
#25668=CARTESIAN_POINT('Ctrl Pts',(177.114388934016,-4.60641880221569,129.080966036777));
#25669=CARTESIAN_POINT('Ctrl Pts',(177.106344406022,-4.65612247536795,129.213817756923));
#25670=CARTESIAN_POINT('Ctrl Pts',(177.098299878028,-4.7001285599589,129.348964844431));
#25671=CARTESIAN_POINT('Ctrl Pts',(177.090255350033,-4.73823142587321,129.485897111295));
#25672=CARTESIAN_POINT('Ctrl Pts',(177.088369420506,-4.74716412148423,129.517999007829));
#25673=CARTESIAN_POINT('Ctrl Pts',(177.086483490979,-4.75577257872343,129.550198923862));
#25674=CARTESIAN_POINT('Ctrl Pts',(177.084597561451,-4.76405452823403,129.582490119308));
#25675=CARTESIAN_POINT('Ctrl Pts',(178.834794689177,-4.76405452823405,129.582490119308));
#25676=CARTESIAN_POINT('Ctrl Pts',(178.834348169157,-4.76600152135323,129.59008141593));
#25677=CARTESIAN_POINT('Ctrl Pts',(178.833901649136,-4.76793019492675,129.597676684138));
#25678=CARTESIAN_POINT('Ctrl Pts',(178.833455129116,-4.76984053507245,129.605275828037));
#25679=CARTESIAN_POINT('Ctrl Pts',(178.823192962182,-4.81374501544364,129.779923502642));
#25680=CARTESIAN_POINT('Ctrl Pts',(178.812930795248,-4.84807446073973,129.95706774057));
#25681=CARTESIAN_POINT('Ctrl Pts',(178.802668628314,-4.87259841686327,130.13580416484));
#25682=CARTESIAN_POINT('Ctrl Pts',(178.792640946099,-4.89656201443736,130.310456562743));
#25683=CARTESIAN_POINT('Ctrl Pts',(178.782613263885,-4.91116315740482,130.486629512172));
#25684=CARTESIAN_POINT('Ctrl Pts',(178.772585581671,-4.9162311945412,130.663456734298));
#25685=CARTESIAN_POINT('Ctrl Pts',(178.77001019979,-4.91753280449775,130.708870780548));
#25686=CARTESIAN_POINT('Ctrl Pts',(178.76743481791,-4.91820583999571,130.754327852339));
#25687=CARTESIAN_POINT('Ctrl Pts',(178.764859436029,-4.91824789753406,130.799812991619));
#25688=CARTESIAN_POINT('',(179.11014056404,-4.9182496345238,130.80625666781));
#25689=CARTESIAN_POINT('Ctrl Pts',(179.180279212536,-4.76405452823405,129.582490119308));
#25690=CARTESIAN_POINT('Ctrl Pts',(179.172592770908,-4.79783235438911,129.714189350837));
#25691=CARTESIAN_POINT('Ctrl Pts',(179.16490632928,-4.82611955095255,129.847191517955));
#25692=CARTESIAN_POINT('Ctrl Pts',(179.157219887652,-4.84884024883698,129.980994779218));
#25693=CARTESIAN_POINT('Ctrl Pts',(179.149373333716,-4.87203422987842,130.117585227311));
#25694=CARTESIAN_POINT('Ctrl Pts',(179.141526779781,-4.88942719215613,130.255010073371));
#25695=CARTESIAN_POINT('Ctrl Pts',(179.133680225846,-4.90099431101235,130.392732355751));
#25696=CARTESIAN_POINT('Ctrl Pts',(179.125833671911,-4.91256142986858,130.530454638131));
#25697=CARTESIAN_POINT('Ctrl Pts',(179.117987117976,-4.91830275159455,130.668473919319));
#25698=CARTESIAN_POINT('Ctrl Pts',(179.11014056404,-4.9182496345238,130.80625666781));
#25699=CARTESIAN_POINT('Ctrl Pts',(179.110140564008,-4.91824963452358,130.806256668381));
#25700=CARTESIAN_POINT('Ctrl Pts',(179.104198294929,-4.9182094084543,130.910600839437));
#25701=CARTESIAN_POINT('Ctrl Pts',(179.09825602585,-4.91484884784317,131.014877292883));
#25702=CARTESIAN_POINT('Ctrl Pts',(179.09231375677,-4.90817921990328,131.11893939595));
#25703=CARTESIAN_POINT('Ctrl Pts',(179.084539422651,-4.89945327441634,131.255084957113));
#25704=CARTESIAN_POINT('Ctrl Pts',(179.076765088532,-4.88504450286705,131.391082820901));
#25705=CARTESIAN_POINT('Ctrl Pts',(179.068990754413,-4.86495766475957,131.526420159846));
#25706=CARTESIAN_POINT('Ctrl Pts',(179.061226001466,-4.84489558188487,131.661590707615));
#25707=CARTESIAN_POINT('Ctrl Pts',(179.053461248519,-4.81916941265581,131.796101967218));
#25708=CARTESIAN_POINT('Ctrl Pts',(179.045696495572,-4.78783586718883,131.929443179585));
#25709=CARTESIAN_POINT('Ctrl Pts',(179.037939454687,-4.75653344264092,132.062651955581));
#25710=CARTESIAN_POINT('Ctrl Pts',(179.030182413802,-4.71963481392058,132.194692618852));
#25711=CARTESIAN_POINT('Ctrl Pts',(179.022425372917,-4.67724817964733,132.325061945403));
#25712=CARTESIAN_POINT('Ctrl Pts',(179.014674181676,-4.63489350946472,132.455332959431));
#25713=CARTESIAN_POINT('Ctrl Pts',(179.006922990436,-4.58705919165299,132.583934775123));
#25714=CARTESIAN_POINT('Ctrl Pts',(178.999171799196,-4.53390386652968,132.710377089574));
#25715=CARTESIAN_POINT('Ctrl Pts',(178.991423902419,-4.48077113383746,132.836765662669));
#25716=CARTESIAN_POINT('Ctrl Pts',(178.983676005642,-4.42232204312134,132.960996200391));
#25717=CARTESIAN_POINT('Ctrl Pts',(178.975928108865,-4.35876411544756,133.082596436876));
#25718=CARTESIAN_POINT('Ctrl Pts',(178.968181832781,-4.29521948272209,133.204171237213));
#25719=CARTESIAN_POINT('Ctrl Pts',(178.960435556697,-4.22656831964791,133.323116484425));
#25720=CARTESIAN_POINT('Ctrl Pts',(178.952689280612,-4.15306486639283,133.438983034163));
#25721=CARTESIAN_POINT('Ctrl Pts',(178.944942947347,-4.07956087055197,133.554850439201));
#25722=CARTESIAN_POINT('Ctrl Pts',(178.937196614082,-4.00120472249036,133.667638771277));
#25723=CARTESIAN_POINT('Ctrl Pts',(178.929450280816,-3.91829467942949,133.776926826695));
#25724=CARTESIAN_POINT('Ctrl Pts',(178.921702212813,-3.83536606923948,133.886239356415));
#25725=CARTESIAN_POINT('Ctrl Pts',(178.91395414481,-3.74788177099222,133.992049738264));
#25726=CARTESIAN_POINT('Ctrl Pts',(178.906206076807,-3.65618084862433,134.093969205932));
#25727=CARTESIAN_POINT('Ctrl Pts',(178.898449774065,-3.56438246542475,134.195996994824));
#25728=CARTESIAN_POINT('Ctrl Pts',(178.890693471324,-3.4683587677859,134.294125317703));
#25729=CARTESIAN_POINT('Ctrl Pts',(178.882937168582,-3.3684866595003,134.388001320436));
#25730=CARTESIAN_POINT('Ctrl Pts',(178.875176726068,-3.2685612464633,134.481927427618));
#25731=CARTESIAN_POINT('Ctrl Pts',(178.867416283553,-3.1647836256717,134.571596436813));
#25732=CARTESIAN_POINT('Ctrl Pts',(178.859655841039,-3.0575636481392,134.656695961235));
#25733=CARTESIAN_POINT('Ctrl Pts',(178.851882940774,-2.95017155158026,134.741932094967));
#25734=CARTESIAN_POINT('Ctrl Pts',(178.844110040508,-2.83932637193757,134.822583855418));
#25735=CARTESIAN_POINT('Ctrl Pts',(178.836337140243,-2.7254675236648,134.898381848575));
#25736=CARTESIAN_POINT('Ctrl Pts',(178.828846804481,-2.61574773132176,134.971424393755));
#25737=CARTESIAN_POINT('Ctrl Pts',(178.821356468719,-2.50322983824925,135.039959777996));
#25738=CARTESIAN_POINT('Ctrl Pts',(178.813866132957,-2.38832672171129,135.10378831586));
#25739=CARTESIAN_POINT('Ctrl Pts',(178.806091798838,-2.26906701858384,135.170036932139));
#25740=CARTESIAN_POINT('Ctrl Pts',(178.798317464719,-2.1468598711432,135.231424591867));
#25741=CARTESIAN_POINT('Ctrl Pts',(178.7905431306,-2.02213930829118,135.287678103576));
#25742=CARTESIAN_POINT('Ctrl Pts',(178.782778377653,-1.8975724523863,135.34386228786));
#25743=CARTESIAN_POINT('Ctrl Pts',(178.775013624706,-1.77049869726083,135.39492475452));
#25744=CARTESIAN_POINT('Ctrl Pts',(178.767248871759,-1.64137841218754,135.440637137631));
#25745=CARTESIAN_POINT('Ctrl Pts',(178.759491830874,-1.51238637120182,135.486304118559));
#25746=CARTESIAN_POINT('Ctrl Pts',(178.751734789989,-1.38135221148386,135.526631460963));
#25747=CARTESIAN_POINT('Ctrl Pts',(178.743977749104,-1.24875779362943,135.561438190546));
#25748=CARTESIAN_POINT('Ctrl Pts',(178.736226557863,-1.11626336625679,135.596218672103));
#25749=CARTESIAN_POINT('Ctrl Pts',(178.728475366623,-0.982211399327259,
135.625486728446));
#25750=CARTESIAN_POINT('Ctrl Pts',(178.720724175383,-0.847100147526754,
135.649110807468));
#25751=CARTESIAN_POINT('Ctrl Pts',(178.712976278606,-0.712046321612475,
135.672724845628));
#25752=CARTESIAN_POINT('Ctrl Pts',(178.705228381829,-0.575934490605304,
135.690699610382));
#25753=CARTESIAN_POINT('Ctrl Pts',(178.697480485052,-0.439274155356607,
135.702954423847));
#25754=CARTESIAN_POINT('Ctrl Pts',(178.689734208968,-0.302642406504035,
135.715206673869));
#25755=CARTESIAN_POINT('Ctrl Pts',(178.681987932884,-0.165462770780643,
135.721741317591));
#25756=CARTESIAN_POINT('Ctrl Pts',(178.6742416568,-0.0282505490694401,135.722529480972));
#25757=CARTESIAN_POINT('Ctrl Pts',(178.666495323534,0.10896268551119,135.723317650172));
#25758=CARTESIAN_POINT('Ctrl Pts',(178.658748990269,0.246208115600862,135.718359252141));
#25759=CARTESIAN_POINT('Ctrl Pts',(178.651002657004,0.382970155287087,135.707677548243));
#25760=CARTESIAN_POINT('Ctrl Pts',(178.643254589001,0.519762821883836,135.69699345225));
#25761=CARTESIAN_POINT('Ctrl Pts',(178.635506520998,0.6560714929648,135.680583530403));
#25762=CARTESIAN_POINT('Ctrl Pts',(178.627758452995,0.791385816082687,135.658522909105));
#25763=CARTESIAN_POINT('Ctrl Pts',(178.620002150253,0.926843952873513,135.636438841517));
#25764=CARTESIAN_POINT('Ctrl Pts',(178.612245847511,1.06130524413376,135.608692140596));
#25765=CARTESIAN_POINT('Ctrl Pts',(178.604489544769,1.19426909797958,135.575409179896));
#25766=CARTESIAN_POINT('Ctrl Pts',(178.596729102255,1.32730391863779,135.542108455078));
#25767=CARTESIAN_POINT('Ctrl Pts',(178.588968659741,1.45883933457868,135.503265693328));
#25768=CARTESIAN_POINT('Ctrl Pts',(178.581208217227,1.58839099146788,135.459056861224));
#25769=CARTESIAN_POINT('Ctrl Pts',(178.573435316961,1.71815061617768,135.414777061178));
#25770=CARTESIAN_POINT('Ctrl Pts',(178.565662416696,1.84591975356253,135.365114118798));
#25771=CARTESIAN_POINT('Ctrl Pts',(178.55788951643,1.97123424056386,135.310292111866));
#25772=CARTESIAN_POINT('Ctrl Pts',(178.550399180668,2.09199323031518,135.257463022974));
#25773=CARTESIAN_POINT('Ctrl Pts',(178.542908844906,2.21047265971088,135.199843582111));
#25774=CARTESIAN_POINT('Ctrl Pts',(178.535418509144,2.32628135749008,135.137673219755));
#25775=CARTESIAN_POINT('Ctrl Pts',(178.527644175025,2.44648097724423,135.073145649215));
#25776=CARTESIAN_POINT('Ctrl Pts',(178.519869840906,2.56418410222925,135.003510844547));
#25777=CARTESIAN_POINT('Ctrl Pts',(178.512095506787,2.67892628550298,134.928986299897));
#25778=CARTESIAN_POINT('Ctrl Pts',(178.50433075384,2.7935270592906,134.854553600087));
#25779=CARTESIAN_POINT('Ctrl Pts',(178.496566000893,2.90517382725016,134.775243361484));
#25780=CARTESIAN_POINT('Ctrl Pts',(178.488801247946,3.01342561782393,134.691319468434));
#25781=CARTESIAN_POINT('Ctrl Pts',(178.481044207061,3.12156989119321,134.607478929778));
#25782=CARTESIAN_POINT('Ctrl Pts',(178.473287166176,3.22632559050266,134.519034093746));
#25783=CARTESIAN_POINT('Ctrl Pts',(178.465530125291,3.32727999952759,134.426292542277));
#25784=CARTESIAN_POINT('Ctrl Pts',(178.457778934051,3.42815827804732,134.333620927934));
#25785=CARTESIAN_POINT('Ctrl Pts',(178.45002774281,3.52524068528896,134.236659310972));
#25786=CARTESIAN_POINT('Ctrl Pts',(178.44227655157,3.61814722391349,134.135755780045));
#25787=CARTESIAN_POINT('Ctrl Pts',(178.434528654793,3.7110142747808,134.03489513581));
#25788=CARTESIAN_POINT('Ctrl Pts',(178.426780758016,3.79970872281605,133.930096196904));
#25789=CARTESIAN_POINT('Ctrl Pts',(178.419032861239,3.88388729377466,133.821744012456));
#25790=CARTESIAN_POINT('Ctrl Pts',(178.411286585155,3.9680482563909,133.713414492949));
#25791=CARTESIAN_POINT('Ctrl Pts',(178.403540309071,4.04769498113156,133.601533514834));
#25792=CARTESIAN_POINT('Ctrl Pts',(178.395794032987,4.12252464273607,133.486519008216));
#25793=CARTESIAN_POINT('Ctrl Pts',(178.388047699721,4.19735485671613,133.371503652587));
#25794=CARTESIAN_POINT('Ctrl Pts',(178.380301366456,4.26736772339357,133.253355050009));
#25795=CARTESIAN_POINT('Ctrl Pts',(178.372555033191,4.33230412643069,133.132519550846));
#25796=CARTESIAN_POINT('Ctrl Pts',(178.364806965188,4.39725507152502,133.011656991411));
#25797=CARTESIAN_POINT('Ctrl Pts',(178.357058897185,4.45712710576504,132.888106682375));
#25798=CARTESIAN_POINT('Ctrl Pts',(178.349310829182,4.51170757715973,132.762338605363));
#25799=CARTESIAN_POINT('Ctrl Pts',(178.34155452644,4.56634605732897,132.636436860543));
#25800=CARTESIAN_POINT('Ctrl Pts',(178.333798223698,4.61568158434175,132.508312998465));
#25801=CARTESIAN_POINT('Ctrl Pts',(178.326041920956,4.65954989770892,132.378456489253));
#25802=CARTESIAN_POINT('Ctrl Pts',(178.318281478442,4.70344162491581,132.248530671711));
#25803=CARTESIAN_POINT('Ctrl Pts',(178.310521035928,4.74186021461869,132.116870739491));
#25804=CARTESIAN_POINT('Ctrl Pts',(178.302760593414,4.77469190713376,131.983979307843));
#25805=CARTESIAN_POINT('Ctrl Pts',(178.294987693148,4.80757630399631,131.850874547072));
#25806=CARTESIAN_POINT('Ctrl Pts',(178.287214792883,4.83485580373611,131.716534719739));
#25807=CARTESIAN_POINT('Ctrl Pts',(178.279441892618,4.85646803786491,131.581471458886));
#25808=CARTESIAN_POINT('Ctrl Pts',(178.271951556856,4.87729461284502,131.451318087769));
#25809=CARTESIAN_POINT('Ctrl Pts',(178.264461221094,4.89285877098853,131.320493273089));
#25810=CARTESIAN_POINT('Ctrl Pts',(178.256970885332,4.90315051431672,131.189455536327));
#25811=CARTESIAN_POINT('Ctrl Pts',(178.249196551213,4.91383247222137,131.053449463947));
#25812=CARTESIAN_POINT('Ctrl Pts',(178.241422217093,4.91886815300688,130.916783178524));
#25813=CARTESIAN_POINT('Ctrl Pts',(178.233647882974,4.91818949574107,130.779964993322));
#25814=CARTESIAN_POINT('Ctrl Pts',(178.225883130027,4.91751167485968,130.643315424305));
#25815=CARTESIAN_POINT('Ctrl Pts',(178.21811837708,4.91113353014638,130.506514715195));
#25816=CARTESIAN_POINT('Ctrl Pts',(178.210353624133,4.89903871907738,130.370076503787));
#25817=CARTESIAN_POINT('Ctrl Pts',(178.202596583248,4.88695592074523,130.233773804734));
#25818=CARTESIAN_POINT('Ctrl Pts',(178.194839542363,4.86916778958114,130.097833273809));
#25819=CARTESIAN_POINT('Ctrl Pts',(178.187082501478,4.84571001977967,129.962768396412));
#25820=CARTESIAN_POINT('Ctrl Pts',(178.179331310238,4.82226993966489,129.827805372489));
#25821=CARTESIAN_POINT('Ctrl Pts',(178.171580118998,4.793168797703,129.693717071373));
#25822=CARTESIAN_POINT('Ctrl Pts',(178.163828927758,4.75849405289253,129.561011346007));
#25823=CARTESIAN_POINT('Ctrl Pts',(178.156081030981,4.72383404577358,129.428362024114));
#25824=CARTESIAN_POINT('Ctrl Pts',(178.148333134204,4.68360524605732,129.297094486689));
#25825=CARTESIAN_POINT('Ctrl Pts',(178.140585237426,4.63794605836684,129.167705668538));
#25826=CARTESIAN_POINT('Ctrl Pts',(178.132838961342,4.59229642159413,129.038343915737));
#25827=CARTESIAN_POINT('Ctrl Pts',(178.125092685258,4.54121878627432,128.910860468985));
#25828=CARTESIAN_POINT('Ctrl Pts',(178.117346409174,4.48490108438993,128.785736005178));
#25829=CARTESIAN_POINT('Ctrl Pts',(178.109600075909,4.42858296678106,128.660610617731));
#25830=CARTESIAN_POINT('Ctrl Pts',(178.101853742643,4.36702486588853,128.537844604495));
#25831=CARTESIAN_POINT('Ctrl Pts',(178.094107409378,4.30046225020525,128.417897230657));
#25832=CARTESIAN_POINT('Ctrl Pts',(178.086359341375,4.23388472828575,128.297922995436));
#25833=CARTESIAN_POINT('Ctrl Pts',(178.078611273372,4.16230065112997,128.180768997448));
#25834=CARTESIAN_POINT('Ctrl Pts',(178.070863205369,4.08599048399426,128.066868183383));
#25835=CARTESIAN_POINT('Ctrl Pts',(178.063106902627,4.00959921350474,127.952846314178));
#25836=CARTESIAN_POINT('Ctrl Pts',(178.055350599885,3.92847203712003,127.842084860995));
#25837=CARTESIAN_POINT('Ctrl Pts',(178.047594297143,3.84293197311061,127.734986591393));
#25838=CARTESIAN_POINT('Ctrl Pts',(178.039833854629,3.75734625379343,127.62783116022));
#25839=CARTESIAN_POINT('Ctrl Pts',(178.032073412115,3.66734321017411,127.524343103294));
#25840=CARTESIAN_POINT('Ctrl Pts',(178.024312969601,3.57328421681137,127.42488980568));
#25841=CARTESIAN_POINT('Ctrl Pts',(178.016540069336,3.47907423160235,127.325276856804));
#25842=CARTESIAN_POINT('Ctrl Pts',(178.00876716907,3.38079556611414,127.229711882971));
#25843=CARTESIAN_POINT('Ctrl Pts',(178.000994268805,3.27884496002266,127.138523906713));
#25844=CARTESIAN_POINT('Ctrl Pts',(177.993503933043,3.18060051525979,127.05065084308));
#25845=CARTESIAN_POINT('Ctrl Pts',(177.98601359728,3.07894670116865,126.966842268125));
#25846=CARTESIAN_POINT('Ctrl Pts',(177.978523261518,2.97426388070669,126.88735443549));
#25847=CARTESIAN_POINT('Ctrl Pts',(177.970748927399,2.86561197929017,126.804852797521));
#25848=CARTESIAN_POINT('Ctrl Pts',(177.96297459328,2.75335267124101,126.726744671128));
#25849=CARTESIAN_POINT('Ctrl Pts',(177.955200259161,2.63787682630871,126.653362073634));
#25850=CARTESIAN_POINT('Ctrl Pts',(177.947435506214,2.52254329503498,126.580069913634));
#25851=CARTESIAN_POINT('Ctrl Pts',(177.939670753267,2.40400144105069,126.511491902602));
#25852=CARTESIAN_POINT('Ctrl Pts',(177.93190600032,2.28267456884699,126.447919423743));
#25853=CARTESIAN_POINT('Ctrl Pts',(177.924148959435,2.16146820020326,126.384410085966));
#25854=CARTESIAN_POINT('Ctrl Pts',(177.91639191855,2.03748266210701,126.325896567003));
#25855=CARTESIAN_POINT('Ctrl Pts',(177.908634877665,1.91116925795102,126.272626387719));
#25856=CARTESIAN_POINT('Ctrl Pts',(177.900883686425,1.78495110771554,126.219396379892));
#25857=CARTESIAN_POINT('Ctrl Pts',(177.893132495185,1.65640894434316,126.17140199277));
#25858=CARTESIAN_POINT('Ctrl Pts',(177.885381303944,1.52601731262292,126.128844151541));
#25859=CARTESIAN_POINT('Ctrl Pts',(177.877633407167,1.3956811008245,126.086304398529));
#25860=CARTESIAN_POINT('Ctrl Pts',(177.86988551039,1.26349735500979,126.049196716703));
#25861=CARTESIAN_POINT('Ctrl Pts',(177.862137613613,1.12995897158237,126.017673267734));
#25862=CARTESIAN_POINT('Ctrl Pts',(177.854391337529,0.996448521506018,125.986156412791));
#25863=CARTESIAN_POINT('Ctrl Pts',(177.846645061445,0.861584377703353,125.960221557053));
#25864=CARTESIAN_POINT('Ctrl Pts',(177.838898785361,0.72587252908902,125.939970405626));
#25865=CARTESIAN_POINT('Ctrl Pts',(177.831152452096,0.590159678680649,125.91971910471));
#25866=CARTESIAN_POINT('Ctrl Pts',(177.82340611883,0.453599497657837,125.905151649526));
#25867=CARTESIAN_POINT('Ctrl Pts',(177.815659785565,0.316705655302379,125.896318177815));
#25868=CARTESIAN_POINT('Ctrl Pts',(177.807911717562,0.179781156520127,125.887482727909));
#25869=CARTESIAN_POINT('Ctrl Pts',(177.800163649559,0.042523237797915,125.884383841828));
#25870=CARTESIAN_POINT('Ctrl Pts',(177.792415581556,-0.0945522522296156,
125.887019574472));
#25871=CARTESIAN_POINT('Ctrl Pts',(177.784659278814,-0.231773427719213,
125.889658108404));
#25872=CARTESIAN_POINT('Ctrl Pts',(177.776902976072,-0.368811395686946,
125.898043428593));
#25873=CARTESIAN_POINT('Ctrl Pts',(177.769146673331,-0.505152697112924,
125.912121476324));
#25874=CARTESIAN_POINT('Ctrl Pts',(177.761386230816,-0.641566767996746,
125.926207037933));
#25875=CARTESIAN_POINT('Ctrl Pts',(177.753625788302,-0.777283044745458,
125.945991324944));
#25876=CARTESIAN_POINT('Ctrl Pts',(177.745865345788,-0.911797104123172,
125.971368883307));
#25877=CARTESIAN_POINT('Ctrl Pts',(177.738092445523,-1.04652709741053,125.99678717998));
#25878=CARTESIAN_POINT('Ctrl Pts',(177.730319545257,-1.18005063572303,126.027816601991));
#25879=CARTESIAN_POINT('Ctrl Pts',(177.722546644992,-1.31187645560094,126.064301205729));
#25880=CARTESIAN_POINT('Ctrl Pts',(177.71505630923,-1.43891007487704,126.099459502223));
#25881=CARTESIAN_POINT('Ctrl Pts',(177.707565973468,-1.5643669721172,126.139683153101));
#25882=CARTESIAN_POINT('Ctrl Pts',(177.700075637706,-1.68782595840395,126.18479065959));
#25883=CARTESIAN_POINT('Ctrl Pts',(177.692301143226,-1.81596857280812,126.231609396601));
#25884=CARTESIAN_POINT('Ctrl Pts',(177.684526648747,-1.94236462080105,126.283838170655));
#25885=CARTESIAN_POINT('Ctrl Pts',(177.676752154268,-2.06652346192655,126.341327585669));
#25886=CARTESIAN_POINT('Ctrl Pts',(177.668987278277,-2.19052869558818,126.398745875637));
#25887=CARTESIAN_POINT('Ctrl Pts',(177.661222402286,-2.3123018782479,126.461411693872));
#25888=CARTESIAN_POINT('Ctrl Pts',(177.653457526295,-2.43136903252473,126.529126391213));
#25889=CARTESIAN_POINT('Ctrl Pts',(177.645700399525,-2.55031735970011,126.596773510377));
#25890=CARTESIAN_POINT('Ctrl Pts',(177.637943272756,-2.66656469520047,126.669459289141));
#25891=CARTESIAN_POINT('Ctrl Pts',(177.630186145986,-2.77965883815893,126.746937814117));
#25892=CARTESIAN_POINT('Ctrl Pts',(177.6224349059,-2.89266715687538,126.82435754263));
#25893=CARTESIAN_POINT('Ctrl Pts',(177.614683665815,-3.00252672482441,126.906562557649));
#25894=CARTESIAN_POINT('Ctrl Pts',(177.60693242573,-3.10881198829223,126.993262208452));
#25895=CARTESIAN_POINT('Ctrl Pts',(177.599184669519,-3.21504948075091,127.079922891202));
#25896=CARTESIAN_POINT('Ctrl Pts',(177.591436913309,-3.31771556266314,127.171073943901));
#25897=CARTESIAN_POINT('Ctrl Pts',(177.583689157098,-3.41641581650257,127.266382942219));
#25898=CARTESIAN_POINT('Ctrl Pts',(177.575943074336,-3.51509475193759,127.361671354615));
#25899=CARTESIAN_POINT('Ctrl Pts',(177.568196991574,-3.60980928238566,127.461115654579));
#25900=CARTESIAN_POINT('Ctrl Pts',(177.560450908813,-3.70020036884153,127.5643451403));
#25901=CARTESIAN_POINT('Ctrl Pts',(177.55270482166,-3.79059150653467,127.667574684535));
#25902=CARTESIAN_POINT('Ctrl Pts',(177.544958734507,-3.87665893800549,127.774589124554));
#25903=CARTESIAN_POINT('Ctrl Pts',(177.537212647354,-3.95808286043119,127.884983435279));
#25904=CARTESIAN_POINT('Ctrl Pts',(177.529464878335,-4.03952446199705,127.995401715328));
#25905=CARTESIAN_POINT('Ctrl Pts',(177.521717109316,-4.11632031667493,128.109201011568));
#25906=CARTESIAN_POINT('Ctrl Pts',(177.513969340297,-4.18819326244221,128.225946326004));
#25907=CARTESIAN_POINT('Ctrl Pts',(177.506214060889,-4.26013587907757,128.342804808855));
#25908=CARTESIAN_POINT('Ctrl Pts',(177.498458781481,-4.32714585161612,128.462614679699));
#25909=CARTESIAN_POINT('Ctrl Pts',(177.490703502072,-4.38899120993295,128.584914916128));
#25910=CARTESIAN_POINT('Ctrl Pts',(177.482944104692,-4.4508694074842,128.707280092696));
#25911=CARTESIAN_POINT('Ctrl Pts',(177.475184707312,-4.50757736508188,128.832137914138));
#25912=CARTESIAN_POINT('Ctrl Pts',(177.467425309932,-4.55893121262907,128.959007193147));
#25913=CARTESIAN_POINT('Ctrl Pts',(177.459655143061,-4.61035633565865,129.086052557677));
#25914=CARTESIAN_POINT('Ctrl Pts',(177.45188497619,-4.65641237482056,129.21511458816));
#25915=CARTESIAN_POINT('Ctrl Pts',(177.444114809319,-4.69696510604612,129.345696209594));
#25916=CARTESIAN_POINT('Ctrl Pts',(177.439448488999,-4.72131877012145,129.424116105041));
#25917=CARTESIAN_POINT('Ctrl Pts',(177.434782168678,-4.74368863307899,129.503083803194));
#25918=CARTESIAN_POINT('Ctrl Pts',(177.430115848357,-4.76405452823405,129.582490119308));
#25919=CARTESIAN_POINT('Origin',(213.235140564004,0.,130.804360617566));
#25920=CARTESIAN_POINT('',(175.334949039109,-4.76405452823403,129.582490119308));
#25921=CARTESIAN_POINT('',(175.679864508177,-4.76405452823404,129.582490119308));
#25922=CARTESIAN_POINT('',(213.235140564004,-4.76405452823405,129.582490119308));
#25923=CARTESIAN_POINT('',(177.014859435954,-4.91824992708477,130.805207512282));
#25924=CARTESIAN_POINT('Ctrl Pts',(177.014859435954,-4.91824992708477,130.805207512282));
#25925=CARTESIAN_POINT('Ctrl Pts',(177.006631410613,-4.9182247716926,130.951294745208));
#25926=CARTESIAN_POINT('Ctrl Pts',(176.998403385273,-4.91168649620771,131.097221500934));
#25927=CARTESIAN_POINT('Ctrl Pts',(176.990175359932,-4.89870335558759,131.242411409661));
#25928=CARTESIAN_POINT('Ctrl Pts',(176.981932190048,-4.88569631813616,131.387868555634));
#25929=CARTESIAN_POINT('Ctrl Pts',(176.973689020164,-4.86622075556974,131.532585836547));
#25930=CARTESIAN_POINT('Ctrl Pts',(176.96544585028,-4.84039616539851,131.67599587643));
#25931=CARTESIAN_POINT('Ctrl Pts',(176.957179149515,-4.81449785657614,131.81981529337));
#25932=CARTESIAN_POINT('Ctrl Pts',(176.94891244875,-4.78221432656776,131.962319697986));
#25933=CARTESIAN_POINT('Ctrl Pts',(176.940645747984,-4.7437157708782,132.102953605234));
#25934=CARTESIAN_POINT('Ctrl Pts',(176.932366109354,-4.70515696271938,132.243807612692));
#25935=CARTESIAN_POINT('Ctrl Pts',(176.924086470723,-4.6603638026299,132.382784981659));
#25936=CARTESIAN_POINT('Ctrl Pts',(176.915806832093,-4.60955515649318,132.519348757976));
#25937=CARTESIAN_POINT('Ctrl Pts',(176.907507626756,-4.55862643774319,132.656235266166));
#25938=CARTESIAN_POINT('Ctrl Pts',(176.899208421419,-4.50165392909692,132.790696489665));
#25939=CARTESIAN_POINT('Ctrl Pts',(176.890909216082,-4.43890382996342,132.922217045853));
#25940=CARTESIAN_POINT('Ctrl Pts',(176.888713398197,-4.42230130184235,132.957014978649));
#25941=CARTESIAN_POINT('Ctrl Pts',(176.886517580312,-4.40529456252688,132.991607204195));
#25942=CARTESIAN_POINT('Ctrl Pts',(176.884321762426,-4.38788905353696,133.025984509306));
#25943=CARTESIAN_POINT('Ctrl Pts',(176.876547428307,-4.32626452478983,133.14769799831));
#25944=CARTESIAN_POINT('Ctrl Pts',(176.868773094188,-4.2594743236812,133.267038271011));
#25945=CARTESIAN_POINT('Ctrl Pts',(176.860998760069,-4.18772473627818,133.383535794956));
#25946=CARTESIAN_POINT('Ctrl Pts',(176.853234007122,-4.11606357382926,133.499889746114));
#25947=CARTESIAN_POINT('Ctrl Pts',(176.845469254175,-4.03945538920248,133.613407589607));
#25948=CARTESIAN_POINT('Ctrl Pts',(176.837704501228,-3.95815340865091,133.723642148369));
#25949=CARTESIAN_POINT('Ctrl Pts',(176.829947460343,-3.87693217837241,133.833767220613));
#25950=CARTESIAN_POINT('Ctrl Pts',(176.822190419458,-3.79102666020864,133.940615185065));
#25951=CARTESIAN_POINT('Ctrl Pts',(176.814433378573,-3.70073444346966,134.043766063233));
#25952=CARTESIAN_POINT('Ctrl Pts',(176.806682187332,-3.61051031679379,134.146839154521));
#25953=CARTESIAN_POINT('Ctrl Pts',(176.798930996092,-3.51590633247001,134.246220415883));
#25954=CARTESIAN_POINT('Ctrl Pts',(176.791179804852,-3.41726136002214,134.34152160624));
#25955=CARTESIAN_POINT('Ctrl Pts',(176.783431908075,-3.31865831431899,134.43678229105));
#25956=CARTESIAN_POINT('Ctrl Pts',(176.775684011298,-3.21601797711347,134.527966082846));
#25957=CARTESIAN_POINT('Ctrl Pts',(176.767936114521,-3.10971704901438,134.614720566123));
#25958=CARTESIAN_POINT('Ctrl Pts',(176.760189838437,-3.00343835677783,134.701456902232));
#25959=CARTESIAN_POINT('Ctrl Pts',(176.752443562353,-2.8935008994043,134.783765525669));
#25960=CARTESIAN_POINT('Ctrl Pts',(176.744697286269,-2.78031521967282,134.861333669209));
#25961=CARTESIAN_POINT('Ctrl Pts',(176.736950953003,-2.6671287044304,134.938902385339));
#25962=CARTESIAN_POINT('Ctrl Pts',(176.729204619738,-2.55069424148432,135.011730330731));
#25963=CARTESIAN_POINT('Ctrl Pts',(176.721458286473,-2.43145183458326,135.079547752488));
#25964=CARTESIAN_POINT('Ctrl Pts',(176.71371021847,-2.31218272417198,135.147380361486));
#25965=CARTESIAN_POINT('Ctrl Pts',(176.705962150467,-2.19010475830888,135.210200020811));
#25966=CARTESIAN_POINT('Ctrl Pts',(176.698214082464,-2.06568268021461,135.267782861446));
#25967=CARTESIAN_POINT('Ctrl Pts',(176.690457779722,-1.94112836485505,135.325426901809));
#25968=CARTESIAN_POINT('Ctrl Pts',(176.68270147698,-1.81422531589903,135.377822840822));
#25969=CARTESIAN_POINT('Ctrl Pts',(176.674945174238,-1.68545892071563,135.424794719366));
#25970=CARTESIAN_POINT('Ctrl Pts',(176.667184731724,-1.55662379902994,135.471791668216));
#25971=CARTESIAN_POINT('Ctrl Pts',(176.65942428921,-1.42592372183812,135.513358669661));
#25972=CARTESIAN_POINT('Ctrl Pts',(176.651663846695,-1.2938584297329,135.549369935398));
#25973=CARTESIAN_POINT('Ctrl Pts',(176.64389094643,-1.16158113469664,135.585439009615));
#25974=CARTESIAN_POINT('Ctrl Pts',(176.636118046164,-1.02793462669097,135.615934438973));
#25975=CARTESIAN_POINT('Ctrl Pts',(176.628345145899,-0.893428894747038,
135.640781595162));
#25976=CARTESIAN_POINT('Ctrl Pts',(176.620854810137,-0.763812784960541,
135.664725494637));
#25977=CARTESIAN_POINT('Ctrl Pts',(176.613364474375,-0.633399141475654,
135.683424605516));
#25978=CARTESIAN_POINT('Ctrl Pts',(176.605874138613,-0.502646113807985,
135.696857929448));
#25979=CARTESIAN_POINT('Ctrl Pts',(176.598099804494,-0.366935545353002,
135.71080058194));
#25980=CARTESIAN_POINT('Ctrl Pts',(176.590325470375,-0.230429458897136,
135.719114426593));
#25981=CARTESIAN_POINT('Ctrl Pts',(176.582551136256,-0.0936343880487996,
135.72171922396));
#25982=CARTESIAN_POINT('Ctrl Pts',(176.574786383309,0.0429920951004432,
135.724320811146));
#25983=CARTESIAN_POINT('Ctrl Pts',(176.567021630362,0.179906466873114,135.721227342998));
#25984=CARTESIAN_POINT('Ctrl Pts',(176.559256877415,0.316595629564081,135.712410155808));
#25985=CARTESIAN_POINT('Ctrl Pts',(176.55149983653,0.453149030651684,135.703601725973));
#25986=CARTESIAN_POINT('Ctrl Pts',(176.543742795645,0.589477280162869,135.689080915264));
#25987=CARTESIAN_POINT('Ctrl Pts',(176.53598575476,0.725066184007642,135.668871085363));
#25988=CARTESIAN_POINT('Ctrl Pts',(176.528234563519,0.86055283920516,135.648676495852));
#25989=CARTESIAN_POINT('Ctrl Pts',(176.520483372279,0.995300873369753,135.622801483805));
#25990=CARTESIAN_POINT('Ctrl Pts',(176.512732181039,1.12880048103276,135.591321295963));
#25991=CARTESIAN_POINT('Ctrl Pts',(176.504984284262,1.26224334780143,135.559854488041));
#25992=CARTESIAN_POINT('Ctrl Pts',(176.497236387485,1.39443846368844,135.522787332179));
#25993=CARTESIAN_POINT('Ctrl Pts',(176.489488490708,1.52488571566593,135.480246268077));
#25994=CARTESIAN_POINT('Ctrl Pts',(176.481742214624,1.65530568089043,135.43771410265));
#25995=CARTESIAN_POINT('Ctrl Pts',(176.47399593854,1.78397813797108,135.389710427638));
#25996=CARTESIAN_POINT('Ctrl Pts',(176.466249662456,1.91041803858375,135.336411585986));
#25997=CARTESIAN_POINT('Ctrl Pts',(176.45850332919,2.036858872547,135.283112350893));
#25998=CARTESIAN_POINT('Ctrl Pts',(176.450756995925,2.16106675689199,135.224518023027));
#25999=CARTESIAN_POINT('Ctrl Pts',(176.44301066266,2.28257690809317,135.160852981973));
#26000=CARTESIAN_POINT('Ctrl Pts',(176.435262594657,2.40411427065022,135.097173683575));
#26001=CARTESIAN_POINT('Ctrl Pts',(176.427514526654,2.52295235165426,135.028421593787));
#26002=CARTESIAN_POINT('Ctrl Pts',(176.419766458651,2.6386515986994,134.954866707573));
#26003=CARTESIAN_POINT('Ctrl Pts',(176.412010155909,2.75447381228113,134.881233646349));
#26004=CARTESIAN_POINT('Ctrl Pts',(176.404253853167,2.8671501974432,134.80278780206));
#26005=CARTESIAN_POINT('Ctrl Pts',(176.396497550425,2.97627035106568,134.719842434644));
#26006=CARTESIAN_POINT('Ctrl Pts',(176.388737107911,3.08544874539976,134.636852796787));
#26007=CARTESIAN_POINT('Ctrl Pts',(176.380976665397,3.19106682520322,134.549359099839));
#26008=CARTESIAN_POINT('Ctrl Pts',(176.373216222883,3.29274863921616,134.457713798062));
#26009=CARTESIAN_POINT('Ctrl Pts',(176.365443322617,3.39459368190384,134.365921379111));
#26010=CARTESIAN_POINT('Ctrl Pts',(176.357670422352,3.49248955237282,134.26996431132));
#26011=CARTESIAN_POINT('Ctrl Pts',(176.349897522086,3.58609780218386,134.170231324482));
#26012=CARTESIAN_POINT('Ctrl Pts',(176.342407186324,3.67630315632983,134.074123882926));
#26013=CARTESIAN_POINT('Ctrl Pts',(176.334916850562,3.76252700773423,133.974510517335));
#26014=CARTESIAN_POINT('Ctrl Pts',(176.3274265148,3.84450404888564,133.871765331751));
#26015=CARTESIAN_POINT('Ctrl Pts',(176.319652180681,3.92958927446819,133.765124531226));
#26016=CARTESIAN_POINT('Ctrl Pts',(176.311877846562,4.01036882151141,133.65477193075));
#26017=CARTESIAN_POINT('Ctrl Pts',(176.304103512443,4.08650138850617,133.54109032001));
#26018=CARTESIAN_POINT('Ctrl Pts',(176.296338759496,4.16254012891625,133.427548811695));
#26019=CARTESIAN_POINT('Ctrl Pts',(176.288574006549,4.23394306881452,133.31068677801));
#26020=CARTESIAN_POINT('Ctrl Pts',(176.280809253602,4.30040875076859,133.190920409152));
#26021=CARTESIAN_POINT('Ctrl Pts',(176.273052212717,4.36680841807035,133.071272993939));
#26022=CARTESIAN_POINT('Ctrl Pts',(176.265295171832,4.42828039763348,132.94872732373));
#26023=CARTESIAN_POINT('Ctrl Pts',(176.257538130947,4.48456640983697,132.823728632134));
#26024=CARTESIAN_POINT('Ctrl Pts',(176.249786939707,4.5408099763208,132.698824203024));
#26025=CARTESIAN_POINT('Ctrl Pts',(176.242035748466,4.5918751997365,132.571470789575));
#26026=CARTESIAN_POINT('Ctrl Pts',(176.234284557226,4.63754982499086,132.442137978268));
#26027=CARTESIAN_POINT('Ctrl Pts',(176.226536660449,4.68320503731109,132.312860136855));
#26028=CARTESIAN_POINT('Ctrl Pts',(176.218788763672,4.72347407846985,132.18160493874));
#26029=CARTESIAN_POINT('Ctrl Pts',(176.211040866895,4.75819300246096,132.048861486923));
#26030=CARTESIAN_POINT('Ctrl Pts',(176.203294590811,4.79290466400163,131.916145802175));
#26031=CARTESIAN_POINT('Ctrl Pts',(176.195548314727,4.8220684187313,131.781942860941));
#26032=CARTESIAN_POINT('Ctrl Pts',(176.187802038643,4.84557044849468,131.646756065782));
#26033=CARTESIAN_POINT('Ctrl Pts',(176.180055705377,4.8690726517447,131.511568272705));
#26034=CARTESIAN_POINT('Ctrl Pts',(176.172309372112,4.88691297966808,131.375396996397));
#26035=CARTESIAN_POINT('Ctrl Pts',(176.164563038847,4.89902898231643,131.238754555051));
#26036=CARTESIAN_POINT('Ctrl Pts',(176.156814970844,4.91114769825956,131.102081513577));
#26037=CARTESIAN_POINT('Ctrl Pts',(176.149066902841,4.91753950352483,130.964937486466));
#26038=CARTESIAN_POINT('Ctrl Pts',(176.141318834838,4.91819396370879,130.827838220477));
#26039=CARTESIAN_POINT('Ctrl Pts',(176.133562532096,4.91884911946082,130.690593243756));
#26040=CARTESIAN_POINT('Ctrl Pts',(176.125806229354,4.91375474741247,130.553393514774));
#26041=CARTESIAN_POINT('Ctrl Pts',(176.118049926612,4.90295256911087,130.416753641946));
#26042=CARTESIAN_POINT('Ctrl Pts',(176.110289484098,4.89214462536145,130.280040840304));
#26043=CARTESIAN_POINT('Ctrl Pts',(176.102529041584,4.87562285216725,130.143888878153));
#26044=CARTESIAN_POINT('Ctrl Pts',(176.09476859907,4.85348056844284,130.008804564074));
#26045=CARTESIAN_POINT('Ctrl Pts',(176.086995698805,4.83130273995889,129.873503400662));
#26046=CARTESIAN_POINT('Ctrl Pts',(176.079222798539,4.80348645040933,129.739273693259));
#26047=CARTESIAN_POINT('Ctrl Pts',(176.071449898274,4.77017580952837,129.606610306069));
#26048=CARTESIAN_POINT('Ctrl Pts',(176.063959562512,4.73807609434798,129.478769567164));
#26049=CARTESIAN_POINT('Ctrl Pts',(176.05646922675,4.7008746464984,129.352383541698));
#26050=CARTESIAN_POINT('Ctrl Pts',(176.048978890988,4.65874280511444,129.227877652769));
#26051=CARTESIAN_POINT('Ctrl Pts',(176.041204556869,4.6150135221586,129.098651085218));
#26052=CARTESIAN_POINT('Ctrl Pts',(176.03343022275,4.56583407235678,128.971040688426));
#26053=CARTESIAN_POINT('Ctrl Pts',(176.02565588863,4.51134202571253,128.845540516194));
#26054=CARTESIAN_POINT('Ctrl Pts',(176.017891135683,4.45691713564568,128.720195011708));
#26055=CARTESIAN_POINT('Ctrl Pts',(176.010126382736,4.39719283013072,128.596954912415));
#26056=CARTESIAN_POINT('Ctrl Pts',(176.002361629789,4.33235631666133,128.476298803957));
#26057=CARTESIAN_POINT('Ctrl Pts',(175.994604588904,4.26758419973116,128.355762532847));
#26058=CARTESIAN_POINT('Ctrl Pts',(175.986847548019,4.19771016320102,128.237805487371));
#26059=CARTESIAN_POINT('Ctrl Pts',(175.979090507134,4.12296918827295,128.122885625131));
#26060=CARTESIAN_POINT('Ctrl Pts',(175.971339315894,4.04828457609545,128.008052424854));
#26061=CARTESIAN_POINT('Ctrl Pts',(175.963588124654,3.9687405431181,127.896252175402));
#26062=CARTESIAN_POINT('Ctrl Pts',(175.955836933414,3.88461743668457,127.787917275962));
#26063=CARTESIAN_POINT('Ctrl Pts',(175.948089036637,3.80053008481534,127.679628421744));
#26064=CARTESIAN_POINT('Ctrl Pts',(175.940341139859,3.71186776967313,127.574802296271));
#26065=CARTESIAN_POINT('Ctrl Pts',(175.932593243082,3.61895337064391,127.47384120408));
#26066=CARTESIAN_POINT('Ctrl Pts',(175.924846966998,3.52605840730398,127.372901230774));
#26067=CARTESIAN_POINT('Ctrl Pts',(175.917100690914,3.42891339381489,127.275824970133));
#26068=CARTESIAN_POINT('Ctrl Pts',(175.90935441483,3.32788033551458,127.182980281976));
#26069=CARTESIAN_POINT('Ctrl Pts',(175.901608081565,3.22684653141127,127.090134908461));
#26070=CARTESIAN_POINT('Ctrl Pts',(175.893861748299,3.12192491310012,127.001521434303));
#26071=CARTESIAN_POINT('Ctrl Pts',(175.886115415034,3.01351275266165,126.917469320907));
#26072=CARTESIAN_POINT('Ctrl Pts',(175.878367347031,2.90507631407145,126.833398384623));
#26073=CARTESIAN_POINT('Ctrl Pts',(175.870619279028,2.79314808681636,126.753891081245));
#26074=CARTESIAN_POINT('Ctrl Pts',(175.862871211025,2.67815634320237,126.679234963254));
#26075=CARTESIAN_POINT('Ctrl Pts',(175.855114908283,2.56304238499486,126.604499499852));
#26076=CARTESIAN_POINT('Ctrl Pts',(175.847358605541,2.44485873477475,126.534625734532));
#26077=CARTESIAN_POINT('Ctrl Pts',(175.839602302799,2.32406089869263,126.469856724193));
#26078=CARTESIAN_POINT('Ctrl Pts',(175.831841860285,2.20319858916816,126.405053144683));
#26079=CARTESIAN_POINT('Ctrl Pts',(175.824081417771,2.07971966540841,126.345359919152));
#26080=CARTESIAN_POINT('Ctrl Pts',(175.816320975257,1.95410096097882,126.290972478174));
#26081=CARTESIAN_POINT('Ctrl Pts',(175.808548074991,1.82828060225302,126.236497729648));
#26082=CARTESIAN_POINT('Ctrl Pts',(175.800775174726,1.70031396387985,126.18734592625));
#26083=CARTESIAN_POINT('Ctrl Pts',(175.79300227446,1.57069528396139,126.14366331057));
#26084=CARTESIAN_POINT('Ctrl Pts',(175.785511938698,1.44578856954715,126.101568668));
#26085=CARTESIAN_POINT('Ctrl Pts',(175.778021602936,1.3193481356255,126.064552565761));
#26086=CARTESIAN_POINT('Ctrl Pts',(175.770531267174,1.19182451568294,126.032700802961));
#26087=CARTESIAN_POINT('Ctrl Pts',(175.762756933055,1.05946579893085,125.999641370894));
#26088=CARTESIAN_POINT('Ctrl Pts',(175.754982598936,0.925520864102131,125.972040898323));
#26089=CARTESIAN_POINT('Ctrl Pts',(175.747208264817,0.790479732600394,125.950050691856));
#26090=CARTESIAN_POINT('Ctrl Pts',(175.73944351187,0.655605027224353,125.928087586353));
#26091=CARTESIAN_POINT('Ctrl Pts',(175.731678758923,0.51963719536985,125.911721052089));
#26092=CARTESIAN_POINT('Ctrl Pts',(175.723914005976,0.383080074915559,125.901052273325));
#26093=CARTESIAN_POINT('Ctrl Pts',(175.716156965091,0.246658584918514,125.890394090943));
#26094=CARTESIAN_POINT('Ctrl Pts',(175.708399924206,0.109649358329901,125.885422432471));
#26095=CARTESIAN_POINT('Ctrl Pts',(175.700642883321,-0.0274352990704107,
125.886187138838));
#26096=CARTESIAN_POINT('Ctrl Pts',(175.692891692081,-0.1644165798644,125.886951268534));
#26097=CARTESIAN_POINT('Ctrl Pts',(175.68514050084,-0.301472788870795,125.893443150581));
#26098=CARTESIAN_POINT('Ctrl Pts',(175.6773893096,-0.438088601822157,125.905660643139));
#26099=CARTESIAN_POINT('Ctrl Pts',(175.669641412823,-0.574646349408622,
125.917872942937));
#26100=CARTESIAN_POINT('Ctrl Pts',(175.661893516046,-0.710763684631094,
125.935805978375));
#26101=CARTESIAN_POINT('Ctrl Pts',(175.654145619269,-0.845927613093618,
125.959405557309));
#26102=CARTESIAN_POINT('Ctrl Pts',(175.646399343185,-0.98106326817615,125.983000199721));
#26103=CARTESIAN_POINT('Ctrl Pts',(175.638653067101,-1.11524552828541,126.012258960764));
#26104=CARTESIAN_POINT('Ctrl Pts',(175.630906791017,-1.24796922981086,126.04707611231));
#26105=CARTESIAN_POINT('Ctrl Pts',(175.623160457752,-1.38069391107248,126.081893520869));
#26106=CARTESIAN_POINT('Ctrl Pts',(175.615414124486,-1.51195963409641,126.122269302602));
#26107=CARTESIAN_POINT('Ctrl Pts',(175.607667791221,-1.64127447840742,126.168047303193));
#26108=CARTESIAN_POINT('Ctrl Pts',(175.599919723218,-1.77061828188111,126.213835555451));
#26109=CARTESIAN_POINT('Ctrl Pts',(175.592171655215,-1.89800996880706,126.265028303463));
#26110=CARTESIAN_POINT('Ctrl Pts',(175.584423587212,-2.02297612149675,126.321420658749));
#26111=CARTESIAN_POINT('Ctrl Pts',(175.57666728447,-2.14807508970072,126.377872948502));
#26112=CARTESIAN_POINT('Ctrl Pts',(175.568910981728,-2.27074301713271,126.43953572365));
#26113=CARTESIAN_POINT('Ctrl Pts',(175.561154678986,-2.39052920093837,126.506157132159));
#26114=CARTESIAN_POINT('Ctrl Pts',(175.553394236472,-2.51037931823709,126.57281409852));
#26115=CARTESIAN_POINT('Ctrl Pts',(175.545633793958,-2.62734429390807,126.644434767697));
#26116=CARTESIAN_POINT('Ctrl Pts',(175.537873351444,-2.74100196648704,126.720723601105));
#26117=CARTESIAN_POINT('Ctrl Pts',(175.530100451179,-2.85484209245202,126.79713490012));
#26118=CARTESIAN_POINT('Ctrl Pts',(175.522327550913,-2.96536399050178,126.878229106851));
#26119=CARTESIAN_POINT('Ctrl Pts',(175.514554650648,-3.07217747483731,126.963669452476));
#26120=CARTESIAN_POINT('Ctrl Pts',(175.507064314886,-3.17510801997039,127.046003826326));
#26121=CARTESIAN_POINT('Ctrl Pts',(175.499573979124,-3.27459485814811,127.132373636935));
#26122=CARTESIAN_POINT('Ctrl Pts',(175.492083643362,-3.37032227979657,127.222446214233));
#26123=CARTESIAN_POINT('Ctrl Pts',(175.484426013505,-3.46818774075487,127.314530531821));
#26124=CARTESIAN_POINT('Ctrl Pts',(175.476768383649,-3.56245359475089,127.410795582262));
#26125=CARTESIAN_POINT('Ctrl Pts',(175.469110753793,-3.65273331836966,127.510924362319));
#26126=CARTESIAN_POINT('Ctrl Pts',(175.461462005809,-3.74290832904258,127.610937005784));
#26127=CARTESIAN_POINT('Ctrl Pts',(175.453813257825,-3.82910613282586,127.714804174024));
#26128=CARTESIAN_POINT('Ctrl Pts',(175.446164509841,-3.91097428624597,127.822169611808));
#26129=CARTESIAN_POINT('Ctrl Pts',(175.438522859586,-3.99276646932869,127.929435418805));
#26130=CARTESIAN_POINT('Ctrl Pts',(175.430881209331,-4.07023674784178,128.040192721918));
#26131=CARTESIAN_POINT('Ctrl Pts',(175.423239559076,-4.1430708837805,128.154049934935));
#26132=CARTESIAN_POINT('Ctrl Pts',(175.415603284732,-4.21585378080787,128.267827049251));
#26133=CARTESIAN_POINT('Ctrl Pts',(175.407967010388,-4.28400680640056,128.384699396879));
#26134=CARTESIAN_POINT('Ctrl Pts',(175.400330736044,-4.3472575948339,128.504244432096));
#26135=CARTESIAN_POINT('Ctrl Pts',(175.392697732783,-4.41048128909551,128.623738258882));
#26136=CARTESIAN_POINT('Ctrl Pts',(175.385064729521,-4.46880673517313,128.745902139713));
#26137=CARTESIAN_POINT('Ctrl Pts',(175.377431726259,-4.52200655733599,128.870287258588));
#26138=CARTESIAN_POINT('Ctrl Pts',(175.369798525334,-4.5752077571597,128.994675598536));
#26139=CARTESIAN_POINT('Ctrl Pts',(175.362165324408,-4.62328289879717,129.121284924899));
#26140=CARTESIAN_POINT('Ctrl Pts',(175.354532123482,-4.66605208952326,129.249644900673));
#26141=CARTESIAN_POINT('Ctrl Pts',(175.348004428691,-4.70262707637903,129.359414675293));
#26142=CARTESIAN_POINT('Ctrl Pts',(175.3414767339,-4.73532246569085,129.470464243522));
#26143=CARTESIAN_POINT('Ctrl Pts',(175.334949039109,-4.76405452823403,129.582490119308));
#26144=CARTESIAN_POINT('Ctrl Pts',(177.084597561451,-4.76405452823403,129.582490119308));
#26145=CARTESIAN_POINT('Ctrl Pts',(177.076567484955,-4.79931814076276,129.719982409358));
#26146=CARTESIAN_POINT('Ctrl Pts',(177.068537408458,-4.82865840725863,129.859130859221));
#26147=CARTESIAN_POINT('Ctrl Pts',(177.060507331961,-4.85193039187213,129.999404385882));
#26148=CARTESIAN_POINT('Ctrl Pts',(177.05248775733,-4.87517194100357,130.13949446053));
#26149=CARTESIAN_POINT('Ctrl Pts',(177.044468182699,-4.89236097345581,130.280706334928));
#26150=CARTESIAN_POINT('Ctrl Pts',(177.036448608067,-4.90340326199463,130.422497405459));
#26151=CARTESIAN_POINT('Ctrl Pts',(177.029252217375,-4.91331209458416,130.549734071631));
#26152=CARTESIAN_POINT('Ctrl Pts',(177.022055826683,-4.91827192846218,130.677436781746));
#26153=CARTESIAN_POINT('Ctrl Pts',(177.014859435991,-4.91824992708488,130.805207511627));
#26154=CARTESIAN_POINT('',(177.360140563968,-4.91824793051881,130.799848805581));
#26155=CARTESIAN_POINT('Ctrl Pts',(177.430115848357,-4.76405452823405,129.582490119308));
#26156=CARTESIAN_POINT('Ctrl Pts',(177.427286570202,-4.77640275516735,129.630635668711));
#26157=CARTESIAN_POINT('Ctrl Pts',(177.424457292047,-4.78801440829828,129.678942445579));
#26158=CARTESIAN_POINT('Ctrl Pts',(177.421628013893,-4.79888619662381,129.727385996531));
#26159=CARTESIAN_POINT('Ctrl Pts',(177.410989040785,-4.83976753005932,129.909548939735));
#26160=CARTESIAN_POINT('Ctrl Pts',(177.400350067677,-4.87028956772032,130.094115230531));
#26161=CARTESIAN_POINT('Ctrl Pts',(177.389711094569,-4.89022784483775,130.280094761274));
#26162=CARTESIAN_POINT('Ctrl Pts',(177.379854251049,-4.90870034924447,130.452401911033));
#26163=CARTESIAN_POINT('Ctrl Pts',(177.369997407528,-4.91808837710366,130.625922424611));
#26164=CARTESIAN_POINT('Ctrl Pts',(177.360140564008,-4.91824793051816,130.79984880487));
#26165=CARTESIAN_POINT('Ctrl Pts',(177.360140563968,-4.91824793051882,130.799848805581));
#26166=CARTESIAN_POINT('Ctrl Pts',(177.352487945942,-4.91837180396175,130.934881095582));
#26167=CARTESIAN_POINT('Ctrl Pts',(177.344835327916,-4.91293045659475,131.070080067784));
#26168=CARTESIAN_POINT('Ctrl Pts',(177.33718270989,-4.90190951832219,131.204942864654));
#26169=CARTESIAN_POINT('Ctrl Pts',(177.329535914745,-4.89089696588737,131.339703044352));
#26170=CARTESIAN_POINT('Ctrl Pts',(177.321889119601,-4.87431330117688,131.474127158148));
#26171=CARTESIAN_POINT('Ctrl Pts',(177.314242324456,-4.85219622232653,131.607712895549));
#26172=CARTESIAN_POINT('Ctrl Pts',(177.306598711799,-4.83008834829065,131.74124303646));
#26173=CARTESIAN_POINT('Ctrl Pts',(177.298955099142,-4.80245170335256,131.87393509822));
#26174=CARTESIAN_POINT('Ctrl Pts',(177.291311486484,-4.76937573609459,132.005292818172));
#26175=CARTESIAN_POINT('Ctrl Pts',(177.283669304355,-4.73630595911592,132.136625954081));
#26176=CARTESIAN_POINT('Ctrl Pts',(177.276027122226,-4.69779898193594,132.266624854489));
#26177=CARTESIAN_POINT('Ctrl Pts',(177.268384940097,-4.65399505901825,132.394804911823));
#26178=CARTESIAN_POINT('Ctrl Pts',(177.260742427898,-4.61018924418316,132.522990505329));
#26179=CARTESIAN_POINT('Ctrl Pts',(177.253099915698,-4.56108615912356,132.649356718698));
#26180=CARTESIAN_POINT('Ctrl Pts',(177.245457403499,-4.50687529735599,132.773436064719));
#26181=CARTESIAN_POINT('Ctrl Pts',(177.237812800583,-4.45264960545219,132.897549354373));
#26182=CARTESIAN_POINT('Ctrl Pts',(177.230168197668,-4.39331351973143,133.019374164111));
#26183=CARTESIAN_POINT('Ctrl Pts',(177.222523594753,-4.32910360359455,133.138465382105));
#26184=CARTESIAN_POINT('Ctrl Pts',(177.21487088778,-4.26482561840363,133.257682848926));
#26185=CARTESIAN_POINT('Ctrl Pts',(177.207218180807,-4.19566368022283,133.374160584805));
#26186=CARTESIAN_POINT('Ctrl Pts',(177.199565473833,-4.12189915921267,133.487480142258));
#26187=CARTESIAN_POINT('Ctrl Pts',(177.19190814988,-4.04809013508669,133.600868066906));
#26188=CARTESIAN_POINT('Ctrl Pts',(177.184250825927,-3.96967323333913,133.711093693201));
#26189=CARTESIAN_POINT('Ctrl Pts',(177.176593501974,-3.88697082811644,133.817770786108));
#26190=CARTESIAN_POINT('Ctrl Pts',(177.168925089948,-3.8041486669113,133.924602351185));
#26191=CARTESIAN_POINT('Ctrl Pts',(177.161256677921,-3.71702887440284,134.02787482013));
#26192=CARTESIAN_POINT('Ctrl Pts',(177.153588265894,-3.62597167935547,134.127237750867));
#26193=CARTESIAN_POINT('Ctrl Pts',(177.150118973956,-3.58477618912948,134.172190866761));
#26194=CARTESIAN_POINT('Ctrl Pts',(177.146649682018,-3.54277526702529,134.216344320271));
#26195=CARTESIAN_POINT('Ctrl Pts',(177.14318039008,-3.50000445877035,134.259668397068));
#26196=CARTESIAN_POINT('Ctrl Pts',(177.135406055961,-3.4041593814917,134.356753293475));
#26197=CARTESIAN_POINT('Ctrl Pts',(177.127631721842,-3.30411994611471,134.450001044235));
#26198=CARTESIAN_POINT('Ctrl Pts',(177.119857387723,-3.20022595236407,134.539027525915));
#26199=CARTESIAN_POINT('Ctrl Pts',(177.112092634776,-3.0964599986757,134.627944290412));
#26200=CARTESIAN_POINT('Ctrl Pts',(177.104327881829,-2.98884923252015,134.712649884976));
#26201=CARTESIAN_POINT('Ctrl Pts',(177.096563128882,-2.8777713262827,134.792795806475));
#26202=CARTESIAN_POINT('Ctrl Pts',(177.088806087997,-2.76680374418746,134.872862125915));
#26203=CARTESIAN_POINT('Ctrl Pts',(177.081049047112,-2.65237618995443,134.948377557388));
#26204=CARTESIAN_POINT('Ctrl Pts',(177.073292006227,-2.53490027577508,135.019033043079));
#26205=CARTESIAN_POINT('Ctrl Pts',(177.065540814986,-2.41751295109669,135.089635246917));
#26206=CARTESIAN_POINT('Ctrl Pts',(177.057789623746,-2.2970821757582,135.155384599089));
#26207=CARTESIAN_POINT('Ctrl Pts',(177.050038432506,-2.17404918026736,135.216014867876));
#26208=CARTESIAN_POINT('Ctrl Pts',(177.042290535729,-2.05106847708128,135.276619367182));
#26209=CARTESIAN_POINT('Ctrl Pts',(177.034542638952,-1.92548810347863,135.332108938039));
#26210=CARTESIAN_POINT('Ctrl Pts',(177.026794742175,-1.79777437560963,135.382263014614));
#26211=CARTESIAN_POINT('Ctrl Pts',(177.019048466091,-1.67008736269943,135.432406600038));
#26212=CARTESIAN_POINT('Ctrl Pts',(177.011302190007,-1.54026824682151,135.477216768286));
#26213=CARTESIAN_POINT('Ctrl Pts',(177.003555913923,-1.40880346413521,135.516521041611));
#26214=CARTESIAN_POINT('Ctrl Pts',(176.995809580657,-1.27733771100549,135.555825605072));
#26215=CARTESIAN_POINT('Ctrl Pts',(176.988063247392,-1.14422664140964,135.58962408052));
#26216=CARTESIAN_POINT('Ctrl Pts',(176.980316914127,-1.00997161176771,135.617793945859));
#26217=CARTESIAN_POINT('Ctrl Pts',(176.972568846124,-0.875686516643258,
135.645970119644));
#26218=CARTESIAN_POINT('Ctrl Pts',(176.964820778121,-0.740257334260181,
135.668515094824));
#26219=CARTESIAN_POINT('Ctrl Pts',(176.957072710118,-0.604194969101184,
135.685357595829));
#26220=CARTESIAN_POINT('Ctrl Pts',(176.949316407376,-0.467987995241147,
135.702217997245));
#26221=CARTESIAN_POINT('Ctrl Pts',(176.941560104634,-0.331146882929249,
135.713363769564));
#26222=CARTESIAN_POINT('Ctrl Pts',(176.933803801892,-0.194187566345887,
135.71877556256));
#26223=CARTESIAN_POINT('Ctrl Pts',(176.926043359378,-0.0571551504514058,
135.724190243992));
#26224=CARTESIAN_POINT('Ctrl Pts',(176.918282916864,0.0799952046522575,
135.723864848926));
#26225=CARTESIAN_POINT('Ctrl Pts',(176.91052247435,0.216749215926602,135.717832184584));
#26226=CARTESIAN_POINT('Ctrl Pts',(176.902749574084,0.353722756880248,135.711789836074));
#26227=CARTESIAN_POINT('Ctrl Pts',(176.894976673819,0.490298292835616,135.700021943642));
#26228=CARTESIAN_POINT('Ctrl Pts',(176.887203773553,0.625967402688034,135.682613160565));
#26229=CARTESIAN_POINT('Ctrl Pts',(176.879713437791,0.756704598669194,135.665837230602));
#26230=CARTESIAN_POINT('Ctrl Pts',(176.872223102029,0.886599822452162,135.643823462321));
#26231=CARTESIAN_POINT('Ctrl Pts',(176.864732766267,1.01521039196965,135.616691749412));
#26232=CARTESIAN_POINT('Ctrl Pts',(176.856958432148,1.14869727031917,135.588531329362));
#26233=CARTESIAN_POINT('Ctrl Pts',(176.849184098029,1.28122300236775,135.554768006105));
#26234=CARTESIAN_POINT('Ctrl Pts',(176.84140976391,1.41228074413996,135.515480034672));
#26235=CARTESIAN_POINT('Ctrl Pts',(176.833645010963,1.54317696895822,135.476240482153));
#26236=CARTESIAN_POINT('Ctrl Pts',(176.825880258016,1.67260843229818,135.431489939802));
#26237=CARTESIAN_POINT('Ctrl Pts',(176.818115505069,1.80007778745586,135.381357779637));
#26238=CARTESIAN_POINT('Ctrl Pts',(176.810358464184,1.92742053825299,135.331275411441));
#26239=CARTESIAN_POINT('Ctrl Pts',(176.802601423299,2.05280469757118,135.275822204587));
#26240=CARTESIAN_POINT('Ctrl Pts',(176.794844382414,2.1757477598724,135.215177406768));
#26241=CARTESIAN_POINT('Ctrl Pts',(176.787093191173,2.29859810985412,135.154578341664));
#26242=CARTESIAN_POINT('Ctrl Pts',(176.779341999933,2.41901067771043,135.088795650461));
#26243=CARTESIAN_POINT('Ctrl Pts',(176.771590808693,2.53652297929066,135.018056648135));
#26244=CARTESIAN_POINT('Ctrl Pts',(176.763842911916,2.65398533500795,134.947347711772));
#26245=CARTESIAN_POINT('Ctrl Pts',(176.756095015139,2.76854954191965,134.871686855295));
#26246=CARTESIAN_POINT('Ctrl Pts',(176.748347118362,2.87977797647419,134.791347182469));
#26247=CARTESIAN_POINT('Ctrl Pts',(176.740600842278,2.99098314443811,134.71102431497));
#26248=CARTESIAN_POINT('Ctrl Pts',(176.732854566194,3.09885361121525,134.6260248066));
#26249=CARTESIAN_POINT('Ctrl Pts',(176.72510829011,3.20298133576673,134.536664681443));
#26250=CARTESIAN_POINT('Ctrl Pts',(176.717361956844,3.30710982896542,134.447303896649));
#26251=CARTESIAN_POINT('Ctrl Pts',(176.709615623579,3.40749522811752,134.35358268545));
#26252=CARTESIAN_POINT('Ctrl Pts',(176.701869290313,3.50376345652187,134.255856627015));
#26253=CARTESIAN_POINT('Ctrl Pts',(176.69412122231,3.60005324352857,134.158108683507));
#26254=CARTESIAN_POINT('Ctrl Pts',(176.686373154307,3.69222375077429,134.05635438659));
#26255=CARTESIAN_POINT('Ctrl Pts',(176.678625086304,3.77993885575116,133.950985048489));
#26256=CARTESIAN_POINT('Ctrl Pts',(176.670868783563,3.86774718538536,133.845503722602));
#26257=CARTESIAN_POINT('Ctrl Pts',(176.663112480821,3.95109040303699,133.736399981461));
#26258=CARTESIAN_POINT('Ctrl Pts',(176.655356178079,4.02967335378458,133.624097435834));
#26259=CARTESIAN_POINT('Ctrl Pts',(176.647595735565,4.10829824661905,133.511734950958));
#26260=CARTESIAN_POINT('Ctrl Pts',(176.639835293051,4.18215759955181,133.396170588928));
#26261=CARTESIAN_POINT('Ctrl Pts',(176.632074850536,4.25100103168297,133.277854763735));
#26262=CARTESIAN_POINT('Ctrl Pts',(176.624301950271,4.31995497740302,133.159349007475));
#26263=CARTESIAN_POINT('Ctrl Pts',(176.616529050006,4.38387672944328,133.03808330775));
#26264=CARTESIAN_POINT('Ctrl Pts',(176.60875614974,4.44256269497506,132.914531170795));
#26265=CARTESIAN_POINT('Ctrl Pts',(176.601265813978,4.49911527783851,132.795470465229));
#26266=CARTESIAN_POINT('Ctrl Pts',(176.593775478216,4.55080601244283,132.674286955166));
#26267=CARTESIAN_POINT('Ctrl Pts',(176.586285142454,4.59749648827391,132.551417887036));
#26268=CARTESIAN_POINT('Ctrl Pts',(176.578510808335,4.64595724768758,132.423890200843));
#26269=CARTESIAN_POINT('Ctrl Pts',(176.570736474216,4.689184602897,132.294142648211));
#26270=CARTESIAN_POINT('Ctrl Pts',(176.562962140097,4.7269704305287,132.162643950088));
#26271=CARTESIAN_POINT('Ctrl Pts',(176.55519738715,4.76470969050479,132.031307312359));
#26272=CARTESIAN_POINT('Ctrl Pts',(176.547432634203,4.79702065929808,131.898224195328));
#26273=CARTESIAN_POINT('Ctrl Pts',(176.539667881256,4.82374335321012,131.763882959599));
#26274=CARTESIAN_POINT('Ctrl Pts',(176.531910840371,4.85043950576582,131.62967515348));
#26275=CARTESIAN_POINT('Ctrl Pts',(176.524153799486,4.8715583531125,131.494212096357));
#26276=CARTESIAN_POINT('Ctrl Pts',(176.516396758601,4.88698989538333,131.357996621562));
#26277=CARTESIAN_POINT('Ctrl Pts',(176.508645567361,4.90240980060812,131.221883867917));
#26278=CARTESIAN_POINT('Ctrl Pts',(176.50089437612,4.91215089360298,131.085020212891));
#26279=CARTESIAN_POINT('Ctrl Pts',(176.49314318488,4.91615443691515,130.947917626797));
#26280=CARTESIAN_POINT('Ctrl Pts',(176.485395288103,4.92015627861463,130.810873312959));
#26281=CARTESIAN_POINT('Ctrl Pts',(176.477647391326,4.91842540945625,130.673590660013));
#26282=CARTESIAN_POINT('Ctrl Pts',(176.469899494549,4.91095505315188,130.5365854723));
#26283=CARTESIAN_POINT('Ctrl Pts',(176.462153218465,4.90348625948502,130.39960894312));
#26284=CARTESIAN_POINT('Ctrl Pts',(176.454406942381,4.89028038795833,130.262910153868));
#26285=CARTESIAN_POINT('Ctrl Pts',(176.446660666297,4.87138276243421,130.127003219763));
#26286=CARTESIAN_POINT('Ctrl Pts',(176.438914333031,4.85248499741213,129.991095282423));
#26287=CARTESIAN_POINT('Ctrl Pts',(176.431167999766,4.82789544839928,129.855979599134));
#26288=CARTESIAN_POINT('Ctrl Pts',(176.423421666501,4.79771107662709,129.722163090444));
#26289=CARTESIAN_POINT('Ctrl Pts',(176.415673598498,4.76751994527414,129.588316614474));
#26290=CARTESIAN_POINT('Ctrl Pts',(176.407925530495,4.73173158400299,129.455770273354));
#26291=CARTESIAN_POINT('Ctrl Pts',(176.400177462492,4.6904935324448,129.325018370284));
#26292=CARTESIAN_POINT('Ctrl Pts',(176.39242115975,4.64921165259457,129.194127502535));
#26293=CARTESIAN_POINT('Ctrl Pts',(176.384664857008,4.60246863010648,129.065035256028));
#26294=CARTESIAN_POINT('Ctrl Pts',(176.376908554266,4.55046132227167,128.938218924926));
#26295=CARTESIAN_POINT('Ctrl Pts',(176.369148111752,4.49842625657074,128.811334908129));
#26296=CARTESIAN_POINT('Ctrl Pts',(176.361387669238,4.44112147021729,128.686729582207));
#26297=CARTESIAN_POINT('Ctrl Pts',(176.353627226724,4.37879057226528,128.564857059466));
#26298=CARTESIAN_POINT('Ctrl Pts',(176.345854326458,4.31635961522244,128.442788896133));
#26299=CARTESIAN_POINT('Ctrl Pts',(176.338081426193,4.24888661597369,128.323462643002));
#26300=CARTESIAN_POINT('Ctrl Pts',(176.330308525927,4.17665990182982,128.207305530174));
#26301=CARTESIAN_POINT('Ctrl Pts',(176.322818190165,4.10705881067231,128.095371020979));
#26302=CARTESIAN_POINT('Ctrl Pts',(176.315327854403,4.03304379623021,127.986379494736));
#26303=CARTESIAN_POINT('Ctrl Pts',(176.307837518641,3.95490791204331,127.880683742507));
#26304=CARTESIAN_POINT('Ctrl Pts',(176.300063184522,3.87380948205952,127.770980503707));
#26305=CARTESIAN_POINT('Ctrl Pts',(176.292288850403,3.78801463276585,127.664480384049));
#26306=CARTESIAN_POINT('Ctrl Pts',(176.284514516284,3.69780521660363,127.561611838743));
#26307=CARTESIAN_POINT('Ctrl Pts',(176.276749763336,3.60770697548464,127.458870069725));
#26308=CARTESIAN_POINT('Ctrl Pts',(176.268985010389,3.51320524788856,127.359751261094));
#26309=CARTESIAN_POINT('Ctrl Pts',(176.261220257442,3.41462443032569,127.264653982501));
#26310=CARTESIAN_POINT('Ctrl Pts',(176.253463216557,3.31614152462077,127.169651155866));
#26311=CARTESIAN_POINT('Ctrl Pts',(176.245706175672,3.21358787099731,127.078662180232));
#26312=CARTESIAN_POINT('Ctrl Pts',(176.237949134787,3.10732705976352,126.992051395302));
#26313=CARTESIAN_POINT('Ctrl Pts',(176.230197943547,3.00114638063378,126.905505924237));
#26314=CARTESIAN_POINT('Ctrl Pts',(176.222446752307,2.89126441018347,126.823332318197));
#26315=CARTESIAN_POINT('Ctrl Pts',(176.214695561067,2.77808013450735,126.745856727121));
#26316=CARTESIAN_POINT('Ctrl Pts',(176.20694766429,2.66494396516788,126.668414065239));
#26317=CARTESIAN_POINT('Ctrl Pts',(176.199199767513,2.54850860413817,126.59566566725));
#26318=CARTESIAN_POINT('Ctrl Pts',(176.191451870736,2.42920434947129,126.527896039084));
#26319=CARTESIAN_POINT('Ctrl Pts',(176.183705594652,2.30992505068262,126.460140586864));
#26320=CARTESIAN_POINT('Ctrl Pts',(176.175959318567,2.18777839164242,126.397362025945));
#26321=CARTESIAN_POINT('Ctrl Pts',(176.168213042483,2.06322141069901,126.339800115912));
#26322=CARTESIAN_POINT('Ctrl Pts',(176.160466709218,1.9386635103043,126.282237780969));
#26323=CARTESIAN_POINT('Ctrl Pts',(176.152720375953,1.81169560740304,126.229892337764));
#26324=CARTESIAN_POINT('Ctrl Pts',(176.144974042687,1.68279659852437,126.182956213005));
#26325=CARTESIAN_POINT('Ctrl Pts',(176.137225974684,1.55386872360639,126.136009577226));
#26326=CARTESIAN_POINT('Ctrl Pts',(176.129477906681,1.42300924946788,126.094474804143));
#26327=CARTESIAN_POINT('Ctrl Pts',(176.121729838678,1.29071379616576,126.058494947439));
#26328=CARTESIAN_POINT('Ctrl Pts',(176.113973535936,1.15827773768127,126.022476850915));
#26329=CARTESIAN_POINT('Ctrl Pts',(176.106217233195,1.02440302919617,125.992025567076));
#26330=CARTESIAN_POINT('Ctrl Pts',(176.098460930453,0.889597637980695,125.967233463459));
#26331=CARTESIAN_POINT('Ctrl Pts',(176.090700487939,0.75472029706883,125.94242812755));
#26332=CARTESIAN_POINT('Ctrl Pts',(176.082940045424,0.618911670593171,125.92328804495));
#26333=CARTESIAN_POINT('Ctrl Pts',(176.07517960291,0.482685492741861,125.909853719257));
#26334=CARTESIAN_POINT('Ctrl Pts',(176.067406702645,0.346240632536643,125.896397827591));
#26335=CARTESIAN_POINT('Ctrl Pts',(176.059633802379,0.209377272069173,125.888666018271));
#26336=CARTESIAN_POINT('Ctrl Pts',(176.051860902114,0.0726107000767102,
125.886646641669));
#26337=CARTESIAN_POINT('Ctrl Pts',(176.044370566352,-0.0591840625283202,
125.884700674493));
#26338=CARTESIAN_POINT('Ctrl Pts',(176.03688023059,-0.190888643576832,125.888059020157));
#26339=CARTESIAN_POINT('Ctrl Pts',(176.029389894828,-0.322047827361773,
125.896665816604));
#26340=CARTESIAN_POINT('Ctrl Pts',(176.021615560709,-0.458179951466051,
125.905598942354));
#26341=CARTESIAN_POINT('Ctrl Pts',(176.01384122659,-0.594155730072887,125.920214662816));
#26342=CARTESIAN_POINT('Ctrl Pts',(176.006066892471,-0.729462343550482,
125.940507438055));
#26343=CARTESIAN_POINT('Ctrl Pts',(175.998302139524,-0.864602203719436,
125.960775204261));
#26344=CARTESIAN_POINT('Ctrl Pts',(175.990537386577,-0.99907415670959,125.986706046939));
#26345=CARTESIAN_POINT('Ctrl Pts',(175.98277263363,-1.1323675303472,126.018242478749));
#26346=CARTESIAN_POINT('Ctrl Pts',(175.975015592745,-1.265528515127,126.04974758813));
#26347=CARTESIAN_POINT('Ctrl Pts',(175.96725855186,-1.39751287206479,126.086847117534));
#26348=CARTESIAN_POINT('Ctrl Pts',(175.959501510975,-1.52781754240825,126.129432102646));
#26349=CARTESIAN_POINT('Ctrl Pts',(175.951750319735,-1.65802394898635,126.17198497409));
#26350=CARTESIAN_POINT('Ctrl Pts',(175.943999128495,-1.78655282007018,126.220014946582));
#26351=CARTESIAN_POINT('Ctrl Pts',(175.936247937254,-1.912914094747,126.27336263383));
#26352=CARTESIAN_POINT('Ctrl Pts',(175.928500040477,-2.03922166251126,126.326687646888));
#26353=CARTESIAN_POINT('Ctrl Pts',(175.9207521437,-2.16336310680931,126.385325727652));
#26354=CARTESIAN_POINT('Ctrl Pts',(175.913004246923,-2.28486647813643,126.449068636586));
#26355=CARTESIAN_POINT('Ctrl Pts',(175.905257970839,-2.40634443357779,126.512798211878));
#26356=CARTESIAN_POINT('Ctrl Pts',(175.897511694755,-2.52518506766956,126.581630309873));
#26357=CARTESIAN_POINT('Ctrl Pts',(175.889765418671,-2.64093962349206,126.655310007177));
#26358=CARTESIAN_POINT('Ctrl Pts',(175.882019085406,-2.75669503378842,126.728990248368));
#26359=CARTESIAN_POINT('Ctrl Pts',(175.87427275214,-2.86936399053878,126.807517950335));
#26360=CARTESIAN_POINT('Ctrl Pts',(175.866526418875,-2.97852574443112,126.890594215204));
#26361=CARTESIAN_POINT('Ctrl Pts',(175.858778350872,-3.08771194434152,126.973689084426));
#26362=CARTESIAN_POINT('Ctrl Pts',(175.851030282869,-3.19338906745496,127.061334306757));
#26363=CARTESIAN_POINT('Ctrl Pts',(175.843282214866,-3.29516886390869,127.153190227016));
#26364=CARTESIAN_POINT('Ctrl Pts',(175.835525912124,-3.39705683314104,127.245143772841));
#26365=CARTESIAN_POINT('Ctrl Pts',(175.827769609382,-3.49503891066816,127.341316693889));
#26366=CARTESIAN_POINT('Ctrl Pts',(175.82001330664,-3.58876281634651,127.441331549819));
#26367=CARTESIAN_POINT('Ctrl Pts',(175.812252864126,-3.68253674529536,127.54139978669));
#26368=CARTESIAN_POINT('Ctrl Pts',(175.804492421612,-3.77204771878202,127.645313748276));
#26369=CARTESIAN_POINT('Ctrl Pts',(175.796731979098,-3.85698397410572,127.752663108639));
#26370=CARTESIAN_POINT('Ctrl Pts',(175.788959078833,-3.94205657664672,127.860184795725));
#26371=CARTESIAN_POINT('Ctrl Pts',(175.781186178567,-4.02253955621019,127.97115258526));
#26372=CARTESIAN_POINT('Ctrl Pts',(175.773413278302,-4.09816418780871,128.085126653329));
#26373=CARTESIAN_POINT('Ctrl Pts',(175.76592294254,-4.17103967356237,128.19495747694));
#26374=CARTESIAN_POINT('Ctrl Pts',(175.758432606778,-4.23940374536326,128.30757953891));
#26375=CARTESIAN_POINT('Ctrl Pts',(175.750942271015,-4.30305734633331,128.422579658563));
#26376=CARTESIAN_POINT('Ctrl Pts',(175.742787679911,-4.37235585373531,128.547778178704));
#26377=CARTESIAN_POINT('Ctrl Pts',(175.734633088806,-4.4362732431258,128.67615975229));
#26378=CARTESIAN_POINT('Ctrl Pts',(175.726478497701,-4.49452037997105,128.807245293774));
#26379=CARTESIAN_POINT('Ctrl Pts',(175.718341777153,-4.55263986985782,128.938043564989));
#26380=CARTESIAN_POINT('Ctrl Pts',(175.710205056605,-4.60511374545798,129.071533685418));
#26381=CARTESIAN_POINT('Ctrl Pts',(175.702068336057,-4.65169851612172,129.207211915156));
#26382=CARTESIAN_POINT('Ctrl Pts',(175.694667060097,-4.69407268163103,129.330626749682));
#26383=CARTESIAN_POINT('Ctrl Pts',(175.687265784137,-4.73157464057992,129.455851530296));
#26384=CARTESIAN_POINT('Ctrl Pts',(175.679864508177,-4.76405452823404,129.582490119308));
#26385=CARTESIAN_POINT('Origin',(213.235140564004,0.,130.804360617566));
#26386=CARTESIAN_POINT('',(173.584942037299,-4.76405452823404,129.582490119308));
#26387=CARTESIAN_POINT('',(173.930202354372,-4.76405452823406,129.582490119308));
#26388=CARTESIAN_POINT('',(213.235140564004,-4.76405452823405,129.582490119308));
#26389=CARTESIAN_POINT('',(175.264859436032,-4.91824815910515,130.808615962297));
#26390=CARTESIAN_POINT('Ctrl Pts',(175.264859435991,-4.91824815910454,130.808615963011));
#26391=CARTESIAN_POINT('Ctrl Pts',(175.25319186359,-4.91807026830515,131.014218800192));
#26392=CARTESIAN_POINT('Ctrl Pts',(175.241524291189,-4.90499673116812,131.219285084506));
#26393=CARTESIAN_POINT('Ctrl Pts',(175.229856718788,-4.8792466415552,131.422531527082));
#26394=CARTESIAN_POINT('Ctrl Pts',(175.224449819042,-4.86731372627334,131.516718483985));
#26395=CARTESIAN_POINT('Ctrl Pts',(175.219042919295,-4.85265909434396,131.610515169461));
#26396=CARTESIAN_POINT('Ctrl Pts',(175.213636019548,-4.83530754954034,131.70379597592));
#26397=CARTESIAN_POINT('Ctrl Pts',(175.205861685429,-4.81035855601216,131.837920185781));
#26398=CARTESIAN_POINT('Ctrl Pts',(175.19808735131,-4.77978520791269,131.971217980356));
#26399=CARTESIAN_POINT('Ctrl Pts',(175.190313017191,-4.74365357488158,132.103180783722));
#26400=CARTESIAN_POINT('Ctrl Pts',(175.182548264244,-4.70756647085903,132.234980954727));
#26401=CARTESIAN_POINT('Ctrl Pts',(175.174783511297,-4.6659348137967,132.365449034629));
#26402=CARTESIAN_POINT('Ctrl Pts',(175.16701875835,-4.61887600350787,132.494084715376));
#26403=CARTESIAN_POINT('Ctrl Pts',(175.159261717465,-4.57186393269282,132.622592633351));
#26404=CARTESIAN_POINT('Ctrl Pts',(175.15150467658,-4.51943556909307,132.749271409193));
#26405=CARTESIAN_POINT('Ctrl Pts',(175.143747635695,-4.46175852998218,132.873634374861));
#26406=CARTESIAN_POINT('Ctrl Pts',(175.135996444455,-4.40412498557524,132.99790355745));
#26407=CARTESIAN_POINT('Ctrl Pts',(175.128245253215,-4.34125080777626,133.119860052667));
#26408=CARTESIAN_POINT('Ctrl Pts',(175.120494061975,-4.27335214775605,133.239036054615));
#26409=CARTESIAN_POINT('Ctrl Pts',(175.112746165198,-4.20548234647749,133.358161403582));
#26410=CARTESIAN_POINT('Ctrl Pts',(175.104998268421,-4.13259250353576,133.474508270769));
#26411=CARTESIAN_POINT('Ctrl Pts',(175.097250371644,-4.05494514228876,133.587632604909));
#26412=CARTESIAN_POINT('Ctrl Pts',(175.08950409556,-3.97731402319586,133.700733275878));
#26413=CARTESIAN_POINT('Ctrl Pts',(175.081757819476,-3.89492758635569,133.810612432457));
#26414=CARTESIAN_POINT('Ctrl Pts',(175.074011543391,-3.80809197298378,133.916854567407));
#26415=CARTESIAN_POINT('Ctrl Pts',(175.066265210126,-3.72125571861122,134.023097486612));
#26416=CARTESIAN_POINT('Ctrl Pts',(175.058518876861,-3.62997046959219,134.1257030279));
#26417=CARTESIAN_POINT('Ctrl Pts',(175.050772543595,-3.53458272588869,134.224288689375));
#26418=CARTESIAN_POINT('Ctrl Pts',(175.043024475592,-3.43917362076133,134.322896428426));
#26419=CARTESIAN_POINT('Ctrl Pts',(175.035276407589,-3.33966046460008,134.417482215401));
#26420=CARTESIAN_POINT('Ctrl Pts',(175.027528339586,-3.23642639092771,134.507700634174));
#26421=CARTESIAN_POINT('Ctrl Pts',(175.019772036845,-3.13308259885326,134.598014938155));
#26422=CARTESIAN_POINT('Ctrl Pts',(175.012015734103,-3.02601028431556,134.683952343975));
#26423=CARTESIAN_POINT('Ctrl Pts',(175.004259431361,-2.91562585318813,134.765207616217));
#26424=CARTESIAN_POINT('Ctrl Pts',(174.996498988847,-2.80518250656608,134.846506256844));
#26425=CARTESIAN_POINT('Ctrl Pts',(174.988738546333,-2.69142384503477,134.923117566151));
#26426=CARTESIAN_POINT('Ctrl Pts',(174.980978103818,-2.57479414442493,134.994780426647));
#26427=CARTESIAN_POINT('Ctrl Pts',(174.973205203553,-2.45797721946581,135.066558326728));
#26428=CARTESIAN_POINT('Ctrl Pts',(174.965432303288,-2.33828038706294,135.13337171331));
#26429=CARTESIAN_POINT('Ctrl Pts',(174.957659403022,-2.21617213142889,135.19500568935));
#26430=CARTESIAN_POINT('Ctrl Pts',(174.95016906726,-2.09850281845932,135.254399115114));
#26431=CARTESIAN_POINT('Ctrl Pts',(174.942678731498,-1.9785946413567,135.308983034166));
#26432=CARTESIAN_POINT('Ctrl Pts',(174.935188395736,-1.8568813991624,135.358608583141));
#26433=CARTESIAN_POINT('Ctrl Pts',(174.927414061617,-1.73055336239648,135.410115699889));
#26434=CARTESIAN_POINT('Ctrl Pts',(174.919639727498,-1.60188051118809,135.456444190198));
#26435=CARTESIAN_POINT('Ctrl Pts',(174.911865393379,-1.47132643711803,135.497374742618));
#26436=CARTESIAN_POINT('Ctrl Pts',(174.904100640432,-1.34093325927635,135.53825485179));
#26437=CARTESIAN_POINT('Ctrl Pts',(174.896335887485,-1.20866384105492,135.573750143681));
#26438=CARTESIAN_POINT('Ctrl Pts',(174.888571134538,-1.07500256325419,135.603688961355));
#26439=CARTESIAN_POINT('Ctrl Pts',(174.880814093653,-0.94147403971895,135.633598043374));
#26440=CARTESIAN_POINT('Ctrl Pts',(174.873057052768,-0.806556786714803,
135.657961548872));
#26441=CARTESIAN_POINT('Ctrl Pts',(174.865300011883,-0.670750853076566,
135.676657443048));
#26442=CARTESIAN_POINT('Ctrl Pts',(174.857548820642,-0.535047331749209,
135.695339238504));
#26443=CARTESIAN_POINT('Ctrl Pts',(174.849797629402,-0.398456849447651,
135.70836187665));
#26444=CARTESIAN_POINT('Ctrl Pts',(174.842046438162,-0.26148981951155,135.715654351074));
#26445=CARTESIAN_POINT('Ctrl Pts',(174.834298541385,-0.124581004216886,
135.722943726001));
#26446=CARTESIAN_POINT('Ctrl Pts',(174.826550644608,0.0127036508045441,
135.724507760431));
#26447=CARTESIAN_POINT('Ctrl Pts',(174.818802747831,0.149848652360622,135.720327302145));
#26448=CARTESIAN_POINT('Ctrl Pts',(174.811056471747,0.286964966138925,135.71614771832));
#26449=CARTESIAN_POINT('Ctrl Pts',(174.803310195663,0.423941294021012,135.70622604378));
#26450=CARTESIAN_POINT('Ctrl Pts',(174.795563919579,0.560262581193397,135.690595251987));
#26451=CARTESIAN_POINT('Ctrl Pts',(174.787817586313,0.696584874658464,135.674964344811));
#26452=CARTESIAN_POINT('Ctrl Pts',(174.780071253048,0.832251729344999,135.653624280825));
#26453=CARTESIAN_POINT('Ctrl Pts',(174.772324919783,0.966754043881733,135.626659828641));
#26454=CARTESIAN_POINT('Ctrl Pts',(174.76457685178,1.10128647927914,135.599689337956));
#26455=CARTESIAN_POINT('Ctrl Pts',(174.756828783777,1.23465347231902,135.567092029565));
#26456=CARTESIAN_POINT('Ctrl Pts',(174.749080715774,1.36635732160314,135.529003538698));
#26457=CARTESIAN_POINT('Ctrl Pts',(174.741324413032,1.49820114730575,135.490874566929));
#26458=CARTESIAN_POINT('Ctrl Pts',(174.73356811029,1.62837792208956,135.447242863246));
#26459=CARTESIAN_POINT('Ctrl Pts',(174.725811807548,1.75640576520965,135.398293774507));
#26460=CARTESIAN_POINT('Ctrl Pts',(174.718051365034,1.88450194064447,135.349318560164));
#26461=CARTESIAN_POINT('Ctrl Pts',(174.71029092252,2.01044654017648,135.295020460421));
#26462=CARTESIAN_POINT('Ctrl Pts',(174.702530480006,2.13377973632738,135.235632116734));
#26463=CARTESIAN_POINT('Ctrl Pts',(174.69475757974,2.2573109178738,135.176148437605));
#26464=CARTESIAN_POINT('Ctrl Pts',(174.686984679475,2.37822197393003,135.11155836997));
#26465=CARTESIAN_POINT('Ctrl Pts',(174.679211779209,2.49607887836731,135.042139905763));
#26466=CARTESIAN_POINT('Ctrl Pts',(174.671721443447,2.60965138746606,134.975244977583));
#26467=CARTESIAN_POINT('Ctrl Pts',(174.664231107685,2.72038768310657,134.903866773744));
#26468=CARTESIAN_POINT('Ctrl Pts',(174.656740771923,2.82792804334672,134.828289797379));
#26469=CARTESIAN_POINT('Ctrl Pts',(174.648966437804,2.93954582903031,134.749847296986));
#26470=CARTESIAN_POINT('Ctrl Pts',(174.641192103685,3.04807411910548,134.666632863708));
#26471=CARTESIAN_POINT('Ctrl Pts',(174.633417769566,3.15307781806533,134.578917987076));
#26472=CARTESIAN_POINT('Ctrl Pts',(174.625653016619,3.25795210935062,134.491311211191));
#26473=CARTESIAN_POINT('Ctrl Pts',(174.617888263672,3.35931015510609,134.399215275864));
#26474=CARTESIAN_POINT('Ctrl Pts',(174.610123510724,3.4567457158364,134.302944919615));
#26475=CARTESIAN_POINT('Ctrl Pts',(174.602366469839,3.5540845021942,134.206770180442));
#26476=CARTESIAN_POINT('Ctrl Pts',(174.594609428954,3.64750828016641,134.106429544268));
#26477=CARTESIAN_POINT('Ctrl Pts',(174.586852388069,3.73664408980739,134.002277753548));
#26478=CARTESIAN_POINT('Ctrl Pts',(174.579101196829,3.82571268144092,133.898204504504));
#26479=CARTESIAN_POINT('Ctrl Pts',(174.571350005589,3.91049948782595,133.790326117314));
#26480=CARTESIAN_POINT('Ctrl Pts',(174.563598814349,3.99066887837805,133.679033636475));
#26481=CARTESIAN_POINT('Ctrl Pts',(174.555850917572,4.07080419480064,133.56778845791));
#26482=CARTESIAN_POINT('Ctrl Pts',(174.548103020795,4.14632577066547,133.453132388349));
#26483=CARTESIAN_POINT('Ctrl Pts',(174.540355124018,4.21693885600655,133.335488774575));
#26484=CARTESIAN_POINT('Ctrl Pts',(174.532608847934,4.28753717061244,133.217869769308));
#26485=CARTESIAN_POINT('Ctrl Pts',(174.52486257185,4.35322883587855,133.09726479785));
#26486=CARTESIAN_POINT('Ctrl Pts',(174.517116295765,4.41376319360522,132.974125013365));
#26487=CARTESIAN_POINT('Ctrl Pts',(174.5093699625,4.47429799818273,132.85098431989));
#26488=CARTESIAN_POINT('Ctrl Pts',(174.501623629235,4.52967524677419,132.725309126912));
#26489=CARTESIAN_POINT('Ctrl Pts',(174.493877295969,4.57969107588829,132.59757357534));
#26490=CARTESIAN_POINT('Ctrl Pts',(174.486129227966,4.62971810570053,132.469809418277));
#26491=CARTESIAN_POINT('Ctrl Pts',(174.478381159963,4.67438118435536,132.339984348464));
#26492=CARTESIAN_POINT('Ctrl Pts',(174.47063309196,4.71352540584998,132.208590410337));
#26493=CARTESIAN_POINT('Ctrl Pts',(174.462876789219,4.75271123028905,132.07705682517));
#26494=CARTESIAN_POINT('Ctrl Pts',(174.455120486477,4.78636636878165,131.943951416142));
#26495=CARTESIAN_POINT('Ctrl Pts',(174.447364183735,4.8143862905749,131.809779787676));
#26496=CARTESIAN_POINT('Ctrl Pts',(174.439603741221,4.84242116744409,131.675536547772));
#26497=CARTESIAN_POINT('Ctrl Pts',(174.431843298707,4.86481477074275,131.540226340033));
#26498=CARTESIAN_POINT('Ctrl Pts',(174.424082856192,4.88151428033375,131.40436177873));
#26499=CARTESIAN_POINT('Ctrl Pts',(174.416309955927,4.89824059746005,131.268279115571));
#26500=CARTESIAN_POINT('Ctrl Pts',(174.408537055661,4.90925452348748,131.131640710474));
#26501=CARTESIAN_POINT('Ctrl Pts',(174.400764155396,4.91455533918001,130.994961983346));
#26502=CARTESIAN_POINT('Ctrl Pts',(174.393273819634,4.91966345687014,130.863251872223));
#26503=CARTESIAN_POINT('Ctrl Pts',(174.385783483872,4.91946662512228,130.731504627803));
#26504=CARTESIAN_POINT('Ctrl Pts',(174.37829314811,4.91400976598499,130.600176675239));
#26505=CARTESIAN_POINT('Ctrl Pts',(174.370518813991,4.90834600837489,130.463869383436));
#26506=CARTESIAN_POINT('Ctrl Pts',(174.362744479872,4.89699754063936,130.327582025503));
#26507=CARTESIAN_POINT('Ctrl Pts',(174.354970145753,4.87995759486065,130.191827406334));
#26508=CARTESIAN_POINT('Ctrl Pts',(174.347205392806,4.86293864929222,130.056240092601));
#26509=CARTESIAN_POINT('Ctrl Pts',(174.339440639859,4.84024223014815,129.921184595486));
#26510=CARTESIAN_POINT('Ctrl Pts',(174.331675886912,4.81191355348855,129.787172819638));
#26511=CARTESIAN_POINT('Ctrl Pts',(174.323918846027,4.78361301326998,129.653294146176));
#26512=CARTESIAN_POINT('Ctrl Pts',(174.316161805142,4.74969142825887,129.52045751106));
#26513=CARTESIAN_POINT('Ctrl Pts',(174.308404764257,4.71024565936873,129.389168443019));
#26514=CARTESIAN_POINT('Ctrl Pts',(174.300653573016,4.67082963683975,129.257978381086));
#26515=CARTESIAN_POINT('Ctrl Pts',(174.292902381776,4.6258978343061,129.128333936235));
#26516=CARTESIAN_POINT('Ctrl Pts',(174.285151190536,4.57559783204922,129.000728853085));
#26517=CARTESIAN_POINT('Ctrl Pts',(174.277403293759,4.52531920863508,128.873178005499));
#26518=CARTESIAN_POINT('Ctrl Pts',(174.269655396982,4.46967706655748,128.747665158614));
#26519=CARTESIAN_POINT('Ctrl Pts',(174.261907500205,4.40886825989597,128.6246671232));
#26520=CARTESIAN_POINT('Ctrl Pts',(174.254161224121,4.34807217312593,128.501694816323));
#26521=CARTESIAN_POINT('Ctrl Pts',(174.246414948037,4.28211174461267,128.381236624837));
#26522=CARTESIAN_POINT('Ctrl Pts',(174.238668671953,4.2112310554105,128.263747293889));
#26523=CARTESIAN_POINT('Ctrl Pts',(174.230922338687,4.14034984298321,128.146257095661));
#26524=CARTESIAN_POINT('Ctrl Pts',(174.223176005422,4.06454849935292,128.031736136464));
#26525=CARTESIAN_POINT('Ctrl Pts',(174.215429672157,3.98411573949752,127.92061221717));
#26526=CARTESIAN_POINT('Ctrl Pts',(174.207681604154,3.90366496728322,127.809463412444));
#26527=CARTESIAN_POINT('Ctrl Pts',(174.199933536151,3.81858094418172,127.70171347806));
#26528=CARTESIAN_POINT('Ctrl Pts',(174.192185468148,3.72919391063464,127.597758702862));
#26529=CARTESIAN_POINT('Ctrl Pts',(174.184429165406,3.63971187548456,127.493693443291));
#26530=CARTESIAN_POINT('Ctrl Pts',(174.176672862664,3.54591794955613,127.393431697254));
#26531=CARTESIAN_POINT('Ctrl Pts',(174.168916559922,3.44818101074379,127.297334700974));
#26532=CARTESIAN_POINT('Ctrl Pts',(174.161156117408,3.35039190678437,127.201186414834));
#26533=CARTESIAN_POINT('Ctrl Pts',(174.153395674894,3.24865588640648,127.10920756974));
#26534=CARTESIAN_POINT('Ctrl Pts',(174.145635232379,3.14337567593979,127.021719685306));
#26535=CARTESIAN_POINT('Ctrl Pts',(174.137862332114,3.03792646033292,126.934091357552));
#26536=CARTESIAN_POINT('Ctrl Pts',(174.130089431849,2.92892199637252,126.850968634122));
#26537=CARTESIAN_POINT('Ctrl Pts',(174.122316531583,2.81679553265813,126.772630717176));
#26538=CARTESIAN_POINT('Ctrl Pts',(174.114826195821,2.70874514832878,126.697140580833));
#26539=CARTESIAN_POINT('Ctrl Pts',(174.107335860059,2.59779606795384,126.626093577242));
#26540=CARTESIAN_POINT('Ctrl Pts',(174.099845524297,2.48435657640448,126.559698621155));
#26541=CARTESIAN_POINT('Ctrl Pts',(174.092071190178,2.36661599205441,126.490786280128));
#26542=CARTESIAN_POINT('Ctrl Pts',(174.084296856059,2.24581945395365,126.426667421473));
#26543=CARTESIAN_POINT('Ctrl Pts',(174.07652252194,2.12239474115937,126.367624922801));
#26544=CARTESIAN_POINT('Ctrl Pts',(174.068757768993,1.99912213829291,126.308655188733));
#26545=CARTESIAN_POINT('Ctrl Pts',(174.060993016045,1.87322815466102,126.25474953385));
#26546=CARTESIAN_POINT('Ctrl Pts',(174.053228263098,1.7451679105289,126.206146613568));
#26547=CARTESIAN_POINT('Ctrl Pts',(174.045471222213,1.61723485763655,126.157591966392));
#26548=CARTESIAN_POINT('Ctrl Pts',(174.037714181328,1.48714018910576,126.114329710576));
#26549=CARTESIAN_POINT('Ctrl Pts',(174.029957140443,1.35536157626157,126.076551604916));
#26550=CARTESIAN_POINT('Ctrl Pts',(174.022205949203,1.22368233869441,126.038801988019));
#26551=CARTESIAN_POINT('Ctrl Pts',(174.014454757963,1.09032205872987,126.006528396842));
#26552=CARTESIAN_POINT('Ctrl Pts',(174.006703566723,0.955775908446305,125.979873548941));
#26553=CARTESIAN_POINT('Ctrl Pts',(173.998955669946,0.821286943865748,125.953230030061));
#26554=CARTESIAN_POINT('Ctrl Pts',(173.991207773169,0.6856134941453,125.932200580495));
#26555=CARTESIAN_POINT('Ctrl Pts',(173.983459876392,0.549263118127799,125.916877309199));
#26556=CARTESIAN_POINT('Ctrl Pts',(173.975713600308,0.412941263669539,125.901557243201));
#26557=CARTESIAN_POINT('Ctrl Pts',(173.967967324224,0.275943152834509,125.891941024953));
#26558=CARTESIAN_POINT('Ctrl Pts',(173.960221048139,0.138783307366114,125.88806910301));
#26559=CARTESIAN_POINT('Ctrl Pts',(173.952474714874,0.00162244941485037,
125.884197152486));
#26560=CARTESIAN_POINT('Ctrl Pts',(173.944728381609,-0.135699754742573,
125.886069593912));
#26561=CARTESIAN_POINT('Ctrl Pts',(173.936982048343,-0.272667326619256,
125.893674760021));
#26562=CARTESIAN_POINT('Ctrl Pts',(173.92923398034,-0.409665571433761,125.901281629254));
#26563=CARTESIAN_POINT('Ctrl Pts',(173.921485912337,-0.546308635646817,
125.914623756121));
#26564=CARTESIAN_POINT('Ctrl Pts',(173.913737844334,-0.682084607205077,
125.933637503786));
#26565=CARTESIAN_POINT('Ctrl Pts',(173.905981541593,-0.818004883081849,
125.952671459487));
#26566=CARTESIAN_POINT('Ctrl Pts',(173.898225238851,-0.953055837591119,
125.977389022991));
#26567=CARTESIAN_POINT('Ctrl Pts',(173.890468936109,-1.08673416495545,126.007675103879));
#26568=CARTESIAN_POINT('Ctrl Pts',(173.882708493595,-1.22048384046815,126.03797734936));
#26569=CARTESIAN_POINT('Ctrl Pts',(173.874948051081,-1.35285905187628,126.073853932136));
#26570=CARTESIAN_POINT('Ctrl Pts',(173.867187608566,-1.48337161220605,126.115139816345));
#26571=CARTESIAN_POINT('Ctrl Pts',(173.859414708301,-1.61409368288399,126.156491976321));
#26572=CARTESIAN_POINT('Ctrl Pts',(173.851641808036,-1.74294675961674,126.203270656618));
#26573=CARTESIAN_POINT('Ctrl Pts',(173.84386890777,-1.86946176026684,126.255262268508));
#26574=CARTESIAN_POINT('Ctrl Pts',(173.836378572008,-1.99137762197043,126.305363854347));
#26575=CARTESIAN_POINT('Ctrl Pts',(173.828888236246,-2.11112216627042,126.360305817047));
#26576=CARTESIAN_POINT('Ctrl Pts',(173.821397900484,-2.22829893932381,126.419857578508));
#26577=CARTESIAN_POINT('Ctrl Pts',(173.813622735437,-2.34993150416124,126.481673869385));
#26578=CARTESIAN_POINT('Ctrl Pts',(173.805847570389,-2.469182484828,126.548653319388));
#26579=CARTESIAN_POINT('Ctrl Pts',(173.798072405342,-2.58558251387288,126.620588859158));
#26580=CARTESIAN_POINT('Ctrl Pts',(173.790307006116,-2.70183634127263,126.692434045906));
#26581=CARTESIAN_POINT('Ctrl Pts',(173.78254160689,-2.81524601298638,126.769222731812));
#26582=CARTESIAN_POINT('Ctrl Pts',(173.774776207664,-2.92536462976308,126.850700940073));
#26583=CARTESIAN_POINT('Ctrl Pts',(173.766866450566,-3.03753033887832,126.933693818794));
#26584=CARTESIAN_POINT('Ctrl Pts',(173.758956693467,-3.14628104028566,127.021552147574));
#26585=CARTESIAN_POINT('Ctrl Pts',(173.751046936369,-3.25117224834878,127.113959274342));
#26586=CARTESIAN_POINT('Ctrl Pts',(173.743296109138,-3.35395588905281,127.204509675007));
#26587=CARTESIAN_POINT('Ctrl Pts',(173.735545281908,-3.45303335142762,127.299427539009));
#26588=CARTESIAN_POINT('Ctrl Pts',(173.727794454678,-3.54801762590248,127.398372656814));
#26589=CARTESIAN_POINT('Ctrl Pts',(173.720047155673,-3.64295866294001,127.497272734182));
#26590=CARTESIAN_POINT('Ctrl Pts',(173.712299856667,-3.7338099494695,127.600196136174));
#26591=CARTESIAN_POINT('Ctrl Pts',(173.704552557662,-3.82022046937444,127.706764997109));
#26592=CARTESIAN_POINT('Ctrl Pts',(173.696807107526,-3.90661036767271,127.813308425711));
#26593=CARTESIAN_POINT('Ctrl Pts',(173.689061657391,-3.98856136312799,127.923495277988));
#26594=CARTESIAN_POINT('Ctrl Pts',(173.681316207255,-4.06576222993557,128.036914041364));
#26595=CARTESIAN_POINT('Ctrl Pts',(173.673285026425,-4.14581104706803,128.154516838126));
#26596=CARTESIAN_POINT('Ctrl Pts',(173.665253845595,-4.22075226631428,128.275594224663));
#26597=CARTESIAN_POINT('Ctrl Pts',(173.657222664766,-4.29028791897018,128.399654266504));
#26598=CARTESIAN_POINT('Ctrl Pts',(173.649473245828,-4.35738401790963,128.519361848497));
#26599=CARTESIAN_POINT('Ctrl Pts',(173.64172382689,-4.41944728697983,128.641845955821));
#26600=CARTESIAN_POINT('Ctrl Pts',(173.633974407952,-4.47625713219153,128.766640040793));
#26601=CARTESIAN_POINT('Ctrl Pts',(173.626222377563,-4.53308612156845,128.891476179719));
#26602=CARTESIAN_POINT('Ctrl Pts',(173.618470347174,-4.58465800978425,129.018623486625));
#26603=CARTESIAN_POINT('Ctrl Pts',(173.610718316784,-4.63080065760616,129.147596200995));
#26604=CARTESIAN_POINT('Ctrl Pts',(173.60295954152,-4.67698345315476,129.276681131754));
#26605=CARTESIAN_POINT('Ctrl Pts',(173.595200766255,-4.71772746156828,129.407594268184));
#26606=CARTESIAN_POINT('Ctrl Pts',(173.587441990991,-4.75291059024451,129.539835416694));
#26607=CARTESIAN_POINT('Ctrl Pts',(173.586608673094,-4.75668937359732,129.55403854954));
#26608=CARTESIAN_POINT('Ctrl Pts',(173.585775355196,-4.76040405828026,129.568256992362));
#26609=CARTESIAN_POINT('Ctrl Pts',(173.584942037299,-4.76405452823404,129.582490119308));
#26610=CARTESIAN_POINT('Ctrl Pts',(175.334949039109,-4.76405452823403,129.582490119308));
#26611=CARTESIAN_POINT('Ctrl Pts',(175.327312301175,-4.79766811449444,129.71354898198));
#26612=CARTESIAN_POINT('Ctrl Pts',(175.319675563241,-4.82585603888722,129.845944000492));
#26613=CARTESIAN_POINT('Ctrl Pts',(175.312038825307,-4.84853163743738,129.979179411243));
#26614=CARTESIAN_POINT('Ctrl Pts',(175.304175593761,-4.87187975850474,130.116366374303));
#26615=CARTESIAN_POINT('Ctrl Pts',(175.296312362215,-4.8893834241265,130.254443897876));
#26616=CARTESIAN_POINT('Ctrl Pts',(175.288449130669,-4.90100548934506,130.392865470681));
#26617=CARTESIAN_POINT('Ctrl Pts',(175.280585899123,-4.91262755456361,130.531287043487));
#26618=CARTESIAN_POINT('Ctrl Pts',(175.272722667577,-4.9183680466244,130.670052201154));
#26619=CARTESIAN_POINT('Ctrl Pts',(175.264859436032,-4.91824815910515,130.808615962297));
#26620=CARTESIAN_POINT('',(175.610140563974,-4.9182499975673,130.80451530825));
#26621=CARTESIAN_POINT('Ctrl Pts',(175.679864508177,-4.76405452823404,129.582490119308));
#26622=CARTESIAN_POINT('Ctrl Pts',(175.671751454559,-4.79965799329642,129.721307489228));
#26623=CARTESIAN_POINT('Ctrl Pts',(175.66363840094,-4.82922619760711,129.861823675682));
#26624=CARTESIAN_POINT('Ctrl Pts',(175.655525347322,-4.85260786805939,130.003498618625));
#26625=CARTESIAN_POINT('Ctrl Pts',(175.647426424684,-4.87594881328887,130.144926798034));
#26626=CARTESIAN_POINT('Ctrl Pts',(175.639327502045,-4.89312465678322,130.287509379538));
#26627=CARTESIAN_POINT('Ctrl Pts',(175.631228579407,-4.90403474638115,130.430694631977));
#26628=CARTESIAN_POINT('Ctrl Pts',(175.624199240941,-4.9135039950584,130.554970124867));
#26629=CARTESIAN_POINT('Ctrl Pts',(175.617169902474,-4.91825392331427,130.679699262973));
#26630=CARTESIAN_POINT('Ctrl Pts',(175.610140564008,-4.91824999756732,130.804515307654));
#26631=CARTESIAN_POINT('Ctrl Pts',(175.610140563974,-4.9182499975673,130.80451530825));
#26632=CARTESIAN_POINT('Ctrl Pts',(175.602006617861,-4.91824545490126,130.948945255158));
#26633=CARTESIAN_POINT('Ctrl Pts',(175.593872671748,-4.91187459119385,131.093245944634));
#26634=CARTESIAN_POINT('Ctrl Pts',(175.585738725635,-4.89919723011719,131.236852886759));
#26635=CARTESIAN_POINT('Ctrl Pts',(175.577593375339,-4.8865020947703,131.380661172728));
#26636=CARTESIAN_POINT('Ctrl Pts',(175.569448025042,-4.86748284501924,131.52377344223));
#26637=CARTESIAN_POINT('Ctrl Pts',(175.561302674745,-4.84225068832209,131.665633706629));
#26638=CARTESIAN_POINT('Ctrl Pts',(175.553137416072,-4.81695686070191,131.807840697373));
#26639=CARTESIAN_POINT('Ctrl Pts',(175.544972157399,-4.78541982124724,131.948789238779));
#26640=CARTESIAN_POINT('Ctrl Pts',(175.536806898725,-4.74780158491423,132.087934991253));
#26641=CARTESIAN_POINT('Ctrl Pts',(175.52863104151,-4.7101345199425,132.227261355535));
#26642=CARTESIAN_POINT('Ctrl Pts',(175.520455184294,-4.66637060377285,132.364779946843));
#26643=CARTESIAN_POINT('Ctrl Pts',(175.512279327079,-4.61672068197947,132.499964700801));
#26644=CARTESIAN_POINT('Ctrl Pts',(175.5040846359,-4.56695638626696,132.635460867336));
#26645=CARTESIAN_POINT('Ctrl Pts',(175.49588994472,-4.51127910012212,132.768612141795));
#26646=CARTESIAN_POINT('Ctrl Pts',(175.487695253541,-4.44994722009171,132.898913744345));
#26647=CARTESIAN_POINT('Ctrl Pts',(175.482628384762,-4.41202503592258,132.979480675718));
#26648=CARTESIAN_POINT('Ctrl Pts',(175.477561515982,-4.37194195059445,133.058958661978));
#26649=CARTESIAN_POINT('Ctrl Pts',(175.472494647203,-4.32976738006333,133.137233845377));
#26650=CARTESIAN_POINT('Ctrl Pts',(175.464720313084,-4.26505696088523,133.257335125965));
#26651=CARTESIAN_POINT('Ctrl Pts',(175.456945978965,-4.19524311273341,133.374932142333));
#26652=CARTESIAN_POINT('Ctrl Pts',(175.449171644846,-4.12054403631122,133.489560779066));
#26653=CARTESIAN_POINT('Ctrl Pts',(175.441406891898,-4.04593701982468,133.604048146249));
#26654=CARTESIAN_POINT('Ctrl Pts',(175.433642138951,-3.9664569656865,133.715574088242));
#26655=CARTESIAN_POINT('Ctrl Pts',(175.425877386004,-3.88236842902149,133.823698035583));
#26656=CARTESIAN_POINT('Ctrl Pts',(175.418120345119,-3.79836341027648,133.931714592695));
#26657=CARTESIAN_POINT('Ctrl Pts',(175.410363304234,-3.70975925632101,134.036335572715));
#26658=CARTESIAN_POINT('Ctrl Pts',(175.402606263349,-3.61686417682021,134.137148727983));
#26659=CARTESIAN_POINT('Ctrl Pts',(175.394855072109,-3.52403915022179,134.237885859265));
#26660=CARTESIAN_POINT('Ctrl Pts',(175.387103880869,-3.4269299026427,134.334820595012));
#26661=CARTESIAN_POINT('Ctrl Pts',(175.379352689629,-3.32588510062422,134.427573468055));
#26662=CARTESIAN_POINT('Ctrl Pts',(175.371604792852,-3.22488324534181,134.520286918652));
#26663=CARTESIAN_POINT('Ctrl Pts',(175.363856896075,-3.11994944993998,134.608821777836));
#26664=CARTESIAN_POINT('Ctrl Pts',(175.356108999298,-3.01146928550664,134.692835357737));
#26665=CARTESIAN_POINT('Ctrl Pts',(175.348362723214,-2.90301181278509,134.776831363809));
#26666=CARTESIAN_POINT('Ctrl Pts',(175.340616447129,-2.79100975547024,134.856307732517));
#26667=CARTESIAN_POINT('Ctrl Pts',(175.332870171045,-2.67588150403046,134.93096227497));
#26668=CARTESIAN_POINT('Ctrl Pts',(175.32512383778,-2.56075240274012,135.005617368506));
#26669=CARTESIAN_POINT('Ctrl Pts',(175.317377504515,-2.44249738931157,135.075450352049));
#26670=CARTESIAN_POINT('Ctrl Pts',(175.309631171249,-2.3215632079231,135.140202788831));
#26671=CARTESIAN_POINT('Ctrl Pts',(175.301883103246,-2.20060194416336,135.204969726472));
#26672=CARTESIAN_POINT('Ctrl Pts',(175.294135035243,-2.07696066315284,135.264653668843));
#26673=CARTESIAN_POINT('Ctrl Pts',(175.28638696724,-1.95110966959261,135.319042679431));
#26674=CARTESIAN_POINT('Ctrl Pts',(175.278630664499,-1.82512492009864,135.373489495306));
#26675=CARTESIAN_POINT('Ctrl Pts',(175.270874361757,-1.69692612611241,135.422629982482));
#26676=CARTESIAN_POINT('Ctrl Pts',(175.263118059015,-1.5670030071668,135.466300625549));
#26677=CARTESIAN_POINT('Ctrl Pts',(175.255357616501,-1.43701054434061,135.509994576953));
#26678=CARTESIAN_POINT('Ctrl Pts',(175.247597173987,-1.30529229802676,135.548212758163));
#26679=CARTESIAN_POINT('Ctrl Pts',(175.239836731472,-1.17235105601835,135.580842174523));
#26680=CARTESIAN_POINT('Ctrl Pts',(175.232063831207,-1.03919640492635,135.613523970519));
#26681=CARTESIAN_POINT('Ctrl Pts',(175.224290930941,-0.904815218402296,
135.640598996321));
#26682=CARTESIAN_POINT('Ctrl Pts',(175.216518030676,-0.769719223808543,
135.662005662132));
#26683=CARTESIAN_POINT('Ctrl Pts',(175.209027694914,-0.639534308903681,
135.682634141721));
#26684=CARTESIAN_POINT('Ctrl Pts',(175.201537359152,-0.508685959715356,
135.697999188744));
#26685=CARTESIAN_POINT('Ctrl Pts',(175.19404702339,-0.377632712410248,135.708091503026));
#26686=CARTESIAN_POINT('Ctrl Pts',(175.186272689271,-0.241610541401607,
135.718566470472));
#26687=CARTESIAN_POINT('Ctrl Pts',(175.178498355152,-0.104936750786517,
135.723394162604));
#26688=CARTESIAN_POINT('Ctrl Pts',(175.170724021032,0.0318802431817009,
135.722507292137));
#26689=CARTESIAN_POINT('Ctrl Pts',(175.162959268085,0.168528622432492,135.721621514658));
#26690=CARTESIAN_POINT('Ctrl Pts',(175.155194515138,0.305319466679357,135.715035189939));
#26691=CARTESIAN_POINT('Ctrl Pts',(175.147429762191,0.44173911385091,135.702732757144));
#26692=CARTESIAN_POINT('Ctrl Pts',(175.139672721306,0.578023267105712,135.690442543298));
#26693=CARTESIAN_POINT('Ctrl Pts',(175.131915680421,0.713936570106025,135.672447554386));
#26694=CARTESIAN_POINT('Ctrl Pts',(175.124158639536,0.848965592368096,135.648784265997));
#26695=CARTESIAN_POINT('Ctrl Pts',(175.116407448296,0.98389278819383,135.625138822278));
#26696=CARTESIAN_POINT('Ctrl Pts',(175.108656257056,1.11793664705349,135.595833654446));
#26697=CARTESIAN_POINT('Ctrl Pts',(175.100905065816,1.25058944968992,135.560956994265));
#26698=CARTESIAN_POINT('Ctrl Pts',(175.093157169039,1.38318587134687,135.526095157595));
#26699=CARTESIAN_POINT('Ctrl Pts',(175.085409272261,1.51439203538062,135.485666637616));
#26700=CARTESIAN_POINT('Ctrl Pts',(175.077661375484,1.64371121819141,135.439810595043));
#26701=CARTESIAN_POINT('Ctrl Pts',(175.0699150994,1.77300335021696,135.393964144565));
#26702=CARTESIAN_POINT('Ctrl Pts',(175.062168823316,1.90040891787971,135.342692560288));
#26703=CARTESIAN_POINT('Ctrl Pts',(175.054422547232,2.02544753083894,135.286184505485));
#26704=CARTESIAN_POINT('Ctrl Pts',(175.046676213967,2.15048706680477,135.229676033552));
#26705=CARTESIAN_POINT('Ctrl Pts',(175.038929880701,2.27315925692985,135.167931174969));
#26706=CARTESIAN_POINT('Ctrl Pts',(175.031183547436,2.39300519490094,135.101186096879));
#26707=CARTESIAN_POINT('Ctrl Pts',(175.023435479433,2.51287797153889,135.034426071693));
#26708=CARTESIAN_POINT('Ctrl Pts',(175.01568741143,2.62992289508509,134.962663788988));
#26709=CARTESIAN_POINT('Ctrl Pts',(175.007939343427,2.74370744617025,134.886180372569));
#26710=CARTESIAN_POINT('Ctrl Pts',(175.000183040685,2.85761292883036,134.809615668664));
#26711=CARTESIAN_POINT('Ctrl Pts',(174.992426737943,2.96825079200132,134.728320026146));
#26712=CARTESIAN_POINT('Ctrl Pts',(174.984670435201,3.07521876016915,134.642617075856));
#26713=CARTESIAN_POINT('Ctrl Pts',(174.976909992687,3.18224382036244,134.55686838332));
#26714=CARTESIAN_POINT('Ctrl Pts',(174.969149550173,3.28559478813973,134.466707952717));
#26715=CARTESIAN_POINT('Ctrl Pts',(174.961389107659,3.38490482881226,134.372497717284));
#26716=CARTESIAN_POINT('Ctrl Pts',(174.953616207393,3.48437429077838,134.278136247217));
#26717=CARTESIAN_POINT('Ctrl Pts',(174.945843307128,3.5797895905496,134.179712261912));
#26718=CARTESIAN_POINT('Ctrl Pts',(174.938070406862,3.67082230974587,134.077623001301));
#26719=CARTESIAN_POINT('Ctrl Pts',(174.9305800711,3.75854576030193,133.97924494246));
#26720=CARTESIAN_POINT('Ctrl Pts',(174.923089735338,3.84219953840779,133.877463703698));
#26721=CARTESIAN_POINT('Ctrl Pts',(174.915599399576,3.92152796956395,133.772660037508));
#26722=CARTESIAN_POINT('Ctrl Pts',(174.907825065457,4.0038641622986,133.66388270846));
#26723=CARTESIAN_POINT('Ctrl Pts',(174.900050731338,4.08180135868748,133.551504663133));
#26724=CARTESIAN_POINT('Ctrl Pts',(174.892276397219,4.15500813662662,133.435917276098));
#26725=CARTESIAN_POINT('Ctrl Pts',(174.884511644272,4.22812469375459,133.320472340188));
#26726=CARTESIAN_POINT('Ctrl Pts',(174.876746891325,4.29652222485149,133.201826259415));
#26727=CARTESIAN_POINT('Ctrl Pts',(174.868982138378,4.35990999124917,133.080402781214));
#26728=CARTESIAN_POINT('Ctrl Pts',(174.861225097493,4.42323480002363,132.959099902525));
#26729=CARTESIAN_POINT('Ctrl Pts',(174.853468056608,4.4815595663455,132.835025460387));
#26730=CARTESIAN_POINT('Ctrl Pts',(174.845711015723,4.53463745644448,132.708631134355));
#26731=CARTESIAN_POINT('Ctrl Pts',(174.837959824483,4.58767532009363,132.582332123267));
#26732=CARTESIAN_POINT('Ctrl Pts',(174.830208633243,4.63547403234835,132.453717069458));
#26733=CARTESIAN_POINT('Ctrl Pts',(174.822457442003,4.67783339042948,132.323260822939));
#26734=CARTESIAN_POINT('Ctrl Pts',(174.814709545225,4.72017474465348,132.192860023806));
#26735=CARTESIAN_POINT('Ctrl Pts',(174.806961648448,4.75708122234953,132.060619959483));
#26736=CARTESIAN_POINT('Ctrl Pts',(174.799213751671,4.78840141212789,131.927033757367));
#26737=CARTESIAN_POINT('Ctrl Pts',(174.791467475587,4.81971505039774,131.793475498606));
#26738=CARTESIAN_POINT('Ctrl Pts',(174.783721199503,4.84544463583429,131.658572042538));
#26739=CARTESIAN_POINT('Ctrl Pts',(174.775974923419,4.86548923347927,131.522829532271));
#26740=CARTESIAN_POINT('Ctrl Pts',(174.768228590154,4.88553397908892,131.387086019983));
#26741=CARTESIAN_POINT('Ctrl Pts',(174.760482256888,4.89989359605523,131.250503827908));
#26742=CARTESIAN_POINT('Ctrl Pts',(174.752735923623,4.90851872841307,131.113596701033));
#26743=CARTESIAN_POINT('Ctrl Pts',(174.74498785562,4.9171457923095,130.976658914757));
#26744=CARTESIAN_POINT('Ctrl Pts',(174.737239787617,4.92003579161466,130.839396439));
#26745=CARTESIAN_POINT('Ctrl Pts',(174.729491719614,4.91719145646168,130.70232511884));
#26746=CARTESIAN_POINT('Ctrl Pts',(174.721735416872,4.91434409831544,130.56510811765));
#26747=CARTESIAN_POINT('Ctrl Pts',(174.71397911413,4.90575023937708,130.4280830694));
#26748=CARTESIAN_POINT('Ctrl Pts',(174.706222811389,4.89146471969663,130.291763350247));
#26749=CARTESIAN_POINT('Ctrl Pts',(174.698462368875,4.87717157540419,130.155370873155));
#26750=CARTESIAN_POINT('Ctrl Pts',(174.69070192636,4.85718077423298,130.019684861881));
#26751=CARTESIAN_POINT('Ctrl Pts',(174.682941483846,4.83159853775673,129.885209578592));
#26752=CARTESIAN_POINT('Ctrl Pts',(174.675168583581,4.8059752344034,129.75051842364));
#26753=CARTESIAN_POINT('Ctrl Pts',(174.667395683315,4.77474264822851,129.617042261444));
#26754=CARTESIAN_POINT('Ctrl Pts',(174.65962278305,4.73805747028144,129.485272117574));
#26755=CARTESIAN_POINT('Ctrl Pts',(174.652132447288,4.70270589095705,129.358292150343));
#26756=CARTESIAN_POINT('Ctrl Pts',(174.644642111526,4.66229136261598,129.232896611929));
#26757=CARTESIAN_POINT('Ctrl Pts',(174.637151775764,4.61699602480054,129.109506414551));
#26758=CARTESIAN_POINT('Ctrl Pts',(174.629377441645,4.56998330048471,128.981437840337));
#26759=CARTESIAN_POINT('Ctrl Pts',(174.621603107526,4.51756342660974,128.855123991234));
#26760=CARTESIAN_POINT('Ctrl Pts',(174.613828773407,4.45988653594367,128.731055249559));
#26761=CARTESIAN_POINT('Ctrl Pts',(174.60606402046,4.40228072689065,128.607139411519));
#26762=CARTESIAN_POINT('Ctrl Pts',(174.598299267512,4.33943095516473,128.485463526739));
#26763=CARTESIAN_POINT('Ctrl Pts',(174.590534514565,4.27153658013364,128.366501247733));
#26764=CARTESIAN_POINT('Ctrl Pts',(174.58277747368,4.20370963875299,128.24765712374));
#26765=CARTESIAN_POINT('Ctrl Pts',(174.575020432795,4.13084825746991,128.131521579328));
#26766=CARTESIAN_POINT('Ctrl Pts',(174.56726339191,4.05319902740399,128.018546426571));
#26767=CARTESIAN_POINT('Ctrl Pts',(174.55951220067,3.97560835322643,127.905656469254));
#26768=CARTESIAN_POINT('Ctrl Pts',(174.55176100943,3.89323723741079,127.795922480723));
#26769=CARTESIAN_POINT('Ctrl Pts',(174.54400981819,3.80637697022949,127.689769565276));
#26770=CARTESIAN_POINT('Ctrl Pts',(174.536261921413,3.71955362097885,127.583661767649));
#26771=CARTESIAN_POINT('Ctrl Pts',(174.528514024636,3.6282451623162,127.481132317808));
#26772=CARTESIAN_POINT('Ctrl Pts',(174.520766127859,3.53278463473215,127.382575149846));
#26773=CARTESIAN_POINT('Ctrl Pts',(174.513019851775,3.43734407543255,127.284038597919));
#26774=CARTESIAN_POINT('Ctrl Pts',(174.505273575691,3.33775344658681,127.189472955786));
#26775=CARTESIAN_POINT('Ctrl Pts',(174.497527299606,3.23438402291478,127.099236725601));
#26776=CARTESIAN_POINT('Ctrl Pts',(174.489780966341,3.13101383619319,127.008999829311));
#26777=CARTESIAN_POINT('Ctrl Pts',(174.482034633076,3.02386509351492,126.92309266585));
#26778=CARTESIAN_POINT('Ctrl Pts',(174.47428829981,2.91334334498373,126.841834451502));
#26779=CARTESIAN_POINT('Ctrl Pts',(174.466540231807,2.8027968458733,126.760558039941));
#26780=CARTESIAN_POINT('Ctrl Pts',(174.458792163804,2.68887615276026,126.683932880708));
#26781=CARTESIAN_POINT('Ctrl Pts',(174.451044095801,2.57201673642119,126.612235503728));
#26782=CARTESIAN_POINT('Ctrl Pts',(174.44328779306,2.45503312050375,126.540461925923));
#26783=CARTESIAN_POINT('Ctrl Pts',(174.435531490318,2.335104875987,126.473626797237));
#26784=CARTESIAN_POINT('Ctrl Pts',(174.427775187576,2.21269356315809,126.411961471534));
#26785=CARTESIAN_POINT('Ctrl Pts',(174.420014745062,2.09021691572571,126.350263233191));
#26786=CARTESIAN_POINT('Ctrl Pts',(174.412254302548,1.96525491527737,126.293740456976));
#26787=CARTESIAN_POINT('Ctrl Pts',(174.404493860033,1.83828922721223,126.242576341692));
#26788=CARTESIAN_POINT('Ctrl Pts',(174.396720959768,1.71111972255312,126.191330093227));
#26789=CARTESIAN_POINT('Ctrl Pts',(174.388948059502,1.5819404713301,126.145459826525));
#26790=CARTESIAN_POINT('Ctrl Pts',(174.381175159237,1.45124928260237,126.105099124284));
#26791=CARTESIAN_POINT('Ctrl Pts',(174.373684823475,1.32530904777689,126.066205635232));
#26792=CARTESIAN_POINT('Ctrl Pts',(174.366194487713,1.1979651901758,126.032428171055));
#26793=CARTESIAN_POINT('Ctrl Pts',(174.358704151951,1.06967028604185,126.003841005934));
#26794=CARTESIAN_POINT('Ctrl Pts',(174.350929817832,0.936511041622508,125.974169949759));
#26795=CARTESIAN_POINT('Ctrl Pts',(174.343155483713,0.801905400721561,125.94999655343));
#26796=CARTESIAN_POINT('Ctrl Pts',(174.335381149594,0.666347086299638,125.931459569619));
#26797=CARTESIAN_POINT('Ctrl Pts',(174.327616396647,0.530955835385183,125.912945430984));
#26798=CARTESIAN_POINT('Ctrl Pts',(174.3198516437,0.394614630670574,125.900053936113));
#26799=CARTESIAN_POINT('Ctrl Pts',(174.312086890753,0.257829728039735,125.892873379077));
#26800=CARTESIAN_POINT('Ctrl Pts',(174.304329849868,0.121180682102519,125.885699953872));
#26801=CARTESIAN_POINT('Ctrl Pts',(174.296572808983,-0.0159107968626869,
125.884226198964));
#26802=CARTESIAN_POINT('Ctrl Pts',(174.288815768098,-0.152931298038684,
125.888488865722));
#26803=CARTESIAN_POINT('Ctrl Pts',(174.281064576857,-0.289848470988973,
125.89274831797));
#26804=CARTESIAN_POINT('Ctrl Pts',(174.273313385617,-0.426694383493149,
125.902735569373));
#26805=CARTESIAN_POINT('Ctrl Pts',(174.265562194377,-0.562953933757235,
125.918435328435));
#26806=CARTESIAN_POINT('Ctrl Pts',(174.2578142976,-0.699155570077616,125.934128414681));
#26807=CARTESIAN_POINT('Ctrl Pts',(174.250066400823,-0.834770952254194,
125.955529134883));
#26808=CARTESIAN_POINT('Ctrl Pts',(174.242318504046,-0.969288635856963,
125.982570223646));
#26809=CARTESIAN_POINT('Ctrl Pts',(174.234572227962,-1.10377818126019,126.009605655996));
#26810=CARTESIAN_POINT('Ctrl Pts',(174.226825951878,-1.23717010175166,126.04227903313));
#26811=CARTESIAN_POINT('Ctrl Pts',(174.219079675794,-1.36896209626315,126.080471770282));
#26812=CARTESIAN_POINT('Ctrl Pts',(174.211333342528,-1.50075506363308,126.118664789363));
#26813=CARTESIAN_POINT('Ctrl Pts',(174.203587009263,-1.63094770594155,126.162377140939));
#26814=CARTESIAN_POINT('Ctrl Pts',(174.195840675997,-1.75905224774906,126.211440168419));
#26815=CARTESIAN_POINT('Ctrl Pts',(174.188092607994,-1.8871854776808,126.260514183225));
#26816=CARTESIAN_POINT('Ctrl Pts',(174.180344539991,-2.01322931157661,126.314941118504));
#26817=CARTESIAN_POINT('Ctrl Pts',(174.172596471988,-2.13671571438622,126.374504071537));
#26818=CARTESIAN_POINT('Ctrl Pts',(174.164840169247,-2.26033336001404,126.434130328786));
#26819=CARTESIAN_POINT('Ctrl Pts',(174.157083866505,-2.38138779221869,126.498903337848));
#26820=CARTESIAN_POINT('Ctrl Pts',(174.149327563763,-2.49943488183132,126.568559827398));
#26821=CARTESIAN_POINT('Ctrl Pts',(174.141567121249,-2.61754497673016,126.638253494714));
#26822=CARTESIAN_POINT('Ctrl Pts',(174.133806678735,-2.73264420277672,126.71283562361));
#26823=CARTESIAN_POINT('Ctrl Pts',(174.12604623622,-2.84431807771759,126.79199999877));
#26824=CARTESIAN_POINT('Ctrl Pts',(174.118273335955,-2.95617122147637,126.871291455612));
#26825=CARTESIAN_POINT('Ctrl Pts',(174.110500435689,-3.06458771663076,126.955179618617));
#26826=CARTESIAN_POINT('Ctrl Pts',(174.102727535424,-3.16918609831779,127.043317871634));
#26827=CARTESIAN_POINT('Ctrl Pts',(174.095237199662,-3.26998206536386,127.128252077148));
#26828=CARTESIAN_POINT('Ctrl Pts',(174.0877468639,-3.36723246818446,127.217132526666));
#26829=CARTESIAN_POINT('Ctrl Pts',(174.080256528138,-3.46063018929389,127.309618601988));
#26830=CARTESIAN_POINT('Ctrl Pts',(174.072592942127,-3.55618818451548,127.404243865203));
#26831=CARTESIAN_POINT('Ctrl Pts',(174.064929356116,-3.64803424359307,127.502961956952));
#26832=CARTESIAN_POINT('Ctrl Pts',(174.057265770104,-3.73578973359036,127.605445468816));
#26833=CARTESIAN_POINT('Ctrl Pts',(174.049611137343,-3.82344270020136,127.707809250773));
#26834=CARTESIAN_POINT('Ctrl Pts',(174.041956504581,-3.9070143390471,127.813929404798));
#26835=CARTESIAN_POINT('Ctrl Pts',(174.034301871819,-3.98616111841343,127.923440174279));
#26836=CARTESIAN_POINT('Ctrl Pts',(174.026654411474,-4.06523373698538,128.032848331806));
#26837=CARTESIAN_POINT('Ctrl Pts',(174.019006951128,-4.13988950626791,128.145640462903));
#26838=CARTESIAN_POINT('Ctrl Pts',(174.011359490783,-4.20982401111621,128.261416485673));
#26839=CARTESIAN_POINT('Ctrl Pts',(174.003717703085,-4.27970664072984,128.3771066294));
#26840=CARTESIAN_POINT('Ctrl Pts',(173.996075915387,-4.3448747666291,128.495775917224));
#26841=CARTESIAN_POINT('Ctrl Pts',(173.988434127689,-4.40506665823473,128.616994439029));
#26842=CARTESIAN_POINT('Ctrl Pts',(173.980795658444,-4.46523241146658,128.7381603216));
#26843=CARTESIAN_POINT('Ctrl Pts',(173.973157189198,-4.52042605048181,128.861872875672));
#26844=CARTESIAN_POINT('Ctrl Pts',(173.965518719952,-4.57043148963561,128.987677084023));
#26845=CARTESIAN_POINT('Ctrl Pts',(173.957880796175,-4.6204333578595,129.113472308591));
#26846=CARTESIAN_POINT('Ctrl Pts',(173.950242872399,-4.66524760870487,129.241358518312));
#26847=CARTESIAN_POINT('Ctrl Pts',(173.942604948623,-4.70470621169906,129.370860521961));
#26848=CARTESIAN_POINT('Ctrl Pts',(173.938470750539,-4.72606406831749,129.440956394999));
#26849=CARTESIAN_POINT('Ctrl Pts',(173.934336552455,-4.74585369313538,129.511525339495));
#26850=CARTESIAN_POINT('Ctrl Pts',(173.930202354372,-4.76405452823406,129.582490119308));
#26851=CARTESIAN_POINT('Origin',(213.235140564004,0.,130.804360617566));
#26852=CARTESIAN_POINT('',(171.834603948179,-4.76405452823406,129.582490119308));
#26853=CARTESIAN_POINT('',(172.180231140679,-4.76405452823404,129.582490119308));
#26854=CARTESIAN_POINT('',(213.235140564004,-4.76405452823405,129.582490119308));
#26855=CARTESIAN_POINT('',(173.514859435953,-4.91824918172569,130.801523549609));
#26856=CARTESIAN_POINT('Ctrl Pts',(173.514859435953,-4.91824918172569,130.801523549609));
#26857=CARTESIAN_POINT('Ctrl Pts',(173.507187584774,-4.91832695800124,130.936353983495));
#26858=CARTESIAN_POINT('Ctrl Pts',(173.499515733596,-4.91285613080631,131.071408084697));
#26859=CARTESIAN_POINT('Ctrl Pts',(173.491843882417,-4.90180792317066,131.206184144554));
#26860=CARTESIAN_POINT('Ctrl Pts',(173.484180616626,-4.89077207932404,131.340809379696));
#26861=CARTESIAN_POINT('Ctrl Pts',(173.476517350836,-4.87417130102263,131.475156795457));
#26862=CARTESIAN_POINT('Ctrl Pts',(173.468854085045,-4.85202881415562,131.608723377211));
#26863=CARTESIAN_POINT('Ctrl Pts',(173.461197450555,-4.82990548798381,131.742174378968));
#26864=CARTESIAN_POINT('Ctrl Pts',(173.453540816066,-4.8022500580158,131.874845496675));
#26865=CARTESIAN_POINT('Ctrl Pts',(173.445884181576,-4.7691376287652,132.006238040765));
#26866=CARTESIAN_POINT('Ctrl Pts',(173.438231801396,-4.73604359800506,132.137557578298));
#26867=CARTESIAN_POINT('Ctrl Pts',(173.430579421216,-4.69749869592266,132.267599566633));
#26868=CARTESIAN_POINT('Ctrl Pts',(173.422927041036,-4.65362918335053,132.395875143534));
#26869=CARTESIAN_POINT('Ctrl Pts',(173.415276829414,-4.60977210267183,132.524114369261));
#26870=CARTESIAN_POINT('Ctrl Pts',(173.407626617791,-4.56059354113234,132.650587798968));
#26871=CARTESIAN_POINT('Ctrl Pts',(173.399976406169,-4.50626958902363,132.774821846198));
#26872=CARTESIAN_POINT('Ctrl Pts',(173.392326606852,-4.45194856468911,132.899049197869));
#26873=CARTESIAN_POINT('Ctrl Pts',(173.384676807536,-4.39248286221509,133.021037039006));
#26874=CARTESIAN_POINT('Ctrl Pts',(173.37702700822,-4.32809645737784,133.140332389256));
#26875=CARTESIAN_POINT('Ctrl Pts',(173.369375865516,-4.26369874559336,133.259648689057));
#26876=CARTESIAN_POINT('Ctrl Pts',(173.361724722813,-4.19437880415203,133.376271204381));
#26877=CARTESIAN_POINT('Ctrl Pts',(173.354073580109,-4.12040596640364,133.489772640799));
#26878=CARTESIAN_POINT('Ctrl Pts',(173.346414694795,-4.04635827148544,133.603388935543));
#26879=CARTESIAN_POINT('Ctrl Pts',(173.33875580948,-3.96764849618805,133.713877506441));
#26880=CARTESIAN_POINT('Ctrl Pts',(173.331096924166,-3.8845888314214,133.820840797063));
#26881=CARTESIAN_POINT('Ctrl Pts',(173.323434102541,-3.80148647785632,133.927859061833));
#26882=CARTESIAN_POINT('Ctrl Pts',(173.315771280917,-3.71403004215883,134.031348131974));
#26883=CARTESIAN_POINT('Ctrl Pts',(173.308108459292,-3.62257036387388,134.130945506199));
#26884=CARTESIAN_POINT('Ctrl Pts',(173.300433602329,-3.53096703769839,134.230699309497));
#26885=CARTESIAN_POINT('Ctrl Pts',(173.292758745366,-3.43534819248633,134.326548922592));
#26886=CARTESIAN_POINT('Ctrl Pts',(173.285083888404,-3.33610018744934,134.418170048319));
#26887=CARTESIAN_POINT('Ctrl Pts',(173.278223476555,-3.24738424225639,134.500068467995));
#26888=CARTESIAN_POINT('Ctrl Pts',(173.271363064707,-3.1557691341598,134.578588662547));
#26889=CARTESIAN_POINT('Ctrl Pts',(173.264502652858,-3.06155048147109,134.653528282387));
#26890=CARTESIAN_POINT('Ctrl Pts',(173.256728318739,-2.95478031920592,134.738451120297));
#26891=CARTESIAN_POINT('Ctrl Pts',(173.24895398462,-2.84430491379653,134.819062635927));
#26892=CARTESIAN_POINT('Ctrl Pts',(173.241179650501,-2.73050757389078,134.895022110702));
#26893=CARTESIAN_POINT('Ctrl Pts',(173.233414897554,-2.61685047903623,134.970887972213));
#26894=CARTESIAN_POINT('Ctrl Pts',(173.225650144607,-2.49987991755621,135.042112985306));
#26895=CARTESIAN_POINT('Ctrl Pts',(173.21788539166,-2.38001253793216,135.108396326268));
#26896=CARTESIAN_POINT('Ctrl Pts',(173.210128350775,-2.26026421227955,135.174613833682));
#26897=CARTESIAN_POINT('Ctrl Pts',(173.20237130989,-2.13762513408804,135.235899248413));
#26898=CARTESIAN_POINT('Ctrl Pts',(173.194614269005,-2.01254092950996,135.291994968708));
#26899=CARTESIAN_POINT('Ctrl Pts',(173.186863077765,-1.88755105190373,135.348048386784));
#26900=CARTESIAN_POINT('Ctrl Pts',(173.179111886525,-1.76012007335078,135.398919740851));
#26901=CARTESIAN_POINT('Ctrl Pts',(173.171360695285,-1.63071790280482,135.444397490692));
#26902=CARTESIAN_POINT('Ctrl Pts',(173.163612798508,-1.50137073163291,135.489855911277));
#26903=CARTESIAN_POINT('Ctrl Pts',(173.155864901731,-1.37005440288363,135.529925157737));
#26904=CARTESIAN_POINT('Ctrl Pts',(173.148117004954,-1.23725826848959,135.564442028588));
#26905=CARTESIAN_POINT('Ctrl Pts',(173.140370728869,-1.10448991218415,135.598951679253));
#26906=CARTESIAN_POINT('Ctrl Pts',(173.132624452785,-0.97024274408504,135.62791116618));
#26907=CARTESIAN_POINT('Ctrl Pts',(173.124878176701,-0.835020339381439,
135.65120743744));
#26908=CARTESIAN_POINT('Ctrl Pts',(173.117131843436,-0.69979693649658,135.674503880667));
#26909=CARTESIAN_POINT('Ctrl Pts',(173.109385510171,-0.563598667931364,
135.692136958429));
#26910=CARTESIAN_POINT('Ctrl Pts',(173.101639176905,-0.426937946320922,
135.704045000513));
#26911=CARTESIAN_POINT('Ctrl Pts',(173.093891108902,-0.290246620489972,
135.715955709319));
#26912=CARTESIAN_POINT('Ctrl Pts',(173.086143040899,-0.153093024949944,
135.72213879732));
#26913=CARTESIAN_POINT('Ctrl Pts',(173.078394972896,-0.0159929217430619,
135.722584615002));
#26914=CARTESIAN_POINT('Ctrl Pts',(173.070638670155,0.121252893085441,135.723030906504));
#26915=CARTESIAN_POINT('Ctrl Pts',(173.062882367413,0.258444710425685,135.717727745723));
#26916=CARTESIAN_POINT('Ctrl Pts',(173.055126064671,0.395067985950195,135.706717637304));
#26917=CARTESIAN_POINT('Ctrl Pts',(173.047365622157,0.5317641814305,135.695701652459));
#26918=CARTESIAN_POINT('Ctrl Pts',(173.039605179643,0.667890842593393,135.678972698288));
#26919=CARTESIAN_POINT('Ctrl Pts',(173.031844737128,0.802941303460366,135.656624864873));
#26920=CARTESIAN_POINT('Ctrl Pts',(173.024071836863,0.938208559316431,135.634241156733));
#26921=CARTESIAN_POINT('Ctrl Pts',(173.016298936598,1.07239577962624,135.60622062463));
#26922=CARTESIAN_POINT('Ctrl Pts',(173.008526036332,1.20500832006864,135.57270813123));
#26923=CARTESIAN_POINT('Ctrl Pts',(173.00103570057,1.33280006063679,135.540413901378));
#26924=CARTESIAN_POINT('Ctrl Pts',(172.993545364808,1.45912932548036,135.50302015859));
#26925=CARTESIAN_POINT('Ctrl Pts',(172.986055029046,1.58357095274533,135.460698889226));
#26926=CARTESIAN_POINT('Ctrl Pts',(172.978280694927,1.71273082212963,135.41677299607));
#26927=CARTESIAN_POINT('Ctrl Pts',(172.970506360808,1.84026622840091,135.367399401916));
#26928=CARTESIAN_POINT('Ctrl Pts',(172.962732026688,1.9656833276869,135.312716428475));
#26929=CARTESIAN_POINT('Ctrl Pts',(172.954967273741,2.09094586160686,135.258100846911));
#26930=CARTESIAN_POINT('Ctrl Pts',(172.947202520794,2.2140949279641,135.198189060103));
#26931=CARTESIAN_POINT('Ctrl Pts',(172.939437767847,2.33465222656795,135.133169003656));
#26932=CARTESIAN_POINT('Ctrl Pts',(172.931680726962,2.45508978596318,135.068213526045));
#26933=CARTESIAN_POINT('Ctrl Pts',(172.923923686077,2.57294035845778,134.998160059884));
#26934=CARTESIAN_POINT('Ctrl Pts',(172.916166645192,2.68774634458161,134.923244283038));
#26935=CARTESIAN_POINT('Ctrl Pts',(172.908415453952,2.80246575461867,134.848385000761));
#26936=CARTESIAN_POINT('Ctrl Pts',(172.900664262712,2.91414482213019,134.768670918946));
#26937=CARTESIAN_POINT('Ctrl Pts',(172.892913071472,3.02235157507306,134.68438304265));
#26938=CARTESIAN_POINT('Ctrl Pts',(172.885165174694,3.13051233725909,134.60013099095));
#26939=CARTESIAN_POINT('Ctrl Pts',(172.877417277917,3.23520341239461,134.511309250959));
#26940=CARTESIAN_POINT('Ctrl Pts',(172.86966938114,3.33602298777566,134.418241313927));
#26941=CARTESIAN_POINT('Ctrl Pts',(172.861923105056,3.43682147387489,134.325192844702));
#26942=CARTESIAN_POINT('Ctrl Pts',(172.854176828972,3.53374978392915,134.227900210162));
#26943=CARTESIAN_POINT('Ctrl Pts',(172.846430552888,3.62644060945729,134.126725975045));
#26944=CARTESIAN_POINT('Ctrl Pts',(172.838684219623,3.71913211920805,134.025550993084));
#26945=CARTESIAN_POINT('Ctrl Pts',(172.830937886357,3.80758581791146,133.920494641647));
#26946=CARTESIAN_POINT('Ctrl Pts',(172.823191553092,3.89147284912339,133.81195469374));
#26947=CARTESIAN_POINT('Ctrl Pts',(172.815443485089,3.97537866625415,133.703390439064));
#26948=CARTESIAN_POINT('Ctrl Pts',(172.807695417086,4.05471554185538,133.591341344839));
#26949=CARTESIAN_POINT('Ctrl Pts',(172.799947349083,4.12919657553683,133.476236120481));
#26950=CARTESIAN_POINT('Ctrl Pts',(172.792191046341,4.20375676854742,133.36100856092));
#26951=CARTESIAN_POINT('Ctrl Pts',(172.784434743599,4.27345059755786,133.242718711578));
#26952=CARTESIAN_POINT('Ctrl Pts',(172.776678440857,4.33803569915251,133.12182244797));
#26953=CARTESIAN_POINT('Ctrl Pts',(172.768917998343,4.4026552717605,133.000861658385));
#26954=CARTESIAN_POINT('Ctrl Pts',(172.761157555829,4.46216051426459,132.877292034684));
#26955=CARTESIAN_POINT('Ctrl Pts',(172.753397113315,4.5163567219789,132.751590707292));
#26956=CARTESIAN_POINT('Ctrl Pts',(172.745624213049,4.57063993025715,132.62568759297));
#26957=CARTESIAN_POINT('Ctrl Pts',(172.737851312784,4.61959693329831,132.497646302103));
#26958=CARTESIAN_POINT('Ctrl Pts',(172.730078412518,4.66308224082845,132.367961294776));
#26959=CARTESIAN_POINT('Ctrl Pts',(172.722588076756,4.7049867478969,132.242990664122));
#26960=CARTESIAN_POINT('Ctrl Pts',(172.715097740994,4.74181038645512,132.116494044411));
#26961=CARTESIAN_POINT('Ctrl Pts',(172.707607405232,4.77346804312973,131.988922099178));
#26962=CARTESIAN_POINT('Ctrl Pts',(172.699833071113,4.80632600947932,131.856513224868));
#26963=CARTESIAN_POINT('Ctrl Pts',(172.692058736994,4.83372260870009,131.722526441924));
#26964=CARTESIAN_POINT('Ctrl Pts',(172.684284402875,4.85550728008837,131.587452001447));
#26965=CARTESIAN_POINT('Ctrl Pts',(172.676519649928,4.8772651038161,131.452544028146));
#26966=CARTESIAN_POINT('Ctrl Pts',(172.668754896981,4.89342469923445,131.316551446661));
#26967=CARTESIAN_POINT('Ctrl Pts',(172.660990144034,4.90388564895249,131.179978248273));
#26968=CARTESIAN_POINT('Ctrl Pts',(172.653233103149,4.91433620870783,131.04354069631));
#26969=CARTESIAN_POINT('Ctrl Pts',(172.645476062264,4.9190993567033,130.906524062358));
#26970=CARTESIAN_POINT('Ctrl Pts',(172.637719021379,4.91812603170907,130.769440727451));
#26971=CARTESIAN_POINT('Ctrl Pts',(172.629967830139,4.91715344070678,130.632460768155));
#26972=CARTESIAN_POINT('Ctrl Pts',(172.622216638899,4.91045298995868,130.495414597396));
#26973=CARTESIAN_POINT('Ctrl Pts',(172.614465447658,4.89802760553687,130.358817535588));
#26974=CARTESIAN_POINT('Ctrl Pts',(172.606717550881,4.88560750223493,130.222278531174));
#26975=CARTESIAN_POINT('Ctrl Pts',(172.598969654104,4.8674673401504,130.086188644601));
#26976=CARTESIAN_POINT('Ctrl Pts',(172.591221757327,4.84366209205329,129.951060787198));
#26977=CARTESIAN_POINT('Ctrl Pts',(172.583475481243,4.81986182350088,129.81596119563));
#26978=CARTESIAN_POINT('Ctrl Pts',(172.575729205159,4.79039889378159,129.681823617755));
#26979=CARTESIAN_POINT('Ctrl Pts',(172.567982929075,4.75537979967245,129.549153055699));
#26980=CARTESIAN_POINT('Ctrl Pts',(172.56023659581,4.72036044706037,129.4164815143));
#26981=CARTESIAN_POINT('Ctrl Pts',(172.552490262544,4.6797849479972,129.285277388346));
#26982=CARTESIAN_POINT('Ctrl Pts',(172.544743929279,4.63381020523644,129.156032360104));
#26983=CARTESIAN_POINT('Ctrl Pts',(172.536995861276,4.58782516675081,129.026758388334));
#26984=CARTESIAN_POINT('Ctrl Pts',(172.529247793273,4.53643860955747,128.899444755574));
#26985=CARTESIAN_POINT('Ctrl Pts',(172.52149972527,4.47985614236095,128.774564567158));
#26986=CARTESIAN_POINT('Ctrl Pts',(172.513743422528,4.42321353864481,128.649551654592));
#26987=CARTESIAN_POINT('Ctrl Pts',(172.505987119787,4.36136415519768,128.526977709454));
#26988=CARTESIAN_POINT('Ctrl Pts',(172.498230817045,4.29456052965462,128.407293050802));
#26989=CARTESIAN_POINT('Ctrl Pts',(172.490470374531,4.22772124900527,128.287544512844));
#26990=CARTESIAN_POINT('Ctrl Pts',(172.482709932016,4.15592266198212,128.170688667083));
#26991=CARTESIAN_POINT('Ctrl Pts',(172.474949489502,4.07946094928639,128.057147224735));
#26992=CARTESIAN_POINT('Ctrl Pts',(172.467176589237,4.00287649346144,127.943423515585));
#26993=CARTESIAN_POINT('Ctrl Pts',(172.459403688972,3.92161418512189,127.833025157096));
#26994=CARTESIAN_POINT('Ctrl Pts',(172.451630788706,3.83601138649515,127.72634182211));
#26995=CARTESIAN_POINT('Ctrl Pts',(172.444140452944,3.75352046521824,127.623536695069));
#26996=CARTESIAN_POINT('Ctrl Pts',(172.436650117182,3.66699935259202,127.524181412244));
#26997=CARTESIAN_POINT('Ctrl Pts',(172.42915978142,3.57678119875583,127.428591176575));
#26998=CARTESIAN_POINT('Ctrl Pts',(172.421385447301,3.48314239619632,127.329376608068));
#26999=CARTESIAN_POINT('Ctrl Pts',(172.413611113182,3.38522405208093,127.233903944241));
#27000=CARTESIAN_POINT('Ctrl Pts',(172.405836779063,3.28335724680598,127.142564848774));
#27001=CARTESIAN_POINT('Ctrl Pts',(172.398072026115,3.18161598326433,127.051338320578));
#27002=CARTESIAN_POINT('Ctrl Pts',(172.390307273168,3.07593622899429,126.964235483192));
#27003=CARTESIAN_POINT('Ctrl Pts',(172.382542520221,2.96668772808122,126.88161324021));
#27004=CARTESIAN_POINT('Ctrl Pts',(172.374785479336,2.85754773432011,126.799073058805));
#27005=CARTESIAN_POINT('Ctrl Pts',(172.367028438451,2.74484635750175,126.721004850029));
#27006=CARTESIAN_POINT('Ctrl Pts',(172.359271397566,2.62898815951006,126.64772684495));
#27007=CARTESIAN_POINT('Ctrl Pts',(172.351520206326,2.51321733108573,126.574504099383));
#27008=CARTESIAN_POINT('Ctrl Pts',(172.343769015086,2.39429474898018,126.50606457553));
#27009=CARTESIAN_POINT('Ctrl Pts',(172.336017823846,2.2726555484634,126.442684354873));
#27010=CARTESIAN_POINT('Ctrl Pts',(172.328269927069,2.15106804785209,126.379331072501));
#27011=CARTESIAN_POINT('Ctrl Pts',(172.320522030292,2.02676657130688,126.321032996745));
#27012=CARTESIAN_POINT('Ctrl Pts',(172.312774133515,1.90021235978166,126.268021118561));
#27013=CARTESIAN_POINT('Ctrl Pts',(172.305027857431,1.77368462066922,126.215020329319));
#27014=CARTESIAN_POINT('Ctrl Pts',(172.297281581346,1.64490544424396,126.167303689192));
#27015=CARTESIAN_POINT('Ctrl Pts',(172.289535305262,1.51435726720566,126.125054565408));
#27016=CARTESIAN_POINT('Ctrl Pts',(172.281788971997,1.38380812649077,126.082805129751));
#27017=CARTESIAN_POINT('Ctrl Pts',(172.274042638732,1.25149033107672,126.046023411354));
#27018=CARTESIAN_POINT('Ctrl Pts',(172.266296305466,1.11790235694933,126.014843169761));
#27019=CARTESIAN_POINT('Ctrl Pts',(172.258548237463,0.984284466720592,125.983655945569));
#27020=CARTESIAN_POINT('Ctrl Pts',(172.25080016946,0.849396212419496,125.958072783163));
#27021=CARTESIAN_POINT('Ctrl Pts',(172.243052101457,0.713746767490395,125.938176423108));
#27022=CARTESIAN_POINT('Ctrl Pts',(172.235295798715,0.577953152717437,125.918258916964));
#27023=CARTESIAN_POINT('Ctrl Pts',(172.227539495974,0.441397118690106,125.904040343542));
#27024=CARTESIAN_POINT('Ctrl Pts',(172.219783193232,0.30459403434467,125.895551644226));
#27025=CARTESIAN_POINT('Ctrl Pts',(172.212022750718,0.167717934074336,125.887058414236));
#27026=CARTESIAN_POINT('Ctrl Pts',(172.204262308203,0.0305949114422294,
125.884301159944));
#27027=CARTESIAN_POINT('Ctrl Pts',(172.196501865689,-0.10626014305852,125.887258641351));
#27028=CARTESIAN_POINT('Ctrl Pts',(172.188728965424,-0.243334889442407,
125.890220870369));
#27029=CARTESIAN_POINT('Ctrl Pts',(172.180956065158,-0.380140417683305,
125.898916142451));
#27030=CARTESIAN_POINT('Ctrl Pts',(172.173183164893,-0.516166532458371,
125.913271252888));
#27031=CARTESIAN_POINT('Ctrl Pts',(172.165692829131,-0.647247755330227,
125.927104518902));
#27032=CARTESIAN_POINT('Ctrl Pts',(172.158202493369,-0.777604943426181,
125.946193224104));
#27033=CARTESIAN_POINT('Ctrl Pts',(172.150712157607,-0.906792831796963,
125.970427454737));
#27034=CARTESIAN_POINT('Ctrl Pts',(172.142937823488,-1.0408789182228,125.99558053359));
#27035=CARTESIAN_POINT('Ctrl Pts',(172.135163489369,-1.17413003100894,126.026356702838));
#27036=CARTESIAN_POINT('Ctrl Pts',(172.12738915525,-1.30603769536912,126.062689118951));
#27037=CARTESIAN_POINT('Ctrl Pts',(172.119624402303,-1.43778279532265,126.09897675861));
#27038=CARTESIAN_POINT('Ctrl Pts',(172.111859649356,-1.56818736785014,126.140806917671));
#27039=CARTESIAN_POINT('Ctrl Pts',(172.104094896409,-1.69675128414133,126.188061435075));
#27040=CARTESIAN_POINT('Ctrl Pts',(172.096337855524,-1.82518750893799,126.235269018626));
#27041=CARTESIAN_POINT('Ctrl Pts',(172.088580814639,-1.95178635104295,126.287890105047));
#27042=CARTESIAN_POINT('Ctrl Pts',(172.080823773754,-2.07606139806592,126.345756336632));
#27043=CARTESIAN_POINT('Ctrl Pts',(172.073072582514,-2.20024272830921,126.403578930842));
#27044=CARTESIAN_POINT('Ctrl Pts',(172.065321391273,-2.32210339850782,126.466638632859));
#27045=CARTESIAN_POINT('Ctrl Pts',(172.057570200033,-2.44117593224942,126.534718579841));
#27046=CARTESIAN_POINT('Ctrl Pts',(172.049822303256,-2.56019785698778,126.60276959103));
#27047=CARTESIAN_POINT('Ctrl Pts',(172.042074406479,-2.67643366351317,126.675836409693));
#27048=CARTESIAN_POINT('Ctrl Pts',(172.034326509702,-2.78943970059156,126.753655837005));
#27049=CARTESIAN_POINT('Ctrl Pts',(172.026580233618,-2.90242209924305,126.83145898617));
#27050=CARTESIAN_POINT('Ctrl Pts',(172.018833957534,-3.01217575045164,126.914012544979));
#27051=CARTESIAN_POINT('Ctrl Pts',(172.01108768145,-3.11828561335356,127.001009740241));
#27052=CARTESIAN_POINT('Ctrl Pts',(172.003341348184,-3.22439625953463,127.088007577696));
#27053=CARTESIAN_POINT('Ctrl Pts',(171.995595014919,-3.32686276139793,127.179448869175));
#27054=CARTESIAN_POINT('Ctrl Pts',(171.987848681654,-3.42530314480444,127.274986533016));
#27055=CARTESIAN_POINT('Ctrl Pts',(171.980100613651,-3.52376557325187,127.370545591854));
#27056=CARTESIAN_POINT('Ctrl Pts',(171.972352545648,-3.61819980861456,127.470202576247));
#27057=CARTESIAN_POINT('Ctrl Pts',(171.964604477645,-3.70826101822914,127.573573827451));
#27058=CARTESIAN_POINT('Ctrl Pts',(171.956848174903,-3.79841794596916,127.677054942851));
#27059=CARTESIAN_POINT('Ctrl Pts',(171.949091872161,-3.88419230643845,127.784257915503));
#27060=CARTESIAN_POINT('Ctrl Pts',(171.941335569419,-3.96527949827477,127.894765875499));
#27061=CARTESIAN_POINT('Ctrl Pts',(171.933575126905,-4.04640996878683,128.005332816921));
#27062=CARTESIAN_POINT('Ctrl Pts',(171.925814684391,-4.12284806806102,128.119207936093));
#27063=CARTESIAN_POINT('Ctrl Pts',(171.918054241877,-4.19433335502167,128.235946560321));
#27064=CARTESIAN_POINT('Ctrl Pts',(171.910281341612,-4.26593339651131,128.352872583753));
#27065=CARTESIAN_POINT('Ctrl Pts',(171.902508441346,-4.33256454752172,128.47267095615));
#27066=CARTESIAN_POINT('Ctrl Pts',(171.894735541081,-4.39401262421191,128.594872866804));
#27067=CARTESIAN_POINT('Ctrl Pts',(171.887245205319,-4.45322690853672,128.712632430199));
#27068=CARTESIAN_POINT('Ctrl Pts',(171.879754869556,-4.50762828454832,128.832623535885));
#27069=CARTESIAN_POINT('Ctrl Pts',(171.872264533794,-4.55706854922347,128.954412158776));
#27070=CARTESIAN_POINT('Ctrl Pts',(171.863524797849,-4.61475553043118,129.096515321982));
#27071=CARTESIAN_POINT('Ctrl Pts',(171.854785061903,-4.66584301224399,129.241444733054));
#27072=CARTESIAN_POINT('Ctrl Pts',(171.846045325957,-4.71007753832181,129.388608998991));
#27073=CARTESIAN_POINT('Ctrl Pts',(171.842231533364,-4.72938033064195,129.452827642531));
#27074=CARTESIAN_POINT('Ctrl Pts',(171.838417740772,-4.74737875562519,129.517471534996));
#27075=CARTESIAN_POINT('Ctrl Pts',(171.834603948179,-4.76405452823406,129.582490119308));
#27076=CARTESIAN_POINT('Ctrl Pts',(173.584942037299,-4.76405452823404,129.582490119308));
#27077=CARTESIAN_POINT('Ctrl Pts',(173.577168687926,-4.79810681298591,129.71525946074));
#27078=CARTESIAN_POINT('Ctrl Pts',(173.569395338553,-4.82656714898436,129.849306908375));
#27079=CARTESIAN_POINT('Ctrl Pts',(173.56162198918,-4.84937016082865,129.984121563531));
#27080=CARTESIAN_POINT('Ctrl Pts',(173.55539808501,-4.86762789680362,130.092063900104));
#27081=CARTESIAN_POINT('Ctrl Pts',(173.549174180841,-4.88225986259371,130.200497867035));
#27082=CARTESIAN_POINT('Ctrl Pts',(173.542950276672,-4.89325658827015,130.309160633872));
#27083=CARTESIAN_POINT('Ctrl Pts',(173.533586663111,-4.90980071987285,130.472639397256));
#27084=CARTESIAN_POINT('Ctrl Pts',(173.524223049551,-4.91815425455034,130.636960909544));
#27085=CARTESIAN_POINT('Ctrl Pts',(173.514859435991,-4.91824918172531,130.801523548944));
#27086=CARTESIAN_POINT('',(173.860140564047,-4.91824797895214,130.808819320649));
#27087=CARTESIAN_POINT('Ctrl Pts',(173.930202354372,-4.76405452823406,129.582490119308));
#27088=CARTESIAN_POINT('Ctrl Pts',(173.922561425174,-4.7976937708428,129.713649015693));
#27089=CARTESIAN_POINT('Ctrl Pts',(173.914920495977,-4.82590276153612,129.846160505067));
#27090=CARTESIAN_POINT('Ctrl Pts',(173.907279566779,-4.84859108433937,129.979528780544));
#27091=CARTESIAN_POINT('Ctrl Pts',(173.899423066324,-4.8719195060305,130.116659735421));
#27092=CARTESIAN_POINT('Ctrl Pts',(173.891566565869,-4.88941106084076,130.254696087604));
#27093=CARTESIAN_POINT('Ctrl Pts',(173.883710065413,-4.90102458032567,130.393092912119));
#27094=CARTESIAN_POINT('Ctrl Pts',(173.875853564958,-4.91263809981058,130.531489736635));
#27095=CARTESIAN_POINT('Ctrl Pts',(173.867997064503,-4.91837360391904,130.670246572473));
#27096=CARTESIAN_POINT('Ctrl Pts',(173.860140564047,-4.91824797895214,130.808819320649));
#27097=CARTESIAN_POINT('Ctrl Pts',(173.860140564008,-4.91824797895151,130.808819321346));
#27098=CARTESIAN_POINT('Ctrl Pts',(173.849233599194,-4.91807357721686,131.001196079562));
#27099=CARTESIAN_POINT('Ctrl Pts',(173.83832663438,-4.90660860059347,131.193082194159));
#27100=CARTESIAN_POINT('Ctrl Pts',(173.827419669566,-4.88404528139263,131.38339839855));
#27101=CARTESIAN_POINT('Ctrl Pts',(173.818882747819,-4.86638488790488,131.532359596444));
#27102=CARTESIAN_POINT('Ctrl Pts',(173.810345826072,-4.8419263040771,131.68035995043));
#27103=CARTESIAN_POINT('Ctrl Pts',(173.801808904325,-4.81078058184838,131.826893382719));
#27104=CARTESIAN_POINT('Ctrl Pts',(173.794034570206,-4.7824170501024,131.960337251127));
#27105=CARTESIAN_POINT('Ctrl Pts',(173.786260236087,-4.74845208433762,132.092811447682));
#27106=CARTESIAN_POINT('Ctrl Pts',(173.778485901968,-4.70896471082672,132.223809248087));
#27107=CARTESIAN_POINT('Ctrl Pts',(173.770721149021,-4.66952600197456,132.354645605411));
#27108=CARTESIAN_POINT('Ctrl Pts',(173.762956396074,-4.62457853878966,132.484008816164));
#27109=CARTESIAN_POINT('Ctrl Pts',(173.755191643127,-4.57425245001799,132.611401731101));
#27110=CARTESIAN_POINT('Ctrl Pts',(173.747434602242,-4.52397634582726,132.738668117598));
#27111=CARTESIAN_POINT('Ctrl Pts',(173.739677561357,-4.46833238984024,132.863967741382));
#27112=CARTESIAN_POINT('Ctrl Pts',(173.731920520472,-4.40750056383562,132.986818370259));
#27113=CARTESIAN_POINT('Ctrl Pts',(173.724169329232,-4.34671461158427,133.10957635652));
#27114=CARTESIAN_POINT('Ctrl Pts',(173.716418137991,-4.2807487491259,133.229888674883));
#27115=CARTESIAN_POINT('Ctrl Pts',(173.708666946751,-4.20983099499577,133.347293187666));
#27116=CARTESIAN_POINT('Ctrl Pts',(173.700919049974,-4.13894338280274,133.464647800399));
#27117=CARTESIAN_POINT('Ctrl Pts',(173.693171153197,-4.06310826671952,133.579096731704));
#27118=CARTESIAN_POINT('Ctrl Pts',(173.68542325642,-3.98259941618203,133.690202774152));
#27119=CARTESIAN_POINT('Ctrl Pts',(173.677676980336,-3.90210740636054,133.801285575611));
#27120=CARTESIAN_POINT('Ctrl Pts',(173.669930704252,-3.81694383593146,133.909026562693));
#27121=CARTESIAN_POINT('Ctrl Pts',(173.662184428168,-3.72742534958035,134.013018175768));
#27122=CARTESIAN_POINT('Ctrl Pts',(173.654438094903,-3.63790620242411,134.117010556485));
#27123=CARTESIAN_POINT('Ctrl Pts',(173.646691761637,-3.54403233026384,134.217253211663));
#27124=CARTESIAN_POINT('Ctrl Pts',(173.638945428372,-3.44615988113825,134.313372606165));
#27125=CARTESIAN_POINT('Ctrl Pts',(173.631197360369,-3.34826551415631,134.409513525939));
#27126=CARTESIAN_POINT('Ctrl Pts',(173.623449292366,-3.24637106724771,134.501529073735));
#27127=CARTESIAN_POINT('Ctrl Pts',(173.615701224363,-3.14086836370495,134.589083722943));
#27128=CARTESIAN_POINT('Ctrl Pts',(173.607944921621,-3.03525353063332,134.676731426275));
#27129=CARTESIAN_POINT('Ctrl Pts',(173.600188618879,-2.92602308164329,134.759908510095));
#27130=CARTESIAN_POINT('Ctrl Pts',(173.592432316137,-2.81360107618712,134.838320464488));
#27131=CARTESIAN_POINT('Ctrl Pts',(173.584671873623,-2.70111906772156,134.916774269702));
#27132=CARTESIAN_POINT('Ctrl Pts',(173.576911431109,-2.58544243815103,134.99045766782));
#27133=CARTESIAN_POINT('Ctrl Pts',(173.569150988595,-2.46702198198113,135.059120963687));
#27134=CARTESIAN_POINT('Ctrl Pts',(173.56137808833,-2.34841142678219,135.127894483972));
#27135=CARTESIAN_POINT('Ctrl Pts',(173.553605188064,-2.22704858945512,135.19163161624));
#27136=CARTESIAN_POINT('Ctrl Pts',(173.545832287799,-2.10340728552242,135.250129488494));
#27137=CARTESIAN_POINT('Ctrl Pts',(173.538341952037,-1.98426065442175,135.306500815744));
#27138=CARTESIAN_POINT('Ctrl Pts',(173.530851616275,-1.86299862018901,135.358007069818));
#27139=CARTESIAN_POINT('Ctrl Pts',(173.523361280513,-1.74005863938335,135.404510505777));
#27140=CARTESIAN_POINT('Ctrl Pts',(173.515586946394,-1.61245735183837,135.452777133645));
#27141=CARTESIAN_POINT('Ctrl Pts',(173.507812612275,-1.48264416477591,135.495806985109));
#27142=CARTESIAN_POINT('Ctrl Pts',(173.500038278155,-1.35108811532953,135.533392650352));
#27143=CARTESIAN_POINT('Ctrl Pts',(173.492273525208,-1.21969419695664,135.570931994621));
#27144=CARTESIAN_POINT('Ctrl Pts',(173.484508772261,-1.08656206223956,135.60304039615));
#27145=CARTESIAN_POINT('Ctrl Pts',(173.476744019314,-0.9521803146846,135.629558614626));
#27146=CARTESIAN_POINT('Ctrl Pts',(173.468986978429,-0.817932036975901,
135.656050494833));
#27147=CARTESIAN_POINT('Ctrl Pts',(173.461229937544,-0.682436997426369,
135.676963166011));
#27148=CARTESIAN_POINT('Ctrl Pts',(173.453472896659,-0.546198196186696,
135.692187393648));
#27149=CARTESIAN_POINT('Ctrl Pts',(173.445721705419,-0.410062133686591,
135.707400140576));
#27150=CARTESIAN_POINT('Ctrl Pts',(173.437970514179,-0.273183812861581,
135.716932939106));
#27151=CARTESIAN_POINT('Ctrl Pts',(173.430219322939,-0.136075292818587,
135.720727830985));
#27152=CARTESIAN_POINT('Ctrl Pts',(173.422471426162,0.000974952445806226,
135.724521109934));
#27153=CARTESIAN_POINT('Ctrl Pts',(173.414723529385,0.138254812332943,135.722581321952));
#27154=CARTESIAN_POINT('Ctrl Pts',(173.406975632607,0.275248472784505,135.714902475725));
#27155=CARTESIAN_POINT('Ctrl Pts',(173.399229356523,0.412213477115542,135.707225235747));
#27156=CARTESIAN_POINT('Ctrl Pts',(173.391483080439,0.548892010984102,135.693811347225));
#27157=CARTESIAN_POINT('Ctrl Pts',(173.383736804355,0.684770028742482,135.674706916366));
#27158=CARTESIAN_POINT('Ctrl Pts',(173.37599047109,0.820649049521523,135.655602344482));
#27159=CARTESIAN_POINT('Ctrl Pts',(173.368244137824,0.955727155241739,135.630807200875));
#27160=CARTESIAN_POINT('Ctrl Pts',(173.360497804559,1.08949757349896,135.600419218109));
#27161=CARTESIAN_POINT('Ctrl Pts',(173.352749736556,1.22329794871381,135.570024430165));
#27162=CARTESIAN_POINT('Ctrl Pts',(173.345001668553,1.35578967255406,135.534034397368));
#27163=CARTESIAN_POINT('Ctrl Pts',(173.33725360055,1.4864786669213,135.492597411424));
#27164=CARTESIAN_POINT('Ctrl Pts',(173.329497297808,1.61730655910707,135.451116385759));
#27165=CARTESIAN_POINT('Ctrl Pts',(173.321740995066,1.7463275212036,135.404176960975));
#27166=CARTESIAN_POINT('Ctrl Pts',(173.313984692324,1.87306455918525,135.351976720496));
#27167=CARTESIAN_POINT('Ctrl Pts',(173.30622424981,1.99986924054009,135.299748619176));
#27168=CARTESIAN_POINT('Ctrl Pts',(173.298463807296,2.12438721404093,135.242254271087));
#27169=CARTESIAN_POINT('Ctrl Pts',(173.290703364782,2.24616473863931,135.17973797608));
#27170=CARTESIAN_POINT('Ctrl Pts',(173.282930464517,2.36813775133103,135.117121324366));
#27171=CARTESIAN_POINT('Ctrl Pts',(173.275157564251,2.48736118386485,135.049466809006));
#27172=CARTESIAN_POINT('Ctrl Pts',(173.267384663986,2.60340824542052,134.977063407147));
#27173=CARTESIAN_POINT('Ctrl Pts',(173.259894328224,2.71523670398502,134.907292051318));
#27174=CARTESIAN_POINT('Ctrl Pts',(173.252403992461,2.82411546576469,134.833111256035));
#27175=CARTESIAN_POINT('Ctrl Pts',(173.244913656699,2.92969218608533,134.754814611386));
#27176=CARTESIAN_POINT('Ctrl Pts',(173.23713932258,3.03927187984508,134.673549325659));
#27177=CARTESIAN_POINT('Ctrl Pts',(173.229364988461,3.14564131102171,134.587592500662));
#27178=CARTESIAN_POINT('Ctrl Pts',(173.221590654342,3.24837245383282,134.497226640546));
#27179=CARTESIAN_POINT('Ctrl Pts',(173.213825901395,3.35097698969172,134.406972148277));
#27180=CARTESIAN_POINT('Ctrl Pts',(173.206061148448,3.44995186800253,134.312319688159));
#27181=CARTESIAN_POINT('Ctrl Pts',(173.198296395501,3.54489901325132,134.213594262881));
#27182=CARTESIAN_POINT('Ctrl Pts',(173.190539354616,3.63975185565693,134.114966893088));
#27183=CARTESIAN_POINT('Ctrl Pts',(173.182782313731,3.73058465672387,134.012274888488));
#27184=CARTESIAN_POINT('Ctrl Pts',(173.175025272846,3.81703363049503,133.905882393432));
#27185=CARTESIAN_POINT('Ctrl Pts',(173.167274081606,3.90341741242252,133.799570129784));
#27186=CARTESIAN_POINT('Ctrl Pts',(173.159522890366,3.98542370165354,133.689563232335));
#27187=CARTESIAN_POINT('Ctrl Pts',(173.151771699126,4.06272695581327,133.576261183064));
#27188=CARTESIAN_POINT('Ctrl Pts',(173.144023802348,4.13999735402793,133.463007290186));
#27189=CARTESIAN_POINT('Ctrl Pts',(173.136275905571,4.21256847297687,133.346461353309));
#27190=CARTESIAN_POINT('Ctrl Pts',(173.128528008794,4.28015646190007,133.227054102957));
#27191=CARTESIAN_POINT('Ctrl Pts',(173.12078173271,4.34773031287302,133.107671830027));
#27192=CARTESIAN_POINT('Ctrl Pts',(173.113035456626,4.41032291467358,132.985429774148));
#27193=CARTESIAN_POINT('Ctrl Pts',(173.105289180542,4.46769520352962,132.860785338011));
#27194=CARTESIAN_POINT('Ctrl Pts',(173.097542847277,4.52506791589482,132.736139981778));
#27195=CARTESIAN_POINT('Ctrl Pts',(173.089796514011,4.57722007495053,132.609092565049));
#27196=CARTESIAN_POINT('Ctrl Pts',(173.082050180746,4.62395998300934,132.480122276642));
#27197=CARTESIAN_POINT('Ctrl Pts',(173.074302112743,4.67071035814649,132.351123106232));
#27198=CARTESIAN_POINT('Ctrl Pts',(173.06655404474,4.71204593728985,132.220200574773));
#27199=CARTESIAN_POINT('Ctrl Pts',(173.058805976737,4.74782442117051,132.08785051945));
#27200=CARTESIAN_POINT('Ctrl Pts',(173.051049673995,4.78364093084961,131.955359800913));
#27201=CARTESIAN_POINT('Ctrl Pts',(173.043293371254,4.8138884449104,131.821438905782));
#27202=CARTESIAN_POINT('Ctrl Pts',(173.035537068512,4.83847536896097,131.686595941308));
#27203=CARTESIAN_POINT('Ctrl Pts',(173.027776625998,4.86307541579321,131.551681007084));
#27204=CARTESIAN_POINT('Ctrl Pts',(173.020016183483,4.88200879861843,131.415843409925));
#27205=CARTESIAN_POINT('Ctrl Pts',(173.012255740969,4.89523579570234,131.279596945065));
#27206=CARTESIAN_POINT('Ctrl Pts',(173.004482840704,4.9084840259362,131.143131765284));
#27207=CARTESIAN_POINT('Ctrl Pts',(172.996709940438,4.91600754356677,131.006256796804));
#27208=CARTESIAN_POINT('Ctrl Pts',(172.988937040173,4.91781878238998,130.869487310038));
#27209=CARTESIAN_POINT('Ctrl Pts',(172.981446704411,4.91956417811974,130.737689738616));
#27210=CARTESIAN_POINT('Ctrl Pts',(172.973956368649,4.91600540439234,130.605990420908));
#27211=CARTESIAN_POINT('Ctrl Pts',(172.966466032887,4.90719901596116,130.474844487081));
#27212=CARTESIAN_POINT('Ctrl Pts',(172.958691698768,4.898058730636,130.338726115312));
#27213=CARTESIAN_POINT('Ctrl Pts',(172.950917364649,4.88323609511096,130.202772736801));
#27214=CARTESIAN_POINT('Ctrl Pts',(172.94314303053,4.8627374297386,130.067497162156));
#27215=CARTESIAN_POINT('Ctrl Pts',(172.935378277583,4.84226402713931,129.932388302566));
#27216=CARTESIAN_POINT('Ctrl Pts',(172.927613524635,4.81612857106773,129.79795596762));
#27217=CARTESIAN_POINT('Ctrl Pts',(172.919848771688,4.78438932595254,129.664710741415));
#27218=CARTESIAN_POINT('Ctrl Pts',(172.912091730803,4.75268160470302,129.531597856246));
#27219=CARTESIAN_POINT('Ctrl Pts',(172.904334689918,4.71538126053565,129.399670111312));
#27220=CARTESIAN_POINT('Ctrl Pts',(172.896577649033,4.67259802320951,129.269430398957));
#27221=CARTESIAN_POINT('Ctrl Pts',(172.888826457793,4.62984704905545,129.139288901382));
#27222=CARTESIAN_POINT('Ctrl Pts',(172.881075266553,4.58162153311918,129.010833272575));
#27223=CARTESIAN_POINT('Ctrl Pts',(172.873324075313,4.52808160729683,128.884553330321));
#27224=CARTESIAN_POINT('Ctrl Pts',(172.865576178536,4.47456443737116,128.758327060411));
#27225=CARTESIAN_POINT('Ctrl Pts',(172.857828281759,4.41573750236395,128.634274997043));
#27226=CARTESIAN_POINT('Ctrl Pts',(172.850080384982,4.35180975979507,128.512868772271));
#27227=CARTESIAN_POINT('Ctrl Pts',(172.842334108898,4.28789538953182,128.391487943064));
#27228=CARTESIAN_POINT('Ctrl Pts',(172.834587832814,4.21888251602815,128.272752197324));
#27229=CARTESIAN_POINT('Ctrl Pts',(172.82684155673,4.14502674531517,128.1571099035));
#27230=CARTESIAN_POINT('Ctrl Pts',(172.819095223464,4.07117042941569,128.041466756031));
#27231=CARTESIAN_POINT('Ctrl Pts',(172.811348890199,3.99247135540927,127.928917435545));
#27232=CARTESIAN_POINT('Ctrl Pts',(172.803602556933,3.90922906113504,127.819882235993));
#27233=CARTESIAN_POINT('Ctrl Pts',(172.795854488931,3.8259681253262,127.710822618764));
#27234=CARTESIAN_POINT('Ctrl Pts',(172.788106420928,3.73816218189519,127.605278999132));
#27235=CARTESIAN_POINT('Ctrl Pts',(172.780358352925,3.64615147647902,127.503639109612));
#27236=CARTESIAN_POINT('Ctrl Pts',(172.772602050183,3.55404298099015,127.401891196008));
#27237=CARTESIAN_POINT('Ctrl Pts',(172.764845747441,3.45772105926657,127.304055590757));
#27238=CARTESIAN_POINT('Ctrl Pts',(172.757089444699,3.35756368732163,127.210483999194));
#27239=CARTESIAN_POINT('Ctrl Pts',(172.749329002185,3.25735285837149,127.116862465656));
#27240=CARTESIAN_POINT('Ctrl Pts',(172.741568559671,3.15330279665184,127.027509735182));
#27241=CARTESIAN_POINT('Ctrl Pts',(172.733808117156,3.04582430207586,126.942736945665));
#27242=CARTESIAN_POINT('Ctrl Pts',(172.726035216891,2.93817327347894,126.857828071341));
#27243=CARTESIAN_POINT('Ctrl Pts',(172.718262316626,2.82708313104801,126.777514059061));
#27244=CARTESIAN_POINT('Ctrl Pts',(172.71048941636,2.71299410714415,126.702062964165));
#27245=CARTESIAN_POINT('Ctrl Pts',(172.702999080598,2.60305250663191,126.629354706617));
#27246=CARTESIAN_POINT('Ctrl Pts',(172.695508744836,2.49032653659821,126.561162105588));
#27247=CARTESIAN_POINT('Ctrl Pts',(172.688018409074,2.37522968016847,126.497683588934));
#27248=CARTESIAN_POINT('Ctrl Pts',(172.680244074955,2.25576889144443,126.431798265027));
#27249=CARTESIAN_POINT('Ctrl Pts',(172.672469740836,2.13337546713922,126.370782846162));
#27250=CARTESIAN_POINT('Ctrl Pts',(172.664695406717,2.00848426564509,126.314909201507));
#27251=CARTESIAN_POINT('Ctrl Pts',(172.65693065377,1.883746981395,126.259104416125));
#27252=CARTESIAN_POINT('Ctrl Pts',(172.649165900823,1.75651839828276,126.208428954782));
#27253=CARTESIAN_POINT('Ctrl Pts',(172.641401147875,1.62725957851607,126.16310978114));
#27254=CARTESIAN_POINT('Ctrl Pts',(172.63364410699,1.49812914043149,126.11783561914));
#27255=CARTESIAN_POINT('Ctrl Pts',(172.625887066105,1.36697284509654,126.077907286437));
#27256=CARTESIAN_POINT('Ctrl Pts',(172.61813002522,1.23427310169855,126.043504289874));
#27257=CARTESIAN_POINT('Ctrl Pts',(172.61037883398,1.10167342820917,126.009127236878));
#27258=CARTESIAN_POINT('Ctrl Pts',(172.60262764274,0.967533000303468,125.98026732418));
#27259=CARTESIAN_POINT('Ctrl Pts',(172.5948764515,0.832350470758849,125.957054586756));
#27260=CARTESIAN_POINT('Ctrl Pts',(172.587128554723,0.697225397395445,125.933851715365));
#27261=CARTESIAN_POINT('Ctrl Pts',(172.579380657946,0.561059487848173,125.916291311462));
#27262=CARTESIAN_POINT('Ctrl Pts',(172.571632761169,0.424362486164162,125.904452501812));
#27263=CARTESIAN_POINT('Ctrl Pts',(172.563886485085,0.287694078546057,125.892616168585));
#27264=CARTESIAN_POINT('Ctrl Pts',(172.556140209001,0.150495189021715,125.886499082755));
#27265=CARTESIAN_POINT('Ctrl Pts',(172.548393932916,0.0132812039699516,
125.886128549829));
#27266=CARTESIAN_POINT('Ctrl Pts',(172.540647599651,-0.123933793964279,
125.885758014166));
#27267=CARTESIAN_POINT('Ctrl Pts',(172.532901266386,-0.261163496684503,
125.891134117109));
#27268=CARTESIAN_POINT('Ctrl Pts',(172.52515493312,-0.397892391465982,125.902232028135));
#27269=CARTESIAN_POINT('Ctrl Pts',(172.517406865117,-0.534651905735297,
125.913332424462));
#27270=CARTESIAN_POINT('Ctrl Pts',(172.509658797114,-0.670909999286356,
125.930157147007));
#27271=CARTESIAN_POINT('Ctrl Pts',(172.501910729112,-0.806156550694722,
125.952629516374));
#27272=CARTESIAN_POINT('Ctrl Pts',(172.49415442637,-0.941546843747564,125.975125769643));
#27273=CARTESIAN_POINT('Ctrl Pts',(172.486398123628,-1.07592306077914,126.003281595962));
#27274=CARTESIAN_POINT('Ctrl Pts',(172.478641820886,-1.20878499686194,126.036969098731));
#27275=CARTESIAN_POINT('Ctrl Pts',(172.470881378372,-1.34171784536042,126.070674581534));
#27276=CARTESIAN_POINT('Ctrl Pts',(172.463120935858,-1.47313442803267,126.109917511927));
#27277=CARTESIAN_POINT('Ctrl Pts',(172.455360493343,-1.60255092836956,126.154520449939));
#27278=CARTESIAN_POINT('Ctrl Pts',(172.447587593078,-1.73217517956185,126.199194988546));
#27279=CARTESIAN_POINT('Ctrl Pts',(172.439814692813,-1.85979256821545,126.249246586193));
#27280=CARTESIAN_POINT('Ctrl Pts',(172.432041792547,-1.98493961543744,126.304449753386));
#27281=CARTESIAN_POINT('Ctrl Pts',(172.424551456785,-2.10553725226601,126.357646146402));
#27282=CARTESIAN_POINT('Ctrl Pts',(172.417061121023,-2.22384075911418,126.415625931003));
#27283=CARTESIAN_POINT('Ctrl Pts',(172.409570785261,-2.33945969527697,126.478148487229));
#27284=CARTESIAN_POINT('Ctrl Pts',(172.401795470065,-2.45947750219968,126.54304979432));
#27285=CARTESIAN_POINT('Ctrl Pts',(172.39402015487,-2.5769826467889,126.61305200159));
#27286=CARTESIAN_POINT('Ctrl Pts',(172.386244839674,-2.69151117187928,126.687936116358));
#27287=CARTESIAN_POINT('Ctrl Pts',(172.3784793216,-2.80589538771341,126.762725874973));
#27288=CARTESIAN_POINT('Ctrl Pts',(172.370713803526,-2.9173101231536,126.842385088473));
#27289=CARTESIAN_POINT('Ctrl Pts',(172.362948285453,-3.02531508606934,126.926648445099));
#27290=CARTESIAN_POINT('Ctrl Pts',(172.355192093898,-3.13319033319682,127.010810600007));
#27291=CARTESIAN_POINT('Ctrl Pts',(172.347435902343,-3.23766365768947,127.099565645918));
#27292=CARTESIAN_POINT('Ctrl Pts',(172.339679710788,-3.33832342166466,127.192604840265));
#27293=CARTESIAN_POINT('Ctrl Pts',(172.331928807266,-3.43891455760079,127.285580602142));
#27294=CARTESIAN_POINT('Ctrl Pts',(172.324177903745,-3.5356970197125,127.382834437454));
#27295=CARTESIAN_POINT('Ctrl Pts',(172.316427000224,-3.62829191739539,127.484017137644));
#27296=CARTESIAN_POINT('Ctrl Pts',(172.308679702519,-3.72084373877824,127.58515276638));
#27297=CARTESIAN_POINT('Ctrl Pts',(172.300932404815,-3.80921160902707,127.690213335137));
#27298=CARTESIAN_POINT('Ctrl Pts',(172.29318510711,-3.89305350831285,127.798812839887));
#27299=CARTESIAN_POINT('Ctrl Pts',(172.285439735789,-3.97687456011947,127.907385341122));
#27300=CARTESIAN_POINT('Ctrl Pts',(172.277694364468,-4.05617164293115,128.019494717258));
#27301=CARTESIAN_POINT('Ctrl Pts',(172.269948993146,-4.13064330814986,128.134722266902));
#27302=CARTESIAN_POINT('Ctrl Pts',(172.262201269052,-4.20513759526255,128.249984818656));
#27303=CARTESIAN_POINT('Ctrl Pts',(172.254453544957,-4.27480331843837,128.368367111375));
#27304=CARTESIAN_POINT('Ctrl Pts',(172.246705820862,-4.33938258107259,128.489421767924));
#27305=CARTESIAN_POINT('Ctrl Pts',(172.238957093025,-4.40397021015532,128.610492107487));
#27306=CARTESIAN_POINT('Ctrl Pts',(172.231208365187,-4.46346988910171,128.734235151717));
#27307=CARTESIAN_POINT('Ctrl Pts',(172.22345963735,-4.51767034852206,128.860180151512));
#27308=CARTESIAN_POINT('Ctrl Pts',(172.215704049381,-4.57191879289411,128.986236653402));
#27309=CARTESIAN_POINT('Ctrl Pts',(172.207948461411,-4.62085849667513,129.114498643236));
#27310=CARTESIAN_POINT('Ctrl Pts',(172.200192873442,-4.66432674005495,129.244476287076));
#27311=CARTESIAN_POINT('Ctrl Pts',(172.193538962521,-4.70162034312863,129.355990677374));
#27312=CARTESIAN_POINT('Ctrl Pts',(172.1868850516,-4.73488728942838,129.46876749788));
#27313=CARTESIAN_POINT('Ctrl Pts',(172.180231140679,-4.76405452823404,129.582490119308));
#27314=CARTESIAN_POINT('Origin',(213.235140564004,0.,130.804360617566));
#27315=CARTESIAN_POINT('',(170.084755673967,-4.76405452823406,129.582490119308));
#27316=CARTESIAN_POINT('',(170.429908526381,-4.76405452823404,129.582490119308));
#27317=CARTESIAN_POINT('',(213.235140564004,-4.76405452823405,129.582490119308));
#27318=CARTESIAN_POINT('',(171.764859436045,-4.91824915272082,130.801473705555));
#27319=CARTESIAN_POINT('Ctrl Pts',(171.764859435991,-4.91824915272138,130.801473706505));
#27320=CARTESIAN_POINT('Ctrl Pts',(171.757035919054,-4.91833059512529,130.940222017634));
#27321=CARTESIAN_POINT('Ctrl Pts',(171.749212402117,-4.91253637186168,131.078982524251));
#27322=CARTESIAN_POINT('Ctrl Pts',(171.74138888518,-4.90088999446994,131.217229028327));
#27323=CARTESIAN_POINT('Ctrl Pts',(171.733564120028,-4.88924175893856,131.355497589159));
#27324=CARTESIAN_POINT('Ctrl Pts',(171.725739354875,-4.87173954124688,131.493251605358));
#27325=CARTESIAN_POINT('Ctrl Pts',(171.717914589723,-4.84845876191544,131.629969905611));
#27326=CARTESIAN_POINT('Ctrl Pts',(171.710087010741,-4.82516961068537,131.766737370529));
#27327=CARTESIAN_POINT('Ctrl Pts',(171.70225943176,-4.79609782325277,131.902468003263));
#27328=CARTESIAN_POINT('Ctrl Pts',(171.694431852778,-4.76136992124217,132.036650979287));
#27329=CARTESIAN_POINT('Ctrl Pts',(171.68659989282,-4.72662258255471,132.170909055475));
#27330=CARTESIAN_POINT('Ctrl Pts',(171.678767932861,-4.68621292006633,132.30361738256));
#27331=CARTESIAN_POINT('Ctrl Pts',(171.670935972903,-4.64031719067666,132.434280686898));
#27332=CARTESIAN_POINT('Ctrl Pts',(171.663093341267,-4.59435892464868,132.565122030542));
#27333=CARTESIAN_POINT('Ctrl Pts',(171.655250709631,-4.54289979057624,132.6939124286));
#27334=CARTESIAN_POINT('Ctrl Pts',(171.647408077995,-4.4861642914408,132.8201763365));
#27335=CARTESIAN_POINT('Ctrl Pts',(171.639559178351,-4.42938344802311,132.946541157344));
#27336=CARTESIAN_POINT('Ctrl Pts',(171.631710278708,-4.36731800569649,133.070375125644));
#27337=CARTESIAN_POINT('Ctrl Pts',(171.623861379065,-4.3002378395814,133.191228352807));
#27338=CARTESIAN_POINT('Ctrl Pts',(171.616000175001,-4.23305251444804,133.312271036964));
#27339=CARTESIAN_POINT('Ctrl Pts',(171.608138970937,-4.16083696557177,133.430323326701));
#27340=CARTESIAN_POINT('Ctrl Pts',(171.600277766874,-4.08390400590978,133.544964772313));
#27341=CARTESIAN_POINT('Ctrl Pts',(171.598124147909,-4.06282780949502,133.576371410451));
#27342=CARTESIAN_POINT('Ctrl Pts',(171.595970528945,-4.04139779314482,133.60752225611));
#27343=CARTESIAN_POINT('Ctrl Pts',(171.593816909981,-4.01962089508612,133.638409121436));
#27344=CARTESIAN_POINT('Ctrl Pts',(171.586042575862,-3.94100862225861,133.749907401736));
#27345=CARTESIAN_POINT('Ctrl Pts',(171.578268241743,-3.85762912375874,133.858308927935));
#27346=CARTESIAN_POINT('Ctrl Pts',(171.570493907623,-3.76975455094454,133.963179018192));
#27347=CARTESIAN_POINT('Ctrl Pts',(171.562729154676,-3.68198827568764,134.067919865435));
#27348=CARTESIAN_POINT('Ctrl Pts',(171.554964401729,-3.58973819731478,134.169137639484));
#27349=CARTESIAN_POINT('Ctrl Pts',(171.547199648782,-3.49331967220828,134.266426580292));
#27350=CARTESIAN_POINT('Ctrl Pts',(171.539442607897,-3.39699691134051,134.363618892351));
#27351=CARTESIAN_POINT('Ctrl Pts',(171.531685567012,-3.29651421627276,134.456889860773));
#27352=CARTESIAN_POINT('Ctrl Pts',(171.523928526127,-3.19222689663071,134.5458670659));
#27353=CARTESIAN_POINT('Ctrl Pts',(171.516177334887,-3.08801822086768,134.634777172625));
#27354=CARTESIAN_POINT('Ctrl Pts',(171.508426143647,-2.98001092751311,134.719399708287));
#27355=CARTESIAN_POINT('Ctrl Pts',(171.500674952407,-2.86859657138408,134.799399637794));
#27356=CARTESIAN_POINT('Ctrl Pts',(171.49292705563,-2.7572295693284,134.879365565197));
#27357=CARTESIAN_POINT('Ctrl Pts',(171.485179158853,-2.64245870155574,134.954712566589));
#27358=CARTESIAN_POINT('Ctrl Pts',(171.477431262076,-2.52470776291514,135.025146536607));
#27359=CARTESIAN_POINT('Ctrl Pts',(171.469684985991,-2.40698145523242,135.095565773358));
#27360=CARTESIAN_POINT('Ctrl Pts',(171.461938709907,-2.28627665190136,135.161073822318));
#27361=CARTESIAN_POINT('Ctrl Pts',(171.454192433823,-2.1630448870223,135.221420712157));
#27362=CARTESIAN_POINT('Ctrl Pts',(171.446446100558,-2.03981221247431,135.281768047463));
#27363=CARTESIAN_POINT('Ctrl Pts',(171.438699767293,-1.91405289028095,135.336953975678));
#27364=CARTESIAN_POINT('Ctrl Pts',(171.430953434027,-1.78624137104705,135.38677535511));
#27365=CARTESIAN_POINT('Ctrl Pts',(171.423205366024,-1.65840122930977,135.436607891694));
#27366=CARTESIAN_POINT('Ctrl Pts',(171.415457298021,-1.52850834022933,135.481073346974));
#27367=CARTESIAN_POINT('Ctrl Pts',(171.407709230018,-1.39705498341314,135.520017563933));
#27368=CARTESIAN_POINT('Ctrl Pts',(171.399952927276,-1.26546191640478,135.55900317127));
#27369=CARTESIAN_POINT('Ctrl Pts',(171.392196624535,-1.13230544411911,135.592455707017));
#27370=CARTESIAN_POINT('Ctrl Pts',(171.384440321793,-0.998091329470628,
135.620271409985));
#27371=CARTESIAN_POINT('Ctrl Pts',(171.376679879279,-0.863805580708047,
135.648101959031));
#27372=CARTESIAN_POINT('Ctrl Pts',(171.368919436764,-0.72846145040388,135.670289617296));
#27373=CARTESIAN_POINT('Ctrl Pts',(171.36115899425,-0.592571632618561,135.686782344815));
#27374=CARTESIAN_POINT('Ctrl Pts',(171.353386093985,-0.456463672433956,
135.703301547925));
#27375=CARTESIAN_POINT('Ctrl Pts',(171.345613193719,-0.319808664241963,
135.714107520806));
#27376=CARTESIAN_POINT('Ctrl Pts',(171.337840293454,-0.18312202844603,135.719200328604));
#27377=CARTESIAN_POINT('Ctrl Pts',(171.330349957692,-0.0514042961550611,
135.724108000011));
#27378=CARTESIAN_POINT('Ctrl Pts',(171.32285962193,0.0803424961590377,135.723710671613));
#27379=CARTESIAN_POINT('Ctrl Pts',(171.315369286168,0.211661992236977,135.718053960006));
#27380=CARTESIAN_POINT('Ctrl Pts',(171.307594952049,0.347960506923273,135.71218277246));
#27381=CARTESIAN_POINT('Ctrl Pts',(171.29982061793,0.484230436602179,135.700626911707));
#27382=CARTESIAN_POINT('Ctrl Pts',(171.292046283811,0.619958966672321,135.68338039024));
#27383=CARTESIAN_POINT('Ctrl Pts',(171.284281530864,0.755520223459236,135.666155123569));
#27384=CARTESIAN_POINT('Ctrl Pts',(171.276516777917,0.89054102409612,135.643253199231));
#27385=CARTESIAN_POINT('Ctrl Pts',(171.268752024969,1.0245095333365,135.614720612265));
#27386=CARTESIAN_POINT('Ctrl Pts',(171.260994984084,1.1583449831651,135.586216364267));
#27387=CARTESIAN_POINT('Ctrl Pts',(171.253237943199,1.29112984157983,135.552092663791));
#27388=CARTESIAN_POINT('Ctrl Pts',(171.245480902314,1.42235872784494,135.512447140966));
#27389=CARTESIAN_POINT('Ctrl Pts',(171.237729711074,1.55348865338571,135.472831515139));
#27390=CARTESIAN_POINT('Ctrl Pts',(171.229978519834,1.6830645695557,135.42770246786));
#27391=CARTESIAN_POINT('Ctrl Pts',(171.222227328594,1.8105929568999,135.377208330635));
#27392=CARTESIAN_POINT('Ctrl Pts',(171.214479431817,1.93806714127793,135.326735654766));
#27393=CARTESIAN_POINT('Ctrl Pts',(171.20673153504,2.06349516495256,135.270902567934));
#27394=CARTESIAN_POINT('Ctrl Pts',(171.198983638263,2.18640051728477,135.209906649617));
#27395=CARTESIAN_POINT('Ctrl Pts',(171.191237362179,2.30928016046664,135.14892349033));
#27396=CARTESIAN_POINT('Ctrl Pts',(171.183491086095,2.42963783192029,135.082779821336));
#27397=CARTESIAN_POINT('Ctrl Pts',(171.175744810011,2.54701915847475,135.011720415451));
#27398=CARTESIAN_POINT('Ctrl Pts',(171.167998476745,2.66440135151142,134.940660485022));
#27399=CARTESIAN_POINT('Ctrl Pts',(171.16025214348,2.77880682135337,134.864684947764));
#27400=CARTESIAN_POINT('Ctrl Pts',(171.152505810215,2.88980820699957,134.78408316936));
#27401=CARTESIAN_POINT('Ctrl Pts',(171.144757742212,3.00083445063688,134.703463340746));
#27402=CARTESIAN_POINT('Ctrl Pts',(171.137009674209,3.10845477684925,134.618215439113));
#27403=CARTESIAN_POINT('Ctrl Pts',(171.129261606206,3.21227339982114,134.528670307603));
#27404=CARTESIAN_POINT('Ctrl Pts',(171.121505303464,3.31620236246078,134.439030006461));
#27405=CARTESIAN_POINT('Ctrl Pts',(171.113749000722,3.4163212540074,134.345083607835));
#27406=CARTESIAN_POINT('Ctrl Pts',(171.10599269798,3.51226940002566,134.247200538931));
#27407=CARTESIAN_POINT('Ctrl Pts',(171.098232255466,3.6082687564584,134.149265226886));
#27408=CARTESIAN_POINT('Ctrl Pts',(171.090471812952,3.70009267013737,134.047389348172));
#27409=CARTESIAN_POINT('Ctrl Pts',(171.082711370438,3.78742023470387,133.941976117951));
#27410=CARTESIAN_POINT('Ctrl Pts',(171.074938470172,3.87488798522955,133.836393669055));
#27411=CARTESIAN_POINT('Ctrl Pts',(171.067165569907,3.95784472616718,133.727262832685));
#27412=CARTESIAN_POINT('Ctrl Pts',(171.059392669641,4.03601191500818,133.615017281837));
#27413=CARTESIAN_POINT('Ctrl Pts',(171.051902333879,4.11133752964417,133.506852139491));
#27414=CARTESIAN_POINT('Ctrl Pts',(171.044411998117,4.18221560535061,133.395795066148));
#27415=CARTESIAN_POINT('Ctrl Pts',(171.036921662355,4.24843784895795,133.282254664139));
#27416=CARTESIAN_POINT('Ctrl Pts',(171.029147328236,4.31717092905886,133.164409343279));
#27417=CARTESIAN_POINT('Ctrl Pts',(171.021372994117,4.38110588169799,133.043515367071));
#27418=CARTESIAN_POINT('Ctrl Pts',(171.013598659998,4.4399604805969,132.920000944568));
#27419=CARTESIAN_POINT('Ctrl Pts',(171.005833907051,4.49874254646279,132.796638742552));
#27420=CARTESIAN_POINT('Ctrl Pts',(170.998069154104,4.55245654971177,132.670662869473));
#27421=CARTESIAN_POINT('Ctrl Pts',(170.990304401156,4.60086452782022,132.542528808261));
#27422=CARTESIAN_POINT('Ctrl Pts',(170.982547360271,4.64922442644237,132.414522011606));
#27423=CARTESIAN_POINT('Ctrl Pts',(170.974790319386,4.69228865022188,132.284361655934));
#27424=CARTESIAN_POINT('Ctrl Pts',(170.967033278501,4.72986616751987,132.152525703841));
#27425=CARTESIAN_POINT('Ctrl Pts',(170.959282087261,4.76741534731984,132.020789170265));
#27426=CARTESIAN_POINT('Ctrl Pts',(170.951530896021,4.79948594948081,131.887379929817));
#27427=CARTESIAN_POINT('Ctrl Pts',(170.943779704781,4.82593601017924,131.752793371194));
#27428=CARTESIAN_POINT('Ctrl Pts',(170.936031808004,4.85237482889622,131.61826401545));
#27429=CARTESIAN_POINT('Ctrl Pts',(170.928283911227,4.87319778221532,131.482558719594));
#27430=CARTESIAN_POINT('Ctrl Pts',(170.92053601445,4.88831353370598,131.346185182058));
#27431=CARTESIAN_POINT('Ctrl Pts',(170.912789738366,4.90342612330728,131.209840170926));
#27432=CARTESIAN_POINT('Ctrl Pts',(170.905043462282,4.91283384261687,131.072827584485));
#27433=CARTESIAN_POINT('Ctrl Pts',(170.897297186197,4.9164970261399,130.93566200544));
#27434=CARTESIAN_POINT('Ctrl Pts',(170.889550852932,4.92016023670372,130.798495413869));
#27435=CARTESIAN_POINT('Ctrl Pts',(170.881804519667,4.91807881642764,130.661176218265));
#27436=CARTESIAN_POINT('Ctrl Pts',(170.874058186401,4.91026521779664,130.524220378763));
#27437=CARTESIAN_POINT('Ctrl Pts',(170.866310118398,4.90244986936441,130.38723386895));
#27438=CARTESIAN_POINT('Ctrl Pts',(170.858562050395,4.88889981046437,130.250611267413));
#27439=CARTESIAN_POINT('Ctrl Pts',(170.850813982392,4.8696794569021,130.114864388769));
#27440=CARTESIAN_POINT('Ctrl Pts',(170.843057679651,4.85043867571933,129.978973236726));
#27441=CARTESIAN_POINT('Ctrl Pts',(170.835301376909,4.82551561627538,129.843960054527));
#27442=CARTESIAN_POINT('Ctrl Pts',(170.827545074167,4.79502613480021,129.71032797222));
#27443=CARTESIAN_POINT('Ctrl Pts',(170.819784631653,4.76452038017076,129.576624566447));
#27444=CARTESIAN_POINT('Ctrl Pts',(170.812024189139,4.72844238640119,129.444304106379));
#27445=CARTESIAN_POINT('Ctrl Pts',(170.804263746624,4.68695793210101,129.313854527268));
#27446=CARTESIAN_POINT('Ctrl Pts',(170.796490846359,4.64540688327195,129.183195538912));
#27447=CARTESIAN_POINT('Ctrl Pts',(170.788717946094,4.59843216469574,129.054413800578));
#27448=CARTESIAN_POINT('Ctrl Pts',(170.780945045828,4.54624807871649,128.927978068813));
#27449=CARTESIAN_POINT('Ctrl Pts',(170.773454710066,4.49596101570655,128.80613859437));
#27450=CARTESIAN_POINT('Ctrl Pts',(170.765964374304,4.44083688581637,128.686477801046));
#27451=CARTESIAN_POINT('Ctrl Pts',(170.758474038542,4.38110687021332,128.569391791325));
#27452=CARTESIAN_POINT('Ctrl Pts',(170.750699704423,4.31911217291391,128.447866429957));
#27453=CARTESIAN_POINT('Ctrl Pts',(170.742925370304,4.25195905043413,128.328729996429));
#27454=CARTESIAN_POINT('Ctrl Pts',(170.735151036185,4.17985521698085,128.212451393157));
#27455=CARTESIAN_POINT('Ctrl Pts',(170.727386283238,4.10784024505831,128.096316092871));
#27456=CARTESIAN_POINT('Ctrl Pts',(170.719621530291,4.03088690600835,127.983031944147));
#27457=CARTESIAN_POINT('Ctrl Pts',(170.711856777344,3.94924978596426,127.873045351246));
#27458=CARTESIAN_POINT('Ctrl Pts',(170.704099736459,3.86769374905841,127.763167998579));
#27459=CARTESIAN_POINT('Ctrl Pts',(170.696342695574,3.78146342035344,127.656581995887));
#27460=CARTESIAN_POINT('Ctrl Pts',(170.688585654689,3.69085766605104,127.553706413955));
#27461=CARTESIAN_POINT('Ctrl Pts',(170.680834463449,3.60032023825277,127.4509084113));
#27462=CARTESIAN_POINT('Ctrl Pts',(170.673083272209,3.50541420975416,127.351815552252));
#27463=CARTESIAN_POINT('Ctrl Pts',(170.665332080968,3.40647963018167,127.256815044686));
#27464=CARTESIAN_POINT('Ctrl Pts',(170.657584184191,3.3075871004449,127.161854914871));
#27465=CARTESIAN_POINT('Ctrl Pts',(170.649836287414,3.20466970656614,127.070983947312));
#27466=CARTESIAN_POINT('Ctrl Pts',(170.642088390637,3.09810522004097,126.984553409335));
#27467=CARTESIAN_POINT('Ctrl Pts',(170.634342114553,2.99156302450901,126.898140950763));
#27468=CARTESIAN_POINT('Ctrl Pts',(170.626595838469,2.88137555722152,126.816167320378));
#27469=CARTESIAN_POINT('Ctrl Pts',(170.618849562385,2.76795431101178,126.738944034404));
#27470=CARTESIAN_POINT('Ctrl Pts',(170.61110322912,2.65453222755217,126.661720178385));
#27471=CARTESIAN_POINT('Ctrl Pts',(170.603356895854,2.53787664070854,126.58924695678));
#27472=CARTESIAN_POINT('Ctrl Pts',(170.595610562589,2.41842837322653,126.521792782018));
#27473=CARTESIAN_POINT('Ctrl Pts',(170.587862494586,2.29895335613314,126.45432350136));
#27474=CARTESIAN_POINT('Ctrl Pts',(170.580114426583,2.17668475429278,126.391875696347));
#27475=CARTESIAN_POINT('Ctrl Pts',(170.57236635858,2.0520879901537,126.334671820439));
#27476=CARTESIAN_POINT('Ctrl Pts',(170.564610055838,1.9273588030912,126.27740714757));
#27477=CARTESIAN_POINT('Ctrl Pts',(170.556853753096,1.80029686672665,126.225397700479));
#27478=CARTESIAN_POINT('Ctrl Pts',(170.549097450355,1.67138810173988,126.178817960119));
#27479=CARTESIAN_POINT('Ctrl Pts',(170.54133700784,1.54241053426362,126.132213358749));
#27480=CARTESIAN_POINT('Ctrl Pts',(170.533576565326,1.41158454681163,126.091044355915));
#27481=CARTESIAN_POINT('Ctrl Pts',(170.525816122812,1.27941026051825,126.055435218301));
#27482=CARTESIAN_POINT('Ctrl Pts',(170.518043222547,1.14702379632676,126.019768917739));
#27483=CARTESIAN_POINT('Ctrl Pts',(170.510270322281,1.01328508976567,125.989680403631));
#27484=CARTESIAN_POINT('Ctrl Pts',(170.502497422016,0.878704354646793,125.965242751712));
#27485=CARTESIAN_POINT('Ctrl Pts',(170.495007086254,0.749015968238953,125.941693469995));
#27486=CARTESIAN_POINT('Ctrl Pts',(170.487516750492,0.61854601515919,125.92339138));
#27487=CARTESIAN_POINT('Ctrl Pts',(170.48002641473,0.487752706712771,125.910356085529));
#27488=CARTESIAN_POINT('Ctrl Pts',(170.472252080611,0.352000330221832,125.896826553907));
#27489=CARTESIAN_POINT('Ctrl Pts',(170.464477746492,0.21546957156963,125.888928225334));
#27490=CARTESIAN_POINT('Ctrl Pts',(170.456703412373,0.0786672062396304,
125.886739797173));
#27491=CARTESIAN_POINT('Ctrl Pts',(170.448938659426,-0.0579665624011073,
125.884554066054));
#27492=CARTESIAN_POINT('Ctrl Pts',(170.441173906479,-0.194870884542369,
125.888064240124));
#27493=CARTESIAN_POINT('Ctrl Pts',(170.433409153531,-0.331532577613189,
125.897297421266));
#27494=CARTESIAN_POINT('Ctrl Pts',(170.425652112646,-0.468058536364183,
125.906521431882));
#27495=CARTESIAN_POINT('Ctrl Pts',(170.417895071762,-0.604341958059236,
125.921457111628));
#27496=CARTESIAN_POINT('Ctrl Pts',(170.410138030877,-0.739868722095001,
125.942079533901));
#27497=CARTESIAN_POINT('Ctrl Pts',(170.402386839636,-0.875293284343255,
125.962686404645));
#27498=CARTESIAN_POINT('Ctrl Pts',(170.394635648396,-1.00996193972761,125.988971423506));
#27499=CARTESIAN_POINT('Ctrl Pts',(170.386884457156,-1.143365114166,126.020857792417));
#27500=CARTESIAN_POINT('Ctrl Pts',(170.379136560379,-1.27671158869719,126.052730608771));
#27501=CARTESIAN_POINT('Ctrl Pts',(170.371388663602,-1.40879327259354,126.090199949401));
#27502=CARTESIAN_POINT('Ctrl Pts',(170.363640766825,-1.53911043998262,126.133137853017));
#27503=CARTESIAN_POINT('Ctrl Pts',(170.355894490741,-1.66940034782977,126.176066774951));
#27504=CARTESIAN_POINT('Ctrl Pts',(170.348148214657,-1.79792610223434,126.22446186231));
#27505=CARTESIAN_POINT('Ctrl Pts',(170.340401938573,-1.92420319384619,126.27814529665));
#27506=CARTESIAN_POINT('Ctrl Pts',(170.332655605307,-2.0504812176065,126.331829127269));
#27507=CARTESIAN_POINT('Ctrl Pts',(170.324909272042,-2.17451018565046,126.390801229804));
#27508=CARTESIAN_POINT('Ctrl Pts',(170.317162938777,-2.29582599953964,126.454835811068));
#27509=CARTESIAN_POINT('Ctrl Pts',(170.309414870774,-2.4171689812639,126.518884732433));
#27510=CARTESIAN_POINT('Ctrl Pts',(170.301666802771,-2.53579725410604,126.587998206005));
#27511=CARTESIAN_POINT('Ctrl Pts',(170.293918734768,-2.65127208946793,126.661904900228));
#27512=CARTESIAN_POINT('Ctrl Pts',(170.286162432026,-2.76686965285929,126.735890143364));
#27513=CARTESIAN_POINT('Ctrl Pts',(170.278406129284,-2.87930675394613,126.814678572455));
#27514=CARTESIAN_POINT('Ctrl Pts',(170.270649826542,-2.98817394496498,126.897955679886));
#27515=CARTESIAN_POINT('Ctrl Pts',(170.262889384028,-3.097099241682,126.981277234817));
#27516=CARTESIAN_POINT('Ctrl Pts',(170.255128941514,-3.20245053155298,127.069091991604));
#27517=CARTESIAN_POINT('Ctrl Pts',(170.247368499,-3.30385293780894,127.161046353351));
#27518=CARTESIAN_POINT('Ctrl Pts',(170.239595598734,-3.40541812420926,127.253148328403));
#27519=CARTESIAN_POINT('Ctrl Pts',(170.231822698469,-3.5030214809247,127.349402913082));
#27520=CARTESIAN_POINT('Ctrl Pts',(170.224049798203,-3.59632574424345,127.449420349276));
#27521=CARTESIAN_POINT('Ctrl Pts',(170.216559462441,-3.686238162572,127.545801899737));
#27522=CARTESIAN_POINT('Ctrl Pts',(170.209069126679,-3.77215842577424,127.64567723967));
#27523=CARTESIAN_POINT('Ctrl Pts',(170.201578790917,-3.85382236621166,127.74867145926));
#27524=CARTESIAN_POINT('Ctrl Pts',(170.193812524806,-3.938494657719,127.855459798618));
#27525=CARTESIAN_POINT('Ctrl Pts',(170.186046258694,-4.01886496298055,127.965946739028));
#27526=CARTESIAN_POINT('Ctrl Pts',(170.178279992583,-4.09459191344809,128.079750530815));
#27527=CARTESIAN_POINT('Ctrl Pts',(170.170486299365,-4.17058629888614,128.193956228575));
#27528=CARTESIAN_POINT('Ctrl Pts',(170.162692606147,-4.24190416979371,128.31150198608));
#27529=CARTESIAN_POINT('Ctrl Pts',(170.154898912929,-4.30823965276746,128.431966435137));
#27530=CARTESIAN_POINT('Ctrl Pts',(170.147152164206,-4.37417557090397,128.551705279197));
#27531=CARTESIAN_POINT('Ctrl Pts',(170.139405415483,-4.43518874164617,128.674327418701));
#27532=CARTESIAN_POINT('Ctrl Pts',(170.131658666761,-4.49102105971179,128.799388571944));
#27533=CARTESIAN_POINT('Ctrl Pts',(170.123841501295,-4.54736088487774,128.925586511648));
#27534=CARTESIAN_POINT('Ctrl Pts',(170.116024335829,-4.59842496368119,129.054267699693));
#27535=CARTESIAN_POINT('Ctrl Pts',(170.108207170364,-4.64399504249936,129.184949271508));
#27536=CARTESIAN_POINT('Ctrl Pts',(170.100390004898,-4.68956512131752,129.315630843323));
#27537=CARTESIAN_POINT('Ctrl Pts',(170.092572839433,-4.72964103274668,129.448312422701));
#27538=CARTESIAN_POINT('Ctrl Pts',(170.084755673967,-4.76405452823406,129.582490119308));
#27539=CARTESIAN_POINT('Ctrl Pts',(171.834603948179,-4.76405452823406,129.582490119308));
#27540=CARTESIAN_POINT('Ctrl Pts',(171.825910999201,-4.80206436672034,129.730689902686));
#27541=CARTESIAN_POINT('Ctrl Pts',(171.817218050222,-4.83319925274758,129.880837722785));
#27542=CARTESIAN_POINT('Ctrl Pts',(171.808525101244,-4.85727658297744,130.032319647825));
#27543=CARTESIAN_POINT('Ctrl Pts',(171.799878869647,-4.88122451755313,130.182987483321));
#27544=CARTESIAN_POINT('Ctrl Pts',(171.79123263805,-4.8981904550706,130.334974919894));
#27545=CARTESIAN_POINT('Ctrl Pts',(171.782586406452,-4.90804272339544,130.487659357977));
#27546=CARTESIAN_POINT('Ctrl Pts',(171.776677416316,-4.9147759407161,130.592006648287));
#27547=CARTESIAN_POINT('Ctrl Pts',(171.770768426181,-4.91818764042097,130.696679096119));
#27548=CARTESIAN_POINT('Ctrl Pts',(171.764859436045,-4.91824915272082,130.801473705556));
#27549=CARTESIAN_POINT('',(172.110140563973,-4.91824950728406,130.802159118055));
#27550=CARTESIAN_POINT('Ctrl Pts',(172.180231140679,-4.76405452823404,129.582490119308));
#27551=CARTESIAN_POINT('Ctrl Pts',(172.172465945589,-4.79809305117586,129.715205803652));
#27552=CARTESIAN_POINT('Ctrl Pts',(172.1647007505,-4.82654693481475,129.849209433246));
#27553=CARTESIAN_POINT('Ctrl Pts',(172.156935555411,-4.84934811999046,129.9839912656));
#27554=CARTESIAN_POINT('Ctrl Pts',(172.149159740024,-4.87218048987978,130.118957436304));
#27555=CARTESIAN_POINT('Ctrl Pts',(172.141383924637,-4.88934468447975,130.254703547973));
#27556=CARTESIAN_POINT('Ctrl Pts',(172.133608109249,-4.90082457327812,130.390716368901));
#27557=CARTESIAN_POINT('Ctrl Pts',(172.132779793315,-4.90204746429799,130.405205085667));
#27558=CARTESIAN_POINT('Ctrl Pts',(172.131951477382,-4.90320590135478,130.41969683088));
#27559=CARTESIAN_POINT('Ctrl Pts',(172.131123161448,-4.90429989972426,130.434190986093));
#27560=CARTESIAN_POINT('Ctrl Pts',(172.124128962302,-4.91353748909132,130.556577872414));
#27561=CARTESIAN_POINT('Ctrl Pts',(172.117134763155,-4.91819451989084,130.679314828552));
#27562=CARTESIAN_POINT('Ctrl Pts',(172.110140564008,-4.91824950728378,130.802159117434));
#27563=CARTESIAN_POINT('Ctrl Pts',(172.110140563973,-4.91824950728406,130.802159118055));
#27564=CARTESIAN_POINT('Ctrl Pts',(172.102450296272,-4.91830996705132,130.937228973409));
#27565=CARTESIAN_POINT('Ctrl Pts',(172.094760028571,-4.91280209186903,131.072526111654));
#27566=CARTESIAN_POINT('Ctrl Pts',(172.087069760869,-4.90169598927124,131.207547288058));
#27567=CARTESIAN_POINT('Ctrl Pts',(172.0793884731,-4.89060285527838,131.342410800125));
#27568=CARTESIAN_POINT('Ctrl Pts',(172.071707185331,-4.87392452826556,131.476998596401));
#27569=CARTESIAN_POINT('Ctrl Pts',(172.064025897562,-4.8516831047687,131.610805974303));
#27570=CARTESIAN_POINT('Ctrl Pts',(172.056351646764,-4.82946205705517,131.744490768767));
#27571=CARTESIAN_POINT('Ctrl Pts',(172.048677395965,-4.80168811669321,131.877396174964));
#27572=CARTESIAN_POINT('Ctrl Pts',(172.041003145167,-4.76843526592711,132.009021639249));
#27573=CARTESIAN_POINT('Ctrl Pts',(172.03315616152,-4.734433956477,132.143609743414));
#27574=CARTESIAN_POINT('Ctrl Pts',(172.025309177873,-4.69470417974674,132.276859175735));
#27575=CARTESIAN_POINT('Ctrl Pts',(172.017462194226,-4.64938062361568,132.408244303887));
#27576=CARTESIAN_POINT('Ctrl Pts',(172.009795351173,-4.60509754529266,132.536613267338));
#27577=CARTESIAN_POINT('Ctrl Pts',(172.00212850812,-4.55547487742502,132.663202199823));
#27578=CARTESIAN_POINT('Ctrl Pts',(171.994461665067,-4.50068881193671,132.787535667986));
#27579=CARTESIAN_POINT('Ctrl Pts',(171.986795591432,-4.44590824458666,132.911856658476));
#27580=CARTESIAN_POINT('Ctrl Pts',(171.979129517797,-4.38596547125795,133.033922268786));
#27581=CARTESIAN_POINT('Ctrl Pts',(171.971463444162,-4.3210846192262,133.153277554366));
#27582=CARTESIAN_POINT('Ctrl Pts',(171.963796395263,-4.25619551317209,133.272648024106));
#27583=CARTESIAN_POINT('Ctrl Pts',(171.956129346364,-4.18636727026433,133.389307132091));
#27584=CARTESIAN_POINT('Ctrl Pts',(171.948462297465,-4.11186945341913,133.502825488662));
#27585=CARTESIAN_POINT('Ctrl Pts',(171.94048006748,-4.03430914105516,133.621010417665));
#27586=CARTESIAN_POINT('Ctrl Pts',(171.932497837494,-3.95168740455701,133.73579046403));
#27587=CARTESIAN_POINT('Ctrl Pts',(171.924515607508,-3.86435680919402,133.846716532599));
#27588=CARTESIAN_POINT('Ctrl Pts',(171.916837196073,-3.78035017906484,133.953420548245));
#27589=CARTESIAN_POINT('Ctrl Pts',(171.909158784638,-3.6919868793546,134.056558317157));
#27590=CARTESIAN_POINT('Ctrl Pts',(171.901480373204,-3.59961974551205,134.155766404728));
#27591=CARTESIAN_POINT('Ctrl Pts',(171.893796744521,-3.50718985100099,134.255041901187));
#27592=CARTESIAN_POINT('Ctrl Pts',(171.886113115839,-3.4107509900769,134.350382121039));
#27593=CARTESIAN_POINT('Ctrl Pts',(171.878429487156,-3.31069053982214,134.441462652433));
#27594=CARTESIAN_POINT('Ctrl Pts',(171.870735374791,-3.21049356527748,134.532667455753));
#27595=CARTESIAN_POINT('Ctrl Pts',(171.863041262427,-3.10666544848945,134.619600721057));
#27596=CARTESIAN_POINT('Ctrl Pts',(171.855347150062,-2.99962419783545,134.701980113394));
#27597=CARTESIAN_POINT('Ctrl Pts',(171.854456612586,-2.98723495257262,134.711514928151));
#27598=CARTESIAN_POINT('Ctrl Pts',(171.85356607511,-2.97480269154766,134.720988787297));
#27599=CARTESIAN_POINT('Ctrl Pts',(171.852675537635,-2.96232808469272,134.730401292488));
#27600=CARTESIAN_POINT('Ctrl Pts',(171.844901203515,-2.8534255799377,134.812571849301));
#27601=CARTESIAN_POINT('Ctrl Pts',(171.837126869396,-2.74092905759722,134.890337935185));
#27602=CARTESIAN_POINT('Ctrl Pts',(171.829352535277,-2.62523039615684,134.963368724025));
#27603=CARTESIAN_POINT('Ctrl Pts',(171.82158778233,-2.50967432297672,135.036309508945));
#27604=CARTESIAN_POINT('Ctrl Pts',(171.813823029383,-2.39092429019464,135.104526401701));
#27605=CARTESIAN_POINT('Ctrl Pts',(171.806058276436,-2.26940448721128,135.167729308833));
#27606=CARTESIAN_POINT('Ctrl Pts',(171.798301235551,-2.14800537940892,135.230869441946));
#27607=CARTESIAN_POINT('Ctrl Pts',(171.790544194666,-2.02384232058094,135.289005320549));
#27608=CARTESIAN_POINT('Ctrl Pts',(171.782787153781,-1.89736736539807,135.341890798537));
#27609=CARTESIAN_POINT('Ctrl Pts',(171.775035962541,-1.77098778596248,135.394736395174));
#27610=CARTESIAN_POINT('Ctrl Pts',(171.767284771301,-1.64230013958309,135.442339321861));
#27611=CARTESIAN_POINT('Ctrl Pts',(171.759533580061,-1.51177958039806,135.484500098692));
#27612=CARTESIAN_POINT('Ctrl Pts',(171.751785683284,-1.38131449593287,135.526642956067));
#27613=CARTESIAN_POINT('Ctrl Pts',(171.744037786506,-1.24901841936518,135.563348144159));
#27614=CARTESIAN_POINT('Ctrl Pts',(171.736289889729,-1.1153847079433,135.59446500221));
#27615=CARTESIAN_POINT('Ctrl Pts',(171.728543613645,-0.981778949813042,
135.625575351285));
#27616=CARTESIAN_POINT('Ctrl Pts',(171.720797337561,-0.846836493912149,
135.651099606832));
#27617=CARTESIAN_POINT('Ctrl Pts',(171.713051061477,-0.711063636366915,
135.670937604272));
#27618=CARTESIAN_POINT('Ctrl Pts',(171.705304728212,-0.575289776577245,
135.690775748152));
#27619=CARTESIAN_POINT('Ctrl Pts',(171.697558394946,-0.438685889769167,
135.704927493644));
#27620=CARTESIAN_POINT('Ctrl Pts',(171.689812061681,-0.301765795447225,
135.713344266673));
#27621=CARTESIAN_POINT('Ctrl Pts',(171.682063993678,-0.164815038819777,
135.721762924579));
#27622=CARTESIAN_POINT('Ctrl Pts',(171.674315925675,-0.0275483239237374,
135.724444030416));
#27623=CARTESIAN_POINT('Ctrl Pts',(171.666567857672,0.109518508915834,135.721391099341));
#27624=CARTESIAN_POINT('Ctrl Pts',(171.65881155493,0.246731018016651,135.718334923575));
#27625=CARTESIAN_POINT('Ctrl Pts',(171.651055252188,0.383742829203628,135.70953254579));
#27626=CARTESIAN_POINT('Ctrl Pts',(171.643298949447,0.520040650371349,135.695039587245));
#27627=CARTESIAN_POINT('Ctrl Pts',(171.635538506932,0.656411217790121,135.680538893372));
#27628=CARTESIAN_POINT('Ctrl Pts',(171.627778064418,0.792066649346082,135.660341624338));
#27629=CARTESIAN_POINT('Ctrl Pts',(171.620017621904,0.926502845105625,135.634554768996));
#27630=CARTESIAN_POINT('Ctrl Pts',(171.612244721639,1.06115484978138,135.608726518305));
#27631=CARTESIAN_POINT('Ctrl Pts',(171.604471821373,1.19458332673509,135.5772908403));
#27632=CARTESIAN_POINT('Ctrl Pts',(171.596698921108,1.32629748942126,135.540405173105));
#27633=CARTESIAN_POINT('Ctrl Pts',(171.589208585346,1.45322351052502,135.504860392824));
#27634=CARTESIAN_POINT('Ctrl Pts',(171.581718249584,1.57855739969979,135.464255080619));
#27635=CARTESIAN_POINT('Ctrl Pts',(171.574227913822,1.70187852239886,135.418772016379));
#27636=CARTESIAN_POINT('Ctrl Pts',(171.566453579703,1.82987540294846,135.371564447935));
#27637=CARTESIAN_POINT('Ctrl Pts',(171.558679245584,1.95610933165808,135.318952406585));
#27638=CARTESIAN_POINT('Ctrl Pts',(171.550904911465,2.08009015525429,135.261086771203));
#27639=CARTESIAN_POINT('Ctrl Pts',(171.543140158518,2.20391818356556,135.203292450046));
#27640=CARTESIAN_POINT('Ctrl Pts',(171.535375405571,2.3254982807933,135.140257581115));
#27641=CARTESIAN_POINT('Ctrl Pts',(171.527610652623,2.44435709836126,135.072182244367));
#27642=CARTESIAN_POINT('Ctrl Pts',(171.519853611738,2.56309786367635,135.004174521003));
#27643=CARTESIAN_POINT('Ctrl Pts',(171.512096570853,2.67912239098659,134.931136485563));
#27644=CARTESIAN_POINT('Ctrl Pts',(171.504339529968,2.79197924401099,134.853315416463));
#27645=CARTESIAN_POINT('Ctrl Pts',(171.496588338728,2.90475099080486,134.775553032836));
#27646=CARTESIAN_POINT('Ctrl Pts',(171.488837147488,3.01435949745014,134.693015015954));
#27647=CARTESIAN_POINT('Ctrl Pts',(171.481085956248,3.12038010343401,134.605993302689));
#27648=CARTESIAN_POINT('Ctrl Pts',(171.473338059471,3.22635564783182,134.519008575973));
#27649=CARTESIAN_POINT('Ctrl Pts',(171.465590162694,3.32874602301495,134.427544190675));
#27650=CARTESIAN_POINT('Ctrl Pts',(171.457842265917,3.42715780217672,134.3319337864));
#27651=CARTESIAN_POINT('Ctrl Pts',(171.450095989833,3.52554899571583,134.236343381761));
#27652=CARTESIAN_POINT('Ctrl Pts',(171.442349713749,3.61996296835883,134.13660895543));
#27653=CARTESIAN_POINT('Ctrl Pts',(171.434603437664,3.71004178338641,134.033102327277));
#27654=CARTESIAN_POINT('Ctrl Pts',(171.426857104399,3.80012126335536,133.929594935061));
#27655=CARTESIAN_POINT('Ctrl Pts',(171.419110771134,3.88586526519137,133.82231558038));
#27656=CARTESIAN_POINT('Ctrl Pts',(171.411364437868,3.96695519015602,133.711670298662));
#27657=CARTESIAN_POINT('Ctrl Pts',(171.403616369865,4.04806327464702,133.6010002387));
#27658=CARTESIAN_POINT('Ctrl Pts',(171.395868301862,4.12451497724753,133.486963067057));
#27659=CARTESIAN_POINT('Ctrl Pts',(171.388120233859,4.19603443106404,133.369994674836));
#27660=CARTESIAN_POINT('Ctrl Pts',(171.380363931118,4.2676298966072,133.252901967217));
#27661=CARTESIAN_POINT('Ctrl Pts',(171.372607628376,4.3342824375269,133.132872149886));
#27662=CARTESIAN_POINT('Ctrl Pts',(171.364851325634,4.39576140264166,133.010367134679));
#27663=CARTESIAN_POINT('Ctrl Pts',(171.35709088312,4.45727318093121,132.887796734857));
#27664=CARTESIAN_POINT('Ctrl Pts',(171.349330440606,4.51360572080102,132.762748861069));
#27665=CARTESIAN_POINT('Ctrl Pts',(171.341569998091,4.56457655667485,132.635705456954));
#27666=CARTESIAN_POINT('Ctrl Pts',(171.333797097826,4.61562921545938,132.508458111489));
#27667=CARTESIAN_POINT('Ctrl Pts',(171.326024197561,4.661302840214,132.379209203116));
#27668=CARTESIAN_POINT('Ctrl Pts',(171.318251297295,4.7014646059764,132.248456743609));
#27669=CARTESIAN_POINT('Ctrl Pts',(171.310760961533,4.74016639039183,132.12245746535));
#27670=CARTESIAN_POINT('Ctrl Pts',(171.303270625771,4.77375001978124,131.99506235166));
#27671=CARTESIAN_POINT('Ctrl Pts',(171.295780290009,4.80214190879403,131.866724091291));
#27672=CARTESIAN_POINT('Ctrl Pts',(171.28800595589,4.83161028490836,131.733519846771));
#27673=CARTESIAN_POINT('Ctrl Pts',(171.280231621771,4.85557880637322,131.598877573947));
#27674=CARTESIAN_POINT('Ctrl Pts',(171.272457287652,4.8739094720403,131.463291206366));
#27675=CARTESIAN_POINT('Ctrl Pts',(171.264692534705,4.89221754680019,131.327871936865));
#27676=CARTESIAN_POINT('Ctrl Pts',(171.256927781758,4.90490153863927,131.19151127137));
#27677=CARTESIAN_POINT('Ctrl Pts',(171.249163028811,4.91187392402293,131.054715599549));
#27678=CARTESIAN_POINT('Ctrl Pts',(171.241405987926,4.91883938433513,130.918055795117));
#27679=CARTESIAN_POINT('Ctrl Pts',(171.233648947041,4.92010450764289,130.780962232097));
#27680=CARTESIAN_POINT('Ctrl Pts',(171.225891906156,4.91563332394328,130.643948376642));
#27681=CARTESIAN_POINT('Ctrl Pts',(171.218140714916,4.91116551199808,130.507037844401));
#27682=CARTESIAN_POINT('Ctrl Pts',(171.210389523676,4.90097001597565,130.370207289259));
#27683=CARTESIAN_POINT('Ctrl Pts',(171.202638332436,4.88506291125395,130.233971789142));
#27684=CARTESIAN_POINT('Ctrl Pts',(171.194890435658,4.86916256747607,130.097794192747));
#27685=CARTESIAN_POINT('Ctrl Pts',(171.187142538881,4.84755548852937,129.962211535864));
#27686=CARTESIAN_POINT('Ctrl Pts',(171.179394642104,4.82030971806418,129.827735159964));
#27687=CARTESIAN_POINT('Ctrl Pts',(171.17164836602,4.79306964682682,129.693286913623));
#27688=CARTESIAN_POINT('Ctrl Pts',(171.163902089936,4.76019330773209,129.559944870916));
#27689=CARTESIAN_POINT('Ctrl Pts',(171.156155813852,4.72180004982653,129.428211151862));
#27690=CARTESIAN_POINT('Ctrl Pts',(171.148409480587,4.68340650851073,129.29647646038));
#27691=CARTESIAN_POINT('Ctrl Pts',(171.140663147321,4.63949607651496,129.16635049159));
#27692=CARTESIAN_POINT('Ctrl Pts',(171.132916814056,4.59023815254312,129.038320763702));
#27693=CARTESIAN_POINT('Ctrl Pts',(171.125168746053,4.54096919760087,128.910262364443));
#27694=CARTESIAN_POINT('Ctrl Pts',(171.11742067805,4.48635050808955,128.784301505036));
#27695=CARTESIAN_POINT('Ctrl Pts',(171.109672610047,4.42659969874548,128.660905889897));
#27696=CARTESIAN_POINT('Ctrl Pts',(171.101916307306,4.36678538552995,128.53737912843));
#27697=CARTESIAN_POINT('Ctrl Pts',(171.094160004564,4.30182822723501,128.416423409898));
#27698=CARTESIAN_POINT('Ctrl Pts',(171.086403701822,4.23199217077095,128.298482462301));
#27699=CARTESIAN_POINT('Ctrl Pts',(171.078643259308,4.16211884070077,128.18047856607));
#27700=CARTESIAN_POINT('Ctrl Pts',(171.070882816793,4.0873616367418,128.06549297461));
#27701=CARTESIAN_POINT('Ctrl Pts',(171.063122374279,4.00802740462579,127.953939703689));
#27702=CARTESIAN_POINT('Ctrl Pts',(171.055349474014,3.92856581815739,127.842207357554));
#27703=CARTESIAN_POINT('Ctrl Pts',(171.047576573749,3.84451276084427,127.733918651447));
#27704=CARTESIAN_POINT('Ctrl Pts',(171.039803673483,3.75621542895881,127.629454522301));
#27705=CARTESIAN_POINT('Ctrl Pts',(171.032313337721,3.67112792749383,127.528787927377));
#27706=CARTESIAN_POINT('Ctrl Pts',(171.024823001959,3.58209958233881,127.431672898084));
#27707=CARTESIAN_POINT('Ctrl Pts',(171.017332666197,3.48947147868166,127.33841603319));
#27708=CARTESIAN_POINT('Ctrl Pts',(171.009558332078,3.39333135232187,127.241623305919));
#27709=CARTESIAN_POINT('Ctrl Pts',(171.001783997958,3.29300856624316,127.148680472706));
#27710=CARTESIAN_POINT('Ctrl Pts',(170.994009663839,3.18884408773586,127.059970620969));
#27711=CARTESIAN_POINT('Ctrl Pts',(170.986244910892,3.08480798263913,126.971370096198));
#27712=CARTESIAN_POINT('Ctrl Pts',(170.978480157945,2.97693990023683,126.88699242414));
#27713=CARTESIAN_POINT('Ctrl Pts',(170.970715404998,2.86561857188853,126.807184956809));
#27714=CARTESIAN_POINT('Ctrl Pts',(170.962958364113,2.75440780945225,126.727456755379));
#27715=CARTESIAN_POINT('Ctrl Pts',(170.955201323228,2.63975094224204,126.652289951801));
#27716=CARTESIAN_POINT('Ctrl Pts',(170.947444282343,2.5220605212085,126.581992349655));
#27717=CARTESIAN_POINT('Ctrl Pts',(170.939693091103,2.40445885143709,126.511747759477));
#27718=CARTESIAN_POINT('Ctrl Pts',(170.931941899863,2.28382851551378,126.446365261706));
#27719=CARTESIAN_POINT('Ctrl Pts',(170.924190708623,2.16061155222033,126.38610974387));
#27720=CARTESIAN_POINT('Ctrl Pts',(170.916442811845,2.03744695942353,126.325879836238));
#27721=CARTESIAN_POINT('Ctrl Pts',(170.908694915068,1.91169827633441,126.270772745864));
#27722=CARTESIAN_POINT('Ctrl Pts',(170.900947018291,1.78383248826975,126.221007618255));
#27723=CARTESIAN_POINT('Ctrl Pts',(170.893200742207,1.65599344697153,126.171252900438));
#27724=CARTESIAN_POINT('Ctrl Pts',(170.885454466123,1.52603854566862,126.126838064481));
#27725=CARTESIAN_POINT('Ctrl Pts',(170.877708190039,1.39445474323015,126.087934106787));
#27726=CARTESIAN_POINT('Ctrl Pts',(170.869961856774,1.26286996947003,126.049029861912));
#27727=CARTESIAN_POINT('Ctrl Pts',(170.862215523508,1.12965664550267,126.015636687324));
#27728=CARTESIAN_POINT('Ctrl Pts',(170.854469190243,0.995316498341022,125.987875578595));
#27729=CARTESIAN_POINT('Ctrl Pts',(170.84672112224,0.860946266634589,125.960108252958));
#27730=CARTESIAN_POINT('Ctrl Pts',(170.838973054237,0.725449092400377,125.937975582051));
#27731=CARTESIAN_POINT('Ctrl Pts',(170.831224986234,0.589336094692924,125.921547286095));
#27732=CARTESIAN_POINT('Ctrl Pts',(170.823468683492,0.453078434471974,125.905101529951));
#27733=CARTESIAN_POINT('Ctrl Pts',(170.81571238075,0.316204032101677,125.894372306533));
#27734=CARTESIAN_POINT('Ctrl Pts',(170.807956078008,0.179228878268098,125.889377395652));
#27735=CARTESIAN_POINT('Ctrl Pts',(170.800195635494,0.0421806166707686,
125.884379818837));
#27736=CARTESIAN_POINT('Ctrl Pts',(170.79243519298,-0.0949681127710925,
125.885122650899));
#27737=CARTESIAN_POINT('Ctrl Pts',(170.784674750466,-0.231703129255,125.891571519468));
#27738=CARTESIAN_POINT('Ctrl Pts',(170.7769018502,-0.368657644926318,125.898030740332));
#27739=CARTESIAN_POINT('Ctrl Pts',(170.769128949935,-0.505196730856685,
125.910214267207));
#27740=CARTESIAN_POINT('Ctrl Pts',(170.761356049669,-0.640812225951854,
125.928035899751));
#27741=CARTESIAN_POINT('Ctrl Pts',(170.753865713907,-0.771497756204666,
125.945209671062));
#27742=CARTESIAN_POINT('Ctrl Pts',(170.746375378145,-0.901325375981167,
125.967618693755));
#27743=CARTESIAN_POINT('Ctrl Pts',(170.738885042383,-1.02985277017972,125.995141727325));
#27744=CARTESIAN_POINT('Ctrl Pts',(170.731110708264,-1.16325331959507,126.023708305078));
#27745=CARTESIAN_POINT('Ctrl Pts',(170.723336374145,-1.2956756738514,126.057874834688));
#27746=CARTESIAN_POINT('Ctrl Pts',(170.715562040026,-1.42661322950235,126.097561518825));
#27747=CARTESIAN_POINT('Ctrl Pts',(170.707797287079,-1.55738941631831,126.137199292671));
#27748=CARTESIAN_POINT('Ctrl Pts',(170.700032534132,-1.68668407488329,126.182343572593));
#27749=CARTESIAN_POINT('Ctrl Pts',(170.692267781185,-1.81400025456092,126.232863473418));
#27750=CARTESIAN_POINT('Ctrl Pts',(170.6845107403,-1.94118998201404,126.283333197166));
#27751=CARTESIAN_POINT('Ctrl Pts',(170.676753699415,-2.06640478007488,126.339167773415));
#27752=CARTESIAN_POINT('Ctrl Pts',(170.66899665853,-2.1891626910087,126.400186486722));
#27753=CARTESIAN_POINT('Ctrl Pts',(170.66124546729,-2.31182802924725,126.461159185342));
#27754=CARTESIAN_POINT('Ctrl Pts',(170.65349427605,-2.43203981947728,126.527308066281));
#27755=CARTESIAN_POINT('Ctrl Pts',(170.645743084809,-2.54933627155889,126.598404407973));
#27756=CARTESIAN_POINT('Ctrl Pts',(170.637995188032,-2.66658286951899,126.669470531822));
#27757=CARTESIAN_POINT('Ctrl Pts',(170.630247291255,-2.78091626015609,126.745479731881));
#27758=CARTESIAN_POINT('Ctrl Pts',(170.622499394478,-2.89189965317959,126.826157573673));
#27759=CARTESIAN_POINT('Ctrl Pts',(170.614753118394,-3.0028598308699,126.9068185394));
#27760=CARTESIAN_POINT('Ctrl Pts',(170.60700684231,-3.11047108873344,126.992145974653));
#27761=CARTESIAN_POINT('Ctrl Pts',(170.599260566226,-3.21432634948992,127.081822614876));
#27762=CARTESIAN_POINT('Ctrl Pts',(170.591514232961,-3.31818237688276,127.171499917071));
#27763=CARTESIAN_POINT('Ctrl Pts',(170.583767899695,-3.41828205592868,127.265526232784));
#27764=CARTESIAN_POINT('Ctrl Pts',(170.57602156643,-3.51425239391991,127.363544845932));
#27765=CARTESIAN_POINT('Ctrl Pts',(170.568273498427,-3.6102442238021,127.461585409667));
#27766=CARTESIAN_POINT('Ctrl Pts',(170.560525430424,-3.70210459904195,127.563619770583));
#27767=CARTESIAN_POINT('Ctrl Pts',(170.552777362421,-3.78949858970825,127.669255595226));
#27768=CARTESIAN_POINT('Ctrl Pts',(170.545021059679,-3.87698546374816,127.775003690882));
#27769=CARTESIAN_POINT('Ctrl Pts',(170.537264756937,-3.95999622110164,127.884360594747));
#27770=CARTESIAN_POINT('Ctrl Pts',(170.529508454195,-4.0382369975398,127.996901799667));
#27771=CARTESIAN_POINT('Ctrl Pts',(170.521748011681,-4.11651953343623,128.109503071216));
#27772=CARTESIAN_POINT('Ctrl Pts',(170.513987569167,-4.19002680609195,128.225291700424));
#27773=CARTESIAN_POINT('Ctrl Pts',(170.506227126653,-4.25850980667207,128.343816513312));
#27774=CARTESIAN_POINT('Ctrl Pts',(170.498454226387,-4.32710274224426,128.462531592752));
#27775=CARTESIAN_POINT('Ctrl Pts',(170.490681326122,-4.39065510712692,128.583991286608));
#27776=CARTESIAN_POINT('Ctrl Pts',(170.482908425857,-4.44896475062447,128.70772147117));
#27777=CARTESIAN_POINT('Ctrl Pts',(170.475418090095,-4.50515469170763,128.826953751865));
#27778=CARTESIAN_POINT('Ctrl Pts',(170.467927754333,-4.55647634596472,128.948294029428));
#27779=CARTESIAN_POINT('Ctrl Pts',(170.460437418571,-4.60279263435049,129.071304638185));
#27780=CARTESIAN_POINT('Ctrl Pts',(170.45151081296,-4.65799005846015,129.217902497775));
#27781=CARTESIAN_POINT('Ctrl Pts',(170.442584207349,-4.70622458911788,129.367257882038));
#27782=CARTESIAN_POINT('Ctrl Pts',(170.433657601738,-4.74724902999245,129.518744146866));
#27783=CARTESIAN_POINT('Ctrl Pts',(170.432407909952,-4.75299230005541,129.539951663926));
#27784=CARTESIAN_POINT('Ctrl Pts',(170.431158218167,-4.75859433443983,129.561200906575));
#27785=CARTESIAN_POINT('Ctrl Pts',(170.429908526381,-4.76405452823404,129.582490119308));
#27786=CARTESIAN_POINT('Origin',(213.235140564004,0.,130.804360617566));
#27787=CARTESIAN_POINT('',(168.33498954974,-4.76405452823405,129.582490119308));
#27788=CARTESIAN_POINT('',(168.68000091015,-4.76405452823405,129.582490119308));
#27789=CARTESIAN_POINT('',(213.235140564004,-4.76405452823405,129.582490119308));
#27790=CARTESIAN_POINT('',(170.01485943594,-4.91824845497615,130.808259030672));
#27791=CARTESIAN_POINT('Ctrl Pts',(170.01485943594,-4.91824845497615,130.808259030672));
#27792=CARTESIAN_POINT('Ctrl Pts',(170.005798405087,-4.91812126027409,130.968728208735));
#27793=CARTESIAN_POINT('Ctrl Pts',(169.996737374234,-4.91013668640864,131.128867560345));
#27794=CARTESIAN_POINT('Ctrl Pts',(169.987676343381,-4.89441470293228,131.287980073565));
#27795=CARTESIAN_POINT('Ctrl Pts',(169.978558931458,-4.87859489148667,131.448082643419));
#27796=CARTESIAN_POINT('Ctrl Pts',(169.969441519536,-4.85494118831579,131.607145469039));
#27797=CARTESIAN_POINT('Ctrl Pts',(169.960324107613,-4.82362485110961,131.764478505254));
#27798=CARTESIAN_POINT('Ctrl Pts',(169.951141754702,-4.79208545566063,131.922932184357));
#27799=CARTESIAN_POINT('Ctrl Pts',(169.941959401791,-4.75277395392615,132.079631260207));
#27800=CARTESIAN_POINT('Ctrl Pts',(169.93277704888,-4.70591350270164,132.233892417699));
#27801=CARTESIAN_POINT('Ctrl Pts',(169.929561754955,-4.689504840823,132.287908525272));
#27802=CARTESIAN_POINT('Ctrl Pts',(169.926346461029,-4.67217101099181,132.34162591278));
#27803=CARTESIAN_POINT('Ctrl Pts',(169.923131167104,-4.65392295427785,132.395015890762));
#27804=CARTESIAN_POINT('Ctrl Pts',(169.915356832985,-4.60980055265348,132.524108762849));
#27805=CARTESIAN_POINT('Ctrl Pts',(169.907582498866,-4.56023292849578,132.651568883231));
#27806=CARTESIAN_POINT('Ctrl Pts',(169.899808164747,-4.50535915490091,132.776902619109));
#27807=CARTESIAN_POINT('Ctrl Pts',(169.8920434118,-4.45055300832781,132.902081892359));
#27808=CARTESIAN_POINT('Ctrl Pts',(169.884278658853,-4.39045387898229,133.02513964057));
#27809=CARTESIAN_POINT('Ctrl Pts',(169.876513905906,-4.325250430141,133.145597850113));
#27810=CARTESIAN_POINT('Ctrl Pts',(169.868756865021,-4.26011174228435,133.265936418864));
#27811=CARTESIAN_POINT('Ctrl Pts',(169.860999824136,-4.1898790087351,133.383680245439));
#27812=CARTESIAN_POINT('Ctrl Pts',(169.853242783251,-4.11478860347228,133.49837208956));
#27813=CARTESIAN_POINT('Ctrl Pts',(169.84549159201,-4.03975482446804,133.612977443669));
#27814=CARTESIAN_POINT('Ctrl Pts',(169.83774040077,-3.95987087843147,133.724535070595));
#27815=CARTESIAN_POINT('Ctrl Pts',(169.82998920953,-3.87541842748207,133.832613426437));
#27816=CARTESIAN_POINT('Ctrl Pts',(169.822241312753,-3.79100187107726,133.940645846094));
#27817=CARTESIAN_POINT('Ctrl Pts',(169.814493415976,-3.70202091194556,134.04520162843));
#27818=CARTESIAN_POINT('Ctrl Pts',(169.806745519199,-3.60879965245402,134.145879453507));
#27819=CARTESIAN_POINT('Ctrl Pts',(169.798999243115,-3.51559789284029,134.246536218953));
#27820=CARTESIAN_POINT('Ctrl Pts',(169.791252967031,-3.41815786257564,134.343316353938));
#27821=CARTESIAN_POINT('Ctrl Pts',(169.783506690946,-3.31684268495997,134.435853102169));
#27822=CARTESIAN_POINT('Ctrl Pts',(169.775760357681,-3.21552675945878,134.528390533485));
#27823=CARTESIAN_POINT('Ctrl Pts',(169.768014024416,-3.11033591820378,134.616684251877));
#27824=CARTESIAN_POINT('Ctrl Pts',(169.76026769115,-3.00166843420253,134.700406006626));
#27825=CARTESIAN_POINT('Ctrl Pts',(169.752519623147,-2.89297661487175,134.78414651028));
#27826=CARTESIAN_POINT('Ctrl Pts',(169.744771555144,-2.78080691317856,134.863312774364));
#27827=CARTESIAN_POINT('Ctrl Pts',(169.737023487141,-2.66558847465607,134.93761855124));
#27828=CARTESIAN_POINT('Ctrl Pts',(169.729267184399,-2.55024758060592,135.012003301181));
#27829=CARTESIAN_POINT('Ctrl Pts',(169.721510881658,-2.43185180609838,135.081517032473));
#27830=CARTESIAN_POINT('Ctrl Pts',(169.713754578916,-2.31085739495577,135.145918075746));
#27831=CARTESIAN_POINT('Ctrl Pts',(169.705994136401,-2.18979840545274,135.210353491795));
#27832=CARTESIAN_POINT('Ctrl Pts',(169.698233693887,-2.06613836799405,135.269670613461));
#27833=CARTESIAN_POINT('Ctrl Pts',(169.690473251373,-1.94035470875989,135.323675462395));
#27834=CARTESIAN_POINT('Ctrl Pts',(169.682700351108,-1.81436913042947,135.377767004707));
#27835=CARTESIAN_POINT('Ctrl Pts',(169.674927450842,-1.68625348360705,135.426529094009));
#27836=CARTESIAN_POINT('Ctrl Pts',(169.667154550577,-1.55650244921759,135.469816992679));
#27837=CARTESIAN_POINT('Ctrl Pts',(169.659664214815,-1.43146819175013,135.511531267197));
#27838=CARTESIAN_POINT('Ctrl Pts',(169.652173879053,-1.30491567920915,135.548162356793));
#27839=CARTESIAN_POINT('Ctrl Pts',(169.64468354329,-1.1772957041373,135.579625834025));
#27840=CARTESIAN_POINT('Ctrl Pts',(169.636909209171,-1.04483697892247,135.612282258559));
#27841=CARTESIAN_POINT('Ctrl Pts',(169.629134875052,-0.910808658173165,
135.63947492098));
#27842=CARTESIAN_POINT('Ctrl Pts',(169.621360540933,-0.775701221548527,
135.661054006837));
#27843=CARTESIAN_POINT('Ctrl Pts',(169.613595787986,-0.640760292764631,
135.6826064984));
#27844=CARTESIAN_POINT('Ctrl Pts',(169.605831035039,-0.504743276603272,
135.698559117546));
#27845=CARTESIAN_POINT('Ctrl Pts',(169.598066282092,-0.36815431657947,135.708812213992));
#27846=CARTESIAN_POINT('Ctrl Pts',(169.590309241207,-0.23170101863633,135.719055126917));
#27847=CARTESIAN_POINT('Ctrl Pts',(169.582552200322,-0.0946772946466856,
135.723609753405));
#27848=CARTESIAN_POINT('Ctrl Pts',(169.574795159437,0.0424044002839236,
135.722427812037));
#27849=CARTESIAN_POINT('Ctrl Pts',(169.567043968197,0.179382720841906,135.721246761982));
#27850=CARTESIAN_POINT('Ctrl Pts',(169.559292776957,0.316418535957338,135.71433775805));
#27851=CARTESIAN_POINT('Ctrl Pts',(169.551541585717,0.452996530268747,135.701704510542));
#27852=CARTESIAN_POINT('Ctrl Pts',(169.543793688939,0.589516475289328,135.6890766325));
#27853=CARTESIAN_POINT('Ctrl Pts',(169.536045792162,0.725578598034433,135.670729385781));
#27854=CARTESIAN_POINT('Ctrl Pts',(169.528297895385,0.860670071426506,135.646718523654));
#27855=CARTESIAN_POINT('Ctrl Pts',(169.520551619301,0.995733286594627,135.622712684081));
#27856=CARTESIAN_POINT('Ctrl Pts',(169.512805343217,1.1298258715768,135.59304565392));
#27857=CARTESIAN_POINT('Ctrl Pts',(169.505059067133,1.26244298690241,135.557824698352));
#27858=CARTESIAN_POINT('Ctrl Pts',(169.497312733868,1.39506108117734,135.52260348279));
#27859=CARTESIAN_POINT('Ctrl Pts',(169.489566400602,1.52620330619644,135.481828360368));
#27860=CARTESIAN_POINT('Ctrl Pts',(169.481820067337,1.65537821904303,135.435656981913));
#27861=CARTESIAN_POINT('Ctrl Pts',(169.474071999334,1.78458205971567,135.389475263699));
#27862=CARTESIAN_POINT('Ctrl Pts',(169.466323931331,1.91181734345662,135.337895016334));
#27863=CARTESIAN_POINT('Ctrl Pts',(169.458575863328,2.03661127838026,135.28112256827));
#27864=CARTESIAN_POINT('Ctrl Pts',(169.450819560586,2.1615378457831,135.224289781773));
#27865=CARTESIAN_POINT('Ctrl Pts',(169.443063257844,2.28401752474915,135.162253933268));
#27866=CARTESIAN_POINT('Ctrl Pts',(169.435306955103,2.40360038106265,135.095268245406));
#27867=CARTESIAN_POINT('Ctrl Pts',(169.427546512588,2.52324706234722,135.028246805265));
#27868=CARTESIAN_POINT('Ctrl Pts',(169.419786070074,2.63999350756389,134.956270466679));
#27869=CARTESIAN_POINT('Ctrl Pts',(169.41202562756,2.75341845672161,134.879636051777));
#27870=CARTESIAN_POINT('Ctrl Pts',(169.404252727295,2.86702548567707,134.80287861651));
#27871=CARTESIAN_POINT('Ctrl Pts',(169.396479827029,2.97730004892688,134.721448394762));
#27872=CARTESIAN_POINT('Ctrl Pts',(169.388706926764,3.0838529874878,134.635683341386));
#27873=CARTESIAN_POINT('Ctrl Pts',(169.381216591002,3.1865324583413,134.55303606373));
#27874=CARTESIAN_POINT('Ctrl Pts',(169.37372625524,3.2857559557091,134.466363849468));
#27875=CARTESIAN_POINT('Ctrl Pts',(169.366235919478,3.38120878401291,134.376000328037));
#27876=CARTESIAN_POINT('Ctrl Pts',(169.358461585359,3.48028073531418,134.282210646226));
#27877=CARTESIAN_POINT('Ctrl Pts',(169.35068725124,3.5756042735339,134.184147122356));
#27878=CARTESIAN_POINT('Ctrl Pts',(169.342912917121,3.66678823929541,134.082141432487));
#27879=CARTESIAN_POINT('Ctrl Pts',(169.335148164174,3.75785982896842,133.980261455514));
#27880=CARTESIAN_POINT('Ctrl Pts',(169.327383411226,3.84480173889385,133.874449267929));
#27881=CARTESIAN_POINT('Ctrl Pts',(169.319618658279,3.9272576285798,133.765075156535));
#27882=CARTESIAN_POINT('Ctrl Pts',(169.311861617394,4.00963162191369,133.65580967705));
#27883=CARTESIAN_POINT('Ctrl Pts',(169.304104576509,4.08752822797811,133.542989624214));
#27884=CARTESIAN_POINT('Ctrl Pts',(169.296347535624,4.16062983174815,133.427020043734));
#27885=CARTESIAN_POINT('Ctrl Pts',(169.288596344384,4.23367630903015,133.311137916817));
#27886=CARTESIAN_POINT('Ctrl Pts',(169.280845153144,4.30193477370519,133.192111319117));
#27887=CARTESIAN_POINT('Ctrl Pts',(169.273093961904,4.36512980681248,133.070375805551));
#27888=CARTESIAN_POINT('Ctrl Pts',(169.265346065127,4.42829798034491,132.948692032825));
#27889=CARTESIAN_POINT('Ctrl Pts',(169.25759816835,4.4864068229048,132.824301980472));
#27890=CARTESIAN_POINT('Ctrl Pts',(169.249850271573,4.53922604573536,132.69766724044));
#27891=CARTESIAN_POINT('Ctrl Pts',(169.242103995489,4.59203421992316,132.571058989666));
#27892=CARTESIAN_POINT('Ctrl Pts',(169.234357719405,4.63955482481111,132.442207345761));
#27893=CARTESIAN_POINT('Ctrl Pts',(169.22661144332,4.6816052275686,132.311595023922));
#27894=CARTESIAN_POINT('Ctrl Pts',(169.218865110055,4.72365594073262,132.180981737931));
#27895=CARTESIAN_POINT('Ctrl Pts',(169.21111877679,4.76023625137703,132.048608120225));
#27896=CARTESIAN_POINT('Ctrl Pts',(169.203372443524,4.79121315870816,131.91497284977));
#27897=CARTESIAN_POINT('Ctrl Pts',(169.195624375521,4.8221970031029,131.781307652623));
#27898=CARTESIAN_POINT('Ctrl Pts',(169.187876307518,4.84757485892271,131.646380621303));
#27899=CARTESIAN_POINT('Ctrl Pts',(169.180128239515,4.86726476057517,131.510701054581));
#27900=CARTESIAN_POINT('Ctrl Pts',(169.172371936774,4.88697558888943,131.374877286002));
#27901=CARTESIAN_POINT('Ctrl Pts',(169.164615634032,4.90098633080901,131.238299771856));
#27902=CARTESIAN_POINT('Ctrl Pts',(169.15685933129,4.90926682928844,131.101483927571));
#27903=CARTESIAN_POINT('Ctrl Pts',(169.149098888776,4.91755174731924,130.96459506055));
#27904=CARTESIAN_POINT('Ctrl Pts',(169.141338446262,4.92010032052056,130.827468000632));
#27905=CARTESIAN_POINT('Ctrl Pts',(169.133578003747,4.9169345724426,130.690617605391));
#27906=CARTESIAN_POINT('Ctrl Pts',(169.125805103482,4.91376374242477,130.553547525745));
#27907=CARTESIAN_POINT('Ctrl Pts',(169.118032203217,4.90486028568715,130.416755388647));
#27908=CARTESIAN_POINT('Ctrl Pts',(169.110259302951,4.8902981832823,130.280751277422));
#27909=CARTESIAN_POINT('Ctrl Pts',(169.102768967189,4.87626544997962,130.149691258215));
#27910=CARTESIAN_POINT('Ctrl Pts',(169.095278631427,4.85697838543172,130.019363270828));
#27911=CARTESIAN_POINT('Ctrl Pts',(169.087788295665,4.83254758088737,129.890212412427));
#27912=CARTESIAN_POINT('Ctrl Pts',(169.080013961546,4.80719047496313,129.756164759974));
#27913=CARTESIAN_POINT('Ctrl Pts',(169.072239627427,4.77621155584309,129.622960637581));
#27914=CARTESIAN_POINT('Ctrl Pts',(169.064465293308,4.73967844079104,129.49110841772));
#27915=CARTESIAN_POINT('Ctrl Pts',(169.056700540361,4.70319034953823,129.359418693936));
#27916=CARTESIAN_POINT('Ctrl Pts',(169.048935787414,4.66116178535475,129.229077930797));
#27917=CARTESIAN_POINT('Ctrl Pts',(169.041171034466,4.61371167027568,129.100586076712));
#27918=CARTESIAN_POINT('Ctrl Pts',(169.033413993581,4.56630868331985,128.972221842549));
#27919=CARTESIAN_POINT('Ctrl Pts',(169.025656952696,4.5134949959467,128.845703227379));
#27920=CARTESIAN_POINT('Ctrl Pts',(169.017899911811,4.45543970590349,128.721516386818));
#27921=CARTESIAN_POINT('Ctrl Pts',(169.010148720571,4.3974281958061,128.59742319652));
#27922=CARTESIAN_POINT('Ctrl Pts',(169.002397529331,4.33418311561574,128.475658633566));
#27923=CARTESIAN_POINT('Ctrl Pts',(168.994646338091,4.26592203934227,128.356689843799));
#27924=CARTESIAN_POINT('Ctrl Pts',(168.986898441314,4.19768997584712,128.237771618941));
#27925=CARTESIAN_POINT('Ctrl Pts',(168.979150544537,4.12444635068408,128.121647142274));
#27926=CARTESIAN_POINT('Ctrl Pts',(168.97140264776,4.04645503753438,128.008759663976));
#27927=CARTESIAN_POINT('Ctrl Pts',(168.963656371676,3.96848003848606,127.895895799305));
#27928=CARTESIAN_POINT('Ctrl Pts',(168.955910095592,3.88575954889843,127.786267907652));
#27929=CARTESIAN_POINT('Ctrl Pts',(168.948163819508,3.79860097323011,127.680290562546));
#27930=CARTESIAN_POINT('Ctrl Pts',(168.940417486242,3.71144175417708,127.574312435138));
#27931=CARTESIAN_POINT('Ctrl Pts',(168.932671152977,3.61984463201219,127.471985210009));
#27932=CARTESIAN_POINT('Ctrl Pts',(168.924924819712,3.52415726929668,127.373690332656));
#27933=CARTESIAN_POINT('Ctrl Pts',(168.917176751709,3.42844847805977,127.275373442847));
#27934=CARTESIAN_POINT('Ctrl Pts',(168.909428683706,3.3286478962373,127.181090977803));
#27935=CARTESIAN_POINT('Ctrl Pts',(168.901680615703,3.22513970690524,127.091187185925));
#27936=CARTESIAN_POINT('Ctrl Pts',(168.893924312961,3.12152150783768,127.001187843227));
#27937=CARTESIAN_POINT('Ctrl Pts',(168.886168010219,3.01418812534955,126.915576726758));
#27938=CARTESIAN_POINT('Ctrl Pts',(168.878411707477,2.90355689241722,126.834657803123));
#27939=CARTESIAN_POINT('Ctrl Pts',(168.870651264963,2.79286661226476,126.753695690622));
#27940=CARTESIAN_POINT('Ctrl Pts',(168.862890822449,2.67887529918352,126.677430978408));
#27941=CARTESIAN_POINT('Ctrl Pts',(168.855130379935,2.5620280216982,126.606123430539));
#27942=CARTESIAN_POINT('Ctrl Pts',(168.847357479669,2.44499317058989,126.534701413465));
#27943=CARTESIAN_POINT('Ctrl Pts',(168.839584579404,2.32509353564874,126.468252652342));
#27944=CARTESIAN_POINT('Ctrl Pts',(168.831811679138,2.20279825299001,126.406990617313));
#27945=CARTESIAN_POINT('Ctrl Pts',(168.824321343376,2.08494871189854,126.347955611567));
#27946=CARTESIAN_POINT('Ctrl Pts',(168.816831007614,1.9648749555283,126.293736904589));
#27947=CARTESIAN_POINT('Ctrl Pts',(168.809340671852,1.84301123400021,126.244482038717));
#27948=CARTESIAN_POINT('Ctrl Pts',(168.801566337733,1.71652701243132,126.193359659635));
#27949=CARTESIAN_POINT('Ctrl Pts',(168.793792003614,1.58771374923849,126.147423019814));
#27950=CARTESIAN_POINT('Ctrl Pts',(168.786017669495,1.4570357013638,126.106890018674));
#27951=CARTESIAN_POINT('Ctrl Pts',(168.778252916548,1.32651870250418,126.066406970836));
#27952=CARTESIAN_POINT('Ctrl Pts',(168.770488163601,1.19414186148694,126.031314425968));
#27953=CARTESIAN_POINT('Ctrl Pts',(168.762723410654,1.06039007933355,126.00178256592));
#27954=CARTESIAN_POINT('Ctrl Pts',(168.754966369769,0.926771141335774,125.972280037332));
#27955=CARTESIAN_POINT('Ctrl Pts',(168.747209328884,0.791780359128918,125.948327286392));
#27956=CARTESIAN_POINT('Ctrl Pts',(168.739452287999,0.65591815066357,125.930044825362));
#27957=CARTESIAN_POINT('Ctrl Pts',(168.731701096759,0.520158396946435,125.911776151277));
#27958=CARTESIAN_POINT('Ctrl Pts',(168.723949905518,0.383528910891622,125.899169307894));
#27959=CARTESIAN_POINT('Ctrl Pts',(168.716198714278,0.246540319593697,125.892293747773));
#27960=CARTESIAN_POINT('Ctrl Pts',(168.708450817501,0.109609952101364,125.885421109949));
#27961=CARTESIAN_POINT('Ctrl Pts',(168.700702920724,-0.0276788274098269,
125.88427493003));
#27962=CARTESIAN_POINT('Ctrl Pts',(168.692955023947,-0.164810469842722,
125.888872791162));
#27963=CARTESIAN_POINT('Ctrl Pts',(168.685208747863,-0.301913427292237,
125.89346969052));
#27964=CARTESIAN_POINT('Ctrl Pts',(168.677462471779,-0.438858922544996,
125.903808227928));
#27965=CARTESIAN_POINT('Ctrl Pts',(168.669716195695,-0.575132003533086,
125.919853862426));
#27966=CARTESIAN_POINT('Ctrl Pts',(168.661969862429,-0.711406090458104,
125.935899615369));
#27967=CARTESIAN_POINT('Ctrl Pts',(168.654223529164,-0.84700736493107,125.957652503748));
#27968=CARTESIAN_POINT('Ctrl Pts',(168.646477195899,-0.981426985945333,
125.985026209812));
#27969=CARTESIAN_POINT('Ctrl Pts',(168.638729127896,-1.11587670930163,126.012406046028));
#27970=CARTESIAN_POINT('Ctrl Pts',(168.630981059893,-1.24914386960109,126.045409126682));
#27971=CARTESIAN_POINT('Ctrl Pts',(168.62323299189,-1.38073118057777,126.083898302339));
#27972=CARTESIAN_POINT('Ctrl Pts',(168.615476689148,-1.51245834411457,126.12242838475));
#27973=CARTESIAN_POINT('Ctrl Pts',(168.607720386406,-1.64250171603113,126.166456099657));
#27974=CARTESIAN_POINT('Ctrl Pts',(168.599964083664,-1.77037998194666,126.215794634383));
#27975=CARTESIAN_POINT('Ctrl Pts',(168.59220364115,-1.89832650034323,126.265159502571));
#27976=CARTESIAN_POINT('Ctrl Pts',(168.584443198636,-2.02410525177077,126.319840682847));
#27977=CARTESIAN_POINT('Ctrl Pts',(168.576682756122,-2.14725711896144,126.379604135276));
#27978=CARTESIAN_POINT('Ctrl Pts',(168.568909855856,-2.27060668046215,126.439463525304));
#27979=CARTESIAN_POINT('Ctrl Pts',(168.561136955591,-2.39132058651883,126.504421305426));
#27980=CARTESIAN_POINT('Ctrl Pts',(168.553364055326,-2.50896565912489,126.574198163968));
#27981=CARTESIAN_POINT('Ctrl Pts',(168.545873719564,-2.6223340370115,126.641438457944));
#27982=CARTESIAN_POINT('Ctrl Pts',(168.538383383802,-2.73285256902816,126.713153374356));
#27983=CARTESIAN_POINT('Ctrl Pts',(168.53089304804,-2.84016240082866,126.789057316516));
#27984=CARTESIAN_POINT('Ctrl Pts',(168.52317132459,-2.95078719402167,126.86730604511));
#27985=CARTESIAN_POINT('Ctrl Pts',(168.51544960114,-3.05836308616123,126.950262473689));
#27986=CARTESIAN_POINT('Ctrl Pts',(168.50772787769,-3.16245894428162,127.03765960896));
#27987=CARTESIAN_POINT('Ctrl Pts',(168.500018346955,-3.26639043351439,127.124918742872));
#27988=CARTESIAN_POINT('Ctrl Pts',(168.492308816219,-3.36685252945368,127.216604368201));
#27989=CARTESIAN_POINT('Ctrl Pts',(168.484599285484,-3.46344322780615,127.312406426821));
#27990=CARTESIAN_POINT('Ctrl Pts',(168.476896797498,-3.5599456893932,127.408120969107));
#27991=CARTESIAN_POINT('Ctrl Pts',(168.469194309512,-3.65258350677029,127.507944188805));
#27992=CARTESIAN_POINT('Ctrl Pts',(168.461491821526,-3.7409877692236,127.611525893842));
#27993=CARTESIAN_POINT('Ctrl Pts',(168.453794642419,-3.82933109973314,127.715036206002));
#27994=CARTESIAN_POINT('Ctrl Pts',(168.446097463312,-3.91344642311149,127.822299549752));
#27995=CARTESIAN_POINT('Ctrl Pts',(168.438400284205,-3.99300207612229,127.932929357274));
#27996=CARTESIAN_POINT('Ctrl Pts',(168.430706684397,-4.07252073461947,128.043507720357));
#27997=CARTESIAN_POINT('Ctrl Pts',(168.423013084588,-4.14748371086074,128.15744911039));
#27998=CARTESIAN_POINT('Ctrl Pts',(168.415319484779,-4.2176003035411,128.274334779344));
#27999=CARTESIAN_POINT('Ctrl Pts',(168.407626333773,-4.28771280600053,128.391213629824));
#28000=CARTESIAN_POINT('Ctrl Pts',(168.399933182767,-4.35297927547694,128.511036081975));
#28001=CARTESIAN_POINT('Ctrl Pts',(168.392240031762,-4.41315307034798,128.633355541529));
#28002=CARTESIAN_POINT('Ctrl Pts',(168.384547189035,-4.47332445394333,128.755670099515));
#28003=CARTESIAN_POINT('Ctrl Pts',(168.376854346307,-4.52840339898507,128.88048110705));
#28004=CARTESIAN_POINT('Ctrl Pts',(168.36916150358,-4.57819020506195,129.007319296735));
#28005=CARTESIAN_POINT('Ctrl Pts',(168.361464918195,-4.62800123300544,129.13421919469));
#28006=CARTESIAN_POINT('Ctrl Pts',(168.353768332809,-4.67251484040017,129.263147872706));
#28007=CARTESIAN_POINT('Ctrl Pts',(168.346071747424,-4.71158027578738,129.393618129615));
#28008=CARTESIAN_POINT('Ctrl Pts',(168.342377681529,-4.73033018698689,129.456238850643));
#28009=CARTESIAN_POINT('Ctrl Pts',(168.338683615635,-4.74782577970215,129.519214475088));
#28010=CARTESIAN_POINT('Ctrl Pts',(168.33498954974,-4.76405452823405,129.582490119308));
#28011=CARTESIAN_POINT('Ctrl Pts',(170.084755673967,-4.76405452823406,129.582490119308));
#28012=CARTESIAN_POINT('Ctrl Pts',(170.077020912222,-4.79810525795013,129.715253397679));
#28013=CARTESIAN_POINT('Ctrl Pts',(170.069286150477,-4.82661229531109,129.849481010834));
#28014=CARTESIAN_POINT('Ctrl Pts',(170.061551388732,-4.84946291612859,129.984670134766));
#28015=CARTESIAN_POINT('Ctrl Pts',(170.053769396608,-4.872453068518,130.120684757099));
#28016=CARTESIAN_POINT('Ctrl Pts',(170.045987404485,-4.88971739268245,130.25767228365));
#28017=CARTESIAN_POINT('Ctrl Pts',(170.038205412361,-4.90119355435987,130.395111542795));
#28018=CARTESIAN_POINT('Ctrl Pts',(170.030423420238,-4.91266971603728,130.532550801939));
#28019=CARTESIAN_POINT('Ctrl Pts',(170.022641428114,-4.9183576950795,130.670441390693));
#28020=CARTESIAN_POINT('Ctrl Pts',(170.014859435991,-4.91824845497686,130.808259029769));
#28021=CARTESIAN_POINT('',(170.360140564063,-4.91824882901199,130.800966737464));
#28022=CARTESIAN_POINT('Ctrl Pts',(170.429908526381,-4.76405452823404,129.582490119308));
#28023=CARTESIAN_POINT('Ctrl Pts',(170.421033020534,-4.80283367562411,129.733689426426));
#28024=CARTESIAN_POINT('Ctrl Pts',(170.412157514688,-4.83445442237841,129.886906563728));
#28025=CARTESIAN_POINT('Ctrl Pts',(170.403282008841,-4.85872694272219,130.041500500267));
#28026=CARTESIAN_POINT('Ctrl Pts',(170.39446678309,-4.8828346105065,130.195044475543));
#28027=CARTESIAN_POINT('Ctrl Pts',(170.385651557339,-4.89969344204067,130.349946452333));
#28028=CARTESIAN_POINT('Ctrl Pts',(170.376836331588,-4.90916496957448,130.505559071381));
#28029=CARTESIAN_POINT('Ctrl Pts',(170.371271075747,-4.91514456390694,130.603800915855));
#28030=CARTESIAN_POINT('Ctrl Pts',(170.365705819905,-4.91818076085781,130.702325621825));
#28031=CARTESIAN_POINT('Ctrl Pts',(170.360140564063,-4.91824882901199,130.800966737464));
#28032=CARTESIAN_POINT('Ctrl Pts',(170.360140564008,-4.91824882901267,130.800966738437));
#28033=CARTESIAN_POINT('Ctrl Pts',(170.352360472836,-4.91834398659548,130.938864598804));
#28034=CARTESIAN_POINT('Ctrl Pts',(170.344580381664,-4.91263525214567,131.076802536184));
#28035=CARTESIAN_POINT('Ctrl Pts',(170.336800290492,-4.90113922727987,131.214259797022));
#28036=CARTESIAN_POINT('Ctrl Pts',(170.329020253002,-4.88964328173574,131.351716109415));
#28037=CARTESIAN_POINT('Ctrl Pts',(170.321240215512,-4.87236015654906,131.488691367181));
#28038=CARTESIAN_POINT('Ctrl Pts',(170.313460178022,-4.84935842684873,131.624669041545));
#28039=CARTESIAN_POINT('Ctrl Pts',(170.305678564943,-4.82635203890897,131.760674253689));
#28040=CARTESIAN_POINT('Ctrl Pts',(170.297896951864,-4.79762480510897,131.895681099668));
#28041=CARTESIAN_POINT('Ctrl Pts',(170.290115338785,-4.76329654399539,132.029182684832));
#28042=CARTESIAN_POINT('Ctrl Pts',(170.282330520181,-4.72895414184579,132.162739264064));
#28043=CARTESIAN_POINT('Ctrl Pts',(170.274545701578,-4.68900621523641,132.294788974566));
#28044=CARTESIAN_POINT('Ctrl Pts',(170.266760882975,-4.64362251945257,132.424839855117));
#28045=CARTESIAN_POINT('Ctrl Pts',(170.258966330822,-4.59818207932088,132.555053341473));
#28046=CARTESIAN_POINT('Ctrl Pts',(170.251171778669,-4.54729242388263,132.683262641997));
#28047=CARTESIAN_POINT('Ctrl Pts',(170.243377226516,-4.49117180285544,132.808994973187));
#28048=CARTESIAN_POINT('Ctrl Pts',(170.23557732948,-4.43501269877819,132.934813521591));
#28049=CARTESIAN_POINT('Ctrl Pts',(170.227777432445,-4.37361565378318,133.058151371684));
#28050=CARTESIAN_POINT('Ctrl Pts',(170.219977535409,-4.30724457420593,133.178560954621));
#28051=CARTESIAN_POINT('Ctrl Pts',(170.212164997682,-4.24076593214009,133.29916567608));
#28052=CARTESIAN_POINT('Ctrl Pts',(170.204352459955,-4.16929735363983,133.416832321866));
#28053=CARTESIAN_POINT('Ctrl Pts',(170.196539922227,-4.09314611327394,133.531142229263));
#28054=CARTESIAN_POINT('Ctrl Pts',(170.191689879738,-4.04587123738561,133.602106098782));
#28055=CARTESIAN_POINT('Ctrl Pts',(170.186839837248,-3.99679250347402,133.671776929543));
#28056=CARTESIAN_POINT('Ctrl Pts',(170.181989794758,-3.94599092647641,133.740061329605));
#28057=CARTESIAN_POINT('Ctrl Pts',(170.174215460639,-3.86455897321264,133.849517224542));
#28058=CARTESIAN_POINT('Ctrl Pts',(170.16644112652,-3.77844037158533,133.95575572089));
#28059=CARTESIAN_POINT('Ctrl Pts',(170.158666792401,-3.68791827680057,134.058349223284));
#28060=CARTESIAN_POINT('Ctrl Pts',(170.150902039454,-3.59750774240747,134.160816288355));
#28061=CARTESIAN_POINT('Ctrl Pts',(170.143137286507,-3.50270476897911,134.259647007123));
#28062=CARTESIAN_POINT('Ctrl Pts',(170.13537253356,-3.40383496463212,134.354443799133));
#28063=CARTESIAN_POINT('Ctrl Pts',(170.127615492675,-3.30506335916833,134.449146437634));
#28064=CARTESIAN_POINT('Ctrl Pts',(170.11985845179,-3.20223324142314,134.539822853769));
#28065=CARTESIAN_POINT('Ctrl Pts',(170.112101410905,-3.09570930894535,134.626109816167));
#28066=CARTESIAN_POINT('Ctrl Pts',(170.104350219664,-2.98926570699406,134.712331708896));
#28067=CARTESIAN_POINT('Ctrl Pts',(170.096599028424,-2.87913413731964,134.794170491394));
#28068=CARTESIAN_POINT('Ctrl Pts',(170.088847837184,-2.76571457685697,134.871301229606));
#28069=CARTESIAN_POINT('Ctrl Pts',(170.081099940407,-2.65234322273291,134.948399185197));
#28070=CARTESIAN_POINT('Ctrl Pts',(170.07335204363,-2.53568697992477,135.020792857034));
#28071=CARTESIAN_POINT('Ctrl Pts',(170.065604146853,-2.41617701043069,135.088199050183));
#28072=CARTESIAN_POINT('Ctrl Pts',(170.057857870769,-2.29669203984581,135.15559114341));
#28073=CARTESIAN_POINT('Ctrl Pts',(170.050111594685,-2.17435487023594,135.217997641129));
#28074=CARTESIAN_POINT('Ctrl Pts',(170.042365318601,-2.04962326757815,135.275180175936));
#28075=CARTESIAN_POINT('Ctrl Pts',(170.034618985335,-1.92489074418012,135.332363132851));
#28076=CARTESIAN_POINT('Ctrl Pts',(170.02687265207,-1.79776410786242,135.384321886974));
#28077=CARTESIAN_POINT('Ctrl Pts',(170.019126318805,-1.66872283861668,135.430865470085));
#28078=CARTESIAN_POINT('Ctrl Pts',(170.011378250802,-1.53965267147335,135.477419476308));
#28079=CARTESIAN_POINT('Ctrl Pts',(170.003630182799,-1.40866738590499,135.51855576578));
#28080=CARTESIAN_POINT('Ctrl Pts',(169.995882114796,-1.276263035079,135.554132793975));
#28081=CARTESIAN_POINT('Ctrl Pts',(169.988125812054,-1.14371796333346,135.58974763386));
#28082=CARTESIAN_POINT('Ctrl Pts',(169.980369509312,-1.00975119171394,135.619791308089));
#28083=CARTESIAN_POINT('Ctrl Pts',(169.97261320657,-0.874870966272833,135.644172995631));
#28084=CARTESIAN_POINT('Ctrl Pts',(169.964852764056,-0.739918751194152,
135.668567696414));
#28085=CARTESIAN_POINT('Ctrl Pts',(169.957092321542,-0.604052497947626,
135.687294335615));
#28086=CARTESIAN_POINT('Ctrl Pts',(169.949331879027,-0.467786061620851,
135.700313973456));
#28087=CARTESIAN_POINT('Ctrl Pts',(169.941558978762,-0.331300878313273,
135.713354511576));
#28088=CARTESIAN_POINT('Ctrl Pts',(169.933786078497,-0.194414618819575,
135.720669720093));
#28089=CARTESIAN_POINT('Ctrl Pts',(169.926013178231,-0.0576425340327472,
135.722272816942));
#28090=CARTESIAN_POINT('Ctrl Pts',(169.918522842469,0.0741575409652403,
135.723817637183));
#28091=CARTESIAN_POINT('Ctrl Pts',(169.911032506707,0.205851290320753,135.720058443634));
#28092=CARTESIAN_POINT('Ctrl Pts',(169.903542170945,0.33698367046011,135.711052483614));
#28093=CARTESIAN_POINT('Ctrl Pts',(169.895767836826,0.473087974648075,135.701705059883));
#28094=CARTESIAN_POINT('Ctrl Pts',(169.887993502707,0.6090186381992,135.686675543623));
#28095=CARTESIAN_POINT('Ctrl Pts',(169.880219168587,0.744262860718677,135.665971035592));
#28096=CARTESIAN_POINT('Ctrl Pts',(169.87245441564,0.879340406820976,135.645292044015));
#28097=CARTESIAN_POINT('Ctrl Pts',(169.864689662693,1.01373281238139,135.618952035079));
#28098=CARTESIAN_POINT('Ctrl Pts',(169.856924909746,1.14692958256326,135.587010050165));
#28099=CARTESIAN_POINT('Ctrl Pts',(169.849167868861,1.27999405983516,135.555099790481));
#28100=CARTESIAN_POINT('Ctrl Pts',(169.841410827976,1.41186488722495,135.517598717937));
#28101=CARTESIAN_POINT('Ctrl Pts',(169.833653787091,1.54203933996029,135.474617327482));
#28102=CARTESIAN_POINT('Ctrl Pts',(169.825902595851,1.67211562712836,135.431668349627));
#28103=CARTESIAN_POINT('Ctrl Pts',(169.818151404611,1.80049771616081,135.383247401935));
#28104=CARTESIAN_POINT('Ctrl Pts',(169.810400213371,1.9266960335319,135.329515361536));
#28105=CARTESIAN_POINT('Ctrl Pts',(169.802652316593,2.05284071325161,135.275806158687));
#28106=CARTESIAN_POINT('Ctrl Pts',(169.794904419816,2.17680310838795,135.216790505677));
#28107=CARTESIAN_POINT('Ctrl Pts',(169.787156523039,2.29811190543176,135.152678077528));
#28108=CARTESIAN_POINT('Ctrl Pts',(169.779410246955,2.41939532729038,135.088579060317));
#28109=CARTESIAN_POINT('Ctrl Pts',(169.771663970871,2.53802590969138,135.019385571137));
#28110=CARTESIAN_POINT('Ctrl Pts',(169.763917694787,2.65355567369279,134.945353898062));
#28111=CARTESIAN_POINT('Ctrl Pts',(169.756171361521,2.76908629050859,134.871321678502));
#28112=CARTESIAN_POINT('Ctrl Pts',(169.748425028256,2.88151571407146,134.792451414722));
#28113=CARTESIAN_POINT('Ctrl Pts',(169.740678694991,2.99042410676061,134.709043283828));
#28114=CARTESIAN_POINT('Ctrl Pts',(169.732930626988,3.09935688872904,134.625616474262));
#28115=CARTESIAN_POINT('Ctrl Pts',(169.725182558985,3.20476676044471,134.537650013086));
#28116=CARTESIAN_POINT('Ctrl Pts',(169.717434490982,3.30626650763675,134.445484735607));
#28117=CARTESIAN_POINT('Ctrl Pts',(169.70967818824,3.40787412996818,134.353221503774));
#28118=CARTESIAN_POINT('Ctrl Pts',(169.701921885498,3.50556303635941,134.256750804453));
#28119=CARTESIAN_POINT('Ctrl Pts',(169.694165582756,3.5989820970972,134.156451148455));
#28120=CARTESIAN_POINT('Ctrl Pts',(169.686405140242,3.69245101840044,134.05609795951));
#28121=CARTESIAN_POINT('Ctrl Pts',(169.678644697728,3.78164529892404,133.951912038634));
#28122=CARTESIAN_POINT('Ctrl Pts',(169.670884255214,3.86625442630231,133.844304658761));
#28123=CARTESIAN_POINT('Ctrl Pts',(169.663111354948,3.95099937576314,133.73652453797));
#28124=CARTESIAN_POINT('Ctrl Pts',(169.655338454683,4.03114423475479,133.625312299924));
#28125=CARTESIAN_POINT('Ctrl Pts',(169.647565554417,4.10642161820729,133.511108584411));
#28126=CARTESIAN_POINT('Ctrl Pts',(169.640075218655,4.17896247915849,133.401056461619));
#28127=CARTESIAN_POINT('Ctrl Pts',(169.632584882893,4.24698345148421,133.288226844591));
#28128=CARTESIAN_POINT('Ctrl Pts',(169.625094547131,4.31028673680823,133.173033517946));
#28129=CARTESIAN_POINT('Ctrl Pts',(169.617320213012,4.37599018543632,133.053472601308));
#28130=CARTESIAN_POINT('Ctrl Pts',(169.609545878893,4.43681927168965,132.930986463652));
#28131=CARTESIAN_POINT('Ctrl Pts',(169.601771544774,4.49250278849581,132.806010376604));
#28132=CARTESIAN_POINT('Ctrl Pts',(169.594006791827,4.54811768034397,132.681188311414));
#28133=CARTESIAN_POINT('Ctrl Pts',(169.58624203888,4.59859946276015,132.553882756205));
#28134=CARTESIAN_POINT('Ctrl Pts',(169.578477285933,4.64372187400349,132.424555118051));
#28135=CARTESIAN_POINT('Ctrl Pts',(169.570720245048,4.68879946903203,132.295355929929));
#28136=CARTESIAN_POINT('Ctrl Pts',(169.562963204163,4.72852815794359,132.164139022346));
#28137=CARTESIAN_POINT('Ctrl Pts',(169.555206163278,4.76272916824859,132.031387077107));
#28138=CARTESIAN_POINT('Ctrl Pts',(169.547454972038,4.79690438730564,131.898735241143));
#28139=CARTESIAN_POINT('Ctrl Pts',(169.539703780798,4.82556012768876,131.764551048696));
#28140=CARTESIAN_POINT('Ctrl Pts',(169.531952589557,4.84856711343453,131.629333349855));
#28141=CARTESIAN_POINT('Ctrl Pts',(169.52420469278,4.87156432059757,131.494173122145));
#28142=CARTESIAN_POINT('Ctrl Pts',(169.516456796003,4.88891748283141,131.35798064633));
#28143=CARTESIAN_POINT('Ctrl Pts',(169.508708899226,4.90054824920584,131.221265786286));
#28144=CARTESIAN_POINT('Ctrl Pts',(169.500962623142,4.91217658267468,131.084579524044));
#28145=CARTESIAN_POINT('Ctrl Pts',(169.493216347058,4.91808486806646,130.94737148423));
#28146=CARTESIAN_POINT('Ctrl Pts',(169.485470070974,4.91824658423699,130.810157094182));
#28147=CARTESIAN_POINT('Ctrl Pts',(169.477723737709,4.91840830160127,130.672941691249));
#28148=CARTESIAN_POINT('Ctrl Pts',(169.469977404443,4.91282336463777,130.535720328952));
#28149=CARTESIAN_POINT('Ctrl Pts',(169.462231071178,4.90151738835985,130.399008481632));
#28150=CARTESIAN_POINT('Ctrl Pts',(169.454483003175,4.89020888018696,130.262266018642));
#28151=CARTESIAN_POINT('Ctrl Pts',(169.446734935172,4.87317681550208,130.12603368724));
#28152=CARTESIAN_POINT('Ctrl Pts',(169.438986867169,4.85049864992938,129.990821491566));
#28153=CARTESIAN_POINT('Ctrl Pts',(169.431230564428,4.82779638173237,129.855465590761));
#28154=CARTESIAN_POINT('Ctrl Pts',(169.423474261686,4.79943609029013,129.721132377709));
#28155=CARTESIAN_POINT('Ctrl Pts',(169.415717958944,4.76554643328138,129.588321862123));
#28156=CARTESIAN_POINT('Ctrl Pts',(169.40795751643,4.73163868834225,129.455440461566));
#28157=CARTESIAN_POINT('Ctrl Pts',(169.400197073916,4.69219580972468,129.324083752131));
#28158=CARTESIAN_POINT('Ctrl Pts',(169.392436631401,4.64739597347956,129.194735279736));
#28159=CARTESIAN_POINT('Ctrl Pts',(169.384663731136,4.60252422056019,129.065179165689));
#28160=CARTESIAN_POINT('Ctrl Pts',(169.376890830871,4.55227846893061,128.937638094825));
#28161=CARTESIAN_POINT('Ctrl Pts',(169.369117930605,4.49688491316069,128.812575202345));
#28162=CARTESIAN_POINT('Ctrl Pts',(169.361627594843,4.44350505267042,128.692058661019));
#28163=CARTESIAN_POINT('Ctrl Pts',(169.354137259081,4.3853452974095,128.573843526525));
#28164=CARTESIAN_POINT('Ctrl Pts',(169.346646923319,4.32264686124391,128.458319872933));
#28165=CARTESIAN_POINT('Ctrl Pts',(169.3388725892,4.25757119481492,128.338416104903));
#28166=CARTESIAN_POINT('Ctrl Pts',(169.331098255081,4.18739974516979,128.221032122576));
#28167=CARTESIAN_POINT('Ctrl Pts',(169.323323920962,4.11235212460887,128.106631375087));
#28168=CARTESIAN_POINT('Ctrl Pts',(169.315559168015,4.03739699353317,127.992371616296));
#28169=CARTESIAN_POINT('Ctrl Pts',(169.307794415067,3.95757786093702,127.881088100829));
#28170=CARTESIAN_POINT('Ctrl Pts',(169.30002966212,3.8731606216617,127.773220590891));
#28171=CARTESIAN_POINT('Ctrl Pts',(169.292272621235,3.78882722677847,127.665460216485));
#28172=CARTESIAN_POINT('Ctrl Pts',(169.28451558035,3.69990505295632,127.561109401629));
#28173=CARTESIAN_POINT('Ctrl Pts',(169.276758539465,3.60670356317283,127.460579453988));
#28174=CARTESIAN_POINT('Ctrl Pts',(169.269007348225,3.51357235735718,127.360125316763));
#28175=CARTESIAN_POINT('Ctrl Pts',(169.261256156985,3.41616852358905,127.263486597156));
#28176=CARTESIAN_POINT('Ctrl Pts',(169.253504965745,3.31484188176225,127.171041699357));
#28177=CARTESIAN_POINT('Ctrl Pts',(169.245757068968,3.21355830646176,127.078636093106));
#28178=CARTESIAN_POINT('Ctrl Pts',(169.238009172191,3.10835552744922,126.990421026387));
#28179=CARTESIAN_POINT('Ctrl Pts',(169.230261275414,2.99962015705057,126.906738011936));
#28180=CARTESIAN_POINT('Ctrl Pts',(169.22251499933,2.89090753174728,126.823072502168));
#28181=CARTESIAN_POINT('Ctrl Pts',(169.214768723245,2.77866409449039,126.743937397324));
#28182=CARTESIAN_POINT('Ctrl Pts',(169.207022447161,2.66330915356937,126.669633611461));
#28183=CARTESIAN_POINT('Ctrl Pts',(169.199276113896,2.54795336112462,126.595329277104));
#28184=CARTESIAN_POINT('Ctrl Pts',(169.191529780631,2.42948634786476,126.525856544606));
#28185=CARTESIAN_POINT('Ctrl Pts',(169.183783447365,2.30835564249141,126.461472489801));
#28186=CARTESIAN_POINT('Ctrl Pts',(169.176035379362,2.18719781073601,126.397074016634));
#28187=CARTESIAN_POINT('Ctrl Pts',(169.168287311359,2.06337544503259,126.337766672244));
#28188=CARTESIAN_POINT('Ctrl Pts',(169.160539243356,1.93735949296564,126.283760960716));
#28189=CARTESIAN_POINT('Ctrl Pts',(169.152782940614,1.81120960964558,126.229697851275));
#28190=CARTESIAN_POINT('Ctrl Pts',(169.145026637872,1.68286184272782,126.180947784745));
#28191=CARTESIAN_POINT('Ctrl Pts',(169.137270335131,1.55280640716156,126.13767278524));
#28192=CARTESIAN_POINT('Ctrl Pts',(169.129509892616,1.42268155709341,126.094374688565));
#28193=CARTESIAN_POINT('Ctrl Pts',(169.121749450102,1.29084759789218,126.056557589411));
#28194=CARTESIAN_POINT('Ctrl Pts',(169.113989007588,1.15780765893901,126.0243329516));
#28195=CARTESIAN_POINT('Ctrl Pts',(169.106216107323,1.02455415246505,125.992056583939));
#28196=CARTESIAN_POINT('Ctrl Pts',(169.098443207057,0.890091181320103,125.965390693653));
#28197=CARTESIAN_POINT('Ctrl Pts',(169.090670306792,0.754930657954383,125.944395312733));
#28198=CARTESIAN_POINT('Ctrl Pts',(169.08317997103,0.624683560064065,125.924163166794));
#28199=CARTESIAN_POINT('Ctrl Pts',(169.075689635268,0.493789051041498,125.909196448306));
#28200=CARTESIAN_POINT('Ctrl Pts',(169.068199299506,0.362705693235946,125.899503061776));
#28201=CARTESIAN_POINT('Ctrl Pts',(169.060424965387,0.226652270075251,125.889442147549));
#28202=CARTESIAN_POINT('Ctrl Pts',(169.052650631268,0.0899644186898381,
125.885030465782));
#28203=CARTESIAN_POINT('Ctrl Pts',(169.044876297149,-0.0468492422225645,
125.886333756008));
#28204=CARTESIAN_POINT('Ctrl Pts',(169.037111544202,-0.18349429252528,125.887635440045));
#28205=CARTESIAN_POINT('Ctrl Pts',(169.029346791255,-0.320264456659288,
125.894638078533));
#28206=CARTESIAN_POINT('Ctrl Pts',(169.021582038308,-0.456646027570617,
125.907355668824));
#28207=CARTESIAN_POINT('Ctrl Pts',(169.013824997423,-0.592892142383768,
125.920060627825));
#28208=CARTESIAN_POINT('Ctrl Pts',(169.006067956538,-0.728750045287246,
125.938469206728));
#28209=CARTESIAN_POINT('Ctrl Pts',(168.998310915652,-0.863706419194596,
125.962543367407));
#28210=CARTESIAN_POINT('Ctrl Pts',(168.990559724412,-0.998561021450345,
125.986599373573));
#28211=CARTESIAN_POINT('Ctrl Pts',(168.982808533172,-1.13251506457823,126.016312389062));
#28212=CARTESIAN_POINT('Ctrl Pts',(168.975057341932,-1.26506110021994,126.051592637198));
#28213=CARTESIAN_POINT('Ctrl Pts',(168.967309445155,-1.39755080026042,126.086857890287));
#28214=CARTESIAN_POINT('Ctrl Pts',(168.959561548378,-1.52863330604812,126.127685569434));
#28215=CARTESIAN_POINT('Ctrl Pts',(168.951813651601,-1.65781231984146,126.173935002714));
#28216=CARTESIAN_POINT('Ctrl Pts',(168.944067375517,-1.78696431216984,126.220174761609));
#28217=CARTESIAN_POINT('Ctrl Pts',(168.936321099433,-1.91421323663274,126.271833887122));
#28218=CARTESIAN_POINT('Ctrl Pts',(168.928574823349,-2.03907927934068,126.328722254711));
#28219=CARTESIAN_POINT('Ctrl Pts',(168.920828490083,-2.1639462437813,126.385611042236));
#28220=CARTESIAN_POINT('Ctrl Pts',(168.913082156818,-2.28642993558682,126.44772898677));
#28221=CARTESIAN_POINT('Ctrl Pts',(168.905335823553,-2.4060721693812,126.514838525511));
#28222=CARTESIAN_POINT('Ctrl Pts',(168.89758775555,-2.52574119622397,126.581963092967));
#28223=CARTESIAN_POINT('Ctrl Pts',(168.889839687547,-2.64256715792227,126.654081287759));
#28224=CARTESIAN_POINT('Ctrl Pts',(168.882091619544,-2.75611839275433,126.730910670946));
#28225=CARTESIAN_POINT('Ctrl Pts',(168.874335316802,-2.86979031119055,126.807821709315));
#28226=CARTESIAN_POINT('Ctrl Pts',(168.86657901406,-2.98018022592325,126.889453718875));
#28227=CARTESIAN_POINT('Ctrl Pts',(168.858822711318,-3.08688684832269,126.975481845895));
#28228=CARTESIAN_POINT('Ctrl Pts',(168.851062268804,-3.19365042325931,127.061555888717));
#28229=CARTESIAN_POINT('Ctrl Pts',(168.84330182629,-3.29672649498496,127.152030466498));
#28230=CARTESIAN_POINT('Ctrl Pts',(168.835541383776,-3.39574933211034,127.246542531158));
#28231=CARTESIAN_POINT('Ctrl Pts',(168.82776848351,-3.4949311294847,127.341206314975));
#28232=CARTESIAN_POINT('Ctrl Pts',(168.819995583245,-3.59004641854384,127.439920255738));
#28233=CARTESIAN_POINT('Ctrl Pts',(168.812222682979,-3.68076799149061,127.542286115762));
#28234=CARTESIAN_POINT('Ctrl Pts',(168.804732347217,-3.76819160674695,127.640930718931));
#28235=CARTESIAN_POINT('Ctrl Pts',(168.797242011455,-3.8515352102945,127.742966099573));
#28236=CARTESIAN_POINT('Ctrl Pts',(168.789751675693,-3.93054428769766,127.848010728776));
#28237=CARTESIAN_POINT('Ctrl Pts',(168.781946135203,-4.0128781873223,127.957475795844));
#28238=CARTESIAN_POINT('Ctrl Pts',(168.774140594712,-4.09076778232355,128.070558441467));
#28239=CARTESIAN_POINT('Ctrl Pts',(168.766335054222,-4.16387970994941,128.186863946399));
#28240=CARTESIAN_POINT('Ctrl Pts',(168.758542386704,-4.23687106068391,128.302977639177));
#28241=CARTESIAN_POINT('Ctrl Pts',(168.750749719185,-4.30510023353292,128.422303280493));
#28242=CARTESIAN_POINT('Ctrl Pts',(168.742957051667,-4.36827486879498,128.544414217061));
#28243=CARTESIAN_POINT('Ctrl Pts',(168.735171791586,-4.43138945245822,128.666409079244));
#28244=CARTESIAN_POINT('Ctrl Pts',(168.727386531505,-4.48945887876381,128.791183629434));
#28245=CARTESIAN_POINT('Ctrl Pts',(168.719601271423,-4.54223454595667,128.918283102717));
#28246=CARTESIAN_POINT('Ctrl Pts',(168.711822962697,-4.59496309046274,129.045269090583));
#28247=CARTESIAN_POINT('Ctrl Pts',(168.70404465397,-4.64240713964826,129.174575512534));
#28248=CARTESIAN_POINT('Ctrl Pts',(168.696266345244,-4.68436470074569,129.305724433261));
#28249=CARTESIAN_POINT('Ctrl Pts',(168.690844533546,-4.71361090368806,129.397140803778));
#28250=CARTESIAN_POINT('Ctrl Pts',(168.685422721848,-4.74019235577851,129.489451871063));
#28251=CARTESIAN_POINT('Ctrl Pts',(168.68000091015,-4.76405452823405,129.582490119308));
#28252=CARTESIAN_POINT('Origin',(213.235140564004,0.,130.804360617566));
#28253=CARTESIAN_POINT('',(166.584804846393,-4.76405452823406,129.582490119308));
#28254=CARTESIAN_POINT('',(166.930280810341,-4.76405452823404,129.582490119308));
#28255=CARTESIAN_POINT('',(213.235140564004,-4.76405452823405,129.582490119308));
#28256=CARTESIAN_POINT('',(168.264859436042,-4.91824981607796,130.805705663694));
#28257=CARTESIAN_POINT('Ctrl Pts',(168.264859435991,-4.91824981607772,130.805705664594));
#28258=CARTESIAN_POINT('Ctrl Pts',(168.260721432069,-4.91822995091836,130.878343880455));
#28259=CARTESIAN_POINT('Ctrl Pts',(168.256583428148,-4.91660096545378,130.950958115917));
#28260=CARTESIAN_POINT('Ctrl Pts',(168.252445424226,-4.91336553894317,131.023500169509));
#28261=CARTESIAN_POINT('Ctrl Pts',(168.244671090107,-4.90728693505862,131.159789591416));
#28262=CARTESIAN_POINT('Ctrl Pts',(168.236896755988,-4.89552370805166,131.296041777244));
#28263=CARTESIAN_POINT('Ctrl Pts',(168.229122421869,-4.87807065083757,131.431743903873));
#28264=CARTESIAN_POINT('Ctrl Pts',(168.221357668922,-4.8606391029567,131.567278789759));
#28265=CARTESIAN_POINT('Ctrl Pts',(168.213592915975,-4.8375317264647,131.702264581214));
#28266=CARTESIAN_POINT('Ctrl Pts',(168.205828163028,-4.8087952952739,131.836189513581));
#28267=CARTESIAN_POINT('Ctrl Pts',(168.198071122143,-4.78008740551166,131.969981429817));
#28268=CARTESIAN_POINT('Ctrl Pts',(168.190314081258,-4.74576166859946,132.102714204006));
#28269=CARTESIAN_POINT('Ctrl Pts',(168.182557040373,-4.70591648365769,132.233882604574));
#28270=CARTESIAN_POINT('Ctrl Pts',(168.174805849133,-4.6661013462798,132.36495209003));
#28271=CARTESIAN_POINT('Ctrl Pts',(168.167054657893,-4.62077515877267,132.494459177426));
#28272=CARTESIAN_POINT('Ctrl Pts',(168.159303466652,-4.57008700352293,132.621910573614));
#28273=CARTESIAN_POINT('Ctrl Pts',(168.151555569875,-4.51942039209137,132.749307799559));
#28274=CARTESIAN_POINT('Ctrl Pts',(168.143807673098,-4.46339648981288,132.874650709536));
#28275=CARTESIAN_POINT('Ctrl Pts',(168.136059776321,-4.40221360110317,132.997463094142));
#28276=CARTESIAN_POINT('Ctrl Pts',(168.128313500237,-4.34104351053483,133.120249789044));
#28277=CARTESIAN_POINT('Ctrl Pts',(168.120567224153,-4.27471675424657,133.240506661721));
#28278=CARTESIAN_POINT('Ctrl Pts',(168.112820948069,-4.20347879624994,133.357779712031));
#28279=CARTESIAN_POINT('Ctrl Pts',(168.105074614803,-4.13224031239089,133.475053628023));
#28280=CARTESIAN_POINT('Ctrl Pts',(168.097328281538,-4.05609075746079,133.589343343552));
#28281=CARTESIAN_POINT('Ctrl Pts',(168.089581948273,-3.97532014717889,133.700221938474));
#28282=CARTESIAN_POINT('Ctrl Pts',(168.08183388027,-3.8945314488789,133.81112536389));
#28283=CARTESIAN_POINT('Ctrl Pts',(168.074085812267,-3.80911986614477,133.918615832685));
#28284=CARTESIAN_POINT('Ctrl Pts',(168.066337744264,-3.71941684405539,134.022298062989));
#28285=CARTESIAN_POINT('Ctrl Pts',(168.058581441522,-3.62961848452657,134.126090488002));
#28286=CARTESIAN_POINT('Ctrl Pts',(168.05082513878,-3.53551983077862,134.226066293187));
#28287=CARTESIAN_POINT('Ctrl Pts',(168.043068836038,-3.43749085847617,134.32186536673));
#28288=CARTESIAN_POINT('Ctrl Pts',(168.035308393524,-3.33940956515953,134.417715571124));
#28289=CARTESIAN_POINT('Ctrl Pts',(168.02754795101,-3.2373940640506,134.509384340727));
#28290=CARTESIAN_POINT('Ctrl Pts',(168.019787508496,-3.13184805820872,134.596551383178));
#28291=CARTESIAN_POINT('Ctrl Pts',(168.01201460823,-3.02613262054841,134.683858353904));
#28292=CARTESIAN_POINT('Ctrl Pts',(168.004241707965,-2.91687566451193,134.766648920223));
#28293=CARTESIAN_POINT('Ctrl Pts',(167.996468807699,-2.80451128648739,134.844645199927));
#28294=CARTESIAN_POINT('Ctrl Pts',(167.988978471937,-2.69623163663488,134.919806118402));
#28295=CARTESIAN_POINT('Ctrl Pts',(167.981488136175,-2.58506682753121,134.99051510207));
#28296=CARTESIAN_POINT('Ctrl Pts',(167.973997800413,-2.471425778021,135.056564479828));
#28297=CARTESIAN_POINT('Ctrl Pts',(167.966223466294,-2.35347599357613,135.125118139819));
#28298=CARTESIAN_POINT('Ctrl Pts',(167.958449132175,-2.23248485924698,135.188869038371));
#28299=CARTESIAN_POINT('Ctrl Pts',(167.950674798056,-2.10888101309144,135.247535601192));
#28300=CARTESIAN_POINT('Ctrl Pts',(167.942910045109,-1.98542949762945,135.306129862718));
#28301=CARTESIAN_POINT('Ctrl Pts',(167.935145292162,-1.85937202685914,135.359652089933));
#28302=CARTESIAN_POINT('Ctrl Pts',(167.927380539215,-1.73116444532265,135.407865013757));
#28303=CARTESIAN_POINT('Ctrl Pts',(167.91962349833,-1.60308420136363,135.456030051825));
#28304=CARTESIAN_POINT('Ctrl Pts',(167.911866457445,-1.47285845999743,135.498896143833));
#28305=CARTESIAN_POINT('Ctrl Pts',(167.90410941656,-1.34096547398435,135.53627298574));
#28306=CARTESIAN_POINT('Ctrl Pts',(167.89635822532,-1.20917194949804,135.57362164148));
#28307=CARTESIAN_POINT('Ctrl Pts',(167.88860703408,-1.07571405753944,135.60548918035));
#28308=CARTESIAN_POINT('Ctrl Pts',(167.88085584284,-0.941087402276455,135.631734392589));
#28309=CARTESIAN_POINT('Ctrl Pts',(167.873107946063,-0.806517966933102,
135.657968449912));
#28310=CARTESIAN_POINT('Ctrl Pts',(167.865360049285,-0.670781139232144,
135.678584858759));
#28311=CARTESIAN_POINT('Ctrl Pts',(167.857612152508,-0.534384756013413,
135.693493055437));
#28312=CARTESIAN_POINT('Ctrl Pts',(167.849865876424,-0.398016903977686,
135.708398133641));
#28313=CARTESIAN_POINT('Ctrl Pts',(167.84211960034,-0.260990159248068,135.717597332224));
#28314=CARTESIAN_POINT('Ctrl Pts',(167.834373324256,-0.123819164296225,
135.721051768844));
#28315=CARTESIAN_POINT('Ctrl Pts',(167.826626990991,0.0133528432206947,
135.724506230963));
#28316=CARTESIAN_POINT('Ctrl Pts',(167.818880657725,0.150668712243327,135.722215836658));
#28317=CARTESIAN_POINT('Ctrl Pts',(167.81113432446,0.287612502185891,135.714193823601));
#28318=CARTESIAN_POINT('Ctrl Pts',(167.803386256457,0.424586959740618,135.706170014071));
#28319=CARTESIAN_POINT('Ctrl Pts',(167.795638188454,0.561188782187678,135.692412054519));
#28320=CARTESIAN_POINT('Ctrl Pts',(167.787890120451,0.69690625353351,135.672985139573));
#28321=CARTESIAN_POINT('Ctrl Pts',(167.780133817709,0.832767967023085,135.65353757747));
#28322=CARTESIAN_POINT('Ctrl Pts',(167.772377514968,0.967743064224729,135.628409079807));
#28323=CARTESIAN_POINT('Ctrl Pts',(167.764621212226,1.10132859198792,135.597716268357));
#28324=CARTESIAN_POINT('Ctrl Pts',(167.756860769712,1.23498541836955,135.56700707523));
#28325=CARTESIAN_POINT('Ctrl Pts',(167.749100327197,1.36725082064779,135.530727754023));
#28326=CARTESIAN_POINT('Ctrl Pts',(167.741339884683,1.49763711642252,135.489044825708));
#28327=CARTESIAN_POINT('Ctrl Pts',(167.733566984418,1.62823271985433,135.447294984256));
#28328=CARTESIAN_POINT('Ctrl Pts',(167.725794084152,1.7569428215368,135.400124336193));
#28329=CARTESIAN_POINT('Ctrl Pts',(167.718021183887,1.88329899159583,135.347747896981));
#28330=CARTESIAN_POINT('Ctrl Pts',(167.710530848125,2.00506179660252,135.297275473263));
#28331=CARTESIAN_POINT('Ctrl Pts',(167.703040512363,2.12463856182078,135.241969303848));
#28332=CARTESIAN_POINT('Ctrl Pts',(167.695550176601,2.24163353704436,135.182061172435));
#28333=CARTESIAN_POINT('Ctrl Pts',(167.687775842482,2.36306441231212,135.119881606011));
#28334=CARTESIAN_POINT('Ctrl Pts',(167.680001508363,2.48209851226058,135.052547255923));
#28335=CARTESIAN_POINT('Ctrl Pts',(167.672227174243,2.59826725112435,134.980266549724));
#28336=CARTESIAN_POINT('Ctrl Pts',(167.664462421296,2.71429282239976,134.908074923036));
#28337=CARTESIAN_POINT('Ctrl Pts',(167.656697668349,2.82745973006033,134.830949273907));
#28338=CARTESIAN_POINT('Ctrl Pts',(167.648932915402,2.93732195779911,134.749144867526));
#28339=CARTESIAN_POINT('Ctrl Pts',(167.641175874517,3.04707506882444,134.667421710434));
#28340=CARTESIAN_POINT('Ctrl Pts',(167.633418833632,3.15352972021036,134.581029275831));
#28341=CARTESIAN_POINT('Ctrl Pts',(167.625661792747,3.25626729647943,134.490267067325));
#28342=CARTESIAN_POINT('Ctrl Pts',(167.617910601507,3.35892739754301,134.399573303308));
#28343=CARTESIAN_POINT('Ctrl Pts',(167.610159410267,3.45787571102379,134.304516582246));
#28344=CARTESIAN_POINT('Ctrl Pts',(167.602408219027,3.5527255469913,134.205437542638));
#28345=CARTESIAN_POINT('Ctrl Pts',(167.59466032225,3.64753506924837,134.106400614264));
#28346=CARTESIAN_POINT('Ctrl Pts',(167.586912425473,3.73824930882739,134.003345049419));
#28347=CARTESIAN_POINT('Ctrl Pts',(167.579164528696,3.82451757371098,133.896649153728));
#28348=CARTESIAN_POINT('Ctrl Pts',(167.571418252612,3.91076779313329,133.789975576518));
#28349=CARTESIAN_POINT('Ctrl Pts',(167.563671976527,3.99257364202647,133.679663486915));
#28350=CARTESIAN_POINT('Ctrl Pts',(167.555925700443,4.06962423074853,133.566124851349));
#28351=CARTESIAN_POINT('Ctrl Pts',(167.548179367178,4.14667538824053,133.452585377668));
#28352=CARTESIAN_POINT('Ctrl Pts',(167.540433033913,4.21897099597718,133.335819634003));
#28353=CARTESIAN_POINT('Ctrl Pts',(167.532686700647,4.2862433126994,133.216268851069));
#28354=CARTESIAN_POINT('Ctrl Pts',(167.524938632644,4.35353069459053,133.096691295566));
#28355=CARTESIAN_POINT('Ctrl Pts',(167.517190564641,4.41579235529187,132.974327800382));
#28356=CARTESIAN_POINT('Ctrl Pts',(167.509442496638,4.47280654989458,132.849644125963));
#28357=CARTESIAN_POINT('Ctrl Pts',(167.501686193897,4.52988133986178,132.724827936251));
#28358=CARTESIAN_POINT('Ctrl Pts',(167.493929891155,4.58169736008899,132.597686997497));
#28359=CARTESIAN_POINT('Ctrl Pts',(167.486173588413,4.62808086931449,132.468707495349));
#28360=CARTESIAN_POINT('Ctrl Pts',(167.478413145899,4.67448913481547,132.339659152957));
#28361=CARTESIAN_POINT('Ctrl Pts',(167.470652703385,4.71545899509354,132.208770664785));
#28362=CARTESIAN_POINT('Ctrl Pts',(167.46289226087,4.75086694470893,132.076542340502));
#28363=CARTESIAN_POINT('Ctrl Pts',(167.455119360605,4.7863317343084,131.944101751574));
#28364=CARTESIAN_POINT('Ctrl Pts',(167.447346460339,4.81621668602879,131.810317410283));
#28365=CARTESIAN_POINT('Ctrl Pts',(167.439573560074,4.84044950068023,131.675699641061));
#28366=CARTESIAN_POINT('Ctrl Pts',(167.432083224312,4.86380139148021,131.545975566831));
#28367=CARTESIAN_POINT('Ctrl Pts',(167.42459288855,4.88190490722373,131.415477912168));
#28368=CARTESIAN_POINT('Ctrl Pts',(167.417102552788,4.89474114144904,131.284664917678));
#28369=CARTESIAN_POINT('Ctrl Pts',(167.409328218669,4.90806406539654,131.148892108742));
#28370=CARTESIAN_POINT('Ctrl Pts',(167.40155388455,4.91575460825063,131.012349488279));
#28371=CARTESIAN_POINT('Ctrl Pts',(167.393779550431,4.91773484396511,130.875543950949));
#28372=CARTESIAN_POINT('Ctrl Pts',(167.386014797484,4.91971263921605,130.738907014216));
#28373=CARTESIAN_POINT('Ctrl Pts',(167.378250044537,4.91599412413756,130.602008192495));
#28374=CARTESIAN_POINT('Ctrl Pts',(167.370485291589,4.90655297785485,130.465360709006));
#28375=CARTESIAN_POINT('Ctrl Pts',(167.362728250704,4.89712120865172,130.328848945724));
#28376=CARTESIAN_POINT('Ctrl Pts',(167.354971209819,4.8819781460325,130.192588411405));
#28377=CARTESIAN_POINT('Ctrl Pts',(167.347214168934,4.86114949897587,130.057093188123));
#28378=CARTESIAN_POINT('Ctrl Pts',(167.339462977694,4.84033655896402,129.921700142843));
#28379=CARTESIAN_POINT('Ctrl Pts',(167.331711786454,4.81384662777197,129.787071644726));
#28380=CARTESIAN_POINT('Ctrl Pts',(167.323960595214,4.78175727886192,129.653717150392));
#28381=CARTESIAN_POINT('Ctrl Pts',(167.316212698437,4.74968156878115,129.520419335274));
#28382=CARTESIAN_POINT('Ctrl Pts',(167.30846480166,4.71201126570212,129.388394826284));
#28383=CARTESIAN_POINT('Ctrl Pts',(167.300716904883,4.66887509126163,129.258143153981));
#28384=CARTESIAN_POINT('Ctrl Pts',(167.292970628799,4.62574793997892,129.127918727519));
#28385=CARTESIAN_POINT('Ctrl Pts',(167.285224352715,4.57715731434078,128.99946677103));
#28386=CARTESIAN_POINT('Ctrl Pts',(167.277478076631,4.52328176992806,128.873271522693));
#28387=CARTESIAN_POINT('Ctrl Pts',(167.269731743365,4.46940582781833,128.747075342812));
#28388=CARTESIAN_POINT('Ctrl Pts',(167.2619854101,4.41024504259584,128.623136263893));
#28389=CARTESIAN_POINT('Ctrl Pts',(167.254239076834,4.34602591346543,128.501918040218));
#28390=CARTESIAN_POINT('Ctrl Pts',(167.246491008831,4.28179240290631,128.380672670561));
#28391=CARTESIAN_POINT('Ctrl Pts',(167.238742940829,4.21249847732859,128.26214971403));
#28392=CARTESIAN_POINT('Ctrl Pts',(167.230994872826,4.13841613564653,128.146787485793));
#28393=CARTESIAN_POINT('Ctrl Pts',(167.223238570084,4.06425505837013,128.031302649207));
#28394=CARTESIAN_POINT('Ctrl Pts',(167.215482267342,3.98529561038756,127.918985580898));
#28395=CARTESIAN_POINT('Ctrl Pts',(167.2077259646,3.90185292205769,127.810245249527));
#28396=CARTESIAN_POINT('Ctrl Pts',(167.199965522086,3.81836569785261,127.701446880166));
#28397=CARTESIAN_POINT('Ctrl Pts',(167.192205079572,3.7303907160241,127.596229351402));
#28398=CARTESIAN_POINT('Ctrl Pts',(167.184444637057,3.6382821435583,127.494967001454));
#28399=CARTESIAN_POINT('Ctrl Pts',(167.176671736792,3.54602571023496,127.393542096192));
#28400=CARTESIAN_POINT('Ctrl Pts',(167.168898836527,3.44962270132345,127.296085335592));
#28401=CARTESIAN_POINT('Ctrl Pts',(167.161125936261,3.3494633877416,127.20293338983));
#28402=CARTESIAN_POINT('Ctrl Pts',(167.153635600499,3.25294511749426,127.113167751932));
#28403=CARTESIAN_POINT('Ctrl Pts',(167.146145264737,3.15293913720184,127.02739958149));
#28404=CARTESIAN_POINT('Ctrl Pts',(167.138654928975,3.04982075826178,126.945892475288));
#28405=CARTESIAN_POINT('Ctrl Pts',(167.130880594856,2.94279261464236,126.861295002381));
#28406=CARTESIAN_POINT('Ctrl Pts',(167.123106260737,2.83207236722314,126.781020109271));
#28407=CARTESIAN_POINT('Ctrl Pts',(167.115331926618,2.71804435990667,126.705407346293));
#28408=CARTESIAN_POINT('Ctrl Pts',(167.107567173671,2.60415688191836,126.629887769288));
#28409=CARTESIAN_POINT('Ctrl Pts',(167.099802420724,2.48697007779855,126.559019104257));
#28410=CARTESIAN_POINT('Ctrl Pts',(167.092037667776,2.36690150970268,126.493100905386));
#28411=CARTESIAN_POINT('Ctrl Pts',(167.084280626891,2.24695219540119,126.427248177399));
#28412=CARTESIAN_POINT('Ctrl Pts',(167.076523586006,2.12412715354412,126.366336317706));
#28413=CARTESIAN_POINT('Ctrl Pts',(167.068766545121,1.99887279227081,126.310621570534));
#28414=CARTESIAN_POINT('Ctrl Pts',(167.061015353881,1.87371288628576,126.254948838286));
#28415=CARTESIAN_POINT('Ctrl Pts',(167.053264162641,1.74612766308127,126.204465575916));
#28416=CARTESIAN_POINT('Ctrl Pts',(167.045512971401,1.61658767329015,126.159381892419));
#28417=CARTESIAN_POINT('Ctrl Pts',(167.037765074624,1.48710274145019,126.11431737069));
#28418=CARTESIAN_POINT('Ctrl Pts',(167.030017177847,1.35566506394611,126.074647991562));
#28419=CARTESIAN_POINT('Ctrl Pts',(167.02226928107,1.22276448717305,126.040535466345));
#28420=CARTESIAN_POINT('Ctrl Pts',(167.014523004986,1.08989171033569,126.006430076732));
#28421=CARTESIAN_POINT('Ctrl Pts',(167.006776728902,0.955557021343663,125.977879326144));
#28422=CARTESIAN_POINT('Ctrl Pts',(166.999030452818,0.820264337144804,125.954994733277));
#28423=CARTESIAN_POINT('Ctrl Pts',(166.991284119552,0.684970654246222,125.932109971481));
#28424=CARTESIAN_POINT('Ctrl Pts',(166.983537786287,0.548719347519155,125.914891516073));
#28425=CARTESIAN_POINT('Ctrl Pts',(166.975791453021,0.412023014928205,125.903399477374));
#28426=CARTESIAN_POINT('Ctrl Pts',(166.968043385019,0.275296070141404,125.891904865113));
#28427=CARTESIAN_POINT('Ctrl Pts',(166.960295317016,0.13812429069425,125.886139254118));
#28428=CARTESIAN_POINT('Ctrl Pts',(166.952547249013,0.00102346560978314,
125.886110724055));
#28429=CARTESIAN_POINT('Ctrl Pts',(166.944790946271,-0.136223071863291,
125.88608216367));
#28430=CARTESIAN_POINT('Ctrl Pts',(166.937034643529,-0.273398112743194,
125.891802864587));
#28431=CARTESIAN_POINT('Ctrl Pts',(166.929278340787,-0.409987244455299,
125.903228756263));
#28432=CARTESIAN_POINT('Ctrl Pts',(166.921517898273,-0.54664927789971,125.91466074628));
#28433=CARTESIAN_POINT('Ctrl Pts',(166.913757455759,-0.682724391351298,
125.931803945695));
#28434=CARTESIAN_POINT('Ctrl Pts',(166.905997013244,-0.81770620755624,125.954562722744));
#28435=CARTESIAN_POINT('Ctrl Pts',(166.898224112979,-0.952904708555676,
125.977358034201));
#28436=CARTESIAN_POINT('Ctrl Pts',(166.890451212714,-1.08700602245833,126.005786856256));
#28437=CARTESIAN_POINT('Ctrl Pts',(166.882678312448,-1.21951594814637,126.039702821384));
#28438=CARTESIAN_POINT('Ctrl Pts',(166.875187976686,-1.34720880426391,126.072385855751));
#28439=CARTESIAN_POINT('Ctrl Pts',(166.867697640924,-1.47342367026775,126.11016392816));
#28440=CARTESIAN_POINT('Ctrl Pts',(166.860207305162,-1.59773590974054,126.152863759003));
#28441=CARTESIAN_POINT('Ctrl Pts',(166.852432913953,-1.72676243303172,126.197182892357));
#28442=CARTESIAN_POINT('Ctrl Pts',(166.844658522745,-1.85414789569075,126.246944837167));
#28443=CARTESIAN_POINT('Ctrl Pts',(166.836884131537,-1.97939886630912,126.302009766005));
#28444=CARTESIAN_POINT('Ctrl Pts',(166.829119334888,-2.10449526175076,126.357006737916));
#28445=CARTESIAN_POINT('Ctrl Pts',(166.821354538239,-2.22746205203118,126.417293516249));
#28446=CARTESIAN_POINT('Ctrl Pts',(166.81358974159,-2.34782150329167,126.482680706793));
#28447=CARTESIAN_POINT('Ctrl Pts',(166.805832670334,-2.46806120587771,126.54800284196));
#28448=CARTESIAN_POINT('Ctrl Pts',(166.798075599079,-2.58569839054954,126.61841510528));
#28449=CARTESIAN_POINT('Ctrl Pts',(166.790318527823,-2.70027617224483,126.693680423716));
#28450=CARTESIAN_POINT('Ctrl Pts',(166.782567319501,-2.81476735399967,126.768888855277));
#28451=CARTESIAN_POINT('Ctrl Pts',(166.774816111179,-2.92620340997121,126.848942827103));
#28452=CARTESIAN_POINT('Ctrl Pts',(166.767064902857,-3.03415322304247,126.933560018));
#28453=CARTESIAN_POINT('Ctrl Pts',(166.759317058284,-3.14205618971799,127.018140488033));
#28454=CARTESIAN_POINT('Ctrl Pts',(166.751569213712,-3.24647561586085,127.107279997354));
#28455=CARTESIAN_POINT('Ctrl Pts',(166.74382136914,-3.34701068383153,127.200653839148));
#28456=CARTESIAN_POINT('Ctrl Pts',(166.736075164187,-3.44752447629983,127.294007920917));
#28457=CARTESIAN_POINT('Ctrl Pts',(166.728328959235,-3.54415525947485,127.391594286795));
#28458=CARTESIAN_POINT('Ctrl Pts',(166.720582754283,-3.63653684047063,127.493049265488));
#28459=CARTESIAN_POINT('Ctrl Pts',(166.712836511089,-3.72891887753324,127.594504745042));
#28460=CARTESIAN_POINT('Ctrl Pts',(166.705090267895,-3.81705140741029,127.6998285864));
#28461=CARTESIAN_POINT('Ctrl Pts',(166.697344024701,-3.90060679718677,127.808622031467));
#28462=CARTESIAN_POINT('Ctrl Pts',(166.68959606574,-3.98418069421321,127.917439573933));
#28463=CARTESIAN_POINT('Ctrl Pts',(166.681848106778,-4.06317519580791,128.029727939255));
#28464=CARTESIAN_POINT('Ctrl Pts',(166.674100147817,-4.13730471913056,128.145057565343));
#28465=CARTESIAN_POINT('Ctrl Pts',(166.666344219302,-4.21151049209885,128.260505819514));
#28466=CARTESIAN_POINT('Ctrl Pts',(166.658588290788,-4.28084107984005,128.379001253493));
#28467=CARTESIAN_POINT('Ctrl Pts',(166.650832362274,-4.34505554027724,128.500087323357));
#28468=CARTESIAN_POINT('Ctrl Pts',(166.64307230181,-4.40930421079557,128.621237901499));
#28469=CARTESIAN_POINT('Ctrl Pts',(166.635312241346,-4.4684311546285,128.744981513072));
#28470=CARTESIAN_POINT('Ctrl Pts',(166.627552180882,-4.52224314406754,128.870840509464));
#28471=CARTESIAN_POINT('Ctrl Pts',(166.619780289522,-4.57613717462138,128.996891388975));
#28472=CARTESIAN_POINT('Ctrl Pts',(166.612008398163,-4.62469992236801,129.125063731427));
#28473=CARTESIAN_POINT('Ctrl Pts',(166.604236506803,-4.66778744933132,129.254862831067));
#28474=CARTESIAN_POINT('Ctrl Pts',(166.597759286667,-4.70369729217216,129.363039503006));
#28475=CARTESIAN_POINT('Ctrl Pts',(166.59128206653,-4.73580502071292,129.472345718229));
#28476=CARTESIAN_POINT('Ctrl Pts',(166.584804846393,-4.76405452823406,129.582490119308));
#28477=CARTESIAN_POINT('Ctrl Pts',(168.33498954974,-4.76405452823405,129.582490119308));
#28478=CARTESIAN_POINT('Ctrl Pts',(168.32728426315,-4.79790534790346,129.714473951441));
#28479=CARTESIAN_POINT('Ctrl Pts',(168.31957897656,-4.82624105686554,129.847763448461));
#28480=CARTESIAN_POINT('Ctrl Pts',(168.311873689969,-4.84898620031437,129.981854756395));
#28481=CARTESIAN_POINT('Ctrl Pts',(168.304037980981,-4.87211633608039,130.118215741083));
#28482=CARTESIAN_POINT('Ctrl Pts',(168.296202271994,-4.88946488867095,130.255405497073));
#28483=CARTESIAN_POINT('Ctrl Pts',(168.288366563006,-4.90100765122071,130.392891219948));
#28484=CARTESIAN_POINT('Ctrl Pts',(168.280530854018,-4.91255041377047,130.530376942823));
#28485=CARTESIAN_POINT('Ctrl Pts',(168.27269514503,-4.91828743264541,130.668158205622));
#28486=CARTESIAN_POINT('Ctrl Pts',(168.264859436042,-4.91824981607796,130.805705663694));
#28487=CARTESIAN_POINT('',(168.610140563953,-4.91824876274648,130.807849205066));
#28488=CARTESIAN_POINT('Ctrl Pts',(168.68000091015,-4.76405452823405,129.582490119308));
#28489=CARTESIAN_POINT('Ctrl Pts',(168.672228899302,-4.79826026490074,129.715857767427));
#28490=CARTESIAN_POINT('Ctrl Pts',(168.664456888454,-4.82687611153899,129.850720065033));
#28491=CARTESIAN_POINT('Ctrl Pts',(168.656684877605,-4.84978382879872,129.986570989103));
#28492=CARTESIAN_POINT('Ctrl Pts',(168.648912706895,-4.87269201724581,130.122424707481));
#28493=CARTESIAN_POINT('Ctrl Pts',(168.641140536184,-4.88989176638913,130.259266713356));
#28494=CARTESIAN_POINT('Ctrl Pts',(168.633368365474,-4.90131605062345,130.396581223284));
#28495=CARTESIAN_POINT('Ctrl Pts',(168.625625764985,-4.91269686970111,130.533373302523));
#28496=CARTESIAN_POINT('Ctrl Pts',(168.617883164497,-4.91834609158011,130.670633913812));
#28497=CARTESIAN_POINT('Ctrl Pts',(168.610140564008,-4.91824876274717,130.807849204087));
#28498=CARTESIAN_POINT('Ctrl Pts',(168.610140563953,-4.91824876274648,130.807849205066));
#28499=CARTESIAN_POINT('Ctrl Pts',(168.601280367312,-4.91813738507152,130.964870667785));
#28500=CARTESIAN_POINT('Ctrl Pts',(168.592420170671,-4.91050237173166,131.121592477866));
#28501=CARTESIAN_POINT('Ctrl Pts',(168.58355997403,-4.8954535172796,131.277348907754));
#28502=CARTESIAN_POINT('Ctrl Pts',(168.574657903986,-4.88033354174772,131.433841444534));
#28503=CARTESIAN_POINT('Ctrl Pts',(168.565755833942,-4.85772959459143,131.589359305109));
#28504=CARTESIAN_POINT('Ctrl Pts',(168.556853763897,-4.82780256547689,131.743245834871));
#28505=CARTESIAN_POINT('Ctrl Pts',(168.547897218697,-4.79769240147487,131.89807405491));
#28506=CARTESIAN_POINT('Ctrl Pts',(168.538940673496,-4.7601693460731,132.05125076968));
#28507=CARTESIAN_POINT('Ctrl Pts',(168.529984128295,-4.71544577824053,132.20212818586));
#28508=CARTESIAN_POINT('Ctrl Pts',(168.523757436157,-4.68435344498441,132.307019882386));
#28509=CARTESIAN_POINT('Ctrl Pts',(168.517530744019,-4.64978198049473,132.410800722358));
#28510=CARTESIAN_POINT('Ctrl Pts',(168.511304051881,-4.61181608600089,132.513259517853));
#28511=CARTESIAN_POINT('Ctrl Pts',(168.503529717762,-4.56441378275859,132.641184408302));
#28512=CARTESIAN_POINT('Ctrl Pts',(168.495755383642,-4.51160969578233,132.767338124264));
#28513=CARTESIAN_POINT('Ctrl Pts',(168.487981049523,-4.45355544969984,132.891230742645));
#28514=CARTESIAN_POINT('Ctrl Pts',(168.480216296576,-4.39557275028721,133.014970674448));
#28515=CARTESIAN_POINT('Ctrl Pts',(168.472451543629,-4.33235293013857,133.136454702548));
#28516=CARTESIAN_POINT('Ctrl Pts',(168.464686790682,-4.26409678933356,133.255209783405));
#28517=CARTESIAN_POINT('Ctrl Pts',(168.456929749797,-4.19590844148999,133.373846915042));
#28518=CARTESIAN_POINT('Ctrl Pts',(168.449172708912,-4.12269392104773,133.489760156541));
#28519=CARTESIAN_POINT('Ctrl Pts',(168.441415668027,-4.0447011931447,133.602498448459));
#28520=CARTESIAN_POINT('Ctrl Pts',(168.433664476787,-3.96676728016439,133.715151723554));
#28521=CARTESIAN_POINT('Ctrl Pts',(168.425913285547,-3.88406255337208,133.824634494463));
#28522=CARTESIAN_POINT('Ctrl Pts',(168.418162094307,-3.7968795955622,133.930522545442));
#28523=CARTESIAN_POINT('Ctrl Pts',(168.41041419753,-3.70973369283501,134.036365591176));
#28524=CARTESIAN_POINT('Ctrl Pts',(168.402666300752,-3.6181135927303,134.138616654568));
#28525=CARTESIAN_POINT('Ctrl Pts',(168.394918403975,-3.52235353319592,134.236882817011));
#28526=CARTESIAN_POINT('Ctrl Pts',(168.387172127891,-3.42661350460165,134.335128424291));
#28527=CARTESIAN_POINT('Ctrl Pts',(168.379425851807,-3.32673551176757,134.429390508785));
#28528=CARTESIAN_POINT('Ctrl Pts',(168.371679575723,-3.22309191885105,134.519311700035));
#28529=CARTESIAN_POINT('Ctrl Pts',(168.363933242458,-3.11944756086106,134.609233555062));
#28530=CARTESIAN_POINT('Ctrl Pts',(168.356186909192,-3.01203784263378,134.694814196693));
#28531=CARTESIAN_POINT('Ctrl Pts',(168.348440575927,-2.90126928397905,134.775735644473));
#28532=CARTESIAN_POINT('Ctrl Pts',(168.340692507924,-2.79047591947359,134.85667521405));
#28533=CARTESIAN_POINT('Ctrl Pts',(168.332944439921,-2.67632253340668,134.932953282958));
#28534=CARTESIAN_POINT('Ctrl Pts',(168.325196371918,-2.5592454361998,135.004294647975));
#28535=CARTESIAN_POINT('Ctrl Pts',(168.317440069176,-2.44204390806084,135.075711835444));
#28536=CARTESIAN_POINT('Ctrl Pts',(168.309683766434,-2.32191279590227,135.142181634232));
#28537=CARTESIAN_POINT('Ctrl Pts',(168.301927463692,-2.19931436203489,135.203474096376));
#28538=CARTESIAN_POINT('Ctrl Pts',(168.294167021178,-2.0766504936919,135.264799272153));
#28539=CARTESIAN_POINT('Ctrl Pts',(168.286406578664,-1.95151703617139,135.320941445213));
#28540=CARTESIAN_POINT('Ctrl Pts',(168.27864613615,-1.82439621023559,135.371718883629));
#28541=CARTESIAN_POINT('Ctrl Pts',(168.270873235884,-1.69707131866469,135.422577834498));
#28542=CARTESIAN_POINT('Ctrl Pts',(168.263100335619,-1.56775305247812,135.468054711526));
#28543=CARTESIAN_POINT('Ctrl Pts',(168.255327435354,-1.43693962500906,135.508017447797));
#28544=CARTESIAN_POINT('Ctrl Pts',(168.247837099591,-1.31088159512657,135.546527437944));
#28545=CARTESIAN_POINT('Ctrl Pts',(168.240346763829,-1.1834355203898,135.579917154768));
#28546=CARTESIAN_POINT('Ctrl Pts',(168.232856428067,-1.05505420101026,135.608113701919));
#28547=CARTESIAN_POINT('Ctrl Pts',(168.225082093948,-0.921805264886874,
135.637379329725));
#28548=CARTESIAN_POINT('Ctrl Pts',(168.217307759829,-0.78712667196695,135.661142920815));
#28549=CARTESIAN_POINT('Ctrl Pts',(168.20953342571,-0.651512565239633,135.679267225885));
#28550=CARTESIAN_POINT('Ctrl Pts',(168.201768672763,-0.516065590778632,
135.697369194369));
#28551=CARTESIAN_POINT('Ctrl Pts',(168.194003919816,-0.37968578031111,135.7098456538));
#28552=CARTESIAN_POINT('Ctrl Pts',(168.186239166869,-0.242879656112835,
135.716609851384));
#28553=CARTESIAN_POINT('Ctrl Pts',(168.178482125984,-0.106209409685695,
135.723367330672));
#28554=CARTESIAN_POINT('Ctrl Pts',(168.170725085099,0.0308859198843273,
135.724423819449));
#28555=CARTESIAN_POINT('Ctrl Pts',(168.162968044214,0.167892812299595,135.719744129163));
#28556=CARTESIAN_POINT('Ctrl Pts',(168.155216852974,0.304796386751348,135.715067967868));
#28557=CARTESIAN_POINT('Ctrl Pts',(168.147465661734,0.441611267636705,135.704664250839));
#28558=CARTESIAN_POINT('Ctrl Pts',(168.139714470493,0.577822402089663,135.688549837298));
#28559=CARTESIAN_POINT('Ctrl Pts',(168.131966573716,0.713975643177067,135.672442272812));
#28560=CARTESIAN_POINT('Ctrl Pts',(168.124218676939,0.849525260761727,135.650628885162));
#28561=CARTESIAN_POINT('Ctrl Pts',(168.116470780162,0.983960017515345,135.623178496095));
#28562=CARTESIAN_POINT('Ctrl Pts',(168.108724504078,1.11836665341593,135.595733849057));
#28563=CARTESIAN_POINT('Ctrl Pts',(168.100978227994,1.25165850952432,135.562654624143));
#28564=CARTESIAN_POINT('Ctrl Pts',(168.09323195191,1.38333364803016,135.5240609344));
#28565=CARTESIAN_POINT('Ctrl Pts',(168.085485618645,1.51500975853188,135.485466959768));
#28566=CARTESIAN_POINT('Ctrl Pts',(168.077739285379,1.64506875243519,135.441358549047));
#28567=CARTESIAN_POINT('Ctrl Pts',(168.069992952114,1.77302336989257,135.391905842664));
#28568=CARTESIAN_POINT('Ctrl Pts',(168.062244884111,1.90100664189935,135.342442061689));
#28569=CARTESIAN_POINT('Ctrl Pts',(168.054496816108,2.02688423509956,135.28763174444));
#28570=CARTESIAN_POINT('Ctrl Pts',(168.046748748105,2.15018877678808,135.227693217165));
#28571=CARTESIAN_POINT('Ctrl Pts',(168.038992445363,2.27362436801094,135.16769098651));
#28572=CARTESIAN_POINT('Ctrl Pts',(168.031236142621,2.39448109274114,135.102549829421));
#28573=CARTESIAN_POINT('Ctrl Pts',(168.02347983988,2.51231562517436,135.032534367781));
#28574=CARTESIAN_POINT('Ctrl Pts',(168.015719397365,2.6302130494455,134.96248153678));
#28575=CARTESIAN_POINT('Ctrl Pts',(168.007958954851,2.74508474001502,134.887549430893));
#28576=CARTESIAN_POINT('Ctrl Pts',(168.000198512337,2.85651714856342,134.808045525556));
#28577=CARTESIAN_POINT('Ctrl Pts',(167.992425612072,2.96812843830649,134.728413993492));
#28578=CARTESIAN_POINT('Ctrl Pts',(167.984652711806,3.07628910457113,134.644196236534));
#28579=CARTESIAN_POINT('Ctrl Pts',(167.976879811541,3.18061873924162,134.555740030273));
#28580=CARTESIAN_POINT('Ctrl Pts',(167.969389475779,3.28115572890079,134.470499429919));
#28581=CARTESIAN_POINT('Ctrl Pts',(167.961899140017,3.37813515974809,134.381323395316));
#28582=CARTESIAN_POINT('Ctrl Pts',(167.954408804255,3.47125095244502,134.288553477849));
#28583=CARTESIAN_POINT('Ctrl Pts',(167.946634470136,3.56789725872451,134.192266160764));
#28584=CARTESIAN_POINT('Ctrl Pts',(167.938860136017,3.66068731010971,134.091802047688));
#28585=CARTESIAN_POINT('Ctrl Pts',(167.931085801898,3.74923853851688,133.987502688508));
#28586=CARTESIAN_POINT('Ctrl Pts',(167.923321048951,3.83768063544908,133.883331868967));
#28587=CARTESIAN_POINT('Ctrl Pts',(167.915556296004,3.92189405293988,133.775335503021));
#28588=CARTESIAN_POINT('Ctrl Pts',(167.907791543056,4.00153201574385,133.663892850201));
#28589=CARTESIAN_POINT('Ctrl Pts',(167.900034502171,4.08109088100043,133.552560883795));
#28590=CARTESIAN_POINT('Ctrl Pts',(167.892277461286,4.15608310930224,133.437789758276));
#28591=CARTESIAN_POINT('Ctrl Pts',(167.884520420401,4.22620152525857,133.319992492543));
#28592=CARTESIAN_POINT('Ctrl Pts',(167.876769229161,4.29626706437197,133.202284058645));
#28593=CARTESIAN_POINT('Ctrl Pts',(167.869018037921,4.36146590759516,133.081554361378));
#28594=CARTESIAN_POINT('Ctrl Pts',(167.861266846681,4.4215338404127,132.958245842128));
#28595=CARTESIAN_POINT('Ctrl Pts',(167.853518949904,4.48157624275646,132.834989732287));
#28596=CARTESIAN_POINT('Ctrl Pts',(167.845771053127,4.5364919012276,132.709157331202));
#28597=CARTESIAN_POINT('Ctrl Pts',(167.83802315635,4.58606238124673,132.581215957152));
#28598=CARTESIAN_POINT('Ctrl Pts',(167.830276880266,4.63562249219005,132.453301345678));
#28599=CARTESIAN_POINT('Ctrl Pts',(167.822530604182,4.67983950747819,132.323279003041));
#28600=CARTESIAN_POINT('Ctrl Pts',(167.814784328098,4.71854317197448,132.191636147774));
#28601=CARTESIAN_POINT('Ctrl Pts',(167.807037994832,4.75724712217241,132.059992320749));
#28602=CARTESIAN_POINT('Ctrl Pts',(167.799291661567,4.79043753008965,131.926728332313));
#28603=CARTESIAN_POINT('Ctrl Pts',(167.791545328302,4.81799416383687,131.792346093033));
#28604=CARTESIAN_POINT('Ctrl Pts',(167.783797260299,4.84555696870114,131.657933759783));
#28605=CARTESIAN_POINT('Ctrl Pts',(167.776049192296,4.86748341034595,131.522403060295));
#28606=CARTESIAN_POINT('Ctrl Pts',(167.768301124293,4.8837045464661,131.386265219134));
#28607=CARTESIAN_POINT('Ctrl Pts',(167.760544821551,4.89994292260276,131.249982689056));
#28608=CARTESIAN_POINT('Ctrl Pts',(167.752788518809,4.9104638340566,131.113092117132));
#28609=CARTESIAN_POINT('Ctrl Pts',(167.745032216067,4.91525028628631,130.97610952051));
#28610=CARTESIAN_POINT('Ctrl Pts',(167.737271773553,4.92003929318968,130.839053812151));
#28611=CARTESIAN_POINT('Ctrl Pts',(167.729511331039,4.91908774496876,130.701906371988));
#28612=CARTESIAN_POINT('Ctrl Pts',(167.721750888525,4.91243079644946,130.565181327921));
#28613=CARTESIAN_POINT('Ctrl Pts',(167.713977988259,4.90576316160543,130.428236800676));
#28614=CARTESIAN_POINT('Ctrl Pts',(167.706205087994,4.8933718595932,130.291716414109));
#28615=CARTESIAN_POINT('Ctrl Pts',(167.698432187728,4.87534386398892,130.156128197546));
#28616=CARTESIAN_POINT('Ctrl Pts',(167.690941851966,4.85797123143446,130.025468954179));
#28617=CARTESIAN_POINT('Ctrl Pts',(167.683451516204,4.83536465915356,129.895675587456));
#28618=CARTESIAN_POINT('Ctrl Pts',(167.675961180442,4.80764606064002,129.76719022746));
#28619=CARTESIAN_POINT('Ctrl Pts',(167.668186846323,4.77887650303921,129.633833305989));
#28620=CARTESIAN_POINT('Ctrl Pts',(167.660412512204,4.74450848871262,129.501463100717));
#28621=CARTESIAN_POINT('Ctrl Pts',(167.652638178085,4.70462258586134,129.370586093067));
#28622=CARTESIAN_POINT('Ctrl Pts',(167.644873425138,4.66478583882064,129.239870379632));
#28623=CARTESIAN_POINT('Ctrl Pts',(167.63710867219,4.6194448467148,129.110644572697));
#28624=CARTESIAN_POINT('Ctrl Pts',(167.629343919243,4.56873125083833,128.983405423138));
#28625=CARTESIAN_POINT('Ctrl Pts',(167.621586878358,4.51806802442023,128.856292649297));
#28626=CARTESIAN_POINT('Ctrl Pts',(167.613829837473,4.46204295721851,128.731162966953));
#28627=CARTESIAN_POINT('Ctrl Pts',(167.606072796588,4.40083749792711,128.608498058265));
#28628=CARTESIAN_POINT('Ctrl Pts',(167.598321605348,4.33967819414871,128.485925652139));
#28629=CARTESIAN_POINT('Ctrl Pts',(167.590570414108,4.27334644792807,128.365814668449));
#28630=CARTESIAN_POINT('Ctrl Pts',(167.582819222868,4.20207168333242,128.248626548725));
#28631=CARTESIAN_POINT('Ctrl Pts',(167.575071326091,4.13082721241299,128.131488237077));
#28632=CARTESIAN_POINT('Ctrl Pts',(167.567323429314,4.05464410441463,128.017270651899));
#28633=CARTESIAN_POINT('Ctrl Pts',(167.559575532537,3.9737974582142,127.906410165334));
#28634=CARTESIAN_POINT('Ctrl Pts',(167.551829256453,3.8929677233893,127.795572868393));
#28635=CARTESIAN_POINT('Ctrl Pts',(167.544082980368,3.8074766209286,127.688091588973));
#28636=CARTESIAN_POINT('Ctrl Pts',(167.536336704284,3.71764203452229,127.58437292106));
#28637=CARTESIAN_POINT('Ctrl Pts',(167.528590371019,3.62780678497748,127.480653487519));
#28638=CARTESIAN_POINT('Ctrl Pts',(167.520844037754,3.53362824347411,127.380697016434));
#28639=CARTESIAN_POINT('Ctrl Pts',(167.513097704488,3.43546369331372,127.284875957218));
#28640=CARTESIAN_POINT('Ctrl Pts',(167.505349636485,3.33727715988305,127.189033439541));
#28641=CARTESIAN_POINT('Ctrl Pts',(167.497601568482,3.23510312126705,127.097328449602));
#28642=CARTESIAN_POINT('Ctrl Pts',(167.489853500479,3.12933442017091,127.010095319879));
#28643=CARTESIAN_POINT('Ctrl Pts',(167.482097197737,3.02345330684048,126.922769477747));
#28644=CARTESIAN_POINT('Ctrl Pts',(167.474340894996,2.91397020136689,126.839925239111));
#28645=CARTESIAN_POINT('Ctrl Pts',(167.466584592254,2.80131005762509,126.76185582183));
#28646=CARTESIAN_POINT('Ctrl Pts',(167.45882414974,2.68858978377239,126.683744736551));
#28647=CARTESIAN_POINT('Ctrl Pts',(167.451063707225,2.57268942309025,126.610413759598));
#28648=CARTESIAN_POINT('Ctrl Pts',(167.443303264711,2.45406052798238,126.542111212909));
#28649=CARTESIAN_POINT('Ctrl Pts',(167.435530364446,2.3352411992407,126.473699020908));
#28650=CARTESIAN_POINT('Ctrl Pts',(167.42775746418,2.21368493015196,126.410331570596));
#28651=CARTESIAN_POINT('Ctrl Pts',(167.419984563915,2.08986615151655,126.352210290899));
#28652=CARTESIAN_POINT('Ctrl Pts',(167.412494228153,1.97054849736614,126.296201866117));
#28653=CARTESIAN_POINT('Ctrl Pts',(167.405003892391,1.84913025749133,126.245064930536));
#28654=CARTESIAN_POINT('Ctrl Pts',(167.397513556629,1.72604930567319,126.198935896991));
#28655=CARTESIAN_POINT('Ctrl Pts',(167.38973922251,1.59830170215628,126.151057867117));
#28656=CARTESIAN_POINT('Ctrl Pts',(167.381964888391,1.46835814831326,126.108423321652));
#28657=CARTESIAN_POINT('Ctrl Pts',(167.374190554272,1.33668831038928,126.071238241864));
#28658=CARTESIAN_POINT('Ctrl Pts',(167.366425801325,1.20518074377299,126.034098989364));
#28659=CARTESIAN_POINT('Ctrl Pts',(167.358661048377,1.07195149878536,126.002395944983));
#28660=CARTESIAN_POINT('Ctrl Pts',(167.35089629543,0.937489661342259,125.976286861152));
#28661=CARTESIAN_POINT('Ctrl Pts',(167.343139254545,0.80316137329168,125.950203709231));
#28662=CARTESIAN_POINT('Ctrl Pts',(167.33538221366,0.667603310368305,125.929703535211));
#28663=CARTESIAN_POINT('Ctrl Pts',(167.327625172775,0.531318802865246,125.914894042139));
#28664=CARTESIAN_POINT('Ctrl Pts',(167.319873981535,0.395137068569294,125.90009571702));
#28665=CARTESIAN_POINT('Ctrl Pts',(167.312122790295,0.258230367195635,125.89097957317));
#28666=CARTESIAN_POINT('Ctrl Pts',(167.304371599055,0.121110931884357,125.88760201004));
#28667=CARTESIAN_POINT('Ctrl Pts',(167.296623702278,-0.0159502240090409,
125.884225882465));
#28668=CARTESIAN_POINT('Ctrl Pts',(167.288875805501,-0.153223543977972,
125.886583494134));
#28669=CARTESIAN_POINT('Ctrl Pts',(167.281127908724,-0.290193198117832,
125.894679266372));
#28670=CARTESIAN_POINT('Ctrl Pts',(167.27338163264,-0.427134201158817,125.902773345148));
#28671=CARTESIAN_POINT('Ctrl Pts',(167.265635356555,-0.563771274679385,
125.91660317398));
#28672=CARTESIAN_POINT('Ctrl Pts',(167.257889080471,-0.699590515744292,
125.936121082294));
#28673=CARTESIAN_POINT('Ctrl Pts',(167.250142747206,-0.835410759395936,
125.955639134686));
#28674=CARTESIAN_POINT('Ctrl Pts',(167.242396413941,-0.970412771555679,
125.980845294734));
#28675=CARTESIAN_POINT('Ctrl Pts',(167.234650080675,-1.104090079631,126.011640287883));
#28676=CARTESIAN_POINT('Ctrl Pts',(167.226902012672,-1.23779732381261,126.042442177357));
#28677=CARTESIAN_POINT('Ctrl Pts',(167.219153944669,-1.37017889268054,126.078835302682));
#28678=CARTESIAN_POINT('Ctrl Pts',(167.211405876666,-1.50074116177388,126.120669869037));
#28679=CARTESIAN_POINT('Ctrl Pts',(167.203649573924,-1.63144219400052,126.162548897666));
#28680=CARTESIAN_POINT('Ctrl Pts',(167.195893271183,-1.76031969101819,126.209880800458));
#28681=CARTESIAN_POINT('Ctrl Pts',(167.188136968441,-1.88689726238662,126.262466543097));
#28682=CARTESIAN_POINT('Ctrl Pts',(167.180376525927,-2.01354239201624,126.31508035233));
#28683=CARTESIAN_POINT('Ctrl Pts',(167.172616083412,-2.13788479574006,126.372953423989));
#28684=CARTESIAN_POINT('Ctrl Pts',(167.164855640898,-2.25947147817604,126.435840078321));
#28685=CARTESIAN_POINT('Ctrl Pts',(167.157082740633,-2.38125334234854,126.498827683892));
#28686=CARTESIAN_POINT('Ctrl Pts',(167.149309840367,-2.50027030557501,126.566844760999));
#28687=CARTESIAN_POINT('Ctrl Pts',(167.141536940102,-2.61609645855909,126.639601034827));
#28688=CARTESIAN_POINT('Ctrl Pts',(167.13404660434,-2.72771203913334,126.709712434839));
#28689=CARTESIAN_POINT('Ctrl Pts',(167.126556268578,-2.8363645157687,126.784224276019));
#28690=CARTESIAN_POINT('Ctrl Pts',(167.119065932816,-2.94170243901029,126.862841897222));
#28691=CARTESIAN_POINT('Ctrl Pts',(167.111199886046,-3.05232405293764,126.945402933865));
#28692=CARTESIAN_POINT('Ctrl Pts',(167.103333839276,-3.15966371172855,127.032771436361));
#28693=CARTESIAN_POINT('Ctrl Pts',(167.095467792506,-3.26327073246246,127.124653130665));
#28694=CARTESIAN_POINT('Ctrl Pts',(167.087781493189,-3.36451022366116,127.214435231491));
#28695=CARTESIAN_POINT('Ctrl Pts',(167.080095193872,-3.46218547176523,127.30852623909));
#28696=CARTESIAN_POINT('Ctrl Pts',(167.072408894555,-3.55590447501027,127.406607473634));
#28697=CARTESIAN_POINT('Ctrl Pts',(167.064729576481,-3.64953835600144,127.504599623836));
#28698=CARTESIAN_POINT('Ctrl Pts',(167.057050258406,-3.73922286352088,127.60657450746));
#28699=CARTESIAN_POINT('Ctrl Pts',(167.049370940332,-3.82460012110788,127.712174178148));
#28700=CARTESIAN_POINT('Ctrl Pts',(167.041696852393,-3.90991923100195,127.81770192831));
#28701=CARTESIAN_POINT('Ctrl Pts',(167.034022764454,-3.99093667579042,127.926849245719));
#28702=CARTESIAN_POINT('Ctrl Pts',(167.026348676516,-4.06733278223542,128.039222808875));
#28703=CARTESIAN_POINT('Ctrl Pts',(167.018343021001,-4.14702966813711,128.156451597853));
#28704=CARTESIAN_POINT('Ctrl Pts',(167.010337365487,-4.22169662929612,128.277191330639));
#28705=CARTESIAN_POINT('Ctrl Pts',(167.002331709972,-4.29101887596182,128.400958847441));
#28706=CARTESIAN_POINT('Ctrl Pts',(166.994661686735,-4.35743482925626,128.519537485767));
#28707=CARTESIAN_POINT('Ctrl Pts',(166.986991663498,-4.41894493693751,128.640894790965));
#28708=CARTESIAN_POINT('Ctrl Pts',(166.979321640262,-4.47531821493297,128.764578781783));
#28709=CARTESIAN_POINT('Ctrl Pts',(166.971651727104,-4.53169068387077,128.888260997515));
#28710=CARTESIAN_POINT('Ctrl Pts',(166.963981813945,-4.58292631008536,129.014269466317));
#28711=CARTESIAN_POINT('Ctrl Pts',(166.956311900787,-4.62884177147018,129.142131115604));
#28712=CARTESIAN_POINT('Ctrl Pts',(166.948638803841,-4.67477629240354,129.270045840375));
#28713=CARTESIAN_POINT('Ctrl Pts',(166.940965706896,-4.71538611344544,129.399814902524));
#28714=CARTESIAN_POINT('Ctrl Pts',(166.93329260995,-4.75053746781127,129.530949124991));
#28715=CARTESIAN_POINT('Ctrl Pts',(166.932288676747,-4.75513660320975,129.548106473702));
#28716=CARTESIAN_POINT('Ctrl Pts',(166.931284743544,-4.75964236840377,129.565287175094));
#28717=CARTESIAN_POINT('Ctrl Pts',(166.930280810341,-4.76405452823404,129.582490119308));
#28718=CARTESIAN_POINT('Origin',(213.235140564004,0.,130.804360617566));
#28719=CARTESIAN_POINT('',(164.834593643846,-4.76405452823404,129.582490119308));
#28720=CARTESIAN_POINT('',(165.180124424339,-4.76405452823406,129.582490119308));
#28721=CARTESIAN_POINT('',(213.235140564004,-4.76405452823405,129.582490119308));
#28722=CARTESIAN_POINT('',(166.514859436034,-4.91824789572956,130.799811040474));
#28723=CARTESIAN_POINT('Ctrl Pts',(166.514859435991,-4.91824789573026,130.799811041232));
#28724=CARTESIAN_POINT('Ctrl Pts',(166.50719928455,-4.91837301695292,130.935071369845));
#28725=CARTESIAN_POINT('Ctrl Pts',(166.499539133109,-4.91291410273851,131.070483954823));
#28726=CARTESIAN_POINT('Ctrl Pts',(166.491878981668,-4.9018603121385,131.205544543941));
#28727=CARTESIAN_POINT('Ctrl Pts',(166.484022026496,-4.89052252881979,131.344075094204));
#28728=CARTESIAN_POINT('Ctrl Pts',(166.476165071324,-4.87329844142217,131.48223488994));
#28729=CARTESIAN_POINT('Ctrl Pts',(166.468308116152,-4.85023337199573,131.619479811107));
#28730=CARTESIAN_POINT('Ctrl Pts',(166.460655682011,-4.82776869950276,131.753152168573));
#28731=CARTESIAN_POINT('Ctrl Pts',(166.45300324787,-4.79976345135041,131.885956273128));
#28732=CARTESIAN_POINT('Ctrl Pts',(166.44535081373,-4.76631191956373,132.017395550255));
#28733=CARTESIAN_POINT('Ctrl Pts',(166.43769924852,-4.73286418618494,132.148819902506));
#28734=CARTESIAN_POINT('Ctrl Pts',(166.43004768331,-4.69397149780892,132.278879346447));
#28735=CARTESIAN_POINT('Ctrl Pts',(166.4223961181,-4.64977882485534,132.407089522411));
#28736=CARTESIAN_POINT('Ctrl Pts',(166.414743667661,-4.60558103913832,132.535314531339));
#28737=CARTESIAN_POINT('Ctrl Pts',(166.407091217222,-4.55608218060183,132.661689467338));
#28738=CARTESIAN_POINT('Ctrl Pts',(166.399438766784,-4.50147627089817,132.785747617887));
#28739=CARTESIAN_POINT('Ctrl Pts',(166.39142820768,-4.44431499026091,132.915611268128));
#28740=CARTESIAN_POINT('Ctrl Pts',(166.383417648576,-4.38155730016116,133.042935601766));
#28741=CARTESIAN_POINT('Ctrl Pts',(166.375407089472,-4.31348037665624,133.167212729464));
#28742=CARTESIAN_POINT('Ctrl Pts',(166.367743386369,-4.24835117367229,133.286108676275));
#28743=CARTESIAN_POINT('Ctrl Pts',(166.360079683266,-4.17835399115401,133.402215459577));
#28744=CARTESIAN_POINT('Ctrl Pts',(166.352415980163,-4.10377613867891,133.515117793358));
#28745=CARTESIAN_POINT('Ctrl Pts',(166.344747105723,-4.02914796232981,133.628096311726));
#28746=CARTESIAN_POINT('Ctrl Pts',(166.337078231283,-3.94993319759305,133.737865752398));
#28747=CARTESIAN_POINT('Ctrl Pts',(166.329409356843,-3.86645964211029,133.844043643546));
#28748=CARTESIAN_POINT('Ctrl Pts',(166.321729972862,-3.78287169321013,133.950367042475));
#28749=CARTESIAN_POINT('Ctrl Pts',(166.314050588881,-3.69501357024591,134.05308877026));
#28750=CARTESIAN_POINT('Ctrl Pts',(166.3063712049,-3.60325019743161,134.151862832234));
#28751=CARTESIAN_POINT('Ctrl Pts',(166.305351489112,-3.59106529298784,134.164978659059));
#28752=CARTESIAN_POINT('Ctrl Pts',(166.304331773324,-3.57881157822753,134.178024938227));
#28753=CARTESIAN_POINT('Ctrl Pts',(166.303312057536,-3.56648995038607,134.191000913832));
#28754=CARTESIAN_POINT('Ctrl Pts',(166.295537723417,-3.47254960653709,134.28993001848));
#28755=CARTESIAN_POINT('Ctrl Pts',(166.287763389298,-3.37434113002548,134.385104210327));
#28756=CARTESIAN_POINT('Ctrl Pts',(166.279989055179,-3.27219679180351,134.476132835203));
#28757=CARTESIAN_POINT('Ctrl Pts',(166.272224302232,-3.17017833734954,134.567049275435));
#28758=CARTESIAN_POINT('Ctrl Pts',(166.264459549285,-3.06423396150634,134.653830056546));
#28759=CARTESIAN_POINT('Ctrl Pts',(166.256694796338,-2.95473449293845,134.73611940197));
#28760=CARTESIAN_POINT('Ctrl Pts',(166.248937755453,-2.84534378078619,134.818327016457));
#28761=CARTESIAN_POINT('Ctrl Pts',(166.241180714568,-2.73240531321915,134.896051839404));
#28762=CARTESIAN_POINT('Ctrl Pts',(166.233423673683,-2.61632461883319,134.968976872563));
#28763=CARTESIAN_POINT('Ctrl Pts',(166.225672482442,-2.50033146180196,135.041846912388));
#28764=CARTESIAN_POINT('Ctrl Pts',(166.217921291202,-2.38120112416977,135.109924159801));
#28765=CARTESIAN_POINT('Ctrl Pts',(166.210170099962,-2.25936957948818,135.172933859001));
#28766=CARTESIAN_POINT('Ctrl Pts',(166.202422203185,-2.13758981646312,135.235916777398));
#28767=CARTESIAN_POINT('Ctrl Pts',(166.194674306408,-2.01311147638515,135.293836252184));
#28768=CARTESIAN_POINT('Ctrl Pts',(166.186926409631,-1.88639650112873,135.346462697334));
#28769=CARTESIAN_POINT('Ctrl Pts',(166.179180133547,-1.75970803191326,135.399078134165));
#28770=CARTESIAN_POINT('Ctrl Pts',(166.171433857463,-1.63078421894571,135.446402593758));
#28771=CARTESIAN_POINT('Ctrl Pts',(166.163687581379,-1.50010805479801,135.488254178102));
#28772=CARTESIAN_POINT('Ctrl Pts',(166.155941248113,-1.3694309260286,135.530106071385));
#28773=CARTESIAN_POINT('Ctrl Pts',(166.148194914848,-1.23700179260285,135.566484889558));
#28774=CARTESIAN_POINT('Ctrl Pts',(166.140448581583,-1.10331953531569,135.597258390885));
#28775=CARTESIAN_POINT('Ctrl Pts',(166.13270051358,-0.969607340813889,135.628038783725));
#28776=CARTESIAN_POINT('Ctrl Pts',(166.124952445577,-0.834641844960347,
135.653211274185));
#28777=CARTESIAN_POINT('Ctrl Pts',(166.117204377574,-0.698932470674764,
135.672694671833));
#28778=CARTESIAN_POINT('Ctrl Pts',(166.109448074832,-0.56307886285132,135.692198776668));
#28779=CARTESIAN_POINT('Ctrl Pts',(166.10169177209,-0.426480184895817,135.706001654637));
#28780=CARTESIAN_POINT('Ctrl Pts',(166.093935469348,-0.289651897532332,
135.714073933102));
#28781=CARTESIAN_POINT('Ctrl Pts',(166.086175026834,-0.152750580792108,
135.722150519986));
#28782=CARTESIAN_POINT('Ctrl Pts',(166.07841458432,-0.0156198011707654,
135.724490406195));
#28783=CARTESIAN_POINT('Ctrl Pts',(166.070654141806,0.121225617870744,135.721116398777));
#28784=CARTESIAN_POINT('Ctrl Pts',(166.06288124154,0.258290713327604,135.717736975103));
#28785=CARTESIAN_POINT('Ctrl Pts',(166.055108341275,0.395069142477458,135.708625354329));
#28786=CARTESIAN_POINT('Ctrl Pts',(166.047335441009,0.531050935170631,135.693856293682));
#28787=CARTESIAN_POINT('Ctrl Pts',(166.039845105247,0.66208944718171,135.67962412559));
#28788=CARTESIAN_POINT('Ctrl Pts',(166.032354769485,0.792387932021461,135.660138746365));
#28789=CARTESIAN_POINT('Ctrl Pts',(166.024864433723,0.921501461342684,135.63551142449));
#28790=CARTESIAN_POINT('Ctrl Pts',(166.017090099604,1.05551036937161,135.609950350221));
#28791=CARTESIAN_POINT('Ctrl Pts',(166.009315765485,1.18866719287546,135.578768752975));
#28792=CARTESIAN_POINT('Ctrl Pts',(166.001541431366,1.3204636628719,135.542035023594));
#28793=CARTESIAN_POINT('Ctrl Pts',(165.993776678419,1.45209770549798,135.505346565252));
#28794=CARTESIAN_POINT('Ctrl Pts',(165.986011925472,1.58237435738474,135.463119693283));
#28795=CARTESIAN_POINT('Ctrl Pts',(165.978247172525,1.71079385168009,135.415474090422));
#28796=CARTESIAN_POINT('Ctrl Pts',(165.97049013164,1.83908579792323,135.367875809845));
#28797=CARTESIAN_POINT('Ctrl Pts',(165.962733090755,1.96552389314472,135.314869643834));
#28798=CARTESIAN_POINT('Ctrl Pts',(165.95497604987,2.08962223963026,135.256625429787));
#28799=CARTESIAN_POINT('Ctrl Pts',(165.94722485863,2.21362700258758,135.198425138155));
#28800=CARTESIAN_POINT('Ctrl Pts',(165.93947366739,2.33529517629466,135.134994826264));
#28801=CARTESIAN_POINT('Ctrl Pts',(165.931722476149,2.4541599465604,135.06655277879));
#28802=CARTESIAN_POINT('Ctrl Pts',(165.923974579372,2.57297419612779,134.998139821012));
#28803=CARTESIAN_POINT('Ctrl Pts',(165.916226682595,2.68898707399475,134.924719558978));
#28804=CARTESIAN_POINT('Ctrl Pts',(165.908478785818,2.80175573206886,134.846556540616));
#28805=CARTESIAN_POINT('Ctrl Pts',(165.900732509734,2.91450080137084,134.768409872272));
#28806=CARTESIAN_POINT('Ctrl Pts',(165.89298623365,3.02400267957236,134.685522643484));
#28807=CARTESIAN_POINT('Ctrl Pts',(165.885239957566,3.12984726144414,134.598202889265));
#28808=CARTESIAN_POINT('Ctrl Pts',(165.877493624301,3.23569262463666,134.510882490471));
#28809=CARTESIAN_POINT('Ctrl Pts',(165.869747291035,3.33788033604528,134.419129749757));
#28810=CARTESIAN_POINT('Ctrl Pts',(165.86200095777,3.43602947969742,134.323292909775));
#28811=CARTESIAN_POINT('Ctrl Pts',(165.854252889767,3.53420060316946,134.227434607797));
#28812=CARTESIAN_POINT('Ctrl Pts',(165.846504821764,3.62833107953929,134.12749065968));
#28813=CARTESIAN_POINT('Ctrl Pts',(165.838756753761,3.71807724546604,134.023845771942));
#28814=CARTESIAN_POINT('Ctrl Pts',(165.831000451019,3.80791879468609,133.920090729184));
#28815=CARTESIAN_POINT('Ctrl Pts',(165.823244148277,3.89336646888192,133.81262718544));
#28816=CARTESIAN_POINT('Ctrl Pts',(165.815487845536,3.9741169369108,133.70187293579));
#28817=CARTESIAN_POINT('Ctrl Pts',(165.807727403021,4.05491050389588,133.591059573262));
#28818=CARTESIAN_POINT('Ctrl Pts',(165.799966960507,4.13100165242269,133.476952330271));
#28819=CARTESIAN_POINT('Ctrl Pts',(165.792206517993,4.20213129605263,133.359996670144));
#28820=CARTESIAN_POINT('Ctrl Pts',(165.784433617728,4.27337512330112,133.242853262408));
#28821=CARTESIAN_POINT('Ctrl Pts',(165.776660717462,4.33964134064374,133.122852642606));
#28822=CARTESIAN_POINT('Ctrl Pts',(165.768887817197,4.40071719213011,133.000464271174));
#28823=CARTESIAN_POINT('Ctrl Pts',(165.761397481435,4.45957278257376,132.882525025322));
#28824=CARTESIAN_POINT('Ctrl Pts',(165.753907145673,4.51360869495033,132.762368896355));
#28825=CARTESIAN_POINT('Ctrl Pts',(165.746416809911,4.5626780479461,132.640430358423));
#28826=CARTESIAN_POINT('Ctrl Pts',(165.738642475792,4.61360788037535,132.513868483762));
#28827=CARTESIAN_POINT('Ctrl Pts',(165.730868141673,4.65934843514372,132.384985461987));
#28828=CARTESIAN_POINT('Ctrl Pts',(165.723093807554,4.69968251960326,132.254245881108));
#28829=CARTESIAN_POINT('Ctrl Pts',(165.715329054606,4.73996689590845,132.123667425077));
#28830=CARTESIAN_POINT('Ctrl Pts',(165.707564301659,4.77485794512297,131.991237332471));
#28831=CARTESIAN_POINT('Ctrl Pts',(165.699799548712,4.80418622352931,131.857440762736));
#28832=CARTESIAN_POINT('Ctrl Pts',(165.692042507827,4.83348537267611,131.72377708164));
#28833=CARTESIAN_POINT('Ctrl Pts',(165.684285466942,4.85723266288805,131.588750003741));
#28834=CARTESIAN_POINT('Ctrl Pts',(165.676528426057,4.87530834359445,131.452860129808));
#28835=CARTESIAN_POINT('Ctrl Pts',(165.668777234817,4.89337039328945,131.317072731486));
#28836=CARTESIAN_POINT('Ctrl Pts',(165.661026043577,4.90576929525523,131.180424218176));
#28837=CARTESIAN_POINT('Ctrl Pts',(165.653274852337,4.91243637409762,131.043425322076));
#28838=CARTESIAN_POINT('Ctrl Pts',(165.64552695556,4.91910061925364,130.906484654162));
#28839=CARTESIAN_POINT('Ctrl Pts',(165.637779058782,4.92003786769394,130.769194289339));
#28840=CARTESIAN_POINT('Ctrl Pts',(165.630031162005,4.91523132087079,130.632069802864));
#28841=CARTESIAN_POINT('Ctrl Pts',(165.622284885921,4.91042577947363,130.494973999875));
#28842=CARTESIAN_POINT('Ctrl Pts',(165.614538609837,4.89987884630609,130.358044396697));
#28843=CARTESIAN_POINT('Ctrl Pts',(165.606792333753,4.88362584595713,130.221795892235));
#28844=CARTESIAN_POINT('Ctrl Pts',(165.599046000488,4.86737272563222,130.085546382018));
#28845=CARTESIAN_POINT('Ctrl Pts',(165.591299667222,4.84541350038635,129.949978368762));
#28846=CARTESIAN_POINT('Ctrl Pts',(165.583553333957,4.81783526223934,129.815600561524));
#28847=CARTESIAN_POINT('Ctrl Pts',(165.575805265954,4.79025084813711,129.681192661309));
#28848=CARTESIAN_POINT('Ctrl Pts',(165.568057197951,4.75704499576905,129.547975880401));
#28849=CARTESIAN_POINT('Ctrl Pts',(165.560309129948,4.7183556111945,129.416447295773));
#28850=CARTESIAN_POINT('Ctrl Pts',(165.552552827206,4.67962510708158,129.284778921001));
#28851=CARTESIAN_POINT('Ctrl Pts',(165.544796524464,4.63539953928269,129.15480270236));
#28852=CARTESIAN_POINT('Ctrl Pts',(165.537040221722,4.58586645273807,129.026999669376));
#28853=CARTESIAN_POINT('Ctrl Pts',(165.529279779208,4.53630692889376,128.899128424065));
#28854=CARTESIAN_POINT('Ctrl Pts',(165.521519336694,4.48143439808903,128.773433033736));
#28855=CARTESIAN_POINT('Ctrl Pts',(165.51375889418,4.42148359868764,128.650372258954));
#28856=CARTESIAN_POINT('Ctrl Pts',(165.505985993914,4.36143656094079,128.527113936092));
#28857=CARTESIAN_POINT('Ctrl Pts',(165.498213093649,4.29629515002293,128.406499024503));
#28858=CARTESIAN_POINT('Ctrl Pts',(165.490440193383,4.22633933650766,128.288960276629));
#28859=CARTESIAN_POINT('Ctrl Pts',(165.482949857621,4.15892659302169,128.175694358301));
#28860=CARTESIAN_POINT('Ctrl Pts',(165.475459521859,4.0870435692621,128.065285092158));
#28861=CARTESIAN_POINT('Ctrl Pts',(165.467969186097,4.01097640770038,127.958090897499));
#28862=CARTESIAN_POINT('Ctrl Pts',(165.460194851978,3.9320251365881,127.846832402369));
#28863=CARTESIAN_POINT('Ctrl Pts',(165.452420517859,3.84831608733918,127.73868515679));
#28864=CARTESIAN_POINT('Ctrl Pts',(165.44464618374,3.76012273307307,127.634083012256));
#28865=CARTESIAN_POINT('Ctrl Pts',(165.436881430793,3.6720380692342,127.529609780518));
#28866=CARTESIAN_POINT('Ctrl Pts',(165.429116677846,3.57948034607099,127.428673252809));
#28867=CARTESIAN_POINT('Ctrl Pts',(165.421351924899,3.48276615349908,127.331678227462));
#28868=CARTESIAN_POINT('Ctrl Pts',(165.413594884014,3.3861480188262,127.23477953894));
#28869=CARTESIAN_POINT('Ctrl Pts',(165.405837843129,3.285381904443,127.141814837302));
#28870=CARTESIAN_POINT('Ctrl Pts',(165.398080802244,3.1808242518467,127.053155459038));
#28871=CARTESIAN_POINT('Ctrl Pts',(165.390329611004,3.07634544698982,126.964562939502));
#28872=CARTESIAN_POINT('Ctrl Pts',(165.382578419763,2.96808109202777,126.880269532854));
#28873=CARTESIAN_POINT('Ctrl Pts',(165.374827228523,2.85642375969557,126.800609080876));
#28874=CARTESIAN_POINT('Ctrl Pts',(165.367079331746,2.74481388470817,126.720982486716));
#28875=CARTESIAN_POINT('Ctrl Pts',(165.359331434969,2.62981421819218,126.645985157368));
#28876=CARTESIAN_POINT('Ctrl Pts',(165.351583538192,2.51184944818924,126.575909906947));
#28877=CARTESIAN_POINT('Ctrl Pts',(165.343837262108,2.39390935387319,126.505849314759));
#28878=CARTESIAN_POINT('Ctrl Pts',(165.336090986024,2.27300572567125,126.440708953128));
#28879=CARTESIAN_POINT('Ctrl Pts',(165.32834470994,2.14959085641904,126.380737417914));
#28880=CARTESIAN_POINT('Ctrl Pts',(165.320598376674,2.02617507614617,126.320765440004));
#28881=CARTESIAN_POINT('Ctrl Pts',(165.312852043409,1.90024836947892,126.265962535523));
#28882=CARTESIAN_POINT('Ctrl Pts',(165.305105710144,1.77228580311794,126.21653040116));
#28883=CARTESIAN_POINT('Ctrl Pts',(165.297357642141,1.6442945804275,126.167087196813));
#28884=CARTESIAN_POINT('Ctrl Pts',(165.289609574138,1.5142669554514,126.123017296768));
#28885=CARTESIAN_POINT('Ctrl Pts',(165.281861506135,1.38269567471772,126.084473358995));
#28886=CARTESIAN_POINT('Ctrl Pts',(165.274105203393,1.25098455846129,126.045888456267));
#28887=CARTESIAN_POINT('Ctrl Pts',(165.266348900651,1.11772688493576,126.012841357968));
#28888=CARTESIAN_POINT('Ctrl Pts',(165.258592597909,0.983428730526352,125.985434285438));
#28889=CARTESIAN_POINT('Ctrl Pts',(165.250832155395,0.849058897148156,125.958012584928));
#28890=CARTESIAN_POINT('Ctrl Pts',(165.243071712881,0.713647862149207,125.936236970411));
#28891=CARTESIAN_POINT('Ctrl Pts',(165.235311270367,0.577708475606904,125.920157921146));
#28892=CARTESIAN_POINT('Ctrl Pts',(165.227538370101,0.441550867093239,125.904053060364));
#28893=CARTESIAN_POINT('Ctrl Pts',(165.219765469836,0.304863602213619,125.893663068374));
#28894=CARTESIAN_POINT('Ctrl Pts',(165.21199256957,0.168162098785835,125.888986311266));
#28895=CARTESIAN_POINT('Ctrl Pts',(165.204502233809,0.0364300393395799,
125.88447956606));
#28896=CARTESIAN_POINT('Ctrl Pts',(165.197011898047,-0.0953149334006313,
125.885277884535));
#28897=CARTESIAN_POINT('Ctrl Pts',(165.189521562285,-0.226616604130561,
125.891334261313));
#28898=CARTESIAN_POINT('Ctrl Pts',(165.181747228166,-0.362896617615897,
125.897620267459));
#28899=CARTESIAN_POINT('Ctrl Pts',(165.173972894047,-0.499130744036451,
125.909590833477));
#28900=CARTESIAN_POINT('Ctrl Pts',(165.166198559927,-0.634806152942256,
125.927250386016));
#28901=CARTESIAN_POINT('Ctrl Pts',(165.15843380698,-0.770314354031923,125.944888174736));
#28902=CARTESIAN_POINT('Ctrl Pts',(165.150669054033,-0.905264823681669,
125.968200949866));
#28903=CARTESIAN_POINT('Ctrl Pts',(165.142904301086,-1.03914586900888,125.997141158729));
#28904=CARTESIAN_POINT('Ctrl Pts',(165.135147260201,-1.17289394179475,126.026052623769));
#28905=CARTESIAN_POINT('Ctrl Pts',(165.127390219316,-1.3055743243527,126.060580317619));
#28906=CARTESIAN_POINT('Ctrl Pts',(165.119633178431,-1.43668193544038,126.100625072398));
#28907=CARTESIAN_POINT('Ctrl Pts',(165.111881987191,-1.5676906772581,126.140639629115));
#28908=CARTESIAN_POINT('Ctrl Pts',(165.104130795951,-1.69712863594474,126.186162851875));
#28909=CARTESIAN_POINT('Ctrl Pts',(165.096379604711,-1.82450274580134,126.237044907758));
#28910=CARTESIAN_POINT('Ctrl Pts',(165.088631707934,-1.95182271826396,126.287905337409));
#28911=CARTESIAN_POINT('Ctrl Pts',(165.080883811157,-2.0770802242538,126.344119925384));
#28912=CARTESIAN_POINT('Ctrl Pts',(165.07313591438,-2.19979935670297,126.405489642787));
#28913=CARTESIAN_POINT('Ctrl Pts',(165.065389638296,-2.32249281895531,126.466846522969));
#28914=CARTESIAN_POINT('Ctrl Pts',(165.057643362211,-2.44264861434462,126.533356212941));
#28915=CARTESIAN_POINT('Ctrl Pts',(165.049897086127,-2.55981311680882,126.604772558064));
#28916=CARTESIAN_POINT('Ctrl Pts',(165.042150752862,-2.67697848415435,126.676189430366));
#28917=CARTESIAN_POINT('Ctrl Pts',(165.034404419597,-2.79115218067688,126.752512826607));
#28918=CARTESIAN_POINT('Ctrl Pts',(165.026658086331,-2.90190772808446,126.833452081704));
#28919=CARTESIAN_POINT('Ctrl Pts',(165.018910018328,-3.01268807842886,126.914409462585));
#28920=CARTESIAN_POINT('Ctrl Pts',(165.011161950325,-3.12004844086206,126.999984528609));
#28921=CARTESIAN_POINT('Ctrl Pts',(165.003413882322,-3.22359403837451,127.089845233528));
#28922=CARTESIAN_POINT('Ctrl Pts',(164.995657579581,-3.32724968538063,127.179801443473));
#28923=CARTESIAN_POINT('Ctrl Pts',(164.987901276839,-3.42708217266223,127.274052134413));
#28924=CARTESIAN_POINT('Ctrl Pts',(164.980144974097,-3.52273195186391,127.372226783081));
#28925=CARTESIAN_POINT('Ctrl Pts',(164.972384531583,-3.61843278223297,127.470453830515));
#28926=CARTESIAN_POINT('Ctrl Pts',(164.964624089068,-3.70994619545918,127.572608717754));
#28927=CARTESIAN_POINT('Ctrl Pts',(164.956863646554,-3.79695251391848,127.678287254776));
#28928=CARTESIAN_POINT('Ctrl Pts',(164.949090746289,-3.884098502644,127.784135436366));
#28929=CARTESIAN_POINT('Ctrl Pts',(164.941317846023,-3.96672270260528,127.893518259033));
#28930=CARTESIAN_POINT('Ctrl Pts',(164.933544945758,-4.04454789253535,128.006001204001));
#28931=CARTESIAN_POINT('Ctrl Pts',(164.926054609996,-4.11954394078338,128.114395110595));
#28932=CARTESIAN_POINT('Ctrl Pts',(164.918564274234,-4.19008366865925,128.225667398012));
#28933=CARTESIAN_POINT('Ctrl Pts',(164.911073938471,-4.25596002760316,128.339408831842));
#28934=CARTESIAN_POINT('Ctrl Pts',(164.902985512137,-4.32709650177464,128.462232325726));
#28935=CARTESIAN_POINT('Ctrl Pts',(164.894897085803,-4.39300527178131,128.588297777807));
#28936=CARTESIAN_POINT('Ctrl Pts',(164.886808659469,-4.45339117781636,128.717139958448));
#28937=CARTESIAN_POINT('Ctrl Pts',(164.878731658804,-4.51369178302798,128.845800137282));
#28938=CARTESIAN_POINT('Ctrl Pts',(164.87065465814,-4.56848491366523,128.97722892253));
#28939=CARTESIAN_POINT('Ctrl Pts',(164.862577657476,-4.61751995329873,129.110934344182));
#28940=CARTESIAN_POINT('Ctrl Pts',(164.854514161893,-4.66647300430411,129.244416204801));
#28941=CARTESIAN_POINT('Ctrl Pts',(164.84645066631,-4.70968703439096,129.380166791153));
#28942=CARTESIAN_POINT('Ctrl Pts',(164.838387170727,-4.74695864644254,129.51767236027));
#28943=CARTESIAN_POINT('Ctrl Pts',(164.837122661767,-4.75280354173969,129.539235840088));
#28944=CARTESIAN_POINT('Ctrl Pts',(164.835858152806,-4.75850239489081,129.560842435668));
#28945=CARTESIAN_POINT('Ctrl Pts',(164.834593643846,-4.76405452823405,129.582490119308));
#28946=CARTESIAN_POINT('Ctrl Pts',(166.584804846393,-4.76405452823406,129.582490119308));
#28947=CARTESIAN_POINT('Ctrl Pts',(166.583789791378,-4.76848155150402,129.599751015848));
#28948=CARTESIAN_POINT('Ctrl Pts',(166.582774736364,-4.77281387238167,129.617032490968));
#28949=CARTESIAN_POINT('Ctrl Pts',(166.581759681349,-4.77705133042995,129.634333417482));
#28950=CARTESIAN_POINT('Ctrl Pts',(166.571381405794,-4.82037657551116,129.811224108263));
#28951=CARTESIAN_POINT('Ctrl Pts',(166.561003130238,-4.85389270006441,129.99060470522));
#28952=CARTESIAN_POINT('Ctrl Pts',(166.550624854682,-4.87736871096789,130.171543487764));
#28953=CARTESIAN_POINT('Ctrl Pts',(166.540504395719,-4.9002615320052,130.347987398294));
#28954=CARTESIAN_POINT('Ctrl Pts',(166.530383936756,-4.91360693885465,130.525913383609));
#28955=CARTESIAN_POINT('Ctrl Pts',(166.520263477793,-4.91723477504882,130.704434497104));
#28956=CARTESIAN_POINT('Ctrl Pts',(166.51846213054,-4.91788049603701,130.736209589376));
#28957=CARTESIAN_POINT('Ctrl Pts',(166.516660783287,-4.91821847244596,130.768003468096));
#28958=CARTESIAN_POINT('Ctrl Pts',(166.514859436034,-4.91824789572956,130.799811040473));
#28959=CARTESIAN_POINT('',(166.860140564042,-4.91824956784904,130.806422377193));
#28960=CARTESIAN_POINT('Ctrl Pts',(166.930280810341,-4.76405452823404,129.582490119308));
#28961=CARTESIAN_POINT('Ctrl Pts',(166.922599644049,-4.79781228548173,129.714111102471));
#28962=CARTESIAN_POINT('Ctrl Pts',(166.914918477758,-4.82608624198017,129.847034690638));
#28963=CARTESIAN_POINT('Ctrl Pts',(166.907237311466,-4.84880030962948,129.980759609895));
#28964=CARTESIAN_POINT('Ctrl Pts',(166.899387853562,-4.87201203439566,130.117414394414));
#28965=CARTESIAN_POINT('Ctrl Pts',(166.891538395658,-4.88941736099183,130.254905588925));
#28966=CARTESIAN_POINT('Ctrl Pts',(166.883688937754,-4.9009911797719,130.392695075775));
#28967=CARTESIAN_POINT('Ctrl Pts',(166.87583947985,-4.91256499855197,130.530484562626));
#28968=CARTESIAN_POINT('Ctrl Pts',(166.867990021946,-4.91830735559279,130.66857190133));
#28969=CARTESIAN_POINT('Ctrl Pts',(166.860140564042,-4.91824956784904,130.806422377193));
#28970=CARTESIAN_POINT('Ctrl Pts',(166.860140564008,-4.91824956784879,130.806422377793));
#28971=CARTESIAN_POINT('Ctrl Pts',(166.853633145673,-4.91820166019232,130.920704246058));
#28972=CARTESIAN_POINT('Ctrl Pts',(166.847125727338,-4.91417087231532,131.034898519982));
#28973=CARTESIAN_POINT('Ctrl Pts',(166.840618309003,-4.90617335239805,131.148811047555));
#28974=CARTESIAN_POINT('Ctrl Pts',(166.832843974884,-4.89661881190913,131.284900968948));
#28975=CARTESIAN_POINT('Ctrl Pts',(166.825069640765,-4.88138244972333,131.420808602728));
#28976=CARTESIAN_POINT('Ctrl Pts',(166.817295306646,-4.86047214698298,131.556021159901));
#28977=CARTESIAN_POINT('Ctrl Pts',(166.809530553699,-4.83958761432197,131.69106707968));
#28978=CARTESIAN_POINT('Ctrl Pts',(166.801765800752,-4.81304311352321,131.825419244607));
#28979=CARTESIAN_POINT('Ctrl Pts',(166.794001047804,-4.78089846278784,131.958567250285));
#28980=CARTESIAN_POINT('Ctrl Pts',(166.78624400692,-4.7487857385728,132.091583011487));
#28981=CARTESIAN_POINT('Ctrl Pts',(166.778486966035,-4.71108402450377,132.223396615924));
#28982=CARTESIAN_POINT('Ctrl Pts',(166.77072992515,-4.66790458046289,132.35350550756));
#28983=CARTESIAN_POINT('Ctrl Pts',(166.762978733909,-4.62475769837655,132.483516283068));
#28984=CARTESIAN_POINT('Ctrl Pts',(166.755227542669,-4.57614143107031,132.611824534997));
#28985=CARTESIAN_POINT('Ctrl Pts',(166.747476351429,-4.52221740053542,132.737940935214));
#28986=CARTESIAN_POINT('Ctrl Pts',(166.739728454652,-4.46831628915203,132.864003732596));
#28987=CARTESIAN_POINT('Ctrl Pts',(166.731980557875,-4.4091120548184,132.987876172408));
#28988=CARTESIAN_POINT('Ctrl Pts',(166.724232661098,-4.34481508957225,133.109087260777));
#28989=CARTESIAN_POINT('Ctrl Pts',(166.716486385014,-4.28053157386513,133.230272994398));
#28990=CARTESIAN_POINT('Ctrl Pts',(166.70874010893,-4.2111576292577,133.348798138715));
#28991=CARTESIAN_POINT('Ctrl Pts',(166.700993832846,-4.13695022527647,133.464215105331));
#28992=CARTESIAN_POINT('Ctrl Pts',(166.69324749958,-4.06274227351302,133.579632923929));
#28993=CARTESIAN_POINT('Ctrl Pts',(166.685501166315,-3.98370100261904,133.691942190185));
#28994=CARTESIAN_POINT('Ctrl Pts',(166.67775483305,-3.90012722827645,133.800723523784));
#28995=CARTESIAN_POINT('Ctrl Pts',(166.670006765047,-3.81653473816656,133.909529218207));
#28996=CARTESIAN_POINT('Ctrl Pts',(166.662258697044,-3.72840796297389,134.014805097881));
#28997=CARTESIAN_POINT('Ctrl Pts',(166.654510629041,-3.63608832688384,134.116164467675));
#28998=CARTESIAN_POINT('Ctrl Pts',(166.646754326299,-3.54367057238597,134.217631563414));
#28999=CARTESIAN_POINT('Ctrl Pts',(166.638998023557,-3.44705131889053,134.315173544701));
#29000=CARTESIAN_POINT('Ctrl Pts',(166.631241720815,-3.34660961113019,134.408439858259));
#29001=CARTESIAN_POINT('Ctrl Pts',(166.623481278301,-3.24611429460613,134.501755950856));
#29002=CARTESIAN_POINT('Ctrl Pts',(166.615720835787,-3.14179275586374,134.590791574858));
#29003=CARTESIAN_POINT('Ctrl Pts',(166.607960393273,-3.03405673991014,134.675236844146));
#29004=CARTESIAN_POINT('Ctrl Pts',(166.600187493007,-2.92614777653937,134.759817672478));
#29005=CARTESIAN_POINT('Ctrl Pts',(166.592414592742,-2.81481370044383,134.839793192568));
#29006=CARTESIAN_POINT('Ctrl Pts',(166.584641692476,-2.70049555781372,134.914896690237));
#29007=CARTESIAN_POINT('Ctrl Pts',(166.577151356714,-2.59033316761781,134.987269986591));
#29008=CARTESIAN_POINT('Ctrl Pts',(166.569661020952,-2.47740016490256,135.05511917268));
#29009=CARTESIAN_POINT('Ctrl Pts',(166.56217068519,-2.36211063482431,135.118247080067));
#29010=CARTESIAN_POINT('Ctrl Pts',(166.554396351071,-2.2424498671721,135.183768501249));
#29011=CARTESIAN_POINT('Ctrl Pts',(166.546622016952,-2.11987129983826,135.244411114013));
#29012=CARTESIAN_POINT('Ctrl Pts',(166.538847682833,-1.99481061667704,135.299904374009));
#29013=CARTESIAN_POINT('Ctrl Pts',(166.531082929886,-1.86990405963087,135.355329243521));
#29014=CARTESIAN_POINT('Ctrl Pts',(166.523318176939,-1.74252182716003,135.405617230097));
#29015=CARTESIAN_POINT('Ctrl Pts',(166.515553423992,-1.61312567013595,135.450542774439));
#29016=CARTESIAN_POINT('Ctrl Pts',(166.507796383107,-1.48385803119936,135.495423698098));
#29017=CARTESIAN_POINT('Ctrl Pts',(166.500039342222,-1.35258081526154,135.534952651208));
#29018=CARTESIAN_POINT('Ctrl Pts',(166.492282301337,-1.21977697563239,135.568951596046));
#29019=CARTESIAN_POINT('Ctrl Pts',(166.484531110096,-1.08707328441164,135.602924902016));
#29020=CARTESIAN_POINT('Ctrl Pts',(166.476779918856,-0.952845638188494,
135.631376403718));
#29021=CARTESIAN_POINT('Ctrl Pts',(166.469028727616,-0.817593083212366,
135.654177584502));
#29022=CARTESIAN_POINT('Ctrl Pts',(166.461280830839,-0.682398014180036,
135.676969074177));
#29023=CARTESIAN_POINT('Ctrl Pts',(166.453532934062,-0.54617928751503,135.694114954552));
#29024=CARTESIAN_POINT('Ctrl Pts',(166.445785037285,-0.409446885738032,
135.705537650714));
#29025=CARTESIAN_POINT('Ctrl Pts',(166.438038761201,-0.27274308543183,135.716957957495));
#29026=CARTESIAN_POINT('Ctrl Pts',(166.430292485117,-0.135526213098289,
135.722657428765));
#29027=CARTESIAN_POINT('Ctrl Pts',(166.422546209033,0.00168826416244504,
135.722610327805));
#29028=CARTESIAN_POINT('Ctrl Pts',(166.414799875767,0.138903754309233,135.722563226497));
#29029=CARTESIAN_POINT('Ctrl Pts',(166.407053542502,0.276116458382751,135.716769468446));
#29030=CARTESIAN_POINT('Ctrl Pts',(166.399307209237,0.412810941621637,135.705255453101));
#29031=CARTESIAN_POINT('Ctrl Pts',(166.391559141234,0.549536036642225,135.693738859273));
#29032=CARTESIAN_POINT('Ctrl Pts',(166.383811073231,0.685742290387179,135.676499491893));
#29033=CARTESIAN_POINT('Ctrl Pts',(166.376063005228,0.82091981718061,135.653615582636));
#29034=CARTESIAN_POINT('Ctrl Pts',(166.368306702486,0.956241012258197,135.630707352089));
#29035=CARTESIAN_POINT('Ctrl Pts',(166.360550399744,1.09053091021809,135.602142661205));
#29036=CARTESIAN_POINT('Ctrl Pts',(166.352794097002,1.22328969772295,135.568050928443));
#29037=CARTESIAN_POINT('Ctrl Pts',(166.345033654488,1.35611934259005,135.533940999897));
#29038=CARTESIAN_POINT('Ctrl Pts',(166.337273211974,1.48741587456849,135.494298264403));
#29039=CARTESIAN_POINT('Ctrl Pts',(166.32951276946,1.61669601945638,135.44930163368));
#29040=CARTESIAN_POINT('Ctrl Pts',(166.321739869194,1.7461836963098,135.40423277037));
#29041=CARTESIAN_POINT('Ctrl Pts',(166.313966968929,1.8736481540021,135.353792981125));
#29042=CARTESIAN_POINT('Ctrl Pts',(166.306194068663,1.99862660209961,135.298209165067));
#29043=CARTESIAN_POINT('Ctrl Pts',(166.298703732901,2.11906176880764,135.24464596073));
#29044=CARTESIAN_POINT('Ctrl Pts',(166.291213397139,2.23718825716293,135.186306369506));
#29045=CARTESIAN_POINT('Ctrl Pts',(166.283723061377,2.35261636063335,135.12343219861));
#29046=CARTESIAN_POINT('Ctrl Pts',(166.275948727258,2.47242095572996,135.058174134414));
#29047=CARTESIAN_POINT('Ctrl Pts',(166.268174393139,2.58969801312797,134.987824127587));
#29048=CARTESIAN_POINT('Ctrl Pts',(166.26040005902,2.70398441843893,134.912602495467));
#29049=CARTESIAN_POINT('Ctrl Pts',(166.252635306073,2.81812997596933,134.837473567286));
#29050=CARTESIAN_POINT('Ctrl Pts',(166.244870553126,2.92929189143952,134.757485172552));
#29051=CARTESIAN_POINT('Ctrl Pts',(166.237105800178,3.03703080780086,134.672903875043));
#29052=CARTESIAN_POINT('Ctrl Pts',(166.229348759293,3.14466271635165,134.58840658487));
#29053=CARTESIAN_POINT('Ctrl Pts',(166.221591718408,3.24887808596006,134.499325709842));
#29054=CARTESIAN_POINT('Ctrl Pts',(166.213834677523,3.34926608038664,134.405971338517));
#29055=CARTESIAN_POINT('Ctrl Pts',(166.206083486283,3.44957837144565,134.31268736645));
#29056=CARTESIAN_POINT('Ctrl Pts',(166.198332295043,3.5460687470917,134.215136577794));
#29057=CARTESIAN_POINT('Ctrl Pts',(166.190581103803,3.63835933594067,134.113669367905));
#29058=CARTESIAN_POINT('Ctrl Pts',(166.182833207026,3.73061069882754,134.012245284287));
#29059=CARTESIAN_POINT('Ctrl Pts',(166.175085310249,3.81866556267354,133.906908378783));
#29060=CARTESIAN_POINT('Ctrl Pts',(166.167337413472,3.9021830034975,133.798045782996));
#29061=CARTESIAN_POINT('Ctrl Pts',(166.159591137388,3.98568297427323,133.689205958917));
#29062=CARTESIAN_POINT('Ctrl Pts',(166.151844861304,4.06464717207518,133.576842221478));
#29063=CARTESIAN_POINT('Ctrl Pts',(166.144098585219,4.13877532131262,133.461374336423));
#29064=CARTESIAN_POINT('Ctrl Pts',(166.136352251954,4.21290401774719,133.34590559901));
#29065=CARTESIAN_POINT('Ctrl Pts',(166.128605918689,4.28219638316992,133.227332997261));
#29066=CARTESIAN_POINT('Ctrl Pts',(166.120859585423,4.34639602310532,133.106104450584));
#29067=CARTESIAN_POINT('Ctrl Pts',(166.11311151742,4.41061004010498,132.984848755614));
#29068=CARTESIAN_POINT('Ctrl Pts',(166.105363449417,4.46972887925609,132.860936277613));
#29069=CARTESIAN_POINT('Ctrl Pts',(166.097615381414,4.52354275341914,132.734838283971));
#29070=CARTESIAN_POINT('Ctrl Pts',(166.089859078673,4.57741382160803,132.608606271881));
#29071=CARTESIAN_POINT('Ctrl Pts',(166.082102775931,4.62596850823346,132.480184464286));
#29072=CARTESIAN_POINT('Ctrl Pts',(166.074346473189,4.6690455353932,132.350063322139));
#29073=CARTESIAN_POINT('Ctrl Pts',(166.066586030675,4.71214555405938,132.219872730421));
#29074=CARTESIAN_POINT('Ctrl Pts',(166.058825588161,4.74976198057786,132.087981372694));
#29075=CARTESIAN_POINT('Ctrl Pts',(166.051065145646,4.78178411693426,131.954892547386));
#29076=CARTESIAN_POINT('Ctrl Pts',(166.043292245381,4.81385765806671,131.82159007608));
#29077=CARTESIAN_POINT('Ctrl Pts',(166.035519345116,4.84031888772147,131.687086679696));
#29078=CARTESIAN_POINT('Ctrl Pts',(166.02774644485,4.86110855302137,131.551894361448));
#29079=CARTESIAN_POINT('Ctrl Pts',(166.020256109088,4.88114246162151,131.421616624498));
#29080=CARTESIAN_POINT('Ctrl Pts',(166.012765773326,4.89590996361786,131.29069949025));
#29081=CARTESIAN_POINT('Ctrl Pts',(166.005275437564,4.90540385236735,131.159601532551));
#29082=CARTESIAN_POINT('Ctrl Pts',(165.997501103445,4.91525770479442,131.023532955939));
#29083=CARTESIAN_POINT('Ctrl Pts',(165.989726769326,4.91946136581058,130.886838549007));
#29084=CARTESIAN_POINT('Ctrl Pts',(165.981952435207,4.91794986999179,130.750027029909));
#29085=CARTESIAN_POINT('Ctrl Pts',(165.97418768226,4.91644023695651,130.61338411878));
#29086=CARTESIAN_POINT('Ctrl Pts',(165.966422929313,4.90922946567046,130.476624769847));
#29087=CARTESIAN_POINT('Ctrl Pts',(165.958658176366,4.89630434057168,130.340262710871));
#29088=CARTESIAN_POINT('Ctrl Pts',(165.950901135481,4.88339205288936,130.204036088614));
#29089=CARTESIAN_POINT('Ctrl Pts',(165.943144094596,4.86477674270188,130.068206357755));
#29090=CARTESIAN_POINT('Ctrl Pts',(165.935387053711,4.84049722927385,129.9332867769));
#29091=CARTESIAN_POINT('Ctrl Pts',(165.92763586247,4.81623602521575,129.79846893995));
#29092=CARTESIAN_POINT('Ctrl Pts',(165.91988467123,4.78631918888288,129.664560270091));
#29093=CARTESIAN_POINT('Ctrl Pts',(165.91213347999,4.75083726909839,129.532068078468));
#29094=CARTESIAN_POINT('Ctrl Pts',(165.904385583213,4.71537043007632,129.39963219956));
#29095=CARTESIAN_POINT('Ctrl Pts',(165.896637686436,4.67434331294802,129.268611978341));
#29096=CARTESIAN_POINT('Ctrl Pts',(165.888889789659,4.62789734475546,129.139503497899));
#29097=CARTESIAN_POINT('Ctrl Pts',(165.881143513575,4.58146109205817,129.010422024168));
#29098=CARTESIAN_POINT('Ctrl Pts',(165.873397237491,4.52960837516405,128.883251863452));
#29099=CARTESIAN_POINT('Ctrl Pts',(165.865650961407,4.47253004859038,128.758472539748));
#29100=CARTESIAN_POINT('Ctrl Pts',(165.857904628141,4.4154513006775,128.633692294952));
#29101=CARTESIAN_POINT('Ctrl Pts',(165.850158294876,4.3531470287462,128.511303277918));
#29102=CARTESIAN_POINT('Ctrl Pts',(165.84241196161,4.28585549260425,128.391763311961));
#29103=CARTESIAN_POINT('Ctrl Pts',(165.834663893607,4.21854888698936,128.272196575857));
#29104=CARTESIAN_POINT('Ctrl Pts',(165.826915825604,4.14625298648257,128.155480501057));
#29105=CARTESIAN_POINT('Ctrl Pts',(165.819167757602,4.06925088661325,128.042046318957));
#29106=CARTESIAN_POINT('Ctrl Pts',(165.81141145486,3.99216694799579,127.928491577659));
#29107=CARTESIAN_POINT('Ctrl Pts',(165.803655152118,3.91036703830625,127.818226020779));
#29108=CARTESIAN_POINT('Ctrl Pts',(165.795898849376,3.82417662159077,127.711650442108));
#29109=CARTESIAN_POINT('Ctrl Pts',(165.788138406862,3.73794020245469,127.605017980843));
#29110=CARTESIAN_POINT('Ctrl Pts',(165.780377964348,3.64730886520722,127.502079715383));
#29111=CARTESIAN_POINT('Ctrl Pts',(165.772617521833,3.55264621408882,127.403200824198));
#29112=CARTESIAN_POINT('Ctrl Pts',(165.764844621568,3.45783160207912,127.304163203839));
#29113=CARTESIAN_POINT('Ctrl Pts',(165.757071721303,3.35897302634649,127.209198250736));
#29114=CARTESIAN_POINT('Ctrl Pts',(165.749298821037,3.25646922206972,127.118632566256));
#29115=CARTESIAN_POINT('Ctrl Pts',(165.741808485275,3.1576916892695,127.031359172528));
#29116=CARTESIAN_POINT('Ctrl Pts',(165.734318149513,3.05552959200497,126.948170945971));
#29117=CARTESIAN_POINT('Ctrl Pts',(165.726827813751,2.95036484607499,126.869321820102));
#29118=CARTESIAN_POINT('Ctrl Pts',(165.719053479632,2.84121274683937,126.787483105661));
#29119=CARTESIAN_POINT('Ctrl Pts',(165.711279145513,2.72848005235996,126.710059780701));
#29120=CARTESIAN_POINT('Ctrl Pts',(165.703504811394,2.61255964622808,126.637381477061));
#29121=CARTESIAN_POINT('Ctrl Pts',(165.695740058446,2.49678210163666,126.564792742935));
#29122=CARTESIAN_POINT('Ctrl Pts',(165.687975305499,2.37782499014026,126.496937600407));
#29123=CARTESIAN_POINT('Ctrl Pts',(165.680210552552,2.25611338211947,126.434104850506));
#29124=CARTESIAN_POINT('Ctrl Pts',(165.672453511667,2.13452265978367,126.371334506978));
#29125=CARTESIAN_POINT('Ctrl Pts',(165.664696470782,2.01018323045405,126.313576807297));
#29126=CARTESIAN_POINT('Ctrl Pts',(165.656939429897,1.88354789589149,126.26107652053));
#29127=CARTESIAN_POINT('Ctrl Pts',(165.649188238657,1.75700805801999,126.208615824637));
#29128=CARTESIAN_POINT('Ctrl Pts',(165.641437047417,1.62817612077944,126.161404799373));
#29129=CARTESIAN_POINT('Ctrl Pts',(165.633685856177,1.49752784325534,126.119641477513));
#29130=CARTESIAN_POINT('Ctrl Pts',(165.6259379594,1.36693509473416,126.07789590618));
#29131=CARTESIAN_POINT('Ctrl Pts',(165.618190062623,1.23452791298634,126.041593551853));
#29132=CARTESIAN_POINT('Ctrl Pts',(165.610442165846,1.1008001115345,126.010883572983));
#29133=CARTESIAN_POINT('Ctrl Pts',(165.602695889762,0.967100283055891,125.980180017978));
#29134=CARTESIAN_POINT('Ctrl Pts',(165.594949613677,0.832080765145308,125.955066599076));
#29135=CARTESIAN_POINT('Ctrl Pts',(165.587203337593,0.696248156450435,125.935641939398));
#29136=CARTESIAN_POINT('Ctrl Pts',(165.579457004328,0.5604145450701,125.916217136332));
#29137=CARTESIAN_POINT('Ctrl Pts',(165.571710671063,0.42376821795664,125.902481231632));
#29138=CARTESIAN_POINT('Ctrl Pts',(165.563964337797,0.286823140077404,125.894481235258));
#29139=CARTESIAN_POINT('Ctrl Pts',(165.556216269794,0.149847394297581,125.88647944734));
#29140=CARTESIAN_POINT('Ctrl Pts',(165.548468201791,0.0125731548475351,
125.884216146584));
#29141=CARTESIAN_POINT('Ctrl Pts',(165.540720133788,-0.124483751035951,
125.887686247809));
#29142=CARTESIAN_POINT('Ctrl Pts',(165.532963831046,-0.261686322630102,
125.891160037098));
#29143=CARTESIAN_POINT('Ctrl Pts',(165.525207528305,-0.39867070777771,125.900379390934));
#29144=CARTESIAN_POINT('Ctrl Pts',(165.517451225563,-0.534923786042843,
125.915287126031));
#29145=CARTESIAN_POINT('Ctrl Pts',(165.509690783049,-0.671249586678486,
125.930202817836));
#29146=CARTESIAN_POINT('Ctrl Pts',(165.501930340534,-0.806842916348517,
125.950812881788));
#29147=CARTESIAN_POINT('Ctrl Pts',(165.49416989802,-0.941200003091565,125.977008795223));
#29148=CARTESIAN_POINT('Ctrl Pts',(165.486396997755,-1.07577277175787,126.003246760663));
#29149=CARTESIAN_POINT('Ctrl Pts',(165.478624097489,-1.20910495128956,126.035088403447));
#29150=CARTESIAN_POINT('Ctrl Pts',(165.470851197224,-1.34070623660191,126.072374792393));
#29151=CARTESIAN_POINT('Ctrl Pts',(165.463360861462,-1.46752348370828,126.108305727182));
#29152=CARTESIAN_POINT('Ctrl Pts',(165.4558705257,-1.59273320374189,126.149292324551));
#29153=CARTESIAN_POINT('Ctrl Pts',(165.448380189938,-1.71591532042347,126.195150525193));
#29154=CARTESIAN_POINT('Ctrl Pts',(165.440605662801,-1.84377109877684,126.242748635169));
#29155=CARTESIAN_POINT('Ctrl Pts',(165.432831135663,-1.96984739568884,126.295746095503));
#29156=CARTESIAN_POINT('Ctrl Pts',(165.425056608526,-2.09365448306572,126.353990524187));
#29157=CARTESIAN_POINT('Ctrl Pts',(165.417291707369,-2.21730827949702,126.412162837908));
#29158=CARTESIAN_POINT('Ctrl Pts',(165.409526806212,-2.33869810637646,126.475569028751));
#29159=CARTESIAN_POINT('Ctrl Pts',(165.401761905056,-2.45735119984756,126.544007563756));
#29160=CARTESIAN_POINT('Ctrl Pts',(165.39400476058,-2.57588576582875,126.612377732674));
#29161=CARTESIAN_POINT('Ctrl Pts',(165.386247616105,-2.69168870250206,126.685770047397));
#29162=CARTESIAN_POINT('Ctrl Pts',(165.37849047163,-2.80430931143856,126.763935844318));
#29163=CARTESIAN_POINT('Ctrl Pts',(165.370739221275,-2.91684434772171,126.842042248427));
#29164=CARTESIAN_POINT('Ctrl Pts',(165.36298797092,-3.02620154948531,126.924914693036));
#29165=CARTESIAN_POINT('Ctrl Pts',(165.355236720565,-3.13195713878541,127.012259940723));
#29166=CARTESIAN_POINT('Ctrl Pts',(165.347488990716,-3.23766469542691,127.099565517463));
#29167=CARTESIAN_POINT('Ctrl Pts',(165.339741260867,-3.3397735935151,127.191339606851));
#29168=CARTESIAN_POINT('Ctrl Pts',(165.331993531018,-3.43789145070786,127.287247392825));
#29169=CARTESIAN_POINT('Ctrl Pts',(165.324247485209,-3.53598798108525,127.383134332363));
#29170=CARTESIAN_POINT('Ctrl Pts',(165.3165014394,-3.63009491707408,127.483152907841));
#29171=CARTESIAN_POINT('Ctrl Pts',(165.30875539359,-3.71985548819165,127.586930243887));
#29172=CARTESIAN_POINT('Ctrl Pts',(165.301009353988,-3.80961598738343,127.690707496776));
#29173=CARTESIAN_POINT('Ctrl Pts',(165.293263314386,-3.8950298731532,127.798243208386));
#29174=CARTESIAN_POINT('Ctrl Pts',(165.285517274784,-3.97577981994194,127.909130421909));
#29175=CARTESIAN_POINT('Ctrl Pts',(165.277769563929,-4.05654718900209,128.020041559995));
#29176=CARTESIAN_POINT('Ctrl Pts',(165.270021853074,-4.13264838712059,128.134305322645));
#29177=CARTESIAN_POINT('Ctrl Pts',(165.262274142218,-4.20380891123564,128.251485042785));
#29178=CARTESIAN_POINT('Ctrl Pts',(165.254519060828,-4.27503713162572,128.36877623808));
#29179=CARTESIAN_POINT('Ctrl Pts',(165.246763979437,-4.34131508909183,128.488988595856));
#29180=CARTESIAN_POINT('Ctrl Pts',(165.239008898046,-4.40241364061653,128.611659726105));
#29181=CARTESIAN_POINT('Ctrl Pts',(165.23124970306,-4.46354460118404,128.734395925882));
#29182=CARTESIAN_POINT('Ctrl Pts',(165.223490508073,-4.51949052232472,128.859593140357));
#29183=CARTESIAN_POINT('Ctrl Pts',(165.215731313086,-4.5700704781865,128.986769110404));
#29184=CARTESIAN_POINT('Ctrl Pts',(165.207961665366,-4.62071857240156,129.114116404467));
#29185=CARTESIAN_POINT('Ctrl Pts',(165.200192017647,-4.66598613558932,129.243447409415));
#29186=CARTESIAN_POINT('Ctrl Pts',(165.192422369927,-4.70574199340715,129.37426434319));
#29187=CARTESIAN_POINT('Ctrl Pts',(165.188323054731,-4.7267174350182,129.443284183454));
#29188=CARTESIAN_POINT('Ctrl Pts',(165.184223739535,-4.74615944644796,129.51271746702));
#29189=CARTESIAN_POINT('Ctrl Pts',(165.180124424339,-4.76405452823406,129.582490119308));
#29190=CARTESIAN_POINT('Origin',(213.235140564004,0.,130.804360617566));
#29191=CARTESIAN_POINT('',(163.084942816425,-4.76405452823405,129.582490119308));
#29192=CARTESIAN_POINT('',(163.429862020825,-4.76405452823405,129.582490119308));
#29193=CARTESIAN_POINT('',(213.235140564004,-4.76405452823405,129.582490119308));
#29194=CARTESIAN_POINT('',(164.764859435961,-4.91824995258213,130.80504357138));
#29195=CARTESIAN_POINT('Ctrl Pts',(164.764859435961,-4.91824995258213,130.80504357138));
#29196=CARTESIAN_POINT('Ctrl Pts',(164.756654934105,-4.91822972407168,130.95071794709));
#29197=CARTESIAN_POINT('Ctrl Pts',(164.748450432249,-4.91173310152479,131.096239299343));
#29198=CARTESIAN_POINT('Ctrl Pts',(164.740245930392,-4.89882630855481,131.241034249826));
#29199=CARTESIAN_POINT('Ctrl Pts',(164.732027256984,-4.88589722181341,131.386079303146));
#29200=CARTESIAN_POINT('Ctrl Pts',(164.723808583575,-4.86653588615109,131.530395135098));
#29201=CARTESIAN_POINT('Ctrl Pts',(164.715589910167,-4.84085980131171,131.673417259301));
#29202=CARTESIAN_POINT('Ctrl Pts',(164.707348638168,-4.81511311586655,131.816832646289));
#29203=CARTESIAN_POINT('Ctrl Pts',(164.69910736617,-4.78301701189617,131.958946898958));
#29204=CARTESIAN_POINT('Ctrl Pts',(164.690866094171,-4.74473971050206,132.099207381506));
#29205=CARTESIAN_POINT('Ctrl Pts',(164.6826124805,-4.70640508714233,132.23967791038));
#29206=CARTESIAN_POINT('Ctrl Pts',(164.674358866829,-4.66187088218157,132.37828882621));
#29207=CARTESIAN_POINT('Ctrl Pts',(164.666105253158,-4.61135402128945,132.514505977715));
#29208=CARTESIAN_POINT('Ctrl Pts',(164.65783226147,-4.56071855579518,132.651042942857));
#29209=CARTESIAN_POINT('Ctrl Pts',(164.649559269783,-4.50407247160253,132.785174614601));
#29210=CARTESIAN_POINT('Ctrl Pts',(164.641286278095,-4.44168007449386,132.916388358469));
#29211=CARTESIAN_POINT('Ctrl Pts',(164.638399623616,-4.41990980088975,132.962172127598));
#29212=CARTESIAN_POINT('Ctrl Pts',(164.635512969137,-4.39744031709227,133.007600886824));
#29213=CARTESIAN_POINT('Ctrl Pts',(164.632626314659,-4.37428410091448,133.052653673862));
#29214=CARTESIAN_POINT('Ctrl Pts',(164.62485198054,-4.31191980937317,133.173989781799));
#29215=CARTESIAN_POINT('Ctrl Pts',(164.61707764642,-4.24440438761954,133.29292127249));
#29216=CARTESIAN_POINT('Ctrl Pts',(164.609303312301,-4.17194697607602,133.408979877901));
#29217=CARTESIAN_POINT('Ctrl Pts',(164.601538559354,-4.09957886181654,133.524895451454));
#29218=CARTESIAN_POINT('Ctrl Pts',(164.593773806407,-4.0222810812284,133.637944855961));
#29219=CARTESIAN_POINT('Ctrl Pts',(164.58600905346,-3.94030957796668,133.7476824641));
#29220=CARTESIAN_POINT('Ctrl Pts',(164.578252012575,-3.85841948995763,133.8573110793));
#29221=CARTESIAN_POINT('Ctrl Pts',(164.57049497169,-3.77186514953762,133.963634132834));
#29222=CARTESIAN_POINT('Ctrl Pts',(164.562737930805,-3.68094669703134,134.066233465504));
#29223=CARTESIAN_POINT('Ctrl Pts',(164.554986739565,-3.5900968068374,134.168755427219));
#29224=CARTESIAN_POINT('Ctrl Pts',(164.547235548325,-3.49488961336082,134.267558965971));
#29225=CARTESIAN_POINT('Ctrl Pts',(164.539484357085,-3.39566634318057,134.362257910672));
#29226=CARTESIAN_POINT('Ctrl Pts',(164.531736460308,-3.2964852455369,134.456916605795));
#29227=CARTESIAN_POINT('Ctrl Pts',(164.523988563531,-3.19329174839745,134.547473907302));
#29228=CARTESIAN_POINT('Ctrl Pts',(164.516240666754,-3.08646469064485,134.633579699298));
#29229=CARTESIAN_POINT('Ctrl Pts',(164.508494390669,-2.97965997880984,134.719667479819));
#29230=CARTESIAN_POINT('Ctrl Pts',(164.500748114585,-2.86922352237007,134.80130535776));
#29231=CARTESIAN_POINT('Ctrl Pts',(164.493001838501,-2.75556776040104,134.878183070783));
#29232=CARTESIAN_POINT('Ctrl Pts',(164.485255505236,-2.64191115945102,134.9550613513));
#29233=CARTESIAN_POINT('Ctrl Pts',(164.477509171971,-2.52503552939137,135.027179177735));
#29234=CARTESIAN_POINT('Ctrl Pts',(164.469762838705,-2.40538250788096,135.094269480617));
#29235=CARTESIAN_POINT('Ctrl Pts',(164.462014770702,-2.28570269090592,135.161374807906));
#29236=CARTESIAN_POINT('Ctrl Pts',(164.454266702699,-2.16324458576815,135.2234501801));
#29237=CARTESIAN_POINT('Ctrl Pts',(164.446518634696,-2.03847428983192,135.280274561354));
#29238=CARTESIAN_POINT('Ctrl Pts',(164.438762331954,-1.91357138654042,135.337159336236));
#29239=CARTESIAN_POINT('Ctrl Pts',(164.431006029213,-1.78635173985156,135.388781809596));
#29240=CARTESIAN_POINT('Ctrl Pts',(164.423249726471,-1.65730179925442,135.434968980264));
#29241=CARTESIAN_POINT('Ctrl Pts',(164.415489283957,-1.52818298081836,135.481180802416));
#29242=CARTESIAN_POINT('Ctrl Pts',(164.407728841442,-1.39723229506051,135.521951425254));
#29243=CARTESIAN_POINT('Ctrl Pts',(164.399968398928,-1.26495023902372,135.557158104867));
#29244=CARTESIAN_POINT('Ctrl Pts',(164.392195498663,-1.13245583208708,135.592421301368));
#29245=CARTESIAN_POINT('Ctrl Pts',(164.384422598397,-0.998626165907619,
135.622102621489));
#29246=CARTESIAN_POINT('Ctrl Pts',(164.376649698132,-0.863971674351278,
135.64613054275));
#29247=CARTESIAN_POINT('Ctrl Pts',(164.36915936237,-0.734212212737345,135.669284988551));
#29248=CARTESIAN_POINT('Ctrl Pts',(164.361669026608,-0.603687158718285,
135.687189888116));
#29249=CARTESIAN_POINT('Ctrl Pts',(164.354178690846,-0.472854781144197,
135.699827032367));
#29250=CARTESIAN_POINT('Ctrl Pts',(164.346404356727,-0.337061854208649,
135.712943317785));
#29251=CARTESIAN_POINT('Ctrl Pts',(164.338630022608,-0.200507688162279,
135.720426057109));
#29252=CARTESIAN_POINT('Ctrl Pts',(164.330855688489,-0.0636992956689109,
135.722198095791));
#29253=CARTESIAN_POINT('Ctrl Pts',(164.323090935542,0.0729404927076261,
135.723967950593));
#29254=CARTESIAN_POINT('Ctrl Pts',(164.315326182595,0.209833496955411,135.720041103119));
#29255=CARTESIAN_POINT('Ctrl Pts',(164.307561429647,0.3464664543917,135.71039201356));
#29256=CARTESIAN_POINT('Ctrl Pts',(164.299804388762,0.482963706048382,135.700752507614));
#29257=CARTESIAN_POINT('Ctrl Pts',(164.292047347877,0.619201037416439,135.685402097192));
#29258=CARTESIAN_POINT('Ctrl Pts',(164.284290306992,0.754664406141891,135.66436727359));
#29259=CARTESIAN_POINT('Ctrl Pts',(164.276539115752,0.890025620887144,135.643348312513));
#29260=CARTESIAN_POINT('Ctrl Pts',(164.268787924512,1.02461364994013,135.616653530339));
#29261=CARTESIAN_POINT('Ctrl Pts',(164.261036733272,1.15791915532598,135.584361275749));
#29262=CARTESIAN_POINT('Ctrl Pts',(164.253288836495,1.29116800231614,135.552082746228));
#29263=CARTESIAN_POINT('Ctrl Pts',(164.245540939718,1.4231350306351,135.514211567943));
#29264=CARTESIAN_POINT('Ctrl Pts',(164.237793042941,1.55332090619529,135.470877222581));
#29265=CARTESIAN_POINT('Ctrl Pts',(164.230046766857,1.68347954967679,135.427551941829));
#29266=CARTESIAN_POINT('Ctrl Pts',(164.222300490773,1.81185741075988,135.378765890447));
#29267=CARTESIAN_POINT('Ctrl Pts',(164.214554214689,1.9379705235568,135.324698360736));
#29268=CARTESIAN_POINT('Ctrl Pts',(164.206807881423,2.06408456729207,135.27063043191));
#29269=CARTESIAN_POINT('Ctrl Pts',(164.199061548158,2.18793347004784,135.211281101015));
#29270=CARTESIAN_POINT('Ctrl Pts',(164.191315214892,2.30905382277212,135.146877572748));
#29271=CARTESIAN_POINT('Ctrl Pts',(164.183567146889,2.43020129955965,135.082459621757));
#29272=CARTESIAN_POINT('Ctrl Pts',(164.175819078886,2.54861866528459,135.012985404657));
#29273=CARTESIAN_POINT('Ctrl Pts',(164.168071010884,2.66386801922089,134.938727587088));
#29274=CARTESIAN_POINT('Ctrl Pts',(164.160314708142,2.77923986154201,134.864390847426));
#29275=CARTESIAN_POINT('Ctrl Pts',(164.1525584054,2.89143663695182,134.785260563419));
#29276=CARTESIAN_POINT('Ctrl Pts',(164.144802102658,3.00004985683638,134.701652487441));
#29277=CARTESIAN_POINT('Ctrl Pts',(164.137041660144,3.10872104686674,134.617999787316));
#29278=CARTESIAN_POINT('Ctrl Pts',(164.12928121763,3.21380457084478,134.529864784193));
#29279=CARTESIAN_POINT('Ctrl Pts',(164.121520775115,3.31492662996522,134.437602214329));
#29280=CARTESIAN_POINT('Ctrl Pts',(164.11374787485,3.41621101919216,134.345191536397));
#29281=CARTESIAN_POINT('Ctrl Pts',(164.105974974585,3.51352095796986,134.248640326519));
#29282=CARTESIAN_POINT('Ctrl Pts',(164.098202074319,3.60652037043833,134.148339367515));
#29283=CARTESIAN_POINT('Ctrl Pts',(164.090711738557,3.69613902001243,134.051684601015));
#29284=CARTESIAN_POINT('Ctrl Pts',(164.083221402795,3.78175489905831,133.951548211972));
#29285=CARTESIAN_POINT('Ctrl Pts',(164.075731067033,3.86310498225758,133.848305912501));
#29286=CARTESIAN_POINT('Ctrl Pts',(164.067956732914,3.9475394785869,133.741149149866));
#29287=CARTESIAN_POINT('Ctrl Pts',(164.060182398795,4.02764578137131,133.630306865937));
#29288=CARTESIAN_POINT('Ctrl Pts',(164.052408064676,4.10308492557468,133.516163920909));
#29289=CARTESIAN_POINT('Ctrl Pts',(164.044643311729,4.17843109777495,133.40216164686));
#29290=CARTESIAN_POINT('Ctrl Pts',(164.036878558782,4.24912134237368,133.284867128396));
#29291=CARTESIAN_POINT('Ctrl Pts',(164.029113805834,4.31485674099162,133.16469838306));
#29292=CARTESIAN_POINT('Ctrl Pts',(164.021356764949,4.38052685028495,133.044648991016));
#29293=CARTESIAN_POINT('Ctrl Pts',(164.013599724064,4.44125172063751,132.921731393907));
#29294=CARTESIAN_POINT('Ctrl Pts',(164.005842683179,4.49677578747697,132.796392389316));
#29295=CARTESIAN_POINT('Ctrl Pts',(163.998091491939,4.5522579831857,132.671147903843));
#29296=CARTESIAN_POINT('Ctrl Pts',(163.990340300699,4.60254702410623,132.543486001448));
#29297=CARTESIAN_POINT('Ctrl Pts',(163.982589109459,4.64743351758415,132.413877551971));
#29298=CARTESIAN_POINT('Ctrl Pts',(163.974841212682,4.69230093310496,132.284324189542));
#29299=CARTESIAN_POINT('Ctrl Pts',(163.967093315905,4.73177024052611,132.152826294198));
#29300=CARTESIAN_POINT('Ctrl Pts',(163.959345419128,4.76568047418773,132.019873957865));
#29301=CARTESIAN_POINT('Ctrl Pts',(163.951599143044,4.79958361455951,131.886949432295));
#29302=CARTESIAN_POINT('Ctrl Pts',(163.94385286696,4.82792989755778,131.752571449478));
#29303=CARTESIAN_POINT('Ctrl Pts',(163.936106590876,4.85060857149034,131.617244095492));
#29304=CARTESIAN_POINT('Ctrl Pts',(163.92836025761,4.8732874128317,131.481915742549));
#29305=CARTESIAN_POINT('Ctrl Pts',(163.920613924345,4.8902984970063,131.345638390041));
#29306=CARTESIAN_POINT('Ctrl Pts',(163.91286759108,4.90158249384904,131.208924726815));
#29307=CARTESIAN_POINT('Ctrl Pts',(163.905119523077,4.91286901766464,131.072180447513));
#29308=CARTESIAN_POINT('Ctrl Pts',(163.897371455074,4.91842586988551,130.93500005263));
#29309=CARTESIAN_POINT('Ctrl Pts',(163.889623387071,4.91824575579846,130.797899342888));
#29310=CARTESIAN_POINT('Ctrl Pts',(163.881867084329,4.918065450284,130.66065292088));
#29311=CARTESIAN_POINT('Ctrl Pts',(163.874110781587,4.91213599893044,130.523486744779));
#29312=CARTESIAN_POINT('Ctrl Pts',(163.866354478845,4.90050225507937,130.386915159497));
#29313=CARTESIAN_POINT('Ctrl Pts',(163.858594036331,4.88886230194891,130.250270681848));
#29314=CARTESIAN_POINT('Ctrl Pts',(163.850833593817,4.87151203922687,130.114221815001));
#29315=CARTESIAN_POINT('Ctrl Pts',(163.843073151303,4.84854786918652,129.979274790087));
#29316=CARTESIAN_POINT('Ctrl Pts',(163.835300251037,4.82554683502176,129.844111136229));
#29317=CARTESIAN_POINT('Ctrl Pts',(163.827527350772,4.79691396651585,129.710053241441));
#29318=CARTESIAN_POINT('Ctrl Pts',(163.819754450506,4.76279638311187,129.577595083523));
#29319=CARTESIAN_POINT('Ctrl Pts',(163.812264114744,4.72991905980141,129.449952113286));
#29320=CARTESIAN_POINT('Ctrl Pts',(163.804773778982,4.69194895359856,129.323794885232));
#29321=CARTESIAN_POINT('Ctrl Pts',(163.79728344322,4.64905999013475,129.199547771584));
#29322=CARTESIAN_POINT('Ctrl Pts',(163.789509109101,4.60454487858566,129.070589790859));
#29323=CARTESIAN_POINT('Ctrl Pts',(163.781734774982,4.55458953925968,128.943281127661));
#29324=CARTESIAN_POINT('Ctrl Pts',(163.773960440863,4.49933454705722,128.818114989211));
#29325=CARTESIAN_POINT('Ctrl Pts',(163.766195687916,4.44414765169439,128.693103106841));
#29326=CARTESIAN_POINT('Ctrl Pts',(163.758430934969,4.38367425526831,128.570228849701));
#29327=CARTESIAN_POINT('Ctrl Pts',(163.750666182021,4.31810447509082,128.449969654981));
#29328=CARTESIAN_POINT('Ctrl Pts',(163.742909141136,4.25259981974337,128.329829903389));
#29329=CARTESIAN_POINT('Ctrl Pts',(163.735152100251,4.18200903980121,128.212300386477));
#29330=CARTESIAN_POINT('Ctrl Pts',(163.727395059366,4.10656989983062,128.097837622965));
#29331=CARTESIAN_POINT('Ctrl Pts',(163.719643868126,4.03118764910229,127.983461176713));
#29332=CARTESIAN_POINT('Ctrl Pts',(163.711892676886,3.95096453004045,127.872147205767));
#29333=CARTESIAN_POINT('Ctrl Pts',(163.704141485646,3.86618351693116,127.764326394747));
#29334=CARTESIAN_POINT('Ctrl Pts',(163.696393588869,3.78143853801404,127.656551410448));
#29335=CARTESIAN_POINT('Ctrl Pts',(163.688645692092,3.69213975920012,127.552266939838));
#29336=CARTESIAN_POINT('Ctrl Pts',(163.680897795315,3.59861250283509,127.451873314542));
#29337=CARTESIAN_POINT('Ctrl Pts',(163.673151519231,3.50510481035586,127.351500689427));
#29338=CARTESIAN_POINT('Ctrl Pts',(163.665405243147,3.40737066598672,127.255017576655));
#29339=CARTESIAN_POINT('Ctrl Pts',(163.657658967062,3.3057743076256,127.162789625598));
#29340=CARTESIAN_POINT('Ctrl Pts',(163.649912633797,3.20417719930328,127.070560993735));
#29341=CARTESIAN_POINT('Ctrl Pts',(163.642166300532,3.09871810957786,126.98258784905));
#29342=CARTESIAN_POINT('Ctrl Pts',(163.634419967266,2.9897963086944,126.899197228536));
#29343=CARTESIAN_POINT('Ctrl Pts',(163.626671899263,2.88085011552887,126.815787933272));
#29344=CARTESIAN_POINT('Ctrl Pts',(163.61892383126,2.76843997852202,126.736963441868));
#29345=CARTESIAN_POINT('Ctrl Pts',(163.611175763257,2.65299591245853,126.663008694464));
#29346=CARTESIAN_POINT('Ctrl Pts',(163.603419460516,2.53742915106774,126.588975347075));
#29347=CARTESIAN_POINT('Ctrl Pts',(163.595663157774,2.41882234907478,126.519822293777));
#29348=CARTESIAN_POINT('Ctrl Pts',(163.587906855032,2.29763248374708,126.455789814172));
#29349=CARTESIAN_POINT('Ctrl Pts',(163.580146412518,2.17637793573922,126.391723158505));
#29350=CARTESIAN_POINT('Ctrl Pts',(163.572385970003,2.05253793015106,126.332782690209));
#29351=CARTESIAN_POINT('Ctrl Pts',(163.564625527489,1.92659048135476,126.279160933612));
#29352=CARTESIAN_POINT('Ctrl Pts',(163.556852627224,1.80044085053261,126.225453098612));
#29353=CARTESIAN_POINT('Ctrl Pts',(163.549079726958,1.6721773821065,126.177081175132));
#29354=CARTESIAN_POINT('Ctrl Pts',(163.541306826693,1.54229519524159,126.134188394485));
#29355=CARTESIAN_POINT('Ctrl Pts',(163.533816490931,1.41713455302368,126.092854874455));
#29356=CARTESIAN_POINT('Ctrl Pts',(163.526326155169,1.29047113423111,126.056609136849));
#29357=CARTESIAN_POINT('Ctrl Pts',(163.518835819407,1.16275598628657,126.025534236659));
#29358=CARTESIAN_POINT('Ctrl Pts',(163.511061485288,1.03019847968851,125.993281122183));
#29359=CARTESIAN_POINT('Ctrl Pts',(163.503287151169,0.896088014638653,125.966496521821));
#29360=CARTESIAN_POINT('Ctrl Pts',(163.49551281705,0.760915524507925,125.945328756479));
#29361=CARTESIAN_POINT('Ctrl Pts',(163.487748064103,0.625909622390663,125.924187078515));
#29362=CARTESIAN_POINT('Ctrl Pts',(163.479983311156,0.48984468196566,125.908648522269));
#29363=CARTESIAN_POINT('Ctrl Pts',(163.472218558209,0.353225147713974,125.898811203125));
#29364=CARTESIAN_POINT('Ctrl Pts',(163.464461517324,0.216741305909704,125.888983654545));
#29365=CARTESIAN_POINT('Ctrl Pts',(163.456704476438,0.0797043538883314,
125.884846102236));
#29366=CARTESIAN_POINT('Ctrl Pts',(163.448947435553,-0.05737310866623,125.886445267654));
#29367=CARTESIAN_POINT('Ctrl Pts',(163.441196244313,-0.194347200040018,
125.888043227128));
#29368=CARTESIAN_POINT('Ctrl Pts',(163.433445053073,-0.331361351783681,
125.895369288941));
#29369=CARTESIAN_POINT('Ctrl Pts',(163.425693861833,-0.46790026221552,125.908418174367));
#29370=CARTESIAN_POINT('Ctrl Pts',(163.417945965056,-0.60438113996813,125.921461513668));
#29371=CARTESIAN_POINT('Ctrl Pts',(163.410198068279,-0.740386789774988,
125.940222801703));
#29372=CARTESIAN_POINT('Ctrl Pts',(163.402450171502,-0.875404556627693,
125.964644724589));
#29373=CARTESIAN_POINT('Ctrl Pts',(163.394703895418,-1.01039408067422,125.989061538935));
#29374=CARTESIAN_POINT('Ctrl Pts',(163.386957619334,-1.1443957483139,126.019136563383));
#29375=CARTESIAN_POINT('Ctrl Pts',(163.379211343249,-1.27690504889282,126.054760996691));
#29376=CARTESIAN_POINT('Ctrl Pts',(163.371465009984,-1.40941532762526,126.090385692971));
#29377=CARTESIAN_POINT('Ctrl Pts',(163.363718676719,-1.54043283975595,126.131559778348));
#29378=CARTESIAN_POINT('Ctrl Pts',(163.355972343453,-1.66946662447946,126.17812410694));
#29379=CARTESIAN_POINT('Ctrl Pts',(163.34822427545,-1.79852930542436,126.224698863291));
#29380=CARTESIAN_POINT('Ctrl Pts',(163.340476207447,-1.92560700729007,126.276666132176));
#29381=CARTESIAN_POINT('Ctrl Pts',(163.332728139444,-2.05022756837374,126.333818147084));
#29382=CARTESIAN_POINT('Ctrl Pts',(163.324971836703,-2.17498057767278,126.391030903834));
#29383=CARTESIAN_POINT('Ctrl Pts',(163.317215533961,-2.29727087353789,126.453439251005));
#29384=CARTESIAN_POINT('Ctrl Pts',(163.309459231219,-2.41664929456,126.520788597674));
#29385=CARTESIAN_POINT('Ctrl Pts',(163.301698788705,-2.53609143143998,126.588173890717));
#29386=CARTESIAN_POINT('Ctrl Pts',(163.293938346191,-2.6526182646793,126.660505231934));
#29387=CARTESIAN_POINT('Ctrl Pts',(163.286177903676,-2.76580943966262,126.737484518399));
#29388=CARTESIAN_POINT('Ctrl Pts',(163.278405003411,-2.87918231916858,126.814587378849));
#29389=CARTESIAN_POINT('Ctrl Pts',(163.270632103146,-2.98920852604997,126.896352861255));
#29390=CARTESIAN_POINT('Ctrl Pts',(163.26285920288,-3.09549993174442,126.982441827865));
#29391=CARTESIAN_POINT('Ctrl Pts',(163.255368867118,-3.19792737711045,127.065401243694));
#29392=CARTESIAN_POINT('Ctrl Pts',(163.247878531356,-3.29688661447606,127.152375058692));
#29393=CARTESIAN_POINT('Ctrl Pts',(163.240388195594,-3.39206396517385,127.24302868714));
#29394=CARTESIAN_POINT('Ctrl Pts',(163.232729627453,-3.4893789920271,127.335718389282));
#29395=CARTESIAN_POINT('Ctrl Pts',(163.225071059311,-3.58306797339335,127.432567693409));
#29396=CARTESIAN_POINT('Ctrl Pts',(163.21741249117,-3.67274626851651,127.533257147848));
#29397=CARTESIAN_POINT('Ctrl Pts',(163.209762819814,-3.76232038640117,127.633829633636));
#29398=CARTESIAN_POINT('Ctrl Pts',(163.202113148457,-3.84789281451807,127.738233103802));
#29399=CARTESIAN_POINT('Ctrl Pts',(163.1944634771,-3.92911323611359,127.846109066346));
#29400=CARTESIAN_POINT('Ctrl Pts',(163.186820918863,-4.0102581341281,127.9538847194));
#29401=CARTESIAN_POINT('Ctrl Pts',(163.179178360626,-4.08705883121905,128.065126124343));
#29402=CARTESIAN_POINT('Ctrl Pts',(163.171535802389,-4.15920343475139,128.179439694785));
#29403=CARTESIAN_POINT('Ctrl Pts',(163.163898689599,-4.23129663408036,128.293671814949));
#29404=CARTESIAN_POINT('Ctrl Pts',(163.156261576809,-4.29874012499224,128.410971406206));
#29405=CARTESIAN_POINT('Ctrl Pts',(163.14862446402,-4.36126408326984,128.530914190117));
#29406=CARTESIAN_POINT('Ctrl Pts',(163.140990631086,-4.4237611898318,128.650805463061));
#29407=CARTESIAN_POINT('Ctrl Pts',(163.133356798152,-4.48134278053375,128.773337313375));
#29408=CARTESIAN_POINT('Ctrl Pts',(163.125722965218,-4.5337841800003,128.898059468304));
#29409=CARTESIAN_POINT('Ctrl Pts',(163.118089120101,-4.58622566316061,129.022781822282));
#29410=CARTESIAN_POINT('Ctrl Pts',(163.110455274984,-4.63352677233583,129.149694120223));
#29411=CARTESIAN_POINT('Ctrl Pts',(163.102821429866,-4.67551045595483,129.278324891));
#29412=CARTESIAN_POINT('Ctrl Pts',(163.096861892052,-4.70828598994256,129.378743478318));
#29413=CARTESIAN_POINT('Ctrl Pts',(163.090902354239,-4.73782174831892,129.480208908557));
#29414=CARTESIAN_POINT('Ctrl Pts',(163.084942816425,-4.76405452823405,129.582490119308));
#29415=CARTESIAN_POINT('Ctrl Pts',(164.834593643846,-4.76405452823405,129.582490119308));
#29416=CARTESIAN_POINT('Ctrl Pts',(164.826544756193,-4.79939512201895,129.720282558107));
#29417=CARTESIAN_POINT('Ctrl Pts',(164.818495868541,-4.82878719210012,129.859741089387));
#29418=CARTESIAN_POINT('Ctrl Pts',(164.810446980889,-4.85208430067357,130.000332631948));
#29419=CARTESIAN_POINT('Ctrl Pts',(164.802409401942,-4.8753486767581,130.140726643082));
#29420=CARTESIAN_POINT('Ctrl Pts',(164.794371822994,-4.89253510851404,130.282250151103));
#29421=CARTESIAN_POINT('Ctrl Pts',(164.786334244047,-4.9035478438914,130.424358505509));
#29422=CARTESIAN_POINT('Ctrl Pts',(164.779175974695,-4.91335578813071,130.550920233198));
#29423=CARTESIAN_POINT('Ctrl Pts',(164.772017705343,-4.91826760155312,130.677945492592));
#29424=CARTESIAN_POINT('Ctrl Pts',(164.764859435991,-4.9182499525822,130.805043570854));
#29425=CARTESIAN_POINT('',(165.110140563977,-4.9182479540109,130.799874486988));
#29426=CARTESIAN_POINT('Ctrl Pts',(165.180124424339,-4.76405452823406,129.582490119308));
#29427=CARTESIAN_POINT('Ctrl Pts',(165.176727138268,-4.77888498385569,129.640313840693));
#29428=CARTESIAN_POINT('Ctrl Pts',(165.173329852197,-4.79265305198197,129.698370631477));
#29429=CARTESIAN_POINT('Ctrl Pts',(165.169932566126,-4.80535313457782,129.756618132743));
#29430=CARTESIAN_POINT('Ctrl Pts',(165.159153962061,-4.84564681577433,129.941420572318));
#29431=CARTESIAN_POINT('Ctrl Pts',(165.148375357997,-4.8752919794919,130.128621269865));
#29432=CARTESIAN_POINT('Ctrl Pts',(165.137596753933,-4.89406303010228,130.317195224823));
#29433=CARTESIAN_POINT('Ctrl Pts',(165.128444690625,-4.91000144314016,130.477312505667));
#29434=CARTESIAN_POINT('Ctrl Pts',(165.119292627316,-4.91810068477407,130.638419860766));
#29435=CARTESIAN_POINT('Ctrl Pts',(165.110140564008,-4.91824795401041,130.799874486449));
#29436=CARTESIAN_POINT('Ctrl Pts',(165.110140563977,-4.9182479540109,130.799874486988));
#29437=CARTESIAN_POINT('Ctrl Pts',(165.102489678719,-4.91837106722112,130.934846326012));
#29438=CARTESIAN_POINT('Ctrl Pts',(165.09483879346,-4.91293394198934,131.069989105914));
#29439=CARTESIAN_POINT('Ctrl Pts',(165.087187908201,-4.90192116343657,131.204800338314));
#29440=CARTESIAN_POINT('Ctrl Pts',(165.079543020346,-4.89091701761987,131.339505894405));
#29441=CARTESIAN_POINT('Ctrl Pts',(165.071898132491,-4.87434594577441,131.473880020402));
#29442=CARTESIAN_POINT('Ctrl Pts',(165.064253244635,-4.85224459998632,131.607420642971));
#29443=CARTESIAN_POINT('Ctrl Pts',(165.056611766299,-4.83015311110892,131.740901708172));
#29444=CARTESIAN_POINT('Ctrl Pts',(165.048970287964,-4.80253631707366,131.873549612425));
#29445=CARTESIAN_POINT('Ctrl Pts',(165.041328809628,-4.76948263181031,132.004868213277));
#29446=CARTESIAN_POINT('Ctrl Pts',(165.033688916441,-4.73643580320209,132.136159573404));
#29447=CARTESIAN_POINT('Ctrl Pts',(165.026049023253,-4.69795442381423,132.266121787939));
#29448=CARTESIAN_POINT('Ctrl Pts',(165.018409130065,-4.65417774052173,132.394270244599));
#29449=CARTESIAN_POINT('Ctrl Pts',(165.010769059858,-4.61040004290534,132.522421670512));
#29450=CARTESIAN_POINT('Ctrl Pts',(165.003128989651,-4.56132692786859,132.648758873867));
#29451=CARTESIAN_POINT('Ctrl Pts',(164.995488919444,-4.50714692209329,132.772814245459));
#29452=CARTESIAN_POINT('Ctrl Pts',(164.98784691012,-4.45295316495702,132.896901103393));
#29453=CARTESIAN_POINT('Ctrl Pts',(164.980204900796,-4.39365010120368,133.018704609114));
#29454=CARTESIAN_POINT('Ctrl Pts',(164.972562891472,-4.32947338047244,133.137779420585));
#29455=CARTESIAN_POINT('Ctrl Pts',(164.964912864165,-4.26522932563666,133.256979165142));
#29456=CARTESIAN_POINT('Ctrl Pts',(164.957262836858,-4.19610159699709,133.37344414524));
#29457=CARTESIAN_POINT('Ctrl Pts',(164.949612809551,-4.12237072084906,133.486755574016));
#29458=CARTESIAN_POINT('Ctrl Pts',(164.941958298561,-4.04859663101648,133.600133414647));
#29459=CARTESIAN_POINT('Ctrl Pts',(164.934303787571,-3.97021425596207,133.710353697194));
#29460=CARTESIAN_POINT('Ctrl Pts',(164.926649276581,-3.88754520286731,133.817029759401));
#29461=CARTESIAN_POINT('Ctrl Pts',(164.918983534378,-3.80475485217408,133.923862343906));
#29462=CARTESIAN_POINT('Ctrl Pts',(164.911317792174,-3.7176655262465,134.027140019929));
#29463=CARTESIAN_POINT('Ctrl Pts',(164.90365204997,-3.62663680993003,134.126511804878));
#29464=CARTESIAN_POINT('Ctrl Pts',(164.899596347418,-3.57847638562538,134.179086283798));
#29465=CARTESIAN_POINT('Ctrl Pts',(164.895540644865,-3.52921386058134,134.230568105216));
#29466=CARTESIAN_POINT('Ctrl Pts',(164.891484942312,-3.47890617260596,134.280909898779));
#29467=CARTESIAN_POINT('Ctrl Pts',(164.883710608193,-3.38247188779414,134.377409560238));
#29468=CARTESIAN_POINT('Ctrl Pts',(164.875936274074,-3.2818666803904,134.470046614896));
#29469=CARTESIAN_POINT('Ctrl Pts',(164.868161939955,-3.17743268209208,134.558439014892));
#29470=CARTESIAN_POINT('Ctrl Pts',(164.860397187008,-3.07312738936337,134.646722479156));
#29471=CARTESIAN_POINT('Ctrl Pts',(164.852632434061,-2.96500298998962,134.730771447044));
#29472=CARTESIAN_POINT('Ctrl Pts',(164.844867681114,-2.85343927079618,134.810239720881));
#29473=CARTESIAN_POINT('Ctrl Pts',(164.837110640229,-2.74198635826087,134.889629065709));
#29474=CARTESIAN_POINT('Ctrl Pts',(164.829353599344,-2.62710124023978,134.964446545056));
#29475=CARTESIAN_POINT('Ctrl Pts',(164.821596558459,-2.5091974026208,135.034385612431));
#29476=CARTESIAN_POINT('Ctrl Pts',(164.813845367219,-2.39138247720325,135.104271938211));
#29477=CARTESIAN_POINT('Ctrl Pts',(164.806094175979,-2.2705536981992,135.169286975887));
#29478=CARTESIAN_POINT('Ctrl Pts',(164.798342984739,-2.14715390856942,135.229167184572));
#29479=CARTESIAN_POINT('Ctrl Pts',(164.790595087962,-2.02380656714206,135.28902194257));
#29480=CARTESIAN_POINT('Ctrl Pts',(164.782847191184,-1.89789073948527,135.343746041955));
#29481=CARTESIAN_POINT('Ctrl Pts',(164.775099294407,-1.76987407575634,135.393121759581));
#29482=CARTESIAN_POINT('Ctrl Pts',(164.767353018323,-1.64188419035378,135.442487148871));
#29483=CARTESIAN_POINT('Ctrl Pts',(164.759606742239,-1.51179470751058,135.486506241084));
#29484=CARTESIAN_POINT('Ctrl Pts',(164.751860466155,-1.38009310429455,135.525009522746));
#29485=CARTESIAN_POINT('Ctrl Pts',(164.74411413289,-1.24839052888712,135.563513088631));
#29486=CARTESIAN_POINT('Ctrl Pts',(164.736367799624,-1.11507618461801,135.596500653009));
#29487=CARTESIAN_POINT('Ctrl Pts',(164.728621466359,-0.98065216444509,135.623852747954));
#29488=CARTESIAN_POINT('Ctrl Pts',(164.720873398356,-0.84619804094479,135.651210968211));
#29489=CARTESIAN_POINT('Ctrl Pts',(164.713125330353,-0.710634130087389,
135.672931129812));
#29490=CARTESIAN_POINT('Ctrl Pts',(164.70537726235,-0.574471760764326,135.688945068528));
#29491=CARTESIAN_POINT('Ctrl Pts',(164.697620959608,-0.438164676454887,
135.70497602705));
#29492=CARTESIAN_POINT('Ctrl Pts',(164.689864656867,-0.30125825201202,135.715288602173));
#29493=CARTESIAN_POINT('Ctrl Pts',(164.682108354125,-0.164268529847385,
135.719866584667));
#29494=CARTESIAN_POINT('Ctrl Pts',(164.67434791161,-0.027205692143024,135.724447010567));
#29495=CARTESIAN_POINT('Ctrl Pts',(164.666587469096,0.109940141110505,135.723286748391));
#29496=CARTESIAN_POINT('Ctrl Pts',(164.658827026582,0.24665489611004,135.716421735338));
#29497=CARTESIAN_POINT('Ctrl Pts',(164.651054126317,0.383589117770987,135.709545701956));
#29498=CARTESIAN_POINT('Ctrl Pts',(164.643281226051,0.520090488796811,135.696946653504));
#29499=CARTESIAN_POINT('Ctrl Pts',(164.635508325786,0.655651112811216,135.678712336592));
#29500=CARTESIAN_POINT('Ctrl Pts',(164.628017990024,0.78628376668563,135.661140883028));
#29501=CARTESIAN_POINT('Ctrl Pts',(164.620527654262,0.916042579753152,135.638336813516));
#29502=CARTESIAN_POINT('Ctrl Pts',(164.6130373185,1.04448560797531,135.610422714255));
#29503=CARTESIAN_POINT('Ctrl Pts',(164.605262984381,1.1777985926524,135.581450243436));
#29504=CARTESIAN_POINT('Ctrl Pts',(164.597488650262,1.31011634237424,135.546880823988));
#29505=CARTESIAN_POINT('Ctrl Pts',(164.589714316143,1.44093249891663,135.506795794798));
#29506=CARTESIAN_POINT('Ctrl Pts',(164.581949563196,1.57158743623721,135.466760166823));
#29507=CARTESIAN_POINT('Ctrl Pts',(164.574184810249,1.7007440922588,135.421222567542));
#29508=CARTESIAN_POINT('Ctrl Pts',(164.566420057301,1.82790591701633,135.370315394065));
#29509=CARTESIAN_POINT('Ctrl Pts',(164.558663016416,1.95494144285745,135.319458782311));
#29510=CARTESIAN_POINT('Ctrl Pts',(164.550905975531,2.07998571968843,135.26324335391));
#29511=CARTESIAN_POINT('Ctrl Pts',(164.543148934646,2.20255734204255,135.201851290383));
#29512=CARTESIAN_POINT('Ctrl Pts',(164.535397743406,2.32503653218259,135.14050552309));
#29513=CARTESIAN_POINT('Ctrl Pts',(164.527646552166,2.44504643116031,135.073991065209));
#29514=CARTESIAN_POINT('Ctrl Pts',(164.519895360926,2.5621259471246,135.002538042779));
#29515=CARTESIAN_POINT('Ctrl Pts',(164.512147464149,2.67915570117121,134.93111538979));
#29516=CARTESIAN_POINT('Ctrl Pts',(164.504399567372,2.79325721636496,134.854758550289));
#29517=CARTESIAN_POINT('Ctrl Pts',(164.496651670595,2.90399453972257,134.773743286919));
#29518=CARTESIAN_POINT('Ctrl Pts',(164.488905394511,3.01470869921935,134.692744970196));
#29519=CARTESIAN_POINT('Ctrl Pts',(164.481159118427,3.12205975127329,134.607090398522));
#29520=CARTESIAN_POINT('Ctrl Pts',(164.473412842342,3.22564158613382,134.517098073986));
#29521=CARTESIAN_POINT('Ctrl Pts',(164.465666509077,3.32922418561214,134.427105085147));
#29522=CARTESIAN_POINT('Ctrl Pts',(164.457920175812,3.42903721724155,134.332774535968));
#29523=CARTESIAN_POINT('Ctrl Pts',(164.450173842546,3.52470877576302,134.234464276139));
#29524=CARTESIAN_POINT('Ctrl Pts',(164.442425774543,3.62040175926644,134.136132000411));
#29525=CARTESIAN_POINT('Ctrl Pts',(164.43467770654,3.7119511515193,134.033818520727));
#29526=CARTESIAN_POINT('Ctrl Pts',(164.426929638537,3.79902321826983,133.927917188135));
#29527=CARTESIAN_POINT('Ctrl Pts',(164.419173335796,3.88618782624916,133.821903302347));
#29528=CARTESIAN_POINT('Ctrl Pts',(164.411417033054,3.96886535430429,133.712294248825));
#29529=CARTESIAN_POINT('Ctrl Pts',(164.403660730312,4.04676323162127,133.599515427178));
#29530=CARTESIAN_POINT('Ctrl Pts',(164.395900287798,4.12470268538086,133.486676412079));
#29531=CARTESIAN_POINT('Ctrl Pts',(164.388139845283,4.19785719679812,133.370664588344));
#29532=CARTESIAN_POINT('Ctrl Pts',(164.380379402769,4.26597913140994,133.251931885757));
#29533=CARTESIAN_POINT('Ctrl Pts',(164.372606502504,4.33421042139878,133.133008582896));
#29534=CARTESIAN_POINT('Ctrl Pts',(164.364833602238,4.39739281038346,133.011356020095));
#29535=CARTESIAN_POINT('Ctrl Pts',(164.357060701973,4.45532559167427,132.887448934146));
#29536=CARTESIAN_POINT('Ctrl Pts',(164.349570366211,4.51115237044098,132.768046182875));
#29537=CARTESIAN_POINT('Ctrl Pts',(164.342080030449,4.56210446891386,132.646550261889));
#29538=CARTESIAN_POINT('Ctrl Pts',(164.334589694687,4.60804614078636,132.52339925206));
#29539=CARTESIAN_POINT('Ctrl Pts',(164.326815360568,4.65572970511176,132.395578934262));
#29540=CARTESIAN_POINT('Ctrl Pts',(164.319041026449,4.69816644923869,132.265570648371));
#29541=CARTESIAN_POINT('Ctrl Pts',(164.31126669233,4.73515110688718,132.133844373557));
#29542=CARTESIAN_POINT('Ctrl Pts',(164.303501939383,4.77209018425052,132.002280439605));
#29543=CARTESIAN_POINT('Ctrl Pts',(164.295737186436,4.8035904396895,131.869003102258));
#29544=CARTESIAN_POINT('Ctrl Pts',(164.287972433489,4.8294948652594,131.734501686938));
#29545=CARTESIAN_POINT('Ctrl Pts',(164.280215392603,4.85537356218869,131.60013386032));
#29546=CARTESIAN_POINT('Ctrl Pts',(164.272458351719,4.87566741617433,131.464544756596));
#29547=CARTESIAN_POINT('Ctrl Pts',(164.264701310833,4.89026949027675,131.32823786938));
#29548=CARTESIAN_POINT('Ctrl Pts',(164.256950119593,4.90486055284151,131.192033772249));
#29549=CARTESIAN_POINT('Ctrl Pts',(164.249198928353,4.91376833744172,131.055113356191));
#29550=CARTESIAN_POINT('Ctrl Pts',(164.241447737113,4.9169372242215,130.917988939586));
#29551=CARTESIAN_POINT('Ctrl Pts',(164.233699840336,4.92010476413985,130.780922804516));
#29552=CARTESIAN_POINT('Ctrl Pts',(164.225951943559,4.91753824857641,130.643653231391));
#29553=CARTESIAN_POINT('Ctrl Pts',(164.218204046782,4.90923404121606,130.506696056247));
#29554=CARTESIAN_POINT('Ctrl Pts',(164.210457770698,4.90093157091687,130.369767529591));
#29555=CARTESIAN_POINT('Ctrl Pts',(164.202711494614,4.88689381973439,130.23315166094));
#29556=CARTESIAN_POINT('Ctrl Pts',(164.19496521853,4.86716924025654,130.097362280085));
#29557=CARTESIAN_POINT('Ctrl Pts',(164.187218885264,4.84744451517635,129.961571896865));
#29558=CARTESIAN_POINT('Ctrl Pts',(164.179472551999,4.82203293423624,129.82660840052));
#29559=CARTESIAN_POINT('Ctrl Pts',(164.171726218734,4.79103454264045,129.692978111979));
#29560=CARTESIAN_POINT('Ctrl Pts',(164.163978150731,4.76002920916975,129.55931789786));
#29561=CARTESIAN_POINT('Ctrl Pts',(164.156230082728,4.72343466377439,129.42699186643));
#29562=CARTESIAN_POINT('Ctrl Pts',(164.148482014725,4.68140145231587,129.296493413614));
#29563=CARTESIAN_POINT('Ctrl Pts',(164.140725711983,4.63932356745998,129.165856265489));
#29564=CARTESIAN_POINT('Ctrl Pts',(164.132969409241,4.5917955898666,129.037050948808));
#29565=CARTESIAN_POINT('Ctrl Pts',(164.125213106499,4.53901727860459,128.910553550563));
#29566=CARTESIAN_POINT('Ctrl Pts',(164.117452663985,4.48621079796874,128.783988636848));
#29567=CARTESIAN_POINT('Ctrl Pts',(164.109692221471,4.42814856535426,128.659734450074));
#29568=CARTESIAN_POINT('Ctrl Pts',(164.101931778957,4.36507694961207,128.538243611217));
#29569=CARTESIAN_POINT('Ctrl Pts',(164.094158878691,4.30190408571302,128.416557744479));
#29570=CARTESIAN_POINT('Ctrl Pts',(164.086385978426,4.23370596381108,128.297644429485));
#29571=CARTESIAN_POINT('Ctrl Pts',(164.07861307816,4.1607735065459,128.181929133289));
#29572=CARTESIAN_POINT('Ctrl Pts',(164.071122742398,4.09049232780753,128.070420379579));
#29573=CARTESIAN_POINT('Ctrl Pts',(164.063632406636,4.01581522233693,127.961881423098));
#29574=CARTESIAN_POINT('Ctrl Pts',(164.056142070874,3.93703738578363,127.856663264471));
#29575=CARTESIAN_POINT('Ctrl Pts',(164.048367736755,3.85527266361391,127.74745572738));
#29576=CARTESIAN_POINT('Ctrl Pts',(164.040593402636,3.76883110744344,127.641479838522));
#29577=CARTESIAN_POINT('Ctrl Pts',(164.032819068517,3.67799717261996,127.539162329452));
#29578=CARTESIAN_POINT('Ctrl Pts',(164.02505431557,3.58727518250291,127.436970917568));
#29579=CARTESIAN_POINT('Ctrl Pts',(164.017289562622,3.49217184148334,127.338429204217));
#29580=CARTESIAN_POINT('Ctrl Pts',(164.009524809675,3.39301396626784,127.243933776974));
#29581=CARTESIAN_POINT('Ctrl Pts',(164.00176776879,3.29395457605215,127.149532203921));
#29582=CARTESIAN_POINT('Ctrl Pts',(163.994010727905,3.19084894678977,127.0591691873));
#29583=CARTESIAN_POINT('Ctrl Pts',(163.98625368702,3.08406287989156,126.973206846784));
#29584=CARTESIAN_POINT('Ctrl Pts',(163.97850249578,2.97735734119732,126.887309331139));
#29585=CARTESIAN_POINT('Ctrl Pts',(163.97075130454,2.86697719254218,126.805806130327));
#29586=CARTESIAN_POINT('Ctrl Pts',(163.9630001133,2.75332339799587,126.729020959507));
#29587=CARTESIAN_POINT('Ctrl Pts',(163.955252216523,2.63971790934375,126.652268424432));
#29588=CARTESIAN_POINT('Ctrl Pts',(163.947504319746,2.52284186544447,126.580230149393));
#29589=CARTESIAN_POINT('Ctrl Pts',(163.939756422969,2.40312728824704,126.513188015703));
#29590=CARTESIAN_POINT('Ctrl Pts',(163.932010146885,2.28343775275832,126.446159905781));
#29591=CARTESIAN_POINT('Ctrl Pts',(163.9242638708,2.16091120589356,126.384126049386));
#29592=CARTESIAN_POINT('Ctrl Pts',(163.916517594716,2.03600613701787,126.327323419538));
#29593=CARTESIAN_POINT('Ctrl Pts',(163.908771261451,1.91110014612176,126.270520370386));
#29594=CARTESIAN_POINT('Ctrl Pts',(163.901024928186,1.78381595407159,126.218948786684));
#29595=CARTESIAN_POINT('Ctrl Pts',(163.89327859492,1.65463361987969,126.172798176395));
#29596=CARTESIAN_POINT('Ctrl Pts',(163.885530526917,1.52542235619964,126.126637230998));
#29597=CARTESIAN_POINT('Ctrl Pts',(163.877782458914,1.39431247263143,126.085899806219));
#29598=CARTESIAN_POINT('Ctrl Pts',(163.870034390911,1.26180045085764,126.050725936113));
#29599=CARTESIAN_POINT('Ctrl Pts',(163.86227808817,1.12914759373007,126.015514682799));
#29600=CARTESIAN_POINT('Ctrl Pts',(163.854521785428,0.995090000025596,125.9858788965));
#29601=CARTESIAN_POINT('Ctrl Pts',(163.846765482686,0.860136189870434,125.961907850902));
#29602=CARTESIAN_POINT('Ctrl Pts',(163.839005040172,0.725110350803273,125.937924011235));
#29603=CARTESIAN_POINT('Ctrl Pts',(163.831244597658,0.58918772943176,125.919610988913));
#29604=CARTESIAN_POINT('Ctrl Pts',(163.823484155143,0.45288229698264,125.907006159537));
#29605=CARTESIAN_POINT('Ctrl Pts',(163.815711254878,0.316358054952771,125.894381095769));
#29606=CARTESIAN_POINT('Ctrl Pts',(163.807938354612,0.179450164528416,125.887482555823));
#29607=CARTESIAN_POINT('Ctrl Pts',(163.800165454347,0.0426738339851343,
125.886295753578));
#29608=CARTESIAN_POINT('Ctrl Pts',(163.792675118585,-0.0891303324227685,
125.885152094584));
#29609=CARTESIAN_POINT('Ctrl Pts',(163.785184782823,-0.220812030087202,
125.889312101193));
#29610=CARTESIAN_POINT('Ctrl Pts',(163.777694447061,-0.351916391783413,
125.898717141355));
#29611=CARTESIAN_POINT('Ctrl Pts',(163.769920112942,-0.487991615203079,
125.908478776473));
#29612=CARTESIAN_POINT('Ctrl Pts',(163.762145778823,-0.623875904455109,
125.923921949299));
#29613=CARTESIAN_POINT('Ctrl Pts',(163.754371444704,-0.759056483132193,
125.94503799832));
#29614=CARTESIAN_POINT('Ctrl Pts',(163.746606691757,-0.894070463827218,
125.966128023698));
#29615=CARTESIAN_POINT('Ctrl Pts',(163.73884193881,-1.02838207696434,125.992876954883));
#29616=CARTESIAN_POINT('Ctrl Pts',(163.731077185863,-1.16148100977317,126.025224196994));
#29617=CARTESIAN_POINT('Ctrl Pts',(163.723320144978,-1.29444774684561,126.057539311368));
#29618=CARTESIAN_POINT('Ctrl Pts',(163.715563104093,-1.42620382305366,126.095441579647));
#29619=CARTESIAN_POINT('Ctrl Pts',(163.707806063208,-1.5562468522622,126.138818977271));
#29620=CARTESIAN_POINT('Ctrl Pts',(163.700054871968,-1.68619181501131,126.182163663663));
#29621=CARTESIAN_POINT('Ctrl Pts',(163.692303680728,-1.81442593267833,126.23097513799));
#29622=CARTESIAN_POINT('Ctrl Pts',(163.684552489487,-1.94046012365977,126.285091033774));
#29623=CARTESIAN_POINT('Ctrl Pts',(163.67680459271,-2.06644074674768,126.339183928859));
#29624=CARTESIAN_POINT('Ctrl Pts',(163.669056695933,-2.19022294435144,126.398576607402));
#29625=CARTESIAN_POINT('Ctrl Pts',(163.661308799156,-2.31133604332367,126.463057960836));
#29626=CARTESIAN_POINT('Ctrl Pts',(163.653562523072,-2.43242380804632,126.527525826161));
#29627=CARTESIAN_POINT('Ctrl Pts',(163.645816246988,-2.55084323977889,126.597080065527));
#29628=CARTESIAN_POINT('Ctrl Pts',(163.638069970904,-2.66614714170715,126.671463028553));
#29629=CARTESIAN_POINT('Ctrl Pts',(163.630323637639,-2.78145189478281,126.745846540658));
#29630=CARTESIAN_POINT('Ctrl Pts',(163.622577304373,-2.89364074362766,126.825058635608));
#29631=CARTESIAN_POINT('Ctrl Pts',(163.614830971108,-3.00229476620142,126.908797859845));
#29632=CARTESIAN_POINT('Ctrl Pts',(163.607082903105,-3.11097312109015,126.992555836902));
#29633=CARTESIAN_POINT('Ctrl Pts',(163.599334835102,-3.21611476490606,127.080842722013));
#29634=CARTESIAN_POINT('Ctrl Pts',(163.591586767099,-3.31733352255727,127.173316502905));
#29635=CARTESIAN_POINT('Ctrl Pts',(163.583830464357,-3.41865985670864,127.265888566031));
#29636=CARTESIAN_POINT('Ctrl Pts',(163.576074161615,-3.5160546869873,127.362656149934));
#29637=CARTESIAN_POINT('Ctrl Pts',(163.568317858873,-3.60916803736314,127.463239676837));
#29638=CARTESIAN_POINT('Ctrl Pts',(163.560557416359,-3.70233108513772,127.563876888197));
#29639=CARTESIAN_POINT('Ctrl Pts',(163.552796973845,-3.7912078464149,127.6683338032));
#29640=CARTESIAN_POINT('Ctrl Pts',(163.545036531331,-3.87548906204061,127.776198205722));
#29641=CARTESIAN_POINT('Ctrl Pts',(163.537263631065,-3.95990557335569,127.884235761759));
#29642=CARTESIAN_POINT('Ctrl Pts',(163.5294907308,-4.03971156932458,127.995691418059));
#29643=CARTESIAN_POINT('Ctrl Pts',(163.521717830534,-4.11464100727173,128.110123723049));
#29644=CARTESIAN_POINT('Ctrl Pts',(163.514227494772,-4.18684657141375,128.220396125515));
#29645=CARTESIAN_POINT('Ctrl Pts',(163.50673715901,-4.25452381412898,128.333432252367));
#29646=CARTESIAN_POINT('Ctrl Pts',(163.499246823248,-4.31747619737546,128.44881771887));
#29647=CARTESIAN_POINT('Ctrl Pts',(163.491070124136,-4.38619710823455,128.574776323598));
#29648=CARTESIAN_POINT('Ctrl Pts',(163.482893425024,-4.44948688220427,128.7038996195));
#29649=CARTESIAN_POINT('Ctrl Pts',(163.474716725911,-4.50705826035773,128.835703994322));
#29650=CARTESIAN_POINT('Ctrl Pts',(163.466558243417,-4.56450137700018,128.967214726213));
#29651=CARTESIAN_POINT('Ctrl Pts',(163.458399760922,-4.61625136555339,129.101394325791));
#29652=CARTESIAN_POINT('Ctrl Pts',(163.450241278427,-4.66206679866313,129.237734871798));
#29653=CARTESIAN_POINT('Ctrl Pts',(163.44344819256,-4.70021460021492,129.351257581058));
#29654=CARTESIAN_POINT('Ctrl Pts',(163.436655106692,-4.73424876069842,129.466277884052));
#29655=CARTESIAN_POINT('Ctrl Pts',(163.429862020825,-4.76405452823405,129.582490119308));
#29656=CARTESIAN_POINT('Origin',(213.235140564004,0.,130.804360617566));
#29657=CARTESIAN_POINT('',(161.334944359449,-4.76405452823403,129.582490119308));
#29658=CARTESIAN_POINT('',(161.680195102581,-4.76405452823405,129.582490119308));
#29659=CARTESIAN_POINT('',(213.235140564004,-4.76405452823405,129.582490119308));
#29660=CARTESIAN_POINT('',(163.014859436027,-4.91824810772423,130.808674938719));
#29661=CARTESIAN_POINT('Ctrl Pts',(163.014859435991,-4.91824810772368,130.80867493935));
#29662=CARTESIAN_POINT('Ctrl Pts',(163.003397208645,-4.91807088703354,131.010703292268));
#29663=CARTESIAN_POINT('Ctrl Pts',(162.991934981299,-4.90544232132287,131.21220712713));
#29664=CARTESIAN_POINT('Ctrl Pts',(162.980472753952,-4.88057421730792,131.411961121063));
#29665=CARTESIAN_POINT('Ctrl Pts',(162.974295359895,-4.86717192879038,131.519615514723));
#29666=CARTESIAN_POINT('Ctrl Pts',(162.968117965839,-4.85021539564769,131.626762338073));
#29667=CARTESIAN_POINT('Ctrl Pts',(162.961940571782,-4.82974284417397,131.733213200945));
#29668=CARTESIAN_POINT('Ctrl Pts',(162.954166237662,-4.80397786075843,131.86718305419));
#29669=CARTESIAN_POINT('Ctrl Pts',(162.946391903543,-4.77259365760229,132.000292270418));
#29670=CARTESIAN_POINT('Ctrl Pts',(162.938617569424,-4.73565939896706,132.132032685313));
#29671=CARTESIAN_POINT('Ctrl Pts',(162.930852816477,-4.69877065850475,132.26361074192));
#29672=CARTESIAN_POINT('Ctrl Pts',(162.92308806353,-4.65634557654704,132.393822980838));
#29673=CARTESIAN_POINT('Ctrl Pts',(162.915323310583,-4.60850459624918,132.522169817929));
#29674=CARTESIAN_POINT('Ctrl Pts',(162.907566269698,-4.56071113228747,132.650389179131));
#29675=CARTESIAN_POINT('Ctrl Pts',(162.899809228813,-4.50751261039981,132.776746461578));
#29676=CARTESIAN_POINT('Ctrl Pts',(162.892052187928,-4.44907960724067,132.90075602658));
#29677=CARTESIAN_POINT('Ctrl Pts',(162.884300996688,-4.39069066886354,133.024672075005));
#29678=CARTESIAN_POINT('Ctrl Pts',(162.876549805448,-4.32707527217559,133.146243577686));
#29679=CARTESIAN_POINT('Ctrl Pts',(162.868798614208,-4.25845241201014,133.265004053163));
#29680=CARTESIAN_POINT('Ctrl Pts',(162.861050717431,-4.18985871839095,133.383714052269));
#29681=CARTESIAN_POINT('Ctrl Pts',(162.853302820653,-4.11626198952557,133.499615062655));
#29682=CARTESIAN_POINT('Ctrl Pts',(162.845554923876,-4.03792744697405,133.612264639336));
#29683=CARTESIAN_POINT('Ctrl Pts',(162.837808647792,-3.95960929032012,133.724890652155));
#29684=CARTESIAN_POINT('Ctrl Pts',(162.830062371708,-3.87655551429641,133.834266263303));
#29685=CARTESIAN_POINT('Ctrl Pts',(162.822316095624,-3.78907478375688,133.939977836807));
#29686=CARTESIAN_POINT('Ctrl Pts',(162.814569762359,-3.70159340745443,134.045690190649));
#29687=CARTESIAN_POINT('Ctrl Pts',(162.806823429093,-3.60968526068687,134.147738151674));
#29688=CARTESIAN_POINT('Ctrl Pts',(162.799077095828,-3.51369916539395,134.245741334315));
#29689=CARTESIAN_POINT('Ctrl Pts',(162.791329027825,-3.41769157468039,134.343766464089));
#29690=CARTESIAN_POINT('Ctrl Pts',(162.783580959822,-3.31760449173534,134.437744733782));
#29691=CARTESIAN_POINT('Ctrl Pts',(162.775832891819,-3.21382314562898,134.527333065909));
#29692=CARTESIAN_POINT('Ctrl Pts',(162.768076589077,-3.1099314994731,134.617016613581));
#29693=CARTESIAN_POINT('Ctrl Pts',(162.760320286336,-3.00233804335629,134.70230064761));
#29694=CARTESIAN_POINT('Ctrl Pts',(162.752563983594,-2.89146103349163,134.782882473017));
#29695=CARTESIAN_POINT('Ctrl Pts',(162.74480354108,-2.7805248452284,134.86350730737));
#29696=CARTESIAN_POINT('Ctrl Pts',(162.737043098565,-2.66630193659719,134.939424715985));
#29697=CARTESIAN_POINT('Ctrl Pts',(162.729282656051,-2.54923816469362,135.010376290643));
#29698=CARTESIAN_POINT('Ctrl Pts',(162.721509755786,-2.43198647163091,135.081441763067));
#29699=CARTESIAN_POINT('Ctrl Pts',(162.71373685552,-2.31188514488524,135.147525283159));
#29700=CARTESIAN_POINT('Ctrl Pts',(162.705963955255,-2.18940396812855,135.208414809653));
#29701=CARTESIAN_POINT('Ctrl Pts',(162.698473619493,-2.0713752906576,135.267090848489));
#29702=CARTESIAN_POINT('Ctrl Pts',(162.690983283731,-1.951137067367,135.320943841119));
#29703=CARTESIAN_POINT('Ctrl Pts',(162.683492947969,-1.82912399543438,135.369827567597));
#29704=CARTESIAN_POINT('Ctrl Pts',(162.67571861385,-1.70248476079516,135.420564735422));
#29705=CARTESIAN_POINT('Ctrl Pts',(162.667944279731,-1.57353227892646,135.466109099204));
#29706=CARTESIAN_POINT('Ctrl Pts',(162.660169945612,-1.44273146783083,135.506244173571));
#29707=CARTESIAN_POINT('Ctrl Pts',(162.652405192665,-1.31209185704487,135.546329785046));
#29708=CARTESIAN_POINT('Ctrl Pts',(162.644640439717,-1.17960881955273,135.5810192578));
#29709=CARTESIAN_POINT('Ctrl Pts',(162.63687568677,-1.04576777210489,135.610143886642));
#29710=CARTESIAN_POINT('Ctrl Pts',(162.629118645885,-0.912059657472297,
135.639239588491));
#29711=CARTESIAN_POINT('Ctrl Pts',(162.621361605,-0.776996596599036,135.662781362977));
#29712=CARTESIAN_POINT('Ctrl Pts',(162.613604564115,-0.641079371915657,
135.680650221497));
#29713=CARTESIAN_POINT('Ctrl Pts',(162.605853372875,-0.505264643468831,
135.698505604971));
#29714=CARTESIAN_POINT('Ctrl Pts',(162.598102181635,-0.36859741937794,135.710696536804));
#29715=CARTESIAN_POINT('Ctrl Pts',(162.590350990395,-0.231588535762066,
135.717155118927));
#29716=CARTESIAN_POINT('Ctrl Pts',(162.582603093618,-0.0946378845763739,
135.723610955981));
#29717=CARTESIAN_POINT('Ctrl Pts',(162.574855196841,0.0426537475999879,
135.724339270772));
#29718=CARTESIAN_POINT('Ctrl Pts',(162.567107300064,0.17977076054081,135.719324049389));
#29719=CARTESIAN_POINT('Ctrl Pts',(162.55936102398,0.316859091558426,135.714309877082));
#29720=CARTESIAN_POINT('Ctrl Pts',(162.551614747896,0.453772485537455,135.703554572581));
#29721=CARTESIAN_POINT('Ctrl Pts',(162.543868471811,0.589996097926005,135.687094244023));
#29722=CARTESIAN_POINT('Ctrl Pts',(162.536122138546,0.72622071588627,135.670633793958));
#29723=CARTESIAN_POINT('Ctrl Pts',(162.528375805281,0.861755153953806,135.648468282702));
#29724=CARTESIAN_POINT('Ctrl Pts',(162.520629472015,0.996090836200424,135.620685576343));
#29725=CARTESIAN_POINT('Ctrl Pts',(162.512881404012,1.13045660199162,135.592896648239));
#29726=CARTESIAN_POINT('Ctrl Pts',(162.50513333601,1.26362269498177,135.55948810106));
#29727=CARTESIAN_POINT('Ctrl Pts',(162.497385268007,1.39509224864404,135.520598597171));
#29728=CARTESIAN_POINT('Ctrl Pts',(162.489628965265,1.52670152971249,135.481667761055));
#29729=CARTESIAN_POINT('Ctrl Pts',(162.481872662523,1.6566102940577,135.43724444279));
#29730=CARTESIAN_POINT('Ctrl Pts',(162.474116359781,1.78433779812183,135.387516919144));
#29731=CARTESIAN_POINT('Ctrl Pts',(162.466355917267,1.91213347420086,135.337762854421));
#29732=CARTESIAN_POINT('Ctrl Pts',(162.458595474753,2.03774521232653,135.282699100171));
#29733=CARTESIAN_POINT('Ctrl Pts',(162.450835032238,2.16071460969468,135.222561092641));
#29734=CARTESIAN_POINT('Ctrl Pts',(162.443062131973,2.28388140845611,135.162326546243));
#29735=CARTESIAN_POINT('Ctrl Pts',(162.435289231708,2.40439704623602,135.097001655394));
#29736=CARTESIAN_POINT('Ctrl Pts',(162.427516331442,2.52182919716291,135.026867048921));
#29737=CARTESIAN_POINT('Ctrl Pts',(162.42002599568,2.63499239360999,134.959282012052));
#29738=CARTESIAN_POINT('Ctrl Pts',(162.412535659918,2.74529213817591,134.887231047424));
#29739=CARTESIAN_POINT('Ctrl Pts',(162.405045324156,2.85237044743471,134.81100084263));
#29740=CARTESIAN_POINT('Ctrl Pts',(162.397270990037,2.96350866333462,134.731880346452));
#29741=CARTESIAN_POINT('Ctrl Pts',(162.389496655918,3.07152839275741,134.648006812439));
#29742=CARTESIAN_POINT('Ctrl Pts',(162.381722321799,3.17599620089133,134.559654373642));
#29743=CARTESIAN_POINT('Ctrl Pts',(162.373957568852,3.28033526178828,134.47141082133));
#29744=CARTESIAN_POINT('Ctrl Pts',(162.366192815905,3.3811308155156,134.378699597134));
#29745=CARTESIAN_POINT('Ctrl Pts',(162.358428062957,3.47797854600734,134.281837906638));
#29746=CARTESIAN_POINT('Ctrl Pts',(162.350671022072,3.57473008596778,134.185072420539));
#29747=CARTESIAN_POINT('Ctrl Pts',(162.342913981187,3.66754133108121,134.084164946391));
#29748=CARTESIAN_POINT('Ctrl Pts',(162.335156940302,3.7560414877301,133.97947249039));
#29749=CARTESIAN_POINT('Ctrl Pts',(162.327405749062,3.84447490572244,133.874858983785));
#29750=CARTESIAN_POINT('Ctrl Pts',(162.319654557822,3.92860345484192,133.766466473976));
#29751=CARTESIAN_POINT('Ctrl Pts',(162.311903366582,4.00809389112144,133.654688041294));
#29752=CARTESIAN_POINT('Ctrl Pts',(162.304155469805,4.08755054184511,133.542957117428));
#29753=CARTESIAN_POINT('Ctrl Pts',(162.296407573028,4.16237277443135,133.427843450911));
#29754=CARTESIAN_POINT('Ctrl Pts',(162.288659676251,4.23226842140721,133.309772174907));
#29755=CARTESIAN_POINT('Ctrl Pts',(162.280913400167,4.3021494477205,133.191725596869));
#29756=CARTESIAN_POINT('Ctrl Pts',(162.273167124083,4.36710573917915,133.07072297613));
#29757=CARTESIAN_POINT('Ctrl Pts',(162.265420847999,4.42688938852497,132.947216983323));
#29758=CARTESIAN_POINT('Ctrl Pts',(162.257674514733,4.48667347918008,132.823710078822));
#29759=CARTESIAN_POINT('Ctrl Pts',(162.249928181468,4.54128468118888,132.697700117285));
#29760=CARTESIAN_POINT('Ctrl Pts',(162.242181848203,4.59052202106745,132.569662471809));
#29761=CARTESIAN_POINT('Ctrl Pts',(162.2344337802,4.63977038730688,132.441596153191));
#29762=CARTESIAN_POINT('Ctrl Pts',(162.226685712197,4.68364235640963,132.311501611899));
#29763=CARTESIAN_POINT('Ctrl Pts',(162.218937644194,4.7219860204571,132.179871826211));
#29764=CARTESIAN_POINT('Ctrl Pts',(162.211181341452,4.76037043660705,132.04810214282));
#29765=CARTESIAN_POINT('Ctrl Pts',(162.20342503871,4.79321470114337,131.914794331547));
#29766=CARTESIAN_POINT('Ctrl Pts',(162.195668735968,4.82041736300751,131.780454623754));
#29767=CARTESIAN_POINT('Ctrl Pts',(162.187908293454,4.84763454375136,131.646043214814));
#29768=CARTESIAN_POINT('Ctrl Pts',(162.18014785094,4.86920406050837,131.51059919784));
#29769=CARTESIAN_POINT('Ctrl Pts',(162.172387408426,4.8850762145486,131.374635499138));
#29770=CARTESIAN_POINT('Ctrl Pts',(162.16461450816,4.90097384797955,131.238453539436));
#29771=CARTESIAN_POINT('Ctrl Pts',(162.156841607895,4.9111558131901,131.101750621039));
#29772=CARTESIAN_POINT('Ctrl Pts',(162.149068707629,4.91562452846481,130.965042158681));
#29773=CARTESIAN_POINT('Ctrl Pts',(162.141578371867,4.9199307946833,130.833303393277));
#29774=CARTESIAN_POINT('Ctrl Pts',(162.134088036105,4.91893198371118,130.701559787998));
#29775=CARTESIAN_POINT('Ctrl Pts',(162.126597700343,4.91267579515416,130.570267486085));
#29776=CARTESIAN_POINT('Ctrl Pts',(162.118823366224,4.9061824013065,130.433997196641));
#29777=CARTESIAN_POINT('Ctrl Pts',(162.111049032105,4.89400452400106,130.297781445141));
#29778=CARTESIAN_POINT('Ctrl Pts',(162.103274697986,4.87613851703441,130.162133068178));
#29779=CARTESIAN_POINT('Ctrl Pts',(162.095509945039,4.85829452832462,130.026651865716));
#29780=CARTESIAN_POINT('Ctrl Pts',(162.087745192092,4.83477640854833,129.891737030411));
#29781=CARTESIAN_POINT('Ctrl Pts',(162.079980439144,4.8056324890368,129.757900182187));
#29782=CARTESIAN_POINT('Ctrl Pts',(162.072223398259,4.77651751567699,129.624196262607));
#29783=CARTESIAN_POINT('Ctrl Pts',(162.064466357374,4.74178794485278,129.491568578963));
#29784=CARTESIAN_POINT('Ctrl Pts',(162.056709316489,4.7015437129799,129.360522060996));
#29785=CARTESIAN_POINT('Ctrl Pts',(162.048958125249,4.66132982959531,129.229574366227));
#29786=CARTESIAN_POINT('Ctrl Pts',(162.041206934009,4.61560967701055,129.100205836022));
#29787=CARTESIAN_POINT('Ctrl Pts',(162.033455742769,4.56453383833639,128.972909307489));
#29788=CARTESIAN_POINT('Ctrl Pts',(162.025707845992,4.51347970825616,128.845666883377));
#29789=CARTESIAN_POINT('Ctrl Pts',(162.017959949215,4.45707456477479,128.720495071466));
#29790=CARTESIAN_POINT('Ctrl Pts',(162.010212052438,4.39551816080704,128.597869475387));
#29791=CARTESIAN_POINT('Ctrl Pts',(162.002465776354,4.33397463311198,128.475269529938));
#29792=CARTESIAN_POINT('Ctrl Pts',(161.99471950027,4.26728216349097,128.355215090114));
#29793=CARTESIAN_POINT('Ctrl Pts',(161.986973224185,4.19568759663884,128.238159406844));
#29794=CARTESIAN_POINT('Ctrl Pts',(161.97922689092,4.12409250129193,128.121102859496));
#29795=CARTESIAN_POINT('Ctrl Pts',(161.971480557655,4.04759544050142,128.007045446401));
#29796=CARTESIAN_POINT('Ctrl Pts',(161.963734224389,3.96648772804128,127.896413203014));
#29797=CARTESIAN_POINT('Ctrl Pts',(161.955986156386,3.8853618520713,127.785756184304));
#29798=CARTESIAN_POINT('Ctrl Pts',(161.948238088383,3.79962350094601,127.678526176875));
#29799=CARTESIAN_POINT('Ctrl Pts',(161.94049002038,3.70960532131113,127.575117451962));
#29800=CARTESIAN_POINT('Ctrl Pts',(161.932733717639,3.61949146928364,127.471598823026));
#29801=CARTESIAN_POINT('Ctrl Pts',(161.924977414897,3.5250889594336,127.371909884856));
#29802=CARTESIAN_POINT('Ctrl Pts',(161.917221112155,3.4267688617684,127.276409621518));
#29803=CARTESIAN_POINT('Ctrl Pts',(161.909460669641,3.32839628770669,127.180858386814));
#29804=CARTESIAN_POINT('Ctrl Pts',(161.901700227127,3.22610225092481,127.089500541908));
#29805=CARTESIAN_POINT('Ctrl Pts',(161.893939784612,3.12029142747198,127.002655148945));
#29806=CARTESIAN_POINT('Ctrl Pts',(161.886166884347,3.01431074709191,126.915670344047));
#29807=CARTESIAN_POINT('Ctrl Pts',(161.878393984081,2.90480231112118,126.833212701799));
#29808=CARTESIAN_POINT('Ctrl Pts',(161.870621083816,2.79220105971505,126.755558781883));
#29809=CARTESIAN_POINT('Ctrl Pts',(161.863130748054,2.68369314742319,126.680727777556));
#29810=CARTESIAN_POINT('Ctrl Pts',(161.855640412292,2.5723136394021,126.610357468845));
#29811=CARTESIAN_POINT('Ctrl Pts',(161.84815007653,2.45847208468172,126.544654281286));
#29812=CARTESIAN_POINT('Ctrl Pts',(161.840375742411,2.34031419281256,126.476459937401));
#29813=CARTESIAN_POINT('Ctrl Pts',(161.832601408292,2.21912958310019,126.413077589533));
#29814=CARTESIAN_POINT('Ctrl Pts',(161.824827074173,2.09534774863237,126.354787506042));
#29815=CARTESIAN_POINT('Ctrl Pts',(161.817062321226,1.97171846421286,126.296569259868));
#29816=CARTESIAN_POINT('Ctrl Pts',(161.809297568279,1.8454986740834,126.243430956144));
#29817=CARTESIAN_POINT('Ctrl Pts',(161.801532815331,1.71714494284011,126.195608475415));
#29818=CARTESIAN_POINT('Ctrl Pts',(161.793775774446,1.58891869433217,126.147833492649));
#29819=CARTESIAN_POINT('Ctrl Pts',(161.786018733561,1.45856308652389,126.105363961555));
#29820=CARTESIAN_POINT('Ctrl Pts',(161.778261692676,1.32655694918039,126.068388729655));
#29821=CARTESIAN_POINT('Ctrl Pts',(161.770510501436,1.19465035869195,126.031441381065));
#29822=CARTESIAN_POINT('Ctrl Pts',(161.762759310196,1.06109609107479,125.999980189719));
#29823=CARTESIAN_POINT('Ctrl Pts',(161.755008118956,0.926390177995158,125.974144856276));
#29824=CARTESIAN_POINT('Ctrl Pts',(161.747260222179,0.791741518521931,125.948320503539));
#29825=CARTESIAN_POINT('Ctrl Pts',(161.739512325402,0.65594257028796,125.928117326397));
#29826=CARTESIAN_POINT('Ctrl Pts',(161.731764428625,0.519501443425542,125.913624342446));
#29827=CARTESIAN_POINT('Ctrl Pts',(161.724018152541,0.383088857105533,125.899134390114));
#29828=CARTESIAN_POINT('Ctrl Pts',(161.716271876457,0.246034747878417,125.890352296417));
#29829=CARTESIAN_POINT('Ctrl Pts',(161.708525600373,0.108853874176539,125.887315377122));
#29830=CARTESIAN_POINT('Ctrl Pts',(161.700779267107,-0.0283280121632919,
125.884278435409));
#29831=CARTESIAN_POINT('Ctrl Pts',(161.693032933842,-0.165636273975663,
125.886986761376));
#29832=CARTESIAN_POINT('Ctrl Pts',(161.685286600577,-0.302555013355518,
125.895425547065));
#29833=CARTESIAN_POINT('Ctrl Pts',(161.677538532574,-0.439504414737683,
125.903866222562));
#29834=CARTESIAN_POINT('Ctrl Pts',(161.669790464571,-0.576063729957995,
125.918039887346));
#29835=CARTESIAN_POINT('Ctrl Pts',(161.662042396568,-0.711721443823145,
125.937879789606));
#29836=CARTESIAN_POINT('Ctrl Pts',(161.654286093826,-0.847523336321078,
125.95774077795));
#29837=CARTESIAN_POINT('Ctrl Pts',(161.646529791084,-0.982421325824132,
125.983279976987));
#29838=CARTESIAN_POINT('Ctrl Pts',(161.638773488342,-1.115912816468,126.014379234665));
#29839=CARTESIAN_POINT('Ctrl Pts',(161.631013045828,-1.24947555553986,126.045495090953));
#29840=CARTESIAN_POINT('Ctrl Pts',(161.623252603314,-1.38162992339948,126.082176814503));
#29841=CARTESIAN_POINT('Ctrl Pts',(161.6154921608,-1.5118887467382,126.124256400779));
#29842=CARTESIAN_POINT('Ctrl Pts',(161.607719260534,-1.64235667310394,126.166403536942));
#29843=CARTESIAN_POINT('Ctrl Pts',(161.599946360269,-1.7709226073832,126.21396571579));
#29844=CARTESIAN_POINT('Ctrl Pts',(161.592173460003,-1.89711877630473,126.266726497114));
#29845=CARTESIAN_POINT('Ctrl Pts',(161.584683124241,-2.0187273966176,126.317569291141));
#29846=CARTESIAN_POINT('Ctrl Pts',(161.577192788479,-2.13813527500847,126.373239154922));
#29847=CARTESIAN_POINT('Ctrl Pts',(161.569702452717,-2.25494736857407,126.433503101304));
#29848=CARTESIAN_POINT('Ctrl Pts',(161.561927252093,-2.37620194134867,126.496058945046));
#29849=CARTESIAN_POINT('Ctrl Pts',(161.554152051469,-2.49504352236654,126.563763402027));
#29850=CARTESIAN_POINT('Ctrl Pts',(161.546376850845,-2.61100400698034,126.636406546558));
#29851=CARTESIAN_POINT('Ctrl Pts',(161.538611423511,-2.72681873132558,126.708958379947));
#29852=CARTESIAN_POINT('Ctrl Pts',(161.530845996176,-2.83975923728124,126.78643634234));
#29853=CARTESIAN_POINT('Ctrl Pts',(161.523080568841,-2.94938017522137,126.868583738154));
#29854=CARTESIAN_POINT('Ctrl Pts',(161.515241560116,-3.06003982753177,126.951509522497));
#29855=CARTESIAN_POINT('Ctrl Pts',(161.507402551392,-3.16731630438019,127.039193531912));
#29856=CARTESIAN_POINT('Ctrl Pts',(161.499563542667,-3.27077868745617,127.131325109953));
#29857=CARTESIAN_POINT('Ctrl Pts',(161.491812679121,-3.37307769509291,127.22242072099));
#29858=CARTESIAN_POINT('Ctrl Pts',(161.484061815575,-3.47164763608889,127.31786413449));
#29859=CARTESIAN_POINT('Ctrl Pts',(161.476310952028,-3.56610326796046,127.417313150414));
#29860=CARTESIAN_POINT('Ctrl Pts',(161.468563642612,-3.66051558754889,127.516716564356));
#29861=CARTESIAN_POINT('Ctrl Pts',(161.460816333196,-3.75081708343823,127.620121643056));
#29862=CARTESIAN_POINT('Ctrl Pts',(161.45306902378,-3.83665870011573,127.727148716945));
#29863=CARTESIAN_POINT('Ctrl Pts',(161.44532358911,-3.92247954425601,127.834149891695));
#29864=CARTESIAN_POINT('Ctrl Pts',(161.43757815444,-4.00384241336998,127.944771012093));
#29865=CARTESIAN_POINT('Ctrl Pts',(161.429832719771,-4.08043821489942,128.05859896788));
#29866=CARTESIAN_POINT('Ctrl Pts',(161.421925356411,-4.15863535429632,128.174806649609));
#29867=CARTESIAN_POINT('Ctrl Pts',(161.414017993051,-4.23186362596502,128.294356412229));
#29868=CARTESIAN_POINT('Ctrl Pts',(161.40611062969,-4.29984067448549,128.416777480471));
#29869=CARTESIAN_POINT('Ctrl Pts',(161.398361401453,-4.36645828644137,128.536750315375));
#29870=CARTESIAN_POINT('Ctrl Pts',(161.390612173215,-4.42803258524586,128.659480318208));
#29871=CARTESIAN_POINT('Ctrl Pts',(161.382862944977,-4.48434464039871,128.784500174707));
#29872=CARTESIAN_POINT('Ctrl Pts',(161.374876514056,-4.54238039889116,128.913346869768));
#29873=CARTESIAN_POINT('Ctrl Pts',(161.366890083134,-4.59482641609933,129.044625440944));
#29874=CARTESIAN_POINT('Ctrl Pts',(161.358903652213,-4.64149715716548,129.177803762573));
#29875=CARTESIAN_POINT('Ctrl Pts',(161.350917221292,-4.6881678982316,129.310982084201));
#29876=CARTESIAN_POINT('Ctrl Pts',(161.342930790371,-4.72906326476933,129.446059714126));
#29877=CARTESIAN_POINT('Ctrl Pts',(161.334944359449,-4.76405452823403,129.582490119308));
#29878=CARTESIAN_POINT('Ctrl Pts',(163.084942816425,-4.76405452823405,129.582490119308));
#29879=CARTESIAN_POINT('Ctrl Pts',(163.077305556572,-4.79767232933164,129.713565415566));
#29880=CARTESIAN_POINT('Ctrl Pts',(163.06966829672,-4.82586396033538,129.8459805258));
#29881=CARTESIAN_POINT('Ctrl Pts',(163.062031036868,-4.84854190088311,129.979239718618));
#29882=CARTESIAN_POINT('Ctrl Pts',(163.054169103394,-4.87188698319665,130.116419142774));
#29883=CARTESIAN_POINT('Ctrl Pts',(163.046307169921,-4.88938889275877,130.254492623326));
#29884=CARTESIAN_POINT('Ctrl Pts',(163.038445236447,-4.90100955637683,130.392913912873));
#29885=CARTESIAN_POINT('Ctrl Pts',(163.030583302974,-4.9126302199949,130.53133520242));
#29886=CARTESIAN_POINT('Ctrl Pts',(163.0227213695,-4.91836966325008,130.670103837096));
#29887=CARTESIAN_POINT('Ctrl Pts',(163.014859436027,-4.91824810772423,130.80867493872));
#29888=CARTESIAN_POINT('',(163.360140564019,-4.91824999998649,130.804349090908));
#29889=CARTESIAN_POINT('Ctrl Pts',(163.429862020825,-4.76405452823405,129.582490119308));
#29890=CARTESIAN_POINT('Ctrl Pts',(163.421727513463,-4.79974600044378,129.72165062776));
#29891=CARTESIAN_POINT('Ctrl Pts',(163.4135930061,-4.82937292020494,129.862520536798));
#29892=CARTESIAN_POINT('Ctrl Pts',(163.405458498738,-4.85278248757454,130.004557397524));
#29893=CARTESIAN_POINT('Ctrl Pts',(163.397339092563,-4.87614859659454,130.146330575993));
#29894=CARTESIAN_POINT('Ctrl Pts',(163.389219686388,-4.89332031540393,130.289266059976));
#29895=CARTESIAN_POINT('Ctrl Pts',(163.381100280213,-4.9041954478384,130.432809716745));
#29896=CARTESIAN_POINT('Ctrl Pts',(163.374113708152,-4.91355326228837,130.55632590504));
#29897=CARTESIAN_POINT('Ctrl Pts',(163.367127136091,-4.91824970923526,130.680292043314));
#29898=CARTESIAN_POINT('Ctrl Pts',(163.36014056403,-4.91824999998649,130.804349090714));
#29899=CARTESIAN_POINT('Ctrl Pts',(163.360140564008,-4.91824999998649,130.804349091103));
#29900=CARTESIAN_POINT('Ctrl Pts',(163.352027365337,-4.91825033761171,130.948411080773));
#29901=CARTESIAN_POINT('Ctrl Pts',(163.343914166666,-4.91191672099125,131.092351239516));
#29902=CARTESIAN_POINT('Ctrl Pts',(163.335800967995,-4.8993069962004,131.235607669129));
#29903=CARTESIAN_POINT('Ctrl Pts',(163.327677138385,-4.88668074855336,131.379051811434));
#29904=CARTESIAN_POINT('Ctrl Pts',(163.319553308775,-4.86776201198404,131.521810105082));
#29905=CARTESIAN_POINT('Ctrl Pts',(163.311429479165,-4.8426600497321,131.663329013509));
#29906=CARTESIAN_POINT('Ctrl Pts',(163.30328650322,-4.81749892688766,131.805181455322));
#29907=CARTESIAN_POINT('Ctrl Pts',(163.295143527275,-4.78612550029788,131.945788342313));
#29908=CARTESIAN_POINT('Ctrl Pts',(163.28700055133,-4.74869987052856,132.084607703929));
#29909=CARTESIAN_POINT('Ctrl Pts',(163.278847477325,-4.71122782944042,132.223599214677));
#29910=CARTESIAN_POINT('Ctrl Pts',(163.27069440332,-4.66768870775622,132.360798458793));
#29911=CARTESIAN_POINT('Ctrl Pts',(163.262541329315,-4.61829148051881,132.495681658489));
#29912=CARTESIAN_POINT('Ctrl Pts',(163.254369571787,-4.56878105496329,132.63087395552));
#29913=CARTESIAN_POINT('Ctrl Pts',(163.246197814258,-4.51338580912547,132.76373928711));
#29914=CARTESIAN_POINT('Ctrl Pts',(163.23802605673,-4.4523623286491,132.893775070691));
#29915=CARTESIAN_POINT('Ctrl Pts',(163.232283770965,-4.40948119052899,132.985151084526));
#29916=CARTESIAN_POINT('Ctrl Pts',(163.2265414852,-4.36382188014511,133.07513042235));
#29917=CARTESIAN_POINT('Ctrl Pts',(163.220799199435,-4.31548629801546,133.163547145618));
#29918=CARTESIAN_POINT('Ctrl Pts',(163.213024865316,-4.2500459871878,133.283252290318));
#29919=CARTESIAN_POINT('Ctrl Pts',(163.205250531197,-4.17951758610824,133.400422151176));
#29920=CARTESIAN_POINT('Ctrl Pts',(163.197476197078,-4.10412211663965,133.514593949626));
#29921=CARTESIAN_POINT('Ctrl Pts',(163.189711444131,-4.02881956534892,133.628625041538));
#29922=CARTESIAN_POINT('Ctrl Pts',(163.181946691184,-3.94866209372835,133.739665099564));
#29923=CARTESIAN_POINT('Ctrl Pts',(163.174181938237,-3.86391693387252,133.847275172829));
#29924=CARTESIAN_POINT('Ctrl Pts',(163.166424897352,-3.77925594410389,133.954778366253));
#29925=CARTESIAN_POINT('Ctrl Pts',(163.158667856467,-3.69001657417765,134.058858049254));
#29926=CARTESIAN_POINT('Ctrl Pts',(163.150910815582,-3.59650953751703,134.159103857972));
#29927=CARTESIAN_POINT('Ctrl Pts',(163.143159624342,-3.5030730152402,134.259274070545));
#29928=CARTESIAN_POINT('Ctrl Pts',(163.135408433101,-3.40537549762023,134.355615878763));
#29929=CARTESIAN_POINT('Ctrl Pts',(163.127657241861,-3.30376795466278,134.447751944921));
#29930=CARTESIAN_POINT('Ctrl Pts',(163.119909345084,-3.20220359762173,134.539848850792));
#29931=CARTESIAN_POINT('Ctrl Pts',(163.112161448307,-3.09673280958298,134.627743307833));
#29932=CARTESIAN_POINT('Ctrl Pts',(163.10441355153,-2.98774324052898,134.711094981606));
#29933=CARTESIAN_POINT('Ctrl Pts',(163.096667275446,-2.87877646974333,134.794429220006));
#29934=CARTESIAN_POINT('Ctrl Pts',(163.088920999362,-2.76629269235277,134.873222327888));
#29935=CARTESIAN_POINT('Ctrl Pts',(163.081174723278,-2.65071213058344,134.947174668821));
#29936=CARTESIAN_POINT('Ctrl Pts',(163.073428390012,-2.53513071562447,135.021127555654));
#29937=CARTESIAN_POINT('Ctrl Pts',(163.065682056747,-2.4164527999954,135.090239393522));
#29938=CARTESIAN_POINT('Ctrl Pts',(163.057935723482,-2.29512669277534,135.154254469904));
#29939=CARTESIAN_POINT('Ctrl Pts',(163.050187655479,-2.17377341541524,135.218283882019));
#29940=CARTESIAN_POINT('Ctrl Pts',(163.042439587476,-2.0497711120938,135.277214079013));
#29941=CARTESIAN_POINT('Ctrl Pts',(163.034691519473,-1.92359136891616,135.33083599118));
#29942=CARTESIAN_POINT('Ctrl Pts',(163.026935216731,-1.79727752040557,135.384514893353));
#29943=CARTESIAN_POINT('Ctrl Pts',(163.019178913989,-1.66878196955274,135.432874087623));
#29944=CARTESIAN_POINT('Ctrl Pts',(163.011422611247,-1.5385954221819,135.475753042672));
#29945=CARTESIAN_POINT('Ctrl Pts',(163.003662168733,-1.40833939033111,135.518654883511));
#29946=CARTESIAN_POINT('Ctrl Pts',(162.995901726219,-1.27639093953481,135.556070550276));
#29947=CARTESIAN_POINT('Ctrl Pts',(162.988141283705,-1.14325353610117,135.587890111015));
#29948=CARTESIAN_POINT('Ctrl Pts',(162.98036838344,-1.00990240868793,135.619760751337));
#29949=CARTESIAN_POINT('Ctrl Pts',(162.972595483174,-0.875358898569053,
135.646017259078));
#29950=CARTESIAN_POINT('Ctrl Pts',(162.964822582909,-0.74013509854036,135.666601160609));
#29951=CARTESIAN_POINT('Ctrl Pts',(162.957332247147,-0.609827024251047,
135.686436785472));
#29952=CARTESIAN_POINT('Ctrl Pts',(162.949841911385,-0.478887567978155,
135.701005036775));
#29953=CARTESIAN_POINT('Ctrl Pts',(162.942351575623,-0.347775314005544,
135.710299405756));
#29954=CARTESIAN_POINT('Ctrl Pts',(162.934577241504,-0.211691899072754,
135.719946173562));
#29955=CARTESIAN_POINT('Ctrl Pts',(162.926802907384,-0.0749912531742415,
135.723941804092));
#29956=CARTESIAN_POINT('Ctrl Pts',(162.919028573265,0.0618178072596507,
135.722222106181));
#29957=CARTESIAN_POINT('Ctrl Pts',(162.911263820318,0.198458262753396,135.720504527644));
#29958=CARTESIAN_POINT('Ctrl Pts',(162.903499067371,0.335206479754615,135.71308564026));
#29959=CARTESIAN_POINT('Ctrl Pts',(162.895734314424,0.471548710985654,135.699953010287));
#29960=CARTESIAN_POINT('Ctrl Pts',(162.887977273539,0.607755525191009,135.686833423828));
#29961=CARTESIAN_POINT('Ctrl Pts',(162.880220232654,0.743556769427832,135.668011425468));
#29962=CARTESIAN_POINT('Ctrl Pts',(162.872463191769,0.878439244762312,135.643526615521));
#29963=CARTESIAN_POINT('Ctrl Pts',(162.864712000529,1.01322000417254,135.619060269759));
#29964=CARTESIAN_POINT('Ctrl Pts',(162.856960809289,1.14708299063578,135.588939681869));
#29965=CARTESIAN_POINT('Ctrl Pts',(162.849209618049,1.27952103139354,135.553256172611));
#29966=CARTESIAN_POINT('Ctrl Pts',(162.841461721272,1.41190278245102,135.517587829795));
#29967=CARTESIAN_POINT('Ctrl Pts',(162.833713824494,1.54286041566226,135.476361369703));
#29968=CARTESIAN_POINT('Ctrl Pts',(162.825965927717,1.67189806374138,135.429718974165));
#29969=CARTESIAN_POINT('Ctrl Pts',(162.818219651633,1.80090871992625,135.38308633521));
#29970=CARTESIAN_POINT('Ctrl Pts',(162.810473375549,1.92799982237271,135.331040147025));
#29971=CARTESIAN_POINT('Ctrl Pts',(162.802727099465,2.05269213808747,135.273771993657));
#29972=CARTESIAN_POINT('Ctrl Pts',(162.7949807662,2.1773853742525,135.216503417549));
#29973=CARTESIAN_POINT('Ctrl Pts',(162.787234432934,2.29967943306641,135.154012962516));
#29974=CARTESIAN_POINT('Ctrl Pts',(162.779488099669,2.41911685433489,135.086539584818));
#29975=CARTESIAN_POINT('Ctrl Pts',(162.771740031666,2.5385810227859,135.019051096924));
#29976=CARTESIAN_POINT('Ctrl Pts',(162.763991963663,2.65518694037741,134.946577658138));
#29977=CARTESIAN_POINT('Ctrl Pts',(162.75624389566,2.76850380703408,134.86940301992));
#29978=CARTESIAN_POINT('Ctrl Pts',(162.748487592918,2.88194110820509,134.792146359579));
#29979=CARTESIAN_POINT('Ctrl Pts',(162.740731290176,2.99208205186223,134.710178739205));
#29980=CARTESIAN_POINT('Ctrl Pts',(162.732974987434,3.09852633997754,134.623826232409));
#29981=CARTESIAN_POINT('Ctrl Pts',(162.72521454492,3.20502744061439,134.537427636679));
#29982=CARTESIAN_POINT('Ctrl Pts',(162.717454102406,3.30782766140585,134.446639749864));
#29983=CARTESIAN_POINT('Ctrl Pts',(162.709693659892,3.4065623776501,134.351826731524));
#29984=CARTESIAN_POINT('Ctrl Pts',(162.701920759626,3.50545559162617,134.256861510909));
#29985=CARTESIAN_POINT('Ctrl Pts',(162.694147859361,3.60026998883824,134.15785852916));
#29986=CARTESIAN_POINT('Ctrl Pts',(162.686374959096,3.69067957510331,134.055217018027));
#29987=CARTESIAN_POINT('Ctrl Pts',(162.678884623333,3.77780254517988,133.956306784361));
#29988=CARTESIAN_POINT('Ctrl Pts',(162.671394287571,3.86083520208575,133.854018207079));
#29989=CARTESIAN_POINT('Ctrl Pts',(162.663903951809,3.93952419380693,133.748733587981));
#29990=CARTESIAN_POINT('Ctrl Pts',(162.65612961769,4.02119670256608,133.63945707055));
#29991=CARTESIAN_POINT('Ctrl Pts',(162.648355283571,4.09844837790067,133.526606681492));
#29992=CARTESIAN_POINT('Ctrl Pts',(162.640580949452,4.1709501862553,133.410575805588));
#29993=CARTESIAN_POINT('Ctrl Pts',(162.632816196505,4.24336264261067,133.294687927369));
#29994=CARTESIAN_POINT('Ctrl Pts',(162.625051443558,4.31103667409021,133.175627689647));
#29995=CARTESIAN_POINT('Ctrl Pts',(162.617286690611,4.37368412688342,133.053820601817));
#29996=CARTESIAN_POINT('Ctrl Pts',(162.609529649726,4.43626935734329,132.932134494504));
#29997=CARTESIAN_POINT('Ctrl Pts',(162.601772608841,4.49383776669642,132.807707311771));
#29998=CARTESIAN_POINT('Ctrl Pts',(162.594015567956,4.54614527524743,132.680992227351));
#29999=CARTESIAN_POINT('Ctrl Pts',(162.586264376716,4.5984133382994,132.554372699762));
#30000=CARTESIAN_POINT('Ctrl Pts',(162.578513185476,4.64542824861686,132.425469064563));
#30001=CARTESIAN_POINT('Ctrl Pts',(162.570761994236,4.68699269767674,132.294757381661));
#30002=CARTESIAN_POINT('Ctrl Pts',(162.563014097458,4.72853948073707,132.164101254711));
#30003=CARTESIAN_POINT('Ctrl Pts',(162.555266200681,4.76464029183585,132.031638980285));
#30004=CARTESIAN_POINT('Ctrl Pts',(162.547518303904,4.79514672419508,131.897864598327));
#30005=CARTESIAN_POINT('Ctrl Pts',(162.53977202782,4.82564677526629,131.764118199087));
#30006=CARTESIAN_POINT('Ctrl Pts',(162.532025751736,4.85055468836595,131.629060619178));
#30007=CARTESIAN_POINT('Ctrl Pts',(162.524279475652,4.86977261144262,131.49319860675));
#30008=CARTESIAN_POINT('Ctrl Pts',(162.516533142387,4.88899067638157,131.35733559142));
#30009=CARTESIAN_POINT('Ctrl Pts',(162.508786809121,4.90251861272758,131.220668518832));
#30010=CARTESIAN_POINT('Ctrl Pts',(162.501040475856,4.91031019274151,131.083711424901));
#30011=CARTESIAN_POINT('Ctrl Pts',(162.493292407853,4.91810351762577,130.946723660378));
#30012=CARTESIAN_POINT('Ctrl Pts',(162.48554433985,4.92015790773628,130.809446135531));
#30013=CARTESIAN_POINT('Ctrl Pts',(162.477796271847,4.91647923325096,130.672394669261));
#30014=CARTESIAN_POINT('Ctrl Pts',(162.470039969105,4.91279664902662,130.535197543061));
#30015=CARTESIAN_POINT('Ctrl Pts',(162.462283666364,4.90336883895152,130.398227346826));
#30016=CARTESIAN_POINT('Ctrl Pts',(162.454527363622,4.88825376712604,130.261997113375));
#30017=CARTESIAN_POINT('Ctrl Pts',(162.446766921108,4.87313062793161,130.125694169747));
#30018=CARTESIAN_POINT('Ctrl Pts',(162.439006478593,4.85231423788077,129.990132362101));
#30019=CARTESIAN_POINT('Ctrl Pts',(162.431246036079,4.82591388616612,129.855815296662));
#30020=CARTESIAN_POINT('Ctrl Pts',(162.423473135814,4.79947115426317,129.721282613546));
#30021=CARTESIAN_POINT('Ctrl Pts',(162.415700235549,4.76742663947144,129.58799904597));
#30022=CARTESIAN_POINT('Ctrl Pts',(162.407927335283,4.7299400189492,129.456454656587));
#30023=CARTESIAN_POINT('Ctrl Pts',(162.400436999521,4.69381613150577,129.329692237097));
#30024=CARTESIAN_POINT('Ctrl Pts',(162.392946663759,4.65263903371826,129.204545036676));
#30025=CARTESIAN_POINT('Ctrl Pts',(162.385456327997,4.60659342396651,129.08143285101));
#30026=CARTESIAN_POINT('Ctrl Pts',(162.377681993878,4.55880198092614,128.953652829407));
#30027=CARTESIAN_POINT('Ctrl Pts',(162.369907659759,4.5056141700184,128.827660415257));
#30028=CARTESIAN_POINT('Ctrl Pts',(162.36213332564,4.44718310632606,128.703945067893));
#30029=CARTESIAN_POINT('Ctrl Pts',(162.354368572693,4.38882405369765,128.580382188638));
#30030=CARTESIAN_POINT('Ctrl Pts',(162.346603819745,4.3252347707861,128.459091142629));
#30031=CARTESIAN_POINT('Ctrl Pts',(162.338839066798,4.25661749652277,128.340544360051));
#30032=CARTESIAN_POINT('Ctrl Pts',(162.331082025913,4.18806837390321,128.222115319807));
#30033=CARTESIAN_POINT('Ctrl Pts',(162.323324985028,4.1145013925504,128.106425455026));
#30034=CARTESIAN_POINT('Ctrl Pts',(162.315567944143,4.03616588932347,127.993925068339));
#30035=CARTESIAN_POINT('Ctrl Pts',(162.307816752903,3.95788945950889,127.881509519068));
#30036=CARTESIAN_POINT('Ctrl Pts',(162.300065561663,3.87485188790448,127.772278980015));
#30037=CARTESIAN_POINT('Ctrl Pts',(162.292314370423,3.78734704711624,127.666656774435));
#30038=CARTESIAN_POINT('Ctrl Pts',(162.284566473646,3.69987939821988,127.56107946111));
#30039=CARTESIAN_POINT('Ctrl Pts',(162.276818576869,3.60794850542882,127.459107731407));
#30040=CARTESIAN_POINT('Ctrl Pts',(162.269070680092,3.51188980105184,127.361133484807));
#30041=CARTESIAN_POINT('Ctrl Pts',(162.261324404007,3.41585119008487,127.263179732307));
#30042=CARTESIAN_POINT('Ctrl Pts',(162.253578127923,3.31568675851793,127.169222078682));
#30043=CARTESIAN_POINT('Ctrl Pts',(162.245831851839,3.21176995649636,127.079616759386));
#30044=CARTESIAN_POINT('Ctrl Pts',(162.238085518574,3.10785238738509,126.990010778645));
#30045=CARTESIAN_POINT('Ctrl Pts',(162.230339185309,3.0001826886377,126.904757451653));
#30046=CARTESIAN_POINT('Ctrl Pts',(162.222592852043,2.88916834600419,126.824173520086));
#30047=CARTESIAN_POINT('Ctrl Pts',(162.21484478404,2.77812914247757,126.743571542305));
#30048=CARTESIAN_POINT('Ctrl Pts',(162.207096716037,2.66374412095743,126.667641270352));
#30049=CARTESIAN_POINT('Ctrl Pts',(162.199348648034,2.54645042746821,126.596656578194));
#30050=CARTESIAN_POINT('Ctrl Pts',(162.191592345292,2.42903207284633,126.525596442661));
#30051=CARTESIAN_POINT('Ctrl Pts',(162.18383604255,2.30869920592379,126.459492589539));
#30052=CARTESIAN_POINT('Ctrl Pts',(162.176079739809,2.18591478675273,126.398573558758));
#30053=CARTESIAN_POINT('Ctrl Pts',(162.168319297294,2.06306483384016,126.337622013657));
#30054=CARTESIAN_POINT('Ctrl Pts',(162.16055885478,1.93776107846641,126.281860963844));
#30055=CARTESIAN_POINT('Ctrl Pts',(162.152798412266,1.81048629228962,126.231470672692));
#30056=CARTESIAN_POINT('Ctrl Pts',(162.145025512001,1.68300719332704,126.180999490571));
#30057=CARTESIAN_POINT('Ctrl Pts',(162.137252611735,1.55355111016339,126.135916424507));
#30058=CARTESIAN_POINT('Ctrl Pts',(162.12947971147,1.42261665579041,126.096352024417));
#30059=CARTESIAN_POINT('Ctrl Pts',(162.121989375708,1.29644199863962,126.058225889927));
#30060=CARTESIAN_POINT('Ctrl Pts',(162.114499039946,1.16889488741463,126.025224229775));
#30061=CARTESIAN_POINT('Ctrl Pts',(162.107008704184,1.04042834210103,125.997418561804));
#30062=CARTESIAN_POINT('Ctrl Pts',(162.099234370065,0.907090948673375,125.968558633481));
#30063=CARTESIAN_POINT('Ctrl Pts',(162.091460035946,0.772340651378395,125.945205067771));
#30064=CARTESIAN_POINT('Ctrl Pts',(162.083685701827,0.636672008656077,125.927493609343));
#30065=CARTESIAN_POINT('Ctrl Pts',(162.075920948879,0.501170565410721,125.909803978705));
#30066=CARTESIAN_POINT('Ctrl Pts',(162.068156195932,0.364753412594142,125.897742670294));
#30067=CARTESIAN_POINT('Ctrl Pts',(162.060391442985,0.227927334181593,125.891394894825));
#30068=CARTESIAN_POINT('Ctrl Pts',(162.0526344021,0.0912371533594043,125.885053424055));
#30069=CARTESIAN_POINT('Ctrl Pts',(162.044877361215,-0.045860756782652,
125.884414211196));
#30070=CARTESIAN_POINT('Ctrl Pts',(162.03712032033,-0.182852771223678,125.889510881658));
#30071=CARTESIAN_POINT('Ctrl Pts',(162.02936912909,-0.319741478920505,125.894603708681));
#30072=CARTESIAN_POINT('Ctrl Pts',(162.02161793785,-0.456524060752298,125.905423794956));
#30073=CARTESIAN_POINT('Ctrl Pts',(162.01386674661,-0.592685517552422,125.921952713695));
#30074=CARTESIAN_POINT('Ctrl Pts',(162.006118849833,-0.728789102101644,
125.938474607203));
#30075=CARTESIAN_POINT('Ctrl Pts',(161.998370953056,-0.864271699381087,
125.960700460223));
#30076=CARTESIAN_POINT('Ctrl Pts',(161.990623056278,-0.998622283900166,
125.988559895298));
#30077=CARTESIAN_POINT('Ctrl Pts',(161.982876780194,-1.13294476517327,126.01641350278));
#30078=CARTESIAN_POINT('Ctrl Pts',(161.97513050411,-1.26613532210091,126.049898269033));
#30079=CARTESIAN_POINT('Ctrl Pts',(161.967384228026,-1.39769238478051,126.088892553839));
#30080=CARTESIAN_POINT('Ctrl Pts',(161.959637894761,-1.5292504185841,126.127887126492));
#30081=CARTESIAN_POINT('Ctrl Pts',(161.951891561495,-1.65917455923311,126.172391187746));
#30082=CARTESIAN_POINT('Ctrl Pts',(161.94414522823,-1.78697806698588,126.222233114908));
#30083=CARTESIAN_POINT('Ctrl Pts',(161.936397160227,-1.91481019544817,126.272086203825));
#30084=CARTESIAN_POINT('Ctrl Pts',(161.928649092224,-2.04052038183997,126.327279395291));
#30085=CARTESIAN_POINT('Ctrl Pts',(161.920901024221,-2.16364192013101,126.387592941544));
#30086=CARTESIAN_POINT('Ctrl Pts',(161.913144721479,-2.28689431345844,126.447970589752));
#30087=CARTESIAN_POINT('Ctrl Pts',(161.905388418737,-2.40755221111399,126.513479291409));
#30088=CARTESIAN_POINT('Ctrl Pts',(161.897632115996,-2.52517309476479,126.583853076526));
#30089=CARTESIAN_POINT('Ctrl Pts',(161.889871673481,-2.64285675622289,126.654264422251));
#30090=CARTESIAN_POINT('Ctrl Pts',(161.882111230967,-2.75749984715998,126.72954581097));
#30091=CARTESIAN_POINT('Ctrl Pts',(161.874350788453,-2.86868975702159,126.809388509971));
#30092=CARTESIAN_POINT('Ctrl Pts',(161.866577888188,-2.98005815879725,126.889359379561));
#30093=CARTESIAN_POINT('Ctrl Pts',(161.858804987922,-3.08796199418656,126.97390595029));
#30094=CARTESIAN_POINT('Ctrl Pts',(161.851032087657,-3.19202191534508,127.062679290347));
#30095=CARTESIAN_POINT('Ctrl Pts',(161.843541751895,-3.29229899625859,127.148225495887));
#30096=CARTESIAN_POINT('Ctrl Pts',(161.836051416133,-3.38900655673042,127.237696289461));
#30097=CARTESIAN_POINT('Ctrl Pts',(161.828561080371,-3.48183955840474,127.330749189667));
#30098=CARTESIAN_POINT('Ctrl Pts',(161.82089528468,-3.57684715843069,127.425981839313));
#30099=CARTESIAN_POINT('Ctrl Pts',(161.81322948899,-3.66811543703843,127.525286604809));
#30100=CARTESIAN_POINT('Ctrl Pts',(161.8055636933,-3.75526764309748,127.62833354098));
#30101=CARTESIAN_POINT('Ctrl Pts',(161.797906871543,-3.84231782477862,127.731259845672));
#30102=CARTESIAN_POINT('Ctrl Pts',(161.790250049785,-3.92526125595901,127.837919307829));
#30103=CARTESIAN_POINT('Ctrl Pts',(161.782593228028,-4.00375652939198,127.947943855983));
#30104=CARTESIAN_POINT('Ctrl Pts',(161.774943600683,-4.08217804801826,128.057865024164));
#30105=CARTESIAN_POINT('Ctrl Pts',(161.767293973339,-4.15615948783112,128.171144665205));
#30106=CARTESIAN_POINT('Ctrl Pts',(161.759644345994,-4.22539877314241,128.287380627493));
#30107=CARTESIAN_POINT('Ctrl Pts',(161.752000464105,-4.29458605445738,128.403529287689));
#30108=CARTESIAN_POINT('Ctrl Pts',(161.744356582215,-4.35903806333865,128.522629506138));
#30109=CARTESIAN_POINT('Ctrl Pts',(161.736712700326,-4.41849559837807,128.644249576528));
#30110=CARTESIAN_POINT('Ctrl Pts',(161.729072152544,-4.47792719923437,128.765816598685));
#30111=CARTESIAN_POINT('Ctrl Pts',(161.721431604762,-4.53236848364606,128.889900925101));
#30112=CARTESIAN_POINT('Ctrl Pts',(161.713791056981,-4.58160604699629,129.016046022024));
#30113=CARTESIAN_POINT('Ctrl Pts',(161.706151217946,-4.63083904300368,129.142179417559));
#30114=CARTESIAN_POINT('Ctrl Pts',(161.698511378912,-4.67486912729776,129.270372830139));
#30115=CARTESIAN_POINT('Ctrl Pts',(161.690871539878,-4.71353107987097,129.400149870708));
#30116=CARTESIAN_POINT('Ctrl Pts',(161.687312727445,-4.73154070505558,129.460602995878));
#30117=CARTESIAN_POINT('Ctrl Pts',(161.683753915013,-4.7483861898325,129.521399505681));
#30118=CARTESIAN_POINT('Ctrl Pts',(161.680195102581,-4.76405452823405,129.582490119308));
#30119=CARTESIAN_POINT('Origin',(213.235140564004,0.,130.804360617566));
#30120=CARTESIAN_POINT('',(159.584608960876,-4.76405452823403,129.582490119308));
#30121=CARTESIAN_POINT('',(159.930232377634,-4.76405452823406,129.582490119308));
#30122=CARTESIAN_POINT('',(213.235140564004,-4.76405452823405,129.582490119308));
#30123=CARTESIAN_POINT('',(161.264859435953,-4.91824926289724,130.801667940323));
#30124=CARTESIAN_POINT('Ctrl Pts',(161.264859435953,-4.91824926289724,130.801667940323));
#30125=CARTESIAN_POINT('Ctrl Pts',(161.257183648469,-4.91832310684931,130.936545955766));
#30126=CARTESIAN_POINT('Ctrl Pts',(161.249507860985,-4.91284442854529,131.071648809145));
#30127=CARTESIAN_POINT('Ctrl Pts',(161.241832073501,-4.90178411382868,131.206474486908));
#30128=CARTESIAN_POINT('Ctrl Pts',(161.234164972532,-4.8907363158205,131.341147585495));
#30129=CARTESIAN_POINT('Ctrl Pts',(161.226497871563,-4.87411947684391,131.475543735888));
#30130=CARTESIAN_POINT('Ctrl Pts',(161.218830770594,-4.85195648200004,131.609159573379));
#30131=CARTESIAN_POINT('Ctrl Pts',(161.211170404233,-4.8298129546289,131.742658045745));
#30132=CARTESIAN_POINT('Ctrl Pts',(161.203510037872,-4.80213302772327,131.875377174943));
#30133=CARTESIAN_POINT('Ctrl Pts',(161.195849671511,-4.76899146737869,132.006817871097));
#30134=CARTESIAN_POINT('Ctrl Pts',(161.188193700248,-4.73586892184574,132.13818315378));
#30135=CARTESIAN_POINT('Ctrl Pts',(161.180537728986,-4.69729107296994,132.268271074224));
#30136=CARTESIAN_POINT('Ctrl Pts',(161.172881757723,-4.65338385067269,132.396592322061));
#30137=CARTESIAN_POINT('Ctrl Pts',(161.165228052397,-4.6094896235862,132.524875590687));
#30138=CARTESIAN_POINT('Ctrl Pts',(161.157574347071,-4.5602692887005,132.651392846883));
#30139=CARTESIAN_POINT('Ctrl Pts',(161.149920641744,-4.50589862262322,132.775669995909));
#30140=CARTESIAN_POINT('Ctrl Pts',(161.142267448267,-4.4515315926375,132.899938833779));
#30141=CARTESIAN_POINT('Ctrl Pts',(161.13461425479,-4.39201507725591,133.02196749469));
#30142=CARTESIAN_POINT('Ctrl Pts',(161.126961061312,-4.32757276525213,133.141302427699));
#30143=CARTESIAN_POINT('Ctrl Pts',(161.119306626236,-4.26311999859303,133.260656720745));
#30144=CARTESIAN_POINT('Ctrl Pts',(161.11165219116,-4.1937400371374,133.377316063854));
#30145=CARTESIAN_POINT('Ctrl Pts',(161.103997756084,-4.11970196404595,133.490852528951));
#30146=CARTESIAN_POINT('Ctrl Pts',(161.096335620217,-4.04558940450076,133.604503218099));
#30147=CARTESIAN_POINT('Ctrl Pts',(161.088673484349,-3.96680959271754,133.715024417255));
#30148=CARTESIAN_POINT('Ctrl Pts',(161.081011348482,-3.88367452400827,133.822017863522));
#30149=CARTESIAN_POINT('Ctrl Pts',(161.07334537205,-3.8004977847159,133.929064939134));
#30150=CARTESIAN_POINT('Ctrl Pts',(161.065679395617,-3.71296170020457,134.032580434307));
#30151=CARTESIAN_POINT('Ctrl Pts',(161.058013419185,-3.62141697560164,134.132201081189));
#30152=CARTESIAN_POINT('Ctrl Pts',(161.05033524256,-3.52972656007069,134.231980271608));
#30153=CARTESIAN_POINT('Ctrl Pts',(161.042657065935,-3.43401504249612,134.327851946002));
#30154=CARTESIAN_POINT('Ctrl Pts',(161.034978889311,-3.33466875951926,134.419490950872));
#30155=CARTESIAN_POINT('Ctrl Pts',(161.027588327904,-3.23904386825342,134.507697269354));
#30156=CARTESIAN_POINT('Ctrl Pts',(161.020197766498,-3.14005188541437,134.591982143659));
#30157=CARTESIAN_POINT('Ctrl Pts',(161.012807205091,-3.03806278193107,134.672093492978));
#30158=CARTESIAN_POINT('Ctrl Pts',(161.005032870972,-2.93077764845143,134.756364817182));
#30159=CARTESIAN_POINT('Ctrl Pts',(160.997258536853,-2.81981358471956,134.836302344118));
#30160=CARTESIAN_POINT('Ctrl Pts',(160.989484202734,-2.70555596633218,134.911567694832));
#30161=CARTESIAN_POINT('Ctrl Pts',(160.981719449787,-2.59143916024824,134.986740287728));
#30162=CARTESIAN_POINT('Ctrl Pts',(160.97395469684,-2.47403719909126,135.057251948179));
#30163=CARTESIAN_POINT('Ctrl Pts',(160.966189943893,-2.35376855482247,135.122804394302));
#30164=CARTESIAN_POINT('Ctrl Pts',(160.958432903008,-2.23361936306604,135.188291732812));
#30165=CARTESIAN_POINT('Ctrl Pts',(160.950675862123,-2.11060949537768,135.248829473188));
#30166=CARTESIAN_POINT('Ctrl Pts',(160.942918821238,-1.98518613774831,135.304162731103));
#30167=CARTESIAN_POINT('Ctrl Pts',(160.935167629998,-1.85985736284844,135.359454261778));
#30168=CARTESIAN_POINT('Ctrl Pts',(160.927416438757,-1.73211907692423,135.409548964781));
#30169=CARTESIAN_POINT('Ctrl Pts',(160.919665247517,-1.60244246792842,135.454238164285));
#30170=CARTESIAN_POINT('Ctrl Pts',(160.91191735074,-1.47282097495116,135.498908369686));
#30171=CARTESIAN_POINT('Ctrl Pts',(160.904169453963,-1.34126316631299,135.538177513991));
#30172=CARTESIAN_POINT('Ctrl Pts',(160.896421557186,-1.20825937833372,135.571885377561));
#30173=CARTESIAN_POINT('Ctrl Pts',(160.888675281102,-1.07528341187967,135.605586190174));
#30174=CARTESIAN_POINT('Ctrl Pts',(160.880929005018,-0.940862446452899,
135.633727939933));
#30175=CARTESIAN_POINT('Ctrl Pts',(160.873182728934,-0.8055007360917,135.656200642408));
#30176=CARTESIAN_POINT('Ctrl Pts',(160.865436395668,-0.670138026521058,
135.678673510771));
#30177=CARTESIAN_POINT('Ctrl Pts',(160.857690062403,-0.533834943845108,
135.695477184315));
#30178=CARTESIAN_POINT('Ctrl Pts',(160.849943729138,-0.397104266609258,
135.706553113168));
#30179=CARTESIAN_POINT('Ctrl Pts',(160.842195661135,-0.260342969486592,
135.717631522399));
#30180=CARTESIAN_POINT('Ctrl Pts',(160.834447593132,-0.123154276873177,
135.722979602976));
#30181=CARTESIAN_POINT('Ctrl Pts',(160.826699525129,0.0139460000053123,
135.722590845156));
#30182=CARTESIAN_POINT('Ctrl Pts',(160.818943222387,0.151191988689769,135.72220167416));
#30183=CARTESIAN_POINT('Ctrl Pts',(160.811186919645,0.288348982338473,135.716063486102));
#30184=CARTESIAN_POINT('Ctrl Pts',(160.803430616903,0.424902704895101,135.704221917019));
#30185=CARTESIAN_POINT('Ctrl Pts',(160.795670174389,0.561529310285058,135.692374027733));
#30186=CARTESIAN_POINT('Ctrl Pts',(160.787909731875,0.697551615443923,135.674816741886));
#30187=CARTESIAN_POINT('Ctrl Pts',(160.780149289361,0.832463536533581,135.651647232038));
#30188=CARTESIAN_POINT('Ctrl Pts',(160.772376389095,0.96759203021589,135.628440528436));
#30189=CARTESIAN_POINT('Ctrl Pts',(160.76460348883,1.10160619541511,135.599603679791));
#30190=CARTESIAN_POINT('Ctrl Pts',(160.756830588564,1.23401227879488,135.565284557127));
#30191=CARTESIAN_POINT('Ctrl Pts',(160.749340252802,1.36160506753294,135.532213021016));
#30192=CARTESIAN_POINT('Ctrl Pts',(160.74184991704,1.48770436546009,135.494050968957));
#30193=CARTESIAN_POINT('Ctrl Pts',(160.734359581278,1.61188606552938,135.450972972202));
#30194=CARTESIAN_POINT('Ctrl Pts',(160.726585247159,1.74077615250114,135.406261660106));
#30195=CARTESIAN_POINT('Ctrl Pts',(160.71881091304,1.86800864475521,135.356112636514));
#30196=CARTESIAN_POINT('Ctrl Pts',(160.711036578921,1.99309054957259,135.30066722674));
#30197=CARTESIAN_POINT('Ctrl Pts',(160.703271825974,2.11801830212123,135.245290148479));
#30198=CARTESIAN_POINT('Ctrl Pts',(160.695507073027,2.24080038676023,135.184629828377));
#30199=CARTESIAN_POINT('Ctrl Pts',(160.68774232008,2.3609596561781,135.118877110106));
#30200=CARTESIAN_POINT('Ctrl Pts',(160.679985279195,2.48099958171563,135.053189698361));
#30201=CARTESIAN_POINT('Ctrl Pts',(160.67222823831,2.59842153538011,134.982420140244));
#30202=CARTESIAN_POINT('Ctrl Pts',(160.664471197425,2.71276936081772,134.90680689479));
#30203=CARTESIAN_POINT('Ctrl Pts',(160.656720006185,2.82703095567067,134.831250669872));
#30204=CARTESIAN_POINT('Ctrl Pts',(160.648968814945,2.93822271178586,134.750858242793));
#30205=CARTESIAN_POINT('Ctrl Pts',(160.641217623704,3.04591437568117,134.665913242938));
#30206=CARTESIAN_POINT('Ctrl Pts',(160.633469726927,3.15356026774636,134.581004346975));
#30207=CARTESIAN_POINT('Ctrl Pts',(160.62572183015,3.25770872005666,134.491546968356));
#30208=CARTESIAN_POINT('Ctrl Pts',(160.617973933373,3.35795989653583,134.397867038286));
#30209=CARTESIAN_POINT('Ctrl Pts',(160.610227657289,3.45819010263007,134.304206704038));
#30210=CARTESIAN_POINT('Ctrl Pts',(160.602481381205,3.55452436894585,134.206325841971));
#30211=CARTESIAN_POINT('Ctrl Pts',(160.594735105121,3.64659760084184,134.104589246015));
#30212=CARTESIAN_POINT('Ctrl Pts',(160.586988771856,3.73867151240152,134.002851899063));
#30213=CARTESIAN_POINT('Ctrl Pts',(160.57924243859,3.82648406443302,133.897259051307));
#30214=CARTESIAN_POINT('Ctrl Pts',(160.571496105325,3.90970882794232,133.788210470224));
#30215=CARTESIAN_POINT('Ctrl Pts',(160.563748037322,3.99295222906044,133.679137468468));
#30216=CARTESIAN_POINT('Ctrl Pts',(160.555999969319,4.07160556009345,133.566607504173));
#30217=CARTESIAN_POINT('Ctrl Pts',(160.548251901316,4.14538453564261,133.451051025255));
#30218=CARTESIAN_POINT('Ctrl Pts',(160.540495598574,4.21924192436505,133.335371731537));
#30219=CARTESIAN_POINT('Ctrl Pts',(160.532739295832,4.2882143982227,133.216659827713));
#30220=CARTESIAN_POINT('Ctrl Pts',(160.52498299309,4.35206237333402,133.095372656188));
#30221=CARTESIAN_POINT('Ctrl Pts',(160.517222550576,4.41594442603208,132.974020750047));
#30222=CARTESIAN_POINT('Ctrl Pts',(160.509462108062,4.47469636266918,132.850091190504));
#30223=CARTESIAN_POINT('Ctrl Pts',(160.501701665548,4.5281263865952,132.724062284367));
#30224=CARTESIAN_POINT('Ctrl Pts',(160.493928765283,4.5816421811389,132.597831065442));
#30225=CARTESIAN_POINT('Ctrl Pts',(160.486155865017,4.62981885344024,132.46949413171));
#30226=CARTESIAN_POINT('Ctrl Pts',(160.478382964752,4.67251392583976,132.339546819736));
#30227=CARTESIAN_POINT('Ctrl Pts',(160.47089262899,4.71365692481503,132.21432341987));
#30228=CARTESIAN_POINT('Ctrl Pts',(160.463402293228,4.7497098602883,132.087604987909));
#30229=CARTESIAN_POINT('Ctrl Pts',(160.455911957466,4.78059036377997,131.959842697148));
#30230=CARTESIAN_POINT('Ctrl Pts',(160.448137623347,4.81264171094755,131.827236260299));
#30231=CARTESIAN_POINT('Ctrl Pts',(160.440363289227,4.83922218699506,131.693085188945));
#30232=CARTESIAN_POINT('Ctrl Pts',(160.432588955108,4.86018421830598,131.557880641606));
#30233=CARTESIAN_POINT('Ctrl Pts',(160.424824202161,4.88112041578672,131.422842721789));
#30234=CARTESIAN_POINT('Ctrl Pts',(160.417059449214,4.89645188636241,131.286754291887));
#30235=CARTESIAN_POINT('Ctrl Pts',(160.409294696267,4.90608128244058,131.150119945114));
#30236=CARTESIAN_POINT('Ctrl Pts',(160.401537655382,4.91570111446682,131.013621305499));
#30237=CARTESIAN_POINT('Ctrl Pts',(160.393780614497,4.91963011507136,130.876578215514));
#30238=CARTESIAN_POINT('Ctrl Pts',(160.386023573612,4.91782234294213,130.739503345351));
#30239=CARTESIAN_POINT('Ctrl Pts',(160.378272382372,4.91601593406792,130.602531844412));
#30240=CARTESIAN_POINT('Ctrl Pts',(160.370521191132,4.90848136852386,130.465529000347));
#30241=CARTESIAN_POINT('Ctrl Pts',(160.362769999891,4.89522470922947,130.329010106207));
#30242=CARTESIAN_POINT('Ctrl Pts',(160.355022103114,4.88197368436897,130.192549236239));
#30243=CARTESIAN_POINT('Ctrl Pts',(160.347274206337,4.86300544061307,130.056572295411));
#30244=CARTESIAN_POINT('Ctrl Pts',(160.33952630956,4.8383780719501,129.921591850916));
#30245=CARTESIAN_POINT('Ctrl Pts',(160.331780033476,4.81375585480178,129.78663964142));
#30246=CARTESIAN_POINT('Ctrl Pts',(160.324033757392,4.78347693745298,129.65268389802));
#30247=CARTESIAN_POINT('Ctrl Pts',(160.316287481308,4.74765088879886,129.520228965208));
#30248=CARTESIAN_POINT('Ctrl Pts',(160.308541148043,4.71182457568494,129.387773054644));
#30249=CARTESIAN_POINT('Ctrl Pts',(160.300794814777,4.67045115163675,129.256818354178));
#30250=CARTESIAN_POINT('Ctrl Pts',(160.293048481512,4.62369050951024,129.127855581855));
#30251=CARTESIAN_POINT('Ctrl Pts',(160.285300413509,4.5769193956623,128.998863929213));
#30252=CARTESIAN_POINT('Ctrl Pts',(160.277552345506,4.52475879632425,128.871865459839));
#30253=CARTESIAN_POINT('Ctrl Pts',(160.269804277503,4.46741719631762,128.747332018702));
#30254=CARTESIAN_POINT('Ctrl Pts',(160.262047974761,4.41001465297591,128.622666221941));
#30255=CARTESIAN_POINT('Ctrl Pts',(160.254291672019,4.34742027305976,128.500471042566));
#30256=CARTESIAN_POINT('Ctrl Pts',(160.246535369277,4.27988933074522,128.381195254023));
#30257=CARTESIAN_POINT('Ctrl Pts',(160.238774926763,4.21232234513353,128.261855804401));
#30258=CARTESIAN_POINT('Ctrl Pts',(160.231014484249,4.13981375367094,128.145439182086));
#30259=CARTESIAN_POINT('Ctrl Pts',(160.223254041735,4.06266229864699,128.032365287546));
#30260=CARTESIAN_POINT('Ctrl Pts',(160.215481141469,3.98538699325826,127.919109876753));
#30261=CARTESIAN_POINT('Ctrl Pts',(160.207708241204,3.90345416437802,127.809208230425));
#30262=CARTESIAN_POINT('Ctrl Pts',(160.199935340938,3.81720354003233,127.703047960567));
#30263=CARTESIAN_POINT('Ctrl Pts',(160.192445005176,3.73408834313408,127.600746883919));
#30264=CARTESIAN_POINT('Ctrl Pts',(160.184954669414,3.64696402973765,127.501920120489));
#30265=CARTESIAN_POINT('Ctrl Pts',(160.177464333652,3.55616566253962,127.406880839396));
#30266=CARTESIAN_POINT('Ctrl Pts',(160.169689999533,3.46192464765145,127.308238115074));
#30267=CARTESIAN_POINT('Ctrl Pts',(160.161915665414,3.36342694853327,127.213363276888));
#30268=CARTESIAN_POINT('Ctrl Pts',(160.154141331295,3.26100602361524,127.122645965879));
#30269=CARTESIAN_POINT('Ctrl Pts',(160.146376578348,3.15871132333361,127.032040455849));
#30270=CARTESIAN_POINT('Ctrl Pts',(160.138611825401,3.05250330737112,126.945582534937));
#30271=CARTESIAN_POINT('Ctrl Pts',(160.130847072454,2.94275388553613,126.863626849388));
#30272=CARTESIAN_POINT('Ctrl Pts',(160.123090031569,2.83311346837376,126.78175256338));
#30273=CARTESIAN_POINT('Ctrl Pts',(160.115332990684,2.71993895630499,126.704371846295));
#30274=CARTESIAN_POINT('Ctrl Pts',(160.107575949799,2.60363684088095,126.631800460623));
#30275=CARTESIAN_POINT('Ctrl Pts',(160.099824758559,2.48742242978704,126.559283801597));
#30276=CARTESIAN_POINT('Ctrl Pts',(160.092073567319,2.36808544023483,126.491569461282));
#30277=CARTESIAN_POINT('Ctrl Pts',(160.084322376078,2.24606268001862,126.428930867253));
#30278=CARTESIAN_POINT('Ctrl Pts',(160.076574479301,2.12409178273078,126.366318896297));
#30279=CARTESIAN_POINT('Ctrl Pts',(160.068826582524,1.99943773227024,126.308778559038));
#30280=CARTESIAN_POINT('Ctrl Pts',(160.061078685747,1.8725631671527,126.256538034447));
#30281=CARTESIAN_POINT('Ctrl Pts',(160.053332409663,1.74571514145887,126.204308437448));
#30282=CARTESIAN_POINT('Ctrl Pts',(160.045586133579,1.61664788628163,126.157376596798));
#30283=CARTESIAN_POINT('Ctrl Pts',(160.037839857495,1.48584494559068,126.115922939601));
#30284=CARTESIAN_POINT('Ctrl Pts',(160.03009352423,1.35504103934232,126.074468976402));
#30285=CARTESIAN_POINT('Ctrl Pts',(160.022347190964,1.22250179471075,126.038493395462));
#30286=CARTESIAN_POINT('Ctrl Pts',(160.014600857699,1.0887264926785,126.008126919482));
#30287=CARTESIAN_POINT('Ctrl Pts',(160.006852789696,0.954921232594703,125.97775364314));
#30288=CARTESIAN_POINT('Ctrl Pts',(159.999104721693,0.819879745490189,125.95299205782));
#30289=CARTESIAN_POINT('Ctrl Pts',(159.99135665369,0.684111699040778,125.933921803071));
#30290=CARTESIAN_POINT('Ctrl Pts',(159.983600350948,0.548199356696079,125.914831280229));
#30291=CARTESIAN_POINT('Ctrl Pts',(159.975844048206,0.41155930024387,125.901444225582));
#30292=CARTESIAN_POINT('Ctrl Pts',(159.968087745465,0.274707077420868,125.893788442746));
#30293=CARTESIAN_POINT('Ctrl Pts',(159.96032730295,0.137781812445819,125.886128573788));
#30294=CARTESIAN_POINT('Ctrl Pts',(159.952566860436,0.000644546196039986,
125.884206077341));
#30295=CARTESIAN_POINT('Ctrl Pts',(159.944806417922,-0.136189969668989,
125.887996579513));
#30296=CARTESIAN_POINT('Ctrl Pts',(159.937033517657,-0.273244144446389,
125.891793166536));
#30297=CARTESIAN_POINT('Ctrl Pts',(159.929260617391,-0.409994207408434,
125.901321051594));
#30298=CARTESIAN_POINT('Ctrl Pts',(159.921487717126,-0.545930418302852,
125.916503925633));
#30299=CARTESIAN_POINT('Ctrl Pts',(159.913997381364,-0.676925005528741,
125.931134863958));
#30300=CARTESIAN_POINT('Ctrl Pts',(159.906507045602,-0.807163580043379,
125.951016736695));
#30301=CARTESIAN_POINT('Ctrl Pts',(159.89901670984,-0.936201554223454,125.976036921668));
#30302=CARTESIAN_POINT('Ctrl Pts',(159.891242375721,-1.07013204241472,126.002005754559));
#30303=CARTESIAN_POINT('Ctrl Pts',(159.883468041602,-1.20319334308913,126.033592490941));
#30304=CARTESIAN_POINT('Ctrl Pts',(159.875693707483,-1.33487739777685,126.070727193292));
#30305=CARTESIAN_POINT('Ctrl Pts',(159.867928954535,-1.46639916363593,126.107816130441));
#30306=CARTESIAN_POINT('Ctrl Pts',(159.860164201588,-1.59654668801709,126.150439324133));
#30307=CARTESIAN_POINT('Ctrl Pts',(159.852399448641,-1.72482057065621,126.198475571069));
#30308=CARTESIAN_POINT('Ctrl Pts',(159.844642407756,-1.8529670498674,126.246464107728));
#30309=CARTESIAN_POINT('Ctrl Pts',(159.836885366871,-1.97924322690081,126.299854862287));
#30310=CARTESIAN_POINT('Ctrl Pts',(159.829128325986,-2.1031637232194,126.35847651923));
#30311=CARTESIAN_POINT('Ctrl Pts',(159.821377134746,-2.2269907701264,126.417053969125));
#30312=CARTESIAN_POINT('Ctrl Pts',(159.813625943506,-2.34846532022352,126.480854303279));
#30313=CARTESIAN_POINT('Ctrl Pts',(159.805874752266,-2.46712122586535,126.549657817207));
#30314=CARTESIAN_POINT('Ctrl Pts',(159.798126855489,-2.58572669958301,126.618432087806));
#30315=CARTESIAN_POINT('Ctrl Pts',(159.790378958712,-2.70151557406425,126.692205113056));
#30316=CARTESIAN_POINT('Ctrl Pts',(159.782631061935,-2.81404580846085,126.770710998377));
#30317=CARTESIAN_POINT('Ctrl Pts',(159.774884785851,-2.9265525039582,126.849200461959));
#30318=CARTESIAN_POINT('Ctrl Pts',(159.767138509766,-3.03580159474203,126.932420592869));
#30319=CARTESIAN_POINT('Ctrl Pts',(159.759392233682,-3.14137991505379,127.020062097127));
#30320=CARTESIAN_POINT('Ctrl Pts',(159.751645900417,-3.24695901472074,127.107704248335));
#30321=CARTESIAN_POINT('Ctrl Pts',(159.743899567152,-3.34886698902163,127.199767588299));
#30322=CARTESIAN_POINT('Ctrl Pts',(159.736153233886,-3.44672398367913,127.295902716603));
#30323=CARTESIAN_POINT('Ctrl Pts',(159.728405165883,-3.54460289273218,127.392059373702));
#30324=CARTESIAN_POINT('Ctrl Pts',(159.72065709788,-3.63842873809756,127.492289359676));
#30325=CARTESIAN_POINT('Ctrl Pts',(159.712909029877,-3.72785902894052,127.596206923797));
#30326=CARTESIAN_POINT('Ctrl Pts',(159.705152727135,-3.81738436736076,127.70023493274));
#30327=CARTESIAN_POINT('Ctrl Pts',(159.697396424394,-3.90250456370759,127.807958052048));
#30328=CARTESIAN_POINT('Ctrl Pts',(159.689640121652,-3.98291755986778,127.91895756534));
#30329=CARTESIAN_POINT('Ctrl Pts',(159.681879679138,-4.06337347486506,128.030016322414));
#30330=CARTESIAN_POINT('Ctrl Pts',(159.674119236623,-4.13911696774629,128.144354632149));
#30331=CARTESIAN_POINT('Ctrl Pts',(159.666358794109,-4.20989030911008,128.261526244713));
#30332=CARTESIAN_POINT('Ctrl Pts',(159.658585893844,-4.28077726212446,128.378885951552));
#30333=CARTESIAN_POINT('Ctrl Pts',(159.650812993578,-4.34667793191823,128.499087707091));
#30334=CARTESIAN_POINT('Ctrl Pts',(159.643040093313,-4.40738099240258,128.62166140551));
#30335=CARTESIAN_POINT('Ctrl Pts',(159.635549757551,-4.46587734373642,128.739779241248));
#30336=CARTESIAN_POINT('Ctrl Pts',(159.628059421789,-4.51954729189796,128.860099280391));
#30337=CARTESIAN_POINT('Ctrl Pts',(159.620569086027,-4.56824527864363,128.982186603743));
#30338=CARTESIAN_POINT('Ctrl Pts',(159.611787365971,-4.62533912603141,129.125322603264));
#30339=CARTESIAN_POINT('Ctrl Pts',(159.603005645915,-4.67575140335755,129.271268173422));
#30340=CARTESIAN_POINT('Ctrl Pts',(159.59422392586,-4.71923020496151,129.419424035957));
#30341=CARTESIAN_POINT('Ctrl Pts',(159.591018937532,-4.73509828669941,129.473495198223));
#30342=CARTESIAN_POINT('Ctrl Pts',(159.587813949204,-4.75004329422944,129.527860530574));
#30343=CARTESIAN_POINT('Ctrl Pts',(159.584608960876,-4.76405452823403,129.582490119308));
#30344=CARTESIAN_POINT('Ctrl Pts',(161.334944359449,-4.76405452823403,129.582490119308));
#30345=CARTESIAN_POINT('Ctrl Pts',(161.327171216939,-4.79811130280615,129.715276966481));
#30346=CARTESIAN_POINT('Ctrl Pts',(161.319398074429,-4.82657531939697,129.849344857447));
#30347=CARTESIAN_POINT('Ctrl Pts',(161.311624931919,-4.84938052155759,129.984182819989));
#30348=CARTESIAN_POINT('Ctrl Pts',(161.304834897581,-4.86930143585433,130.101967151689));
#30349=CARTESIAN_POINT('Ctrl Pts',(161.298044863242,-4.8849052060667,130.220338818543));
#30350=CARTESIAN_POINT('Ctrl Pts',(161.291254828904,-4.89618035041408,130.338956450504));
#30351=CARTESIAN_POINT('Ctrl Pts',(161.2824563646,-4.91079057918865,130.492660091562));
#30352=CARTESIAN_POINT('Ctrl Pts',(161.273657900295,-4.91816461835232,130.647062382023));
#30353=CARTESIAN_POINT('Ctrl Pts',(161.264859435991,-4.91824926289688,130.801667939662));
#30354=CARTESIAN_POINT('',(161.610140564037,-4.91824795040022,130.808850704879));
#30355=CARTESIAN_POINT('Ctrl Pts',(161.680195102581,-4.76405452823405,129.582490119308));
#30356=CARTESIAN_POINT('Ctrl Pts',(161.672552391556,-4.79770299521974,129.713684981399));
#30357=CARTESIAN_POINT('Ctrl Pts',(161.664909680531,-4.82591915561794,129.846236774025));
#30358=CARTESIAN_POINT('Ctrl Pts',(161.657266969507,-4.84861163807389,129.979649610222));
#30359=CARTESIAN_POINT('Ctrl Pts',(161.649412568595,-4.87193266307583,130.116757751412));
#30360=CARTESIAN_POINT('Ctrl Pts',(161.641558167684,-4.88941948444408,130.254774881735));
#30361=CARTESIAN_POINT('Ctrl Pts',(161.633703766772,-4.90102992760437,130.393156639927));
#30362=CARTESIAN_POINT('Ctrl Pts',(161.62584936586,-4.91264037076467,130.531538398119));
#30363=CARTESIAN_POINT('Ctrl Pts',(161.617994964949,-4.9183744538122,130.670284324455));
#30364=CARTESIAN_POINT('Ctrl Pts',(161.610140564037,-4.91824795040022,130.808850704879));
#30365=CARTESIAN_POINT('Ctrl Pts',(161.610140564008,-4.91824795039975,130.808850705393));
#30366=CARTESIAN_POINT('Ctrl Pts',(161.599381903105,-4.91807467079718,130.998653685444));
#30367=CARTESIAN_POINT('Ctrl Pts',(161.588623242203,-4.90691076602029,131.187975563161));
#30368=CARTESIAN_POINT('Ctrl Pts',(161.5778645813,-4.88494323448938,131.375773479091));
#30369=CARTESIAN_POINT('Ctrl Pts',(161.568614206386,-4.86605539106516,131.537243493439));
#30370=CARTESIAN_POINT('Ctrl Pts',(161.559363831472,-4.8391815661298,131.697587784437));
#30371=CARTESIAN_POINT('Ctrl Pts',(161.550113456558,-4.80446700205628,131.856159024416));
#30372=CARTESIAN_POINT('Ctrl Pts',(161.542339122439,-4.77529168511808,131.98942776355));
#30373=CARTESIAN_POINT('Ctrl Pts',(161.53456478832,-4.74052094061047,132.121692751278));
#30374=CARTESIAN_POINT('Ctrl Pts',(161.526790454201,-4.7002368779166,132.252447753747));
#30375=CARTESIAN_POINT('Ctrl Pts',(161.519025701254,-4.6600024617297,132.383041612361));
#30376=CARTESIAN_POINT('Ctrl Pts',(161.511260948307,-4.61426836073582,132.512128818347));
#30377=CARTESIAN_POINT('Ctrl Pts',(161.503496195359,-4.56316772755854,132.639213023802));
#30378=CARTESIAN_POINT('Ctrl Pts',(161.495739154474,-4.51211784825061,132.766171007431));
#30379=CARTESIAN_POINT('Ctrl Pts',(161.487982113589,-4.45571218884313,132.89112958915));
#30380=CARTESIAN_POINT('Ctrl Pts',(161.480225072704,-4.39413366326438,133.013607641298));
#30381=CARTESIAN_POINT('Ctrl Pts',(161.472473881464,-4.33260157453067,133.135993331794));
#30382=CARTESIAN_POINT('Ctrl Pts',(161.464722690224,-4.26590455903632,133.25590186812));
#30383=CARTESIAN_POINT('Ctrl Pts',(161.456971498984,-4.19427344425517,133.372872509171));
#30384=CARTESIAN_POINT('Ctrl Pts',(161.449223602207,-4.12267277460866,133.489793434579));
#30385=CARTESIAN_POINT('Ctrl Pts',(161.44147570543,-4.04614238044535,133.603778615534));
#30386=CARTESIAN_POINT('Ctrl Pts',(161.433727808653,-3.96495868753456,133.71439251922));
#30387=CARTESIAN_POINT('Ctrl Pts',(161.425981532569,-3.88379197650217,133.824983284862));
#30388=CARTESIAN_POINT('Ctrl Pts',(161.418235256485,-3.79797413398804,133.932203860928));
#30389=CARTESIAN_POINT('Ctrl Pts',(161.4104889804,-3.70782427974217,134.035648622844));
#30390=CARTESIAN_POINT('Ctrl Pts',(161.402742647135,-3.61767376003062,134.139094148366));
#30391=CARTESIAN_POINT('Ctrl Pts',(161.39499631387,-3.52319142164166,134.238763509375));
#30392=CARTESIAN_POINT('Ctrl Pts',(161.387249980604,-3.42473567982982,134.33428534563));
#30393=CARTESIAN_POINT('Ctrl Pts',(161.379501912601,-3.32625788953721,134.429828573339));
#30394=CARTESIAN_POINT('Ctrl Pts',(161.371753844598,-3.2238052057403,134.52122215588));
#30395=CARTESIAN_POINT('Ctrl Pts',(161.364005776596,-3.11777148691773,134.608132958002));
#30396=CARTESIAN_POINT('Ctrl Pts',(161.356249473854,-3.01162507419694,134.695136129958));
#30397=CARTESIAN_POINT('Ctrl Pts',(161.348493171112,-2.90189032647662,134.777646755954));
#30398=CARTESIAN_POINT('Ctrl Pts',(161.34073686837,-2.78899308811763,134.855372912898));
#30399=CARTESIAN_POINT('Ctrl Pts',(161.332976425856,-2.67603559310322,134.933140554633));
#30400=CARTESIAN_POINT('Ctrl Pts',(161.325215983342,-2.55991257499477,135.006118431091));
#30401=CARTESIAN_POINT('Ctrl Pts',(161.317455540827,-2.44107633991098,135.074059595858));
#30402=CARTESIAN_POINT('Ctrl Pts',(161.309682640562,-2.32204933835285,135.142109825814));
#30403=CARTESIAN_POINT('Ctrl Pts',(161.301909740297,-2.20030076358336,135.205107007143));
#30404=CARTESIAN_POINT('Ctrl Pts',(161.294136840031,-2.07630565728573,135.262851155856));
#30405=CARTESIAN_POINT('Ctrl Pts',(161.286646504269,-1.95681808542466,135.318496159316));
#30406=CARTESIAN_POINT('Ctrl Pts',(161.279156168507,-1.83524476470625,135.369263302679));
#30407=CARTESIAN_POINT('Ctrl Pts',(161.271665832745,-1.71202398207716,135.41501750648));
#30408=CARTESIAN_POINT('Ctrl Pts',(161.263891498626,-1.58413124602475,135.462506494824));
#30409=CARTESIAN_POINT('Ctrl Pts',(161.256117164507,-1.45405852918058,135.50474533933));
#30410=CARTESIAN_POINT('Ctrl Pts',(161.248342830388,-1.32227612255046,135.541529489185));
#30411=CARTESIAN_POINT('Ctrl Pts',(161.24057807744,-1.19065612595883,135.578268305862));
#30412=CARTESIAN_POINT('Ctrl Pts',(161.232813324493,-1.05733100491809,135.609565699404));
#30413=CARTESIAN_POINT('Ctrl Pts',(161.225048571546,-0.922790323222832,
135.635265406719));
#30414=CARTESIAN_POINT('Ctrl Pts',(161.217291530661,-0.788383269229369,
135.660939588723));
#30415=CARTESIAN_POINT('Ctrl Pts',(161.209534489776,-0.652763438723616,
135.681027075674));
#30416=CARTESIAN_POINT('Ctrl Pts',(161.201777448891,-0.516434487478315,
135.695421696989));
#30417=CARTESIAN_POINT('Ctrl Pts',(161.194026257651,-0.380208342955726,
135.709805463207));
#30418=CARTESIAN_POINT('Ctrl Pts',(161.186275066411,-0.243274529318622,
135.718504867927));
#30419=CARTESIAN_POINT('Ctrl Pts',(161.178523875171,-0.106145448995003,
135.721465071018));
#30420=CARTESIAN_POINT('Ctrl Pts',(161.170775978394,0.0309253478116268,
135.724424015944));
#30421=CARTESIAN_POINT('Ctrl Pts',(161.163028081617,0.168190856181115,135.721648602429));
#30422=CARTESIAN_POINT('Ctrl Pts',(161.15528018484,0.305135235141163,135.713135979179));
#30423=CARTESIAN_POINT('Ctrl Pts',(161.147533908756,0.442050968289219,135.704625136585));
#30424=CARTESIAN_POINT('Ctrl Pts',(161.139787632671,0.578645315674485,135.690379495562));
#30425=CARTESIAN_POINT('Ctrl Pts',(161.132041356587,0.714404521834894,135.670448290603));
#30426=CARTESIAN_POINT('Ctrl Pts',(161.124295023322,0.850164730138877,135.650516938516));
#30427=CARTESIAN_POINT('Ctrl Pts',(161.116548690057,0.98508939809787,135.624899995535));
#30428=CARTESIAN_POINT('Ctrl Pts',(161.108802356791,1.11867235762289,135.593698277284));
#30429=CARTESIAN_POINT('Ctrl Pts',(161.101054288788,1.25228523212554,135.562489571624));
#30430=CARTESIAN_POINT('Ctrl Pts',(161.093306220785,1.38455541965632,135.52569369091));
#30431=CARTESIAN_POINT('Ctrl Pts',(161.085558152782,1.51498975396465,135.483461931695));
#30432=CARTESIAN_POINT('Ctrl Pts',(161.07780185004,1.64556271543567,135.441185288063));
#30433=CARTESIAN_POINT('Ctrl Pts',(161.070045547299,1.77429555347097,135.393461345741));
#30434=CARTESIAN_POINT('Ctrl Pts',(161.062289244557,1.90071248562887,135.340490588089));
#30435=CARTESIAN_POINT('Ctrl Pts',(161.054528802043,2.02719689030988,135.287491558348));
#30436=CARTESIAN_POINT('Ctrl Pts',(161.046768359528,2.15136257236546,135.229240299248));
#30437=CARTESIAN_POINT('Ctrl Pts',(161.039007917014,2.27275728627645,135.165983868166));
#30438=CARTESIAN_POINT('Ctrl Pts',(161.031235016749,2.39434687375913,135.102625892246));
#30439=CARTESIAN_POINT('Ctrl Pts',(161.023462116483,2.5131562651213,135.034246883493));
#30440=CARTESIAN_POINT('Ctrl Pts',(161.015689216218,2.6287604365361,134.9611384117));
#30441=CARTESIAN_POINT('Ctrl Pts',(161.008198880456,2.74016210512989,134.890687617006));
#30442=CARTESIAN_POINT('Ctrl Pts',(161.000708544694,2.84858729008048,134.815845420196));
#30443=CARTESIAN_POINT('Ctrl Pts',(160.993218208932,2.95368544040804,134.736907550741));
#30444=CARTESIAN_POINT('Ctrl Pts',(160.985443874813,3.06276841904973,134.654976727972));
#30445=CARTESIAN_POINT('Ctrl Pts',(160.977669540694,3.16861263585589,134.568373994637));
#30446=CARTESIAN_POINT('Ctrl Pts',(160.969895206575,3.27079179265738,134.477384455167));
#30447=CARTESIAN_POINT('Ctrl Pts',(160.962130453628,3.3728450227801,134.386507052172));
#30448=CARTESIAN_POINT('Ctrl Pts',(160.954365700681,3.47124189092529,134.291253857568));
#30449=CARTESIAN_POINT('Ctrl Pts',(160.946600947733,3.56558630733806,134.191952291222));
#30450=CARTESIAN_POINT('Ctrl Pts',(160.938843906848,3.65983701954643,134.092749352591));
#30451=CARTESIAN_POINT('Ctrl Pts',(160.931086865963,3.75004302231244,133.989506325595));
#30452=CARTESIAN_POINT('Ctrl Pts',(160.923329825078,3.8358427530691,133.882589562305));
#30453=CARTESIAN_POINT('Ctrl Pts',(160.915578633838,3.92157778158132,133.775753425777));
#30454=CARTESIAN_POINT('Ctrl Pts',(160.907827442598,4.00291290821725,133.665249370943));
#30455=CARTESIAN_POINT('Ctrl Pts',(160.900076251358,4.07952502839383,133.551478854047));
#30456=CARTESIAN_POINT('Ctrl Pts',(160.892328354581,4.15610458637569,133.437756692656));
#30457=CARTESIAN_POINT('Ctrl Pts',(160.884580457804,4.22796491255238,133.320771154106));
#30458=CARTESIAN_POINT('Ctrl Pts',(160.876832561027,4.29482478340195,133.200954688821));
#30459=CARTESIAN_POINT('Ctrl Pts',(160.869086284943,4.36167066860786,133.081163286558));
#30460=CARTESIAN_POINT('Ctrl Pts',(160.861340008859,4.42351798862189,132.958542476608));
#30461=CARTESIAN_POINT('Ctrl Pts',(160.853593732775,4.48013046844121,132.833551108438));
#30462=CARTESIAN_POINT('Ctrl Pts',(160.845847399509,4.53674336616095,132.70855881761));
#30463=CARTESIAN_POINT('Ctrl Pts',(160.838101066244,4.58812118527195,132.581196289781));
#30464=CARTESIAN_POINT('Ctrl Pts',(160.830354732979,4.63407514859685,132.451943871808));
#30465=CARTESIAN_POINT('Ctrl Pts',(160.822606664976,4.68003940299322,132.322662508651));
#30466=CARTESIAN_POINT('Ctrl Pts',(160.814858596973,4.72057725367482,132.19149078148));
#30467=CARTESIAN_POINT('Ctrl Pts',(160.80711052897,4.75554942231088,132.058925384511));
#30468=CARTESIAN_POINT('Ctrl Pts',(160.799354226228,4.79055875978396,131.926219095459));
#30469=CARTESIAN_POINT('Ctrl Pts',(160.791597923486,4.81999049892845,131.79211655637));
#30470=CARTESIAN_POINT('Ctrl Pts',(160.783841620744,4.84375614004254,131.657126422638));
#30471=CARTESIAN_POINT('Ctrl Pts',(160.77608117823,4.86753446559487,131.522064240608));
#30472=CARTESIAN_POINT('Ctrl Pts',(160.768320735716,4.88564061561917,131.38611390733));
#30473=CARTESIAN_POINT('Ctrl Pts',(160.760560293202,4.89803799673453,131.249789450316));
#30474=CARTESIAN_POINT('Ctrl Pts',(160.752787392936,4.91045527922664,131.113246153181));
#30475=CARTESIAN_POINT('Ctrl Pts',(160.745014492671,4.91714546068101,130.97632792289));
#30476=CARTESIAN_POINT('Ctrl Pts',(160.737241592405,4.91812411126045,130.839549944621));
#30477=CARTESIAN_POINT('Ctrl Pts',(160.729751256643,4.91906718542626,130.707744190383));
#30478=CARTESIAN_POINT('Ctrl Pts',(160.722260920881,4.91470678650708,130.576068976024));
#30479=CARTESIAN_POINT('Ctrl Pts',(160.714770585119,4.90510223871495,130.444979079012));
#30480=CARTESIAN_POINT('Ctrl Pts',(160.706996251,4.89513353157412,130.308918868712));
#30481=CARTESIAN_POINT('Ctrl Pts',(160.699221916881,4.87948358387501,130.173058238692));
#30482=CARTESIAN_POINT('Ctrl Pts',(160.691447582762,4.85816183747676,130.037909951584));
#30483=CARTESIAN_POINT('Ctrl Pts',(160.683682829815,4.83686636822538,129.902928222661));
#30484=CARTESIAN_POINT('Ctrl Pts',(160.675918076868,4.80991306860397,129.768657472374));
#30485=CARTESIAN_POINT('Ctrl Pts',(160.668153323921,4.77736331003202,129.635607920688));
#30486=CARTESIAN_POINT('Ctrl Pts',(160.660396283036,4.74484588033915,129.502690515692));
#30487=CARTESIAN_POINT('Ctrl Pts',(160.652639242151,4.70674314563176,129.370992272855));
#30488=CARTESIAN_POINT('Ctrl Pts',(160.644882201266,4.66316789488435,129.241015407249));
#30489=CARTESIAN_POINT('Ctrl Pts',(160.637131010026,4.61962550457248,129.111136558209));
#30490=CARTESIAN_POINT('Ctrl Pts',(160.629379818786,4.57061893627067,128.98297687179));
#30491=CARTESIAN_POINT('Ctrl Pts',(160.621628627545,4.51631130056807,128.857025181936));
#30492=CARTESIAN_POINT('Ctrl Pts',(160.613880730768,4.46202674705934,128.73112702491));
#30493=CARTESIAN_POINT('Ctrl Pts',(160.606132833991,4.40244576185906,128.60743535619));
#30494=CARTESIAN_POINT('Ctrl Pts',(160.598384937214,4.33778016957377,128.486420527108));
#30495=CARTESIAN_POINT('Ctrl Pts',(160.59063866113,4.27312810393636,128.36543101172));
#30496=CARTESIAN_POINT('Ctrl Pts',(160.582892385046,4.20339373089582,128.247117566827));
#30497=CARTESIAN_POINT('Ctrl Pts',(160.575146108962,4.12883538109347,128.131926996626));
#30498=CARTESIAN_POINT('Ctrl Pts',(160.567399775697,4.05427648091835,128.016735576115));
#30499=CARTESIAN_POINT('Ctrl Pts',(160.559653442431,3.97489374536435,127.904667404507));
#30500=CARTESIAN_POINT('Ctrl Pts',(160.551907109166,3.89098926516945,127.796140944597));
#30501=CARTESIAN_POINT('Ctrl Pts',(160.544159041163,3.80706599514796,127.687590180939));
#30502=CARTESIAN_POINT('Ctrl Pts',(160.53641097316,3.7186192045881,127.582583016486));
#30503=CARTESIAN_POINT('Ctrl Pts',(160.528662905157,3.62599149306077,127.481505105397));
#30504=CARTESIAN_POINT('Ctrl Pts',(160.520906602415,3.53326533569931,127.380319767502));
#30505=CARTESIAN_POINT('Ctrl Pts',(160.513150299673,3.43634964549955,127.283072313795));
#30506=CARTESIAN_POINT('Ctrl Pts',(160.505393996932,3.33562453240203,127.190112142248));
#30507=CARTESIAN_POINT('Ctrl Pts',(160.497633554417,3.23484565927881,127.097102355059));
#30508=CARTESIAN_POINT('Ctrl Pts',(160.489873111903,3.13025360993405,127.008384662343));
#30509=CARTESIAN_POINT('Ctrl Pts',(160.482112669389,3.02226107065443,126.924267695572));
#30510=CARTESIAN_POINT('Ctrl Pts',(160.474339769124,2.91409517216366,126.840015696779));
#30511=CARTESIAN_POINT('Ctrl Pts',(160.466566868858,2.80251819378715,126.76037940976));
#30512=CARTESIAN_POINT('Ctrl Pts',(160.458793968593,2.68797199145841,126.685624205068));
#30513=CARTESIAN_POINT('Ctrl Pts',(160.451303632831,2.57758983210879,126.613586540364));
#30514=CARTESIAN_POINT('Ctrl Pts',(160.443813297069,2.46445084290856,126.546081397761));
#30515=CARTESIAN_POINT('Ctrl Pts',(160.436322961307,2.34896970720894,126.48330468445));
#30516=CARTESIAN_POINT('Ctrl Pts',(160.428548627188,2.22911006914954,126.418147772974));
#30517=CARTESIAN_POINT('Ctrl Pts',(160.420774293068,2.10634749433814,126.357878528096));
#30518=CARTESIAN_POINT('Ctrl Pts',(160.412999958949,1.98111848805488,126.302766166842));
#30519=CARTESIAN_POINT('Ctrl Pts',(160.405235206002,1.85604381532991,126.247721726648));
#30520=CARTESIAN_POINT('Ctrl Pts',(160.397470453055,1.72850911355208,126.197821680701));
#30521=CARTESIAN_POINT('Ctrl Pts',(160.389705700108,1.59897681797892,126.153290181842));
#30522=CARTESIAN_POINT('Ctrl Pts',(160.381948659223,1.46957317570777,126.108802912296));
#30523=CARTESIAN_POINT('Ctrl Pts',(160.374191618338,1.33817625530096,126.069673704969));
#30524=CARTESIAN_POINT('Ctrl Pts',(160.366434577453,1.20526954971698,126.036079126816));
#30525=CARTESIAN_POINT('Ctrl Pts',(160.358683386213,1.07246307011349,126.002509882597));
#30526=CARTESIAN_POINT('Ctrl Pts',(160.350932194973,0.938149449039233,125.974467055463));
#30527=CARTESIAN_POINT('Ctrl Pts',(160.343181003733,0.802828121592549,125.952077642545));
#30528=CARTESIAN_POINT('Ctrl Pts',(160.335433106956,0.66756430931989,125.929697745724));
#30529=CARTESIAN_POINT('Ctrl Pts',(160.327685210178,0.531294027448772,125.912966547714));
#30530=CARTESIAN_POINT('Ctrl Pts',(160.319937313401,0.394527492249022,125.901960070858));
#30531=CARTESIAN_POINT('Ctrl Pts',(160.312191037317,0.25778956566009,125.89095589632));
#30532=CARTESIAN_POINT('Ctrl Pts',(160.304444761233,0.120555981675745,125.885674092408));
#30533=CARTESIAN_POINT('Ctrl Pts',(160.296698485149,-0.0166577166577505,
125.886138826819));
#30534=CARTESIAN_POINT('Ctrl Pts',(160.288952151884,-0.15387242787155,125.886603564661));
#30535=CARTESIAN_POINT('Ctrl Pts',(160.281205818618,-0.291066862178625,
125.892814924147));
#30536=CARTESIAN_POINT('Ctrl Pts',(160.273459485353,-0.427725667555909,
125.904744937146));
#30537=CARTESIAN_POINT('Ctrl Pts',(160.26571141735,-0.564415076725132,125.916677621789));
#30538=CARTESIAN_POINT('Ctrl Pts',(160.257963349347,-0.700568228867815,
125.934331474301));
#30539=CARTESIAN_POINT('Ctrl Pts',(160.250215281344,-0.835675478780135,
125.957626711453));
#30540=CARTESIAN_POINT('Ctrl Pts',(160.242458978602,-0.970926322285506,
125.980946707061));
#30541=CARTESIAN_POINT('Ctrl Pts',(160.23470267586,-1.10512865713056,126.009919997891));
#30542=CARTESIAN_POINT('Ctrl Pts',(160.226946373118,-1.23778306619832,126.044415644824));
#30543=CARTESIAN_POINT('Ctrl Pts',(160.219185930604,-1.37050827691844,126.078929703122));
#30544=CARTESIAN_POINT('Ctrl Pts',(160.21142548809,-1.50168354189003,126.118971876474));
#30545=CARTESIAN_POINT('Ctrl Pts',(160.203665045576,-1.63082613369543,126.164361783067));
#30546=CARTESIAN_POINT('Ctrl Pts',(160.19589214531,-1.76017603665388,126.209824553567));
#30547=CARTESIAN_POINT('Ctrl Pts',(160.188119245045,-1.8874863825716,126.260652067141));
#30548=CARTESIAN_POINT('Ctrl Pts',(160.180346344779,-2.0122950737614,126.316616017144));
#30549=CARTESIAN_POINT('Ctrl Pts',(160.172856009017,-2.13256665465224,126.3705455366));
#30550=CARTESIAN_POINT('Ctrl Pts',(160.165365673255,-2.25051503020531,126.429244393995));
#30551=CARTESIAN_POINT('Ctrl Pts',(160.157875337493,-2.36575123167159,126.492469597104));
#30552=CARTESIAN_POINT('Ctrl Pts',(160.150099986099,-2.48537229916469,126.558100589727));
#30553=CARTESIAN_POINT('Ctrl Pts',(160.142324634705,-2.60244967655088,126.628817140122));
#30554=CARTESIAN_POINT('Ctrl Pts',(160.134549283311,-2.7165207419171,126.704397432215));
#30555=CARTESIAN_POINT('Ctrl Pts',(160.126783736502,-2.83044796561676,126.77988241885));
#30556=CARTESIAN_POINT('Ctrl Pts',(160.119018189693,-2.94137609787276,126.860218728868));
#30557=CARTESIAN_POINT('Ctrl Pts',(160.111252642884,-3.04886646503335,126.945138371971));
#30558=CARTESIAN_POINT('Ctrl Pts',(160.103496441674,-3.1562274708204,127.029955816877));
#30559=CARTESIAN_POINT('Ctrl Pts',(160.095740240463,-3.26015864667098,127.119345368188));
#30560=CARTESIAN_POINT('Ctrl Pts',(160.087984039253,-3.36025024047125,127.212995781753));
#30561=CARTESIAN_POINT('Ctrl Pts',(160.080233136657,-3.46027345714688,127.306582218457));
#30562=CARTESIAN_POINT('Ctrl Pts',(160.07248223406,-3.55646202584206,127.404423460644));
#30563=CARTESIAN_POINT('Ctrl Pts',(160.064731331464,-3.64843918916843,127.506167999564));
#30564=CARTESIAN_POINT('Ctrl Pts',(160.056984045247,-3.74037343823166,127.607865067006));
#30565=CARTESIAN_POINT('Ctrl Pts',(160.049236759029,-3.82809993053074,127.713461517755));
#30566=CARTESIAN_POINT('Ctrl Pts',(160.041489472812,-3.91127900413893,127.822569274383));
#30567=CARTESIAN_POINT('Ctrl Pts',(160.033744123531,-3.99443728174649,127.931649752455));
#30568=CARTESIAN_POINT('Ctrl Pts',(160.02599877425,-4.07305016753664,128.044239477975));
#30569=CARTESIAN_POINT('Ctrl Pts',(160.018253424969,-4.1468187700814,128.159917925693));
#30570=CARTESIAN_POINT('Ctrl Pts',(160.010505830616,-4.22060875523721,128.275629904035));
#30571=CARTESIAN_POINT('Ctrl Pts',(160.002758236264,-4.28955143620647,128.394432066875));
#30572=CARTESIAN_POINT('Ctrl Pts',(159.995010641911,-4.35339165714536,128.515875498104));
#30573=CARTESIAN_POINT('Ctrl Pts',(159.987262048063,-4.41724011393877,128.637334596423));
#30574=CARTESIAN_POINT('Ctrl Pts',(159.979513454214,-4.47598462469449,128.761435292019));
#30575=CARTESIAN_POINT('Ctrl Pts',(159.971764860365,-4.52941679935757,128.887705583347));
#30576=CARTESIAN_POINT('Ctrl Pts',(159.96400967179,-4.58289444944049,129.014083341656));
#30577=CARTESIAN_POINT('Ctrl Pts',(159.956254483215,-4.6310505857517,129.142634021231));
#30578=CARTESIAN_POINT('Ctrl Pts',(159.94849929464,-4.67372549519188,129.272866883301));
#30579=CARTESIAN_POINT('Ctrl Pts',(159.942410322305,-4.707231623442,129.375118980286));
#30580=CARTESIAN_POINT('Ctrl Pts',(159.936321349969,-4.73735977013598,129.478407662633));
#30581=CARTESIAN_POINT('Ctrl Pts',(159.930232377634,-4.76405452823406,129.582490119308));
#30582=CARTESIAN_POINT('Origin',(213.235140564004,0.,130.804360617566));
#30583=CARTESIAN_POINT('',(157.83474697768,-4.76405452823405,129.582490119308));
#30584=CARTESIAN_POINT('',(158.179915040683,-4.76405452823403,129.582490119308));
#30585=CARTESIAN_POINT('',(213.235140564004,-4.76405452823405,129.582490119308));
#30586=CARTESIAN_POINT('',(159.514859436045,-4.91824907623685,130.801346219555));
#30587=CARTESIAN_POINT('Ctrl Pts',(159.514859435991,-4.91824907623744,130.801346220521));
#30588=CARTESIAN_POINT('Ctrl Pts',(159.507046905898,-4.91833398470203,130.93988171244));
#30589=CARTESIAN_POINT('Ctrl Pts',(159.499234375806,-4.9125612288758,131.078436147646));
#30590=CARTESIAN_POINT('Ctrl Pts',(159.491421845713,-4.90095264269885,131.216484696604));
#30591=CARTESIAN_POINT('Ctrl Pts',(159.483608395001,-4.88934268857953,131.354549513044));
#30592=CARTESIAN_POINT('Ctrl Pts',(159.475794944289,-4.87189556608927,131.492107944224));
#30593=CARTESIAN_POINT('Ctrl Pts',(159.467981493577,-4.84868503514287,131.628639995254));
#30594=CARTESIAN_POINT('Ctrl Pts',(159.460165539454,-4.82546706759599,131.765215790838));
#30595=CARTESIAN_POINT('Ctrl Pts',(159.45234958533,-4.79648207834992,131.900764175359));
#30596=CARTESIAN_POINT('Ctrl Pts',(159.444533631207,-4.7618549636528,132.034775331244));
#30597=CARTESIAN_POINT('Ctrl Pts',(159.436713589575,-4.72720974002225,132.168856570909));
#30598=CARTESIAN_POINT('Ctrl Pts',(159.428893547944,-4.68691661062925,132.301398612136));
#30599=CARTESIAN_POINT('Ctrl Pts',(159.421073506313,-4.64115025576767,132.431907042676));
#30600=CARTESIAN_POINT('Ctrl Pts',(159.413243026568,-4.59532281242605,132.562589674584));
#30601=CARTESIAN_POINT('Ctrl Pts',(159.405412546822,-4.54400768117739,132.691232915173));
#30602=CARTESIAN_POINT('Ctrl Pts',(159.397582067076,-4.48742784772967,132.817361952369));
#30603=CARTESIAN_POINT('Ctrl Pts',(159.389745547182,-4.43080437064702,132.943588280938));
#30604=CARTESIAN_POINT('Ctrl Pts',(159.381909027288,-4.36890826923445,133.06729620146));
#30605=CARTESIAN_POINT('Ctrl Pts',(159.374072507394,-4.30200796832913,133.188036456042));
#30606=CARTESIAN_POINT('Ctrl Pts',(159.366223609298,-4.23500199483128,133.308967426294));
#30607=CARTESIAN_POINT('Ctrl Pts',(159.358374711203,-4.16297623535751,133.426921045389));
#30608=CARTESIAN_POINT('Ctrl Pts',(159.350525813108,-4.0862421534414,133.541477371732));
#30609=CARTESIAN_POINT('Ctrl Pts',(159.34772436281,-4.05885401385308,133.582365130839));
#30610=CARTESIAN_POINT('Ctrl Pts',(159.344922912512,-4.03086643201579,133.622820408351));
#30611=CARTESIAN_POINT('Ctrl Pts',(159.342121462214,-4.0022947631806,133.662825186372));
#30612=CARTESIAN_POINT('Ctrl Pts',(159.334347128095,-3.92300522517745,133.773842865649));
#30613=CARTESIAN_POINT('Ctrl Pts',(159.326572793976,-3.83896740064877,133.881734828746));
#30614=CARTESIAN_POINT('Ctrl Pts',(159.318798459857,-3.75045608194201,133.986068058536));
#30615=CARTESIAN_POINT('Ctrl Pts',(159.31103370691,-3.66205384552502,134.090272706945));
#30616=CARTESIAN_POINT('Ctrl Pts',(159.303268953963,-3.56918933501307,134.190927053252));
#30617=CARTESIAN_POINT('Ctrl Pts',(159.295504201015,-3.47218037092224,134.287627264592));
#30618=CARTESIAN_POINT('Ctrl Pts',(159.28774716013,-3.37526775750219,134.384231431918));
#30619=CARTESIAN_POINT('Ctrl Pts',(159.279990119245,-3.27421915728784,134.47688900556));
#30620=CARTESIAN_POINT('Ctrl Pts',(159.27223307836,-3.16939214034595,134.565229735631));
#30621=CARTESIAN_POINT('Ctrl Pts',(159.26448188712,-3.06464417427273,134.65350384727));
#30622=CARTESIAN_POINT('Ctrl Pts',(159.25673069588,-2.95612376064952,134.737467344022));
#30623=CARTESIAN_POINT('Ctrl Pts',(159.24897950464,-2.84422448649254,134.816787580507));
#30624=CARTESIAN_POINT('Ctrl Pts',(159.241231607863,-2.7323727725124,134.896074103775));
#30625=CARTESIAN_POINT('Ctrl Pts',(159.233483711086,-2.61714537259464,134.970721066314));
#30626=CARTESIAN_POINT('Ctrl Pts',(159.225735814309,-2.49896786403922,135.040436947969));
#30627=CARTESIAN_POINT('Ctrl Pts',(159.217989538225,-2.3808150756709,135.110138246564));
#30628=CARTESIAN_POINT('Ctrl Pts',(159.210243262141,-2.2597137426329,135.174910317414));
#30629=CARTESIAN_POINT('Ctrl Pts',(159.202496986057,-2.13611691230614,135.234505942435));
#30630=CARTESIAN_POINT('Ctrl Pts',(159.194750652791,-2.01251916961573,135.294102007377));
#30631=CARTESIAN_POINT('Ctrl Pts',(159.187004319526,-1.88642624504282,135.348521380436));
#30632=CARTESIAN_POINT('Ctrl Pts',(159.17925798626,-1.75831381698292,135.397563811798));
#30633=CARTESIAN_POINT('Ctrl Pts',(159.171509918257,-1.63017269903276,135.446617225873));
#30634=CARTESIAN_POINT('Ctrl Pts',(159.163761850255,-1.50001154271935,135.490291162427));
#30635=CARTESIAN_POINT('Ctrl Pts',(159.156013782252,-1.36832355692679,135.528434463947));
#30636=CARTESIAN_POINT('Ctrl Pts',(159.14825747951,-1.236495611576,135.566618304621));
#30637=CARTESIAN_POINT('Ctrl Pts',(159.140501176768,-1.10313797129142,135.599259659329));
#30638=CARTESIAN_POINT('Ctrl Pts',(159.132744874026,-0.968757021240737,
135.626257847526));
#30639=CARTESIAN_POINT('Ctrl Pts',(159.124984431512,-0.834304348030785,
135.653270445469));
#30640=CARTESIAN_POINT('Ctrl Pts',(159.117223988998,-0.698827662766445,
135.674633814512));
#30641=CARTESIAN_POINT('Ctrl Pts',(159.109463546483,-0.56283996679113,135.690299036568));
#30642=CARTESIAN_POINT('Ctrl Pts',(159.101690646218,-0.426633971293907,
135.70598940583));
#30643=CARTESIAN_POINT('Ctrl Pts',(159.093917745953,-0.289915715978825,
135.715963320679));
#30644=CARTESIAN_POINT('Ctrl Pts',(159.086144845687,-0.153200611303244,
135.720223983771));
#30645=CARTESIAN_POINT('Ctrl Pts',(159.078654509925,-0.021455445046401,
135.724329761028));
#30646=CARTESIAN_POINT('Ctrl Pts',(159.071164174163,0.110286487655596,135.723130459872));
#30647=CARTESIAN_POINT('Ctrl Pts',(159.063673838401,0.241569116679861,135.716674474026));
#30648=CARTESIAN_POINT('Ctrl Pts',(159.055899504282,0.377829366485305,135.709973707514));
#30649=CARTESIAN_POINT('Ctrl Pts',(159.048125170163,0.51402642759366,135.697588547125));
#30650=CARTESIAN_POINT('Ctrl Pts',(159.040350836044,0.64964745845715,135.679516127108));
#30651=CARTESIAN_POINT('Ctrl Pts',(159.032586083097,0.785101348520533,135.661465979734));
#30652=CARTESIAN_POINT('Ctrl Pts',(159.024821330149,0.919980237020838,135.637742569779));
#30653=CARTESIAN_POINT('Ctrl Pts',(159.017056577202,1.05377257817957,135.608395007116));
#30654=CARTESIAN_POINT('Ctrl Pts',(159.009299536317,1.18743203489955,135.579076592865));
#30655=CARTESIAN_POINT('Ctrl Pts',(159.001542495432,1.32000671246847,135.5441452255));
#30656=CARTESIAN_POINT('Ctrl Pts',(158.993785454547,1.45099183381639,135.503701609737));
#30657=CARTESIAN_POINT('Ctrl Pts',(158.986034263307,1.58187817826525,135.463288492819));
#30658=CARTESIAN_POINT('Ctrl Pts',(158.978283072067,1.71117698037423,135.417371516297));
#30659=CARTESIAN_POINT('Ctrl Pts',(158.970531880827,1.83839563276808,135.366102013121));
#30660=CARTESIAN_POINT('Ctrl Pts',(158.96278398405,1.96556021384085,135.314854300851));
#30661=CARTESIAN_POINT('Ctrl Pts',(158.955036087273,2.09064604177785,135.258258732497));
#30662=CARTESIAN_POINT('Ctrl Pts',(158.947288190496,2.21317781749103,135.196515784527));
#30663=CARTESIAN_POINT('Ctrl Pts',(158.939541914412,2.335683962198,135.134785751852));
#30664=CARTESIAN_POINT('Ctrl Pts',(158.931795638327,2.45563676841574,135.067910657039));
#30665=CARTESIAN_POINT('Ctrl Pts',(158.924049362243,2.57258336139334,134.996138034269));
#30666=CARTESIAN_POINT('Ctrl Pts',(158.916303028978,2.68953081764425,134.92436488169));
#30667=CARTESIAN_POINT('Ctrl Pts',(158.908556695713,2.80347168315822,134.847694333515));
#30668=CARTESIAN_POINT('Ctrl Pts',(158.900810362447,2.91398036630329,134.766418351534));
#30669=CARTESIAN_POINT('Ctrl Pts',(158.893062294444,3.02451379710167,134.685124168362));
#30670=CARTESIAN_POINT('Ctrl Pts',(158.885314226441,3.1316132011848,134.599222730702));
#30671=CARTESIAN_POINT('Ctrl Pts',(158.877566158438,3.23488481400627,134.509047284831));
#30672=CARTESIAN_POINT('Ctrl Pts',(158.869809855697,3.33826618512695,134.418775999423));
#30673=CARTESIAN_POINT('Ctrl Pts',(158.862053552955,3.43781134330879,134.324221889295));
#30674=CARTESIAN_POINT('Ctrl Pts',(158.854297250213,3.53316186960717,134.225756570339));
#30675=CARTESIAN_POINT('Ctrl Pts',(158.846536807699,3.62856328735242,134.127238697478));
#30676=CARTESIAN_POINT('Ctrl Pts',(158.838776365184,3.7197653523574,134.024805748063));
#30677=CARTESIAN_POINT('Ctrl Pts',(158.83101592267,3.80644961869418,133.918862883233));
#30678=CARTESIAN_POINT('Ctrl Pts',(158.823243022405,3.89327303831072,133.812749949511));
#30679=CARTESIAN_POINT('Ctrl Pts',(158.815470122139,3.97556393187606,133.703116153854));
#30680=CARTESIAN_POINT('Ctrl Pts',(158.807697221874,4.05304640193297,133.590396856792));
#30681=CARTESIAN_POINT('Ctrl Pts',(158.800206886112,4.12771218903637,133.4817751901));
#30682=CARTESIAN_POINT('Ctrl Pts',(158.79271655035,4.19791291560811,133.370288719424));
#30683=CARTESIAN_POINT('Ctrl Pts',(158.785226214588,4.26344277961622,133.256347307464));
#30684=CARTESIAN_POINT('Ctrl Pts',(158.777451880469,4.33145722833588,133.138085772237));
#30685=CARTESIAN_POINT('Ctrl Pts',(158.76967754635,4.39465508046152,133.016804845711));
#30686=CARTESIAN_POINT('Ctrl Pts',(158.761903212231,4.45275672157375,132.892934446996));
#30687=CARTESIAN_POINT('Ctrl Pts',(158.754138459284,4.51078675760594,132.769216707477));
#30688=CARTESIAN_POINT('Ctrl Pts',(158.746373706337,4.5637329147631,132.642916196056));
#30689=CARTESIAN_POINT('Ctrl Pts',(158.738608953389,4.61136000758437,132.514489835769));
#30690=CARTESIAN_POINT('Ctrl Pts',(158.730851912504,4.65893979650574,132.386191030354));
#30691=CARTESIAN_POINT('Ctrl Pts',(158.723094871619,4.70121089937608,132.255770942098));
#30692=CARTESIAN_POINT('Ctrl Pts',(158.715337830734,4.73798519758984,132.123708687606));
#30693=CARTESIAN_POINT('Ctrl Pts',(158.707586639494,4.7747317640193,131.991746022288));
#30694=CARTESIAN_POINT('Ctrl Pts',(158.699835448254,4.8059896720736,131.858144030747));
#30695=CARTESIAN_POINT('Ctrl Pts',(158.692084257014,4.83161997613111,131.723398956674));
#30696=CARTESIAN_POINT('Ctrl Pts',(158.684336360237,4.8572393866256,131.588711152853));
#30697=CARTESIAN_POINT('Ctrl Pts',(158.67658846346,4.87723587748997,131.452881616076));
#30698=CARTESIAN_POINT('Ctrl Pts',(158.668840566683,4.89152120449035,131.316418591355));
#30699=CARTESIAN_POINT('Ctrl Pts',(158.661094290599,4.90580354330827,131.179984111758));
#30700=CARTESIAN_POINT('Ctrl Pts',(158.653348014515,4.91437705381214,131.042916796386));
#30701=CARTESIAN_POINT('Ctrl Pts',(158.64560173843,4.91720520365298,130.905731459863));
#30702=CARTESIAN_POINT('Ctrl Pts',(158.637855405165,4.9200333743706,130.768545110669));
#30703=CARTESIAN_POINT('Ctrl Pts',(158.6301090719,4.91711609173894,130.631241129468));
#30704=CARTESIAN_POINT('Ctrl Pts',(158.622362738634,4.90846894880806,130.494335391033));
#30705=CARTESIAN_POINT('Ctrl Pts',(158.614614670631,4.89981986940952,130.357398993507));
#30706=CARTESIAN_POINT('Ctrl Pts',(158.606866602628,4.88543840100705,130.220861406325));
#30707=CARTESIAN_POINT('Ctrl Pts',(158.599118534625,4.86539207377361,130.085234042504));
#30708=CARTESIAN_POINT('Ctrl Pts',(158.591362231884,4.845324441065,129.949462532305));
#30709=CARTESIAN_POINT('Ctrl Pts',(158.583605929142,4.8195799798263,129.814603565325));
#30710=CARTESIAN_POINT('Ctrl Pts',(158.5758496264,4.78827760683634,129.681159557039));
#30711=CARTESIAN_POINT('Ctrl Pts',(158.568089183886,4.75695852682736,129.547644325667));
#30712=CARTESIAN_POINT('Ctrl Pts',(158.560328741372,4.72007572930198,129.415545934178));
#30713=CARTESIAN_POINT('Ctrl Pts',(158.552568298857,4.67779795999857,129.285351299644));
#30714=CARTESIAN_POINT('Ctrl Pts',(158.544795398592,4.63545232266669,129.154947665125));
#30715=CARTESIAN_POINT('Ctrl Pts',(158.537022498327,4.5876945434294,129.026454261262));
#30716=CARTESIAN_POINT('Ctrl Pts',(158.529249598061,4.53474177411445,128.900338531402));
#30717=CARTESIAN_POINT('Ctrl Pts',(158.521759262299,4.48371397134414,128.778807425988));
#30718=CARTESIAN_POINT('Ctrl Pts',(158.514268926537,4.42786245356357,128.659484405926));
#30719=CARTESIAN_POINT('Ctrl Pts',(158.506778590775,4.36742080884511,128.542764159095));
#30720=CARTESIAN_POINT('Ctrl Pts',(158.499004256656,4.30468750079616,128.421618428629));
#30721=CARTESIAN_POINT('Ctrl Pts',(158.491229922537,4.23681040522234,128.302892982541));
#30722=CARTESIAN_POINT('Ctrl Pts',(158.483455588418,4.16400008682413,128.187055450141));
#30723=CARTESIAN_POINT('Ctrl Pts',(158.475690835471,4.09127950063627,128.071360677148));
#30724=CARTESIAN_POINT('Ctrl Pts',(158.467926082524,4.0136379945863,127.958547064133));
#30725=CARTESIAN_POINT('Ctrl Pts',(158.460161329576,3.93133286748008,127.849059457351));
#30726=CARTESIAN_POINT('Ctrl Pts',(158.452404288691,3.84910948698593,127.739680595202));
#30727=CARTESIAN_POINT('Ctrl Pts',(158.444647247806,3.76223193667793,127.633621475787));
#30728=CARTESIAN_POINT('Ctrl Pts',(158.436890206921,3.6710016282233,127.531299342844));
#30729=CARTESIAN_POINT('Ctrl Pts',(158.429139015681,3.57984011725463,127.429054371819));
#30730=CARTESIAN_POINT('Ctrl Pts',(158.421387824441,3.48433264078649,127.330541068666));
#30731=CARTESIAN_POINT('Ctrl Pts',(158.413636633201,3.38482159918926,127.236144564107));
#30732=CARTESIAN_POINT('Ctrl Pts',(158.405888736424,3.28535285243901,127.141788180581));
#30733=CARTESIAN_POINT('Ctrl Pts',(158.398140839647,3.18188420800949,127.051545384038));
#30734=CARTESIAN_POINT('Ctrl Pts',(158.39039294287,3.07479556866096,126.965765135695));
#30735=CARTESIAN_POINT('Ctrl Pts',(158.382646666786,2.96772932994706,126.88000283073));
#30736=CARTESIAN_POINT('Ctrl Pts',(158.374900390702,2.85704490742315,126.798701461515));
#30737=CARTESIAN_POINT('Ctrl Pts',(158.367154114618,2.74315568258615,126.722170033628));
#30738=CARTESIAN_POINT('Ctrl Pts',(158.359407781352,2.62926561704496,126.645638040803));
#30739=CARTESIAN_POINT('Ctrl Pts',(158.351661448087,2.51217102648917,126.573876277627));
#30740=CARTESIAN_POINT('Ctrl Pts',(158.343915114821,2.39231435939962,126.507150468142));
#30741=CARTESIAN_POINT('Ctrl Pts',(158.336167046819,2.27243085124042,126.440409715875));
#30742=CARTESIAN_POINT('Ctrl Pts',(158.328418978816,2.14978437724043,126.378707351558));
#30743=CARTESIAN_POINT('Ctrl Pts',(158.320670910813,2.02484170536205,126.322262991373));
#30744=CARTESIAN_POINT('Ctrl Pts',(158.312914608071,1.89976624292512,126.26575864145));
#30745=CARTESIAN_POINT('Ctrl Pts',(158.305158305329,1.7723900644575,126.214523620045));
#30746=CARTESIAN_POINT('Ctrl Pts',(158.297402002587,1.64320014375113,126.16872944694));
#30747=CARTESIAN_POINT('Ctrl Pts',(158.289641560073,1.51394127049389,126.122910832107));
#30748=CARTESIAN_POINT('Ctrl Pts',(158.281881117559,1.38286709953899,126.082538966958));
#30749=CARTESIAN_POINT('Ctrl Pts',(158.274120675044,1.25047849920119,126.047735071495));
#30750=CARTESIAN_POINT('Ctrl Pts',(158.266347774779,1.11787737692959,126.012875305729));
#30751=CARTESIAN_POINT('Ctrl Pts',(158.258574874514,0.983957990911603,125.983601454559));
#30752=CARTESIAN_POINT('Ctrl Pts',(158.250801974248,0.849230990338732,125.959983486546));
#30753=CARTESIAN_POINT('Ctrl Pts',(158.243311638486,0.71940165559325,125.937224091161));
#30754=CARTESIAN_POINT('Ctrl Pts',(158.235821302724,0.588822709801794,125.919716547896));
#30755=CARTESIAN_POINT('Ctrl Pts',(158.228330966962,0.457952475113953,125.907477670932));
#30756=CARTESIAN_POINT('Ctrl Pts',(158.220556632843,0.322120255700965,125.894774753227));
#30757=CARTESIAN_POINT('Ctrl Pts',(158.212782298724,0.185543947279615,125.887707672472));
#30758=CARTESIAN_POINT('Ctrl Pts',(158.205007964605,0.048730794997183,125.886352039684));
#30759=CARTESIAN_POINT('Ctrl Pts',(158.197243211658,-0.0879137473025429,
125.884998077593));
#30760=CARTESIAN_POINT('Ctrl Pts',(158.189478458711,-0.224794165498482,
125.889341562095));
#30761=CARTESIAN_POINT('Ctrl Pts',(158.181713705764,-0.361397121550913,
125.899406470682));
#30762=CARTESIAN_POINT('Ctrl Pts',(158.173956664879,-0.497864401621396,
125.90946138266));
#30763=CARTESIAN_POINT('Ctrl Pts',(158.166199623994,-0.634054380578433,
125.925226381552));
#30764=CARTESIAN_POINT('Ctrl Pts',(158.158442583109,-0.769453099079439,
125.946673411619));
#30765=CARTESIAN_POINT('Ctrl Pts',(158.150691391868,-0.904749712353483,
125.968104268314));
#30766=CARTESIAN_POINT('Ctrl Pts',(158.142940200628,-1.03925586826959,125.995208566503));
#30767=CARTESIAN_POINT('Ctrl Pts',(158.135189009388,-1.17246246967853,126.027906407622));
#30768=CARTESIAN_POINT('Ctrl Pts',(158.127441112611,-1.30561245472861,126.060590351285));
#30769=CARTESIAN_POINT('Ctrl Pts',(158.119693215834,-1.43746360494574,126.098863016394));
#30770=CARTESIAN_POINT('Ctrl Pts',(158.111945319057,-1.56751698265293,126.142593402057));
#30771=CARTESIAN_POINT('Ctrl Pts',(158.104199042973,-1.69754315599708,126.186314640266));
#30772=CARTESIAN_POINT('Ctrl Pts',(158.096452766889,-1.82577193448391,126.235491203724));
#30773=CARTESIAN_POINT('Ctrl Pts',(158.088706490805,-1.95171990017145,126.289942327933));
#30774=CARTESIAN_POINT('Ctrl Pts',(158.080960157539,-2.07766879557827,126.344393854087));
#30775=CARTESIAN_POINT('Ctrl Pts',(158.073213824274,-2.20133648572639,126.404119863538));
#30776=CARTESIAN_POINT('Ctrl Pts',(158.065467491009,-2.32226025524325,126.468891742183));
#30777=CARTESIAN_POINT('Ctrl Pts',(158.057719423006,-2.44321110480003,126.53367812604));
#30778=CARTESIAN_POINT('Ctrl Pts',(158.049971355003,-2.56141646640514,126.603512443068));
#30779=CARTESIAN_POINT('Ctrl Pts',(158.042223287,-2.67643927126129,126.67812069607));
#30780=CARTESIAN_POINT('Ctrl Pts',(158.034466984258,-2.7915843237232,126.75280824361));
#30781=CARTESIAN_POINT('Ctrl Pts',(158.026710681516,-2.9035397340804,126.832279649482));
#30782=CARTESIAN_POINT('Ctrl Pts',(158.018954378774,-3.01189797665267,126.916217919473));
#30783=CARTESIAN_POINT('Ctrl Pts',(158.01119393626,-3.12031405328153,127.000200989846));
#30784=CARTESIAN_POINT('Ctrl Pts',(158.003433493746,-3.2251288378874,127.088655422833));
#30785=CARTESIAN_POINT('Ctrl Pts',(157.995673051232,-3.32596961309159,127.181225346107));
#30786=CARTESIAN_POINT('Ctrl Pts',(157.987900150966,-3.42697226686039,127.27394387084));
#30787=CARTESIAN_POINT('Ctrl Pts',(157.980127250701,-3.52398788623438,127.370790811479));
#30788=CARTESIAN_POINT('Ctrl Pts',(157.972354350435,-3.61668158631872,127.471374364117));
#30789=CARTESIAN_POINT('Ctrl Pts',(157.964864014673,-3.70600563692349,127.56830145126));
#30790=CARTESIAN_POINT('Ctrl Pts',(157.957373678911,-3.79131633867925,127.668697961763));
#30791=CARTESIAN_POINT('Ctrl Pts',(157.949883343149,-3.87235181102435,127.772187384692));
#30792=CARTESIAN_POINT('Ctrl Pts',(157.942108314672,-3.95646727996599,127.879610234073));
#30793=CARTESIAN_POINT('Ctrl Pts',(157.934333286195,-4.03624745410983,127.990712287173));
#30794=CARTESIAN_POINT('Ctrl Pts',(157.926558257717,-4.11135287214958,128.105108753962));
#30795=CARTESIAN_POINT('Ctrl Pts',(157.918795709745,-4.1863377306947,128.219321591121));
#30796=CARTESIAN_POINT('Ctrl Pts',(157.911033161772,-4.25666256443127,128.336817987588));
#30797=CARTESIAN_POINT('Ctrl Pts',(157.903270613799,-4.32202819273545,128.457180316929));
#30798=CARTESIAN_POINT('Ctrl Pts',(157.895515248821,-4.38733333561691,128.577431270206));
#30799=CARTESIAN_POINT('Ctrl Pts',(157.887759883844,-4.44768821420025,128.700542541763));
#30800=CARTESIAN_POINT('Ctrl Pts',(157.880004518866,-4.50283681842229,128.826067502489));
#30801=CARTESIAN_POINT('Ctrl Pts',(157.872255468489,-4.557940519357,128.951490257848));
#30802=CARTESIAN_POINT('Ctrl Pts',(157.864506418111,-4.60784622703961,129.079322434733));
#30803=CARTESIAN_POINT('Ctrl Pts',(157.856757367734,-4.65234404438156,129.209093255897));
#30804=CARTESIAN_POINT('Ctrl Pts',(157.849420571049,-4.69447455364886,129.331960198822));
#30805=CARTESIAN_POINT('Ctrl Pts',(157.842083774365,-4.73175751323662,129.456564548009));
#30806=CARTESIAN_POINT('Ctrl Pts',(157.83474697768,-4.76405452823405,129.582490119308));
#30807=CARTESIAN_POINT('Ctrl Pts',(159.584608960876,-4.76405452823403,129.582490119308));
#30808=CARTESIAN_POINT('Ctrl Pts',(159.575875008844,-4.80223670963421,129.731361865092));
#30809=CARTESIAN_POINT('Ctrl Pts',(159.567141056811,-4.83348102434377,129.882197515467));
#30810=CARTESIAN_POINT('Ctrl Pts',(159.558407104779,-4.85760317562201,130.034377208208));
#30811=CARTESIAN_POINT('Ctrl Pts',(159.549722762089,-4.88158831171254,130.185692511661));
#30812=CARTESIAN_POINT('Ctrl Pts',(159.541038419399,-4.89853187053611,130.338336438866));
#30813=CARTESIAN_POINT('Ctrl Pts',(159.53235407671,-4.90830056874771,130.491680926299));
#30814=CARTESIAN_POINT('Ctrl Pts',(159.526522529822,-4.9148602617138,130.594651939817));
#30815=CARTESIAN_POINT('Ctrl Pts',(159.520690982934,-4.91818569755605,130.697938462117));
#30816=CARTESIAN_POINT('Ctrl Pts',(159.514859436045,-4.91824907623685,130.801346219555));
#30817=CARTESIAN_POINT('',(159.860140563974,-4.91824957733792,130.80232161894));
#30818=CARTESIAN_POINT('Ctrl Pts',(159.930232377634,-4.76405452823406,129.582490119308));
#30819=CARTESIAN_POINT('Ctrl Pts',(159.92246762958,-4.79809608066164,129.715217615571));
#30820=CARTESIAN_POINT('Ctrl Pts',(159.914702881527,-4.82655266194119,129.849235873015));
#30821=CARTESIAN_POINT('Ctrl Pts',(159.906938133473,-4.84935554201804,129.984035139723));
#30822=CARTESIAN_POINT('Ctrl Pts',(159.899162618928,-4.87219004025057,130.119021317214));
#30823=CARTESIAN_POINT('Ctrl Pts',(159.891387104383,-4.88935514236526,130.254790279368));
#30824=CARTESIAN_POINT('Ctrl Pts',(159.883611589838,-4.90083404844994,130.390828645339));
#30825=CARTESIAN_POINT('Ctrl Pts',(159.882216964452,-4.90289291847507,130.415228645818));
#30826=CARTESIAN_POINT('Ctrl Pts',(159.880822339066,-4.90476899633132,130.439637318142));
#30827=CARTESIAN_POINT('Ctrl Pts',(159.879427713681,-4.90646236201941,130.464051709973));
#30828=CARTESIAN_POINT('Ctrl Pts',(159.87299866379,-4.91426856761627,130.576599025358));
#30829=CARTESIAN_POINT('Ctrl Pts',(159.866569613899,-4.91820276995444,130.689417998646));
#30830=CARTESIAN_POINT('Ctrl Pts',(159.860140564008,-4.91824957733767,130.802321618344));
#30831=CARTESIAN_POINT('Ctrl Pts',(159.860140563974,-4.91824957733792,130.80232161894));
#30832=CARTESIAN_POINT('Ctrl Pts',(159.852445159348,-4.91830560453543,130.937464299746));
#30833=CARTESIAN_POINT('Ctrl Pts',(159.844749754723,-4.91278728852856,131.072834611119));
#30834=CARTESIAN_POINT('Ctrl Pts',(159.837054350097,-4.90166458996473,131.207928839786));
#30835=CARTESIAN_POINT('Ctrl Pts',(159.829368007524,-4.89055498940976,131.342863982473));
#30836=CARTESIAN_POINT('Ctrl Pts',(159.821681664951,-4.87385416547425,131.477523294776));
#30837=CARTESIAN_POINT('Ctrl Pts',(159.813995322378,-4.85158406506426,131.611401584379));
#30838=CARTESIAN_POINT('Ctrl Pts',(159.806316102376,-4.82933460130636,131.745155815283));
#30839=CARTESIAN_POINT('Ctrl Pts',(159.798636882374,-4.80152619300176,131.878130071634));
#30840=CARTESIAN_POINT('Ctrl Pts',(159.790957662372,-4.76823267337784,132.00982328187));
#30841=CARTESIAN_POINT('Ctrl Pts',(159.783041930184,-4.73391374712471,132.145572509384));
#30842=CARTESIAN_POINT('Ctrl Pts',(159.775126197997,-4.69376641371811,132.279960076937));
#30843=CARTESIAN_POINT('Ctrl Pts',(159.767210465809,-4.64792874228581,132.412446892967));
#30844=CARTESIAN_POINT('Ctrl Pts',(159.759538874211,-4.60350481703267,132.540847490738));
#30845=CARTESIAN_POINT('Ctrl Pts',(159.751867282613,-4.55373652964841,132.667462452084));
#30846=CARTESIAN_POINT('Ctrl Pts',(159.744195691015,-4.498800346222,132.791815901927));
#30847=CARTESIAN_POINT('Ctrl Pts',(159.736524941261,-4.44387019123,132.916155705816));
#30848=CARTESIAN_POINT('Ctrl Pts',(159.728854191507,-4.3837734292531,133.03823412636));
#30849=CARTESIAN_POINT('Ctrl Pts',(159.721183441753,-4.31873446334889,133.157595773173));
#30850=CARTESIAN_POINT('Ctrl Pts',(159.713511792458,-4.25368787039606,133.276971417396));
#30851=CARTESIAN_POINT('Ctrl Pts',(159.705840143164,-4.18369811216107,133.393629303588));
#30852=CARTESIAN_POINT('Ctrl Pts',(159.698168493869,-4.10903503364523,133.507139586475));
#30853=CARTESIAN_POINT('Ctrl Pts',(159.690494203257,-4.03434624893852,133.620688950485));
#30854=CARTESIAN_POINT('Ctrl Pts',(159.682819912645,-3.95498116330527,133.731088222441));
#30855=CARTESIAN_POINT('Ctrl Pts',(159.675145622034,-3.87125202192377,133.837937853314));
#30856=CARTESIAN_POINT('Ctrl Pts',(159.667462889337,-3.78743077450296,133.944905023866));
#30857=CARTESIAN_POINT('Ctrl Pts',(159.65978015664,-3.69923613639072,134.048314445649));
#30858=CARTESIAN_POINT('Ctrl Pts',(159.652097423944,-3.60701976937073,134.147800679219));
#30859=CARTESIAN_POINT('Ctrl Pts',(159.644409615416,-3.5147424768062,134.247352641392));
#30860=CARTESIAN_POINT('Ctrl Pts',(159.636721806889,-3.41843844804785,134.342975974839));
#30861=CARTESIAN_POINT('Ctrl Pts',(159.629033998361,-3.31849409145874,134.434344092384));
#30862=CARTESIAN_POINT('Ctrl Pts',(159.621335500479,-3.21841076929584,134.525839250848));
#30863=CARTESIAN_POINT('Ctrl Pts',(159.613637002596,-3.1146773236678,134.613067132168));
#30864=CARTESIAN_POINT('Ctrl Pts',(159.605938504713,-3.00771107946218,134.695743035805));
#30865=CARTESIAN_POINT('Ctrl Pts',(159.604285699765,-2.98474629588517,134.71349288061));
#30866=CARTESIAN_POINT('Ctrl Pts',(159.602632894816,-2.96163260066913,134.731033077885));
#30867=CARTESIAN_POINT('Ctrl Pts',(159.600980089868,-2.93837427568491,134.748361083906));
#30868=CARTESIAN_POINT('Ctrl Pts',(159.593205755749,-2.82897359313902,134.829867197833));
#30869=CARTESIAN_POINT('Ctrl Pts',(159.58543142163,-2.71600577086117,134.90694704463));
#30870=CARTESIAN_POINT('Ctrl Pts',(159.577657087511,-2.59986469390879,134.979272189787));
#30871=CARTESIAN_POINT('Ctrl Pts',(159.569892334564,-2.48386675045409,135.051508200667));
#30872=CARTESIAN_POINT('Ctrl Pts',(159.562127581617,-2.36470366224649,135.119000964367));
#30873=CARTESIAN_POINT('Ctrl Pts',(159.554362828669,-2.24280137670867,135.181462974963));
#30874=CARTESIAN_POINT('Ctrl Pts',(159.546605787784,-2.12102016623907,135.24386294741));
#30875=CARTESIAN_POINT('Ctrl Pts',(159.538848746899,-1.99650551827106,135.301241933109));
#30876=CARTESIAN_POINT('Ctrl Pts',(159.531091706014,-1.86971097746101,135.353356542302));
#30877=CARTESIAN_POINT('Ctrl Pts',(159.523340514774,-1.74301205340064,135.405431851462));
#30878=CARTESIAN_POINT('Ctrl Pts',(159.515589323534,-1.61403701877965,135.452250537947));
#30879=CARTESIAN_POINT('Ctrl Pts',(159.507838132294,-1.48326223322349,135.493616017946));
#30880=CARTESIAN_POINT('Ctrl Pts',(159.500090235517,-1.35254303043986,135.534963916512));
#30881=CARTESIAN_POINT('Ctrl Pts',(159.49234233874,-1.22002597011408,135.570863100774));
#30882=CARTESIAN_POINT('Ctrl Pts',(159.484594441963,-1.08620531746851,135.601165915971));
#30883=CARTESIAN_POINT('Ctrl Pts',(159.476848165879,-0.952412657218591,
135.631462392471));
#30884=CARTESIAN_POINT('Ctrl Pts',(159.469101889795,-0.817317328100775,
135.656164742082));
#30885=CARTESIAN_POINT('Ctrl Pts',(159.46135561371,-0.681426226591078,135.67517588405));
#30886=CARTESIAN_POINT('Ctrl Pts',(159.453609280445,-0.54553412196414,135.694187166354));
#30887=CARTESIAN_POINT('Ctrl Pts',(159.44586294718,-0.40884662041825,135.707507103015));
#30888=CARTESIAN_POINT('Ctrl Pts',(159.438116613914,-0.271877827622247,
135.715090248624));
#30889=CARTESIAN_POINT('Ctrl Pts',(159.430368545911,-0.134878361614726,
135.722675092425));
#30890=CARTESIAN_POINT('Ctrl Pts',(159.422620477908,0.00240213069945419,
135.724520567133));
#30891=CARTESIAN_POINT('Ctrl Pts',(159.414872409906,0.13944783995033,135.720633327906));
#30892=CARTESIAN_POINT('Ctrl Pts',(159.407116107164,0.27663920301177,135.716741957275));
#30893=CARTESIAN_POINT('Ctrl Pts',(159.399359804422,0.413594893115202,135.707105712795));
#30894=CARTESIAN_POINT('Ctrl Pts',(159.39160350168,0.549801966247687,135.691783339248));
#30895=CARTESIAN_POINT('Ctrl Pts',(159.383843059166,0.686081737196404,135.676452787688));
#30896=CARTESIAN_POINT('Ctrl Pts',(159.376082616652,0.821611708862234,135.655430119748));
#30897=CARTESIAN_POINT('Ctrl Pts',(159.368322174137,0.9558884419229,135.628825390896));
#30898=CARTESIAN_POINT('Ctrl Pts',(159.360549273872,1.09038072791596,135.602177953771));
#30899=CARTESIAN_POINT('Ctrl Pts',(159.352776373607,1.22361537485448,135.569930641185));
#30900=CARTESIAN_POINT('Ctrl Pts',(159.345003473341,1.35510256365665,135.532243875904));
#30901=CARTESIAN_POINT('Ctrl Pts',(159.337513137579,1.48180986195065,135.495927119468));
#30902=CARTESIAN_POINT('Ctrl Pts',(159.330022801817,1.60689425291996,135.454559616627));
#30903=CARTESIAN_POINT('Ctrl Pts',(159.322532466055,1.72993622244429,135.408326704406));
#30904=CARTESIAN_POINT('Ctrl Pts',(159.314758131936,1.85764336563999,135.360340857267));
#30905=CARTESIAN_POINT('Ctrl Pts',(159.306983797817,1.98355469109857,135.306961368943));
#30906=CARTESIAN_POINT('Ctrl Pts',(159.299209463698,2.10718097307052,135.248342099214));
#30907=CARTESIAN_POINT('Ctrl Pts',(159.29144471075,2.23065489669891,135.189795072496));
#30908=CARTESIAN_POINT('Ctrl Pts',(159.283679957803,2.35184903019095,135.126021278895));
#30909=CARTESIAN_POINT('Ctrl Pts',(159.275915204856,2.47029125168392,135.057223676066));
#30910=CARTESIAN_POINT('Ctrl Pts',(159.268158163971,2.588615834692,134.988494403987));
#30911=CARTESIAN_POINT('Ctrl Pts',(159.260401123086,2.70419360908349,134.914751447543));
#30912=CARTESIAN_POINT('Ctrl Pts',(159.252644082201,2.81657465219533,134.836244828591));
#30913=CARTESIAN_POINT('Ctrl Pts',(159.244892890961,2.92887094788952,134.757797412089));
#30914=CARTESIAN_POINT('Ctrl Pts',(159.237141699721,3.0379749914075,134.674593706355));
#30915=CARTESIAN_POINT('Ctrl Pts',(159.229390508481,3.14346390720701,134.586928227879));
#30916=CARTESIAN_POINT('Ctrl Pts',(159.221642611704,3.24890798740281,134.49930000957));
#30917=CARTESIAN_POINT('Ctrl Pts',(159.213894714927,3.3507396958555,134.407214039619));
#30918=CARTESIAN_POINT('Ctrl Pts',(159.20614681815,3.44856764400671,134.311006346352));
#30919=CARTESIAN_POINT('Ctrl Pts',(159.198400542065,3.54637512866016,134.214818777659));
#30920=CARTESIAN_POINT('Ctrl Pts',(159.190654265981,3.6401802402699,134.114511474527));
#30921=CARTESIAN_POINT('Ctrl Pts',(159.182907989897,3.72962731212147,134.010458428797));
#30922=CARTESIAN_POINT('Ctrl Pts',(159.175161656632,3.81907504425073,133.906404614971));
#30923=CARTESIAN_POINT('Ctrl Pts',(159.167415323366,3.9041644175673,133.798605299852));
#30924=CARTESIAN_POINT('Ctrl Pts',(159.159668990101,3.98457931088853,133.687468450745));
#30925=CARTESIAN_POINT('Ctrl Pts',(159.151920922098,4.06501221256767,133.576306713311));
#30926=CARTESIAN_POINT('Ctrl Pts',(159.144172854095,4.14076832206378,133.461806271299));
#30927=CARTESIAN_POINT('Ctrl Pts',(159.136424786092,4.21157443098738,133.344404687017));
#30928=CARTESIAN_POINT('Ctrl Pts',(159.12866848335,4.28245579348614,133.226878326934));
#30929=CARTESIAN_POINT('Ctrl Pts',(159.120912180608,4.34837644392194,133.106445000543));
#30930=CARTESIAN_POINT('Ctrl Pts',(159.113155877867,4.40910854717513,132.98356801516));
#30931=CARTESIAN_POINT('Ctrl Pts',(159.105395435352,4.46987306498049,132.860625446629));
#30932=CARTESIAN_POINT('Ctrl Pts',(159.097634992838,4.52544335923817,132.735236977529));
#30933=CARTESIAN_POINT('Ctrl Pts',(159.089874550324,4.57563990148032,132.607885653289));
#30934=CARTESIAN_POINT('Ctrl Pts',(159.082101650059,4.62591702366828,132.480329893398));
#30935=CARTESIAN_POINT('Ctrl Pts',(159.074328749793,4.67080302740583,132.35080535139));
#30936=CARTESIAN_POINT('Ctrl Pts',(159.066555849528,4.71016812173062,132.219810838355));
#30937=CARTESIAN_POINT('Ctrl Pts',(159.059065513766,4.74810219572142,132.093578305826));
#30938=CARTESIAN_POINT('Ctrl Pts',(159.051575178004,4.78090971266741,131.96598111939));
#30939=CARTESIAN_POINT('Ctrl Pts',(159.044084842242,4.80851984422631,131.837472407346));
#30940=CARTESIAN_POINT('Ctrl Pts',(159.036310508123,4.83717682231556,131.704091248423));
#30941=CARTESIAN_POINT('Ctrl Pts',(159.028536174004,4.86032529396847,131.569305567015));
#30942=CARTESIAN_POINT('Ctrl Pts',(159.020761839885,4.87783026730727,131.433610127571));
#30943=CARTESIAN_POINT('Ctrl Pts',(159.012997086938,4.89531366733088,131.298081920628));
#30944=CARTESIAN_POINT('Ctrl Pts',(159.005232333991,4.90716735809032,131.161646570522));
#30945=CARTESIAN_POINT('Ctrl Pts',(158.997467581044,4.91330690021019,131.024810990319));
#30946=CARTESIAN_POINT('Ctrl Pts',(158.989710540158,4.91944034445029,130.888111317143));
#30947=CARTESIAN_POINT('Ctrl Pts',(158.981953499273,4.91987091688834,130.751012592984));
#30948=CARTESIAN_POINT('Ctrl Pts',(158.974196458388,4.91456577380205,130.614028493442));
#30949=CARTESIAN_POINT('Ctrl Pts',(158.966445267148,4.90926463136541,130.477147694675));
#30950=CARTESIAN_POINT('Ctrl Pts',(158.958694075908,4.89823639781546,130.340381737563));
#30951=CARTESIAN_POINT('Ctrl Pts',(158.950942884668,4.88150028365789,130.204245592635));
#30952=CARTESIAN_POINT('Ctrl Pts',(158.943194987891,4.8647712827954,130.068167309201));
#30953=CARTESIAN_POINT('Ctrl Pts',(158.935447091114,4.84233927406236,129.932718692773));
#30954=CARTESIAN_POINT('Ctrl Pts',(158.927699194337,4.81427541252908,129.798410661148));
#30955=CARTESIAN_POINT('Ctrl Pts',(158.919952918253,4.78621742135064,129.664130723867));
#30956=CARTESIAN_POINT('Ctrl Pts',(158.912206642169,4.75253000051732,129.530991279286));
#30957=CARTESIAN_POINT('Ctrl Pts',(158.904460366084,4.71333555341149,129.399493711611));
#30958=CARTESIAN_POINT('Ctrl Pts',(158.896714032819,4.67414081698108,129.267995173251));
#30959=CARTESIAN_POINT('Ctrl Pts',(158.888967699554,4.62943908483753,129.138138910657));
#30960=CARTESIAN_POINT('Ctrl Pts',(158.881221366288,4.57940272020786,129.010411401826));
#30961=CARTESIAN_POINT('Ctrl Pts',(158.873473298285,4.52935515028136,128.882655289306));
#30962=CARTESIAN_POINT('Ctrl Pts',(158.865725230282,4.47397071322438,128.757029243127));
#30963=CARTESIAN_POINT('Ctrl Pts',(158.857977162279,4.41346986679087,128.633999634359));
#30964=CARTESIAN_POINT('Ctrl Pts',(158.850220859538,4.35290471933774,128.510839268258));
#30965=CARTESIAN_POINT('Ctrl Pts',(158.842464556796,4.2872124727583,128.390281203415));
#30966=CARTESIAN_POINT('Ctrl Pts',(158.834708254054,4.21665977017082,128.272767552889));
#30967=CARTESIAN_POINT('Ctrl Pts',(158.82694781154,4.14606941148154,128.155191181788));
#30968=CARTESIAN_POINT('Ctrl Pts',(158.819187369026,4.07061364266819,128.040662789065));
#30969=CARTESIAN_POINT('Ctrl Pts',(158.811426926511,3.99060182400884,127.929594514956));
#30970=CARTESIAN_POINT('Ctrl Pts',(158.803654026246,3.91046156327514,127.818347944193));
#30971=CARTESIAN_POINT('Ctrl Pts',(158.795881125981,3.82575087918032,127.710572899243));
#30972=CARTESIAN_POINT('Ctrl Pts',(158.788108225715,3.73681928043525,127.606648196496));
#30973=CARTESIAN_POINT('Ctrl Pts',(158.780617889953,3.65112056930974,127.506501418464));
#30974=CARTESIAN_POINT('Ctrl Pts',(158.773127554191,3.56150270689706,127.409930129295));
#30975=CARTESIAN_POINT('Ctrl Pts',(158.765637218429,3.4683086384193,127.317238845794));
#30976=CARTESIAN_POINT('Ctrl Pts',(158.75786288431,3.37158108850939,127.221033144106));
#30977=CARTESIAN_POINT('Ctrl Pts',(158.750088550191,3.27069439177339,127.128702726181));
#30978=CARTESIAN_POINT('Ctrl Pts',(158.742314216072,3.1659918411462,127.040628596779));
#30979=CARTESIAN_POINT('Ctrl Pts',(158.734549463125,3.0614183270553,126.952663010871));
#30980=CARTESIAN_POINT('Ctrl Pts',(158.726784710178,2.95303861235956,126.86894352577));
#30981=CARTESIAN_POINT('Ctrl Pts',(158.71901995723,2.8412335358318,126.789815181609));
#30982=CARTESIAN_POINT('Ctrl Pts',(158.711262916345,2.72953950568233,126.710765428835));
#30983=CARTESIAN_POINT('Ctrl Pts',(158.70350587546,2.61442720113072,126.636297966818));
#30984=CARTESIAN_POINT('Ctrl Pts',(158.695748834575,2.4963110391717,126.566718082121));
#30985=CARTESIAN_POINT('Ctrl Pts',(158.687997643335,2.37828394952865,126.497190668156));
#30986=CARTESIAN_POINT('Ctrl Pts',(158.680246452095,2.2572578467844,126.432543692865));
#30987=CARTESIAN_POINT('Ctrl Pts',(158.672495260855,2.13367637397629,126.373039348053));
#30988=CARTESIAN_POINT('Ctrl Pts',(158.664747364078,2.01014742659118,126.313560294176));
#30989=CARTESIAN_POINT('Ctrl Pts',(158.656999467301,1.88406562083364,126.259219692735));
#30990=CARTESIAN_POINT('Ctrl Pts',(158.649251570524,1.7558992673692,126.210233842503));
#30991=CARTESIAN_POINT('Ctrl Pts',(158.64150529444,1.62775972354296,126.161258239055));
#30992=CARTESIAN_POINT('Ctrl Pts',(158.633759018356,1.49753686429052,126.117635298371));
#30993=CARTESIAN_POINT('Ctrl Pts',(158.626012742271,1.36571868036245,126.079533049431));
#30994=CARTESIAN_POINT('Ctrl Pts',(158.618266409006,1.23389952338227,126.041430519228));
#30995=CARTESIAN_POINT('Ctrl Pts',(158.610520075741,1.10048539381718,126.008848870652));
#30996=CARTESIAN_POINT('Ctrl Pts',(158.602773742475,0.965978745918657,125.981906042878));
#30997=CARTESIAN_POINT('Ctrl Pts',(158.595025674472,0.831441976189031,125.954957181444));
#30998=CARTESIAN_POINT('Ctrl Pts',(158.587277606469,0.695812584553893,125.933649730362));
#30999=CARTESIAN_POINT('Ctrl Pts',(158.579529538466,0.559602105004731,125.918050297235));
#31000=CARTESIAN_POINT('Ctrl Pts',(158.571773235725,0.423246859336932,125.902434284845));
#31001=CARTESIAN_POINT('Ctrl Pts',(158.564016932983,0.286309681103846,125.892538453551));
#31002=CARTESIAN_POINT('Ctrl Pts',(158.556260630241,0.149306659662162,125.888377441854));
#31003=CARTESIAN_POINT('Ctrl Pts',(158.548500187727,0.0122305155829474,
125.8842142093));
#31004=CARTESIAN_POINT('Ctrl Pts',(158.540739745212,-0.124911150981226,
125.885791890843));
#31005=CARTESIAN_POINT('Ctrl Pts',(158.532979302698,-0.261604377988794,
125.893072984784));
#31006=CARTESIAN_POINT('Ctrl Pts',(158.525206402433,-0.398517037099548,
125.900365766984));
#31007=CARTESIAN_POINT('Ctrl Pts',(158.517433502167,-0.534979428690864,
125.913380220297));
#31008=CARTESIAN_POINT('Ctrl Pts',(158.509660601902,-0.670483925809493,
125.932027052658));
#31009=CARTESIAN_POINT('Ctrl Pts',(158.50217026614,-0.801062493141713,125.949996025694));
#31010=CARTESIAN_POINT('Ctrl Pts',(158.494679930378,-0.93075129743161,125.973194930771));
#31011=CARTESIAN_POINT('Ctrl Pts',(158.487189594616,-1.05910876979799,126.001499837131));
#31012=CARTESIAN_POINT('Ctrl Pts',(158.479415260497,-1.19233295474349,126.03087793262));
#31013=CARTESIAN_POINT('Ctrl Pts',(158.471640926378,-1.32454487415725,126.065849921659));
#31014=CARTESIAN_POINT('Ctrl Pts',(158.463866592259,-1.45523841972807,126.10633292456));
#31015=CARTESIAN_POINT('Ctrl Pts',(158.456101839312,-1.58577089718448,126.146766035778));
#31016=CARTESIAN_POINT('Ctrl Pts',(158.448337086364,-1.71478835417376,126.192696532566));
#31017=CARTESIAN_POINT('Ctrl Pts',(158.440572333417,-1.8417946460021,126.243990507097));
#31018=CARTESIAN_POINT('Ctrl Pts',(158.432815292532,-1.96867479339024,126.295233535729));
#31019=CARTESIAN_POINT('Ctrl Pts',(158.425058251647,-2.09354739059707,126.351829295509));
#31020=CARTESIAN_POINT('Ctrl Pts',(158.417301210762,-2.21593158888361,126.413594140527));
#31021=CARTESIAN_POINT('Ctrl Pts',(158.409550019522,-2.33822349629563,126.475312408196));
#31022=CARTESIAN_POINT('Ctrl Pts',(158.401798828282,-2.4580303922667,126.542191826837));
#31023=CARTESIAN_POINT('Ctrl Pts',(158.394047637042,-2.57489188750593,126.614000868075));
#31024=CARTESIAN_POINT('Ctrl Pts',(158.386299740265,-2.69170371349151,126.685779388554));
#31025=CARTESIAN_POINT('Ctrl Pts',(158.378551843488,-2.80557229622117,126.762483160139));
#31026=CARTESIAN_POINT('Ctrl Pts',(158.370803946711,-2.91606252405755,126.843835094572));
#31027=CARTESIAN_POINT('Ctrl Pts',(158.363057670626,-3.02652963972008,126.925170011934));
#31028=CARTESIAN_POINT('Ctrl Pts',(158.355311394542,-3.13361949147905,127.011150926538));
#31029=CARTESIAN_POINT('Ctrl Pts',(158.347565118458,-3.23692694087578,127.10145810171));
#31030=CARTESIAN_POINT('Ctrl Pts',(158.339818785193,-3.3402351528646,127.191765943509));
#31031=CARTESIAN_POINT('Ctrl Pts',(158.332072451928,-3.43976061242328,127.28639985229));
#31032=CARTESIAN_POINT('Ctrl Pts',(158.324326118662,-3.53513250518679,127.385000848066));
#31033=CARTESIAN_POINT('Ctrl Pts',(158.316578050659,-3.63052575582409,127.483623924852));
#31034=CARTESIAN_POINT('Ctrl Pts',(158.308829982656,-3.7217633169883,127.586215575485));
#31035=CARTESIAN_POINT('Ctrl Pts',(158.301081914653,-3.8085126531988,127.692381434968));
#31036=CARTESIAN_POINT('Ctrl Pts',(158.293325611912,-3.89535418763626,127.79866012879));
#31037=CARTESIAN_POINT('Ctrl Pts',(158.28556930917,-3.97769772047951,127.908520316566));
#31038=CARTESIAN_POINT('Ctrl Pts',(158.277813006428,-4.05525197703981,128.021535710172));
#31039=CARTESIAN_POINT('Ctrl Pts',(158.270052563914,-4.13284762664232,128.134611423496));
#31040=CARTESIAN_POINT('Ctrl Pts',(158.2622921214,-4.20564869912791,128.250845367041));
#31041=CARTESIAN_POINT('Ctrl Pts',(158.254531678885,-4.27340893669931,128.369784859402));
#31042=CARTESIAN_POINT('Ctrl Pts',(158.24675877862,-4.34127794901937,128.488915283995));
#31043=CARTESIAN_POINT('Ctrl Pts',(158.238985878355,-4.404089776793,128.610759588768));
#31044=CARTESIAN_POINT('Ctrl Pts',(158.231212978089,-4.46164515919564,128.734842428246));
#31045=CARTESIAN_POINT('Ctrl Pts',(158.223722642327,-4.51710825847412,128.854414543962));
#31046=CARTESIAN_POINT('Ctrl Pts',(158.216232306565,-4.56769032914941,128.976064982847));
#31047=CARTESIAN_POINT('Ctrl Pts',(158.208741970803,-4.61325695891121,129.099355252895));
#31048=CARTESIAN_POINT('Ctrl Pts',(158.199766254412,-4.6678597375636,129.247094757892));
#31049=CARTESIAN_POINT('Ctrl Pts',(158.190790538021,-4.71540475201521,129.39757591567));
#31050=CARTESIAN_POINT('Ctrl Pts',(158.18181482163,-4.75564619449548,129.55016273235));
#31051=CARTESIAN_POINT('Ctrl Pts',(158.181181561314,-4.75848533373057,129.560928132179));
#31052=CARTESIAN_POINT('Ctrl Pts',(158.180548300999,-4.76128813747417,129.571704003721));
#31053=CARTESIAN_POINT('Ctrl Pts',(158.179915040683,-4.76405452823403,129.582490119308));
#31054=CARTESIAN_POINT('Origin',(213.235140564004,0.,130.804360617566));
#31055=CARTESIAN_POINT('',(156.084992794976,-4.76405452823404,129.582490119308));
#31056=CARTESIAN_POINT('',(156.429992618608,-4.76405452823404,129.582490119308));
#31057=CARTESIAN_POINT('',(213.235140564004,-4.76405452823405,129.582490119308));
#31058=CARTESIAN_POINT('',(157.764859435939,-4.9182485252746,130.8081693095));
#31059=CARTESIAN_POINT('Ctrl Pts',(157.764859435939,-4.9182485252746,130.8081693095));
#31060=CARTESIAN_POINT('Ctrl Pts',(157.755849159831,-4.91812493258219,130.967767299479));
#31061=CARTESIAN_POINT('Ctrl Pts',(157.746838883724,-4.91022897793391,131.127042622001));
#31062=CARTESIAN_POINT('Ctrl Pts',(157.737828607616,-4.89467815940805,131.285306330005));
#31063=CARTESIAN_POINT('Ctrl Pts',(157.728765898902,-4.87903684754533,131.444491006319));
#31064=CARTESIAN_POINT('Ctrl Pts',(157.719703190188,-4.85565143099362,131.602652156559));
#31065=CARTESIAN_POINT('Ctrl Pts',(157.710640481474,-4.8246906293771,131.759108434165));
#31066=CARTESIAN_POINT('Ctrl Pts',(157.701515594764,-4.79351740996534,131.916638136741));
#31067=CARTESIAN_POINT('Ctrl Pts',(157.692390708053,-4.75466458056885,132.072439391437));
#31068=CARTESIAN_POINT('Ctrl Pts',(157.683265821343,-4.70835263847484,132.225838191876));
#31069=CARTESIAN_POINT('Ctrl Pts',(157.679322454008,-4.68833869139834,132.292130282745));
#31070=CARTESIAN_POINT('Ctrl Pts',(157.675379086672,-4.66693229571562,132.357973975118));
#31071=CARTESIAN_POINT('Ctrl Pts',(157.671435719337,-4.64415395773542,132.423316169566));
#31072=CARTESIAN_POINT('Ctrl Pts',(157.663661385218,-4.59924654864364,132.552138064279));
#31073=CARTESIAN_POINT('Ctrl Pts',(157.655887051098,-4.54890395692894,132.679294090923));
#31074=CARTESIAN_POINT('Ctrl Pts',(157.648112716979,-4.49326825799374,132.804291472422));
#31075=CARTESIAN_POINT('Ctrl Pts',(157.640347964032,-4.43770112508511,132.92913480582));
#31076=CARTESIAN_POINT('Ctrl Pts',(157.632583211085,-4.37685402179583,133.051824433599));
#31077=CARTESIAN_POINT('Ctrl Pts',(157.624818458138,-4.31091851771169,133.17188349943));
#31078=CARTESIAN_POINT('Ctrl Pts',(157.617061417253,-4.24504850169973,133.291823320905));
#31079=CARTESIAN_POINT('Ctrl Pts',(157.609304376368,-4.17410032930813,133.409137439376));
#31080=CARTESIAN_POINT('Ctrl Pts',(157.601547335483,-4.09831315348778,133.523370061913));
#31081=CARTESIAN_POINT('Ctrl Pts',(157.593796144243,-4.02258312936639,133.637516540741));
#31082=CARTESIAN_POINT('Ctrl Pts',(157.586044953003,-3.94202158045546,133.748585824509));
#31083=CARTESIAN_POINT('Ctrl Pts',(157.578293761763,-3.85691279058616,133.856148091869));
#31084=CARTESIAN_POINT('Ctrl Pts',(157.570545864986,-3.77184017422281,133.963664642397));
#31085=CARTESIAN_POINT('Ctrl Pts',(157.562797968209,-3.68222440297854,134.067676835203));
#31086=CARTESIAN_POINT('Ctrl Pts',(157.555050071432,-3.58839201616392,134.167785330687));
#31087=CARTESIAN_POINT('Ctrl Pts',(157.547303795347,-3.49457925706182,134.267872885631));
#31088=CARTESIAN_POINT('Ctrl Pts',(157.539557519263,-3.39655190398407,134.364058082384));
#31089=CARTESIAN_POINT('Ctrl Pts',(157.531811243179,-3.29467530605241,134.45597638188));
#31090=CARTESIAN_POINT('Ctrl Pts',(157.524064909914,-3.19279795609091,134.547895359897));
#31091=CARTESIAN_POINT('Ctrl Pts',(157.516318576649,-3.08707159485389,134.635547115904));
#31092=CARTESIAN_POINT('Ctrl Pts',(157.508572243383,-2.97789648612514,134.718605829663));
#31093=CARTESIAN_POINT('Ctrl Pts',(157.50082417538,-2.86869692838775,134.801683143845));
#31094=CARTESIAN_POINT('Ctrl Pts',(157.493076107377,-2.75604739741964,134.880165132349));
#31095=CARTESIAN_POINT('Ctrl Pts',(157.485328039374,-2.64037877327346,134.953768165174));
#31096=CARTESIAN_POINT('Ctrl Pts',(157.477571736632,-2.52458721513698,135.027449424178));
#31097=CARTESIAN_POINT('Ctrl Pts',(157.469815433891,-2.40577048441605,135.096241158857));
#31098=CARTESIAN_POINT('Ctrl Pts',(157.462059131149,-2.28438628758989,135.159904481605));
#31099=CARTESIAN_POINT('Ctrl Pts',(157.454298688635,-2.16293730436299,135.223601783386));
#31100=CARTESIAN_POINT('Ctrl Pts',(157.44653824612,-2.03891847788247,135.282165052296));
#31101=CARTESIAN_POINT('Ctrl Pts',(157.438777803606,-1.91280840628421,135.33540321981));
#31102=CARTESIAN_POINT('Ctrl Pts',(157.431004903341,-1.78649589160353,135.388726849956));
#31103=CARTESIAN_POINT('Ctrl Pts',(157.423232003075,-1.65808578978925,135.436708159504));
#31104=CARTESIAN_POINT('Ctrl Pts',(157.41545910281,-1.52807365366,135.479205424775));
#31105=CARTESIAN_POINT('Ctrl Pts',(157.407968767048,-1.40278778615982,135.52015780741));
#31106=CARTESIAN_POINT('Ctrl Pts',(157.400478431286,-1.27601463450529,135.556017857252));
#31107=CARTESIAN_POINT('Ctrl Pts',(157.392988095524,-1.14820549682072,135.586703892528));
#31108=CARTESIAN_POINT('Ctrl Pts',(157.385213761405,-1.01555043683414,135.618553398157));
#31109=CARTESIAN_POINT('Ctrl Pts',(157.377439427286,-0.881359069864842,
135.644929688331));
#31110=CARTESIAN_POINT('Ctrl Pts',(157.369665093167,-0.746122778447592,
135.665685937063));
#31111=CARTESIAN_POINT('Ctrl Pts',(157.36190034022,-0.6110531536731,135.686416605573));
#31112=CARTESIAN_POINT('Ctrl Pts',(157.354135587273,-0.474941549471379,
135.701540954972));
#31113=CARTESIAN_POINT('Ctrl Pts',(157.346370834325,-0.338292706616414,
135.710962405683));
#31114=CARTESIAN_POINT('Ctrl Pts',(157.33861379344,-0.201779585318584,135.720374498876));
#31115=CARTESIAN_POINT('Ctrl Pts',(157.330856752555,-0.064730674756998,
135.724094938677));
#31116=CARTESIAN_POINT('Ctrl Pts',(157.32309971167,0.0723412855547204,135.722078564023));
#31117=CARTESIAN_POINT('Ctrl Pts',(157.31534852043,0.209309878834764,135.720063709933));
#31118=CARTESIAN_POINT('Ctrl Pts',(157.30759732919,0.346301097925988,135.712320658107));
#31119=CARTESIAN_POINT('Ctrl Pts',(157.29984613795,0.482799659600159,135.698856255647));
#31120=CARTESIAN_POINT('Ctrl Pts',(157.292098241173,0.61924020574454,135.685397575916));
#31121=CARTESIAN_POINT('Ctrl Pts',(157.284350344396,0.755188122675336,135.666222420369));
#31122=CARTESIAN_POINT('Ctrl Pts',(157.276602447619,0.890130932202471,135.641389662965));
#31123=CARTESIAN_POINT('Ctrl Pts',(157.268856171535,1.02504551460288,135.616562100039));
#31124=CARTESIAN_POINT('Ctrl Pts',(157.261109895451,1.15895502352692,135.586079359915));
#31125=CARTESIAN_POINT('Ctrl Pts',(157.253363619366,1.29135528181109,135.550051778887));
#31126=CARTESIAN_POINT('Ctrl Pts',(157.245617286101,1.42375651744388,135.514023931911));
#31127=CARTESIAN_POINT('Ctrl Pts',(157.237870952836,1.55464810295783,135.472451265011));
#31128=CARTESIAN_POINT('Ctrl Pts',(157.23012461957,1.68353956420689,135.425494417647));
#31129=CARTESIAN_POINT('Ctrl Pts',(157.222376551567,1.8124598898049,135.378527054622));
#31130=CARTESIAN_POINT('Ctrl Pts',(157.214628483564,1.93937883256479,135.326173245634));
#31131=CARTESIAN_POINT('Ctrl Pts',(157.206880415561,2.06382486534054,135.26864219333));
#31132=CARTESIAN_POINT('Ctrl Pts',(157.19912411282,2.18840316084093,135.211049996338));
#31133=CARTESIAN_POINT('Ctrl Pts',(157.191367810078,2.31050294072448,135.148269728644));
#31134=CARTESIAN_POINT('Ctrl Pts',(157.183611507336,2.42967582054979,135.080557347083));
#31135=CARTESIAN_POINT('Ctrl Pts',(157.175851064822,2.54891230652936,135.012808825386));
#31136=CARTESIAN_POINT('Ctrl Pts',(157.168090622308,2.66521844830249,134.940123151606));
#31137=CARTESIAN_POINT('Ctrl Pts',(157.160330179793,2.77817480052365,134.862799706703));
#31138=CARTESIAN_POINT('Ctrl Pts',(157.152557279528,2.89131248030919,134.785352135342));
#31139=CARTESIAN_POINT('Ctrl Pts',(157.144784379263,3.00108931155435,134.703252149742));
#31140=CARTESIAN_POINT('Ctrl Pts',(157.137011478997,3.10711819971322,134.616840067414));
#31141=CARTESIAN_POINT('Ctrl Pts',(157.129521143235,3.2092926707166,134.533569281937));
#31142=CARTESIAN_POINT('Ctrl Pts',(157.122030807473,3.30798673133394,134.446294671919));
#31143=CARTESIAN_POINT('Ctrl Pts',(157.114540471711,3.40288772271461,134.355351776257));
#31144=CARTESIAN_POINT('Ctrl Pts',(157.106766137592,3.50138691402832,134.260960753063));
#31145=CARTESIAN_POINT('Ctrl Pts',(157.098991803473,3.59611174562021,134.162318784651));
#31146=CARTESIAN_POINT('Ctrl Pts',(157.091217469354,3.6866730843672,134.05975992203));
#31147=CARTESIAN_POINT('Ctrl Pts',(157.083452716407,3.77712281435786,133.957327454041));
#31148=CARTESIAN_POINT('Ctrl Pts',(157.07568796346,3.86341900463223,133.850987986828));
#31149=CARTESIAN_POINT('Ctrl Pts',(157.067923210513,3.94520757534147,133.741113969478));
#31150=CARTESIAN_POINT('Ctrl Pts',(157.060166169628,4.02691491248923,133.631349080552));
#31151=CARTESIAN_POINT('Ctrl Pts',(157.052409128742,4.10412330762623,133.518056939259));
#31152=CARTESIAN_POINT('Ctrl Pts',(157.044652087857,4.17651761724043,133.401644517216));
#31153=CARTESIAN_POINT('Ctrl Pts',(157.036900896617,4.2488573337426,133.285319882686));
#31154=CARTESIAN_POINT('Ctrl Pts',(157.029149705377,4.31638998506244,133.165879981625));
#31155=CARTESIAN_POINT('Ctrl Pts',(157.021398514137,4.37884280868842,133.043762037432));
#31156=CARTESIAN_POINT('Ctrl Pts',(157.01365061736,4.44126908819839,132.921695996623));
#31157=CARTESIAN_POINT('Ctrl Pts',(157.005902720583,4.49861965658127,132.796954523911));
#31158=CARTESIAN_POINT('Ctrl Pts',(156.998154823806,4.5506670391882,132.670000604527));
#31159=CARTESIAN_POINT('Ctrl Pts',(156.990408547722,4.6027035346047,132.543073241165));
#31160=CARTESIAN_POINT('Ctrl Pts',(156.982662271638,4.64943890251702,132.413934713173));
#31161=CARTESIAN_POINT('Ctrl Pts',(156.974915995553,4.69069345190272,132.28306883854));
#31162=CARTESIAN_POINT('Ctrl Pts',(156.967169662288,4.73194830582011,132.152201997885));
#31163=CARTESIAN_POINT('Ctrl Pts',(156.959423329023,4.76772214293298,132.019608158022));
#31164=CARTESIAN_POINT('Ctrl Pts',(156.951676995757,4.79788500051228,131.885786798292));
#31165=CARTESIAN_POINT('Ctrl Pts',(156.943928927754,4.8280546128544,131.751935470196));
#31166=CARTESIAN_POINT('Ctrl Pts',(156.936180859751,4.8526106593448,131.61685645655));
#31167=CARTESIAN_POINT('Ctrl Pts',(156.928432791748,4.87147427615589,131.481059545636));
#31168=CARTESIAN_POINT('Ctrl Pts',(156.920676489007,4.89035794144341,131.34511830815));
#31169=CARTESIAN_POINT('Ctrl Pts',(156.912920186265,4.90353703768245,131.208458037106));
#31170=CARTESIAN_POINT('Ctrl Pts',(156.905163883523,4.91098454586627,131.071594321957));
#31171=CARTESIAN_POINT('Ctrl Pts',(156.897403441009,4.91843602900945,130.934657558523));
#31172=CARTESIAN_POINT('Ctrl Pts',(156.889642998495,4.92014982365658,130.797517525363));
#31173=CARTESIAN_POINT('Ctrl Pts',(156.88188255598,4.91615108703395,130.660688936449));
#31174=CARTESIAN_POINT('Ctrl Pts',(156.874109655715,4.91214593128431,130.523640698137));
#31175=CARTESIAN_POINT('Ctrl Pts',(156.866336755449,4.90240994694233,130.386905293349));
#31176=CARTESIAN_POINT('Ctrl Pts',(156.858563855184,4.88702021871189,130.250992345616));
#31177=CARTESIAN_POINT('Ctrl Pts',(156.851073519422,4.87218994586699,130.120020175877));
#31178=CARTESIAN_POINT('Ctrl Pts',(156.84358318366,4.8521098952129,129.989812009002));
#31179=CARTESIAN_POINT('Ctrl Pts',(156.836092847898,4.82689336538216,129.860812260708));
#31180=CARTESIAN_POINT('Ctrl Pts',(156.828318513779,4.80072074315854,129.726921447749));
#31181=CARTESIAN_POINT('Ctrl Pts',(156.82054417966,4.76893154670519,129.593908370793));
#31182=CARTESIAN_POINT('Ctrl Pts',(156.812769845541,4.73159648664064,129.462280981289));
#31183=CARTESIAN_POINT('Ctrl Pts',(156.805005092594,4.69430743870088,129.330815810778));
#31184=CARTESIAN_POINT('Ctrl Pts',(156.797240339646,4.6514862319889,129.200733302351));
#31185=CARTESIAN_POINT('Ctrl Pts',(156.789475586699,4.60325482966432,129.072532671241));
#31186=CARTESIAN_POINT('Ctrl Pts',(156.781718545814,4.55507133144848,128.944459370806));
#31187=CARTESIAN_POINT('Ctrl Pts',(156.773961504929,4.50148846786972,128.818264591638));
#31188=CARTESIAN_POINT('Ctrl Pts',(156.766204464044,4.44267829290953,128.694433451001));
#31189=CARTESIAN_POINT('Ctrl Pts',(156.758453272804,4.38391246715974,128.57069569239));
#31190=CARTESIAN_POINT('Ctrl Pts',(156.750702081564,4.31992734329849,128.449318376205));
#31191=CARTESIAN_POINT('Ctrl Pts',(156.742950890324,4.25094333495383,128.3307673152));
#31192=CARTESIAN_POINT('Ctrl Pts',(156.735202993547,4.18198864665293,128.212266641558));
#31193=CARTESIAN_POINT('Ctrl Pts',(156.72745509677,4.10803949587497,128.096590171144));
#31194=CARTESIAN_POINT('Ctrl Pts',(156.719707199993,4.02936244960184,127.984179539649));
#31195=CARTESIAN_POINT('Ctrl Pts',(156.711960923909,3.95070186087074,127.871792422035));
#31196=CARTESIAN_POINT('Ctrl Pts',(156.704214647824,3.86731556780952,127.762670104633));
#31197=CARTESIAN_POINT('Ctrl Pts',(156.69646837174,3.77951349280804,127.65722528203));
#31198=CARTESIAN_POINT('Ctrl Pts',(156.688722038475,3.69171076967156,127.551779681056));
#31199=CARTESIAN_POINT('Ctrl Pts',(156.68097570521,3.5994924497257,127.450011929495));
#31200=CARTESIAN_POINT('Ctrl Pts',(156.673229371944,3.50320851105733,127.352301349454));
#31201=CARTESIAN_POINT('Ctrl Pts',(156.665481303941,3.40690301026851,127.254568887807));
#31202=CARTESIAN_POINT('Ctrl Pts',(156.657733235938,3.30653035339417,127.160895684067));
#31203=CARTESIAN_POINT('Ctrl Pts',(156.649985167935,3.20247681193,127.071623641626));
#31204=CARTESIAN_POINT('Ctrl Pts',(156.642228865193,3.09831268112366,126.982256719796));
#31205=CARTESIAN_POINT('Ctrl Pts',(156.634472562452,2.99046014810908,126.897300558266));
#31206=CARTESIAN_POINT('Ctrl Pts',(156.62671625971,2.8793383884614,126.817056577587));
#31207=CARTESIAN_POINT('Ctrl Pts',(156.618955817196,2.76815731978472,126.736769768279));
#31208=CARTESIAN_POINT('Ctrl Pts',(156.611195374681,2.65370387374858,126.661200366551));
#31209=CARTESIAN_POINT('Ctrl Pts',(156.603434932167,2.53642469188915,126.59060542239));
#31210=CARTESIAN_POINT('Ctrl Pts',(156.595662031902,2.41895724307548,126.519897152957));
#31211=CARTESIAN_POINT('Ctrl Pts',(156.587889131636,2.29865533712734,126.454179486085));
#31212=CARTESIAN_POINT('Ctrl Pts',(156.580116231371,2.17598940092134,126.393663032197));
#31213=CARTESIAN_POINT('Ctrl Pts',(156.572625895609,2.05778268047426,126.33534650384));
#31214=CARTESIAN_POINT('Ctrl Pts',(156.565135559847,1.93738110413567,126.281859724446));
#31215=CARTESIAN_POINT('Ctrl Pts',(156.557645224085,1.81521981211289,126.233347590215));
#31216=CARTESIAN_POINT('Ctrl Pts',(156.549870889966,1.688426737572,126.18299610367));
#31217=CARTESIAN_POINT('Ctrl Pts',(156.542096555847,1.55933623162569,126.137844437843));
#31218=CARTESIAN_POINT('Ctrl Pts',(156.534322221728,1.42841386903006,126.098107662054));
#31219=CARTESIAN_POINT('Ctrl Pts',(156.526557468781,1.2976528565455,126.05841985829));
#31220=CARTESIAN_POINT('Ctrl Pts',(156.518792715834,1.16506484988346,126.02413377901));
#31221=CARTESIAN_POINT('Ctrl Pts',(156.511027962886,1.03113577702658,125.99541665118));
#31222=CARTESIAN_POINT('Ctrl Pts',(156.503270922001,0.897339724412969,125.966728045607));
#31223=CARTESIAN_POINT('Ctrl Pts',(156.495513881116,0.762205636079137,125.943597465663));
#31224=CARTESIAN_POINT('Ctrl Pts',(156.487756840231,0.62623465429642,125.926142375189));
#31225=CARTESIAN_POINT('Ctrl Pts',(156.480005648991,0.490366209288719,125.908700447735));
#31226=CARTESIAN_POINT('Ctrl Pts',(156.472254457751,0.35366251322796,125.896925540389));
#31227=CARTESIAN_POINT('Ctrl Pts',(156.464503266511,0.21663460652543,125.890883996094));
#31228=CARTESIAN_POINT('Ctrl Pts',(156.456755369734,0.0796649403385415,
125.884845019616));
#31229=CARTESIAN_POINT('Ctrl Pts',(156.449007472957,-0.0576282726520325,
125.884534576701));
#31230=CARTESIAN_POINT('Ctrl Pts',(156.44125957618,-0.194729385867471,125.889967111875));
#31231=CARTESIAN_POINT('Ctrl Pts',(156.433513300096,-0.331801820485583,
125.895398510679));
#31232=CARTESIAN_POINT('Ctrl Pts',(156.425767024012,-0.468681844843868,
125.906570482638));
#31233=CARTESIAN_POINT('Ctrl Pts',(156.418020747927,-0.604854726675913,
125.92344535277));
#31234=CARTESIAN_POINT('Ctrl Pts',(156.410274414662,-0.741028613705098,
125.940320347469));
#31235=CARTESIAN_POINT('Ctrl Pts',(156.402528081397,-0.876494959794615,
125.962898276263));
#31236=CARTESIAN_POINT('Ctrl Pts',(156.394781748131,-1.01074545880611,125.991089725542));
#31237=CARTESIAN_POINT('Ctrl Pts',(156.387033680128,-1.14502602228603,126.019287488101));
#31238=CARTESIAN_POINT('Ctrl Pts',(156.379285612125,-1.27808981433431,126.053101192314));
#31239=CARTESIAN_POINT('Ctrl Pts',(156.371537544122,-1.40944039276611,126.092390664167));
#31240=CARTESIAN_POINT('Ctrl Pts',(156.363781241381,-1.54093057215585,126.131721893338));
#31241=CARTESIAN_POINT('Ctrl Pts',(156.356024938639,-1.67070352547269,126.176540403429));
#31242=CARTESIAN_POINT('Ctrl Pts',(156.348268635897,-1.79827908443529,126.226656455327));
#31243=CARTESIAN_POINT('Ctrl Pts',(156.340508193383,-1.92592273431503,126.27679925567));
#31244=CARTESIAN_POINT('Ctrl Pts',(156.332747750869,-2.05136629548881,126.332245073791));
#31245=CARTESIAN_POINT('Ctrl Pts',(156.324987308354,-2.17415208386269,126.392757079312));
#31246=CARTESIAN_POINT('Ctrl Pts',(156.317214408089,-2.29713497888443,126.453366224076));
#31247=CARTESIAN_POINT('Ctrl Pts',(156.309441507823,-2.41745123194715,126.519057620489));
#31248=CARTESIAN_POINT('Ctrl Pts',(156.301668607558,-2.53466937331946,126.589549325176));
#31249=CARTESIAN_POINT('Ctrl Pts',(156.294178271796,-2.64762633999865,126.65747847884));
#31250=CARTESIAN_POINT('Ctrl Pts',(156.286687936034,-2.75770627531209,126.729864824214));
#31251=CARTESIAN_POINT('Ctrl Pts',(156.279197600272,-2.8645520700704,126.806420585455));
#31252=CARTESIAN_POINT('Ctrl Pts',(156.271105733385,-2.97997839755708,126.88912435857));
#31253=CARTESIAN_POINT('Ctrl Pts',(156.263013866497,-3.09202648001146,126.976979076286));
#31254=CARTESIAN_POINT('Ctrl Pts',(156.25492199961,-3.200202032726,127.069673212677));
#31255=CARTESIAN_POINT('Ctrl Pts',(156.247218857282,-3.30318094853596,127.15791442271));
#31256=CARTESIAN_POINT('Ctrl Pts',(156.239515714955,-3.40265032657603,127.250540669921));
#31257=CARTESIAN_POINT('Ctrl Pts',(156.231812572627,-3.49821192172148,127.34723805491));
#31258=CARTESIAN_POINT('Ctrl Pts',(156.224116381523,-3.59368728322783,127.443848181337));
#31259=CARTESIAN_POINT('Ctrl Pts',(156.216420190418,-3.68526159703673,127.544521858844));
#31260=CARTESIAN_POINT('Ctrl Pts',(156.208723999314,-3.77257014628933,127.64890541208));
#31261=CARTESIAN_POINT('Ctrl Pts',(156.201033021136,-3.859819558099,127.753218262316));
#31262=CARTESIAN_POINT('Ctrl Pts',(156.193342042959,-3.94280869879852,127.861235685983));
#31263=CARTESIAN_POINT('Ctrl Pts',(156.185651064781,-4.02121049843016,127.972568042215));
#31264=CARTESIAN_POINT('Ctrl Pts',(156.177963565501,-4.09957683419471,128.083850038941));
#31265=CARTESIAN_POINT('Ctrl Pts',(156.170276066221,-4.1733597297056,128.19844365986));
#31266=CARTESIAN_POINT('Ctrl Pts',(156.162588566941,-4.242273434718,128.315927542801));
#31267=CARTESIAN_POINT('Ctrl Pts',(156.154901463274,-4.311183593297,128.433405379792));
#31268=CARTESIAN_POINT('Ctrl Pts',(156.147214359608,-4.37522485144858,128.553772844428));
#31269=CARTESIAN_POINT('Ctrl Pts',(156.139527255941,-4.43415583624978,128.676581239352));
#31270=CARTESIAN_POINT('Ctrl Pts',(156.131840359425,-4.49308523299093,128.799386324861));
#31271=CARTESIAN_POINT('Ctrl Pts',(156.12415346291,-4.54690446386079,128.924631848696));
#31272=CARTESIAN_POINT('Ctrl Pts',(156.116466566394,-4.59541935318012,129.051846985403));
#31273=CARTESIAN_POINT('Ctrl Pts',(156.108776075186,-4.6439569299483,129.179121612854));
#31274=CARTESIAN_POINT('Ctrl Pts',(156.101085583978,-4.68718507680773,129.308367318422));
#31275=CARTESIAN_POINT('Ctrl Pts',(156.093395092771,-4.72495878294843,129.439095968519));
#31276=CARTESIAN_POINT('Ctrl Pts',(156.090594326839,-4.73871542168699,129.486705456596));
#31277=CARTESIAN_POINT('Ctrl Pts',(156.087793560907,-4.75174911450255,129.53451149793));
#31278=CARTESIAN_POINT('Ctrl Pts',(156.084992794976,-4.76405452823404,129.582490119308));
#31279=CARTESIAN_POINT('Ctrl Pts',(157.83474697768,-4.76405452823405,129.582490119308));
#31280=CARTESIAN_POINT('Ctrl Pts',(157.827003930467,-4.79813988220165,129.71538839711));
#31281=CARTESIAN_POINT('Ctrl Pts',(157.819260883253,-4.82667131339279,129.84975804506));
#31282=CARTESIAN_POINT('Ctrl Pts',(157.81151783604,-4.84953480182535,129.98509553935));
#31283=CARTESIAN_POINT('Ctrl Pts',(157.803741436032,-4.87249677360888,130.121015993234));
#31284=CARTESIAN_POINT('Ctrl Pts',(157.795965036024,-4.8897417613054,130.2579122657));
#31285=CARTESIAN_POINT('Ctrl Pts',(157.788188636015,-4.90120637170618,130.395265073167));
#31286=CARTESIAN_POINT('Ctrl Pts',(157.780412236007,-4.91267098210696,130.532617880635));
#31287=CARTESIAN_POINT('Ctrl Pts',(157.772635835999,-4.91835519303655,130.670426824793));
#31288=CARTESIAN_POINT('Ctrl Pts',(157.764859435991,-4.91824852527531,130.808169308574));
#31289=CARTESIAN_POINT('',(158.110140564063,-4.91824875213615,130.800857103449));
#31290=CARTESIAN_POINT('Ctrl Pts',(158.179915040683,-4.76405452823403,129.582490119308));
#31291=CARTESIAN_POINT('Ctrl Pts',(158.170991527053,-4.80303679988543,129.734481404838));
#31292=CARTESIAN_POINT('Ctrl Pts',(158.162068013422,-4.83478472549672,129.888508569464));
#31293=CARTESIAN_POINT('Ctrl Pts',(158.153144499792,-4.8591067013772,130.043923159828));
#31294=CARTESIAN_POINT('Ctrl Pts',(158.14428513534,-4.88325383191697,130.198220508848));
#31295=CARTESIAN_POINT('Ctrl Pts',(158.135425770889,-4.90008131355361,130.353885259974));
#31296=CARTESIAN_POINT('Ctrl Pts',(158.126566406437,-4.90944903895876,130.51026336092));
#31297=CARTESIAN_POINT('Ctrl Pts',(158.121091125646,-4.91523849792619,130.606908443869));
#31298=CARTESIAN_POINT('Ctrl Pts',(158.115615844854,-4.9181796317636,130.703825615994));
#31299=CARTESIAN_POINT('Ctrl Pts',(158.110140564063,-4.91824875213615,130.800857103449));
#31300=CARTESIAN_POINT('Ctrl Pts',(158.110140564008,-4.91824875213684,130.800857104418));
#31301=CARTESIAN_POINT('Ctrl Pts',(158.102369830278,-4.91834685045954,130.93856800569));
#31302=CARTESIAN_POINT('Ctrl Pts',(158.094599096547,-4.91265677724765,131.076325466706));
#31303=CARTESIAN_POINT('Ctrl Pts',(158.086828362817,-4.90119353514655,131.213609922437));
#31304=CARTESIAN_POINT('Ctrl Pts',(158.079057967618,-4.88973079244064,131.350888397383));
#31305=CARTESIAN_POINT('Ctrl Pts',(158.071287572418,-4.87249541273953,131.487693522148));
#31306=CARTESIAN_POINT('Ctrl Pts',(158.063517177219,-4.84955438502098,131.623509767125));
#31307=CARTESIAN_POINT('Ctrl Pts',(158.055745478988,-4.82660951027941,131.759348787378));
#31308=CARTESIAN_POINT('Ctrl Pts',(158.047973780758,-4.79795714719638,131.894198215901));
#31309=CARTESIAN_POINT('Ctrl Pts',(158.040202082527,-4.76371555994939,132.027551987057));
#31310=CARTESIAN_POINT('Ctrl Pts',(158.032427439215,-4.72946099687106,132.160956292552));
#31311=CARTESIAN_POINT('Ctrl Pts',(158.024652795903,-4.68961308972873,132.292863437657));
#31312=CARTESIAN_POINT('Ctrl Pts',(158.016878152591,-4.6443400861399,132.422782140771));
#31313=CARTESIAN_POINT('Ctrl Pts',(158.009093984334,-4.59901161725824,132.552860011123));
#31314=CARTESIAN_POINT('Ctrl Pts',(158.001309816077,-4.54824490514241,132.680944208087));
#31315=CARTESIAN_POINT('Ctrl Pts',(157.993525647821,-4.49225675065279,132.806562492681));
#31316=CARTESIAN_POINT('Ctrl Pts',(157.985736342952,-4.43623165073384,132.932263670192));
#31317=CARTESIAN_POINT('Ctrl Pts',(157.977947038083,-4.37497841552365,133.05549534717));
#31318=CARTESIAN_POINT('Ctrl Pts',(157.970157733214,-4.30875957135957,133.17581038906));
#31319=CARTESIAN_POINT('Ctrl Pts',(157.96235569651,-4.24243249065822,133.296322089222));
#31320=CARTESIAN_POINT('Ctrl Pts',(157.954553659806,-4.17112378757189,133.413907300181));
#31321=CARTESIAN_POINT('Ctrl Pts',(157.946751623102,-4.09513946182071,133.528147659671));
#31322=CARTESIAN_POINT('Ctrl Pts',(157.941265864398,-4.04171345369319,133.608472204427));
#31323=CARTESIAN_POINT('Ctrl Pts',(157.935780105694,-3.98597681923433,133.687143779075));
#31324=CARTESIAN_POINT('Ctrl Pts',(157.93029434699,-3.92804737291623,133.764027304648));
#31325=CARTESIAN_POINT('Ctrl Pts',(157.922520012871,-3.84595063929811,133.872985472209));
#31326=CARTESIAN_POINT('Ctrl Pts',(157.914745678752,-3.7591869293676,133.978697771831));
#31327=CARTESIAN_POINT('Ctrl Pts',(157.906971344633,-3.66804199597895,134.080738339721));
#31328=CARTESIAN_POINT('Ctrl Pts',(157.899206591686,-3.57700939057493,134.182653151731));
#31329=CARTESIAN_POINT('Ctrl Pts',(157.891441838739,-3.48160656298945,134.280904946787));
#31330=CARTESIAN_POINT('Ctrl Pts',(157.883677085792,-3.38216153549143,134.37509813387));
#31331=CARTESIAN_POINT('Ctrl Pts',(157.875920044907,-3.28281527819636,134.469197766953));
#31332=CARTESIAN_POINT('Ctrl Pts',(157.868163004022,-3.17943509257304,134.55924654695));
#31333=CARTESIAN_POINT('Ctrl Pts',(157.860405963137,-3.07238788050573,134.644883469239));
#31334=CARTESIAN_POINT('Ctrl Pts',(157.852654771897,-2.9654213935741,134.730455812058));
#31335=CARTESIAN_POINT('Ctrl Pts',(157.844903580657,-2.85479368848489,134.811622676149));
#31336=CARTESIAN_POINT('Ctrl Pts',(157.837152389417,-2.74090671272816,134.888061568251));
#31337=CARTESIAN_POINT('Ctrl Pts',(157.829404492639,-2.62706814197413,134.964467971784));
#31338=CARTESIAN_POINT('Ctrl Pts',(157.821656595862,-2.50997337970784,135.036150182672));
#31339=CARTESIAN_POINT('Ctrl Pts',(157.813908699085,-2.39005530382696,135.102827635835));
#31340=CARTESIAN_POINT('Ctrl Pts',(157.806162423001,-2.2701623122223,135.169491141513));
#31341=CARTESIAN_POINT('Ctrl Pts',(157.798416146917,-2.14744752317223,135.23115178191));
#31342=CARTESIAN_POINT('Ctrl Pts',(157.790669870833,-2.02237014518254,135.287573980587));
#31343=CARTESIAN_POINT('Ctrl Pts',(157.782923537568,-1.89729184390009,135.343996595761));
#31344=CARTESIAN_POINT('Ctrl Pts',(157.775177204302,-1.76985127526052,135.395180531291));
#31345=CARTESIAN_POINT('Ctrl Pts',(157.767430871037,-1.6405290728496,135.440937741225));
#31346=CARTESIAN_POINT('Ctrl Pts',(157.759682803034,-1.5111779096282,135.486705198168));
#31347=CARTESIAN_POINT('Ctrl Pts',(157.751934735031,-1.37994464264407,135.527043380868));
#31348=CARTESIAN_POINT('Ctrl Pts',(157.744186667028,-1.24732617749561,135.561813767039));
#31349=CARTESIAN_POINT('Ctrl Pts',(157.736430364286,-1.11456676386411,135.596621107591));
#31350=CARTESIAN_POINT('Ctrl Pts',(157.728674061545,-0.980419589966094,
135.625848731418));
#31351=CARTESIAN_POINT('Ctrl Pts',(157.720917758803,-0.845393445290692,
135.649408913007));
#31352=CARTESIAN_POINT('Ctrl Pts',(157.713157316289,-0.71029523309618,135.672981669375));
#31353=CARTESIAN_POINT('Ctrl Pts',(157.705396873774,-0.574317502768465,
135.690880905169));
#31354=CARTESIAN_POINT('Ctrl Pts',(157.69763643126,-0.437974336912093,135.703070809311));
#31355=CARTESIAN_POINT('Ctrl Pts',(157.689863530995,-0.30141230090205,135.71528028177));
#31356=CARTESIAN_POINT('Ctrl Pts',(157.682090630729,-0.164484047843235,
135.721762089238));
#31357=CARTESIAN_POINT('Ctrl Pts',(157.674317730464,-0.0277047386209147,
135.722532585885));
#31358=CARTESIAN_POINT('Ctrl Pts',(157.666827394702,0.104102298185345,135.723275073038));
#31359=CARTESIAN_POINT('Ctrl Pts',(157.65933705894,0.235770724281695,135.718714291907));
#31360=CARTESIAN_POINT('Ctrl Pts',(157.651846723178,0.366845853006052,135.708910258729));
#31361=CARTESIAN_POINT('Ctrl Pts',(157.644072389059,0.502890735075081,135.698734502653));
#31362=CARTESIAN_POINT('Ctrl Pts',(157.63629805494,0.638727391214445,135.682877816325));
#31363=CARTESIAN_POINT('Ctrl Pts',(157.62852372082,0.77384307375465,135.661350421931));
#31364=CARTESIAN_POINT('Ctrl Pts',(157.620758967873,0.908792238291439,135.639849558126));
#31365=CARTESIAN_POINT('Ctrl Pts',(157.612994214926,1.04302181476096,135.612691952491));
#31366=CARTESIAN_POINT('Ctrl Pts',(157.605229461979,1.1760216771865,135.579939752842));
#31367=CARTESIAN_POINT('Ctrl Pts',(157.597472421094,1.30888944227443,135.54722008314));
#31368=CARTESIAN_POINT('Ctrl Pts',(157.589715380209,1.44052954673107,135.508916970248));
#31369=CARTESIAN_POINT('Ctrl Pts',(157.581958339324,1.57043994771253,135.465143967297));
#31370=CARTESIAN_POINT('Ctrl Pts',(157.574207148084,1.70025238224965,135.421403973907));
#31371=CARTESIAN_POINT('Ctrl Pts',(157.566455956844,1.82833734060721,135.372202425128));
#31372=CARTESIAN_POINT('Ctrl Pts',(157.558704765604,1.95420623763486,135.317703175282));
#31373=CARTESIAN_POINT('Ctrl Pts',(157.550956868827,2.0800216370236,135.26322708907));
#31374=CARTESIAN_POINT('Ctrl Pts',(157.543208972049,2.20362249039337,135.2034579352));
#31375=CARTESIAN_POINT('Ctrl Pts',(157.535461075272,2.32453876931873,135.138608253827));
#31376=CARTESIAN_POINT('Ctrl Pts',(157.527714799188,2.44542975516502,135.073772137609));
#31377=CARTESIAN_POINT('Ctrl Pts',(157.519968523104,2.56363693920783,135.003857792397));
#31378=CARTESIAN_POINT('Ctrl Pts',(157.51222224702,2.67871391090342,134.929124228494));
#31379=CARTESIAN_POINT('Ctrl Pts',(157.504475913755,2.79379173207135,134.854390112923));
#31380=CARTESIAN_POINT('Ctrl Pts',(157.496729580489,2.90573896689588,134.774836920613));
#31381=CARTESIAN_POINT('Ctrl Pts',(157.488983247224,3.01413761279812,134.690767378781));
#31382=CARTESIAN_POINT('Ctrl Pts',(157.481235179221,3.12256053382531,134.606679010157));
#31383=CARTESIAN_POINT('Ctrl Pts',(157.473487111218,3.22743297572324,134.518072518988));
#31384=CARTESIAN_POINT('Ctrl Pts',(157.465739043215,3.3283698061565,134.425291091348));
#31385=CARTESIAN_POINT('Ctrl Pts',(157.457982740473,3.42941391345437,134.332411054503));
#31386=CARTESIAN_POINT('Ctrl Pts',(157.450226437731,3.52651376536795,134.23534748246));
#31387=CARTESIAN_POINT('Ctrl Pts',(157.442470134989,3.61932054279237,134.134481016444));
#31388=CARTESIAN_POINT('Ctrl Pts',(157.434709692475,3.71217685398844,134.033560714958));
#31389=CARTESIAN_POINT('Ctrl Pts',(157.426949249961,3.80073527267693,133.928833773503));
#31390=CARTESIAN_POINT('Ctrl Pts',(157.419188807447,3.88468779578029,133.820713347572));
#31391=CARTESIAN_POINT('Ctrl Pts',(157.411415907181,3.96877508692653,133.712419357136));
#31392=CARTESIAN_POINT('Ctrl Pts',(157.403643006916,4.04824148056073,133.600721315091));
#31393=CARTESIAN_POINT('Ctrl Pts',(157.39587010665,4.1228222788664,133.486061480709));
#31394=CARTESIAN_POINT('Ctrl Pts',(157.388379770888,4.19469187729538,133.375569820118));
#31395=CARTESIAN_POINT('Ctrl Pts',(157.380889435126,4.2620247634462,133.262328230597));
#31396=CARTESIAN_POINT('Ctrl Pts',(157.373399099364,4.32462566143182,133.146751693152));
#31397=CARTESIAN_POINT('Ctrl Pts',(157.365624765245,4.38960009149224,133.026793036161));
#31398=CARTESIAN_POINT('Ctrl Pts',(157.357850431126,4.44968244283791,132.903938883975));
#31399=CARTESIAN_POINT('Ctrl Pts',(157.350076097007,4.50460416304322,132.778626151073));
#31400=CARTESIAN_POINT('Ctrl Pts',(157.34231134406,4.55945819713687,132.653467854915));
#31401=CARTESIAN_POINT('Ctrl Pts',(157.334546591113,4.60916409919449,132.525857361444));
#31402=CARTESIAN_POINT('Ctrl Pts',(157.326781838166,4.65349842038315,132.396257446507));
#31403=CARTESIAN_POINT('Ctrl Pts',(157.319024797281,4.69778870809917,132.266786252031));
#31404=CARTESIAN_POINT('Ctrl Pts',(157.311267756396,4.73671790636995,132.135329935787));
#31405=CARTESIAN_POINT('Ctrl Pts',(157.303510715511,4.77011018423933,132.002372258877));
#31406=CARTESIAN_POINT('Ctrl Pts',(157.295759524271,4.803477280732,131.869514846386));
#31407=CARTESIAN_POINT('Ctrl Pts',(157.288008333031,4.83131567292508,131.735158704436));
#31408=CARTESIAN_POINT('Ctrl Pts',(157.280257141791,4.85349912389242,131.599803460815));
#31409=CARTESIAN_POINT('Ctrl Pts',(157.272509245013,4.8756731463014,131.464505746782));
#31410=CARTESIAN_POINT('Ctrl Pts',(157.264761348236,4.89219694476504,131.328210160674));
#31411=CARTESIAN_POINT('Ctrl Pts',(157.257013451459,4.90299527349092,131.191427033864));
#31412=CARTESIAN_POINT('Ctrl Pts',(157.249267175375,4.91379134343922,131.054672519135));
#31413=CARTESIAN_POINT('Ctrl Pts',(157.241520899291,4.91886429508151,130.917431056058));
#31414=CARTESIAN_POINT('Ctrl Pts',(157.233774623207,4.91819074531745,130.780218223862));
#31415=CARTESIAN_POINT('Ctrl Pts',(157.226028289942,4.91751719058141,130.643004378793));
#31416=CARTESIAN_POINT('Ctrl Pts',(157.218281956676,4.91109705171341,130.505819555986));
#31417=CARTESIAN_POINT('Ctrl Pts',(157.210535623411,4.89895908109086,130.369179064306));
#31418=CARTESIAN_POINT('Ctrl Pts',(157.202787555408,4.88681839225398,130.232507972936));
#31419=CARTESIAN_POINT('Ctrl Pts',(157.195039487405,4.86895735826512,130.096381844615));
#31420=CARTESIAN_POINT('Ctrl Pts',(157.187291419402,4.84545653785333,129.961310202541));
#31421=CARTESIAN_POINT('Ctrl Pts',(157.17953511666,4.82193074048988,129.826095004717));
#31422=CARTESIAN_POINT('Ctrl Pts',(157.171778813919,4.79275325010191,129.691936917693));
#31423=CARTESIAN_POINT('Ctrl Pts',(157.164022511177,4.75805576568542,129.559335158739));
#31424=CARTESIAN_POINT('Ctrl Pts',(157.156262068662,4.72333976217676,129.426662626234));
#31425=CARTESIAN_POINT('Ctrl Pts',(157.148501626148,4.68309800877048,129.295548450532));
#31426=CARTESIAN_POINT('Ctrl Pts',(157.140741183634,4.63751162169754,129.166475083983));
#31427=CARTESIAN_POINT('Ctrl Pts',(157.132968283369,4.59185205530909,129.037194517407));
#31428=CARTESIAN_POINT('Ctrl Pts',(157.125195383103,4.54083085591796,128.909961669736));
#31429=CARTESIAN_POINT('Ctrl Pts',(157.117422482838,4.48467703313857,128.785238290678));
#31430=CARTESIAN_POINT('Ctrl Pts',(157.109932147076,4.43056454325988,128.665048920607));
#31431=CARTESIAN_POINT('Ctrl Pts',(157.102441811314,4.37168625648756,128.547190011304));
#31432=CARTESIAN_POINT('Ctrl Pts',(157.094951475552,4.30828575671004,128.432050161275));
#31433=CARTESIAN_POINT('Ctrl Pts',(157.087177141433,4.2424814077137,128.312544748836));
#31434=CARTESIAN_POINT('Ctrl Pts',(157.079402807314,4.17159670856506,128.195590094893));
#31435=CARTESIAN_POINT('Ctrl Pts',(157.071628473195,4.095854088642,128.081648303153));
#31436=CARTESIAN_POINT('Ctrl Pts',(157.063863720247,4.02020481472882,127.967846934489));
#31437=CARTESIAN_POINT('Ctrl Pts',(157.0560989673,3.93970974665174,127.857051362563));
#31438=CARTESIAN_POINT('Ctrl Pts',(157.048334214353,3.85463745128303,127.749699722857));
#31439=CARTESIAN_POINT('Ctrl Pts',(157.040577173468,3.76964965091695,127.642454706311));
#31440=CARTESIAN_POINT('Ctrl Pts',(157.032820132583,3.68009391158809,127.538647119345));
#31441=CARTESIAN_POINT('Ctrl Pts',(157.025063091698,3.58628219428691,127.438686378214));
#31442=CARTESIAN_POINT('Ctrl Pts',(157.017311900458,3.49254122113127,127.338801018254));
#31443=CARTESIAN_POINT('Ctrl Pts',(157.009560709218,3.39455092471505,127.242757013922));
#31444=CARTESIAN_POINT('Ctrl Pts',(157.001809517978,3.29266342190441,127.150930632942));
#31445=CARTESIAN_POINT('Ctrl Pts',(156.994061621201,3.19081922400085,127.059143280623));
#31446=CARTESIAN_POINT('Ctrl Pts',(156.986313724424,3.08508140400256,126.971570247501));
#31447=CARTESIAN_POINT('Ctrl Pts',(156.978565827646,2.97583864595741,126.888550686565));
#31448=CARTESIAN_POINT('Ctrl Pts',(156.970819551562,2.86661873914209,126.805548491531));
#31449=CARTESIAN_POINT('Ctrl Pts',(156.963073275478,2.75389566365159,126.727098110539));
#31450=CARTESIAN_POINT('Ctrl Pts',(156.955326999394,2.63809055175585,126.65349789962));
#31451=CARTESIAN_POINT('Ctrl Pts',(156.947580666129,2.52228458501323,126.579897145401));
#31452=CARTESIAN_POINT('Ctrl Pts',(156.939834332863,2.40339686643112,126.511146842406));
#31453=CARTESIAN_POINT('Ctrl Pts',(156.932087999598,2.28187648131301,126.447501337473));
#31454=CARTESIAN_POINT('Ctrl Pts',(156.924339931595,2.16032888254787,126.383841579572));
#31455=CARTESIAN_POINT('Ctrl Pts',(156.916591863592,2.0361477903483,126.325289075894));
#31456=CARTESIAN_POINT('Ctrl Pts',(156.908843795589,1.90980542497134,126.272051459835));
#31457=CARTESIAN_POINT('Ctrl Pts',(156.901087492847,1.78332878142448,126.218757262204));
#31458=CARTESIAN_POINT('Ctrl Pts',(156.893331190105,1.65468663700184,126.170789388187));
#31459=CARTESIAN_POINT('Ctrl Pts',(156.885574887364,1.52437018385685,126.128306874818));
#31460=CARTESIAN_POINT('Ctrl Pts',(156.877814444849,1.39398417689715,126.085801687253));
#31461=CARTESIAN_POINT('Ctrl Pts',(156.870054002335,1.26192245685782,126.048787799491));
#31462=CARTESIAN_POINT('Ctrl Pts',(156.862293559821,1.12868882231008,126.017373610597));
#31463=CARTESIAN_POINT('Ctrl Pts',(156.854520659556,0.995241309304005,125.985908992858));
#31464=CARTESIAN_POINT('Ctrl Pts',(156.84674775929,0.860618506603748,125.9600621109));
#31465=CARTESIAN_POINT('Ctrl Pts',(156.838974859025,0.725332682606731,125.939889879444));
#31466=CARTESIAN_POINT('Ctrl Pts',(156.831484523263,0.594964839077581,125.920450959413));
#31467=CARTESIAN_POINT('Ctrl Pts',(156.823994187501,0.463981648562595,125.906281310252));
#31468=CARTESIAN_POINT('Ctrl Pts',(156.816503851739,0.332841713031933,125.897386044923));
#31469=CARTESIAN_POINT('Ctrl Pts',(156.80872951762,0.196729566985446,125.888153512905));
#31470=CARTESIAN_POINT('Ctrl Pts',(156.800955183501,0.0600173929501631,
125.884573970625));
#31471=CARTESIAN_POINT('Ctrl Pts',(156.793180849382,-0.0767857996245379,
125.88671006029));
#31472=CARTESIAN_POINT('Ctrl Pts',(156.785416096435,-0.213420394490518,
125.888843517416));
#31473=CARTESIAN_POINT('Ctrl Pts',(156.777651343487,-0.350145397541858,
125.89667858497));
#31474=CARTESIAN_POINT('Ctrl Pts',(156.76988659054,-0.486447026036527,125.910226132965));
#31475=CARTESIAN_POINT('Ctrl Pts',(156.762129549655,-0.622613277832677,
125.923760225345));
#31476=CARTESIAN_POINT('Ctrl Pts',(156.75437250877,-0.758356605358593,125.942995468796));
#31477=CARTESIAN_POINT('Ctrl Pts',(156.746615467885,-0.893163932587293,
125.967890701188));
#31478=CARTESIAN_POINT('Ctrl Pts',(156.738864276645,-1.02786960056188,125.992767159893));
#31479=CARTESIAN_POINT('Ctrl Pts',(156.731113085405,-1.1616402902725,126.02329504115));
#31480=CARTESIAN_POINT('Ctrl Pts',(156.723361894165,-1.29396910925877,126.059381480964));
#31481=CARTESIAN_POINT('Ctrl Pts',(156.715613997388,-1.426241684967,126.095452583079));
#31482=CARTESIAN_POINT('Ctrl Pts',(156.707866100611,-1.55707323242829,126.137077442202));
#31483=CARTESIAN_POINT('Ctrl Pts',(156.700118203834,-1.68596831940623,126.184112367909));
#31484=CARTESIAN_POINT('Ctrl Pts',(156.692371927749,-1.81483644431075,126.231137454924));
#31485=CARTESIAN_POINT('Ctrl Pts',(156.684625651665,-1.94176854738642,126.283570223634));
#31486=CARTESIAN_POINT('Ctrl Pts',(156.676879375581,-2.06628598097567,126.341217632256));
#31487=CARTESIAN_POINT('Ctrl Pts',(156.669133042316,-2.19080433372386,126.398865466418));
#31488=CARTESIAN_POINT('Ctrl Pts',(156.661386709051,-2.31290762663056,126.461727853047));
#31489=CARTESIAN_POINT('Ctrl Pts',(156.653640375785,-2.43213912892105,126.529564444639));
#31490=CARTESIAN_POINT('Ctrl Pts',(156.645892307782,-2.55139733227917,126.597416227765));
#31491=CARTESIAN_POINT('Ctrl Pts',(156.638144239779,-2.66778212554129,126.670244239161));
#31492=CARTESIAN_POINT('Ctrl Pts',(156.630396171776,-2.78086357426937,126.747763417473));
#31493=CARTESIAN_POINT('Ctrl Pts',(156.622639869035,-2.89406520730764,126.825364984091));
#31494=CARTESIAN_POINT('Ctrl Pts',(156.614883566293,-3.00395615955874,126.907667455941));
#31495=CARTESIAN_POINT('Ctrl Pts',(156.607127263551,-3.11013712730472,126.994343542557));
#31496=CARTESIAN_POINT('Ctrl Pts',(156.599366821037,-3.21637476703048,127.08106589081));
#31497=CARTESIAN_POINT('Ctrl Pts',(156.591606378522,-3.31889818456083,127.172166245612));
#31498=CARTESIAN_POINT('Ctrl Pts',(156.583845936008,-3.41734386525934,127.267279339298));
#31499=CARTESIAN_POINT('Ctrl Pts',(156.576073035743,-3.51594757970393,127.362545116966));
#31500=CARTESIAN_POINT('Ctrl Pts',(156.568300135477,-3.61046020672136,127.46183622255));
#31501=CARTESIAN_POINT('Ctrl Pts',(156.560527235212,-3.70055696876274,127.564752433936));
#31502=CARTESIAN_POINT('Ctrl Pts',(156.55303689945,-3.78737848656463,127.663927381809));
#31503=CARTESIAN_POINT('Ctrl Pts',(156.545546563688,-3.87009942762595,127.766468208144));
#31504=CARTESIAN_POINT('Ctrl Pts',(156.538056227926,-3.9484676047014,127.871991841794));
#31505=CARTESIAN_POINT('Ctrl Pts',(156.530240313066,-4.03024217652106,127.982102224358));
#31506=CARTESIAN_POINT('Ctrl Pts',(156.522424398206,-4.10753741834068,128.095810972429));
#31507=CARTESIAN_POINT('Ctrl Pts',(156.514608483347,-4.18002188035116,128.21272018296));
#31508=CARTESIAN_POINT('Ctrl Pts',(156.506805570645,-4.2523857609046,128.329434909286));
#31509=CARTESIAN_POINT('Ctrl Pts',(156.499002657942,-4.31995460066225,128.449339168763));
#31510=CARTESIAN_POINT('Ctrl Pts',(156.49119974524,-4.38243817600167,128.572003411377));
#31511=CARTESIAN_POINT('Ctrl Pts',(156.483404320061,-4.44486179332591,128.694549947786));
#31512=CARTESIAN_POINT('Ctrl Pts',(156.475608894881,-4.50220967899097,128.819850858168));
#31513=CARTESIAN_POINT('Ctrl Pts',(156.467813469701,-4.55423554785991,128.947448762601));
#31514=CARTESIAN_POINT('Ctrl Pts',(156.460025184181,-4.60621376737362,129.074929802905));
#31515=CARTESIAN_POINT('Ctrl Pts',(156.45223689866,-4.65287953135542,129.204703292622));
#31516=CARTESIAN_POINT('Ctrl Pts',(156.44444861314,-4.69403331291715,129.33628898453));
#31517=CARTESIAN_POINT('Ctrl Pts',(156.439629948296,-4.71949543547048,129.417701940679));
#31518=CARTESIAN_POINT('Ctrl Pts',(156.434811283452,-4.74284850274732,129.499808147782));
#31519=CARTESIAN_POINT('Ctrl Pts',(156.429992618608,-4.76405452823405,129.582490119308));
#31520=CARTESIAN_POINT('Origin',(213.235140564004,0.,130.804360617566));
#31521=CARTESIAN_POINT('',(154.334814618358,-4.76405452823406,129.582490119308));
#31522=CARTESIAN_POINT('',(154.680281909745,-4.76405452823406,129.582490119308));
#31523=CARTESIAN_POINT('',(213.235140564004,-4.76405452823405,129.582490119308));
#31524=CARTESIAN_POINT('',(156.014859436047,-4.91824976483825,130.805881527989));
#31525=CARTESIAN_POINT('Ctrl Pts',(156.014859435991,-4.91824976483794,130.80588152897));
#31526=CARTESIAN_POINT('Ctrl Pts',(156.010156282814,-4.91822423215231,130.888447893331));
#31527=CARTESIAN_POINT('Ctrl Pts',(156.005453129637,-4.91611967239412,130.970979563799));
#31528=CARTESIAN_POINT('Ctrl Pts',(156.000749976459,-4.91194054100773,131.053405159977));
#31529=CARTESIAN_POINT('Ctrl Pts',(155.99297564234,-4.90503241735089,131.189655054569));
#31530=CARTESIAN_POINT('Ctrl Pts',(155.985201308221,-4.89244000256113,131.325833109858));
#31531=CARTESIAN_POINT('Ctrl Pts',(155.977426974102,-4.87416121135011,131.461426480528));
#31532=CARTESIAN_POINT('Ctrl Pts',(155.969662221155,-4.85590494711567,131.596852744487));
#31533=CARTESIAN_POINT('Ctrl Pts',(155.961897468208,-4.83197630192374,131.731695373808));
#31534=CARTESIAN_POINT('Ctrl Pts',(155.954132715261,-4.80242516407676,131.865442898043));
#31535=CARTESIAN_POINT('Ctrl Pts',(155.946375674376,-4.77290337683641,131.999057582352));
#31536=CARTESIAN_POINT('Ctrl Pts',(155.938618633491,-4.73777029383005,132.131578946807));
#31537=CARTESIAN_POINT('Ctrl Pts',(155.930861592606,-4.69712738784296,132.262502368177));
#31538=CARTESIAN_POINT('Ctrl Pts',(155.923110401365,-4.65651513098748,132.393327059177));
#31539=CARTESIAN_POINT('Ctrl Pts',(155.915359210125,-4.61040143687021,132.522555833738));
#31540=CARTESIAN_POINT('Ctrl Pts',(155.907608018885,-4.55893838793106,132.649696315359));
#31541=CARTESIAN_POINT('Ctrl Pts',(155.899860122108,-4.50749721216053,132.776782758883));
#31542=CARTESIAN_POINT('Ctrl Pts',(155.892112225331,-4.45071135000565,132.901782313152));
#31543=CARTESIAN_POINT('Ctrl Pts',(155.884364328554,-4.38878200102981,133.024219984719));
#31544=CARTESIAN_POINT('Ctrl Pts',(155.87661805247,-4.32686560633869,133.146632044965));
#31545=CARTESIAN_POINT('Ctrl Pts',(155.868871776386,-4.25980804121466,133.266482939769));
#31546=CARTESIAN_POINT('Ctrl Pts',(155.861125500301,-4.18785752874912,133.383320171611));
#31547=CARTESIAN_POINT('Ctrl Pts',(155.853379167036,-4.11590648516133,133.500158265918));
#31548=CARTESIAN_POINT('Ctrl Pts',(155.845632833771,-4.03906262716851,133.613982319968));
#31549=CARTESIAN_POINT('Ctrl Pts',(155.837886500505,-3.95761856390068,133.724367186937));
#31550=CARTESIAN_POINT('Ctrl Pts',(155.830138432502,-3.87615626179946,133.834776773831));
#31551=CARTESIAN_POINT('Ctrl Pts',(155.822390364499,-3.79009193655109,133.94174532653));
#31552=CARTESIAN_POINT('Ctrl Pts',(155.814642296496,-3.6997594332865,134.044879588087));
#31553=CARTESIAN_POINT('Ctrl Pts',(155.806885993755,-3.60933092356253,134.148123461964));
#31554=CARTESIAN_POINT('Ctrl Pts',(155.799129691013,-3.51462543214212,134.247524609615));
#31555=CARTESIAN_POINT('Ctrl Pts',(155.791373388271,-3.41601511993789,134.342725178045));
#31556=CARTESIAN_POINT('Ctrl Pts',(155.783612945757,-3.31735217644088,134.437976557885));
#31557=CARTESIAN_POINT('Ctrl Pts',(155.775852503242,-3.21478055162372,134.529022631768));
#31558=CARTESIAN_POINT('Ctrl Pts',(155.768092060728,-3.10870589077663,134.61554557072));
#31559=CARTESIAN_POINT('Ctrl Pts',(155.760319160463,-3.00246094946708,134.702207403975));
#31560=CARTESIAN_POINT('Ctrl Pts',(155.752546260197,-2.89270204803302,134.784331358275));
#31561=CARTESIAN_POINT('Ctrl Pts',(155.744773359932,-2.77986496636764,134.861642199027));
#31562=CARTESIAN_POINT('Ctrl Pts',(155.73728302417,-2.67112979684147,134.936142595982));
#31563=CARTESIAN_POINT('Ctrl Pts',(155.729792688408,-2.55953662171019,135.006173577832));
#31564=CARTESIAN_POINT('Ctrl Pts',(155.722302352646,-2.44549561639506,135.071529966525));
#31565=CARTESIAN_POINT('Ctrl Pts',(155.714528018527,-2.32713071170023,135.13936436256));
#31566=CARTESIAN_POINT('Ctrl Pts',(155.706753684408,-2.20575374924236,135.202377572579));
#31567=CARTESIAN_POINT('Ctrl Pts',(155.698979350289,-2.0817950731603,135.26029063675));
#31568=CARTESIAN_POINT('Ctrl Pts',(155.691214597342,-1.95798916506796,135.318132328245));
#31569=CARTESIAN_POINT('Ctrl Pts',(155.683449844395,-1.83160822486209,135.370886216214));
#31570=CARTESIAN_POINT('Ctrl Pts',(155.675685091447,-1.7031095329633,135.418317810825));
#31571=CARTESIAN_POINT('Ctrl Pts',(155.667928050562,-1.57473846777695,135.465702295708));
#31572=CARTESIAN_POINT('Ctrl Pts',(155.660171009677,-1.4442542011232,135.507774872457));
#31573=CARTESIAN_POINT('Ctrl Pts',(155.652413968792,-1.31213613533616,135.544348151816));
#31574=CARTESIAN_POINT('Ctrl Pts',(155.644662777552,-1.1801177008102,135.580893850981));
#31575=CARTESIAN_POINT('Ctrl Pts',(155.636911586312,-1.04646829476294,135.611948403351));
#31576=CARTESIAN_POINT('Ctrl Pts',(155.629160395072,-0.911684371763793,
135.637373618664));
#31577=CARTESIAN_POINT('Ctrl Pts',(155.621412498295,-0.776957735527394,
135.662788027582));
#31578=CARTESIAN_POINT('Ctrl Pts',(155.613664601518,-0.641097924783222,
135.682577785858));
#31579=CARTESIAN_POINT('Ctrl Pts',(155.605916704741,-0.504613318248974,
135.696655422823));
#31580=CARTESIAN_POINT('Ctrl Pts',(155.598170428657,-0.368157261352146,
135.71073011505));
#31581=CARTESIAN_POINT('Ctrl Pts',(155.590424152573,-0.231077057277963,
135.719095022505));
#31582=CARTESIAN_POINT('Ctrl Pts',(155.582677876489,-0.0938875756508093,
135.721714396342));
#31583=CARTESIAN_POINT('Ctrl Pts',(155.574931543223,0.0433029186779331,
135.724333789514));
#31584=CARTESIAN_POINT('Ctrl Pts',(155.567185209958,0.18060230127532,135.721207556975));
#31585=CARTESIAN_POINT('Ctrl Pts',(155.559438876692,0.317494721696234,135.712352076829));
#31586=CARTESIAN_POINT('Ctrl Pts',(155.55169080869,0.454417798225463,135.703494613559));
#31587=CARTESIAN_POINT('Ctrl Pts',(155.543942740687,0.590933341152365,135.688905374846));
#31588=CARTESIAN_POINT('Ctrl Pts',(155.536194672684,0.726530040822484,135.668652669066));
#31589=CARTESIAN_POINT('Ctrl Pts',(155.528438369942,0.86227085427868,135.648378438469));
#31590=CARTESIAN_POINT('Ctrl Pts',(155.5206820672,0.99709048640669,135.622428774651));
#31591=CARTESIAN_POINT('Ctrl Pts',(155.512925764458,1.13048670328439,135.590923358845));
#31592=CARTESIAN_POINT('Ctrl Pts',(155.505165321944,1.26395411773961,135.559401127649));
#31593=CARTESIAN_POINT('Ctrl Pts',(155.49740487943,1.3959962269207,135.522317341569));
#31594=CARTESIAN_POINT('Ctrl Pts',(155.489644436916,1.52612637112357,135.479841487152));
#31595=CARTESIAN_POINT('Ctrl Pts',(155.48187153665,1.65646541178632,135.437297446722));
#31596=CARTESIAN_POINT('Ctrl Pts',(155.474098636385,1.78488598764526,135.389344177701));
#31597=CARTESIAN_POINT('Ctrl Pts',(155.466325736119,1.91092098636537,135.336199543032));
#31598=CARTESIAN_POINT('Ctrl Pts',(155.458835400357,2.03237429541947,135.284986849697));
#31599=CARTESIAN_POINT('Ctrl Pts',(155.451345064595,2.15161218080537,135.228953807267));
#31600=CARTESIAN_POINT('Ctrl Pts',(155.443854728833,2.26824031058236,135.168334604192));
#31601=CARTESIAN_POINT('Ctrl Pts',(155.436080394714,2.38929043134765,135.105417005608));
#31602=CARTESIAN_POINT('Ctrl Pts',(155.428306060595,2.50791244256908,135.037359308717));
#31603=CARTESIAN_POINT('Ctrl Pts',(155.420531726476,2.62363903592074,134.964372789627));
#31604=CARTESIAN_POINT('Ctrl Pts',(155.412766973529,2.73922300658888,134.891476219898));
#31605=CARTESIAN_POINT('Ctrl Pts',(155.405002220582,2.85191833181156,134.813663120641));
#31606=CARTESIAN_POINT('Ctrl Pts',(155.397237467635,2.96128055741714,134.731191467343));
#31607=CARTESIAN_POINT('Ctrl Pts',(155.38948042675,3.0705341629184,134.648801726054));
#31608=CARTESIAN_POINT('Ctrl Pts',(155.381723385865,3.17646094667556,134.561762872424));
#31609=CARTESIAN_POINT('Ctrl Pts',(155.37396634498,3.27864412413066,134.470376952746));
#31610=CARTESIAN_POINT('Ctrl Pts',(155.36621515374,3.38075024445686,134.3790599479));
#31611=CARTESIAN_POINT('Ctrl Pts',(155.3584639625,3.47911808741322,134.28340266155));
#31612=CARTESIAN_POINT('Ctrl Pts',(155.35071277126,3.57336304379692,134.183748079774));
#31613=CARTESIAN_POINT('Ctrl Pts',(155.342964874482,3.66756794356007,134.084135853853));
#31614=CARTESIAN_POINT('Ctrl Pts',(155.335216977705,3.75765317394044,133.980529995064));
#31615=CARTESIAN_POINT('Ctrl Pts',(155.327469080928,3.8432703522719,133.873310936787));
#31616=CARTESIAN_POINT('Ctrl Pts',(155.319722804844,3.92886962133535,133.766114306426));
#31617=CARTESIAN_POINT('Ctrl Pts',(155.31197652876,4.01000245355591,133.655306285229));
#31618=CARTESIAN_POINT('Ctrl Pts',(155.304230252676,4.08636047280824,133.541300724468));
#31619=CARTESIAN_POINT('Ctrl Pts',(155.296483919411,4.1627190557181,133.427294322145));
#31620=CARTESIAN_POINT('Ctrl Pts',(155.288737586145,4.23430253776083,133.310090657995));
#31621=CARTESIAN_POINT('Ctrl Pts',(155.28099125288,4.30084586853458,133.190132584374));
#31622=CARTESIAN_POINT('Ctrl Pts',(155.273243184877,4.36740410122585,133.070147646975));
#31623=CARTESIAN_POINT('Ctrl Pts',(155.265495116874,4.42891974703676,132.947407414503));
#31624=CARTESIAN_POINT('Ctrl Pts',(155.257747048871,4.4851739003829,132.822378988598));
#31625=CARTESIAN_POINT('Ctrl Pts',(155.249990746129,4.54148784131269,132.697217680995));
#31626=CARTESIAN_POINT('Ctrl Pts',(155.242234443388,4.59252895852806,132.569763679046));
#31627=CARTESIAN_POINT('Ctrl Pts',(155.234478140646,4.63812647353636,132.440504217004));
#31628=CARTESIAN_POINT('Ctrl Pts',(155.226717698132,4.68374832531135,132.311175765294));
#31629=CARTESIAN_POINT('Ctrl Pts',(155.218957255618,4.72392067113484,132.180040307015));
#31630=CARTESIAN_POINT('Ctrl Pts',(155.211196813103,4.75852305338228,132.047598894378));
#31631=CARTESIAN_POINT('Ctrl Pts',(155.203423912838,4.79318098244553,131.914944875027));
#31632=CARTESIAN_POINT('Ctrl Pts',(155.195651012573,4.82225099720917,131.780981094267));
#31633=CARTESIAN_POINT('Ctrl Pts',(155.187878112307,4.84566390631248,131.646218307179));
#31634=CARTESIAN_POINT('Ctrl Pts',(155.180387776545,4.86822569719661,131.516354486847));
#31635=CARTESIAN_POINT('Ctrl Pts',(155.172897440783,4.88553450126068,131.385749048762));
#31636=CARTESIAN_POINT('Ctrl Pts',(155.165407105021,4.89757420183388,131.254860340131));
#31637=CARTESIAN_POINT('Ctrl Pts',(155.157632770902,4.91007039131358,131.119008946331));
#31638=CARTESIAN_POINT('Ctrl Pts',(155.149858436783,4.91692961799356,130.982422041169));
#31639=CARTESIAN_POINT('Ctrl Pts',(155.142084102664,4.91807704288308,130.845606984271));
#31640=CARTESIAN_POINT('Ctrl Pts',(155.134319349716,4.91922305367398,130.708960539704));
#31641=CARTESIAN_POINT('Ctrl Pts',(155.126554596769,4.91467126550661,130.572086890057));
#31642=CARTESIAN_POINT('Ctrl Pts',(155.118789843822,4.90439848212926,130.435499409266));
#31643=CARTESIAN_POINT('Ctrl Pts',(155.111032802937,4.89413590182518,130.299047589087));
#31644=CARTESIAN_POINT('Ctrl Pts',(155.103275762052,4.87816366322405,130.16288175948));
#31645=CARTESIAN_POINT('Ctrl Pts',(155.095518721167,4.85651060419171,130.027515836497));
#31646=CARTESIAN_POINT('Ctrl Pts',(155.087767529927,4.83487387389963,129.89225199401));
#31647=CARTESIAN_POINT('Ctrl Pts',(155.080016338687,4.80756491162441,129.757787241978));
#31648=CARTESIAN_POINT('Ctrl Pts',(155.072265147447,4.77466439059804,129.624630555367));
#31649=CARTESIAN_POINT('Ctrl Pts',(155.06451725067,4.74177785317077,129.491530463901));
#31650=CARTESIAN_POINT('Ctrl Pts',(155.056769353893,4.70330457737588,129.359737710847));
#31651=CARTESIAN_POINT('Ctrl Pts',(155.049021457116,4.65937632324956,129.229751033942));
#31652=CARTESIAN_POINT('Ctrl Pts',(155.041275181032,4.61545725796702,129.099791547447));
#31653=CARTESIAN_POINT('Ctrl Pts',(155.033528904947,4.56608560908237,128.971637755806));
#31654=CARTESIAN_POINT('Ctrl Pts',(155.025782628863,4.5114428765635,128.845772801305));
#31655=CARTESIAN_POINT('Ctrl Pts',(155.018036295598,4.45679974068441,128.719906917699));
#31656=CARTESIAN_POINT('Ctrl Pts',(155.010289962333,4.39688559922266,128.596330263575));
#31657=CARTESIAN_POINT('Ctrl Pts',(155.002543629067,4.33192977019051,128.475505205859));
#31658=CARTESIAN_POINT('Ctrl Pts',(154.994795561064,4.26695939475083,128.354653090209));
#31659=CARTESIAN_POINT('Ctrl Pts',(154.987047493061,4.19694527015171,128.236554141426));
#31660=CARTESIAN_POINT('Ctrl Pts',(154.979299425058,4.12216205841675,128.121645010825));
#31661=CARTESIAN_POINT('Ctrl Pts',(154.971543122316,4.0472993661944,128.006613753433));
#31662=CARTESIAN_POINT('Ctrl Pts',(154.963786819575,3.96765767527319,127.89477941467));
#31663=CARTESIAN_POINT('Ctrl Pts',(154.956030516833,3.88355459968167,127.786549037333));
#31664=CARTESIAN_POINT('Ctrl Pts',(154.948270074319,3.79940663574637,127.678260894184));
#31665=CARTESIAN_POINT('Ctrl Pts',(154.940509631804,3.71079279492847,127.573580843542));
#31666=CARTESIAN_POINT('Ctrl Pts',(154.93274918929,3.6180695163552,127.472881060774));
#31667=CARTESIAN_POINT('Ctrl Pts',(154.924976289025,3.52519739014357,127.372019625776));
#31668=CARTESIAN_POINT('Ctrl Pts',(154.917203388759,3.42820292039307,127.275151503302));
#31669=CARTESIAN_POINT('Ctrl Pts',(154.909430488494,3.3274784201976,127.1826109816));
#31670=CARTESIAN_POINT('Ctrl Pts',(154.901940152732,3.23041550929518,127.093434540959));
#31671=CARTESIAN_POINT('Ctrl Pts',(154.89444981697,3.129889286686,127.008276724391));
#31672=CARTESIAN_POINT('Ctrl Pts',(154.886959481208,3.02627666140226,126.927398839169));
#31673=CARTESIAN_POINT('Ctrl Pts',(154.879185147089,2.91873553193722,126.843454444346));
#31674=CARTESIAN_POINT('Ctrl Pts',(154.87141081297,2.80752867984863,126.763855024115));
#31675=CARTESIAN_POINT('Ctrl Pts',(154.863636478851,2.69304250885731,126.688937782912));
#31676=CARTESIAN_POINT('Ctrl Pts',(154.855871725904,2.57869743183989,126.614112870514));
#31677=CARTESIAN_POINT('Ctrl Pts',(154.848106972957,2.46108140124111,126.543958867854));
#31678=CARTESIAN_POINT('Ctrl Pts',(154.84034222001,2.3406137949513,126.478772781747));
#31679=CARTESIAN_POINT('Ctrl Pts',(154.832585179125,2.22026583878635,126.41365143938));
#31680=CARTESIAN_POINT('Ctrl Pts',(154.82482813824,2.09707228481409,126.353488379135));
#31681=CARTESIAN_POINT('Ctrl Pts',(154.817071097355,1.97148109273428,126.298537123077));
#31682=CARTESIAN_POINT('Ctrl Pts',(154.809319906114,1.84598460994937,126.243627306188));
#31683=CARTESIAN_POINT('Ctrl Pts',(154.801568714874,1.71809444465663,126.193921626622));
#31684=CARTESIAN_POINT('Ctrl Pts',(154.793817523634,1.58828241776373,126.149627325107));
#31685=CARTESIAN_POINT('Ctrl Pts',(154.786069626857,1.45852556444507,126.105351849852));
#31686=CARTESIAN_POINT('Ctrl Pts',(154.77832173008,1.32684884340647,126.066483304155));
#31687=CARTESIAN_POINT('Ctrl Pts',(154.770573833303,1.19374307635,126.033180414496));
#31688=CARTESIAN_POINT('Ctrl Pts',(154.762827557219,1.06066515215057,125.999884491084));
#31689=CARTESIAN_POINT('Ctrl Pts',(154.755081281135,0.926159155546655,125.972152002855));
#31690=CARTESIAN_POINT('Ctrl Pts',(154.747335005051,0.790729672995634,125.950091398956));
#31691=CARTESIAN_POINT('Ctrl Pts',(154.739588671785,0.655299190735075,125.928030632211));
#31692=CARTESIAN_POINT('Ctrl Pts',(154.73184233852,0.518945594803852,125.911641896197));
#31693=CARTESIAN_POINT('Ctrl Pts',(154.724096005255,0.382181839577906,125.900982179795));
#31694=CARTESIAN_POINT('Ctrl Pts',(154.716347937252,0.245387457057136,125.890320076223));
#31695=CARTESIAN_POINT('Ctrl Pts',(154.708599869249,0.108183122174561,125.885389575607));
#31696=CARTESIAN_POINT('Ctrl Pts',(154.700851801246,-0.028915336419939,
125.886195617709));
#31697=CARTESIAN_POINT('Ctrl Pts',(154.693095498504,-0.166159504887726,
125.887002516482));
#31698=CARTESIAN_POINT('Ctrl Pts',(154.685339195762,-0.303297180701629,
125.893558134816));
#31699=CARTESIAN_POINT('Ctrl Pts',(154.67758289302,-0.439814229087802,125.90581527161));
#31700=CARTESIAN_POINT('Ctrl Pts',(154.669822450506,-0.57640414073324,125.918078950406));
#31701=CARTESIAN_POINT('Ctrl Pts',(154.662062007992,-0.712372377507485,
125.936050160035));
#31702=CARTESIAN_POINT('Ctrl Pts',(154.654301565478,-0.847213153676408,
125.959630188044));
#31703=CARTESIAN_POINT('Ctrl Pts',(154.646528665212,-0.982270388229838,
125.983248068807));
#31704=CARTESIAN_POINT('Ctrl Pts',(154.638755764947,-1.11619616323684,126.012492676901));
#31705=CARTESIAN_POINT('Ctrl Pts',(154.630982864681,-1.24849717771664,126.047214639174));
#31706=CARTESIAN_POINT('Ctrl Pts',(154.623492528919,-1.3759887170752,126.080674370659));
#31707=CARTESIAN_POINT('Ctrl Pts',(154.616002193157,-1.50197127876108,126.119220048841));
#31708=CARTESIAN_POINT('Ctrl Pts',(154.608511857395,-1.6260212890266,126.162675812441));
#31709=CARTESIAN_POINT('Ctrl Pts',(154.600737434001,-1.7547761716397,126.207779732458));
#31710=CARTESIAN_POINT('Ctrl Pts',(154.592963010608,-1.88185687821755,126.258316418503));
#31711=CARTESIAN_POINT('Ctrl Pts',(154.585188587214,-2.00677083157016,126.314143040203));
#31712=CARTESIAN_POINT('Ctrl Pts',(154.577423765877,-2.1315305058499,126.369900711404));
#31713=CARTESIAN_POINT('Ctrl Pts',(154.56965894454,-2.25412839810567,126.430935160395));
#31714=CARTESIAN_POINT('Ctrl Pts',(154.561894123203,-2.37408793177902,126.497054086254));
#31715=CARTESIAN_POINT('Ctrl Pts',(154.554137034724,-2.49392799971371,126.563107165356));
#31716=CARTESIAN_POINT('Ctrl Pts',(154.546379946246,-2.61113459777468,126.634234457001));
#31717=CARTESIAN_POINT('Ctrl Pts',(154.538622857767,-2.72525228965192,126.710196109361));
#31718=CARTESIAN_POINT('Ctrl Pts',(154.530871639664,-2.8392836200523,126.786100275801));
#31719=CARTESIAN_POINT('Ctrl Pts',(154.52312042156,-2.95023037306813,126.866831304994));
#31720=CARTESIAN_POINT('Ctrl Pts',(154.515369203456,-3.05766315679506,126.952104255111));
#31721=CARTESIAN_POINT('Ctrl Pts',(154.50762138725,-3.16504878982158,127.037339780159));
#31722=CARTESIAN_POINT('Ctrl Pts',(154.499873571045,-3.26892321592966,127.127113018156));
#31723=CARTESIAN_POINT('Ctrl Pts',(154.492125754839,-3.36888760615964,127.221096831635));
#31724=CARTESIAN_POINT('Ctrl Pts',(154.484379588851,-3.46883070483132,127.315060627367));
#31725=CARTESIAN_POINT('Ctrl Pts',(154.476633422864,-3.56486513965299,127.413232946955));
#31726=CARTESIAN_POINT('Ctrl Pts',(154.468887256877,-3.65662694395631,127.515247902071));
#31727=CARTESIAN_POINT('Ctrl Pts',(154.461141063254,-3.74838907563266,127.617263221139));
#31728=CARTESIAN_POINT('Ctrl Pts',(154.453394869631,-3.83587828503477,127.723120912351));
#31729=CARTESIAN_POINT('Ctrl Pts',(154.445648676008,-3.9187693788703,127.832420238331));
#31730=CARTESIAN_POINT('Ctrl Pts',(154.437900777239,-4.00167871926914,127.941743624038));
#31731=CARTESIAN_POINT('Ctrl Pts',(154.43015287847,-4.07998769403529,128.054509840464));
#31732=CARTESIAN_POINT('Ctrl Pts',(154.422404979701,-4.15341334672048,128.170287605331));
#31733=CARTESIAN_POINT('Ctrl Pts',(154.414649257282,-4.22691314295054,128.286182279938));
#31734=CARTESIAN_POINT('Ctrl Pts',(154.406893534862,-4.29551955865376,128.405094246168));
#31735=CARTESIAN_POINT('Ctrl Pts',(154.399137812442,-4.35899445312151,128.526565538952));
#31736=CARTESIAN_POINT('Ctrl Pts',(154.391377962452,-4.42250312872119,128.648101478363));
#31737=CARTESIAN_POINT('Ctrl Pts',(154.383618112462,-4.48087467518851,128.772199104847));
#31738=CARTESIAN_POINT('Ctrl Pts',(154.375858262472,-4.53391878889429,128.898379642264));
#31739=CARTESIAN_POINT('Ctrl Pts',(154.368086922269,-4.58704144640668,129.024747018504));
#31740=CARTESIAN_POINT('Ctrl Pts',(154.360315582066,-4.63482077540106,129.153203101052));
#31741=CARTESIAN_POINT('Ctrl Pts',(154.352544241863,-4.6771158768101,129.283252423718));
#31742=CARTESIAN_POINT('Ctrl Pts',(154.346634367361,-4.70928005117857,129.382151089317));
#31743=CARTESIAN_POINT('Ctrl Pts',(154.34072449286,-4.738273635472,129.481970809709));
#31744=CARTESIAN_POINT('Ctrl Pts',(154.334814618358,-4.76405452823406,129.582490119308));
#31745=CARTESIAN_POINT('Ctrl Pts',(156.084992794976,-4.76405452823404,129.582490119308));
#31746=CARTESIAN_POINT('Ctrl Pts',(156.077293740712,-4.79788100655492,129.714379044893));
#31747=CARTESIAN_POINT('Ctrl Pts',(156.069594686447,-4.82620048638222,129.847572500239));
#31748=CARTESIAN_POINT('Ctrl Pts',(156.061895632183,-4.84893743113397,129.981567295128));
#31749=CARTESIAN_POINT('Ctrl Pts',(156.05405626616,-4.87208874635078,130.118004084141));
#31750=CARTESIAN_POINT('Ctrl Pts',(156.046216900138,-4.88945202110533,130.255271272325));
#31751=CARTESIAN_POINT('Ctrl Pts',(156.038377534115,-4.90100290378361,130.392834677187));
#31752=CARTESIAN_POINT('Ctrl Pts',(156.030538168092,-4.91255378646188,130.530398082049));
#31753=CARTESIAN_POINT('Ctrl Pts',(156.02269880207,-4.91829232350721,130.668257273153));
#31754=CARTESIAN_POINT('Ctrl Pts',(156.014859436047,-4.91824976483825,130.805881527989));
#31755=CARTESIAN_POINT('',(156.360140563953,-4.91824883972711,130.807738934152));
#31756=CARTESIAN_POINT('Ctrl Pts',(156.429992618608,-4.76405452823405,129.582490119308));
#31757=CARTESIAN_POINT('Ctrl Pts',(156.422210727339,-4.79830114839348,129.716017171545));
#31758=CARTESIAN_POINT('Ctrl Pts',(156.414428836071,-4.82694553781918,129.851046419521));
#31759=CARTESIAN_POINT('Ctrl Pts',(156.406646944802,-4.84986811108228,129.987070970252));
#31760=CARTESIAN_POINT('Ctrl Pts',(156.398865314921,-4.87278991439169,130.12309095201));
#31761=CARTESIAN_POINT('Ctrl Pts',(156.391083685041,-4.88999020947882,130.260105791632));
#31762=CARTESIAN_POINT('Ctrl Pts',(156.38330205516,-4.9014005977705,130.397598718324));
#31763=CARTESIAN_POINT('Ctrl Pts',(156.37558155811,-4.91272134554554,130.534011494484));
#31764=CARTESIAN_POINT('Ctrl Pts',(156.367861061059,-4.91834283735024,130.670894495926));
#31765=CARTESIAN_POINT('Ctrl Pts',(156.360140564008,-4.91824883972778,130.807738933169));
#31766=CARTESIAN_POINT('Ctrl Pts',(156.360140563953,-4.91824883972711,130.807738934152));
#31767=CARTESIAN_POINT('Ctrl Pts',(156.351323954703,-4.91814149682635,130.964011765196));
#31768=CARTESIAN_POINT('Ctrl Pts',(156.342507345453,-4.91058202809959,131.119992202956));
#31769=CARTESIAN_POINT('Ctrl Pts',(156.333690736203,-4.89567786746431,131.275021090221));
#31770=CARTESIAN_POINT('Ctrl Pts',(156.3248350287,-4.8807076126391,131.430737470661));
#31771=CARTESIAN_POINT('Ctrl Pts',(156.315979321197,-4.85832749074473,131.585493680049));
#31772=CARTESIAN_POINT('Ctrl Pts',(156.307123613693,-4.82869601254221,131.738639955323));
#31773=CARTESIAN_POINT('Ctrl Pts',(156.298215535422,-4.79888930008775,131.892691905055));
#31774=CARTESIAN_POINT('Ctrl Pts',(156.28930745715,-4.7617453046484,132.045114662076));
#31775=CARTESIAN_POINT('Ctrl Pts',(156.280399378879,-4.71747396232134,132.195267687546));
#31776=CARTESIAN_POINT('Ctrl Pts',(156.273469120624,-4.68303198434525,132.312082921158));
#31777=CARTESIAN_POINT('Ctrl Pts',(156.266538862368,-4.64427720768572,132.427524809799));
#31778=CARTESIAN_POINT('Ctrl Pts',(156.259608604113,-4.6013280870806,132.541301289421));
#31779=CARTESIAN_POINT('Ctrl Pts',(156.251834269994,-4.55314794697554,132.668935258443));
#31780=CARTESIAN_POINT('Ctrl Pts',(156.244059935875,-4.49957690486087,132.794765203604));
#31781=CARTESIAN_POINT('Ctrl Pts',(156.236285601756,-4.440769564856,132.918302133869));
#31782=CARTESIAN_POINT('Ctrl Pts',(156.228520848809,-4.38203469964196,133.041686815908));
#31783=CARTESIAN_POINT('Ctrl Pts',(156.220756095862,-4.31807654304976,133.162783756201));
#31784=CARTESIAN_POINT('Ctrl Pts',(156.212991342914,-4.24909877098898,133.2811211423));
#31785=CARTESIAN_POINT('Ctrl Pts',(156.205234302029,-4.18018950862385,133.399340994038));
#31786=CARTESIAN_POINT('Ctrl Pts',(156.197477261144,-4.10627074787576,133.514806410367));
#31787=CARTESIAN_POINT('Ctrl Pts',(156.189720220259,-4.02759319501525,133.627067849634));
#31788=CARTESIAN_POINT('Ctrl Pts',(156.181969029019,-3.94897497350953,133.739244631676));
#31789=CARTESIAN_POINT('Ctrl Pts',(156.174217837779,-3.86560532634282,133.848221926976));
#31790=CARTESIAN_POINT('Ctrl Pts',(156.166466646539,-3.77777941321032,133.953577308685));
#31791=CARTESIAN_POINT('Ctrl Pts',(156.158718749762,-3.68999082843352,134.058887911547));
#31792=CARTESIAN_POINT('Ctrl Pts',(156.150970852985,-3.59774999459174,134.16057936291));
#31793=CARTESIAN_POINT('Ctrl Pts',(156.143222956208,-3.50139353524727,134.258260786046));
#31794=CARTESIAN_POINT('Ctrl Pts',(156.135476680124,-3.4050572315969,134.355921776335));
#31795=CARTESIAN_POINT('Ctrl Pts',(156.12773040404,-3.30460728920746,134.44957412868));
#31796=CARTESIAN_POINT('Ctrl Pts',(156.119984127955,-3.20041824075269,134.53886274593));
#31797=CARTESIAN_POINT('Ctrl Pts',(156.11223779469,-3.09622842319807,134.628152022289));
#31798=CARTESIAN_POINT('Ctrl Pts',(156.104491461425,-2.98829974136769,134.713077244867));
#31799=CARTESIAN_POINT('Ctrl Pts',(156.096745128159,-2.87704064317679,134.793322913704));
#31800=CARTESIAN_POINT('Ctrl Pts',(156.088997060156,-2.76575662928249,134.873586553002));
#31801=CARTESIAN_POINT('Ctrl Pts',(156.081248992153,-2.65114103195784,134.949168324592));
#31802=CARTESIAN_POINT('Ctrl Pts',(156.07350092415,-2.53363182878062,135.019795686297));
#31803=CARTESIAN_POINT('Ctrl Pts',(156.065744621409,-2.4159977354236,135.090498111603));
#31804=CARTESIAN_POINT('Ctrl Pts',(156.057988318667,-2.29546422848449,135.156235406683));
#31805=CARTESIAN_POINT('Ctrl Pts',(156.050232015925,-2.17249496146798,135.216780441755));
#31806=CARTESIAN_POINT('Ctrl Pts',(156.042471573411,-2.04946006205101,135.277357791535));
#31807=CARTESIAN_POINT('Ctrl Pts',(156.034711130897,-1.92398716962091,135.332737201539));
#31808=CARTESIAN_POINT('Ctrl Pts',(156.026950688382,-1.79655960225933,135.382739878618));
#31809=CARTESIAN_POINT('Ctrl Pts',(156.019177788117,-1.66892747685422,135.432822824433));
#31810=CARTESIAN_POINT('Ctrl Pts',(156.011404887851,-1.53933477597712,135.47751166189));
#31811=CARTESIAN_POINT('Ctrl Pts',(156.003631987586,-1.40828050765929,135.516677359281));
#31812=CARTESIAN_POINT('Ctrl Pts',(155.996141651824,-1.28199039210069,135.55441928492));
#31813=CARTESIAN_POINT('Ctrl Pts',(155.988651316062,-1.15434342596211,135.587032582679));
#31814=CARTESIAN_POINT('Ctrl Pts',(155.9811609803,-1.02579284480649,135.614447113882));
#31815=CARTESIAN_POINT('Ctrl Pts',(155.973386646181,-0.892368229294299,
135.642901075369));
#31816=CARTESIAN_POINT('Ctrl Pts',(155.965612312062,-0.75754747593295,135.665844399354));
#31817=CARTESIAN_POINT('Ctrl Pts',(155.957837977943,-0.621825554031741,
135.683142847063));
#31818=CARTESIAN_POINT('Ctrl Pts',(155.950073224996,-0.48627089726946,135.700419975981));
#31819=CARTESIAN_POINT('Ctrl Pts',(155.942308472049,-0.349817665854264,
135.712066021637));
#31820=CARTESIAN_POINT('Ctrl Pts',(155.934543719101,-0.212972900766116,
135.717997316187));
#31821=CARTESIAN_POINT('Ctrl Pts',(155.926786678216,-0.0762640518279205,
135.723922719693));
#31822=CARTESIAN_POINT('Ctrl Pts',(155.919029637331,0.0608351688299815,
135.724144650713));
#31823=CARTESIAN_POINT('Ctrl Pts',(155.911272596446,0.197811036221584,135.718631047289));
#31824=CARTESIAN_POINT('Ctrl Pts',(155.903521405206,0.334683609045929,135.713121601716));
#31825=CARTESIAN_POINT('Ctrl Pts',(155.895770213966,0.471432624689744,135.701885246432));
#31826=CARTESIAN_POINT('Ctrl Pts',(155.888019022726,0.607543142456625,135.684941975617));
#31827=CARTESIAN_POINT('Ctrl Pts',(155.880271125949,0.743595809622773,135.668005906144));
#31828=CARTESIAN_POINT('Ctrl Pts',(155.872523229172,0.879010131504822,135.64536779365));
#31829=CARTESIAN_POINT('Ctrl Pts',(155.864775332395,1.01327529918402,135.617099570653));
#31830=CARTESIAN_POINT('Ctrl Pts',(155.857029056311,1.14751238148461,135.58883726076));
#31831=CARTESIAN_POINT('Ctrl Pts',(155.849282780227,1.28060040537247,135.554947263365));
#31832=CARTESIAN_POINT('Ctrl Pts',(155.841536504143,1.41203817349923,135.515552744733));
#31833=CARTESIAN_POINT('Ctrl Pts',(155.833790170877,1.54347691186965,135.476157935299));
#31834=CARTESIAN_POINT('Ctrl Pts',(155.826043837612,1.67326499566543,135.431258635794));
#31835=CARTESIAN_POINT('Ctrl Pts',(155.818297504347,1.80091620975991,135.38102794958));
#31836=CARTESIAN_POINT('Ctrl Pts',(155.810549436344,1.92859601045877,135.330786014553));
#31837=CARTESIAN_POINT('Ctrl Pts',(155.802801368341,2.05413762548057,135.275210460173));
#31838=CARTESIAN_POINT('Ctrl Pts',(155.795053300338,2.17707501979339,135.214522453677));
#31839=CARTESIAN_POINT('Ctrl Pts',(155.787296997596,2.3001430734319,135.153769947246));
#31840=CARTESIAN_POINT('Ctrl Pts',(155.779540694854,2.42060102625438,135.087894307885));
#31841=CARTESIAN_POINT('Ctrl Pts',(155.771784392112,2.53800717149881,135.017162851225));
#31842=CARTESIAN_POINT('Ctrl Pts',(155.764023949598,2.65547597993806,134.946393643056));
#31843=CARTESIAN_POINT('Ctrl Pts',(155.756263507084,2.76988940920439,134.870763668902));
#31844=CARTESIAN_POINT('Ctrl Pts',(155.74850306457,2.88083579033065,134.790582915889));
#31845=CARTESIAN_POINT('Ctrl Pts',(155.740730164304,2.99196027243722,134.710273449614));
#31846=CARTESIAN_POINT('Ctrl Pts',(155.732957264039,3.09960627734477,134.625398848341));
#31847=CARTESIAN_POINT('Ctrl Pts',(155.725184363773,3.2033955209944,134.536309196871));
#31848=CARTESIAN_POINT('Ctrl Pts',(155.717694028011,3.30341176420874,134.450458178634));
#31849=CARTESIAN_POINT('Ctrl Pts',(155.710203692249,3.39984655841918,134.360693454934));
#31850=CARTESIAN_POINT('Ctrl Pts',(155.702713356487,3.49239590907836,134.267358434018));
#31851=CARTESIAN_POINT('Ctrl Pts',(155.694939022368,3.58845429649688,134.170484587416));
#31852=CARTESIAN_POINT('Ctrl Pts',(155.687164688249,3.68063107512587,134.069457496327));
#31853=CARTESIAN_POINT('Ctrl Pts',(155.67939035413,3.76854576308079,133.964621033112));
#31854=CARTESIAN_POINT('Ctrl Pts',(155.671625601183,3.85635210403997,133.859913771468));
#31855=CARTESIAN_POINT('Ctrl Pts',(155.663860848236,3.9399065567186,133.751406775469));
#31856=CARTESIAN_POINT('Ctrl Pts',(155.656096095288,4.01886466095661,133.63948140854));
#31857=CARTESIAN_POINT('Ctrl Pts',(155.648339054403,4.09774434289234,133.527667207463));
#31858=CARTESIAN_POINT('Ctrl Pts',(155.640582013518,4.17203653734483,133.412441709409));
#31859=CARTESIAN_POINT('Ctrl Pts',(155.632824972634,4.2414365887779,133.294219795487));
#31860=CARTESIAN_POINT('Ctrl Pts',(155.625073781393,4.31078430509233,133.176087033629));
#31861=CARTESIAN_POINT('Ctrl Pts',(155.617322590153,4.3752470243975,133.05496268934));
#31862=CARTESIAN_POINT('Ctrl Pts',(155.609571398913,4.43456323033953,132.931290804154));
#31863=CARTESIAN_POINT('Ctrl Pts',(155.601823502136,4.49385422531172,132.807671482819));
#31864=CARTESIAN_POINT('Ctrl Pts',(155.594075605359,4.54800288878193,132.681507125917));
#31865=CARTESIAN_POINT('Ctrl Pts',(155.586327708582,4.59679363491687,132.553266372742));
#31866=CARTESIAN_POINT('Ctrl Pts',(155.578581432498,4.64557417507955,132.425052444768));
#31867=CARTESIAN_POINT('Ctrl Pts',(155.570835156414,4.6889988882244,132.294763349622));
#31868=CARTESIAN_POINT('Ctrl Pts',(155.56308888033,4.72690048820667,132.1628873332));
#31869=CARTESIAN_POINT('Ctrl Pts',(155.555342547064,4.76480236796994,132.0310103433));
#31870=CARTESIAN_POINT('Ctrl Pts',(155.547596213799,4.79718094522331,131.897546784504));
#31871=CARTESIAN_POINT('Ctrl Pts',(155.539849880534,4.82391904557718,131.762999289964));
#31872=CARTESIAN_POINT('Ctrl Pts',(155.532101812531,4.85066313374322,131.628421664447));
#31873=CARTESIAN_POINT('Ctrl Pts',(155.524353744528,4.87176415530583,131.492760003555));
#31874=CARTESIAN_POINT('Ctrl Pts',(155.516605676525,4.88715628120619,131.356525942054));
#31875=CARTESIAN_POINT('Ctrl Pts',(155.508849373783,4.90256476604114,131.220147089371));
#31876=CARTESIAN_POINT('Ctrl Pts',(155.501093071041,4.91225219080136,131.083195009938));
#31877=CARTESIAN_POINT('Ctrl Pts',(155.493336768299,4.91620470240323,130.946185814793));
#31878=CARTESIAN_POINT('Ctrl Pts',(155.485576325785,4.92015932357955,130.809103493714));
#31879=CARTESIAN_POINT('Ctrl Pts',(155.477815883271,4.91837293759324,130.671964386921));
#31880=CARTESIAN_POINT('Ctrl Pts',(155.470055440757,4.91088382826134,130.535282398787));
#31881=CARTESIAN_POINT('Ctrl Pts',(155.462282540491,4.90338269674628,130.398380996592));
#31882=CARTESIAN_POINT('Ctrl Pts',(155.454509640226,4.89016058597404,130.261938568805));
#31883=CARTESIAN_POINT('Ctrl Pts',(155.44673673996,4.871307560428,130.126462605903));
#31884=CARTESIAN_POINT('Ctrl Pts',(155.439246404198,4.85313988984843,129.995911535495));
#31885=CARTESIAN_POINT('Ctrl Pts',(155.431756068436,4.82974364735219,129.866258186166));
#31886=CARTESIAN_POINT('Ctrl Pts',(155.424265732674,4.80124343554559,129.737943937684));
#31887=CARTESIAN_POINT('Ctrl Pts',(155.416491398555,4.77166262954591,129.60476461547));
#31888=CARTESIAN_POINT('Ctrl Pts',(155.408717064436,4.73648947696845,129.47260607057));
#31889=CARTESIAN_POINT('Ctrl Pts',(155.400942730317,4.69580762761774,129.341974284579));
#31890=CARTESIAN_POINT('Ctrl Pts',(155.39317797737,4.65517591501052,129.21150349059));
#31891=CARTESIAN_POINT('Ctrl Pts',(155.385413224423,4.60904912880283,129.082556081398));
#31892=CARTESIAN_POINT('Ctrl Pts',(155.377648471476,4.55756193171374,128.955627997338));
#31893=CARTESIAN_POINT('Ctrl Pts',(155.369891430591,4.50612587243467,128.828825980041));
#31894=CARTESIAN_POINT('Ctrl Pts',(155.362134389706,4.44934014335527,128.704039656547));
#31895=CARTESIAN_POINT('Ctrl Pts',(155.354377348821,4.3873891219437,128.581749595558));
#31896=CARTESIAN_POINT('Ctrl Pts',(155.346626157581,4.32548481827929,128.459551754456));
#31897=CARTESIAN_POINT('Ctrl Pts',(155.338874966341,4.25842315138301,128.339846776311));
#31898=CARTESIAN_POINT('Ctrl Pts',(155.3311237751,4.18643634999695,128.223094697533));
#31899=CARTESIAN_POINT('Ctrl Pts',(155.323375878323,4.11448014492177,128.106392241503));
#31900=CARTESIAN_POINT('Ctrl Pts',(155.315627981546,4.03760317356018,127.992640520714));
#31901=CARTESIAN_POINT('Ctrl Pts',(155.307880084769,3.9560831860132,127.882274224619));
#31902=CARTESIAN_POINT('Ctrl Pts',(155.300133808685,3.87458025069021,127.771931014774));
#31903=CARTESIAN_POINT('Ctrl Pts',(155.292387532601,3.78843646312696,127.664972135339));
#31904=CARTESIAN_POINT('Ctrl Pts',(155.284641256517,3.69797217617701,127.561802237718));
#31905=CARTESIAN_POINT('Ctrl Pts',(155.276894923252,3.60750722144029,127.458631578521));
#31906=CARTESIAN_POINT('Ctrl Pts',(155.269148589986,3.51272196143669,127.35925025091));
#31907=CARTESIAN_POINT('Ctrl Pts',(155.261402256721,3.41397594005339,127.264028522517));
#31908=CARTESIAN_POINT('Ctrl Pts',(155.253654188718,3.31520780518326,127.168785469877));
#31909=CARTESIAN_POINT('Ctrl Pts',(155.245906120715,3.21247742531274,127.077704141392));
#31910=CARTESIAN_POINT('Ctrl Pts',(155.238158052712,3.10617967104525,126.991116472001));
#31911=CARTESIAN_POINT('Ctrl Pts',(155.23040174997,2.99976894225953,126.904436776205));
#31912=CARTESIAN_POINT('Ctrl Pts',(155.222645447228,2.88978356885973,126.822260527218));
#31913=CARTESIAN_POINT('Ctrl Pts',(155.214889144486,2.77665028174771,126.744878350654));
#31914=CARTESIAN_POINT('Ctrl Pts',(155.207128701972,2.66345661199391,126.667454872893));
#31915=CARTESIAN_POINT('Ctrl Pts',(155.199368259458,2.54711201220644,126.594830772986));
#31916=CARTESIAN_POINT('Ctrl Pts',(155.191607816944,2.42806953802891,126.52725161954));
#31917=CARTESIAN_POINT('Ctrl Pts',(155.183834916679,2.30883596630377,126.459563982038));
#31918=CARTESIAN_POINT('Ctrl Pts',(155.176062016413,2.18689621371526,126.396937653289));
#31919=CARTESIAN_POINT('Ctrl Pts',(155.168289116148,2.06272592842871,126.339571170494));
#31920=CARTESIAN_POINT('Ctrl Pts',(155.160798780386,1.94306954577844,126.284290103845));
#31921=CARTESIAN_POINT('Ctrl Pts',(155.153308444624,1.82134227046019,126.233893223002));
#31922=CARTESIAN_POINT('Ctrl Pts',(155.145818108862,1.69798279852588,126.188514272809));
#31923=CARTESIAN_POINT('Ctrl Pts',(155.138043774742,1.56994611471888,126.141414765926));
#31924=CARTESIAN_POINT('Ctrl Pts',(155.130269440623,1.43974543984953,126.099572013674));
#31925=CARTESIAN_POINT('Ctrl Pts',(155.122495106504,1.30785168532758,126.063189134516));
#31926=CARTESIAN_POINT('Ctrl Pts',(155.114730353557,1.17612047807048,126.026851094005));
#31927=CARTESIAN_POINT('Ctrl Pts',(155.10696560061,1.04270071608255,125.995959641236));
#31928=CARTESIAN_POINT('Ctrl Pts',(155.099200847663,0.908082436501846,125.970669548516));
#31929=CARTESIAN_POINT('Ctrl Pts',(155.091443806778,0.773597861694302,125.945404574272));
#31930=CARTESIAN_POINT('Ctrl Pts',(155.083686765893,0.637917519969964,125.925729960477));
#31931=CARTESIAN_POINT('Ctrl Pts',(155.075929725008,0.501545387915416,125.91175034427));
#31932=CARTESIAN_POINT('Ctrl Pts',(155.068178533768,0.365276095146332,125.8977812702));
#31933=CARTESIAN_POINT('Ctrl Pts',(155.060427342528,0.228316437781679,125.889498685201));
#31934=CARTESIAN_POINT('Ctrl Pts',(155.052676151288,0.0911789827905253,
125.886955869572));
#31935=CARTESIAN_POINT('Ctrl Pts',(155.04492825451,-0.0459001851239494,
125.884414134707));
#31936=CARTESIAN_POINT('Ctrl Pts',(155.037180357733,-0.183156610284839,
125.887607324356));
#31937=CARTESIAN_POINT('Ctrl Pts',(155.029432460956,-0.320074445430811,
125.896536719759));
#31938=CARTESIAN_POINT('Ctrl Pts',(155.021686184872,-0.456963640317278,
125.905464247326));
#31939=CARTESIAN_POINT('Ctrl Pts',(155.013939908788,-0.593513996175859,
125.920125568571));
#31940=CARTESIAN_POINT('Ctrl Pts',(155.006193632704,-0.729211909777027,
125.940469885535));
#31941=CARTESIAN_POINT('Ctrl Pts',(154.998447299439,-0.864910825069366,
125.960814352676));
#31942=CARTESIAN_POINT('Ctrl Pts',(154.990700966173,-0.999756898903957,
125.986841841278));
#31943=CARTESIAN_POINT('Ctrl Pts',(154.982954632908,-1.13324427238443,126.018449995583));
#31944=CARTESIAN_POINT('Ctrl Pts',(154.975206564905,-1.26676153943657,126.050065228316));
#31945=CARTESIAN_POINT('Ctrl Pts',(154.967458496902,-1.39891912029712,126.087263523545));
#31946=CARTESIAN_POINT('Ctrl Pts',(154.959710428899,-1.52922431149447,126.129892084392));
#31947=CARTESIAN_POINT('Ctrl Pts',(154.951954126157,-1.65966799259981,126.172565951381));
#31948=CARTESIAN_POINT('Ctrl Pts',(154.944197823415,-1.78825497908933,126.220681491126));
#31949=CARTESIAN_POINT('Ctrl Pts',(154.936441520673,-1.91451010092752,126.274036773077));
#31950=CARTESIAN_POINT('Ctrl Pts',(154.928681078159,-2.04083260892575,126.327420532349));
#31951=CARTESIAN_POINT('Ctrl Pts',(154.920920635645,-2.16482041905922,126.386049439258));
#31952=CARTESIAN_POINT('Ctrl Pts',(154.913160193131,-2.28602203986124,126.449675061091));
#31953=CARTESIAN_POINT('Ctrl Pts',(154.905387292865,-2.40741822426469,126.513402820422));
#31954=CARTESIAN_POINT('Ctrl Pts',(154.8976143926,-2.52601894312855,126.582143127366));
#31955=CARTESIAN_POINT('Ctrl Pts',(154.889841492334,-2.64140006203276,126.655603119857));
#31956=CARTESIAN_POINT('Ctrl Pts',(154.882351156572,-2.75258678663672,126.726392656587));
#31957=CARTESIAN_POINT('Ctrl Pts',(154.87486082081,-2.86078367546688,126.801564515699));
#31958=CARTESIAN_POINT('Ctrl Pts',(154.867370485048,-2.96564107926591,126.880821902137));
#31959=CARTESIAN_POINT('Ctrl Pts',(154.859575127744,-3.07476848751448,126.963306808811));
#31960=CARTESIAN_POINT('Ctrl Pts',(154.85177977044,-3.18064515146998,127.050494249024));
#31961=CARTESIAN_POINT('Ctrl Pts',(154.843984413136,-3.28283355226151,127.142095344453));
#31962=CARTESIAN_POINT('Ctrl Pts',(154.836302734693,-3.38353175053798,127.232360630909));
#31963=CARTESIAN_POINT('Ctrl Pts',(154.82862105625,-3.48064819156846,127.326911468719));
#31964=CARTESIAN_POINT('Ctrl Pts',(154.820939377807,-3.57379280059238,127.425427637921));
#31965=CARTESIAN_POINT('Ctrl Pts',(154.813264691756,-3.66685262299287,127.523854130936));
#31966=CARTESIAN_POINT('Ctrl Pts',(154.805590005705,-3.75594752972872,127.62623848939));
#31967=CARTESIAN_POINT('Ctrl Pts',(154.797915319653,-3.84072175893283,127.732221390096));
#31968=CARTESIAN_POINT('Ctrl Pts',(154.7902458715,-3.92543813055292,127.838131958507));
#31969=CARTESIAN_POINT('Ctrl Pts',(154.782576423347,-4.00583944108695,127.947635873119));
#31970=CARTESIAN_POINT('Ctrl Pts',(154.774906975194,-4.08160830550919,128.060338623686));
#31971=CARTESIAN_POINT('Ctrl Pts',(154.767021553074,-4.15951084395384,128.176215117622));
#31972=CARTESIAN_POINT('Ctrl Pts',(154.759136130953,-4.23251587964388,128.295472954516));
#31973=CARTESIAN_POINT('Ctrl Pts',(154.751250708832,-4.30032435264736,128.417648752986));
#31974=CARTESIAN_POINT('Ctrl Pts',(154.74358536649,-4.36624031139867,128.536414661369));
#31975=CARTESIAN_POINT('Ctrl Pts',(154.735920024148,-4.42724573367112,128.657937438946));
#31976=CARTESIAN_POINT('Ctrl Pts',(154.728254681806,-4.48311152563272,128.781764733253));
#31977=CARTESIAN_POINT('Ctrl Pts',(154.720259219796,-4.5413832631991,128.910924839001));
#31978=CARTESIAN_POINT('Ctrl Pts',(154.712263757786,-4.59406258058145,129.042591971584));
#31979=CARTESIAN_POINT('Ctrl Pts',(154.704268295776,-4.64094485693375,129.176228590549));
#31980=CARTESIAN_POINT('Ctrl Pts',(154.696272833765,-4.68782713328608,129.309865209513));
#31981=CARTESIAN_POINT('Ctrl Pts',(154.688277371755,-4.72891223230369,129.445470840835));
#31982=CARTESIAN_POINT('Ctrl Pts',(154.680281909745,-4.76405452823406,129.582490119308));
#31983=CARTESIAN_POINT('Origin',(213.235140564004,0.,130.804360617566));
#31984=CARTESIAN_POINT('',(152.584590056215,-4.76405452823403,129.582490119308));
#31985=CARTESIAN_POINT('',(152.930132636296,-4.76405452823406,129.582490119308));
#31986=CARTESIAN_POINT('',(213.235140564004,-4.76405452823405,129.582490119308));
#31987=CARTESIAN_POINT('',(154.264859436025,-4.91824789998526,130.799815643358));
#31988=CARTESIAN_POINT('Ctrl Pts',(154.264859435991,-4.91824789998582,130.799815643966));
#31989=CARTESIAN_POINT('Ctrl Pts',(154.257201974255,-4.91837282331536,130.934998806114));
#31990=CARTESIAN_POINT('Ctrl Pts',(154.249544512518,-4.91292008139986,131.070338875953));
#31991=CARTESIAN_POINT('Ctrl Pts',(154.241887050782,-4.90187769675906,131.205332073553));
#31992=CARTESIAN_POINT('Ctrl Pts',(154.233959115739,-4.89044527813835,131.345093438159));
#31993=CARTESIAN_POINT('Ctrl Pts',(154.226031180697,-4.87302102558022,131.484482540111));
#31994=CARTESIAN_POINT('Ctrl Pts',(154.218103245655,-4.84965056909455,131.622940131224));
#31995=CARTESIAN_POINT('Ctrl Pts',(154.210453950955,-4.82710150581549,131.756531402126));
#31996=CARTESIAN_POINT('Ctrl Pts',(154.202804656255,-4.79901723311674,131.889255105444));
#31997=CARTESIAN_POINT('Ctrl Pts',(154.195155361554,-4.76549141676183,132.020614957443));
#31998=CARTESIAN_POINT('Ctrl Pts',(154.187507083778,-4.73197005744568,132.151957346006));
#31999=CARTESIAN_POINT('Ctrl Pts',(154.179858806002,-4.69300869217524,132.281935854467));
#32000=CARTESIAN_POINT('Ctrl Pts',(154.172210528225,-4.64875168296609,132.410066335504));
#32001=CARTESIAN_POINT('Ctrl Pts',(154.16456151096,-4.60449039468026,132.538209205091));
#32002=CARTESIAN_POINT('Ctrl Pts',(154.156912493695,-4.55493257575353,132.664503312174));
#32003=CARTESIAN_POINT('Ctrl Pts',(154.149263476429,-4.50027166529154,132.788482085892));
#32004=CARTESIAN_POINT('Ctrl Pts',(154.14161196291,-4.44559291626051,132.91250132004));
#32005=CARTESIAN_POINT('Ctrl Pts',(154.13396044939,-4.38580792617314,133.034203350896));
#32006=CARTESIAN_POINT('Ctrl Pts',(154.126308935871,-4.32115699401076,133.153144408299));
#32007=CARTESIAN_POINT('Ctrl Pts',(154.118649094412,-4.25643569549892,133.272214921656));
#32008=CARTESIAN_POINT('Ctrl Pts',(154.110989252953,-4.1868380770245,133.388518111072));
#32009=CARTESIAN_POINT('Ctrl Pts',(154.103329411493,-4.11264897603279,133.50163729274));
#32010=CARTESIAN_POINT('Ctrl Pts',(154.095664596587,-4.03841170491251,133.614829921389));
#32011=CARTESIAN_POINT('Ctrl Pts',(154.087999781681,-3.95957725044642,133.724834101816));
#32012=CARTESIAN_POINT('Ctrl Pts',(154.080334966775,-3.87647115193746,133.831265715301));
#32013=CARTESIAN_POINT('Ctrl Pts',(154.07265943833,-3.79324889140172,133.937846094186));
#32014=CARTESIAN_POINT('Ctrl Pts',(154.064983909885,-3.70574333233295,134.040843638029));
#32015=CARTESIAN_POINT('Ctrl Pts',(154.05730838144,-3.61431743326588,134.139910430429));
#32016=CARTESIAN_POINT('Ctrl Pts',(154.055411124216,-3.5917185400876,134.164398019633));
#32017=CARTESIAN_POINT('Ctrl Pts',(154.053513866993,-3.56888027694123,134.188645634285));
#32018=CARTESIAN_POINT('Ctrl Pts',(154.051616609769,-3.54580843086088,134.21264840385));
#32019=CARTESIAN_POINT('Ctrl Pts',(154.04384227565,-3.4512676179694,134.311003834035));
#32020=CARTESIAN_POINT('Ctrl Pts',(154.036067941531,-3.35248160871389,134.405578439652));
#32021=CARTESIAN_POINT('Ctrl Pts',(154.028293607412,-3.24978504591324,134.4959835964));
#32022=CARTESIAN_POINT('Ctrl Pts',(154.020528854465,-3.14721504744805,134.586277336873));
#32023=CARTESIAN_POINT('Ctrl Pts',(154.012764101518,-3.04074437526277,134.67241159665));
#32024=CARTESIAN_POINT('Ctrl Pts',(154.004999348571,-2.93074601686428,134.754032863099));
#32025=CARTESIAN_POINT('Ctrl Pts',(153.997242307686,-2.82085691038576,134.835573062156));
#32026=CARTESIAN_POINT('Ctrl Pts',(153.989485266801,-2.70744740224859,134.912608956533));
#32027=CARTESIAN_POINT('Ctrl Pts',(153.981728225916,-2.59092494319348,134.984826022427));
#32028=CARTESIAN_POINT('Ctrl Pts',(153.973977034675,-2.47449035463095,135.056988628869));
#32029=CARTESIAN_POINT('Ctrl Pts',(153.966225843435,-2.35494781867991,135.12433943479));
#32030=CARTESIAN_POINT('Ctrl Pts',(153.958474652195,-2.23273497333086,135.186606343374));
#32031=CARTESIAN_POINT('Ctrl Pts',(153.950726755418,-2.11057407170164,135.248846786861));
#32032=CARTESIAN_POINT('Ctrl Pts',(153.942978858641,-1.98574546563632,135.306007453546));
#32033=CARTESIAN_POINT('Ctrl Pts',(153.935230961864,-1.85871248600596,135.357861573629));
#32034=CARTESIAN_POINT('Ctrl Pts',(153.92748468578,-1.73170607893638,135.409704846948));
#32035=CARTESIAN_POINT('Ctrl Pts',(153.919738409696,-1.60249657721068,135.456243633885));
#32036=CARTESIAN_POINT('Ctrl Pts',(153.911992133612,-1.47156807171687,135.497298979915));
#32037=CARTESIAN_POINT('Ctrl Pts',(153.904245800346,-1.34063859973858,135.538354629006));
#32038=CARTESIAN_POINT('Ctrl Pts',(153.896499467081,-1.20799047172617,135.57392663944));
#32039=CARTESIAN_POINT('Ctrl Pts',(153.888753133815,-1.07412336422445,135.603885808762));
#32040=CARTESIAN_POINT('Ctrl Pts',(153.881005065812,-0.940226278112406,
135.633851687233));
#32041=CARTESIAN_POINT('Ctrl Pts',(153.873256997809,-0.805110050762888,
135.658202138023));
#32042=CARTESIAN_POINT('Ctrl Pts',(153.865508929806,-0.669284589886382,
135.676859073209));
#32043=CARTESIAN_POINT('Ctrl Pts',(153.857752627065,-0.533314772093666,
135.695535837207));
#32044=CARTESIAN_POINT('Ctrl Pts',(153.849996324323,-0.396634602959449,
135.708506944516));
#32045=CARTESIAN_POINT('Ctrl Pts',(153.842240021581,-0.259759712457097,
135.7157461608));
#32046=CARTESIAN_POINT('Ctrl Pts',(153.834479579067,-0.122811767703994,
135.722989240871));
#32047=CARTESIAN_POINT('Ctrl Pts',(153.826719136552,0.0143307147535147,
135.724494329748));
#32048=CARTESIAN_POINT('Ctrl Pts',(153.818958694038,0.151153059825974,135.720287367936));
#32049=CARTESIAN_POINT('Ctrl Pts',(153.811185793773,0.28819504427298,135.716073652735));
#32050=CARTESIAN_POINT('Ctrl Pts',(153.803412893507,0.424915474213501,135.706129591658));
#32051=CARTESIAN_POINT('Ctrl Pts',(153.795639993242,0.560804844014884,135.690533044879));
#32052=CARTESIAN_POINT('Ctrl Pts',(153.78814965748,0.691754292938122,135.67550347186));
#32053=CARTESIAN_POINT('Ctrl Pts',(153.780659321718,0.821931750613826,135.655225289794));
#32054=CARTESIAN_POINT('Ctrl Pts',(153.773168985956,0.950892974261133,135.629812473507));
#32055=CARTESIAN_POINT('Ctrl Pts',(153.765394651837,1.08474380190108,135.603436122565));
#32056=CARTESIAN_POINT('Ctrl Pts',(153.757620317718,1.21770834708445,135.571444539663));
#32057=CARTESIAN_POINT('Ctrl Pts',(153.749845983599,1.34927876656043,135.533909208352));
#32058=CARTESIAN_POINT('Ctrl Pts',(153.742081230652,1.48068703725302,135.496420135983));
#32059=CARTESIAN_POINT('Ctrl Pts',(153.734316477705,1.61070422845986,135.453401015423));
#32060=CARTESIAN_POINT('Ctrl Pts',(153.726551724758,1.73883131113119,135.404974569413));
#32061=CARTESIAN_POINT('Ctrl Pts',(153.718794683873,1.86683113617794,135.356596221232));
#32062=CARTESIAN_POINT('Ctrl Pts',(153.711037642988,1.99294422521703,135.302821372729));
#32063=CARTESIAN_POINT('Ctrl Pts',(153.703280602103,2.11668572338516,135.243822815954));
#32064=CARTESIAN_POINT('Ctrl Pts',(153.695529410862,2.240333907127,135.18486875045));
#32065=CARTESIAN_POINT('Ctrl Pts',(153.687778219622,2.36161370829242,135.120698985069));
#32066=CARTESIAN_POINT('Ctrl Pts',(153.680027028382,2.48005965010008,135.051534642073));
#32067=CARTESIAN_POINT('Ctrl Pts',(153.672279131605,2.59845524922262,134.982399695768));
#32068=CARTESIAN_POINT('Ctrl Pts',(153.664531234828,2.7140190476654,134.908274590725));
#32069=CARTESIAN_POINT('Ctrl Pts',(153.656783338051,2.82630981591932,134.829426565714));
#32070=CARTESIAN_POINT('Ctrl Pts',(153.649037061967,2.9385770953653,134.750595034009));
#32071=CARTESIAN_POINT('Ctrl Pts',(153.641290785883,3.04757238666269,134.667042771917));
#32072=CARTESIAN_POINT('Ctrl Pts',(153.633544509799,3.1528834673512,134.579080329519));
#32073=CARTESIAN_POINT('Ctrl Pts',(153.625798176533,3.25819532542193,134.491117237802));
#32074=CARTESIAN_POINT('Ctrl Pts',(153.618051843268,3.35982261855329,134.39874415145));
#32075=CARTESIAN_POINT('Ctrl Pts',(153.610305510003,3.45738655768207,134.302311625407));
#32076=CARTESIAN_POINT('Ctrl Pts',(153.602557442,3.55497234557872,134.205857503969));
#32077=CARTESIAN_POINT('Ctrl Pts',(153.594809373997,3.64849269074929,134.105342408655));
#32078=CARTESIAN_POINT('Ctrl Pts',(153.587061305994,3.73760627803798,134.001153130832));
#32079=CARTESIAN_POINT('Ctrl Pts',(153.579305003252,3.82681457630779,133.896853119404));
#32080=CARTESIAN_POINT('Ctrl Pts',(153.57154870051,3.91160650626362,133.788871422465));
#32081=CARTESIAN_POINT('Ctrl Pts',(153.563792397768,3.99168128562,133.677627673816));
#32082=CARTESIAN_POINT('Ctrl Pts',(153.556031955254,4.07179880329717,133.566324551029));
#32083=CARTESIAN_POINT('Ctrl Pts',(153.54827151274,4.14719393885572,133.451756233763));
#32084=CARTESIAN_POINT('Ctrl Pts',(153.540511070226,4.217610322319,133.334369754223));
#32085=CARTESIAN_POINT('Ctrl Pts',(153.53273816996,4.28813974441229,133.216794835485));
#32086=CARTESIAN_POINT('Ctrl Pts',(153.524965269695,4.35367425616248,133.096393057743));
#32087=CARTESIAN_POINT('Ctrl Pts',(153.517192369429,4.41400396329998,132.973635167841));
#32088=CARTESIAN_POINT('Ctrl Pts',(153.509702033667,4.4721405336219,132.855339836445));
#32089=CARTESIAN_POINT('Ctrl Pts',(153.502211697905,4.52544402037737,132.734857001755));
#32090=CARTESIAN_POINT('Ctrl Pts',(153.494721362143,4.57377018974149,132.612622023982));
#32091=CARTESIAN_POINT('Ctrl Pts',(153.486947028024,4.62392866050528,132.485752469874));
#32092=CARTESIAN_POINT('Ctrl Pts',(153.479172693905,4.66888382027217,132.356593400263));
#32093=CARTESIAN_POINT('Ctrl Pts',(153.471398359786,4.70842130849739,132.225610716665));
#32094=CARTESIAN_POINT('Ctrl Pts',(153.463633606839,4.7479100703018,132.094789457518));
#32095=CARTESIAN_POINT('Ctrl Pts',(153.455868853892,4.78199433350404,131.962149426815));
#32096=CARTESIAN_POINT('Ctrl Pts',(153.448104100945,4.81050761082926,131.828176806466));
#32097=CARTESIAN_POINT('Ctrl Pts',(153.44034706006,4.83899256836557,131.694337249612));
#32098=CARTESIAN_POINT('Ctrl Pts',(153.432590019175,4.86191747044678,131.559168116956));
#32099=CARTESIAN_POINT('Ctrl Pts',(153.424832978289,4.87916561601989,131.423170728948));
#32100=CARTESIAN_POINT('Ctrl Pts',(153.417081787049,4.89640075463227,131.287275897629));
#32101=CARTESIAN_POINT('Ctrl Pts',(153.409330595809,4.9079676085891,131.150554440464));
#32102=CARTESIAN_POINT('Ctrl Pts',(153.401579404569,4.91380061274046,131.013517498236));
#32103=CARTESIAN_POINT('Ctrl Pts',(153.393831507792,4.91963113770944,130.876538800363));
#32104=CARTESIAN_POINT('Ctrl Pts',(153.386083611015,4.91973264336635,130.739245273915));
#32105=CARTESIAN_POINT('Ctrl Pts',(153.378335714238,4.91409146992764,130.602152586854));
#32106=CARTESIAN_POINT('Ctrl Pts',(153.370589438154,4.90845147650081,130.465088576628));
#32107=CARTESIAN_POINT('Ctrl Pts',(153.36284316207,4.89707120938373,130.328225712614));
#32108=CARTESIAN_POINT('Ctrl Pts',(153.355096885986,4.87998912684664,130.192078669148));
#32109=CARTESIAN_POINT('Ctrl Pts',(153.34735055272,4.86290691821352,130.055930620675));
#32110=CARTESIAN_POINT('Ctrl Pts',(153.339604219455,4.84012285884581,129.920498791218));
#32111=CARTESIAN_POINT('Ctrl Pts',(153.33185788619,4.8117271358061,129.786291350253));
#32112=CARTESIAN_POINT('Ctrl Pts',(153.324109818187,4.7833250537411,129.652053854462));
#32113=CARTESIAN_POINT('Ctrl Pts',(153.316361750184,4.74930888824381,129.519041675201));
#32114=CARTESIAN_POINT('Ctrl Pts',(153.308613682181,4.70981956866713,129.387751040759));
#32115=CARTESIAN_POINT('Ctrl Pts',(153.300857379439,4.67028827937163,129.256320869069));
#32116=CARTESIAN_POINT('Ctrl Pts',(153.293101076697,4.62527232883565,129.12661627217));
#32117=CARTESIAN_POINT('Ctrl Pts',(153.285344773955,4.57496218668788,128.999117129037));
#32118=CARTESIAN_POINT('Ctrl Pts',(153.277584331441,4.52462519250233,128.871549935773));
#32119=CARTESIAN_POINT('Ctrl Pts',(153.269823888927,4.46898853484091,128.746190898957));
#32120=CARTESIAN_POINT('Ctrl Pts',(153.262063446413,4.40828974032399,128.623497341738));
#32121=CARTESIAN_POINT('Ctrl Pts',(153.254290546147,4.34749350671365,128.500606825929));
#32122=CARTESIAN_POINT('Ctrl Pts',(153.246517645882,4.28161908551396,128.380390683314));
#32123=CARTESIAN_POINT('Ctrl Pts',(153.238744745616,4.21094907639826,128.263279954053));
#32124=CARTESIAN_POINT('Ctrl Pts',(153.231254409854,4.14284810012079,128.150426494784));
#32125=CARTESIAN_POINT('Ctrl Pts',(153.223764074092,4.07029431564631,128.040456846637));
#32126=CARTESIAN_POINT('Ctrl Pts',(153.21627373833,3.99357604194475,127.933727680441));
#32127=CARTESIAN_POINT('Ctrl Pts',(153.208499404211,3.91394897157787,127.82295184547));
#32128=CARTESIAN_POINT('Ctrl Pts',(153.200725070092,3.82958315028404,127.715316164351));
#32129=CARTESIAN_POINT('Ctrl Pts',(153.192950735973,3.74075468709309,127.611252815833));
#32130=CARTESIAN_POINT('Ctrl Pts',(153.185185983026,3.65203569704401,127.50731771609));
#32131=CARTESIAN_POINT('Ctrl Pts',(153.177421230079,3.55886525946724,127.406946483633));
#32132=CARTESIAN_POINT('Ctrl Pts',(153.169656477132,3.46156242253508,127.31054198212));
#32133=CARTESIAN_POINT('Ctrl Pts',(153.161899436247,3.36435622815283,127.214233230916));
#32134=CARTESIAN_POINT('Ctrl Pts',(153.154142395362,3.26302607820749,127.121883643638));
#32135=CARTESIAN_POINT('Ctrl Pts',(153.146385354477,3.15793066802292,127.033862380136));
#32136=CARTESIAN_POINT('Ctrl Pts',(153.138634163237,3.05291451110415,126.945907494153));
#32137=CARTESIAN_POINT('Ctrl Pts',(153.130882971996,2.94413904413805,126.862274685124));
#32138=CARTESIAN_POINT('Ctrl Pts',(153.123131780756,2.83199886477588,126.783295398944));
#32139=CARTESIAN_POINT('Ctrl Pts',(153.115383883979,2.71990634798167,126.704349681068));
#32140=CARTESIAN_POINT('Ctrl Pts',(153.107635987202,2.60445228211273,126.630053776858));
#32141=CARTESIAN_POINT('Ctrl Pts',(153.099888090425,2.48606312978482,126.560697909807));
#32142=CARTESIAN_POINT('Ctrl Pts',(153.092141814341,2.36769874191547,126.491356550508));
#32143=CARTESIAN_POINT('Ctrl Pts',(153.084395538257,2.2464008259076,126.426953370479));
#32144=CARTESIAN_POINT('Ctrl Pts',(153.076649262173,2.12262317949043,126.367734207737));
#32145=CARTESIAN_POINT('Ctrl Pts',(153.068902928908,1.99884461937461,126.308514607853));
#32146=CARTESIAN_POINT('Ctrl Pts',(153.061156595642,1.8725866450032,126.254479270349));
#32147=CARTESIAN_POINT('Ctrl Pts',(153.053410262377,1.74432554205993,126.20582699631));
#32148=CARTESIAN_POINT('Ctrl Pts',(153.045662194374,1.61603571593231,126.157163826933));
#32149=CARTESIAN_POINT('Ctrl Pts',(153.037914126371,1.48574223407726,126.11388625846));
#32150=CARTESIAN_POINT('Ctrl Pts',(153.030166058368,1.35393876316582,126.076143946548));
#32151=CARTESIAN_POINT('Ctrl Pts',(153.022409755626,1.2219952099567,126.038361521657));
#32152=CARTESIAN_POINT('Ctrl Pts',(153.014653452884,1.08853883831998,126.006126212926));
#32153=CARTESIAN_POINT('Ctrl Pts',(153.006897150143,0.954076337514759,125.979537159169));
#32154=CARTESIAN_POINT('Ctrl Pts',(152.999136707628,0.819542070024268,125.952933914034));
#32155=CARTESIAN_POINT('Ctrl Pts',(152.991376265114,0.684000989532066,125.931982988373));
#32156=CARTESIAN_POINT('Ctrl Pts',(152.9836158226,0.547966243895212,125.916731738646));
#32157=CARTESIAN_POINT('Ctrl Pts',(152.975842922335,0.411713123208111,125.901456006259));
#32158=CARTESIAN_POINT('Ctrl Pts',(152.968070022069,0.274965143996772,125.891898260949));
#32159=CARTESIAN_POINT('Ctrl Pts',(152.960297121804,0.138237704583411,125.888053731342));
#32160=CARTESIAN_POINT('Ctrl Pts',(152.952806786042,0.00648065198873604,
125.884348960071));
#32161=CARTESIAN_POINT('Ctrl Pts',(152.94531645028,-0.12525702023226,125.885949232798));
#32162=CARTESIAN_POINT('Ctrl Pts',(152.937826114518,-0.25651939136301,125.892804767903));
#32163=CARTESIAN_POINT('Ctrl Pts',(152.930051780399,-0.392758615191718,
125.899920232706));
#32164=CARTESIAN_POINT('Ctrl Pts',(152.92227744628,-0.52891734927641,125.912719872733));
#32165=CARTESIAN_POINT('Ctrl Pts',(152.914503112161,-0.6644827457224,125.931204992805));
#32166=CARTESIAN_POINT('Ctrl Pts',(152.906738359213,-0.799881069933328,
125.949667331619));
#32167=CARTESIAN_POINT('Ctrl Pts',(152.898973606266,-0.934687127784761,
125.97380115663));
#32168=CARTESIAN_POINT('Ctrl Pts',(152.891208853319,-1.06838952534121,126.003555801221));
#32169=CARTESIAN_POINT('Ctrl Pts',(152.883451812434,-1.20195912779154,126.03328089308));
#32170=CARTESIAN_POINT('Ctrl Pts',(152.875694771549,-1.33442687221691,126.06861561036));
#32171=CARTESIAN_POINT('Ctrl Pts',(152.867937730664,-1.46528829039603,126.109457712443));
#32172=CARTESIAN_POINT('Ctrl Pts',(152.860186539424,-1.59605102496232,126.15026901518));
#32173=CARTESIAN_POINT('Ctrl Pts',(152.852435348184,-1.72520947268672,126.196579320095));
#32174=CARTESIAN_POINT('Ctrl Pts',(152.844684156944,-1.85227148908113,126.248235795611));
#32175=CARTESIAN_POINT('Ctrl Pts',(152.836936260167,-1.97927950072866,126.299870315746));
#32176=CARTESIAN_POINT('Ctrl Pts',(152.82918836339,-2.1041924918347,126.356846340187));
#32177=CARTESIAN_POINT('Ctrl Pts',(152.821440466612,-2.22653577569419,126.418961946743));
#32178=CARTESIAN_POINT('Ctrl Pts',(152.813694190528,-2.34885346797617,126.481064560054));
#32179=CARTESIAN_POINT('Ctrl Pts',(152.805947914444,-2.46860217379645,126.548304440186));
#32180=CARTESIAN_POINT('Ctrl Pts',(152.79820163836,-2.58532977391074,126.620432675712));
#32181=CARTESIAN_POINT('Ctrl Pts',(152.790455305095,-2.70205823568137,126.692561443671));
#32182=CARTESIAN_POINT('Ctrl Pts',(152.782708971829,-2.81576521465385,126.769578433514));
#32183=CARTESIAN_POINT('Ctrl Pts',(152.774962638564,-2.92602600979875,126.851190389448));
#32184=CARTESIAN_POINT('Ctrl Pts',(152.767214570561,-3.03631149708442,126.932820621813));
#32185=CARTESIAN_POINT('Ctrl Pts',(152.759466502558,-3.14314895066318,127.019047635328));
#32186=CARTESIAN_POINT('Ctrl Pts',(152.751718434555,-3.24614562209954,127.109536986779));
#32187=CARTESIAN_POINT('Ctrl Pts',(152.743962131813,-3.34925175962384,127.200122511389));
#32188=CARTESIAN_POINT('Ctrl Pts',(152.736205829071,-3.44850866653318,127.294979164767));
#32189=CARTESIAN_POINT('Ctrl Pts',(152.728449526329,-3.54355905661403,127.393734241841));
#32190=CARTESIAN_POINT('Ctrl Pts',(152.720689083815,-3.63866017795002,127.492542027474));
#32191=CARTESIAN_POINT('Ctrl Pts',(152.712928641301,-3.72955004985057,127.59525209014));
#32192=CARTESIAN_POINT('Ctrl Pts',(152.705168198787,-3.81591146103389,127.701458301338));
#32193=CARTESIAN_POINT('Ctrl Pts',(152.697395298521,-3.90241150722139,127.807835004176));
#32194=CARTESIAN_POINT('Ctrl Pts',(152.689622398256,-3.98436833205943,127.917718757189));
#32195=CARTESIAN_POINT('Ctrl Pts',(152.681849497991,-4.06150736445639,128.03067336213));
#32196=CARTESIAN_POINT('Ctrl Pts',(152.674359162229,-4.13584219872345,128.139521782665));
#32197=CARTESIAN_POINT('Ctrl Pts',(152.666868826467,-4.20570327366286,128.251221403806));
#32198=CARTESIAN_POINT('Ctrl Pts',(152.659378490705,-4.270886035677,128.365361738362));
#32199=CARTESIAN_POINT('Ctrl Pts',(152.651270040263,-4.34144778513971,128.488921118812));
#32200=CARTESIAN_POINT('Ctrl Pts',(152.643161589822,-4.40673476032177,128.615703962037));
#32201=CARTESIAN_POINT('Ctrl Pts',(152.63505313938,-4.46645369419116,128.745240791003));
#32202=CARTESIAN_POINT('Ctrl Pts',(152.62664262552,-4.52839733246053,128.879603244518));
#32203=CARTESIAN_POINT('Ctrl Pts',(152.618232111659,-4.58434981356175,129.016928573631));
#32204=CARTESIAN_POINT('Ctrl Pts',(152.609821597798,-4.63403356683683,129.15666041306));
#32205=CARTESIAN_POINT('Ctrl Pts',(152.601411083937,-4.68371732011193,129.296392252489));
#32206=CARTESIAN_POINT('Ctrl Pts',(152.593000570076,-4.72713212829472,129.43853024232));
#32207=CARTESIAN_POINT('Ctrl Pts',(152.584590056215,-4.76405452823404,129.582490119308));
#32208=CARTESIAN_POINT('Ctrl Pts',(154.334814618358,-4.76405452823406,129.582490119308));
#32209=CARTESIAN_POINT('Ctrl Pts',(154.333231156766,-4.77096212897711,129.609422749768));
#32210=CARTESIAN_POINT('Ctrl Pts',(154.331647695174,-4.77763918936648,129.636405591418));
#32211=CARTESIAN_POINT('Ctrl Pts',(154.330064233582,-4.78408511039337,129.663434362713));
#32212=CARTESIAN_POINT('Ctrl Pts',(154.319196767322,-4.82832415579875,129.848935710869));
#32213=CARTESIAN_POINT('Ctrl Pts',(154.308329301063,-4.86178997871693,130.037097735734));
#32214=CARTESIAN_POINT('Ctrl Pts',(154.297461834803,-4.88422663702635,130.226854582392));
#32215=CARTESIAN_POINT('Ctrl Pts',(154.287250081402,-4.90530952942634,130.405162025733));
#32216=CARTESIAN_POINT('Ctrl Pts',(154.277038328001,-4.91665437759487,130.584877919004));
#32217=CARTESIAN_POINT('Ctrl Pts',(154.266826574599,-4.91809324692398,130.76509387514));
#32218=CARTESIAN_POINT('Ctrl Pts',(154.266170861741,-4.9181856390023,130.776665827086));
#32219=CARTESIAN_POINT('Ctrl Pts',(154.265515148883,-4.91823720272719,130.788239831339));
#32220=CARTESIAN_POINT('Ctrl Pts',(154.264859436025,-4.91824789998526,130.799815643358));
#32221=CARTESIAN_POINT('',(154.610140564044,-4.91824949728461,130.806584344098));
#32222=CARTESIAN_POINT('Ctrl Pts',(154.680281909745,-4.76405452823406,129.582490119308));
#32223=CARTESIAN_POINT('Ctrl Pts',(154.672605721356,-4.79779352713309,129.714037963955));
#32224=CARTESIAN_POINT('Ctrl Pts',(154.664929532968,-4.82605516076123,129.846888324421));
#32225=CARTESIAN_POINT('Ctrl Pts',(154.657253344579,-4.8487630813234,129.980540465048));
#32226=CARTESIAN_POINT('Ctrl Pts',(154.64940121449,-4.87199147766924,130.117255973033));
#32227=CARTESIAN_POINT('Ctrl Pts',(154.641549084401,-4.88940843558675,130.254810015955));
#32228=CARTESIAN_POINT('Ctrl Pts',(154.633696954311,-4.9009885182294,130.39266339061));
#32229=CARTESIAN_POINT('Ctrl Pts',(154.625844824222,-4.91256860087204,130.530516765264));
#32230=CARTESIAN_POINT('Ctrl Pts',(154.617992694133,-4.91831185401273,130.668669028351));
#32231=CARTESIAN_POINT('Ctrl Pts',(154.610140564044,-4.91824949728461,130.806584344098));
#32232=CARTESIAN_POINT('Ctrl Pts',(154.610140564008,-4.91824949728433,130.806584344722));
#32233=CARTESIAN_POINT('Ctrl Pts',(154.603067996417,-4.91819333134041,130.930807374822));
#32234=CARTESIAN_POINT('Ctrl Pts',(154.595995428826,-4.91343124279772,131.054919660382));
#32235=CARTESIAN_POINT('Ctrl Pts',(154.588922861235,-4.90398568483504,131.178669935421));
#32236=CARTESIAN_POINT('Ctrl Pts',(154.581148527116,-4.89360290339115,131.314699174184));
#32237=CARTESIAN_POINT('Ctrl Pts',(154.573374192997,-4.87753951515781,131.450511541849));
#32238=CARTESIAN_POINT('Ctrl Pts',(154.565599858878,-4.85580652262352,131.585594306898));
#32239=CARTESIAN_POINT('Ctrl Pts',(154.557835105931,-4.83410031406017,131.720510594511));
#32240=CARTESIAN_POINT('Ctrl Pts',(154.550070352984,-4.80673846530788,131.854698686293));
#32241=CARTESIAN_POINT('Ctrl Pts',(154.542305600037,-4.7737839004359,131.987648551435));
#32242=CARTESIAN_POINT('Ctrl Pts',(154.534548559152,-4.74086206650237,132.120466368896));
#32243=CARTESIAN_POINT('Ctrl Pts',(154.526791518267,-4.70235866413532,132.252048030097));
#32244=CARTESIAN_POINT('Ctrl Pts',(154.519034477382,-4.65838801035674,132.381891665585));
#32245=CARTESIAN_POINT('Ctrl Pts',(154.511283286142,-4.6144505151903,132.511637384977));
#32246=CARTESIAN_POINT('Ctrl Pts',(154.503532094902,-4.5650540998833,132.639647318632));
#32247=CARTESIAN_POINT('Ctrl Pts',(154.495780903662,-4.51036336211174,132.765433131325));
#32248=CARTESIAN_POINT('Ctrl Pts',(154.488033006885,-4.45569586936251,132.891165481692));
#32249=CARTESIAN_POINT('Ctrl Pts',(154.480285110107,-4.39573868524584,133.014675233456));
#32250=CARTESIAN_POINT('Ctrl Pts',(154.47253721333,-4.33070506497477,133.135492682187));
#32251=CARTESIAN_POINT('Ctrl Pts',(154.464790937246,-4.2656850483351,133.256284858511));
#32252=CARTESIAN_POINT('Ctrl Pts',(154.457044661162,-4.19559089287126,133.37438550794));
#32253=CARTESIAN_POINT('Ctrl Pts',(154.449298385078,-4.12068228794628,133.489348614617));
#32254=CARTESIAN_POINT('Ctrl Pts',(154.441552051813,-4.04577313006293,133.604312569924));
#32255=CARTESIAN_POINT('Ctrl Pts',(154.433805718547,-3.96604966523966,133.7161386087));
#32256=CARTESIAN_POINT('Ctrl Pts',(154.426059385282,-3.881815256472,133.824409189546));
#32257=CARTESIAN_POINT('Ctrl Pts',(154.418311317279,-3.7975619839926,133.932704016839));
#32258=CARTESIAN_POINT('Ctrl Pts',(154.410563249276,-3.70879599742448,134.037441493301));
#32259=CARTESIAN_POINT('Ctrl Pts',(154.402815181273,-3.61586106855026,134.138237009312));
#32260=CARTESIAN_POINT('Ctrl Pts',(154.395058878531,-3.5228273673277,134.239139651998));
#32261=CARTESIAN_POINT('Ctrl Pts',(154.38730257579,-3.42561613823736,134.336091677238));
#32262=CARTESIAN_POINT('Ctrl Pts',(154.379546273048,-3.32460855290637,134.428744845603));
#32263=CARTESIAN_POINT('Ctrl Pts',(154.371785830534,-3.2235470567857,134.521447465754));
#32264=CARTESIAN_POINT('Ctrl Pts',(154.364025388019,-3.11868546576502,134.609846405316));
#32265=CARTESIAN_POINT('Ctrl Pts',(154.356264945505,-3.0104374035875,134.693634290321));
#32266=CARTESIAN_POINT('Ctrl Pts',(154.34849204524,-2.90201557201087,134.777556679077));
#32267=CARTESIAN_POINT('Ctrl Pts',(154.340719144974,-2.79019672498729,134.856852995285));
#32268=CARTESIAN_POINT('Ctrl Pts',(154.332946244709,-2.67542352410029,134.931259214478));
#32269=CARTESIAN_POINT('Ctrl Pts',(154.325455908947,-2.56482261816187,135.002960580185));
#32270=CARTESIAN_POINT('Ctrl Pts',(154.317965573185,-2.45147869058044,135.070121053944));
#32271=CARTESIAN_POINT('Ctrl Pts',(154.310475237423,-2.33580701906053,135.132545991624));
#32272=CARTESIAN_POINT('Ctrl Pts',(154.302700903304,-2.21574962095726,135.197337789789));
#32273=CARTESIAN_POINT('Ctrl Pts',(154.294926569185,-2.09280417592404,135.257233108455));
#32274=CARTESIAN_POINT('Ctrl Pts',(154.287152235066,-1.96740800662316,135.311964060414));
#32275=CARTESIAN_POINT('Ctrl Pts',(154.279387482119,-1.84216637689392,135.366627561367));
#32276=CARTESIAN_POINT('Ctrl Pts',(154.271622729171,-1.71448038727301,135.416139204418));
#32277=CARTESIAN_POINT('Ctrl Pts',(154.263857976224,-1.58481315312012,135.460276245259));
#32278=CARTESIAN_POINT('Ctrl Pts',(154.256100935339,-1.4552747062923,135.504369448569));
#32279=CARTESIAN_POINT('Ctrl Pts',(154.248343894454,-1.32375929865986,135.543098547625));
#32280=CARTESIAN_POINT('Ctrl Pts',(154.240586853569,-1.19075095835084,135.576288447876));
#32281=CARTESIAN_POINT('Ctrl Pts',(154.232835662329,-1.05784292066591,135.609453319365));
#32282=CARTESIAN_POINT('Ctrl Pts',(154.225084471089,-0.923444569003787,
135.637087212145));
#32283=CARTESIAN_POINT('Ctrl Pts',(154.217333279849,-0.788055722685048,
135.659064649785));
#32284=CARTESIAN_POINT('Ctrl Pts',(154.209585383072,-0.652724420237518,
135.681032746428));
#32285=CARTESIAN_POINT('Ctrl Pts',(154.201837486295,-0.516403845549539,
135.697349107077));
#32286=CARTESIAN_POINT('Ctrl Pts',(154.194089589518,-0.379604443913512,
135.707939262664));
#32287=CARTESIAN_POINT('Ctrl Pts',(154.186343313434,-0.242833657763301,
135.718527203019));
#32288=CARTESIAN_POINT('Ctrl Pts',(154.17859703735,-0.105584633441303,135.723391290643));
#32289=CARTESIAN_POINT('Ctrl Pts',(154.170850761266,0.0316270148360211,
135.722508927086));
#32290=CARTESIAN_POINT('Ctrl Pts',(154.163104428,0.168839675978609,135.721626557015));
#32291=CARTESIAN_POINT('Ctrl Pts',(154.155358094735,0.306014569568859,135.714997653635));
#32292=CARTESIAN_POINT('Ctrl Pts',(154.147611761469,0.442636431096155,135.7026517535));
#32293=CARTESIAN_POINT('Ctrl Pts',(154.139863693466,0.579288888141884,135.690303088586));
#32294=CARTESIAN_POINT('Ctrl Pts',(154.132115625464,0.715387677377987,135.672234914485));
#32295=CARTESIAN_POINT('Ctrl Pts',(154.124367557461,0.850423398793978,135.648528565241));
#32296=CARTESIAN_POINT('Ctrl Pts',(154.116611254719,0.985602637781775,135.624797020607));
#32297=CARTESIAN_POINT('Ctrl Pts',(154.108854951977,1.11971616627986,135.595415398235));
#32298=CARTESIAN_POINT('Ctrl Pts',(154.101098649235,1.25226496801818,135.560516156694));
#32299=CARTESIAN_POINT('Ctrl Pts',(154.093338206721,1.38488451504305,135.525598288376));
#32300=CARTESIAN_POINT('Ctrl Pts',(154.085577764207,1.515937297818,135.485157048113));
#32301=CARTESIAN_POINT('Ctrl Pts',(154.077817321692,1.6449411401815,135.439374286137));
#32302=CARTESIAN_POINT('Ctrl Pts',(154.070044421427,1.77415207096519,135.393518029607));
#32303=CARTESIAN_POINT('Ctrl Pts',(154.062271521162,1.90130712572271,135.342303262562));
#32304=CARTESIAN_POINT('Ctrl Pts',(154.054498620896,2.02594490379417,135.285959697057));
#32305=CARTESIAN_POINT('Ctrl Pts',(154.047008285134,2.14605178468941,135.231664362078));
#32306=CARTESIAN_POINT('Ctrl Pts',(154.039517949372,2.26382095478368,135.172606782289));
#32307=CARTESIAN_POINT('Ctrl Pts',(154.03202761361,2.3788641867144,135.109031132677));
#32308=CARTESIAN_POINT('Ctrl Pts',(154.024253279491,2.49826931775002,135.043044992987));
#32309=CARTESIAN_POINT('Ctrl Pts',(154.016478945372,2.61511596181641,134.971982390848));
#32310=CARTESIAN_POINT('Ctrl Pts',(154.008704611253,2.72894235423973,134.896066458623));
#32311=CARTESIAN_POINT('Ctrl Pts',(154.000939858306,2.84262846580737,134.820244085999));
#32312=CARTESIAN_POINT('Ctrl Pts',(153.993175105359,2.95330140964259,134.739580499134));
#32313=CARTESIAN_POINT('Ctrl Pts',(153.985410352411,3.06052345948639,134.654344931357));
#32314=CARTESIAN_POINT('Ctrl Pts',(153.977653311526,3.16763901487864,134.569194020746));
#32315=CARTESIAN_POINT('Ctrl Pts',(153.969896270641,3.27131019304707,134.479480407646));
#32316=CARTESIAN_POINT('Ctrl Pts',(153.962139229756,3.37112805296117,134.385516675746));
#32317=CARTESIAN_POINT('Ctrl Pts',(153.954388038516,3.47087063945059,134.291623802627));
#32318=CARTESIAN_POINT('Ctrl Pts',(153.946636847276,3.56676540801466,134.193487457058));
#32319=CARTESIAN_POINT('Ctrl Pts',(153.938885656036,3.65843662722632,134.091460328112));
#32320=CARTESIAN_POINT('Ctrl Pts',(153.931137759259,3.75006888372446,133.989476563417));
#32321=CARTESIAN_POINT('Ctrl Pts',(153.923389862482,3.83748090047573,133.883605594613));
#32322=CARTESIAN_POINT('Ctrl Pts',(153.915641965705,3.92033411639544,133.77423662143));
#32323=CARTESIAN_POINT('Ctrl Pts',(153.907895689621,4.00317000120849,133.664890525878));
#32324=CARTESIAN_POINT('Ctrl Pts',(153.900149413537,4.08144874602431,133.552048192795));
#32325=CARTESIAN_POINT('Ctrl Pts',(153.892403137453,4.15487263604879,133.436131208008));
#32326=CARTESIAN_POINT('Ctrl Pts',(153.884656804187,4.22829706807172,133.320213367548));
#32327=CARTESIAN_POINT('Ctrl Pts',(153.876910470922,4.29686636458563,133.201221160378));
#32328=CARTESIAN_POINT('Ctrl Pts',(153.869164137657,4.360326862478,133.079604058355));
#32329=CARTESIAN_POINT('Ctrl Pts',(153.861416069654,4.42380157190886,132.957959721025));
#32330=CARTESIAN_POINT('Ctrl Pts',(153.853668001651,4.48216502530064,132.833689665681));
#32331=CARTESIAN_POINT('Ctrl Pts',(153.845919933648,4.53521030813904,132.707266428017));
#32332=CARTESIAN_POINT('Ctrl Pts',(153.838163630906,4.58831196813531,132.580708826232));
#32333=CARTESIAN_POINT('Ctrl Pts',(153.830407328164,4.63608401516158,132.451993831836));
#32334=CARTESIAN_POINT('Ctrl Pts',(153.822651025422,4.67836815987875,132.321612878442));
#32335=CARTESIAN_POINT('Ctrl Pts',(153.814890582908,4.72067487291712,132.191162336807));
#32336=CARTESIAN_POINT('Ctrl Pts',(153.807130140394,4.75748774236063,132.059044440857));
#32337=CARTESIAN_POINT('Ctrl Pts',(153.79936969788,4.78869913596625,131.925763153543));
#32338=CARTESIAN_POINT('Ctrl Pts',(153.791596797614,4.8199606328717,131.792267911275));
#32339=CARTESIAN_POINT('Ctrl Pts',(153.783823897349,4.84560261191078,131.657605929912));
#32340=CARTESIAN_POINT('Ctrl Pts',(153.776050997083,4.86556893801303,131.522289563871));
#32341=CARTESIAN_POINT('Ctrl Pts',(153.768560661321,4.88480943786941,131.391892288577));
#32342=CARTESIAN_POINT('Ctrl Pts',(153.761070325559,4.89877973650338,131.260887685943));
#32343=CARTESIAN_POINT('Ctrl Pts',(153.753579989797,4.90747541887456,131.129734365189));
#32344=CARTESIAN_POINT('Ctrl Pts',(153.745805655678,4.9165008006858,130.993608326416));
#32345=CARTESIAN_POINT('Ctrl Pts',(153.738031321559,4.91987228616429,130.856890863237));
#32346=CARTESIAN_POINT('Ctrl Pts',(153.73025698744,4.91752800780147,130.720091079843));
#32347=CARTESIAN_POINT('Ctrl Pts',(153.722492234493,4.91518661855221,130.583459889955));
#32348=CARTESIAN_POINT('Ctrl Pts',(153.714727481546,4.9071434878911,130.446746968868));
#32349=CARTESIAN_POINT('Ctrl Pts',(153.706962728598,4.89338852770775,130.31046611527));
#32350=CARTESIAN_POINT('Ctrl Pts',(153.699205687713,4.87964722914476,130.174320617737));
#32351=CARTESIAN_POINT('Ctrl Pts',(153.691448646828,4.86020542973101,130.038606720166));
#32352=CARTESIAN_POINT('Ctrl Pts',(153.683691605943,4.83510507236268,129.903837435348));
#32353=CARTESIAN_POINT('Ctrl Pts',(153.675940414703,4.81002364336909,129.769169781096));
#32354=CARTESIAN_POINT('Ctrl Pts',(153.668189223463,4.77929222124466,129.635445704528));
#32355=CARTESIAN_POINT('Ctrl Pts',(153.660438032223,4.74300444128178,129.503171956195));
#32356=CARTESIAN_POINT('Ctrl Pts',(153.652690135446,4.70673208459338,129.370954427733));
#32357=CARTESIAN_POINT('Ctrl Pts',(153.644942238669,4.664908170328,129.240186377722));
#32358=CARTESIAN_POINT('Ctrl Pts',(153.637194341892,4.61767714270585,129.111363019153));
#32359=CARTESIAN_POINT('Ctrl Pts',(153.629448065808,4.5704559947965,128.982566607653));
#32360=CARTESIAN_POINT('Ctrl Pts',(153.621701789724,4.51783011774968,128.855714445311));
#32361=CARTESIAN_POINT('Ctrl Pts',(153.61395551364,4.45999328154526,128.731284885454));
#32362=CARTESIAN_POINT('Ctrl Pts',(153.606209180374,4.40215601840248,128.606854407086));
#32363=CARTESIAN_POINT('Ctrl Pts',(153.598462847109,4.33910788414023,128.484846921424));
#32364=CARTESIAN_POINT('Ctrl Pts',(153.590716513844,4.27108992105236,128.365718792946));
#32365=CARTESIAN_POINT('Ctrl Pts',(153.582968445841,4.20305672581325,128.24656398655));
#32366=CARTESIAN_POINT('Ctrl Pts',(153.575220377838,4.13005168090679,128.130290159894));
#32367=CARTESIAN_POINT('Ctrl Pts',(153.567472309835,4.05236050164516,128.017326813105));
#32368=CARTESIAN_POINT('Ctrl Pts',(153.559716007093,3.97458675127365,127.904243407527));
#32369=CARTESIAN_POINT('Ctrl Pts',(153.551959704351,3.89211713940521,127.79447783288));
#32370=CARTESIAN_POINT('Ctrl Pts',(153.544203401609,3.80527956380148,127.688428894339));
#32371=CARTESIAN_POINT('Ctrl Pts',(153.536442959095,3.71839564036896,127.582323354286));
#32372=CARTESIAN_POINT('Ctrl Pts',(153.528682516581,3.62713936787112,127.479938694708));
#32373=CARTESIAN_POINT('Ctrl Pts',(153.520922074067,3.53187656675667,127.381637873946));
#32374=CARTESIAN_POINT('Ctrl Pts',(153.513149173801,3.43646084133686,127.283179251979));
#32375=CARTESIAN_POINT('Ctrl Pts',(153.505376273536,3.33702601860097,127.188817838566));
#32376=CARTESIAN_POINT('Ctrl Pts',(153.49760337327,3.23397281445536,127.09887780181));
#32377=CARTESIAN_POINT('Ctrl Pts',(153.490113037508,3.13466585385538,127.012207311935));
#32378=CARTESIAN_POINT('Ctrl Pts',(153.482622701746,3.03199925907132,126.929642516345));
#32379=CARTESIAN_POINT('Ctrl Pts',(153.475132365984,2.92635648459142,126.851435019026));
#32380=CARTESIAN_POINT('Ctrl Pts',(153.467358031865,2.816708232208,126.770262260676));
#32381=CARTESIAN_POINT('Ctrl Pts',(153.459583697746,2.70350632864995,126.6935266061));
#32382=CARTESIAN_POINT('Ctrl Pts',(153.451809363627,2.5871456567919,126.621555289435));
#32383=CARTESIAN_POINT('Ctrl Pts',(153.44404461068,2.47092838906247,126.549672670985));
#32384=CARTESIAN_POINT('Ctrl Pts',(153.436279857733,2.35156042805369,126.482542911357));
#32385=CARTESIAN_POINT('Ctrl Pts',(153.428515104785,2.2294685942844,126.420452218706));
#32386=CARTESIAN_POINT('Ctrl Pts',(153.4207580639,2.10749802384572,126.358423195405));
#32387=CARTESIAN_POINT('Ctrl Pts',(153.413001023015,1.98280931072624,126.301423455239));
#32388=CARTESIAN_POINT('Ctrl Pts',(153.40524398213,1.85585673827628,126.249695006405));
#32389=CARTESIAN_POINT('Ctrl Pts',(153.39749279089,1.72899990174875,126.198005566396));
#32390=CARTESIAN_POINT('Ctrl Pts',(153.38974159965,1.59988296455461,126.151579652412));
#32391=CARTESIAN_POINT('Ctrl Pts',(153.38199040841,1.46898288244637,126.110612397478));
#32392=CARTESIAN_POINT('Ctrl Pts',(153.374242511633,1.33813843636481,126.06966255472));
#32393=CARTESIAN_POINT('Ctrl Pts',(153.366494614856,1.20551272508072,126.034166873089));
#32394=CARTESIAN_POINT('Ctrl Pts',(153.358746718079,1.07160046093737,126.004271502287));
#32395=CARTESIAN_POINT('Ctrl Pts',(153.351000441995,0.937716208352806,125.974382384953));
#32396=CARTESIAN_POINT('Ctrl Pts',(153.343254165911,0.802546319532186,125.950091333472));
#32397=CARTESIAN_POINT('Ctrl Pts',(153.335507889826,0.666597984084025,125.931493885332));
#32398=CARTESIAN_POINT('Ctrl Pts',(153.327761556561,0.530648645096227,125.912896299909));
#32399=CARTESIAN_POINT('Ctrl Pts',(153.320015223296,0.393921235372095,125.899992454681));
#32400=CARTESIAN_POINT('Ctrl Pts',(153.31226889003,0.256929996519377,125.892826230087));
#32401=CARTESIAN_POINT('Ctrl Pts',(153.304520822027,0.119908079428549,125.885658400667));
#32402=CARTESIAN_POINT('Ctrl Pts',(153.296772754024,-0.0173773940019696,
125.884230769104));
#32403=CARTESIAN_POINT('Ctrl Pts',(153.289024686021,-0.154410637047434,
125.888535110322));
#32404=CARTESIAN_POINT('Ctrl Pts',(153.28126838328,-0.291589520654324,125.892844026246));
#32405=CARTESIAN_POINT('Ctrl Pts',(153.273512080538,-0.428515246974978,
125.902897072102));
#32406=CARTESIAN_POINT('Ctrl Pts',(153.265755777796,-0.564675053171283,
125.918633942155));
#32407=CARTESIAN_POINT('Ctrl Pts',(153.257995335282,-0.700907531955895,
125.934379211449));
#32408=CARTESIAN_POINT('Ctrl Pts',(153.250234892768,-0.836372890086373,
125.955814288627));
#32409=CARTESIAN_POINT('Ctrl Pts',(153.242474450253,-0.97056802554333,125.982827586434));
#32410=CARTESIAN_POINT('Ctrl Pts',(153.234701549988,-1.10497858294505,126.009884248386));
#32411=CARTESIAN_POINT('Ctrl Pts',(153.226928649722,-1.23811446302291,126.042536932039));
#32412=CARTESIAN_POINT('Ctrl Pts',(153.219155749457,-1.36948633723559,126.08062372453));
#32413=CARTESIAN_POINT('Ctrl Pts',(153.211665413695,-1.49608251291339,126.11732596618));
#32414=CARTESIAN_POINT('Ctrl Pts',(153.204175077933,-1.6210404160491,126.159073991267));
#32415=CARTESIAN_POINT('Ctrl Pts',(153.196684742171,-1.74394109856774,126.20568118677));
#32416=CARTESIAN_POINT('Ctrl Pts',(153.188910182228,-1.87150530312345,126.254056913406));
#32417=CARTESIAN_POINT('Ctrl Pts',(153.181135622284,-1.99725717652517,126.307821103664));
#32418=CARTESIAN_POINT('Ctrl Pts',(153.173361062341,-2.12070792118543,126.366818395173));
#32419=CARTESIAN_POINT('Ctrl Pts',(153.165596135869,-2.24400569780601,126.425742583032));
#32420=CARTESIAN_POINT('Ctrl Pts',(153.157831209397,-2.365007669715,126.489886802918));
#32421=CARTESIAN_POINT('Ctrl Pts',(153.150066282924,-2.48324230409938,126.559046645475));
#32422=CARTESIAN_POINT('Ctrl Pts',(153.142309120592,-2.60135871582199,126.628137335192));
#32423=CARTESIAN_POINT('Ctrl Pts',(153.13455195826,-2.71671296144106,126.702233470816));
#32424=CARTESIAN_POINT('Ctrl Pts',(153.126794795928,-2.82885586166695,126.78108364768));
#32425=CARTESIAN_POINT('Ctrl Pts',(153.119043535151,-2.94091344493543,126.859873836287));
#32426=CARTESIAN_POINT('Ctrl Pts',(153.111292274374,-3.04976422741467,126.943410642797));
#32427=CARTESIAN_POINT('Ctrl Pts',(153.103541013597,-3.15498622263056,127.031398253917));
#32428=CARTESIAN_POINT('Ctrl Pts',(153.095793309482,-3.26015993678443,127.119345491964));
#32429=CARTESIAN_POINT('Ctrl Pts',(153.088045605367,-3.36170787752173,127.211739220715));
#32430=CARTESIAN_POINT('Ctrl Pts',(153.080297901253,-3.4592397120966,127.308242244748));
#32431=CARTESIAN_POINT('Ctrl Pts',(153.072551891767,-3.5567502138597,127.404724160998));
#32432=CARTESIAN_POINT('Ctrl Pts',(153.064805882282,-3.65024607946991,127.505313309501));
#32433=CARTESIAN_POINT('Ctrl Pts',(153.057059872797,-3.73937282004578,127.609634655108));
#32434=CARTESIAN_POINT('Ctrl Pts',(153.049313880113,-3.82849936729201,127.713955774426));
#32435=CARTESIAN_POINT('Ctrl Pts',(153.04156788743,-3.91325655476401,127.822008777284));
#32436=CARTESIAN_POINT('Ctrl Pts',(153.033821894747,-3.99332954576843,127.933384790187));
#32437=CARTESIAN_POINT('Ctrl Pts',(153.026074241422,-4.07341970340675,128.044784680696));
#32438=CARTESIAN_POINT('Ctrl Pts',(153.018326588096,-4.14882343868998,128.159508681186));
#32439=CARTESIAN_POINT('Ctrl Pts',(153.01057893477,-4.21926891751633,128.277118471633));
#32440=CARTESIAN_POINT('Ctrl Pts',(153.002824048872,-4.28978015845497,128.394838052919));
#32441=CARTESIAN_POINT('Ctrl Pts',(152.995069162973,-4.35532369948918,128.515448467746));
#32442=CARTESIAN_POINT('Ctrl Pts',(152.987314277075,-4.4156732325677,128.638485975375));
#32443=CARTESIAN_POINT('Ctrl Pts',(152.979555281955,-4.47605474414673,128.761588679118));
#32444=CARTESIAN_POINT('Ctrl Pts',(152.971796286834,-4.53123660676934,128.887120680812));
#32445=CARTESIAN_POINT('Ctrl Pts',(152.964037291714,-4.5810408449334,129.01459866704));
#32446=CARTESIAN_POINT('Ctrl Pts',(152.956268153135,-4.63091019297496,129.142243307279));
#32447=CARTESIAN_POINT('Ctrl Pts',(152.948499014556,-4.67538775094528,129.271838643228));
#32448=CARTESIAN_POINT('Ctrl Pts',(152.940729875978,-4.71434539745154,129.40288620252));
#32449=CARTESIAN_POINT('Ctrl Pts',(152.93719746275,-4.73205836580928,129.462469916612));
#32450=CARTESIAN_POINT('Ctrl Pts',(152.933665049523,-4.74863091835531,129.522353698477));
#32451=CARTESIAN_POINT('Ctrl Pts',(152.930132636296,-4.76405452823406,129.582490119308));
#32452=CARTESIAN_POINT('Origin',(213.235140564004,0.,130.804360617566));
#32453=CARTESIAN_POINT('',(150.83493632599,-4.76405452823404,129.582490119308));
#32454=CARTESIAN_POINT('',(151.179859891219,-4.76405452823403,129.582490119308));
#32455=CARTESIAN_POINT('',(213.235140564004,-4.76405452823405,129.582490119308));
#32456=CARTESIAN_POINT('',(152.514859435946,-4.91824997270806,130.804878746085));
#32457=CARTESIAN_POINT('Ctrl Pts',(152.514859435946,-4.91824997270806,130.804878746085));
#32458=CARTESIAN_POINT('Ctrl Pts',(152.506677763759,-4.91823466848991,130.95015152646));
#32459=CARTESIAN_POINT('Ctrl Pts',(152.498496091571,-4.91177859513664,131.095278734219));
#32460=CARTESIAN_POINT('Ctrl Pts',(152.490314419384,-4.89894595758979,131.23968988044));
#32461=CARTESIAN_POINT('Ctrl Pts',(152.482119495279,-4.88609253492128,131.384334930505));
#32462=CARTESIAN_POINT('Ctrl Pts',(152.473924571174,-4.8668419583285,131.528261284787));
#32463=CARTESIAN_POINT('Ctrl Pts',(152.465729647069,-4.84130974263598,131.670907233945));
#32464=CARTESIAN_POINT('Ctrl Pts',(152.457513011982,-4.81570988391617,131.813931097968));
#32465=CARTESIAN_POINT('Ctrl Pts',(152.449296376895,-4.78379516239512,131.95566745651));
#32466=CARTESIAN_POINT('Ctrl Pts',(152.441079741808,-4.74573183950992,132.095566398982));
#32467=CARTESIAN_POINT('Ctrl Pts',(152.432851336312,-4.70761399054798,132.235665748037));
#32468=CARTESIAN_POINT('Ctrl Pts',(152.424622930817,-4.66333005474041,132.373922121759));
#32469=CARTESIAN_POINT('Ctrl Pts',(152.416394525321,-4.6130950350023,132.509804038069));
#32470=CARTESIAN_POINT('Ctrl Pts',(152.408146922173,-4.56274281218702,132.646002979809));
#32471=CARTESIAN_POINT('Ctrl Pts',(152.399899319025,-4.50641186754353,132.779816091296));
#32472=CARTESIAN_POINT('Ctrl Pts',(152.391651715877,-4.44436463416552,132.910733343623));
#32473=CARTESIAN_POINT('Ctrl Pts',(152.388078099548,-4.41748009542755,132.967458676085));
#32474=CARTESIAN_POINT('Ctrl Pts',(152.38450448322,-4.3895229399061,133.023640680006));
#32475=CARTESIAN_POINT('Ctrl Pts',(152.380930866891,-4.36051705758569,133.079239527092));
#32476=CARTESIAN_POINT('Ctrl Pts',(152.373156532772,-4.29741531418191,133.200193757808));
#32477=CARTESIAN_POINT('Ctrl Pts',(152.365382198653,-4.22917717359203,133.318712059438));
#32478=CARTESIAN_POINT('Ctrl Pts',(152.357607864534,-4.15601462284397,133.434327445723));
#32479=CARTESIAN_POINT('Ctrl Pts',(152.349843111587,-4.08294223840114,133.549800346377));
#32480=CARTESIAN_POINT('Ctrl Pts',(152.34207835864,-4.00495772614946,133.662377122809));
#32481=CARTESIAN_POINT('Ctrl Pts',(152.334313605693,-3.92231973766197,133.771613713958));
#32482=CARTESIAN_POINT('Ctrl Pts',(152.326556564808,-3.83976382638955,133.880741809784));
#32483=CARTESIAN_POINT('Ctrl Pts',(152.318799523923,-3.75256387101605,133.986536012562));
#32484=CARTESIAN_POINT('Ctrl Pts',(152.311042483038,-3.661022551759,134.088579997877));
#32485=CARTESIAN_POINT('Ctrl Pts',(152.303291291798,-3.56955026452293,134.19054703103));
#32486=CARTESIAN_POINT('Ctrl Pts',(152.295540100558,-3.47374338983093,134.288769185972));
#32487=CARTESIAN_POINT('Ctrl Pts',(152.287788909318,-3.37394549867287,134.382862375912));
#32488=CARTESIAN_POINT('Ctrl Pts',(152.280041012541,-3.27419002428064,134.476915573737));
#32489=CARTESIAN_POINT('Ctrl Pts',(152.272293115763,-3.17044719108015,134.56684302932));
#32490=CARTESIAN_POINT('Ctrl Pts',(152.264545218986,-3.06309796218986,134.652296939353));
#32491=CARTESIAN_POINT('Ctrl Pts',(152.256798942902,-2.95577118844407,134.737732974271));
#32492=CARTESIAN_POINT('Ctrl Pts',(152.249052666818,-2.84483982520137,134.818697081595));
#32493=CARTESIAN_POINT('Ctrl Pts',(152.241306390734,-2.73071819255062,134.89488151537));
#32494=CARTESIAN_POINT('Ctrl Pts',(152.233560057469,-2.61659571748002,134.971066511521));
#32495=CARTESIAN_POINT('Ctrl Pts',(152.225813724203,-2.49928325117612,135.042471546646));
#32496=CARTESIAN_POINT('Ctrl Pts',(152.218067390938,-2.37922404884293,135.108832244596));
#32497=CARTESIAN_POINT('Ctrl Pts',(152.210319322935,-2.25913796008374,135.175207803564));
#32498=CARTESIAN_POINT('Ctrl Pts',(152.202571254932,-2.13630425340141,135.236536588402));
#32499=CARTESIAN_POINT('Ctrl Pts',(152.194823186929,-2.01119036303242,135.292600404626));
#32500=CARTESIAN_POINT('Ctrl Pts',(152.187066884187,-1.88594350013187,135.348723806141));
#32501=CARTESIAN_POINT('Ctrl Pts',(152.179310581445,-1.75841196988084,135.399570900957));
#32502=CARTESIAN_POINT('Ctrl Pts',(152.171554278703,-1.62908326586283,135.444971652267));
#32503=CARTESIAN_POINT('Ctrl Pts',(152.163793836189,-1.49968553522143,135.490396635324));
#32504=CARTESIAN_POINT('Ctrl Pts',(152.156033393675,-1.36848909332313,135.530369368785));
#32505=CARTESIAN_POINT('Ctrl Pts',(152.148272951161,-1.23599517511472,135.564770157678));
#32506=CARTESIAN_POINT('Ctrl Pts',(152.140500050895,-1.10328856590655,135.599226169773));
#32507=CARTESIAN_POINT('Ctrl Pts',(152.13272715063,-0.96928070066067,135.628092280804));
#32508=CARTESIAN_POINT('Ctrl Pts',(152.124954250364,-0.834482439163498,
135.651300076774));
#32509=CARTESIAN_POINT('Ctrl Pts',(152.117463914602,-0.70458443400849,135.673664210904));
#32510=CARTESIAN_POINT('Ctrl Pts',(152.10997357884,-0.573952806110955,135.69077423568));
#32511=CARTESIAN_POINT('Ctrl Pts',(152.102483243078,-0.44304592667414,135.702614731978));
#32512=CARTESIAN_POINT('Ctrl Pts',(152.094708908959,-0.307175673114855,
135.714904164292));
#32513=CARTESIAN_POINT('Ctrl Pts',(152.08693457484,-0.170578487542805,135.721555521011));
#32514=CARTESIAN_POINT('Ctrl Pts',(152.079160240721,-0.0337618428896808,
135.722494735345));
#32515=CARTESIAN_POINT('Ctrl Pts',(152.071395487774,0.102886187476517,135.723432792182));
#32516=CARTESIAN_POINT('Ctrl Pts',(152.063630734827,0.239752751578779,135.718672710891));
#32517=CARTESIAN_POINT('Ctrl Pts',(152.05586598188,0.376324440775884,135.708192076515));
#32518=CARTESIAN_POINT('Ctrl Pts',(152.048108940995,0.512760485045863,135.697721851652));
#32519=CARTESIAN_POINT('Ctrl Pts',(152.04035190011,0.648901849946454,135.681542410334));
#32520=CARTESIAN_POINT('Ctrl Pts',(152.032594859225,0.784234663907718,135.659683372484));
#32521=CARTESIAN_POINT('Ctrl Pts',(152.024843667985,0.919465422341192,135.637840818705));
#32522=CARTESIAN_POINT('Ctrl Pts',(152.017092476745,1.05388845907374,135.61032725559));
#32523=CARTESIAN_POINT('Ctrl Pts',(152.009341285505,1.186994922498,135.577224130853));
#32524=CARTESIAN_POINT('Ctrl Pts',(152.001593388727,1.32004481212471,135.544135075826));
#32525=CARTESIAN_POINT('Ctrl Pts',(151.99384549195,1.45177886278894,135.505461278448));
#32526=CARTESIAN_POINT('Ctrl Pts',(151.986097595173,1.5816985378464,135.461335257595));
#32527=CARTESIAN_POINT('Ctrl Pts',(151.978351319089,1.71159103650858,135.417218466955));
#32528=CARTESIAN_POINT('Ctrl Pts',(151.970605043005,1.83966954450535,135.367651846987));
#32529=CARTESIAN_POINT('Ctrl Pts',(151.962858766921,1.96545119631883,135.312817632709));
#32530=CARTESIAN_POINT('Ctrl Pts',(151.955112433656,2.0912337766239,135.257983013657));
#32531=CARTESIAN_POINT('Ctrl Pts',(151.94736610039,2.21471910852384,135.197880878944));
#32532=CARTESIAN_POINT('Ctrl Pts',(151.939619767125,2.33544517461206,135.13274124996));
#32533=CARTESIAN_POINT('Ctrl Pts',(151.931871699122,2.45619827646565,135.067587033408));
#32534=CARTESIAN_POINT('Ctrl Pts',(151.924123631119,2.57419053891233,134.997393263388));
#32535=CARTESIAN_POINT('Ctrl Pts',(151.916375563116,2.68898572913251,134.922435266115));
#32536=CARTESIAN_POINT('Ctrl Pts',(151.908619260374,2.80390292504701,134.847397602591));
#32537=CARTESIAN_POINT('Ctrl Pts',(151.900862957633,2.91561593321185,134.767585811067));
#32538=CARTESIAN_POINT('Ctrl Pts',(151.893106654891,3.02371819465574,134.683318124656));
#32539=CARTESIAN_POINT('Ctrl Pts',(151.885346212377,3.13187815353146,134.599005462043));
#32540=CARTESIAN_POINT('Ctrl Pts',(151.877585769862,3.23642322777542,134.510232418621));
#32541=CARTESIAN_POINT('Ctrl Pts',(151.869825327348,3.33698178488827,134.417355999493));
#32542=CARTESIAN_POINT('Ctrl Pts',(151.862052427083,3.4377017675242,134.324330486891));
#32543=CARTESIAN_POINT('Ctrl Pts',(151.854279526817,3.53442216875508,134.227188712666));
#32544=CARTESIAN_POINT('Ctrl Pts',(151.846506626552,3.62680929775357,134.126323498188));
#32545=CARTESIAN_POINT('Ctrl Pts',(151.83901629079,3.71583792190436,134.029124988319));
#32546=CARTESIAN_POINT('Ctrl Pts',(151.831525955028,3.80084265606436,133.928469286415));
#32547=CARTESIAN_POINT('Ctrl Pts',(151.824035619266,3.88156276685469,133.824733698738));
#32548=CARTESIAN_POINT('Ctrl Pts',(151.816261285147,3.96534340517948,133.717064944725));
#32549=CARTESIAN_POINT('Ctrl Pts',(151.808486951028,4.04477349533657,133.605737084644));
#32550=CARTESIAN_POINT('Ctrl Pts',(151.800712616909,4.11951642132331,133.491137034938));
#32551=CARTESIAN_POINT('Ctrl Pts',(151.792947863962,4.19416723333374,133.376678219551));
#32552=CARTESIAN_POINT('Ctrl Pts',(151.785183111014,4.26414216317996,133.2589555627));
#32553=CARTESIAN_POINT('Ctrl Pts',(151.777418358067,4.32914484261244,133.138388893783));
#32554=CARTESIAN_POINT('Ctrl Pts',(151.769661317182,4.39408296046729,133.017941973382));
#32555=CARTESIAN_POINT('Ctrl Pts',(151.761904276297,4.45405847142686,132.89465700413));
#32556=CARTESIAN_POINT('Ctrl Pts',(151.754147235412,4.50881853543756,132.768982331025));
#32557=CARTESIAN_POINT('Ctrl Pts',(151.746396044172,4.56353730445802,132.643402430169));
#32558=CARTESIAN_POINT('Ctrl Pts',(151.738644852932,4.61304829940446,132.515436769388));
#32559=CARTESIAN_POINT('Ctrl Pts',(151.730893661692,4.65714499782038,132.385557484429));
#32560=CARTESIAN_POINT('Ctrl Pts',(151.723145764915,4.70122295396318,132.25573340163));
#32561=CARTESIAN_POINT('Ctrl Pts',(151.715397868138,4.73989106509696,132.123997681761));
#32562=CARTESIAN_POINT('Ctrl Pts',(151.707649971361,4.77299135187286,131.99084138751));
#32563=CARTESIAN_POINT('Ctrl Pts',(151.699903695277,4.80608471478233,131.857712946685));
#32564=CARTESIAN_POINT('Ctrl Pts',(151.692157419193,4.83361247566719,131.723164901711));
#32565=CARTESIAN_POINT('Ctrl Pts',(151.684411143109,4.85546695340222,131.587702003501));
#32566=CARTESIAN_POINT('Ctrl Pts',(151.676664809843,4.87732159246204,131.452238105335));
#32567=CARTESIAN_POINT('Ctrl Pts',(151.668918476578,4.89350280253579,131.315859726433));
#32568=CARTESIAN_POINT('Ctrl Pts',(151.661172143312,4.90395437544017,131.179079907303));
#32569=CARTESIAN_POINT('Ctrl Pts',(151.653424075309,4.91440828890183,131.042269457282));
#32570=CARTESIAN_POINT('Ctrl Pts',(151.645676007307,4.91912998216698,130.905057777897));
#32571=CARTESIAN_POINT('Ctrl Pts',(151.637927939304,4.91811530048297,130.767960704719));
#32572=CARTESIAN_POINT('Ctrl Pts',(151.630171636562,4.91709954038319,130.63071792314));
#32573=CARTESIAN_POINT('Ctrl Pts',(151.62241533382,4.91033522944226,130.493590382665));
#32574=CARTESIAN_POINT('Ctrl Pts',(151.614659031078,4.89787035113423,130.357092145639));
#32575=CARTESIAN_POINT('Ctrl Pts',(151.606898588564,4.88539881994532,130.220521055394));
#32576=CARTESIAN_POINT('Ctrl Pts',(151.59913814605,4.86722071061565,130.08458032519));
#32577=CARTESIAN_POINT('Ctrl Pts',(151.591377703535,4.84343550520494,129.949775589953));
#32578=CARTESIAN_POINT('Ctrl Pts',(151.58360480327,4.81961211767097,129.814754454188));
#32579=CARTESIAN_POINT('Ctrl Pts',(151.575831903005,4.79016373121001,129.68087333958));
#32580=CARTESIAN_POINT('Ctrl Pts',(151.568059002739,4.75524046952243,129.548625319218));
#32581=CARTESIAN_POINT('Ctrl Pts',(151.560568666977,4.72158675636345,129.421184847509));
#32582=CARTESIAN_POINT('Ctrl Pts',(151.553078331215,4.68284939880394,129.29526109167));
#32583=CARTESIAN_POINT('Ctrl Pts',(151.545587995453,4.63920490252708,129.171277357328));
#32584=CARTESIAN_POINT('Ctrl Pts',(151.537813661334,4.59390561190859,129.042592742015));
#32585=CARTESIAN_POINT('Ctrl Pts',(151.530039327215,4.54317623417197,128.915590529881));
#32586=CARTESIAN_POINT('Ctrl Pts',(151.522264993096,4.48716034390543,128.790763063291));
#32587=CARTESIAN_POINT('Ctrl Pts',(151.514500240149,4.43121348821737,128.666089435397));
#32588=CARTESIAN_POINT('Ctrl Pts',(151.506735487202,4.3699932417442,128.543585573561));
#32589=CARTESIAN_POINT('Ctrl Pts',(151.498970734254,4.30369262457101,128.423727748829));
#32590=CARTESIAN_POINT('Ctrl Pts',(151.491213693369,4.23745785810548,128.303988968578));
#32591=CARTESIAN_POINT('Ctrl Pts',(151.483456652484,4.16615295051874,128.186891335329));
#32592=CARTESIAN_POINT('Ctrl Pts',(151.475699611599,4.09001844093084,128.072889912004));
#32593=CARTESIAN_POINT('Ctrl Pts',(151.467948420359,4.01394134496887,127.958974458038));
#32594=CARTESIAN_POINT('Ctrl Pts',(151.460197229119,3.9330421125199,127.848150890379));
#32595=CARTESIAN_POINT('Ctrl Pts',(151.452446037879,3.84760633432665,127.740848163119));
#32596=CARTESIAN_POINT('Ctrl Pts',(151.444698141102,3.76220686861815,127.633591042382));
#32597=CARTESIAN_POINT('Ctrl Pts',(151.436950244325,3.67227493513176,127.529852090934));
#32598=CARTESIAN_POINT('Ctrl Pts',(151.429202347548,3.57813828711793,127.430029652654));
#32599=CARTESIAN_POINT('Ctrl Pts',(151.421456071464,3.48402133046152,127.330228095077));
#32600=CARTESIAN_POINT('Ctrl Pts',(151.41370979538,3.38570167678715,127.234341705391));
#32601=CARTESIAN_POINT('Ctrl Pts',(151.405963519296,3.28354578305581,127.142733908974));
#32602=CARTESIAN_POINT('Ctrl Pts',(151.39821718603,3.1813891352329,127.051125436329));
#32603=CARTESIAN_POINT('Ctrl Pts',(151.390470852765,3.07539648191876,126.963795880994));
#32604=CARTESIAN_POINT('Ctrl Pts',(151.382724519499,2.96596907672791,126.881069843433));
#32605=CARTESIAN_POINT('Ctrl Pts',(151.374976451496,2.85651716602838,126.79832527995));
#32606=CARTESIAN_POINT('Ctrl Pts',(151.367228383494,2.74362928466882,126.720186521392));
#32607=CARTESIAN_POINT('Ctrl Pts',(151.359480315491,2.62773717397821,126.646935884995));
#32608=CARTESIAN_POINT('Ctrl Pts',(151.351724012749,2.51172189177319,126.57360739695));
#32609=CARTESIAN_POINT('Ctrl Pts',(151.343967710007,2.39269633302623,126.505177618167));
#32610=CARTESIAN_POINT('Ctrl Pts',(151.336211407265,2.27111892918819,126.441884042043));
#32611=CARTESIAN_POINT('Ctrl Pts',(151.328450964751,2.14947663582905,126.378556684233));
#32612=CARTESIAN_POINT('Ctrl Pts',(151.320690522237,2.02528013734966,126.320371157231));
#32613=CARTESIAN_POINT('Ctrl Pts',(151.312930079722,1.89900861121593,126.267517071991));
#32614=CARTESIAN_POINT('Ctrl Pts',(151.305157179457,1.77253438281858,126.214578140681));
#32615=CARTESIAN_POINT('Ctrl Pts',(151.297384279192,1.64397883718975,126.166987889558));
#32616=CARTESIAN_POINT('Ctrl Pts',(151.289611378926,1.5138379562108,126.124886533351));
#32617=CARTESIAN_POINT('Ctrl Pts',(151.282121043164,1.38842802406032,126.08431566749));
#32618=CARTESIAN_POINT('Ctrl Pts',(151.274630707402,1.26154631395382,126.048841637614));
#32619=CARTESIAN_POINT('Ctrl Pts',(151.26714037164,1.13364437053645,126.018544751525));
#32620=CARTESIAN_POINT('Ctrl Pts',(151.259366037521,1.00089298605965,125.987099149791));
#32621=CARTESIAN_POINT('Ctrl Pts',(151.251591703402,0.866621960301331,125.961131414152));
#32622=CARTESIAN_POINT('Ctrl Pts',(151.243817369283,0.731323120408024,125.940786874313));
#32623=CARTESIAN_POINT('Ctrl Pts',(151.236052616336,0.596191024243065,125.920467407302));
#32624=CARTESIAN_POINT('Ctrl Pts',(151.228287863389,0.460034017184144,125.905757404861));
#32625=CARTESIAN_POINT('Ctrl Pts',(151.220523110442,0.323357131622324,125.896751909862));
#32626=CARTESIAN_POINT('Ctrl Pts',(151.212766069557,0.186815995470143,125.887755359248));
#32627=CARTESIAN_POINT('Ctrl Pts',(151.205009028672,0.0497563959710257,
125.884452066421));
#32628=CARTESIAN_POINT('Ctrl Pts',(151.197251987787,-0.0873087922816362,
125.886885631632));
#32629=CARTESIAN_POINT('Ctrl Pts',(151.189500796546,-0.224270618609951,
125.889317361672));
#32630=CARTESIAN_POINT('Ctrl Pts',(151.181749605306,-0.361237635981154,
125.89747733178));
#32631=CARTESIAN_POINT('Ctrl Pts',(151.173998414066,-0.497694584393988,
125.911357126543));
#32632=CARTESIAN_POINT('Ctrl Pts',(151.166250517289,-0.634093534963498,
125.925231022022));
#32633=CARTESIAN_POINT('Ctrl Pts',(151.158502620512,-0.769982459615248,
125.944819867447));
#32634=CARTESIAN_POINT('Ctrl Pts',(151.150754723735,-0.904849061725005,
125.970063229321));
#32635=CARTESIAN_POINT('Ctrl Pts',(151.143008447651,-1.03968745264899,125.995301310827));
#32636=CARTESIAN_POINT('Ctrl Pts',(151.135262171567,-1.17350356233794,126.02619148424));
#32637=CARTESIAN_POINT('Ctrl Pts',(151.127515895483,-1.30579355178939,126.062621879233));
#32638=CARTESIAN_POINT('Ctrl Pts',(151.119769562217,-1.43808451777555,126.099052543147));
#32639=CARTESIAN_POINT('Ctrl Pts',(151.112023228952,-1.56884896411093,126.141023406447));
#32640=CARTESIAN_POINT('Ctrl Pts',(151.104276895686,-1.69759690785262,126.188372337582));
#32641=CARTESIAN_POINT('Ctrl Pts',(151.096528827684,-1.82637368380359,126.235731872182));
#32642=CARTESIAN_POINT('Ctrl Pts',(151.088780759681,-1.95313269169805,126.288471736274));
#32643=CARTESIAN_POINT('Ctrl Pts',(151.081032691678,-2.07740304331496,126.346381293015));
#32644=CARTESIAN_POINT('Ctrl Pts',(151.073276388936,-2.20180547094041,126.404352396721));
#32645=CARTESIAN_POINT('Ctrl Pts',(151.065520086194,-2.32371360372672,126.467504003351));
#32646=CARTESIAN_POINT('Ctrl Pts',(151.057763783452,-2.44267983835396,126.535578792525));
#32647=CARTESIAN_POINT('Ctrl Pts',(151.050003340938,-2.56170956884274,126.603689915264));
#32648=CARTESIAN_POINT('Ctrl Pts',(151.042242898424,-2.67779394170561,126.676729248257));
#32649=CARTESIAN_POINT('Ctrl Pts',(151.034482455909,-2.79051442475252,126.754396135284));
#32650=CARTESIAN_POINT('Ctrl Pts',(151.026709555644,-2.90341585672563,126.832187700092));
#32651=CARTESIAN_POINT('Ctrl Pts',(151.018936655379,-3.012942295377,126.914621428324));
#32652=CARTESIAN_POINT('Ctrl Pts',(151.011163755113,-3.11870768376315,127.00135582586));
#32653=CARTESIAN_POINT('Ctrl Pts',(151.003673419351,-3.22062823387432,127.084937209575));
#32654=CARTESIAN_POINT('Ctrl Pts',(150.996183083589,-3.31905620345581,127.172511806115));
#32655=CARTESIAN_POINT('Ctrl Pts',(150.988692747827,-3.4136799563702,127.263743126509));
#32656=CARTESIAN_POINT('Ctrl Pts',(150.981032940029,-3.51044461198812,127.357038594377));
#32657=CARTESIAN_POINT('Ctrl Pts',(150.973373132231,-3.6035565650681,127.454472638766));
#32658=CARTESIAN_POINT('Ctrl Pts',(150.965713324432,-3.69263305694419,127.555723338758));
#32659=CARTESIAN_POINT('Ctrl Pts',(150.958062429611,-3.78160589912683,127.656856223108));
#32660=CARTESIAN_POINT('Ctrl Pts',(150.95041153479,-3.86655235126987,127.761796635112));
#32661=CARTESIAN_POINT('Ctrl Pts',(150.942760639969,-3.94712422251413,127.87018382764));
#32662=CARTESIAN_POINT('Ctrl Pts',(150.93511687513,-4.02762100763716,127.978470012536));
#32663=CARTESIAN_POINT('Ctrl Pts',(150.927473110291,-4.10375107923227,128.090196269446));
#32664=CARTESIAN_POINT('Ctrl Pts',(150.919829345452,-4.17520488840337,128.204966995516));
#32665=CARTESIAN_POINT('Ctrl Pts',(150.912191096375,-4.24660713631114,128.319654902718));
#32666=CARTESIAN_POINT('Ctrl Pts',(150.904552847297,-4.31333962266588,128.4373825674));
#32667=CARTESIAN_POINT('Ctrl Pts',(150.89691459822,-4.37513506165698,128.557723963641));
#32668=CARTESIAN_POINT('Ctrl Pts',(150.889279639307,-4.43690388236004,128.678013523015));
#32669=CARTESIAN_POINT('Ctrl Pts',(150.881644680393,-4.49373970237022,128.80091421611));
#32670=CARTESIAN_POINT('Ctrl Pts',(150.874009721479,-4.54542054193341,128.925974299614));
#32671=CARTESIAN_POINT('Ctrl Pts',(150.866374930831,-4.59710024251206,129.051031626941));
#32672=CARTESIAN_POINT('Ctrl Pts',(150.858740140183,-4.64362502598018,129.178247880934));
#32673=CARTESIAN_POINT('Ctrl Pts',(150.851105349535,-4.68482067447721,129.307150441775));
#32674=CARTESIAN_POINT('Ctrl Pts',(150.84571567502,-4.71390217088837,129.398147415904));
#32675=CARTESIAN_POINT('Ctrl Pts',(150.840326000505,-4.74032891330032,129.489984306768));
#32676=CARTESIAN_POINT('Ctrl Pts',(150.83493632599,-4.76405452823404,129.582490119308));
#32677=CARTESIAN_POINT('Ctrl Pts',(152.584590056215,-4.76405452823404,129.582490119308));
#32678=CARTESIAN_POINT('Ctrl Pts',(152.576521756221,-4.79947459936531,129.720592439074));
#32679=CARTESIAN_POINT('Ctrl Pts',(152.568453456227,-4.82892004477874,129.860370932365));
#32680=CARTESIAN_POINT('Ctrl Pts',(152.560385156233,-4.85224291862247,130.0012904331));
#32681=CARTESIAN_POINT('Ctrl Pts',(152.552329006894,-4.87553066881171,130.141997712653));
#32682=CARTESIAN_POINT('Ctrl Pts',(152.544272857554,-4.89271417596742,130.283842236169));
#32683=CARTESIAN_POINT('Ctrl Pts',(152.536216708215,-4.90369615824396,130.42627722713));
#32684=CARTESIAN_POINT('Ctrl Pts',(152.529097617474,-4.91340076090857,130.552144757965));
#32685=CARTESIAN_POINT('Ctrl Pts',(152.521978526732,-4.91826328929538,130.678473032375));
#32686=CARTESIAN_POINT('Ctrl Pts',(152.514859435991,-4.91824997270814,130.804878745294));
#32687=CARTESIAN_POINT('',(152.860140563967,-4.91824798336883,130.799906789047));
#32688=CARTESIAN_POINT('Ctrl Pts',(152.930132636296,-4.76405452823406,129.582490119308));
#32689=CARTESIAN_POINT('Ctrl Pts',(152.92616746365,-4.78136769973006,129.649993912207));
#32690=CARTESIAN_POINT('Ctrl Pts',(152.922202291004,-4.79723310715757,129.7178160321));
#32691=CARTESIAN_POINT('Ctrl Pts',(152.918237118358,-4.81164200840415,129.785889093438));
#32692=CARTESIAN_POINT('Ctrl Pts',(152.907308734836,-4.85135427644649,129.973504763228));
#32693=CARTESIAN_POINT('Ctrl Pts',(152.896380351314,-4.88010455357513,130.163515281877));
#32694=CARTESIAN_POINT('Ctrl Pts',(152.885451967792,-4.89766574652585,130.354857227359));
#32695=CARTESIAN_POINT('Ctrl Pts',(152.877014833197,-4.9112236664385,130.502580606975));
#32696=CARTESIAN_POINT('Ctrl Pts',(152.868577698603,-4.91811322570068,130.651097395188));
#32697=CARTESIAN_POINT('Ctrl Pts',(152.860140564008,-4.91824798336817,130.799906788326));
#32698=CARTESIAN_POINT('Ctrl Pts',(152.860140563967,-4.91824798336883,130.799906789047));
#32699=CARTESIAN_POINT('Ctrl Pts',(152.85249111539,-4.91837016011845,130.934823423101));
#32700=CARTESIAN_POINT('Ctrl Pts',(152.844841666814,-4.91293664648777,131.069915127919));
#32701=CARTESIAN_POINT('Ctrl Pts',(152.837192218237,-4.90193101268551,131.204679751972));
#32702=CARTESIAN_POINT('Ctrl Pts',(152.82954893775,-4.89093425321401,131.339335709331));
#32703=CARTESIAN_POINT('Ctrl Pts',(152.821905657263,-4.87437434403013,131.473664710837));
#32704=CARTESIAN_POINT('Ctrl Pts',(152.814262376776,-4.85228692064385,131.607164891501));
#32705=CARTESIAN_POINT('Ctrl Pts',(152.806622729055,-4.83020999516479,131.740601621011));
#32706=CARTESIAN_POINT('Ctrl Pts',(152.798983081334,-4.80261084430478,131.873209916207));
#32707=CARTESIAN_POINT('Ctrl Pts',(152.791343433614,-4.76957687614594,132.004493728947));
#32708=CARTESIAN_POINT('Ctrl Pts',(152.783705522536,-4.73655041726043,132.135747698284));
#32709=CARTESIAN_POINT('Ctrl Pts',(152.776067611458,-4.69809169541259,132.265677393132));
#32710=CARTESIAN_POINT('Ctrl Pts',(152.76842970038,-4.65433897773422,132.393798173069));
#32711=CARTESIAN_POINT('Ctrl Pts',(152.760791762406,-4.61058610598386,132.521919404174));
#32712=CARTESIAN_POINT('Ctrl Pts',(152.753153824432,-4.56153933179913,132.648231326355));
#32713=CARTESIAN_POINT('Ctrl Pts',(152.745515886457,-4.5073862417989,132.772266186881));
#32714=CARTESIAN_POINT('Ctrl Pts',(152.737876158235,-4.45322045891165,132.89633011981));
#32715=CARTESIAN_POINT('Ctrl Pts',(152.730236430012,-4.39394614191575,133.018115560744));
#32716=CARTESIAN_POINT('Ctrl Pts',(152.722596701789,-4.32979805238567,133.137176917247));
#32717=CARTESIAN_POINT('Ctrl Pts',(152.714949039957,-4.26558334714713,133.256361915103));
#32718=CARTESIAN_POINT('Ctrl Pts',(152.707301378124,-4.19648495599278,133.372816825593));
#32719=CARTESIAN_POINT('Ctrl Pts',(152.699653716292,-4.12278258597115,133.486122503214));
#32720=CARTESIAN_POINT('Ctrl Pts',(152.692001702043,-4.04903827065087,133.599492665063));
#32721=CARTESIAN_POINT('Ctrl Pts',(152.684349687793,-3.97068499342522,133.709709698357));
#32722=CARTESIAN_POINT('Ctrl Pts',(152.676697673543,-3.88804361829641,133.816386494733));
#32723=CARTESIAN_POINT('Ctrl Pts',(152.669034281977,-3.80527936870936,133.92322190238));
#32724=CARTESIAN_POINT('Ctrl Pts',(152.661370890411,-3.71821455089191,134.026506256536));
#32725=CARTESIAN_POINT('Ctrl Pts',(152.653707498844,-3.62720812907893,134.12588801484));
#32726=CARTESIAN_POINT('Ctrl Pts',(152.649068164078,-3.57211382089796,134.186052661582));
#32727=CARTESIAN_POINT('Ctrl Pts',(152.644428829312,-3.51557562191086,134.244787764669));
#32728=CARTESIAN_POINT('Ctrl Pts',(152.639789494546,-3.45767897429468,134.302022575678));
#32729=CARTESIAN_POINT('Ctrl Pts',(152.632015160426,-3.36065905535762,134.397933426358));
#32730=CARTESIAN_POINT('Ctrl Pts',(152.624240826307,-3.2594918038901,134.489956352213));
#32731=CARTESIAN_POINT('Ctrl Pts',(152.616466492188,-3.15452167088433,134.577711395114));
#32732=CARTESIAN_POINT('Ctrl Pts',(152.608701739241,-3.04968090418608,134.665358287767));
#32733=CARTESIAN_POINT('Ctrl Pts',(152.600936986294,-2.94104687818329,134.748747514514));
#32734=CARTESIAN_POINT('Ctrl Pts',(152.593172233347,-2.82900148006827,134.827535195964));
#32735=CARTESIAN_POINT('Ctrl Pts',(152.585415192462,-2.71706736702215,134.906244624379));
#32736=CARTESIAN_POINT('Ctrl Pts',(152.577658151577,-2.6017289423239,134.980361379209));
#32737=CARTESIAN_POINT('Ctrl Pts',(152.569901110692,-2.48340155023599,135.04958143665));
#32738=CARTESIAN_POINT('Ctrl Pts',(152.562149919452,-2.36516338975504,135.118749294707));
#32739=CARTESIAN_POINT('Ctrl Pts',(152.554398728212,-2.24394108444064,135.183027608733));
#32740=CARTESIAN_POINT('Ctrl Pts',(152.546647536971,-2.12017907329689,135.242155538431));
#32741=CARTESIAN_POINT('Ctrl Pts',(152.538899640194,-1.99646966430934,135.301258337182));
#32742=CARTESIAN_POINT('Ctrl Pts',(152.531151743417,-1.87022304845567,135.355214937274));
#32743=CARTESIAN_POINT('Ctrl Pts',(152.52340384664,-1.74190819257132,135.403810466315));
#32744=CARTESIAN_POINT('Ctrl Pts',(152.515657570556,-1.61362017738854,135.452395830218));
#32745=CARTESIAN_POINT('Ctrl Pts',(152.507911294472,-1.48326514809356,135.495622215254));
#32746=CARTESIAN_POINT('Ctrl Pts',(152.500165018388,-1.35133160459901,135.533323078499));
#32747=CARTESIAN_POINT('Ctrl Pts',(152.492418685122,-1.21939708720092,135.571024220043));
#32748=CARTESIAN_POINT('Ctrl Pts',(152.484672351857,-1.0858844082703,135.603199650986));
#32749=CARTESIAN_POINT('Ctrl Pts',(152.476926018592,-0.951296378697564,
135.629732961995));
#32750=CARTESIAN_POINT('Ctrl Pts',(152.469177950589,-0.816678209069185,
135.656272214955));
#32751=CARTESIAN_POINT('Ctrl Pts',(152.461429882586,-0.680984593108801,
135.677166758128));
#32752=CARTESIAN_POINT('Ctrl Pts',(152.453681814583,-0.544727265169134,
135.692351541154));
#32753=CARTESIAN_POINT('Ctrl Pts',(152.445925511841,-0.408325121319524,
135.707552462748));
#32754=CARTESIAN_POINT('Ctrl Pts',(152.438169209099,-0.27135845786369,135.717031458539));
#32755=CARTESIAN_POINT('Ctrl Pts',(152.430412906357,-0.134343406322409,
135.720775460892));
#32756=CARTESIAN_POINT('Ctrl Pts',(152.422652463843,0.00274477427746336,
135.724521461532));
#32757=CARTESIAN_POINT('Ctrl Pts',(152.414892021329,0.139881003691061,135.722526375239));
#32758=CARTESIAN_POINT('Ctrl Pts',(152.407131578815,0.276551436399757,135.714829267861));
#32759=CARTESIAN_POINT('Ctrl Pts',(152.399358678549,0.413441264619928,135.707119804402));
#32760=CARTESIAN_POINT('Ctrl Pts',(152.391585778284,0.549863412607578,135.693690066792));
#32761=CARTESIAN_POINT('Ctrl Pts',(152.383812878018,0.685310527535069,135.674630891724));
#32762=CARTESIAN_POINT('Ctrl Pts',(152.376322542256,0.815833798663701,135.656264565677));
#32763=CARTESIAN_POINT('Ctrl Pts',(152.368832206494,0.945451392757213,135.632671039947));
#32764=CARTESIAN_POINT('Ctrl Pts',(152.361341870732,1.07372212018233,135.6039755887));
#32765=CARTESIAN_POINT('Ctrl Pts',(152.353567536613,1.20685627122519,135.574192140697));
#32766=CARTESIAN_POINT('Ctrl Pts',(152.345793202494,1.3389611355373,135.538817906041));
#32767=CARTESIAN_POINT('Ctrl Pts',(152.338018868375,1.469530859409,135.497937304459));
#32768=CARTESIAN_POINT('Ctrl Pts',(152.330254115428,1.59993966776525,135.457107084564));
#32769=CARTESIAN_POINT('Ctrl Pts',(152.322489362481,1.72881673052121,135.410784115765));
#32770=CARTESIAN_POINT('Ctrl Pts',(152.314724609534,1.85566631285052,135.35910381536));
#32771=CARTESIAN_POINT('Ctrl Pts',(152.306967568649,1.98238990638692,135.307474844558));
#32772=CARTESIAN_POINT('Ctrl Pts',(152.299210527764,2.10708966716845,135.250499277694));
#32773=CARTESIAN_POINT('Ctrl Pts',(152.291453486879,2.2292853076384,135.188362223365));
#32774=CARTESIAN_POINT('Ctrl Pts',(152.283702295639,2.35138879942496,135.126272027072));
#32775=CARTESIAN_POINT('Ctrl Pts',(152.275951104399,2.47099158251282,135.059028267233));
#32776=CARTESIAN_POINT('Ctrl Pts',(152.268199913158,2.58763397443632,134.986863872417));
#32777=CARTESIAN_POINT('Ctrl Pts',(152.260452016381,2.70422679023167,134.914730149395));
#32778=CARTESIAN_POINT('Ctrl Pts',(152.252704119604,2.81786138563387,134.8376801563));
#32779=CARTESIAN_POINT('Ctrl Pts',(152.244956222827,2.9281034943823,134.755992304437));
#32780=CARTESIAN_POINT('Ctrl Pts',(152.237209946743,3.03832254285825,134.674321539912));
#32781=CARTESIAN_POINT('Ctrl Pts',(152.229463670659,3.14515020225643,134.588015078895));
#32782=CARTESIAN_POINT('Ctrl Pts',(152.221717394575,3.24818230916322,134.49739388968));
#32783=CARTESIAN_POINT('Ctrl Pts',(152.21397106131,3.35121517662934,134.40677203152));
#32784=CARTESIAN_POINT('Ctrl Pts',(152.206224728044,3.45045214212701,134.311835639813));
#32785=CARTESIAN_POINT('Ctrl Pts',(152.198478394779,3.54552348562038,134.212944821516));
#32786=CARTESIAN_POINT('Ctrl Pts',(152.190730326776,3.6406161196821,134.114031857305));
#32787=CARTESIAN_POINT('Ctrl Pts',(152.182982258773,3.73154100454593,134.011162986117));
#32788=CARTESIAN_POINT('Ctrl Pts',(152.17523419077,3.81796680658291,133.904733583248));
#32789=CARTESIAN_POINT('Ctrl Pts',(152.167477888028,3.90448446299083,133.798191065943));
#32790=CARTESIAN_POINT('Ctrl Pts',(152.159721585287,3.98649323780333,133.688080761642));
#32791=CARTESIAN_POINT('Ctrl Pts',(152.151965282545,4.06370315515527,133.574829843037));
#32792=CARTESIAN_POINT('Ctrl Pts',(152.144204840031,4.14095428176486,133.461518479006));
#32793=CARTESIAN_POINT('Ctrl Pts',(152.136444397516,4.21340124089931,133.345063492427));
#32794=CARTESIAN_POINT('Ctrl Pts',(152.128683955002,4.28079915370848,133.225918312131));
#32795=CARTESIAN_POINT('Ctrl Pts',(152.120911054737,4.34830525963057,133.106581869415));
#32796=CARTESIAN_POINT('Ctrl Pts',(152.113138154471,4.41074594431306,132.98454695142));
#32797=CARTESIAN_POINT('Ctrl Pts',(152.105365254206,4.46792339464244,132.860289507899));
#32798=CARTESIAN_POINT('Ctrl Pts',(152.097874918444,4.52302230063149,132.740549135435));
#32799=CARTESIAN_POINT('Ctrl Pts',(152.090384582682,4.57323387492497,132.618745305601));
#32800=CARTESIAN_POINT('Ctrl Pts',(152.08289424692,4.61842504045398,132.495316917477));
#32801=CARTESIAN_POINT('Ctrl Pts',(152.075119912801,4.66532964275923,132.367208704502));
#32802=CARTESIAN_POINT('Ctrl Pts',(152.067345578682,4.70697420329463,132.236944502857));
#32803=CARTESIAN_POINT('Ctrl Pts',(152.059571244563,4.74315632047991,132.104995532518));
#32804=CARTESIAN_POINT('Ctrl Pts',(152.051806491616,4.7792938464394,131.973209177492));
#32805=CARTESIAN_POINT('Ctrl Pts',(152.044041738668,4.80998222127051,131.839742558469));
#32806=CARTESIAN_POINT('Ctrl Pts',(152.036276985721,4.83506741860027,131.705085947559));
#32807=CARTESIAN_POINT('Ctrl Pts',(152.028519944836,4.86012770095843,131.570563079492));
#32808=CARTESIAN_POINT('Ctrl Pts',(152.020762903951,4.87959580958676,131.43485295347));
#32809=CARTESIAN_POINT('Ctrl Pts',(152.013005863066,4.89336787443554,131.298459704736));
#32810=CARTESIAN_POINT('Ctrl Pts',(152.005254671826,4.90712955366309,131.162169311212));
#32811=CARTESIAN_POINT('Ctrl Pts',(151.997503480586,4.91520369978747,131.02519720776));
#32812=CARTESIAN_POINT('Ctrl Pts',(151.989752289346,4.91753781261068,130.888056041839));
#32813=CARTESIAN_POINT('Ctrl Pts',(151.982004392569,4.91987093337366,130.750973164572));
#32814=CARTESIAN_POINT('Ctrl Pts',(151.974256495792,4.91646886650844,130.613721757843));
#32815=CARTESIAN_POINT('Ctrl Pts',(151.966508599015,4.90733111580762,130.476817670265));
#32816=CARTESIAN_POINT('Ctrl Pts',(151.958762322931,4.89819527652724,130.339942220071));
#32817=CARTESIAN_POINT('Ctrl Pts',(151.951016046847,4.88332616586303,130.203414334371));
#32818=CARTESIAN_POINT('Ctrl Pts',(151.943269770762,4.86277536333299,130.067747538493));
#32819=CARTESIAN_POINT('Ctrl Pts',(151.935523437497,4.8422244091016,129.932079741153));
#32820=CARTESIAN_POINT('Ctrl Pts',(151.927777104232,4.81599173786964,129.797273432875));
#32821=CARTESIAN_POINT('Ctrl Pts',(151.920030770966,4.78418047510694,129.663834316201));
#32822=CARTESIAN_POINT('Ctrl Pts',(151.912282702963,4.75236208843253,129.530365316762));
#32823=CARTESIAN_POINT('Ctrl Pts',(151.90453463496,4.71496271493733,129.398264498411));
#32824=CARTESIAN_POINT('Ctrl Pts',(151.896786566957,4.67213590113458,129.268024331517));
#32825=CARTESIAN_POINT('Ctrl Pts',(151.889030264216,4.62926357048447,129.137645743825));
#32826=CARTESIAN_POINT('Ctrl Pts',(151.881273961474,4.58095239895237,129.009132129898));
#32827=CARTESIAN_POINT('Ctrl Pts',(151.873517658732,4.52740503998275,128.882958351918));
#32828=CARTESIAN_POINT('Ctrl Pts',(151.865757216218,4.47382910117527,128.756717231193));
#32829=CARTESIAN_POINT('Ctrl Pts',(151.857996773704,4.4150115738168,128.632818787851));
#32830=CARTESIAN_POINT('Ctrl Pts',(151.850236331189,4.35120157742595,128.511714134764));
#32831=CARTESIAN_POINT('Ctrl Pts',(151.842463430924,4.28728914756418,128.390415073736));
#32832=CARTESIAN_POINT('Ctrl Pts',(151.834690530658,4.21836843011531,128.271919103256));
#32833=CARTESIAN_POINT('Ctrl Pts',(151.826917630393,4.1447329322676,128.156649911564));
#32834=CARTESIAN_POINT('Ctrl Pts',(151.819427294631,4.0737742702435,128.045571045337));
#32835=CARTESIAN_POINT('Ctrl Pts',(151.811936958869,3.99843784093229,127.93748868057));
#32836=CARTESIAN_POINT('Ctrl Pts',(151.804446623107,3.91902097115459,127.832752014444));
#32837=CARTESIAN_POINT('Ctrl Pts',(151.796672288988,3.83659298662095,127.724044225787));
#32838=CARTESIAN_POINT('Ctrl Pts',(151.788897954869,3.74950792669753,127.618596494705));
#32839=CARTESIAN_POINT('Ctrl Pts',(151.78112362075,3.65805283909787,127.516833813285));
#32840=CARTESIAN_POINT('Ctrl Pts',(151.773358867803,3.56671046171992,127.415196545275));
#32841=CARTESIAN_POINT('Ctrl Pts',(151.765594114856,3.47100903136664,127.317235578704));
#32842=CARTESIAN_POINT('Ctrl Pts',(151.757829361908,3.37127777283058,127.223345504373));
#32843=CARTESIAN_POINT('Ctrl Pts',(151.750072321023,3.27164556878627,127.129548682987));
#32844=CARTESIAN_POINT('Ctrl Pts',(151.742315280138,3.16799178450195,127.039814973813));
#32845=CARTESIAN_POINT('Ctrl Pts',(151.734558239253,3.06068441893629,126.954504263079));
#32846=CARTESIAN_POINT('Ctrl Pts',(151.726807048013,2.95345797469032,126.869257885817));
#32847=CARTESIAN_POINT('Ctrl Pts',(151.719055856773,2.84258373800712,126.788428110365));
#32848=CARTESIAN_POINT('Ctrl Pts',(151.711304665533,2.72846463607351,126.712336205103));
#32849=CARTESIAN_POINT('Ctrl Pts',(151.703556768756,2.6143940378023,126.636276640929));
#32850=CARTESIAN_POINT('Ctrl Pts',(151.695808871979,2.49708164191867,126.564951158246));
#32851=CARTESIAN_POINT('Ctrl Pts',(151.688060975202,2.37696117825879,126.498639003301));
#32852=CARTESIAN_POINT('Ctrl Pts',(151.680314699118,2.25686584121033,126.432340719429));
#32853=CARTESIAN_POINT('Ctrl Pts',(151.672568423034,2.13396394678784,126.371053866246));
#32854=CARTESIAN_POINT('Ctrl Pts',(151.66482214695,2.00871541838373,126.315012621426));
#32855=CARTESIAN_POINT('Ctrl Pts',(151.657075813684,1.8834659654236,126.258970962922));
#32856=CARTESIAN_POINT('Ctrl Pts',(151.649329480419,1.75587020078702,126.208175149726));
#32857=CARTESIAN_POINT('Ctrl Pts',(151.641583147154,1.62640932818071,126.162811764036));
#32858=CARTESIAN_POINT('Ctrl Pts',(151.633835079151,1.49691946370956,126.11743821953));
#32859=CARTESIAN_POINT('Ctrl Pts',(151.626087011148,1.36556402903665,126.077499652596));
#32860=CARTESIAN_POINT('Ctrl Pts',(151.618338943145,1.23284034907297,126.043133072468));
#32861=CARTESIAN_POINT('Ctrl Pts',(151.610582640403,1.09997560880265,126.00872996713));
#32862=CARTESIAN_POINT('Ctrl Pts',(151.602826337661,0.965740097432175,125.979910776536));
#32863=CARTESIAN_POINT('Ctrl Pts',(151.595070034919,0.830642869100312,125.956761677213));
#32864=CARTESIAN_POINT('Ctrl Pts',(151.587309592405,0.695473535310081,125.933600222518));
#32865=CARTESIAN_POINT('Ctrl Pts',(151.579549149891,0.559441955705539,125.91611493907));
#32866=CARTESIAN_POINT('Ctrl Pts',(151.571788707377,0.423062319506636,125.904340073087));
#32867=CARTESIAN_POINT('Ctrl Pts',(151.564015807111,0.286463754608351,125.892546305044));
#32868=CARTESIAN_POINT('Ctrl Pts',(151.556242906846,0.149516407399585,125.8864812901));
#32869=CARTESIAN_POINT('Ctrl Pts',(151.54847000658,0.0127353866029482,125.886127106189));
#32870=CARTESIAN_POINT('Ctrl Pts',(151.540979670818,-0.119073299558426,
125.885785797756));
#32871=CARTESIAN_POINT('Ctrl Pts',(151.533489335056,-0.250727234327518,
125.890747311159));
#32872=CARTESIAN_POINT('Ctrl Pts',(151.525998999294,-0.381771915817088,
125.900950246529));
#32873=CARTESIAN_POINT('Ctrl Pts',(151.518224665175,-0.517785196234352,
125.911540029295));
#32874=CARTESIAN_POINT('Ctrl Pts',(151.510450331056,-0.653572960888895,
125.927810082231));
#32875=CARTESIAN_POINT('Ctrl Pts',(151.502675996937,-0.788622495599073,
125.949748622572));
#32876=CARTESIAN_POINT('Ctrl Pts',(151.49491124399,-0.923505593827125,125.971660125623));
#32877=CARTESIAN_POINT('Ctrl Pts',(151.487146491043,-1.0576518901447,125.999226154124));
#32878=CARTESIAN_POINT('Ctrl Pts',(151.479381738095,-1.19055145009452,126.032383007897));
#32879=CARTESIAN_POINT('Ctrl Pts',(151.47162469721,-1.32331901232838,126.065506929817));
#32880=CARTESIAN_POINT('Ctrl Pts',(151.463867656325,-1.45484192553694,126.104210532487));
#32881=CARTESIAN_POINT('Ctrl Pts',(151.45611061544,-1.58461849481841,126.148378735258));
#32882=CARTESIAN_POINT('Ctrl Pts',(151.4483594242,-1.71429719857956,126.192513630444));
#32883=CARTESIAN_POINT('Ctrl Pts',(151.44060823296,-1.84223181106679,126.242104797879));
#32884=CARTESIAN_POINT('Ctrl Pts',(151.43285704172,-1.967934248109,126.296986896915));
#32885=CARTESIAN_POINT('Ctrl Pts',(151.425109144943,-2.093583258262,126.351845669594));
#32886=CARTESIAN_POINT('Ctrl Pts',(151.417361248166,-2.21700162237641,126.411990745098));
#32887=CARTESIAN_POINT('Ctrl Pts',(151.409613351389,-2.33771996110309,126.477208153652));
#32888=CARTESIAN_POINT('Ctrl Pts',(151.401867075304,-2.45841304815582,126.542411920129));
#32889=CARTESIAN_POINT('Ctrl Pts',(151.39412079922,-2.57640688945399,126.61268572351));
#32890=CARTESIAN_POINT('Ctrl Pts',(151.386374523136,-2.69125586485991,126.68776919597));
#32891=CARTESIAN_POINT('Ctrl Pts',(151.378628189871,-2.80610568805457,126.762853222679));
#32892=CARTESIAN_POINT('Ctrl Pts',(151.370881856606,-2.9178102717946,126.842746775379));
#32893=CARTESIAN_POINT('Ctrl Pts',(151.36313552334,-3.02595253683478,126.927145855998));
#32894=CARTESIAN_POINT('Ctrl Pts',(151.355387455337,-3.13411901958545,127.011563837205));
#32895=CARTESIAN_POINT('Ctrl Pts',(151.347639387334,-3.23872128804158,127.100489113594));
#32896=CARTESIAN_POINT('Ctrl Pts',(151.339891319331,-3.339375256192,127.193577328468));
#32897=CARTESIAN_POINT('Ctrl Pts',(151.332135016589,-3.44013620057762,127.286764478604));
#32898=CARTESIAN_POINT('Ctrl Pts',(151.324378713847,-3.5369401746064,127.384123139604));
#32899=CARTESIAN_POINT('Ctrl Pts',(151.316622411106,-3.62943951933013,127.485271610319));
#32900=CARTESIAN_POINT('Ctrl Pts',(151.308861968591,-3.72198823373946,127.58647406702));
#32901=CARTESIAN_POINT('Ctrl Pts',(151.301101526077,-3.81022748944611,127.69147006475));
#32902=CARTESIAN_POINT('Ctrl Pts',(151.293341083563,-3.89385054230238,127.799845512476));
#32903=CARTESIAN_POINT('Ctrl Pts',(151.285568183298,-3.97760783430676,127.908394934092));
#32904=CARTESIAN_POINT('Ctrl Pts',(151.277795283032,-4.05673388944061,128.020334327126));
#32905=CARTESIAN_POINT('Ctrl Pts',(151.270022382767,-4.1309653571986,128.135220628707));
#32906=CARTESIAN_POINT('Ctrl Pts',(151.262532047005,-4.20249832412462,128.245930523843));
#32907=CARTESIAN_POINT('Ctrl Pts',(151.255041711243,-4.26948622994854,128.359376526981));
#32908=CARTESIAN_POINT('Ctrl Pts',(151.247551375481,-4.33173506274729,128.475143064681));
#32909=CARTESIAN_POINT('Ctrl Pts',(151.239351872804,-4.39987746482186,128.601870098814));
#32910=CARTESIAN_POINT('Ctrl Pts',(151.231152370127,-4.46253770433376,128.731743506672));
#32911=CARTESIAN_POINT('Ctrl Pts',(151.22295286745,-4.51943039138935,128.864275052472));
#32912=CARTESIAN_POINT('Ctrl Pts',(151.214771930565,-4.57619425870915,128.996506512627));
#32913=CARTESIAN_POINT('Ctrl Pts',(151.20659099368,-4.62721648224196,129.131383810757));
#32914=CARTESIAN_POINT('Ctrl Pts',(151.198410056794,-4.67225768868374,129.268394747816));
#32915=CARTESIAN_POINT('Ctrl Pts',(151.192226668269,-4.70630113419362,129.371951573632));
#32916=CARTESIAN_POINT('Ctrl Pts',(151.186043279744,-4.73692864470159,129.476726711108));
#32917=CARTESIAN_POINT('Ctrl Pts',(151.179859891219,-4.76405452823403,129.582490119308));
#32918=CARTESIAN_POINT('Origin',(213.235140564004,0.,130.804360617566));
#32919=CARTESIAN_POINT('',(149.084946415013,-4.76405452823403,129.582490119308));
#32920=CARTESIAN_POINT('',(149.43018764199,-4.76405452823406,129.582490119308));
#32921=CARTESIAN_POINT('',(213.235140564004,-4.76405452823405,129.582490119308));
#32922=CARTESIAN_POINT('',(150.764859436022,-4.91824806144419,130.808727378438));
#32923=CARTESIAN_POINT('Ctrl Pts',(150.764859435991,-4.9182480614437,130.808727378982));
#32924=CARTESIAN_POINT('Ctrl Pts',(150.75358626954,-4.91807160662695,131.007467011822));
#32925=CARTESIAN_POINT('Ctrl Pts',(150.742313103089,-4.90584570983701,131.205693402104));
#32926=CARTESIAN_POINT('Ctrl Pts',(150.731039936638,-4.88177550045476,131.402232698918));
#32927=CARTESIAN_POINT('Ctrl Pts',(150.72410833243,-4.86697529632734,131.523080077754));
#32928=CARTESIAN_POINT('Ctrl Pts',(150.717176728222,-4.84769794250399,131.643290400273));
#32929=CARTESIAN_POINT('Ctrl Pts',(150.710245124014,-4.82399917091086,131.762596006994));
#32930=CARTESIAN_POINT('Ctrl Pts',(150.702470789895,-4.79741915233895,131.89640653932));
#32931=CARTESIAN_POINT('Ctrl Pts',(150.694696455776,-4.76522525707937,132.02932224479));
#32932=CARTESIAN_POINT('Ctrl Pts',(150.686922121657,-4.7274897414526,132.160835389525));
#32933=CARTESIAN_POINT('Ctrl Pts',(150.67915736871,-4.68980073147629,132.292186456063));
#32934=CARTESIAN_POINT('Ctrl Pts',(150.671392615763,-4.64658379670008,132.422138028934));
#32935=CARTESIAN_POINT('Ctrl Pts',(150.663627862816,-4.59796241915813,132.550191266429));
#32936=CARTESIAN_POINT('Ctrl Pts',(150.655870821931,-4.54938933305391,132.678117319643));
#32937=CARTESIAN_POINT('Ctrl Pts',(150.648113781046,-4.49542262416883,132.80414842648));
#32938=CARTESIAN_POINT('Ctrl Pts',(150.640356740161,-4.43623582221752,132.927799995597));
#32939=CARTESIAN_POINT('Ctrl Pts',(150.632605548921,-4.37709365349398,133.051358318104));
#32940=CARTESIAN_POINT('Ctrl Pts',(150.624854357681,-4.31273939520922,133.17254032337));
#32941=CARTESIAN_POINT('Ctrl Pts',(150.617103166441,-4.24339487774415,133.290880871663));
#32942=CARTESIAN_POINT('Ctrl Pts',(150.609355269663,-4.17407983354872,133.409171122066));
#32943=CARTESIAN_POINT('Ctrl Pts',(150.601607372886,-4.09977894591339,133.524621980896));
#32944=CARTESIAN_POINT('Ctrl Pts',(150.593859476109,-4.02076012477245,133.636792625848));
#32945=CARTESIAN_POINT('Ctrl Pts',(150.586113200025,-3.94175783266545,133.748939807119));
#32946=CARTESIAN_POINT('Ctrl Pts',(150.578366923941,-3.85803979504627,133.857807819881));
#32947=CARTESIAN_POINT('Ctrl Pts',(150.570620647857,-3.7699171889696,133.962984914758));
#32948=CARTESIAN_POINT('Ctrl Pts',(150.562874314592,-3.68179393239183,134.068162786028));
#32949=CARTESIAN_POINT('Ctrl Pts',(150.555127981326,-3.58926629356591,134.169649385364));
#32950=CARTESIAN_POINT('Ctrl Pts',(150.547381648061,-3.49268540348365,134.267066457627));
#32951=CARTESIAN_POINT('Ctrl Pts',(150.539633580058,-3.39608288478092,134.364505345767));
#32952=CARTESIAN_POINT('Ctrl Pts',(150.531885512055,-3.29542558381622,134.457872615778));
#32953=CARTESIAN_POINT('Ctrl Pts',(150.524137444052,-3.19110081093237,134.54682754153));
#32954=CARTESIAN_POINT('Ctrl Pts',(150.51638114131,-3.08666516043819,134.635877009636));
#32955=CARTESIAN_POINT('Ctrl Pts',(150.508624838568,-2.97855454965732,134.720504511643));
#32956=CARTESIAN_POINT('Ctrl Pts',(150.500868535826,-2.86718906964377,134.800409904226));
#32957=CARTESIAN_POINT('Ctrl Pts',(150.493108093312,-2.75576415052027,134.880357944723));
#32958=CARTESIAN_POINT('Ctrl Pts',(150.485347650798,-2.6410812273607,134.955578639499));
#32959=CARTESIAN_POINT('Ctrl Pts',(150.477587208284,-2.52358772200415,135.025816299182));
#32960=CARTESIAN_POINT('Ctrl Pts',(150.469814308018,-2.40590560564229,135.096166710592));
#32961=CARTESIAN_POINT('Ctrl Pts',(150.462041407753,-2.28540423495246,135.161517915445));
#32962=CARTESIAN_POINT('Ctrl Pts',(150.454268507487,-2.16255467565798,135.22166073611));
#32963=CARTESIAN_POINT('Ctrl Pts',(150.446778171725,-2.04417100728164,135.279617213754));
#32964=CARTESIAN_POINT('Ctrl Pts',(150.439287835963,-1.92360719327457,135.332737284421));
#32965=CARTESIAN_POINT('Ctrl Pts',(150.431797500201,-1.8012988128428,135.380877376997));
#32966=CARTESIAN_POINT('Ctrl Pts',(150.424023166082,-1.6743530729938,135.430842715814));
#32967=CARTESIAN_POINT('Ctrl Pts',(150.416248831963,-1.54512573884652,135.475601265406));
#32968=CARTESIAN_POINT('Ctrl Pts',(150.408474497844,-1.41408303759758,135.5149393745));
#32969=CARTESIAN_POINT('Ctrl Pts',(150.400709744897,-1.28320183476636,135.554229002891));
#32970=CARTESIAN_POINT('Ctrl Pts',(150.39294499195,-1.15051008721139,135.588111371076));
#32971=CARTESIAN_POINT('Ctrl Pts',(150.385180239002,-1.01649422964589,135.616420731862));
#32972=CARTESIAN_POINT('Ctrl Pts',(150.377423198117,-0.882611478519405,
135.644701975391));
#32973=CARTESIAN_POINT('Ctrl Pts',(150.369666157232,-0.747407614588527,
135.667421146515));
#32974=CARTESIAN_POINT('Ctrl Pts',(150.361909116347,-0.611384135322865,
135.684462307242));
#32975=CARTESIAN_POINT('Ctrl Pts',(150.354157925107,-0.475463232421164,
135.701490617096));
#32976=CARTESIAN_POINT('Ctrl Pts',(150.346406733867,-0.338724330795074,
135.712849390875));
#32977=CARTESIAN_POINT('Ctrl Pts',(150.338655542627,-0.201678670413874,
135.718473841374));
#32978=CARTESIAN_POINT('Ctrl Pts',(150.33090764585,-0.0646912580939631,
135.724095901331));
#32979=CARTESIAN_POINT('Ctrl Pts',(150.323159749073,0.0726022638453508,
135.723988469494));
#32980=CARTESIAN_POINT('Ctrl Pts',(150.315411852296,0.209686207249513,135.718138670855));
#32981=CARTESIAN_POINT('Ctrl Pts',(150.307665576212,0.346741475647902,135.712290095868));
#32982=CARTESIAN_POINT('Ctrl Pts',(150.299919300128,0.483586862347687,135.700701559949));
#32983=CARTESIAN_POINT('Ctrl Pts',(150.292173024043,0.619707752136331,135.683412304569));
#32984=CARTESIAN_POINT('Ctrl Pts',(150.284426690778,0.755829646738368,135.666122921563));
#32985=CARTESIAN_POINT('Ctrl Pts',(150.276680357513,0.891226645908353,135.643132784389));
#32986=CARTESIAN_POINT('Ctrl Pts',(150.268934024247,1.02539071800664,135.614532853352));
#32987=CARTESIAN_POINT('Ctrl Pts',(150.261185956244,1.15958483521864,135.585926517559));
#32988=CARTESIAN_POINT('Ctrl Pts',(150.253437888241,1.29254509364041,135.551707969557));
#32989=CARTESIAN_POINT('Ctrl Pts',(150.245689820238,1.42377548002807,135.512018893713));
#32990=CARTESIAN_POINT('Ctrl Pts',(150.237933517497,1.55514533963208,135.472287635846));
#32991=CARTESIAN_POINT('Ctrl Pts',(150.230177214755,1.68478127972169,135.42707434912));
#32992=CARTESIAN_POINT('Ctrl Pts',(150.222420912013,1.81220371174026,135.376570233239));
#32993=CARTESIAN_POINT('Ctrl Pts',(150.214660469499,1.93969415294749,135.326039161791));
#32994=CARTESIAN_POINT('Ctrl Pts',(150.206900026985,2.06496837507746,135.270211793442));
#32995=CARTESIAN_POINT('Ctrl Pts',(150.19913958447,2.18756941698641,135.209326350505));
#32996=CARTESIAN_POINT('Ctrl Pts',(150.191366684205,2.31036726897179,135.14834316885));
#32997=CARTESIAN_POINT('Ctrl Pts',(150.18359378394,2.43048302272403,135.082285875427));
#32998=CARTESIAN_POINT('Ctrl Pts',(150.175820883674,2.54748606864897,135.011437725552));
#32999=CARTESIAN_POINT('Ctrl Pts',(150.168330547912,2.66023575914113,134.943165084381));
#33000=CARTESIAN_POINT('Ctrl Pts',(150.16084021215,2.77009486543544,134.870444028838));
#33001=CARTESIAN_POINT('Ctrl Pts',(150.153349876388,2.8767071558873,134.793563420353));
#33002=CARTESIAN_POINT('Ctrl Pts',(150.145575542269,2.98736168373615,134.71376786023));
#33003=CARTESIAN_POINT('Ctrl Pts',(150.13780120815,3.09486884979585,134.629238333447));
#33004=CARTESIAN_POINT('Ctrl Pts',(150.130026874031,3.19879689601085,134.540251606416));
#33005=CARTESIAN_POINT('Ctrl Pts',(150.122262121084,3.30259686019714,134.451374547574));
#33006=CARTESIAN_POINT('Ctrl Pts',(150.114497368137,3.40282618687997,134.358051469958));
#33007=CARTESIAN_POINT('Ctrl Pts',(150.10673261519,3.49908249840483,134.260602034461));
#33008=CARTESIAN_POINT('Ctrl Pts',(150.098975574305,3.59524320680414,134.163249387117));
#33009=CARTESIAN_POINT('Ctrl Pts',(150.09121853342,3.68743847990409,134.061778814159));
#33010=CARTESIAN_POINT('Ctrl Pts',(150.083461492535,3.77529970415513,133.956549572294));
#33011=CARTESIAN_POINT('Ctrl Pts',(150.075710301295,3.86309467157351,133.851399684618));
#33012=CARTESIAN_POINT('Ctrl Pts',(150.067959110055,3.94656184601318,133.742497068714));
#33013=CARTESIAN_POINT('Ctrl Pts',(150.060207918814,4.02537038247279,133.63023682618));
#33014=CARTESIAN_POINT('Ctrl Pts',(150.052460022037,4.10414542320216,133.518024297244));
#33015=CARTESIAN_POINT('Ctrl Pts',(150.04471212526,4.17826553994447,133.40245729935));
#33016=CARTESIAN_POINT('Ctrl Pts',(150.036964228483,4.24744115854621,133.283962736291));
#33017=CARTESIAN_POINT('Ctrl Pts',(150.029217952399,4.31660230709979,133.165492959741));
#33018=CARTESIAN_POINT('Ctrl Pts',(150.021471676315,4.38082081777171,133.044097173518));
#33019=CARTESIAN_POINT('Ctrl Pts',(150.013725400231,4.43985154343156,132.920229548948));
#33020=CARTESIAN_POINT('Ctrl Pts',(150.005979066966,4.49888270484277,132.796361010016));
#33021=CARTESIAN_POINT('Ctrl Pts',(149.9982327337,4.55272583663069,132.670020949264));
#33022=CARTESIAN_POINT('Ctrl Pts',(149.990486400435,4.60118286276593,132.541685954367));
#33023=CARTESIAN_POINT('Ctrl Pts',(149.982738332432,4.6496507405162,132.413322219736));
#33024=CARTESIAN_POINT('Ctrl Pts',(149.974990264429,4.69272997437489,132.282963027667));
#33025=CARTESIAN_POINT('Ctrl Pts',(149.967242196426,4.7302716601366,132.151102272008));
#33026=CARTESIAN_POINT('Ctrl Pts',(149.959485893684,4.7678532456487,132.019101373168));
#33027=CARTESIAN_POINT('Ctrl Pts',(149.951729590943,4.79988541917236,131.88559609942));
#33028=CARTESIAN_POINT('Ctrl Pts',(149.943973288201,4.82626981310267,131.751093290306));
#33029=CARTESIAN_POINT('Ctrl Pts',(149.936212845687,4.85266828917847,131.616518692994));
#33030=CARTESIAN_POINT('Ctrl Pts',(149.928452403172,4.87341292012736,131.480945885714));
#33031=CARTESIAN_POINT('Ctrl Pts',(149.920691960658,4.88845713046823,131.344888087797));
#33032=CARTESIAN_POINT('Ctrl Pts',(149.912919060393,4.9035254911111,131.208611877824));
#33033=CARTESIAN_POINT('Ctrl Pts',(149.905146160127,4.91287511820822,131.071849511704));
#33034=CARTESIAN_POINT('Ctrl Pts',(149.897373259862,4.91651156747513,130.935116379899));
#33035=CARTESIAN_POINT('Ctrl Pts',(149.8898829241,4.92001582265155,130.803353841844));
#33036=CARTESIAN_POINT('Ctrl Pts',(149.882392588338,4.91821506946645,130.671618757515));
#33037=CARTESIAN_POINT('Ctrl Pts',(149.874902252576,4.91115978331515,130.54036697134));
#33038=CARTESIAN_POINT('Ctrl Pts',(149.867127918457,4.90383699384507,130.4041387338));
#33039=CARTESIAN_POINT('Ctrl Pts',(149.859353584338,4.89083015822545,130.267999636258));
#33040=CARTESIAN_POINT('Ctrl Pts',(149.851579250219,4.87213875210234,130.132462528));
#33041=CARTESIAN_POINT('Ctrl Pts',(149.843814497272,4.85347038146679,129.997092457115));
#33042=CARTESIAN_POINT('Ctrl Pts',(149.836049744324,4.82913143253088,129.86232328294));
#33043=CARTESIAN_POINT('Ctrl Pts',(149.828284991377,4.7991733501061,129.728666321713));
#33044=CARTESIAN_POINT('Ctrl Pts',(149.820527950492,4.76924502247113,129.595142110464));
#33045=CARTESIAN_POINT('Ctrl Pts',(149.812770909607,4.73370875275085,129.462728292858));
#33046=CARTESIAN_POINT('Ctrl Pts',(149.805013868722,4.69266754916007,129.331929180942));
#33047=CARTESIAN_POINT('Ctrl Pts',(149.797262677482,4.65165729506016,129.201228705652));
#33048=CARTESIAN_POINT('Ctrl Pts',(149.789511486242,4.60515048660142,129.072140883893));
#33049=CARTESIAN_POINT('Ctrl Pts',(149.781760295002,4.55330070414402,128.945157626997));
#33050=CARTESIAN_POINT('Ctrl Pts',(149.774012398225,4.50147295922729,128.818228341372));
#33051=CARTESIAN_POINT('Ctrl Pts',(149.766264501448,4.44430690445549,128.693402202724));
#33052=CARTESIAN_POINT('Ctrl Pts',(149.758516604671,4.3820051841767,128.571153589915));
#33053=CARTESIAN_POINT('Ctrl Pts',(149.750770328587,4.31971649607473,128.448930548881));
#33054=CARTESIAN_POINT('Ctrl Pts',(149.743024052503,4.25229445666001,128.329284309379));
#33055=CARTESIAN_POINT('Ctrl Pts',(149.735277776418,4.17998866512098,128.21266661133));
#33056=CARTESIAN_POINT('Ctrl Pts',(149.727531443153,4.10768233983702,128.096048052435));
#33057=CARTESIAN_POINT('Ctrl Pts',(149.719785109888,4.03049239651298,127.982458411881));
#33058=CARTESIAN_POINT('Ctrl Pts',(149.712038776622,3.94871273692421,127.872321943921));
#33059=CARTESIAN_POINT('Ctrl Pts',(149.704290708619,3.86691476334772,127.762160811662));
#33060=CARTESIAN_POINT('Ctrl Pts',(149.696542640616,3.78052526126477,127.655454704635));
#33061=CARTESIAN_POINT('Ctrl Pts',(149.688794572614,3.68987927119882,127.552595861856));
#33062=CARTESIAN_POINT('Ctrl Pts',(149.681038269872,3.5991369414959,127.449627699475));
#33063=CARTESIAN_POINT('Ctrl Pts',(149.67328196713,3.50412934584402,127.350515263182));
#33064=CARTESIAN_POINT('Ctrl Pts',(149.665525664388,3.40522973261341,127.255615271584));
#33065=CARTESIAN_POINT('Ctrl Pts',(149.657765221874,3.30627733368134,127.160664629004));
#33066=CARTESIAN_POINT('Ctrl Pts',(149.65000477936,3.20342907103866,127.069931169583));
#33067=CARTESIAN_POINT('Ctrl Pts',(149.642244336845,3.0970915554587,126.983731486179));
#33068=CARTESIAN_POINT('Ctrl Pts',(149.63447143658,2.99058333745853,126.89739342739));
#33069=CARTESIAN_POINT('Ctrl Pts',(149.626698536315,2.88057498735286,126.815603921823));
#33070=CARTESIAN_POINT('Ctrl Pts',(149.618925636049,2.76750312073579,126.738636876432));
#33071=CARTESIAN_POINT('Ctrl Pts',(149.611435300287,2.65854170128125,126.66446777701));
#33072=CARTESIAN_POINT('Ctrl Pts',(149.603944964525,2.5467358928218,126.594776770777));
#33073=CARTESIAN_POINT('Ctrl Pts',(149.596454628763,2.43249649337023,126.529767786402));
#33074=CARTESIAN_POINT('Ctrl Pts',(149.588680294644,2.31392567236601,126.462293966625));
#33075=CARTESIAN_POINT('Ctrl Pts',(149.580905960525,2.19235748158222,126.399650478201));
#33076=CARTESIAN_POINT('Ctrl Pts',(149.573131626406,2.06822311222214,126.342114969849));
#33077=CARTESIAN_POINT('Ctrl Pts',(149.565366873459,1.94424172737818,126.284650368869));
#33078=CARTESIAN_POINT('Ctrl Pts',(149.557602120512,1.81770080787187,126.232281385362));
#33079=CARTESIAN_POINT('Ctrl Pts',(149.549837367564,1.68905834571211,126.185241116267));
#33080=CARTESIAN_POINT('Ctrl Pts',(149.542080326679,1.56054365305936,126.13824756823));
#33081=CARTESIAN_POINT('Ctrl Pts',(149.534323285794,1.42993193634857,126.096572335583));
#33082=CARTESIAN_POINT('Ctrl Pts',(149.526566244909,1.29770316604169,126.060401347574));
#33083=CARTESIAN_POINT('Ctrl Pts',(149.518815053669,1.16557411047886,126.024257636388));
#33084=CARTESIAN_POINT('Ctrl Pts',(149.511063862429,1.03183080411126,125.993610010679));
#33085=CARTESIAN_POINT('Ctrl Pts',(149.503312671189,0.896970119812349,125.968595149032));
#33086=CARTESIAN_POINT('Ctrl Pts',(149.495564774412,0.762166754901932,125.943590919369));
#33087=CARTESIAN_POINT('Ctrl Pts',(149.487816877635,0.626247340234282,125.924214763287));
#33088=CARTESIAN_POINT('Ctrl Pts',(149.480068980858,0.489720518402962,125.910552603723));
#33089=CARTESIAN_POINT('Ctrl Pts',(149.472322704774,0.353222255039544,125.896893301988));
#33090=CARTESIAN_POINT('Ctrl Pts',(149.46457642869,0.216117226010545,125.888945658266));
#33091=CARTESIAN_POINT('Ctrl Pts',(149.456830152605,0.0789204073626937,
125.886743854153));
#33092=CARTESIAN_POINT('Ctrl Pts',(149.44908381934,-0.0582774240408593,
125.884542033787));
#33093=CARTESIAN_POINT('Ctrl Pts',(149.441337486075,-0.195566655500435,
125.888086143937));
#33094=CARTESIAN_POINT('Ctrl Pts',(149.433591152809,-0.332431488809621,
125.897358236504));
#33095=CARTESIAN_POINT('Ctrl Pts',(149.425843084806,-0.469326972049227,
125.906632405492));
#33096=CARTESIAN_POINT('Ctrl Pts',(149.418095016803,-0.605797478021365,
125.921637082982));
#33097=CARTESIAN_POINT('Ctrl Pts',(149.4103469488,-0.741331907347136,125.942302404664));
#33098=CARTESIAN_POINT('Ctrl Pts',(149.402590646059,-0.877010384277369,
125.962989689695));
#33099=CARTESIAN_POINT('Ctrl Pts',(149.394834343317,-1.0117504100798,125.9893495779));
#33100=CARTESIAN_POINT('Ctrl Pts',(149.387078040575,-1.14505011742713,126.021260859974));
#33101=CARTESIAN_POINT('Ctrl Pts',(149.379317598061,-1.27842097084193,126.053189174059));
#33102=CARTESIAN_POINT('Ctrl Pts',(149.371557155546,-1.41034959812453,126.09067467913));
#33103=CARTESIAN_POINT('Ctrl Pts',(149.363796713032,-1.54034985768378,126.133546408198));
#33104=CARTESIAN_POINT('Ctrl Pts',(149.356023812767,-1.67055880520047,126.176486958771));
#33105=CARTESIAN_POINT('Ctrl Pts',(149.348250912501,-1.79883283296839,126.224830873735));
#33106=CARTESIAN_POINT('Ctrl Pts',(149.340478012236,-1.92470549391604,126.278358869423));
#33107=CARTESIAN_POINT('Ctrl Pts',(149.332987676474,-2.04600236658388,126.329940987639));
#33108=CARTESIAN_POINT('Ctrl Pts',(149.325497340712,-2.16506915436073,126.386336689635));
#33109=CARTESIAN_POINT('Ctrl Pts',(149.31800700495,-2.28151223992148,126.447310587834));
#33110=CARTESIAN_POINT('Ctrl Pts',(149.310231768601,-2.40238432632126,126.510603674373));
#33111=CARTESIAN_POINT('Ctrl Pts',(149.302456532253,-2.52081210212507,126.579030637407));
#33112=CARTESIAN_POINT('Ctrl Pts',(149.294681295904,-2.63632874284507,126.652378702607));
#33113=CARTESIAN_POINT('Ctrl Pts',(149.286915840311,-2.75170007094013,126.725634500582));
#33114=CARTESIAN_POINT('Ctrl Pts',(149.279150384718,-2.86416722390513,126.803798874773));
#33115=CARTESIAN_POINT('Ctrl Pts',(149.271384929125,-2.97328641825445,126.886612420256));
#33116=CARTESIAN_POINT('Ctrl Pts',(149.263616657703,-3.08244518026236,126.969455994719));
#33117=CARTESIAN_POINT('Ctrl Pts',(149.255848386282,-3.18825320822307,127.056951928444));
#33118=CARTESIAN_POINT('Ctrl Pts',(149.248080114861,-3.29029285746525,127.14879554844));
#33119=CARTESIAN_POINT('Ctrl Pts',(149.240329214054,-3.39210433606394,127.240433797112));
#33120=CARTESIAN_POINT('Ctrl Pts',(149.232578313248,-3.4901639627876,127.336400067624));
#33121=CARTESIAN_POINT('Ctrl Pts',(149.224827412442,-3.5840882724255,127.436350178455));
#33122=CARTESIAN_POINT('Ctrl Pts',(149.217080091668,-3.67796919975373,127.536254123744));
#33123=CARTESIAN_POINT('Ctrl Pts',(149.209332770893,-3.76771834363505,127.6401379636));
#33124=CARTESIAN_POINT('Ctrl Pts',(149.201585450118,-3.85298861839908,127.747620234578));
#33125=CARTESIAN_POINT('Ctrl Pts',(149.193840029964,-3.93823797414069,127.855076137352));
#33126=CARTESIAN_POINT('Ctrl Pts',(149.186094609809,-4.01901040555093,127.966128407808));
#33127=CARTESIAN_POINT('Ctrl Pts',(149.178349189654,-4.09499896150973,128.080362348893));
#33128=CARTESIAN_POINT('Ctrl Pts',(149.170565625101,-4.17136174349028,128.195158865654));
#33129=CARTESIAN_POINT('Ctrl Pts',(149.162782060547,-4.24289315910445,128.313168160968));
#33130=CARTESIAN_POINT('Ctrl Pts',(149.154998495994,-4.30932586238927,128.433940048502));
#33131=CARTESIAN_POINT('Ctrl Pts',(149.1472494548,-4.37546390889053,128.554176262276));
#33132=CARTESIAN_POINT('Ctrl Pts',(149.139500413606,-4.43654823085717,128.677150246));
#33133=CARTESIAN_POINT('Ctrl Pts',(149.131751372412,-4.49236156400216,128.802393924343));
#33134=CARTESIAN_POINT('Ctrl Pts',(149.123950546179,-4.54854788466556,128.928474577045));
#33135=CARTESIAN_POINT('Ctrl Pts',(149.116149719945,-4.59939234242686,129.056855005353));
#33136=CARTESIAN_POINT('Ctrl Pts',(149.108348893712,-4.64472317883897,129.187038864031));
#33137=CARTESIAN_POINT('Ctrl Pts',(149.100548067479,-4.69005401525106,129.31722272271));
#33138=CARTESIAN_POINT('Ctrl Pts',(149.092747241246,-4.72987114286435,129.449209618557));
#33139=CARTESIAN_POINT('Ctrl Pts',(149.084946415013,-4.76405452823403,129.582490119308));
#33140=CARTESIAN_POINT('Ctrl Pts',(150.83493632599,-4.76405452823404,129.582490119308));
#33141=CARTESIAN_POINT('Ctrl Pts',(150.827298245854,-4.79767773639729,129.713586497633));
#33142=CARTESIAN_POINT('Ctrl Pts',(150.819660165717,-4.82587389977647,129.846026514504));
#33143=CARTESIAN_POINT('Ctrl Pts',(150.812022085581,-4.84855461702794,129.979314444193));
#33144=CARTESIAN_POINT('Ctrl Pts',(150.804161643988,-4.87189562027245,130.116482681196));
#33145=CARTESIAN_POINT('Ctrl Pts',(150.796301202394,-4.8893950646696,130.254548500785));
#33146=CARTESIAN_POINT('Ctrl Pts',(150.788440760801,-4.90101392815764,130.392965991319));
#33147=CARTESIAN_POINT('Ctrl Pts',(150.780580319208,-4.91263279164569,130.531383481853));
#33148=CARTESIAN_POINT('Ctrl Pts',(150.772719877615,-4.9183710980918,130.670152180157));
#33149=CARTESIAN_POINT('Ctrl Pts',(150.764859436022,-4.91824806144419,130.808727378438));
#33150=CARTESIAN_POINT('',(151.110140564062,-4.91824999678873,130.804182888505));
#33151=CARTESIAN_POINT('Ctrl Pts',(151.179859891219,-4.76405452823403,129.582490119308));
#33152=CARTESIAN_POINT('Ctrl Pts',(151.171703248589,-4.79983687266862,129.722004937186));
#33153=CARTESIAN_POINT('Ctrl Pts',(151.16354660596,-4.82952429123457,129.863239908004));
#33154=CARTESIAN_POINT('Ctrl Pts',(151.15538996333,-4.85296245138542,130.005650089312));
#33155=CARTESIAN_POINT('Ctrl Pts',(151.147249438033,-4.87635429829,130.147778871494));
#33156=CARTESIAN_POINT('Ctrl Pts',(151.139108912735,-4.89352145798313,130.291077910992));
#33157=CARTESIAN_POINT('Ctrl Pts',(151.130968387437,-4.9043601863316,130.434990579223));
#33158=CARTESIAN_POINT('Ctrl Pts',(151.124025779645,-4.913603943599,130.557725805171));
#33159=CARTESIAN_POINT('Ctrl Pts',(151.117083171854,-4.91824554201133,130.68090699426));
#33160=CARTESIAN_POINT('Ctrl Pts',(151.110140564062,-4.91824999678873,130.804182888505));
#33161=CARTESIAN_POINT('Ctrl Pts',(151.110140564008,-4.91824999678877,130.804182889472));
#33162=CARTESIAN_POINT('Ctrl Pts',(151.102047498551,-4.91825518973788,130.947886798916));
#33163=CARTESIAN_POINT('Ctrl Pts',(151.093954433094,-4.91195784762291,131.09147629153));
#33164=CARTESIAN_POINT('Ctrl Pts',(151.085861367638,-4.89941385205013,131.234391975538));
#33165=CARTESIAN_POINT('Ctrl Pts',(151.07775840512,-4.88685451634673,131.377482432029));
#33166=CARTESIAN_POINT('Ctrl Pts',(151.069655442603,-4.86803331533055,131.519897100418));
#33167=CARTESIAN_POINT('Ctrl Pts',(151.061552480086,-4.84305758079219,131.661084804006));
#33168=CARTESIAN_POINT('Ctrl Pts',(151.053431098674,-4.8180250737541,131.802593442254));
#33169=CARTESIAN_POINT('Ctrl Pts',(151.045309717261,-4.78681012220712,131.942869206641));
#33170=CARTESIAN_POINT('Ctrl Pts',(151.037188335849,-4.74957092612867,132.081372395183));
#33171=CARTESIAN_POINT('Ctrl Pts',(151.029057337182,-4.71228763178285,132.220039597756));
#33172=CARTESIAN_POINT('Ctrl Pts',(151.020926338514,-4.66896595889947,132.356929714758));
#33173=CARTESIAN_POINT('Ctrl Pts',(151.012795339847,-4.61981302748866,132.491521147434));
#33174=CARTESIAN_POINT('Ctrl Pts',(151.00464579797,-4.57054799999613,132.6264195236));
#33175=CARTESIAN_POINT('Ctrl Pts',(150.996496256093,-4.51542525160003,132.759008420918));
#33176=CARTESIAN_POINT('Ctrl Pts',(150.988346714217,-4.4546995750925,132.888787339274));
#33177=CARTESIAN_POINT('Ctrl Pts',(150.981932393367,-4.40690376290869,132.99093340275));
#33178=CARTESIAN_POINT('Ctrl Pts',(150.975518072518,-4.35563793521106,133.091339153192));
#33179=CARTESIAN_POINT('Ctrl Pts',(150.969103751668,-4.30104530403734,133.189773025331));
#33180=CARTESIAN_POINT('Ctrl Pts',(150.961329417549,-4.23487752647494,133.309077598426));
#33181=CARTESIAN_POINT('Ctrl Pts',(150.95355508343,-4.16363718592351,133.425815962002));
#33182=CARTESIAN_POINT('Ctrl Pts',(150.945780749311,-4.08754811721538,133.539526691491));
#33183=CARTESIAN_POINT('Ctrl Pts',(150.938015996364,-4.01155282148424,133.653097282668));
#33184=CARTESIAN_POINT('Ctrl Pts',(150.930251243417,-3.93072090264591,133.763647342098));
#33185=CARTESIAN_POINT('Ctrl Pts',(150.92248649047,-3.84532225986233,133.870739553756));
#33186=CARTESIAN_POINT('Ctrl Pts',(150.914729449585,-3.76000843621474,133.977725399919));
#33187=CARTESIAN_POINT('Ctrl Pts',(150.9069724087,-3.67013715711599,134.081259929191));
#33188=CARTESIAN_POINT('Ctrl Pts',(150.899215367815,-3.57602162823383,134.180934676713));
#33189=CARTESIAN_POINT('Ctrl Pts',(150.891464176575,-3.48197707260397,134.280534258733));
#33190=CARTESIAN_POINT('Ctrl Pts',(150.883712985334,-3.38369490516131,134.37627956944));
#33191=CARTESIAN_POINT('Ctrl Pts',(150.875961794094,-3.28152838637055,134.467795414576));
#33192=CARTESIAN_POINT('Ctrl Pts',(150.868213897317,-3.17940529107565,134.559272363037));
#33193=CARTESIAN_POINT('Ctrl Pts',(150.86046600054,-3.07340141865898,134.646523160974));
#33194=CARTESIAN_POINT('Ctrl Pts',(150.852718103763,-2.96390648363309,134.729209839992));
#33195=CARTESIAN_POINT('Ctrl Pts',(150.844971827679,-2.85443445258724,134.811879222739));
#33196=CARTESIAN_POINT('Ctrl Pts',(150.837225551595,-2.74147312324885,134.889986150088));
#33197=CARTESIAN_POINT('Ctrl Pts',(150.829479275511,-2.62544453403033,134.96323354917));
#33198=CARTESIAN_POINT('Ctrl Pts',(150.821732942245,-2.50941508831524,135.036481488948));
#33199=CARTESIAN_POINT('Ctrl Pts',(150.81398660898,-2.39031866814014,135.104869620177));
#33200=CARTESIAN_POINT('Ctrl Pts',(150.806240275715,-2.26860513087272,135.168144964057));
#33201=CARTESIAN_POINT('Ctrl Pts',(150.798492207712,-2.14686433670245,135.231434478011));
#33202=CARTESIAN_POINT('Ctrl Pts',(150.790744139709,-2.02250560602092,135.289608745949));
#33203=CARTESIAN_POINT('Ctrl Pts',(150.782996071706,-1.8960017888625,135.342461572716));
#33204=CARTESIAN_POINT('Ctrl Pts',(150.775239768964,-1.76936352194175,135.395370572095));
#33205=CARTESIAN_POINT('Ctrl Pts',(150.767483466222,-1.64057597567256,135.442946681492));
#33206=CARTESIAN_POINT('Ctrl Pts',(150.75972716348,-1.51013082398722,135.485032359629));
#33207=CARTESIAN_POINT('Ctrl Pts',(150.751966720966,-1.37961604979662,135.527140500159));
#33208=CARTESIAN_POINT('Ctrl Pts',(150.744206278452,-1.24744228391585,135.563752266027));
#33209=CARTESIAN_POINT('Ctrl Pts',(150.736445835938,-1.11411365251201,135.594760792059));
#33210=CARTESIAN_POINT('Ctrl Pts',(150.728672935672,-0.980570990152776,
135.625819095731));
#33211=CARTESIAN_POINT('Ctrl Pts',(150.720900035407,-0.845870141998508,
135.651256112465));
#33212=CARTESIAN_POINT('Ctrl Pts',(150.713127135141,-0.710523547302674,
135.671016486972));
#33213=CARTESIAN_POINT('Ctrl Pts',(150.705636799379,-0.580097142239193,
135.690058522094));
#33214=CARTESIAN_POINT('Ctrl Pts',(150.698146463617,-0.449071430888062,
135.703829437846));
#33215=CARTESIAN_POINT('Ctrl Pts',(150.690656127855,-0.317905028657354,
135.71232551712));
#33216=CARTESIAN_POINT('Ctrl Pts',(150.682881793736,-0.181765412421204,
135.721143727822));
#33217=CARTESIAN_POINT('Ctrl Pts',(150.675107459617,-0.0450429767317745,
135.724307148691));
#33218=CARTESIAN_POINT('Ctrl Pts',(150.667333125498,0.0917530806579278,
135.72175468706));
#33219=CARTESIAN_POINT('Ctrl Pts',(150.659568372551,0.228380549132573,135.719205371109));
#33220=CARTESIAN_POINT('Ctrl Pts',(150.651803619603,0.365081071632927,135.710954195969));
#33221=CARTESIAN_POINT('Ctrl Pts',(150.644038866656,0.501340834712195,135.696991855453));
#33222=CARTESIAN_POINT('Ctrl Pts',(150.636281825771,0.637465262673801,135.683043382531));
#33223=CARTESIAN_POINT('Ctrl Pts',(150.628524784886,0.773149415981377,135.663395072181));
#33224=CARTESIAN_POINT('Ctrl Pts',(150.620767744001,0.90788034626783,135.638089647969));
#33225=CARTESIAN_POINT('Ctrl Pts',(150.613016552761,1.0425096749123,135.612803306774));
#33226=CARTESIAN_POINT('Ctrl Pts',(150.605265361521,1.17618682863727,135.581868414955));
#33227=CARTESIAN_POINT('Ctrl Pts',(150.597514170281,1.30840519997636,135.545379378885));
#33228=CARTESIAN_POINT('Ctrl Pts',(150.589766273504,1.44056737498005,135.508905851628));
#33229=CARTESIAN_POINT('Ctrl Pts',(150.582018376727,1.57127162468564,135.466882979082));
#33230=CARTESIAN_POINT('Ctrl Pts',(150.57427047995,1.70002295649571,135.419455958931));
#33231=CARTESIAN_POINT('Ctrl Pts',(150.566524203866,1.82874735630267,135.372038859489));
#33232=CARTESIAN_POINT('Ctrl Pts',(150.558777927781,1.95551928412539,135.319219995985));
#33233=CARTESIAN_POINT('Ctrl Pts',(150.551031651697,2.07986068207613,135.261193866147));
#33234=CARTESIAN_POINT('Ctrl Pts',(150.543285318432,2.20420299788708,135.203167307972));
#33235=CARTESIAN_POINT('Ctrl Pts',(150.535538985167,2.32611439373893,135.139933572094));
#33236=CARTESIAN_POINT('Ctrl Pts',(150.527792651901,2.44513887250762,135.071734395038));
#33237=CARTESIAN_POINT('Ctrl Pts',(150.520044583898,2.56419000598339,135.003519945248));
#33238=CARTESIAN_POINT('Ctrl Pts',(150.512296515895,2.6803525967454,134.930338035909));
#33239=CARTESIAN_POINT('Ctrl Pts',(150.504548447892,2.79319757997576,134.852475035628));
#33240=CARTESIAN_POINT('Ctrl Pts',(150.49679214515,2.90616249619667,134.774529281624));
#33241=CARTESIAN_POINT('Ctrl Pts',(150.489035842408,3.01580243902672,134.691892720734));
#33242=CARTESIAN_POINT('Ctrl Pts',(150.481279539667,3.12171910275717,134.604893857255));
#33243=CARTESIAN_POINT('Ctrl Pts',(150.473519097152,3.22769229740017,134.517848559863));
#33244=CARTESIAN_POINT('Ctrl Pts',(150.465758654638,3.32993796190583,134.426436581015));
#33245=CARTESIAN_POINT('Ctrl Pts',(150.457998212124,3.42809369507061,134.331024293098));
#33246=CARTESIAN_POINT('Ctrl Pts',(150.450225311859,3.52640699653218,134.235458840906));
#33247=CARTESIAN_POINT('Ctrl Pts',(150.442452411593,3.6206169778027,134.135880531306));
#33248=CARTESIAN_POINT('Ctrl Pts',(150.434679511328,3.71040008097605,134.032690573068));
#33249=CARTESIAN_POINT('Ctrl Pts',(150.427189175566,3.79691934219794,133.933251829734));
#33250=CARTESIAN_POINT('Ctrl Pts',(150.419698839804,3.87932780109678,133.830459704274));
#33251=CARTESIAN_POINT('Ctrl Pts',(150.412208504042,3.95737443753222,133.724698033631));
#33252=CARTESIAN_POINT('Ctrl Pts',(150.404434169923,4.03838023591081,133.614926377098));
#33253=CARTESIAN_POINT('Ctrl Pts',(150.396659835804,4.11494352760169,133.501607826023));
#33254=CARTESIAN_POINT('Ctrl Pts',(150.388885501685,4.1867376797905,133.385137760816));
#33255=CARTESIAN_POINT('Ctrl Pts',(150.381120748738,4.258443352103,133.268811234556));
#33256=CARTESIAN_POINT('Ctrl Pts',(150.373355995791,4.32539137627902,133.149341251707));
#33257=CARTESIAN_POINT('Ctrl Pts',(150.365591242844,4.38729619404333,133.027155067854));
#33258=CARTESIAN_POINT('Ctrl Pts',(150.357834201959,4.44913952707024,132.905090241041));
#33259=CARTESIAN_POINT('Ctrl Pts',(150.350077161074,4.50594944623636,132.780314928407));
#33260=CARTESIAN_POINT('Ctrl Pts',(150.342320120188,4.55748463496566,132.653283781073));
#33261=CARTESIAN_POINT('Ctrl Pts',(150.334568928948,4.60898096060829,132.526348428914));
#33262=CARTESIAN_POINT('Ctrl Pts',(150.326817737708,4.65521032683379,132.397160988897));
#33263=CARTESIAN_POINT('Ctrl Pts',(150.319066546468,4.69597832668656,132.266198713181));
#33264=CARTESIAN_POINT('Ctrl Pts',(150.311318649691,4.7367289990517,132.135292099925));
#33265=CARTESIAN_POINT('Ctrl Pts',(150.303570752914,4.77202280582424,132.002612523835));
#33266=CARTESIAN_POINT('Ctrl Pts',(150.295822856137,4.80171435033717,131.868654919095));
#33267=CARTESIAN_POINT('Ctrl Pts',(150.288076580053,4.83139968401905,131.734725335397));
#33268=CARTESIAN_POINT('Ctrl Pts',(150.280330303969,4.85548500180989,131.599518636256));
#33269=CARTESIAN_POINT('Ctrl Pts',(150.272584027885,4.87387553819101,131.463542156084));
#33270=CARTESIAN_POINT('Ctrl Pts',(150.264837694619,4.89226621032692,131.327564672164));
#33271=CARTESIAN_POINT('Ctrl Pts',(150.257091361354,4.90496196477,131.190817783313));
#33272=CARTESIAN_POINT('Ctrl Pts',(150.249345028088,4.91191970372013,131.05381579732));
#33273=CARTESIAN_POINT('Ctrl Pts',(150.241596960085,4.91887900080767,130.916783130682));
#33274=CARTESIAN_POINT('Ctrl Pts',(150.233848892082,4.92009770559724,130.779495643613));
#33275=CARTESIAN_POINT('Ctrl Pts',(150.226100824079,4.91558482809408,130.642469109724));
#33276=CARTESIAN_POINT('Ctrl Pts',(150.218344521338,4.911067154251,130.505296942405));
#33277=CARTESIAN_POINT('Ctrl Pts',(150.210588218596,4.90080574239001,130.368386673666));
#33278=CARTESIAN_POINT('Ctrl Pts',(150.202831915854,4.8848616785139,130.232250973978));
#33279=CARTESIAN_POINT('Ctrl Pts',(150.19507147334,4.86890910481085,130.096042614568));
#33280=CARTESIAN_POINT('Ctrl Pts',(150.187311030826,4.84726789723923,129.960610033843));
#33281=CARTESIAN_POINT('Ctrl Pts',(150.179550588311,4.82005040856081,129.826456163423));
#33282=CARTESIAN_POINT('Ctrl Pts',(150.171777688046,4.79278922795327,129.6920869373));
#33283=CARTESIAN_POINT('Ctrl Pts',(150.164004787781,4.75993397196585,129.559000903218));
#33284=CARTESIAN_POINT('Ctrl Pts',(150.156231887515,4.72164729794882,129.427687142746));
#33285=CARTESIAN_POINT('Ctrl Pts',(150.148741551753,4.68475244097071,129.301146968227));
#33286=CARTESIAN_POINT('Ctrl Pts',(150.141251215991,4.64281429956983,129.176252743177));
#33287=CARTESIAN_POINT('Ctrl Pts',(150.133760880229,4.59602012411946,129.053423131192));
#33288=CARTESIAN_POINT('Ctrl Pts',(150.12598654611,4.54745173328399,128.925936397135));
#33289=CARTESIAN_POINT('Ctrl Pts',(150.118212211991,4.49349795623729,128.800270086635));
#33290=CARTESIAN_POINT('Ctrl Pts',(150.110437877872,4.43431488470314,128.676912717898));
#33291=CARTESIAN_POINT('Ctrl Pts',(150.102673124925,4.37520475101538,128.553707376095));
#33292=CARTESIAN_POINT('Ctrl Pts',(150.094908371978,4.31087831324231,128.432805663342));
#33293=CARTESIAN_POINT('Ctrl Pts',(150.087143619031,4.24154068238491,128.314678769985));
#33294=CARTESIAN_POINT('Ctrl Pts',(150.079386578146,4.17227191864001,128.196669201924));
#33295=CARTESIAN_POINT('Ctrl Pts',(150.071629537261,4.09800206326972,128.081429303705));
#33296=CARTESIAN_POINT('Ctrl Pts',(150.063872496376,4.01898318963348,127.969407851832));
#33297=CARTESIAN_POINT('Ctrl Pts',(150.056121305136,3.94002390474433,127.857470876207));
#33298=CARTESIAN_POINT('Ctrl Pts',(150.048370113896,3.85632295433952,127.74874783421));
#33299=CARTESIAN_POINT('Ctrl Pts',(150.040618922655,3.76817678246907,127.643660252368));
#33300=CARTESIAN_POINT('Ctrl Pts',(150.032871025878,3.68006807507323,127.538617335552));
#33301=CARTESIAN_POINT('Ctrl Pts',(150.025123129101,3.58751815468715,127.437207104586));
#33302=CARTESIAN_POINT('Ctrl Pts',(150.017375232324,3.49086483300824,127.339819409821));
#33303=CARTESIAN_POINT('Ctrl Pts',(150.00962895624,3.39423172912051,127.242452086461));
#33304=CARTESIAN_POINT('Ctrl Pts',(150.001882680156,3.29349720646282,127.149105902979));
#33305=CARTESIAN_POINT('Ctrl Pts',(149.994136404072,3.18903687676764,127.060134814931));
#33306=CARTESIAN_POINT('Ctrl Pts',(149.986390070807,3.08457577597028,126.971163070119));
#33307=CARTESIAN_POINT('Ctrl Pts',(149.978643737541,2.97638911089388,126.886566738691));
#33308=CARTESIAN_POINT('Ctrl Pts',(149.970897404276,2.86488628783513,126.80666007597));
#33309=CARTESIAN_POINT('Ctrl Pts',(149.963149336273,2.7533584944923,126.726735518707));
#33310=CARTESIAN_POINT('Ctrl Pts',(149.95540126827,2.6385133831456,126.651502947658));
#33311=CARTESIAN_POINT('Ctrl Pts',(149.947653200267,2.52078975886876,126.581233570687));
#33312=CARTESIAN_POINT('Ctrl Pts',(149.939896897525,2.40294101652282,126.510889510586));
#33313=CARTESIAN_POINT('Ctrl Pts',(149.932140594783,2.28220798617316,126.44551938253));
#33314=CARTESIAN_POINT('Ctrl Pts',(149.924384292042,2.15905501048179,126.385348904048));
#33315=CARTESIAN_POINT('Ctrl Pts',(149.916623849527,2.03583630433914,126.325146310769));
#33316=CARTESIAN_POINT('Ctrl Pts',(149.908863407013,1.91019543721665,126.270149053603));
#33317=CARTESIAN_POINT('Ctrl Pts',(149.901102964499,1.78261626914211,126.220534453815));
#33318=CARTESIAN_POINT('Ctrl Pts',(149.893330064234,1.65483229966107,126.170840208266));
#33319=CARTESIAN_POINT('Ctrl Pts',(149.885557163968,1.52510418159966,126.126546013409));
#33320=CARTESIAN_POINT('Ctrl Pts',(149.877784263703,1.39393131340587,126.087779381543));
#33321=CARTESIAN_POINT('Ctrl Pts',(149.870293927941,1.26752690937505,126.050422014392));
#33322=CARTESIAN_POINT('Ctrl Pts',(149.862803592179,1.13978127082817,126.018197381151));
#33323=CARTESIAN_POINT('Ctrl Pts',(149.855313256417,1.01114784470684,125.99117424068));
#33324=CARTESIAN_POINT('Ctrl Pts',(149.847538922298,0.877637243137432,125.963126509623));
#33325=CARTESIAN_POINT('Ctrl Pts',(149.839764588179,0.742747282670678,125.940593639907));
#33326=CARTESIAN_POINT('Ctrl Pts',(149.83199025406,0.606973338899836,125.923708363168));
#33327=CARTESIAN_POINT('Ctrl Pts',(149.824225501112,0.471366724380364,125.906843896022));
#33328=CARTESIAN_POINT('Ctrl Pts',(149.816460748165,0.334878678450548,125.895613221009));
#33329=CARTESIAN_POINT('Ctrl Pts',(149.808695995218,0.198016494397925,125.890098462324));
#33330=CARTESIAN_POINT('Ctrl Pts',(149.800938954333,0.0612902437953645,
125.884589180975));
#33331=CARTESIAN_POINT('Ctrl Pts',(149.793181913448,-0.0758090173103959,
125.884784533851));
#33332=CARTESIAN_POINT('Ctrl Pts',(149.785424872563,-0.212767468727311,
125.890715019158));
#33333=CARTESIAN_POINT('Ctrl Pts',(149.777673681323,-0.34962263871105,125.896641032241));
#33334=CARTESIAN_POINT('Ctrl Pts',(149.769922490083,-0.486336821343375,
125.908293552443));
#33335=CARTESIAN_POINT('Ctrl Pts',(149.762171298843,-0.622395139168448,
125.925651018375));
#33336=CARTESIAN_POINT('Ctrl Pts',(149.754423402066,-0.758395628578369,
125.94300110692));
#33337=CARTESIAN_POINT('Ctrl Pts',(149.746675505288,-0.89374042060341,125.966051269171));
#33338=CARTESIAN_POINT('Ctrl Pts',(149.738927608511,-1.02791892762871,125.994728018217));
#33339=CARTESIAN_POINT('Ctrl Pts',(149.731181332427,-1.16206936740281,126.023398768704));
#33340=CARTESIAN_POINT('Ctrl Pts',(149.723435056343,-1.29505362534163,126.057693683287));
#33341=CARTESIAN_POINT('Ctrl Pts',(149.715688780259,-1.42637088129404,126.0974880708));
#33342=CARTESIAN_POINT('Ctrl Pts',(149.707942446994,-1.55768910660073,126.137282752067));
#33343=CARTESIAN_POINT('Ctrl Pts',(149.700196113728,-1.68733993120418,126.182576873884));
#33344=CARTESIAN_POINT('Ctrl Pts',(149.692449780463,-1.81483766909694,126.233195853819));
#33345=CARTESIAN_POINT('Ctrl Pts',(149.68470171246,-1.94236395922391,126.283826169522));
#33346=CARTESIAN_POINT('Ctrl Pts',(149.676953644457,-2.06773583987514,126.339783571972));
#33347=CARTESIAN_POINT('Ctrl Pts',(149.669205576454,-2.19048795133432,126.400845476504));
#33348=CARTESIAN_POINT('Ctrl Pts',(149.661449273712,-2.31337052519833,126.461972278356));
#33349=CARTESIAN_POINT('Ctrl Pts',(149.65369297097,-2.43362741728175,126.528214245158));
#33350=CARTESIAN_POINT('Ctrl Pts',(149.645936668228,-2.55081773648536,126.599302718115));
#33351=CARTESIAN_POINT('Ctrl Pts',(149.638176225714,-2.66807060369137,126.670429133131));
#33352=CARTESIAN_POINT('Ctrl Pts',(149.6304157832,-2.7822533113771,126.746406992095));
#33353=CARTESIAN_POINT('Ctrl Pts',(149.622655340686,-2.89295513597643,126.826925056337));
#33354=CARTESIAN_POINT('Ctrl Pts',(149.61488244042,-3.00383466897184,126.907572375323));
#33355=CARTESIAN_POINT('Ctrl Pts',(149.607109540155,-3.1112218461797,126.992774220874));
#33356=CARTESIAN_POINT('Ctrl Pts',(149.599336639889,-3.214739450831,127.082179358442));
#33357=CARTESIAN_POINT('Ctrl Pts',(149.591846304127,-3.31449392980714,127.168334394062));
#33358=CARTESIAN_POINT('Ctrl Pts',(149.584355968365,-3.41065506439533,127.258392216318));
#33359=CARTESIAN_POINT('Ctrl Pts',(149.576865632604,-3.50291990667291,127.352008493298));
#33360=CARTESIAN_POINT('Ctrl Pts',(149.569197320369,-3.59737703667771,127.447849169195));
#33361=CARTESIAN_POINT('Ctrl Pts',(149.561529008135,-3.68806722165813,127.54774133921));
#33362=CARTESIAN_POINT('Ctrl Pts',(149.5538606959,-3.77461559262725,127.651352499848));
#33363=CARTESIAN_POINT('Ctrl Pts',(149.546201379826,-3.86106242847899,127.75484210798));
#33364=CARTESIAN_POINT('Ctrl Pts',(149.538542063751,-3.94337685520339,127.862041727308));
#33365=CARTESIAN_POINT('Ctrl Pts',(149.530882747676,-4.02121958990375,127.97258095236));
#33366=CARTESIAN_POINT('Ctrl Pts',(149.52323064977,-4.09898896532333,128.083016004838));
#33367=CARTESIAN_POINT('Ctrl Pts',(149.515578551863,-4.17229479881784,128.196784077586));
#33368=CARTESIAN_POINT('Ctrl Pts',(149.507926453956,-4.24083735305767,128.313480932111));
#33369=CARTESIAN_POINT('Ctrl Pts',(149.500280175115,-4.30932778386069,128.430089044086));
#33370=CARTESIAN_POINT('Ctrl Pts',(149.492633896274,-4.37306194064365,128.549621160038));
#33371=CARTESIAN_POINT('Ctrl Pts',(149.484987617433,-4.43178314844268,128.67164376161));
#33372=CARTESIAN_POINT('Ctrl Pts',(149.477344690191,-4.49047861693751,128.793612876938));
#33373=CARTESIAN_POINT('Ctrl Pts',(149.469701762948,-4.54416533374774,128.918069944154));
#33374=CARTESIAN_POINT('Ctrl Pts',(149.462058835706,-4.59263257083703,129.04455689789));
#33375=CARTESIAN_POINT('Ctrl Pts',(149.454416774795,-4.6410943141279,129.171029514232));
#33376=CARTESIAN_POINT('Ctrl Pts',(149.446774713884,-4.68433760733893,129.299531185077));
#33377=CARTESIAN_POINT('Ctrl Pts',(149.439132652973,-4.72220003377671,129.429584307216));
#33378=CARTESIAN_POINT('Ctrl Pts',(149.436150982645,-4.7369726552922,129.480326579464));
#33379=CARTESIAN_POINT('Ctrl Pts',(149.433169312318,-4.7509266820847,129.531304846415));
#33380=CARTESIAN_POINT('Ctrl Pts',(149.43018764199,-4.76405452823406,129.582490119308));
#33381=CARTESIAN_POINT('Origin',(213.235140564004,0.,130.804360617566));
#33382=CARTESIAN_POINT('',(147.334614341604,-4.76405452823404,129.582490119308));
#33383=CARTESIAN_POINT('',(147.680233368326,-4.76405452823403,129.582490119308));
#33384=CARTESIAN_POINT('',(213.235140564004,-4.76405452823405,129.582490119308));
#33385=CARTESIAN_POINT('',(149.014859435954,-4.918249342247,130.80181700066));
#33386=CARTESIAN_POINT('Ctrl Pts',(149.014859435953,-4.918249342247,130.80181700066));
#33387=CARTESIAN_POINT('Ctrl Pts',(149.007179426612,-4.91831912604006,130.936748520212));
#33388=CARTESIAN_POINT('Ctrl Pts',(148.99949941727,-4.91283197951487,131.071905857874));
#33389=CARTESIAN_POINT('Ctrl Pts',(148.991819407929,-4.90175849519354,131.206786657104));
#33390=CARTESIAN_POINT('Ctrl Pts',(148.984148181936,-4.89069767521578,131.34151319804));
#33391=CARTESIAN_POINT('Ctrl Pts',(148.976476955943,-4.87406325677253,131.475963433587));
#33392=CARTESIAN_POINT('Ctrl Pts',(148.968805729951,-4.85187782821074,131.609633616379));
#33393=CARTESIAN_POINT('Ctrl Pts',(148.961141337866,-4.82971216352713,131.743184719153));
#33394=CARTESIAN_POINT('Ctrl Pts',(148.953476945781,-4.80200539131236,131.875956758268));
#33395=CARTESIAN_POINT('Ctrl Pts',(148.945812553697,-4.7688319828449,132.007450216015));
#33396=CARTESIAN_POINT('Ctrl Pts',(148.938116687181,-4.73552234515806,132.139483662021));
#33397=CARTESIAN_POINT('Ctrl Pts',(148.930420820666,-4.69670110519183,132.270227594894));
#33398=CARTESIAN_POINT('Ctrl Pts',(148.92272495415,-4.65249580553531,132.399185323286));
#33399=CARTESIAN_POINT('Ctrl Pts',(148.915067460644,-4.60851092165367,132.527500044668));
#33400=CARTESIAN_POINT('Ctrl Pts',(148.907409967138,-4.55919568686713,132.654045953508));
#33401=CARTESIAN_POINT('Ctrl Pts',(148.899752473632,-4.50472583585498,132.778348511724));
#33402=CARTESIAN_POINT('Ctrl Pts',(148.892095580377,-4.45026025459386,132.902641326182));
#33403=CARTESIAN_POINT('Ctrl Pts',(148.884438687122,-4.39064102149756,133.024690772476));
#33404=CARTESIAN_POINT('Ctrl Pts',(148.876781793867,-4.32609179803745,133.144042821938));
#33405=CARTESIAN_POINT('Ctrl Pts',(148.86912374989,-4.26153287374632,133.263412808316));
#33406=CARTESIAN_POINT('Ctrl Pts',(148.861465705913,-4.19204267667199,133.380084239163));
#33407=CARTESIAN_POINT('Ctrl Pts',(148.853807661936,-4.11789028459296,133.49362867162));
#33408=CARTESIAN_POINT('Ctrl Pts',(148.846083003218,-4.04309286587704,133.60816078878));
#33409=CARTESIAN_POINT('Ctrl Pts',(148.8383583445,-3.96355197716302,133.719510895084));
#33410=CARTESIAN_POINT('Ctrl Pts',(148.830633685783,-3.87958705625758,133.827271025669));
#33411=CARTESIAN_POINT('Ctrl Pts',(148.822964187473,-3.79622171385506,133.934261660409));
#33412=CARTESIAN_POINT('Ctrl Pts',(148.815294689164,-3.70849562683673,134.037713159311));
#33413=CARTESIAN_POINT('Ctrl Pts',(148.807625190855,-3.61675985563495,134.137261937612));
#33414=CARTESIAN_POINT('Ctrl Pts',(148.799872951933,-3.52403441423975,134.237884674931));
#33415=CARTESIAN_POINT('Ctrl Pts',(148.792120713011,-3.42721257078373,134.334519698674));
#33416=CARTESIAN_POINT('Ctrl Pts',(148.784368474089,-3.32669194495889,134.426832669335));
#33417=CARTESIAN_POINT('Ctrl Pts',(148.776616235168,-3.22617131913406,134.519145639995));
#33418=CARTESIAN_POINT('Ctrl Pts',(148.768863996246,-3.12195227097812,134.607136339945));
#33419=CARTESIAN_POINT('Ctrl Pts',(148.761111757324,-3.01446250585793,134.690515383305));
#33420=CARTESIAN_POINT('Ctrl Pts',(148.753337423205,-2.90666637665375,134.774132071098));
#33421=CARTESIAN_POINT('Ctrl Pts',(148.745563089086,-2.79521776641346,134.853392647225));
#33422=CARTESIAN_POINT('Ctrl Pts',(148.737788754967,-2.68050410340236,134.927961084893));
#33423=CARTESIAN_POINT('Ctrl Pts',(148.73002400202,-2.56593181472891,135.002437623627));
#33424=CARTESIAN_POINT('Ctrl Pts',(148.722259249073,-2.44810280426747,135.072233318599));
#33425=CARTESIAN_POINT('Ctrl Pts',(148.714494496126,-2.3274373519524,135.137052440814));
#33426=CARTESIAN_POINT('Ctrl Pts',(148.706737455241,-2.20689174626573,135.201807183762));
#33427=CARTESIAN_POINT('Ctrl Pts',(148.698980414356,-2.08351564725758,135.261595006534));
#33428=CARTESIAN_POINT('Ctrl Pts',(148.691223373471,-1.95775778418675,135.316163751675));
#33429=CARTESIAN_POINT('Ctrl Pts',(148.683472182231,-1.83209475609824,135.370691346101));
#33430=CARTESIAN_POINT('Ctrl Pts',(148.675720990991,-1.70405389619313,135.420007541762));
#33431=CARTESIAN_POINT('Ctrl Pts',(148.66796979975,-1.57410765396314,135.463906534953));
#33432=CARTESIAN_POINT('Ctrl Pts',(148.660221902973,-1.44421664235275,135.5077868699));
#33433=CARTESIAN_POINT('Ctrl Pts',(148.652474006196,-1.31242222874879,135.546254456916));
#33434=CARTESIAN_POINT('Ctrl Pts',(148.644726109419,-1.17921571568869,135.57915206415));
#33435=CARTESIAN_POINT('Ctrl Pts',(148.636979833335,-1.04603706655952,135.612042789914));
#33436=CARTESIAN_POINT('Ctrl Pts',(148.629233557251,-0.911447284823557,
135.639365759701));
#33437=CARTESIAN_POINT('Ctrl Pts',(148.621487281167,-0.775951284682872,
135.661014060658));
#33438=CARTESIAN_POINT('Ctrl Pts',(148.613740947901,-0.640454284341493,
135.682662521418));
#33439=CARTESIAN_POINT('Ctrl Pts',(148.605994614636,-0.504051438315701,
135.698636168077));
#33440=CARTESIAN_POINT('Ctrl Pts',(148.598248281371,-0.367255872060017,
135.708879573278));
#33441=CARTESIAN_POINT('Ctrl Pts',(148.590500213368,-0.230429671385745,
135.719125272418));
#33442=CARTESIAN_POINT('Ctrl Pts',(148.582752145365,-0.0932109652763536,
135.723638147398));
#33443=CARTESIAN_POINT('Ctrl Pts',(148.575004077362,0.0438844049726258,
135.722414828481));
#33444=CARTESIAN_POINT('Ctrl Pts',(148.56724777462,0.181125481812562,135.721190209407));
#33445=CARTESIAN_POINT('Ctrl Pts',(148.559491471878,0.318242569367009,135.714217221526));
#33446=CARTESIAN_POINT('Ctrl Pts',(148.551735169136,0.454721678907472,135.701544630571));
#33447=CARTESIAN_POINT('Ctrl Pts',(148.543974726622,0.591273631458189,135.688865275873));
#33448=CARTESIAN_POINT('Ctrl Pts',(148.536214284108,0.727186540256706,135.670480308943));
#33449=CARTESIAN_POINT('Ctrl Pts',(148.528453841594,0.861954922358426,135.646489981216));
#33450=CARTESIAN_POINT('Ctrl Pts',(148.520680941328,0.996939646631087,135.622461142085));
#33451=CARTESIAN_POINT('Ctrl Pts',(148.512908041063,1.13077579077568,135.592809045459));
#33452=CARTESIAN_POINT('Ctrl Pts',(148.505135140797,1.26297051073684,135.557684565238));
#33453=CARTESIAN_POINT('Ctrl Pts',(148.497644805035,1.39035961964847,135.523836948346));
#33454=CARTESIAN_POINT('Ctrl Pts',(148.490154469273,1.51622427800469,135.484908001123));
#33455=CARTESIAN_POINT('Ctrl Pts',(148.482664133511,1.64014144928102,135.441074873249));
#33456=CARTESIAN_POINT('Ctrl Pts',(148.474889799392,1.76875697777074,135.395579799007));
#33457=CARTESIAN_POINT('Ctrl Pts',(148.467115465273,1.89568184136087,135.344657204267));
#33458=CARTESIAN_POINT('Ctrl Pts',(148.459341131154,2.02042391675374,135.288451412712));
#33459=CARTESIAN_POINT('Ctrl Pts',(148.451576378207,2.14501225868712,135.232314889771));
#33460=CARTESIAN_POINT('Ctrl Pts',(148.44381162526,2.26742281187251,135.170908284166));
#33461=CARTESIAN_POINT('Ctrl Pts',(148.436046872313,2.38717959955839,135.104425340562));
#33462=CARTESIAN_POINT('Ctrl Pts',(148.428289831428,2.50681744311466,135.038008428754));
#33463=CARTESIAN_POINT('Ctrl Pts',(148.420532790543,2.62380642683538,134.966525401073));
#33464=CARTESIAN_POINT('Ctrl Pts',(148.412775749658,2.73769185438608,134.890217488888));
#33465=CARTESIAN_POINT('Ctrl Pts',(148.405024558417,2.85149140004965,134.813967121093));
#33466=CARTESIAN_POINT('Ctrl Pts',(148.397273367177,2.96219172451724,134.732899327719));
#33467=CARTESIAN_POINT('Ctrl Pts',(148.389522175937,3.06936430881091,134.647300351975));
#33468=CARTESIAN_POINT('Ctrl Pts',(148.38177427916,3.17649134189743,134.561737758078));
#33469=CARTESIAN_POINT('Ctrl Pts',(148.374026382383,3.28009331212357,134.471648055707));
#33470=CARTESIAN_POINT('Ctrl Pts',(148.366278485606,3.37977237485689,134.377359603943));
#33471=CARTESIAN_POINT('Ctrl Pts',(148.358532209522,3.47943058687919,134.283090875291));
#33472=CARTESIAN_POINT('Ctrl Pts',(148.350785933438,3.57516723975498,134.184625412707));
#33473=CARTESIAN_POINT('Ctrl Pts',(148.343039657354,3.66661946621151,134.082330225799));
#33474=CARTESIAN_POINT('Ctrl Pts',(148.335293324088,3.75807236774757,133.980034283771));
#33475=CARTESIAN_POINT('Ctrl Pts',(148.327546990823,3.84524051918084,133.873908852477));
#33476=CARTESIAN_POINT('Ctrl Pts',(148.319800657557,3.92779993106341,133.764355679055));
#33477=CARTESIAN_POINT('Ctrl Pts',(148.312052589554,4.01037783155359,133.654777971959));
#33478=CARTESIAN_POINT('Ctrl Pts',(148.304304521552,4.08834470348989,133.541771307433));
#33479=CARTESIAN_POINT('Ctrl Pts',(148.296556453549,4.16141888699936,133.425767855945));
#33480=CARTESIAN_POINT('Ctrl Pts',(148.288800150807,4.23457073462087,133.309641114608));
#33481=CARTESIAN_POINT('Ctrl Pts',(148.281043848065,4.3028192975253,133.190511555216));
#33482=CARTESIAN_POINT('Ctrl Pts',(148.273287545323,4.36592778024305,133.068837970114));
#33483=CARTESIAN_POINT('Ctrl Pts',(148.265527102809,4.42906994585831,132.947099444156));
#33484=CARTESIAN_POINT('Ctrl Pts',(148.257766660295,4.48706639955389,132.822814541027));
#33485=CARTESIAN_POINT('Ctrl Pts',(148.25000621778,4.5397282598225,132.696462726193));
#33486=CARTESIAN_POINT('Ctrl Pts',(148.242233317515,4.59247465758425,132.569908080209));
#33487=CARTESIAN_POINT('Ctrl Pts',(148.23446041725,4.6398692139415,132.441280259184));
#33488=CARTESIAN_POINT('Ctrl Pts',(148.226687516984,4.68177246912884,132.311075457809));
#33489=CARTESIAN_POINT('Ctrl Pts',(148.219197181222,4.72215243544235,132.185603928929));
#33490=CARTESIAN_POINT('Ctrl Pts',(148.21170684546,4.75743333187616,132.058668380314));
#33491=CARTESIAN_POINT('Ctrl Pts',(148.204216509698,4.78753553789668,131.930720478302));
#33492=CARTESIAN_POINT('Ctrl Pts',(148.196442175579,4.81877907820772,131.797921392696));
#33493=CARTESIAN_POINT('Ctrl Pts',(148.18866784146,4.8445424461326,131.663611003948));
#33494=CARTESIAN_POINT('Ctrl Pts',(148.180893507341,4.86468106061032,131.528281359802));
#33495=CARTESIAN_POINT('Ctrl Pts',(148.173128754394,4.88479485604551,131.393118497348));
#33496=CARTESIAN_POINT('Ctrl Pts',(148.165364001446,4.89929763366519,131.256939261837));
#33497=CARTESIAN_POINT('Ctrl Pts',(148.157599248499,4.90809511928264,131.120248829714));
#33498=CARTESIAN_POINT('Ctrl Pts',(148.149842207614,4.91688386711335,130.983694160455));
#33499=CARTESIAN_POINT('Ctrl Pts',(148.142085166729,4.91997857473634,130.846629692619));
#33500=CARTESIAN_POINT('Ctrl Pts',(148.134328125844,4.9173364224597,130.709568366558));
#33501=CARTESIAN_POINT('Ctrl Pts',(148.126576934604,4.91469626265065,130.572610399508));
#33502=CARTESIAN_POINT('Ctrl Pts',(148.118825743364,4.90632786150677,130.435655958828));
#33503=CARTESIAN_POINT('Ctrl Pts',(148.111074552124,4.89224041857029,130.299220291115));
#33504=CARTESIAN_POINT('Ctrl Pts',(148.103326655347,4.87815896317286,130.1628426122));
#33505=CARTESIAN_POINT('Ctrl Pts',(148.09557875857,4.85836334062089,130.026983655794));
#33506=CARTESIAN_POINT('Ctrl Pts',(148.087830861793,4.83291476396836,129.892155625957));
#33507=CARTESIAN_POINT('Ctrl Pts',(148.080084585709,4.80747151060945,129.757355799237));
#33508=CARTESIAN_POINT('Ctrl Pts',(148.072338309624,4.77637772762758,129.623586854091));
#33509=CARTESIAN_POINT('Ctrl Pts',(148.06459203354,4.73974605197591,129.491352458689));
#33510=CARTESIAN_POINT('Ctrl Pts',(148.056845700275,4.70311410591752,129.359117087162));
#33511=CARTESIAN_POINT('Ctrl Pts',(148.04909936701,4.66094428999194,129.228416664759));
#33512=CARTESIAN_POINT('Ctrl Pts',(148.041353033744,4.6133994812327,129.099740927118));
#33513=CARTESIAN_POINT('Ctrl Pts',(148.033604965741,4.5658440251431,128.971036373438));
#33514=CARTESIAN_POINT('Ctrl Pts',(148.025856897738,4.5129113164903,128.844357773423));
#33515=CARTESIAN_POINT('Ctrl Pts',(148.018108829735,4.45481270848735,128.720175694197));
#33516=CARTESIAN_POINT('Ctrl Pts',(148.010352526993,4.39665235259258,128.595861632779));
#33517=CARTESIAN_POINT('Ctrl Pts',(148.002596224252,4.33331529566538,128.474049747155));
#33518=CARTESIAN_POINT('Ctrl Pts',(147.99483992151,4.26505953896349,128.35518724853));
#33519=CARTESIAN_POINT('Ctrl Pts',(147.987079478996,4.19676735210905,128.23626130941));
#33520=CARTESIAN_POINT('Ctrl Pts',(147.979319036481,4.12355144303966,128.120288224402));
#33521=CARTESIAN_POINT('Ctrl Pts',(147.971558593967,4.04571310456317,128.007686067665));
#33522=CARTESIAN_POINT('Ctrl Pts',(147.963785693702,3.96774981307556,127.894903151949));
#33523=CARTESIAN_POINT('Ctrl Pts',(147.956012793436,3.88514949970579,127.785502290229));
#33524=CARTESIAN_POINT('Ctrl Pts',(147.948239893171,3.79825424568981,127.679869019306));
#33525=CARTESIAN_POINT('Ctrl Pts',(147.940749557409,3.7145178530339,127.578075783855));
#33526=CARTESIAN_POINT('Ctrl Pts',(147.933259221647,3.62679356729015,127.479781201881));
#33527=CARTESIAN_POINT('Ctrl Pts',(147.925768885885,3.53541835129655,127.385296397079));
#33528=CARTESIAN_POINT('Ctrl Pts',(147.917994551766,3.44057861621496,127.287229172184));
#33529=CARTESIAN_POINT('Ctrl Pts',(147.910220217647,3.34150521196224,127.192955675261));
#33530=CARTESIAN_POINT('Ctrl Pts',(147.902445883528,3.23853396264591,127.102863510274));
#33531=CARTESIAN_POINT('Ctrl Pts',(147.894681130581,3.13568961619176,127.01288237583));
#33532=CARTESIAN_POINT('Ctrl Pts',(147.886916377634,3.02895727411363,126.927072575122));
#33533=CARTESIAN_POINT('Ctrl Pts',(147.879151624686,2.91871099816158,126.845786483902));
#33534=CARTESIAN_POINT('Ctrl Pts',(147.871394583801,2.80857422036444,126.764581127174));
#33535=CARTESIAN_POINT('Ctrl Pts',(147.863637542916,2.69493076676894,126.687890769153));
#33536=CARTESIAN_POINT('Ctrl Pts',(147.855880502031,2.57818904353077,126.616028692047));
#33537=CARTESIAN_POINT('Ctrl Pts',(147.848129310791,2.46153535613417,126.544220806693));
#33538=CARTESIAN_POINT('Ctrl Pts',(147.840378119551,2.34178838121044,126.477234159095));
#33539=CARTESIAN_POINT('Ctrl Pts',(147.832626928311,2.21938658289212,126.415339512789));
#33540=CARTESIAN_POINT('Ctrl Pts',(147.824879031534,2.09703680860363,126.353471173359));
#33541=CARTESIAN_POINT('Ctrl Pts',(147.817131134757,1.9720348033289,126.296690706776));
#33542=CARTESIAN_POINT('Ctrl Pts',(147.80938323798,1.8448445860021,126.24522347157));
#33543=CARTESIAN_POINT('Ctrl Pts',(147.801636961896,1.71768097412686,126.193767002201));
#33544=CARTESIAN_POINT('Ctrl Pts',(147.793890685811,1.58833042283198,126.147621700105));
#33545=CARTESIAN_POINT('Ctrl Pts',(147.786144409727,1.4572775654392,126.106965045574));
#33546=CARTESIAN_POINT('Ctrl Pts',(147.778398076462,1.32622374064434,126.066308090925));
#33547=CARTESIAN_POINT('Ctrl Pts',(147.770651743197,1.19346795808586,126.031139980531));
#33548=CARTESIAN_POINT('Ctrl Pts',(147.762905409931,1.05951028524192,126.001588395404));
#33549=CARTESIAN_POINT('Ctrl Pts',(147.755157341928,0.92552261350576,125.972030192406));
#33550=CARTESIAN_POINT('Ctrl Pts',(147.747409273925,0.790332897609332,125.948091101723));
#33551=CARTESIAN_POINT('Ctrl Pts',(147.739661205922,0.65445128057406,125.929847658936));
#33552=CARTESIAN_POINT('Ctrl Pts',(147.731904903181,0.518425246939145,125.911584826801));
#33553=CARTESIAN_POINT('Ctrl Pts',(147.724148600439,0.381706231309343,125.899029786992));
#33554=CARTESIAN_POINT('Ctrl Pts',(147.716392297697,0.244809941117924,125.892207204324));
#33555=CARTESIAN_POINT('Ctrl Pts',(147.708631855183,0.107840585254747,125.885380980237));
#33556=CARTESIAN_POINT('Ctrl Pts',(147.700871412669,-0.029305842940348,
125.884293312873));
#33557=CARTESIAN_POINT('Ctrl Pts',(147.693110970154,-0.166114749715804,
125.888916695352));
#33558=CARTESIAN_POINT('Ctrl Pts',(147.685338069889,-0.30314327429402,125.893547499696));
#33559=CARTESIAN_POINT('Ctrl Pts',(147.677565169624,-0.439832804653475,
125.903907644672));
#33560=CARTESIAN_POINT('Ctrl Pts',(147.669792269358,-0.575674074501106,
125.919917719707));
#33561=CARTESIAN_POINT('Ctrl Pts',(147.662301933596,-0.706577172025894,
125.935345788187));
#33562=CARTESIAN_POINT('Ctrl Pts',(147.654811597834,-0.836692306918456,
125.956020091728));
#33563=CARTESIAN_POINT('Ctrl Pts',(147.647321262072,-0.965575585355786,
125.981825303909));
#33564=CARTESIAN_POINT('Ctrl Pts',(147.639546927953,-1.0993455124684,126.008608928554));
#33565=CARTESIAN_POINT('Ctrl Pts',(147.631772593834,-1.23221207039511,126.041005061611));
#33566=CARTESIAN_POINT('Ctrl Pts',(147.623998259715,-1.36366763580874,126.078940674159));
#33567=CARTESIAN_POINT('Ctrl Pts',(147.616233506768,-1.49496119398665,126.116829534455));
#33568=CARTESIAN_POINT('Ctrl Pts',(147.608468753821,-1.62484684755778,126.160244183359));
#33569=CARTESIAN_POINT('Ctrl Pts',(147.600704000874,-1.75282594330959,126.209060379827));
#33570=CARTESIAN_POINT('Ctrl Pts',(147.592946959989,-1.88067792841945,126.257828091361));
#33571=CARTESIAN_POINT('Ctrl Pts',(147.585189919104,-2.0066267611702,126.311986535644));
#33572=CARTESIAN_POINT('Ctrl Pts',(147.577432878219,-2.13018811486396,126.371361445697));
#33573=CARTESIAN_POINT('Ctrl Pts',(147.569681686979,-2.25365628998014,126.430691580669));
#33574=CARTESIAN_POINT('Ctrl Pts',(147.561930495739,-2.37474021869379,126.495230182816));
#33575=CARTESIAN_POINT('Ctrl Pts',(147.554179304498,-2.49297509939969,126.564754714151));
#33576=CARTESIAN_POINT('Ctrl Pts',(147.546431407721,-2.61115972712664,126.634249695705));
#33577=CARTESIAN_POINT('Ctrl Pts',(147.538683510944,-2.72649737896388,126.708726193855));
#33578=CARTESIAN_POINT('Ctrl Pts',(147.530935614167,-2.83854764082894,126.78791562812));
#33579=CARTESIAN_POINT('Ctrl Pts',(147.523189338083,-2.95057446419478,126.867088497663));
#33580=CARTESIAN_POINT('Ctrl Pts',(147.515443061999,-3.05931494628822,126.950972116921));
#33581=CARTESIAN_POINT('Ctrl Pts',(147.507696785915,-3.16435781176599,127.039254682587));
#33582=CARTESIAN_POINT('Ctrl Pts',(147.49995045265,-3.26940145264633,127.127537899935));
#33583=CARTESIAN_POINT('Ctrl Pts',(147.492204119384,-3.37074712314723,127.220219876943));
#33584=CARTESIAN_POINT('Ctrl Pts',(147.484457786119,-3.4680171029287,127.316948907387));
#33585=CARTESIAN_POINT('Ctrl Pts',(147.476709718116,-3.56530886564702,127.413699599626));
#33586=CARTESIAN_POINT('Ctrl Pts',(147.468961650113,-3.65852284426262,127.514498873121));
#33587=CARTESIAN_POINT('Ctrl Pts',(147.46121358211,-3.7473189024605,127.618958899452));
#33588=CARTESIAN_POINT('Ctrl Pts',(147.453457279369,-3.83620933416645,127.723529947143));
#33589=CARTESIAN_POINT('Ctrl Pts',(147.445700976627,-3.9206722122305,127.831769221386));
#33590=CARTESIAN_POINT('Ctrl Pts',(147.437944673885,-4.0004080329813,127.943256174845));
#33591=CARTESIAN_POINT('Ctrl Pts',(147.430184231371,-4.0801864111405,128.054802632248));
#33592=CARTESIAN_POINT('Ctrl Pts',(147.422423788856,-4.15523249092599,128.169599895699));
#33593=CARTESIAN_POINT('Ctrl Pts',(147.414663346342,-4.22529126416093,128.287200154762));
#33594=CARTESIAN_POINT('Ctrl Pts',(147.406890446077,-4.29546250195816,128.4049891962));
#33595=CARTESIAN_POINT('Ctrl Pts',(147.399117545811,-4.36063024856198,128.52558988076));
#33596=CARTESIAN_POINT('Ctrl Pts',(147.391344645546,-4.42058604346647,128.648530824932));
#33597=CARTESIAN_POINT('Ctrl Pts',(147.383854309784,-4.47836229420734,128.767002556115));
#33598=CARTESIAN_POINT('Ctrl Pts',(147.376363974022,-4.53129882576064,128.887647070215));
#33599=CARTESIAN_POINT('Ctrl Pts',(147.36887363826,-4.57925273005628,129.010028570042));
#33600=CARTESIAN_POINT('Ctrl Pts',(147.360048375184,-4.6357529770913,129.154220895448));
#33601=CARTESIAN_POINT('Ctrl Pts',(147.351223112107,-4.68548683024461,129.301206282813));
#33602=CARTESIAN_POINT('Ctrl Pts',(147.342397849031,-4.72820390052873,129.450377258169));
#33603=CARTESIAN_POINT('Ctrl Pts',(147.339803346556,-4.74076211478789,129.494231414301));
#33604=CARTESIAN_POINT('Ctrl Pts',(147.33720884408,-4.75271418880937,129.538274308005));
#33605=CARTESIAN_POINT('Ctrl Pts',(147.334614341604,-4.76405452823404,129.582490119308));
#33606=CARTESIAN_POINT('Ctrl Pts',(149.084946415013,-4.76405452823403,129.582490119308));
#33607=CARTESIAN_POINT('Ctrl Pts',(149.077173469471,-4.79811573982622,129.715294266355));
#33608=CARTESIAN_POINT('Ctrl Pts',(149.069400523929,-4.82658340099087,129.849382389387));
#33609=CARTESIAN_POINT('Ctrl Pts',(149.061627578387,-4.84939077464027,129.984243444637));
#33610=CARTESIAN_POINT('Ctrl Pts',(149.054271512637,-4.87097493977352,130.111871611355));
#33611=CARTESIAN_POINT('Ctrl Pts',(149.046915446886,-4.88749009678853,130.240191692275));
#33612=CARTESIAN_POINT('Ctrl Pts',(149.039559381136,-4.89892268279498,130.368769512863));
#33613=CARTESIAN_POINT('Ctrl Pts',(149.031326066088,-4.91171866445289,130.512680910767));
#33614=CARTESIAN_POINT('Ctrl Pts',(149.023092751039,-4.91817453086599,130.657164349066));
#33615=CARTESIAN_POINT('Ctrl Pts',(149.014859435991,-4.91824934224666,130.801817000001));
#33616=CARTESIAN_POINT('',(149.360140564045,-4.91824792773029,130.808875468254));
#33617=CARTESIAN_POINT('Ctrl Pts',(149.43018764199,-4.76405452823406,129.582490119308));
#33618=CARTESIAN_POINT('Ctrl Pts',(149.422542844658,-4.79771342147254,129.7137256332));
#33619=CARTESIAN_POINT('Ctrl Pts',(149.414898047325,-4.82593757969098,129.846322570406));
#33620=CARTESIAN_POINT('Ctrl Pts',(149.407253249992,-4.84863465409383,129.979784936612));
#33621=CARTESIAN_POINT('Ctrl Pts',(149.399401135668,-4.87194724372685,130.116866629151));
#33622=CARTESIAN_POINT('Ctrl Pts',(149.391549021343,-4.8894286189972,130.254860913363));
#33623=CARTESIAN_POINT('Ctrl Pts',(149.383696907019,-4.90103558399918,130.393224062546));
#33624=CARTESIAN_POINT('Ctrl Pts',(149.375844792694,-4.91264254900116,130.531587211729));
#33625=CARTESIAN_POINT('Ctrl Pts',(149.36799267837,-4.91837511993864,130.670318767624));
#33626=CARTESIAN_POINT('Ctrl Pts',(149.360140564045,-4.91824792773029,130.808875468254));
#33627=CARTESIAN_POINT('Ctrl Pts',(149.360140564008,-4.91824792772968,130.808875468915));
#33628=CARTESIAN_POINT('Ctrl Pts',(149.349520212843,-4.91807589430529,130.996279874428));
#33629=CARTESIAN_POINT('Ctrl Pts',(149.338899861678,-4.90718913097012,131.183212342436));
#33630=CARTESIAN_POINT('Ctrl Pts',(149.328279510512,-4.8857697338849,131.368662992144));
#33631=CARTESIAN_POINT('Ctrl Pts',(149.318325676605,-4.86569458592999,131.542475038132));
#33632=CARTESIAN_POINT('Ctrl Pts',(149.308371842698,-4.83636785883871,131.714986206173));
#33633=CARTESIAN_POINT('Ctrl Pts',(149.298418008791,-4.79797539097165,131.885385691341));
#33634=CARTESIAN_POINT('Ctrl Pts',(149.290643674672,-4.76798936994312,132.018474362879));
#33635=CARTESIAN_POINT('Ctrl Pts',(149.282869340553,-4.73241413513519,132.150525240653));
#33636=CARTESIAN_POINT('Ctrl Pts',(149.275095006434,-4.69133487599886,132.281032600011));
#33637=CARTESIAN_POINT('Ctrl Pts',(149.267330253487,-4.65030624337806,132.411379120712));
#33638=CARTESIAN_POINT('Ctrl Pts',(149.259565500539,-4.6037871992689,132.540185538557));
#33639=CARTESIAN_POINT('Ctrl Pts',(149.251800747592,-4.5519139152385,132.666956325378));
#33640=CARTESIAN_POINT('Ctrl Pts',(149.244043706707,-4.5000921524851,132.793601201665));
#33641=CARTESIAN_POINT('Ctrl Pts',(149.236286665822,-4.44292687978926,132.918214110932));
#33642=CARTESIAN_POINT('Ctrl Pts',(149.228529624937,-4.38060393645091,133.040315047882));
#33643=CARTESIAN_POINT('Ctrl Pts',(149.220778433697,-4.3183279913289,133.162323907566));
#33644=CARTESIAN_POINT('Ctrl Pts',(149.213027242457,-4.25090229428091,133.2818242186));
#33645=CARTESIAN_POINT('Ctrl Pts',(149.205276051217,-4.17856047316595,133.39835665353));
#33646=CARTESIAN_POINT('Ctrl Pts',(149.19752815444,-4.10624939925472,133.514839559066));
#33647=CARTESIAN_POINT('Ctrl Pts',(149.189780257663,-4.02902656287279,133.628356765908));
#33648=CARTESIAN_POINT('Ctrl Pts',(149.182032360886,-3.94717103587984,133.738474431993));
#33649=CARTESIAN_POINT('Ctrl Pts',(149.174286084802,-3.86533263129856,133.848569063836));
#33650=CARTESIAN_POINT('Ctrl Pts',(149.166539808717,-3.77886369671074,133.955265255788));
#33651=CARTESIAN_POINT('Ctrl Pts',(149.158793532633,-3.68808581510577,134.058159333362));
#33652=CARTESIAN_POINT('Ctrl Pts',(149.151047199368,-3.59730726339924,134.161054170476));
#33653=CARTESIAN_POINT('Ctrl Pts',(149.143300866103,-3.50221995985908,134.260146544032));
#33654=CARTESIAN_POINT('Ctrl Pts',(149.135554532837,-3.40318457367438,134.355067282443));
#33655=CARTESIAN_POINT('Ctrl Pts',(149.127806464834,-3.30412700920148,134.450009277696));
#33656=CARTESIAN_POINT('Ctrl Pts',(149.120058396831,-3.20111988493779,134.54077750836));
#33657=CARTESIAN_POINT('Ctrl Pts',(149.112310328828,-3.0945590799535,134.627041242883));
#33658=CARTESIAN_POINT('Ctrl Pts',(149.104554026086,-2.98788502087758,134.713396659531));
#33659=CARTESIAN_POINT('Ctrl Pts',(149.096797723345,-2.87765004068806,134.795237770239));
#33660=CARTESIAN_POINT('Ctrl Pts',(149.089041420603,-2.76428175287462,134.872275249564));
#33661=CARTESIAN_POINT('Ctrl Pts',(149.081280978089,-2.65085295699241,134.949353846111));
#33662=CARTESIAN_POINT('Ctrl Pts',(149.073520535574,-2.5342878533267,135.021623496688));
#33663=CARTESIAN_POINT('Ctrl Pts',(149.06576009306,-2.41504024284893,135.088840012769));
#33664=CARTESIAN_POINT('Ctrl Pts',(149.057987192795,-2.2956012055206,135.156164430769));
#33665=CARTESIAN_POINT('Ctrl Pts',(149.050214292529,-2.17347140474658,135.218419326775));
#33666=CARTESIAN_POINT('Ctrl Pts',(149.042441392264,-2.04912709076797,135.275407612217));
#33667=CARTESIAN_POINT('Ctrl Pts',(149.034951056502,-1.92930300580758,135.330324229939));
#33668=CARTESIAN_POINT('Ctrl Pts',(149.02746072074,-1.80742290355297,135.380350381393));
#33669=CARTESIAN_POINT('Ctrl Pts',(149.019970384978,-1.68392588509735,135.425353657595));
#33670=CARTESIAN_POINT('Ctrl Pts',(149.012196050859,-1.55574643965011,135.472063246694));
#33671=CARTESIAN_POINT('Ctrl Pts',(149.00442171674,-1.42541901291683,135.513509519065));
#33672=CARTESIAN_POINT('Ctrl Pts',(148.996647382621,-1.29341513234875,135.549490790481));
#33673=CARTESIAN_POINT('Ctrl Pts',(148.988882629674,-1.16157393476604,135.585427718196));
#33674=CARTESIAN_POINT('Ctrl Pts',(148.981117876727,-1.02806076781331,135.615912944016));
#33675=CARTESIAN_POINT('Ctrl Pts',(148.97335312378,-0.893366137432455,135.640793187859));
#33676=CARTESIAN_POINT('Ctrl Pts',(148.965596082895,-0.75880528765736,135.665648720292));
#33677=CARTESIAN_POINT('Ctrl Pts',(148.95783904201,-0.623065691638389,135.684910278667));
#33678=CARTESIAN_POINT('Ctrl Pts',(148.950082001125,-0.48665164210719,135.698474760262));
#33679=CARTESIAN_POINT('Ctrl Pts',(148.942330809884,-0.350340463471888,
135.712029012775));
#33680=CARTESIAN_POINT('Ctrl Pts',(148.934579618644,-0.213356231155399,
135.719894701325));
#33681=CARTESIAN_POINT('Ctrl Pts',(148.926828427404,-0.076211671919524,
135.722020105937));
#33682=CARTESIAN_POINT('Ctrl Pts',(148.919080530627,0.060874597220272,135.724144607195));
#33683=CARTESIAN_POINT('Ctrl Pts',(148.91133263385,0.198120667647949,135.720533670992));
#33684=CARTESIAN_POINT('Ctrl Pts',(148.903584737073,0.33501069059189,135.711187586157));
#33685=CARTESIAN_POINT('Ctrl Pts',(148.895838460989,0.471872079094039,135.701843456321));
#33686=CARTESIAN_POINT('Ctrl Pts',(148.888092184905,0.608377178442163,135.686766590674));
#33687=CARTESIAN_POINT('Ctrl Pts',(148.880345908821,0.744012542397229,135.666009350173));
#33688=CARTESIAN_POINT('Ctrl Pts',(148.872599575555,0.879648907581739,135.645251956446));
#33689=CARTESIAN_POINT('Ctrl Pts',(148.86485324229,1.01441513809635,135.618814163338));
#33690=CARTESIAN_POINT('Ctrl Pts',(148.857106909024,1.14780568892352,135.586799865792));
#33691=CARTESIAN_POINT('Ctrl Pts',(148.849358841021,1.28122611163969,135.554778398866));
#33692=CARTESIAN_POINT('Ctrl Pts',(148.841610773019,1.41326986154048,135.517178033721));
#33693=CARTESIAN_POINT('Ctrl Pts',(148.833862705016,1.54344470249761,135.474153066148));
#33694=CARTESIAN_POINT('Ctrl Pts',(148.826106402274,1.67375789482481,135.431082371127));
#33695=CARTESIAN_POINT('Ctrl Pts',(148.818350099532,1.80219783855624,135.382575679695));
#33696=CARTESIAN_POINT('Ctrl Pts',(148.81059379679,1.92828998046452,135.328836367721));
#33697=CARTESIAN_POINT('Ctrl Pts',(148.802833354276,2.05444942154553,135.275068373458));
#33698=CARTESIAN_POINT('Ctrl Pts',(148.795072911762,2.1782582111508,135.21606236187));
#33699=CARTESIAN_POINT('Ctrl Pts',(148.787312469247,2.29926561604861,135.152068138704));
#33700=CARTESIAN_POINT('Ctrl Pts',(148.779539568982,2.4204672727753,135.087971186329));
#33701=CARTESIAN_POINT('Ctrl Pts',(148.771766668717,2.53885822044009,135.018870217994));
#33702=CARTESIAN_POINT('Ctrl Pts',(148.763993768451,2.65401521795891,134.945059385328));
#33703=CARTESIAN_POINT('Ctrl Pts',(148.756503432689,2.76498596855541,134.873931762347));
#33704=CARTESIAN_POINT('Ctrl Pts',(148.749013096927,2.87295355894489,134.798430937313));
#33705=CARTESIAN_POINT('Ctrl Pts',(148.741522761165,2.97756924483162,134.718854768121));
#33706=CARTESIAN_POINT('Ctrl Pts',(148.733748427046,3.08615146624547,134.636261444289));
#33707=CARTESIAN_POINT('Ctrl Pts',(148.725974092927,3.19146654658486,134.549016011712));
#33708=CARTESIAN_POINT('Ctrl Pts',(148.718199758808,3.29308993109058,134.457406164538));
#33709=CARTESIAN_POINT('Ctrl Pts',(148.710435005861,3.39458807385724,134.365909218313));
#33710=CARTESIAN_POINT('Ctrl Pts',(148.702670252913,3.49240328570476,134.270058818865));
#33711=CARTESIAN_POINT('Ctrl Pts',(148.694905499966,3.58614147731454,134.170184791106));
#33712=CARTESIAN_POINT('Ctrl Pts',(148.687148459081,3.67978656683091,134.070409959639));
#33713=CARTESIAN_POINT('Ctrl Pts',(148.679391418196,3.76936242867941,133.966619735954));
#33714=CARTESIAN_POINT('Ctrl Pts',(148.671634377311,3.85450973708102,133.85918266627));
#33715=CARTESIAN_POINT('Ctrl Pts',(148.663883186071,3.93959283523504,133.751826615715));
#33716=CARTESIAN_POINT('Ctrl Pts',(148.656131994831,4.02025378537295,133.640829498264));
#33717=CARTESIAN_POINT('Ctrl Pts',(148.648380803591,4.09617193267615,133.526594729551));
#33718=CARTESIAN_POINT('Ctrl Pts',(148.640632906814,4.17205781274156,133.412408513663));
#33719=CARTESIAN_POINT('Ctrl Pts',(148.632885010037,4.24320468333521,133.294987708382));
#33720=CARTESIAN_POINT('Ctrl Pts',(148.62513711326,4.30933395859403,133.174766468008));
#33721=CARTESIAN_POINT('Ctrl Pts',(148.617390837176,4.37544940103404,133.054570375325));
#33722=CARTESIAN_POINT('Ctrl Pts',(148.609644561091,4.43654914748633,132.931575355064));
#33723=CARTESIAN_POINT('Ctrl Pts',(148.601898285007,4.49239972047262,132.80624168646));
#33724=CARTESIAN_POINT('Ctrl Pts',(148.594151951742,4.54825070573514,132.680907092672));
#33725=CARTESIAN_POINT('Ctrl Pts',(148.586405618477,4.59885228107741,132.553234173209));
#33726=CARTESIAN_POINT('Ctrl Pts',(148.578659285211,4.64401859682732,132.423704415165));
#33727=CARTESIAN_POINT('Ctrl Pts',(148.570911217208,4.68919502726045,132.29414564983));
#33728=CARTESIAN_POINT('Ctrl Pts',(148.563163149205,4.72893364733518,132.162729587564));
#33729=CARTESIAN_POINT('Ctrl Pts',(148.555415081202,4.76309820481994,132.029953761207));
#33730=CARTESIAN_POINT('Ctrl Pts',(148.547658778461,4.79729907280299,131.897036819122));
#33731=CARTESIAN_POINT('Ctrl Pts',(148.539902475719,4.82591394642714,131.762757605292));
#33732=CARTESIAN_POINT('Ctrl Pts',(148.532146172977,4.84885742396003,131.627625304412));
#33733=CARTESIAN_POINT('Ctrl Pts',(148.524385730463,4.87181314711771,131.492420879354));
#33734=CARTESIAN_POINT('Ctrl Pts',(148.516625287949,4.88909139341091,131.356362847647));
#33735=CARTESIAN_POINT('Ctrl Pts',(148.508864845434,4.90065869916805,131.219965450031));
#33736=CARTESIAN_POINT('Ctrl Pts',(148.501091945169,4.91224457379128,131.083349095205));
#33737=CARTESIAN_POINT('Ctrl Pts',(148.493319044903,4.91810117116215,130.946392676658));
#33738=CARTESIAN_POINT('Ctrl Pts',(148.485546144638,4.91824719723337,130.809611275244));
#33739=CARTESIAN_POINT('Ctrl Pts',(148.478055808876,4.9183879148891,130.677802222303));
#33740=CARTESIAN_POINT('Ctrl Pts',(148.470565473114,4.9132260523543,130.546155990567));
#33741=CARTESIAN_POINT('Ctrl Pts',(148.463075137352,4.90282370110143,130.415126987958));
#33742=CARTESIAN_POINT('Ctrl Pts',(148.455300803233,4.89202694153906,130.279129980888));
#33743=CARTESIAN_POINT('Ctrl Pts',(148.447526469114,4.87555026158044,130.143367133725));
#33744=CARTESIAN_POINT('Ctrl Pts',(148.439752134995,4.85340622424147,130.008351142124));
#33745=CARTESIAN_POINT('Ctrl Pts',(148.431987382048,4.83128947744946,129.873501545665));
#33746=CARTESIAN_POINT('Ctrl Pts',(148.424222629101,4.80351933304268,129.73939735549));
#33747=CARTESIAN_POINT('Ctrl Pts',(148.416457876153,4.77016026715726,129.606548408522));
#33748=CARTESIAN_POINT('Ctrl Pts',(148.408700835268,4.73683433396637,129.473831409002));
#33749=CARTESIAN_POINT('Ctrl Pts',(148.400943794383,4.69793062062983,129.34236754839));
#33750=CARTESIAN_POINT('Ctrl Pts',(148.393186753498,4.65356497115811,129.212658345874));
#33751=CARTESIAN_POINT('Ctrl Pts',(148.385435562258,4.60923277816776,129.083046958076));
#33752=CARTESIAN_POINT('Ctrl Pts',(148.377684371018,4.55944697345686,128.955187963051));
#33753=CARTESIAN_POINT('Ctrl Pts',(148.369933179778,4.50437364026346,128.829569192782));
#33754=CARTESIAN_POINT('Ctrl Pts',(148.362185283001,4.4493237147058,128.704003813842));
#33755=CARTESIAN_POINT('Ctrl Pts',(148.354437386224,4.3889908871078,128.580677123211));
#33756=CARTESIAN_POINT('Ctrl Pts',(148.346689489447,4.32358984131344,128.460058174068));
#33757=CARTESIAN_POINT('Ctrl Pts',(148.338943213363,4.25820247600797,128.339464455809));
#33758=CARTESIAN_POINT('Ctrl Pts',(148.331196937279,4.18774918746342,128.221577695912));
#33759=CARTESIAN_POINT('Ctrl Pts',(148.323450661194,4.11249102135881,128.106843117763));
#33760=CARTESIAN_POINT('Ctrl Pts',(148.315704327929,4.03723229971554,127.99210769267));
#33761=CARTESIAN_POINT('Ctrl Pts',(148.307957994664,3.95716884417045,127.880524822668));
#33762=CARTESIAN_POINT('Ctrl Pts',(148.300211661398,3.87260528716628,127.772511123889));
#33763=CARTESIAN_POINT('Ctrl Pts',(148.292463593395,3.78802279273987,127.66447323619));
#33764=CARTESIAN_POINT('Ctrl Pts',(148.284715525392,3.69893843247959,127.560006417994));
#33765=CARTESIAN_POINT('Ctrl Pts',(148.27696745739,3.60569714719512,127.459494230816));
#33766=CARTESIAN_POINT('Ctrl Pts',(148.269211154648,3.51235676396302,127.358875218089));
#33767=CARTESIAN_POINT('Ctrl Pts',(148.261454851906,3.41485089653373,127.262219519467));
#33768=CARTESIAN_POINT('Ctrl Pts',(148.253698549164,3.31356177468985,127.169874212609));
#33769=CARTESIAN_POINT('Ctrl Pts',(148.24593810665,3.21221859179179,127.077479618281));
#33770=CARTESIAN_POINT('Ctrl Pts',(148.238177664136,3.10708843051879,126.98940025079));
#33771=CARTESIAN_POINT('Ctrl Pts',(148.230417221621,2.99858584823882,126.90594222375));
#33772=CARTESIAN_POINT('Ctrl Pts',(148.222644321356,2.8899090879814,126.822350222477));
#33773=CARTESIAN_POINT('Ctrl Pts',(148.21487142109,2.7778494081853,126.74339461167));
#33774=CARTESIAN_POINT('Ctrl Pts',(148.207098520825,2.66285027198336,126.669338067265));
#33775=CARTESIAN_POINT('Ctrl Pts',(148.199608185063,2.55203164404766,126.597973664786));
#33776=CARTESIAN_POINT('Ctrl Pts',(148.192117849301,2.43848382808754,126.531158482037));
#33777=CARTESIAN_POINT('Ctrl Pts',(148.184627513539,2.32262269231376,126.469085898284));
#33778=CARTESIAN_POINT('Ctrl Pts',(148.17685317942,2.20236864636197,126.404659813651));
#33779=CARTESIAN_POINT('Ctrl Pts',(148.169078845301,2.07924147005676,126.34513897606));
#33780=CARTESIAN_POINT('Ctrl Pts',(148.161304511182,1.95367929939125,126.290789940416));
#33781=CARTESIAN_POINT('Ctrl Pts',(148.153539758235,1.82827187287941,126.236507885101));
#33782=CARTESIAN_POINT('Ctrl Pts',(148.145775005288,1.70043577828129,126.187385103614));
#33783=CARTESIAN_POINT('Ctrl Pts',(148.13801025234,1.57063480676853,126.14364292967));
#33784=CARTESIAN_POINT('Ctrl Pts',(148.130253211455,1.44096275541034,126.099944201069));
#33785=CARTESIAN_POINT('Ctrl Pts',(148.12249617057,1.30933007889283,126.061615569065));
#33786=CARTESIAN_POINT('Ctrl Pts',(148.114739129685,1.17622133602967,126.028830654183));
#33787=CARTESIAN_POINT('Ctrl Pts',(148.106987938445,1.04321297150498,125.99607046266));
#33788=CARTESIAN_POINT('Ctrl Pts',(148.099236747205,0.908731134302753,125.96884576023));
#33789=CARTESIAN_POINT('Ctrl Pts',(148.091485555965,0.773276023335518,125.947280501464));
#33790=CARTESIAN_POINT('Ctrl Pts',(148.083737659188,0.63787848440392,125.925724408509));
#33791=CARTESIAN_POINT('Ctrl Pts',(148.075989762411,0.501508879754367,125.909823036373));
#33792=CARTESIAN_POINT('Ctrl Pts',(148.068241865634,0.364677878973141,125.89964930016));
#33793=CARTESIAN_POINT('Ctrl Pts',(148.06049558955,0.227875500287496,125.889477692074));
#33794=CARTESIAN_POINT('Ctrl Pts',(148.052749313466,0.0906123070840266,
125.885031365799));
#33795=CARTESIAN_POINT('Ctrl Pts',(148.045003037381,-0.0465960200271926,
125.886331350327));
#33796=CARTESIAN_POINT('Ctrl Pts',(148.037256704116,-0.183805359979067,
125.887631344452));
#33797=CARTESIAN_POINT('Ctrl Pts',(148.029510370851,-0.320959442082866,
125.894677730318));
#33798=CARTESIAN_POINT('Ctrl Pts',(148.021764037585,-0.457543094113758,
125.907439403218));
#33799=CARTESIAN_POINT('Ctrl Pts',(148.014015969582,-0.59415733310647,125.920203934007));
#33800=CARTESIAN_POINT('Ctrl Pts',(148.00626790158,-0.730200498635566,125.938686262315));
#33801=CARTESIAN_POINT('Ctrl Pts',(147.998519833577,-0.865163440602921,
125.962803504039));
#33802=CARTESIAN_POINT('Ctrl Pts',(147.990763530835,-1.00026982279112,125.986946377854));
#33803=CARTESIAN_POINT('Ctrl Pts',(147.983007228093,-1.13429330253283,126.01673605958));
#33804=CARTESIAN_POINT('Ctrl Pts',(147.975250925351,-1.26673526902769,126.052038572428));
#33805=CARTESIAN_POINT('Ctrl Pts',(147.967490482837,-1.39924792378792,126.087359927291));
#33806=CARTESIAN_POINT('Ctrl Pts',(147.959730040323,-1.53017701031113,126.128199859823));
#33807=CARTESIAN_POINT('Ctrl Pts',(147.951969597808,-1.65904090815876,126.174375053058));
#33808=CARTESIAN_POINT('Ctrl Pts',(147.944196697543,-1.78811166977517,126.220624370812));
#33809=CARTESIAN_POINT('Ctrl Pts',(147.936423797278,-1.91511025542533,126.27222591688));
#33810=CARTESIAN_POINT('Ctrl Pts',(147.928650897012,-2.039575965751,126.328948575929));
#33811=CARTESIAN_POINT('Ctrl Pts',(147.92116056125,-2.15951703399633,126.383609223445));
#33812=CARTESIAN_POINT('Ctrl Pts',(147.913670225488,-2.27710590763376,126.443024978527));
#33813=CARTESIAN_POINT('Ctrl Pts',(147.906179889726,-2.39195510428361,126.506950485685));
#33814=CARTESIAN_POINT('Ctrl Pts',(147.898404501985,-2.51117499830053,126.573308739907));
#33815=CARTESIAN_POINT('Ctrl Pts',(147.890629114244,-2.62782026801909,126.644737020951));
#33816=CARTESIAN_POINT('Ctrl Pts',(147.882853726503,-2.74142964393392,126.721010697481));
#33817=CARTESIAN_POINT('Ctrl Pts',(147.87508815081,-2.85489565200044,126.797188121454));
#33818=CARTESIAN_POINT('Ctrl Pts',(147.867322575116,-2.96533306815711,126.878198557428));
#33819=CARTESIAN_POINT('Ctrl Pts',(147.859556999423,-3.07230485350154,126.963771346419));
#33820=CARTESIAN_POINT('Ctrl Pts',(147.851800787942,-3.17914764563016,127.049240946432));
#33821=CARTESIAN_POINT('Ctrl Pts',(147.844044576462,-3.28253282694053,127.139261699393));
#33822=CARTESIAN_POINT('Ctrl Pts',(147.836288364982,-3.38205254619534,127.233519871009));
#33823=CARTESIAN_POINT('Ctrl Pts',(147.828537462695,-3.4815041433458,127.327713522095));
#33824=CARTESIAN_POINT('Ctrl Pts',(147.820786560408,-3.57709525984537,127.426138553648));
#33825=CARTESIAN_POINT('Ctrl Pts',(147.813035658121,-3.66845128540179,127.528441169665));
#33826=CARTESIAN_POINT('Ctrl Pts',(147.805288382774,-3.75976456202871,127.63069591443));
#33827=CARTESIAN_POINT('Ctrl Pts',(147.797541107426,-3.84684643162001,127.736824341951));
#33828=CARTESIAN_POINT('Ctrl Pts',(147.789793832079,-3.92935960264885,127.8464363157));
#33829=CARTESIAN_POINT('Ctrl Pts',(147.782048504219,-4.01185203175431,127.956020735506));
#33830=CARTESIAN_POINT('Ctrl Pts',(147.774303176359,-4.08977781411566,128.069086645999));
#33831=CARTESIAN_POINT('Ctrl Pts',(147.7665578485,-4.16284062645161,128.185211713578));
#33832=CARTESIAN_POINT('Ctrl Pts',(147.758810381406,-4.23592361849478,128.301368854516));
#33833=CARTESIAN_POINT('Ctrl Pts',(147.751062914313,-4.30414074378607,128.420586512747));
#33834=CARTESIAN_POINT('Ctrl Pts',(147.743315447219,-4.36723959620254,128.542414249532));
#33835=CARTESIAN_POINT('Ctrl Pts',(147.735566984875,-4.43034655438534,128.664257636479));
#33836=CARTESIAN_POINT('Ctrl Pts',(147.727818522531,-4.48833375736234,128.788711418972));
#33837=CARTESIAN_POINT('Ctrl Pts',(147.720070060187,-4.54099570167479,128.915302360161));
#33838=CARTESIAN_POINT('Ctrl Pts',(147.712315261109,-4.59370071320322,129.041996828089));
#33839=CARTESIAN_POINT('Ctrl Pts',(147.704560462032,-4.64107162368983,129.170831581822));
#33840=CARTESIAN_POINT('Ctrl Pts',(147.696805662955,-4.68295173121227,129.301314994294));
#33841=CARTESIAN_POINT('Ctrl Pts',(147.691281564745,-4.71278484805569,129.394264299363));
#33842=CARTESIAN_POINT('Ctrl Pts',(147.685757466536,-4.7398327621419,129.488049820932));
#33843=CARTESIAN_POINT('Ctrl Pts',(147.680233368326,-4.76405452823403,129.582490119308));
#33844=CARTESIAN_POINT('Origin',(213.235140564004,0.,130.804360617566));
#33845=CARTESIAN_POINT('',(145.584738356252,-4.76405452823403,129.582490119308));
#33846=CARTESIAN_POINT('',(145.92992189461,-4.76405452823405,129.582490119308));
#33847=CARTESIAN_POINT('',(213.235140564004,-4.76405452823405,129.582490119308));
#33848=CARTESIAN_POINT('',(147.264859436046,-4.91824899899375,130.801222720669));
#33849=CARTESIAN_POINT('Ctrl Pts',(147.264859435991,-4.91824899899438,130.801222721645));
#33850=CARTESIAN_POINT('Ctrl Pts',(147.257057493982,-4.91833725438135,130.939551710121));
#33851=CARTESIAN_POINT('Ctrl Pts',(147.249255551972,-4.91258528675101,131.077906330366));
#33852=CARTESIAN_POINT('Ctrl Pts',(147.241453609963,-4.90101327064487,131.215763076799));
#33853=CARTESIAN_POINT('Ctrl Pts',(147.233651063793,-4.8894403584344,131.35363049847));
#33854=CARTESIAN_POINT('Ctrl Pts',(147.225848517623,-4.8720465317177,131.490999587807));
#33855=CARTESIAN_POINT('Ctrl Pts',(147.218045971453,-4.84890390699558,131.627351482171));
#33856=CARTESIAN_POINT('Ctrl Pts',(147.210241222478,-4.82575474867703,131.763741871229));
#33857=CARTESIAN_POINT('Ctrl Pts',(147.202436473504,-4.79685362473761,131.899114115955));
#33858=CARTESIAN_POINT('Ctrl Pts',(147.194631724529,-4.76232382245233,132.032959361096));
#33859=CARTESIAN_POINT('Ctrl Pts',(147.186823173015,-4.7277771969581,132.166869816762));
#33860=CARTESIAN_POINT('Ctrl Pts',(147.179014621501,-4.68759652835638,132.299251421062));
#33861=CARTESIAN_POINT('Ctrl Pts',(147.171206069987,-4.64195493632828,132.429610577295));
#33862=CARTESIAN_POINT('Ctrl Pts',(147.163387307618,-4.59625366105695,132.560140197721));
#33863=CARTESIAN_POINT('Ctrl Pts',(147.15556854525,-4.54507732862304,132.68864172716));
#33864=CARTESIAN_POINT('Ctrl Pts',(147.147749782881,-4.48864742345066,132.814641038415));
#33865=CARTESIAN_POINT('Ctrl Pts',(147.139925203294,-4.43217553400683,132.940734094101));
#33866=CARTESIAN_POINT('Ctrl Pts',(147.132100623708,-4.37044245397524,133.064320880399));
#33867=CARTESIAN_POINT('Ctrl Pts',(147.124276044121,-4.30371517452387,133.184952720189));
#33868=CARTESIAN_POINT('Ctrl Pts',(147.116439008637,-4.23688167234614,133.305776593028));
#33869=CARTESIAN_POINT('Ctrl Pts',(147.108601973152,-4.16503829201448,133.423635799085));
#33870=CARTESIAN_POINT('Ctrl Pts',(147.100764937668,-4.08849516546904,133.538110852031));
#33871=CARTESIAN_POINT('Ctrl Pts',(147.097318629928,-4.05483560503897,133.588450838601));
#33872=CARTESIAN_POINT('Ctrl Pts',(147.093872322187,-4.02026774482163,133.638136842638));
#33873=CARTESIAN_POINT('Ctrl Pts',(147.090426014447,-3.98482032476812,133.687135329855));
#33874=CARTESIAN_POINT('Ctrl Pts',(147.082651680328,-3.90485645969203,133.797668294309));
#33875=CARTESIAN_POINT('Ctrl Pts',(147.074877346209,-3.82016342318674,133.905046696327));
#33876=CARTESIAN_POINT('Ctrl Pts',(147.06710301209,-3.73101863840657,134.008839199545));
#33877=CARTESIAN_POINT('Ctrl Pts',(147.059338259143,-3.64198371660671,134.112503787779));
#33878=CARTESIAN_POINT('Ctrl Pts',(147.051573506196,-3.54850821508408,134.21259097656));
#33879=CARTESIAN_POINT('Ctrl Pts',(147.043808753249,-3.45091240671159,134.30869887517));
#33880=CARTESIAN_POINT('Ctrl Pts',(147.036051712364,-3.35341353187163,134.40471131806));
#33881=CARTESIAN_POINT('Ctrl Pts',(147.028294671479,-3.25180277090356,134.49675206346));
#33882=CARTESIAN_POINT('Ctrl Pts',(147.020537630594,-3.14643994106533,134.584453044977));
#33883=CARTESIAN_POINT('Ctrl Pts',(147.012786439353,-3.04115656615668,134.672087890501));
#33884=CARTESIAN_POINT('Ctrl Pts',(147.005035248113,-2.93212705352909,134.755389237044));
#33885=CARTESIAN_POINT('Ctrl Pts',(146.997284056873,-2.81974700781337,134.834026841266));
#33886=CARTESIAN_POINT('Ctrl Pts',(146.989536160096,-2.70741472661507,134.912631022408));
#33887=CARTESIAN_POINT('Ctrl Pts',(146.981788263319,-2.59173506434583,134.986575180023));
#33888=CARTESIAN_POINT('Ctrl Pts',(146.974040366542,-2.47313536498654,135.055570389966));
#33889=CARTESIAN_POINT('Ctrl Pts',(146.966294090458,-2.35456047412757,135.1245511676));
#33890=CARTESIAN_POINT('Ctrl Pts',(146.958547814374,-2.23306709883701,135.188584860186));
#33891=CARTESIAN_POINT('Ctrl Pts',(146.95080153829,-2.10910978298848,135.247427012051));
#33892=CARTESIAN_POINT('Ctrl Pts',(146.943055205024,-1.98515155211544,135.306269598275));
#33893=CARTESIAN_POINT('Ctrl Pts',(146.935308871759,-1.85872969758267,135.359920399648));
#33894=CARTESIAN_POINT('Ctrl Pts',(146.927562538494,-1.7303211079499,135.408182065655));
#33895=CARTESIAN_POINT('Ctrl Pts',(146.919814470491,-1.60188376210385,135.456454539527));
#33896=CARTESIAN_POINT('Ctrl Pts',(146.912066402488,-1.47145916172775,135.499335339002));
#33897=CARTESIAN_POINT('Ctrl Pts',(146.904318334485,-1.33954142670635,135.536676311667));
#33898=CARTESIAN_POINT('Ctrl Pts',(146.896562031743,-1.20748348794619,135.574056970763));
#33899=CARTESIAN_POINT('Ctrl Pts',(146.888805729001,-1.07392962127918,135.605885934894));
#33900=CARTESIAN_POINT('Ctrl Pts',(146.881049426259,-0.939386815361894,
135.632065607893));
#33901=CARTESIAN_POINT('Ctrl Pts',(146.873288983745,-0.804772199897945,
135.658259253771));
#33902=CARTESIAN_POINT('Ctrl Pts',(146.865528541231,-0.669167979811934,
135.678797541964));
#33903=CARTESIAN_POINT('Ctrl Pts',(146.857768098717,-0.533087444720832,
135.693634678077));
#33904=CARTESIAN_POINT('Ctrl Pts',(146.849995198451,-0.396788461074094,
135.708495632077));
#33905=CARTESIAN_POINT('Ctrl Pts',(146.842222298186,-0.260012024781023,
135.717637119308));
#33906=CARTESIAN_POINT('Ctrl Pts',(146.83444939792,-0.123273517254129,135.721065479813));
#33907=CARTESIAN_POINT('Ctrl Pts',(146.826959062158,0.0084942011015726,
135.724369210779));
#33908=CARTESIAN_POINT('Ctrl Pts',(146.819468726396,0.140226392444292,135.722367981306));
#33909=CARTESIAN_POINT('Ctrl Pts',(146.811978390634,0.271467289687367,135.715112960449));
#33910=CARTESIAN_POINT('Ctrl Pts',(146.804204056515,0.407684225438265,135.707582863271));
#33911=CARTESIAN_POINT('Ctrl Pts',(146.796429722396,0.543803371143854,135.694368862182));
#33912=CARTESIAN_POINT('Ctrl Pts',(146.788655388277,0.679311877313508,135.675471213297));
#33913=CARTESIAN_POINT('Ctrl Pts',(146.78089063533,0.814653381359636,135.656596854075));
#33914=CARTESIAN_POINT('Ctrl Pts',(146.773125882383,0.94938535973654,135.632052837582));
#33915=CARTESIAN_POINT('Ctrl Pts',(146.765361129436,1.08299657508922,135.601891386706));
#33916=CARTESIAN_POINT('Ctrl Pts',(146.757604088551,1.21647508589972,135.571759892608));
#33917=CARTESIAN_POINT('Ctrl Pts',(146.749847047666,1.34883467001885,135.536022152749));
#33918=CARTESIAN_POINT('Ctrl Pts',(146.742090006781,1.47957117274723,135.4947819427));
#33919=CARTESIAN_POINT('Ctrl Pts',(146.73433881554,1.61020908606156,135.453572832216));
#33920=CARTESIAN_POINT('Ctrl Pts',(146.7265876243,1.73922598289392,135.406869627921));
#33921=CARTESIAN_POINT('Ctrl Pts',(146.71883643306,1.86613018620254,135.354826658604));
#33922=CARTESIAN_POINT('Ctrl Pts',(146.711088536283,1.99298045183982,135.302805808938));
#33923=CARTESIAN_POINT('Ctrl Pts',(146.703340639506,2.1177194489379,135.24544985623));
#33924=CARTESIAN_POINT('Ctrl Pts',(146.695592742729,2.23987310757214,135.182962166517));
#33925=CARTESIAN_POINT('Ctrl Pts',(146.687846466645,2.36200121429415,135.120487547882));
#33926=CARTESIAN_POINT('Ctrl Pts',(146.680100190561,2.48154471038079,135.052883505332));
#33927=CARTESIAN_POINT('Ctrl Pts',(146.672353914477,2.59805223628271,134.980400325237));
#33928=CARTESIAN_POINT('Ctrl Pts',(146.664607581211,2.71456062221672,134.907916610088));
#33929=CARTESIAN_POINT('Ctrl Pts',(146.656861247946,2.82803266128193,134.830553892052));
#33930=CARTESIAN_POINT('Ctrl Pts',(146.649114914681,2.93804454698588,134.748606718208));
#33931=CARTESIAN_POINT('Ctrl Pts',(146.641366846678,3.04808106908861,134.666641192862));
#33932=CARTESIAN_POINT('Ctrl Pts',(146.633618778675,3.15465558243492,134.580089402286));
#33933=CARTESIAN_POINT('Ctrl Pts',(146.625870710672,3.25737635833861,134.489286983538));
#33934=CARTESIAN_POINT('Ctrl Pts',(146.61811440793,3.3602063071056,134.398388058899));
#33935=CARTESIAN_POINT('Ctrl Pts',(146.610358105188,3.45917404324022,134.303229741008));
#33936=CARTESIAN_POINT('Ctrl Pts',(146.602601802446,3.55392341656995,134.204185820669));
#33937=CARTESIAN_POINT('Ctrl Pts',(146.594841359932,3.64872336049306,134.105089037608));
#33938=CARTESIAN_POINT('Ctrl Pts',(146.587080917418,3.739300197298,134.002102813182));
#33939=CARTESIAN_POINT('Ctrl Pts',(146.579320474904,3.82533795328772,133.895634239495));
#33940=CARTESIAN_POINT('Ctrl Pts',(146.571547574638,3.91151382472149,133.788994753002));
#33941=CARTESIAN_POINT('Ctrl Pts',(146.563774674373,3.99313582159533,133.67886206058));
#33942=CARTESIAN_POINT('Ctrl Pts',(146.556001774107,4.06993070172686,133.565673194157));
#33943=CARTESIAN_POINT('Ctrl Pts',(146.548511438345,4.14393389453164,133.456599028134));
#33944=CARTESIAN_POINT('Ctrl Pts',(146.541021102583,4.21345467065687,133.344687291295));
#33945=CARTESIAN_POINT('Ctrl Pts',(146.533530766821,4.27828972683423,133.230349091521));
#33946=CARTESIAN_POINT('Ctrl Pts',(146.525756432702,4.34558302387209,133.111675724153));
#33947=CARTESIAN_POINT('Ctrl Pts',(146.517982098583,4.40804143366448,132.990012341417));
#33948=CARTESIAN_POINT('Ctrl Pts',(146.510207764464,4.46538796401225,132.865790556554));
#33949=CARTESIAN_POINT('Ctrl Pts',(146.502443011517,4.52266381988654,132.741721863938));
#33950=CARTESIAN_POINT('Ctrl Pts',(146.49467825857,4.57484016901265,132.615101394286));
#33951=CARTESIAN_POINT('Ctrl Pts',(146.486913505623,4.6216846117074,132.48638749381));
#33952=CARTESIAN_POINT('Ctrl Pts',(146.479156464738,4.66848252784132,132.357801433795));
#33953=CARTESIAN_POINT('Ctrl Pts',(146.471399423853,4.70995894343115,132.22712644572));
#33954=CARTESIAN_POINT('Ctrl Pts',(146.463642382968,4.7459286598755,132.094842782446));
#33955=CARTESIAN_POINT('Ctrl Pts',(146.455891191727,4.78187125127707,131.96265887531));
#33956=CARTESIAN_POINT('Ctrl Pts',(146.448140000487,4.81231530695156,131.828869083345));
#33957=CARTESIAN_POINT('Ctrl Pts',(146.440388809247,4.83712490462788,131.693970486851));
#33958=CARTESIAN_POINT('Ctrl Pts',(146.43264091247,4.86192395756323,131.559129225859));
#33959=CARTESIAN_POINT('Ctrl Pts',(146.424893015693,4.88109324499556,131.423180481373));
#33960=CARTESIAN_POINT('Ctrl Pts',(146.417145118916,4.89454761815763,131.286633026156));
#33961=CARTESIAN_POINT('Ctrl Pts',(146.409398842832,4.90799917695487,131.150114133724));
#33962=CARTESIAN_POINT('Ctrl Pts',(146.401652566748,4.91573816095844,131.012997168499));
#33963=CARTESIAN_POINT('Ctrl Pts',(146.393906290663,4.91773117231896,130.875797157952));
#33964=CARTESIAN_POINT('Ctrl Pts',(146.386159957398,4.91972419839145,130.738596134625));
#33965=CARTESIAN_POINT('Ctrl Pts',(146.378413624133,4.91597116150519,130.601312455677));
#33966=CARTESIAN_POINT('Ctrl Pts',(146.370667290867,4.90649079469751,130.464461891401));
#33967=CARTESIAN_POINT('Ctrl Pts',(146.362919222864,4.89700830482741,130.32758068039));
#33968=CARTESIAN_POINT('Ctrl Pts',(146.355171154861,4.88179595983298,130.191133167013));
#33969=CARTESIAN_POINT('Ctrl Pts',(146.347423086858,4.8609244017522,130.055630343736));
#33970=CARTESIAN_POINT('Ctrl Pts',(146.339666784117,4.84003066113115,129.919983506445));
#33971=CARTESIAN_POINT('Ctrl Pts',(146.331910481375,4.81346575206809,129.785283751932));
#33972=CARTESIAN_POINT('Ctrl Pts',(146.324154178633,4.78135164748417,129.652032762483));
#33973=CARTESIAN_POINT('Ctrl Pts',(146.316393736119,4.74922040263571,129.518710652969));
#33974=CARTESIAN_POINT('Ctrl Pts',(146.308633293604,4.7115341680602,129.386839225015));
#33975=CARTESIAN_POINT('Ctrl Pts',(146.30087285109,4.66846465037193,129.256904359468));
#33976=CARTESIAN_POINT('Ctrl Pts',(146.293099950825,4.62532599367029,129.126760910939));
#33977=CARTESIAN_POINT('Ctrl Pts',(146.285327050559,4.57678692345388,128.998560602919));
#33978=CARTESIAN_POINT('Ctrl Pts',(146.277554150294,4.52306743298746,128.872769548228));
#33979=CARTESIAN_POINT('Ctrl Pts',(146.270063814532,4.4713007813112,128.751551315223));
#33980=CARTESIAN_POINT('Ctrl Pts',(146.26257347877,4.41472394523929,128.632570489983));
#33981=CARTESIAN_POINT('Ctrl Pts',(146.255083143008,4.35357291109338,128.516220331156));
#33982=CARTESIAN_POINT('Ctrl Pts',(146.247308808889,4.2901033169008,128.395458720691));
#33983=CARTESIAN_POINT('Ctrl Pts',(146.23953447477,4.22150476344376,128.277148661457));
#33984=CARTESIAN_POINT('Ctrl Pts',(146.231760140651,4.14799065811385,128.161756492333));
#33985=CARTESIAN_POINT('Ctrl Pts',(146.223995387704,4.07456715234876,128.046506533744));
#33986=CARTESIAN_POINT('Ctrl Pts',(146.216230634757,3.99624035633337,127.934167636789));
#33987=CARTESIAN_POINT('Ctrl Pts',(146.20846588181,3.91327027201179,127.825183073228));
#33988=CARTESIAN_POINT('Ctrl Pts',(146.200708840925,3.83038259474738,127.716306754671));
#33989=CARTESIAN_POINT('Ctrl Pts',(146.19295180004,3.74286104211641,127.610778448594));
#33990=CARTESIAN_POINT('Ctrl Pts',(146.185194759155,3.6510095600827,127.509013556226));
#33991=CARTESIAN_POINT('Ctrl Pts',(146.177443567914,3.5592273439659,127.407325405554));
#33992=CARTESIAN_POINT('Ctrl Pts',(146.169692376674,3.46312195859176,127.309395308741));
#33993=CARTESIAN_POINT('Ctrl Pts',(146.161941185434,3.3630381423868,127.215606305085));
#33994=CARTESIAN_POINT('Ctrl Pts',(146.154193288657,3.26299686447389,127.121857164258));
#33995=CARTESIAN_POINT('Ctrl Pts',(146.14644539188,3.15898080356209,127.032245882711));
#33996=CARTESIAN_POINT('Ctrl Pts',(146.138697495103,3.0513719795989,126.947119102621));
#33997=CARTESIAN_POINT('Ctrl Pts',(146.130951219019,2.94378566508189,126.862010129217));
#33998=CARTESIAN_POINT('Ctrl Pts',(146.123204942935,2.83260838877351,126.781384033824));
#33999=CARTESIAN_POINT('Ctrl Pts',(146.115458666851,2.71825540551634,126.705547299924));
#34000=CARTESIAN_POINT('Ctrl Pts',(146.107712333585,2.60390157813147,126.629710006214));
#34001=CARTESIAN_POINT('Ctrl Pts',(146.09996600032,2.48637232284625,126.558662360626));
#34002=CARTESIAN_POINT('Ctrl Pts',(146.092219667054,2.36611169748163,126.492667388968));
#34003=CARTESIAN_POINT('Ctrl Pts',(146.084471599052,2.24582414058411,126.426657638193));
#34004=CARTESIAN_POINT('Ctrl Pts',(146.076723531049,2.12280433913469,126.365703000977));
#34005=CARTESIAN_POINT('Ctrl Pts',(146.068975463046,1.99752038931368,126.310020248082));
#34006=CARTESIAN_POINT('Ctrl Pts',(146.061219160304,1.87210328621955,126.254278314894));
#34007=CARTESIAN_POINT('Ctrl Pts',(146.053462857562,1.74441758561998,126.203819617707));
#34008=CARTESIAN_POINT('Ctrl Pts',(146.04570655482,1.614951296374,126.158812708778));
#34009=CARTESIAN_POINT('Ctrl Pts',(146.037946112306,1.48541590707125,126.113781778307));
#34010=CARTESIAN_POINT('Ctrl Pts',(146.030185669792,1.35409840961538,126.074208546838));
#34011=CARTESIAN_POINT('Ctrl Pts',(146.022425227278,1.22150040094184,126.040211183197));
#34012=CARTESIAN_POINT('Ctrl Pts',(146.014652327012,1.08868953417309,126.00615924397));
#34013=CARTESIAN_POINT('Ctrl Pts',(146.006879426747,0.954594431129953,125.97770114049));
#34014=CARTESIAN_POINT('Ctrl Pts',(145.999106526481,0.819726157461254,125.954903731556));
#34015=CARTESIAN_POINT('Ctrl Pts',(145.991616190719,0.689760685252308,125.932935065859));
#34016=CARTESIAN_POINT('Ctrl Pts',(145.984125854957,0.55907758540045,125.916222718075));
#34017=CARTESIAN_POINT('Ctrl Pts',(145.976635519195,0.428135273916304,125.904780712132));
#34018=CARTESIAN_POINT('Ctrl Pts',(145.968861185076,0.292228244893996,125.892904879057));
#34019=CARTESIAN_POINT('Ctrl Pts',(145.961086850957,0.155611447588727,125.886669307992));
#34020=CARTESIAN_POINT('Ctrl Pts',(145.953312516838,0.0187925780154328,
125.886146520812));
#34021=CARTESIAN_POINT('Ctrl Pts',(145.945547763891,-0.117857674529477,
125.88562437792));
#34022=CARTESIAN_POINT('Ctrl Pts',(145.937783010943,-0.254709116625827,
125.890801011904));
#34023=CARTESIAN_POINT('Ctrl Pts',(145.930018257996,-0.391248273787048,
125.901697274978));
#34024=CARTESIAN_POINT('Ctrl Pts',(145.922261217111,-0.527651818331677,
125.912582715729));
#34025=CARTESIAN_POINT('Ctrl Pts',(145.914504176226,-0.663743307980828,
125.92917644959));
#34026=CARTESIAN_POINT('Ctrl Pts',(145.906747135341,-0.799008963697667,
125.951447292724));
#34027=CARTESIAN_POINT('Ctrl Pts',(145.898995944101,-0.934172614531225,
125.973701341241));
#34028=CARTESIAN_POINT('Ctrl Pts',(145.891244752861,-1.0685112868035,126.001623914399));
#34029=CARTESIAN_POINT('Ctrl Pts',(145.883493561621,-1.20151637916289,126.035132016094));
#34030=CARTESIAN_POINT('Ctrl Pts',(145.875745664844,-1.33446494081028,126.068625875951));
#34031=CARTESIAN_POINT('Ctrl Pts',(145.867997768067,-1.4660806715554,126.107700447331));
#34032=CARTESIAN_POINT('Ctrl Pts',(145.86024987129,-1.59586544040504,126.152221694595));
#34033=CARTESIAN_POINT('Ctrl Pts',(145.852503595206,-1.72562306107897,126.196733628974));
#34034=CARTESIAN_POINT('Ctrl Pts',(145.844757319122,-1.85355011208393,126.246689846275));
#34035=CARTESIAN_POINT('Ctrl Pts',(145.837011043038,-1.97916428479939,126.301906642646));
#34036=CARTESIAN_POINT('Ctrl Pts',(145.829264709772,-2.10477938476983,126.357123846615));
#34037=CARTESIAN_POINT('Ctrl Pts',(145.821518376507,-2.22808121447012,126.417601549812));
#34038=CARTESIAN_POINT('Ctrl Pts',(145.813772043242,-2.34860845873968,126.483108325691));
#34039=CARTESIAN_POINT('Ctrl Pts',(145.806023975239,-2.46916269425025,126.548629771358));
#34040=CARTESIAN_POINT('Ctrl Pts',(145.798275907236,-2.58694076447469,126.619182344105));
#34041=CARTESIAN_POINT('Ctrl Pts',(145.790527839233,-2.7015072766123,126.694489391249));
#34042=CARTESIAN_POINT('Ctrl Pts',(145.782771536491,-2.81619555140222,126.769876475618));
#34043=CARTESIAN_POINT('Ctrl Pts',(145.775015233749,-2.92766512248064,126.850027913428));
#34044=CARTESIAN_POINT('Ctrl Pts',(145.767258931007,-3.03551040135156,126.934624235616));
#34045=CARTESIAN_POINT('Ctrl Pts',(145.759498488493,-3.14341324049483,127.019265709408));
#34046=CARTESIAN_POINT('Ctrl Pts',(145.751738045979,-3.24768763588538,127.108356540883));
#34047=CARTESIAN_POINT('Ctrl Pts',(145.743977603465,-3.34796304334593,127.201538595471));
#34048=CARTESIAN_POINT('Ctrl Pts',(145.736204703199,-3.44839942179278,127.294870234166));
#34049=CARTESIAN_POINT('Ctrl Pts',(145.728431802934,-3.54482370887592,127.392305942068));
#34050=CARTESIAN_POINT('Ctrl Pts',(145.720658902668,-3.63690341092675,127.493451883987));
#34051=CARTESIAN_POINT('Ctrl Pts',(145.713168566906,-3.72563578387244,127.590920916145));
#34052=CARTESIAN_POINT('Ctrl Pts',(145.705678231144,-3.81033376296251,127.691834876987));
#34053=CARTESIAN_POINT('Ctrl Pts',(145.698187895382,-3.89073776441627,127.795815668418));
#34054=CARTESIAN_POINT('Ctrl Pts',(145.690403729643,-3.97429584423556,127.903875405656));
#34055=CARTESIAN_POINT('Ctrl Pts',(145.682619563903,-4.05348493014445,128.015594995365));
#34056=CARTESIAN_POINT('Ctrl Pts',(145.674835398163,-4.12796746956741,128.130586574627));
#34057=CARTESIAN_POINT('Ctrl Pts',(145.667063832803,-4.20232944265324,128.245392014781));
#34058=CARTESIAN_POINT('Ctrl Pts',(145.659292267444,-4.27199983210114,128.363458572807));
#34059=CARTESIAN_POINT('Ctrl Pts',(145.651520702085,-4.33668159389262,128.484365829707));
#34060=CARTESIAN_POINT('Ctrl Pts',(145.643756385211,-4.40130302745182,128.605160317244));
#34061=CARTESIAN_POINT('Ctrl Pts',(145.635992068337,-4.46094490469177,128.728789893477));
#34062=CARTESIAN_POINT('Ctrl Pts',(145.628227751463,-4.5153535379215,128.854805414429));
#34063=CARTESIAN_POINT('Ctrl Pts',(145.620469954524,-4.56971648255395,128.980715116284));
#34064=CARTESIAN_POINT('Ctrl Pts',(145.612712157585,-4.61885477749342,129.10900641855));
#34065=CARTESIAN_POINT('Ctrl Pts',(145.604954360646,-4.66256100658676,129.239206336878));
#34066=CARTESIAN_POINT('Ctrl Pts',(145.598215692514,-4.70052562147025,129.352302109716));
#34067=CARTESIAN_POINT('Ctrl Pts',(145.591477024383,-4.73439227538181,129.466837445625));
#34068=CARTESIAN_POINT('Ctrl Pts',(145.584738356252,-4.76405452823403,129.582490119308));
#34069=CARTESIAN_POINT('Ctrl Pts',(147.334614341604,-4.76405452823404,129.582490119308));
#34070=CARTESIAN_POINT('Ctrl Pts',(147.32583785793,-4.80241575731761,129.732059969292));
#34071=CARTESIAN_POINT('Ctrl Pts',(147.317061374255,-4.83377339724143,129.883610054808));
#34072=CARTESIAN_POINT('Ctrl Pts',(147.308284890581,-4.85794144089961,130.03651426621));
#34073=CARTESIAN_POINT('Ctrl Pts',(147.299561109063,-4.88196435718438,130.188500298761));
#34074=CARTESIAN_POINT('Ctrl Pts',(147.290837327545,-4.8988836733556,130.34182405967));
#34075=CARTESIAN_POINT('Ctrl Pts',(147.282113546027,-4.90856448932769,130.495851757707));
#34076=CARTESIAN_POINT('Ctrl Pts',(147.276362176033,-4.91494680809417,130.597398349501));
#34077=CARTESIAN_POINT('Ctrl Pts',(147.27061080604,-4.9181839396096,130.699250520337));
#34078=CARTESIAN_POINT('Ctrl Pts',(147.264859436046,-4.91824899899375,130.801222720669));
#34079=CARTESIAN_POINT('',(147.610140563976,-4.91824964343576,130.802487827118));
#34080=CARTESIAN_POINT('Ctrl Pts',(147.680233368326,-4.76405452823403,129.582490119308));
#34081=CARTESIAN_POINT('Ctrl Pts',(147.672469059238,-4.79809904943347,129.715229190767));
#34082=CARTESIAN_POINT('Ctrl Pts',(147.66470475015,-4.82655828705133,129.849261833059));
#34083=CARTESIAN_POINT('Ctrl Pts',(147.656940441062,-4.84936284072016,129.984078287181));
#34084=CARTESIAN_POINT('Ctrl Pts',(147.64916521746,-4.87219945141112,130.119084256699));
#34085=CARTESIAN_POINT('Ctrl Pts',(147.641389993857,-4.88936546244613,130.254875851216));
#34086=CARTESIAN_POINT('Ctrl Pts',(147.633614770255,-4.90084340470038,130.390939542747));
#34087=CARTESIAN_POINT('Ctrl Pts',(147.631653935474,-4.90373802864088,130.425253465069));
#34088=CARTESIAN_POINT('Ctrl Pts',(147.629693100694,-4.90627115089988,130.45958470123));
#34089=CARTESIAN_POINT('Ctrl Pts',(147.627732265913,-4.90844301354763,130.493925044129));
#34090=CARTESIAN_POINT('Ctrl Pts',(147.621868365278,-4.91493799562629,130.596620263797));
#34091=CARTESIAN_POINT('Ctrl Pts',(147.616004464643,-4.918210435478,130.69952144019));
#34092=CARTESIAN_POINT('Ctrl Pts',(147.610140564008,-4.91824964343554,130.802487826551));
#34093=CARTESIAN_POINT('Ctrl Pts',(147.610140563976,-4.91824964343576,130.802487827118));
#34094=CARTESIAN_POINT('Ctrl Pts',(147.602439734443,-4.91830113368513,130.937709523106));
#34095=CARTESIAN_POINT('Ctrl Pts',(147.59473890491,-4.91277175834642,131.073158991306));
#34096=CARTESIAN_POINT('Ctrl Pts',(147.587038075378,-4.90163137916255,131.208332009262));
#34097=CARTESIAN_POINT('Ctrl Pts',(147.579346385036,-4.89050422115882,131.343344606573));
#34098=CARTESIAN_POINT('Ctrl Pts',(147.571654694695,-4.87377933677944,131.478081012467));
#34099=CARTESIAN_POINT('Ctrl Pts',(147.563963004353,-4.85147857154113,131.612035510315));
#34100=CARTESIAN_POINT('Ctrl Pts',(147.556278517553,-4.8291986917631,131.745864555009));
#34101=CARTESIAN_POINT('Ctrl Pts',(147.548594030753,-4.80135338499484,131.878912757415));
#34102=CARTESIAN_POINT('Ctrl Pts',(147.540909543953,-4.76801638328633,132.01067849906));
#34103=CARTESIAN_POINT('Ctrl Pts',(147.532925173043,-4.73337841804295,132.147586347562));
#34104=CARTESIAN_POINT('Ctrl Pts',(147.524940802132,-4.69281146874443,132.283109172404));
#34105=CARTESIAN_POINT('Ctrl Pts',(147.516956431222,-4.6464570671264,132.416694263513));
#34106=CARTESIAN_POINT('Ctrl Pts',(147.509279785587,-4.60188920839122,132.545130857705));
#34107=CARTESIAN_POINT('Ctrl Pts',(147.501603139952,-4.55197186160213,132.671775895844));
#34108=CARTESIAN_POINT('Ctrl Pts',(147.493926494318,-4.49688180943077,132.796153040112));
#34109=CARTESIAN_POINT('Ctrl Pts',(147.486250759867,-4.44179829620614,132.92051542136));
#34110=CARTESIAN_POINT('Ctrl Pts',(147.478575025416,-4.38154346000645,133.042610079365));
#34111=CARTESIAN_POINT('Ctrl Pts',(147.470899290966,-4.31634202060979,133.161981160321));
#34112=CARTESIAN_POINT('Ctrl Pts',(147.463222729902,-4.25113355955972,133.28136509655));
#34113=CARTESIAN_POINT('Ctrl Pts',(147.455546168839,-4.1809776271877,133.398024522358));
#34114=CARTESIAN_POINT('Ctrl Pts',(147.447869607775,-4.10614438988712,133.511529122092));
#34115=CARTESIAN_POINT('Ctrl Pts',(147.44019048198,-4.0312861508724,133.625071643606));
#34116=CARTESIAN_POINT('Ctrl Pts',(147.432511356185,-3.95174771837245,133.735456909927));
#34117=CARTESIAN_POINT('Ctrl Pts',(147.424832230389,-3.86784166952686,133.842284889494));
#34118=CARTESIAN_POINT('Ctrl Pts',(147.41714468187,-3.78384358970452,133.949230041584));
#34119=CARTESIAN_POINT('Ctrl Pts',(147.409457133352,-3.69546857816107,134.052609805367));
#34120=CARTESIAN_POINT('Ctrl Pts',(147.401769584833,-3.60306865499176,134.152058233826));
#34121=CARTESIAN_POINT('Ctrl Pts',(147.394077036228,-3.51060863365079,134.251571344902));
#34122=CARTESIAN_POINT('Ctrl Pts',(147.386384487622,-3.41411877119594,134.347147750118));
#34123=CARTESIAN_POINT('Ctrl Pts',(147.378691939017,-3.3139858621897,134.438460336576));
#34124=CARTESIAN_POINT('Ctrl Pts',(147.370988573147,-3.21371214624986,134.529901326826));
#34125=CARTESIAN_POINT('Ctrl Pts',(147.363285207277,-3.10978546467493,134.617066278072));
#34126=CARTESIAN_POINT('Ctrl Pts',(147.355581841407,-3.00262359945466,134.699669922679));
#34127=CARTESIAN_POINT('Ctrl Pts',(147.353482774971,-2.9734233929154,134.722178335335));
#34128=CARTESIAN_POINT('Ctrl Pts',(147.351383708536,-2.94398312849165,134.744348332494));
#34129=CARTESIAN_POINT('Ctrl Pts',(147.3492846421,-2.91431158413388,134.76617472894));
#34130=CARTESIAN_POINT('Ctrl Pts',(147.341510307981,-2.80441677767962,134.847013379741));
#34131=CARTESIAN_POINT('Ctrl Pts',(147.333735973862,-2.69098184152859,134.923404131228));
#34132=CARTESIAN_POINT('Ctrl Pts',(147.325961639743,-2.57440265271451,134.995020952668));
#34133=CARTESIAN_POINT('Ctrl Pts',(147.318196886796,-2.4579671373319,135.066549512776));
#34134=CARTESIAN_POINT('Ctrl Pts',(147.310432133849,-2.33839540933109,135.133315646451));
#34135=CARTESIAN_POINT('Ctrl Pts',(147.302667380902,-2.21611515837309,135.195034445958));
#34136=CARTESIAN_POINT('Ctrl Pts',(147.294910340017,-2.09395635788373,135.256691945484));
#34137=CARTESIAN_POINT('Ctrl Pts',(147.287153299132,-1.96909473471167,135.31331191208));
#34138=CARTESIAN_POINT('Ctrl Pts',(147.279396258247,-1.84198530669273,135.364653721351));
#34139=CARTESIAN_POINT('Ctrl Pts',(147.271645067007,-1.7149717328821,135.415956813364));
#34140=CARTESIAN_POINT('Ctrl Pts',(147.263893875767,-1.58571408923612,135.461989524764));
#34141=CARTESIAN_POINT('Ctrl Pts',(147.256142684526,-1.45468992321589,135.502558175119));
#34142=CARTESIAN_POINT('Ctrl Pts',(147.248394787749,-1.32372144596189,135.543109582714));
#34143=CARTESIAN_POINT('Ctrl Pts',(147.240646890972,-1.19098831234639,135.578201432888));
#34144=CARTESIAN_POINT('Ctrl Pts',(147.232898994195,-1.05698567725058,135.607689082348));
#34145=CARTESIAN_POINT('Ctrl Pts',(147.225152718111,-0.9230110726171,135.637170563628));
#34146=CARTESIAN_POINT('Ctrl Pts',(147.217406442027,-0.78776787628935,135.661050091948));
#34147=CARTESIAN_POINT('Ctrl Pts',(147.209660165943,-0.651763566309817,
135.679233673978));
#34148=CARTESIAN_POINT('Ctrl Pts',(147.201913832678,-0.51575825237755,135.697417390235));
#34149=CARTESIAN_POINT('Ctrl Pts',(147.194167499412,-0.378992201099509,
135.70990502449));
#34150=CARTESIAN_POINT('Ctrl Pts',(147.186421166147,-0.241979785258479,
135.716654261682));
#34151=CARTESIAN_POINT('Ctrl Pts',(147.178673098144,-0.104936686436712,
135.72340501032));
#34152=CARTESIAN_POINT('Ctrl Pts',(147.170925030141,0.0323524963162291,
135.724414785513));
#34153=CARTESIAN_POINT('Ctrl Pts',(147.163176962138,0.169372003699001,135.719693382177));
#34154=CARTESIAN_POINT('Ctrl Pts',(147.155420659396,0.306537137044632,135.714966960878));
#34155=CARTESIAN_POINT('Ctrl Pts',(147.147664356654,0.443431631121024,135.704497206777));
#34156=CARTESIAN_POINT('Ctrl Pts',(147.139908053913,0.579542909015048,135.688345986003));
#34157=CARTESIAN_POINT('Ctrl Pts',(147.132147611398,0.715726833596269,135.672186144837));
#34158=CARTESIAN_POINT('Ctrl Pts',(147.124387168884,0.851126323258618,135.650338856992));
#34159=CARTESIAN_POINT('Ctrl Pts',(147.11662672637,0.985238617946266,135.622917240478));
#34160=CARTESIAN_POINT('Ctrl Pts',(147.108853826105,1.11956620159551,135.59545160435));
#34161=CARTESIAN_POINT('Ctrl Pts',(147.101080925839,1.25260208145998,135.56239385212));
#34162=CARTESIAN_POINT('Ctrl Pts',(147.093308025574,1.38385742407199,135.523907385248));
#34163=CARTESIAN_POINT('Ctrl Pts',(147.085817689812,1.51034130436829,135.486819998389));
#34164=CARTESIAN_POINT('Ctrl Pts',(147.07832735405,1.63517156208169,135.444691837802));
#34165=CARTESIAN_POINT('Ctrl Pts',(147.070837018288,1.75792981906361,135.397710790778));
#34166=CARTESIAN_POINT('Ctrl Pts',(147.063062684169,1.8853424926702,135.348948443077));
#34167=CARTESIAN_POINT('Ctrl Pts',(147.055288350049,2.01092654918722,135.294803485775));
#34168=CARTESIAN_POINT('Ctrl Pts',(147.04751401593,2.13419370851755,135.235432753858));
#34169=CARTESIAN_POINT('Ctrl Pts',(147.039749262983,2.25730895209079,135.176135191062));
#34170=CARTESIAN_POINT('Ctrl Pts',(147.031984510036,2.37811263095337,135.111624835952));
#34171=CARTESIAN_POINT('Ctrl Pts',(147.024219757089,2.49613386745074,135.042107516363));
#34172=CARTESIAN_POINT('Ctrl Pts',(147.016462716204,2.6140378835921,134.972659242356));
#34173=CARTESIAN_POINT('Ctrl Pts',(147.008705675319,2.72916462228905,134.898214097482));
#34174=CARTESIAN_POINT('Ctrl Pts',(147.000948634434,2.84106569116859,134.819024837767));
#34175=CARTESIAN_POINT('Ctrl Pts',(146.993197443194,2.95288237458132,134.73989529529));
#34176=CARTESIAN_POINT('Ctrl Pts',(146.985446251954,3.06147791208037,134.656028983848));
#34177=CARTESIAN_POINT('Ctrl Pts',(146.977695060714,3.16643122876389,134.567722988639));
#34178=CARTESIAN_POINT('Ctrl Pts',(146.969947163937,3.27133993748831,134.479454525834));
#34179=CARTESIAN_POINT('Ctrl Pts',(146.962199267159,3.37260920579902,134.38675038351));
#34180=CARTESIAN_POINT('Ctrl Pts',(146.954451370382,3.46984969788895,134.289948966261));
#34181=CARTESIAN_POINT('Ctrl Pts',(146.946705094298,3.5670698493642,134.193167797782));
#34182=CARTESIAN_POINT('Ctrl Pts',(146.938958818214,3.66026262395762,134.092291334772));
#34183=CARTESIAN_POINT('Ctrl Pts',(146.93121254213,3.7490746381389,133.98769572719));
#34184=CARTESIAN_POINT('Ctrl Pts',(146.923466208865,3.83788730791041,133.883099347506));
#34185=CARTESIAN_POINT('Ctrl Pts',(146.915719875599,3.92231889969002,133.774784066492));
#34186=CARTESIAN_POINT('Ctrl Pts',(146.907973542334,4.00205578156489,133.663159768214));
#34187=CARTESIAN_POINT('Ctrl Pts',(146.900225474331,4.08181051996143,133.551510472447));
#34188=CARTESIAN_POINT('Ctrl Pts',(146.892477406328,4.15686822918267,133.436551002923));
#34189=CARTESIAN_POINT('Ctrl Pts',(146.884729338325,4.22695836946702,133.318720576938));
#34190=CARTESIAN_POINT('Ctrl Pts',(146.876973035583,4.29712300238664,133.200764919374));
#34191=CARTESIAN_POINT('Ctrl Pts',(146.869216732841,4.36230931962478,133.079932546624));
#34192=CARTESIAN_POINT('Ctrl Pts',(146.861460430099,4.4222923105662,132.956688144316));
#34193=CARTESIAN_POINT('Ctrl Pts',(146.853699987585,4.48230731623595,132.83337796276));
#34194=CARTESIAN_POINT('Ctrl Pts',(146.845939545071,4.53711330570396,132.707653544664));
#34195=CARTESIAN_POINT('Ctrl Pts',(146.838179102557,4.58653369426326,132.579999019349));
#34196=CARTESIAN_POINT('Ctrl Pts',(146.830406202291,4.6360334168176,132.452139571658));
#34197=CARTESIAN_POINT('Ctrl Pts',(146.822633302026,4.68013013627093,132.322344195595));
#34198=CARTESIAN_POINT('Ctrl Pts',(146.81486040176,4.71869710047028,132.191112483082));
#34199=CARTESIAN_POINT('Ctrl Pts',(146.807370065998,4.75586205837629,132.064651373874));
#34200=CARTESIAN_POINT('Ctrl Pts',(146.799879730236,4.787892247185,131.93685684285));
#34201=CARTESIAN_POINT('Ctrl Pts',(146.792389394474,4.81471959818696,131.808182441066));
#34202=CARTESIAN_POINT('Ctrl Pts',(146.784615060355,4.84256411635641,131.674629310227));
#34203=CARTESIAN_POINT('Ctrl Pts',(146.776840726236,4.86489168042236,131.539705214769));
#34204=CARTESIAN_POINT('Ctrl Pts',(146.769066392117,4.88157031277973,131.403905731705));
#34205=CARTESIAN_POINT('Ctrl Pts',(146.76130163917,4.89822839021328,131.268273609367));
#34206=CARTESIAN_POINT('Ctrl Pts',(146.753536886223,4.90925134065023,131.131768630313));
#34207=CARTESIAN_POINT('Ctrl Pts',(146.745772133276,4.91455781200336,130.994898212221));
#34208=CARTESIAN_POINT('Ctrl Pts',(146.738015092391,4.91985901289433,130.858163735757));
#34209=CARTESIAN_POINT('Ctrl Pts',(146.730258051506,4.9194550185077,130.721064930705));
#34210=CARTESIAN_POINT('Ctrl Pts',(146.722501010621,4.91331611261889,130.584115663073));
#34211=CARTESIAN_POINT('Ctrl Pts',(146.714749819381,4.90718183612675,130.447269669949));
#34212=CARTESIAN_POINT('Ctrl Pts',(146.706998628141,4.89532127370488,130.310573378783));
#34213=CARTESIAN_POINT('Ctrl Pts',(146.699247436901,4.8777567702748,130.17454163362));
#34214=CARTESIAN_POINT('Ctrl Pts',(146.691499540124,4.86019973222719,130.038567705578));
#34215=CARTESIAN_POINT('Ctrl Pts',(146.683751643347,4.83694362493432,129.903258148703));
#34216=CARTESIAN_POINT('Ctrl Pts',(146.67600374657,4.80806271224981,129.769123438185));
#34217=CARTESIAN_POINT('Ctrl Pts',(146.668257470485,4.77918784082964,129.635016785756));
#34218=CARTESIAN_POINT('Ctrl Pts',(146.660511194401,4.74469058655765,129.502084872833));
#34219=CARTESIAN_POINT('Ctrl Pts',(146.652764918317,4.70469640261632,129.370828329227));
#34220=CARTESIAN_POINT('Ctrl Pts',(146.645018585052,4.664701923447,129.239570816716));
#34221=CARTESIAN_POINT('Ctrl Pts',(146.637272251787,4.61921054759512,129.109989072189));
#34222=CARTESIAN_POINT('Ctrl Pts',(146.629525918521,4.5683975964239,128.982568515407));
#34223=CARTESIAN_POINT('Ctrl Pts',(146.621777850518,4.51757326604481,128.855119423676));
#34224=CARTESIAN_POINT('Ctrl Pts',(146.614029782515,4.46142513373345,128.729832845844));
#34225=CARTESIAN_POINT('Ctrl Pts',(146.606281714512,4.40017649209229,128.607173802355));
#34226=CARTESIAN_POINT('Ctrl Pts',(146.598525411771,4.33886275466562,128.484384395373));
#34227=CARTESIAN_POINT('Ctrl Pts',(146.590769109029,4.27243785405228,128.364228451542));
#34228=CARTESIAN_POINT('Ctrl Pts',(146.583012806287,4.20117111969791,128.247146452597));
#34229=CARTESIAN_POINT('Ctrl Pts',(146.575252363773,4.12986634814147,128.130001963464));
#34230=CARTESIAN_POINT('Ctrl Pts',(146.567491921259,4.05371481051523,128.015935013368));
#34231=CARTESIAN_POINT('Ctrl Pts',(146.559731478744,3.97302837018012,127.905355851747));
#34232=CARTESIAN_POINT('Ctrl Pts',(146.551958578479,3.89221240480812,127.794599178639));
#34233=CARTESIAN_POINT('Ctrl Pts',(146.544185678214,3.8068472329173,127.687341788488));
#34234=CARTESIAN_POINT('Ctrl Pts',(146.536412777948,3.71728466270584,127.583960363108));
#34235=CARTESIAN_POINT('Ctrl Pts',(146.528922442186,3.63097791751464,127.484337112941));
#34236=CARTESIAN_POINT('Ctrl Pts',(146.521432106424,3.54077385866447,127.388313142378));
#34237=CARTESIAN_POINT('Ctrl Pts',(146.513941770662,3.4470172787037,127.296190874977));
#34238=CARTESIAN_POINT('Ctrl Pts',(146.506167436543,3.34970588951856,127.200575763808));
#34239=CARTESIAN_POINT('Ctrl Pts',(146.498393102424,3.24825902051891,127.108861182511));
#34240=CARTESIAN_POINT('Ctrl Pts',(146.490618768305,3.14302227756331,127.021426039062));
#34241=CARTESIAN_POINT('Ctrl Pts',(146.482854015357,3.03791522948806,126.934098651614));
#34242=CARTESIAN_POINT('Ctrl Pts',(146.47508926241,2.92902789854883,126.851040455726));
#34243=CARTESIAN_POINT('Ctrl Pts',(146.467324509463,2.81674321681961,126.772594166865));
#34244=CARTESIAN_POINT('Ctrl Pts',(146.459567468578,2.70457005781979,126.694225791964));
#34245=CARTESIAN_POINT('Ctrl Pts',(146.451810427693,2.58900658145499,126.620460430928));
#34246=CARTESIAN_POINT('Ctrl Pts',(146.444053386808,2.47046905540772,126.551600841988));
#34247=CARTESIAN_POINT('Ctrl Pts',(146.436302195568,2.35202091943036,126.4827931806));
#34248=CARTESIAN_POINT('Ctrl Pts',(146.428551004328,2.23060353453201,126.418884123306));
#34249=CARTESIAN_POINT('Ctrl Pts',(146.420799813088,2.10666213156628,126.360133156474));
#34250=CARTESIAN_POINT('Ctrl Pts',(146.413051916311,1.98277340700314,126.30140716037));
#34251=CARTESIAN_POINT('Ctrl Pts',(146.405304019534,1.85636315058457,126.247835061472));
#34252=CARTESIAN_POINT('Ctrl Pts',(146.397556122757,1.72790098097139,126.199630303806));
#34253=CARTESIAN_POINT('Ctrl Pts',(146.389809846673,1.599465682875,126.151435629536));
#34254=CARTESIAN_POINT('Ctrl Pts',(146.382063570588,1.46897969112893,126.108606200591));
#34255=CARTESIAN_POINT('Ctrl Pts',(146.374317294504,1.33693201028251,126.071307072297));
#34256=CARTESIAN_POINT('Ctrl Pts',(146.366570961239,1.20488335468966,126.034007668669));
#34257=CARTESIAN_POINT('Ctrl Pts',(146.358824627974,1.07127336323652,126.00223875343));
#34258=CARTESIAN_POINT('Ctrl Pts',(146.351078294708,0.936605198794484,125.976115204987));
#34259=CARTESIAN_POINT('Ctrl Pts',(146.343330226705,0.801906876351253,125.949985806357));
#34260=CARTESIAN_POINT('Ctrl Pts',(146.335582158702,0.666150293112305,125.929504364656));
#34261=CARTESIAN_POINT('Ctrl Pts',(146.327834090699,0.529847379050967,125.9147343724));
#34262=CARTESIAN_POINT('Ctrl Pts',(146.320077787957,0.393399600630261,125.899948682421));
#34263=CARTESIAN_POINT('Ctrl Pts',(146.312321485216,0.25640472079204,125.890886609946));
#34264=CARTESIAN_POINT('Ctrl Pts',(146.304565182474,0.119378908439775,125.887559651621));
#34265=CARTESIAN_POINT('Ctrl Pts',(146.29680473996,-0.0177200387142628,
125.884230917598));
#34266=CARTESIAN_POINT('Ctrl Pts',(146.289044297445,-0.154849560565692,
125.886643390159));
#34267=CARTESIAN_POINT('Ctrl Pts',(146.281283854931,-0.291495932878982,
125.89475643967));
#34268=CARTESIAN_POINT('Ctrl Pts',(146.273510954666,-0.428361662080005,
125.902882512968));
#34269=CARTESIAN_POINT('Ctrl Pts',(146.2657380544,-0.564742302667943,125.916727410463));
#34270=CARTESIAN_POINT('Ctrl Pts',(146.257965154135,-0.700130780640822,
125.936198751677));
#34271=CARTESIAN_POINT('Ctrl Pts',(146.250474818373,-0.830597546414922,
125.954962260591));
#34272=CARTESIAN_POINT('Ctrl Pts',(146.242984482611,-0.960142729551186,
125.978950188408));
#34273=CARTESIAN_POINT('Ctrl Pts',(146.235494146849,-1.08832552375138,126.008035918711));
#34274=CARTESIAN_POINT('Ctrl Pts',(146.22771981273,-1.22136840755523,126.038224443318));
#34275=CARTESIAN_POINT('Ctrl Pts',(146.219945478611,-1.35336499296447,126.074000595887));
#34276=CARTESIAN_POINT('Ctrl Pts',(146.212171144492,-1.48380968555717,126.115278417439));
#34277=CARTESIAN_POINT('Ctrl Pts',(146.204406391545,-1.61409361672415,126.156505367765));
#34278=CARTESIAN_POINT('Ctrl Pts',(146.196641638598,-1.74282909134756,126.203220379447));
#34279=CARTESIAN_POINT('Ctrl Pts',(146.188876885651,-1.86952078906091,126.255286526966));
#34280=CARTESIAN_POINT('Ctrl Pts',(146.181119844766,-1.99608665479422,126.307300961653));
#34281=CARTESIAN_POINT('Ctrl Pts',(146.173362803881,-2.1206124239477,126.364655807788));
#34282=CARTESIAN_POINT('Ctrl Pts',(146.165605762996,-2.24261837459615,126.427164495798));
#34283=CARTESIAN_POINT('Ctrl Pts',(146.157854571756,-2.36453231960794,126.48962604552));
#34284=CARTESIAN_POINT('Ctrl Pts',(146.150103380515,-2.48392988182947,126.55723352362));
#34285=CARTESIAN_POINT('Ctrl Pts',(146.142352189275,-2.60035208987876,126.629752603493));
#34286=CARTESIAN_POINT('Ctrl Pts',(146.134604292498,-2.71672481538424,126.702240860822));
#34287=CARTESIAN_POINT('Ctrl Pts',(146.126856395721,-2.83012437076388,126.779636361646));
#34288=CARTESIAN_POINT('Ctrl Pts',(146.119108498944,-2.94011733915678,126.861659374194));
#34289=CARTESIAN_POINT('Ctrl Pts',(146.11136222286,-3.05008729939216,126.943665229296));
#34290=CARTESIAN_POINT('Ctrl Pts',(146.103615946776,-3.15665177679296,127.030296437195));
#34291=CARTESIAN_POINT('Ctrl Pts',(146.095869670692,-3.25940758673466,127.121230800951));
#34292=CARTESIAN_POINT('Ctrl Pts',(146.088123337426,-3.3621641551964,127.212165835964));
#34293=CARTESIAN_POINT('Ctrl Pts',(146.080377004161,-3.46111170731605,127.307403831119));
#34294=CARTESIAN_POINT('Ctrl Pts',(146.072630670896,-3.55588162081195,127.406583555828));
#34295=CARTESIAN_POINT('Ctrl Pts',(146.064882602893,-3.65067275737241,127.505785491148));
#34296=CARTESIAN_POINT('Ctrl Pts',(146.05713453489,-3.74128412361966,127.608930629927));
#34297=CARTESIAN_POINT('Ctrl Pts',(146.049386466887,-3.82738559084586,127.715622590234));
#34298=CARTESIAN_POINT('Ctrl Pts',(146.041630164145,-3.9135785677364,127.822427944027));
#34299=CARTESIAN_POINT('Ctrl Pts',(146.033873861403,-3.9952518248,127.932787344805));
#34300=CARTESIAN_POINT('Ctrl Pts',(146.026117558661,-4.0721166876814,128.046272739269));
#34301=CARTESIAN_POINT('Ctrl Pts',(146.018357116147,-4.14902257565452,128.159818704306));
#34302=CARTESIAN_POINT('Ctrl Pts',(146.010596673633,-4.22111475029939,128.276493655097));
#34303=CARTESIAN_POINT('Ctrl Pts',(146.002836231119,-4.28814971398151,128.395843419583));
#34304=CARTESIAN_POINT('Ctrl Pts',(145.995063330853,-4.35529228813831,128.515384774906));
#34305=CARTESIAN_POINT('Ctrl Pts',(145.987290430588,-4.41736125128767,128.63760917561));
#34306=CARTESIAN_POINT('Ctrl Pts',(145.979517530322,-4.47416023985968,128.762040072069));
#34307=CARTESIAN_POINT('Ctrl Pts',(145.97202719456,-4.52889444212961,128.881947592021));
#34308=CARTESIAN_POINT('Ctrl Pts',(145.964536858798,-4.57873505488728,129.003903684428));
#34309=CARTESIAN_POINT('Ctrl Pts',(145.957046523036,-4.62355033753805,129.127469047204));
#34310=CARTESIAN_POINT('Ctrl Pts',(145.948004980227,-4.67764661698982,129.27662411217));
#34311=CARTESIAN_POINT('Ctrl Pts',(145.938963437419,-4.72456322357162,129.428514121794));
#34312=CARTESIAN_POINT('Ctrl Pts',(145.92992189461,-4.76405452823405,129.582490119308));
#34313=CARTESIAN_POINT('Origin',(213.235140564004,0.,130.804360617566));
#34314=CARTESIAN_POINT('',(143.834995515417,-4.76405452823405,129.582490119308));
#34315=CARTESIAN_POINT('',(144.179984458271,-4.76405452823405,129.582490119308));
#34316=CARTESIAN_POINT('',(213.235140564004,-4.76405452823405,129.582490119308));
#34317=CARTESIAN_POINT('',(145.514859435938,-4.9182485978174,130.808074452137));
#34318=CARTESIAN_POINT('Ctrl Pts',(145.514859435938,-4.9182485978174,130.808074452137));
#34319=CARTESIAN_POINT('Ctrl Pts',(145.50589805865,-4.91812871707833,130.966833078993));
#34320=CARTESIAN_POINT('Ctrl Pts',(145.496936681362,-4.91031794769265,131.125276220947));
#34321=CARTESIAN_POINT('Ctrl Pts',(145.487975304074,-4.89493134552557,131.282722598801));
#34322=CARTESIAN_POINT('Ctrl Pts',(145.478965112646,-4.87946092992949,131.441026613752));
#34323=CARTESIAN_POINT('Ctrl Pts',(145.469954921218,-4.85633203283539,131.598322856858));
#34324=CARTESIAN_POINT('Ctrl Pts',(145.46094472979,-4.82571087920542,131.753938193554));
#34325=CARTESIAN_POINT('Ctrl Pts',(145.451874947198,-4.7948872048858,131.910582731359));
#34326=CARTESIAN_POINT('Ctrl Pts',(145.442805164606,-4.75647192550071,132.065523938142));
#34327=CARTESIAN_POINT('Ctrl Pts',(145.433735382015,-4.7106829381227,132.218096561432));
#34328=CARTESIAN_POINT('Ctrl Pts',(145.429070345199,-4.68713140205463,132.296572191626));
#34329=CARTESIAN_POINT('Ctrl Pts',(145.424405308384,-4.66162988630557,132.374421556298));
#34330=CARTESIAN_POINT('Ctrl Pts',(145.419740271569,-4.63421287035937,132.451556457379));
#34331=CARTESIAN_POINT('Ctrl Pts',(145.41196593745,-4.58852211786071,132.580102601175));
#34332=CARTESIAN_POINT('Ctrl Pts',(145.404191603331,-4.53740642405227,132.706949822268));
#34333=CARTESIAN_POINT('Ctrl Pts',(145.396417269212,-4.48101086137801,132.831606217564));
#34334=CARTESIAN_POINT('Ctrl Pts',(145.388652516265,-4.42468480119456,132.956108984995));
#34335=CARTESIAN_POINT('Ctrl Pts',(145.380887763318,-4.36309197867349,133.07842594603));
#34336=CARTESIAN_POINT('Ctrl Pts',(145.373123010371,-4.29642686261107,133.198081419317));
#34337=CARTESIAN_POINT('Ctrl Pts',(145.365365969486,-4.22982795928184,133.3176180491));
#34338=CARTESIAN_POINT('Ctrl Pts',(145.357608928601,-4.15816697705891,133.43449811235));
#34339=CARTESIAN_POINT('Ctrl Pts',(145.349851887716,-4.08168583900318,133.54826728037));
#34340=CARTESIAN_POINT('Ctrl Pts',(145.342100696476,-4.00526237596834,133.661950654176));
#34341=CARTESIAN_POINT('Ctrl Pts',(145.334349505236,-3.92402620942064,133.772527479074));
#34342=CARTESIAN_POINT('Ctrl Pts',(145.326598313996,-3.83826423436866,133.879569672194));
#34343=CARTESIAN_POINT('Ctrl Pts',(145.318850417219,-3.75253871044404,133.986566369527));
#34344=CARTESIAN_POINT('Ctrl Pts',(145.311102520442,-3.66229144783274,134.090031118592));
#34345=CARTESIAN_POINT('Ctrl Pts',(145.303354623665,-3.5678514106888,134.189566574926));
#34346=CARTESIAN_POINT('Ctrl Pts',(145.295608347581,-3.47343112836475,134.289081210588));
#34347=CARTESIAN_POINT('Ctrl Pts',(145.287862071496,-3.37482008491364,134.38466790493));
#34348=CARTESIAN_POINT('Ctrl Pts',(145.280115795412,-3.27238584174091,134.475964349626));
#34349=CARTESIAN_POINT('Ctrl Pts',(145.272369462147,-3.16995084242179,134.567261468251));
#34350=CARTESIAN_POINT('Ctrl Pts',(145.264623128882,-3.06369287893197,134.654268013904));
#34351=CARTESIAN_POINT('Ctrl Pts',(145.256876795616,-2.95401419099952,134.736660608904));
#34352=CARTESIAN_POINT('Ctrl Pts',(145.249128727613,-2.84431094128552,134.819071655153));
#34353=CARTESIAN_POINT('Ctrl Pts',(145.24138065961,-2.73118575531252,134.896866459899));
#34354=CARTESIAN_POINT('Ctrl Pts',(145.233632591607,-2.61507123168629,134.969764021284));
#34355=CARTESIAN_POINT('Ctrl Pts',(145.225876288866,-2.49883330016253,135.042739059065));
#34356=CARTESIAN_POINT('Ctrl Pts',(145.218119986124,-2.37960001602614,135.110806248029));
#34357=CARTESIAN_POINT('Ctrl Pts',(145.210363683382,-2.25783053145275,135.173729491184));
#34358=CARTESIAN_POINT('Ctrl Pts',(145.202603240868,-2.135996054839,135.236686318368));
#34359=CARTESIAN_POINT('Ctrl Pts',(145.194842798354,-2.01162303490017,135.294493564439));
#34360=CARTESIAN_POINT('Ctrl Pts',(145.187082355839,-1.88519122399317,135.346963077773));
#34361=CARTESIAN_POINT('Ctrl Pts',(145.179309455574,-1.75855645351921,135.399516819828));
#34362=CARTESIAN_POINT('Ctrl Pts',(145.171536555309,-1.6298566549969,135.446715571655));
#34363=CARTESIAN_POINT('Ctrl Pts',(145.163763655043,-1.49958823477567,135.488420628777));
#34364=CARTESIAN_POINT('Ctrl Pts',(145.156273319281,-1.3740553997549,135.528609602023));
#34365=CARTESIAN_POINT('Ctrl Pts',(145.148782983519,-1.24706630661079,135.563697283306));
#34366=CARTESIAN_POINT('Ctrl Pts',(145.141292647757,-1.11907274232627,135.593604739542));
#34367=CARTESIAN_POINT('Ctrl Pts',(145.133518313638,-0.98622626314995,135.624646146072));
#34368=CARTESIAN_POINT('Ctrl Pts',(145.125743979519,-0.851876822471075,
135.650205086615));
#34369=CARTESIAN_POINT('Ctrl Pts',(145.1179696454,-0.716516687491695,135.670137729092));
#34370=CARTESIAN_POINT('Ctrl Pts',(145.110204892453,-0.581323371781241,
135.690045806368));
#34371=CARTESIAN_POINT('Ctrl Pts',(145.102440139506,-0.445122223204724,
135.704341325579));
#34372=CARTESIAN_POINT('Ctrl Pts',(145.094675386558,-0.308418561091736,
135.71293078144));
#34373=CARTESIAN_POINT('Ctrl Pts',(145.086918345673,-0.171850674983235,
135.721511706133));
#34374=CARTESIAN_POINT('Ctrl Pts',(145.079161304788,-0.0347816562475976,
135.724397821385));
#34375=CARTESIAN_POINT('Ctrl Pts',(145.071404263903,0.102275490193226,135.721547088161));
#34376=CARTESIAN_POINT('Ctrl Pts',(145.063653072663,0.239229280773723,135.718698504698));
#34377=CARTESIAN_POINT('Ctrl Pts',(145.055901881423,0.376170827580724,135.7101216919));
#34378=CARTESIAN_POINT('Ctrl Pts',(145.048150690183,0.512584898613247,135.695826633416));
#34379=CARTESIAN_POINT('Ctrl Pts',(145.040402793406,0.648940990026757,135.681537650713));
#34380=CARTESIAN_POINT('Ctrl Pts',(145.032654896629,0.784769663543133,135.66153529688));
#34381=CARTESIAN_POINT('Ctrl Pts',(145.024906999852,0.919558808849843,135.635881564387));
#34382=CARTESIAN_POINT('Ctrl Pts',(145.017160723768,1.05431975917307,135.610233198101));
#34383=CARTESIAN_POINT('Ctrl Pts',(145.009414447684,1.18804122997288,135.578935877563));
#34384=CARTESIAN_POINT('Ctrl Pts',(145.0016681716,1.32021972507534,135.542103006091));
#34385=CARTESIAN_POINT('Ctrl Pts',(144.993921838334,1.45239919588937,135.505269862726));
#34386=CARTESIAN_POINT('Ctrl Pts',(144.986175505069,1.58303529166219,135.462901191839));
#34387=CARTESIAN_POINT('Ctrl Pts',(144.978429171803,1.7116385251931,135.415160615568));
#34388=CARTESIAN_POINT('Ctrl Pts',(144.9706811038,1.84027055852649,135.367409348126));
#34389=CARTESIAN_POINT('Ctrl Pts',(144.962933035798,1.96686845727731,135.314283917504));
#34390=CARTESIAN_POINT('Ctrl Pts',(144.955184967795,2.09096197651175,135.255996392793));
#34391=CARTESIAN_POINT('Ctrl Pts',(144.947428665053,2.2151873838152,135.197646919408));
#34392=CARTESIAN_POINT('Ctrl Pts',(144.939672362311,2.33690274016403,135.13412455887));
#34393=CARTESIAN_POINT('Ctrl Pts',(144.931916059569,2.4556612275063,135.065687992718));
#34394=CARTESIAN_POINT('Ctrl Pts',(144.924155617055,2.57448309982909,134.997214899911));
#34395=CARTESIAN_POINT('Ctrl Pts',(144.916395174541,2.69034462839187,134.923822584331));
#34396=CARTESIAN_POINT('Ctrl Pts',(144.908634732026,2.80282819803734,134.845812974676));
#34397=CARTESIAN_POINT('Ctrl Pts',(144.900861831761,2.91549233629462,134.76767813707));
#34398=CARTESIAN_POINT('Ctrl Pts',(144.893088931496,3.02476736771428,134.684911429862));
#34399=CARTESIAN_POINT('Ctrl Pts',(144.88531603123,3.13026827653164,134.597855520612));
#34400=CARTESIAN_POINT('Ctrl Pts',(144.877825695468,3.23193396157277,134.513964312945));
#34401=CARTESIAN_POINT('Ctrl Pts',(144.870335359706,3.33009492829537,134.426090541163));
#34402=CARTESIAN_POINT('Ctrl Pts',(144.862845023944,3.42444056616217,134.334571641191));
#34403=CARTESIAN_POINT('Ctrl Pts',(144.855070689825,3.52236334756429,134.23958277431));
#34404=CARTESIAN_POINT('Ctrl Pts',(144.847296355706,3.61648596246463,134.140366016569));
#34405=CARTESIAN_POINT('Ctrl Pts',(144.839522021587,3.70642131841318,134.037257781553));
#34406=CARTESIAN_POINT('Ctrl Pts',(144.83175726864,3.79624583707327,133.934276618221));
#34407=CARTESIAN_POINT('Ctrl Pts',(144.823992515693,3.88189310995933,133.827413811828));
#34408=CARTESIAN_POINT('Ctrl Pts',(144.816227762745,3.96301133098612,133.717043959946));
#34409=CARTESIAN_POINT('Ctrl Pts',(144.80847072186,4.04404898425213,133.606783728956));
#34410=CARTESIAN_POINT('Ctrl Pts',(144.800713680975,4.12056630747607,133.493023697289));
#34411=CARTESIAN_POINT('Ctrl Pts',(144.79295664009,4.1922506403365,133.376172747388));
#34412=CARTESIAN_POINT('Ctrl Pts',(144.78520544885,4.26388091548393,133.259409915697));
#34413=CARTESIAN_POINT('Ctrl Pts',(144.77745425761,4.33068525100124,133.139561137164));
#34414=CARTESIAN_POINT('Ctrl Pts',(144.76970306637,4.39239355093347,133.017065287471));
#34415=CARTESIAN_POINT('Ctrl Pts',(144.761955169593,4.45407562319214,132.894621501781));
#34416=CARTESIAN_POINT('Ctrl Pts',(144.754207272816,4.51066579225154,132.769533231052));
#34417=CARTESIAN_POINT('Ctrl Pts',(144.746459376039,4.56193940599989,132.642264836639));
#34418=CARTESIAN_POINT('Ctrl Pts',(144.738713099955,4.61320229441356,132.51502306403));
#34419=CARTESIAN_POINT('Ctrl Pts',(144.730966823871,4.65915069355398,132.385602437227));
#34420=CARTESIAN_POINT('Ctrl Pts',(144.723220547787,4.69960786086538,132.254487859084));
#34421=CARTESIAN_POINT('Ctrl Pts',(144.715474214521,4.74006532682238,132.123372313083));
#34422=CARTESIAN_POINT('Ctrl Pts',(144.707727881256,4.77503136479106,131.990563164376));
#34423=CARTESIAN_POINT('Ctrl Pts',(144.699981547991,4.80437905492279,131.856560674171));
#34424=CARTESIAN_POINT('Ctrl Pts',(144.692233479988,4.83373331726623,131.722528175037));
#34425=CARTESIAN_POINT('Ctrl Pts',(144.684485411985,4.85746664449393,131.587302184467));
#34426=CARTESIAN_POINT('Ctrl Pts',(144.676737343982,4.87550327746544,131.451392961366));
#34427=CARTESIAN_POINT('Ctrl Pts',(144.66898104124,4.89355907998513,131.315339292326));
#34428=CARTESIAN_POINT('Ctrl Pts',(144.661224738498,4.90590604218744,131.178601328381));
#34429=CARTESIAN_POINT('Ctrl Pts',(144.653468435756,4.91252028410558,131.041694813904));
#34430=CARTESIAN_POINT('Ctrl Pts',(144.645707993242,4.91913805624378,130.904715228297));
#34431=CARTESIAN_POINT('Ctrl Pts',(144.637947550728,4.92001700883151,130.767567303671));
#34432=CARTESIAN_POINT('Ctrl Pts',(144.630187108214,4.91518543183898,130.630765591319));
#34433=CARTESIAN_POINT('Ctrl Pts',(144.622414207948,4.91034609877014,130.493744272713));
#34434=CARTESIAN_POINT('Ctrl Pts',(144.614641307683,4.89977794759441,130.357070667015));
#34435=CARTESIAN_POINT('Ctrl Pts',(144.606868407417,4.88356116381054,130.221253919078));
#34436=CARTESIAN_POINT('Ctrl Pts',(144.599378071655,4.86793390096474,130.09037445203));
#34437=CARTESIAN_POINT('Ctrl Pts',(144.591887735893,4.84706160827821,129.960290930578));
#34438=CARTESIAN_POINT('Ctrl Pts',(144.584397400131,4.82106028756894,129.831447072524));
#34439=CARTESIAN_POINT('Ctrl Pts',(144.576623066012,4.7940731188822,129.697718060432));
#34440=CARTESIAN_POINT('Ctrl Pts',(144.568848731893,4.76147482305602,129.564900957762));
#34441=CARTESIAN_POINT('Ctrl Pts',(144.561074397774,4.72333920144347,129.433503276116));
#34442=CARTESIAN_POINT('Ctrl Pts',(144.553309644827,4.6852505785763,129.302267530369));
#34443=CARTESIAN_POINT('Ctrl Pts',(144.54554489188,4.64163831609154,129.172448096909));
#34444=CARTESIAN_POINT('Ctrl Pts',(144.537780138932,4.59262741375395,129.044543439296));
#34445=CARTESIAN_POINT('Ctrl Pts',(144.530023098047,4.54366518973551,128.916765818392));
#34446=CARTESIAN_POINT('Ctrl Pts',(144.522266057162,4.48931513548404,128.79089955142));
#34447=CARTESIAN_POINT('Ctrl Pts',(144.514509016277,4.42975225483972,128.667428699314));
#34448=CARTESIAN_POINT('Ctrl Pts',(144.506757825037,4.37023429102696,128.544050957538));
#34449=CARTESIAN_POINT('Ctrl Pts',(144.499006633797,4.30551149448725,128.423065385804));
#34450=CARTESIAN_POINT('Ctrl Pts',(144.491255442557,4.23580711029935,128.304936446514));
#34451=CARTESIAN_POINT('Ctrl Pts',(144.48350754578,4.1661323523342,128.186857715175));
#34452=CARTESIAN_POINT('Ctrl Pts',(144.475759649003,4.09148041615446,128.071633537448));
#34453=CARTESIAN_POINT('Ctrl Pts',(144.468011752226,4.01212055216497,127.959703918174));
#34454=CARTESIAN_POINT('Ctrl Pts',(144.460265476142,3.93277728854825,127.847797712163));
#34455=CARTESIAN_POINT('Ctrl Pts',(144.452519200058,3.84872828192332,127.739185012578));
#34456=CARTESIAN_POINT('Ctrl Pts',(144.444772923973,3.76028596112699,127.634276619775));
#34457=CARTESIAN_POINT('Ctrl Pts',(144.437026590708,3.6718429874695,127.529367452562));
#34458=CARTESIAN_POINT('Ctrl Pts',(144.429280257443,3.57900688692668,127.428162945609));
#34459=CARTESIAN_POINT('Ctrl Pts',(144.421533924177,3.48212994014246,127.331040283582));
#34460=CARTESIAN_POINT('Ctrl Pts',(144.413785856174,3.38523129843776,127.233895871609));
#34461=CARTESIAN_POINT('Ctrl Pts',(144.406037788171,3.28429028585757,127.140835400269));
#34462=CARTESIAN_POINT('Ctrl Pts',(144.398289720168,3.17969524800384,127.052198415272));
#34463=CARTESIAN_POINT('Ctrl Pts',(144.390533417427,3.0749890452991,126.963467225833));
#34464=CARTESIAN_POINT('Ctrl Pts',(144.382777114685,2.96662135827354,126.879169167326));
#34465=CARTESIAN_POINT('Ctrl Pts',(144.375020811943,2.8550131895684,126.799603103073));
#34466=CARTESIAN_POINT('Ctrl Pts',(144.367260369429,2.74334545222313,126.719994572015));
#34467=CARTESIAN_POINT('Ctrl Pts',(144.359499926915,2.62843411434688,126.645123281025));
#34468=CARTESIAN_POINT('Ctrl Pts',(144.3517394844,2.5107273739368,126.575243556492));
#34469=CARTESIAN_POINT('Ctrl Pts',(144.343966584135,2.3928316802175,126.505251654822));
#34470=CARTESIAN_POINT('Ctrl Pts',(144.336193683869,2.27213196109396,126.440267517394));
#34471=CARTESIAN_POINT('Ctrl Pts',(144.328420783604,2.14909991677226,126.380498887106));
#34472=CARTESIAN_POINT('Ctrl Pts',(144.320930447842,2.03054039716113,126.322902997077));
#34473=CARTESIAN_POINT('Ctrl Pts',(144.31344011208,1.90981546237683,126.270150127238));
#34474=CARTESIAN_POINT('Ctrl Pts',(144.305949776318,1.78736112658887,126.222382522282));
#34475=CARTESIAN_POINT('Ctrl Pts',(144.298175442199,1.66026389743988,126.172803794066));
#34476=CARTESIAN_POINT('Ctrl Pts',(144.29040110808,1.53090093223615,126.128438775345));
#34477=CARTESIAN_POINT('Ctrl Pts',(144.282626773961,1.39973910629574,126.089499697368));
#34478=CARTESIAN_POINT('Ctrl Pts',(144.274862021014,1.26873892558363,126.050608608325));
#34479=CARTESIAN_POINT('Ctrl Pts',(144.267097268067,1.13594466637413,126.017130265116));
#34480=CARTESIAN_POINT('Ctrl Pts',(144.259332515119,1.00184326560478,125.989228933628));
#34481=CARTESIAN_POINT('Ctrl Pts',(144.251575474234,0.867875056237084,125.961355314137));
#34482=CARTESIAN_POINT('Ctrl Pts',(144.243818433349,0.732602669219422,125.939047762299));
#34483=CARTESIAN_POINT('Ctrl Pts',(144.236061392464,0.596527952573879,125.922420689187));
#34484=CARTESIAN_POINT('Ctrl Pts',(144.228310201224,0.460555850930619,125.90580615468));
#34485=CARTESIAN_POINT('Ctrl Pts',(144.220559009984,0.323783010469462,125.894863619695));
#34486=CARTESIAN_POINT('Ctrl Pts',(144.212807818744,0.186720865981622,125.889656315097));
#34487=CARTESIAN_POINT('Ctrl Pts',(144.205059921967,0.049716976561534,125.884451223742));
#34488=CARTESIAN_POINT('Ctrl Pts',(144.19731202519,-0.0875755824579162,
125.884976529335));
#34489=CARTESIAN_POINT('Ctrl Pts',(144.189564128413,-0.224641086123712,
125.891243537247));
#34490=CARTESIAN_POINT('Ctrl Pts',(144.181817852329,-0.361677918640931,
125.897509234235));
#34491=CARTESIAN_POINT('Ctrl Pts',(144.174071576245,-0.498487399965087,
125.909514226762));
#34492=CARTESIAN_POINT('Ctrl Pts',(144.166325300161,-0.634555036704846,
125.927217707225));
#34493=CARTESIAN_POINT('Ctrl Pts',(144.158578966895,-0.77062367786499,125.94492131837));
#34494=CARTESIAN_POINT('Ctrl Pts',(144.15083263363,-0.905950075816032,125.968323450946));
#34495=CARTESIAN_POINT('Ctrl Pts',(144.143086300364,-1.04002647812338,125.997331598795));
#34496=CARTESIAN_POINT('Ctrl Pts',(144.135338232361,-1.1741329059114,126.026346242818));
#34497=CARTESIAN_POINT('Ctrl Pts',(144.127590164358,-1.30698839898089,126.060969317612));
#34498=CARTESIAN_POINT('Ctrl Pts',(144.119842096355,-1.43809737762394,126.101057629774));
#34499=CARTESIAN_POINT('Ctrl Pts',(144.112085793614,-1.56934570044976,126.141188548272));
#34500=CARTESIAN_POINT('Ctrl Pts',(144.104329490872,-1.69884342638246,126.186796192781));
#34501=CARTESIAN_POINT('Ctrl Pts',(144.09657318813,-1.82611155103295,126.237687904782));
#34502=CARTESIAN_POINT('Ctrl Pts',(144.088812745616,-1.95344760251353,126.288606779222));
#34503=CARTESIAN_POINT('Ctrl Pts',(144.081052303102,-2.07855132507632,126.344815180623));
#34504=CARTESIAN_POINT('Ctrl Pts',(144.073291860587,-2.20096648476092,126.406073496941));
#34505=CARTESIAN_POINT('Ctrl Pts',(144.065518960322,-2.3235781561274,126.467430150546));
#34506=CARTESIAN_POINT('Ctrl Pts',(144.057746060057,-2.44349229783324,126.533852729033));
#34507=CARTESIAN_POINT('Ctrl Pts',(144.049973159791,-2.56027916441055,126.605056667768));
#34508=CARTESIAN_POINT('Ctrl Pts',(144.042482824029,-2.6728205342191,126.673672163979));
#34509=CARTESIAN_POINT('Ctrl Pts',(144.034992488267,-2.78245779377563,126.746727256012));
#34510=CARTESIAN_POINT('Ctrl Pts',(144.027502152505,-2.88883559228039,126.823931999531));
#34511=CARTESIAN_POINT('Ctrl Pts',(144.019481042626,-3.00275144833393,126.906607563163));
#34512=CARTESIAN_POINT('Ctrl Pts',(144.011459932748,-3.11331865693512,126.994325096411));
#34513=CARTESIAN_POINT('Ctrl Pts',(144.003438822869,-3.22005684860705,127.086778479369));
#34514=CARTESIAN_POINT('Ctrl Pts',(143.995741301339,-3.3224889983866,127.175502099495));
#34515=CARTESIAN_POINT('Ctrl Pts',(143.988043779809,-3.42139467126964,127.268586646072));
#34516=CARTESIAN_POINT('Ctrl Pts',(143.980346258278,-3.51637759337915,127.365716744863));
#34517=CARTESIAN_POINT('Ctrl Pts',(143.972655696484,-3.61127463640881,127.462759023197));
#34518=CARTESIAN_POINT('Ctrl Pts',(143.96496513469,-3.70225570535656,127.563839297074));
#34519=CARTESIAN_POINT('Ctrl Pts',(143.957274572896,-3.78895824126995,127.668602573901));
#34520=CARTESIAN_POINT('Ctrl Pts',(143.949589228179,-3.87560196043033,127.773294782035));
#34521=CARTESIAN_POINT('Ctrl Pts',(143.941903883463,-3.95797266707612,127.881664717766));
#34522=CARTESIAN_POINT('Ctrl Pts',(143.934218538747,-4.03574562371058,127.993321606239));
#34523=CARTESIAN_POINT('Ctrl Pts',(143.926536672775,-4.11348337668676,128.10492795361));
#34524=CARTESIAN_POINT('Ctrl Pts',(143.918854806803,-4.18662729394016,128.219817966861));
#34525=CARTESIAN_POINT('Ctrl Pts',(143.911172940831,-4.25489411663926,128.337569357915));
#34526=CARTESIAN_POINT('Ctrl Pts',(143.903491513211,-4.32315704381489,128.455314029698));
#34527=CARTESIAN_POINT('Ctrl Pts',(143.895810085591,-4.38654322345769,128.575919414166));
#34528=CARTESIAN_POINT('Ctrl Pts',(143.888128657971,-4.44481391950573,128.698936127477));
#34529=CARTESIAN_POINT('Ctrl Pts',(143.880447426527,-4.50308312737967,128.821949699066));
#34530=CARTESIAN_POINT('Ctrl Pts',(143.872766195083,-4.55623694672054,128.947374114459));
#34531=CARTESIAN_POINT('Ctrl Pts',(143.865084963639,-4.60408395472253,129.074738115294));
#34532=CARTESIAN_POINT('Ctrl Pts',(143.85740026354,-4.65195256925087,129.202159630564));
#34533=CARTESIAN_POINT('Ctrl Pts',(143.849715563442,-4.69450945444632,129.331522104781));
#34534=CARTESIAN_POINT('Ctrl Pts',(143.842030863343,-4.73161245236431,129.46233727085));
#34535=CARTESIAN_POINT('Ctrl Pts',(143.839685747368,-4.74293505858744,129.502257727323));
#34536=CARTESIAN_POINT('Ctrl Pts',(143.837340631392,-4.75375011671748,129.542313375196));
#34537=CARTESIAN_POINT('Ctrl Pts',(143.834995515417,-4.76405452823405,129.582490119308));
#34538=CARTESIAN_POINT('Ctrl Pts',(145.584738356252,-4.76405452823403,129.582490119308));
#34539=CARTESIAN_POINT('Ctrl Pts',(145.576986652373,-4.79817595935304,129.715529061376));
#34540=CARTESIAN_POINT('Ctrl Pts',(145.569234948494,-4.82673275080714,129.850046531733));
#34541=CARTESIAN_POINT('Ctrl Pts',(145.561483244616,-4.84960957421066,129.985538267954));
#34542=CARTESIAN_POINT('Ctrl Pts',(145.553712609845,-4.87254226645113,130.121360896519));
#34543=CARTESIAN_POINT('Ctrl Pts',(145.545941975074,-4.8897671214549,130.258162172932));
#34544=CARTESIAN_POINT('Ctrl Pts',(145.538171340304,-4.90121969823317,130.395424764221));
#34545=CARTESIAN_POINT('Ctrl Pts',(145.530400705533,-4.91267227501144,130.53268735551));
#34546=CARTESIAN_POINT('Ctrl Pts',(145.522630070762,-4.91835254938408,130.670410868192));
#34547=CARTESIAN_POINT('Ctrl Pts',(145.514859435991,-4.91824859781811,130.808074451192));
#34548=CARTESIAN_POINT('',(145.860140564062,-4.91824867625418,130.800752151961));
#34549=CARTESIAN_POINT('Ctrl Pts',(145.92992189461,-4.76405452823405,129.582490119308));
#34550=CARTESIAN_POINT('Ctrl Pts',(145.920948441898,-4.80324843157597,129.735306553588));
#34551=CARTESIAN_POINT('Ctrl Pts',(145.911974989186,-4.83512838164778,129.890177542899));
#34552=CARTESIAN_POINT('Ctrl Pts',(145.903001536475,-4.85950097047483,130.046446783114));
#34553=CARTESIAN_POINT('Ctrl Pts',(145.894096396557,-4.88368801649093,130.201526382199));
#34554=CARTESIAN_POINT('Ctrl Pts',(145.885191256639,-4.90048149046819,130.357982889292));
#34555=CARTESIAN_POINT('Ctrl Pts',(145.876286116722,-4.90973963625009,130.515155211782));
#34556=CARTESIAN_POINT('Ctrl Pts',(145.870904265835,-4.91533482740309,130.610142826905));
#34557=CARTESIAN_POINT('Ctrl Pts',(145.865522414949,-4.91817871119236,130.705391516625));
#34558=CARTESIAN_POINT('Ctrl Pts',(145.860140564062,-4.91824867625418,130.800752151961));
#34559=CARTESIAN_POINT('Ctrl Pts',(145.860140564008,-4.91824867625488,130.800752152921));
#34560=CARTESIAN_POINT('Ctrl Pts',(145.852378814537,-4.91834958041379,130.938282043005));
#34561=CARTESIAN_POINT('Ctrl Pts',(145.844617065067,-4.91267751355959,131.075864905963));
#34562=CARTESIAN_POINT('Ctrl Pts',(145.836855315596,-4.90124589904416,131.212982324775));
#34563=CARTESIAN_POINT('Ctrl Pts',(145.8290941807,-4.88981518968292,131.350088886643));
#34564=CARTESIAN_POINT('Ctrl Pts',(145.821333045803,-4.87262587158808,131.486729690643));
#34565=CARTESIAN_POINT('Ctrl Pts',(145.813571910907,-4.84974336629735,131.622390166882));
#34566=CARTESIAN_POINT('Ctrl Pts',(145.805809737665,-4.82685779960359,131.758068792856));
#34567=CARTESIAN_POINT('Ctrl Pts',(145.798047564423,-4.79827759397041,131.89276644696));
#34568=CARTESIAN_POINT('Ctrl Pts',(145.79028539118,-4.76411947705081,132.025977853399));
#34569=CARTESIAN_POINT('Ctrl Pts',(145.782520526355,-4.72994951558522,132.159235451748));
#34570=CARTESIAN_POINT('Ctrl Pts',(145.774755661529,-4.69019788940373,132.291005400603));
#34571=CARTESIAN_POINT('Ctrl Pts',(145.766990796703,-4.64503135568583,132.420797058381));
#34572=CARTESIAN_POINT('Ctrl Pts',(145.759216610126,-4.599810599364,132.550744531563));
#34573=CARTESIAN_POINT('Ctrl Pts',(145.751442423549,-4.54916207961528,132.678708602936));
#34574=CARTESIAN_POINT('Ctrl Pts',(145.743668236972,-4.49330116536668,132.804217537402));
#34575=CARTESIAN_POINT('Ctrl Pts',(145.735889117777,-4.4374048081052,132.929806105629));
#34576=CARTESIAN_POINT('Ctrl Pts',(145.728109998581,-4.37628963952763,133.052936085945));
#34577=CARTESIAN_POINT('Ctrl Pts',(145.720330879385,-4.31021682307232,133.173160735897));
#34578=CARTESIAN_POINT('Ctrl Pts',(145.712538932775,-4.24403505553835,133.293583630846));
#34579=CARTESIAN_POINT('Ctrl Pts',(145.704746986164,-4.17287950881536,133.41109129229));
#34580=CARTESIAN_POINT('Ctrl Pts',(145.696955039554,-4.0970549255999,133.525265613908));
#34581=CARTESIAN_POINT('Ctrl Pts',(145.69083632611,-4.03751282144295,133.614922280144));
#34582=CARTESIAN_POINT('Ctrl Pts',(145.684717612666,-3.975092507965,133.702524059789));
#34583=CARTESIAN_POINT('Ctrl Pts',(145.678598899223,-3.90995826411787,133.787883608152));
#34584=CARTESIAN_POINT('Ctrl Pts',(145.670824565104,-3.82719979227,133.896340010851));
#34585=CARTESIAN_POINT('Ctrl Pts',(145.663050230985,-3.73979418909744,134.001522196541));
#34586=CARTESIAN_POINT('Ctrl Pts',(145.655275896866,-3.64802979451386,134.103006048775));
#34587=CARTESIAN_POINT('Ctrl Pts',(145.647511143918,-3.55637849134542,134.204364831232));
#34588=CARTESIAN_POINT('Ctrl Pts',(145.639746390971,-3.46037934478948,134.30203406182));
#34589=CARTESIAN_POINT('Ctrl Pts',(145.631981638024,-3.36036277911229,134.395620153614));
#34590=CARTESIAN_POINT('Ctrl Pts',(145.624224597139,-3.26044555129847,134.489113294382));
#34591=CARTESIAN_POINT('Ctrl Pts',(145.616467556254,-3.15651912858829,134.578531101451));
#34592=CARTESIAN_POINT('Ctrl Pts',(145.608710515369,-3.04895260360576,134.663514810322));
#34593=CARTESIAN_POINT('Ctrl Pts',(145.600959324129,-2.94146719537606,134.748434432318));
#34594=CARTESIAN_POINT('Ctrl Pts',(145.593208132889,-2.8303474542221,134.828926370334));
#34595=CARTESIAN_POINT('Ctrl Pts',(145.585456941649,-2.7159972832948,134.904670583853));
#34596=CARTESIAN_POINT('Ctrl Pts',(145.577709044872,-2.60169571424069,134.980382604062));
#34597=CARTESIAN_POINT('Ctrl Pts',(145.569961148095,-2.48416677150554,135.051350697791));
#34598=CARTESIAN_POINT('Ctrl Pts',(145.562213251318,-2.36384503284604,135.117296940211));
#34599=CARTESIAN_POINT('Ctrl Pts',(145.554466975233,-2.24354846290036,135.183229388098));
#34600=CARTESIAN_POINT('Ctrl Pts',(145.546720699149,-2.12046060165158,135.244141886315));
#34601=CARTESIAN_POINT('Ctrl Pts',(145.538974423065,-1.99504208311807,135.299801658119));
#34602=CARTESIAN_POINT('Ctrl Pts',(145.5312280898,-1.86962263877354,135.355461840791));
#34603=CARTESIAN_POINT('Ctrl Pts',(145.523481756535,-1.74187286016913,135.405869061088));
#34604=CARTESIAN_POINT('Ctrl Pts',(145.515735423269,-1.61227451667469,135.450838202294));
#34605=CARTESIAN_POINT('Ctrl Pts',(145.507987355266,-1.48264715052979,135.495817414028));
#34606=CARTESIAN_POINT('Ctrl Pts',(145.500239287263,-1.35117076502652,135.53535599521));
#34607=CARTESIAN_POINT('Ctrl Pts',(145.49249121926,-1.21834309978122,135.569318450928));
#34608=CARTESIAN_POINT('Ctrl Pts',(145.484734916518,-1.08537426371269,135.603317002347));
#34609=CARTESIAN_POINT('Ctrl Pts',(145.476978613777,-0.951051658409011,
135.631727492731));
#34610=CARTESIAN_POINT('Ctrl Pts',(145.469222311035,-0.815884597942765,
135.654465295337));
#34611=CARTESIAN_POINT('Ctrl Pts',(145.461461868521,-0.680645394746499,
135.677215233794));
#34612=CARTESIAN_POINT('Ctrl Pts',(145.453701426006,-0.544561226042542,
135.694286402916));
#34613=CARTESIAN_POINT('Ctrl Pts',(145.445940983492,-0.408146382902866,
135.705646121658));
#34614=CARTESIAN_POINT('Ctrl Pts',(145.438168083227,-0.271512554546641,
135.717024076029));
#34615=CARTESIAN_POINT('Ctrl Pts',(145.430395182961,-0.134547381849304,
135.722672242263));
#34616=CARTESIAN_POINT('Ctrl Pts',(145.422622282696,0.00223408340109133,
135.722610110157));
#34617=CARTESIAN_POINT('Ctrl Pts',(145.415131946934,0.134043197857729,135.722550236709));
#34618=CARTESIAN_POINT('Ctrl Pts',(145.407641611172,0.265681421673301,135.717188036997));
#34619=CARTESIAN_POINT('Ctrl Pts',(145.40015127541,0.39669444194589,135.706586293953));
#34620=CARTESIAN_POINT('Ctrl Pts',(145.392376941291,0.532674860702761,135.695582582599));
#34621=CARTESIAN_POINT('Ctrl Pts',(145.384602607172,0.668412475953023,135.678899313778));
#34622=CARTESIAN_POINT('Ctrl Pts',(145.376828273053,0.803394611752564,135.656549830726));
#34623=CARTESIAN_POINT('Ctrl Pts',(145.369063520106,0.938210394133524,135.634227891415));
#34624=CARTESIAN_POINT('Ctrl Pts',(145.361298767158,1.07227216758641,135.606253695416));
#34625=CARTESIAN_POINT('Ctrl Pts',(145.353534014211,1.20507019389738,135.572692494678));
#34626=CARTESIAN_POINT('Ctrl Pts',(145.345776973326,1.33773632333645,135.539164627397));
#34627=CARTESIAN_POINT('Ctrl Pts',(145.338019932441,1.46914082688648,135.500060893493));
#34628=CARTESIAN_POINT('Ctrl Pts',(145.330262891556,1.5987823622354,135.455497900071));
#34629=CARTESIAN_POINT('Ctrl Pts',(145.322511700316,1.7283261338945,135.410968511948));
#34630=CARTESIAN_POINT('Ctrl Pts',(145.314760509076,1.85610921534232,135.360988185263));
#34631=CARTESIAN_POINT('Ctrl Pts',(145.307009317836,1.98164402790863,135.305723745459));
#34632=CARTESIAN_POINT('Ctrl Pts',(145.299261421059,2.10712548483043,135.250482794516));
#34633=CARTESIAN_POINT('Ctrl Pts',(145.291513524282,2.23036021635847,135.189962354554));
#34634=CARTESIAN_POINT('Ctrl Pts',(145.283765627505,2.35087949656811,135.124377822985));
#34635=CARTESIAN_POINT('Ctrl Pts',(145.276019351421,2.47137356674247,135.058807010286));
#34636=CARTESIAN_POINT('Ctrl Pts',(145.268273075336,2.58915297221669,134.988174399745));
#34637=CARTESIAN_POINT('Ctrl Pts',(145.260526799252,2.70377288738724,134.912741714291));
#34638=CARTESIAN_POINT('Ctrl Pts',(145.252780465987,2.81839364865598,134.837308472011));
#34639=CARTESIAN_POINT('Ctrl Pts',(145.245034132722,2.92985454649591,134.757075299044));
#34640=CARTESIAN_POINT('Ctrl Pts',(145.237287799456,3.03773942885925,134.672347461501));
#34641=CARTESIAN_POINT('Ctrl Pts',(145.229539731453,3.1456484712939,134.587600649746));
#34642=CARTESIAN_POINT('Ctrl Pts',(145.22179166345,3.24997959728711,134.49835741193));
#34643=CARTESIAN_POINT('Ctrl Pts',(145.214043595447,3.35034977071012,134.404963272179));
#34644=CARTESIAN_POINT('Ctrl Pts',(145.206287292706,3.4508266187478,134.311469872024));
#34645=CARTESIAN_POINT('Ctrl Pts',(145.198530989964,3.54733381811295,134.213817023985));
#34646=CARTESIAN_POINT('Ctrl Pts',(145.190774687222,3.63952487323465,134.112387485596));
#34647=CARTESIAN_POINT('Ctrl Pts',(145.183014244708,3.73176513349839,134.010903811207));
#34648=CARTESIAN_POINT('Ctrl Pts',(145.175253802194,3.81968440878661,133.90563972987));
#34649=CARTESIAN_POINT('Ctrl Pts',(145.167493359679,3.90297721672312,133.797010264324));
#34650=CARTESIAN_POINT('Ctrl Pts',(145.159720459414,3.98640373366926,133.688206417116));
#34651=CARTESIAN_POINT('Ctrl Pts',(145.151947559149,4.06518871728958,133.576026710085));
#34652=CARTESIAN_POINT('Ctrl Pts',(145.144174658883,4.13907016682952,133.460915005596));
#34653=CARTESIAN_POINT('Ctrl Pts',(145.136684323121,4.21026583958247,133.349987901515));
#34654=CARTESIAN_POINT('Ctrl Pts',(145.129193987359,4.27690814451405,133.236338535707));
#34655=CARTESIAN_POINT('Ctrl Pts',(145.121703651597,4.3388043354624,133.120383070193));
#34656=CARTESIAN_POINT('Ctrl Pts',(145.113929317478,4.40304733930367,133.00003111796));
#34657=CARTESIAN_POINT('Ctrl Pts',(145.106154983359,4.46238072936799,132.876813503651));
#34658=CARTESIAN_POINT('Ctrl Pts',(145.09838064924,4.51653861782784,132.751168768404));
#34659=CARTESIAN_POINT('Ctrl Pts',(145.090615896293,4.57062976153049,132.625678879064));
#34660=CARTESIAN_POINT('Ctrl Pts',(145.082851143346,4.61955794135898,132.497768175986));
#34661=CARTESIAN_POINT('Ctrl Pts',(145.075086390399,4.66310252966831,132.367900786638));
#34662=CARTESIAN_POINT('Ctrl Pts',(145.067329349514,4.70660386887837,132.238162383412));
#34663=CARTESIAN_POINT('Ctrl Pts',(145.059572308629,4.7447321339722,132.106471529671));
#34664=CARTESIAN_POINT('Ctrl Pts',(145.051815267744,4.77731444204252,131.973313047886));
#34665=CARTESIAN_POINT('Ctrl Pts',(145.044064076504,4.80987217954111,131.840254981948));
#34666=CARTESIAN_POINT('Ctrl Pts',(145.036312885264,4.83689219198253,131.705731869111));
#34667=CARTESIAN_POINT('Ctrl Pts',(145.028561694023,4.85825128615566,131.570244096345));
#34668=CARTESIAN_POINT('Ctrl Pts',(145.020813797246,4.87960130214394,131.434813909498));
#34669=CARTESIAN_POINT('Ctrl Pts',(145.013065900469,4.8952951245419,131.29842026358));
#34670=CARTESIAN_POINT('Ctrl Pts',(145.005318003692,4.90526061548313,131.161573938552));
#34671=CARTESIAN_POINT('Ctrl Pts',(144.997571727608,4.91522402185848,131.024756238826));
#34672=CARTESIAN_POINT('Ctrl Pts',(144.989825451524,4.91946145177116,130.887486438019));
#34673=CARTESIAN_POINT('Ctrl Pts',(144.98207917544,4.91795266103117,130.750280248148));
#34674=CARTESIAN_POINT('Ctrl Pts',(144.974332842175,4.91644385915363,130.613073045451));
#34675=CARTESIAN_POINT('Ctrl Pts',(144.966586508909,4.90918875628171,130.475929845569));
#34676=CARTESIAN_POINT('Ctrl Pts',(144.958840175644,4.89621924109144,130.339365772793));
#34677=CARTESIAN_POINT('Ctrl Pts',(144.951092107641,4.88324682146822,130.20277111744));
#34678=CARTESIAN_POINT('Ctrl Pts',(144.943344039638,4.86455748002248,130.066756236403));
#34679=CARTESIAN_POINT('Ctrl Pts',(144.935595971635,4.84023487560304,129.931830153057));
#34680=CARTESIAN_POINT('Ctrl Pts',(144.927839668893,4.81588642083022,129.796760668664));
#34681=CARTESIAN_POINT('Ctrl Pts',(144.920083366151,4.78589281267913,129.662782678944));
#34682=CARTESIAN_POINT('Ctrl Pts',(144.912327063409,4.75038878658295,129.53039459023));
#34683=CARTESIAN_POINT('Ctrl Pts',(144.904566620895,4.71486581091898,129.397935842006));
#34684=CARTESIAN_POINT('Ctrl Pts',(144.896806178381,4.67382667389694,129.267069058522));
#34685=CARTESIAN_POINT('Ctrl Pts',(144.889045735867,4.62745542521647,129.13827558068));
#34686=CARTESIAN_POINT('Ctrl Pts',(144.881272835601,4.58100973729097,129.009275352114));
#34687=CARTESIAN_POINT('Ctrl Pts',(144.873499935336,4.52921498074763,128.882355442295));
#34688=CARTESIAN_POINT('Ctrl Pts',(144.865727035071,4.47230297175938,128.75797619833));
#34689=CARTESIAN_POINT('Ctrl Pts',(144.858236699309,4.41745985765125,128.638118453177));
#34690=CARTESIAN_POINT('Ctrl Pts',(144.850746363547,4.35786522112499,128.520620136372));
#34691=CARTESIAN_POINT('Ctrl Pts',(144.843256027785,4.29376500706537,128.405868356457));
#34692=CARTESIAN_POINT('Ctrl Pts',(144.835481693666,4.22723441390598,128.286765727927));
#34693=CARTESIAN_POINT('Ctrl Pts',(144.827707359547,4.15563909191235,128.170244736165));
#34694=CARTESIAN_POINT('Ctrl Pts',(144.819933025427,4.0792042792977,128.056766122329));
#34695=CARTESIAN_POINT('Ctrl Pts',(144.81216827248,4.00286366575849,127.943427360742));
#34696=CARTESIAN_POINT('Ctrl Pts',(144.804403519533,3.92169564497463,127.833123837928));
#34697=CARTESIAN_POINT('Ctrl Pts',(144.796638766586,3.83597144589743,127.726292046407));
#34698=CARTESIAN_POINT('Ctrl Pts',(144.788881725701,3.750332389303,127.619566361726));
#34699=CARTESIAN_POINT('Ctrl Pts',(144.781124684816,3.66014640298863,127.516305849278));
#34700=CARTESIAN_POINT('Ctrl Pts',(144.773367643931,3.5657279343978,127.416918018738));
#34701=CARTESIAN_POINT('Ctrl Pts',(144.765616452691,3.47138066750932,127.317605137334));
#34702=CARTESIAN_POINT('Ctrl Pts',(144.757865261451,3.37280753951247,127.222159407223));
#34703=CARTESIAN_POINT('Ctrl Pts',(144.750114070211,3.27036295119792,127.130954945722));
#34704=CARTESIAN_POINT('Ctrl Pts',(144.742366173434,3.16796190456571,127.03978924855));
#34705=CARTESIAN_POINT('Ctrl Pts',(144.734618276657,3.06169296173569,126.952861494076));
#34706=CARTESIAN_POINT('Ctrl Pts',(144.726870379879,2.95194686407482,126.870508462975));
#34707=CARTESIAN_POINT('Ctrl Pts',(144.719124103795,2.84222372293164,126.788172658353));
#34708=CARTESIAN_POINT('Ctrl Pts',(144.711377827711,2.72902518620294,126.71040990822));
#34709=CARTESIAN_POINT('Ctrl Pts',(144.703631551627,2.61277419453387,126.637515999527));
#34710=CARTESIAN_POINT('Ctrl Pts',(144.695885218362,2.4965223447265,126.564621552749));
#34711=CARTESIAN_POINT('Ctrl Pts',(144.688138885096,2.37721832625067,126.496596226825));
#34712=CARTESIAN_POINT('Ctrl Pts',(144.680392551831,2.25531276437078,126.433691630172));
#34713=CARTESIAN_POINT('Ctrl Pts',(144.672644483828,2.13337990258558,126.370772946471));
#34714=CARTESIAN_POINT('Ctrl Pts',(144.664896415825,2.00884468546454,126.312977453191));
#34715=CARTESIAN_POINT('Ctrl Pts',(144.657148347822,1.88218058843893,126.260509905339));
#34716=CARTESIAN_POINT('Ctrl Pts',(144.64939204508,1.75538187130373,126.207986594354));
#34717=CARTESIAN_POINT('Ctrl Pts',(144.641635742338,1.62645011625809,126.160802690316));
#34718=CARTESIAN_POINT('Ctrl Pts',(144.633879439596,1.49587747445835,126.119114237288));
#34719=CARTESIAN_POINT('Ctrl Pts',(144.626118997082,1.36523514210817,126.077403533877));
#34720=CARTESIAN_POINT('Ctrl Pts',(144.618358554568,1.23295055482595,126.041194229071));
#34721=CARTESIAN_POINT('Ctrl Pts',(144.610598112054,1.09952816170457,126.010591653158));
#34722=CARTESIAN_POINT('Ctrl Pts',(144.602825211788,0.965891587112881,125.979939951274));
#34723=CARTESIAN_POINT('Ctrl Pts',(144.595052311523,0.831113941354601,125.95491303541));
#34724=CARTESIAN_POINT('Ctrl Pts',(144.587279411257,0.695707829792073,125.935564700908));
#34725=CARTESIAN_POINT('Ctrl Pts',(144.579789075495,0.565224071451377,125.916919727101));
#34726=CARTESIAN_POINT('Ctrl Pts',(144.572298739733,0.434157053073168,125.903547672329));
#34727=CARTESIAN_POINT('Ctrl Pts',(144.564808403971,0.302965399254829,125.895450857817));
#34728=CARTESIAN_POINT('Ctrl Pts',(144.557034069852,0.166799574008043,125.887047050123));
#34729=CARTESIAN_POINT('Ctrl Pts',(144.549259735733,0.0300681432426362,
125.884299779971));
#34730=CARTESIAN_POINT('Ctrl Pts',(144.541485401614,-0.106719511701879,
125.887268589922));
#34731=CARTESIAN_POINT('Ctrl Pts',(144.533720648667,-0.243338588086971,
125.89023374108));
#34732=CARTESIAN_POINT('Ctrl Pts',(144.52595589572,-0.380013363661367,125.898900947369));
#34733=CARTESIAN_POINT('Ctrl Pts',(144.518191142773,-0.516229999033403,
125.91327795106));
#34734=CARTESIAN_POINT('Ctrl Pts',(144.510434101888,-0.652311342122083,
125.927640675307));
#34735=CARTESIAN_POINT('Ctrl Pts',(144.502677061003,-0.787935064251584,
125.947701870537));
#34736=CARTESIAN_POINT('Ctrl Pts',(144.494920020118,-0.922588349466602,
125.973417252143));
#34737=CARTESIAN_POINT('Ctrl Pts',(144.487168828878,-1.05714009159165,125.999113241579));
#34738=CARTESIAN_POINT('Ctrl Pts',(144.479417637638,-1.19072247096256,126.030454857382));
#34739=CARTESIAN_POINT('Ctrl Pts',(144.471666446397,-1.32282916980003,126.067346151679));
#34740=CARTESIAN_POINT('Ctrl Pts',(144.46391854962,-1.45487971976697,126.104221766191));
#34741=CARTESIAN_POINT('Ctrl Pts',(144.456170652843,-1.58545546089066,126.146642262865));
#34742=CARTESIAN_POINT('Ctrl Pts',(144.448422756066,-1.71406184479824,126.194460938104));
#34743=CARTESIAN_POINT('Ctrl Pts',(144.440676479982,-1.84264132702257,126.242269610706));
#34744=CARTESIAN_POINT('Ctrl Pts',(144.432930203898,-1.96925190519468,126.295474079697));
#34745=CARTESIAN_POINT('Ctrl Pts',(144.425183927814,-2.09341611562539,126.353878393207));
#34746=CARTESIAN_POINT('Ctrl Pts',(144.417437594549,-2.21758124260792,126.412283137843));
#34747=CARTESIAN_POINT('Ctrl Pts',(144.409691261283,-2.3392996120335,126.475887637179));
#34748=CARTESIAN_POINT('Ctrl Pts',(144.401944928018,-2.45811596465303,126.544448767913));
#34749=CARTESIAN_POINT('Ctrl Pts',(144.394196860015,-2.57695892537096,126.613025252436));
#34750=CARTESIAN_POINT('Ctrl Pts',(144.386448792012,-2.69289823751659,126.686560381769));
#34751=CARTESIAN_POINT('Ctrl Pts',(144.378700724009,-2.80550570986693,126.764766482705));
#34752=CARTESIAN_POINT('Ctrl Pts',(144.370944421267,-2.91823286277919,126.843055702016));
#34753=CARTESIAN_POINT('Ctrl Pts',(144.363188118525,-3.02762078049908,126.92602558641));
#34754=CARTESIAN_POINT('Ctrl Pts',(144.355431815784,-3.13327215901682,127.013346420807));
#34755=CARTESIAN_POINT('Ctrl Pts',(144.347671373269,-3.2389799268568,127.100713860962));
#34756=CARTESIAN_POINT('Ctrl Pts',(144.339910930755,-3.3409468911488,127.192436617028));
#34757=CARTESIAN_POINT('Ctrl Pts',(144.332150488241,-3.43881176747942,127.28814721529));
#34758=CARTESIAN_POINT('Ctrl Pts',(144.324377587976,-3.53683374519725,127.384011456701));
#34759=CARTESIAN_POINT('Ctrl Pts',(144.31660468771,-3.63074020797275,127.483876047837));
#34760=CARTESIAN_POINT('Ctrl Pts',(144.308831787445,-3.72020882053998,127.587338796988));
#34761=CARTESIAN_POINT('Ctrl Pts',(144.301341451683,-3.80642502368255,127.6870404146));
#34762=CARTESIAN_POINT('Ctrl Pts',(144.293851115921,-3.88852023700126,127.790082886937));
#34763=CARTESIAN_POINT('Ctrl Pts',(144.286360780158,-3.96624460978605,127.896081614815));
#34764=CARTESIAN_POINT('Ctrl Pts',(144.278534089727,-4.04745920737628,128.006840231723));
#34765=CARTESIAN_POINT('Ctrl Pts',(144.270707399296,-4.12415900736794,128.121178041885));
#34766=CARTESIAN_POINT('Ctrl Pts',(144.262880708865,-4.19601447399703,128.238693921265));
#34767=CARTESIAN_POINT('Ctrl Pts',(144.255067153101,-4.26774935356702,128.35601258678));
#34768=CARTESIAN_POINT('Ctrl Pts',(144.247253597336,-4.33465589462292,128.476498373107));
#34769=CARTESIAN_POINT('Ctrl Pts',(144.239440041572,-4.39644600918776,128.599718798404));
#34770=CARTESIAN_POINT('Ctrl Pts',(144.231634058566,-4.45817623787452,128.722819800661));
#34771=CARTESIAN_POINT('Ctrl Pts',(144.22382807556,-4.51479973331902,128.848649828656));
#34772=CARTESIAN_POINT('Ctrl Pts',(144.216022092555,-4.56607252489284,128.976748853564));
#34773=CARTESIAN_POINT('Ctrl Pts',(144.208223432298,-4.61729721774736,129.104727709493));
#34774=CARTESIAN_POINT('Ctrl Pts',(144.200424772042,-4.66318106056448,129.234970968362));
#34775=CARTESIAN_POINT('Ctrl Pts',(144.192626111785,-4.70352698732374,129.366996035417));
#34776=CARTESIAN_POINT('Ctrl Pts',(144.188412227281,-4.72532727993827,129.438333722401));
#34777=CARTESIAN_POINT('Ctrl Pts',(144.184198342776,-4.7455115290801,129.510191247036));
#34778=CARTESIAN_POINT('Ctrl Pts',(144.179984458271,-4.76405452823405,129.582490119308));
#34779=CARTESIAN_POINT('Origin',(213.235140564004,0.,130.804360617566));
#34780=CARTESIAN_POINT('',(142.084824010153,-4.76405452823403,129.582490119308));
#34781=CARTESIAN_POINT('',(142.430282519794,-4.76405452823406,129.582490119308));
#34782=CARTESIAN_POINT('',(213.235140564004,-4.76405452823405,129.582490119308));
#34783=CARTESIAN_POINT('',(143.764859436021,-4.91824970830014,130.806054520038));
#34784=CARTESIAN_POINT('Ctrl Pts',(143.764859435991,-4.91824970829996,130.806054520568));
#34785=CARTESIAN_POINT('Ctrl Pts',(143.759591133558,-4.9182178511643,130.898551757986));
#34786=CARTESIAN_POINT('Ctrl Pts',(143.754322831125,-4.91557679471082,130.991000951387));
#34787=CARTESIAN_POINT('Ctrl Pts',(143.749054528692,-4.91033352930923,131.083300922007));
#34788=CARTESIAN_POINT('Ctrl Pts',(143.741280194573,-4.90259614186322,131.219506240495));
#34789=CARTESIAN_POINT('Ctrl Pts',(143.733505860454,-4.88917500590729,131.355605119116));
#34790=CARTESIAN_POINT('Ctrl Pts',(143.725731526335,-4.87007115802673,131.491084709364));
#34791=CARTESIAN_POINT('Ctrl Pts',(143.717966773388,-4.85099085393131,131.626397333126));
#34792=CARTESIAN_POINT('Ctrl Pts',(143.710202020441,-4.82624182672417,131.761091803671));
#34793=CARTESIAN_POINT('Ctrl Pts',(143.702437267494,-4.79587707724921,131.89465696371));
#34794=CARTESIAN_POINT('Ctrl Pts',(143.694680226609,-4.76554248647153,132.02808946495));
#34795=CARTESIAN_POINT('Ctrl Pts',(143.686923185724,-4.72960335924045,132.160394509042));
#34796=CARTESIAN_POINT('Ctrl Pts',(143.679166144839,-4.68816423824603,132.2910680998));
#34797=CARTESIAN_POINT('Ctrl Pts',(143.671414953599,-4.64675636681517,132.421643148587));
#34798=CARTESIAN_POINT('Ctrl Pts',(143.663663762358,-4.59985687484779,132.550588821693));
#34799=CARTESIAN_POINT('Ctrl Pts',(143.655912571118,-4.54762083920157,132.677413677508));
#34800=CARTESIAN_POINT('Ctrl Pts',(143.648164674341,-4.49540700526386,132.804184629377));
#34801=CARTESIAN_POINT('Ctrl Pts',(143.640416777564,-4.43786128745369,132.928836196033));
#34802=CARTESIAN_POINT('Ctrl Pts',(143.632668880787,-4.37518777302663,133.050894617589));
#34803=CARTESIAN_POINT('Ctrl Pts',(143.624922604703,-4.3125273685477,133.172927507154));
#34804=CARTESIAN_POINT('Ctrl Pts',(143.617176328619,-4.24474147943085,133.292367982967));
#34805=CARTESIAN_POINT('Ctrl Pts',(143.609430052535,-4.1720810786493,133.408765066893));
#34806=CARTESIAN_POINT('Ctrl Pts',(143.601683719269,-4.09942014150519,133.525163010037));
#34807=CARTESIAN_POINT('Ctrl Pts',(143.593937386004,-4.0218848279271,133.638517184816));
#34808=CARTESIAN_POINT('Ctrl Pts',(143.586191052739,-3.93977032961307,133.748404233479));
#34809=CARTESIAN_POINT('Ctrl Pts',(143.578442984736,-3.85763744232646,133.858315890585));
#34810=CARTESIAN_POINT('Ctrl Pts',(143.570694916733,-3.77092356370936,133.964758563429));
#34811=CARTESIAN_POINT('Ctrl Pts',(143.56294684873,-3.67996492657399,134.06734103456));
#34812=CARTESIAN_POINT('Ctrl Pts',(143.555190545988,-3.58890961751671,134.170032531562));
#34813=CARTESIAN_POINT('Ctrl Pts',(143.547434243246,-3.4936007977708,134.268855338332));
#34814=CARTESIAN_POINT('Ctrl Pts',(143.539677940504,-3.39441279970635,134.363453873957));
#34815=CARTESIAN_POINT('Ctrl Pts',(143.53191749799,-3.29517186202071,134.458102899669));
#34816=CARTESIAN_POINT('Ctrl Pts',(143.524157055476,-3.19204791432472,134.548522904085));
#34817=CARTESIAN_POINT('Ctrl Pts',(143.516396612962,-3.08544852910806,134.6343985334));
#34818=CARTESIAN_POINT('Ctrl Pts',(143.508623712696,-2.97867802109489,134.720412017898));
#34819=CARTESIAN_POINT('Ctrl Pts',(143.500850812431,-2.86842124141996,134.801866317045));
#34820=CARTESIAN_POINT('Ctrl Pts',(143.493077912165,-2.75511563733355,134.878488854063));
#34821=CARTESIAN_POINT('Ctrl Pts',(143.485587576403,-2.64592897735447,134.95232596886));
#34822=CARTESIAN_POINT('Ctrl Pts',(143.478097240641,-2.53391157132072,135.021676353868));
#34823=CARTESIAN_POINT('Ctrl Pts',(143.470606904879,-2.41947483603103,135.086337331691));
#34824=CARTESIAN_POINT('Ctrl Pts',(143.46283257076,-2.30069919714137,135.153449950141));
#34825=CARTESIAN_POINT('Ctrl Pts',(143.455058236641,-2.17894090422282,135.21572313665));
#34826=CARTESIAN_POINT('Ctrl Pts',(143.447283902522,-2.05463199154863,135.272880556182));
#34827=CARTESIAN_POINT('Ctrl Pts',(143.439519149575,-1.93047627849945,135.329967534302));
#34828=CARTESIAN_POINT('Ctrl Pts',(143.431754396628,-1.80377655195029,135.381951128208));
#34829=CARTESIAN_POINT('Ctrl Pts',(143.42398964368,-1.67499151125555,135.428599636012));
#34830=CARTESIAN_POINT('Ctrl Pts',(143.416232602796,-1.54633438167882,135.475201811861));
#34831=CARTESIAN_POINT('Ctrl Pts',(143.40847556191,-1.41559642487995,135.516479314335));
#34832=CARTESIAN_POINT('Ctrl Pts',(143.400718521025,-1.28325817500237,135.55224767591));
#34833=CARTESIAN_POINT('Ctrl Pts',(143.392967329785,-1.15101972242861,135.587989064285));
#34834=CARTESIAN_POINT('Ctrl Pts',(143.385216138545,-1.01718375472078,135.618229479418));
#34835=CARTESIAN_POINT('Ctrl Pts',(143.377464947305,-0.882247558453494,
135.642833755665));
#34836=CARTESIAN_POINT('Ctrl Pts',(143.369717050528,-0.747368713669025,
135.667427574438));
#34837=CARTESIAN_POINT('Ctrl Pts',(143.361969153751,-0.611390954216804,
135.686389948826));
#34838=CARTESIAN_POINT('Ctrl Pts',(143.354221256974,-0.474823181854244,
135.699636504426));
#34839=CARTESIAN_POINT('Ctrl Pts',(143.34647498089,-0.338283976525602,135.712880289132));
#34840=CARTESIAN_POINT('Ctrl Pts',(143.338728704806,-0.20115539266414,135.720410595494));
#34841=CARTESIAN_POINT('Ctrl Pts',(143.330982428722,-0.0639525079682787,
135.722194809487));
#34842=CARTESIAN_POINT('Ctrl Pts',(143.323236095456,0.0732513895281564,
135.72397903665));
#34843=CARTESIAN_POINT('Ctrl Pts',(143.315489762191,0.210529198021276,135.72001708172));
#34844=CARTESIAN_POINT('Ctrl Pts',(143.307743428925,0.347365176321654,135.710328462628));
#34845=CARTESIAN_POINT('Ctrl Pts',(143.299995360922,0.484231798090526,135.700637673836));
#34846=CARTESIAN_POINT('Ctrl Pts',(143.292247292919,0.620656002863723,135.68521769657));
#34847=CARTESIAN_POINT('Ctrl Pts',(143.284499224916,0.756126906272655,135.664139950428));
#34848=CARTESIAN_POINT('Ctrl Pts',(143.276742922175,0.891741789769901,135.643039802606));
#34849=CARTESIAN_POINT('Ctrl Pts',(143.268986619433,1.02640096103342,135.616269934209));
#34850=CARTESIAN_POINT('Ctrl Pts',(143.261230316691,1.15960292397994,135.58395308149));
#34851=CARTESIAN_POINT('Ctrl Pts',(143.253469874177,1.29287598082477,135.551618980294));
#34852=CARTESIAN_POINT('Ctrl Pts',(143.245709431663,1.42468990403993,135.513732103493));
#34853=CARTESIAN_POINT('Ctrl Pts',(143.237948989148,1.55455907465073,135.470464896932));
#34854=CARTESIAN_POINT('Ctrl Pts',(143.230176088883,1.68463672278345,135.42712823401));
#34855=CARTESIAN_POINT('Ctrl Pts',(143.222403188618,1.81276301414729,135.378394120956));
#34856=CARTESIAN_POINT('Ctrl Pts',(143.214630288352,1.93847217125534,135.324483260124));
#34857=CARTESIAN_POINT('Ctrl Pts',(143.20713995259,2.05961148386025,135.272532194877));
#34858=CARTESIAN_POINT('Ctrl Pts',(143.199649616828,2.17850607101054,135.215774355758));
#34859=CARTESIAN_POINT('Ctrl Pts',(143.192159281066,2.2947630336431,135.154446327288));
#34860=CARTESIAN_POINT('Ctrl Pts',(143.184384946947,2.4154279143493,135.090793027978));
#34861=CARTESIAN_POINT('Ctrl Pts',(143.176610612828,2.53363344126155,135.022014506187));
#34862=CARTESIAN_POINT('Ctrl Pts',(143.168836278709,2.64891360080973,134.948324878747));
#34863=CARTESIAN_POINT('Ctrl Pts',(143.161071525762,2.76405168786412,134.874726067187));
#34864=CARTESIAN_POINT('Ctrl Pts',(143.153306772815,2.87627125468223,134.796228401195));
#34865=CARTESIAN_POINT('Ctrl Pts',(143.145542019867,2.98512942569717,134.713092556998));
#34866=CARTESIAN_POINT('Ctrl Pts',(143.137784978982,3.09387947724198,134.630039284494));
#34867=CARTESIAN_POINT('Ctrl Pts',(143.130027938098,3.1992744682146,134.542357237094));
#34868=CARTESIAN_POINT('Ctrl Pts',(143.122270897213,3.30089946042062,134.45035099258));
#34869=CARTESIAN_POINT('Ctrl Pts',(143.114519705972,3.40244781642952,134.358414130691));
#34870=CARTESIAN_POINT('Ctrl Pts',(143.106768514732,3.50023154380476,134.262159823669));
#34871=CARTESIAN_POINT('Ctrl Pts',(143.099017323492,3.59386812832307,134.161933392462));
#34872=CARTESIAN_POINT('Ctrl Pts',(143.091269426715,3.68746491479512,134.061749560162));
#34873=CARTESIAN_POINT('Ctrl Pts',(143.083521529938,3.77691779783553,133.957597246583));
#34874=CARTESIAN_POINT('Ctrl Pts',(143.075773633161,3.86188071703885,133.849858998761));
#34875=CARTESIAN_POINT('Ctrl Pts',(143.068027357077,3.9468258638311,133.742143287458));
#34876=CARTESIAN_POINT('Ctrl Pts',(143.060281080993,4.02728267297213,133.630843440699));
#34877=CARTESIAN_POINT('Ctrl Pts',(143.052534804909,4.10294529328026,133.516375179262));
#34878=CARTESIAN_POINT('Ctrl Pts',(143.044788471643,4.17860847211264,133.401906072846));
#34879=CARTESIAN_POINT('Ctrl Pts',(143.037042138378,4.24947717590922,133.284268831235));
#34880=CARTESIAN_POINT('Ctrl Pts',(143.029295805113,4.3152890549469,133.163907912018));
#34881=CARTESIAN_POINT('Ctrl Pts',(143.02154773711,4.38111567209856,133.043520038807));
#34882=CARTESIAN_POINT('Ctrl Pts',(143.013799669107,4.44188302353416,132.920407617231));
#34883=CARTESIAN_POINT('Ctrl Pts',(143.006051601104,4.49737505110536,132.795039072816));
#34884=CARTESIAN_POINT('Ctrl Pts',(142.998295298362,4.55292605626385,132.669537285219));
#34885=CARTESIAN_POINT('Ctrl Pts',(142.99053899562,4.60319037911991,132.54177494293));
#34886=CARTESIAN_POINT('Ctrl Pts',(142.982782692878,4.64800021027819,132.41224031075));
#34887=CARTESIAN_POINT('Ctrl Pts',(142.975022250364,4.69283395779258,132.282636542037));
#34888=CARTESIAN_POINT('Ctrl Pts',(142.96726180785,4.73220730056031,132.151258972923));
#34889=CARTESIAN_POINT('Ctrl Pts',(142.959501365336,4.76600283323565,132.018609379595));
#34890=CARTESIAN_POINT('Ctrl Pts',(142.95172846507,4.79985261750025,131.885746845365));
#34891=CARTESIAN_POINT('Ctrl Pts',(142.943955564805,4.82810661810689,131.751608589213));
#34892=CARTESIAN_POINT('Ctrl Pts',(142.936182664539,4.85069875408796,131.616705777944));
#34893=CARTESIAN_POINT('Ctrl Pts',(142.928692328777,4.87246960902022,131.486707023663));
#34894=CARTESIAN_POINT('Ctrl Pts',(142.921201993015,4.88898306002035,131.355998641791));
#34895=CARTESIAN_POINT('Ctrl Pts',(142.913711657253,4.90022578080569,131.22503906915));
#34896=CARTESIAN_POINT('Ctrl Pts',(142.905937323134,4.91189477276663,131.08911412451));
#34897=CARTESIAN_POINT('Ctrl Pts',(142.898162989015,4.9179224291013,130.952487995927));
#34898=CARTESIAN_POINT('Ctrl Pts',(142.890388654896,4.91823700064761,130.815668489195));
#34899=CARTESIAN_POINT('Ctrl Pts',(142.882623901949,4.91855118451261,130.679017600276));
#34900=CARTESIAN_POINT('Ctrl Pts',(142.874859149002,4.91316629192455,130.542174194608));
#34901=CARTESIAN_POINT('Ctrl Pts',(142.867094396054,4.90206225211436,130.405651777815));
#34902=CARTESIAN_POINT('Ctrl Pts',(142.859337355169,4.89096924099305,130.269264957011));
#34903=CARTESIAN_POINT('Ctrl Pts',(142.851580314284,4.87416841826721,130.133198877792));
#34904=CARTESIAN_POINT('Ctrl Pts',(142.843823273399,4.85169174962129,129.997967271142));
#34905=CARTESIAN_POINT('Ctrl Pts',(142.836072082159,4.82923203080603,129.862837643699));
#34906=CARTESIAN_POINT('Ctrl Pts',(142.828320890919,4.80110504939137,129.728541620392));
#34907=CARTESIAN_POINT('Ctrl Pts',(142.820569699679,4.7673945753897,129.595587675676));
#34908=CARTESIAN_POINT('Ctrl Pts',(142.812821802902,4.73369842923874,129.462690239934));
#34909=CARTESIAN_POINT('Ctrl Pts',(142.805073906125,4.69442360636946,129.331134126444));
#34910=CARTESIAN_POINT('Ctrl Pts',(142.797326009348,4.64970490033501,129.201417261642));
#34911=CARTESIAN_POINT('Ctrl Pts',(142.789579733264,4.60499554848984,129.071727530812));
#34912=CARTESIAN_POINT('Ctrl Pts',(142.78183345718,4.5548447058434,128.943876652803));
#34913=CARTESIAN_POINT('Ctrl Pts',(142.774087181095,4.49943681002503,128.818346656112));
#34914=CARTESIAN_POINT('Ctrl Pts',(142.76634084783,4.44402850519818,128.692815732786));
#34915=CARTESIAN_POINT('Ctrl Pts',(142.758594514565,4.38336322763782,128.569606082636));
#34916=CARTESIAN_POINT('Ctrl Pts',(142.750848181299,4.31767310566619,128.449178668097));
#34917=CARTESIAN_POINT('Ctrl Pts',(142.743100113296,4.25196827284723,128.328724284673));
#34918=CARTESIAN_POINT('Ctrl Pts',(142.735352045293,4.181236543626,128.211053719839));
#34919=CARTESIAN_POINT('Ctrl Pts',(142.72760397729,4.10575523295771,128.096601944874));
#34920=CARTESIAN_POINT('Ctrl Pts',(142.719847674549,4.03019369985416,127.9820285292));
#34921=CARTESIAN_POINT('Ctrl Pts',(142.712091371807,3.94987271714661,127.870681064046));
#34922=CARTESIAN_POINT('Ctrl Pts',(142.704335069065,3.86511237076399,127.762964651259));
#34923=CARTESIAN_POINT('Ctrl Pts',(142.696574626551,3.7803067852324,127.65519074698));
#34924=CARTESIAN_POINT('Ctrl Pts',(142.688814184036,3.69105736904373,127.551052053417));
#34925=CARTESIAN_POINT('Ctrl Pts',(142.681053741522,3.59772282025836,127.450918569298));
#34926=CARTESIAN_POINT('Ctrl Pts',(142.673280841257,3.50423844256942,127.350624342021));
#34927=CARTESIAN_POINT('Ctrl Pts',(142.665507940991,3.40665610614584,127.254348447156));
#34928=CARTESIAN_POINT('Ctrl Pts',(142.657735040726,3.30537015172036,127.162422778638));
#34929=CARTESIAN_POINT('Ctrl Pts',(142.650244704964,3.20776619686285,127.073838839717));
#34930=CARTESIAN_POINT('Ctrl Pts',(142.642754369202,3.10672345697104,126.989294532576));
#34931=CARTESIAN_POINT('Ctrl Pts',(142.63526403344,3.00262042474543,126.909048865292));
#34932=CARTESIAN_POINT('Ctrl Pts',(142.627489699321,2.89457029441094,126.825760659143));
#34933=CARTESIAN_POINT('Ctrl Pts',(142.619715365202,2.78288095846386,126.746839661379));
#34934=CARTESIAN_POINT('Ctrl Pts',(142.611941031083,2.66794086612493,126.672620718037));
#34935=CARTESIAN_POINT('Ctrl Pts',(142.604176278136,2.55314242717736,126.598493242909));
#34936=CARTESIAN_POINT('Ctrl Pts',(142.596411525189,2.43510152840496,126.529056502202));
#34937=CARTESIAN_POINT('Ctrl Pts',(142.588646772241,2.31423934789276,126.464604944355));
#34938=CARTESIAN_POINT('Ctrl Pts',(142.580889731356,2.19349720940202,126.400217400704));
#34939=CARTESIAN_POINT('Ctrl Pts',(142.573132690471,2.0699397082969,126.340805369271));
#34940=CARTESIAN_POINT('Ctrl Pts',(142.565375649586,1.94401633923829,126.286619640565));
#34941=CARTESIAN_POINT('Ctrl Pts',(142.557624458346,1.81818792997186,126.232474773739));
#34942=CARTESIAN_POINT('Ctrl Pts',(142.549873267106,1.689997561608,126.18354851884));
#34943=CARTESIAN_POINT('Ctrl Pts',(142.542122075866,1.55991830784575,126.140045240649));
#34944=CARTESIAN_POINT('Ctrl Pts',(142.534374179089,1.42989434123632,126.096560452511));
#34945=CARTESIAN_POINT('Ctrl Pts',(142.526626282312,1.29798345599256,126.058494180533));
#34946=CARTESIAN_POINT('Ctrl Pts',(142.518878385535,1.16467743093587,126.026002160484));
#34947=CARTESIAN_POINT('Ctrl Pts',(142.511132109451,1.03139929062587,125.993516937064));
#34948=CARTESIAN_POINT('Ctrl Pts',(142.503385833367,0.896726970579325,125.966603738833));
#34949=CARTESIAN_POINT('Ctrl Pts',(142.495639557283,0.761165708065515,125.945367941366));
#34950=CARTESIAN_POINT('Ctrl Pts',(142.487893224017,0.625603444869398,125.924131987141));
#34951=CARTESIAN_POINT('Ctrl Pts',(142.480146890752,0.48915261236676,125.908573577813));
#34952=CARTESIAN_POINT('Ctrl Pts',(142.472400557487,0.352326502337162,125.898746578707));
#34953=CARTESIAN_POINT('Ctrl Pts',(142.464652489484,0.215469751048862,125.888917378912));
#34954=CARTESIAN_POINT('Ctrl Pts',(142.456904421481,0.0782379448882408,
125.884822171377));
#34955=CARTESIAN_POINT('Ctrl Pts',(142.449156353478,-0.0588530669821975,
125.886462755775));
#34956=CARTESIAN_POINT('Ctrl Pts',(142.441400050736,-0.196089780811549,
125.888105083806));
#34957=CARTESIAN_POINT('Ctrl Pts',(142.433643747994,-0.333185009872422,
125.895495376637));
#34958=CARTESIAN_POINT('Ctrl Pts',(142.425887445252,-0.469624916243211,
125.908583304356));
#34959=CARTESIAN_POINT('Ctrl Pts',(142.418127002738,-0.60613764470025,125.921678217496));
#34960=CARTESIAN_POINT('Ctrl Pts',(142.410366560224,-0.741993966444115,
125.94047677141));
#34961=CARTESIAN_POINT('Ctrl Pts',(142.40260611771,-0.876688706002444,125.964877176612));
#34962=CARTESIAN_POINT('Ctrl Pts',(142.394833217444,-1.01159966951435,125.989316751511));
#34963=CARTESIAN_POINT('Ctrl Pts',(142.387060317179,-1.14534494295683,126.019376061976));
#34964=CARTESIAN_POINT('Ctrl Pts',(142.379287416913,-1.2774321437656,126.054902734757));
#34965=CARTESIAN_POINT('Ctrl Pts',(142.371797081151,-1.40471764211793,126.089137923497));
#34966=CARTESIAN_POINT('Ctrl Pts',(142.364306745389,-1.53046323115435,126.128449779128));
#34967=CARTESIAN_POINT('Ctrl Pts',(142.356816409627,-1.65424641549254,126.172659865215));
#34968=CARTESIAN_POINT('Ctrl Pts',(142.3490419539,-1.78272488654235,126.218546907916));
#34969=CARTESIAN_POINT('Ctrl Pts',(142.341267498174,-1.90949612757785,126.269856469942));
#34970=CARTESIAN_POINT('Ctrl Pts',(142.333493042447,-2.03406843387499,126.326442723185));
#34971=CARTESIAN_POINT('Ctrl Pts',(142.325728196272,-2.15848676360114,126.382959033457));
#34972=CARTESIAN_POINT('Ctrl Pts',(142.317963350097,-2.2807112140519,126.444738897361));
#34973=CARTESIAN_POINT('Ctrl Pts',(142.310198503922,-2.40026638362756,126.511587114325));
#34974=CARTESIAN_POINT('Ctrl Pts',(142.302441398069,-2.51970237562632,126.5783686942));
#34975=CARTESIAN_POINT('Ctrl Pts',(142.294684292217,-2.63647404299896,126.650208382986));
#34976=CARTESIAN_POINT('Ctrl Pts',(142.286927186364,-2.75012741506298,126.726863558901));
#34977=CARTESIAN_POINT('Ctrl Pts',(142.279175958326,-2.86369466822685,126.803460650668));
#34978=CARTESIAN_POINT('Ctrl Pts',(142.271424730288,-2.97414800643865,126.884865748838));
#34979=CARTESIAN_POINT('Ctrl Pts',(142.263673502249,-3.08105977891318,126.970791301476));
#34980=CARTESIAN_POINT('Ctrl Pts',(142.255925713781,-3.1879241098019,127.056678725064));
#34981=CARTESIAN_POINT('Ctrl Pts',(142.248177925313,-3.2912496973339,127.147082368081));
#34982=CARTESIAN_POINT('Ctrl Pts',(142.240430136845,-3.39063971587617,127.241672674506));
#34983=CARTESIAN_POINT('Ctrl Pts',(142.232684009192,-3.49000842918814,127.336242704567));
#34984=CARTESIAN_POINT('Ctrl Pts',(142.224937881539,-3.58544296877462,127.434997343353));
#34985=CARTESIAN_POINT('Ctrl Pts',(142.217191753886,-3.67658160752567,127.537568499034));
#34986=CARTESIAN_POINT('Ctrl Pts',(142.2094456092,-3.767720446674,127.64013988025));
#34987=CARTESIAN_POINT('Ctrl Pts',(142.201699464515,-3.8545631066173,127.746527502757));
#34988=CARTESIAN_POINT('Ctrl Pts',(142.193953319829,-3.93678684557427,127.856328664718));
#34989=CARTESIAN_POINT('Ctrl Pts',(142.186205480617,-4.01902857158532,127.966153846499));
#34990=CARTESIAN_POINT('Ctrl Pts',(142.178457641405,-4.09664913200355,128.079393740599));
#34991=CARTESIAN_POINT('Ctrl Pts',(142.170709802193,-4.16936820707962,128.195615360494));
#34992=CARTESIAN_POINT('Ctrl Pts',(142.162954283335,-4.24215936118452,128.31195217907));
#34993=CARTESIAN_POINT('Ctrl Pts',(142.155198764477,-4.31003911935539,128.431276294259));
#34994=CARTESIAN_POINT('Ctrl Pts',(142.147443245619,-4.3727721504203,128.553128336568));
#34995=CARTESIAN_POINT('Ctrl Pts',(142.13968360357,-4.43553853325875,128.675045161044));
#34996=CARTESIAN_POINT('Ctrl Pts',(142.13192396152,-4.49315257281768,128.79949223612));
#34997=CARTESIAN_POINT('Ctrl Pts',(142.124164319471,-4.54542689597396,128.925989675538));
#34998=CARTESIAN_POINT('Ctrl Pts',(142.116393520392,-4.59777638061022,129.052668996502));
#34999=CARTESIAN_POINT('Ctrl Pts',(142.108622721312,-4.64477067816591,129.181404203919));
#35000=CARTESIAN_POINT('Ctrl Pts',(142.100851922233,-4.68627193195673,129.311699087863));
#35001=CARTESIAN_POINT('Ctrl Pts',(142.095509284873,-4.71480518146293,129.401280391881));
#35002=CARTESIAN_POINT('Ctrl Pts',(142.090166647513,-4.74074295468664,129.491598647849));
#35003=CARTESIAN_POINT('Ctrl Pts',(142.084824010153,-4.76405452823403,129.582490119308));
#35004=CARTESIAN_POINT('Ctrl Pts',(143.834995515417,-4.76405452823405,129.582490119308));
#35005=CARTESIAN_POINT('Ctrl Pts',(143.827302392399,-4.7978580186573,129.714289415429));
#35006=CARTESIAN_POINT('Ctrl Pts',(143.819609269382,-4.82616221601706,129.84739236389));
#35007=CARTESIAN_POINT('Ctrl Pts',(143.811916146364,-4.84889145772445,129.981296407612));
#35008=CARTESIAN_POINT('Ctrl Pts',(143.804073361307,-4.87206287417234,130.117805421027));
#35009=CARTESIAN_POINT('Ctrl Pts',(143.79623057625,-4.88944012954329,130.255146585595));
#35010=CARTESIAN_POINT('Ctrl Pts',(143.788387791193,-4.90099868268711,130.3927844098));
#35011=CARTESIAN_POINT('Ctrl Pts',(143.780545006136,-4.91255723583092,130.530422234005));
#35012=CARTESIAN_POINT('Ctrl Pts',(143.772702221078,-4.91829713317609,130.668356284091));
#35013=CARTESIAN_POINT('Ctrl Pts',(143.764859436021,-4.91824970830014,130.806054520038));
#35014=CARTESIAN_POINT('',(144.110140563953,-4.91824891722445,130.807624161739));
#35015=CARTESIAN_POINT('Ctrl Pts',(144.179984458271,-4.76405452823405,129.582490119308));
#35016=CARTESIAN_POINT('Ctrl Pts',(144.172192290088,-4.7983435952176,129.716182671068));
#35017=CARTESIAN_POINT('Ctrl Pts',(144.164400121904,-4.82701755785097,129.851385085608));
#35018=CARTESIAN_POINT('Ctrl Pts',(144.15660795372,-4.84995547360527,129.987589556285));
#35019=CARTESIAN_POINT('Ctrl Pts',(144.148816480302,-4.872891344169,130.123781882698));
#35020=CARTESIAN_POINT('Ctrl Pts',(144.141025006883,-4.89009211292143,130.26097571021));
#35021=CARTESIAN_POINT('Ctrl Pts',(144.133233533465,-4.90148799701282,130.39865323824));
#35022=CARTESIAN_POINT('Ctrl Pts',(144.125535876979,-4.91274666355443,130.534672994666));
#35023=CARTESIAN_POINT('Ctrl Pts',(144.117838220494,-4.91833946612017,130.671164497436));
#35024=CARTESIAN_POINT('Ctrl Pts',(144.110140564008,-4.9182489172251,130.807624160758));
#35025=CARTESIAN_POINT('Ctrl Pts',(144.110140563953,-4.91824891722444,130.807624161739));
#35026=CARTESIAN_POINT('Ctrl Pts',(144.101366046741,-4.91814570099509,130.963173797746));
#35027=CARTESIAN_POINT('Ctrl Pts',(144.09259152953,-4.91065911423936,131.118438323462));
#35028=CARTESIAN_POINT('Ctrl Pts',(144.083817012319,-4.89589425273592,131.272764853806));
#35029=CARTESIAN_POINT('Ctrl Pts',(144.075005960534,-4.88106791458293,131.427733955569));
#35030=CARTESIAN_POINT('Ctrl Pts',(144.06619490875,-4.85890267712743,131.581757060317));
#35031=CARTESIAN_POINT('Ctrl Pts',(144.057383856965,-4.8295547027173,131.734190944003));
#35032=CARTESIAN_POINT('Ctrl Pts',(144.048522408935,-4.80003886778996,131.887496698101));
#35033=CARTESIAN_POINT('Ctrl Pts',(144.039660960905,-4.76325799042229,132.039194826826));
#35034=CARTESIAN_POINT('Ctrl Pts',(144.030799512875,-4.71941960498347,132.188651647154));
#35035=CARTESIAN_POINT('Ctrl Pts',(144.023170727366,-4.68167931259706,132.317318431796));
#35036=CARTESIAN_POINT('Ctrl Pts',(144.015541941856,-4.63870923365158,132.444324367405));
#35037=CARTESIAN_POINT('Ctrl Pts',(144.007913156346,-4.59066958425604,132.569278698012));
#35038=CARTESIAN_POINT('Ctrl Pts',(144.000138822227,-4.54171339262111,132.696617016085));
#35039=CARTESIAN_POINT('Ctrl Pts',(143.992364488108,-4.48737738046281,132.822118527769));
#35040=CARTESIAN_POINT('Ctrl Pts',(143.984590153989,-4.42781912566329,132.945295192211));
#35041=CARTESIAN_POINT('Ctrl Pts',(143.976825401042,-4.36833427108993,133.068320052422));
#35042=CARTESIAN_POINT('Ctrl Pts',(143.969060648094,-4.30364014804724,133.189025417617));
#35043=CARTESIAN_POINT('Ctrl Pts',(143.961295895147,-4.23394330072747,133.306940723921));
#35044=CARTESIAN_POINT('Ctrl Pts',(143.953538854262,-4.16431567729903,133.424738915081));
#35045=CARTESIAN_POINT('Ctrl Pts',(143.945781813377,-4.08969541533217,133.539752227625));
#35046=CARTESIAN_POINT('Ctrl Pts',(143.938024772492,-4.01033595294006,133.651532654352));
#35047=CARTESIAN_POINT('Ctrl Pts',(143.930273581252,-3.93103633613595,133.76322878659));
#35048=CARTESIAN_POINT('Ctrl Pts',(143.922522390012,-3.84700485788766,133.871696568087));
#35049=CARTESIAN_POINT('Ctrl Pts',(143.914771198772,-3.75853924385391,133.976515376545));
#35050=CARTESIAN_POINT('Ctrl Pts',(143.907023301995,-3.67011123006587,134.081289634212));
#35051=CARTESIAN_POINT('Ctrl Pts',(143.899275405218,-3.57725308050513,134.182417705331));
#35052=CARTESIAN_POINT('Ctrl Pts',(143.891527508441,-3.4803037918747,134.27951076954));
#35053=CARTESIAN_POINT('Ctrl Pts',(143.883781232357,-3.38337478294551,134.376583523972));
#35054=CARTESIAN_POINT('Ctrl Pts',(143.876034956273,-3.2823566132104,134.469622673846));
#35055=CARTESIAN_POINT('Ctrl Pts',(143.868288680188,-3.17762596998102,134.558275408475));
#35056=CARTESIAN_POINT('Ctrl Pts',(143.860542346923,-3.07289455365394,134.646928797518));
#35057=CARTESIAN_POINT('Ctrl Pts',(143.852796013658,-2.96445090755763,134.731195454108));
#35058=CARTESIAN_POINT('Ctrl Pts',(143.845049680392,-2.85270539257755,134.810762370468));
#35059=CARTESIAN_POINT('Ctrl Pts',(143.837301612389,-2.74093485296409,134.890347105288));
#35060=CARTESIAN_POINT('Ctrl Pts',(143.829553544386,-2.62586129150441,134.965229778851));
#35061=CARTESIAN_POINT('Ctrl Pts',(143.821805476384,-2.50792433670316,135.035140520122));
#35062=CARTESIAN_POINT('Ctrl Pts',(143.814049173642,-2.38986203710288,135.105125563361));
#35063=CARTESIAN_POINT('Ctrl Pts',(143.8062928709,-2.26893060179689,135.170127918812));
#35064=CARTESIAN_POINT('Ctrl Pts',(143.798536568158,-2.1455950583029,135.229923283294));
#35065=CARTESIAN_POINT('Ctrl Pts',(143.790776125644,-2.0221936869157,135.289750562362));
#35066=CARTESIAN_POINT('Ctrl Pts',(143.78301568313,-1.89638600902053,135.344365157204));
#35067=CARTESIAN_POINT('Ctrl Pts',(143.775255240615,-1.76865642210888,135.393591220078));
#35068=CARTESIAN_POINT('Ctrl Pts',(143.76748234035,-1.64072179232507,135.442896304999));
#35069=CARTESIAN_POINT('Ctrl Pts',(143.759709440085,-1.51085945886281,135.486795446921));
#35070=CARTESIAN_POINT('Ctrl Pts',(143.751936539819,-1.37956920596051,135.525162654134));
#35071=CARTESIAN_POINT('Ctrl Pts',(143.744446204057,-1.25305168445153,135.562135116723));
#35072=CARTESIAN_POINT('Ctrl Pts',(143.736955868295,-1.12520855691546,135.59397078692));
#35073=CARTESIAN_POINT('Ctrl Pts',(143.729465532533,-0.996493477471868,
135.620602286321));
#35074=CARTESIAN_POINT('Ctrl Pts',(143.721691198414,-0.862898126668925,
135.648243527117));
#35075=CARTESIAN_POINT('Ctrl Pts',(143.713916864295,-0.727940208698602,
135.670365733823));
#35076=CARTESIAN_POINT('Ctrl Pts',(143.706142530176,-0.592115500849083,
135.686837683171));
#35077=CARTESIAN_POINT('Ctrl Pts',(143.698377777229,-0.456458184813031,
135.703289332313));
#35078=CARTESIAN_POINT('Ctrl Pts',(143.690613024282,-0.31993658877468,135.714104532645));
#35079=CARTESIAN_POINT('Ctrl Pts',(143.682848271334,-0.183058253629607,
135.719202704376));
#35080=CARTESIAN_POINT('Ctrl Pts',(143.675091230449,-0.0463158679766459,
135.724295812531));
#35081=CARTESIAN_POINT('Ctrl Pts',(143.667334189564,0.0907821635074765,
135.723683177569));
#35082=CARTESIAN_POINT('Ctrl Pts',(143.659577148679,0.227721930184656,135.717335865317));
#35083=CARTESIAN_POINT('Ctrl Pts',(143.651825957439,0.364558429518408,135.710993339622));
#35084=CARTESIAN_POINT('Ctrl Pts',(143.644074766199,0.501236512635953,135.698924762449));
#35085=CARTESIAN_POINT('Ctrl Pts',(143.636323574959,0.637241370091793,135.681153262199));
#35086=CARTESIAN_POINT('Ctrl Pts',(143.628575678182,0.773188421855305,135.66338931531));
#35087=CARTESIAN_POINT('Ctrl Pts',(143.620827781405,0.908462430207474,135.639927316836));
#35088=CARTESIAN_POINT('Ctrl Pts',(143.613079884628,1.04255303356731,135.610842307399));
#35089=CARTESIAN_POINT('Ctrl Pts',(143.605333608544,1.17661558806359,135.581763381919));
#35090=CARTESIAN_POINT('Ctrl Pts',(143.59758733246,1.30949484810539,135.547063867852));
#35091=CARTESIAN_POINT('Ctrl Pts',(143.589841056375,1.44069037537835,135.506869980108));
#35092=CARTESIAN_POINT('Ctrl Pts',(143.58209472311,1.57188687110684,135.466675795661));
#35093=CARTESIAN_POINT('Ctrl Pts',(143.574348389845,1.70139923545008,135.420987271131));
#35094=CARTESIAN_POINT('Ctrl Pts',(143.566602056579,1.82874231601914,135.369980466404));
#35095=CARTESIAN_POINT('Ctrl Pts',(143.558853988576,1.95611391418808,135.318962239056));
#35096=CARTESIAN_POINT('Ctrl Pts',(143.551105920573,2.08131489904073,135.262623506919));
#35097=CARTESIAN_POINT('Ctrl Pts',(143.543357852571,2.20388059048747,135.201188270019));
#35098=CARTESIAN_POINT('Ctrl Pts',(143.535601549829,2.32657654620975,135.139687739017));
#35099=CARTESIAN_POINT('Ctrl Pts',(143.527845247087,2.44663126351085,135.07308005843));
#35100=CARTESIAN_POINT('Ctrl Pts',(143.520088944345,2.56360467103868,135.00163522773));
#35101=CARTESIAN_POINT('Ctrl Pts',(143.512328501831,2.68064051079619,134.930152264773));
#35102=CARTESIAN_POINT('Ctrl Pts',(143.504568059317,2.79459143912766,134.853827224848));
#35103=CARTESIAN_POINT('Ctrl Pts',(143.496807616802,2.90504768167286,134.772972595287));
#35104=CARTESIAN_POINT('Ctrl Pts',(143.489034716537,3.0156812383844,134.691988170696));
#35105=CARTESIAN_POINT('Ctrl Pts',(143.481261816272,3.12280859307257,134.606459870167));
#35106=CARTESIAN_POINT('Ctrl Pts',(143.473488916006,3.22605359975275,134.516740074737));
#35107=CARTESIAN_POINT('Ctrl Pts',(143.465998580244,3.32554539038173,134.430281819861));
#35108=CARTESIAN_POINT('Ctrl Pts',(143.458508244482,3.4214319745268,134.33993173333));
#35109=CARTESIAN_POINT('Ctrl Pts',(143.45101790872,3.51341145369641,134.24603506753));
#35110=CARTESIAN_POINT('Ctrl Pts',(143.443243574601,3.60887836277513,134.148578281107));
#35111=CARTESIAN_POINT('Ctrl Pts',(143.435469240482,3.70043845300352,134.046991955602));
#35112=CARTESIAN_POINT('Ctrl Pts',(143.427694906363,3.78771334279514,133.941622273104));
#35113=CARTESIAN_POINT('Ctrl Pts',(143.419930153416,3.87488067408505,133.836382449324));
#35114=CARTESIAN_POINT('Ctrl Pts',(143.412165400469,3.95777306581054,133.72736884404));
#35115=CARTESIAN_POINT('Ctrl Pts',(143.404400647521,4.03604838566099,133.614964910437));
#35116=CARTESIAN_POINT('Ctrl Pts',(143.396643606636,4.11424596136026,133.502672618005));
#35117=CARTESIAN_POINT('Ctrl Pts',(143.388886565751,4.18783536903886,133.386997017139));
#35118=CARTESIAN_POINT('Ctrl Pts',(143.381129524866,4.25651448430425,133.268354835783));
#35119=CARTESIAN_POINT('Ctrl Pts',(143.373378333626,4.32514180811459,133.14980212342));
#35120=CARTESIAN_POINT('Ctrl Pts',(143.365627142386,4.38886601481198,133.028287620415));
#35121=CARTESIAN_POINT('Ctrl Pts',(143.357875951146,4.44742829589468,132.904256952001));
#35122=CARTESIAN_POINT('Ctrl Pts',(143.350128054369,4.50596568644573,132.78027899993));
#35123=CARTESIAN_POINT('Ctrl Pts',(143.342380157592,4.55934534841643,132.653787362278));
#35124=CARTESIAN_POINT('Ctrl Pts',(143.334632260815,4.60735455270819,132.525251981987));
#35125=CARTESIAN_POINT('Ctrl Pts',(143.326885984731,4.6553537145094,132.396743488527));
#35126=CARTESIAN_POINT('Ctrl Pts',(143.319139708647,4.69798451639225,132.266192468781));
#35127=CARTESIAN_POINT('Ctrl Pts',(143.311393432563,4.73508264740282,132.13408817792));
#35128=CARTESIAN_POINT('Ctrl Pts',(143.303647099297,4.77218105226334,132.001982911895));
#35129=CARTESIAN_POINT('Ctrl Pts',(143.295900766032,4.80374659905278,131.868324728279));
#35130=CARTESIAN_POINT('Ctrl Pts',(143.288154432767,4.82966517522317,131.733616964188));
#35131=CARTESIAN_POINT('Ctrl Pts',(143.280406364764,4.85558955567897,131.598879033226));
#35132=CARTESIAN_POINT('Ctrl Pts',(143.272658296761,4.87586437525329,131.463091437923));
#35133=CARTESIAN_POINT('Ctrl Pts',(143.264910228758,4.890426920573,131.326766204285));
#35134=CARTESIAN_POINT('Ctrl Pts',(143.257153926016,4.90500494313918,131.190296082565));
#35135=CARTESIAN_POINT('Ctrl Pts',(143.249397623274,4.9138585222347,131.053287570433));
#35136=CARTESIAN_POINT('Ctrl Pts',(143.241641320532,4.91697694674696,130.916256853691));
#35137=CARTESIAN_POINT('Ctrl Pts',(143.233880878018,4.92009703565629,130.779152999529));
#35138=CARTESIAN_POINT('Ctrl Pts',(143.226120435504,4.91747587809979,130.642027307844));
#35139=CARTESIAN_POINT('Ctrl Pts',(143.21835999299,4.90915488546698,130.505393440445));
#35140=CARTESIAN_POINT('Ctrl Pts',(143.210587092724,4.90082053523809,130.368540236233));
#35141=CARTESIAN_POINT('Ctrl Pts',(143.202814192459,4.88676810565601,130.232180823148));
#35142=CARTESIAN_POINT('Ctrl Pts',(143.195041292193,4.86709074877401,130.09682213402));
#35143=CARTESIAN_POINT('Ctrl Pts',(143.187550956431,4.84812871337881,129.966384074189));
#35144=CARTESIAN_POINT('Ctrl Pts',(143.180060620669,4.82394366762322,129.836875546604));
#35145=CARTESIAN_POINT('Ctrl Pts',(143.172570284907,4.79466289860887,129.708737164365));
#35146=CARTESIAN_POINT('Ctrl Pts',(143.164795950788,4.76427194033785,129.575740376418));
#35147=CARTESIAN_POINT('Ctrl Pts',(143.157021616669,4.72829495286353,129.443798389073));
#35148=CARTESIAN_POINT('Ctrl Pts',(143.14924728255,4.68681866449419,129.31341666535));
#35149=CARTESIAN_POINT('Ctrl Pts',(143.141482529603,4.64539349194345,129.18319562545));
#35150=CARTESIAN_POINT('Ctrl Pts',(143.133717776656,4.59848262087887,129.054531392195));
#35151=CARTESIAN_POINT('Ctrl Pts',(143.125953023708,4.54622373045415,128.927919077002));
#35152=CARTESIAN_POINT('Ctrl Pts',(143.118195982823,4.49401674429614,128.801432514945));
#35153=CARTESIAN_POINT('Ctrl Pts',(143.110438941938,4.43647245755512,128.676994174302));
#35154=CARTESIAN_POINT('Ctrl Pts',(143.102681901054,4.37377816964122,128.555083492517));
#35155=CARTESIAN_POINT('Ctrl Pts',(143.094930709813,4.31113115997752,128.433264744525));
#35156=CARTESIAN_POINT('Ctrl Pts',(143.087179518573,4.24334205740033,128.313970207636));
#35157=CARTESIAN_POINT('Ctrl Pts',(143.079428327333,4.17064588672128,128.197658496096));
#35158=CARTESIAN_POINT('Ctrl Pts',(143.071680430556,4.09798061385399,128.081396220136));
#35159=CARTESIAN_POINT('Ctrl Pts',(143.063932533779,4.02041262783363,127.968114578849));
#35160=CARTESIAN_POINT('Ctrl Pts',(143.056184637002,3.93822231969323,127.858246562888));
#35161=CARTESIAN_POINT('Ctrl Pts',(143.048438360918,3.85604920399347,127.748401528948));
#35162=CARTESIAN_POINT('Ctrl Pts',(143.040692084834,3.76925592341749,127.641969012899));
#35163=CARTESIAN_POINT('Ctrl Pts',(143.03294580875,3.67816528811141,127.539351708569));
#35164=CARTESIAN_POINT('Ctrl Pts',(143.025199475484,3.58707398039498,127.436733646741));
#35165=CARTESIAN_POINT('Ctrl Pts',(143.017453142219,3.49168551419383,127.337931145218));
#35166=CARTESIAN_POINT('Ctrl Pts',(143.009706808953,3.39236168065779,127.243312276122));
#35167=CARTESIAN_POINT('Ctrl Pts',(143.00195874095,3.29301560423786,127.148672217786));
#35168=CARTESIAN_POINT('Ctrl Pts',(142.994210672948,3.18973268982494,127.058217925808));
#35169=CARTESIAN_POINT('Ctrl Pts',(142.986462604945,3.08290982128859,126.972278925287));
#35170=CARTESIAN_POINT('Ctrl Pts',(142.978706302203,2.97597342013635,126.886248587773));
#35171=CARTESIAN_POINT('Ctrl Pts',(142.970949999461,2.86548985435889,126.804743373508));
#35172=CARTESIAN_POINT('Ctrl Pts',(142.963193696719,2.75188761607232,126.728051305086));
#35173=CARTESIAN_POINT('Ctrl Pts',(142.955433254205,2.63822474485057,126.651318303799));
#35174=CARTESIAN_POINT('Ctrl Pts',(142.947672811691,2.52144021714982,126.579403772049));
#35175=CARTESIAN_POINT('Ctrl Pts',(142.939912369176,2.40198857506541,126.512550516017));
#35176=CARTESIAN_POINT('Ctrl Pts',(142.932139468911,2.28234517860079,126.445589941204));
#35177=CARTESIAN_POINT('Ctrl Pts',(142.924366568646,2.16002646103501,126.383707054661));
#35178=CARTESIAN_POINT('Ctrl Pts',(142.91659366838,2.03550927027305,126.327097494504));
#35179=CARTESIAN_POINT('Ctrl Pts',(142.909103332618,1.91551859303516,126.272545834449));
#35180=CARTESIAN_POINT('Ctrl Pts',(142.901612996856,1.79348679292343,126.222890875819));
#35181=CARTESIAN_POINT('Ctrl Pts',(142.894122661094,1.6698533720046,126.178263690511));
#35182=CARTESIAN_POINT('Ctrl Pts',(142.886348326975,1.54153235235402,126.131944451909));
#35183=CARTESIAN_POINT('Ctrl Pts',(142.878573992856,1.41107938109231,126.09089504337));
#35184=CARTESIAN_POINT('Ctrl Pts',(142.870799658737,1.27896659734406,126.055315713022));
#35185=CARTESIAN_POINT('Ctrl Pts',(142.86303490579,1.14701663079471,126.019780231019));
#35186=CARTESIAN_POINT('Ctrl Pts',(142.855270152843,1.01341129572504,125.989701514557));
#35187=CARTESIAN_POINT('Ctrl Pts',(142.847505399896,0.878641562336831,125.965231350081));
#35188=CARTESIAN_POINT('Ctrl Pts',(142.839748359011,0.744005684147697,125.940785489716));
#35189=CARTESIAN_POINT('Ctrl Pts',(142.831991318126,0.608208091307349,125.921937165197));
#35190=CARTESIAN_POINT('Ctrl Pts',(142.824234277241,0.471753388020811,125.908787943875));
#35191=CARTESIAN_POINT('Ctrl Pts',(142.816483086,0.335401586287345,125.895648638482));
#35192=CARTESIAN_POINT('Ctrl Pts',(142.80873189476,0.198394048022155,125.888199919248));
#35193=CARTESIAN_POINT('Ctrl Pts',(142.80098070352,0.0612436550299411,125.886491945344));
#35194=CARTESIAN_POINT('Ctrl Pts',(142.793232806743,-0.0758484453865517,
125.884784697375));
#35195=CARTESIAN_POINT('Ctrl Pts',(142.785484909966,-0.213082889652012,
125.888813346679));
#35196=CARTESIAN_POINT('Ctrl Pts',(142.777737013189,-0.349943832263288,
125.898576034366));
#35197=CARTESIAN_POINT('Ctrl Pts',(142.769990737105,-0.48677614651575,125.908336679909));
#35198=CARTESIAN_POINT('Ctrl Pts',(142.762244461021,-0.62323472478866,125.923828950288));
#35199=CARTESIAN_POINT('Ctrl Pts',(142.754498184937,-0.758806282589974,
125.944998922034));
#35200=CARTESIAN_POINT('Ctrl Pts',(142.746751851671,-0.89437884114973,125.966169050053));
#35201=CARTESIAN_POINT('Ctrl Pts',(142.739005518406,-1.02906397988825,125.993016902751));
#35202=CARTESIAN_POINT('Ctrl Pts',(142.731259185141,-1.1623564723501,126.025437046961));
#35203=CARTESIAN_POINT('Ctrl Pts',(142.723511117138,-1.29567881474137,126.057864451438));
#35204=CARTESIAN_POINT('Ctrl Pts',(142.715763049135,-1.4276075104468,126.095866538174));
#35205=CARTESIAN_POINT('Ctrl Pts',(142.708014981132,-1.55765079524142,126.139287513896));
#35206=CARTESIAN_POINT('Ctrl Pts',(142.70025867839,-1.68783229158674,126.182754637948));
#35207=CARTESIAN_POINT('Ctrl Pts',(142.692502375648,-1.81612400270989,126.231652031708));
#35208=CARTESIAN_POINT('Ctrl Pts',(142.684746072906,-1.94205199658775,126.285774875871));
#35209=CARTESIAN_POINT('Ctrl Pts',(142.676985630392,-2.06804720202769,126.339926607026));
#35210=CARTESIAN_POINT('Ctrl Pts',(142.669225187878,-2.191675824157,126.399309176669));
#35211=CARTESIAN_POINT('Ctrl Pts',(142.661464745364,-2.31248789215451,126.463671408335));
#35212=CARTESIAN_POINT('Ctrl Pts',(142.653691845098,-2.43349389840871,126.528136959968));
#35213=CARTESIAN_POINT('Ctrl Pts',(142.645918944833,-2.55167397811675,126.597597949552));
#35214=CARTESIAN_POINT('Ctrl Pts',(142.638146044567,-2.66660578745136,126.67175893862));
#35215=CARTESIAN_POINT('Ctrl Pts',(142.630655708805,-2.7773595360207,126.743223988934));
#35216=CARTESIAN_POINT('Ctrl Pts',(142.623165373043,-2.88509682777075,126.819053080459));
#35217=CARTESIAN_POINT('Ctrl Pts',(142.615675037281,-2.98946982659814,126.89894729522));
#35218=CARTESIAN_POINT('Ctrl Pts',(142.607950349053,-3.09710837592991,126.981341185148));
#35219=CARTESIAN_POINT('Ctrl Pts',(142.600225660824,-3.2015278714696,127.06833394483));
#35220=CARTESIAN_POINT('Ctrl Pts',(142.592500972595,-3.30230372306345,127.159642084793));
#35221=CARTESIAN_POINT('Ctrl Pts',(142.584823606184,-3.40246221687705,127.250390866638));
#35222=CARTESIAN_POINT('Ctrl Pts',(142.577146239772,-3.49902125553019,127.345402067541));
#35223=CARTESIAN_POINT('Ctrl Pts',(142.56946887336,-3.59159267859491,127.444353907221));
#35224=CARTESIAN_POINT('Ctrl Pts',(142.561798511355,-3.68407964457878,127.543215468679));
#35225=CARTESIAN_POINT('Ctrl Pts',(142.55412814935,-3.77258595742159,127.646010229757));
#35226=CARTESIAN_POINT('Ctrl Pts',(142.546457787346,-3.85675795738575,127.752377472029));
#35227=CARTESIAN_POINT('Ctrl Pts',(142.53879267214,-3.94087238072502,127.858671955345));
#35228=CARTESIAN_POINT('Ctrl Pts',(142.531127556934,-4.02065814070938,127.968533746617));
#35229=CARTESIAN_POINT('Ctrl Pts',(142.523462441729,-4.09580012770525,128.081567129916));
#35230=CARTESIAN_POINT('Ctrl Pts',(142.515697448234,-4.17192123280728,128.1960733653));
#35231=CARTESIAN_POINT('Ctrl Pts',(142.50793245474,-4.243276407309,128.313834122567));
#35232=CARTESIAN_POINT('Ctrl Pts',(142.500167461245,-4.30958178691302,128.434405368113));
#35233=CARTESIAN_POINT('Ctrl Pts',(142.492506496131,-4.37499886683234,128.553361308838));
#35234=CARTESIAN_POINT('Ctrl Pts',(142.484845531017,-4.43550044605301,128.675052525963));
#35235=CARTESIAN_POINT('Ctrl Pts',(142.477184565903,-4.49085929893384,128.799026276445));
#35236=CARTESIAN_POINT('Ctrl Pts',(142.469367558218,-4.54734573007758,128.925525189551));
#35237=CARTESIAN_POINT('Ctrl Pts',(142.461550550533,-4.59847746135096,129.054400245879));
#35238=CARTESIAN_POINT('Ctrl Pts',(142.453733542848,-4.64406441275163,129.185148218678));
#35239=CARTESIAN_POINT('Ctrl Pts',(142.445916535164,-4.68965136415229,129.315896191477));
#35240=CARTESIAN_POINT('Ctrl Pts',(142.438099527479,-4.72969341376038,129.448516655478));
#35241=CARTESIAN_POINT('Ctrl Pts',(142.430282519794,-4.76405452823406,129.582490119308));
#35242=CARTESIAN_POINT('Origin',(213.235140564004,0.,130.804360617566));
#35243=CARTESIAN_POINT('',(140.334586805861,-4.76405452823407,129.582490119308));
#35244=CARTESIAN_POINT('',(140.680140489264,-4.76405452823406,129.582490119308));
#35245=CARTESIAN_POINT('',(213.235140564004,-4.76405452823405,129.582490119308));
#35246=CARTESIAN_POINT('',(142.01485943596,-4.91824791031056,130.799826830428));
#35247=CARTESIAN_POINT('Ctrl Pts',(142.01485943596,-4.91824791031056,130.799826830428));
#35248=CARTESIAN_POINT('Ctrl Pts',(142.007204362131,-4.9183724598586,130.93493805991));
#35249=CARTESIAN_POINT('Ctrl Pts',(141.999549288301,-4.91292527910308,131.070210728423));
#35250=CARTESIAN_POINT('Ctrl Pts',(141.991894214472,-4.90189328219073,131.205141495994));
#35251=CARTESIAN_POINT('Ctrl Pts',(141.983895337286,-4.89036581813378,131.34613225095));
#35252=CARTESIAN_POINT('Ctrl Pts',(141.975896460099,-4.87274017314778,131.486749237213));
#35253=CARTESIAN_POINT('Ctrl Pts',(141.967897582913,-4.8490622793132,131.626417838106));
#35254=CARTESIAN_POINT('Ctrl Pts',(141.960251120509,-4.82642758686816,131.759932915398));
#35255=CARTESIAN_POINT('Ctrl Pts',(141.952604658105,-4.79826264535518,131.892580951809));
#35256=CARTESIAN_POINT('Ctrl Pts',(141.9449581957,-4.76466051954016,132.023865925482));
#35257=CARTESIAN_POINT('Ctrl Pts',(141.937312894906,-4.73106349838228,132.155130955036));
#35258=CARTESIAN_POINT('Ctrl Pts',(141.929667594112,-4.69203103485191,132.285032944037));
#35259=CARTESIAN_POINT('Ctrl Pts',(141.922022293318,-4.64770690713896,132.413087930641));
#35260=CARTESIAN_POINT('Ctrl Pts',(141.914376395698,-4.60337931929056,132.541152913777));
#35261=CARTESIAN_POINT('Ctrl Pts',(141.906730498079,-4.55375937765899,132.667370227804));
#35262=CARTESIAN_POINT('Ctrl Pts',(141.899084600459,-4.49903996263695,132.791273418143));
#35263=CARTESIAN_POINT('Ctrl Pts',(141.891436347327,-4.44430368991786,132.915214779987));
#35264=CARTESIAN_POINT('Ctrl Pts',(141.883788094196,-4.38446498243226,133.036840232908));
#35265=CARTESIAN_POINT('Ctrl Pts',(141.876139841064,-4.31976361211479,133.155706061764));
#35266=CARTESIAN_POINT('Ctrl Pts',(141.868483341257,-4.25499247799666,133.274700056869));
#35267=CARTESIAN_POINT('Ctrl Pts',(141.86082684145,-4.18534840864223,133.390928135706));
#35268=CARTESIAN_POINT('Ctrl Pts',(141.853170341643,-4.11111575725234,133.503973607046));
#35269=CARTESIAN_POINT('Ctrl Pts',(141.845508990916,-4.03683607435818,133.617090700489));
#35270=CARTESIAN_POINT('Ctrl Pts',(141.837847640188,-3.95796225631683,133.727020847084));
#35271=CARTESIAN_POINT('Ctrl Pts',(141.83018628946,-3.87481940199019,133.833379875422));
#35272=CARTESIAN_POINT('Ctrl Pts',(141.82251410854,-3.79155901575509,133.939889254378));
#35273=CARTESIAN_POINT('Ctrl Pts',(141.814841927619,-3.70401781001808,134.042817136548));
#35274=CARTESIAN_POINT('Ctrl Pts',(141.807169746698,-3.61255838303633,134.141815484924));
#35275=CARTESIAN_POINT('Ctrl Pts',(141.804753551799,-3.58375512576284,134.172992969762));
#35276=CARTESIAN_POINT('Ctrl Pts',(141.8023373569,-3.55456350779432,134.20378101864));
#35277=CARTESIAN_POINT('Ctrl Pts',(141.799921162002,-3.52499552010276,134.234169598509));
#35278=CARTESIAN_POINT('Ctrl Pts',(141.792146827883,-3.42985774141342,134.331947709633));
#35279=CARTESIAN_POINT('Ctrl Pts',(141.784372493764,-3.33049785996596,134.425919224525));
#35280=CARTESIAN_POINT('Ctrl Pts',(141.776598159645,-3.22725287804554,134.515697563149));
#35281=CARTESIAN_POINT('Ctrl Pts',(141.768833406697,-3.12413513633827,134.605365257993));
#35282=CARTESIAN_POINT('Ctrl Pts',(141.76106865375,-3.01714211312096,134.690849804701));
#35283=CARTESIAN_POINT('Ctrl Pts',(141.753303900803,-2.90664894092162,134.771799967668));
#35284=CARTESIAN_POINT('Ctrl Pts',(141.745546859918,-2.7962655120984,134.852669729792));
#35285=CARTESIAN_POINT('Ctrl Pts',(141.737789819033,-2.6823891658225,134.929013841008));
#35286=CARTESIAN_POINT('Ctrl Pts',(141.730032778148,-2.56542925988115,135.000520263605));
#35287=CARTESIAN_POINT('Ctrl Pts',(141.722281586908,-2.44855755431465,135.071972762653));
#35288=CARTESIAN_POINT('Ctrl Pts',(141.714530395668,-2.32860724973823,135.138594631373));
#35289=CARTESIAN_POINT('Ctrl Pts',(141.706779204428,-2.20601763236454,135.200116442017));
#35290=CARTESIAN_POINT('Ctrl Pts',(141.699031307651,-2.08348011884859,135.261612104251));
#35291=CARTESIAN_POINT('Ctrl Pts',(141.691283410874,-1.95830587236612,135.318011844726));
#35292=CARTESIAN_POINT('Ctrl Pts',(141.683535514097,-1.83095959561589,135.369091718269));
#35293=CARTESIAN_POINT('Ctrl Pts',(141.675789238013,-1.70363995696132,135.420160907003));
#35294=CARTESIAN_POINT('Ctrl Pts',(141.668042961928,-1.57414955438306,135.465912296774));
#35295=CARTESIAN_POINT('Ctrl Pts',(141.660296685844,-1.44297355914704,135.506169883168));
#35296=CARTESIAN_POINT('Ctrl Pts',(141.652550352579,-1.31179659559975,135.546427766735));
#35297=CARTESIAN_POINT('Ctrl Pts',(141.644804019314,-1.178934388326,135.581191651297));
#35298=CARTESIAN_POINT('Ctrl Pts',(141.637057686048,-1.04488739110477,135.610335378466));
#35299=CARTESIAN_POINT('Ctrl Pts',(141.629309618045,-0.910810374987649,
135.639485632171));
#35300=CARTESIAN_POINT('Ctrl Pts',(141.621561550042,-0.775548422923046,
135.663013140978));
#35301=CARTESIAN_POINT('Ctrl Pts',(141.613813482039,-0.639611908517401,
135.680842922361));
#35302=CARTESIAN_POINT('Ctrl Pts',(141.606057179298,-0.503530919166858,
135.698691653449));
#35303=CARTESIAN_POINT('Ctrl Pts',(141.598300876556,-0.366774323587707,
135.710830509449));
#35304=CARTESIAN_POINT('Ctrl Pts',(141.590544573814,-0.229857901895721,
135.717236395299));
#35305=CARTESIAN_POINT('Ctrl Pts',(141.5827841313,-0.0928684037868652,135.723645700163));
#35306=CARTESIAN_POINT('Ctrl Pts',(141.575023688786,0.0442806996410358,
135.724315935938));
#35307=CARTESIAN_POINT('Ctrl Pts',(141.567263246271,0.181074900741475,135.719276175622));
#35308=CARTESIAN_POINT('Ctrl Pts',(141.559490346006,0.318088696037493,135.714228325035));
#35309=CARTESIAN_POINT('Ctrl Pts',(141.551717445741,0.45474606054288,135.703452192135));
#35310=CARTESIAN_POINT('Ctrl Pts',(141.543944545475,0.590537972021914,135.68702873716));
#35311=CARTESIAN_POINT('Ctrl Pts',(141.536454209713,0.721393505480238,135.671202316141));
#35312=CARTESIAN_POINT('Ctrl Pts',(141.528963873951,0.851445112221208,135.650132082649));
#35313=CARTESIAN_POINT('Ctrl Pts',(141.521473538189,0.980249251491861,135.62393471363));
#35314=CARTESIAN_POINT('Ctrl Pts',(141.51369920407,1.11393703885156,135.596744063402));
#35315=CARTESIAN_POINT('Ctrl Pts',(141.505924869951,1.24670437866469,135.563943680303));
#35316=CARTESIAN_POINT('Ctrl Pts',(141.498150535832,1.37804387223028,135.525608137948));
#35317=CARTESIAN_POINT('Ctrl Pts',(141.490385782885,1.50922150160793,135.487319840722));
#35318=CARTESIAN_POINT('Ctrl Pts',(141.482621029937,1.63897441430036,135.443510065661));
#35319=CARTESIAN_POINT('Ctrl Pts',(141.47485627699,1.76680433755179,135.394304570961));
#35320=CARTESIAN_POINT('Ctrl Pts',(141.467099236105,1.89450729832135,135.345147947853));
#35321=CARTESIAN_POINT('Ctrl Pts',(141.45934219522,2.02029070801094,135.290606409506));
#35322=CARTESIAN_POINT('Ctrl Pts',(141.451585154335,2.14367077257473,135.230855696216));
#35323=CARTESIAN_POINT('Ctrl Pts',(141.443833963095,2.2669577952725,135.171150041403));
#35324=CARTESIAN_POINT('Ctrl Pts',(141.436082771855,2.38784472982894,135.106243200366));
#35325=CARTESIAN_POINT('Ctrl Pts',(141.428331580615,2.50586745412087,135.036359124758));
#35326=CARTESIAN_POINT('Ctrl Pts',(141.420583683838,2.62384001560638,134.966504751747));
#35327=CARTESIAN_POINT('Ctrl Pts',(141.412835787061,2.7389504523662,134.891677550429));
#35328=CARTESIAN_POINT('Ctrl Pts',(141.405087890284,2.85075916982444,134.81214744051));
#35329=CARTESIAN_POINT('Ctrl Pts',(141.397341614199,2.96254449930937,134.732633966575));
#35330=CARTESIAN_POINT('Ctrl Pts',(141.389595338115,3.07102916484228,134.648419767238));
#35331=CARTESIAN_POINT('Ctrl Pts',(141.381849062031,3.1758028420069,134.559817896141));
#35332=CARTESIAN_POINT('Ctrl Pts',(141.374102728766,3.28057729258664,134.471215371005));
#35333=CARTESIAN_POINT('Ctrl Pts',(141.366356395501,3.38164040160441,134.378225361934));
#35334=CARTESIAN_POINT('Ctrl Pts',(141.358610062235,3.47861552094251,134.281200723173));
#35335=CARTESIAN_POINT('Ctrl Pts',(141.350861994232,3.57561235718655,134.184154356417));
#35336=CARTESIAN_POINT('Ctrl Pts',(141.343113926229,3.66851910572709,134.083071838529));
#35337=CARTESIAN_POINT('Ctrl Pts',(141.335365858226,3.75699681224093,133.978342031392));
#35338=CARTESIAN_POINT('Ctrl Pts',(141.327609555484,3.8455685539141,133.873500916169));
#35339=CARTESIAN_POINT('Ctrl Pts',(141.319853252742,3.92970159763366,133.765005067337));
#35340=CARTESIAN_POINT('Ctrl Pts',(141.312096950001,4.00909772111698,133.653275941867));
#35341=CARTESIAN_POINT('Ctrl Pts',(141.304336507486,4.08853622070192,133.541487183198));
#35342=CARTESIAN_POINT('Ctrl Pts',(141.296576064972,4.16323254949747,133.426462037028));
#35343=CARTESIAN_POINT('Ctrl Pts',(141.288815622458,4.23293306348885,133.308649087875));
#35344=CARTESIAN_POINT('Ctrl Pts',(141.281042722193,4.30274546693306,133.190647014917));
#35345=CARTESIAN_POINT('Ctrl Pts',(141.273269821927,4.36754584468517,133.069848540767));
#35346=CARTESIAN_POINT('Ctrl Pts',(141.265496921662,4.42712717193409,132.946725681233));
#35347=CARTESIAN_POINT('Ctrl Pts',(141.2580065859,4.4845425678604,132.828078647773));
#35348=CARTESIAN_POINT('Ctrl Pts',(141.250516250138,4.53711165381283,132.7072735719));
#35349=CARTESIAN_POINT('Ctrl Pts',(141.243025914376,4.58469284879999,132.58474668375));
#35350=CARTESIAN_POINT('Ctrl Pts',(141.235251580257,4.63407809925764,132.457574151393));
#35351=CARTESIAN_POINT('Ctrl Pts',(141.227477246138,4.67824619819302,132.328143819984));
#35352=CARTESIAN_POINT('Ctrl Pts',(141.219702912019,4.7169856251077,132.196922887279));
#35353=CARTESIAN_POINT('Ctrl Pts',(141.211938159072,4.75567730914099,132.065863672646));
#35354=CARTESIAN_POINT('Ctrl Pts',(141.204173406125,4.78895352332623,131.93301861887));
#35355=CARTESIAN_POINT('Ctrl Pts',(141.196408653177,4.81665074300047,131.798874912311));
#35356=CARTESIAN_POINT('Ctrl Pts',(141.188651612292,4.84432045340566,131.664864439173));
#35357=CARTESIAN_POINT('Ctrl Pts',(141.180894571408,4.86642211786545,131.529558260502));
#35358=CARTESIAN_POINT('Ctrl Pts',(141.173137530523,4.88284208916889,131.393458397854));
#35359=CARTESIAN_POINT('Ctrl Pts',(141.165386339282,4.8992496780443,131.257461169171));
#35360=CARTESIAN_POINT('Ctrl Pts',(141.157635148042,4.9099840553782,131.120671834415));
#35361=CARTESIAN_POINT('Ctrl Pts',(141.149883956802,4.91498276869447,130.983601924012));
#35362=CARTESIAN_POINT('Ctrl Pts',(141.142136060025,4.91997935742423,130.846590271977));
#35363=CARTESIAN_POINT('Ctrl Pts',(141.134388163248,4.91924511653648,130.709298671366));
#35364=CARTESIAN_POINT('Ctrl Pts',(141.126640266471,4.91276952551801,130.572242863739));
#35365=CARTESIAN_POINT('Ctrl Pts',(141.118893990387,4.90629528905358,130.435215725233));
#35366=CARTESIAN_POINT('Ctrl Pts',(141.111147714303,4.89408210968696,130.298424671887));
#35367=CARTESIAN_POINT('Ctrl Pts',(141.103401438219,4.87617157794461,130.162384134395));
#35368=CARTESIAN_POINT('Ctrl Pts',(141.095655104953,4.85826091399083,130.026342592682));
#35369=CARTESIAN_POINT('Ctrl Pts',(141.087908771688,4.834652864773,129.8910519655));
#35370=CARTESIAN_POINT('Ctrl Pts',(141.080162438423,4.80544070905459,129.757019863914));
#35371=CARTESIAN_POINT('Ctrl Pts',(141.07241437042,4.7762220114765,129.622957746768));
#35372=CARTESIAN_POINT('Ctrl Pts',(141.064666302417,4.74139679333162,129.49015509797));
#35373=CARTESIAN_POINT('Ctrl Pts',(141.056918234414,4.70110900204418,129.359107278736));
#35374=CARTESIAN_POINT('Ctrl Pts',(141.049161931672,4.6607783924126,129.22792018032));
#35375=CARTESIAN_POINT('Ctrl Pts',(141.04140562893,4.61497372722213,129.098492011415));
#35376=CARTESIAN_POINT('Ctrl Pts',(141.033649326188,4.56388839373205,128.971301482661));
#35377=CARTESIAN_POINT('Ctrl Pts',(141.025888883674,4.5127757944613,128.844043068493));
#35378=CARTESIAN_POINT('Ctrl Pts',(141.01812844116,4.45637707158025,128.719025030416));
#35379=CARTESIAN_POINT('Ctrl Pts',(141.010367998646,4.39493253116425,128.596703237216));
#35380=CARTESIAN_POINT('Ctrl Pts',(141.00259509838,4.33338935451723,128.474185082214));
#35381=CARTESIAN_POINT('Ctrl Pts',(140.994822198115,4.26678436403662,128.354372163224));
#35382=CARTESIAN_POINT('Ctrl Pts',(140.987049297849,4.19540277802365,128.237693792158));
#35383=CARTESIAN_POINT('Ctrl Pts',(140.979558962087,4.12661609246075,128.125256973773));
#35384=CARTESIAN_POINT('Ctrl Pts',(140.972068626325,4.05339423577779,128.015731018587));
#35385=CARTESIAN_POINT('Ctrl Pts',(140.964578290563,3.9760276927594,127.909470835742));
#35386=CARTESIAN_POINT('Ctrl Pts',(140.956803956444,3.89572777374833,127.799181765768));
#35387=CARTESIAN_POINT('Ctrl Pts',(140.949029622325,3.81070830661618,127.692061637589));
#35388=CARTESIAN_POINT('Ctrl Pts',(140.941255288206,3.72124802607181,127.588540941192));
#35389=CARTESIAN_POINT('Ctrl Pts',(140.933490535259,3.63189799732804,127.485147824801));
#35390=CARTESIAN_POINT('Ctrl Pts',(140.925725782312,3.53811829780334,127.385345606889));
#35391=CARTESIAN_POINT('Ctrl Pts',(140.917961029364,3.4402304221042,127.289535201513));
#35392=CARTESIAN_POINT('Ctrl Pts',(140.910203988479,3.34243977002346,127.193819956384));
#35393=CARTESIAN_POINT('Ctrl Pts',(140.902446947594,3.24054933934156,127.102088905514));
#35394=CARTESIAN_POINT('Ctrl Pts',(140.89468990671,3.13492006591731,127.014709018433));
#35395=CARTESIAN_POINT('Ctrl Pts',(140.886938715469,3.02937044834976,126.927395025205));
#35396=CARTESIAN_POINT('Ctrl Pts',(140.879187524229,2.92008790009538,126.844425912841));
#35397=CARTESIAN_POINT('Ctrl Pts',(140.871436332989,2.80746902909971,126.766130719065));
#35398=CARTESIAN_POINT('Ctrl Pts',(140.863688436212,2.69489802412811,126.687868802836));
#35399=CARTESIAN_POINT('Ctrl Pts',(140.855940539435,2.57899383709904,126.614277076825));
#35400=CARTESIAN_POINT('Ctrl Pts',(140.848192642658,2.46018468939969,126.54564316315));
#35401=CARTESIAN_POINT('Ctrl Pts',(140.840446366574,2.34140039401272,126.477023606211));
#35402=CARTESIAN_POINT('Ctrl Pts',(140.83270009049,2.21971268493754,126.413359994267));
#35403=CARTESIAN_POINT('Ctrl Pts',(140.824953814406,2.09557684798133,126.354895398385));
#35404=CARTESIAN_POINT('Ctrl Pts',(140.81720748114,1.9714400946824,126.29643037093));
#35405=CARTESIAN_POINT('Ctrl Pts',(140.809461147875,1.84485553114223,126.243164602702));
#35406=CARTESIAN_POINT('Ctrl Pts',(140.801714814609,1.71630064437875,126.195293991816));
#35407=CARTESIAN_POINT('Ctrl Pts',(140.793966746606,1.58771696863963,126.147412660638));
#35408=CARTESIAN_POINT('Ctrl Pts',(140.786218678603,1.45716245797747,126.104929027404));
#35409=CARTESIAN_POINT('Ctrl Pts',(140.7784706106,1.32513168091329,126.067989739907));
#35410=CARTESIAN_POINT('Ctrl Pts',(140.770714307859,1.19296057996833,126.031011192895));
#35411=CARTESIAN_POINT('Ctrl Pts',(140.762958005117,1.05931045549533,125.999588868223));
#35412=CARTESIAN_POINT('Ctrl Pts',(140.755201702375,0.924688590851678,125.973818818508));
#35413=CARTESIAN_POINT('Ctrl Pts',(140.747441259861,0.789994874465482,125.948035014541));
#35414=CARTESIAN_POINT('Ctrl Pts',(140.739680817347,0.654328771004443,125.92790955408));
#35415=CARTESIAN_POINT('Ctrl Pts',(140.731920374832,0.518203707090394,125.913486669031));
#35416=CARTESIAN_POINT('Ctrl Pts',(140.724147474567,0.381860123139134,125.899040631087));
#35417=CARTESIAN_POINT('Ctrl Pts',(140.716374574301,0.245056496842509,125.890315486622));
#35418=CARTESIAN_POINT('Ctrl Pts',(140.708601674036,0.108308187928903,125.887303326978));
#35419=CARTESIAN_POINT('Ctrl Pts',(140.701111338274,-0.0234689755073049,
125.884400666923));
#35420=CARTESIAN_POINT('Ctrl Pts',(140.693621002512,-0.155194465620334,
125.886802834603));
#35421=CARTESIAN_POINT('Ctrl Pts',(140.68613066675,-0.286412673175626,125.894457274002));
#35422=CARTESIAN_POINT('Ctrl Pts',(140.678356332631,-0.422606058953481,
125.902401933796));
#35423=CARTESIAN_POINT('Ctrl Pts',(140.670581998512,-0.558684355290657,
125.916030173536));
#35424=CARTESIAN_POINT('Ctrl Pts',(140.662807664393,-0.694134715851532,
125.935340176168));
#35425=CARTESIAN_POINT('Ctrl Pts',(140.655042911446,-0.829418145948654,
125.954626380948));
#35426=CARTESIAN_POINT('Ctrl Pts',(140.647278158498,-0.964074796713364,
125.979580361551));
#35427=CARTESIAN_POINT('Ctrl Pts',(140.639513405551,-1.09759359210719,126.010148339301));
#35428=CARTESIAN_POINT('Ctrl Pts',(140.631756364666,-1.23097977475124,126.040685956505));
#35429=CARTESIAN_POINT('Ctrl Pts',(140.623999323781,-1.36322997240307,126.076826387874));
#35430=CARTESIAN_POINT('Ctrl Pts',(140.616242282896,-1.49384034855565,126.118464323843));
#35431=CARTESIAN_POINT('Ctrl Pts',(140.608491091656,-1.62435223040652,126.160070860321));
#35432=CARTESIAN_POINT('Ctrl Pts',(140.600739900416,-1.7532263811522,126.207166531343));
#35433=CARTESIAN_POINT('Ctrl Pts',(140.592988709176,-1.87997159575207,126.259595512342));
#35434=CARTESIAN_POINT('Ctrl Pts',(140.585240812399,-2.00666294025565,126.312002209625));
#35435=CARTESIAN_POINT('Ctrl Pts',(140.577492915622,-2.13122678778079,126.369737559263));
#35436=CARTESIAN_POINT('Ctrl Pts',(140.569745018845,-2.25318968957502,126.432596753255));
#35437=CARTESIAN_POINT('Ctrl Pts',(140.561998742761,-2.37512707935907,126.495442798459));
#35438=CARTESIAN_POINT('Ctrl Pts',(140.554252466677,-2.49446425827756,126.563410377152));
#35439=CARTESIAN_POINT('Ctrl Pts',(140.546506190592,-2.6107506306574,126.636247830342));
#35440=CARTESIAN_POINT('Ctrl Pts',(140.538759857327,-2.72703786143737,126.709085821201));
#35441=CARTESIAN_POINT('Ctrl Pts',(140.531013524062,-2.84027390940619,126.786793550753));
#35442=CARTESIAN_POINT('Ctrl Pts',(140.523267190796,-2.95003586653442,126.869075183362));
#35443=CARTESIAN_POINT('Ctrl Pts',(140.515519122793,-3.05982240409213,126.951375242372));
#35444=CARTESIAN_POINT('Ctrl Pts',(140.50777105479,-3.16613298991541,127.038251008205));
#35445=CARTESIAN_POINT('Ctrl Pts',(140.500022986787,-3.26857691869624,127.129365653071));
#35446=CARTESIAN_POINT('Ctrl Pts',(140.492266684045,-3.37112972610326,127.220577135665));
#35447=CARTESIAN_POINT('Ctrl Pts',(140.484510381304,-3.46980737463951,127.316036236534));
#35448=CARTESIAN_POINT('Ctrl Pts',(140.476754078562,-3.56425485347275,127.415368082609));
#35449=CARTESIAN_POINT('Ctrl Pts',(140.468993636048,-3.65875274176908,127.51475294508));
#35450=CARTESIAN_POINT('Ctrl Pts',(140.461233193533,-3.74901570438674,127.618014377215));
#35451=CARTESIAN_POINT('Ctrl Pts',(140.453472751019,-3.83472900814064,127.72474432708));
#35452=CARTESIAN_POINT('Ctrl Pts',(140.445699850754,-3.92057990649899,127.831645609336));
#35453=CARTESIAN_POINT('Ctrl Pts',(140.437926950488,-4.00186631927342,127.942026220913));
#35454=CARTESIAN_POINT('Ctrl Pts',(140.430154050223,-4.07831633572203,128.055448300252));
#35455=CARTESIAN_POINT('Ctrl Pts',(140.422663714461,-4.15198720150614,128.164747201312));
#35456=CARTESIAN_POINT('Ctrl Pts',(140.415173378699,-4.22116703478364,128.27687001711));
#35457=CARTESIAN_POINT('Ctrl Pts',(140.407683042937,-4.28565378449886,128.391405022883));
#35458=CARTESIAN_POINT('Ctrl Pts',(140.399553936778,-4.3556399174246,128.515707490818));
#35459=CARTESIAN_POINT('Ctrl Pts',(140.391424830619,-4.42030332323987,128.643214966403));
#35460=CARTESIAN_POINT('Ctrl Pts',(140.38329572446,-4.47935262289568,128.773453642282));
#35461=CARTESIAN_POINT('Ctrl Pts',(140.37517757136,-4.53832236023881,128.903516836143));
#35462=CARTESIAN_POINT('Ctrl Pts',(140.36705941826,-4.59169291274071,129.036303595815));
#35463=CARTESIAN_POINT('Ctrl Pts',(140.35894126516,-4.63921774360707,129.17131383627));
#35464=CARTESIAN_POINT('Ctrl Pts',(140.350823112061,-4.68674257447341,129.306324076725));
#35465=CARTESIAN_POINT('Ctrl Pts',(140.342704958961,-4.72842150515073,129.443557503113));
#35466=CARTESIAN_POINT('Ctrl Pts',(140.334586805861,-4.76405452823407,129.582490119308));
#35467=CARTESIAN_POINT('Ctrl Pts',(142.084824010153,-4.76405452823403,129.582490119308));
#35468=CARTESIAN_POINT('Ctrl Pts',(142.082672268707,-4.77344323938914,129.619096561608));
#35469=CARTESIAN_POINT('Ctrl Pts',(142.080520527261,-4.78240609402808,129.655795966851));
#35470=CARTESIAN_POINT('Ctrl Pts',(142.078368785814,-4.79094161432327,129.692577585385));
#35471=CARTESIAN_POINT('Ctrl Pts',(142.067783894177,-4.83292972472065,129.873514494464));
#35472=CARTESIAN_POINT('Ctrl Pts',(142.05719900254,-4.86468194816004,130.056909269468));
#35473=CARTESIAN_POINT('Ctrl Pts',(142.046614110902,-4.88596847754098,130.241781646242));
#35474=CARTESIAN_POINT('Ctrl Pts',(142.036029219265,-4.90725500692191,130.426654023016));
#35475=CARTESIAN_POINT('Ctrl Pts',(142.025444327628,-4.91807569203257,130.613004631307));
#35476=CARTESIAN_POINT('Ctrl Pts',(142.014859435991,-4.91824791031005,130.79982682988));
#35477=CARTESIAN_POINT('',(142.360140564045,-4.91824942331981,130.806742321652));
#35478=CARTESIAN_POINT('Ctrl Pts',(142.430282519794,-4.76405452823406,129.582490119308));
#35479=CARTESIAN_POINT('Ctrl Pts',(142.422611012822,-4.79777606720098,129.713969887945));
#35480=CARTESIAN_POINT('Ctrl Pts',(142.414939505849,-4.82602628670489,129.846752319787));
#35481=CARTESIAN_POINT('Ctrl Pts',(142.407267998877,-4.84872853961549,129.980337188519));
#35482=CARTESIAN_POINT('Ctrl Pts',(142.399413426405,-4.8719725373614,130.117109798705));
#35483=CARTESIAN_POINT('Ctrl Pts',(142.391558853933,-4.88940039608235,130.254723178035));
#35484=CARTESIAN_POINT('Ctrl Pts',(142.383704281461,-4.90098631039045,130.392637108563));
#35485=CARTESIAN_POINT('Ctrl Pts',(142.375849708989,-4.91257222469854,130.530551039091));
#35486=CARTESIAN_POINT('Ctrl Pts',(142.367995136517,-4.91831623997429,130.668765074869));
#35487=CARTESIAN_POINT('Ctrl Pts',(142.360140564045,-4.91824942331981,130.806742321652));
#35488=CARTESIAN_POINT('Ctrl Pts',(142.360140564008,-4.9182494233195,130.806742322295));
#35489=CARTESIAN_POINT('Ctrl Pts',(142.352502847162,-4.9181844513777,130.940910177508));
#35490=CARTESIAN_POINT('Ctrl Pts',(142.344865130315,-4.91262993299218,131.074940705202));
#35491=CARTESIAN_POINT('Ctrl Pts',(142.337227413469,-4.90161629827904,131.208514953118));
#35492=CARTESIAN_POINT('Ctrl Pts',(142.32945307935,-4.89040566061798,131.344478468636));
#35493=CARTESIAN_POINT('Ctrl Pts',(142.321678745231,-4.87351584157187,131.480190537609));
#35494=CARTESIAN_POINT('Ctrl Pts',(142.313904411111,-4.85096096456765,131.615138504993));
#35495=CARTESIAN_POINT('Ctrl Pts',(142.306139658164,-4.82843388443355,131.749920161068));
#35496=CARTESIAN_POINT('Ctrl Pts',(142.298374905217,-4.80025570163112,131.883939207315));
#35497=CARTESIAN_POINT('Ctrl Pts',(142.29061015227,-4.7664924437661,132.016686005414));
#35498=CARTESIAN_POINT('Ctrl Pts',(142.282853111385,-4.73276272004476,132.149300957521));
#35499=CARTESIAN_POINT('Ctrl Pts',(142.2750960705,-4.69345905613744,132.280645799681));
#35500=CARTESIAN_POINT('Ctrl Pts',(142.267339029615,-4.64869882196989,132.410219367617));
#35501=CARTESIAN_POINT('Ctrl Pts',(142.259587838375,-4.60397234184315,132.539695223118));
#35502=CARTESIAN_POINT('Ctrl Pts',(142.251836647135,-4.55379760893742,132.667402095045));
#35503=CARTESIAN_POINT('Ctrl Pts',(142.244085455895,-4.49834219051421,132.792852659174));
#35504=CARTESIAN_POINT('Ctrl Pts',(142.236337559118,-4.44291034212314,132.918249903467));
#35505=CARTESIAN_POINT('Ctrl Pts',(142.22858966234,-4.38220242995891,133.041392390484));
#35506=CARTESIAN_POINT('Ctrl Pts',(142.220841765563,-4.31643456450761,133.161811722642));
#35507=CARTESIAN_POINT('Ctrl Pts',(142.213095489479,-4.25068045627592,133.282205865672));
#35508=CARTESIAN_POINT('Ctrl Pts',(142.205349213395,-4.17986868732026,133.39987764395));
#35509=CARTESIAN_POINT('Ctrl Pts',(142.197602937311,-4.10426165721733,133.514382630686));
#35510=CARTESIAN_POINT('Ctrl Pts',(142.189856604046,-4.02865406900058,133.628888462672));
#35511=CARTESIAN_POINT('Ctrl Pts',(142.18211027078,-3.94825136443048,133.740227130211));
#35512=CARTESIAN_POINT('Ctrl Pts',(142.174363937515,-3.86335944257491,133.8479829463));
#35513=CARTESIAN_POINT('Ctrl Pts',(142.166615869512,-3.77844850976184,133.955762893557));
#35514=CARTESIAN_POINT('Ctrl Pts',(142.158867801509,-3.68904660107439,134.059958085721));
#35515=CARTESIAN_POINT('Ctrl Pts',(142.151119733506,-3.5954998231538,134.160186012935));
#35516=CARTESIAN_POINT('Ctrl Pts',(142.143363430764,-3.5018536226046,134.260520463582));
#35517=CARTESIAN_POINT('Ctrl Pts',(142.135607128022,-3.40405402011725,134.356878940183));
#35518=CARTESIAN_POINT('Ctrl Pts',(142.12785082528,-3.30248430008892,134.448915530058));
#35519=CARTESIAN_POINT('Ctrl Pts',(142.120090382766,-3.20086036924273,134.541001242632));
#35520=CARTESIAN_POINT('Ctrl Pts',(142.112329940252,-3.09546261162876,134.628760222098));
#35521=CARTESIAN_POINT('Ctrl Pts',(142.104569497738,-2.98670651439929,134.711887618029));
#35522=CARTESIAN_POINT('Ctrl Pts',(142.096796597472,-2.87777583222768,134.795148457435));
#35523=CARTESIAN_POINT('Ctrl Pts',(142.089023697207,-2.76547635776458,134.873762631406));
#35524=CARTESIAN_POINT('Ctrl Pts',(142.081250796941,-2.65025235158391,134.947468814973));
#35525=CARTESIAN_POINT('Ctrl Pts',(142.073760461179,-2.53921702826021,135.018495593113));
#35526=CARTESIAN_POINT('Ctrl Pts',(142.066270125417,-2.42546637581353,135.084964865886));
#35527=CARTESIAN_POINT('Ctrl Pts',(142.058779789655,-2.30941684910832,135.14668452068));
#35528=CARTESIAN_POINT('Ctrl Pts',(142.051005455536,-2.18896726932503,135.210744294945));
#35529=CARTESIAN_POINT('Ctrl Pts',(142.043231121417,-2.06565950238112,135.269890100069));
#35530=CARTESIAN_POINT('Ctrl Pts',(142.035456787298,-1.93993249354175,135.323856715916));
#35531=CARTESIAN_POINT('Ctrl Pts',(142.027692034351,-1.81436043200432,135.377756822732));
#35532=CARTESIAN_POINT('Ctrl Pts',(142.019927281404,-1.68637541668486,135.426490287587));
#35533=CARTESIAN_POINT('Ctrl Pts',(142.012162528457,-1.55644191027044,135.469837189413));
#35534=CARTESIAN_POINT('Ctrl Pts',(142.004405487572,-1.42663745564651,135.513141038485));
#35535=CARTESIAN_POINT('Ctrl Pts',(141.996648446687,-1.29488872967157,135.551068848366));
#35536=CARTESIAN_POINT('Ctrl Pts',(141.988891405802,-1.16168081735598,135.583448474164));
#35537=CARTESIAN_POINT('Ctrl Pts',(141.981140214562,-1.02857335816314,135.615803682236));
#35538=CARTESIAN_POINT('Ctrl Pts',(141.973389023322,-0.894009281242463,
135.642618942111));
#35539=CARTESIAN_POINT('Ctrl Pts',(141.965637832082,-0.758489160464665,
135.663771822224));
#35540=CARTESIAN_POINT('Ctrl Pts',(141.957889935304,-0.623026639353269,
135.684915711799));
#35541=CARTESIAN_POINT('Ctrl Pts',(141.950142038527,-0.486609268051492,
135.700401948114));
#35542=CARTESIAN_POINT('Ctrl Pts',(141.94239414175,-0.349747935708725,135.710159170704));
#35543=CARTESIAN_POINT('Ctrl Pts',(141.934647865666,-0.212915231806296,
135.719914352293));
#35544=CARTESIAN_POINT('Ctrl Pts',(141.926901589582,-0.0756391413089238,
135.72394287603));
#35545=CARTESIAN_POINT('Ctrl Pts',(141.919155313498,0.061564593556896,135.722225282573));
#35546=CARTESIAN_POINT('Ctrl Pts',(141.911408980233,0.198769341229425,135.720507676437));
#35547=CARTESIAN_POINT('Ctrl Pts',(141.903662646967,0.335901341270046,135.713043873362));
#35548=CARTESIAN_POINT('Ctrl Pts',(141.895916313702,0.472445518512196,135.699866545919));
#35549=CARTESIAN_POINT('Ctrl Pts',(141.888168245699,0.609020273876202,135.686686267505));
#35550=CARTESIAN_POINT('Ctrl Pts',(141.880420177696,0.74500655541295,135.667789956206));
#35551=CARTESIAN_POINT('Ctrl Pts',(141.872672109693,0.879895467653373,135.643262045422));
#35552=CARTESIAN_POINT('Ctrl Pts',(141.864915806951,1.01492774143492,135.618708066082));
#35553=CARTESIAN_POINT('Ctrl Pts',(141.85715950421,1.14885993084504,135.58851060097));
#35554=CARTESIAN_POINT('Ctrl Pts',(141.849403201468,1.28119383517219,135.552805143852));
#35555=CARTESIAN_POINT('Ctrl Pts',(141.841642758954,1.41359837008866,135.517080629657));
#35556=CARTESIAN_POINT('Ctrl Pts',(141.833882316439,1.54440254745099,135.475842383191));
#35557=CARTESIAN_POINT('Ctrl Pts',(141.826121873925,1.67312530700521,135.429275186459));
#35558=CARTESIAN_POINT('Ctrl Pts',(141.81834897366,1.80205470376054,135.382633235929));
#35559=CARTESIAN_POINT('Ctrl Pts',(141.810576073394,1.9288956438059,135.330645388866));
#35560=CARTESIAN_POINT('Ctrl Pts',(141.802803173129,2.05318813335255,135.273544161745));
#35561=CARTESIAN_POINT('Ctrl Pts',(141.795312837367,2.1729622778313,135.218518708059));
#35562=CARTESIAN_POINT('Ctrl Pts',(141.787822501605,2.29036976568558,135.158745328104));
#35563=CARTESIAN_POINT('Ctrl Pts',(141.780332165843,2.4050238631082,135.094470555596));
#35564=CARTESIAN_POINT('Ctrl Pts',(141.772557831724,2.52402510548203,135.027758785552));
#35565=CARTESIAN_POINT('Ctrl Pts',(141.764783497605,2.64043700642165,134.95598622135));
#35566=CARTESIAN_POINT('Ctrl Pts',(141.757009163486,2.75379916807868,134.879378802113));
#35567=CARTESIAN_POINT('Ctrl Pts',(141.749244410539,2.86702162100286,134.802865794674));
#35568=CARTESIAN_POINT('Ctrl Pts',(141.741479657591,2.97720149217645,134.721530004696));
#35569=CARTESIAN_POINT('Ctrl Pts',(141.733714904644,3.08390270235017,134.635643325085));
#35570=CARTESIAN_POINT('Ctrl Pts',(141.725957863759,3.19049793537773,134.549841949336));
#35571=CARTESIAN_POINT('Ctrl Pts',(141.718200822874,3.29362108053269,134.459498922534));
#35572=CARTESIAN_POINT('Ctrl Pts',(141.710443781989,3.3928651071469,134.364929311919));
#35573=CARTESIAN_POINT('Ctrl Pts',(141.702692590749,3.49203429306856,134.270431016983));
#35574=CARTESIAN_POINT('Ctrl Pts',(141.694941399509,3.58732990113477,134.171712750978));
#35575=CARTESIAN_POINT('Ctrl Pts',(141.687190208269,3.6783783537984,134.069129483628));
#35576=CARTESIAN_POINT('Ctrl Pts',(141.679442311492,3.76938810844097,133.966589816902));
#35577=CARTESIAN_POINT('Ctrl Pts',(141.671694414715,3.8561540390132,133.860188707885));
#35578=CARTESIAN_POINT('Ctrl Pts',(141.663946517938,3.93833995987237,133.750317410014));
#35579=CARTESIAN_POINT('Ctrl Pts',(141.656200241854,4.02050868920862,133.64046909485));
#35580=CARTESIAN_POINT('Ctrl Pts',(141.64845396577,4.09809908039066,133.527152347535));
#35581=CARTESIAN_POINT('Ctrl Pts',(141.640707689685,4.17081599045296,133.410790558363));
#35582=CARTESIAN_POINT('Ctrl Pts',(141.63296135642,4.24353343729492,133.294427910234));
#35583=CARTESIAN_POINT('Ctrl Pts',(141.625215023155,4.3113771240395,133.175020506944));
#35584=CARTESIAN_POINT('Ctrl Pts',(141.617468689889,4.37409612833673,133.053019356141));
#35585=CARTESIAN_POINT('Ctrl Pts',(141.609720621886,4.43682917812006,132.930990884026));
#35586=CARTESIAN_POINT('Ctrl Pts',(141.601972553883,4.49443508307323,132.806367856213));
#35587=CARTESIAN_POINT('Ctrl Pts',(141.59422448588,4.54670980897447,132.679624059186));
#35588=CARTESIAN_POINT('Ctrl Pts',(141.586468183139,4.59904009307651,132.552745557343));
#35589=CARTESIAN_POINT('Ctrl Pts',(141.578711880397,4.64602773029276,132.423742145728));
#35590=CARTESIAN_POINT('Ctrl Pts',(141.570955577655,4.68751742571277,132.293106212401));
#35591=CARTESIAN_POINT('Ctrl Pts',(141.563195135141,4.72902926543247,132.162400554742));
#35592=CARTESIAN_POINT('Ctrl Pts',(141.555434692627,4.76503721368654,132.030061016245));
#35593=CARTESIAN_POINT('Ctrl Pts',(141.547674250112,4.79543670799164,131.896592205713));
#35594=CARTESIAN_POINT('Ctrl Pts',(141.539901349847,4.82588500226374,131.762909139198));
#35595=CARTESIAN_POINT('Ctrl Pts',(141.532128449582,4.85070678051408,131.628093562804));
#35596=CARTESIAN_POINT('Ctrl Pts',(141.524355549316,4.86984902755901,131.492658163169));
#35597=CARTESIAN_POINT('Ctrl Pts',(141.516865213554,4.8882954057074,131.362146181451));
#35598=CARTESIAN_POINT('Ctrl Pts',(141.509374877792,4.90146798330419,131.231058964857));
#35599=CARTESIAN_POINT('Ctrl Pts',(141.50188454203,4.90936513707526,131.099855140984));
#35600=CARTESIAN_POINT('Ctrl Pts',(141.494110207911,4.91756171383188,130.96367668425));
#35601=CARTESIAN_POINT('Ctrl Pts',(141.486335873792,4.92010089884113,130.82694123094));
#35602=CARTESIAN_POINT('Ctrl Pts',(141.478561539673,4.91692392480242,130.690158252417));
#35603=CARTESIAN_POINT('Ctrl Pts',(141.470796786726,4.91375086610027,130.55354384669));
#35604=CARTESIAN_POINT('Ctrl Pts',(141.463032033779,4.90487567410532,130.416882419396));
#35605=CARTESIAN_POINT('Ctrl Pts',(141.455267280831,4.89029138853252,130.280687821113));
#35606=CARTESIAN_POINT('Ctrl Pts',(141.447510239946,4.87572158827778,130.144628493226));
#35607=CARTESIAN_POINT('Ctrl Pts',(141.439753199061,4.85545402006082,130.00903545787));
#35608=CARTESIAN_POINT('Ctrl Pts',(141.431996158176,4.8295337488552,129.874421463014));
#35609=CARTESIAN_POINT('Ctrl Pts',(141.424244966936,4.8036330243277,129.739908981619));
#35610=CARTESIAN_POINT('Ctrl Pts',(141.416493775696,4.77208815517582,129.606374453538));
#35611=CARTESIAN_POINT('Ctrl Pts',(141.408742584456,4.73499585969154,129.474324049947));
#35612=CARTESIAN_POINT('Ctrl Pts',(141.400994687679,4.69791932942232,129.3423297713));
#35613=CARTESIAN_POINT('Ctrl Pts',(141.393246790902,4.65530016782035,129.211818738156));
#35614=CARTESIAN_POINT('Ctrl Pts',(141.385498894125,4.60728583093167,129.083285275056));
#35615=CARTESIAN_POINT('Ctrl Pts',(141.377752618041,4.5592815376072,128.954778698386));
#35616=CARTESIAN_POINT('Ctrl Pts',(141.370006341957,4.50588445047884,128.828249234971));
#35617=CARTESIAN_POINT('Ctrl Pts',(141.362260065873,4.44729124780882,128.704174049743));
#35618=CARTESIAN_POINT('Ctrl Pts',(141.354513732607,4.38869761261713,128.580097948621));
#35619=CARTESIAN_POINT('Ctrl Pts',(141.346767399342,4.32490795229567,128.458476515363));
#35620=CARTESIAN_POINT('Ctrl Pts',(141.339021066076,4.25616608269245,128.339764638701));
#35621=CARTESIAN_POINT('Ctrl Pts',(141.331272998073,4.18740881882415,128.221026177337));
#35622=CARTESIAN_POINT('Ctrl Pts',(141.323524930071,4.11369733474675,128.105198907396));
#35623=CARTESIAN_POINT('Ctrl Pts',(141.315776862068,4.03531995496797,127.992710581815));
#35624=CARTESIAN_POINT('Ctrl Pts',(141.308020559326,3.95685927477721,127.880102702304));
#35625=CARTESIAN_POINT('Ctrl Pts',(141.300264256584,3.87372301667154,127.770841177293));
#35626=CARTESIAN_POINT('Ctrl Pts',(141.292507953842,3.78624149997771,127.665322808564));
#35627=CARTESIAN_POINT('Ctrl Pts',(141.284747511328,3.6987132917644,127.559748121503));
#35628=CARTESIAN_POINT('Ctrl Pts',(141.276987068814,3.60683546555084,127.457920861709));
#35629=CARTESIAN_POINT('Ctrl Pts',(141.269226626299,3.51097604443836,127.360201753942));
#35630=CARTESIAN_POINT('Ctrl Pts',(141.261453726034,3.41496274127311,127.262325778789));
#35631=CARTESIAN_POINT('Ctrl Pts',(141.253680825769,3.31495535612773,127.168571401663));
#35632=CARTESIAN_POINT('Ctrl Pts',(141.245907925503,3.21135657078749,127.079260345391));
#35633=CARTESIAN_POINT('Ctrl Pts',(141.238417589741,3.11152386224369,126.993195970975));
#35634=CARTESIAN_POINT('Ctrl Pts',(141.230927253979,3.00835657428851,126.911257665823));
#35635=CARTESIAN_POINT('Ctrl Pts',(141.223436918217,2.90223968589053,126.833694695061));
#35636=CARTESIAN_POINT('Ctrl Pts',(141.215662584098,2.79209934341573,126.753190900688));
#35637=CARTESIAN_POINT('Ctrl Pts',(141.207888249979,2.67843242551728,126.677145759963));
#35638=CARTESIAN_POINT('Ctrl Pts',(141.20011391586,2.56163579972067,126.605884097197));
#35639=CARTESIAN_POINT('Ctrl Pts',(141.192349162913,2.44498311532701,126.534710258061));
#35640=CARTESIAN_POINT('Ctrl Pts',(141.184584409966,2.32520872802974,126.468308368852));
#35641=CARTESIAN_POINT('Ctrl Pts',(141.176819657018,2.20274119266995,126.406962034243));
#35642=CARTESIAN_POINT('Ctrl Pts',(141.169062616133,2.08039529379269,126.345676629678));
#35643=CARTESIAN_POINT('Ctrl Pts',(141.161305575248,1.95536191726943,126.289436961172));
#35644=CARTESIAN_POINT('Ctrl Pts',(141.153548534363,1.82809681120627,126.238482267089));
#35645=CARTESIAN_POINT('Ctrl Pts',(141.145797343123,1.70092767674957,126.187565998336));
#35646=CARTESIAN_POINT('Ctrl Pts',(141.138046151883,1.57153052407757,126.141926915961));
#35647=CARTESIAN_POINT('Ctrl Pts',(141.130294960643,1.44038348793601,126.101757246009));
#35648=CARTESIAN_POINT('Ctrl Pts',(141.122547063866,1.30929219278326,126.061604649238));
#35649=CARTESIAN_POINT('Ctrl Pts',(141.114799167089,1.17645286645757,126.026916955608));
#35650=CARTESIAN_POINT('Ctrl Pts',(141.107051270312,1.04236110179102,125.997837300659));
#35651=CARTESIAN_POINT('Ctrl Pts',(141.099304994228,0.908297386230965,125.968763728547));
#35652=CARTESIAN_POINT('Ctrl Pts',(141.091558718144,0.772982135270482,125.945295944603));
#35653=CARTESIAN_POINT('Ctrl Pts',(141.083812442059,0.63692311068484,125.927526397134));
#35654=CARTESIAN_POINT('Ctrl Pts',(141.076066108794,0.500863081742386,125.909756718495));
#35655=CARTESIAN_POINT('Ctrl Pts',(141.068319775529,0.364059655892093,125.897685410896));
#35656=CARTESIAN_POINT('Ctrl Pts',(141.060573442263,0.227027332326683,125.891353223629));
#35657=CARTESIAN_POINT('Ctrl Pts',(141.05282537426,0.0899643213225272,125.885019618313));
#35658=CARTESIAN_POINT('Ctrl Pts',(141.045077306257,-0.0473272989246117,
125.884427708844));
#35659=CARTESIAN_POINT('Ctrl Pts',(141.037329238254,-0.18433180131469,125.889566130558));
#35660=CARTESIAN_POINT('Ctrl Pts',(141.029572935513,-0.321481913720284,
125.894710013448));
#35661=CARTESIAN_POINT('Ctrl Pts',(141.021816632771,-0.458343907380787,
125.905596378804));
#35662=CARTESIAN_POINT('Ctrl Pts',(141.014060330029,-0.59440539605652,125.922161800676));
#35663=CARTESIAN_POINT('Ctrl Pts',(141.006299887515,-0.730539504845583,
125.938736064013));
#35664=CARTESIAN_POINT('Ctrl Pts',(140.998539445001,-0.865871871717929,
125.960995360133));
#35665=CARTESIAN_POINT('Ctrl Pts',(140.990779002486,-0.999900083238783,
125.988825041325));
#35666=CARTESIAN_POINT('Ctrl Pts',(140.983006102221,-1.13414344874324,126.016699397192));
#35667=CARTESIAN_POINT('Ctrl Pts',(140.975233201955,-1.2670780959682,126.050161911757));
#35668=CARTESIAN_POINT('Ctrl Pts',(140.96746030169,-1.39821569104805,126.089047696475));
#35669=CARTESIAN_POINT('Ctrl Pts',(140.959969965928,-1.52458610423091,126.126519884971));
#35670=CARTESIAN_POINT('Ctrl Pts',(140.952479630166,-1.64928756010908,126.169027790788));
#35671=CARTESIAN_POINT('Ctrl Pts',(140.944989294404,-1.77190225433616,126.216382254106));
#35672=CARTESIAN_POINT('Ctrl Pts',(140.937214701506,-1.89917015809501,126.265533812311));
#35673=CARTESIAN_POINT('Ctrl Pts',(140.929440108609,-2.02459294751934,126.32006274775));
#35674=CARTESIAN_POINT('Ctrl Pts',(140.921665515711,-2.14768277363802,126.37981072336));
#35675=CARTESIAN_POINT('Ctrl Pts',(140.913900563774,-2.27061996100675,126.439484607905));
#35676=CARTESIAN_POINT('Ctrl Pts',(140.906135611837,-2.39122959307165,126.504364485944));
#35677=CARTESIAN_POINT('Ctrl Pts',(140.898370659899,-2.50904138553715,126.574243079227));
#35678=CARTESIAN_POINT('Ctrl Pts',(140.89061347956,-2.62673526538269,126.644051734112));
#35679=CARTESIAN_POINT('Ctrl Pts',(140.88285629922,-2.74163654429565,126.718848949515));
#35680=CARTESIAN_POINT('Ctrl Pts',(140.87509911888,-2.85329757877115,126.798380588974));
#35681=CARTESIAN_POINT('Ctrl Pts',(140.866975842646,-2.97022839485252,126.881665680769));
#35682=CARTESIAN_POINT('Ctrl Pts',(140.858852566412,-3.08360526868429,126.970142791753));
#35683=CARTESIAN_POINT('Ctrl Pts',(140.850729290178,-3.1929453900343,127.063467301958));
#35684=CARTESIAN_POINT('Ctrl Pts',(140.842981731391,-3.29722831647514,127.152475370659));
#35685=CARTESIAN_POINT('Ctrl Pts',(140.835234172603,-3.39783919195002,127.245892214331));
#35686=CARTESIAN_POINT('Ctrl Pts',(140.827486613816,-3.49439138665629,127.343376379035));
#35687=CARTESIAN_POINT('Ctrl Pts',(140.819740679673,-3.59092333459718,127.440840101541));
#35688=CARTESIAN_POINT('Ctrl Pts',(140.811994745531,-3.68339802026635,127.542369170494));
#35689=CARTESIAN_POINT('Ctrl Pts',(140.804248811388,-3.77146507988114,127.64758469683));
#35690=CARTESIAN_POINT('Ctrl Pts',(140.796502824113,-3.859532743589,127.752800944889));
#35691=CARTESIAN_POINT('Ctrl Pts',(140.788756836837,-3.94319247059463,127.861703400579));
#35692=CARTESIAN_POINT('Ctrl Pts',(140.781010849561,-4.0221339254761,127.973879784203));
#35693=CARTESIAN_POINT('Ctrl Pts',(140.773263131714,-4.10109301708202,128.086081229742));
#35694=CARTESIAN_POINT('Ctrl Pts',(140.765515413867,-4.1753315146918,128.201557738712));
#35695=CARTESIAN_POINT('Ctrl Pts',(140.757767696019,-4.24458241120132,128.31986807038));
#35696=CARTESIAN_POINT('Ctrl Pts',(140.750012840577,-4.31389710518594,128.43828739559));
#35697=CARTESIAN_POINT('Ctrl Pts',(140.742257985135,-4.37821482655643,128.55954541827));
#35698=CARTESIAN_POINT('Ctrl Pts',(140.734503129693,-4.43731438705389,128.683176020944));
#35699=CARTESIAN_POINT('Ctrl Pts',(140.72674409703,-4.49644578205236,128.806873218337));
#35700=CARTESIAN_POINT('Ctrl Pts',(140.718985064366,-4.55035326234016,128.932945183225));
#35701=CARTESIAN_POINT('Ctrl Pts',(140.711226031703,-4.5988641806459,129.060906772329));
#35702=CARTESIAN_POINT('Ctrl Pts',(140.703457242644,-4.64743609775488,129.189029263434));
#35703=CARTESIAN_POINT('Ctrl Pts',(140.695688453585,-4.69059778190035,129.319045752601));
#35704=CARTESIAN_POINT('Ctrl Pts',(140.687919664526,-4.72822661721739,129.450456588937));
#35705=CARTESIAN_POINT('Ctrl Pts',(140.685326606105,-4.74078633116139,129.49431876271));
#35706=CARTESIAN_POINT('Ctrl Pts',(140.682733547685,-4.75273006249754,129.538336199274));
#35707=CARTESIAN_POINT('Ctrl Pts',(140.680140489264,-4.76405452823406,129.582490119308));
#35708=CARTESIAN_POINT('Origin',(213.235140564004,0.,130.804360617566));
#35709=CARTESIAN_POINT('',(138.584929581679,-4.76405452823406,129.582490119308));
#35710=CARTESIAN_POINT('',(138.929858124837,-4.76405452823407,129.582490119308));
#35711=CARTESIAN_POINT('',(213.235140564004,-4.76405452823405,129.582490119308));
#35712=CARTESIAN_POINT('',(140.264859435961,-4.9182499873584,130.804713249272));
#35713=CARTESIAN_POINT('Ctrl Pts',(140.264859435961,-4.9182499873584,130.804713249272));
#35714=CARTESIAN_POINT('Ctrl Pts',(140.256699920237,-4.9182395995136,130.949595336183));
#35715=CARTESIAN_POINT('Ctrl Pts',(140.248540404513,-4.91182300637272,131.094339296179));
#35716=CARTESIAN_POINT('Ctrl Pts',(140.240380888789,-4.89906240695556,131.23837743205));
#35717=CARTESIAN_POINT('Ctrl Pts',(140.232208991226,-4.88628244368213,131.382634141803));
#35718=CARTESIAN_POINT('Ctrl Pts',(140.224037093662,-4.86713928737667,131.526182566396));
#35719=CARTESIAN_POINT('Ctrl Pts',(140.215865196099,-4.84174648071891,131.668463666366));
#35720=CARTESIAN_POINT('Ctrl Pts',(140.207672433166,-4.81628883841023,131.811108053777));
#35721=CARTESIAN_POINT('Ctrl Pts',(140.199479670233,-4.78454969417094,131.952478325094));
#35722=CARTESIAN_POINT('Ctrl Pts',(140.1912869073,-4.74669336420818,132.092027177154));
#35723=CARTESIAN_POINT('Ctrl Pts',(140.183082921663,-4.70878517745716,132.23176718761));
#35724=CARTESIAN_POINT('Ctrl Pts',(140.174878936027,-4.6647431774351,132.369680489536));
#35725=CARTESIAN_POINT('Ctrl Pts',(140.16667495039,-4.61478046118432,132.505238143307));
#35726=CARTESIAN_POINT('Ctrl Pts',(140.158451938574,-4.56470187447502,132.641110174051));
#35727=CARTESIAN_POINT('Ctrl Pts',(140.150228926759,-4.50867524175657,132.774615333103));
#35728=CARTESIAN_POINT('Ctrl Pts',(140.142005914943,-4.44696114355522,132.905246061899));
#35729=CARTESIAN_POINT('Ctrl Pts',(140.137749083004,-4.41501341561366,132.972870074986));
#35730=CARTESIAN_POINT('Ctrl Pts',(140.133492251064,-4.3815422660966,133.039724218812));
#35731=CARTESIAN_POINT('Ctrl Pts',(140.129235419124,-4.34658843369518,133.105741083844));
#35732=CARTESIAN_POINT('Ctrl Pts',(140.121461085005,-4.28275157668732,133.226308955337));
#35733=CARTESIAN_POINT('Ctrl Pts',(140.113686750886,-4.21379324585066,133.344409676167));
#35734=CARTESIAN_POINT('Ctrl Pts',(140.105912416767,-4.13992826696339,133.459577559154));
#35735=CARTESIAN_POINT('Ctrl Pts',(140.09814766382,-4.06615432006105,133.574603508018));
#35736=CARTESIAN_POINT('Ctrl Pts',(140.090382910873,-3.98748596589034,133.686703484803));
#35737=CARTESIAN_POINT('Ctrl Pts',(140.082618157926,-3.90418455435782,133.79543501116));
#35738=CARTESIAN_POINT('Ctrl Pts',(140.074861117041,-3.82096587896162,133.904058543832));
#35739=CARTESIAN_POINT('Ctrl Pts',(140.067104076156,-3.733123539861,134.009319975609));
#35740=CARTESIAN_POINT('Ctrl Pts',(140.059347035271,-3.64096274595035,134.110804832293));
#35741=CARTESIAN_POINT('Ctrl Pts',(140.051595844031,-3.54887145121118,134.212213158457));
#35742=CARTESIAN_POINT('Ctrl Pts',(140.043844652791,-3.45246844546252,134.309850289931));
#35743=CARTESIAN_POINT('Ctrl Pts',(140.03609346155,-3.35209963137398,134.403334238453));
#35744=CARTESIAN_POINT('Ctrl Pts',(140.028345564773,-3.25177347670899,134.496778453803));
#35745=CARTESIAN_POINT('Ctrl Pts',(140.020597667996,-3.14748515167631,134.586072731168));
#35746=CARTESIAN_POINT('Ctrl Pts',(140.012849771219,-3.0396177295135,134.670871592712));
#35747=CARTESIAN_POINT('Ctrl Pts',(140.005103495135,-2.93177287089005,134.755652716163));
#35748=CARTESIAN_POINT('Ctrl Pts',(139.997357219051,-2.82035071144692,134.835940052717));
#35749=CARTESIAN_POINT('Ctrl Pts',(139.989610942967,-2.70576743693359,134.911428384201));
#35750=CARTESIAN_POINT('Ctrl Pts',(139.981864609702,-2.59118331659255,134.986917272923));
#35751=CARTESIAN_POINT('Ctrl Pts',(139.974118276436,-2.47343836110084,135.057606870798));
#35752=CARTESIAN_POINT('Ctrl Pts',(139.966371943171,-2.35297742678264,135.123235504797));
#35753=CARTESIAN_POINT('Ctrl Pts',(139.958623875168,-2.23248951607342,135.188878835873));
#35754=CARTESIAN_POINT('Ctrl Pts',(139.950875807165,-2.10928475949464,135.249458760793));
#35755=CARTESIAN_POINT('Ctrl Pts',(139.943127739162,-1.98383191083405,135.304759934522));
#35756=CARTESIAN_POINT('Ctrl Pts',(139.93537143642,-1.85824572939299,135.360119882997));
#35757=CARTESIAN_POINT('Ctrl Pts',(139.927615133678,-1.73040704130752,135.410189715111));
#35758=CARTESIAN_POINT('Ctrl Pts',(139.919858830936,-1.60080436619132,135.454802364721));
#35759=CARTESIAN_POINT('Ctrl Pts',(139.912098388422,-1.47113251822506,135.499438825445));
#35760=CARTESIAN_POINT('Ctrl Pts',(139.904337945908,-1.33969518171868,135.538612188323));
#35761=CARTESIAN_POINT('Ctrl Pts',(139.896577503394,-1.20699431094952,135.572205811764));
#35762=CARTESIAN_POINT('Ctrl Pts',(139.888804603129,-1.07408041696197,135.605853362671));
#35763=CARTESIAN_POINT('Ctrl Pts',(139.881031702863,-0.939899318360345,
135.633903194968));
#35764=CARTESIAN_POINT('Ctrl Pts',(139.873258802598,-0.804962281921439,
135.656290005674));
#35765=CARTESIAN_POINT('Ctrl Pts',(139.865768466836,-0.674930546644616,
135.677862999421));
#35766=CARTESIAN_POINT('Ctrl Pts',(139.858278131074,-0.544197185472536,
135.694177515392));
#35767=CARTESIAN_POINT('Ctrl Pts',(139.850787795312,-0.413220654976473,
135.705220924982));
#35768=CARTESIAN_POINT('Ctrl Pts',(139.843013461193,-0.277278109515476,
135.716683048803));
#35769=CARTESIAN_POINT('Ctrl Pts',(139.835239127074,-0.140642966076507,
135.722502776448));
#35770=CARTESIAN_POINT('Ctrl Pts',(139.827464792955,-0.00382313905452457,
135.722609131632));
#35771=CARTESIAN_POINT('Ctrl Pts',(139.819700040008,0.1328280697585,135.722715355742));
#35772=CARTESIAN_POINT('Ctrl Pts',(139.81193528706,0.269663122074555,135.717122217021));
#35773=CARTESIAN_POINT('Ctrl Pts',(139.804170534113,0.406168482318487,135.705810426191));
#35774=CARTESIAN_POINT('Ctrl Pts',(139.796413493228,0.542538263514051,135.694509870391));
#35775=CARTESIAN_POINT('Ctrl Pts',(139.788656452343,0.678578617178914,135.677501997711));
#35776=CARTESIAN_POINT('Ctrl Pts',(139.780899411458,0.813775861568878,135.654819555608));
#35777=CARTESIAN_POINT('Ctrl Pts',(139.773148220218,0.948871152665259,135.632154218511));
#35778=CARTESIAN_POINT('Ctrl Pts',(139.765397028978,1.08312421598248,135.60382289398));
#35779=CARTESIAN_POINT('Ctrl Pts',(139.757645837738,1.21602670513635,135.569910125744));
#35780=CARTESIAN_POINT('Ctrl Pts',(139.749897940961,1.34887270718713,135.536011771339));
#35781=CARTESIAN_POINT('Ctrl Pts',(139.742150044184,1.48036889874304,135.496536787939));
#35782=CARTESIAN_POINT('Ctrl Pts',(139.734402147407,1.61001755907654,135.451620726702));
#35783=CARTESIAN_POINT('Ctrl Pts',(139.726655871323,1.73963909970521,135.406714060936));
#35784=CARTESIAN_POINT('Ctrl Pts',(139.718909595239,1.86741350861953,135.356368709092));
#35785=CARTESIAN_POINT('Ctrl Pts',(139.711163319155,1.99285903856431,135.300769842149));
#35786=CARTESIAN_POINT('Ctrl Pts',(139.703416985889,2.11830549451942,135.245170564788));
#35787=CARTESIAN_POINT('Ctrl Pts',(139.695670652624,2.24142267976915,135.184317853363));
#35788=CARTESIAN_POINT('Ctrl Pts',(139.687924319358,2.36174998567253,135.118444537435));
#35789=CARTESIAN_POINT('Ctrl Pts',(139.680176251356,2.4821042380417,135.052556469635));
#35790=CARTESIAN_POINT('Ctrl Pts',(139.672428183353,2.59966702496357,134.981645747752));
#35791=CARTESIAN_POINT('Ctrl Pts',(139.66468011535,2.71400379768974,134.905990348371));
#35792=CARTESIAN_POINT('Ctrl Pts',(139.656923812608,2.82846208889875,134.830254541532));
#35793=CARTESIAN_POINT('Ctrl Pts',(139.649167509866,2.93968719025207,134.749764199948));
#35794=CARTESIAN_POINT('Ctrl Pts',(139.641411207124,3.0472744874863,134.664840025673));
#35795=CARTESIAN_POINT('Ctrl Pts',(139.63365076461,3.15491920730045,134.579870524809));
#35796=CARTESIAN_POINT('Ctrl Pts',(139.625890322096,3.2589219578543,134.490462730605));
#35797=CARTESIAN_POINT('Ctrl Pts',(139.618129879581,3.35891328672535,134.396975903783));
#35798=CARTESIAN_POINT('Ctrl Pts',(139.610356979316,3.45906513055431,134.303339003607));
#35799=CARTESIAN_POINT('Ctrl Pts',(139.602584079051,3.55519241022837,134.205610264659));
#35800=CARTESIAN_POINT('Ctrl Pts',(139.594811178785,3.64696383231787,134.104184532302));
#35801=CARTESIAN_POINT('Ctrl Pts',(139.587320843023,3.73539913205683,134.006445880792));
#35802=CARTESIAN_POINT('Ctrl Pts',(139.579830507261,3.81978957144916,133.905274595861));
#35803=CARTESIAN_POINT('Ctrl Pts',(139.572340171499,3.89987671871707,133.801049563938));
#35804=CARTESIAN_POINT('Ctrl Pts',(139.56456583738,3.98300039451491,133.692872808252));
#35805=CARTESIAN_POINT('Ctrl Pts',(139.556791503261,4.06175132873342,133.581063497316));
#35806=CARTESIAN_POINT('Ctrl Pts',(139.549017169142,4.13579526687686,133.466010589478));
#35807=CARTESIAN_POINT('Ctrl Pts',(139.541252416195,4.20974795248405,133.351099474067));
#35808=CARTESIAN_POINT('Ctrl Pts',(139.533487663247,4.27900497463091,133.232953041084));
#35809=CARTESIAN_POINT('Ctrl Pts',(139.5257229103,4.34327252617964,133.111992916229));
#35810=CARTESIAN_POINT('Ctrl Pts',(139.517965869415,4.40747624629011,132.991152930675));
#35811=CARTESIAN_POINT('Ctrl Pts',(139.51020882853,4.46670017544205,132.86750515765));
#35812=CARTESIAN_POINT('Ctrl Pts',(139.502451787645,4.52069420746963,132.741499472953));
#35813=CARTESIAN_POINT('Ctrl Pts',(139.494700596405,4.57464752217768,132.615588810124));
#35814=CARTESIAN_POINT('Ctrl Pts',(139.486949405165,4.62337863650188,132.487324132771));
#35815=CARTESIAN_POINT('Ctrl Pts',(139.479198213925,4.6666839058364,132.357178825054));
#35816=CARTESIAN_POINT('Ctrl Pts',(139.471450317148,4.70997076927626,132.227088832565));
#35817=CARTESIAN_POINT('Ctrl Pts',(139.463702420371,4.74783625126156,132.095120169686));
#35818=CARTESIAN_POINT('Ctrl Pts',(139.455954523594,4.7801253646084,131.961764851672));
#35819=CARTESIAN_POINT('Ctrl Pts',(139.44820824751,4.8124077237688,131.828437428716));
#35820=CARTESIAN_POINT('Ctrl Pts',(139.440461971426,4.83911594248892,131.693724307312));
#35821=CARTESIAN_POINT('Ctrl Pts',(139.432715695341,4.8601454142007,131.558130884507));
#35822=CARTESIAN_POINT('Ctrl Pts',(139.424969362076,4.88117504114725,131.422536460782));
#35823=CARTESIAN_POINT('Ctrl Pts',(139.417223028811,4.89652577751942,131.286062109037));
#35824=CARTESIAN_POINT('Ctrl Pts',(139.409476695545,4.90614453919853,131.14922120243));
#35825=CARTESIAN_POINT('Ctrl Pts',(139.401728627542,4.91576545493262,131.01234965125));
#35826=CARTESIAN_POINT('Ctrl Pts',(139.393980559539,4.91965181427796,130.875111771793));
#35827=CARTESIAN_POINT('Ctrl Pts',(139.386232491536,4.91780260259638,130.738023415362));
#35828=CARTESIAN_POINT('Ctrl Pts',(139.378476188795,4.91595142555062,130.600789359794));
#35829=CARTESIAN_POINT('Ctrl Pts',(139.370719886053,4.90835250567635,130.463705536255));
#35830=CARTESIAN_POINT('Ctrl Pts',(139.362963583311,4.895056954802,130.327285705477));
#35831=CARTESIAN_POINT('Ctrl Pts',(139.355203140797,4.88175430769182,130.190793063328));
#35832=CARTESIAN_POINT('Ctrl Pts',(139.347442698283,4.86274902535104,130.054965507103));
#35833=CARTESIAN_POINT('Ctrl Pts',(139.339682255768,4.83814366593952,129.920308056782));
#35834=CARTESIAN_POINT('Ctrl Pts',(139.331909355503,4.81349880782071,129.785434442367));
#35835=CARTESIAN_POINT('Ctrl Pts',(139.324136455238,4.78323599462548,129.651735068953));
#35836=CARTESIAN_POINT('Ctrl Pts',(139.316363554972,4.74750834874858,129.519702086647));
#35837=CARTESIAN_POINT('Ctrl Pts',(139.30887321921,4.71307949279179,129.392468835819));
#35838=CARTESIAN_POINT('Ctrl Pts',(139.301382883448,4.67357631930266,129.266783218347));
#35839=CARTESIAN_POINT('Ctrl Pts',(139.293892547686,4.62917790747561,129.143067457573));
#35840=CARTESIAN_POINT('Ctrl Pts',(139.286118213567,4.5830961163696,129.014660976127));
#35841=CARTESIAN_POINT('Ctrl Pts',(139.278343879448,4.53159458001806,128.887969921171));
#35842=CARTESIAN_POINT('Ctrl Pts',(139.270569545329,4.47481986737682,128.763485751968));
#35843=CARTESIAN_POINT('Ctrl Pts',(139.262804792382,4.41811512449481,128.639154998378));
#35844=CARTESIAN_POINT('Ctrl Pts',(139.255040039435,4.35615029651326,128.517026071271));
#35845=CARTESIAN_POINT('Ctrl Pts',(139.247275286487,4.28912129913806,128.397574057902));
#35846=CARTESIAN_POINT('Ctrl Pts',(139.239518245602,4.22215887590799,128.278240685956));
#35847=CARTESIAN_POINT('Ctrl Pts',(139.231761204717,4.15014248290613,128.161579275467));
#35848=CARTESIAN_POINT('Ctrl Pts',(139.224004163832,4.07331542489305,128.048043416693));
#35849=CARTESIAN_POINT('Ctrl Pts',(139.216252972592,3.99654630276211,127.934593176194));
#35850=CARTESIAN_POINT('Ctrl Pts',(139.208501781352,3.91497395467671,127.824264118428));
#35851=CARTESIAN_POINT('Ctrl Pts',(139.200750590112,3.82888657725357,127.717483451071));
#35852=CARTESIAN_POINT('Ctrl Pts',(139.193002693335,3.74283578926224,127.610748168346));
#35853=CARTESIAN_POINT('Ctrl Pts',(139.185254796558,3.6522740335642,127.507558580146));
#35854=CARTESIAN_POINT('Ctrl Pts',(139.177506899781,3.55753148216963,127.408311027841));
#35855=CARTESIAN_POINT('Ctrl Pts',(139.169760623697,3.46280874887439,127.309084235984));
#35856=CARTESIAN_POINT('Ctrl Pts',(139.162014347613,3.36390722916566,127.213798122489));
#35857=CARTESIAN_POINT('Ctrl Pts',(139.154268071529,3.26119558548824,127.122813875272));
#35858=CARTESIAN_POINT('Ctrl Pts',(139.146521738263,3.15848318361686,127.031828956431));
#35859=CARTESIAN_POINT('Ctrl Pts',(139.138775404998,3.05196089431073,126.945146226476));
#35860=CARTESIAN_POINT('Ctrl Pts',(139.131029071732,2.9420319396852,126.863087837312));
#35861=CARTESIAN_POINT('Ctrl Pts',(139.123281003729,2.83207836723248,126.78101107174));
#35862=CARTESIAN_POINT('Ctrl Pts',(139.115532935726,2.71871692462217,126.703560941487));
#35863=CARTESIAN_POINT('Ctrl Pts',(139.107784867724,2.60238106372923,126.631017130427));
#35864=CARTESIAN_POINT('Ctrl Pts',(139.100028564982,2.48592155969885,126.558396218941));
#35865=CARTESIAN_POINT('Ctrl Pts',(139.09227226224,2.36648165473367,126.490692250363));
#35866=CARTESIAN_POINT('Ctrl Pts',(139.084515959498,2.24452121748061,126.428139923088));
#35867=CARTESIAN_POINT('Ctrl Pts',(139.076755516984,2.12249568626994,126.365554209752));
#35868=CARTESIAN_POINT('Ctrl Pts',(139.06899507447,1.99794729704609,126.308125780131));
#35869=CARTESIAN_POINT('Ctrl Pts',(139.061234631955,1.87135637261259,126.256041324774));
#35870=CARTESIAN_POINT('Ctrl Pts',(139.05346173169,1.74456223318907,126.203873258826));
#35871=CARTESIAN_POINT('Ctrl Pts',(139.045688831425,1.61571937403047,126.157066443535));
#35872=CARTESIAN_POINT('Ctrl Pts',(139.037915931159,1.48532462135564,126.11575807185));
#35873=CARTESIAN_POINT('Ctrl Pts',(139.030425595397,1.35967004638484,126.075951363525));
#35874=CARTESIAN_POINT('Ctrl Pts',(139.022935259635,1.23257474661397,126.041250355883));
#35875=CARTESIAN_POINT('Ctrl Pts',(139.015444923873,1.10449074717846,126.011732606558));
#35876=CARTESIAN_POINT('Ctrl Pts',(139.007670589754,0.971550403974258,125.981095682796));
#35877=CARTESIAN_POINT('Ctrl Pts',(138.999896255635,0.837123792969694,125.955945774123));
#35878=CARTESIAN_POINT('Ctrl Pts',(138.992121921516,0.701703616862046,125.936425213662));
#35879=CARTESIAN_POINT('Ctrl Pts',(138.984357168569,0.566450334018694,125.916928710547));
#35880=CARTESIAN_POINT('Ctrl Pts',(138.976592415622,0.430206305673608,125.903047806997));
#35881=CARTESIAN_POINT('Ctrl Pts',(138.968827662675,0.293477133413694,125.894874469845));
#35882=CARTESIAN_POINT('Ctrl Pts',(138.96107062179,0.156883762495212,125.886709250567));
#35883=CARTESIAN_POINT('Ctrl Pts',(138.953313580905,0.0198065943118101,
125.884240339626));
#35884=CARTESIAN_POINT('Ctrl Pts',(138.94555654002,-0.117241240638398,125.887508214453));
#35885=CARTESIAN_POINT('Ctrl Pts',(138.937805348779,-0.254185726750192,
125.890773624951));
#35886=CARTESIAN_POINT('Ctrl Pts',(138.930054157539,-0.391100534385532,
125.899767200984));
#35887=CARTESIAN_POINT('Ctrl Pts',(138.922302966299,-0.527470464316749,
125.914477390763));
#35888=CARTESIAN_POINT('Ctrl Pts',(138.914555069522,-0.663782433390052,
125.929181328318));
#35889=CARTESIAN_POINT('Ctrl Pts',(138.906807172745,-0.799549597472776,
125.949597005261));
#35890=CARTESIAN_POINT('Ctrl Pts',(138.899059275968,-0.934260037308206,
125.97566087072));
#35891=CARTESIAN_POINT('Ctrl Pts',(138.891312999884,-1.06894229862355,126.001719284181));
#35892=CARTESIAN_POINT('Ctrl Pts',(138.8835667238,-1.20256789175668,126.033423461912));
#35893=CARTESIAN_POINT('Ctrl Pts',(138.875820447716,-1.33463366802653,126.070658468648));
#35894=CARTESIAN_POINT('Ctrl Pts',(138.86807411445,-1.46670041917602,126.107893750245));
#35895=CARTESIAN_POINT('Ctrl Pts',(138.860327781185,-1.59720695419146,126.150659836222));
#35896=CARTESIAN_POINT('Ctrl Pts',(138.85258144792,-1.72566428614893,126.198791615368));
#35897=CARTESIAN_POINT('Ctrl Pts',(138.844833379917,-1.85415038523523,126.246934173291));
#35898=CARTESIAN_POINT('Ctrl Pts',(138.837085311914,-1.98058600205685,126.300444678296));
#35899=CARTESIAN_POINT('Ctrl Pts',(138.829337243911,-2.10450153932347,126.359109631009));
#35900=CARTESIAN_POINT('Ctrl Pts',(138.821580941169,-2.22854877549763,126.417836933532));
#35901=CARTESIAN_POINT('Ctrl Pts',(138.813824638427,-2.35007022785446,126.481729459515));
#35902=CARTESIAN_POINT('Ctrl Pts',(138.806068335685,-2.46861986774926,126.550527168657));
#35903=CARTESIAN_POINT('Ctrl Pts',(138.798307893171,-2.5872327811565,126.619361597209));
#35904=CARTESIAN_POINT('Ctrl Pts',(138.790547450657,-2.70287039209385,126.693106215479));
#35905=CARTESIAN_POINT('Ctrl Pts',(138.782787008143,-2.81511600630547,126.771457825092));
#35906=CARTESIAN_POINT('Ctrl Pts',(138.775014107877,-2.92754180714165,126.849935211665));
#35907=CARTESIAN_POINT('Ctrl Pts',(138.767241207612,-3.03656441902054,126.93303413111));
#35908=CARTESIAN_POINT('Ctrl Pts',(138.759468307346,-3.14179987092302,127.020410745598));
#35909=CARTESIAN_POINT('Ctrl Pts',(138.751977971584,-3.24320974907617,127.10461100006));
#35910=CARTESIAN_POINT('Ctrl Pts',(138.744487635822,-3.34110280358922,127.192783133033));
#35911=CARTESIAN_POINT('Ctrl Pts',(138.73699730006,-3.43516945240252,127.284588764764));
#35912=CARTESIAN_POINT('Ctrl Pts',(138.729335950167,-3.5313837654499,127.37849043876));
#35913=CARTESIAN_POINT('Ctrl Pts',(138.721674600274,-3.62391849594263,127.476509765588));
#35914=CARTESIAN_POINT('Ctrl Pts',(138.714013250381,-3.71239276697578,127.578322334128));
#35915=CARTESIAN_POINT('Ctrl Pts',(138.706360830996,-3.80076390733441,127.680016224111));
#35916=CARTESIAN_POINT('Ctrl Pts',(138.698708411611,-3.88508373587602,127.785494264888));
#35917=CARTESIAN_POINT('Ctrl Pts',(138.691055992225,-3.96500618700098,127.894393435699));
#35918=CARTESIAN_POINT('Ctrl Pts',(138.68341072122,-4.0448539799082,128.003190880175));
#35919=CARTESIAN_POINT('Ctrl Pts',(138.675765450214,-4.12031232660955,128.115402777161));
#35920=CARTESIAN_POINT('Ctrl Pts',(138.668120179208,-4.19107402046465,128.230631490893));
#35921=CARTESIAN_POINT('Ctrl Pts',(138.660480495053,-4.26178400456586,128.34577600019));
#35922=CARTESIAN_POINT('Ctrl Pts',(138.652840810899,-4.32780395415916,128.463932597832));
#35923=CARTESIAN_POINT('Ctrl Pts',(138.645201126745,-4.38886911884744,128.584673495441));
#35924=CARTESIAN_POINT('Ctrl Pts',(138.63756474466,-4.4499078895902,128.705362205708));
#35925=CARTESIAN_POINT('Ctrl Pts',(138.629928362575,-4.50599595419598,128.828632634724));
#35926=CARTESIAN_POINT('Ctrl Pts',(138.62229198049,-4.5569140238837,128.954031554553));
#35927=CARTESIAN_POINT('Ctrl Pts',(138.614655941915,-4.60782980310321,129.079424833511));
#35928=CARTESIAN_POINT('Ctrl Pts',(138.607019903341,-4.65357589110573,129.206946042359));
#35929=CARTESIAN_POINT('Ctrl Pts',(138.599383864766,-4.69398089638185,129.336121397649));
#35930=CARTESIAN_POINT('Ctrl Pts',(138.594565770404,-4.71947515315274,129.417626885738));
#35931=CARTESIAN_POINT('Ctrl Pts',(138.589747676042,-4.74284398389356,129.49979052884));
#35932=CARTESIAN_POINT('Ctrl Pts',(138.584929581679,-4.76405452823406,129.582490119308));
#35933=CARTESIAN_POINT('Ctrl Pts',(140.334586805861,-4.76405452823407,129.582490119308));
#35934=CARTESIAN_POINT('Ctrl Pts',(140.326498474831,-4.79955665325446,129.720912365943));
#35935=CARTESIAN_POINT('Ctrl Pts',(140.318410143802,-4.82905709203218,129.861021019605));
#35936=CARTESIAN_POINT('Ctrl Pts',(140.310321812772,-4.85240638469056,130.002278738757));
#35937=CARTESIAN_POINT('Ctrl Pts',(140.302246511742,-4.87571806251177,130.143308897006));
#35938=CARTESIAN_POINT('Ctrl Pts',(140.294171210711,-4.89289829758937,130.285484095697));
#35939=CARTESIAN_POINT('Ctrl Pts',(140.28609590968,-4.90384827356347,130.428255349897));
#35940=CARTESIAN_POINT('Ctrl Pts',(140.279017085117,-4.91344704376335,130.553408908539));
#35941=CARTESIAN_POINT('Ctrl Pts',(140.271938260554,-4.91825899936649,130.679020142658));
#35942=CARTESIAN_POINT('Ctrl Pts',(140.264859435991,-4.91824998735844,130.804713248748));
#35943=CARTESIAN_POINT('',(140.610140563957,-4.9182480184558,130.799945704706));
#35944=CARTESIAN_POINT('Ctrl Pts',(140.680140489264,-4.76405452823406,129.582490119308));
#35945=CARTESIAN_POINT('Ctrl Pts',(140.675607549706,-4.78385088850951,129.659675827571));
#35946=CARTESIAN_POINT('Ctrl Pts',(140.671074610149,-4.80175451530272,129.737278628265));
#35947=CARTESIAN_POINT('Ctrl Pts',(140.666541670591,-4.8177525850657,129.815197793966));
#35948=CARTESIAN_POINT('Ctrl Pts',(140.655452150913,-4.85689074413086,130.005821584622));
#35949=CARTESIAN_POINT('Ctrl Pts',(140.644362631235,-4.88472582398956,130.198838737255));
#35950=CARTESIAN_POINT('Ctrl Pts',(140.633273111557,-4.90102881052903,130.393143326022));
#35951=CARTESIAN_POINT('Ctrl Pts',(140.625562262374,-4.91236472715027,130.528248670805));
#35952=CARTESIAN_POINT('Ctrl Pts',(140.617851413191,-4.91812596406356,130.663976169357));
#35953=CARTESIAN_POINT('Ctrl Pts',(140.610140564008,-4.91824801845499,130.799945703804));
#35954=CARTESIAN_POINT('Ctrl Pts',(140.610140563957,-4.9182480184558,130.799945704706));
#35955=CARTESIAN_POINT('Ctrl Pts',(140.60249225751,-4.91836908283874,130.934812389576));
#35956=CARTESIAN_POINT('Ctrl Pts',(140.594843951064,-4.91293857030097,131.069858143507));
#35957=CARTESIAN_POINT('Ctrl Pts',(140.587195644617,-4.90193906657004,131.204581119458));
#35958=CARTESIAN_POINT('Ctrl Pts',(140.579553673181,-4.89094867361067,131.339192505806));
#35959=CARTESIAN_POINT('Ctrl Pts',(140.571911701746,-4.87439849772661,131.473481246169));
#35960=CARTESIAN_POINT('Ctrl Pts',(140.56426973031,-4.85232318791553,131.606945655127));
#35961=CARTESIAN_POINT('Ctrl Pts',(140.556631611151,-4.83025900615042,131.740342785388));
#35962=CARTESIAN_POINT('Ctrl Pts',(140.548993491992,-4.8026752939131,131.87291601369));
#35963=CARTESIAN_POINT('Ctrl Pts',(140.541355372833,-4.7696584828474,132.00416936045));
#35964=CARTESIAN_POINT('Ctrl Pts',(140.533719138739,-4.73664982023216,132.135390314277));
#35965=CARTESIAN_POINT('Ctrl Pts',(140.526082904645,-4.69821082266585,132.265291643392));
#35966=CARTESIAN_POINT('Ctrl Pts',(140.518446670551,-4.65447880598773,132.393388656057));
#35967=CARTESIAN_POINT('Ctrl Pts',(140.510810556802,-4.61074747851223,132.521483649954));
#35968=CARTESIAN_POINT('Ctrl Pts',(140.503174443053,-4.56172342825247,132.6477740024));
#35969=CARTESIAN_POINT('Ctrl Pts',(140.495538329304,-4.5075933291255,132.771791795962));
#35970=CARTESIAN_POINT('Ctrl Pts',(140.487900571483,-4.45345157567036,132.895836290825));
#35971=CARTESIAN_POINT('Ctrl Pts',(140.480262813661,-4.39420174905913,133.017606884614));
#35972=CARTESIAN_POINT('Ctrl Pts',(140.47262505584,-4.33007774905487,133.136657714773));
#35973=CARTESIAN_POINT('Ctrl Pts',(140.464979447087,-4.26588783531267,133.255830918539));
#35974=CARTESIAN_POINT('Ctrl Pts',(140.457333838334,-4.19681393595512,133.372278421314));
#35975=CARTESIAN_POINT('Ctrl Pts',(140.449688229581,-4.12313496391443,133.485580700261));
#35976=CARTESIAN_POINT('Ctrl Pts',(140.44203839766,-4.04941529418598,133.598945563424));
#35977=CARTESIAN_POINT('Ctrl Pts',(140.43438856574,-3.97108572103642,133.709161416099));
#35978=CARTESIAN_POINT('Ctrl Pts',(140.42673873382,-3.88846638952164,133.815840685582));
#35979=CARTESIAN_POINT('Ctrl Pts',(140.419077375535,-3.80572257154178,133.922680693781));
#35980=CARTESIAN_POINT('Ctrl Pts',(140.411416017251,-3.71867634798768,134.025973170753));
#35981=CARTESIAN_POINT('Ctrl Pts',(140.403754658966,-3.62768608616077,134.125365995878));
#35982=CARTESIAN_POINT('Ctrl Pts',(140.398534454903,-3.56568823711147,134.193089082337));
#35983=CARTESIAN_POINT('Ctrl Pts',(140.393314250841,-3.50186008474626,134.259002485839));
#35984=CARTESIAN_POINT('Ctrl Pts',(140.388094046778,-3.4363236504197,134.323005645423));
#35985=CARTESIAN_POINT('Ctrl Pts',(140.380319712659,-3.33872169246614,134.418324131314));
#35986=CARTESIAN_POINT('Ctrl Pts',(140.37254537854,-3.23699614572452,134.509729518424));
#35987=CARTESIAN_POINT('Ctrl Pts',(140.364771044421,-3.13149376771814,134.596843952433));
#35988=CARTESIAN_POINT('Ctrl Pts',(140.357006291474,-3.0261214119637,134.683851025688));
#35989=CARTESIAN_POINT('Ctrl Pts',(140.349241538527,-2.91698178480588,134.766577421275));
#35990=CARTESIAN_POINT('Ctrl Pts',(140.341476785579,-2.80445885965293,134.844681590832));
#35991=CARTESIAN_POINT('Ctrl Pts',(140.333719744694,-2.69204769385554,134.922708186226));
#35992=CARTESIAN_POINT('Ctrl Pts',(140.325962703809,-2.57626023638771,134.996121470117));
#35993=CARTESIAN_POINT('Ctrl Pts',(140.318205662924,-2.45751367449571,135.06461995265));
#35994=CARTESIAN_POINT('Ctrl Pts',(140.310454471684,-2.33885666031007,135.133066779944));
#35995=CARTESIAN_POINT('Ctrl Pts',(140.302703280444,-2.21724532062262,135.196605988461));
#35996=CARTESIAN_POINT('Ctrl Pts',(140.294952089204,-2.09312567401196,135.254979448166));
#35997=CARTESIAN_POINT('Ctrl Pts',(140.287204192427,-1.96905878156185,135.313328097594));
#35998=CARTESIAN_POINT('Ctrl Pts',(140.27945629565,-1.84248605562609,135.366515199012));
#35999=CARTESIAN_POINT('Ctrl Pts',(140.271708398873,-1.71387776234049,135.414328738742));
#36000=CARTESIAN_POINT('Ctrl Pts',(140.263962122789,-1.58529637113728,135.46213227691));
#36001=CARTESIAN_POINT('Ctrl Pts',(140.256215846705,-1.45468062574428,135.504564352998));
#36002=CARTESIAN_POINT('Ctrl Pts',(140.248469570621,-1.32252003081739,135.541461400807));
#36003=CARTESIAN_POINT('Ctrl Pts',(140.240723237355,-1.19035846031128,135.578358720982));
#36004=CARTESIAN_POINT('Ctrl Pts',(140.23297690409,-1.05665239408112,135.609720826216));
#36005=CARTESIAN_POINT('Ctrl Pts',(140.225230570825,-0.92190534231808,135.635434370088));
#36006=CARTESIAN_POINT('Ctrl Pts',(140.217482502822,-0.787128114886699,
135.661153672329));
#36007=CARTESIAN_POINT('Ctrl Pts',(140.209734434819,-0.651309821999467,
135.681221822821));
#36008=CARTESIAN_POINT('Ctrl Pts',(140.201986366816,-0.514962584507861,
135.695576887479));
#36009=CARTESIAN_POINT('Ctrl Pts',(140.194230064074,-0.378470435549882,
135.70994720887));
#36010=CARTESIAN_POINT('Ctrl Pts',(140.186473761332,-0.241448608431359,
135.71859227408));
#36011=CARTESIAN_POINT('Ctrl Pts',(140.17871745859,-0.104413304656748,135.721502157558));
#36012=CARTESIAN_POINT('Ctrl Pts',(140.170957016076,0.0326951389856347,
135.724413594127));
#36013=CARTESIAN_POINT('Ctrl Pts',(140.163196573562,0.169816682925836,135.721583757646));
#36014=CARTESIAN_POINT('Ctrl Pts',(140.155436131048,0.306437728970503,135.713054841162));
#36015=CARTESIAN_POINT('Ctrl Pts',(140.147663230782,0.443278091246834,135.704512233304));
#36016=CARTESIAN_POINT('Ctrl Pts',(140.139890330517,0.579615961023312,135.69025230418));
#36017=CARTESIAN_POINT('Ctrl Pts',(140.132117430251,0.714944547821106,135.670368977201));
#36018=CARTESIAN_POINT('Ctrl Pts',(140.124627094489,0.845353599618035,135.651208459241));
#36019=CARTESIAN_POINT('Ctrl Pts',(140.117136758727,0.974825171711792,135.626826351559));
#36020=CARTESIAN_POINT('Ctrl Pts',(140.109646422965,1.10291884522271,135.597350611646));
#36021=CARTESIAN_POINT('Ctrl Pts',(140.101872088846,1.2358692292968,135.566757290096));
#36022=CARTESIAN_POINT('Ctrl Pts',(140.094097754727,1.36775631300523,135.530579551038));
#36023=CARTESIAN_POINT('Ctrl Pts',(140.086323420608,1.49807476589744,135.488904891909));
#36024=CARTESIAN_POINT('Ctrl Pts',(140.07855866766,1.62823261294354,135.447281593073));
#36025=CARTESIAN_POINT('Ctrl Pts',(140.070793914713,1.75682530684741,135.40017497127));
#36026=CARTESIAN_POINT('Ctrl Pts',(140.063029161766,1.88335794629106,135.347723458969));
#36027=CARTESIAN_POINT('Ctrl Pts',(140.055272120881,2.00976491173341,135.29532404225));
#36028=CARTESIAN_POINT('Ctrl Pts',(140.047515079996,2.13411553567006,135.237590448173));
#36029=CARTESIAN_POINT('Ctrl Pts',(140.039758039111,2.25593066625146,135.174710705553));
#36030=CARTESIAN_POINT('Ctrl Pts',(140.032006847871,2.37765393509472,135.111878381036));
#36031=CARTESIAN_POINT('Ctrl Pts',(140.024255656631,2.49684517036757,135.04390781098));
#36032=CARTESIAN_POINT('Ctrl Pts',(140.016504465391,2.61304611602351,134.971034717857));
#36033=CARTESIAN_POINT('Ctrl Pts',(140.008756568614,2.7291976731781,134.898192597742));
#36034=CARTESIAN_POINT('Ctrl Pts',(140.001008671837,2.84236113801716,134.82045230617));
#36035=CARTESIAN_POINT('Ctrl Pts',(139.99326077506,2.95210394709466,134.738094892787));
#36036=CARTESIAN_POINT('Ctrl Pts',(139.985514498976,3.06182380034236,134.655754706799));
#36037=CARTESIAN_POINT('Ctrl Pts',(139.977768222891,3.16812410854656,134.568799554557));
#36038=CARTESIAN_POINT('Ctrl Pts',(139.970021946807,3.27060266960694,134.477552858664));
#36039=CARTESIAN_POINT('Ctrl Pts',(139.962275613542,3.37308198714057,134.386305489208));
#36040=CARTESIAN_POINT('Ctrl Pts',(139.954529280277,3.47173920924471,134.290766772877));
#36041=CARTESIAN_POINT('Ctrl Pts',(139.946782947011,3.56620681480678,134.191299060545));
#36042=CARTESIAN_POINT('Ctrl Pts',(139.939034879008,3.66069557573445,134.091809073107));
#36043=CARTESIAN_POINT('Ctrl Pts',(139.931286811005,3.75099258395434,133.98838862226));
#36044=CARTESIAN_POINT('Ctrl Pts',(139.923538743002,3.83676891873799,133.881435092893));
#36045=CARTESIAN_POINT('Ctrl Pts',(139.91578244026,3.92263641763087,133.774367892042));
#36046=CARTESIAN_POINT('Ctrl Pts',(139.908026137518,4.00397340033536,133.663760417141));
#36047=CARTESIAN_POINT('Ctrl Pts',(139.900269834777,4.0804924966803,133.550041598131));
#36048=CARTESIAN_POINT('Ctrl Pts',(139.892509392262,4.15705243357075,133.436262083963));
#36049=CARTESIAN_POINT('Ctrl Pts',(139.884748949748,4.22878915587345,133.319368249822));
#36050=CARTESIAN_POINT('Ctrl Pts',(139.876988507234,4.29546054942528,133.199815006786));
#36051=CARTESIAN_POINT('Ctrl Pts',(139.869215606969,4.36223896981695,133.08006984627));
#36052=CARTESIAN_POINT('Ctrl Pts',(139.861442706703,4.42393563643457,132.957657095128));
#36053=CARTESIAN_POINT('Ctrl Pts',(139.853669806438,4.48035563707092,132.833053898441));
#36054=CARTESIAN_POINT('Ctrl Pts',(139.846179470676,4.53472462857017,132.712980341811));
#36055=CARTESIAN_POINT('Ctrl Pts',(139.838689134914,4.58419381807425,132.590873116617));
#36056=CARTESIAN_POINT('Ctrl Pts',(139.831198799152,4.62863280268317,132.467171923886));
#36057=CARTESIAN_POINT('Ctrl Pts',(139.823424465033,4.67475670490096,132.338780562833));
#36058=CARTESIAN_POINT('Ctrl Pts',(139.815650130914,4.71560753869031,132.208265272421));
#36059=CARTESIAN_POINT('Ctrl Pts',(139.807875796795,4.75098577467072,132.076098495974));
#36060=CARTESIAN_POINT('Ctrl Pts',(139.800111043848,4.78632041013706,131.944094603266));
#36061=CARTESIAN_POINT('Ctrl Pts',(139.792346290901,4.81619576719131,131.810443648223));
#36062=CARTESIAN_POINT('Ctrl Pts',(139.784581537953,4.84046080673972,131.675636831471));
#36063=CARTESIAN_POINT('Ctrl Pts',(139.776824497069,4.86470174590874,131.54096390675));
#36064=CARTESIAN_POINT('Ctrl Pts',(139.769067456183,4.88334338778184,131.40513778722));
#36065=CARTESIAN_POINT('Ctrl Pts',(139.761310415299,4.89628493304807,131.26866323107));
#36066=CARTESIAN_POINT('Ctrl Pts',(139.753559224058,4.90921671899439,131.132291591443));
#36067=CARTESIAN_POINT('Ctrl Pts',(139.745808032818,4.91645692745254,130.995272876148));
#36068=CARTESIAN_POINT('Ctrl Pts',(139.738056841578,4.91795617982778,130.858120042728));
#36069=CARTESIAN_POINT('Ctrl Pts',(139.730308944801,4.91945479498077,130.721025502921));
#36070=CARTESIAN_POINT('Ctrl Pts',(139.722561048024,4.91521730287863,130.583797348489));
#36071=CARTESIAN_POINT('Ctrl Pts',(139.714813151247,4.90524634744008,130.44695142151));
#36072=CARTESIAN_POINT('Ctrl Pts',(139.707066875163,4.89527747771046,130.310134119748));
#36073=CARTESIAN_POINT('Ctrl Pts',(139.699320599079,4.87957755854499,130.17369927609));
#36074=CARTESIAN_POINT('Ctrl Pts',(139.691574322995,4.85820129448045,130.038160092371));
#36075=CARTESIAN_POINT('Ctrl Pts',(139.683827989729,4.83682487262119,129.902619908134));
#36076=CARTESIAN_POINT('Ctrl Pts',(139.676081656464,4.80977208315887,129.76797578322));
#36077=CARTESIAN_POINT('Ctrl Pts',(139.668335323199,4.77714912800754,129.634732783049));
#36078=CARTESIAN_POINT('Ctrl Pts',(139.660587255196,4.74451886717173,129.501459944033));
#36079=CARTESIAN_POINT('Ctrl Pts',(139.652839187193,4.70631605142454,129.369589233806));
#36080=CARTESIAN_POINT('Ctrl Pts',(139.64509111919,4.6626972222413,129.239612178933));
#36081=CARTESIAN_POINT('Ctrl Pts',(139.637334816448,4.61903203444713,129.109496982899));
#36082=CARTESIAN_POINT('Ctrl Pts',(139.629578513706,4.56993945916475,128.981279833845));
#36083=CARTESIAN_POINT('Ctrl Pts',(139.621822210964,4.51562503670479,128.855434351545));
#36084=CARTESIAN_POINT('Ctrl Pts',(139.61406176845,4.4612816250022,128.729521701722));
#36085=CARTESIAN_POINT('Ctrl Pts',(139.606301325936,4.40171098240527,128.605983592915));
#36086=CARTESIAN_POINT('Ctrl Pts',(139.598540883422,4.33716496986913,128.485269613177));
#36087=CARTESIAN_POINT('Ctrl Pts',(139.590767983156,4.27251534234354,128.364361852641));
#36088=CARTESIAN_POINT('Ctrl Pts',(139.582995082891,4.2028745832306,128.246287617585));
#36089=CARTESIAN_POINT('Ctrl Pts',(139.575222182625,4.12853877339113,128.131468801741));
#36090=CARTESIAN_POINT('Ctrl Pts',(139.567731846863,4.05690525747929,128.020823939062));
#36091=CARTESIAN_POINT('Ctrl Pts',(139.560241511101,3.980912295945,127.913202171038));
#36092=CARTESIAN_POINT('Ctrl Pts',(139.552751175339,3.9008593357625,127.808950878466));
#36093=CARTESIAN_POINT('Ctrl Pts',(139.54497684122,3.81777114326387,127.700746866451));
#36094=CARTESIAN_POINT('Ctrl Pts',(139.537202507101,3.73004580655604,127.595831200548));
#36095=CARTESIAN_POINT('Ctrl Pts',(139.529428172982,3.63797295508169,127.494627117631));
#36096=CARTESIAN_POINT('Ctrl Pts',(139.521663420035,3.54601357516793,127.393547759701));
#36097=CARTESIAN_POINT('Ctrl Pts',(139.513898667088,3.44971760173233,127.29617116989));
#36098=CARTESIAN_POINT('Ctrl Pts',(139.506133914141,3.34941665545385,127.202889927602));
#36099=CARTESIAN_POINT('Ctrl Pts',(139.498376873256,3.24921532948975,127.10970133356));
#36100=CARTESIAN_POINT('Ctrl Pts',(139.490619832371,3.14501723111356,127.02060025695));
#36101=CARTESIAN_POINT('Ctrl Pts',(139.482862791486,3.03719254319538,126.935944337218));
#36102=CARTESIAN_POINT('Ctrl Pts',(139.475111600246,2.92944916671276,126.851352257174));
#36103=CARTESIAN_POINT('Ctrl Pts',(139.467360409006,2.81808495048683,126.77119890226));
#36104=CARTESIAN_POINT('Ctrl Pts',(139.459609217766,2.70350476989094,126.695803082168));
#36105=CARTESIAN_POINT('Ctrl Pts',(139.451861320988,2.58897328892809,126.620439307311));
#36106=CARTESIAN_POINT('Ctrl Pts',(139.444113424211,2.47122888811353,126.549829259974));
#36107=CARTESIAN_POINT('Ctrl Pts',(139.436365527434,2.3507069890986,126.484249540996));
#36108=CARTESIAN_POINT('Ctrl Pts',(139.42861925135,2.2302103006668,126.418683539882));
#36109=CARTESIAN_POINT('Ctrl Pts',(139.420872975266,2.10693761286098,126.358145960917));
#36110=CARTESIAN_POINT('Ctrl Pts',(139.413126699182,1.9813502660582,126.302868177753));
#36111=CARTESIAN_POINT('Ctrl Pts',(139.405380365917,1.85576199219824,126.247589986542));
#36112=CARTESIAN_POINT('Ctrl Pts',(139.397634032651,1.72785938308289,126.197571826109));
#36113=CARTESIAN_POINT('Ctrl Pts',(139.389887699386,1.59812476928206,126.152997345975));
#36114=CARTESIAN_POINT('Ctrl Pts',(139.382139631383,1.46836110231381,126.108412883694));
#36115=CARTESIAN_POINT('Ctrl Pts',(139.37439156338,1.33676498395961,126.069274654544));
#36116=CARTESIAN_POINT('Ctrl Pts',(139.366643495377,1.20383456393023,126.03571663786));
#36117=CARTESIAN_POINT('Ctrl Pts',(139.358887192635,1.07076286386856,126.002122955317));
#36118=CARTESIAN_POINT('Ctrl Pts',(139.351130889893,0.936354408977907,125.974121428334));
#36119=CARTESIAN_POINT('Ctrl Pts',(139.343374587152,0.801118768546406,125.951795133084));
#36120=CARTESIAN_POINT('Ctrl Pts',(139.335614144637,0.665810948781648,125.929456921618));
#36121=CARTESIAN_POINT('Ctrl Pts',(139.327853702123,0.529675451643455,125.912800024967));
#36122=CARTESIAN_POINT('Ctrl Pts',(139.320093259609,0.393226665291511,125.9018555587));
#36123=CARTESIAN_POINT('Ctrl Pts',(139.312320359344,0.256558839234639,125.890893523405));
#36124=CARTESIAN_POINT('Ctrl Pts',(139.304547459078,0.119577109875557,125.885662258204));
#36125=CARTESIAN_POINT('Ctrl Pts',(139.296774558813,-0.0172035327036181,
125.886140705752));
#36126=CARTESIAN_POINT('Ctrl Pts',(139.289284223051,-0.14901185439539,125.886601760527));
#36127=CARTESIAN_POINT('Ctrl Pts',(139.281793887289,-0.28063314778043,125.892364596873));
#36128=CARTESIAN_POINT('Ctrl Pts',(139.274303551527,-0.411613293150797,
125.903365049378));
#36129=CARTESIAN_POINT('Ctrl Pts',(139.266529217408,-0.547559590543532,
125.914782587383));
#36130=CARTESIAN_POINT('Ctrl Pts',(139.258754883288,-0.683245798935054,
125.931878917537));
#36131=CARTESIAN_POINT('Ctrl Pts',(139.250980549169,-0.818159285368155,
125.954639136257));
#36132=CARTESIAN_POINT('Ctrl Pts',(139.243215796222,-0.952906502987066,
125.977371305042));
#36133=CARTESIAN_POINT('Ctrl Pts',(139.235451043275,-1.08688251164536,126.005753409389));
#36134=CARTESIAN_POINT('Ctrl Pts',(139.227686290328,-1.21957777409472,126.039718646186));
#36135=CARTESIAN_POINT('Ctrl Pts',(139.219929249443,-1.35214124173875,126.073650148231));
#36136=CARTESIAN_POINT('Ctrl Pts',(139.212172208558,-1.48342611831749,126.113153651117));
#36137=CARTESIAN_POINT('Ctrl Pts',(139.204415167673,-1.61293141875301,126.158111022366));
#36138=CARTESIAN_POINT('Ctrl Pts',(139.196663976433,-1.74233905823345,126.203034490911));
#36139=CARTESIAN_POINT('Ctrl Pts',(139.188912785193,-1.86996942487607,126.253403513835));
#36140=CARTESIAN_POINT('Ctrl Pts',(139.181161593953,-1.99533545002837,126.309049782445));
#36141=CARTESIAN_POINT('Ctrl Pts',(139.173413697175,-2.1206481912759,126.364672399906));
#36142=CARTESIAN_POINT('Ctrl Pts',(139.165665800398,-2.24369814858787,126.425567643674));
#36143=CARTESIAN_POINT('Ctrl Pts',(139.157917903621,-2.36401725380633,126.491518690692));
#36144=CARTESIAN_POINT('Ctrl Pts',(139.150171627537,-2.484311190862,126.557455942172));
#36145=CARTESIAN_POINT('Ctrl Pts',(139.142425351453,-2.60187506942021,126.628446705544));
#36146=CARTESIAN_POINT('Ctrl Pts',(139.134679075369,-2.71626486253243,126.704227905193));
#36147=CARTESIAN_POINT('Ctrl Pts',(139.126932742104,-2.83065550004381,126.780009664241));
#36148=CARTESIAN_POINT('Ctrl Pts',(139.119186408838,-2.94187167942476,126.860581714205));
#36149=CARTESIAN_POINT('Ctrl Pts',(139.111440075573,-3.04949817968013,126.945637523766));
#36150=CARTESIAN_POINT('Ctrl Pts',(139.10369200757,-3.15714878214377,127.030712380985));
#36151=CARTESIAN_POINT('Ctrl Pts',(139.095943939567,-3.26120779916445,127.120272753491));
#36152=CARTESIAN_POINT('Ctrl Pts',(139.088195871564,-3.36129324804418,127.213971952929));
#36153=CARTESIAN_POINT('Ctrl Pts',(139.080439568822,-3.46148506893041,127.307770736992));
#36154=CARTESIAN_POINT('Ctrl Pts',(139.07268326608,-3.55769459960266,127.405716867427));
#36155=CARTESIAN_POINT('Ctrl Pts',(139.064926963338,-3.64957651107725,127.507426533861));
#36156=CARTESIAN_POINT('Ctrl Pts',(139.057166520824,-3.74150746269457,127.609190485807));
#36157=CARTESIAN_POINT('Ctrl Pts',(139.04940607831,-3.82910594309253,127.7147216756));
#36158=CARTESIAN_POINT('Ctrl Pts',(139.041645635796,-3.91206773449635,127.823604152638));
#36159=CARTESIAN_POINT('Ctrl Pts',(139.03387273553,-3.99516270353274,127.932661417493));
#36160=CARTESIAN_POINT('Ctrl Pts',(139.026099835265,-4.0736058857865,128.045080399306));
#36161=CARTESIAN_POINT('Ctrl Pts',(139.018326935,-4.147136632681,128.160416440323));
#36162=CARTESIAN_POINT('Ctrl Pts',(139.010836599238,-4.21799435171278,128.271559725735));
#36163=CARTESIAN_POINT('Ctrl Pts',(139.003346263476,-4.28429043838581,128.385411401379));
#36164=CARTESIAN_POINT('Ctrl Pts',(138.995855927714,-4.34583341408507,128.501554720509));
#36165=CARTESIAN_POINT('Ctrl Pts',(138.987632903478,-4.4133963908017,128.629058928373));
#36166=CARTESIAN_POINT('Ctrl Pts',(138.979409879243,-4.47542512871843,128.759691239174));
#36167=CARTESIAN_POINT('Ctrl Pts',(138.971186855008,-4.53163609976733,128.89295869181));
#36168=CARTESIAN_POINT('Ctrl Pts',(138.962982749488,-4.58771774621055,129.025919535958));
#36169=CARTESIAN_POINT('Ctrl Pts',(138.954778643968,-4.63800818801278,129.161503136765));
#36170=CARTESIAN_POINT('Ctrl Pts',(138.946574538448,-4.68227009606823,129.299192915958));
#36171=CARTESIAN_POINT('Ctrl Pts',(138.941002400578,-4.71233229523069,129.392710293463));
#36172=CARTESIAN_POINT('Ctrl Pts',(138.935430262708,-4.73961446584328,129.487198686976));
#36173=CARTESIAN_POINT('Ctrl Pts',(138.929858124837,-4.76405452823407,129.582490119308));
#36174=CARTESIAN_POINT('Origin',(213.235140564004,0.,130.804360617566));
#36175=CARTESIAN_POINT('',(136.834948208849,-4.76405452823407,129.582490119308));
#36176=CARTESIAN_POINT('',(137.180179986924,-4.76405452823403,129.582490119308));
#36177=CARTESIAN_POINT('',(213.235140564004,-4.76405452823405,129.582490119308));
#36178=CARTESIAN_POINT('',(138.514859436043,-4.91824802050565,130.808773246294));
#36179=CARTESIAN_POINT('Ctrl Pts',(138.514859435991,-4.91824802050483,130.808773247205));
#36180=CARTESIAN_POINT('Ctrl Pts',(138.503760886087,-4.91807243545752,131.004477596301));
#36181=CARTESIAN_POINT('Ctrl Pts',(138.492662336184,-4.90621248966243,131.19967933262));
#36182=CARTESIAN_POINT('Ctrl Pts',(138.48156378628,-4.88286716168191,131.393250542653));
#36183=CARTESIAN_POINT('Ctrl Pts',(138.473892416269,-4.86673076093358,131.527047875508));
#36184=CARTESIAN_POINT('Ctrl Pts',(138.466221046258,-4.84510800141887,131.66006707746));
#36185=CARTESIAN_POINT('Ctrl Pts',(138.458549676247,-4.81807674258383,131.79194330528));
#36186=CARTESIAN_POINT('Ctrl Pts',(138.450775342128,-4.79068267378781,131.92558955829));
#36187=CARTESIAN_POINT('Ctrl Pts',(138.443001008009,-4.75768027938131,132.058306827762));
#36188=CARTESIAN_POINT('Ctrl Pts',(138.43522667389,-4.71914490506628,132.189587829069));
#36189=CARTESIAN_POINT('Ctrl Pts',(138.427461920942,-4.68065702215611,132.320707038274));
#36190=CARTESIAN_POINT('Ctrl Pts',(138.419697167995,-4.63664983598088,132.450393129695));
#36191=CARTESIAN_POINT('Ctrl Pts',(138.411932415048,-4.58724986287797,132.578148022535));
#36192=CARTESIAN_POINT('Ctrl Pts',(138.404175374163,-4.53789895452477,132.705776027414));
#36193=CARTESIAN_POINT('Ctrl Pts',(138.396418333278,-4.48316605839848,132.831476288512));
#36194=CARTESIAN_POINT('Ctrl Pts',(138.388661292393,-4.42322765084366,132.954765279789));
#36195=CARTESIAN_POINT('Ctrl Pts',(138.380910101153,-4.36333444330832,133.077961297879));
#36196=CARTESIAN_POINT('Ctrl Pts',(138.373158909913,-4.29824370809723,133.198749315287));
#36197=CARTESIAN_POINT('Ctrl Pts',(138.365407718673,-4.22818010291886,133.316665551244));
#36198=CARTESIAN_POINT('Ctrl Pts',(138.357659821896,-4.1581462766416,133.434531669654));
#36199=CARTESIAN_POINT('Ctrl Pts',(138.349911925119,-4.08314398348298,133.549528098856));
#36200=CARTESIAN_POINT('Ctrl Pts',(138.342164028342,-4.00344381182405,133.661215655552));
#36201=CARTESIAN_POINT('Ctrl Pts',(138.334417752258,-3.92376031172279,133.77287984962));
#36202=CARTESIAN_POINT('Ctrl Pts',(138.326671476173,-3.83938111471063,133.881236229854));
#36203=CARTESIAN_POINT('Ctrl Pts',(138.318925200089,-3.75061989851219,133.985874948727));
#36204=CARTESIAN_POINT('Ctrl Pts',(138.311178866824,-3.66185802709886,134.09051444002));
#36205=CARTESIAN_POINT('Ctrl Pts',(138.303432533559,-3.56871432486036,134.191435917044));
#36206=CARTESIAN_POINT('Ctrl Pts',(138.295686200293,-3.47154221882925,134.288263269103));
#36207=CARTESIAN_POINT('Ctrl Pts',(138.28793813229,-3.37434835177861,134.385112304976));
#36208=CARTESIAN_POINT('Ctrl Pts',(138.280190064287,-3.27312456268692,134.477865115547));
#36209=CARTESIAN_POINT('Ctrl Pts',(138.272441996284,-3.1682602288177,134.566183338667));
#36210=CARTESIAN_POINT('Ctrl Pts',(138.264685693542,-3.06328444388646,134.654595427445));
#36211=CARTESIAN_POINT('Ctrl Pts',(138.256929390801,-2.95466068451977,134.738563261528));
#36212=CARTESIAN_POINT('Ctrl Pts',(138.249173088059,-2.84281086104595,134.817789260362));
#36213=CARTESIAN_POINT('Ctrl Pts',(138.241412645545,-2.73090133995354,134.897057544498));
#36214=CARTESIAN_POINT('Ctrl Pts',(138.23365220303,-2.6157626518835,134.971578738105));
#36215=CARTESIAN_POINT('Ctrl Pts',(138.225891760516,-2.49784376683901,135.041099880131));
#36216=CARTESIAN_POINT('Ctrl Pts',(138.218118860251,-2.37973558793199,135.110732623667));
#36217=CARTESIAN_POINT('Ctrl Pts',(138.210345959985,-2.25883863852052,135.175349091667));
#36218=CARTESIAN_POINT('Ctrl Pts',(138.20257305972,-2.13562524892375,135.234742977889));
#36219=CARTESIAN_POINT('Ctrl Pts',(138.195082723958,-2.01689097639495,135.291977746742));
#36220=CARTESIAN_POINT('Ctrl Pts',(138.187592388196,-1.89600603921056,135.34436292706));
#36221=CARTESIAN_POINT('Ctrl Pts',(138.180102052434,-1.77340688246443,135.391757601884));
#36222=CARTESIAN_POINT('Ctrl Pts',(138.172327718315,-1.6461593414268,135.440949260209));
#36223=CARTESIAN_POINT('Ctrl Pts',(138.164553384196,-1.51666194356741,135.484920337067));
#36224=CARTESIAN_POINT('Ctrl Pts',(138.156779050077,-1.38538220800074,135.5234600232));
#36225=CARTESIAN_POINT('Ctrl Pts',(138.14901429713,-1.25426426297534,135.561952212615));
#36226=CARTESIAN_POINT('Ctrl Pts',(138.141249544183,-1.12136872229903,135.595026220709));
#36227=CARTESIAN_POINT('Ctrl Pts',(138.133484791235,-0.987183020622717,
135.622519264424));
#36228=CARTESIAN_POINT('Ctrl Pts',(138.12572775035,-0.853130594077,135.649985001661));
#36229=CARTESIAN_POINT('Ctrl Pts',(138.117970709465,-0.717790937117477,
135.671880727557));
#36230=CARTESIAN_POINT('Ctrl Pts',(138.11021366858,-0.581666243669646,135.688093559023));
#36231=CARTESIAN_POINT('Ctrl Pts',(138.10246247734,-0.44564420291241,135.704294164268));
#36232=CARTESIAN_POINT('Ctrl Pts',(138.0947112861,-0.308838690661705,135.714820359089));
#36233=CARTESIAN_POINT('Ctrl Pts',(138.08696009486,-0.171761331792822,135.719610469547));
#36234=CARTESIAN_POINT('Ctrl Pts',(138.079212198083,-0.0347422344578371,
135.72439854408));
#36235=CARTESIAN_POINT('Ctrl Pts',(138.071464301306,0.102548089782278,135.723455369598));
#36236=CARTESIAN_POINT('Ctrl Pts',(138.063716404529,0.239593883953647,135.71677121047));
#36237=CARTESIAN_POINT('Ctrl Pts',(138.055970128445,0.37661101109924,135.710088449524));
#36238=CARTESIAN_POINT('Ctrl Pts',(138.048223852361,0.51338331966346,135.697667111602));
#36239=CARTESIAN_POINT('Ctrl Pts',(138.040477576277,0.649396442842379,135.67954957006));
#36240=CARTESIAN_POINT('Ctrl Pts',(138.032731243011,0.785410570039183,135.661431894779));
#36241=CARTESIAN_POINT('Ctrl Pts',(138.024984909746,0.92066511312588,135.637617983595));
#36242=CARTESIAN_POINT('Ctrl Pts',(138.017238576481,1.05465260357668,135.608201887661));
#36243=CARTESIAN_POINT('Ctrl Pts',(138.009490508478,1.18867009959695,135.578779204197));
#36244=CARTESIAN_POINT('Ctrl Pts',(138.001742440475,1.32141959655889,135.543751923354));
#36245=CARTESIAN_POINT('Ctrl Pts',(137.993994372472,1.45240595288155,135.503264746247));
#36246=CARTESIAN_POINT('Ctrl Pts',(137.98623806973,1.58353152306256,135.462734538886));
#36247=CARTESIAN_POINT('Ctrl Pts',(137.978481766988,1.71288983518903,135.416732959096));
#36248=CARTESIAN_POINT('Ctrl Pts',(137.970725464246,1.84000247347685,135.365454122429));
#36249=CARTESIAN_POINT('Ctrl Pts',(137.962965021732,1.96718295560701,135.314147916702));
#36250=CARTESIAN_POINT('Ctrl Pts',(137.955204579218,2.09211501965882,135.257559002958));
#36251=CARTESIAN_POINT('Ctrl Pts',(137.947444136704,2.21434316308179,135.195928380747));
#36252=CARTESIAN_POINT('Ctrl Pts',(137.939671236438,2.33676751797156,135.134198823591));
#36253=CARTESIAN_POINT('Ctrl Pts',(137.931898336173,2.45647893676274,135.06741157537));
#36254=CARTESIAN_POINT('Ctrl Pts',(137.924125435907,2.57304854209484,134.995852507398));
#36255=CARTESIAN_POINT('Ctrl Pts',(137.916635100145,2.68538054865303,134.926894791791));
#36256=CARTESIAN_POINT('Ctrl Pts',(137.909144764383,2.79479494580824,134.853506340039));
#36257=CARTESIAN_POINT('Ctrl Pts',(137.901654428621,2.90093726689751,134.7759781767));
#36258=CARTESIAN_POINT('Ctrl Pts',(137.893880094502,3.01110400635121,134.695510509485));
#36259=CARTESIAN_POINT('Ctrl Pts',(137.886105760383,3.11809462533035,134.610328122204));
#36260=CARTESIAN_POINT('Ctrl Pts',(137.878331426264,3.22147905853459,134.520710404376));
#36261=CARTESIAN_POINT('Ctrl Pts',(137.870566673317,3.32473607966456,134.431203132376));
#36262=CARTESIAN_POINT('Ctrl Pts',(137.86280192037,3.42439546526849,134.33727165946));
#36263=CARTESIAN_POINT('Ctrl Pts',(137.855037167422,3.5200567910136,134.239238089986));
#36264=CARTESIAN_POINT('Ctrl Pts',(137.847280126537,3.61562310458133,134.141301888836));
#36265=CARTESIAN_POINT('Ctrl Pts',(137.839523085652,3.707198989338,134.039271977097));
#36266=CARTESIAN_POINT('Ctrl Pts',(137.831766044767,3.79441802546119,133.933509848676));
#36267=CARTESIAN_POINT('Ctrl Pts',(137.824014853527,3.88157128903082,133.827827476298));
#36268=CARTESIAN_POINT('Ctrl Pts',(137.816263662287,3.96437399588384,133.718418789726));
#36269=CARTESIAN_POINT('Ctrl Pts',(137.808512471047,4.04249771224427,133.605680897184));
#36270=CARTESIAN_POINT('Ctrl Pts',(137.80076457427,4.12058822394123,133.492990921254));
#36271=CARTESIAN_POINT('Ctrl Pts',(137.793016677493,4.19400347829145,133.376974874361));
#36272=CARTESIAN_POINT('Ctrl Pts',(137.785268780716,4.26245650519108,133.258061415107));
#36273=CARTESIAN_POINT('Ctrl Pts',(137.777522504632,4.33089521319321,133.139172829986));
#36274=CARTESIAN_POINT('Ctrl Pts',(137.769776228548,4.39437356343792,133.017388376643));
#36275=CARTESIAN_POINT('Ctrl Pts',(137.762029952464,4.45264917800659,132.893163710272));
#36276=CARTESIAN_POINT('Ctrl Pts',(137.754283619198,4.51092522275257,132.768938126902));
#36277=CARTESIAN_POINT('Ctrl Pts',(137.746537285933,4.56399828914259,132.642272648513));
#36278=CARTESIAN_POINT('Ctrl Pts',(137.738790952667,4.61167320594162,132.513645059694));
#36279=CARTESIAN_POINT('Ctrl Pts',(137.731042884664,4.65935879920771,132.384988665618));
#36280=CARTESIAN_POINT('Ctrl Pts',(137.723294816662,4.70164370150549,132.254369653278));
#36281=CARTESIAN_POINT('Ctrl Pts',(137.715546748659,4.73838201786046,132.122282813796));
#36282=CARTESIAN_POINT('Ctrl Pts',(137.707790445917,4.77515938013527,131.99005559085));
#36283=CARTESIAN_POINT('Ctrl Pts',(137.700034143175,4.80637827568231,131.856357801712));
#36284=CARTESIAN_POINT('Ctrl Pts',(137.692277840433,4.83194342399536,131.72169687533));
#36285=CARTESIAN_POINT('Ctrl Pts',(137.684517397919,4.85752221719785,131.586964076356));
#36286=CARTESIAN_POINT('Ctrl Pts',(137.676756955405,4.87744119363868,131.451267502469));
#36287=CARTESIAN_POINT('Ctrl Pts',(137.66899651289,4.8916569028114,131.31512064701));
#36288=CARTESIAN_POINT('Ctrl Pts',(137.661223612625,4.90589543230249,131.178755236532));
#36289=CARTESIAN_POINT('Ctrl Pts',(137.65345071236,4.91441237483225,131.041938490467));
#36290=CARTESIAN_POINT('Ctrl Pts',(137.645677812094,4.91721642334132,130.905185755911));
#36291=CARTESIAN_POINT('Ctrl Pts',(137.638187476332,4.91991853762411,130.773404327717));
#36292=CARTESIAN_POINT('Ctrl Pts',(137.63069714057,4.91731590895363,130.641682645831));
#36293=CARTESIAN_POINT('Ctrl Pts',(137.623206804808,4.90946178664443,130.510476238978));
#36294=CARTESIAN_POINT('Ctrl Pts',(137.615432470689,4.90130987290062,130.374295101329));
#36295=CARTESIAN_POINT('Ctrl Pts',(137.60765813657,4.88747456093996,130.23823770243));
#36296=CARTESIAN_POINT('Ctrl Pts',(137.599883802451,4.86795844827736,130.102816885255));
#36297=CARTESIAN_POINT('Ctrl Pts',(137.592119049504,4.84846638747943,129.967562962134));
#36298=CARTESIAN_POINT('Ctrl Pts',(137.584354296557,4.82330751127265,129.832944443011));
#36299=CARTESIAN_POINT('Ctrl Pts',(137.57658954361,4.79253637604242,129.699472321488));
#36300=CARTESIAN_POINT('Ctrl Pts',(137.568832502725,4.76179580313749,129.566132766358));
#36301=CARTESIAN_POINT('Ctrl Pts',(137.56107546184,4.72545415133071,129.433937721434));
#36302=CARTESIAN_POINT('Ctrl Pts',(137.553318420955,4.68361749681892,129.303390862377));
#36303=CARTESIAN_POINT('Ctrl Pts',(137.545567229715,4.64181239165377,129.172942449722));
#36304=CARTESIAN_POINT('Ctrl Pts',(137.537816038475,4.59452065064799,129.044140119804));
#36305=CARTESIAN_POINT('Ctrl Pts',(137.530064847234,4.54189884572014,128.917474839956));
#36306=CARTESIAN_POINT('Ctrl Pts',(137.522316950457,4.48929940646308,128.790863396231));
#36307=CARTESIAN_POINT('Ctrl Pts',(137.51456905368,4.43137455871004,128.666387556323));
#36308=CARTESIAN_POINT('Ctrl Pts',(137.506821156903,4.36832983073338,128.544520456753));
#36309=CARTESIAN_POINT('Ctrl Pts',(137.499074880819,4.30529829035469,128.422678849152));
#36310=CARTESIAN_POINT('Ctrl Pts',(137.491328604735,4.23714917949465,128.303445243509));
#36311=CARTESIAN_POINT('Ctrl Pts',(137.483582328651,4.16413484258633,128.187269851991));
#36312=CARTESIAN_POINT('Ctrl Pts',(137.475835995386,4.09111996670282,128.071093602893));
#36313=CARTESIAN_POINT('Ctrl Pts',(137.46808966212,4.013240001147,127.957975943986));
#36314=CARTESIAN_POINT('Ctrl Pts',(137.460343328855,3.93079142480495,127.848339332599));
#36315=CARTESIAN_POINT('Ctrl Pts',(137.452595260852,3.84832438467595,127.738678168852));
#36316=CARTESIAN_POINT('Ctrl Pts',(137.444847192849,3.76128693283012,127.632499916262));
#36317=CARTESIAN_POINT('Ctrl Pts',(137.437099124846,3.67001649125362,127.53019476709));
#36318=CARTESIAN_POINT('Ctrl Pts',(137.429342822104,3.57864904636561,127.427780886787));
#36319=CARTESIAN_POINT('Ctrl Pts',(137.421586519362,3.48303988545323,127.329248625019));
#36320=CARTESIAN_POINT('Ctrl Pts',(137.413830216621,3.38356442141867,127.234952421715));
#36321=CARTESIAN_POINT('Ctrl Pts',(137.406069774106,3.28403586433368,127.140605889688));
#36322=CARTESIAN_POINT('Ctrl Pts',(137.398309331592,3.18063718691026,127.050500177914));
#36323=CARTESIAN_POINT('Ctrl Pts',(137.390548889078,3.07377691957879,126.96494939823));
#36324=CARTESIAN_POINT('Ctrl Pts',(137.382775988813,2.96674511065966,126.879261284839));
#36325=CARTESIAN_POINT('Ctrl Pts',(137.375003088547,2.85624092281886,126.798142946693));
#36326=CARTESIAN_POINT('Ctrl Pts',(137.367230188282,2.7427026309104,126.721865627869));
#36327=CARTESIAN_POINT('Ctrl Pts',(137.35973985252,2.63329174189834,126.648361181716));
#36328=CARTESIAN_POINT('Ctrl Pts',(137.352249516758,2.52106377600558,126.579352060385));
#36329=CARTESIAN_POINT('Ctrl Pts',(137.344759180996,2.40643076500545,126.515039688126));
#36330=CARTESIAN_POINT('Ctrl Pts',(137.336984846877,2.28745140855148,126.448288892724));
#36331=CARTESIAN_POINT('Ctrl Pts',(137.329210512758,2.1655041414502,126.386386585021));
#36332=CARTESIAN_POINT('Ctrl Pts',(137.321436178638,2.0410218370425,126.329607783809));
#36333=CARTESIAN_POINT('Ctrl Pts',(137.313671425691,1.91669294594976,126.272898957395));
#36334=CARTESIAN_POINT('Ctrl Pts',(137.305906672744,1.78983558608679,126.221301234658));
#36335=CARTESIAN_POINT('Ctrl Pts',(137.298141919797,1.66090915990418,126.17504492029));
#36336=CARTESIAN_POINT('Ctrl Pts',(137.290384878912,1.5321107852656,126.128834548346));
#36337=CARTESIAN_POINT('Ctrl Pts',(137.282627838027,1.40124779951728,126.087955158435));
#36338=CARTESIAN_POINT('Ctrl Pts',(137.274870797142,1.26880129603253,126.052589754647));
#36339=CARTESIAN_POINT('Ctrl Pts',(137.267119605902,1.13645467148634,126.017251020185));
#36340=CARTESIAN_POINT('Ctrl Pts',(137.259368414662,1.00252728227598,125.987418095772));
#36341=CARTESIAN_POINT('Ctrl Pts',(137.251617223422,0.867516824070355,125.963224632856));
#36342=CARTESIAN_POINT('Ctrl Pts',(137.243869326645,0.732563748910991,125.939041452807));
#36343=CARTESIAN_POINT('Ctrl Pts',(137.236121429868,0.596528904353548,125.920493035777));
#36344=CARTESIAN_POINT('Ctrl Pts',(137.228373533091,0.459921446604906,125.907662206856));
#36345=CARTESIAN_POINT('Ctrl Pts',(137.220627257006,0.32334256419151,125.894834061868));
#36346=CARTESIAN_POINT('Ctrl Pts',(137.212880980922,0.186191695837987,125.887721162624));
#36347=CARTESIAN_POINT('Ctrl Pts',(137.205134704838,0.0489840161228252,
125.886354555282));
#36348=CARTESIAN_POINT('Ctrl Pts',(137.197388371573,-0.0882246764282594,
125.884987937851));
#36349=CARTESIAN_POINT('Ctrl Pts',(137.189642038308,-0.225489790231987,
125.889367700857));
#36350=CARTESIAN_POINT('Ctrl Pts',(137.181895705042,-0.362295645893674,
125.899472756721));
#36351=CARTESIAN_POINT('Ctrl Pts',(137.174147637039,-0.499132138278191,
125.909580075542));
#36352=CARTESIAN_POINT('Ctrl Pts',(137.166399569036,-0.63550877803731,125.925415209735));
#36353=CARTESIAN_POINT('Ctrl Pts',(137.158651501033,-0.770914900545521,
125.946905185077));
#36354=CARTESIAN_POINT('Ctrl Pts',(137.150895198291,-0.906464934292087,
125.96841800022));
#36355=CARTESIAN_POINT('Ctrl Pts',(137.14313889555,-1.04104200355258,125.995597600818));
#36356=CARTESIAN_POINT('Ctrl Pts',(137.135382592808,-1.17414498813358,126.028319724803));
#36357=CARTESIAN_POINT('Ctrl Pts',(137.127622150293,-1.30731901378509,126.061059313571));
#36358=CARTESIAN_POINT('Ctrl Pts',(137.119861707779,-1.43901701182668,126.099347211123));
#36359=CARTESIAN_POINT('Ctrl Pts',(137.112101265265,-1.56875389039883,126.143009494355));
#36360=CARTESIAN_POINT('Ctrl Pts',(137.104328365,-1.69869903412606,126.186741868161));
#36361=CARTESIAN_POINT('Ctrl Pts',(137.096555464734,-1.8266764021414,126.23586572784));
#36362=CARTESIAN_POINT('Ctrl Pts',(137.088782564469,-1.95222089085743,126.290158954392));
#36363=CARTESIAN_POINT('Ctrl Pts',(137.081292228707,-2.07320152117996,126.342478485403));
#36364=CARTESIAN_POINT('Ctrl Pts',(137.073801892945,-2.19192280627911,126.399597935849));
#36365=CARTESIAN_POINT('Ctrl Pts',(137.066311557183,-2.30799256899358,126.461279526454));
#36366=CARTESIAN_POINT('Ctrl Pts',(137.058536284961,-2.4284776888173,126.525307518425));
#36367=CARTESIAN_POINT('Ctrl Pts',(137.05076101274,-2.54648726911118,126.594454459831));
#36368=CARTESIAN_POINT('Ctrl Pts',(137.042985740518,-2.66155578285581,126.668504735497));
#36369=CARTESIAN_POINT('Ctrl Pts',(137.035220256517,-2.77647943787687,126.742461789932));
#36370=CARTESIAN_POINT('Ctrl Pts',(137.027454772516,-2.88846906809892,126.821309685809));
#36371=CARTESIAN_POINT('Ctrl Pts',(137.019689288515,-2.99708247263446,126.904786318399));
#36372=CARTESIAN_POINT('Ctrl Pts',(137.011933107671,-3.10556575681877,126.988162944835));
#36373=CARTESIAN_POINT('Ctrl Pts',(137.004176926827,-3.2106805629706,127.076157027058));
#36374=CARTESIAN_POINT('Ctrl Pts',(136.996420745982,-3.31201302418701,127.168462820582));
#36375=CARTESIAN_POINT('Ctrl Pts',(136.988669840552,-3.41327656350487,127.260705831751));
#36376=CARTESIAN_POINT('Ctrl Pts',(136.980918935122,-3.51076258802983,127.357254457942));
#36377=CARTESIAN_POINT('Ctrl Pts',(136.973168029692,-3.60408968145251,127.457762250485));
#36378=CARTESIAN_POINT('Ctrl Pts',(136.965420717481,-3.69737350964463,127.558223448919));
#36379=CARTESIAN_POINT('Ctrl Pts',(136.95767340527,-3.78650197791445,127.662639875589));
#36380=CARTESIAN_POINT('Ctrl Pts',(136.94992609306,-3.87113027098331,127.770628017686));
#36381=CARTESIAN_POINT('Ctrl Pts',(136.942180694645,-3.95573765857231,127.878589483788));
#36382=CARTESIAN_POINT('Ctrl Pts',(136.93443529623,-4.03584684328171,127.990120601348));
#36383=CARTESIAN_POINT('Ctrl Pts',(136.926689897815,-4.11115334144958,128.10480486419));
#36384=CARTESIAN_POINT('Ctrl Pts',(136.918942015748,-4.18648398752441,128.219525901878));
#36385=CARTESIAN_POINT('Ctrl Pts',(136.91119413368,-4.25700864966831,128.337401781762));
#36386=CARTESIAN_POINT('Ctrl Pts',(136.903446251613,-4.32246617463714,128.457986983292));
#36387=CARTESIAN_POINT('Ctrl Pts',(136.89569736074,-4.38793222244506,128.578587885511));
#36388=CARTESIAN_POINT('Ctrl Pts',(136.887948469866,-4.44832963932198,128.701898464539));
#36389=CARTESIAN_POINT('Ctrl Pts',(136.880199578993,-4.50344373176889,128.827449487219));
#36390=CARTESIAN_POINT('Ctrl Pts',(136.872443501781,-4.55860893714959,128.9531169462));
#36391=CARTESIAN_POINT('Ctrl Pts',(136.864687424568,-4.60848087711548,129.081028639127));
#36392=CARTESIAN_POINT('Ctrl Pts',(136.856931347356,-4.65289325216137,129.21069583271));
#36393=CARTESIAN_POINT('Ctrl Pts',(136.84960363452,-4.69485275330791,129.33320157018));
#36394=CARTESIAN_POINT('Ctrl Pts',(136.842275921685,-4.7319394296721,129.45727383743));
#36395=CARTESIAN_POINT('Ctrl Pts',(136.834948208849,-4.76405452823407,129.582490119308));
#36396=CARTESIAN_POINT('Ctrl Pts',(138.584929581679,-4.76405452823406,129.582490119308));
#36397=CARTESIAN_POINT('Ctrl Pts',(138.577290381644,-4.79768433680502,129.713612232523));
#36398=CARTESIAN_POINT('Ctrl Pts',(138.569651181608,-4.82588585814068,129.84608197248));
#36399=CARTESIAN_POINT('Ctrl Pts',(138.562011981572,-4.84856978594709,129.979403592442));
#36400=CARTESIAN_POINT('Ctrl Pts',(138.554153223984,-4.87190567045693,130.116556996943));
#36401=CARTESIAN_POINT('Ctrl Pts',(138.546294466396,-4.88940194006727,130.254611535898));
#36402=CARTESIAN_POINT('Ctrl Pts',(138.538435708807,-4.90101860449271,130.393021705091));
#36403=CARTESIAN_POINT('Ctrl Pts',(138.530576951219,-4.91263526891816,130.531431874284));
#36404=CARTESIAN_POINT('Ctrl Pts',(138.522718193631,-4.91837235026494,130.670197211417));
#36405=CARTESIAN_POINT('Ctrl Pts',(138.514859436043,-4.91824802050565,130.808773246294));
#36406=CARTESIAN_POINT('',(138.860140564037,-4.91824998799066,130.804016917383));
#36407=CARTESIAN_POINT('Ctrl Pts',(138.929858124837,-4.76405452823407,129.582490119308));
#36408=CARTESIAN_POINT('Ctrl Pts',(138.921678643293,-4.79993071147542,129.722370813269));
#36409=CARTESIAN_POINT('Ctrl Pts',(138.913499161748,-4.82968047010897,129.863982586788));
#36410=CARTESIAN_POINT('Ctrl Pts',(138.905319680203,-4.85314793322502,130.006777894124));
#36411=CARTESIAN_POINT('Ctrl Pts',(138.897157381201,-4.87656609851148,130.149273233001));
#36412=CARTESIAN_POINT('Ctrl Pts',(138.888995082198,-4.89372823319955,130.292946829293));
#36413=CARTESIAN_POINT('Ctrl Pts',(138.880832783196,-4.90452904142768,130.437239460055));
#36414=CARTESIAN_POINT('Ctrl Pts',(138.87393537681,-4.91365607336216,130.559171395245));
#36415=CARTESIAN_POINT('Ctrl Pts',(138.867037970423,-4.91824142933335,130.681545011985));
#36416=CARTESIAN_POINT('Ctrl Pts',(138.860140564037,-4.91824998799067,130.804016917383));
#36417=CARTESIAN_POINT('Ctrl Pts',(138.860140564008,-4.9182499879907,130.804016917894));
#36418=CARTESIAN_POINT('Ctrl Pts',(138.852067034098,-4.91826000602782,130.947372338169));
#36419=CARTESIAN_POINT('Ctrl Pts',(138.843993504189,-4.91199799204111,131.090620741002));
#36420=CARTESIAN_POINT('Ctrl Pts',(138.835919974279,-4.89951787644956,131.233205159156));
#36421=CARTESIAN_POINT('Ctrl Pts',(138.827837244499,-4.88702353963818,131.375952053717));
#36422=CARTESIAN_POINT('Ctrl Pts',(138.819754514719,-4.86829699567183,131.518033115249));
#36423=CARTESIAN_POINT('Ctrl Pts',(138.811671784939,-4.84344365772086,131.658899438793));
#36424=CARTESIAN_POINT('Ctrl Pts',(138.803571331097,-4.81853582059472,131.800074658408));
#36425=CARTESIAN_POINT('Ctrl Pts',(138.795470877255,-4.78747438949765,131.940029478287));
#36426=CARTESIAN_POINT('Ctrl Pts',(138.787370423413,-4.75041567751435,132.078226369255));
#36427=CARTESIAN_POINT('Ctrl Pts',(138.779260814515,-4.71331508212753,132.216579449034));
#36428=CARTESIAN_POINT('Ctrl Pts',(138.771151205617,-4.67020378374145,132.353170311098));
#36429=CARTESIAN_POINT('Ctrl Pts',(138.763041596719,-4.6212870625238,132.487479433411));
#36430=CARTESIAN_POINT('Ctrl Pts',(138.754913574557,-4.57225927349625,132.62209351116));
#36431=CARTESIAN_POINT('Ctrl Pts',(138.746785552396,-4.51739983376362,132.75441517391));
#36432=CARTESIAN_POINT('Ctrl Pts',(138.738657530234,-4.45696176081644,132.88394589476));
#36433=CARTESIAN_POINT('Ctrl Pts',(138.731574454789,-4.40429366741349,132.996824015646));
#36434=CARTESIAN_POINT('Ctrl Pts',(138.724491379345,-4.34738992070749,133.10758294576));
#36435=CARTESIAN_POINT('Ctrl Pts',(138.7174083039,-4.28644493324192,133.215910512713));
#36436=CARTESIAN_POINT('Ctrl Pts',(138.709633969781,-4.21955214081599,133.334810093328));
#36437=CARTESIAN_POINT('Ctrl Pts',(138.701859635662,-4.14760250062957,133.45111263384));
#36438=CARTESIAN_POINT('Ctrl Pts',(138.694085301543,-4.07082265219019,133.564358080774));
#36439=CARTESIAN_POINT('Ctrl Pts',(138.686320548596,-3.99413742805201,133.677463962816));
#36440=CARTESIAN_POINT('Ctrl Pts',(138.678555795649,-3.91263405725212,133.787519927177));
#36441=CARTESIAN_POINT('Ctrl Pts',(138.670791042702,-3.82658509601864,133.894090308887));
#36442=CARTESIAN_POINT('Ctrl Pts',(138.663034001817,-3.74062159982659,134.000554843391));
#36443=CARTESIAN_POINT('Ctrl Pts',(138.655276960932,-3.65012174176799,134.103540382423));
#36444=CARTESIAN_POINT('Ctrl Pts',(138.647519920047,-3.55540120814913,134.202640375266));
#36445=CARTESIAN_POINT('Ctrl Pts',(138.639768728807,-3.46075210402123,134.301665636033));
#36446=CARTESIAN_POINT('Ctrl Pts',(138.632017537567,-3.3618889286371,134.396810901353));
#36447=CARTESIAN_POINT('Ctrl Pts',(138.624266346327,-3.25916721983027,134.487703134314));
#36448=CARTESIAN_POINT('Ctrl Pts',(138.61651844955,-3.15648917049015,134.578556735651));
#36449=CARTESIAN_POINT('Ctrl Pts',(138.608770552772,-3.04995614170784,134.665160641375));
#36450=CARTESIAN_POINT('Ctrl Pts',(138.601022655995,-2.93995989808493,134.747179261652));
#36451=CARTESIAN_POINT('Ctrl Pts',(138.593276379911,-2.8299866633048,134.829180725402));
#36452=CARTESIAN_POINT('Ctrl Pts',(138.585530103827,-2.71655196784174,134.906598577936));
#36453=CARTESIAN_POINT('Ctrl Pts',(138.577783827743,-2.6000796506556,134.979138320959));
#36454=CARTESIAN_POINT('Ctrl Pts',(138.570037494478,-2.48360647369751,135.051678599453));
#36455=CARTESIAN_POINT('Ctrl Pts',(138.562291161212,-2.36409596213738,135.119340489895));
#36456=CARTESIAN_POINT('Ctrl Pts',(138.554544827947,-2.24199950496182,135.181873756581));
#36457=CARTESIAN_POINT('Ctrl Pts',(138.546796759944,-2.11987570513131,135.244421027159));
#36458=CARTESIAN_POINT('Ctrl Pts',(138.539048691941,-1.99516515524824,135.301837210372));
#36459=CARTESIAN_POINT('Ctrl Pts',(138.531300623938,-1.86834195175459,135.353918993256));
#36460=CARTESIAN_POINT('Ctrl Pts',(138.523544321196,-1.7413839590508,135.40605612928));
#36461=CARTESIAN_POINT('Ctrl Pts',(138.515788018455,-1.61230918963471,135.452847390853));
#36462=CARTESIAN_POINT('Ctrl Pts',(138.508031715713,-1.48161026732753,135.494138232576));
#36463=CARTESIAN_POINT('Ctrl Pts',(138.500271273199,-1.35084158707007,135.535451112465));
#36464=CARTESIAN_POINT('Ctrl Pts',(138.492510830684,-1.21844740385234,135.571257620773));
#36465=CARTESIAN_POINT('Ctrl Pts',(138.48475038817,-1.0849324850198,135.601453963067));
#36466=CARTESIAN_POINT('Ctrl Pts',(138.476977487905,-0.951203236186739,
135.63169877921));
#36467=CARTESIAN_POINT('Ctrl Pts',(138.469204587639,-0.816350041386251,
135.65631536236));
#36468=CARTESIAN_POINT('Ctrl Pts',(138.461431687374,-0.680885667340857,
135.675251477615));
#36469=CARTESIAN_POINT('Ctrl Pts',(138.453941351612,-0.550345764507372,
135.693499217384));
#36470=CARTESIAN_POINT('Ctrl Pts',(138.44645101585,-0.419238653289755,135.706472287298));
#36471=CARTESIAN_POINT('Ctrl Pts',(138.438960680088,-0.288022963226061,
135.714169762039));
#36472=CARTESIAN_POINT('Ctrl Pts',(138.431186345969,-0.151832190390304,
135.722159088875));
#36473=CARTESIAN_POINT('Ctrl Pts',(138.42341201185,-0.015093031210281,135.724490182861));
#36474=CARTESIAN_POINT('Ctrl Pts',(138.415637677731,0.121684954106831,135.721105052092));
#36475=CARTESIAN_POINT('Ctrl Pts',(138.407872924784,0.258294372781518,135.717724093195));
#36476=CARTESIAN_POINT('Ctrl Pts',(138.400108171837,0.394942135293119,135.708640936049));
#36477=CARTESIAN_POINT('Ctrl Pts',(138.392343418889,0.531114381065231,135.69384940237));
#36478=CARTESIAN_POINT('Ctrl Pts',(138.384586378004,0.667151378642781,135.679072559851));
#36479=CARTESIAN_POINT('Ctrl Pts',(138.376829337119,0.802713413195336,135.658598665586));
#36480=CARTESIAN_POINT('Ctrl Pts',(138.369072296234,0.93728780593003,135.632473564811));
#36481=CARTESIAN_POINT('Ctrl Pts',(138.361321104994,1.07176071506823,135.606368165178));
#36482=CARTESIAN_POINT('Ctrl Pts',(138.353569913754,1.20524708259767,135.574620115734));
#36483=CARTESIAN_POINT('Ctrl Pts',(138.345818722514,1.33724088511658,135.537326904967));
#36484=CARTESIAN_POINT('Ctrl Pts',(138.338070825737,1.46917858674854,135.500049544809));
#36485=CARTESIAN_POINT('Ctrl Pts',(138.33032292896,1.59962460965452,135.457231816984));
#36486=CARTESIAN_POINT('Ctrl Pts',(138.322575032183,1.72808485426766,135.409021929644));
#36487=CARTESIAN_POINT('Ctrl Pts',(138.314828756099,1.856518227767,135.360822126774));
#36488=CARTESIAN_POINT('Ctrl Pts',(138.307082480015,1.98296628338582,135.307232545174));
#36489=CARTESIAN_POINT('Ctrl Pts',(138.299336203931,2.10695215605658,135.248450589044));
#36490=CARTESIAN_POINT('Ctrl Pts',(138.291589870665,2.23093894396279,135.189668198998));
#36491=CARTESIAN_POINT('Ctrl Pts',(138.2838435374,2.35246315938058,135.125693525426));
#36492=CARTESIAN_POINT('Ctrl Pts',(138.276097204134,2.47107028515328,135.056771076157));
#36493=CARTESIAN_POINT('Ctrl Pts',(138.268349136131,2.5897039721696,134.987833192183));
#36494=CARTESIAN_POINT('Ctrl Pts',(138.260601068128,2.70541893165399,134.913945524074));
#36495=CARTESIAN_POINT('Ctrl Pts',(138.252853000125,2.8177878499451,134.835397046972));
#36496=CARTESIAN_POINT('Ctrl Pts',(138.245096697384,2.93027619525954,134.756765087614));
#36497=CARTESIAN_POINT('Ctrl Pts',(138.237340394642,3.03941107451428,134.673462648338));
#36498=CARTESIAN_POINT('Ctrl Pts',(138.2295840919,3.14479618907911,134.585820651951));
#36499=CARTESIAN_POINT('Ctrl Pts',(138.221823649386,3.25023755085296,134.498131878392));
#36500=CARTESIAN_POINT('Ctrl Pts',(138.214063206872,3.35192487032253,134.406099194816));
#36501=CARTESIAN_POINT('Ctrl Pts',(138.206302764357,3.44949798321141,134.31009117286));
#36502=CARTESIAN_POINT('Ctrl Pts',(138.198529864092,3.54722772912304,134.213929030304));
#36503=CARTESIAN_POINT('Ctrl Pts',(138.190756963826,3.64082980346662,134.113779082763));
#36504=CARTESIAN_POINT('Ctrl Pts',(138.182984063561,3.72998309660246,134.010044501164));
#36505=CARTESIAN_POINT('Ctrl Pts',(138.175493727799,3.81589544296935,133.910080932898));
#36506=CARTESIAN_POINT('Ctrl Pts',(138.168003392037,3.89767665018792,133.806789068257));
#36507=CARTESIAN_POINT('Ctrl Pts',(138.160513056275,3.97507803929305,133.700554265102));
#36508=CARTESIAN_POINT('Ctrl Pts',(138.152738722156,4.05541412559163,133.590291537097));
#36509=CARTESIAN_POINT('Ctrl Pts',(138.144964388037,4.13128619655803,133.476509023064));
#36510=CARTESIAN_POINT('Ctrl Pts',(138.137190053918,4.20237003222244,133.359604084396));
#36511=CARTESIAN_POINT('Ctrl Pts',(138.12942530097,4.27336626341243,133.242843220617));
#36512=CARTESIAN_POINT('Ctrl Pts',(138.121660548023,4.33958579950162,133.122967919644));
#36513=CARTESIAN_POINT('Ctrl Pts',(138.113895795076,4.40074568833152,133.000407167421));
#36514=CARTESIAN_POINT('Ctrl Pts',(138.106138754191,4.46184483229747,132.877968144266));
#36515=CARTESIAN_POINT('Ctrl Pts',(138.098381713306,4.51789415616363,132.752849325327));
#36516=CARTESIAN_POINT('Ctrl Pts',(138.090624672421,4.56865511541544,132.625506822265));
#36517=CARTESIAN_POINT('Ctrl Pts',(138.082873481181,4.61937779543301,132.498260349174));
#36518=CARTESIAN_POINT('Ctrl Pts',(138.075122289941,4.66481990452005,132.368793891428));
#36519=CARTESIAN_POINT('Ctrl Pts',(138.067371098701,4.7047899444922,132.237585875753));
#36520=CARTESIAN_POINT('Ctrl Pts',(138.059623201924,4.74474299613117,132.106433626985));
#36521=CARTESIAN_POINT('Ctrl Pts',(138.051875305147,4.7792284907526,131.97354166572));
#36522=CARTESIAN_POINT('Ctrl Pts',(138.04412740837,4.80810404718821,131.839405802045));
#36523=CARTESIAN_POINT('Ctrl Pts',(138.036381132286,4.83697356347986,131.705297996701));
#36524=CARTESIAN_POINT('Ctrl Pts',(138.028634856202,4.86023539347157,131.569947188461));
#36525=CARTESIAN_POINT('Ctrl Pts',(138.020888580117,4.87779786168906,131.433861279203));
#36526=CARTESIAN_POINT('Ctrl Pts',(138.013142246852,4.89536045954871,131.29777436539));
#36527=CARTESIAN_POINT('Ctrl Pts',(138.005395913587,4.90722356164297,131.160952727481));
#36528=CARTESIAN_POINT('Ctrl Pts',(137.997649580321,4.91334720170772,131.023910926085));
#36529=CARTESIAN_POINT('Ctrl Pts',(137.989901512318,4.91947221311921,130.886838435128));
#36530=CARTESIAN_POINT('Ctrl Pts',(137.982153444315,4.91985518742833,130.749546073077));
#36531=CARTESIAN_POINT('Ctrl Pts',(137.974405376312,4.91450827413372,130.612549549139));
#36532=CARTESIAN_POINT('Ctrl Pts',(137.966649073571,4.90915567807605,130.475407423665));
#36533=CARTESIAN_POINT('Ctrl Pts',(137.958892770829,4.89806104466963,130.338562155683));
#36534=CARTESIAN_POINT('Ctrl Pts',(137.951136468087,4.88128857955614,130.202526034317));
#36535=CARTESIAN_POINT('Ctrl Pts',(137.943376025573,4.86450716247296,130.066417306376));
#36536=CARTESIAN_POINT('Ctrl Pts',(137.935615583059,4.84204193930341,129.931118971075));
#36537=CARTESIAN_POINT('Ctrl Pts',(137.927855140544,4.81400832221518,129.797133266794));
#36538=CARTESIAN_POINT('Ctrl Pts',(137.920082240279,4.78592970307612,129.662932476766));
#36539=CARTESIAN_POINT('Ctrl Pts',(137.912309340013,4.7522649233566,129.530048907728));
#36540=CARTESIAN_POINT('Ctrl Pts',(137.904536439748,4.71317961457157,129.398970642048));
#36541=CARTESIAN_POINT('Ctrl Pts',(137.897046103986,4.67551515521117,129.272657401493));
#36542=CARTESIAN_POINT('Ctrl Pts',(137.889555768224,4.63281752423003,129.148020779814));
#36543=CARTESIAN_POINT('Ctrl Pts',(137.882065432462,4.58527651705627,129.025478293006));
#36544=CARTESIAN_POINT('Ctrl Pts',(137.874291098343,4.53593297814532,128.898289570563));
#36545=CARTESIAN_POINT('Ctrl Pts',(137.866516764224,4.48121523423676,128.772954020323));
#36546=CARTESIAN_POINT('Ctrl Pts',(137.858742430105,4.42128234791134,128.649959201268));
#36547=CARTESIAN_POINT('Ctrl Pts',(137.850977677158,4.36142332351201,128.527115962335));
#36548=CARTESIAN_POINT('Ctrl Pts',(137.843212924211,4.29636211451729,128.406608062896));
#36549=CARTESIAN_POINT('Ctrl Pts',(137.835448171264,4.22630669639728,128.288905435996));
#36550=CARTESIAN_POINT('Ctrl Pts',(137.827691130379,4.15632085830635,128.171319713005));
#36551=CARTESIAN_POINT('Ctrl Pts',(137.819934089494,4.08135088101514,128.056534051604));
#36552=CARTESIAN_POINT('Ctrl Pts',(137.812177048609,4.00165156504272,127.944995685542));
#36553=CARTESIAN_POINT('Ctrl Pts',(137.804425857369,3.92201235094423,127.833541431428));
#36554=CARTESIAN_POINT('Ctrl Pts',(137.796674666129,3.83765112330837,127.72532991526));
#36555=CARTESIAN_POINT('Ctrl Pts',(137.788923474888,3.74886688664438,127.620780851215));
#36556=CARTESIAN_POINT('Ctrl Pts',(137.781175578111,3.66012038564932,127.516276223311));
#36557=CARTESIAN_POINT('Ctrl Pts',(137.773427681334,3.56695486713926,127.415431248875));
#36558=CARTESIAN_POINT('Ctrl Pts',(137.765679784557,3.46971050968245,127.318633714681));
#36559=CARTESIAN_POINT('Ctrl Pts',(137.757933508473,3.372486493649,127.221856428444));
#36560=CARTESIAN_POINT('Ctrl Pts',(137.750187232389,3.27118561265513,127.129125174081));
#36561=CARTESIAN_POINT('Ctrl Pts',(137.742440956305,3.16618562610208,127.040791614138));
#36562=CARTESIAN_POINT('Ctrl Pts',(137.73469462304,3.06118486446276,126.952457402136));
#36563=CARTESIAN_POINT('Ctrl Pts',(137.726948289774,2.95248524195363,126.868521201019));
#36564=CARTESIAN_POINT('Ctrl Pts',(137.719201956509,2.84049807024734,126.789294768116));
#36565=CARTESIAN_POINT('Ctrl Pts',(137.711453888506,2.7284858197908,126.710050593002));
#36566=CARTESIAN_POINT('Ctrl Pts',(137.703705820503,2.61318487424444,126.635518510629));
#36567=CARTESIAN_POINT('Ctrl Pts',(137.6959577525,2.49503568147119,126.565967052701));
#36568=CARTESIAN_POINT('Ctrl Pts',(137.688201449758,2.37676091832962,126.496341674657));
#36569=CARTESIAN_POINT('Ctrl Pts',(137.680445147016,2.25563219835964,126.431707693982));
#36570=CARTESIAN_POINT('Ctrl Pts',(137.672688844275,2.13211522962672,126.372287997437));
#36571=CARTESIAN_POINT('Ctrl Pts',(137.66492840176,2.00853233616872,126.312836586811));
#36572=CARTESIAN_POINT('Ctrl Pts',(137.657167959246,1.88255901296629,126.258605160237));
#36573=CARTESIAN_POINT('Ctrl Pts',(137.649407516732,1.75468019048728,126.2097680903));
#36574=CARTESIAN_POINT('Ctrl Pts',(137.641634616467,1.62659608556954,126.160852622762));
#36575=CARTESIAN_POINT('Ctrl Pts',(137.633861716201,1.49660073973325,126.11734894045));
#36576=CARTESIAN_POINT('Ctrl Pts',(137.626088815936,1.36519431837731,126.079381513319));
#36577=CARTESIAN_POINT('Ctrl Pts',(137.618598480174,1.23856485143018,126.042794297799));
#36578=CARTESIAN_POINT('Ctrl Pts',(137.611108144412,1.11062541922513,126.011347885567));
#36579=CARTESIAN_POINT('Ctrl Pts',(137.60361780865,0.981829878857104,125.985108273946));
#36580=CARTESIAN_POINT('Ctrl Pts',(137.595843474531,0.848151016429937,125.957873779476));
#36581=CARTESIAN_POINT('Ctrl Pts',(137.588069140411,0.713126391188011,125.936162440718));
#36582=CARTESIAN_POINT('Ctrl Pts',(137.580294806292,0.5772521775216,125.920103971356));
#36583=CARTESIAN_POINT('Ctrl Pts',(137.572530053345,0.441545416679736,125.904065292623));
#36584=CARTESIAN_POINT('Ctrl Pts',(137.564765300398,0.304991535250185,125.893665667163));
#36585=CARTESIAN_POINT('Ctrl Pts',(137.557000547451,0.168098317034786,125.888984129614));
#36586=CARTESIAN_POINT('Ctrl Pts',(137.549243506566,0.0313410630940389,
125.884307241834));
#36587=CARTESIAN_POINT('Ctrl Pts',(137.541486465681,-0.105754468711179,
125.885337153207));
#36588=CARTESIAN_POINT('Ctrl Pts',(137.533729424796,-0.242674282057496,
125.892101233603));
#36589=CARTESIAN_POINT('Ctrl Pts',(137.525978233556,-0.379490843106835,
125.898860213155));
#36590=CARTESIAN_POINT('Ctrl Pts',(137.518227042316,-0.516131560542711,
125.911344735497));
#36591=CARTESIAN_POINT('Ctrl Pts',(137.510475851076,-0.652081697699105,
125.929530105433));
#36592=CARTESIAN_POINT('Ctrl Pts',(137.502727954298,-0.787974052421266,
125.947707746102));
#36593=CARTESIAN_POINT('Ctrl Pts',(137.494980057521,-0.9231760239406,125.971581363451));
#36594=CARTESIAN_POINT('Ctrl Pts',(137.487232160744,-1.05717748143791,126.001074363839));
#36595=CARTESIAN_POINT('Ctrl Pts',(137.47948588466,-1.19115090871906,126.030561194928));
#36596=CARTESIAN_POINT('Ctrl Pts',(137.471739608576,-1.3239239398884,126.065664987028));
#36597=CARTESIAN_POINT('Ctrl Pts',(137.463993332492,-1.45499652310436,126.106258002653));
#36598=CARTESIAN_POINT('Ctrl Pts',(137.456246999227,-1.58607007386799,126.146851317926));
#36599=CARTESIAN_POINT('Ctrl Pts',(137.448500665961,-1.71544277816592,126.192933821916));
#36600=CARTESIAN_POINT('Ctrl Pts',(137.440754332696,-1.84263002172215,126.244327978917));
#36601=CARTESIAN_POINT('Ctrl Pts',(137.433006264693,-1.96984574798051,126.295733645282));
#36602=CARTESIAN_POINT('Ctrl Pts',(137.42525819669,-2.0948746771903,126.352453185193));
#36603=CARTESIAN_POINT('Ctrl Pts',(137.417510128687,-2.21725281319327,126.414261185334));
#36604=CARTESIAN_POINT('Ctrl Pts',(137.409753825945,-2.33976101413508,126.476134875752));
#36605=CARTESIAN_POINT('Ctrl Pts',(137.401997523203,-2.45961244448321,126.543107653079));
#36606=CARTESIAN_POINT('Ctrl Pts',(137.394241220461,-2.57636785670945,126.614908179667));
#36607=CARTESIAN_POINT('Ctrl Pts',(137.386480777947,-2.69318558481478,126.686747028358));
#36608=CARTESIAN_POINT('Ctrl Pts',(137.378720335433,-2.8069036781665,126.763418542179));
#36609=CARTESIAN_POINT('Ctrl Pts',(137.370959892919,-2.91711331540635,126.844608988034));
#36610=CARTESIAN_POINT('Ctrl Pts',(137.363186992653,-3.02749987093992,126.925929768001));
#36611=CARTESIAN_POINT('Ctrl Pts',(137.355414092388,-3.13436641069527,127.011783731186));
#36612=CARTESIAN_POINT('Ctrl Pts',(137.347641192122,-3.23733786295673,127.101817353326));
#36613=CARTESIAN_POINT('Ctrl Pts',(137.34015085636,-3.33656604355934,127.188578026521));
#36614=CARTESIAN_POINT('Ctrl Pts',(137.332660520598,-3.43217718898026,127.279219540335));
#36615=CARTESIAN_POINT('Ctrl Pts',(137.325170184836,-3.52387045295582,127.373395725107));
#36616=CARTESIAN_POINT('Ctrl Pts',(137.317499047477,-3.61777700737291,127.469845133021));
#36617=CARTESIAN_POINT('Ctrl Pts',(137.309827910118,-3.70788874961435,127.570325501121));
#36618=CARTESIAN_POINT('Ctrl Pts',(137.302156772759,-3.79383269335377,127.674501745773));
#36619=CARTESIAN_POINT('Ctrl Pts',(137.294494655402,-3.87967558108404,127.778555496215));
#36620=CARTESIAN_POINT('Ctrl Pts',(137.286832538045,-3.96136016024525,127.886296176482));
#36621=CARTESIAN_POINT('Ctrl Pts',(137.279170420688,-4.03854927230723,127.997351027692));
#36622=CARTESIAN_POINT('Ctrl Pts',(137.27151554709,-4.1156654098467,128.108300887737));
#36623=CARTESIAN_POINT('Ctrl Pts',(137.263860673493,-4.18829430409693,128.222558359869));
#36624=CARTESIAN_POINT('Ctrl Pts',(137.256205799895,-4.25613855508317,128.339717101267));
#36625=CARTESIAN_POINT('Ctrl Pts',(137.248556819799,-4.32393057264981,128.456785641924));
#36626=CARTESIAN_POINT('Ctrl Pts',(137.240907839703,-4.38694507721455,128.576750659864));
#36627=CARTESIAN_POINT('Ctrl Pts',(137.233258859608,-4.44492791759091,128.699176808508));
#36628=CARTESIAN_POINT('Ctrl Pts',(137.225613250521,-4.50288520414662,128.821549002295));
#36629=CARTESIAN_POINT('Ctrl Pts',(137.217967641434,-4.55581506643461,128.946379806153));
#36630=CARTESIAN_POINT('Ctrl Pts',(137.210322032347,-4.60350944859244,129.073209607625));
#36631=CARTESIAN_POINT('Ctrl Pts',(137.202677441345,-4.65119747979308,129.200022520511));
#36632=CARTESIAN_POINT('Ctrl Pts',(137.195032850343,-4.69365127397722,129.328833526159));
#36633=CARTESIAN_POINT('Ctrl Pts',(137.187388259341,-4.73071121066212,129.459163790401));
#36634=CARTESIAN_POINT('Ctrl Pts',(137.184985501868,-4.74235945185325,129.500127658345));
#36635=CARTESIAN_POINT('Ctrl Pts',(137.182582744396,-4.75347520330263,129.541241491964));
#36636=CARTESIAN_POINT('Ctrl Pts',(137.180179986924,-4.76405452823403,129.582490119308));
#36637=CARTESIAN_POINT('Origin',(213.235140564004,0.,130.804360617566));
#36638=CARTESIAN_POINT('',(135.084620084674,-4.76405452823407,129.582490119308));
#36639=CARTESIAN_POINT('',(135.430234117584,-4.76405452823404,129.582490119308));
#36640=CARTESIAN_POINT('',(213.235140564004,-4.76405452823405,129.582490119308));
#36641=CARTESIAN_POINT('',(136.764859435954,-4.91824941924801,130.801970519943));
#36642=CARTESIAN_POINT('Ctrl Pts',(136.764859435954,-4.91824941924801,130.801970519943));
#36643=CARTESIAN_POINT('Ctrl Pts',(136.75717491875,-4.91831502016731,130.936961526231));
#36644=CARTESIAN_POINT('Ctrl Pts',(136.749490401545,-4.91281878792003,131.072179136748));
#36645=CARTESIAN_POINT('Ctrl Pts',(136.74180588434,-4.9017310665055,131.207120613289));
#36646=CARTESIAN_POINT('Ctrl Pts',(136.734130242886,-4.89065615160033,131.341906230098));
#36647=CARTESIAN_POINT('Ctrl Pts',(136.726454601431,-4.87400262499367,131.476415951784));
#36648=CARTESIAN_POINT('Ctrl Pts',(136.718778959976,-4.85179282326919,131.6101456153));
#36649=CARTESIAN_POINT('Ctrl Pts',(136.711110247597,-4.82960307112644,131.74375455627));
#36650=CARTESIAN_POINT('Ctrl Pts',(136.703441535218,-4.80186708723321,131.876584447115));
#36651=CARTESIAN_POINT('Ctrl Pts',(136.695772822839,-4.76865909261835,132.008135314463));
#36652=CARTESIAN_POINT('Ctrl Pts',(136.688007968119,-4.7350347707001,132.141335429785));
#36653=CARTESIAN_POINT('Ctrl Pts',(136.680243113399,-4.69580032358549,132.273223816898));
#36654=CARTESIAN_POINT('Ctrl Pts',(136.672478258679,-4.65108650847972,132.403290682684));
#36655=CARTESIAN_POINT('Ctrl Pts',(136.664816681235,-4.60696741422874,132.531627580284));
#36656=CARTESIAN_POINT('Ctrl Pts',(136.657155103791,-4.55751396328245,132.658190728913));
#36657=CARTESIAN_POINT('Ctrl Pts',(136.649493526347,-4.5029020747524,132.78250519461));
#36658=CARTESIAN_POINT('Ctrl Pts',(136.641832628041,-4.44829502712893,132.906808640826));
#36659=CARTESIAN_POINT('Ctrl Pts',(136.634171729735,-4.38853061224154,133.02886343381));
#36660=CARTESIAN_POINT('Ctrl Pts',(136.626510831429,-4.32383268073799,133.148215137685));
#36661=CARTESIAN_POINT('Ctrl Pts',(136.618848864003,-4.25912572029284,133.267583497727));
#36662=CARTESIAN_POINT('Ctrl Pts',(136.611186896577,-4.18948406511449,133.38424766647));
#36663=CARTESIAN_POINT('Ctrl Pts',(136.603524929152,-4.11517699189767,133.497778778167));
#36664=CARTESIAN_POINT('Ctrl Pts',(136.595682544186,-4.03912019845103,133.613983224639));
#36665=CARTESIAN_POINT('Ctrl Pts',(136.587840159219,-3.95817577314425,133.726904853683));
#36666=CARTESIAN_POINT('Ctrl Pts',(136.579997774253,-3.87267802707688,133.836117197685));
#36667=CARTESIAN_POINT('Ctrl Pts',(136.57232439521,-3.78902278498877,133.942975980481));
#36668=CARTESIAN_POINT('Ctrl Pts',(136.564651016167,-3.70100879126266,134.046283463396));
#36669=CARTESIAN_POINT('Ctrl Pts',(136.556977637124,-3.60898789791708,134.145676139211));
#36670=CARTESIAN_POINT('Ctrl Pts',(136.549050749196,-3.51392686880833,134.248352495693));
#36671=CARTESIAN_POINT('Ctrl Pts',(136.541123861268,-3.41458996194518,134.34685058651));
#36672=CARTESIAN_POINT('Ctrl Pts',(136.533196973341,-3.31140286017304,134.440814131656));
#36673=CARTESIAN_POINT('Ctrl Pts',(136.525270085413,-3.2082157584009,134.534777676802));
#36674=CARTESIAN_POINT('Ctrl Pts',(136.517343197485,-3.10117886344023,134.624206435075));
#36675=CARTESIAN_POINT('Ctrl Pts',(136.509416309557,-2.99075052776747,134.708793270738));
#36676=CARTESIAN_POINT('Ctrl Pts',(136.501641975438,-2.88244739726414,134.791752223673));
#36677=CARTESIAN_POINT('Ctrl Pts',(136.493867641319,-2.77051837028484,134.870332911962));
#36678=CARTESIAN_POINT('Ctrl Pts',(136.4860933072,-2.6553529134072,134.944201673423));
#36679=CARTESIAN_POINT('Ctrl Pts',(136.478328554253,-2.54032938766237,135.017979398238));
#36680=CARTESIAN_POINT('Ctrl Pts',(136.470563801305,-2.4220776940936,135.087056541428));
#36681=CARTESIAN_POINT('Ctrl Pts',(136.462799048358,-2.30101990503478,135.151139937837));
#36682=CARTESIAN_POINT('Ctrl Pts',(136.455042007473,-2.18008235227893,135.215159685713));
#36683=CARTESIAN_POINT('Ctrl Pts',(136.447284966588,-2.05634459369694,135.274195375423));
#36684=CARTESIAN_POINT('Ctrl Pts',(136.439527925703,-1.93025688518774,135.327997585724));
#36685=CARTESIAN_POINT('Ctrl Pts',(136.431776734463,-1.80426426040036,135.38175922336));
#36686=CARTESIAN_POINT('Ctrl Pts',(136.424025543223,-1.67592557111555,135.43029508425));
#36687=CARTESIAN_POINT('Ctrl Pts',(136.416274351983,-1.54571451085721,135.473402244434));
#36688=CARTESIAN_POINT('Ctrl Pts',(136.408526455206,-1.41555879377297,135.516491082925));
#36689=CARTESIAN_POINT('Ctrl Pts',(136.400778558429,-1.28353265889378,135.554155687223));
#36690=CARTESIAN_POINT('Ctrl Pts',(136.393030661652,-1.15012835676926,135.586241819087));
#36691=CARTESIAN_POINT('Ctrl Pts',(136.385284385568,-1.01675195994888,135.618321239223));
#36692=CARTESIAN_POINT('Ctrl Pts',(136.377538109484,-0.881998349177671,
135.644824416577));
#36693=CARTESIAN_POINT('Ctrl Pts',(136.369791833399,-0.746373080111705,
135.66564751383));
#36694=CARTESIAN_POINT('Ctrl Pts',(136.362045500134,-0.610746809890719,
135.686470764794));
#36695=CARTESIAN_POINT('Ctrl Pts',(136.354299166869,-0.474249254972687,
135.701613792659));
#36696=CARTESIAN_POINT('Ctrl Pts',(136.346552833603,-0.337393868707141,
135.711024294634));
#36697=CARTESIAN_POINT('Ctrl Pts',(136.3388047656,-0.200507834627103,135.720436904026));
#36698=CARTESIAN_POINT('Ctrl Pts',(136.331056697597,-0.0632641997119973,
135.724114406181));
#36699=CARTESIAN_POINT('Ctrl Pts',(136.323308629594,0.0738211837874544,
135.722056571499));
#36700=CARTESIAN_POINT('Ctrl Pts',(136.315552326853,0.211052263264013,135.719996549725));
#36701=CARTESIAN_POINT('Ctrl Pts',(136.307796024111,0.348124363799805,135.712189020407));
#36702=CARTESIAN_POINT('Ctrl Pts',(136.300039721369,0.48452380304023,135.698685877169));
#36703=CARTESIAN_POINT('Ctrl Pts',(136.292279278855,0.620996042768379,135.685175526897));
#36704=CARTESIAN_POINT('Ctrl Pts',(136.284518836341,0.756794518903235,135.665963560145));
#36705=CARTESIAN_POINT('Ctrl Pts',(136.276758393826,0.891414368124566,135.64115330351));
#36706=CARTESIAN_POINT('Ctrl Pts',(136.268985493561,1.02625032107885,135.616303219248));
#36707=CARTESIAN_POINT('Ctrl Pts',(136.261212593296,1.15990348482117,135.58583697341));
#36708=CARTESIAN_POINT('Ctrl Pts',(136.25343969303,1.29188194283965,135.549908437182));
#36709=CARTESIAN_POINT('Ctrl Pts',(136.245949357268,1.41906265147647,135.515285993745));
#36710=CARTESIAN_POINT('Ctrl Pts',(136.238459021506,1.54468800630241,135.475591593885));
#36711=CARTESIAN_POINT('Ctrl Pts',(136.230968685744,1.66833605699124,135.431004959143));
#36712=CARTESIAN_POINT('Ctrl Pts',(136.223194351625,1.79667226110305,135.384727808592));
#36713=CARTESIAN_POINT('Ctrl Pts',(136.215420017506,1.92328479278158,135.33303352966));
#36714=CARTESIAN_POINT('Ctrl Pts',(136.207645683387,2.04768241638631,135.276069439048));
#36715=CARTESIAN_POINT('Ctrl Pts',(136.19988093044,2.17192673103751,135.219175551587));
#36716=CARTESIAN_POINT('Ctrl Pts',(136.192116177493,2.29396121680107,135.157024935923));
#36717=CARTESIAN_POINT('Ctrl Pts',(136.184351424545,2.41331108512305,135.089814230537));
#36718=CARTESIAN_POINT('Ctrl Pts',(136.176594383661,2.53254241347303,135.02267027977));
#36719=CARTESIAN_POINT('Ctrl Pts',(136.168837342776,2.64909409217947,134.950476431355));
#36720=CARTESIAN_POINT('Ctrl Pts',(136.161080301891,2.76251290177618,134.873476680057));
#36721=CARTESIAN_POINT('Ctrl Pts',(136.15332911065,2.87584618136699,134.79653499487));
#36722=CARTESIAN_POINT('Ctrl Pts',(136.14557791941,2.98605097214634,134.714794839199));
#36723=CARTESIAN_POINT('Ctrl Pts',(136.13782672817,3.0927005055194,134.628545059465));
#36724=CARTESIAN_POINT('Ctrl Pts',(136.130078831393,3.19930470999545,134.542331938188));
#36725=CARTESIAN_POINT('Ctrl Pts',(136.122330934616,3.30235635912813,134.451613250372));
#36726=CARTESIAN_POINT('Ctrl Pts',(136.114583037839,3.40145961447108,134.356719770808));
#36727=CARTESIAN_POINT('Ctrl Pts',(136.106836761755,3.50054213954944,134.261846140914));
#36728=CARTESIAN_POINT('Ctrl Pts',(136.099090485671,3.59567763142809,134.162799726488));
#36729=CARTESIAN_POINT('Ctrl Pts',(136.091344209587,3.68650546364902,134.059949739213));
#36730=CARTESIAN_POINT('Ctrl Pts',(136.083597876321,3.77733396634038,133.957098992723));
#36731=CARTESIAN_POINT('Ctrl Pts',(136.075851543056,3.86385448712737,133.850444910409));
#36732=CARTESIAN_POINT('Ctrl Pts',(136.068105209791,3.94574548811367,133.74039120418));
#36733=CARTESIAN_POINT('Ctrl Pts',(136.060357141788,4.02765482802196,133.630312852186));
#36734=CARTESIAN_POINT('Ctrl Pts',(136.052609073785,4.10493235177089,133.516833674932));
#36735=CARTESIAN_POINT('Ctrl Pts',(136.044861005782,4.17729903545029,133.400387549423));
#36736=CARTESIAN_POINT('Ctrl Pts',(136.03710470304,4.24974263130219,133.283817663586));
#36737=CARTESIAN_POINT('Ctrl Pts',(136.029348400298,4.31726475427772,133.164274863015));
#36738=CARTESIAN_POINT('Ctrl Pts',(136.021592097556,4.37963140609379,133.042219372996));
#36739=CARTESIAN_POINT('Ctrl Pts',(136.013831655042,4.44203134486979,132.920098738288));
#36740=CARTESIAN_POINT('Ctrl Pts',(136.006071212528,4.49927016654367,132.795463096995));
#36741=CARTESIAN_POINT('Ctrl Pts',(135.998310770013,4.55116191175006,132.668793055477));
#36742=CARTESIAN_POINT('Ctrl Pts',(135.990537869748,4.60313695819259,132.541919671963));
#36743=CARTESIAN_POINT('Ctrl Pts',(135.982764969483,4.64974764238295,132.413005729998));
#36744=CARTESIAN_POINT('Ctrl Pts',(135.974992069217,4.6908575276175,132.282548264008));
#36745=CARTESIAN_POINT('Ctrl Pts',(135.967501733455,4.73047296497443,132.156833255509));
#36746=CARTESIAN_POINT('Ctrl Pts',(135.960011397693,4.76498051502194,132.029685293886));
#36747=CARTESIAN_POINT('Ctrl Pts',(135.952521061931,4.79430330812283,131.901556521779));
#36748=CARTESIAN_POINT('Ctrl Pts',(135.944746727812,4.82473788383648,131.768569708335));
#36749=CARTESIAN_POINT('Ctrl Pts',(135.936972393693,4.84968318896769,131.634104979115));
#36750=CARTESIAN_POINT('Ctrl Pts',(135.929198059574,4.86899764036849,131.498655252851));
#36751=CARTESIAN_POINT('Ctrl Pts',(135.921433306627,4.88828828843411,131.36337245627));
#36752=CARTESIAN_POINT('Ctrl Pts',(135.91366855368,4.90196183569212,131.227107461321));
#36753=CARTESIAN_POINT('Ctrl Pts',(135.905903800732,4.90992708485487,131.090366008964));
#36754=CARTESIAN_POINT('Ctrl Pts',(135.898146759847,4.91788442281987,130.953760370144));
#36755=CARTESIAN_POINT('Ctrl Pts',(135.890389718962,4.92014472278587,130.816679603432));
#36756=CARTESIAN_POINT('Ctrl Pts',(135.882632678077,4.91666828826785,130.67963690033));
#36757=CARTESIAN_POINT('Ctrl Pts',(135.874881486837,4.91319447535613,130.542697542196));
#36758=CARTESIAN_POINT('Ctrl Pts',(135.867130295597,4.90399254870659,130.405796579796));
#36759=CARTESIAN_POINT('Ctrl Pts',(135.859379104357,4.8890748441433,130.269449194183));
#36760=CARTESIAN_POINT('Ctrl Pts',(135.85163120758,4.87416348000244,130.133159759847));
#36761=CARTESIAN_POINT('Ctrl Pts',(135.843883310803,4.85354121218845,129.997423822165));
#36762=CARTESIAN_POINT('Ctrl Pts',(135.836135414026,4.82727237055267,129.862753203089));
#36763=CARTESIAN_POINT('Ctrl Pts',(135.828389137942,4.8010090237923,129.728110754202));
#36764=CARTESIAN_POINT('Ctrl Pts',(135.820642861857,4.76910152736892,129.594533564167));
#36765=CARTESIAN_POINT('Ctrl Pts',(135.812896585773,4.73166558211992,129.462524606169));
#36766=CARTESIAN_POINT('Ctrl Pts',(135.805150252508,4.69422936052725,129.330514673711));
#36767=CARTESIAN_POINT('Ctrl Pts',(135.797403919243,4.65126471534227,129.200073372522));
#36768=CARTESIAN_POINT('Ctrl Pts',(135.789657585977,4.60293750174063,129.071689437691));
#36769=CARTESIAN_POINT('Ctrl Pts',(135.781909517974,4.55459946559474,128.943276752168));
#36770=CARTESIAN_POINT('Ctrl Pts',(135.774161449971,4.50089660906874,128.816922715636));
#36771=CARTESIAN_POINT('Ctrl Pts',(135.766413381968,4.44204314593543,128.693096599934));
#36772=CARTESIAN_POINT('Ctrl Pts',(135.758657079226,4.38312713264093,128.569138880362));
#36773=CARTESIAN_POINT('Ctrl Pts',(135.750900776485,4.31904974568052,128.447714802273));
#36774=CARTESIAN_POINT('Ctrl Pts',(135.743144473743,4.25007170383332,128.329269998058));
#36775=CARTESIAN_POINT('Ctrl Pts',(135.735384031229,4.18105684632821,128.210761976285));
#36776=CARTESIAN_POINT('Ctrl Pts',(135.727623588714,4.10713633269439,128.09523672601));
#36777=CARTESIAN_POINT('Ctrl Pts',(135.7198631462,4.02861399509353,127.983110479589));
#36778=CARTESIAN_POINT('Ctrl Pts',(135.712090245935,3.94996560646557,127.870804238163));
#36779=CARTESIAN_POINT('Ctrl Pts',(135.704317345669,3.86670086939134,127.76190821494));
#36780=CARTESIAN_POINT('Ctrl Pts',(135.696544445404,3.77916420564075,127.656805857232));
#36781=CARTESIAN_POINT('Ctrl Pts',(135.689054109642,3.69480972010988,127.555524234964));
#36782=CARTESIAN_POINT('Ctrl Pts',(135.68156377388,3.60648871267436,127.457765476787));
#36783=CARTESIAN_POINT('Ctrl Pts',(135.674073438118,3.51454003382728,127.363838649445));
#36784=CARTESIAN_POINT('Ctrl Pts',(135.666299103999,3.41910509287365,127.266350557895));
#36785=CARTESIAN_POINT('Ctrl Pts',(135.65852476988,3.31945965468791,127.172681895573));
#36786=CARTESIAN_POINT('Ctrl Pts',(135.650750435761,3.21594189661092,127.083218215007));
#36787=CARTESIAN_POINT('Ctrl Pts',(135.642985682814,3.11255171491932,126.993864790432));
#36788=CARTESIAN_POINT('Ctrl Pts',(135.635220929867,3.00529900173171,126.908706289641));
#36789=CARTESIAN_POINT('Ctrl Pts',(135.62745617692,2.89455995687888,126.828092804838));
#36790=CARTESIAN_POINT('Ctrl Pts',(135.619699136035,2.7839308996064,126.747559386485));
#36791=CARTESIAN_POINT('Ctrl Pts',(135.61194209515,2.6698227155848,126.671562229316));
#36792=CARTESIAN_POINT('Ctrl Pts',(135.604185054265,2.55264571044068,126.600412123654));
#36793=CARTESIAN_POINT('Ctrl Pts',(135.596433863024,2.43555706938795,126.529315672839));
#36794=CARTESIAN_POINT('Ctrl Pts',(135.588682671784,2.31540454636224,126.463059200173));
#36795=CARTESIAN_POINT('Ctrl Pts',(135.580931480544,2.19262824558685,126.40191079512));
#36796=CARTESIAN_POINT('Ctrl Pts',(135.573183583767,2.06990412801395,126.34078837977));
#36797=CARTESIAN_POINT('Ctrl Pts',(135.56543568699,1.94455879992063,126.284769887883));
#36798=CARTESIAN_POINT('Ctrl Pts',(135.557687790213,1.81705764346521,126.2340778492));
#36799=CARTESIAN_POINT('Ctrl Pts',(135.549941514129,1.68958315750312,126.183396414198));
#36800=CARTESIAN_POINT('Ctrl Pts',(135.542195238045,1.55995410322297,126.138039360588));
#36801=CARTESIAN_POINT('Ctrl Pts',(135.534448961961,1.4286561853403,126.098181215271));
#36802=CARTESIAN_POINT('Ctrl Pts',(135.526702628695,1.29735729824623,126.05832277573));
#36803=CARTESIAN_POINT('Ctrl Pts',(135.51895629543,1.16438989707475,126.023963439048));
#36804=CARTESIAN_POINT('Ctrl Pts',(135.511209962165,1.0302548172695,125.99522783982));
#36805=CARTESIAN_POINT('Ctrl Pts',(135.503461894162,0.89608969884316,125.966485805454));
#36806=CARTESIAN_POINT('Ctrl Pts',(135.495713826159,0.760756763659207,125.943370096479));
#36807=CARTESIAN_POINT('Ctrl Pts',(135.487965758156,0.624766611181083,125.925954141671));
#36808=CARTESIAN_POINT('Ctrl Pts',(135.480209455414,0.488631926750602,125.908519676979));
#36809=CARTESIAN_POINT('Ctrl Pts',(135.472453152672,0.351839018116533,125.89679711724));
#36810=CARTESIAN_POINT('Ctrl Pts',(135.46469684993,0.21490373329901,125.890807987552));
#36811=CARTESIAN_POINT('Ctrl Pts',(135.456936407416,0.077895361997031,125.884815661286));
#36812=CARTESIAN_POINT('Ctrl Pts',(135.449175964902,-0.059255146132568,
125.884562863309));
#36813=CARTESIAN_POINT('Ctrl Pts',(135.441415522388,-0.196033374314634,
125.890018954774));
#36814=CARTESIAN_POINT('Ctrl Pts',(135.433642622122,-0.333031171051272,
125.895483804841));
#36815=CARTESIAN_POINT('Ctrl Pts',(135.425869721857,-0.469655103727329,
125.906675825836));
#36816=CARTESIAN_POINT('Ctrl Pts',(135.418096821591,-0.605396398879946,
125.923512508608));
#36817=CARTESIAN_POINT('Ctrl Pts',(135.410606485829,-0.736203156042354,
125.939737135551));
#36818=CARTESIAN_POINT('Ctrl Pts',(135.403116150067,-0.866190029849771,
125.961203103802));
#36819=CARTESIAN_POINT('Ctrl Pts',(135.395625814305,-0.994913836728182,
125.98779238697));
#36820=CARTESIAN_POINT('Ctrl Pts',(135.387851480186,-1.12851824586895,126.015389810891));
#36821=CARTESIAN_POINT('Ctrl Pts',(135.380077146067,-1.26118513762943,126.048594140172));
#36822=CARTESIAN_POINT('Ctrl Pts',(135.372302811948,-1.39240734263527,126.0873292572));
#36823=CARTESIAN_POINT('Ctrl Pts',(135.364538059001,-1.52346782800121,126.126016636658));
#36824=CARTESIAN_POINT('Ctrl Pts',(135.356773306054,-1.65308679780187,126.170221132028));
#36825=CARTESIAN_POINT('Ctrl Pts',(135.349008553107,-1.78076636435417,126.219815469126));
#36826=CARTESIAN_POINT('Ctrl Pts',(135.341251512222,-1.90831911776118,126.269360548429));
#36827=CARTESIAN_POINT('Ctrl Pts',(135.333494471336,-2.03393593914977,126.324284675575));
#36828=CARTESIAN_POINT('Ctrl Pts',(135.325737430451,-2.15713357160803,126.38441063858));
#36829=CARTESIAN_POINT('Ctrl Pts',(135.317986239211,-2.28023829977349,126.444491260128));
#36830=CARTESIAN_POINT('Ctrl Pts',(135.310235047971,-2.40092712029292,126.509765738766));
#36831=CARTESIAN_POINT('Ctrl Pts',(135.302483856731,-2.51873659482472,126.580008711251));
#36832=CARTESIAN_POINT('Ctrl Pts',(135.294735959954,-2.6364959971867,126.650221828598));
#36833=CARTESIAN_POINT('Ctrl Pts',(135.286988063177,-2.7513781525014,126.725399039894));
#36834=CARTESIAN_POINT('Ctrl Pts',(135.2792401664,-2.86294428977179,126.805269088711));
#36835=CARTESIAN_POINT('Ctrl Pts',(135.271493890316,-2.97448708981135,126.885122430434));
#36836=CARTESIAN_POINT('Ctrl Pts',(135.263747614231,-3.08271493379622,126.969666429702));
#36837=CARTESIAN_POINT('Ctrl Pts',(135.256001338147,-3.18721845203829,127.058586785434));
#36838=CARTESIAN_POINT('Ctrl Pts',(135.248255004882,-3.29172274170203,127.147507797556));
#36839=CARTESIAN_POINT('Ctrl Pts',(135.240508671617,-3.39250235300254,127.240804977244));
#36840=CARTESIAN_POINT('Ctrl Pts',(135.232762338351,-3.48918171353372,127.338124325499));
#36841=CARTESIAN_POINT('Ctrl Pts',(135.225014270348,-3.5858827247369,127.435465467747));
#36842=CARTESIAN_POINT('Ctrl Pts',(135.217266202345,-3.67848138252594,127.536830293611));
#36843=CARTESIAN_POINT('Ctrl Pts',(135.209518134342,-3.76663991770947,127.641828911351));
#36844=CARTESIAN_POINT('Ctrl Pts',(135.2017618316,-3.8548921488333,127.74693912287));
#36845=CARTESIAN_POINT('Ctrl Pts',(135.194005528859,-3.93869457881135,127.855690541202));
#36846=CARTESIAN_POINT('Ctrl Pts',(135.186249226117,-4.01775026951237,127.967660803639));
#36847=CARTESIAN_POINT('Ctrl Pts',(135.178488783603,-4.09684815461596,128.079690827977));
#36848=CARTESIAN_POINT('Ctrl Pts',(135.170728341088,-4.17119404044526,128.194942791289));
#36849=CARTESIAN_POINT('Ctrl Pts',(135.162967898574,-4.24053564949736,128.312967339129));
#36850=CARTESIAN_POINT('Ctrl Pts',(135.155194998309,-4.30998857185626,128.431181350451));
#36851=CARTESIAN_POINT('Ctrl Pts',(135.147422098043,-4.37442098045509,128.55217649513));
#36852=CARTESIAN_POINT('Ctrl Pts',(135.139649197778,-4.43362728809547,128.675480129433));
#36853=CARTESIAN_POINT('Ctrl Pts',(135.132158862016,-4.4906812973207,128.794301366043));
#36854=CARTESIAN_POINT('Ctrl Pts',(135.124668526254,-4.54288245068104,128.915265884571));
#36855=CARTESIAN_POINT('Ctrl Pts',(135.117178190492,-4.59009049557536,129.037937025975));
#36856=CARTESIAN_POINT('Ctrl Pts',(135.108307742422,-4.64599673583467,129.183210619059));
#36857=CARTESIAN_POINT('Ctrl Pts',(135.099437294352,-4.69504882930383,129.33126094761));
#36858=CARTESIAN_POINT('Ctrl Pts',(135.090566846281,-4.73699786693891,129.481472008833));
#36859=CARTESIAN_POINT('Ctrl Pts',(135.088584592412,-4.74637209939055,129.51503924861));
#36860=CARTESIAN_POINT('Ctrl Pts',(135.086602338543,-4.75539180591618,129.548714296466));
#36861=CARTESIAN_POINT('Ctrl Pts',(135.084620084674,-4.76405452823407,129.582490119308));
#36862=CARTESIAN_POINT('Ctrl Pts',(136.834948208849,-4.76405452823407,129.582490119308));
#36863=CARTESIAN_POINT('Ctrl Pts',(136.827100829603,-4.79844716391908,129.716586483863));
#36864=CARTESIAN_POINT('Ctrl Pts',(136.819253450356,-4.82713745802811,129.851994585027));
#36865=CARTESIAN_POINT('Ctrl Pts',(136.81140607111,-4.85005629057773,129.988188429405));
#36866=CARTESIAN_POINT('Ctrl Pts',(136.803558691863,-4.87297512312734,130.124382273783));
#36867=CARTESIAN_POINT('Ctrl Pts',(136.795711312616,-4.89012250416789,130.261361450188));
#36868=CARTESIAN_POINT('Ctrl Pts',(136.78786393337,-4.90148348379414,130.398598716208));
#36869=CARTESIAN_POINT('Ctrl Pts',(136.780195767577,-4.91258500859702,130.532701844876));
#36870=CARTESIAN_POINT('Ctrl Pts',(136.772527601784,-4.9181839578989,130.667266752074));
#36871=CARTESIAN_POINT('Ctrl Pts',(136.764859435991,-4.91824941924769,130.801970519299));
#36872=CARTESIAN_POINT('',(137.110140564041,-4.91824791103875,130.808893614699));
#36873=CARTESIAN_POINT('Ctrl Pts',(137.180179986924,-4.76405452823403,129.582490119308));
#36874=CARTESIAN_POINT('Ctrl Pts',(137.172532796993,-4.79772505387415,129.713770987757));
#36875=CARTESIAN_POINT('Ctrl Pts',(137.164885607063,-4.82595803982301,129.846417925077));
#36876=CARTESIAN_POINT('Ctrl Pts',(137.157238417133,-4.84866013835519,129.979934802089));
#36877=CARTESIAN_POINT('Ctrl Pts',(137.149388774951,-4.8719632538637,130.116986414428));
#36878=CARTESIAN_POINT('Ctrl Pts',(137.141539132769,-4.88943846897025,130.254954226966));
#36879=CARTESIAN_POINT('Ctrl Pts',(137.133689490587,-4.90104155255462,130.393295218106));
#36880=CARTESIAN_POINT('Ctrl Pts',(137.125839848405,-4.91264463613899,130.531636209247));
#36881=CARTESIAN_POINT('Ctrl Pts',(137.117990206223,-4.91837560247917,130.670349922381));
#36882=CARTESIAN_POINT('Ctrl Pts',(137.110140564041,-4.91824791103875,130.808893614699));
#36883=CARTESIAN_POINT('Ctrl Pts',(137.110140564008,-4.9182479110382,130.808893615287));
#36884=CARTESIAN_POINT('Ctrl Pts',(137.099570896844,-4.9180759724748,130.995444884955));
#36885=CARTESIAN_POINT('Ctrl Pts',(137.08900122968,-4.90728645279196,131.181526057821));
#36886=CARTESIAN_POINT('Ctrl Pts',(137.078431562516,-4.88606103454535,131.366135153477));
#36887=CARTESIAN_POINT('Ctrl Pts',(137.067861895352,-4.86483561629874,131.550744249132));
#36888=CARTESIAN_POINT('Ctrl Pts',(137.057292228188,-4.83317444821162,131.733881895428));
#36889=CARTESIAN_POINT('Ctrl Pts',(137.046722561024,-4.7913059891444,131.914572300485));
#36890=CARTESIAN_POINT('Ctrl Pts',(137.038948226905,-4.76051037516862,132.047475972777));
#36891=CARTESIAN_POINT('Ctrl Pts',(137.031173892785,-4.72413196831382,132.179307847402));
#36892=CARTESIAN_POINT('Ctrl Pts',(137.023399558666,-4.68225903494216,132.30956272765));
#36893=CARTESIAN_POINT('Ctrl Pts',(137.015634805719,-4.64043770621858,132.4396570804));
#36894=CARTESIAN_POINT('Ctrl Pts',(137.007870052772,-4.59313544277444,132.568177937136));
#36895=CARTESIAN_POINT('Ctrl Pts',(137.000105299825,-4.54049143007457,132.694630607784));
#36896=CARTESIAN_POINT('Ctrl Pts',(136.99234825894,-4.48789970415026,132.820957683857));
#36897=CARTESIAN_POINT('Ctrl Pts',(136.984591218055,-4.42997693644635,132.945220303095));
#36898=CARTESIAN_POINT('Ctrl Pts',(136.97683417717,-4.36691188474811,133.066939600352));
#36899=CARTESIAN_POINT('Ctrl Pts',(136.96908298593,-4.30389439089588,133.18856710814));
#36900=CARTESIAN_POINT('Ctrl Pts',(136.96133179469,-4.23574251077828,133.307654765755));
#36901=CARTESIAN_POINT('Ctrl Pts',(136.95358060345,-4.16269266398234,133.42374467641));
#36902=CARTESIAN_POINT('Ctrl Pts',(136.945832706673,-4.08967386531995,133.539785245757));
#36903=CARTESIAN_POINT('Ctrl Pts',(136.938084809895,-4.01176144824017,133.652830272064));
#36904=CARTESIAN_POINT('Ctrl Pts',(136.930336913118,-3.92923712035187,133.762447620098));
#36905=CARTESIAN_POINT('Ctrl Pts',(136.922590637034,-3.84673005477401,133.872042038546));
#36906=CARTESIAN_POINT('Ctrl Pts',(136.91484436095,-3.75961323225081,133.978209892716));
#36907=CARTESIAN_POINT('Ctrl Pts',(136.907098084866,-3.66821068709465,134.08054947317));
#36908=CARTESIAN_POINT('Ctrl Pts',(136.899351751601,-3.5768074672256,134.182889809071));
#36909=CARTESIAN_POINT('Ctrl Pts',(136.891605418335,-3.48111872202904,134.28140152327));
#36910=CARTESIAN_POINT('Ctrl Pts',(136.88385908507,-3.38150736126393,134.375717646514));
#36911=CARTESIAN_POINT('Ctrl Pts',(136.876111017067,-3.2818736932253,134.470054891201));
#36912=CARTESIAN_POINT('Ctrl Pts',(136.868362949064,-3.17831594546179,134.560194406537));
#36913=CARTESIAN_POINT('Ctrl Pts',(136.860614881061,-3.07123200296568,134.645807876928));
#36914=CARTESIAN_POINT('Ctrl Pts',(136.852858578319,-2.96403425038109,134.731512338334));
#36915=CARTESIAN_POINT('Ctrl Pts',(136.845102275577,-2.85330312252009,134.812680901104));
#36916=CARTESIAN_POINT('Ctrl Pts',(136.837345972835,-2.73946798615575,134.889026848157));
#36917=CARTESIAN_POINT('Ctrl Pts',(136.829585530321,-2.62557209255163,134.96541354334));
#36918=CARTESIAN_POINT('Ctrl Pts',(136.821825087807,-2.50856922269159,135.036972290057));
#36919=CARTESIAN_POINT('Ctrl Pts',(136.814064645293,-2.38891465558407,135.10346166672));
#36920=CARTESIAN_POINT('Ctrl Pts',(136.806291745027,-2.26906800834291,135.170057778033));
#36921=CARTESIAN_POINT('Ctrl Pts',(136.798518844762,-2.14656150712895,135.231568081838));
#36922=CARTESIAN_POINT('Ctrl Pts',(136.790745944496,-2.02187259309354,135.287798392287));
#36923=CARTESIAN_POINT('Ctrl Pts',(136.783255608734,-1.90171643515751,135.341984589315));
#36924=CARTESIAN_POINT('Ctrl Pts',(136.775765272972,-1.77953406767676,135.391267895124));
#36925=CARTESIAN_POINT('Ctrl Pts',(136.76827493721,-1.65576538962007,135.435518576115));
#36926=CARTESIAN_POINT('Ctrl Pts',(136.760500603091,-1.52730398451464,135.481447035127));
#36927=CARTESIAN_POINT('Ctrl Pts',(136.752726268972,-1.3967266772231,135.522099199557));
#36928=CARTESIAN_POINT('Ctrl Pts',(136.744951934853,-1.26450621416956,135.557276259235));
#36929=CARTESIAN_POINT('Ctrl Pts',(136.737187181906,-1.13244870101984,135.592409966331));
#36930=CARTESIAN_POINT('Ctrl Pts',(136.729422428959,-0.998752435534629,
135.622081894788));
#36931=CARTESIAN_POINT('Ctrl Pts',(136.721657676012,-0.863908847627266,
135.646141753211));
#36932=CARTESIAN_POINT('Ctrl Pts',(136.713900635127,-0.729199188272466,
135.670177715044));
#36933=CARTESIAN_POINT('Ctrl Pts',(136.706143594242,-0.593344856621078,
135.688612631098));
#36934=CARTESIAN_POINT('Ctrl Pts',(136.698386553357,-0.456850763676913,
135.701346470336));
#36935=CARTESIAN_POINT('Ctrl Pts',(136.690635362117,-0.320459601989821,
135.714070706886));
#36936=CARTESIAN_POINT('Ctrl Pts',(136.682884170877,-0.183430026995121,
135.721102387801));
#36937=CARTESIAN_POINT('Ctrl Pts',(136.675132979637,-0.0462750707891389,
135.722392915175));
#36938=CARTESIAN_POINT('Ctrl Pts',(136.667385082859,0.0908215909015406,
135.723682894041));
#36939=CARTESIAN_POINT('Ctrl Pts',(136.659637186082,0.228043137683621,135.719236568955));
#36940=CARTESIAN_POINT('Ctrl Pts',(136.651889289305,0.364873732101145,135.709057368857));
#36941=CARTESIAN_POINT('Ctrl Pts',(136.644143013221,0.501675704508042,135.698880298028));
#36942=CARTESIAN_POINT('Ctrl Pts',(136.636396737137,0.638086497572104,135.682972766436));
#36943=CARTESIAN_POINT('Ctrl Pts',(136.628650461053,0.773592993303272,135.66139025956));
#36944=CARTESIAN_POINT('Ctrl Pts',(136.620904127788,0.909100489312608,135.639807593367));
#36945=CARTESIAN_POINT('Ctrl Pts',(136.613157794522,1.04370328857031,135.612549929794));
#36946=CARTESIAN_POINT('Ctrl Pts',(136.605411461257,1.17689648786341,135.579724239255));
#36947=CARTESIAN_POINT('Ctrl Pts',(136.597663393254,1.31011951484991,135.546891197631));
#36948=CARTESIAN_POINT('Ctrl Pts',(136.589915325251,1.44193193419066,135.508487741349));
#36949=CARTESIAN_POINT('Ctrl Pts',(136.582167257248,1.57184245811965,135.464671159724));
#36950=CARTESIAN_POINT('Ctrl Pts',(136.574410954507,1.70189105249951,135.420808009315));
#36951=CARTESIAN_POINT('Ctrl Pts',(136.566654651765,1.8300333425375,135.371520366207));
#36952=CARTESIAN_POINT('Ctrl Pts',(136.558898349023,1.95579602180523,135.317014491241));
#36953=CARTESIAN_POINT('Ctrl Pts',(136.551137906509,2.0816258244017,135.262479524848));
#36954=CARTESIAN_POINT('Ctrl Pts',(136.543377463995,2.20507313377636,135.202720947261));
#36955=CARTESIAN_POINT('Ctrl Pts',(136.53561702148,2.32568874568705,135.13799130334));
#36956=CARTESIAN_POINT('Ctrl Pts',(136.527844121215,2.44649798048564,135.073157749649));
#36957=CARTESIAN_POINT('Ctrl Pts',(136.52007122095,2.56446609743282,135.003337382293));
#36958=CARTESIAN_POINT('Ctrl Pts',(136.512298320684,2.67917165387063,134.928826923841));
#36959=CARTESIAN_POINT('Ctrl Pts',(136.504807984922,2.78970737440746,134.857025108233));
#36960=CARTESIAN_POINT('Ctrl Pts',(136.49731764916,2.89721336945666,134.780868452687));
#36961=CARTESIAN_POINT('Ctrl Pts',(136.489827313398,3.00134271432949,134.700656932484));
#36962=CARTESIAN_POINT('Ctrl Pts',(136.482052979279,3.10942015496139,134.617404168113));
#36963=CARTESIAN_POINT('Ctrl Pts',(136.47427864516,3.21420219634503,134.529519269206));
#36964=CARTESIAN_POINT('Ctrl Pts',(136.466504311041,3.31526604286314,134.437292508964));
#36965=CARTESIAN_POINT('Ctrl Pts',(136.458739558094,3.41620533722269,134.345179409962));
#36966=CARTESIAN_POINT('Ctrl Pts',(136.450974805146,3.51343526819386,134.248735357442));
#36967=CARTESIAN_POINT('Ctrl Pts',(136.443210052199,3.60656376149745,134.148292569139));
#36968=CARTESIAN_POINT('Ctrl Pts',(136.435453011314,3.69959975826861,134.04794954203));
#36969=CARTESIAN_POINT('Ctrl Pts',(136.427695970429,3.78854215993315,133.943615967642));
#36970=CARTESIAN_POINT('Ctrl Pts',(136.419938929544,3.87303389081492,133.835662572683));
#36971=CARTESIAN_POINT('Ctrl Pts',(136.412187738304,3.95746190582512,133.72779058622));
#36972=CARTESIAN_POINT('Ctrl Pts',(136.404436547064,4.03744569054372,133.61630451919));
#36973=CARTESIAN_POINT('Ctrl Pts',(136.396685355824,4.11266705179859,133.501609731673));
#36974=CARTESIAN_POINT('Ctrl Pts',(136.388937459047,4.18785644196844,133.386963692499));
#36975=CARTESIAN_POINT('Ctrl Pts',(136.38118956227,4.25828722060567,133.269111971559));
#36976=CARTESIAN_POINT('Ctrl Pts',(136.373441665493,4.32368344982922,133.148490410938));
#36977=CARTESIAN_POINT('Ctrl Pts',(136.365695389409,4.38906599957139,133.027894081747));
#36978=CARTESIAN_POINT('Ctrl Pts',(136.357949113325,4.44941590838845,132.904529408799));
#36979=CARTESIAN_POINT('Ctrl Pts',(136.35020283724,4.5045025049783,132.778858084048));
#36980=CARTESIAN_POINT('Ctrl Pts',(136.342456503975,4.55958950820486,132.65318583162));
#36981=CARTESIAN_POINT('Ctrl Pts',(136.33471017071,4.60941296471849,132.525207251489));
#36982=CARTESIAN_POINT('Ctrl Pts',(136.326963837444,4.65378995923906,132.395404953147));
#36983=CARTESIAN_POINT('Ctrl Pts',(136.319215769441,4.69817689167987,132.265573586482));
#36984=CARTESIAN_POINT('Ctrl Pts',(136.311467701438,4.73711480861872,132.133918058791));
#36985=CARTESIAN_POINT('Ctrl Pts',(136.303719633435,4.7704704889721,132.000936723105));
#36986=CARTESIAN_POINT('Ctrl Pts',(136.295963330694,4.80386162013951,131.867814053272));
#36987=CARTESIAN_POINT('Ctrl Pts',(136.288207027952,4.8316585679088,131.733363140467));
#36988=CARTESIAN_POINT('Ctrl Pts',(136.28045072521,4.85377903168164,131.598093679815));
#36989=CARTESIAN_POINT('Ctrl Pts',(136.272690282696,4.87591130181205,131.46275202178));
#36990=CARTESIAN_POINT('Ctrl Pts',(136.264929840182,4.89236100412251,131.326591333323));
#36991=CARTESIAN_POINT('Ctrl Pts',(136.257169397667,4.9030978058908,131.190126049362));
#36992=CARTESIAN_POINT('Ctrl Pts',(136.249396497402,4.91385184332644,131.053441699213));
#36993=CARTESIAN_POINT('Ctrl Pts',(136.241623597137,4.91887463959558,130.916452167381));
#36994=CARTESIAN_POINT('Ctrl Pts',(136.233850696871,4.91818803574769,130.779672411307));
#36995=CARTESIAN_POINT('Ctrl Pts',(136.226360361109,4.91752639167913,130.647864943895));
#36996=CARTESIAN_POINT('Ctrl Pts',(136.218870025347,4.91156325680349,130.516252572982));
#36997=CARTESIAN_POINT('Ctrl Pts',(136.211379689585,4.90036348755281,130.385289320101));
#36998=CARTESIAN_POINT('Ctrl Pts',(136.203605355466,4.88873907564683,130.249360555681));
#36999=CARTESIAN_POINT('Ctrl Pts',(136.195831021347,4.87143627397818,130.113700522116));
#37000=CARTESIAN_POINT('Ctrl Pts',(136.188056687228,4.84847076625396,129.978821829089));
#37001=CARTESIAN_POINT('Ctrl Pts',(136.180291934281,4.82553356146554,129.844109361996));
#37002=CARTESIAN_POINT('Ctrl Pts',(136.172527181334,4.79694760130631,129.710176701212));
#37003=CARTESIAN_POINT('Ctrl Pts',(136.164762428386,4.76278046423991,129.57753328173));
#37004=CARTESIAN_POINT('Ctrl Pts',(136.157005387501,4.72864726245571,129.445021605562));
#37005=CARTESIAN_POINT('Ctrl Pts',(136.149248346617,4.68894401208142,129.313796998616));
#37006=CARTESIAN_POINT('Ctrl Pts',(136.141491305732,4.64378960787083,129.184360265612));
#37007=CARTESIAN_POINT('Ctrl Pts',(136.133740114491,4.59866925494771,129.055021141855));
#37008=CARTESIAN_POINT('Ctrl Pts',(136.125988923251,4.54810605865902,128.927467576084));
#37009=CARTESIAN_POINT('Ctrl Pts',(136.118237732011,4.49226906873743,128.802186380252));
#37010=CARTESIAN_POINT('Ctrl Pts',(136.110489835234,4.43645581102606,128.676958432269));
#37011=CARTESIAN_POINT('Ctrl Pts',(136.102741938457,4.37537337668544,128.554001289642));
#37012=CARTESIAN_POINT('Ctrl Pts',(136.09499404168,4.30923930084178,128.433782690017));
#37013=CARTESIAN_POINT('Ctrl Pts',(136.087247765596,4.24311905882105,128.313589237532));
#37014=CARTESIAN_POINT('Ctrl Pts',(136.079501489512,4.17194946544494,128.196133530968));
#37015=CARTESIAN_POINT('Ctrl Pts',(136.071755213427,4.09599427175701,128.081859196403));
#37016=CARTESIAN_POINT('Ctrl Pts',(136.064008880162,4.02003851738514,127.967584018291));
#37017=CARTESIAN_POINT('Ctrl Pts',(136.056262546897,3.93929730862969,127.85649058464));
#37018=CARTESIAN_POINT('Ctrl Pts',(136.048516213631,3.85407780834988,127.748993649478));
#37019=CARTESIAN_POINT('Ctrl Pts',(136.040768145628,3.76883922375391,127.641472641122));
#37020=CARTESIAN_POINT('Ctrl Pts',(136.033020077625,3.67912059484687,127.53755004024));
#37021=CARTESIAN_POINT('Ctrl Pts',(136.025272009622,3.58526919089529,127.437607301489));
#37022=CARTESIAN_POINT('Ctrl Pts',(136.017515706881,3.49131804055468,127.337558342405));
#37023=CARTESIAN_POINT('Ctrl Pts',(136.009759404139,3.39322560901152,127.241497980479));
#37024=CARTESIAN_POINT('Ctrl Pts',(136.002003101397,3.29137623172681,127.1497709602));
#37025=CARTESIAN_POINT('Ctrl Pts',(135.994242658883,3.18947249436276,127.057994982449));
#37026=CARTESIAN_POINT('Ctrl Pts',(135.986482216369,3.08380811679827,126.970557203995));
#37027=CARTESIAN_POINT('Ctrl Pts',(135.978721773854,2.97479951212098,126.887761209255));
#37028=CARTESIAN_POINT('Ctrl Pts',(135.970948873589,2.86561591715413,126.804832303033));
#37029=CARTESIAN_POINT('Ctrl Pts',(135.963175973324,2.753077688351,126.726560294169));
#37030=CARTESIAN_POINT('Ctrl Pts',(135.955403073058,2.63762987961105,126.653205154242));
#37031=CARTESIAN_POINT('Ctrl Pts',(135.947912737296,2.52637888951411,126.582516658423));
#37032=CARTESIAN_POINT('Ctrl Pts',(135.940422401534,2.41242645434999,126.516393911388));
#37033=CARTESIAN_POINT('Ctrl Pts',(135.932932065772,2.29618961177886,126.455027757315));
#37034=CARTESIAN_POINT('Ctrl Pts',(135.925157731653,2.17554561399248,126.391334886858));
#37035=CARTESIAN_POINT('Ctrl Pts',(135.917383397534,2.05205839871615,126.332564662121));
#37036=CARTESIAN_POINT('Ctrl Pts',(135.909609063415,1.92616771642072,126.27898096601));
#37037=CARTESIAN_POINT('Ctrl Pts',(135.901844310468,1.80043218314012,126.225463307015));
#37038=CARTESIAN_POINT('Ctrl Pts',(135.89407955752,1.67229943273503,126.177119610253));
#37039=CARTESIAN_POINT('Ctrl Pts',(135.886314804573,1.54223459510521,126.134168382105));
#37040=CARTESIAN_POINT('Ctrl Pts',(135.878557763688,1.41229893970581,126.091259813722));
#37041=CARTESIAN_POINT('Ctrl Pts',(135.870800722803,1.28043538477516,126.053733177323));
#37042=CARTESIAN_POINT('Ctrl Pts',(135.863043681918,1.14712953702657,126.021759140568));
#37043=CARTESIAN_POINT('Ctrl Pts',(135.855292490678,1.01392421625455,125.989809215683));
#37044=CARTESIAN_POINT('Ctrl Pts',(135.847541299438,0.87927914619829,125.963403646777));
#37045=CARTESIAN_POINT('Ctrl Pts',(135.839790108198,0.743695271049467,125.942663341273));
#37046=CARTESIAN_POINT('Ctrl Pts',(135.832042211421,0.6081690226644,125.921931850952));
#37047=CARTESIAN_POINT('Ctrl Pts',(135.824294314644,0.471705148462137,125.906860893922));
#37048=CARTESIAN_POINT('Ctrl Pts',(135.816546417867,0.334814752422365,125.897520275344));
#37049=CARTESIAN_POINT('Ctrl Pts',(135.808800141783,0.197952990902429,125.888181610622));
#37050=CARTESIAN_POINT('Ctrl Pts',(135.801053865698,0.0606652748179095,
125.884570926744));
#37051=CARTESIAN_POINT('Ctrl Pts',(135.793307589614,-0.0765325967660386,
125.886706113218));
#37052=CARTESIAN_POINT('Ctrl Pts',(135.785561256349,-0.213731481113414,
125.888841315454));
#37053=CARTESIAN_POINT('Ctrl Pts',(135.777814923084,-0.350840128718959,
125.896722466594));
#37054=CARTESIAN_POINT('Ctrl Pts',(135.770068589818,-0.487343566245976,
125.910315326507));
#37055=CARTESIAN_POINT('Ctrl Pts',(135.762320521815,-0.623877572771378,
125.923911230447));
#37056=CARTESIAN_POINT('Ctrl Pts',(135.754572453812,-0.759805710557421,
125.943221349683));
#37057=CARTESIAN_POINT('Ctrl Pts',(135.746824385809,-0.894619343478421,
125.968159702305));
#37058=CARTESIAN_POINT('Ctrl Pts',(135.739068083068,-1.02957625793288,125.993124559705));
#37059=CARTESIAN_POINT('Ctrl Pts',(135.731311780326,-1.16341591628201,126.023729528458));
#37060=CARTESIAN_POINT('Ctrl Pts',(135.723555477584,-1.2956405325183,126.059837599074));
#37061=CARTESIAN_POINT('Ctrl Pts',(135.71579503507,-1.42793572101357,126.095964941655));
#37062=CARTESIAN_POINT('Ctrl Pts',(135.708034592555,-1.55861377746305,126.13760112003));
#37063=CARTESIAN_POINT('Ctrl Pts',(135.700274150041,-1.68719420625387,126.184559888867));
#37064=CARTESIAN_POINT('Ctrl Pts',(135.692501249776,-1.81598104376382,126.231594040089));
#37065=CARTESIAN_POINT('Ctrl Pts',(135.68472834951,-1.94266316316723,126.283967706538));
#37066=CARTESIAN_POINT('Ctrl Pts',(135.676955449245,-2.06678128050621,126.341446972754));
#37067=CARTESIAN_POINT('Ctrl Pts',(135.669465113483,-2.1863873916445,126.396836722861));
#37068=CARTESIAN_POINT('Ctrl Pts',(135.661974777721,-2.30361240606622,126.456967173955));
#37069=CARTESIAN_POINT('Ctrl Pts',(135.654484441959,-2.41807034211935,126.52159061638));
#37070=CARTESIAN_POINT('Ctrl Pts',(135.646709017723,-2.53688464341573,126.588673681336));
#37071=CARTESIAN_POINT('Ctrl Pts',(135.638933593486,-2.65309348094871,126.660811054195));
#37072=CARTESIAN_POINT('Ctrl Pts',(135.63115816925,-2.76623695472661,126.737775296587));
#37073=CARTESIAN_POINT('Ctrl Pts',(135.623392564522,-2.87923754069221,126.814642341572));
#37074=CARTESIAN_POINT('Ctrl Pts',(135.615626959795,-2.98918014595701,126.896323907967));
#37075=CARTESIAN_POINT('Ctrl Pts',(135.607861355068,-3.09562938257853,126.982546678058));
#37076=CARTESIAN_POINT('Ctrl Pts',(135.600105132703,-3.20195000779408,127.068665274254));
#37077=CARTESIAN_POINT('Ctrl Pts',(135.592348910338,-3.30478536874702,127.159313901849));
#37078=CARTESIAN_POINT('Ctrl Pts',(135.584592687973,-3.40372953011546,127.254176347937));
#37079=CARTESIAN_POINT('Ctrl Pts',(135.57684178538,-3.50260582850577,127.34897373058));
#37080=CARTESIAN_POINT('Ctrl Pts',(135.569090882787,-3.59759595600647,127.447978912464));
#37081=CARTESIAN_POINT('Ctrl Pts',(135.561339980194,-3.68832746322366,127.550835823357));
#37082=CARTESIAN_POINT('Ctrl Pts',(135.5535927151,-3.77901639014381,127.653644463502));
#37083=CARTESIAN_POINT('Ctrl Pts',(135.545845450005,-3.86545041598168,127.760300942952));
#37084=CARTESIAN_POINT('Ctrl Pts',(135.538098184911,-3.94729463202187,127.870413080456));
#37085=CARTESIAN_POINT('Ctrl Pts',(135.530352877854,-4.02911816282088,127.980497388308));
#37086=CARTESIAN_POINT('Ctrl Pts',(135.522607570797,-4.10635396062298,128.094035301791));
#37087=CARTESIAN_POINT('Ctrl Pts',(135.51486226374,-4.17870828117702,128.210602694528));
#37088=CARTESIAN_POINT('Ctrl Pts',(135.507114921424,-4.25108161451235,128.327200718059));
#37089=CARTESIAN_POINT('Ctrl Pts',(135.499367579107,-4.3185706968598,128.446829481985));
#37090=CARTESIAN_POINT('Ctrl Pts',(135.491620236791,-4.38092588068271,128.569037041333));
#37091=CARTESIAN_POINT('Ctrl Pts',(135.483871903469,-4.44328904069723,128.691260232916));
#37092=CARTESIAN_POINT('Ctrl Pts',(135.476123570148,-4.5005168236209,128.816062525076));
#37093=CARTESIAN_POINT('Ctrl Pts',(135.468375236827,-4.5524066197537,128.942969462832));
#37094=CARTESIAN_POINT('Ctrl Pts',(135.460620817355,-4.60433717421597,129.069976083284));
#37095=CARTESIAN_POINT('Ctrl Pts',(135.452866397883,-4.65092122662039,129.199090286265));
#37096=CARTESIAN_POINT('Ctrl Pts',(135.44511197841,-4.6920050906097,129.329819572972));
#37097=CARTESIAN_POINT('Ctrl Pts',(135.440152691468,-4.71828000015651,129.413426611108));
#37098=CARTESIAN_POINT('Ctrl Pts',(135.435193404526,-4.74230625146068,129.497693918245));
#37099=CARTESIAN_POINT('Ctrl Pts',(135.430234117584,-4.76405452823404,129.582490119308));
#37100=CARTESIAN_POINT('Origin',(213.235140564004,0.,130.804360617566));
#37101=CARTESIAN_POINT('',(133.334729823376,-4.76405452823402,129.582490119308));
#37102=CARTESIAN_POINT('',(133.679929079587,-4.76405452823404,129.582490119308));
#37103=CARTESIAN_POINT('',(213.235140564004,-4.76405452823405,129.582490119308));
#37104=CARTESIAN_POINT('',(135.014859436046,-4.91824892140636,130.801103381751));
#37105=CARTESIAN_POINT('Ctrl Pts',(135.014859435991,-4.91824892140701,130.801103382733));
#37106=CARTESIAN_POINT('Ctrl Pts',(135.00706768985,-4.9183404006375,130.939232086896));
#37107=CARTESIAN_POINT('Ctrl Pts',(134.999275943709,-4.91260854852309,131.07739304955));
#37108=CARTESIAN_POINT('Ctrl Pts',(134.991484197567,-4.90107189874953,131.215064045586));
#37109=CARTESIAN_POINT('Ctrl Pts',(134.983692153207,-4.88953480742615,131.352740310795));
#37110=CARTESIAN_POINT('Ctrl Pts',(134.975900108848,-4.87219250742866,131.489926188914));
#37111=CARTESIAN_POINT('Ctrl Pts',(134.968108064488,-4.84911548938473,131.626103906622));
#37112=CARTESIAN_POINT('Ctrl Pts',(134.960314108631,-4.82603281022766,131.762315030616));
#37113=CARTESIAN_POINT('Ctrl Pts',(134.952520152775,-4.79721267620561,131.897517122828));
#37114=CARTESIAN_POINT('Ctrl Pts',(134.944726196918,-4.76277678234938,132.031202247123));
#37115=CARTESIAN_POINT('Ctrl Pts',(134.936928715398,-4.72832531111852,132.164947845041));
#37116=CARTESIAN_POINT('Ctrl Pts',(134.929131233878,-4.68825311816046,132.297174736941));
#37117=CARTESIAN_POINT('Ctrl Pts',(134.921333752358,-4.64273177880704,132.427390097445));
#37118=CARTESIAN_POINT('Ctrl Pts',(134.913526281164,-4.59715212019576,132.557772282196));
#37119=CARTESIAN_POINT('Ctrl Pts',(134.90571880997,-4.54610950054951,132.686137426018));
#37120=CARTESIAN_POINT('Ctrl Pts',(134.897911338777,-4.48982391918956,132.81201204079));
#37121=CARTESIAN_POINT('Ctrl Pts',(134.890098268532,-4.43349797318495,132.93797692529));
#37122=CARTESIAN_POINT('Ctrl Pts',(134.882285198288,-4.3719217447522,133.061447378862));
#37123=CARTESIAN_POINT('Ctrl Pts',(134.874472128044,-4.30536080807937,133.181975257232));
#37124=CARTESIAN_POINT('Ctrl Pts',(134.866646520133,-4.23869306078745,133.302696547203));
#37125=CARTESIAN_POINT('Ctrl Pts',(134.858820912222,-4.16702482837157,133.420465503421));
#37126=CARTESIAN_POINT('Ctrl Pts',(134.85099530431,-4.09066492895952,133.534863044132));
#37127=CARTESIAN_POINT('Ctrl Pts',(134.846907058433,-4.05077307040069,133.594626487361));
#37128=CARTESIAN_POINT('Ctrl Pts',(134.842818812556,-4.00960142714413,133.653470343483));
#37129=CARTESIAN_POINT('Ctrl Pts',(134.838730566679,-3.9671982273736,133.711338651061));
#37130=CARTESIAN_POINT('Ctrl Pts',(134.83095623256,-3.88656299831506,133.821382804852));
#37131=CARTESIAN_POINT('Ctrl Pts',(134.823181898441,-3.80121788816482,133.928243666845));
#37132=CARTESIAN_POINT('Ctrl Pts',(134.815407564322,-3.71144294060409,134.031491597421));
#37133=CARTESIAN_POINT('Ctrl Pts',(134.807642811375,-3.62177863264288,134.13461228415));
#37134=CARTESIAN_POINT('Ctrl Pts',(134.799878058428,-3.52769560387842,134.234128606638));
#37135=CARTESIAN_POINT('Ctrl Pts',(134.792113305481,-3.42951656767255,134.329640631205));
#37136=CARTESIAN_POINT('Ctrl Pts',(134.784356264596,-3.3314350442696,134.425057791882));
#37137=CARTESIAN_POINT('Ctrl Pts',(134.776599223711,-3.22926588777218,134.516478298438));
#37138=CARTESIAN_POINT('Ctrl Pts',(134.768842182826,-3.1233711492963,134.603536281607));
#37139=CARTESIAN_POINT('Ctrl Pts',(134.761090991586,-3.01755626686638,134.690528613674));
#37140=CARTESIAN_POINT('Ctrl Pts',(134.753339800346,-2.90802169536307,134.773164723247));
#37141=CARTESIAN_POINT('Ctrl Pts',(134.745588609106,-2.79516504237249,134.85111678126));
#37142=CARTESIAN_POINT('Ctrl Pts',(134.737840712329,-2.68235635646991,134.92903570757));
#37143=CARTESIAN_POINT('Ctrl Pts',(134.730092815552,-2.56622871840148,135.002274320232));
#37144=CARTESIAN_POINT('Ctrl Pts',(134.722344918774,-2.44721122299368,135.070546301822));
#37145=CARTESIAN_POINT('Ctrl Pts',(134.71459864269,-2.32821862348028,135.138804002385));
#37146=CARTESIAN_POINT('Ctrl Pts',(134.706852366606,-2.20633770791888,135.202096943917));
#37147=CARTESIAN_POINT('Ctrl Pts',(134.699106090522,-2.08202449983253,135.260183442208));
#37148=CARTESIAN_POINT('Ctrl Pts',(134.691359757257,-1.9577103740944,135.31827036928));
#37149=CARTESIAN_POINT('Ctrl Pts',(134.683613423991,-1.83096427420974,135.371150610916));
#37150=CARTESIAN_POINT('Ctrl Pts',(134.675867090726,-1.70226428123129,135.418629723215));
#37151=CARTESIAN_POINT('Ctrl Pts',(134.668119022723,-1.57353546678149,135.466119468131));
#37152=CARTESIAN_POINT('Ctrl Pts',(134.66037095472,-1.44285225527326,135.508205541562));
#37153=CARTESIAN_POINT('Ctrl Pts',(134.652622886717,-1.31070965928222,135.54474280169));
#37154=CARTESIAN_POINT('Ctrl Pts',(134.644866583975,-1.17842662056782,135.581318894053));
#37155=CARTESIAN_POINT('Ctrl Pts',(134.637110281234,-1.04468147640565,135.612334288174));
#37156=CARTESIAN_POINT('Ctrl Pts',(134.629353978492,-0.909981800154545,
135.637694475876));
#37157=CARTESIAN_POINT('Ctrl Pts',(134.621593535978,-0.775210230630404,
135.663068199074));
#37158=CARTESIAN_POINT('Ctrl Pts',(134.613833093463,-0.639483500586702,
135.682780645364));
#37159=CARTESIAN_POINT('Ctrl Pts',(134.606072650949,-0.503315168893812,
135.696789145737));
#37160=CARTESIAN_POINT('Ctrl Pts',(134.598299750684,-0.366928247706432,
135.710820133799));
#37161=CARTESIAN_POINT('Ctrl Pts',(134.590526850418,-0.230098698736417,
135.719128854669));
#37162=CARTESIAN_POINT('Ctrl Pts',(134.582753950153,-0.0933418552538072,
135.721724785548));
#37163=CARTESIAN_POINT('Ctrl Pts',(134.575263614391,0.0384435324981373,
135.724226347802));
#37164=CARTESIAN_POINT('Ctrl Pts',(134.567773278629,0.17016110109541,135.721423264168));
#37165=CARTESIAN_POINT('Ctrl Pts',(134.560282942867,0.30135540337624,135.713369477138));
#37166=CARTESIAN_POINT('Ctrl Pts',(134.552508608748,0.437523977503984,135.705010328325));
#37167=CARTESIAN_POINT('Ctrl Pts',(134.544734274629,0.573560163861853,135.690967976185));
#37168=CARTESIAN_POINT('Ctrl Pts',(134.53695994051,0.70895112402018,135.671245798691));
#37169=CARTESIAN_POINT('Ctrl Pts',(134.529195187563,0.844175226920348,135.651547927017));
#37170=CARTESIAN_POINT('Ctrl Pts',(134.521430434615,0.978755302631332,135.626184213474));
#37171=CARTESIAN_POINT('Ctrl Pts',(134.513665681668,1.11218044116573,135.595209992029));
#37172=CARTESIAN_POINT('Ctrl Pts',(134.505908640783,1.24547305997129,135.564266534616));
#37173=CARTESIAN_POINT('Ctrl Pts',(134.498151599898,1.37761264600742,135.527723746538));
#37174=CARTESIAN_POINT('Ctrl Pts',(134.490394559013,1.50809568562692,135.485688470376));
#37175=CARTESIAN_POINT('Ctrl Pts',(134.482643367773,1.6384803269714,135.443684893343));
#37176=CARTESIAN_POINT('Ctrl Pts',(134.474892176533,1.76721053775918,135.39619719188));
#37177=CARTESIAN_POINT('Ctrl Pts',(134.467140985293,1.89379558950122,135.343382684893));
#37178=CARTESIAN_POINT('Ctrl Pts',(134.459393088516,2.02032683921959,135.290590625481));
#37179=CARTESIAN_POINT('Ctrl Pts',(134.451645191739,2.14471438322918,135.232476413766));
#37180=CARTESIAN_POINT('Ctrl Pts',(134.443897294962,2.26648539833556,135.169246297814));
#37181=CARTESIAN_POINT('Ctrl Pts',(134.436151018878,2.3882309415705,135.106029408239));
#37182=CARTESIAN_POINT('Ctrl Pts',(134.428404742794,2.50736069779764,135.037698923044));
#37183=CARTESIAN_POINT('Ctrl Pts',(134.42065846671,2.62342483939446,134.964507871516));
#37184=CARTESIAN_POINT('Ctrl Pts',(134.412912133444,2.73948983775018,134.891316279708));
#37185=CARTESIAN_POINT('Ctrl Pts',(134.405165800179,2.85248884561819,134.813264258516));
#37186=CARTESIAN_POINT('Ctrl Pts',(134.397419466914,2.96199985734986,134.730648929389));
#37187=CARTESIAN_POINT('Ctrl Pts',(134.389671398911,3.07153539331361,134.648015099132));
#37188=CARTESIAN_POINT('Ctrl Pts',(134.381923330908,3.17758106676573,134.560816162849));
#37189=CARTESIAN_POINT('Ctrl Pts',(134.374175262905,3.27974719939589,134.46939013594));
#37190=CARTESIAN_POINT('Ctrl Pts',(134.366418960163,3.38202191540753,134.377866940363));
#37191=CARTESIAN_POINT('Ctrl Pts',(134.358662657421,3.48040856220899,134.282107940835));
#37192=CARTESIAN_POINT('Ctrl Pts',(134.350906354679,3.57455327159708,134.182489089222));
#37193=CARTESIAN_POINT('Ctrl Pts',(134.343145912165,3.66874822885115,134.082817068029));
#37194=CARTESIAN_POINT('Ctrl Pts',(134.335385469651,3.7586964810979,133.979281384785));
#37195=CARTESIAN_POINT('Ctrl Pts',(134.327625027137,3.84408453857975,133.872291047473));
#37196=CARTESIAN_POINT('Ctrl Pts',(134.319852126871,3.92960966855198,133.765128959774));
#37197=CARTESIAN_POINT('Ctrl Pts',(134.312079226606,4.01055974420107,133.654501451593));
#37198=CARTESIAN_POINT('Ctrl Pts',(134.30430632634,4.08666418874456,133.540847210066));
#37199=CARTESIAN_POINT('Ctrl Pts',(134.296815990578,4.16000204503434,133.431324586495));
#37200=CARTESIAN_POINT('Ctrl Pts',(134.289325654816,4.2288402945944,133.318991730424));
#37201=CARTESIAN_POINT('Ctrl Pts',(134.281835319054,4.29297814045349,133.204260979683));
#37202=CARTESIAN_POINT('Ctrl Pts',(134.274060984935,4.35954779223176,133.085180177658));
#37203=CARTESIAN_POINT('Ctrl Pts',(134.266286650816,4.4212644452716,132.963138846995));
#37204=CARTESIAN_POINT('Ctrl Pts',(134.258512316697,4.47785373985819,132.838570279066));
#37205=CARTESIAN_POINT('Ctrl Pts',(134.25074756375,4.53437329319673,132.714155230763));
#37206=CARTESIAN_POINT('Ctrl Pts',(134.242982810803,4.58577790087803,132.587219494849));
#37207=CARTESIAN_POINT('Ctrl Pts',(134.235218057855,4.63183795760822,132.458222823725));
#37208=CARTESIAN_POINT('Ctrl Pts',(134.22746101697,4.67785226684053,132.329354273913));
#37209=CARTESIAN_POINT('Ctrl Pts',(134.219703976086,4.71853245822587,132.19842922823));
#37210=CARTESIAN_POINT('Ctrl Pts',(134.211946935201,4.75369626002962,132.065929057993));
#37211=CARTESIAN_POINT('Ctrl Pts',(134.20419574396,4.78883354453696,131.933528807164));
#37212=CARTESIAN_POINT('Ctrl Pts',(134.19644455272,4.81846261971568,131.799556172407));
#37213=CARTESIAN_POINT('Ctrl Pts',(134.18869336148,4.84245059168189,131.66450905221));
#37214=CARTESIAN_POINT('Ctrl Pts',(134.180945464703,4.86642836812017,131.52951933064));
#37215=CARTESIAN_POINT('Ctrl Pts',(134.173197567926,4.88476974179557,131.393456416076));
#37216=CARTESIAN_POINT('Ctrl Pts',(134.165449671149,4.89739266256268,131.256829590179));
#37217=CARTESIAN_POINT('Ctrl Pts',(134.157703395065,4.91001294288687,131.120231343669));
#37218=CARTESIAN_POINT('Ctrl Pts',(134.149957118981,4.91691711361933,130.983069809512));
#37219=CARTESIAN_POINT('Ctrl Pts',(134.142210842897,4.91807491264784,130.845860208937));
#37220=CARTESIAN_POINT('Ctrl Pts',(134.134464509631,4.91923272022296,130.708649595512));
#37221=CARTESIAN_POINT('Ctrl Pts',(134.126718176366,4.91464406815236,130.571391305913));
#37222=CARTESIAN_POINT('Ctrl Pts',(134.118971843101,4.90433082876644,130.434600986845));
#37223=CARTESIAN_POINT('Ctrl Pts',(134.111223775098,4.89401527980205,130.297780034533));
#37224=CARTESIAN_POINT('Ctrl Pts',(134.103475707095,4.87797262191486,130.161427651074));
#37225=CARTESIAN_POINT('Ctrl Pts',(134.095727639092,4.85627660639018,130.026054389448));
#37226=CARTESIAN_POINT('Ctrl Pts',(134.08797133635,4.83455753208206,129.890537251508));
#37227=CARTESIAN_POINT('Ctrl Pts',(134.080215033608,4.80717315956721,129.756001700811));
#37228=CARTESIAN_POINT('Ctrl Pts',(134.072458730866,4.77424851338938,129.622948667864));
#37229=CARTESIAN_POINT('Ctrl Pts',(134.064698288352,4.7413062943365,129.489824620506));
#37230=CARTESIAN_POINT('Ctrl Pts',(134.056937845838,4.70281801918803,129.358185042631));
#37231=CARTESIAN_POINT('Ctrl Pts',(134.049177403323,4.65895834907157,129.228514760854));
#37232=CARTESIAN_POINT('Ctrl Pts',(134.041404503058,4.61502827151903,129.09863632083));
#37233=CARTESIAN_POINT('Ctrl Pts',(134.033631602792,4.56570970895668,128.970733859162));
#37234=CARTESIAN_POINT('Ctrl Pts',(134.025858702527,4.51122548793434,128.845272140873));
#37235=CARTESIAN_POINT('Ctrl Pts',(134.018368366765,4.45872190558375,128.724371272063));
#37236=CARTESIAN_POINT('Ctrl Pts',(134.010878031003,4.40142184769512,128.60573705052));
#37237=CARTESIAN_POINT('Ctrl Pts',(134.003387695241,4.33956369009485,128.489761291093));
#37238=CARTESIAN_POINT('Ctrl Pts',(133.995613361122,4.27536016164765,128.369388275496));
#37239=CARTESIAN_POINT('Ctrl Pts',(133.987839027003,4.2060426922519,128.251497987139));
#37240=CARTESIAN_POINT('Ctrl Pts',(133.980064692884,4.13182752408236,128.136555457189));
#37241=CARTESIAN_POINT('Ctrl Pts',(133.972299939937,4.05770381947484,128.021754583634));
#37242=CARTESIAN_POINT('Ctrl Pts',(133.96453518699,3.97869463592205,127.909894565498));
#37243=CARTESIAN_POINT('Ctrl Pts',(133.956770434042,3.89506266887186,127.801417083621));
#37244=CARTESIAN_POINT('Ctrl Pts',(133.949013393157,3.81151376627034,127.693047343108));
#37245=CARTESIAN_POINT('Ctrl Pts',(133.941256352272,3.7233514544595,127.588053760759));
#37246=CARTESIAN_POINT('Ctrl Pts',(133.933499311387,3.63088220243694,127.4868498799));
#37247=CARTESIAN_POINT('Ctrl Pts',(133.925748120147,3.53848268219638,127.385722317675));
#37248=CARTESIAN_POINT('Ctrl Pts',(133.917996928907,3.44178294913729,127.288379056039));
#37249=CARTESIAN_POINT('Ctrl Pts',(133.910245737667,3.34113006696793,127.195201028672));
#37250=CARTESIAN_POINT('Ctrl Pts',(133.90249784089,3.24051996495884,127.102062604454));
#37251=CARTESIAN_POINT('Ctrl Pts',(133.894749944113,3.13596034191829,127.013086158482));
#37252=CARTESIAN_POINT('Ctrl Pts',(133.887002047336,3.02783532082514,126.928616001049));
#37253=CARTESIAN_POINT('Ctrl Pts',(133.879255771252,2.9197329171555,126.844163512951));
#37254=CARTESIAN_POINT('Ctrl Pts',(133.871509495168,2.80806690677753,126.764215679009));
#37255=CARTESIAN_POINT('Ctrl Pts',(133.863763219083,2.69325440249207,126.689076449254));
#37256=CARTESIAN_POINT('Ctrl Pts',(133.856016885818,2.57844105068655,126.613936664839));
#37257=CARTESIAN_POINT('Ctrl Pts',(133.848270552553,2.46048148576158,126.543605769535));
#37258=CARTESIAN_POINT('Ctrl Pts',(133.840524219287,2.33982135842349,126.478344081171));
#37259=CARTESIAN_POINT('Ctrl Pts',(133.832776151284,2.21913421008648,126.413067777904));
#37260=CARTESIAN_POINT('Ctrl Pts',(133.825028083281,2.09574563973077,126.352863126485));
#37261=CARTESIAN_POINT('Ctrl Pts',(133.817280015278,1.97012505440905,126.297944044224));
#37262=CARTESIAN_POINT('Ctrl Pts',(133.809523712537,1.84437095803453,126.24296659331));
#37263=CARTESIAN_POINT('Ctrl Pts',(133.801767409795,1.71638046674353,126.193286090107));
#37264=CARTESIAN_POINT('Ctrl Pts',(133.794011107053,1.58664260637883,126.149068113102));
#37265=CARTESIAN_POINT('Ctrl Pts',(133.786250664539,1.45683550101181,126.104826535631));
#37266=CARTESIAN_POINT('Ctrl Pts',(133.778490222024,1.32527954307293,126.066053404241));
#37267=CARTESIAN_POINT('Ctrl Pts',(133.77072977951,1.19247703953137,126.032863832207));
#37268=CARTESIAN_POINT('Ctrl Pts',(133.762956879245,1.05946134962138,125.999620981326));
#37269=CARTESIAN_POINT('Ctrl Pts',(133.755183978979,0.925195498496844,125.971979680061));
#37270=CARTESIAN_POINT('Ctrl Pts',(133.747411078714,0.790190949326217,125.950003674973));
#37271=CARTESIAN_POINT('Ctrl Pts',(133.739920742952,0.660094155574433,125.928826553023));
#37272=CARTESIAN_POINT('Ctrl Pts',(133.73243040719,0.529311744174783,125.912910020001));
#37273=CARTESIAN_POINT('Ctrl Pts',(133.724940071428,0.398302208012137,125.902265309069));
#37274=CARTESIAN_POINT('Ctrl Pts',(133.717165737309,0.262325405465818,125.891217000685));
#37275=CARTESIAN_POINT('Ctrl Pts',(133.70939140319,0.125673181662655,125.885813170373));
#37276=CARTESIAN_POINT('Ctrl Pts',(133.701617069071,-0.0111463353276202,
125.886123248171));
#37277=CARTESIAN_POINT('Ctrl Pts',(133.693852316124,-0.14779723449093,125.886432943827));
#37278=CARTESIAN_POINT('Ctrl Pts',(133.686087563176,-0.284614629405755,
125.892442535471));
#37279=CARTESIAN_POINT('Ctrl Pts',(133.678322810229,-0.421084928165682,
125.904169749266));
#37280=CARTESIAN_POINT('Ctrl Pts',(133.670565769344,-0.55741968270108,125.915885315427));
#37281=CARTESIAN_POINT('Ctrl Pts',(133.662808728459,-0.693407640122305,
125.933307169369));
#37282=CARTESIAN_POINT('Ctrl Pts',(133.655051687574,-0.828535220736507,
125.956401000315));
#37283=CARTESIAN_POINT('Ctrl Pts',(133.647300496334,-0.963560900591121,
125.979477416023));
#37284=CARTESIAN_POINT('Ctrl Pts',(133.639549305094,-1.09772711125099,126.008217229468));
#37285=CARTESIAN_POINT('Ctrl Pts',(133.631798113854,-1.23052576600856,126.042534350083));
#37286=CARTESIAN_POINT('Ctrl Pts',(133.624050217077,-1.36326797779543,126.076836885007));
#37287=CARTESIAN_POINT('Ctrl Pts',(133.6163023203,-1.49464341199928,126.116711914735));
#37288=CARTESIAN_POINT('Ctrl Pts',(133.608554423523,-1.62415476276908,126.162022373849));
#37289=CARTESIAN_POINT('Ctrl Pts',(133.600808147439,-1.75363902255623,126.207323354992));
#37290=CARTESIAN_POINT('Ctrl Pts',(133.593061871355,-1.88125960569524,126.258057374989));
#37291=CARTESIAN_POINT('Ctrl Pts',(133.58531559527,-2.00653533075908,126.314037797443));
#37292=CARTESIAN_POINT('Ctrl Pts',(133.577569262005,-2.1318119805791,126.370018633132));
#37293=CARTESIAN_POINT('Ctrl Pts',(133.56982292874,-2.25474338083662,126.431245789052));
#37294=CARTESIAN_POINT('Ctrl Pts',(133.562076595474,-2.37486963367725,126.497485034787));
#37295=CARTESIAN_POINT('Ctrl Pts',(133.554328527472,-2.49502278795956,126.563739114342));
#37296=CARTESIAN_POINT('Ctrl Pts',(133.546580459469,-2.61236920249317,126.635007328455));
#37297=CARTESIAN_POINT('Ctrl Pts',(133.538832391466,-2.72647517660756,126.711010379211));
#37298=CARTESIAN_POINT('Ctrl Pts',(133.531076088724,-2.84070242390967,126.787094206913));
#37299=CARTESIAN_POINT('Ctrl Pts',(133.523319785982,-2.95168202516372,126.867922706621));
#37300=CARTESIAN_POINT('Ctrl Pts',(133.51556348324,-3.05901034408721,126.953173946257));
#37301=CARTESIAN_POINT('Ctrl Pts',(133.507803040726,-3.1663959473658,127.038470687047));
#37302=CARTESIAN_POINT('Ctrl Pts',(133.500042598212,-3.27012608961524,127.128194615716));
#37303=CARTESIAN_POINT('Ctrl Pts',(133.492282155698,-3.36983241359037,127.221985348723));
#37304=CARTESIAN_POINT('Ctrl Pts',(133.484509255432,-3.46969879500853,127.315926642942));
#37305=CARTESIAN_POINT('Ctrl Pts',(133.476736355167,-3.5655281767636,127.413947507589));
#37306=CARTESIAN_POINT('Ctrl Pts',(133.468963454901,-3.65699046873391,127.51565209079));
#37307=CARTESIAN_POINT('Ctrl Pts',(133.461473119139,-3.74512787601217,127.613659456214));
#37308=CARTESIAN_POINT('Ctrl Pts',(133.453982783377,-3.82920999392396,127.715087127994));
#37309=CARTESIAN_POINT('Ctrl Pts',(133.446492447615,-3.90897954508848,127.819555434882));
#37310=CARTESIAN_POINT('Ctrl Pts',(133.438698763919,-3.99197964950509,127.928254559463));
#37311=CARTESIAN_POINT('Ctrl Pts',(133.430905080222,-4.07057665885007,128.040594229956));
#37312=CARTESIAN_POINT('Ctrl Pts',(133.423111396526,-4.14443493069619,128.156183477017));
#37313=CARTESIAN_POINT('Ctrl Pts',(133.415330435805,-4.21817263094185,128.271584027807));
#37314=CARTESIAN_POINT('Ctrl Pts',(133.407549475083,-4.28718679338726,128.390223265882));
#37315=CARTESIAN_POINT('Ctrl Pts',(133.399768514361,-4.35118251058085,128.511677948265));
#37316=CARTESIAN_POINT('Ctrl Pts',(133.391994871904,-4.41511803757263,128.633018398287));
#37317=CARTESIAN_POINT('Ctrl Pts',(133.384221229447,-4.47404432737747,128.757168684957));
#37318=CARTESIAN_POINT('Ctrl Pts',(133.37644758699,-4.52771001302225,128.883677119309));
#37319=CARTESIAN_POINT('Ctrl Pts',(133.368680664419,-4.58132930764104,129.010076194095));
#37320=CARTESIAN_POINT('Ctrl Pts',(133.360913741847,-4.62969690070071,129.138829002326));
#37321=CARTESIAN_POINT('Ctrl Pts',(133.353146819275,-4.67260785241139,129.269460321103));
#37322=CARTESIAN_POINT('Ctrl Pts',(133.347007820642,-4.70652479589331,129.372711702843));
#37323=CARTESIAN_POINT('Ctrl Pts',(133.340868822009,-4.73703364669907,129.477136112303));
#37324=CARTESIAN_POINT('Ctrl Pts',(133.334729823376,-4.76405452823402,129.582490119308));
#37325=CARTESIAN_POINT('Ctrl Pts',(135.084620084674,-4.76405452823407,129.582490119308));
#37326=CARTESIAN_POINT('Ctrl Pts',(135.07579945711,-4.80260188508095,129.732785678617));
#37327=CARTESIAN_POINT('Ctrl Pts',(135.066978829546,-4.83407694623485,129.885078300731));
#37328=CARTESIAN_POINT('Ctrl Pts',(135.058158201982,-4.85829197544408,130.038735288939));
#37329=CARTESIAN_POINT('Ctrl Pts',(135.049393588783,-4.88235322993912,130.191416496393));
#37330=CARTESIAN_POINT('Ctrl Pts',(135.040628975584,-4.8992462793229,130.345444623537));
#37331=CARTESIAN_POINT('Ctrl Pts',(135.031864362385,-4.90883460055151,130.50017987043));
#37332=CARTESIAN_POINT('Ctrl Pts',(135.026196053605,-4.91503562325125,130.600251275586));
#37333=CARTESIAN_POINT('Ctrl Pts',(135.020527744826,-4.91818237243618,130.70061805634));
#37334=CARTESIAN_POINT('Ctrl Pts',(135.014859436046,-4.91824892140636,130.801103381751));
#37335=CARTESIAN_POINT('',(135.360140563978,-4.91824970511146,130.80265748193));
#37336=CARTESIAN_POINT('Ctrl Pts',(135.430234117584,-4.76405452823404,129.582490119308));
#37337=CARTESIAN_POINT('Ctrl Pts',(135.422470239396,-4.79810195755941,129.715240529506));
#37338=CARTESIAN_POINT('Ctrl Pts',(135.414706361208,-4.82656381027021,129.849287313936));
#37339=CARTESIAN_POINT('Ctrl Pts',(135.40694248302,-4.8493700162653,129.984120708852));
#37340=CARTESIAN_POINT('Ctrl Pts',(135.399167540465,-4.87220872357314,130.119146255954));
#37341=CARTESIAN_POINT('Ctrl Pts',(135.39139259791,-4.88937564496455,130.254960265062));
#37342=CARTESIAN_POINT('Ctrl Pts',(135.383617655355,-4.90085264228569,130.391049063044));
#37343=CARTESIAN_POINT('Ctrl Pts',(135.381090709619,-4.90458279839146,130.435279487302));
#37344=CARTESIAN_POINT('Ctrl Pts',(135.378563763883,-4.90771232449835,130.479538949501));
#37345=CARTESIAN_POINT('Ctrl Pts',(135.376036818146,-4.91024178091484,130.523809881587));
#37346=CARTESIAN_POINT('Ctrl Pts',(135.370738066767,-4.91554579693871,130.616641579199));
#37347=CARTESIAN_POINT('Ctrl Pts',(135.365439315388,-4.9182174890166,130.709625109034));
#37348=CARTESIAN_POINT('Ctrl Pts',(135.360140564008,-4.91824970511128,130.802657481398));
#37349=CARTESIAN_POINT('Ctrl Pts',(135.360140563978,-4.91824970511146,130.80265748193));
#37350=CARTESIAN_POINT('Ctrl Pts',(135.352434020783,-4.91829656042319,130.937964452346));
#37351=CARTESIAN_POINT('Ctrl Pts',(135.344727477589,-4.9127555070284,131.073499126688));
#37352=CARTESIAN_POINT('Ctrl Pts',(135.337020934394,-4.9015963568133,131.208756732006));
#37353=CARTESIAN_POINT('Ctrl Pts',(135.329323602338,-4.89045054441684,131.343852672559));
#37354=CARTESIAN_POINT('Ctrl Pts',(135.321626270282,-4.8737000241861,131.478671809661));
#37355=CARTESIAN_POINT('Ctrl Pts',(135.313928938225,-4.85136658957273,131.612707867254));
#37356=CARTESIAN_POINT('Ctrl Pts',(135.306238885862,-4.82905427663341,131.746617161275));
#37357=CARTESIAN_POINT('Ctrl Pts',(135.298548833498,-4.80116961870553,131.879744458713));
#37358=CARTESIAN_POINT('Ctrl Pts',(135.290858781135,-4.76778629558902,132.011587564786));
#37359=CARTESIAN_POINT('Ctrl Pts',(135.282805881684,-4.73282781524928,132.149651550072));
#37360=CARTESIAN_POINT('Ctrl Pts',(135.274752982234,-4.69183914262272,132.286306757394));
#37361=CARTESIAN_POINT('Ctrl Pts',(135.266700082784,-4.64496535698311,132.420986701398));
#37362=CARTESIAN_POINT('Ctrl Pts',(135.259018075935,-4.60025043851293,132.549463687704));
#37363=CARTESIAN_POINT('Ctrl Pts',(135.251336069085,-4.55018055014769,132.676142878261));
#37364=CARTESIAN_POINT('Ctrl Pts',(135.243654062235,-4.49493283453246,132.800547451392));
#37365=CARTESIAN_POINT('Ctrl Pts',(135.235973032723,-4.43969214776671,132.924936197244));
#37366=CARTESIAN_POINT('Ctrl Pts',(135.228292003211,-4.37927510531011,133.047050537171));
#37367=CARTESIAN_POINT('Ctrl Pts',(135.220610973699,-4.3139067855382,133.16643413636));
#37368=CARTESIAN_POINT('Ctrl Pts',(135.212929187623,-4.24853202714298,133.285829494548));
#37369=CARTESIAN_POINT('Ctrl Pts',(135.205247401548,-4.1782052128679,133.4024932277));
#37370=CARTESIAN_POINT('Ctrl Pts',(135.197565615473,-4.10319687070256,133.515994535107));
#37371=CARTESIAN_POINT('Ctrl Pts',(135.189881338679,-4.02816420806,133.629532643833));
#37372=CARTESIAN_POINT('Ctrl Pts',(135.182197061884,-3.94844721793339,133.739905955303));
#37373=CARTESIAN_POINT('Ctrl Pts',(135.17451278509,-3.86435884791437,133.846713943044));
#37374=CARTESIAN_POINT('Ctrl Pts',(135.166820103302,-3.78017850277946,133.953638756417));
#37375=CARTESIAN_POINT('Ctrl Pts',(135.159127421514,-3.69161748003889,134.056990148703));
#37376=CARTESIAN_POINT('Ctrl Pts',(135.151434739725,-3.59902819490115,134.156401654726));
#37377=CARTESIAN_POINT('Ctrl Pts',(135.143737131849,-3.50637961926161,134.255876819931));
#37378=CARTESIAN_POINT('Ctrl Pts',(135.136039523973,-3.40969792771429,134.35140679649));
#37379=CARTESIAN_POINT('Ctrl Pts',(135.128341916097,-3.30937033630008,134.442663936383));
#37380=CARTESIAN_POINT('Ctrl Pts',(135.120633362036,-3.20890007662033,134.53405084614));
#37381=CARTESIAN_POINT('Ctrl Pts',(135.112924807975,-3.10477387357521,134.621152537841));
#37382=CARTESIAN_POINT('Ctrl Pts',(135.105216253913,-2.9974100002693,134.703683168059));
#37383=CARTESIAN_POINT('Ctrl Pts',(135.10267390072,-2.96200039115256,134.73090254145));
#37384=CARTESIAN_POINT('Ctrl Pts',(135.100131547527,-2.92623882241581,134.757625063772));
#37385=CARTESIAN_POINT('Ctrl Pts',(135.097589194333,-2.89014090169641,134.783841567494));
#37386=CARTESIAN_POINT('Ctrl Pts',(135.089814860214,-2.77975604352618,134.864009759663));
#37387=CARTESIAN_POINT('Ctrl Pts',(135.082040526095,-2.66585819687516,134.939708585154));
#37388=CARTESIAN_POINT('Ctrl Pts',(135.074266191976,-2.54884521608402,135.010614429088));
#37389=CARTESIAN_POINT('Ctrl Pts',(135.066501439029,-2.43197644333395,135.081432887907));
#37390=CARTESIAN_POINT('Ctrl Pts',(135.058736686082,-2.31200050631387,135.147469917514));
#37391=CARTESIAN_POINT('Ctrl Pts',(135.050971933135,-2.18934682107491,135.20844321892));
#37392=CARTESIAN_POINT('Ctrl Pts',(135.04321489225,-2.06681495720533,135.269355960784));
#37393=CARTESIAN_POINT('Ctrl Pts',(135.035457851365,-1.94161098562287,135.325214810203));
#37394=CARTESIAN_POINT('Ctrl Pts',(135.02770081048,-1.81419138048192,135.375781917062));
#37395=CARTESIAN_POINT('Ctrl Pts',(135.019949619239,-1.68686786345621,135.426310890873));
#37396=CARTESIAN_POINT('Ctrl Pts',(135.012198427999,-1.55733240047529,135.471555921429));
#37397=CARTESIAN_POINT('Ctrl Pts',(135.004447236759,-1.42606370914016,135.511326238853));
#37398=CARTESIAN_POINT('Ctrl Pts',(134.996699339982,-1.29485081050081,135.55107965283));
#37399=CARTESIAN_POINT('Ctrl Pts',(134.988951443205,-1.1619065220706,135.585362868575));
#37400=CARTESIAN_POINT('Ctrl Pts',(134.981203546428,-1.02772687004141,135.614034259623));
#37401=CARTESIAN_POINT('Ctrl Pts',(134.973457270344,-0.89357528550275,135.642699653233));
#37402=CARTESIAN_POINT('Ctrl Pts',(134.96571099426,-0.75818923345157,135.665755475399));
#37403=CARTESIAN_POINT('Ctrl Pts',(134.957964718176,-0.622076754692063,
135.683110823692));
#37404=CARTESIAN_POINT('Ctrl Pts',(134.95021838491,-0.485963271181158,135.700466300098));
#37405=CARTESIAN_POINT('Ctrl Pts',(134.942472051645,-0.349123738087069,
135.712121169213));
#37406=CARTESIAN_POINT('Ctrl Pts',(134.93472571838,-0.212072776246219,135.718036247894));
#37407=CARTESIAN_POINT('Ctrl Pts',(134.926977650377,-0.0749911227926161,
135.723952651215));
#37408=CARTESIAN_POINT('Ctrl Pts',(134.919229582374,0.0623016630979726,
135.724126689477));
#37409=CARTESIAN_POINT('Ctrl Pts',(134.911481514371,0.199289891304434,135.718571296986));
#37410=CARTESIAN_POINT('Ctrl Pts',(134.903725211629,0.336423712230015,135.713010000157));
#37411=CARTESIAN_POINT('Ctrl Pts',(134.895968908887,0.473251937603753,135.701707124396));
#37412=CARTESIAN_POINT('Ctrl Pts',(134.888212606145,0.609262376606084,135.684727654885));
#37413=CARTESIAN_POINT('Ctrl Pts',(134.880452163631,0.745345408474906,135.667739122921));
#37414=CARTESIAN_POINT('Ctrl Pts',(134.872691721117,0.880609398856398,135.645068024731));
#37415=CARTESIAN_POINT('Ctrl Pts',(134.864931278603,1.01455228559113,135.616830536672));
#37416=CARTESIAN_POINT('Ctrl Pts',(134.857158378337,1.14871018933854,135.58854771929));
#37417=CARTESIAN_POINT('Ctrl Pts',(134.849385478072,1.28154237243552,135.554680752383));
#37418=CARTESIAN_POINT('Ctrl Pts',(134.841612577806,1.4125610051424,135.515396010052));
#37419=CARTESIAN_POINT('Ctrl Pts',(134.834122242044,1.53881678053471,135.477539367056));
#37420=CARTESIAN_POINT('Ctrl Pts',(134.826631906282,1.66338827936151,135.434652109796));
#37421=CARTESIAN_POINT('Ctrl Pts',(134.81914157052,1.78585827494905,135.386924668869));
#37422=CARTESIAN_POINT('Ctrl Pts',(134.811367236401,1.91297175764289,135.337387627513));
#37423=CARTESIAN_POINT('Ctrl Pts',(134.803592902282,2.03822389165481,135.282479207595));
#37424=CARTESIAN_POINT('Ctrl Pts',(134.795818568163,2.16112736063343,135.222359213494));
#37425=CARTESIAN_POINT('Ctrl Pts',(134.788053815216,2.28387936207048,135.162313311912));
#37426=CARTESIAN_POINT('Ctrl Pts',(134.780289062269,2.40428810987845,135.097068785749));
#37427=CARTESIAN_POINT('Ctrl Pts',(134.772524309322,2.52188398805953,135.02683432539));
#37428=CARTESIAN_POINT('Ctrl Pts',(134.764767268437,2.63936306835699,134.956669622888));
#37429=CARTESIAN_POINT('Ctrl Pts',(134.757010227552,2.75403450529529,134.881525048174));
#37430=CARTESIAN_POINT('Ctrl Pts',(134.749253186667,2.86545145340681,134.801656082086));
#37431=CARTESIAN_POINT('Ctrl Pts',(134.741501995427,2.97678438113099,134.721847345806));
#37432=CARTESIAN_POINT('Ctrl Pts',(134.733750804187,3.0848673885647,134.637321536352));
#37433=CARTESIAN_POINT('Ctrl Pts',(134.725999612946,3.18928121704955,134.548378296621));
#37434=CARTESIAN_POINT('Ctrl Pts',(134.718251716169,3.29365066687183,134.459472860139));
#37435=CARTESIAN_POINT('Ctrl Pts',(134.710503819392,3.39435374247058,134.366153980629));
#37436=CARTESIAN_POINT('Ctrl Pts',(134.702755922615,3.49100317521703,134.26876242641));
#37437=CARTESIAN_POINT('Ctrl Pts',(134.695009646531,3.58763239098567,134.171391244406));
#37438=CARTESIAN_POINT('Ctrl Pts',(134.687263370447,3.68020937527026,134.069949359533));
#37439=CARTESIAN_POINT('Ctrl Pts',(134.679517094363,3.76838304081943,133.964815065927));
#37440=CARTESIAN_POINT('Ctrl Pts',(134.671770761098,3.85655735724633,133.859679996244));
#37441=CARTESIAN_POINT('Ctrl Pts',(134.664024427832,3.94032803884466,133.750852762998));
#37442=CARTESIAN_POINT('Ctrl Pts',(134.656278094567,4.01938395459308,133.638745151827));
#37443=CARTESIAN_POINT('Ctrl Pts',(134.648530026564,4.09845757436607,133.526612434934));
#37444=CARTESIAN_POINT('Ctrl Pts',(134.640781958561,4.17281410202161,133.411198197762));
#37445=CARTESIAN_POINT('Ctrl Pts',(134.633033890558,4.24218567645094,133.292943296324));
#37446=CARTESIAN_POINT('Ctrl Pts',(134.625277587816,4.31163097981501,133.17456271217));
#37447=CARTESIAN_POINT('Ctrl Pts',(134.617521285074,4.37608054835242,133.053335770549));
#37448=CARTESIAN_POINT('Ctrl Pts',(134.609764982333,4.43531220429017,132.929728518183));
#37449=CARTESIAN_POINT('Ctrl Pts',(134.602004539818,4.49457547394611,132.806055292906));
#37450=CARTESIAN_POINT('Ctrl Pts',(134.594244097304,4.54861512776828,132.679999584579));
#37451=CARTESIAN_POINT('Ctrl Pts',(134.58648365479,4.59725753135398,132.552046588474));
#37452=CARTESIAN_POINT('Ctrl Pts',(134.578710754525,4.64597802004418,132.423888190861));
#37453=CARTESIAN_POINT('Ctrl Pts',(134.570937854259,4.68928382119304,132.293826790359));
#37454=CARTESIAN_POINT('Ctrl Pts',(134.563164953994,4.72705122615383,132.162362741209));
#37455=CARTESIAN_POINT('Ctrl Pts',(134.555674618232,4.7634456908141,132.035677741382));
#37456=CARTESIAN_POINT('Ctrl Pts',(134.54818428247,4.79469736459525,131.907690601243));
#37457=CARTESIAN_POINT('Ctrl Pts',(134.540693946708,4.820740940943,131.778855277796));
#37458=CARTESIAN_POINT('Ctrl Pts',(134.532919612589,4.84777196740363,131.645135123902));
#37459=CARTESIAN_POINT('Ctrl Pts',(134.525145278469,4.86927779652637,131.510077614055));
#37460=CARTESIAN_POINT('Ctrl Pts',(134.51737094435,4.88512946986935,131.374179119472));
#37461=CARTESIAN_POINT('Ctrl Pts',(134.509606191403,4.90096160744162,131.238448107638));
#37462=CARTESIAN_POINT('Ctrl Pts',(134.501841438456,4.91115340909654,131.101878557876));
#37463=CARTESIAN_POINT('Ctrl Pts',(134.494076685509,4.91562661304959,130.964978373678));
#37464=CARTESIAN_POINT('Ctrl Pts',(134.486319644624,4.92009537415343,130.828214160673));
#37465=CARTESIAN_POINT('Ctrl Pts',(134.478562603739,4.91885682791216,130.691120354972));
#37466=CARTESIAN_POINT('Ctrl Pts',(134.470805562854,4.91188438670001,130.554210993955));
#37467=CARTESIAN_POINT('Ctrl Pts',(134.463054371614,4.90491720346003,130.417404877353));
#37468=CARTESIAN_POINT('Ctrl Pts',(134.455303180374,4.89222475166342,130.280783317462));
#37469=CARTESIAN_POINT('Ctrl Pts',(134.447551989134,4.87383250981955,130.14486101277));
#37470=CARTESIAN_POINT('Ctrl Pts',(134.439804092357,4.8554480851691,130.008996478684));
#37471=CARTESIAN_POINT('Ctrl Pts',(134.432056195579,4.8313687410798,129.873830995308));
#37472=CARTESIAN_POINT('Ctrl Pts',(134.424308298802,4.80167184743674,129.739874576308));
#37473=CARTESIAN_POINT('Ctrl Pts',(134.416562022718,4.77198116574363,129.605946178103));
#37474=CARTESIAN_POINT('Ctrl Pts',(134.408815746634,4.73667535634123,129.473226722679));
#37475=CARTESIAN_POINT('Ctrl Pts',(134.40106947055,4.69588291756345,129.342216066902));
#37476=CARTESIAN_POINT('Ctrl Pts',(134.393323137285,4.65509017766517,129.211204444035));
#37477=CARTESIAN_POINT('Ctrl Pts',(134.385576804019,4.60881084380448,129.081902019275));
#37478=CARTESIAN_POINT('Ctrl Pts',(134.377830470754,4.55722318898415,128.954793136157));
#37479=CARTESIAN_POINT('Ctrl Pts',(134.370082402751,4.50562398146631,128.827655787887));
#37480=CARTESIAN_POINT('Ctrl Pts',(134.362334334748,4.44871423448981,128.702713320944));
#37481=CARTESIAN_POINT('Ctrl Pts',(134.354586266745,4.38672006723145,128.580429387908));
#37482=CARTESIAN_POINT('Ctrl Pts',(134.346829964003,4.32466001183421,128.458015490053));
#37483=CARTESIAN_POINT('Ctrl Pts',(134.339073661261,4.257504918586,128.338266119657));
#37484=CARTESIAN_POINT('Ctrl Pts',(134.331317358519,4.18552679327976,128.22162011081));
#37485=CARTESIAN_POINT('Ctrl Pts',(134.323556916005,4.11351025108077,128.104911844477));
#37486=CARTESIAN_POINT('Ctrl Pts',(134.315796473491,4.03666576646497,127.991310563801));
#37487=CARTESIAN_POINT('Ctrl Pts',(134.308036030977,3.95530769431998,127.881224612219));
#37488=CARTESIAN_POINT('Ctrl Pts',(134.300263130711,3.8738190189749,127.770961940896));
#37489=CARTESIAN_POINT('Ctrl Pts',(134.292490230446,3.78780252252585,127.664226180007));
#37490=CARTESIAN_POINT('Ctrl Pts',(134.284717330181,3.69761229962191,127.561391862831));
#37491=CARTESIAN_POINT('Ctrl Pts',(134.277226994418,3.61070071849538,127.462295832108));
#37492=CARTESIAN_POINT('Ctrl Pts',(134.269736658656,3.51991380575471,127.366822738357));
#37493=CARTESIAN_POINT('Ctrl Pts',(134.262246322894,3.42559818849807,127.275272900682));
#37494=CARTESIAN_POINT('Ctrl Pts',(134.254471988775,3.32770656594715,127.180251923087));
#37495=CARTESIAN_POINT('Ctrl Pts',(134.246697654656,3.225703283835,127.089156576933));
#37496=CARTESIAN_POINT('Ctrl Pts',(134.238923320537,3.11993624813733,127.00236365938));
#37497=CARTESIAN_POINT('Ctrl Pts',(134.23115856759,3.01429956085856,126.91567770634));
#37498=CARTESIAN_POINT('Ctrl Pts',(134.223393814643,2.90490864853648,126.833283877418));
#37499=CARTESIAN_POINT('Ctrl Pts',(134.215629061696,2.79214852235655,126.755522550712));
#37500=CARTESIAN_POINT('Ctrl Pts',(134.207872020811,2.67950039112358,126.677838457653));
#37501=CARTESIAN_POINT('Ctrl Pts',(134.200114979926,2.56349002519221,126.604777930999));
#37502=CARTESIAN_POINT('Ctrl Pts',(134.192357939041,2.44453552750779,126.536641189434));
#37503=CARTESIAN_POINT('Ctrl Pts',(134.184606747801,2.32567073433508,126.468555830316));
#37504=CARTESIAN_POINT('Ctrl Pts',(134.17685555656,2.20386656644816,126.405387059193));
#37505=CARTESIAN_POINT('Ctrl Pts',(134.16910436532,2.07956982601877,126.347391647379));
#37506=CARTESIAN_POINT('Ctrl Pts',(134.161356468543,1.95532591502003,126.289420885162));
#37507=CARTESIAN_POINT('Ctrl Pts',(134.153608571766,1.82859189211915,126.236619273941));
#37508=CARTESIAN_POINT('Ctrl Pts',(134.145860674989,1.69983866657038,126.189197395086));
#37509=CARTESIAN_POINT('Ctrl Pts',(134.138114398905,1.5711123734208,126.141785435866));
#37510=CARTESIAN_POINT('Ctrl Pts',(134.130368122821,1.44036808438728,126.099751105718));
#37511=CARTESIAN_POINT('Ctrl Pts',(134.122621846737,1.30809579969763,126.063256480204));
#37512=CARTESIAN_POINT('Ctrl Pts',(134.114875513472,1.17582253860448,126.026761585294));
#37513=CARTESIAN_POINT('Ctrl Pts',(134.107129180206,1.04202163623152,125.9958065806));
#37514=CARTESIAN_POINT('Ctrl Pts',(134.099382846941,0.907196945425237,125.970503279507));
#37515=CARTESIAN_POINT('Ctrl Pts',(134.091634778938,0.772342061563523,125.945194311914));
#37516=CARTESIAN_POINT('Ctrl Pts',(134.083886710935,0.636463317230123,125.925539638541));
#37517=CARTESIAN_POINT('Ctrl Pts',(134.076138642932,0.500073019410448,125.911599634465));
#37518=CARTESIAN_POINT('Ctrl Pts',(134.06838234019,0.363537764359557,125.897644814786));
#37519=CARTESIAN_POINT('Ctrl Pts',(134.060626037448,0.226490259311975,125.889416836927));
#37520=CARTESIAN_POINT('Ctrl Pts',(134.052869734706,0.0894467335911126,
125.886924055255));
#37521=CARTESIAN_POINT('Ctrl Pts',(134.045109292192,-0.0476699363857279,
125.884429943111));
#37522=CARTESIAN_POINT('Ctrl Pts',(134.037348849678,-0.184782232139447,
125.887677117296));
#37523=CARTESIAN_POINT('Ctrl Pts',(134.029588407164,-0.321376686276765,
125.896621821744));
#37524=CARTESIAN_POINT('Ctrl Pts',(134.021815506898,-0.458190413958243,
125.905580885025));
#37525=CARTESIAN_POINT('Ctrl Pts',(134.014042606633,-0.594484249908106,
125.920255713675));
#37526=CARTESIAN_POINT('Ctrl Pts',(134.006269706368,-0.729751691865504,
125.940550842223));
#37527=CARTESIAN_POINT('Ctrl Pts',(133.998779370606,-0.860101821587794,
125.960108191728));
#37528=CARTESIAN_POINT('Ctrl Pts',(133.991289034844,-0.989498583226331,
125.984884253403));
#37529=CARTESIAN_POINT('Ctrl Pts',(133.983798699082,-1.11750194940005,126.014749729865));
#37530=CARTESIAN_POINT('Ctrl Pts',(133.976024364963,-1.25035860210971,126.045747564945));
#37531=CARTESIAN_POINT('Ctrl Pts',(133.968250030844,-1.38213496233291,126.082326555345));
#37532=CARTESIAN_POINT('Ctrl Pts',(133.960475696725,-1.51232596827186,126.124397665983));
#37533=CARTESIAN_POINT('Ctrl Pts',(133.952710943778,-1.64235652543133,126.166416927737));
#37534=CARTESIAN_POINT('Ctrl Pts',(133.94494619083,-1.77080524734935,126.213914723271));
#37535=CARTESIAN_POINT('Ctrl Pts',(133.937181437883,-1.89717765634108,126.266751114449));
#37536=CARTESIAN_POINT('Ctrl Pts',(133.929424396998,-2.02342455047483,126.319535027778));
#37537=CARTESIAN_POINT('Ctrl Pts',(133.921667356113,-2.14759887722674,126.377646834961));
#37538=CARTESIAN_POINT('Ctrl Pts',(133.913910315228,-2.26922205926168,126.440897049681));
#37539=CARTESIAN_POINT('Ctrl Pts',(133.906159123988,-2.39075352430895,126.504099566922));
#37540=CARTESIAN_POINT('Ctrl Pts',(133.898407932748,-2.50973732846206,126.572432599263));
#37541=CARTESIAN_POINT('Ctrl Pts',(133.890656741508,-2.62571593525527,126.64565903055));
#37542=CARTESIAN_POINT('Ctrl Pts',(133.882908844731,-2.74164524804667,126.718854338651));
#37543=CARTESIAN_POINT('Ctrl Pts',(133.875160947954,-2.8545715740142,126.796938700795));
#37544=CARTESIAN_POINT('Ctrl Pts',(133.867413051177,-2.96406320713384,126.879629752065));
#37545=CARTESIAN_POINT('Ctrl Pts',(133.859666775093,-3.07353193696434,126.96230350615));
#37546=CARTESIAN_POINT('Ctrl Pts',(133.851920499008,-3.17956709122067,127.049581797194));
#37547=CARTESIAN_POINT('Ctrl Pts',(133.844174222924,-3.28176745405261,127.141139979927));
#37548=CARTESIAN_POINT('Ctrl Pts',(133.836427889659,-3.38396857130433,127.232698838523));
#37549=CARTESIAN_POINT('Ctrl Pts',(133.828681556394,-3.48233454944653,127.328537390972));
#37550=CARTESIAN_POINT('Ctrl Pts',(133.820935223128,-3.57649897194036,127.428292169473));
#37551=CARTESIAN_POINT('Ctrl Pts',(133.813187155125,-3.67068448190404,127.528069287365));
#37552=CARTESIAN_POINT('Ctrl Pts',(133.805439087122,-3.76066629559726,127.631764092208));
#37553=CARTESIAN_POINT('Ctrl Pts',(133.797691019119,-3.84611670331799,127.738978199831));
#37554=CARTESIAN_POINT('Ctrl Pts',(133.789934716377,-3.93165792874857,127.846306255883));
#37555=CARTESIAN_POINT('Ctrl Pts',(133.782178413635,-4.0126578835994,127.957160780254));
#37556=CARTESIAN_POINT('Ctrl Pts',(133.774422110894,-4.08883050454563,128.071111970334));
#37557=CARTESIAN_POINT('Ctrl Pts',(133.766661668379,-4.16504378111342,128.185123979595));
#37558=CARTESIAN_POINT('Ctrl Pts',(133.758901225865,-4.23642438651551,128.302235614199));
#37559=CARTESIAN_POINT('Ctrl Pts',(133.751140783351,-4.30273159230308,128.421991228261));
#37560=CARTESIAN_POINT('Ctrl Pts',(133.743367883086,-4.36914524030373,128.541939084666));
#37561=CARTESIAN_POINT('Ctrl Pts',(133.73559498282,-4.43046903884042,128.664539052231));
#37562=CARTESIAN_POINT('Ctrl Pts',(133.727822082555,-4.48650952887424,128.789313394839));
#37563=CARTESIAN_POINT('Ctrl Pts',(133.720331746793,-4.54051280593823,128.909551875806));
#37564=CARTESIAN_POINT('Ctrl Pts',(133.71284141103,-4.58961011391488,129.031809102606));
#37565=CARTESIAN_POINT('Ctrl Pts',(133.705351075268,-4.63367238880688,129.155644979347));
#37566=CARTESIAN_POINT('Ctrl Pts',(133.696877076708,-4.68352110932786,129.295743510919));
#37567=CARTESIAN_POINT('Ctrl Pts',(133.688403078147,-4.72704813717389,129.438202762215));
#37568=CARTESIAN_POINT('Ctrl Pts',(133.679929079587,-4.76405452823404,129.582490119308));
#37569=CARTESIAN_POINT('Origin',(213.235140564004,0.,130.804360617566));
#37570=CARTESIAN_POINT('',(131.584997718909,-4.76405452823404,129.582490119308));
#37571=CARTESIAN_POINT('',(131.929976442121,-4.76405452823405,129.582490119308));
#37572=CARTESIAN_POINT('',(213.235140564004,-4.76405452823405,129.582490119308));
#37573=CARTESIAN_POINT('',(133.264859435937,-4.91824867220211,130.807974601818));
#37574=CARTESIAN_POINT('Ctrl Pts',(133.264859435937,-4.91824867220211,130.807974601818));
#37575=CARTESIAN_POINT('Ctrl Pts',(133.255945198427,-4.91813260923259,130.965923974559));
#37576=CARTESIAN_POINT('Ctrl Pts',(133.247030960918,-4.91040380121572,131.123565068945));
#37577=CARTESIAN_POINT('Ctrl Pts',(133.238116723408,-4.89517488915305,131.280223903716));
#37578=CARTESIAN_POINT('Ctrl Pts',(133.22915699462,-4.87986826066354,131.43768220235));
#37579=CARTESIAN_POINT('Ctrl Pts',(133.220197265831,-4.85698489393969,131.594148056893));
#37580=CARTESIAN_POINT('Ctrl Pts',(133.211237537043,-4.82668855896882,131.748956095651));
#37581=CARTESIAN_POINT('Ctrl Pts',(133.202220640543,-4.79619891768544,131.904751889898));
#37582=CARTESIAN_POINT('Ctrl Pts',(133.193203744043,-4.75820149578884,132.058868513842));
#37583=CARTESIAN_POINT('Ctrl Pts',(133.184186847543,-4.71291164423838,132.21064895788));
#37584=CARTESIAN_POINT('Ctrl Pts',(133.178806172963,-4.6858857209641,132.301221271426));
#37585=CARTESIAN_POINT('Ctrl Pts',(133.173425498383,-4.65626395683687,132.390962109657));
#37586=CARTESIAN_POINT('Ctrl Pts',(133.168044823802,-4.62410006052217,132.479735707741));
#37587=CARTESIAN_POINT('Ctrl Pts',(133.160270489683,-4.57762765770432,132.608001337296));
#37588=CARTESIAN_POINT('Ctrl Pts',(133.152496155564,-4.52574075591298,132.734535052467));
#37589=CARTESIAN_POINT('Ctrl Pts',(133.144721821445,-4.46858741925803,132.858845842373));
#37590=CARTESIAN_POINT('Ctrl Pts',(133.136957068498,-4.4115045189826,132.98300343034));
#37591=CARTESIAN_POINT('Ctrl Pts',(133.129192315551,-4.3491682595744,133.104943192132));
#37592=CARTESIAN_POINT('Ctrl Pts',(133.121427562604,-4.28177600183403,133.224190638997));
#37593=CARTESIAN_POINT('Ctrl Pts',(133.113670521719,-4.21445067903416,133.343319647616));
#37594=CARTESIAN_POINT('Ctrl Pts',(133.105913480834,-4.1420795424037,133.45976132461));
#37595=CARTESIAN_POINT('Ctrl Pts',(133.098156439949,-4.06490727614898,133.573062822356));
#37596=CARTESIAN_POINT('Ctrl Pts',(133.090405248709,-3.9877932061006,133.686278878562));
#37597=CARTESIAN_POINT('Ctrl Pts',(133.082654057469,-3.9058854321526,133.796359147123));
#37598=CARTESIAN_POINT('Ctrl Pts',(133.074902866228,-3.81947344985998,133.902877299515));
#37599=CARTESIAN_POINT('Ctrl Pts',(133.067154969451,-3.73309819496483,134.00935017885));
#37600=CARTESIAN_POINT('Ctrl Pts',(133.059407072674,-3.64222278513193,134.112263650251));
#37601=CARTESIAN_POINT('Ctrl Pts',(133.051659175897,-3.54717859716893,134.211222379112));
#37602=CARTESIAN_POINT('Ctrl Pts',(133.043912899813,-3.45215429040106,134.310160407941));
#37603=CARTESIAN_POINT('Ctrl Pts',(133.036166623729,-3.35296321064494,134.405145057872));
#37604=CARTESIAN_POINT('Ctrl Pts',(133.028420347645,-3.24997511796952,134.495816264744));
#37605=CARTESIAN_POINT('Ctrl Pts',(133.020674014379,-3.14698626505947,134.586488140929));
#37606=CARTESIAN_POINT('Ctrl Pts',(133.012927681114,-3.04020063674487,134.672846252169));
#37607=CARTESIAN_POINT('Ctrl Pts',(133.005181347849,-2.93002243379298,134.754569675321));
#37608=CARTESIAN_POINT('Ctrl Pts',(132.997433279846,-2.81981955719653,134.836311399867));
#37609=CARTESIAN_POINT('Ctrl Pts',(132.989685211843,-2.70622290811392,134.913416138139));
#37610=CARTESIAN_POINT('Ctrl Pts',(132.98193714384,-2.58966678767391,134.985605526839));
#37611=CARTESIAN_POINT('Ctrl Pts',(132.974180841098,-2.4729867900019,135.05787163928));
#37612=CARTESIAN_POINT('Ctrl Pts',(132.966424538356,-2.35334137068296,135.125211760273));
#37613=CARTESIAN_POINT('Ctrl Pts',(132.958668235614,-2.2311911105751,135.187392592192));
#37614=CARTESIAN_POINT('Ctrl Pts',(132.9509077931,-2.10897565519547,135.249606611892));
#37615=CARTESIAN_POINT('Ctrl Pts',(132.943147350586,-1.98425305048594,135.306655693055));
#37616=CARTESIAN_POINT('Ctrl Pts',(132.935386908072,-1.85750418524707,135.358354607932));
#37617=CARTESIAN_POINT('Ctrl Pts',(132.927614007806,-1.73055185147756,135.410136514496));
#37618=CARTESIAN_POINT('Ctrl Pts',(132.919841107541,-1.60156712526531,135.456550959638));
#37619=CARTESIAN_POINT('Ctrl Pts',(132.912068207275,-1.47104724809604,135.497462263212));
#37620=CARTESIAN_POINT('Ctrl Pts',(132.904577871513,-1.34527209722028,135.536886337853));
#37621=CARTESIAN_POINT('Ctrl Pts',(132.897087535751,-1.21807176821434,135.571200350389));
#37622=CARTESIAN_POINT('Ctrl Pts',(132.889597199989,-1.0898985201787,135.600328119355));
#37623=CARTESIAN_POINT('Ctrl Pts',(132.88182286587,-0.956865544487872,135.630560276534));
#37624=CARTESIAN_POINT('Ctrl Pts',(132.874048531751,-0.822363008467457,
135.655300920351));
#37625=CARTESIAN_POINT('Ctrl Pts',(132.866274197632,-0.686884045745631,
135.67440921796));
#37626=CARTESIAN_POINT('Ctrl Pts',(132.858509444685,-0.551572048737166,
135.6934939663));
#37627=CARTESIAN_POINT('Ctrl Pts',(132.850744691738,-0.415286402769419,
135.706960125599));
#37628=CARTESIAN_POINT('Ctrl Pts',(132.84297993879,-0.278532987002799,135.714717268325));
#37629=CARTESIAN_POINT('Ctrl Pts',(132.835222897905,-0.141915396656605,
135.722466706547));
#37630=CARTESIAN_POINT('Ctrl Pts',(132.82746585702,-0.00483134888954567,
135.724518390304));
#37631=CARTESIAN_POINT('Ctrl Pts',(132.819708816135,0.132205904977683,135.720833404147));
#37632=CARTESIAN_POINT('Ctrl Pts',(132.811957624895,0.269139817985589,135.717151196866));
#37633=CARTESIAN_POINT('Ctrl Pts',(132.804206433655,0.406026618089016,135.707740940912));
#37634=CARTESIAN_POINT('Ctrl Pts',(132.796455242415,0.542351143606349,135.692615756113));
#37635=CARTESIAN_POINT('Ctrl Pts',(132.788707345638,0.678617727563854,135.677496999921));
#37636=CARTESIAN_POINT('Ctrl Pts',(132.780959448861,0.81432212448434,135.656668188996));
#37637=CARTESIAN_POINT('Ctrl Pts',(132.773211552084,0.948952610909251,135.630194432022));
#37638=CARTESIAN_POINT('Ctrl Pts',(132.765465276,1.08355493553879,135.603726212787));
#37639=CARTESIAN_POINT('Ctrl Pts',(132.757718999916,1.21708341311615,135.571615471568));
#37640=CARTESIAN_POINT('Ctrl Pts',(132.749972723831,1.34903524711421,135.533978674507));
#37641=CARTESIAN_POINT('Ctrl Pts',(132.742226390566,1.48098805515064,135.49634159962));
#37642=CARTESIAN_POINT('Ctrl Pts',(132.734480057301,1.61136382041381,135.453178494732));
#37643=CARTESIAN_POINT('Ctrl Pts',(132.726733724035,1.73967406078651,135.404655958599));
#37644=CARTESIAN_POINT('Ctrl Pts',(132.718985656032,1.86801303534789,135.35612255618));
#37645=CARTESIAN_POINT('Ctrl Pts',(132.711237588029,1.99428519895787,135.302227472506));
#37646=CARTESIAN_POINT('Ctrl Pts',(132.703489520026,2.11802160631991,135.243185635255));
#37647=CARTESIAN_POINT('Ctrl Pts',(132.695733217285,2.24188952220817,135.184081047637));
#37648=CARTESIAN_POINT('Ctrl Pts',(132.687976914543,2.36321594481492,135.1198189481));
#37649=CARTESIAN_POINT('Ctrl Pts',(132.680220611801,2.48155563903464,135.050660733299));
#37650=CARTESIAN_POINT('Ctrl Pts',(132.672460169287,2.59995849471239,134.981465606677));
#37651=CARTESIAN_POINT('Ctrl Pts',(132.664699726773,2.71537111677318,134.907369368877));
#37652=CARTESIAN_POINT('Ctrl Pts',(132.656939284258,2.82737773572283,134.828676485144));
#37653=CARTESIAN_POINT('Ctrl Pts',(132.649166383993,2.9395641576407,134.749857276608));
#37654=CARTESIAN_POINT('Ctrl Pts',(132.641393483728,3.04833334000829,134.666426914743));
#37655=CARTESIAN_POINT('Ctrl Pts',(132.633620583462,3.1533023601091,134.578730404462));
#37656=CARTESIAN_POINT('Ctrl Pts',(132.6261302477,3.25445549192795,134.494221883223));
#37657=CARTESIAN_POINT('Ctrl Pts',(132.618639911938,3.35207972736444,134.405752205873));
#37658=CARTESIAN_POINT('Ctrl Pts',(132.611149576176,3.44586651570447,134.313660692858));
#37659=CARTESIAN_POINT('Ctrl Pts',(132.603375242057,3.54320925863056,134.218077502137));
#37660=CARTESIAN_POINT('Ctrl Pts',(132.595600907938,3.63672616909146,134.11828963158));
#37661=CARTESIAN_POINT('Ctrl Pts',(132.587826573819,3.72603220965407,134.014635844882));
#37662=CARTESIAN_POINT('Ctrl Pts',(132.580061820872,3.81522818850313,133.911109802213));
#37663=CARTESIAN_POINT('Ctrl Pts',(132.572297067925,3.90022337030979,133.80372761648));
#37664=CARTESIAN_POINT('Ctrl Pts',(132.564532314978,3.98066823578871,133.69286601986));
#37665=CARTESIAN_POINT('Ctrl Pts',(132.556775274093,4.0610332022931,133.582114532541));
#37666=CARTESIAN_POINT('Ctrl Pts',(132.549018233208,4.13685661822656,133.467890825918));
#37667=CARTESIAN_POINT('Ctrl Pts',(132.541261192323,4.20782831804404,133.350605678114));
#37668=CARTESIAN_POINT('Ctrl Pts',(132.533510001083,4.27874649755062,133.233408975953));
#37669=CARTESIAN_POINT('Ctrl Pts',(132.525758809843,4.34482004180623,133.113155760989));
#37670=CARTESIAN_POINT('Ctrl Pts',(132.518007618602,4.40578153142101,132.990286544923));
#37671=CARTESIAN_POINT('Ctrl Pts',(132.510259721825,4.46671711077654,132.867469551551));
#37672=CARTESIAN_POINT('Ctrl Pts',(132.502511825048,4.52254478354295,132.742039117997));
#37673=CARTESIAN_POINT('Ctrl Pts',(132.494763928271,4.57304272847009,132.614460964532));
#37674=CARTESIAN_POINT('Ctrl Pts',(132.487017652187,4.62353011031576,132.486909497667));
#37675=CARTESIAN_POINT('Ctrl Pts',(132.479271376103,4.66868983804943,132.357211567781));
#37676=CARTESIAN_POINT('Ctrl Pts',(132.471525100019,4.70834812413129,132.225853144627));
#37677=CARTESIAN_POINT('Ctrl Pts',(132.463778766754,4.7480067029616,132.094493751815));
#37678=CARTESIAN_POINT('Ctrl Pts',(132.456032433488,4.78216364610665,131.961474215556));
#37679=CARTESIAN_POINT('Ctrl Pts',(132.448286100223,4.81069508130131,131.827295560387));
#37680=CARTESIAN_POINT('Ctrl Pts',(132.44053803222,4.83923290591303,131.693086856838));
#37681=CARTESIAN_POINT('Ctrl Pts',(132.432789964217,4.8621426344308,131.557718900193));
#37682=CARTESIAN_POINT('Ctrl Pts',(132.425041896214,4.87935161520858,131.421702401071));
#37683=CARTESIAN_POINT('Ctrl Pts',(132.417285593472,4.89657888589594,131.285541341995));
#37684=CARTESIAN_POINT('Ctrl Pts',(132.40952929073,4.9080932565402,131.148730752025));
#37685=CARTESIAN_POINT('Ctrl Pts',(132.401772987989,4.91387398709938,131.01178651134));
#37686=CARTESIAN_POINT('Ctrl Pts',(132.394012545474,4.91965780300853,130.874769179391));
#37687=CARTESIAN_POINT('Ctrl Pts',(132.38625210296,4.91970188096682,130.737618445364));
#37688=CARTESIAN_POINT('Ctrl Pts',(132.378491660446,4.91403764264012,130.600848678811));
#37689=CARTESIAN_POINT('Ctrl Pts',(132.370718760181,4.90836431157521,130.463859357287));
#37690=CARTESIAN_POINT('Ctrl Pts',(132.362945859915,4.89696438517229,130.32725261517));
#37691=CARTESIAN_POINT('Ctrl Pts',(132.35517295965,4.87992114675371,130.191537099768));
#37692=CARTESIAN_POINT('Ctrl Pts',(132.347682623888,4.86349747298099,130.060755185199));
#37693=CARTESIAN_POINT('Ctrl Pts',(132.340192288126,4.84183371169264,129.930801129464));
#37694=CARTESIAN_POINT('Ctrl Pts',(132.332701952364,4.81504856359359,129.802117936009));
#37695=CARTESIAN_POINT('Ctrl Pts',(132.324927618245,4.78724784846318,129.668555680161));
#37696=CARTESIAN_POINT('Ctrl Pts',(132.317153284125,4.75384166120601,129.535939473364));
#37697=CARTESIAN_POINT('Ctrl Pts',(132.309378950006,4.71490689117494,129.404776368565));
#37698=CARTESIAN_POINT('Ctrl Pts',(132.301614197059,4.67602010476827,129.273774910571));
#37699=CARTESIAN_POINT('Ctrl Pts',(132.293849444112,4.63161840257915,129.144223362585));
#37700=CARTESIAN_POINT('Ctrl Pts',(132.286084691165,4.58182981634555,129.016619418022));
#37701=CARTESIAN_POINT('Ctrl Pts',(132.27832765028,4.53209068083769,128.889142211496));
#37702=CARTESIAN_POINT('Ctrl Pts',(132.270570609395,4.47697544987471,128.763609120742));
#37703=CARTESIAN_POINT('Ctrl Pts',(132.26281356851,4.41666207067068,128.640503132425));
#37704=CARTESIAN_POINT('Ctrl Pts',(132.25506237727,4.35639417425512,128.517489979292));
#37705=CARTESIAN_POINT('Ctrl Pts',(132.24731118603,4.29093610336416,128.396900635174));
#37706=CARTESIAN_POINT('Ctrl Pts',(132.23955999479,4.22051392625481,128.279198194911));
#37707=CARTESIAN_POINT('Ctrl Pts',(132.231812098013,4.15012168044925,128.161545781325));
#37708=CARTESIAN_POINT('Ctrl Pts',(132.224064201235,4.07476972512276,128.04677816596));
#37709=CARTESIAN_POINT('Ctrl Pts',(132.216316304458,3.99472998412593,127.935333706499));
#37710=CARTESIAN_POINT('Ctrl Pts',(132.208570028374,3.91470698571745,127.823912558817));
#37711=CARTESIAN_POINT('Ctrl Pts',(132.20082375229,3.82999837999571,127.715813501733));
#37712=CARTESIAN_POINT('Ctrl Pts',(132.193077476206,3.74091909066729,127.611445426149));
#37713=CARTESIAN_POINT('Ctrl Pts',(132.185331142941,3.65183914377579,127.507076580143));
#37714=CARTESIAN_POINT('Ctrl Pts',(132.177584809675,3.55838870271194,127.40643906797));
#37715=CARTESIAN_POINT('Ctrl Pts',(132.16983847641,3.46092233762285,127.309907922874));
#37716=CARTESIAN_POINT('Ctrl Pts',(132.162090408407,3.36343414561709,127.213355160297));
#37717=CARTESIAN_POINT('Ctrl Pts',(132.154342340404,3.26192851773738,127.120910869745));
#37718=CARTESIAN_POINT('Ctrl Pts',(132.146594272401,3.15679585930167,127.032912226669));
#37719=CARTESIAN_POINT('Ctrl Pts',(132.138837969659,3.05155146462541,126.944820057589));
#37720=CARTESIAN_POINT('Ctrl Pts',(132.131081666917,2.94267263919339,126.861183225799));
#37721=CARTESIAN_POINT('Ctrl Pts',(132.123325364175,2.83058219711254,126.782298026321));
#37722=CARTESIAN_POINT('Ctrl Pts',(132.115564921661,2.71843192898778,126.703370723438));
#37723=CARTESIAN_POINT('Ctrl Pts',(132.107804479147,2.60306695735331,126.629200317569));
#37724=CARTESIAN_POINT('Ctrl Pts',(132.100044036633,2.48493702005917,126.560038402083));
#37725=CARTESIAN_POINT('Ctrl Pts',(132.092271136367,2.3666174501026,126.490765461751));
#37726=CARTESIAN_POINT('Ctrl Pts',(132.084498236102,2.24552439037618,126.426517261777));
#37727=CARTESIAN_POINT('Ctrl Pts',(132.076725335836,2.12213079693651,126.367498669838));
#37728=CARTESIAN_POINT('Ctrl Pts',(132.069235000074,2.00322287142732,126.310625552375));
#37729=CARTESIAN_POINT('Ctrl Pts',(132.061744664312,1.88217905170354,126.258608546867));
#37730=CARTESIAN_POINT('Ctrl Pts',(132.05425432855,1.75943620974022,126.211587241233));
#37731=CARTESIAN_POINT('Ctrl Pts',(132.046479994431,1.6320395356177,126.162783108504));
#37732=CARTESIAN_POINT('Ctrl Pts',(132.038705660312,1.50240890474879,126.119206380851));
#37733=CARTESIAN_POINT('Ctrl Pts',(132.030931326193,1.37101247571331,126.081066443588));
#37734=CARTESIAN_POINT('Ctrl Pts',(132.023166573246,1.23977798103348,126.042973510388));
#37735=CARTESIAN_POINT('Ctrl Pts',(132.015401820299,1.10678239001659,126.010304143802));
#37736=CARTESIAN_POINT('Ctrl Pts',(132.007637067352,0.972513630511448,125.983219642551));
#37737=CARTESIAN_POINT('Ctrl Pts',(131.999880026467,0.838378228631015,125.956162042008));
#37738=CARTESIAN_POINT('Ctrl Pts',(131.992122985582,0.702972555497661,125.934678344893));
#37739=CARTESIAN_POINT('Ctrl Pts',(131.984365944697,0.566799146288047,125.918879905265));
#37740=CARTESIAN_POINT('Ctrl Pts',(131.976614753456,0.430728426505499,125.903093379363));
#37741=CARTESIAN_POINT('Ctrl Pts',(131.968863562216,0.29389150981188,125.892983622218));
#37742=CARTESIAN_POINT('Ctrl Pts',(131.961112370976,0.156800206426934,125.888610750276));
#37743=CARTESIAN_POINT('Ctrl Pts',(131.953364474199,0.0197671705030495,
125.884239736921));
#37744=CARTESIAN_POINT('Ctrl Pts',(131.945616577422,-0.11751964711912,125.885600771556));
#37745=CARTESIAN_POINT('Ctrl Pts',(131.937868680645,-0.254544462222737,
125.892702019979));
#37746=CARTESIAN_POINT('Ctrl Pts',(131.930122404561,-0.391540614688948,
125.899801782974));
#37747=CARTESIAN_POINT('Ctrl Pts',(131.922376128477,-0.528274483453441,
125.91263935122));
#37748=CARTESIAN_POINT('Ctrl Pts',(131.914629852393,-0.664231833064708,
125.931170786004));
#37749=CARTESIAN_POINT('Ctrl Pts',(131.906883519127,-0.800190186282245,
125.949702357582));
#37750=CARTESIAN_POINT('Ctrl Pts',(131.899137185862,-0.935371621525342,
125.973927826765));
#37751=CARTESIAN_POINT('Ctrl Pts',(131.891390852596,-1.06926895887812,126.003751598277));
#37752=CARTESIAN_POINT('Ctrl Pts',(131.883642784594,-1.20319628161123,126.033582048615));
#37753=CARTESIAN_POINT('Ctrl Pts',(131.875894716591,-1.33583855269275,126.069013211019));
#37754=CARTESIAN_POINT('Ctrl Pts',(131.868146648588,-1.46670107325562,126.109898878004));
#37755=CARTESIAN_POINT('Ctrl Pts',(131.860390345846,-1.59770267606254,126.150827998763));
#37756=CARTESIAN_POINT('Ctrl Pts',(131.852634043104,-1.72692037602514,126.197223087681));
#37757=CARTESIAN_POINT('Ctrl Pts',(131.844877740362,-1.85387635039624,126.248888573975));
#37758=CARTESIAN_POINT('Ctrl Pts',(131.837117297848,-1.98090008499362,126.300581635694));
#37759=CARTESIAN_POINT('Ctrl Pts',(131.829356855334,-2.10565933318112,126.357550537551));
#37760=CARTESIAN_POINT('Ctrl Pts',(131.821596412819,-2.22769932803784,126.419552894717));
#37761=CARTESIAN_POINT('Ctrl Pts',(131.813823512554,-2.34993523232842,126.481654783571));
#37762=CARTESIAN_POINT('Ctrl Pts',(131.806050612289,-2.4694428192147,126.548806082817));
#37763=CARTESIAN_POINT('Ctrl Pts',(131.798277712023,-2.58579408341668,126.620719617113));
#37764=CARTESIAN_POINT('Ctrl Pts',(131.790787376261,-2.69791568609289,126.690018913299));
#37765=CARTESIAN_POINT('Ctrl Pts',(131.783297040499,-2.80710620724367,126.763740044908));
#37766=CARTESIAN_POINT('Ctrl Pts',(131.775806704737,-2.91301206762658,126.841590909854));
#37767=CARTESIAN_POINT('Ctrl Pts',(131.767856330328,-3.02542241463406,126.924223190181));
#37768=CARTESIAN_POINT('Ctrl Pts',(131.759905955918,-3.13451423036537,127.011789730077));
#37769=CARTESIAN_POINT('Ctrl Pts',(131.751955581509,-3.23982082542546,127.103989814303));
#37770=CARTESIAN_POINT('Ctrl Pts',(131.744263365086,-3.34170799176701,127.193196053598));
#37771=CARTESIAN_POINT('Ctrl Pts',(131.736571148663,-3.44005156374033,127.286739352508));
#37772=CARTESIAN_POINT('Ctrl Pts',(131.728878932241,-3.53445722420859,127.384302841338));
#37773=CARTESIAN_POINT('Ctrl Pts',(131.721193684871,-3.62877735431287,127.48177793885));
#37774=CARTESIAN_POINT('Ctrl Pts',(131.713508437502,-3.71916639214806,127.583265698873));
#37775=CARTESIAN_POINT('Ctrl Pts',(131.705823190132,-3.80526392249755,127.688409792755));
#37776=CARTESIAN_POINT('Ctrl Pts',(131.698143165122,-3.89130294695759,127.793482438029));
#37777=CARTESIAN_POINT('Ctrl Pts',(131.690463140112,-3.97305601293349,127.902206167732));
#37778=CARTESIAN_POINT('Ctrl Pts',(131.682783115101,-4.05020070095915,128.014189055735));
#37779=CARTESIAN_POINT('Ctrl Pts',(131.67510657014,-4.12731043241603,128.126121200937));
#37780=CARTESIAN_POINT('Ctrl Pts',(131.66743002518,-4.19981571551304,128.24130923787));
#37781=CARTESIAN_POINT('Ctrl Pts',(131.659753480219,-4.2674357676132,128.35932993641));
#37782=CARTESIAN_POINT('Ctrl Pts',(131.652077418928,-4.33505155922955,128.477343198911));
#37783=CARTESIAN_POINT('Ctrl Pts',(131.644401357637,-4.39778252739333,128.598188425893));
#37784=CARTESIAN_POINT('Ctrl Pts',(131.636725296346,-4.45539255642993,128.72141553173));
#37785=CARTESIAN_POINT('Ctrl Pts',(131.629049422028,-4.51300118220605,128.844639636011));
#37786=CARTESIAN_POINT('Ctrl Pts',(131.62137354771,-4.56548895383169,128.970245139823));
#37787=CARTESIAN_POINT('Ctrl Pts',(131.613697673393,-4.61266718327577,129.097760336648));
#37788=CARTESIAN_POINT('Ctrl Pts',(131.606018456807,-4.65986595530053,129.225331056777));
#37789=CARTESIAN_POINT('Ctrl Pts',(131.598339240222,-4.70175043836995,129.354812753454));
#37790=CARTESIAN_POINT('Ctrl Pts',(131.590660023636,-4.73818130706446,129.485717009958));
#37791=CARTESIAN_POINT('Ctrl Pts',(131.588772588727,-4.7471354617718,129.517891289809));
#37792=CARTESIAN_POINT('Ctrl Pts',(131.586885153818,-4.75576040176345,129.55015144608));
#37793=CARTESIAN_POINT('Ctrl Pts',(131.584997718909,-4.76405452823404,129.582490119308));
#37794=CARTESIAN_POINT('Ctrl Pts',(133.334729823376,-4.76405452823402,129.582490119308));
#37795=CARTESIAN_POINT('Ctrl Pts',(133.32696908606,-4.79821351346672,129.715675484296));
#37796=CARTESIAN_POINT('Ctrl Pts',(133.319208348743,-4.8267966455201,129.85034665783));
#37797=CARTESIAN_POINT('Ctrl Pts',(133.311447611427,-4.84968727538676,129.985998598988));
#37798=CARTESIAN_POINT('Ctrl Pts',(133.303682915521,-4.87258958128452,130.121719733361));
#37799=CARTESIAN_POINT('Ctrl Pts',(133.295918219615,-4.88979349900938,130.258422254787));
#37800=CARTESIAN_POINT('Ctrl Pts',(133.288153523709,-4.90123355226953,130.395590842989));
#37801=CARTESIAN_POINT('Ctrl Pts',(133.280388827803,-4.91267360552968,130.532759431192));
#37802=CARTESIAN_POINT('Ctrl Pts',(133.272624131897,-4.91834976816577,130.670393697661));
#37803=CARTESIAN_POINT('Ctrl Pts',(133.264859435991,-4.91824867220281,130.807974600859));
#37804=CARTESIAN_POINT('',(133.610140564061,-4.91824860178181,130.800652036803));
#37805=CARTESIAN_POINT('Ctrl Pts',(133.679929079587,-4.76405452823404,129.582490119308));
#37806=CARTESIAN_POINT('Ctrl Pts',(133.670903636898,-4.80346910439079,129.736166953544));
#37807=CARTESIAN_POINT('Ctrl Pts',(133.66187819421,-4.83548620139363,129.891917696107));
#37808=CARTESIAN_POINT('Ctrl Pts',(133.652852751521,-4.85991057754177,130.049077729638));
#37809=CARTESIAN_POINT('Ctrl Pts',(133.643900109645,-4.88413794236419,130.20497008262));
#37810=CARTESIAN_POINT('Ctrl Pts',(133.634947467769,-4.90089450501078,130.362248961787));
#37811=CARTESIAN_POINT('Ctrl Pts',(133.625994825893,-4.91003684997578,130.520245861913));
#37812=CARTESIAN_POINT('Ctrl Pts',(133.620710071949,-4.91543358585336,130.613511598736));
#37813=CARTESIAN_POINT('Ctrl Pts',(133.615425318005,-4.91817800441632,130.707027166196));
#37814=CARTESIAN_POINT('Ctrl Pts',(133.610140564061,-4.91824860178181,130.800652036803));
#37815=CARTESIAN_POINT('Ctrl Pts',(133.610140564008,-4.91824860178252,130.800652037749));
#37816=CARTESIAN_POINT('Ctrl Pts',(133.602387431034,-4.91835217342056,130.938006790535));
#37817=CARTESIAN_POINT('Ctrl Pts',(133.59463429806,-4.91269746273253,131.075420857256));
#37818=CARTESIAN_POINT('Ctrl Pts',(133.586881165086,-4.90129633382327,131.212376929189));
#37819=CARTESIAN_POINT('Ctrl Pts',(133.579128914385,-4.88989650231452,131.349317416097));
#37820=CARTESIAN_POINT('Ctrl Pts',(133.571376663685,-4.87275158523712,131.485799623771));
#37821=CARTESIAN_POINT('Ctrl Pts',(133.563624412985,-4.84992545578321,131.621309903535));
#37822=CARTESIAN_POINT('Ctrl Pts',(133.55587138114,-4.82709702628796,131.756833837794));
#37823=CARTESIAN_POINT('Ctrl Pts',(133.548118349296,-4.79858630945917,131.891385265033));
#37824=CARTESIAN_POINT('Ctrl Pts',(133.540365317452,-4.76450851464186,132.024459661253));
#37825=CARTESIAN_POINT('Ctrl Pts',(133.532609840892,-4.73041997428373,132.157576019001));
#37826=CARTESIAN_POINT('Ctrl Pts',(133.524854364331,-4.69076095872476,132.289214041575));
#37827=CARTESIAN_POINT('Ctrl Pts',(133.517098887771,-4.64569675226893,132.418883689082));
#37828=CARTESIAN_POINT('Ctrl Pts',(133.509334287436,-4.60057953092724,132.548705883857));
#37829=CARTESIAN_POINT('Ctrl Pts',(133.5015696871,-4.55004454557834,132.676554709826));
#37830=CARTESIAN_POINT('Ctrl Pts',(133.493805086764,-4.49430575041075,132.801958896581));
#37831=CARTESIAN_POINT('Ctrl Pts',(133.486035753666,-4.43853298073561,132.927439521039));
#37832=CARTESIAN_POINT('Ctrl Pts',(133.478266420568,-4.37755025445433,133.050472188914));
#37833=CARTESIAN_POINT('Ctrl Pts',(133.47049708747,-4.31161738938312,133.170610509287));
#37834=CARTESIAN_POINT('Ctrl Pts',(133.462714826863,-4.24557481763773,133.290948729596));
#37835=CARTESIAN_POINT('Ctrl Pts',(133.454932566257,-4.17456585152711,133.408382646762));
#37836=CARTESIAN_POINT('Ctrl Pts',(133.44715030565,-4.09889399462122,133.522494367652));
#37837=CARTESIAN_POINT('Ctrl Pts',(133.440401354252,-4.0332696586797,133.621454618038));
#37838=CARTESIAN_POINT('Ctrl Pts',(133.433652402854,-3.96413924999595,133.717916702468));
#37839=CARTESIAN_POINT('Ctrl Pts',(133.426903451456,-3.89172427037809,133.811629356114));
#37840=CARTESIAN_POINT('Ctrl Pts',(133.419129117337,-3.80830712694628,133.919579975059));
#37841=CARTESIAN_POINT('Ctrl Pts',(133.411354783218,-3.72026286937863,134.024228149251));
#37842=CARTESIAN_POINT('Ctrl Pts',(133.403580449099,-3.62788241396373,134.12515152531));
#37843=CARTESIAN_POINT('Ctrl Pts',(133.395815696151,-3.53561580920398,134.225950522327));
#37844=CARTESIAN_POINT('Ctrl Pts',(133.388050943204,-3.43902390096166,134.323033569277));
#37845=CARTESIAN_POINT('Ctrl Pts',(133.380286190257,-3.33843950325637,134.416009097914));
#37846=CARTESIAN_POINT('Ctrl Pts',(133.372529149372,-3.23795500739293,134.508892281945));
#37847=CARTESIAN_POINT('Ctrl Pts',(133.364772108487,-3.13348619862717,134.597675802676));
#37848=CARTESIAN_POINT('Ctrl Pts',(133.357015067602,-3.025404346646,134.682003149027));
#37849=CARTESIAN_POINT('Ctrl Pts',(133.349263876362,-2.91740400002994,134.766266903471));
#37850=CARTESIAN_POINT('Ctrl Pts',(133.341512685122,-2.8057963403945,134.846080932754));
#37851=CARTESIAN_POINT('Ctrl Pts',(133.333761493882,-2.6909872115847,134.921127660962));
#37852=CARTESIAN_POINT('Ctrl Pts',(133.326013597105,-2.57622687971727,134.996142492308));
#37853=CARTESIAN_POINT('Ctrl Pts',(133.318265700328,-2.45826811159151,135.06639383913));
#37854=CARTESIAN_POINT('Ctrl Pts',(133.310517803551,-2.33754716871975,135.131606427144));
#37855=CARTESIAN_POINT('Ctrl Pts',(133.302771527467,-2.21685147806679,135.19680537409));
#37856=CARTESIAN_POINT('Ctrl Pts',(133.295025251383,-2.09339510568538,135.256967472991));
#37857=CARTESIAN_POINT('Ctrl Pts',(133.287278975298,-1.96764009403749,135.311862755429));
#37858=CARTESIAN_POINT('Ctrl Pts',(133.279532642033,-1.84188415409466,135.36675844309));
#37859=CARTESIAN_POINT('Ctrl Pts',(133.271786308768,-1.7138298993406,135.416387080296));
#37860=CARTESIAN_POINT('Ctrl Pts',(133.264039975502,-1.58396021707708,135.460566486427));
#37861=CARTESIAN_POINT('Ctrl Pts',(133.256291907499,-1.45406145139839,135.50475578623));
#37862=CARTESIAN_POINT('Ctrl Pts',(133.248543839496,-1.32234681928177,135.543493300778));
#37863=CARTESIAN_POINT('Ctrl Pts',(133.240795771493,-1.1893148759176,135.576646567551));
#37864=CARTESIAN_POINT('Ctrl Pts',(133.233039468752,-1.0561415446212,135.60983507001));
#37865=CARTESIAN_POINT('Ctrl Pts',(133.22528316601,-0.92164848528549,135.637427374189));
#37866=CARTESIAN_POINT('Ctrl Pts',(133.217526863268,-0.786345517693598,
135.659341955254));
#37867=CARTESIAN_POINT('Ctrl Pts',(133.209766420754,-0.650970334833916,
135.681268232792));
#37868=CARTESIAN_POINT('Ctrl Pts',(133.20200597824,-0.514784770402567,135.697510702665));
#37869=CARTESIAN_POINT('Ctrl Pts',(133.194245535725,-0.378303304881688,
135.708039815068));
#37870=CARTESIAN_POINT('Ctrl Pts',(133.18647263546,-0.241602747196285,135.718585829738));
#37871=CARTESIAN_POINT('Ctrl Pts',(133.178699735195,-0.104605730155504,
135.723400145443));
#37872=CARTESIAN_POINT('Ctrl Pts',(133.170926834929,0.032172822635227,135.722505386885));
#37873=CARTESIAN_POINT('Ctrl Pts',(133.163436499167,0.163979130507997,135.721643155055));
#37874=CARTESIAN_POINT('Ctrl Pts',(133.155946163405,0.295582274140959,135.715479735461));
#37875=CARTESIAN_POINT('Ctrl Pts',(133.148455827643,0.426528331227084,135.704080675402));
#37876=CARTESIAN_POINT('Ctrl Pts',(133.140681493524,0.562439247867539,135.692249416517));
#37877=CARTESIAN_POINT('Ctrl Pts',(133.132907159405,0.698072792421624,135.674740183407));
#37878=CARTESIAN_POINT('Ctrl Pts',(133.125132825286,0.83291637966798,135.651569439866));
#37879=CARTESIAN_POINT('Ctrl Pts',(133.117368072339,0.967593784244372,135.628427252195));
#37880=CARTESIAN_POINT('Ctrl Pts',(133.109603319392,1.10148278697197,135.599637502428));
#37881=CARTESIAN_POINT('Ctrl Pts',(133.101838566444,1.23407405628833,135.565268544222));
#37882=CARTESIAN_POINT('Ctrl Pts',(133.094081525559,1.3665336340868,135.53093372175));
#37883=CARTESIAN_POINT('Ctrl Pts',(133.086324484674,1.49769766748849,135.491030815838));
#37884=CARTESIAN_POINT('Ctrl Pts',(133.078567443789,1.62706553329057,135.445679483242));
#37885=CARTESIAN_POINT('Ctrl Pts',(133.070816252549,1.7563358417788,135.400362350438));
#37886=CARTESIAN_POINT('Ctrl Pts',(133.063065061309,1.88381231126709,135.349605097887));
#37887=CARTESIAN_POINT('Ctrl Pts',(133.055313870069,2.00900838763274,135.293577515971));
#37888=CARTESIAN_POINT('Ctrl Pts',(133.047565973292,2.13415125232605,135.237573747271));
#37889=CARTESIAN_POINT('Ctrl Pts',(133.039818076515,2.25701529550406,135.176304263823));
#37890=CARTESIAN_POINT('Ctrl Pts',(133.032070179738,2.37713311111174,135.109987312317));
#37891=CARTESIAN_POINT('Ctrl Pts',(133.024323903654,2.49722580066175,135.043684232889));
#37892=CARTESIAN_POINT('Ctrl Pts',(133.01657762757,2.61457306320791,134.972335974335));
#37893=CARTESIAN_POINT('Ctrl Pts',(133.008831351485,2.72873167457004,134.896206962518));
#37894=CARTESIAN_POINT('Ctrl Pts',(133.00108501822,2.84289112862511,134.820077388734));
#37895=CARTESIAN_POINT('Ctrl Pts',(132.993338684955,2.95386155925588,134.739167208181));
#37896=CARTESIAN_POINT('Ctrl Pts',(132.985592351689,3.06122868036634,134.653784214548));
#37897=CARTESIAN_POINT('Ctrl Pts',(132.977844283686,3.16861984559913,134.568382099986));
#37898=CARTESIAN_POINT('Ctrl Pts',(132.970096215683,3.27240578965933,134.478505422464));
#37899=CARTESIAN_POINT('Ctrl Pts',(132.962348147681,3.37220558681838,134.384502031356));
#37900=CARTESIAN_POINT('Ctrl Pts',(132.954591844939,3.47211145238954,134.290398732325));
#37901=CARTESIAN_POINT('Ctrl Pts',(132.946835542197,3.5680224230967,134.192160226852));
#37902=CARTESIAN_POINT('Ctrl Pts',(132.939079239455,3.65959433974247,134.090171374598));
#37903=CARTESIAN_POINT('Ctrl Pts',(132.931318796941,3.75121513107732,133.988128087822));
#37904=CARTESIAN_POINT('Ctrl Pts',(132.923558354427,3.83849200508441,133.882330767201));
#37905=CARTESIAN_POINT('Ctrl Pts',(132.915797911912,3.92112201140862,133.773196287344));
#37906=CARTESIAN_POINT('Ctrl Pts',(132.908025011647,4.00388466275459,133.663886615132));
#37907=CARTESIAN_POINT('Ctrl Pts',(132.900252111382,4.08198531695467,133.551229399973));
#37908=CARTESIAN_POINT('Ctrl Pts',(132.892479211116,4.15516468002477,133.435670090884));
#37909=CARTESIAN_POINT('Ctrl Pts',(132.884988875354,4.22568378891998,133.324311653757));
#37910=CARTESIAN_POINT('Ctrl Pts',(132.877498539592,4.29163304317731,133.210258722982));
#37911=CARTESIAN_POINT('Ctrl Pts',(132.87000820383,4.35282223350238,133.093928626171));
#37912=CARTESIAN_POINT('Ctrl Pts',(132.862233869711,4.41633143057632,132.973187838382));
#37913=CARTESIAN_POINT('Ctrl Pts',(132.854459535592,4.47491366073867,132.849611327824));
#37914=CARTESIAN_POINT('Ctrl Pts',(132.846685201473,4.52830571061255,132.723639246044));
#37915=CARTESIAN_POINT('Ctrl Pts',(132.838920448526,4.58163195955671,132.597822413597));
#37916=CARTESIAN_POINT('Ctrl Pts',(132.831155695579,4.62978060410419,132.46961624069));
#37917=CARTESIAN_POINT('Ctrl Pts',(132.823390942631,4.67253384597332,132.339486189216));
#37918=CARTESIAN_POINT('Ctrl Pts',(132.815633901746,4.71524462471988,132.209485384743));
#37919=CARTESIAN_POINT('Ctrl Pts',(132.807876860861,4.75257054378033,132.077564873356));
#37920=CARTESIAN_POINT('Ctrl Pts',(132.800119819976,4.78434167470252,131.944210520933));
#37921=CARTESIAN_POINT('Ctrl Pts',(132.792368628736,4.81608884676777,131.810956732063));
#37922=CARTESIAN_POINT('Ctrl Pts',(132.784617437496,4.84228947822081,131.676271633143));
#37923=CARTESIAN_POINT('Ctrl Pts',(132.776866246256,4.86282342413051,131.540656351784));
#37924=CARTESIAN_POINT('Ctrl Pts',(132.769118349479,4.88334864256545,131.405098710537));
#37925=CARTESIAN_POINT('Ctrl Pts',(132.761370452702,4.89821190735741,131.268612058927));
#37926=CARTESIAN_POINT('Ctrl Pts',(132.753622555925,4.90734419123914,131.131707606572));
#37927=CARTESIAN_POINT('Ctrl Pts',(132.745876279841,4.91647456484395,130.994831791678));
#37928=CARTESIAN_POINT('Ctrl Pts',(132.738130003757,4.91987631600756,130.857538739724));
#37929=CARTESIAN_POINT('Ctrl Pts',(132.730383727673,4.91753234020049,130.720344276404));
#37930=CARTESIAN_POINT('Ctrl Pts',(132.722637394407,4.91518834709071,130.583148800344));
#37931=CARTESIAN_POINT('Ctrl Pts',(132.714891061142,4.90709854905556,130.446052305279));
#37932=CARTESIAN_POINT('Ctrl Pts',(132.707144727876,4.893297969888,130.309569711839));
#37933=CARTESIAN_POINT('Ctrl Pts',(132.699396659873,4.87949430017642,130.173056554069));
#37934=CARTESIAN_POINT('Ctrl Pts',(132.691648591871,4.85997734381448,130.0371579604));
#37935=CARTESIAN_POINT('Ctrl Pts',(132.683900523868,4.83483385667072,129.902382435518));
#37936=CARTESIAN_POINT('Ctrl Pts',(132.676144221126,4.80966364672962,129.767463669605));
#37937=CARTESIAN_POINT('Ctrl Pts',(132.668387918384,4.77885503223973,129.633670741792));
#37938=CARTESIAN_POINT('Ctrl Pts',(132.660631615642,4.7425457800787,129.501501229006));
#37939=CARTESIAN_POINT('Ctrl Pts',(132.652871173128,4.70621714857652,129.369261173372));
#37940=CARTESIAN_POINT('Ctrl Pts',(132.645110730614,4.66438214865916,129.238646631421));
#37941=CARTESIAN_POINT('Ctrl Pts',(132.637350288099,4.61722775667497,129.110137814777));
#37942=CARTESIAN_POINT('Ctrl Pts',(132.629577387834,4.56999766827467,128.981422704372));
#37943=CARTESIAN_POINT('Ctrl Pts',(132.621804487569,4.51743127385306,128.854820435469));
#37944=CARTESIAN_POINT('Ctrl Pts',(132.614031587303,4.45976318755155,128.730789935515));
#37945=CARTESIAN_POINT('Ctrl Pts',(132.606541251541,4.40419148144425,128.611268256649));
#37946=CARTESIAN_POINT('Ctrl Pts',(132.599050915779,4.34388270346346,128.494134886282));
#37947=CARTESIAN_POINT('Ctrl Pts',(132.591560580017,4.27908515037673,128.379775428647));
#37948=CARTESIAN_POINT('Ctrl Pts',(132.583786245898,4.21183077836993,128.261079997417));
#37949=CARTESIAN_POINT('Ctrl Pts',(132.576011911779,4.13952748652236,128.144996985566));
#37950=CARTESIAN_POINT('Ctrl Pts',(132.56823757766,4.06240331353629,128.031985754625));
#37951=CARTESIAN_POINT('Ctrl Pts',(132.560472824713,3.98537418920069,127.919113799925));
#37952=CARTESIAN_POINT('Ctrl Pts',(132.552708071766,3.90353622342103,127.809306413561));
#37953=CARTESIAN_POINT('Ctrl Pts',(132.544943318818,3.81716329717726,127.702998428917));
#37954=CARTESIAN_POINT('Ctrl Pts',(132.537186277934,3.7308761577417,127.596796030862));
#37955=CARTESIAN_POINT('Ctrl Pts',(132.529429237049,3.64006326631725,127.494086419289));
#37956=CARTESIAN_POINT('Ctrl Pts',(132.521672196164,3.54504154514848,127.395275182193));
#37957=CARTESIAN_POINT('Ctrl Pts',(132.513921004923,3.4500914805988,127.29653845942));
#37958=CARTESIAN_POINT('Ctrl Pts',(132.506169813683,3.3509391736837,127.201694540305));
#37959=CARTESIAN_POINT('Ctrl Pts',(132.498418622443,3.24794129598594,127.111115377898));
#37960=CARTESIAN_POINT('Ctrl Pts',(132.490670725666,3.14498719513334,127.020574714051));
#37961=CARTESIAN_POINT('Ctrl Pts',(132.482922828889,3.03819106730616,126.934295459365));
#37962=CARTESIAN_POINT('Ctrl Pts',(132.475174932112,2.92794569671138,126.85261200972));
#37963=CARTESIAN_POINT('Ctrl Pts',(132.467428656028,2.81772338707158,126.770945646493));
#37964=CARTESIAN_POINT('Ctrl Pts',(132.459682379944,2.70405358371796,126.693873408746));
#37965=CARTESIAN_POINT('Ctrl Pts',(132.45193610386,2.58736101999869,126.621688503392));
#37966=CARTESIAN_POINT('Ctrl Pts',(132.444189770594,2.47066759488149,126.549503065185));
#37967=CARTESIAN_POINT('Ctrl Pts',(132.436443437329,2.35095169736611,126.482205237036));
#37968=CARTESIAN_POINT('Ctrl Pts',(132.428697104064,2.22866547597977,126.420043879615));
#37969=CARTESIAN_POINT('Ctrl Pts',(132.420949036061,2.10635186944144,126.35786860159));
#37970=CARTESIAN_POINT('Ctrl Pts',(132.413200968058,1.98146714209708,126.30083226034));
#37971=CARTESIAN_POINT('Ctrl Pts',(132.405452900055,1.85448600700744,126.2491367249));
#37972=CARTESIAN_POINT('Ctrl Pts',(132.397696597313,1.72736991485685,126.197386246831));
#37973=CARTESIAN_POINT('Ctrl Pts',(132.389940294571,1.59815332680166,126.15098806119));
#37974=CARTESIAN_POINT('Ctrl Pts',(132.382183991829,1.4673293347643,126.110095213284));
#37975=CARTESIAN_POINT('Ctrl Pts',(132.374423549315,1.336435518023,126.069180539634));
#37976=CARTESIAN_POINT('Ctrl Pts',(132.366663106801,1.20393296535165,126.033777159531));
#37977=CARTESIAN_POINT('Ctrl Pts',(132.358902664286,1.07032675767217,126.00398733059));
#37978=CARTESIAN_POINT('Ctrl Pts',(132.351129764021,0.936506073447491,125.974149680372));
#37979=CARTESIAN_POINT('Ctrl Pts',(132.343356863756,0.801578578866621,125.949943657982));
#37980=CARTESIAN_POINT('Ctrl Pts',(132.33558396349,0.666057197262066,125.931419937394));
#37981=CARTESIAN_POINT('Ctrl Pts',(132.328093627728,0.535462359236508,125.913569600708));
#37982=CARTESIAN_POINT('Ctrl Pts',(132.320603291966,0.404316369734703,125.900995635831));
#37983=CARTESIAN_POINT('Ctrl Pts',(132.313112956204,0.273077858986737,125.893697572169));
#37984=CARTESIAN_POINT('Ctrl Pts',(132.305338622085,0.136863400214587,125.886122800204));
#37985=CARTESIAN_POINT('Ctrl Pts',(132.297564287966,0.000117779352706487,
125.88420790398));
#37986=CARTESIAN_POINT('Ctrl Pts',(132.289789953847,-0.136649269244567,
125.888009324207));
#37987=CARTESIAN_POINT('Ctrl Pts',(132.2820252009,-0.273247764677482,125.891806059523));
#37988=CARTESIAN_POINT('Ctrl Pts',(132.274260447953,-0.409867248239707,
125.90130508338));
#37989=CARTESIAN_POINT('Ctrl Pts',(132.266495695005,-0.545993842930439,
125.916511010021));
#37990=CARTESIAN_POINT('Ctrl Pts',(132.25873865412,-0.681985234767812,125.93170183392));
#37991=CARTESIAN_POINT('Ctrl Pts',(132.250981613236,-0.817484325914376,
125.952588237553));
#37992=CARTESIAN_POINT('Ctrl Pts',(132.243224572351,-0.951978579489092,
125.979122815479));
#37993=CARTESIAN_POINT('Ctrl Pts',(132.23547338111,-1.08637140990116,126.005637383472));
#37994=CARTESIAN_POINT('Ctrl Pts',(132.22772218987,-1.21976052898902,126.037791572446));
#37995=CARTESIAN_POINT('Ctrl Pts',(132.21997099863,-1.3516402124162,126.075486354205));
#37996=CARTESIAN_POINT('Ctrl Pts',(132.212223101853,-1.48346384346045,126.113165114676));
#37997=CARTESIAN_POINT('Ctrl Pts',(132.204475205076,-1.61377893971469,126.156379676994));
#37998=CARTESIAN_POINT('Ctrl Pts',(132.196727308299,-1.74209185499535,126.204980329825));
#37999=CARTESIAN_POINT('Ctrl Pts',(132.188981032215,-1.87037792998007,126.253570816447));
#38000=CARTESIAN_POINT('Ctrl Pts',(132.181234756131,-1.99666229164767,126.307545014208));
#38001=CARTESIAN_POINT('Ctrl Pts',(132.173488480047,-2.1204686779699,126.366704068412));
#38002=CARTESIAN_POINT('Ctrl Pts',(132.165742146781,-2.24427597820225,126.425863559314));
#38003=CARTESIAN_POINT('Ctrl Pts',(132.157995813516,-2.36560491382767,126.490207814469));
#38004=CARTESIAN_POINT('Ctrl Pts',(132.150249480251,-2.48400171399254,126.559490943785));
#38005=CARTESIAN_POINT('Ctrl Pts',(132.142501412248,-2.60242502830046,126.628789588579));
#38006=CARTESIAN_POINT('Ctrl Pts',(132.134753344245,-2.71791456315555,126.703029110977));
#38007=CARTESIAN_POINT('Ctrl Pts',(132.127005276242,-2.83004388641667,126.781919236582));
#38008=CARTESIAN_POINT('Ctrl Pts',(132.1192489735,-2.94229238205684,126.860893207551));
#38009=CARTESIAN_POINT('Ctrl Pts',(132.111492670758,-3.05117321183601,126.944527430008));
#38010=CARTESIAN_POINT('Ctrl Pts',(132.103736368016,-3.15629108617485,127.03248977648));
#38011=CARTESIAN_POINT('Ctrl Pts',(132.095975925502,-3.26146506508811,127.120499071105));
#38012=CARTESIAN_POINT('Ctrl Pts',(132.088215482988,-3.36287179771774,127.212840829614));
#38013=CARTESIAN_POINT('Ctrl Pts',(132.080455040474,-3.46015224326087,127.309145385859));
#38014=CARTESIAN_POINT('Ctrl Pts',(132.072682140208,-3.55758885201153,127.405604538728));
#38015=CARTESIAN_POINT('Ctrl Pts',(132.064909239943,-3.65088567080659,127.506038914897));
#38016=CARTESIAN_POINT('Ctrl Pts',(132.057136339677,-3.73972281860737,127.610044367962));
#38017=CARTESIAN_POINT('Ctrl Pts',(132.049646003915,-3.82533051231844,127.710268960833));
#38018=CARTESIAN_POINT('Ctrl Pts',(132.042155668153,-3.90679695582707,127.813809260897));
#38019=CARTESIAN_POINT('Ctrl Pts',(132.034665332391,-3.98387464421675,127.920279155182));
#38020=CARTESIAN_POINT('Ctrl Pts',(132.026827458088,-4.06452860318,128.031689067232));
#38021=CARTESIAN_POINT('Ctrl Pts',(132.018989583785,-4.14063184094279,128.146659040027));
#38022=CARTESIAN_POINT('Ctrl Pts',(132.011151709482,-4.21185673676159,128.264784690074));
#38023=CARTESIAN_POINT('Ctrl Pts',(132.003327105895,-4.28296103797626,128.382710335392));
#38024=CARTESIAN_POINT('Ctrl Pts',(131.995502502307,-4.34920325460927,128.503780689803));
#38025=CARTESIAN_POINT('Ctrl Pts',(131.98767789872,-4.41029743374626,128.627560303253));
#38026=CARTESIAN_POINT('Ctrl Pts',(131.979860958591,-4.47133177692381,128.751218686302));
#38027=CARTESIAN_POINT('Ctrl Pts',(131.972044018461,-4.52722794482337,128.877580708845));
#38028=CARTESIAN_POINT('Ctrl Pts',(131.964227078332,-4.57774427904976,129.006183657941));
#38029=CARTESIAN_POINT('Ctrl Pts',(131.956417638901,-4.62821214062265,129.134663206827));
#38030=CARTESIAN_POINT('Ctrl Pts',(131.948608199471,-4.67331031006328,129.265379045104));
#38031=CARTESIAN_POINT('Ctrl Pts',(131.940798760041,-4.71284417704997,129.397846193415));
#38032=CARTESIAN_POINT('Ctrl Pts',(131.937191320734,-4.73110618253503,129.459037166457));
#38033=CARTESIAN_POINT('Ctrl Pts',(131.933583881427,-4.74818152974977,129.520601539124));
#38034=CARTESIAN_POINT('Ctrl Pts',(131.929976442121,-4.76405452823405,129.582490119308));
#38035=CARTESIAN_POINT('Origin',(213.235140564004,0.,130.804360617566));
#38036=CARTESIAN_POINT('',(129.834833026848,-4.76405452823404,129.582490119308));
#38037=CARTESIAN_POINT('',(130.180282649887,-4.76405452823405,129.582490119308));
#38038=CARTESIAN_POINT('',(213.235140564004,-4.76405452823405,129.582490119308));
#38039=CARTESIAN_POINT('',(131.514859436023,-4.91824964687546,130.80622435291));
#38040=CARTESIAN_POINT('Ctrl Pts',(131.514859435991,-4.91824964687524,130.806224353474));
#38041=CARTESIAN_POINT('Ctrl Pts',(131.509025984302,-4.91821083134048,130.908655437895));
#38042=CARTESIAN_POINT('Ctrl Pts',(131.503192532613,-4.91497231306959,131.011022270698));
#38043=CARTESIAN_POINT('Ctrl Pts',(131.497359080925,-4.90854456339616,131.113186347799));
#38044=CARTESIAN_POINT('Ctrl Pts',(131.489584746806,-4.89997819887275,131.249342043044));
#38045=CARTESIAN_POINT('Ctrl Pts',(131.481810412686,-4.88572883907578,131.385356701805));
#38046=CARTESIAN_POINT('Ctrl Pts',(131.474036078567,-4.86580064242577,131.520717491386));
#38047=CARTESIAN_POINT('Ctrl Pts',(131.46627132562,-4.8458970054971,131.655911460891));
#38048=CARTESIAN_POINT('Ctrl Pts',(131.458506572673,-4.82032851335909,131.790452781506));
#38049=CARTESIAN_POINT('Ctrl Pts',(131.450741819726,-4.78915127743318,131.923830628044));
#38050=CARTESIAN_POINT('Ctrl Pts',(131.442984778841,-4.75800500717745,132.057076001825));
#38051=CARTESIAN_POINT('Ctrl Pts',(131.435227737956,-4.72126116745904,132.189159822943));
#38052=CARTESIAN_POINT('Ctrl Pts',(131.427470697071,-4.67902736699891,132.319578740931));
#38053=CARTESIAN_POINT('Ctrl Pts',(131.419719505831,-4.63682541537638,132.449899308999));
#38054=CARTESIAN_POINT('Ctrl Pts',(131.411968314591,-4.58914186343657,132.578557102521));
#38055=CARTESIAN_POINT('Ctrl Pts',(131.404217123351,-4.5361347767085,132.70506163299));
#38056=CARTESIAN_POINT('Ctrl Pts',(131.396469226574,-4.48315021940624,132.83151239566));
#38057=CARTESIAN_POINT('Ctrl Pts',(131.388721329797,-4.42484677831832,132.955811355693));
#38058=CARTESIAN_POINT('Ctrl Pts',(131.38097343302,-4.36143142082994,133.077486004318));
#38059=CARTESIAN_POINT('Ctrl Pts',(131.373227156935,-4.29802932846723,133.199135201229));
#38060=CARTESIAN_POINT('Ctrl Pts',(131.365480880851,-4.22951762718827,133.31816083214));
#38061=CARTESIAN_POINT('Ctrl Pts',(131.357734604767,-4.15615003054825,133.434113455016));
#38062=CARTESIAN_POINT('Ctrl Pts',(131.349988271502,-4.08278189232539,133.550066933827));
#38063=CARTESIAN_POINT('Ctrl Pts',(131.342241938237,-4.00455799626143,133.662947028955));
#38064=CARTESIAN_POINT('Ctrl Pts',(131.334495604971,-3.92177610568397,133.772332187407));
#38065=CARTESIAN_POINT('Ctrl Pts',(131.326747536968,-3.83897567667592,133.881741841908));
#38066=CARTESIAN_POINT('Ctrl Pts',(131.318999468965,-3.75161545790435,133.987654690624));
#38067=CARTESIAN_POINT('Ctrl Pts',(131.311251400962,-3.66003405740353,134.089681570098));
#38068=CARTESIAN_POINT('Ctrl Pts',(131.30349509822,-3.56835532310054,134.191816884954));
#38069=CARTESIAN_POINT('Ctrl Pts',(131.295738795479,-3.47244670673212,134.290057688929));
#38070=CARTESIAN_POINT('Ctrl Pts',(131.287982492737,-3.37268469825481,134.384050686365));
#38071=CARTESIAN_POINT('Ctrl Pts',(131.280222050223,-3.27286944378979,134.478093850694));
#38072=CARTESIAN_POINT('Ctrl Pts',(131.272461607708,-3.16919699451058,134.567884435097));
#38073=CARTESIAN_POINT('Ctrl Pts',(131.264701165194,-3.06207683500362,134.653109572621));
#38074=CARTESIAN_POINT('Ctrl Pts',(131.256928264929,-2.95478471670686,134.738471521101));
#38075=CARTESIAN_POINT('Ctrl Pts',(131.249155364663,-2.84403414439618,134.819253146776));
#38076=CARTESIAN_POINT('Ctrl Pts',(131.241382464398,-2.73026421646917,134.895184540783));
#38077=CARTESIAN_POINT('Ctrl Pts',(131.233892128636,-2.62063011199177,134.968355637359));
#38078=CARTESIAN_POINT('Ctrl Pts',(131.226401792874,-2.50819262590463,135.03702285572));
#38079=CARTESIAN_POINT('Ctrl Pts',(131.218911457112,-2.39336440113872,135.100986026636));
#38080=CARTESIAN_POINT('Ctrl Pts',(131.211137122993,-2.2741824293291,135.167374380618));
#38081=CARTESIAN_POINT('Ctrl Pts',(131.203362788874,-2.15204731774808,135.228905236061));
#38082=CARTESIAN_POINT('Ctrl Pts',(131.195588454755,-2.0273927747941,135.285304892963));
#38083=CARTESIAN_POINT('Ctrl Pts',(131.187823701808,-1.9028918574237,135.341635042329));
#38084=CARTESIAN_POINT('Ctrl Pts',(131.180058948861,-1.77587803943621,135.392846415902));
#38085=CARTESIAN_POINT('Ctrl Pts',(131.172294195913,-1.64681142212257,135.438710108322));
#38086=CARTESIAN_POINT('Ctrl Pts',(131.164537155028,-1.51787299559294,135.484528248275));
#38087=CARTESIAN_POINT('Ctrl Pts',(131.156780114143,-1.38688619319223,135.525009146921));
#38088=CARTESIAN_POINT('Ctrl Pts',(131.149023073258,-1.25433266306687,135.559971265302));
#38089=CARTESIAN_POINT('Ctrl Pts',(131.141271882018,-1.12187909258979,135.594907018478));
#38090=CARTESIAN_POINT('Ctrl Pts',(131.133520690778,-0.987861522562395,
135.624332175803));
#38091=CARTESIAN_POINT('Ctrl Pts',(131.125769499538,-0.85277805313735,135.648114601264));
#38092=CARTESIAN_POINT('Ctrl Pts',(131.118021602761,-0.717751997790004,
135.671886918559));
#38093=CARTESIAN_POINT('Ctrl Pts',(131.110273705984,-0.581661328335614,
135.690021206402));
#38094=CARTESIAN_POINT('Ctrl Pts',(131.102525809207,-0.445015450713763,
135.702436189781));
#38095=CARTESIAN_POINT('Ctrl Pts',(131.094779533123,-0.308398156463766,
135.714848576213));
#38096=CARTESIAN_POINT('Ctrl Pts',(131.087033257039,-0.171226274165125,
135.721544002444));
#38097=CARTESIAN_POINT('Ctrl Pts',(131.079286980955,-0.0340150705038945,
135.722492990477));
#38098=CARTESIAN_POINT('Ctrl Pts',(131.071540647689,0.103197146019178,135.723441985516));
#38099=CARTESIAN_POINT('Ctrl Pts',(131.063794314424,0.24044829352818,135.718644455007));
#38100=CARTESIAN_POINT('Ctrl Pts',(131.056047981159,0.377222759200355,135.708123055984));
#38101=CARTESIAN_POINT('Ctrl Pts',(131.048299913156,0.514027854565697,135.697599300767));
#38102=CARTESIAN_POINT('Ctrl Pts',(131.040551845153,0.65035566593594,135.681349156341));
#38103=CARTESIAN_POINT('Ctrl Pts',(131.03280377715,0.78569575315938,135.65944715088));
#38104=CARTESIAN_POINT('Ctrl Pts',(131.025047474408,0.921179681438274,135.637521867708));
#38105=CARTESIAN_POINT('Ctrl Pts',(131.017291171666,1.05567340199217,135.609932786697));
#38106=CARTESIAN_POINT('Ctrl Pts',(131.009534868924,1.18867617515979,135.576805694579));
#38107=CARTESIAN_POINT('Ctrl Pts',(131.00177442641,1.32174993591217,135.543660921535));
#38108=CARTESIAN_POINT('Ctrl Pts',(130.994013983896,1.45333078874808,135.504972357927));
#38109=CARTESIAN_POINT('Ctrl Pts',(130.986253541381,1.58293417341703,135.460915402504));
#38110=CARTESIAN_POINT('Ctrl Pts',(130.978480641116,1.71274560894469,135.416787722945));
#38111=CARTESIAN_POINT('Ctrl Pts',(130.970707740851,1.84057286804668,135.367274571719));
#38112=CARTESIAN_POINT('Ctrl Pts',(130.962934840585,1.9659515253437,135.312599482411));
#38113=CARTESIAN_POINT('Ctrl Pts',(130.955444504823,2.08677235263906,135.259911970317));
#38114=CARTESIAN_POINT('Ctrl Pts',(130.947954169061,2.20531923587244,135.20243143769));
#38115=CARTESIAN_POINT('Ctrl Pts',(130.940463833299,2.32120072341737,135.140396856357));
#38116=CARTESIAN_POINT('Ctrl Pts',(130.93268949918,2.44147589278306,135.076010215018));
#38117=CARTESIAN_POINT('Ctrl Pts',(130.924915165061,2.55926055523696,135.00651341694));
#38118=CARTESIAN_POINT('Ctrl Pts',(130.917140830942,2.67409000923304,134.932123411746));
#38119=CARTESIAN_POINT('Ctrl Pts',(130.909376077995,2.78877794618959,134.857825085586));
#38120=CARTESIAN_POINT('Ctrl Pts',(130.901611325047,2.9005175962659,134.778645761619));
#38121=CARTESIAN_POINT('Ctrl Pts',(130.8938465721,3.0088676789107,134.694848807152));
#38122=CARTESIAN_POINT('Ctrl Pts',(130.886089531215,3.11711014672594,134.611135081001));
#38123=CARTESIAN_POINT('Ctrl Pts',(130.87833249033,3.22196943946388,134.522813088922));
#38124=CARTESIAN_POINT('Ctrl Pts',(130.870575449445,3.32303248066937,134.430189928898));
#38125=CARTESIAN_POINT('Ctrl Pts',(130.862824258205,3.42401930944933,134.33763661672));
#38126=CARTESIAN_POINT('Ctrl Pts',(130.855073066965,3.52121529783151,134.240788855765));
#38127=CARTESIAN_POINT('Ctrl Pts',(130.847321875725,3.61424004074636,134.139994289054));
#38128=CARTESIAN_POINT('Ctrl Pts',(130.839573978948,3.70722524566402,134.039242562723));
#38129=CARTESIAN_POINT('Ctrl Pts',(130.831826082171,3.79604246665503,133.934547653756));
#38130=CARTESIAN_POINT('Ctrl Pts',(130.824078185394,3.88034797839801,133.82629420867));
#38131=CARTESIAN_POINT('Ctrl Pts',(130.81633190931,3.96463585524536,133.71806340787));
#38132=CARTESIAN_POINT('Ctrl Pts',(130.808585633225,4.04441365995016,133.606275859806));
#38133=CARTESIAN_POINT('Ctrl Pts',(130.800839357141,4.11937807760781,133.491349139355));
#38134=CARTESIAN_POINT('Ctrl Pts',(130.793093023876,4.19434304863571,133.37642157054));
#38135=CARTESIAN_POINT('Ctrl Pts',(130.785346690611,4.26449434812018,133.258355110561));
#38136=CARTESIAN_POINT('Ctrl Pts',(130.777600357345,4.32957233673832,133.137595805765));
#38137=CARTESIAN_POINT('Ctrl Pts',(130.769852289342,4.39466489912074,133.01680945776));
#38138=CARTESIAN_POINT('Ctrl Pts',(130.762104221339,4.45468170442435,132.893329409056));
#38139=CARTESIAN_POINT('Ctrl Pts',(130.754356153336,4.50940954994301,132.767625391707));
#38140=CARTESIAN_POINT('Ctrl Pts',(130.746599850595,4.56419556086724,132.641787774632));
#38141=CARTESIAN_POINT('Ctrl Pts',(130.738843547853,4.61368122680096,132.513721826283));
#38142=CARTESIAN_POINT('Ctrl Pts',(130.731087245111,4.65770171366438,132.383916823919));
#38143=CARTESIAN_POINT('Ctrl Pts',(130.723326802597,4.7017456955871,132.254042540716));
#38144=CARTESIAN_POINT('Ctrl Pts',(130.715566360082,4.74031857630529,132.122427729011));
#38145=CARTESIAN_POINT('Ctrl Pts',(130.707805917568,4.77330600710254,131.989574870374));
#38146=CARTESIAN_POINT('Ctrl Pts',(130.700033017303,4.80634639225217,131.856508744534));
#38147=CARTESIAN_POINT('Ctrl Pts',(130.692260117037,4.83378333173931,131.722200983532));
#38148=CARTESIAN_POINT('Ctrl Pts',(130.684487216772,4.85555385743811,131.587163146955));
#38149=CARTESIAN_POINT('Ctrl Pts',(130.67699688101,4.87653296969101,131.457034275879));
#38150=CARTESIAN_POINT('Ctrl Pts',(130.669506545248,4.8922504557149,131.326227793669));
#38151=CARTESIAN_POINT('Ctrl Pts',(130.662016209486,4.90269578010907,131.195202209775));
#38152=CARTESIAN_POINT('Ctrl Pts',(130.654241875367,4.91353714215249,131.059208751043));
#38153=CARTESIAN_POINT('Ctrl Pts',(130.646467541248,4.91873300478485,130.922548461771));
#38154=CARTESIAN_POINT('Ctrl Pts',(130.638693207129,4.91821471133141,130.785729575101));
#38155=CARTESIAN_POINT('Ctrl Pts',(130.630928454182,4.91769705662832,130.649079305481));
#38156=CARTESIAN_POINT('Ctrl Pts',(130.623163701235,4.91147925915879,130.512271214574));
#38157=CARTESIAN_POINT('Ctrl Pts',(130.615398948287,4.89954437438008,130.375818920668));
#38158=CARTESIAN_POINT('Ctrl Pts',(130.607641907402,4.88762134349718,130.239502153103));
#38159=CARTESIAN_POINT('Ctrl Pts',(130.599884866517,4.86999255920737,130.10354086625));
#38160=CARTESIAN_POINT('Ctrl Pts',(130.592127825632,4.84669311382913,129.96844858699));
#38161=CARTESIAN_POINT('Ctrl Pts',(130.584376634392,4.82341123874389,129.83345818187));
#38162=CARTESIAN_POINT('Ctrl Pts',(130.576625443152,4.79446728044548,129.699335863676));
#38163=CARTESIAN_POINT('Ctrl Pts',(130.568874251912,4.75994810262256,129.566589587512));
#38164=CARTESIAN_POINT('Ctrl Pts',(130.561126355135,4.72544359637106,129.433899732058));
#38165=CARTESIAN_POINT('Ctrl Pts',(130.553378458358,4.68536868177046,129.302585132992));
#38166=CARTESIAN_POINT('Ctrl Pts',(130.545630561581,4.63986118089606,129.173142887));
#38167=CARTESIAN_POINT('Ctrl Pts',(130.537884285497,4.59436319920982,129.043727717535));
#38168=CARTESIAN_POINT('Ctrl Pts',(130.530138009413,4.54343502115958,128.916184490721));
#38169=CARTESIAN_POINT('Ctrl Pts',(130.522391733329,4.48726401520176,128.790994103397));
#38170=CARTESIAN_POINT('Ctrl Pts',(130.514645400063,4.43109259460237,128.665802791947));
#38171=CARTESIAN_POINT('Ctrl Pts',(130.506899066798,4.36967842891768,128.54296471135));
#38172=CARTESIAN_POINT('Ctrl Pts',(130.499152733532,4.30325644817831,128.422939402469));
#38173=CARTESIAN_POINT('Ctrl Pts',(130.491404665529,4.23681959269689,128.302887214753));
#38174=CARTESIAN_POINT('Ctrl Pts',(130.483656597526,4.16537287984385,128.185649394194));
#38175=CARTESIAN_POINT('Ctrl Pts',(130.475908529524,4.08919626723004,128.071659215917));
#38176=CARTESIAN_POINT('Ctrl Pts',(130.468152226782,4.01293869320583,127.957547887523));
#38177=CARTESIAN_POINT('Ctrl Pts',(130.46039592404,3.93194139503565,127.846691421999));
#38178=CARTESIAN_POINT('Ctrl Pts',(130.452639621298,3.84652691868793,127.739492965234));
#38179=CARTESIAN_POINT('Ctrl Pts',(130.444879178784,3.76106685406228,127.632237293426));
#38180=CARTESIAN_POINT('Ctrl Pts',(130.43711873627,3.67118516967286,127.52864381584));
#38181=CARTESIAN_POINT('Ctrl Pts',(130.429358293755,3.57724280922148,127.429080340852));
#38182=CARTESIAN_POINT('Ctrl Pts',(130.42158539349,3.48314964415336,127.329357037736));
#38183=CARTESIAN_POINT('Ctrl Pts',(130.413812493225,3.38498305700623,127.23367693802));
#38184=CARTESIAN_POINT('Ctrl Pts',(130.406039592959,3.28313940153916,127.142369529024));
#38185=CARTESIAN_POINT('Ctrl Pts',(130.398549257197,3.18499801947666,127.054381374334));
#38186=CARTESIAN_POINT('Ctrl Pts',(130.391058921435,3.08344250647774,126.970453709439));
#38187=CARTESIAN_POINT('Ctrl Pts',(130.383568585673,2.978852924886,126.890843233626));
#38188=CARTESIAN_POINT('Ctrl Pts',(130.375794251554,2.87029779751921,126.808214302426));
#38189=CARTESIAN_POINT('Ctrl Pts',(130.368019917435,2.75813011640286,126.729974651574));
#38190=CARTESIAN_POINT('Ctrl Pts',(130.360245583316,2.64274036186352,126.656456756303));
#38191=CARTESIAN_POINT('Ctrl Pts',(130.352480830369,2.52749281488413,126.583029465268));
#38192=CARTESIAN_POINT('Ctrl Pts',(130.344716077422,2.40903142198699,126.514312559517));
#38193=CARTESIAN_POINT('Ctrl Pts',(130.336951324474,2.2877791458449,126.450597918206));
#38194=CARTESIAN_POINT('Ctrl Pts',(130.329194283589,2.16664729917275,126.386946559175));
#38195=CARTESIAN_POINT('Ctrl Pts',(130.321437242704,2.04273042940345,126.328287758088));
#38196=CARTESIAN_POINT('Ctrl Pts',(130.313680201819,1.91647954950282,126.274869564607));
#38197=CARTESIAN_POINT('Ctrl Pts',(130.305929010579,1.79032387637273,126.221491654201));
#38198=CARTESIAN_POINT('Ctrl Pts',(130.298177819339,1.66183805507885,126.17334663695));
#38199=CARTESIAN_POINT('Ctrl Pts',(130.290426628099,1.53149639458168,126.130635994112));
#38200=CARTESIAN_POINT('Ctrl Pts',(130.282678731322,1.4012101327673,126.087943504436));
#38201=CARTESIAN_POINT('Ctrl Pts',(130.274930834545,1.26906997132464,126.050680916738));
#38202=CARTESIAN_POINT('Ctrl Pts',(130.267182937768,1.1355686279714,126.019000970302));
#38203=CARTESIAN_POINT('Ctrl Pts',(130.259436661684,1.00209521022124,125.987327650627));
#38204=CARTESIAN_POINT('Ctrl Pts',(130.2516903856,0.867261557064295,125.961234739672));
#38205=CARTESIAN_POINT('Ctrl Pts',(130.243944109515,0.731573537860023,125.940824535536));
#38206=CARTESIAN_POINT('Ctrl Pts',(130.23619777625,0.595884517037618,125.920414180738));
#38207=CARTESIAN_POINT('Ctrl Pts',(130.228451442985,0.459341504199096,125.905686674618));
#38208=CARTESIAN_POINT('Ctrl Pts',(130.220705109719,0.322458109507423,125.896692756951));
#38209=CARTESIAN_POINT('Ctrl Pts',(130.212957041716,0.185544060728592,125.887696825159));
#38210=CARTESIAN_POINT('Ctrl Pts',(130.205208973713,0.0482898684647223,
125.884437062453));
#38211=CARTESIAN_POINT('Ctrl Pts',(130.19746090571,-0.0887886167240415,
125.886912128355));
#38212=CARTESIAN_POINT('Ctrl Pts',(130.189704602969,-0.226012790558119,
125.889389824787));
#38213=CARTESIAN_POINT('Ctrl Pts',(130.181948300227,-0.363060492751894,
125.897614518265));
#38214=CARTESIAN_POINT('Ctrl Pts',(130.174191997485,-0.499418201276451,
125.911532751931));
#38215=CARTESIAN_POINT('Ctrl Pts',(130.166431554971,-0.635848688015792,
125.925458414177));
#38216=CARTESIAN_POINT('Ctrl Pts',(130.158671112457,-0.771588060523373,
125.945083615789));
#38217=CARTESIAN_POINT('Ctrl Pts',(130.150910669942,-0.906131772308056,
125.970303494019));
#38218=CARTESIAN_POINT('Ctrl Pts',(130.143137769677,-1.04089146560313,125.995563857437));
#38219=CARTESIAN_POINT('Ctrl Pts',(130.135364869412,-1.17445128150084,126.026436756413));
#38220=CARTESIAN_POINT('Ctrl Pts',(130.127591969146,-1.30631977409885,126.06276682325));
#38221=CARTESIAN_POINT('Ctrl Pts',(130.120101633384,-1.43339451483387,126.097776200647));
#38222=CARTESIAN_POINT('Ctrl Pts',(130.112611297622,-1.55889847167166,126.137852777012));
#38223=CARTESIAN_POINT('Ctrl Pts',(130.10512096186,-1.68241024325098,126.182815547364));
#38224=CARTESIAN_POINT('Ctrl Pts',(130.097346473652,-1.81060754203999,126.229484019783));
#38225=CARTESIAN_POINT('Ctrl Pts',(130.089571985444,-1.93706461948167,126.281564563924));
#38226=CARTESIAN_POINT('Ctrl Pts',(130.081797497236,-2.0612906615337,126.338908359264));
#38227=CARTESIAN_POINT('Ctrl Pts',(130.074032626073,-2.18536303591096,126.396181220301));
#38228=CARTESIAN_POINT('Ctrl Pts',(130.066267754911,-2.30720951455965,126.458704215773));
#38229=CARTESIAN_POINT('Ctrl Pts',(130.058502883748,-2.42635588845429,126.526279252624));
#38230=CARTESIAN_POINT('Ctrl Pts',(130.05074576037,-2.54538337815762,126.593786863138));
#38231=CARTESIAN_POINT('Ctrl Pts',(130.042988636993,-2.66171578683055,126.666336291502));
#38232=CARTESIAN_POINT('Ctrl Pts',(130.035231513615,-2.77490062623944,126.74368215492));
#38233=CARTESIAN_POINT('Ctrl Pts',(130.027480275489,-2.8879995934364,126.820969336801));
#38234=CARTESIAN_POINT('Ctrl Pts',(130.019729037363,-2.9979554232324,126.9030454906));
#38235=CARTESIAN_POINT('Ctrl Pts',(130.011977799238,-3.10434222180379,126.989620464892));
#38236=CARTESIAN_POINT('Ctrl Pts',(130.00423003788,-3.21068130127053,127.076156606543));
#38237=CARTESIAN_POINT('Ctrl Pts',(129.996482276521,-3.31345423189615,127.167187307716));
#38238=CARTESIAN_POINT('Ctrl Pts',(129.988734515163,-3.412266205948,127.262380606012));
#38239=CARTESIAN_POINT('Ctrl Pts',(129.980988425214,-3.51105686349139,127.35755336845));
#38240=CARTESIAN_POINT('Ctrl Pts',(129.973242335264,-3.60588798304674,127.456886670484));
#38241=CARTESIAN_POINT('Ctrl Pts',(129.965496245315,-3.69640009032173,127.56001023039));
#38242=CARTESIAN_POINT('Ctrl Pts',(129.957750148934,-3.78691227274952,127.66313387592));
#38243=CARTESIAN_POINT('Ctrl Pts',(129.950004052553,-3.87310517804813,127.770047491654));
#38244=CARTESIAN_POINT('Ctrl Pts',(129.942257956172,-3.9546585277464,127.880346426181));
#38245=CARTESIAN_POINT('Ctrl Pts',(129.934510175881,-4.03622960618354,127.990669338398));
#38246=CARTESIAN_POINT('Ctrl Pts',(129.92676239559,-4.11315889006694,128.104378719303));
#38247=CARTESIAN_POINT('Ctrl Pts',(129.919014615299,-4.18516870655706,128.221039894126));
#38248=CARTESIAN_POINT('Ctrl Pts',(129.911259297473,-4.25724857878879,128.337814564379));
#38249=CARTESIAN_POINT('Ctrl Pts',(129.903503979647,-4.32439922019065,128.45754643047));
#38250=CARTESIAN_POINT('Ctrl Pts',(129.895748661821,-4.38638811719911,128.579774735251));
#38251=CARTESIAN_POINT('Ctrl Pts',(129.887989225181,-4.44840993623201,128.702067954936));
#38252=CARTESIAN_POINT('Ctrl Pts',(129.880229788541,-4.50526438665995,128.826859899736));
#38253=CARTESIAN_POINT('Ctrl Pts',(129.8724703519,-4.55676703219201,128.953669590725));
#38254=CARTESIAN_POINT('Ctrl Pts',(129.864700083919,-4.60834156989123,129.080656294438));
#38255=CARTESIAN_POINT('Ctrl Pts',(129.856929815938,-4.65454924940357,129.209666002495));
#38256=CARTESIAN_POINT('Ctrl Pts',(129.849159547956,-4.69525525982363,129.340201777959));
#38257=CARTESIAN_POINT('Ctrl Pts',(129.84438404092,-4.72027265171207,129.420427391242));
#38258=CARTESIAN_POINT('Ctrl Pts',(129.839608533884,-4.7432129639482,129.501229176473));
#38259=CARTESIAN_POINT('Ctrl Pts',(129.834833026848,-4.76405452823404,129.582490119308));
#38260=CARTESIAN_POINT('Ctrl Pts',(131.584997718909,-4.76405452823404,129.582490119308));
#38261=CARTESIAN_POINT('Ctrl Pts',(131.577310227301,-4.79783637010872,129.714205008067));
#38262=CARTESIAN_POINT('Ctrl Pts',(131.569622735692,-4.82612622203509,129.847222924197));
#38263=CARTESIAN_POINT('Ctrl Pts',(131.561935244083,-4.84884825233541,129.981041913586));
#38264=CARTESIAN_POINT('Ctrl Pts',(131.554089276073,-4.87203869363109,130.117619559889));
#38265=CARTESIAN_POINT('Ctrl Pts',(131.546243308063,-4.88942919083452,130.25503123002));
#38266=CARTESIAN_POINT('Ctrl Pts',(131.538397340053,-4.90099496924391,130.392740192968));
#38267=CARTESIAN_POINT('Ctrl Pts',(131.530551372043,-4.9125607476533,130.530449155917));
#38268=CARTESIAN_POINT('Ctrl Pts',(131.522705404033,-4.9183018535908,130.668454974763));
#38269=CARTESIAN_POINT('Ctrl Pts',(131.514859436023,-4.91824964687546,130.806224352909));
#38270=CARTESIAN_POINT('',(131.860140563953,-4.91824899481853,130.807505051778));
#38271=CARTESIAN_POINT('Ctrl Pts',(131.929976442121,-4.76405452823405,129.582490119308));
#38272=CARTESIAN_POINT('Ctrl Pts',(131.922173593699,-4.79838763563934,129.716354384004));
#38273=CARTESIAN_POINT('Ctrl Pts',(131.914370745277,-4.82709221949561,129.851736299158));
#38274=CARTESIAN_POINT('Ctrl Pts',(131.906567896855,-4.85004596951037,129.988127099425));
#38275=CARTESIAN_POINT('Ctrl Pts',(131.898766189335,-4.87299636331966,130.124497957176));
#38276=CARTESIAN_POINT('Ctrl Pts',(131.890964481814,-4.89019752581795,130.26187703042));
#38277=CARTESIAN_POINT('Ctrl Pts',(131.883162774293,-4.90157827896259,130.399745445208));
#38278=CARTESIAN_POINT('Ctrl Pts',(131.875488704198,-4.91277284081155,130.535358306391));
#38279=CARTESIAN_POINT('Ctrl Pts',(131.867814634103,-4.9183359839254,130.671444256286));
#38280=CARTESIAN_POINT('Ctrl Pts',(131.860140564008,-4.91824899481915,130.807505050802));
#38281=CARTESIAN_POINT('Ctrl Pts',(131.860140563953,-4.91824899481853,130.807505051778));
#38282=CARTESIAN_POINT('Ctrl Pts',(131.851406713904,-4.91814999258943,130.962355680208));
#38283=CARTESIAN_POINT('Ctrl Pts',(131.842672863855,-4.91073377224643,131.116928504414));
#38284=CARTESIAN_POINT('Ctrl Pts',(131.833939013806,-4.89610311273186,131.270576631874));
#38285=CARTESIAN_POINT('Ctrl Pts',(131.825171001558,-4.88141522582029,131.424825749494));
#38286=CARTESIAN_POINT('Ctrl Pts',(131.81640298931,-4.859456461858,131.578142736764));
#38287=CARTESIAN_POINT('Ctrl Pts',(131.807634977062,-4.83038066305623,131.729890580599));
#38288=CARTESIAN_POINT('Ctrl Pts',(131.798818421842,-4.80114388983702,131.882478556839));
#38289=CARTESIAN_POINT('Ctrl Pts',(131.790001866623,-4.76471115565391,132.033479782782));
#38290=CARTESIAN_POINT('Ctrl Pts',(131.781185311404,-4.72128763113361,132.182267060909));
#38291=CARTESIAN_POINT('Ctrl Pts',(131.772862777129,-4.68029727127292,132.322717292447));
#38292=CARTESIAN_POINT('Ctrl Pts',(131.764540242853,-4.63307809789463,132.461194792037));
#38293=CARTESIAN_POINT('Ctrl Pts',(131.756217708578,-4.57984097248172,132.597190706916));
#38294=CARTESIAN_POINT('Ctrl Pts',(131.748443374459,-4.53011054340665,132.72422865547));
#38295=CARTESIAN_POINT('Ctrl Pts',(131.74066904034,-4.47501157464565,132.849397083174));
#38296=CARTESIAN_POINT('Ctrl Pts',(131.732894706221,-4.41470461200455,132.972208917435));
#38297=CARTESIAN_POINT('Ctrl Pts',(131.725129953274,-4.35447197230511,133.094869397087));
#38298=CARTESIAN_POINT('Ctrl Pts',(131.717365200327,-4.28904428007655,133.215178714402));
#38299=CARTESIAN_POINT('Ctrl Pts',(131.70960044738,-4.21863094014019,133.332667571516));
#38300=CARTESIAN_POINT('Ctrl Pts',(131.701843406495,-4.14828753572565,133.450039737041));
#38301=CARTESIAN_POINT('Ctrl Pts',(131.69408636561,-4.0729685376213,133.564596683941));
#38302=CARTESIAN_POINT('Ctrl Pts',(131.686329324725,-3.99293010639168,133.675891956063));
#38303=CARTESIAN_POINT('Ctrl Pts',(131.678578133485,-3.91295203276555,133.787103299555));
#38304=CARTESIAN_POINT('Ctrl Pts',(131.670826942245,-3.82826183725292,133.895057547937));
#38305=CARTESIAN_POINT('Ctrl Pts',(131.663075751004,-3.73915980044368,133.999335899043));
#38306=CARTESIAN_POINT('Ctrl Pts',(131.655327854227,-3.65009563437707,134.103569929067));
#38307=CARTESIAN_POINT('Ctrl Pts',(131.64757995745,-3.55662360999035,134.204130872604));
#38308=CARTESIAN_POINT('Ctrl Pts',(131.639832060673,-3.45908508456563,134.300631980066));
#38309=CARTESIAN_POINT('Ctrl Pts',(131.632085784589,-3.3615669620978,134.397112901576));
#38310=CARTESIAN_POINT('Ctrl Pts',(131.624339508505,-3.25998430828257,134.489535401377));
#38311=CARTESIAN_POINT('Ctrl Pts',(131.616593232421,-3.15471595111122,134.577548968325));
#38312=CARTESIAN_POINT('Ctrl Pts',(131.608846899156,-3.04944681687263,134.665563184969));
#38313=CARTESIAN_POINT('Ctrl Pts',(131.60110056589,-2.94049222492938,134.749168153039));
#38314=CARTESIAN_POINT('Ctrl Pts',(131.593354232625,-2.82826443393104,134.828053368542));
#38315=CARTESIAN_POINT('Ctrl Pts',(131.585606164622,-2.71601151029719,134.906956249843));
#38316=CARTESIAN_POINT('Ctrl Pts',(131.577858096619,-2.60048424879594,134.981137050572));
#38317=CARTESIAN_POINT('Ctrl Pts',(131.570110028616,-2.48212391256823,135.050328580841));
#38318=CARTESIAN_POINT('Ctrl Pts',(131.562353725874,-2.36363778156667,135.119593648691));
#38319=CARTESIAN_POINT('Ctrl Pts',(131.554597423132,-2.24231289905267,135.183858655828));
#38320=CARTESIAN_POINT('Ctrl Pts',(131.546841120391,-2.11861564932518,135.24290213398));
#38321=CARTESIAN_POINT('Ctrl Pts',(131.539080677876,-1.99485237865097,135.301977125415));
#38322=CARTESIAN_POINT('Ctrl Pts',(131.531320235362,-1.8687145771405,135.35582488133));
#38323=CARTESIAN_POINT('Ctrl Pts',(131.523559792848,-1.74068770374561,135.40427250591));
#38324=CARTESIAN_POINT('Ctrl Pts',(131.515786892583,-1.61245531024786,135.452797902918));
#38325=CARTESIAN_POINT('Ctrl Pts',(131.508013992317,-1.48232815629695,135.495905722608));
#38326=CARTESIAN_POINT('Ctrl Pts',(131.500241092052,-1.35080678381879,135.533473017931));
#38327=CARTESIAN_POINT('Ctrl Pts',(131.49275075629,-1.22406654451229,135.569674647443));
#38328=CARTESIAN_POINT('Ctrl Pts',(131.485260420528,-1.09603199285238,135.600731510395));
#38329=CARTESIAN_POINT('Ctrl Pts',(131.477770084766,-0.967157184704948,
135.626578991154));
#38330=CARTESIAN_POINT('Ctrl Pts',(131.469995750647,-0.833396049036143,
135.653406487003));
#38331=CARTESIAN_POINT('Ctrl Pts',(131.462221416528,-0.698305967372166,
135.674706756683));
#38332=CARTESIAN_POINT('Ctrl Pts',(131.454447082409,-0.562383506608875,
135.690351597295));
#38333=CARTESIAN_POINT('Ctrl Pts',(131.446682329462,-0.426628558130827,
135.70597715704));
#38334=CARTESIAN_POINT('Ctrl Pts',(131.438917576514,-0.290043656327314,
135.715961111286));
#38335=CARTESIAN_POINT('Ctrl Pts',(131.431152823567,-0.153136823202405,
135.720225971283));
#38336=CARTESIAN_POINT('Ctrl Pts',(131.423395782682,-0.0163659678742974,
135.724486595362));
#38337=CARTESIAN_POINT('Ctrl Pts',(131.415638741797,0.12072579421784,135.72303941712));
#38338=CARTESIAN_POINT('Ctrl Pts',(131.407881700912,0.257624385826948,135.71585863124));
#38339=CARTESIAN_POINT('Ctrl Pts',(131.400130509672,0.394419741143208,135.708683260447));
#38340=CARTESIAN_POINT('Ctrl Pts',(131.392379318432,0.53102182707775,135.695782908591));
#38341=CARTESIAN_POINT('Ctrl Pts',(131.384628127192,0.666915984512446,135.677183837436));
#38342=CARTESIAN_POINT('Ctrl Pts',(131.376880230415,0.802752383305229,135.658592671382));
#38343=CARTESIAN_POINT('Ctrl Pts',(131.369132333638,0.937881065499304,135.634307656319));
#38344=CARTESIAN_POINT('Ctrl Pts',(131.361384436861,1.07179213576307,135.604406938198));
#38345=CARTESIAN_POINT('Ctrl Pts',(131.353638160777,1.20567519471773,135.574512474663));
#38346=CARTESIAN_POINT('Ctrl Pts',(131.345891884693,1.33834076702356,135.539004729726));
#38347=CARTESIAN_POINT('Ctrl Pts',(131.338145608608,1.46928919194417,135.498012962269));
#38348=CARTESIAN_POINT('Ctrl Pts',(131.330399275343,1.60023858349621,135.45702089222));
#38349=CARTESIAN_POINT('Ctrl Pts',(131.322652942078,1.72947042925848,135.410544835671));
#38350=CARTESIAN_POINT('Ctrl Pts',(131.314906608812,1.85650065755731,135.358763802506));
#38351=CARTESIAN_POINT('Ctrl Pts',(131.307158540809,1.9835593333951,135.306971173337));
#38352=CARTESIAN_POINT('Ctrl Pts',(131.299410472806,2.10841504871024,135.249871351095));
#38353=CARTESIAN_POINT('Ctrl Pts',(131.291662404804,2.23060449557428,135.187691160295));
#38354=CARTESIAN_POINT('Ctrl Pts',(131.283906102062,2.35292380683652,135.125444883649));
#38355=CARTESIAN_POINT('Ctrl Pts',(131.27614979932,2.47257083994451,135.058107630008));
#38356=CARTESIAN_POINT('Ctrl Pts',(131.268393496578,2.58910717526307,134.985952072682));
#38357=CARTESIAN_POINT('Ctrl Pts',(131.260633054064,2.70570570953271,134.913758003763));
#38358=CARTESIAN_POINT('Ctrl Pts',(131.25287261155,2.81918991443573,134.836740726321));
#38359=CARTESIAN_POINT('Ctrl Pts',(131.245112169035,2.92915192540314,134.755215216309));
#38360=CARTESIAN_POINT('Ctrl Pts',(131.23733926877,3.03929045715253,134.67355883431));
#38361=CARTESIAN_POINT('Ctrl Pts',(131.229566368505,3.14589519197781,134.587380003809));
#38362=CARTESIAN_POINT('Ctrl Pts',(131.221793468239,3.24859213590686,134.497033389018));
#38363=CARTESIAN_POINT('Ctrl Pts',(131.214303132477,3.34755578724603,134.409971101245));
#38364=CARTESIAN_POINT('Ctrl Pts',(131.206812796715,3.4428906082135,134.319038999838));
#38365=CARTESIAN_POINT('Ctrl Pts',(131.199322460953,3.53429680756048,134.22458416853));
#38366=CARTESIAN_POINT('Ctrl Pts',(131.191548126834,3.62916870073795,134.126548053584));
#38367=CARTESIAN_POINT('Ctrl Pts',(131.183773792715,3.7201087097729,134.02440625798));
#38368=CARTESIAN_POINT('Ctrl Pts',(131.175999458596,3.80674056739808,133.918507260713));
#38369=CARTESIAN_POINT('Ctrl Pts',(131.168234705649,3.89326565900124,133.812738774496));
#38370=CARTESIAN_POINT('Ctrl Pts',(131.160469952702,3.97549291816558,133.703222599466));
#38371=CARTESIAN_POINT('Ctrl Pts',(131.152705199755,4.05308255310777,133.590344264358));
#38372=CARTESIAN_POINT('Ctrl Pts',(131.14494815887,4.13059512493071,133.477578041605));
#38373=CARTESIAN_POINT('Ctrl Pts',(131.137191117985,4.20347901895293,133.361456624327));
#38374=CARTESIAN_POINT('Ctrl Pts',(131.1294340771,4.27143465312082,133.242398571868));
#38375=CARTESIAN_POINT('Ctrl Pts',(131.121682885859,4.33933904141637,133.123430302013));
#38376=CARTESIAN_POINT('Ctrl Pts',(131.113931694619,4.40232237418207,133.001530143058));
#38377=CARTESIAN_POINT('Ctrl Pts',(131.106180503379,4.46012856035861,132.877145287418));
#38378=CARTESIAN_POINT('Ctrl Pts',(131.098432606602,4.51791017736398,132.75281329866));
#38379=CARTESIAN_POINT('Ctrl Pts',(131.090684709825,4.57051885983218,132.625999067452));
#38380=CARTESIAN_POINT('Ctrl Pts',(131.082936813048,4.61774474328205,132.49717382297));
#38381=CARTESIAN_POINT('Ctrl Pts',(131.075190536964,4.66496074809519,132.368375525953));
#38382=CARTESIAN_POINT('Ctrl Pts',(131.06744426088,4.70679605901602,132.237567419224));
#38383=CARTESIAN_POINT('Ctrl Pts',(131.059697984796,4.74308934636998,132.105239749097));
#38384=CARTESIAN_POINT('Ctrl Pts',(131.05195165153,4.77938290163272,131.972911102156));
#38385=CARTESIAN_POINT('Ctrl Pts',(131.044205318265,4.81013424828529,131.839063246475));
#38386=CARTESIAN_POINT('Ctrl Pts',(131.036458985,4.83523233984983,131.704200204476));
#38387=CARTESIAN_POINT('Ctrl Pts',(131.028710916997,4.86033605195797,131.569306960834));
#38388=CARTESIAN_POINT('Ctrl Pts',(131.020962848994,4.87978391825313,131.43339846278));
#38389=CARTESIAN_POINT('Ctrl Pts',(131.013214780991,4.89351634337174,131.296987108585));
#38390=CARTESIAN_POINT('Ctrl Pts',(131.005458478249,4.90726336347519,131.16043077478));
#38391=CARTESIAN_POINT('Ctrl Pts',(130.997702175507,4.91528276883339,131.023370906849));
#38392=CARTESIAN_POINT('Ctrl Pts',(130.989945872765,4.91756699070171,130.886323746234));
#38393=CARTESIAN_POINT('Ctrl Pts',(130.982185430251,4.91985243172801,130.749203439421));
#38394=CARTESIAN_POINT('Ctrl Pts',(130.974424987737,4.91639659972929,130.612096244088));
#38395=CARTESIAN_POINT('Ctrl Pts',(130.966664545223,4.90724403213303,130.475515560442));
#38396=CARTESIAN_POINT('Ctrl Pts',(130.958891644957,4.89807677202273,130.338715625358));
#38397=CARTESIAN_POINT('Ctrl Pts',(130.951118744692,4.88319454434876,130.202444279825));
#38398=CARTESIAN_POINT('Ctrl Pts',(130.943345844426,4.8626935852825,130.067207880236));
#38399=CARTESIAN_POINT('Ctrl Pts',(130.935855508664,4.84293788771695,129.936887664411));
#38400=CARTESIAN_POINT('Ctrl Pts',(130.928365172902,4.8179649348879,129.807528757558));
#38401=CARTESIAN_POINT('Ctrl Pts',(130.92087483714,4.78790469367565,129.679570989778));
#38402=CARTESIAN_POINT('Ctrl Pts',(130.913100503021,4.75670470928147,129.546761664343));
#38403=CARTESIAN_POINT('Ctrl Pts',(130.905326168902,4.71992522005083,129.415041123711));
#38404=CARTESIAN_POINT('Ctrl Pts',(130.897551834783,4.67765602958201,129.2849142936));
#38405=CARTESIAN_POINT('Ctrl Pts',(130.889787081836,4.63543893211273,129.154947833177));
#38406=CARTESIAN_POINT('Ctrl Pts',(130.882022328889,4.58774571449083,129.026571543559));
#38407=CARTESIAN_POINT('Ctrl Pts',(130.874257575941,4.53471706720284,128.900279688897));
#38408=CARTESIAN_POINT('Ctrl Pts',(130.866500535056,4.48174108871494,128.774113269086));
#38409=CARTESIAN_POINT('Ctrl Pts',(130.858743494171,4.42344037663695,128.650027522404));
#38410=CARTESIAN_POINT('Ctrl Pts',(130.850986453286,4.36000514538059,128.528500737267));
#38411=CARTESIAN_POINT('Ctrl Pts',(130.843235262046,4.29661775112552,128.407065596423));
#38412=CARTESIAN_POINT('Ctrl Pts',(130.835484070806,4.22810372481749,128.288185921294));
#38413=CARTESIAN_POINT('Ctrl Pts',(130.827732879566,4.15470087862873,128.172318886966));
#38414=CARTESIAN_POINT('Ctrl Pts',(130.819984982789,4.08132923060768,128.056501099217));
#38415=CARTESIAN_POINT('Ctrl Pts',(130.812237086012,4.00307310423874,127.943693735123));
#38416=CARTESIAN_POINT('Ctrl Pts',(130.804489189235,3.92021552109696,127.834328070497));
#38417=CARTESIAN_POINT('Ctrl Pts',(130.796742913151,3.83737526997536,127.72498528281));
#38418=CARTESIAN_POINT('Ctrl Pts',(130.788996637067,3.74993571254349,127.619083074042));
#38419=CARTESIAN_POINT('Ctrl Pts',(130.781250360982,3.65822210427816,127.517022165524));
#38420=CARTESIAN_POINT('Ctrl Pts',(130.773504027717,3.56650781900381,127.414960503617));
#38421=CARTESIAN_POINT('Ctrl Pts',(130.765757694452,3.47051968125969,127.316740489343));
#38422=CARTESIAN_POINT('Ctrl Pts',(130.758011361186,3.37062171605196,127.222727985682));
#38423=CARTESIAN_POINT('Ctrl Pts',(130.750263293183,3.27070137938763,127.128694428572));
#38424=CARTESIAN_POINT('Ctrl Pts',(130.74251522518,3.16686975761869,127.038870524918));
#38425=CARTESIAN_POINT('Ctrl Pts',(130.734767157177,3.05952573317417,126.953583377768));
#38426=CARTESIAN_POINT('Ctrl Pts',(130.727010854436,2.95206762222299,126.868205586424));
#38427=CARTESIAN_POINT('Ctrl Pts',(130.719254551694,2.84108995807692,126.787374427085));
#38428=CARTESIAN_POINT('Ctrl Pts',(130.711498248952,2.72702297818842,126.711375308659));
#38429=CARTESIAN_POINT('Ctrl Pts',(130.703737806438,2.61289511731818,126.635335627214));
#38430=CARTESIAN_POINT('Ctrl Pts',(130.695977363924,2.49567498919772,126.564133328442));
#38431=CARTESIAN_POINT('Ctrl Pts',(130.688216921409,2.37581860553092,126.498008447096));
#38432=CARTESIAN_POINT('Ctrl Pts',(130.680444021144,2.25576981775671,126.43177741622));
#38433=CARTESIAN_POINT('Ctrl Pts',(130.672671120879,2.13307666777857,126.370640264976));
#38434=CARTESIAN_POINT('Ctrl Pts',(130.664898220613,2.00821718557131,126.314789725145));
#38435=CARTESIAN_POINT('Ctrl Pts',(130.657407884851,1.88789666004443,126.260969493116));
#38436=CARTESIAN_POINT('Ctrl Pts',(130.649917549089,1.76556485707241,126.212058296681));
#38437=CARTESIAN_POINT('Ctrl Pts',(130.642427213327,1.64166206845087,126.168184529936));
#38438=CARTESIAN_POINT('Ctrl Pts',(130.634652879208,1.51306146793932,126.12264727599));
#38439=CARTESIAN_POINT('Ctrl Pts',(130.626878545089,1.3823610342681,126.082392732265));
#38440=CARTESIAN_POINT('Ctrl Pts',(130.61910421097,1.25003411678139,126.047618269132));
#38441=CARTESIAN_POINT('Ctrl Pts',(130.611339458023,1.11787028039417,126.012886662418));
#38442=CARTESIAN_POINT('Ctrl Pts',(130.603574705075,0.984084323037445,125.983621796842));
#38443=CARTESIAN_POINT('Ctrl Pts',(130.595809952128,0.849168129783613,125.95997246736));
#38444=CARTESIAN_POINT('Ctrl Pts',(130.588052911243,0.714385937194814,125.936346626725));
#38445=CARTESIAN_POINT('Ctrl Pts',(130.580295870358,0.578476125268148,125.918325289914));
#38446=CARTESIAN_POINT('Ctrl Pts',(130.572538829473,0.441943907128777,125.906006950725));
#38447=CARTESIAN_POINT('Ctrl Pts',(130.564787638233,0.305514648997078,125.893697900892));
#38448=CARTESIAN_POINT('Ctrl Pts',(130.557036446993,0.168464306696063,125.887083323438));
#38449=CARTESIAN_POINT('Ctrl Pts',(130.549285255753,0.031306057861031,125.886210254549));
#38450=CARTESIAN_POINT('Ctrl Pts',(130.541537358976,-0.105793895059336,
125.885337556738));
#38451=CARTESIAN_POINT('Ctrl Pts',(130.533789462199,-0.24300127315662,125.890201516415));
#38452=CARTESIAN_POINT('Ctrl Pts',(130.526041565422,-0.379800251800693,
125.900797134625));
#38453=CARTESIAN_POINT('Ctrl Pts',(130.518295289338,-0.516570615047478,
125.91139053646));
#38454=CARTESIAN_POINT('Ctrl Pts',(130.510549013253,-0.652932359211966,
125.927713181901));
#38455=CARTESIAN_POINT('Ctrl Pts',(130.502802737169,-0.788372537559546,
125.949708023969));
#38456=CARTESIAN_POINT('Ctrl Pts',(130.495056403904,-0.923813715695663,
125.971703028398));
#38457=CARTESIAN_POINT('Ctrl Pts',(130.487310070639,-1.05833292853073,125.999370250335));
#38458=CARTESIAN_POINT('Ctrl Pts',(130.479563737373,-1.19142560077159,126.032601183109));
#38459=CARTESIAN_POINT('Ctrl Pts',(130.47181566937,-1.32454807819361,126.065839557721));
#38460=CARTESIAN_POINT('Ctrl Pts',(130.464067601367,-1.45624300007764,126.104644027783));
#38461=CARTESIAN_POINT('Ctrl Pts',(130.456319533364,-1.58601955966783,126.148855809401));
#38462=CARTESIAN_POINT('Ctrl Pts',(130.448563230623,-1.7159340473301,126.193114579826));
#38463=CARTESIAN_POINT('Ctrl Pts',(130.440806927881,-1.84392572919052,126.242792015689));
#38464=CARTESIAN_POINT('Ctrl Pts',(130.433050625139,-1.96952192880009,126.297680416523));
#38465=CARTESIAN_POINT('Ctrl Pts',(130.425290182625,-2.09518516288311,126.352598112949));
#38466=CARTESIAN_POINT('Ctrl Pts',(130.41752974011,-2.21845001590423,126.412732144884));
#38467=CARTESIAN_POINT('Ctrl Pts',(130.409769297596,-2.33886805436165,126.477828601414));
#38468=CARTESIAN_POINT('Ctrl Pts',(130.401996397331,-2.45947939854453,126.543029556556));
#38469=CARTESIAN_POINT('Ctrl Pts',(130.394223497065,-2.57723445989045,126.613208654877));
#38470=CARTESIAN_POINT('Ctrl Pts',(130.3864505968,-2.69171270081496,126.688067892459));
#38471=CARTESIAN_POINT('Ctrl Pts',(130.378960261038,-2.80202936932844,126.760205808195));
#38472=CARTESIAN_POINT('Ctrl Pts',(130.371469925276,-2.90930307175307,126.836689322256));
#38473=CARTESIAN_POINT('Ctrl Pts',(130.363979589514,-3.01318779802863,126.917217404831));
#38474=CARTESIAN_POINT('Ctrl Pts',(130.356297479428,-3.11973227464586,126.999807239916));
#38475=CARTESIAN_POINT('Ctrl Pts',(130.348615369343,-3.22306642030545,127.086926619262));
#38476=CARTESIAN_POINT('Ctrl Pts',(130.340933259257,-3.32277383898975,127.178294280966));
#38477=CARTESIAN_POINT('Ctrl Pts',(130.33325992669,-3.42236733276733,127.269557546703));
#38478=CARTESIAN_POINT('Ctrl Pts',(130.325586594123,-3.51834204516812,127.365059177432));
#38479=CARTESIAN_POINT('Ctrl Pts',(130.317913261555,-3.61031183691572,127.464475664049));
#38480=CARTESIAN_POINT('Ctrl Pts',(130.310246939852,-3.70219759898305,127.563801317194));
#38481=CARTESIAN_POINT('Ctrl Pts',(130.302580618148,-3.79008544596941,127.667034421855));
#38482=CARTESIAN_POINT('Ctrl Pts',(130.294914296444,-3.87362394279327,127.773812711276));
#38483=CARTESIAN_POINT('Ctrl Pts',(130.287253225158,-3.95710522679259,127.880517871687));
#38484=CARTESIAN_POINT('Ctrl Pts',(130.279592153871,-4.03624283920432,127.990763073242));
#38485=CARTESIAN_POINT('Ctrl Pts',(130.271931082584,-4.11072408185366,128.104151258022));
#38486=CARTESIAN_POINT('Ctrl Pts',(130.264272468355,-4.18518143688101,128.217503076947));
#38487=CARTESIAN_POINT('Ctrl Pts',(130.256613854127,-4.25498516717711,128.333995543411));
#38488=CARTESIAN_POINT('Ctrl Pts',(130.248955239899,-4.3198647706816,128.453201025891));
#38489=CARTESIAN_POINT('Ctrl Pts',(130.241298355174,-4.3847297227764,128.572379588843));
#38490=CARTESIAN_POINT('Ctrl Pts',(130.233641470449,-4.44467257160386,128.694269595334));
#38491=CARTESIAN_POINT('Ctrl Pts',(130.225984585724,-4.49946819602265,128.818417764541));
#38492=CARTESIAN_POINT('Ctrl Pts',(130.21832467224,-4.55428549540717,128.942615041818));
#38493=CARTESIAN_POINT('Ctrl Pts',(130.210664758757,-4.60395133706325,129.069071900715));
#38494=CARTESIAN_POINT('Ctrl Pts',(130.203004845274,-4.64828828671816,129.197313926876));
#38495=CARTESIAN_POINT('Ctrl Pts',(130.195430780145,-4.69212833073771,129.324118682634));
#38496=CARTESIAN_POINT('Ctrl Pts',(130.187856715016,-4.73075824526441,129.452668417351));
#38497=CARTESIAN_POINT('Ctrl Pts',(130.180282649887,-4.76405452823405,129.582490119308));
#38498=CARTESIAN_POINT('Origin',(213.235140564004,0.,130.804360617566));
#38499=CARTESIAN_POINT('',(128.084583899672,-4.76405452823402,129.582490119308));
#38500=CARTESIAN_POINT('',(128.430147988268,-4.76405452823404,129.582490119308));
#38501=CARTESIAN_POINT('',(213.235140564004,-4.76405452823405,129.582490119308));
#38502=CARTESIAN_POINT('',(129.764859435955,-4.91824792667793,130.799844620641));
#38503=CARTESIAN_POINT('Ctrl Pts',(129.764859435955,-4.91824792667793,130.799844620641));
#38504=CARTESIAN_POINT('Ctrl Pts',(129.757206450161,-4.91837192626011,130.934889151915));
#38505=CARTESIAN_POINT('Ctrl Pts',(129.749553464366,-4.91292969583926,131.070099530846));
#38506=CARTESIAN_POINT('Ctrl Pts',(129.741900478572,-4.90190706987218,131.204972825115));
#38507=CARTESIAN_POINT('Ctrl Pts',(129.734253281609,-4.8908927815808,131.339744099249));
#38508=CARTESIAN_POINT('Ctrl Pts',(129.726606084645,-4.87430652785045,131.474178396558));
#38509=CARTESIAN_POINT('Ctrl Pts',(129.718958887681,-4.85218621156504,131.607773357568));
#38510=CARTESIAN_POINT('Ctrl Pts',(129.711314829052,-4.83007497323841,131.741313492529));
#38511=CARTESIAN_POINT('Ctrl Pts',(129.703670770422,-4.80243425226872,131.874014579584));
#38512=CARTESIAN_POINT('Ctrl Pts',(129.696026711792,-4.76935369971396,132.005380329946));
#38513=CARTESIAN_POINT('Ctrl Pts',(129.688384053555,-4.73627920752195,132.13672201408));
#38514=CARTESIAN_POINT('Ctrl Pts',(129.680741395318,-4.69776696330622,132.266728457751));
#38515=CARTESIAN_POINT('Ctrl Pts',(129.673098737082,-4.65395741868477,132.394915051582));
#38516=CARTESIAN_POINT('Ctrl Pts',(129.665455718965,-4.61014581114452,132.523107681508));
#38517=CARTESIAN_POINT('Ctrl Pts',(129.657812700848,-4.56103653761683,132.649479910392));
#38518=CARTESIAN_POINT('Ctrl Pts',(129.650169682731,-4.50681928080383,132.77356427201));
#38519=CARTESIAN_POINT('Ctrl Pts',(129.642524544391,-4.45258698377443,132.897683055429));
#38520=CARTESIAN_POINT('Ctrl Pts',(129.634879406052,-4.39324404718015,133.019512341041));
#38521=CARTESIAN_POINT('Ctrl Pts',(129.627234267712,-4.32902721326783,133.138607058987));
#38522=CARTESIAN_POINT('Ctrl Pts',(129.619581008545,-4.26474216687697,133.25782828186));
#38523=CARTESIAN_POINT('Ctrl Pts',(129.611927749378,-4.19557307996666,133.374308784386));
#38524=CARTESIAN_POINT('Ctrl Pts',(129.604274490211,-4.12180148796512,133.487630182166));
#38525=CARTESIAN_POINT('Ctrl Pts',(129.596616588164,-4.04798514213191,133.601020326826));
#38526=CARTESIAN_POINT('Ctrl Pts',(129.588958686117,-3.96956096589173,133.711247224781));
#38527=CARTESIAN_POINT('Ctrl Pts',(129.58130078407,-3.88685148376183,133.817924721029));
#38528=CARTESIAN_POINT('Ctrl Pts',(129.573631821169,-3.80402253843159,133.924756299187));
#38529=CARTESIAN_POINT('Ctrl Pts',(129.565962858267,-3.71689619156054,134.02802793669));
#38530=CARTESIAN_POINT('Ctrl Pts',(129.558293895366,-3.62583279854373,134.127389293263));
#38531=CARTESIAN_POINT('Ctrl Pts',(129.554937834989,-3.58598200658362,134.170871406311));
#38532=CARTESIAN_POINT('Ctrl Pts',(129.551581774612,-3.5453776831429,134.213605178592));
#38533=CARTESIAN_POINT('Ctrl Pts',(129.548225714235,-3.50405198933578,134.255563700338));
#38534=CARTESIAN_POINT('Ctrl Pts',(129.540451380116,-3.40832077021414,134.352760869197));
#38535=CARTESIAN_POINT('Ctrl Pts',(129.532677045997,-3.30839069839188,134.446125811215));
#38536=CARTESIAN_POINT('Ctrl Pts',(129.524902711878,-3.20460112313271,134.535274004944));
#38537=CARTESIAN_POINT('Ctrl Pts',(129.51713795893,-3.10093945924917,134.624312331492));
#38538=CARTESIAN_POINT('Ctrl Pts',(129.509373205983,-2.99342804966562,134.709143997468));
#38539=CARTESIAN_POINT('Ctrl Pts',(129.501608453036,-2.88244415803053,134.789420057315));
#38540=CARTESIAN_POINT('Ctrl Pts',(129.493851412151,-2.77157049716099,134.869616385848));
#38541=CARTESIAN_POINT('Ctrl Pts',(129.486094371266,-2.65723153247605,134.945265884942));
#38542=CARTESIAN_POINT('Ctrl Pts',(129.478337330381,-2.53983851364061,135.016059014546));
#38543=CARTESIAN_POINT('Ctrl Pts',(129.470586139141,-2.42253402179426,135.086798758501));
#38544=CARTESIAN_POINT('Ctrl Pts',(129.462834947901,-2.30218039339522,135.152689221322));
#38545=CARTESIAN_POINT('Ctrl Pts',(129.455083756661,-2.17921854660036,135.213463654313));
#38546=CARTESIAN_POINT('Ctrl Pts',(129.447335859884,-2.05630896187026,135.27421225655));
#38547=CARTESIAN_POINT('Ctrl Pts',(129.439587963107,-1.93079371334835,135.329848980901));
#38548=CARTESIAN_POINT('Ctrl Pts',(129.43184006633,-1.80313885834133,135.38015271512));
#38549=CARTESIAN_POINT('Ctrl Pts',(129.424093790246,-1.67551070597798,135.430445926883));
#38550=CARTESIAN_POINT('Ctrl Pts',(129.416347514162,-1.54574420086184,135.475408224152));
#38551=CARTESIAN_POINT('Ctrl Pts',(129.408601238078,-1.41432557665855,135.514866559151));
#38552=CARTESIAN_POINT('Ctrl Pts',(129.400854904812,-1.28290598235291,135.554325185423));
#38553=CARTESIAN_POINT('Ctrl Pts',(129.393108571547,-1.1498346190758,135.588279655925));
#38554=CARTESIAN_POINT('Ctrl Pts',(129.385362238282,-1.01561269929587,135.616606861009));
#38555=CARTESIAN_POINT('Ctrl Pts',(129.377614170279,-0.881360721447727,
135.644940409774));
#38556=CARTESIAN_POINT('Ctrl Pts',(129.369866102276,-0.745958056850334,
135.667644104776));
#38557=CARTESIAN_POINT('Ctrl Pts',(129.362118034273,-0.609915526094017,
135.684646071669));
#38558=CARTESIAN_POINT('Ctrl Pts',(129.354361731531,-0.4737284077169,135.701666108454));
#38559=CARTESIAN_POINT('Ctrl Pts',(129.346605428789,-0.336900453258914,
135.712972263337));
#38560=CARTESIAN_POINT('Ctrl Pts',(129.338849126047,-0.199947573865809,
135.71854458138));
#38561=CARTESIAN_POINT('Ctrl Pts',(129.331088683533,-0.0629215985974926,
135.724119873537));
#38562=CARTESIAN_POINT('Ctrl Pts',(129.323328241019,0.0742290436902866,
135.723955231374));
#38563=CARTESIAN_POINT('Ctrl Pts',(129.315567798505,0.210990031859213,135.718082859305));
#38564=CARTESIAN_POINT('Ctrl Pts',(129.307794898239,0.347970560907605,135.712201060382));
#38565=CARTESIAN_POINT('Ctrl Pts',(129.300021997974,0.484559796088881,135.700593254973));
#38566=CARTESIAN_POINT('Ctrl Pts',(129.292249097708,0.620249217426277,135.683343500379));
#38567=CARTESIAN_POINT('Ctrl Pts',(129.284758761946,0.751005986519056,135.666720817814));
#38568=CARTESIAN_POINT('Ctrl Pts',(129.277268426184,0.880926923214471,135.644859313661));
#38569=CARTESIAN_POINT('Ctrl Pts',(129.269778090422,1.00956920522302,135.617878362663));
#38570=CARTESIAN_POINT('Ctrl Pts',(129.262003756303,1.14308899845174,135.589874420708));
#38571=CARTESIAN_POINT('Ctrl Pts',(129.254229422184,1.27565421315145,135.556266452844));
#38572=CARTESIAN_POINT('Ctrl Pts',(129.246455088065,1.40675791397285,135.517132119981));
#38573=CARTESIAN_POINT('Ctrl Pts',(129.238690335118,1.53770004120033,135.478046016686));
#38574=CARTESIAN_POINT('Ctrl Pts',(129.230925582171,1.66718386733653,135.433447210511));
#38575=CARTESIAN_POINT('Ctrl Pts',(129.223160829223,1.79471189438333,135.38346449045));
#38576=CARTESIAN_POINT('Ctrl Pts',(129.215403788338,1.92211325879585,135.333531413931));
#38577=CARTESIAN_POINT('Ctrl Pts',(129.207646747453,2.04756232818574,135.278225206796));
#38578=CARTESIAN_POINT('Ctrl Pts',(129.199889706568,2.17057638725182,135.217724551076));
#38579=CARTESIAN_POINT('Ctrl Pts',(129.192138515328,2.29349768045864,135.157269519371));
#38580=CARTESIAN_POINT('Ctrl Pts',(129.184387324088,2.41398726889542,135.091628007826));
#38581=CARTESIAN_POINT('Ctrl Pts',(129.176636132848,2.53158240229536,135.021026789186));
#38582=CARTESIAN_POINT('Ctrl Pts',(129.168888236071,2.64912755462682,134.950455577949));
#38583=CARTESIAN_POINT('Ctrl Pts',(129.161140339294,2.7637803642438,134.874929053105));
#38584=CARTESIAN_POINT('Ctrl Pts',(129.153392442517,2.87510288779291,134.794719805296));
#38585=CARTESIAN_POINT('Ctrl Pts',(129.145646166433,2.98640212506993,134.714527335534));
#38586=CARTESIAN_POINT('Ctrl Pts',(129.137899890349,3.09437214489886,134.62965431954));
#38587=CARTESIAN_POINT('Ctrl Pts',(129.130153614265,3.19860453611217,134.54041630292));
#38588=CARTESIAN_POINT('Ctrl Pts',(129.122407280999,3.30283769674538,134.451177627564));
#38589=CARTESIAN_POINT('Ctrl Pts',(129.114660947734,3.40333287671913,134.357574141552));
#38590=CARTESIAN_POINT('Ctrl Pts',(129.106914614469,3.49971558281811,134.259960985357));
#38591=CARTESIAN_POINT('Ctrl Pts',(129.099166546466,3.59611987315585,134.162325969373));
#38592=CARTESIAN_POINT('Ctrl Pts',(129.091418478463,3.68840958237244,134.060679774562));
#38593=CARTESIAN_POINT('Ctrl Pts',(129.08367041046,3.77624812953736,133.955413318913));
#38594=CARTESIAN_POINT('Ctrl Pts',(129.075914107718,3.8641800325555,133.850034984823));
#38595=CARTESIAN_POINT('Ctrl Pts',(129.068157804976,3.94765107245801,133.74102900445));
#38596=CARTESIAN_POINT('Ctrl Pts',(129.060401502234,4.02636559801586,133.628818642323));
#38597=CARTESIAN_POINT('Ctrl Pts',(129.05264105972,4.10512213588609,133.516548390147));
#38598=CARTESIAN_POINT('Ctrl Pts',(129.044880617206,4.17911689001905,133.401070677372));
#38599=CARTESIAN_POINT('Ctrl Pts',(129.037120174691,4.24809895176071,133.282835624208));
#38600=CARTESIAN_POINT('Ctrl Pts',(129.029347274426,4.31719174963176,133.164410769641));
#38601=CARTESIAN_POINT('Ctrl Pts',(129.021574374161,4.38125559218418,133.043220075315));
#38602=CARTESIAN_POINT('Ctrl Pts',(129.013801473895,4.44008633173679,132.919736808513));
#38603=CARTESIAN_POINT('Ctrl Pts',(129.006311138133,4.496778425721,132.800742469494));
#38604=CARTESIAN_POINT('Ctrl Pts',(128.998820802371,4.54861116290541,132.679619628911));
#38605=CARTESIAN_POINT('Ctrl Pts',(128.991330466609,4.59544562037844,132.556805370659));
#38606=CARTESIAN_POINT('Ctrl Pts',(128.98355613249,4.64405582054163,132.429334572478));
#38607=CARTESIAN_POINT('Ctrl Pts',(128.975781798371,4.68743522198056,132.299637775358));
#38608=CARTESIAN_POINT('Ctrl Pts',(128.968007464252,4.72537515208118,132.168183455985));
#38609=CARTESIAN_POINT('Ctrl Pts',(128.960242711305,4.76326832460866,132.036891142313));
#38610=CARTESIAN_POINT('Ctrl Pts',(128.952477958358,4.79573525671448,131.903845988088));
#38611=CARTESIAN_POINT('Ctrl Pts',(128.944713205411,4.82261539240705,131.769536166064));
#38612=CARTESIAN_POINT('Ctrl Pts',(128.936956164526,4.84946883036996,131.635359742448));
#38613=CARTESIAN_POINT('Ctrl Pts',(128.929199123641,4.8707464382231,131.499921531583));
#38614=CARTESIAN_POINT('Ctrl Pts',(128.921442082756,4.88633762680884,131.363724237524));
#38615=CARTESIAN_POINT('Ctrl Pts',(128.913690891515,4.901917057958,131.227629650904));
#38616=CARTESIAN_POINT('Ctrl Pts',(128.905939700275,4.91181856090263,131.090777507335));
#38617=CARTESIAN_POINT('Ctrl Pts',(128.898188509035,4.9159827981546,130.953679707933));
#38618=CARTESIAN_POINT('Ctrl Pts',(128.890440612258,4.92014526549464,130.816640178753));
#38619=CARTESIAN_POINT('Ctrl Pts',(128.882692715481,4.91857530526971,130.67935559137));
#38620=CARTESIAN_POINT('Ctrl Pts',(128.874944818704,4.91126553662678,130.54234174183));
#38621=CARTESIAN_POINT('Ctrl Pts',(128.86719854262,4.90395729702987,130.405356552634));
#38622=CARTESIAN_POINT('Ctrl Pts',(128.859452266536,4.89091165797746,130.268642378798));
#38623=CARTESIAN_POINT('Ctrl Pts',(128.851705990451,4.87217334071108,130.132713388312));
#38624=CARTESIAN_POINT('Ctrl Pts',(128.843959657186,4.85343488512271,129.99678339443));
#38625=CARTESIAN_POINT('Ctrl Pts',(128.836213323921,4.82900372085949,129.861638982765));
#38626=CARTESIAN_POINT('Ctrl Pts',(128.828466990655,4.79897621492929,129.727787187166));
#38627=CARTESIAN_POINT('Ctrl Pts',(128.820718922652,4.76894198454746,129.593905416387));
#38628=CARTESIAN_POINT('Ctrl Pts',(128.812970854649,4.73330900421599,129.461317219101));
#38629=CARTESIAN_POINT('Ctrl Pts',(128.805222786647,4.69222423409643,129.3305170711));
#38630=CARTESIAN_POINT('Ctrl Pts',(128.797466483905,4.65109579859405,129.199577907145));
#38631=CARTESIAN_POINT('Ctrl Pts',(128.789710181163,4.60450411605752,129.070430962242));
#38632=CARTESIAN_POINT('Ctrl Pts',(128.781953878421,4.55264548421063,128.943553760959));
#38633=CARTESIAN_POINT('Ctrl Pts',(128.774193435907,4.50075917385051,128.816608841493));
#38634=CARTESIAN_POINT('Ctrl Pts',(128.766432993393,4.44360047562489,128.691936434745));
#38635=CARTESIAN_POINT('Ctrl Pts',(128.758672550878,4.38141246615946,128.569990938242));
#38636=CARTESIAN_POINT('Ctrl Pts',(128.750899650613,4.31912462698037,128.447849684002));
#38637=CARTESIAN_POINT('Ctrl Pts',(128.743126750347,4.25179153529079,128.328444428349));
#38638=CARTESIAN_POINT('Ctrl Pts',(128.735353850082,4.17970101745098,128.212202739037));
#38639=CARTESIAN_POINT('Ctrl Pts',(128.72786351432,4.11023117151975,128.100186727927));
#38640=CARTESIAN_POINT('Ctrl Pts',(128.720373178558,4.03634395589248,127.991108524229));
#38641=CARTESIAN_POINT('Ctrl Pts',(128.712882842796,3.9583320104045,127.885321262246));
#38642=CARTESIAN_POINT('Ctrl Pts',(128.705108508677,3.87736221829223,127.775523044072));
#38643=CARTESIAN_POINT('Ctrl Pts',(128.697334174558,3.79169225574934,127.668922438209));
#38644=CARTESIAN_POINT('Ctrl Pts',(128.689559840439,3.70160347283512,127.56594822993));
#38645=CARTESIAN_POINT('Ctrl Pts',(128.681795087492,3.61162571629437,127.463100928159));
#38646=CARTESIAN_POINT('Ctrl Pts',(128.674030334544,3.51724022986249,127.363871423));
#38647=CARTESIAN_POINT('Ctrl Pts',(128.666265581597,3.41877094266708,127.268658664053));
#38648=CARTESIAN_POINT('Ctrl Pts',(128.658508540712,3.32039945655615,127.173540471761));
#38649=CARTESIAN_POINT('Ctrl Pts',(128.650751499827,3.21795252072476,127.082431356426));
#38650=CARTESIAN_POINT('Ctrl Pts',(128.642994458942,3.11179329819212,126.995696083661));
#38651=CARTESIAN_POINT('Ctrl Pts',(128.635243267702,3.00571413115434,126.909026218639));
#38652=CARTESIAN_POINT('Ctrl Pts',(128.627492076462,2.89592855111529,126.826723877389));
#38653=CARTESIAN_POINT('Ctrl Pts',(128.619740885222,2.7828351616183,126.749115677274));
#38654=CARTESIAN_POINT('Ctrl Pts',(128.611992988445,2.66978983982918,126.671540462716));
#38655=CARTESIAN_POINT('Ctrl Pts',(128.604245091668,2.55343982651217,126.598655641873));
#38656=CARTESIAN_POINT('Ctrl Pts',(128.596497194891,2.43421508595795,126.530746224831));
#38657=CARTESIAN_POINT('Ctrl Pts',(128.588750918807,2.31501528464934,126.462851012974));
#38658=CARTESIAN_POINT('Ctrl Pts',(128.581004642722,2.19294229168991,126.399929328193));
#38659=CARTESIAN_POINT('Ctrl Pts',(128.573258366638,2.06845286409403,126.342221465599));
#38660=CARTESIAN_POINT('Ctrl Pts',(128.565512033373,1.94396251754531,126.284513177017));
#38661=CARTESIAN_POINT('Ctrl Pts',(128.557765700108,1.81705605547426,126.232018951848));
#38662=CARTESIAN_POINT('Ctrl Pts',(128.550019366842,1.68821214853949,126.184931777977));
#38663=CARTESIAN_POINT('Ctrl Pts',(128.542271298839,1.55933938790537,126.137834059261));
#38664=CARTESIAN_POINT('Ctrl Pts',(128.534523230836,1.42852868618266,126.096145935512));
#38665=CARTESIAN_POINT('Ctrl Pts',(128.526775162833,1.29627549541593,126.06001104123));
#38666=CARTESIAN_POINT('Ctrl Pts',(128.519018860092,1.16388174438403,126.023837742351));
#38667=CARTESIAN_POINT('Ctrl Pts',(128.51126255735,1.03004281952939,125.993229566104));
#38668=CARTESIAN_POINT('Ctrl Pts',(128.503506254608,0.895266579510176,125.968279475348));
#38669=CARTESIAN_POINT('Ctrl Pts',(128.495745812094,0.760418405353534,125.943316067978));
#38670=CARTESIAN_POINT('Ctrl Pts',(128.487985369579,0.624632306081089,125.924016818474));
#38671=CARTESIAN_POINT('Ctrl Pts',(128.480224927065,0.48842196805422,125.910422832549));
#38672=CARTESIAN_POINT('Ctrl Pts',(128.4724520268,0.351992973100564,125.89680702435));
#38673=CARTESIAN_POINT('Ctrl Pts',(128.464679126534,0.215138769027454,125.888914804045));
#38674=CARTESIAN_POINT('Ctrl Pts',(128.456906226269,0.0783746578725998,
125.886735125979));
#38675=CARTESIAN_POINT('Ctrl Pts',(128.449415890507,-0.0534177333533048,
125.884634684701));
#38676=CARTESIAN_POINT('Ctrl Pts',(128.441925554745,-0.185126160221312,
125.887838658321));
#38677=CARTESIAN_POINT('Ctrl Pts',(128.434435218983,-0.316295341861633,
125.896291718374));
#38678=CARTESIAN_POINT('Ctrl Pts',(128.426660884864,-0.452437842892243,
125.905065278768));
#38679=CARTESIAN_POINT('Ctrl Pts',(128.418886550745,-0.588430659050207,
125.919521613221));
#38680=CARTESIAN_POINT('Ctrl Pts',(128.411112216626,-0.723760964562665,
125.939655782874));
#38681=CARTESIAN_POINT('Ctrl Pts',(128.403347463679,-0.858924487568211,
125.959765138962));
#38682=CARTESIAN_POINT('Ctrl Pts',(128.395582710732,-0.993426741493978,
125.985538350479));
#38683=CARTESIAN_POINT('Ctrl Pts',(128.387817957784,-1.12675698713663,126.01691852868));
#38684=CARTESIAN_POINT('Ctrl Pts',(128.380060916899,-1.2599548073004,126.048267539645));
#38685=CARTESIAN_POINT('Ctrl Pts',(128.372303876014,-1.39198255759903,126.085212345906));
#38686=CARTESIAN_POINT('Ctrl Pts',(128.364546835129,-1.52233705190963,126.127644572852));
#38687=CARTESIAN_POINT('Ctrl Pts',(128.356795643889,-1.65259324488082,126.170044801326));
#38688=CARTESIAN_POINT('Ctrl Pts',(128.349044452649,-1.7811783231702,126.217924093309));
#38689=CARTESIAN_POINT('Ctrl Pts',(128.341293261409,-1.90760203938644,126.271123637016));
#38690=CARTESIAN_POINT('Ctrl Pts',(128.333545364632,-2.03397202215126,126.324300569498));
#38691=CARTESIAN_POINT('Ctrl Pts',(128.325797467855,-2.15818211033594,126.382793104929));
#38692=CARTESIAN_POINT('Ctrl Pts',(128.318049571078,-2.2797601106843,126.446393557086));
#38693=CARTESIAN_POINT('Ctrl Pts',(128.310303294994,-2.40131267953607,126.509980705399));
#38694=CARTESIAN_POINT('Ctrl Pts',(128.30255701891,-2.52023390947012,126.578673464091));
#38695=CARTESIAN_POINT('Ctrl Pts',(128.294810742826,-2.63607474508163,126.652217435926));
#38696=CARTESIAN_POINT('Ctrl Pts',(128.28706440956,-2.75191643580355,126.725761950645));
#38697=CARTESIAN_POINT('Ctrl Pts',(128.279318076295,-2.8646773567641,126.804157540416));
#38698=CARTESIAN_POINT('Ctrl Pts',(128.27157174303,-2.97393640860482,126.887105800724));
#38699=CARTESIAN_POINT('Ctrl Pts',(128.263823675027,-3.08321992825324,126.970072636719));
#38700=CARTESIAN_POINT('Ctrl Pts',(128.256075607024,-3.18899970694241,127.057593935656));
#38701=CARTESIAN_POINT('Ctrl Pts',(128.248327539021,-3.29088709696956,127.149330497649));
#38702=CARTESIAN_POINT('Ctrl Pts',(128.240571236279,-3.39288277412696,127.241164558352));
#38703=CARTESIAN_POINT('Ctrl Pts',(128.232814933537,-3.49097750775328,127.33722256944));
#38704=CARTESIAN_POINT('Ctrl Pts',(128.225058630795,-3.58481857555258,127.437127503736));
#38705=CARTESIAN_POINT('Ctrl Pts',(128.217298188281,-3.67870972915533,127.537085760304));
#38706=CARTESIAN_POINT('Ctrl Pts',(128.209537745767,-3.76834243776297,127.640894735516));
#38707=CARTESIAN_POINT('Ctrl Pts',(128.201777303253,-3.85340445794956,127.748144469131));
#38708=CARTESIAN_POINT('Ctrl Pts',(128.194004402987,-3.93860302724253,127.85556636954));
#38709=CARTESIAN_POINT('Ctrl Pts',(128.186231502722,-4.01921601585577,127.966439749486));
#38710=CARTESIAN_POINT('Ctrl Pts',(128.178458602456,-4.09497418347289,128.080325100325));
#38711=CARTESIAN_POINT('Ctrl Pts',(128.170968266694,-4.16797835087439,128.190070431802));
#38712=CARTESIAN_POINT('Ctrl Pts',(128.163477930932,-4.23647437900702,128.302612287507));
#38713=CARTESIAN_POINT('Ctrl Pts',(128.15598759517,-4.30026272684413,128.417537720362));
#38714=CARTESIAN_POINT('Ctrl Pts',(128.147837182824,-4.36967234401632,128.542590814985));
#38715=CARTESIAN_POINT('Ctrl Pts',(128.139686770478,-4.43371036204155,128.670830503645));
#38716=CARTESIAN_POINT('Ctrl Pts',(128.131536358132,-4.49208728454085,128.801778561678));
#38717=CARTESIAN_POINT('Ctrl Pts',(128.123403750017,-4.55033668512407,128.932440569221));
#38718=CARTESIAN_POINT('Ctrl Pts',(128.115271141902,-4.60294950846619,129.065798845733));
#38719=CARTESIAN_POINT('Ctrl Pts',(128.107138533787,-4.6496818656245,129.201350445738));
#38720=CARTESIAN_POINT('Ctrl Pts',(128.099620322415,-4.69288371846655,129.326661485713));
#38721=CARTESIAN_POINT('Ctrl Pts',(128.092102111043,-4.73106039665717,129.453846501046));
#38722=CARTESIAN_POINT('Ctrl Pts',(128.084583899671,-4.76405452823402,129.582490119308));
#38723=CARTESIAN_POINT('Ctrl Pts',(129.834833026848,-4.76405452823404,129.582490119308));
#38724=CARTESIAN_POINT('Ctrl Pts',(129.832113130581,-4.7759248683824,129.628772395389));
#38725=CARTESIAN_POINT('Ctrl Pts',(129.829393234315,-4.78711453292458,129.675203598535));
#38726=CARTESIAN_POINT('Ctrl Pts',(129.826673338048,-4.79762058815034,129.721762005588));
#38727=CARTESIAN_POINT('Ctrl Pts',(129.816060175579,-4.83861570710667,129.903435087876));
#38728=CARTESIAN_POINT('Ctrl Pts',(129.805447013111,-4.86930468188327,130.087512672684));
#38729=CARTESIAN_POINT('Ctrl Pts',(129.794833850643,-4.8894632274617,130.273011005917));
#38730=CARTESIAN_POINT('Ctrl Pts',(129.784842379092,-4.9084409388886,130.44764333862));
#38731=CARTESIAN_POINT('Ctrl Pts',(129.774850907542,-4.91808603712119,130.623535186195));
#38732=CARTESIAN_POINT('Ctrl Pts',(129.764859435991,-4.91824792667734,130.79984462));
#38733=CARTESIAN_POINT('',(130.110140564045,-4.91824934646016,130.806896074964));
#38734=CARTESIAN_POINT('Ctrl Pts',(130.180282649887,-4.76405452823405,129.582490119308));
#38735=CARTESIAN_POINT('Ctrl Pts',(130.172615528694,-4.79775989417285,129.713906829553));
#38736=CARTESIAN_POINT('Ctrl Pts',(130.164948407501,-4.82599960023451,129.846626582253));
#38737=CARTESIAN_POINT('Ctrl Pts',(130.157281286307,-4.84869666132585,129.980149631867));
#38738=CARTESIAN_POINT('Ctrl Pts',(130.149424499264,-4.8719551922682,130.116975715581));
#38739=CARTESIAN_POINT('Ctrl Pts',(130.14156771222,-4.88939322364667,130.254644908175));
#38740=CARTESIAN_POINT('Ctrl Pts',(130.133710925176,-4.90098454109159,130.392616048104));
#38741=CARTESIAN_POINT('Ctrl Pts',(130.125854138133,-4.91257585853652,130.530587188034));
#38742=CARTESIAN_POINT('Ctrl Pts',(130.117997351089,-4.91832050694874,130.668859826868));
#38743=CARTESIAN_POINT('Ctrl Pts',(130.110140564045,-4.91824934646016,130.806896074964));
#38744=CARTESIAN_POINT('Ctrl Pts',(130.110140564008,-4.91824934645982,130.806896075623));
#38745=CARTESIAN_POINT('Ctrl Pts',(130.101937697906,-4.91817505144483,130.951012602406));
#38746=CARTESIAN_POINT('Ctrl Pts',(130.093734831804,-4.91176691442507,131.094961645225));
#38747=CARTESIAN_POINT('Ctrl Pts',(130.085531965701,-4.89906528052872,131.238344994725));
#38748=CARTESIAN_POINT('Ctrl Pts',(130.077757631582,-4.88702720206481,131.374237748821));
#38749=CARTESIAN_POINT('Ctrl Pts',(130.069983297463,-4.86931157806441,131.509844490242));
#38750=CARTESIAN_POINT('Ctrl Pts',(130.062208963344,-4.84593565236954,131.644652659414));
#38751=CARTESIAN_POINT('Ctrl Pts',(130.054444210397,-4.82258853541397,131.779294689566));
#38752=CARTESIAN_POINT('Ctrl Pts',(130.04667945745,-4.79359506271441,131.913139724154));
#38753=CARTESIAN_POINT('Ctrl Pts',(130.038914704503,-4.75902436296635,132.045678536229));
#38754=CARTESIAN_POINT('Ctrl Pts',(130.031157663618,-4.72448799932461,132.178085708886));
#38755=CARTESIAN_POINT('Ctrl Pts',(130.023400622733,-4.68438553028882,132.309188864972));
#38756=CARTESIAN_POINT('Ctrl Pts',(130.015643581848,-4.63883737433938,132.43848756396));
#38757=CARTESIAN_POINT('Ctrl Pts',(130.007892390607,-4.59332356660868,132.567688757794));
#38758=CARTESIAN_POINT('Ctrl Pts',(130.000141199367,-4.5423723753476,132.695087835769));
#38759=CARTESIAN_POINT('Ctrl Pts',(129.992390008127,-4.48615433119391,132.820198502717));
#38760=CARTESIAN_POINT('Ctrl Pts',(129.98464211135,-4.42996018120862,132.945255994295));
#38761=CARTESIAN_POINT('Ctrl Pts',(129.976894214573,-4.36850379055091,133.068026653475));
#38762=CARTESIAN_POINT('Ctrl Pts',(129.969146317796,-4.3020041169719,133.188043406877));
#38763=CARTESIAN_POINT('Ctrl Pts',(129.961400041712,-4.23551835369103,133.308035055362));
#38764=CARTESIAN_POINT('Ctrl Pts',(129.953653765628,-4.16399159519987,133.425273602118));
#38765=CARTESIAN_POINT('Ctrl Pts',(129.945907489543,-4.08768894156549,133.53931622589));
#38766=CARTESIAN_POINT('Ctrl Pts',(129.938161156278,-4.01138572468225,133.653359691499));
#38767=CARTESIAN_POINT('Ctrl Pts',(129.930414823013,-3.93030675971699,133.764206862106));
#38768=CARTESIAN_POINT('Ctrl Pts',(129.922668489747,-3.84476047047476,133.871443920506));
#38769=CARTESIAN_POINT('Ctrl Pts',(129.914920421744,-3.75919502373425,133.978704993902));
#38770=CARTESIAN_POINT('Ctrl Pts',(129.907172353741,-3.66916050574849,134.082354040776));
#38771=CARTESIAN_POINT('Ctrl Pts',(129.899424285738,-3.57500534519222,134.18201066521));
#38772=CARTESIAN_POINT('Ctrl Pts',(129.891667982997,-3.48075011541079,134.28177320589));
#38773=CARTESIAN_POINT('Ctrl Pts',(129.883911680255,-3.38236576352666,134.377534563251));
#38774=CARTESIAN_POINT('Ctrl Pts',(129.876155377513,-3.28023767250429,134.468951164187));
#38775=CARTESIAN_POINT('Ctrl Pts',(129.868394934999,-3.17805507264471,134.560416556915));
#38776=CARTESIAN_POINT('Ctrl Pts',(129.860634492485,-3.07212505399012,134.647532324345));
#38777=CARTESIAN_POINT('Ctrl Pts',(129.85287404997,-2.96286495170588,134.729996150885));
#38778=CARTESIAN_POINT('Ctrl Pts',(129.845101149705,-2.8534294554058,134.812592355679));
#38779=CARTESIAN_POINT('Ctrl Pts',(129.837328249439,-2.74065351480153,134.890521474336));
#38780=CARTESIAN_POINT('Ctrl Pts',(129.829555349174,-2.62498297299513,134.963524891069));
#38781=CARTESIAN_POINT('Ctrl Pts',(129.822065013412,-2.51351734674053,135.033874449719));
#38782=CARTESIAN_POINT('Ctrl Pts',(129.81457467765,-2.39936418450045,135.099650058462));
#38783=CARTESIAN_POINT('Ctrl Pts',(129.807084341888,-2.2829411028674,135.160662143326));
#38784=CARTESIAN_POINT('Ctrl Pts',(129.799310007769,-2.16210380470743,135.223987519932));
#38785=CARTESIAN_POINT('Ctrl Pts',(129.79153567365,-2.03843828506735,135.282381619845));
#38786=CARTESIAN_POINT('Ctrl Pts',(129.783761339531,-1.9123850955499,135.335581899827));
#38787=CARTESIAN_POINT('Ctrl Pts',(129.775996586584,-1.78648725532292,135.38871661522));
#38788=CARTESIAN_POINT('Ctrl Pts',(129.768231833637,-1.65820795683645,135.436670096041));
#38789=CARTESIAN_POINT('Ctrl Pts',(129.760467080689,-1.52801299289409,135.479225252617));
#38790=CARTESIAN_POINT('Ctrl Pts',(129.752710039804,-1.39794734042551,135.521738142811));
#38791=CARTESIAN_POINT('Ctrl Pts',(129.74495299892,-1.26597017810524,135.558863258087));
#38792=CARTESIAN_POINT('Ctrl Pts',(129.737195958035,-1.13256762985092,135.590431409595));
#38793=CARTESIAN_POINT('Ctrl Pts',(129.729444766794,-0.999265681495784,
135.621975755315));
#38794=CARTESIAN_POINT('Ctrl Pts',(129.721693575554,-0.864540865637652,
135.647971388635));
#38795=CARTESIAN_POINT('Ctrl Pts',(129.713942384314,-0.728894492148465,
135.668298927394));
#38796=CARTESIAN_POINT('Ctrl Pts',(129.706194487537,-0.593305771986403,
135.688617826407));
#38797=CARTESIAN_POINT('Ctrl Pts',(129.69844659076,-0.456796659066359,135.703273364538));
#38798=CARTESIAN_POINT('Ctrl Pts',(129.690698693983,-0.319878467463521,
135.712197292574));
#38799=CARTESIAN_POINT('Ctrl Pts',(129.682952417899,-0.182988916194844,
135.721119353916));
#38800=CARTESIAN_POINT('Ctrl Pts',(129.675206141815,-0.0456908463379253,
135.724312164487));
#38801=CARTESIAN_POINT('Ctrl Pts',(129.667459865731,0.0914998909817206,
135.721759404776));
#38802=CARTESIAN_POINT('Ctrl Pts',(129.659713532465,0.228691641012224,135.71920662622));
#38803=CARTESIAN_POINT('Ctrl Pts',(129.6519671992,0.365775666026927,135.710908200026));
#38804=CARTESIAN_POINT('Ctrl Pts',(129.644220865934,0.502237099289631,135.696899933565));
#38805=CARTESIAN_POINT('Ctrl Pts',(129.636472797931,0.638729092144156,135.682888530051));
#38806=CARTESIAN_POINT('Ctrl Pts',(129.628724729928,0.774597826959905,135.663164781763));
#38807=CARTESIAN_POINT('Ctrl Pts',(129.620976661925,0.909334931666526,135.637816218329));
#38808=CARTESIAN_POINT('Ctrl Pts',(129.613220359184,1.04421523657142,135.612440714141));
#38809=CARTESIAN_POINT('Ctrl Pts',(129.605464056442,1.17796112398719,135.581428525266));
#38810=CARTESIAN_POINT('Ctrl Pts',(129.5977077537,1.3100752272218,135.544918175651));
#38811=CARTESIAN_POINT('Ctrl Pts',(129.589947311186,1.44225984373128,135.508388339364));
#38812=CARTESIAN_POINT('Ctrl Pts',(129.582186868672,1.5728105686842,135.466354614792));
#38813=CARTESIAN_POINT('Ctrl Pts',(129.574426426157,1.70124747556007,135.419004708869));
#38814=CARTESIAN_POINT('Ctrl Pts',(129.566653525892,1.82989056076095,135.371578792674));
#38815=CARTESIAN_POINT('Ctrl Pts',(129.558880625626,1.95641268595657,135.318819792021));
#38816=CARTESIAN_POINT('Ctrl Pts',(129.551107725361,2.08035528127459,135.260963019191));
#38817=CARTESIAN_POINT('Ctrl Pts',(129.543617389599,2.19979225106051,135.205209485786));
#38818=CARTESIAN_POINT('Ctrl Pts',(129.536127053837,2.31683370609582,135.144722520591));
#38819=CARTESIAN_POINT('Ctrl Pts',(129.528636718075,2.43109442045933,135.079751006912));
#38820=CARTESIAN_POINT('Ctrl Pts',(129.520862383956,2.54968736453638,135.012316078544));
#38821=CARTESIAN_POINT('Ctrl Pts',(129.513088049837,2.66566020866326,134.939836211839));
#38822=CARTESIAN_POINT('Ctrl Pts',(129.505313715718,2.77855393887726,134.862540144306));
#38823=CARTESIAN_POINT('Ctrl Pts',(129.497548962771,2.8913085376583,134.785339337268));
#38824=CARTESIAN_POINT('Ctrl Pts',(129.489784209823,3.00099125341456,134.703334358105));
#38825=CARTESIAN_POINT('Ctrl Pts',(129.482019456876,3.1071676700656,134.616799749224));
#38826=CARTESIAN_POINT('Ctrl Pts',(129.474262415991,3.21323863080279,134.530351087736));
#38827=CARTESIAN_POINT('Ctrl Pts',(129.466505375106,3.31580992167811,134.439381994927));
#38828=CARTESIAN_POINT('Ctrl Pts',(129.458748334221,3.41447643746844,134.344210009909));
#38829=CARTESIAN_POINT('Ctrl Pts',(129.450997142981,3.51306854807163,134.249109794826));
#38830=CARTESIAN_POINT('Ctrl Pts',(129.443245951741,3.60776146442614,134.149813266428));
#38831=CARTESIAN_POINT('Ctrl Pts',(129.435494760501,3.6981837767078,134.046677661933));
#38832=CARTESIAN_POINT('Ctrl Pts',(129.427746863724,3.7885676570947,133.943585892822));
#38833=CARTESIAN_POINT('Ctrl Pts',(129.419998966947,3.87468428634427,133.836658586325));
#38834=CARTESIAN_POINT('Ctrl Pts',(129.41225107017,3.95619986671324,133.726289035087));
#38835=CARTESIAN_POINT('Ctrl Pts',(129.404504794086,4.03769839578008,133.61594257078));
#38836=CARTESIAN_POINT('Ctrl Pts',(129.396758518002,4.11459755818775,133.502155608229));
#38837=CARTESIAN_POINT('Ctrl Pts',(129.389012241917,4.18660479373594,133.385353326499));
#38838=CARTESIAN_POINT('Ctrl Pts',(129.381265908652,4.25861256082518,133.268550182562));
#38839=CARTESIAN_POINT('Ctrl Pts',(129.373519575387,4.32572812382767,133.148732007838));
#38840=CARTESIAN_POINT('Ctrl Pts',(129.365773242121,4.38770331045398,133.026351329052));
#38841=CARTESIAN_POINT('Ctrl Pts',(129.358025174118,4.44969237599364,132.903943243962));
#38842=CARTESIAN_POINT('Ctrl Pts',(129.350277106115,4.50653859790028,132.778971861631));
#38843=CARTESIAN_POINT('Ctrl Pts',(129.342529038112,4.55804082980524,132.651912201779));
#38844=CARTESIAN_POINT('Ctrl Pts',(129.334772735371,4.60959779889515,132.524717501409));
#38845=CARTESIAN_POINT('Ctrl Pts',(129.327016432629,4.65579928515726,132.395430452844));
#38846=CARTESIAN_POINT('Ctrl Pts',(129.319260129887,4.6964929938642,132.264544380345));
#38847=CARTESIAN_POINT('Ctrl Pts',(129.311499687373,4.7372084220288,132.133588450009));
#38848=CARTESIAN_POINT('Ctrl Pts',(129.303739244859,4.7724101148057,132.001032172856));
#38849=CARTESIAN_POINT('Ctrl Pts',(129.295978802344,4.80199658334589,131.867380784841));
#38850=CARTESIAN_POINT('Ctrl Pts',(129.288205902079,4.83163054671193,131.733514847754));
#38851=CARTESIAN_POINT('Ctrl Pts',(129.280433001814,4.85563120439344,131.598550671972));
#38852=CARTESIAN_POINT('Ctrl Pts',(129.272660101548,4.8739486630581,131.463001257349));
#38853=CARTESIAN_POINT('Ctrl Pts',(129.265169765786,4.89160023596136,131.332379405377));
#38854=CARTESIAN_POINT('Ctrl Pts',(129.257679430024,4.90397460440636,131.201214432306));
#38855=CARTESIAN_POINT('Ctrl Pts',(129.250189094262,4.91107293694543,131.06996496712));
#38856=CARTESIAN_POINT('Ctrl Pts',(129.242414760143,4.91844040492024,130.933739138569));
#38857=CARTESIAN_POINT('Ctrl Pts',(129.234640426024,4.9201471953698,130.79699076191));
#38858=CARTESIAN_POINT('Ctrl Pts',(129.226866091905,4.91613764337911,130.660229656802));
#38859=CARTESIAN_POINT('Ctrl Pts',(129.219101338958,4.91213303280291,130.523637097532));
#38860=CARTESIAN_POINT('Ctrl Pts',(129.211336586011,4.9024261083476,130.387032228071));
#38861=CARTESIAN_POINT('Ctrl Pts',(129.203571833064,4.88701303781143,130.250928931844));
#38862=CARTESIAN_POINT('Ctrl Pts',(129.195814792179,4.87161527575421,130.11496081533));
#38863=CARTESIAN_POINT('Ctrl Pts',(129.188057751294,4.85052268975622,129.97949366664));
#38864=CARTESIAN_POINT('Ctrl Pts',(129.180300710409,4.82378346519847,129.845039949917));
#38865=CARTESIAN_POINT('Ctrl Pts',(129.172549519169,4.79706440489794,129.710687625789));
#38866=CARTESIAN_POINT('Ctrl Pts',(129.164798327929,4.76470725762534,129.577347594365));
#38867=CARTESIAN_POINT('Ctrl Pts',(129.157047136688,4.72681182108834,129.445525428693));
#38868=CARTESIAN_POINT('Ctrl Pts',(129.149299239911,4.68893249112276,129.313759290958));
#38869=CARTESIAN_POINT('Ctrl Pts',(129.141551343134,4.64551966145292,129.183510110814));
#38870=CARTESIAN_POINT('Ctrl Pts',(129.133803446357,4.59672379448664,129.055271306038));
#38871=CARTESIAN_POINT('Ctrl Pts',(129.126057170273,4.54793813456381,128.927059326056));
#38872=CARTESIAN_POINT('Ctrl Pts',(129.118310894189,4.49377181600263,128.800857250165));
#38873=CARTESIAN_POINT('Ctrl Pts',(129.110564618105,4.43442441805971,128.677141037218));
#38874=CARTESIAN_POINT('Ctrl Pts',(129.10281828484,4.37507658202782,128.553423911027));
#38875=CARTESIAN_POINT('Ctrl Pts',(129.095071951574,4.3105477593965,128.432193036901));
#38876=CARTESIAN_POINT('Ctrl Pts',(129.087325618309,4.24108453053319,128.313901810966));
#38877=CARTESIAN_POINT('Ctrl Pts',(129.079577550306,4.17160574586141,128.195584094531));
#38878=CARTESIAN_POINT('Ctrl Pts',(129.071829482303,4.09719055401924,128.080207673327));
#38879=CARTESIAN_POINT('Ctrl Pts',(129.0640814143,4.01812987802596,127.968198537251));
#38880=CARTESIAN_POINT('Ctrl Pts',(129.056325111558,3.93898517540535,127.856070356533));
#38881=CARTESIAN_POINT('Ctrl Pts',(129.048568808816,3.85518535170712,127.747316929886));
#38882=CARTESIAN_POINT('Ctrl Pts',(129.040812506075,3.76706313558302,127.642333040989));
#38883=CARTESIAN_POINT('Ctrl Pts',(129.03305206356,3.67889388597881,127.53729311903));
#38884=CARTESIAN_POINT('Ctrl Pts',(129.025291621046,3.58639791061611,127.436027032265));
#38885=CARTESIAN_POINT('Ctrl Pts',(129.017531178532,3.48994542161163,127.338893258512));
#38886=CARTESIAN_POINT('Ctrl Pts',(129.009758278267,3.39333809850922,127.241603557001));
#38887=CARTESIAN_POINT('Ctrl Pts',(129.001985378001,3.29276185676482,127.148459690266));
#38888=CARTESIAN_POINT('Ctrl Pts',(128.994212477736,3.18862132912109,127.059780923932));
#38889=CARTESIAN_POINT('Ctrl Pts',(128.986722141974,3.08826657197116,126.974325854123));
#38890=CARTESIAN_POINT('Ctrl Pts',(128.979231806212,2.98460241374662,126.893017075662));
#38891=CARTESIAN_POINT('Ctrl Pts',(128.97174147045,2.87801534363086,126.816101505582));
#38892=CARTESIAN_POINT('Ctrl Pts',(128.963967136331,2.76738699235537,126.736269658284));
#38893=CARTESIAN_POINT('Ctrl Pts',(128.956192802212,2.65325927208579,126.660917849291));
#38894=CARTESIAN_POINT('Ctrl Pts',(128.948418468093,2.53603102029232,126.59036848105));
#38895=CARTESIAN_POINT('Ctrl Pts',(128.940653715146,2.4189472418422,126.519906058601));
#38896=CARTESIAN_POINT('Ctrl Pts',(128.932888962198,2.29877086654001,126.454234500356));
#38897=CARTESIAN_POINT('Ctrl Pts',(128.925124209251,2.1759321676689,126.393634797));
#38898=CARTESIAN_POINT('Ctrl Pts',(128.917367168366,2.0532154739253,126.333095282125));
#38899=CARTESIAN_POINT('Ctrl Pts',(128.909610127481,1.927842067156,126.277617769262));
#38900=CARTESIAN_POINT('Ctrl Pts',(128.901853086596,1.80026914333493,126.227438718073));
#38901=CARTESIAN_POINT('Ctrl Pts',(128.894101895356,1.67279242324808,126.177297507298));
#38902=CARTESIAN_POINT('Ctrl Pts',(128.886350704116,1.54311984995728,126.132446947704));
#38903=CARTESIAN_POINT('Ctrl Pts',(128.878599512876,1.41173071948402,126.093076351236));
#38904=CARTESIAN_POINT('Ctrl Pts',(128.870851616099,1.28039743289614,126.053722488322));
#38905=CARTESIAN_POINT('Ctrl Pts',(128.863103719322,1.14734941393881,126.019844068058));
#38906=CARTESIAN_POINT('Ctrl Pts',(128.855355822545,1.01308311756862,125.991581206519));
#38907=CARTESIAN_POINT('Ctrl Pts',(128.847609546461,0.87884490681319,125.963324256962));
#38908=CARTESIAN_POINT('Ctrl Pts',(128.839863270377,0.743389307869076,125.940680610161));
#38909=CARTESIAN_POINT('Ctrl Pts',(128.832116994292,0.607224635862987,125.923739621822));
#38910=CARTESIAN_POINT('Ctrl Pts',(128.824370661027,0.471058958720221,125.906798508428));
#38911=CARTESIAN_POINT('Ctrl Pts',(128.816624327762,0.334184586044954,125.895560185765));
#38912=CARTESIAN_POINT('Ctrl Pts',(128.808877994496,0.197116255549933,125.890062270467));
#38913=CARTESIAN_POINT('Ctrl Pts',(128.801129926493,0.060017229552756,125.884563123949));
#38914=CARTESIAN_POINT('Ctrl Pts',(128.79338185849,-0.0772754501194973,
125.884806958507));
#38915=CARTESIAN_POINT('Ctrl Pts',(128.785633790487,-0.214246135101939,
125.890779270311));
#38916=CARTESIAN_POINT('Ctrl Pts',(128.777877487746,-0.351362394158446,
125.896757929559));
#38917=CARTESIAN_POINT('Ctrl Pts',(128.770121185004,-0.488155583687352,
125.908477211017));
#38918=CARTESIAN_POINT('Ctrl Pts',(128.762364882262,-0.624113713034071,
125.925870570871));
#38919=CARTESIAN_POINT('Ctrl Pts',(128.754604439748,-0.760144407328043,
125.943273214084));
#38920=CARTESIAN_POINT('Ctrl Pts',(128.746843997234,-0.895338768151558,
125.966355904321));
#38921=CARTESIAN_POINT('Ctrl Pts',(128.739083554719,-1.02919508927156,125.995000937659));
#38922=CARTESIAN_POINT('Ctrl Pts',(128.731310654454,-1.16326628844153,126.023691954547));
#38923=CARTESIAN_POINT('Ctrl Pts',(128.723537754188,-1.29599477687142,126.057963060058));
#38924=CARTESIAN_POINT('Ctrl Pts',(128.715764853923,-1.42689323346668,126.097646396075));
#38925=CARTESIAN_POINT('Ctrl Pts',(128.708274518161,-1.55303320145113,126.135887142871));
#38926=CARTESIAN_POINT('Ctrl Pts',(128.700784182399,-1.67747358921217,126.179153354272));
#38927=CARTESIAN_POINT('Ctrl Pts',(128.693293846637,-1.79979775161385,126.227253330667));
#38928=CARTESIAN_POINT('Ctrl Pts',(128.685519220637,-1.92676463849925,126.27717890663));
#38929=CARTESIAN_POINT('Ctrl Pts',(128.677744594637,-2.05185369561391,126.332470574193));
#38930=CARTESIAN_POINT('Ctrl Pts',(128.669969968637,-2.1745780406785,126.392967027384));
#38931=CARTESIAN_POINT('Ctrl Pts',(128.662204991085,-2.29715008266293,126.453388403408));
#38932=CARTESIAN_POINT('Ctrl Pts',(128.654440013534,-2.41736290449301,126.519001541467));
#38933=CARTESIAN_POINT('Ctrl Pts',(128.646675035982,-2.53474748781889,126.589596302032));
#38934=CARTESIAN_POINT('Ctrl Pts',(128.638917837483,-2.65201447377654,126.660120339869));
#38935=CARTESIAN_POINT('Ctrl Pts',(128.631160638985,-2.76645852706476,126.735615867966));
#38936=CARTESIAN_POINT('Ctrl Pts',(128.623403440486,-2.87763355655261,126.815826027431));
#38937=CARTESIAN_POINT('Ctrl Pts',(128.615351129977,-2.99303808802988,126.899087672743));
#38938=CARTESIAN_POINT('Ctrl Pts',(128.607298819468,-3.10491955705152,126.987429589041));
#38939=CARTESIAN_POINT('Ctrl Pts',(128.599246508959,-3.21280959593889,127.080513472107));
#38940=CARTESIAN_POINT('Ctrl Pts',(128.591498952426,-3.31661634490334,127.170074430484));
#38941=CARTESIAN_POINT('Ctrl Pts',(128.583751395894,-3.41672795085056,127.264024689781));
#38942=CARTESIAN_POINT('Ctrl Pts',(128.576003839361,-3.51275955805842,127.362020810143));
#38943=CARTESIAN_POINT('Ctrl Pts',(128.56825793343,-3.60877070591622,127.459996052619));
#38944=CARTESIAN_POINT('Ctrl Pts',(128.560512027499,-3.70070331117244,127.56201516205));
#38945=CARTESIAN_POINT('Ctrl Pts',(128.552766121569,-3.78820897605295,127.667697451676));
#38946=CARTESIAN_POINT('Ctrl Pts',(128.54502018846,-3.87571494796172,127.773380112106));
#38947=CARTESIAN_POINT('Ctrl Pts',(128.537274255352,-3.95879369977514,127.882725676861));
#38948=CARTESIAN_POINT('Ctrl Pts',(128.529528322243,-4.03713703291781,127.995320276107));
#38949=CARTESIAN_POINT('Ctrl Pts',(128.521780684535,-4.11549760659178,128.107939653348));
#38950=CARTESIAN_POINT('Ctrl Pts',(128.514033046827,-4.18912046547083,128.223809166609));
#38951=CARTESIAN_POINT('Ctrl Pts',(128.506285409119,-4.25774088705439,128.342486209477));
#38952=CARTESIAN_POINT('Ctrl Pts',(128.498530775566,-4.32642327047889,128.461270413564));
#38953=CARTESIAN_POINT('Ctrl Pts',(128.490776142012,-4.39009400275787,128.582866869874));
#38954=CARTESIAN_POINT('Ctrl Pts',(128.483021508458,-4.44853431613953,128.706808353466));
#38955=CARTESIAN_POINT('Ctrl Pts',(128.475262715865,-4.50700597278432,128.83081631053));
#38956=CARTESIAN_POINT('Ctrl Pts',(128.467503923273,-4.56024146973399,128.957171441148));
#38957=CARTESIAN_POINT('Ctrl Pts',(128.45974513068,-4.6080706728571,129.085387745048));
#38958=CARTESIAN_POINT('Ctrl Pts',(128.451976857346,-4.65595832016514,129.213760720957));
#38959=CARTESIAN_POINT('Ctrl Pts',(128.444208584013,-4.6984263645923,129.343999039703));
#38960=CARTESIAN_POINT('Ctrl Pts',(128.436440310679,-4.73535478389164,129.475602500686));
#38961=CARTESIAN_POINT('Ctrl Pts',(128.434342869875,-4.74532549039541,129.511135553799));
#38962=CARTESIAN_POINT('Ctrl Pts',(128.432245429071,-4.75489264477029,129.546768074734));
#38963=CARTESIAN_POINT('Ctrl Pts',(128.430147988268,-4.76405452823404,129.582490119308));
#38964=CARTESIAN_POINT('Origin',(213.235140564004,0.,130.804360617566));
#38965=CARTESIAN_POINT('',(126.334922597491,-4.76405452823406,129.582490119308));
#38966=CARTESIAN_POINT('',(126.679856726692,-4.76405452823408,129.582490119308));
#38967=CARTESIAN_POINT('',(213.235140564004,-4.76405452823405,129.582490119308));
#38968=CARTESIAN_POINT('',(128.014859435962,-4.91824999645718,130.804547296181));
#38969=CARTESIAN_POINT('Ctrl Pts',(128.014859435962,-4.91824999645718,130.804547296181));
#38970=CARTESIAN_POINT('Ctrl Pts',(128.006721423039,-4.91824451169638,130.949049250926));
#38971=CARTESIAN_POINT('Ctrl Pts',(127.998583410116,-4.91186636222894,131.09342051706));
#38972=CARTESIAN_POINT('Ctrl Pts',(127.990445397193,-4.89917575400125,131.23709609555));
#38973=CARTESIAN_POINT('Ctrl Pts',(127.982295826442,-4.88646712222452,131.380975726028));
#38974=CARTESIAN_POINT('Ctrl Pts',(127.97414625569,-4.86742816844376,131.524157369783));
#38975=CARTESIAN_POINT('Ctrl Pts',(127.965996684939,-4.84217047593194,131.666084555097));
#38976=CARTESIAN_POINT('Ctrl Pts',(127.957827054933,-4.81685061444324,131.808361078256));
#38977=CARTESIAN_POINT('Ctrl Pts',(127.949657424928,-4.78528146592727,131.949376644164));
#38978=CARTESIAN_POINT('Ctrl Pts',(127.941487794922,-4.74762541554514,132.088586445125));
#38979=CARTESIAN_POINT('Ctrl Pts',(127.933307467654,-4.70992005856948,132.227978526516));
#38980=CARTESIAN_POINT('Ctrl Pts',(127.925127140387,-4.66611199179819,132.365559810819));
#38981=CARTESIAN_POINT('Ctrl Pts',(127.91694681312,-4.61641242277826,132.500803780575));
#38982=CARTESIAN_POINT('Ctrl Pts',(127.908747621784,-4.56659824513116,132.636359626792));
#38983=CARTESIAN_POINT('Ctrl Pts',(127.900548430448,-4.51086552640424,132.769567077166));
#38984=CARTESIAN_POINT('Ctrl Pts',(127.892349239112,-4.44947301394585,132.899920915116));
#38985=CARTESIAN_POINT('Ctrl Pts',(127.887412816527,-4.41251090724346,132.978402024203));
#38986=CARTESIAN_POINT('Ctrl Pts',(127.882476393942,-4.37349812256339,133.055849260602));
#38987=CARTESIAN_POINT('Ctrl Pts',(127.877539971357,-4.33249874537039,133.1321573621));
#38988=CARTESIAN_POINT('Ctrl Pts',(127.869765637238,-4.26792914025671,133.252334406682));
#38989=CARTESIAN_POINT('Ctrl Pts',(127.861991303119,-4.19825317444962,133.370013170446));
#38990=CARTESIAN_POINT('Ctrl Pts',(127.854216969,-4.12368850451715,133.484729282547));
#38991=CARTESIAN_POINT('Ctrl Pts',(127.846452216053,-4.04921572887634,133.599304017292));
#38992=CARTESIAN_POINT('Ctrl Pts',(127.838687463106,-3.96986644787174,133.710923040524));
#38993=CARTESIAN_POINT('Ctrl Pts',(127.830922710159,-3.88590470005901,133.819145473001));
#38994=CARTESIAN_POINT('Ctrl Pts',(127.823165669274,-3.80202634423779,133.927260417433));
#38995=CARTESIAN_POINT('Ctrl Pts',(127.815408628389,-3.71354487644034,134.031985177708));
#38996=CARTESIAN_POINT('Ctrl Pts',(127.807651587504,-3.62076802292836,134.132907145202));
#38997=CARTESIAN_POINT('Ctrl Pts',(127.799900396264,-3.52806113316356,134.233753006655));
#38998=CARTESIAN_POINT('Ctrl Pts',(127.792149205023,-3.4310655686078,134.33080149668));
#38999=CARTESIAN_POINT('Ctrl Pts',(127.784398013783,-3.33012955079288,134.423672739701));
#39000=CARTESIAN_POINT('Ctrl Pts',(127.776650117006,-3.22923643347787,134.516504509967));
#39001=CARTESIAN_POINT('Ctrl Pts',(127.768902220229,-3.12440648105544,134.60516230028));
#39002=CARTESIAN_POINT('Ctrl Pts',(127.761154323452,-3.0160248626873,134.689302971083));
#39003=CARTESIAN_POINT('Ctrl Pts',(127.753408047368,-2.90766591541735,134.773426041472));
#39004=CARTESIAN_POINT('Ctrl Pts',(127.745661771284,-2.79575708856317,134.853033632177));
#39005=CARTESIAN_POINT('Ctrl Pts',(127.7379154952,-2.6807164181129,134.927823064122));
#39006=CARTESIAN_POINT('Ctrl Pts',(127.730169161934,-2.56567489845846,135.002613048146));
#39007=CARTESIAN_POINT('Ctrl Pts',(127.722422828669,-2.44750181686188,135.072584589343));
#39008=CARTESIAN_POINT('Ctrl Pts',(127.714676495404,-2.3266436142832,135.137478727497));
#39009=CARTESIAN_POINT('Ctrl Pts',(127.706928427401,-2.20575834634802,135.202387398244));
#39010=CARTESIAN_POINT('Ctrl Pts',(127.699180359398,-2.08218710527059,135.262216218435));
#39011=CARTESIAN_POINT('Ctrl Pts',(127.691432291395,-1.95639994702006,135.316752700464));
#39012=CARTESIAN_POINT('Ctrl Pts',(127.683675988653,-1.83047910068086,135.371347144515));
#39013=CARTESIAN_POINT('Ctrl Pts',(127.675919685911,-1.70233799187077,135.420637858573));
#39014=CARTESIAN_POINT('Ctrl Pts',(127.668163383169,-1.57246614813139,135.464460753344));
#39015=CARTESIAN_POINT('Ctrl Pts',(127.660402940655,-1.44252498787864,135.508307037714));
#39016=CARTESIAN_POINT('Ctrl Pts',(127.652642498141,-1.31085162722338,135.546679578427));
#39017=CARTESIAN_POINT('Ctrl Pts',(127.644882055627,-1.17794872117338,135.57946479159));
#39018=CARTESIAN_POINT('Ctrl Pts',(127.637109155361,-1.04483246758002,135.612302634488));
#39019=CARTESIAN_POINT('Ctrl Pts',(127.629336255096,-0.910483107752943,
135.639535148655));
#39020=CARTESIAN_POINT('Ctrl Pts',(127.62156335483,-0.77541229651415,135.661100144544));
#39021=CARTESIAN_POINT('Ctrl Pts',(127.614073019068,-0.64525164948536,135.681881198514));
#39022=CARTESIAN_POINT('Ctrl Pts',(127.606582683306,-0.514421399407542,
135.697399601139));
#39023=CARTESIAN_POINT('Ctrl Pts',(127.599092347544,-0.383380071231758,
135.707645514804));
#39024=CARTESIAN_POINT('Ctrl Pts',(127.591318013425,-0.247370271270378,
135.718279905399));
#39025=CARTESIAN_POINT('Ctrl Pts',(127.583543679306,-0.110702233030291,
135.723267788318));
#39026=CARTESIAN_POINT('Ctrl Pts',(127.575769345187,0.026115706451228,135.72254128041));
#39027=CARTESIAN_POINT('Ctrl Pts',(127.56800459224,0.162765030050107,135.721815667858));
#39028=CARTESIAN_POINT('Ctrl Pts',(127.560239839293,0.299563500106598,135.715389678964));
#39029=CARTESIAN_POINT('Ctrl Pts',(127.552475086346,0.43599747314086,135.703247150842));
#39030=CARTESIAN_POINT('Ctrl Pts',(127.544718045461,0.572295938029814,135.691116682851));
#39031=CARTESIAN_POINT('Ctrl Pts',(127.536961004575,0.70823023943381,135.673281009041));
#39032=CARTESIAN_POINT('Ctrl Pts',(127.52920396369,0.843286904469057,135.649776003191));
#39033=CARTESIAN_POINT('Ctrl Pts',(127.52145277245,0.978241722222339,135.626288722649));
#39034=CARTESIAN_POINT('Ctrl Pts',(127.51370158121,1.11231983732729,135.59714068653));
#39035=CARTESIAN_POINT('Ctrl Pts',(127.50595038997,1.24501342745985,135.562419531445));
#39036=CARTESIAN_POINT('Ctrl Pts',(127.498202493193,1.37765061927708,135.527713133777));
#39037=CARTESIAN_POINT('Ctrl Pts',(127.490454596416,1.50890407908477,135.487438427117));
#39038=CARTESIAN_POINT('Ctrl Pts',(127.482706699639,1.63827692051537,135.441733989876));
#39039=CARTESIAN_POINT('Ctrl Pts',(127.474960423555,1.7676226999365,135.396039113018));
#39040=CARTESIAN_POINT('Ctrl Pts',(127.467214147471,1.89508827504052,135.344916894862));
#39041=CARTESIAN_POINT('Ctrl Pts',(127.459467871387,2.0201930346862,135.288555435491));
#39042=CARTESIAN_POINT('Ctrl Pts',(127.451721538121,2.14529871782679,135.232193560072));
#39043=CARTESIAN_POINT('Ctrl Pts',(127.443975204856,2.26804319427376,135.170592526856));
#39044=CARTESIAN_POINT('Ctrl Pts',(127.43622887159,2.38796728121975,135.103987964944));
#39045=CARTESIAN_POINT('Ctrl Pts',(127.428480803587,2.50791822433343,135.037368487403));
#39046=CARTESIAN_POINT('Ctrl Pts',(127.420732735585,2.6250471793982,134.965743441278));
#39047=CARTESIAN_POINT('Ctrl Pts',(127.412984667582,2.73892129783921,134.889393443229));
#39048=CARTESIAN_POINT('Ctrl Pts',(127.40522836484,2.8529164430485,134.812962299493));
#39049=CARTESIAN_POINT('Ctrl Pts',(127.397472062098,2.96364951610314,134.731796390447));
#39050=CARTESIAN_POINT('Ctrl Pts',(127.389715759356,3.07071786244071,134.646218875205));
#39051=CARTESIAN_POINT('Ctrl Pts',(127.381955316842,3.17784335437855,134.560595684666));
#39052=CARTESIAN_POINT('Ctrl Pts',(127.374194874328,3.28129992738204,134.47055645272));
#39053=CARTESIAN_POINT('Ctrl Pts',(127.366434431814,3.38072032279577,134.376462682392));
#39054=CARTESIAN_POINT('Ctrl Pts',(127.358661531548,3.48030031665428,134.282217864391));
#39055=CARTESIAN_POINT('Ctrl Pts',(127.350888631283,3.57583091273973,134.183905782095));
#39056=CARTESIAN_POINT('Ctrl Pts',(127.343115731017,3.66698322729635,134.081923290228));
#39057=CARTESIAN_POINT('Ctrl Pts',(127.335625395255,3.75482192562014,133.983648118819));
#39058=CARTESIAN_POINT('Ctrl Pts',(127.328135059493,3.83859494312531,133.881964999801));
#39059=CARTESIAN_POINT('Ctrl Pts',(127.320644723731,3.91804615921147,133.77725438573));
#39060=CARTESIAN_POINT('Ctrl Pts',(127.312870389612,4.00050979230403,133.668573636901));
#39061=CARTESIAN_POINT('Ctrl Pts',(127.305096055493,4.07857865243919,133.556287018243));
#39062=CARTESIAN_POINT('Ctrl Pts',(127.297321721374,4.15192085901405,133.440785515602));
#39063=CARTESIAN_POINT('Ctrl Pts',(127.289556968427,4.22517267787409,133.32542635824));
#39064=CARTESIAN_POINT('Ctrl Pts',(127.28179221548,4.29370922597723,133.206860527086));
#39065=CARTESIAN_POINT('Ctrl Pts',(127.274027462533,4.35723926818454,133.085511428514));
#39066=CARTESIAN_POINT('Ctrl Pts',(127.266270421648,4.4207062114583,132.964282855578));
#39067=CARTESIAN_POINT('Ctrl Pts',(127.258513380763,4.47917636423823,132.840276860593));
#39068=CARTESIAN_POINT('Ctrl Pts',(127.250756339878,4.53240236351408,132.713944833492));
#39069=CARTESIAN_POINT('Ctrl Pts',(127.243005148638,4.58558822464981,132.587708074355));
#39070=CARTESIAN_POINT('Ctrl Pts',(127.235253957398,4.63353765260243,132.459149133325));
#39071=CARTESIAN_POINT('Ctrl Pts',(127.227502766157,4.67604988816291,132.328742625434));
#39072=CARTESIAN_POINT('Ctrl Pts',(127.21975486938,4.71854405488926,132.198391543787));
#39073=CARTESIAN_POINT('Ctrl Pts',(127.212006972603,4.75560550460681,132.066194828046));
#39074=CARTESIAN_POINT('Ctrl Pts',(127.204259075826,4.78708224803971,131.932645427799));
#39075=CARTESIAN_POINT('Ctrl Pts',(127.196512799742,4.81855240721645,131.799123963208));
#39076=CARTESIAN_POINT('Ctrl Pts',(127.188766523658,4.84444009408906,131.664250757218));
#39077=CARTESIAN_POINT('Ctrl Pts',(127.181020247574,4.86464378052288,131.528531834282));
#39078=CARTESIAN_POINT('Ctrl Pts',(127.173273914309,4.88484761609573,131.3928119095));
#39079=CARTESIAN_POINT('Ctrl Pts',(127.165527581043,4.89936730993927,131.256246642019));
#39080=CARTESIAN_POINT('Ctrl Pts',(127.157781247778,4.90815290396647,131.119349718624));
#39081=CARTESIAN_POINT('Ctrl Pts',(127.150033179775,4.91694046546654,130.982422138113));
#39082=CARTESIAN_POINT('Ctrl Pts',(127.142285111772,4.9199913468817,130.845163143983));
#39083=CARTESIAN_POINT('Ctrl Pts',(127.134537043769,4.91730767372589,130.708088584158));
#39084=CARTESIAN_POINT('Ctrl Pts',(127.126780741027,4.91462114833031,130.57086833986));
#39085=CARTESIAN_POINT('Ctrl Pts',(127.119024438286,4.90618790110359,130.433833312948));
#39086=CARTESIAN_POINT('Ctrl Pts',(127.111268135544,4.89206217033457,130.297496943506));
#39087=CARTESIAN_POINT('Ctrl Pts',(127.10350769303,4.87792890023772,130.161087807239));
#39088=CARTESIAN_POINT('Ctrl Pts',(127.095747250515,4.85809714913368,130.025378458131));
#39089=CARTESIAN_POINT('Ctrl Pts',(127.087986808001,4.83267254748213,129.890873282507));
#39090=CARTESIAN_POINT('Ctrl Pts',(127.080213907736,4.80720713200292,129.756152187235));
#39091=CARTESIAN_POINT('Ctrl Pts',(127.07244100747,4.77613101347324,129.622639509294));
#39092=CARTESIAN_POINT('Ctrl Pts',(127.064668107205,4.73960030730825,129.490826457575));
#39093=CARTESIAN_POINT('Ctrl Pts',(127.057177771443,4.70439758432741,129.363805142302));
#39094=CARTESIAN_POINT('Ctrl Pts',(127.049687435681,4.66413005871302,129.238362320521));
#39095=CARTESIAN_POINT('Ctrl Pts',(127.042197099919,4.61897937653492,129.114919117648));
#39096=CARTESIAN_POINT('Ctrl Pts',(127.0344227658,4.57211679251908,128.986795528219));
#39097=CARTESIAN_POINT('Ctrl Pts',(127.026648431681,4.51984500596098,128.860420325024));
#39098=CARTESIAN_POINT('Ctrl Pts',(127.018874097562,4.46231357475289,128.736284066015));
#39099=CARTESIAN_POINT('Ctrl Pts',(127.011109344615,4.40485304589202,128.61230079385));
#39100=CARTESIAN_POINT('Ctrl Pts',(127.003344591667,4.34214593253155,128.490551327005));
#39101=CARTESIAN_POINT('Ctrl Pts',(126.99557983872,4.27439103873849,128.371509551337));
#39102=CARTESIAN_POINT('Ctrl Pts',(126.987822797835,4.20670344006116,128.252586009639));
#39103=CARTESIAN_POINT('Ctrl Pts',(126.98006575695,4.13397823023816,128.13636514484));
#39104=CARTESIAN_POINT('Ctrl Pts',(126.972308716065,4.05646147065486,128.023299057731));
#39105=CARTESIAN_POINT('Ctrl Pts',(126.964557524825,3.97900316706291,127.910318234638));
#39106=CARTESIAN_POINT('Ctrl Pts',(126.956806333585,3.89676072603435,127.800487775049));
#39107=CARTESIAN_POINT('Ctrl Pts',(126.949055142345,3.81002493938064,127.694233124392));
#39108=CARTESIAN_POINT('Ctrl Pts',(126.941307245568,3.72332601775002,127.588023634795));
#39109=CARTESIAN_POINT('Ctrl Pts',(126.933559348791,3.63213779563943,127.48538723357));
#39110=CARTESIAN_POINT('Ctrl Pts',(126.925811452014,3.53679285158414,127.386718244894));
#39111=CARTESIAN_POINT('Ctrl Pts',(126.91806517593,3.44146785163575,127.288069895643));
#39112=CARTESIAN_POINT('Ctrl Pts',(126.910318899846,3.34198813072477,127.1933875892));
#39113=CARTESIAN_POINT('Ctrl Pts',(126.902572623761,3.23872454311893,127.10303026264));
#39114=CARTESIAN_POINT('Ctrl Pts',(126.894826290496,3.13546019324474,127.012672269082));
#39115=CARTESIAN_POINT('Ctrl Pts',(126.887079957231,3.02841221516904,126.926639576566));
#39116=CARTESIAN_POINT('Ctrl Pts',(126.879333623965,2.91798578456649,126.845251876502));
#39117=CARTESIAN_POINT('Ctrl Pts',(126.871585555962,2.80753462473053,126.763845950227));
#39118=CARTESIAN_POINT('Ctrl Pts',(126.863837487959,2.6937038215193,126.687087318223));
#39119=CARTESIAN_POINT('Ctrl Pts',(126.856089419956,2.57692852129203,126.615253020637));
#39120=CARTESIAN_POINT('Ctrl Pts',(126.848333117215,2.46002911088596,126.543342376704));
#39121=CARTESIAN_POINT('Ctrl Pts',(126.840576814473,2.34017928559209,126.476366727126));
#39122=CARTESIAN_POINT('Ctrl Pts',(126.832820511731,2.2178403342128,126.414557966599));
#39123=CARTESIAN_POINT('Ctrl Pts',(126.825060069217,2.09543608685151,126.352716216875));
#39124=CARTESIAN_POINT('Ctrl Pts',(126.817299626703,1.97054042206953,126.296047012666));
#39125=CARTESIAN_POINT('Ctrl Pts',(126.809539184188,1.8436347902095,126.244734117201));
#39126=CARTESIAN_POINT('Ctrl Pts',(126.801766283923,1.71652543816315,126.193338849721));
#39127=CARTESIAN_POINT('Ctrl Pts',(126.793993383657,1.58740003979422,126.147317204707));
#39128=CARTESIAN_POINT('Ctrl Pts',(126.786220483392,1.45675624724891,126.10680334824));
#39129=CARTESIAN_POINT('Ctrl Pts',(126.77873014763,1.33086168563537,126.067762272504));
#39130=CARTESIAN_POINT('Ctrl Pts',(126.771239811868,1.20355750576431,126.033835572956));
#39131=CARTESIAN_POINT('Ctrl Pts',(126.763749476106,1.07529619651151,126.005098054185));
#39132=CARTESIAN_POINT('Ctrl Pts',(126.755975141987,0.942171820733176,125.975270943656));
#39133=CARTESIAN_POINT('Ctrl Pts',(126.748200807868,0.807594605709832,125.950939793889));
#39134=CARTESIAN_POINT('Ctrl Pts',(126.740426473749,0.672058111432231,125.932243936147));
#39135=CARTESIAN_POINT('Ctrl Pts',(126.732661720802,0.536688653770675,125.91357111938));
#39136=CARTESIAN_POINT('Ctrl Pts',(126.724896967855,0.400362652712045,125.900519829082));
#39137=CARTESIAN_POINT('Ctrl Pts',(126.717132214907,0.263586260303849,125.893178952643));
#39138=CARTESIAN_POINT('Ctrl Pts',(126.709375174022,0.126945716136708,125.885845367265));
#39139=CARTESIAN_POINT('Ctrl Pts',(126.701618133137,-0.010143941286047,
125.884210929698));
#39140=CARTESIAN_POINT('Ctrl Pts',(126.693861092252,-0.14716934457583,125.888312993049));
#39141=CARTESIAN_POINT('Ctrl Pts',(126.686109901012,-0.284091415942997,
125.892411963002));
#39142=CARTESIAN_POINT('Ctrl Pts',(126.678358709772,-0.420948940414114,
125.902238811701));
#39143=CARTESIAN_POINT('Ctrl Pts',(126.670607518532,-0.557226798625999,
125.917778851403));
#39144=CARTESIAN_POINT('Ctrl Pts',(126.662859621755,-0.693446735112906,
125.933312286174));
#39145=CARTESIAN_POINT('Ctrl Pts',(126.655111724978,-0.829087107724373,
125.954554038125));
#39146=CARTESIAN_POINT('Ctrl Pts',(126.647363828201,-0.96363639354055,125.981437441364));
#39147=CARTESIAN_POINT('Ctrl Pts',(126.639617552117,-1.09815753454668,126.008315221175));
#39148=CARTESIAN_POINT('Ctrl Pts',(126.631871276032,-1.23158765957864,126.040832228413));
#39149=CARTESIAN_POINT('Ctrl Pts',(126.624124999948,-1.3634243289211,126.078870467137));
#39150=CARTESIAN_POINT('Ctrl Pts',(126.616378666683,-1.49526197145191,126.116908986649));
#39151=CARTESIAN_POINT('Ctrl Pts',(126.608632333418,-1.62550575917977,126.160468710591));
#39152=CARTESIAN_POINT('Ctrl Pts',(126.600886000152,-1.75366771931936,126.209381554206));
#39153=CARTESIAN_POINT('Ctrl Pts',(126.593137932149,-1.88185838044132,126.258305351513));
#39154=CARTESIAN_POINT('Ctrl Pts',(126.585389864146,-2.00796592107178,126.312584514579));
#39155=CARTESIAN_POINT('Ctrl Pts',(126.577641796143,-2.13152205225228,126.372002689413));
#39156=CARTESIAN_POINT('Ctrl Pts',(126.569885493401,-2.25520950035924,126.43148401459));
#39157=CARTESIAN_POINT('Ctrl Pts',(126.562129190659,-2.37633976926454,126.496115092365));
#39158=CARTESIAN_POINT('Ctrl Pts',(126.554372887918,-2.49446842152646,126.565633172152));
#39159=CARTESIAN_POINT('Ctrl Pts',(126.546612445403,-2.61266012260688,126.635188355831));
#39160=CARTESIAN_POINT('Ctrl Pts',(126.538852002889,-2.72784668662439,126.709635526744));
#39161=CARTESIAN_POINT('Ctrl Pts',(126.531091560375,-2.8396132726981,126.788668955596));
#39162=CARTESIAN_POINT('Ctrl Pts',(126.52331866011,-2.95155927641802,126.867829255924));
#39163=CARTESIAN_POINT('Ctrl Pts',(126.515545759844,-3.06007402165151,126.951590287322));
#39164=CARTESIAN_POINT('Ctrl Pts',(126.507772859579,-3.16477563753202,127.039605880988));
#39165=CARTESIAN_POINT('Ctrl Pts',(126.500282523817,-3.26567108594768,127.124421886127));
#39166=CARTESIAN_POINT('Ctrl Pts',(126.492792188055,-3.36302559792996,127.213188288283));
#39167=CARTESIAN_POINT('Ctrl Pts',(126.485301852293,-3.45653165696864,127.305564829459));
#39168=CARTESIAN_POINT('Ctrl Pts',(126.477638656649,-3.55219562278178,127.400073210711));
#39169=CARTESIAN_POINT('Ctrl Pts',(126.469975461006,-3.6441528984451,127.498678419363));
#39170=CARTESIAN_POINT('Ctrl Pts',(126.462312265362,-3.7320244887104,127.601053532979));
#39171=CARTESIAN_POINT('Ctrl Pts',(126.454658019157,-3.81979345842112,127.703309088147));
#39172=CARTESIAN_POINT('Ctrl Pts',(126.447003772952,-3.9034859687367,127.809325493409));
#39173=CARTESIAN_POINT('Ctrl Pts',(126.439349526747,-3.98275807885899,127.918737435689));
#39174=CARTESIAN_POINT('Ctrl Pts',(126.431702448918,-4.06195594883983,128.028046911187));
#39175=CARTESIAN_POINT('Ctrl Pts',(126.424055371089,-4.13674141584888,128.140745276162));
#39176=CARTESIAN_POINT('Ctrl Pts',(126.416408293261,-4.20680961415279,128.256432845283));
#39177=CARTESIAN_POINT('Ctrl Pts',(126.408766874152,-4.2768259630699,128.372034807386));
#39178=CARTESIAN_POINT('Ctrl Pts',(126.401125455043,-4.34213178084251,128.490621229099));
#39179=CARTESIAN_POINT('Ctrl Pts',(126.393484035934,-4.40246484959004,128.611762544361));
#39180=CARTESIAN_POINT('Ctrl Pts',(126.385845932466,-4.46277173958543,128.732851295937));
#39181=CARTESIAN_POINT('Ctrl Pts',(126.378207828999,-4.51810999373234,128.856492375637));
#39182=CARTESIAN_POINT('Ctrl Pts',(126.370569725531,-4.56826300964923,128.982231056538));
#39183=CARTESIAN_POINT('Ctrl Pts',(126.362932135452,-4.61841265457045,129.107961286013));
#39184=CARTESIAN_POINT('Ctrl Pts',(126.355294545374,-4.66337759932938,129.23578846447));
#39185=CARTESIAN_POINT('Ctrl Pts',(126.347656955295,-4.70298927148318,129.365237629488));
#39186=CARTESIAN_POINT('Ctrl Pts',(126.343412169361,-4.72500447092223,129.437182312208));
#39187=CARTESIAN_POINT('Ctrl Pts',(126.339167383426,-4.7453669856379,129.509627674349));
#39188=CARTESIAN_POINT('Ctrl Pts',(126.334922597491,-4.76405452823406,129.582490119308));
#39189=CARTESIAN_POINT('Ctrl Pts',(128.084583899671,-4.76405452823402,129.582490119308));
#39190=CARTESIAN_POINT('Ctrl Pts',(128.076474900419,-4.79964136864725,129.721242669974));
#39191=CARTESIAN_POINT('Ctrl Pts',(128.068365901168,-4.82919846761125,129.861692018109));
#39192=CARTESIAN_POINT('Ctrl Pts',(128.060256901916,-4.85257484534123,130.003298552017));
#39193=CARTESIAN_POINT('Ctrl Pts',(128.052161851861,-4.87591101074747,130.144661492677));
#39194=CARTESIAN_POINT('Ctrl Pts',(128.044066801806,-4.89308760105199,130.287177319227));
#39195=CARTESIAN_POINT('Ctrl Pts',(128.035971751751,-4.90400426091189,130.430294752433));
#39196=CARTESIAN_POINT('Ctrl Pts',(128.028934313165,-4.91349466836051,130.554714013595));
#39197=CARTESIAN_POINT('Ctrl Pts',(128.021896874578,-4.91825473945302,130.679587598279));
#39198=CARTESIAN_POINT('Ctrl Pts',(128.014859435991,-4.9182499964572,130.804547295668));
#39199=CARTESIAN_POINT('',(128.360140563977,-4.9182480591004,130.799991217711));
#39200=CARTESIAN_POINT('Ctrl Pts',(128.430147988268,-4.76405452823404,129.582490119308));
#39201=CARTESIAN_POINT('Ctrl Pts',(128.425047399786,-4.78633453593721,129.669359531197));
#39202=CARTESIAN_POINT('Ctrl Pts',(128.419946811305,-4.80621721630481,129.756758400623));
#39203=CARTESIAN_POINT('Ctrl Pts',(128.414846222823,-4.82368463813426,129.84454314829));
#39204=CARTESIAN_POINT('Ctrl Pts',(128.403582817055,-4.8622571794244,130.038394355244));
#39205=CARTESIAN_POINT('Ctrl Pts',(128.392319411286,-4.88915397073168,130.234639638687));
#39206=CARTESIAN_POINT('Ctrl Pts',(128.381056005517,-4.90414358667604,130.432125821014));
#39207=CARTESIAN_POINT('Ctrl Pts',(128.374084191681,-4.91342184708737,130.554365659184));
#39208=CARTESIAN_POINT('Ctrl Pts',(128.367112377844,-4.91813886456444,130.677080574109));
#39209=CARTESIAN_POINT('Ctrl Pts',(128.360140564008,-4.91824805909993,130.799991217172));
#39210=CARTESIAN_POINT('Ctrl Pts',(128.360140563977,-4.91824805910041,130.799991217711));
#39211=CARTESIAN_POINT('Ctrl Pts',(128.352493106526,-4.91836783574399,130.934813221745));
#39212=CARTESIAN_POINT('Ctrl Pts',(128.344845649074,-4.91293971375226,131.069818158709));
#39213=CARTESIAN_POINT('Ctrl Pts',(128.337198191623,-4.90194532537492,131.204504453624));
#39214=CARTESIAN_POINT('Ctrl Pts',(128.329557232397,-4.89096027918952,131.339076302407));
#39215=CARTESIAN_POINT('Ctrl Pts',(128.321916273171,-4.8744184074605,131.473329647834));
#39216=CARTESIAN_POINT('Ctrl Pts',(128.314275313945,-4.85235340333965,131.606762955298));
#39217=CARTESIAN_POINT('Ctrl Pts',(128.306638422809,-4.83030014675143,131.740125222117));
#39218=CARTESIAN_POINT('Ctrl Pts',(128.299001531673,-4.80272967054546,131.872667922253));
#39219=CARTESIAN_POINT('Ctrl Pts',(128.291364640537,-4.76972745995375,132.003895119055));
#39220=CARTESIAN_POINT('Ctrl Pts',(128.283729779861,-4.73673402383204,132.135087425798));
#39221=CARTESIAN_POINT('Ctrl Pts',(128.276094919185,-4.69831182247926,132.264964533653));
#39222=CARTESIAN_POINT('Ctrl Pts',(128.268460058509,-4.6545972495114,132.393041676602));
#39223=CARTESIAN_POINT('Ctrl Pts',(128.260825462576,-4.61088419237095,132.521114378405));
#39224=CARTESIAN_POINT('Ctrl Pts',(128.253190866643,-4.56187925896366,132.647386857705));
#39225=CARTESIAN_POINT('Ctrl Pts',(128.24555627071,-4.50776823846932,132.771391011522));
#39226=CARTESIAN_POINT('Ctrl Pts',(128.237920174223,-4.45364658263779,132.895419537935));
#39227=CARTESIAN_POINT('Ctrl Pts',(128.230284077736,-4.39441700591012,133.017178482913));
#39228=CARTESIAN_POINT('Ctrl Pts',(128.22264798125,-4.33031257306284,133.13622169449));
#39229=CARTESIAN_POINT('Ctrl Pts',(128.215004114817,-4.26614291212615,133.255386035931));
#39230=CARTESIAN_POINT('Ctrl Pts',(128.207360248384,-4.19708868173679,133.3718287705));
#39231=CARTESIAN_POINT('Ctrl Pts',(128.199716381951,-4.12342802636981,133.485129979866));
#39232=CARTESIAN_POINT('Ctrl Pts',(128.192068419599,-4.04972790039472,133.598491900987));
#39233=CARTESIAN_POINT('Ctrl Pts',(128.184420457248,-3.97141666865398,133.708708617251));
#39234=CARTESIAN_POINT('Ctrl Pts',(128.176772494896,-3.88881378195585,133.815392074022));
#39235=CARTESIAN_POINT('Ctrl Pts',(128.169112854212,-3.80608476179517,133.922238434953));
#39236=CARTESIAN_POINT('Ctrl Pts',(128.161453213528,-3.71905125886355,134.025540453863));
#39237=CARTESIAN_POINT('Ctrl Pts',(128.153793572844,-3.62807106759501,134.124945414101));
#39238=CARTESIAN_POINT('Ctrl Pts',(128.147995248233,-3.5591993405899,134.200194665493));
#39239=CARTESIAN_POINT('Ctrl Pts',(128.142196923622,-3.48806677687409,134.273211467254));
#39240=CARTESIAN_POINT('Ctrl Pts',(128.136398599011,-3.41484099230444,134.343858330488));
#39241=CARTESIAN_POINT('Ctrl Pts',(128.128624264892,-3.31666061201087,134.438580919527));
#39242=CARTESIAN_POINT('Ctrl Pts',(128.120849930773,-3.21438053947274,134.52936538083));
#39243=CARTESIAN_POINT('Ctrl Pts',(128.113075596654,-3.10834982589523,134.61583597789));
#39244=CARTESIAN_POINT('Ctrl Pts',(128.105310843707,-3.00244978569605,134.702200007668));
#39245=CARTESIAN_POINT('Ctrl Pts',(128.09754609076,-2.89280860159226,134.784260506639));
#39246=CARTESIAN_POINT('Ctrl Pts',(128.089781337812,-2.77981231897982,134.861678270123));
#39247=CARTESIAN_POINT('Ctrl Pts',(128.082024296928,-2.66692826586855,134.939019141192));
#39248=CARTESIAN_POINT('Ctrl Pts',(128.074267256043,-2.55069606617825,135.011726233786));
#39249=CARTESIAN_POINT('Ctrl Pts',(128.066510215158,-2.43153473468002,135.079500603174));
#39250=CARTESIAN_POINT('Ctrl Pts',(128.058759023917,-2.31246326366873,135.147223863383));
#39251=CARTESIAN_POINT('Ctrl Pts',(128.051007832677,-2.19046739596087,135.210021611924));
#39252=CARTESIAN_POINT('Ctrl Pts',(128.043256641437,-2.06599471318216,135.267638438585));
#39253=CARTESIAN_POINT('Ctrl Pts',(128.03550874466,-1.94157493461371,135.325230776559));
#39254=CARTESIAN_POINT('Ctrl Pts',(128.027760847883,-1.81468078879465,135.377646408435));
#39255=CARTESIAN_POINT('Ctrl Pts',(128.020012951106,-1.68578382373529,135.424676187106));
#39256=CARTESIAN_POINT('Ctrl Pts',(128.012266675022,-1.5569138211425,135.471696128161));
#39257=CARTESIAN_POINT('Ctrl Pts',(128.004520398938,-1.42604219966607,135.513332322966));
#39258=CARTESIAN_POINT('Ctrl Pts',(127.996774122854,-1.2936594505664,135.549424188105));
#39259=CARTESIAN_POINT('Ctrl Pts',(127.989027789588,-1.16127572424744,135.585516319667));
#39260=CARTESIAN_POINT('Ctrl Pts',(127.981281456323,-1.0273812252448,135.616063937058));
#39261=CARTESIAN_POINT('Ctrl Pts',(127.973535123058,-0.892480144392583,
135.640956760967));
#39262=CARTESIAN_POINT('Ctrl Pts',(127.965787055055,-0.757548853378283,
135.665855159452));
#39263=CARTESIAN_POINT('Ctrl Pts',(127.958038987052,-0.621610916361356,
135.685096173629));
#39264=CARTESIAN_POINT('Ctrl Pts',(127.950290919049,-0.485178821715212,
135.698620987986));
#39265=CARTESIAN_POINT('Ctrl Pts',(127.942534616307,-0.348601725415501,
135.712160176676));
#39266=CARTESIAN_POINT('Ctrl Pts',(127.934778313565,-0.211529812028351,
135.719970990961));
#39267=CARTESIAN_POINT('Ctrl Pts',(127.927022010823,-0.0744793339138556,
135.722046647735));
#39268=CARTESIAN_POINT('Ctrl Pts',(127.919261568309,0.0626442921672268,
135.72412341235));
#39269=CARTESIAN_POINT('Ctrl Pts',(127.911501125795,0.199746069544796,135.720458930541));
#39270=CARTESIAN_POINT('Ctrl Pts',(127.903740683281,0.336312666382312,135.711098520993));
#39271=CARTESIAN_POINT('Ctrl Pts',(127.895967783015,0.473098492045071,135.701723085285));
#39272=CARTESIAN_POINT('Ctrl Pts',(127.88819488275,0.609347031560676,135.686633493054));
#39273=CARTESIAN_POINT('Ctrl Pts',(127.880421982484,0.744552075578421,135.665926750949));
#39274=CARTESIAN_POINT('Ctrl Pts',(127.872931646722,0.874842075685719,135.645972751076));
#39275=CARTESIAN_POINT('Ctrl Pts',(127.86544131096,1.00416282816048,135.62080296493));
#39276=CARTESIAN_POINT('Ctrl Pts',(127.857950975198,1.13207470119655,135.590548028586));
#39277=CARTESIAN_POINT('Ctrl Pts',(127.850176641079,1.2648363917761,135.559145967136));
#39278=CARTESIAN_POINT('Ctrl Pts',(127.84240230696,1.39650080775607,135.522166064256));
#39279=CARTESIAN_POINT('Ctrl Pts',(127.834627972841,1.52656316067025,135.47969889185));
#39280=CARTESIAN_POINT('Ctrl Pts',(127.826863219894,1.65646522335865,135.437284056439));
#39281=CARTESIAN_POINT('Ctrl Pts',(127.819098466947,1.78476878336023,135.389395527186));
#39282=CARTESIAN_POINT('Ctrl Pts',(127.811333713999,1.91097979120411,135.3361747466));
#39283=CARTESIAN_POINT('Ctrl Pts',(127.803576673114,2.03706544449549,135.283006825644));
#39284=CARTESIAN_POINT('Ctrl Pts',(127.795819632229,2.16106232372884,135.224517343693));
#39285=CARTESIAN_POINT('Ctrl Pts',(127.788062591344,2.28249243051693,135.160897242815));
#39286=CARTESIAN_POINT('Ctrl Pts',(127.780311400104,2.40383096591732,135.097325118349));
#39287=CARTESIAN_POINT('Ctrl Pts',(127.772560208864,2.52260623670097,135.02863025675));
#39288=CARTESIAN_POINT('Ctrl Pts',(127.764809017624,2.63836143022142,134.955051165658));
#39289=CARTESIAN_POINT('Ctrl Pts',(127.757061120847,2.75406742469644,134.881503347643));
#39290=CARTESIAN_POINT('Ctrl Pts',(127.74931322407,2.86675556565846,134.803075638288));
#39291=CARTESIAN_POINT('Ctrl Pts',(127.741565327293,2.97599500850477,134.72005171517));
#39292=CARTESIAN_POINT('Ctrl Pts',(127.733819051209,3.08521160081472,134.637045158866));
#39293=CARTESIAN_POINT('Ctrl Pts',(127.726072775125,3.19098061882793,134.549444537554));
#39294=CARTESIAN_POINT('Ctrl Pts',(127.71832649904,3.29290183666117,134.457575716163));
#39295=CARTESIAN_POINT('Ctrl Pts',(127.710580165775,3.39482380685327,134.365706216617));
#39296=CARTESIAN_POINT('Ctrl Pts',(127.70283383251,3.49289762978401,134.269568715884));
#39297=CARTESIAN_POINT('Ctrl Pts',(127.695087499244,3.58675799688275,134.16952779533));
#39298=CARTESIAN_POINT('Ctrl Pts',(127.687339431241,3.68063938336017,134.069464471305));
#39299=CARTESIAN_POINT('Ctrl Pts',(127.679591363239,3.77030516894693,133.96549627308));
#39300=CARTESIAN_POINT('Ctrl Pts',(127.671843295236,3.85542885800333,133.858022580419));
#39301=CARTESIAN_POINT('Ctrl Pts',(127.664086992494,3.94064301752938,133.750434663438));
#39302=CARTESIAN_POINT('Ctrl Pts',(127.656330689752,4.02130519415403,133.639334116538));
#39303=CARTESIAN_POINT('Ctrl Pts',(127.64857438701,4.09713063404873,133.525151611016));
#39304=CARTESIAN_POINT('Ctrl Pts',(127.640813944496,4.17299654426377,133.410908162853));
#39305=CARTESIAN_POINT('Ctrl Pts',(127.633053501982,4.24402037150442,133.293579812694));
#39306=CARTESIAN_POINT('Ctrl Pts',(127.625293059467,4.30996277526624,133.173622937006));
#39307=CARTESIAN_POINT('Ctrl Pts',(127.617520159202,4.37601103562876,133.053473495892));
#39308=CARTESIAN_POINT('Ctrl Pts',(127.609747258937,4.43696139798907,132.930687447654));
#39309=CARTESIAN_POINT('Ctrl Pts',(127.601974358671,4.49262185826876,132.805743115018));
#39310=CARTESIAN_POINT('Ctrl Pts',(127.594484022909,4.54625892061693,132.685340823589));
#39311=CARTESIAN_POINT('Ctrl Pts',(127.586993687147,4.59498389223406,132.56293472776));
#39312=CARTESIAN_POINT('Ctrl Pts',(127.579503351385,4.63866904922118,132.438965314212));
#39313=CARTESIAN_POINT('Ctrl Pts',(127.571729017266,4.6840105422134,132.310295562669));
#39314=CARTESIAN_POINT('Ctrl Pts',(127.563954683147,4.72406613551407,132.179534019784));
#39315=CARTESIAN_POINT('Ctrl Pts',(127.556180349028,4.7586391793361,132.047154334716));
#39316=CARTESIAN_POINT('Ctrl Pts',(127.548415596081,4.79316961497151,131.914937795779));
#39317=CARTESIAN_POINT('Ctrl Pts',(127.540650843134,4.82223084720667,131.7811074572));
#39318=CARTESIAN_POINT('Ctrl Pts',(127.532886090187,4.84567482982384,131.646155429923));
#39319=CARTESIAN_POINT('Ctrl Pts',(127.525129049302,4.86909552754698,131.511337438902));
#39320=CARTESIAN_POINT('Ctrl Pts',(127.517372008417,4.88691001189204,131.37540035895));
#39321=CARTESIAN_POINT('Ctrl Pts',(127.509614967532,4.89902055802202,131.238849552497));
#39322=CARTESIAN_POINT('Ctrl Pts',(127.501863776291,4.91112197149492,131.10240172007));
#39323=CARTESIAN_POINT('Ctrl Pts',(127.494112585051,4.91752797399816,130.965341470211));
#39324=CARTESIAN_POINT('Ctrl Pts',(127.486361393811,4.91819231037008,130.828182051541));
#39325=CARTESIAN_POINT('Ctrl Pts',(127.478613497034,4.91885636438132,130.691080929282));
#39326=CARTESIAN_POINT('Ctrl Pts',(127.470865600257,4.91378360406405,130.553881112188));
#39327=CARTESIAN_POINT('Ctrl Pts',(127.46311770348,4.90297981336515,130.417098416682));
#39328=CARTESIAN_POINT('Ctrl Pts',(127.455371427396,4.89217828258636,130.280344333167));
#39329=CARTESIAN_POINT('Ctrl Pts',(127.447625151312,4.8756481366858,130.144007587195));
#39330=CARTESIAN_POINT('Ctrl Pts',(127.439878875228,4.85344720319195,130.00860103809));
#39331=CARTESIAN_POINT('Ctrl Pts',(127.432132541962,4.83124610581588,129.873193489445));
#39332=CARTESIAN_POINT('Ctrl Pts',(127.424386208697,4.80337420057413,129.738716537183));
#39333=CARTESIAN_POINT('Ctrl Pts',(127.416639875431,4.76994076188964,129.605674590884));
#39334=CARTESIAN_POINT('Ctrl Pts',(127.408891807429,4.73649983601844,129.472602850763));
#39335=CARTESIAN_POINT('Ctrl Pts',(127.401143739426,4.69749499363828,129.340967135178));
#39336=CARTESIAN_POINT('Ctrl Pts',(127.393395671423,4.65308576538586,129.211258008672));
#39337=CARTESIAN_POINT('Ctrl Pts',(127.385639368681,4.60862933847702,129.081411025763));
#39338=CARTESIAN_POINT('Ctrl Pts',(127.377883065939,4.55875717858758,128.953495092716));
#39339=CARTESIAN_POINT('Ctrl Pts',(127.370126763197,4.50367770527798,128.827982569347));
#39340=CARTESIAN_POINT('Ctrl Pts',(127.362366320683,4.44856883439518,128.702403056165));
#39341=CARTESIAN_POINT('Ctrl Pts',(127.354605878169,4.38824728397169,128.579229859643));
#39342=CARTESIAN_POINT('Ctrl Pts',(127.346845435654,4.32296764706629,128.458911026354));
#39343=CARTESIAN_POINT('Ctrl Pts',(127.339072535389,4.25758321749239,128.338399046591));
#39344=CARTESIAN_POINT('Ctrl Pts',(127.331299635124,4.18722499727909,128.220750922245));
#39345=CARTESIAN_POINT('Ctrl Pts',(127.323526734858,4.11219162998841,128.106386736901));
#39346=CARTESIAN_POINT('Ctrl Pts',(127.316036399096,4.03988591459579,127.996179977759));
#39347=CARTESIAN_POINT('Ctrl Pts',(127.308546063334,3.96323923678638,127.889022794443));
#39348=CARTESIAN_POINT('Ctrl Pts',(127.301055727572,3.88255315259187,127.785260738496));
#39349=CARTESIAN_POINT('Ctrl Pts',(127.293281393453,3.79880783099182,127.677564512662));
#39350=CARTESIAN_POINT('Ctrl Pts',(127.285507059334,3.71044546819425,127.573184799627));
#39351=CARTESIAN_POINT('Ctrl Pts',(127.277732725215,3.61775826463864,127.472543065367));
#39352=CARTESIAN_POINT('Ctrl Pts',(127.269967972268,3.52518528977797,127.372025363051));
#39353=CARTESIAN_POINT('Ctrl Pts',(127.26220321932,3.42829834154304,127.275236758326));
#39354=CARTESIAN_POINT('Ctrl Pts',(127.254438466373,3.32743142421089,127.182567804652));
#39355=CARTESIAN_POINT('Ctrl Pts',(127.246681425488,3.22666468932314,127.08999089109));
#39356=CARTESIAN_POINT('Ctrl Pts',(127.238924384603,3.12192613795301,127.001525748717));
#39357=CARTESIAN_POINT('Ctrl Pts',(127.231167343718,3.0135881231648,126.917527756943));
#39358=CARTESIAN_POINT('Ctrl Pts',(127.223416152478,2.90533180691615,126.833593108708));
#39359=CARTESIAN_POINT('Ctrl Pts',(127.215664961238,2.79348173778971,126.754119144443));
#39360=CARTESIAN_POINT('Ctrl Pts',(127.207913769998,2.6784447243425,126.679422203342));
#39361=CARTESIAN_POINT('Ctrl Pts',(127.200165873221,2.5634566046944,126.604757010433));
#39362=CARTESIAN_POINT('Ctrl Pts',(127.192417976444,2.44528456201122,126.534865014925));
#39363=CARTESIAN_POINT('Ctrl Pts',(127.184670079667,2.3243656936248,126.470020161995));
#39364=CARTESIAN_POINT('Ctrl Pts',(127.176923803583,2.20347211885877,126.40518887321));
#39365=CARTESIAN_POINT('Ctrl Pts',(127.169177527499,2.07983320558443,126.345402811706));
#39366=CARTESIAN_POINT('Ctrl Pts',(127.161431251415,1.95391169406834,126.290890538538));
#39367=CARTESIAN_POINT('Ctrl Pts',(127.153684918149,1.82798925302869,126.236377862972));
#39368=CARTESIAN_POINT('Ctrl Pts',(127.145938584884,1.69978453891325,126.187139208746));
#39369=CARTESIAN_POINT('Ctrl Pts',(127.138192251619,1.56978099128221,126.14335528589));
#39370=CARTESIAN_POINT('Ctrl Pts',(127.130444183616,1.43974833025745,126.099561557929));
#39371=CARTESIAN_POINT('Ctrl Pts',(127.122696115612,1.3079164045647,126.061225116843));
#39372=CARTESIAN_POINT('Ctrl Pts',(127.11494804761,1.17478417025543,126.028476907108));
#39373=CARTESIAN_POINT('Ctrl Pts',(127.107191744868,1.04151044142369,125.995693892187));
#39374=CARTESIAN_POINT('Ctrl Pts',(127.099435442126,0.906934023568071,125.968511066422));
#39375=CARTESIAN_POINT('Ctrl Pts',(127.091679139384,0.771564982243835,125.947008402555));
#39376=CARTESIAN_POINT('Ctrl Pts',(127.08391869687,0.636123690385901,125.925494262068));
#39377=CARTESIAN_POINT('Ctrl Pts',(127.076158254356,0.499889320265314,125.909666369441));
#39378=CARTESIAN_POINT('Ctrl Pts',(127.068397811841,0.363376439920618,125.899552708441));
#39379=CARTESIAN_POINT('Ctrl Pts',(127.060624911576,0.226644416981721,125.889422812095));
#39380=CARTESIAN_POINT('Ctrl Pts',(127.052852011311,0.0896333813806602,
125.885025490484));
#39381=CARTESIAN_POINT('Ctrl Pts',(127.045079111045,-0.0471418145240442,
125.886336551762));
#39382=CARTESIAN_POINT('Ctrl Pts',(127.037588775283,-0.178944887541407,
125.887599952661));
#39383=CARTESIAN_POINT('Ctrl Pts',(127.030098439521,-0.310528662267972,
125.894163898406));
#39384=CARTESIAN_POINT('Ctrl Pts',(127.022608103759,-0.441439418002701,
125.90596146042));
#39385=CARTESIAN_POINT('Ctrl Pts',(127.01483376964,-0.577313694830587,125.918206330582));
#39386=CARTESIAN_POINT('Ctrl Pts',(127.007059435521,-0.712893319056468,
125.936128304444));
#39387=CARTESIAN_POINT('Ctrl Pts',(126.999285101402,-0.847665757943376,
125.959709358155));
#39388=CARTESIAN_POINT('Ctrl Pts',(126.991520348455,-0.98227210184468,125.983261350325));
#39389=CARTESIAN_POINT('Ctrl Pts',(126.983755595508,-1.11607285831267,126.012458478809));
#39390=CARTESIAN_POINT('Ctrl Pts',(126.975990842561,-1.2485589061891,126.047230840035));
#39391=CARTESIAN_POINT('Ctrl Pts',(126.968233801676,-1.38091336705452,126.081968664861));
#39392=CARTESIAN_POINT('Ctrl Pts',(126.960476760791,-1.51195534219338,126.122270604144));
#39393=CARTESIAN_POINT('Ctrl Pts',(126.952719719906,-1.64118457491573,126.168015477959));
#39394=CARTESIAN_POINT('Ctrl Pts',(126.944968528666,-1.77031635486887,126.213725855208));
#39395=CARTESIAN_POINT('Ctrl Pts',(126.937217337425,-1.89763774627782,126.264870867178));
#39396=CARTESIAN_POINT('Ctrl Pts',(126.929466146185,-2.02266271405707,126.32127924337));
#39397=CARTESIAN_POINT('Ctrl Pts',(126.921718249408,-2.1476345428897,126.377663644497));
#39398=CARTESIAN_POINT('Ctrl Pts',(126.913970352631,-2.27031153373802,126.439306800033));
#39399=CARTESIAN_POINT('Ctrl Pts',(126.906222455854,-2.39022694697982,126.505989041675));
#39400=CARTESIAN_POINT('Ctrl Pts',(126.89847617977,-2.51011727650225,126.572657334829));
#39401=CARTESIAN_POINT('Ctrl Pts',(126.890729903686,-2.62724683594767,126.644362427603));
#39402=CARTESIAN_POINT('Ctrl Pts',(126.882983627602,-2.74117320801024,126.72083854634));
#39403=CARTESIAN_POINT('Ctrl Pts',(126.875237294336,-2.85510042105127,126.797315229606));
#39404=CARTESIAN_POINT('Ctrl Pts',(126.867490961071,-2.96582407491677,126.878562791207));
#39405=CARTESIAN_POINT('Ctrl Pts',(126.859744627806,-3.07293082224783,126.964272177936));
#39406=CARTESIAN_POINT('Ctrl Pts',(126.851996559803,-3.18006155539146,127.050000758687));
#39407=CARTESIAN_POINT('Ctrl Pts',(126.8442484918,-3.28357346503124,127.140192908618));
#39408=CARTESIAN_POINT('Ctrl Pts',(126.836500423797,-3.38308668593686,127.234499620561));
#39409=CARTESIAN_POINT('Ctrl Pts',(126.828744121055,-3.48270567067891,127.328906562801));
#39410=CARTESIAN_POINT('Ctrl Pts',(126.820987818313,-3.57831719291506,127.427436533241));
#39411=CARTESIAN_POINT('Ctrl Pts',(126.813231515572,-3.66957826642248,127.529703626506));
#39412=CARTESIAN_POINT('Ctrl Pts',(126.805471073057,-3.76088804871265,127.632025302797));
#39413=CARTESIAN_POINT('Ctrl Pts',(126.797710630543,-3.84784250780809,127.738087774154));
#39414=CARTESIAN_POINT('Ctrl Pts',(126.789950188029,-3.93013996357985,127.847473245823));
#39415=CARTESIAN_POINT('Ctrl Pts',(126.782177287764,-4.0125695305337,127.957034312762));
#39416=CARTESIAN_POINT('Ctrl Pts',(126.774404387498,-4.09032693316647,128.069928717626));
#39417=CARTESIAN_POINT('Ctrl Pts',(126.766631487233,-4.16315423448871,128.185710224261));
#39418=CARTESIAN_POINT('Ctrl Pts',(126.759141151471,-4.23333407996803,128.297282781495));
#39419=CARTESIAN_POINT('Ctrl Pts',(126.751650815709,-4.29893589086485,128.411535910829));
#39420=CARTESIAN_POINT('Ctrl Pts',(126.744160479946,-4.35977072896749,128.528051707655));
#39421=CARTESIAN_POINT('Ctrl Pts',(126.735913192433,-4.42675336053556,128.656342255212));
#39422=CARTESIAN_POINT('Ctrl Pts',(126.727665904919,-4.48814858008666,128.787742683637));
#39423=CARTESIAN_POINT('Ctrl Pts',(126.719418617406,-4.54367471349653,128.92175519942));
#39424=CARTESIAN_POINT('Ctrl Pts',(126.711190605967,-4.59907106776353,129.055454492791));
#39425=CARTESIAN_POINT('Ctrl Pts',(126.702962594528,-4.64862556553197,129.191753406355));
#39426=CARTESIAN_POINT('Ctrl Pts',(126.694734583089,-4.69210291139784,129.330130875853));
#39427=CARTESIAN_POINT('Ctrl Pts',(126.689775297624,-4.71830809730973,129.413535399335));
#39428=CARTESIAN_POINT('Ctrl Pts',(126.684816012158,-4.74230640943244,129.497694534175));
#39429=CARTESIAN_POINT('Ctrl Pts',(126.679856726692,-4.76405452823407,129.582490119308));
#39430=CARTESIAN_POINT('Origin',(213.235140564004,0.,130.804360617566));
#39431=CARTESIAN_POINT('',(124.584949745809,-4.76405452823405,129.582490119308));
#39432=CARTESIAN_POINT('',(124.930172151781,-4.76405452823403,129.582490119308));
#39433=CARTESIAN_POINT('',(213.235140564004,-4.76405452823405,129.582490119308));
#39434=CARTESIAN_POINT('',(126.264859436032,-4.91824798511455,130.808812517913));
#39435=CARTESIAN_POINT('Ctrl Pts',(126.264859435991,-4.91824798511388,130.808812518644));
#39436=CARTESIAN_POINT('Ctrl Pts',(126.253922671906,-4.91807338114146,131.001706659933));
#39437=CARTESIAN_POINT('Ctrl Pts',(126.242985907822,-4.90654741857509,131.194108271543));
#39438=CARTESIAN_POINT('Ctrl Pts',(126.232049143737,-4.8838633796719,131.384930640216));
#39439=CARTESIAN_POINT('Ctrl Pts',(126.223650838651,-4.86644438098075,131.531462508034));
#39440=CARTESIAN_POINT('Ctrl Pts',(126.215252533566,-4.84244679529329,131.677064071246));
#39441=CARTESIAN_POINT('Ctrl Pts',(126.20685422848,-4.81197577865153,131.821254008326));
#39442=CARTESIAN_POINT('Ctrl Pts',(126.199079894361,-4.78376867472872,131.954731029709));
#39443=CARTESIAN_POINT('Ctrl Pts',(126.191305560242,-4.74995900409119,132.087244945294));
#39444=CARTESIAN_POINT('Ctrl Pts',(126.183531226123,-4.71062519903041,132.218288938507));
#39445=CARTESIAN_POINT('Ctrl Pts',(126.175766473176,-4.67133986936906,132.34917143171));
#39446=CARTESIAN_POINT('Ctrl Pts',(126.168001720229,-4.62654406249727,132.478587236115));
#39447=CARTESIAN_POINT('Ctrl Pts',(126.160236967282,-4.57636732436756,132.606039050295));
#39448=CARTESIAN_POINT('Ctrl Pts',(126.152479926396,-4.5262404224815,132.733364277536));
#39449=CARTESIAN_POINT('Ctrl Pts',(126.144722885511,-4.47074336726166,132.858729035026));
#39450=CARTESIAN_POINT('Ctrl Pts',(126.136965844626,-4.41005557514316,132.981650879945));
#39451=CARTESIAN_POINT('Ctrl Pts',(126.129214653386,-4.34941354816091,133.104480028544));
#39452=CARTESIAN_POINT('Ctrl Pts',(126.121463462146,-4.28358874798467,133.224869582249));
#39453=CARTESIAN_POINT('Ctrl Pts',(126.113712270906,-4.21280865132573,133.34235713644));
#39454=CARTESIAN_POINT('Ctrl Pts',(126.105964374129,-4.1420586380958,133.459794755286));
#39455=CARTESIAN_POINT('Ctrl Pts',(126.098216477352,-4.06635771865141,133.574332493623));
#39456=CARTESIAN_POINT('Ctrl Pts',(126.090468580575,-3.98597914979362,133.685532823442));
#39457=CARTESIAN_POINT('Ctrl Pts',(126.082722304491,-3.90561739439972,133.796709892548));
#39458=CARTESIAN_POINT('Ctrl Pts',(126.074976028407,-3.82058016469699,133.904550625068));
#39459=CARTESIAN_POINT('Ctrl Pts',(126.067229752322,-3.73118362745657,134.008647090511));
#39460=CARTESIAN_POINT('Ctrl Pts',(126.059483419057,-3.64178643031121,134.112744324372));
#39461=CARTESIAN_POINT('Ctrl Pts',(126.051737085792,-3.54803011613398,134.213096939402));
#39462=CARTESIAN_POINT('Ctrl Pts',(126.043990752526,-3.45027039490185,134.309330983284));
#39463=CARTESIAN_POINT('Ctrl Pts',(126.036242684523,-3.35248878105783,134.405586578114));
#39464=CARTESIAN_POINT('Ctrl Pts',(126.02849461652,-3.25070225472393,134.497721492255));
#39465=CARTESIAN_POINT('Ctrl Pts',(126.020746548517,-3.14530224565585,134.585399740079));
#39466=CARTESIAN_POINT('Ctrl Pts',(126.012990245775,-3.03979021620393,134.673171173387));
#39467=CARTESIAN_POINT('Ctrl Pts',(126.005233943034,-2.93065733334482,134.756476228086));
#39468=CARTESIAN_POINT('Ctrl Pts',(125.997477640292,-2.81832731104713,134.835019897424));
#39469=CARTESIAN_POINT('Ctrl Pts',(125.989717197778,-2.70593733483443,134.913605487883));
#39470=CARTESIAN_POINT('Ctrl Pts',(125.981956755263,-2.59034714836053,134.987424418911));
#39471=CARTESIAN_POINT('Ctrl Pts',(125.974196312749,-2.47200725315596,135.056226467148));
#39472=CARTESIAN_POINT('Ctrl Pts',(125.966423412484,-2.3534773882458,135.125138962542));
#39473=CARTESIAN_POINT('Ctrl Pts',(125.958650512218,-2.23218933999362,135.189018299303));
#39474=CARTESIAN_POINT('Ctrl Pts',(125.950877611953,-2.10861668581204,135.247661050219));
#39475=CARTESIAN_POINT('Ctrl Pts',(125.943387276191,-1.98953620887186,135.304171989427));
#39476=CARTESIAN_POINT('Ctrl Pts',(125.935896940429,-1.86833462794485,135.355820338244));
#39477=CARTESIAN_POINT('Ctrl Pts',(125.928406604667,-1.74544923784005,135.402467839089));
#39478=CARTESIAN_POINT('Ctrl Pts',(125.920632270548,-1.61790461081815,135.450883994107));
#39479=CARTESIAN_POINT('Ctrl Pts',(125.912857936429,-1.4881419478203,135.494065968866));
#39480=CARTESIAN_POINT('Ctrl Pts',(125.90508360231,-1.3566300425547,135.531805803937));
#39481=CARTESIAN_POINT('Ctrl Pts',(125.897318849363,-1.22528021395888,135.569499128033));
#39482=CARTESIAN_POINT('Ctrl Pts',(125.889554096416,-1.09218580465443,135.601763550466));
#39483=CARTESIAN_POINT('Ctrl Pts',(125.881789343468,-0.957835231167931,
135.628439258346));
#39484=CARTESIAN_POINT('Ctrl Pts',(125.874032302583,-0.823618096564934,
135.655088471538));
#39485=CARTESIAN_POINT('Ctrl Pts',(125.866275261698,-0.688147661637522,
135.67615994085));
#39486=CARTESIAN_POINT('Ctrl Pts',(125.858518220813,-0.551926798158095,
135.691543842285));
#39487=CARTESIAN_POINT('Ctrl Pts',(125.850767029573,-0.415808659891554,
135.7069161426));
#39488=CARTESIAN_POINT('Ctrl Pts',(125.843015838333,-0.278941606394287,
135.716609368413));
#39489=CARTESIAN_POINT('Ctrl Pts',(125.835264647093,-0.141837628489148,
135.72056496133));
#39490=CARTESIAN_POINT('Ctrl Pts',(125.827516750316,-0.00479192343189372,
135.724518873015));
#39491=CARTESIAN_POINT('Ctrl Pts',(125.819768853539,0.132490115765808,135.722739990836));
#39492=CARTESIAN_POINT('Ctrl Pts',(125.812020956762,0.269492682422311,135.715221718903));
#39493=CARTESIAN_POINT('Ctrl Pts',(125.804274680678,0.406466591095302,135.70770501963));
#39494=CARTESIAN_POINT('Ctrl Pts',(125.796528404594,0.543160753375989,135.694451339984));
#39495=CARTESIAN_POINT('Ctrl Pts',(125.788782128509,0.679061069929106,135.675506183632));
#39496=CARTESIAN_POINT('Ctrl Pts',(125.781035795244,0.814962389667395,135.656560887431));
#39497=CARTESIAN_POINT('Ctrl Pts',(125.773289461979,0.950069464764186,135.63192408467));
#39498=CARTESIAN_POINT('Ctrl Pts',(125.765543128713,1.08387540861196,135.601692913864));
#39499=CARTESIAN_POINT('Ctrl Pts',(125.75779506071,1.21771131737312,135.571454972997));
#39500=CARTESIAN_POINT('Ctrl Pts',(125.750046992707,1.35024513379401,135.535620257262));
#39501=CARTESIAN_POINT('Ctrl Pts',(125.742298924704,1.48098260630426,135.494336479159));
#39502=CARTESIAN_POINT('Ctrl Pts',(125.734542621963,1.61185902815617,135.453008824165));
#39503=CARTESIAN_POINT('Ctrl Pts',(125.726786319221,1.74093491889981,135.406220655915));
#39504=CARTESIAN_POINT('Ctrl Pts',(125.719030016479,1.86773305325146,135.354168998618));
#39505=CARTESIAN_POINT('Ctrl Pts',(125.711269573965,1.99459886358531,135.302089559784));
#39506=CARTESIAN_POINT('Ctrl Pts',(125.703509131451,2.11918414015567,135.244741197567));
#39507=CARTESIAN_POINT('Ctrl Pts',(125.695748688936,2.24103485588412,135.182367679828));
#39508=CARTESIAN_POINT('Ctrl Pts',(125.687975788671,2.36308117719877,135.11989403458));
#39509=CARTESIAN_POINT('Ctrl Pts',(125.680202888406,2.48238382507819,135.052379306389));
#39510=CARTESIAN_POINT('Ctrl Pts',(125.67242998814,2.59851567028782,134.980111971965));
#39511=CARTESIAN_POINT('Ctrl Pts',(125.664939652378,2.71042583040586,134.910471737179));
#39512=CARTESIAN_POINT('Ctrl Pts',(125.657449316616,2.81939146402898,134.836418608654));
#39513=CARTESIAN_POINT('Ctrl Pts',(125.649958980854,2.9250598826108,134.758245763298));
#39514=CARTESIAN_POINT('Ctrl Pts',(125.642184646735,3.03473475140013,134.677108970751));
#39515=CARTESIAN_POINT('Ctrl Pts',(125.634410312616,3.14120485872182,134.591276879437));
#39516=CARTESIAN_POINT('Ctrl Pts',(125.626635978497,3.24404184796695,134.501031491628));
#39517=CARTESIAN_POINT('Ctrl Pts',(125.61887122555,3.34675209981358,134.410897323195));
#39518=CARTESIAN_POINT('Ctrl Pts',(125.611106472603,3.4458378514233,134.316360935645));
#39519=CARTESIAN_POINT('Ctrl Pts',(125.603341719655,3.54090064662295,134.217746864864));
#39520=CARTESIAN_POINT('Ctrl Pts',(125.59558467877,3.63586902411424,134.119230738969));
#39521=CARTESIAN_POINT('Ctrl Pts',(125.587827637885,3.72682212714961,134.016645269205));
#39522=CARTESIAN_POINT('Ctrl Pts',(125.580070597,3.81339574321152,133.910354173283));
#39523=CARTESIAN_POINT('Ctrl Pts',(125.57231940576,3.89990407343612,133.804143232303));
#39524=CARTESIAN_POINT('Ctrl Pts',(125.56456821452,3.98203924441768,133.694232529241));
#39525=CARTESIAN_POINT('Ctrl Pts',(125.55681702328,4.05947524577584,133.581021164236));
#39526=CARTESIAN_POINT('Ctrl Pts',(125.549069126503,4.13687833476775,133.467857917081));
#39527=CARTESIAN_POINT('Ctrl Pts',(125.541321229726,4.20958600629661,133.351397120205));
#39528=CARTESIAN_POINT('Ctrl Pts',(125.533573332949,4.27731390494205,133.232069171139));
#39529=CARTESIAN_POINT('Ctrl Pts',(125.525827056865,4.34502763637119,133.112766182907));
#39530=CARTESIAN_POINT('Ctrl Pts',(125.518080780781,4.40776347397505,132.990597575213));
#39531=CARTESIAN_POINT('Ctrl Pts',(125.510334504697,4.46528181802819,132.86602047023));
#39532=CARTESIAN_POINT('Ctrl Pts',(125.502588171431,4.52280058666864,132.741442445648));
#39533=CARTESIAN_POINT('Ctrl Pts',(125.494841838166,4.57510162101877,132.614456243258));
#39534=CARTESIAN_POINT('Ctrl Pts',(125.4870955049,4.62199266187001,132.485540826859));
#39535=CARTESIAN_POINT('Ctrl Pts',(125.479347436897,4.6688942036447,132.356596540747));
#39536=CARTESIAN_POINT('Ctrl Pts',(125.471599368895,4.71038320749897,132.225722548274));
#39537=CARTESIAN_POINT('Ctrl Pts',(125.463851300892,4.74631679309538,132.093414519496));
#39538=CARTESIAN_POINT('Ctrl Pts',(125.45609499815,4.78228856933421,131.960965872171));
#39539=CARTESIAN_POINT('Ctrl Pts',(125.448338695408,4.812693030077,131.827080521866));
#39540=CARTESIAN_POINT('Ctrl Pts',(125.440582392666,4.83743798544688,131.692266468124));
#39541=CARTESIAN_POINT('Ctrl Pts',(125.432821950152,4.86219614794451,131.557380460063));
#39542=CARTESIAN_POINT('Ctrl Pts',(125.425061507638,4.88128873177235,131.421565147856));
#39543=CARTESIAN_POINT('Ctrl Pts',(125.417301065123,4.89467541300868,131.285334279826));
#39544=CARTESIAN_POINT('Ctrl Pts',(125.409528164858,4.90808358373416,131.148884721913));
#39545=CARTESIAN_POINT('Ctrl Pts',(125.401755264593,4.91576752609823,131.012018665699));
#39546=CARTESIAN_POINT('Ctrl Pts',(125.393982364327,4.91773906994455,130.875251395816));
#39547=CARTESIAN_POINT('Ctrl Pts',(125.386492028565,4.91963894320605,130.743455960688));
#39548=CARTESIAN_POINT('Ctrl Pts',(125.379001692803,4.91623453549151,130.611752562238));
#39549=CARTESIAN_POINT('Ctrl Pts',(125.371511357041,4.90758186806153,130.480596396606));
#39550=CARTESIAN_POINT('Ctrl Pts',(125.363737022922,4.89860113211608,130.344467405092));
#39551=CARTESIAN_POINT('Ctrl Pts',(125.355962688803,4.88393785648686,130.208496746491));
#39552=CARTESIAN_POINT('Ctrl Pts',(125.348188354684,4.86359776046143,130.073197238468));
#39553=CARTESIAN_POINT('Ctrl Pts',(125.340423601737,4.84328273178652,129.938064474996));
#39554=CARTESIAN_POINT('Ctrl Pts',(125.33265884879,4.81730486058022,129.803601599262));
#39555=CARTESIAN_POINT('Ctrl Pts',(125.324894095842,4.7857218127802,129.670319263303));
#39556=CARTESIAN_POINT('Ctrl Pts',(125.317137054957,4.7541701337085,129.537169305238));
#39557=CARTESIAN_POINT('Ctrl Pts',(125.309380014072,4.71702444646845,129.405197931532));
#39558=CARTESIAN_POINT('Ctrl Pts',(125.301622973187,4.67439389130825,129.274908162797));
#39559=CARTESIAN_POINT('Ctrl Pts',(125.293871781947,4.63179548418129,129.144716646589));
#39560=CARTESIAN_POINT('Ctrl Pts',(125.286120590707,4.58372056304116,129.01620458133));
#39561=CARTESIAN_POINT('Ctrl Pts',(125.278369399467,4.53032868556305,128.889861972159));
#39562=CARTESIAN_POINT('Ctrl Pts',(125.27062150269,4.47695950105715,128.763573061967));
#39563=CARTESIAN_POINT('Ctrl Pts',(125.262873605913,4.41827800674933,128.639452133297));
#39564=CARTESIAN_POINT('Ctrl Pts',(125.255125709136,4.35449260722029,128.517971062795));
#39565=CARTESIAN_POINT('Ctrl Pts',(125.247379433052,4.29072055022178,128.396515403515));
#39566=CARTESIAN_POINT('Ctrl Pts',(125.239633156967,4.22184689320682,128.277698849975));
#39567=CARTESIAN_POINT('Ctrl Pts',(125.231886880883,4.14812671650236,128.16197006991));
#39568=CARTESIAN_POINT('Ctrl Pts',(125.224140547618,4.07440599561236,128.046240435563));
#39569=CARTESIAN_POINT('Ctrl Pts',(125.216394214353,3.99583889369552,127.93359894992));
#39570=CARTESIAN_POINT('Ctrl Pts',(125.208647881087,3.91272445576253,127.824466257731));
#39571=CARTESIAN_POINT('Ctrl Pts',(125.200899813084,3.82959140492744,127.715309126032));
#39572=CARTESIAN_POINT('Ctrl Pts',(125.193151745081,3.74190922852344,127.609662662353));
#39573=CARTESIAN_POINT('Ctrl Pts',(125.185403677078,3.65001771749608,127.507914997741));
#39574=CARTESIAN_POINT('Ctrl Pts',(125.177647374337,3.55802854307727,127.4060591945));
#39575=CARTESIAN_POINT('Ctrl Pts',(125.169891071595,3.46182135973703,127.308110758407));
#39576=CARTESIAN_POINT('Ctrl Pts',(125.162134768853,3.36177373099847,127.214421837577));
#39577=CARTESIAN_POINT('Ctrl Pts',(125.154374326339,3.261672703828,127.120682912149));
#39578=CARTESIAN_POINT('Ctrl Pts',(125.146613883825,3.15772744310006,127.031208286924));
#39579=CARTESIAN_POINT('Ctrl Pts',(125.13885344131,3.05034838376378,126.946309581075));
#39580=CARTESIAN_POINT('Ctrl Pts',(125.131080541045,2.9427969500288,126.861274588287));
#39581=CARTESIAN_POINT('Ctrl Pts',(125.12330764078,2.83180101922627,126.780830423432));
#39582=CARTESIAN_POINT('Ctrl Pts',(125.115534740514,2.71780050922964,126.705245657659));
#39583=CARTESIAN_POINT('Ctrl Pts',(125.108044404752,2.60794420492189,126.632408588509));
#39584=CARTESIAN_POINT('Ctrl Pts',(125.10055406899,2.49529824024551,126.564083909241));
#39585=CARTESIAN_POINT('Ctrl Pts',(125.093063733228,2.3802758654664,126.500470532216));
#39586=CARTESIAN_POINT('Ctrl Pts',(125.085289399109,2.26089238238665,126.434445234665));
#39587=CARTESIAN_POINT('Ctrl Pts',(125.07751506499,2.1385705577689,126.373286401496));
#39588=CARTESIAN_POINT('Ctrl Pts',(125.069740730871,2.01374493105133,126.317266411383));
#39589=CARTESIAN_POINT('Ctrl Pts',(125.061975977924,1.88907314076279,126.2613154609));
#39590=CARTESIAN_POINT('Ctrl Pts',(125.054211224977,1.76190404128946,126.210490910905));
#39591=CARTESIAN_POINT('Ctrl Pts',(125.04644647203,1.63269842850033,126.16502026531));
#39592=CARTESIAN_POINT('Ctrl Pts',(125.038689431145,1.50362114454748,126.119594781801));
#39593=CARTESIAN_POINT('Ctrl Pts',(125.03093239026,1.37251173893809,126.079512749428));
#39594=CARTESIAN_POINT('Ctrl Pts',(125.023175349375,1.23985241012979,126.044954240338));
#39595=CARTESIAN_POINT('Ctrl Pts',(125.015424158135,1.10729312075292,126.010421792089));
#39596=CARTESIAN_POINT('Ctrl Pts',(125.007672966895,0.973186611428278,125.981404674443));
#39597=CARTESIAN_POINT('Ctrl Pts',(124.999921775654,0.838031382177934,125.958033506755));
#39598=CARTESIAN_POINT('Ctrl Pts',(124.992173878877,0.702933597505588,125.934672272437));
#39599=CARTESIAN_POINT('Ctrl Pts',(124.9844259821,0.566788363879681,125.916952281776));
#39600=CARTESIAN_POINT('Ctrl Pts',(124.976678085323,0.430105332253433,125.904953258949));
#39601=CARTESIAN_POINT('Ctrl Pts',(124.968931809239,0.293450891770855,125.89295674606));
#39602=CARTESIAN_POINT('Ctrl Pts',(124.961185533155,0.156259266268752,125.886678854866));
#39603=CARTESIAN_POINT('Ctrl Pts',(124.953439257071,0.0190458097673841,
125.886147494934));
#39604=CARTESIAN_POINT('Ctrl Pts',(124.945692923806,-0.118168659612549,
125.88561613108));
#39605=CARTESIAN_POINT('Ctrl Pts',(124.93794659054,-0.255404569351039,125.890831384647));
#39606=CARTESIAN_POINT('Ctrl Pts',(124.930200257275,-0.392146377973822,
125.901769029361));
#39607=CARTESIAN_POINT('Ctrl Pts',(124.922452189272,-0.528918808976545,
125.912709123484));
#39608=CARTESIAN_POINT('Ctrl Pts',(124.914704121269,-0.665196529035951,
125.929374127604));
#39609=CARTESIAN_POINT('Ctrl Pts',(124.906956053266,-0.800469327202789,
125.951687960287));
#39610=CARTESIAN_POINT('Ctrl Pts',(124.899199750524,-0.935885894909286,
125.974025508376));
#39611=CARTESIAN_POINT('Ctrl Pts',(124.891443447782,-1.070295020825,126.002023814217));
#39612=CARTESIAN_POINT('Ctrl Pts',(124.883687145041,-1.20319635045958,126.035555567583));
#39613=CARTESIAN_POINT('Ctrl Pts',(124.875926702526,-1.33616861353546,126.069105217856));
#39614=CARTESIAN_POINT('Ctrl Pts',(124.868166260012,-1.46763110221842,126.108194089115));
#39615=CARTESIAN_POINT('Ctrl Pts',(124.860405817498,-1.59709979235588,126.152645308591));
#39616=CARTESIAN_POINT('Ctrl Pts',(124.852632917233,-1.72677631712843,126.197167885109));
#39617=CARTESIAN_POINT('Ctrl Pts',(124.844860016967,-1.85445228314264,126.2470698692));
#39618=CARTESIAN_POINT('Ctrl Pts',(124.837087116702,-1.97966394752975,126.302126314761));
#39619=CARTESIAN_POINT('Ctrl Pts',(124.82959678094,-2.10032385252699,126.355181319848));
#39620=CARTESIAN_POINT('Ctrl Pts',(124.822106445178,-2.21869523568927,126.413022402162));
#39621=CARTESIAN_POINT('Ctrl Pts',(124.814616109416,-2.33438737455136,126.475409399542));
#39622=CARTESIAN_POINT('Ctrl Pts',(124.806840801173,-2.45448106187394,126.540169932366));
#39623=CARTESIAN_POINT('Ctrl Pts',(124.79906549293,-2.5720680717935,126.610034297799));
#39624=CARTESIAN_POINT('Ctrl Pts',(124.791290184687,-2.68668419202054,126.684784047717));
#39625=CARTESIAN_POINT('Ctrl Pts',(124.783524672129,-2.80115591367417,126.759439624519));
#39626=CARTESIAN_POINT('Ctrl Pts',(124.775759159571,-2.91266386903581,126.83896812665));
#39627=CARTESIAN_POINT('Ctrl Pts',(124.767993647013,-3.02076745621588,126.923104759217));
#39628=CARTESIAN_POINT('Ctrl Pts',(124.760237457247,-3.12874126095208,127.007140382576));
#39629=CARTESIAN_POINT('Ctrl Pts',(124.75248126748,-3.23331853092937,127.095772879485));
#39630=CARTESIAN_POINT('Ctrl Pts',(124.744725077714,-3.33408726690759,127.188693990353));
#39631=CARTESIAN_POINT('Ctrl Pts',(124.736974173943,-3.43478732700543,127.281551773651));
#39632=CARTESIAN_POINT('Ctrl Pts',(124.729223270173,-3.53168373067039,127.378692092438));
#39633=CARTESIAN_POINT('Ctrl Pts',(124.721472366403,-3.62439717815534,127.479766182529));
#39634=CARTESIAN_POINT('Ctrl Pts',(124.713725066416,-3.71706751851891,127.580793278217));
#39635=CARTESIAN_POINT('Ctrl Pts',(124.705977766429,-3.80555850919785,127.685750218183));
#39636=CARTESIAN_POINT('Ctrl Pts',(124.698230466441,-3.88952767779987,127.79425139926));
#39637=CARTESIAN_POINT('Ctrl Pts',(124.690485090805,-3.97347598930845,127.902725629741));
#39638=CARTESIAN_POINT('Ctrl Pts',(124.682739715169,-4.05290447591747,128.014742039753));
#39639=CARTESIAN_POINT('Ctrl Pts',(124.674994339533,-4.12751119792334,128.129882280859));
#39640=CARTESIAN_POINT('Ctrl Pts',(124.667246590171,-4.20214078465265,128.245057808996));
#39641=CARTESIAN_POINT('Ctrl Pts',(124.65949884081,-4.27194543615605,128.363358756285));
#39642=CARTESIAN_POINT('Ctrl Pts',(124.651751091448,-4.33666672914206,128.484338043785));
#39643=CARTESIAN_POINT('Ctrl Pts',(124.644002337527,-4.4013964137794,128.605333017251));
#39644=CARTESIAN_POINT('Ctrl Pts',(124.636253583606,-4.46104124962412,128.729006674073));
#39645=CARTESIAN_POINT('Ctrl Pts',(124.628504829684,-4.51538941372329,128.854888508267));
#39646=CARTESIAN_POINT('Ctrl Pts',(124.620749163676,-4.56978605777646,128.98088263228));
#39647=CARTESIAN_POINT('Ctrl Pts',(124.612993497668,-4.61887644198245,129.109088506853));
#39648=CARTESIAN_POINT('Ctrl Pts',(124.605237831659,-4.66249726811931,129.239016474165));
#39649=CARTESIAN_POINT('Ctrl Pts',(124.598475136376,-4.70053324786056,129.352309549289));
#39650=CARTESIAN_POINT('Ctrl Pts',(124.591712441093,-4.73441128232443,129.466911553406));
#39651=CARTESIAN_POINT('Ctrl Pts',(124.584949745809,-4.76405452823405,129.582490119308));
#39652=CARTESIAN_POINT('Ctrl Pts',(126.334922597491,-4.76405452823406,129.582490119308));
#39653=CARTESIAN_POINT('Ctrl Pts',(126.327281976563,-4.79769213240394,129.713642627445));
#39654=CARTESIAN_POINT('Ctrl Pts',(126.319641355634,-4.82589983755495,129.846146911425));
#39655=CARTESIAN_POINT('Ctrl Pts',(126.312000734706,-4.84858740908575,129.979507176672));
#39656=CARTESIAN_POINT('Ctrl Pts',(126.304143851594,-4.87191713572563,130.116642106631));
#39657=CARTESIAN_POINT('Ctrl Pts',(126.296286968481,-4.88940952022633,130.25468174393));
#39658=CARTESIAN_POINT('Ctrl Pts',(126.288430085369,-4.90102358601449,130.393081063212));
#39659=CARTESIAN_POINT('Ctrl Pts',(126.280573202257,-4.91263765180265,130.531480382494));
#39660=CARTESIAN_POINT('Ctrl Pts',(126.272716319145,-4.91837341917953,130.670238922525));
#39661=CARTESIAN_POINT('Ctrl Pts',(126.264859436032,-4.91824798511455,130.808812517913));
#39662=CARTESIAN_POINT('',(126.610140564052,-4.91824997363776,130.803851390504));
#39663=CARTESIAN_POINT('Ctrl Pts',(126.679856726692,-4.76405452823407,129.582490119308));
#39664=CARTESIAN_POINT('Ctrl Pts',(126.671653679144,-4.80002762432874,129.722748675014));
#39665=CARTESIAN_POINT('Ctrl Pts',(126.663450631596,-4.82984162546053,129.864749417658));
#39666=CARTESIAN_POINT('Ctrl Pts',(126.655247584047,-4.85333911657205,130.007942083093));
#39667=CARTESIAN_POINT('Ctrl Pts',(126.647062836702,-4.87678418706063,130.150815299584));
#39668=CARTESIAN_POINT('Ctrl Pts',(126.638878089357,-4.89394079707537,130.294874821921));
#39669=CARTESIAN_POINT('Ctrl Pts',(126.630693342012,-4.90470209545733,130.439558729802));
#39670=CARTESIAN_POINT('Ctrl Pts',(126.623842416025,-4.91370968672766,130.560664330568));
#39671=CARTESIAN_POINT('Ctrl Pts',(126.616991490039,-4.91823737879227,130.68220703363));
#39672=CARTESIAN_POINT('Ctrl Pts',(126.610140564052,-4.91824997363776,130.803851390504));
#39673=CARTESIAN_POINT('Ctrl Pts',(126.610140564008,-4.91824997363784,130.803851391281));
#39674=CARTESIAN_POINT('Ctrl Pts',(126.602085987719,-4.91826478126958,130.946867642582));
#39675=CARTESIAN_POINT('Ctrl Pts',(126.59403141143,-4.91203717351668,131.089784258798));
#39676=CARTESIAN_POINT('Ctrl Pts',(126.585976835141,-4.89961914306179,131.232046618556));
#39677=CARTESIAN_POINT('Ctrl Pts',(126.577913721954,-4.88718795096255,131.374459759597));
#39678=CARTESIAN_POINT('Ctrl Pts',(126.569850608766,-4.86855327872846,131.516216918705));
#39679=CARTESIAN_POINT('Ctrl Pts',(126.561787495578,-4.84381863382357,131.656771378364));
#39680=CARTESIAN_POINT('Ctrl Pts',(126.553707322419,-4.81903165524257,131.797623223798));
#39681=CARTESIAN_POINT('Ctrl Pts',(126.545627149259,-4.78811896234214,131.937266942921));
#39682=CARTESIAN_POINT('Ctrl Pts',(126.537546976099,-4.75123499494181,132.075167088017));
#39683=CARTESIAN_POINT('Ctrl Pts',(126.529458092486,-4.71431126650594,132.213215889914));
#39684=CARTESIAN_POINT('Ctrl Pts',(126.521369208874,-4.67140352368006,132.349517039915));
#39685=CARTESIAN_POINT('Ctrl Pts',(126.513280325261,-4.62271522172352,132.483552995272));
#39686=CARTESIAN_POINT('Ctrl Pts',(126.505173147772,-4.57391680595623,132.617892087301));
#39687=CARTESIAN_POINT('Ctrl Pts',(126.497065970283,-4.51931181977965,132.749955421507));
#39688=CARTESIAN_POINT('Ctrl Pts',(126.488958792793,-4.45915152249253,132.879246340191));
#39689=CARTESIAN_POINT('Ctrl Pts',(126.48121014724,-4.40165175507547,133.002819495389));
#39690=CARTESIAN_POINT('Ctrl Pts',(126.473461501687,-4.33907763532179,133.123859981535));
#39691=CARTESIAN_POINT('Ctrl Pts',(126.465712856134,-4.27168572665355,133.241958639227));
#39692=CARTESIAN_POINT('Ctrl Pts',(126.457938522015,-4.20407039810127,133.360448821494));
#39693=CARTESIAN_POINT('Ctrl Pts',(126.450164187896,-4.13141412440042,133.476311229307));
#39694=CARTESIAN_POINT('Ctrl Pts',(126.442389853777,-4.05394634133551,133.589087197335));
#39695=CARTESIAN_POINT('Ctrl Pts',(126.434625100829,-3.97657403038968,133.701724179062));
#39696=CARTESIAN_POINT('Ctrl Pts',(126.426860347882,-3.89440222776585,133.811281970189));
#39697=CARTESIAN_POINT('Ctrl Pts',(126.419095594935,-3.80770613665861,133.917326572946));
#39698=CARTESIAN_POINT('Ctrl Pts',(126.41133855405,-3.72109615333132,134.023265850708));
#39699=CARTESIAN_POINT('Ctrl Pts',(126.403581513165,-3.62997106981866,134.125698583334));
#39700=CARTESIAN_POINT('Ctrl Pts',(126.39582447228,-3.53464904136758,134.22422014931));
#39701=CARTESIAN_POINT('Ctrl Pts',(126.38807328104,-3.43939889599953,134.322667419407));
#39702=CARTESIAN_POINT('Ctrl Pts',(126.3803220898,-3.3399583760858,134.417209113696));
#39703=CARTESIAN_POINT('Ctrl Pts',(126.37257089856,-3.23668528365419,134.507474366437));
#39704=CARTESIAN_POINT('Ctrl Pts',(126.364823001783,-3.13345608504191,134.597701254038));
#39705=CARTESIAN_POINT('Ctrl Pts',(126.357075105006,-3.02639784751469,134.683655058407));
#39706=CARTESIAN_POINT('Ctrl Pts',(126.349327208229,-2.91590437124619,134.765002580714));
#39707=CARTESIAN_POINT('Ctrl Pts',(126.341580932145,-2.80543400783096,134.846333086872));
#39708=CARTESIAN_POINT('Ctrl Pts',(126.33383465606,-2.69153014960811,134.923058995845));
#39709=CARTESIAN_POINT('Ctrl Pts',(126.326088379976,-2.57461842037946,134.994888394821));
#39710=CARTESIAN_POINT('Ctrl Pts',(126.318342046711,-2.45770582813507,135.066718324024));
#39711=CARTESIAN_POINT('Ctrl Pts',(126.310595713446,-2.33778565369613,135.133651466443));
#39712=CARTESIAN_POINT('Ctrl Pts',(126.30284938018,-2.21531080094182,135.195440338743));
#39713=CARTESIAN_POINT('Ctrl Pts',(126.295101312177,-2.09280852079317,135.257243048232));
#39714=CARTESIAN_POINT('Ctrl Pts',(126.287353244174,-1.96775077290358,135.313899019142));
#39715=CARTESIAN_POINT('Ctrl Pts',(126.279605176171,-1.84061288255488,135.365207828236));
#39716=CARTESIAN_POINT('Ctrl Pts',(126.27184887343,-1.71333986854343,135.416571168942));
#39717=CARTESIAN_POINT('Ctrl Pts',(126.264092570688,-1.5839826588938,135.462575848824));
#39718=CARTESIAN_POINT('Ctrl Pts',(126.256336267946,-1.45303480906168,135.503070324087));
#39719=CARTESIAN_POINT('Ctrl Pts',(126.248575825432,-1.32201706841934,135.543586412471));
#39720=CARTESIAN_POINT('Ctrl Pts',(126.240815382918,-1.18940737378025,135.578586336396));
#39721=CARTESIAN_POINT('Ctrl Pts',(126.233054940403,-1.05571111496386,135.607969376014));
#39722=CARTESIAN_POINT('Ctrl Pts',(126.225282040138,-0.921800235043832,
135.637399583897));
#39723=CARTESIAN_POINT('Ctrl Pts',(126.217509139873,-0.7867996906322,135.661194821285));
#39724=CARTESIAN_POINT('Ctrl Pts',(126.209736239607,-0.651222556919777,
135.679305975604));
#39725=CARTESIAN_POINT('Ctrl Pts',(126.202245903845,-0.520573993515626,
135.696758743845));
#39726=CARTESIAN_POINT('Ctrl Pts',(126.194755568083,-0.389390340648915,
135.7089334872));
#39727=CARTESIAN_POINT('Ctrl Pts',(126.187265232321,-0.258130224993057,
135.715832072176));
#39728=CARTESIAN_POINT('Ctrl Pts',(126.179490898202,-0.121893342156839,
135.722992219098));
#39729=CARTESIAN_POINT('Ctrl Pts',(126.171716564083,0.0148574735939531,
135.72449089982));
#39730=CARTESIAN_POINT('Ctrl Pts',(126.163942229964,0.151612318479945,135.720273225352));
#39731=CARTESIAN_POINT('Ctrl Pts',(126.156177477017,0.288198625241561,135.71606074879));
#39732=CARTESIAN_POINT('Ctrl Pts',(126.14841272407,0.424788564230456,135.706145946218));
#39733=CARTESIAN_POINT('Ctrl Pts',(126.140647971122,0.560868246781902,135.690525767482));
#39734=CARTESIAN_POINT('Ctrl Pts',(126.132890930237,0.696812773073972,135.674921102928));
#39735=CARTESIAN_POINT('Ctrl Pts',(126.125133889353,0.832247665570025,135.653622383415));
#39736=CARTESIAN_POINT('Ctrl Pts',(126.117376848468,0.966660534048905,135.626678574152));
#39737=CARTESIAN_POINT('Ctrl Pts',(126.109625657227,1.10097204073836,135.599755083425));
#39738=CARTESIAN_POINT('Ctrl Pts',(126.101874465987,1.2342626756864,135.567195052793));
#39739=CARTESIAN_POINT('Ctrl Pts',(126.094123274747,1.36602701830681,135.529099049242));
#39740=CARTESIAN_POINT('Ctrl Pts',(126.08637537797,1.49773535756677,135.491019237509));
#39741=CARTESIAN_POINT('Ctrl Pts',(126.078627481193,1.62791831994757,135.447408241031));
#39742=CARTESIAN_POINT('Ctrl Pts',(126.070879584416,1.75608271722196,135.398417272939));
#39743=CARTESIAN_POINT('Ctrl Pts',(126.063133308332,1.88422030526735,135.349436552701));
#39744=CARTESIAN_POINT('Ctrl Pts',(126.055387032248,2.01033980310264,135.295078238788));
#39745=CARTESIAN_POINT('Ctrl Pts',(126.047640756164,2.13396555615088,135.235542634552));
#39746=CARTESIAN_POINT('Ctrl Pts',(126.039894422898,2.25759222177643,135.176006590838));
#39747=CARTESIAN_POINT('Ctrl Pts',(126.032148089633,2.37872475363574,135.111293350177));
#39748=CARTESIAN_POINT('Ctrl Pts',(126.024401756368,2.49691013138188,135.041650182642));
#39749=CARTESIAN_POINT('Ctrl Pts',(126.016653688365,2.61512197592384,134.971991419002));
#39750=CARTESIAN_POINT('Ctrl Pts',(126.008905620362,2.73038501627021,134.897400730059));
#39751=CARTESIAN_POINT('Ctrl Pts',(126.001157552359,2.84227370575046,134.818169686779));
#39752=CARTESIAN_POINT('Ctrl Pts',(125.993401249617,2.95428131186139,134.738854435804));
#39753=CARTESIAN_POINT('Ctrl Pts',(125.985644946875,3.06290708350767,134.654889204942));
#39754=CARTESIAN_POINT('Ctrl Pts',(125.977888644133,3.16775674382266,134.566607323255));
#39755=CARTESIAN_POINT('Ctrl Pts',(125.970128201619,3.27266236555832,134.478278322869));
#39756=CARTESIAN_POINT('Ctrl Pts',(125.962367759105,3.37378757193022,134.38562834487));
#39757=CARTESIAN_POINT('Ctrl Pts',(125.954607316591,3.47077444893512,134.289028146487));
#39758=CARTESIAN_POINT('Ctrl Pts',(125.946834416325,3.56791701788514,134.192272876891));
#39759=CARTESIAN_POINT('Ctrl Pts',(125.93906151606,3.66090771684249,134.091555002503));
#39760=CARTESIAN_POINT('Ctrl Pts',(125.931288615794,3.74942789633278,133.987279641466));
#39761=CARTESIAN_POINT('Ctrl Pts',(125.923798280032,3.83473014433063,133.886794952455));
#39762=CARTESIAN_POINT('Ctrl Pts',(125.91630794427,3.91588106943581,133.783007176151));
#39763=CARTESIAN_POINT('Ctrl Pts',(125.908817608508,3.99263434307331,133.676303177056));
#39764=CARTESIAN_POINT('Ctrl Pts',(125.901043274389,4.07229774040865,133.565553463405));
#39765=CARTESIAN_POINT('Ctrl Pts',(125.89326894027,4.1474757791831,133.451311202667));
#39766=CARTESIAN_POINT('Ctrl Pts',(125.885494606151,4.21784666428545,133.333975722493));
#39767=CARTESIAN_POINT('Ctrl Pts',(125.877729853204,4.28813082356114,133.216784847812));
#39768=CARTESIAN_POINT('Ctrl Pts',(125.869965100257,4.35361941777396,133.09650867074));
#39769=CARTESIAN_POINT('Ctrl Pts',(125.862200347309,4.41403211136707,132.973577891681));
#39770=CARTESIAN_POINT('Ctrl Pts',(125.854443306424,4.4743848022214,132.850769209205));
#39771=CARTESIAN_POINT('Ctrl Pts',(125.846686265539,4.52967145385982,132.725311520285));
#39772=CARTESIAN_POINT('Ctrl Pts',(125.838929224654,4.57965630266858,132.597662380217));
#39773=CARTESIAN_POINT('Ctrl Pts',(125.831178033414,4.62960345751375,132.470109501359));
#39774=CARTESIAN_POINT('Ctrl Pts',(125.823426842174,4.67425662558844,132.340368823311));
#39775=CARTESIAN_POINT('Ctrl Pts',(125.815675650934,4.7134272245756,132.208919929638));
#39776=CARTESIAN_POINT('Ctrl Pts',(125.807927754157,4.75258117501339,132.077526905252));
#39777=CARTESIAN_POINT('Ctrl Pts',(125.80017985738,4.78625707961104,131.944427483174));
#39778=CARTESIAN_POINT('Ctrl Pts',(125.792431960603,4.81431557797499,131.810118331018));
#39779=CARTESIAN_POINT('Ctrl Pts',(125.784685684519,4.84236820710598,131.675837273441));
#39780=CARTESIAN_POINT('Ctrl Pts',(125.776939408435,4.86480568732303,131.540347371576));
#39781=CARTESIAN_POINT('Ctrl Pts',(125.76919313235,4.88153943659325,131.404157075946));
#39782=CARTESIAN_POINT('Ctrl Pts',(125.761446799085,4.8982733093882,131.26796577499));
#39783=CARTESIAN_POINT('Ctrl Pts',(125.75370046582,4.90930331954209,131.131074457999));
#39784=CARTESIAN_POINT('Ctrl Pts',(125.745954132554,4.91459263380777,130.993997919335));
#39785=CARTESIAN_POINT('Ctrl Pts',(125.738206064551,4.91988313257869,130.856890683332));
#39786=CARTESIAN_POINT('Ctrl Pts',(125.730457996548,4.91943036221618,130.719598533718));
#39787=CARTESIAN_POINT('Ctrl Pts',(125.722709928545,4.91324961126213,130.582637096187));
#39788=CARTESIAN_POINT('Ctrl Pts',(125.714953625804,4.90706229133238,130.445530094411));
#39789=CARTESIAN_POINT('Ctrl Pts',(125.707197323062,4.89513484749634,130.308754898037));
#39790=CARTESIAN_POINT('Ctrl Pts',(125.69944102032,4.87753460265541,130.172823395861));
#39791=CARTESIAN_POINT('Ctrl Pts',(125.691680577806,4.85992496403381,130.036819342948));
#39792=CARTESIAN_POINT('Ctrl Pts',(125.683920135292,4.83663655772362,129.901660266602));
#39793=CARTESIAN_POINT('Ctrl Pts',(125.676159692777,4.80778785102174,129.76784769335));
#39794=CARTESIAN_POINT('Ctrl Pts',(125.668386792512,4.77889283381485,129.633820312275));
#39795=CARTESIAN_POINT('Ctrl Pts',(125.660613892246,4.74441977782415,129.501144132331));
#39796=CARTESIAN_POINT('Ctrl Pts',(125.652840991981,4.70453728259173,129.370306218596));
#39797=CARTESIAN_POINT('Ctrl Pts',(125.645350656219,4.66610461651938,129.244224592588));
#39798=CARTESIAN_POINT('Ctrl Pts',(125.637860320457,4.6226490781343,129.119850192736));
#39799=CARTESIAN_POINT('Ctrl Pts',(125.630369984695,4.57436300088649,128.997599371961));
#39800=CARTESIAN_POINT('Ctrl Pts',(125.622595650576,4.5242461423431,128.870713374157));
#39801=CARTESIAN_POINT('Ctrl Pts',(125.614821316457,4.46876645915886,128.745713228533));
#39802=CARTESIAN_POINT('Ctrl Pts',(125.607046982338,4.40808597887739,128.623085516776));
#39803=CARTESIAN_POINT('Ctrl Pts',(125.599282229391,4.34748028186456,128.500608932715));
#39804=CARTESIAN_POINT('Ctrl Pts',(125.591517476444,4.28168671251511,128.380499312054));
#39805=CARTESIAN_POINT('Ctrl Pts',(125.583752723496,4.21091610306165,128.263225313125));
#39806=CARTESIAN_POINT('Ctrl Pts',(125.575995682611,4.14021578397538,128.146067792386));
#39807=CARTESIAN_POINT('Ctrl Pts',(125.568238641726,4.06454846280301,128.031740621227));
#39808=CARTESIAN_POINT('Ctrl Pts',(125.560481600841,3.98417165778152,127.92068947407));
#39809=CARTESIAN_POINT('Ctrl Pts',(125.552730409601,3.90385546553339,127.809722071446));
#39810=CARTESIAN_POINT('Ctrl Pts',(125.544979218361,3.81883708670207,127.702026090923));
#39811=CARTESIAN_POINT('Ctrl Pts',(125.537228027121,3.72941807517629,127.598019418778));
#39812=CARTESIAN_POINT('Ctrl Pts',(125.529480130344,3.64003706911622,127.494056952243));
#39813=CARTESIAN_POINT('Ctrl Pts',(125.521732233567,3.54625940476471,127.393780971186));
#39814=CARTESIAN_POINT('Ctrl Pts',(125.51398433679,3.44842761495544,127.297577184431));
#39815=CARTESIAN_POINT('Ctrl Pts',(125.506238060706,3.35061628944766,127.201393521434));
#39816=CARTESIAN_POINT('Ctrl Pts',(125.498491784621,3.24875280385875,127.109280632382));
#39817=CARTESIAN_POINT('Ctrl Pts',(125.490745508537,3.14321705126064,127.021587873776));
#39818=CARTESIAN_POINT('Ctrl Pts',(125.482999175272,3.03768051962172,126.933894467841));
#39819=CARTESIAN_POINT('Ctrl Pts',(125.475252842007,2.92847196758488,126.850621507323));
#39820=CARTESIAN_POINT('Ctrl Pts',(125.467506508741,2.8160045969575,126.772078240002));
#39821=CARTESIAN_POINT('Ctrl Pts',(125.459758440738,2.70351204004265,126.693517383461));
#39822=CARTESIAN_POINT('Ctrl Pts',(125.452010372735,2.58775953281585,126.619688551576));
#39823=CARTESIAN_POINT('Ctrl Pts',(125.444262304732,2.46918914960827,126.550857589948));
#39824=CARTESIAN_POINT('Ctrl Pts',(125.436506001991,2.35049274838578,126.481953473954));
#39825=CARTESIAN_POINT('Ctrl Pts',(125.428749699249,2.2289728272646,126.418058035696));
#39826=CARTESIAN_POINT('Ctrl Pts',(125.420993396507,2.10509644245668,126.359391322908));
#39827=CARTESIAN_POINT('Ctrl Pts',(125.413232953993,1.98115394109267,126.300693297928));
#39828=CARTESIAN_POINT('Ctrl Pts',(125.405472511479,1.85485282979789,126.24722971151));
#39829=CARTESIAN_POINT('Ctrl Pts',(125.397712068964,1.72667909151098,126.1991719811));
#39830=CARTESIAN_POINT('Ctrl Pts',(125.389939168699,1.5982995973603,126.151037104154));
#39831=CARTESIAN_POINT('Ctrl Pts',(125.382166268433,1.46804184077466,126.108325546431));
#39832=CARTESIAN_POINT('Ctrl Pts',(125.374393368168,1.33640673556999,126.071158730933));
#39833=CARTESIAN_POINT('Ctrl Pts',(125.366903032406,1.20955689800798,126.035343022797));
#39834=CARTESIAN_POINT('Ctrl Pts',(125.359412696644,1.0814284129874,126.004675996831));
#39835=CARTESIAN_POINT('Ctrl Pts',(125.351922360882,0.952475530938753,125.979220886381));
#39836=CARTESIAN_POINT('Ctrl Pts',(125.344148026763,0.818633361173232,125.952800637681));
#39837=CARTESIAN_POINT('Ctrl Pts',(125.336373692644,0.683479074543296,125.931911634402));
#39838=CARTESIAN_POINT('Ctrl Pts',(125.328599358525,0.547509625850272,125.916680567471));
#39839=CARTESIAN_POINT('Ctrl Pts',(125.320834605577,0.411707747350917,125.901468271468));
#39840=CARTESIAN_POINT('Ctrl Pts',(125.31306985263,0.275093090476897,125.891900080925));
#39841=CARTESIAN_POINT('Ctrl Pts',(125.305305099683,0.138173910728253,125.888051937988));
#39842=CARTESIAN_POINT('Ctrl Pts',(125.297548058798,0.00139072103915638,
125.884207617081));
#39843=CARTESIAN_POINT('Ctrl Pts',(125.289791017913,-0.135696001340689,
125.886072048786));
#39844=CARTESIAN_POINT('Ctrl Pts',(125.282033977028,-0.27257210300288,125.893669473627));
#39845=CARTESIAN_POINT('Ctrl Pts',(125.274282785788,-0.409344985331323,
125.90126116919));
#39846=CARTESIAN_POINT('Ctrl Pts',(125.266531594548,-0.545907174300209,
125.914577231053));
#39847=CARTESIAN_POINT('Ctrl Pts',(125.258780403308,-0.681744093107058,
125.933589831128));
#39848=CARTESIAN_POINT('Ctrl Pts',(125.251032506531,-0.817523277600494,
125.952594350342));
#39849=CARTESIAN_POINT('Ctrl Pts',(125.243284609754,-0.952577418655537,
125.977290538144));
#39850=CARTESIAN_POINT('Ctrl Pts',(125.235536712977,-1.08639686115177,126.007598697001));
#39851=CARTESIAN_POINT('Ctrl Pts',(125.227790436893,-1.22018831150554,126.037900516045));
#39852=CARTESIAN_POINT('Ctrl Pts',(125.220044160809,-1.35274519595211,126.07381188488));
#39853=CARTESIAN_POINT('Ctrl Pts',(125.212297884724,-1.48356824948902,126.115202024427));
#39854=CARTESIAN_POINT('Ctrl Pts',(125.204551551459,-1.61439226873209,126.156592469507));
#39855=CARTESIAN_POINT('Ctrl Pts',(125.196805218194,-1.74348205877243,126.203461648067));
#39856=CARTESIAN_POINT('Ctrl Pts',(125.189058884928,-1.87035409502309,126.255629077705));
#39857=CARTESIAN_POINT('Ctrl Pts',(125.181310816925,-1.99725454338729,126.307808189876));
#39858=CARTESIAN_POINT('Ctrl Pts',(125.173562748922,-2.12193588816264,126.365287765485));
#39859=CARTESIAN_POINT('Ctrl Pts',(125.165814680919,-2.24393551394253,126.427839570916));
#39860=CARTESIAN_POINT('Ctrl Pts',(125.158058378177,-2.36606480237567,126.49045785715));
#39861=CARTESIAN_POINT('Ctrl Pts',(125.150302075436,-2.48550632984962,126.558158963301));
#39862=CARTESIAN_POINT('Ctrl Pts',(125.142545772694,-2.60182250868369,126.630668882925));
#39863=CARTESIAN_POINT('Ctrl Pts',(125.13478533018,-2.71820076896485,126.703217503277));
#39864=CARTESIAN_POINT('Ctrl Pts',(125.127024887665,-2.83145003411709,126.780579830863));
#39865=CARTESIAN_POINT('Ctrl Pts',(125.119264445151,-2.94116340013911,126.862439649791));
#39866=CARTESIAN_POINT('Ctrl Pts',(125.111491544886,-3.05105288779586,126.944430877367));
#39867=CARTESIAN_POINT('Ctrl Pts',(125.10371864462,-3.15739483011924,127.030933776837));
#39868=CARTESIAN_POINT('Ctrl Pts',(125.095945744355,-3.25981631434529,127.121592547319));
#39869=CARTESIAN_POINT('Ctrl Pts',(125.088455408593,-3.3585145196348,127.208955643138));
#39870=CARTESIAN_POINT('Ctrl Pts',(125.080965072831,-3.45357213297964,127.300177489754));
#39871=CARTESIAN_POINT('Ctrl Pts',(125.073474737069,-3.54469042092311,127.394910092582));
#39872=CARTESIAN_POINT('Ctrl Pts',(125.06580046413,-3.63804626419334,127.49196900602));
#39873=CARTESIAN_POINT('Ctrl Pts',(125.058126191191,-3.7275791791741,127.593038430459));
#39874=CARTESIAN_POINT('Ctrl Pts',(125.050451918251,-3.81291806288186,127.697780680038));
#39875=CARTESIAN_POINT('Ctrl Pts',(125.042786690845,-3.89815635911944,127.802399471735));
#39876=CARTESIAN_POINT('Ctrl Pts',(125.035121463439,-3.97921020139492,127.910682173425));
#39877=CARTESIAN_POINT('Ctrl Pts',(125.027456236033,-4.05574455568276,128.022253653132));
#39878=CARTESIAN_POINT('Ctrl Pts',(125.019798279898,-4.13220630911704,128.133719295602));
#39879=CARTESIAN_POINT('Ctrl Pts',(125.012140323763,-4.20415687476356,128.248467182711));
#39880=CARTESIAN_POINT('Ctrl Pts',(125.004482367629,-4.27130118908144,128.366088849561));
#39881=CARTESIAN_POINT('Ctrl Pts',(124.996830380284,-4.33839316955069,128.483618839333));
#39882=CARTESIAN_POINT('Ctrl Pts',(124.989178392939,-4.40068615589158,128.604017803311));
#39883=CARTESIAN_POINT('Ctrl Pts',(124.981526405594,-4.45792851807693,128.72684855016));
#39884=CARTESIAN_POINT('Ctrl Pts',(124.973877810681,-4.51514550244192,128.849624841245));
#39885=CARTESIAN_POINT('Ctrl Pts',(124.966229215767,-4.56731614805962,128.974830406805));
#39886=CARTESIAN_POINT('Ctrl Pts',(124.958580620853,-4.61423506686561,129.10200407142));
#39887=CARTESIAN_POINT('Ctrl Pts',(124.950933189818,-4.66114684606942,129.229158384152));
#39888=CARTESIAN_POINT('Ctrl Pts',(124.943285758782,-4.70280834798796,129.358279823902));
#39889=CARTESIAN_POINT('Ctrl Pts',(124.935638327747,-4.73906274128495,129.488888308217));
#39890=CARTESIAN_POINT('Ctrl Pts',(124.933816269092,-4.74770062645131,129.520006773778));
#39891=CARTESIAN_POINT('Ctrl Pts',(124.931994210437,-4.75603178956365,129.551209582994));
#39892=CARTESIAN_POINT('Ctrl Pts',(124.930172151781,-4.76405452823403,129.582490119308));
#39893=CARTESIAN_POINT('Origin',(213.235140564004,0.,130.804360617566));
#39894=CARTESIAN_POINT('',(122.834626183723,-4.76405452823408,129.582490119308));
#39895=CARTESIAN_POINT('',(123.180234630229,-4.76405452823405,129.582490119308));
#39896=CARTESIAN_POINT('',(213.235140564004,-4.76405452823405,129.582490119308));
#39897=CARTESIAN_POINT('',(124.514859435955,-4.91824949338178,130.802128275784));
#39898=CARTESIAN_POINT('Ctrl Pts',(124.514859435955,-4.91824949338178,130.802128275784));
#39899=CARTESIAN_POINT('Ctrl Pts',(124.507170124347,-4.91831079412571,130.937184813825));
#39900=CARTESIAN_POINT('Ctrl Pts',(124.499480812739,-4.91280485829688,131.07246854448));
#39901=CARTESIAN_POINT('Ctrl Pts',(124.49179150113,-4.9017018271335,131.207476308623));
#39902=CARTESIAN_POINT('Ctrl Pts',(124.484111153086,-4.89061173896633,131.34232669187));
#39903=CARTESIAN_POINT('Ctrl Pts',(124.476430805041,-4.87393756511142,131.476901353473));
#39904=CARTESIAN_POINT('Ctrl Pts',(124.468750456997,-4.85170143636514,131.610695681217));
#39905=CARTESIAN_POINT('Ctrl Pts',(124.461077128925,-4.82948563182929,131.744367718606));
#39906=CARTESIAN_POINT('Ctrl Pts',(124.453403800853,-4.80171805088814,131.877260448722));
#39907=CARTESIAN_POINT('Ctrl Pts',(124.445730472781,-4.76847270988192,132.008873414348));
#39908=CARTESIAN_POINT('Ctrl Pts',(124.43789673899,-4.73453239756891,132.143237659761));
#39909=CARTESIAN_POINT('Ctrl Pts',(124.430063005198,-4.69488278740763,132.276267617716));
#39910=CARTESIAN_POINT('Ctrl Pts',(124.422229271407,-4.64965792528211,132.407440228927));
#39911=CARTESIAN_POINT('Ctrl Pts',(124.414563307727,-4.60540161536512,132.535803599461));
#39912=CARTESIAN_POINT('Ctrl Pts',(124.406897344048,-4.55580659448187,132.662387982753));
#39913=CARTESIAN_POINT('Ctrl Pts',(124.399231380368,-4.50104900655704,132.786718028093));
#39914=CARTESIAN_POINT('Ctrl Pts',(124.391566171814,-4.44629681245654,132.911035826465));
#39915=CARTESIAN_POINT('Ctrl Pts',(124.38390096326,-4.38638322374303,133.033099362377));
#39916=CARTESIAN_POINT('Ctrl Pts',(124.376235754706,-4.32153231921454,133.152453775106));
#39917=CARTESIAN_POINT('Ctrl Pts',(124.368569555993,-4.2566730375258,133.271823605523));
#39918=CARTESIAN_POINT('Ctrl Pts',(124.360903357281,-4.18687536283241,133.388483265375));
#39919=CARTESIAN_POINT('Ctrl Pts',(124.353237158568,-4.11240880817546,133.50200345103));
#39920=CARTESIAN_POINT('Ctrl Pts',(124.34527746717,-4.03509137658085,133.619869642496));
#39921=CARTESIAN_POINT('Ctrl Pts',(124.337317775772,-3.9527407162197,133.734350795783));
#39922=CARTESIAN_POINT('Ctrl Pts',(124.329358084373,-3.8657064068974,133.845001510235));
#39923=CARTESIAN_POINT('Ctrl Pts',(124.321680515349,-3.78175693148386,133.95173033367));
#39924=CARTESIAN_POINT('Ctrl Pts',(124.314002946324,-3.69345047191876,134.054895356447));
#39925=CARTESIAN_POINT('Ctrl Pts',(124.3063253773,-3.60113970192494,134.154133133681));
#39926=CARTESIAN_POINT('Ctrl Pts',(124.298642580328,-3.50876607403826,134.253438485669));
#39927=CARTESIAN_POINT('Ctrl Pts',(124.290959783357,-3.41238299107311,134.348810988535));
#39928=CARTESIAN_POINT('Ctrl Pts',(124.283276986385,-3.31237767471077,134.439926213533));
#39929=CARTESIAN_POINT('Ctrl Pts',(124.275583724379,-3.21223613724717,134.531165550095));
#39930=CARTESIAN_POINT('Ctrl Pts',(124.267890462373,-3.10846282832349,134.618135785211));
#39931=CARTESIAN_POINT('Ctrl Pts',(124.260197200367,-3.00147560165349,134.700554564892));
#39932=CARTESIAN_POINT('Ctrl Pts',(124.259371754175,-2.98999643991024,134.709397662634));
#39933=CARTESIAN_POINT('Ctrl Pts',(124.258546307982,-2.97848030367339,134.718188406198));
#39934=CARTESIAN_POINT('Ctrl Pts',(124.25772086179,-2.96692772631653,134.726926477984));
#39935=CARTESIAN_POINT('Ctrl Pts',(124.249946527671,-2.85812160772622,134.809224621986));
#39936=CARTESIAN_POINT('Ctrl Pts',(124.242172193552,-2.745716311579,134.8871225106));
#39937=CARTESIAN_POINT('Ctrl Pts',(124.234397859433,-2.63010332833298,134.96028885862));
#39938=CARTESIAN_POINT('Ctrl Pts',(124.226633106486,-2.51463282775627,135.033365035656));
#39939=CARTESIAN_POINT('Ctrl Pts',(124.218868353539,-2.39596283294063,135.101721067383));
#39940=CARTESIAN_POINT('Ctrl Pts',(124.211103600591,-2.27451719297946,135.165066363353));
#39941=CARTESIAN_POINT('Ctrl Pts',(124.203346559706,-2.15319217454014,135.228348743882));
#39942=CARTESIAN_POINT('Ctrl Pts',(124.195589518821,-2.02909734153275,135.286630112939));
#39943=CARTESIAN_POINT('Ctrl Pts',(124.187832477936,-1.90268445981187,135.339663794741));
#39944=CARTESIAN_POINT('Ctrl Pts',(124.180081286696,-1.77636690702827,135.39265748343));
#39945=CARTESIAN_POINT('Ctrl Pts',(124.172330095456,-1.6477351440007,135.440411211034));
#39946=CARTESIAN_POINT('Ctrl Pts',(124.164578904216,-1.51726409073234,135.48272494086));
#39947=CARTESIAN_POINT('Ctrl Pts',(124.156831007439,-1.38684849114206,135.525020686223));
#39948=CARTESIAN_POINT('Ctrl Pts',(124.149083110662,-1.25459552726443,135.561880912126));
#39949=CARTESIAN_POINT('Ctrl Pts',(124.141335213885,-1.1209983794208,135.593154379656));
#39950=CARTESIAN_POINT('Ctrl Pts',(124.133588937801,-0.987429177220381,
135.624421305451));
#39951=CARTESIAN_POINT('Ctrl Pts',(124.125842661717,-0.852516730758256,
135.650103708287));
#39952=CARTESIAN_POINT('Ctrl Pts',(124.118096385632,-0.716767218410962,
135.670100830228));
#39953=CARTESIAN_POINT('Ctrl Pts',(124.110350052367,-0.581016703991329,
135.690098099783));
#39954=CARTESIAN_POINT('Ctrl Pts',(124.102603719102,-0.444429498147779,
135.704409947723));
#39955=CARTESIAN_POINT('Ctrl Pts',(124.094857385836,-0.307519363098675,
135.712987197763));
#39956=CARTESIAN_POINT('Ctrl Pts',(124.087109317833,-0.170578567974468,
135.721566368619));
#39957=CARTESIAN_POINT('Ctrl Pts',(124.07936124983,-0.0333150898662861,
135.724408361678));
#39958=CARTESIAN_POINT('Ctrl Pts',(124.071613181827,0.103755227135066,135.721516087484));
#39959=CARTESIAN_POINT('Ctrl Pts',(124.063856879086,0.240971224100578,135.718620739346));
#39960=CARTESIAN_POINT('Ctrl Pts',(124.056100576344,0.377993258361073,135.709978957901));
#39961=CARTESIAN_POINT('Ctrl Pts',(124.048344273602,0.514307972970508,135.695645762744));
#39962=CARTESIAN_POINT('Ctrl Pts',(124.040583831088,0.650695442847857,135.681304917529));
#39963=CARTESIAN_POINT('Ctrl Pts',(124.032823388573,0.786374454257362,135.661266662862));
#39964=CARTESIAN_POINT('Ctrl Pts',(124.025062946059,0.920840782211044,135.635637396671));
#39965=CARTESIAN_POINT('Ctrl Pts',(124.017290045794,1.05552296745144,135.609966988107));
#39966=CARTESIAN_POINT('Ctrl Pts',(124.009517145528,1.18898819822462,135.578687721994));
#39967=CARTESIAN_POINT('Ctrl Pts',(124.001744245263,1.3207455037904,135.541956461105));
#39968=CARTESIAN_POINT('Ctrl Pts',(123.994253909501,1.44771309942099,135.50656047407));
#39969=CARTESIAN_POINT('Ctrl Pts',(123.986763573739,1.5730944956195,135.466102092464));
#39970=CARTESIAN_POINT('Ctrl Pts',(123.979273237977,1.69646884389354,135.42076360303));
#39971=CARTESIAN_POINT('Ctrl Pts',(123.971498903858,1.82452096808229,135.373706090987));
#39972=CARTESIAN_POINT('Ctrl Pts',(123.963724569739,1.9508164761754,135.321242043413));
#39973=CARTESIAN_POINT('Ctrl Pts',(123.95595023562,2.07486503839237,135.263521764571));
#39974=CARTESIAN_POINT('Ctrl Pts',(123.948185482673,2.19876072184295,135.205872620814));
#39975=CARTESIAN_POINT('Ctrl Pts',(123.940420729726,2.3204146181523,135.142980298104));
#39976=CARTESIAN_POINT('Ctrl Pts',(123.932655976778,2.43935314455744,135.075044321452));
#39977=CARTESIAN_POINT('Ctrl Pts',(123.924898935894,2.55817353954084,135.00717581977));
#39978=CARTESIAN_POINT('Ctrl Pts',(123.917141895009,2.67428359436808,134.93427382579));
#39979=CARTESIAN_POINT('Ctrl Pts',(123.909384854124,2.78723158323549,134.856585088633));
#39980=CARTESIAN_POINT('Ctrl Pts',(123.901633662883,2.90009439714611,134.778954937157));
#39981=CARTESIAN_POINT('Ctrl Pts',(123.893882471643,3.00979957055717,134.696545448101));
#39982=CARTESIAN_POINT('Ctrl Pts',(123.886131280403,3.115922101071,134.609648060396));
#39983=CARTESIAN_POINT('Ctrl Pts',(123.878383383626,3.2219995266786,134.522787606398));
#39984=CARTESIAN_POINT('Ctrl Pts',(123.870635486849,3.3244970361011,134.431443294751));
#39985=CARTESIAN_POINT('Ctrl Pts',(123.862887590072,3.42302081174617,134.3359483037));
#39986=CARTESIAN_POINT('Ctrl Pts',(123.855141313988,3.52152397834137,134.240473288142));
#39987=CARTESIAN_POINT('Ctrl Pts',(123.847395037904,3.61605478394241,134.140849592074));
#39988=CARTESIAN_POINT('Ctrl Pts',(123.83964876182,3.70625485626919,134.037448615577));
#39989=CARTESIAN_POINT('Ctrl Pts',(123.831902428554,3.79645559443236,133.934046875797));
#39990=CARTESIAN_POINT('Ctrl Pts',(123.824156095289,3.88232527852341,133.826868094568));
#39991=CARTESIAN_POINT('Ctrl Pts',(123.816409762024,3.96354483411237,133.716317933613));
#39992=CARTESIAN_POINT('Ctrl Pts',(123.808661694021,4.04478257825766,133.605743015716));
#39993=CARTESIAN_POINT('Ctrl Pts',(123.800913626018,4.1213678902718,133.491795530748));
#39994=CARTESIAN_POINT('Ctrl Pts',(123.793165558015,4.1930243925468,133.374911046172));
#39995=CARTESIAN_POINT('Ctrl Pts',(123.785409255273,4.26475705220518,133.257902335375));
#39996=CARTESIAN_POINT('Ctrl Pts',(123.777652952531,4.33155023319489,133.137950723328));
#39997=CARTESIAN_POINT('Ctrl Pts',(123.769896649789,4.39317274309023,133.015517851204));
#39998=CARTESIAN_POINT('Ctrl Pts',(123.762136207275,4.45482814277455,132.893019632969));
#39999=CARTESIAN_POINT('Ctrl Pts',(123.754375764761,4.51130721142138,132.768037871932));
#40000=CARTESIAN_POINT('Ctrl Pts',(123.746615322247,4.56242691869805,132.641054297535));
#40001=CARTESIAN_POINT('Ctrl Pts',(123.738842421981,4.61362868786701,132.513866877832));
#40002=CARTESIAN_POINT('Ctrl Pts',(123.731069521716,4.65945377271454,132.384671591879));
#40003=CARTESIAN_POINT('Ctrl Pts',(123.72329662145,4.69976876465451,132.253966295424));
#40004=CARTESIAN_POINT('Ctrl Pts',(123.715806285688,4.73861820509072,132.12801246572));
#40005=CARTESIAN_POINT('Ctrl Pts',(123.708315949926,4.77235113006234,132.000656802601));
#40006=CARTESIAN_POINT('Ctrl Pts',(123.700825614164,4.80089342367698,131.872351908259));
#40007=CARTESIAN_POINT('Ctrl Pts',(123.693051280045,4.83051790702883,131.739182294851));
#40008=CARTESIAN_POINT('Ctrl Pts',(123.685276945926,4.8546442250089,131.604568207798));
#40009=CARTESIAN_POINT('Ctrl Pts',(123.677502611807,4.87313379762867,131.469003418557));
#40010=CARTESIAN_POINT('Ctrl Pts',(123.66973785886,4.89160058350265,131.333605700803));
#40011=CARTESIAN_POINT('Ctrl Pts',(123.661973105913,4.90444439372064,131.197259995765));
#40012=CARTESIAN_POINT('Ctrl Pts',(123.654208352965,4.91157711127343,131.060472590178));
#40013=CARTESIAN_POINT('Ctrl Pts',(123.64645131208,4.91870274451059,130.92382104377));
#40014=CARTESIAN_POINT('Ctrl Pts',(123.638694271195,4.92012855306334,130.786729057759));
#40015=CARTESIAN_POINT('Ctrl Pts',(123.63093723031,4.91581796512449,130.649710055785));
#40016=CARTESIAN_POINT('Ctrl Pts',(123.62318603907,4.91151062783351,130.512794380905));
#40017=CARTESIAN_POINT('Ctrl Pts',(123.61543484783,4.90147551665914,130.375951969703));
#40018=CARTESIAN_POINT('Ctrl Pts',(123.60768365659,4.88572810325017,130.239697918593));
#40019=CARTESIAN_POINT('Ctrl Pts',(123.599935759813,4.86998738291205,130.10350177909));
#40020=CARTESIAN_POINT('Ctrl Pts',(123.592187863036,4.84853923400185,129.967893889879));
#40021=CARTESIAN_POINT('Ctrl Pts',(123.584439966259,4.82145110078454,129.833385671832));
#40022=CARTESIAN_POINT('Ctrl Pts',(123.576693690175,4.7943686338207,129.698905590004));
#40023=CARTESIAN_POINT('Ctrl Pts',(123.568947414091,4.76164860629984,129.565525104832));
#40024=CARTESIAN_POINT('Ctrl Pts',(123.561201138006,4.72340977865622,129.433746475878));
#40025=CARTESIAN_POINT('Ctrl Pts',(123.553454804741,4.68517066874234,129.301966874165));
#40026=CARTESIAN_POINT('Ctrl Pts',(123.545708471476,4.64141278636882,129.171789527742));
#40027=CARTESIAN_POINT('Ctrl Pts',(123.53796213821,4.59230495870758,129.043702153034));
#40028=CARTESIAN_POINT('Ctrl Pts',(123.530214070207,4.5431861336888,128.915586094046));
#40029=CARTESIAN_POINT('Ctrl Pts',(123.522466002204,4.4887151192683,128.789561303092));
#40030=CARTESIAN_POINT('Ctrl Pts',(123.514717934201,4.42910898184085,128.666095739335));
#40031=CARTESIAN_POINT('Ctrl Pts',(123.50696163146,4.36943949430127,128.542498954908));
#40032=CARTESIAN_POINT('Ctrl Pts',(123.499205328718,4.30462415171893,128.421467183767));
#40033=CARTESIAN_POINT('Ctrl Pts',(123.491449025976,4.23492638073328,128.30344446298));
#40034=CARTESIAN_POINT('Ctrl Pts',(123.483688583462,4.16519140994861,128.185358749913));
#40035=CARTESIAN_POINT('Ctrl Pts',(123.475928140947,4.09056903090241,128.0702856152));
#40036=CARTESIAN_POINT('Ctrl Pts',(123.468167698433,4.01136560385153,127.958639433975));
#40037=CARTESIAN_POINT('Ctrl Pts',(123.460394798168,3.93203503242825,127.846814028389));
#40038=CARTESIAN_POINT('Ctrl Pts',(123.452621897902,3.84810895705507,127.738426878845));
#40039=CARTESIAN_POINT('Ctrl Pts',(123.444848997637,3.75993412727321,127.633859328958));
#40040=CARTESIAN_POINT('Ctrl Pts',(123.437358661875,3.67496467465328,127.533093072899));
#40041=CARTESIAN_POINT('Ctrl Pts',(123.429868326113,3.58605021829274,127.435873761006));
#40042=CARTESIAN_POINT('Ctrl Pts',(123.422377990351,3.49353148378359,127.342508391616));
#40043=CARTESIAN_POINT('Ctrl Pts',(123.414603656232,3.39750487333459,127.245603045868));
#40044=CARTESIAN_POINT('Ctrl Pts',(123.406829322113,3.29729109361403,127.152542689075));
#40045=CARTESIAN_POINT('Ctrl Pts',(123.399054987994,3.19323066266481,127.063710808039));
#40046=CARTESIAN_POINT('Ctrl Pts',(123.391290235047,3.0892984768965,126.974988404357));
#40047=CARTESIAN_POINT('Ctrl Pts',(123.3835254821,2.98152936688766,126.890484359063));
#40048=CARTESIAN_POINT('Ctrl Pts',(123.375760729152,2.87030165660958,126.810546467838));
#40049=CARTESIAN_POINT('Ctrl Pts',(123.368003688267,2.75918441926176,126.730687972055));
#40050=CARTESIAN_POINT('Ctrl Pts',(123.360246647382,2.64461573313438,126.655386831842));
#40051=CARTESIAN_POINT('Ctrl Pts',(123.352489606497,2.52700778812089,126.584951334115));
#40052=CARTESIAN_POINT('Ctrl Pts',(123.344738415257,2.40948853217287,126.514568952344));
#40053=CARTESIAN_POINT('Ctrl Pts',(123.336987224017,2.28893491333921,126.449045109768));
#40054=CARTESIAN_POINT('Ctrl Pts',(123.329236032777,2.16578865962575,126.388645211843));
#40055=CARTESIAN_POINT('Ctrl Pts',(123.321488136,2.04269474635566,126.328270985487));
#40056=CARTESIAN_POINT('Ctrl Pts',(123.313740239223,1.91701074016089,126.273016544083));
#40057=CARTESIAN_POINT('Ctrl Pts',(123.305992342446,1.78920336917902,126.223101580334));
#40058=CARTESIAN_POINT('Ctrl Pts',(123.298246066362,1.66142273274387,126.17319705772));
#40059=CARTESIAN_POINT('Ctrl Pts',(123.290499790277,1.53151997893062,126.128629933317));
#40060=CARTESIAN_POINT('Ctrl Pts',(123.282753514193,1.39998186585056,126.089571774172));
#40061=CARTESIAN_POINT('Ctrl Pts',(123.275007180928,1.26844278178604,126.050513326709));
#40062=CARTESIAN_POINT('Ctrl Pts',(123.267260847663,1.13526868915776,126.016964036937));
#40063=CARTESIAN_POINT('Ctrl Pts',(123.259514514397,1.00096117281618,125.989045488417));
#40064=CARTESIAN_POINT('Ctrl Pts',(123.251766446394,0.866623579237726,125.961120687731));
#40065=CARTESIAN_POINT('Ctrl Pts',(123.244018378391,0.7311524395782,125.938829217025));
#40066=CARTESIAN_POINT('Ctrl Pts',(123.236270310388,0.595058790822629,125.922241395551));
#40067=CARTESIAN_POINT('Ctrl Pts',(123.228514007647,0.458820500117439,125.905635944344));
#40068=CARTESIAN_POINT('Ctrl Pts',(123.220757704905,0.321958767390716,125.894746299058));
#40069=CARTESIAN_POINT('Ctrl Pts',(123.213001402163,0.184989562134513,125.88959084428));
#40070=CARTESIAN_POINT('Ctrl Pts',(123.205240959649,0.0479472522894938,
125.884432637882));
#40071=CARTESIAN_POINT('Ctrl Pts',(123.197480517134,-0.089202253611909,
125.885014718659));
#40072=CARTESIAN_POINT('Ctrl Pts',(123.18972007462,-0.225944734832842,125.891303316933));
#40073=CARTESIAN_POINT('Ctrl Pts',(123.181947174355,-0.36290672722415,125.897602010223));
#40074=CARTESIAN_POINT('Ctrl Pts',(123.174174274089,-0.499459999566706,
125.909625492513));
#40075=CARTESIAN_POINT('Ctrl Pts',(123.166401373824,-0.635096290080667,
125.927288159131));
#40076=CARTESIAN_POINT('Ctrl Pts',(123.158911038062,-0.76580185978642,125.944308743328));
#40077=CARTESIAN_POINT('Ctrl Pts',(123.1514207023,-0.895655655795518,125.96656558086));
#40078=CARTESIAN_POINT('Ctrl Pts',(123.143930366538,-1.02421522120527,125.993937949738));
#40079=CARTESIAN_POINT('Ctrl Pts',(123.136156032419,-1.15764916161348,126.022348150302));
#40080=CARTESIAN_POINT('Ctrl Pts',(123.1283816983,-1.29011147118705,126.056359445411));
#40081=CARTESIAN_POINT('Ctrl Pts',(123.120607364181,-1.42109545329787,126.095892631574));
#40082=CARTESIAN_POINT('Ctrl Pts',(123.112842611234,-1.55191800935639,126.135377096617));
#40083=CARTESIAN_POINT('Ctrl Pts',(123.105077858287,-1.68126549230711,126.18036980044));
#40084=CARTESIAN_POINT('Ctrl Pts',(123.09731310534,-1.80864079844571,126.230740440431));
#40085=CARTESIAN_POINT('Ctrl Pts',(123.089556064455,-1.93588959363475,126.281061051592));
#40086=CARTESIAN_POINT('Ctrl Pts',(123.08179902357,-2.06116974888277,126.336748826367));
#40087=CARTESIAN_POINT('Ctrl Pts',(123.074041982685,-2.18399909497111,126.397623614333));
#40088=CARTESIAN_POINT('Ctrl Pts',(123.066290791445,-2.30673581449443,126.458452496148));
#40089=CARTESIAN_POINT('Ctrl Pts',(123.058539600204,-2.42702505465063,126.524460432507));
#40090=CARTESIAN_POINT('Ctrl Pts',(123.050788408964,-2.54440475753456,126.595419243261));
#40091=CARTESIAN_POINT('Ctrl Pts',(123.043040512187,-2.6617345709134,126.666347894628));
#40092=CARTESIAN_POINT('Ctrl Pts',(123.03529261541,-2.77615697270482,126.742223033352));
#40093=CARTESIAN_POINT('Ctrl Pts',(123.027544718633,-2.88723485125613,126.822770737105));
#40094=CARTESIAN_POINT('Ctrl Pts',(123.019798442549,-2.99828949470972,126.903301592014));
#40095=CARTESIAN_POINT('Ctrl Pts',(123.012052166465,-3.10600069016326,126.988502838482));
#40096=CARTESIAN_POINT('Ctrl Pts',(123.004305890381,-3.20996098875319,127.078057689303));
#40097=CARTESIAN_POINT('Ctrl Pts',(122.996559557115,-3.31392205475493,127.167613201197));
#40098=CARTESIAN_POINT('Ctrl Pts',(122.98881322385,-3.41413187242903,127.261522126404));
#40099=CARTESIAN_POINT('Ctrl Pts',(122.981066890585,-3.51021703122026,127.359428186265));
#40100=CARTESIAN_POINT('Ctrl Pts',(122.973318822582,-3.60632370761607,127.457356171509));
#40101=CARTESIAN_POINT('Ctrl Pts',(122.965570754579,-3.69830361330064,127.55928279363));
#40102=CARTESIAN_POINT('Ctrl Pts',(122.957822686576,-3.78582135872236,127.664816112014));
#40103=CARTESIAN_POINT('Ctrl Pts',(122.950066383834,-3.8734321190455,127.770461592465));
#40104=CARTESIAN_POINT('Ctrl Pts',(122.942310081092,-3.95657099560802,127.879721125062));
#40105=CARTESIAN_POINT('Ctrl Pts',(122.93455377835,-4.03494362682191,127.992170547377));
#40106=CARTESIAN_POINT('Ctrl Pts',(122.926793335836,-4.11335808786905,128.104679987335));
#40107=CARTESIAN_POINT('Ctrl Pts',(122.919032893322,-4.18700102482841,128.220382379805));
#40108=CARTESIAN_POINT('Ctrl Pts',(122.911272450808,-4.25562290021923,128.338826842979));
#40109=CARTESIAN_POINT('Ctrl Pts',(122.903499550542,-4.32435493353634,128.45746144372));
#40110=CARTESIAN_POINT('Ctrl Pts',(122.895726650277,-4.38804961656374,128.578846564999));
#40111=CARTESIAN_POINT('Ctrl Pts',(122.887953750011,-4.44650424302869,128.70250832037));
#40112=CARTESIAN_POINT('Ctrl Pts',(122.880463414249,-4.5028338965828,128.821674659447));
#40113=CARTESIAN_POINT('Ctrl Pts',(122.872973078488,-4.55429773741881,128.942954700019));
#40114=CARTESIAN_POINT('Ctrl Pts',(122.865482742726,-4.60075817360164,129.06591093738));
#40115=CARTESIAN_POINT('Ctrl Pts',(122.856565377702,-4.65607006905499,129.212292312697));
#40116=CARTESIAN_POINT('Ctrl Pts',(122.847648012679,-4.70443694400042,129.361434294279));
#40117=CARTESIAN_POINT('Ctrl Pts',(122.838730647656,-4.74561132962465,129.512711992499));
#40118=CARTESIAN_POINT('Ctrl Pts',(122.837362493012,-4.75192854628791,129.535921907631));
#40119=CARTESIAN_POINT('Ctrl Pts',(122.835994338368,-4.75807654452855,129.559182051569));
#40120=CARTESIAN_POINT('Ctrl Pts',(122.834626183723,-4.76405452823408,129.582490119308));
#40121=CARTESIAN_POINT('Ctrl Pts',(124.584949745809,-4.76405452823405,129.582490119308));
#40122=CARTESIAN_POINT('Ctrl Pts',(124.576819535775,-4.79969206700382,129.721440342096));
#40123=CARTESIAN_POINT('Ctrl Pts',(124.56868932574,-4.82920735029006,129.861801844806));
#40124=CARTESIAN_POINT('Ctrl Pts',(124.560559115706,-4.85252381590777,130.002989493462));
#40125=CARTESIAN_POINT('Ctrl Pts',(124.552428905671,-4.87584028152547,130.144177142117));
#40126=CARTESIAN_POINT('Ctrl Pts',(124.544298695637,-4.89295794227717,130.286190445843));
#40127=CARTESIAN_POINT('Ctrl Pts',(124.536168485602,-4.90386265852004,130.428442955208));
#40128=CARTESIAN_POINT('Ctrl Pts',(124.529065469065,-4.91338964238377,130.552722884288));
#40129=CARTESIAN_POINT('Ctrl Pts',(124.521962452528,-4.91819286668434,130.677369535755));
#40130=CARTESIAN_POINT('Ctrl Pts',(124.514859435991,-4.9182494933815,130.802128275159));
#40131=CARTESIAN_POINT('',(124.860140563954,-4.91824790038655,130.808905157512));
#40132=CARTESIAN_POINT('Ctrl Pts',(124.930172151781,-4.76405452823403,129.582490119308));
#40133=CARTESIAN_POINT('Ctrl Pts',(124.922522261014,-4.79773789748411,129.713821064798));
#40134=CARTESIAN_POINT('Ctrl Pts',(124.914872370247,-4.82598054335935,129.846522875123));
#40135=CARTESIAN_POINT('Ctrl Pts',(124.907222479479,-4.84868809827559,129.980099258445));
#40136=CARTESIAN_POINT('Ctrl Pts',(124.899375493568,-4.8719807006071,130.117117162357));
#40137=CARTESIAN_POINT('Ctrl Pts',(124.891528507656,-4.88944903983335,130.255054876221));
#40138=CARTESIAN_POINT('Ctrl Pts',(124.883681521744,-4.90104783706232,130.393370153775));
#40139=CARTESIAN_POINT('Ctrl Pts',(124.875834535832,-4.9126466342913,130.53168543133));
#40140=CARTESIAN_POINT('Ctrl Pts',(124.86798754992,-4.91837590184352,130.670377817801));
#40141=CARTESIAN_POINT('Ctrl Pts',(124.860140564008,-4.91824790038743,130.80890515656));
#40142=CARTESIAN_POINT('Ctrl Pts',(124.860140563954,-4.91824790038655,130.808905157512));
#40143=CARTESIAN_POINT('Ctrl Pts',(124.849923153069,-4.91808123209384,130.989278966611));
#40144=CARTESIAN_POINT('Ctrl Pts',(124.839705742184,-4.90798857365373,131.169211590381));
#40145=CARTESIAN_POINT('Ctrl Pts',(124.8294883313,-4.88813519968135,131.347791691518));
#40146=CARTESIAN_POINT('Ctrl Pts',(124.818986074523,-4.86772834380638,131.531350334552));
#40147=CARTESIAN_POINT('Ctrl Pts',(124.808483817746,-4.83700889931984,131.713480411591));
#40148=CARTESIAN_POINT('Ctrl Pts',(124.797981560969,-4.79620387198005,131.893218496678));
#40149=CARTESIAN_POINT('Ctrl Pts',(124.796996745065,-4.79237750963129,131.910072866991));
#40150=CARTESIAN_POINT('Ctrl Pts',(124.79601192916,-4.78846249740315,131.926906219906));
#40151=CARTESIAN_POINT('Ctrl Pts',(124.795027113256,-4.78445904371179,131.943717770326));
#40152=CARTESIAN_POINT('Ctrl Pts',(124.787252779137,-4.75285497793157,132.076431518577));
#40153=CARTESIAN_POINT('Ctrl Pts',(124.779478445018,-4.71567474704518,132.208039504975));
#40154=CARTESIAN_POINT('Ctrl Pts',(124.771704110899,-4.67300969105515,132.338037079472));
#40155=CARTESIAN_POINT('Ctrl Pts',(124.763939357952,-4.63039721593357,132.467874443577));
#40156=CARTESIAN_POINT('Ctrl Pts',(124.756174605005,-4.58231348595731,132.596104976815));
#40157=CARTESIAN_POINT('Ctrl Pts',(124.748409852058,-4.52890069533131,132.72223484554));
#40158=CARTESIAN_POINT('Ctrl Pts',(124.740652811173,-4.47554095504197,132.848239440302));
#40159=CARTESIAN_POINT('Ctrl Pts',(124.732895770288,-4.41686283867964,132.972147164914));
#40160=CARTESIAN_POINT('Ctrl Pts',(124.725138729403,-4.35305801552037,133.093480312124));
#40161=CARTESIAN_POINT('Ctrl Pts',(124.717387538162,-4.28930130807453,133.214721961065));
#40162=CARTESIAN_POINT('Ctrl Pts',(124.709636346922,-4.22042577028052,133.333392552423));
#40163=CARTESIAN_POINT('Ctrl Pts',(124.701885155682,-4.14667060469276,133.449035637049));
#40164=CARTESIAN_POINT('Ctrl Pts',(124.694137258905,-4.07294678701781,133.564629570279));
#40165=CARTESIAN_POINT('Ctrl Pts',(124.686389362128,-3.99434767631359,133.677198227128));
#40166=CARTESIAN_POINT('Ctrl Pts',(124.678641465351,-3.91115760549944,133.786311195199));
#40167=CARTESIAN_POINT('Ctrl Pts',(124.670895189267,-3.82798493625478,133.895401339189));
#40168=CARTESIAN_POINT('Ctrl Pts',(124.663148913183,-3.74022345394225,134.00103692149));
#40169=CARTESIAN_POINT('Ctrl Pts',(124.655402637099,-3.64819963218999,134.102818212593));
#40170=CARTESIAN_POINT('Ctrl Pts',(124.647656303833,-3.55617513113883,134.204600255022));
#40171=CARTESIAN_POINT('Ctrl Pts',(124.639909970568,-3.45988849006804,134.302527659474));
#40172=CARTESIAN_POINT('Ctrl Pts',(124.632163637303,-3.35970484585868,134.396235672633));
#40173=CARTESIAN_POINT('Ctrl Pts',(124.6244155693,-3.25949876621689,134.489964671052));
#40174=CARTESIAN_POINT('Ctrl Pts',(124.616667501297,-3.15539423232435,134.579472130908));
#40175=CARTESIAN_POINT('Ctrl Pts',(124.608919433294,-3.04779112035167,134.664432164727));
#40176=CARTESIAN_POINT('Ctrl Pts',(124.601163130552,-2.94007364651095,134.749482495082));
#40177=CARTESIAN_POINT('Ctrl Pts',(124.59340682781,-2.82885047416152,134.829975502182));
#40178=CARTESIAN_POINT('Ctrl Pts',(124.585650525068,-2.71455270744954,134.905627087936));
#40179=CARTESIAN_POINT('Ctrl Pts',(124.577890082554,-2.60019393657795,134.981319051219));
#40180=CARTESIAN_POINT('Ctrl Pts',(124.57012964004,-2.48275763610817,135.052164242439));
#40181=CARTESIAN_POINT('Ctrl Pts',(124.562369197526,-2.36270054621509,135.117924015896));
#40182=CARTESIAN_POINT('Ctrl Pts',(124.55459629726,-2.24245073002315,135.18378935278));
#40183=CARTESIAN_POINT('Ctrl Pts',(124.546823396995,-2.11957206789316,135.244552785097));
#40184=CARTESIAN_POINT('Ctrl Pts',(124.539050496729,-1.99454317419499,135.300023036918));
#40185=CARTESIAN_POINT('Ctrl Pts',(124.531560160967,-1.8740593957116,135.353476805364));
#40186=CARTESIAN_POINT('Ctrl Pts',(124.524069825205,-1.75157929051489,135.402015439318));
#40187=CARTESIAN_POINT('Ctrl Pts',(124.516579489443,-1.62754353914853,135.445511885374));
#40188=CARTESIAN_POINT('Ctrl Pts',(124.508805155324,-1.49880493456936,135.490657512403));
#40189=CARTESIAN_POINT('Ctrl Pts',(124.501030821205,-1.36798258530955,135.530514062511));
#40190=CARTESIAN_POINT('Ctrl Pts',(124.493256487086,-1.23555043924825,135.564885606953));
#40191=CARTESIAN_POINT('Ctrl Pts',(124.485491734139,-1.10328150397109,135.599214791537));
#40192=CARTESIAN_POINT('Ctrl Pts',(124.477726981192,-0.969407094117519,
135.628072323127));
#40193=CARTESIAN_POINT('Ctrl Pts',(124.469962228245,-0.834419545362218,
135.651310904583));
#40194=CARTESIAN_POINT('Ctrl Pts',(124.46220518736,-0.699566068143424,135.674526405153));
#40195=CARTESIAN_POINT('Ctrl Pts',(124.454448146475,-0.563602034991586,
135.692133995775));
#40196=CARTESIAN_POINT('Ctrl Pts',(124.44669110559,-0.427032956473006,135.704036720798));
#40197=CARTESIAN_POINT('Ctrl Pts',(124.43893991435,-0.290566865758703,135.715930469885));
#40198=CARTESIAN_POINT('Ctrl Pts',(124.43118872311,-0.153497025767011,135.722127882601));
#40199=CARTESIAN_POINT('Ctrl Pts',(124.423437531869,-0.0163367549181919,
135.722583484917));
#40200=CARTESIAN_POINT('Ctrl Pts',(124.415689635092,0.120765219156459,135.72303889359));
#40201=CARTESIAN_POINT('Ctrl Pts',(124.407941738315,0.257957157498372,135.717757344381));
#40202=CARTESIAN_POINT('Ctrl Pts',(124.400193841538,0.394723253081784,135.706745406215));
#40203=CARTESIAN_POINT('Ctrl Pts',(124.392447565454,0.531460740146428,135.695735771509));
#40204=CARTESIAN_POINT('Ctrl Pts',(124.38470128937,0.667772172174718,135.678998163431));
#40205=CARTESIAN_POINT('Ctrl Pts',(124.376955013286,0.803144778439342,135.656591189928));
#40206=CARTESIAN_POINT('Ctrl Pts',(124.369208680021,0.938518383993701,135.634184051022));
#40207=CARTESIAN_POINT('Ctrl Pts',(124.361462346755,1.07295276423854,135.606107527026));
#40208=CARTESIAN_POINT('Ctrl Pts',(124.35371601349,1.20594367647488,135.572471659863));
#40209=CARTESIAN_POINT('Ctrl Pts',(124.345967945487,1.33896437110383,135.53882826018));
#40210=CARTESIAN_POINT('Ctrl Pts',(124.338219877484,1.47054057552723,135.499623135816));
#40211=CARTESIAN_POINT('Ctrl Pts',(124.330471809481,1.60018196854618,135.455016563778));
#40212=CARTESIAN_POINT('Ctrl Pts',(124.322715506739,1.72996114598048,135.410362583345));
#40213=CARTESIAN_POINT('Ctrl Pts',(124.314959203998,1.85780103396559,135.360295814932));
#40214=CARTESIAN_POINT('Ctrl Pts',(124.307202901256,1.98322959041068,135.305025396709));
#40215=CARTESIAN_POINT('Ctrl Pts',(124.299442458742,2.10872509185302,135.249725479));
#40216=CARTESIAN_POINT('Ctrl Pts',(124.291682016227,2.23180634661166,135.18921654979));
#40217=CARTESIAN_POINT('Ctrl Pts',(124.283921573713,2.35202569607938,135.123753883695));
#40218=CARTESIAN_POINT('Ctrl Pts',(124.276148673448,2.47243803231935,135.058186131117));
#40219=CARTESIAN_POINT('Ctrl Pts',(124.268375773182,2.58997894719704,134.987648951959));
#40220=CARTESIAN_POINT('Ctrl Pts',(124.260602872917,2.70422881209734,134.912441628734));
#40221=CARTESIAN_POINT('Ctrl Pts',(124.253112537155,2.81432540663117,134.839968281144));
#40222=CARTESIAN_POINT('Ctrl Pts',(124.245622201393,2.92136582266444,134.763158617099));
#40223=CARTESIAN_POINT('Ctrl Pts',(124.238131865631,3.02500496797082,134.682314718152));
#40224=CARTESIAN_POINT('Ctrl Pts',(124.230357531512,3.13257362297132,134.598405598205));
#40225=CARTESIAN_POINT('Ctrl Pts',(124.222583197393,3.23681874266201,134.509884489575));
#40226=CARTESIAN_POINT('Ctrl Pts',(124.214808863274,3.3373193062344,134.417044233763));
#40227=CARTESIAN_POINT('Ctrl Pts',(124.207044110327,3.43769601184418,134.324318395268));
#40228=CARTESIAN_POINT('Ctrl Pts',(124.199279357379,3.53433705904816,134.227284263446));
#40229=CARTESIAN_POINT('Ctrl Pts',(124.191514604432,3.62685240313502,134.126276436544));
#40230=CARTESIAN_POINT('Ctrl Pts',(124.183757563547,3.71927585967788,134.025368932039));
#40231=CARTESIAN_POINT('Ctrl Pts',(124.176000522662,3.80758150536502,133.920495873066));
#40232=CARTESIAN_POINT('Ctrl Pts',(124.168243481777,3.89141452785478,133.812030153087));
#40233=CARTESIAN_POINT('Ctrl Pts',(124.160492290537,3.97518433121009,133.703646227951));
#40234=CARTESIAN_POINT('Ctrl Pts',(124.152741099297,4.05448798668088,133.5916753425));
#40235=CARTESIAN_POINT('Ctrl Pts',(124.144989908057,4.12900977453227,133.476524786235));
#40236=CARTESIAN_POINT('Ctrl Pts',(124.13724201128,4.20349988863593,133.361423172028));
#40237=CARTESIAN_POINT('Ctrl Pts',(124.129494114503,4.27321196547824,133.243144902466));
#40238=CARTESIAN_POINT('Ctrl Pts',(124.121746217726,4.3378727253851,133.122127491274));
#40239=CARTESIAN_POINT('Ctrl Pts',(124.113999941642,4.40251995965491,133.001135394316));
#40240=CARTESIAN_POINT('Ctrl Pts',(124.106253665558,4.46211779454859,132.877405640006));
#40241=CARTESIAN_POINT('Ctrl Pts',(124.098507389473,4.51643837348782,132.751401315905));
#40242=CARTESIAN_POINT('Ctrl Pts',(124.090761056208,4.57075935340923,132.625396061668));
#40243=CARTESIAN_POINT('Ctrl Pts',(124.083014722943,4.61980284486769,132.497116563162));
#40244=CARTESIAN_POINT('Ctrl Pts',(124.075268389677,4.66338887375304,132.367046534395));
#40245=CARTESIAN_POINT('Ctrl Pts',(124.067520321674,4.70698466342732,132.236947377348));
#40246=CARTESIAN_POINT('Ctrl Pts',(124.059772253671,4.74512043437139,132.105057262777));
#40247=CARTESIAN_POINT('Ctrl Pts',(124.052024185668,4.7776660015863,131.971875345433));
#40248=CARTESIAN_POINT('Ctrl Pts',(124.044267882927,4.81024615861737,131.838551880762));
#40249=CARTESIAN_POINT('Ctrl Pts',(124.036511580185,4.83722415050561,131.70393425111));
#40250=CARTESIAN_POINT('Ctrl Pts',(124.028755277443,4.85852078083644,131.568532643147));
#40251=CARTESIAN_POINT('Ctrl Pts',(124.020994834929,4.87982877782012,131.433058767269));
#40252=CARTESIAN_POINT('Ctrl Pts',(124.013234392415,4.89544932659802,131.296800467547));
#40253=CARTESIAN_POINT('Ctrl Pts',(124.0054739499,4.90535522652129,131.160272354012));
#40254=CARTESIAN_POINT('Ctrl Pts',(123.997701049635,4.91527702827452,131.023525073429));
#40255=CARTESIAN_POINT('Ctrl Pts',(123.98992814937,4.91946583732034,130.886507504509));
#40256=CARTESIAN_POINT('Ctrl Pts',(123.982155249104,4.91794662899568,130.7497344622));
#40257=CARTESIAN_POINT('Ctrl Pts',(123.974664913342,4.91648264772027,130.61793346449));
#40258=CARTESIAN_POINT('Ctrl Pts',(123.96717457758,4.90971846146985,130.486359831343));
#40259=CARTESIAN_POINT('Ctrl Pts',(123.959684241818,4.89772168923275,130.355467181081));
#40260=CARTESIAN_POINT('Ctrl Pts',(123.951909907699,4.88527005572995,130.219611696201));
#40261=CARTESIAN_POINT('Ctrl Pts',(123.94413557358,4.86714177351287,130.084059503168));
#40262=CARTESIAN_POINT('Ctrl Pts',(123.936361239461,4.8433556463987,129.949323106694));
#40263=CARTESIAN_POINT('Ctrl Pts',(123.928596486514,4.81959883356039,129.814752760788));
#40264=CARTESIAN_POINT('Ctrl Pts',(123.920831733567,4.79019811691197,129.680996592319));
#40265=CARTESIAN_POINT('Ctrl Pts',(123.913066980619,4.7552241747404,129.548563615474));
#40266=CARTESIAN_POINT('Ctrl Pts',(123.905309939734,4.72028496918125,129.416262172928));
#40267=CARTESIAN_POINT('Ctrl Pts',(123.897552898849,4.67978365298778,129.285281682224));
#40268=CARTESIAN_POINT('Ctrl Pts',(123.889795857965,4.63384216725141,129.156122215058));
#40269=CARTESIAN_POINT('Ctrl Pts',(123.882044666724,4.58793532634682,129.02706014805));
#40270=CARTESIAN_POINT('Ctrl Pts',(123.874293475484,4.53659661211821,128.899816738079));
#40271=CARTESIAN_POINT('Ctrl Pts',(123.866542284244,4.47999803452869,128.774877759023));
#40272=CARTESIAN_POINT('Ctrl Pts',(123.858794387467,4.42342351284446,128.649991882366));
#40273=CARTESIAN_POINT('Ctrl Pts',(123.85104649069,4.36159373519336,128.527408843965));
#40274=CARTESIAN_POINT('Ctrl Pts',(123.843298593913,4.294729079923,128.407595048604));
#40275=CARTESIAN_POINT('Ctrl Pts',(123.835552317829,4.22787841129708,128.287806315705));
#40276=CARTESIAN_POINT('Ctrl Pts',(123.827806041745,4.15599515030506,128.170786014839));
#40277=CARTESIAN_POINT('Ctrl Pts',(123.820059765661,4.07934574358167,128.056976158335));
#40278=CARTESIAN_POINT('Ctrl Pts',(123.812313432395,4.00269577104978,127.943165461713));
#40279=CARTESIAN_POINT('Ctrl Pts',(123.80456709913,3.92127980097931,127.832565581022));
#40280=CARTESIAN_POINT('Ctrl Pts',(123.796820765865,3.83540751526397,127.725589392815));
#40281=CARTESIAN_POINT('Ctrl Pts',(123.789072697862,3.74951599904564,127.618589248032));
#40282=CARTESIAN_POINT('Ctrl Pts',(123.781324629859,3.65916642604875,127.515214715355));
#40283=CARTESIAN_POINT('Ctrl Pts',(123.773576561856,3.56470838112846,127.415845128445));
#40284=CARTESIAN_POINT('Ctrl Pts',(123.765820259114,3.47014994507397,127.316369930356));
#40285=CARTESIAN_POINT('Ctrl Pts',(123.758063956372,3.37147458426828,127.220908464678));
#40286=CARTESIAN_POINT('Ctrl Pts',(123.75030765363,3.26906872560912,127.129803129957));
#40287=CARTESIAN_POINT('Ctrl Pts',(123.742547211116,3.16660820985967,127.038649169575));
#40288=CARTESIAN_POINT('Ctrl Pts',(123.734786768602,3.06041353143619,126.951856220198));
#40289=CARTESIAN_POINT('Ctrl Pts',(123.727026326087,2.95090294371566,126.869725325792));
#40290=CARTESIAN_POINT('Ctrl Pts',(123.719253425822,2.8412165598779,126.787462587584));
#40291=CARTESIAN_POINT('Ctrl Pts',(123.711480525557,2.72820395221347,126.709877081059));
#40292=CARTESIAN_POINT('Ctrl Pts',(123.703707625291,2.61231174889679,126.637226063814));
#40293=CARTESIAN_POINT('Ctrl Pts',(123.696217289529,2.50063251908489,126.567216094041));
#40294=CARTESIAN_POINT('Ctrl Pts',(123.688726953767,2.38627968726607,126.501788232925));
#40295=CARTESIAN_POINT('Ctrl Pts',(123.681236618005,2.26967144509646,126.441130782477));
#40296=CARTESIAN_POINT('Ctrl Pts',(123.673462283886,2.14864196598328,126.378173486359));
#40297=CARTESIAN_POINT('Ctrl Pts',(123.665687949767,2.02479928760008,126.320156052226));
#40298=CARTESIAN_POINT('Ctrl Pts',(123.657913615648,1.89858475860032,126.267339681212));
#40299=CARTESIAN_POINT('Ctrl Pts',(123.650148862701,1.77252577772743,126.214588401655));
#40300=CARTESIAN_POINT('Ctrl Pts',(123.642384109754,1.64410111952157,126.167025581009));
#40301=CARTESIAN_POINT('Ctrl Pts',(123.634619356806,1.51377723537512,126.124866890232));
#40302=CARTESIAN_POINT('Ctrl Pts',(123.626862315921,1.38358279074764,126.08275007206));
#40303=CARTESIAN_POINT('Ctrl Pts',(123.619105275036,1.25149324365598,126.046026821829));
#40304=CARTESIAN_POINT('Ctrl Pts',(123.611348234151,1.11799523071876,126.01486484801));
#40305=CARTESIAN_POINT('Ctrl Pts',(123.603597042911,0.984597889671743,125.983726373679));
#40306=CARTESIAN_POINT('Ctrl Pts',(123.595845851671,0.849794576084234,125.958140916765));
#40307=CARTESIAN_POINT('Ctrl Pts',(123.588094660431,0.71408696086437,125.938226333062));
#40308=CARTESIAN_POINT('Ctrl Pts',(123.580346763654,0.578437025000908,125.918320213589));
#40309=CARTESIAN_POINT('Ctrl Pts',(123.572598866877,0.441883937965077,125.904080230124));
#40310=CARTESIAN_POINT('Ctrl Pts',(123.5648509701,0.304939219190822,125.895573075301));
#40311=CARTESIAN_POINT('Ctrl Pts',(123.557104694016,0.168023146299548,125.887067699991));
#40312=CARTESIAN_POINT('Ctrl Pts',(123.549358417932,0.0307159945808324,
125.884292792305));
#40313=CARTESIAN_POINT('Ctrl Pts',(123.541612141847,-0.106466337558215,
125.887263101605));
#40314=CARTESIAN_POINT('Ctrl Pts',(123.533865808582,-0.243649682346075,
125.890233432831));
#40315=CARTESIAN_POINT('Ctrl Pts',(123.526119475317,-0.380707814842109,
125.898949057206));
#40316=CARTESIAN_POINT('Ctrl Pts',(123.518373142051,-0.517125979680275,
125.913372600443));
#40317=CARTESIAN_POINT('Ctrl Pts',(123.510625074048,-0.653574694420693,
125.927799373733));
#40318=CARTESIAN_POINT('Ctrl Pts',(123.502877006045,-0.789382767596694,
125.947936568353));
#40319=CARTESIAN_POINT('Ctrl Pts',(123.495128938042,-0.924042095902742,
125.973695107773));
#40320=CARTESIAN_POINT('Ctrl Pts',(123.487372635301,-1.05884454174529,125.999481023676));
#40321=CARTESIAN_POINT('Ctrl Pts',(123.479616332559,-1.192495419224,126.030900145379));
#40322=CARTESIAN_POINT('Ctrl Pts',(123.471860029817,-1.32449778556986,126.067812435765));
#40323=CARTESIAN_POINT('Ctrl Pts',(123.464099587303,-1.45657060555316,126.104744427352));
#40324=CARTESIAN_POINT('Ctrl Pts',(123.456339144789,-1.5869927896053,126.147175308726));
#40325=CARTESIAN_POINT('Ctrl Pts',(123.448578702274,-1.71528498474409,126.194915913091));
#40326=CARTESIAN_POINT('Ctrl Pts',(123.440805802009,-1.84378312590385,126.242733154913));
#40327=CARTESIAN_POINT('Ctrl Pts',(123.433032901743,-1.97014408480792,126.295877001017));
#40328=CARTESIAN_POINT('Ctrl Pts',(123.425260001478,-2.09391000991764,126.354110744484));
#40329=CARTESIAN_POINT('Ctrl Pts',(123.417769665716,-2.21317673190098,126.410227544694));
#40330=CARTESIAN_POINT('Ctrl Pts',(123.410279329954,-2.3300335432915,126.471070463645));
#40331=CARTESIAN_POINT('Ctrl Pts',(123.402788994192,-2.44409597746751,126.53638944669));
#40332=CARTESIAN_POINT('Ctrl Pts',(123.395013533312,-2.56250028176348,126.604194844679));
#40333=CARTESIAN_POINT('Ctrl Pts',(123.387238072432,-2.67826837869846,126.677038644254));
#40334=CARTESIAN_POINT('Ctrl Pts',(123.379462611551,-2.79094175485048,126.754690608351));
#40335=CARTESIAN_POINT('Ctrl Pts',(123.371696977641,-2.90347272943427,126.832244432482));
#40336=CARTESIAN_POINT('Ctrl Pts',(123.36393134373,-3.01291644728908,126.914594108902));
#40337=CARTESIAN_POINT('Ctrl Pts',(123.356165709819,-3.11883918758244,127.001463671224));
#40338=CARTESIAN_POINT('Ctrl Pts',(123.348409475956,-3.2246337118387,127.088228080761));
#40339=CARTESIAN_POINT('Ctrl Pts',(123.340653242093,-3.32691544683841,127.179501232828));
#40340=CARTESIAN_POINT('Ctrl Pts',(123.33289700823,-3.42528038814454,127.274964447526));
#40341=CARTESIAN_POINT('Ctrl Pts',(123.325146104715,-3.5235777297045,127.370362056644));
#40342=CARTESIAN_POINT('Ctrl Pts',(123.317395201201,-3.61796335350893,127.469943728431));
#40343=CARTESIAN_POINT('Ctrl Pts',(123.309644297686,-3.70806698478605,127.573351131532));
#40344=CARTESIAN_POINT('Ctrl Pts',(123.301897042228,-3.79812820769994,127.67670986469));
#40345=CARTESIAN_POINT('Ctrl Pts',(123.29414978677,-3.88391119257016,127.783890451748));
#40346=CARTESIAN_POINT('Ctrl Pts',(123.286402531312,-3.96508342581776,127.894498681184));
#40347=CARTESIAN_POINT('Ctrl Pts',(123.27865724444,-4.04623503311629,128.005078804954));
#40348=CARTESIAN_POINT('Ctrl Pts',(123.270911957568,-4.12277799061117,128.119084522027));
#40349=CARTESIAN_POINT('Ctrl Pts',(123.263166670696,-4.19442114387112,128.236089928883));
#40350=CARTESIAN_POINT('Ctrl Pts',(123.255419450676,-4.26608217855897,128.353124539141));
#40351=CARTESIAN_POINT('Ctrl Pts',(123.247672230656,-4.33284075699117,128.473160004255));
#40352=CARTESIAN_POINT('Ctrl Pts',(123.239925010636,-4.39444999898795,128.595742889462));
#40353=CARTESIAN_POINT('Ctrl Pts',(123.232176803857,-4.45606708812261,128.718341387989));
#40354=CARTESIAN_POINT('Ctrl Pts',(123.224428597077,-4.51253336610795,128.843487599983));
#40355=CARTESIAN_POINT('Ctrl Pts',(123.216680390298,-4.56364912406604,128.970705869553));
#40356=CARTESIAN_POINT('Ctrl Pts',(123.208926340544,-4.61480342876115,129.098020075276));
#40357=CARTESIAN_POINT('Ctrl Pts',(123.201172290789,-4.66059901697531,129.22740909341));
#40358=CARTESIAN_POINT('Ctrl Pts',(123.193418241035,-4.70088522222651,129.358379569989));
#40359=CARTESIAN_POINT('Ctrl Pts',(123.1890237041,-4.7237170614039,129.432605892364));
#40360=CARTESIAN_POINT('Ctrl Pts',(123.184629167164,-4.74478022412167,129.507339900102));
#40361=CARTESIAN_POINT('Ctrl Pts',(123.180234630229,-4.76405452823405,129.582490119308));
#40362=CARTESIAN_POINT('Origin',(213.235140564004,0.,130.804360617566));
#40363=CARTESIAN_POINT('',(121.084721392599,-4.76405452823403,129.582490119308));
#40364=CARTESIAN_POINT('',(121.429936586327,-4.76405452823403,129.582490119308));
#40365=CARTESIAN_POINT('',(213.235140564004,-4.76405452823405,129.582490119308));
#40366=CARTESIAN_POINT('',(122.764859436046,-4.91824884389311,130.800988371423));
#40367=CARTESIAN_POINT('Ctrl Pts',(122.764859435991,-4.91824884389379,130.800988372406));
#40368=CARTESIAN_POINT('Ctrl Pts',(122.757077499762,-4.91834342005838,130.938922920481));
#40369=CARTESIAN_POINT('Ctrl Pts',(122.749295563533,-4.91263101685004,131.07689628956));
#40370=CARTESIAN_POINT('Ctrl Pts',(122.741513627304,-4.90112854599004,131.214387492516));
#40371=CARTESIAN_POINT('Ctrl Pts',(122.733731688858,-4.88962607185356,131.351878734637));
#40372=CARTESIAN_POINT('Ctrl Pts',(122.725949750412,-4.87233355806728,131.488887425918));
#40373=CARTESIAN_POINT('Ctrl Pts',(122.718167811966,-4.84931988728419,131.624896840587));
#40374=CARTESIAN_POINT('Ctrl Pts',(122.710384244513,-4.82630139900788,131.760934726352));
#40375=CARTESIAN_POINT('Ctrl Pts',(122.702600677061,-4.79755943368696,131.895972538746));
#40376=CARTESIAN_POINT('Ctrl Pts',(122.694817109608,-4.7632141111743,132.029503218903));
#40377=CARTESIAN_POINT('Ctrl Pts',(122.687030285658,-4.72885441923102,132.16308976576));
#40378=CARTESIAN_POINT('Ctrl Pts',(122.679243461708,-4.68888679902929,132.295167551827));
#40379=CARTESIAN_POINT('Ctrl Pts',(122.671456637758,-4.64348129810139,132.425244480365));
#40380=CARTESIAN_POINT('Ctrl Pts',(122.663660039455,-4.59801880225171,132.555484687013));
#40381=CARTESIAN_POINT('Ctrl Pts',(122.655863441152,-4.54710492090752,132.683718655831));
#40382=CARTESIAN_POINT('Ctrl Pts',(122.648066842848,-4.49095818467999,132.809473493679));
#40383=CARTESIAN_POINT('Ctrl Pts',(122.640264859057,-4.43477266518489,132.93531519648));
#40384=CARTESIAN_POINT('Ctrl Pts',(122.632462875266,-4.37334726035518,133.05867401179));
#40385=CARTESIAN_POINT('Ctrl Pts',(122.624660891475,-4.30694614418969,133.179102282158));
#40386=CARTESIAN_POINT('Ctrl Pts',(122.61684628404,-4.24043759072811,133.299725405994));
#40387=CARTESIAN_POINT('Ctrl Pts',(122.609031676606,-4.16893744484744,133.417408184763));
#40388=CARTESIAN_POINT('Ctrl Pts',(122.601217069171,-4.0927532286261,133.531731892635));
#40389=CARTESIAN_POINT('Ctrl Pts',(122.596489752418,-4.04666685453286,133.600890117659));
#40390=CARTESIAN_POINT('Ctrl Pts',(122.591762435665,-3.99886717083042,133.668819733568));
#40391=CARTESIAN_POINT('Ctrl Pts',(122.587035118912,-3.94942912399173,133.735434253124));
#40392=CARTESIAN_POINT('Ctrl Pts',(122.579260784793,-3.86812551891892,133.844985518526));
#40393=CARTESIAN_POINT('Ctrl Pts',(122.571486450674,-3.7821314976183,133.951324880725));
#40394=CARTESIAN_POINT('Ctrl Pts',(122.563712116555,-3.69172971392083,134.054024412769));
#40395=CARTESIAN_POINT('Ctrl Pts',(122.555947363608,-3.60143934234245,134.156597376818));
#40396=CARTESIAN_POINT('Ctrl Pts',(122.548182610661,-3.50675227261767,134.255539145399));
#40397=CARTESIAN_POINT('Ctrl Pts',(122.540417857714,-3.40799364663902,134.350451756689));
#40398=CARTESIAN_POINT('Ctrl Pts',(122.532660816829,-3.30933310911974,134.445270099436));
#40399=CARTESIAN_POINT('Ctrl Pts',(122.524903775944,-3.20660934300837,134.536066979527));
#40400=CARTESIAN_POINT('Ctrl Pts',(122.517146735059,-3.10018661986303,134.622478738384));
#40401=CARTESIAN_POINT('Ctrl Pts',(122.509395543819,-2.99384415092098,134.708825333462));
#40402=CARTESIAN_POINT('Ctrl Pts',(122.501644352579,-2.88380857938552,134.790793143953));
#40403=CARTESIAN_POINT('Ctrl Pts',(122.493893161339,-2.77047950106459,134.868056767216));
#40404=CARTESIAN_POINT('Ctrl Pts',(122.486145264561,-2.65719859062533,134.945287551378));
#40405=CARTESIAN_POINT('Ctrl Pts',(122.478397367784,-2.54062727991032,135.017817905205));
#40406=CARTESIAN_POINT('Ctrl Pts',(122.470649471007,-2.42119639869134,135.085364128598));
#40407=CARTESIAN_POINT('Ctrl Pts',(122.462903194923,-2.30179049983808,135.152896222776));
#40408=CARTESIAN_POINT('Ctrl Pts',(122.455156918839,-2.17952656034801,135.215446067909));
#40409=CARTESIAN_POINT('Ctrl Pts',(122.447410642755,-2.05486206649551,135.27277476021));
#40410=CARTESIAN_POINT('Ctrl Pts',(122.43966430949,-1.93019665239795,135.330103875698));
#40411=CARTESIAN_POINT('Ctrl Pts',(122.431917976224,-1.8031310037848,135.382211598101));
#40412=CARTESIAN_POINT('Ctrl Pts',(122.424171642959,-1.67414437648625,135.428906397335));
#40413=CARTESIAN_POINT('Ctrl Pts',(122.416423574956,-1.54512886352728,135.475611653545));
#40414=CARTESIAN_POINT('Ctrl Pts',(122.408675506953,-1.41419188340241,135.516901441418));
#40415=CARTESIAN_POINT('Ctrl Pts',(122.40092743895,-1.28182932303529,135.552633635107));
#40416=CARTESIAN_POINT('Ctrl Pts',(122.393171136208,-1.14932608616351,135.588403805397));
#40417=CARTESIAN_POINT('Ctrl Pts',(122.385414833466,-1.0153946204819,135.61860448022));
#40418=CARTESIAN_POINT('Ctrl Pts',(122.377658530724,-0.880543065243223,
135.643144242895));
#40419=CARTESIAN_POINT('Ctrl Pts',(122.36989808821,-0.745619535668938,135.667697103181));
#40420=CARTESIAN_POINT('Ctrl Pts',(122.362137645696,-0.609775325071402,
135.686582977114));
#40421=CARTESIAN_POINT('Ctrl Pts',(122.354377203182,-0.473524242544293,
135.699762322659));
#40422=CARTESIAN_POINT('Ctrl Pts',(122.346604302916,-0.337054437683895,
135.712962824858));
#40423=CARTESIAN_POINT('Ctrl Pts',(122.338831402651,-0.200176846306303,
135.720438471486));
#40424=CARTESIAN_POINT('Ctrl Pts',(122.331058502385,-0.0634067344431984,
135.722201876546));
#40425=CARTESIAN_POINT('Ctrl Pts',(122.323568166623,0.0683914393515826,
135.723901177391));
#40426=CARTESIAN_POINT('Ctrl Pts',(122.316077830861,0.200089504363081,135.720296343466));
#40427=CARTESIAN_POINT('Ctrl Pts',(122.308587495099,0.331232350231125,135.711444088698));
#40428=CARTESIAN_POINT('Ctrl Pts',(122.30081316098,0.467347516959299,135.702256198001));
#40429=CARTESIAN_POINT('Ctrl Pts',(122.293038826861,0.603295703098704,135.687386015155));
#40430=CARTESIAN_POINT('Ctrl Pts',(122.285264492742,0.73856410028404,135.666840039864));
#40431=CARTESIAN_POINT('Ctrl Pts',(122.277499739795,0.873665791258854,135.646319385651));
#40432=CARTESIAN_POINT('Ctrl Pts',(122.269734986848,1.00808897738918,135.62013691492));
#40433=CARTESIAN_POINT('Ctrl Pts',(122.261970233901,1.14132309498719,135.588351070666));
#40434=CARTESIAN_POINT('Ctrl Pts',(122.254213193016,1.2744248825815,135.55659679656));
#40435=CARTESIAN_POINT('Ctrl Pts',(122.246456152131,1.40633957405435,135.519250314369));
#40436=CARTESIAN_POINT('Ctrl Pts',(122.238699111246,1.53656431546861,135.476421529725));
#40437=CARTESIAN_POINT('Ctrl Pts',(122.230947920006,1.66669085339236,135.433625042602));
#40438=CARTESIAN_POINT('Ctrl Pts',(122.223196728765,1.79512960799016,135.385354603645));
#40439=CARTESIAN_POINT('Ctrl Pts',(122.215445537525,1.92139081750991,135.33177051605));
#40440=CARTESIAN_POINT('Ctrl Pts',(122.207697640748,2.0475983626474,135.278209203121));
#40441=CARTESIAN_POINT('Ctrl Pts',(122.199949743971,2.17162984434234,135.219338885842));
#40442=CARTESIAN_POINT('Ctrl Pts',(122.192201847194,2.29301370365112,135.155368686665));
#40443=CARTESIAN_POINT('Ctrl Pts',(122.18445557111,2.41437217207336,135.091411868676));
#40444=CARTESIAN_POINT('Ctrl Pts',(122.176709295026,2.53308377404431,135.022357472847));
#40445=CARTESIAN_POINT('Ctrl Pts',(122.168963018942,2.64870023053681,134.948461262007));
#40446=CARTESIAN_POINT('Ctrl Pts',(122.161216685677,2.7643175404838,134.874564505681));
#40447=CARTESIAN_POINT('Ctrl Pts',(122.153470352411,2.87683932993553,134.795826073578));
#40448=CARTESIAN_POINT('Ctrl Pts',(122.145724019146,2.98584540972476,134.71254565051));
#40449=CARTESIAN_POINT('Ctrl Pts',(122.137975951143,3.09487590066947,134.629246577369));
#40450=CARTESIAN_POINT('Ctrl Pts',(122.13022788314,3.20038880466551,134.541403726566));
#40451=CARTESIAN_POINT('Ctrl Pts',(122.122479815137,3.30199650821807,134.449357479323));
#40452=CARTESIAN_POINT('Ctrl Pts',(122.114723512395,3.40371220164725,134.357213404232));
#40453=CARTESIAN_POINT('Ctrl Pts',(122.106967209653,3.50151411336226,134.260857271452));
#40454=CARTESIAN_POINT('Ctrl Pts',(122.099210906912,3.59505067024195,134.160667179978));
#40455=CARTESIAN_POINT('Ctrl Pts',(122.091450464397,3.68863715039857,134.060423614036));
#40456=CARTESIAN_POINT('Ctrl Pts',(122.083690021883,3.7779534850219,133.956342308526));
#40457=CARTESIAN_POINT('Ctrl Pts',(122.075929579369,3.86268867991028,133.848834172155));
#40458=CARTESIAN_POINT('Ctrl Pts',(122.068156679104,3.94755989925581,133.74115345418));
#40459=CARTESIAN_POINT('Ctrl Pts',(122.060383778838,4.02783505404528,133.630035229584));
#40460=CARTESIAN_POINT('Ctrl Pts',(122.052610878573,4.10324624292248,133.515919824451));
#40461=CARTESIAN_POINT('Ctrl Pts',(122.045120542811,4.17591604513422,133.405952801735));
#40462=CARTESIAN_POINT('Ctrl Pts',(122.037630207049,4.24406921730083,133.29320298897));
#40463=CARTESIAN_POINT('Ctrl Pts',(122.030139871287,4.30750747618878,133.178083938654));
#40464=CARTESIAN_POINT('Ctrl Pts',(122.022365537168,4.37335101594443,133.058600114555));
#40465=CARTESIAN_POINT('Ctrl Pts',(122.014591203049,4.43432362529838,132.936185358251));
#40466=CARTESIAN_POINT('Ctrl Pts',(122.00681686893,4.49015358718661,132.811274623191));
#40467=CARTESIAN_POINT('Ctrl Pts',(121.999052115983,4.54591474363659,132.686517829448));
#40468=CARTESIAN_POINT('Ctrl Pts',(121.991287363035,4.59654570505646,132.559271530921));
#40469=CARTESIAN_POINT('Ctrl Pts',(121.983522610088,4.64181966904977,132.429996869168));
#40470=CARTESIAN_POINT('Ctrl Pts',(121.975765569203,4.68704866630361,132.300850604832));
#40471=CARTESIAN_POINT('Ctrl Pts',(121.968008528318,4.72693112606523,132.169680353015));
#40472=CARTESIAN_POINT('Ctrl Pts',(121.960251487433,4.76128771022092,132.036968585656));
#40473=CARTESIAN_POINT('Ctrl Pts',(121.952500296193,4.79561838580935,131.904356897273));
#40474=CARTESIAN_POINT('Ctrl Pts',(121.944749104953,4.82443138257623,131.770206384128));
#40475=CARTESIAN_POINT('Ctrl Pts',(121.936997913713,4.8475968399493,131.635015744447));
#40476=CARTESIAN_POINT('Ctrl Pts',(121.929250016936,4.87075245138502,131.499882564394));
#40477=CARTESIAN_POINT('Ctrl Pts',(121.921502120159,4.88826523165698,131.363710521612));
#40478=CARTESIAN_POINT('Ctrl Pts',(121.913754223382,4.90005623228201,131.227009387793));
#40479=CARTESIAN_POINT('Ctrl Pts',(121.906007947298,4.91184476648389,131.090336848903));
#40480=CARTESIAN_POINT('Ctrl Pts',(121.898261671214,4.91791386810852,130.953135828385));
#40481=CARTESIAN_POINT('Ctrl Pts',(121.89051539513,4.91823641190225,130.815921722135));
#40482=CARTESIAN_POINT('Ctrl Pts',(121.882769061864,4.91855895807692,130.678706603002));
#40483=CARTESIAN_POINT('Ctrl Pts',(121.875022728599,4.91313486085608,130.541478788909));
#40484=CARTESIAN_POINT('Ctrl Pts',(121.867276395333,4.90198913105274,130.404753783865));
#40485=CARTESIAN_POINT('Ctrl Pts',(121.85952832733,4.89084090524046,130.267998160203));
#40486=CARTESIAN_POINT('Ctrl Pts',(121.851780259328,4.87396852892708,130.13174595925));
#40487=CARTESIAN_POINT('Ctrl Pts',(121.844032191325,4.85144885991235,129.996507275582));
#40488=CARTESIAN_POINT('Ctrl Pts',(121.836275888583,4.82890525672543,129.861124858631));
#40489=CARTESIAN_POINT('Ctrl Pts',(121.828519585841,4.80070243549678,129.726758497014));
#40490=CARTESIAN_POINT('Ctrl Pts',(121.820763283099,4.76696846775993,129.593908350898));
#40491=CARTESIAN_POINT('Ctrl Pts',(121.813002840585,4.73321649518879,129.460987298658));
#40492=CARTESIAN_POINT('Ctrl Pts',(121.805242398071,4.69392760566475,129.329584448815));
#40493=CARTESIAN_POINT('Ctrl Pts',(121.797481955556,4.64927940835654,129.200183555789));
#40494=CARTESIAN_POINT('Ctrl Pts',(121.789709055291,4.60455953779834,129.070574936962));
#40495=CARTESIAN_POINT('Ctrl Pts',(121.781936155026,4.5544633104076,128.94297506112));
#40496=CARTESIAN_POINT('Ctrl Pts',(121.77416325476,4.49921637776227,128.817847328263));
#40497=CARTESIAN_POINT('Ctrl Pts',(121.766672918998,4.44597781027703,128.697268303674));
#40498=CARTESIAN_POINT('Ctrl Pts',(121.759182583236,4.38795665384656,128.578985081864));
#40499=CARTESIAN_POINT('Ctrl Pts',(121.751692247474,4.32539366496889,128.463388019361));
#40500=CARTESIAN_POINT('Ctrl Pts',(121.743917913355,4.26045858135254,128.343408059098));
#40501=CARTESIAN_POINT('Ctrl Pts',(121.736143579236,4.19042476460252,128.225941910086));
#40502=CARTESIAN_POINT('Ctrl Pts',(121.728369245117,4.11551128366383,128.111453278548));
#40503=CARTESIAN_POINT('Ctrl Pts',(121.72060449217,4.04069012689533,127.997105744017));
#40504=CARTESIAN_POINT('Ctrl Pts',(121.712839739223,3.96100148351983,127.885728749714));
#40505=CARTESIAN_POINT('Ctrl Pts',(121.705074986275,3.87671073275472,127.777762369195));
#40506=CARTESIAN_POINT('Ctrl Pts',(121.69731794539,3.79250370075155,127.669903222406));
#40507=CARTESIAN_POINT('Ctrl Pts',(121.689560904506,3.70370389664788,127.56544825436));
#40508=CARTESIAN_POINT('Ctrl Pts',(121.681803863621,3.61062030111874,127.464809135159));
#40509=CARTESIAN_POINT('Ctrl Pts',(121.67405267238,3.51760690065301,127.364245908699));
#40510=CARTESIAN_POINT('Ctrl Pts',(121.66630148114,3.42031640315355,127.26749308933));
#40511=CARTESIAN_POINT('Ctrl Pts',(121.6585502899,3.3190981847498,127.174929490999));
#40512=CARTESIAN_POINT('Ctrl Pts',(121.650802393123,3.21792298678888,127.082405234667));
#40513=CARTESIAN_POINT('Ctrl Pts',(121.643054496346,3.11282367611486,126.994066921327));
#40514=CARTESIAN_POINT('Ctrl Pts',(121.635306599569,3.00418646450419,126.910256516622));
#40515=CARTESIAN_POINT('Ctrl Pts',(121.627560323485,2.89557197745617,126.826463643247));
#40516=CARTESIAN_POINT('Ctrl Pts',(121.619814047401,2.7834213708336,126.747197033253));
#40517=CARTESIAN_POINT('Ctrl Pts',(121.612067771317,2.66815359993932,126.672758091956));
#40518=CARTESIAN_POINT('Ctrl Pts',(121.604321438051,2.55288497816469,126.598318601167));
#40519=CARTESIAN_POINT('Ctrl Pts',(121.596575104786,2.43449947463561,126.528707062284));
#40520=CARTESIAN_POINT('Ctrl Pts',(121.588828771521,2.31344431643005,126.46418107551));
#40521=CARTESIAN_POINT('Ctrl Pts',(121.581080703518,2.1923620487613,126.39964063859));
#40522=CARTESIAN_POINT('Ctrl Pts',(121.573332635515,2.06860928170925,126.340188203873));
#40523=CARTESIAN_POINT('Ctrl Pts',(121.565584567512,1.94265671580499,126.286034827294));
#40524=CARTESIAN_POINT('Ctrl Pts',(121.55782826477,1.81657028601448,126.231823895862));
#40525=CARTESIAN_POINT('Ctrl Pts',(121.550071962028,1.68827974676689,126.182923427572));
#40526=CARTESIAN_POINT('Ctrl Pts',(121.542315659286,1.5582751227677,126.139496021003));
#40527=CARTESIAN_POINT('Ctrl Pts',(121.534555216772,1.42820111138641,126.09604543592));
#40528=CARTESIAN_POINT('Ctrl Pts',(121.526794774258,1.29641156781885,126.058073841363));
#40529=CARTESIAN_POINT('Ctrl Pts',(121.519034331744,1.16340949045483,126.025693290788));
#40530=CARTESIAN_POINT('Ctrl Pts',(121.511261431478,1.03019390634876,125.993260760078));
#40531=CARTESIAN_POINT('Ctrl Pts',(121.503488531213,0.89576228241315,125.966437285288));
#40532=CARTESIAN_POINT('Ctrl Pts',(121.495715630947,0.76062646038363,125.945283498373));
#40533=CARTESIAN_POINT('Ctrl Pts',(121.488225295185,0.630403165870012,125.924898704896));
#40534=CARTESIAN_POINT('Ctrl Pts',(121.480734959423,0.499526289109342,125.909778576429));
#40535=CARTESIAN_POINT('Ctrl Pts',(121.473244623661,0.368454382871144,125.899931554949));
#40536=CARTESIAN_POINT('Ctrl Pts',(121.465470289542,0.232412845470919,125.889711180657));
#40537=CARTESIAN_POINT('Ctrl Pts',(121.457695955423,0.0957302588679489,
125.885139291338));
#40538=CARTESIAN_POINT('Ctrl Pts',(121.449921621304,-0.0410848356421021,
125.886282222626));
#40539=CARTESIAN_POINT('Ctrl Pts',(121.442156868357,-0.177731317775314,
125.887423745352));
#40540=CARTESIAN_POINT('Ctrl Pts',(121.43439211541,-0.314509595690544,125.894266071969));
#40541=CARTESIAN_POINT('Ctrl Pts',(121.426627362463,-0.450905979092884,
125.906823801929));
#40542=CARTESIAN_POINT('Ctrl Pts',(121.418870321578,-0.587166891684377,
125.919369059375));
#40543=CARTESIAN_POINT('Ctrl Pts',(121.411113280693,-0.723046277793696,
125.937618387826));
#40544=CARTESIAN_POINT('Ctrl Pts',(121.403356239808,-0.858030776102852,
125.961534350833));
#40545=CARTESIAN_POINT('Ctrl Pts',(121.395605048567,-0.992913481551806,
125.985432278626));
#40546=CARTESIAN_POINT('Ctrl Pts',(121.387853857327,-1.12690225902049,126.014988267395));
#40547=CARTESIAN_POINT('Ctrl Pts',(121.380102666087,-1.25948955527277,126.050113135297));
#40548=CARTESIAN_POINT('Ctrl Pts',(121.37235476931,-1.39202049838762,126.085223074194));
#40549=CARTESIAN_POINT('Ctrl Pts',(121.364606872533,-1.52315076788515,126.125897084687));
#40550=CARTESIAN_POINT('Ctrl Pts',(121.356858975756,-1.65238390148433,126.171995076655));
#40551=CARTESIAN_POINT('Ctrl Pts',(121.349112699672,-1.78159000229808,126.218083425917));
#40552=CARTESIAN_POINT('Ctrl Pts',(121.341366423588,-1.9088993885437,126.269593368643));
#40553=CARTESIAN_POINT('Ctrl Pts',(121.333620147504,-2.03383202381809,126.326335342806));
#40554=CARTESIAN_POINT('Ctrl Pts',(121.325873814238,-2.15876558131646,126.383077735825));
#40555=CARTESIAN_POINT('Ctrl Pts',(121.318127480973,-2.28132199686403,126.445052075673));
#40556=CARTESIAN_POINT('Ctrl Pts',(121.310381147707,-2.40104280695426,126.512021336746));
#40557=CARTESIAN_POINT('Ctrl Pts',(121.302633079704,-2.52079042769038,126.57900559512));
#40558=CARTESIAN_POINT('Ctrl Pts',(121.294885011701,-2.6377008382199,126.650986809731));
#40559=CARTESIAN_POINT('Ctrl Pts',(121.287136943698,-2.75134204607348,126.727683047779));
#40560=CARTESIAN_POINT('Ctrl Pts',(121.279380640957,-2.86510403315464,126.8044607995));
#40561=CARTESIAN_POINT('Ctrl Pts',(121.271624338215,-2.97558955219394,126.885963365975));
#40562=CARTESIAN_POINT('Ctrl Pts',(121.263868035473,-3.0823969340792,126.971866364044));
#40563=CARTESIAN_POINT('Ctrl Pts',(121.256107592959,-3.18926132228037,127.05781521113));
#40564=CARTESIAN_POINT('Ctrl Pts',(121.248347150444,-3.29244336763037,127.148168912241));
#40565=CARTESIAN_POINT('Ctrl Pts',(121.24058670793,-3.39157691346575,127.242564848218));
#40566=CARTESIAN_POINT('Ctrl Pts',(121.232813807665,-3.49086959726937,127.337112316931));
#40567=CARTESIAN_POINT('Ctrl Pts',(121.225040907399,-3.58610052270303,127.435714706125));
#40568=CARTESIAN_POINT('Ctrl Pts',(121.217268007134,-3.67694201542359,127.537974161907));
#40569=CARTESIAN_POINT('Ctrl Pts',(121.209777671372,-3.76448119106748,127.636516228894));
#40570=CARTESIAN_POINT('Ctrl Pts',(121.20228733561,-3.84794433210451,127.738453853171));
#40571=CARTESIAN_POINT('Ctrl Pts',(121.194796999848,-3.92707647708734,127.843405804401));
#40572=CARTESIAN_POINT('Ctrl Pts',(121.186993411415,-4.00951800052268,127.952746941921));
#40573=CARTESIAN_POINT('Ctrl Pts',(121.179189822982,-4.08752191368574,128.065709362174));
#40574=CARTESIAN_POINT('Ctrl Pts',(121.171386234549,-4.16075448563075,128.181898954776));
#40575=CARTESIAN_POINT('Ctrl Pts',(121.163595494578,-4.23386648151851,128.297897243391));
#40576=CARTESIAN_POINT('Ctrl Pts',(121.155804754607,-4.30222257832876,128.417111797096));
#40577=CARTESIAN_POINT('Ctrl Pts',(121.148014014637,-4.36553000502787,128.539116516437));
#40578=CARTESIAN_POINT('Ctrl Pts',(121.14023066725,-4.42877735971003,128.66100546627));
#40579=CARTESIAN_POINT('Ctrl Pts',(121.132447319863,-4.48698539601392,128.785678974622));
#40580=CARTESIAN_POINT('Ctrl Pts',(121.124663972476,-4.53990506589921,128.912682776304));
#40581=CARTESIAN_POINT('Ctrl Pts',(121.116887539582,-4.59277772353407,129.039573751611));
#40582=CARTESIAN_POINT('Ctrl Pts',(121.109111106688,-4.64037122070024,129.168790542686));
#40583=CARTESIAN_POINT('Ctrl Pts',(121.101334673793,-4.68248308927141,129.299855655398));
#40584=CARTESIAN_POINT('Ctrl Pts',(121.095796913395,-4.71247183105595,129.393189861536));
#40585=CARTESIAN_POINT('Ctrl Pts',(121.090259152997,-4.73968170673913,129.487460858209));
#40586=CARTESIAN_POINT('Ctrl Pts',(121.084721392599,-4.76405452823403,129.582490119308));
#40587=CARTESIAN_POINT('Ctrl Pts',(122.834626183723,-4.76405452823408,129.582490119308));
#40588=CARTESIAN_POINT('Ctrl Pts',(122.825759709209,-4.80279549980021,129.733540579468));
#40589=CARTESIAN_POINT('Ctrl Pts',(122.816893234695,-4.83439229329883,129.886605462658));
#40590=CARTESIAN_POINT('Ctrl Pts',(122.808026760181,-4.85865542249204,130.041045120547));
#40591=CARTESIAN_POINT('Ctrl Pts',(122.799219852322,-4.88275554738768,130.194447223563));
#40592=CARTESIAN_POINT('Ctrl Pts',(122.790412944462,-4.89962012903744,130.349205529587));
#40593=CARTESIAN_POINT('Ctrl Pts',(122.781606036603,-4.90911101441911,130.504673930159));
#40594=CARTESIAN_POINT('Ctrl Pts',(122.776023836418,-4.91512674922489,130.603216545616));
#40595=CARTESIAN_POINT('Ctrl Pts',(122.770441636232,-4.91818100174923,130.70204406795));
#40596=CARTESIAN_POINT('Ctrl Pts',(122.764859436046,-4.91824884389311,130.800988371423));
#40597=CARTESIAN_POINT('',(123.110140563952,-4.91824976192362,130.802830310975));
#40598=CARTESIAN_POINT('Ctrl Pts',(123.180234630229,-4.76405452823405,129.582490119308));
#40599=CARTESIAN_POINT('Ctrl Pts',(123.172471174879,-4.79810480510647,129.715251632049));
#40600=CARTESIAN_POINT('Ctrl Pts',(123.164707719529,-4.8265692317211,129.849312316196));
#40601=CARTESIAN_POINT('Ctrl Pts',(123.15694426418,-4.8493770688196,129.984162405603));
#40602=CARTESIAN_POINT('Ctrl Pts',(123.14916959278,-4.87221785694477,130.119207316154));
#40603=CARTESIAN_POINT('Ctrl Pts',(123.141394921381,-4.88938569015853,130.25504352242));
#40604=CARTESIAN_POINT('Ctrl Pts',(123.133620249982,-4.90086176145776,130.391157208116));
#40605=CARTESIAN_POINT('Ctrl Pts',(123.130527290115,-4.90542723132088,130.445306656459));
#40606=CARTESIAN_POINT('Ctrl Pts',(123.127434330247,-4.90909247502338,130.499500032022));
#40607=CARTESIAN_POINT('Ctrl Pts',(123.124341370379,-4.91185859746714,130.553705114957));
#40608=CARTESIAN_POINT('Ctrl Pts',(123.119607768255,-4.9160919931895,130.636662963314));
#40609=CARTESIAN_POINT('Ctrl Pts',(123.114874166132,-4.91822390503836,130.719728964701));
#40610=CARTESIAN_POINT('Ctrl Pts',(123.110140564008,-4.91824976192331,130.80283030999));
#40611=CARTESIAN_POINT('Ctrl Pts',(123.110140563952,-4.91824976192362,130.802830310975));
#40612=CARTESIAN_POINT('Ctrl Pts',(123.102428017502,-4.91829189100263,130.938228886704));
#40613=CARTESIAN_POINT('Ctrl Pts',(123.094715471052,-4.91273854065694,131.07385488417));
#40614=CARTESIAN_POINT('Ctrl Pts',(123.087002924603,-4.90155952306506,131.209202937921));
#40615=CARTESIAN_POINT('Ctrl Pts',(123.079299655817,-4.89039395306417,131.344388177251));
#40616=CARTESIAN_POINT('Ctrl Pts',(123.071596387031,-4.87361620922271,131.479295745428));
#40617=CARTESIAN_POINT('Ctrl Pts',(123.063893118246,-4.85124808336885,131.613418771292));
#40618=CARTESIAN_POINT('Ctrl Pts',(123.056197200275,-4.8289013022153,131.74741381076));
#40619=CARTESIAN_POINT('Ctrl Pts',(123.048501282305,-4.80097481726048,131.880625407544));
#40620=CARTESIAN_POINT('Ctrl Pts',(123.040805364335,-4.76754230610144,132.012550760728));
#40621=CARTESIAN_POINT('Ctrl Pts',(123.033114877499,-4.73413338880946,132.144383012043));
#40622=CARTESIAN_POINT('Ctrl Pts',(123.025424390663,-4.69522627500157,132.274930442014));
#40623=CARTESIAN_POINT('Ctrl Pts',(123.017733903828,-4.65094582541877,132.403699853476));
#40624=CARTESIAN_POINT('Ctrl Pts',(123.010046117276,-4.60668092358835,132.532424051418));
#40625=CARTESIAN_POINT('Ctrl Pts',(123.002358330724,-4.55704656498262,132.659371096231));
#40626=CARTESIAN_POINT('Ctrl Pts',(122.994670544172,-4.5022175488539,132.784062667192));
#40627=CARTESIAN_POINT('Ctrl Pts',(122.986983894752,-4.44739664270996,132.90873579451));
#40628=CARTESIAN_POINT('Ctrl Pts',(122.979297245332,-4.38738276700006,133.031153747441));
#40629=CARTESIAN_POINT('Ctrl Pts',(122.971610595913,-4.32239877614302,133.150858408423));
#40630=CARTESIAN_POINT('Ctrl Pts',(122.963923353924,-4.25740977562546,133.27057229752));
#40631=CARTESIAN_POINT('Ctrl Pts',(122.956236111935,-4.18745008770041,133.387572129125));
#40632=CARTESIAN_POINT('Ctrl Pts',(122.948548869946,-4.11278817141666,133.501425043855));
#40633=CARTESIAN_POINT('Ctrl Pts',(122.940859305564,-4.03810369901763,133.615312354695));
#40634=CARTESIAN_POINT('Ctrl Pts',(122.933169741182,-3.95871439066999,133.72605052528));
#40635=CARTESIAN_POINT('Ctrl Pts',(122.9254801768,-3.8749313152967,133.833236706849));
#40636=CARTESIAN_POINT('Ctrl Pts',(122.917782267932,-3.79105732103234,133.940539203661));
#40637=CARTESIAN_POINT('Ctrl Pts',(122.910084359065,-3.70278028615443,134.044281702914));
#40638=CARTESIAN_POINT('Ctrl Pts',(122.902386450197,-3.6104509844101,134.14409515068));
#40639=CARTESIAN_POINT('Ctrl Pts',(122.894683774628,-3.51806451049176,134.243970404954));
#40640=CARTESIAN_POINT('Ctrl Pts',(122.88698109906,-3.42162105445613,134.339911483451));
#40641=CARTESIAN_POINT('Ctrl Pts',(122.879278423491,-3.32150645419486,134.431587924648));
#40642=CARTESIAN_POINT('Ctrl Pts',(122.871564556849,-3.22124639930248,134.523397560833));
#40643=CARTESIAN_POINT('Ctrl Pts',(122.863850690207,-3.11730485552744,134.610929935339));
#40644=CARTESIAN_POINT('Ctrl Pts',(122.856136823565,-3.01009907664712,134.693896143984));
#40645=CARTESIAN_POINT('Ctrl Pts',(122.852722464565,-2.96264699678834,134.730619156487));
#40646=CARTESIAN_POINT('Ctrl Pts',(122.849308105566,-2.91455575475838,134.766448159479));
#40647=CARTESIAN_POINT('Ctrl Pts',(122.845893746566,-2.86586312402484,134.801360944918));
#40648=CARTESIAN_POINT('Ctrl Pts',(122.838119412447,-2.75499230449017,134.880855707794));
#40649=CARTESIAN_POINT('Ctrl Pts',(122.830345078328,-2.64063576786579,134.95585980224));
#40650=CARTESIAN_POINT('Ctrl Pts',(122.822570744209,-2.52319333105665,135.026052041227));
#40651=CARTESIAN_POINT('Ctrl Pts',(122.814805991262,-2.4058956315549,135.096157774553));
#40652=CARTESIAN_POINT('Ctrl Pts',(122.807041238315,-2.28551993126846,135.161463253064));
#40653=CARTESIAN_POINT('Ctrl Pts',(122.799276485368,-2.16249735672644,135.221688796981));
#40654=CARTESIAN_POINT('Ctrl Pts',(122.791519444483,-2.03959696993951,135.281854524039));
#40655=CARTESIAN_POINT('Ctrl Pts',(122.783762403598,-1.91405528942545,135.33695018641));
#40656=CARTESIAN_POINT('Ctrl Pts',(122.776005362713,-1.78633022874239,135.386740717076));
#40657=CARTESIAN_POINT('Ctrl Pts',(122.768254171473,-1.65870148652097,135.436493700315));
#40658=CARTESIAN_POINT('Ctrl Pts',(122.760502980232,-1.52889300418891,135.480949373456));
#40659=CARTESIAN_POINT('Ctrl Pts',(122.752751788992,-1.3973846517481,135.519919884245));
#40660=CARTESIAN_POINT('Ctrl Pts',(122.745003892215,-1.26593219386545,135.558873831527));
#40661=CARTESIAN_POINT('Ctrl Pts',(122.737255995438,-1.13278167691982,135.592347142465));
#40662=CARTESIAN_POINT('Ctrl Pts',(122.729508098661,-0.998429980033417,
135.620201212672));
#40663=CARTESIAN_POINT('Ctrl Pts',(122.721761822577,-0.86410638662562,135.648049456408));
#40664=CARTESIAN_POINT('Ctrl Pts',(122.714015546493,-0.728582495630703,
135.670280718076));
#40665=CARTESIAN_POINT('Ctrl Pts',(122.706269270409,-0.59236689178891,135.686807189523));
#40666=CARTESIAN_POINT('Ctrl Pts',(122.698522937143,-0.456150282434567,
135.703333782964));
#40667=CARTESIAN_POINT('Ctrl Pts',(122.690776603878,-0.319242338163657,
135.714155455064));
#40668=CARTESIAN_POINT('Ctrl Pts',(122.683030270613,-0.182157908796801,
135.719236156047));
#40669=CARTESIAN_POINT('Ctrl Pts',(122.67528220261,-0.0450427803222785,
135.724317994819));
#40670=CARTESIAN_POINT('Ctrl Pts',(122.667534134607,0.092248521271429,135.7236562897));
#40671=CARTESIAN_POINT('Ctrl Pts',(122.659786066604,0.229200394152558,135.71726711391));
#40672=CARTESIAN_POINT('Ctrl Pts',(122.652029763862,0.366297821113747,135.710871147628));
#40673=CARTESIAN_POINT('Ctrl Pts',(122.64427346112,0.503054707564457,135.698735569038));
#40674=CARTESIAN_POINT('Ctrl Pts',(122.636517158378,0.638959267758077,135.680928479971));
#40675=CARTESIAN_POINT('Ctrl Pts',(122.628756715864,0.774936364307664,135.663111886725));
#40676=CARTESIAN_POINT('Ctrl Pts',(122.62099627335,0.910059843151345,135.639617818276));
#40677=CARTESIAN_POINT('Ctrl Pts',(122.613235830835,1.04382835863018,135.610565505023));
#40678=CARTESIAN_POINT('Ctrl Pts',(122.60546293057,1.17781161120547,135.581466554418));
#40679=CARTESIAN_POINT('Ctrl Pts',(122.597690030305,1.31043517538972,135.546791627786));
#40680=CARTESIAN_POINT('Ctrl Pts',(122.589917130039,1.441212243248,135.506710065705));
#40681=CARTESIAN_POINT('Ctrl Pts',(122.582426794277,1.56723523528109,135.468085569365));
#40682=CARTESIAN_POINT('Ctrl Pts',(122.574936458515,1.69154335917757,135.424440804636));
#40683=CARTESIAN_POINT('Ctrl Pts',(122.567446122753,1.81372055519902,135.375968738364));
#40684=CARTESIAN_POINT('Ctrl Pts',(122.559671788634,1.94053013674339,135.325658838967));
#40685=CARTESIAN_POINT('Ctrl Pts',(122.551897454515,2.06544570698642,135.269988991084));
#40686=CARTESIAN_POINT('Ctrl Pts',(122.544123120396,2.18798093138022,135.209121962567));
#40687=CARTESIAN_POINT('Ctrl Pts',(122.536358367449,2.31036514206116,135.148329947223));
#40688=CARTESIAN_POINT('Ctrl Pts',(122.528593614502,2.4303744970247,135.082353667665));
#40689=CARTESIAN_POINT('Ctrl Pts',(122.520828861555,2.54754065933153,135.011404669101));
#40690=CARTESIAN_POINT('Ctrl Pts',(122.51307182067,2.66459045055429,134.940526138081));
#40691=CARTESIAN_POINT('Ctrl Pts',(122.505314779784,2.77880233654142,134.864684918038));
#40692=CARTESIAN_POINT('Ctrl Pts',(122.497557738899,2.88973103528868,134.78413920515));
#40693=CARTESIAN_POINT('Ctrl Pts',(122.489806547659,3.00057608184155,134.70365423241));
#40694=CARTESIAN_POINT('Ctrl Pts',(122.482055356419,3.10814255415416,134.61847205708));
#40695=CARTESIAN_POINT('Ctrl Pts',(122.474304165179,3.21201302534738,134.52889486865));
#40696=CARTESIAN_POINT('Ctrl Pts',(122.466556268402,3.31583934881922,134.439355752915));
#40697=CARTESIAN_POINT('Ctrl Pts',(122.458808371625,3.41597250011656,134.345425594184));
#40698=CARTESIAN_POINT('Ctrl Pts',(122.451060474848,3.5120272921393,134.247447511876));
#40699=CARTESIAN_POINT('Ctrl Pts',(122.443314198764,3.60806199157032,134.14948992447));
#40700=CARTESIAN_POINT('Ctrl Pts',(122.43556792268,3.70001975507199,134.047486376701));
#40701=CARTESIAN_POINT('Ctrl Pts',(122.427821646595,3.78755180468155,133.941817292861));
#40702=CARTESIAN_POINT('Ctrl Pts',(122.42007531333,3.87508450043256,133.836147428996));
#40703=CARTESIAN_POINT('Ctrl Pts',(122.412328980065,3.95819116769659,133.726812276151));
#40704=CARTESIAN_POINT('Ctrl Pts',(122.404582646799,4.03656318787289,133.614225506277));
#40705=CARTESIAN_POINT('Ctrl Pts',(122.396834578796,4.11495275891997,133.501613523376));
#40706=CARTESIAN_POINT('Ctrl Pts',(122.389086510793,4.18860534970106,133.385748795274));
#40707=CARTESIAN_POINT('Ctrl Pts',(122.38133844279,4.25725578768592,133.267073800362));
#40708=CARTESIAN_POINT('Ctrl Pts',(122.373582140049,4.32597918817317,133.148272676253));
#40709=CARTESIAN_POINT('Ctrl Pts',(122.365825837307,4.38968961980737,133.02665565787));
#40710=CARTESIAN_POINT('Ctrl Pts',(122.358069534565,4.44816774589062,132.902690135759));
#40711=CARTESIAN_POINT('Ctrl Pts',(122.350309092051,4.5066770835107,132.778658449516));
#40712=CARTESIAN_POINT('Ctrl Pts',(122.342548649537,4.55994839922792,132.652276121997));
#40713=CARTESIAN_POINT('Ctrl Pts',(122.334788207022,4.60781101537796,132.524029396448));
#40714=CARTESIAN_POINT('Ctrl Pts',(122.327015306757,4.65575046484836,132.39557679787));
#40715=CARTESIAN_POINT('Ctrl Pts',(122.319242406491,4.69826374298029,132.265254192401));
#40716=CARTESIAN_POINT('Ctrl Pts',(122.311469506226,4.73523018921738,132.133562678061));
#40717=CARTESIAN_POINT('Ctrl Pts',(122.303979170464,4.77085281202079,132.006658481979));
#40718=CARTESIAN_POINT('Ctrl Pts',(122.296488834702,4.80132481273146,131.878483475337));
#40719=CARTESIAN_POINT('Ctrl Pts',(122.28899849894,4.82658364937024,131.749492004269));
#40720=CARTESIAN_POINT('Ctrl Pts',(122.281224164821,4.85280018247748,131.61560978237));
#40721=CARTESIAN_POINT('Ctrl Pts',(122.273449830702,4.87348347975067,131.48042386274));
#40722=CARTESIAN_POINT('Ctrl Pts',(122.265675496583,4.88850760668973,131.344431392406));
#40723=CARTESIAN_POINT('Ctrl Pts',(122.257910743636,4.90351321773507,131.208606520639));
#40724=CARTESIAN_POINT('Ctrl Pts',(122.250145990689,4.91287349294705,131.071977460805));
#40725=CARTESIAN_POINT('Ctrl Pts',(122.242381237741,4.91651326374388,130.935052583388));
#40726=CARTESIAN_POINT('Ctrl Pts',(122.234624196857,4.92014941946904,130.79826370169));
#40727=CARTESIAN_POINT('Ctrl Pts',(122.226867155971,4.918076367268,130.661179975402));
#40728=CARTESIAN_POINT('Ctrl Pts',(122.219110115086,4.91027064909904,130.524315594228));
#40729=CARTESIAN_POINT('Ctrl Pts',(122.211358923846,4.90247081728285,130.387554423547));
#40730=CARTESIAN_POINT('Ctrl Pts',(122.203607732606,4.88894694643506,130.251012657494));
#40731=CARTESIAN_POINT('Ctrl Pts',(122.195856541366,4.86972764770875,130.115204829924));
#40732=CARTESIAN_POINT('Ctrl Pts',(122.188108644589,4.85051651769716,129.979454724303));
#40733=CARTESIAN_POINT('Ctrl Pts',(122.180360747812,4.82561482908048,129.844438323033));
#40734=CARTESIAN_POINT('Ctrl Pts',(122.172612851035,4.79510305490826,129.710665159356));
#40735=CARTESIAN_POINT('Ctrl Pts',(122.164866574951,4.76459766314141,129.576919978141));
#40736=CARTESIAN_POINT('Ctrl Pts',(122.157120298867,4.72848460687843,129.444417898183));
#40737=CARTESIAN_POINT('Ctrl Pts',(122.149374022783,4.68689542484307,129.313657984884));
#40738=CARTESIAN_POINT('Ctrl Pts',(122.141627689517,4.64530593580589,129.182897106345));
#40739=CARTESIAN_POINT('Ctrl Pts',(122.133881356252,4.59824035883419,129.0538787927));
#40740=CARTESIAN_POINT('Ctrl Pts',(122.126135022987,4.54587991196435,128.927086293313));
#40741=CARTESIAN_POINT('Ctrl Pts',(122.118386954984,4.4935077393355,128.800265399625));
#40742=CARTESIAN_POINT('Ctrl Pts',(122.110638886981,4.4358384865056,128.675671673359));
#40743=CARTESIAN_POINT('Ctrl Pts',(122.102890818978,4.37310109084685,128.553767382054));
#40744=CARTESIAN_POINT('Ctrl Pts',(122.095134516236,4.3102970171372,128.431733529416));
#40745=CARTESIAN_POINT('Ctrl Pts',(122.087378213494,4.24241421971074,128.312395169812));
#40746=CARTESIAN_POINT('Ctrl Pts',(122.079621910752,4.16972737062844,128.196189473425));
#40747=CARTESIAN_POINT('Ctrl Pts',(122.071861468238,4.09700172638623,128.079921754558));
#40748=CARTESIAN_POINT('Ctrl Pts',(122.064101025724,4.01946714228137,127.96679035284));
#40749=CARTESIAN_POINT('Ctrl Pts',(122.05634058321,3.9374404530796,127.857201690573));
#40750=CARTESIAN_POINT('Ctrl Pts',(122.048567682944,3.85528208735434,127.747437106858));
#40751=CARTESIAN_POINT('Ctrl Pts',(122.040794782679,3.76861745372003,127.641226930364));
#40752=CARTESIAN_POINT('Ctrl Pts',(122.033021882413,3.67780292015556,127.538943531956));
#40753=CARTESIAN_POINT('Ctrl Pts',(122.025531546651,3.59028972363337,127.440378392715));
#40754=CARTESIAN_POINT('Ctrl Pts',(122.018041210889,3.4989233211436,127.345459713566));
#40755=CARTESIAN_POINT('Ctrl Pts',(122.010550875127,3.40405216148986,127.254485698029));
#40756=CARTESIAN_POINT('Ctrl Pts',(122.002776541008,3.30558393298314,127.160062375044));
#40757=CARTESIAN_POINT('Ctrl Pts',(121.995002206889,3.20302801752754,127.069589639606));
#40758=CARTESIAN_POINT('Ctrl Pts',(121.98722787277,3.09673460832412,126.983442164091));
#40759=CARTESIAN_POINT('Ctrl Pts',(121.979463119823,2.99057219624776,126.89740085764));
#40760=CARTESIAN_POINT('Ctrl Pts',(121.971698366875,2.88068175606293,126.815674448817));
#40761=CARTESIAN_POINT('Ctrl Pts',(121.963933613928,2.76745036379981,126.738600965741));
#40762=CARTESIAN_POINT('Ctrl Pts',(121.956176573043,2.65433143455208,126.661604033137));
#40763=CARTESIAN_POINT('Ctrl Pts',(121.948419532158,2.53787847786143,126.589251048151));
#40764=CARTESIAN_POINT('Ctrl Pts',(121.940662491273,2.41851141644303,126.521839678792));
#40765=CARTESIAN_POINT('Ctrl Pts',(121.932911300033,2.29923437065411,126.454479144872));
#40766=CARTESIAN_POINT('Ctrl Pts',(121.925160108793,2.17704793327744,126.392053000662));
#40767=CARTESIAN_POINT('Ctrl Pts',(121.917408917553,2.05240046124638,126.334815292908));
#40768=CARTESIAN_POINT('Ctrl Pts',(121.909661020776,1.92780596771602,126.277601912705));
#40769=CARTESIAN_POINT('Ctrl Pts',(121.901913123999,1.80075287450881,126.225572745745));
#40770=CARTESIAN_POINT('Ctrl Pts',(121.894165227222,1.67171336402272,126.178935502936));
#40771=CARTESIAN_POINT('Ctrl Pts',(121.886418951138,1.54270084582046,126.132308015633));
#40772=CARTESIAN_POINT('Ctrl Pts',(121.878672675054,1.41170310427758,126.091070341882));
#40773=CARTESIAN_POINT('Ctrl Pts',(121.870926398969,1.27921111714325,126.055381571468));
#40774=CARTESIAN_POINT('Ctrl Pts',(121.863180065704,1.14671815198298,126.019692537608));
#40775=CARTESIAN_POINT('Ctrl Pts',(121.855433732439,1.01273129673073,125.989552590508));
#40776=CARTESIAN_POINT('Ctrl Pts',(121.847687399173,0.877755075537518,125.965070474387));
#40777=CARTESIAN_POINT('Ctrl Pts',(121.83993933117,0.742748627355887,125.940582875666));
#40778=CARTESIAN_POINT('Ctrl Pts',(121.832191263167,0.606752756966128,125.921755698932));
#40779=CARTESIAN_POINT('Ctrl Pts',(121.824443195164,0.470280129382032,125.908646199587));
#40780=CARTESIAN_POINT('Ctrl Pts',(121.816686892423,0.333662457065015,125.89552276731));
#40781=CARTESIAN_POINT('Ctrl Pts',(121.808930589681,0.196567405153723,125.888129188958));
#40782=CARTESIAN_POINT('Ctrl Pts',(121.801174286939,0.0595112442624678,
125.88647067631));
#40783=CARTESIAN_POINT('Ctrl Pts',(121.793413844425,-0.0776180676289099,
125.884811278464));
#40784=CARTESIAN_POINT('Ctrl Pts',(121.785653401911,-0.214708056538748,
125.888893033948));
#40785=CARTESIAN_POINT('Ctrl Pts',(121.777892959396,-0.351245530942734,
125.898669061884));
#40786=CARTESIAN_POINT('Ctrl Pts',(121.770120059131,-0.488002187421583,
125.908460783167));
#40787=CARTESIAN_POINT('Ctrl Pts',(121.762347158866,-0.624204168315074,
125.923964999191));
#40788=CARTESIAN_POINT('Ctrl Pts',(121.7545742586,-0.759345561872103,125.94508316303));
#40789=CARTESIAN_POINT('Ctrl Pts',(121.747083922838,-0.889574225371972,
125.965433628419));
#40790=CARTESIAN_POINT('Ctrl Pts',(121.739593587076,-1.01881777066954,125.990996905867));
#40791=CARTESIAN_POINT('Ctrl Pts',(121.732103251314,-1.14663696560631,126.021641021812));
#40792=CARTESIAN_POINT('Ctrl Pts',(121.724328917195,-1.27930246416974,126.053447018729));
#40793=CARTESIAN_POINT('Ctrl Pts',(121.716554583076,-1.41085371618547,126.090827491513));
#40794=CARTESIAN_POINT('Ctrl Pts',(121.708780248957,-1.54078621119515,126.133690332276));
#40795=CARTESIAN_POINT('Ctrl Pts',(121.70101549601,-1.67055857601678,126.176500348419));
#40796=CARTESIAN_POINT('Ctrl Pts',(121.693250743063,-1.79871578551457,126.224779167758));
#40797=CARTESIAN_POINT('Ctrl Pts',(121.685485990116,-1.9247642230084,126.278383844722));
#40798=CARTESIAN_POINT('Ctrl Pts',(121.677728949231,-2.05068746741723,126.331935280765));
#40799=CARTESIAN_POINT('Ctrl Pts',(121.669971908346,-2.17450575044197,126.390801895643));
#40800=CARTESIAN_POINT('Ctrl Pts',(121.662214867461,-2.2957416570714,126.454791293313));
#40801=CARTESIAN_POINT('Ctrl Pts',(121.654463676221,-2.41688613876073,126.51873243608));
#40802=CARTESIAN_POINT('Ctrl Pts',(121.646712484981,-2.53545177585653,126.587788490556));
#40803=CARTESIAN_POINT('Ctrl Pts',(121.63896129374,-2.65098248376344,126.661719559825));
#40804=CARTESIAN_POINT('Ctrl Pts',(121.631213396963,-2.76646408803754,126.735619206418));
#40805=CARTESIAN_POINT('Ctrl Pts',(121.623465500186,-2.87891300006648,126.814389536439));
#40806=CARTESIAN_POINT('Ctrl Pts',(121.615717603409,-2.9878992406602,126.897745562283));
#40807=CARTESIAN_POINT('Ctrl Pts',(121.607971327325,-3.09686268368186,126.981084151844));
#40808=CARTESIAN_POINT('Ctrl Pts',(121.600225051241,-3.20236458562215,127.069006291904));
#40809=CARTESIAN_POINT('Ctrl Pts',(121.592478775157,-3.30400571427236,127.161184900893));
#40810=CARTESIAN_POINT('Ctrl Pts',(121.584732441892,-3.40564759321437,127.253364190324));
#40811=CARTESIAN_POINT('Ctrl Pts',(121.576986108626,-3.50342835239185,127.349799748736));
#40812=CARTESIAN_POINT('Ctrl Pts',(121.569239775361,-3.59698379458653,127.450125884578));
#40813=CARTESIAN_POINT('Ctrl Pts',(121.561491707358,-3.69056018787395,127.550474487763));
#40814=CARTESIAN_POINT('Ctrl Pts',(121.553743639355,-3.77990911470321,127.654715116222));
#40815=CARTESIAN_POINT('Ctrl Pts',(121.545995571352,-3.86470529652155,127.762447398301));
#40816=CARTESIAN_POINT('Ctrl Pts',(121.53823926861,-3.94959160073084,127.870294179531));
#40817=CARTESIAN_POINT('Ctrl Pts',(121.530482965868,-4.02991525188601,127.981639719741));
#40818=CARTESIAN_POINT('Ctrl Pts',(121.522726663126,-4.10539280829276,128.096052482933));
#40819=CARTESIAN_POINT('Ctrl Pts',(121.514966220612,-4.180910649344,128.210526311662));
#40820=CARTESIAN_POINT('Ctrl Pts',(121.507205778098,-4.25157704046853,128.328070290464));
#40821=CARTESIAN_POINT('Ctrl Pts',(121.499445335584,-4.31715403132347,128.448227316514));
#40822=CARTESIAN_POINT('Ctrl Pts',(121.491672435318,-4.38283629218579,128.568577229289));
#40823=CARTESIAN_POINT('Ctrl Pts',(121.483899535053,-4.44341265373388,128.691548220728));
#40824=CARTESIAN_POINT('Ctrl Pts',(121.476126634787,-4.49869256862852,128.816661385925));
#40825=CARTESIAN_POINT('Ctrl Pts',(121.468636299025,-4.55196291937478,128.937226372426));
#40826=CARTESIAN_POINT('Ctrl Pts',(121.461145963263,-4.60031510325118,129.05978020333));
#40827=CARTESIAN_POINT('Ctrl Pts',(121.453655627501,-4.64362273764029,129.183882005251));
#40828=CARTESIAN_POINT('Ctrl Pts',(121.445749280443,-4.68933566675726,129.314876388909));
#40829=CARTESIAN_POINT('Ctrl Pts',(121.437842933385,-4.72953256361434,129.4478895032));
#40830=CARTESIAN_POINT('Ctrl Pts',(121.429936586327,-4.76405452823403,129.582490119308));
#40831=CARTESIAN_POINT('Origin',(213.235140564004,0.,130.804360617566));
#40832=CARTESIAN_POINT('',(119.334999413688,-4.76405452823402,129.582490119308));
#40833=CARTESIAN_POINT('',(119.679968582935,-4.76405452823404,129.582490119308));
#40834=CARTESIAN_POINT('',(213.235140564004,-4.76405452823405,129.582490119308));
#40835=CARTESIAN_POINT('',(121.014859435936,-4.9182487480187,130.807869907024));
#40836=CARTESIAN_POINT('Ctrl Pts',(121.014859435936,-4.9182487480187,130.807869907024));
#40837=CARTESIAN_POINT('Ctrl Pts',(121.005990668755,-4.91813660439169,130.965038547478));
#40838=CARTESIAN_POINT('Ctrl Pts',(120.997121901573,-4.91048672634217,131.121906140279));
#40839=CARTESIAN_POINT('Ctrl Pts',(120.988253134392,-4.89540936564683,131.277805656865));
#40840=CARTESIAN_POINT('Ctrl Pts',(120.979341933319,-4.88025986515247,131.434451097094));
#40841=CARTESIAN_POINT('Ctrl Pts',(120.970430732247,-4.85761174710443,131.590119028022));
#40842=CARTESIAN_POINT('Ctrl Pts',(120.961519531174,-4.82762636292375,131.744151425408));
#40843=CARTESIAN_POINT('Ctrl Pts',(120.952553434066,-4.79745625855732,131.899132714857));
#40844=CARTESIAN_POINT('Ctrl Pts',(120.943587336958,-4.75985829917768,132.052458112461));
#40845=CARTESIAN_POINT('Ctrl Pts',(120.93462123985,-4.71504533913386,132.203478379733));
#40846=CARTESIAN_POINT('Ctrl Pts',(120.928530618578,-4.68460413775154,132.306065630483));
#40847=CARTESIAN_POINT('Ctrl Pts',(120.922439997307,-4.65083464287957,132.407589637772));
#40848=CARTESIAN_POINT('Ctrl Pts',(120.916349376035,-4.61381590295559,132.507852876467));
#40849=CARTESIAN_POINT('Ctrl Pts',(120.908575041916,-4.56656357187052,132.63583323885));
#40850=CARTESIAN_POINT('Ctrl Pts',(120.900800707797,-4.51390738478452,132.762048759346));
#40851=CARTESIAN_POINT('Ctrl Pts',(120.893026373678,-4.4559983919868,132.886009337478));
#40852=CARTESIAN_POINT('Ctrl Pts',(120.885261620731,-4.39816076684725,133.009817145276));
#40853=CARTESIAN_POINT('Ctrl Pts',(120.877496867784,-4.33508338044493,133.131375189303));
#40854=CARTESIAN_POINT('Ctrl Pts',(120.869732114837,-4.26696647827154,133.250210190988));
#40855=CARTESIAN_POINT('Ctrl Pts',(120.861975073952,-4.19891723076567,133.368927164073));
#40856=CARTESIAN_POINT('Ctrl Pts',(120.854218033067,-4.12583862146679,133.484926140023));
#40857=CARTESIAN_POINT('Ctrl Pts',(120.846460992182,-4.04797808665986,133.597755769066));
#40858=CARTESIAN_POINT('Ctrl Pts',(120.838709800942,-3.97017626708778,133.710500312408));
#40859=CARTESIAN_POINT('Ctrl Pts',(120.830958609702,-3.88759992086172,133.820079945569));
#40860=CARTESIAN_POINT('Ctrl Pts',(120.823207418461,-3.80054113335574,133.926070110163));
#40861=CARTESIAN_POINT('Ctrl Pts',(120.815459521684,-3.71351934815694,134.03201522611));
#40862=CARTESIAN_POINT('Ctrl Pts',(120.807711624907,-3.62201915852423,134.134373606349));
#40863=CARTESIAN_POINT('Ctrl Pts',(120.79996372813,-3.52637434163955,134.232751940785));
#40864=CARTESIAN_POINT('Ctrl Pts',(120.792217452046,-3.43074953158863,134.331109696595));
#40865=CARTESIAN_POINT('Ctrl Pts',(120.784471175962,-3.33098209108957,134.425488782424));
#40866=CARTESIAN_POINT('Ctrl Pts',(120.776724899878,-3.22744396517328,134.515531391616));
#40867=CARTESIAN_POINT('Ctrl Pts',(120.768978566613,-3.12390507496221,134.605574665483));
#40868=CARTESIAN_POINT('Ctrl Pts',(120.761232233347,-3.01659573880367,134.691281142278));
#40869=CARTESIAN_POINT('Ctrl Pts',(120.753485900082,-2.90592210352628,134.77233236529));
#40870=CARTESIAN_POINT('Ctrl Pts',(120.745737832079,-2.79522368365555,134.853401739162));
#40871=CARTESIAN_POINT('Ctrl Pts',(120.737989764076,-2.68115978082898,134.929813553817));
#40872=CARTESIAN_POINT('Ctrl Pts',(120.730241696073,-2.56416638260516,135.001292094826));
#40873=CARTESIAN_POINT('Ctrl Pts',(120.722485393331,-2.44704864240539,135.07284660408));
#40874=CARTESIAN_POINT('Ctrl Pts',(120.714729090589,-2.3269955214092,135.13945716179));
#40875=CARTESIAN_POINT('Ctrl Pts',(120.706972787847,-2.20446901208997,135.200893278338));
#40876=CARTESIAN_POINT('Ctrl Pts',(120.699212345333,-2.08187710668343,135.262362185191));
#40877=CARTESIAN_POINT('Ctrl Pts',(120.691451902819,-1.95680953884554,135.318650987472));
#40878=CARTESIAN_POINT('Ctrl Pts',(120.683691460305,-1.82974831600096,135.369577388169));
#40879=CARTESIAN_POINT('Ctrl Pts',(120.675918560039,-1.7024831232016,135.420585540445));
#40880=CARTESIAN_POINT('Ctrl Pts',(120.668145659774,-1.57321824887618,135.466213958996));
#40881=CARTESIAN_POINT('Ctrl Pts',(120.660372759508,-1.44245175122122,135.50632999304));
#40882=CARTESIAN_POINT('Ctrl Pts',(120.652882423746,-1.31643894513546,135.544987708202));
#40883=CARTESIAN_POINT('Ctrl Pts',(120.645392087984,-1.18903209372321,135.578526780472));
#40884=CARTESIAN_POINT('Ctrl Pts',(120.637901752222,-1.06068391144384,135.606873782827));
#40885=CARTESIAN_POINT('Ctrl Pts',(120.630127418103,-0.927469368824172,
135.636295570392));
#40886=CARTESIAN_POINT('Ctrl Pts',(120.622353083984,-0.792818721502979,
135.660217000709));
#40887=CARTESIAN_POINT('Ctrl Pts',(120.614578749865,-0.657225951261317,
135.678500245386));
#40888=CARTESIAN_POINT('Ctrl Pts',(120.606813996918,-0.521800286990796,
135.696760957598));
#40889=CARTESIAN_POINT('Ctrl Pts',(120.599049243971,-0.3854351937467,135.709397257991));
#40890=CARTESIAN_POINT('Ctrl Pts',(120.591284491024,-0.248637091774711,
135.716321800138));
#40891=CARTESIAN_POINT('Ctrl Pts',(120.583527450139,-0.111974859606116,
135.723239464732));
#40892=CARTESIAN_POINT('Ctrl Pts',(120.575770409253,0.0251191374923183,
135.724456640969));
#40893=CARTESIAN_POINT('Ctrl Pts',(120.568013368368,0.162131420819873,135.719937538425));
#40894=CARTESIAN_POINT('Ctrl Pts',(120.560262177128,0.299040382118771,135.715421843772));
#40895=CARTESIAN_POINT('Ctrl Pts',(120.552510985888,0.435867363127998,135.705178493363));
#40896=CARTESIAN_POINT('Ctrl Pts',(120.544759794648,0.572097291574801,135.689223742718));
#40897=CARTESIAN_POINT('Ctrl Pts',(120.537011897871,0.708269318668056,135.673275773268));
#40898=CARTESIAN_POINT('Ctrl Pts',(120.529264001094,0.843844410416449,135.651621277072));
#40899=CARTESIAN_POINT('Ctrl Pts',(120.521516104317,0.978311249177513,135.624328476612));
#40900=CARTESIAN_POINT('Ctrl Pts',(120.513769828233,1.11274996037468,135.597041385217));
#40901=CARTESIAN_POINT('Ctrl Pts',(120.506023552149,1.2460804967827,135.564118413192));
#40902=CARTESIAN_POINT('Ctrl Pts',(120.498277276064,1.37780078015259,135.525679085188));
#40903=CARTESIAN_POINT('Ctrl Pts',(120.490530942799,1.50952203585168,135.487239473434));
#40904=CARTESIAN_POINT('Ctrl Pts',(120.482784609534,1.63963263948338,135.44328353397));
#40905=CARTESIAN_POINT('Ctrl Pts',(120.475038276268,1.76764513211481,135.393980835995));
#40906=CARTESIAN_POINT('Ctrl Pts',(120.467290208265,1.8956862922563,135.344667097022));
#40907=CARTESIAN_POINT('Ctrl Pts',(120.459542140262,2.02162804166398,135.2900043574));
#40908=CARTESIAN_POINT('Ctrl Pts',(120.451794072259,2.14500275205556,135.230210395425));
#40909=CARTESIAN_POINT('Ctrl Pts',(120.444037769518,2.26850858655761,135.170352883716));
#40910=CARTESIAN_POINT('Ctrl Pts',(120.436281466776,2.38944157962719,135.105353426436));
#40911=CARTESIAN_POINT('Ctrl Pts',(120.428525164034,2.50735809560362,135.035476125669));
#40912=CARTESIAN_POINT('Ctrl Pts',(120.42076472152,2.62533754717509,134.965561529283));
#40913=CARTESIAN_POINT('Ctrl Pts',(120.413004279006,2.74029698607688,134.890764114926));
#40914=CARTESIAN_POINT('Ctrl Pts',(120.405243836491,2.85182250388439,134.811390873109));
#40915=CARTESIAN_POINT('Ctrl Pts',(120.397470936226,2.96352705235385,134.731890214318));
#40916=CARTESIAN_POINT('Ctrl Pts',(120.38969803596,3.07178635518746,134.647799289339));
#40917=CARTESIAN_POINT('Ctrl Pts',(120.381925135695,3.17621959690619,134.559465427652));
#40918=CARTESIAN_POINT('Ctrl Pts',(120.374434799933,3.2768564272362,134.474342724337));
#40919=CARTESIAN_POINT('Ctrl Pts',(120.366944464171,3.37394031388461,134.385280419695));
#40920=CARTESIAN_POINT('Ctrl Pts',(120.359454128409,3.46716477739389,134.292619706123));
#40921=CARTESIAN_POINT('Ctrl Pts',(120.35167979429,3.56392387477278,134.196445733431));
#40922=CARTESIAN_POINT('Ctrl Pts',(120.343905460171,3.6568316154907,134.096090447735));
#40923=CARTESIAN_POINT('Ctrl Pts',(120.336131126052,3.74550503139918,133.991894950285));
#40924=CARTESIAN_POINT('Ctrl Pts',(120.328366373105,3.83406916524751,133.887827864474));
#40925=CARTESIAN_POINT('Ctrl Pts',(120.320601620158,3.91840910644715,133.779930278488));
#40926=CARTESIAN_POINT('Ctrl Pts',(120.312836867211,3.99817763546422,133.668581045147));
#40927=CARTESIAN_POINT('Ctrl Pts',(120.305079826326,4.07786693725367,133.557342405435));
#40928=CARTESIAN_POINT('Ctrl Pts',(120.297322785441,4.15299363623217,133.442659256459));
#40929=CARTESIAN_POINT('Ctrl Pts',(120.289565744556,4.22325007312434,133.324944256796));
#40930=CARTESIAN_POINT('Ctrl Pts',(120.281814553315,4.29345352909089,133.20731802693));
#40931=CARTESIAN_POINT('Ctrl Pts',(120.274063362075,4.35879383370537,133.086664831562));
#40932=CARTESIAN_POINT('Ctrl Pts',(120.266312170835,4.41900625405234,132.963426802088));
#40933=CARTESIAN_POINT('Ctrl Pts',(120.258564274058,4.47919308251453,132.840241152064));
#40934=CARTESIAN_POINT('Ctrl Pts',(120.250816377281,4.53425619027309,132.714473203555));
#40935=CARTESIAN_POINT('Ctrl Pts',(120.243068480504,4.5839765951592,132.586590018494));
#40936=CARTESIAN_POINT('Ctrl Pts',(120.23532220442,4.63368659960846,132.458733583839));
#40937=CARTESIAN_POINT('Ctrl Pts',(120.227575928336,4.67805598252515,132.328763156874));
#40938=CARTESIAN_POINT('Ctrl Pts',(120.219829652252,4.71691391782517,132.197165756244));
#40939=CARTESIAN_POINT('Ctrl Pts',(120.212083318986,4.75577213996561,132.065567384191));
#40940=CARTESIAN_POINT('Ctrl Pts',(120.204336985721,4.789118722589,131.932342389469));
#40941=CARTESIAN_POINT('Ctrl Pts',(120.196590652456,4.81683284560382,131.797992541375));
#40942=CARTESIAN_POINT('Ctrl Pts',(120.188842584453,4.84455317500433,131.663612606564));
#40943=CARTESIAN_POINT('Ctrl Pts',(120.18109451645,4.86663845588384,131.528107699954));
#40944=CARTESIAN_POINT('Ctrl Pts',(120.173346448447,4.88301914678287,131.391988964952));
#40945=CARTESIAN_POINT('Ctrl Pts',(120.165590145705,4.89941724727513,131.255725561339));
#40946=CARTESIAN_POINT('Ctrl Pts',(120.157833842963,4.91009859969219,131.118847414909));
#40947=CARTESIAN_POINT('Ctrl Pts',(120.150077540221,4.9150456046854,130.981870522537));
#40948=CARTESIAN_POINT('Ctrl Pts',(120.142317097707,4.91999525004413,130.844820521472));
#40949=CARTESIAN_POINT('Ctrl Pts',(120.134556655193,4.91920445173975,130.707672060215));
#40950=CARTESIAN_POINT('Ctrl Pts',(120.126796212678,4.91270776196941,130.570939307516));
#40951=CARTESIAN_POINT('Ctrl Pts',(120.119023312413,4.9062006431359,130.433987059263));
#40952=CARTESIAN_POINT('Ctrl Pts',(120.111250412148,4.89396936393437,130.29745224274));
#40953=CARTESIAN_POINT('Ctrl Pts',(120.103477511882,4.87610030242466,130.161842988863));
#40954=CARTESIAN_POINT('Ctrl Pts',(120.09598717612,4.85888082631016,130.031163472942));
#40955=CARTESIAN_POINT('Ctrl Pts',(120.088496840358,4.83642639917832,129.901343698418));
#40956=CARTESIAN_POINT('Ctrl Pts',(120.081006504596,4.80885841622255,129.772825937962));
#40957=CARTESIAN_POINT('Ctrl Pts',(120.073232170477,4.78024518481408,129.639435387557));
#40958=CARTESIAN_POINT('Ctrl Pts',(120.065457836358,4.74603234400435,129.507024990775));
#40959=CARTESIAN_POINT('Ctrl Pts',(120.057683502239,4.70629986829687,129.376101323121));
#40960=CARTESIAN_POINT('Ctrl Pts',(120.049918749292,4.66661635931472,129.245339007187));
#40961=CARTESIAN_POINT('Ctrl Pts',(120.042153996344,4.62142686274248,129.116060145254));
#40962=CARTESIAN_POINT('Ctrl Pts',(120.034389243397,4.57086243754707,128.988761642153));
#40963=CARTESIAN_POINT('Ctrl Pts',(120.026632202512,4.52034823365161,128.86158957372));
#40964=CARTESIAN_POINT('Ctrl Pts',(120.018875161627,4.46446986829211,128.736394310857));
#40965=CARTESIAN_POINT('Ctrl Pts',(120.011118120742,4.40340822546264,128.613657748068));
#40966=CARTESIAN_POINT('Ctrl Pts',(120.003366929502,4.34239262969302,128.491013741875));
#40967=CARTESIAN_POINT('Ctrl Pts',(119.995615738262,4.27620171002332,128.370825093854));
#40968=CARTESIAN_POINT('Ctrl Pts',(119.987864547022,4.20506434951178,128.253553514125));
#40969=CARTESIAN_POINT('Ctrl Pts',(119.980116650245,4.1339572242761,128.136331777945));
#40970=CARTESIAN_POINT('Ctrl Pts',(119.972368753468,4.05790804199699,128.022024977698));
#40971=CARTESIAN_POINT('Ctrl Pts',(119.964620856691,3.97719138989455,127.911069807667));
#40972=CARTESIAN_POINT('Ctrl Pts',(119.956874580607,3.89649162197569,127.800137847065));
#40973=CARTESIAN_POINT('Ctrl Pts',(119.949128304522,3.81112655606539,127.692556438132));
#40974=CARTESIAN_POINT('Ctrl Pts',(119.941382028438,3.72141359907042,127.588732547165));
#40975=CARTESIAN_POINT('Ctrl Pts',(119.933635695173,3.63169997983478,127.484907889793));
#40976=CARTESIAN_POINT('Ctrl Pts',(119.925889361908,3.53763866109004,127.384841101558));
#40977=CARTESIAN_POINT('Ctrl Pts',(119.918143028642,3.43958648934775,127.288905050389));
#40978=CARTESIAN_POINT('Ctrl Pts',(119.910394960639,3.34151235950144,127.192947515006));
#40979=CARTESIAN_POINT('Ctrl Pts',(119.902646892636,3.23944587765031,127.101122830801));
#40980=CARTESIAN_POINT('Ctrl Pts',(119.894898824633,3.13377949436166,127.013765790468));
#40981=CARTESIAN_POINT('Ctrl Pts',(119.887142521891,3.0280008075834,126.926315906034));
#40982=CARTESIAN_POINT('Ctrl Pts',(119.87938621915,2.91861487828964,126.843343400155));
#40983=CARTESIAN_POINT('Ctrl Pts',(119.871629916408,2.80604631638542,126.765141988574));
#40984=CARTESIAN_POINT('Ctrl Pts',(119.863869473894,2.69341767325027,126.686898838544));
#40985=CARTESIAN_POINT('Ctrl Pts',(119.856109031379,2.57760334274872,126.613432066208));
#40986=CARTESIAN_POINT('Ctrl Pts',(119.848348588865,2.45905458591844,126.54499052259));
#40987=CARTESIAN_POINT('Ctrl Pts',(119.8405756886,2.34031552409944,126.476439110531));
#40988=CARTESIAN_POINT('Ctrl Pts',(119.832802788334,2.21883361091768,126.412929228752));
#40989=CARTESIAN_POINT('Ctrl Pts',(119.825029888069,2.09508304075466,126.354662862118));
#40990=CARTESIAN_POINT('Ctrl Pts',(119.817539552307,1.97583111552721,126.298514624675));
#40991=CARTESIAN_POINT('Ctrl Pts',(119.810049216545,1.85447289619021,126.24723541101));
#40992=CARTESIAN_POINT('Ctrl Pts',(119.802558880783,1.73144609633575,126.20096214709));
#40993=CARTESIAN_POINT('Ctrl Pts',(119.794784546664,1.60375469797044,126.152934418303));
#40994=CARTESIAN_POINT('Ctrl Pts',(119.787010212545,1.4738612049472,126.11014759647));
#40995=CARTESIAN_POINT('Ctrl Pts',(119.779235878426,1.34223504175979,126.072808213209));
#40996=CARTESIAN_POINT('Ctrl Pts',(119.771471125479,1.21077109605474,126.035514847402));
#40997=CARTESIAN_POINT('Ctrl Pts',(119.763706372532,1.07757910143104,126.003655668015));
#40998=CARTESIAN_POINT('Ctrl Pts',(119.755941619585,0.943147958568414,125.977389000626));
#40999=CARTESIAN_POINT('Ctrl Pts',(119.7481845787,0.808850334612117,125.951148421661));
#41000=CARTESIAN_POINT('Ctrl Pts',(119.740427537815,0.673316392870307,125.930489375354));
#41001=CARTESIAN_POINT('Ctrl Pts',(119.73267049693,0.537049337052604,125.915520154627));
#41002=CARTESIAN_POINT('Ctrl Pts',(119.724919305689,0.40088504128151,125.900562222306));
#41003=CARTESIAN_POINT('Ctrl Pts',(119.717168114449,0.263989118897879,125.891285617622));
#41004=CARTESIAN_POINT('Ctrl Pts',(119.709416923209,0.126873736584666,125.887747340374));
#41005=CARTESIAN_POINT('Ctrl Pts',(119.701669026432,-0.0101833680332993,
125.884210566987));
#41006=CARTESIAN_POINT('Ctrl Pts',(119.693921129655,-0.147459357044499,
125.886407280231));
#41007=CARTESIAN_POINT('Ctrl Pts',(119.686173232878,-0.284438406080855,
125.894342506026));
#41008=CARTESIAN_POINT('Ctrl Pts',(119.678426956794,-0.421388802053079,
125.902276071944));
#41009=CARTESIAN_POINT('Ctrl Pts',(119.67068068071,-0.55804199153395,125.915945740208));
#41010=CARTESIAN_POINT('Ctrl Pts',(119.662934404626,-0.693884016066977,
125.935304442623));
#41011=CARTESIAN_POINT('Ctrl Pts',(119.65518807136,-0.829727043354971,125.95466328794));
#41012=CARTESIAN_POINT('Ctrl Pts',(119.647441738095,-0.964758506692176,
125.979711196047));
#41013=CARTESIAN_POINT('Ctrl Pts',(119.63969540483,-1.09847181747517,126.01034948609));
#41014=CARTESIAN_POINT('Ctrl Pts',(119.631947336827,-1.23221507242701,126.040994637366));
#41015=CARTESIAN_POINT('Ctrl Pts',(119.624199268824,-1.36463920641229,126.077232574465));
#41016=CARTESIAN_POINT('Ctrl Pts',(119.616451200821,-1.49525041973602,126.118914081239));
#41017=CARTESIAN_POINT('Ctrl Pts',(119.608694898079,-1.62600044821156,126.160639887615));
#41018=CARTESIAN_POINT('Ctrl Pts',(119.600938595337,-1.75493333399475,126.207820701756));
#41019=CARTESIAN_POINT('Ctrl Pts',(119.593182292595,-1.88157245368625,126.260258047858));
#41020=CARTESIAN_POINT('Ctrl Pts',(119.585421850081,-2.00827916448905,126.31272338135));
#41021=CARTESIAN_POINT('Ctrl Pts',(119.577661407567,-2.13268931530129,126.37045067266));
#41022=CARTESIAN_POINT('Ctrl Pts',(119.569900965053,-2.25434962309309,126.433194773153));
#41023=CARTESIAN_POINT('Ctrl Pts',(119.562128064787,-2.37620523081136,126.496039596047));
#41024=CARTESIAN_POINT('Ctrl Pts',(119.554355164522,-2.49530183448049,126.563917127737));
#41025=CARTESIAN_POINT('Ctrl Pts',(119.546582264257,-2.61121318486823,126.636537592812));
#41026=CARTESIAN_POINT('Ctrl Pts',(119.539091928495,-2.72291086570622,126.706518121062));
#41027=CARTESIAN_POINT('Ctrl Pts',(119.531601592733,-2.8316506023576,126.780902560483));
#41028=CARTESIAN_POINT('Ctrl Pts',(119.524111256971,-2.93708060023924,126.859396662065));
#41029=CARTESIAN_POINT('Ctrl Pts',(119.516231596834,-3.04799052175957,126.941970643107));
#41030=CARTESIAN_POINT('Ctrl Pts',(119.508351936697,-3.15561253471809,127.029372439893));
#41031=CARTESIAN_POINT('Ctrl Pts',(119.50047227656,-3.25949339448024,127.121306738807));
#41032=CARTESIAN_POINT('Ctrl Pts',(119.492785051891,-3.36083729687221,127.210995836847));
#41033=CARTESIAN_POINT('Ctrl Pts',(119.485097827223,-3.45862030751185,127.304998364797));
#41034=CARTESIAN_POINT('Ctrl Pts',(119.477410602554,-3.55245005209682,127.402995937051));
#41035=CARTESIAN_POINT('Ctrl Pts',(119.469730357079,-3.64619460911075,127.500904537782));
#41036=CARTESIAN_POINT('Ctrl Pts',(119.462050111604,-3.73599276293087,127.602800683898));
#41037=CARTESIAN_POINT('Ctrl Pts',(119.45436986613,-3.82148622846593,127.708326692018));
#41038=CARTESIAN_POINT('Ctrl Pts',(119.446694849426,-3.90692148938258,127.813780857208));
#41039=CARTESIAN_POINT('Ctrl Pts',(119.439019832722,-3.98805764091882,127.922859659899));
#41040=CARTESIAN_POINT('Ctrl Pts',(119.431344816019,-4.06457456773828,128.035170005529));
#41041=CARTESIAN_POINT('Ctrl Pts',(119.423316032491,-4.14461841198534,128.152657105267));
#41042=CARTESIAN_POINT('Ctrl Pts',(119.415287248964,-4.21960674024664,128.273680422712));
#41043=CARTESIAN_POINT('Ctrl Pts',(119.407258465436,-4.28922167208049,128.39775294072));
#41044=CARTESIAN_POINT('Ctrl Pts',(119.399587505903,-4.35573403016929,128.516295838476));
#41045=CARTESIAN_POINT('Ctrl Pts',(119.39191654637,-4.4173414144964,128.637621624153));
#41046=CARTESIAN_POINT('Ctrl Pts',(119.384245586837,-4.47381247445167,128.761278385755));
#41047=CARTESIAN_POINT('Ctrl Pts',(119.37657473415,-4.53028274783441,128.884933424971));
#41048=CARTESIAN_POINT('Ctrl Pts',(119.368903881464,-4.58161667923464,129.010919009614));
#41049=CARTESIAN_POINT('Ctrl Pts',(119.361233028778,-4.62763056527772,129.138762102375));
#41050=CARTESIAN_POINT('Ctrl Pts',(119.353558968967,-4.67366368937961,129.266658645369));
#41051=CARTESIAN_POINT('Ctrl Pts',(119.345884909155,-4.71437220104739,129.396413868271));
#41052=CARTESIAN_POINT('Ctrl Pts',(119.338210849343,-4.74962193958152,129.527538588642));
#41053=CARTESIAN_POINT('Ctrl Pts',(119.337140370791,-4.75453903561341,129.545829585087));
#41054=CARTESIAN_POINT('Ctrl Pts',(119.33606989224,-4.75934999365132,129.564147210371));
#41055=CARTESIAN_POINT('Ctrl Pts',(119.334999413688,-4.76405452823402,129.582490119308));
#41056=CARTESIAN_POINT('Ctrl Pts',(121.084721392599,-4.76405452823403,129.582490119308));
#41057=CARTESIAN_POINT('Ctrl Pts',(121.076951239219,-4.79825256998917,129.715827765084));
#41058=CARTESIAN_POINT('Ctrl Pts',(121.069181085838,-4.82686303770906,129.850658621233));
#41059=CARTESIAN_POINT('Ctrl Pts',(121.061410932458,-4.84976794993014,129.98647682733));
#41060=CARTESIAN_POINT('Ctrl Pts',(121.053640539447,-4.87267356853512,130.12229922204));
#41061=CARTESIAN_POINT('Ctrl Pts',(121.045870146437,-4.88987320487444,130.259108647659));
#41062=CARTESIAN_POINT('Ctrl Pts',(121.038099753426,-4.90130009637116,130.396389506074));
#41063=CARTESIAN_POINT('Ctrl Pts',(121.030352980948,-4.91269225226841,130.533253056517));
#41064=CARTESIAN_POINT('Ctrl Pts',(121.022606208469,-4.91834670424102,130.670584793771));
#41065=CARTESIAN_POINT('Ctrl Pts',(121.014859435991,-4.91824874801939,130.807869906056));
#41066=CARTESIAN_POINT('',(121.36014056406,-4.91824852912944,130.800556906732));
#41067=CARTESIAN_POINT('Ctrl Pts',(121.429936586327,-4.76405452823403,129.582490119308));
#41068=CARTESIAN_POINT('Ctrl Pts',(121.420856971801,-4.80369940204384,129.737064880598));
#41069=CARTESIAN_POINT('Ctrl Pts',(121.411777357275,-4.83585906930173,129.893733636719));
#41070=CARTESIAN_POINT('Ctrl Pts',(121.402697742749,-4.86033642164795,130.051822956779));
#41071=CARTESIAN_POINT('Ctrl Pts',(121.393695775175,-4.88460444883132,130.208560330265));
#41072=CARTESIAN_POINT('Ctrl Pts',(121.384693807601,-4.90132092246141,130.36669396795));
#41073=CARTESIAN_POINT('Ctrl Pts',(121.375691840026,-4.91034075570341,130.525547552273));
#41074=CARTESIAN_POINT('Ctrl Pts',(121.370508081371,-4.91553480225507,130.617022958717));
#41075=CARTESIAN_POINT('Ctrl Pts',(121.365324322716,-4.9181775165785,130.708736737056));
#41076=CARTESIAN_POINT('Ctrl Pts',(121.36014056406,-4.91824852912944,130.800556906732));
#41077=CARTESIAN_POINT('Ctrl Pts',(121.360140564008,-4.91824852913016,130.800556907659));
#41078=CARTESIAN_POINT('Ctrl Pts',(121.352395684946,-4.91835462656282,130.937742327915));
#41079=CARTESIAN_POINT('Ctrl Pts',(121.344650805883,-4.91271662615867,131.074993328622));
#41080=CARTESIAN_POINT('Ctrl Pts',(121.336905926821,-4.90134485319712,131.211793670396));
#41081=CARTESIAN_POINT('Ctrl Pts',(121.329162189819,-4.88997475711792,131.348573839582));
#41082=CARTESIAN_POINT('Ctrl Pts',(121.321418452817,-4.87287260227552,131.484903092875));
#41083=CARTESIAN_POINT('Ctrl Pts',(121.313674715815,-4.85010073300231,131.620268665222));
#41084=CARTESIAN_POINT('Ctrl Pts',(121.30593044775,-4.82732730204311,131.755643520888));
#41085=CARTESIAN_POINT('Ctrl Pts',(121.298186179686,-4.79888344729425,131.890054178806));
#41086=CARTESIAN_POINT('Ctrl Pts',(121.290441911621,-4.76488287839154,132.022996829777));
#41087=CARTESIAN_POINT('Ctrl Pts',(121.282695439375,-4.73087263221228,132.15597731902));
#41088=CARTESIAN_POINT('Ctrl Pts',(121.274948967129,-4.69130262112038,132.28748859148));
#41089=CARTESIAN_POINT('Ctrl Pts',(121.267202494883,-4.64633667445302,132.41704117184));
#41090=CARTESIAN_POINT('Ctrl Pts',(121.259447091804,-4.60131888698141,132.546743112114));
#41091=CARTESIAN_POINT('Ctrl Pts',(121.251691688725,-4.55089286580262,132.674481480011));
#41092=CARTESIAN_POINT('Ctrl Pts',(121.243936285647,-4.49527116784955,132.799785431985));
#41093=CARTESIAN_POINT('Ctrl Pts',(121.236176345659,-4.4396169312176,132.92516268674));
#41094=CARTESIAN_POINT('Ctrl Pts',(121.228416405671,-4.37876113520666,133.048102338447));
#41095=CARTESIAN_POINT('Ctrl Pts',(121.220656465684,-4.312962269487,133.168158308673));
#41096=CARTESIAN_POINT('Ctrl Pts',(121.212883493517,-4.24705290000236,133.288415902993));
#41097=CARTESIAN_POINT('Ctrl Pts',(121.205110521351,-4.17618407452121,133.405779804192));
#41098=CARTESIAN_POINT('Ctrl Pts',(121.197337549185,-4.10065807548136,133.519832291233));
#41099=CARTESIAN_POINT('Ctrl Pts',(121.189961034019,-4.02898424655723,133.628067581709));
#41100=CARTESIAN_POINT('Ctrl Pts',(121.182584518854,-3.95311672216256,133.733320667862));
#41101=CARTESIAN_POINT('Ctrl Pts',(121.175208003689,-3.8733460673644,133.835263668627));
#41102=CARTESIAN_POINT('Ctrl Pts',(121.16743366957,-3.78927334340142,133.942704503668));
#41103=CARTESIAN_POINT('Ctrl Pts',(121.159659335451,-3.70059369395087,134.046814788587));
#41104=CARTESIAN_POINT('Ctrl Pts',(121.151885001332,-3.60760060089622,134.147173948716));
#41105=CARTESIAN_POINT('Ctrl Pts',(121.144120248384,-3.51472211351787,134.247409425149));
#41106=CARTESIAN_POINT('Ctrl Pts',(121.136355495437,-3.41754102283757,134.343902691014));
#41107=CARTESIAN_POINT('Ctrl Pts',(121.12859074249,-3.31639252029569,134.436264211252));
#41108=CARTESIAN_POINT('Ctrl Pts',(121.120833701605,-3.21534447987269,134.528533996725));
#41109=CARTESIAN_POINT('Ctrl Pts',(121.11307666072,-3.1103371561816,134.616679941212));
#41110=CARTESIAN_POINT('Ctrl Pts',(121.105319619835,-3.00174398221468,134.700347800263));
#41111=CARTESIAN_POINT('Ctrl Pts',(121.097568428595,-2.89323269920491,134.78395256473));
#41112=CARTESIAN_POINT('Ctrl Pts',(121.089817237355,-2.78114125675095,134.863085727742));
#41113=CARTESIAN_POINT('Ctrl Pts',(121.082066046115,-2.66587742435323,134.937432189753));
#41114=CARTESIAN_POINT('Ctrl Pts',(121.074318149338,-2.5506625821588,135.011747052536));
#41115=CARTESIAN_POINT('Ctrl Pts',(121.066570252561,-2.43227835964799,135.081279049261));
#41116=CARTESIAN_POINT('Ctrl Pts',(121.058822355784,-2.31116268592292,135.145755566393));
#41117=CARTESIAN_POINT('Ctrl Pts',(121.0510760797,-2.19007234698567,135.210218596427));
#41118=CARTESIAN_POINT('Ctrl Pts',(121.043329803616,-2.06625203819268,135.269628066684));
#41119=CARTESIAN_POINT('Ctrl Pts',(121.035583527532,-1.94016519332837,135.323756825589));
#41120=CARTESIAN_POINT('Ctrl Pts',(121.027837194266,-1.81407741771963,135.377885984061));
#41121=CARTESIAN_POINT('Ctrl Pts',(121.020090861001,-1.68572343191319,135.426734199168));
#41122=CARTESIAN_POINT('Ctrl Pts',(121.012344527735,-1.55558722324916,135.47012223314));
#41123=CARTESIAN_POINT('Ctrl Pts',(121.004596459732,-1.42542187148351,135.513519983561));
#41124=CARTESIAN_POINT('Ctrl Pts',(120.996848391729,-1.29347387348796,135.551454996042));
#41125=CARTESIAN_POINT('Ctrl Pts',(120.989100323726,-1.16024258155281,135.583797845363));
#41126=CARTESIAN_POINT('Ctrl Pts',(120.981344020985,-1.02686968981539,135.616175069049));
#41127=CARTESIAN_POINT('Ctrl Pts',(120.973587718243,-0.892211160137485,
135.642948164581));
#41128=CARTESIAN_POINT('Ctrl Pts',(120.965831415501,-0.756777299121249,
135.664038712053));
#41129=CARTESIAN_POINT('Ctrl Pts',(120.958070972987,-0.621271152975369,
135.685140516185));
#41130=CARTESIAN_POINT('Ctrl Pts',(120.950310530473,-0.484989239222823,
135.700553684938));
#41131=CARTESIAN_POINT('Ctrl Pts',(120.942550087958,-0.348446208691673,
135.710251800842));
#41132=CARTESIAN_POINT('Ctrl Pts',(120.934777187693,-0.211683987166286,
135.719965485024));
#41133=CARTESIAN_POINT('Ctrl Pts',(120.927004287428,-0.0746602022566778,
135.723945771804));
#41134=CARTESIAN_POINT('Ctrl Pts',(120.919231387162,0.0621103696950562,
135.722218419951));
#41135=CARTESIAN_POINT('Ctrl Pts',(120.9117410514,0.193908986852247,135.720553861689));
#41136=CARTESIAN_POINT('Ctrl Pts',(120.904250715638,0.325472173699212,135.713589450599));
#41137=CARTESIAN_POINT('Ctrl Pts',(120.896760379876,0.456346415344077,135.701393495922));
#41138=CARTESIAN_POINT('Ctrl Pts',(120.888986045757,0.592182793639085,135.688735127917));
#41139=CARTESIAN_POINT('Ctrl Pts',(120.881211711638,0.727707241546074,135.670400579329));
#41140=CARTESIAN_POINT('Ctrl Pts',(120.873437377519,0.862407283560495,135.6464094339));
#41141=CARTESIAN_POINT('Ctrl Pts',(120.865672624572,0.996941319811804,135.622447855413));
#41142=CARTESIAN_POINT('Ctrl Pts',(120.857907871625,1.13065259050813,135.592843618691));
#41143=CARTESIAN_POINT('Ctrl Pts',(120.850143118677,1.26303218961186,135.557668176572));
#41144=CARTESIAN_POINT('Ctrl Pts',(120.842386077792,1.39528030743136,135.522527671198));
#41145=CARTESIAN_POINT('Ctrl Pts',(120.834629036907,1.52619901035321,135.481827071894));
#41146=CARTESIAN_POINT('Ctrl Pts',(120.826871996022,1.6552884128346,135.435689080635));
#41147=CARTESIAN_POINT('Ctrl Pts',(120.819120804782,1.7842804679935,135.389585882394));
#41148=CARTESIAN_POINT('Ctrl Pts',(120.811369613542,1.91144560183515,135.338053584806));
#41149=CARTESIAN_POINT('Ctrl Pts',(120.803618422302,2.0362983028138,135.281264936898));
#41150=CARTESIAN_POINT('Ctrl Pts',(120.795870525525,2.16109793806382,135.224500425682));
#41151=CARTESIAN_POINT('Ctrl Pts',(120.788122628748,2.28358674011956,135.162484169111));
#41152=CARTESIAN_POINT('Ctrl Pts',(120.780374731971,2.4032986401155,135.095437255068));
#41153=CARTESIAN_POINT('Ctrl Pts',(120.772628455887,2.52298549896256,135.028404365795));
#41154=CARTESIAN_POINT('Ctrl Pts',(120.764882179803,2.63989627023486,134.956343103065));
#41155=CARTESIAN_POINT('Ctrl Pts',(120.757135903718,2.75358934759938,134.879520585872));
#41156=CARTESIAN_POINT('Ctrl Pts',(120.749389570453,2.86728326422069,134.802697501594));
#41157=CARTESIAN_POINT('Ctrl Pts',(120.741643237188,2.97775911559259,134.72111331161));
#41158=CARTESIAN_POINT('Ctrl Pts',(120.733896903922,3.08460449692238,134.635078325785));
#41159=CARTESIAN_POINT('Ctrl Pts',(120.726148835919,3.19147380553415,134.549024073022));
#41160=CARTESIAN_POINT('Ctrl Pts',(120.718400767916,3.29471072183496,134.458517286208));
#41161=CARTESIAN_POINT('Ctrl Pts',(120.710652699913,3.39393644461178,134.363908127073));
#41162=CARTESIAN_POINT('Ctrl Pts',(120.702896397172,3.49326762566778,134.269198416197));
#41163=CARTESIAN_POINT('Ctrl Pts',(120.69514009443,3.5885788137006,134.170377893556));
#41164=CARTESIAN_POINT('Ctrl Pts',(120.687383791688,3.67952819863928,134.06783350667));
#41165=CARTESIAN_POINT('Ctrl Pts',(120.679623349174,3.77052612600321,133.965234388758));
#41166=CARTESIAN_POINT('Ctrl Pts',(120.67186290666,3.85715736465253,133.858907749212));
#41167=CARTESIAN_POINT('Ctrl Pts',(120.664102464145,3.93912150747921,133.749272299063));
#41168=CARTESIAN_POINT('Ctrl Pts',(120.65632956388,4.02121722642428,133.639460852356));
#41169=CARTESIAN_POINT('Ctrl Pts',(120.648556663615,4.09863065715541,133.526330303625));
#41170=CARTESIAN_POINT('Ctrl Pts',(120.640783763349,4.17110522206723,133.410327672028));
#41171=CARTESIAN_POINT('Ctrl Pts',(120.633293427587,4.24094515399218,133.298542028284));
#41172=CARTESIAN_POINT('Ctrl Pts',(120.625803091825,4.30619891380052,133.184089758817));
#41173=CARTESIAN_POINT('Ctrl Pts',(120.618312756063,4.36667883611359,133.067389341365));
#41174=CARTESIAN_POINT('Ctrl Pts',(120.610538421944,4.42945187306359,132.946264192114));
#41175=CARTESIAN_POINT('Ctrl Pts',(120.602764087825,4.48728077253792,132.82233336448));
#41176=CARTESIAN_POINT('Ctrl Pts',(120.594989753706,4.53990500536383,132.696038604109));
#41177=CARTESIAN_POINT('Ctrl Pts',(120.587225000759,4.59246438352587,132.569899490743));
#41178=CARTESIAN_POINT('Ctrl Pts',(120.579460247812,4.63983170862671,132.441402598735));
#41179=CARTESIAN_POINT('Ctrl Pts',(120.571695494864,4.68179201981861,132.311014707151));
#41180=CARTESIAN_POINT('Ctrl Pts',(120.56393845398,4.72371065543776,132.180756318659));
#41181=CARTESIAN_POINT('Ctrl Pts',(120.556181413095,4.76023284533896,132.04861103799));
#41182=CARTESIAN_POINT('Ctrl Pts',(120.54842437221,4.79119162182193,131.915065756423));
#41183=CARTESIAN_POINT('Ctrl Pts',(120.540673180969,4.8221270520509,131.78162118239));
#41184=CARTESIAN_POINT('Ctrl Pts',(120.532921989729,4.84750733164166,131.646779088193));
#41185=CARTESIAN_POINT('Ctrl Pts',(120.525170798489,4.86721536839511,131.511041323514));
#41186=CARTESIAN_POINT('Ctrl Pts',(120.517422901712,4.88691502870719,131.375361251005));
#41187=CARTESIAN_POINT('Ctrl Pts',(120.509675004935,4.90094718512941,131.238786651265));
#41188=CARTESIAN_POINT('Ctrl Pts',(120.501927108158,4.90924592355149,131.101829144629));
#41189=CARTESIAN_POINT('Ctrl Pts',(120.494180832074,4.9175429260564,130.964900286551));
#41190=CARTESIAN_POINT('Ctrl Pts',(120.48643455599,4.9201088724178,130.827589070895));
#41191=CARTESIAN_POINT('Ctrl Pts',(120.478688279906,4.91692979840053,130.690411417916));
#41192=CARTESIAN_POINT('Ctrl Pts',(120.47094194664,4.91375070091604,130.553232752322));
#41193=CARTESIAN_POINT('Ctrl Pts',(120.463195613375,4.90482650748803,130.416188042234));
#41194=CARTESIAN_POINT('Ctrl Pts',(120.45544928011,4.89019537572859,130.279791985543));
#41195=CARTESIAN_POINT('Ctrl Pts',(120.447701212107,4.87556096742863,130.143365383901));
#41196=CARTESIAN_POINT('Ctrl Pts',(120.439953144104,4.85521711935837,130.00758811337));
#41197=CARTESIAN_POINT('Ctrl Pts',(120.432205076101,4.82925368119135,129.872968141109));
#41198=CARTESIAN_POINT('Ctrl Pts',(120.424448773359,4.80326264877332,129.73820509314));
#41199=CARTESIAN_POINT('Ctrl Pts',(120.416692470617,4.77164016956917,129.604602184982));
#41200=CARTESIAN_POINT('Ctrl Pts',(120.408936167875,4.73452703679601,129.472656145715));
#41201=CARTESIAN_POINT('Ctrl Pts',(120.401175725361,4.69739409562638,129.340639682874));
#41202=CARTESIAN_POINT('Ctrl Pts',(120.393415282847,4.65476478302499,129.210282222427));
#41203=CARTESIAN_POINT('Ctrl Pts',(120.385654840332,4.60682899506041,129.082062828921));
#41204=CARTESIAN_POINT('Ctrl Pts',(120.377881940067,4.55881625631354,128.953637606263));
#41205=CARTESIAN_POINT('Ctrl Pts',(120.370109039802,4.50548017188069,128.82735766957));
#41206=CARTESIAN_POINT('Ctrl Pts',(120.362336139536,4.44705814517803,128.703680509623));
#41207=CARTESIAN_POINT('Ctrl Pts',(120.354845803774,4.39075990630207,128.584499325965));
#41208=CARTESIAN_POINT('Ctrl Pts',(120.347355468012,4.32973922163128,128.467735242457));
#41209=CARTESIAN_POINT('Ctrl Pts',(120.33986513225,4.26424673061527,128.353772344735));
#41210=CARTESIAN_POINT('Ctrl Pts',(120.332090798131,4.19627107189652,128.235488509108));
#41211=CARTESIAN_POINT('Ctrl Pts',(120.324316464012,4.12326248942005,128.119847778666));
#41212=CARTESIAN_POINT('Ctrl Pts',(120.316542129893,4.04545181392711,128.007308118292));
#41213=CARTESIAN_POINT('Ctrl Pts',(120.308777376946,3.96773703313763,127.894907152992));
#41214=CARTESIAN_POINT('Ctrl Pts',(120.301012623999,3.88523215489806,127.785599972031));
#41215=CARTESIAN_POINT('Ctrl Pts',(120.293247871051,3.79821370206821,127.679819733545));
#41216=CARTESIAN_POINT('Ctrl Pts',(120.285490830166,3.71128167719251,127.574144557483));
#41217=CARTESIAN_POINT('Ctrl Pts',(120.277733789281,3.61984524576229,127.471989652727));
#41218=CARTESIAN_POINT('Ctrl Pts',(120.269976748396,3.52422379307952,127.373758670561));
#41219=CARTESIAN_POINT('Ctrl Pts',(120.262225557156,3.42867444927786,127.275601765143));
#41220=CARTESIAN_POINT('Ctrl Pts',(120.254474365916,3.32894663756933,127.181363171502));
#41221=CARTESIAN_POINT('Ctrl Pts',(120.246723174676,3.2253992871122,127.091412664632));
#41222=CARTESIAN_POINT('Ctrl Pts',(120.238975277899,3.12189594704131,127.001500389128));
#41223=CARTESIAN_POINT('Ctrl Pts',(120.231227381122,3.01457659158679,126.915872831339));
#41224=CARTESIAN_POINT('Ctrl Pts',(120.223479484345,2.9038360332409,126.834861989962));
#41225=CARTESIAN_POINT('Ctrl Pts',(120.215733208261,2.79311863943267,126.753868094307));
#41226=CARTESIAN_POINT('Ctrl Pts',(120.207986932177,2.67898178153047,126.677489224887));
#41227=CARTESIAN_POINT('Ctrl Pts',(120.200240656093,2.56185196984684,126.606015997708));
#41228=CARTESIAN_POINT('Ctrl Pts',(120.192494322827,2.44472129353754,126.53454224293));
#41229=CARTESIAN_POINT('Ctrl Pts',(120.184747989562,2.32459795309918,126.467974406302));
#41230=CARTESIAN_POINT('Ctrl Pts',(120.177001656297,2.20193560356723,126.406558591526));
#41231=CARTESIAN_POINT('Ctrl Pts',(120.169253588294,2.07924578465308,126.345129023104));
#41232=CARTESIAN_POINT('Ctrl Pts',(120.161505520291,1.95401617473662,126.288853947388));
#41233=CARTESIAN_POINT('Ctrl Pts',(120.153757452288,1.82672270691737,126.237932339959));
#41234=CARTESIAN_POINT('Ctrl Pts',(120.146001149546,1.69929395008502,126.186956612438));
#41235=CARTESIAN_POINT('Ctrl Pts',(120.138244846804,1.56979731718857,126.141345864496));
#41236=CARTESIAN_POINT('Ctrl Pts',(120.130488544062,1.43872682264481,126.101250137011));
#41237=CARTESIAN_POINT('Ctrl Pts',(120.122728101548,1.30758637183148,126.06113300923));
#41238=CARTESIAN_POINT('Ctrl Pts',(120.114967659034,1.17487076370234,126.026536865717));
#41239=CARTESIAN_POINT('Ctrl Pts',(120.10720721652,1.04108569229251,125.997560887621));
#41240=CARTESIAN_POINT('Ctrl Pts',(120.099434316254,0.907085857209262,125.968538394712));
#41241=CARTESIAN_POINT('Ctrl Pts',(120.091661415989,0.77201351359351,125.94515416276));
#41242=CARTESIAN_POINT('Ctrl Pts',(120.083888515723,0.636381883741304,125.927455742489));
#41243=CARTESIAN_POINT('Ctrl Pts',(120.076398179961,0.505680805268763,125.910400704375));
#41244=CARTESIAN_POINT('Ctrl Pts',(120.068907844199,0.374460704304341,125.898625295326));
#41245=CARTESIAN_POINT('Ctrl Pts',(120.061417508437,0.243180199716132,125.892126252945));
#41246=CARTESIAN_POINT('Ctrl Pts',(120.053643174318,0.106922154895483,125.885380797396));
#41247=CARTESIAN_POINT('Ctrl Pts',(120.045868840199,-0.0298325889035889,
125.884298346058));
#41248=CARTESIAN_POINT('Ctrl Pts',(120.03809450608,-0.166573963200332,125.888932235697));
#41249=CARTESIAN_POINT('Ctrl Pts',(120.030329753133,-0.303146815974181,
125.893560414481));
#41250=CARTESIAN_POINT('Ctrl Pts',(120.022565000186,-0.439705945039631,
125.903890903918));
#41251=CARTESIAN_POINT('Ctrl Pts',(120.014800247239,-0.575737454828614,
125.919925190047));
#41252=CARTESIAN_POINT('Ctrl Pts',(120.007043206354,-0.71163385620409,125.935943550696));
#41253=CARTESIAN_POINT('Ctrl Pts',(119.999286165469,-0.847003295399503,
125.95765438878));
#41254=CARTESIAN_POINT('Ctrl Pts',(119.991529124584,-0.981333533600314,
125.985007179777));
#41255=CARTESIAN_POINT('Ctrl Pts',(119.983777933343,-1.1155624723242,126.012339343821));
#41256=CARTESIAN_POINT('Ctrl Pts',(119.976026742103,-1.24875338834668,126.045304914481));
#41257=CARTESIAN_POINT('Ctrl Pts',(119.968275550863,-1.38040116951393,126.083801786908));
#41258=CARTESIAN_POINT('Ctrl Pts',(119.960527654086,-1.511992996862,126.122282297137));
#41259=CARTESIAN_POINT('Ctrl Pts',(119.952779757309,-1.64204261937261,126.166289323769));
#41260=CARTESIAN_POINT('Ctrl Pts',(119.945031860532,-1.77005731134371,126.215670153277));
#41261=CARTESIAN_POINT('Ctrl Pts',(119.937285584448,-1.89804522540093,126.26504065338));
#41262=CARTESIAN_POINT('Ctrl Pts',(119.929539308364,-2.02399869105035,126.319782579878));
#41263=CARTESIAN_POINT('Ctrl Pts',(119.921793032279,-2.14744266557274,126.379694182615));
#41264=CARTESIAN_POINT('Ctrl Pts',(119.914046699014,-2.27088755133017,126.439606227607));
#41265=CARTESIAN_POINT('Ctrl Pts',(119.906300365749,-2.39182255726741,126.50468785428));
#41266=CARTESIAN_POINT('Ctrl Pts',(119.898554032483,-2.5097954177409,126.574690414869));
#41267=CARTESIAN_POINT('Ctrl Pts',(119.89080596448,-2.62779469741926,126.644708652046));
#41268=CARTESIAN_POINT('Ctrl Pts',(119.883057896477,-2.74283017547651,126.719649816536));
#41269=CARTESIAN_POINT('Ctrl Pts',(119.875309828474,-2.85447719465501,126.799221043507));
#41270=CARTESIAN_POINT('Ctrl Pts',(119.867553525733,-2.96624287361364,126.878876839724));
#41271=CARTESIAN_POINT('Ctrl Pts',(119.859797222991,-3.07461258083279,126.963172301148));
#41272=CARTESIAN_POINT('Ctrl Pts',(119.852040920249,-3.17919305581108,127.051772900219));
#41273=CARTESIAN_POINT('Ctrl Pts',(119.844280477735,-3.28382934853765,127.140420788098));
#41274=CARTESIAN_POINT('Ctrl Pts',(119.836520035221,-3.38467209184157,127.233378127291));
#41275=CARTESIAN_POINT('Ctrl Pts',(119.828759592706,-3.48136450183492,127.33027307292));
#41276=CARTESIAN_POINT('Ctrl Pts',(119.820986692441,-3.57821213106887,127.427323562918));
#41277=CARTESIAN_POINT('Ctrl Pts',(119.813213792175,-3.67089584873541,127.528324002488));
#41278=CARTESIAN_POINT('Ctrl Pts',(119.80544089191,-3.75909823987637,127.632868305506));
#41279=CARTESIAN_POINT('Ctrl Pts',(119.797950556148,-3.84409425192963,127.733612159776));
#41280=CARTESIAN_POINT('Ctrl Pts',(119.790460220386,-3.92492890685757,127.83764645084));
#41281=CARTESIAN_POINT('Ctrl Pts',(119.782969884624,-4.00135705470864,127.94458356625));
#41282=CARTESIAN_POINT('Ctrl Pts',(119.775120410701,-4.08144969309127,128.056647981717));
#41283=CARTESIAN_POINT('Ctrl Pts',(119.767270936778,-4.1569552162601,128.172253364202));
#41284=CARTESIAN_POINT('Ctrl Pts',(119.759421462855,-4.22754791932674,128.290992030929));
#41285=CARTESIAN_POINT('Ctrl Pts',(119.75158539947,-4.29802001734926,128.409527836998));
#41286=CARTESIAN_POINT('Ctrl Pts',(119.743749336086,-4.36359582221846,128.531185938641));
#41287=CARTESIAN_POINT('Ctrl Pts',(119.735913272701,-4.42399151533761,128.655527879841));
#41288=CARTESIAN_POINT('Ctrl Pts',(119.728084969267,-4.48432739939225,128.779746686843));
#41289=CARTESIAN_POINT('Ctrl Pts',(119.720256665833,-4.53949321192236,128.906643705212));
#41290=CARTESIAN_POINT('Ctrl Pts',(119.7124283624,-4.58924960431368,129.035753501272));
#41291=CARTESIAN_POINT('Ctrl Pts',(119.704607732563,-4.63895722362022,129.164736739059));
#41292=CARTESIAN_POINT('Ctrl Pts',(119.696787102726,-4.68326584723437,129.295928080183));
#41293=CARTESIAN_POINT('Ctrl Pts',(119.68896647289,-4.72198331519722,129.428840122081));
#41294=CARTESIAN_POINT('Ctrl Pts',(119.685967176238,-4.73683188550948,129.479813336584));
#41295=CARTESIAN_POINT('Ctrl Pts',(119.682967879587,-4.7508586051796,129.531039415595));
#41296=CARTESIAN_POINT('Ctrl Pts',(119.679968582935,-4.76405452823404,129.582490119308));
#41297=CARTESIAN_POINT('Origin',(213.235140564004,0.,130.804360617566));
#41298=CARTESIAN_POINT('',(117.5848416735,-4.76405452823405,129.582490119308));
#41299=CARTESIAN_POINT('',(117.930282309765,-4.76405452823403,129.582490119308));
#41300=CARTESIAN_POINT('',(213.235140564004,-4.76405452823405,129.582490119308));
#41301=CARTESIAN_POINT('',(119.264859436025,-4.91824958100419,130.806390753538));
#41302=CARTESIAN_POINT('Ctrl Pts',(119.264859435991,-4.91824958100395,130.806390754133));
#41303=CARTESIAN_POINT('Ctrl Pts',(119.258460835046,-4.91820319810624,130.918758892777));
#41304=CARTESIAN_POINT('Ctrl Pts',(119.252062234102,-4.9143062059521,131.031043513497));
#41305=CARTESIAN_POINT('Ctrl Pts',(119.245663633157,-4.90657370955902,131.143060329943));
#41306=CARTESIAN_POINT('Ctrl Pts',(119.237889299038,-4.89717868538792,131.279161356646));
#41307=CARTESIAN_POINT('Ctrl Pts',(119.230114964919,-4.88210162976514,131.415086755473));
#41308=CARTESIAN_POINT('Ctrl Pts',(119.2223406308,-4.86134982279231,131.550323728542));
#41309=CARTESIAN_POINT('Ctrl Pts',(119.214575877853,-4.84062359056692,131.685394034129));
#41310=CARTESIAN_POINT('Ctrl Pts',(119.206811124906,-4.8142365809479,131.819777219336));
#41311=CARTESIAN_POINT('Ctrl Pts',(119.199046371959,-4.78224801385495,131.952962810007));
#41312=CARTESIAN_POINT('Ctrl Pts',(119.191289331074,-4.75029121825784,132.086016118872));
#41313=CARTESIAN_POINT('Ctrl Pts',(119.183532290189,-4.71274402760884,132.217873822601));
#41314=CARTESIAN_POINT('Ctrl Pts',(119.175775249304,-4.66971711267233,132.348033235097));
#41315=CARTESIAN_POINT('Ctrl Pts',(119.168024058064,-4.62672264466707,132.478094493368));
#41316=CARTESIAN_POINT('Ctrl Pts',(119.160272866824,-4.5782567996865,132.606459639844));
#41317=CARTESIAN_POINT('Ctrl Pts',(119.152521675584,-4.52448062607383,132.732639157296));
#41318=CARTESIAN_POINT('Ctrl Pts',(119.144773778807,-4.47072730876942,132.858765045086));
#41319=CARTESIAN_POINT('Ctrl Pts',(119.13702588203,-4.41166830485938,132.982706792553));
#41320=CARTESIAN_POINT('Ctrl Pts',(119.129277985253,-4.34751345418928,133.103993159548));
#41321=CARTESIAN_POINT('Ctrl Pts',(119.121531709169,-4.28337202333095,133.225254156049));
#41322=CARTESIAN_POINT('Ctrl Pts',(119.113785433085,-4.21413704861652,133.343860531519));
#41323=CARTESIAN_POINT('Ctrl Pts',(119.106039157,-4.14006497478168,133.459364396676));
#41324=CARTESIAN_POINT('Ctrl Pts',(119.098292823735,-4.06599235416361,133.574869114456));
#41325=CARTESIAN_POINT('Ctrl Pts',(119.09054649047,-3.98708277422921,133.687270947119));
#41326=CARTESIAN_POINT('Ctrl Pts',(119.082800157205,-3.90363655890191,133.796150162053));
#41327=CARTESIAN_POINT('Ctrl Pts',(119.075052089202,-3.82017165637327,133.905053759733));
#41328=CARTESIAN_POINT('Ctrl Pts',(119.067304021199,-3.73216833461281,134.010432859682));
#41329=CARTESIAN_POINT('Ctrl Pts',(119.059555953196,-3.63996756432957,134.111900366855));
#41330=CARTESIAN_POINT('Ctrl Pts',(119.051799650454,-3.54766880197041,134.213475714903));
#41331=CARTESIAN_POINT('Ctrl Pts',(119.044043347712,-3.45116394290887,134.311130875734));
#41332=CARTESIAN_POINT('Ctrl Pts',(119.03628704497,-3.35083162073693,134.404514852036));
#41333=CARTESIAN_POINT('Ctrl Pts',(119.028526602456,-3.25044574818363,134.497948670178));
#41334=CARTESIAN_POINT('Ctrl Pts',(119.020766159942,-3.14622863894206,134.587106507345));
#41335=CARTESIAN_POINT('Ctrl Pts',(119.013005717428,-3.0385916745218,134.671677995029));
#41336=CARTESIAN_POINT('Ctrl Pts',(119.005232817162,-2.93078192169069,134.756385244373));
#41337=CARTESIAN_POINT('Ctrl Pts',(118.997459916897,-2.81954166064776,134.836491203183));
#41338=CARTESIAN_POINT('Ctrl Pts',(118.989687016631,-2.70531162466699,134.911728640515));
#41339=CARTESIAN_POINT('Ctrl Pts',(118.982196680869,-2.59523413822036,134.984231007489));
#41340=CARTESIAN_POINT('Ctrl Pts',(118.974706345107,-2.48238073848909,135.052212514715));
#41341=CARTESIAN_POINT('Ctrl Pts',(118.967216009345,-2.36716527924578,135.115475508546));
#41342=CARTESIAN_POINT('Ctrl Pts',(118.959441675226,-2.24758139084821,135.181137138016));
#41343=CARTESIAN_POINT('Ctrl Pts',(118.951667341107,-2.12507398636641,135.241923382344));
#41344=CARTESIAN_POINT('Ctrl Pts',(118.943893006988,-2.00007843225282,135.297563186707));
#41345=CARTESIAN_POINT('Ctrl Pts',(118.936128254041,-1.87523692398849,135.353134419984));
#41346=CARTESIAN_POINT('Ctrl Pts',(118.928363501094,-1.74791372110643,135.403571675569));
#41347=CARTESIAN_POINT('Ctrl Pts',(118.920598748146,-1.61857030978488,135.448648853107));
#41348=CARTESIAN_POINT('Ctrl Pts',(118.912841707261,-1.48935536416287,135.493681259357));
#41349=CARTESIAN_POINT('Ctrl Pts',(118.905084666376,-1.35812456992417,135.533364054141));
#41350=CARTESIAN_POINT('Ctrl Pts',(118.897327625491,-1.22536067137054,135.567518633794));
#41351=CARTESIAN_POINT('Ctrl Pts',(118.889576434251,-1.09269689110566,135.601647457213));
#41352=CARTESIAN_POINT('Ctrl Pts',(118.881825243011,-0.958502684828784,
135.63025626637));
#41353=CARTESIAN_POINT('Ctrl Pts',(118.874074051771,-0.823276947813364,
135.653215959778));
#41354=CARTESIAN_POINT('Ctrl Pts',(118.866326154994,-0.688108685343347,
135.676165894704));
#41355=CARTESIAN_POINT('Ctrl Pts',(118.858578258217,-0.551910148776666,
135.693471424028));
#41356=CARTESIAN_POINT('Ctrl Pts',(118.85083036144,-0.415191229358849,135.705054375144));
#41357=CARTESIAN_POINT('Ctrl Pts',(118.843084085356,-0.278500908591656,
135.716634903357));
#41358=CARTESIAN_POINT('Ctrl Pts',(118.835337809272,-0.141290810810461,
135.722495201356));
#41359=CARTESIAN_POINT('Ctrl Pts',(118.827591533188,-0.00407637259556072,
135.722608928264));
#41360=CARTESIAN_POINT('Ctrl Pts',(118.819845199922,0.133139078505059,135.722722656012));
#41361=CARTESIAN_POINT('Ctrl Pts',(118.812098866657,0.270358479138243,135.7170897277));
#41362=CARTESIAN_POINT('Ctrl Pts',(118.804352533391,0.407066363954133,135.70573593862));
#41363=CARTESIAN_POINT('Ctrl Pts',(118.796604465388,0.543804863552962,135.694379606938));
#41364=CARTESIAN_POINT('Ctrl Pts',(118.788856397385,0.680031229843201,135.677299897507));
#41365=CARTESIAN_POINT('Ctrl Pts',(118.781108329383,0.815235485804568,135.654574444315));
#41366=CARTESIAN_POINT('Ctrl Pts',(118.773352026641,0.950583438458122,135.631824838241));
#41367=CARTESIAN_POINT('Ctrl Pts',(118.765595723899,1.08490672458792,135.603417566941));
#41368=CARTESIAN_POINT('Ctrl Pts',(118.757839421157,1.21770537950975,135.56948146296));
#41369=CARTESIAN_POINT('Ctrl Pts',(118.750078978643,1.35057491307229,135.535527246259));
#41370=CARTESIAN_POINT('Ctrl Pts',(118.742318536129,1.48191781975181,135.496038429462));
#41371=CARTESIAN_POINT('Ctrl Pts',(118.734558093614,1.61125061597757,135.451193357725));
#41372=CARTESIAN_POINT('Ctrl Pts',(118.726785193349,1.74079102868946,135.406276296697));
#41373=CARTESIAN_POINT('Ctrl Pts',(118.719012293084,1.86831451884324,135.355985942027));
#41374=CARTESIAN_POINT('Ctrl Pts',(118.711239392818,1.99335803037674,135.300548650248));
#41375=CARTESIAN_POINT('Ctrl Pts',(118.703749057056,2.11385589530083,135.247126643663));
#41376=CARTESIAN_POINT('Ctrl Pts',(118.696258721294,2.23205068181748,135.188925547492));
#41377=CARTESIAN_POINT('Ctrl Pts',(118.688768385532,2.34755240024224,135.12618671201));
#41378=CARTESIAN_POINT('Ctrl Pts',(118.680994051413,2.46743340142664,135.061069114512));
#41379=CARTESIAN_POINT('Ctrl Pts',(118.673219717294,2.58479283486809,134.990856615378));
#41380=CARTESIAN_POINT('Ctrl Pts',(118.665445383175,2.69916732826432,134.91576898898));
#41381=CARTESIAN_POINT('Ctrl Pts',(118.657680630228,2.8134008653193,134.840773901371));
#41382=CARTESIAN_POINT('Ctrl Pts',(118.649915877281,2.92465645809992,134.760915853448));
#41383=CARTESIAN_POINT('Ctrl Pts',(118.642151124333,3.03249443742238,134.676460893838));
#41384=CARTESIAN_POINT('Ctrl Pts',(118.634394083448,3.14022531054352,134.592089816084));
#41385=CARTESIAN_POINT('Ctrl Pts',(118.626637042563,3.24454501944707,134.503131152129));
#41386=CARTESIAN_POINT('Ctrl Pts',(118.618880001678,3.34504236472383,134.409894508781));
#41387=CARTESIAN_POINT('Ctrl Pts',(118.611128810438,3.4454639241707,134.316728175912));
#41388=CARTESIAN_POINT('Ctrl Pts',(118.603377619198,3.54206857192666,134.219290549752));
#41389=CARTESIAN_POINT('Ctrl Pts',(118.595626427958,3.63447802617195,134.117931582518));
#41390=CARTESIAN_POINT('Ctrl Pts',(118.587878531181,3.72684820393416,134.016615695549));
#41391=CARTESIAN_POINT('Ctrl Pts',(118.580130634404,3.81502647172089,133.911382070703));
#41392=CARTESIAN_POINT('Ctrl Pts',(118.572382737627,3.89867145203174,133.802617439723));
#41393=CARTESIAN_POINT('Ctrl Pts',(118.564636461543,3.98229893561589,133.69387555996));
#41394=CARTESIAN_POINT('Ctrl Pts',(118.556890185459,4.06139477968857,133.581604452919));
#41395=CARTESIAN_POINT('Ctrl Pts',(118.549143909375,4.13565821686171,133.466223532106));
#41396=CARTESIAN_POINT('Ctrl Pts',(118.541397576109,4.20992220223071,133.350841759577));
#41397=CARTESIAN_POINT('Ctrl Pts',(118.533651242844,4.27935349792102,133.232350456224));
#41398=CARTESIAN_POINT('Ctrl Pts',(118.525904909579,4.34369518463098,133.111197240631));
#41399=CARTESIAN_POINT('Ctrl Pts',(118.518156841576,4.40805128021553,132.990016893615));
#41400=CARTESIAN_POINT('Ctrl Pts',(118.510408773573,4.46731531544255,132.866173793381));
#41401=CARTESIAN_POINT('Ctrl Pts',(118.50266070557,4.52127695094842,132.740138961107));
#41402=CARTESIAN_POINT('Ctrl Pts',(118.494904402828,4.57529593752266,132.613970177513));
#41403=CARTESIAN_POINT('Ctrl Pts',(118.487148100086,4.62400111282458,132.485605368636));
#41404=CARTESIAN_POINT('Ctrl Pts',(118.479391797344,4.66723062419794,132.35553480606));
#41405=CARTESIAN_POINT('Ctrl Pts',(118.47163135483,4.71048320846318,132.225394820908));
#41406=CARTESIAN_POINT('Ctrl Pts',(118.463870912316,4.74825419779972,132.093547643647));
#41407=CARTESIAN_POINT('Ctrl Pts',(118.456110469802,4.7804323043577,131.960496442611));
#41408=CARTESIAN_POINT('Ctrl Pts',(118.448337569536,4.81266206606895,131.827231655976));
#41409=CARTESIAN_POINT('Ctrl Pts',(118.440564669271,4.83928092775092,131.692759366947));
#41410=CARTESIAN_POINT('Ctrl Pts',(118.432791769005,4.86022903645285,131.55759150894));
#41411=CARTESIAN_POINT('Ctrl Pts',(118.425301433243,4.88041562863846,131.427337343038));
#41412=CARTESIAN_POINT('Ctrl Pts',(118.417811097481,4.89533656726942,131.29643760757));
#41413=CARTESIAN_POINT('Ctrl Pts',(118.410320761719,4.90498410821736,131.165350867621));
#41414=CARTESIAN_POINT('Ctrl Pts',(118.4025464276,4.91499743861261,131.029293934085));
#41415=CARTESIAN_POINT('Ctrl Pts',(118.394772093481,4.91936131500807,130.892604548121));
#41416=CARTESIAN_POINT('Ctrl Pts',(118.386997759362,4.91801017576041,130.755791351388));
#41417=CARTESIAN_POINT('Ctrl Pts',(118.379233006415,4.91666070167111,130.619146764692));
#41418=CARTESIAN_POINT('Ctrl Pts',(118.371468253468,4.90961022972284,130.48237905802));
#41419=CARTESIAN_POINT('Ctrl Pts',(118.36370350052,4.8968449422271,130.346001943289));
#41420=CARTESIAN_POINT('Ctrl Pts',(118.355946459635,4.88409233339485,130.209760280231));
#41421=CARTESIAN_POINT('Ctrl Pts',(118.34818941875,4.86563624078206,130.073908823839));
#41422=CARTESIAN_POINT('Ctrl Pts',(118.340432377865,4.84151488204095,129.938960877864));
#41423=CARTESIAN_POINT('Ctrl Pts',(118.332681186625,4.81741171340409,129.804114697185));
#41424=CARTESIAN_POINT('Ctrl Pts',(118.324929995385,4.78765185075088,129.670171054056));
#41425=CARTESIAN_POINT('Ctrl Pts',(118.317178804145,4.75232524822748,129.537637365407));
#41426=CARTESIAN_POINT('Ctrl Pts',(118.309430907368,4.71701366045253,129.405160007111));
#41427=CARTESIAN_POINT('Ctrl Pts',(118.301683010591,4.67614013911124,129.274091788381));
#41428=CARTESIAN_POINT('Ctrl Pts',(118.293935113814,4.62984552969398,129.144928957728));
#41429=CARTESIAN_POINT('Ctrl Pts',(118.28618883773,4.58356060411099,129.015793145155));
#41430=CARTESIAN_POINT('Ctrl Pts',(118.278442561646,4.53185697781919,128.888562295696));
#41431=CARTESIAN_POINT('Ctrl Pts',(118.270696285561,4.47492494315906,128.763716156717));
#41432=CARTESIAN_POINT('Ctrl Pts',(118.262949952296,4.41799248823963,128.638869096153));
#41433=CARTESIAN_POINT('Ctrl Pts',(118.255203619031,4.35583171015494,128.516407136919));
#41434=CARTESIAN_POINT('Ctrl Pts',(118.247457285765,4.28868033193859,128.396788381278));
#41435=CARTESIAN_POINT('Ctrl Pts',(118.239709217762,4.22151391563672,128.277142837847));
#41436=CARTESIAN_POINT('Ctrl Pts',(118.231961149759,4.149354866636,128.160342105854));
#41437=CARTESIAN_POINT('Ctrl Pts',(118.224213081757,4.07248577482895,128.046817748214));
#41438=CARTESIAN_POINT('Ctrl Pts',(118.216456779015,3.99553498563633,127.933172735535));
#41439=CARTESIAN_POINT('Ctrl Pts',(118.208700476273,3.91386437338798,127.822811377468));
#41440=CARTESIAN_POINT('Ctrl Pts',(118.200944173531,3.82779893213975,127.716134849004));
#41441=CARTESIAN_POINT('Ctrl Pts',(118.193183731017,3.74168755517409,127.609401384065));
#41442=CARTESIAN_POINT('Ctrl Pts',(118.185423288503,3.65117693318272,127.50635696115));
#41443=CARTESIAN_POINT('Ctrl Pts',(118.177662845988,3.55663024213399,127.407367184655));
#41444=CARTESIAN_POINT('Ctrl Pts',(118.169889945723,3.46193177634333,127.308218500984));
#41445=CARTESIAN_POINT('Ctrl Pts',(118.162117045458,3.36318457607143,127.213137741877));
#41446=CARTESIAN_POINT('Ctrl Pts',(118.154344145192,3.26078699341668,127.122451975833));
#41447=CARTESIAN_POINT('Ctrl Pts',(118.14685380943,3.16211182081559,127.035062865809));
#41448=CARTESIAN_POINT('Ctrl Pts',(118.139363473668,3.06004729788793,126.951754953132));
#41449=CARTESIAN_POINT('Ctrl Pts',(118.131873137906,2.95497504253706,126.872782618787));
#41450=CARTESIAN_POINT('Ctrl Pts',(118.124098803787,2.84591894068824,126.790816024381));
#41451=CARTESIAN_POINT('Ctrl Pts',(118.116324469668,2.73327707081743,126.713260619641));
#41452=CARTESIAN_POINT('Ctrl Pts',(118.108550135549,2.61744192988759,126.640446496674));
#41453=CARTESIAN_POINT('Ctrl Pts',(118.100785382602,2.50174954541655,126.567722110605));
#41454=CARTESIAN_POINT('Ctrl Pts',(118.093020629655,2.38287204802507,126.499727586142));
#41455=CARTESIAN_POINT('Ctrl Pts',(118.085255876708,2.26123416930068,126.436752222336));
#41456=CARTESIAN_POINT('Ctrl Pts',(118.077498835822,2.13971710303224,126.373839406548));
#41457=CARTESIAN_POINT('Ctrl Pts',(118.069741794938,2.01544545638394,126.315936009431));
#41458=CARTESIAN_POINT('Ctrl Pts',(118.061984754053,1.88887174391407,126.263287330606));
#41459=CARTESIAN_POINT('Ctrl Pts',(118.054233562812,1.76239348166538,126.210678354559));
#41460=CARTESIAN_POINT('Ctrl Pts',(118.046482371572,1.63361696853104,126.163316358986));
#41461=CARTESIAN_POINT('Ctrl Pts',(118.038731180332,1.50301773115734,126.12139993416));
#41462=CARTESIAN_POINT('Ctrl Pts',(118.030983283555,1.37247400194338,126.079501324933));
#41463=CARTESIAN_POINT('Ctrl Pts',(118.023235386778,1.24010946080412,126.043043802292));
#41464=CARTESIAN_POINT('Ctrl Pts',(118.015487490001,1.10641774609574,126.012177103381));
#41465=CARTESIAN_POINT('Ctrl Pts',(118.007741213917,0.972753996812022,125.981316861118));
#41466=CARTESIAN_POINT('Ctrl Pts',(117.999994937833,0.837764006855314,125.956045204321));
#41467=CARTESIAN_POINT('Ctrl Pts',(117.992248661749,0.701954258930055,125.936461349825));
#41468=CARTESIAN_POINT('Ctrl Pts',(117.984502328483,0.566143508488181,125.916877350766));
#41469=CARTESIAN_POINT('Ctrl Pts',(117.976755995218,0.429513374965579,125.902981293588));
#41470=CARTESIAN_POINT('Ctrl Pts',(117.969009661952,0.292577767876609,125.894820790633));
#41471=CARTESIAN_POINT('Ctrl Pts',(117.961261593949,0.155611495007877,125.88665846019));
#41472=CARTESIAN_POINT('Ctrl Pts',(117.953513525946,0.0183400026455234,
125.884234263106));
#41473=CARTESIAN_POINT('Ctrl Pts',(117.945765457943,-0.118720876367694,
125.887543718798));
#41474=CARTESIAN_POINT('Ctrl Pts',(117.938009155202,-0.255927425314266,
125.890856691818));
#41475=CARTESIAN_POINT('Ctrl Pts',(117.93025285246,-0.392922522287937,125.899915481174));
#41476=CARTESIAN_POINT('Ctrl Pts',(117.922496549718,-0.529192980181233,
125.914663505042));
#41477=CARTESIAN_POINT('Ctrl Pts',(117.914736107204,-0.665536169721116,
125.929419400374));
#41478=CARTESIAN_POINT('Ctrl Pts',(117.90697566469,-0.801153563120145,125.949870522464));
#41479=CARTESIAN_POINT('Ctrl Pts',(117.899215222175,-0.935541261564568,
125.97590893919));
#41480=CARTESIAN_POINT('Ctrl Pts',(117.89144232191,-1.07014469107282,126.001989155094));
#41481=CARTESIAN_POINT('Ctrl Pts',(117.883669421644,-1.2035141003177,126.033674498575));
#41482=CARTESIAN_POINT('Ctrl Pts',(117.875896521379,-1.33515899826947,126.070806613243));
#41483=CARTESIAN_POINT('Ctrl Pts',(117.868406185617,-1.46201827258748,126.106588882013));
#41484=CARTESIAN_POINT('Ctrl Pts',(117.860915849855,-1.58727594663287,126.147428694059));
#41485=CARTESIAN_POINT('Ctrl Pts',(117.853425514093,-1.71051172868069,126.193142482567));
#41486=CARTESIAN_POINT('Ctrl Pts',(117.845650993255,-1.83842310487397,126.24059066281));
#41487=CARTESIAN_POINT('Ctrl Pts',(117.837876472418,-1.96456133225279,126.293440266656));
#41488=CARTESIAN_POINT('Ctrl Pts',(117.83010195158,-2.0884365056399,126.351539486596));
#41489=CARTESIAN_POINT('Ctrl Pts',(117.82233705528,-2.21215832664063,126.409566782084));
#41490=CARTESIAN_POINT('Ctrl Pts',(117.814572158981,-2.33362231744179,126.472830598264));
#41491=CARTESIAN_POINT('Ctrl Pts',(117.806807262681,-2.452355479164,126.541129956868));
#41492=CARTESIAN_POINT('Ctrl Pts',(117.799050121627,-2.57097005530141,126.609361101005));
#41493=CARTESIAN_POINT('Ctrl Pts',(117.791292980572,-2.68685889348965,126.682617585103));
#41494=CARTESIAN_POINT('Ctrl Pts',(117.783535839518,-2.79957100471094,126.760651274391));
#41495=CARTESIAN_POINT('Ctrl Pts',(117.775784591152,-2.91219749451705,126.838625685622));
#41496=CARTESIAN_POINT('Ctrl Pts',(117.768033342786,-3.02165174067263,126.921369856849));
#41497=CARTESIAN_POINT('Ctrl Pts',(117.760282094421,-3.12750962209338,127.008591047872));
#41498=CARTESIAN_POINT('Ctrl Pts',(117.752534359545,-3.23331952020366,127.095772703233));
#41499=CARTESIAN_POINT('Ctrl Pts',(117.744786624668,-3.33553599594384,127.187427092607));
#41500=CARTESIAN_POINT('Ctrl Pts',(117.737038889792,-3.43376627398198,127.283219859493));
#41501=CARTESIAN_POINT('Ctrl Pts',(117.729292836917,-3.53197522663689,127.378991830169));
#41502=CARTESIAN_POINT('Ctrl Pts',(117.721546784042,-3.62619942358062,127.478900118195));
#41503=CARTESIAN_POINT('Ctrl Pts',(117.713800731166,-3.7160816565156,127.58257226564));
#41504=CARTESIAN_POINT('Ctrl Pts',(117.706054682458,-3.80596384110301,127.686244357319));
#41505=CARTESIAN_POINT('Ctrl Pts',(117.698308633749,-3.89150381048676,127.793680008845));
#41506=CARTESIAN_POINT('Ctrl Pts',(117.69056258504,-3.9723837612152,127.904472634189));
#41507=CARTESIAN_POINT('Ctrl Pts',(117.682814863035,-4.05328118357907,128.015289192885));
#41508=CARTESIAN_POINT('Ctrl Pts',(117.67506714103,-4.12951635417953,128.12946385244));
#41509=CARTESIAN_POINT('Ctrl Pts',(117.667319419025,-4.20081425720144,128.246560265898));
#41510=CARTESIAN_POINT('Ctrl Pts',(117.659564299703,-4.27218023354459,128.363768479864));
#41511=CARTESIAN_POINT('Ctrl Pts',(117.651809180381,-4.33859932528608,128.483903684194));
#41512=CARTESIAN_POINT('Ctrl Pts',(117.644054061059,-4.39984184444552,128.606503750897));
#41513=CARTESIAN_POINT('Ctrl Pts',(117.636294827299,-4.46111685550754,128.729168862432));
#41514=CARTESIAN_POINT('Ctrl Pts',(117.628535593538,-4.51720966197646,128.854301085703));
#41515=CARTESIAN_POINT('Ctrl Pts',(117.620776359778,-4.56793877061906,128.981418366595));
#41516=CARTESIAN_POINT('Ctrl Pts',(117.613006612876,-4.61873661314919,129.108707881243));
#41517=CARTESIAN_POINT('Ctrl Pts',(117.605236865974,-4.66415611414588,129.237987456855));
#41518=CARTESIAN_POINT('Ctrl Pts',(117.597467119072,-4.70406551180002,129.368759446212));
#41519=CARTESIAN_POINT('Ctrl Pts',(117.593258637215,-4.72568242906647,129.439592068122));
#41520=CARTESIAN_POINT('Ctrl Pts',(117.589050155357,-4.74568364887164,129.510862339491));
#41521=CARTESIAN_POINT('Ctrl Pts',(117.5848416735,-4.76405452823405,129.582490119308));
#41522=CARTESIAN_POINT('Ctrl Pts',(119.334999413688,-4.76405452823402,129.582490119308));
#41523=CARTESIAN_POINT('Ctrl Pts',(119.327317254803,-4.7978160474119,129.71412577018));
#41524=CARTESIAN_POINT('Ctrl Pts',(119.319635095917,-4.82609248166911,129.847064070791));
#41525=CARTESIAN_POINT('Ctrl Pts',(119.311952937031,-4.84880778827108,129.98080364024));
#41526=CARTESIAN_POINT('Ctrl Pts',(119.304104020197,-4.87201617995309,130.117446317601));
#41527=CARTESIAN_POINT('Ctrl Pts',(119.296255103362,-4.88941918290399,130.254925008655));
#41528=CARTESIAN_POINT('Ctrl Pts',(119.288406186528,-4.90099174565895,130.392701812871));
#41529=CARTESIAN_POINT('Ctrl Pts',(119.280557269694,-4.91256430841392,130.530478617087));
#41530=CARTESIAN_POINT('Ctrl Pts',(119.272708352859,-4.91830647709806,130.668553094539));
#41531=CARTESIAN_POINT('Ctrl Pts',(119.264859436025,-4.91824958100419,130.806390753538));
#41532=CARTESIAN_POINT('',(119.610140563954,-4.91824907209079,130.807381772652));
#41533=CARTESIAN_POINT('Ctrl Pts',(119.679968582935,-4.76405452823404,129.582490119308));
#41534=CARTESIAN_POINT('Ctrl Pts',(119.672154643786,-4.79843330157376,129.716532434789));
#41535=CARTESIAN_POINT('Ctrl Pts',(119.664340704637,-4.82716957323685,129.852100309024));
#41536=CARTESIAN_POINT('Ctrl Pts',(119.656526765489,-4.85013965485316,129.98868397151));
#41537=CARTESIAN_POINT('Ctrl Pts',(119.648714426812,-4.873105031675,130.12523965856));
#41538=CARTESIAN_POINT('Ctrl Pts',(119.640902088135,-4.89030649992739,130.262810344994));
#41539=CARTESIAN_POINT('Ctrl Pts',(119.633089749459,-4.90167147584519,130.400876038696));
#41540=CARTESIAN_POINT('Ctrl Pts',(119.625440020975,-4.91279989507929,130.53606795925));
#41541=CARTESIAN_POINT('Ctrl Pts',(119.617790292492,-4.9183323969573,130.67173412575));
#41542=CARTESIAN_POINT('Ctrl Pts',(119.610140564008,-4.91824907209139,130.807381771687));
#41543=CARTESIAN_POINT('Ctrl Pts',(119.610140563954,-4.91824907209079,130.807381772653));
#41544=CARTESIAN_POINT('Ctrl Pts',(119.601339038692,-4.91815320121794,130.963453479642));
#41545=CARTESIAN_POINT('Ctrl Pts',(119.59253751343,-4.9106240938899,131.119247980167));
#41546=CARTESIAN_POINT('Ctrl Pts',(119.583735988168,-4.89576630750545,131.274100252677));
#41547=CARTESIAN_POINT('Ctrl Pts',(119.575009108628,-4.88103452998284,131.42763922332));
#41548=CARTESIAN_POINT('Ctrl Pts',(119.566282229087,-4.8590980702172,131.580251715686));
#41549=CARTESIAN_POINT('Ctrl Pts',(119.557555349547,-4.83010909763408,131.731306768889));
#41550=CARTESIAN_POINT('Ctrl Pts',(119.548716501424,-4.80074818750619,131.88429990546));
#41551=CARTESIAN_POINT('Ctrl Pts',(119.539877653302,-4.76415267188377,132.035695156408));
#41552=CARTESIAN_POINT('Ctrl Pts',(119.531038805179,-4.72053075406594,132.184857796997));
#41553=CARTESIAN_POINT('Ctrl Pts',(119.522199957057,-4.67690883624814,132.334020437587));
#41554=CARTESIAN_POINT('Ctrl Pts',(119.513361108934,-4.62626066231785,132.48095029492));
#41555=CARTESIAN_POINT('Ctrl Pts',(119.504522260812,-4.56884265301679,132.625036281839));
#41556=CARTESIAN_POINT('Ctrl Pts',(119.496747926693,-4.51833982928082,132.751769153437));
#41557=CARTESIAN_POINT('Ctrl Pts',(119.488973592573,-4.46247994562957,132.876599858998));
#41558=CARTESIAN_POINT('Ctrl Pts',(119.481199258454,-4.40142650984342,132.999042312242));
#41559=CARTESIAN_POINT('Ctrl Pts',(119.473434505507,-4.34044831696042,133.121333866106));
#41560=CARTESIAN_POINT('Ctrl Pts',(119.46566975256,-4.27428947999307,133.241242677434));
#41561=CARTESIAN_POINT('Ctrl Pts',(119.457904999613,-4.20316225663219,133.358300731767));
#41562=CARTESIAN_POINT('Ctrl Pts',(119.450147958728,-4.13210567783217,133.475242522389));
#41563=CARTESIAN_POINT('Ctrl Pts',(119.442390917843,-4.05609073456338,133.589338858695));
#41564=CARTESIAN_POINT('Ctrl Pts',(119.434633876958,-3.97537630034961,133.700144852125));
#41565=CARTESIAN_POINT('Ctrl Pts',(119.426882685718,-3.89472273351878,133.810867285893));
#41566=CARTESIAN_POINT('Ctrl Pts',(119.419131494478,-3.80937695896858,133.918304000875));
#41567=CARTESIAN_POINT('Ctrl Pts',(119.411380303238,-3.71964180109306,134.022038030555));
#41568=CARTESIAN_POINT('Ctrl Pts',(119.40363240646,-3.62994478305321,134.125727970506));
#41569=CARTESIAN_POINT('Ctrl Pts',(119.395884509683,-3.53586234748065,134.225718060139));
#41570=CARTESIAN_POINT('Ctrl Pts',(119.388136612906,-3.43773819958743,134.32162363497));
#41571=CARTESIAN_POINT('Ctrl Pts',(119.380390336822,-3.33963457715071,134.417509148422));
#41572=CARTESIAN_POINT('Ctrl Pts',(119.372644060738,-3.23749120343779,134.509311573402));
#41573=CARTESIAN_POINT('Ctrl Pts',(119.364897784654,-3.13168903308198,134.596682711294));
#41574=CARTESIAN_POINT('Ctrl Pts',(119.357151451389,-3.02588608171858,134.684054494139));
#41575=CARTESIAN_POINT('Ctrl Pts',(119.349405118123,-2.91642458128109,134.766994675676));
#41576=CARTESIAN_POINT('Ctrl Pts',(119.341658784858,-2.80371867290681,134.845195267201));
#41577=CARTESIAN_POINT('Ctrl Pts',(119.333910716855,-2.69098752482564,134.923413371207));
#41578=CARTESIAN_POINT('Ctrl Pts',(119.326162648852,-2.57501084418768,134.996889550307));
#41579=CARTESIAN_POINT('Ctrl Pts',(119.318414580849,-2.45623151241898,135.065359305655));
#41580=CARTESIAN_POINT('Ctrl Pts',(119.310658278107,-2.33732594056315,135.133901831475));
#41581=CARTESIAN_POINT('Ctrl Pts',(119.302901975365,-2.2156121065791,135.197427108934));
#41582=CARTESIAN_POINT('Ctrl Pts',(119.295145672623,-2.09155773426502,135.255716512879));
#41583=CARTESIAN_POINT('Ctrl Pts',(119.287385230109,-1.96743715039724,135.314037027633));
#41584=CARTESIAN_POINT('Ctrl Pts',(119.279624787595,-1.84097389935401,135.367115949275));
#41585=CARTESIAN_POINT('Ctrl Pts',(119.271864345081,-1.71265448355867,135.414783340316));
#41586=CARTESIAN_POINT('Ctrl Pts',(119.264091444815,-1.58412907804535,135.462527251284));
#41587=CARTESIAN_POINT('Ctrl Pts',(119.25631854455,-1.45374192551523,135.504842151366));
#41588=CARTESIAN_POINT('Ctrl Pts',(119.248545644284,-1.32199430703389,135.54160814273));
#41589=CARTESIAN_POINT('Ctrl Pts',(119.241055308522,-1.19503604633702,135.577037597699));
#41590=CARTESIAN_POINT('Ctrl Pts',(119.23356497276,-1.06681481492169,135.607314502583));
#41591=CARTESIAN_POINT('Ctrl Pts',(119.226074636998,-0.937785053574844,
135.632377006912));
#41592=CARTESIAN_POINT('Ctrl Pts',(119.218300302879,-0.803863089608314,
135.65838976371));
#41593=CARTESIAN_POINT('Ctrl Pts',(119.21052596876,-0.668645850063405,135.678867307075));
#41594=CARTESIAN_POINT('Ctrl Pts',(119.202751634641,-0.532630673043177,
135.693684459227));
#41595=CARTESIAN_POINT('Ctrl Pts',(119.194986881694,-0.396783122572601,
135.708483350563));
#41596=CARTESIAN_POINT('Ctrl Pts',(119.187222128747,-0.260139976207619,
135.717635688765));
#41597=CARTESIAN_POINT('Ctrl Pts',(119.1794573758,-0.123209718235847,135.721067078992));
#41598=CARTESIAN_POINT('Ctrl Pts',(119.171700334915,0.0135845386731426,
135.724495061115));
#41599=CARTESIAN_POINT('Ctrl Pts',(119.16394329403,0.150664951387716,135.722213393219));
#41600=CARTESIAN_POINT('Ctrl Pts',(119.156186253145,0.287517295101176,135.714199399799));
#41601=CARTESIAN_POINT('Ctrl Pts',(119.148435061904,0.424266437397779,135.706191449794));
#41602=CARTESIAN_POINT('Ctrl Pts',(119.140683870664,0.560787464308823,135.692459801282));
#41603=CARTESIAN_POINT('Ctrl Pts',(119.132932679424,0.696565886114431,135.673033848417));
#41604=CARTESIAN_POINT('Ctrl Pts',(119.125184782647,0.832286598468855,135.653616152099));
#41605=CARTESIAN_POINT('Ctrl Pts',(119.11743688587,0.967264947261899,135.628509020339));
#41606=CARTESIAN_POINT('Ctrl Pts',(119.109688989093,1.10099152230572,135.597793701516));
#41607=CARTESIAN_POINT('Ctrl Pts',(119.101942713009,1.23469012463285,135.567084807676));
#41608=CARTESIAN_POINT('Ctrl Pts',(119.094196436925,1.36713709323124,135.530770147622));
#41609=CARTESIAN_POINT('Ctrl Pts',(119.086450160841,1.49783356345753,135.488982019417));
#41610=CARTESIAN_POINT('Ctrl Pts',(119.078703827575,1.62853099845539,135.447193582742));
#41611=CARTESIAN_POINT('Ctrl Pts',(119.07095749431,1.75747753690324,135.399931716361));
#41612=CARTESIAN_POINT('Ctrl Pts',(119.063211161045,1.88419020578014,135.347378373523));
#41613=CARTESIAN_POINT('Ctrl Pts',(119.055463093042,2.01093125108067,135.294813261729));
#41614=CARTESIAN_POINT('Ctrl Pts',(119.047715025039,2.13543707028372,135.236954465237));
#41615=CARTESIAN_POINT('Ctrl Pts',(119.039966957036,2.25724574479005,135.174031624647));
#41616=CARTESIAN_POINT('Ctrl Pts',(119.032210654294,2.37918387900528,135.111041908914));
#41617=CARTESIAN_POINT('Ctrl Pts',(119.024454351552,2.49841879435542,135.042977577426));
#41618=CARTESIAN_POINT('Ctrl Pts',(119.01669804881,2.61451373916802,134.970113967226));
#41619=CARTESIAN_POINT('Ctrl Pts',(119.008937606296,2.73067064734831,134.897211467523));
#41620=CARTESIAN_POINT('Ctrl Pts',(119.001177163782,2.84368392362401,134.819504806466));
#41621=CARTESIAN_POINT('Ctrl Pts',(118.993416721268,2.95314762833095,134.737311436961));
#41622=CARTESIAN_POINT('Ctrl Pts',(118.985643821002,3.06278705389435,134.654986123363));
#41623=CARTESIAN_POINT('Ctrl Pts',(118.977870920737,3.16886521857905,134.568159956276));
#41624=CARTESIAN_POINT('Ctrl Pts',(118.970098020471,3.27101029428391,134.477189869953));
#41625=CARTESIAN_POINT('Ctrl Pts',(118.962607684709,3.36944213919967,134.389526775406));
#41626=CARTESIAN_POINT('Ctrl Pts',(118.955117348947,3.46422166432354,134.298016028646));
#41627=CARTESIAN_POINT('Ctrl Pts',(118.947627013185,3.55505119675834,134.203006531886));
#41628=CARTESIAN_POINT('Ctrl Pts',(118.939852679066,3.64932455852177,134.10439472118));
#41629=CARTESIAN_POINT('Ctrl Pts',(118.932078344947,3.73964111654788,134.001701240381));
#41630=CARTESIAN_POINT('Ctrl Pts',(118.924304010828,3.82562673183133,133.895276852471));
#41631=CARTESIAN_POINT('Ctrl Pts',(118.916539257881,3.91150637752863,133.788983623107));
#41632=CARTESIAN_POINT('Ctrl Pts',(118.908774504934,3.99306545717046,133.678968936492));
#41633=CARTESIAN_POINT('Ctrl Pts',(118.901009751987,4.06996653209188,133.565620382628));
#41634=CARTESIAN_POINT('Ctrl Pts',(118.893252711102,4.14679122778152,133.452384408146));
#41635=CARTESIAN_POINT('Ctrl Pts',(118.885495670217,4.21896690740773,133.33582147738));
#41636=CARTESIAN_POINT('Ctrl Pts',(118.877738629332,4.28619654235699,133.216351965558));
#41637=CARTESIAN_POINT('Ctrl Pts',(118.869987438092,4.35337547891562,133.096972546624));
#41638=CARTESIAN_POINT('Ctrl Pts',(118.862236246851,4.41561560387903,132.974691248772));
#41639=CARTESIAN_POINT('Ctrl Pts',(118.854485055611,4.47266355311984,132.849956815033));
#41640=CARTESIAN_POINT('Ctrl Pts',(118.846737158834,4.52968725546043,132.725275396756));
#41641=CARTESIAN_POINT('Ctrl Pts',(118.838989262057,4.58152300899197,132.598143271139));
#41642=CARTESIAN_POINT('Ctrl Pts',(118.83124136528,4.62796382162741,132.469032936134));
#41643=CARTESIAN_POINT('Ctrl Pts',(118.823495089196,4.67439491984602,132.339949608228));
#41644=CARTESIAN_POINT('Ctrl Pts',(118.815748813112,4.71543318958196,132.208889261659));
#41645=CARTESIAN_POINT('Ctrl Pts',(118.808002537028,4.75092028841816,132.076343115715));
#41646=CARTESIAN_POINT('Ctrl Pts',(118.800256203763,4.78640764921203,131.943795991345));
#41647=CARTESIAN_POINT('Ctrl Pts',(118.792509870497,4.8163436562252,131.809763423379));
#41648=CARTESIAN_POINT('Ctrl Pts',(118.784763537232,4.8406203331648,131.674750100873));
#41649=CARTESIAN_POINT('Ctrl Pts',(118.777015469229,4.86490244669787,131.53970654307));
#41650=CARTESIAN_POINT('Ctrl Pts',(118.769267401226,4.88352263906591,131.403682178403));
#41651=CARTESIAN_POINT('Ctrl Pts',(118.761519333223,4.89642443512322,131.267189758425));
#41652=CARTESIAN_POINT('Ctrl Pts',(118.753763030481,4.90933994336293,131.130552272679));
#41653=CARTESIAN_POINT('Ctrl Pts',(118.746006727739,4.91652487782168,130.993446127754));
#41654=CARTESIAN_POINT('Ctrl Pts',(118.738250424998,4.91797481240323,130.856387601597));
#41655=CARTESIAN_POINT('Ctrl Pts',(118.730489982483,4.91942552085853,130.719255923179));
#41656=CARTESIAN_POINT('Ctrl Pts',(118.722729539969,4.91513514247457,130.582172304754));
#41657=CARTESIAN_POINT('Ctrl Pts',(118.714969097455,4.90515133906645,130.445649865909));
#41658=CARTESIAN_POINT('Ctrl Pts',(118.70719619719,4.89515150877079,130.308908269125));
#41659=CARTESIAN_POINT('Ctrl Pts',(118.699423296924,4.87944003447119,130.172730040728));
#41660=CARTESIAN_POINT('Ctrl Pts',(118.691650396659,4.8581162328911,130.037620941913));
#41661=CARTESIAN_POINT('Ctrl Pts',(118.684160060897,4.83756760520995,129.90742339916));
#41662=CARTESIAN_POINT('Ctrl Pts',(118.676669725135,4.81180767068963,129.778218906481));
#41663=CARTESIAN_POINT('Ctrl Pts',(118.669179389373,4.78096907117315,129.650446494684));
#41664=CARTESIAN_POINT('Ctrl Pts',(118.661405055254,4.7489612167827,129.517829553059));
#41665=CARTESIAN_POINT('Ctrl Pts',(118.653630721135,4.71138058867321,129.386335340093));
#41666=CARTESIAN_POINT('Ctrl Pts',(118.645856387016,4.66832006240529,129.256468225491));
#41667=CARTESIAN_POINT('Ctrl Pts',(118.638091634069,4.6253126043876,129.1267611605));
#41668=CARTESIAN_POINT('Ctrl Pts',(118.630326881121,4.57683880749814,128.998677571551));
#41669=CARTESIAN_POINT('Ctrl Pts',(118.622562128174,4.52304236834297,128.872710857212));
#41670=CARTESIAN_POINT('Ctrl Pts',(118.614805087289,4.46929936056956,128.74686925479));
#41671=CARTESIAN_POINT('Ctrl Pts',(118.607048046404,4.41024438350894,128.623140700112));
#41672=CARTESIAN_POINT('Ctrl Pts',(118.599291005519,4.34607055952594,128.502002314842));
#41673=CARTESIAN_POINT('Ctrl Pts',(118.591539814279,4.28194512952285,128.380955280971));
#41674=CARTESIAN_POINT('Ctrl Pts',(118.583788623039,4.21270871829655,128.262494872732));
#41675=CARTESIAN_POINT('Ctrl Pts',(118.576037431799,4.13860191656769,128.14707680911));
#41676=CARTESIAN_POINT('Ctrl Pts',(118.568289535022,4.06452661220632,128.031707801244));
#41677=CARTESIAN_POINT('Ctrl Pts',(118.560541638245,3.98558524529838,127.919378894462));
#41678=CARTESIAN_POINT('Ctrl Pts',(118.552793741468,3.90206345747345,127.810519633754));
#41679=CARTESIAN_POINT('Ctrl Pts',(118.545047465384,3.81855914060607,127.701683144057));
#41680=CARTESIAN_POINT('Ctrl Pts',(118.5373011893,3.73047654642335,127.596315166817));
#41681=CARTESIAN_POINT('Ctrl Pts',(118.529554913216,3.63814336368036,127.494814436017));
#41682=CARTESIAN_POINT('Ctrl Pts',(118.52180857995,3.54580949935478,127.393312955961));
#41683=CARTESIAN_POINT('Ctrl Pts',(118.514062246685,3.44922524694357,127.295679068516));
#41684=CARTESIAN_POINT('Ctrl Pts',(118.506315913419,3.34875685182013,127.202276413957));
#41685=CARTESIAN_POINT('Ctrl Pts',(118.498567845417,3.24826595749627,127.108852842522));
#41686=CARTESIAN_POINT('Ctrl Pts',(118.490819777414,3.14388947589027,127.019662655649));
#41687=CARTESIAN_POINT('Ctrl Pts',(118.483071709411,3.03602827320992,126.935030522217));
#41688=CARTESIAN_POINT('Ctrl Pts',(118.475315406669,2.92805243435972,126.850308440747));
#41689=CARTESIAN_POINT('Ctrl Pts',(118.467559103927,2.81658478416331,126.770154331563));
#41690=CARTESIAN_POINT('Ctrl Pts',(118.459802801185,2.70205728946686,126.694850979308));
#41691=CARTESIAN_POINT('Ctrl Pts',(118.452042358671,2.58746866799806,126.619507435385));
#41692=CARTESIAN_POINT('Ctrl Pts',(118.444281916157,2.46981728309294,126.549020008017));
#41693=CARTESIAN_POINT('Ctrl Pts',(118.436521473643,2.34956059916619,126.483625951639));
#41694=CARTESIAN_POINT('Ctrl Pts',(118.428748573377,2.22911086853451,126.418126918915));
#41695=CARTESIAN_POINT('Ctrl Pts',(118.420975673112,2.10604783258396,126.357737768429));
#41696=CARTESIAN_POINT('Ctrl Pts',(118.413202772846,1.9808506856456,126.302648318487));
#41697=CARTESIAN_POINT('Ctrl Pts',(118.405712437084,1.86020477035019,126.249561508812));
#41698=CARTESIAN_POINT('Ctrl Pts',(118.398222101322,1.73757749756692,126.201395886994));
#41699=CARTESIAN_POINT('Ctrl Pts',(118.39073176556,1.61340993250517,126.158277164571));
#41700=CARTESIAN_POINT('Ctrl Pts',(118.382957431441,1.48453451647501,126.113523582682));
#41701=CARTESIAN_POINT('Ctrl Pts',(118.375183097322,1.35359146354676,126.074065395416));
#41702=CARTESIAN_POINT('Ctrl Pts',(118.367408763203,1.22105531574398,126.04009708808));
#41703=CARTESIAN_POINT('Ctrl Pts',(118.359644010256,1.08868250689827,126.006170643646));
#41704=CARTESIAN_POINT('Ctrl Pts',(118.351879257308,0.954720884742169,125.977720713375));
#41705=CARTESIAN_POINT('Ctrl Pts',(118.344114504361,0.819663230991687,125.954893095223));
#41706=CARTESIAN_POINT('Ctrl Pts',(118.336357463476,0.684739718406982,125.932088149783));
#41707=CARTESIAN_POINT('Ctrl Pts',(118.328600422591,0.548722723582106,125.914894468466));
#41708=CARTESIAN_POINT('Ctrl Pts',(118.320843381706,0.412118049841507,125.903407467872));
#41709=CARTESIAN_POINT('Ctrl Pts',(118.313092190466,0.27561639074782,125.891929129715));
#41710=CARTESIAN_POINT('Ctrl Pts',(118.305340999226,0.138528322861724,125.886148939147));
#41711=CARTESIAN_POINT('Ctrl Pts',(118.297589807986,0.00136730063314124,
125.886110807625));
#41712=CARTESIAN_POINT('Ctrl Pts',(118.289841911209,-0.135735424502011,
125.886072692309));
#41713=CARTESIAN_POINT('Ctrl Pts',(118.282094014432,-0.272910652161346,
125.891771782123));
#41714=CARTESIAN_POINT('Ctrl Pts',(118.274346117655,-0.409642597701834,
125.903199938232));
#41715=CARTESIAN_POINT('Ctrl Pts',(118.266599841571,-0.546345941866914,
125.914625703818));
#41716=CARTESIAN_POINT('Ctrl Pts',(118.258853565486,-0.682605798988489,
125.931778119478));
#41717=CARTESIAN_POINT('Ctrl Pts',(118.251107289402,-0.817909579096792,
125.954597016841));
#41718=CARTESIAN_POINT('Ctrl Pts',(118.243360956137,-0.953214357986863,
125.977416082647));
#41719=CARTESIAN_POINT('Ctrl Pts',(118.235614622872,-1.08756266025981,126.005901648605));
#41720=CARTESIAN_POINT('Ctrl Pts',(118.227868289606,-1.22045058048202,126.039942138559));
#41721=CARTESIAN_POINT('Ctrl Pts',(118.220120221603,-1.3533682600324,126.073990251646));
#41722=CARTESIAN_POINT('Ctrl Pts',(118.2123721536,-1.48482452809123,126.11359566712));
#41723=CARTESIAN_POINT('Ctrl Pts',(118.204624085597,-1.61432955355883,126.158596616349));
#41724=CARTESIAN_POINT('Ctrl Pts',(118.196867782855,-1.74397221850879,126.203645393122));
#41725=CARTESIAN_POINT('Ctrl Pts',(118.189111480114,-1.87165912832753,126.254101030273));
#41726=CARTESIAN_POINT('Ctrl Pts',(118.181355177372,-1.99691887965533,126.309752953868));
#41727=CARTESIAN_POINT('Ctrl Pts',(118.173594734858,-2.12224548588399,126.365434580569));
#41728=CARTESIAN_POINT('Ctrl Pts',(118.165834292343,-2.24514200217239,126.426317846507));
#41729=CARTESIAN_POINT('Ctrl Pts',(118.158073849829,-2.36516154895495,126.49214611573));
#41730=CARTESIAN_POINT('Ctrl Pts',(118.150300949564,-2.48537376176875,126.558080058334));
#41731=CARTESIAN_POINT('Ctrl Pts',(118.142528049298,-2.60269944129539,126.628974664881));
#41732=CARTESIAN_POINT('Ctrl Pts',(118.134755149033,-2.71671987177647,126.70452937704));
#41733=CARTESIAN_POINT('Ctrl Pts',(118.127264813271,-2.82659537240865,126.7773374851));
#41734=CARTESIAN_POINT('Ctrl Pts',(118.119774477509,-2.93340151044071,126.854472587573));
#41735=CARTESIAN_POINT('Ctrl Pts',(118.112284141747,-3.03679411467708,126.935631553964));
#41736=CARTESIAN_POINT('Ctrl Pts',(118.104605799054,-3.14278186642054,127.018827605026));
#41737=CARTESIAN_POINT('Ctrl Pts',(118.096927456361,-3.2455358106779,127.106529833381));
#41738=CARTESIAN_POINT('Ctrl Pts',(118.089249113669,-3.34464148734229,127.1984548529));
#41739=CARTESIAN_POINT('Ctrl Pts',(118.081579549546,-3.44363385751248,127.290274775497));
#41740=CARTESIAN_POINT('Ctrl Pts',(118.073909985423,-3.53898596087357,127.386307622067));
#41741=CARTESIAN_POINT('Ctrl Pts',(118.0662404213,-3.63031383490147,127.486227931457));
#41742=CARTESIAN_POINT('Ctrl Pts',(118.058577866454,-3.72155824364189,127.586056922864));
#41743=CARTESIAN_POINT('Ctrl Pts',(118.050915311608,-3.80878546702297,127.689766018797));
#41744=CARTESIAN_POINT('Ctrl Pts',(118.043252756762,-3.89164647165308,127.796991201919));
#41745=CARTESIAN_POINT('Ctrl Pts',(118.03559544818,-3.97445074446253,127.904142971981));
#41746=CARTESIAN_POINT('Ctrl Pts',(118.027938139598,-4.05289449986584,128.014805724947));
#41747=CARTESIAN_POINT('Ctrl Pts',(118.020280831016,-4.12666764679549,128.128580881603));
#41748=CARTESIAN_POINT('Ctrl Pts',(118.012626026437,-4.20041666929017,128.242318832833));
#41749=CARTESIAN_POINT('Ctrl Pts',(118.004971221859,-4.26949789797453,128.359166830722));
#41750=CARTESIAN_POINT('Ctrl Pts',(117.997316417281,-4.3336436268644,128.478695986146));
#41751=CARTESIAN_POINT('Ctrl Pts',(117.989663330027,-4.39777496492372,128.598198325696));
#41752=CARTESIAN_POINT('Ctrl Pts',(117.982010242772,-4.45697281923355,128.720380271036));
#41753=CARTESIAN_POINT('Ctrl Pts',(117.974357155518,-4.51101501937698,128.844787562675));
#41754=CARTESIAN_POINT('Ctrl Pts',(117.966701217411,-4.56507735078616,128.969241197287));
#41755=CARTESIAN_POINT('Ctrl Pts',(117.959045279304,-4.61398002821263,129.095921467083));
#41756=CARTESIAN_POINT('Ctrl Pts',(117.951389341198,-4.65754870950382,129.224353313438));
#41757=CARTESIAN_POINT('Ctrl Pts',(117.944353664054,-4.69758758793953,129.342379999834));
#41758=CARTESIAN_POINT('Ctrl Pts',(117.937317986909,-4.73312221386927,129.461885495063));
#41759=CARTESIAN_POINT('Ctrl Pts',(117.930282309765,-4.76405452823403,129.582490119308));
#41760=CARTESIAN_POINT('Origin',(213.235140564004,0.,130.804360617566));
#41761=CARTESIAN_POINT('',(115.834581344104,-4.76405452823405,129.582490119308));
#41762=CARTESIAN_POINT('',(116.180155138321,-4.76405452823404,129.582490119308));
#41763=CARTESIAN_POINT('',(213.235140564004,-4.76405452823405,129.582490119308));
#41764=CARTESIAN_POINT('',(117.514859435962,-4.91824794902791,130.799869027345));
#41765=CARTESIAN_POINT('Ctrl Pts',(117.514859435962,-4.91824794902791,130.799869027345));
#41766=CARTESIAN_POINT('Ctrl Pts',(117.507208240132,-4.91837122232531,130.934852098431));
#41767=CARTESIAN_POINT('Ctrl Pts',(117.499557044301,-4.91293333160114,131.070005300327));
#41768=CARTESIAN_POINT('Ctrl Pts',(117.491905848471,-4.90191906084059,131.204826076086));
#41769=CARTESIAN_POINT('Ctrl Pts',(117.48426061674,-4.89091337569394,131.339541759175));
#41770=CARTESIAN_POINT('Ctrl Pts',(117.47661538501,-4.87433999035582,131.473925132035));
#41771=CARTESIAN_POINT('Ctrl Pts',(117.468970153279,-4.85223575605224,131.607474077912));
#41772=CARTESIAN_POINT('Ctrl Pts',(117.46132828765,-4.83014125397164,131.740964223826));
#41773=CARTESIAN_POINT('Ctrl Pts',(117.453686422022,-4.80252080945946,131.873620276622));
#41774=CARTESIAN_POINT('Ctrl Pts',(117.446044556393,-4.76946303344324,132.004946072716));
#41775=CARTESIAN_POINT('Ctrl Pts',(117.438404246385,-4.73641198685376,132.136245135393));
#41776=CARTESIAN_POINT('Ctrl Pts',(117.430763936377,-4.69792590751848,132.266214089369));
#41777=CARTESIAN_POINT('Ctrl Pts',(117.42312362637,-4.65414423417374,132.394368325097));
#41778=CARTESIAN_POINT('Ctrl Pts',(117.415483110102,-4.61036137888763,132.522526020509));
#41779=CARTESIAN_POINT('Ctrl Pts',(117.407842593835,-4.56128277577274,132.648868519189));
#41780=CARTESIAN_POINT('Ctrl Pts',(117.400202077567,-4.50709713560817,132.772928237104));
#41781=CARTESIAN_POINT('Ctrl Pts',(117.392559593207,-4.45289753795934,132.897019911116));
#41782=CARTESIAN_POINT('Ctrl Pts',(117.384917108846,-4.39358844892161,133.018827266335));
#41783=CARTESIAN_POINT('Ctrl Pts',(117.377274624486,-4.32940569209491,133.137905006635));
#41784=CARTESIAN_POINT('Ctrl Pts',(117.369624105701,-4.26515546094297,133.257107931495));
#41785=CARTESIAN_POINT('Ctrl Pts',(117.361973586917,-4.19602152499452,133.373575158077));
#41786=CARTESIAN_POINT('Ctrl Pts',(117.354323068132,-4.12228457112978,133.486887966378));
#41787=CARTESIAN_POINT('Ctrl Pts',(117.346668040157,-4.04850415695003,133.600267560871));
#41788=CARTESIAN_POINT('Ctrl Pts',(117.339013012182,-3.97011555708345,133.710488708695));
#41789=CARTESIAN_POINT('Ctrl Pts',(117.331357984208,-3.88744052455226,133.817164831346));
#41790=CARTESIAN_POINT('Ctrl Pts',(117.323691752811,-3.80464449399681,133.92399707852));
#41791=CARTESIAN_POINT('Ctrl Pts',(117.316025521414,-3.71754976648684,134.027273636758));
#41792=CARTESIAN_POINT('Ctrl Pts',(117.308359290018,-3.62651604905118,134.126643629062));
#41793=CARTESIAN_POINT('Ctrl Pts',(117.304416282168,-3.5796942608856,134.177753051601));
#41794=CARTESIAN_POINT('Ctrl Pts',(117.300473274318,-3.53183101738966,134.2278296636));
#41795=CARTESIAN_POINT('Ctrl Pts',(117.296530266467,-3.48297861463481,134.276829916566));
#41796=CARTESIAN_POINT('Ctrl Pts',(117.288755932348,-3.3866575024361,134.373442541485));
#41797=CARTESIAN_POINT('Ctrl Pts',(117.280981598229,-3.28616094318428,134.466197450955));
#41798=CARTESIAN_POINT('Ctrl Pts',(117.27320726411,-3.18183062054689,134.554712196372));
#41799=CARTESIAN_POINT('Ctrl Pts',(117.265442511163,-3.07762887570802,134.643117855275));
#41800=CARTESIAN_POINT('Ctrl Pts',(117.257677758216,-2.96960306363289,134.727293497052));
#41801=CARTESIAN_POINT('Ctrl Pts',(117.249913005269,-2.85813256511082,134.80689247912));
#41802=CARTESIAN_POINT('Ctrl Pts',(117.242155964384,-2.74677278065935,134.886412402357));
#41803=CARTESIAN_POINT('Ctrl Pts',(117.234398923499,-2.63197543443788,134.96136448611));
#41804=CARTESIAN_POINT('Ctrl Pts',(117.226641882614,-2.51415365274995,135.031441699455));
#41805=CARTESIAN_POINT('Ctrl Pts',(117.218890691374,-2.39642072138412,135.101466067029));
#41806=CARTESIAN_POINT('Ctrl Pts',(117.211139500134,-2.27566822890966,135.166622682356));
#41807=CARTESIAN_POINT('Ctrl Pts',(117.203388308894,-2.15233870908931,135.226647485676));
#41808=CARTESIAN_POINT('Ctrl Pts',(117.195640412117,-2.02906160760456,135.286646776853));
#41809=CARTESIAN_POINT('Ctrl Pts',(117.187892515339,-1.90321000805651,135.341518423441));
#41810=CARTESIAN_POINT('Ctrl Pts',(117.180144618562,-1.77525130508993,135.391044154314));
#41811=CARTESIAN_POINT('Ctrl Pts',(117.172398342478,-1.64731936832553,135.440559525472));
#41812=CARTESIAN_POINT('Ctrl Pts',(117.164652066394,-1.51728156921669,135.484731064144));
#41813=CARTESIAN_POINT('Ctrl Pts',(117.15690579031,-1.38562518581118,135.523388685606));
#41814=CARTESIAN_POINT('Ctrl Pts',(117.149159457045,-1.2539678305485,135.562046592429));
#41815=CARTESIAN_POINT('Ctrl Pts',(117.141413123779,-1.12069224227625,135.595190390674));
#41816=CARTESIAN_POINT('Ctrl Pts',(117.133666790514,-0.986300373580139,
135.622700023998));
#41817=CARTESIAN_POINT('Ctrl Pts',(117.125918722511,-0.851878408756472,
135.650215817914));
#41818=CARTESIAN_POINT('Ctrl Pts',(117.118170654508,-0.716340049020913,
135.672094857818));
#41819=CARTESIAN_POINT('Ctrl Pts',(117.110422586505,-0.580196543019012,
135.688268380205));
#41820=CARTESIAN_POINT('Ctrl Pts',(117.102666283763,-0.443908342078803,
135.704459092005));
#41821=CARTESIAN_POINT('Ctrl Pts',(117.094909981022,-0.307014098951865,
135.714932126815));
#41822=CARTESIAN_POINT('Ctrl Pts',(117.08715367828,-0.170029836696684,135.719670670567));
#41823=CARTESIAN_POINT('Ctrl Pts',(117.079393235766,-0.0329724618161275,
135.724411743423));
#41824=CARTESIAN_POINT('Ctrl Pts',(117.071632793251,0.104174637164699,135.723412229423));
#41825=CARTESIAN_POINT('Ctrl Pts',(117.063872350737,0.240897344674072,135.716707463202));
#41826=CARTESIAN_POINT('Ctrl Pts',(117.056099450472,0.377839531611117,135.709991933895));
#41827=CARTESIAN_POINT('Ctrl Pts',(117.048326550206,0.514355576104106,135.697552886109));
#41828=CARTESIAN_POINT('Ctrl Pts',(117.040553649941,0.6499374792786,135.679477471092));
#41829=CARTESIAN_POINT('Ctrl Pts',(117.033063314179,0.780590638762682,135.662059142939));
#41830=CARTESIAN_POINT('Ctrl Pts',(117.025572978417,0.910376091141495,135.639407178212));
#41831=CARTESIAN_POINT('Ctrl Pts',(117.018082642655,1.03885174899798,135.611643645026));
#41832=CARTESIAN_POINT('Ctrl Pts',(117.010308308536,1.17219860047123,135.582827449041));
#41833=CARTESIAN_POINT('Ctrl Pts',(117.002533974417,1.30455677780528,135.548413141765));
#41834=CARTESIAN_POINT('Ctrl Pts',(116.994759640298,1.43541982778716,135.508481468532));
#41835=CARTESIAN_POINT('Ctrl Pts',(116.986994887351,1.56612160075525,135.468599007518));
#41836=CARTESIAN_POINT('Ctrl Pts',(116.979230134403,1.69533154226387,135.423212822854));
#41837=CARTESIAN_POINT('Ctrl Pts',(116.971465381456,1.82255294750759,135.37245472956));
#41838=CARTESIAN_POINT('Ctrl Pts',(116.963708340571,1.94964799465829,135.321747049919));
#41839=CARTESIAN_POINT('Ctrl Pts',(116.955951299686,2.07475807518674,135.265678223388));
#41840=CARTESIAN_POINT('Ctrl Pts',(116.948194258801,2.19740157042359,135.204429867112));
#41841=CARTESIAN_POINT('Ctrl Pts',(116.940443067561,2.31995257924716,135.143227698698));
#41842=CARTESIAN_POINT('Ctrl Pts',(116.932691876321,2.44004035677962,135.076853949013));
#41843=CARTESIAN_POINT('Ctrl Pts',(116.924940685081,2.55720354175795,135.005538203496));
#41844=CARTESIAN_POINT('Ctrl Pts',(116.917192788304,2.67431692925667,134.934252769074));
#41845=CARTESIAN_POINT('Ctrl Pts',(116.909444891527,2.78850786322893,134.858029719367));
#41846=CARTESIAN_POINT('Ctrl Pts',(116.90169699475,2.899340067772,134.777144305852));
#41847=CARTESIAN_POINT('Ctrl Pts',(116.893950718666,3.01014908860722,134.696275811822));
#41848=CARTESIAN_POINT('Ctrl Pts',(116.886204442582,3.11760046186363,134.610747124173));
#41849=CARTESIAN_POINT('Ctrl Pts',(116.878458166497,3.22128770475625,134.520876268776));
#41850=CARTESIAN_POINT('Ctrl Pts',(116.870711833232,3.32497571304462,134.431004749972));
#41851=CARTESIAN_POINT('Ctrl Pts',(116.862965499967,3.42489924008829,134.336791255532));
#41852=CARTESIAN_POINT('Ctrl Pts',(116.855219166701,3.52068596145132,134.238593198994));
#41853=CARTESIAN_POINT('Ctrl Pts',(116.847471098698,3.61649413358633,134.140373151682));
#41854=CARTESIAN_POINT('Ctrl Pts',(116.839723030695,3.70816338364981,134.038167046484));
#41855=CARTESIAN_POINT('Ctrl Pts',(116.831974962692,3.79535951657608,133.932367843011));
#41856=CARTESIAN_POINT('Ctrl Pts',(116.824218659951,3.88264832259008,133.826456194885));
#41857=CARTESIAN_POINT('Ctrl Pts',(116.816462357209,3.96545426562535,133.716944122229));
#41858=CARTESIAN_POINT('Ctrl Pts',(116.808706054467,4.04348427646189,133.604256681441));
#41859=CARTESIAN_POINT('Ctrl Pts',(116.800945611953,4.12155593426476,133.491509095974));
#41860=CARTESIAN_POINT('Ctrl Pts',(116.793185169439,4.19484637183213,133.375583095662));
#41861=CARTESIAN_POINT('Ctrl Pts',(116.785424726924,4.26310742516818,133.256930319731));
#41862=CARTESIAN_POINT('Ctrl Pts',(116.777651826659,4.33147805720694,133.13808707183));
#41863=CARTESIAN_POINT('Ctrl Pts',(116.769878926393,4.3948029906503,133.016508648094));
#41864=CARTESIAN_POINT('Ctrl Pts',(116.762106026128,4.45288096251175,132.892669549741));
#41865=CARTESIAN_POINT('Ctrl Pts',(116.754615690366,4.50884765380629,132.773332314545));
#41866=CARTESIAN_POINT('Ctrl Pts',(116.747125354604,4.55994212154052,132.651896197504));
#41867=CARTESIAN_POINT('Ctrl Pts',(116.739635018842,4.60602810603052,132.528799120081));
#41868=CARTESIAN_POINT('Ctrl Pts',(116.731860684723,4.65386145463017,132.401034779553));
#41869=CARTESIAN_POINT('Ctrl Pts',(116.724086350604,4.69645055113279,132.271076322685));
#41870=CARTESIAN_POINT('Ctrl Pts',(116.716312016485,4.73358957854112,132.139393487733));
#41871=CARTESIAN_POINT('Ctrl Pts',(116.708547263538,4.77068283541728,132.007872940107));
#41872=CARTESIAN_POINT('Ctrl Pts',(116.700782510591,4.80233928236949,131.87463261547));
#41873=CARTESIAN_POINT('Ctrl Pts',(116.693017757644,4.82840133802701,131.740161654881));
#41874=CARTESIAN_POINT('Ctrl Pts',(116.685260716759,4.85443750848347,131.605824252744));
#41875=CARTESIAN_POINT('Ctrl Pts',(116.677503675874,4.87489027128026,131.470259028397));
#41876=CARTESIAN_POINT('Ctrl Pts',(116.669746634989,4.88965209941101,131.333969349769));
#41877=CARTESIAN_POINT('Ctrl Pts',(116.661995443748,4.90440279553233,131.197782448247));
#41878=CARTESIAN_POINT('Ctrl Pts',(116.654244252508,4.91347105718386,131.060872566974));
#41879=CARTESIAN_POINT('Ctrl Pts',(116.646493061268,4.91680066406422,130.923751958783));
#41880=CARTESIAN_POINT('Ctrl Pts',(116.638745164491,4.92012885577285,130.786689630508));
#41881=CARTESIAN_POINT('Ctrl Pts',(116.630997267714,4.91772323438627,130.649417143483));
#41882=CARTESIAN_POINT('Ctrl Pts',(116.623249370937,4.90957955898512,130.512450329129));
#41883=CARTESIAN_POINT('Ctrl Pts',(116.615503094853,4.90143758706532,130.37551216528));
#41884=CARTESIAN_POINT('Ctrl Pts',(116.607756818769,4.88755997173819,130.238879936949));
#41885=CARTESIAN_POINT('Ctrl Pts',(116.600010542685,4.86799456330315,130.103067530368));
#41886=CARTESIAN_POINT('Ctrl Pts',(116.592264209419,4.84842901044069,129.967254121252));
#41887=CARTESIAN_POINT('Ctrl Pts',(116.584517876154,4.82317563643801,129.832260932931));
#41888=CARTESIAN_POINT('Ctrl Pts',(116.576771542888,4.79233389297649,129.698594403247));
#41889=CARTESIAN_POINT('Ctrl Pts',(116.569023474885,4.76148524272035,129.564897939871));
#41890=CARTESIAN_POINT('Ctrl Pts',(116.561275406882,4.7250458205954,129.432529107202));
#41891=CARTESIAN_POINT('Ctrl Pts',(116.553527338879,4.68316559405484,129.301981477282));
#41892=CARTESIAN_POINT('Ctrl Pts',(116.545771036138,4.6412408567112,129.171295099787));
#41893=CARTESIAN_POINT('Ctrl Pts',(116.538014733396,4.59386388330079,129.042434164474));
#41894=CARTESIAN_POINT('Ctrl Pts',(116.530258430654,4.54123387473806,128.915874992142));
#41895=CARTESIAN_POINT('Ctrl Pts',(116.52249798814,4.48857577595502,128.78924827137));
#41896=CARTESIAN_POINT('Ctrl Pts',(116.514737545626,4.43065922042154,128.664926115733));
#41897=CARTESIAN_POINT('Ctrl Pts',(116.506977103111,4.36773004630638,128.543361434662));
#41898=CARTESIAN_POINT('Ctrl Pts',(116.499204202846,4.30469985269439,128.421601607173));
#41899=CARTESIAN_POINT('Ctrl Pts',(116.49143130258,4.23664115484876,128.302608439464));
#41900=CARTESIAN_POINT('Ctrl Pts',(116.483658402315,4.16384437652324,128.186807739285));
#41901=CARTESIAN_POINT('Ctrl Pts',(116.476168066553,4.09369394445397,128.075216686243));
#41902=CARTESIAN_POINT('Ctrl Pts',(116.468677730791,4.01914410779989,127.966590275964));
#41903=CARTESIAN_POINT('Ctrl Pts',(116.461187395029,3.9404896506031,127.861279854829));
#41904=CARTESIAN_POINT('Ctrl Pts',(116.45341306091,3.85885298575508,127.751976557069));
#41905=CARTESIAN_POINT('Ctrl Pts',(116.445638726791,3.77253570233343,127.645899423646));
#41906=CARTESIAN_POINT('Ctrl Pts',(116.437864392672,3.68182175532233,127.543475519232));
#41907=CARTESIAN_POINT('Ctrl Pts',(116.430099639725,3.59121960514365,127.441177843127));
#41908=CARTESIAN_POINT('Ctrl Pts',(116.422334886778,3.49623182929369,127.342524727706));
#41909=CARTESIAN_POINT('Ctrl Pts',(116.41457013383,3.39718477941786,127.247913143331));
#41910=CARTESIAN_POINT('Ctrl Pts',(116.406813092945,3.29823610446814,127.153395528515));
#41911=CARTESIAN_POINT('Ctrl Pts',(116.39905605206,3.19523645969594,127.062911724797));
#41912=CARTESIAN_POINT('Ctrl Pts',(116.391299011175,3.08855122182369,126.976824280355));
#41913=CARTESIAN_POINT('Ctrl Pts',(116.383547819935,2.98194643611958,126.890801755124));
#41914=CARTESIAN_POINT('Ctrl Pts',(116.375796628695,2.87166189244234,126.809169234732));
#41915=CARTESIAN_POINT('Ctrl Pts',(116.368045437455,2.75809817516269,126.73225090408));
#41916=CARTESIAN_POINT('Ctrl Pts',(116.360297540678,2.64458272549207,126.65536526577));
#41917=CARTESIAN_POINT('Ctrl Pts',(116.352549643901,2.52779119727969,126.58319005087));
#41918=CARTESIAN_POINT('Ctrl Pts',(116.344801747124,2.40815528178724,126.516007646867));
#41919=CARTESIAN_POINT('Ctrl Pts',(116.33705547104,2.28854439154942,126.448839295975));
#41920=CARTESIAN_POINT('Ctrl Pts',(116.329309194956,2.16609063816533,126.386661869944));
#41921=CARTESIAN_POINT('Ctrl Pts',(116.321562918872,2.04125223293124,126.329712879022));
#41922=CARTESIAN_POINT('Ctrl Pts',(116.313816585606,1.9164129061684,126.272763467716));
#41923=CARTESIAN_POINT('Ctrl Pts',(116.306070252341,1.78918924813218,126.221042730798));
#41924=CARTESIAN_POINT('Ctrl Pts',(116.298323919076,1.66006109538457,126.174740738776));
#41925=CARTESIAN_POINT('Ctrl Pts',(116.290575851073,1.53090402528291,126.128428377743));
#41926=CARTESIAN_POINT('Ctrl Pts',(116.28282778307,1.39984197973823,126.087537308249));
#41927=CARTESIAN_POINT('Ctrl Pts',(116.275079715067,1.26737127595946,126.052208146172));
#41928=CARTESIAN_POINT('Ctrl Pts',(116.267323412325,1.13475978073966,126.016841435842));
#41929=CARTESIAN_POINT('Ctrl Pts',(116.259567109583,1.00073701495387,125.987048542217));
#41930=CARTESIAN_POINT('Ctrl Pts',(116.251810806841,0.865811393742108,125.962919334955));
#41931=CARTESIAN_POINT('Ctrl Pts',(116.244050364327,0.730813758663684,125.938777249209));
#41932=CARTESIAN_POINT('Ctrl Pts',(116.236289921813,0.594912695183648,125.920304925802));
#41933=CARTESIAN_POINT('Ctrl Pts',(116.228529479299,0.458622130368095,125.907540342731));
#41934=CARTESIAN_POINT('Ctrl Pts',(116.220756579033,0.322112779838777,125.894755268817));
#41935=CARTESIAN_POINT('Ctrl Pts',(116.212983678768,0.185213069172185,125.887696265121));
#41936=CARTESIAN_POINT('Ctrl Pts',(116.205210778502,0.048438223620664,125.886349149402));
#41937=CARTESIAN_POINT('Ctrl Pts',(116.19772044274,-0.0833645117811219,
125.885051004733));
#41938=CARTESIAN_POINT('Ctrl Pts',(116.190230106978,-0.215050994901615,
125.889056665568));
#41939=CARTESIAN_POINT('Ctrl Pts',(116.182739771216,-0.346166290106392,
125.898308033044));
#41940=CARTESIAN_POINT('Ctrl Pts',(116.174965437097,-0.482252861579623,
125.90791016893));
#41941=CARTESIAN_POINT('Ctrl Pts',(116.167191102978,-0.618155158294855,
125.923194062412));
#41942=CARTESIAN_POINT('Ctrl Pts',(116.159416768859,-0.753360394044942,
125.944151653007));
#41943=CARTESIAN_POINT('Ctrl Pts',(116.151652015912,-0.888399001425789,
125.965083415243));
#41944=CARTESIAN_POINT('Ctrl Pts',(116.143887262965,-1.02274187448304,125.991674902639));
#41945=CARTESIAN_POINT('Ctrl Pts',(116.136122510017,-1.15587862977411,126.023866118486));
#41946=CARTESIAN_POINT('Ctrl Pts',(116.128365469132,-1.28888315176256,126.056025361564));
#41947=CARTESIAN_POINT('Ctrl Pts',(116.120608428247,-1.42068356237032,126.093773173713));
#41948=CARTESIAN_POINT('Ctrl Pts',(116.112851387362,-1.55077734450439,126.136998119294));
#41949=CARTESIAN_POINT('Ctrl Pts',(116.105100196122,-1.68077302190555,126.180190468608));
#41950=CARTESIAN_POINT('Ctrl Pts',(116.097349004882,-1.80906426297203,126.228851607367));
#41951=CARTESIAN_POINT('Ctrl Pts',(116.089597813642,-1.93516179612806,126.282819742454));
#41952=CARTESIAN_POINT('Ctrl Pts',(116.081849916865,-2.06120573446865,126.336764939644));
#41953=CARTESIAN_POINT('Ctrl Pts',(116.074102020088,-2.18505746066304,126.396012493406));
#41954=CARTESIAN_POINT('Ctrl Pts',(116.066354123311,-2.30624605444866,126.46035184699));
#41955=CARTESIAN_POINT('Ctrl Pts',(116.058607847227,-2.42740929819307,126.524677742168));
#41956=CARTESIAN_POINT('Ctrl Pts',(116.050861571143,-2.54591017247284,126.594093135423));
#41957=CARTESIAN_POINT('Ctrl Pts',(116.043115295059,-2.66130117879128,126.668340900705));
#41958=CARTESIAN_POINT('Ctrl Pts',(116.035368961793,-2.77669303689976,126.742589214066));
#41959=CARTESIAN_POINT('Ctrl Pts',(116.027622628528,-2.88897465245562,126.82166975908));
#41960=CARTESIAN_POINT('Ctrl Pts',(116.019876295262,-2.9977267503754,126.905281573409));
#41961=CARTESIAN_POINT('Ctrl Pts',(116.01212822726,-3.10650320257339,126.988912112024));
#41962=CARTESIAN_POINT('Ctrl Pts',(116.004380159257,-3.21174825441974,127.07707570093));
#41963=CARTESIAN_POINT('Ctrl Pts',(115.996632091254,-3.31307533021835,127.169430780719));
#41964=CARTESIAN_POINT('Ctrl Pts',(115.988875788512,-3.414510097639,127.261884016587));
#41965=CARTESIAN_POINT('Ctrl Pts',(115.98111948577,-3.51201828141911,127.358537378428));
#41966=CARTESIAN_POINT('Ctrl Pts',(115.973363183028,-3.60524946086931,127.459011698933));
#41967=CARTESIAN_POINT('Ctrl Pts',(115.965602740514,-3.69853040060692,127.559539645607));
#41968=CARTESIAN_POINT('Ctrl Pts',(115.957842298,-3.78752953383121,127.663892317217));
#41969=CARTESIAN_POINT('Ctrl Pts',(115.950081855486,-3.87193711844573,127.771657860403));
#41970=CARTESIAN_POINT('Ctrl Pts',(115.94230895522,-3.95648020160871,127.879596398407));
#41971=CARTESIAN_POINT('Ctrl Pts',(115.934536054955,-4.03641677891657,127.990958438268));
#41972=CARTESIAN_POINT('Ctrl Pts',(115.926763154689,-4.11148029045516,128.105302840545));
#41973=CARTESIAN_POINT('Ctrl Pts',(115.919272818927,-4.18381505427524,128.215490535782));
#41974=CARTESIAN_POINT('Ctrl Pts',(115.911782483165,-4.25162473911524,128.32844726111));
#41975=CARTESIAN_POINT('Ctrl Pts',(115.904292147403,-4.31471232137161,128.44375886244));
#41976=CARTESIAN_POINT('Ctrl Pts',(115.896119758503,-4.38354451706451,128.569570478998));
#41977=CARTESIAN_POINT('Ctrl Pts',(115.887947369603,-4.44695528377166,128.698550318887));
#41978=CARTESIAN_POINT('Ctrl Pts',(115.879774980703,-4.50465700191711,128.830215648832));
#41979=CARTESIAN_POINT('Ctrl Pts',(115.871620741564,-4.56223057241044,128.961588568022));
#41980=CARTESIAN_POINT('Ctrl Pts',(115.863466502426,-4.61412024000921,129.09563478355));
#41981=CARTESIAN_POINT('Ctrl Pts',(115.855312263288,-4.66008418077987,129.231847186607));
#41982=CARTESIAN_POINT('Ctrl Pts',(115.848401956893,-4.69903630230064,129.347280328057));
#41983=CARTESIAN_POINT('Ctrl Pts',(115.841491650499,-4.73373342589427,129.464268601472));
#41984=CARTESIAN_POINT('Ctrl Pts',(115.834581344104,-4.76405452823405,129.582490119308));
#41985=CARTESIAN_POINT('Ctrl Pts',(117.5848416735,-4.76405452823405,129.582490119308));
#41986=CARTESIAN_POINT('Ctrl Pts',(117.58155374576,-4.77840700162319,129.638450195223));
#41987=CARTESIAN_POINT('Ctrl Pts',(117.57826581802,-4.7917644510224,129.694628467612));
#41988=CARTESIAN_POINT('Ctrl Pts',(117.57497789028,-4.80412178438199,129.75098654188));
#41989=CARTESIAN_POINT('Ctrl Pts',(117.564226926074,-4.84452816163197,129.935267854337));
#41990=CARTESIAN_POINT('Ctrl Pts',(117.553475961867,-4.87434350039962,130.121948280994));
#41991=CARTESIAN_POINT('Ctrl Pts',(117.542724997661,-4.89334244972931,130.310009798636));
#41992=CARTESIAN_POINT('Ctrl Pts',(117.533436477104,-4.90975698967351,130.472489483155));
#41993=CARTESIAN_POINT('Ctrl Pts',(117.524147956548,-4.91809829573002,130.636000128652));
#41994=CARTESIAN_POINT('Ctrl Pts',(117.514859435991,-4.91824794902745,130.799869026841));
#41995=CARTESIAN_POINT('',(117.860140564046,-4.91824926722357,130.807045381015));
#41996=CARTESIAN_POINT('Ctrl Pts',(117.930282309765,-4.76405452823403,129.582490119308));
#41997=CARTESIAN_POINT('Ctrl Pts',(117.922619279463,-4.79774499717081,129.713848746368));
#41998=CARTESIAN_POINT('Ctrl Pts',(117.914956249162,-4.82597508279731,129.846511022407));
#41999=CARTESIAN_POINT('Ctrl Pts',(117.90729321886,-4.848667424413,129.979977654413));
#42000=CARTESIAN_POINT('Ctrl Pts',(117.899434443058,-4.87193942232638,130.116853576439));
#42001=CARTESIAN_POINT('Ctrl Pts',(117.891575667255,-4.88938690047608,130.254575048808));
#42002=CARTESIAN_POINT('Ctrl Pts',(117.883716891453,-4.90098319599923,130.39260003782));
#42003=CARTESIAN_POINT('Ctrl Pts',(117.87585811565,-4.91257949152238,130.530625026831));
#42004=CARTESIAN_POINT('Ctrl Pts',(117.867999339848,-4.91832464875417,130.668953081738));
#42005=CARTESIAN_POINT('Ctrl Pts',(117.860140564046,-4.91824926722357,130.807045381015));
#42006=CARTESIAN_POINT('Ctrl Pts',(117.860140564008,-4.91824926722321,130.807045381675));
#42007=CARTESIAN_POINT('Ctrl Pts',(117.85137254865,-4.9181651642284,130.961114594403));
#42008=CARTESIAN_POINT('Ctrl Pts',(117.842604533292,-4.91084215645057,131.114982470872));
#42009=CARTESIAN_POINT('Ctrl Pts',(117.833836517934,-4.89633272611262,131.268158954884));
#42010=CARTESIAN_POINT('Ctrl Pts',(117.826062183815,-4.88346765292127,131.403975912001));
#42011=CARTESIAN_POINT('Ctrl Pts',(117.818287849696,-4.86492688042555,131.539472300911));
#42012=CARTESIAN_POINT('Ctrl Pts',(117.810513515577,-4.84073077224359,131.674135676506));
#42013=CARTESIAN_POINT('Ctrl Pts',(117.80274876263,-4.81656448360249,131.808633091525));
#42014=CARTESIAN_POINT('Ctrl Pts',(117.794984009683,-4.7867567953695,131.942299154777));
#42015=CARTESIAN_POINT('Ctrl Pts',(117.787219256735,-4.7513799347683,132.074625069553));
#42016=CARTESIAN_POINT('Ctrl Pts',(117.779462215851,-4.71603821096378,132.206819556364));
#42017=CARTESIAN_POINT('Ctrl Pts',(117.771705174966,-4.67513842281126,132.337676168301));
#42018=CARTESIAN_POINT('Ctrl Pts',(117.763948134081,-4.62880403288357,132.46669520713));
#42019=CARTESIAN_POINT('Ctrl Pts',(117.75619694284,-4.58250458407985,132.595616951698));
#42020=CARTESIAN_POINT('Ctrl Pts',(117.7484457516,-4.53077882247863,132.7227035149));
#42021=CARTESIAN_POINT('Ctrl Pts',(117.74069456036,-4.47380023577484,132.847469648646));
#42022=CARTESIAN_POINT('Ctrl Pts',(117.732946663583,-4.41684586649028,132.972182753457));
#42023=CARTESIAN_POINT('Ctrl Pts',(117.725198766806,-4.35464327462833,133.094577035488));
#42024=CARTESIAN_POINT('Ctrl Pts',(117.717450870029,-4.28741425709157,133.214186762869));
#42025=CARTESIAN_POINT('Ctrl Pts',(117.709704593945,-4.22019930241598,133.333771470475));
#42026=CARTESIAN_POINT('Ctrl Pts',(117.701958317861,-4.14796020483971,133.450572441392));
#42027=CARTESIAN_POINT('Ctrl Pts',(117.694212041777,-4.07096475509683,133.564148476308));
#42028=CARTESIAN_POINT('Ctrl Pts',(117.686465708511,-3.99396873699097,133.677725349617));
#42029=CARTESIAN_POINT('Ctrl Pts',(117.678719375246,-3.91221651604153,133.78807691581));
#42030=CARTESIAN_POINT('Ctrl Pts',(117.670973041981,-3.82601902936198,133.894791242812));
#42031=CARTESIAN_POINT('Ctrl Pts',(117.663224973978,-3.73980223935306,134.001529467748));
#42032=CARTESIAN_POINT('Ctrl Pts',(117.655476905975,-3.64913844833108,134.104628528579));
#42033=CARTESIAN_POINT('Ctrl Pts',(117.647728837972,-3.55437839409314,134.20371015742));
#42034=CARTESIAN_POINT('Ctrl Pts',(117.63997253523,-3.45951762774183,134.302897091394));
#42035=CARTESIAN_POINT('Ctrl Pts',(117.632216232488,-3.36055217212944,134.398057781045));
#42036=CARTESIAN_POINT('Ctrl Pts',(117.624459929746,-3.25786949450717,134.488851005565));
#42037=CARTESIAN_POINT('Ctrl Pts',(117.616699487232,-3.15513201204807,134.579692689163));
#42038=CARTESIAN_POINT('Ctrl Pts',(117.608939044718,-3.0486736576287,134.66616201645));
#42039=CARTESIAN_POINT('Ctrl Pts',(117.601178602204,-2.938913598963,134.747959217871));
#42040=CARTESIAN_POINT('Ctrl Pts',(117.593405701938,-2.82897734370708,134.829887727422));
#42041=CARTESIAN_POINT('Ctrl Pts',(117.585632801673,-2.71572911591568,134.907128903073));
#42042=CARTESIAN_POINT('Ctrl Pts',(117.577859901407,-2.59961632469809,134.979426847803));
#42043=CARTESIAN_POINT('Ctrl Pts',(117.570369565645,-2.48772452591102,135.049096580134));
#42044=CARTESIAN_POINT('Ctrl Pts',(117.562879229883,-2.37317308386355,135.114176087509));
#42045=CARTESIAN_POINT('Ctrl Pts',(117.555388894121,-2.2563807614013,135.174478341619));
#42046=CARTESIAN_POINT('Ctrl Pts',(117.547614560002,-2.13516022253541,135.23706697402));
#42047=CARTESIAN_POINT('Ctrl Pts',(117.539840225883,-2.01114153267069,135.294707204907));
#42048=CARTESIAN_POINT('Ctrl Pts',(117.532065891764,-1.88476683342271,135.347139177669));
#42049=CARTESIAN_POINT('Ctrl Pts',(117.524301138817,-1.75854787969721,135.39950653271));
#42050=CARTESIAN_POINT('Ctrl Pts',(117.51653638587,-1.62997905148056,135.446678252565));
#42051=CARTESIAN_POINT('Ctrl Pts',(117.508771632922,-1.49952745443278,135.488440086992));
#42052=CARTESIAN_POINT('Ctrl Pts',(117.501014592037,-1.36920542375024,135.530160442977));
#42053=CARTESIAN_POINT('Ctrl Pts',(117.493257551152,-1.237004715547,135.566481487964));
#42054=CARTESIAN_POINT('Ctrl Pts',(117.485500510267,-1.10341247463453,135.597236995413));
#42055=CARTESIAN_POINT('Ctrl Pts',(117.477749319027,-0.969920976670225,
135.627969309894));
#42056=CARTESIAN_POINT('Ctrl Pts',(117.469998127787,-0.835040414152658,
135.653144353381));
#42057=CARTESIAN_POINT('Ctrl Pts',(117.462246936547,-0.699272814378756,
135.672645797542));
#42058=CARTESIAN_POINT('Ctrl Pts',(117.45449903977,-0.563562919456384,135.692138953068));
#42059=CARTESIAN_POINT('Ctrl Pts',(117.446751142993,-0.426967123313924,
135.70596324995));
#42060=CARTESIAN_POINT('Ctrl Pts',(117.439003246216,-0.289997146005428,
135.714053552751));
#42061=CARTESIAN_POINT('Ctrl Pts',(117.431256970132,-0.153055819863362,
135.722142163236));
#42062=CARTESIAN_POINT('Ctrl Pts',(117.423510694048,-0.0157408582775557,
135.72449914233));
#42063=CARTESIAN_POINT('Ctrl Pts',(117.415764417964,0.121431797842503,135.721111310958));
#42064=CARTESIAN_POINT('Ctrl Pts',(117.408018084698,0.258605466539949,135.717723454578));
#42065=CARTESIAN_POINT('Ctrl Pts',(117.400271751433,0.395636436829494,135.708590712764));
#42066=CARTESIAN_POINT('Ctrl Pts',(117.392525418167,0.53201006948388,135.693752026368));
#42067=CARTESIAN_POINT('Ctrl Pts',(117.384777350165,0.668414242067658,135.678910016951));
#42068=CARTESIAN_POINT('Ctrl Pts',(117.377029282162,0.804160395496203,135.658359562546));
#42069=CARTESIAN_POINT('Ctrl Pts',(117.369281214159,0.938740699935791,135.632191285763));
#42070=CARTESIAN_POINT('Ctrl Pts',(117.361524911417,1.07346403792456,135.605995197024));
#42071=CARTESIAN_POINT('Ctrl Pts',(117.353768608675,1.20701866734276,135.574169433555));
#42072=CARTESIAN_POINT('Ctrl Pts',(117.346012305933,1.338908073948,135.536855544348));
#42073=CARTESIAN_POINT('Ctrl Pts',(117.338251863419,1.47086787390065,135.499521739595));
#42074=CARTESIAN_POINT('Ctrl Pts',(117.330491420905,1.60116030883881,135.456694094493));
#42075=CARTESIAN_POINT('Ctrl Pts',(117.32273097839,1.72930660375927,135.408563233948));
#42076=CARTESIAN_POINT('Ctrl Pts',(117.314958078125,1.85765861048863,135.360355109472));
#42077=CARTESIAN_POINT('Ctrl Pts',(117.30718517786,1.98385723251042,135.306826910234));
#42078=CARTESIAN_POINT('Ctrl Pts',(117.299412277594,2.10744534086116,135.248216735599));
#42079=CARTESIAN_POINT('Ctrl Pts',(117.291921941832,2.22654071017419,135.191737188442));
#42080=CARTESIAN_POINT('Ctrl Pts',(117.28443160607,2.34321179537716,135.130538879374));
#42081=CARTESIAN_POINT('Ctrl Pts',(117.276941270308,2.45707489270949,135.064873032067));
#42082=CARTESIAN_POINT('Ctrl Pts',(117.269166936189,2.5752551439847,134.996717444201));
#42083=CARTESIAN_POINT('Ctrl Pts',(117.26139260207,2.69078463388255,134.923532960761));
#42084=CARTESIAN_POINT('Ctrl Pts',(117.253618267951,2.80320574933492,134.845551109166));
#42085=CARTESIAN_POINT('Ctrl Pts',(117.245853515004,2.91548831580978,134.767665363233));
#42086=CARTESIAN_POINT('Ctrl Pts',(117.238088762057,3.02466981181543,134.684994233611));
#42087=CARTESIAN_POINT('Ctrl Pts',(117.230324009109,3.13031750053771,134.597814902031));
#42088=CARTESIAN_POINT('Ctrl Pts',(117.222566968224,3.23586025848617,134.510722158192));
#42089=CARTESIAN_POINT('Ctrl Pts',(117.214809927339,3.33787589426502,134.419130370269));
#42090=CARTESIAN_POINT('Ctrl Pts',(117.207052886454,3.43596124310754,134.323359537481));
#42091=CARTESIAN_POINT('Ctrl Pts',(117.199301695214,3.5339726250255,134.227660926223));
#42092=CARTESIAN_POINT('Ctrl Pts',(117.191550503974,3.62805934078759,134.127789814901));
#42093=CARTESIAN_POINT('Ctrl Pts',(117.183799312734,3.71785216205539,134.024105694991));
#42094=CARTESIAN_POINT('Ctrl Pts',(117.176051415957,3.80760681897891,133.920465643597));
#42095=CARTESIAN_POINT('Ctrl Pts',(117.16830351918,3.89307095582263,133.81301610185));
#42096=CARTESIAN_POINT('Ctrl Pts',(117.160555622403,3.97391317511178,133.70215238703));
#42097=CARTESIAN_POINT('Ctrl Pts',(117.152809346319,4.05473848395141,133.591311862509));
#42098=CARTESIAN_POINT('Ctrl Pts',(117.145063070235,4.13094356805814,133.477058901138));
#42099=CARTESIAN_POINT('Ctrl Pts',(117.137316794151,4.20223846083776,133.359820455003));
#42100=CARTESIAN_POINT('Ctrl Pts',(117.129570460885,4.27353387990004,133.242581143442));
#42101=CARTESIAN_POINT('Ctrl Pts',(117.12182412762,4.33991883216861,133.122356637188));
#42102=CARTESIAN_POINT('Ctrl Pts',(117.114077794354,4.40114790461073,132.999600965282));
#42103=CARTESIAN_POINT('Ctrl Pts',(117.106329726351,4.46239068887909,132.876817803094));
#42104=CARTESIAN_POINT('Ctrl Pts',(117.098581658349,4.51847512128156,132.751502697105));
#42105=CARTESIAN_POINT('Ctrl Pts',(117.090833590346,4.56920295075611,132.624131882671));
#42106=CARTESIAN_POINT('Ctrl Pts',(117.083077287604,4.61998469437154,132.496625697019));
#42107=CARTESIAN_POINT('Ctrl Pts',(117.075320984862,4.6653983176665,132.367059802284));
#42108=CARTESIAN_POINT('Ctrl Pts',(117.06756468212,4.70529453174012,132.235928440645));
#42109=CARTESIAN_POINT('Ctrl Pts',(117.059804239606,4.74521203962446,132.104727090251));
#42110=CARTESIAN_POINT('Ctrl Pts',(117.052043797092,4.77960617251255,131.971958986364));
#42111=CARTESIAN_POINT('Ctrl Pts',(117.044283354577,4.8083785189504,131.838129973369));
#42112=CARTESIAN_POINT('Ctrl Pts',(117.036510454312,4.83719705331301,131.704086126161));
#42113=CARTESIAN_POINT('Ctrl Pts',(117.028737554047,4.86037570107255,131.568978352137));
#42114=CARTESIAN_POINT('Ctrl Pts',(117.020964653781,4.87786769259683,131.433319945361));
#42115=CARTESIAN_POINT('Ctrl Pts',(117.013474318019,4.89472380616945,131.302593063375));
#42116=CARTESIAN_POINT('Ctrl Pts',(117.005983982257,4.90629950692592,131.171355194195));
#42117=CARTESIAN_POINT('Ctrl Pts',(116.998493646495,4.91259875520174,131.040064951193));
#42118=CARTESIAN_POINT('Ctrl Pts',(116.990719312376,4.91913684139058,130.903796798721));
#42119=CARTESIAN_POINT('Ctrl Pts',(116.982944978257,4.92001117403477,130.767040565976));
#42120=CARTESIAN_POINT('Ctrl Pts',(116.975170644138,4.91516919266761,130.630306402014));
#42121=CARTESIAN_POINT('Ctrl Pts',(116.967405891191,4.91033317860973,130.49374075069));
#42122=CARTESIAN_POINT('Ctrl Pts',(116.959641138244,4.89979488138778,130.357197501004));
#42123=CARTESIAN_POINT('Ctrl Pts',(116.951876385297,4.88355359702528,130.221190550192));
#42124=CARTESIAN_POINT('Ctrl Pts',(116.944119344412,4.86732844373538,130.0853186834));
#42125=CARTESIAN_POINT('Ctrl Pts',(116.936362303527,4.84541162154993,129.94998244116));
#42126=CARTESIAN_POINT('Ctrl Pts',(116.928605262642,4.81785443447189,129.815693984803));
#42127=CARTESIAN_POINT('Ctrl Pts',(116.920854071402,4.79031802848298,129.681506796415));
#42128=CARTESIAN_POINT('Ctrl Pts',(116.913102880162,4.75714980209572,129.548366202613));
#42129=CARTESIAN_POINT('Ctrl Pts',(116.905351688922,4.71845262873539,129.416777159579));
#42130=CARTESIAN_POINT('Ctrl Pts',(116.897603792144,4.67977190270598,129.285244045398));
#42131=CARTESIAN_POINT('Ctrl Pts',(116.889855895367,4.63556701364667,129.155261544686));
#42132=CARTESIAN_POINT('Ctrl Pts',(116.88210799859,4.58599142475161,129.02732215017));
#42133=CARTESIAN_POINT('Ctrl Pts',(116.874361722506,4.53642620600101,128.899409517818));
#42134=CARTESIAN_POINT('Ctrl Pts',(116.866615446422,4.48149266315989,128.773539505914));
#42135=CARTESIAN_POINT('Ctrl Pts',(116.858869170338,4.42139326908373,128.650186849598));
#42136=CARTESIAN_POINT('Ctrl Pts',(116.851122837073,4.36129343136754,128.526833282721));
#42137=CARTESIAN_POINT('Ctrl Pts',(116.843376503807,4.2960278375656,128.405997459982));
#42138=CARTESIAN_POINT('Ctrl Pts',(116.835630170542,4.22584582342771,128.288131268099));
#42139=CARTESIAN_POINT('Ctrl Pts',(116.827882102539,4.15564809251435,128.1702386809));
#42140=CARTESIAN_POINT('Ctrl Pts',(116.820134034536,4.0805319503897,128.055317383748));
#42141=CARTESIAN_POINT('Ctrl Pts',(116.812385966533,4.00079090780434,127.943791587717));
#42142=CARTESIAN_POINT('Ctrl Pts',(116.804629663791,3.92096511548993,127.832147260743));
#42143=CARTESIAN_POINT('Ctrl Pts',(116.796873361049,3.83650483143241,127.723905962357));
#42144=CARTESIAN_POINT('Ctrl Pts',(116.789117058308,3.74774518127914,127.61946044351));
#42145=CARTESIAN_POINT('Ctrl Pts',(116.781356615793,3.65893815742809,127.514959178946));
#42146=CARTESIAN_POINT('Ctrl Pts',(116.773596173279,3.56582746038873,127.414258017662));
#42147=CARTESIAN_POINT('Ctrl Pts',(116.765835730765,3.46878547757482,127.317713177249));
#42148=CARTESIAN_POINT('Ctrl Pts',(116.7580628305,3.37158771435505,127.221013354488));
#42149=CARTESIAN_POINT('Ctrl Pts',(116.750289930234,3.27044634290115,127.128483449624));
#42150=CARTESIAN_POINT('Ctrl Pts',(116.742517029969,3.16576793191937,127.040440259252));
#42151=CARTESIAN_POINT('Ctrl Pts',(116.735026694207,3.06489484484521,126.955597660617));
#42152=CARTESIAN_POINT('Ctrl Pts',(116.727536358445,2.96073765766425,126.874921421774));
#42153=CARTESIAN_POINT('Ctrl Pts',(116.720046022683,2.85368435545317,126.79865610251));
#42154=CARTESIAN_POINT('Ctrl Pts',(116.712271688563,2.74257209475132,126.719499160486));
#42155=CARTESIAN_POINT('Ctrl Pts',(116.704497354444,2.62798780115533,126.644843475414));
#42156=CARTESIAN_POINT('Ctrl Pts',(116.696723020325,2.51033226730108,126.575009015932));
#42157=CARTESIAN_POINT('Ctrl Pts',(116.688958267378,2.3928217333772,126.505260621179));
#42158=CARTESIAN_POINT('Ctrl Pts',(116.681193514431,2.27224782325015,126.440321827383));
#42159=CARTESIAN_POINT('Ctrl Pts',(116.673428761484,2.14904251270113,126.380471000826));
#42160=CARTESIAN_POINT('Ctrl Pts',(116.665671720599,2.02595957140337,126.320679618953));
#42161=CARTESIAN_POINT('Ctrl Pts',(116.657914679714,1.90025078014564,126.265966317472));
#42162=CARTESIAN_POINT('Ctrl Pts',(116.650157638829,1.77237476582821,126.216564768582));
#42163=CARTESIAN_POINT('Ctrl Pts',(116.642406447589,1.6445951838079,126.167200473784));
#42164=CARTESIAN_POINT('Ctrl Pts',(116.634655256349,1.51465199496312,126.123140098927));
#42165=CARTESIAN_POINT('Ctrl Pts',(116.626904065109,1.38302563883066,126.084570034835));
#42166=CARTESIAN_POINT('Ctrl Pts',(116.619156168331,1.2514552274108,126.046016364049));
#42167=CARTESIAN_POINT('Ctrl Pts',(116.611408271554,1.11820344596504,126.012948472528));
#42168=CARTESIAN_POINT('Ctrl Pts',(116.603660374777,0.983767593178136,125.98550345169));
#42169=CARTESIAN_POINT('Ctrl Pts',(116.595914098693,0.849359861473531,125.958064171759));
#42170=CARTESIAN_POINT('Ctrl Pts',(116.588167822609,0.713768933902753,125.93624550117));
#42171=CARTESIAN_POINT('Ctrl Pts',(116.580421546525,0.577503660108147,125.920133699715));
#42172=CARTESIAN_POINT('Ctrl Pts',(116.57267521326,0.441237380434337,125.904021779326));
#42173=CARTESIAN_POINT('Ctrl Pts',(116.564928879994,0.304297132864337,125.89361685804));
#42174=CARTESIAN_POINT('Ctrl Pts',(116.557182546729,0.167197874557127,125.888953418438));
#42175=CARTESIAN_POINT('Ctrl Pts',(116.549434478726,0.0300679138215044,
125.884288934491));
#42176=CARTESIAN_POINT('Ctrl Pts',(116.541686410723,-0.107220737845377,
125.88536850404));
#42177=CARTESIAN_POINT('Ctrl Pts',(116.53393834272,-0.244152529921328,125.892174484628));
#42178=CARTESIAN_POINT('Ctrl Pts',(116.526182039978,-0.381229854735314,
125.898987698692));
#42179=CARTESIAN_POINT('Ctrl Pts',(116.518425737236,-0.51794917121065,125.911539461991));
#42180=CARTESIAN_POINT('Ctrl Pts',(116.510669434494,-0.653798903249842,
125.929760115308));
#42181=CARTESIAN_POINT('Ctrl Pts',(116.50290899198,-0.789721142381565,125.947990493538));
#42182=CARTESIAN_POINT('Ctrl Pts',(116.495148549466,-0.92477248747973,125.971895722552));
#42183=CARTESIAN_POINT('Ctrl Pts',(116.487388106952,-1.05845195810392,126.001355046584));
#42184=CARTESIAN_POINT('Ctrl Pts',(116.479615206686,-1.19234602288186,126.030861661337));
#42185=CARTESIAN_POINT('Ctrl Pts',(116.471842306421,-1.32486343421377,126.065940087866));
#42186=CARTESIAN_POINT('Ctrl Pts',(116.464069406155,-1.45551790183405,126.106419504702));
#42187=CARTESIAN_POINT('Ctrl Pts',(116.456579070393,-1.58142275045652,126.145427392773));
#42188=CARTESIAN_POINT('Ctrl Pts',(116.449088734631,-1.70559745891545,126.189450306511));
#42189=CARTESIAN_POINT('Ctrl Pts',(116.441598398869,-1.82762655672429,126.238294013622));
#42190=CARTESIAN_POINT('Ctrl Pts',(116.433823739619,-1.95428772175633,126.28899176488));
#42191=CARTESIAN_POINT('Ctrl Pts',(116.426049080369,-2.07903841053544,126.345044123271));
#42192=CARTESIAN_POINT('Ctrl Pts',(116.418274421118,-2.20139272551441,126.406286819805));
#42193=CARTESIAN_POINT('Ctrl Pts',(116.410509417803,-2.32359507945858,126.467453454424));
#42194=CARTESIAN_POINT('Ctrl Pts',(116.402744414487,-2.44340663531066,126.533797427219));
#42195=CARTESIAN_POINT('Ctrl Pts',(116.394979411171,-2.56035965804851,126.605105745099));
#42196=CARTESIAN_POINT('Ctrl Pts',(116.387222194363,-2.67719540387604,126.676342557181));
#42197=CARTESIAN_POINT('Ctrl Pts',(116.379464977555,-2.79117798951135,126.752533605028));
#42198=CARTESIAN_POINT('Ctrl Pts',(116.371707760747,-2.90186289272959,126.833419316779));
#42199=CARTESIAN_POINT('Ctrl Pts',(116.363726401479,-3.01574600312155,126.916642196978));
#42200=CARTESIAN_POINT('Ctrl Pts',(116.355745042211,-3.12613759040226,127.004834978786));
#42201=CARTESIAN_POINT('Ctrl Pts',(116.347763682943,-3.23258342274687,127.097665664177));
#42202=CARTESIAN_POINT('Ctrl Pts',(116.340016127709,-3.33591105628094,127.187776989623));
#42203=CARTESIAN_POINT('Ctrl Pts',(116.332268572475,-3.43552055662054,127.282258021064));
#42204=CARTESIAN_POINT('Ctrl Pts',(116.324521017241,-3.53102885228761,127.380763341774));
#42205=CARTESIAN_POINT('Ctrl Pts',(116.316775138562,-3.62651648016286,127.479247346142));
#42206=CARTESIAN_POINT('Ctrl Pts',(116.309029259882,-3.71790439738277,127.58175362649));
#42207=CARTESIAN_POINT('Ctrl Pts',(116.301283381203,-3.80484618139089,127.687899708385));
#42208=CARTESIAN_POINT('Ctrl Pts',(116.293537501295,-3.89178797918496,127.79404580711));
#42209=CARTESIAN_POINT('Ctrl Pts',(116.285791621387,-3.97428339523463,127.903831405719));
#42210=CARTESIAN_POINT('Ctrl Pts',(116.27804574148,-4.05202637596742,128.01684105513));
#42211=CARTESIAN_POINT('Ctrl Pts',(116.270298182938,-4.12978620462031,128.129875195208));
#42212=CARTESIAN_POINT('Ctrl Pts',(116.262550624397,-4.20279132786444,128.246134453958));
#42213=CARTESIAN_POINT('Ctrl Pts',(116.254803065856,-4.27077931482062,128.365174870928));
#42214=CARTESIAN_POINT('Ctrl Pts',(116.247048651461,-4.33882746469416,128.484320627373));
#42215=CARTESIAN_POINT('Ctrl Pts',(116.239294237065,-4.40184942114921,128.606252115559));
#42216=CARTESIAN_POINT('Ctrl Pts',(116.23153982267,-4.45962884239706,128.730501015143));
#42217=CARTESIAN_POINT('Ctrl Pts',(116.223781267413,-4.51743911788667,128.854816263707));
#42218=CARTESIAN_POINT('Ctrl Pts',(116.216022712156,-4.57000113067515,128.981451028912));
#42219=CARTESIAN_POINT('Ctrl Pts',(116.208264156899,-4.61714726400384,129.109918466001));
#42220=CARTESIAN_POINT('Ctrl Pts',(116.20049639022,-4.66434937205099,129.238538427339));
#42221=CARTESIAN_POINT('Ctrl Pts',(116.192728623541,-4.7061226463963,129.368995032754));
#42222=CARTESIAN_POINT('Ctrl Pts',(116.184960856862,-4.74234966060826,129.500787543654));
#42223=CARTESIAN_POINT('Ctrl Pts',(116.183358950682,-4.74982056960365,129.52796642871));
#42224=CARTESIAN_POINT('Ctrl Pts',(116.181757044501,-4.75705577794431,129.555202098149));
#42225=CARTESIAN_POINT('Ctrl Pts',(116.180155138321,-4.76405452823404,129.582490119308));
#42226=CARTESIAN_POINT('Origin',(213.235140564004,0.,130.804360617566));
#42227=CARTESIAN_POINT('',(114.08491538754,-4.76405452823405,129.582490119308));
#42228=CARTESIAN_POINT('',(114.429855701321,-4.76405452823407,129.582490119308));
#42229=CARTESIAN_POINT('',(213.235140564004,-4.76405452823405,129.582490119308));
#42230=CARTESIAN_POINT('',(115.76485943597,-4.91824999995734,130.80438110132));
#42231=CARTESIAN_POINT('Ctrl Pts',(115.764859435949,-4.91824999995734,130.80438110169));
#42232=CARTESIAN_POINT('Ctrl Pts',(115.756742290709,-4.91824939965866,130.948513163258));
#42233=CARTESIAN_POINT('Ctrl Pts',(115.748625145469,-4.91190868767493,131.092521964845));
#42234=CARTESIAN_POINT('Ctrl Pts',(115.740508000229,-4.89928608984441,131.235845115963));
#42235=CARTESIAN_POINT('Ctrl Pts',(115.732380078311,-4.88664673369991,131.379358549177));
#42236=CARTESIAN_POINT('Ctrl Pts',(115.724252156393,-4.8677088783086,131.522184184355));
#42237=CARTESIAN_POINT('Ctrl Pts',(115.716124234475,-4.84258216027101,131.663768020097));
#42238=CARTESIAN_POINT('Ctrl Pts',(115.707977022248,-4.81739580802846,131.805687882194));
#42239=CARTESIAN_POINT('Ctrl Pts',(115.69982981002,-4.785991283619,131.946359723495));
#42240=CARTESIAN_POINT('Ctrl Pts',(115.691682597793,-4.74852905514042,132.085241125259));
#42241=CARTESIAN_POINT('Ctrl Pts',(115.683525192704,-4.7110199581972,132.224296279582));
#42242=CARTESIAN_POINT('Ctrl Pts',(115.675367787615,-4.66743813284541,132.361556207261));
#42243=CARTESIAN_POINT('Ctrl Pts',(115.667210382525,-4.61799291307658,132.496496698759));
#42244=CARTESIAN_POINT('Ctrl Pts',(115.659034265724,-4.56843427431116,132.631746720991));
#42245=CARTESIAN_POINT('Ctrl Pts',(115.650858148923,-4.51298547576976,132.764666360837));
#42246=CARTESIAN_POINT('Ctrl Pts',(115.642682032122,-4.45190345035901,132.894752621756));
#42247=CARTESIAN_POINT('Ctrl Pts',(115.637069529278,-4.40997363823737,132.984050454355));
#42248=CARTESIAN_POINT('Ctrl Pts',(115.631457026434,-4.36539032889249,133.072013675603));
#42249=CARTESIAN_POINT('Ctrl Pts',(115.62584452359,-4.31824851471123,133.158487382992));
#42250=CARTESIAN_POINT('Ctrl Pts',(115.618070189471,-4.25294855414198,133.278269147458));
#42251=CARTESIAN_POINT('Ctrl Pts',(115.610295855351,-4.18255753523278,133.395521593527));
#42252=CARTESIAN_POINT('Ctrl Pts',(115.602521521232,-4.10729593727613,133.509781683895));
#42253=CARTESIAN_POINT('Ctrl Pts',(115.594756768285,-4.0321270925127,133.623900958912));
#42254=CARTESIAN_POINT('Ctrl Pts',(115.586992015338,-3.95209982499075,133.735034892506));
#42255=CARTESIAN_POINT('Ctrl Pts',(115.579227262391,-3.86748085213096,133.842744220882));
#42256=CARTESIAN_POINT('Ctrl Pts',(115.571470221506,-3.78294592402805,133.950346570835));
#42257=CARTESIAN_POINT('Ctrl Pts',(115.563713180621,-3.69382860624714,134.054530778995));
#42258=CARTESIAN_POINT('Ctrl Pts',(115.555956139736,-3.60043913101427,134.154886117597));
#42259=CARTESIAN_POINT('Ctrl Pts',(115.548204948496,-3.50712008151108,134.255165777459));
#42260=CARTESIAN_POINT('Ctrl Pts',(115.540453757256,-3.40953555235383,134.351622029868));
#42261=CARTESIAN_POINT('Ctrl Pts',(115.532702566016,-3.30803607103304,134.443877126011));
#42262=CARTESIAN_POINT('Ctrl Pts',(115.524954669239,-3.20657972969932,134.536093011277));
#42263=CARTESIAN_POINT('Ctrl Pts',(115.517206772462,-3.10121203439929,134.624111029292));
#42264=CARTESIAN_POINT('Ctrl Pts',(115.509458875685,-2.99232023594627,134.70759039149));
#42265=CARTESIAN_POINT('Ctrl Pts',(115.5017125996,-2.88345121530997,134.791052291605));
#42266=CARTESIAN_POINT('Ctrl Pts',(115.493966323516,-2.77105986786696,134.869977186573));
#42267=CARTESIAN_POINT('Ctrl Pts',(115.486220047432,-2.65556606435359,134.94406494763));
#42268=CARTESIAN_POINT('Ctrl Pts',(115.478473714167,-2.54007140829127,135.018153255587));
#42269=CARTESIAN_POINT('Ctrl Pts',(115.470727380902,-2.42147457953653,135.087404147284));
#42270=CARTESIAN_POINT('Ctrl Pts',(115.462981047636,-2.30022358714223,135.151561384917));
#42271=CARTESIAN_POINT('Ctrl Pts',(115.455232979633,-2.17894544142913,135.215732990118));
#42272=CARTESIAN_POINT('Ctrl Pts',(115.44748491163,-2.05501229483079,135.274808488602));
#42273=CARTESIAN_POINT('Ctrl Pts',(115.439736843627,-1.92889548807974,135.328578258061));
#42274=CARTESIAN_POINT('Ctrl Pts',(115.431980540886,-1.8026446428854,135.382405174671));
#42275=CARTESIAN_POINT('Ctrl Pts',(115.424224238144,-1.67420586166634,135.430914944186));
#42276=CARTESIAN_POINT('Ctrl Pts',(115.416467935402,-1.54406966175244,135.473946460246));
#42277=CARTESIAN_POINT('Ctrl Pts',(115.408707492888,-1.41386400423032,135.517000943522));
#42278=CARTESIAN_POINT('Ctrl Pts',(115.400947050374,-1.28195949863064,135.55457124016));
#42279=CARTESIAN_POINT('Ctrl Pts',(115.393186607859,-1.14885948206551,135.586546828178));
#42280=CARTESIAN_POINT('Ctrl Pts',(115.385413707594,-1.01554580153763,135.618573746248));
#42281=CARTESIAN_POINT('Ctrl Pts',(115.377640807328,-0.881033158849612,
135.644987933173));
#42282=CARTESIAN_POINT('Ctrl Pts',(115.369867907063,-0.745833577909087,
135.665730315147));
#42283=CARTESIAN_POINT('Ctrl Pts',(115.362377571301,-0.615548842282759,
135.68571865929));
#42284=CARTESIAN_POINT('Ctrl Pts',(115.354887235539,-0.484626551266065,
135.700440373528));
#42285=CARTESIAN_POINT('Ctrl Pts',(115.347396899777,-0.353525281199007,
135.709888411601));
#42286=CARTESIAN_POINT('Ctrl Pts',(115.339622565658,-0.217453266630271,
135.719694674909));
#42287=CARTESIAN_POINT('Ctrl Pts',(115.331848231539,-0.0807573978733542,
135.723850528275));
#42288=CARTESIAN_POINT('Ctrl Pts',(115.32407389742,0.0560535842287742,135.722291184196));
#42289=CARTESIAN_POINT('Ctrl Pts',(115.316309144473,0.192695959022425,135.72073376187));
#42290=CARTESIAN_POINT('Ctrl Pts',(115.308544391526,0.329452777701594,135.713475160918));
#42291=CARTESIAN_POINT('Ctrl Pts',(115.300779638578,0.465810307915003,135.700502345451));
#42292=CARTESIAN_POINT('Ctrl Pts',(115.293022597693,0.602032405907284,135.687542414768));
#42293=CARTESIAN_POINT('Ctrl Pts',(115.285265556808,0.737855617954568,135.668879600736));
#42294=CARTESIAN_POINT('Ctrl Pts',(115.277508515923,0.8727666990604,135.644552902126));
#42295=CARTESIAN_POINT('Ctrl Pts',(115.269757324683,1.00757604267033,135.620244548468));
#42296=CARTESIAN_POINT('Ctrl Pts',(115.262006133443,1.14147424124929,135.590280880853));
#42297=CARTESIAN_POINT('Ctrl Pts',(115.254254942203,1.27395401535093,135.554752625524));
#42298=CARTESIAN_POINT('Ctrl Pts',(115.246507045426,1.40637748201465,135.519239470652));
#42299=CARTESIAN_POINT('Ctrl Pts',(115.238759148649,1.53738334642888,135.478166533124));
#42300=CARTESIAN_POINT('Ctrl Pts',(115.231011251872,1.66647557499834,135.431675413475));
#42301=CARTESIAN_POINT('Ctrl Pts',(115.223264975788,1.7955408002565,135.385194018765));
#42302=CARTESIAN_POINT('Ctrl Pts',(115.215518699704,1.92269281826643,135.333296828651));
#42303=CARTESIAN_POINT('Ctrl Pts',(115.20777242362,2.04745217181012,135.276174865346));
#42304=CARTESIAN_POINT('Ctrl Pts',(115.200026090354,2.17221244629894,135.21905248038));
#42305=CARTESIAN_POINT('Ctrl Pts',(115.192279757089,2.29457966560127,135.156705408022));
#42306=CARTESIAN_POINT('Ctrl Pts',(115.184533423824,2.41409608975856,135.089372068182));
#42307=CARTESIAN_POINT('Ctrl Pts',(115.176785355821,2.53363927879037,135.022023649508));
#42308=CARTESIAN_POINT('Ctrl Pts',(115.169037287818,2.65033006174147,134.949686933236));
#42309=CARTESIAN_POINT('Ctrl Pts',(115.161289219815,2.76373730624994,134.872645165695));
#42310=CARTESIAN_POINT('Ctrl Pts',(115.153532917073,2.87726508132752,134.795521517246));
#42311=CARTESIAN_POINT('Ctrl Pts',(115.145776614331,2.98750202282875,134.713683048371));
#42312=CARTESIAN_POINT('Ctrl Pts',(115.138020311589,3.09404745081275,134.627455363269));
#42313=CARTESIAN_POINT('Ctrl Pts',(115.130259869075,3.20064974529975,134.541181655854));
#42314=CARTESIAN_POINT('Ctrl Pts',(115.122499426561,3.30355630713151,134.450514322602));
#42315=CARTESIAN_POINT('Ctrl Pts',(115.114738984047,3.40240208502859,134.355817095448));
#42316=CARTESIAN_POINT('Ctrl Pts',(115.106966083781,3.50140653894346,134.260967851899));
#42317=CARTESIAN_POINT('Ctrl Pts',(115.099193183516,3.59633691151905,134.162076069245));
#42318=CARTESIAN_POINT('Ctrl Pts',(115.09142028325,3.68686674086039,134.059540596866));
#42319=CARTESIAN_POINT('Ctrl Pts',(115.083929947488,3.77410558287503,133.960732547179));
#42320=CARTESIAN_POINT('Ctrl Pts',(115.076439611726,3.85725807425426,133.858541361978));
#42321=CARTESIAN_POINT('Ctrl Pts',(115.068949275964,3.93607041506568,133.753349045849));
#42322=CARTESIAN_POINT('Ctrl Pts',(115.061174941845,4.01787094973278,133.644168331082));
#42323=CARTESIAN_POINT('Ctrl Pts',(115.053400607726,4.09525484291431,133.531408565524));
#42324=CARTESIAN_POINT('Ctrl Pts',(115.045626273607,4.16789260019818,133.41546274803));
#42325=CARTESIAN_POINT('Ctrl Pts',(115.03786152066,4.24044083793802,133.299659823393));
#42326=CARTESIAN_POINT('Ctrl Pts',(115.030096767713,4.30825437235047,133.180678987568));
#42327=CARTESIAN_POINT('Ctrl Pts',(115.022332014765,4.37104455108726,133.058945411915));
#42328=CARTESIAN_POINT('Ctrl Pts',(115.01457497388,4.43377236573335,132.937332743766));
#42329=CARTESIAN_POINT('Ctrl Pts',(115.006817932995,4.49148657550821,132.812973121908));
#42330=CARTESIAN_POINT('Ctrl Pts',(114.99906089211,4.54394256972332,132.686319433682));
#42331=CARTESIAN_POINT('Ctrl Pts',(114.99130970087,4.59635900646514,132.559761255987));
#42332=CARTESIAN_POINT('Ctrl Pts',(114.98355850963,4.64352497126251,132.430912815079));
#42333=CARTESIAN_POINT('Ctrl Pts',(114.97580731839,4.68524259774243,132.300249939274));
#42334=CARTESIAN_POINT('Ctrl Pts',(114.968059421613,4.72694249311824,132.169642598677));
#42335=CARTESIAN_POINT('Ctrl Pts',(114.960311524836,4.76319853724232,132.03722272867));
#42336=CARTESIAN_POINT('Ctrl Pts',(114.952563628059,4.7938617443789,131.903484194913));
#42337=CARTESIAN_POINT('Ctrl Pts',(114.944817351975,4.82451853743356,131.769773636375));
#42338=CARTESIAN_POINT('Ctrl Pts',(114.937071075891,4.84958473318081,131.634745343574));
#42339=CARTESIAN_POINT('Ctrl Pts',(114.929324799806,4.86896188568153,131.498905949622));
#42340=CARTESIAN_POINT('Ctrl Pts',(114.921578466541,4.88833918121999,131.363065552934));
#42341=CARTESIAN_POINT('Ctrl Pts',(114.913832133276,4.90202729450218,131.226414430193));
#42342=CARTESIAN_POINT('Ctrl Pts',(114.90608580001,4.90997939532392,131.089466562777));
#42343=CARTESIAN_POINT('Ctrl Pts',(114.898337732007,4.91793327696351,130.952488026835));
#42344=CARTESIAN_POINT('Ctrl Pts',(114.890589664004,4.92014856739681,130.815213004216));
#42345=CARTESIAN_POINT('Ctrl Pts',(114.882841596001,4.91663053221111,130.678157320345));
#42346=CARTESIAN_POINT('Ctrl Pts',(114.87508529326,4.91310875801575,130.540955972062));
#42347=CARTESIAN_POINT('Ctrl Pts',(114.867328990518,4.90384149593349,130.403974819662));
#42348=CARTESIAN_POINT('Ctrl Pts',(114.859572687776,4.88888610870378,130.267726963549));
#42349=CARTESIAN_POINT('Ctrl Pts',(114.851812245262,4.8739227393336,130.131406387854));
#42350=CARTESIAN_POINT('Ctrl Pts',(114.844051802748,4.85326525433895,129.995820274624));
#42351=CARTESIAN_POINT('Ctrl Pts',(114.836291360233,4.82702235256512,129.861472357836));
#42352=CARTESIAN_POINT('Ctrl Pts',(114.828518459968,4.80073732335564,129.726908773845));
#42353=CARTESIAN_POINT('Ctrl Pts',(114.820745559703,4.76884905102829,129.593587738739));
#42354=CARTESIAN_POINT('Ctrl Pts',(114.812972659437,4.73151663823373,129.461999501987));
#42355=CARTESIAN_POINT('Ctrl Pts',(114.805482323675,4.695541352679,129.335194829093));
#42356=CARTESIAN_POINT('Ctrl Pts',(114.797991987913,4.65451096706779,129.209999451336));
#42357=CARTESIAN_POINT('Ctrl Pts',(114.790501652151,4.60860968761438,129.086833380598));
#42358=CARTESIAN_POINT('Ctrl Pts',(114.782727318032,4.56096804719903,128.958997430852));
#42359=CARTESIAN_POINT('Ctrl Pts',(114.774952983913,4.50792794738468,128.832942762299));
#42360=CARTESIAN_POINT('Ctrl Pts',(114.767178649794,4.44964192945812,128.709159013398));
#42361=CARTESIAN_POINT('Ctrl Pts',(114.759413896847,4.39142774383952,128.585527816905));
#42362=CARTESIAN_POINT('Ctrl Pts',(114.7516491439,4.32798066873539,128.464162321793));
#42363=CARTESIAN_POINT('Ctrl Pts',(114.743884390952,4.25950238920709,128.345535194963));
#42364=CARTESIAN_POINT('Ctrl Pts',(114.736127350067,4.19109212327139,128.227025890268));
#42365=CARTESIAN_POINT('Ctrl Pts',(114.728370309182,4.11766079148668,128.111249877766));
#42366=CARTESIAN_POINT('Ctrl Pts',(114.720613268297,4.03945720274524,127.998657752028));
#42367=CARTESIAN_POINT('Ctrl Pts',(114.712862077057,3.96131258793835,127.886150532887));
#42368=CARTESIAN_POINT('Ctrl Pts',(114.705110885817,3.87840310149067,127.776822741284));
#42369=CARTESIAN_POINT('Ctrl Pts',(114.697359694577,3.79102211963303,127.671098044631));
#42370=CARTESIAN_POINT('Ctrl Pts',(114.6896117978,3.70367827702366,127.565418283795));
#42371=CARTESIAN_POINT('Ctrl Pts',(114.681863901023,3.61186696751373,127.463338872775));
#42372=CARTESIAN_POINT('Ctrl Pts',(114.674116004246,3.51592316383981,127.365252103943));
#42373=CARTESIAN_POINT('Ctrl Pts',(114.666369728162,3.41999942954131,127.267185852748));
#42374=CARTESIAN_POINT('Ctrl Pts',(114.658623452078,3.31994519368586,127.173110861847));
#42375=CARTESIAN_POINT('Ctrl Pts',(114.650877175994,3.21613348862195,127.083383804165));
#42376=CARTESIAN_POINT('Ctrl Pts',(114.643130842728,3.11232101724375,126.993656084139));
#42377=CARTESIAN_POINT('Ctrl Pts',(114.635384509463,3.00475131710103,126.908276617037));
#42378=CARTESIAN_POINT('Ctrl Pts',(114.627638176197,2.89383150241384,126.827562621925));
#42379=CARTESIAN_POINT('Ctrl Pts',(114.619890108195,2.78288684800306,126.746830551472));
#42380=CARTESIAN_POINT('Ctrl Pts',(114.612142040192,2.66859090223326,126.670766262036));
#42381=CARTESIAN_POINT('Ctrl Pts',(114.604393972189,2.55138048982342,126.59964413977));
#42382=CARTESIAN_POINT('Ctrl Pts',(114.596637669447,2.43404550479245,126.528446428066));
#42383=CARTESIAN_POINT('Ctrl Pts',(114.588881366705,2.3137902002494,126.462201579296));
#42384=CARTESIAN_POINT('Ctrl Pts',(114.581125063963,2.19107726805885,126.401138675863));
#42385=CARTESIAN_POINT('Ctrl Pts',(114.573364621449,2.06829884028149,126.34004318132));
#42386=CARTESIAN_POINT('Ctrl Pts',(114.565604178935,1.94306052799632,126.284135302421));
#42387=CARTESIAN_POINT('Ctrl Pts',(114.557843736421,1.81584489124477,126.233595868266));
#42388=CARTESIAN_POINT('Ctrl Pts',(114.550070836155,1.68842503665952,126.182975303726));
#42389=CARTESIAN_POINT('Ctrl Pts',(114.54229793589,1.55902188386952,126.137740534335));
#42390=CARTESIAN_POINT('Ctrl Pts',(114.534525035624,1.42813389250766,126.098022694343));
#42391=CARTESIAN_POINT('Ctrl Pts',(114.527034699862,1.30200400931841,126.059748697877));
#42392=CARTESIAN_POINT('Ctrl Pts',(114.5195443641,1.17449566664806,126.026597563588));
#42393=CARTESIAN_POINT('Ctrl Pts',(114.512054028338,1.04606180034561,125.998641340251));
#42394=CARTESIAN_POINT('Ctrl Pts',(114.504279694219,0.912758324965945,125.969625148209));
#42395=CARTESIAN_POINT('Ctrl Pts',(114.4965053601,0.778035492732118,125.946113658947));
#42396=CARTESIAN_POINT('Ctrl Pts',(114.488731025981,0.64238770263931,125.928243196708));
#42397=CARTESIAN_POINT('Ctrl Pts',(114.480966273034,0.506907086324599,125.910394758216));
#42398=CARTESIAN_POINT('Ctrl Pts',(114.473201520087,0.37050416416255,125.89817356479));
#42399=CARTESIAN_POINT('Ctrl Pts',(114.46543676714,0.233685619905608,125.891665421083));
#42400=CARTESIAN_POINT('Ctrl Pts',(114.457679726255,0.0970029657557192,
125.885163741355));
#42401=CARTESIAN_POINT('Ctrl Pts',(114.44992268537,-0.0400941009984268,
125.884363837726));
#42402=CARTESIAN_POINT('Ctrl Pts',(114.442165644485,-0.177091995100775,
125.889299937598));
#42403=CARTESIAN_POINT('Ctrl Pts',(114.434414453245,-0.313986578025586,
125.894232315118));
#42404=CARTESIAN_POINT('Ctrl Pts',(114.426663262005,-0.45078174802656,125.904892072344));
#42405=CARTESIAN_POINT('Ctrl Pts',(114.418912070764,-0.586962484692938,
125.921261386129));
#42406=CARTESIAN_POINT('Ctrl Pts',(114.411164173987,-0.723085340913494,
125.937623742518));
#42407=CARTESIAN_POINT('Ctrl Pts',(114.40341627721,-0.858593895849701,125.959690782356));
#42408=CARTESIAN_POINT('Ctrl Pts',(114.395668380433,-0.992977041873242,
125.9873927272));
#42409=CARTESIAN_POINT('Ctrl Pts',(114.387922104349,-1.1273320778396,126.015088877395));
#42410=CARTESIAN_POINT('Ctrl Pts',(114.380175828265,-1.26056179046783,126.048417509212));
#42411=CARTESIAN_POINT('Ctrl Pts',(114.372429552181,-1.39216446762645,126.0872575704));
#42412=CARTESIAN_POINT('Ctrl Pts',(114.364683218916,-1.52376811624605,126.126097918298));
#42413=CARTESIAN_POINT('Ctrl Pts',(114.35693688565,-1.65374433045467,126.170449666082));
#42414=CARTESIAN_POINT('Ctrl Pts',(114.349190552385,-1.78160616968763,126.220141761683));
#42415=CARTESIAN_POINT('Ctrl Pts',(114.341442484382,-1.90949664269312,126.269844985485));
#42416=CARTESIAN_POINT('Ctrl Pts',(114.333694416379,-2.03527143417113,126.324890795277));
#42417=CARTESIAN_POINT('Ctrl Pts',(114.325946348376,-2.1584635808476,126.38505999047));
#42418=CARTESIAN_POINT('Ctrl Pts',(114.318190045634,-2.28178665760349,126.445293134199));
#42419=CARTESIAN_POINT('Ctrl Pts',(114.310433742892,-2.40252125453057,126.510660368837));
#42420=CARTESIAN_POINT('Ctrl Pts',(114.30267744015,-2.52022454185894,126.580896243251));
#42421=CARTESIAN_POINT('Ctrl Pts',(114.294916997636,-2.63799065097566,126.651169604664));
#42422=CARTESIAN_POINT('Ctrl Pts',(114.287156555122,-2.7527218997929,126.726316569552));
#42423=CARTESIAN_POINT('Ctrl Pts',(114.279396112608,-2.86400531617679,126.806028889031));
#42424=CARTESIAN_POINT('Ctrl Pts',(114.271623212343,-2.97546737458009,126.885869169801));
#42425=CARTESIAN_POINT('Ctrl Pts',(114.263850312077,-3.08347023211437,126.970289209355));
#42426=CARTESIAN_POINT('Ctrl Pts',(114.256077411812,-3.187634132216,127.05894052075));
#42427=CARTESIAN_POINT('Ctrl Pts',(114.24858707605,-3.28801141217507,127.144369133676));
#42428=CARTESIAN_POINT('Ctrl Pts',(114.241096740288,-3.38482377411824,127.233726515743));
#42429=CARTESIAN_POINT('Ctrl Pts',(114.233606404526,-3.47776577847991,127.326670543316));
#42430=CARTESIAN_POINT('Ctrl Pts',(114.225941058105,-3.57287935991102,127.421786195231));
#42431=CARTESIAN_POINT('Ctrl Pts',(114.218275711685,-3.66425891122612,127.520977943977));
#42432=CARTESIAN_POINT('Ctrl Pts',(114.210610365264,-3.75152731893948,127.62391633449));
#42433=CARTESIAN_POINT('Ctrl Pts',(114.202953988676,-3.83869360693815,127.726734268594));
#42434=CARTESIAN_POINT('Ctrl Pts',(114.195297612088,-3.921758057678,127.833289824629));
#42435=CARTESIAN_POINT('Ctrl Pts',(114.1876412355,-4.00037885486759,127.943215378326));
#42436=CARTESIAN_POINT('Ctrl Pts',(114.179992048955,-4.07892581988254,128.053037701796));
#42437=CARTESIAN_POINT('Ctrl Pts',(114.172342862411,-4.1530371968604,128.166223404336));
#42438=CARTESIAN_POINT('Ctrl Pts',(114.164693675866,-4.22241045974782,128.282370734178));
#42439=CARTESIAN_POINT('Ctrl Pts',(114.157050220695,-4.29173174271236,128.398431037274));
#42440=CARTESIAN_POINT('Ctrl Pts',(114.149406765524,-4.35632177014896,128.517448207599));
#42441=CARTESIAN_POINT('Ctrl Pts',(114.141763310354,-4.41592085388093,128.638990885913));
#42442=CARTESIAN_POINT('Ctrl Pts',(114.134123186136,-4.47549396483498,128.760480596953));
#42443=CARTESIAN_POINT('Ctrl Pts',(114.126483061919,-4.53008028209918,128.884493265514));
#42444=CARTESIAN_POINT('Ctrl Pts',(114.118842937702,-4.57946588518187,129.010572651012));
#42445=CARTESIAN_POINT('Ctrl Pts',(114.111203491232,-4.62884710732094,129.136640852143));
#42446=CARTESIAN_POINT('Ctrl Pts',(114.103564044761,-4.67302838144765,129.264775032536));
#42447=CARTESIAN_POINT('Ctrl Pts',(114.095924598291,-4.71184394696733,129.394499035024));
#42448=CARTESIAN_POINT('Ctrl Pts',(114.092254861374,-4.73048965831579,129.456814146835));
#42449=CARTESIAN_POINT('Ctrl Pts',(114.088585124457,-4.74789794643968,129.519495852102));
#42450=CARTESIAN_POINT('Ctrl Pts',(114.08491538754,-4.76405452823405,129.582490119308));
#42451=CARTESIAN_POINT('Ctrl Pts',(115.834581344104,-4.76405452823405,129.582490119308));
#42452=CARTESIAN_POINT('Ctrl Pts',(115.826451019897,-4.7997288353145,129.721583701182));
#42453=CARTESIAN_POINT('Ctrl Pts',(115.81832069569,-4.82934431273923,129.862384632814));
#42454=CARTESIAN_POINT('Ctrl Pts',(115.810190371483,-4.85274845500096,130.004350933258));
#42455=CARTESIAN_POINT('Ctrl Pts',(115.802074958176,-4.87610967439746,130.14605686952));
#42456=CARTESIAN_POINT('Ctrl Pts',(115.793959544868,-4.89328222023574,130.288923585756));
#42457=CARTESIAN_POINT('Ctrl Pts',(115.78584413156,-4.9041641939585,130.432397418855));
#42458=CARTESIAN_POINT('Ctrl Pts',(115.778849233037,-4.91354366719489,130.556061472082));
#42459=CARTESIAN_POINT('Ctrl Pts',(115.771854334514,-4.91825051724227,130.680176209359));
#42460=CARTESIAN_POINT('Ctrl Pts',(115.764859435991,-4.91824999995734,130.804381100951));
#42461=CARTESIAN_POINT('',(116.110140563973,-4.91824810509851,130.800043304177));
#42462=CARTESIAN_POINT('Ctrl Pts',(116.180155138321,-4.76405452823404,129.582490119308));
#42463=CARTESIAN_POINT('Ctrl Pts',(116.174487017233,-4.78881862777827,129.679044967583));
#42464=CARTESIAN_POINT('Ctrl Pts',(116.168818896145,-4.8106211484576,129.77625532962));
#42465=CARTESIAN_POINT('Ctrl Pts',(116.163150775057,-4.82943794779455,129.873924069003));
#42466=CARTESIAN_POINT('Ctrl Pts',(116.151699131444,-4.86745465149391,130.071250057303));
#42467=CARTESIAN_POINT('Ctrl Pts',(116.140247487831,-4.89338666919524,130.270973357238));
#42468=CARTESIAN_POINT('Ctrl Pts',(116.128795844218,-4.90699959386499,130.471887989657));
#42469=CARTESIAN_POINT('Ctrl Pts',(116.122577417482,-4.91439163099023,130.580987867742));
#42470=CARTESIAN_POINT('Ctrl Pts',(116.116358990745,-4.91815189245368,130.690438661909));
#42471=CARTESIAN_POINT('Ctrl Pts',(116.110140564008,-4.91824810509796,130.800043303551));
#42472=CARTESIAN_POINT('Ctrl Pts',(116.110140563973,-4.91824810509851,130.800043304177));
#42473=CARTESIAN_POINT('Ctrl Pts',(116.102493663682,-4.9183664193317,130.934825911027));
#42474=CARTESIAN_POINT('Ctrl Pts',(116.094846763391,-4.91294007719472,131.069795177394));
#42475=CARTESIAN_POINT('Ctrl Pts',(116.0871998631,-4.90194978904778,131.204449767824));
#42476=CARTESIAN_POINT('Ctrl Pts',(116.079559620593,-4.89096906960994,131.338987121055));
#42477=CARTESIAN_POINT('Ctrl Pts',(116.071919378086,-4.87443407244818,131.473209943396));
#42478=CARTESIAN_POINT('Ctrl Pts',(116.064279135579,-4.85237756615036,131.606616822292));
#42479=CARTESIAN_POINT('Ctrl Pts',(116.056643173303,-4.8303334163909,131.739948963729));
#42480=CARTESIAN_POINT('Ctrl Pts',(116.049007211028,-4.80277397434707,131.872465673803));
#42481=CARTESIAN_POINT('Ctrl Pts',(116.041371248752,-4.76978380949576,132.003671033252));
#42482=CARTESIAN_POINT('Ctrl Pts',(116.033737459343,-4.7368030322277,132.134839057293));
#42483=CARTESIAN_POINT('Ctrl Pts',(116.026103669934,-4.6983947023943,132.264696081564));
#42484=CARTESIAN_POINT('Ctrl Pts',(116.018469880525,-4.65469432108969,132.392757243008));
#42485=CARTESIAN_POINT('Ctrl Pts',(116.010836497449,-4.61099626587797,132.520811587986));
#42486=CARTESIAN_POINT('Ctrl Pts',(116.003203114373,-4.56200684971436,132.647069878375));
#42487=CARTESIAN_POINT('Ctrl Pts',(115.995569731297,-4.50791100562389,132.771063805105));
#42488=CARTESIAN_POINT('Ctrl Pts',(115.987934988556,-4.45380552593009,132.89507981775));
#42489=CARTESIAN_POINT('Ctrl Pts',(115.980300245814,-4.39459197150539,133.016830295155));
#42490=CARTESIAN_POINT('Ctrl Pts',(115.972665503073,-4.33050259955188,133.135868777057));
#42491=CARTESIAN_POINT('Ctrl Pts',(115.96502306968,-4.26634866891172,133.255027169138));
#42492=CARTESIAN_POINT('Ctrl Pts',(115.957380636288,-4.19730930403953,133.371467754463));
#42493=CARTESIAN_POINT('Ctrl Pts',(115.949738202896,-4.12366190715808,133.484770201557));
#42494=CARTESIAN_POINT('Ctrl Pts',(115.942091798843,-4.04997624643288,133.598131515459));
#42495=CARTESIAN_POINT('Ctrl Pts',(115.934445394789,-3.97167802053146,133.708351116492));
#42496=CARTESIAN_POINT('Ctrl Pts',(115.926798990736,-3.88908601119759,133.815040451093));
#42497=CARTESIAN_POINT('Ctrl Pts',(115.919140753492,-3.80636618662677,133.921894892739));
#42498=CARTESIAN_POINT('Ctrl Pts',(115.911482516249,-3.71933956651517,134.025207847914));
#42499=CARTESIAN_POINT('Ctrl Pts',(115.903824279005,-3.62836339690442,134.124625986856));
#42500=CARTESIAN_POINT('Ctrl Pts',(115.897450569751,-3.55264680107667,134.207368567428));
#42501=CARTESIAN_POINT('Ctrl Pts',(115.891076860498,-3.47419521953665,134.287413918513));
#42502=CARTESIAN_POINT('Ctrl Pts',(115.884703151244,-3.39323179600188,134.364579858161));
#42503=CARTESIAN_POINT('Ctrl Pts',(115.876928817125,-3.29447663147852,134.458703040368));
#42504=CARTESIAN_POINT('Ctrl Pts',(115.869154483006,-3.19164582316973,134.548863211813));
#42505=CARTESIAN_POINT('Ctrl Pts',(115.861380148886,-3.08509070302833,134.634686767725));
#42506=CARTESIAN_POINT('Ctrl Pts',(115.853615395939,-2.97866690254939,134.720404553774));
#42507=CARTESIAN_POINT('Ctrl Pts',(115.845850642992,-2.8685282242941,134.801796115346));
#42508=CARTESIAN_POINT('Ctrl Pts',(115.838085890045,-2.75506277134103,134.878524604014));
#42509=CARTESIAN_POINT('Ctrl Pts',(115.83032884916,-2.64171001387542,134.955176884865));
#42510=CARTESIAN_POINT('Ctrl Pts',(115.822571808275,-2.52503737898898,135.027175091975));
#42511=CARTESIAN_POINT('Ctrl Pts',(115.81481476739,-2.40546569345085,135.094222836814));
#42512=CARTESIAN_POINT('Ctrl Pts',(115.80706357615,-2.28598417785108,135.161220020427));
#42513=CARTESIAN_POINT('Ctrl Pts',(115.79931238491,-2.16360830272458,135.223273981998));
#42514=CARTESIAN_POINT('Ctrl Pts',(115.79156119367,-2.03878719615887,135.280132040603));
#42515=CARTESIAN_POINT('Ctrl Pts',(115.783813296893,-1.91401914189283,135.336965933018));
#42516=CARTESIAN_POINT('Ctrl Pts',(115.776065400116,-1.78680827829982,135.388608153071));
#42517=CARTESIAN_POINT('Ctrl Pts',(115.768317503339,-1.65762741779125,135.434852427977));
#42518=CARTESIAN_POINT('Ctrl Pts',(115.760571227254,-1.52847357913397,135.481087029578));
#42519=CARTESIAN_POINT('Ctrl Pts',(115.75282495117,-1.39735093106992,135.521925800256));
#42520=CARTESIAN_POINT('Ctrl Pts',(115.745078675086,-1.26475093328867,135.557211145328));
#42521=CARTESIAN_POINT('Ctrl Pts',(115.737332341821,-1.13214995668436,135.592496750868));
#42522=CARTESIAN_POINT('Ctrl Pts',(115.729586008556,-0.998071986418951,
135.622228748464));
#42523=CARTESIAN_POINT('Ctrl Pts',(115.72183967529,-0.863021875286548,135.646299929998));
#42524=CARTESIAN_POINT('Ctrl Pts',(115.714091607287,-0.727941520618037,
135.670376502107));
#42525=CARTESIAN_POINT('Ctrl Pts',(115.706343539284,-0.59188897670176,135.688789666985));
#42526=CARTESIAN_POINT('Ctrl Pts',(115.698595471281,-0.455377080442616,
135.701483729875));
#42527=CARTESIAN_POINT('Ctrl Pts',(115.690839168539,-0.318720097715708,
135.714191284165));
#42528=CARTESIAN_POINT('Ctrl Pts',(115.683082865798,-0.18160317731009,135.721167558091));
#42529=CARTESIAN_POINT('Ctrl Pts',(115.675326563056,-0.0445426033115799,
135.722408911248));
#42530=CARTESIAN_POINT('Ctrl Pts',(115.667566120542,0.092591124042088,135.723650926953));
#42531=CARTESIAN_POINT('Ctrl Pts',(115.659805678027,0.229668054500501,135.719151935606));
#42532=CARTESIAN_POINT('Ctrl Pts',(115.652045235513,0.366175141605675,135.708960379847));
#42533=CARTESIAN_POINT('Ctrl Pts',(115.644272335248,0.502901362005599,135.698752463699));
#42534=CARTESIAN_POINT('Ctrl Pts',(115.636499434982,0.639055522520417,135.682833767511));
#42535=CARTESIAN_POINT('Ctrl Pts',(115.628726534717,0.774132013685305,135.661304377575));
#42536=CARTESIAN_POINT('Ctrl Pts',(115.621236198955,0.904298134159657,135.640557635192));
#42537=CARTESIAN_POINT('Ctrl Pts',(115.613745863193,1.03346327498792,135.614601103258));
#42538=CARTESIAN_POINT('Ctrl Pts',(115.606255527431,1.16118860772819,135.583568091592));
#42539=CARTESIAN_POINT('Ctrl Pts',(115.598481193312,1.29375668528011,135.551358453856));
#42540=CARTESIAN_POINT('Ctrl Pts',(115.590706859193,1.42519355465844,135.513577757456));
#42541=CARTESIAN_POINT('Ctrl Pts',(115.582932525074,1.55499498808643,135.470319645411));
#42542=CARTESIAN_POINT('Ctrl Pts',(115.575167772127,1.68463645284814,135.427114845122));
#42543=CARTESIAN_POINT('Ctrl Pts',(115.56740301918,1.81264612461156,135.378446182946));
#42544=CARTESIAN_POINT('Ctrl Pts',(115.559638266232,1.93853082406011,135.32445810619));
#42545=CARTESIAN_POINT('Ctrl Pts',(115.551881225347,2.06429049305043,135.270523651154));
#42546=CARTESIAN_POINT('Ctrl Pts',(115.544124184462,2.18792903283064,135.21128044868));
#42547=CARTESIAN_POINT('Ctrl Pts',(115.536367143578,2.30896961618832,135.146922347009));
#42548=CARTESIAN_POINT('Ctrl Pts',(115.528615952337,2.42991892190044,135.082612778282));
#42549=CARTESIAN_POINT('Ctrl Pts',(115.520864761097,2.54827382693229,135.013196170655));
#42550=CARTESIAN_POINT('Ctrl Pts',(115.513113569857,2.66357897896477,134.938913808095));
#42551=CARTESIAN_POINT('Ctrl Pts',(115.50536567308,2.77883512323209,134.864663017521));
#42552=CARTESIAN_POINT('Ctrl Pts',(115.497617776303,2.89104376461658,134.785550796552));
#42553=CARTESIAN_POINT('Ctrl Pts',(115.489869879526,2.99977579332402,134.70186344018));
#42554=CARTESIAN_POINT('Ctrl Pts',(115.482123603442,3.1084850776352,134.6181935894));
#42555=CARTESIAN_POINT('Ctrl Pts',(115.474377327358,3.21371888614757,134.52995074509));
#42556=CARTESIAN_POINT('Ctrl Pts',(115.466631051274,3.31507898402545,134.437463202434));
#42557=CARTESIAN_POINT('Ctrl Pts',(115.458884718008,3.41643983012026,134.344974977055));
#42558=CARTESIAN_POINT('Ctrl Pts',(115.451138384743,3.51392661971633,134.248242254331));
#42559=CARTESIAN_POINT('Ctrl Pts',(115.443392051478,3.60717627032161,134.147631832608));
#42560=CARTESIAN_POINT('Ctrl Pts',(115.435643983475,3.70044680353997,134.046998879878));
#42561=CARTESIAN_POINT('Ctrl Pts',(115.427895915472,3.78947804389538,133.942486786857));
#42562=CARTESIAN_POINT('Ctrl Pts',(115.420147847469,3.87394593293532,133.834496913377));
#42563=CARTESIAN_POINT('Ctrl Pts',(115.412391544727,3.95850359545262,133.726392266976));
#42564=CARTESIAN_POINT('Ctrl Pts',(115.404635241985,4.03848797703091,133.614802764948));
#42565=CARTESIAN_POINT('Ctrl Pts',(115.396878939243,4.11361695073589,133.500160803989));
#42566=CARTESIAN_POINT('Ctrl Pts',(115.389118496729,4.18878602303633,133.385457655164));
#42567=CARTESIAN_POINT('Ctrl Pts',(115.381358054215,4.2590943234009,133.267699136632));
#42568=CARTESIAN_POINT('Ctrl Pts',(115.373597611701,4.32430529385268,133.147343073338));
#42569=CARTESIAN_POINT('Ctrl Pts',(115.365824711435,4.38962094674335,133.026793803808));
#42570=CARTESIAN_POINT('Ctrl Pts',(115.35805181117,4.44982274630815,132.903639008355));
#42571=CARTESIAN_POINT('Ctrl Pts',(115.350278910904,4.50472160371224,132.778358169628));
#42572=CARTESIAN_POINT('Ctrl Pts',(115.342788575142,4.55762474936841,132.657631604951));
#42573=CARTESIAN_POINT('Ctrl Pts',(115.33529823938,4.60560369757696,132.534931174291));
#42574=CARTESIAN_POINT('Ctrl Pts',(115.327807903618,4.64853340817278,132.410698133657));
#42575=CARTESIAN_POINT('Ctrl Pts',(115.320033569499,4.69309081179363,132.281754759529));
#42576=CARTESIAN_POINT('Ctrl Pts',(115.31225923538,4.73234968033078,132.150751809587));
#42577=CARTESIAN_POINT('Ctrl Pts',(115.304484901261,4.76611625087749,132.018164121277));
#42578=CARTESIAN_POINT('Ctrl Pts',(115.296720148314,4.79984120714382,131.885739835444));
#42579=CARTESIAN_POINT('Ctrl Pts',(115.288955395367,4.8280872376851,131.751735072462));
#42580=CARTESIAN_POINT('Ctrl Pts',(115.281190642419,4.85070929464554,131.616642835357));
#42581=CARTESIAN_POINT('Ctrl Pts',(115.273433601534,4.87330888306012,131.481684773766));
#42582=CARTESIAN_POINT('Ctrl Pts',(115.265676560649,4.89029554975478,131.34564177059));
#42583=CARTESIAN_POINT('Ctrl Pts',(115.257919519764,4.9015746479877,131.209019773776));
#42584=CARTESIAN_POINT('Ctrl Pts',(115.250168328524,4.91284524056479,131.072500804673));
#42585=CARTESIAN_POINT('Ctrl Pts',(115.242417137284,4.91841679973631,130.935404099068));
#42586=CARTESIAN_POINT('Ctrl Pts',(115.234665946044,4.91824619548765,130.798243177641));
#42587=CARTESIAN_POINT('Ctrl Pts',(115.226918049267,4.91807566375034,130.661140553263));
#42588=CARTESIAN_POINT('Ctrl Pts',(115.21917015249,4.91216782319093,130.523974157495));
#42589=CARTESIAN_POINT('Ctrl Pts',(115.211422255713,4.90053159757012,130.387259761996));
#42590=CARTESIAN_POINT('Ctrl Pts',(115.203675979629,4.88889780599686,130.250573964202));
#42591=CARTESIAN_POINT('Ctrl Pts',(115.195929703545,4.87153804589188,130.114340367924));
#42592=CARTESIAN_POINT('Ctrl Pts',(115.188183427461,4.84851326563254,129.979071470972));
#42593=CARTESIAN_POINT('Ctrl Pts',(115.180437094195,4.82548831540953,129.843801575497));
#42594=CARTESIAN_POINT('Ctrl Pts',(115.17269076093,4.79679832719209,129.709496778979));
#42595=CARTESIAN_POINT('Ctrl Pts',(115.164944427664,4.76255564386286,129.57666081647));
#42596=CARTESIAN_POINT('Ctrl Pts',(115.157196359661,4.7283052921221,129.443795106269));
#42597=CARTESIAN_POINT('Ctrl Pts',(115.149448291659,4.68849986844778,129.312399263134));
#42598=CARTESIAN_POINT('Ctrl Pts',(115.141700223656,4.64330188672649,129.182962871415));
#42599=CARTESIAN_POINT('Ctrl Pts',(115.133943920914,4.5980558680523,129.053388913159));
#42600=CARTESIAN_POINT('Ctrl Pts',(115.126187618172,4.54740597158711,128.92577893609));
#42601=CARTESIAN_POINT('Ctrl Pts',(115.11843131543,4.4915634884181,128.800604022565));
#42602=CARTESIAN_POINT('Ctrl Pts',(115.110670872916,4.43569120043451,128.67536229942));
#42603=CARTESIAN_POINT('Ctrl Pts',(115.102910430402,4.3746209774216,128.55255857941));
#42604=CARTESIAN_POINT('Ctrl Pts',(115.095149987887,4.3086101351078,128.432639351028));
#42605=CARTESIAN_POINT('Ctrl Pts',(115.087377087622,4.24249332632962,128.312527617655));
#42606=CARTESIAN_POINT('Ctrl Pts',(115.079604187357,4.17142025216563,128.195309963512));
#42607=CARTESIAN_POINT('Ctrl Pts',(115.071831287091,4.0956921078127,128.081404646475));
#42608=CARTESIAN_POINT('Ctrl Pts',(115.064340951329,4.02271687225504,127.971640074623));
#42609=CARTESIAN_POINT('Ctrl Pts',(115.056850615567,3.94541931834231,127.864951446765));
#42610=CARTESIAN_POINT('Ctrl Pts',(115.049360279805,3.86410309998936,127.761682472387));
#42611=CARTESIAN_POINT('Ctrl Pts',(115.041585945686,3.77970375250179,127.654498023456));
#42612=CARTESIAN_POINT('Ctrl Pts',(115.033811611567,3.69070763791452,127.550658131118));
#42613=CARTESIAN_POINT('Ctrl Pts',(115.026037277448,3.59740951683628,127.450582474833));
#42614=CARTESIAN_POINT('Ctrl Pts',(115.018272524501,3.5042263773541,127.35063015285));
#42615=CARTESIAN_POINT('Ctrl Pts',(115.010507771554,3.40675204450105,127.254433119747));
#42616=CARTESIAN_POINT('Ctrl Pts',(115.002743018607,3.30532289377565,127.162379888569));
#42617=CARTESIAN_POINT('Ctrl Pts',(114.994985977722,3.20399448391265,127.070418085959));
#42618=CARTESIAN_POINT('Ctrl Pts',(114.987228936837,3.09871936067409,126.98259215593));
#42619=CARTESIAN_POINT('Ctrl Pts',(114.979471895952,2.98987203352079,126.89925520469));
#42620=CARTESIAN_POINT('Ctrl Pts',(114.971720704712,2.88110678898383,126.815981098494));
#42621=CARTESIAN_POINT('Ctrl Pts',(114.963969513471,2.76877501160242,126.737189469815));
#42622=CARTESIAN_POINT('Ctrl Pts',(114.956218322231,2.65328542804283,126.663194175628));
#42623=CARTESIAN_POINT('Ctrl Pts',(114.948470425454,2.53784493063656,126.589230331414));
#42624=CARTESIAN_POINT('Ctrl Pts',(114.940722528677,2.41924962499331,126.520058977607));
#42625=CARTESIAN_POINT('Ctrl Pts',(114.9329746319,2.29793826792855,126.455951393575));
#42626=CARTESIAN_POINT('Ctrl Pts',(114.925228355816,2.1766522865846,126.391857219467));
#42627=CARTESIAN_POINT('Ctrl Pts',(114.917482079732,2.05265172932757,126.332824890819));
#42628=CARTESIAN_POINT('Ctrl Pts',(114.909735803648,1.92640071916654,126.279080147618));
#42629=CARTESIAN_POINT('Ctrl Pts',(114.901989470382,1.80014877704923,126.225335007685));
#42630=CARTESIAN_POINT('Ctrl Pts',(114.894243137117,1.67164670860619,126.176877684221));
#42631=CARTESIAN_POINT('Ctrl Pts',(114.886496803852,1.54137904447387,126.133885941074));
#42632=CARTESIAN_POINT('Ctrl Pts',(114.878748735849,1.41108220780182,126.090884570224));
#42633=CARTESIAN_POINT('Ctrl Pts',(114.871000667846,1.27901935985217,126.053351337773));
#42634=CARTESIAN_POINT('Ctrl Pts',(114.863252599843,1.1456902445281,126.021414148485));
#42635=CARTESIAN_POINT('Ctrl Pts',(114.855496297101,1.01221942543308,125.989443015972));
#42636=CARTESIAN_POINT('Ctrl Pts',(114.847739994359,0.877480031390909,125.963079898695));
#42637=CARTESIAN_POINT('Ctrl Pts',(114.839983691617,0.74198260532327,125.942401662999));
#42638=CARTESIAN_POINT('Ctrl Pts',(114.832223249103,0.60641286019959,125.921712390705));
#42639=CARTESIAN_POINT('Ctrl Pts',(114.824462806589,0.470084665311837,125.906714088612));
#42640=CARTESIAN_POINT('Ctrl Pts',(114.816702364075,0.333512749509917,125.897431607644));
#42641=CARTESIAN_POINT('Ctrl Pts',(114.808929463809,0.196721596344467,125.888134225614));
#42642=CARTESIAN_POINT('Ctrl Pts',(114.801156563544,0.0596863314958162,
125.884571010537));
#42643=CARTESIAN_POINT('Ctrl Pts',(114.793383663279,-0.0770783494791731,
125.886714636963));
#42644=CARTESIAN_POINT('Ctrl Pts',(114.785893327516,-0.208871289813787,
125.888780337169));
#42645=CARTESIAN_POINT('Ctrl Pts',(114.778402991754,-0.340412669999736,
125.896145149085));
#42646=CARTESIAN_POINT('Ctrl Pts',(114.770912655992,-0.471249185155597,
125.908739383444));
#42647=CARTESIAN_POINT('Ctrl Pts',(114.763138321873,-0.607046406547911,
125.921811132026));
#42648=CARTESIAN_POINT('Ctrl Pts',(114.755363987754,-0.742514422655864,
125.94055808549));
#42649=CARTESIAN_POINT('Ctrl Pts',(114.747589653635,-0.877140819954839,
125.964959100388));
#42650=CARTESIAN_POINT('Ctrl Pts',(114.739824900688,-1.01160130225087,125.989330043215));
#42651=CARTESIAN_POINT('Ctrl Pts',(114.732060147741,-1.14522184849222,126.019341113925));
#42652=CARTESIAN_POINT('Ctrl Pts',(114.724295394794,-1.27749377247639,126.054919311077));
#42653=CARTESIAN_POINT('Ctrl Pts',(114.716538353909,-1.4096343221214,126.090462171462));
#42654=CARTESIAN_POINT('Ctrl Pts',(114.708781313024,-1.54042854001318,126.131561053741));
#42655=CARTESIAN_POINT('Ctrl Pts',(114.701024272139,-1.66937691638695,126.178091735029));
#42656=CARTESIAN_POINT('Ctrl Pts',(114.693273080898,-1.79822805178685,126.224587327167));
#42657=CARTESIAN_POINT('Ctrl Pts',(114.685521889658,-1.92523575002078,126.276506432986));
#42658=CARTESIAN_POINT('Ctrl Pts',(114.677770698418,-2.04991502758049,126.333674826527));
#42659=CARTESIAN_POINT('Ctrl Pts',(114.670022801641,-2.17454131312105,126.390818921975));
#42660=CARTESIAN_POINT('Ctrl Pts',(114.662274904864,-2.29684079166465,126.453207705069));
#42661=CARTESIAN_POINT('Ctrl Pts',(114.654527008087,-2.41634806941997,126.5206186704));
#42662=CARTESIAN_POINT('Ctrl Pts',(114.646780732003,-2.5358303488293,126.58801553481));
#42663=CARTESIAN_POINT('Ctrl Pts',(114.639034455919,-2.65252124888335,126.660432299929));
#42664=CARTESIAN_POINT('Ctrl Pts',(114.631288179835,-2.765979978313,126.737600503904));
#42665=CARTESIAN_POINT('Ctrl Pts',(114.623541846569,-2.87943954526891,126.814769277517));
#42666=CARTESIAN_POINT('Ctrl Pts',(114.615795513304,-2.98966657071328,126.896689340097));
#42667=CARTESIAN_POINT('Ctrl Pts',(114.608049180039,-3.09624959624012,126.983049128001));
#42668=CARTESIAN_POINT('Ctrl Pts',(114.600301112036,-3.20285649029659,127.06942825558));
#42669=CARTESIAN_POINT('Ctrl Pts',(114.592553044033,-3.30581745688504,127.160248840835));
#42670=CARTESIAN_POINT('Ctrl Pts',(114.58480497603,-3.40475476231889,127.255159570715));
#42671=CARTESIAN_POINT('Ctrl Pts',(114.577048673288,-3.50379721949826,127.350171172848));
#42672=CARTESIAN_POINT('Ctrl Pts',(114.569292370546,-3.59880719037784,127.449281332231));
#42673=CARTESIAN_POINT('Ctrl Pts',(114.561536067804,-3.68944404420507,127.55210206278));
#42674=CARTESIAN_POINT('Ctrl Pts',(114.55377562529,-3.78012927365021,127.654977671849));
#42675=CARTESIAN_POINT('Ctrl Pts',(114.546015182776,-3.86643648931334,127.761567494588));
#42676=CARTESIAN_POINT('Ctrl Pts',(114.538254740262,-3.94806655989022,127.871451907569));
#42677=CARTESIAN_POINT('Ctrl Pts',(114.530481839996,-4.02982767030333,127.981512716765));
#42678=CARTESIAN_POINT('Ctrl Pts',(114.522708939731,-4.10689641198569,128.094878361338));
#42679=CARTESIAN_POINT('Ctrl Pts',(114.514936039465,-4.17901756909294,128.211101043263));
#42680=CARTESIAN_POINT('Ctrl Pts',(114.507445703703,-4.248516940477,128.323098737953));
#42681=CARTESIAN_POINT('Ctrl Pts',(114.499955367941,-4.31342204469588,128.437749087283));
#42682=CARTESIAN_POINT('Ctrl Pts',(114.492465032179,-4.37354649094247,128.554633044266));
#42683=CARTESIAN_POINT('Ctrl Pts',(114.484192714557,-4.43994785558427,128.683719542903));
#42684=CARTESIAN_POINT('Ctrl Pts',(114.475920396934,-4.50070748873984,128.81589775137));
#42685=CARTESIAN_POINT('Ctrl Pts',(114.467648079312,-4.55554556162818,128.95066493099));
#42686=CARTESIAN_POINT('Ctrl Pts',(114.4593954003,-4.61025344808148,129.085112171237));
#42687=CARTESIAN_POINT('Ctrl Pts',(114.451142721288,-4.65906768654208,129.222135836395));
#42688=CARTESIAN_POINT('Ctrl Pts',(114.442890042275,-4.70175500412639,129.361210263766));
#42689=CARTESIAN_POINT('Ctrl Pts',(114.438545261957,-4.72422855689706,129.434428649447));
#42690=CARTESIAN_POINT('Ctrl Pts',(114.434200481639,-4.74500467371644,129.508215025666));
#42691=CARTESIAN_POINT('Ctrl Pts',(114.429855701321,-4.76405452823407,129.582490119308));
#42692=CARTESIAN_POINT('Origin',(213.235140564004,0.,130.804360617566));
#42693=CARTESIAN_POINT('',(112.334951030737,-4.76405452823405,129.582490119308));
#42694=CARTESIAN_POINT('',(112.680164151027,-4.76405452823403,129.582490119308));
#42695=CARTESIAN_POINT('',(213.235140564004,-4.76405452823405,129.582490119308));
#42696=CARTESIAN_POINT('',(114.014859436022,-4.91824795544417,130.808845176549));
#42697=CARTESIAN_POINT('Ctrl Pts',(114.014859435991,-4.91824795544367,130.808845177098));
#42698=CARTESIAN_POINT('Ctrl Pts',(114.004073030885,-4.9180744502827,130.999129506488));
#42699=CARTESIAN_POINT('Ctrl Pts',(113.993286625778,-4.90685453025112,131.188930927681));
#42700=CARTESIAN_POINT('Ctrl Pts',(113.982500220672,-4.88477617430655,131.377199852803));
#42701=CARTESIAN_POINT('Ctrl Pts',(113.973386407352,-4.86612139428455,131.536274894077));
#42702=CARTESIAN_POINT('Ctrl Pts',(113.964272594033,-4.83971544491623,131.694256767633));
#42703=CARTESIAN_POINT('Ctrl Pts',(113.955158780713,-4.80569650518746,131.850527030011));
#42704=CARTESIAN_POINT('Ctrl Pts',(113.947384446594,-4.77667741136257,131.983829873726));
#42705=CARTESIAN_POINT('Ctrl Pts',(113.939610112474,-4.74206171732388,132.116135525075));
#42706=CARTESIAN_POINT('Ctrl Pts',(113.931835778355,-4.70193093904607,132.24693765431));
#42707=CARTESIAN_POINT('Ctrl Pts',(113.924071025408,-4.66184961836592,132.377578581611));
#42708=CARTESIAN_POINT('Ctrl Pts',(113.916306272461,-4.61626685072272,132.50671930345));
#42709=CARTESIAN_POINT('Ctrl Pts',(113.908541519514,-4.56531520688374,132.633863316196));
#42710=CARTESIAN_POINT('Ctrl Pts',(113.900784478629,-4.51441416893574,132.760881047717));
#42711=CARTESIAN_POINT('Ctrl Pts',(113.893027437744,-4.45815501108632,132.88590565616));
#42712=CARTESIAN_POINT('Ctrl Pts',(113.885270396859,-4.39672008321279,133.008455799806));
#42713=CARTESIAN_POINT('Ctrl Pts',(113.877519205619,-4.33533148389617,133.130913527435));
#42714=CARTESIAN_POINT('Ctrl Pts',(113.869768014379,-4.26877505791689,133.250900156359));
#42715=CARTESIAN_POINT('Ctrl Pts',(113.862016823139,-4.19728109255979,133.36795467524));
#42716=CARTESIAN_POINT('Ctrl Pts',(113.854268926362,-4.12581751404513,133.484959442827));
#42717=CARTESIAN_POINT('Ctrl Pts',(113.846521029584,-4.04942077344058,133.599034246062));
#42718=CARTESIAN_POINT('Ctrl Pts',(113.838773132807,-3.96836678584156,133.709743228433));
#42719=CARTESIAN_POINT('Ctrl Pts',(113.831026856723,-3.88732975298949,133.820429052872));
#42720=CARTESIAN_POINT('Ctrl Pts',(113.823280580639,-3.80163764168207,133.927750141598));
#42721=CARTESIAN_POINT('Ctrl Pts',(113.815534304555,-3.71160909602127,134.03130049628));
#42722=CARTESIAN_POINT('Ctrl Pts',(113.80778797129,-3.62157988579013,134.134851615346));
#42723=CARTESIAN_POINT('Ctrl Pts',(113.800041638024,-3.52721443384914,134.23463164978));
#42724=CARTESIAN_POINT('Ctrl Pts',(113.792295304759,-3.42887071993867,134.330268819497));
#42725=CARTESIAN_POINT('Ctrl Pts',(113.784547236756,-3.33050498263553,134.425927406496));
#42726=CARTESIAN_POINT('Ctrl Pts',(113.776799168753,-3.22815949079723,134.517441010115));
#42727=CARTESIAN_POINT('Ctrl Pts',(113.76905110075,-3.12222771216706,134.604476033692));
#42728=CARTESIAN_POINT('Ctrl Pts',(113.761294798008,-3.01618334798175,134.691603559128));
#42729=CARTESIAN_POINT('Ctrl Pts',(113.753538495266,-2.90654538558959,134.774242747543));
#42730=CARTESIAN_POINT('Ctrl Pts',(113.745782192525,-2.79373932689858,134.85210117692));
#42731=CARTESIAN_POINT('Ctrl Pts',(113.73802175001,-2.68087306021744,134.930001161685));
#42732=CARTESIAN_POINT('Ctrl Pts',(113.730261307496,-2.56483565857648,135.003115094745));
#42733=CARTESIAN_POINT('Ctrl Pts',(113.722500864982,-2.44607913834008,135.07119549971));
#42734=CARTESIAN_POINT('Ctrl Pts',(113.714727964717,-2.32713197959469,135.139385193384));
#42735=CARTESIAN_POINT('Ctrl Pts',(113.706955064451,-2.20545732687521,135.202525031834));
#42736=CARTESIAN_POINT('Ctrl Pts',(113.699182164186,-2.08152998713914,135.260414474415));
#42737=CARTESIAN_POINT('Ctrl Pts',(113.691691828424,-1.96210771835727,135.316199489944));
#42738=CARTESIAN_POINT('Ctrl Pts',(113.684201492662,-1.84059398485557,135.367109093414));
#42739=CARTESIAN_POINT('Ctrl Pts',(113.6767111569,-1.71742691495417,135.41300769174));
#42740=CARTESIAN_POINT('Ctrl Pts',(113.668936822781,-1.58958992816093,135.460646549372));
#42741=CARTESIAN_POINT('Ctrl Pts',(113.661162488662,-1.45956680842768,135.503037821909));
#42742=CARTESIAN_POINT('Ctrl Pts',(113.653388154543,-1.32782760668504,135.539976407453));
#42743=CARTESIAN_POINT('Ctrl Pts',(113.645623401596,-1.19625076173477,135.576869469491));
#42744=CARTESIAN_POINT('Ctrl Pts',(113.637858648648,-1.06296241566424,135.608323110693));
#42745=CARTESIAN_POINT('Ctrl Pts',(113.630093895701,-0.928451948777212,
135.63418049426));
#42746=CARTESIAN_POINT('Ctrl Pts',(113.622336854816,-0.794075079582346,
135.66001219591));
#42747=CARTESIAN_POINT('Ctrl Pts',(113.614579813931,-0.658478886593955,
135.680258627828));
#42748=CARTESIAN_POINT('Ctrl Pts',(113.606822773046,-0.522166900797256,
135.694813029175));
#42749=CARTESIAN_POINT('Ctrl Pts',(113.599071581806,-0.385957708929306,
135.709356454934));
#42750=CARTESIAN_POINT('Ctrl Pts',(113.591320390566,-0.2490341858447,135.718216352552));
#42751=CARTESIAN_POINT('Ctrl Pts',(113.583569199326,-0.111908669341853,
135.721337281353));
#42752=CARTESIAN_POINT('Ctrl Pts',(113.575821302549,0.025158565158725,135.724456883676));
#42753=CARTESIAN_POINT('Ctrl Pts',(113.568073405772,0.162427232277614,135.721842359718));
#42754=CARTESIAN_POINT('Ctrl Pts',(113.560325508995,0.299381494738817,135.713490253572));
#42755=CARTESIAN_POINT('Ctrl Pts',(113.552579232911,0.436307109320613,135.705139894506));
#42756=CARTESIAN_POINT('Ctrl Pts',(113.544832956827,0.572918060065281,135.691054364256));
#42757=CARTESIAN_POINT('Ctrl Pts',(113.537086680742,0.708700534156355,135.671282295114));
#42758=CARTESIAN_POINT('Ctrl Pts',(113.529340347477,0.844484010562807,135.651510080019));
#42759=CARTESIAN_POINT('Ctrl Pts',(113.521594014212,0.979438611227399,135.626051298607));
#42760=CARTESIAN_POINT('Ctrl Pts',(113.513847680946,1.11305805024376,135.595006173155));
#42761=CARTESIAN_POINT('Ctrl Pts',(113.506099612943,1.24670741240704,135.563954095363));
#42762=CARTESIAN_POINT('Ctrl Pts',(113.49835154494,1.37902063719763,135.527313272605));
#42763=CARTESIAN_POINT('Ctrl Pts',(113.490603476938,1.5095043813704,135.485234423291));
#42764=CARTESIAN_POINT('Ctrl Pts',(113.482847174196,1.64012680521926,135.443110852076));
#42765=CARTESIAN_POINT('Ctrl Pts',(113.475090871454,1.76891549162545,135.39553782912));
#42766=CARTESIAN_POINT('Ctrl Pts',(113.467334568712,1.89539442348939,135.342715279986));
#42767=CARTESIAN_POINT('Ctrl Pts',(113.459574126198,2.02194086096757,135.289864537866));
#42768=CARTESIAN_POINT('Ctrl Pts',(113.451813683684,2.14617473350313,135.231758852242));
#42769=CARTESIAN_POINT('Ctrl Pts',(113.444053241169,2.26764350631388,135.168644750247));
#42770=CARTESIAN_POINT('Ctrl Pts',(113.436280340904,2.38930727158216,135.105429331893));
#42771=CARTESIAN_POINT('Ctrl Pts',(113.428507440639,2.50819672774641,135.037189625513));
#42772=CARTESIAN_POINT('Ctrl Pts',(113.420734540373,2.62388650952542,134.964216702532));
#42773=CARTESIAN_POINT('Ctrl Pts',(113.413244204611,2.73537067633226,134.893896529109));
#42774=CARTESIAN_POINT('Ctrl Pts',(113.405753868849,2.84388350866272,134.819181467877));
#42775=CARTESIAN_POINT('Ctrl Pts',(113.398263533087,2.94907410915593,134.740366837227));
#42776=CARTESIAN_POINT('Ctrl Pts',(113.390489198968,3.05825304323831,134.6585639259));
#42777=CARTESIAN_POINT('Ctrl Pts',(113.382714864849,3.16419869361358,134.572085311093));
#42778=CARTESIAN_POINT('Ctrl Pts',(113.37494053073,3.26648442823714,134.48121559738));
#42779=CARTESIAN_POINT('Ctrl Pts',(113.367175777783,3.36864410483431,134.390457872468));
#42780=CARTESIAN_POINT('Ctrl Pts',(113.359411024835,3.46715255079093,134.295320073365));
#42781=CARTESIAN_POINT('Ctrl Pts',(113.351646271888,3.5616132928583,134.196129155458));
#42782=CARTESIAN_POINT('Ctrl Pts',(113.343889231003,3.65598021518499,134.09703675537));
#42783=CARTESIAN_POINT('Ctrl Pts',(113.336132190118,3.74630716619833,133.993899528923));
#42784=CARTESIAN_POINT('Ctrl Pts',(113.328375149233,3.83223215418175,133.887083404155));
#42785=CARTESIAN_POINT('Ctrl Pts',(113.320623957993,3.91809234546334,133.780347830258));
#42786=CARTESIAN_POINT('Ctrl Pts',(113.312872766753,3.99955693702449,133.669939183488));
#42787=CARTESIAN_POINT('Ctrl Pts',(113.305121575513,4.07630235396087,133.556258541108));
#42788=CARTESIAN_POINT('Ctrl Pts',(113.297373678736,4.15301515204781,133.442626216033));
#42789=CARTESIAN_POINT('Ctrl Pts',(113.289625781959,4.22501254654578,133.325724984672));
#42790=CARTESIAN_POINT('Ctrl Pts',(113.281877885182,4.29201280725482,133.205986967534));
#42791=CARTESIAN_POINT('Ctrl Pts',(113.274131609098,4.35899905295368,133.086273997007));
#42792=CARTESIAN_POINT('Ctrl Pts',(113.266385333014,4.42099005321708,132.963725761965));
#42793=CARTESIAN_POINT('Ctrl Pts',(113.258639056929,4.47774899539122,132.838800834622));
#42794=CARTESIAN_POINT('Ctrl Pts',(113.250892723664,4.53450835654698,132.713874985111));
#42795=CARTESIAN_POINT('Ctrl Pts',(113.243146390399,4.5860354208231,132.58657276424));
#42796=CARTESIAN_POINT('Ctrl Pts',(113.235400057133,4.63214084816174,132.457374297271));
#42797=CARTESIAN_POINT('Ctrl Pts',(113.22765198913,4.67825660049113,132.328146897201));
#42798=CARTESIAN_POINT('Ctrl Pts',(113.219903921127,4.71894816851154,132.197022774176));
#42799=CARTESIAN_POINT('Ctrl Pts',(113.212155853124,4.75407569181712,132.064498458825));
#42800=CARTESIAN_POINT('Ctrl Pts',(113.204399550383,4.78924054907252,131.931833295055));
#42801=CARTESIAN_POINT('Ctrl Pts',(113.196643247641,4.8188294483625,131.797765344753));
#42802=CARTESIAN_POINT('Ctrl Pts',(113.188886944899,4.84275329385569,131.662803159237));
#42803=CARTESIAN_POINT('Ctrl Pts',(113.181126502385,4.86668990822556,131.527768940338));
#42804=CARTESIAN_POINT('Ctrl Pts',(113.173366059871,4.88495539195758,131.391839922498));
#42805=CARTESIAN_POINT('Ctrl Pts',(113.165605617356,4.89751254920902,131.255530089982));
#42806=CARTESIAN_POINT('Ctrl Pts',(113.157832717091,4.91008986432404,131.119001440822));
#42807=CARTESIAN_POINT('Ctrl Pts',(113.150059816826,4.91694052179098,130.982091146081));
#42808=CARTESIAN_POINT('Ctrl Pts',(113.14228691656,4.91807948791812,130.845314408832));
#42809=CARTESIAN_POINT('Ctrl Pts',(113.134796580798,4.91917704975766,130.713509850501));
#42810=CARTESIAN_POINT('Ctrl Pts',(113.127306245036,4.91497098915063,130.581829615806));
#42811=CARTESIAN_POINT('Ctrl Pts',(113.119815909274,4.90552009722783,130.450728551438));
#42812=CARTESIAN_POINT('Ctrl Pts',(113.112041575155,4.89571087186524,130.314656750367));
#42813=CARTESIAN_POINT('Ctrl Pts',(113.104267241036,4.88022017592059,130.178777870509));
#42814=CARTESIAN_POINT('Ctrl Pts',(113.096492906917,4.85905685024213,130.04360468521));
#42815=CARTESIAN_POINT('Ctrl Pts',(113.08872815397,4.83791960647114,129.908598088781));
#42816=CARTESIAN_POINT('Ctrl Pts',(113.080963401023,4.81112370288492,129.774295839008));
#42817=CARTESIAN_POINT('Ctrl Pts',(113.073198648075,4.77872991283661,129.641208227438));
#42818=CARTESIAN_POINT('Ctrl Pts',(113.06544160719,4.74636829675727,129.50825280036));
#42819=CARTESIAN_POINT('Ctrl Pts',(113.057684566305,4.70841995053111,129.376509988119));
#42820=CARTESIAN_POINT('Ctrl Pts',(113.04992752542,4.66499707441347,129.246482137641));
#42821=CARTESIAN_POINT('Ctrl Pts',(113.04217633418,4.62160694382445,129.116552342176));
#42822=CARTESIAN_POINT('Ctrl Pts',(113.03442514294,4.57275062398401,128.988335303638));
#42823=CARTESIAN_POINT('Ctrl Pts',(113.0266739517,4.51859065241145,128.862320046816));
#42824=CARTESIAN_POINT('Ctrl Pts',(113.018926054923,4.46445370027158,128.736358349839));
#42825=CARTESIAN_POINT('Ctrl Pts',(113.011178158146,4.40501773387347,128.612596931754));
#42826=CARTESIAN_POINT('Ctrl Pts',(113.003430261369,4.34049402638364,128.491506391847));
#42827=CARTESIAN_POINT('Ctrl Pts',(112.995683985285,4.27598381586244,128.37044118147));
#42828=CARTESIAN_POINT('Ctrl Pts',(112.987937709201,4.20638816483134,128.252046082824));
#42829=CARTESIAN_POINT('Ctrl Pts',(112.980191433116,4.1319648800591,128.136768202586));
#42830=CARTESIAN_POINT('Ctrl Pts',(112.972445099851,4.05754104591108,128.021489471393));
#42831=CARTESIAN_POINT('Ctrl Pts',(112.964698766586,3.97828971896613,127.909328332985));
#42832=CARTESIAN_POINT('Ctrl Pts',(112.95695243332,3.89451249927829,127.800703603947));
#42833=CARTESIAN_POINT('Ctrl Pts',(112.949204365317,3.81071651826298,127.692054549153));
#42834=CARTESIAN_POINT('Ctrl Pts',(112.941456297314,3.72239286639619,127.586943789153));
#42835=CARTESIAN_POINT('Ctrl Pts',(112.933708229311,3.6298836909918,127.485757379399));
#42836=CARTESIAN_POINT('Ctrl Pts',(112.92595192657,3.53727619573492,127.384463427525));
#42837=CARTESIAN_POINT('Ctrl Pts',(112.918195623828,3.4404745549594,127.287102446621));
#42838=CARTESIAN_POINT('Ctrl Pts',(112.910439321086,3.33985846881852,127.194024279943));
#42839=CARTESIAN_POINT('Ctrl Pts',(112.902678878572,3.2391886808429,127.100896434645));
#42840=CARTESIAN_POINT('Ctrl Pts',(112.894918436058,3.13470068854024,127.012056211482));
#42841=CARTESIAN_POINT('Ctrl Pts',(112.887157993543,3.02680681616963,126.927812725422));
#42842=CARTESIAN_POINT('Ctrl Pts',(112.879385093278,2.91873974297679,126.843434004239));
#42843=CARTESIAN_POINT('Ctrl Pts',(112.871612193013,2.80725618220763,126.763666993564));
#42844=CARTESIAN_POINT('Ctrl Pts',(112.863839292747,2.69279767845374,126.688777581663));
#42845=CARTESIAN_POINT('Ctrl Pts',(112.856348956985,2.58250002961489,126.61661058852));
#42846=CARTESIAN_POINT('Ctrl Pts',(112.848858621223,2.4694402402913,126.548972883109));
#42847=CARTESIAN_POINT('Ctrl Pts',(112.841368285461,2.35403276392831,126.486060858534));
#42848=CARTESIAN_POINT('Ctrl Pts',(112.833593951342,2.2342495780216,126.420763505426));
#42849=CARTESIAN_POINT('Ctrl Pts',(112.825819617223,2.11155772856749,126.360350413054));
#42850=CARTESIAN_POINT('Ctrl Pts',(112.818045283104,1.98639340499948,126.305091309881));
#42851=CARTESIAN_POINT('Ctrl Pts',(112.810280530157,1.86138333527402,126.249900308614));
#42852=CARTESIAN_POINT('Ctrl Pts',(112.80251577721,1.73390720848793,126.199850814684));
#42853=CARTESIAN_POINT('Ctrl Pts',(112.794751024262,1.60442719685361,126.155167522792));
#42854=CARTESIAN_POINT('Ctrl Pts',(112.786993983377,1.47507578659228,126.110528610975));
#42855=CARTESIAN_POINT('Ctrl Pts',(112.779236942492,1.34372481942865,126.071245421395));
#42856=CARTESIAN_POINT('Ctrl Pts',(112.771479901607,1.21085758103656,126.037495087582));
#42857=CARTESIAN_POINT('Ctrl Pts',(112.763728710367,1.07809053886251,126.003770205159));
#42858=CARTESIAN_POINT('Ctrl Pts',(112.755977519127,0.943809878789901,125.975569969518));
#42859=CARTESIAN_POINT('Ctrl Pts',(112.748226327887,0.808514886721858,125.953021963086));
#42860=CARTESIAN_POINT('Ctrl Pts',(112.74047843111,0.673277398634464,125.930483540158));
#42861=CARTESIAN_POINT('Ctrl Pts',(112.732730534333,0.537026820851626,125.913592632487));
#42862=CARTESIAN_POINT('Ctrl Pts',(112.724982637556,0.400273280187613,125.902425860384));
#42863=CARTESIAN_POINT('Ctrl Pts',(112.717236361472,0.263548345416242,125.891261424129));
#42864=CARTESIAN_POINT('Ctrl Pts',(112.709490085388,0.126321046451539,125.885818773613));
#42865=CARTESIAN_POINT('Ctrl Pts',(112.701743809303,-0.0108931023410998,
125.886122680782));
#42866=CARTESIAN_POINT('Ctrl Pts',(112.693997476038,-0.148108264017321,
125.886426590194));
#42867=CARTESIAN_POINT('Ctrl Pts',(112.686251142773,-0.28530988436353,125.892477141069));
#42868=CARTESIAN_POINT('Ctrl Pts',(112.678504809507,-0.421982578929462,
125.904246969335));
#42869=CARTESIAN_POINT('Ctrl Pts',(112.670756741504,-0.55868588039772,125.916019433372));
#42870=CARTESIAN_POINT('Ctrl Pts',(112.663008673501,-0.694859630936441,
125.93351368989));
#42871=CARTESIAN_POINT('Ctrl Pts',(112.655260605498,-0.829994092178677,
125.956650553067));
#42872=CARTESIAN_POINT('Ctrl Pts',(112.647504302757,-0.965272175934534,
125.979812006376));
#42873=CARTESIAN_POINT('Ctrl Pts',(112.639748000015,-1.09950837792602,126.008627979973));
#42874=CARTESIAN_POINT('Ctrl Pts',(112.631991697273,-1.23220312790668,126.042968120189));
#42875=CARTESIAN_POINT('Ctrl Pts',(112.624231254759,-1.36496870107086,126.077326588772));
#42876=CARTESIAN_POINT('Ctrl Pts',(112.616470812244,-1.49619080900436,126.117214985287));
#42877=CARTESIAN_POINT('Ctrl Pts',(112.60871036973,-1.62538651319723,126.162453493849));
#42878=CARTESIAN_POINT('Ctrl Pts',(112.600937469465,-1.75478961380384,126.20776462328));
#42879=CARTESIAN_POINT('Ctrl Pts',(112.593164569199,-1.88215944673707,126.258442882647));
#42880=CARTESIAN_POINT('Ctrl Pts',(112.585391668934,-2.00703364703102,126.31426050708));
#42881=CARTESIAN_POINT('Ctrl Pts',(112.577901333172,-2.12736835560448,126.368049020269));
#42882=CARTESIAN_POINT('Ctrl Pts',(112.57041099741,-2.24538545053348,126.426609591129));
#42883=CARTESIAN_POINT('Ctrl Pts',(112.562920661648,-2.3606956785272,126.489699683508));
#42884=CARTESIAN_POINT('Ctrl Pts',(112.555145317235,-2.48039348186472,126.555190365485));
#42885=CARTESIAN_POINT('Ctrl Pts',(112.547369972822,-2.59755356213865,126.625769574031));
#42886=CARTESIAN_POINT('Ctrl Pts',(112.53959462841,-2.71171303900294,126.701216036077));
#42887=CARTESIAN_POINT('Ctrl Pts',(112.531829087145,-2.82572858368351,126.77656737528));
#42888=CARTESIAN_POINT('Ctrl Pts',(112.524063545881,-2.93675072985558,126.856773543025));
#42889=CARTESIAN_POINT('Ctrl Pts',(112.516298004617,-3.04434049096868,126.94156706399));
#42890=CARTESIAN_POINT('Ctrl Pts',(112.508541805313,-3.15180082139576,127.026258578189));
#42891=CARTESIAN_POINT('Ctrl Pts',(112.50078560601,-3.25583668553785,127.115526213941));
#42892=CARTESIAN_POINT('Ctrl Pts',(112.493029406706,-3.35603796700677,127.209059207877));
#42893=CARTESIAN_POINT('Ctrl Pts',(112.48527850398,-3.45617082271927,127.302528329718));
#42894=CARTESIAN_POINT('Ctrl Pts',(112.477527601253,-3.55247402070944,127.400256749436));
#42895=CARTESIAN_POINT('Ctrl Pts',(112.469776698526,-3.64457039176469,127.50189340017));
#42896=CARTESIAN_POINT('Ctrl Pts',(112.462029410145,-3.73662381710103,127.603482656431));
#42897=CARTESIAN_POINT('Ctrl Pts',(112.454282121764,-3.82447405730881,127.70897622806));
#42898=CARTESIAN_POINT('Ctrl Pts',(112.446534833383,-3.90778099548178,127.817986435744));
#42899=CARTESIAN_POINT('Ctrl Pts',(112.438789479906,-3.99106712754004,127.926969417859));
#42900=CARTESIAN_POINT('Ctrl Pts',(112.43104412643,-4.06981197963845,128.039466977067));
#42901=CARTESIAN_POINT('Ctrl Pts',(112.423298772953,-4.14371616711926,128.155058938094));
#42902=CARTESIAN_POINT('Ctrl Pts',(112.415551153812,-4.21764197299036,128.270684711983));
#42903=CARTESIAN_POINT('Ctrl Pts',(112.407803534671,-4.28672406924796,128.389406369999));
#42904=CARTESIAN_POINT('Ctrl Pts',(112.40005591553,-4.35070677162548,128.510775291089));
#42905=CARTESIAN_POINT('Ctrl Pts',(112.392307296076,-4.41469773496383,128.632159882412));
#42906=CARTESIAN_POINT('Ctrl Pts',(112.384558676621,-4.47358781771709,128.756192067992));
#42907=CARTESIAN_POINT('Ctrl Pts',(112.376810057166,-4.52716807485757,128.882400086106));
#42908=CARTESIAN_POINT('Ctrl Pts',(112.369054792459,-4.5807942826802,129.008716340814));
#42909=CARTESIAN_POINT('Ctrl Pts',(112.361299527752,-4.62910142171835,129.137211792758));
#42910=CARTESIAN_POINT('Ctrl Pts',(112.353544263044,-4.67192919959215,129.267395876104));
#42911=CARTESIAN_POINT('Ctrl Pts',(112.347346518942,-4.70615570477945,129.37143457307));
#42912=CARTESIAN_POINT('Ctrl Pts',(112.341148774839,-4.73688366297584,129.476551328042));
#42913=CARTESIAN_POINT('Ctrl Pts',(112.334951030737,-4.76405452823405,129.582490119308));
#42914=CARTESIAN_POINT('Ctrl Pts',(114.08491538754,-4.76405452823405,129.582490119308));
#42915=CARTESIAN_POINT('Ctrl Pts',(114.077273043215,-4.79770112579015,129.713677692521));
#42916=CARTESIAN_POINT('Ctrl Pts',(114.06963069889,-4.82591584136121,129.846221348947));
#42917=CARTESIAN_POINT('Ctrl Pts',(114.061988354565,-4.84860748928013,129.979625219152));
#42918=CARTESIAN_POINT('Ctrl Pts',(114.054133534808,-4.87193001922921,130.116738035696));
#42919=CARTESIAN_POINT('Ctrl Pts',(114.046278715051,-4.88941780736256,130.2547591488));
#42920=CARTESIAN_POINT('Ctrl Pts',(114.038423895294,-4.90102887405486,130.393144083146));
#42921=CARTESIAN_POINT('Ctrl Pts',(114.030569075537,-4.91263994074715,130.531529017491));
#42922=CARTESIAN_POINT('Ctrl Pts',(114.022714255779,-4.9183743044535,130.67027731309));
#42923=CARTESIAN_POINT('Ctrl Pts',(114.014859436022,-4.91824795544417,130.808845176549));
#42924=CARTESIAN_POINT('',(114.360140564037,-4.91824995380443,130.803686523594));
#42925=CARTESIAN_POINT('Ctrl Pts',(114.429855701321,-4.76405452823407,129.582490119308));
#42926=CARTESIAN_POINT('Ctrl Pts',(114.421628335829,-4.8001277250803,129.723138966325));
#42927=CARTESIAN_POINT('Ctrl Pts',(114.413400970338,-4.8300079357871,129.865541295514));
#42928=CARTESIAN_POINT('Ctrl Pts',(114.405173604846,-4.85353619530554,130.009144003454));
#42929=CARTESIAN_POINT('Ctrl Pts',(114.396965713327,-4.87700876401274,130.152406807319));
#42930=CARTESIAN_POINT('Ctrl Pts',(114.388757821807,-4.89415931337737,130.296864013968));
#42931=CARTESIAN_POINT('Ctrl Pts',(114.380549930287,-4.90487943354696,130.441950897956));
#42932=CARTESIAN_POINT('Ctrl Pts',(114.373746808204,-4.91376481977387,130.562206359675));
#42933=CARTESIAN_POINT('Ctrl Pts',(114.366943686121,-4.91823339802076,130.682894044141));
#42934=CARTESIAN_POINT('Ctrl Pts',(114.360140564037,-4.91824995380443,130.803686523594));
#42935=CARTESIAN_POINT('Ctrl Pts',(114.360140564008,-4.9182499538045,130.803686524113));
#42936=CARTESIAN_POINT('Ctrl Pts',(114.352104374385,-4.91826951031294,130.946372669984));
#42937=CARTESIAN_POINT('Ctrl Pts',(114.344068184762,-4.91207540979104,131.088966543765));
#42938=CARTESIAN_POINT('Ctrl Pts',(114.336031995138,-4.8997177208193,131.230915794289));
#42939=CARTESIAN_POINT('Ctrl Pts',(114.327987899649,-4.88734787456491,131.373004692054));
#42940=CARTESIAN_POINT('Ctrl Pts',(114.319943804161,-4.86880237640859,131.514447356263));
#42941=CARTESIAN_POINT('Ctrl Pts',(114.311899708672,-4.84418284113059,131.654699176139));
#42942=CARTESIAN_POINT('Ctrl Pts',(114.303742850313,-4.8192181869443,131.796917058916));
#42943=CARTESIAN_POINT('Ctrl Pts',(114.295585991954,-4.78800800756211,131.937910097035));
#42944=CARTESIAN_POINT('Ctrl Pts',(114.287429133595,-4.75071072483695,132.077125588572));
#42945=CARTESIAN_POINT('Ctrl Pts',(114.279360225711,-4.71381559617151,132.214840003596));
#42946=CARTESIAN_POINT('Ctrl Pts',(114.271291317826,-4.67096416418026,132.350814710882));
#42947=CARTESIAN_POINT('Ctrl Pts',(114.263222409942,-4.62235864862707,132.484534294887));
#42948=CARTESIAN_POINT('Ctrl Pts',(114.255021576346,-4.57295843851214,132.620440178636));
#42949=CARTESIAN_POINT('Ctrl Pts',(114.24682074275,-4.51761451060067,132.754016210855));
#42950=CARTESIAN_POINT('Ctrl Pts',(114.238619909154,-4.45658795979715,132.884746836298));
#42951=CARTESIAN_POINT('Ctrl Pts',(114.230419075558,-4.39556140899363,133.015477461742));
#42952=CARTESIAN_POINT('Ctrl Pts',(114.222218241962,-4.32885246381835,133.143362382982));
#42953=CARTESIAN_POINT('Ctrl Pts',(114.214017408366,-4.25676823117942,133.26791643965));
#42954=CARTESIAN_POINT('Ctrl Pts',(114.206243074247,-4.18843287201148,133.385992832871));
#42955=CARTESIAN_POINT('Ctrl Pts',(114.198468740128,-4.11507265710095,133.501410814662));
#42956=CARTESIAN_POINT('Ctrl Pts',(114.190694406009,-4.03691981000747,133.61371312483));
#42957=CARTESIAN_POINT('Ctrl Pts',(114.182929653062,-3.95886327931348,133.725877032436));
#42958=CARTESIAN_POINT('Ctrl Pts',(114.175164900115,-3.87602608977212,133.834932590625));
#42959=CARTESIAN_POINT('Ctrl Pts',(114.167400147168,-3.78868608134673,133.940447484907));
#42960=CARTESIAN_POINT('Ctrl Pts',(114.159643106283,-3.70143282024905,134.045857580308));
#42961=CARTESIAN_POINT('Ctrl Pts',(114.151886065398,-3.60968588795588,134.147733710845));
#42962=CARTESIAN_POINT('Ctrl Pts',(114.144129024513,-3.5137658968655,134.245673199202));
#42963=CARTESIAN_POINT('Ctrl Pts',(114.136377833272,-3.41791823978629,134.343538830629));
#42964=CARTESIAN_POINT('Ctrl Pts',(114.128626642032,-3.3179040601478,134.43747345061));
#42965=CARTESIAN_POINT('Ctrl Pts',(114.120875450792,-3.21408341091365,134.527108378319));
#42966=CARTESIAN_POINT('Ctrl Pts',(114.113127554015,-3.11030688822499,134.616705208792));
#42967=CARTESIAN_POINT('Ctrl Pts',(114.105379657238,-3.00272740903509,134.702005726759));
#42968=CARTESIAN_POINT('Ctrl Pts',(114.097631760461,-2.89174079449725,134.782679136732));
#42969=CARTESIAN_POINT('Ctrl Pts',(114.089885484377,-2.78077739596666,134.863335671567));
#42970=CARTESIAN_POINT('Ctrl Pts',(114.082139208293,-2.66640859573317,134.939366793872));
#42971=CARTESIAN_POINT('Ctrl Pts',(114.074392932209,-2.54906178666891,135.010483187136));
#42972=CARTESIAN_POINT('Ctrl Pts',(114.066646598943,-2.43171411137709,135.081600105365));
#42973=CARTESIAN_POINT('Ctrl Pts',(114.058900265678,-2.31138871774528,135.147802019528));
#42974=CARTESIAN_POINT('Ctrl Pts',(114.051153932413,-2.1885400077627,135.208844207832));
#42975=CARTESIAN_POINT('Ctrl Pts',(114.04340586441,-2.06566378666363,135.269900066111));
#42976=CARTESIAN_POINT('Ctrl Pts',(114.035657796407,-1.94026347482909,135.325793725309));
#42977=CARTESIAN_POINT('Ctrl Pts',(114.027909728404,-1.81281560876735,135.376327659345));
#42978=CARTESIAN_POINT('Ctrl Pts',(114.020153425662,-1.68523228959656,135.426915301446));
#42979=CARTESIAN_POINT('Ctrl Pts',(114.01239712292,-1.5555974330923,135.472131694917));
#42980=CARTESIAN_POINT('Ctrl Pts',(114.004640820178,-1.42440550805593,135.511828303182));
#42981=CARTESIAN_POINT('Ctrl Pts',(113.996880377664,-1.29314356193897,135.551546098722));
#42982=CARTESIAN_POINT('Ctrl Pts',(113.98911993515,-1.16032326977921,135.585738141329));
#42983=CARTESIAN_POINT('Ctrl Pts',(113.981359492636,-1.02645062514271,135.614306789473));
#42984=CARTESIAN_POINT('Ctrl Pts',(113.97358659237,-0.892363076252286,135.642921298547));
#42985=CARTESIAN_POINT('Ctrl Pts',(113.965813692105,-0.757220184724024,
135.665894308434));
#42986=CARTESIAN_POINT('Ctrl Pts',(113.958040791839,-0.621535315204801,
135.683179830701));
#42987=CARTESIAN_POINT('Ctrl Pts',(113.950550456077,-0.490782932461883,
135.699836980694));
#42988=CARTESIAN_POINT('Ctrl Pts',(113.943060120315,-0.359527599005925,
135.71121294635));
#42989=CARTESIAN_POINT('Ctrl Pts',(113.935569784553,-0.228227921651108,
135.717312385931));
#42990=CARTESIAN_POINT('Ctrl Pts',(113.927795450434,-0.0919499771221869,
135.723643087618));
#42991=CARTESIAN_POINT('Ctrl Pts',(113.920021116315,0.0448074278476511,
135.724309299543));
#42992=CARTESIAN_POINT('Ctrl Pts',(113.912246782196,0.181534064801489,135.719259237662));
#42993=CARTESIAN_POINT('Ctrl Pts',(113.904482029249,0.318092198394799,135.71421539953));
#42994=CARTESIAN_POINT('Ctrl Pts',(113.896717276302,0.454619252471153,135.703469318929));
#42995=CARTESIAN_POINT('Ctrl Pts',(113.888952523355,0.590601329319836,135.687021073947));
#42996=CARTESIAN_POINT('Ctrl Pts',(113.88119548247,0.726448346852689,135.670589165594));
#42997=CARTESIAN_POINT('Ctrl Pts',(113.873438441585,0.861751078703154,135.648466410065));
#42998=CARTESIAN_POINT('Ctrl Pts',(113.8656814007,0.995997442208604,135.620704890727));
#42999=CARTESIAN_POINT('Ctrl Pts',(113.85793020946,1.13014256948723,135.592964306567));
#43000=CARTESIAN_POINT('Ctrl Pts',(113.85017901822,1.26323253272058,135.559593501269));
#43001=CARTESIAN_POINT('Ctrl Pts',(113.842427826979,1.39476253286651,135.520696116596));
#43002=CARTESIAN_POINT('Ctrl Pts',(113.834679930202,1.52623662925371,135.48181526435));
#43003=CARTESIAN_POINT('Ctrl Pts',(113.826932033425,1.65615170713195,135.43741261524));
#43004=CARTESIAN_POINT('Ctrl Pts',(113.819184136648,1.78401550788889,135.387642381773));
#43005=CARTESIAN_POINT('Ctrl Pts',(113.811437860564,1.91185256229505,135.337882559166));
#43006=CARTESIAN_POINT('Ctrl Pts',(113.80369158448,2.03763882894259,135.282757527206));
#43007=CARTESIAN_POINT('Ctrl Pts',(113.795945308396,2.16089988137072,135.22247048098));
#43008=CARTESIAN_POINT('Ctrl Pts',(113.788198975131,2.28416184368394,135.162182989728));
#43009=CARTESIAN_POINT('Ctrl Pts',(113.780452641865,2.40489820337418,135.09673357995));
#43010=CARTESIAN_POINT('Ctrl Pts',(113.7727063086,2.522657453691,135.026372274802));
#43011=CARTESIAN_POINT('Ctrl Pts',(113.764958240597,2.64044307537546,134.955995212728));
#43012=CARTESIAN_POINT('Ctrl Pts',(113.757210172594,2.75524992546965,134.880704266935));
#43013=CARTESIAN_POINT('Ctrl Pts',(113.749462104591,2.8666542400627,134.800793593412));
#43014=CARTESIAN_POINT('Ctrl Pts',(113.741705801849,2.97817695648711,134.720797989874));
#43015=CARTESIAN_POINT('Ctrl Pts',(113.733949499108,3.08628959535703,134.63617307879));
#43016=CARTESIAN_POINT('Ctrl Pts',(113.726193196366,3.19059991617947,134.547254583119));
#43017=CARTESIAN_POINT('Ctrl Pts',(113.718432753852,3.29496591056093,134.45828862897));
#43018=CARTESIAN_POINT('Ctrl Pts',(113.710672311337,3.39552525660378,134.365024789726));
#43019=CARTESIAN_POINT('Ctrl Pts',(113.702911868823,3.49192230384059,134.267835994473));
#43020=CARTESIAN_POINT('Ctrl Pts',(113.695138968558,3.5884740961753,134.170491183138));
#43021=CARTESIAN_POINT('Ctrl Pts',(113.687366068292,3.68084997394178,134.06920911404));
#43022=CARTESIAN_POINT('Ctrl Pts',(113.679593168027,3.7687337596386,133.964396837526));
#43023=CARTESIAN_POINT('Ctrl Pts',(113.672102832265,3.8534227483598,133.863394751269));
#43024=CARTESIAN_POINT('Ctrl Pts',(113.664612496503,3.93394038427291,133.759114909199));
#43025=CARTESIAN_POINT('Ctrl Pts',(113.657122160741,4.01004269832085,133.651945668121));
#43026=CARTESIAN_POINT('Ctrl Pts',(113.649347826622,4.08903045473632,133.540713072694));
#43027=CARTESIAN_POINT('Ctrl Pts',(113.641573492503,4.1635116755688,133.426015298541));
#43028=CARTESIAN_POINT('Ctrl Pts',(113.633799158384,4.23316700248996,133.308253624771));
#43029=CARTESIAN_POINT('Ctrl Pts',(113.626034405437,4.30273648544601,133.190637081739));
#43030=CARTESIAN_POINT('Ctrl Pts',(113.618269652489,4.36749171107854,133.069964485445));
#43031=CARTESIAN_POINT('Ctrl Pts',(113.610504899542,4.42715497082029,132.946668234796));
#43032=CARTESIAN_POINT('Ctrl Pts',(113.602747858657,4.4867589721712,132.823494443722));
#43033=CARTESIAN_POINT('Ctrl Pts',(113.594990817772,4.54128090291414,132.697702533702));
#43034=CARTESIAN_POINT('Ctrl Pts',(113.587233776887,4.59048778907245,132.569751486716));
#43035=CARTESIAN_POINT('Ctrl Pts',(113.579482585647,4.63965756793541,132.441896928608));
#43036=CARTESIAN_POINT('Ctrl Pts',(113.571731394407,4.6835201403585,132.311886837845));
#43037=CARTESIAN_POINT('Ctrl Pts',(113.563980203167,4.72188984687997,132.180201937062));
#43038=CARTESIAN_POINT('Ctrl Pts',(113.55623230639,4.76024324525248,132.048573005875));
#43039=CARTESIAN_POINT('Ctrl Pts',(113.548484409613,4.79310831195328,131.915271055031));
#43040=CARTESIAN_POINT('Ctrl Pts',(113.540736512836,4.82034871252759,131.780793591269));
#43041=CARTESIAN_POINT('Ctrl Pts',(113.532990236752,4.84758341499731,131.646344257293));
#43042=CARTESIAN_POINT('Ctrl Pts',(113.525243960668,4.86919571401053,131.510720282432));
#43043=CARTESIAN_POINT('Ctrl Pts',(113.517497684584,4.88510012425823,131.374430647012));
#43044=CARTESIAN_POINT('Ctrl Pts',(113.509751351318,4.90100465190866,131.238140005532));
#43045=CARTESIAN_POINT('Ctrl Pts',(113.502005018053,4.91120116140113,131.101184082018));
#43046=CARTESIAN_POINT('Ctrl Pts',(113.494258684788,4.91565595387034,130.964077885509));
#43047=CARTESIAN_POINT('Ctrl Pts',(113.486510616785,4.92011174395943,130.826940985017));
#43048=CARTESIAN_POINT('Ctrl Pts',(113.478762548782,4.91882324570292,130.68965413525));
#43049=CARTESIAN_POINT('Ctrl Pts',(113.471014480779,4.91180888611941,130.552732859283));
#43050=CARTESIAN_POINT('Ctrl Pts',(113.463258178037,4.90478707159103,130.415666061754));
#43051=CARTESIAN_POINT('Ctrl Pts',(113.455501875295,4.89202725930124,130.278966005245));
#43052=CARTESIAN_POINT('Ctrl Pts',(113.447745572553,4.87359988691645,130.14314415925));
#43053=CARTESIAN_POINT('Ctrl Pts',(113.439985130039,4.8551626792882,130.007249821047));
#43054=CARTESIAN_POINT('Ctrl Pts',(113.432224687525,4.83105195279801,129.872235012025));
#43055=CARTESIAN_POINT('Ctrl Pts',(113.424464245011,4.80138922548218,129.738600528276));
#43056=CARTESIAN_POINT('Ctrl Pts',(113.416691344745,4.77167888092311,129.60475152259));
#43057=CARTESIAN_POINT('Ctrl Pts',(113.40891844448,4.73639882607318,129.472287648105));
#43058=CARTESIAN_POINT('Ctrl Pts',(113.401145544214,4.6957206222541,129.341694934562));
#43059=CARTESIAN_POINT('Ctrl Pts',(113.393655208452,4.65652117360567,129.215849595098));
#43060=CARTESIAN_POINT('Ctrl Pts',(113.38616487269,4.61230933807669,129.09174202581));
#43061=CARTESIAN_POINT('Ctrl Pts',(113.378674536928,4.56327998001207,128.969787401115));
#43062=CARTESIAN_POINT('Ctrl Pts',(113.370900202809,4.51239165893472,128.843208829757));
#43063=CARTESIAN_POINT('Ctrl Pts',(113.36312586869,4.45615209229471,128.718548720674));
#43064=CARTESIAN_POINT('Ctrl Pts',(113.355351534571,4.39472626659451,128.596292660232));
#43065=CARTESIAN_POINT('Ctrl Pts',(113.347586781624,4.33337614273474,128.474187269458));
#43066=CARTESIAN_POINT('Ctrl Pts',(113.339822028676,4.26685265103566,128.354480378281));
#43067=CARTESIAN_POINT('Ctrl Pts',(113.332057275729,4.19536947267995,128.237639352955));
#43068=CARTESIAN_POINT('Ctrl Pts',(113.324300234844,4.12395729242486,128.120914375783));
#43069=CARTESIAN_POINT('Ctrl Pts',(113.316543193959,4.04759543125197,128.007049931303));
#43070=CARTESIAN_POINT('Ctrl Pts',(113.308786153074,3.96654411557375,127.896490118093));
#43071=CARTESIAN_POINT('Ctrl Pts',(113.301034961834,3.88555392132284,127.786013678897));
#43072=CARTESIAN_POINT('Ctrl Pts',(113.293283770594,3.79988154168427,127.678837224734));
#43073=CARTESIAN_POINT('Ctrl Pts',(113.285532579354,3.70983106875204,127.575376798495));
#43074=CARTESIAN_POINT('Ctrl Pts',(113.277784682577,3.61981886967329,127.471960345697));
#43075=CARTESIAN_POINT('Ctrl Pts',(113.2700367858,3.52543253444647,127.372257073783));
#43076=CARTESIAN_POINT('Ctrl Pts',(113.262288889023,3.42701693747799,127.276650599333));
#43077=CARTESIAN_POINT('Ctrl Pts',(113.254542612939,3.32862192693073,127.181064123697));
#43078=CARTESIAN_POINT('Ctrl Pts',(113.246796336855,3.22619961133592,127.089573013233));
#43079=CARTESIAN_POINT('Ctrl Pts',(113.23905006077,3.12013200335912,127.002524305451));
#43080=CARTESIAN_POINT('Ctrl Pts',(113.231303727505,3.01406361241533,126.915474955096));
#43081=CARTESIAN_POINT('Ctrl Pts',(113.22355739424,2.90435017761357,126.832868320885));
#43082=CARTESIAN_POINT('Ctrl Pts',(113.215811060974,2.79140677558456,126.755011129596));
#43083=CARTESIAN_POINT('Ctrl Pts',(113.208062992971,2.67843808066414,126.677136502729));
#43084=CARTESIAN_POINT('Ctrl Pts',(113.200314924968,2.56223830100829,126.604013657088));
#43085=CARTESIAN_POINT('Ctrl Pts',(113.192566856965,2.44325112103519,126.535905742314));
#43086=CARTESIAN_POINT('Ctrl Pts',(113.184810554224,2.32413748007085,126.467725441638));
#43087=CARTESIAN_POINT('Ctrl Pts',(113.177054251482,2.20223086076412,126.404570913466));
#43088=CARTESIAN_POINT('Ctrl Pts',(113.16929794874,2.0779996501665,126.346659358351));
#43089=CARTESIAN_POINT('Ctrl Pts',(113.161537506226,1.95370213363082,126.288716894095));
#43090=CARTESIAN_POINT('Ctrl Pts',(113.153777063712,1.82707791437718,126.236023128946));
#43091=CARTESIAN_POINT('Ctrl Pts',(113.146016621197,1.6986140098067,126.188746518858));
#43092=CARTESIAN_POINT('Ctrl Pts',(113.138243720932,1.56994388357256,126.14139401616));
#43093=CARTESIAN_POINT('Ctrl Pts',(113.130470820666,1.43942854298673,126.099476165719));
#43094=CARTESIAN_POINT('Ctrl Pts',(113.122697920401,1.30756963172069,126.063111339084));
#43095=CARTESIAN_POINT('Ctrl Pts',(113.115207584639,1.180504124012,126.028068465496));
#43096=CARTESIAN_POINT('Ctrl Pts',(113.107717248877,1.05219133402489,125.998181962175));
#43097=CARTESIAN_POINT('Ctrl Pts',(113.100226913115,0.923085888692947,125.973512296143));
#43098=CARTESIAN_POINT('Ctrl Pts',(113.092452578996,0.789085371159932,125.947907272225));
#43099=CARTESIAN_POINT('Ctrl Pts',(113.084678244877,0.653806431333827,125.927841378475));
#43100=CARTESIAN_POINT('Ctrl Pts',(113.076903910758,0.517746786012154,125.913438278367));
#43101=CARTESIAN_POINT('Ctrl Pts',(113.069139157811,0.381854822043895,125.899052928793));
#43102=CARTESIAN_POINT('Ctrl Pts',(113.061374404864,0.245184452031789,125.890316527718));
#43103=CARTESIAN_POINT('Ctrl Pts',(113.053609651917,0.108244384340495,125.887301921988));
#43104=CARTESIAN_POINT('Ctrl Pts',(113.045852611032,-0.0285596725451436,
125.884290310407));
#43105=CARTESIAN_POINT('Ctrl Pts',(113.038095570147,-0.165632505700293,
125.886989193357));
#43106=CARTESIAN_POINT('Ctrl Pts',(113.030338529262,-0.302459823683665,
125.895419681116));
#43107=CARTESIAN_POINT('Ctrl Pts',(113.022587338021,-0.439183959122743,
125.903843811378));
#43108=CARTESIAN_POINT('Ctrl Pts',(113.014836146781,-0.575662559263489,
125.91799091933));
#43109=CARTESIAN_POINT('Ctrl Pts',(113.007084955541,-0.711381226234788,
125.937830045027));
#43110=CARTESIAN_POINT('Ctrl Pts',(112.999337058764,-0.847042209151933,
125.957660738565));
#43111=CARTESIAN_POINT('Ctrl Pts',(112.991589161987,-0.981943515261864,
125.983178581694));
#43112=CARTESIAN_POINT('Ctrl Pts',(112.98384126521,-1.11557598402841,126.01430077594));
#43113=CARTESIAN_POINT('Ctrl Pts',(112.976094989126,-1.24918049976328,126.045416460094));
#43114=CARTESIAN_POINT('Ctrl Pts',(112.968348713042,-1.38151632554283,126.082134074954));
#43115=CARTESIAN_POINT('Ctrl Pts',(112.960602436958,-1.5120850017042,126.124319804697));
#43116=CARTESIAN_POINT('Ctrl Pts',(112.952856103692,-1.64265464169388,126.166505845845));
#43117=CARTESIAN_POINT('Ctrl Pts',(112.945109770427,-1.77145673400635,126.21415996222));
#43118=CARTESIAN_POINT('Ctrl Pts',(112.937363437161,-1.89800886166085,126.267098731411));
#43119=CARTESIAN_POINT('Ctrl Pts',(112.929615369158,-2.02458932978722,126.320049355872));
#43120=CARTESIAN_POINT('Ctrl Pts',(112.921867301155,-2.14891847001423,126.378286837252));
#43121=CARTESIAN_POINT('Ctrl Pts',(112.914119233152,-2.27053506482922,126.441580130092));
#43122=CARTESIAN_POINT('Ctrl Pts',(112.906362930411,-2.39228091520811,126.504940691798));
#43123=CARTESIAN_POINT('Ctrl Pts',(112.898606627669,-2.51130811385827,126.573367618083));
#43124=CARTESIAN_POINT('Ctrl Pts',(112.890850324927,-2.6271807491615,126.646584243862));
#43125=CARTESIAN_POINT('Ctrl Pts',(112.883089882413,-2.74311522917913,126.719839947558));
#43126=CARTESIAN_POINT('Ctrl Pts',(112.875329439899,-2.85589146963866,126.79789022222));
#43127=CARTESIAN_POINT('Ctrl Pts',(112.867568997384,-2.96510449897364,126.880416380874));
#43128=CARTESIAN_POINT('Ctrl Pts',(112.859796097119,-3.07449284675872,126.963075017845));
#43129=CARTESIAN_POINT('Ctrl Pts',(112.852023196853,-3.18030625111083,127.050223648203));
#43130=CARTESIAN_POINT('Ctrl Pts',(112.844250296588,-3.28217397203618,127.141504207633));
#43131=CARTESIAN_POINT('Ctrl Pts',(112.836759960826,-3.38033854471555,127.229466488805));
#43132=CARTESIAN_POINT('Ctrl Pts',(112.829269625064,-3.47483910359065,127.321265287964));
#43133=CARTESIAN_POINT('Ctrl Pts',(112.821779289302,-3.56537903908143,127.416550798497));
#43134=CARTESIAN_POINT('Ctrl Pts',(112.814101568287,-3.65818400637564,127.514220060582));
#43135=CARTESIAN_POINT('Ctrl Pts',(112.806423847272,-3.74713767467342,127.615879466278));
#43136=CARTESIAN_POINT('Ctrl Pts',(112.798746126257,-3.83187082516827,127.721188705115));
#43137=CARTESIAN_POINT('Ctrl Pts',(112.791077478074,-3.91650384573452,127.826373499075));
#43138=CARTESIAN_POINT('Ctrl Pts',(112.783408829892,-3.99692601563795,127.935199241451));
#43139=CARTESIAN_POINT('Ctrl Pts',(112.775740181709,-4.07280442560457,128.047288407181));
#43140=CARTESIAN_POINT('Ctrl Pts',(112.767775512486,-4.15161185322238,128.163704378719));
#43141=CARTESIAN_POINT('Ctrl Pts',(112.759810843262,-4.22551736617257,128.283640488079));
#43142=CARTESIAN_POINT('Ctrl Pts',(112.751846174039,-4.29419299984012,128.406634706911));
#43143=CARTESIAN_POINT('Ctrl Pts',(112.744191036869,-4.3601996827535,128.524848984219));
#43144=CARTESIAN_POINT('Ctrl Pts',(112.736535899699,-4.42137513354883,128.645887747828));
#43145=CARTESIAN_POINT('Ctrl Pts',(112.728880762529,-4.47747202685312,128.76931091025));
#43146=CARTESIAN_POINT('Ctrl Pts',(112.721228978975,-4.53354434483844,128.892680002591));
#43147=CARTESIAN_POINT('Ctrl Pts',(112.713577195422,-4.58454236614004,129.018431050676));
#43148=CARTESIAN_POINT('Ctrl Pts',(112.705925411868,-4.63026525524111,129.146100466502));
#43149=CARTESIAN_POINT('Ctrl Pts',(112.69827489598,-4.67598056945924,129.273748731414));
#43150=CARTESIAN_POINT('Ctrl Pts',(112.690624380093,-4.71642235479985,129.40331435413));
#43151=CARTESIAN_POINT('Ctrl Pts',(112.682973864205,-4.75143853263936,129.53431536914));
#43152=CARTESIAN_POINT('Ctrl Pts',(112.682037293146,-4.7557251898085,129.550352426146));
#43153=CARTESIAN_POINT('Ctrl Pts',(112.681100722086,-4.75993059748163,129.566410975894));
#43154=CARTESIAN_POINT('Ctrl Pts',(112.680164151027,-4.76405452823403,129.582490119308));
#43155=CARTESIAN_POINT('Origin',(213.235140564004,0.,130.804360617566));
#43156=CARTESIAN_POINT('',(110.584632631705,-4.76405452823407,129.582490119308));
#43157=CARTESIAN_POINT('',(110.930234911077,-4.76405452823406,129.582490119308));
#43158=CARTESIAN_POINT('',(213.235140564004,-4.76405452823405,129.582490119308));
#43159=CARTESIAN_POINT('',(112.264859435957,-4.91824956414205,130.802290033936));
#43160=CARTESIAN_POINT('Ctrl Pts',(112.264859435957,-4.91824956414205,130.802290033936));
#43161=CARTESIAN_POINT('Ctrl Pts',(112.257165042791,-4.91830645312108,130.937418213418));
#43162=CARTESIAN_POINT('Ctrl Pts',(112.249470649625,-4.91279019552954,131.07277397242));
#43163=CARTESIAN_POINT('Ctrl Pts',(112.241776256459,-4.90167077659974,131.207853691023));
#43164=CARTESIAN_POINT('Ctrl Pts',(112.234090909914,-4.89056443123831,131.342774590722));
#43165=CARTESIAN_POINT('Ctrl Pts',(112.22640556337,-4.87386806018489,131.47741970112));
#43166=CARTESIAN_POINT('Ctrl Pts',(112.218720216826,-4.85160363543908,131.611283926868));
#43167=CARTESIAN_POINT('Ctrl Pts',(112.211041976725,-4.82935979803793,131.745024371787));
#43168=CARTESIAN_POINT('Ctrl Pts',(112.203363736624,-4.80155821467893,131.877984976763));
#43169=CARTESIAN_POINT('Ctrl Pts',(112.195685496523,-4.76827274359631,132.009664772199));
#43170=CARTESIAN_POINT('Ctrl Pts',(112.187782993086,-4.73401508217962,132.145190624794));
#43171=CARTESIAN_POINT('Ctrl Pts',(112.179880489648,-4.69394830635821,132.279359272445));
#43172=CARTESIAN_POINT('Ctrl Pts',(112.17197798621,-4.64820982799618,132.411634227571));
#43173=CARTESIAN_POINT('Ctrl Pts',(112.164307332625,-4.603813261035,132.540028396177));
#43174=CARTESIAN_POINT('Ctrl Pts',(112.15663667904,-4.55407327827764,132.66663803191));
#43175=CARTESIAN_POINT('Ctrl Pts',(112.148966025455,-4.4991662897558,132.790987346377));
#43176=CARTESIAN_POINT('Ctrl Pts',(112.141296200005,-4.44426522907564,132.915323235903));
#43177=CARTESIAN_POINT('Ctrl Pts',(112.133626374556,-4.38419843324348,133.037398923964));
#43178=CARTESIAN_POINT('Ctrl Pts',(112.125956549106,-4.31919024906225,133.156759107386));
#43179=CARTESIAN_POINT('Ctrl Pts',(112.11828580975,-4.25417431876513,133.27613351329));
#43180=CARTESIAN_POINT('Ctrl Pts',(112.110615070395,-4.18421602040058,133.392791420241));
#43181=CARTESIAN_POINT('Ctrl Pts',(112.102944331039,-4.10958514162716,133.506303071842));
#43182=CARTESIAN_POINT('Ctrl Pts',(112.094867754621,-4.03100575473559,133.625820302972));
#43183=CARTESIAN_POINT('Ctrl Pts',(112.086791178203,-3.94724614939418,133.741848862472));
#43184=CARTESIAN_POINT('Ctrl Pts',(112.078714601785,-3.85867157109584,133.853923991054));
#43185=CARTESIAN_POINT('Ctrl Pts',(112.07103253183,-3.7744234848383,133.960524725502));
#43186=CARTESIAN_POINT('Ctrl Pts',(112.063350461875,-3.68581995801667,134.063548816537));
#43187=CARTESIAN_POINT('Ctrl Pts',(112.05566839192,-3.59321451679928,134.16263286662));
#43188=CARTESIAN_POINT('Ctrl Pts',(112.047981149009,-3.50054671688989,134.261783637963));
#43189=CARTESIAN_POINT('Ctrl Pts',(112.040293906098,-3.40387192149152,134.356988807403));
#43190=CARTESIAN_POINT('Ctrl Pts',(112.032606663187,-3.30357817157142,134.447924028132));
#43191=CARTESIAN_POINT('Ctrl Pts',(112.024908858096,-3.20314661922482,134.53898419278));
#43192=CARTESIAN_POINT('Ctrl Pts',(112.017211053004,-3.09908649696322,134.625762449481));
#43193=CARTESIAN_POINT('Ctrl Pts',(112.009513247913,-2.99181647378796,134.707976537411));
#43194=CARTESIAN_POINT('Ctrl Pts',(112.008350636616,-2.97561531784006,134.720393457071));
#43195=CARTESIAN_POINT('Ctrl Pts',(112.007188025319,-2.95934099060744,134.732706349626));
#43196=CARTESIAN_POINT('Ctrl Pts',(112.006025414022,-2.94299498426938,134.744914333107));
#43197=CARTESIAN_POINT('Ctrl Pts',(111.998251079903,-2.83368990944292,134.826548618589));
#43198=CARTESIAN_POINT('Ctrl Pts',(111.990476745784,-2.72081250934746,134.903760820993));
#43199=CARTESIAN_POINT('Ctrl Pts',(111.982702411665,-2.60475628381479,134.976222044367));
#43200=CARTESIAN_POINT('Ctrl Pts',(111.974937658718,-2.48884308720792,135.048593965759));
#43201=CARTESIAN_POINT('Ctrl Pts',(111.967172905771,-2.36975918850557,135.116226353066));
#43202=CARTESIAN_POINT('Ctrl Pts',(111.959408152824,-2.24793019785474,135.178831201314));
#43203=CARTESIAN_POINT('Ctrl Pts',(111.951651111939,-2.12622220947482,135.241373869543));
#43204=CARTESIAN_POINT('Ctrl Pts',(111.943894071054,-2.00177490042135,135.298898758311));
#43205=CARTESIAN_POINT('Ctrl Pts',(111.936137030169,-1.87504152976425,135.35116194643));
#43206=CARTESIAN_POINT('Ctrl Pts',(111.928385838929,-1.74840372972773,135.403385722472));
#43207=CARTESIAN_POINT('Ctrl Pts',(111.920634647688,-1.61948365945458,135.450355547259));
#43208=CARTESIAN_POINT('Ctrl Pts',(111.912883456448,-1.48875744782896,135.491874278776));
#43209=CARTESIAN_POINT('Ctrl Pts',(111.905135559671,-1.3580867983307,135.533375363725));
#43210=CARTESIAN_POINT('Ctrl Pts',(111.897387662894,-1.22561190613693,135.569429845365));
#43211=CARTESIAN_POINT('Ctrl Pts',(111.889639766117,-1.0918268630657,135.599889489712));
#43212=CARTESIAN_POINT('Ctrl Pts',(111.881893490033,-0.958069804941316,
135.630342762558));
#43213=CARTESIAN_POINT('Ctrl Pts',(111.874147213949,-0.823003522018772,
135.655203439204));
#43214=CARTESIAN_POINT('Ctrl Pts',(111.866400937865,-0.687134796638426,
135.674373844832));
#43215=CARTESIAN_POINT('Ctrl Pts',(111.858654604599,-0.551265068305921,
135.693544391973));
#43216=CARTESIAN_POINT('Ctrl Pts',(111.850908271334,-0.414593272826536,
135.707024529658));
#43217=CARTESIAN_POINT('Ctrl Pts',(111.843161938069,-0.277633462249825,
135.714768209929));
#43218=CARTESIAN_POINT('Ctrl Pts',(111.835413870066,-0.140642980473522,
135.722513624345));
#43219=CARTESIAN_POINT('Ctrl Pts',(111.827665802063,-0.00336474552146701,
135.724520002997));
#43220=CARTESIAN_POINT('Ctrl Pts',(111.81991773406,0.133685425790239,135.720793396465));
#43221=CARTESIAN_POINT('Ctrl Pts',(111.812161431318,0.270881255655212,135.717062829251));
#43222=CARTESIAN_POINT('Ctrl Pts',(111.804405128576,0.407848146238273,135.707587115905));
#43223=CARTESIAN_POINT('Ctrl Pts',(111.796648825834,0.544073085024587,135.69242439995));
#43224=CARTESIAN_POINT('Ctrl Pts',(111.78888838332,0.68037073116257,135.677253591197));
#43225=CARTESIAN_POINT('Ctrl Pts',(111.781127940806,0.815925250210358,135.656389791139));
#43226=CARTESIAN_POINT('Ctrl Pts',(111.773367498292,0.950233074196477,135.629942465095));
#43227=CARTESIAN_POINT('Ctrl Pts',(111.765594598026,1.08475650102476,135.603452683455));
#43228=CARTESIAN_POINT('Ctrl Pts',(111.757821697761,1.2180288532253,135.571361556134));
#43229=CARTESIAN_POINT('Ctrl Pts',(111.750048797495,1.34956012402267,135.533828931674));
#43230=CARTESIAN_POINT('Ctrl Pts',(111.742558461733,1.4763099018183,135.497660712652));
#43231=CARTESIAN_POINT('Ctrl Pts',(111.735068125971,1.60144269333784,135.4564398485));
#43232=CARTESIAN_POINT('Ctrl Pts',(111.727577790209,1.72453876751733,135.410351184407));
#43233=CARTESIAN_POINT('Ctrl Pts',(111.71980345609,1.85230206676458,135.362515054606));
#43234=CARTESIAN_POINT('Ctrl Pts',(111.712029121971,1.97827587134586,135.309283182464));
#43235=CARTESIAN_POINT('Ctrl Pts',(111.704254787852,2.10197077551009,135.250808854238));
#43236=CARTESIAN_POINT('Ctrl Pts',(111.696490034905,2.22551323676003,135.192406590395));
#43237=CARTESIAN_POINT('Ctrl Pts',(111.688725281958,2.34678203568538,135.128774891138));
#43238=CARTESIAN_POINT('Ctrl Pts',(111.680960529011,2.46530481286291,135.060116160613));
#43239=CARTESIAN_POINT('Ctrl Pts',(111.673203488126,2.58370987154654,134.991525622908));
#43240=CARTESIAN_POINT('Ctrl Pts',(111.665446447241,2.69937399999404,134.917918184773));
#43241=CARTESIAN_POINT('Ctrl Pts',(111.657689406356,2.81184698280311,134.839543340542));
#43242=CARTESIAN_POINT('Ctrl Pts',(111.649938215116,2.92423514886092,134.76122759939));
#43243=CARTESIAN_POINT('Ctrl Pts',(111.642187023876,3.03343663973857,134.678151830663));
#43244=CARTESIAN_POINT('Ctrl Pts',(111.634435832636,3.13902823498417,134.590610055));
#43245=CARTESIAN_POINT('Ctrl Pts',(111.626687935859,3.24457495098547,134.503105486928));
#43246=CARTESIAN_POINT('Ctrl Pts',(111.618940039082,3.34651452261505,134.411138936247));
#43247=CARTESIAN_POINT('Ctrl Pts',(111.611192142305,3.44445516772763,134.31504597231));
#43248=CARTESIAN_POINT('Ctrl Pts',(111.60344586622,3.54237532576874,134.218973108949));
#43249=CARTESIAN_POINT('Ctrl Pts',(111.595699590136,3.63629794221854,134.118775822833));
#43250=CARTESIAN_POINT('Ctrl Pts',(111.587953314052,3.72586691225441,134.014827688674));
#43251=CARTESIAN_POINT('Ctrl Pts',(111.580206980787,3.81543654346802,133.910878787193));
#43252=CARTESIAN_POINT('Ctrl Pts',(111.572460647522,3.90065220893055,133.803179278599));
#43253=CARTESIAN_POINT('Ctrl Pts',(111.564714314256,3.98119730950177,133.692136759395));
#43254=CARTESIAN_POINT('Ctrl Pts',(111.556966246253,4.06176044758986,133.581069372988));
#43255=CARTESIAN_POINT('Ctrl Pts',(111.54921817825,4.13765070997256,133.466657802671));
#43256=CARTESIAN_POINT('Ctrl Pts',(111.541470110247,4.20859437558527,133.349339290226));
#43257=CARTESIAN_POINT('Ctrl Pts',(111.533713807505,4.27961344097,133.231896090269));
#43258=CARTESIAN_POINT('Ctrl Pts',(111.525957504764,4.34567520492794,133.111540111597));
#43259=CARTESIAN_POINT('Ctrl Pts',(111.518201202022,4.40655128945769,132.988734394162));
#43260=CARTESIAN_POINT('Ctrl Pts',(111.510440759508,4.46745986538682,132.865863131617));
#43261=CARTESIAN_POINT('Ctrl Pts',(111.502680316993,4.5231770881539,132.740539882081));
#43262=CARTESIAN_POINT('Ctrl Pts',(111.494919874479,4.57352286324126,132.613247480228));
#43263=CARTESIAN_POINT('Ctrl Pts',(111.487146974214,4.62394945783614,132.48575073731));
#43264=CARTESIAN_POINT('Ctrl Pts',(111.479374073948,4.66898724527533,132.356278894748));
#43265=CARTESIAN_POINT('Ctrl Pts',(111.471601173683,4.70850585003369,132.225330611161));
#43266=CARTESIAN_POINT('Ctrl Pts',(111.464110837921,4.74658785396819,132.09914262752));
#43267=CARTESIAN_POINT('Ctrl Pts',(111.456620502159,4.77954490387742,131.971583982118));
#43268=CARTESIAN_POINT('Ctrl Pts',(111.449130166397,4.80730564036021,131.843107719926));
#43269=CARTESIAN_POINT('Ctrl Pts',(111.441355832278,4.8361189336041,131.709760241205));
#43270=CARTESIAN_POINT('Ctrl Pts',(111.433581498159,4.85942537042342,131.575001784493));
#43271=CARTESIAN_POINT('Ctrl Pts',(111.425807164039,4.8770893791242,131.439326955677));
#43272=CARTESIAN_POINT('Ctrl Pts',(111.418042411092,4.89473161851294,131.303819333961));
#43273=CARTESIAN_POINT('Ctrl Pts',(111.410277658145,4.90674521575874,131.167397971176));
#43274=CARTESIAN_POINT('Ctrl Pts',(111.402512905198,4.91304513739603,131.030569681065));
#43275=CARTESIAN_POINT('Ctrl Pts',(111.394755864313,4.91933880186232,130.893877290742));
#43276=CARTESIAN_POINT('Ctrl Pts',(111.386998823428,4.91993006616789,130.756779165427));
#43277=CARTESIAN_POINT('Ctrl Pts',(111.379241782543,4.91478548453854,130.61978894187));
#43278=CARTESIAN_POINT('Ctrl Pts',(111.371490591303,4.90964478247818,130.482902023705));
#43279=CARTESIAN_POINT('Ctrl Pts',(111.363739400063,4.89877685863359,130.346123234446));
#43280=CARTESIAN_POINT('Ctrl Pts',(111.355988208823,4.88220031990499,130.209967566783));
#43281=CARTESIAN_POINT('Ctrl Pts',(111.348240312046,4.86563082664764,130.073869768911));
#43282=CARTESIAN_POINT('Ctrl Pts',(111.340492415269,4.84335759141013,129.93839495317));
#43283=CARTESIAN_POINT('Ctrl Pts',(111.332744518491,4.81545117037186,129.804054120404));
#43284=CARTESIAN_POINT('Ctrl Pts',(111.324998242407,4.78755058675529,129.669741388845));
#43285=CARTESIAN_POINT('Ctrl Pts',(111.317251966323,4.75401924058959,129.536562550998));
#43286=CARTESIAN_POINT('Ctrl Pts',(111.309505690239,4.7149789475052,129.405019134195));
#43287=CARTESIAN_POINT('Ctrl Pts',(111.301759356974,4.67593836623427,129.273474746368));
#43288=CARTESIAN_POINT('Ctrl Pts',(111.294013023709,4.6313888681365,129.14356617848));
#43289=CARTESIAN_POINT('Ctrl Pts',(111.286266690443,4.58150224612414,129.01578011022));
#43290=CARTESIAN_POINT('Ctrl Pts',(111.27851862244,4.53160445234873,128.887965425155));
#43291=CARTESIAN_POINT('Ctrl Pts',(111.270770554437,4.47636729847742,128.762274549675));
#43292=CARTESIAN_POINT('Ctrl Pts',(111.263022486434,4.41601069548345,128.639174112926));
#43293=CARTESIAN_POINT('Ctrl Pts',(111.255266183692,4.35558994477336,128.515942843567));
#43294=CARTESIAN_POINT('Ctrl Pts',(111.247509880951,4.2900390483252,128.395307864252));
#43295=CARTESIAN_POINT('Ctrl Pts',(111.239753578209,4.21962413087738,128.277711600267));
#43296=CARTESIAN_POINT('Ctrl Pts',(111.231993135694,4.14917163086796,128.160052571615));
#43297=CARTESIAN_POINT('Ctrl Pts',(111.22423269318,4.07385015156888,128.045435816543));
#43298=CARTESIAN_POINT('Ctrl Pts',(111.216472250666,3.99396856997989,127.934273837604));
#43299=CARTESIAN_POINT('Ctrl Pts',(111.208699350401,3.91395875538463,127.822933411588));
#43300=CARTESIAN_POINT('Ctrl Pts',(111.200926450135,3.82937445162395,127.715059152049));
#43301=CARTESIAN_POINT('Ctrl Pts',(111.19315354987,3.7405647231614,127.611030284772));
#43302=CARTESIAN_POINT('Ctrl Pts',(111.185663214108,3.65498345202751,127.510783128855));
#43303=CARTESIAN_POINT('Ctrl Pts',(111.178172878346,3.56547884150072,127.414106865743));
#43304=CARTESIAN_POINT('Ctrl Pts',(111.170682542584,3.47239347964619,127.321306413995));
#43305=CARTESIAN_POINT('Ctrl Pts',(111.162908208465,3.3757787580033,127.224987404912));
#43306=CARTESIAN_POINT('Ctrl Pts',(111.155133874346,3.27500035020651,127.132538802033));
#43307=CARTESIAN_POINT('Ctrl Pts',(111.147359540227,3.17040110238271,127.044342012225));
#43308=CARTESIAN_POINT('Ctrl Pts',(111.13959478728,3.0659307637839,126.956253917078));
#43309=CARTESIAN_POINT('Ctrl Pts',(111.131830034333,2.95764925037871,126.87240745861));
#43310=CARTESIAN_POINT('Ctrl Pts',(111.124065281385,2.84593699626002,126.793148123093));
#43311=CARTESIAN_POINT('Ctrl Pts',(111.1163082405,2.7343356963266,126.713967509064));
#43312=CARTESIAN_POINT('Ctrl Pts',(111.108551199615,2.61931075347786,126.639365176118));
#43313=CARTESIAN_POINT('Ctrl Pts',(111.10079415873,2.50127622660025,126.569646896339));
#43314=CARTESIAN_POINT('Ctrl Pts',(111.09304296749,2.38333071047802,126.499981191659));
#43315=CARTESIAN_POINT('Ctrl Pts',(111.08529177625,2.26238046299699,126.435192407183));
#43316=CARTESIAN_POINT('Ctrl Pts',(111.07754058501,2.13886881957718,126.375543254529));
#43317=CARTESIAN_POINT('Ctrl Pts',(111.069792688233,2.01540967190009,126.315919454355));
#43318=CARTESIAN_POINT('Ctrl Pts',(111.062044791456,1.8893916448709,126.261431110907));
#43319=CARTESIAN_POINT('Ctrl Pts',(111.054296894679,1.76128279531167,126.21229507171));
#43320=CARTESIAN_POINT('Ctrl Pts',(111.046550618595,1.63320074336187,126.163169310713));
#43321=CARTESIAN_POINT('Ctrl Pts',(111.038804342511,1.50302910360973,126.119393766969));
#43322=CARTESIAN_POINT('Ctrl Pts',(111.031058066427,1.37125566952536,126.081137041311));
#43323=CARTESIAN_POINT('Ctrl Pts',(111.023311733161,1.2394812627197,126.04288003325));
#43324=CARTESIAN_POINT('Ctrl Pts',(111.015565399896,1.10610541344974,126.01014203357));
#43325=CARTESIAN_POINT('Ctrl Pts',(111.00781906663,0.971630437386399,125.983041570288));
#43326=CARTESIAN_POINT('Ctrl Pts',(111.000070998627,0.837125346584189,125.955935038046));
#43327=CARTESIAN_POINT('Ctrl Pts',(110.992322930624,0.701521022381416,125.934468631627));
#43328=CARTESIAN_POINT('Ctrl Pts',(110.984574862621,0.565328920347991,125.918709558156));
#43329=CARTESIAN_POINT('Ctrl Pts',(110.97681855988,0.428992071728189,125.902933735753));
#43330=CARTESIAN_POINT('Ctrl Pts',(110.969062257138,0.292066586370765,125.89287740844));
#43331=CARTESIAN_POINT('Ctrl Pts',(110.961305954396,0.155068536120264,125.88855581961));
#43332=CARTESIAN_POINT('Ctrl Pts',(110.953545511882,0.0179973658855062,
125.884231924218));
#43333=CARTESIAN_POINT('Ctrl Pts',(110.945785069368,-0.119146055662212,
125.885648862181));
#43334=CARTESIAN_POINT('Ctrl Pts',(110.938024626853,-0.255847722878992,
125.892769734237));
#43335=CARTESIAN_POINT('Ctrl Pts',(110.930251726588,-0.392768835747792,
125.899902037349));
#43336=CARTESIAN_POINT('Ctrl Pts',(110.922478826322,-0.529246387724954,
125.912756535399));
#43337=CARTESIAN_POINT('Ctrl Pts',(110.914705926057,-0.664772647547478,
125.931244531367));
#43338=CARTESIAN_POINT('Ctrl Pts',(110.907215590295,-0.795372186455674,
125.949060442113));
#43339=CARTESIAN_POINT('Ctrl Pts',(110.899725254533,-0.925088092888324,
125.972107324191));
#43340=CARTESIAN_POINT('Ctrl Pts',(110.892234918771,-1.05347865300944,126.000261764487));
#43341=CARTESIAN_POINT('Ctrl Pts',(110.884460584652,-1.18673718024092,126.029483688944));
#43342=CARTESIAN_POINT('Ctrl Pts',(110.876686250533,-1.31898999918757,126.064300689578));
#43343=CARTESIAN_POINT('Ctrl Pts',(110.868911916414,-1.44973090474329,126.104630479959));
#43344=CARTESIAN_POINT('Ctrl Pts',(110.861147163467,-1.58031068381783,126.144910567478));
#43345=CARTESIAN_POINT('Ctrl Pts',(110.853382410519,-1.70938188690138,126.190689812532));
#43346=CARTESIAN_POINT('Ctrl Pts',(110.845617657572,-1.83644821268875,126.241834888914));
#43347=CARTESIAN_POINT('Ctrl Pts',(110.837860616687,-1.96338833440977,126.292929167285));
#43348=CARTESIAN_POINT('Ctrl Pts',(110.830103575802,-2.08832718121577,126.349378526158));
#43349=CARTESIAN_POINT('Ctrl Pts',(110.822346534917,-2.21078368944838,126.410999883348));
#43350=CARTESIAN_POINT('Ctrl Pts',(110.814595343677,-2.33314785227431,126.472574771392));
#43351=CARTESIAN_POINT('Ctrl Pts',(110.806844152437,-2.45303305470429,126.539313719524));
#43352=CARTESIAN_POINT('Ctrl Pts',(110.799092961197,-2.56997863639138,126.610985739143));
#43353=CARTESIAN_POINT('Ctrl Pts',(110.79134506442,-2.68687451308767,126.682627296242));
#43354=CARTESIAN_POINT('Ctrl Pts',(110.783597167643,-2.80083292139165,126.759197550812));
#43355=CARTESIAN_POINT('Ctrl Pts',(110.775849270866,-2.9114184251922,126.840419924777));
#43356=CARTESIAN_POINT('Ctrl Pts',(110.768102994782,-3.02198079688953,126.921625308772));
#43357=CARTESIAN_POINT('Ctrl Pts',(110.760356718698,-3.12917135253408,127.007480645277));
#43358=CARTESIAN_POINT('Ctrl Pts',(110.752610442613,-3.23258457918507,127.097666672699));
#43359=CARTESIAN_POINT('Ctrl Pts',(110.744864109348,-3.33599856920837,127.187853365853));
#43360=CARTESIAN_POINT('Ctrl Pts',(110.737117776083,-3.43563487994359,127.282370556746));
#43361=CARTESIAN_POINT('Ctrl Pts',(110.729371442817,-3.53112227652322,127.380859700268));
#43362=CARTESIAN_POINT('Ctrl Pts',(110.721623374814,-3.62663105684415,127.479370899751));
#43363=CARTESIAN_POINT('Ctrl Pts',(110.713875306811,-3.71798880207566,127.581855541202));
#43364=CARTESIAN_POINT('Ctrl Pts',(110.706127238808,-3.80486251473392,127.687919649655));
#43365=CARTESIAN_POINT('Ctrl Pts',(110.698370936067,-3.89182855780733,127.794096484305));
#43366=CARTESIAN_POINT('Ctrl Pts',(110.690614633325,-3.97430080021255,127.903860082515));
#43367=CARTESIAN_POINT('Ctrl Pts',(110.682858330583,-4.05198746781253,128.016784497854));
#43368=CARTESIAN_POINT('Ctrl Pts',(110.675097888069,-4.12971559912601,128.129769184353));
#43369=CARTESIAN_POINT('Ctrl Pts',(110.667337445555,-4.20265285834884,128.245917718584));
#43370=CARTESIAN_POINT('Ctrl Pts',(110.65957700304,-4.27055245726914,128.364777708089));
#43371=CARTESIAN_POINT('Ctrl Pts',(110.651804102775,-4.33856105465366,128.483828502201));
#43372=CARTESIAN_POINT('Ctrl Pts',(110.64403120251,-4.40151565187973,128.605599102109));
#43373=CARTESIAN_POINT('Ctrl Pts',(110.636258302244,-4.45921643111155,128.729614396216));
#43374=CARTESIAN_POINT('Ctrl Pts',(110.628767966482,-4.51481964167916,128.849121422008));
#43375=CARTESIAN_POINT('Ctrl Pts',(110.62127763072,-4.56554426297981,128.97071249055));
#43376=CARTESIAN_POINT('Ctrl Pts',(110.613787294958,-4.61125536884304,129.093949267681));
#43377=CARTESIAN_POINT('Ctrl Pts',(110.604821183356,-4.66597265917731,129.241466646374));
#43378=CARTESIAN_POINT('Ctrl Pts',(110.595855071755,-4.71365072512056,129.391728716157));
#43379=CARTESIAN_POINT('Ctrl Pts',(110.586888960154,-4.75404349510082,129.544101315204));
#43380=CARTESIAN_POINT('Ctrl Pts',(110.586136850671,-4.75743178499588,129.556882873337));
#43381=CARTESIAN_POINT('Ctrl Pts',(110.585384741188,-4.76076883944629,129.569679268592));
#43382=CARTESIAN_POINT('Ctrl Pts',(110.584632631705,-4.76405452823407,129.582490119308));
#43383=CARTESIAN_POINT('Ctrl Pts',(112.334951030737,-4.76405452823405,129.582490119308));
#43384=CARTESIAN_POINT('Ctrl Pts',(112.327186197236,-4.79809550206713,129.71521535964));
#43385=CARTESIAN_POINT('Ctrl Pts',(112.319421363735,-4.82655156713842,129.849230819445));
#43386=CARTESIAN_POINT('Ctrl Pts',(112.311656530233,-4.84935412252618,129.984026748438));
#43387=CARTESIAN_POINT('Ctrl Pts',(112.303880958532,-4.87218821219024,130.119009090401));
#43388=CARTESIAN_POINT('Ctrl Pts',(112.296105386831,-4.88935313945802,130.254773669745));
#43389=CARTESIAN_POINT('Ctrl Pts',(112.288329815129,-4.90083223329311,130.390807134187));
#43390=CARTESIAN_POINT('Ctrl Pts',(112.287044222698,-4.90273015626524,130.413298546911));
#43391=CARTESIAN_POINT('Ctrl Pts',(112.285758630266,-4.90447276423942,130.435797314352));
#43392=CARTESIAN_POINT('Ctrl Pts',(112.284473037835,-4.90606011881192,130.458301123977));
#43393=CARTESIAN_POINT('Ctrl Pts',(112.277935170553,-4.9141325944039,130.572744019767));
#43394=CARTESIAN_POINT('Ctrl Pts',(112.271397303272,-4.91820122599546,130.687472648211));
#43395=CARTESIAN_POINT('Ctrl Pts',(112.264859435991,-4.91824956414179,130.802290033335));
#43396=CARTESIAN_POINT('',(112.610140563967,-4.91824789580415,130.808910114032));
#43397=CARTESIAN_POINT('Ctrl Pts',(112.680164151027,-4.76405452823403,129.582490119308));
#43398=CARTESIAN_POINT('Ctrl Pts',(112.672511249089,-4.79775195816247,129.713875887169));
#43399=CARTESIAN_POINT('Ctrl Pts',(112.66485834715,-4.82600509894512,129.846637463952));
#43400=CARTESIAN_POINT('Ctrl Pts',(112.657205445212,-4.84871854275895,129.980278367056));
#43401=CARTESIAN_POINT('Ctrl Pts',(112.649361298345,-4.87199959229714,130.117258937285));
#43402=CARTESIAN_POINT('Ctrl Pts',(112.641517151477,-4.8894603380112,130.255162923673));
#43403=CARTESIAN_POINT('Ctrl Pts',(112.63367300461,-4.901054442012,130.393448925186));
#43404=CARTESIAN_POINT('Ctrl Pts',(112.625828857743,-4.91264854601281,130.5317349267));
#43405=CARTESIAN_POINT('Ctrl Pts',(112.617984710875,-4.91837601863491,130.67040249058));
#43406=CARTESIAN_POINT('Ctrl Pts',(112.610140564008,-4.91824789580482,130.808910113306));
#43407=CARTESIAN_POINT('Ctrl Pts',(112.610140563967,-4.91824789580415,130.808910114032));
#43408=CARTESIAN_POINT('Ctrl Pts',(112.600025508912,-4.91808268093644,130.987516182108));
#43409=CARTESIAN_POINT('Ctrl Pts',(112.589910453858,-4.90818496828126,131.165688321249));
#43410=CARTESIAN_POINT('Ctrl Pts',(112.579795398803,-4.88871656797851,131.342536592942));
#43411=CARTESIAN_POINT('Ctrl Pts',(112.56942060632,-4.86874825223235,131.523926027792));
#43412=CARTESIAN_POINT('Ctrl Pts',(112.559045813837,-4.83871138131471,131.703923091685));
#43413=CARTESIAN_POINT('Ctrl Pts',(112.548671021353,-4.79882824532939,131.881593430995));
#43414=CARTESIAN_POINT('Ctrl Pts',(112.546891236065,-4.79198633318692,131.912072600245));
#43415=CARTESIAN_POINT('Ctrl Pts',(112.545111450777,-4.78485476703272,131.942483348665));
#43416=CARTESIAN_POINT('Ctrl Pts',(112.543331665489,-4.77743480839001,131.972821020867));
#43417=CARTESIAN_POINT('Ctrl Pts',(112.53555733137,-4.74502346190569,132.105339927322));
#43418=CARTESIAN_POINT('Ctrl Pts',(112.527782997251,-4.70704278471488,132.23671914871));
#43419=CARTESIAN_POINT('Ctrl Pts',(112.520008663132,-4.66358718707587,132.366454600347));
#43420=CARTESIAN_POINT('Ctrl Pts',(112.512243910184,-4.62018514457724,132.496030164635));
#43421=CARTESIAN_POINT('Ctrl Pts',(112.504479157237,-4.57132172982918,132.623965622747));
#43422=CARTESIAN_POINT('Ctrl Pts',(112.49671440429,-4.51714214050766,132.74976801576));
#43423=CARTESIAN_POINT('Ctrl Pts',(112.488957363405,-4.46301636311794,132.875445460064));
#43424=CARTESIAN_POINT('Ctrl Pts',(112.48120032252,-4.40358507243615,132.998993698604));
#43425=CARTESIAN_POINT('Ctrl Pts',(112.473443281635,-4.3390428421268,133.119936199724));
#43426=CARTESIAN_POINT('Ctrl Pts',(112.465692090395,-4.27454928361557,133.240787497163));
#43427=CARTESIAN_POINT('Ctrl Pts',(112.457940899155,-4.20495264035351,133.359036624882));
#43428=CARTESIAN_POINT('Ctrl Pts',(112.450189707915,-4.1304948889987,133.474228598283));
#43429=CARTESIAN_POINT('Ctrl Pts',(112.442441811138,-4.05606878417434,133.589371612022));
#43430=CARTESIAN_POINT('Ctrl Pts',(112.434693914361,-3.97678589236462,133.701459728137));
#43431=CARTESIAN_POINT('Ctrl Pts',(112.426946017584,-3.89293316126326,133.810064273025));
#43432=CARTESIAN_POINT('Ctrl Pts',(112.419199741499,-3.80909797034559,133.918646100182));
#43433=CARTESIAN_POINT('Ctrl Pts',(112.411453465415,-3.72069508027764,134.023745496248));
#43434=CARTESIAN_POINT('Ctrl Pts',(112.403707189331,-3.62805339190574,134.124964726457));
#43435=CARTESIAN_POINT('Ctrl Pts',(112.395960856066,-3.53541101967394,134.226184703843));
#43436=CARTESIAN_POINT('Ctrl Pts',(112.388214522801,-3.43853005066551,134.323524169814));
#43437=CARTESIAN_POINT('Ctrl Pts',(112.380468189535,-3.33777783535336,134.416620600502));
#43438=CARTESIAN_POINT('Ctrl Pts',(112.372720121532,-3.23700305728123,134.509737879491));
#43439=CARTESIAN_POINT('Ctrl Pts',(112.364972053529,-3.13235559489112,134.598609967135));
#43440=CARTESIAN_POINT('Ctrl Pts',(112.357223985526,-3.02423730071441,134.682913416158));
#43441=CARTESIAN_POINT('Ctrl Pts',(112.349467682784,-2.91600409712795,134.76730646389));
#43442=CARTESIAN_POINT('Ctrl Pts',(112.341711380043,-2.80429300170543,134.847120932622));
#43443=CARTESIAN_POINT('Ctrl Pts',(112.333955077301,-2.68953683999136,134.922075353779));
#43444=CARTESIAN_POINT('Ctrl Pts',(112.326194634787,-2.57471942945855,134.997069780369));
#43445=CARTESIAN_POINT('Ctrl Pts',(112.318434192272,-2.45685405002427,135.067198790898));
#43446=CARTESIAN_POINT('Ctrl Pts',(112.310673749758,-2.33639888610519,135.132226524397));
#43447=CARTESIAN_POINT('Ctrl Pts',(112.302900849493,-2.2157503568634,135.197358646186));
#43448=CARTESIAN_POINT('Ctrl Pts',(112.295127949227,-2.09250408713119,135.257372955404));
#43449=CARTESIAN_POINT('Ctrl Pts',(112.287355048962,-1.96713984676166,135.312081093126));
#43450=CARTESIAN_POINT('Ctrl Pts',(112.2798647132,-1.84633291230294,135.36480045224));
#43451=CARTESIAN_POINT('Ctrl Pts',(112.272374377438,-1.72355960793693,135.412592615722));
#43452=CARTESIAN_POINT('Ctrl Pts',(112.264884041676,-1.59926137945267,135.455333215065));
#43453=CARTESIAN_POINT('Ctrl Pts',(112.257109707557,-1.47025034585598,135.499694337224));
#43454=CARTESIAN_POINT('Ctrl Pts',(112.249335373438,-1.33918780229806,135.538753796111));
#43455=CARTESIAN_POINT('Ctrl Pts',(112.241561039319,-1.20654888055078,135.572318551665));
#43456=CARTESIAN_POINT('Ctrl Pts',(112.233796286372,-1.07407342442037,135.605841941658));
#43457=CARTESIAN_POINT('Ctrl Pts',(112.226031533425,-0.9400258309641,135.633884007054));
#43458=CARTESIAN_POINT('Ctrl Pts',(112.218266780477,-0.804899323374295,
135.65630045043));
#43459=CARTESIAN_POINT('Ctrl Pts',(112.210509739592,-0.669907025336778,
135.678694629479));
#43460=CARTESIAN_POINT('Ctrl Pts',(112.202752698707,-0.533838328881824,
135.695474242211));
#43461=CARTESIAN_POINT('Ctrl Pts',(112.194995657822,-0.397199325406341,
135.706545411961));
#43462=CARTESIAN_POINT('Ctrl Pts',(112.187244466582,-0.260663362466276,
135.717608232856));
#43463=CARTESIAN_POINT('Ctrl Pts',(112.179493275342,-0.123558336651192,
135.722971147728));
#43464=CARTESIAN_POINT('Ctrl Pts',(112.171742084102,0.0136021663159125,
135.722591808103));
#43465=CARTESIAN_POINT('Ctrl Pts',(112.163994187325,0.15070437241038,135.722212629708));
#43466=CARTESIAN_POINT('Ctrl Pts',(112.156246290548,0.287861618614307,135.716096052085));
#43467=CARTESIAN_POINT('Ctrl Pts',(112.148498393771,0.424558147445553,135.704251783902));
#43468=CARTESIAN_POINT('Ctrl Pts',(112.140752117687,0.561226082309897,135.692409993284));
#43469=CARTESIAN_POINT('Ctrl Pts',(112.133005841603,0.697433102231994,135.674842928939));
#43470=CARTESIAN_POINT('Ctrl Pts',(112.125259565519,0.832666802748191,135.651612319108));
#43471=CARTESIAN_POINT('Ctrl Pts',(112.117513232253,0.967901501528752,135.628381537794));
#43472=CARTESIAN_POINT('Ctrl Pts',(112.109766898988,1.10216248124526,135.599487193761));
#43473=CARTESIAN_POINT('Ctrl Pts',(112.102020565722,1.23494617839759,135.565042396362));
#43474=CARTESIAN_POINT('Ctrl Pts',(112.09427249772,1.36775961153815,135.53058988529));
#43475=CARTESIAN_POINT('Ctrl Pts',(112.086524429717,1.49909472543948,135.490584545604));
#43476=CARTESIAN_POINT('Ctrl Pts',(112.078776361714,1.62846218363884,135.445189636067));
#43477=CARTESIAN_POINT('Ctrl Pts',(112.071020058972,1.75796713511235,135.39974648028));
#43478=CARTESIAN_POINT('Ctrl Pts',(112.06326375623,1.88549988389046,135.348902441804));
#43479=CARTESIAN_POINT('Ctrl Pts',(112.055507453488,2.01058966971157,135.29286952839));
#43480=CARTESIAN_POINT('Ctrl Pts',(112.047747010974,2.13574621971792,135.236806708523));
#43481=CARTESIAN_POINT('Ctrl Pts',(112.03998656846,2.25845685903948,135.175549669872));
#43482=CARTESIAN_POINT('Ctrl Pts',(112.032226125945,2.37827549129213,135.109356407346));
#43483=CARTESIAN_POINT('Ctrl Pts',(112.02445322568,2.49828646705019,135.043056885518));
#43484=CARTESIAN_POINT('Ctrl Pts',(112.016680325415,2.61539582433666,134.97180550834));
#43485=CARTESIAN_POINT('Ctrl Pts',(112.008907425149,2.7291857641288,134.895904107177));
#43486=CARTESIAN_POINT('Ctrl Pts',(112.001417089387,2.83883915299046,134.82276191313));
#43487=CARTESIAN_POINT('Ctrl Pts',(111.993926753625,2.94541002358644,134.745302086796));
#43488=CARTESIAN_POINT('Ctrl Pts',(111.986436417863,3.04855512894029,134.663828804805));
#43489=CARTESIAN_POINT('Ctrl Pts',(111.978662083744,3.15561101231339,134.579266438565));
#43490=CARTESIAN_POINT('Ctrl Pts',(111.970887749625,3.25931534746992,134.490112400395));
#43491=CARTESIAN_POINT('Ctrl Pts',(111.963113415506,3.3592489040113,134.396662089241));
#43492=CARTESIAN_POINT('Ctrl Pts',(111.955348662559,3.45905930137556,134.303326947244));
#43493=CARTESIAN_POINT('Ctrl Pts',(111.947583909612,3.55510788374279,134.205706331756));
#43494=CARTESIAN_POINT('Ctrl Pts',(111.939819156664,3.6470066504228,134.104137209136));
#43495=CARTESIAN_POINT('Ctrl Pts',(111.932062115779,3.73881414195219,134.0026689664));
#43496=CARTESIAN_POINT('Ctrl Pts',(111.924305074894,3.82647975946374,133.897260308953));
#43497=CARTESIAN_POINT('Ctrl Pts',(111.916548034009,3.909650967098,133.78828628319));
#43498=CARTESIAN_POINT('Ctrl Pts',(111.908796842769,3.9927594546776,133.679394435587));
#43499=CARTESIAN_POINT('Ctrl Pts',(111.901045651529,4.07138004227451,133.566942880837));
#43500=CARTESIAN_POINT('Ctrl Pts',(111.893294460289,4.14519949529019,133.451340822771));
#43501=CARTESIAN_POINT('Ctrl Pts',(111.885546563512,4.21898757306915,133.335787898663));
#43502=CARTESIAN_POINT('Ctrl Pts',(111.877798666735,4.28797836490992,133.217087463325));
#43503=CARTESIAN_POINT('Ctrl Pts',(111.870050769958,4.35190125947188,133.095678685907));
#43504=CARTESIAN_POINT('Ctrl Pts',(111.862304493874,4.41581078274232,132.974295304588));
#43505=CARTESIAN_POINT('Ctrl Pts',(111.85455821779,4.47465433529296,132.850205053766));
#43506=CARTESIAN_POINT('Ctrl Pts',(111.846811941705,4.52820688371257,132.723872399452));
#43507=CARTESIAN_POINT('Ctrl Pts',(111.83906560844,4.58175982744488,132.597538812578));
#43508=CARTESIAN_POINT('Ctrl Pts',(111.831319275175,4.63002153652351,132.468963149141));
#43509=CARTESIAN_POINT('Ctrl Pts',(111.823572941909,4.67281498467728,132.338630209742));
#43510=CARTESIAN_POINT('Ctrl Pts',(111.815824873906,4.71561801612706,132.208268083185));
#43511=CARTESIAN_POINT('Ctrl Pts',(111.808076805903,4.75295022794133,132.076148268971));
#43512=CARTESIAN_POINT('Ctrl Pts',(111.8003287379,4.78468447602984,131.942770705074));
#43513=CARTESIAN_POINT('Ctrl Pts',(111.792572435159,4.81645245165488,131.809251385914));
#43514=CARTESIAN_POINT('Ctrl Pts',(111.784816132417,4.84261048798266,131.674472027722));
#43515=CARTESIAN_POINT('Ctrl Pts',(111.777059829675,4.86308249571701,131.538943289803));
#43516=CARTESIAN_POINT('Ctrl Pts',(111.769299387161,4.8835654299783,131.403342216116));
#43517=CARTESIAN_POINT('Ctrl Pts',(111.761538944647,4.89835624639847,131.266991354232));
#43518=CARTESIAN_POINT('Ctrl Pts',(111.753778502132,4.90743087740996,131.130405470222));
#43519=CARTESIAN_POINT('Ctrl Pts',(111.746005601867,4.91652007582474,130.993600326426));
#43520=CARTESIAN_POINT('Ctrl Pts',(111.738232701602,4.91987474242937,130.856559797655));
#43521=CARTESIAN_POINT('Ctrl Pts',(111.730459801336,4.91752298592275,130.719798537286));
#43522=CARTESIAN_POINT('Ctrl Pts',(111.722969465574,4.91525672168886,130.588008893211));
#43523=CARTESIAN_POINT('Ctrl Pts',(111.715479129812,4.9076917347131,130.456478873341));
#43524=CARTESIAN_POINT('Ctrl Pts',(111.70798879405,4.89489840403446,130.325661675974));
#43525=CARTESIAN_POINT('Ctrl Pts',(111.700214459931,4.88162001033469,130.189884504809));
#43526=CARTESIAN_POINT('Ctrl Pts',(111.692440125812,4.86266691931936,130.054445175243));
#43527=CARTESIAN_POINT('Ctrl Pts',(111.684665791693,4.83806105421889,129.91985606803));
#43528=CARTESIAN_POINT('Ctrl Pts',(111.676901038746,4.81348551364809,129.785432829863));
#43529=CARTESIAN_POINT('Ctrl Pts',(111.669136285799,4.78327112996479,129.651858110093));
#43530=CARTESIAN_POINT('Ctrl Pts',(111.661371532851,4.74749167866028,129.519640483237));
#43531=CARTESIAN_POINT('Ctrl Pts',(111.653614491966,4.71174776401121,129.387554176792));
#43532=CARTESIAN_POINT('Ctrl Pts',(111.645857451081,4.67044988278964,129.25682265586));
#43533=CARTESIAN_POINT('Ctrl Pts',(111.638100410196,4.62372301790605,129.127945240583));
#43534=CARTESIAN_POINT('Ctrl Pts',(111.630349218956,4.57703139011475,128.999165012767));
#43535=CARTESIAN_POINT('Ctrl Pts',(111.622598027716,4.52491906032104,128.872236473647));
#43536=CARTESIAN_POINT('Ctrl Pts',(111.614846836476,4.46756099234455,128.747644341027));
#43537=CARTESIAN_POINT('Ctrl Pts',(111.607098939699,4.41022730307703,128.623105163387));
#43538=CARTESIAN_POINT('Ctrl Pts',(111.599351042922,4.34765247324044,128.500900771571));
#43539=CARTESIAN_POINT('Ctrl Pts',(111.591603146145,4.28005971623759,128.381496220217));
#43540=CARTESIAN_POINT('Ctrl Pts',(111.583856870061,4.21248109818238,128.262116645721));
#43541=CARTESIAN_POINT('Ctrl Pts',(111.576110593977,4.13988683323489,128.145536086782));
#43542=CARTESIAN_POINT('Ctrl Pts',(111.568364317892,4.06254605374773,128.032194925606));
#43543=CARTESIAN_POINT('Ctrl Pts',(111.560617984627,3.98520470334852,127.918852927771));
#43544=CARTESIAN_POINT('Ctrl Pts',(111.552871651362,3.90311698886153,127.808750698358));
#43545=CARTESIAN_POINT('Ctrl Pts',(111.545125318096,3.81659509973955,127.702299221148));
#43546=CARTESIAN_POINT('Ctrl Pts',(111.537377250093,3.7300538346404,127.595823904869));
#43547=CARTESIAN_POINT('Ctrl Pts',(111.52962918209,3.63907666549011,127.493001270978));
#43548=CARTESIAN_POINT('Ctrl Pts',(111.521881114087,3.54401547977851,127.394208518086));
#43549=CARTESIAN_POINT('Ctrl Pts',(111.514124811346,3.44885326190744,127.29531076708));
#43550=CARTESIAN_POINT('Ctrl Pts',(111.506368508604,3.34959862829066,127.200451735011));
#43551=CARTESIAN_POINT('Ctrl Pts',(111.498612205862,3.24664008294344,127.109971461789));
#43552=CARTESIAN_POINT('Ctrl Pts',(111.490851763348,3.14362658552047,127.01944289652));
#43553=CARTESIAN_POINT('Ctrl Pts',(111.483091320833,3.03690554132065,126.933297992364));
#43554=CARTESIAN_POINT('Ctrl Pts',(111.475330878319,2.92689702851175,126.851835241684));
#43555=CARTESIAN_POINT('Ctrl Pts',(111.467557978054,2.81671192027207,126.770241719765));
#43556=CARTESIAN_POINT('Ctrl Pts',(111.459785077788,2.70322912146974,126.69334559054));
#43557=CARTESIAN_POINT('Ctrl Pts',(111.452012177523,2.58689681800423,126.621401388085));
#43558=CARTESIAN_POINT('Ctrl Pts',(111.444521841761,2.47479348679355,126.552072538606));
#43559=CARTESIAN_POINT('Ctrl Pts',(111.437031505999,2.36004449570761,126.487341987861));
#43560=CARTESIAN_POINT('Ctrl Pts',(111.429541170237,2.24306917490219,126.427395488723));
#43561=CARTESIAN_POINT('Ctrl Pts',(111.421766836118,2.12165869925411,126.36517609985));
#43562=CARTESIAN_POINT('Ctrl Pts',(111.413992501999,1.9974651468001,126.307913606181));
#43563=CARTESIAN_POINT('Ctrl Pts',(111.40621816788,1.87093144802186,126.255866517394));
#43564=CARTESIAN_POINT('Ctrl Pts',(111.398453414933,1.74455369071881,126.203883571992));
#43565=CARTESIAN_POINT('Ctrl Pts',(111.390688661986,1.61584188353536,126.157103389921));
#43566=CARTESIAN_POINT('Ctrl Pts',(111.382923909038,1.48526378207196,126.115738798719));
#43567=CARTESIAN_POINT('Ctrl Pts',(111.375166868153,1.35481537261976,126.074415291413));
#43568=CARTESIAN_POINT('Ctrl Pts',(111.367409827268,1.22250472799417,126.038496788143));
#43569=CARTESIAN_POINT('Ctrl Pts',(111.359652786383,1.08881949668664,126.00814803198));
#43570=CARTESIAN_POINT('Ctrl Pts',(111.351901595143,0.955235078452045,125.97782216205));
#43571=CARTESIAN_POINT('Ctrl Pts',(111.344150403903,0.82027851651953,125.953057765207));
#43572=CARTESIAN_POINT('Ctrl Pts',(111.336399212663,0.684452189924092,125.933969641247));
#43573=CARTESIAN_POINT('Ctrl Pts',(111.328651315886,0.548683593140558,125.914889630249));
#43574=CARTESIAN_POINT('Ctrl Pts',(111.320903419109,0.41204635329608,125.901481148018));
#43575=CARTESIAN_POINT('Ctrl Pts',(111.313155522332,0.275052386324319,125.893807772185));
#43576=CARTESIAN_POINT('Ctrl Pts',(111.305409246248,0.1380870755372,125.886136001458));
#43577=CARTESIAN_POINT('Ctrl Pts',(111.297662970164,0.000765576151350478,
125.884196972789));
#43578=CARTESIAN_POINT('Ctrl Pts',(111.28991669408,-0.136396133200972,125.888002294849));
#43579=CARTESIAN_POINT('Ctrl Pts',(111.282170360814,-0.273558855049874,
125.891807644999));
#43580=CARTESIAN_POINT('Ctrl Pts',(111.274424027549,-0.410561393696745,
125.901357419647));
#43581=CARTESIAN_POINT('Ctrl Pts',(111.266677694283,-0.546889230820648,
125.916611111739));
#43582=CARTESIAN_POINT('Ctrl Pts',(111.258929626281,-0.683247597618353,
125.931868219789));
#43583=CARTESIAN_POINT('Ctrl Pts',(111.251181558278,-0.818930573765801,
125.952831743602));
#43584=CARTESIAN_POINT('Ctrl Pts',(111.243433490275,-0.953430607605556,
125.979409515329));
#43585=CARTESIAN_POINT('Ctrl Pts',(111.235677187533,-1.08807358968194,126.006015534227));
#43586=CARTESIAN_POINT('Ctrl Pts',(111.227920884791,-1.22153073380778,126.038247644632));
#43587=CARTESIAN_POINT('Ctrl Pts',(111.220164582049,-1.35330595886695,126.07596278699));
#43588=CARTESIAN_POINT('Ctrl Pts',(111.212404139535,-1.48515151633141,126.113698059055));
#43589=CARTESIAN_POINT('Ctrl Pts',(111.204643697021,-1.61531299514427,126.156922071135));
#43590=CARTESIAN_POINT('Ctrl Pts',(111.196883254507,-1.74331220271663,126.205442741983));
#43591=CARTESIAN_POINT('Ctrl Pts',(111.189110354241,-1.87151688598021,126.254041302519));
#43592=CARTESIAN_POINT('Ctrl Pts',(111.181337453976,-1.997552002033,126.307953359013));
#43593=CARTESIAN_POINT('Ctrl Pts',(111.17356455371,-2.12096114872149,126.366939421859));
#43594=CARTESIAN_POINT('Ctrl Pts',(111.166074217948,-2.23988406207946,126.423781192743));
#43595=CARTESIAN_POINT('Ctrl Pts',(111.158583882186,-2.35636834026842,126.485334324995));
#43596=CARTESIAN_POINT('Ctrl Pts',(111.151093546424,-2.47003104594351,126.551346428244));
#43597=CARTESIAN_POINT('Ctrl Pts',(111.143318048751,-2.58802096408834,126.619871654813));
#43598=CARTESIAN_POINT('Ctrl Pts',(111.135542551079,-2.70334402827948,126.693419189844));
#43599=CARTESIAN_POINT('Ctrl Pts',(111.127767053406,-2.81554312866998,126.771756006015));
#43600=CARTESIAN_POINT('Ctrl Pts',(111.120001390163,-2.92760031993348,126.849993741988));
#43601=CARTESIAN_POINT('Ctrl Pts',(111.112235726919,-3.03654109228594,126.93300848329));
#43602=CARTESIAN_POINT('Ctrl Pts',(111.104470063675,-3.14193340809388,127.020521625008));
#43603=CARTESIAN_POINT('Ctrl Pts',(111.0967138177,-3.24719791669754,127.107928641247));
#43604=CARTESIAN_POINT('Ctrl Pts',(111.088957571725,-3.34892224050942,127.1998229446));
#43605=CARTESIAN_POINT('Ctrl Pts',(111.081201325749,-3.44670432087686,127.29588339989));
#43606=CARTESIAN_POINT('Ctrl Pts',(111.073450420698,-3.54441906883546,127.391877708277));
#43607=CARTESIAN_POINT('Ctrl Pts',(111.065699515648,-3.6381966964812,127.49203218828));
#43608=CARTESIAN_POINT('Ctrl Pts',(111.057948610597,-3.72766911730934,127.595986260612));
#43609=CARTESIAN_POINT('Ctrl Pts',(111.050201364159,-3.81709930501157,127.699891264132));
#43610=CARTESIAN_POINT('Ctrl Pts',(111.042454117721,-3.90222807564878,127.807591995144));
#43611=CARTESIAN_POINT('Ctrl Pts',(111.034706871283,-3.98272532301652,127.918692226378));
#43612=CARTESIAN_POINT('Ctrl Pts',(111.026961603978,-4.06320200634288,128.02976407565));
#43613=CARTESIAN_POINT('Ctrl Pts',(111.019216336672,-4.13904929327087,128.144233379648));
#43614=CARTESIAN_POINT('Ctrl Pts',(111.011471069367,-4.20997862988462,128.261672473413));
#43615=CARTESIAN_POINT('Ctrl Pts',(111.003723969164,-4.28092475173514,128.379139358824));
#43616=CARTESIAN_POINT('Ctrl Pts',(110.995976868962,-4.34695039166321,128.499577105967));
#43617=CARTESIAN_POINT('Ctrl Pts',(110.98822976876,-4.40781144552144,128.622530806781));
#43618=CARTESIAN_POINT('Ctrl Pts',(110.980481686043,-4.46868021799213,128.745500101015));
#43619=CARTESIAN_POINT('Ctrl Pts',(110.972733603326,-4.52438293361868,128.870985630572));
#43620=CARTESIAN_POINT('Ctrl Pts',(110.964985520609,-4.57472279130914,128.998510555912));
#43621=CARTESIAN_POINT('Ctrl Pts',(110.95723183069,-4.62509907940227,129.126127769641));
#43622=CARTESIAN_POINT('Ctrl Pts',(110.949478140771,-4.67010462351842,129.255786959791));
#43623=CARTESIAN_POINT('Ctrl Pts',(110.941724450852,-4.70959178128307,129.386993933828));
#43624=CARTESIAN_POINT('Ctrl Pts',(110.93789460426,-4.72909601193425,129.451802120325));
#43625=CARTESIAN_POINT('Ctrl Pts',(110.934064757668,-4.747254666173,129.516987712106));
#43626=CARTESIAN_POINT('Ctrl Pts',(110.930234911077,-4.76405452823406,129.582490119308));
#43627=CARTESIAN_POINT('Origin',(213.235140564004,0.,130.804360617566));
#43628=CARTESIAN_POINT('',(108.834713077301,-4.76405452823407,129.582490119308));
#43629=CARTESIAN_POINT('',(109.179944404822,-4.76405452823403,129.582490119308));
#43630=CARTESIAN_POINT('',(213.235140564004,-4.76405452823405,129.582490119308));
#43631=CARTESIAN_POINT('',(110.514859436046,-4.91824876687394,130.800877853875));
#43632=CARTESIAN_POINT('Ctrl Pts',(110.514859435991,-4.91824876687464,130.800877854854));
#43633=CARTESIAN_POINT('Ctrl Pts',(110.507086929701,-4.91834630934749,130.938624289666));
#43634=CARTESIAN_POINT('Ctrl Pts',(110.499314423412,-4.91265269404362,131.07641604133));
#43635=CARTESIAN_POINT('Ctrl Pts',(110.491541917122,-4.901183229966,131.213733319147));
#43636=CARTESIAN_POINT('Ctrl Pts',(110.483769695216,-4.88971418553847,131.351045572736));
#43637=CARTESIAN_POINT('Ctrl Pts',(110.475997473311,-4.87246974426606,131.487883001353));
#43638=CARTESIAN_POINT('Ctrl Pts',(110.468225251405,-4.84951719909121,131.6237298861));
#43639=CARTESIAN_POINT('Ctrl Pts',(110.460451674612,-4.82656065272929,131.759600452265));
#43640=CARTESIAN_POINT('Ctrl Pts',(110.452678097819,-4.79789408591347,131.894479749222));
#43641=CARTESIAN_POINT('Ctrl Pts',(110.444904521026,-4.76363606073343,132.027861554787));
#43642=CARTESIAN_POINT('Ctrl Pts',(110.437127949555,-4.72936483805523,132.161294744112));
#43643=CARTESIAN_POINT('Ctrl Pts',(110.429351378083,-4.68949796532972,132.293228919119));
#43644=CARTESIAN_POINT('Ctrl Pts',(110.421574806612,-4.6442039791409,132.423172670471));
#43645=CARTESIAN_POINT('Ctrl Pts',(110.413788670456,-4.59885428425325,132.553276244306));
#43646=CARTESIAN_POINT('Ctrl Pts',(110.406002534301,-4.5480642721441,132.681384139421));
#43647=CARTESIAN_POINT('Ctrl Pts',(110.398216398145,-4.49205102133843,132.807024015192));
#43648=CARTESIAN_POINT('Ctrl Pts',(110.390425085613,-4.43600053181788,132.932747418834));
#43649=CARTESIAN_POINT('Ctrl Pts',(110.38263377308,-4.37472005680413,133.055999188144));
#43650=CARTESIAN_POINT('Ctrl Pts',(110.374842460547,-4.30847238702395,133.176332108278));
#43651=CARTESIAN_POINT('Ctrl Pts',(110.367038434071,-4.24211661362025,133.296861388899));
#43652=CARTESIAN_POINT('Ctrl Pts',(110.359234407595,-4.17077765399009,133.414461975275));
#43653=CARTESIAN_POINT('Ctrl Pts',(110.351430381119,-4.09476175193706,133.528715450801));
#43654=CARTESIAN_POINT('Ctrl Pts',(110.346066811128,-4.04251736086828,133.60723985287));
#43655=CARTESIAN_POINT('Ctrl Pts',(110.340703241137,-3.98806466406905,133.684183871582));
#43656=CARTESIAN_POINT('Ctrl Pts',(110.335339671145,-3.93151367305878,133.75942124318));
#43657=CARTESIAN_POINT('Ctrl Pts',(110.327565337026,-3.84954470470652,133.868475560729));
#43658=CARTESIAN_POINT('Ctrl Pts',(110.319791002907,-3.76290495879544,133.974289482691));
#43659=CARTESIAN_POINT('Ctrl Pts',(110.312016668788,-3.6718796888324,134.076436810634));
#43660=CARTESIAN_POINT('Ctrl Pts',(110.304251915841,-3.58096659937936,134.178458251124));
#43661=CARTESIAN_POINT('Ctrl Pts',(110.296487162894,-3.485678997358,134.276821799475));
#43662=CARTESIAN_POINT('Ctrl Pts',(110.288722409947,-3.38634444114331,134.371131480467));
#43663=CARTESIAN_POINT('Ctrl Pts',(110.280965369061,-3.28710854541023,134.465347491754));
#43664=CARTESIAN_POINT('Ctrl Pts',(110.273208328176,-3.18383397615189,134.555517380869));
#43665=CARTESIAN_POINT('Ctrl Pts',(110.265451287291,-3.07688721187026,134.641279713394));
#43666=CARTESIAN_POINT('Ctrl Pts',(110.257700096051,-2.97002109697588,134.726977371877));
#43667=CARTESIAN_POINT('Ctrl Pts',(110.249948904811,-2.85948860281737,134.808273845938));
#43668=CARTESIAN_POINT('Ctrl Pts',(110.242197713571,-2.74569129861734,134.884846171418));
#43669=CARTESIAN_POINT('Ctrl Pts',(110.234449816794,-2.63194236130693,134.961385951618));
#43670=CARTESIAN_POINT('Ctrl Pts',(110.226701920017,-2.51493169753785,135.03320535897));
#43671=CARTESIAN_POINT('Ctrl Pts',(110.21895402324,-2.39509185606264,135.100023321215));
#43672=CARTESIAN_POINT('Ctrl Pts',(110.211207747156,-2.27527708249874,135.166827306583));
#43673=CARTESIAN_POINT('Ctrl Pts',(110.203461471072,-2.15263464961498,135.228631737509));
#43674=CARTESIAN_POINT('Ctrl Pts',(110.195715194987,-2.02762348948471,135.285200499484));
#43675=CARTESIAN_POINT('Ctrl Pts',(110.187968861722,-1.90261140655054,135.341769679037));
#43676=CARTESIAN_POINT('Ctrl Pts',(110.180222528457,-1.77523091767329,135.393102951336));
#43677=CARTESIAN_POINT('Ctrl Pts',(110.172476195191,-1.64596243570163,135.439011707212));
#43678=CARTESIAN_POINT('Ctrl Pts',(110.164728127188,-1.51666500494999,135.484930744036));
#43679=CARTESIAN_POINT('Ctrl Pts',(110.156980059185,-1.38547910812564,135.525422716342));
#43680=CARTESIAN_POINT('Ctrl Pts',(110.149231991182,-1.25290148812496,135.560348519522));
#43681=CARTESIAN_POINT('Ctrl Pts',(110.141475688441,-1.12018296305187,135.595311442262));
#43682=CARTESIAN_POINT('Ctrl Pts',(110.133719385699,-0.986070138730447,
135.62469627869));
#43683=CARTESIAN_POINT('Ctrl Pts',(110.125963082957,-0.851071701478091,
135.648414707008));
#43684=CARTESIAN_POINT('Ctrl Pts',(110.118202640443,-0.716001211494864,
135.672145794566));
#43685=CARTESIAN_POINT('Ctrl Pts',(110.110442197929,-0.580044554100888,
135.690204396321));
#43686=CARTESIAN_POINT('Ctrl Pts',(110.102681755414,-0.44371576957375,135.70255409867));
#43687=CARTESIAN_POINT('Ctrl Pts',(110.094908855149,-0.307168137979082,
135.714923625858));
#43688=CARTESIAN_POINT('Ctrl Pts',(110.087135954883,-0.170247576243332,
135.72156592123));
#43689=CARTESIAN_POINT('Ctrl Pts',(110.079363054618,-0.0334692640664809,
135.722496735127));
#43690=CARTESIAN_POINT('Ctrl Pts',(110.071872718856,0.0983368119382216,
135.723393711595));
#43691=CARTESIAN_POINT('Ctrl Pts',(110.064382383094,0.230010493240583,135.718987260958));
#43692=CARTESIAN_POINT('Ctrl Pts',(110.056892047332,0.361097023146372,135.709336866476));
#43693=CARTESIAN_POINT('Ctrl Pts',(110.049117713213,0.497153738677194,135.699320574355));
#43694=CARTESIAN_POINT('Ctrl Pts',(110.041343379094,0.63300888698788,135.683623111824));
#43695=CARTESIAN_POINT('Ctrl Pts',(110.033569044975,0.768149708779823,135.662254100075));
#43696=CARTESIAN_POINT('Ctrl Pts',(110.025804292028,0.903123981586423,135.640911423723));
#43697=CARTESIAN_POINT('Ctrl Pts',(110.018039539081,1.0373852970355,135.613911166004));
#43698=CARTESIAN_POINT('Ctrl Pts',(110.010274786134,1.17042345665789,135.581314876778));
#43699=CARTESIAN_POINT('Ctrl Pts',(110.002517745249,1.30332948090445,135.548750962646));
#43700=CARTESIAN_POINT('Ctrl Pts',(109.994760704364,1.43501438966582,135.51060217023));
#43701=CARTESIAN_POINT('Ctrl Pts',(109.987003663479,1.56497600734838,135.466981464142));
#43702=CARTESIAN_POINT('Ctrl Pts',(109.979252472238,1.69483961996419,135.423393652767));
#43703=CARTESIAN_POINT('Ctrl Pts',(109.971501280998,1.82298215902628,135.374342264996));
#43704=CARTESIAN_POINT('Ctrl Pts',(109.963750089758,1.94891484766775,135.319990582371));
#43705=CARTESIAN_POINT('Ctrl Pts',(109.956002192981,2.07479401155744,135.26566200066));
#43706=CARTESIAN_POINT('Ctrl Pts',(109.948254296204,2.19846483490563,135.206037759278));
#43707=CARTESIAN_POINT('Ctrl Pts',(109.940506399427,2.31945704049337,135.141329847317));
#43708=CARTESIAN_POINT('Ctrl Pts',(109.932760123343,2.44042393711999,135.076635470856));
#43709=CARTESIAN_POINT('Ctrl Pts',(109.925013847259,2.55871298593247,135.00685972323));
#43710=CARTESIAN_POINT('Ctrl Pts',(109.917267571175,2.67387747311014,134.932261091329));
#43711=CARTESIAN_POINT('Ctrl Pts',(109.909521237909,2.78904281040582,134.857661908758));
#43712=CARTESIAN_POINT('Ctrl Pts',(109.901774904644,2.90108321190439,134.778239983425));
#43713=CARTESIAN_POINT('Ctrl Pts',(109.894028571379,3.00958032049026,134.694297552404));
#43714=CARTESIAN_POINT('Ctrl Pts',(109.886280503376,3.11810172625134,134.610336323057));
#43715=CARTESIAN_POINT('Ctrl Pts',(109.878532435373,3.22307795097219,134.521852812784));
#43716=CARTESIAN_POINT('Ctrl Pts',(109.87078436737,3.32412346033668,134.429189756014));
#43717=CARTESIAN_POINT('Ctrl Pts',(109.863028064628,3.42527636207105,134.336428215843));
#43718=CARTESIAN_POINT('Ctrl Pts',(109.855271761886,3.52248991461387,134.239478520324));
#43719=CARTESIAN_POINT('Ctrl Pts',(109.847515459144,3.61541485295376,134.13872090157));
#43720=CARTESIAN_POINT('Ctrl Pts',(109.83975501663,3.70838938813142,134.037909505441));
#43721=CARTESIAN_POINT('Ctrl Pts',(109.831994574116,3.79707049548166,133.933286434437));
#43722=CARTESIAN_POINT('Ctrl Pts',(109.824234131602,3.88114968788277,133.825264482761));
#43723=CARTESIAN_POINT('Ctrl Pts',(109.816461231336,3.96536385166748,133.717069124658));
#43724=CARTESIAN_POINT('Ctrl Pts',(109.808688331071,4.04496111097209,133.605464301174));
#43725=CARTESIAN_POINT('Ctrl Pts',(109.800915430805,4.11967624979386,133.490891961024));
#43726=CARTESIAN_POINT('Ctrl Pts',(109.793425095043,4.19167530512428,133.380484614029));
#43727=CARTESIAN_POINT('Ctrl Pts',(109.785934759281,4.25914087445923,133.267322022551));
#43728=CARTESIAN_POINT('Ctrl Pts',(109.778444423519,4.32187719565033,133.151818938435));
#43729=CARTESIAN_POINT('Ctrl Pts',(109.7706700894,4.38699218352695,133.03193651978));
#43730=CARTESIAN_POINT('Ctrl Pts',(109.762895755281,4.44721848983267,132.909152873958));
#43731=CARTESIAN_POINT('Ctrl Pts',(109.755121421162,4.50228705022288,132.78390460038));
#43732=CARTESIAN_POINT('Ctrl Pts',(109.747356668215,4.55728774353399,132.658810684106));
#43733=CARTESIAN_POINT('Ctrl Pts',(109.739591915268,4.6071431825434,132.531258538125));
#43734=CARTESIAN_POINT('Ctrl Pts',(109.73182716232,4.65162937615635,132.401710676063));
#43735=CARTESIAN_POINT('Ctrl Pts',(109.724070121435,4.69607138545471,132.272291482763));
#43736=CARTESIAN_POINT('Ctrl Pts',(109.71631308055,4.7351546357335,132.140880885374));
#43737=CARTESIAN_POINT('Ctrl Pts',(109.708556039665,4.76870272914536,132.007962438577));
#43738=CARTESIAN_POINT('Ctrl Pts',(109.700804848425,4.80222552367885,131.875144226616));
#43739=CARTESIAN_POINT('Ctrl Pts',(109.693053657185,4.83022137435755,131.74082080608));
#43740=CARTESIAN_POINT('Ctrl Pts',(109.685302465945,4.85256345873285,131.605491656455));
#43741=CARTESIAN_POINT('Ctrl Pts',(109.677554569168,4.87489604712636,131.470220025327));
#43742=CARTESIAN_POINT('Ctrl Pts',(109.669806672391,4.89157958505243,131.333943900234));
#43743=CARTESIAN_POINT('Ctrl Pts',(109.662058775614,4.90253822861556,131.197173524002));
#43744=CARTESIAN_POINT('Ctrl Pts',(109.65431249953,4.91349457986669,131.060431757185));
#43745=CARTESIAN_POINT('Ctrl Pts',(109.646566223446,4.91872838749074,130.92319633434));
#43746=CARTESIAN_POINT('Ctrl Pts',(109.638819947362,4.91821566409774,130.785982806934));
#43747=CARTESIAN_POINT('Ctrl Pts',(109.631073614096,4.91770293691993,130.648768266649));
#43748=CARTESIAN_POINT('Ctrl Pts',(109.623327280831,4.91144359554072,130.511576013088));
#43749=CARTESIAN_POINT('Ctrl Pts',(109.615580947565,4.89946578832898,130.374921388462));
#43750=CARTESIAN_POINT('Ctrl Pts',(109.607832879562,4.88748529877037,130.23823616098));
#43751=CARTESIAN_POINT('Ctrl Pts',(109.60008481156,4.86978382924282,130.102089191408));
#43752=CARTESIAN_POINT('Ctrl Pts',(109.592336743557,4.84644134121256,129.966990097016));
#43753=CARTESIAN_POINT('Ctrl Pts',(109.584580440815,4.82307404450828,129.831747417699));
#43754=CARTESIAN_POINT('Ctrl Pts',(109.576824138073,4.79405381963168,129.697555224158));
#43755=CARTESIAN_POINT('Ctrl Pts',(109.569067835331,4.75951178036033,129.564912887683));
#43756=CARTESIAN_POINT('Ctrl Pts',(109.561307392817,4.72495130496253,129.432199756));
#43757=CARTESIAN_POINT('Ctrl Pts',(109.553546950303,4.68486325692695,129.301038503369));
#43758=CARTESIAN_POINT('Ctrl Pts',(109.545786507788,4.63942818688215,129.171911794091));
#43759=CARTESIAN_POINT('Ctrl Pts',(109.538013607523,4.59392018042941,129.042577799157));
#43760=CARTESIAN_POINT('Ctrl Pts',(109.530240707258,4.54304814454427,128.9152852374));
#43761=CARTESIAN_POINT('Ctrl Pts',(109.522467806992,4.4870405474712,128.790496126631));
#43762=CARTESIAN_POINT('Ctrl Pts',(109.51497747123,4.43306896762663,128.670243414364));
#43763=CARTESIAN_POINT('Ctrl Pts',(109.507487135468,4.37432886265035,128.552315575316));
#43764=CARTESIAN_POINT('Ctrl Pts',(109.499996799706,4.31106336079069,128.437101493231));
#43765=CARTESIAN_POINT('Ctrl Pts',(109.492222465587,4.24539912819849,128.317519034204));
#43766=CARTESIAN_POINT('Ctrl Pts',(109.484448131468,4.17465155922289,128.200481377287));
#43767=CARTESIAN_POINT('Ctrl Pts',(109.476673797349,4.09904254146147,128.08645088658));
#43768=CARTESIAN_POINT('Ctrl Pts',(109.468909044402,4.02352670505702,127.972560928261));
#43769=CARTESIAN_POINT('Ctrl Pts',(109.461144291455,3.94316155475029,127.861671084906));
#43770=CARTESIAN_POINT('Ctrl Pts',(109.453379538508,3.85821514369443,127.754219806478));
#43771=CARTESIAN_POINT('Ctrl Pts',(109.445622497623,3.77335310261134,127.646875250173));
#43772=CARTESIAN_POINT('Ctrl Pts',(109.437865456738,3.68391909672332,127.542962767047));
#43773=CARTESIAN_POINT('Ctrl Pts',(109.430108415853,3.5902246069335,127.442892138721));
#43774=CARTESIAN_POINT('Ctrl Pts',(109.422357224612,3.4966007728874,127.342896974434));
#43775=CARTESIAN_POINT('Ctrl Pts',(109.414606033372,3.39872311608172,127.246738182542));
#43776=CARTESIAN_POINT('Ctrl Pts',(109.406854842132,3.29694331212077,127.154792443225));
#43777=CARTESIAN_POINT('Ctrl Pts',(109.399106945355,3.19520676729191,127.0628857833));
#43778=CARTESIAN_POINT('Ctrl Pts',(109.391359048578,3.08957166347778,126.975188875999));
#43779=CARTESIAN_POINT('Ctrl Pts',(109.383611151801,2.98042628694114,126.892041329649));
#43780=CARTESIAN_POINT('Ctrl Pts',(109.375864875717,2.87130374126437,126.808911175973));
#43781=CARTESIAN_POINT('Ctrl Pts',(109.368118599633,2.75867269417907,126.73032872718));
#43782=CARTESIAN_POINT('Ctrl Pts',(109.360372323549,2.6429539279655,126.656592832702));
#43783=CARTESIAN_POINT('Ctrl Pts',(109.352625990283,2.52723430754237,126.582856393923));
#43784=CARTESIAN_POINT('Ctrl Pts',(109.344879657018,2.40842725222696,126.513966790943));
#43785=CARTESIAN_POINT('Ctrl Pts',(109.337133323753,2.28698154889673,126.450178896794));
#43786=CARTESIAN_POINT('Ctrl Pts',(109.32938525575,2.16550864864279,126.386376717788));
#43787=CARTESIAN_POINT('Ctrl Pts',(109.321637187747,2.04139627059726,126.327678702805));
#43788=CARTESIAN_POINT('Ctrl Pts',(109.313889119744,1.91511639132759,126.274293038581));
#43789=CARTESIAN_POINT('Ctrl Pts',(109.306132817002,1.78870230029983,126.220850635438));
#43790=CARTESIAN_POINT('Ctrl Pts',(109.29837651426,1.66011646694844,126.172732014087));
#43791=CARTESIAN_POINT('Ctrl Pts',(109.290620211518,1.52984989668365,126.130096787173));
#43792=CARTESIAN_POINT('Ctrl Pts',(109.282859769004,1.39951379922787,126.087438804556));
#43793=CARTESIAN_POINT('Ctrl Pts',(109.27509932649,1.26749555354112,126.050270153882));
#43794=CARTESIAN_POINT('Ctrl Pts',(109.267338883976,1.13429883079499,126.018699824639));
#43795=CARTESIAN_POINT('Ctrl Pts',(109.25956598371,1.00088828884504,125.987078815901));
#43796=CARTESIAN_POINT('Ctrl Pts',(109.251793083445,0.866295873511378,125.961074161539));
#43797=CARTESIAN_POINT('Ctrl Pts',(109.244020183179,0.73103378613032,125.94074337666));
#43798=CARTESIAN_POINT('Ctrl Pts',(109.236529847417,0.600688816332127,125.921151667022));
#43799=CARTESIAN_POINT('Ctrl Pts',(109.229039511656,0.46972232390649,125.906828503393));
#43800=CARTESIAN_POINT('Ctrl Pts',(109.221549175894,0.338592904515696,125.897779536252));
#43801=CARTESIAN_POINT('Ctrl Pts',(109.213774841774,0.20249167333058,125.888387474771));
#43802=CARTESIAN_POINT('Ctrl Pts',(109.206000507655,0.0657837887511484,
125.884647695859));
#43803=CARTESIAN_POINT('Ctrl Pts',(109.198226173536,-0.0710218135452183,
125.886623438283));
#43804=CARTESIAN_POINT('Ctrl Pts',(109.190461420589,-0.207658815163144,
125.888596745782));
#43805=CARTESIAN_POINT('Ctrl Pts',(109.182696667642,-0.344392907709876,
125.896271553826));
#43806=CARTESIAN_POINT('Ctrl Pts',(109.174931914695,-0.480710321536931,
125.909659334621));
#43807=CARTESIAN_POINT('Ctrl Pts',(109.16717487381,-0.616892342986928,125.923033818483));
#43808=CARTESIAN_POINT('Ctrl Pts',(109.159417832925,-0.752658122724326,
125.942109945206));
#43809=CARTESIAN_POINT('Ctrl Pts',(109.15166079204,-0.887494536828826,125.96684715406));
#43810=CARTESIAN_POINT('Ctrl Pts',(109.1439096008,-1.02222926974439,125.991565708393));
#43811=CARTESIAN_POINT('Ctrl Pts',(109.13615840956,-1.15603564901901,126.021936777276));
#43812=CARTESIAN_POINT('Ctrl Pts',(109.128407218319,-1.28840667369546,126.057868090902));
#43813=CARTESIAN_POINT('Ctrl Pts',(109.120659321542,-1.42072143715549,126.093784132761));
#43814=CARTESIAN_POINT('Ctrl Pts',(109.112911424765,-1.55160168286634,126.135255616829));
#43815=CARTESIAN_POINT('Ctrl Pts',(109.105163527988,-1.68055181051363,126.182139433473));
#43816=CARTESIAN_POINT('Ctrl Pts',(109.097417251904,-1.80947496457415,126.229013443033));
#43817=CARTESIAN_POINT('Ctrl Pts',(109.08967097582,-1.93646843643001,126.281297399768));
#43818=CARTESIAN_POINT('Ctrl Pts',(109.081924699736,-2.06105335248994,126.338798823045));
#43819=CARTESIAN_POINT('Ctrl Pts',(109.07417836647,-2.18563918820699,126.396300670783));
#43820=CARTESIAN_POINT('Ctrl Pts',(109.066432033205,-2.30781607767081,126.459019898078));
#43821=CARTESIAN_POINT('Ctrl Pts',(109.05868569994,-2.42712700871127,126.526716692917));
#43822=CARTESIAN_POINT('Ctrl Pts',(109.050937631937,-2.5464646586083,126.594428647985));
#43823=CARTESIAN_POINT('Ctrl Pts',(109.043189563934,-2.66293473297472,126.667120195803));
#43824=CARTESIAN_POINT('Ctrl Pts',(109.035441495931,-2.77610696355001,126.744506779134));
#43825=CARTESIAN_POINT('Ctrl Pts',(109.027685193189,-2.88939947491825,126.821975609847));
#43826=CARTESIAN_POINT('Ctrl Pts',(109.019928890447,-2.99938681766151,126.904149222982));
#43827=CARTESIAN_POINT('Ctrl Pts',(109.012172587705,-3.10566930472197,126.990700796317));
#43828=CARTESIAN_POINT('Ctrl Pts',(109.004412145191,-3.21200851794623,127.077298564833));
#43829=CARTESIAN_POINT('Ctrl Pts',(108.996651702677,-3.31463864294787,127.168278690297));
#43830=CARTESIAN_POINT('Ctrl Pts',(108.988891260162,-3.41319573721326,127.263276331366));
#43831=CARTESIAN_POINT('Ctrl Pts',(108.981118359897,-3.51191104407552,127.358426471083));
#43832=CARTESIAN_POINT('Ctrl Pts',(108.973345459632,-3.60653998437088,127.457606731077));
#43833=CARTESIAN_POINT('Ctrl Pts',(108.965572559366,-3.69675731167684,127.560417270178));
#43834=CARTESIAN_POINT('Ctrl Pts',(108.958082223604,-3.78369501188966,127.659490387216));
#43835=CARTESIAN_POINT('Ctrl Pts',(108.950591887842,-3.86653608329424,127.761934186653));
#43836=CARTESIAN_POINT('Ctrl Pts',(108.943101552081,-3.94502788982435,127.867365893191));
#43837=CARTESIAN_POINT('Ctrl Pts',(108.935287665741,-4.02691020782528,127.977351800049));
#43838=CARTESIAN_POINT('Ctrl Pts',(108.927473779402,-4.10431997379332,128.09093976861));
#43839=CARTESIAN_POINT('Ctrl Pts',(108.919659893063,-4.17692536949992,128.207732511709));
#43840=CARTESIAN_POINT('Ctrl Pts',(108.911858983755,-4.24941018468157,128.324331289467));
#43841=CARTESIAN_POINT('Ctrl Pts',(108.904058074448,-4.31710632009062,128.444123916064));
#43842=CARTESIAN_POINT('Ctrl Pts',(108.89625716514,-4.37972314083985,128.566681401929));
#43843=CARTESIAN_POINT('Ctrl Pts',(108.888463727543,-4.44227998719784,128.689121502234));
#43844=CARTESIAN_POINT('Ctrl Pts',(108.880670289947,-4.49976702168279,128.814320853177));
#43845=CARTESIAN_POINT('Ctrl Pts',(108.87287685235,-4.55193751326061,128.941822580942));
#43846=CARTESIAN_POINT('Ctrl Pts',(108.865090518563,-4.60406045082571,129.069208089393));
#43847=CARTESIAN_POINT('Ctrl Pts',(108.857304184776,-4.65087634985271,129.198891440245));
#43848=CARTESIAN_POINT('Ctrl Pts',(108.849517850989,-4.69218520904243,129.330392834152));
#43849=CARTESIAN_POINT('Ctrl Pts',(108.844582926426,-4.71836647861593,129.413737509136));
#43850=CARTESIAN_POINT('Ctrl Pts',(108.839648001863,-4.74233653958104,129.497812011167));
#43851=CARTESIAN_POINT('Ctrl Pts',(108.834713077301,-4.76405452823406,129.582490119308));
#43852=CARTESIAN_POINT('Ctrl Pts',(110.584632631705,-4.76405452823407,129.582490119308));
#43853=CARTESIAN_POINT('Ctrl Pts',(110.57571850841,-4.8029970434331,129.734326395034));
#43854=CARTESIAN_POINT('Ctrl Pts',(110.566804385115,-4.83472011272508,129.888195027331));
#43855=CARTESIAN_POINT('Ctrl Pts',(110.55789026182,-4.85903247671165,130.043449024303));
#43856=CARTESIAN_POINT('Ctrl Pts',(110.549039520694,-4.88317197228292,130.197599117416));
#43857=CARTESIAN_POINT('Ctrl Pts',(110.540188779568,-4.90000568966876,130.353114794605));
#43858=CARTESIAN_POINT('Ctrl Pts',(110.531338038442,-4.90939383791824,130.509343318564));
#43859=CARTESIAN_POINT('Ctrl Pts',(110.525845170977,-4.91522022616582,130.606300461948));
#43860=CARTESIAN_POINT('Ctrl Pts',(110.520352303511,-4.91817983312127,130.70353178788));
#43861=CARTESIAN_POINT('Ctrl Pts',(110.514859436046,-4.91824876687394,130.800877853875));
#43862=CARTESIAN_POINT('',(110.860140563956,-4.91824981345875,130.803006027984));
#43863=CARTESIAN_POINT('Ctrl Pts',(110.930234911077,-4.76405452823406,129.582490119308));
#43864=CARTESIAN_POINT('Ctrl Pts',(110.922471870508,-4.79810759213842,129.715262498644));
#43865=CARTESIAN_POINT('Ctrl Pts',(110.914708829939,-4.82657455152162,129.849336840364));
#43866=CARTESIAN_POINT('Ctrl Pts',(110.90694578937,-4.84938399854219,129.984203378262));
#43867=CARTESIAN_POINT('Ctrl Pts',(110.899171379239,-4.87222685172807,130.119267438435));
#43868=CARTESIAN_POINT('Ctrl Pts',(110.891396969109,-4.88939559826073,130.255125624766));
#43869=CARTESIAN_POINT('Ctrl Pts',(110.883622558978,-4.90087076246386,130.391263979808));
#43870=CARTESIAN_POINT('Ctrl Pts',(110.879963680189,-4.90627133102083,130.455334916539));
#43871=CARTESIAN_POINT('Ctrl Pts',(110.8763048014,-4.91041155883166,130.519467917546));
#43872=CARTESIAN_POINT('Ctrl Pts',(110.872645922612,-4.91329340329261,130.583609636455));
#43873=CARTESIAN_POINT('Ctrl Pts',(110.868477469744,-4.9165766038306,130.656684408145));
#43874=CARTESIAN_POINT('Ctrl Pts',(110.864309016876,-4.91822966004416,130.729832970459));
#43875=CARTESIAN_POINT('Ctrl Pts',(110.860140564008,-4.9182498134585,130.80300602708));
#43876=CARTESIAN_POINT('Ctrl Pts',(110.860140563956,-4.91824981345875,130.803006027984));
#43877=CARTESIAN_POINT('Ctrl Pts',(110.852421723757,-4.91828713207212,130.938502613616));
#43878=CARTESIAN_POINT('Ctrl Pts',(110.844702883558,-4.91272086582082,131.074226120841));
#43879=CARTESIAN_POINT('Ctrl Pts',(110.836984043359,-4.90152087846242,131.209670548973));
#43880=CARTESIAN_POINT('Ctrl Pts',(110.829274541677,-4.89033444123204,131.3449511118));
#43881=CARTESIAN_POINT('Ctrl Pts',(110.821565039995,-4.87352787326834,131.479952875333));
#43882=CARTESIAN_POINT('Ctrl Pts',(110.813855538313,-4.85112301637002,131.614168337056));
#43883=CARTESIAN_POINT('Ctrl Pts',(110.806153453313,-4.82873971335402,131.748254681048));
#43884=CARTESIAN_POINT('Ctrl Pts',(110.798451368313,-4.80076890139968,131.881555839073));
#43885=CARTESIAN_POINT('Ctrl Pts',(110.790749283312,-4.76728430710159,132.013568373811));
#43886=CARTESIAN_POINT('Ctrl Pts',(110.783052700285,-4.73382363247239,132.145486605596));
#43887=CARTESIAN_POINT('Ctrl Pts',(110.775356117257,-4.69485711086892,132.276117662544));
#43888=CARTESIAN_POINT('Ctrl Pts',(110.767659534229,-4.65050965366092,132.404967697304));
#43889=CARTESIAN_POINT('Ctrl Pts',(110.759965746648,-4.60617830372207,132.533770932939));
#43890=CARTESIAN_POINT('Ctrl Pts',(110.752271959066,-4.55647003202619,132.660794057457));
#43891=CARTESIAN_POINT('Ctrl Pts',(110.744578171485,-4.50155969320645,132.785558081475));
#43892=CARTESIAN_POINT('Ctrl Pts',(110.736885594092,-4.44665799146452,132.910302480835));
#43893=CARTESIAN_POINT('Ctrl Pts',(110.729193016698,-4.38655600965109,133.032788123049));
#43894=CARTESIAN_POINT('Ctrl Pts',(110.721500439305,-4.3214766702694,133.152556190941));
#43895=CARTESIAN_POINT('Ctrl Pts',(110.713807346968,-4.25639297445367,133.272332276149));
#43896=CARTESIAN_POINT('Ctrl Pts',(110.706114254631,-4.186331447955,133.389390076323));
#43897=CARTESIAN_POINT('Ctrl Pts',(110.698421162294,-4.11156063904084,133.503295995449));
#43898=CARTESIAN_POINT('Ctrl Pts',(110.690725829826,-4.03676805781946,133.617235082529));
#43899=CARTESIAN_POINT('Ctrl Pts',(110.683030497359,-3.95726368435546,133.728020131229));
#43900=CARTESIAN_POINT('Ctrl Pts',(110.675335164891,-3.87335870781698,133.835247514677));
#43901=CARTESIAN_POINT('Ctrl Pts',(110.66763150882,-3.78936297603294,133.942590879893));
#43902=CARTESIAN_POINT('Ctrl Pts',(110.659927852748,-3.70095738281575,134.046368584067));
#43903=CARTESIAN_POINT('Ctrl Pts',(110.652224196677,-3.60849287329806,134.146210740755));
#43904=CARTESIAN_POINT('Ctrl Pts',(110.644515856566,-3.51597214276631,134.246113604273));
#43905=CARTESIAN_POINT('Ctrl Pts',(110.636807516456,-3.41938786237572,134.342075875924));
#43906=CARTESIAN_POINT('Ctrl Pts',(110.629099176346,-3.31912609810012,134.433766217304));
#43907=CARTESIAN_POINT('Ctrl Pts',(110.621379496337,-3.21871683666944,134.525591446242));
#43908=CARTESIAN_POINT('Ctrl Pts',(110.613659816328,-3.11461959280639,134.613131942647));
#43909=CARTESIAN_POINT('Ctrl Pts',(110.605940136319,-3.0072519563348,134.696097856078));
#43910=CARTESIAN_POINT('Ctrl Pts',(110.602026190479,-2.95281561782933,134.738162305817));
#43911=CARTESIAN_POINT('Ctrl Pts',(110.598112244639,-2.89753904253257,134.779051527273));
#43912=CARTESIAN_POINT('Ctrl Pts',(110.594198298799,-2.8414791507417,134.818732212025));
#43913=CARTESIAN_POINT('Ctrl Pts',(110.58642396468,-2.73012647820146,134.897550599899));
#43914=CARTESIAN_POINT('Ctrl Pts',(110.578649630561,-2.61531548912708,134.971857183996));
#43915=CARTESIAN_POINT('Ctrl Pts',(110.570875296441,-2.49744794817247,135.041333217037));
#43916=CARTESIAN_POINT('Ctrl Pts',(110.563110543494,-2.37972566842837,135.110723627076));
#43917=CARTESIAN_POINT('Ctrl Pts',(110.555345790547,-2.25895466544133,135.175295134574));
#43918=CARTESIAN_POINT('Ctrl Pts',(110.5475810376,-2.13556776024288,135.234770689321));
#43919=CARTESIAN_POINT('Ctrl Pts',(110.539823996715,-2.01230340465831,135.29418717211));
#43920=CARTESIAN_POINT('Ctrl Pts',(110.53206695583,-1.88642866720647,135.348517605844));
#43921=CARTESIAN_POINT('Ctrl Pts',(110.524309914945,-1.75840288388109,135.397529715309));
#43922=CARTESIAN_POINT('Ctrl Pts',(110.516558723705,-1.63047364579473,135.446504864361));
#43923=CARTESIAN_POINT('Ctrl Pts',(110.508807532465,-1.5003969542134,135.490169532765));
#43924=CARTESIAN_POINT('Ctrl Pts',(110.501056341225,-1.3686538137581,135.528338792853));
#43925=CARTESIAN_POINT('Ctrl Pts',(110.493308444448,-1.2369666676515,135.566491829987));
#43926=CARTESIAN_POINT('Ctrl Pts',(110.485560547671,-1.10361485613204,135.599153995753));
#43927=CARTESIAN_POINT('Ctrl Pts',(110.477812650894,-0.969096092840138,
135.626189712976));
#43928=CARTESIAN_POINT('Ctrl Pts',(110.47006637481,-0.83460546797363,135.653219774909));
#43929=CARTESIAN_POINT('Ctrl Pts',(110.462320098726,-0.698948759922859,
135.674625652294));
#43930=CARTESIAN_POINT('Ctrl Pts',(110.454573822641,-0.562635078518343,
135.6903226345));
#43931=CARTESIAN_POINT('Ctrl Pts',(110.446827489376,-0.426320390877383,
135.706019732578));
#43932=CARTESIAN_POINT('Ctrl Pts',(110.439081156111,-0.28934910860414,135.716007806661));
#43933=CARTESIAN_POINT('Ctrl Pts',(110.431334822845,-0.152236291425476,
135.72025394168));
#43934=CARTESIAN_POINT('Ctrl Pts',(110.423586754842,-0.0150927687817969,
135.724501027592));
#43935=CARTESIAN_POINT('Ctrl Pts',(110.41583868684,0.122191961135122,135.723003603613));
#43936=CARTESIAN_POINT('Ctrl Pts',(110.408090618837,0.259102403888672,135.715780881278));
#43937=CARTESIAN_POINT('Ctrl Pts',(110.400334316095,0.39615835668985,135.708550482548));
#43938=CARTESIAN_POINT('Ctrl Pts',(110.392578013353,0.532838836640757,135.695582650818));
#43939=CARTESIAN_POINT('Ctrl Pts',(110.384821710611,0.668632482032181,135.676948602043));
#43940=CARTESIAN_POINT('Ctrl Pts',(110.377061268097,0.80449860458091,135.658304607715));
#43941=CARTESIAN_POINT('Ctrl Pts',(110.369300825583,0.939476564836288,135.633988439589));
#43942=CARTESIAN_POINT('Ctrl Pts',(110.361540383068,1.07306575221742,135.604122377687));
#43943=CARTESIAN_POINT('Ctrl Pts',(110.353767482803,1.20686938882162,135.57420837213));
#43944=CARTESIAN_POINT('Ctrl Pts',(110.345994582538,1.33927941967796,135.538726770666));
#43945=CARTESIAN_POINT('Ctrl Pts',(110.338221682272,1.46981007669505,135.497849874073));
#43946=CARTESIAN_POINT('Ctrl Pts',(110.33073134651,1.59559561554375,135.458458955633));
#43947=CARTESIAN_POINT('Ctrl Pts',(110.323241010748,1.71963575822971,135.414058300707));
#43948=CARTESIAN_POINT('Ctrl Pts',(110.315750674986,1.84151562736709,135.364843405239));
#43949=CARTESIAN_POINT('Ctrl Pts',(110.307976340867,1.96801660878642,135.313762512052));
#43950=CARTESIAN_POINT('Ctrl Pts',(110.300202006748,2.0925909864683,135.257333299071));
#43951=CARTESIAN_POINT('Ctrl Pts',(110.292427672629,2.21475342568958,135.195721491589));
#43952=CARTESIAN_POINT('Ctrl Pts',(110.284662919682,2.3367653106224,135.134185615153));
#43953=CARTESIAN_POINT('Ctrl Pts',(110.276898166734,2.45637082575065,135.067480026976));
#43954=CARTESIAN_POINT('Ctrl Pts',(110.269133413787,2.57310293054794,134.995819119246));
#43955=CARTESIAN_POINT('Ctrl Pts',(110.261376372902,2.6897190953728,134.92422938614));
#43956=CARTESIAN_POINT('Ctrl Pts',(110.253619332017,2.80346719824521,134.847694331092));
#43957=CARTESIAN_POINT('Ctrl Pts',(110.245862291132,2.91390353712436,134.766474856055));
#43958=CARTESIAN_POINT('Ctrl Pts',(110.238111099892,3.02425659510152,134.685316629255));
#43959=CARTESIAN_POINT('Ctrl Pts',(110.230359908652,3.13130254637744,134.599481244506));
#43960=CARTESIAN_POINT('Ctrl Pts',(110.222608717412,3.23462581132014,134.509273426694));
#43961=CARTESIAN_POINT('Ctrl Pts',(110.214860820635,3.33790516111914,134.419103949611));
#43962=CARTESIAN_POINT('Ctrl Pts',(110.207112923858,3.4374646776445,134.324565992275));
#43963=CARTESIAN_POINT('Ctrl Pts',(110.199365027081,3.53292126959806,134.226005012491));
#43964=CARTESIAN_POINT('Ctrl Pts',(110.191618750997,3.62835789409032,134.127464649539));
#43965=CARTESIAN_POINT('Ctrl Pts',(110.183872474913,3.7196930292803,134.024903218652));
#43966=CARTESIAN_POINT('Ctrl Pts',(110.176126198829,3.80658021941792,133.918703260185));
#43967=CARTESIAN_POINT('Ctrl Pts',(110.168379865563,3.89346805093704,133.812502517774));
#43968=CARTESIAN_POINT('Ctrl Pts',(110.160633532298,3.97590762431884,133.702663496784));
#43969=CARTESIAN_POINT('Ctrl Pts',(110.152887199032,4.05359284481915,133.58960174015));
#43970=CARTESIAN_POINT('Ctrl Pts',(110.145139131029,4.13129546238618,133.476514664119));
#43971=CARTESIAN_POINT('Ctrl Pts',(110.137391063026,4.20424138706917,133.360203738496));
#43972=CARTESIAN_POINT('Ctrl Pts',(110.129642995023,4.2721681447425,133.241113047656));
#43973=CARTESIAN_POINT('Ctrl Pts',(110.121886692282,4.34016709578204,133.121895785812));
#43974=CARTESIAN_POINT('Ctrl Pts',(110.11413038954,4.40313602969954,132.99989319723));
#43975=CARTESIAN_POINT('Ctrl Pts',(110.106374086798,4.4608584589998,132.875573998961));
#43976=CARTESIAN_POINT('Ctrl Pts',(110.098613644284,4.51861169649858,132.751188447793));
#43977=CARTESIAN_POINT('Ctrl Pts',(110.09085320177,4.57111270012231,132.624484184228));
#43978=CARTESIAN_POINT('Ctrl Pts',(110.083092759255,4.61819375526957,132.495948481465));
#43979=CARTESIAN_POINT('Ctrl Pts',(110.07531985899,4.66535038910622,132.36720644178));
#43980=CARTESIAN_POINT('Ctrl Pts',(110.067546958725,4.70706956887608,132.236627460496));
#43981=CARTESIAN_POINT('Ctrl Pts',(110.059774058459,4.74323368658421,132.104713360845));
#43982=CARTESIAN_POINT('Ctrl Pts',(110.052283722697,4.77808314752173,131.977594670987));
#43983=CARTESIAN_POINT('Ctrl Pts',(110.044793386935,4.80777434601102,131.849236547414));
#43984=CARTESIAN_POINT('Ctrl Pts',(110.037303051173,4.83224750696555,131.720093708551));
#43985=CARTESIAN_POINT('Ctrl Pts',(110.029528717054,4.85764857525613,131.586054379701));
#43986=CARTESIAN_POINT('Ctrl Pts',(110.021754382935,4.87750857425258,131.450745059652));
#43987=CARTESIAN_POINT('Ctrl Pts',(110.013980048816,4.89170459806314,131.314663652818));
#43988=CARTESIAN_POINT('Ctrl Pts',(110.006215295869,4.90588312654309,131.178749954157));
#43989=CARTESIAN_POINT('Ctrl Pts',(109.998450542922,4.91441152846365,131.042066447092));
#43990=CARTESIAN_POINT('Ctrl Pts',(109.990685789974,4.91721773123116,130.905121950258));
#43991=CARTESIAN_POINT('Ctrl Pts',(109.982928749089,4.92002114683852,130.768313468629));
#43992=CARTESIAN_POINT('Ctrl Pts',(109.975171708204,4.91711366549537,130.631244901442));
#43993=CARTESIAN_POINT('Ctrl Pts',(109.967414667319,4.90847495961329,130.49443057167));
#43994=CARTESIAN_POINT('Ctrl Pts',(109.959663476079,4.89984276824651,130.357719414647));
#43995=CARTESIAN_POINT('Ctrl Pts',(109.951912284839,4.88548797947955,130.221262502037));
#43996=CARTESIAN_POINT('Ctrl Pts',(109.944161093599,4.86544233604906,130.085574183998));
#43997=CARTESIAN_POINT('Ctrl Pts',(109.936413196822,4.84540521255178,129.949943537114));
#43998=CARTESIAN_POINT('Ctrl Pts',(109.928665300045,4.81968210214892,129.815081221031));
#43999=CARTESIAN_POINT('Ctrl Pts',(109.920917403268,4.78835657807249,129.681496269691));
#44000=CARTESIAN_POINT('Ctrl Pts',(109.913171127184,4.75703760662045,129.547939261442));
#44001=CARTESIAN_POINT('Ctrl Pts',(109.9054248511,4.7201186416795,129.415659466865));
#44002=CARTESIAN_POINT('Ctrl Pts',(109.897678575016,4.67773425748905,129.2851551414));
#44003=CARTESIAN_POINT('Ctrl Pts',(109.88993224175,4.6353495604267,129.154649852581));
#44004=CARTESIAN_POINT('Ctrl Pts',(109.882185908485,4.58749948437617,129.025920430873));
#44005=CARTESIAN_POINT('Ctrl Pts',(109.87443957522,4.5343681856923,128.899449013559));
#44006=CARTESIAN_POINT('Ctrl Pts',(109.866691507217,4.48122498862258,128.772949273848));
#44007=CARTESIAN_POINT('Ctrl Pts',(109.858943439214,4.4227983668947,128.648708905126));
#44008=CARTESIAN_POINT('Ctrl Pts',(109.851195371211,4.35932006759288,128.527188772759));
#44009=CARTESIAN_POINT('Ctrl Pts',(109.843439068469,4.2957743027989,128.405539487349));
#44010=CARTESIAN_POINT('Ctrl Pts',(109.835682765727,4.22716631661626,128.286616560664));
#44011=CARTESIAN_POINT('Ctrl Pts',(109.827926462985,4.1537734371959,128.17085548278));
#44012=CARTESIAN_POINT('Ctrl Pts',(109.820166020471,4.08034138578597,128.055032619723));
#44013=CARTESIAN_POINT('Ctrl Pts',(109.812405577957,4.00211957526458,127.942375289088));
#44014=CARTESIAN_POINT('Ctrl Pts',(109.804645135443,3.91942730853519,127.833287976985));
#44015=CARTESIAN_POINT('Ctrl Pts',(109.796872235177,3.83660229683811,127.724025548244));
#44016=CARTESIAN_POINT('Ctrl Pts',(109.789099334912,3.74929273740831,127.618344891802));
#44017=CARTESIAN_POINT('Ctrl Pts',(109.781326434646,3.65785725834914,127.516616202311));
#44018=CARTESIAN_POINT('Ctrl Pts',(109.773836098884,3.5697456892651,127.41858560692));
#44019=CARTESIAN_POINT('Ctrl Pts',(109.766345763122,3.47780318264203,127.324224859619));
#44020=CARTESIAN_POINT('Ctrl Pts',(109.75885542736,3.38237999607707,127.233830037297));
#44021=CARTESIAN_POINT('Ctrl Pts',(109.751081093241,3.28333881039114,127.140007867812));
#44022=CARTESIAN_POINT('Ctrl Pts',(109.743306759122,3.18023406183943,127.050161095591));
#44023=CARTESIAN_POINT('Ctrl Pts',(109.735532425003,3.07341821787181,126.964662254341));
#44024=CARTESIAN_POINT('Ctrl Pts',(109.727767672056,2.96673401488562,126.879268782771));
#44025=CARTESIAN_POINT('Ctrl Pts',(109.720002919109,2.8563481188693,126.798212822449));
#44026=CARTESIAN_POINT('Ctrl Pts',(109.712238166162,2.7426496563545,126.721830038991));
#44027=CARTESIAN_POINT('Ctrl Pts',(109.704481125277,2.62906412075577,126.645523119991));
#44028=CARTESIAN_POINT('Ctrl Pts',(109.696724084392,2.5121728885132,126.573880357739));
#44029=CARTESIAN_POINT('Ctrl Pts',(109.688967043507,2.39239768655144,126.50719685854));
#44030=CARTESIAN_POINT('Ctrl Pts',(109.681215852266,2.27271280800103,126.440563645888));
#44031=CARTESIAN_POINT('Ctrl Pts',(109.673464661026,2.15014862879788,126.378882441815));
#44032=CARTESIAN_POINT('Ctrl Pts',(109.665713469786,2.02515504402298,126.322404559083));
#44033=CARTESIAN_POINT('Ctrl Pts',(109.657965573009,1.90021458485566,126.265950680959));
#44034=CARTESIAN_POINT('Ctrl Pts',(109.650217676232,1.77284712934111,126.214695886219));
#44035=CARTESIAN_POINT('Ctrl Pts',(109.642469779455,1.64352611552412,126.168845007616));
#44036=CARTESIAN_POINT('Ctrl Pts',(109.634723503371,1.51423215287529,126.123003720028));
#44037=CARTESIAN_POINT('Ctrl Pts',(109.626977227287,1.38298581299231,126.08256423075));
#44038=CARTESIAN_POINT('Ctrl Pts',(109.619230951203,1.25027903295238,126.047682637898));
#44039=CARTESIAN_POINT('Ctrl Pts',(109.611484617937,1.11757127330078,126.012800787558));
#44040=CARTESIAN_POINT('Ctrl Pts',(109.603738284672,0.983403430101634,125.983477014899));
#44041=CARTESIAN_POINT('Ctrl Pts',(109.595991951406,0.848280680115232,125.959816990944));
#44042=CARTESIAN_POINT('Ctrl Pts',(109.588243883403,0.713127670325847,125.936151668491));
#44043=CARTESIAN_POINT('Ctrl Pts',(109.5804958154,0.577019713255284,125.918152686044));
#44044=CARTESIAN_POINT('Ctrl Pts',(109.572747747397,0.440469812948712,125.905874177207));
#44045=CARTESIAN_POINT('Ctrl Pts',(109.564991444656,0.303774785783503,125.893582618625));
#44046=CARTESIAN_POINT('Ctrl Pts',(109.557235141914,0.166637267115951,125.887023713752));
#44047=CARTESIAN_POINT('Ctrl Pts',(109.549478839172,0.0295735497205978,
125.886199531585));
#44048=CARTESIAN_POINT('Ctrl Pts',(109.541718396658,-0.107563322707545,
125.885374909527));
#44049=CARTESIAN_POINT('Ctrl Pts',(109.533957954144,-0.244625924852864,
125.890291095059));
#44050=CARTESIAN_POINT('Ctrl Pts',(109.526197511629,-0.381101360076507,
125.900898084228));
#44051=CARTESIAN_POINT('Ctrl Pts',(109.518424611364,-0.517795877784491,
125.911522100678));
#44052=CARTESIAN_POINT('Ctrl Pts',(109.510651711099,-0.65390095660709,125.927855129561));
#44053=CARTESIAN_POINT('Ctrl Pts',(109.502878810833,-0.788911294049677,
125.949795546149));
#44054=CARTESIAN_POINT('Ctrl Pts',(109.495388475071,-0.919013665655613,
125.97093837333));
#44055=CARTESIAN_POINT('Ctrl Pts',(109.487898139309,-1.04809920544465,125.997287919293));
#44056=CARTESIAN_POINT('Ctrl Pts',(109.480407803547,-1.17572949275671,126.028709539193));
#44057=CARTESIAN_POINT('Ctrl Pts',(109.472633469428,-1.30819892120478,126.061322519363));
#44058=CARTESIAN_POINT('Ctrl Pts',(109.464859135309,-1.43952019033272,126.099503089383));
#44059=CARTESIAN_POINT('Ctrl Pts',(109.45708480119,-1.56918935971647,126.143156071973));
#44060=CARTESIAN_POINT('Ctrl Pts',(109.449320048243,-1.69869872343773,126.186755256164));
#44061=CARTESIAN_POINT('Ctrl Pts',(109.441555295296,-1.82655967160295,126.235813310318));
#44062=CARTESIAN_POINT('Ctrl Pts',(109.433790542348,-1.95227946682784,126.290184286728));
#44063=CARTESIAN_POINT('Ctrl Pts',(109.426033501463,-2.07787439537986,126.344501261117));
#44064=CARTESIAN_POINT('Ctrl Pts',(109.418276460578,-2.20133204654564,126.404120502365));
#44065=CARTESIAN_POINT('Ctrl Pts',(109.410519419693,-2.3221761853287,126.468846711834));
#44066=CARTESIAN_POINT('Ctrl Pts',(109.402768228453,-2.44292919460732,126.533524110766));
#44067=CARTESIAN_POINT('Ctrl Pts',(109.395017037213,-2.56107227115304,126.603300628479));
#44068=CARTESIAN_POINT('Ctrl Pts',(109.387265845973,-2.67615079914131,126.677933596188));
#44069=CARTESIAN_POINT('Ctrl Pts',(109.379517949196,-2.79118041568475,126.752534842895));
#44070=CARTESIAN_POINT('Ctrl Pts',(109.371770052419,-2.90314774693929,126.831988221928));
#44071=CARTESIAN_POINT('Ctrl Pts',(109.364022155642,-3.01162455648183,126.916006133559));
#44072=CARTESIAN_POINT('Ctrl Pts',(109.356275879557,-3.12007867501439,127.000006470454));
#44073=CARTESIAN_POINT('Ctrl Pts',(109.348529603473,-3.22504341522704,127.088569201543));
#44074=CARTESIAN_POINT('Ctrl Pts',(109.340783327389,-3.32612154334628,127.181364821076));
#44075=CARTESIAN_POINT('Ctrl Pts',(109.333036994124,-3.42720041760151,127.274161125604));
#44076=CARTESIAN_POINT('Ctrl Pts',(109.325290660859,-3.52439233451243,127.371190116524));
#44077=CARTESIAN_POINT('Ctrl Pts',(109.317544327593,-3.61733532967677,127.472083892087));
#44078=CARTESIAN_POINT('Ctrl Pts',(109.30979625959,-3.71029913878046,127.573000262111));
#44079=CARTESIAN_POINT('Ctrl Pts',(109.302048191587,-3.79901186788861,127.67778285151));
#44080=CARTESIAN_POINT('Ctrl Pts',(109.294300123584,-3.883150681651,127.786029315987));
#44081=CARTESIAN_POINT('Ctrl Pts',(109.286543820842,-3.96737891914557,127.894390826093));
#44082=CARTESIAN_POINT('Ctrl Pts',(109.2787875181,-4.04702329018245,128.006223256191));
#44083=CARTESIAN_POINT('Ctrl Pts',(109.271031215359,-4.12180298520095,128.121093352889));
#44084=CARTESIAN_POINT('Ctrl Pts',(109.263270772844,-4.19662259239436,128.236024759216));
#44085=CARTESIAN_POINT('Ctrl Pts',(109.25551033033,-4.26657215067226,128.35399672658));
#44086=CARTESIAN_POINT('Ctrl Pts',(109.247749887816,-4.33141649661511,128.474550712155));
#44087=CARTESIAN_POINT('Ctrl Pts',(109.239976987551,-4.39636493645869,128.59529822169));
#44088=CARTESIAN_POINT('Ctrl Pts',(109.232204087285,-4.45619161633874,128.718635680268));
#44089=CARTESIAN_POINT('Ctrl Pts',(109.22443118702,-4.51070890767654,128.84408303194));
#44090=CARTESIAN_POINT('Ctrl Pts',(109.216940851258,-4.56324435815248,128.964970056394));
#44091=CARTESIAN_POINT('Ctrl Pts',(109.209450515496,-4.61084962622054,129.087815950126));
#44092=CARTESIAN_POINT('Ctrl Pts',(109.201960179734,-4.65340101532632,129.212179078589));
#44093=CARTESIAN_POINT('Ctrl Pts',(109.194621588097,-4.69509037054069,129.334022777397));
#44094=CARTESIAN_POINT('Ctrl Pts',(109.18728299646,-4.73201650924825,129.457574369527));
#44095=CARTESIAN_POINT('Ctrl Pts',(109.179944404822,-4.76405452823403,129.582490119308));
#44096=CARTESIAN_POINT('Origin',(213.235140564004,0.,130.804360617566));
#44097=CARTESIAN_POINT('',(107.085000608365,-4.76405452823403,129.582490119308));
#44098=CARTESIAN_POINT('',(107.429960893282,-4.76405452823407,129.582490119308));
#44099=CARTESIAN_POINT('',(213.235140564004,-4.76405452823405,129.582490119308));
#44100=CARTESIAN_POINT('',(108.764859435936,-4.91824882485165,130.807760521293));
#44101=CARTESIAN_POINT('Ctrl Pts',(108.764859435936,-4.91824882485165,130.807760521293));
#44102=CARTESIAN_POINT('Ctrl Pts',(108.756034552605,-4.91814069778781,130.964175481081));
#44103=CARTESIAN_POINT('Ctrl Pts',(108.747209669273,-4.91056689496297,131.120296647971));
#44104=CARTESIAN_POINT('Ctrl Pts',(108.738384785941,-4.89563530303815,131.275463623443));
#44105=CARTESIAN_POINT('Ctrl Pts',(108.729520287116,-4.88063668219459,131.431327153887));
#44106=CARTESIAN_POINT('Ctrl Pts',(108.720655788291,-4.85821417577054,131.586227746882));
#44107=CARTESIAN_POINT('Ctrl Pts',(108.711791289465,-4.82852675013294,131.739514340625));
#44108=CARTESIAN_POINT('Ctrl Pts',(108.702874025054,-4.79866261124519,131.893713366874));
#44109=CARTESIAN_POINT('Ctrl Pts',(108.693956760643,-4.76144689983342,132.046278963872));
#44110=CARTESIAN_POINT('Ctrl Pts',(108.685039496232,-4.71709001905848,132.196569227868));
#44111=CARTESIAN_POINT('Ctrl Pts',(108.678244306911,-4.68328891272221,132.311094350146));
#44112=CARTESIAN_POINT('Ctrl Pts',(108.671449117589,-4.64534204592225,132.424298633557));
#44113=CARTESIAN_POINT('Ctrl Pts',(108.664653928267,-4.60336077874322,132.535906921662));
#44114=CARTESIAN_POINT('Ctrl Pts',(108.656879594148,-4.55533027034333,132.663597274515));
#44115=CARTESIAN_POINT('Ctrl Pts',(108.649105260029,-4.50190674915696,132.789489923373));
#44116=CARTESIAN_POINT('Ctrl Pts',(108.64133092591,-4.44324424605536,132.913095696327));
#44117=CARTESIAN_POINT('Ctrl Pts',(108.633566172963,-4.38465403924595,133.036549136213));
#44118=CARTESIAN_POINT('Ctrl Pts',(108.625801420016,-4.32083786320501,133.157720958096));
#44119=CARTESIAN_POINT('Ctrl Pts',(108.618036667069,-4.25199884069516,133.276139111126));
#44120=CARTESIAN_POINT('Ctrl Pts',(108.610279626184,-4.18322819007303,133.394439649577));
#44121=CARTESIAN_POINT('Ctrl Pts',(108.602522585299,-4.10944481606034,133.509991626097));
#44122=CARTESIAN_POINT('Ctrl Pts',(108.594765544414,-4.03089889785178,133.622345205494));
#44123=CARTESIAN_POINT('Ctrl Pts',(108.587014353174,-3.95241221173119,133.734614058182));
#44124=CARTESIAN_POINT('Ctrl Pts',(108.579263161934,-3.86917035312413,133.843688995428));
#44125=CARTESIAN_POINT('Ctrl Pts',(108.571511970694,-3.7814679864004,133.94914724472));
#44126=CARTESIAN_POINT('Ctrl Pts',(108.563764073917,-3.69380289552201,134.054560671444));
#44127=CARTESIAN_POINT('Ctrl Pts',(108.55601617714,-3.60168131666245,134.156360167594));
#44128=CARTESIAN_POINT('Ctrl Pts',(108.548268280362,-3.50543941500974,134.25415446216));
#44129=CARTESIAN_POINT('Ctrl Pts',(108.540522004278,-3.40921764508805,134.351928300267));
#44130=CARTESIAN_POINT('Ctrl Pts',(108.532775728194,-3.308877540765,134.445698324743));
#44131=CARTESIAN_POINT('Ctrl Pts',(108.52502945211,-3.20479321825092,134.535108999694));
#44132=CARTESIAN_POINT('Ctrl Pts',(108.517283118845,-3.10070812741009,134.624520334655));
#44133=CARTESIAN_POINT('Ctrl Pts',(108.509536785579,-2.99287905979412,134.70957200112));
#44134=CARTESIAN_POINT('Ctrl Pts',(108.501790452314,-2.88171409324305,134.78994802061));
#44135=CARTESIAN_POINT('Ctrl Pts',(108.494042384311,-2.77052423206849,134.870342039752));
#44136=CARTESIAN_POINT('Ctrl Pts',(108.486294316308,-2.65599730217761,134.946058099321));
#44137=CARTESIAN_POINT('Ctrl Pts',(108.478546248305,-2.53857096140315,135.016823143977));
#44138=CARTESIAN_POINT('Ctrl Pts',(108.470789945563,-2.42101981851632,135.087663398565));
#44139=CARTESIAN_POINT('Ctrl Pts',(108.463033642822,-2.30056344445518,135.153541924713));
#44140=CARTESIAN_POINT('Ctrl Pts',(108.45527734008,-2.17766522618921,135.214231049353));
#44141=CARTESIAN_POINT('Ctrl Pts',(108.447516897566,-2.05470141344358,135.274952565605));
#44142=CARTESIAN_POINT('Ctrl Pts',(108.439756455051,-1.92929351690171,135.330479003201));
#44143=CARTESIAN_POINT('Ctrl Pts',(108.431996012537,-1.80192464475143,135.380631002622));
#44144=CARTESIAN_POINT('Ctrl Pts',(108.424223112272,-1.67435130878047,135.430863510484));
#44145=CARTESIAN_POINT('Ctrl Pts',(108.416450212006,-1.54481107629906,135.475704211666));
#44146=CARTESIAN_POINT('Ctrl Pts',(108.408677311741,-1.41380280375881,135.515023489666));
#44147=CARTESIAN_POINT('Ctrl Pts',(108.401186975979,-1.2875570119156,135.552913412872));
#44148=CARTESIAN_POINT('Ctrl Pts',(108.393696640217,-1.1599483592065,135.585676302073));
#44149=CARTESIAN_POINT('Ctrl Pts',(108.386206304455,-1.03142999867423,135.613241487408));
#44150=CARTESIAN_POINT('Ctrl Pts',(108.378431970336,-0.898038825439874,
135.641851815124));
#44151=CARTESIAN_POINT('Ctrl Pts',(108.370657636217,-0.763245056347442,
135.664953145524));
#44152=CARTESIAN_POINT('Ctrl Pts',(108.362883302098,-0.627543503026194,
135.682410659776));
#44153=CARTESIAN_POINT('Ctrl Pts',(108.355118549151,-0.492009189741419,
135.699846659203));
#44154=CARTESIAN_POINT('Ctrl Pts',(108.347353796204,-0.355569702279653,
135.711652632446));
#44155=CARTESIAN_POINT('Ctrl Pts',(108.339589043256,-0.218731983206265,
135.717744317423));
#44156=CARTESIAN_POINT('Ctrl Pts',(108.331832002371,-0.0820301732845349,
135.723829952053));
#44157=CARTESIAN_POINT('Ctrl Pts',(108.324074961486,0.0550686930768079,
135.724212575665));
#44158=CARTESIAN_POINT('Ctrl Pts',(108.316317920601,0.192050928824161,135.718859524193));
#44159=CARTESIAN_POINT('Ctrl Pts',(108.308566729361,0.328929865201878,135.713510509498));
#44160=CARTESIAN_POINT('Ctrl Pts',(108.300815538121,0.465691956942546,135.702434444206));
#44161=CARTESIAN_POINT('Ctrl Pts',(108.293064346881,0.601822240268474,135.685650718924));
#44162=CARTESIAN_POINT('Ctrl Pts',(108.285316450104,0.737894664592687,135.668874127174));
#44163=CARTESIAN_POINT('Ctrl Pts',(108.277568553327,0.873335427383866,135.646394748121));
#44164=CARTESIAN_POINT('Ctrl Pts',(108.26982065655,1.00763363576269,135.61828391552));
#44165=CARTESIAN_POINT('Ctrl Pts',(108.262074380466,1.14190375185145,135.590178963098));
#44166=CARTESIAN_POINT('Ctrl Pts',(108.254328104382,1.27503140647794,135.556444980241));
#44167=CARTESIAN_POINT('Ctrl Pts',(108.246581828298,1.40651525827599,135.517204545677));
#44168=CARTESIAN_POINT('Ctrl Pts',(108.238835495032,1.53800008065797,135.47796382145));
#44169=CARTESIAN_POINT('Ctrl Pts',(108.231089161767,1.66784070136172,135.433216676214));
#44170=CARTESIAN_POINT('Ctrl Pts',(108.223342828502,1.79555070270169,135.383135643326));
#44171=CARTESIAN_POINT('Ctrl Pts',(108.215594760499,1.92328930381108,135.333043395139));
#44172=CARTESIAN_POINT('Ctrl Pts',(108.207846692496,2.04889597219868,135.277615025115));
#44173=CARTESIAN_POINT('Ctrl Pts',(108.200098624493,2.17190441392461,135.217071154104));
#44174=CARTESIAN_POINT('Ctrl Pts',(108.192342321751,2.29504359048615,135.156462936346));
#44175=CARTESIAN_POINT('Ctrl Pts',(108.184586019009,2.41557867280187,135.090728529902));
#44176=CARTESIAN_POINT('Ctrl Pts',(108.176829716267,2.53306764109497,135.020134732499));
#44177=CARTESIAN_POINT('Ctrl Pts',(108.169069273753,2.65061931678806,134.94950325706));
#44178=CARTESIAN_POINT('Ctrl Pts',(108.161308831239,2.7651213126664,134.874007437792));
#44179=CARTESIAN_POINT('Ctrl Pts',(108.153548388725,2.87616159671256,134.793956779096));
#44180=CARTESIAN_POINT('Ctrl Pts',(108.145775488459,2.98738013248029,134.713777615976));
#44181=CARTESIAN_POINT('Ctrl Pts',(108.138002588194,3.09512554419143,134.629029243903));
#44182=CARTESIAN_POINT('Ctrl Pts',(108.130229687928,3.19901913771574,134.540061304054));
#44183=CARTESIAN_POINT('Ctrl Pts',(108.122739352166,3.29913593742404,134.454327572915));
#44184=CARTESIAN_POINT('Ctrl Pts',(108.115249016404,3.39567587780697,134.364675941216));
#44185=CARTESIAN_POINT('Ctrl Pts',(108.107758680642,3.48833456202035,134.271449460661));
#44186=CARTESIAN_POINT('Ctrl Pts',(108.099984346523,3.58450642840799,134.174688269761));
#44187=CARTESIAN_POINT('Ctrl Pts',(108.092210012404,3.67680155665234,134.073769287628));
#44188=CARTESIAN_POINT('Ctrl Pts',(108.084435678285,3.76483906208055,133.969035940428));
#44189=CARTESIAN_POINT('Ctrl Pts',(108.076670925338,3.85276806915139,133.864431667718));
#44190=CARTESIAN_POINT('Ctrl Pts',(108.068906172391,3.93644964449626,133.756022679665));
#44191=CARTESIAN_POINT('Ctrl Pts',(108.061141419443,4.0155388811991,133.64418993569));
#44192=CARTESIAN_POINT('Ctrl Pts',(108.053384378558,4.09454956535708,133.532468265574));
#44193=CARTESIAN_POINT('Ctrl Pts',(108.045627337673,4.16897676353303,133.417329923871));
#44194=CARTESIAN_POINT('Ctrl Pts',(108.037870296788,4.23851533412164,133.299189434322));
#44195=CARTESIAN_POINT('Ctrl Pts',(108.030119105548,4.30800146513324,133.181138035435));
#44196=CARTESIAN_POINT('Ctrl Pts',(108.022367914308,4.37260610889755,133.060089330511));
#44197=CARTESIAN_POINT('Ctrl Pts',(108.014616723068,4.43206722878328,132.936487054259));
#44198=CARTESIAN_POINT('Ctrl Pts',(108.006868826291,4.49150307610689,132.812937312272));
#44199=CARTESIAN_POINT('Ctrl Pts',(107.999120929514,4.54579957847373,132.686836509186));
#44200=CARTESIAN_POINT('Ctrl Pts',(107.991373032737,4.59474060091079,132.558653031288));
#44201=CARTESIAN_POINT('Ctrl Pts',(107.983626756653,4.64367138594099,132.43049636661));
#44202=CARTESIAN_POINT('Ctrl Pts',(107.975880480569,4.68724877991678,132.300258258669));
#44203=CARTESIAN_POINT('Ctrl Pts',(107.968134204485,4.72530492453977,132.168426756952));
#44204=CARTESIAN_POINT('Ctrl Pts',(107.960387871219,4.7633613500846,132.036594282085));
#44205=CARTESIAN_POINT('Ctrl Pts',(107.952641537954,4.7958963365164,131.9031687656));
#44206=CARTESIAN_POINT('Ctrl Pts',(107.944895204688,4.82279212039432,131.768652702965));
#44207=CARTESIAN_POINT('Ctrl Pts',(107.937147136685,4.84969392739654,131.63410651639));
#44208=CARTESIAN_POINT('Ctrl Pts',(107.929399068683,4.8709539422595,131.498469680999));
#44209=CARTESIAN_POINT('Ctrl Pts',(107.92165100068,4.88650573628719,131.362253754047));
#44210=CARTESIAN_POINT('Ctrl Pts',(107.913894697938,4.90207405894664,131.225893055187));
#44211=CARTESIAN_POINT('Ctrl Pts',(107.906138395196,4.91192199733498,131.088952424369));
#44212=CARTESIAN_POINT('Ctrl Pts',(107.898382092454,4.91603509344909,130.951947956037));
#44213=CARTESIAN_POINT('Ctrl Pts',(107.89062164994,4.92015038484644,130.814870364296));
#44214=CARTESIAN_POINT('Ctrl Pts',(107.882861207426,4.91852473958268,130.677729257896));
#44215=CARTESIAN_POINT('Ctrl Pts',(107.875100764911,4.91119583910588,130.541038585732));
#44216=CARTESIAN_POINT('Ctrl Pts',(107.867327864646,4.90385517362742,130.404128485567));
#44217=CARTESIAN_POINT('Ctrl Pts',(107.859554964381,4.8907929948618,130.267670653986));
#44218=CARTESIAN_POINT('Ctrl Pts',(107.851782064115,4.87209877240557,130.132172686683));
#44219=CARTESIAN_POINT('Ctrl Pts',(107.844291728353,4.85408413202345,130.00160041179));
#44220=CARTESIAN_POINT('Ctrl Pts',(107.836801392591,4.83083987110543,129.871919728997));
#44221=CARTESIAN_POINT('Ctrl Pts',(107.829311056829,4.80249007483505,129.743572163815));
#44222=CARTESIAN_POINT('Ctrl Pts',(107.82153672271,4.77306538742247,129.61035826169));
#44223=CARTESIAN_POINT('Ctrl Pts',(107.813762388591,4.73804716082972,129.478158581438));
#44224=CARTESIAN_POINT('Ctrl Pts',(107.805988054472,4.69751845174746,129.347479202353));
#44225=CARTESIAN_POINT('Ctrl Pts',(107.798223301525,4.65703969067701,129.216960873925));
#44226=CARTESIAN_POINT('Ctrl Pts',(107.790458548578,4.61106407423523,129.087959488522));
#44227=CARTESIAN_POINT('Ctrl Pts',(107.78269379563,4.55972568376157,128.960971143975));
#44228=CARTESIAN_POINT('Ctrl Pts',(107.774936754745,4.50843828330107,128.834108926043));
#44229=CARTESIAN_POINT('Ctrl Pts',(107.76717971386,4.45179885413864,128.709256130229));
#44230=CARTESIAN_POINT('Ctrl Pts',(107.759422672975,4.38999121034556,128.586893541015));
#44231=CARTESIAN_POINT('Ctrl Pts',(107.751671481735,4.32823017617746,128.464623226381));
#44232=CARTESIAN_POINT('Ctrl Pts',(107.743920290495,4.26130886045816,128.344839728093));
#44233=CARTESIAN_POINT('Ctrl Pts',(107.736169099255,4.18945895256576,128.228003354439));
#44234=CARTESIAN_POINT('Ctrl Pts',(107.728421202478,4.11763958280088,128.111216639361));
#44235=CARTESIAN_POINT('Ctrl Pts',(107.720673305701,4.04089599159981,127.997374889912));
#44236=CARTESIAN_POINT('Ctrl Pts',(107.712925408924,3.95950541937726,127.886913120794));
#44237=CARTESIAN_POINT('Ctrl Pts',(107.70517913284,3.87813187230783,127.776474457897));
#44238=CARTESIAN_POINT('Ctrl Pts',(107.697432856756,3.79211350944316,127.669414683585));
#44239=CARTESIAN_POINT('Ctrl Pts',(107.689686580671,3.70177020912853,127.566138824466));
#44240=CARTESIAN_POINT('Ctrl Pts',(107.681940247406,3.61142624192018,127.462862202988));
#44241=CARTESIAN_POINT('Ctrl Pts',(107.674193914141,3.51675753097159,127.363369846705));
#44242=CARTESIAN_POINT('Ctrl Pts',(107.666447580875,3.41812318593567,127.268032444408));
#44243=CARTESIAN_POINT('Ctrl Pts',(107.658699512872,3.31946675242206,127.172673691962));
#44244=CARTESIAN_POINT('Ctrl Pts',(107.650951444869,3.21684319871082,127.0814720167));
#44245=CARTESIAN_POINT('Ctrl Pts',(107.643203376866,3.11064700607623,126.994759816158));
#44246=CARTESIAN_POINT('Ctrl Pts',(107.635447074125,3.00433794686436,126.907955456858));
#44247=CARTESIAN_POINT('Ctrl Pts',(107.627690771383,2.89444896704493,126.825650351465));
#44248=CARTESIAN_POINT('Ctrl Pts',(107.619934468641,2.78140645658704,126.748135625562));
#44249=CARTESIAN_POINT('Ctrl Pts',(107.612174026127,2.66830361193761,126.670579527716));
#44250=CARTESIAN_POINT('Ctrl Pts',(107.604413583612,2.55204421411191,126.59781911125));
#44251=CARTESIAN_POINT('Ctrl Pts',(107.596653141098,2.4330810306136,126.530100475627));
#44252=CARTESIAN_POINT('Ctrl Pts',(107.588880240833,2.31392687685209,126.462273132038));
#44253=CARTESIAN_POINT('Ctrl Pts',(107.581107340567,2.19206061177229,126.399503921837));
#44254=CARTESIAN_POINT('Ctrl Pts',(107.573334440302,2.06795765050916,126.341991939588));
#44255=CARTESIAN_POINT('Ctrl Pts',(107.56584410454,1.94836614448477,126.286570662758));
#44256=CARTESIAN_POINT('Ctrl Pts',(107.558353768778,1.8266980225053,126.236031141104));
#44257=CARTESIAN_POINT('Ctrl Pts',(107.550863433016,1.70339182356023,126.19050763357));
#44258=CARTESIAN_POINT('Ctrl Pts',(107.543089098897,1.57541043260377,126.143258088411));
#44259=CARTESIAN_POINT('Ctrl Pts',(107.535314764778,1.44525889067726,126.101262757879));
#44260=CARTESIAN_POINT('Ctrl Pts',(107.527540430659,1.31340787079371,126.064725312246));
#44261=CARTESIAN_POINT('Ctrl Pts',(107.519775677712,1.1817193455084,126.028232895749));
#44262=CARTESIAN_POINT('Ctrl Pts',(107.512010924765,1.04833588275632,125.997185084115));
#44263=CARTESIAN_POINT('Ctrl Pts',(107.504246171817,0.91374733793175,125.971737223909));
#44264=CARTESIAN_POINT('Ctrl Pts',(107.496489130932,0.779292468347171,125.946314638876));
#44265=CARTESIAN_POINT('Ctrl Pts',(107.488732090047,0.643635280256703,125.926481008906));
#44266=CARTESIAN_POINT('Ctrl Pts',(107.480975049162,0.507279627256514,125.91234156177));
#44267=CARTESIAN_POINT('Ctrl Pts',(107.473223857922,0.371026801114852,125.898212777301));
#44268=CARTESIAN_POINT('Ctrl Pts',(107.465472666682,0.234076945769885,125.889769668827));
#44269=CARTESIAN_POINT('Ctrl Pts',(107.457721475442,0.0969425653892498,
125.887066117384));
#44270=CARTESIAN_POINT('Ctrl Pts',(107.449973578665,-0.0401335292214509,
125.884363715024));
#44271=CARTESIAN_POINT('Ctrl Pts',(107.442225681888,-0.177393602809493,
125.887396025476));
#44272=CARTESIAN_POINT('Ctrl Pts',(107.434477785111,-0.314321809969613,
125.896164934601));
#44273=CARTESIAN_POINT('Ctrl Pts',(107.426731509027,-0.451221374700625,
125.904932009459));
#44274=CARTESIAN_POINT('Ctrl Pts',(107.418985232943,-0.587788821163742,
125.919433271207));
#44275=CARTESIAN_POINT('Ctrl Pts',(107.411238956858,-0.723510486942408,
125.93961852391));
#44276=CARTESIAN_POINT('Ctrl Pts',(107.403492623593,-0.859233154587487,
125.959803925617));
#44277=CARTESIAN_POINT('Ctrl Pts',(107.395746290328,-0.99410964237823,125.985673344488));
#44278=CARTESIAN_POINT('Ctrl Pts',(107.387999957062,-1.12763397179549,126.017125017749));
#44279=CARTESIAN_POINT('Ctrl Pts',(107.380251889059,-1.26118820306053,126.048583734395));
#44280=CARTESIAN_POINT('Ctrl Pts',(107.372503821056,-1.39338929292455,126.085627103379));
#44281=CARTESIAN_POINT('Ctrl Pts',(107.364755753053,-1.52374435916254,126.128102905418));
#44282=CARTESIAN_POINT('Ctrl Pts',(107.356999450312,-1.65423796831636,126.170623851246));
#44283=CARTESIAN_POINT('Ctrl Pts',(107.34924314757,-1.78288126226469,126.218588642307));
#44284=CARTESIAN_POINT('Ctrl Pts',(107.341486844828,-1.90919883461748,126.271795905133));
#44285=CARTESIAN_POINT('Ctrl Pts',(107.333726402314,-2.03558382646206,126.325031566276));
#44286=CARTESIAN_POINT('Ctrl Pts',(107.3259659598,-2.15964026983527,126.383515107933));
#44287=CARTESIAN_POINT('Ctrl Pts',(107.318205517285,-2.28091638239481,126.446998626748));
#44288=CARTESIAN_POINT('Ctrl Pts',(107.31043261702,-2.40238717813653,126.510584054944));
#44289=CARTESIAN_POINT('Ctrl Pts',(107.302659716754,-2.52106838542017,126.57918530385));
#44290=CARTESIAN_POINT('Ctrl Pts',(107.294886816489,-2.63653552685606,126.652510008726));
#44291=CARTESIAN_POINT('Ctrl Pts',(107.287396480727,-2.74780514685642,126.723169175885));
#44292=CARTESIAN_POINT('Ctrl Pts',(107.279906144965,-2.85609006961675,126.798214166777));
#44293=CARTESIAN_POINT('Ctrl Pts',(107.272415809203,-2.9610402982491,126.877348596367));
#44294=CARTESIAN_POINT('Ctrl Pts',(107.264606842501,-3.07045499830437,126.959849320667));
#44295=CARTESIAN_POINT('Ctrl Pts',(107.2567978758,-3.17661290686497,127.04707268425));
#44296=CARTESIAN_POINT('Ctrl Pts',(107.248988909098,-3.27907398866812,127.138728770348));
#44297=CARTESIAN_POINT('Ctrl Pts',(107.24130636499,-3.37987628562483,127.228900998145));
#44298=CARTESIAN_POINT('Ctrl Pts',(107.233623820881,-3.47710021184727,127.323363256761));
#44299=CARTESIAN_POINT('Ctrl Pts',(107.225941276772,-3.57035532253909,127.421795624352));
#44300=CARTESIAN_POINT('Ctrl Pts',(107.218265722842,-3.66352558245395,127.520138430494));
#44301=CARTESIAN_POINT('Ctrl Pts',(107.210590168911,-3.75273393443584,127.622443874409));
#44302=CARTESIAN_POINT('Ctrl Pts',(107.20291461498,-3.83762421044486,127.72835289945));
#44303=CARTESIAN_POINT('Ctrl Pts',(107.195244297365,-3.92245657372734,127.83418967263));
#44304=CARTESIAN_POINT('Ctrl Pts',(107.18757397975,-4.00297647128173,127.943624826383));
#44305=CARTESIAN_POINT('Ctrl Pts',(107.179903662135,-4.07886607850665,128.056264080669));
#44306=CARTESIAN_POINT('Ctrl Pts',(107.171995074321,-4.15711311507403,128.17240235271));
#44307=CARTESIAN_POINT('Ctrl Pts',(107.164086486507,-4.23043721623045,128.291946705557));
#44308=CARTESIAN_POINT('Ctrl Pts',(107.156177898692,-4.29853633508979,128.414429982921));
#44309=CARTESIAN_POINT('Ctrl Pts',(107.148511678719,-4.3645484775137,128.533159618273));
#44310=CARTESIAN_POINT('Ctrl Pts',(107.140845458746,-4.42565100790585,128.654650303783));
#44311=CARTESIAN_POINT('Ctrl Pts',(107.133179238773,-4.48161447020671,128.778449759968));
#44312=CARTESIAN_POINT('Ctrl Pts',(107.125149467038,-4.54023186304472,128.908120103045));
#44313=CARTESIAN_POINT('Ctrl Pts',(107.117119695303,-4.59321060406721,129.040323138286));
#44314=CARTESIAN_POINT('Ctrl Pts',(107.109089923569,-4.64034318807285,129.174514563668));
#44315=CARTESIAN_POINT('Ctrl Pts',(107.101060151834,-4.6874757720785,129.308705989051));
#44316=CARTESIAN_POINT('Ctrl Pts',(107.0930303801,-4.728762059849,129.444885320713));
#44317=CARTESIAN_POINT('Ctrl Pts',(107.085000608365,-4.76405452823403,129.582490119308));
#44318=CARTESIAN_POINT('Ctrl Pts',(108.834713077301,-4.76405452823406,129.582490119308));
#44319=CARTESIAN_POINT('Ctrl Pts',(108.826933119087,-4.79829315580961,129.715986008582));
#44320=CARTESIAN_POINT('Ctrl Pts',(108.819153160872,-4.82693196985436,129.850982631195));
#44321=CARTESIAN_POINT('Ctrl Pts',(108.811373202658,-4.84985164498987,129.986973265028));
#44322=CARTESIAN_POINT('Ctrl Pts',(108.803593423799,-4.87277079174911,130.122960763815));
#44323=CARTESIAN_POINT('Ctrl Pts',(108.795813644939,-4.88997098710633,130.259941849649));
#44324=CARTESIAN_POINT('Ctrl Pts',(108.788033866079,-4.90138409773953,130.39739994511));
#44325=CARTESIAN_POINT('Ctrl Pts',(108.78030905605,-4.91271656786181,130.533886816213));
#44326=CARTESIAN_POINT('Ctrl Pts',(108.77258424602,-4.91834347321842,130.670843599752));
#44327=CARTESIAN_POINT('Ctrl Pts',(108.764859435991,-4.91824882485232,130.80776052032));
#44328=CARTESIAN_POINT('',(109.110140564059,-4.91824845869996,130.800466905272));
#44329=CARTESIAN_POINT('Ctrl Pts',(109.179944404822,-4.76405452823403,129.582490119308));
#44330=CARTESIAN_POINT('Ctrl Pts',(109.170808292833,-4.80393996454638,129.738002830144));
#44331=CARTESIAN_POINT('Ctrl Pts',(109.161672180843,-4.83624795301888,129.895630417634));
#44332=CARTESIAN_POINT('Ctrl Pts',(109.152536068854,-4.86077948173073,130.054690094946));
#44333=CARTESIAN_POINT('Ctrl Pts',(109.143482846257,-4.88508844273259,130.21230666822));
#44334=CARTESIAN_POINT('Ctrl Pts',(109.13442962366,-4.90176134354085,130.371329371744));
#44335=CARTESIAN_POINT('Ctrl Pts',(109.125376401064,-4.91065141233991,130.531073645714));
#44336=CARTESIAN_POINT('Ctrl Pts',(109.120297788729,-4.91563849981933,130.62068585082));
#44337=CARTESIAN_POINT('Ctrl Pts',(109.115219176394,-4.918177252701,130.710524770806));
#44338=CARTESIAN_POINT('Ctrl Pts',(109.110140564059,-4.91824845869996,130.800466905272));
#44339=CARTESIAN_POINT('Ctrl Pts',(109.110140564008,-4.91824845870068,130.800466906176));
#44340=CARTESIAN_POINT('Ctrl Pts',(109.102364397004,-4.9183574864379,130.938182686036));
#44341=CARTESIAN_POINT('Ctrl Pts',(109.094588230001,-4.91267786849137,131.075970964058));
#44342=CARTESIAN_POINT('Ctrl Pts',(109.086812062997,-4.90121868070611,131.213308666097));
#44343=CARTESIAN_POINT('Ctrl Pts',(109.079076477325,-4.88981929476085,131.349929646547));
#44344=CARTESIAN_POINT('Ctrl Pts',(109.071340891652,-4.8727005703394,131.48610435019));
#44345=CARTESIAN_POINT('Ctrl Pts',(109.06360530598,-4.84992360522252,131.621320889553));
#44346=CARTESIAN_POINT('Ctrl Pts',(109.055869424027,-4.82714576772626,131.756542607839));
#44347=CARTESIAN_POINT('Ctrl Pts',(109.048133542075,-4.79870932295161,131.890805702541));
#44348=CARTESIAN_POINT('Ctrl Pts',(109.040397660122,-4.76472675750061,132.023607101612));
#44349=CARTESIAN_POINT('Ctrl Pts',(109.032659799947,-4.73073550201525,132.156442460706));
#44350=CARTESIAN_POINT('Ctrl Pts',(109.024921939771,-4.69119540060019,132.287815001019));
#44351=CARTESIAN_POINT('Ctrl Pts',(109.017184079596,-4.64626909585595,132.417235861159));
#44352=CARTESIAN_POINT('Ctrl Pts',(109.00937811929,-4.60094739921181,132.547795741302));
#44353=CARTESIAN_POINT('Ctrl Pts',(109.001572158984,-4.5501443666063,132.676369038117));
#44354=CARTESIAN_POINT('Ctrl Pts',(108.993766198677,-4.49407649494377,132.802474608332));
#44355=CARTESIAN_POINT('Ctrl Pts',(108.986015200061,-4.4384033966153,132.927692270465));
#44356=CARTESIAN_POINT('Ctrl Pts',(108.978264201445,-4.377539595994,133.050476523415));
#44357=CARTESIAN_POINT('Ctrl Pts',(108.970513202828,-4.31174283950206,133.170381908363));
#44358=CARTESIAN_POINT('Ctrl Pts',(108.962679761677,-4.24524624397538,133.291562652056));
#44359=CARTESIAN_POINT('Ctrl Pts',(108.954846320526,-4.17371137008288,133.409802584944));
#44360=CARTESIAN_POINT('Ctrl Pts',(108.947012879375,-4.09744815581249,133.524673407105));
#44361=CARTESIAN_POINT('Ctrl Pts',(108.939179438224,-4.02118494154209,133.639544229266));
#44362=CARTESIAN_POINT('Ctrl Pts',(108.931345997072,-3.94019367744347,133.751045650442));
#44363=CARTESIAN_POINT('Ctrl Pts',(108.923512555921,-3.85482433608878,133.858785669912));
#44364=CARTESIAN_POINT('Ctrl Pts',(108.915738221802,-3.77009914694037,133.96571273979));
#44365=CARTESIAN_POINT('Ctrl Pts',(108.907963887683,-3.68078739166395,134.069281277589));
#44366=CARTESIAN_POINT('Ctrl Pts',(108.900189553564,-3.58718510686284,134.169072502944));
#44367=CARTESIAN_POINT('Ctrl Pts',(108.892424800617,-3.4936981785124,134.268740744531));
#44368=CARTESIAN_POINT('Ctrl Pts',(108.88466004767,-3.39593150647519,134.364640653717));
#44369=CARTESIAN_POINT('Ctrl Pts',(108.876895294723,-3.29422264719171,134.456384743065));
#44370=CARTESIAN_POINT('Ctrl Pts',(108.869138253838,-3.19261480658105,134.548037710891));
#44371=CARTESIAN_POINT('Ctrl Pts',(108.861381212953,-3.08707285904919,134.635542812854));
#44372=CARTESIAN_POINT('Ctrl Pts',(108.853624172068,-2.97797238705606,134.718548084261));
#44373=CARTESIAN_POINT('Ctrl Pts',(108.845872980828,-2.86895418857785,134.801490760747));
#44374=CARTESIAN_POINT('Ctrl Pts',(108.838121789588,-2.75638311689477,134.879940125178));
#44375=CARTESIAN_POINT('Ctrl Pts',(108.830370598348,-2.64066885205257,134.953583566059));
#44376=CARTESIAN_POINT('Ctrl Pts',(108.82262270157,-2.52500376885939,135.027195706513));
#44377=CARTESIAN_POINT('Ctrl Pts',(108.814874804793,-2.40619847873435,135.096005776607));
#44378=CARTESIAN_POINT('Ctrl Pts',(108.807126908016,-2.2846925621417,135.159743833656));
#44379=CARTESIAN_POINT('Ctrl Pts',(108.799380631932,-2.16321206196751,135.223468558077));
#44380=CARTESIAN_POINT('Ctrl Pts',(108.791634355848,-2.03903240497035,135.282123198249));
#44381=CARTESIAN_POINT('Ctrl Pts',(108.783888079764,-1.9126183990844,135.335483427862));
#44382=CARTESIAN_POINT('Ctrl Pts',(108.776141746499,-1.78620346003888,135.388844051367));
#44383=CARTESIAN_POINT('Ctrl Pts',(108.768395413233,-1.65755449938448,135.436910034288));
#44384=CARTESIAN_POINT('Ctrl Pts',(108.760649079968,-1.52715658656531,135.47950508834));
#44385=CARTESIAN_POINT('Ctrl Pts',(108.752901011965,-1.39672947203777,135.52210968126));
#44386=CARTESIAN_POINT('Ctrl Pts',(108.745152943962,-1.264552997545,135.559240785977));
#44387=CARTESIAN_POINT('Ctrl Pts',(108.737404875959,-1.1311272939735,135.590772019371));
#44388=CARTESIAN_POINT('Ctrl Pts',(108.729648573217,-0.997559783976367,
135.622336764534));
#44389=CARTESIAN_POINT('Ctrl Pts',(108.721892270475,-0.862740773777352,
135.648289659332));
#44390=CARTESIAN_POINT('Ctrl Pts',(108.714135967734,-0.72718103788804,135.668555391692));
#44391=CARTESIAN_POINT('Ctrl Pts',(108.706375525219,-0.591548949686152,
135.688831940484));
#44392=CARTESIAN_POINT('Ctrl Pts',(108.698615082705,-0.45517573658895,135.703415236976));
#44393=CARTESIAN_POINT('Ctrl Pts',(108.690854640191,-0.31857620069985,135.712281997015));
#44394=CARTESIAN_POINT('Ctrl Pts',(108.683081739926,-0.181757383108912,
135.721162990764));
#44395=CARTESIAN_POINT('Ctrl Pts',(108.67530883966,-0.0447119077972331,
135.724309101127));
#44396=CARTESIAN_POINT('Ctrl Pts',(108.667535939395,0.0920456152316443,
135.721749219987));
#44397=CARTESIAN_POINT('Ctrl Pts',(108.660045603633,0.223831657826546,135.719282396973));
#44398=CARTESIAN_POINT('Ctrl Pts',(108.652555267871,0.355350012764772,135.711517252458));
#44399=CARTESIAN_POINT('Ctrl Pts',(108.645064932109,0.486147589374755,135.698524855089));
#44400=CARTESIAN_POINT('Ctrl Pts',(108.63729059799,0.621904395857443,135.685039847024));
#44401=CARTESIAN_POINT('Ctrl Pts',(108.629516263871,0.757314725209164,135.665880662352));
#44402=CARTESIAN_POINT('Ctrl Pts',(108.621741929752,0.891866230632137,135.641070004035));
#44403=CARTESIAN_POINT('Ctrl Pts',(108.613977176804,1.02625191334962,135.616289922637));
#44404=CARTESIAN_POINT('Ctrl Pts',(108.606212423857,1.1597804972938,135.585872295956));
#44405=CARTESIAN_POINT('Ctrl Pts',(108.59844767091,1.29194352080965,135.549891673363));
#44406=CARTESIAN_POINT('Ctrl Pts',(108.590690630025,1.42397527814763,135.513946787232));
#44407=CARTESIAN_POINT('Ctrl Pts',(108.58293358914,1.55464379934905,135.472450002712));
#44408=CARTESIAN_POINT('Ctrl Pts',(108.575176548255,1.68344995505456,135.425527062451));
#44409=CARTESIAN_POINT('Ctrl Pts',(108.567425357015,1.81215897703661,135.378639507143));
#44410=CARTESIAN_POINT('Ctrl Pts',(108.559674165775,1.93900806308132,135.326334074065));
#44411=CARTESIAN_POINT('Ctrl Pts',(108.551922974535,2.06351276221074,135.268786464491));
#44412=CARTESIAN_POINT('Ctrl Pts',(108.544175077758,2.18796454352116,135.211263314187));
#44413=CARTESIAN_POINT('Ctrl Pts',(108.53642718098,2.3100735655871,135.14850258253));
#44414=CARTESIAN_POINT('Ctrl Pts',(108.528679284203,2.42937511400288,135.080728190397));
#44415=CARTESIAN_POINT('Ctrl Pts',(108.520933008119,2.54865170710675,135.012967975207));
#44416=CARTESIAN_POINT('Ctrl Pts',(108.513186732035,2.66512165493384,134.940196378557));
#44417=CARTESIAN_POINT('Ctrl Pts',(108.505440455951,2.77834498536226,134.862683202676));
#44418=CARTESIAN_POINT('Ctrl Pts',(108.497694122686,2.89156915157935,134.78516945461));
#44419=CARTESIAN_POINT('Ctrl Pts',(108.48994778942,3.00154632996856,134.702914278329));
#44420=CARTESIAN_POINT('Ctrl Pts',(108.482201456155,3.1078660123223,134.616230488371));
#44421=CARTESIAN_POINT('Ctrl Pts',(108.474453388152,3.2142095042316,134.52952728618));
#44422=CARTESIAN_POINT('Ctrl Pts',(108.466705320149,3.3168935672912,134.438393743834));
#44423=CARTESIAN_POINT('Ctrl Pts',(108.458957252146,3.41554153884024,134.34318232245));
#44424=CARTESIAN_POINT('Ctrl Pts',(108.451200949404,3.51429435462757,134.247869709234));
#44425=CARTESIAN_POINT('Ctrl Pts',(108.443444646662,3.60900222819488,134.148470831253));
#44426=CARTESIAN_POINT('Ctrl Pts',(108.43568834392,3.69932571126356,134.045374709557));
#44427=CARTESIAN_POINT('Ctrl Pts',(108.427927901406,3.78969740269467,133.942223562357));
#44428=CARTESIAN_POINT('Ctrl Pts',(108.420167458892,3.87567979583365,133.835371543859));
#44429=CARTESIAN_POINT('Ctrl Pts',(108.412407016378,3.95697503795119,133.725239185999));
#44430=CARTESIAN_POINT('Ctrl Pts',(108.404634116112,4.03840078240848,133.614930033901));
#44431=CARTESIAN_POINT('Ctrl Pts',(108.396861215847,4.11512412108769,133.501330343692));
#44432=CARTESIAN_POINT('Ctrl Pts',(108.389088315582,4.18689120226974,133.384888688108));
#44433=CARTESIAN_POINT('Ctrl Pts',(108.381597979819,4.25604936928113,133.272679980003));
#44434=CARTESIAN_POINT('Ctrl Pts',(108.374107644057,4.32060521663931,133.157832612914));
#44435=CARTESIAN_POINT('Ctrl Pts',(108.366617308295,4.38037362983542,133.040766199195));
#44436=CARTESIAN_POINT('Ctrl Pts',(108.358842974176,4.44240818058346,132.91926117682));
#44437=CARTESIAN_POINT('Ctrl Pts',(108.351068640057,4.49948160649857,132.794980624413));
#44438=CARTESIAN_POINT('Ctrl Pts',(108.343294305938,4.55133607226615,132.668367865349));
#44439=CARTESIAN_POINT('Ctrl Pts',(108.335529552991,4.60312663203904,132.541911145196));
#44440=CARTESIAN_POINT('Ctrl Pts',(108.327764800044,4.64971088247962,132.413128295585));
#44441=CARTESIAN_POINT('Ctrl Pts',(108.320000047097,4.69087670813955,132.282487395462));
#44442=CARTESIAN_POINT('Ctrl Pts',(108.312243006212,4.73200164732102,132.151976249724));
#44443=CARTESIAN_POINT('Ctrl Pts',(108.304485965327,4.76771875471989,132.019611096464));
#44444=CARTESIAN_POINT('Ctrl Pts',(108.296728924442,4.79786402957485,131.885879834322));
#44445=CARTESIAN_POINT('Ctrl Pts',(108.288977733202,4.82798657164354,131.752249419964));
#44446=CARTESIAN_POINT('Ctrl Pts',(108.281226541962,4.85254555889622,131.617255327113));
#44447=CARTESIAN_POINT('Ctrl Pts',(108.273475350722,4.8714269562047,131.481400108927));
#44448=CARTESIAN_POINT('Ctrl Pts',(108.265727453944,4.89030032841571,131.345602632832));
#44449=CARTESIAN_POINT('Ctrl Pts',(108.257979557167,4.90350085650142,131.208945145784));
#44450=CARTESIAN_POINT('Ctrl Pts',(108.25023166039,4.91096574195096,131.071939659877));
#44451=CARTESIAN_POINT('Ctrl Pts',(108.242485384306,4.9184290659074,130.934962832564));
#44452=CARTESIAN_POINT('Ctrl Pts',(108.234739108222,4.92015911238442,130.797638541323));
#44453=CARTESIAN_POINT('Ctrl Pts',(108.226992832138,4.91614505795859,130.660482781854));
#44454=CARTESIAN_POINT('Ctrl Pts',(108.219246498873,4.91213097390194,130.523326009932));
#44455=CARTESIAN_POINT('Ctrl Pts',(108.211500165607,4.90237271577029,130.386338163064));
#44456=CARTESIAN_POINT('Ctrl Pts',(108.203753832342,4.88691157358095,130.250033697328));
#44457=CARTESIAN_POINT('Ctrl Pts',(108.196005764339,4.87144696897595,130.113698707152));
#44458=CARTESIAN_POINT('Ctrl Pts',(108.188257696336,4.85027698304612,129.978047791037));
#44459=CARTESIAN_POINT('Ctrl Pts',(108.180509628333,4.82349455594055,129.84358835979));
#44460=CARTESIAN_POINT('Ctrl Pts',(108.172753325591,4.7966836641528,129.70898602346));
#44461=CARTESIAN_POINT('Ctrl Pts',(108.164997022849,4.76424849201689,129.57557808566));
#44462=CARTESIAN_POINT('Ctrl Pts',(108.157240720108,4.72633285387229,129.443860409221));
#44463=CARTESIAN_POINT('Ctrl Pts',(108.149480277593,4.68839697901004,129.312072431092));
#44464=CARTESIAN_POINT('Ctrl Pts',(108.141719835079,4.64497493336955,129.181976882592));
#44465=CARTESIAN_POINT('Ctrl Pts',(108.133959392565,4.5962595257029,129.054051663442));
#44466=CARTESIAN_POINT('Ctrl Pts',(108.1261864923,4.54746591573906,128.925921087374));
#44467=CARTESIAN_POINT('Ctrl Pts',(108.118413592034,4.49336211768305,128.79996816224));
#44468=CARTESIAN_POINT('Ctrl Pts',(108.110640691769,4.43418831542878,128.676648925204));
#44469=CARTESIAN_POINT('Ctrl Pts',(108.103150356007,4.3771656299363,128.557812653056));
#44470=CARTESIAN_POINT('Ctrl Pts',(108.095660020245,4.31543529971967,128.441422183144));
#44471=CARTESIAN_POINT('Ctrl Pts',(108.088169684483,4.24925029762302,128.327860068273));
#44472=CARTESIAN_POINT('Ctrl Pts',(108.080395350364,4.18055587105537,128.2099922113));
#44473=CARTESIAN_POINT('Ctrl Pts',(108.072621016245,4.10684470330988,128.094798047376));
#44474=CARTESIAN_POINT('Ctrl Pts',(108.064846682126,4.02835040861327,127.982734127769));
#44475=CARTESIAN_POINT('Ctrl Pts',(108.057081929179,3.94995285111975,127.870808316927));
#44476=CARTESIAN_POINT('Ctrl Pts',(108.049317176231,3.86678411766896,127.762005391786));
#44477=CARTESIAN_POINT('Ctrl Pts',(108.041552423284,3.77912336275388,127.656756819184));
#44478=CARTESIAN_POINT('Ctrl Pts',(108.033795382399,3.69154967373626,127.551612780948));
#44479=CARTESIAN_POINT('Ctrl Pts',(108.026038341514,3.59949309051094,127.450016368397));
#44480=CARTESIAN_POINT('Ctrl Pts',(108.018281300629,3.50327544960236,127.352369281147));
#44481=CARTESIAN_POINT('Ctrl Pts',(108.010530109389,3.40713036716506,127.254795830325));
#44482=CARTESIAN_POINT('Ctrl Pts',(108.002778918149,3.30683074611415,127.161166054202));
#44483=CARTESIAN_POINT('Ctrl Pts',(107.995027726909,3.20273775988312,127.071847536019));
#44484=CARTESIAN_POINT('Ctrl Pts',(107.987279830132,3.09868901594844,126.98256698059));
#44485=CARTESIAN_POINT('Ctrl Pts',(107.979531933355,2.99085040962496,126.897594292659));
#44486=CARTESIAN_POINT('Ctrl Pts',(107.971784036578,2.87961876706026,126.817259061436));
#44487=CARTESIAN_POINT('Ctrl Pts',(107.964037760494,2.76841039175723,126.736940634612));
#44488=CARTESIAN_POINT('Ctrl Pts',(107.95629148441,2.65381070868957,126.661257963765));
#44489=CARTESIAN_POINT('Ctrl Pts',(107.948545208326,2.53624798932969,126.590499063229));
#44490=CARTESIAN_POINT('Ctrl Pts',(107.94079887506,2.41868440214852,126.519739640366));
#44491=CARTESIAN_POINT('Ctrl Pts',(107.933052541795,2.29815807000165,126.453904261954));
#44492=CARTESIAN_POINT('Ctrl Pts',(107.92530620853,2.1751241376225,126.393236265609));
#44493=CARTESIAN_POINT('Ctrl Pts',(107.917558140527,2.05206265264758,126.332554683086));
#44494=CARTESIAN_POINT('Ctrl Pts',(107.909810072524,1.9264928005869,126.277042958196));
#44495=CARTESIAN_POINT('Ctrl Pts',(107.902062004521,1.79889171694289,126.226897165695));
#44496=CARTESIAN_POINT('Ctrl Pts',(107.894305701779,1.67115501734827,126.176698077649));
#44497=CARTESIAN_POINT('Ctrl Pts',(107.886549399037,1.54138313815597,126.131876457527));
#44498=CARTESIAN_POINT('Ctrl Pts',(107.878793096295,1.41007099797125,126.092579336227));
#44499=CARTESIAN_POINT('Ctrl Pts',(107.871032653781,1.27868877254367,126.053261240869));
#44500=CARTESIAN_POINT('Ctrl Pts',(107.863272211267,1.14576502678259,126.019473615918));
#44501=CARTESIAN_POINT('Ctrl Pts',(107.855511768753,1.01180604909759,125.991312562382));
#44502=CARTESIAN_POINT('Ctrl Pts',(107.847738868487,0.877632028569192,125.963106302223));
#44503=CARTESIAN_POINT('Ctrl Pts',(107.839965968222,0.742419841074156,125.940544727221));
#44504=CARTESIAN_POINT('Ctrl Pts',(107.832193067956,0.606682988854484,125.923672263088));
#44505=CARTESIAN_POINT('Ctrl Pts',(107.824702732194,0.475880513111934,125.907413155526));
#44506=CARTESIAN_POINT('Ctrl Pts',(107.817212396432,0.344591163094445,125.896436738648));
#44507=CARTESIAN_POINT('Ctrl Pts',(107.80972206067,0.213273529313823,125.890736958372));
#44508=CARTESIAN_POINT('Ctrl Pts',(107.801947726551,0.0769769475366263,
125.884821069194));
#44509=CARTESIAN_POINT('Ctrl Pts',(107.794173392432,-0.0597818517023291,
125.884571102853));
#44510=CARTESIAN_POINT('Ctrl Pts',(107.786399058313,-0.19649248469664,125.890037290193));
#44511=CARTESIAN_POINT('Ctrl Pts',(107.778634305366,-0.333034634054338,
125.895496740947));
#44512=CARTESIAN_POINT('Ctrl Pts',(107.770869552419,-0.469528348374439,
125.906658313162));
#44513=CARTESIAN_POINT('Ctrl Pts',(107.763104799471,-0.605459732564249,
125.923520364624));
#44514=CARTESIAN_POINT('Ctrl Pts',(107.755347758586,-0.741256107786986,
125.940365668457));
#44515=CARTESIAN_POINT('Ctrl Pts',(107.747590717701,-0.876490878867187,
125.962900136489));
#44516=CARTESIAN_POINT('Ctrl Pts',(107.739833676816,-1.01065212403799,125.991070126989));
#44517=CARTESIAN_POINT('Ctrl Pts',(107.732082485576,-1.14471219716983,126.019218874281));
#44518=CARTESIAN_POINT('Ctrl Pts',(107.724331294336,-1.27769997468739,126.052994605075));
#44519=CARTESIAN_POINT('Ctrl Pts',(107.716580103096,-1.40911097533662,126.092292141654));
#44520=CARTESIAN_POINT('Ctrl Pts',(107.708832206319,-1.5404661228048,126.131572975731));
#44521=CARTESIAN_POINT('Ctrl Pts',(107.701084309542,-1.67024545253506,126.176370835979));
#44522=CARTESIAN_POINT('Ctrl Pts',(107.693336412765,-1.79795717756498,126.22653001234));
#44523=CARTESIAN_POINT('Ctrl Pts',(107.685590136681,-1.92564218805543,126.276678696483));
#44524=CARTESIAN_POINT('Ctrl Pts',(107.677843860597,-2.05126009043464,126.332186323235));
#44525=CARTESIAN_POINT('Ctrl Pts',(107.670097584512,-2.17433707889527,126.39284825446));
#44526=CARTESIAN_POINT('Ctrl Pts',(107.662351251247,-2.29741497588203,126.453510633477));
#44527=CARTESIAN_POINT('Ctrl Pts',(107.654604917982,-2.41795157083984,126.519327220045));
#44528=CARTESIAN_POINT('Ctrl Pts',(107.646858584716,-2.53549612009413,126.590046617935));
#44529=CARTESIAN_POINT('Ctrl Pts',(107.639110516713,-2.65306699263562,126.660781852944));
#44530=CARTESIAN_POINT('Ctrl Pts',(107.63136244871,-2.76764415121255,126.736421882554));
#44531=CARTESIAN_POINT('Ctrl Pts',(107.623614380707,-2.87880472918655,126.816671262349));
#44532=CARTESIAN_POINT('Ctrl Pts',(107.615858077966,-2.99008344994534,126.897005932139));
#44533=CARTESIAN_POINT('Ctrl Pts',(107.608101775224,-3.09793801892514,126.98195950893));
#44534=CARTESIAN_POINT('Ctrl Pts',(107.600345472482,-3.20197721927498,127.071195077472));
#44535=CARTESIAN_POINT('Ctrl Pts',(107.592585029968,-3.30607194847888,127.160478273724));
#44536=CARTESIAN_POINT('Ctrl Pts',(107.584824587453,-3.40634696569246,127.254047749035));
#44537=CARTESIAN_POINT('Ctrl Pts',(107.577064144939,-3.50244775716352,127.351529493569));
#44538=CARTESIAN_POINT('Ctrl Pts',(107.569291244674,-3.59870281815634,127.449167724454));
#44539=CARTESIAN_POINT('Ctrl Pts',(107.561518344408,-3.69077000026521,127.550730484816));
#44540=CARTESIAN_POINT('Ctrl Pts',(107.553745444143,-3.77833436637443,127.65580976386));
#44541=CARTESIAN_POINT('Ctrl Pts',(107.546255108381,-3.86271554721265,127.75706914643));
#44542=CARTESIAN_POINT('Ctrl Pts',(107.538764772619,-3.94291541820318,127.861593573468));
#44543=CARTESIAN_POINT('Ctrl Pts',(107.531274436857,-4.01869119344353,127.968993947409));
#44544=CARTESIAN_POINT('Ctrl Pts',(107.523412939756,-4.09822181214448,128.081716227862));
#44545=CARTESIAN_POINT('Ctrl Pts',(107.515551442654,-4.17312843613846,128.197960419511));
#44546=CARTESIAN_POINT('Ctrl Pts',(107.507689945552,-4.24308727707193,128.317315499027));
#44547=CARTESIAN_POINT('Ctrl Pts',(107.499842002833,-4.31292549863128,128.436464792758));
#44548=CARTESIAN_POINT('Ctrl Pts',(107.491994060113,-4.37783274116075,128.558713964327));
#44549=CARTESIAN_POINT('Ctrl Pts',(107.484146117394,-4.43752731946132,128.683621512552));
#44550=CARTESIAN_POINT('Ctrl Pts',(107.476306037269,-4.49716209173173,128.808403920022));
#44551=CARTESIAN_POINT('Ctrl Pts',(107.468465957145,-4.55159442764522,128.935839064882));
#44552=CARTESIAN_POINT('Ctrl Pts',(107.460625877021,-4.60058728572763,129.065458754636));
#44553=CARTESIAN_POINT('Ctrl Pts',(107.452793638437,-4.64953114182543,129.194948800554));
#44554=CARTESIAN_POINT('Ctrl Pts',(107.444961399853,-4.69304622271882,129.326618685661));
#44555=CARTESIAN_POINT('Ctrl Pts',(107.437129161269,-4.73094281329889,129.459978543974));
#44556=CARTESIAN_POINT('Ctrl Pts',(107.434739738607,-4.74250412765164,129.500663344913));
#44557=CARTESIAN_POINT('Ctrl Pts',(107.432350315945,-4.75354286155822,129.541505290476));
#44558=CARTESIAN_POINT('Ctrl Pts',(107.429960893282,-4.76405452823407,129.582490119308));
#44559=CARTESIAN_POINT('Origin',(213.235140564004,0.,130.804360617566));
#44560=CARTESIAN_POINT('',(105.334849955158,-4.76405452823402,129.582490119308));
#44561=CARTESIAN_POINT('',(105.680281509498,-4.76405452823405,129.582490119308));
#44562=CARTESIAN_POINT('',(213.235140564004,-4.76405452823405,129.582490119308));
#44563=CARTESIAN_POINT('',(107.014859436026,-4.91824951115124,130.806553460605));
#44564=CARTESIAN_POINT('Ctrl Pts',(107.014859435991,-4.91824951115096,130.806553461225));
#44565=CARTESIAN_POINT('Ctrl Pts',(107.007895685791,-4.91819497880655,130.928862078681));
#44566=CARTESIAN_POINT('Ctrl Pts',(107.000931935591,-4.91357844965842,131.051064671271));
#44567=CARTESIAN_POINT('Ctrl Pts',(106.99396818539,-4.90442104082865,131.172921761445));
#44568=CARTESIAN_POINT('Ctrl Pts',(106.986193851271,-4.89419770514593,131.308963076332));
#44569=CARTESIAN_POINT('Ctrl Pts',(106.978419517152,-4.87829351238314,131.444794178459));
#44570=CARTESIAN_POINT('Ctrl Pts',(106.970645183033,-4.85671886405327,131.579902323762));
#44571=CARTESIAN_POINT('Ctrl Pts',(106.962880430086,-4.83517080454929,131.71484396035));
#44572=CARTESIAN_POINT('Ctrl Pts',(106.955115677139,-4.80796625522953,131.849064030531));
#44573=CARTESIAN_POINT('Ctrl Pts',(106.947350924192,-4.77516754231759,131.982052430094));
#44574=CARTESIAN_POINT('Ctrl Pts',(106.939593883307,-4.74240140554971,132.114908743704));
#44575=CARTESIAN_POINT('Ctrl Pts',(106.931836842422,-4.70405225529482,132.246535444009));
#44576=CARTESIAN_POINT('Ctrl Pts',(106.924079801537,-4.66023382025977,132.376430527909));
#44577=CARTESIAN_POINT('Ctrl Pts',(106.916328610297,-4.61644842904743,132.506227656916));
#44578=CARTESIAN_POINT('Ctrl Pts',(106.908577419057,-4.56720208694562,132.63429539973));
#44579=CARTESIAN_POINT('Ctrl Pts',(106.900826227816,-4.51265881914401,132.760145228535));
#44580=CARTESIAN_POINT('Ctrl Pts',(106.893078331039,-4.45813873368621,132.885941567805));
#44581=CARTESIAN_POINT('Ctrl Pts',(106.885330434262,-4.39832635540693,133.009521509999));
#44582=CARTESIAN_POINT('Ctrl Pts',(106.877582537485,-4.33343438883644,133.130415101053));
#44583=CARTESIAN_POINT('Ctrl Pts',(106.869836261401,-4.2685559962664,133.251283403774));
#44584=CARTESIAN_POINT('Ctrl Pts',(106.862089985317,-4.1986003136435,133.3694661288));
#44585=CARTESIAN_POINT('Ctrl Pts',(106.854343709233,-4.12382650738129,133.4845169562));
#44586=CARTESIAN_POINT('Ctrl Pts',(106.846597375968,-4.04905214915587,133.599568632879));
#44587=CARTESIAN_POINT('Ctrl Pts',(106.838851042702,-3.96945980937418,133.711488037986));
#44588=CARTESIAN_POINT('Ctrl Pts',(106.831104709437,-3.88535236142688,133.819857274844));
#44589=CARTESIAN_POINT('Ctrl Pts',(106.823356641434,-3.80122607819977,133.928250780241));
#44590=CARTESIAN_POINT('Ctrl Pts',(106.815608573431,-3.7125829144453,134.033092226561));
#44591=CARTESIAN_POINT('Ctrl Pts',(106.807860505428,-3.61976619091251,134.133996601518));
#44592=CARTESIAN_POINT('Ctrl Pts',(106.800104202686,-3.52685082066141,134.235008218845));
#44593=CARTESIAN_POINT('Ctrl Pts',(106.792347899944,-3.42975329492943,134.332074117884));
#44594=CARTESIAN_POINT('Ctrl Pts',(106.784591597202,-3.32885437691362,134.424845612674));
#44595=CARTESIAN_POINT('Ctrl Pts',(106.776831154688,-3.22790160610719,134.517666622405));
#44596=CARTESIAN_POINT('Ctrl Pts',(106.769070712174,-3.12314369870628,134.606188408559));
#44597=CARTESIAN_POINT('Ctrl Pts',(106.76131026966,-3.01499391789975,134.690103112576));
#44598=CARTESIAN_POINT('Ctrl Pts',(106.753537369395,-2.90667052546398,134.774152523925));
#44599=CARTESIAN_POINT('Ctrl Pts',(106.745764469129,-2.79494469773725,134.853579847515));
#44600=CARTESIAN_POINT('Ctrl Pts',(106.737991568864,-2.68025878653837,134.92812054022));
#44601=CARTESIAN_POINT('Ctrl Pts',(106.730501233102,-2.56974199708748,134.999951490988));
#44602=CARTESIAN_POINT('Ctrl Pts',(106.72301089734,-2.45647686553973,135.067244767998));
#44603=CARTESIAN_POINT('Ctrl Pts',(106.715520561578,-2.3408784411738,135.129805240509));
#44604=CARTESIAN_POINT('Ctrl Pts',(106.707746227459,-2.22089706741315,135.19473771235));
#44605=CARTESIAN_POINT('Ctrl Pts',(106.699971893339,-2.09802190958741,135.254777093107));
#44606=CARTESIAN_POINT('Ctrl Pts',(106.69219755922,-1.97268997607033,135.309654983178));
#44607=CARTESIAN_POINT('Ctrl Pts',(106.684432806273,-1.84751250296006,135.364465241153));
#44608=CARTESIAN_POINT('Ctrl Pts',(106.676668053326,-1.71988463319152,135.414126509778));
#44609=CARTESIAN_POINT('Ctrl Pts',(106.668903300379,-1.59026922072971,135.458415502083));
#44610=CARTESIAN_POINT('Ctrl Pts',(106.661146259494,-1.46078254412282,135.502660505937));
#44611=CARTESIAN_POINT('Ctrl Pts',(106.653389218609,-1.32931262085163,135.541543726399));
#44612=CARTESIAN_POINT('Ctrl Pts',(106.645632177724,-1.19634327348498,135.574889501714));
#44613=CARTESIAN_POINT('Ctrl Pts',(106.637880986484,-1.06347419933763,135.60821013072));
#44614=CARTESIAN_POINT('Ctrl Pts',(106.630129795244,-0.929108329427115,
135.636001531599));
#44615=CARTESIAN_POINT('Ctrl Pts',(106.622378604004,-0.793745335660902,
135.658137642174));
#44616=CARTESIAN_POINT('Ctrl Pts',(106.614630707227,-0.658439874777875,
135.680264344312));
#44617=CARTESIAN_POINT('Ctrl Pts',(106.606882810449,-0.522138517985745,
135.696740473855));
#44618=CARTESIAN_POINT('Ctrl Pts',(106.599134913672,-0.385351622941781,
135.707490963498));
#44619=CARTESIAN_POINT('Ctrl Pts',(106.591388637588,-0.248593340767475,
135.71823920437));
#44620=CARTESIAN_POINT('Ctrl Pts',(106.583642361504,-0.111350111874335,
135.723264156981));
#44621=CARTESIAN_POINT('Ctrl Pts',(106.57589608542,0.0258624763627931,135.722542618551));
#44622=CARTESIAN_POINT('Ctrl Pts',(106.568149752155,0.163076077471984,135.721821074795));
#44623=CARTESIAN_POINT('Ctrl Pts',(106.560403418889,0.30025864651403,135.715352957408));
#44624=CARTESIAN_POINT('Ctrl Pts',(106.552657085624,0.436894884712721,135.703167198991));
#44625=CARTESIAN_POINT('Ctrl Pts',(106.544909017621,0.573561721649587,135.690978711657));
#44626=CARTESIAN_POINT('Ctrl Pts',(106.537160949618,0.709681594941662,135.673070070116));
#44627=CARTESIAN_POINT('Ctrl Pts',(106.529412881615,0.844745009597477,135.649522011293));
#44628=CARTESIAN_POINT('Ctrl Pts',(106.521656578873,0.979951971257663,135.625948925312));
#44629=CARTESIAN_POINT('Ctrl Pts',(106.513900276131,1.11409984556473,135.596724516365));
#44630=CARTESIAN_POINT('Ctrl Pts',(106.506143973389,1.24668946133791,135.561980658037));
#44631=CARTESIAN_POINT('Ctrl Pts',(106.498383530875,1.37934984418123,135.527218255865));
#44632=CARTESIAN_POINT('Ctrl Pts',(106.490623088361,1.51044993774469,135.486930649152));
#44633=CARTESIAN_POINT('Ctrl Pts',(106.482862645847,1.63950735305299,135.44129912285));
#44634=CARTESIAN_POINT('Ctrl Pts',(106.475089745581,1.7687719427816,135.395594344771));
#44635=CARTESIAN_POINT('Ctrl Pts',(106.467316845316,1.89598693855749,135.344528650185));
#44636=CARTESIAN_POINT('Ctrl Pts',(106.45954394505,2.0206906707943,135.288331210184));
#44637=CARTESIAN_POINT('Ctrl Pts',(106.452053609288,2.14086110825507,135.23417668868));
#44638=CARTESIAN_POINT('Ctrl Pts',(106.444563273526,2.25869941830432,135.175257185627));
#44639=CARTESIAN_POINT('Ctrl Pts',(106.437072937764,2.37381708765086,135.111816420807));
#44640=CARTESIAN_POINT('Ctrl Pts',(106.429298603645,2.49329947841942,135.045970280107));
#44641=CARTESIAN_POINT('Ctrl Pts',(106.421524269526,2.61022933405147,134.975044681666));
#44642=CARTESIAN_POINT('Ctrl Pts',(106.413749935407,2.72414462865895,134.899262216463));
#44643=CARTESIAN_POINT('Ctrl Pts',(106.40598518246,2.83791953284665,134.823573146376));
#44644=CARTESIAN_POINT('Ctrl Pts',(106.398220429513,2.9486869457147,134.743039333666));
#44645=CARTESIAN_POINT('Ctrl Pts',(106.390455676566,3.05600882573884,134.657929498423));
#44646=CARTESIAN_POINT('Ctrl Pts',(106.382698635681,3.16322411215877,134.572904195467));
#44647=CARTESIAN_POINT('Ctrl Pts',(106.374941594796,3.26700037162276,134.483312156033));
#44648=CARTESIAN_POINT('Ctrl Pts',(106.367184553911,3.36692829700471,134.389465484279));
#44649=CARTESIAN_POINT('Ctrl Pts',(106.359433362671,3.4667808659608,134.29568958303));
#44650=CARTESIAN_POINT('Ctrl Pts',(106.351682171431,3.56279059336993,134.197665702254));
#44651=CARTESIAN_POINT('Ctrl Pts',(106.34393098019,3.65458133467947,134.095746090389));
#44652=CARTESIAN_POINT('Ctrl Pts',(106.336183083413,3.74633306247542,133.993869797079));
#44653=CARTESIAN_POINT('Ctrl Pts',(106.328435186636,3.83386910957983,133.888101355824));
#44654=CARTESIAN_POINT('Ctrl Pts',(106.320687289859,3.91685045896313,133.778829569265));
#44655=CARTESIAN_POINT('Ctrl Pts',(106.312941013775,3.999814450437,133.669580640008));
#44656=CARTESIAN_POINT('Ctrl Pts',(106.305194737691,4.07822540295203,133.556830134237));
#44657=CARTESIAN_POINT('Ctrl Pts',(106.297448461607,4.15178510778171,133.440999288545));
#44658=CARTESIAN_POINT('Ctrl Pts',(106.289702128342,4.22534535561237,133.325167587816));
#44659=CARTESIAN_POINT('Ctrl Pts',(106.281955795076,4.29405407470617,133.206255831828));
#44660=CARTESIAN_POINT('Ctrl Pts',(106.274209461811,4.35765707530295,133.084713194814));
#44661=CARTESIAN_POINT('Ctrl Pts',(106.266461393808,4.42127431935072,132.963143339169));
#44662=CARTESIAN_POINT('Ctrl Pts',(106.258713325805,4.47978338845044,132.838941776458));
#44663=CARTESIAN_POINT('Ctrl Pts',(106.250965257802,4.53297681437517,132.712580799525));
#44664=CARTESIAN_POINT('Ctrl Pts',(106.24320895506,4.58622677490601,132.586085524643));
#44665=CARTESIAN_POINT('Ctrl Pts',(106.235452652319,4.63414965478795,132.457426611842));
#44666=CARTESIAN_POINT('Ctrl Pts',(106.227696349577,4.67658658878576,132.327095308866));
#44667=CARTESIAN_POINT('Ctrl Pts',(106.219935907063,4.719046172653,132.19669444415));
#44668=CARTESIAN_POINT('Ctrl Pts',(106.212175464548,4.75601387098987,132.064619786979));
#44669=CARTESIAN_POINT('Ctrl Pts',(106.204415022034,4.78738146093688,131.931375173806));
#44670=CARTESIAN_POINT('Ctrl Pts',(106.196642121769,4.81879940492397,131.797916664551));
#44671=CARTESIAN_POINT('Ctrl Pts',(106.188869221503,4.84459920242897,131.663284830417));
#44672=CARTESIAN_POINT('Ctrl Pts',(106.181096321238,4.86472411789404,131.527991959673));
#44673=CARTESIAN_POINT('Ctrl Pts',(106.173605985476,4.88411744199042,131.397617325563));
#44674=CARTESIAN_POINT('Ctrl Pts',(106.166115649714,4.89824128032734,131.266629187376));
#44675=CARTESIAN_POINT('Ctrl Pts',(106.158625313952,4.90709068033576,131.135486148841));
#44676=CARTESIAN_POINT('Ctrl Pts',(106.150850979833,4.91627560803518,130.99937078214));
#44677=CARTESIAN_POINT('Ctrl Pts',(106.143076645714,4.91980733648867,130.86265736456));
#44678=CARTESIAN_POINT('Ctrl Pts',(106.135302311595,4.91762340151374,130.725854927426));
#44679=CARTESIAN_POINT('Ctrl Pts',(106.127537558648,4.91544215804349,130.589221087069));
#44680=CARTESIAN_POINT('Ctrl Pts',(106.1197728057,4.9075592728743,130.45249883261));
#44681=CARTESIAN_POINT('Ctrl Pts',(106.112008052753,4.89396405568395,130.31620195056));
#44682=CARTESIAN_POINT('Ctrl Pts',(106.104251011868,4.88038234145496,130.180040440494));
#44683=CARTESIAN_POINT('Ctrl Pts',(106.096493970983,4.86109962441651,130.044303848589));
#44684=CARTESIAN_POINT('Ctrl Pts',(106.088736930098,4.83615724613833,129.909505236444));
#44685=CARTESIAN_POINT('Ctrl Pts',(106.080985738858,4.81123367710164,129.77480827698));
#44686=CARTESIAN_POINT('Ctrl Pts',(106.073234547618,4.78065901285627,129.641048272248));
#44687=CARTESIAN_POINT('Ctrl Pts',(106.065483356378,4.74452629467262,129.508732082198));
#44688=CARTESIAN_POINT('Ctrl Pts',(106.057735459601,4.70840893385807,129.376472130058));
#44689=CARTESIAN_POINT('Ctrl Pts',(106.049987562824,4.66673832035942,129.245655148444));
#44690=CARTESIAN_POINT('Ctrl Pts',(106.042239666047,4.61965831786306,129.116776519306));
#44691=CARTESIAN_POINT('Ctrl Pts',(106.034493389963,4.57258816348829,128.9879248488));
#44692=CARTESIAN_POINT('Ctrl Pts',(106.026747113879,4.52011100485186,128.861011091283));
#44693=CARTESIAN_POINT('Ctrl Pts',(106.019000837794,4.46242005112696,128.736513826868));
#44694=CARTESIAN_POINT('Ctrl Pts',(106.011254504529,4.40472867154055,128.612015643443));
#44695=CARTESIAN_POINT('Ctrl Pts',(106.003508171264,4.34182358444637,128.489934343445));
#44696=CARTESIAN_POINT('Ctrl Pts',(105.995761837998,4.27394529707205,128.370726573562));
#44697=CARTESIAN_POINT('Ctrl Pts',(105.988013769995,4.20605180882591,128.251492107925));
#44698=CARTESIAN_POINT('Ctrl Pts',(105.980265701992,4.1331830975575,128.135132792592));
#44699=CARTESIAN_POINT('Ctrl Pts',(105.972517633989,4.05562437496958,128.022078462275));
#44700=CARTESIAN_POINT('Ctrl Pts',(105.964761331248,3.97798322204833,127.90890397647));
#44701=CARTESIAN_POINT('Ctrl Pts',(105.957005028506,3.89564232205637,127.799041815341));
#44702=CARTESIAN_POINT('Ctrl Pts',(105.949248725764,3.80892910509421,127.692891168115));
#44703=CARTESIAN_POINT('Ctrl Pts',(105.94148828325,3.72216960667721,127.586683865092));
#44704=CARTESIAN_POINT('Ctrl Pts',(105.933727840736,3.6310334009882,127.484192315198));
#44705=CARTESIAN_POINT('Ctrl Pts',(105.925967398221,3.53588588280445,127.385779905299));
#44706=CARTESIAN_POINT('Ctrl Pts',(105.918194497956,3.44058562537771,127.287209515063));
#44707=CARTESIAN_POINT('Ctrl Pts',(105.910421597691,3.34126147109483,127.192731619818));
#44708=CARTESIAN_POINT('Ctrl Pts',(105.902648697425,3.23831375563247,127.102670857121));
#44709=CARTESIAN_POINT('Ctrl Pts',(105.895158361663,3.13910844893701,127.015884029998));
#44710=CARTESIAN_POINT('Ctrl Pts',(105.887668025901,3.03653869811844,126.933198956544));
#44711=CARTESIAN_POINT('Ctrl Pts',(105.880177690139,2.93098766249886,126.854867690014));
#44712=CARTESIAN_POINT('Ctrl Pts',(105.87240335602,2.82143462728206,126.773566469706));
#44713=CARTESIAN_POINT('Ctrl Pts',(105.864629021901,2.70832274264279,126.696698184921));
#44714=CARTESIAN_POINT('Ctrl Pts',(105.856854687782,2.59204650763631,126.624590532412));
#44715=CARTESIAN_POINT('Ctrl Pts',(105.849089934835,2.47591357269765,126.55257174614));
#44716=CARTESIAN_POINT('Ctrl Pts',(105.841325181888,2.35662437586141,126.485302122525));
#44717=CARTESIAN_POINT('Ctrl Pts',(105.83356042894,2.23460540189126,126.4230683698));
#44718=CARTESIAN_POINT('Ctrl Pts',(105.825803388055,2.11270761888615,126.360896428514));
#44719=CARTESIAN_POINT('Ctrl Pts',(105.81804634717,1.98808580029047,126.303750580998));
#44720=CARTESIAN_POINT('Ctrl Pts',(105.810289306285,1.86119394548687,126.251873367745));
#44721=CARTESIAN_POINT('Ctrl Pts',(105.802538115045,1.73439778081807,126.200035275502));
#44722=CARTESIAN_POINT('Ctrl Pts',(105.794786923805,1.60533534770429,126.153458056623));
#44723=CARTESIAN_POINT('Ctrl Pts',(105.787035732565,1.4744833728568,126.112337403038));
#44724=CARTESIAN_POINT('Ctrl Pts',(105.779287835788,1.3436870135893,126.071234226828));
#44725=CARTESIAN_POINT('Ctrl Pts',(105.771539939011,1.21110299757035,126.035583120192));
#44726=CARTESIAN_POINT('Ctrl Pts',(105.763792042234,1.07722586550265,126.005530812583));
#44727=CARTESIAN_POINT('Ctrl Pts',(105.75604576615,0.943376737644913,125.975484791269));
#44728=CARTESIAN_POINT('Ctrl Pts',(105.748299490066,0.808235412992326,125.951035325081));
#44729=CARTESIAN_POINT('Ctrl Pts',(105.740553213982,0.672308968826403,125.932278545912));
#44730=CARTESIAN_POINT('Ctrl Pts',(105.732806880716,0.536381521282347,125.913521628284));
#44731=CARTESIAN_POINT('Ctrl Pts',(105.725060547451,0.399669329955497,125.90045753497));
#44732=CARTESIAN_POINT('Ctrl Pts',(105.717314214185,0.2626865846685,125.893130749118));
#44733=CARTESIAN_POINT('Ctrl Pts',(105.709566146183,0.125673163045561,125.885802322483));
#44734=CARTESIAN_POINT('Ctrl Pts',(105.70181807818,-0.011610542769554,125.88421378085));
#44735=CARTESIAN_POINT('Ctrl Pts',(105.694070010177,-0.148648736765858,
125.888357503698));
#44736=CARTESIAN_POINT('Ctrl Pts',(105.686313707435,-0.285832576585611,
125.892505630545));
#44737=CARTESIAN_POINT('Ctrl Pts',(105.678557404693,-0.422769991935293,
125.902398180101));
#44738=CARTESIAN_POINT('Ctrl Pts',(105.670801101951,-0.558948149645208,
125.917975447677));
#44739=CARTESIAN_POINT('Ctrl Pts',(105.663040659437,-0.695198989738231,
125.933561029311));
#44740=CARTESIAN_POINT('Ctrl Pts',(105.655280216923,-0.830689378675953,
125.954837314055));
#44741=CARTESIAN_POINT('Ctrl Pts',(105.647519774409,-0.964916083994161,
125.981693304414));
#44742=CARTESIAN_POINT('Ctrl Pts',(105.639746874143,-1.09935826193583,126.008592406392));
#44743=CARTESIAN_POINT('Ctrl Pts',(105.631973973878,-1.23253232247518,126.041089020265));
#44744=CARTESIAN_POINT('Ctrl Pts',(105.624201073612,-1.36394874763043,126.079021806821));
#44745=CARTESIAN_POINT('Ctrl Pts',(105.61671073785,-1.49058785471391,126.115575641038));
#44746=CARTESIAN_POINT('Ctrl Pts',(105.609220402088,-1.6155946044973,126.157177175431));
#44747=CARTESIAN_POINT('Ctrl Pts',(105.601730066326,-1.73854983046595,126.203640288152));
#44748=CARTESIAN_POINT('Ctrl Pts',(105.593955512711,-1.86617054426714,126.251866425464));
#44749=CARTESIAN_POINT('Ctrl Pts',(105.586180959096,-1.9919852468701,126.305483138132));
#44750=CARTESIAN_POINT('Ctrl Pts',(105.57840640548,-2.11550496011297,126.364335637204));
#44751=CARTESIAN_POINT('Ctrl Pts',(105.570641483894,-2.2388716426454,126.423115222897));
#44752=CARTESIAN_POINT('Ctrl Pts',(105.562876562308,-2.35994864367044,126.487117521491));
#44753=CARTESIAN_POINT('Ctrl Pts',(105.555111640722,-2.47826419198246,126.55613867689));
#44754=CARTESIAN_POINT('Ctrl Pts',(105.54735448184,-2.59646145853393,126.625090830845));
#44755=CARTESIAN_POINT('Ctrl Pts',(105.539597322958,-2.71190243083685,126.699051660647));
#44756=CARTESIAN_POINT('Ctrl Pts',(105.531840164076,-2.82413763580126,126.777770288696));
#44757=CARTESIAN_POINT('Ctrl Pts',(105.524088905317,-2.93628747425554,126.856429043066));
#44758=CARTESIAN_POINT('Ctrl Pts',(105.516337646559,-3.04523608008542,126.939838168783));
#44759=CARTESIAN_POINT('Ctrl Pts',(105.5085863878,-3.15056112065854,127.02770234768));
#44760=CARTESIAN_POINT('Ctrl Pts',(105.500838678779,-3.25583792697191,127.115526288629));
#44761=CARTESIAN_POINT('Ctrl Pts',(105.493090969758,-3.35749417033841,127.207800973286));
#44762=CARTESIAN_POINT('Ctrl Pts',(105.485343260737,-3.45513912225318,127.304189663402));
#44763=CARTESIAN_POINT('Ctrl Pts',(105.477597244306,-3.5527627423227,127.400557296119));
#44764=CARTESIAN_POINT('Ctrl Pts',(105.469851227876,-3.6463765364184,127.501036871708));
#44765=CARTESIAN_POINT('Ctrl Pts',(105.462105211445,-3.73562557533219,127.6052537698));
#44766=CARTESIAN_POINT('Ctrl Pts',(105.454359209777,-3.82487444415469,127.709470469275));
#44767=CARTESIAN_POINT('Ctrl Pts',(105.446613208109,-3.90975832038601,127.817424179934));
#44768=CARTESIAN_POINT('Ctrl Pts',(105.438867206441,-3.9899618872133,127.928706396161));
#44769=CARTESIAN_POINT('Ctrl Pts',(105.431119542087,-4.07018266980003,128.040012499204));
#44770=CARTESIAN_POINT('Ctrl Pts',(105.423371877734,-4.14572091591109,128.154648212115));
#44771=CARTESIAN_POINT('Ctrl Pts',(105.41562421338,-4.21630427677361,128.272175531882));
#44772=CARTESIAN_POINT('Ctrl Pts',(105.407869290037,-4.28695376903883,128.389812966078));
#44773=CARTESIAN_POINT('Ctrl Pts',(105.400114366693,-4.35263890466126,128.51034708153));
#44774=CARTESIAN_POINT('Ctrl Pts',(105.39235944335,-4.41313282912109,128.633314396263));
#44775=CARTESIAN_POINT('Ctrl Pts',(105.384600409942,-4.47365881500711,128.756346882954));
#44776=CARTESIAN_POINT('Ctrl Pts',(105.376841376535,-4.52898795015834,128.881814781216));
#44777=CARTESIAN_POINT('Ctrl Pts',(105.369082343127,-4.57894169052388,129.009234979266));
#44778=CARTESIAN_POINT('Ctrl Pts',(105.361313107293,-4.62896111553639,129.136822723343));
#44779=CARTESIAN_POINT('Ctrl Pts',(105.353543871459,-4.67359090372758,129.266367524707));
#44780=CARTESIAN_POINT('Ctrl Pts',(105.345774635624,-4.71270234562357,129.397371042603));
#44781=CARTESIAN_POINT('Ctrl Pts',(105.342133075469,-4.7310344791148,129.458774403397));
#44782=CARTESIAN_POINT('Ctrl Pts',(105.338491515313,-4.74815499509428,129.520498080905));
#44783=CARTESIAN_POINT('Ctrl Pts',(105.334849955158,-4.76405452823403,129.582490119308));
#44784=CARTESIAN_POINT('Ctrl Pts',(107.085000608365,-4.76405452823403,129.582490119308));
#44785=CARTESIAN_POINT('Ctrl Pts',(107.077323484576,-4.79779703768306,129.714051651536));
#44786=CARTESIAN_POINT('Ctrl Pts',(107.069646360786,-4.82606097313593,129.846915698217));
#44787=CARTESIAN_POINT('Ctrl Pts',(107.061969236997,-4.84877003991418,129.980581422314));
#44788=CARTESIAN_POINT('Ctrl Pts',(107.054117603501,-4.87199530946124,130.117285519477));
#44789=CARTESIAN_POINT('Ctrl Pts',(107.046265970006,-4.88941008467352,130.254827733819));
#44790=CARTESIAN_POINT('Ctrl Pts',(107.038414336511,-4.90098899494674,130.39266906566));
#44791=CARTESIAN_POINT('Ctrl Pts',(107.030562703016,-4.91256790521996,130.530510397501));
#44792=CARTESIAN_POINT('Ctrl Pts',(107.022711069521,-4.91831099639246,130.668650404071));
#44793=CARTESIAN_POINT('Ctrl Pts',(107.014859436026,-4.91824951115124,130.806553460605));
#44794=CARTESIAN_POINT('',(107.360140563954,-4.91824914862615,130.807254496995));
#44795=CARTESIAN_POINT('Ctrl Pts',(107.429960893282,-4.76405452823407,129.582490119308));
#44796=CARTESIAN_POINT('Ctrl Pts',(107.422135445397,-4.79848062666256,129.716716954592));
#44797=CARTESIAN_POINT('Ctrl Pts',(107.414309997512,-4.82724967230215,129.852477377668));
#44798=CARTESIAN_POINT('Ctrl Pts',(107.406484549627,-4.85023658873154,129.989260564916));
#44799=CARTESIAN_POINT('Ctrl Pts',(107.398661175943,-4.87321741228365,130.12600749662));
#44800=CARTESIAN_POINT('Ctrl Pts',(107.39083780226,-4.89041908976492,130.263776279477));
#44801=CARTESIAN_POINT('Ctrl Pts',(107.383014428576,-4.90176762153945,130.40204575713));
#44802=CARTESIAN_POINT('Ctrl Pts',(107.375389807053,-4.91282784480339,130.536802510146));
#44803=CARTESIAN_POINT('Ctrl Pts',(107.367765185531,-4.91832871155599,130.67203447485));
#44804=CARTESIAN_POINT('Ctrl Pts',(107.360140564008,-4.91824914862671,130.807254496045));
#44805=CARTESIAN_POINT('Ctrl Pts',(107.360140563954,-4.91824914862615,130.807254496995));
#44806=CARTESIAN_POINT('Ctrl Pts',(107.351197751379,-4.91815583034193,130.965852179838));
#44807=CARTESIAN_POINT('Ctrl Pts',(107.342254938803,-4.91038646992283,131.124168952794));
#44808=CARTESIAN_POINT('Ctrl Pts',(107.333312126227,-4.89505025752853,131.281504242452));
#44809=CARTESIAN_POINT('Ctrl Pts',(107.324624727898,-4.88015206025675,131.434345903932));
#44810=CARTESIAN_POINT('Ctrl Pts',(107.31593732957,-4.85811346436008,131.586261223086));
#44811=CARTESIAN_POINT('Ctrl Pts',(107.307249931241,-4.82908541778232,131.736625113437));
#44812=CARTESIAN_POINT('Ctrl Pts',(107.298179411542,-4.79877721061071,131.893620174324));
#44813=CARTESIAN_POINT('Ctrl Pts',(107.289108891842,-4.76084924803436,132.048923574273));
#44814=CARTESIAN_POINT('Ctrl Pts',(107.280038372143,-4.71552915031273,132.201846894798));
#44815=CARTESIAN_POINT('Ctrl Pts',(107.270967852443,-4.67020905259109,132.354770215322));
#44816=CARTESIAN_POINT('Ctrl Pts',(107.261897332744,-4.61749699331532,132.505313243214));
#44817=CARTESIAN_POINT('Ctrl Pts',(107.252826813044,-4.55767503340629,132.652814390957));
#44818=CARTESIAN_POINT('Ctrl Pts',(107.245052478925,-4.50640168641018,132.779237489467));
#44819=CARTESIAN_POINT('Ctrl Pts',(107.237278144806,-4.44978295777727,132.903725847237));
#44820=CARTESIAN_POINT('Ctrl Pts',(107.229503810687,-4.38798531120369,133.025794382314));
#44821=CARTESIAN_POINT('Ctrl Pts',(107.22173905774,-4.32626382470649,133.14771247883));
#44822=CARTESIAN_POINT('Ctrl Pts',(107.213974304793,-4.25937629454039,133.267216340907));
#44823=CARTESIAN_POINT('Ctrl Pts',(107.206209551845,-4.18753782340043,133.383839254828));
#44824=CARTESIAN_POINT('Ctrl Pts',(107.19845251096,-4.1157707032428,133.500346337226));
#44825=CARTESIAN_POINT('Ctrl Pts',(107.190695470075,-4.03906263157148,133.613977835055));
#44826=CARTESIAN_POINT('Ctrl Pts',(107.18293842919,-3.95767518527689,133.724290443836));
#44827=CARTESIAN_POINT('Ctrl Pts',(107.17518723795,-3.87634911388864,133.834519865021));
#44828=CARTESIAN_POINT('Ctrl Pts',(107.16743604671,-3.79035092281963,133.941435065496));
#44829=CARTESIAN_POINT('Ctrl Pts',(107.15968485547,-3.69998596904676,134.044620929849));
#44830=CARTESIAN_POINT('Ctrl Pts',(107.151936958693,-3.60965942278974,134.147762937458));
#44831=CARTESIAN_POINT('Ctrl Pts',(107.144189061916,-3.51497006229068,134.247178468017));
#44832=CARTESIAN_POINT('Ctrl Pts',(107.136441165139,-3.41626392795545,134.3424849564));
#44833=CARTESIAN_POINT('Ctrl Pts',(107.128694889055,-3.31757844081566,134.437771508721));
#44834=CARTESIAN_POINT('Ctrl Pts',(107.120948612971,-3.21487813216536,134.528950457107));
#44835=CARTESIAN_POINT('Ctrl Pts',(107.113202336886,-3.10854606916345,134.615675928373));
#44836=CARTESIAN_POINT('Ctrl Pts',(107.105456003621,-3.00221322124248,134.702402039826));
#44837=CARTESIAN_POINT('Ctrl Pts',(107.097709670356,-2.89224886844685,134.784674361452));
#44838=CARTESIAN_POINT('Ctrl Pts',(107.08996333709,-2.77906901905547,134.862187431247));
#44839=CARTESIAN_POINT('Ctrl Pts',(107.082215269087,-2.66586382382171,134.939717859556));
#44840=CARTESIAN_POINT('Ctrl Pts',(107.074467201084,-2.54944202160618,135.01248669434));
#44841=CARTESIAN_POINT('Ctrl Pts',(107.066719133081,-2.43024809570893,135.080232137596));
#44842=CARTESIAN_POINT('Ctrl Pts',(107.05896283034,-2.31092748908857,135.148049581516));
#44843=CARTESIAN_POINT('Ctrl Pts',(107.051206527598,-2.18882921378542,135.210832775345));
#44844=CARTESIAN_POINT('Ctrl Pts',(107.043450224856,-2.0644223157652,135.268365945147));
#44845=CARTESIAN_POINT('Ctrl Pts',(107.035689782342,-1.93994901803767,135.325929822134));
#44846=CARTESIAN_POINT('Ctrl Pts',(107.027929339828,-1.81316500360393,135.378237942642));
#44847=CARTESIAN_POINT('Ctrl Pts',(107.020168897313,-1.68455780033125,135.425123333811));
#44848=CARTESIAN_POINT('Ctrl Pts',(107.012395997048,-1.55574414535866,135.472083989573));
#44849=CARTESIAN_POINT('Ctrl Pts',(107.004623096783,-1.42510182579334,135.513604402052));
#44850=CARTESIAN_POINT('Ctrl Pts',(106.996850196517,-1.29313284326542,135.549567727079));
#44851=CARTESIAN_POINT('Ctrl Pts',(106.989359860755,-1.16596126566158,135.584223694655));
#44852=CARTESIAN_POINT('Ctrl Pts',(106.981869524993,-1.03755810577401,135.613719519549));
#44853=CARTESIAN_POINT('Ctrl Pts',(106.974379189231,-0.908378172471304,
135.637996118747));
#44854=CARTESIAN_POINT('Ctrl Pts',(106.966604855112,-0.774300342734789,
135.663193172583));
#44855=CARTESIAN_POINT('Ctrl Pts',(106.958830520993,-0.638960955833597,
135.68284723083));
#44856=CARTESIAN_POINT('Ctrl Pts',(106.951056186874,-0.502858102648951,
135.696836145466));
#44857=CARTESIAN_POINT('Ctrl Pts',(106.943291433927,-0.366922984067087,
135.710807820015));
#44858=CARTESIAN_POINT('Ctrl Pts',(106.93552668098,-0.230226656502972,135.719128203029));
#44859=CARTESIAN_POINT('Ctrl Pts',(106.927761928032,-0.093278047685706,
135.721725996335));
#44860=CARTESIAN_POINT('Ctrl Pts',(106.920004887147,0.0435345418426454,
135.724321209476));
#44861=CARTESIAN_POINT('Ctrl Pts',(106.912247846263,0.180598525614519,135.721205136474));
#44862=CARTESIAN_POINT('Ctrl Pts',(106.904490805378,0.317399550318383,135.712358232476));
#44863=CARTESIAN_POINT('Ctrl Pts',(106.896739614137,0.454097412305267,135.703517999996));
#44864=CARTESIAN_POINT('Ctrl Pts',(106.888988422897,0.590532321355654,135.68895556366));
#44865=CARTESIAN_POINT('Ctrl Pts',(106.881237231657,0.72618997621252,135.66870344892));
#44866=CARTESIAN_POINT('Ctrl Pts',(106.87348933488,0.86178997294747,135.64845994187));
#44867=CARTESIAN_POINT('Ctrl Pts',(106.865741438103,0.996612986666924,135.622531623766));
#44868=CARTESIAN_POINT('Ctrl Pts',(106.857993541326,1.13015011120318,135.591002842409));
#44869=CARTESIAN_POINT('Ctrl Pts',(106.850247265242,1.26365930265171,135.559480656192));
#44870=CARTESIAN_POINT('Ctrl Pts',(106.842500989158,1.39588275967132,135.522360426674));
#44871=CARTESIAN_POINT('Ctrl Pts',(106.834754713074,1.52632243219733,135.479777486196));
#44872=CARTESIAN_POINT('Ctrl Pts',(106.827008379808,1.65676306759938,135.437194231381));
#44873=CARTESIAN_POINT('Ctrl Pts',(106.819262046543,1.78541952057131,135.389148306474));
#44874=CARTESIAN_POINT('Ctrl Pts',(106.811515713278,1.91180993464163,135.335824601347));
#44875=CARTESIAN_POINT('Ctrl Pts',(106.803767645275,2.03822865296876,135.282488954746));
#44876=CARTESIAN_POINT('Ctrl Pts',(106.796019577272,2.1623799624507,135.223873327984));
#44877=CARTESIAN_POINT('Ctrl Pts',(106.788271509269,2.283803350934,135.160210169234));
#44878=CARTESIAN_POINT('Ctrl Pts',(106.780515206527,2.40535578963962,135.096479348521));
#44879=CARTESIAN_POINT('Ctrl Pts',(106.772758903785,2.52417416893811,135.027690461335));
#44880=CARTESIAN_POINT('Ctrl Pts',(106.765002601043,2.63982342130372,134.954121498248));
#44881=CARTESIAN_POINT('Ctrl Pts',(106.757242158529,2.75553439915754,134.88051326919));
#44882=CARTESIAN_POINT('Ctrl Pts',(106.749481716015,2.86807255905725,134.802120103969));
#44883=CARTESIAN_POINT('Ctrl Pts',(106.741721273501,2.97703390128575,134.719261920676));
#44884=CARTESIAN_POINT('Ctrl Pts',(106.733948373235,3.08617015793393,134.636270726073));
#44885=CARTESIAN_POINT('Ctrl Pts',(106.72617547297,3.19171782171265,134.548800439777));
#44886=CARTESIAN_POINT('Ctrl Pts',(106.718402572704,3.29330724416999,134.45721025285));
#44887=CARTESIAN_POINT('Ctrl Pts',(106.710912236942,3.39120363523365,134.36894959992));
#44888=CARTESIAN_POINT('Ctrl Pts',(106.70342190118,3.48542435242331,134.27686359877));
#44889=CARTESIAN_POINT('Ctrl Pts',(106.695931565418,3.57567385222377,134.181302957172));
#44890=CARTESIAN_POINT('Ctrl Pts',(106.688157231299,3.66934518923912,134.082119104803));
#44891=CARTESIAN_POINT('Ctrl Pts',(106.68038289718,3.75903494954317,133.978877744152));
#44892=CARTESIAN_POINT('Ctrl Pts',(106.672608563061,3.84437113625636,133.871931909194));
#44893=CARTESIAN_POINT('Ctrl Pts',(106.664843810114,3.92960215374607,133.765117875419));
#44894=CARTESIAN_POINT('Ctrl Pts',(106.657079057167,4.01049003166381,133.654608753854));
#44895=CARTESIAN_POINT('Ctrl Pts',(106.649314304219,4.08669969696697,133.540794181406));
#44896=CARTESIAN_POINT('Ctrl Pts',(106.641557263334,4.16283366975624,133.427092651196));
#44897=CARTESIAN_POINT('Ctrl Pts',(106.633800222449,4.23429846049034,133.310092526223));
#44898=CARTESIAN_POINT('Ctrl Pts',(106.626043181564,4.30079960500237,133.190215982024));
#44899=CARTESIAN_POINT('Ctrl Pts',(106.618291990324,4.36725060048396,133.070429837659));
#44900=CARTESIAN_POINT('Ctrl Pts',(106.610540799084,4.42874521131446,132.947771932091));
#44901=CARTESIAN_POINT('Ctrl Pts',(106.602789607844,4.48503280968691,132.822692542333));
#44902=CARTESIAN_POINT('Ctrl Pts',(106.595041711067,4.54129648432857,132.697666314652));
#44903=CARTESIAN_POINT('Ctrl Pts',(106.58729381429,4.59235738813069,132.570221005554));
#44904=CARTESIAN_POINT('Ctrl Pts',(106.579545917513,4.63801140907041,132.440830364256));
#44905=CARTESIAN_POINT('Ctrl Pts',(106.571799641429,4.68365588017314,132.311466788692));
#44906=CARTESIAN_POINT('Ctrl Pts',(106.564053365344,4.72389558803606,132.180159058771));
#44907=CARTESIAN_POINT('Ctrl Pts',(106.55630708926,4.75857518336706,132.047399348557));
#44908=CARTESIAN_POINT('Ctrl Pts',(106.548560755995,4.79325503469494,131.914638658341));
#44909=CARTESIAN_POINT('Ctrl Pts',(106.54081442273,4.82237459277903,131.780426344716));
#44910=CARTESIAN_POINT('Ctrl Pts',(106.533068089464,4.84582895551257,131.645267744671));
#44911=CARTESIAN_POINT('Ctrl Pts',(106.525320021461,4.86928857068803,131.510078876795));
#44912=CARTESIAN_POINT('Ctrl Pts',(106.517571953458,4.88708039915095,131.373943685948));
#44913=CARTESIAN_POINT('Ctrl Pts',(106.509823885455,4.89915108806627,131.237375257964));
#44914=CARTESIAN_POINT('Ctrl Pts',(106.502067582713,4.91123460585341,131.10066168343));
#44915=CARTESIAN_POINT('Ctrl Pts',(106.494311279972,4.91758480317241,130.963514342028));
#44916=CARTESIAN_POINT('Ctrl Pts',(106.48655497723,4.91820039673943,130.826449529086));
#44917=CARTESIAN_POINT('Ctrl Pts',(106.478794534716,4.91881631886727,130.689311560525));
#44918=CARTESIAN_POINT('Ctrl Pts',(106.471034092201,4.91369155307972,130.552256598693));
#44919=CARTESIAN_POINT('Ctrl Pts',(106.463273649687,4.90287688381336,130.415797463538));
#44920=CARTESIAN_POINT('Ctrl Pts',(106.455500749422,4.89204485387983,130.279119272064));
#44921=CARTESIAN_POINT('Ctrl Pts',(106.447727849156,4.87550471514916,130.143039206938));
#44922=CARTESIAN_POINT('Ctrl Pts',(106.439954948891,4.85335886121664,130.008062415414));
#44923=CARTESIAN_POINT('Ctrl Pts',(106.432464613129,4.8320180648569,129.87799237025));
#44924=CARTESIAN_POINT('Ctrl Pts',(106.424974277367,4.80547210318921,129.748947079465));
#44925=CARTESIAN_POINT('Ctrl Pts',(106.417483941605,4.77385628810415,129.621364758305));
#44926=CARTESIAN_POINT('Ctrl Pts',(106.409709607486,4.74104174978028,129.488945114659));
#44927=CARTESIAN_POINT('Ctrl Pts',(106.401935273367,4.702661375356,129.357682101927));
#44928=CARTESIAN_POINT('Ctrl Pts',(106.394160939248,4.65881110891264,129.228079515106));
#44929=CARTESIAN_POINT('Ctrl Pts',(106.386396186301,4.6150148840037,129.098636651891));
#44930=CARTESIAN_POINT('Ctrl Pts',(106.378631433354,4.56576230406105,128.970850509794));
#44931=CARTESIAN_POINT('Ctrl Pts',(106.370866680407,4.5112000664855,128.845213603521));
#44932=CARTESIAN_POINT('Ctrl Pts',(106.363109639522,4.45669202089354,128.719701481595));
#44933=CARTESIAN_POINT('Ctrl Pts',(106.355352598637,4.39688496715423,128.596334703727));
#44934=CARTESIAN_POINT('Ctrl Pts',(106.347595557752,4.33197492842929,128.475589207152));
#44935=CARTESIAN_POINT('Ctrl Pts',(106.339844366511,4.26711383886943,128.354934765696));
#44936=CARTESIAN_POINT('Ctrl Pts',(106.332093175271,4.19715760830539,128.23689801394));
#44937=CARTESIAN_POINT('Ctrl Pts',(106.324341984031,4.12234959709103,128.121933197884));
#44938=CARTESIAN_POINT('Ctrl Pts',(106.316594087254,4.04757338127701,128.007017244941));
#44939=CARTESIAN_POINT('Ctrl Pts',(106.308846190477,3.96794969903147,127.89517095786));
#44940=CARTESIAN_POINT('Ctrl Pts',(106.3010982937,3.88376680145399,127.786822134891));
#44941=CARTESIAN_POINT('Ctrl Pts',(106.293352017616,3.7996015131239,127.67849597616));
#44942=CARTESIAN_POINT('Ctrl Pts',(106.285605741532,3.71087914612315,127.573666134896));
#44943=CARTESIAN_POINT('Ctrl Pts',(106.277859465448,3.61792981034243,127.47272934296));
#44944=CARTESIAN_POINT('Ctrl Pts',(106.270113132182,3.52497978843088,127.371791805931));
#44945=CARTESIAN_POINT('Ctrl Pts',(106.262366798917,3.42780300031751,127.274747663174));
#44946=CARTESIAN_POINT('Ctrl Pts',(106.254620465652,3.32676789817163,127.181958318788));
#44947=CARTESIAN_POINT('Ctrl Pts',(106.246872397649,3.22571016991516,127.089148194871));
#44948=CARTESIAN_POINT('Ctrl Pts',(106.239124329646,3.12079269618089,127.000595029755));
#44949=CARTESIAN_POINT('Ctrl Pts',(106.231376261643,3.0124183121011,126.916621046116));
#44950=CARTESIAN_POINT('Ctrl Pts',(106.223619958901,2.90392874643616,126.832557813928));
#44951=CARTESIAN_POINT('Ctrl Pts',(106.215863656159,2.79197524066403,126.753083725039));
#44952=CARTESIAN_POINT('Ctrl Pts',(106.208107353417,2.67699147501793,126.678478929347));
#44953=CARTESIAN_POINT('Ctrl Pts',(106.200346910903,2.56194633907393,126.603834314829));
#44954=CARTESIAN_POINT('Ctrl Pts',(106.192586468389,2.44386805699931,126.534064370803));
#44955=CARTESIAN_POINT('Ctrl Pts',(106.184826025875,2.3232155289681,126.469403562593));
#44956=CARTESIAN_POINT('Ctrl Pts',(106.177053125609,2.20236931878787,126.404638955113));
#44957=CARTESIAN_POINT('Ctrl Pts',(106.169280225344,2.07894095701078,126.345000043127));
#44958=CARTESIAN_POINT('Ctrl Pts',(106.161507325078,1.95341078456747,126.290673724434));
#44959=CARTESIAN_POINT('Ctrl Pts',(106.154016989316,1.83244395008245,126.238322304264));
#44960=CARTESIAN_POINT('Ctrl Pts',(106.146526653554,1.7095257514868,126.190904041858));
#44961=CARTESIAN_POINT('Ctrl Pts',(106.139036317792,1.5850980110598,126.148541961536));
#44962=CARTESIAN_POINT('Ctrl Pts',(106.131261983673,1.45595255503697,126.104573710064));
#44963=CARTESIAN_POINT('Ctrl Pts',(106.123487649554,1.32477173499468,126.065913341397));
#44964=CARTESIAN_POINT('Ctrl Pts',(106.115713315435,1.19203126805155,126.032752448564));
#44965=CARTESIAN_POINT('Ctrl Pts',(106.107948562488,1.05945439187075,125.999632423568));
#44966=CARTESIAN_POINT('Ctrl Pts',(106.100183809541,0.925322068912722,125.971998482826));
#44967=CARTESIAN_POINT('Ctrl Pts',(106.092419056594,0.790127959276913,125.949993421889));
#44968=CARTESIAN_POINT('Ctrl Pts',(106.084662015709,0.655068126336514,125.928010216688));
#44969=CARTESIAN_POINT('Ctrl Pts',(106.076904974824,0.518948988773026,125.911644827984));
#44970=CARTESIAN_POINT('Ctrl Pts',(106.069147933939,0.382276921367454,125.90098959164));
#44971=CARTESIAN_POINT('Ctrl Pts',(106.061396742699,0.245707919431345,125.890342390492));
#44972=CARTESIAN_POINT('Ctrl Pts',(106.053645551458,0.108587205809336,125.885396800998));
#44973=CARTESIAN_POINT('Ctrl Pts',(106.045894360218,-0.0285715072602836,
125.886193608255));
#44974=CARTESIAN_POINT('Ctrl Pts',(106.038146463441,-0.165671924218207,
125.886990076848));
#44975=CARTESIAN_POINT('Ctrl Pts',(106.030398566664,-0.302809918360973,
125.893524085617));
#44976=CARTESIAN_POINT('Ctrl Pts',(106.022650669887,-0.439469764145238,
125.905784356151));
#44977=CARTESIAN_POINT('Ctrl Pts',(106.014904393803,-0.57610102363581,125.9180420621));
#44978=CARTESIAN_POINT('Ctrl Pts',(106.007158117719,-0.712253944555239,
125.936023612391));
#44979=CARTESIAN_POINT('Ctrl Pts',(105.999411841635,-0.847416312692825,
125.959665719486));
#44980=CARTESIAN_POINT('Ctrl Pts',(105.99166550837,-0.982579678568309,125.983308001101));
#44981=CARTESIAN_POINT('Ctrl Pts',(105.983919175104,-1.1167520919532,126.012610855536));
#44982=CARTESIAN_POINT('Ctrl Pts',(105.976172841839,-1.24943033594581,126.047459641288));
#44983=CARTESIAN_POINT('Ctrl Pts',(105.968424773836,-1.38213829231104,126.082316231183));
#44984=CARTESIAN_POINT('Ctrl Pts',(105.960676705833,-1.51335103538431,126.122721124477));
#44985=CARTESIAN_POINT('Ctrl Pts',(105.95292863783,-1.64257972787296,126.16850957379));
#44986=CARTESIAN_POINT('Ctrl Pts',(105.945172335088,-1.7719457661539,126.214346687612));
#44987=CARTESIAN_POINT('Ctrl Pts',(105.937416032346,-1.89932317244547,126.265578656399));
#44988=CARTESIAN_POINT('Ctrl Pts',(105.929659729605,-2.02424183394526,126.321992040552));
#44989=CARTESIAN_POINT('Ctrl Pts',(105.92189928709,-2.14922716829608,126.378435534226));
#44990=CARTESIAN_POINT('Ctrl Pts',(105.914138844576,-2.27175079387615,126.440065778115));
#44991=CARTESIAN_POINT('Ctrl Pts',(105.906378402062,-2.3913674016154,126.506623420739));
#44992=CARTESIAN_POINT('Ctrl Pts',(105.898605501797,-2.51117602855246,126.5732879076));
#44993=CARTESIAN_POINT('Ctrl Pts',(105.890832601531,-2.6280679787137,126.644895395346));
#44994=CARTESIAN_POINT('Ctrl Pts',(105.883059701266,-2.74162637368244,126.721142782374));
#44995=CARTESIAN_POINT('Ctrl Pts',(105.875569365504,-2.85105663495688,126.794618384827));
#44996=CARTESIAN_POINT('Ctrl Pts',(105.868079029742,-2.95739125085624,126.872402217443));
#44997=CARTESIAN_POINT('Ctrl Pts',(105.86058869398,-3.06028790180302,126.954189060274));
#44998=CARTESIAN_POINT('Ctrl Pts',(105.852913814628,-3.16571967507078,127.037990931281));
#44999=CARTESIAN_POINT('Ctrl Pts',(105.845238935276,-3.26789399701385,127.126275793685));
#45000=CARTESIAN_POINT('Ctrl Pts',(105.837564055923,-3.36639833683841,127.218758115861));
#45001=CARTESIAN_POINT('Ctrl Pts',(105.829897956767,-3.46478998597824,127.311134636646));
#45002=CARTESIAN_POINT('Ctrl Pts',(105.822231857611,-3.55951970969645,127.407698799645));
#45003=CARTESIAN_POINT('Ctrl Pts',(105.814565758455,-3.65020571628105,127.508123172944));
#45004=CARTESIAN_POINT('Ctrl Pts',(105.806906667801,-3.74080881589757,127.608455736265));
#45005=CARTESIAN_POINT('Ctrl Pts',(105.799247577146,-3.82737528171168,127.712641196918));
#45006=CARTESIAN_POINT('Ctrl Pts',(105.791588486492,-3.90955847607444,127.820313770639));
#45007=CARTESIAN_POINT('Ctrl Pts',(105.783934638994,-3.99168541057586,127.927912635323));
#45008=CARTESIAN_POINT('Ctrl Pts',(105.776280791497,-4.06943479897665,128.038993547196));
#45009=CARTESIAN_POINT('Ctrl Pts',(105.768626943999,-4.14249915075095,128.153156391459));
#45010=CARTESIAN_POINT('Ctrl Pts',(105.76097564897,-4.2155391364183,128.267281163749));
#45011=CARTESIAN_POINT('Ctrl Pts',(105.753324353941,-4.28389697206781,128.384485489604));
#45012=CARTESIAN_POINT('Ctrl Pts',(105.745673058913,-4.34730773998133,128.504339209753));
#45013=CARTESIAN_POINT('Ctrl Pts',(105.738023470259,-4.41070436615869,128.624166200377));
#45014=CARTESIAN_POINT('Ctrl Pts',(105.730373881606,-4.46915593470218,128.746641053295));
#45015=CARTESIAN_POINT('Ctrl Pts',(105.722724292953,-4.52244321646789,128.871308518857));
#45016=CARTESIAN_POINT('Ctrl Pts',(105.715072029486,-4.57574913107084,128.996019576595));
#45017=CARTESIAN_POINT('Ctrl Pts',(105.70741976602,-4.62388699108354,129.122924409893));
#45018=CARTESIAN_POINT('Ctrl Pts',(105.699767502553,-4.66668553437845,129.251547304343));
#45019=CARTESIAN_POINT('Ctrl Pts',(105.693272171535,-4.70301344010398,129.360723926349));
#45020=CARTESIAN_POINT('Ctrl Pts',(105.686776840516,-4.73549524688595,129.47113791478));
#45021=CARTESIAN_POINT('Ctrl Pts',(105.680281509498,-4.76405452823405,129.582490119308));
#45022=CARTESIAN_POINT('Origin',(213.235140564004,0.,130.804360617566));
#45023=CARTESIAN_POINT('',(103.584579145176,-4.76405452823405,129.582490119308));
#45024=CARTESIAN_POINT('',(103.930161944428,-4.76405452823404,129.582490119308));
#45025=CARTESIAN_POINT('',(213.235140564004,-4.76405452823405,129.582490119308));
#45026=CARTESIAN_POINT('',(105.264859435952,-4.91824797726599,130.799900054936));
#45027=CARTESIAN_POINT('Ctrl Pts',(105.264859435952,-4.91824797726599,130.799900054936));
#45028=CARTESIAN_POINT('Ctrl Pts',(105.257209733691,-4.91837034801499,130.93482691028));
#45029=CARTESIAN_POINT('Ctrl Pts',(105.249560031429,-4.91293618644247,131.069928051336));
#45030=CARTESIAN_POINT('Ctrl Pts',(105.241910329167,-4.90192925582662,131.20470126423));
#45031=CARTESIAN_POINT('Ctrl Pts',(105.234266762425,-4.8909311534284,131.339366380934));
#45032=CARTESIAN_POINT('Ctrl Pts',(105.226623195683,-4.87436920604566,131.473703692978));
#45033=CARTESIAN_POINT('Ctrl Pts',(105.218979628941,-4.85227924260771,131.607211297492));
#45034=CARTESIAN_POINT('Ctrl Pts',(105.211339652271,-4.83019965450653,131.740656195414));
#45035=CARTESIAN_POINT('Ctrl Pts',(105.203699675602,-4.80259727797285,131.873271763944));
#45036=CARTESIAN_POINT('Ctrl Pts',(105.196059698933,-4.76955971249369,132.004561938786));
#45037=CARTESIAN_POINT('Ctrl Pts',(105.188421429977,-4.73652953168282,132.135822767204));
#45038=CARTESIAN_POINT('Ctrl Pts',(105.180783161021,-4.69806667542035,132.265758400346));
#45039=CARTESIAN_POINT('Ctrl Pts',(105.173144892065,-4.65430959729121,132.393884205017));
#45040=CARTESIAN_POINT('Ctrl Pts',(105.165506567533,-4.61055220078228,132.522010941941));
#45041=CARTESIAN_POINT('Ctrl Pts',(105.157868243,-4.56150063627449,132.648327442905));
#45042=CARTESIAN_POINT('Ctrl Pts',(105.150229918468,-4.50734266928378,132.772365984468));
#45043=CARTESIAN_POINT('Ctrl Pts',(105.142589775233,-4.4531718071604,132.896434059884));
#45044=CARTESIAN_POINT('Ctrl Pts',(105.134949631999,-4.39389228649692,133.018222728364));
#45045=CARTESIAN_POINT('Ctrl Pts',(105.127309488764,-4.32973903783793,133.137286447232));
#45046=CARTESIAN_POINT('Ctrl Pts',(105.119661395806,-4.26551903642628,133.256474054307));
#45047=CARTESIAN_POINT('Ctrl Pts',(105.112013302848,-4.19641537389779,133.372930696015));
#45048=CARTESIAN_POINT('Ctrl Pts',(105.10436520989,-4.12270791310648,133.486237297376));
#45049=CARTESIAN_POINT('Ctrl Pts',(105.096712739397,-4.04895826441624,133.599608751975));
#45050=CARTESIAN_POINT('Ctrl Pts',(105.089060268904,-3.97059980482833,133.709826249315));
#45051=CARTESIAN_POINT('Ctrl Pts',(105.081407798411,-3.88795353957172,133.816502768367));
#45052=CARTESIAN_POINT('Ctrl Pts',(105.073743978962,-3.80518470621165,133.923337493462));
#45053=CARTESIAN_POINT('Ctrl Pts',(105.066080159514,-3.7181156304839,134.026620448661));
#45054=CARTESIAN_POINT('Ctrl Pts',(105.058416340065,-3.6271053942907,134.126000200845));
#45055=CARTESIAN_POINT('Ctrl Pts',(105.053889166277,-3.57334379949745,134.184705838706));
#45056=CARTESIAN_POINT('Ctrl Pts',(105.049361992489,-3.51820760852765,134.242050180961));
#45057=CARTESIAN_POINT('Ctrl Pts',(105.0448348187,-3.46177617688253,134.297967459165));
#45058=CARTESIAN_POINT('Ctrl Pts',(105.037060484581,-3.36486874082114,134.393991960127));
#45059=CARTESIAN_POINT('Ctrl Pts',(105.029286150462,-3.26380941807688,134.486133399984));
#45060=CARTESIAN_POINT('Ctrl Pts',(105.021511816343,-3.15894221405989,134.57401141714));
#45061=CARTESIAN_POINT('Ctrl Pts',(105.013747063396,-3.05420424949947,134.661781132495));
#45062=CARTESIAN_POINT('Ctrl Pts',(105.005982310449,-2.94566803786873,134.745297630913));
#45063=CARTESIAN_POINT('Ctrl Pts',(104.998217557502,-2.83371506303976,134.824216585633));
#45064=CARTESIAN_POINT('Ctrl Pts',(104.990460516617,-2.72187328148395,134.903057156934));
#45065=CARTESIAN_POINT('Ctrl Pts',(104.982703475732,-2.60662180758364,134.977309047969));
#45066=CARTESIAN_POINT('Ctrl Pts',(104.974946434847,-2.48837562897248,135.046667748319));
#45067=CARTESIAN_POINT('Ctrl Pts',(104.967195243607,-2.37021862072443,135.115974144733));
#45068=CARTESIAN_POINT('Ctrl Pts',(104.959444052367,-2.2490717387028,135.180394498164));
#45069=CARTESIAN_POINT('Ctrl Pts',(104.951692861126,-2.12537911587788,135.239667447571));
#45070=CARTESIAN_POINT('Ctrl Pts',(104.943944964349,-2.00173906571718,135.298915204394));
#45071=CARTESIAN_POINT('Ctrl Pts',(104.936197067572,-1.8755557786207,135.35301973993));
#45072=CARTESIAN_POINT('Ctrl Pts',(104.928449170795,-1.74729796925173,135.401765632262));
#45073=CARTESIAN_POINT('Ctrl Pts',(104.920702894711,-1.61906698865174,135.450501328003));
#45074=CARTESIAN_POINT('Ctrl Pts',(104.912956618627,-1.48876271414915,135.493880471287));
#45075=CARTESIAN_POINT('Ctrl Pts',(104.905210342543,-1.35687345011762,135.531735946738));
#45076=CARTESIAN_POINT('Ctrl Pts',(104.897464009277,-1.22498321250932,135.56959170163));
#45077=CARTESIAN_POINT('Ctrl Pts',(104.889717676012,-1.09150833781755,135.601923599463));
#45078=CARTESIAN_POINT('Ctrl Pts',(104.881971342747,-0.956951500145035,
135.628614641648));
#45079=CARTESIAN_POINT('Ctrl Pts',(104.874223274744,-0.822364529401955,
135.655311661106));
#45080=CARTESIAN_POINT('Ctrl Pts',(104.866475206741,-0.686695496952768,
135.676365235176));
#45081=CARTESIAN_POINT('Ctrl Pts',(104.858727138738,-0.55045606055374,135.691709713743));
#45082=CARTESIAN_POINT('Ctrl Pts',(104.850970835996,-0.414071827260159,
135.707070500603));
#45083=CARTESIAN_POINT('Ctrl Pts',(104.843214533254,-0.277116368131101,
135.71671002726));
#45084=CARTESIAN_POINT('Ctrl Pts',(104.835458230512,-0.14010579901636,135.720614621132));
#45085=CARTESIAN_POINT('Ctrl Pts',(104.827697787998,-0.00302210323538782,
135.724521299004));
#45086=CARTESIAN_POINT('Ctrl Pts',(104.819937345484,0.134116370401911,135.722686950205));
#45087=CARTESIAN_POINT('Ctrl Pts',(104.81217690297,0.270795730941145,135.715150038281));
#45088=CARTESIAN_POINT('Ctrl Pts',(104.804404002704,0.407694501323553,135.707601027437));
#45089=CARTESIAN_POINT('Ctrl Pts',(104.796631102439,0.544132296475826,135.694331198206));
#45090=CARTESIAN_POINT('Ctrl Pts',(104.788858202173,0.679601657449962,135.675430792557));
#45091=CARTESIAN_POINT('Ctrl Pts',(104.781367866411,0.810146365927796,135.657217464261));
#45092=CARTESIAN_POINT('Ctrl Pts',(104.773877530649,0.939791524745636,135.633775878336));
#45093=CARTESIAN_POINT('Ctrl Pts',(104.766387194887,1.06809579774052,135.605230791748));
#45094=CARTESIAN_POINT('Ctrl Pts',(104.758612860768,1.20126476624147,135.575603409527));
#45095=CARTESIAN_POINT('Ctrl Pts',(104.750838526649,1.33341100162869,135.540384038075));
#45096=CARTESIAN_POINT('Ctrl Pts',(104.74306419253,1.46402855159239,135.499656504155));
#45097=CARTESIAN_POINT('Ctrl Pts',(104.735299439583,1.59448512709965,135.458979163281));
#45098=CARTESIAN_POINT('Ctrl Pts',(104.727534686635,1.7234163960596,135.412807281929));
#45099=CARTESIAN_POINT('Ctrl Pts',(104.719769933688,1.85032646526505,135.361275696261));
#45100=CARTESIAN_POINT('Ctrl Pts',(104.712012892803,1.97711048560039,135.309795292491));
#45101=CARTESIAN_POINT('Ctrl Pts',(104.704255851918,2.10187694126749,135.252965924214));
#45102=CARTESIAN_POINT('Ctrl Pts',(104.696498811033,2.22414532807544,135.190972136962));
#45103=CARTESIAN_POINT('Ctrl Pts',(104.688747619793,2.34632151134144,135.129025099708));
#45104=CARTESIAN_POINT('Ctrl Pts',(104.680996428553,2.46600302807129,135.061921571389));
#45105=CARTESIAN_POINT('Ctrl Pts',(104.673245237313,2.58272992310162,134.989893941626));
#45106=CARTESIAN_POINT('Ctrl Pts',(104.665497340536,2.69940720608816,134.917896925527));
#45107=CARTESIAN_POINT('Ctrl Pts',(104.657749443759,2.81313203302882,134.84098017543));
#45108=CARTESIAN_POINT('Ctrl Pts',(104.650001546982,2.92346981163792,134.759421593448));
#45109=CARTESIAN_POINT('Ctrl Pts',(104.642255270898,3.03378450996235,134.677880071762));
#45110=CARTESIAN_POINT('Ctrl Pts',(104.634508994813,3.14071325499609,134.591698881754));
#45111=CARTESIAN_POINT('Ctrl Pts',(104.626762718729,3.24385150739914,134.501198517778));
#45112=CARTESIAN_POINT('Ctrl Pts',(104.619016385464,3.34699052114512,134.410697485749));
#45113=CARTESIAN_POINT('Ctrl Pts',(104.611270052199,3.44633869255544,134.315877473996));
#45114=CARTESIAN_POINT('Ctrl Pts',(104.603523718933,3.5415258797701,134.21709815588));
#45115=CARTESIAN_POINT('Ctrl Pts',(104.59577565093,3.6367343834955,134.118296716821));
#45116=CARTESIAN_POINT('Ctrl Pts',(104.588027582927,3.72777977756826,134.015534488521));
#45117=CARTESIAN_POINT('Ctrl Pts',(104.580279514924,3.81433026517127,133.909206457652));
#45118=CARTESIAN_POINT('Ctrl Pts',(104.572523212182,3.90097273966252,133.802765420086));
#45119=CARTESIAN_POINT('Ctrl Pts',(104.564766909441,3.98311051742606,133.692751313156));
#45120=CARTESIAN_POINT('Ctrl Pts',(104.557010606699,4.06045312211073,133.579590969382));
#45121=CARTESIAN_POINT('Ctrl Pts',(104.549250164185,4.13783700687236,133.466370228525));
#45122=CARTESIAN_POINT('Ctrl Pts',(104.54148972167,4.2104204120701,133.350000236358));
#45123=CARTESIAN_POINT('Ctrl Pts',(104.533729279156,4.27795792756222,133.230934134381));
#45124=CARTESIAN_POINT('Ctrl Pts',(104.525956378891,4.34560386026981,133.111676896927));
#45125=CARTESIAN_POINT('Ctrl Pts',(104.518183478625,4.40818753807545,132.989715248914));
#45126=CARTESIAN_POINT('Ctrl Pts',(104.51041057836,4.46551059014517,132.865524907913));
#45127=CARTESIAN_POINT('Ctrl Pts',(104.502920242598,4.52074980488344,132.745849198626));
#45128=CARTESIAN_POINT('Ctrl Pts',(104.495429906836,4.57110410984297,132.624104304988));
#45129=CARTESIAN_POINT('Ctrl Pts',(104.487939571074,4.61643991361667,132.500728969802));
#45130=CARTESIAN_POINT('Ctrl Pts',(104.480165236955,4.66349463817047,132.372675821281));
#45131=CARTESIAN_POINT('Ctrl Pts',(104.472390902836,4.70529185158218,132.242460520324));
#45132=CARTESIAN_POINT('Ctrl Pts',(104.464616568717,4.74162860009793,132.110554049349));
#45133=CARTESIAN_POINT('Ctrl Pts',(104.45685181577,4.7779205668186,131.978810141311));
#45134=CARTESIAN_POINT('Ctrl Pts',(104.449087062823,4.80876535557601,131.845379583531));
#45135=CARTESIAN_POINT('Ctrl Pts',(104.441322309876,4.8340083654595,131.710752467247));
#45136=CARTESIAN_POINT('Ctrl Pts',(104.433565268991,4.8592263036297,131.576259064512));
#45137=CARTESIAN_POINT('Ctrl Pts',(104.425808228106,4.87885346348556,131.440571850102));
#45138=CARTESIAN_POINT('Ctrl Pts',(104.418051187221,4.8927853841564,131.304194837168));
#45139=CARTESIAN_POINT('Ctrl Pts',(104.410299995981,4.90670679865746,131.167920667201));
#45140=CARTESIAN_POINT('Ctrl Pts',(104.402548804741,4.91494148298815,131.030958121469));
#45141=CARTESIAN_POINT('Ctrl Pts',(104.394797613501,4.91743633611711,130.893819785543));
#45142=CARTESIAN_POINT('Ctrl Pts',(104.387049716724,4.91993012886695,130.756739737068));
#45143=CARTESIAN_POINT('Ctrl Pts',(104.379301819946,4.91668893545993,130.619484437085));
#45144=CARTESIAN_POINT('Ctrl Pts',(104.371553923169,4.90771165506752,130.482569733272));
#45145=CARTESIAN_POINT('Ctrl Pts',(104.363807647085,4.89873625252865,130.345683669065));
#45146=CARTESIAN_POINT('Ctrl Pts',(104.356061371001,4.88402717516698,130.209138449196));
#45147=CARTESIAN_POINT('Ctrl Pts',(104.348315094917,4.86363540056671,130.073447659099));
#45148=CARTESIAN_POINT('Ctrl Pts',(104.340568761652,4.84324347543904,129.937755867365));
#45149=CARTESIAN_POINT('Ctrl Pts',(104.332822428387,4.81716882747013,129.802918904611));
#45150=CARTESIAN_POINT('Ctrl Pts',(104.325076095121,4.78551398932964,129.669442593905));
#45151=CARTESIAN_POINT('Ctrl Pts',(104.317328027118,4.75385206230745,129.535936392105));
#45152=CARTESIAN_POINT('Ctrl Pts',(104.309579959115,4.71660754866543,129.403791829029));
#45153=CARTESIAN_POINT('Ctrl Pts',(104.301831891112,4.67393341759135,129.273501554679));
#45154=CARTESIAN_POINT('Ctrl Pts',(104.29407558837,4.63121393194308,129.143072806276));
#45155=CARTESIAN_POINT('Ctrl Pts',(104.286319285629,4.58305342323004,129.014502655542));
#45156=CARTESIAN_POINT('Ctrl Pts',(104.278562982887,4.52965398817584,128.888266201859));
#45157=CARTESIAN_POINT('Ctrl Pts',(104.270802540373,4.47622605223547,128.761962371981));
#45158=CARTESIAN_POINT('Ctrl Pts',(104.263042097859,4.41755378551381,128.637995074258));
#45159=CARTESIAN_POINT('Ctrl Pts',(104.255281655344,4.35388577861308,128.516815713244));
#45160=CARTESIAN_POINT('Ctrl Pts',(104.247508755079,4.29011556617529,128.395441824361));
#45161=CARTESIAN_POINT('Ctrl Pts',(104.239735854814,4.22133378411373,128.276865153931));
#45162=CARTESIAN_POINT('Ctrl Pts',(104.231962954548,4.14783344281394,128.161509733923));
#45163=CARTESIAN_POINT('Ctrl Pts',(104.224472618786,4.07700502405559,128.050347773993));
#45164=CARTESIAN_POINT('Ctrl Pts',(104.216982283024,4.00179532884505,127.942177182324));
#45165=CARTESIAN_POINT('Ctrl Pts',(104.209491947262,3.92250127450789,127.837347504352));
#45166=CARTESIAN_POINT('Ctrl Pts',(104.201717613143,3.84020076200073,127.728543177278));
#45167=CARTESIAN_POINT('Ctrl Pts',(104.193943279024,3.75323935621899,127.622993447023));
#45168=CARTESIAN_POINT('Ctrl Pts',(104.186168944905,3.66190360654968,127.52112364183));
#45169=CARTESIAN_POINT('Ctrl Pts',(104.178404191957,3.57068042002887,127.419379382068));
#45170=CARTESIAN_POINT('Ctrl Pts',(104.17063943901,3.47509387456759,127.321306312013));
#45171=CARTESIAN_POINT('Ctrl Pts',(104.162874686063,3.37547273223597,127.227299408077));
#45172=CARTESIAN_POINT('Ctrl Pts',(104.155117645178,3.27595053502713,127.133385873123));
#45173=CARTESIAN_POINT('Ctrl Pts',(104.147360604293,3.17240199800395,127.043530733932));
#45174=CARTESIAN_POINT('Ctrl Pts',(104.139603563408,3.06519469805296,126.958094307815));
#45175=CARTESIAN_POINT('Ctrl Pts',(104.131852372168,2.95806824396119,126.872722309971));
#45176=CARTESIAN_POINT('Ctrl Pts',(104.124101180928,2.84728882327914,126.79176263536));
#45177=CARTESIAN_POINT('Ctrl Pts',(104.116349989688,2.73325898636117,126.715537024407));
#45178=CARTESIAN_POINT('Ctrl Pts',(104.108602092911,2.61927761516574,126.639343811371));
#45179=CARTESIAN_POINT('Ctrl Pts',(104.100854196134,2.50204889981095,126.567880876892));
#45180=CARTESIAN_POINT('Ctrl Pts',(104.093106299357,2.38200624253308,126.501427975398));
#45181=CARTESIAN_POINT('Ctrl Pts',(104.085360023273,2.26198869559121,126.434988974418));
#45182=CARTESIAN_POINT('Ctrl Pts',(104.077613747188,2.13915871935098,126.373558111144));
#45183=CARTESIAN_POINT('Ctrl Pts',(104.069867471104,2.01397596241131,126.317370102162));
#45184=CARTESIAN_POINT('Ctrl Pts',(104.062121137839,1.88879228140165,126.261181678412));
#45185=CARTESIAN_POINT('Ctrl Pts',(104.054374804574,1.76125614171982,126.210236346277));
#45186=CARTESIAN_POINT('Ctrl Pts',(104.046628471308,1.63184852805071,126.16472125184));
#45187=CARTESIAN_POINT('Ctrl Pts',(104.038880403305,1.50241193444324,126.119195964613));
#45188=CARTESIAN_POINT('Ctrl Pts',(104.031132335302,1.37110340162787,126.079103464606));
#45189=CARTESIAN_POINT('Ctrl Pts',(104.023384267299,1.23842009358668,126.044581343871));
#45190=CARTESIAN_POINT('Ctrl Pts',(104.015627964558,1.10559576814675,126.010022532614));
#45191=CARTESIAN_POINT('Ctrl Pts',(104.007871661816,0.971394127692739,125.981046025599));
#45192=CARTESIAN_POINT('Ctrl Pts',(104.000115359074,0.836324125007024,125.957738595948));
#45193=CARTESIAN_POINT('Ctrl Pts',(103.99235491656,0.70118203139372,125.934418726421));
#45194=CARTESIAN_POINT('Ctrl Pts',(103.984594474045,0.565171039569875,125.91677401361));
#45195=CARTESIAN_POINT('Ctrl Pts',(103.976834031531,0.428805298262543,125.904839306389));
#45196=CARTESIAN_POINT('Ctrl Pts',(103.969061131266,0.292220650561469,125.892885440516));
#45197=CARTESIAN_POINT('Ctrl Pts',(103.961288231,0.155280506170268,125.886659915002));
#45198=CARTESIAN_POINT('Ctrl Pts',(103.953515330735,0.0184999944640169,
125.886145411548));
#45199=CARTESIAN_POINT('Ctrl Pts',(103.946024994973,-0.113308201112205,
125.885649611591));
#45200=CARTESIAN_POINT('Ctrl Pts',(103.938534659211,-0.244967860791525,
125.89045681121));
#45201=CARTESIAN_POINT('Ctrl Pts',(103.931044323449,-0.376024411032684,
125.900506143297));
#45202=CARTESIAN_POINT('Ctrl Pts',(103.92326998933,-0.512050010210392,125.910936498864));
#45203=CARTESIAN_POINT('Ctrl Pts',(103.915495655211,-0.647856751573124,
125.927047385025));
#45204=CARTESIAN_POINT('Ctrl Pts',(103.907721321092,-0.782931907480926,
125.94882761997));
#45205=CARTESIAN_POINT('Ctrl Pts',(103.899956568144,-0.917840595330902,
125.970581012721));
#45206=CARTESIAN_POINT('Ctrl Pts',(103.892191815197,-1.05201910939418,125.997989790637));
#45207=CARTESIAN_POINT('Ctrl Pts',(103.88442706225,-1.18495744090136,126.030990851274));
#45208=CARTESIAN_POINT('Ctrl Pts',(103.876670021365,-1.31776373618322,126.063959134792));
#45209=CARTESIAN_POINT('Ctrl Pts',(103.86891298048,-1.44933192318762,126.10250855407));
#45210=CARTESIAN_POINT('Ctrl Pts',(103.861155939595,-1.57916017247244,126.14652461657));
#45211=CARTESIAN_POINT('Ctrl Pts',(103.853404748355,-1.70889051726429,126.190507486214));
#45212=CARTESIAN_POINT('Ctrl Pts',(103.845653557115,-1.83688316722717,126.239948668593));
#45213=CARTESIAN_POINT('Ctrl Pts',(103.837902365875,-1.962649844731,126.29468339525));
#45214=CARTESIAN_POINT('Ctrl Pts',(103.830154469098,-2.08836306804272,126.349394858188));
#45215=CARTESIAN_POINT('Ctrl Pts',(103.822406572321,-2.21185184287539,126.409395234841));
#45216=CARTESIAN_POINT('Ctrl Pts',(103.814658675544,-2.33264653941025,126.474471105733));
#45217=CARTESIAN_POINT('Ctrl Pts',(103.80691239946,-2.45341596829855,126.539533364157));
#45218=CARTESIAN_POINT('Ctrl Pts',(103.799166123375,-2.57149209583039,126.609668819761));
#45219=CARTESIAN_POINT('Ctrl Pts',(103.791419847291,-2.68642899699944,126.684617627211));
#45220=CARTESIAN_POINT('Ctrl Pts',(103.783673514026,-2.80136674660659,126.759566987915));
#45221=CARTESIAN_POINT('Ctrl Pts',(103.775927180761,-2.91316489612109,126.839329557813));
#45222=CARTESIAN_POINT('Ctrl Pts',(103.768180847495,-3.02140601027084,126.923601827896));
#45223=CARTESIAN_POINT('Ctrl Pts',(103.760432779492,-3.12967136426799,127.00789297017));
#45224=CARTESIAN_POINT('Ctrl Pts',(103.752684711489,-3.23437778937837,127.096695582112));
#45225=CARTESIAN_POINT('Ctrl Pts',(103.744936643486,-3.33514079623731,127.189665757447));
#45226=CARTESIAN_POINT('Ctrl Pts',(103.737180340744,-3.43601089521875,127.28273474259));
#45227=CARTESIAN_POINT('Ctrl Pts',(103.729424038002,-3.53292891595121,127.379979873659));
#45228=CARTESIAN_POINT('Ctrl Pts',(103.721667735261,-3.62554675233683,127.481019857259));
#45229=CARTESIAN_POINT('Ctrl Pts',(103.713907292746,-3.71821402165047,127.58211376894));
#45230=CARTESIAN_POINT('Ctrl Pts',(103.706146850232,-3.80657628159641,127.687006270122));
#45231=CARTESIAN_POINT('Ctrl Pts',(103.698386407718,-3.89032630288535,127.795283629588));
#45232=CARTESIAN_POINT('Ctrl Pts',(103.690613507453,-3.97421076714333,127.903734805484));
#45233=CARTESIAN_POINT('Ctrl Pts',(103.682840607187,-4.05346797106655,128.015581378699));
#45234=CARTESIAN_POINT('Ctrl Pts',(103.675067706922,-4.12783404502062,128.130380595339));
#45235=CARTESIAN_POINT('Ctrl Pts',(103.66757737116,-4.19949672486927,128.241006571292));
#45236=CARTESIAN_POINT('Ctrl Pts',(103.660087035398,-4.26661755370495,128.354373980592));
#45237=CARTESIAN_POINT('Ctrl Pts',(103.652596699636,-4.329002032648,128.470067477485));
#45238=CARTESIAN_POINT('Ctrl Pts',(103.644401642804,-4.39725589557558,128.596645886287));
#45239=CARTESIAN_POINT('Ctrl Pts',(103.636206585971,-4.46003750102258,128.726374192205));
#45240=CARTESIAN_POINT('Ctrl Pts',(103.628011529139,-4.51706109976003,128.858765057452));
#45241=CARTESIAN_POINT('Ctrl Pts',(103.619834970596,-4.57395598200442,128.990857083478));
#45242=CARTESIAN_POINT('Ctrl Pts',(103.611658412052,-4.62511864185374,129.125599385668));
#45243=CARTESIAN_POINT('Ctrl Pts',(103.603481853508,-4.67030931125085,129.262480596376));
#45244=CARTESIAN_POINT('Ctrl Pts',(103.597180950731,-4.70513349954493,129.367962040206));
#45245=CARTESIAN_POINT('Ctrl Pts',(103.590880047953,-4.73641218697444,129.474713050268));
#45246=CARTESIAN_POINT('Ctrl Pts',(103.584579145176,-4.76405452823405,129.582490119308));
#45247=CARTESIAN_POINT('Ctrl Pts',(105.334849955158,-4.76405452823403,129.582490119308));
#45248=CARTESIAN_POINT('Ctrl Pts',(105.330994117609,-4.78088962480231,129.64812990532));
#45249=CARTESIAN_POINT('Ctrl Pts',(105.327138280061,-4.79635579169737,129.714070555088));
#45250=CARTESIAN_POINT('Ctrl Pts',(105.323282442513,-4.81044496211385,129.780250111335));
#45251=CARTESIAN_POINT('Ctrl Pts',(105.312383741536,-4.8502686459327,129.967309650353));
#45252=CARTESIAN_POINT('Ctrl Pts',(105.30148504056,-4.87919273195189,130.156764553182));
#45253=CARTESIAN_POINT('Ctrl Pts',(105.290586339583,-4.89699044628828,130.347559094515));
#45254=CARTESIAN_POINT('Ctrl Pts',(105.282010705053,-4.9109945642069,130.497685633495));
#45255=CARTESIAN_POINT('Ctrl Pts',(105.273435070522,-4.91811079454292,130.648641435253));
#45256=CARTESIAN_POINT('Ctrl Pts',(105.264859435991,-4.91824797726537,130.799900054249));
#45257=CARTESIAN_POINT('',(105.610140564046,-4.91824918613665,130.807190028493));
#45258=CARTESIAN_POINT('Ctrl Pts',(105.680281509498,-4.76405452823405,129.582490119308));
#45259=CARTESIAN_POINT('Ctrl Pts',(105.67262227585,-4.79773136595739,129.713795598474));
#45260=CARTESIAN_POINT('Ctrl Pts',(105.664963042202,-4.8259527168751,129.846405555949));
#45261=CARTESIAN_POINT('Ctrl Pts',(105.657303808554,-4.84864080799001,129.979821123306));
#45262=CARTESIAN_POINT('Ctrl Pts',(105.649443267802,-4.87192520861973,130.116743242706));
#45263=CARTESIAN_POINT('Ctrl Pts',(105.641582727051,-4.88938140979562,130.254513451776));
#45264=CARTESIAN_POINT('Ctrl Pts',(105.6337221863,-4.90098226160684,130.392588916359));
#45265=CARTESIAN_POINT('Ctrl Pts',(105.625861645548,-4.91258311341805,130.530664380942));
#45266=CARTESIAN_POINT('Ctrl Pts',(105.618001104797,-4.91832865954961,130.669044648147));
#45267=CARTESIAN_POINT('Ctrl Pts',(105.610140564046,-4.91824918613665,130.807190028493));
#45268=CARTESIAN_POINT('Ctrl Pts',(105.610140564008,-4.91824918613627,130.807190029158));
#45269=CARTESIAN_POINT('Ctrl Pts',(105.600807399395,-4.91815482384702,130.971216095075));
#45270=CARTESIAN_POINT('Ctrl Pts',(105.591474234781,-4.90985562625394,131.13500317217));
#45271=CARTESIAN_POINT('Ctrl Pts',(105.582141070167,-4.89341873628665,131.297955728825));
#45272=CARTESIAN_POINT('Ctrl Pts',(105.574366736048,-4.87972714508784,131.433691856217));
#45273=CARTESIAN_POINT('Ctrl Pts',(105.566592401929,-4.86036191113187,131.569072871748));
#45274=CARTESIAN_POINT('Ctrl Pts',(105.55881806781,-4.83534651705842,131.703586463764));
#45275=CARTESIAN_POINT('Ctrl Pts',(105.551053314863,-4.81036195222251,131.8379342798));
#45276=CARTESIAN_POINT('Ctrl Pts',(105.543288561915,-4.77974115299095,131.971416418671));
#45277=CARTESIAN_POINT('Ctrl Pts',(105.535523808968,-4.74355944243922,132.103524532761));
#45278=CARTESIAN_POINT('Ctrl Pts',(105.527766768083,-4.70741366807248,132.235501435211));
#45279=CARTESIAN_POINT('Ctrl Pts',(105.520009727198,-4.66571807635992,132.366106654058));
#45280=CARTESIAN_POINT('Ctrl Pts',(105.512252686313,-4.61859916939185,132.494841251881));
#45281=CARTESIAN_POINT('Ctrl Pts',(105.504501495073,-4.57151579515805,132.623478769942));
#45282=CARTESIAN_POINT('Ctrl Pts',(105.496750303833,-4.51901737993361,132.750248109131));
#45283=CARTESIAN_POINT('Ctrl Pts',(105.488999112593,-4.46128036204199,132.87466508642));
#45284=CARTESIAN_POINT('Ctrl Pts',(105.481251215816,-4.40356788392312,132.999029183175));
#45285=CARTESIAN_POINT('Ctrl Pts',(105.473503319039,-4.3406213957967,133.121042552691));
#45286=CARTESIAN_POINT('Ctrl Pts',(105.465755422262,-4.27266552549797,133.24024082187));
#45287=CARTESIAN_POINT('Ctrl Pts',(105.458009146177,-4.20472387010231,133.359414157341));
#45288=CARTESIAN_POINT('Ctrl Pts',(105.450262870093,-4.13177511028703,133.475773224316));
#45289=CARTESIAN_POINT('Ctrl Pts',(105.442516594009,-4.05408971753009,133.588878461775));
#45290=CARTESIAN_POINT('Ctrl Pts',(105.434770260744,-3.97640375131739,133.701984534151));
#45291=CARTESIAN_POINT('Ctrl Pts',(105.427023927479,-3.89398130374241,133.811836406812));
#45292=CARTESIAN_POINT('Ctrl Pts',(105.419277594213,-3.80713581370514,133.918024048077));
#45293=CARTESIAN_POINT('Ctrl Pts',(105.41152952621,-3.72027087522229,134.024235469329));
#45294=CARTESIAN_POINT('Ctrl Pts',(105.403781458207,-3.6289811707438,134.126780723745));
#45295=CARTESIAN_POINT('Ctrl Pts',(105.396033390204,-3.53361973419242,134.225283685486));
#45296=CARTESIAN_POINT('Ctrl Pts',(105.388277087462,-3.43815694637166,134.323891337347));
#45297=CARTESIAN_POINT('Ctrl Pts',(105.380520784721,-3.33861405423218,134.418447833072));
#45298=CARTESIAN_POINT('Ctrl Pts',(105.372764481979,-3.23538059495422,134.508614316801));
#45299=CARTESIAN_POINT('Ctrl Pts',(105.365004039465,-3.13209203687054,134.598828925096));
#45300=CARTESIAN_POINT('Ctrl Pts',(105.35724359695,-3.02510929153961,134.684648608087));
#45301=CARTESIAN_POINT('Ctrl Pts',(105.349483154436,-2.91485334369152,134.765776153365));
#45302=CARTESIAN_POINT('Ctrl Pts',(105.341710254171,-2.80442040320796,134.847033931781));
#45303=CARTESIAN_POINT('Ctrl Pts',(105.333937353905,-2.69070408468396,134.923584302226));
#45304=CARTESIAN_POINT('Ctrl Pts',(105.32616445364,-2.57415334665718,134.995174095925));
#45305=CARTESIAN_POINT('Ctrl Pts',(105.318674117878,-2.46183952153143,135.064161420299));
#45306=CARTESIAN_POINT('Ctrl Pts',(105.311183782116,-2.3468940444245,135.12854241476));
#45307=CARTESIAN_POINT('Ctrl Pts',(105.303693446354,-2.22973680891774,135.188132603591));
#45308=CARTESIAN_POINT('Ctrl Pts',(105.295919112235,-2.10813752121747,135.249982172544));
#45309=CARTESIAN_POINT('Ctrl Pts',(105.288144778116,-1.98377025668619,135.306866398525));
#45310=CARTESIAN_POINT('Ctrl Pts',(105.280370443997,-1.85707873056852,135.35852812118));
#45311=CARTESIAN_POINT('Ctrl Pts',(105.27260569105,-1.73054334043396,135.410126175379));
#45312=CARTESIAN_POINT('Ctrl Pts',(105.264840938102,-1.60168974665206,135.456514386301));
#45313=CARTESIAN_POINT('Ctrl Pts',(105.257076185155,-1.47098635043047,135.497481351081));
#45314=CARTESIAN_POINT('Ctrl Pts',(105.24931914427,-1.3404127706647,135.538407626894));
#45315=CARTESIAN_POINT('Ctrl Pts',(105.241562103385,-1.20799341532432,135.573923255702));
#45316=CARTESIAN_POINT('Ctrl Pts',(105.2338050625,-1.07421643206328,135.603864979434));
#45317=CARTESIAN_POINT('Ctrl Pts',(105.22605387126,-0.940540331066034,135.633784123878));
#45318=CARTESIAN_POINT('Ctrl Pts',(105.21830268002,-0.805509019937553,135.658137644663));
#45319=CARTESIAN_POINT('Ctrl Pts',(105.21055148878,-0.669625224796948,135.676812271591));
#45320=CARTESIAN_POINT('Ctrl Pts',(105.202803592003,-0.533799183894003,
135.695478961306));
#45321=CARTESIAN_POINT('Ctrl Pts',(105.195055695226,-0.397121766136255,
135.708471504673));
#45322=CARTESIAN_POINT('Ctrl Pts',(105.187307798449,-0.260105078594647,
135.715727882452));
#45323=CARTESIAN_POINT('Ctrl Pts',(105.179561522365,-0.123117051990335,
135.722982742352));
#45324=CARTESIAN_POINT('Ctrl Pts',(105.171815246281,0.0142097130680153,
135.724503802631));
#45325=CARTESIAN_POINT('Ctrl Pts',(105.164068970196,0.151359205005327,135.720281025136));
#45326=CARTESIAN_POINT('Ctrl Pts',(105.156322636931,0.288509709349126,135.716058216469));
#45327=CARTESIAN_POINT('Ctrl Pts',(105.148576303666,0.425482547180669,135.706091497453));
#45328=CARTESIAN_POINT('Ctrl Pts',(105.1408299704,0.561763325851781,135.690422940974));
#45329=CARTESIAN_POINT('Ctrl Pts',(105.133081902397,0.698074623658279,135.67475087563));
#45330=CARTESIAN_POINT('Ctrl Pts',(105.125333834394,0.833693165576224,135.653374476612));
#45331=CARTESIAN_POINT('Ctrl Pts',(105.117585766391,0.968111682826347,135.626387456155));
#45332=CARTESIAN_POINT('Ctrl Pts',(105.10982946365,1.1026730616762,135.599371753572));
#45333=CARTESIAN_POINT('Ctrl Pts',(105.102073160908,1.23603148418099,135.566733594824));
#45334=CARTESIAN_POINT('Ctrl Pts',(105.094316858166,1.36769130694644,135.528617548704));
#45335=CARTESIAN_POINT('Ctrl Pts',(105.086556415652,1.4994214005236,135.490481158902));
#45336=CARTESIAN_POINT('Ctrl Pts',(105.078795973138,1.62945071741313,135.446861180265));
#45337=CARTESIAN_POINT('Ctrl Pts',(105.071035530623,1.75730165187032,135.397951148603));
#45338=CARTESIAN_POINT('Ctrl Pts',(105.063262630358,1.88535782399748,135.348962602216));
#45339=CARTESIAN_POINT('Ctrl Pts',(105.055489730093,2.01122826650921,135.294667187901));
#45340=CARTESIAN_POINT('Ctrl Pts',(105.047716829827,2.13445730828998,135.235305783283));
#45341=CARTESIAN_POINT('Ctrl Pts',(105.040226494065,2.25320666400672,135.178102315245));
#45342=CARTESIAN_POINT('Ctrl Pts',(105.032736158303,2.36950305608668,135.116194930029));
#45343=CARTESIAN_POINT('Ctrl Pts',(105.025245822541,2.48296431714824,135.049837182366));
#45344=CARTESIAN_POINT('Ctrl Pts',(105.017471488422,2.60072749640885,134.980963460532));
#45345=CARTESIAN_POINT('Ctrl Pts',(105.009697154303,2.71580935108983,134.907077072235));
#45346=CARTESIAN_POINT('Ctrl Pts',(105.001922820184,2.8277536859747,134.828412326224));
#45347=CARTESIAN_POINT('Ctrl Pts',(104.994158067237,2.93956005947158,134.749844527483));
#45348=CARTESIAN_POINT('Ctrl Pts',(104.98639331429,3.04823628996613,134.666510310809));
#45349=CARTESIAN_POINT('Ctrl Pts',(104.978628561342,3.15335133594567,134.578689486993));
#45350=CARTESIAN_POINT('Ctrl Pts',(104.970871520457,3.25836198017967,134.490955888057));
#45351=CARTESIAN_POINT('Ctrl Pts',(104.963114479572,3.35981818063514,134.398744798986));
#45352=CARTESIAN_POINT('Ctrl Pts',(104.955357438687,3.45731872794115,134.302378667252));
#45353=CARTESIAN_POINT('Ctrl Pts',(104.947606247447,3.55474574932591,134.206085205967));
#45354=CARTESIAN_POINT('Ctrl Pts',(104.939855056207,3.64822277807761,134.105643212481));
#45355=CARTESIAN_POINT('Ctrl Pts',(104.932103864967,3.73738278102539,134.001414419208));
#45356=CARTESIAN_POINT('Ctrl Pts',(104.92435596819,3.82650488859355,133.897229925953));
#45357=CARTESIAN_POINT('Ctrl Pts',(104.916608071413,3.91131336612629,133.789262130538));
#45358=CARTESIAN_POINT('Ctrl Pts',(104.908860174636,3.99147922869732,133.677908360231));
#45359=CARTESIAN_POINT('Ctrl Pts',(104.901113898552,4.07162832229813,133.566577882733));
#45360=CARTESIAN_POINT('Ctrl Pts',(104.893367622468,4.14713650429643,133.451863156228));
#45361=CARTESIAN_POINT('Ctrl Pts',(104.885621346383,4.21771641244897,133.334192890002));
#45362=CARTESIAN_POINT('Ctrl Pts',(104.877875013118,4.28829684160625,133.216521755161));
#45363=CARTESIAN_POINT('Ctrl Pts',(104.870128679853,4.35394872322201,133.095895372343));
#45364=CARTESIAN_POINT('Ctrl Pts',(104.862382346587,4.41442941261409,132.972769256072));
#45365=CARTESIAN_POINT('Ctrl Pts',(104.854634278584,4.4749236462372,132.849615566561));
#45366=CARTESIAN_POINT('Ctrl Pts',(104.846886210581,4.53024421090618,132.723961380512));
#45367=CARTESIAN_POINT('Ctrl Pts',(104.839138142578,4.5801957582119,132.596284131268));
#45368=CARTESIAN_POINT('Ctrl Pts',(104.831381839837,4.63020039461657,132.468471185124));
#45369=CARTESIAN_POINT('Ctrl Pts',(104.823625537095,4.6748244721258,132.338631245329));
#45370=CARTESIAN_POINT('Ctrl Pts',(104.815869234353,4.71392171319714,132.207259453672));
#45371=CARTESIAN_POINT('Ctrl Pts',(104.808108791839,4.75303982164326,132.075817544935));
#45372=CARTESIAN_POINT('Ctrl Pts',(104.800348349325,4.78662512015525,131.942842534084));
#45373=CARTESIAN_POINT('Ctrl Pts',(104.79258790681,4.81458227832083,131.808840855191));
#45374=CARTESIAN_POINT('Ctrl Pts',(104.784815006545,4.84258431579862,131.674624064907));
#45375=CARTESIAN_POINT('Ctrl Pts',(104.777042106279,4.86494009474285,131.539377699109));
#45376=CARTESIAN_POINT('Ctrl Pts',(104.769269206014,4.88160597095454,131.403615327052));
#45377=CARTESIAN_POINT('Ctrl Pts',(104.761778870252,4.89766600058711,131.272788259184));
#45378=CARTESIAN_POINT('Ctrl Pts',(104.75428853449,4.90844260471322,131.141482356961));
#45379=CARTESIAN_POINT('Ctrl Pts',(104.746798198728,4.91394253530475,131.01015620115));
#45380=CARTESIAN_POINT('Ctrl Pts',(104.739023864609,4.91965099743632,130.873850774226));
#45381=CARTESIAN_POINT('Ctrl Pts',(104.73124953049,4.91969283987632,130.737091752946));
#45382=CARTESIAN_POINT('Ctrl Pts',(104.723475196371,4.91401860855399,130.600389596867));
#45383=CARTESIAN_POINT('Ctrl Pts',(104.715710443424,4.90835137021465,130.463855913978));
#45384=CARTESIAN_POINT('Ctrl Pts',(104.707945690477,4.89698209072647,130.327379343729));
#45385=CARTESIAN_POINT('Ctrl Pts',(104.700180937529,4.87991319436435,130.191473778118));
#45386=CARTESIAN_POINT('Ctrl Pts',(104.692423896644,4.86286125107073,130.055703195831));
#45387=CARTESIAN_POINT('Ctrl Pts',(104.68466685576,4.84012100483368,129.920502874975));
#45388=CARTESIAN_POINT('Ctrl Pts',(104.676909814875,4.811746876377,129.786384655091));
#45389=CARTESIAN_POINT('Ctrl Pts',(104.669158623634,4.78339414507133,129.652367574801));
#45390=CARTESIAN_POINT('Ctrl Pts',(104.661407432394,4.74941606863021,129.519431352194));
#45391=CARTESIAN_POINT('Ctrl Pts',(104.653656241154,4.70991859238451,129.388080307878));
#45392=CARTESIAN_POINT('Ctrl Pts',(104.645908344377,4.67043790361981,129.256785091259));
#45393=CARTESIAN_POINT('Ctrl Pts',(104.6381604476,4.62544259319947,129.127074086529));
#45394=CARTESIAN_POINT('Ctrl Pts',(104.630412550823,4.57508911941733,128.999438843115));
#45395=CARTESIAN_POINT('Ctrl Pts',(104.622666274739,4.52474617849641,128.871830298242));
#45396=CARTESIAN_POINT('Ctrl Pts',(104.614919998655,4.46904744695803,128.746297014485));
#45397=CARTESIAN_POINT('Ctrl Pts',(104.607173722571,4.40819828375385,128.623312485679));
#45398=CARTESIAN_POINT('Ctrl Pts',(104.599427389305,4.34734867137498,128.500327049028));
#45399=CARTESIAN_POINT('Ctrl Pts',(104.59168105604,4.28134872484304,128.379890755291));
#45400=CARTESIAN_POINT('Ctrl Pts',(104.583934722775,4.21045052605094,128.262453965036));
#45401=CARTESIAN_POINT('Ctrl Pts',(104.576186654772,4.13953645009884,128.144990875626));
#45402=CARTESIAN_POINT('Ctrl Pts',(104.568438586769,4.0637221411481,128.030528960977));
#45403=CARTESIAN_POINT('Ctrl Pts',(104.560690518766,3.98330368680443,127.919490637621));
#45404=CARTESIAN_POINT('Ctrl Pts',(104.552934216024,3.90279976277044,127.808334301413));
#45405=CARTESIAN_POINT('Ctrl Pts',(104.545177913282,3.81768214806065,127.700609142209));
#45406=CARTESIAN_POINT('Ctrl Pts',(104.53742161054,3.72828835289985,127.596705863679));
#45407=CARTESIAN_POINT('Ctrl Pts',(104.529661168026,3.63884684557892,127.492747128842));
#45408=CARTESIAN_POINT('Ctrl Pts',(104.521900725512,3.54512487711405,127.392614624558));
#45409=CARTESIAN_POINT('Ctrl Pts',(104.514140282998,3.44749699641711,127.296662294991));
#45410=CARTESIAN_POINT('Ctrl Pts',(104.506367382732,3.34971239477908,127.200555934226));
#45411=CARTESIAN_POINT('Ctrl Pts',(104.498594482467,3.24800964144666,127.108643419962));
#45412=CARTESIAN_POINT('Ctrl Pts',(104.490821582201,3.14279722602412,127.021239068026));
#45413=CARTESIAN_POINT('Ctrl Pts',(104.483331246439,3.04140954691542,126.93701208444));
#45414=CARTESIAN_POINT('Ctrl Pts',(104.475840910677,2.93676319036127,126.856971374702));
#45415=CARTESIAN_POINT('Ctrl Pts',(104.468350574915,2.82924762295476,126.781359132293));
#45416=CARTESIAN_POINT('Ctrl Pts',(104.460576240796,2.71765557013216,126.702880028732));
#45417=CARTESIAN_POINT('Ctrl Pts',(104.452801906677,2.60261894917284,126.628923233976));
#45418=CARTESIAN_POINT('Ctrl Pts',(104.445027572558,2.48454049302679,126.559806270993));
#45419=CARTESIAN_POINT('Ctrl Pts',(104.437262819611,2.36660755802506,126.490774488491));
#45420=CARTESIAN_POINT('Ctrl Pts',(104.429498066664,2.24564058098356,126.426570865473));
#45421=CARTESIAN_POINT('Ctrl Pts',(104.421733313716,2.12207322417457,126.367471133508));
#45422=CARTESIAN_POINT('Ctrl Pts',(104.413976272831,1.99862859620628,126.30843010023));
#45423=CARTESIAN_POINT('Ctrl Pts',(104.406219231946,1.87258907864562,126.254483037553));
#45424=CARTESIAN_POINT('Ctrl Pts',(104.398462191061,1.74441471232456,126.205860821554));
#45425=CARTESIAN_POINT('Ctrl Pts',(104.390710999821,1.61633700329036,126.157275271946));
#45426=CARTESIAN_POINT('Ctrl Pts',(104.382959808581,1.48612801398442,126.114006714498));
#45427=CARTESIAN_POINT('Ctrl Pts',(104.375208617341,1.35426930965596,126.07623861201));
#45428=CARTESIAN_POINT('Ctrl Pts',(104.367460720564,1.2224666487942,126.038486561973));
#45429=CARTESIAN_POINT('Ctrl Pts',(104.359712823787,1.08901604255386,126.006230424538));
#45430=CARTESIAN_POINT('Ctrl Pts',(104.35196492701,0.954415614920289,125.979604261386));
#45431=CARTESIAN_POINT('Ctrl Pts',(104.344218650926,0.819843342794435,125.952983667854));
#45432=CARTESIAN_POINT('Ctrl Pts',(104.336472374842,0.684122110968675,125.931990781976));
#45433=CARTESIAN_POINT('Ctrl Pts',(104.328726098757,0.547761284745379,125.916708764433));
#45434=CARTESIAN_POINT('Ctrl Pts',(104.320979765492,0.411399451937533,125.901426634082));
#45435=CARTESIAN_POINT('Ctrl Pts',(104.313233432227,0.274398403843937,125.89185549973));
#45436=CARTESIAN_POINT('Ctrl Pts',(104.305487098961,0.137273297987871,125.888026708629));
#45437=CARTESIAN_POINT('Ctrl Pts',(104.297739030958,0.000117483915200584,
125.884197060098));
#45438=CARTESIAN_POINT('Ctrl Pts',(104.289990962955,-0.137162052464567,
125.886112324635));
#45439=CARTESIAN_POINT('Ctrl Pts',(104.282242894952,-0.274049877575846,
125.893751721808));
#45440=CARTESIAN_POINT('Ctrl Pts',(104.274486592211,-0.411083188696826,
125.901399238222));
#45441=CARTESIAN_POINT('Ctrl Pts',(104.266730289469,-0.547723565934234,
125.914783018251));
#45442=CARTESIAN_POINT('Ctrl Pts',(104.258973986727,-0.683459866704315,
125.93383028986));
#45443=CARTESIAN_POINT('Ctrl Pts',(104.251213544213,-0.819268614025057,
125.952887727571));
#45444=CARTESIAN_POINT('Ctrl Pts',(104.243453101698,-0.954171939020441,
125.977614609547));
#45445=CARTESIAN_POINT('Ctrl Pts',(104.235692659184,-1.0876696056067,126.007887132646));
#45446=CARTESIAN_POINT('Ctrl Pts',(104.227919758919,-1.22138157449873,126.038208251887));
#45447=CARTESIAN_POINT('Ctrl Pts',(104.220146858653,-1.3536829982512,126.074092699589));
#45448=CARTESIAN_POINT('Ctrl Pts',(104.212373958388,-1.48408863544707,126.115366697263));
#45449=CARTESIAN_POINT('Ctrl Pts',(104.204883622626,-1.60975369925739,126.155140281158));
#45450=CARTESIAN_POINT('Ctrl Pts',(104.197393286864,-1.73365812707501,126.199918265949));
#45451=CARTESIAN_POINT('Ctrl Pts',(104.189902951102,-1.85538763845819,126.249503893853));
#45452=CARTESIAN_POINT('Ctrl Pts',(104.182128258453,-1.98173838792778,126.300971949358));
#45453=CARTESIAN_POINT('Ctrl Pts',(104.174353565804,-2.10614608482347,126.357782929116));
#45454=CARTESIAN_POINT('Ctrl Pts',(104.166578873156,-2.22812583433463,126.419769607122));
#45455=CARTESIAN_POINT('Ctrl Pts',(104.158813843926,-2.3499539712278,126.481679239859));
#45456=CARTESIAN_POINT('Ctrl Pts',(104.151048814697,-2.4693598201718,126.548751595043));
#45457=CARTESIAN_POINT('Ctrl Pts',(104.143283785468,-2.58587694680721,126.620770833843));
#45458=CARTESIAN_POINT('Ctrl Pts',(104.135526550199,-2.70227712219174,126.692717785072));
#45459=CARTESIAN_POINT('Ctrl Pts',(104.12776931493,-2.81579401519334,126.769601533965));
#45460=CARTESIAN_POINT('Ctrl Pts',(104.120012079662,-2.92598468896782,126.851159805259));
#45461=CARTESIAN_POINT('Ctrl Pts',(104.11210165736,-3.03835136769242,126.934328659336));
#45462=CARTESIAN_POINT('Ctrl Pts',(104.104191235059,-3.14725870223143,127.022358424044));
#45463=CARTESIAN_POINT('Ctrl Pts',(104.096280812758,-3.25226629346806,127.114923395052));
#45464=CARTESIAN_POINT('Ctrl Pts',(104.088533257867,-3.35511188704357,127.205582549076));
#45465=CARTESIAN_POINT('Ctrl Pts',(104.080785702977,-3.45421645976481,127.30059169383));
#45466=CARTESIAN_POINT('Ctrl Pts',(104.073038148086,-3.54919873451535,127.399603444813));
#45467=CARTESIAN_POINT('Ctrl Pts',(104.065292295697,-3.64416013719751,127.498593438262));
#45468=CARTESIAN_POINT('Ctrl Pts',(104.057546443309,-3.73500077404149,127.601584005824));
#45469=CARTESIAN_POINT('Ctrl Pts',(104.04980059092,-3.82137620686658,127.708190895459));
#45470=CARTESIAN_POINT('Ctrl Pts',(104.042054763247,-3.90775136408046,127.814797444927));
#45471=CARTESIAN_POINT('Ctrl Pts',(104.034308935575,-3.98966110018621,127.925019989339));
#45472=CARTESIAN_POINT('Ctrl Pts',(104.026563107902,-4.06680151471503,128.038441511299));
#45473=CARTESIAN_POINT('Ctrl Pts',(104.018529677612,-4.14680615318612,128.156074374886));
#45474=CARTESIAN_POINT('Ctrl Pts',(104.010496247323,-4.2216801926709,128.277147994697));
#45475=CARTESIAN_POINT('Ctrl Pts',(104.002462817033,-4.29113456301106,128.401165406054));
#45476=CARTESIAN_POINT('Ctrl Pts',(103.994708493788,-4.35817586653774,128.520874056161));
#45477=CARTESIAN_POINT('Ctrl Pts',(103.986954170543,-4.42016766575189,128.643324982946));
#45478=CARTESIAN_POINT('Ctrl Pts',(103.979199847298,-4.47689781571174,128.768048016275));
#45479=CARTESIAN_POINT('Ctrl Pts',(103.971441345739,-4.53365853396177,128.89283825496));
#45480=CARTESIAN_POINT('Ctrl Pts',(103.963682844179,-4.58515180761465,129.019902677904));
#45481=CARTESIAN_POINT('Ctrl Pts',(103.95592434262,-4.63121437594359,129.148753035271));
#45482=CARTESIAN_POINT('Ctrl Pts',(103.948156950967,-4.67732972515105,129.277751036056));
#45483=CARTESIAN_POINT('Ctrl Pts',(103.940389559314,-4.71800183383925,129.408538683573));
#45484=CARTESIAN_POINT('Ctrl Pts',(103.932622167662,-4.75311776225026,129.54061436112));
#45485=CARTESIAN_POINT('Ctrl Pts',(103.93180209325,-4.75682527123209,129.554558795539));
#45486=CARTESIAN_POINT('Ctrl Pts',(103.930982018839,-4.76047089301986,129.568517579997));
#45487=CARTESIAN_POINT('Ctrl Pts',(103.930161944428,-4.76405452823404,129.582490119308));
#45488=CARTESIAN_POINT('Origin',(213.235140564004,0.,130.804360617566));
#45489=CARTESIAN_POINT('',(101.834907966042,-4.76405452823403,129.582490119308));
#45490=CARTESIAN_POINT('',(102.179855052771,-4.76405452823403,129.582490119308));
#45491=CARTESIAN_POINT('',(213.235140564004,-4.76405452823405,129.582490119308));
#45492=CARTESIAN_POINT('',(103.514859436023,-4.91824999784073,130.804214879153));
#45493=CARTESIAN_POINT('Ctrl Pts',(103.514859435991,-4.91824999784074,130.80421487972));
#45494=CARTESIAN_POINT('Ctrl Pts',(103.506762540919,-4.91825425810335,130.947986981988));
#45495=CARTESIAN_POINT('Ctrl Pts',(103.498665645847,-4.91195000582023,131.091643240942));
#45496=CARTESIAN_POINT('Ctrl Pts',(103.490568750775,-4.89939349982138,131.234623788669));
#45497=CARTESIAN_POINT('Ctrl Pts',(103.482461820269,-4.88682143106815,131.377781549002));
#45498=CARTESIAN_POINT('Ctrl Pts',(103.474354889763,-4.86798167668567,131.520261592361));
#45499=CARTESIAN_POINT('Ctrl Pts',(103.466247959256,-4.84298193936281,131.661512294637));
#45500=CARTESIAN_POINT('Ctrl Pts',(103.458122472384,-4.81792497886648,131.803086312848));
#45501=CARTESIAN_POINT('Ctrl Pts',(103.449996985511,-4.78667990419565,131.943425031803));
#45502=CARTESIAN_POINT('Ctrl Pts',(103.441871498638,-4.74940528021162,132.081988320302));
#45503=CARTESIAN_POINT('Ctrl Pts',(103.433736303412,-4.71208612040582,132.220717164593));
#45504=CARTESIAN_POINT('Ctrl Pts',(103.425601108185,-4.66872313664903,132.357666024962));
#45505=CARTESIAN_POINT('Ctrl Pts',(103.417465912958,-4.61952380494145,132.492312891204));
#45506=CARTESIAN_POINT('Ctrl Pts',(103.409312148305,-4.57021217065619,132.627267102883));
#45507=CARTESIAN_POINT('Ctrl Pts',(103.401158383651,-4.51503767883914,132.759908502117));
#45508=CARTESIAN_POINT('Ctrl Pts',(103.393004618998,-4.4542554661105,132.889736196479));
#45509=CARTESIAN_POINT('Ctrl Pts',(103.38671943794,-4.40740260386084,132.989811511395));
#45510=CARTESIAN_POINT('Ctrl Pts',(103.380434256881,-4.35721869783343,133.088215438985));
#45511=CARTESIAN_POINT('Ctrl Pts',(103.374149075823,-4.30383826976654,133.184730170848));
#45512=CARTESIAN_POINT('Ctrl Pts',(103.366374741704,-4.23781037345589,133.304112216641));
#45513=CARTESIAN_POINT('Ctrl Pts',(103.358600407585,-4.16670690980976,133.420934000183));
#45514=CARTESIAN_POINT('Ctrl Pts',(103.350826073466,-4.09075117267524,133.534733834867));
#45515=CARTESIAN_POINT('Ctrl Pts',(103.343061320519,-4.01488904419838,133.648393421426));
#45516=CARTESIAN_POINT('Ctrl Pts',(103.335296567572,-3.9341867555989,133.759038147273));
#45517=CARTESIAN_POINT('Ctrl Pts',(103.327531814624,-3.84891369327921,133.86623038034));
#45518=CARTESIAN_POINT('Ctrl Pts',(103.319774773739,-3.76372532536722,133.973316148569));
#45519=CARTESIAN_POINT('Ctrl Pts',(103.312017732854,-3.67397545987754,134.076955944029));
#45520=CARTESIAN_POINT('Ctrl Pts',(103.304260691969,-3.57997682350484,134.176740935037));
#45521=CARTESIAN_POINT('Ctrl Pts',(103.296509500729,-3.48604907223497,134.276450677408));
#45522=CARTESIAN_POINT('Ctrl Pts',(103.288758309489,-3.38787919450686,134.372311117979));
#45523=CARTESIAN_POINT('Ctrl Pts',(103.281007118249,-3.28582001078081,134.463946648697));
#45524=CARTESIAN_POINT('Ctrl Pts',(103.273259221472,-3.18380420493035,134.55554323187));
#45525=CARTESIAN_POINT('Ctrl Pts',(103.265511324695,-3.07790267119138,134.642918216047));
#45526=CARTESIAN_POINT('Ctrl Pts',(103.257763427918,-2.96850472767904,134.725733176282));
#45527=CARTESIAN_POINT('Ctrl Pts',(103.250017151834,-2.85912966785807,134.808530813412));
#45528=CARTESIAN_POINT('Ctrl Pts',(103.242270875749,-2.74625996452902,134.886770088052));
#45529=CARTESIAN_POINT('Ctrl Pts',(103.234524599665,-2.63031730761799,134.960153432872));
#45530=CARTESIAN_POINT('Ctrl Pts',(103.2267782664,-2.51437379484491,135.03353731939));
#45531=CARTESIAN_POINT('Ctrl Pts',(103.219031933135,-2.39535761358128,135.10206499547));
#45532=CARTESIAN_POINT('Ctrl Pts',(103.211285599869,-2.27371832437165,135.165482955212));
#45533=CARTESIAN_POINT('Ctrl Pts',(103.203537531866,-2.15205179488608,135.228915116967));
#45534=CARTESIAN_POINT('Ctrl Pts',(103.195789463863,-2.02776133515433,135.287235104679));
#45535=CARTESIAN_POINT('Ctrl Pts',(103.18804139586,-1.90131955320651,135.34023616911));
#45536=CARTESIAN_POINT('Ctrl Pts',(103.180285093118,-1.77474338742851,135.393293563703));
#45537=CARTESIAN_POINT('Ctrl Pts',(103.172528790377,-1.64601169314672,135.441020591127));
#45538=CARTESIAN_POINT('Ctrl Pts',(103.164772487635,-1.51561595930304,135.483259133927));
#45539=CARTESIAN_POINT('Ctrl Pts',(103.15701204512,-1.38515062932988,135.525520220709));
#45540=CARTESIAN_POINT('Ctrl Pts',(103.149251602606,-1.25301986655555,135.562286881093));
#45541=CARTESIAN_POINT('Ctrl Pts',(103.141491160092,-1.11972767154515,135.593451659097));
#45542=CARTESIAN_POINT('Ctrl Pts',(103.133718259827,-0.986221504070382,
135.62466646557));
#45543=CARTESIAN_POINT('Ctrl Pts',(103.125945359561,-0.851550562937025,
135.650261346466));
#45544=CARTESIAN_POINT('Ctrl Pts',(103.118172459296,-0.716227222165132,
135.670180345909));
#45545=CARTESIAN_POINT('Ctrl Pts',(103.110682123534,-0.585823225691153,
135.689375239548));
#45546=CARTESIAN_POINT('Ctrl Pts',(103.103191787772,-0.454813745110329,
135.703299719881));
#45547=CARTESIAN_POINT('Ctrl Pts',(103.09570145201,-0.323657391158878,135.711949532262));
#45548=CARTESIAN_POINT('Ctrl Pts',(103.087927117891,-0.187528204181233,
135.720927304908));
#45549=CARTESIAN_POINT('Ctrl Pts',(103.080152783772,-0.0508095702230775,
135.724250974724));
#45550=CARTESIAN_POINT('Ctrl Pts',(103.072378449653,0.0859893849184933,
135.721858852256));
#45551=CARTESIAN_POINT('Ctrl Pts',(103.064613696706,0.222619747573554,135.719469677866));
#45552=CARTESIAN_POINT('Ctrl Pts',(103.056848943759,0.359329847301274,135.711378733828));
#45553=CARTESIAN_POINT('Ctrl Pts',(103.049084190812,0.495605881915482,135.697576111728));
#45554=CARTESIAN_POINT('Ctrl Pts',(103.041327149927,0.631746565251048,135.683787198587));
#45555=CARTESIAN_POINT('Ctrl Pts',(103.033570109042,0.767453654962441,135.664297935892));
#45556=CARTESIAN_POINT('Ctrl Pts',(103.025813068157,0.902214152959024,135.639150445956));
#45557=CARTESIAN_POINT('Ctrl Pts',(103.018061876916,1.03687302701615,135.614021919937));
#45558=CARTESIAN_POINT('Ctrl Pts',(103.010310685676,1.17058634742248,135.58324373114));
#45559=CARTESIAN_POINT('Ctrl Pts',(103.002559494436,1.30284739640677,135.54690969208));
#45560=CARTESIAN_POINT('Ctrl Pts',(102.994811597659,1.43505223091689,135.510591095957));
#45561=CARTESIAN_POINT('Ctrl Pts',(102.987063700882,1.56580564546732,135.468721449535));
#45562=CARTESIAN_POINT('Ctrl Pts',(102.979315804105,1.69461247761578,135.421445370222));
#45563=CARTESIAN_POINT('Ctrl Pts',(102.971569528021,1.82339236615171,135.374179180046));
#45564=CARTESIAN_POINT('Ctrl Pts',(102.963823251937,1.95022611540291,135.321508941043));
#45565=CARTESIAN_POINT('Ctrl Pts',(102.956076975853,2.07463543984101,135.26362859048));
#45566=CARTESIAN_POINT('Ctrl Pts',(102.948330642587,2.19904568264041,135.205747812657));
#45567=CARTESIAN_POINT('Ctrl Pts',(102.940584309322,2.32103111043598,135.14265701145));
#45568=CARTESIAN_POINT('Ctrl Pts',(102.932837976057,2.44013544307972,135.074597388745));
#45569=CARTESIAN_POINT('Ctrl Pts',(102.925089908054,2.55926644831302,135.006522524559));
#45570=CARTESIAN_POINT('Ctrl Pts',(102.917341840051,2.67551473513075,134.933476818601));
#45571=CARTESIAN_POINT('Ctrl Pts',(102.909593772048,2.78845090335968,134.85574613638));
#45572=CARTESIAN_POINT('Ctrl Pts',(102.901837469306,2.90150710149216,134.777932841064));
#45573=CARTESIAN_POINT('Ctrl Pts',(102.894081166564,3.01124382656967,134.695424844914));
#45574=CARTESIAN_POINT('Ctrl Pts',(102.886324863822,3.11726238812015,134.60855018515));
#45575=CARTESIAN_POINT('Ctrl Pts',(102.878564421308,3.22333753496915,134.521629157763));
#45576=CARTESIAN_POINT('Ctrl Pts',(102.870803978794,3.32569027238873,134.430337082917));
#45577=CARTESIAN_POINT('Ctrl Pts',(102.86304353628,3.42395777000255,134.335039907977));
#45578=CARTESIAN_POINT('Ctrl Pts',(102.855270636014,3.52238301532733,134.239589753553));
#45579=CARTESIAN_POINT('Ctrl Pts',(102.847497735749,3.61670964671316,134.140121935012));
#45580=CARTESIAN_POINT('Ctrl Pts',(102.839724835483,3.70661363622307,134.037037281612));
#45581=CARTESIAN_POINT('Ctrl Pts',(102.832234499721,3.7932493892609,133.937700015016));
#45582=CARTESIAN_POINT('Ctrl Pts',(102.824744163959,3.87577827326778,133.835004550364));
#45583=CARTESIAN_POINT('Ctrl Pts',(102.817253828197,3.95394881838397,133.729334430115));
#45584=CARTESIAN_POINT('Ctrl Pts',(102.809479494078,4.03508322347669,133.619657795142));
#45585=CARTESIAN_POINT('Ctrl Pts',(102.801705159959,4.11177928221597,133.50642906104));
#45586=CARTESIAN_POINT('Ctrl Pts',(102.79393082584,4.18370989859002,133.390043225107));
#45587=CARTESIAN_POINT('Ctrl Pts',(102.786166072892,4.25555186690805,133.273800824315));
#45588=CARTESIAN_POINT('Ctrl Pts',(102.778401319945,4.32263987477437,133.154409392698));
#45589=CARTESIAN_POINT('Ctrl Pts',(102.770636566998,4.38468786332751,133.032295850846));
#45590=CARTESIAN_POINT('Ctrl Pts',(102.762879526113,4.44667422494365,132.910303593885));
#45591=CARTESIAN_POINT('Ctrl Pts',(102.755122485228,4.50363035309214,132.785594953347));
#45592=CARTESIAN_POINT('Ctrl Pts',(102.747365444343,4.5553143984703,132.658624297194));
#45593=CARTESIAN_POINT('Ctrl Pts',(102.739614253103,4.60695946850756,132.531749390602));
#45594=CARTESIAN_POINT('Ctrl Pts',(102.731863061863,4.65334022239725,132.402616224343));
#45595=CARTESIAN_POINT('Ctrl Pts',(102.724111870623,4.69426169393441,132.271701822385));
#45596=CARTESIAN_POINT('Ctrl Pts',(102.716363973846,4.73516577275474,132.14084306254));
#45597=CARTESIAN_POINT('Ctrl Pts',(102.708616077069,4.77061506780431,132.008204945136));
#45598=CARTESIAN_POINT('Ctrl Pts',(102.700868180292,4.80046360240816,131.874282233599));
#45599=CARTESIAN_POINT('Ctrl Pts',(102.693121904208,4.83030589334202,131.740387535806));
#45600=CARTESIAN_POINT('Ctrl Pts',(102.685375628123,4.85454966912681,131.605209159719));
#45601=CARTESIAN_POINT('Ctrl Pts',(102.677629352039,4.87309956966692,131.469254328329));
#45602=CARTESIAN_POINT('Ctrl Pts',(102.669883018774,4.89164960713816,131.333298493351));
#45603=CARTESIAN_POINT('Ctrl Pts',(102.662136685509,4.90450563264091,131.196566579008));
#45604=CARTESIAN_POINT('Ctrl Pts',(102.654390352243,4.91162394558918,131.059572842224));
#45605=CARTESIAN_POINT('Ctrl Pts',(102.64664228424,4.91874385263427,130.922548426643));
#45606=CARTESIAN_POINT('Ctrl Pts',(102.638894216237,4.92012346999734,130.78526246231));
#45607=CARTESIAN_POINT('Ctrl Pts',(102.631146148234,4.91577120314387,130.648230733042));
#45608=CARTESIAN_POINT('Ctrl Pts',(102.623389845493,4.9114143106494,130.511053364822));
#45609=CARTESIAN_POINT('Ctrl Pts',(102.615633542751,4.90131337711345,130.37413116282));
#45610=CARTESIAN_POINT('Ctrl Pts',(102.607877240009,4.88552888760048,130.237976868751));
#45611=CARTESIAN_POINT('Ctrl Pts',(102.600116797495,4.86973597343017,130.101749905037));
#45612=CARTESIAN_POINT('Ctrl Pts',(102.59235635498,4.84825352001566,129.966292051878));
#45613=CARTESIAN_POINT('Ctrl Pts',(102.584595912466,4.82119329055999,129.832106372237));
#45614=CARTESIAN_POINT('Ctrl Pts',(102.576823012201,4.79408962162168,129.697705285832));
#45615=CARTESIAN_POINT('Ctrl Pts',(102.569050111935,4.76139037712837,129.56458083382));
#45616=CARTESIAN_POINT('Ctrl Pts',(102.56127721167,4.72325764107054,129.433222288086));
#45617=CARTESIAN_POINT('Ctrl Pts',(102.553786875908,4.68651112601932,129.306638956363));
#45618=CARTESIAN_POINT('Ctrl Pts',(102.546296540146,4.64471940080725,129.181695661791));
#45619=CARTESIAN_POINT('Ctrl Pts',(102.538806204384,4.59806922496722,129.058811287152));
#45620=CARTESIAN_POINT('Ctrl Pts',(102.531031870265,4.54965029353087,128.931267714098));
#45621=CARTESIAN_POINT('Ctrl Pts',(102.523257536146,4.49584384588066,128.805538251188));
#45622=CARTESIAN_POINT('Ctrl Pts',(102.515483202027,4.43680540104545,128.682111599247));
#45623=CARTESIAN_POINT('Ctrl Pts',(102.50771844908,4.3778397158172,128.558837059625));
#45624=CARTESIAN_POINT('Ctrl Pts',(102.499953696133,4.31365503002414,128.437860033489));
#45625=CARTESIAN_POINT('Ctrl Pts',(102.492188943186,4.24445590224847,128.31965195127));
#45626=CARTESIAN_POINT('Ctrl Pts',(102.484431902301,4.17532550402208,128.201561274984));
#45627=CARTESIAN_POINT('Ctrl Pts',(102.476674861416,4.10119077130081,128.086234404903));
#45628=CARTESIAN_POINT('Ctrl Pts',(102.468917820531,4.02230325126411,127.974120412677));
#45629=CARTESIAN_POINT('Ctrl Pts',(102.46116662929,3.94347522092014,127.862090966485));
#45630=CARTESIAN_POINT('Ctrl Pts',(102.45341543805,3.85990176129532,127.753269894051));
#45631=CARTESIAN_POINT('Ctrl Pts',(102.44566424681,3.77187882216869,127.64807906907));
#45632=CARTESIAN_POINT('Ctrl Pts',(102.437916350033,3.68389329513897,127.542932952996));
#45633=CARTESIAN_POINT('Ctrl Pts',(102.430168453256,3.59146230033177,127.441414314772));
#45634=CARTESIAN_POINT('Ctrl Pts',(102.422420556479,3.49492319227238,127.343913400425));
#45635=CARTESIAN_POINT('Ctrl Pts',(102.414674280395,3.39840427811325,127.246432881169));
#45636=CARTESIAN_POINT('Ctrl Pts',(102.406928004311,3.29777923486006,127.152968691791));
#45637=CARTESIAN_POINT('Ctrl Pts',(102.399181728227,3.19342325911923,127.063875227858));
#45638=CARTESIAN_POINT('Ctrl Pts',(102.391435394961,3.08906651304643,126.974781106258));
#45639=CARTESIAN_POINT('Ctrl Pts',(102.383689061696,2.98097907687159,126.890058028336));
#45640=CARTESIAN_POINT('Ctrl Pts',(102.375942728431,2.86956998827437,126.810020729062));
#45641=CARTESIAN_POINT('Ctrl Pts',(102.368194660428,2.75813595038452,126.72996550599));
#45642=CARTESIAN_POINT('Ctrl Pts',(102.360446592425,2.64337909733524,126.654598377711));
#45643=CARTESIAN_POINT('Ctrl Pts',(102.352698524422,2.5257379160186,126.584191066223));
#45644=CARTESIAN_POINT('Ctrl Pts',(102.34494222168,2.40797170425388,126.513708925005));
#45645=CARTESIAN_POINT('Ctrl Pts',(102.337185918938,2.28731537656628,126.448197331769));
#45646=CARTESIAN_POINT('Ctrl Pts',(102.329429616196,2.16423301073741,126.387882548138));
#45647=CARTESIAN_POINT('Ctrl Pts',(102.321669173682,2.04108495214395,126.327535572692));
#45648=CARTESIAN_POINT('Ctrl Pts',(102.313908731168,1.91550863310748,126.27239109079));
#45649=CARTESIAN_POINT('Ctrl Pts',(102.306148288654,1.78798770548679,126.222626990703));
#45650=CARTESIAN_POINT('Ctrl Pts',(102.298375388389,1.66026206995221,126.172783004865));
#45651=CARTESIAN_POINT('Ctrl Pts',(102.290602488123,1.53058595782255,126.12833678729));
#45652=CARTESIAN_POINT('Ctrl Pts',(102.282829587858,1.39945861774678,126.08941643553));
#45653=CARTESIAN_POINT('Ctrl Pts',(102.275339252096,1.27309808676921,126.051910936591));
#45654=CARTESIAN_POINT('Ctrl Pts',(102.267848916333,1.14539030616624,126.019536595987));
#45655=CARTESIAN_POINT('Ctrl Pts',(102.260358580571,1.01678864197639,125.992362704012));
#45656=CARTESIAN_POINT('Ctrl Pts',(102.252584246452,0.883311006604902,125.964158505664));
#45657=CARTESIAN_POINT('Ctrl Pts',(102.244809912333,0.748447549364895,125.941467548134));
#45658=CARTESIAN_POINT('Ctrl Pts',(102.237035578214,0.612693489935831,125.924423143593));
#45659=CARTESIAN_POINT('Ctrl Pts',(102.229270825267,0.477106735251679,125.907399744756));
#45660=CARTESIAN_POINT('Ctrl Pts',(102.22150607232,0.340631946446295,125.896009101064));
#45661=CARTESIAN_POINT('Ctrl Pts',(102.213741319372,0.203776320201726,125.89033393125));
#45662=CARTESIAN_POINT('Ctrl Pts',(102.205984278487,0.0670566208946548,
125.884664398095));
#45663=CARTESIAN_POINT('Ctrl Pts',(102.198227237602,-0.0700427750091018,
125.884699058044));
#45664=CARTESIAN_POINT('Ctrl Pts',(102.190470196717,-0.207008083417117,
125.890469011527));
#45665=CARTESIAN_POINT('Ctrl Pts',(102.182719005477,-0.343870105220161,
125.896234613843));
#45666=CARTESIAN_POINT('Ctrl Pts',(102.174967814237,-0.480597851755358,
125.907726884596));
#45667=CARTESIAN_POINT('Ctrl Pts',(102.167216622997,-0.616676420648657,
125.924924865892));
#45668=CARTESIAN_POINT('Ctrl Pts',(102.15946872622,-0.752697152520348,125.942115537587));
#45669=CARTESIAN_POINT('Ctrl Pts',(102.151720829443,-0.888068868461948,
125.965007047609));
#45670=CARTESIAN_POINT('Ctrl Pts',(102.143972932666,-1.02228089507594,125.993526507553));
#45671=CARTESIAN_POINT('Ctrl Pts',(102.136226656582,-1.15646484742743,126.022040001841));
#45672=CARTESIAN_POINT('Ctrl Pts',(102.128480380498,-1.28948921077608,126.056179023231));
#45673=CARTESIAN_POINT('Ctrl Pts',(102.120734104414,-1.42085301916542,126.095819467653));
#45674=CARTESIAN_POINT('Ctrl Pts',(102.112987771148,-1.55221779725219,126.135460204691));
#45675=CARTESIAN_POINT('Ctrl Pts',(102.105241437883,-1.68192162162514,126.180602332847));
#45676=CARTESIAN_POINT('Ctrl Pts',(102.097495104617,-1.80947860198397,126.231071839076));
#45677=CARTESIAN_POINT('Ctrl Pts',(102.089747036614,-1.93706414784448,126.281552647601));
#45678=CARTESIAN_POINT('Ctrl Pts',(102.081998968611,-2.06250152953885,126.337363064376));
#45679=CARTESIAN_POINT('Ctrl Pts',(102.074250900608,-2.18532512678099,126.398281050336));
#45680=CARTESIAN_POINT('Ctrl Pts',(102.066494597867,-2.30827926240373,126.459263780656));
#45681=CARTESIAN_POINT('Ctrl Pts',(102.058738295125,-2.42861371348762,126.525364749951));
#45682=CARTESIAN_POINT('Ctrl Pts',(102.050981992383,-2.54588727434374,126.596315816375));
#45683=CARTESIAN_POINT('Ctrl Pts',(102.043221549869,-2.66322342763066,126.667304751518));
#45684=CARTESIAN_POINT('Ctrl Pts',(102.035461107355,-2.77749510983936,126.743148725783));
#45685=CARTESIAN_POINT('Ctrl Pts',(102.02770066484,-2.88829123288586,126.823536982119));
#45686=CARTESIAN_POINT('Ctrl Pts',(102.019927764575,-2.99926521570494,126.90405428482));
#45687=CARTESIAN_POINT('Ctrl Pts',(102.012154864309,-3.10675218345438,126.989130204315));
#45688=CARTESIAN_POINT('Ctrl Pts',(102.004381964044,-3.21037450794547,127.078413948432));
#45689=CARTESIAN_POINT('Ctrl Pts',(101.996891628282,-3.31022989993145,127.164452003557));
#45690=CARTESIAN_POINT('Ctrl Pts',(101.98940129252,-3.40649652441835,127.254397054364));
#45691=CARTESIAN_POINT('Ctrl Pts',(101.981910956758,-3.4988710301033,127.34790512426));
#45692=CARTESIAN_POINT('Ctrl Pts',(101.974243153007,-3.5934341583345,127.443628674158));
#45693=CARTESIAN_POINT('Ctrl Pts',(101.966575349257,-3.68423567913244,127.543407681893));
#45694=CARTESIAN_POINT('Ctrl Pts',(101.958907545506,-3.77090036107563,127.646910138249));
#45695=CARTESIAN_POINT('Ctrl Pts',(101.951248733512,-3.85746341447274,127.750291221008));
#45696=CARTESIAN_POINT('Ctrl Pts',(101.943589921519,-3.93989901778072,127.857386766542));
#45697=CARTESIAN_POINT('Ctrl Pts',(101.935931109525,-4.01786747906985,127.967826820282));
#45698=CARTESIAN_POINT('Ctrl Pts',(101.928279510985,-4.09576250574849,128.078162856036));
#45699=CARTESIAN_POINT('Ctrl Pts',(101.920627912444,-4.16919852661075,128.191836809296));
#45700=CARTESIAN_POINT('Ctrl Pts',(101.912976313904,-4.23787535416553,128.308444844737));
#45701=CARTESIAN_POINT('Ctrl Pts',(101.905330520193,-4.30650008054961,128.424964416349));
#45702=CARTESIAN_POINT('Ctrl Pts',(101.897684726482,-4.3703725950023,128.544413295145));
#45703=CARTESIAN_POINT('Ctrl Pts',(101.890038932771,-4.42923573631129,128.666358312917));
#45704=CARTESIAN_POINT('Ctrl Pts',(101.882396487143,-4.48807310152065,128.788249931111));
#45705=CARTESIAN_POINT('Ctrl Pts',(101.874754041516,-4.54190528299562,128.912635151929));
#45706=CARTESIAN_POINT('Ctrl Pts',(101.867111595889,-4.59052103767788,129.039056206101));
#45707=CARTESIAN_POINT('Ctrl Pts',(101.8594699867,-4.63913147153866,129.165463423938));
#45708=CARTESIAN_POINT('Ctrl Pts',(101.851828377512,-4.68252646635379,129.29390565779));
#45709=CARTESIAN_POINT('Ctrl Pts',(101.844186768323,-4.7205430662157,129.42390553952));
#45710=CARTESIAN_POINT('Ctrl Pts',(101.841093834229,-4.73593024906338,129.476522868729));
#45711=CARTESIAN_POINT('Ctrl Pts',(101.838000900136,-4.75043689666253,129.529395180487));
#45712=CARTESIAN_POINT('Ctrl Pts',(101.834907966042,-4.76405452823403,129.582490119308));
#45713=CARTESIAN_POINT('Ctrl Pts',(103.584579145176,-4.76405452823405,129.582490119308));
#45714=CARTESIAN_POINT('Ctrl Pts',(103.576426818607,-4.79981914816621,129.72193582962));
#45715=CARTESIAN_POINT('Ctrl Pts',(103.568274492038,-4.82949477661317,129.863099609191));
#45716=CARTESIAN_POINT('Ctrl Pts',(103.56012216547,-4.85292737657309,130.005437004066));
#45717=CARTESIAN_POINT('Ctrl Pts',(103.551985756864,-4.87631422281494,130.147496475662));
#45718=CARTESIAN_POINT('Ctrl Pts',(103.543849348258,-4.893482295562,130.290724669727));
#45719=CARTESIAN_POINT('Ctrl Pts',(103.535712939652,-4.90432814903514,130.434565445773));
#45720=CARTESIAN_POINT('Ctrl Pts',(103.528761771776,-4.91359407358562,130.557452757631));
#45721=CARTESIAN_POINT('Ctrl Pts',(103.521810603899,-4.91824634039976,130.680786823101));
#45722=CARTESIAN_POINT('Ctrl Pts',(103.514859436023,-4.91824999784073,130.804214879153));
#45723=CARTESIAN_POINT('',(103.860140563968,-4.91824815621127,130.800101929457));
#45724=CARTESIAN_POINT('Ctrl Pts',(103.930161944428,-4.76405452823404,129.582490119308));
#45725=CARTESIAN_POINT('Ctrl Pts',(103.923926405382,-4.79130314982063,129.688732081319));
#45726=CARTESIAN_POINT('Ctrl Pts',(103.917690866335,-4.81496624846374,129.795769395495));
#45727=CARTESIAN_POINT('Ctrl Pts',(103.911455327289,-4.8350123008557,129.903339467385));
#45728=CARTESIAN_POINT('Ctrl Pts',(103.899799266646,-4.87248428212411,130.104419642177));
#45729=CARTESIAN_POINT('Ctrl Pts',(103.888143206003,-4.89742086526062,130.3079032426));
#45730=CARTESIAN_POINT('Ctrl Pts',(103.876487145359,-4.9095839965138,130.512524972595));
#45731=CARTESIAN_POINT('Ctrl Pts',(103.871038284909,-4.91526989733962,130.608179523988));
#45732=CARTESIAN_POINT('Ctrl Pts',(103.865589424458,-4.91816501337355,130.70408244416));
#45733=CARTESIAN_POINT('Ctrl Pts',(103.860140564008,-4.91824815621066,130.800101928748));
#45734=CARTESIAN_POINT('Ctrl Pts',(103.860140563968,-4.91824815621127,130.800101929457));
#45735=CARTESIAN_POINT('Ctrl Pts',(103.85249393019,-4.91836483431793,130.934850440796));
#45736=CARTESIAN_POINT('Ctrl Pts',(103.844847296412,-4.91293966118262,131.069789198067));
#45737=CARTESIAN_POINT('Ctrl Pts',(103.837200662635,-4.90195245746252,131.204417072678));
#45738=CARTESIAN_POINT('Ctrl Pts',(103.829560842582,-4.89097504416677,131.338924983735));
#45739=CARTESIAN_POINT('Ctrl Pts',(103.82192102253,-4.87444549097799,131.473122163232));
#45740=CARTESIAN_POINT('Ctrl Pts',(103.814281202478,-4.85239567383066,131.606507291865));
#45741=CARTESIAN_POINT('Ctrl Pts',(103.806645871143,-4.83035881188223,131.739814051102));
#45742=CARTESIAN_POINT('Ctrl Pts',(103.799010539807,-4.80280820171784,131.872309311373));
#45743=CARTESIAN_POINT('Ctrl Pts',(103.791375208472,-4.7698275283597,132.003497145323));
#45744=CARTESIAN_POINT('Ctrl Pts',(103.783742189454,-4.73685684301134,132.134645249783));
#45745=CARTESIAN_POINT('Ctrl Pts',(103.776109170435,-4.69845946167205,132.264486324024));
#45746=CARTESIAN_POINT('Ctrl Pts',(103.768476151417,-4.65477002326167,132.392535385356));
#45747=CARTESIAN_POINT('Ctrl Pts',(103.76084367754,-4.61108370510527,132.520575301557));
#45748=CARTESIAN_POINT('Ctrl Pts',(103.753211203664,-4.56210621177099,132.646823077398));
#45749=CARTESIAN_POINT('Ctrl Pts',(103.745578729788,-4.50802164934403,132.770810177444));
#45750=CARTESIAN_POINT('Ctrl Pts',(103.737945034529,-4.45392843206285,132.894817118462));
#45751=CARTESIAN_POINT('Ctrl Pts',(103.73031133927,-4.39472668245777,133.016562294646));
#45752=CARTESIAN_POINT('Ctrl Pts',(103.722677644011,-4.33064787817129,133.135598918939));
#45753=CARTESIAN_POINT('Ctrl Pts',(103.715036335704,-4.2665051684046,133.25475425788));
#45754=CARTESIAN_POINT('Ctrl Pts',(103.707395027398,-4.19747588163011,133.371195294228));
#45755=CARTESIAN_POINT('Ctrl Pts',(103.699753719092,-4.12383670458569,133.484501266191));
#45756=CARTESIAN_POINT('Ctrl Pts',(103.6921085634,-4.05016045033656,133.597864287525));
#45757=CARTESIAN_POINT('Ctrl Pts',(103.684463407707,-3.97186991796053,133.70808877289));
#45758=CARTESIAN_POINT('Ctrl Pts',(103.676818252015,-3.88928324582296,133.814785653381));
#45759=CARTESIAN_POINT('Ctrl Pts',(103.669161105421,-3.80656704216425,133.921649880598));
#45760=CARTESIAN_POINT('Ctrl Pts',(103.661503958827,-3.71954149868936,134.024975142375));
#45761=CARTESIAN_POINT('Ctrl Pts',(103.653846812233,-3.62856333795136,134.12440747943));
#45762=CARTESIAN_POINT('Ctrl Pts',(103.646900442648,-3.54603025321083,134.214609978948));
#45763=CARTESIAN_POINT('Ctrl Pts',(103.639954073062,-3.4602449279693,134.301609058963));
#45764=CARTESIAN_POINT('Ctrl Pts',(103.633007703477,-3.37149686224685,134.385169460601));
#45765=CARTESIAN_POINT('Ctrl Pts',(103.625233369358,-3.27217057290244,134.478689748207));
#45766=CARTESIAN_POINT('Ctrl Pts',(103.617459035238,-3.16879283925618,134.568222288876));
#45767=CARTESIAN_POINT('Ctrl Pts',(103.609684701119,-3.06171726098981,134.653395623416));
#45768=CARTESIAN_POINT('Ctrl Pts',(103.601919948172,-2.9547736438041,134.738463989433));
#45769=CARTESIAN_POINT('Ctrl Pts',(103.594155195225,-2.84414155262642,134.819183597613));
#45770=CARTESIAN_POINT('Ctrl Pts',(103.586390442278,-2.73021113383673,134.895219968262));
#45771=CARTESIAN_POINT('Ctrl Pts',(103.578633401393,-2.61639387234488,134.971180818516));
#45772=CARTESIAN_POINT('Ctrl Pts',(103.570876360508,-2.49928512560967,135.042467472221));
#45773=CARTESIAN_POINT('Ctrl Pts',(103.563119319623,-2.37930751680441,135.108786108033));
#45774=CARTESIAN_POINT('Ctrl Pts',(103.555368128383,-2.25942038404725,135.175054732445));
#45775=CARTESIAN_POINT('Ctrl Pts',(103.547616937143,-2.13666903618474,135.236362607613));
#45776=CARTESIAN_POINT('Ctrl Pts',(103.539865745903,-2.01150413112362,135.292459791267));
#45777=CARTESIAN_POINT('Ctrl Pts',(103.532117849126,-1.88639242448628,135.348533132121));
#45778=CARTESIAN_POINT('Ctrl Pts',(103.524369952349,-1.75886955696481,135.39940002673));
#45779=CARTESIAN_POINT('Ctrl Pts',(103.516622055572,-1.6294095878515,135.444857084273));
#45780=CARTESIAN_POINT('Ctrl Pts',(103.508875779487,-1.49997669897281,135.490304633179));
#45781=CARTESIAN_POINT('Ctrl Pts',(103.501129503403,-1.36860788311919,135.530344466433));
#45782=CARTESIAN_POINT('Ctrl Pts',(103.493383227319,-1.23579555019815,135.564821983926));
#45783=CARTESIAN_POINT('Ctrl Pts',(103.485636894054,-1.10298223688664,135.599299755925));
#45784=CARTESIAN_POINT('Ctrl Pts',(103.477890560789,-0.968725763667167,
135.628215031995));
#45785=CARTESIAN_POINT('Ctrl Pts',(103.470144227523,-0.833531626586319,
135.651463679187));
#45786=CARTESIAN_POINT('Ctrl Pts',(103.46239615952,-0.698307213715842,135.674717532753));
#45787=CARTESIAN_POINT('Ctrl Pts',(103.454648091517,-0.562145104377292,
135.692302166028));
#45788=CARTESIAN_POINT('Ctrl Pts',(103.446900023514,-0.425558465003698,
135.704165007066));
#45789=CARTESIAN_POINT('Ctrl Pts',(103.439143720772,-0.288826659724283,
135.716040456073));
#45790=CARTESIAN_POINT('Ctrl Pts',(103.431387418031,-0.151669813218047,
135.722181931132));
#45791=CARTESIAN_POINT('Ctrl Pts',(103.423631115289,-0.0146042221654386,
135.722588934673));
#45792=CARTESIAN_POINT('Ctrl Pts',(103.415870672775,0.122534524920174,135.722996155445));
#45793=CARTESIAN_POINT('Ctrl Pts',(103.40811023026,0.259581529023418,135.717662821271));
#45794=CARTESIAN_POINT('Ctrl Pts',(103.400349787746,0.396024048075988,135.706640496953));
#45795=CARTESIAN_POINT('Ctrl Pts',(103.392576887481,0.532685596772845,135.695600478622));
#45796=CARTESIAN_POINT('Ctrl Pts',(103.384803987215,0.668740333044529,135.678853268351));
#45797=CARTESIAN_POINT('Ctrl Pts',(103.37703108695,0.803683266047643,135.656502028363));
#45798=CARTESIAN_POINT('Ctrl Pts',(103.369540751188,0.933720683534809,135.634963312249));
#45799=CARTESIAN_POINT('Ctrl Pts',(103.362050415426,1.06272542645402,135.608220996356));
#45800=CARTESIAN_POINT('Ctrl Pts',(103.354560079664,1.19025948598856,135.576411059306));
#45801=CARTESIAN_POINT('Ctrl Pts',(103.346785745545,1.32262903815395,135.543395038825));
#45802=CARTESIAN_POINT('Ctrl Pts',(103.339011411426,1.45383349048909,135.504814948884));
#45803=CARTESIAN_POINT('Ctrl Pts',(103.331237077307,1.58336919459099,135.460767500144));
#45804=CARTESIAN_POINT('Ctrl Pts',(103.32347232436,1.71274525751454,135.416774335948));
#45805=CARTESIAN_POINT('Ctrl Pts',(103.315707571413,1.84045629759499,135.367327344283));
#45806=CARTESIAN_POINT('Ctrl Pts',(103.307942818465,1.96601002394501,135.312573971906));
#45807=CARTESIAN_POINT('Ctrl Pts',(103.30018577758,2.09143904856393,135.25787498135));
#45808=CARTESIAN_POINT('Ctrl Pts',(103.292428736695,2.21471466741992,135.197880253631));
#45809=CARTESIAN_POINT('Ctrl Pts',(103.28467169581,2.33536124214426,135.132786535979));
#45810=CARTESIAN_POINT('Ctrl Pts',(103.27692050457,2.45591683634859,135.067741906006));
#45811=CARTESIAN_POINT('Ctrl Pts',(103.26916931333,2.57384698994551,134.997606124607));
#45812=CARTESIAN_POINT('Ctrl Pts',(103.26141812209,2.68869782781654,134.922623243139));
#45813=CARTESIAN_POINT('Ctrl Pts',(103.253670225313,2.80349985101726,134.847672231397));
#45814=CARTESIAN_POINT('Ctrl Pts',(103.245922328536,2.91522483489166,134.767878430345));
#45815=CARTESIAN_POINT('Ctrl Pts',(103.238174431759,3.02344542035482,134.683530741785));
#45816=CARTESIAN_POINT('Ctrl Pts',(103.230428155675,3.13164336840455,134.599200696944));
#45817=CARTESIAN_POINT('Ctrl Pts',(103.222681879591,3.23633806793841,134.510318899509));
#45818=CARTESIAN_POINT('Ctrl Pts',(103.214935603506,3.33713328992503,134.417216062747));
#45819=CARTESIAN_POINT('Ctrl Pts',(103.207189270241,3.43792925595908,134.324112538721));
#45820=CARTESIAN_POINT('Ctrl Pts',(103.199442936976,3.53482539981158,134.226788178471));
#45821=CARTESIAN_POINT('Ctrl Pts',(103.19169660371,3.62746087852322,134.125611983736));
#45822=CARTESIAN_POINT('Ctrl Pts',(103.183948535707,3.72011710230821,134.024413131292));
#45823=CARTESIAN_POINT('Ctrl Pts',(103.176200467704,3.80851049834654,133.919361016208));
#45824=CARTESIAN_POINT('Ctrl Pts',(103.168452399701,3.89231945738096,133.810858963515));
#45825=CARTESIAN_POINT('Ctrl Pts',(103.16069609696,3.97621748957416,133.70224159355));
#45826=CARTESIAN_POINT('Ctrl Pts',(103.152939794218,4.05552111225531,133.590167271384));
#45827=CARTESIAN_POINT('Ctrl Pts',(103.145183491476,4.12995083583871,133.475070103088));
#45828=CARTESIAN_POINT('Ctrl Pts',(103.137423048962,4.20442028480668,133.359911503967));
#45829=CARTESIAN_POINT('Ctrl Pts',(103.129662606447,4.27401045299499,133.241727180648));
#45830=CARTESIAN_POINT('Ctrl Pts',(103.121902163933,4.33848757372001,133.120976389587));
#45831=CARTESIAN_POINT('Ctrl Pts',(103.114129263668,4.40306819884322,133.000031758637));
#45832=CARTESIAN_POINT('Ctrl Pts',(103.106356363402,4.46251920481258,132.876512779516));
#45833=CARTESIAN_POINT('Ctrl Pts',(103.098583463137,4.51665442504361,132.750900077026));
#45834=CARTESIAN_POINT('Ctrl Pts',(103.091093127375,4.56882169366067,132.629853712671));
#45835=CARTESIAN_POINT('Ctrl Pts',(103.083602791613,4.61605284058172,132.506863493891));
#45836=CARTESIAN_POINT('Ctrl Pts',(103.076112455851,4.65822551400895,132.382371429676));
#45837=CARTESIAN_POINT('Ctrl Pts',(103.068338121732,4.70199717716743,132.253159211008));
#45838=CARTESIAN_POINT('Ctrl Pts',(103.060563787613,4.74045786618925,132.121919708371));
#45839=CARTESIAN_POINT('Ctrl Pts',(103.052789453494,4.77341671222796,131.989128929905));
#45840=CARTESIAN_POINT('Ctrl Pts',(103.045024700547,4.80633493943454,131.856501804206));
#45841=CARTESIAN_POINT('Ctrl Pts',(103.0372599476,4.83376472161489,131.722327582417));
#45842=CARTESIAN_POINT('Ctrl Pts',(103.029495194652,4.85556401464997,131.587100141377));
#45843=CARTESIAN_POINT('Ctrl Pts',(103.021738153767,4.87734165631981,131.452007010138));
#45844=CARTESIAN_POINT('Ctrl Pts',(103.013981112883,4.89349987591688,131.315863124864));
#45845=CARTESIAN_POINT('Ctrl Pts',(103.006224071998,4.90394710830169,131.179175000267));
#45846=CARTESIAN_POINT('Ctrl Pts',(102.998472880757,4.91438646234729,131.042589953248));
#45847=CARTESIAN_POINT('Ctrl Pts',(102.990721689517,4.91912337173111,130.905461872065));
#45848=CARTESIAN_POINT('Ctrl Pts',(102.982970498277,4.91811783318378,130.768304530429));
#45849=CARTESIAN_POINT('Ctrl Pts',(102.9752226015,4.91711272201716,130.631205484321));
#45850=CARTESIAN_POINT('Ctrl Pts',(102.967474704723,4.91037002013292,130.494077592631));
#45851=CARTESIAN_POINT('Ctrl Pts',(102.959726807946,4.89790179077492,130.357436563141));
#45852=CARTESIAN_POINT('Ctrl Pts',(102.951980531862,4.88543616950173,130.220824116009));
#45853=CARTESIAN_POINT('Ctrl Pts',(102.944234255778,4.86724743846475,130.084698717611));
#45854=CARTESIAN_POINT('Ctrl Pts',(102.936487979694,4.84339966463173,129.949572485252));
#45855=CARTESIAN_POINT('Ctrl Pts',(102.928741646428,4.81955171475988,129.814445255421));
#45856=CARTESIAN_POINT('Ctrl Pts',(102.920995313163,4.79004470668492,129.680317591362));
#45857=CARTESIAN_POINT('Ctrl Pts',(102.913248979898,4.75499404758626,129.547692534929));
#45858=CARTESIAN_POINT('Ctrl Pts',(102.905500911895,4.71993553913543,129.415037778033));
#45859=CARTESIAN_POINT('Ctrl Pts',(102.897752843892,4.67933100917168,129.283886676271));
#45860=CARTESIAN_POINT('Ctrl Pts',(102.890004775889,4.63334594880947,129.154727815652));
#45861=CARTESIAN_POINT('Ctrl Pts',(102.882248473147,4.58731201497794,129.025431683459));
#45862=CARTESIAN_POINT('Ctrl Pts',(102.874492170405,4.53588625878769,128.898132391004));
#45863=CARTESIAN_POINT('Ctrl Pts',(102.866735867663,4.47928283502318,128.773299725725));
#45864=CARTESIAN_POINT('Ctrl Pts',(102.858975425149,4.42264920030707,128.648400433494));
#45865=CARTESIAN_POINT('Ctrl Pts',(102.851214982635,4.3608325676844,128.525970740534));
#45866=CARTESIAN_POINT('Ctrl Pts',(102.843454540121,4.29409296601832,128.406455560711));
#45867=CARTESIAN_POINT('Ctrl Pts',(102.835681639855,4.22724622801887,128.286748524511));
#45868=CARTESIAN_POINT('Ctrl Pts',(102.82790873959,4.15546093354346,128.169965684115));
#45869=CARTESIAN_POINT('Ctrl Pts',(102.820135839324,4.07904081826292,128.056523456189));
#45870=CARTESIAN_POINT('Ctrl Pts',(102.812645503562,4.00539876666256,127.94720513899));
#45871=CARTESIAN_POINT('Ctrl Pts',(102.8051551678,3.92745320093368,127.840989019974));
#45872=CARTESIAN_POINT('Ctrl Pts',(102.797664832038,3.84550986162237,127.738216953831));
#45873=CARTESIAN_POINT('Ctrl Pts',(102.789890497919,3.76045961569588,127.631548253563));
#45874=CARTESIAN_POINT('Ctrl Pts',(102.7821161638,3.67083304710242,127.528252029747));
#45875=CARTESIAN_POINT('Ctrl Pts',(102.774341829681,3.57692746569745,127.428746159776));
#45876=CARTESIAN_POINT('Ctrl Pts',(102.766577076734,3.48313761452899,127.329362921897));
#45877=CARTESIAN_POINT('Ctrl Pts',(102.758812323787,3.38507950900481,127.233761025032));
#45878=CARTESIAN_POINT('Ctrl Pts',(102.751047570839,3.28309188338035,127.142326927418));
#45879=CARTESIAN_POINT('Ctrl Pts',(102.743290529954,3.18120555330349,127.050983643438));
#45880=CARTESIAN_POINT('Ctrl Pts',(102.735533489069,3.07539775920484,126.963800180176));
#45881=CARTESIAN_POINT('Ctrl Pts',(102.727776448184,2.96604515306411,126.881127357551));
#45882=CARTESIAN_POINT('Ctrl Pts',(102.720025256944,2.85677501057386,126.798516879145));
#45883=CARTESIAN_POINT('Ctrl Pts',(102.712274065704,2.74396568743165,126.720410505705));
#45884=CARTESIAN_POINT('Ctrl Pts',(102.704522874464,2.62802781326745,126.647119600354));
#45885=CARTESIAN_POINT('Ctrl Pts',(102.696774977687,2.51213921579291,126.573859845593));
#45886=CARTESIAN_POINT('Ctrl Pts',(102.68902708091,2.39312504178207,126.505411696658));
#45887=CARTESIAN_POINT('Ctrl Pts',(102.681279184133,2.27142569127575,126.442043757053));
#45888=CARTESIAN_POINT('Ctrl Pts',(102.673532908049,2.14975179765018,126.378689072656));
#45889=CARTESIAN_POINT('Ctrl Pts',(102.665786631964,2.02539419129638,126.320412664328));
#45890=CARTESIAN_POINT('Ctrl Pts',(102.65804035588,1.89881836076769,126.267437442626));
#45891=CARTESIAN_POINT('Ctrl Pts',(102.650294022615,1.77224159588514,126.214461829873));
#45892=CARTESIAN_POINT('Ctrl Pts',(102.64254768935,1.64344693480621,126.166787632774));
#45893=CARTESIAN_POINT('Ctrl Pts',(102.634801356084,1.51291998128912,126.124589662411));
#45894=CARTESIAN_POINT('Ctrl Pts',(102.627053288081,1.38236379716589,126.082382242104));
#45895=CARTESIAN_POINT('Ctrl Pts',(102.619305220078,1.25007492059564,126.045653609097));
#45896=CARTESIAN_POINT('Ctrl Pts',(102.611557152075,1.11655386481506,126.0145286237));
#45897=CARTESIAN_POINT('Ctrl Pts',(102.603800849334,0.982890901267192,125.983370558297));
#45898=CARTESIAN_POINT('Ctrl Pts',(102.596044546592,0.847993523856434,125.957828126403));
#45899=CARTESIAN_POINT('Ctrl Pts',(102.58828824385,0.712372733952538,125.937975085118));
#45900=CARTESIAN_POINT('Ctrl Pts',(102.580527801336,0.576679559149422,125.918111447667));
#45901=CARTESIAN_POINT('Ctrl Pts',(102.572767358822,0.440262591185438,125.903943291874));
#45902=CARTESIAN_POINT('Ctrl Pts',(102.565006916307,0.303636700648433,125.895492334905));
#45903=CARTESIAN_POINT('Ctrl Pts',(102.557234016042,0.166791486102861,125.887027811709));
#45904=CARTESIAN_POINT('Ctrl Pts',(102.549461115776,0.0297370698987304,
125.884298835203));
#45905=CARTESIAN_POINT('Ctrl Pts',(102.541688215511,-0.107012028281012,
125.887274947344));
#45906=CARTESIAN_POINT('Ctrl Pts',(102.534197879749,-0.23878995229145,125.890142870312));
#45907=CARTESIAN_POINT('Ctrl Pts',(102.526707543987,-0.370284063617012,
125.898308275492));
#45908=CARTESIAN_POINT('Ctrl Pts',(102.519217208225,-0.50104148999333,125.911698715513));
#45909=CARTESIAN_POINT('Ctrl Pts',(102.511442874106,-0.636756623933761,
125.925596858136));
#45910=CARTESIAN_POINT('Ctrl Pts',(102.503668539987,-0.772108012106316,
125.945168096527));
#45911=CARTESIAN_POINT('Ctrl Pts',(102.495894205868,-0.906583379186386,
125.970388168422));
#45912=CARTESIAN_POINT('Ctrl Pts',(102.488129452921,-1.04089301739485,125.995577158832));
#45913=CARTESIAN_POINT('Ctrl Pts',(102.480364699974,-1.17432840205142,126.026401059698));
#45914=CARTESIAN_POINT('Ctrl Pts',(102.472599947026,-1.30638130075887,126.062783774413));
#45915=CARTESIAN_POINT('Ctrl Pts',(102.464842906141,-1.43830304266579,126.099130353302));
#45916=CARTESIAN_POINT('Ctrl Pts',(102.457085865256,-1.56884465668163,126.141024655642));
#45917=CARTESIAN_POINT('Ctrl Pts',(102.449328824371,-1.69750739847636,126.188339420191));
#45918=CARTESIAN_POINT('Ctrl Pts',(102.441577633131,-1.82607311469665,126.235618504307));
#45919=CARTESIAN_POINT('Ctrl Pts',(102.433826441891,-1.95276241343844,126.288309780094));
#45920=CARTESIAN_POINT('Ctrl Pts',(102.426075250651,-2.07709138074198,126.346236072587));
#45921=CARTESIAN_POINT('Ctrl Pts',(102.418327353874,-2.20136750491775,126.40413774486));
#45922=CARTESIAN_POINT('Ctrl Pts',(102.410579457097,-2.32328493930456,126.467269843673));
#45923=CARTESIAN_POINT('Ctrl Pts',(102.40283156032,-2.44237965318738,126.535407034755));
#45924=CARTESIAN_POINT('Ctrl Pts',(102.395085284236,-2.56144945502352,126.603529973005));
#45925=CARTESIAN_POINT('Ctrl Pts',(102.387339008152,-2.67769737166177,126.676655727039));
#45926=CARTESIAN_POINT('Ctrl Pts',(102.379592732068,-2.79068425420331,126.754513156754));
#45927=CARTESIAN_POINT('Ctrl Pts',(102.371846398802,-2.90367197078797,126.832371161196));
#45928=CARTESIAN_POINT('Ctrl Pts',(102.364100065537,-3.01339828330809,126.914960689177));
#45929=CARTESIAN_POINT('Ctrl Pts',(102.356353732272,-3.11945363755738,127.001967678162));
#45930=CARTESIAN_POINT('Ctrl Pts',(102.348605664269,-3.22553274216849,127.088994151759));
#45931=CARTESIAN_POINT('Ctrl Pts',(102.340857596266,-3.32793895044865,127.180439806947));
#45932=CARTESIAN_POINT('Ctrl Pts',(102.333109528263,-3.42629667425205,127.275951037811));
#45933=CARTESIAN_POINT('Ctrl Pts',(102.325353225521,-3.52475893381458,127.371563779147));
#45934=CARTESIAN_POINT('Ctrl Pts',(102.317596922779,-3.61916383270866,127.471250454908));
#45935=CARTESIAN_POINT('Ctrl Pts',(102.309840620037,-3.70917310827423,127.574621012682));
#45936=CARTESIAN_POINT('Ctrl Pts',(102.302080177523,-3.79923042450018,127.678046742436));
#45937=CARTESIAN_POINT('Ctrl Pts',(102.294319735009,-3.88488719858575,127.78515996683));
#45938=CARTESIAN_POINT('Ctrl Pts',(102.286559292495,-3.96584685913581,127.895539249317));
#45939=CARTESIAN_POINT('Ctrl Pts',(102.278786392229,-4.04693648332046,128.006095722427));
#45940=CARTESIAN_POINT('Ctrl Pts',(102.271013491964,-4.12331370824213,128.119928405902));
#45941=CARTESIAN_POINT('Ctrl Pts',(102.263240591698,-4.19472604865866,128.236587956444));
#45942=CARTESIAN_POINT('Ctrl Pts',(102.255750255936,-4.26354237062437,128.349006638477));
#45943=CARTESIAN_POINT('Ctrl Pts',(102.248259920174,-4.32774836308428,128.464049959393));
#45944=CARTESIAN_POINT('Ctrl Pts',(102.240769584412,-4.38716018954261,128.581297745357));
#45945=CARTESIAN_POINT('Ctrl Pts',(102.232471443257,-4.45297936479825,128.711190277413));
#45946=CARTESIAN_POINT('Ctrl Pts',(102.224173302102,-4.51310129049722,128.844156401856));
#45947=CARTESIAN_POINT('Ctrl Pts',(102.215875160946,-4.56724797383606,128.979688316031));
#45948=CARTESIAN_POINT('Ctrl Pts',(102.207597026909,-4.62126410756482,129.114893457863));
#45949=CARTESIAN_POINT('Ctrl Pts',(102.199318892872,-4.66933361053416,129.252651766697));
#45950=CARTESIAN_POINT('Ctrl Pts',(102.191040758835,-4.71122522047061,129.392432862863));
#45951=CARTESIAN_POINT('Ctrl Pts',(102.187312190147,-4.73009369305051,129.455391908461));
#45952=CARTESIAN_POINT('Ctrl Pts',(102.183583621459,-4.74770947080646,129.518760988469));
#45953=CARTESIAN_POINT('Ctrl Pts',(102.179855052771,-4.76405452823403,129.582490119308));
#45954=CARTESIAN_POINT('Origin',(213.235140564004,0.,130.804360617566));
#45955=CARTESIAN_POINT('',(100.084952068471,-4.76405452823407,129.582490119308));
#45956=CARTESIAN_POINT('',(100.43015599918,-4.76405452823403,129.582490119308));
#45957=CARTESIAN_POINT('',(213.235140564004,-4.76405452823405,129.582490119308));
#45958=CARTESIAN_POINT('',(101.764859436032,-4.91824793163316,130.808871214655));
#45959=CARTESIAN_POINT('Ctrl Pts',(101.764859435991,-4.91824793163249,130.808871215387));
#45960=CARTESIAN_POINT('Ctrl Pts',(101.754213180585,-4.91807564840936,130.996724719397));
#45961=CARTESIAN_POINT('Ctrl Pts',(101.74356692518,-4.90713724480048,131.184104547583));
#45962=CARTESIAN_POINT('Ctrl Pts',(101.732920669774,-4.88561573720794,131.369994713821));
#45963=CARTESIAN_POINT('Ctrl Pts',(101.723101557498,-4.86576630739908,131.541442452369));
#45964=CARTESIAN_POINT('Ctrl Pts',(101.713282445222,-4.83691494772115,131.711623822433));
#45965=CARTESIAN_POINT('Ctrl Pts',(101.703463332945,-4.79923915487164,131.879761285618));
#45966=CARTESIAN_POINT('Ctrl Pts',(101.695688998826,-4.76940914645777,132.012885012079));
#45967=CARTESIAN_POINT('Ctrl Pts',(101.687914664707,-4.73398871171512,132.144977496555));
#45968=CARTESIAN_POINT('Ctrl Pts',(101.680140330588,-4.69306244728092,132.275532914893));
#45969=CARTESIAN_POINT('Ctrl Pts',(101.672375577641,-4.65218662081001,132.405927435345));
#45970=CARTESIAN_POINT('Ctrl Pts',(101.664610824694,-4.60581858148159,132.53478828926));
#45971=CARTESIAN_POINT('Ctrl Pts',(101.656846071747,-4.55409391996521,132.661619789205));
#45972=CARTESIAN_POINT('Ctrl Pts',(101.649089030862,-4.5024206321118,132.788325318315));
#45973=CARTESIAN_POINT('Ctrl Pts',(101.641331989977,-4.4454014563364,132.91300514488));
#45974=CARTESIAN_POINT('Ctrl Pts',(101.633574949092,-4.38322166920146,133.035179046113));
#45975=CARTESIAN_POINT('Ctrl Pts',(101.625823757852,-4.32108877232769,133.157260815055));
#45976=CARTESIAN_POINT('Ctrl Pts',(101.618072566612,-4.25380318681832,133.276840073049));
#45977=CARTESIAN_POINT('Ctrl Pts',(101.610321375372,-4.18159800199837,133.393457219121));
#45978=CARTESIAN_POINT('Ctrl Pts',(101.602573478595,-4.10942350630805,133.510024799795));
#45979=CARTESIAN_POINT('Ctrl Pts',(101.594825581818,-4.03233377545255,133.623632440844));
#45980=CARTESIAN_POINT('Ctrl Pts',(101.58707768504,-3.95060737259751,133.733845973406));
#45981=CARTESIAN_POINT('Ctrl Pts',(101.579331408956,-3.86889806514414,133.844036451672));
#45982=CARTESIAN_POINT('Ctrl Pts',(101.571585132872,-3.78255424758454,133.950833919784));
#45983=CARTESIAN_POINT('Ctrl Pts',(101.563838856788,-3.69189702954403,134.053834326606));
#45984=CARTESIAN_POINT('Ctrl Pts',(101.556092523523,-3.60123914229259,134.156835493754));
#45985=CARTESIAN_POINT('Ctrl Pts',(101.548346190257,-3.50626804933434,134.256039250205));
#45986=CARTESIAN_POINT('Ctrl Pts',(101.540599856992,-3.40734398690799,134.351076001887));
#45987=CARTESIAN_POINT('Ctrl Pts',(101.532851788989,-3.3083977711239,134.446134036392));
#45988=CARTESIAN_POINT('Ctrl Pts',(101.525103720986,-3.20549710623059,134.537022938417));
#45989=CARTESIAN_POINT('Ctrl Pts',(101.517355652983,-3.09903748337889,134.623411512633));
#45990=CARTESIAN_POINT('Ctrl Pts',(101.509599350241,-2.99246471397299,134.709891901654));
#45991=CARTESIAN_POINT('Ctrl Pts',(101.5018430475,-2.8823257347227,134.79186216156));
#45992=CARTESIAN_POINT('Ctrl Pts',(101.494086744758,-2.76904781970824,134.869032465904));
#45993=CARTESIAN_POINT('Ctrl Pts',(101.486326302244,-2.65570944485981,134.946243958362));
#45994=CARTESIAN_POINT('Ctrl Pts',(101.478565859729,-2.53922912786052,135.018650184191));
#45995=CARTESIAN_POINT('Ctrl Pts',(101.470805417215,-2.42006038315897,135.086006423137));
#45996=CARTESIAN_POINT('Ctrl Pts',(101.46303251695,-2.30070033820905,135.153470788298));
#45997=CARTESIAN_POINT('Ctrl Pts',(101.455259616684,-2.17864358972124,135.215868788766));
#45998=CARTESIAN_POINT('Ctrl Pts',(101.447486716419,-2.05436615660382,135.273002777898));
#45999=CARTESIAN_POINT('Ctrl Pts',(101.439996380657,-1.93460652121634,135.328059802614));
#46000=CARTESIAN_POINT('Ctrl Pts',(101.432506044895,-1.81278513787602,135.378228774261));
#46001=CARTESIAN_POINT('Ctrl Pts',(101.425015709133,-1.68934095217909,135.42337676928));
#46002=CARTESIAN_POINT('Ctrl Pts',(101.417241375014,-1.56121634266132,135.470236564251));
#46003=CARTESIAN_POINT('Ctrl Pts',(101.409467040895,-1.43093758424745,135.511835563741));
#46004=CARTESIAN_POINT('Ctrl Pts',(101.401692706776,-1.29897596767261,135.547971530985));
#46005=CARTESIAN_POINT('Ctrl Pts',(101.393927953829,-1.16717698199653,135.584062963879));
#46006=CARTESIAN_POINT('Ctrl Pts',(101.386163200882,-1.03369963820886,135.614704658324));
#46007=CARTESIAN_POINT('Ctrl Pts',(101.378398447934,-0.89903426225641,135.639742759423));
#46008=CARTESIAN_POINT('Ctrl Pts',(101.370641407049,-0.764502637853893,
135.664755992327));
#46009=CARTESIAN_POINT('Ctrl Pts',(101.362884366164,-0.628785711371234,
135.684176636613));
#46010=CARTESIAN_POINT('Ctrl Pts',(101.355127325279,-0.492387654347936,
135.697900998553));
#46011=CARTESIAN_POINT('Ctrl Pts',(101.347376134039,-0.356092456160276,
135.711615010844));
#46012=CARTESIAN_POINT('Ctrl Pts',(101.339624942799,-0.219117537239844,
135.71964125196));
#46013=CARTESIAN_POINT('Ctrl Pts',(101.331873751559,-0.081975563375735,
135.721927400998));
#46014=CARTESIAN_POINT('Ctrl Pts',(101.324125854782,0.0551081214910062,
135.724212578361));
#46015=CARTESIAN_POINT('Ctrl Pts',(101.316377958005,0.192358329989765,135.720762509506));
#46016=CARTESIAN_POINT('Ctrl Pts',(101.308630061228,0.329259213364727,135.711576878636));
#46017=CARTESIAN_POINT('Ctrl Pts',(101.300883785144,0.466131460026223,135.702393169203));
#46018=CARTESIAN_POINT('Ctrl Pts',(101.29313750906,0.602654137065751,135.687476310294));
#46019=CARTESIAN_POINT('Ctrl Pts',(101.285391232976,0.738313737225168,135.666878061023));
#46020=CARTESIAN_POINT('Ctrl Pts',(101.27764489971,0.873974338792844,135.646279659701));
#46021=CARTESIAN_POINT('Ctrl Pts',(101.269898566445,1.00877146423259,135.619999843022));
#46022=CARTESIAN_POINT('Ctrl Pts',(101.262152233179,1.14219944709981,135.588141913314));
#46023=CARTESIAN_POINT('Ctrl Pts',(101.254404165176,1.27565731023858,135.556276849243));
#46024=CARTESIAN_POINT('Ctrl Pts',(101.246656097174,1.4077450404833,135.5188312772));
#46025=CARTESIAN_POINT('Ctrl Pts',(101.238908029171,1.53797022119512,135.475958915924));
#46026=CARTESIAN_POINT('Ctrl Pts',(101.231151726429,1.66833380677878,135.433040989392));
#46027=CARTESIAN_POINT('Ctrl Pts',(101.223395423687,1.7968305165352,135.384684874565));
#46028=CARTESIAN_POINT('Ctrl Pts',(101.215639120945,1.92298555918795,135.331093390953));
#46029=CARTESIAN_POINT('Ctrl Pts',(101.207878678431,2.0492079345855,135.277473303953));
#46030=CARTESIAN_POINT('Ctrl Pts',(101.200118235917,2.17308579955428,135.218612448048));
#46031=CARTESIAN_POINT('Ctrl Pts',(101.192357793403,2.29416812837713,135.154760100514));
#46032=CARTESIAN_POINT('Ctrl Pts',(101.184584893137,2.41544482930339,135.090805251524));
#46033=CARTESIAN_POINT('Ctrl Pts',(101.176811992872,2.53391668825988,135.021843095604));
#46034=CARTESIAN_POINT('Ctrl Pts',(101.169039092606,2.64916011968079,134.948167288104));
#46035=CARTESIAN_POINT('Ctrl Pts',(101.161548756844,2.76021416208956,134.877169781784));
#46036=CARTESIAN_POINT('Ctrl Pts',(101.154058421082,2.86827017214438,134.801795556439));
#46037=CARTESIAN_POINT('Ctrl Pts',(101.14656808532,2.97297905667257,134.722342060999));
#46038=CARTESIAN_POINT('Ctrl Pts',(101.138793751201,3.0816580103826,134.639876062131));
#46039=CARTESIAN_POINT('Ctrl Pts',(101.131019417082,3.18707527795657,134.552754128327));
#46040=CARTESIAN_POINT('Ctrl Pts',(101.123245082963,3.2888059677232,134.461263455921));
#46041=CARTESIAN_POINT('Ctrl Pts',(101.115480330016,3.39041128350656,134.369885537592));
#46042=CARTESIAN_POINT('Ctrl Pts',(101.107715577069,3.48833877354339,134.274149852301));
#46043=CARTESIAN_POINT('Ctrl Pts',(101.099950824121,3.58219396220099,134.174385762824));
#46044=CARTESIAN_POINT('Ctrl Pts',(101.092193783236,3.67595593256203,134.074720760447));
#46045=CARTESIAN_POINT('Ctrl Pts',(101.084436742351,3.76565338445493,133.971035599106));
#46046=CARTESIAN_POINT('Ctrl Pts',(101.076679701466,3.85092656037782,133.863698403603));
#46047=CARTESIAN_POINT('Ctrl Pts',(101.068928510226,3.93613543113548,133.756442151915));
#46048=CARTESIAN_POINT('Ctrl Pts',(101.061177318986,4.01692642457587,133.64553965267));
#46049=CARTESIAN_POINT('Ctrl Pts',(101.053426127746,4.09297841326089,133.531393945393));
#46050=CARTESIAN_POINT('Ctrl Pts',(101.045678230969,4.16899807782195,133.417296753087));
#46051=CARTESIAN_POINT('Ctrl Pts',(101.037930334192,4.24028252739919,133.29995941906));
#46052=CARTESIAN_POINT('Ctrl Pts',(101.030182437415,4.30655266745259,133.179815770785));
#46053=CARTESIAN_POINT('Ctrl Pts',(101.022436161331,4.37280894522136,133.059697253972));
#46054=CARTESIAN_POINT('Ctrl Pts',(101.014689885247,4.43405281104514,132.936773932651));
#46055=CARTESIAN_POINT('Ctrl Pts',(101.006943609163,4.49005024811696,132.811505812086));
#46056=CARTESIAN_POINT('Ctrl Pts',(100.999197275897,4.54604809854909,132.686236766821));
#46057=CARTESIAN_POINT('Ctrl Pts',(100.991450942632,4.59679928339698,132.5586232447));
#46058=CARTESIAN_POINT('Ctrl Pts',(100.983704609366,4.64211738876953,132.429146514656));
#46059=CARTESIAN_POINT('Ctrl Pts',(100.975956541363,4.68744564281757,132.299640789197));
#46060=CARTESIAN_POINT('Ctrl Pts',(100.968208473361,4.72733826716322,132.168271394474));
#46061=CARTESIAN_POINT('Ctrl Pts',(100.960460405358,4.76165842651478,132.035535703287));
#46062=CARTESIAN_POINT('Ctrl Pts',(100.952704102616,4.79601506174014,131.902658939028));
#46063=CARTESIAN_POINT('Ctrl Pts',(100.944947799874,4.82478730314989,131.768413356666));
#46064=CARTESIAN_POINT('Ctrl Pts',(100.937191497132,4.8478891522596,131.633308040449));
#46065=CARTESIAN_POINT('Ctrl Pts',(100.929431054618,4.87100333152177,131.498130614456));
#46066=CARTESIAN_POINT('Ctrl Pts',(100.921670612104,4.88844103832387,131.362092927881));
#46067=CARTESIAN_POINT('Ctrl Pts',(100.913910169589,4.90016820628043,131.225709181891));
#46068=CARTESIAN_POINT('Ctrl Pts',(100.906137269324,4.91191419972807,131.089106500603));
#46069=CARTESIAN_POINT('Ctrl Pts',(100.898364369059,4.91793131844436,130.952157040596));
#46070=CARTESIAN_POINT('Ctrl Pts',(100.890591468793,4.9182376646476,130.815375904293));
#46071=CARTESIAN_POINT('Ctrl Pts',(100.883101133031,4.91853287439472,130.683567106826));
#46072=CARTESIAN_POINT('Ctrl Pts',(100.875610797269,4.91352531675243,130.551914915346));
#46073=CARTESIAN_POINT('Ctrl Pts',(100.868120461507,4.90327655054314,130.420873810239));
#46074=CARTESIAN_POINT('Ctrl Pts',(100.860346127388,4.89263919924793,130.284864241802));
#46075=CARTESIAN_POINT('Ctrl Pts',(100.852571793269,4.8763216570013,130.149082175728));
#46076=CARTESIAN_POINT('Ctrl Pts',(100.84479745915,4.85433588588463,130.014040322045));
#46077=CARTESIAN_POINT('Ctrl Pts',(100.837032706203,4.83237721026595,129.879164895377));
#46078=CARTESIAN_POINT('Ctrl Pts',(100.829267953256,4.80476426723189,129.745028248185));
#46079=CARTESIAN_POINT('Ctrl Pts',(100.821503200308,4.77156093529912,129.612140292615));
#46080=CARTESIAN_POINT('Ctrl Pts',(100.813746159424,4.73839058138372,129.479384323235));
#46081=CARTESIAN_POINT('Ctrl Pts',(100.805989118539,4.69964098236137,129.347874954238));
#46082=CARTESIAN_POINT('Ctrl Pts',(100.798232077654,4.65542739433689,129.218113840246));
#46083=CARTESIAN_POINT('Ctrl Pts',(100.790480886413,4.61124714812307,129.08845058012));
#46084=CARTESIAN_POINT('Ctrl Pts',(100.782729695173,4.56161123997121,128.960533319433));
#46085=CARTESIAN_POINT('Ctrl Pts',(100.774978503933,4.50668518122186,128.834850084501));
#46086=CARTESIAN_POINT('Ctrl Pts',(100.767230607156,4.45178246751264,128.709220268296));
#46087=CARTESIAN_POINT('Ctrl Pts',(100.759482710379,4.39159423144577,128.585822946821));
#46088=CARTESIAN_POINT('Ctrl Pts',(100.751734813602,4.32633460694478,128.465127424562));
#46089=CARTESIAN_POINT('Ctrl Pts',(100.743988537518,4.26108863335041,128.344457149204));
#46090=CARTESIAN_POINT('Ctrl Pts',(100.736242261434,4.19077356719554,128.226487892627));
#46091=CARTESIAN_POINT('Ctrl Pts',(100.728495985349,4.11564993213761,128.11166518388));
#46092=CARTESIAN_POINT('Ctrl Pts',(100.720749652084,4.04052574253412,127.996841627537));
#46093=CARTESIAN_POINT('Ctrl Pts',(100.713003318819,3.96059312724813,127.885164992536));
#46094=CARTESIAN_POINT('Ctrl Pts',(100.705256985554,3.87615623020115,127.777052251778));
#46095=CARTESIAN_POINT('Ctrl Pts',(100.697508917551,3.79170042409646,127.66891529992));
#46096=CARTESIAN_POINT('Ctrl Pts',(100.689760849547,3.70273856963225,127.564344138517));
#46097=CARTESIAN_POINT('Ctrl Pts',(100.682012781545,3.6096151578123,127.463722733121));
#46098=CARTESIAN_POINT('Ctrl Pts',(100.674256478803,3.51639277332208,127.362994386097));
#46099=CARTESIAN_POINT('Ctrl Pts',(100.666500176061,3.41900026213164,127.26622446813));
#46100=CARTESIAN_POINT('Ctrl Pts',(100.658743873319,3.31781944695446,127.173760504649));
#46101=CARTESIAN_POINT('Ctrl Pts',(100.650983430805,3.21658462852966,127.081247190367));
#46102=CARTESIAN_POINT('Ctrl Pts',(100.643222988291,3.1115577764932,126.993044661274));
#46103=CARTESIAN_POINT('Ctrl Pts',(100.635462545776,3.00315308913531,126.909459516676));
#46104=CARTESIAN_POINT('Ctrl Pts',(100.627689645511,2.89457438094963,126.825740193783));
#46105=CARTESIAN_POINT('Ctrl Pts',(100.619916745246,2.78260732127804,126.746653293083));
#46106=CARTESIAN_POINT('Ctrl Pts',(100.61214384498,2.6676950650687,126.672462010109));
#46107=CARTESIAN_POINT('Ctrl Pts',(100.604653509218,2.55696015881852,126.600967767147));
#46108=CARTESIAN_POINT('Ctrl Pts',(100.597163173456,2.44349073431964,126.534019541934));
#46109=CARTESIAN_POINT('Ctrl Pts',(100.589672837694,2.32770243283911,126.471811201038));
#46110=CARTESIAN_POINT('Ctrl Pts',(100.581898503575,2.20752398271535,126.40724421199));
#46111=CARTESIAN_POINT('Ctrl Pts',(100.574124169456,2.08446665481643,126.347579099044));
#46112=CARTESIAN_POINT('Ctrl Pts',(100.566349835337,1.95896827240795,126.293082930458));
#46113=CARTESIAN_POINT('Ctrl Pts',(100.55858508239,1.83362455553967,126.238653923529));
#46114=CARTESIAN_POINT('Ctrl Pts',(100.550820329442,1.7058461251156,126.189381340265));
#46115=CARTESIAN_POINT('Ctrl Pts',(100.543055576495,1.57609651256555,126.145487057833));
#46116=CARTESIAN_POINT('Ctrl Pts',(100.53529853561,1.44647576915993,126.101636371821));
#46117=CARTESIAN_POINT('Ctrl Pts',(100.527541494725,1.31488810770054,126.063153480686));
#46118=CARTESIAN_POINT('Ctrl Pts',(100.51978445384,1.18181788316917,126.030212572781));
#46119=CARTESIAN_POINT('Ctrl Pts',(100.5120332626,1.04884800792934,125.997296505871));
#46120=CARTESIAN_POINT('Ctrl Pts',(100.50428207136,0.914398172927853,125.969914197207));
#46121=CARTESIAN_POINT('Ctrl Pts',(100.49653088012,0.778968431447635,125.948190187556));
#46122=CARTESIAN_POINT('Ctrl Pts',(100.488782983343,0.643596251220161,125.926475411187));
#46123=CARTESIAN_POINT('Ctrl Pts',(100.481035086566,0.507245378095775,125.910414212405));
#46124=CARTESIAN_POINT('Ctrl Pts',(100.473287189789,0.370426395846859,125.900080104814));
#46125=CARTESIAN_POINT('Ctrl Pts',(100.465540913705,0.233636033179553,125.889748158895));
#46126=CARTESIAN_POINT('Ctrl Pts',(100.45779463762,0.0963781457603969,125.885140950738));
#46127=CARTESIAN_POINT('Ctrl Pts',(100.450048361536,-0.0408316108026457,
125.886280113746));
#46128=CARTESIAN_POINT('Ctrl Pts',(100.442302028271,-0.178042380216942,
125.887419285162));
#46129=CARTESIAN_POINT('Ctrl Pts',(100.434555695006,-0.315204627114432,
125.89430490914));
#46130=CARTESIAN_POINT('Ctrl Pts',(100.42680936174,-0.451803143166616,125.906906484823));
#46131=CARTESIAN_POINT('Ctrl Pts',(100.419061293737,-0.588432249509362,
125.91951088254));
#46132=CARTESIAN_POINT('Ctrl Pts',(100.411313225734,-0.724496984559048,
125.937833743201));
#46133=CARTESIAN_POINT('Ctrl Pts',(100.403565157731,-0.859488101419582,
125.961792779526));
#46134=CARTESIAN_POINT('Ctrl Pts',(100.395808854989,-0.994622688445529,
125.9857772798));
#46135=CARTESIAN_POINT('Ctrl Pts',(100.388052552248,-1.12868099234083,126.015409853366));
#46136=CARTESIAN_POINT('Ctrl Pts',(100.380296249506,-1.26116424561469,126.050557107945));
#46137=CARTESIAN_POINT('Ctrl Pts',(100.372535806992,-1.3937182091898,126.085723121672));
#46138=CARTESIAN_POINT('Ctrl Pts',(100.364775364477,-1.52469507389019,126.126409565364));
#46139=CARTESIAN_POINT('Ctrl Pts',(100.357014921963,-1.65361300474393,126.172433686683));
#46140=CARTESIAN_POINT('Ctrl Pts',(100.349242021698,-1.78273788610517,126.218531690006));
#46141=CARTESIAN_POINT('Ctrl Pts',(100.341469121432,-1.90979686622148,126.269984346747));
#46142=CARTESIAN_POINT('Ctrl Pts',(100.333696221167,-2.03432897516291,126.32656108171));
#46143=CARTESIAN_POINT('Ctrl Pts',(100.326205885405,-2.15433402826569,126.381081109848));
#46144=CARTESIAN_POINT('Ctrl Pts',(100.318715549643,-2.27199246179451,126.440358999271));
#46145=CARTESIAN_POINT('Ctrl Pts',(100.311225213881,-2.38691650605695,126.504149848823));
#46146=CARTESIAN_POINT('Ctrl Pts',(100.30344983315,-2.50621398853184,126.570368261213));
#46147=CARTESIAN_POINT('Ctrl Pts',(100.295674452419,-2.62294279564377,126.641659705483));
#46148=CARTESIAN_POINT('Ctrl Pts',(100.287899071688,-2.73664139615496,126.717800091726));
#46149=CARTESIAN_POINT('Ctrl Pts',(100.280133501568,-2.85019653710222,126.7938444076));
#46150=CARTESIAN_POINT('Ctrl Pts',(100.272367931448,-2.96072875769736,126.874725275215));
#46151=CARTESIAN_POINT('Ctrl Pts',(100.264602361327,-3.06780070301104,126.960172548662));
#46152=CARTESIAN_POINT('Ctrl Pts',(100.256846151872,-3.17474358315738,127.045516823451));
#46153=CARTESIAN_POINT('Ctrl Pts',(100.249089942417,-3.27823419171602,127.13541629879));
#46154=CARTESIAN_POINT('Ctrl Pts',(100.241333732962,-3.37786431027174,127.229557718959));
#46155=CARTESIAN_POINT('Ctrl Pts',(100.233582830663,-3.47742625730071,127.323634723221));
#46156=CARTESIAN_POINT('Ctrl Pts',(100.225831928365,-3.57313268662067,127.42194763052));
#46157=CARTESIAN_POINT('Ctrl Pts',(100.218081026066,-3.66460857344863,127.524143084245));
#46158=CARTESIAN_POINT('Ctrl Pts',(100.210333748674,-3.75604167925621,127.626290743672));
#46159=CARTESIAN_POINT('Ctrl Pts',(100.202586471281,-3.84324791968253,127.732317045537));
#46160=CARTESIAN_POINT('Ctrl Pts',(100.194839193889,-3.92588954582157,127.841832248671));
#46161=CARTESIAN_POINT('Ctrl Pts',(100.187093861953,-4.00851041942263,127.951319950913));
#46162=CARTESIAN_POINT('Ctrl Pts',(100.179348530017,-4.08656872574872,128.064294498307));
#46163=CARTESIAN_POINT('Ctrl Pts',(100.17160319808,-4.15976764618254,128.180333904235));
#46164=CARTESIAN_POINT('Ctrl Pts',(100.163855706677,-4.23298697512897,128.296405662987));
#46165=CARTESIAN_POINT('Ctrl Pts',(100.156108215273,-4.30134399763379,128.415543659899));
#46166=CARTESIAN_POINT('Ctrl Pts',(100.148360723869,-4.36458577743344,128.537297748141));
#46167=CARTESIAN_POINT('Ctrl Pts',(100.140612236397,-4.42783568800787,128.65906748988));
#46168=CARTESIAN_POINT('Ctrl Pts',(100.132863748925,-4.48596887283135,128.783453642227));
#46169=CARTESIAN_POINT('Ctrl Pts',(100.125115261453,-4.53877927208194,128.909983204847));
#46170=CARTESIAN_POINT('Ctrl Pts',(100.117360388149,-4.59163319445624,129.036617045448));
#46171=CARTESIAN_POINT('Ctrl Pts',(100.109605514844,-4.63915542495276,129.165397460993));
#46172=CARTESIAN_POINT('Ctrl Pts',(100.10185064154,-4.68118868151468,129.295832994167));
#46173=CARTESIAN_POINT('Ctrl Pts',(100.09621778385,-4.71172010906225,129.390576617584));
#46174=CARTESIAN_POINT('Ctrl Pts',(100.090584926161,-4.73935655762074,129.486193106731));
#46175=CARTESIAN_POINT('Ctrl Pts',(100.084952068471,-4.76405452823407,129.582490119308));
#46176=CARTESIAN_POINT('Ctrl Pts',(101.834907966042,-4.76405452823403,129.582490119308));
#46177=CARTESIAN_POINT('Ctrl Pts',(101.827263594172,-4.79771132031781,129.71371744083));
#46178=CARTESIAN_POINT('Ctrl Pts',(101.819619222302,-4.82593387413391,129.846305308646));
#46179=CARTESIAN_POINT('Ctrl Pts',(101.811974850433,-4.84863003077733,129.979757751245));
#46180=CARTESIAN_POINT('Ctrl Pts',(101.804122281366,-4.87194432534955,130.116844818761));
#46181=CARTESIAN_POINT('Ctrl Pts',(101.796269712299,-4.88942680470606,130.254843783683));
#46182=CARTESIAN_POINT('Ctrl Pts',(101.788417143233,-4.9010344707148,130.393210791632));
#46183=CARTESIAN_POINT('Ctrl Pts',(101.780564574166,-4.91264213672354,130.531577799582));
#46184=CARTESIAN_POINT('Ctrl Pts',(101.772712005099,-4.91837500595534,130.670312392003));
#46185=CARTESIAN_POINT('Ctrl Pts',(101.764859436032,-4.91824793163316,130.808871214656));
#46186=CARTESIAN_POINT('',(102.110140564045,-4.91824992859335,130.803522529585));
#46187=CARTESIAN_POINT('Ctrl Pts',(102.179855052771,-4.76405452823403,129.582490119308));
#46188=CARTESIAN_POINT('Ctrl Pts',(102.171602591026,-4.80023113444554,129.72354215787));
#46189=CARTESIAN_POINT('Ctrl Pts',(102.16335012928,-4.83017959017385,129.866359169411));
#46190=CARTESIAN_POINT('Ctrl Pts',(102.155097667534,-4.8537393744369,130.010385084227));
#46191=CARTESIAN_POINT('Ctrl Pts',(102.146865913599,-4.87724004039645,130.154049596424));
#46192=CARTESIAN_POINT('Ctrl Pts',(102.138634159663,-4.89438395406626,130.298916657161));
#46193=CARTESIAN_POINT('Ctrl Pts',(102.130402405727,-4.90506114365806,130.444418622967));
#46194=CARTESIAN_POINT('Ctrl Pts',(102.1236484585,-4.91382150938374,130.56379932922));
#46195=CARTESIAN_POINT('Ctrl Pts',(102.116894511272,-4.91822949455648,130.683607076022));
#46196=CARTESIAN_POINT('Ctrl Pts',(102.110140564044,-4.91824992859335,130.803522529585));
#46197=CARTESIAN_POINT('Ctrl Pts',(102.110140564008,-4.91824992859346,130.803522530233));
#46198=CARTESIAN_POINT('Ctrl Pts',(102.102122208341,-4.91827418807359,130.945887390996));
#46199=CARTESIAN_POINT('Ctrl Pts',(102.094103852674,-4.91211271718102,131.088167320966));
#46200=CARTESIAN_POINT('Ctrl Pts',(102.086085497007,-4.89981367422495,131.229812166368));
#46201=CARTESIAN_POINT('Ctrl Pts',(102.078059836677,-4.88750342692988,131.371586049198));
#46202=CARTESIAN_POINT('Ctrl Pts',(102.070034176346,-4.86904448769284,131.512723345161));
#46203=CARTESIAN_POINT('Ctrl Pts',(102.062008516015,-4.84453659176315,131.652681472884));
#46204=CARTESIAN_POINT('Ctrl Pts',(102.053701303064,-4.81916892080687,131.797549548949));
#46205=CARTESIAN_POINT('Ctrl Pts',(102.045394090112,-4.78732024247637,131.941153806296));
#46206=CARTESIAN_POINT('Ctrl Pts',(102.037086877161,-4.74915763238618,132.082908561621));
#46207=CARTESIAN_POINT('Ctrl Pts',(102.02903725149,-4.71217835574289,132.220267832916));
#46208=CARTESIAN_POINT('Ctrl Pts',(102.020987625819,-4.66927105687257,132.355890290011));
#46209=CARTESIAN_POINT('Ctrl Pts',(102.012938000147,-4.62063717517419,132.489262738729));
#46210=CARTESIAN_POINT('Ctrl Pts',(102.004501993556,-4.56966887387285,132.62903704656));
#46211=CARTESIAN_POINT('Ctrl Pts',(101.996065986965,-4.51241084531998,132.76633959036));
#46212=CARTESIAN_POINT('Ctrl Pts',(101.987629980373,-4.44914929363851,132.900608128099));
#46213=CARTESIAN_POINT('Ctrl Pts',(101.979193973782,-4.38588774195708,133.034876665838));
#46214=CARTESIAN_POINT('Ctrl Pts',(101.97075796719,-4.31662293608384,133.166110848154));
#46215=CARTESIAN_POINT('Ctrl Pts',(101.962321960599,-4.2416929995932,133.293782952105));
#46216=CARTESIAN_POINT('Ctrl Pts',(101.95454762648,-4.17264014200159,133.411441180918));
#46217=CARTESIAN_POINT('Ctrl Pts',(101.946773292361,-4.09857870427127,133.52641045983));
#46218=CARTESIAN_POINT('Ctrl Pts',(101.938998958242,-4.01974368913189,133.638234950733));
#46219=CARTESIAN_POINT('Ctrl Pts',(101.931234205295,-3.94100583110288,133.749921627945));
#46220=CARTESIAN_POINT('Ctrl Pts',(101.923469452348,-3.85750632420618,133.858470912103));
#46221=CARTESIAN_POINT('Ctrl Pts',(101.9157046994,-3.76952563487839,133.963452188017));
#46222=CARTESIAN_POINT('Ctrl Pts',(101.907947658515,-3.68163232921173,134.068329195048));
#46223=CARTESIAN_POINT('Ctrl Pts',(101.90019061763,-3.58926694785408,134.169644948438));
#46224=CARTESIAN_POINT('Ctrl Pts',(101.892433576745,-3.49275254847463,134.266998729992));
#46225=CARTESIAN_POINT('Ctrl Pts',(101.884682385505,-3.39631093135439,134.364279096302));
#46226=CARTESIAN_POINT('Ctrl Pts',(101.876931194265,-3.29572679805333,134.457603161193));
#46227=CARTESIAN_POINT('Ctrl Pts',(101.869180003025,-3.19136243912891,134.546604442415));
#46228=CARTESIAN_POINT('Ctrl Pts',(101.861432106248,-3.08704243784112,134.635567895717));
#46229=CARTESIAN_POINT('Ctrl Pts',(101.853684209471,-2.97894570338572,134.720211966438));
#46230=CARTESIAN_POINT('Ctrl Pts',(101.845936312694,-2.86747006322841,134.800208274696));
#46231=CARTESIAN_POINT('Ctrl Pts',(101.83819003661,-2.75601774137181,134.88018784945));
#46232=CARTESIAN_POINT('Ctrl Pts',(101.830443760526,-2.64118823710544,134.955521367725));
#46233=CARTESIAN_POINT('Ctrl Pts',(101.822697484442,-2.52341069653454,135.025922120033));
#46234=CARTESIAN_POINT('Ctrl Pts',(101.814951151176,-2.40563228655666,135.096323392024));
#46235=CARTESIAN_POINT('Ctrl Pts',(101.807204817911,-2.28490613243383,135.161791624795));
#46236=CARTESIAN_POINT('Ctrl Pts',(101.799458484645,-2.16168811742724,135.222084867163));
#46237=CARTESIAN_POINT('Ctrl Pts',(101.791710416642,-2.03844250860028,135.282391611784));
#46238=CARTESIAN_POINT('Ctrl Pts',(101.783962348639,-1.91270427957439,135.337520888111));
#46239=CARTESIAN_POINT('Ctrl Pts',(101.776214280636,-1.78495116042607,135.387278074535));
#46240=CARTESIAN_POINT('Ctrl Pts',(101.768457977895,-1.65706226374269,135.437088143489));
#46241=CARTESIAN_POINT('Ctrl Pts',(101.760701675153,-1.52715456405104,135.481514575038));
#46242=CARTESIAN_POINT('Ctrl Pts',(101.752945372411,-1.39572342517542,135.520411845332));
#46243=CARTESIAN_POINT('Ctrl Pts',(101.745184929897,-1.2642221375434,135.559329876271));
#46244=CARTESIAN_POINT('Ctrl Pts',(101.737424487382,-1.13119616956762,135.592712770561));
#46245=CARTESIAN_POINT('Ctrl Pts',(101.729664044868,-0.997152099810959,
135.620465968609));
#46246=CARTESIAN_POINT('Ctrl Pts',(101.721891144603,-0.862892850613838,
135.648263718554));
#46247=CARTESIAN_POINT('Ctrl Pts',(101.714118244337,-0.727612619738735,
135.670413649664));
#46248=CARTESIAN_POINT('Ctrl Pts',(101.706345344072,-0.591825042265724,
135.686872899358));
#46249=CARTESIAN_POINT('Ctrl Pts',(101.69885500831,-0.460973685263137,135.702733813866));
#46250=CARTESIAN_POINT('Ctrl Pts',(101.691364672548,-0.329651534934086,
135.713310580282));
#46251=CARTESIAN_POINT('Ctrl Pts',(101.683874336786,-0.198317161239635,
135.718610648451));
#46252=CARTESIAN_POINT('Ctrl Pts',(101.676100002667,-0.0620032048473757,
135.724111670316));
#46253=CARTESIAN_POINT('Ctrl Pts',(101.668325668548,0.0747557217455648,
135.723945388758));
#46254=CARTESIAN_POINT('Ctrl Pts',(101.660551334429,0.211449084311424,135.718063126596));
#46255=CARTESIAN_POINT('Ctrl Pts',(101.652786581482,0.347973984524278,135.712188113796));
#46256=CARTESIAN_POINT('Ctrl Pts',(101.645021828535,0.484433094627608,135.700611153365));
#46257=CARTESIAN_POINT('Ctrl Pts',(101.637257075588,0.620312526907382,135.683335451633));
#46258=CARTESIAN_POINT('Ctrl Pts',(101.629500034703,0.756057001819729,135.666076908372));
#46259=CARTESIAN_POINT('Ctrl Pts',(101.621742993818,0.891222559332021,135.643130936594));
#46260=CARTESIAN_POINT('Ctrl Pts',(101.613985952933,1.02529744331558,135.614552735895));
#46261=CARTESIAN_POINT('Ctrl Pts',(101.606234761692,1.15927122038591,135.585996086239));
#46262=CARTESIAN_POINT('Ctrl Pts',(101.598483570452,1.2921555802066,135.551815742842));
#46263=CARTESIAN_POINT('Ctrl Pts',(101.590732379212,1.4234463639851,135.512118418405));
#46264=CARTESIAN_POINT('Ctrl Pts',(101.582984482435,1.55468134567855,135.472437966389));
#46265=CARTESIAN_POINT('Ctrl Pts',(101.575236585658,1.68432372500326,135.427245310004));
#46266=CARTESIAN_POINT('Ctrl Pts',(101.567488688881,1.81188219120261,135.376697655417));
#46267=CARTESIAN_POINT('Ctrl Pts',(101.559742412797,1.93941397492059,135.32616057431));
#46268=CARTESIAN_POINT('Ctrl Pts',(101.551996136713,2.06486234932414,135.270270866981));
#46269=CARTESIAN_POINT('Ctrl Pts',(101.544249860629,2.18775413364865,135.209234612722));
#46270=CARTESIAN_POINT('Ctrl Pts',(101.536503527363,2.31064682513239,135.148197907907));
#46271=CARTESIAN_POINT('Ctrl Pts',(101.528757194098,2.43098253872352,135.082014754265));
#46272=CARTESIAN_POINT('Ctrl Pts',(101.521010860832,2.5483112979989,135.010937918768));
#46273=CARTESIAN_POINT('Ctrl Pts',(101.513262792829,2.66566633223666,134.939845166107));
#46274=CARTESIAN_POINT('Ctrl Pts',(101.505514724826,2.78001273786896,134.863856753399));
#46275=CARTESIAN_POINT('Ctrl Pts',(101.497766656824,2.89092854944727,134.783269410752));
#46276=CARTESIAN_POINT('Ctrl Pts',(101.490010354082,3.00196224366982,134.702596418918));
#46277=CARTESIAN_POINT('Ctrl Pts',(101.48225405134,3.10955774360974,134.617314963419));
#46278=CARTESIAN_POINT('Ctrl Pts',(101.474497748598,3.21332485968227,134.527763148672));
#46279=CARTESIAN_POINT('Ctrl Pts',(101.466737306084,3.31714735938924,134.438163537425));
#46280=CARTESIAN_POINT('Ctrl Pts',(101.45897686357,3.4171371188395,134.344289292863));
#46281=CARTESIAN_POINT('Ctrl Pts',(101.451216421055,3.51294076428022,134.246515502105));
#46282=CARTESIAN_POINT('Ctrl Pts',(101.44344352079,3.60889820223751,134.148584756179));
#46283=CARTESIAN_POINT('Ctrl Pts',(101.435670620525,3.70065583579107,134.046742245416));
#46284=CARTESIAN_POINT('Ctrl Pts',(101.427897720259,3.7878999711285,133.941396937283));
#46285=CARTESIAN_POINT('Ctrl Pts',(101.420407384497,3.87197256239157,133.83988119645));
#46286=CARTESIAN_POINT('Ctrl Pts',(101.412917048735,3.95185392550212,133.73511315274));
#46287=CARTESIAN_POINT('Ctrl Pts',(101.405426712973,4.02730245996136,133.627482640874));
#46288=CARTESIAN_POINT('Ctrl Pts',(101.397652378854,4.10561164853672,133.515771285438));
#46289=CARTESIAN_POINT('Ctrl Pts',(101.389878044735,4.17939329149829,133.400622248037));
#46290=CARTESIAN_POINT('Ctrl Pts',(101.382103710616,4.24833047913458,133.282438744372));
#46291=CARTESIAN_POINT('Ctrl Pts',(101.374338957669,4.31718270784833,133.164400891313));
#46292=CARTESIAN_POINT('Ctrl Pts',(101.366574204722,4.38120216537198,133.043336347365));
#46293=CARTESIAN_POINT('Ctrl Pts',(101.358809451774,4.44011378041843,132.919679193913));
#46294=CARTESIAN_POINT('Ctrl Pts',(101.351052410889,4.49896688361818,132.79614485849));
#46295=CARTESIAN_POINT('Ctrl Pts',(101.343295370004,4.55272207313581,132.670023388635));
#46296=CARTESIAN_POINT('Ctrl Pts',(101.335538329119,4.6011491732647,132.541775176002));
#46297=CARTESIAN_POINT('Ctrl Pts',(101.327787137879,4.64953975414088,132.413623676343));
#46298=CARTESIAN_POINT('Ctrl Pts',(101.320035946639,4.69261010556833,132.283348990438));
#46299=CARTESIAN_POINT('Ctrl Pts',(101.312284755399,4.73017749782027,132.151432962177));
#46300=CARTESIAN_POINT('Ctrl Pts',(101.304536858622,4.76772892292823,132.019573001747));
#46301=CARTESIAN_POINT('Ctrl Pts',(101.296788961845,4.79978193390504,131.88607346169));
#46302=CARTESIAN_POINT('Ctrl Pts',(101.289041065068,4.8262032272866,131.751432669433));
#46303=CARTESIAN_POINT('Ctrl Pts',(101.281294788984,4.85261899390317,131.616820041128));
#46304=CARTESIAN_POINT('Ctrl Pts',(101.2735485129,4.87340531086086,131.481067018867));
#46305=CARTESIAN_POINT('Ctrl Pts',(101.265802236815,4.8884797927422,131.344683093918));
#46306=CARTESIAN_POINT('Ctrl Pts',(101.25805590355,4.90355438589991,131.208298162214));
#46307=CARTESIAN_POINT('Ctrl Pts',(101.250309570285,4.91291701689544,131.071282707129));
#46308=CARTESIAN_POINT('Ctrl Pts',(101.242563237019,4.91653712249402,130.934151933293));
#46309=CARTESIAN_POINT('Ctrl Pts',(101.234815169016,4.92015803879016,130.796990449971));
#46310=CARTESIAN_POINT('Ctrl Pts',(101.227067101013,4.91803386038523,130.659713987266));
#46311=CARTESIAN_POINT('Ctrl Pts',(101.21931903301,4.91018615209169,130.52283794653));
#46312=CARTESIAN_POINT('Ctrl Pts',(101.211562730269,4.90233010316038,130.38581643231));
#46313=CARTESIAN_POINT('Ctrl Pts',(101.203806427527,4.88873839523614,130.249196581135));
#46314=CARTESIAN_POINT('Ctrl Pts',(101.196050124785,4.86948457814034,130.11348942425));
#46315=CARTESIAN_POINT('Ctrl Pts',(101.188289682271,4.85022048470262,129.97770983637));
#46316=CARTESIAN_POINT('Ctrl Pts',(101.180529239757,4.82528833146388,129.842844297696));
#46317=CARTESIAN_POINT('Ctrl Pts',(101.172768797242,4.79481268269693,129.709392855324));
#46318=CARTESIAN_POINT('Ctrl Pts',(101.164995896977,4.76428811171308,129.57572718485));
#46319=CARTESIAN_POINT('Ctrl Pts',(101.157222996712,4.72820236531896,129.443480524322));
#46320=CARTESIAN_POINT('Ctrl Pts',(101.149450096446,4.68672996025863,129.313137850132));
#46321=CARTESIAN_POINT('Ctrl Pts',(101.141959760684,4.6467651815851,129.187533460463));
#46322=CARTESIAN_POINT('Ctrl Pts',(101.134469424922,4.60179868719937,129.063697320594));
#46323=CARTESIAN_POINT('Ctrl Pts',(101.12697908916,4.55202786512049,128.942043411055));
#46324=CARTESIAN_POINT('Ctrl Pts',(101.119204755041,4.50036996719478,128.81577695656));
#46325=CARTESIAN_POINT('Ctrl Pts',(101.111430420922,4.44337260107701,128.691461503345));
#46326=CARTESIAN_POINT('Ctrl Pts',(101.103656086803,4.38120370611486,128.569581624461));
#46327=CARTESIAN_POINT('Ctrl Pts',(101.095891333856,4.31911142875964,128.447851951634));
#46328=CARTESIAN_POINT('Ctrl Pts',(101.088126580909,4.25186047976347,128.328552225725));
#46329=CARTESIAN_POINT('Ctrl Pts',(101.080361827962,4.17966738134106,128.212148503588));
#46330=CARTESIAN_POINT('Ctrl Pts',(101.072604787077,4.1075459861218,128.09586039527));
#46331=CARTESIAN_POINT('Ctrl Pts',(101.064847746192,4.0304924145653,127.982462896758));
#46332=CARTESIAN_POINT('Ctrl Pts',(101.057090705307,3.94876959161668,127.872398514328));
#46333=CARTESIAN_POINT('Ctrl Pts',(101.049339514067,3.86710839648473,127.762417132305));
#46334=CARTESIAN_POINT('Ctrl Pts',(101.041588322827,3.78078519066078,127.655764175967));
#46335=CARTESIAN_POINT('Ctrl Pts',(101.033837131587,3.69010659317586,127.552853829398));
#46336=CARTESIAN_POINT('Ctrl Pts',(101.02608923481,3.59946653651344,127.449987222472));
#46337=CARTESIAN_POINT('Ctrl Pts',(101.018341338032,3.50447502793151,127.350860354241));
#46338=CARTESIAN_POINT('Ctrl Pts',(101.010593441255,3.40547927062977,127.25585473483));
#46339=CARTESIAN_POINT('Ctrl Pts',(101.002847165171,3.30650422110637,127.160868988547));
#46340=CARTESIAN_POINT('Ctrl Pts',(100.995100889087,3.20352687080224,127.070003046907));
#46341=CARTESIAN_POINT('Ctrl Pts',(100.987354613003,3.09693133782097,126.983601615571));
#46342=CARTESIAN_POINT('Ctrl Pts',(100.979608279738,2.99033501797548,126.89719954644));
#46343=CARTESIAN_POINT('Ctrl Pts',(100.971861946472,2.88012076588038,126.815262299557));
#46344=CARTESIAN_POINT('Ctrl Pts',(100.964115613207,2.76670551760895,126.738094069326));
#46345=CARTESIAN_POINT('Ctrl Pts',(100.956367545204,2.65326487077887,126.660908557806));
#46346=CARTESIAN_POINT('Ctrl Pts',(100.948619477201,2.53662212451889,126.588494408001));
#46347=CARTESIAN_POINT('Ctrl Pts',(100.940871409198,2.41722255689327,126.521112063846));
#46348=CARTESIAN_POINT('Ctrl Pts',(100.933115106456,2.29769608998664,126.453658104934));
#46349=CARTESIAN_POINT('Ctrl Pts',(100.925358803714,2.17540728978875,126.391246827062));
#46350=CARTESIAN_POINT('Ctrl Pts',(100.917602500973,2.05082585683438,126.334092575553));
#46351=CARTESIAN_POINT('Ctrl Pts',(100.909842058458,1.926177931018,126.2769078191));
#46352=CARTESIAN_POINT('Ctrl Pts',(100.902081615944,1.79923529591329,126.224985827807));
#46353=CARTESIAN_POINT('Ctrl Pts',(100.89432117343,1.67048598533729,126.178492089896));
#46354=CARTESIAN_POINT('Ctrl Pts',(100.886548273165,1.5415299949383,126.131923716108));
#46355=CARTESIAN_POINT('Ctrl Pts',(100.878775372899,1.41076190664602,126.090801126231));
#46356=CARTESIAN_POINT('Ctrl Pts',(100.871002472634,1.27868407539881,126.055239635971));
#46357=CARTESIAN_POINT('Ctrl Pts',(100.863512136872,1.1514076060016,126.020970895457));
#46358=CARTESIAN_POINT('Ctrl Pts',(100.85602180111,1.02291526572459,125.991866022236));
#46359=CARTESIAN_POINT('Ctrl Pts',(100.848531465348,0.8936620411581,125.967982714766));
#46360=CARTESIAN_POINT('Ctrl Pts',(100.840757131229,0.759508141296226,125.943193864434));
#46361=CARTESIAN_POINT('Ctrl Pts',(100.83298279711,0.62410956108497,125.923951823762));
#46362=CARTESIAN_POINT('Ctrl Pts',(100.82520846299,0.487964760875024,125.91037722419));
#46363=CARTESIAN_POINT('Ctrl Pts',(100.817443710043,0.351987746964005,125.896819354098));
#46364=CARTESIAN_POINT('Ctrl Pts',(100.809678957096,0.215266728184087,125.888915066222));
#46365=CARTESIAN_POINT('Ctrl Pts',(100.801914204149,0.078310846914143,125.886734109406));
#46366=CARTESIAN_POINT('Ctrl Pts',(100.794157163264,-0.0585090078438774,
125.884555318747));
#46367=CARTESIAN_POINT('Ctrl Pts',(100.786400122379,-0.195562872490565,
125.888088552935));
#46368=CARTESIAN_POINT('Ctrl Pts',(100.778643081494,-0.332336336609006,
125.897351791217));
#46369=CARTESIAN_POINT('Ctrl Pts',(100.770891890254,-0.469006658793839,
125.906608044019));
#46370=CARTESIAN_POINT('Ctrl Pts',(100.763140699014,-0.60539661283996,125.921585673834));
#46371=CARTESIAN_POINT('Ctrl Pts',(100.755389507774,-0.740991998868861,
125.942250590005));
#46372=CARTESIAN_POINT('Ctrl Pts',(100.747641610997,-0.876529753241944,
125.962906723035));
#46373=CARTESIAN_POINT('Ctrl Pts',(100.73989371422,-1.01127322558911,125.989245275916));
#46374=CARTESIAN_POINT('Ctrl Pts',(100.732145817443,-1.14471376882555,126.021180352307));
#46375=CARTESIAN_POINT('Ctrl Pts',(100.724399541358,-1.27812639917681,126.053108748568));
#46376=CARTESIAN_POINT('Ctrl Pts',(100.716653265274,-1.41023626253643,126.090631248869));
#46377=CARTESIAN_POINT('Ctrl Pts',(100.70890698919,-1.54054572305174,126.133611005599));
#46378=CARTESIAN_POINT('Ctrl Pts',(100.701160655925,-1.67085614548207,126.176591079596));
#46379=CARTESIAN_POINT('Ctrl Pts',(100.69341432266,-1.79936576725781,126.225028367945));
#46380=CARTESIAN_POINT('Ctrl Pts',(100.685667989394,-1.92559329688056,126.278736515024));
#46381=CARTESIAN_POINT('Ctrl Pts',(100.677919921391,-2.05184909428363,126.33245668967));
#46382=CARTESIAN_POINT('Ctrl Pts',(100.670171853388,-2.17582142290059,126.391449918809));
#46383=CARTESIAN_POINT('Ctrl Pts',(100.662423785385,-2.29705048020335,126.455482353703));
#46384=CARTESIAN_POINT('Ctrl Pts',(100.654667482643,-2.41840838119069,126.519582843031));
#46385=CARTESIAN_POINT('Ctrl Pts',(100.646911179901,-2.53701684042041,126.588733053866));
#46386=CARTESIAN_POINT('Ctrl Pts',(100.63915487716,-2.65244163848967,126.66265367273));
#46387=CARTESIAN_POINT('Ctrl Pts',(100.631394434645,-2.76792804224895,126.736613745253));
#46388=CARTESIAN_POINT('Ctrl Pts',(100.623633992131,-2.88022707905069,126.81534907481));
#46389=CARTESIAN_POINT('Ctrl Pts',(100.615873549617,-2.98893572476966,126.898538515153));
#46390=CARTESIAN_POINT('Ctrl Pts',(100.608100649352,-3.09781887925745,126.981861498572));
#46391=CARTESIAN_POINT('Ctrl Pts',(100.600327749086,-3.20309982468353,127.069652630493));
#46392=CARTESIAN_POINT('Ctrl Pts',(100.592554848821,-3.30441000756219,127.161551596436));
#46393=CARTESIAN_POINT('Ctrl Pts',(100.585064513059,-3.40203731010833,127.250109803489));
#46394=CARTESIAN_POINT('Ctrl Pts',(100.577574177297,-3.49597731276188,127.342482153554));
#46395=CARTESIAN_POINT('Ctrl Pts',(100.570083841535,-3.58593554081042,127.438317040954));
#46396=CARTESIAN_POINT('Ctrl Pts',(100.562402357742,-3.67818943872558,127.536597566379));
#46397=CARTESIAN_POINT('Ctrl Pts',(100.55472087395,-3.76656340649161,127.638847946972));
#46398=CARTESIAN_POINT('Ctrl Pts',(100.547039390158,-3.85069011045177,127.744725224947));
#46399=CARTESIAN_POINT('Ctrl Pts',(100.539367008347,-3.934717130587,127.8504770463));
#46400=CARTESIAN_POINT('Ctrl Pts',(100.531694626536,-4.01450664646612,127.959846909533));
#46401=CARTESIAN_POINT('Ctrl Pts',(100.524022244724,-4.08972787390997,128.072454876172));
#46402=CARTESIAN_POINT('Ctrl Pts',(100.516200057596,-4.1664178160439,128.187261543635));
#46403=CARTESIAN_POINT('Ctrl Pts',(100.508377870467,-4.23835890669656,128.305433798632));
#46404=CARTESIAN_POINT('Ctrl Pts',(100.500555683338,-4.30524298001553,128.426532628512));
#46405=CARTESIAN_POINT('Ctrl Pts',(100.492896842392,-4.37073035215044,128.545102621994));
#46406=CARTESIAN_POINT('Ctrl Pts',(100.485238001445,-4.43136962217265,128.666477797822));
#46407=CARTESIAN_POINT('Ctrl Pts',(100.477579160499,-4.48691512220699,128.790216693064));
#46408=CARTESIAN_POINT('Ctrl Pts',(100.469675300279,-4.5442376167169,128.91791420481));
#46409=CARTESIAN_POINT('Ctrl Pts',(100.461771440059,-4.59613473198388,129.048128836655));
#46410=CARTESIAN_POINT('Ctrl Pts',(100.453867579839,-4.64238822044992,129.180348710858));
#46411=CARTESIAN_POINT('Ctrl Pts',(100.445963719619,-4.68864170891593,129.312568585062));
#46412=CARTESIAN_POINT('Ctrl Pts',(100.4380598594,-4.72925140293648,129.446793261984));
#46413=CARTESIAN_POINT('Ctrl Pts',(100.43015599918,-4.76405452823403,129.582490119308));
#46414=CARTESIAN_POINT('Origin',(213.235140564004,0.,130.804360617566));
#46415=CARTESIAN_POINT('',(98.3346394208835,-4.76405452823406,129.582490119308));
#46416=CARTESIAN_POINT('',(98.680234964937,-4.76405452823403,129.582490119308));
#46417=CARTESIAN_POINT('',(213.235140564004,-4.76405452823405,129.582490119308));
#46418=CARTESIAN_POINT('',(100.014859435958,-4.91824963103853,130.802455548176));
#46419=CARTESIAN_POINT('Ctrl Pts',(100.014859435958,-4.91824963103853,130.802455548176));
#46420=CARTESIAN_POINT('Ctrl Pts',(100.007159673393,-4.91830200268018,130.937661545693));
#46421=CARTESIAN_POINT('Ctrl Pts',(99.9994599108281,-4.91277480486665,131.073095304347));
#46422=CARTESIAN_POINT('Ctrl Pts',(99.991760148263,-4.90163791460517,131.208252702912));
#46423=CARTESIAN_POINT('Ctrl Pts',(99.984069510433,-4.89051422230582,131.343249930892));
#46424=CARTESIAN_POINT('Ctrl Pts',(99.9763788726031,-4.8737940927686,131.477971056342));
#46425=CARTESIAN_POINT('Ctrl Pts',(99.9686882347731,-4.85149938723206,131.611910466298));
#46426=CARTESIAN_POINT('Ctrl Pts',(99.9610047852629,-4.82922552021042,131.745724685168));
#46427=CARTESIAN_POINT('Ctrl Pts',(99.9533213357526,-4.80138750806904,131.878758250946));
#46428=CARTESIAN_POINT('Ctrl Pts',(99.9456378862424,-4.76805909856987,132.010509652737));
#46429=CARTESIAN_POINT('Ctrl Pts',(99.9376667229096,-4.73348267617179,132.147194606755));
#46430=CARTESIAN_POINT('Ctrl Pts',(99.9296955595768,-4.69299668467984,132.282499065602));
#46431=CARTESIAN_POINT('Ctrl Pts',(99.921724396244,-4.64674198262771,132.415872953661));
#46432=CARTESIAN_POINT('Ctrl Pts',(99.91404874757,-4.60220207952328,132.544302276243));
#46433=CARTESIAN_POINT('Ctrl Pts',(99.906373098896,-4.55231370292702,132.670941207271));
#46434=CARTESIAN_POINT('Ctrl Pts',(99.898697450222,-4.49725357121119,132.795313499662));
#46435=CARTESIAN_POINT('Ctrl Pts',(99.8910226996253,-4.44219988172028,132.919671240068));
#46436=CARTESIAN_POINT('Ctrl Pts',(99.8833479490286,-4.38197580186486,133.041762504411));
#46437=CARTESIAN_POINT('Ctrl Pts',(99.875673198432,-4.31680598721369,133.161131529483));
#46438=CARTESIAN_POINT('Ctrl Pts',(99.8679976074016,-4.25162903605579,133.280513626217));
#46439=CARTESIAN_POINT('Ctrl Pts',(99.8603220163711,-4.18150546430801,133.397172540643));
#46440=CARTESIAN_POINT('Ctrl Pts',(99.8526464253407,-4.10670537338365,133.510678048822));
#46441=CARTESIAN_POINT('Ctrl Pts',(99.8449682550301,-4.03188014688457,133.624221699016));
#46442=CARTESIAN_POINT('Ctrl Pts',(99.8372900847196,-3.95237549516136,133.734609502517));
#46443=CARTESIAN_POINT('Ctrl Pts',(99.829611914409,-3.86850392847026,133.841441521643));
#46444=CARTESIAN_POINT('Ctrl Pts',(99.8219253177721,-3.78454031782061,133.948390782432));
#46445=CARTESIAN_POINT('Ctrl Pts',(99.8142387211352,-3.69620047320614,134.05177615626));
#46446=CARTESIAN_POINT('Ctrl Pts',(99.8065521244983,-3.60383634289496,134.15123179467));
#46447=CARTESIAN_POINT('Ctrl Pts',(99.7988605133256,-3.51141195662625,134.250752315353));
#46448=CARTESIAN_POINT('Ctrl Pts',(99.7911689021529,-3.41495834033394,134.346337716751));
#46449=CARTESIAN_POINT('Ctrl Pts',(99.7834772909802,-3.31486221150036,134.437660987927));
#46450=CARTESIAN_POINT('Ctrl Pts',(99.7757748872528,-3.21462563186727,134.529112400188));
#46451=CARTESIAN_POINT('Ctrl Pts',(99.7680724835255,-3.11073664445713,134.616289492766));
#46452=CARTESIAN_POINT('Ctrl Pts',(99.7603700797981,-3.00361294062392,134.698907107906));
#46453=CARTESIAN_POINT('Ctrl Pts',(99.7583567086171,-2.97561132116425,134.720502953988));
#46454=CARTESIAN_POINT('Ctrl Pts',(99.7563433374361,-2.94738882210631,134.741787501222));
#46455=CARTESIAN_POINT('Ctrl Pts',(99.7543299662552,-2.91895318845925,134.762756169565));
#46456=CARTESIAN_POINT('Ctrl Pts',(99.7465556321361,-2.80915320773641,134.843723571537));
#46457=CARTESIAN_POINT('Ctrl Pts',(99.738781298017,-2.69580788640631,134.920247226605));
#46458=CARTESIAN_POINT('Ctrl Pts',(99.7310069638979,-2.57931271909312,134.992000640255));
#46459=CARTESIAN_POINT('Ctrl Pts',(99.7232422109509,-2.46296112166225,135.063665624235));
#46460=CARTESIAN_POINT('Ctrl Pts',(99.7154774580038,-2.34346773177088,135.130571860979));
#46461=CARTESIAN_POINT('Ctrl Pts',(99.7077127050567,-2.22125990484847,135.192433941659));
#46462=CARTESIAN_POINT('Ctrl Pts',(99.6999556641717,-2.09917345646267,135.254234580047));
#46463=CARTESIAN_POINT('Ctrl Pts',(99.6921986232867,-1.97437828280437,135.31100085692));
#46464=CARTESIAN_POINT('Ctrl Pts',(99.6844415824017,-1.8473291193632,135.362491614724));
#46465=CARTESIAN_POINT('Ctrl Pts',(99.6766903911616,-1.72037576468422,135.413943542948));
#46466=CARTESIAN_POINT('Ctrl Pts',(99.6689391999214,-1.59117216434632,135.460127724433));
#46467=CARTESIAN_POINT('Ctrl Pts',(99.6611880086813,-1.46019563847152,135.50084991915));
#46468=CARTESIAN_POINT('Ctrl Pts',(99.6534401119042,-1.32927478111422,135.541554805847));
#46469=CARTESIAN_POINT('Ctrl Pts',(99.6456922151272,-1.19658286951013,135.576802207212));
#46470=CARTESIAN_POINT('Ctrl Pts',(99.6379443183501,-1.06261488866523,135.606446899682));
#46471=CARTESIAN_POINT('Ctrl Pts',(99.630198042266,-0.928674931034093,135.636085391122));
#46472=CARTESIAN_POINT('Ctrl Pts',(99.6224517661819,-0.793459816582142,
135.660123420356));
#46473=CARTESIAN_POINT('Ctrl Pts',(99.6147054900978,-0.657476912834559,
135.678466399306));
#46474=CARTESIAN_POINT('Ctrl Pts',(99.6069591568325,-0.521493005292072,
135.696809513659));
#46475=CARTESIAN_POINT('Ctrl Pts',(99.5992128235672,-0.384741684600638,
135.709457441578));
#46476=CARTESIAN_POINT('Ctrl Pts',(99.5914664903018,-0.247737273592604,
135.716367265136));
#46477=CARTESIAN_POINT('Ctrl Pts',(99.5837184222989,-0.11070218139702,135.723278636102));
#46478=CARTESIAN_POINT('Ctrl Pts',(99.5759703542959,0.0265857235032949,
135.724449326));
#46479=CARTESIAN_POINT('Ctrl Pts',(99.568222286293,0.163610670680727,135.719888525221));
#46480=CARTESIAN_POINT('Ctrl Pts',(99.5604659835511,0.300781249603198,135.71532287717));
#46481=CARTESIAN_POINT('Ctrl Pts',(99.5527096808093,0.437687921150294,135.705013583047));
#46482=CARTESIAN_POINT('Ctrl Pts',(99.5449533780674,0.573818036248256,135.689021908155));
#46483=CARTESIAN_POINT('Ctrl Pts',(99.5371929355533,0.710020808087536,135.673021698024));
#46484=CARTESIAN_POINT('Ctrl Pts',(99.5294324930391,0.84544581175113,135.651333125692));
#46485=CARTESIAN_POINT('Ctrl Pts',(99.5216720505249,0.979590154943948,135.62406871981));
#46486=CARTESIAN_POINT('Ctrl Pts',(99.5138991502595,1.11394983854523,135.596760546683));
#46487=CARTESIAN_POINT('Ctrl Pts',(99.5061262499941,1.24702437371728,135.563858747301));
#46488=CARTESIAN_POINT('Ctrl Pts',(99.4983533497286,1.3783247358068,135.525526150055));
#46489=CARTESIAN_POINT('Ctrl Pts',(99.4908630139665,1.50485199900952,135.488587039273));
#46490=CARTESIAN_POINT('Ctrl Pts',(99.4833726782045,1.62973154901008,135.446605220029));
#46491=CARTESIAN_POINT('Ctrl Pts',(99.4758823424424,1.75254478772631,135.399768089109));
#46492=CARTESIAN_POINT('Ctrl Pts',(99.4681080083233,1.88001452771585,135.351155114135));
#46493=CARTESIAN_POINT('Ctrl Pts',(99.4603336742042,2.0056619607795,135.297157389952));
#46494=CARTESIAN_POINT('Ctrl Pts',(99.4525593400851,2.12899862333067,135.237931179129));
#46495=CARTESIAN_POINT('Ctrl Pts',(99.4447945871381,2.25218328446766,135.178777959318));
#46496=CARTESIAN_POINT('Ctrl Pts',(99.437029834191,2.37306249234812,135.11440924141));
#46497=CARTESIAN_POINT('Ctrl Pts',(99.429265081244,2.49116512839206,135.045030301187));
#46498=CARTESIAN_POINT('Ctrl Pts',(99.421508040359,2.60915046323331,134.975720269106));
#46499=CARTESIAN_POINT('Ctrl Pts',(99.413750999474,2.72436437932463,134.901410114367));
#46500=CARTESIAN_POINT('Ctrl Pts',(99.405993958589,2.83635818834796,134.82235206727));
#46501=CARTESIAN_POINT('Ctrl Pts',(99.3982427673489,2.94826754196849,134.743353638461));
#46502=CARTESIAN_POINT('Ctrl Pts',(99.3904915761088,3.05696130381164,134.659614668465));
#46503=CARTESIAN_POINT('Ctrl Pts',(99.3827403848687,3.16201805105393,134.571431748738));
#46504=CARTESIAN_POINT('Ctrl Pts',(99.3749924880916,3.26703014637637,134.483286309104));
#46505=CARTESIAN_POINT('Ctrl Pts',(99.3672445913145,3.36840800280452,134.390700927245));
#46506=CARTESIAN_POINT('Ctrl Pts',(99.3594966945374,3.46576188815781,134.294013551182));
#46507=CARTESIAN_POINT('Ctrl Pts',(99.3517504184533,3.56309540917699,134.197346400034));
#46508=CARTESIAN_POINT('Ctrl Pts',(99.3440041423693,3.65640635613809,134.096579236717));
#46509=CARTESIAN_POINT('Ctrl Pts',(99.3362578662852,3.74534090487162,133.992087796732));
#46510=CARTESIAN_POINT('Ctrl Pts',(99.3285115330198,3.83427611009972,133.887595585416));
#46511=CARTESIAN_POINT('Ctrl Pts',(99.3207651997545,3.91883459923561,133.779379340302));
#46512=CARTESIAN_POINT('Ctrl Pts',(99.3130188664891,3.99870226016051,133.66784857757));
#46513=CARTESIAN_POINT('Ctrl Pts',(99.3052707984862,4.07858780689437,133.556292838296));
#46514=CARTESIAN_POINT('Ctrl Pts',(99.2975227304832,4.15378020750377,133.441421422194));
#46515=CARTESIAN_POINT('Ctrl Pts',(99.2897746624802,4.22400840761036,133.32367322916));
#46516=CARTESIAN_POINT('Ctrl Pts',(99.2820183597384,4.29431124708375,133.205799891946));
#46517=CARTESIAN_POINT('Ctrl Pts',(99.2742620569965,4.35963914606689,133.085044006483));
#46518=CARTESIAN_POINT('Ctrl Pts',(99.2665057542547,4.41976654944531,132.961869994348));
#46519=CARTESIAN_POINT('Ctrl Pts',(99.2587453117405,4.47992604462927,132.838630240535));
#46520=CARTESIAN_POINT('Ctrl Pts',(99.2509848692264,4.5348793568942,132.712970146399));
#46521=CARTESIAN_POINT('Ctrl Pts',(99.2432244267122,4.58444933421086,132.585373633957));
#46522=CARTESIAN_POINT('Ctrl Pts',(99.2354515264468,4.63409888565576,132.457572292265));
#46523=CARTESIAN_POINT('Ctrl Pts',(99.2276786261814,4.67834770679495,132.327828690721));
#46524=CARTESIAN_POINT('Ctrl Pts',(99.2199057259159,4.71706845999541,132.196642272339));
#46525=CARTESIAN_POINT('Ctrl Pts',(99.2124153901538,4.75438161628592,132.070224810701));
#46526=CARTESIAN_POINT('Ctrl Pts',(99.2049250543917,4.78656156989748,131.942467909748));
#46527=CARTESIAN_POINT('Ctrl Pts',(99.1974347186295,4.81353972056436,131.81382504044));
#46528=CARTESIAN_POINT('Ctrl Pts',(99.1896603845104,4.84154075601318,131.680304637645));
#46529=CARTESIAN_POINT('Ctrl Pts',(99.1818860503913,4.86402644804321,131.5454068048));
#46530=CARTESIAN_POINT('Ctrl Pts',(99.1741117162723,4.88086423827874,131.409626963889));
#46531=CARTESIAN_POINT('Ctrl Pts',(99.1663469633251,4.89768127744267,131.274014459498));
#46532=CARTESIAN_POINT('Ctrl Pts',(99.1585822103781,4.90886421654812,131.137522494107));
#46533=CARTESIAN_POINT('Ctrl Pts',(99.150817457431,4.9143311088241,131.000658389697));
#46534=CARTESIAN_POINT('Ctrl Pts',(99.143060416546,4.91979257130559,130.863930220645));
#46535=CARTESIAN_POINT('Ctrl Pts',(99.1353033756609,4.91954926945457,130.726831036248));
#46536=CARTESIAN_POINT('Ctrl Pts',(99.1275463347759,4.9135708847692,130.589874667331));
#46537=CARTESIAN_POINT('Ctrl Pts',(99.1197951435358,4.90759700843023,130.453021578277));
#46538=CARTESIAN_POINT('Ctrl Pts',(99.1120439522957,4.89589667463061,130.31631147935));
#46539=CARTESIAN_POINT('Ctrl Pts',(99.1042927610556,4.87849162483249,130.180259240433));
#46540=CARTESIAN_POINT('Ctrl Pts',(99.0965448642785,4.86109397264482,130.044264827347));
#46541=CARTESIAN_POINT('Ctrl Pts',(99.0887969675014,4.83799647642319,129.908928105145));
#46542=CARTESIAN_POINT('Ctrl Pts',(99.0810490707244,4.80927280164692,129.77475963571));
#46543=CARTESIAN_POINT('Ctrl Pts',(99.0733027946403,4.78055513524419,129.640619231426));
#46544=CARTESIAN_POINT('Ctrl Pts',(99.0655565185561,4.74621371295018,129.507646975896));
#46545=CARTESIAN_POINT('Ctrl Pts',(99.057810242472,4.70637340107757,129.376343645633));
#46546=CARTESIAN_POINT('Ctrl Pts',(99.0500639092067,4.6665327951129,129.245039346118));
#46547=CARTESIAN_POINT('Ctrl Pts',(99.0423175759414,4.62119333208913,129.115404370574));
#46548=CARTESIAN_POINT('Ctrl Pts',(99.034571242676,4.57052976429298,128.987924343921));
#46549=CARTESIAN_POINT('Ctrl Pts',(99.0268231746731,4.51985485074218,128.860415769001));
#46550=CARTESIAN_POINT('Ctrl Pts',(99.0190751066701,4.46385360425319,128.735063466515));
#46551=CARTESIAN_POINT('Ctrl Pts',(99.0113270386671,4.40274877222889,128.612332718305));
#46552=CARTESIAN_POINT('Ctrl Pts',(99.0035707359253,4.3415789972618,128.489471530396));
#46553=CARTESIAN_POINT('Ctrl Pts',(98.9958144331834,4.27529497596077,128.36923781308));
#46554=CARTESIAN_POINT('Ctrl Pts',(98.9880581304416,4.20416552130183,128.25207236347));
#46555=CARTESIAN_POINT('Ctrl Pts',(98.9802976879274,4.13299810271118,128.134844379131));
#46556=CARTESIAN_POINT('Ctrl Pts',(98.9725372454132,4.05698031422455,128.020688250865));
#46557=CARTESIAN_POINT('Ctrl Pts',(98.964776802899,3.97642353813905,127.910014593361));
#46558=CARTESIAN_POINT('Ctrl Pts',(98.9570039026336,3.89573744516513,127.799163272676));
#46559=CARTESIAN_POINT('Ctrl Pts',(98.9492310023682,3.81049804731964,127.691805900461));
#46560=CARTESIAN_POINT('Ctrl Pts',(98.9414581021027,3.72105671105376,127.588319570623));
#46561=CARTESIAN_POINT('Ctrl Pts',(98.9339677663407,3.63486679264991,127.48859522954));
#46562=CARTESIAN_POINT('Ctrl Pts',(98.9264774305786,3.54477534458148,127.392465597583));
#46563=CARTESIAN_POINT('Ctrl Pts',(98.9189870948165,3.45112680469209,127.30023350223));
#46564=CARTESIAN_POINT('Ctrl Pts',(98.9112127606974,3.35392755194935,127.204504398948));
#46565=CARTESIAN_POINT('Ctrl Pts',(98.9034384265783,3.25258825045728,127.112670975699));
#46566=CARTESIAN_POINT('Ctrl Pts',(98.8956640924592,3.14745406172249,127.025112545284));
#46567=CARTESIAN_POINT('Ctrl Pts',(98.8878993395122,3.04244944147934,126.937662022809));
#46568=CARTESIAN_POINT('Ctrl Pts',(98.8801345865651,2.93365953708844,126.854476258127));
#46569=CARTESIAN_POINT('Ctrl Pts',(98.872369833618,2.82146687866708,126.7758984153));
#46570=CARTESIAN_POINT('Ctrl Pts',(98.864612792733,2.70938565157577,126.697398617094));
#46571=CARTESIAN_POINT('Ctrl Pts',(98.856855751848,2.59390871429774,126.623497855831));
#46572=CARTESIAN_POINT('Ctrl Pts',(98.8490987109631,2.47545197936939,126.554499377439));
#46573=CARTESIAN_POINT('Ctrl Pts',(98.841347519723,2.35708457358679,126.485552931336));
#46574=CARTESIAN_POINT('Ctrl Pts',(98.8335963284829,2.23574217931364,126.421501605732));
#46575=CARTESIAN_POINT('Ctrl Pts',(98.8258451372428,2.11186972295615,126.362605408669));
#46576=CARTESIAN_POINT('Ctrl Pts',(98.8180972404657,1.98804991569626,126.303734244061));
#46577=CARTESIAN_POINT('Ctrl Pts',(98.8103493436886,1.86170253747707,126.250014017653));
#46578=CARTESIAN_POINT('Ctrl Pts',(98.8026014469116,1.73329695646108,126.201658723762));
#46579=CARTESIAN_POINT('Ctrl Pts',(98.7948551708274,1.60491823512436,126.153313544756));
#46580=CARTESIAN_POINT('Ctrl Pts',(98.7871088947433,1.47448253299151,126.11033120379));
#46581=CARTESIAN_POINT('Ctrl Pts',(98.7793626186592,1.34247866081608,126.072877329235));
#46582=CARTESIAN_POINT('Ctrl Pts',(98.7716162853939,1.21047381421841,126.035423178204));
#46583=CARTESIAN_POINT('Ctrl Pts',(98.7638699521285,1.07690115059797,126.003497681735));
#46584=CARTESIAN_POINT('Ctrl Pts',(98.7561236188632,0.942263697832593,125.97721630791));
#46585=CARTESIAN_POINT('Ctrl Pts',(98.7483755508602,0.807596093943093,125.950929048553));
#46586=CARTESIAN_POINT('Ctrl Pts',(98.7406274828573,0.671863610066019,125.930288501868));
#46587=CARTESIAN_POINT('Ctrl Pts',(98.7328794148543,0.535578101404049,125.915358760357));
#46588=CARTESIAN_POINT('Ctrl Pts',(98.7251231121125,0.399147746881654,125.900413151338));
#46589=CARTESIAN_POINT('Ctrl Pts',(98.7173668093706,0.262163582717695,125.891190514639));
#46590=CARTESIAN_POINT('Ctrl Pts',(98.7096105066288,0.125141763985987,125.887702951894));
#46591=CARTESIAN_POINT('Ctrl Pts',(98.7018500641146,-0.0119531874161191,
125.884213527733));
#46592=CARTESIAN_POINT('Ctrl Pts',(98.6940896216004,-0.149085442710467,
125.886465270376));
#46593=CARTESIAN_POINT('Ctrl Pts',(98.6863291790862,-0.285741230392769,
125.894418152348));
#46594=CARTESIAN_POINT('Ctrl Pts',(98.6785562788208,-0.422616390077281,
125.902383800991));
#46595=CARTESIAN_POINT('Ctrl Pts',(98.6707833785554,-0.559013164463572,
125.916068838473));
#46596=CARTESIAN_POINT('Ctrl Pts',(98.6630104782899,-0.694424371619658,
125.935381478711));
#46597=CARTESIAN_POINT('Ctrl Pts',(98.6555201425279,-0.824913040315651,
125.953992055832));
#46598=CARTESIAN_POINT('Ctrl Pts',(98.6480298067659,-0.954486250500531,
125.977828128445));
#46599=CARTESIAN_POINT('Ctrl Pts',(98.6405394710038,-1.08270304777291,126.006763596885));
#46600=CARTESIAN_POINT('Ctrl Pts',(98.6327651368848,-1.21578122388396,126.036796162407));
#46601=CARTESIAN_POINT('Ctrl Pts',(98.6249908027657,-1.34781965152687,126.072417578408));
#46602=CARTESIAN_POINT('Ctrl Pts',(98.6172164686466,-1.47831263587522,126.113542478572));
#46603=CARTESIAN_POINT('Ctrl Pts',(98.6094517156995,-1.60864479928285,126.154616695973));
#46604=CARTESIAN_POINT('Ctrl Pts',(98.6016869627524,-1.73743493971715,126.201180785891));
#46605=CARTESIAN_POINT('Ctrl Pts',(98.5939222098053,-1.86418757666274,126.253098403464));
#46606=CARTESIAN_POINT('Ctrl Pts',(98.5861651689203,-1.99081432110224,126.304964455726));
#46607=CARTESIAN_POINT('Ctrl Pts',(98.5784081280354,-2.11540722981075,126.362173306946));
#46608=CARTESIAN_POINT('Ctrl Pts',(98.5706510871504,-2.23748636251614,126.424538949957));
#46609=CARTESIAN_POINT('Ctrl Pts',(98.5628998959103,-2.35947343439792,126.486857562552));
#46610=CARTESIAN_POINT('Ctrl Pts',(98.5551487046702,-2.47895015671362,126.55432504942));
#46611=CARTESIAN_POINT('Ctrl Pts',(98.5473975134301,-2.59545728374445,126.626707622072));
#46612=CARTESIAN_POINT('Ctrl Pts',(98.539649616653,-2.7119148921386,126.6990594302));
#46613=CARTESIAN_POINT('Ctrl Pts',(98.5319017198759,-2.82540508418448,126.776321963277));
#46614=CARTESIAN_POINT('Ctrl Pts',(98.5241538230988,-2.93549411544786,126.858215997729));
#46615=CARTESIAN_POINT('Ctrl Pts',(98.5164075470147,-3.04556011845922,126.940092901714));
#46616=CARTESIAN_POINT('Ctrl Pts',(98.5086612709306,-3.15222606230903,127.026599146855));
#46617=CARTESIAN_POINT('Ctrl Pts',(98.5009149948465,-3.25508838500562,127.117413009001));
#46618=CARTESIAN_POINT('Ctrl Pts',(98.4931686615812,-3.35795146700837,127.208227541515));
#46619=CARTESIAN_POINT('Ctrl Pts',(98.4854223283158,-3.45701057874577,127.303349495727));
#46620=CARTESIAN_POINT('Ctrl Pts',(98.4776759950505,-3.5518966747943,127.402418073359));
#46621=CARTESIAN_POINT('Ctrl Pts',(98.4699279270476,-3.64680401992537,127.501508836711));
#46622=CARTESIAN_POINT('Ctrl Pts',(98.4621798590446,-3.73753621940716,127.604547699883));
#46623=CARTESIAN_POINT('Ctrl Pts',(98.4544317910417,-3.82376268016293,127.711138668159));
#46624=CARTESIAN_POINT('Ctrl Pts',(98.4466754882999,-3.91008078342812,127.817842922586));
#46625=CARTESIAN_POINT('Ctrl Pts',(98.438919185558,-3.99188333563701,127.928106519079));
#46626=CARTESIAN_POINT('Ctrl Pts',(98.4311628828162,-4.06888116091525,128.041501742985));
#46627=CARTESIAN_POINT('Ctrl Pts',(98.423402440302,-4.14592008225131,128.154957489338));
#46628=CARTESIAN_POINT('Ctrl Pts',(98.4156419977878,-4.21814896102131,128.271547861405));
#46629=CARTESIAN_POINT('Ctrl Pts',(98.4078815552736,-4.28532376742706,128.39081897284));
#46630=CARTESIAN_POINT('Ctrl Pts',(98.4001086550082,-4.35260640879552,128.510281548853));
#46631=CARTESIAN_POINT('Ctrl Pts',(98.3923357547427,-4.41481858741458,128.632433115135));
#46632=CARTESIAN_POINT('Ctrl Pts',(98.3845628544773,-4.47176338128977,128.756797352547));
#46633=CARTESIAN_POINT('Ctrl Pts',(98.3770725187151,-4.52663808847352,128.876640636677));
#46634=CARTESIAN_POINT('Ctrl Pts',(98.3695821829529,-4.57662161061937,128.998538227587));
#46635=CARTESIAN_POINT('Ctrl Pts',(98.3620918471907,-4.62158169232119,129.122050977903));
#46636=CARTESIAN_POINT('Ctrl Pts',(98.3529410384216,-4.67650861722246,129.27294428824));
#46637=CARTESIAN_POINT('Ctrl Pts',(98.3437902296526,-4.72408470636501,129.426648390468));
#46638=CARTESIAN_POINT('Ctrl Pts',(98.3346394208835,-4.76405452823406,129.582490119308));
#46639=CARTESIAN_POINT('Ctrl Pts',(100.084952068471,-4.76405452823407,129.582490119308));
#46640=CARTESIAN_POINT('Ctrl Pts',(100.077187675489,-4.79809848252394,129.715226980395));
#46641=CARTESIAN_POINT('Ctrl Pts',(100.069423282507,-4.8265572118817,129.849256871815));
#46642=CARTESIAN_POINT('Ctrl Pts',(100.061658889525,-4.84936144496104,129.984070035744));
#46643=CARTESIAN_POINT('Ctrl Pts',(100.053883610672,-4.87219765013864,130.119072211061));
#46644=CARTESIAN_POINT('Ctrl Pts',(100.046108331819,-4.88936348605365,130.254859464739));
#46645=CARTESIAN_POINT('Ctrl Pts',(100.038333052966,-4.90084161242132,130.39091829697));
#46646=CARTESIAN_POINT('Ctrl Pts',(100.036481232,-4.90357533238947,130.42332312809));
#46647=CARTESIAN_POINT('Ctrl Pts',(100.034629411034,-4.9059866557627,130.455743372047));
#46648=CARTESIAN_POINT('Ctrl Pts',(100.032777590068,-4.90807578324186,130.488172116107));
#46649=CARTESIAN_POINT('Ctrl Pts',(100.026804872043,-4.91481389107284,130.592765242415));
#46650=CARTESIAN_POINT('Ctrl Pts',(100.020832154017,-4.91820900626066,130.697576041031));
#46651=CARTESIAN_POINT('Ctrl Pts',(100.014859435991,-4.91824963103831,130.802455547603));
#46652=CARTESIAN_POINT('',(100.360140563971,-4.91824789728292,130.808908515121));
#46653=CARTESIAN_POINT('Ctrl Pts',(100.43015599918,-4.76405452823403,129.582490119308));
#46654=CARTESIAN_POINT('Ctrl Pts',(100.422499773494,-4.79776724258496,129.713935480901));
#46655=CARTESIAN_POINT('Ctrl Pts',(100.414843547808,-4.82603171654888,129.846761741419));
#46656=CARTESIAN_POINT('Ctrl Pts',(100.407187322122,-4.84875148222177,129.980472199058));
#46657=CARTESIAN_POINT('Ctrl Pts',(100.399346195769,-4.87201993859153,130.117411813425));
#46658=CARTESIAN_POINT('Ctrl Pts',(100.391505069417,-4.88947237101566,130.255278441819));
#46659=CARTESIAN_POINT('Ctrl Pts',(100.383663943065,-4.90106137271956,130.393531597977));
#46660=CARTESIAN_POINT('Ctrl Pts',(100.375822816713,-4.91265037442346,130.531784754135));
#46661=CARTESIAN_POINT('Ctrl Pts',(100.36798169036,-4.91837595373029,130.670423987494));
#46662=CARTESIAN_POINT('Ctrl Pts',(100.360140564008,-4.91824789728353,130.80890851446));
#46663=CARTESIAN_POINT('Ctrl Pts',(100.360140563971,-4.91824789728292,130.808908515121));
#46664=CARTESIAN_POINT('Ctrl Pts',(100.350122548475,-4.91808428919946,130.985839746017));
#46665=CARTESIAN_POINT('Ctrl Pts',(100.340104532979,-4.90836974886036,131.162344238964));
#46666=CARTESIAN_POINT('Ctrl Pts',(100.330086517483,-4.88926273780238,131.3375518996));
#46667=CARTESIAN_POINT('Ctrl Pts',(100.319830746939,-4.86970226484551,131.516917719681));
#46668=CARTESIAN_POINT('Ctrl Pts',(100.309574976395,-4.84029819124037,131.694924725954));
#46669=CARTESIAN_POINT('Ctrl Pts',(100.299319205851,-4.80126838982909,131.870664941541));
#46670=CARTESIAN_POINT('Ctrl Pts',(100.296758209808,-4.79152215315772,131.914549503385));
#46671=CARTESIAN_POINT('Ctrl Pts',(100.294197213765,-4.78117592073932,131.958292825173));
#46672=CARTESIAN_POINT('Ctrl Pts',(100.291636217722,-4.77023354346506,132.001880973677));
#46673=CARTESIAN_POINT('Ctrl Pts',(100.283861883603,-4.73701611729094,132.134200127798));
#46674=CARTESIAN_POINT('Ctrl Pts',(100.276087549484,-4.69823640118361,132.265345715872));
#46675=CARTESIAN_POINT('Ctrl Pts',(100.268313215365,-4.65399187215868,132.394814237255));
#46676=CARTESIAN_POINT('Ctrl Pts',(100.260548462417,-4.60980187056156,132.524123200256));
#46677=CARTESIAN_POINT('Ctrl Pts',(100.25278370947,-4.56016058169338,132.651758842545));
#46678=CARTESIAN_POINT('Ctrl Pts',(100.245018956523,-4.50521620132081,132.777229098194));
#46679=CARTESIAN_POINT('Ctrl Pts',(100.237261915638,-4.45032639248137,132.902574735017));
#46680=CARTESIAN_POINT('Ctrl Pts',(100.229504874753,-4.39014412972855,133.025758909359));
#46681=CARTESIAN_POINT('Ctrl Pts',(100.221747833868,-4.32486688390532,133.146306282819));
#46682=CARTESIAN_POINT('Ctrl Pts',(100.213996642628,-4.25963886416082,133.266762750568));
#46683=CARTESIAN_POINT('Ctrl Pts',(100.206245451388,-4.18932369435945,133.384586032884));
#46684=CARTESIAN_POINT('Ctrl Pts',(100.198494260148,-4.11416611629642,133.499322626578));
#46685=CARTESIAN_POINT('Ctrl Pts',(100.190746363371,-4.03904048220912,133.614010454159));
#46686=CARTESIAN_POINT('Ctrl Pts',(100.182998466594,-3.95907674715038,133.725613876076));
#46687=CARTESIAN_POINT('Ctrl Pts',(100.175250569816,-3.87456446295535,133.833705973398));
#46688=CARTESIAN_POINT('Ctrl Pts',(100.167504293732,-3.7900698569083,133.941775460184));
#46689=CARTESIAN_POINT('Ctrl Pts',(100.159758017648,-3.70102883488634,134.046334775518));
#46690=CARTESIAN_POINT('Ctrl Pts',(100.152011741564,-3.60777271276643,134.146988194117));
#46691=CARTESIAN_POINT('Ctrl Pts',(100.144265408299,-3.51451590225101,134.247642355716));
#46692=CARTESIAN_POINT('Ctrl Pts',(100.136519075033,-3.41704419526475,134.344390276256));
#46693=CARTESIAN_POINT('Ctrl Pts',(100.128772741768,-3.31572714226006,134.436871674752));
#46694=CARTESIAN_POINT('Ctrl Pts',(100.121024673765,-3.21438740000391,134.529373783816));
#46695=CARTESIAN_POINT('Ctrl Pts',(100.113276605762,-3.10920088686629,134.61760720606));
#46696=CARTESIAN_POINT('Ctrl Pts',(100.105528537759,-3.00057141684857,134.701250946391));
#46697=CARTESIAN_POINT('Ctrl Pts',(100.097772235017,-2.89182649413733,134.784983584285));
#46698=CARTESIAN_POINT('Ctrl Pts',(100.090015932275,-2.77963161513725,134.864116557094));
#46699=CARTESIAN_POINT('Ctrl Pts',(100.082259629534,-2.66442131075266,134.938371036192));
#46700=CARTESIAN_POINT('Ctrl Pts',(100.074499187019,-2.54914951515972,135.012665147141));
#46701=CARTESIAN_POINT('Ctrl Pts',(100.066738744505,-2.43085942430564,135.082075378324));
#46702=CARTESIAN_POINT('Ctrl Pts',(100.058978301991,-2.31001064987067,135.146368662237));
#46703=CARTESIAN_POINT('Ctrl Pts',(100.051205401726,-2.18896787825445,135.210765155437));
#46704=CARTESIAN_POINT('Ctrl Pts',(100.04343250146,-2.06535856785564,135.270028117703));
#46705=CARTESIAN_POINT('Ctrl Pts',(100.035659601195,-1.93966362623258,135.323972114096));
#46706=CARTESIAN_POINT('Ctrl Pts',(100.028169265433,-1.81853801234627,135.375955110343));
#46707=CARTESIAN_POINT('Ctrl Pts',(100.020678929671,-1.69547605822335,135.422999032394));
#46708=CARTESIAN_POINT('Ctrl Pts',(100.013188593909,-1.57091995854025,135.464982201256));
#46709=CARTESIAN_POINT('Ctrl Pts',(100.00541425979,-1.44164127647739,135.508557174727));
#46710=CARTESIAN_POINT('Ctrl Pts',(99.9976399256709,-1.31034339519215,135.54681809503));
#46711=CARTESIAN_POINT('Ctrl Pts',(99.9898655915518,-1.17750261274296,135.579574817943));
#46712=CARTESIAN_POINT('Ctrl Pts',(99.9821008386047,-1.04482554468581,135.612291171123));
#46713=CARTESIAN_POINT('Ctrl Pts',(99.9743360856576,-0.910609734809486,
135.639516731215));
#46714=CARTESIAN_POINT('Ctrl Pts',(99.9665713327105,-0.775349275547373,
135.661110205861));
#46715=CARTESIAN_POINT('Ctrl Pts',(99.9588142918255,-0.640223158880329,
135.682682233564));
#46716=CARTESIAN_POINT('Ctrl Pts',(99.9510572509405,-0.504054841197791,
135.698633246633));
#46717=CARTESIAN_POINT('Ctrl Pts',(99.9433002100555,-0.367350975973875,
135.708872450863));
#46718=CARTESIAN_POINT('Ctrl Pts',(99.9355490188154,-0.230750200198219,
135.719103933629));
#46719=CARTESIAN_POINT('Ctrl Pts',(99.9277978275753,-0.0936150690367489,
135.723632151932));
#46720=CARTESIAN_POINT('Ctrl Pts',(99.9200466363352,0.0435405835159097,
135.722417884423));
#46721=CARTESIAN_POINT('Ctrl Pts',(99.9122987395581,0.180637941257673,135.721204133011));
#46722=CARTESIAN_POINT('Ctrl Pts',(99.9045508427809,0.317755412911561,135.714252753627));
#46723=CARTESIAN_POINT('Ctrl Pts',(99.8968029460039,0.45437730965064,135.70157659432));
#46724=CARTESIAN_POINT('Ctrl Pts',(99.8890566699198,0.590970628034148,135.688903086593));
#46725=CARTESIAN_POINT('Ctrl Pts',(99.8813103938356,0.727068188648891,135.670507216934));
#46726=CARTESIAN_POINT('Ctrl Pts',(99.8735641177515,0.862157972282204,135.646453831593));
#46727=CARTESIAN_POINT('Ctrl Pts',(99.8658177844862,0.99724875311752,135.622400268696));
#46728=CARTESIAN_POINT('Ctrl Pts',(99.8580714512209,1.13133135721577,135.592689175317));
#46729=CARTESIAN_POINT('Ctrl Pts',(99.8503251179555,1.26390291893541,135.557436724048));
#46730=CARTESIAN_POINT('Ctrl Pts',(99.8425770499525,1.39650416913711,135.522176378236));
#46731=CARTESIAN_POINT('Ctrl Pts',(99.8348289819496,1.52759332584556,135.48137230564));
#46732=CARTESIAN_POINT('Ctrl Pts',(99.8270809139466,1.65668205546671,135.435190740729));
#46733=CARTESIAN_POINT('Ctrl Pts',(99.8193246112047,1.78590798212587,135.388960093501));
#46734=CARTESIAN_POINT('Ctrl Pts',(99.8115683084629,1.9131288659241,135.337340669008));
#46735=CARTESIAN_POINT('Ctrl Pts',(99.803812005721,2.03787524587325,135.280547336723));
#46736=CARTESIAN_POINT('Ctrl Pts',(99.7960515632068,2.1626882067215,135.223723692126));
#46737=CARTESIAN_POINT('Ctrl Pts',(99.7882911206927,2.28502368351798,135.161720813935));
#46738=CARTESIAN_POINT('Ctrl Pts',(99.7805306781785,2.40443715863196,135.094799407794));
#46739=CARTESIAN_POINT('Ctrl Pts',(99.7727577779131,2.52404232685722,135.02777057347));
#46740=CARTESIAN_POINT('Ctrl Pts',(99.7649848776476,2.64071578702214,134.955807638518));
#46741=CARTESIAN_POINT('Ctrl Pts',(99.7572119773822,2.75404158517801,134.879214971971));
#46742=CARTESIAN_POINT('Ctrl Pts',(99.7497216416201,2.86324770512137,134.805406641777));
#46743=CARTESIAN_POINT('Ctrl Pts',(99.742231305858,2.96934508125772,134.727299523456));
#46744=CARTESIAN_POINT('Ctrl Pts',(99.7347409700959,3.07199232457968,134.645199877444));
#46745=CARTESIAN_POINT('Ctrl Pts',(99.7269666359768,3.17853146933025,134.559987398401));
#46746=CARTESIAN_POINT('Ctrl Pts',(99.7191923018577,3.28169117715037,134.470203734325));
#46747=CARTESIAN_POINT('Ctrl Pts',(99.7114179677386,3.38105402358604,134.376146830666));
#46748=CARTESIAN_POINT('Ctrl Pts',(99.7036532147915,3.48029441419379,134.282205843735));
#46749=CARTESIAN_POINT('Ctrl Pts',(99.6958884618445,3.57574697260873,134.184002361948));
#46750=CARTESIAN_POINT('Ctrl Pts',(99.6881237088974,3.66702575653928,134.081875707291));
#46751=CARTESIAN_POINT('Ctrl Pts',(99.6803666680124,3.75821388109476,133.979850486268));
#46752=CARTESIAN_POINT('Ctrl Pts',(99.6726096271274,3.84523622194897,133.873910136304));
#46753=CARTESIAN_POINT('Ctrl Pts',(99.6648525862424,3.92774253278796,133.764431842829));
#46754=CARTESIAN_POINT('Ctrl Pts',(99.6571013950023,4.01018662497609,133.655036107787));
#46755=CARTESIAN_POINT('Ctrl Pts',(99.6493502037621,4.08812123138416,133.542108050672));
#46756=CARTESIAN_POINT('Ctrl Pts',(99.641599012522,4.16123561415702,133.426058774481));
#46757=CARTESIAN_POINT('Ctrl Pts',(99.6338511157449,4.23431892136685,133.310058822328));
#46758=CARTESIAN_POINT('Ctrl Pts',(99.6261032189679,4.30258587172688,133.190940619703));
#46759=CARTESIAN_POINT('Ctrl Pts',(99.6183553221908,4.36576853225753,133.069144974906));
#46760=CARTESIAN_POINT('Ctrl Pts',(99.6106090461067,4.42893797633766,132.947374807132));
#46761=CARTESIAN_POINT('Ctrl Pts',(99.6028627700226,4.48702506607574,132.822928658009));
#46762=CARTESIAN_POINT('Ctrl Pts',(99.5951164939385,4.5398075995663,132.696272354783));
#46763=CARTESIAN_POINT('Ctrl Pts',(99.5873701606731,4.59259052268554,132.56961511661));
#46764=CARTESIAN_POINT('Ctrl Pts',(99.5796238274078,4.64006866102898,132.44074805266));
#46765=CARTESIAN_POINT('Ctrl Pts',(99.5718774941424,4.68206794272422,132.310157032163));
#46766=CARTESIAN_POINT('Ctrl Pts',(99.5641294261394,4.72407662986739,132.179536766713));
#46767=CARTESIAN_POINT('Ctrl Pts',(99.5563813581365,4.76060389919301,132.047192148604));
#46768=CARTESIAN_POINT('Ctrl Pts',(99.5486332901335,4.79152565223085,131.913623880508));
#46769=CARTESIAN_POINT('Ctrl Pts',(99.5408769873916,4.8224802692758,131.779913654468));
#46770=CARTESIAN_POINT('Ctrl Pts',(99.5331206846498,4.84781738074743,131.644977562033));
#46771=CARTESIAN_POINT('Ctrl Pts',(99.5253643819079,4.86746400728748,131.509326716227));
#46772=CARTESIAN_POINT('Ctrl Pts',(99.5176039393938,4.88712111982367,131.373603469479));
#46773=CARTESIAN_POINT('Ctrl Pts',(99.5098434968796,4.90108165580695,131.237165097963));
#46774=CARTESIAN_POINT('Ctrl Pts',(99.5020830543654,4.90932468164281,131.100526504718));
#46775=CARTESIAN_POINT('Ctrl Pts',(99.4943101541,4.91758093991554,130.963668567074));
#46776=CARTESIAN_POINT('Ctrl Pts',(99.4865372538345,4.92010133977055,130.826610156539));
#46777=CARTESIAN_POINT('Ctrl Pts',(99.4787643535691,4.91691712222713,130.689865745848));
#46778=CARTESIAN_POINT('Ctrl Pts',(99.4712740178071,4.91384865901198,130.558092338925));
#46779=CARTESIAN_POINT('Ctrl Pts',(99.4637836820451,4.90548315163427,130.426610806224));
#46780=CARTESIAN_POINT('Ctrl Pts',(99.4562933462831,4.89189373657571,130.295873909233));
#46781=CARTESIAN_POINT('Ctrl Pts',(99.448519012164,4.87778907471478,130.160180083056));
#46782=CARTESIAN_POINT('Ctrl Pts',(99.4407446780449,4.85801187721498,130.024858635711));
#46783=CARTESIAN_POINT('Ctrl Pts',(99.4329703439258,4.83258718590767,129.890421805007));
#46784=CARTESIAN_POINT('Ctrl Pts',(99.4252055909787,4.80719382826012,129.756150655683));
#46785=CARTESIAN_POINT('Ctrl Pts',(99.4174408380317,4.77616689714709,129.622762334272));
#46786=CARTESIAN_POINT('Ctrl Pts',(99.4096760850846,4.73958326253042,129.490764956778));
#46787=CARTESIAN_POINT('Ctrl Pts',(99.4019190441996,4.70303596329543,129.35889868094));
#46788=CARTESIAN_POINT('Ctrl Pts',(99.3941620033146,4.66094304735403,129.228420974086));
#46789=CARTESIAN_POINT('Ctrl Pts',(99.3864049624296,4.61343253480448,129.099830386298));
#46790=CARTESIAN_POINT('Ctrl Pts',(99.3786537711894,4.565957850302,128.971336769672));
#46791=CARTESIAN_POINT('Ctrl Pts',(99.3709025799493,4.51307383598483,128.844727804787));
#46792=CARTESIAN_POINT('Ctrl Pts',(99.3631513887092,4.45495840304577,128.72048713541));
#46793=CARTESIAN_POINT('Ctrl Pts',(99.3554034919321,4.39686767071599,128.596299271633));
#46794=CARTESIAN_POINT('Ctrl Pts',(99.347655595155,4.33355010742735,128.474478054732));
#46795=CARTESIAN_POINT('Ctrl Pts',(99.339907698378,4.26523175336659,128.355487171964));
#46796=CARTESIAN_POINT('Ctrl Pts',(99.3321614222939,4.19692769003272,128.236521179524));
#46797=CARTESIAN_POINT('Ctrl Pts',(99.3244151462097,4.12362511113706,128.120384682449));
#46798=CARTESIAN_POINT('Ctrl Pts',(99.3166688701256,4.04559582477728,128.007516416499));
#46799=CARTESIAN_POINT('Ctrl Pts',(99.3089225368603,3.96756596242304,127.89464731738));
#46800=CARTESIAN_POINT('Ctrl Pts',(99.3011762035949,3.8848095453101,127.785046819124));
#46801=CARTESIAN_POINT('Ctrl Pts',(99.2934298703296,3.79764125888202,127.67912399751));
#46802=CARTESIAN_POINT('Ctrl Pts',(99.2856818023266,3.71045345172064,127.573177455216));
#46803=CARTESIAN_POINT('Ctrl Pts',(99.2779337343236,3.61885205760961,127.470910530241));
#46804=CARTESIAN_POINT('Ctrl Pts',(99.2701856663207,3.5231912536341,127.372698272169));
#46805=CARTESIAN_POINT('Ctrl Pts',(99.2624293635788,3.42742878021768,127.27438163294));
#46806=CARTESIAN_POINT('Ctrl Pts',(99.254673060837,3.32759855170705,127.180128549516));
#46807=CARTESIAN_POINT('Ctrl Pts',(99.2469167580951,3.22409113483882,127.090276690572));
#46808=CARTESIAN_POINT('Ctrl Pts',(99.2391563155809,3.12052847294559,127.000376874985));
#46809=CARTESIAN_POINT('Ctrl Pts',(99.2313958730668,3.01328501755718,126.914883208183));
#46810=CARTESIAN_POINT('Ctrl Pts',(99.2236354305526,2.90278265606604,126.83409161986));
#46811=CARTESIAN_POINT('Ctrl Pts',(99.2158625302872,2.79210290637438,126.753170337708));
#46812=CARTESIAN_POINT('Ctrl Pts',(99.2080896300217,2.67815412158125,126.676966435197));
#46813=CARTESIAN_POINT('Ctrl Pts',(99.2003167297563,2.56138602870343,126.605731713452));
#46814=CARTESIAN_POINT('Ctrl Pts',(99.1928263939943,2.44886275012272,126.537086553272));
#46815=CARTESIAN_POINT('Ctrl Pts',(99.1853360582323,2.33372185183422,126.473055711512));
#46816=CARTESIAN_POINT('Ctrl Pts',(99.1778457224702,2.21638378695495,126.413822385023));
#46817=CARTESIAN_POINT('Ctrl Pts',(99.1700713883511,2.09459681368174,126.352343208956));
#46818=CARTESIAN_POINT('Ctrl Pts',(99.1622970542321,1.9700569891946,126.295837777632));
#46819=CARTESIAN_POINT('Ctrl Pts',(99.154522720113,1.84320880939055,126.244561899696));
#46820=CARTESIAN_POINT('Ctrl Pts',(99.1467579671659,1.71651695863145,126.193349214697));
#46821=CARTESIAN_POINT('Ctrl Pts',(99.1389932142188,1.58752277193361,126.147353404658));
#46822=CARTESIAN_POINT('Ctrl Pts',(99.1312284612717,1.45669529177267,126.106784445812));
#46823=CARTESIAN_POINT('Ctrl Pts',(99.1234714203867,1.32599775130947,126.066255780629));
#46824=CARTESIAN_POINT('Ctrl Pts',(99.1157143795017,1.19347091196947,126.031143355294));
#46825=CARTESIAN_POINT('Ctrl Pts',(99.1079573386168,1.05960341604697,126.00160894137));
#46826=CARTESIAN_POINT('Ctrl Pts',(99.1002061473766,0.925836870644291,125.972096799578));
#46827=CARTESIAN_POINT('Ctrl Pts',(99.0924549561365,0.790732061231549,125.948154380459));
#46828=CARTESIAN_POINT('Ctrl Pts',(99.0847037648964,0.654792056354769,125.929893423561));
#46829=CARTESIAN_POINT('Ctrl Pts',(99.0769558681193,0.51890982960638,125.911640228056));
#46830=CARTESIAN_POINT('Ctrl Pts',(99.0692079713422,0.382193500096363,125.899063743913));
#46831=CARTESIAN_POINT('Ctrl Pts',(99.0614600745651,0.24515536128886,125.892224431411));
#46832=CARTESIAN_POINT('Ctrl Pts',(99.053713798481,0.108145887905796,125.885386549546));
#46833=CARTESIAN_POINT('Ctrl Pts',(99.0459675223969,-0.0291848706485858,
125.884283471747));
#46834=CARTESIAN_POINT('Ctrl Pts',(99.0382212463128,-0.166320874636657,
125.888923665559));
#46835=CARTESIAN_POINT('Ctrl Pts',(99.0304749130475,-0.303457890931464,
125.893563893623));
#46836=CARTESIAN_POINT('Ctrl Pts',(99.0227285797821,-0.440399759049679,
125.903947464675));
#46837=CARTESIAN_POINT('Ctrl Pts',(99.0149822465168,-0.576632216781138,
125.92003074039));
#46838=CARTESIAN_POINT('Ctrl Pts',(99.0072341785138,-0.712895182826937,
125.936117617844));
#46839=CARTESIAN_POINT('Ctrl Pts',(98.9994861105109,-0.848448034163486,
125.957906694038));
#46840=CARTESIAN_POINT('Ctrl Pts',(98.9917380425079,-0.982783789588957,
125.985302713222));
#46841=CARTESIAN_POINT('Ctrl Pts',(98.9839817397661,-1.117262318654,126.012727849221));
#46842=CARTESIAN_POINT('Ctrl Pts',(98.9762254370242,-1.25052078412346,126.045771753956));
#46843=CARTESIAN_POINT('Ctrl Pts',(98.9684691342824,-1.38206398491655,126.084288350736));
#46844=CARTESIAN_POINT('Ctrl Pts',(98.9607086917682,-1.51367739427659,126.122825504984));
#46845=CARTESIAN_POINT('Ctrl Pts',(98.952948249254,-1.64357334466874,126.166841046089));
#46846=CARTESIAN_POINT('Ctrl Pts',(98.9451878067398,-1.77127482161698,126.216139985468));
#46847=CARTESIAN_POINT('Ctrl Pts',(98.9374149064744,-1.89918129631281,126.265518063882));
#46848=CARTESIAN_POINT('Ctrl Pts',(98.929642006209,-2.02488589923686,126.320196333034));
#46849=CARTESIAN_POINT('Ctrl Pts',(98.9218691059435,-2.1479336945329,126.379932529509));
#46850=CARTESIAN_POINT('Ctrl Pts',(98.9143787701815,-2.26650839253174,126.437497164775));
#46851=CARTESIAN_POINT('Ctrl Pts',(98.9068884344194,-2.38261582114992,126.499758229454));
#46852=CARTESIAN_POINT('Ctrl Pts',(98.8993980986574,-2.49587458650939,126.566461006802));
#46853=CARTESIAN_POINT('Ctrl Pts',(98.8916225640437,-2.61344574464242,126.635703530845));
#46854=CARTESIAN_POINT('Ctrl Pts',(98.8838470294301,-2.72831950036794,126.709952084004));
#46855=CARTESIAN_POINT('Ctrl Pts',(98.8760714948165,-2.84004016436807,126.788970857247));
#46856=CARTESIAN_POINT('Ctrl Pts',(98.8679116394048,-2.95728283770591,126.871895285791));
#46857=CARTESIAN_POINT('Ctrl Pts',(98.8597517839932,-3.07105237575799,126.960073382573));
#46858=CARTESIAN_POINT('Ctrl Pts',(98.8515919285816,-3.18085032049864,127.053177564037));
#46859=CARTESIAN_POINT('Ctrl Pts',(98.8438359823462,-3.2852133163126,127.141673130355));
#46860=CARTESIAN_POINT('Ctrl Pts',(98.8360800361107,-3.38598806948694,127.234618568138));
#46861=CARTESIAN_POINT('Ctrl Pts',(98.8283240898753,-3.48277611758001,127.331688220504));
#46862=CARTESIAN_POINT('Ctrl Pts',(98.8205734095931,-3.57949845076016,127.428691966761));
#46863=CARTESIAN_POINT('Ctrl Pts',(98.8128227293109,-3.67223918936309,127.529814080812));
#46864=CARTESIAN_POINT('Ctrl Pts',(98.8050720490286,-3.760634296572,127.634689853915));
#46865=CARTESIAN_POINT('Ctrl Pts',(98.7973249525395,-3.84898853126834,127.739517134103));
#46866=CARTESIAN_POINT('Ctrl Pts',(98.7895778560505,-3.93300088211774,127.848094320907));
#46867=CARTESIAN_POINT('Ctrl Pts',(98.7818307595614,-4.01234570138409,127.960021496595));
#46868=CARTESIAN_POINT('Ctrl Pts',(98.7740855674892,-4.09167101584442,128.071921157975));
#46869=CARTESIAN_POINT('Ctrl Pts',(98.766340375417,-4.16633085777311,128.187168849741));
#46870=CARTESIAN_POINT('Ctrl Pts',(98.7585951833448,-4.23604149092616,128.305333697012));
#46871=CARTESIAN_POINT('Ctrl Pts',(98.7508481870581,-4.30576836291918,128.423526070358));
#46872=CARTESIAN_POINT('Ctrl Pts',(98.7431011907714,-4.37054352053089,128.544636622193));
#46873=CARTESIAN_POINT('Ctrl Pts',(98.7353541944847,-4.43012799617072,128.668207767219));
#46874=CARTESIAN_POINT('Ctrl Pts',(98.7276061435344,-4.48972058354506,128.791795735022));
#46875=CARTESIAN_POINT('Ctrl Pts',(98.7198580925841,-4.54412091917249,128.917844607592));
#46876=CARTESIAN_POINT('Ctrl Pts',(98.7121100416338,-4.59313758346951,129.045875416656));
#46877=CARTESIAN_POINT('Ctrl Pts',(98.7043566509114,-4.64218802888359,129.173994461502));
#46878=CARTESIAN_POINT('Ctrl Pts',(98.6966032601891,-4.68584726356118,129.304097801933));
#46879=CARTESIAN_POINT('Ctrl Pts',(98.6888498694667,-4.72397323480069,129.435689751584));
#46880=CARTESIAN_POINT('Ctrl Pts',(98.6859782346235,-4.73809400742304,129.48442765752));
#46881=CARTESIAN_POINT('Ctrl Pts',(98.6831065997802,-4.75145625339996,129.533369636936));
#46882=CARTESIAN_POINT('Ctrl Pts',(98.680234964937,-4.76405452823403,129.582490119308));
#46883=CARTESIAN_POINT('Origin',(213.235140564004,0.,130.804360617566));
#46884=CARTESIAN_POINT('',(96.5847048906856,-4.76405452823403,129.582490119308));
#46885=CARTESIAN_POINT('',(96.929952524335,-4.76405452823408,129.582490119308));
#46886=CARTESIAN_POINT('',(213.235140564004,-4.76405452823405,129.582490119308));
#46887=CARTESIAN_POINT('',(98.2648594360458,-4.91824869076816,130.800771988677));
#46888=CARTESIAN_POINT('Ctrl Pts',(98.264859435991,-4.91824869076887,130.800771989647));
#46889=CARTESIAN_POINT('Ctrl Pts',(98.2570959853869,-4.9183490653254,130.938336273932));
#46890=CARTESIAN_POINT('Ctrl Pts',(98.2493325347827,-4.9126735820973,131.075952301792));
#46891=CARTESIAN_POINT('Ctrl Pts',(98.2415690841786,-4.90123596697668,131.213101438275));
#46892=CARTESIAN_POINT('Ctrl Pts',(98.2338061956604,-4.8897991799573,131.350240644946));
#46893=CARTESIAN_POINT('Ctrl Pts',(98.2260433071422,-4.87260112265808,131.486912640666));
#46894=CARTESIAN_POINT('Ctrl Pts',(98.218280418624,-4.84970751694911,131.622602673774));
#46895=CARTESIAN_POINT('Ctrl Pts',(98.2105164413888,-4.82681070049466,131.758311736918));
#46896=CARTESIAN_POINT('Ctrl Pts',(98.2027524641536,-4.7982168100034,131.893038180506));
#46897=CARTESIAN_POINT('Ctrl Pts',(98.1949884869183,-4.76404286757597,132.026276579651));
#46898=CARTESIAN_POINT('Ctrl Pts',(98.1872217698146,-4.72985686533635,132.159561997957));
#46899=CARTESIAN_POINT('Ctrl Pts',(98.1794550527109,-4.69008698798128,132.291357950785));
#46900=CARTESIAN_POINT('Ctrl Pts',(98.1716883356072,-4.64490027831379,132.421173676339));
#46901=CARTESIAN_POINT('Ctrl Pts',(98.1639122580396,-4.59965910952808,132.551145856081));
#46902=CARTESIAN_POINT('Ctrl Pts',(98.1561361804719,-4.54898819716927,132.679132674873));
#46903=CARTESIAN_POINT('Ctrl Pts',(98.1483601029043,-4.49310318454982,132.804662303684));
#46904=CARTESIAN_POINT('Ctrl Pts',(98.1405790537656,-4.43718244230799,132.93027218883));
#46905=CARTESIAN_POINT('Ctrl Pts',(98.1327980046268,-4.37604113030625,133.053421406858));
#46906=CARTESIAN_POINT('Ctrl Pts',(98.1250169554881,-4.30994067306685,133.173663143024));
#46907=CARTESIAN_POINT('Ctrl Pts',(98.1172230976868,-4.2437314055069,133.294102813402));
#46908=CARTESIAN_POINT('Ctrl Pts',(98.1094292398855,-4.17254688458937,133.411625108483));
#46909=CARTESIAN_POINT('Ctrl Pts',(98.1016353820842,-4.09669209365738,133.525811876043));
#46910=CARTESIAN_POINT('Ctrl Pts',(98.0956383291821,-4.03832495305826,133.613673895499));
#46911=CARTESIAN_POINT('Ctrl Pts',(98.08964127628,-3.9771935914175,133.699561650248));
#46912=CARTESIAN_POINT('Ctrl Pts',(98.0836442233779,-3.91345253844182,133.783298732375));
#46913=CARTESIAN_POINT('Ctrl Pts',(98.0758698892588,-3.83082124420054,133.891852061025));
#46914=CARTESIAN_POINT('Ctrl Pts',(98.0680955551398,-3.7435389841468,133.997136621775));
#46915=CARTESIAN_POINT('Ctrl Pts',(98.0603212210207,-3.65189360089321,134.09872796051));
#46916=CARTESIAN_POINT('Ctrl Pts',(98.0525564680736,-3.5603611623839,134.200194097));
#46917=CARTESIAN_POINT('Ctrl Pts',(98.0447917151265,-3.46447655898354,134.297975780222));
#46918=CARTESIAN_POINT('Ctrl Pts',(98.0370269621794,-3.3645697534118,134.391679036236));
#46919=CARTESIAN_POINT('Ctrl Pts',(98.0292699212944,-3.26476217668785,134.485289224854));
#46920=CARTESIAN_POINT('Ctrl Pts',(98.0215128804093,-3.16094063116001,134.574828781714));
#46921=CARTESIAN_POINT('Ctrl Pts',(98.0137558395244,-3.05347378869415,134.659938509952));
#46922=CARTESIAN_POINT('Ctrl Pts',(98.0060046482842,-2.94608798781016,134.744984056283));
#46923=CARTESIAN_POINT('Ctrl Pts',(97.9982534570441,-2.83506266685036,134.825606181443));
#46924=CARTESIAN_POINT('Ctrl Pts',(97.990502265804,-2.72080135357165,134.901484371726));
#46925=CARTESIAN_POINT('Ctrl Pts',(97.9827543690269,-2.60658860439903,134.977330311754));
#46926=CARTESIAN_POINT('Ctrl Pts',(97.9750064722498,-2.48914292344931,135.048436111337));
#46927=CARTESIAN_POINT('Ctrl Pts',(97.9672585754728,-2.36889856242752,135.11452333647));
#46928=CARTESIAN_POINT('Ctrl Pts',(97.9595122993887,-2.24867935393405,135.18059673758));
#46929=CARTESIAN_POINT('Ctrl Pts',(97.9517660233046,-2.12566297221762,135.241653464115));
#46930=CARTESIAN_POINT('Ctrl Pts',(97.9440197472205,-2.00030977814471,135.297460199587));
#46931=CARTESIAN_POINT('Ctrl Pts',(97.9362734139551,-1.8749556587429,135.353267347012));
#46932=CARTESIAN_POINT('Ctrl Pts',(97.9285270806897,-1.74726504973267,135.403824267034));
#46933=CARTESIAN_POINT('Ctrl Pts',(97.9207807474244,-1.61771950317931,135.448945278387));
#46934=CARTESIAN_POINT('Ctrl Pts',(97.9130326794214,-1.48814494579918,135.494076394277));
#46935=CARTESIAN_POINT('Ctrl Pts',(97.9052846114185,-1.35671499341734,135.533769050572));
#46936=CARTESIAN_POINT('Ctrl Pts',(97.8975365434155,-1.22392722649592,135.567887169055));
#46937=CARTESIAN_POINT('Ctrl Pts',(97.8897802406737,-1.09099833115553,135.602041548681));
#46938=CARTESIAN_POINT('Ctrl Pts',(97.8820239379318,-0.95670911779455,135.630609457849));
#46939=CARTESIAN_POINT('Ctrl Pts',(97.87426763519,-0.821568800945488,135.653505672915));
#46940=CARTESIAN_POINT('Ctrl Pts',(97.8665071926758,-0.686356355639959,
135.67641410838));
#46941=CARTESIAN_POINT('Ctrl Pts',(97.8587467501616,-0.550292289373433,
135.693644768788));
#46942=CARTESIAN_POINT('Ctrl Pts',(97.8509863076474,-0.413890854559451,
135.70516437032));
#46943=CARTESIAN_POINT('Ctrl Pts',(97.843213407382,-0.277270456053341,135.71670246414));
#46944=CARTESIAN_POINT('Ctrl Pts',(97.8354405071166,-0.140311997601334,
135.722511162123));
#46945=CARTESIAN_POINT('Ctrl Pts',(97.8276676068512,-0.00353055348150193,
135.722609350366));
#46946=CARTESIAN_POINT('Ctrl Pts',(97.8201772710891,0.128278540613648,135.72270396922));
#46947=CARTESIAN_POINT('Ctrl Pts',(97.812686935327,0.259922958993352,135.717496065152));
#46948=CARTESIAN_POINT('Ctrl Pts',(97.805196599565,0.390948315480429,135.707047888556));
#46949=CARTESIAN_POINT('Ctrl Pts',(97.7974222654459,0.526941538182246,135.696203566168));
#46950=CARTESIAN_POINT('Ctrl Pts',(97.7896479313268,0.662698614501715,135.679679405626));
#46951=CARTESIAN_POINT('Ctrl Pts',(97.7818735972077,0.797706853207384,135.657488149256));
#46952=CARTESIAN_POINT('Ctrl Pts',(97.7741088442606,0.93254870632488,135.635324241625));
#46953=CARTESIAN_POINT('Ctrl Pts',(97.7663440913135,1.06664317599071,135.607507197424));
#46954=CARTESIAN_POINT('Ctrl Pts',(97.7585793383664,1.19948044785995,135.574101671093));
#46955=CARTESIAN_POINT('Ctrl Pts',(97.7508222974815,1.33218578387774,135.540729323602));
#46956=CARTESIAN_POINT('Ctrl Pts',(97.7430652565965,1.46363603029548,135.501779634579));
#46957=CARTESIAN_POINT('Ctrl Pts',(97.7353082157115,1.59332970847138,135.457368623427));
#46958=CARTESIAN_POINT('Ctrl Pts',(97.7275570244714,1.72292558363578,135.412991102964));
#46959=CARTESIAN_POINT('Ctrl Pts',(97.7198058332313,1.85076715879369,135.363160583994));
#46960=CARTESIAN_POINT('Ctrl Pts',(97.7120546419912,1.9763666600752,135.30804332036));
#46961=CARTESIAN_POINT('Ctrl Pts',(97.7043067452141,2.10191277821837,135.252949483033));
#46962=CARTESIAN_POINT('Ctrl Pts',(97.696558848437,2.22521836055197,135.192573526946));
#46963=CARTESIAN_POINT('Ctrl Pts',(97.6888109516599,2.34581442900797,135.127130299975));
#46964=CARTESIAN_POINT('Ctrl Pts',(97.6810646755758,2.46638527136635,135.061700762317));
#46965=CARTESIAN_POINT('Ctrl Pts',(97.6733183994917,2.58424738377636,134.99120624846));
#46966=CARTESIAN_POINT('Ctrl Pts',(97.6655721234076,2.69895563417696,134.915907959777));
#46967=CARTESIAN_POINT('Ctrl Pts',(97.6578257901422,2.8136647313278,134.84060911526));
#46968=CARTESIAN_POINT('Ctrl Pts',(97.6500794568769,2.9252195931753,134.760506639707));
#46969=CARTESIAN_POINT('Ctrl Pts',(97.6423331236116,3.0332037101579,134.675905311249));
#46970=CARTESIAN_POINT('Ctrl Pts',(97.6345850556086,3.14121200943464,134.59128503691));
#46971=CARTESIAN_POINT('Ctrl Pts',(97.6268369876056,3.24564766494756,134.502164145956));
#46972=CARTESIAN_POINT('Ctrl Pts',(97.6190889196027,3.34612723584534,134.408887713321));
#46973=CARTESIAN_POINT('Ctrl Pts',(97.6113326168608,3.44671359762679,134.315512145384));
#46974=CARTESIAN_POINT('Ctrl Pts',(97.603576314119,3.54333518871336,134.217972479631));
#46975=CARTESIAN_POINT('Ctrl Pts',(97.5958200113771,3.63564506514554,134.116651067207));
#46976=CARTESIAN_POINT('Ctrl Pts',(97.5880595688629,3.72800421013829,134.015275576495));
#46977=CARTESIAN_POINT('Ctrl Pts',(97.5802991263488,3.81604680410408,133.910114616843));
#46978=CARTESIAN_POINT('Ctrl Pts',(97.5725386838346,3.89946687843218,133.801582852655));
#46979=CARTESIAN_POINT('Ctrl Pts',(97.5647657835692,3.98302086606922,133.692876863644));
#46980=CARTESIAN_POINT('Ctrl Pts',(97.5569928833038,4.06193728038319,133.580789576828));
#46981=CARTESIAN_POINT('Ctrl Pts',(97.5492199830384,4.13595360055248,133.465764547182));
#46982=CARTESIAN_POINT('Ctrl Pts',(97.5417296472763,4.20727924104815,133.354920967094));
#46983=CARTESIAN_POINT('Ctrl Pts',(97.5342393115142,4.27405470758821,133.241349790189));
#46984=CARTESIAN_POINT('Ctrl Pts',(97.5267489757521,4.33608676636349,133.125466952284));
#46985=CARTESIAN_POINT('Ctrl Pts',(97.5189746416331,4.4004707895011,133.005190381359));
#46986=CARTESIAN_POINT('Ctrl Pts',(97.511200307514,4.45994856105055,132.882042395813));
#46987=CARTESIAN_POINT('Ctrl Pts',(97.5034259733949,4.51425367935687,132.756461224838));
#46988=CARTESIAN_POINT('Ctrl Pts',(97.4956612204478,4.56849187145831,132.631034821433));
#46989=CARTESIAN_POINT('Ctrl Pts',(97.4878964675007,4.61756994064574,132.50318155449));
#46990=CARTESIAN_POINT('Ctrl Pts',(97.4801317145536,4.66126671542612,132.373365292562));
#46991=CARTESIAN_POINT('Ctrl Pts',(97.4723746736686,4.70492008995378,132.243677965976));
#46992=CARTESIAN_POINT('Ctrl Pts',(97.4646176327836,4.74320268250534,132.112031892484));
#46993=CARTESIAN_POINT('Ctrl Pts',(97.4568605918986,4.77594104203629,131.978911691591));
#46994=CARTESIAN_POINT('Ctrl Pts',(97.4491094006584,4.80865471331567,131.845891877677));
#46995=CARTESIAN_POINT('Ctrl Pts',(97.4413582094183,4.83583238050986,131.711400527154));
#46996=CARTESIAN_POINT('Ctrl Pts',(97.4336070181782,4.85735026399335,131.575937882254));
#46997=CARTESIAN_POINT('Ctrl Pts',(97.4258591214011,4.87885900180233,131.440532812592));
#46998=CARTESIAN_POINT('Ctrl Pts',(97.418111224624,4.8947126791678,131.30415765495));
#46999=CARTESIAN_POINT('Ctrl Pts',(97.4103633278469,4.90483855959238,131.167323104382));
#47000=CARTESIAN_POINT('Ctrl Pts',(97.4026170517628,4.91496232190106,131.030517176653));
#47001=CARTESIAN_POINT('Ctrl Pts',(97.3948707756787,4.91936064158377,130.89325243679));
#47002=CARTESIAN_POINT('Ctrl Pts',(97.3871244995946,4.91801267000309,130.756044572726));
#47003=CARTESIAN_POINT('Ctrl Pts',(97.3793781663292,4.916664688472,130.618835695824));
#47004=CARTESIAN_POINT('Ctrl Pts',(97.3716318330639,4.9095703348766,130.481684086506));
#47005=CARTESIAN_POINT('Ctrl Pts',(97.3638854997985,4.89676089409853,130.345104906086));
#47006=CARTESIAN_POINT('Ctrl Pts',(97.3561374317955,4.88394858473499,130.208495139705));
#47007=CARTESIAN_POINT('Ctrl Pts',(97.3483893637925,4.8654186779277,130.07245844649));
#47008=CARTESIAN_POINT('Ctrl Pts',(97.3406412957895,4.84125423584634,129.937503947522));
#47009=CARTESIAN_POINT('Ctrl Pts',(97.3328849930477,4.8170641115084,129.802406017306));
#47010=CARTESIAN_POINT('Ctrl Pts',(97.3251286903058,4.78722755833888,129.668392964381));
#47011=CARTESIAN_POINT('Ctrl Pts',(97.317372387564,4.75187872750089,129.535963352659));
#47012=CARTESIAN_POINT('Ctrl Pts',(97.3096119450498,4.71651102992761,129.403463059266));
#47013=CARTESIAN_POINT('Ctrl Pts',(97.3018515025356,4.67562530885795,129.272548264076));
#47014=CARTESIAN_POINT('Ctrl Pts',(97.2940910600215,4.62940504968989,129.143700523385));
#47015=CARTESIAN_POINT('Ctrl Pts',(97.286318159756,4.58311059365847,129.014645944862));
#47016=CARTESIAN_POINT('Ctrl Pts',(97.2785452594906,4.53146463436087,128.887665414063));
#47017=CARTESIAN_POINT('Ctrl Pts',(97.2707723592251,4.47469844824211,128.763219549487));
#47018=CARTESIAN_POINT('Ctrl Pts',(97.2632820234631,4.41999585597459,128.643297605549));
#47019=CARTESIAN_POINT('Ctrl Pts',(97.2557916877012,4.36053897908826,128.525729519124));
#47020=CARTESIAN_POINT('Ctrl Pts',(97.2483013519392,4.29657330857259,128.410902686755));
#47021=CARTESIAN_POINT('Ctrl Pts',(97.2405270178201,4.23018236021695,128.291722160136));
#47022=CARTESIAN_POINT('Ctrl Pts',(97.232752683701,4.15872366059314,128.175117332189));
#47023=CARTESIAN_POINT('Ctrl Pts',(97.2249783495819,4.08242190772916,128.061549207754));
#47024=CARTESIAN_POINT('Ctrl Pts',(97.2172135966348,4.00621418995636,127.948121045883));
#47025=CARTESIAN_POINT('Ctrl Pts',(97.2094488436878,3.92517551067917,127.837722462541));
#47026=CARTESIAN_POINT('Ctrl Pts',(97.2016840907407,3.83957658705373,127.730790267851));
#47027=CARTESIAN_POINT('Ctrl Pts',(97.1939270498557,3.75406268148615,127.623964279724));
#47028=CARTESIAN_POINT('Ctrl Pts',(97.1861700089707,3.6639977878252,127.520598132035));
#47029=CARTESIAN_POINT('Ctrl Pts',(97.1784129680857,3.56969587566003,127.421099702739));
#47030=CARTESIAN_POINT('Ctrl Pts',(97.1706617768456,3.47546507730038,127.321676305983));
#47031=CARTESIAN_POINT('Ctrl Pts',(97.1629105856055,3.37700388808234,127.226115104769));
#47032=CARTESIAN_POINT('Ctrl Pts',(97.1551593943654,3.27466627005367,127.13479063155));
#47033=CARTESIAN_POINT('Ctrl Pts',(97.1474114975883,3.17237214824225,127.043504973667));
#47034=CARTESIAN_POINT('Ctrl Pts',(97.1396636008112,3.06620516563591,126.956452722045));
#47035=CARTESIAN_POINT('Ctrl Pts',(97.1319157040341,2.95655566859566,126.873971115113));
#47036=CARTESIAN_POINT('Ctrl Pts',(97.12416942795,2.84692910786626,126.791506761554));
#47037=CARTESIAN_POINT('Ctrl Pts',(97.1164231518659,2.73382179390314,126.713611385864));
#47038=CARTESIAN_POINT('Ctrl Pts',(97.1086768757818,2.61765632037175,126.640581270516));
#47039=CARTESIAN_POINT('Ctrl Pts',(97.1009305425164,2.5014899893333,126.567550616077));
#47040=CARTESIAN_POINT('Ctrl Pts',(97.093184209251,2.38226578467078,126.499385501728));
#47041=CARTESIAN_POINT('Ctrl Pts',(97.0854378759856,2.26043403643116,126.436338063888));
#47042=CARTESIAN_POINT('Ctrl Pts',(97.0776898079827,2.13857500481642,126.373276507011));
#47043=CARTESIAN_POINT('Ctrl Pts',(97.0699417399797,2.01410761480864,126.315335086839));
#47044=CARTESIAN_POINT('Ctrl Pts',(97.0621936719767,1.88750510152241,126.262719113195));
#47045=CARTESIAN_POINT('Ctrl Pts',(97.0544373692349,1.76076803357838,126.210047218668));
#47046=CARTESIAN_POINT('Ctrl Pts',(97.046681066493,1.63189167091894,126.162712227308));
#47047=CARTESIAN_POINT('Ctrl Pts',(97.0389247637511,1.50136798146454,126.120870759914));
#47048=CARTESIAN_POINT('Ctrl Pts',(97.031164321237,1.37077462758691,126.079006960468));
#47049=CARTESIAN_POINT('Ctrl Pts',(97.0234038787228,1.23853257176621,126.042642630976));
#47050=CARTESIAN_POINT('Ctrl Pts',(97.0156434362086,1.10514613929213,126.011883692915));
#47051=CARTESIAN_POINT('Ctrl Pts',(97.0078705359432,0.971545583075235,125.981075377877));
#47052=CARTESIAN_POINT('Ctrl Pts',(97.0000976356777,0.83679736371519,125.955890507554));
#47053=CARTESIAN_POINT('Ctrl Pts',(96.9923247354123,0.701414023169202,125.936383478076));
#47054=CARTESIAN_POINT('Ctrl Pts',(96.9848343996503,0.570952208062481,125.917585578254));
#47055=CARTESIAN_POINT('Ctrl Pts',(96.9773440638883,0.439900952978621,125.904059910211));
#47056=CARTESIAN_POINT('Ctrl Pts',(96.9698537281263,0.308718879479279,125.895809332721));
#47057=CARTESIAN_POINT('Ctrl Pts',(96.9620793940072,0.172562997791085,125.887245932078));
#47058=CARTESIAN_POINT('Ctrl Pts',(96.9543050598881,0.0358348809967539,
125.884338402151));
#47059=CARTESIAN_POINT('Ctrl Pts',(96.946530725769,-0.10095615970339,125.8871468825));
#47060=CARTESIAN_POINT('Ctrl Pts',(96.9387659728219,-0.237578617671331,
125.889951901649));
#47061=CARTESIAN_POINT('Ctrl Pts',(96.9310012198748,-0.374263458117102,
125.898458906728));
#47062=CARTESIAN_POINT('Ctrl Pts',(96.9232364669277,-0.510496851076634,
125.912676242267));
#47063=CARTESIAN_POINT('Ctrl Pts',(96.9154794260428,-0.646594935109353,
125.926879456949));
#47064=CARTESIAN_POINT('Ctrl Pts',(96.9077223851578,-0.782242077623067,
125.946781675071));
#47065=CARTESIAN_POINT('Ctrl Pts',(96.8999653442728,-0.91692541110914,125.972339213126));
#47066=CARTESIAN_POINT('Ctrl Pts',(96.8922141530327,-1.05150717884621,125.997877478043));
#47067=CARTESIAN_POINT('Ctrl Pts',(96.8844629617925,-1.18512620168211,126.02906250163));
#47068=CARTESIAN_POINT('Ctrl Pts',(96.8767117705524,-1.31727604972572,126.06579892953));
#47069=CARTESIAN_POINT('Ctrl Pts',(96.8689638737753,-1.44936973055835,126.102519743469));
#47070=CARTESIAN_POINT('Ctrl Pts',(96.8612159769982,-1.57999510266655,126.14478716437));
#47071=CARTESIAN_POINT('Ctrl Pts',(96.8534680802212,-1.70865744606722,126.192455068392));
#47072=CARTESIAN_POINT('Ctrl Pts',(96.8457218041371,-1.83729287607921,126.240113001317));
#47073=CARTESIAN_POINT('Ctrl Pts',(96.837975528053,-1.96396572775514,126.293169034659));
#47074=CARTESIAN_POINT('Ctrl Pts',(96.8302292519689,-2.08819830806037,126.351427776313));
#47075=CARTESIAN_POINT('Ctrl Pts',(96.8224829187036,-2.21243180542237,126.409686948019));
#47076=CARTESIAN_POINT('Ctrl Pts',(96.8147365854383,-2.33422464149312,126.473148738675));
#47077=CARTESIAN_POINT('Ctrl Pts',(96.8069902521729,-2.45312127237363,126.541570558751));
#47078=CARTESIAN_POINT('Ctrl Pts',(96.79924218417,-2.57204452933009,126.61000770142));
#47079=CARTESIAN_POINT('Ctrl Pts',(96.791494116167,-2.68806995169109,126.683406888832));
#47080=CARTESIAN_POINT('Ctrl Pts',(96.783746048164,-2.80076901134863,126.761480949858));
#47081=CARTESIAN_POINT('Ctrl Pts',(96.7759897454222,-2.91358784890822,126.839637988925));
#47082=CARTESIAN_POINT('Ctrl Pts',(96.7682334426803,-3.02307293973397,126.922479603747));
#47083=CARTESIAN_POINT('Ctrl Pts',(96.7604771399385,-3.12882659363299,127.009676545146));
#47084=CARTESIAN_POINT('Ctrl Pts',(96.7527166974243,-3.23463669144135,127.096920026179));
#47085=CARTESIAN_POINT('Ctrl Pts',(96.7449562549102,-3.33671109309735,127.188523204692));
#47086=CARTESIAN_POINT('Ctrl Pts',(96.737195812396,-3.43468808372314,127.284119030682));
#47087=CARTESIAN_POINT('Ctrl Pts',(96.7294229121306,-3.53282235571221,127.379868315578));
#47088=CARTESIAN_POINT('Ctrl Pts',(96.7216500118651,-3.6268458043593,127.479622771209));
#47089=CARTESIAN_POINT('Ctrl Pts',(96.7138771115997,-3.71643562321466,127.582980583947));
#47090=CARTESIAN_POINT('Ctrl Pts',(96.7063867758376,-3.8027686264921,127.682581079849));
#47091=CARTESIAN_POINT('Ctrl Pts',(96.6988964400755,-3.88498455856165,127.785527258357));
#47092=CARTESIAN_POINT('Ctrl Pts',(96.6914061043134,-3.9628331180997,127.891434813397));
#47093=CARTESIAN_POINT('Ctrl Pts',(96.6835815201943,-4.04415558774659,128.002068381716));
#47094=CARTESIAN_POINT('Ctrl Pts',(96.6757569360752,-4.1209701239629,128.116284831714));
#47095=CARTESIAN_POINT('Ctrl Pts',(96.6679323519561,-4.19294682236243,128.233683662493));
#47096=CARTESIAN_POINT('Ctrl Pts',(96.660120876721,-4.26480293490392,128.350885809638));
#47097=CARTESIAN_POINT('Ctrl Pts',(96.6523094014859,-4.33183715470952,128.471259392883));
#47098=CARTESIAN_POINT('Ctrl Pts',(96.6444979262508,-4.3937609826322,128.594372497689));
#47099=CARTESIAN_POINT('Ctrl Pts',(96.636694006948,-4.45562491249,128.717366516886));
#47100=CARTESIAN_POINT('Ctrl Pts',(96.6288900876451,-4.51238811216936,128.843094445365));
#47101=CARTESIAN_POINT('Ctrl Pts',(96.6210861683423,-4.56380616556344,128.971096767035));
#47102=CARTESIAN_POINT('Ctrl Pts',(96.6132895369372,-4.61517620083963,129.098979550329));
#47103=CARTESIAN_POINT('Ctrl Pts',(96.6054929055322,-4.66121088771008,129.229132141857));
#47104=CARTESIAN_POINT('Ctrl Pts',(96.5976962741271,-4.70171268672026,129.361072401708));
#47105=CARTESIAN_POINT('Ctrl Pts',(96.5933658129799,-4.72420848752097,129.434355610745));
#47106=CARTESIAN_POINT('Ctrl Pts',(96.5890353518328,-4.74499823409669,129.508189917686));
#47107=CARTESIAN_POINT('Ctrl Pts',(96.5847048906856,-4.76405452823403,129.582490119308));
#47108=CARTESIAN_POINT('Ctrl Pts',(98.3346394208835,-4.76405452823406,129.582490119308));
#47109=CARTESIAN_POINT('Ctrl Pts',(98.3256757393383,-4.80320699701511,129.735145000864));
#47110=CARTESIAN_POINT('Ctrl Pts',(98.3167120577931,-4.83506113694242,129.889850790442));
#47111=CARTESIAN_POINT('Ctrl Pts',(98.3077483762479,-4.85942388963773,130.045952730398));
#47112=CARTESIAN_POINT('Ctrl Pts',(98.2988521815638,-4.88360321706305,130.200879390991));
#47113=CARTESIAN_POINT('Ctrl Pts',(98.2899559868796,-4.90040345683945,130.357181120761));
#47114=CARTESIAN_POINT('Ctrl Pts',(98.2810597921955,-4.90968317106223,130.51419821082));
#47115=CARTESIAN_POINT('Ctrl Pts',(98.2756596734789,-4.91531609168038,130.609509853266));
#47116=CARTESIAN_POINT('Ctrl Pts',(98.2702595547623,-4.91817887198582,130.705084709376));
#47117=CARTESIAN_POINT('Ctrl Pts',(98.2648594360457,-4.91824869076816,130.800771988677));
#47118=CARTESIAN_POINT('',(98.6101405639625,-4.91824985933626,130.803184335762));
#47119=CARTESIAN_POINT('Ctrl Pts',(98.680234964937,-4.76405452823403,129.582490119308));
#47120=CARTESIAN_POINT('Ctrl Pts',(98.6724723310953,-4.79811031872045,129.715273129546));
#47121=CARTESIAN_POINT('Ctrl Pts',(98.6647096972535,-4.82657976979179,129.849360886975));
#47122=CARTESIAN_POINT('Ctrl Pts',(98.6569470634118,-4.84939080559483,129.984243627672));
#47123=CARTESIAN_POINT('Ctrl Pts',(98.6491729046658,-4.87223570812522,130.119326623941));
#47124=CARTESIAN_POINT('Ctrl Pts',(98.6413987459199,-4.88940536950229,130.255206573573));
#47125=CARTESIAN_POINT('Ctrl Pts',(98.6336245871739,-4.90087964554873,130.391369379952));
#47126=CARTESIAN_POINT('Ctrl Pts',(98.6293998830641,-4.90711510108216,130.465364211612));
#47127=CARTESIAN_POINT('Ctrl Pts',(98.6251751789543,-4.91166953074298,130.539442574513));
#47128=CARTESIAN_POINT('Ctrl Pts',(98.6209504748445,-4.91454614522429,130.613522337965));
#47129=CARTESIAN_POINT('Ctrl Pts',(98.6173471712325,-4.91699964612792,130.676705905923));
#47130=CARTESIAN_POINT('Ctrl Pts',(98.6137438676204,-4.91823473268887,130.739937093408));
#47131=CARTESIAN_POINT('Ctrl Pts',(98.6101405640085,-4.91824985933606,130.803184334955));
#47132=CARTESIAN_POINT('Ctrl Pts',(98.6101405639625,-4.91824985933626,130.803184335762));
#47133=CARTESIAN_POINT('Ctrl Pts',(98.6024151385632,-4.91828229060402,130.938785411579));
#47134=CARTESIAN_POINT('Ctrl Pts',(98.5946897131639,-4.91270248946855,131.074612686756));
#47135=CARTESIAN_POINT('Ctrl Pts',(98.5869642877645,-4.90148042372996,131.210159481897));
#47136=CARTESIAN_POINT('Ctrl Pts',(98.5792482557868,-4.8902720030128,131.345541464339));
#47137=CARTESIAN_POINT('Ctrl Pts',(98.5715322238092,-4.87343499719098,131.480643254024));
#47138=CARTESIAN_POINT('Ctrl Pts',(98.5638161918315,-4.85099135081706,131.614956680225));
#47139=CARTESIAN_POINT('Ctrl Pts',(98.5561076368954,-4.82856945293771,131.749139953118));
#47140=CARTESIAN_POINT('Ctrl Pts',(98.5483990819594,-4.80055178889892,131.882535994059));
#47141=CARTESIAN_POINT('Ctrl Pts',(98.5406905270234,-4.76701218668155,132.014640698593));
#47142=CARTESIAN_POINT('Ctrl Pts',(98.5329875398277,-4.73349680947091,132.14664998645));
#47143=CARTESIAN_POINT('Ctrl Pts',(98.525284552632,-4.69446752830021,132.277369411346));
#47144=CARTESIAN_POINT('Ctrl Pts',(98.5175815654363,-4.65004935656035,132.406304450555));
#47145=CARTESIAN_POINT('Ctrl Pts',(98.5098814630934,-4.60564781991039,132.535191202186));
#47146=CARTESIAN_POINT('Ctrl Pts',(98.5021813607504,-4.55586153363794,132.662294522571));
#47147=CARTESIAN_POINT('Ctrl Pts',(98.4944812584075,-4.5008654577651,132.787134733192));
#47148=CARTESIAN_POINT('Ctrl Pts',(98.4867824355351,-4.44587852019431,132.911954200014));
#47149=CARTESIAN_POINT('Ctrl Pts',(98.4790836126627,-4.38568367425209,133.034510942316));
#47150=CARTESIAN_POINT('Ctrl Pts',(98.4713847897903,-4.32050395869148,133.154345427183));
#47151=CARTESIAN_POINT('Ctrl Pts',(98.4636855262004,-4.25532051193083,133.274186771952));
#47152=CARTESIAN_POINT('Ctrl Pts',(98.4559862626104,-4.18515181732883,133.391305201108));
#47153=CARTESIAN_POINT('Ctrl Pts',(98.4482869990204,-4.11026655844159,133.505266369542));
#47154=CARTESIAN_POINT('Ctrl Pts',(98.4405855745342,-4.03536028205367,133.619259522627));
#47155=CARTESIAN_POINT('Ctrl Pts',(98.4328841500479,-3.95573502574528,133.730093321226));
#47156=CARTESIAN_POINT('Ctrl Pts',(98.4251827255616,-3.87170214278111,133.837363350846));
#47157=CARTESIAN_POINT('Ctrl Pts',(98.4174729964773,-3.78757864550064,133.944749051856));
#47158=CARTESIAN_POINT('Ctrl Pts',(98.409763267393,-3.69903827632902,134.048562998609));
#47159=CARTESIAN_POINT('Ctrl Pts',(98.4020535383087,-3.60643219335031,134.148434465026));
#47160=CARTESIAN_POINT('Ctrl Pts',(98.3943392058232,-3.51377081621609,134.248365563686));
#47161=CARTESIAN_POINT('Ctrl Pts',(98.3866248733376,-3.41703917144957,134.34434921535));
#47162=CARTESIAN_POINT('Ctrl Pts',(98.3789105408521,-3.31662359250585,134.436053199288));
#47163=CARTESIAN_POINT('Ctrl Pts',(98.3711847186851,-3.21605845519007,134.527893766599));
#47164=CARTESIAN_POINT('Ctrl Pts',(98.3634588965182,-3.1117987301916,134.615441683928));
#47165=CARTESIAN_POINT('Ctrl Pts',(98.3557330743512,-3.00426238077046,134.698406150169));
#47166=CARTESIAN_POINT('Ctrl Pts',(98.3513229999113,-2.94287819463539,134.745764148332));
#47167=CARTESIAN_POINT('Ctrl Pts',(98.3469129254714,-2.8804268792548,134.791629486694));
#47168=CARTESIAN_POINT('Ctrl Pts',(98.3425028510316,-2.81698988540556,134.835954725115));
#47169=CARTESIAN_POINT('Ctrl Pts',(98.3347285169125,-2.70515948607426,134.914093817343));
#47170=CARTESIAN_POINT('Ctrl Pts',(98.3269541827934,-2.58989829891362,134.987700137634));
#47171=CARTESIAN_POINT('Ctrl Pts',(98.3191798486743,-2.47161002143893,135.056457390268));
#47172=CARTESIAN_POINT('Ctrl Pts',(98.3114150957272,-2.35346752369467,135.125129905733));
#47173=CARTESIAN_POINT('Ctrl Pts',(98.3036503427802,-2.23230569322079,135.188965049496));
#47174=CARTESIAN_POINT('Ctrl Pts',(98.2958855898331,-2.1085590295129,135.247688411186));
#47175=CARTESIAN_POINT('Ctrl Pts',(98.2881285489481,-1.98493527273594,135.306353448006));
#47176=CARTESIAN_POINT('Ctrl Pts',(98.2803715080631,-1.85873214268023,135.359916639869));
#47177=CARTESIAN_POINT('Ctrl Pts',(98.2726144671781,-1.73041038075421,135.408148511972));
#47178=CARTESIAN_POINT('Ctrl Pts',(98.264863275938,-1.60218538726696,135.456344012045));
#47179=CARTESIAN_POINT('Ctrl Pts',(98.2571120846979,-1.47184530647509,135.499216057703));
#47180=CARTESIAN_POINT('Ctrl Pts',(98.2493608934577,-1.33987225979488,135.536582652713));
#47181=CARTESIAN_POINT('Ctrl Pts',(98.2416129966807,-1.20795530517992,135.573933365924));
#47182=CARTESIAN_POINT('Ctrl Pts',(98.2338650999036,-1.07440714048701,135.60578317621));
#47183=CARTESIAN_POINT('Ctrl Pts',(98.2261172031265,-0.939726295431838,
135.63199953863));
#47184=CARTESIAN_POINT('Ctrl Pts',(98.2183709270424,-0.805073622705975,
135.658210417153));
#47185=CARTESIAN_POINT('Ctrl Pts',(98.2106246509583,-0.669289124408354,
135.67879011705));
#47186=CARTESIAN_POINT('Ctrl Pts',(98.2028783748742,-0.532882416594516,
135.693657028358));
#47187=CARTESIAN_POINT('Ctrl Pts',(98.1951320416089,-0.396474701857627,
135.708524049411));
#47188=CARTESIAN_POINT('Ctrl Pts',(98.1873857083435,-0.259445157103111,
135.717678155366));
#47189=CARTESIAN_POINT('Ctrl Pts',(98.1796393750782,-0.122309032878326,
135.721089567079));
#47190=CARTESIAN_POINT('Ctrl Pts',(98.1718913070752,0.014857802030737,135.724501742753));
#47191=CARTESIAN_POINT('Ctrl Pts',(98.1641432390723,0.152130873134605,135.722168655401));
#47192=CARTESIAN_POINT('Ctrl Pts',(98.1563951710693,0.288994812493648,135.714112654161));
#47193=CARTESIAN_POINT('Ctrl Pts',(98.1486388683274,0.426004212476236,135.706048090908));
#47194=CARTESIAN_POINT('Ctrl Pts',(98.1408825655856,0.562603221182044,135.692248486566));
#47195=CARTESIAN_POINT('Ctrl Pts',(98.1331262628437,0.69828091988794,135.672788168575));
#47196=CARTESIAN_POINT('Ctrl Pts',(98.1253658203296,0.834031033866721,135.653317464026));
#47197=CARTESIAN_POINT('Ctrl Pts',(98.1176053778154,0.968858473875881,135.628180097266));
#47198=CARTESIAN_POINT('Ctrl Pts',(98.1098449353013,1.10226338296286,135.597501393412));
#47199=CARTESIAN_POINT('Ctrl Pts',(98.1020720350358,1.23588244545332,135.566773441379));
#47200=CARTESIAN_POINT('Ctrl Pts',(98.0942991347704,1.36807403647961,135.530486479867));
#47201=CARTESIAN_POINT('Ctrl Pts',(98.0865262345049,1.49835344579429,135.488815763469));
#47202=CARTESIAN_POINT('Ctrl Pts',(98.0790358987429,1.62389687042671,135.448659882574));
#47203=CARTESIAN_POINT('Ctrl Pts',(98.0715455629808,1.74766443554663,135.403504982735));
#47204=CARTESIAN_POINT('Ctrl Pts',(98.0640552272188,1.86924246149423,135.353549081748));
#47205=CARTESIAN_POINT('Ctrl Pts',(98.0562808930997,1.99543015524821,135.301699087592));
#47206=CARTESIAN_POINT('Ctrl Pts',(98.0485065589806,2.11965872421962,135.244512600519));
#47207=CARTESIAN_POINT('Ctrl Pts',(98.0407322248615,2.24144385149432,135.182158297119));
#47208=CARTESIAN_POINT('Ctrl Pts',(98.0329674719144,2.3630788894839,135.119880839825));
#47209=CARTESIAN_POINT('Ctrl Pts',(98.0252027189673,2.48227613275066,135.05244841483));
#47210=CARTESIAN_POINT('Ctrl Pts',(98.0174379660202,2.59856985448748,134.980078253356));
#47211=CARTESIAN_POINT('Ctrl Pts',(98.0096809251352,2.71474807166018,134.907779970947));
#47212=CARTESIAN_POINT('Ctrl Pts',(98.0019238842502,2.82802817644063,134.830553916928));
#47213=CARTESIAN_POINT('Ctrl Pts',(97.9941668433652,2.93796806319306,134.748663689359));
#47214=CARTESIAN_POINT('Ctrl Pts',(97.986415652125,3.04782504342185,134.666835215848));
#47215=CARTESIAN_POINT('Ctrl Pts',(97.9786644608849,3.15434650703443,134.58034980234));
#47216=CARTESIAN_POINT('Ctrl Pts',(97.9709132696448,3.25711873704543,134.48951469783));
#47217=CARTESIAN_POINT('Ctrl Pts',(97.9631653728677,3.35984728611713,134.398718200663));
#47218=CARTESIAN_POINT('Ctrl Pts',(97.9554174760906,3.45882947865587,134.30357594786));
#47219=CARTESIAN_POINT('Ctrl Pts',(97.9476695793135,3.55368433336097,134.204435722814));
#47220=CARTESIAN_POINT('Ctrl Pts',(97.9399233032294,3.64851934647537,134.105316235765));
#47221=CARTESIAN_POINT('Ctrl Pts',(97.9321770271453,3.73922846889674,134.002200722212));
#47222=CARTESIAN_POINT('Ctrl Pts',(97.9244307510611,3.82546757992572,133.895473824396));
#47223=CARTESIAN_POINT('Ctrl Pts',(97.9166844177958,3.91170732755224,133.788746138746));
#47224=CARTESIAN_POINT('Ctrl Pts',(97.9089380845304,3.99347675222295,133.678407319736));
#47225=CARTESIAN_POINT('Ctrl Pts',(97.9011917512651,4.07047229439274,133.564874765887));
#47226=CARTESIAN_POINT('Ctrl Pts',(97.8934436832621,4.14748507918008,133.451316787211));
#47227=CARTESIAN_POINT('Ctrl Pts',(97.8856956152591,4.21972163472643,133.334563974013));
#47228=CARTESIAN_POINT('Ctrl Pts',(97.8779475472562,4.28692219503683,133.215062000193));
#47229=CARTESIAN_POINT('Ctrl Pts',(97.8701912445143,4.3541941769026,133.095433018253));
#47230=CARTESIAN_POINT('Ctrl Pts',(97.8624349417724,4.41641927976647,132.973049380323));
#47231=CARTESIAN_POINT('Ctrl Pts',(97.8546786390306,4.47338387335798,132.848381112591));
#47232=CARTESIAN_POINT('Ctrl Pts',(97.8469181965164,4.53037887066826,132.72364630565));
#47233=CARTESIAN_POINT('Ctrl Pts',(97.8391577540022,4.58210761675472,132.596624801111));
#47234=CARTESIAN_POINT('Ctrl Pts',(97.8313973114881,4.62840536629358,132.46780488407));
#47235=CARTESIAN_POINT('Ctrl Pts',(97.8236244112226,4.67477743709015,132.338778173862));
#47236=CARTESIAN_POINT('Ctrl Pts',(97.8158515109572,4.71570097257844,132.207947655416));
#47237=CARTESIAN_POINT('Ctrl Pts',(97.8080786106917,4.75106142168296,132.075815858578));
#47238=CARTESIAN_POINT('Ctrl Pts',(97.8005882749297,4.78513642939482,131.948487385375));
#47239=CARTESIAN_POINT('Ctrl Pts',(97.7930979391677,4.81404572544429,131.819950901228));
#47240=CARTESIAN_POINT('Ctrl Pts',(97.7856076034057,4.83773230385249,131.690661480006));
#47241=CARTESIAN_POINT('Ctrl Pts',(97.7778332692866,4.86231696608044,131.556470011082));
#47242=CARTESIAN_POINT('Ctrl Pts',(97.7700589351675,4.88135293088056,131.42104230455));
#47243=CARTESIAN_POINT('Ctrl Pts',(97.7622846010484,4.89472032552374,131.284877003764));
#47244=CARTESIAN_POINT('Ctrl Pts',(97.7545198481013,4.90807124604772,131.148879514542));
#47245=CARTESIAN_POINT('Ctrl Pts',(97.7467550951542,4.91576745865379,131.012146625102));
#47246=CARTESIAN_POINT('Ctrl Pts',(97.7389903422071,4.9177399894071,130.875187583379));
#47247=CARTESIAN_POINT('Ctrl Pts',(97.7312333013221,4.91971056101505,130.738364571308));
#47248=CARTESIAN_POINT('Ctrl Pts',(97.7234762604371,4.91596875826757,130.601316242348));
#47249=CARTESIAN_POINT('Ctrl Pts',(97.7157192195521,4.90649738478277,130.464557033683));
#47250=CARTESIAN_POINT('Ctrl Pts',(97.707968028312,4.89703315373438,130.3279009562));
#47251=CARTESIAN_POINT('Ctrl Pts',(97.7002168370719,4.88184797897018,130.191533953494));
#47252=CARTESIAN_POINT('Ctrl Pts',(97.6924656458317,4.86097673363409,130.055970172966));
#47253=CARTESIAN_POINT('Ctrl Pts',(97.6847177490546,4.84011435913408,129.920464010662));
#47254=CARTESIAN_POINT('Ctrl Pts',(97.6769698522775,4.81357078012432,129.78576077714));
#47255=CARTESIAN_POINT('Ctrl Pts',(97.6692219555005,4.7814326669225,129.652368988175));
#47256=CARTESIAN_POINT('Ctrl Pts',(97.6614756794164,4.74930127632112,129.519005101897));
#47257=CARTESIAN_POINT('Ctrl Pts',(97.6537294033323,4.71157777074786,129.386952494377));
#47258=CARTESIAN_POINT('Ctrl Pts',(97.6459831272482,4.66839975497106,129.256708592631));
#47259=CARTESIAN_POINT('Ctrl Pts',(97.6382367939828,4.62522142046395,129.126463729454));
#47260=CARTESIAN_POINT('Ctrl Pts',(97.6304904607175,4.57658861843661,128.998027969798));
#47261=CARTESIAN_POINT('Ctrl Pts',(97.6227441274521,4.52268843673838,128.871882321001));
#47262=CARTESIAN_POINT('Ctrl Pts',(97.6149960594491,4.46877618446803,128.745708422762));
#47263=CARTESIAN_POINT('Ctrl Pts',(97.6072479914461,4.40959435886156,128.621826015355));
#47264=CARTESIAN_POINT('Ctrl Pts',(97.5994999234431,4.34537750812776,128.500694544899));
#47265=CARTESIAN_POINT('Ctrl Pts',(97.5917436207013,4.28109240696095,128.379434334475));
#47266=CARTESIAN_POINT('Ctrl Pts',(97.5839873179594,4.2117617743161,128.260931247441));
#47267=CARTESIAN_POINT('Ctrl Pts',(97.5762310152175,4.13766558415761,128.145619077631));
#47268=CARTESIAN_POINT('Ctrl Pts',(97.5684705727034,4.06352984663144,128.030245362243));
#47269=CARTESIAN_POINT('Ctrl Pts',(97.5607101301892,3.98462370823129,127.91806627725));
#47270=CARTESIAN_POINT('Ctrl Pts',(97.552949687675,3.90126892816643,127.809484357581));
#47271=CARTESIAN_POINT('Ctrl Pts',(97.5451767874096,3.81778033960878,127.700728132575));
#47272=CARTESIAN_POINT('Ctrl Pts',(97.5374038871442,3.7298290896713,127.59558091222));
#47273=CARTESIAN_POINT('Ctrl Pts',(97.5296309868788,3.63777605329274,127.494410701239));
#47274=CARTESIAN_POINT('Ctrl Pts',(97.5221406511168,3.54906937665477,127.396918282261));
#47275=CARTESIAN_POINT('Ctrl Pts',(97.5146503153548,3.45655417286324,127.303118963381));
#47276=CARTESIAN_POINT('Ctrl Pts',(97.5071599795928,3.36058249532988,127.213306683888));
#47277=CARTESIAN_POINT('Ctrl Pts',(97.4993856454738,3.26097202247225,127.12008914452));
#47278=CARTESIAN_POINT('Ctrl Pts',(97.4916113113547,3.15732226140873,127.030871664821));
#47279=CARTESIAN_POINT('Ctrl Pts',(97.4838369772356,3.04998794077722,126.946024626026));
#47280=CARTESIAN_POINT('Ctrl Pts',(97.4760722242885,2.9427859001033,126.861282153624));
#47281=CARTESIAN_POINT('Ctrl Pts',(97.4683074713414,2.83190863864512,126.780899645361));
#47282=CARTESIAN_POINT('Ctrl Pts',(97.4605427183944,2.71774731901665,126.705210391912));
#47283=CARTESIAN_POINT('Ctrl Pts',(97.4527856775094,2.60369938602014,126.629596314097));
#47284=CARTESIAN_POINT('Ctrl Pts',(97.4450286366244,2.48637420967266,126.558666429327));
#47285=CARTESIAN_POINT('Ctrl Pts',(97.4372715957394,2.36619530548107,126.49271327127));
#47286=CARTESIAN_POINT('Ctrl Pts',(97.4295204044993,2.2461070291359,126.426809849003));
#47287=CARTESIAN_POINT('Ctrl Pts',(97.4217692132591,2.12316964976652,126.365875870686));
#47288=CARTESIAN_POINT('Ctrl Pts',(97.414018022019,1.99783458393054,126.310159905787));
#47289=CARTESIAN_POINT('Ctrl Pts',(97.4062701252419,1.87255278884078,126.25446762166));
#47290=CARTESIAN_POINT('Ctrl Pts',(97.3985222284649,1.74487569066665,126.203989098405));
#47291=CARTESIAN_POINT('Ctrl Pts',(97.3907743316878,1.61527796555632,126.15892628303));
#47292=CARTESIAN_POINT('Ctrl Pts',(97.3830280556036,1.4857073494961,126.113872893824));
#47293=CARTESIAN_POINT('Ctrl Pts',(97.3752817795196,1.3542172746543,126.074233087518));
#47294=CARTESIAN_POINT('Ctrl Pts',(97.3675355034354,1.22130061920716,126.040159964778));
#47295=CARTESIAN_POINT('Ctrl Pts',(97.3597891701701,1.08838298259992,126.006086590518));
#47296=CARTESIAN_POINT('Ctrl Pts',(97.3520428369047,0.954039123093512,125.977580078904));
#47297=CARTESIAN_POINT('Ctrl Pts',(97.3442965036394,0.818774851338005,125.954743023846));
#47298=CARTESIAN_POINT('Ctrl Pts',(97.3365484356364,0.683480288086327,125.931900854588));
#47299=CARTESIAN_POINT('Ctrl Pts',(97.3288003676334,0.547265287866364,125.914730733388));
#47300=CARTESIAN_POINT('Ctrl Pts',(97.3210522996304,0.410643174745097,125.903283670044));
#47301=CARTESIAN_POINT('Ctrl Pts',(97.3132959968886,0.273875858016367,125.891824440624));
#47302=CARTESIAN_POINT('Ctrl Pts',(97.3055396941468,0.136700954273868,125.886100452274));
#47303=CARTESIAN_POINT('Ctrl Pts',(97.2977833914049,-0.000365240678962547,
125.886110631128));
#47304=CARTESIAN_POINT('Ctrl Pts',(97.2900229488907,-0.137504591987303,
125.886120815415));
#47305=CARTESIAN_POINT('Ctrl Pts',(97.2822625063765,-0.274534728463636,
125.891871248824));
#47306=CARTESIAN_POINT('Ctrl Pts',(97.2745020638624,-0.41094306736016,125.90330880618));
#47307=CARTESIAN_POINT('Ctrl Pts',(97.2667291635969,-0.547570381031765,
125.914764724119));
#47308=CARTESIAN_POINT('Ctrl Pts',(97.2589562633315,-0.683573514359819,
125.931925960635));
#47309=CARTESIAN_POINT('Ctrl Pts',(97.2511833630661,-0.818447792830363,
125.954687816963));
#47310=CARTESIAN_POINT('Ctrl Pts',(97.243693027304,-0.948419051550785,125.976622222479));
#47311=CARTESIAN_POINT('Ctrl Pts',(97.236202691542,-1.07734180251876,126.003757060566));
#47312=CARTESIAN_POINT('Ctrl Pts',(97.22871235578,-1.20477845281854,126.035955020081));
#47313=CARTESIAN_POINT('Ctrl Pts',(97.2209380216609,-1.33704690244797,126.069373775018));
#47314=CARTESIAN_POINT('Ctrl Pts',(97.2131636875418,-1.46813332253031,126.108353027479));
#47315=CARTESIAN_POINT('Ctrl Pts',(97.2053893534227,-1.59753436134945,126.15279453432));
#47316=CARTESIAN_POINT('Ctrl Pts',(97.1976246004756,-1.72677592495342,126.197181270975));
#47317=CARTESIAN_POINT('Ctrl Pts',(97.1898598475285,-1.85433587385178,126.24701674208));
#47318=CARTESIAN_POINT('Ctrl Pts',(97.1820950945814,-1.97972236821465,126.302152003198));
#47319=CARTESIAN_POINT('Ctrl Pts',(97.1743380536963,-2.10498432694351,126.357232503197));
#47320=CARTESIAN_POINT('Ctrl Pts',(97.1665810128113,-2.22807677148156,126.417602161604));
#47321=CARTESIAN_POINT('Ctrl Pts',(97.1588239719263,-2.34852466449414,126.483062784419));
#47322=CARTESIAN_POINT('Ctrl Pts',(97.1510727806863,-2.46888172681226,126.548474042868));
#47323=CARTESIAN_POINT('Ctrl Pts',(97.1433215894462,-2.58659786497023,126.618968438223));
#47324=CARTESIAN_POINT('Ctrl Pts',(97.1355703982062,-2.70121994876031,126.694300538818));
#47325=CARTESIAN_POINT('Ctrl Pts',(97.1278225014291,-2.81579331510837,126.769600621261));
#47326=CARTESIAN_POINT('Ctrl Pts',(97.120074604652,-2.92727491659795,126.849734105133));
#47327=CARTESIAN_POINT('Ctrl Pts',(97.1123267078749,-3.03523827544131,126.934410789235));
#47328=CARTESIAN_POINT('Ctrl Pts',(97.1045804317908,-3.14317905067756,127.019069760801));
#47329=CARTESIAN_POINT('Ctrl Pts',(97.0968341557066,-3.24760273965558,127.108269801194));
#47330=CARTESIAN_POINT('Ctrl Pts',(97.0890878796225,-3.34811412175674,127.201678992694));
#47331=CARTESIAN_POINT('Ctrl Pts',(97.0813415463572,-3.44862624580946,127.295088873718));
#47332=CARTESIAN_POINT('Ctrl Pts',(97.0735952130919,-3.54522571897084,127.392707701699));
#47333=CARTESIAN_POINT('Ctrl Pts',(97.0658488798266,-3.63755282306729,127.494165378325));
#47334=CARTESIAN_POINT('Ctrl Pts',(97.0581008118236,-3.72990060317879,127.595645775694));
#47335=CARTESIAN_POINT('Ctrl Pts',(97.0503527438206,-3.81797384728278,127.700966443276));
#47336=CARTESIAN_POINT('Ctrl Pts',(97.0426046758177,-3.90145217519436,127.809723079036));
#47337=CARTESIAN_POINT('Ctrl Pts',(97.0348483730758,-3.98501922486635,127.918595302644));
#47338=CARTESIAN_POINT('Ctrl Pts',(97.0270920703339,-4.06398136453394,128.030910478637));
#47339=CARTESIAN_POINT('Ctrl Pts',(97.0193357675921,-4.13806042717554,128.146233652287));
#47340=CARTESIAN_POINT('Ctrl Pts',(97.0115753250779,-4.21217902804339,128.261618377387));
#47341=CARTESIAN_POINT('Ctrl Pts',(97.0038148825637,-4.28140916146843,128.380013961819));
#47342=CARTESIAN_POINT('Ctrl Pts',(96.9960544400495,-4.34551845966848,128.500960439746));
#47343=CARTESIAN_POINT('Ctrl Pts',(96.9882815397841,-4.40973067180539,128.622101071697));
#47344=CARTESIAN_POINT('Ctrl Pts',(96.9805086395186,-4.4688054531182,128.745800427099));
#47345=CARTESIAN_POINT('Ctrl Pts',(96.9727357392532,-4.52255810074129,128.871577316748));
#47346=CARTESIAN_POINT('Ctrl Pts',(96.9652454034911,-4.57435670422879,128.992781899647));
#47347=CARTESIAN_POINT('Ctrl Pts',(96.957755067729,-4.62121329245976,129.11591530411));
#47348=CARTESIAN_POINT('Ctrl Pts',(96.9502647319669,-4.66300685952642,129.240535150799));
#47349=CARTESIAN_POINT('Ctrl Pts',(96.9434939960896,-4.70078530003539,129.353182713445));
#47350=CARTESIAN_POINT('Ctrl Pts',(96.9367232602123,-4.73449998266919,129.467257394704));
#47351=CARTESIAN_POINT('Ctrl Pts',(96.929952524335,-4.76405452823407,129.582490119308));
#47352=CARTESIAN_POINT('Origin',(213.235140564004,0.,130.804360617566));
#47353=CARTESIAN_POINT('',(94.8350013119177,-4.76405452823406,129.582490119308));
#47354=CARTESIAN_POINT('',(95.1799533855057,-4.76405452823404,129.582490119308));
#47355=CARTESIAN_POINT('',(213.235140564004,-4.76405452823405,129.582490119308));
#47356=CARTESIAN_POINT('',(96.5148594359362,-4.91824890228215,130.807646603022));
#47357=CARTESIAN_POINT('Ctrl Pts',(96.5148594359362,-4.91824890228215,130.807646603022));
#47358=CARTESIAN_POINT('Ctrl Pts',(96.5060769269297,-4.91814488454752,130.963333569976));
#47359=CARTESIAN_POINT('Ctrl Pts',(96.4972944179233,-4.91064446456671,131.118734022512));
#47360=CARTESIAN_POINT('Ctrl Pts',(96.4885119089168,-4.89585318662738,131.273193890159));
#47361=CARTESIAN_POINT('Ctrl Pts',(96.4796923871704,-4.88099957277427,131.428304708795));
#47362=CARTESIAN_POINT('Ctrl Pts',(96.470872865424,-4.85879362968525,131.58246682585));
#47363=CARTESIAN_POINT('Ctrl Pts',(96.4620533436776,-4.82939196962361,131.73503578444));
#47364=CARTESIAN_POINT('Ctrl Pts',(96.4531830551799,-4.79982106832561,131.888482957359));
#47365=CARTESIAN_POINT('Ctrl Pts',(96.4443127666822,-4.76297146670377,132.04031840757));
#47366=CARTESIAN_POINT('Ctrl Pts',(96.4354424781845,-4.7190511585257,132.189907161612));
#47367=CARTESIAN_POINT('Ctrl Pts',(96.4279478122898,-4.68194210216631,132.316297383692));
#47368=CARTESIAN_POINT('Ctrl Pts',(96.4204531463951,-4.63978623720257,132.441084028861));
#47369=CARTESIAN_POINT('Ctrl Pts',(96.4129584805004,-4.59273507530652,132.563896803767));
#47370=CARTESIAN_POINT('Ctrl Pts',(96.4051841463814,-4.54392816938009,132.691292415476));
#47371=CARTESIAN_POINT('Ctrl Pts',(96.3974098122623,-4.48973929372166,132.816857527698));
#47372=CARTESIAN_POINT('Ctrl Pts',(96.3896354781432,-4.43032545407694,132.940103915216));
#47373=CARTESIAN_POINT('Ctrl Pts',(96.3818707251961,-4.37098483667964,133.063198412577));
#47374=CARTESIAN_POINT('Ctrl Pts',(96.374105972249,-4.30643223573233,133.183979522251));
#47375=CARTESIAN_POINT('Ctrl Pts',(96.366341219302,-4.23687364374173,133.301976438597));
#47376=CARTESIAN_POINT('Ctrl Pts',(96.358584178417,-4.1673841383253,133.419856158744));
#47377=CARTESIAN_POINT('Ctrl Pts',(96.350827137532,-4.09289873366908,133.534956854013));
#47378=CARTESIAN_POINT('Ctrl Pts',(96.343070096647,-4.01367034260699,133.64683022046));
#47379=CARTESIAN_POINT('Ctrl Pts',(96.3353189054069,-3.93450169829108,133.758619222331));
#47380=CARTESIAN_POINT('Ctrl Pts',(96.3275677141668,-3.85059741186087,133.867185421851));
#47381=CARTESIAN_POINT('Ctrl Pts',(96.3198165229267,-3.76225471576301,133.972107848047));
#47382=CARTESIAN_POINT('Ctrl Pts',(96.3120686261496,-3.67394956766743,134.076985679413));
#47383=CARTESIAN_POINT('Ctrl Pts',(96.3043207293725,-3.58121001318023,134.178222519257));
#47384=CARTESIAN_POINT('Ctrl Pts',(96.2965728325955,-3.48437459303877,134.275429150149));
#47385=CARTESIAN_POINT('Ctrl Pts',(96.2888265565114,-3.38755942877967,134.372615447509));
#47386=CARTESIAN_POINT('Ctrl Pts',(96.2810802804273,-3.28665037877241,134.465772935949));
#47387=CARTESIAN_POINT('Ctrl Pts',(96.2733340043432,-3.1820237165437,134.554548363513));
#47388=CARTESIAN_POINT('Ctrl Pts',(96.2655876710778,-3.07739628198474,134.643324446398));
#47389=CARTESIAN_POINT('Ctrl Pts',(96.2578413378125,-2.9690514785574,134.727718150913));
#47390=CARTESIAN_POINT('Ctrl Pts',(96.2500950045471,-2.8573992999917,134.807415988518));
#47391=CARTESIAN_POINT('Ctrl Pts',(96.2423469365442,-2.74572211769482,134.887131673901));
#47392=CARTESIAN_POINT('Ctrl Pts',(96.2345988685412,-2.63073640457746,134.962149172698));
#47393=CARTESIAN_POINT('Ctrl Pts',(96.2268508005383,-2.51288147252894,135.032198098776));
#47394=CARTESIAN_POINT('Ctrl Pts',(96.2190944977964,-2.39490128285606,135.102321473686));
#47395=CARTESIAN_POINT('Ctrl Pts',(96.2113381950546,-2.27404611928539,135.167465527119));
#47396=CARTESIAN_POINT('Ctrl Pts',(96.2035818923127,-2.15078074611151,135.227405410992));
#47397=CARTESIAN_POINT('Ctrl Pts',(96.1958214497986,-2.02744958249652,135.287377286586));
#47398=CARTESIAN_POINT('Ctrl Pts',(96.1880610072844,-1.90170600428682,135.342139301944));
#47399=CARTESIAN_POINT('Ctrl Pts',(96.1803005647702,-1.77403420253166,135.391515041689));
#47400=CARTESIAN_POINT('Ctrl Pts',(96.1725276645048,-1.64615745066616,135.440970043754));
#47401=CARTESIAN_POINT('Ctrl Pts',(96.1647547642394,-1.51634666018989,135.485021365978));
#47402=CARTESIAN_POINT('Ctrl Pts',(96.156981863974,-1.38510146732424,135.523542430944));
#47403=CARTESIAN_POINT('Ctrl Pts',(96.1494915282119,-1.25862736780407,135.56066315817));
#47404=CARTESIAN_POINT('Ctrl Pts',(96.1420011924497,-1.13082164237983,135.592648650262));
#47405=CARTESIAN_POINT('Ctrl Pts',(96.1345108566876,-1.00213786588589,135.619430997141));
#47406=CARTESIAN_POINT('Ctrl Pts',(96.1267365225685,-0.868575004895484,
135.647228804841));
#47407=CARTESIAN_POINT('Ctrl Pts',(96.1189621884494,-0.733643108864154,
135.669509179295));
#47408=CARTESIAN_POINT('Ctrl Pts',(96.1111878543303,-0.597837800933942,
135.686140316229));
#47409=CARTESIAN_POINT('Ctrl Pts',(96.1034231013832,-0.462199860908578,
135.702750956772));
#47410=CARTESIAN_POINT('Ctrl Pts',(96.0956583484362,-0.325691035044379,
135.713726165392));
#47411=CARTESIAN_POINT('Ctrl Pts',(96.0878935954891,-0.188818769441456,
135.718984767469));
#47412=CARTESIAN_POINT('Ctrl Pts',(96.0801365546041,-0.0520824473022909,
135.724238146628));
#47413=CARTESIAN_POINT('Ctrl Pts',(96.072379513719,0.0850162080731771,135.723786203438));
#47414=CARTESIAN_POINT('Ctrl Pts',(96.064622472834,0.221963320313328,135.717599401396));
#47415=CARTESIAN_POINT('Ctrl Pts',(96.0568712815939,0.358807159670751,135.71141726487));
#47416=CARTESIAN_POINT('Ctrl Pts',(96.0491200903538,0.495499294373461,135.699508895121));
#47417=CARTESIAN_POINT('Ctrl Pts',(96.0413688991137,0.631524888220994,135.68189681713));
#47418=CARTESIAN_POINT('Ctrl Pts',(96.0336210023366,0.767492667562634,135.664292224742));
#47419=CARTESIAN_POINT('Ctrl Pts',(96.0258731055595,0.902794082589508,135.640988795814));
#47420=CARTESIAN_POINT('Ctrl Pts',(96.0181252087825,1.03691868411676,135.612060972729));
#47421=CARTESIAN_POINT('Ctrl Pts',(96.0103789326983,1.17101522966885,135.58313920072));
#47422=CARTESIAN_POINT('Ctrl Pts',(96.0026326566142,1.30393506941985,135.548595457055));
#47423=CARTESIAN_POINT('Ctrl Pts',(95.9948863805301,1.43517761746382,135.50855537));
#47424=CARTESIAN_POINT('Ctrl Pts',(95.9871400472648,1.56642113431028,135.468514987378));
#47425=CARTESIAN_POINT('Ctrl Pts',(95.9793937139994,1.69598696079417,135.422978294492));
#47426=CARTESIAN_POINT('Ctrl Pts',(95.971647380734,1.82338973850166,135.372120782464));
#47427=CARTESIAN_POINT('Ctrl Pts',(95.963899312731,1.95082104717796,135.321251881248));
#47428=CARTESIAN_POINT('Ctrl Pts',(95.9561512447281,2.07608798014407,135.265059934742));
#47429=CARTESIAN_POINT('Ctrl Pts',(95.9484031767252,2.19872559508115,135.20376839817));
#47430=CARTESIAN_POINT('Ctrl Pts',(95.9406468739833,2.32149355073488,135.142411720223));
#47431=CARTESIAN_POINT('Ctrl Pts',(95.9328905712414,2.44162625582511,135.075944800427));
#47432=CARTESIAN_POINT('Ctrl Pts',(95.9251342684996,2.55868332283812,135.004637122265));
#47433=CARTESIAN_POINT('Ctrl Pts',(95.9173738259854,2.67580286673239,134.933291385049));
#47434=CARTESIAN_POINT('Ctrl Pts',(95.9096133834712,2.78984317667386,134.857099958395));
#47435=CARTESIAN_POINT('Ctrl Pts',(95.901852940957,2.90039411232023,134.776374849126));
#47436=CARTESIAN_POINT('Ctrl Pts',(95.8940800406916,3.01112251414267,134.695520152746));
#47437=CARTESIAN_POINT('Ctrl Pts',(95.8863071404261,3.11835004218567,134.610117473961));
#47438=CARTESIAN_POINT('Ctrl Pts',(95.8785342401607,3.22170013770037,134.520518752689));
#47439=CARTESIAN_POINT('Ctrl Pts',(95.8710439043987,3.32129319691959,134.434177170621));
#47440=CARTESIAN_POINT('Ctrl Pts',(95.8635535686367,3.4172856137117,134.343939533942));
#47441=CARTESIAN_POINT('Ctrl Pts',(95.8560632328747,3.50937508512537,134.250150740949));
#47442=CARTESIAN_POINT('Ctrl Pts',(95.8482888987556,3.60495615683794,134.152805917362));
#47443=CARTESIAN_POINT('Ctrl Pts',(95.8405145646365,3.69663525257884,134.051326978382));
#47444=CARTESIAN_POINT('Ctrl Pts',(95.8327402305174,3.78403358526469,133.946059662365));
#47445=CARTESIAN_POINT('Ctrl Pts',(95.8249754775703,3.87132420731645,133.840922078907));
#47446=CARTESIAN_POINT('Ctrl Pts',(95.8172107246233,3.95434431595511,133.73200570592));
#47447=CARTESIAN_POINT('Ctrl Pts',(95.8094459716762,4.03275132966307,133.619693595315));
#47448=CARTESIAN_POINT('Ctrl Pts',(95.8016889307912,4.11108046841973,133.507493034682));
#47449=CARTESIAN_POINT('Ctrl Pts',(95.7939318899062,4.18480540786601,133.391903766746));
#47450=CARTESIAN_POINT('Ctrl Pts',(95.7861748490212,4.25362353537386,133.273342165049));
#47451=CARTESIAN_POINT('Ctrl Pts',(95.778423657781,4.32238976659642,133.154869971579));
#47452=CARTESIAN_POINT('Ctrl Pts',(95.7706724665409,4.38625635556175,133.033430242604));
#47453=CARTESIAN_POINT('Ctrl Pts',(95.7629212753008,4.44496397163262,132.909468299702));
#47454=CARTESIAN_POINT('Ctrl Pts',(95.7551733785237,4.50364663540059,132.785559043933));
#47455=CARTESIAN_POINT('Ctrl Pts',(95.7474254817466,4.55717452039897,132.659130058982));
#47456=CARTESIAN_POINT('Ctrl Pts',(95.7396775849696,4.60533434685947,132.530651038132));
#47457=CARTESIAN_POINT('Ctrl Pts',(95.7319313088855,4.65348409932249,132.402198892323));
#47458=CARTESIAN_POINT('Ctrl Pts',(95.7241850328014,4.69626788958109,132.271697929427));
#47459=CARTESIAN_POINT('Ctrl Pts',(95.7164387567173,4.73352083334267,132.139637211688));
#47460=CARTESIAN_POINT('Ctrl Pts',(95.708692423452,4.770774052097,132.007575519108));
#47461=CARTESIAN_POINT('Ctrl Pts',(95.7009460901865,4.8024962367413,131.873954424991));
#47462=CARTESIAN_POINT('Ctrl Pts',(95.6931997569212,4.82857268484914,131.739277132357));
#47463=CARTESIAN_POINT('Ctrl Pts',(95.6854516889182,4.85465497259673,131.604569679676));
#47464=CARTESIAN_POINT('Ctrl Pts',(95.6777036209153,4.8750889336455,131.468805941577));
#47465=CARTESIAN_POINT('Ctrl Pts',(95.6699555529123,4.8898112545244,131.332497870206));
#47466=CARTESIAN_POINT('Ctrl Pts',(95.6621992501705,4.90454922246114,131.196044928995));
#47467=CARTESIAN_POINT('Ctrl Pts',(95.6544429474286,4.91356338190181,131.059046888174));
#47468=CARTESIAN_POINT('Ctrl Pts',(95.6466866446868,4.91684241672453,130.922019920634));
#47469=CARTESIAN_POINT('Ctrl Pts',(95.6389262021726,4.92012320166686,130.784919817676));
#47470=CARTESIAN_POINT('Ctrl Pts',(95.6311657596585,4.91766276968259,130.647791147948));
#47471=CARTESIAN_POINT('Ctrl Pts',(95.6234053171443,4.90950193007445,130.511147621443));
#47472=CARTESIAN_POINT('Ctrl Pts',(95.6156324168789,4.90132798996209,130.374284742619));
#47473=CARTESIAN_POINT('Ctrl Pts',(95.6078595166134,4.8874353956562,130.237908952476));
#47474=CARTESIAN_POINT('Ctrl Pts',(95.600086616348,4.86791670497473,130.102527292675));
#47475=CARTESIAN_POINT('Ctrl Pts',(95.592596280586,4.84910756786409,129.972067097213));
#47476=CARTESIAN_POINT('Ctrl Pts',(95.5851059448239,4.8250743344845,129.842530311516));
#47477=CARTESIAN_POINT('Ctrl Pts',(95.5776156090619,4.79594377541159,129.714357697574));
#47478=CARTESIAN_POINT('Ctrl Pts',(95.5698412749428,4.76570872233749,129.581325380018));
#47479=CARTESIAN_POINT('Ctrl Pts',(95.5620669408237,4.72988640757497,129.449341315004));
#47480=CARTESIAN_POINT('Ctrl Pts',(95.5542926067046,4.68856296692414,129.318911066862));
#47481=CARTESIAN_POINT('Ctrl Pts',(95.5465278537575,4.64729045372073,129.188641562343));
#47482=CARTESIAN_POINT('Ctrl Pts',(95.5387631008105,4.60053042105274,129.059922433664));
#47483=CARTESIAN_POINT('Ctrl Pts',(95.5309983478634,4.54841996766372,128.933248953272));
#47484=CARTESIAN_POINT('Ctrl Pts',(95.5232413069784,4.49636127111167,128.806701286766));
#47485=CARTESIAN_POINT('Ctrl Pts',(95.5154842660934,4.43896287694115,128.682195584467));
#47486=CARTESIAN_POINT('Ctrl Pts',(95.5077272252084,4.37641152248942,128.560211503019));
#47487=CARTESIAN_POINT('Ctrl Pts',(95.4999760339683,4.31390733850062,128.438319410716));
#47488=CARTESIAN_POINT('Ctrl Pts',(95.4922248427281,4.24625810652563,128.318945500782));
#47489=CARTESIAN_POINT('Ctrl Pts',(95.484473651488,4.17369831367707,128.202548662618));
#47490=CARTESIAN_POINT('Ctrl Pts',(95.4767257547109,4.10116936067607,128.086201296216));
#47491=CARTESIAN_POINT('Ctrl Pts',(95.4689778579339,4.02373420431497,127.972828816012));
#47492=CARTESIAN_POINT('Ctrl Pts',(95.4612299611568,3.94167272792981,127.86286454101));
#47493=CARTESIAN_POINT('Ctrl Pts',(95.4534836850727,3.85962841703646,127.752923268163));
#47494=CARTESIAN_POINT('Ctrl Pts',(95.4457374089886,3.7729599446594,127.64638909561));
#47495=CARTESIAN_POINT('Ctrl Pts',(95.4379911329045,3.68198964872925,127.543665095265));
#47496=CARTESIAN_POINT('Ctrl Pts',(95.4302447996391,3.59101868127703,127.440940336636));
#47497=CARTESIAN_POINT('Ctrl Pts',(95.4224984663738,3.49574608610839,127.342026099029));
#47498=CARTESIAN_POINT('Ctrl Pts',(95.4147521331084,3.39653322271067,127.247290878367));
#47499=CARTESIAN_POINT('Ctrl Pts',(95.4070040651054,3.29729814128009,127.15253444241));
#47500=CARTESIAN_POINT('Ctrl Pts',(95.3992559971025,3.19412131846217,127.061959155604));
#47501=CARTESIAN_POINT('Ctrl Pts',(95.3915079290995,3.08739925162051,126.975895008005));
#47502=CARTESIAN_POINT('Ctrl Pts',(95.3837516263577,2.9805637592962,126.889739390406));
#47503=CARTESIAN_POINT('Ctrl Pts',(95.3759953236158,2.87017580092754,126.808104735347));
#47504=CARTESIAN_POINT('Ctrl Pts',(95.3682390208739,2.75666353074768,126.731279567458));
#47505=CARTESIAN_POINT('Ctrl Pts',(95.3604785783598,2.64309067565135,126.654413395665));
#47506=CARTESIAN_POINT('Ctrl Pts',(95.3527181358456,2.52639051853612,126.582362031234));
#47507=CARTESIAN_POINT('Ctrl Pts',(95.3449576933314,2.40701731659418,126.515368812944));
#47508=CARTESIAN_POINT('Ctrl Pts',(95.337184793066,2.28745248619112,126.448268051192));
#47509=CARTESIAN_POINT('Ctrl Pts',(95.3294118928006,2.1652063850125,126.386241838504));
#47510=CARTESIAN_POINT('Ctrl Pts',(95.3216389925351,2.04075563133009,126.329486371769));
#47511=CARTESIAN_POINT('Ctrl Pts',(95.3141486567731,1.92082897601657,126.274794109209));
#47512=CARTESIAN_POINT('Ctrl Pts',(95.3066583210111,1.7988554598522,126.224996152327));
#47513=CARTESIAN_POINT('Ctrl Pts',(95.2991679852491,1.67527443097365,126.180224088069));
#47514=CARTESIAN_POINT('Ctrl Pts',(95.29139365113,1.54700778982344,126.133754477387));
#47515=CARTESIAN_POINT('Ctrl Pts',(95.2836193170109,1.41660302180681,126.092552194308));
#47516=CARTESIAN_POINT('Ctrl Pts',(95.2758449828918,1.28453203101504,126.056818040211));
#47517=CARTESIAN_POINT('Ctrl Pts',(95.2680802299447,1.15262380591599,126.021127925266));
#47518=CARTESIAN_POINT('Ctrl Pts',(95.2603154769976,1.0190538176086,125.990892631872));
#47519=CARTESIAN_POINT('Ctrl Pts',(95.2525507240505,0.884312858049897,125.966264521829));
#47520=CARTESIAN_POINT('Ctrl Pts',(95.2447936831655,0.749705725111924,125.941660872772));
#47521=CARTESIAN_POINT('Ctrl Pts',(95.2370366422805,0.613930317500038,125.922653394081));
#47522=CARTESIAN_POINT('Ctrl Pts',(95.2292796013955,0.477491120026485,125.909344244478));
#47523=CARTESIAN_POINT('Ctrl Pts',(95.2215284101554,0.341154812412719,125.896045131409));
#47524=CARTESIAN_POINT('Ctrl Pts',(95.2137772189152,0.204156098833551,125.888435832006));
#47525=CARTESIAN_POINT('Ctrl Pts',(95.2060260276751,0.0670078019502721,
125.886567106551));
#47526=CARTESIAN_POINT('Ctrl Pts',(95.198278130898,-0.0700822032480007,
125.884699175355));
#47527=CARTESIAN_POINT('Ctrl Pts',(95.1905302341209,-0.207321275190314,
125.888566970652));
#47528=CARTESIAN_POINT('Ctrl Pts',(95.1827823373439,-0.344193566549059,
125.898169238171));
#47529=CARTESIAN_POINT('Ctrl Pts',(95.1750360612598,-0.48103722717517,125.907769497103));
#47530=CARTESIAN_POINT('Ctrl Pts',(95.1672897851757,-0.617513870063609,
125.923101814986));
#47531=CARTESIAN_POINT('Ctrl Pts',(95.1595435090915,-0.753110147871704,
125.944112870005));
#47532=CARTESIAN_POINT('Ctrl Pts',(95.1517971758262,-0.888707426620626,
125.965124080123));
#47533=CARTESIAN_POINT('Ctrl Pts',(95.1440508425608,-1.02342394096716,125.991814051157));
#47534=CARTESIAN_POINT('Ctrl Pts',(95.1363045092955,-1.15675434122567,126.024077942184));
#47535=CARTESIAN_POINT('Ctrl Pts',(95.1285564412925,-1.29011459990268,126.056349058486));
#47536=CARTESIAN_POINT('Ctrl Pts',(95.1208083732895,-1.42208774688537,126.094196486698));
#47537=CARTESIAN_POINT('Ctrl Pts',(95.1130603052866,-1.55218183568265,126.137465010047));
#47538=CARTESIAN_POINT('Ctrl Pts',(95.1053040025447,-1.68241419002592,126.180779519698));
#47539=CARTESIAN_POINT('Ctrl Pts',(95.0975476998029,-1.81076312521467,126.229526510326));
#47540=CARTESIAN_POINT('Ctrl Pts',(95.089791397061,-1.9367544694845,126.28350171826));
#47541=CARTESIAN_POINT('Ctrl Pts',(95.0820309545469,-2.06281305912837,126.337505734388));
#47542=CARTESIAN_POINT('Ctrl Pts',(95.0742705120327,-2.18651119810527,126.396743359262));
#47543=CARTESIAN_POINT('Ctrl Pts',(95.0665100695185,-2.30739862150147,126.460963943994));
#47544=CARTESIAN_POINT('Ctrl Pts',(95.058737169253,-2.4284801041215,126.525287621311));
#47545=CARTESIAN_POINT('Ctrl Pts',(95.0509642689876,-2.54674151724374,126.594610045389));
#47546=CARTESIAN_POINT('Ctrl Pts',(95.0431913687222,-2.66176017105028,126.668636272991));
#47547=CARTESIAN_POINT('Ctrl Pts',(95.0357010329602,-2.77259760707675,126.739971460759));
#47548=CARTESIAN_POINT('Ctrl Pts',(95.0282106971981,-2.88042370340878,126.8156742223));
#47549=CARTESIAN_POINT('Ctrl Pts',(95.020720361436,-2.98489027382289,126.895446047543));
#47550=CARTESIAN_POINT('Ctrl Pts',(95.0129820677061,-3.09281507619549,126.977858616847));
#47551=CARTESIAN_POINT('Ctrl Pts',(95.0052437739762,-3.19751468618271,127.064889917331));
#47552=CARTESIAN_POINT('Ctrl Pts',(94.9975054802462,-3.29856204254205,127.156255422537));
#47553=CARTESIAN_POINT('Ctrl Pts',(94.9898273074911,-3.39882433364356,127.246911083502));
#47554=CARTESIAN_POINT('Ctrl Pts',(94.9821491347359,-3.49549059162687,127.341833600504));
#47555=CARTESIAN_POINT('Ctrl Pts',(94.9744709619808,-3.58817228842645,127.440701495261));
#47556=CARTESIAN_POINT('Ctrl Pts',(94.966799791251,-3.68076946516975,127.539479228525));
#47557=CARTESIAN_POINT('Ctrl Pts',(94.9591286205212,-3.76938903420821,127.642194895289));
#47558=CARTESIAN_POINT('Ctrl Pts',(94.9514574497914,-3.85367693199277,127.748488047198));
#47559=CARTESIAN_POINT('Ctrl Pts',(94.943791524058,-3.93790719975773,127.854708523474));
#47560=CARTESIAN_POINT('Ctrl Pts',(94.9361255983246,-4.01781143930909,127.964501307338));
#47561=CARTESIAN_POINT('Ctrl Pts',(94.9284596725912,-4.09307410386974,128.077470916326));
#47562=CARTESIAN_POINT('Ctrl Pts',(94.9206714758684,-4.16953720276554,128.192242382824));
#47563=CARTESIAN_POINT('Ctrl Pts',(94.9128832791456,-4.24120910544823,128.310292574397));
#47564=CARTESIAN_POINT('Ctrl Pts',(94.9050950824228,-4.30780306291853,128.431173765755));
#47565=CARTESIAN_POINT('Ctrl Pts',(94.8974332980193,-4.37331611592385,128.550092901929));
#47566=CARTESIAN_POINT('Ctrl Pts',(94.8897715136158,-4.43391464534115,128.671751456445));
#47567=CARTESIAN_POINT('Ctrl Pts',(94.8821097292122,-4.48937106750423,128.795696762971));
#47568=CARTESIAN_POINT('Ctrl Pts',(94.8742583263298,-4.54619995877645,128.92270954298));
#47569=CARTESIAN_POINT('Ctrl Pts',(94.8664069234474,-4.59762869126989,129.052123353862));
#47570=CARTESIAN_POINT('Ctrl Pts',(94.858555520565,-4.64346444194557,129.183428466337));
#47571=CARTESIAN_POINT('Ctrl Pts',(94.8507041176826,-4.68930019262124,129.314733578813));
#47572=CARTESIAN_POINT('Ctrl Pts',(94.8428527148001,-4.7295428368851,129.447929558527));
#47573=CARTESIAN_POINT('Ctrl Pts',(94.8350013119177,-4.76405452823406,129.582490119308));
#47574=CARTESIAN_POINT('Ctrl Pts',(96.5847048906856,-4.76405452823403,129.582490119308));
#47575=CARTESIAN_POINT('Ctrl Pts',(96.5769147324208,-4.79833529931696,129.716150325477));
#47576=CARTESIAN_POINT('Ctrl Pts',(96.569124574156,-4.82700348682742,129.851318908786));
#47577=CARTESIAN_POINT('Ctrl Pts',(96.5613344158913,-4.84993841038099,129.98748824197));
#47578=CARTESIAN_POINT('Ctrl Pts',(96.553544867975,-4.87287153701372,130.123646906468));
#47579=CARTESIAN_POINT('Ctrl Pts',(96.5457553200588,-4.89007222053425,130.260805787351));
#47580=CARTESIAN_POINT('Ctrl Pts',(96.5379657721426,-4.90147094549081,130.398447285672));
#47581=CARTESIAN_POINT('Ctrl Pts',(96.530263660092,-4.9127417224079,130.534543790151));
#47582=CARTESIAN_POINT('Ctrl Pts',(96.5225615480415,-4.91834012405208,130.671111761788));
#47583=CARTESIAN_POINT('Ctrl Pts',(96.514859435991,-4.9182489022828,130.80764660205));
#47584=CARTESIAN_POINT('',(96.8601405640579,-4.91824839088665,130.800382170524));
#47585=CARTESIAN_POINT('Ctrl Pts',(96.929952524335,-4.76405452823407,129.582490119308));
#47586=CARTESIAN_POINT('Ctrl Pts',(96.9207574310496,-4.80419149538206,129.738983545055));
#47587=CARTESIAN_POINT('Ctrl Pts',(96.9115623377642,-4.83665391359241,129.897613593837));
#47588=CARTESIAN_POINT('Ctrl Pts',(96.9023672444788,-4.86124082596128,130.057687533474));
#47589=CARTESIAN_POINT('Ctrl Pts',(96.8932607227116,-4.88559090547952,130.216219564682));
#47590=CARTESIAN_POINT('Ctrl Pts',(96.8841542009443,-4.90221640676791,130.376167729082));
#47591=CARTESIAN_POINT('Ctrl Pts',(96.8750476791771,-4.91096885746551,130.536838761442));
#47592=CARTESIAN_POINT('Ctrl Pts',(96.870078640804,-4.91574469444108,130.624510053034));
#47593=CARTESIAN_POINT('Ctrl Pts',(96.865109602431,-4.91817721769542,130.712396222853));
#47594=CARTESIAN_POINT('Ctrl Pts',(96.8601405640579,-4.91824839088665,130.800382170524));
#47595=CARTESIAN_POINT('Ctrl Pts',(96.8601405640084,-4.91824839088736,130.8003821714));
#47596=CARTESIAN_POINT('Ctrl Pts',(96.8522937533478,-4.91836078334458,130.939324361083));
#47597=CARTESIAN_POINT('Ctrl Pts',(96.8444469426872,-4.91258087579584,131.078346812634));
#47598=CARTESIAN_POINT('Ctrl Pts',(96.8366001320266,-4.90091673110298,131.216911532357));
#47599=CARTESIAN_POINT('Ctrl Pts',(96.8288723439396,-4.88942951135199,131.353374464453));
#47600=CARTESIAN_POINT('Ctrl Pts',(96.8211445558527,-4.87223536073034,131.489393051659));
#47601=CARTESIAN_POINT('Ctrl Pts',(96.8134167677656,-4.84939441297877,131.624456276541));
#47602=CARTESIAN_POINT('Ctrl Pts',(96.805688903088,-4.82655323884909,131.759520840045));
#47603=CARTESIAN_POINT('Ctrl Pts',(96.7979610384104,-4.79806522128852,131.893629635197));
#47604=CARTESIAN_POINT('Ctrl Pts',(96.7902331737327,-4.76404190096828,132.026280348284));
#47605=CARTESIAN_POINT('Ctrl Pts',(96.7825035423692,-4.73001080249401,132.158961386974));
#47606=CARTESIAN_POINT('Ctrl Pts',(96.7747739110056,-4.6904419807485,132.290183300077));
#47607=CARTESIAN_POINT('Ctrl Pts',(96.7670442796421,-4.64549716040654,132.419457888678));
#47608=CARTESIAN_POINT('Ctrl Pts',(96.7591086820181,-4.59935472582714,132.552177169831));
#47609=CARTESIAN_POINT('Ctrl Pts',(96.7511730843941,-4.54754591949674,132.682843477103));
#47610=CARTESIAN_POINT('Ctrl Pts',(96.7432374867701,-4.49029844563479,132.810950493856));
#47611=CARTESIAN_POINT('Ctrl Pts',(96.7354949775542,-4.43444391331513,132.93594041961));
#47612=CARTESIAN_POINT('Ctrl Pts',(96.7277524683382,-4.37341256186794,133.058493840385));
#47613=CARTESIAN_POINT('Ctrl Pts',(96.7200099591223,-4.30746209298632,133.178166292002));
#47614=CARTESIAN_POINT('Ctrl Pts',(96.7119778172943,-4.23904454191752,133.302315463477));
#47615=CARTESIAN_POINT('Ctrl Pts',(96.7039456754663,-4.16533294617827,133.423363531095));
#47616=CARTESIAN_POINT('Ctrl Pts',(96.6959135336382,-4.08666308125691,133.540848863985));
#47617=CARTESIAN_POINT('Ctrl Pts',(96.6878813918102,-4.00799321633556,133.658334196876));
#47618=CARTESIAN_POINT('Ctrl Pts',(96.6798492499822,-3.92436541508682,133.772256464385));
#47619=CARTESIAN_POINT('Ctrl Pts',(96.6718171081542,-3.83615976287862,133.882194488354));
#47620=CARTESIAN_POINT('Ctrl Pts',(96.6640427740351,-3.75078524806782,133.988603830847));
#47621=CARTESIAN_POINT('Ctrl Pts',(96.656268439916,-3.66084469644549,134.091626783757));
#47622=CARTESIAN_POINT('Ctrl Pts',(96.6484941057969,-3.56663668836502,134.190846376536));
#47623=CARTESIAN_POINT('Ctrl Pts',(96.6407293528498,-3.47254478323504,134.289943690035));
#47624=CARTESIAN_POINT('Ctrl Pts',(96.6329645999027,-3.37419615262093,134.385246688935));
#47625=CARTESIAN_POINT('Ctrl Pts',(96.6251998469557,-3.27193070545506,134.476369947783));
#47626=CARTESIAN_POINT('Ctrl Pts',(96.6174428060707,-3.16976682977294,134.567402701726));
#47627=CARTESIAN_POINT('Ctrl Pts',(96.6096857651856,-3.06369416929632,134.654263718631));
#47628=CARTESIAN_POINT('Ctrl Pts',(96.6019287243006,-2.95409044203545,134.736603326603));
#47629=CARTESIAN_POINT('Ctrl Pts',(96.5941775330605,-2.84456936779828,134.818880841636));
#47630=CARTESIAN_POINT('Ctrl Pts',(96.5864263418204,-2.73152283824858,134.896643500518));
#47631=CARTESIAN_POINT('Ctrl Pts',(96.5786751505803,-2.6153624287966,134.969581191382));
#47632=CARTESIAN_POINT('Ctrl Pts',(96.5709272538032,-2.49925139061693,135.042487881782));
#47633=CARTESIAN_POINT('Ctrl Pts',(96.5631793570262,-2.38002943525141,135.110573475463));
#47634=CARTESIAN_POINT('Ctrl Pts',(96.5554314602491,-2.25813777823766,135.173570710591));
#47635=CARTESIAN_POINT('Ctrl Pts',(96.547685184165,-2.13627161833095,135.236554768056));
#47636=CARTESIAN_POINT('Ctrl Pts',(96.5399389080808,-2.01173721465227,135.294452404676));
#47637=CARTESIAN_POINT('Ctrl Pts',(96.5321926319967,-1.88500073206192,135.347042127712));
#47638=CARTESIAN_POINT('Ctrl Pts',(96.5244462987314,-1.75826331393148,135.399632238954));
#47639=CARTESIAN_POINT('Ctrl Pts',(96.516699965466,-1.62932414556343,135.446914208585));
#47640=CARTESIAN_POINT('Ctrl Pts',(96.5089536322007,-1.4986693605315,135.488714704343));
#47641=CARTESIAN_POINT('Ctrl Pts',(96.5012055641977,-1.36798531626644,135.530524561032));
#47642=CARTESIAN_POINT('Ctrl Pts',(96.4934574961947,-1.235585263124,135.56685038208));
#47643=CARTESIAN_POINT('Ctrl Pts',(96.4857094281917,-1.10197009205432,135.597568831145));
#47644=CARTESIAN_POINT('Ctrl Pts',(96.4779531254499,-0.968212913190873,
135.628319928142));
#47645=CARTESIAN_POINT('Ctrl Pts',(96.470196822708,-0.833238418238962,135.653451660511));
#47646=CARTESIAN_POINT('Ctrl Pts',(96.4624405199662,-0.697557830692655,
135.672891826806));
#47647=CARTESIAN_POINT('Ctrl Pts',(96.454680077452,-0.561804826331418,135.692342368902));
#47648=CARTESIAN_POINT('Ctrl Pts',(96.4469196349378,-0.425345367248886,
135.706095252743));
#47649=CARTESIAN_POINT('Ctrl Pts',(96.4391591924236,-0.288694387747627,
135.714130328355));
#47650=CARTESIAN_POINT('Ctrl Pts',(96.4313862921582,-0.151824043962769,
135.722178302584));
#47651=CARTESIAN_POINT('Ctrl Pts',(96.4236133918928,-0.014761956519537,
135.724490119951));
#47652=CARTESIAN_POINT('Ctrl Pts',(96.4158404916273,0.121977449986141,135.72109780438));
#47653=CARTESIAN_POINT('Ctrl Pts',(96.4083501558653,0.253746034639001,135.717828808024));
#47654=CARTESIAN_POINT('Ctrl Pts',(96.4008598201033,0.385214684207991,135.709263217823));
#47655=CARTESIAN_POINT('Ctrl Pts',(96.3933694843413,0.515930749031297,135.695474859199));
#47656=CARTESIAN_POINT('Ctrl Pts',(96.3855951502222,0.651602953183148,135.681163710767));
#47657=CARTESIAN_POINT('Ctrl Pts',(96.3778208161031,0.786894146299921,135.661180599962));
#47658=CARTESIAN_POINT('Ctrl Pts',(96.370046481984,0.921292129275798,135.635551348125));
#47659=CARTESIAN_POINT('Ctrl Pts',(96.362281729037,1.05552447874915,135.60995368205));
#47660=CARTESIAN_POINT('Ctrl Pts',(96.3545169760899,1.18886542799099,135.578723792547));
#47661=CARTESIAN_POINT('Ctrl Pts',(96.3467522231428,1.32080697857008,135.541939322755));
#47662=CARTESIAN_POINT('Ctrl Pts',(96.3389951822578,1.45261748294063,135.505191387817));
#47663=CARTESIAN_POINT('Ctrl Pts',(96.3312381413729,1.58303098045092,135.46289995576));
#47664=CARTESIAN_POINT('Ctrl Pts',(96.3234811004879,1.71154911642052,135.415193805243));
#47665=CARTESIAN_POINT('Ctrl Pts',(96.3157299092478,1.83997033586431,135.367523630304));
#47666=CARTESIAN_POINT('Ctrl Pts',(96.3079787180076,1.96649867367134,135.314446999934));
#47667=CARTESIAN_POINT('Ctrl Pts',(96.3002275267675,2.09065075738291,135.256142561143));
#47668=CARTESIAN_POINT('Ctrl Pts',(96.2924796299904,2.21475007314721,135.197862903293));
#47669=CARTESIAN_POINT('Ctrl Pts',(96.2847317332133,2.33647479042863,135.13436002217));
#47670=CARTESIAN_POINT('Ctrl Pts',(96.2769838364362,2.45536156650153,135.065860663354));
#47671=CARTESIAN_POINT('Ctrl Pts',(96.2692375603521,2.57422347402385,134.997375633126));
#47672=CARTESIAN_POINT('Ctrl Pts',(96.261491284268,2.69024828256869,134.923896399135));
#47673=CARTESIAN_POINT('Ctrl Pts',(96.2537450081839,2.80299767052856,134.845695436844));
#47674=CARTESIAN_POINT('Ctrl Pts',(96.2459986749186,2.91574789077865,134.767493897292));
#47675=CARTESIAN_POINT('Ctrl Pts',(96.2382523416532,3.0252223209407,134.684570782709));
#47676=CARTESIAN_POINT('Ctrl Pts',(96.2305060083879,3.13101236460376,134.597241400717));
#47677=CARTESIAN_POINT('Ctrl Pts',(96.2227579403849,3.23682609921375,134.509892461916));
#47678=CARTESIAN_POINT('Ctrl Pts',(96.2150098723819,3.33895350403678,134.418135541027));
#47679=CARTESIAN_POINT('Ctrl Pts',(96.2072618043789,3.43702006892149,134.322325385487));
#47680=CARTESIAN_POINT('Ctrl Pts',(96.1995055016371,3.5351908601183,134.226413401773));
#47681=CARTESIAN_POINT('Ctrl Pts',(96.1917491988953,3.62929190978506,134.126439851716));
#47682=CARTESIAN_POINT('Ctrl Pts',(96.1839928961534,3.71898614401388,134.022795815474));
#47683=CARTESIAN_POINT('Ctrl Pts',(96.1762324536392,3.80872825075628,133.919096461289));
#47684=CARTESIAN_POINT('Ctrl Pts',(96.168472011125,3.89405861227602,133.811723023279));
#47685=CARTESIAN_POINT('Ctrl Pts',(96.1607115686109,3.97468194125959,133.701097838704));
#47686=CARTESIAN_POINT('Ctrl Pts',(96.1529386683454,4.05543469396812,133.590295068761));
#47687=CARTESIAN_POINT('Ctrl Pts',(96.14516576808,4.13146509758381,133.476230446552));
#47688=CARTESIAN_POINT('Ctrl Pts',(96.1373928678146,4.20252203568043,133.359354081769));
#47689=CARTESIAN_POINT('Ctrl Pts',(96.1299025320525,4.27099587509585,133.24672646724));
#47690=CARTESIAN_POINT('Ctrl Pts',(96.1224121962905,4.33485141786226,133.131488258241));
#47691=CARTESIAN_POINT('Ctrl Pts',(96.1149218605284,4.39390610720005,133.014060186197));
#47692=CARTESIAN_POINT('Ctrl Pts',(96.1071475264093,4.45519987303315,132.892179793111));
#47693=CARTESIAN_POINT('Ctrl Pts',(96.0993731922903,4.51151571051237,132.767554121192));
#47694=CARTESIAN_POINT('Ctrl Pts',(96.0915988581712,4.56259848773544,132.640628055118));
#47695=CARTESIAN_POINT('Ctrl Pts',(96.0838341052241,4.61361831000094,132.513858414078));
#47696=CARTESIAN_POINT('Ctrl Pts',(96.076069352277,4.65941775958474,132.38479437896));
#47697=CARTESIAN_POINT('Ctrl Pts',(96.0683045993299,4.69978757429792,132.253905311246));
#47698=CARTESIAN_POINT('Ctrl Pts',(96.060547558445,4.74011729314194,132.123146244399));
#47699=CARTESIAN_POINT('Ctrl Pts',(96.05279051756,4.77502799452796,131.990566123389));
#47700=CARTESIAN_POINT('Ctrl Pts',(96.045033476675,4.80435865071069,131.856653836133));
#47701=CARTESIAN_POINT('Ctrl Pts',(96.0372822854349,4.83366718841754,131.722842533173));
#47702=CARTESIAN_POINT('Ctrl Pts',(96.0295310941947,4.85740397329008,131.587701443924));
#47703=CARTESIAN_POINT('Ctrl Pts',(96.0217799029546,4.87545803149665,131.451733806395));
#47704=CARTESIAN_POINT('Ctrl Pts',(96.0140320061775,4.89350441624688,131.31582395874));
#47705=CARTESIAN_POINT('Ctrl Pts',(96.0062841094004,4.90587282684568,131.179088648277));
#47706=CARTESIAN_POINT('Ctrl Pts',(95.9985362126233,4.91250358270869,131.042040259888));
#47707=CARTESIAN_POINT('Ctrl Pts',(95.9907899365392,4.91913295156051,130.905020539067));
#47708=CARTESIAN_POINT('Ctrl Pts',(95.9830436604551,4.92002703404573,130.767688260843));
#47709=CARTESIAN_POINT('Ctrl Pts',(95.975297384371,4.91517814795374,130.630559477242));
#47710=CARTESIAN_POINT('Ctrl Pts',(95.9675510511057,4.91032922606837,130.493429681386));
#47711=CARTESIAN_POINT('Ctrl Pts',(95.9598047178404,4.89973726482899,130.356503773872));
#47712=CARTESIAN_POINT('Ctrl Pts',(95.952058384575,4.88344668512806,130.220295949903));
#47713=CARTESIAN_POINT('Ctrl Pts',(95.9443103165721,4.86715245726478,130.084057623137));
#47714=CARTESIAN_POINT('Ctrl Pts',(95.9365622485691,4.8451571179372,129.948538088034));
#47715=CARTESIAN_POINT('Ctrl Pts',(95.9288141805661,4.81755669432605,129.814244180244));
#47716=CARTESIAN_POINT('Ctrl Pts',(95.9210578778243,4.78992693665619,129.679807543292));
#47717=CARTESIAN_POINT('Ctrl Pts',(95.9133015750825,4.75668027348595,129.546599519332));
#47718=CARTESIAN_POINT('Ctrl Pts',(95.9055452723406,4.71796353494803,129.415115086567));
#47719=CARTESIAN_POINT('Ctrl Pts',(95.8977848298264,4.6792261321209,129.283560476601));
#47720=CARTESIAN_POINT('Ctrl Pts',(95.8900243873122,4.63501296246106,129.153731660787));
#47721=CARTESIAN_POINT('Ctrl Pts',(95.8822639447981,4.58551974025954,129.026105356308));
#47722=CARTESIAN_POINT('Ctrl Pts',(95.8744910445326,4.53594706714405,128.898274174756));
#47723=CARTESIAN_POINT('Ctrl Pts',(95.8667181442672,4.48107756030123,128.772652928414));
#47724=CARTESIAN_POINT('Ctrl Pts',(95.8589452440018,4.42115417520255,128.649696183927));
#47725=CARTESIAN_POINT('Ctrl Pts',(95.8514549082397,4.36340915608987,128.531209226811));
#47726=CARTESIAN_POINT('Ctrl Pts',(95.8439645724777,4.30097146776716,128.415196683385));
#47727=CARTESIAN_POINT('Ctrl Pts',(95.8364742367156,4.23409640709906,128.30203955945));
#47728=CARTESIAN_POINT('Ctrl Pts',(95.8286999025965,4.16468575817969,128.184592048768));
#47729=CARTESIAN_POINT('Ctrl Pts',(95.8209255684774,4.09027473655954,128.069848719925));
#47730=CARTESIAN_POINT('Ctrl Pts',(95.8131512343583,4.01109973129416,127.958264693653));
#47731=CARTESIAN_POINT('Ctrl Pts',(95.8053864814112,3.93202230214679,127.846818184722));
#47732=CARTESIAN_POINT('Ctrl Pts',(95.7976217284642,3.84819279533263,127.738523547134));
#47733=CARTESIAN_POINT('Ctrl Pts',(95.7898569755171,3.75989298663368,127.63381054044));
#47734=CARTESIAN_POINT('Ctrl Pts',(95.782099934632,3.67168087854936,127.529201536181));
#47735=CARTESIAN_POINT('Ctrl Pts',(95.774342893747,3.57900755471945,127.428167380526));
#47736=CARTESIAN_POINT('Ctrl Pts',(95.766585852862,3.48219729096509,127.331107806541));
#47737=CARTESIAN_POINT('Ctrl Pts',(95.7588346616219,3.3854600325841,127.234121425935));
#47738=CARTESIAN_POINT('Ctrl Pts',(95.7510834703818,3.28459231883076,127.141103936817));
#47739=CARTESIAN_POINT('Ctrl Pts',(95.7433322791417,3.17995755403037,127.052420717053));
#47740=CARTESIAN_POINT('Ctrl Pts',(95.7355843823646,3.07536726179589,126.963775190022));
#47741=CARTESIAN_POINT('Ctrl Pts',(95.7278364855875,2.96701340060214,126.879460520642));
#47742=CARTESIAN_POINT('Ctrl Pts',(95.7200885888104,2.8552947955475,126.799803876425));
#47743=CARTESIAN_POINT('Ctrl Pts',(95.7123423127263,2.7435995596166,126.72016389466));
#47744=CARTESIAN_POINT('Ctrl Pts',(95.7045960366422,2.62854129791653,126.645180226836));
#47745=CARTESIAN_POINT('Ctrl Pts',(95.6968497605581,2.51055002720985,126.575138274939));
#47746=CARTESIAN_POINT('Ctrl Pts',(95.6891034272928,2.39255788551865,126.505095806008));
#47747=CARTESIAN_POINT('Ctrl Pts',(95.6813570940274,2.27163302781073,126.439995325366));
#47748=CARTESIAN_POINT('Ctrl Pts',(95.6736107607621,2.14823207165186,126.380077395526));
#47749=CARTESIAN_POINT('Ctrl Pts',(95.6658626927591,2.02480348070446,126.32014604748));
#47750=CARTESIAN_POINT('Ctrl Pts',(95.6581146247561,1.8988980395363,126.265399730425));
#47751=CARTESIAN_POINT('Ctrl Pts',(95.6503665567531,1.7709940683723,126.216031611022));
#47752=CARTESIAN_POINT('Ctrl Pts',(95.6426102540113,1.64295415934549,126.166611022595));
#47753=CARTESIAN_POINT('Ctrl Pts',(95.6348539512694,1.51291184260174,126.122580191177));
#47754=CARTESIAN_POINT('Ctrl Pts',(95.6270976485276,1.38136292259538,126.084083132229));
#47755=CARTESIAN_POINT('Ctrl Pts',(95.6193372060134,1.24974379096955,126.045565526242));
#47756=CARTESIAN_POINT('Ctrl Pts',(95.6115767634992,1.11661683311413,126.012587671866));
#47757=CARTESIAN_POINT('Ctrl Pts',(95.603816320985,0.982488913052441,125.985242586408));
#47758=CARTESIAN_POINT('Ctrl Pts',(95.5960434207196,0.848145678946153,125.957853604192));
#47759=CARTESIAN_POINT('Ctrl Pts',(95.5882705204542,0.712798657908766,125.936115522167));
#47760=CARTESIAN_POINT('Ctrl Pts',(95.5804976201887,0.576961613100181,125.920069639388));
#47761=CARTESIAN_POINT('Ctrl Pts',(95.5730072844267,0.446062587022976,125.904607064866));
#47762=CARTESIAN_POINT('Ctrl Pts',(95.5655169486646,0.314708852929088,125.894430046893));
#47763=CARTESIAN_POINT('Ctrl Pts',(95.5580266129026,0.183358955980787,125.88952973993));
#47764=CARTESIAN_POINT('Ctrl Pts',(95.5502522787835,0.0470288877670453,
125.884443636339));
#47765=CARTESIAN_POINT('Ctrl Pts',(95.5424779446644,-0.0897288992641427,
125.885026164257));
#47766=CARTESIAN_POINT('Ctrl Pts',(95.5347036105453,-0.226403725093196,
125.891324446748));
#47767=CARTESIAN_POINT('Ctrl Pts',(95.5269388575982,-0.362910111414581,
125.897614967169));
#47768=CARTESIAN_POINT('Ctrl Pts',(95.5191741046511,-0.499333353163979,
125.909607208567));
#47769=CARTESIAN_POINT('Ctrl Pts',(95.511409351704,-0.635159574766587,125.927296400531));
#47770=CARTESIAN_POINT('Ctrl Pts',(95.5036523108189,-0.77085089185127,125.94496802334));
#47771=CARTESIAN_POINT('Ctrl Pts',(95.4958952699339,-0.90594598364137,125.968325286296));
#47772=CARTESIAN_POINT('Ctrl Pts',(95.4881382290489,-1.03993326438723,125.99731143245));
#47773=CARTESIAN_POINT('Ctrl Pts',(95.4803870378088,-1.17381950428168,126.026275719927));
#47774=CARTESIAN_POINT('Ctrl Pts',(95.4726358465687,-1.30659921538332,126.060860359283));
#47775=CARTESIAN_POINT('Ctrl Pts',(95.4648846553285,-1.43776856603156,126.100957103829));
#47776=CARTESIAN_POINT('Ctrl Pts',(95.4571367585514,-1.56888216620698,126.14103680619));
#47777=CARTESIAN_POINT('Ctrl Pts',(95.4493888617744,-1.69838639413649,126.186623840053));
#47778=CARTESIAN_POINT('Ctrl Pts',(95.4416409649973,-1.82579041982071,126.2375595046));
#47779=CARTESIAN_POINT('Ctrl Pts',(95.4338946889132,-1.95316779532917,126.288484514503));
#47780=CARTESIAN_POINT('Ctrl Pts',(95.4261484128291,-2.07844547962043,126.344755784654));
#47781=CARTESIAN_POINT('Ctrl Pts',(95.418402136745,-2.20115092135606,126.406165796516));
#47782=CARTESIAN_POINT('Ctrl Pts',(95.4106558034796,-2.32385726887573,126.467576261693));
#47783=CARTESIAN_POINT('Ctrl Pts',(95.4029094702142,-2.44399098632657,126.534125369298));
#47784=CARTESIAN_POINT('Ctrl Pts',(95.3951631369488,-2.56110286870544,126.605558983956));
#47785=CARTESIAN_POINT('Ctrl Pts',(95.3874150689459,-2.67824097747775,126.677008595676));
#47786=CARTESIAN_POINT('Ctrl Pts',(95.3796670009429,-2.79235557087524,126.753344687536));
#47787=CARTESIAN_POINT('Ctrl Pts',(95.37191893294,-2.90302558854828,126.834269246485));
#47788=CARTESIAN_POINT('Ctrl Pts',(95.3641626301981,-3.01381322763347,126.915279813018));
#47789=CARTESIAN_POINT('Ctrl Pts',(95.3564063274562,-3.12114866178335,127.00088835719));
#47790=CARTESIAN_POINT('Ctrl Pts',(95.3486500247144,-3.22464273229404,127.090755588546));
#47791=CARTESIAN_POINT('Ctrl Pts',(95.3408895822002,-3.32819204070653,127.180670784749));
#47792=CARTESIAN_POINT('Ctrl Pts',(95.333129139686,-3.42789561610189,127.274848928926));
#47793=CARTESIAN_POINT('Ctrl Pts',(95.3253686971718,-3.52340122800027,127.372913860143));
#47794=CARTESIAN_POINT('Ctrl Pts',(95.3175957969064,-3.61906015398533,127.471136213894));
#47795=CARTESIAN_POINT('Ctrl Pts',(95.309822896641,-3.71050738895328,127.573257531603));
#47796=CARTESIAN_POINT('Ctrl Pts',(95.3020499963755,-3.79743048530101,127.678867892921));
#47797=CARTESIAN_POINT('Ctrl Pts',(95.2945596606136,-3.88119370814933,127.780639051588));
#47798=CARTESIAN_POINT('Ctrl Pts',(95.2870693248516,-3.96075582336749,127.885649741409));
#47799=CARTESIAN_POINT('Ctrl Pts',(95.2795789890897,-4.03587641809858,127.993509394122));
#47800=CARTESIAN_POINT('Ctrl Pts',(95.2717050370586,-4.11484430128238,128.106893060561));
#47801=CARTESIAN_POINT('Ctrl Pts',(95.2638310850276,-4.1891508090201,128.223779619484));
#47802=CARTESIAN_POINT('Ctrl Pts',(95.2559571329966,-4.25847407000337,128.343754664227));
#47803=CARTESIAN_POINT('Ctrl Pts',(95.2480968834774,-4.327676692354,128.463520924426));
#47804=CARTESIAN_POINT('Ctrl Pts',(95.2402366339582,-4.39191315701078,128.586364638088));
#47805=CARTESIAN_POINT('Ctrl Pts',(95.232376384439,-4.45090391106428,128.71184121814));
#47806=CARTESIAN_POINT('Ctrl Pts',(95.2245241066918,-4.50983483739389,128.837190541332));
#47807=CARTESIAN_POINT('Ctrl Pts',(95.2166718289445,-4.56353047892363,128.965167078036));
#47808=CARTESIAN_POINT('Ctrl Pts',(95.2088195511973,-4.61175609847826,129.095299837298));
#47809=CARTESIAN_POINT('Ctrl Pts',(95.2009752780905,-4.65993255666154,129.225299938755));
#47810=CARTESIAN_POINT('Ctrl Pts',(95.1931310049836,-4.7026499690485,129.357451531393));
#47811=CARTESIAN_POINT('Ctrl Pts',(95.1852867318768,-4.73972105968052,129.491262243901));
#47812=CARTESIAN_POINT('Ctrl Pts',(95.1835089497531,-4.74812264403829,129.521588354354));
#47813=CARTESIAN_POINT('Ctrl Pts',(95.1817311676294,-4.75623441118283,129.551999601612));
#47814=CARTESIAN_POINT('Ctrl Pts',(95.1799533855056,-4.76405452823405,129.582490119308));
#47815=CARTESIAN_POINT('Origin',(213.235140564004,0.,130.804360617566));
#47816=CARTESIAN_POINT('',(93.084857876857,-4.76405452823403,129.582490119308));
#47817=CARTESIAN_POINT('',(93.4302802594722,-4.76405452823405,129.582490119308));
#47818=CARTESIAN_POINT('',(213.235140564004,-4.76405452823405,129.582490119308));
#47819=CARTESIAN_POINT('',(94.7648594360276,-4.91824943780232,130.806712224922));
#47820=CARTESIAN_POINT('Ctrl Pts',(94.7648594359911,-4.91824943780201,130.806712225562));
#47821=CARTESIAN_POINT('Ctrl Pts',(94.7573305365351,-4.91818620258719,130.938964948065));
#47822=CARTESIAN_POINT('Ctrl Pts',(94.7498016370792,-4.91278901830967,131.071085735199));
#47823=CARTESIAN_POINT('Ctrl Pts',(94.7422727376233,-4.90208663697329,131.202769535774));
#47824=CARTESIAN_POINT('Ctrl Pts',(94.7344984035042,-4.89103536860852,131.338746097785));
#47825=CARTESIAN_POINT('Ctrl Pts',(94.7267240693851,-4.87430462804154,131.474477869941));
#47826=CARTESIAN_POINT('Ctrl Pts',(94.718949735266,-4.85190793781127,131.609452180995));
#47827=CARTESIAN_POINT('Ctrl Pts',(94.7111849823189,-4.82953884950005,131.744260148273));
#47828=CARTESIAN_POINT('Ctrl Pts',(94.7034202293718,-4.80151776855422,131.878312129854));
#47829=CARTESIAN_POINT('Ctrl Pts',(94.6956554764247,-4.76791012519175,132.011098410375));
#47830=CARTESIAN_POINT('Ctrl Pts',(94.6878984355397,-4.73433586141442,132.143752805691));
#47831=CARTESIAN_POINT('Ctrl Pts',(94.6801413946547,-4.69518617259555,132.275143625096));
#47832=CARTESIAN_POINT('Ctrl Pts',(94.6723843537697,-4.65057784117023,132.40476956709));
#47833=CARTESIAN_POINT('Ctrl Pts',(94.6646331625296,-4.60600314923467,132.534297757153));
#47834=CARTESIAN_POINT('Ctrl Pts',(94.6568819712895,-4.55597813485301,132.662063350706));
#47835=CARTESIAN_POINT('Ctrl Pts',(94.6491307800494,-4.5006697939834,132.787578827453));
#47836=CARTESIAN_POINT('Ctrl Pts',(94.6413828832723,-4.44538496063406,132.913040956774));
#47837=CARTESIAN_POINT('Ctrl Pts',(94.6336349864952,-4.38482142435525,133.036254514394));
#47838=CARTESIAN_POINT('Ctrl Pts',(94.6258870897181,-4.3191947464801,133.156750849751));
#47839=CARTESIAN_POINT('Ctrl Pts',(94.618140813634,-4.25358179629116,133.277221979872));
#47840=CARTESIAN_POINT('Ctrl Pts',(94.6103945375499,-4.18290799799347,133.39497667515));
#47841=CARTESIAN_POINT('Ctrl Pts',(94.6026482614658,-4.10743523007492,133.509570201543));
#47842=CARTESIAN_POINT('Ctrl Pts',(94.5949019282004,-4.03196190503353,133.624164573839));
#47843=CARTESIAN_POINT('Ctrl Pts',(94.587155594935,-3.951689754728,133.735597404176));
#47844=CARTESIAN_POINT('Ctrl Pts',(94.5794092616697,-3.86692419079314,133.843452647294));
#47845=CARTESIAN_POINT('Ctrl Pts',(94.5716611936667,-3.78213964419796,133.951332043847));
#47846=CARTESIAN_POINT('Ctrl Pts',(94.5639131256637,-3.69285992315453,134.0556319516));
#47847=CARTESIAN_POINT('Ctrl Pts',(94.5561650576607,-3.59943068573003,134.155969455292));
#47848=CARTESIAN_POINT('Ctrl Pts',(94.5484087549189,-3.50590215060024,134.256413598877));
#47849=CARTESIAN_POINT('Ctrl Pts',(94.540652452177,-3.40821555618238,134.352886639311));
#47850=CARTESIAN_POINT('Ctrl Pts',(94.5328961494351,-3.30675378116922,134.445042214908));
#47851=CARTESIAN_POINT('Ctrl Pts',(94.525135706921,-3.20523785295179,134.53724697671));
#47852=CARTESIAN_POINT('Ctrl Pts',(94.5173752644068,-3.09994302923442,134.625129431645));
#47853=CARTESIAN_POINT('Ctrl Pts',(94.5096148218926,-2.99128443957162,134.708384242504));
#47854=CARTESIAN_POINT('Ctrl Pts',(94.5018419216272,-2.88245142149436,134.791772701377));
#47855=CARTESIAN_POINT('Ctrl Pts',(94.4940690213618,-2.77024416712548,134.870518446537));
#47856=CARTESIAN_POINT('Ctrl Pts',(94.4862961210963,-2.65510663043712,134.944359632482));
#47857=CARTESIAN_POINT('Ctrl Pts',(94.4788057853343,-2.54415463322166,135.015516505324));
#47858=CARTESIAN_POINT('Ctrl Pts',(94.4713154495723,-2.4304819669379,135.08211905854));
#47859=CARTESIAN_POINT('Ctrl Pts',(94.4638251138103,-2.31450486099081,135.14397469153));
#47860=CARTESIAN_POINT('Ctrl Pts',(94.4560507796912,-2.19413044782092,135.208175599646));
#47861=CARTESIAN_POINT('Ctrl Pts',(94.4482764455721,-2.07089208983531,135.267465892051));
#47862=CARTESIAN_POINT('Ctrl Pts',(94.440502111453,-1.94522842113553,135.321579834308));
#47863=CARTESIAN_POINT('Ctrl Pts',(94.4327373585059,-1.81971962167662,135.375627085968));
#47864=CARTESIAN_POINT('Ctrl Pts',(94.4249726055589,-1.69179181431925,135.424510527416));
#47865=CARTESIAN_POINT('Ctrl Pts',(94.4172078526118,-1.56190920366396,135.468009693345));
#47866=CARTESIAN_POINT('Ctrl Pts',(94.4094508117268,-1.43215559424861,135.511465655288));
#47867=CARTESIAN_POINT('Ctrl Pts',(94.4016937708417,-1.30045141361129,135.549547860595));
#47868=CARTESIAN_POINT('Ctrl Pts',(94.3939367299567,-1.1672815446597,135.582083595931));
#47869=CARTESIAN_POINT('Ctrl Pts',(94.3861855387166,-1.03421210014219,135.614594795816));
#47870=CARTESIAN_POINT('Ctrl Pts',(94.3784343474765,-0.899679545574676,
135.641567758598));
#47871=CARTESIAN_POINT('Ctrl Pts',(94.3706831562363,-0.764184310983108,
135.662879466078));
#47872=CARTESIAN_POINT('Ctrl Pts',(94.3629352594592,-0.628746665480602,
135.684182115514));
#47873=CARTESIAN_POINT('Ctrl Pts',(94.3551873626822,-0.492347539159849,
135.699828234747));
#47874=CARTESIAN_POINT('Ctrl Pts',(94.3474394659051,-0.355497737178362,
135.709745864553));
#47875=CARTESIAN_POINT('Ctrl Pts',(94.339693189821,-0.218676561225309,135.719661419805));
#47876=CARTESIAN_POINT('Ctrl Pts',(94.3319469137369,-0.0814052868184683,
135.723850840828));
#47877=CARTESIAN_POINT('Ctrl Pts',(94.3242006376528,0.0558003669780375,
135.722294063796));
#47878=CARTESIAN_POINT('Ctrl Pts',(94.3164543043874,0.193007033595418,135.720737275272));
#47879=CARTESIAN_POINT('Ctrl Pts',(94.3087079711221,0.330147687695843,135.71343420849));
#47880=CARTESIAN_POINT('Ctrl Pts',(94.3009616378567,0.46670721617134,135.700416932282));
#47881=CARTESIAN_POINT('Ctrl Pts',(94.2932135698538,0.603297326206309,135.687396740946));
#47882=CARTESIAN_POINT('Ctrl Pts',(94.2854655018508,0.739305662528221,135.668659830907));
#47883=CARTESIAN_POINT('Ctrl Pts',(94.2777174338478,0.874223231053945,135.644290039033));
#47884=CARTESIAN_POINT('Ctrl Pts',(94.269961131106,1.00928419157722,135.619894346655));
#47885=CARTESIAN_POINT('Ctrl Pts',(94.2622048283641,1.14325168316288,135.589853882983));
#47886=CARTESIAN_POINT('Ctrl Pts',(94.2544485256223,1.27562734663058,135.554303557753));
#47887=CARTESIAN_POINT('Ctrl Pts',(94.2466880831081,1.40807366297571,135.518734258244));
#47888=CARTESIAN_POINT('Ctrl Pts',(94.2389276405939,1.53892608546125,135.477649354486));
#47889=CARTESIAN_POINT('Ctrl Pts',(94.2311671980797,1.66770333758238,135.431233064513));
#47890=CARTESIAN_POINT('Ctrl Pts',(94.2233942978143,1.79668731438083,135.38474226299));
#47891=CARTESIAN_POINT('Ctrl Pts',(94.2156213975489,1.9235891017804,135.332903120746));
#47892=CARTESIAN_POINT('Ctrl Pts',(94.2078484972835,2.04794843377789,135.27594761494));
#47893=CARTESIAN_POINT('Ctrl Pts',(94.2003581615215,2.16778699081442,135.221062585233));
#47894=CARTESIAN_POINT('Ctrl Pts',(94.1928678257595,2.28526445785325,135.161426858583));
#47895=CARTESIAN_POINT('Ctrl Pts',(94.1853774899975,2.39999381239291,135.097286515246));
#47896=CARTESIAN_POINT('Ctrl Pts',(94.1776031558784,2.51907316528185,135.030714271297));
#47897=CARTESIAN_POINT('Ctrl Pts',(94.1698288217593,2.63556911022584,134.959078201723));
#47898=CARTESIAN_POINT('Ctrl Pts',(94.1620544876402,2.74902098487157,134.882603705862));
#47899=CARTESIAN_POINT('Ctrl Pts',(94.1542897346931,2.8623330402212,134.806223457983));
#47900=CARTESIAN_POINT('Ctrl Pts',(94.146524981746,2.97260816864958,134.725016864697));
#47901=CARTESIAN_POINT('Ctrl Pts',(94.1387602287989,3.07940997252379,134.639255307596));
#47902=CARTESIAN_POINT('Ctrl Pts',(94.1310031879139,3.18610569934069,134.553578930083));
#47903=CARTESIAN_POINT('Ctrl Pts',(94.1232461470289,3.28933466389771,134.463356835035));
#47904=CARTESIAN_POINT('Ctrl Pts',(94.1154891061439,3.38868946651886,134.368903612398));
#47905=CARTESIAN_POINT('Ctrl Pts',(94.1077379149038,3.48796934491049,134.274521617671));
#47906=CARTESIAN_POINT('Ctrl Pts',(94.0999867236637,3.583380594297,134.175915114588));
#47907=CARTESIAN_POINT('Ctrl Pts',(94.0922355324236,3.67454922133108,134.073438634762));
#47908=CARTESIAN_POINT('Ctrl Pts',(94.0844876356465,3.76567909926674,133.971005710174));
#47909=CARTESIAN_POINT('Ctrl Pts',(94.0767397388694,3.85256968200841,133.864706371799));
#47910=CARTESIAN_POINT('Ctrl Pts',(94.0689918420923,3.93488432555971,133.754931478766));
#47911=CARTESIAN_POINT('Ctrl Pts',(94.0612455660082,4.01718175066207,133.645179548275));
#47912=CARTESIAN_POINT('Ctrl Pts',(94.0534992899241,4.09490490607276,133.531953821786));
#47913=CARTESIAN_POINT('Ctrl Pts',(94.04575301384,4.16775815277707,133.415677343369));
#47914=CARTESIAN_POINT('Ctrl Pts',(94.0380066805747,4.2406119372675,133.299400006626));
#47915=CARTESIAN_POINT('Ctrl Pts',(94.0302603473094,4.30859553373807,133.180072204323));
#47916=CARTESIAN_POINT('Ctrl Pts',(94.022514014044,4.3714574913892,133.058144649694));
#47917=CARTESIAN_POINT('Ctrl Pts',(94.014765946041,4.43433352653985,132.936189790236));
#47918=CARTESIAN_POINT('Ctrl Pts',(94.007017878038,4.49208546143721,132.811634367381));
#47919=CARTESIAN_POINT('Ctrl Pts',(93.9992698100351,4.54450870667887,132.684951928144));
#47920=CARTESIAN_POINT('Ctrl Pts',(93.9915135072932,4.59698766796945,132.558134849302));
#47921=CARTESIAN_POINT('Ctrl Pts',(93.9837572045514,4.64412647663145,132.42918660008));
#47922=CARTESIAN_POINT('Ctrl Pts',(93.9760009018095,4.68576926073752,132.298599386179));
#47923=CARTESIAN_POINT('Ctrl Pts',(93.9682404592953,4.72743427085134,132.167942473951));
#47924=CARTESIAN_POINT('Ctrl Pts',(93.9604800167812,4.76359730833694,132.035645230945));
#47925=CARTESIAN_POINT('Ctrl Pts',(93.952719574267,4.79415321933547,131.902212143063));
#47926=CARTESIAN_POINT('Ctrl Pts',(93.9449466740016,4.82475818139496,131.768564856542));
#47927=CARTESIAN_POINT('Ctrl Pts',(93.9371737737361,4.84973795870201,131.633778466133));
#47928=CARTESIAN_POINT('Ctrl Pts',(93.9294008734707,4.86903893519409,131.49836559598));
#47929=CARTESIAN_POINT('Ctrl Pts',(93.9219105377087,4.88763827257452,131.367875324742));
#47930=CARTESIAN_POINT('Ctrl Pts',(93.9144202019466,4.90096448725339,131.236803637648));
#47931=CARTESIAN_POINT('Ctrl Pts',(93.9069298661845,4.90901541840449,131.10560916008));
#47932=CARTESIAN_POINT('Ctrl Pts',(93.8991555320654,4.91737160305718,130.96944040402));
#47933=CARTESIAN_POINT('Ctrl Pts',(93.8913811979463,4.92007105269916,130.832708020789));
#47934=CARTESIAN_POINT('Ctrl Pts',(93.8836068638272,4.91705440292345,130.69592141252));
#47935=CARTESIAN_POINT('Ctrl Pts',(93.8758421108801,4.91404147089899,130.55930338152));
#47936=CARTESIAN_POINT('Ctrl Pts',(93.8680773579331,4.90532646461207,130.422631645567));
#47937=CARTESIAN_POINT('Ctrl Pts',(93.860312604986,4.89090182150286,130.286420046728));
#47938=CARTESIAN_POINT('Ctrl Pts',(93.852555564101,4.87649150515253,130.150343735169));
#47939=CARTESIAN_POINT('Ctrl Pts',(93.844798523216,4.85638287821656,130.014727037521));
#47940=CARTESIAN_POINT('Ctrl Pts',(93.837041482331,4.83062040465032,129.880082754218));
#47941=CARTESIAN_POINT('Ctrl Pts',(93.8292902910908,4.80487735876579,129.745540007216));
#47942=CARTESIAN_POINT('Ctrl Pts',(93.8215390998507,4.77348902588368,129.611968597406));
#47943=CARTESIAN_POINT('Ctrl Pts',(93.8137879086106,4.73655153095094,129.47987480898));
#47944=CARTESIAN_POINT('Ctrl Pts',(93.8060400118335,4.69962973543887,129.347837163937));
#47945=CARTESIAN_POINT('Ctrl Pts',(93.7982921150564,4.65716357390278,129.21727626691));
#47946=CARTESIAN_POINT('Ctrl Pts',(93.7905442182794,4.60929992289413,129.088686614934));
#47947=CARTESIAN_POINT('Ctrl Pts',(93.7827979421952,4.56144628392941,128.96012386114));
#47948=CARTESIAN_POINT('Ctrl Pts',(93.7750516661111,4.5081975375087,128.8335318984));
#47949=CARTESIAN_POINT('Ctrl Pts',(93.767305390027,4.44974980247846,128.709388121841));
#47950=CARTESIAN_POINT('Ctrl Pts',(93.7595590567616,4.39130163600036,128.585243428881));
#47951=CARTESIAN_POINT('Ctrl Pts',(93.7518127234963,4.32765457086784,128.463547311887));
#47952=CARTESIAN_POINT('Ctrl Pts',(93.7440663902309,4.25905188959048,128.344754945049));
#47953=CARTESIAN_POINT('Ctrl Pts',(93.7363183222279,4.19043384521836,128.225935975485));
#47954=CARTESIAN_POINT('Ctrl Pts',(93.728570254225,4.11685817185928,128.110022388548));
#47955=CARTESIAN_POINT('Ctrl Pts',(93.720822186222,4.03861269245762,127.997442274824));
#47956=CARTESIAN_POINT('Ctrl Pts',(93.7130658834802,3.96028405282926,127.884742509616));
#47957=CARTESIAN_POINT('Ctrl Pts',(93.7053095807383,3.87727591626608,127.775383616408));
#47958=CARTESIAN_POINT('Ctrl Pts',(93.6975532779964,3.78991813678017,127.669762783871));
#47959=CARTESIAN_POINT('Ctrl Pts',(93.6897928354823,3.70251373181701,127.564085578316));
#47960=CARTESIAN_POINT('Ctrl Pts',(93.6820323929681,3.61075531951605,127.462150699305));
#47961=CARTESIAN_POINT('Ctrl Pts',(93.6742719504539,3.51501049992361,127.364319302708));
#47962=CARTESIAN_POINT('Ctrl Pts',(93.6664990501885,3.41911198224693,127.26633085847));
#47963=CARTESIAN_POINT('Ctrl Pts',(93.658726149923,3.31921455444623,127.172459328));
#47964=CARTESIAN_POINT('Ctrl Pts',(93.6509532496576,3.21572052094178,127.083026905885));
#47965=CARTESIAN_POINT('Ctrl Pts',(93.6434629138956,3.11598875624116,126.99684557758));
#47966=CARTESIAN_POINT('Ctrl Pts',(93.6359725781336,3.01291757829159,126.914786407275));
#47967=CARTESIAN_POINT('Ctrl Pts',(93.6284822423716,2.90689167363581,126.837099111155));
#47968=CARTESIAN_POINT('Ctrl Pts',(93.6207079082525,2.79684576457891,126.75646627759));
#47969=CARTESIAN_POINT('Ctrl Pts',(93.6129335741334,2.68326805657351,126.680287961144));
#47970=CARTESIAN_POINT('Ctrl Pts',(93.6051592400143,2.56655503614888,126.608889451068));
#47971=CARTESIAN_POINT('Ctrl Pts',(93.5973944870672,2.44998585409105,126.537578933274));
#47972=CARTESIAN_POINT('Ctrl Pts',(93.5896297341201,2.33028937811493,126.47103670321));
#47973=CARTESIAN_POINT('Ctrl Pts',(93.581864981173,2.20789383035681,126.409546867659));
#47974=CARTESIAN_POINT('Ctrl Pts',(93.574107940288,2.0856198475822,126.34811810468));
#47975=CARTESIAN_POINT('Ctrl Pts',(93.566350899403,1.96065247494643,126.291731924326));
#47976=CARTESIAN_POINT('Ctrl Pts',(93.558593858518,1.83344717983344,126.240628098973));
#47977=CARTESIAN_POINT('Ctrl Pts',(93.5508426672779,1.70633781122309,126.189562811413));
#47978=CARTESIAN_POINT('Ctrl Pts',(93.5430914760378,1.57699424058588,126.143772095165));
#47979=CARTESIAN_POINT('Ctrl Pts',(93.5353402847976,1.44589437703271,126.103448736562));
#47980=CARTESIAN_POINT('Ctrl Pts',(93.5275923880206,1.31485023441875,126.063142516461));
#47981=CARTESIAN_POINT('Ctrl Pts',(93.5198444912435,1.18205165646947,126.028299146896));
#47982=CARTESIAN_POINT('Ctrl Pts',(93.5120965944664,1.04799406790868,125.999062344188));
#47983=CARTESIAN_POINT('Ctrl Pts',(93.5043503183824,0.913964521305467,125.969831657189));
#47984=CARTESIAN_POINT('Ctrl Pts',(93.4966040422982,0.77867686966836,125.946205287594));
#47985=CARTESIAN_POINT('Ctrl Pts',(93.4888577662142,0.642638766066019,125.928276278791));
#47986=CARTESIAN_POINT('Ctrl Pts',(93.4811114329488,0.506599658261301,125.910347137639));
#47987=CARTESIAN_POINT('Ctrl Pts',(93.4733650996835,0.369810475050688,125.898115492285));
#47988=CARTESIAN_POINT('Ctrl Pts',(93.4656187664181,0.232785667511623,125.891622695032));
#47989=CARTESIAN_POINT('Ctrl Pts',(93.4578706984151,0.0957301742169731,
125.885128443762));
#47990=CARTESIAN_POINT('Ctrl Pts',(93.4501226304122,-0.0415606579529346,
125.884375616444));
#47991=CARTESIAN_POINT('Ctrl Pts',(93.4423745624092,-0.178571088931887,
125.889353452902));
#47992=CARTESIAN_POINT('Ctrl Pts',(93.4346182596674,-0.315727136227329,
125.894336579864));
#47993=CARTESIAN_POINT('Ctrl Pts',(93.4268619569255,-0.452601795686883,
125.905062523048));
#47994=CARTESIAN_POINT('Ctrl Pts',(93.4191056541837,-0.588682607081849,
125.921468457112));
#47995=CARTESIAN_POINT('Ctrl Pts',(93.4113452116695,-0.724836048903355,
125.937883147517));
#47996=CARTESIAN_POINT('Ctrl Pts',(93.4035847691554,-0.860194412733907,
125.959983806516));
#47997=CARTESIAN_POINT('Ctrl Pts',(93.3958243266412,-0.994255151106295,
125.987656375348));
#47998=CARTESIAN_POINT('Ctrl Pts',(93.3880514263758,-1.12853109567718,126.015373366645));
#47999=CARTESIAN_POINT('Ctrl Pts',(93.3802785261103,-1.26150487269735,126.048680046737));
#48000=CARTESIAN_POINT('Ctrl Pts',(93.3725056258449,-1.39268795537226,126.087412099566));
#48001=CARTESIAN_POINT('Ctrl Pts',(93.3650152900828,-1.51910220256204,126.124736144715));
#48002=CARTESIAN_POINT('Ctrl Pts',(93.3575249543208,-1.64385339591185,126.167097859895));
#48003=CARTESIAN_POINT('Ctrl Pts',(93.3500346185588,-1.76652350964976,126.214308575121));
#48004=CARTESIAN_POINT('Ctrl Pts',(93.3422600320179,-1.89384883197644,126.26331088995));
#48005=CARTESIAN_POINT('Ctrl Pts',(93.334485445477,-2.01933534701955,126.317692732156));
#48006=CARTESIAN_POINT('Ctrl Pts',(93.3267108589361,-2.14249502174921,126.377296336998));
#48007=CARTESIAN_POINT('Ctrl Pts',(93.3189459119137,-2.26550199382955,126.436826040797));
#48008=CARTESIAN_POINT('Ctrl Pts',(93.3111809648912,-2.38618751743574,126.501564456171));
#48009=CARTESIAN_POINT('Ctrl Pts',(93.3034160178688,-2.50408106651856,126.571304856676));
#48010=CARTESIAN_POINT('Ctrl Pts',(93.2956588410081,-2.62185664287882,126.640975469945));
#48011=CARTESIAN_POINT('Ctrl Pts',(93.2879016641474,-2.73684547044058,126.715637909341));
#48012=CARTESIAN_POINT('Ctrl Pts',(93.2801444872867,-2.84859960869798,126.795038563674));
#48013=CARTESIAN_POINT('Ctrl Pts',(93.2720075451855,-2.96582485299805,126.878326406495));
#48014=CARTESIAN_POINT('Ctrl Pts',(93.2638706030843,-3.07949028666099,126.966827943532));
#48015=CARTESIAN_POINT('Ctrl Pts',(93.255733660983,-3.18911028308469,127.060197337897));
#48016=CARTESIAN_POINT('Ctrl Pts',(93.2479861016518,-3.29348455730325,127.14909866146));
#48017=CARTESIAN_POINT('Ctrl Pts',(93.2402385423207,-3.39419123848658,127.242412495729));
#48018=CARTESIAN_POINT('Ctrl Pts',(93.2324909829895,-3.49084335641013,127.339797770177));
#48019=CARTESIAN_POINT('Ctrl Pts',(93.2247450433043,-3.5874752689745,127.437162685998));
#48020=CARTESIAN_POINT('Ctrl Pts',(93.2169991036192,-3.68005402955596,127.538597071215));
#48021=CARTESIAN_POINT('Ctrl Pts',(93.2092531639341,-3.76822889688579,127.643722384048));
#48022=CARTESIAN_POINT('Ctrl Pts',(93.2015071661177,-3.8564044259445,127.748848485819));
#48023=CARTESIAN_POINT('Ctrl Pts',(93.1937611683014,-3.94017574517851,127.857665270521));
#48024=CARTESIAN_POINT('Ctrl Pts',(93.186015170485,-4.01923210866512,127.969760765881));
#48025=CARTESIAN_POINT('Ctrl Pts',(93.1782674370955,-4.09830618557037,128.081881377427));
#48026=CARTESIAN_POINT('Ctrl Pts',(93.170519703706,-4.17266297993153,128.197281841703));
#48027=CARTESIAN_POINT('Ctrl Pts',(93.1627719703165,-4.24203504556325,128.315521182264));
#48028=CARTESIAN_POINT('Ctrl Pts',(93.1550170718371,-4.31147126635622,128.433869870354));
#48029=CARTESIAN_POINT('Ctrl Pts',(93.1472621733577,-4.37591335644257,128.555062339154));
#48030=CARTESIAN_POINT('Ctrl Pts',(93.1395072748783,-4.43513966213504,128.678632685808));
#48031=CARTESIAN_POINT('Ctrl Pts',(93.1317481956758,-4.49439789716756,128.80226965015));
#48032=CARTESIAN_POINT('Ctrl Pts',(93.1239891164731,-4.54843459148819,128.92828668781));
#48033=CARTESIAN_POINT('Ctrl Pts',(93.1162300372706,-4.59707661442089,129.056198821952));
#48034=CARTESIAN_POINT('Ctrl Pts',(93.1084611478687,-4.64578013794245,129.184272681925));
#48035=CARTESIAN_POINT('Ctrl Pts',(93.1006922584668,-4.68907524859617,129.314246052368));
#48036=CARTESIAN_POINT('Ctrl Pts',(93.0929233690649,-4.7268388313816,129.445619389575));
#48037=CARTESIAN_POINT('Ctrl Pts',(93.0902348716622,-4.73990727514232,129.491082371165));
#48038=CARTESIAN_POINT('Ctrl Pts',(93.0875463742596,-4.75231372960658,129.536712923651));
#48039=CARTESIAN_POINT('Ctrl Pts',(93.084857876857,-4.76405452823403,129.582490119308));
#48040=CARTESIAN_POINT('Ctrl Pts',(94.8350013119177,-4.76405452823406,129.582490119308));
#48041=CARTESIAN_POINT('Ctrl Pts',(94.8273289265629,-4.79777932866022,129.713982604325));
#48042=CARTESIAN_POINT('Ctrl Pts',(94.8196565412081,-4.82603167565206,129.846777706001));
#48043=CARTESIAN_POINT('Ctrl Pts',(94.8119841558533,-4.84873498274878,129.980375102179));
#48044=CARTESIAN_POINT('Ctrl Pts',(94.8041300358823,-4.87197605960158,130.117136999407));
#48045=CARTESIAN_POINT('Ctrl Pts',(94.7962759159114,-4.889401876088,130.254739227271));
#48046=CARTESIAN_POINT('Ctrl Pts',(94.7884217959404,-4.90098670095333,130.392641757689));
#48047=CARTESIAN_POINT('Ctrl Pts',(94.7805676759695,-4.91257152581865,130.530544288107));
#48048=CARTESIAN_POINT('Ctrl Pts',(94.7727135559985,-4.91831540452579,130.668746675627));
#48049=CARTESIAN_POINT('Ctrl Pts',(94.7648594360275,-4.91824943780232,130.806712224922));
#48050=CARTESIAN_POINT('',(95.110140563956,-4.91824922401509,130.807123401486));
#48051=CARTESIAN_POINT('Ctrl Pts',(95.1799533855056,-4.76405452823405,129.582490119308));
#48052=CARTESIAN_POINT('Ctrl Pts',(95.172116002983,-4.79852964635118,129.716908081614));
#48053=CARTESIAN_POINT('Ctrl Pts',(95.1642786204605,-4.82733257278166,129.852867781761));
#48054=CARTESIAN_POINT('Ctrl Pts',(95.1564412379379,-4.85033683341142,129.989857293477));
#48055=CARTESIAN_POINT('Ctrl Pts',(95.1486064182765,-4.873333571539,130.126802008973));
#48056=CARTESIAN_POINT('Ctrl Pts',(95.1407715986151,-4.89053535270011,130.264775493699));
#48057=CARTESIAN_POINT('Ctrl Pts',(95.1329367789537,-4.90186675161587,130.403255379626));
#48058=CARTESIAN_POINT('Ctrl Pts',(95.1253380406386,-4.91285670911659,130.537562544377));
#48059=CARTESIAN_POINT('Ctrl Pts',(95.1177393023236,-4.91832493420278,130.672345688801));
#48060=CARTESIAN_POINT('Ctrl Pts',(95.1101405640085,-4.91824922401561,130.807123400555));
#48061=CARTESIAN_POINT('Ctrl Pts',(95.110140563956,-4.91824922401509,130.807123401486));
#48062=CARTESIAN_POINT('Ctrl Pts',(95.1015424548622,-4.91816355654752,130.959626806792));
#48063=CARTESIAN_POINT('Ctrl Pts',(95.0929443457683,-4.91098067842199,131.111875745966));
#48064=CARTESIAN_POINT('Ctrl Pts',(95.0843462366745,-4.89679575169032,131.263244512171));
#48065=CARTESIAN_POINT('Ctrl Pts',(95.0756985162661,-4.88252897756011,131.415486680119));
#48066=CARTESIAN_POINT('Ctrl Pts',(95.0670507958577,-4.86117920513635,131.566838266414));
#48067=CARTESIAN_POINT('Ctrl Pts',(95.0584030754493,-4.83289334049698,131.716679104653));
#48068=CARTESIAN_POINT('Ctrl Pts',(95.0497295757736,-4.80452315434503,131.866966625582));
#48069=CARTESIAN_POINT('Ctrl Pts',(95.0410560760979,-4.76917557784388,132.015734171589));
#48070=CARTESIAN_POINT('Ctrl Pts',(95.0323825764223,-4.72704749906738,132.162375714706));
#48071=CARTESIAN_POINT('Ctrl Pts',(95.0236768895022,-4.68476308353893,132.309561442681));
#48072=CARTESIAN_POINT('Ctrl Pts',(95.0149712025821,-4.63564786483374,132.454605157963));
#48073=CARTESIAN_POINT('Ctrl Pts',(95.006265515662,-4.57994812761617,132.596916951645));
#48074=CARTESIAN_POINT('Ctrl Pts',(95.0045541322003,-4.56899854833866,132.624892923254));
#48075=CARTESIAN_POINT('Ctrl Pts',(95.0028427487386,-4.55779465553684,132.65276339691));
#48076=CARTESIAN_POINT('Ctrl Pts',(95.0011313652769,-4.54633852747124,132.680524004942));
#48077=CARTESIAN_POINT('Ctrl Pts',(94.9933570311578,-4.49429655716773,132.806632645708));
#48078=CARTESIAN_POINT('Ctrl Pts',(94.9855826970387,-4.43692108158099,132.930774042726));
#48079=CARTESIAN_POINT('Ctrl Pts',(94.9778083629196,-4.37438151415451,133.05246413634));
#48080=CARTESIAN_POINT('Ctrl Pts',(94.9700436099725,-4.31191902115552,133.174004257789));
#48081=CARTESIAN_POINT('Ctrl Pts',(94.9622788570254,-4.24430527633272,133.293098742356));
#48082=CARTESIAN_POINT('Ctrl Pts',(94.9545141040783,-4.17175821941467,133.40928219436));
#48083=CARTESIAN_POINT('Ctrl Pts',(94.9467570631933,-4.09928321725629,133.525350251322));
#48084=CARTESIAN_POINT('Ctrl Pts',(94.9390000223083,-4.02188485962807,133.638512700018));
#48085=CARTESIAN_POINT('Ctrl Pts',(94.9312429814233,-3.93982741709419,133.748327836475));
#48086=CARTESIAN_POINT('Ctrl Pts',(94.9234917901832,-3.85783185471631,133.858060160484));
#48087=CARTESIAN_POINT('Ctrl Pts',(94.9157405989431,-3.77118443382339,133.964449884669));
#48088=CARTESIAN_POINT('Ctrl Pts',(94.907989407703,-3.68019303266012,134.067083760105));
#48089=CARTESIAN_POINT('Ctrl Pts',(94.9002415109259,-3.58924030526937,134.169674013406));
#48090=CARTESIAN_POINT('Ctrl Pts',(94.8924936141488,-3.49394752859292,134.268511301012));
#48091=CARTESIAN_POINT('Ctrl Pts',(94.8847457173717,-3.39466306540784,134.363215171331));
#48092=CARTESIAN_POINT('Ctrl Pts',(94.8769994412876,-3.29539937039219,134.457899231642));
#48093=CARTESIAN_POINT('Ctrl Pts',(94.8692531652036,-3.19214593240241,134.548451324765));
#48094=CARTESIAN_POINT('Ctrl Pts',(94.8615068891195,-3.0852879169283,134.63452791576));
#48095=CARTESIAN_POINT('Ctrl Pts',(94.8537605558541,-2.97842911265261,134.720605142153));
#48096=CARTESIAN_POINT('Ctrl Pts',(94.8460142225888,-2.86796598226844,134.802206555236));
#48097=CARTESIAN_POINT('Ctrl Pts',(94.8382678893234,-2.75431638578097,134.879029231026));
#48098=CARTESIAN_POINT('Ctrl Pts',(94.8305198213205,-2.64064133825442,134.955869110722));
#48099=CARTESIAN_POINT('Ctrl Pts',(94.8227717533175,-2.52377872851369,135.027927904713));
#48100=CARTESIAN_POINT('Ctrl Pts',(94.8150236853145,-2.4041746252623,135.094946525545));
#48101=CARTESIAN_POINT('Ctrl Pts',(94.8072673825727,-2.28444340534651,135.162036374565));
#48102=CARTESIAN_POINT('Ctrl Pts',(94.7995110798309,-2.16196521312088,135.224075158309));
#48103=CARTESIAN_POINT('Ctrl Pts',(94.791754777089,-2.037210399338,135.280849962056));
#48104=CARTESIAN_POINT('Ctrl Pts',(94.7839943345748,-1.91238900015462,135.337655068224));
#48105=CARTESIAN_POINT('Ctrl Pts',(94.7762338920607,-1.78528892035869,135.389190449303));
#48106=CARTESIAN_POINT('Ctrl Pts',(94.7684734495465,-1.65639869519593,135.435292103245));
#48107=CARTESIAN_POINT('Ctrl Pts',(94.7607005492811,-1.5273015640014,135.481467763655));
#48108=CARTESIAN_POINT('Ctrl Pts',(94.7529276490156,-1.39640891840004,135.522192149977));
#48109=CARTESIAN_POINT('Ctrl Pts',(94.7451547487502,-1.26422346198469,135.557351476033));
#48110=CARTESIAN_POINT('Ctrl Pts',(94.7376644129881,-1.13684327986367,135.591232672026));
#48111=CARTESIAN_POINT('Ctrl Pts',(94.730174077226,-1.0082629495304,135.619946323951));
#48112=CARTESIAN_POINT('Ctrl Pts',(94.7226837414639,-0.878937631082016,
135.643436118441));
#48113=CARTESIAN_POINT('Ctrl Pts',(94.7149094073448,-0.744708903878587,
135.667816535628));
#48114=CARTESIAN_POINT('Ctrl Pts',(94.7071350732257,-0.609252384671647,
135.686646380469));
#48115=CARTESIAN_POINT('Ctrl Pts',(94.6993607391066,-0.473066898663637,
135.699806539225));
#48116=CARTESIAN_POINT('Ctrl Pts',(94.6915959861596,-0.337049249095979,
135.712950479261));
#48117=CARTESIAN_POINT('Ctrl Pts',(94.6838312332125,-0.200304805665102,
135.720438598774));
#48118=CARTESIAN_POINT('Ctrl Pts',(94.6760664802654,-0.0633429206830855,
135.722202698896));
#48119=CARTESIAN_POINT('Ctrl Pts',(94.6683094393804,0.0734829318239427,
135.723965046889));
#48120=CARTESIAN_POINT('Ctrl Pts',(94.6605523984954,0.21052540769693,135.720014684248));
#48121=CARTESIAN_POINT('Ctrl Pts',(94.6527953576104,0.347270044179051,135.710335197496));
#48122=CARTESIAN_POINT('Ctrl Pts',(94.6450441663703,0.483911560466989,135.70066301012));
#48123=CARTESIAN_POINT('Ctrl Pts',(94.6372929751302,0.620255296011304,135.685270325576));
#48124=CARTESIAN_POINT('Ctrl Pts',(94.6295417838901,0.755787157075454,135.664192799411));
#48125=CARTESIAN_POINT('Ctrl Pts',(94.621793887113,0.891261413483313,135.643124231758));
#48126=CARTESIAN_POINT('Ctrl Pts',(94.6140459903359,1.02592409621296,135.616375688094));
#48127=CARTESIAN_POINT('Ctrl Pts',(94.6062980935588,1.15926682197451,135.584034612513));
#48128=CARTESIAN_POINT('Ctrl Pts',(94.5985518174748,1.29258165531247,135.551700301987));
#48129=CARTESIAN_POINT('Ctrl Pts',(94.5908055413907,1.42457670116469,135.513775878507));
#48130=CARTESIAN_POINT('Ctrl Pts',(94.5830592653066,1.55475474250059,135.470399703683));
#48131=CARTESIAN_POINT('Ctrl Pts',(94.5753129320412,1.68493374478114,135.427023208666));
#48132=CARTESIAN_POINT('Ctrl Pts',(94.5675665987759,1.813295344865,135.378195005592));
#48133=CARTESIAN_POINT('Ctrl Pts',(94.5598202655106,1.93935882068549,135.324102914106));
#48134=CARTESIAN_POINT('Ctrl Pts',(94.5520721975076,2.06545052754733,135.269998709071));
#48135=CARTESIAN_POINT('Ctrl Pts',(94.5443241295046,2.18924272683591,135.21062842406));
#48136=CARTESIAN_POINT('Ctrl Pts',(94.5365760615016,2.31027632990805,135.146227306211));
#48137=CARTESIAN_POINT('Ctrl Pts',(94.5288197587598,2.43143856893385,135.081757742088));
#48138=CARTESIAN_POINT('Ctrl Pts',(94.5210634560179,2.54983600932203,135.012246848201));
#48139=CARTESIAN_POINT('Ctrl Pts',(94.5133071532761,2.66503528381516,134.937975258352));
#48140=CARTESIAN_POINT('Ctrl Pts',(94.5055467107619,2.78029604362976,134.863664027519));
#48141=CARTESIAN_POINT('Ctrl Pts',(94.4977862682478,2.89235491701066,134.78458726302));
#48142=CARTESIAN_POINT('Ctrl Pts',(94.4900258257336,3.00080985915818,134.701067336281));
#48143=CARTESIAN_POINT('Ctrl Pts',(94.4822529254682,3.10943890280701,134.617413335941));
#48144=CARTESIAN_POINT('Ctrl Pts',(94.4744800252028,3.21445215457224,134.52930217168));
#48145=CARTESIAN_POINT('Ctrl Pts',(94.4667071249373,3.31548215934863,134.437095278058));
#48146=CARTESIAN_POINT('Ctrl Pts',(94.4592167891753,3.41283946897272,134.348240337274));
#48147=CARTESIAN_POINT('Ctrl Pts',(94.4517264534132,3.50649788684419,134.255582494017));
#48148=CARTESIAN_POINT('Ctrl Pts',(94.4442361176511,3.59616400978133,134.159474248615));
#48149=CARTESIAN_POINT('Ctrl Pts',(94.436461783532,3.68922985102259,134.059722029878));
#48150=CARTESIAN_POINT('Ctrl Pts',(94.4286874494129,3.77828949011739,133.955936615023));
#48151=CARTESIAN_POINT('Ctrl Pts',(94.4209131152939,3.86297308609639,133.848473295933));
#48152=CARTESIAN_POINT('Ctrl Pts',(94.4131483623468,3.94755231711168,133.74114241578));
#48153=CARTESIAN_POINT('Ctrl Pts',(94.4053836093997,4.02776599597515,133.630142954221));
#48154=CARTESIAN_POINT('Ctrl Pts',(94.3976188564526,4.10328142768276,133.51586658063));
#48155=CARTESIAN_POINT('Ctrl Pts',(94.3898618155676,4.17872185639902,133.401703707945));
#48156=CARTESIAN_POINT('Ctrl Pts',(94.3821047746826,4.24947311008669,133.284270724247));
#48157=CARTESIAN_POINT('Ctrl Pts',(94.3743477337976,4.31524329993689,133.163991589741));
#48158=CARTESIAN_POINT('Ctrl Pts',(94.3665965425574,4.38096389197532,133.043803158666));
#48159=CARTESIAN_POINT('Ctrl Pts',(94.3588453513173,4.44171070996742,132.920773190514));
#48160=CARTESIAN_POINT('Ctrl Pts',(94.3510941600772,4.4972358717138,132.7953534796));
#48161=CARTESIAN_POINT('Ctrl Pts',(94.3433462633001,4.5527374337853,132.669987075409));
#48162=CARTESIAN_POINT('Ctrl Pts',(94.335598366523,4.60302159577734,132.542233305363));
#48163=CARTESIAN_POINT('Ctrl Pts',(94.3278504697459,4.64788713329477,132.412567152391));
#48164=CARTESIAN_POINT('Ctrl Pts',(94.3201041936618,4.69274328590893,132.282928122782));
#48165=CARTESIAN_POINT('Ctrl Pts',(94.3123579175777,4.73218294080165,132.151377875167));
#48166=CARTESIAN_POINT('Ctrl Pts',(94.3046116414936,4.7660537475623,132.018409520143));
#48167=CARTESIAN_POINT('Ctrl Pts',(94.2968653082282,4.79992480434952,131.885440183576));
#48168=CARTESIAN_POINT('Ctrl Pts',(94.2891189749629,4.82822683446862,131.75105309758));
#48169=CARTESIAN_POINT('Ctrl Pts',(94.2813726416975,4.85085801388609,131.615754228348));
#48170=CARTESIAN_POINT('Ctrl Pts',(94.2736245736945,4.87349426139927,131.480425059872));
#48171=CARTESIAN_POINT('Ctrl Pts',(94.2658765056916,4.89045706667438,131.344184087385));
#48172=CARTESIAN_POINT('Ctrl Pts',(94.2581284376886,4.90169620116392,131.207544711988));
#48173=CARTESIAN_POINT('Ctrl Pts',(94.2503721349467,4.91294728073934,131.070760114637));
#48174=CARTESIAN_POINT('Ctrl Pts',(94.2426158322048,4.91846250560974,130.933576658805));
#48175=CARTESIAN_POINT('Ctrl Pts',(94.234859529463,4.91824373535125,130.796510638064));
#48176=CARTESIAN_POINT('Ctrl Pts',(94.2270990869488,4.91802484832848,130.659371461059));
#48177=CARTESIAN_POINT('Ctrl Pts',(94.2193386444346,4.9120658850375,130.522350234443));
#48178=CARTESIAN_POINT('Ctrl Pts',(94.2115782019205,4.90042075065456,130.38595945952));
#48179=CARTESIAN_POINT('Ctrl Pts',(94.203805301655,4.8887569224681,130.249349738018));
#48180=CARTESIAN_POINT('Ctrl Pts',(94.1960324013896,4.8713887322074,130.113372878659));
#48181=CARTESIAN_POINT('Ctrl Pts',(94.1882595011242,4.84842164654532,129.978533396042));
#48182=CARTESIAN_POINT('Ctrl Pts',(94.1807691653621,4.82628947229773,129.848595668258));
#48183=CARTESIAN_POINT('Ctrl Pts',(94.1732788296002,4.79895846715251,129.719714361185));
#48184=CARTESIAN_POINT('Ctrl Pts',(94.1657884938381,4.7665666080338,129.592326858268));
#48185=CARTESIAN_POINT('Ctrl Pts',(94.158014159719,4.73294660173122,129.46010941946));
#48186=CARTESIAN_POINT('Ctrl Pts',(94.1502398256,4.69376790319095,129.32908247096));
#48187=CARTESIAN_POINT('Ctrl Pts',(94.1424654914809,4.64912952145985,129.199749214394));
#48188=CARTESIAN_POINT('Ctrl Pts',(94.1347007385338,4.60454615254482,129.070575349507));
#48189=CARTESIAN_POINT('Ctrl Pts',(94.1269359855867,4.55451661462139,128.943091389425));
#48190=CARTESIAN_POINT('Ctrl Pts',(94.1191712326396,4.49919060044921,128.81778894674));
#48191=CARTESIAN_POINT('Ctrl Pts',(94.1114141917546,4.44391953685423,128.692610956207));
#48192=CARTESIAN_POINT('Ctrl Pts',(94.1036571508696,4.38336262260845,128.569610526551));
#48193=CARTESIAN_POINT('Ctrl Pts',(94.0959001099846,4.31771877440675,128.44926239294));
#48194=CARTESIAN_POINT('Ctrl Pts',(94.0881489187445,4.25212442874161,128.329005014793));
#48195=CARTESIAN_POINT('Ctrl Pts',(94.0803977275043,4.18145097109365,128.211396293416));
#48196=CARTESIAN_POINT('Ctrl Pts',(94.0726465362642,4.10594452243216,128.096888984989));
#48197=CARTESIAN_POINT('Ctrl Pts',(94.0648986394871,4.0304701660256,127.982430345222));
#48198=CARTESIAN_POINT('Ctrl Pts',(94.0571507427101,3.95016711892722,127.871070822348));
#48199=CARTESIAN_POINT('Ctrl Pts',(94.049402845933,3.86532623102535,127.763236452023));
#48200=CARTESIAN_POINT('Ctrl Pts',(94.0416565698489,3.78050309000828,127.655424638324));
#48201=CARTESIAN_POINT('Ctrl Pts',(94.0339102937648,3.69114423782945,127.551136817544));
#48202=CARTESIAN_POINT('Ctrl Pts',(94.0261640176807,3.59758219328283,127.450767704722));
#48203=CARTESIAN_POINT('Ctrl Pts',(94.0184176844154,3.50401945808245,127.350397850999));
#48204=CARTESIAN_POINT('Ctrl Pts',(94.01067135115,3.40625373518845,127.253947048936));
#48205=CARTESIAN_POINT('Ctrl Pts',(94.0029250178847,3.30465566991289,127.161774453065));
#48206=CARTESIAN_POINT('Ctrl Pts',(93.9951769498817,3.20303485245505,127.069581215781));
#48207=CARTESIAN_POINT('Ctrl Pts',(93.9874288818787,3.09758027434805,126.981668353791));
#48208=CARTESIAN_POINT('Ctrl Pts',(93.9796808138758,2.98869672472144,126.898355631632));
#48209=CARTESIAN_POINT('Ctrl Pts',(93.9719245111339,2.87969745236249,126.814954363721));
#48210=CARTESIAN_POINT('Ctrl Pts',(93.964168208392,2.76726223949295,126.736163240068));
#48211=CARTESIAN_POINT('Ctrl Pts',(93.9564119056502,2.65182646366289,126.662259765448));
#48212=CARTESIAN_POINT('Ctrl Pts',(93.948651463136,2.53632907628349,126.588316846318));
#48213=CARTESIAN_POINT('Ctrl Pts',(93.9408910206219,2.41782827247352,126.519266970985));
#48214=CARTESIAN_POINT('Ctrl Pts',(93.9331305781077,2.29678437116164,126.455341806973));
#48215=CARTESIAN_POINT('Ctrl Pts',(93.9253576778423,2.17554615943368,126.391314024613));
#48216=CARTESIAN_POINT('Ctrl Pts',(93.9175847775768,2.05175704551348,126.33242756107));
#48217=CARTESIAN_POINT('Ctrl Pts',(93.9098118773114,1.925898499132,126.278866386707));
#48218=CARTESIAN_POINT('Ctrl Pts',(93.9023215415494,1.8046152279297,126.227252295944));
#48219=CARTESIAN_POINT('Ctrl Pts',(93.8948312057873,1.68141065830259,126.180583150053));
#48220=CARTESIAN_POINT('Ctrl Pts',(93.8873408700253,1.55672735322792,126.138979281575));
#48221=CARTESIAN_POINT('Ctrl Pts',(93.8795665359062,1.42731664274494,126.095797989779));
#48222=CARTESIAN_POINT('Ctrl Pts',(93.8717922017871,1.29590291654227,126.057936872284));
#48223=CARTESIAN_POINT('Ctrl Pts',(93.864017867668,1.16296304920575,126.025584622745));
#48224=CARTESIAN_POINT('Ctrl Pts',(93.8562531147209,1.03018701837464,125.993272244461));
#48225=CARTESIAN_POINT('Ctrl Pts',(93.8484883617738,0.895888964937103,125.966455317233));
#48226=CARTESIAN_POINT('Ctrl Pts',(93.8407236088267,0.760563409083274,125.945273628916));
#48227=CARTESIAN_POINT('Ctrl Pts',(93.8329665679417,0.625372260479276,125.924112978551));
#48228=CARTESIAN_POINT('Ctrl Pts',(93.8252095270567,0.489156024122194,125.908576488886));
#48229=CARTESIAN_POINT('Ctrl Pts',(93.8174524861717,0.352421627485681,125.898753411625));
#48230=CARTESIAN_POINT('Ctrl Pts',(93.8097012949316,0.215790343321218,125.888937742023));
#48231=CARTESIAN_POINT('Ctrl Pts',(93.8019501036915,0.0786420650212302,
125.884826936862));
#48232=CARTESIAN_POINT('Ctrl Pts',(93.7941989124513,-0.0585092564234095,
125.886458653373));
#48233=CARTESIAN_POINT('Ctrl Pts',(93.7864510156743,-0.195602284897711,
125.888089676361));
#48234=CARTESIAN_POINT('Ctrl Pts',(93.7787031188972,-0.332697963825081,
125.895458361964));
#48235=CARTESIAN_POINT('Ctrl Pts',(93.7709552221201,-0.469280645872262,
125.908550292614));
#48236=CARTESIAN_POINT('Ctrl Pts',(93.763208946036,-0.605834757766741,125.921639484713));
#48237=CARTESIAN_POINT('Ctrl Pts',(93.7554626699519,-0.741875697287455,
125.940449503322));
#48238=CARTESIAN_POINT('Ctrl Pts',(93.7477163938678,-0.876891644963057,
125.964913944082));
#48239=CARTESIAN_POINT('Ctrl Pts',(93.7399700606024,-1.01190858929571,125.989378565433));
#48240=CARTESIAN_POINT('Ctrl Pts',(93.7322237273371,-1.14590014198443,126.019497622516));
#48241=CARTESIAN_POINT('Ctrl Pts',(93.7244773940717,-1.2783637933063,126.05515341273));
#48242=CARTESIAN_POINT('Ctrl Pts',(93.7167293260688,-1.41085710894435,126.090817187811));
#48243=CARTESIAN_POINT('Ctrl Pts',(93.7089812580658,-1.5418214648957,126.132020061705));
#48244=CARTESIAN_POINT('Ctrl Pts',(93.7012331900628,-1.67076903578876,126.178594314395));
#48245=CARTESIAN_POINT('Ctrl Pts',(93.6934768873209,-1.79985365369474,126.225218066755));
#48246=CARTESIAN_POINT('Ctrl Pts',(93.6857205845791,-1.92691683644267,126.277224468759));
#48247=CARTESIAN_POINT('Ctrl Pts',(93.6779642818372,-2.05148977920767,126.334397223051));
#48248=CARTESIAN_POINT('Ctrl Pts',(93.6702038393231,-2.17612921030305,126.391600492163));
#48249=CARTESIAN_POINT('Ctrl Pts',(93.6624433968089,-2.29827540501672,126.453975430271));
#48250=CARTESIAN_POINT('Ctrl Pts',(93.6546829542947,-2.41748464127521,126.521259979979));
#48251=CARTESIAN_POINT('Ctrl Pts',(93.6469100540293,-2.53688524278272,126.588652540819));
#48252=CARTESIAN_POINT('Ctrl Pts',(93.6391371537639,-2.65333913210431,126.660970256323));
#48253=CARTESIAN_POINT('Ctrl Pts',(93.6313642534984,-2.76643128361256,126.737907492845));
#48254=CARTESIAN_POINT('Ctrl Pts',(93.6238739177364,-2.8754122505514,126.812047867027));
#48255=CARTESIAN_POINT('Ctrl Pts',(93.6163835819744,-2.98127140405043,126.890477547477));
#48256=CARTESIAN_POINT('Ctrl Pts',(93.6088932462124,-3.083668288835,126.972889236108));
#48257=CARTESIAN_POINT('Ctrl Pts',(93.601221527421,-3.18854477637049,127.057296573827));
#48258=CARTESIAN_POINT('Ctrl Pts',(93.5935498086296,-3.29013999903654,127.146163892061));
#48259=CARTESIAN_POINT('Ctrl Pts',(93.5858780898382,-3.38804334928593,127.239203492577));
#48260=CARTESIAN_POINT('Ctrl Pts',(93.578215153484,-3.48583462164936,127.332136583135));
#48261=CARTESIAN_POINT('Ctrl Pts',(93.5705522171298,-3.57994213498176,127.429232187488));
#48262=CARTESIAN_POINT('Ctrl Pts',(93.5628892807756,-3.66998626290684,127.530160884414));
#48263=CARTESIAN_POINT('Ctrl Pts',(93.5552333529899,-3.75994803592049,127.630997271334));
#48264=CARTESIAN_POINT('Ctrl Pts',(93.5475774252043,-3.84585354721556,127.735659482425));
#48265=CARTESIAN_POINT('Ctrl Pts',(93.5399214974187,-3.92735854934403,127.843779950299));
#48266=CARTESIAN_POINT('Ctrl Pts',(93.5322708107495,-4.0088077545497,127.95182640076));
#48267=CARTESIAN_POINT('Ctrl Pts',(93.5246201240804,-4.08586220121889,128.06332607961));
#48268=CARTESIAN_POINT('Ctrl Pts',(93.5169694374112,-4.15821699315964,128.177877322302));
#48269=CARTESIAN_POINT('Ctrl Pts',(93.5093213530922,-4.23054717391102,128.292389600854));
#48270=CARTESIAN_POINT('Ctrl Pts',(93.5016732687731,-4.29818066069358,128.409951042302));
#48271=CARTESIAN_POINT('Ctrl Pts',(93.494025184454,-4.36085531655467,128.53013020475));
#48272=CARTESIAN_POINT('Ctrl Pts',(93.4863787967934,-4.42351606860911,128.650282706535));
#48273=CARTESIAN_POINT('Ctrl Pts',(93.4787324091328,-4.48121999544925,128.773051416107));
#48274=CARTESIAN_POINT('Ctrl Pts',(93.4710860214722,-4.53375080004373,128.897980082205));
#48275=CARTESIAN_POINT('Ctrl Pts',(93.4634371328192,-4.58629878649579,129.022949610166));
#48276=CARTESIAN_POINT('Ctrl Pts',(93.4557882441662,-4.63367011290399,129.1500801358));
#48277=CARTESIAN_POINT('Ctrl Pts',(93.4481393555132,-4.67569658534787,129.278895277328));
#48278=CARTESIAN_POINT('Ctrl Pts',(93.4421863234996,-4.70840525025724,129.379150451139));
#48279=CARTESIAN_POINT('Ctrl Pts',(93.4362332914858,-4.73787732419656,129.480425598061));
#48280=CARTESIAN_POINT('Ctrl Pts',(93.4302802594722,-4.76405452823405,129.582490119308));
#48281=CARTESIAN_POINT('Origin',(213.235140564004,0.,130.804360617566));
#48282=CARTESIAN_POINT('',(91.3345773084523,-4.76405452823402,129.582490119308));
#48283=CARTESIAN_POINT('',(91.6801684115835,-4.76405452823408,129.582490119308));
#48284=CARTESIAN_POINT('',(213.235140564004,-4.76405452823405,129.582490119308));
#48285=CARTESIAN_POINT('',(93.0148594359418,-4.91824801126209,130.799937698111));
#48286=CARTESIAN_POINT('Ctrl Pts',(93.0148594359418,-4.91824801126209,130.799937698111));
#48287=CARTESIAN_POINT('Ctrl Pts',(93.0072109324117,-4.91836930348058,130.934813591398));
#48288=CARTESIAN_POINT('Ctrl Pts',(92.9995624288815,-4.91293826055421,131.069867794249));
#48289=CARTESIAN_POINT('Ctrl Pts',(92.9919139253514,-4.90193765537652,131.204598403516));
#48290=CARTESIAN_POINT('Ctrl Pts',(92.9842717249816,-4.89094611583876,131.339217980782));
#48291=CARTESIAN_POINT('Ctrl Pts',(92.9766295246119,-4.87439417693943,131.473514095127));
#48292=CARTESIAN_POINT('Ctrl Pts',(92.9689873242421,-4.85231667526038,131.606985028788));
#48293=CARTESIAN_POINT('Ctrl Pts',(92.9613489341719,-4.8302501811303,131.740389415616));
#48294=CARTESIAN_POINT('Ctrl Pts',(92.9537105441017,-4.80266366750942,131.872969043028));
#48295=CARTESIAN_POINT('Ctrl Pts',(92.9460721540315,-4.76964375173622,132.004227920239));
#48296=CARTESIAN_POINT('Ctrl Pts',(92.9384356206848,-4.73663186237339,132.135454891323));
#48297=CARTESIAN_POINT('Ctrl Pts',(92.9307990873382,-4.69818929472312,132.265361359725));
#48298=CARTESIAN_POINT('Ctrl Pts',(92.9231625539915,-4.65445354555209,132.393462645378));
#48299=CARTESIAN_POINT('Ctrl Pts',(92.9155261128608,-4.61071832451822,132.521562384126));
#48300=CARTESIAN_POINT('Ctrl Pts',(92.9078896717301,-4.5616901795235,132.647856601963));
#48301=CARTESIAN_POINT('Ctrl Pts',(92.9002532305995,-4.50755595806729,132.771877414799));
#48302=CARTESIAN_POINT('Ctrl Pts',(92.8926151174588,-4.45340988384364,132.895925382173));
#48303=CARTESIAN_POINT('Ctrl Pts',(92.8849770043181,-4.39415567179046,133.017698585535));
#48304=CARTESIAN_POINT('Ctrl Pts',(92.8773388911774,-4.33002738554203,133.136751215848));
#48305=CARTESIAN_POINT('Ctrl Pts',(92.8696929113169,-4.26583305166541,133.255926462004));
#48306=CARTESIAN_POINT('Ctrl Pts',(92.8620469314565,-4.19675481207021,133.372375185258));
#48307=CARTESIAN_POINT('Ctrl Pts',(92.854400951596,-4.12307173061472,133.485677936853));
#48308=CARTESIAN_POINT('Ctrl Pts',(92.846750723838,-4.04934771285196,133.599043636361));
#48309=CARTESIAN_POINT('Ctrl Pts',(92.83910049608,-3.97101399334953,133.709259556717));
#48310=CARTESIAN_POINT('Ctrl Pts',(92.831450268322,-3.88839085368846,133.81593821601));
#48311=CARTESIAN_POINT('Ctrl Pts',(92.8237885431259,-3.80564354067381,133.922777201418));
#48312=CARTESIAN_POINT('Ctrl Pts',(92.8161268179297,-3.7185941946397,134.026068003277));
#48313=CARTESIAN_POINT('Ctrl Pts',(92.8084650927336,-3.62760129596635,134.125458613712));
#48314=CARTESIAN_POINT('Ctrl Pts',(92.8033565188001,-3.56693037154647,134.191728842506));
#48315=CARTESIAN_POINT('Ctrl Pts',(92.7982479448665,-3.50450699143506,134.256265915611));
#48316=CARTESIAN_POINT('Ctrl Pts',(92.793139370933,-3.44044546173787,134.318975544881));
#48317=CARTESIAN_POINT('Ctrl Pts',(92.7853650368139,-3.34295529275445,134.414408363662));
#48318=CARTESIAN_POINT('Ctrl Pts',(92.7775907026948,-3.2413369513081,134.50593291957));
#48319=CARTESIAN_POINT('Ctrl Pts',(92.7698163685757,-3.13593675180432,134.593170952115));
#48320=CARTESIAN_POINT('Ctrl Pts',(92.7620516156286,-3.0306664486267,134.680301471581));
#48321=CARTESIAN_POINT('Ctrl Pts',(92.7542868626816,-2.9216238592902,134.763155731905));
#48322=CARTESIAN_POINT('Ctrl Pts',(92.7465221097345,-2.80919255661363,134.841391734905));
#48323=CARTESIAN_POINT('Ctrl Pts',(92.7387650688495,-2.69687292229196,134.919550032805));
#48324=CARTESIAN_POINT('Ctrl Pts',(92.7310080279645,-2.5811715913987,134.99309897969));
#48325=CARTESIAN_POINT('Ctrl Pts',(92.7232509870795,-2.4625053975201,135.061736596932));
#48326=CARTESIAN_POINT('Ctrl Pts',(92.7154997958394,-2.34392869074138,135.130322454014));
#48327=CARTESIAN_POINT('Ctrl Pts',(92.7077486045993,-2.22239190831499,135.194004158428));
#48328=CARTESIAN_POINT('Ctrl Pts',(92.6999974133592,-2.0983407659613,135.252523057541));
#48329=CARTESIAN_POINT('Ctrl Pts',(92.6922495165821,-1.97434234865203,135.311017084561));
#48330=CARTESIAN_POINT('Ctrl Pts',(92.684501619805,-1.84783204977505,135.364352504182));
#48331=CARTESIAN_POINT('Ctrl Pts',(92.6767537230279,-1.71927988664383,135.412316751676));
#48332=CARTESIAN_POINT('Ctrl Pts',(92.6690074469438,-1.59075461385388,135.460270966083));
#48333=CARTESIAN_POINT('Ctrl Pts',(92.6612611708597,-1.46018869242984,135.502856106548));
#48334=CARTESIAN_POINT('Ctrl Pts',(92.6535148947756,-1.32807143497694,135.53990803324));
#48335=CARTESIAN_POINT('Ctrl Pts',(92.6457685615102,-1.19595320226419,135.576960233441));
#48336=CARTESIAN_POINT('Ctrl Pts',(92.6380222282448,-1.06228398711339,135.608479032793));
#48337=CARTESIAN_POINT('Ctrl Pts',(92.6302758949795,-0.927567166517519,
135.634350494791));
#48338=CARTESIAN_POINT('Ctrl Pts',(92.6225278269765,-0.79282017702392,135.660227750524));
#48339=CARTESIAN_POINT('Ctrl Pts',(92.6147797589735,-0.657025499126192,
135.680455078613));
#48340=CARTESIAN_POINT('Ctrl Pts',(92.6070316909705,-0.520695180731654,
135.694969944763));
#48341=CARTESIAN_POINT('Ctrl Pts',(92.5992753882286,-0.384219968852467,
135.709500237485));
#48342=CARTESIAN_POINT('Ctrl Pts',(92.5915190854868,-0.247208368656059,
135.718305898791));
#48343=CARTESIAN_POINT('Ctrl Pts',(92.583762782745,-0.11017656965865,135.721376398098));
#48344=CARTESIAN_POINT('Ctrl Pts',(92.5760023402308,0.0269283673357381,
135.724448536223));
#48345=CARTESIAN_POINT('Ctrl Pts',(92.5682418977166,0.164053133912697,135.721779420596));
#48346=CARTESIAN_POINT('Ctrl Pts',(92.5604814552025,0.300684082777564,135.713410642251));
#48347=CARTESIAN_POINT('Ctrl Pts',(92.552708554937,0.437534363771167,135.705028429601));
#48348=CARTESIAN_POINT('Ctrl Pts',(92.5449356546716,0.573888853830151,135.690928310645));
#48349=CARTESIAN_POINT('Ctrl Pts',(92.5371627544062,0.709240652737029,135.671203614726));
#48350=CARTESIAN_POINT('Ctrl Pts',(92.5296724186441,0.839672072823583,135.652195961187));
#48351=CARTESIAN_POINT('Ctrl Pts',(92.522182082882,0.969172134028587,135.627965622701));
#48352=CARTESIAN_POINT('Ctrl Pts',(92.51469174712,1.09730026779709,135.598640040461));
#48353=CARTESIAN_POINT('Ctrl Pts',(92.5069174130009,1.23028641870085,135.568202569857));
#48354=CARTESIAN_POINT('Ctrl Pts',(92.4991430788818,1.3622158154141,135.532179439297));
#48355=CARTESIAN_POINT('Ctrl Pts',(92.4913687447627,1.4925830252785,135.490657553863));
#48356=CARTESIAN_POINT('Ctrl Pts',(92.4836039918156,1.62278956920763,135.449186840443));
#48357=CARTESIAN_POINT('Ctrl Pts',(92.4758392388686,1.75143738802246,135.40223097332));
#48358=CARTESIAN_POINT('Ctrl Pts',(92.4680744859215,1.8780314184895,135.349927804801));
#48359=CARTESIAN_POINT('Ctrl Pts',(92.4603174450365,2.00449971398099,135.297676584526));
#48360=CARTESIAN_POINT('Ctrl Pts',(92.4525604041514,2.12891792151989,135.240088780337));
#48361=CARTESIAN_POINT('Ctrl Pts',(92.4448033632664,2.25080666919891,135.177351859312));
#48362=CARTESIAN_POINT('Ctrl Pts',(92.4370521720263,2.37260349962482,135.114662248688));
#48363=CARTESIAN_POINT('Ctrl Pts',(92.4293009807862,2.49187432071027,135.04683142828));
#48364=CARTESIAN_POINT('Ctrl Pts',(92.4215497895461,2.60816060043538,134.974094583281));
#48365=CARTESIAN_POINT('Ctrl Pts',(92.4138018927691,2.72439745538974,134.901388653382));
#48366=CARTESIAN_POINT('Ctrl Pts',(92.406053995992,2.83765196118316,134.823781053074));
#48367=CARTESIAN_POINT('Ctrl Pts',(92.3983060992149,2.947491225251,134.741552324807));
#48368=CARTESIAN_POINT('Ctrl Pts',(92.3905598231308,3.05730751331267,134.659340797018));
#48369=CARTESIAN_POINT('Ctrl Pts',(92.3828135470468,3.16370966783957,134.572510298126));
#48370=CARTESIAN_POINT('Ctrl Pts',(92.3750672709627,3.26629510792696,134.481383779097));
#48371=CARTESIAN_POINT('Ctrl Pts',(92.3673209376973,3.36888130527698,134.390256587391));
#48372=CARTESIAN_POINT('Ctrl Pts',(92.3595746044319,3.4676504396714,134.294833571915));
#48373=CARTESIAN_POINT('Ctrl Pts',(92.3518282711666,3.56223456554194,134.195476652525));
#48374=CARTESIAN_POINT('Ctrl Pts',(92.3440802031636,3.65683987287185,134.096097482842));
#48375=CARTESIAN_POINT('Ctrl Pts',(92.3363321351606,3.74725803723358,133.992782939333));
#48376=CARTESIAN_POINT('Ctrl Pts',(92.3285840671576,3.83315967235341,133.885930021091));
#48377=CARTESIAN_POINT('Ctrl Pts',(92.3208277644158,3.91915260475304,133.778963538297));
#48378=CARTESIAN_POINT('Ctrl Pts',(92.3130714616739,4.0006191735992,133.668451473707));
#48379=CARTESIAN_POINT('Ctrl Pts',(92.305315158932,4.07727150617325,133.554822420145));
#48380=CARTESIAN_POINT('Ctrl Pts',(92.2975547164179,4.15396475040527,133.441132719336));
#48381=CARTESIAN_POINT('Ctrl Pts',(92.2897942739037,4.22583843362858,133.324323047446));
#48382=CARTESIAN_POINT('Ctrl Pts',(92.2820338313895,4.29264990864926,133.204848031462));
#48383=CARTESIAN_POINT('Ctrl Pts',(92.274260931124,4.35956863538084,133.085181223576));
#48384=CARTESIAN_POINT('Ctrl Pts',(92.2664880308587,4.42140873848766,132.962840870619));
#48385=CARTESIAN_POINT('Ctrl Pts',(92.2587151305932,4.47797474663897,132.83830388889));
#48386=CARTESIAN_POINT('Ctrl Pts',(92.2512247948313,4.53248443791231,132.718294140137));
#48387=CARTESIAN_POINT('Ctrl Pts',(92.2437344590693,4.58209671420049,132.596244981204));
#48388=CARTESIAN_POINT('Ctrl Pts',(92.2362441233073,4.62668065732355,132.472595959971));
#48389=CARTESIAN_POINT('Ctrl Pts',(92.2284697891882,4.67295501420153,132.344258748514));
#48390=CARTESIAN_POINT('Ctrl Pts',(92.2206954550691,4.71395879571134,132.213791428643));
#48391=CARTESIAN_POINT('Ctrl Pts',(92.21292112095,4.74949191886304,132.081666209488));
#48392=CARTESIAN_POINT('Ctrl Pts',(92.2051563680029,4.78498125061609,131.949703822857));
#48393=CARTESIAN_POINT('Ctrl Pts',(92.1973916150559,4.81501323821375,131.816087976252));
#48394=CARTESIAN_POINT('Ctrl Pts',(92.1896268621088,4.83943626693423,131.68130969293));
#48395=CARTESIAN_POINT('Ctrl Pts',(92.1818698212237,4.86383503835838,131.546665273299));
#48396=CARTESIAN_POINT('Ctrl Pts',(92.1741127803387,4.88263586798179,131.410861096765));
#48397=CARTESIAN_POINT('Ctrl Pts',(92.1663557394537,4.8957373649403,131.274401803025));
#48398=CARTESIAN_POINT('Ctrl Pts',(92.1586045482136,4.90882898195795,131.1380454143));
#48399=CARTESIAN_POINT('Ctrl Pts',(92.1508533569735,4.91622978382848,131.001035279306));
#48400=CARTESIAN_POINT('Ctrl Pts',(92.1431021657333,4.91788979075825,130.863884297356));
#48401=CARTESIAN_POINT('Ctrl Pts',(92.1353542689562,4.91954909214079,130.726791608233));
#48402=CARTESIAN_POINT('Ctrl Pts',(92.1276063721792,4.9154724468168,130.589558581337));
#48403=CARTESIAN_POINT('Ctrl Pts',(92.1198584754021,4.90566189408938,130.45270106149));
#48404=CARTESIAN_POINT('Ctrl Pts',(92.112112199318,4.89585339351811,130.315872169287));
#48405=CARTESIAN_POINT('Ctrl Pts',(92.1043659232339,4.88031339917199,130.179419017614));
#48406=CARTESIAN_POINT('Ctrl Pts',(92.0966196471498,4.85909601403103,130.043854872073));
#48407=CARTESIAN_POINT('Ctrl Pts',(92.0888733138844,4.83787847226814,129.908289725828));
#48408=CARTESIAN_POINT('Ctrl Pts',(92.0811269806191,4.8109835165383,129.773613985074));
#48409=CARTESIAN_POINT('Ctrl Pts',(92.0733806473537,4.77851675670007,129.640332839359));
#48410=CARTESIAN_POINT('Ctrl Pts',(92.0656325793508,4.74604272615621,129.507021846257));
#48411=CARTESIAN_POINT('Ctrl Pts',(92.0578845113478,4.70799450110639,129.37510644944));
#48412=CARTESIAN_POINT('Ctrl Pts',(92.0501364433448,4.6645280468046,129.245078358617));
#48413=CARTESIAN_POINT('Ctrl Pts',(92.042380140603,4.62101539583777,129.114912072391));
#48414=CARTESIAN_POINT('Ctrl Pts',(92.0346238378611,4.57207313642727,128.98663747045));
#48415=CARTESIAN_POINT('Ctrl Pts',(92.0268675351193,4.51790625361711,128.860728413154));
#48416=CARTESIAN_POINT('Ctrl Pts',(92.0191070926051,4.46371046031056,128.734752154403));
#48417=CARTESIAN_POINT('Ctrl Pts',(92.0113466500909,4.40428465652239,128.611144308248));
#48418=CARTESIAN_POINT('Ctrl Pts',(92.0035862075767,4.33988017607665,128.490354757635));
#48419=CARTESIAN_POINT('Ctrl Pts',(91.9958133073113,4.27537230784138,128.369371304912));
#48420=CARTESIAN_POINT('Ctrl Pts',(91.9880404070458,4.2058699902978,128.251215525663));
#48421=CARTESIAN_POINT('Ctrl Pts',(91.9802675067804,4.13166880960557,128.136309660363));
#48422=CARTESIAN_POINT('Ctrl Pts',(91.9727771710183,4.06016502873254,128.025580912696));
#48423=CARTESIAN_POINT('Ctrl Pts',(91.9652868352563,3.98429826188994,127.917870147941));
#48424=CARTESIAN_POINT('Ctrl Pts',(91.9577964994942,3.90436754868442,127.813525097635));
#48425=CARTESIAN_POINT('Ctrl Pts',(91.9500221653751,3.82140623819378,127.705223773033));
#48426=CARTESIAN_POINT('Ctrl Pts',(91.942247831256,3.73380393243871,127.600205357129));
#48427=CARTESIAN_POINT('Ctrl Pts',(91.9344734971369,3.64184976459086,127.49889342598));
#48428=CARTESIAN_POINT('Ctrl Pts',(91.9267087441898,3.55000892203682,127.397706352732));
#48429=CARTESIAN_POINT('Ctrl Pts',(91.9189439912427,3.45382714895903,127.300216962177));
#48430=CARTESIAN_POINT('Ctrl Pts',(91.9111792382956,3.35363560566992,127.206818222141));
#48431=CARTESIAN_POINT('Ctrl Pts',(91.9034221974106,3.25354357403432,127.113512247049));
#48432=CARTESIAN_POINT('Ctrl Pts',(91.8956651565256,3.14944998179012,127.024289102003));
#48433=CARTESIAN_POINT('Ctrl Pts',(91.8879081156406,3.04172459236721,126.939506860088));
#48434=CARTESIAN_POINT('Ctrl Pts',(91.8801569244005,2.93408043949786,126.854788553122));
#48435=CARTESIAN_POINT('Ctrl Pts',(91.8724057331603,2.82281024678311,126.774504724283));
#48436=CARTESIAN_POINT('Ctrl Pts',(91.8646545419201,2.70831851564428,126.698974657596));
#48437=CARTESIAN_POINT('Ctrl Pts',(91.8569066451431,2.59387544654557,126.623476693203));
#48438=CARTESIAN_POINT('Ctrl Pts',(91.849158748366,2.47621388800146,126.55272868723));
#48439=CARTESIAN_POINT('Ctrl Pts',(91.8414108515889,2.35576893716289,126.487007750681));
#48440=CARTESIAN_POINT('Ctrl Pts',(91.8336645755048,2.23534918081146,126.421300561535));
#48441=CARTESIAN_POINT('Ctrl Pts',(91.8259182994207,2.11214753322513,126.360618537362));
#48442=CARTESIAN_POINT('Ctrl Pts',(91.8181720233366,1.98662506327313,126.305193592385));
#48443=CARTESIAN_POINT('Ctrl Pts',(91.8104256900712,1.86110166674277,126.249768238274));
#48444=CARTESIAN_POINT('Ctrl Pts',(91.8026793568058,1.73325777131264,126.199600198719));
#48445=CARTESIAN_POINT('Ctrl Pts',(91.7949330235405,1.60357549196744,126.154873688446));
#48446=CARTESIAN_POINT('Ctrl Pts',(91.7871849555375,1.4738641711753,126.110137161981));
#48447=CARTESIAN_POINT('Ctrl Pts',(91.7794368875345,1.34231401677578,126.070844717105));
#48448=CARTESIAN_POINT('Ctrl Pts',(91.7716888195315,1.20942302110151,126.03713091694));
#48449=CARTESIAN_POINT('Ctrl Pts',(91.7639325167897,1.07639078729545,126.003381285347));
#48450=CARTESIAN_POINT('Ctrl Pts',(91.7561762140478,0.942015245064114,125.975222238676));
#48451=CARTESIAN_POINT('Ctrl Pts',(91.748419911306,0.806805865972816,125.952737450302));
#48452=CARTESIAN_POINT('Ctrl Pts',(91.7406594687918,0.671524321564729,125.93024066112));
#48453=CARTESIAN_POINT('Ctrl Pts',(91.7328990262776,0.535408441334497,125.913424212737));
#48454=CARTESIAN_POINT('Ctrl Pts',(91.7251385837635,0.398972576618193,125.90231982361));
#48455=CARTESIAN_POINT('Ctrl Pts',(91.717365683498,0.26231769293964,125.891197608733));
#48456=CARTESIAN_POINT('Ctrl Pts',(91.7095927832326,0.125342189191165,125.885805792091));
#48457=CARTESIAN_POINT('Ctrl Pts',(91.7018198829672,-0.0114389202177289,
125.886123919968));
#48458=CARTESIAN_POINT('Ctrl Pts',(91.6943295472052,-0.143247691767026,
125.886430483095));
#48459=CARTESIAN_POINT('Ctrl Pts',(91.6868392114433,-0.27487564930785,125.892039043366));
#48460=CARTESIAN_POINT('Ctrl Pts',(91.6793488756814,-0.405868598236534,
125.902885967681));
#48461=CARTESIAN_POINT('Ctrl Pts',(91.6715745415623,-0.541828184639833,
125.914144156429));
#48462=CARTESIAN_POINT('Ctrl Pts',(91.6638002074432,-0.677534338281038,
125.931081438273));
#48463=CARTESIAN_POINT('Ctrl Pts',(91.6560258733241,-0.812474409086707,
125.953683510493));
#48464=CARTESIAN_POINT('Ctrl Pts',(91.648261120377,-0.947248178315323,125.976257727679));
#48465=CARTESIAN_POINT('Ctrl Pts',(91.6404963674299,-1.08125736135097,126.004482780474));
#48466=CARTESIAN_POINT('Ctrl Pts',(91.6327316144828,-1.21399234299605,126.038292463034));
#48467=CARTESIAN_POINT('Ctrl Pts',(91.6249745735978,-1.34659549038584,126.07206856534));
#48468=CARTESIAN_POINT('Ctrl Pts',(91.6172175327129,-1.47792657847998,126.111418163285));
#48469=CARTESIAN_POINT('Ctrl Pts',(91.6094604918279,-1.60748448408262,126.156223711672));
#48470=CARTESIAN_POINT('Ctrl Pts',(91.6017093005877,-1.73694468906136,126.200995471847));
#48471=CARTESIAN_POINT('Ctrl Pts',(91.5939581093476,-1.86463400510768,126.251214865784));
#48472=CARTESIAN_POINT('Ctrl Pts',(91.5862069181074,-1.99006516663053,126.306714155797));
#48473=CARTESIAN_POINT('Ctrl Pts',(91.5784590213303,-2.11544301656323,126.362189857131));
#48474=CARTESIAN_POINT('Ctrl Pts',(91.5707111245532,-2.23856426411182,126.422940833338));
#48475=CARTESIAN_POINT('Ctrl Pts',(91.5629632277762,-2.35896058730359,126.488750810129));
#48476=CARTESIAN_POINT('Ctrl Pts',(91.5552169516921,-2.47933172617984,126.554547020891));
#48477=CARTESIAN_POINT('Ctrl Pts',(91.547470675608,-2.5969787316091,126.62539993995));
#48478=CARTESIAN_POINT('Ctrl Pts',(91.5397243995239,-2.71145726859929,126.701047012312));
#48479=CARTESIAN_POINT('Ctrl Pts',(91.5319780662586,-2.82593665064412,126.776694643084));
#48480=CARTESIAN_POINT('Ctrl Pts',(91.5242317329932,-2.93724719139532,126.857136282234));
#48481=CARTESIAN_POINT('Ctrl Pts',(91.5164853997279,-3.04497331086037,126.942065885331));
#48482=CARTESIAN_POINT('Ctrl Pts',(91.5087373317249,-3.15272355484296,127.027014507824));
#48483=CARTESIAN_POINT('Ctrl Pts',(91.500989263722,-3.25688747328116,127.116452852188));
#48484=CARTESIAN_POINT('Ctrl Pts',(91.493241195719,-3.35708267738909,127.210034678023));
#48485=CARTESIAN_POINT('Ctrl Pts',(91.4854848929772,-3.45738437015242,127.303715963736));
#48486=CARTESIAN_POINT('Ctrl Pts',(91.4777285902353,-3.55370863650405,127.401549260579));
#48487=CARTESIAN_POINT('Ctrl Pts',(91.4699722874934,-3.64570969783685,127.5031511632));
#48488=CARTESIAN_POINT('Ctrl Pts',(91.4622118449793,-3.73775986290624,127.604807293815));
#48489=CARTESIAN_POINT('Ctrl Pts',(91.4544514024651,-3.82548197527734,127.710235737739));
#48490=CARTESIAN_POINT('Ctrl Pts',(91.4466909599509,-3.90857132985244,127.819020901226));
#48491=CARTESIAN_POINT('Ctrl Pts',(91.4389180596855,-3.99179406683566,127.927980696316));
#48492=CARTESIAN_POINT('Ctrl Pts',(91.4311451594201,-4.07036896046935,128.040307658369));
#48493=CARTESIAN_POINT('Ctrl Pts',(91.4233722591547,-4.14403484117663,128.155557435445));
#48494=CARTESIAN_POINT('Ctrl Pts',(91.4158819233926,-4.21502278156739,128.266617592828));
#48495=CARTESIAN_POINT('Ctrl Pts',(91.4083915876306,-4.28145226721218,128.380391485229));
#48496=CARTESIAN_POINT('Ctrl Pts',(91.4009012518685,-4.34313133116246,128.496462590621));
#48497=CARTESIAN_POINT('Ctrl Pts',(91.3926828135285,-4.41080594549865,128.623816457394));
#48498=CARTESIAN_POINT('Ctrl Pts',(91.3844643751885,-4.47295643192316,128.754301941354));
#48499=CARTESIAN_POINT('Ctrl Pts',(91.3762459368485,-4.5292989044717,128.887426999401));
#48500=CARTESIAN_POINT('Ctrl Pts',(91.3680463489467,-4.58551214561941,129.020246711641));
#48501=CARTESIAN_POINT('Ctrl Pts',(91.3598467610449,-4.6359438082404,129.155693628935));
#48502=CARTESIAN_POINT('Ctrl Pts',(91.3516471731431,-4.68035617042155,129.293252024348));
#48503=CARTESIAN_POINT('Ctrl Pts',(91.3459572182461,-4.71117532142097,129.388708171044));
#48504=CARTESIAN_POINT('Ctrl Pts',(91.3402672633492,-4.73909685092036,129.485180514248));
#48505=CARTESIAN_POINT('Ctrl Pts',(91.3345773084523,-4.76405452823403,129.582490119308));
#48506=CARTESIAN_POINT('Ctrl Pts',(93.084857876857,-4.76405452823403,129.582490119308));
#48507=CARTESIAN_POINT('Ctrl Pts',(93.0804342494867,-4.78337272363488,129.657811469982));
#48508=CARTESIAN_POINT('Ctrl Pts',(93.0760106221163,-4.80088849673471,129.733529841816));
#48509=CARTESIAN_POINT('Ctrl Pts',(93.0715869947459,-4.81658988703912,129.809551629583));
#48510=CARTESIAN_POINT('Ctrl Pts',(93.0605294465413,-4.855837966869,129.999579973393));
#48511=CARTESIAN_POINT('Ctrl Pts',(93.0494718983367,-4.88385096599703,130.192001803521));
#48512=CARTESIAN_POINT('Ctrl Pts',(93.0384143501322,-4.90040027604376,130.385719724855));
#48513=CARTESIAN_POINT('Ctrl Pts',(93.0305627120851,-4.91215145180274,130.523273093232));
#48514=CARTESIAN_POINT('Ctrl Pts',(93.022711074038,-4.9181234976515,130.661479671936));
#48515=CARTESIAN_POINT('Ctrl Pts',(93.014859435991,-4.91824801126131,130.799937697244));
#48516=CARTESIAN_POINT('',(93.3601405640463,-4.91824910373096,130.807329817729));
#48517=CARTESIAN_POINT('Ctrl Pts',(93.4302802594722,-4.76405452823405,129.582490119308));
#48518=CARTESIAN_POINT('Ctrl Pts',(93.4226245287869,-4.79771899093888,129.713747348465));
#48519=CARTESIAN_POINT('Ctrl Pts',(93.4149687981016,-4.82593248599096,129.846310103717));
#48520=CARTESIAN_POINT('Ctrl Pts',(93.4073130674163,-4.84861679233564,129.979679913547));
#48521=CARTESIAN_POINT('Ctrl Pts',(93.3994509835213,-4.87191253338415,130.116644584464));
#48522=CARTESIAN_POINT('Ctrl Pts',(93.3915888996263,-4.88937673586048,130.25445997831));
#48523=CARTESIAN_POINT('Ctrl Pts',(93.3837268157313,-4.90098172523436,130.392582532405));
#48524=CARTESIAN_POINT('Ctrl Pts',(93.3758647318363,-4.91258671460823,130.5307050865));
#48525=CARTESIAN_POINT('Ctrl Pts',(93.3680026479413,-4.9183325338315,130.669134345982));
#48526=CARTESIAN_POINT('Ctrl Pts',(93.3601405640462,-4.91824910373096,130.807329817729));
#48527=CARTESIAN_POINT('Ctrl Pts',(93.3601405640084,-4.91824910373056,130.807329818395));
#48528=CARTESIAN_POINT('Ctrl Pts',(93.3502422501388,-4.9181440657384,130.981317042771));
#48529=CARTESIAN_POINT('Ctrl Pts',(93.3403439362691,-4.90880728885546,131.155023738731));
#48530=CARTESIAN_POINT('Ctrl Pts',(93.3304456223994,-4.89032341902961,131.32773421242));
#48531=CARTESIAN_POINT('Ctrl Pts',(93.3226712882803,-4.87580581717025,131.463384480334));
#48532=CARTESIAN_POINT('Ctrl Pts',(93.3148969541612,-4.85561683933991,131.598645105893));
#48533=CARTESIAN_POINT('Ctrl Pts',(93.3071226200421,-4.82978308632962,131.733003929879));
#48534=CARTESIAN_POINT('Ctrl Pts',(93.299357867095,-4.8039811711111,131.867197168623));
#48535=CARTESIAN_POINT('Ctrl Pts',(93.291593114148,-4.77254839554594,132.000490436883));
#48536=CARTESIAN_POINT('Ctrl Pts',(93.2838283612009,-4.73556317577024,132.132375854974));
#48537=CARTESIAN_POINT('Ctrl Pts',(93.2760713203159,-4.69861469023621,132.26413028261));
#48538=CARTESIAN_POINT('Ctrl Pts',(93.2683142794309,-4.65612484000902,132.394479268743));
#48539=CARTESIAN_POINT('Ctrl Pts',(93.2605572385459,-4.60822316200892,132.522924655251));
#48540=CARTESIAN_POINT('Ctrl Pts',(93.2528060473058,-4.56035760703691,132.651273180094));
#48541=CARTESIAN_POINT('Ctrl Pts',(93.2450548560657,-4.5070884835375,132.777720597787));
#48542=CARTESIAN_POINT('Ctrl Pts',(93.2373036648256,-4.44859517392466,132.901783808301));
#48543=CARTESIAN_POINT('Ctrl Pts',(93.2295557680485,-4.3901267255287,133.025794288642));
#48544=CARTESIAN_POINT('Ctrl Pts',(93.2218078712715,-4.32643867364319,133.147422224393));
#48545=CARTESIAN_POINT('Ctrl Pts',(93.2140599744944,-4.25775846871242,133.266204618434));
#48546=CARTESIAN_POINT('Ctrl Pts',(93.2063136984103,-4.18909263019994,133.384962165758));
#48547=CARTESIAN_POINT('Ctrl Pts',(93.1985674223262,-4.11543691128902,133.500875017062));
#48548=CARTESIAN_POINT('Ctrl Pts',(93.1908211462421,-4.03706445417912,133.613505265907));
#48549=CARTESIAN_POINT('Ctrl Pts',(93.1830748129768,-3.95869141854148,133.726136346163));
#48550=CARTESIAN_POINT('Ctrl Pts',(93.1753284797114,-3.8756017985349,133.835484454692));
#48551=CARTESIAN_POINT('Ctrl Pts',(93.1675821464461,-3.78811152323129,133.941141475398));
#48552=CARTESIAN_POINT('Ctrl Pts',(93.1598340784431,-3.7006016550872,134.046822157262));
#48553=CARTESIAN_POINT('Ctrl Pts',(93.1520860104401,-3.60868941992628,134.148809805409));
#48554=CARTESIAN_POINT('Ctrl Pts',(93.1443379424372,-3.5127301347151,134.246730449987));
#48555=CARTESIAN_POINT('Ctrl Pts',(93.1365816396953,-3.41666886283366,134.344755165792));
#48556=CARTESIAN_POINT('Ctrl Pts',(93.1288253369535,-3.31655222276564,134.438703963766));
#48557=CARTESIAN_POINT('Ctrl Pts',(93.1210690342116,-3.21277180718587,134.528240365551));
#48558=CARTESIAN_POINT('Ctrl Pts',(93.1133085916975,-3.10893600087347,134.617824555609));
#48559=CARTESIAN_POINT('Ctrl Pts',(93.1055481491833,-3.00143282891633,134.702991414223));
#48560=CARTESIAN_POINT('Ctrl Pts',(93.0977877066691,-2.89068507746093,134.783446297147));
#48561=CARTESIAN_POINT('Ctrl Pts',(93.0900148064037,-2.77975954388325,134.864030333391));
#48562=CARTESIAN_POINT('Ctrl Pts',(93.0822419061383,-2.66557934842697,134.939887062027));
#48563=CARTESIAN_POINT('Ctrl Pts',(93.0744690058728,-2.54859498242178,135.01076605191));
#48564=CARTESIAN_POINT('Ctrl Pts',(93.0669786701108,-2.43586329278592,135.079068411977));
#48565=CARTESIAN_POINT('Ctrl Pts',(93.0594883343487,-2.32052803996489,135.142748507863));
#48566=CARTESIAN_POINT('Ctrl Pts',(93.0519979985866,-2.20301023271641,135.201624423281));
#48567=CARTESIAN_POINT('Ctrl Pts',(93.0442236644676,-2.0810367020881,135.262732636926));
#48568=CARTESIAN_POINT('Ctrl Pts',(93.0364493303484,-1.95632547136498,135.318858750135));
#48569=CARTESIAN_POINT('Ctrl Pts',(93.0286749962294,-1.82932181297873,135.369748308339));
#48570=CARTESIAN_POINT('Ctrl Pts',(93.0209102432823,-1.70247467525088,135.420575149711));
#48571=CARTESIAN_POINT('Ctrl Pts',(93.0131454903352,-1.57334109062139,135.466178132769));
#48572=CARTESIAN_POINT('Ctrl Pts',(93.0053807373881,-1.44239073848878,135.506348709854));
#48573=CARTESIAN_POINT('Ctrl Pts',(92.9976236965031,-1.31157044809198,135.546479388957));
#48574=CARTESIAN_POINT('Ctrl Pts',(92.9898666556181,-1.17893735246257,135.581188285542));
#48575=CARTESIAN_POINT('Ctrl Pts',(92.9821096147331,-1.04498058400846,135.610315116055));
#48576=CARTESIAN_POINT('Ctrl Pts',(92.974358423493,-0.911124833395652,135.639419981798));
#48577=CARTESIAN_POINT('Ctrl Pts',(92.9666072322529,-0.775947777291451,
135.662951077451));
#48578=CARTESIAN_POINT('Ctrl Pts',(92.9588560410128,-0.639952822008436,
135.680798195153));
#48579=CARTESIAN_POINT('Ctrl Pts',(92.9511081442357,-0.504015668209016,
135.698637727354));
#48580=CARTESIAN_POINT('Ctrl Pts',(92.9433602474586,-0.367261693468156,
135.710798035764));
#48581=CARTESIAN_POINT('Ctrl Pts',(92.9356123506815,-0.230203372897379,
135.717220219631));
#48582=CARTESIAN_POINT('Ctrl Pts',(92.9278660745974,-0.0931737219726303,
135.723641060116));
#48583=CARTESIAN_POINT('Ctrl Pts',(92.9201197985133,0.0441597578643789,
135.724326145217));
#48584=CARTESIAN_POINT('Ctrl Pts',(92.9123735224292,0.181281003493984,135.719268578075));
#48585=CARTESIAN_POINT('Ctrl Pts',(92.9046271891639,0.318403261321476,135.714210973599));
#48586=CARTESIAN_POINT('Ctrl Pts',(92.8968808558986,0.45531289111586,135.703410646702));
#48587=CARTESIAN_POINT('Ctrl Pts',(92.8891345226332,0.591495765869051,135.686912800744));
#48588=CARTESIAN_POINT('Ctrl Pts',(92.8813864546302,0.727709137832818,135.670411260208));
#48589=CARTESIAN_POINT('Ctrl Pts',(92.8736383866273,0.863195042845044,135.648209708688));
#48590=CARTESIAN_POINT('Ctrl Pts',(92.8658903186243,0.997446791977944,135.620404944571));
#48591=CARTESIAN_POINT('Ctrl Pts',(92.8581340158824,1.13184122546744,135.592570629219));
#48592=CARTESIAN_POINT('Ctrl Pts',(92.8503777131406,1.26499849941334,135.559121284612));
#48593=CARTESIAN_POINT('Ctrl Pts',(92.8426214103987,1.3964238596358,135.520204493983));
#48594=CARTESIAN_POINT('Ctrl Pts',(92.8348609678846,1.52791936553024,135.481266932291));
#48595=CARTESIAN_POINT('Ctrl Pts',(92.8271005253704,1.65768074608685,135.436856236473));
#48596=CARTESIAN_POINT('Ctrl Pts',(92.8193400828562,1.78523158251724,135.387168846074));
#48597=CARTESIAN_POINT('Ctrl Pts',(92.8115671825908,1.9129871748737,135.337401693066));
#48598=CARTESIAN_POINT('Ctrl Pts',(92.8037942823254,2.03852477369988,135.282341075608));
#48599=CARTESIAN_POINT('Ctrl Pts',(92.7960213820599,2.16139018261328,135.222230640666));
#48600=CARTESIAN_POINT('Ctrl Pts',(92.7885310462979,2.2797891244343,135.164305371442));
#48601=CARTESIAN_POINT('Ctrl Pts',(92.7810407105358,2.39570651398725,135.101691204079));
#48602=CARTESIAN_POINT('Ctrl Pts',(92.7735503747737,2.50876173443079,135.03464401497));
#48603=CARTESIAN_POINT('Ctrl Pts',(92.7657760406546,2.62610347791886,134.965054711309));
#48604=CARTESIAN_POINT('Ctrl Pts',(92.7580017065355,2.74073343298251,134.890469156042));
#48605=CARTESIAN_POINT('Ctrl Pts',(92.7502273724164,2.85219683916137,134.811124430567));
#48606=CARTESIAN_POINT('Ctrl Pts',(92.7424626194694,2.96352287665397,134.731877490375));
#48607=CARTESIAN_POINT('Ctrl Pts',(92.7346978665223,3.07168981459971,134.647883274631));
#48608=CARTESIAN_POINT('Ctrl Pts',(92.7269331135752,3.1762683227598,134.559424212811));
#48609=CARTESIAN_POINT('Ctrl Pts',(92.7191760726902,3.28074296207123,134.471053009778));
#48610=CARTESIAN_POINT('Ctrl Pts',(92.7114190318052,3.38163596770642,134.378226036477));
#48611=CARTESIAN_POINT('Ctrl Pts',(92.7036619909202,3.4785481005572,134.281268176678));
#48612=CARTESIAN_POINT('Ctrl Pts',(92.69591079968,3.5753871512148,134.184383433556));
#48613=CARTESIAN_POINT('Ctrl Pts',(92.6881596084399,3.66825102913052,134.083374279821));
#48614=CARTESIAN_POINT('Ctrl Pts',(92.6804084171998,3.7567749099017,133.978604675422));
#48615=CARTESIAN_POINT('Ctrl Pts',(92.6726605204227,3.84526116566209,133.873879600899));
#48616=CARTESIAN_POINT('Ctrl Pts',(92.6649126236457,3.92941084127455,133.765397552604));
#48617=CARTESIAN_POINT('Ctrl Pts',(92.6571647268686,4.00889737655199,133.653557853065));
#48618=CARTESIAN_POINT('Ctrl Pts',(92.6494184507845,4.08836728495977,133.54174154798));
#48619=CARTESIAN_POINT('Ctrl Pts',(92.6416721747004,4.16317576686614,133.426569307138));
#48620=CARTESIAN_POINT('Ctrl Pts',(92.6339258986163,4.23303807502707,133.308471581136));
#48621=CARTESIAN_POINT('Ctrl Pts',(92.6261795653509,4.30290089889565,133.190372983363));
#48622=CARTESIAN_POINT('Ctrl Pts',(92.6184332320856,4.36781727710403,133.069349193835));
#48623=CARTESIAN_POINT('Ctrl Pts',(92.6106868988202,4.4275473423119,132.945857195683));
#48624=CARTESIAN_POINT('Ctrl Pts',(92.6029388308173,4.48729078365374,132.822337542354));
#48625=CARTESIAN_POINT('Ctrl Pts',(92.5951907628143,4.54184543066538,132.696348932408));
#48626=CARTESIAN_POINT('Ctrl Pts',(92.5874426948113,4.59101884482935,132.56836997948));
#48627=CARTESIAN_POINT('Ctrl Pts',(92.5796863920694,4.64024452108309,132.440255008999));
#48628=CARTESIAN_POINT('Ctrl Pts',(92.5719300893276,4.68407739924502,132.310145835412));
#48629=CARTESIAN_POINT('Ctrl Pts',(92.5641737865857,4.72237421855145,132.178538481767));
#48630=CARTESIAN_POINT('Ctrl Pts',(92.5564133440716,4.76069147802347,132.046860885315));
#48631=CARTESIAN_POINT('Ctrl Pts',(92.5486529015574,4.7934666976438,131.913683894938));
#48632=CARTESIAN_POINT('Ctrl Pts',(92.5408924590433,4.82060763157436,131.779514515629));
#48633=CARTESIAN_POINT('Ctrl Pts',(92.5331195587778,4.84779213454149,131.645129755721));
#48634=CARTESIAN_POINT('Ctrl Pts',(92.5253466585124,4.86932421626879,131.509749809753));
#48635=CARTESIAN_POINT('Ctrl Pts',(92.517573758247,4.88516335960771,131.37388850314));
#48636=CARTESIAN_POINT('Ctrl Pts',(92.5100834224849,4.9004267101899,131.242966097236));
#48637=CARTESIAN_POINT('Ctrl Pts',(92.5025930867229,4.91040381835462,131.111597027558));
#48638=CARTESIAN_POINT('Ctrl Pts',(92.4951027509609,4.91510422745994,130.980239825278));
#48639=CARTESIAN_POINT('Ctrl Pts',(92.4873284168418,4.91998285400513,130.843902174749));
#48640=CARTESIAN_POINT('Ctrl Pts',(92.4795540827227,4.91919220469049,130.707145432589));
#48641=CARTESIAN_POINT('Ctrl Pts',(92.4717797486036,4.91268593367374,130.570480349941));
#48642=CARTESIAN_POINT('Ctrl Pts',(92.4640149956565,4.90618768105453,130.433983694794));
#48643=CARTESIAN_POINT('Ctrl Pts',(92.4562502427094,4.89398784059295,130.29757886117));
#48644=CARTESIAN_POINT('Ctrl Pts',(92.4484854897623,4.87609196472543,130.161779716792));
#48645=CARTESIAN_POINT('Ctrl Pts',(92.4407284488774,4.85821386329412,130.026115450037));
#48646=CARTESIAN_POINT('Ctrl Pts',(92.4329714079923,4.83465103565366,129.891056060464));
#48647=CARTESIAN_POINT('Ctrl Pts',(92.4252143671073,4.80546101723211,129.757113046854));
#48648=CARTESIAN_POINT('Ctrl Pts',(92.4174631758672,4.77629301123049,129.623271040712));
#48649=CARTESIAN_POINT('Ctrl Pts',(92.4097119846271,4.74150634380554,129.490544115301));
#48650=CARTESIAN_POINT('Ctrl Pts',(92.401960793387,4.70121002826787,129.359435936964));
#48651=CARTESIAN_POINT('Ctrl Pts',(92.3942128966099,4.66093083973923,129.2283834831));
#48652=CARTESIAN_POINT('Ctrl Pts',(92.3864649998328,4.61514677527553,129.098948780839));
#48653=CARTESIAN_POINT('Ctrl Pts',(92.3787171030557,4.56401728247269,128.971622418098));
#48654=CARTESIAN_POINT('Ctrl Pts',(92.3709708269716,4.51289848485752,128.844322689286));
#48655=CARTESIAN_POINT('Ctrl Pts',(92.3632245508875,4.45643662855871,128.719130785358));
#48656=CARTESIAN_POINT('Ctrl Pts',(92.3554782748034,4.39483995101448,128.596518941298));
#48657=CARTESIAN_POINT('Ctrl Pts',(92.347731941538,4.33324281877761,128.473906192144));
#48658=CARTESIAN_POINT('Ctrl Pts',(92.3399856082727,4.26651096516788,128.35387389022));
#48659=CARTESIAN_POINT('Ctrl Pts',(92.3322392750073,4.19489920888033,128.236870853256));
#48660=CARTESIAN_POINT('Ctrl Pts',(92.3244912070044,4.12327141563648,128.119841614274));
#48661=CARTESIAN_POINT('Ctrl Pts',(92.3167431390014,4.04676174918654,128.005843323556));
#48662=CARTESIAN_POINT('Ctrl Pts',(92.3089950709984,3.96566886301975,127.89529658744));
#48663=CARTESIAN_POINT('Ctrl Pts',(92.3012387682566,3.88448979036846,127.784632360936));
#48664=CARTESIAN_POINT('Ctrl Pts',(92.2934824655147,3.79871799907069,127.67742733271));
#48665=CARTESIAN_POINT('Ctrl Pts',(92.2857261627728,3.70869337142207,127.574070144672));
#48666=CARTESIAN_POINT('Ctrl Pts',(92.2779657202587,3.61862069491903,127.47065779179));
#48667=CARTESIAN_POINT('Ctrl Pts',(92.2702052777445,3.52429092793046,127.371097654954));
#48668=CARTESIAN_POINT('Ctrl Pts',(92.2624448352304,3.4260807669873,127.275741391781));
#48669=CARTESIAN_POINT('Ctrl Pts',(92.2546719349649,3.32771295037511,127.180232054269));
#48670=CARTESIAN_POINT('Ctrl Pts',(92.2468990346995,3.2254525837968,127.088940336457));
#48671=CARTESIAN_POINT('Ctrl Pts',(92.2391261344341,3.11971006261793,127.002178061757));
#48672=CARTESIAN_POINT('Ctrl Pts',(92.231635798672,3.01781154843319,126.918569814283));
#48673=CARTESIAN_POINT('Ctrl Pts',(92.22414546291,2.9126799002159,126.839167599589));
#48674=CARTESIAN_POINT('Ctrl Pts',(92.2166551271479,2.80470605164371,126.764211235876));
#48675=CARTESIAN_POINT('Ctrl Pts',(92.2088807930288,2.69263834178503,126.68641287885));
#48676=CARTESIAN_POINT('Ctrl Pts',(92.2011064589097,2.57715365618677,126.613157714904));
#48677=CARTESIAN_POINT('Ctrl Pts',(92.1933321247906,2.45865665318967,126.544760809576));
#48678=CARTESIAN_POINT('Ctrl Pts',(92.1855673718435,2.34030568715847,126.476448197321));
#48679=CARTESIAN_POINT('Ctrl Pts',(92.1778026188965,2.21895012567846,126.412982124173));
#48680=CARTESIAN_POINT('Ctrl Pts',(92.1700378659494,2.09502530144347,126.354635676762));
#48681=CARTESIAN_POINT('Ctrl Pts',(92.1622808250644,1.97122356109095,126.296347179866));
#48682=CARTESIAN_POINT('Ctrl Pts',(92.1545237841794,1.84485798766824,126.24316835502));
#48683=CARTESIAN_POINT('Ctrl Pts',(92.1467667432944,1.71639001889204,126.195327273626));
#48684=CARTESIAN_POINT('Ctrl Pts',(92.1390155520542,1.58801892881042,126.147522269564));
#48685=CARTESIAN_POINT('Ctrl Pts',(92.1312643608141,1.45754896398517,126.105047132858));
#48686=CARTESIAN_POINT('Ctrl Pts',(92.123513169574,1.32546279753335,126.068082391484));
#48687=CARTESIAN_POINT('Ctrl Pts',(92.1157652727969,1.19343277122579,126.031133361112));
#48688=CARTESIAN_POINT('Ctrl Pts',(92.1080173760198,1.05978828525221,125.999690173027));
#48689=CARTESIAN_POINT('Ctrl Pts',(92.1002694792428,0.925028270440346,125.973883854203));
#48690=CARTESIAN_POINT('Ctrl Pts',(92.0925232031587,0.790296444518492,125.948082933505));
#48691=CARTESIAN_POINT('Ctrl Pts',(92.0847769270745,0.654449937638121,125.927916610237));
#48692=CARTESIAN_POINT('Ctrl Pts',(92.0770306509904,0.517998611886916,125.913464942888));
#48693=CARTESIAN_POINT('Ctrl Pts',(92.069284317725,0.381546278883022,125.89901316886));
#48694=CARTESIAN_POINT('Ctrl Pts',(92.0615379844597,0.244489506890172,125.890276176104));
#48695=CARTESIAN_POINT('Ctrl Pts',(92.0537916511944,0.1073436347066,125.887282175382));
#48696=CARTESIAN_POINT('Ctrl Pts',(92.0460435831914,-0.0298329503441449,
125.884287504175));
#48697=CARTESIAN_POINT('Ctrl Pts',(92.0382955151884,-0.167098284493242,
125.887038392729));
#48698=CARTESIAN_POINT('Ctrl Pts',(92.0305474471855,-0.303937070211306,
125.895510923406));
#48699=CARTESIAN_POINT('Ctrl Pts',(92.0227911444436,-0.440921289819233,
125.90399245879));
#48700=CARTESIAN_POINT('Ctrl Pts',(92.0150348417018,-0.57747766455898,125.918207759607));
#48701=CARTESIAN_POINT('Ctrl Pts',(92.0072785389599,-0.713095504301106,
125.938080943704));
#48702=CARTESIAN_POINT('Ctrl Pts',(91.9995180964457,-0.848785727367769,
125.957964734717));
#48703=CARTESIAN_POINT('Ctrl Pts',(91.9917576539316,-0.983536033368037,
125.98351235339));
#48704=CARTESIAN_POINT('Ctrl Pts',(91.9839972114174,-1.11684694911122,126.014596953797));
#48705=CARTESIAN_POINT('Ctrl Pts',(91.976224311152,-1.25037186737114,126.045731453964));
#48706=CARTESIAN_POINT('Ctrl Pts',(91.9684514108865,-1.38245240106622,126.082420593129));
#48707=CARTESIAN_POINT('Ctrl Pts',(91.9606785106211,-1.51260437560883,126.124487642218));
#48708=CARTESIAN_POINT('Ctrl Pts',(91.9531881748591,-1.63802499804342,126.165025448113));
#48709=CARTESIAN_POINT('Ctrl Pts',(91.9456978390971,-1.76165455389711,126.210556844692));
#48710=CARTESIAN_POINT('Ctrl Pts',(91.9382075033351,-1.88307996812429,126.260882555976));
#48711=CARTESIAN_POINT('Ctrl Pts',(91.9304327771396,-2.00911561976703,126.313119016164));
#48712=CARTESIAN_POINT('Ctrl Pts',(91.9226580509441,-2.13317571388074,126.37068651974));
#48713=CARTESIAN_POINT('Ctrl Pts',(91.9148833247487,-2.25477637635929,126.433414889796));
#48714=CARTESIAN_POINT('Ctrl Pts',(91.9071182694565,-2.37622578100307,126.496065232666));
#48715=CARTESIAN_POINT('Ctrl Pts',(91.8993532141643,-2.49522149708592,126.56386349092));
#48716=CARTESIAN_POINT('Ctrl Pts',(91.8915881588722,-2.61129840819856,126.636590987915));
#48717=CARTESIAN_POINT('Ctrl Pts',(91.883830904992,-2.72725869891749,126.709245416897));
#48718=CARTESIAN_POINT('Ctrl Pts',(91.8760736511119,-2.840305691509,126.786819022479));
#48719=CARTESIAN_POINT('Ctrl Pts',(91.8683163972317,-2.94999805092592,126.869046835663));
#48720=CARTESIAN_POINT('Ctrl Pts',(91.8604768978297,-3.06085341280244,126.952146461156));
#48721=CARTESIAN_POINT('Ctrl Pts',(91.8526373984277,-3.16828222908446,127.039999384072));
#48722=CARTESIAN_POINT('Ctrl Pts',(91.8447978990257,-3.27185763377978,127.1322861784));
#48723=CARTESIAN_POINT('Ctrl Pts',(91.8370503435242,-3.37421827638199,127.223490606699));
#48724=CARTESIAN_POINT('Ctrl Pts',(91.8293027880226,-3.47281511362822,127.319025190661));
#48725=CARTESIAN_POINT('Ctrl Pts',(91.8215552325211,-3.56726867283482,127.418540587158));
#48726=CARTESIAN_POINT('Ctrl Pts',(91.8138094054638,-3.66170115988376,127.518033782225));
#48727=CARTESIAN_POINT('Ctrl Pts',(91.8060635784066,-3.75199193937431,127.621505739236));
#48728=CARTESIAN_POINT('Ctrl Pts',(91.7983177513493,-3.83779856660814,127.728570438662));
#48729=CARTESIAN_POINT('Ctrl Pts',(91.7905719749466,-3.92360463270164,127.835634437929));
#48730=CARTESIAN_POINT('Ctrl Pts',(91.7828261985438,-4.00492636114638,127.946290827345));
#48731=CARTESIAN_POINT('Ctrl Pts',(91.7750804221411,-4.0814620126222,128.060121032176));
#48732=CARTESIAN_POINT('Ctrl Pts',(91.767171087928,-4.159613771112,128.17635484616));
#48733=CARTESIAN_POINT('Ctrl Pts',(91.7592617537148,-4.23277481175118,128.295897670547));
#48734=CARTESIAN_POINT('Ctrl Pts',(91.7513524195017,-4.30067131094419,128.418274001845));
#48735=CARTESIAN_POINT('Ctrl Pts',(91.7435983649255,-4.36723483526734,128.538247785498));
#48736=CARTESIAN_POINT('Ctrl Pts',(91.7358443103493,-4.42873849149336,128.660944467187));
#48737=CARTESIAN_POINT('Ctrl Pts',(91.7280902557731,-4.48497180747443,128.785893142312));
#48738=CARTESIAN_POINT('Ctrl Pts',(91.7201032817415,-4.54289428274695,128.914595076725));
#48739=CARTESIAN_POINT('Ctrl Pts',(91.7121163077099,-4.59522464169714,129.045686007565));
#48740=CARTESIAN_POINT('Ctrl Pts',(91.7041293336783,-4.6417874480562,129.178632365499));
#48741=CARTESIAN_POINT('Ctrl Pts',(91.6961423596467,-4.68835025441526,129.311578723434));
#48742=CARTESIAN_POINT('Ctrl Pts',(91.6881553856151,-4.7291454272762,129.446380064493));
#48743=CARTESIAN_POINT('Ctrl Pts',(91.6801684115835,-4.76405452823407,129.582490119308));
#48744=CARTESIAN_POINT('Origin',(213.235140564004,0.,130.804360617566));
#48745=CARTESIAN_POINT('',(89.5849003473043,-4.76405452823408,129.582490119308));
#48746=CARTESIAN_POINT('',(89.9298547845941,-4.76405452823405,129.582490119308));
#48747=CARTESIAN_POINT('',(213.235140564004,-4.76405452823405,129.582490119308));
#48748=CARTESIAN_POINT('',(91.2648594360222,-4.91824999011832,130.804048846578));
#48749=CARTESIAN_POINT('Ctrl Pts',(91.2648594359911,-4.91824999011835,130.80404884713));
#48750=CARTESIAN_POINT('Ctrl Pts',(91.2567821902965,-4.91825908170041,130.947470635016));
#48751=CARTESIAN_POINT('Ctrl Pts',(91.2487049446019,-4.91199033781274,131.090783981988));
#48752=CARTESIAN_POINT('Ctrl Pts',(91.2406276989073,-4.89949806352798,131.233431460185));
#48753=CARTESIAN_POINT('Ctrl Pts',(91.2325411218347,-4.88699135732701,131.376243734351));
#48754=CARTESIAN_POINT('Ctrl Pts',(91.2244545447621,-4.86824680681819,131.5183882668));
#48755=CARTESIAN_POINT('Ctrl Pts',(91.2163679676895,-4.84337019359417,131.659315721828));
#48756=CARTESIAN_POINT('Ctrl Pts',(91.2082635352129,-4.8184386520642,131.800554348891));
#48757=CARTESIAN_POINT('Ctrl Pts',(91.2001591027363,-4.78734803810946,131.940570190156));
#48758=CARTESIAN_POINT('Ctrl Pts',(91.1920546702598,-4.75025502706789,132.078825305314));
#48759=CARTESIAN_POINT('Ctrl Pts',(91.1839409951308,-4.71311971351996,132.217238092705));
#48760=CARTESIAN_POINT('Ctrl Pts',(91.1758273200019,-4.66996844606161,132.353885823443));
#48761=CARTESIAN_POINT('Ctrl Pts',(91.1677136448729,-4.62100685794723,132.488248583348));
#48762=CARTESIAN_POINT('Ctrl Pts',(91.1595815322751,-4.57193400980094,132.622916668417));
#48763=CARTESIAN_POINT('Ctrl Pts',(91.1514494196773,-4.51702456936365,132.755289085));
#48764=CARTESIAN_POINT('Ctrl Pts',(91.1433173070796,-4.45653189461077,132.884866934504));
#48765=CARTESIAN_POINT('Ctrl Pts',(91.1363627474049,-4.40479873039393,132.995681544613));
#48766=CARTESIAN_POINT('Ctrl Pts',(91.1294081877302,-4.34898303515304,133.104452624606));
#48767=CARTESIAN_POINT('Ctrl Pts',(91.1224536280556,-4.28926854451115,133.210884753237));
#48768=CARTESIAN_POINT('Ctrl Pts',(91.1146792939365,-4.2225151591471,133.329862656611));
#48769=CARTESIAN_POINT('Ctrl Pts',(91.1069049598174,-4.1507018855291,133.446249448752));
#48770=CARTESIAN_POINT('Ctrl Pts',(91.0991306256983,-4.07405482378452,133.559584810857));
#48771=CARTESIAN_POINT('Ctrl Pts',(91.0913658727512,-3.9975022226934,133.672780497258));
#48772=CARTESIAN_POINT('Ctrl Pts',(91.0836011198041,-3.91612790346948,133.782931915379));
#48773=CARTESIAN_POINT('Ctrl Pts',(91.075836366857,-3.83020391151471,133.889603081088));
#48774=CARTESIAN_POINT('Ctrl Pts',(91.068079325972,-3.74436526048018,133.996168299491));
#48775=CARTESIAN_POINT('Ctrl Pts',(91.060322285087,-3.6539861729963,134.09925984184));
#48776=CARTESIAN_POINT('Ctrl Pts',(91.052565244202,-3.5593818586381,134.198470787684));
#48777=CARTESIAN_POINT('Ctrl Pts',(91.0448140529619,-3.46484888612909,134.297606917782));
#48778=CARTESIAN_POINT('Ctrl Pts',(91.0370628617217,-3.36609729755123,134.392867994372));
#48779=CARTESIAN_POINT('Ctrl Pts',(91.0293116704816,-3.2634821932607,134.483880564077));
#48780=CARTESIAN_POINT('Ctrl Pts',(91.0215637737045,-3.16091070312698,134.574854451011));
#48781=CARTESIAN_POINT('Ctrl Pts',(91.0138158769274,-3.0544792551696,134.661583163637));
#48782=CARTESIAN_POINT('Ctrl Pts',(91.0060679801503,-2.94457922037927,134.743730653169));
#48783=CARTESIAN_POINT('Ctrl Pts',(90.9983217040662,-2.83470217430705,134.825860959218));
#48784=CARTESIAN_POINT('Ctrl Pts',(90.9905754279821,-2.7213582975207,134.903411714345));
#48785=CARTESIAN_POINT('Ctrl Pts',(90.982829151898,-2.60497108351019,134.97608792368));
#48786=CARTESIAN_POINT('Ctrl Pts',(90.9750828186327,-2.48858301035571,135.048764669494));
#48787=CARTESIAN_POINT('Ctrl Pts',(90.9673364853673,-2.3691518867714,135.116566590639));
#48788=CARTESIAN_POINT('Ctrl Pts',(90.959590152102,-2.24712880813484,135.179242922514));
#48789=CARTESIAN_POINT('Ctrl Pts',(90.951842084099,-2.12507840327604,135.24193329032));
#48790=CARTESIAN_POINT('Ctrl Pts',(90.944094016096,-2.00043523604083,135.299495606191));
#48791=CARTESIAN_POINT('Ctrl Pts',(90.9363459480931,-1.87367316424428,135.35172600162));
#48792=CARTESIAN_POINT('Ctrl Pts',(90.9285896453512,-1.74677636820917,135.404011908135));
#48793=CARTESIAN_POINT('Ctrl Pts',(90.9208333426094,-1.61775653106513,135.450954424926));
#48794=CARTESIAN_POINT('Ctrl Pts',(90.9130770398675,-1.48710609515371,135.492398429301));
#48795=CARTESIAN_POINT('Ctrl Pts',(90.9053165973534,-1.35638592717075,135.533864553589));
#48796=CARTESIAN_POINT('Ctrl Pts',(90.8975561548392,-1.22403380337619,135.569826215315));
#48797=CARTESIAN_POINT('Ctrl Pts',(90.889795712325,-1.09055436911228,135.600179028485));
#48798=CARTESIAN_POINT('Ctrl Pts',(90.8820228120596,-0.956860661810738,
135.630580566685));
#48799=CARTESIAN_POINT('Ctrl Pts',(90.8742499117942,-0.822036412513276,
135.655355193125));
#48800=CARTESIAN_POINT('Ctrl Pts',(90.8664770115287,-0.686594326366148,
135.674450071929));
#48801=CARTESIAN_POINT('Ctrl Pts',(90.8589866757667,-0.556075901208769,
135.692850803793));
#48802=CARTESIAN_POINT('Ctrl Pts',(90.8514963400047,-0.424984085664462,
135.705977534244));
#48803=CARTESIAN_POINT('Ctrl Pts',(90.8440060042427,-0.293777507871708,
135.713828800411));
#48804=CARTESIAN_POINT('Ctrl Pts',(90.8362316701236,-0.157596192802371,
135.721977749721));
#48805=CARTESIAN_POINT('Ctrl Pts',(90.8284573360045,-0.0208598598023733,
135.724469112826));
#48806=CARTESIAN_POINT('Ctrl Pts',(90.8206830018854,0.115921999242919,135.721244300611));
#48807=CARTESIAN_POINT('Ctrl Pts',(90.8129182489383,0.252535286871484,135.718023462689));
#48808=CARTESIAN_POINT('Ctrl Pts',(90.8051534959913,0.389193601805164,135.709100475377));
#48809=CARTESIAN_POINT('Ctrl Pts',(90.7973887430442,0.525383091062019,135.694468558105));
#48810=CARTESIAN_POINT('Ctrl Pts',(90.7896317021592,0.661437314998209,135.67985117346));
#48811=CARTESIAN_POINT('Ctrl Pts',(90.7818746612742,0.797023253698014,135.659536184282));
#48812=CARTESIAN_POINT('Ctrl Pts',(90.7741176203892,0.931628174985949,135.63356883487));
#48813=CARTESIAN_POINT('Ctrl Pts',(90.7663664291491,1.06613158965539,135.607621067637));
#48814=CARTESIAN_POINT('Ctrl Pts',(90.7586152379089,1.19965507709207,135.576029498155));
#48815=CARTESIAN_POINT('Ctrl Pts',(90.7508640466688,1.33169249997644,135.538891021736));
#48816=CARTESIAN_POINT('Ctrl Pts',(90.7431161498917,1.46367380343406,135.50176833016));
#48817=CARTESIAN_POINT('Ctrl Pts',(90.7353682531147,1.59416992300471,135.459103526339));
#48818=CARTESIAN_POINT('Ctrl Pts',(90.7276203563376,1.72268658574751,135.411044239195));
#48819=CARTESIAN_POINT('Ctrl Pts',(90.7198740802535,1.85117636557488,135.362995005018));
#48820=CARTESIAN_POINT('Ctrl Pts',(90.7121278041695,1.9776871461959,135.309553668841));
#48821=CARTESIAN_POINT('Ctrl Pts',(90.7043815280854,2.10174183149495,135.250917075798));
#48822=CARTESIAN_POINT('Ctrl Pts',(90.69663519482,2.22579743253743,135.192280049913));
#48823=CARTESIAN_POINT('Ctrl Pts',(90.6888888615547,2.34739654861116,135.128447857709));
#48824=CARTESIAN_POINT('Ctrl Pts',(90.6811425282894,2.46608437628631,135.059664474112));
#48825=CARTESIAN_POINT('Ctrl Pts',(90.6733944602864,2.58479878327754,134.990865686954));
#48826=CARTESIAN_POINT('Ctrl Pts',(90.6656463922834,2.70060026633855,134.917113698047));
#48827=CARTESIAN_POINT('Ctrl Pts',(90.6578983242805,2.81306117339638,134.838696981484));
#48828=CARTESIAN_POINT('Ctrl Pts',(90.6501420215387,2.92564160524469,134.760196922701));
#48829=CARTESIAN_POINT('Ctrl Pts',(90.6423857187968,3.03487404756369,134.677022456641));
#48830=CARTESIAN_POINT('Ctrl Pts',(90.6346294160549,3.14036181412377,134.589504041387));
#48831=CARTESIAN_POINT('Ctrl Pts',(90.6268689735408,3.24590588268112,134.501938914919));
#48832=CARTESIAN_POINT('Ctrl Pts',(90.6191085310266,3.34770100297013,134.41002548134));
#48833=CARTESIAN_POINT('Ctrl Pts',(90.6113480885124,3.44538657896237,134.314131889886));
#48834=CARTESIAN_POINT('Ctrl Pts',(90.603575188247,3.54322896851331,134.218084361527));
#48835=CARTESIAN_POINT('Ctrl Pts',(90.5958022879816,3.63694836340132,134.118044192917));
#48836=CARTESIAN_POINT('Ctrl Pts',(90.5880293877162,3.72622318165434,134.014414178334));
#48837=CARTESIAN_POINT('Ctrl Pts',(90.5805390519541,3.81225263539495,133.91455137581));
#48838=CARTESIAN_POINT('Ctrl Pts',(90.573048716192,3.89415485389067,133.811355437125));
#48839=CARTESIAN_POINT('Ctrl Pts',(90.5655583804299,3.97168070667275,133.705211428405));
#48840=CARTESIAN_POINT('Ctrl Pts',(90.5577840463108,4.05214597572579,133.595042937333));
#48841=CARTESIAN_POINT('Ctrl Pts',(90.5500097121917,4.12815135802207,133.481349430419));
#48842=CARTESIAN_POINT('Ctrl Pts',(90.5422353780726,4.19937216807081,133.364527888768));
#48843=CARTESIAN_POINT('Ctrl Pts',(90.5344706251255,4.27050520483626,133.247850319226));
#48844=CARTESIAN_POINT('Ctrl Pts',(90.5267058721785,4.33686520018545,133.12805271591));
#48845=CARTESIAN_POINT('Ctrl Pts',(90.5189411192314,4.39816869934376,133.005563732822));
#48846=CARTESIAN_POINT('Ctrl Pts',(90.5111840783464,4.45941131100252,132.883196407519));
#48847=CARTESIAN_POINT('Ctrl Pts',(90.5034270374614,4.51560724699439,132.758143369425));
#48848=CARTESIAN_POINT('Ctrl Pts',(90.4956699965764,4.56651742836434,132.630860450291));
#48849=CARTESIAN_POINT('Ctrl Pts',(90.4879188053363,4.6173892179705,132.503673516196));
#48850=CARTESIAN_POINT('Ctrl Pts',(90.4801676140961,4.6629830422971,132.374260409662));
#48851=CARTESIAN_POINT('Ctrl Pts',(90.472416422856,4.70310684253171,132.243099332633));
#48852=CARTESIAN_POINT('Ctrl Pts',(90.4646685260789,4.74321358908094,132.11199400256));
#48853=CARTESIAN_POINT('Ctrl Pts',(90.4569206293018,4.77785482146942,131.979142552712));
#48854=CARTESIAN_POINT('Ctrl Pts',(90.4491727325247,4.8068875774922,131.845040625951));
#48855=CARTESIAN_POINT('Ctrl Pts',(90.4414264564406,4.83591426048827,131.710966750422));
#48856=CARTESIAN_POINT('Ctrl Pts',(90.4336801803565,4.85933471794867,131.575643300133));
#48857=CARTESIAN_POINT('Ctrl Pts',(90.4259339042724,4.87705667915491,131.439578069161));
#48858=CARTESIAN_POINT('Ctrl Pts',(90.4181875710071,4.89477877118064,131.303511833786));
#48859=CARTESIAN_POINT('Ctrl Pts',(90.4104412377417,4.90680223251936,131.166704194493));
#48860=CARTESIAN_POINT('Ctrl Pts',(90.4026949044763,4.91308649382261,131.029669664694));
#48861=CARTESIAN_POINT('Ctrl Pts',(90.3949468364734,4.91937216244262,130.892604446962));
#48862=CARTESIAN_POINT('Ctrl Pts',(90.3871987684704,4.91991605561335,130.755312628097));
#48863=CARTESIAN_POINT('Ctrl Pts',(90.3794507004674,4.91472971836706,130.618309931194));
#48864=CARTESIAN_POINT('Ctrl Pts',(90.3716943977255,4.90953786901984,130.481161626194));
#48865=CARTESIAN_POINT('Ctrl Pts',(90.3639380949837,4.89860363832411,130.344303448292));
#48866=CARTESIAN_POINT('Ctrl Pts',(90.3561817922418,4.88199063142803,130.208247761515));
#48867=CARTESIAN_POINT('Ctrl Pts',(90.3484213497276,4.86536875766992,130.072119457721));
#48868=CARTESIAN_POINT('Ctrl Pts',(90.3406609072134,4.84306213187583,129.936794884074));
#48869=CARTESIAN_POINT('Ctrl Pts',(90.3329004646993,4.81518557746513,129.802776413881));
#48870=CARTESIAN_POINT('Ctrl Pts',(90.3251275644338,4.78726427313458,129.668542805342));
#48871=CARTESIAN_POINT('Ctrl Pts',(90.3173546641684,4.75375526815799,129.5356198694));
#48872=CARTESIAN_POINT('Ctrl Pts',(90.309581763903,4.71482362185967,129.404495882224));
#48873=CARTESIAN_POINT('Ctrl Pts',(90.302091428141,4.67730723896732,129.278138582264));
#48874=CARTESIAN_POINT('Ctrl Pts',(90.2946010923789,4.63475572276177,129.153452000694));
#48875=CARTESIAN_POINT('Ctrl Pts',(90.2871107566169,4.58735837917409,129.030853875678));
#48876=CARTESIAN_POINT('Ctrl Pts',(90.2793364224978,4.53816395089799,128.90360740549));
#48877=CARTESIAN_POINT('Ctrl Pts',(90.2715620883788,4.4835931492296,128.778207807174));
#48878=CARTESIAN_POINT('Ctrl Pts',(90.2637877542597,4.42380446517697,128.655142825815));
#48879=CARTESIAN_POINT('Ctrl Pts',(90.2560230013126,4.36408946533396,128.532229511046));
#48880=CARTESIAN_POINT('Ctrl Pts',(90.2482582483655,4.29916954723883,128.411645436735));
#48881=CARTESIAN_POINT('Ctrl Pts',(90.2404934954184,4.22925213541458,128.293860779368));
#48882=CARTESIAN_POINT('Ctrl Pts',(90.2327364545334,4.15940416654941,128.176193107384));
#48883=CARTESIAN_POINT('Ctrl Pts',(90.2249794136484,4.0845687799809,128.061319653203));
#48884=CARTESIAN_POINT('Ctrl Pts',(90.2172223727634,4.00500025185449,127.949687948915));
#48885=CARTESIAN_POINT('Ctrl Pts',(90.2094711815233,3.92549172697409,127.838140426963));
#48886=CARTESIAN_POINT('Ctrl Pts',(90.2017199902832,3.84125739101632,127.7298301061));
#48887=CARTESIAN_POINT('Ctrl Pts',(90.193968799043,3.75259575634186,127.625177050676));
#48888=CARTESIAN_POINT('Ctrl Pts',(90.186220902266,3.66397180522734,127.520568475592));
#48889=CARTESIAN_POINT('Ctrl Pts',(90.1784730054889,3.5709245501868,127.419614371973));
#48890=CARTESIAN_POINT('Ctrl Pts',(90.1707251087118,3.47379371503351,127.322702925045));
#48891=CARTESIAN_POINT('Ctrl Pts',(90.1629788326277,3.3766831975569,127.225811749902));
#48892=CARTESIAN_POINT('Ctrl Pts',(90.1552325565436,3.27549107560323,127.132961825398));
#48893=CARTESIAN_POINT('Ctrl Pts',(90.1474862804595,3.17059469613377,127.044505256605));
#48894=CARTESIAN_POINT('Ctrl Pts',(90.1397399471941,3.06569754234328,126.956048034845));
#48895=CARTESIAN_POINT('Ctrl Pts',(90.1319936139288,2.9570963753553,126.871984485549));
#48896=CARTESIAN_POINT('Ctrl Pts',(90.1242472806634,2.84520214115207,126.792626847924));
#48897=CARTESIAN_POINT('Ctrl Pts',(90.1164992126605,2.73328284901083,126.713251438707));
#48898=CARTESIAN_POINT('Ctrl Pts',(90.1087511446575,2.61806934103788,126.638584264343));
#48899=CARTESIAN_POINT('Ctrl Pts',(90.1010030766545,2.50000175005002,126.5688943726));
#48900=CARTESIAN_POINT('Ctrl Pts',(90.0932467739127,2.38180867542152,126.499130413611));
#48901=CARTESIAN_POINT('Ctrl Pts',(90.0854904711708,2.26075579555368,126.434354503466));
#48902=CARTESIAN_POINT('Ctrl Pts',(90.077734168429,2.13730855694855,126.374790074625));
#48903=CARTESIAN_POINT('Ctrl Pts',(90.0699737259148,2.01379543083509,126.315193854454));
#48904=CARTESIAN_POINT('Ctrl Pts',(90.0622132834007,1.88788575832351,126.260814812948));
#48905=CARTESIAN_POINT('Ctrl Pts',(90.0544528408865,1.76006426516806,126.211827890957));
#48906=CARTESIAN_POINT('Ctrl Pts',(90.0466799406211,1.63203758160441,126.162762330809));
#48907=CARTESIAN_POINT('Ctrl Pts',(90.0389070403556,1.50209331533099,126.11910631202));
#48908=CARTESIAN_POINT('Ctrl Pts',(90.0311341400902,1.37073148551301,126.080984890703));
#48909=CARTESIAN_POINT('Ctrl Pts',(90.0236438043282,1.24414498908985,126.044249279072));
#48910=CARTESIAN_POINT('Ctrl Pts',(90.0161534685662,1.11624250281998,126.012652931799));
#48911=CARTESIAN_POINT('Ctrl Pts',(90.0086631328042,0.98747780613174,125.986262378126));
#48912=CARTESIAN_POINT('Ctrl Pts',(90.0008887986851,0.853830956830725,125.958871218588));
#48913=CARTESIAN_POINT('Ctrl Pts',(89.993114464566,0.718831871998949,125.937001633612));
#48914=CARTESIAN_POINT('Ctrl Pts',(89.9853401304469,0.582976573649635,125.920783918355));
#48915=CARTESIAN_POINT('Ctrl Pts',(89.9775753774998,0.447288704814077,125.904586189983));
#48916=CARTESIAN_POINT('Ctrl Pts',(89.9698106245527,0.310747106489839,125.894026518108));
#48917=CARTESIAN_POINT('Ctrl Pts',(89.9620458716057,0.173859469494193,125.889184532483));
#48918=CARTESIAN_POINT('Ctrl Pts',(89.9542888307206,0.0371077912286443,
125.884347355987));
#48919=CARTESIAN_POINT('Ctrl Pts',(89.9465317898356,-0.0999888535562237,
125.88521657823));
#48920=CARTESIAN_POINT('Ctrl Pts',(89.9387747489505,-0.236916500970071,
125.891820171517));
#48921=CARTESIAN_POINT('Ctrl Pts',(89.9310235577104,-0.373740890178559,
125.898418784983));
#48922=CARTESIAN_POINT('Ctrl Pts',(89.9232723664704,-0.51039614675082,125.910743143411));
#48923=CARTESIAN_POINT('Ctrl Pts',(89.9155211752303,-0.646367505429397,
125.928769154941));
#48924=CARTESIAN_POINT('Ctrl Pts',(89.9077732784532,-0.782281072654214,
125.946787504935));
#48925=CARTESIAN_POINT('Ctrl Pts',(89.9000253816761,-0.917510933352707,
125.970502636888));
#48926=CARTESIAN_POINT('Ctrl Pts',(89.892277484899,-1.05154686728138,125.999838555132));
#48927=CARTESIAN_POINT('Ctrl Pts',(89.8845312088149,-1.18555476378207,126.029168336935));
#48928=CARTESIAN_POINT('Ctrl Pts',(89.8767849327307,-1.31836884858427,126.064116482865));
#48929=CARTESIAN_POINT('Ctrl Pts',(89.8690386566466,-1.44948892046989,126.104555841627));
#48930=CARTESIAN_POINT('Ctrl Pts',(89.8612923233813,-1.58060996025446,126.144995498905));
#48931=CARTESIAN_POINT('Ctrl Pts',(89.8535459901159,-1.71003658856958,126.190926334675));
#48932=CARTESIAN_POINT('Ctrl Pts',(89.8457996568505,-1.83728398338421,126.242171381366));
#48933=CARTESIAN_POINT('Ctrl Pts',(89.8380515888476,-1.96455987436968,126.293427904029));
#48934=CARTESIAN_POINT('Ctrl Pts',(89.8303035208446,-2.08965519815141,126.350000859712));
#48935=CARTESIAN_POINT('Ctrl Pts',(89.8225554528417,-2.21210569468498,126.4116653791));
#48936=CARTESIAN_POINT('Ctrl Pts',(89.8147991500998,-2.33468633306404,126.473395436273));
#48937=CARTESIAN_POINT('Ctrl Pts',(89.8070428473579,-2.45461617926756,126.540227690829));
#48938=CARTESIAN_POINT('Ctrl Pts',(89.7992865446161,-2.57145566803669,126.611891320144));
#48939=CARTESIAN_POINT('Ctrl Pts',(89.7915261021019,-2.68835751755942,126.683593198497));
#48940=CARTESIAN_POINT('Ctrl Pts',(89.7837656595877,-2.80216539878034,126.760131371712));
#48941=CARTESIAN_POINT('Ctrl Pts',(89.7760052170735,-2.91247012289832,126.841192586089));
#48942=CARTESIAN_POINT('Ctrl Pts',(89.7682323168081,-3.02295191795154,126.922383927122));
#48943=CARTESIAN_POINT('Ctrl Pts',(89.7604594165426,-3.12991901294711,127.008112574038));
#48944=CARTESIAN_POINT('Ctrl Pts',(89.7526865162772,-3.23299592206444,127.098025442435));
#48945=CARTESIAN_POINT('Ctrl Pts',(89.7451961805151,-3.33232572590036,127.184669751588));
#48946=CARTESIAN_POINT('Ctrl Pts',(89.7377058447531,-3.42804304573703,127.27519913819));
#48947=CARTESIAN_POINT('Ctrl Pts',(89.730215508991,-3.5198466297751,127.369267785435));
#48948=CARTESIAN_POINT('Ctrl Pts',(89.7225449396728,-3.61385920509875,127.465599926247));
#48949=CARTESIAN_POINT('Ctrl Pts',(89.7148743703545,-3.70408235314633,127.565966974299));
#48950=CARTESIAN_POINT('Ctrl Pts',(89.7072038010363,-3.79014272504406,127.670034344458));
#48951=CARTESIAN_POINT('Ctrl Pts',(89.6995422470002,-3.87610194949049,127.773979403395));
#48952=CARTESIAN_POINT('Ctrl Pts',(89.6918806929641,-3.95790787116681,127.881615831503));
#48953=CARTESIAN_POINT('Ctrl Pts',(89.684219138928,-4.03522292249679,127.992571324561));
#48954=CARTESIAN_POINT('Ctrl Pts',(89.6765648235771,-4.11246492607275,128.103421986161));
#48955=CARTESIAN_POINT('Ctrl Pts',(89.6689105082262,-4.18522426871552,128.21758514882));
#48956=CARTESIAN_POINT('Ctrl Pts',(89.6612561928753,-4.25320310047533,128.334654876267));
#48957=CARTESIAN_POINT('Ctrl Pts',(89.6536077566286,-4.32112971925222,128.451634685138));
#48958=CARTESIAN_POINT('Ctrl Pts',(89.6459593203818,-4.38428293318778,128.571516269498));
#48959=CARTESIAN_POINT('Ctrl Pts',(89.6383108841352,-4.44240810535641,128.693864636057));
#48960=CARTESIAN_POINT('Ctrl Pts',(89.6306658150064,-4.50050768872443,128.816159140446));
#48961=CARTESIAN_POINT('Ctrl Pts',(89.6230207458776,-4.55358346182154,128.940917903946));
#48962=CARTESIAN_POINT('Ctrl Pts',(89.6153756767489,-4.60142685460908,129.067681613207));
#48963=CARTESIAN_POINT('Ctrl Pts',(89.607731596945,-4.64926405613048,129.194428918366));
#48964=CARTESIAN_POINT('Ctrl Pts',(89.6000875171411,-4.69187007989412,129.323180278017));
#48965=CARTESIAN_POINT('Ctrl Pts',(89.5924434373372,-4.72908476756752,129.45345709634));
#48966=CARTESIAN_POINT('Ctrl Pts',(89.5899290739929,-4.74132577615913,129.496308984991));
#48967=CARTESIAN_POINT('Ctrl Pts',(89.5874147106486,-4.75298386921147,129.5393257878));
#48968=CARTESIAN_POINT('Ctrl Pts',(89.5849003473043,-4.76405452823408,129.582490119308));
#48969=CARTESIAN_POINT('Ctrl Pts',(91.3345773084523,-4.76405452823403,129.582490119308));
#48970=CARTESIAN_POINT('Ctrl Pts',(91.3264022802331,-4.7999124076053,129.722299446757));
#48971=CARTESIAN_POINT('Ctrl Pts',(91.318227252014,-4.8296500169407,129.863837736042));
#48972=CARTESIAN_POINT('Ctrl Pts',(91.3100522237949,-4.85311178198504,130.006557951452));
#48973=CARTESIAN_POINT('Ctrl Pts',(91.3018941690471,-4.87652483434178,130.148981842812));
#48974=CARTESIAN_POINT('Ctrl Pts',(91.2937361142993,-4.89368797434029,130.292582447441));
#48975=CARTESIAN_POINT('Ctrl Pts',(91.2855780595515,-4.90449620518163,130.436801049796));
#48976=CARTESIAN_POINT('Ctrl Pts',(91.2786718517084,-4.91364592173953,130.558889424231));
#48977=CARTESIAN_POINT('Ctrl Pts',(91.2717656438653,-4.91824221661868,130.681420327672));
#48978=CARTESIAN_POINT('Ctrl Pts',(91.2648594360222,-4.91824999011832,130.804048846578));
#48979=CARTESIAN_POINT('',(91.6101405639636,-4.91824821216763,130.800167049889));
#48980=CARTESIAN_POINT('Ctrl Pts',(91.6801684115835,-4.76405452823407,129.582490119308));
#48981=CARTESIAN_POINT('Ctrl Pts',(91.6733655675631,-4.79378808787393,129.698420817074));
#48982=CARTESIAN_POINT('Ctrl Pts',(91.6665627235426,-4.81925245143363,129.815300578257));
#48983=CARTESIAN_POINT('Ctrl Pts',(91.6597598795222,-4.84040749075737,129.932788253433));
#48984=CARTESIAN_POINT('Ctrl Pts',(91.6478811714655,-4.87734712002086,130.13793800984));
#48985=CARTESIAN_POINT('Ctrl Pts',(91.636002463409,-4.90125243413717,130.345500572299));
#48986=CARTESIAN_POINT('Ctrl Pts',(91.6241237553524,-4.91188095687709,130.554143655774));
#48987=CARTESIAN_POINT('Ctrl Pts',(91.619462691571,-4.91605146280719,130.636012720573));
#48988=CARTESIAN_POINT('Ctrl Pts',(91.6148016277897,-4.91817819283374,130.718047855595));
#48989=CARTESIAN_POINT('Ctrl Pts',(91.6101405640084,-4.91824821216696,130.800167049099));
#48990=CARTESIAN_POINT('Ctrl Pts',(91.6101405639636,-4.91824821216763,130.800167049889));
#48991=CARTESIAN_POINT('Ctrl Pts',(91.6024939071275,-4.91836308159171,130.934886788097));
#48992=CARTESIAN_POINT('Ctrl Pts',(91.5948472502914,-4.91293846637897,131.069800215564));
#48993=CARTESIAN_POINT('Ctrl Pts',(91.5872005934553,-4.90195333028209,131.204406377744));
#48994=CARTESIAN_POINT('Ctrl Pts',(91.5795609026991,-4.89097820160899,131.338889914141));
#48995=CARTESIAN_POINT('Ctrl Pts',(91.5719212119429,-4.87445266018738,131.473066342139));
#48996=CARTESIAN_POINT('Ctrl Pts',(91.5642815211867,-4.85240772185146,131.606434406825));
#48997=CARTESIAN_POINT('Ctrl Pts',(91.556646523981,-4.83037632713072,131.739720534981));
#48998=CARTESIAN_POINT('Ctrl Pts',(91.5490115267753,-4.80283234498052,131.872198890597));
#48999=CARTESIAN_POINT('Ctrl Pts',(91.5413765295696,-4.76985860792635,132.003373512781));
#49000=CARTESIAN_POINT('Ctrl Pts',(91.5337439811993,-4.73689544680993,132.13450606225));
#49001=CARTESIAN_POINT('Ctrl Pts',(91.5261114328291,-4.69850609087948,132.264335318513));
#49002=CARTESIAN_POINT('Ctrl Pts',(91.5184788844588,-4.6548243478885,132.392376156786));
#49003=CARTESIAN_POINT('Ctrl Pts',(91.5108470172819,-4.61114650342711,132.520405567608));
#49004=CARTESIAN_POINT('Ctrl Pts',(91.503215150105,-4.56217734141902,132.646646495816));
#49005=CARTESIAN_POINT('Ctrl Pts',(91.4955832829282,-4.50810017087201,132.770630159588));
#49006=CARTESIAN_POINT('Ctrl Pts',(91.4879503300651,-4.45401530747093,132.8946314609));
#49007=CARTESIAN_POINT('Ctrl Pts',(91.480317377202,-4.39482115247596,133.016374489488));
#49008=CARTESIAN_POINT('Ctrl Pts',(91.4726844243389,-4.33074843260344,133.135412113351));
#49009=CARTESIAN_POINT('Ctrl Pts',(91.4650439343352,-4.26661244428113,133.254567280623));
#49010=CARTESIAN_POINT('Ctrl Pts',(91.4574034443316,-4.19758846088063,133.37101135136));
#49011=CARTESIAN_POINT('Ctrl Pts',(91.4497629543279,-4.12395248100192,133.484323116732));
#49012=CARTESIAN_POINT('Ctrl Pts',(91.4421187382377,-4.05028059059438,133.597690141577));
#49013=CARTESIAN_POINT('Ctrl Pts',(91.4344745221474,-3.97199245886475,133.707921490589));
#49014=CARTESIAN_POINT('Ctrl Pts',(91.4268303060572,-3.88940560700759,133.814627563649));
#49015=CARTESIAN_POINT('Ctrl Pts',(91.4191739385419,-3.80668747315459,133.921503259184));
#49016=CARTESIAN_POINT('Ctrl Pts',(91.4115175710265,-3.7196572275666,134.024842174677));
#49017=CARTESIAN_POINT('Ctrl Pts',(91.4038612035112,-3.62867109466048,134.124289705555));
#49018=CARTESIAN_POINT('Ctrl Pts',(91.3963448875772,-3.53934929562656,134.221918125225));
#49019=CARTESIAN_POINT('Ctrl Pts',(91.3888285716432,-3.44621541074271,134.315796117543));
#49020=CARTESIAN_POINT('Ctrl Pts',(91.3813122557092,-3.34963699643573,134.405626374853));
#49021=CARTESIAN_POINT('Ctrl Pts',(91.3735379215901,-3.24974326284253,134.49854030243));
#49022=CARTESIAN_POINT('Ctrl Pts',(91.365763587471,-3.14582243455883,134.587441894661));
#49023=CARTESIAN_POINT('Ctrl Pts',(91.357989253352,-3.0382303658925,134.671961851699));
#49024=CARTESIAN_POINT('Ctrl Pts',(91.3502245004049,-2.93077089483532,134.756377645444));
#49025=CARTESIAN_POINT('Ctrl Pts',(91.3424597474578,-2.81964949024835,134.836422309136));
#49026=CARTESIAN_POINT('Ctrl Pts',(91.3346949945108,-2.70525832735585,134.911763744211));
#49027=CARTESIAN_POINT('Ctrl Pts',(91.3269379536258,-2.59098077937866,134.98703034911));
#49028=CARTESIAN_POINT('Ctrl Pts',(91.3191809127408,-2.47344026030279,135.057602807858));
#49029=CARTESIAN_POINT('Ctrl Pts',(91.3114238718558,-2.35306117404527,135.12318987718));
#49030=CARTESIAN_POINT('Ctrl Pts',(91.3036726806157,-2.23277286659336,135.188727486783));
#49031=CARTESIAN_POINT('Ctrl Pts',(91.2959214893755,-2.10965059459207,135.249287003763));
#49032=CARTESIAN_POINT('Ctrl Pts',(91.2881702981354,-1.98414652906802,135.304621233762));
#49033=CARTESIAN_POINT('Ctrl Pts',(91.2804224013584,-1.85869580611949,135.359931945238));
#49034=CARTESIAN_POINT('Ctrl Pts',(91.2726745045812,-1.7308656600761,135.410021629511));
#49035=CARTESIAN_POINT('Ctrl Pts',(91.2649266078042,-1.6011313795446,135.454689785263));
#49036=CARTESIAN_POINT('Ctrl Pts',(91.2571803317201,-1.47142423662783,135.4993485974));
#49037=CARTESIAN_POINT('Ctrl Pts',(91.249434055636,-1.33981412090444,135.53858800954));
#49038=CARTESIAN_POINT('Ctrl Pts',(91.2416877795519,-1.20679437425347,135.572256421877));
#49039=CARTESIAN_POINT('Ctrl Pts',(91.2339414462865,-1.07377364568095,135.605925082748));
#49040=CARTESIAN_POINT('Ctrl Pts',(91.2261951130212,-0.93934364443041,135.634022565825));
#49041=CARTESIAN_POINT('Ctrl Pts',(91.2184487797558,-0.804010491069592,
135.656447817189));
#49042=CARTESIAN_POINT('Ctrl Pts',(91.2107007117529,-0.668647030787413,
135.678878090533));
#49043=CARTESIAN_POINT('Ctrl Pts',(91.2029526437499,-0.532380401563536,
135.695633540598));
#49044=CARTESIAN_POINT('Ctrl Pts',(91.1952045757469,-0.395724080343547,
135.706664720203));
#49045=CARTESIAN_POINT('Ctrl Pts',(91.1874482730051,-0.25892251915932,135.717707623878));
#49046=CARTESIAN_POINT('Ctrl Pts',(91.1796919702632,-0.121730828950221,
135.723014072495));
#49047=CARTESIAN_POINT('Ctrl Pts',(91.1719356675214,0.0153347001402445,
135.722586711339));
#49048=CARTESIAN_POINT('Ctrl Pts',(91.1641752250072,0.152473385230736,135.722159122088));
#49049=CARTESIAN_POINT('Ctrl Pts',(91.156414782493,0.289485384651345,135.715991642716));
#49050=CARTESIAN_POINT('Ctrl Pts',(91.1486543399788,0.425858279723248,135.704138958276));
#49051=CARTESIAN_POINT('Ctrl Pts',(91.1408814397134,0.562450092673031,135.692267246855));
#49052=CARTESIAN_POINT('Ctrl Pts',(91.133108539448,0.698400363143223,135.674692143074));
#49053=CARTESIAN_POINT('Ctrl Pts',(91.1253356391826,0.833204737624504,135.651519881269));
#49054=CARTESIAN_POINT('Ctrl Pts',(91.1178453034205,0.963108633542396,135.629189989547));
#49055=CARTESIAN_POINT('Ctrl Pts',(91.1103549676584,1.09194819823657,135.601662880641));
#49056=CARTESIAN_POINT('Ctrl Pts',(91.1028646318964,1.21928625874606,135.569077196937));
#49057=CARTESIAN_POINT('Ctrl Pts',(91.0950902977773,1.3514523805225,135.535256017131));
#49058=CARTESIAN_POINT('Ctrl Pts',(91.0873159636582,1.4824195539852,135.495877963249));
#49059=CARTESIAN_POINT('Ctrl Pts',(91.0795416295391,1.61168472876788,135.451042810008));
#49060=CARTESIAN_POINT('Ctrl Pts',(91.071776876592,1.74079059577531,135.406262912087));
#49061=CARTESIAN_POINT('Ctrl Pts',(91.0640121236449,1.8681982717929,135.356039423211));
#49062=CARTESIAN_POINT('Ctrl Pts',(91.0562473706978,1.99341637260455,135.300522784118));
#49063=CARTESIAN_POINT('Ctrl Pts',(91.0484903298129,2.11851010503312,135.245061284933));
#49064=CARTESIAN_POINT('Ctrl Pts',(91.0407332889279,2.24141823494115,135.184317255096));
#49065=CARTESIAN_POINT('Ctrl Pts',(91.0329762480429,2.36166633042866,135.118490333536));
#49066=CARTESIAN_POINT('Ctrl Pts',(91.0252250568027,2.48182374589196,135.052713052571));
#49067=CARTESIAN_POINT('Ctrl Pts',(91.0174738655626,2.59932477810744,134.981860696308));
#49068=CARTESIAN_POINT('Ctrl Pts',(91.0097226743225,2.71371704597576,134.906180074451));
#49069=CARTESIAN_POINT('Ctrl Pts',(91.0019747775454,2.8280606940788,134.830531618877));
#49070=CARTESIAN_POINT('Ctrl Pts',(90.9942268807683,2.93929788043286,134.750059194531));
#49071=CARTESIAN_POINT('Ctrl Pts',(90.9864789839913,3.04700301249826,134.665054299319));
#49072=CARTESIAN_POINT('Ctrl Pts',(90.9787327079072,3.1546856149719,134.580067185298));
#49073=CARTESIAN_POINT('Ctrl Pts',(90.9709864318231,3.25883732602677,134.490549728285));
#49074=CARTESIAN_POINT('Ctrl Pts',(90.963240155739,3.35906393711825,134.396835047378));
#49075=CARTESIAN_POINT('Ctrl Pts',(90.9554938224737,3.45929128805959,134.30311967469));
#49076=CARTESIAN_POINT('Ctrl Pts',(90.9477474892083,3.55559319564597,134.205207283306));
#49077=CARTESIAN_POINT('Ctrl Pts',(90.940001155943,3.64761106982197,134.103469064679));
#49078=CARTESIAN_POINT('Ctrl Pts',(90.93225308794,3.73964955076301,134.001708062483));
#49079=CARTESIAN_POINT('Ctrl Pts',(90.924505019937,3.82740182703436,133.896119818081));
#49080=CARTESIAN_POINT('Ctrl Pts',(90.9167569519341,3.91054875049141,133.787109606759));
#49081=CARTESIAN_POINT('Ctrl Pts',(90.9090006491922,3.99378404348823,133.677983538087));
#49082=CARTESIAN_POINT('Ctrl Pts',(90.9012443464504,4.07240396864752,133.565428548738));
#49083=CARTESIAN_POINT('Ctrl Pts',(90.8934880437085,4.14613168408876,133.449880438073));
#49084=CARTESIAN_POINT('Ctrl Pts',(90.8857276011944,4.21989875023162,133.334270655902));
#49085=CARTESIAN_POINT('Ctrl Pts',(90.8779671586802,4.28876820755461,133.215664907159));
#49086=CARTESIAN_POINT('Ctrl Pts',(90.8702067161661,4.35250908932965,133.094523862796));
#49087=CARTESIAN_POINT('Ctrl Pts',(90.8624338159006,4.4163522936268,132.973188352075));
#49088=CARTESIAN_POINT('Ctrl Pts',(90.8546609156352,4.47505030302207,132.849309766327));
#49089=CARTESIAN_POINT('Ctrl Pts',(90.8468880153697,4.52841988007978,132.723369854698));
#49090=CARTESIAN_POINT('Ctrl Pts',(90.8393976796076,4.57984933858214,132.602008176079));
#49091=CARTESIAN_POINT('Ctrl Pts',(90.8319073438455,4.62633093404965,132.478732726624));
#49092=CARTESIAN_POINT('Ctrl Pts',(90.8244170080834,4.66774500758555,132.353986251924));
#49093=CARTESIAN_POINT('Ctrl Pts',(90.8166426739643,4.71072930830667,132.224509976721));
#49094=CARTESIAN_POINT('Ctrl Pts',(90.8088683398452,4.74839039263825,132.093038784518));
#49095=CARTESIAN_POINT('Ctrl Pts',(90.8010940057261,4.78054029286684,131.960049836507));
#49096=CARTESIAN_POINT('Ctrl Pts',(90.7933292527791,4.81265057121667,131.827224785489));
#49097=CARTESIAN_POINT('Ctrl Pts',(90.785564499832,4.83926308861544,131.692886076769));
#49098=CARTESIAN_POINT('Ctrl Pts',(90.7777997468849,4.86023880994435,131.557528442696));
#49099=CARTESIAN_POINT('Ctrl Pts',(90.7700427059999,4.88119369789114,131.422305247733));
#49100=CARTESIAN_POINT('Ctrl Pts',(90.7622856651149,4.89652287164194,131.28606552522));
#49101=CARTESIAN_POINT('Ctrl Pts',(90.7545286242299,4.90613785105258,131.149316337868));
#49102=CARTESIAN_POINT('Ctrl Pts',(90.7467774329897,4.91574557973249,131.012670274142));
#49103=CARTESIAN_POINT('Ctrl Pts',(90.7390262417496,4.91964766380053,130.875515898711));
#49104=CARTESIAN_POINT('Ctrl Pts',(90.7312750505095,4.91780722821489,130.73836721928));
#49105=CARTESIAN_POINT('Ctrl Pts',(90.7235271537324,4.91596757486348,130.601276831697));
#49106=CARTESIAN_POINT('Ctrl Pts',(90.7157792569553,4.90839026150749,130.464192525409));
#49107=CARTESIAN_POINT('Ctrl Pts',(90.7080313601782,4.8950904904269,130.327629925212));
#49108=CARTESIAN_POINT('Ctrl Pts',(90.7002850840941,4.88179350137171,130.191095890967));
#49109=CARTESIAN_POINT('Ctrl Pts',(90.69253880801,4.86277647339259,130.055083734626));
#49110=CARTESIAN_POINT('Ctrl Pts',(90.6847925319259,4.83810658967367,129.920105174011));
#49111=CARTESIAN_POINT('Ctrl Pts',(90.6770461986606,4.81343652384725,129.785125617015));
#49112=CARTESIAN_POINT('Ctrl Pts',(90.6692998653952,4.78311358930753,129.651180055564));
#49113=CARTESIAN_POINT('Ctrl Pts',(90.6615535321299,4.7472562532542,129.518770819676));
#49114=CARTESIAN_POINT('Ctrl Pts',(90.6538054641269,4.71139088719918,129.386331931658));
#49115=CARTESIAN_POINT('Ctrl Pts',(90.6460573961239,4.66998875556181,129.255430431122));
#49116=CARTESIAN_POINT('Ctrl Pts',(90.638309328121,4.6232183205521,129.126553887632));
#49117=CARTESIAN_POINT('Ctrl Pts',(90.6305530253791,4.57639817736729,128.997540372618));
#49118=CARTESIAN_POINT('Ctrl Pts',(90.6227967226373,4.52419846705199,128.870556481898));
#49119=CARTESIAN_POINT('Ctrl Pts',(90.6150404198955,4.46683620015233,128.746070690586));
#49120=CARTESIAN_POINT('Ctrl Pts',(90.6072799773813,4.40944331728365,128.621518457458));
#49121=CARTESIAN_POINT('Ctrl Pts',(90.5995195348671,4.34688256568907,128.499467328225));
#49122=CARTESIAN_POINT('Ctrl Pts',(90.5917590923529,4.27941667773097,128.38036062564));
#49123=CARTESIAN_POINT('Ctrl Pts',(90.5839861920874,4.21184248754027,128.261062722402));
#49124=CARTESIAN_POINT('Ctrl Pts',(90.576213291822,4.13934763278347,128.144719023184));
#49125=CARTESIAN_POINT('Ctrl Pts',(90.5684403915566,4.06223837835029,128.031744088012));
#49126=CARTESIAN_POINT('Ctrl Pts',(90.5609500557946,3.98793223954252,127.9228760763));
#49127=CARTESIAN_POINT('Ctrl Pts',(90.5534597200326,3.90934155030137,127.817136402007));
#49128=CARTESIAN_POINT('Ctrl Pts',(90.5459693842705,3.82677412647474,127.714865052357));
#49129=CARTESIAN_POINT('Ctrl Pts',(90.5381950501515,3.74107613367761,127.608716053401));
#49130=CARTESIAN_POINT('Ctrl Pts',(90.5304207160324,3.65082243222353,127.505967325787));
#49131=CARTESIAN_POINT('Ctrl Pts',(90.5226463819133,3.55631287019784,127.407034929357));
#49132=CARTESIAN_POINT('Ctrl Pts',(90.5148816289662,3.4619197827609,127.308224458264));
#49133=CARTESIAN_POINT('Ctrl Pts',(90.5071168760191,3.36328153814516,127.213221240201));
#49134=CARTESIAN_POINT('Ctrl Pts',(90.499352123072,3.26073921681105,127.122409664274));
#49135=CARTESIAN_POINT('Ctrl Pts',(90.491595082187,3.15829874195586,127.031688283683));
#49136=CARTESIAN_POINT('Ctrl Pts',(90.483838041302,3.05196219774392,126.945150517803));
#49137=CARTESIAN_POINT('Ctrl Pts',(90.476081000417,2.94210836471689,126.863144887266));
#49138=CARTESIAN_POINT('Ctrl Pts',(90.4683298091768,2.83233737331973,126.781201097813));
#49139=CARTESIAN_POINT('Ctrl Pts',(90.4605786179367,2.71905468460876,126.703782873872));
#49140=CARTESIAN_POINT('Ctrl Pts',(90.4528274266965,2.60267281596168,126.631199073179));
#49141=CARTESIAN_POINT('Ctrl Pts',(90.4450795299194,2.48634041271368,126.558646122537));
#49142=CARTESIAN_POINT('Ctrl Pts',(90.4373316331424,2.36691178044942,126.490923714845));
#49143=CARTESIAN_POINT('Ctrl Pts',(90.4295837363653,2.24482894611593,126.428297767791));
#49144=CARTESIAN_POINT('Ctrl Pts',(90.4218374602812,2.12277164887941,126.365684920735));
#49145=CARTESIAN_POINT('Ctrl Pts',(90.4140911841971,1.99806160154545,126.30816659218));
#49146=CARTESIAN_POINT('Ctrl Pts',(90.406344908113,1.87116564096279,126.255962854993));
#49147=CARTESIAN_POINT('Ctrl Pts',(90.3985985748476,1.7442687436634,126.20375873245));
#49148=CARTESIAN_POINT('Ctrl Pts',(90.3908522415823,1.61518626248192,126.156869428302));
#49149=CARTESIAN_POINT('Ctrl Pts',(90.3831059083169,1.48440485630412,126.115466794383));
#49150=CARTESIAN_POINT('Ctrl Pts',(90.3753578403139,1.35359416253691,126.074054888632));
#49151=CARTESIAN_POINT('Ctrl Pts',(90.367609772311,1.22108415935881,126.038132216061));
#49152=CARTESIAN_POINT('Ctrl Pts',(90.359861704308,1.0873761107933,126.007820587901));
#49153=CARTESIAN_POINT('Ctrl Pts',(90.3521054015661,0.953525955722621,125.977476744183));
#49154=CARTESIAN_POINT('Ctrl Pts',(90.3443490988243,0.818475593614946,125.952755944155));
#49155=CARTESIAN_POINT('Ctrl Pts',(90.3365927960824,0.682736465352775,125.933728832943));
#49156=CARTESIAN_POINT('Ctrl Pts',(90.3288323535683,0.546924889030731,125.914691566389));
#49157=CARTESIAN_POINT('Ctrl Pts',(90.3210719110541,0.410424202971469,125.901354081903));
#49158=CARTESIAN_POINT('Ctrl Pts',(90.3133114685399,0.273749400421997,125.893734962085));
#49159=CARTESIAN_POINT('Ctrl Pts',(90.3055385682745,0.136855195346147,125.886103611379));
#49160=CARTESIAN_POINT('Ctrl Pts',(90.297765668009,-0.000213293611603577,
125.884208974567));
#49161=CARTESIAN_POINT('Ctrl Pts',(90.2899927677436,-0.136941741707901,
125.888017462143));
#49162=CARTESIAN_POINT('Ctrl Pts',(90.2825024319816,-0.26869976631716,125.891687501602));
#49163=CARTESIAN_POINT('Ctrl Pts',(90.2750120962196,-0.400141736222104,
125.900653197474));
#49164=CARTESIAN_POINT('Ctrl Pts',(90.2675217604576,-0.530815228556763,
125.914839346968));
#49165=CARTESIAN_POINT('Ctrl Pts',(90.2597474263385,-0.6664432460714,125.929563368632));
#49166=CARTESIAN_POINT('Ctrl Pts',(90.2519730922194,-0.801672990813378,
125.94995816673));
#49167=CARTESIAN_POINT('Ctrl Pts',(90.2441987581003,-0.935992344640633,
125.975996361084));
#49168=CARTESIAN_POINT('Ctrl Pts',(90.2364340051532,-1.07014616186876,126.00200246569));
#49169=CARTESIAN_POINT('Ctrl Pts',(90.2286692522061,-1.20339144044358,126.03363805452));
#49170=CARTESIAN_POINT('Ctrl Pts',(90.220904499259,-1.33522042060583,126.070823938623));
#49171=CARTESIAN_POINT('Ctrl Pts',(90.213147458374,-1.46691846636626,126.107972889182));
#49172=CARTESIAN_POINT('Ctrl Pts',(90.205390417489,-1.59720263923891,126.150661059174));
#49173=CARTESIAN_POINT('Ctrl Pts',(90.197633376604,-1.72557497880962,126.198758153718));
#49174=CARTESIAN_POINT('Ctrl Pts',(90.1898821853638,-1.85385051180152,126.246818977869));
#49175=CARTESIAN_POINT('Ctrl Pts',(90.1821309941237,-1.9802167165337,126.300280471128));
#49176=CARTESIAN_POINT('Ctrl Pts',(90.1743798028835,-2.10419076652649,126.358962516095));
#49177=CARTESIAN_POINT('Ctrl Pts',(90.1666319061064,-2.22811212424007,126.417619619626));
#49178=CARTESIAN_POINT('Ctrl Pts',(90.1588840093293,-2.34964299677482,126.481492694776));
#49179=CARTESIAN_POINT('Ctrl Pts',(90.1511361125522,-2.4683207336868,126.550353586759));
#49180=CARTESIAN_POINT('Ctrl Pts',(90.1433898364681,-2.58697364577476,126.619200074529));
#49181=CARTESIAN_POINT('Ctrl Pts',(90.135643560384,-2.70277427138817,126.693032107776));
#49182=CARTESIAN_POINT('Ctrl Pts',(90.1278972842998,-2.81528512027138,126.771575878198));
#49183=CARTESIAN_POINT('Ctrl Pts',(90.1201509510345,-2.9277967996838,126.850120228412));
#49184=CARTESIAN_POINT('Ctrl Pts',(90.1124046177692,-3.03701833333117,126.933376161409));
#49185=CARTESIAN_POINT('Ctrl Pts',(90.1046582845038,-3.14254208638309,127.0210271274));
#49186=CARTESIAN_POINT('Ctrl Pts',(90.0969102165008,-3.24808947074835,127.108697722217));
#49187=CARTESIAN_POINT('Ctrl Pts',(90.0891621484978,-3.34993712602023,127.200765058785));
#49188=CARTESIAN_POINT('Ctrl Pts',(90.0814140804948,-3.44771162351129,127.29687325143));
#49189=CARTESIAN_POINT('Ctrl Pts',(90.073657777753,-3.54559003690134,127.393083589005));
#49190=CARTESIAN_POINT('Ctrl Pts',(90.0659014750111,-3.63938636560129,127.493343087217));
#49191=CARTESIAN_POINT('Ctrl Pts',(90.0581451722692,-3.72876472757801,127.597259641783));
#49192=CARTESIAN_POINT('Ctrl Pts',(90.0503847297551,-3.81819079347783,127.701231659743));
#49193=CARTESIAN_POINT('Ctrl Pts',(90.0426242872409,-3.90319395194257,127.808864316674));
#49194=CARTESIAN_POINT('Ctrl Pts',(90.0348638447267,-3.98348020247577,127.919734378522));
#49195=CARTESIAN_POINT('Ctrl Pts',(90.0270909444613,-4.06389533562576,128.030782418835));
#49196=CARTESIAN_POINT('Ctrl Pts',(90.0193180441958,-4.13957821360021,128.145077923101));
#49197=CARTESIAN_POINT('Ctrl Pts',(90.0115451439304,-4.21027909111514,128.262170019397));
#49198=CARTESIAN_POINT('Ctrl Pts',(90.0040548081685,-4.27840981364644,128.375005523054));
#49199=CARTESIAN_POINT('Ctrl Pts',(89.9965644724066,-4.34191431516899,128.490437552582));
#49200=CARTESIAN_POINT('Ctrl Pts',(89.9890741366447,-4.40061132031051,128.608044822865));
#49201=CARTESIAN_POINT('Ctrl Pts',(89.98074935034,-4.46584738449569,128.738753969171));
#49202=CARTESIAN_POINT('Ctrl Pts',(89.9724245640352,-4.52532942677357,128.872518646867));
#49203=CARTESIAN_POINT('Ctrl Pts',(89.9640997777305,-4.57878128013611,129.008825864025));
#49204=CARTESIAN_POINT('Ctrl Pts',(89.9557953738861,-4.63210226163665,129.144799345714));
#49205=CARTESIAN_POINT('Ctrl Pts',(89.9474909700418,-4.67942238345934,129.283302669902));
#49206=CARTESIAN_POINT('Ctrl Pts',(89.9391865661974,-4.72051238125432,129.423800614913));
#49207=CARTESIAN_POINT('Ctrl Pts',(89.9360759723297,-4.73590352763438,129.476427155527));
#49208=CARTESIAN_POINT('Ctrl Pts',(89.9329653784619,-4.75042102772514,129.529333307741));
#49209=CARTESIAN_POINT('Ctrl Pts',(89.9298547845941,-4.76405452823405,129.582490119308));
#49210=CARTESIAN_POINT('Origin',(213.235140564004,0.,130.804360617566));
#49211=CARTESIAN_POINT('',(87.8349528638408,-4.76405452823403,129.582490119308));
#49212=CARTESIAN_POINT('',(88.1801477108009,-4.76405452823403,129.582490119308));
#49213=CARTESIAN_POINT('',(213.235140564004,-4.76405452823405,129.582490119308));
#49214=CARTESIAN_POINT('',(89.5148594360324,-4.91824791378463,130.808890634465));
#49215=CARTESIAN_POINT('Ctrl Pts',(89.5148594359911,-4.91824791378396,130.808890635194));
#49216=CARTESIAN_POINT('Ctrl Pts',(89.5043441766185,-4.91807698000317,130.994473734362));
#49217=CARTESIAN_POINT('Ctrl Pts',(89.4938289172459,-4.90739846811374,131.179592062533));
#49218=CARTESIAN_POINT('Ctrl Pts',(89.4833136578734,-4.88639072837316,131.363260172199));
#49219=CARTESIAN_POINT('Ctrl Pts',(89.4727984003083,-4.8653829922438,131.546928250292));
#49220=CARTESIAN_POINT('Ctrl Pts',(89.4622831427433,-4.83404617532037,131.729146731365));
#49221=CARTESIAN_POINT('Ctrl Pts',(89.4517678851783,-4.79260396698406,131.908955691857));
#49222=CARTESIAN_POINT('Ctrl Pts',(89.4439935510592,-4.76196414934318,132.041895368116));
#49223=CARTESIAN_POINT('Ctrl Pts',(89.4362192169401,-4.72574028641383,132.173769790985));
#49224=CARTESIAN_POINT('Ctrl Pts',(89.428444882821,-4.68402005236109,132.304073660644));
#49225=CARTESIAN_POINT('Ctrl Pts',(89.4206801298739,-4.64235123476817,132.43421694243));
#49226=CARTESIAN_POINT('Ctrl Pts',(89.4129153769269,-4.59519964193923,132.562793153437));
#49227=CARTESIAN_POINT('Ctrl Pts',(89.4051506239798,-4.54270387942175,132.689307440791));
#49228=CARTESIAN_POINT('Ctrl Pts',(89.3973935830948,-4.49026025643574,132.815696072372));
#49229=CARTESIAN_POINT('Ctrl Pts',(89.3896365422098,-4.43248317560102,132.940026497001));
#49230=CARTESIAN_POINT('Ctrl Pts',(89.3818795013248,-4.36956083329973,133.061819628621));
#49231=CARTESIAN_POINT('Ctrl Pts',(89.3741283100847,-4.30668594122627,133.183520915092));
#49232=CARTESIAN_POINT('Ctrl Pts',(89.3663771188446,-4.23867368947907,133.302688371102));
#49233=CARTESIAN_POINT('Ctrl Pts',(89.3586259276045,-4.1657599607861,133.418863823074));
#49234=CARTESIAN_POINT('Ctrl Pts',(89.3508780308274,-4.09287722237272,133.53498989738));
#49235=CARTESIAN_POINT('Ctrl Pts',(89.3431301340503,-4.01509735785471,133.64812616647));
#49236=CARTESIAN_POINT('Ctrl Pts',(89.3353822372732,-3.93270156814569,133.757840165219));
#49237=CARTESIAN_POINT('Ctrl Pts',(89.3276359611891,-3.85032301385957,133.867531214165));
#49238=CARTESIAN_POINT('Ctrl Pts',(89.319889685105,-3.76333068954983,133.973801104242));
#49239=CARTESIAN_POINT('Ctrl Pts',(89.3121434090209,-3.6720481584663,134.076247746488));
#49240=CARTESIAN_POINT('Ctrl Pts',(89.3043970757555,-3.58076495355592,134.178695144971));
#49241=CARTESIAN_POINT('Ctrl Pts',(89.2966507424901,-3.4851917387692,134.277318947407));
#49242=CARTESIAN_POINT('Ctrl Pts',(89.2889044092248,-3.38569099349451,134.371751759433));
#49243=CARTESIAN_POINT('Ctrl Pts',(89.2811563412218,-3.2861679657178,134.466205719032));
#49244=CARTESIAN_POINT('Ctrl Pts',(89.2734082732188,-3.1827159407914,134.556466551543));
#49245=CARTESIAN_POINT('Ctrl Pts',(89.2656602052159,-3.07573241861856,134.642205475238));
#49246=CARTESIAN_POINT('Ctrl Pts',(89.257903902474,-2.96863519308523,134.728035523281));
#49247=CARTESIAN_POINT('Ctrl Pts',(89.2501475997321,-2.85799927821717,134.809333817241));
#49248=CARTESIAN_POINT('Ctrl Pts',(89.2423912969903,-2.74425370443405,134.885813136976));
#49249=CARTESIAN_POINT('Ctrl Pts',(89.2346308544761,-2.63044742121331,134.962333276027));
#49250=CARTESIAN_POINT('Ctrl Pts',(89.2268704119619,-2.51352850507649,135.034029111586));
#49251=CARTESIAN_POINT('Ctrl Pts',(89.2191099694478,-2.39395195175127,135.100658688604));
#49252=CARTESIAN_POINT('Ctrl Pts',(89.2113370691823,-2.27418344352713,135.167395225334));
#49253=CARTESIAN_POINT('Ctrl Pts',(89.2035641689169,-2.15174912212869,135.22904907564));
#49254=CARTESIAN_POINT('Ctrl Pts',(89.1957912686514,-2.02712620077586,135.285425494203));
#49255=CARTESIAN_POINT('Ctrl Pts',(89.1883009328894,-1.90703363652032,135.339752487947));
#49256=CARTESIAN_POINT('Ctrl Pts',(89.1808105971274,-1.78490911747776,135.389178968742));
#49257=CARTESIAN_POINT('Ctrl Pts',(89.1733202613653,-1.66119239025523,135.433574687477));
#49258=CARTESIAN_POINT('Ctrl Pts',(89.1655459272463,-1.53278490571734,135.479653683381));
#49259=CARTESIAN_POINT('Ctrl Pts',(89.1577715931272,-1.40225533615003,135.520458868357));
#49260=CARTESIAN_POINT('Ctrl Pts',(89.1499972590081,-1.27007619462908,135.55579087827));
#49261=CARTESIAN_POINT('Ctrl Pts',(89.142232506061,-1.13805995208687,135.591079344639));
#49262=CARTESIAN_POINT('Ctrl Pts',(89.1344677531139,-1.00439855663392,135.620907956887));
#49263=CARTESIAN_POINT('Ctrl Pts',(89.1267030001668,-0.869583261690838,
135.645125847722));
#49264=CARTESIAN_POINT('Ctrl Pts',(89.1189459592818,-0.734901867199259,
135.669319685007));
#49265=CARTESIAN_POINT('Ctrl Pts',(89.1111889183968,-0.599069236262726,
135.68791382202));
#49266=CARTESIAN_POINT('Ctrl Pts',(89.1034318775118,-0.462590162292759,
135.700807635992));
#49267=CARTESIAN_POINT('Ctrl Pts',(89.0956806862717,-0.326214008254124,
135.713691726638));
#49268=CARTESIAN_POINT('Ctrl Pts',(89.0879294950315,-0.189192769153895,
135.720884013836));
#49269=CARTESIAN_POINT('Ctrl Pts',(89.0801783037914,-0.0520394197748442,
135.722335298396));
#49270=CARTESIAN_POINT('Ctrl Pts',(89.0724304070143,0.0850556357720356,
135.723785966122));
#49271=CARTESIAN_POINT('Ctrl Pts',(89.0646825102372,0.222282299794044,135.719500480213));
#49272=CARTESIAN_POINT('Ctrl Pts',(89.0569346134602,0.359124731170519,135.709481664998));
#49273=CARTESIAN_POINT('Ctrl Pts',(89.0491883373761,0.495938538060332,135.699464945503));
#49274=CARTESIAN_POINT('Ctrl Pts',(89.041442061292,0.632367882496771,135.683717310684));
#49275=CARTESIAN_POINT('Ctrl Pts',(89.0336957852079,0.767899581808212,135.66229364456));
#49276=CARTESIAN_POINT('Ctrl Pts',(89.0259494519425,0.90343228158387,135.640869820291));
#49277=CARTESIAN_POINT('Ctrl Pts',(89.0182031186771,1.03806693684196,135.613769942154));
#49278=CARTESIAN_POINT('Ctrl Pts',(89.0104567854118,1.17129851933729,135.581100388696));
#49279=CARTESIAN_POINT('Ctrl Pts',(89.0027087174088,1.30455993812167,135.548423519119));
#49280=CARTESIAN_POINT('Ctrl Pts',(88.9949606494058,1.43641727926142,135.51017458535));
#49281=CARTESIAN_POINT('Ctrl Pts',(88.9872125814028,1.56637907097063,135.466510300762));
#49282=CARTESIAN_POINT('Ctrl Pts',(88.979456278661,1.69647898761862,135.422799609253));
#49283=CARTESIAN_POINT('Ctrl Pts',(88.9716999759192,1.82467895923258,135.373662194409));
#49284=CARTESIAN_POINT('Ctrl Pts',(88.9639436731774,1.95050543795275,135.319303762171));
#49285=CARTESIAN_POINT('Ctrl Pts',(88.9561832306632,2.07639907405327,135.264916317202));
#49286=CARTESIAN_POINT('Ctrl Pts',(88.948422788149,2.19991634111552,135.205302472128));
#49287=CARTESIAN_POINT('Ctrl Pts',(88.9406623456348,2.32060773920036,135.140714245127));
#49288=CARTESIAN_POINT('Ctrl Pts',(88.9328894453694,2.44149288183189,135.076022335371));
#49289=CARTESIAN_POINT('Ctrl Pts',(88.925116545104,2.55954275356234,135.006340285328));
#49290=CARTESIAN_POINT('Ctrl Pts',(88.9173436448386,2.67433556423744,134.931964323393));
#49291=CARTESIAN_POINT('Ctrl Pts',(88.9098533090765,2.78495536709909,134.860292115016));
#49292=CARTESIAN_POINT('Ctrl Pts',(88.9023629733145,2.89255055082243,134.784261518578));
#49293=CARTESIAN_POINT('Ctrl Pts',(88.8948726375524,2.99677383935875,134.704172102527));
#49294=CARTESIAN_POINT('Ctrl Pts',(88.8870983034333,3.10494878555767,134.621046071925));
#49295=CARTESIAN_POINT('Ctrl Pts',(88.8793239693143,3.20983376405457,134.53328404746));
#49296=CARTESIAN_POINT('Ctrl Pts',(88.8715496351952,3.31100563929601,134.441175806581));
#49297=CARTESIAN_POINT('Ctrl Pts',(88.8637848822481,3.41205282924321,134.349181080877));
#49298=CARTESIAN_POINT('Ctrl Pts',(88.856020129301,3.50939573462108,134.252851056919));
#49299=CARTESIAN_POINT('Ctrl Pts',(88.8482553763539,3.60264189203036,134.152517492667));
#49300=CARTESIAN_POINT('Ctrl Pts',(88.8404983354689,3.6957954360415,134.052283581126));
#49301=CARTESIAN_POINT('Ctrl Pts',(88.8327412945839,3.78486006504195,133.948054326982));
#49302=CARTESIAN_POINT('Ctrl Pts',(88.8249842536989,3.86947826907545,133.840200038163));
#49303=CARTESIAN_POINT('Ctrl Pts',(88.8172330624588,3.95403266186306,133.732427083103));
#49304=CARTESIAN_POINT('Ctrl Pts',(88.8094818712187,4.03414706344264,133.621034840917));
#49305=CARTESIAN_POINT('Ctrl Pts',(88.8017306799786,4.1095028057418,133.506428298454));
#49306=CARTESIAN_POINT('Ctrl Pts',(88.7939827832015,4.18482651984035,133.391870466829));
#49307=CARTESIAN_POINT('Ctrl Pts',(88.7862348864244,4.25539538302532,133.274101378114));
#49308=CARTESIAN_POINT('Ctrl Pts',(88.7784869896473,4.32093294675865,133.153556550671));
#49309=CARTESIAN_POINT('Ctrl Pts',(88.7707407135633,4.38645680144647,133.033036938607));
#49310=CARTESIAN_POINT('Ctrl Pts',(88.7629944374792,4.44695126341655,132.909743085976));
#49311=CARTESIAN_POINT('Ctrl Pts',(88.755248161395,4.50218512038031,132.784136414046));
#49312=CARTESIAN_POINT('Ctrl Pts',(88.7475018281297,4.55741938506786,132.658528814916));
#49313=CARTESIAN_POINT('Ctrl Pts',(88.7397554948643,4.60739280988365,132.530608720311));
#49314=CARTESIAN_POINT('Ctrl Pts',(88.732009161599,4.65192191401102,132.400858525001));
#49315=CARTESIAN_POINT('Ctrl Pts',(88.724261093596,4.69646099012249,132.271079273035));
#49316=CARTESIAN_POINT('Ctrl Pts',(88.716513025593,4.73555319255742,132.139469474556));
#49317=CARTESIAN_POINT('Ctrl Pts',(88.7087649575901,4.76906471620876,132.006527326102));
#49318=CARTESIAN_POINT('Ctrl Pts',(88.7010086548482,4.80261185630625,131.873443885151));
#49319=CARTESIAN_POINT('Ctrl Pts',(88.6932523521064,4.83056637366972,131.739025645249));
#49320=CARTESIAN_POINT('Ctrl Pts',(88.6854960493645,4.85284537034838,131.603782204708));
#49321=CARTESIAN_POINT('Ctrl Pts',(88.6777356068504,4.87513625799839,131.46846658067));
#49322=CARTESIAN_POINT('Ctrl Pts',(88.6699751643362,4.89174554170988,131.332325266288));
#49323=CARTESIAN_POINT('Ctrl Pts',(88.662214721822,4.902642285817,131.195872660572));
#49324=CARTESIAN_POINT('Ctrl Pts',(88.6544418215566,4.91355652234512,131.05920100902));
#49325=CARTESIAN_POINT('Ctrl Pts',(88.6466689212912,4.91873987934418,130.92221745846));
#49326=CARTESIAN_POINT('Ctrl Pts',(88.6388960210257,4.91821359427175,130.785436991578));
#49327=CARTESIAN_POINT('Ctrl Pts',(88.6314056852637,4.91770644098734,130.653628839197));
#49328=CARTESIAN_POINT('Ctrl Pts',(88.6239153495017,4.91189757186654,130.522009569351));
#49329=CARTESIAN_POINT('Ctrl Pts',(88.6164250137396,4.90085131114236,130.39103327928));
#49330=CARTESIAN_POINT('Ctrl Pts',(88.6086506796205,4.88938622808539,130.255090983363));
#49331=CARTESIAN_POINT('Ctrl Pts',(88.6008763455014,4.87224244418924,130.119410762527));
#49332=CARTESIAN_POINT('Ctrl Pts',(88.5931020113824,4.84943504232513,129.984505244485));
#49333=CARTESIAN_POINT('Ctrl Pts',(88.5853372584353,4.82665574854547,129.849765985439));
#49334=CARTESIAN_POINT('Ctrl Pts',(88.5775725054882,4.79822678927128,129.715799911309));
#49335=CARTESIAN_POINT('Ctrl Pts',(88.5698077525411,4.76421514581565,129.583116535951));
#49336=CARTESIAN_POINT('Ctrl Pts',(88.5620507116561,4.73023728320381,129.450564943591));
#49337=CARTESIAN_POINT('Ctrl Pts',(88.5542936707711,4.69068786726586,129.319293890966));
#49338=CARTESIAN_POINT('Ctrl Pts',(88.5465366298861,4.64568520568527,129.189804321806));
#49339=CARTESIAN_POINT('Ctrl Pts',(88.538785438646,4.60071648096183,129.060412401738));
#49340=CARTESIAN_POINT('Ctrl Pts',(88.5310342474059,4.55030282377528,128.932799658923));
#49341=CARTESIAN_POINT('Ctrl Pts',(88.5232830561657,4.49461271315434,128.80745310312));
#49342=CARTESIAN_POINT('Ctrl Pts',(88.5155351593886,4.43894627231599,128.682159822946));
#49343=CARTESIAN_POINT('Ctrl Pts',(88.5077872626115,4.37800799687756,128.559131170614));
#49344=CARTESIAN_POINT('Ctrl Pts',(88.5000393658345,4.31201487358479,128.438835138421));
#49345=CARTESIAN_POINT('Ctrl Pts',(88.4922930897503,4.24603555463073,128.318564269565));
#49346=CARTESIAN_POINT('Ctrl Pts',(88.4845468136662,4.17500367890266,128.20102522645));
#49347=CARTESIAN_POINT('Ctrl Pts',(88.4768005375821,4.09918247729292,128.08666194399));
#49348=CARTESIAN_POINT('Ctrl Pts',(88.4690542043168,4.02336071598834,127.972297817327));
#49349=CARTESIAN_POINT('Ctrl Pts',(88.4613078710514,3.94274977429366,127.861109823953));
#49350=CARTESIAN_POINT('Ctrl Pts',(88.4535615377861,3.8576563287277,127.753513077631));
#49351=CARTESIAN_POINT('Ctrl Pts',(88.4458134697831,3.77254382707466,127.645892235764));
#49352=CARTESIAN_POINT('Ctrl Pts',(88.4380654017801,3.68294706652733,127.541864547881));
#49353=CARTESIAN_POINT('Ctrl Pts',(88.4303173337771,3.58921286901418,127.441811875406));
#49354=CARTESIAN_POINT('Ctrl Pts',(88.4225610310352,3.4953790496804,127.34165286576));
#49355=CARTESIAN_POINT('Ctrl Pts',(88.4148047282934,3.39739927699039,127.245477596574));
#49356=CARTESIAN_POINT('Ctrl Pts',(88.4070484255516,3.29565748206928,127.153631262577));
#49357=CARTESIAN_POINT('Ctrl Pts',(88.3992879830374,3.19386138448877,127.061735907426));
#49358=CARTESIAN_POINT('Ctrl Pts',(88.3915275405232,3.0882995645272,126.97417434078));
#49359=CARTESIAN_POINT('Ctrl Pts',(88.383767098009,2.97938807915765,126.891250634921));
#49360=CARTESIAN_POINT('Ctrl Pts',(88.3759941977436,2.87030175940308,126.808193812568));
#49361=CARTESIAN_POINT('Ctrl Pts',(88.3682212974782,2.75785534980964,126.729789952438));
#49362=CARTESIAN_POINT('Ctrl Pts',(88.3604483972127,2.64249359926074,126.656299547576));
#49363=CARTESIAN_POINT('Ctrl Pts',(88.3529580614507,2.53132553892318,126.585480704042));
#49364=CARTESIAN_POINT('Ctrl Pts',(88.3454677256887,2.41745068390158,126.519224439819));
#49365=CARTESIAN_POINT('Ctrl Pts',(88.3379773899267,2.30128584788295,126.457722087755));
#49366=CARTESIAN_POINT('Ctrl Pts',(88.3302030558076,2.18071658679904,126.393887855321));
#49367=CARTESIAN_POINT('Ctrl Pts',(88.3224287216885,2.05729834039006,126.334972932714));
#49368=CARTESIAN_POINT('Ctrl Pts',(88.3146543875694,1.93147054953006,126.28124171809));
#49369=CARTESIAN_POINT('Ctrl Pts',(88.3068896346223,1.80579783017681,126.227576722386));
#49370=CARTESIAN_POINT('Ctrl Pts',(88.2991248816753,1.6777218309918,126.179082875603));
#49371=CARTESIAN_POINT('Ctrl Pts',(88.2913601287282,1.54770742544596,126.135979229149));
#49372=CARTESIAN_POINT('Ctrl Pts',(88.2836030878432,1.4178221520406,126.092918393844));
#49373=CARTESIAN_POINT('Ctrl Pts',(88.2758460469582,1.28600267231488,126.055237227153));
#49374=CARTESIAN_POINT('Ctrl Pts',(88.2680890060732,1.15273439261057,126.023106965793));
#49375=CARTESIAN_POINT('Ctrl Pts',(88.260337814833,1.01956661155247,125.991000934113));
#49376=CARTESIAN_POINT('Ctrl Pts',(88.2525866235929,0.884952583710046,125.964437567087));
#49377=CARTESIAN_POINT('Ctrl Pts',(88.2448354323528,0.749393111216389,125.943538359207));
#49378=CARTESIAN_POINT('Ctrl Pts',(88.2370875355757,0.6138912551148,125.922648034047));
#49379=CARTESIAN_POINT('Ctrl Pts',(88.2293396387986,0.477445139180659,125.907417139308));
#49380=CARTESIAN_POINT('Ctrl Pts',(88.2215917420216,0.340565785224577,125.897916079162));
#49381=CARTESIAN_POINT('Ctrl Pts',(88.2138454659375,0.203715063478565,125.888417006433));
#49382=CARTESIAN_POINT('Ctrl Pts',(88.2060991898533,0.0664316737464815,
125.884645411356));
#49383=CARTESIAN_POINT('Ctrl Pts',(88.1983529137692,-0.0707686062289486,
125.886619787991));
#49384=CARTESIAN_POINT('Ctrl Pts',(88.1906065805039,-0.207969898985678,
125.888594179199));
#49385=CARTESIAN_POINT('Ctrl Pts',(88.1828602472385,-0.345087689836836,
125.896314621131));
#49386=CARTESIAN_POINT('Ctrl Pts',(88.1751139139732,-0.481606965666912,
125.909747477274));
#49387=CARTESIAN_POINT('Ctrl Pts',(88.1673658459702,-0.618156814042252,
125.923183341611));
#49388=CARTESIAN_POINT('Ctrl Pts',(88.1596177779672,-0.754107491674002,
125.942334127454));
#49389=CARTESIAN_POINT('Ctrl Pts',(88.1518697099643,-0.888950262007253,
125.967114449117));
#49390=CARTESIAN_POINT('Ctrl Pts',(88.1441134072224,-1.02393634484146,125.991921107601));
#49391=CARTESIAN_POINT('Ctrl Pts',(88.1363571044805,-1.15781178306082,126.022369183089));
#49392=CARTESIAN_POINT('Ctrl Pts',(88.1286008017387,-1.2900786304122,126.058322249637));
#49393=CARTESIAN_POINT('Ctrl Pts',(88.1208403592245,-1.42241607256257,126.094294505419));
#49394=CARTESIAN_POINT('Ctrl Pts',(88.1130799167104,-1.55314284063411,126.135777488636));
#49395=CARTESIAN_POINT('Ctrl Pts',(88.1053194741962,-1.68177822104757,126.182585517271));
#49396=CARTESIAN_POINT('Ctrl Pts',(88.0975465739308,-1.81062009839329,126.229468686308));
#49397=CARTESIAN_POINT('Ctrl Pts',(88.0897736736653,-1.93736351747529,126.281693833825));
#49398=CARTESIAN_POINT('Ctrl Pts',(88.0820007733999,-2.06154892048095,126.339027582846));
#49399=CARTESIAN_POINT('Ctrl Pts',(88.0745104376379,-2.1812198712832,126.394277105674));
#49400=CARTESIAN_POINT('Ctrl Pts',(88.0670201018759,-2.29851528353681,126.454270117095));
#49401=CARTESIAN_POINT('Ctrl Pts',(88.0595297661138,-2.41304888551663,126.518759360029));
#49402=CARTESIAN_POINT('Ctrl Pts',(88.051754348916,-2.53194162502168,126.585703057148));
#49403=CARTESIAN_POINT('Ctrl Pts',(88.0439789317182,-2.6482348313707,126.657704103374));
#49404=CARTESIAN_POINT('Ctrl Pts',(88.0362035145204,-2.7614683395498,126.734535600177));
#49405=CARTESIAN_POINT('Ctrl Pts',(88.0284379153951,-2.87455886700438,126.811270081324));
#49406=CARTESIAN_POINT('Ctrl Pts',(88.0206723162697,-2.98459706372859,126.892822658075));
#49407=CARTESIAN_POINT('Ctrl Pts',(88.0129067171443,-3.09114722263641,126.978920523866));
#49408=CARTESIAN_POINT('Ctrl Pts',(88.0051504969231,-3.19756869556548,127.06491440494));
#49409=CARTESIAN_POINT('Ctrl Pts',(87.9973942767018,-3.300510218846,127.15544239732));
#49410=CARTESIAN_POINT('Ctrl Pts',(87.9896380564805,-3.39956548708786,127.250188764447));
#49411=CARTESIAN_POINT('Ctrl Pts',(87.9818871539942,-3.49855284213875,127.344870172605));
#49412=CARTESIAN_POINT('Ctrl Pts',(87.974136251508,-3.59365896174388,127.443763932585));
#49413=CARTESIAN_POINT('Ctrl Pts',(87.9663853490217,-3.68451097936713,127.546514411033));
#49414=CARTESIAN_POINT('Ctrl Pts',(87.958638082001,-3.77532038396717,127.64921669563));
#49415=CARTESIAN_POINT('Ctrl Pts',(87.9508908149804,-3.86187939899171,127.755771806658));
#49416=CARTESIAN_POINT('Ctrl Pts',(87.9431435479597,-3.94385265596307,127.865787955447));
#49417=CARTESIAN_POINT('Ctrl Pts',(87.9353982369455,-4.02580521657647,127.975776327695));
#49418=CARTESIAN_POINT('Ctrl Pts',(87.9276529259312,-4.10317409112435,128.089223684663));
#49419=CARTESIAN_POINT('Ctrl Pts',(87.9199076149169,-4.17566503793127,128.205706243953));
#49420=CARTESIAN_POINT('Ctrl Pts',(87.9121602487679,-4.24817521942896,128.322219710633));
#49421=CARTESIAN_POINT('Ctrl Pts',(87.9044128826188,-4.31580467586253,128.441769659617));
#49422=CARTESIAN_POINT('Ctrl Pts',(87.8966655164698,-4.37830322785507,128.563904434675));
#49423=CARTESIAN_POINT('Ctrl Pts',(87.8889171584985,-4.44080978094808,128.686054845497));
#49424=CARTESIAN_POINT('Ctrl Pts',(87.8811688005273,-4.49818395030201,128.810790389823));
#49425=CARTESIAN_POINT('Ctrl Pts',(87.873420442556,-4.55022256848223,128.937636845881));
#49426=CARTESIAN_POINT('Ctrl Pts',(87.8656659507611,-4.6023023819335,129.064583717251));
#49427=CARTESIAN_POINT('Ctrl Pts',(87.8579114589662,-4.64903806660193,129.193644473272));
#49428=CARTESIAN_POINT('Ctrl Pts',(87.8501569671712,-4.69027535515693,129.3243267817));
#49429=CARTESIAN_POINT('Ctrl Pts',(87.8450889327278,-4.71722644418757,129.409735659262));
#49430=CARTESIAN_POINT('Ctrl Pts',(87.8400208982843,-4.7418299522699,129.495836834929));
#49431=CARTESIAN_POINT('Ctrl Pts',(87.8349528638408,-4.76405452823403,129.582490119308));
#49432=CARTESIAN_POINT('Ctrl Pts',(89.5849003473043,-4.76405452823408,129.582490119308));
#49433=CARTESIAN_POINT('Ctrl Pts',(89.5772536419592,-4.7977227201108,129.71376188845));
#49434=CARTESIAN_POINT('Ctrl Pts',(89.569606936614,-4.8259539416985,129.846398820212));
#49435=CARTESIAN_POINT('Ctrl Pts',(89.5619602312689,-4.84865503925609,129.979904813537));
#49436=CARTESIAN_POINT('Ctrl Pts',(89.5541100987295,-4.8719600597287,130.116962499835));
#49437=CARTESIAN_POINT('Ctrl Pts',(89.54625996619,-4.88943651653312,130.254935691279));
#49438=CARTESIAN_POINT('Ctrl Pts',(89.5384098336506,-4.90104037889306,130.39328122504));
#49439=CARTESIAN_POINT('Ctrl Pts',(89.5305597011112,-4.912644241253,130.531626758801));
#49440=CARTESIAN_POINT('Ctrl Pts',(89.5227095685718,-4.91837552381983,130.670344177938));
#49441=CARTESIAN_POINT('Ctrl Pts',(89.5148594360324,-4.91824791378463,130.808890634465));
#49442=CARTESIAN_POINT('',(89.8601405640521,-4.91824989813527,130.803359621866));
#49443=CARTESIAN_POINT('Ctrl Pts',(89.9298547845941,-4.76405452823405,129.582490119308));
#49444=CARTESIAN_POINT('Ctrl Pts',(89.9215764202743,-4.80033798051544,129.723958749075));
#49445=CARTESIAN_POINT('Ctrl Pts',(89.9132980559544,-4.8303567890655,129.867204046601));
#49446=CARTESIAN_POINT('Ctrl Pts',(89.9050196916345,-4.85394887088816,130.011666842326));
#49447=CARTESIAN_POINT('Ctrl Pts',(89.8967633333281,-4.87747823891274,130.155745618927));
#49448=CARTESIAN_POINT('Ctrl Pts',(89.8885069750216,-4.8946148997633,130.301035139103));
#49449=CARTESIAN_POINT('Ctrl Pts',(89.8802506167151,-4.90524731660639,130.446964723038));
#49450=CARTESIAN_POINT('Ctrl Pts',(89.8735472658275,-4.91387979332768,130.565445192234));
#49451=CARTESIAN_POINT('Ctrl Pts',(89.8668439149397,-4.91822567592008,130.684347215093));
#49452=CARTESIAN_POINT('Ctrl Pts',(89.8601405640521,-4.91824989813527,130.803359621866));
#49453=CARTESIAN_POINT('Ctrl Pts',(89.8601405640085,-4.91824989813543,130.80335962264));
#49454=CARTESIAN_POINT('Ctrl Pts',(89.8521395031509,-4.9182788095368,130.945411788095));
#49455=CARTESIAN_POINT('Ctrl Pts',(89.8441384422934,-4.9121491106778,131.087386340008));
#49456=CARTESIAN_POINT('Ctrl Pts',(89.8361373814359,-4.89990706363619,131.228735251855));
#49457=CARTESIAN_POINT('Ctrl Pts',(89.8281295892336,-4.88765471728043,131.370203081466));
#49458=CARTESIAN_POINT('Ctrl Pts',(89.8201217970312,-4.86927979946688,131.511043870025));
#49459=CARTESIAN_POINT('Ctrl Pts',(89.8121140048289,-4.84488017921743,131.650716991398));
#49460=CARTESIAN_POINT('Ctrl Pts',(89.8040983150251,-4.82045649509702,131.79052786393));
#49461=CARTESIAN_POINT('Ctrl Pts',(89.7960826252213,-4.78999632098478,131.929168425915));
#49462=CARTESIAN_POINT('Ctrl Pts',(89.7880669354174,-4.75364812777663,132.066110410427));
#49463=CARTESIAN_POINT('Ctrl Pts',(89.7800364422495,-4.71723280677881,132.203305299195));
#49464=CARTESIAN_POINT('Ctrl Pts',(89.7720059490815,-4.67490783011908,132.338795001309));
#49465=CARTESIAN_POINT('Ctrl Pts',(89.7639754559136,-4.62687122199029,132.472067353661));
#49466=CARTESIAN_POINT('Ctrl Pts',(89.7559363960225,-4.57878336964621,132.605481877524));
#49467=CARTESIAN_POINT('Ctrl Pts',(89.7478973361315,-4.52497186587371,132.736674008009));
#49468=CARTESIAN_POINT('Ctrl Pts',(89.7398582762404,-4.46568186199103,132.865153807089));
#49469=CARTESIAN_POINT('Ctrl Pts',(89.7318046094637,-4.4062841288068,132.993867052587));
#49470=CARTESIAN_POINT('Ctrl Pts',(89.7237509426869,-4.34138816872011,133.119857807639));
#49471=CARTESIAN_POINT('Ctrl Pts',(89.7156972759102,-4.27128431534761,133.242661944303));
#49472=CARTESIAN_POINT('Ctrl Pts',(89.7140070215508,-4.25657134707327,133.268435325932));
#49473=CARTESIAN_POINT('Ctrl Pts',(89.7123167671913,-4.24162913377656,133.294068454993));
#49474=CARTESIAN_POINT('Ctrl Pts',(89.7106265128319,-4.22646059051327,133.3195572181));
#49475=CARTESIAN_POINT('Ctrl Pts',(89.7028521787128,-4.15669279327702,133.436792922634));
#49476=CARTESIAN_POINT('Ctrl Pts',(89.6950778445937,-4.08193287710072,133.55130923844));
#49477=CARTESIAN_POINT('Ctrl Pts',(89.6873035104746,-4.00241861517591,133.662651766381));
#49478=CARTESIAN_POINT('Ctrl Pts',(89.6795387575275,-3.92300234747264,133.773857074607));
#49479=CARTESIAN_POINT('Ctrl Pts',(89.6717740045805,-3.83884361732605,133.881896062399));
#49480=CARTESIAN_POINT('Ctrl Pts',(89.6640092516334,-3.75022550725323,133.986339829825));
#49481=CARTESIAN_POINT('Ctrl Pts',(89.6562522107484,-3.66169541393663,134.090679862229));
#49482=CARTESIAN_POINT('Ctrl Pts',(89.6484951698634,-3.56871500614797,134.19143148418));
#49483=CARTESIAN_POINT('Ctrl Pts',(89.6407381289784,-3.47160977485632,134.28819595145));
#49484=CARTESIAN_POINT('Ctrl Pts',(89.6329869377383,-3.37457777137482,134.384887447884));
#49485=CARTESIAN_POINT('Ctrl Pts',(89.6252357464982,-3.2734274115934,134.477597499527));
#49486=CARTESIAN_POINT('Ctrl Pts',(89.617484555258,-3.16852321023861,134.565961836286));
#49487=CARTESIAN_POINT('Ctrl Pts',(89.609736658481,-3.0636635959678,134.654288615845));
#49488=CARTESIAN_POINT('Ctrl Pts',(89.6019887617039,-2.95505361181128,134.738273102803));
#49489=CARTESIAN_POINT('Ctrl Pts',(89.5942408649268,-2.84309307680544,134.817589345052));
#49490=CARTESIAN_POINT('Ctrl Pts',(89.5864945888427,-2.73115596153001,134.896888996053));
#49491=CARTESIAN_POINT('Ctrl Pts',(89.5787483127586,-2.61587000828068,134.971522118788));
#49492=CARTESIAN_POINT('Ctrl Pts',(89.5710020366745,-2.49766610049364,135.041204621414));
#49493=CARTESIAN_POINT('Ctrl Pts',(89.5632557034092,-2.37946132015228,135.110887638421));
#49494=CARTESIAN_POINT('Ctrl Pts',(89.5555093701438,-2.25833887909073,135.175619763851));
#49495=CARTESIAN_POINT('Ctrl Pts',(89.5477630368785,-2.13475612494927,135.235161826094));
#49496=CARTESIAN_POINT('Ctrl Pts',(89.5400149688755,-2.01114569530671,135.294717222368));
#49497=CARTESIAN_POINT('Ctrl Pts',(89.5322669008725,-1.88507420836676,135.349080072989));
#49498=CARTESIAN_POINT('Ctrl Pts',(89.5245188328696,-1.75702057007165,135.398058668031));
#49499=CARTESIAN_POINT('Ctrl Pts',(89.5167625301277,-1.6288308348459,135.447089318106));
#49500=CARTESIAN_POINT('Ctrl Pts',(89.5090062273859,-1.49865510574455,135.490724141497));
#49501=CARTESIAN_POINT('Ctrl Pts',(89.501249924644,-1.36698962325895,135.528820632467));
#49502=CARTESIAN_POINT('Ctrl Pts',(89.4934894821298,-1.23525386694098,135.566937456682));
#49503=CARTESIAN_POINT('Ctrl Pts',(89.4857290396157,-1.10202715247588,135.599509965641));
#49504=CARTESIAN_POINT('Ctrl Pts',(89.4779685971015,-0.967816624651894,
135.626446685187));
#49505=CARTESIAN_POINT('Ctrl Pts',(89.4701956968361,-0.833390650173906,
135.653426645947));
#49506=CARTESIAN_POINT('Ctrl Pts',(89.4624227965706,-0.69797809281063,135.674752677509));
#49507=CARTESIAN_POINT('Ctrl Pts',(89.4546498963052,-0.5620928390424,135.690385044725));
#49508=CARTESIAN_POINT('Ctrl Pts',(89.4471595605432,-0.431147356522391,
135.705449136018));
#49509=CARTESIAN_POINT('Ctrl Pts',(89.4396692247811,-0.299763255507869,
135.715226311269));
#49510=CARTESIAN_POINT('Ctrl Pts',(89.4321788890191,-0.168399052114349,
135.71972681163));
#49511=CARTESIAN_POINT('Ctrl Pts',(89.4244045549,-0.0320541350223629,135.724397949831));
#49512=CARTESIAN_POINT('Ctrl Pts',(89.4166302207808,0.104701245541517,135.72339918095));
#49513=CARTESIAN_POINT('Ctrl Pts',(89.4088558866618,0.241356268496753,135.716684936476));
#49514=CARTESIAN_POINT('Ctrl Pts',(89.4010911337147,0.377842876349129,135.709978966709));
#49515=CARTESIAN_POINT('Ctrl Pts',(89.3933263807676,0.514228985937299,135.697571555438));
#49516=CARTESIAN_POINT('Ctrl Pts',(89.3855616278205,0.650000738586185,135.679469037113));
#49517=CARTESIAN_POINT('Ctrl Pts',(89.3778045869355,0.785637640816571,135.661384498464));
#49518=CARTESIAN_POINT('Ctrl Pts',(89.3700475460505,0.920661015381237,135.63761616071));
#49519=CARTESIAN_POINT('Ctrl Pts',(89.3622905051655,1.05455945164876,135.608222337624));
#49520=CARTESIAN_POINT('Ctrl Pts',(89.3545393139254,1.18835691406383,135.578850680649));
#49521=CARTESIAN_POINT('Ctrl Pts',(89.3467881226853,1.32103074639363,135.54386206572));
#49522=CARTESIAN_POINT('Ctrl Pts',(89.3390369314451,1.452077448777,135.503366272516));
#49523=CARTESIAN_POINT('Ctrl Pts',(89.331289034668,1.58306845281589,135.462887691105));
#49524=CARTESIAN_POINT('Ctrl Pts',(89.323541137891,1.71243332964075,135.416906702075));
#49525=CARTESIAN_POINT('Ctrl Pts',(89.3157932411139,1.83968173455635,135.36558349943));
#49526=CARTESIAN_POINT('Ctrl Pts',(89.3080469650298,1.96690352184888,135.314271032493));
#49527=CARTESIAN_POINT('Ctrl Pts',(89.3003006889457,2.09200935547267,135.257618720809));
#49528=CARTESIAN_POINT('Ctrl Pts',(89.2925544128616,2.21452731789317,135.195835520239));
#49529=CARTESIAN_POINT('Ctrl Pts',(89.2848080795962,2.33704618471353,135.134051863599));
#49530=CARTESIAN_POINT('Ctrl Pts',(89.2770617463309,2.45697679312138,135.067137418533));
#49531=CARTESIAN_POINT('Ctrl Pts',(89.2693154130656,2.57387071369496,134.995347686466));
#49532=CARTESIAN_POINT('Ctrl Pts',(89.2615673450626,2.69079081185164,134.923541877586));
#49533=CARTESIAN_POINT('Ctrl Pts',(89.2538192770596,2.80467253587353,134.84685881374));
#49534=CARTESIAN_POINT('Ctrl Pts',(89.2460712090566,2.91509573441053,134.765597788163));
#49535=CARTESIAN_POINT('Ctrl Pts',(89.2383149063148,3.02563629203691,134.684250397402));
#49536=CARTESIAN_POINT('Ctrl Pts',(89.2305586035729,3.13271066605606,134.598315557623));
#49537=CARTESIAN_POINT('Ctrl Pts',(89.222802300831,3.23593073225011,134.508133742175));
#49538=CARTESIAN_POINT('Ctrl Pts',(89.2150418583169,3.33920589010144,134.417903793978));
#49539=CARTESIAN_POINT('Ctrl Pts',(89.2072814158027,3.43862235780159,134.323422622641));
#49540=CARTESIAN_POINT('Ctrl Pts',(89.1995209732885,3.5338290514067,134.225067459424));
#49541=CARTESIAN_POINT('Ctrl Pts',(89.1917480730231,3.62918857924831,134.126554407767));
#49542=CARTESIAN_POINT('Ctrl Pts',(89.1839751727576,3.720324568476,134.024155229151));
#49543=CARTESIAN_POINT('Ctrl Pts',(89.1762022724922,3.80692582059041,133.918280793008));
#49544=CARTESIAN_POINT('Ctrl Pts',(89.1687119367301,3.89037889905559,133.816255159299));
#49545=CARTESIAN_POINT('Ctrl Pts',(89.1612216009681,3.96962102933123,133.711002796168));
#49546=CARTESIAN_POINT('Ctrl Pts',(89.153731265206,4.04441298842942,133.602915001801));
#49547=CARTESIAN_POINT('Ctrl Pts',(89.1459569310869,4.1220407073889,133.49072902586));
#49548=CARTESIAN_POINT('Ctrl Pts',(89.1381825969679,4.19512003847368,133.375132992101));
#49549=CARTESIAN_POINT('Ctrl Pts',(89.1304082628488,4.26333653233225,133.256532037875));
#49550=CARTESIAN_POINT('Ctrl Pts',(89.1226435099017,4.33146895545883,133.138077248725));
#49551=CARTESIAN_POINT('Ctrl Pts',(89.1148787569546,4.39475027260884,133.016625243214));
#49552=CARTESIAN_POINT('Ctrl Pts',(89.1071140040075,4.45290805996824,132.892611769121));
#49553=CARTESIAN_POINT('Ctrl Pts',(89.0993569631225,4.51100808419343,132.768721466959));
#49554=CARTESIAN_POINT('Ctrl Pts',(89.0915999222374,4.5639945405674,132.642275110746));
#49555=CARTESIAN_POINT('Ctrl Pts',(89.0838428813524,4.61164006018283,132.513734484752));
#49556=CARTESIAN_POINT('Ctrl Pts',(89.0760916901123,4.65924964994126,132.385290792243));
#49557=CARTESIAN_POINT('Ctrl Pts',(89.0683404988721,4.70152618438521,132.254756338572));
#49558=CARTESIAN_POINT('Ctrl Pts',(89.060589307632,4.73828987029396,132.12261407103));
#49559=CARTESIAN_POINT('Ctrl Pts',(89.0528414108549,4.7750379306555,131.990527967476));
#49560=CARTESIAN_POINT('Ctrl Pts',(89.0450935140778,4.8062776981722,131.856835785081));
#49561=CARTESIAN_POINT('Ctrl Pts',(89.0373456173007,4.83187890531025,131.722036653495));
#49562=CARTESIAN_POINT('Ctrl Pts',(89.0295993412166,4.85747475722766,131.587265718981));
#49563=CARTESIAN_POINT('Ctrl Pts',(89.0218530651325,4.87743432188516,131.451388679697));
#49564=CARTESIAN_POINT('Ctrl Pts',(89.0141067890484,4.89167831680965,131.314915518977));
#49565=CARTESIAN_POINT('Ctrl Pts',(89.006360455783,4.90592241688007,131.178441350842));
#49566=CARTESIAN_POINT('Ctrl Pts',(88.9986141225177,4.91445082244292,131.041371441343));
#49567=CARTESIAN_POINT('Ctrl Pts',(88.9908677892523,4.91723610702654,130.904221171613));
#49568=CARTESIAN_POINT('Ctrl Pts',(88.9831197212494,4.92002201535532,130.767040188031));
#49569=CARTESIAN_POINT('Ctrl Pts',(88.9753716532464,4.91706223551421,130.629779199217));
#49570=CARTESIAN_POINT('Ctrl Pts',(88.9676235852434,4.90838146931043,130.492953465705));
#49571=CARTESIAN_POINT('Ctrl Pts',(88.9598672825016,4.89969147708502,130.355982312176));
#49572=CARTESIAN_POINT('Ctrl Pts',(88.9521109797597,4.88526837717211,130.219447728834));
#49573=CARTESIAN_POINT('Ctrl Pts',(88.9443546770178,4.8651888288226,130.083860289738));
#49574=CARTESIAN_POINT('Ctrl Pts',(88.9365942345037,4.84509856341354,129.948200483544));
#49575=CARTESIAN_POINT('Ctrl Pts',(88.9288337919895,4.81934590729644,129.813489212709));
#49576=CARTESIAN_POINT('Ctrl Pts',(88.9210733494753,4.78805846636481,129.680225756808));
#49577=CARTESIAN_POINT('Ctrl Pts',(88.9133004492099,4.75672080005546,129.546748374577));
#49578=CARTESIAN_POINT('Ctrl Pts',(88.9055275489444,4.71983069928783,129.414723828453));
#49579=CARTESIAN_POINT('Ctrl Pts',(88.897754648679,4.67756562976158,129.284636023512));
#49580=CARTESIAN_POINT('Ctrl Pts',(88.8902643129171,4.63683700197232,129.159277237953));
#49581=CARTESIAN_POINT('Ctrl Pts',(88.8827739771551,4.59111751497956,129.035717116296));
#49582=CARTESIAN_POINT('Ctrl Pts',(88.8752836413932,4.54060707316218,128.914368429844));
#49583=CARTESIAN_POINT('Ctrl Pts',(88.8675093072741,4.48818151259042,128.788418771061));
#49584=CARTESIAN_POINT('Ctrl Pts',(88.859734973155,4.43042845905312,128.664452580269));
#49585=CARTESIAN_POINT('Ctrl Pts',(88.8519606390359,4.36751879852014,128.542953399245));
#49586=CARTESIAN_POINT('Ctrl Pts',(88.8441958860888,4.30468666852132,128.421603955104));
#49587=CARTESIAN_POINT('Ctrl Pts',(88.8364311331417,4.23671075423634,128.302715815156));
#49588=CARTESIAN_POINT('Ctrl Pts',(88.8286663801946,4.16381041088863,128.186753709592));
#49589=CARTESIAN_POINT('Ctrl Pts',(88.8209093393096,4.0909824731898,128.070906779225));
#49590=CARTESIAN_POINT('Ctrl Pts',(88.8131522984246,4.01324004649786,127.957980428667));
#49591=CARTESIAN_POINT('Ctrl Pts',(88.8053952575396,3.93084874454786,127.848415555494));
#49592=CARTESIAN_POINT('Ctrl Pts',(88.7976440662995,3.84851957451912,127.738933306044));
#49593=CARTESIAN_POINT('Ctrl Pts',(88.7898928750593,3.76154874124641,127.632807799592));
#49594=CARTESIAN_POINT('Ctrl Pts',(88.7821416838191,3.67024537933595,127.530451346074));
#49595=CARTESIAN_POINT('Ctrl Pts',(88.7743937870421,3.57898082379033,127.428138396779));
#49596=CARTESIAN_POINT('Ctrl Pts',(88.766645890265,3.48338766179843,127.329591605414));
#49597=CARTESIAN_POINT('Ctrl Pts',(88.7588979934879,3.38381541248751,127.23519036151));
#49598=CARTESIAN_POINT('Ctrl Pts',(88.7511517174038,3.28426399154462,127.140808864312));
#49599=CARTESIAN_POINT('Ctrl Pts',(88.7434054413197,3.18073542239457,127.050571458568));
#49600=CARTESIAN_POINT('Ctrl Pts',(88.7356591652356,3.07361591434535,126.964820505315));
#49601=CARTESIAN_POINT('Ctrl Pts',(88.7279128319703,2.96649561556424,126.879068919069));
#49602=CARTESIAN_POINT('Ctrl Pts',(88.7201664987049,2.85578463020576,126.797804095729));
#49603=CARTESIAN_POINT('Ctrl Pts',(88.7124201654396,2.74190173833597,126.721327686054));
#49604=CARTESIAN_POINT('Ctrl Pts',(88.7046720974366,2.62799334318199,126.644834150018));
#49605=CARTESIAN_POINT('Ctrl Pts',(88.6969240294336,2.51091195255865,126.573131379383));
#49606=CARTESIAN_POINT('Ctrl Pts',(88.6891759614306,2.3911044216764,126.506477102725));
#49607=CARTESIAN_POINT('Ctrl Pts',(88.6814196586888,2.27116955792493,126.439751985109));
#49608=CARTESIAN_POINT('Ctrl Pts',(88.6736633559469,2.14850310829263,126.37808627021));
#49609=CARTESIAN_POINT('Ctrl Pts',(88.6659070532051,2.02357606939264,126.321691440181));
#49610=CARTESIAN_POINT('Ctrl Pts',(88.6581466106909,1.89858235317024,126.265266510532));
#49611=CARTESIAN_POINT('Ctrl Pts',(88.6503861681768,1.77132600612046,126.214118217084));
#49612=CARTESIAN_POINT('Ctrl Pts',(88.6426257256626,1.64229606039197,126.168409074191));
#49613=CARTESIAN_POINT('Ctrl Pts',(88.6348528253972,1.51305898433995,126.122626554924));
#49614=CARTESIAN_POINT('Ctrl Pts',(88.6270799251317,1.38204299400097,126.082300749423));
#49615=CARTESIAN_POINT('Ctrl Pts',(88.6193070248663,1.24975113696537,126.047543913282));
#49616=CARTESIAN_POINT('Ctrl Pts',(88.6118166891043,1.1222684221569,126.014050575683));
#49617=CARTESIAN_POINT('Ctrl Pts',(88.6043263533424,0.993601292921839,125.985728411053));
#49618=CARTESIAN_POINT('Ctrl Pts',(88.5968360175804,0.86420507864751,125.962632347151));
#49619=CARTESIAN_POINT('Ctrl Pts',(88.5890616834613,0.729902767578985,125.938660588965));
#49620=CARTESIAN_POINT('Ctrl Pts',(88.5812873493422,0.594389564226906,125.920243114391));
#49621=CARTESIAN_POINT('Ctrl Pts',(88.5735130152231,0.45816465402444,125.907497518366));
#49622=CARTESIAN_POINT('Ctrl Pts',(88.565748262276,0.322107628848937,125.894767630149));
#49623=CARTESIAN_POINT('Ctrl Pts',(88.5579835093289,0.185341027548832,125.887695748369));
#49624=CARTESIAN_POINT('Ctrl Pts',(88.5502187563818,0.0483744076508083,
125.886348521283));
#49625=CARTESIAN_POINT('Ctrl Pts',(88.5424617154968,-0.0884561750692558,
125.885002632282));
#49626=CARTESIAN_POINT('Ctrl Pts',(88.5347046746118,-0.225485992625819,
125.889370086782));
#49627=CARTESIAN_POINT('Ctrl Pts',(88.5269476337268,-0.362200534688017,
125.899465732334));
#49628=CARTESIAN_POINT('Ctrl Pts',(88.5191964424866,-0.498811979251213,
125.909553764682));
#49629=CARTESIAN_POINT('Ctrl Pts',(88.5114452512465,-0.635108233224452,
125.92536136136));
#49630=CARTESIAN_POINT('Ctrl Pts',(88.5036940600063,-0.770575313775685,
125.946851302258));
#49631=CARTESIAN_POINT('Ctrl Pts',(88.4959461632292,-0.905984817203335,
125.968332109359));
#49632=CARTESIAN_POINT('Ctrl Pts',(88.4881982664521,-1.04056546281879,125.99549039601));
#49633=CARTESIAN_POINT('Ctrl Pts',(88.480450369675,-1.17380913583667,126.028237171179));
#49634=CARTESIAN_POINT('Ctrl Pts',(88.4727040935909,-1.30702493715075,126.060977096429));
#49635=CARTESIAN_POINT('Ctrl Pts',(88.4649578175068,-1.43890394271133,126.099303091761));
#49636=CARTESIAN_POINT('Ctrl Pts',(88.4572115414227,-1.56894935891606,126.143075282848));
#49637=CARTESIAN_POINT('Ctrl Pts',(88.4494652081574,-1.69899573508643,126.186847797052));
#49638=CARTESIAN_POINT('Ctrl Pts',(88.441718874892,-1.82720812435417,126.236066462513));
#49639=CARTESIAN_POINT('Ctrl Pts',(88.4339725416267,-1.95310637853767,126.290541997305));
#49640=CARTESIAN_POINT('Ctrl Pts',(88.4262244736237,-2.07903282676219,126.345029731515));
#49641=CARTESIAN_POINT('Ctrl Pts',(88.4184764056207,-2.20264374992861,126.404776522398));
#49642=CARTESIAN_POINT('Ctrl Pts',(88.4107283376177,-2.32348077753159,126.4695457266));
#49643=CARTESIAN_POINT('Ctrl Pts',(88.4029720348758,-2.44444623216557,126.534383768283));
#49644=CARTESIAN_POINT('Ctrl Pts',(88.395215732134,-2.56263155689463,126.604254701281));
#49645=CARTESIAN_POINT('Ctrl Pts',(88.3874594293921,-2.67760424062142,126.678876574074));
#49646=CARTESIAN_POINT('Ctrl Pts',(88.3796989868779,-2.79263828873143,126.753538274807));
#49647=CARTESIAN_POINT('Ctrl Pts',(88.3719385443638,-2.90445596059346,126.832955741693));
#49648=CARTESIAN_POINT('Ctrl Pts',(88.3641781018496,-3.01265619445776,126.91680538111));
#49649=CARTESIAN_POINT('Ctrl Pts',(88.3564052015841,-3.12103012094296,127.000789623413));
#49650=CARTESIAN_POINT('Ctrl Pts',(88.3486323013187,-3.22577470621888,127.089220003765));
#49651=CARTESIAN_POINT('Ctrl Pts',(88.3408594010533,-3.32652359696477,127.181733970872));
#49652=CARTESIAN_POINT('Ctrl Pts',(88.3333690652913,-3.4236100117603,127.270884822246));
#49653=CARTESIAN_POINT('Ctrl Pts',(88.3258787295293,-3.51698597720932,127.363827300324));
#49654=CARTESIAN_POINT('Ctrl Pts',(88.3183883937673,-3.60635916437889,127.460208013393));
#49655=CARTESIAN_POINT('Ctrl Pts',(88.3107028301196,-3.69806177160779,127.559100790464));
#49656=CARTESIAN_POINT('Ctrl Pts',(88.3030172664718,-3.78585555100518,127.661943210462));
#49657=CARTESIAN_POINT('Ctrl Pts',(88.2953317028241,-3.86937505516217,127.76838964521));
#49658=CARTESIAN_POINT('Ctrl Pts',(88.2876552722435,-3.95279530970278,127.874709585339));
#49659=CARTESIAN_POINT('Ctrl Pts',(88.279978841663,-4.03195114367966,127.984624712708));
#49660=CARTESIAN_POINT('Ctrl Pts',(88.2723024110824,-4.10651389843591,128.097752654736));
#49661=CARTESIAN_POINT('Ctrl Pts',(88.2646228527257,-4.18110703392854,128.21092669096));
#49662=CARTESIAN_POINT('Ctrl Pts',(88.2569432943689,-4.25110307235286,128.327315865827));
#49663=CARTESIAN_POINT('Ctrl Pts',(88.2492637360121,-4.31621279932073,128.446503511319));
#49664=CARTESIAN_POINT('Ctrl Pts',(88.2416008776309,-4.38118093860825,128.565431971232));
#49665=CARTESIAN_POINT('Ctrl Pts',(88.2339380192497,-4.44128377905166,128.687146405816));
#49666=CARTESIAN_POINT('Ctrl Pts',(88.2262751608685,-4.49627730081323,128.811203951197));
#49667=CARTESIAN_POINT('Ctrl Pts',(88.2185872525239,-4.55145059696731,128.935667041979));
#49668=CARTESIAN_POINT('Ctrl Pts',(88.2108993441793,-4.60148089862532,129.062488243117));
#49669=CARTESIAN_POINT('Ctrl Pts',(88.2032114358347,-4.64616873835184,129.191196299444));
#49670=CARTESIAN_POINT('Ctrl Pts',(88.1955235274901,-4.69085657807836,129.319904355771));
#49671=CARTESIAN_POINT('Ctrl Pts',(88.1878356191455,-4.73020181031948,129.450498885946));
#49672=CARTESIAN_POINT('Ctrl Pts',(88.1801477108009,-4.76405452823403,129.582490119308));
#49673=CARTESIAN_POINT('Origin',(213.235140564004,0.,130.804360617566));
#49674=CARTESIAN_POINT('',(86.0846345799593,-4.7702492504123,129.580946905181));
#49675=CARTESIAN_POINT('',(86.430234796612,-4.76405452823404,129.582490119308));
#49676=CARTESIAN_POINT('',(213.235140564004,-4.76405452823405,129.582490119308));
#49677=CARTESIAN_POINT('',(87.7648579073645,-4.92391445715771,130.802649439709));
#49678=CARTESIAN_POINT('Ctrl Pts',(87.764857441322,-4.9256415109711,130.802657025058));
#49679=CARTESIAN_POINT('Ctrl Pts',(87.6774498003774,-4.91862979770035,132.339650290333));
#49680=CARTESIAN_POINT('Ctrl Pts',(87.4972262848284,-3.31659732523356,135.521305288248));
#49681=CARTESIAN_POINT('Ctrl Pts',(87.2241868946751,2.10597827242213,136.227139918491));
#49682=CARTESIAN_POINT('Ctrl Pts',(86.9457392708622,5.70067050458257,131.963686123471));
#49683=CARTESIAN_POINT('Ctrl Pts',(86.6672916470494,4.0567250362683,126.634868824723));
#49684=CARTESIAN_POINT('Ctrl Pts',(86.3888440232364,-1.31515255834102,125.1376107926));
#49685=CARTESIAN_POINT('Ctrl Pts',(86.1946250008731,-4.21909290079494,127.725505074334));
#49686=CARTESIAN_POINT('Ctrl Pts',(86.0932218531139,-4.7337430531318,129.434338303608));
#49687=CARTESIAN_POINT('Ctrl Pts',(86.0846345799591,-4.77024925041304,129.580946905184));
#49688=CARTESIAN_POINT('Ctrl Pts',(87.8349528638408,-4.76405452823403,129.582490119308));
#49689=CARTESIAN_POINT('Ctrl Pts',(87.8271889033113,-4.79810140232196,129.715238364644));
#49690=CARTESIAN_POINT('Ctrl Pts',(87.8194249427818,-4.82656275471006,129.849282444912));
#49691=CARTESIAN_POINT('Ctrl Pts',(87.8116609822523,-4.84936864420704,129.984112597098));
#49692=CARTESIAN_POINT('Ctrl Pts',(87.8038859863517,-4.87220694904848,130.119134391264));
#49693=CARTESIAN_POINT('Ctrl Pts',(87.796110990451,-4.88937369504103,130.254944101439));
#49694=CARTESIAN_POINT('Ctrl Pts',(87.7883359945504,-4.90085087283581,130.391028082282));
#49695=CARTESIAN_POINT('Ctrl Pts',(87.7859180438006,-4.90442016740642,130.433348923054));
#49696=CARTESIAN_POINT('Ctrl Pts',(87.7835000930507,-4.90743957424586,130.475696300847));
#49697=CARTESIAN_POINT('Ctrl Pts',(87.7810821423009,-4.90990957711857,130.518054824716));
#49698=CARTESIAN_POINT('Ctrl Pts',(87.7756745735309,-4.91543355662776,130.612786543645));
#49699=CARTESIAN_POINT('Ctrl Pts',(87.770267004761,-4.91821617968026,130.707679669371));
#49700=CARTESIAN_POINT('Ctrl Pts',(87.764859435991,-4.91824969360065,130.802624559646));
#49701=CARTESIAN_POINT('',(88.1101405639545,-4.91824790478202,130.8089003981));
#49702=CARTESIAN_POINT('Ctrl Pts',(88.1801477108009,-4.76405452823403,129.582490119308));
#49703=CARTESIAN_POINT('Ctrl Pts',(88.1724878463956,-4.79778375826004,129.713999875267));
#49704=CARTESIAN_POINT('Ctrl Pts',(88.1648279819903,-4.82606040748949,129.846895763953));
#49705=CARTESIAN_POINT('Ctrl Pts',(88.1571681175851,-4.84878692862279,129.980680835541));
#49706=CARTESIAN_POINT('Ctrl Pts',(88.149330191989,-4.87204175041555,130.117575874605));
#49707=CARTESIAN_POINT('Ctrl Pts',(88.1414922663929,-4.88948514735401,130.255401512422));
#49708=CARTESIAN_POINT('Ctrl Pts',(88.1336543407968,-4.9010686352311,130.393618246664));
#49709=CARTESIAN_POINT('Ctrl Pts',(88.1258164152007,-4.91265212310819,130.531834980907));
#49710=CARTESIAN_POINT('Ctrl Pts',(88.1179784896046,-4.9183757082134,130.670442363389));
#49711=CARTESIAN_POINT('Ctrl Pts',(88.1101405640085,-4.9182479047829,130.808900397146));
#49712=CARTESIAN_POINT('Ctrl Pts',(88.1101405639545,-4.91824790478202,130.8089003981));
#49713=CARTESIAN_POINT('Ctrl Pts',(88.1002146810802,-4.91808605556142,130.984242484372));
#49714=CARTESIAN_POINT('Ctrl Pts',(88.0902887982059,-4.90854396835757,131.159164971997));
#49715=CARTESIAN_POINT('Ctrl Pts',(88.0803629153316,-4.88977686091136,131.332816209831));
#49716=CARTESIAN_POINT('Ctrl Pts',(88.0702186323547,-4.87059681909521,131.510288311625));
#49717=CARTESIAN_POINT('Ctrl Pts',(88.0600743493779,-4.8417813266888,131.68643285966));
#49718=CARTESIAN_POINT('Ctrl Pts',(88.049930066401,-4.80354409539745,131.860365913988));
#49719=CARTESIAN_POINT('Ctrl Pts',(88.0466003009189,-4.79099308383976,131.917457803265));
#49720=CARTESIAN_POINT('Ctrl Pts',(88.0432705354368,-4.77742733571033,131.974311603233));
#49721=CARTESIAN_POINT('Ctrl Pts',(88.0399407699546,-4.76285551578117,132.030896551933));
#49722=CARTESIAN_POINT('Ctrl Pts',(88.0321664358355,-4.72883324080123,132.163011050585));
#49723=CARTESIAN_POINT('Ctrl Pts',(88.0243921017164,-4.68925592277407,132.293918145695));
#49724=CARTESIAN_POINT('Ctrl Pts',(88.0166177675973,-4.64422410186059,132.42311493932));
#49725=CARTESIAN_POINT('Ctrl Pts',(88.0088530146503,-4.5992477786418,132.552152509443));
#49726=CARTESIAN_POINT('Ctrl Pts',(88.0010882617032,-4.54883045512982,132.679483606324));
#49727=CARTESIAN_POINT('Ctrl Pts',(87.9933235087561,-4.49312331969054,132.804617075262));
#49728=CARTESIAN_POINT('Ctrl Pts',(87.9855664678711,-4.43747151336355,132.929626259873));
#49729=CARTESIAN_POINT('Ctrl Pts',(87.9778094269861,-4.37654050861573,133.052441805383));
#49730=CARTESIAN_POINT('Ctrl Pts',(87.9700523861011,-4.31053066615113,133.172589584256));
#49731=CARTESIAN_POINT('Ctrl Pts',(87.9623011948609,-4.24457060222231,133.292646758755));
#49732=CARTESIAN_POINT('Ctrl Pts',(87.9545500036208,-4.1735395114369,133.410039829681));
#49733=CARTESIAN_POINT('Ctrl Pts',(87.9467988123807,-4.09768489165824,133.524316792061));
#49734=CARTESIAN_POINT('Ctrl Pts',(87.9390509156036,-4.02186251211626,133.638545183685));
#49735=CARTESIAN_POINT('Ctrl Pts',(87.9313030188266,-3.94122089689439,133.749659775897));
#49736=CARTESIAN_POINT('Ctrl Pts',(87.9235551220495,-3.85605219123975,133.857235420262));
#49737=CARTESIAN_POINT('Ctrl Pts',(87.9158088459654,-3.7709013010423,133.964788562121));
#49738=CARTESIAN_POINT('Ctrl Pts',(87.9080625698812,-3.68122544651445,134.068803922239));
#49739=CARTESIAN_POINT('Ctrl Pts',(87.9003162937971,-3.58735834628673,134.168887799478));
#49740=CARTESIAN_POINT('Ctrl Pts',(87.8925699605318,-3.49349055315347,134.268972415514));
#49741=CARTESIAN_POINT('Ctrl Pts',(87.8848236272664,-3.39543172003968,134.365125205593));
#49742=CARTESIAN_POINT('Ctrl Pts',(87.877077294001,-3.29355358368351,134.456988144964));
#49743=CARTESIAN_POINT('Ctrl Pts',(87.869329225998,-3.191652632425,134.548871656404));
#49744=CARTESIAN_POINT('Ctrl Pts',(87.8615811579951,-3.08593096626504,134.636463143726));
#49745=CARTESIAN_POINT('Ctrl Pts',(87.8538330899921,-2.9767943457115,134.719444075915));
#49746=CARTESIAN_POINT('Ctrl Pts',(87.8460767872502,-2.8675417334589,134.802513201227));
#49747=CARTESIAN_POINT('Ctrl Pts',(87.8383204845084,-2.75486722830405,134.880961745812));
#49748=CARTESIAN_POINT('Ctrl Pts',(87.8305641817665,-2.63920705040945,134.954513531323));
#49749=CARTESIAN_POINT('Ctrl Pts',(87.8228037392523,-2.52348514119538,135.028104573637));
#49750=CARTESIAN_POINT('Ctrl Pts',(87.8150432967381,-2.40477472220454,135.096793453451));
#49751=CARTESIAN_POINT('Ctrl Pts',(87.8072828542239,-2.28353681534967,135.160349905368));
#49752=CARTESIAN_POINT('Ctrl Pts',(87.7995099539585,-2.16210428664381,135.224008383743));
#49753=CARTESIAN_POINT('Ctrl Pts',(87.7917370536931,-2.03813651596725,135.282517803047));
#49754=CARTESIAN_POINT('Ctrl Pts',(87.7839641534276,-1.91211553076332,135.335695659197));
#49755=CARTESIAN_POINT('Ctrl Pts',(87.7764738176656,-1.79067572579969,135.386940366329));
#49756=CARTESIAN_POINT('Ctrl Pts',(87.7689834819036,-1.66732968202179,135.433234303722));
#49757=CARTESIAN_POINT('Ctrl Pts',(87.7614931461416,-1.54252032660781,135.474458486401));
#49758=CARTESIAN_POINT('Ctrl Pts',(87.7537188120225,-1.41297878654797,135.517245696497));
#49759=CARTESIAN_POINT('Ctrl Pts',(87.7459444779035,-1.28145043282677,135.554706660444));
#49760=CARTESIAN_POINT('Ctrl Pts',(87.7381701437844,-1.14841271213979,135.586654136903));
#49761=CARTESIAN_POINT('Ctrl Pts',(87.7304053908373,-1.01553894855373,135.618562240953));
#49762=CARTESIAN_POINT('Ctrl Pts',(87.7226406378902,-0.881159895673808,
135.644970286889));
#49763=CARTESIAN_POINT('Ctrl Pts',(87.7148758849431,-0.745770496865722,
135.665739992651));
#49764=CARTESIAN_POINT('Ctrl Pts',(87.7071188440581,-0.610515568717097,
135.686489069649));
#49765=CARTESIAN_POINT('Ctrl Pts',(87.6993618031731,-0.474252675574064,
135.701610891983));
#49766=CARTESIAN_POINT('Ctrl Pts',(87.6916047622881,-0.337489014213713,
135.711017751276));
#49767=CARTESIAN_POINT('Ctrl Pts',(87.683853571048,-0.200828487394539,135.720417516782));
#49768=CARTESIAN_POINT('Ctrl Pts',(87.6761023798079,-0.063668332479496,
135.72411087072));
#49769=CARTESIAN_POINT('Ctrl Pts',(87.6683511885678,0.0734773873054794,
135.722061720323));
#49770=CARTESIAN_POINT('Ctrl Pts',(87.6606032917907,0.210564816501158,135.720013440869));
#49771=CARTESIAN_POINT('Ctrl Pts',(87.6528553950136,0.3476374326663,135.712227517309));
#49772=CARTESIAN_POINT('Ctrl Pts',(87.6451074982366,0.484179634738213,135.698719936599));
#49773=CARTESIAN_POINT('Ctrl Pts',(87.6373612221525,0.620693275125056,135.685215181384));
#49774=CARTESIAN_POINT('Ctrl Pts',(87.6296149460684,0.7566763332871,135.665991188077));
#49775=CARTESIAN_POINT('Ctrl Pts',(87.6218686699843,0.891617194235736,135.641115918534));
#49776=CARTESIAN_POINT('Ctrl Pts',(87.6141223367189,1.02655905128706,135.616240465367));
#49777=CARTESIAN_POINT('Ctrl Pts',(87.6063760034536,1.16045831128667,135.585713723598));
#49778=CARTESIAN_POINT('Ctrl Pts',(87.5986296701883,1.29281282508547,135.54965492475));
#49779=CARTESIAN_POINT('Ctrl Pts',(87.5908816021854,1.42519697875995,135.513588050784));
#49780=CARTESIAN_POINT('Ctrl Pts',(87.5831335341824,1.55603532071835,135.471986757289));
#49781=CARTESIAN_POINT('Ctrl Pts',(87.5753854661794,1.68484053833069,135.425020248279));
#49782=CARTESIAN_POINT('Ctrl Pts',(87.5676291634375,1.8137826516612,135.378003822703));
#49783=CARTESIAN_POINT('Ctrl Pts',(87.5598728606957,1.94068695626284,135.325610924969));
#49784=CARTESIAN_POINT('Ctrl Pts',(87.5521165579539,2.06508530781696,135.268059278311));
#49785=CARTESIAN_POINT('Ctrl Pts',(87.5443561154397,2.18955005451696,135.210476914606));
#49786=CARTESIAN_POINT('Ctrl Pts',(87.5365956729255,2.31150583560229,135.147730494415));
#49787=CARTESIAN_POINT('Ctrl Pts',(87.5288352304114,2.43050972866737,135.080083424455));
#49788=CARTESIAN_POINT('Ctrl Pts',(87.5210623301459,2.54970465734618,135.012327761414));
#49789=CARTESIAN_POINT('Ctrl Pts',(87.5132894298805,2.66593789701143,134.9396559353));
#49790=CARTESIAN_POINT('Ctrl Pts',(87.5055165296151,2.77879535420176,134.862374841539));
#49791=CARTESIAN_POINT('Ctrl Pts',(87.498026193853,2.88755015855358,134.787903110194));
#49792=CARTESIAN_POINT('Ctrl Pts',(87.4905358580909,2.99317010875273,134.709151594175));
#49793=CARTESIAN_POINT('Ctrl Pts',(87.4830455223288,3.09531568641119,134.626428626374));
#49794=CARTESIAN_POINT('Ctrl Pts',(87.4752711882097,3.20133414469208,134.540569192108));
#49795=CARTESIAN_POINT('Ctrl Pts',(87.4674968540906,3.30394540255489,134.450159229093));
#49796=CARTESIAN_POINT('Ctrl Pts',(87.4597225199715,3.40273385695808,134.355499218242));
#49797=CARTESIAN_POINT('Ctrl Pts',(87.4519577670245,3.50140056342012,134.260955867394));
#49798=CARTESIAN_POINT('Ctrl Pts',(87.4441930140774,3.59625356085309,134.162173158274));
#49799=CARTESIAN_POINT('Ctrl Pts',(87.4364282611303,3.68690897966526,134.059492755923));
#49800=CARTESIAN_POINT('Ctrl Pts',(87.4286712202453,3.77747435823745,133.956914337194));
#49801=CARTESIAN_POINT('Ctrl Pts',(87.4209141793603,3.86385019778957,133.85044622037));
#49802=CARTESIAN_POINT('Ctrl Pts',(87.4131571384753,3.94568855453173,133.740467715943));
#49803=CARTESIAN_POINT('Ctrl Pts',(87.4054059472351,4.02746519633245,133.630572147161));
#49804=CARTESIAN_POINT('Ctrl Pts',(87.397654755995,4.10471093365639,133.517171772271));
#49805=CARTESIAN_POINT('Ctrl Pts',(87.3899035647549,4.17711753690626,133.400679578204));
#49806=CARTESIAN_POINT('Ctrl Pts',(87.3821556679778,4.24949336541828,133.284236896427));
#49807=CARTESIAN_POINT('Ctrl Pts',(87.3744077712007,4.31703394464075,133.164705340483));
#49808=CARTESIAN_POINT('Ctrl Pts',(87.3666598744236,4.37947402988349,133.042527341489));
#49809=CARTESIAN_POINT('Ctrl Pts',(87.3589135983395,4.44190105400645,132.920374899498));
#49810=CARTESIAN_POINT('Ctrl Pts',(87.3511673222554,4.49922952849361,132.795577463472));
#49811=CARTESIAN_POINT('Ctrl Pts',(87.3434210461713,4.55124009117904,132.668602204632));
#49812=CARTESIAN_POINT('Ctrl Pts',(87.3356747129059,4.6032510377946,132.541626008489));
#49813=CARTESIAN_POINT('Ctrl Pts',(87.3279283796406,4.64994384608303,132.412472319243));
#49814=CARTESIAN_POINT('Ctrl Pts',(87.3201820463753,4.69114740502095,132.281628056747));
#49815=CARTESIAN_POINT('Ctrl Pts',(87.3124339783723,4.73236019121023,132.150754492586));
#49816=CARTESIAN_POINT('Ctrl Pts',(87.3046859103693,4.76808116451588,132.018189974659));
#49817=CARTESIAN_POINT('Ctrl Pts',(87.2969378423663,4.79818927668619,131.884435951787));
#49818=CARTESIAN_POINT('Ctrl Pts',(87.2891815396245,4.82832938811641,131.750539773548));
#49819=CARTESIAN_POINT('Ctrl Pts',(87.2814252368826,4.85284463585599,131.615451946977));
#49820=CARTESIAN_POINT('Ctrl Pts',(87.2736689341407,4.87166515318884,131.479684019874));
#49821=CARTESIAN_POINT('Ctrl Pts',(87.2659084916266,4.89049571559848,131.343843629341));
#49822=CARTESIAN_POINT('Ctrl Pts',(87.2581480491124,4.90362545383212,131.207322803966));
#49823=CARTESIAN_POINT('Ctrl Pts',(87.2503876065982,4.91103656904408,131.070636564681));
#49824=CARTESIAN_POINT('Ctrl Pts',(87.2426147063328,4.9184595812361,130.933730904509));
#49825=CARTESIAN_POINT('Ctrl Pts',(87.2348418060673,4.9201456209472,130.79665969096));
#49826=CARTESIAN_POINT('Ctrl Pts',(87.2270689058019,4.91612906035938,130.659937197062));
#49827=CARTESIAN_POINT('Ctrl Pts',(87.2195785700399,4.91225851186607,130.528184910202));
#49828=CARTESIAN_POINT('Ctrl Pts',(87.2120882342779,4.90309279407344,130.396756736768));
#49829=CARTESIAN_POINT('Ctrl Pts',(87.204597898516,4.88870779819585,130.266104984656));
#49830=CARTESIAN_POINT('Ctrl Pts',(87.1968235643969,4.87377739082723,130.130499531651));
#49831=CARTESIAN_POINT('Ctrl Pts',(87.1890492302778,4.85317681969433,129.995300980914));
#49832=CARTESIAN_POINT('Ctrl Pts',(87.1812748961587,4.82693424430148,129.861021408326));
#49833=CARTESIAN_POINT('Ctrl Pts',(87.1735101432116,4.80072401053742,129.72690732331));
#49834=CARTESIAN_POINT('Ctrl Pts',(87.1657453902645,4.76888568170904,129.593710343012));
#49835=CARTESIAN_POINT('Ctrl Pts',(87.1579806373174,4.73149921940028,129.461938106091));
#49836=CARTESIAN_POINT('Ctrl Pts',(87.1502235964324,4.69414988985295,129.330296747214));
#49837=CARTESIAN_POINT('Ctrl Pts',(87.1424665555474,4.65126349896016,129.200077689336));
#49838=CARTESIAN_POINT('Ctrl Pts',(87.1347095146624,4.60297109926411,129.071778694008));
#49839=CARTESIAN_POINT('Ctrl Pts',(87.1269583234223,4.55471511724237,128.943576449951));
#49840=CARTESIAN_POINT('Ctrl Pts',(87.1192071321822,4.50106137803836,128.817291750842));
#49841=CARTESIAN_POINT('Ctrl Pts',(87.1114559409421,4.44219073362551,128.693407148493));
#49842=CARTESIAN_POINT('Ctrl Pts',(87.103708044165,4.38334511080693,128.569575200405));
#49843=CARTESIAN_POINT('Ctrl Pts',(87.0959601473879,4.31928716032181,128.448141672548));
#49844=CARTESIAN_POINT('Ctrl Pts',(87.0882122506108,4.25024574076486,128.329568867618));
#49845=CARTESIAN_POINT('Ctrl Pts',(87.0804659745267,4.18121876318452,128.211020865563));
#49846=CARTESIAN_POINT('Ctrl Pts',(87.0727196984426,4.10721058659468,128.095332733831));
#49847=CARTESIAN_POINT('Ctrl Pts',(87.0649734223585,4.02849568476616,127.982941545482));
#49848=CARTESIAN_POINT('Ctrl Pts',(87.0572270890931,3.94978020188212,127.870549527486));
#49849=CARTESIAN_POINT('Ctrl Pts',(87.0494807558278,3.86635814871267,127.761454821673));
#49850=CARTESIAN_POINT('Ctrl Pts',(87.0417344225625,3.77854669503138,127.656064580665));
#49851=CARTESIAN_POINT('Ctrl Pts',(87.0339863545595,3.69071557658399,127.550650738243));
#49852=CARTESIAN_POINT('Ctrl Pts',(87.0262382865565,3.59849335183553,127.448943311723));
#49853=CARTESIAN_POINT('Ctrl Pts',(87.0184902185535,3.50223647434234,127.351315187763));
#49854=CARTESIAN_POINT('Ctrl Pts',(87.0107339158117,3.40587729389422,127.25358330347));
#49855=CARTESIAN_POINT('Ctrl Pts',(87.0029776130699,3.30547516973552,127.159939661273));
#49856=CARTESIAN_POINT('Ctrl Pts',(86.995221310328,3.20142271685164,127.070719546102));
#49857=CARTESIAN_POINT('Ctrl Pts',(86.9874608678139,3.09731472804061,126.981451811468));
#49858=CARTESIAN_POINT('Ctrl Pts',(86.9797004252997,2.98955283540926,126.896612550017));
#49859=CARTESIAN_POINT('Ctrl Pts',(86.9719399827855,2.87856071994148,126.816495117814));
#49860=CARTESIAN_POINT('Ctrl Pts',(86.96416708252,2.76739043007645,126.736249073997));
#49861=CARTESIAN_POINT('Ctrl Pts',(86.9563941822546,2.65297988170643,126.660740221963));
#49862=CARTESIAN_POINT('Ctrl Pts',(86.9486212819892,2.53578032630071,126.590217620556));
#49863=CARTESIAN_POINT('Ctrl Pts',(86.9411309462271,2.42284126994121,126.522258693346));
#49864=CARTESIAN_POINT('Ctrl Pts',(86.933640610465,2.30731273103825,126.458929933258));
#49865=CARTESIAN_POINT('Ctrl Pts',(86.926150274703,2.18961627009005,126.40041197433));
#49866=CARTESIAN_POINT('Ctrl Pts',(86.9183759405839,2.06745731205271,126.339675289204));
#49867=CARTESIAN_POINT('Ctrl Pts',(86.9106016064648,1.94257583040136,126.283929014055));
#49868=CARTESIAN_POINT('Ctrl Pts',(86.9028272723457,1.81541786997739,126.233426247017));
#49869=CARTESIAN_POINT('Ctrl Pts',(86.8950625193986,1.68841662037529,126.182985720125));
#49870=CARTESIAN_POINT('Ctrl Pts',(86.8872977664515,1.55914483409,126.137775986509));
#49871=CARTESIAN_POINT('Ctrl Pts',(86.8795330135044,1.42807282309185,126.098004163318));
#49872=CARTESIAN_POINT('Ctrl Pts',(86.8717759726194,1.2971309946629,126.058271842062));
#49873=CARTESIAN_POINT('Ctrl Pts',(86.8640189317344,1.1643928714391,126.023966795765));
#49874=CARTESIAN_POINT('Ctrl Pts',(86.8562618908494,1.03034807141074,125.99524781849));
#49875=CARTESIAN_POINT('Ctrl Pts',(86.8485106996093,0.896404355608625,125.966550498418));
#49876=CARTESIAN_POINT('Ctrl Pts',(86.8407595083692,0.761156305074167,125.94343094422));
#49877=CARTESIAN_POINT('Ctrl Pts',(86.8330083171291,0.625107659223032,125.925997831048));
#49878=CARTESIAN_POINT('Ctrl Pts',(86.825260420352,0.4891168376756,125.908572127415));
#49879=CARTESIAN_POINT('Ctrl Pts',(86.8175125235749,0.35232648457384,125.896828107388));
#49880=CARTESIAN_POINT('Ctrl Pts',(86.8097646267978,0.215249251929158,125.89082311165));
#49881=CARTESIAN_POINT('Ctrl Pts',(86.8020183507137,0.0782006928865948,
125.884819372027));
#49882=CARTESIAN_POINT('Ctrl Pts',(86.7942720746296,-0.0591342359945297,
125.884552285972));
#49883=CARTESIAN_POINT('Ctrl Pts',(86.7865257985455,-0.196239452993261,
125.890027179592));
#49884=CARTESIAN_POINT('Ctrl Pts',(86.7787794652801,-0.333345682071464,
125.895502113627));
#49885=CARTESIAN_POINT('Ctrl Pts',(86.7710331320148,-0.470221805229798,
125.906719096315));
#49886=CARTESIAN_POINT('Ctrl Pts',(86.7632867987494,-0.606353835425051,
125.923631359682));
#49887=CARTESIAN_POINT('Ctrl Pts',(86.7555387307465,-0.742516351444593,
125.940547410433));
#49888=CARTESIAN_POINT('Ctrl Pts',(86.7477906627435,-0.877934055009452,
125.963161231607));
#49889=CARTESIAN_POINT('Ctrl Pts',(86.7400425947405,-1.01210055415978,125.991374483078));
#49890=CARTESIAN_POINT('Ctrl Pts',(86.7322862919987,-1.14640964706219,126.019617719929));
#49891=CARTESIAN_POINT('Ctrl Pts',(86.7245299892569,-1.27946449593388,126.05347219454));
#49892=CARTESIAN_POINT('Ctrl Pts',(86.716773686515,-1.41077079807924,126.092788818497));
#49893=CARTESIAN_POINT('Ctrl Pts',(86.7090132440008,-1.54214718235162,126.13212642692));
#49894=CARTESIAN_POINT('Ctrl Pts',(86.7012528014866,-1.67177279098091,126.176931866037));
#49895=CARTESIAN_POINT('Ctrl Pts',(86.6934923589724,-1.79917180527986,126.227007247158));
#49896=CARTESIAN_POINT('Ctrl Pts',(86.685719458707,-1.92677533178653,126.277163013726));
#49897=CARTESIAN_POINT('Ctrl Pts',(86.6779465584416,-2.05214476355159,126.332605469414));
#49898=CARTESIAN_POINT('Ctrl Pts',(86.6701736581761,-2.1748266478739,126.39308958597));
#49899=CARTESIAN_POINT('Ctrl Pts',(86.6626833224141,-2.29304873668383,126.451374952539));
#49900=CARTESIAN_POINT('Ctrl Pts',(86.6551929866521,-2.40877501332709,126.514341642537));
#49901=CARTESIAN_POINT('Ctrl Pts',(86.6477026508901,-2.52162564152507,126.581732622288));
#49902=CARTESIAN_POINT('Ctrl Pts',(86.6399270791868,-2.63877368123814,126.651689886136));
#49903=CARTESIAN_POINT('Ctrl Pts',(86.6321515074835,-2.75319386935908,126.726636714134));
#49904=CARTESIAN_POINT('Ctrl Pts',(86.6243759357803,-2.86443195400119,126.80633452418));
#49905=CARTESIAN_POINT('Ctrl Pts',(86.6162867216482,-2.98015703771763,126.889247096518));
#49906=CARTESIAN_POINT('Ctrl Pts',(86.6081975075162,-3.09243753941397,126.977301815903));
#49907=CARTESIAN_POINT('Ctrl Pts',(86.6001082933842,-3.20078964714923,127.070176811538));
#49908=CARTESIAN_POINT('Ctrl Pts',(86.5923522785462,-3.30467867043511,127.159226233703));
#49909=CARTESIAN_POINT('Ctrl Pts',(86.5845962637082,-3.40495611958501,127.252706476487));
#49910=CARTESIAN_POINT('Ctrl Pts',(86.5768402488702,-3.5012252238783,127.350289831641));
#49911=CARTESIAN_POINT('Ctrl Pts',(86.5690895258958,-3.59742864457262,127.447806606495));
#49912=CARTESIAN_POINT('Ctrl Pts',(86.5613388029213,-3.68962888826259,127.54942064671));
#49913=CARTESIAN_POINT('Ctrl Pts',(86.5535880799469,-3.77746381088411,127.65476537056));
#49914=CARTESIAN_POINT('Ctrl Pts',(86.5458409666259,-3.8652578271761,127.760061033446));
#49915=CARTESIAN_POINT('Ctrl Pts',(86.5380938533049,-3.94869031867422,127.869083622547));
#49916=CARTESIAN_POINT('Ctrl Pts',(86.5303467399839,-4.02743771144179,127.981431546024));
#49917=CARTESIAN_POINT('Ctrl Pts',(86.5226015569098,-4.1061654837518,128.093751477239));
#49918=CARTESIAN_POINT('Ctrl Pts',(86.5148563738356,-4.18021025782734,128.209394773103));
#49919=CARTESIAN_POINT('Ctrl Pts',(86.5071111907615,-4.24929053015312,128.327929101685));
#49920=CARTESIAN_POINT('Ctrl Pts',(86.4993643122063,-4.31838592468953,128.446489378356));
#49921=CARTESIAN_POINT('Ctrl Pts',(86.4916174336511,-4.38251444595739,128.567941616334));
#49922=CARTESIAN_POINT('Ctrl Pts',(86.483870555096,-4.44143950327054,128.691827019895));
#49923=CARTESIAN_POINT('Ctrl Pts',(86.4761226398207,-4.50037244618458,128.815729002326));
#49924=CARTESIAN_POINT('Ctrl Pts',(86.4683747245455,-4.55410037778972,128.942064442426));
#49925=CARTESIAN_POINT('Ctrl Pts',(86.4606268092702,-4.60243436192303,129.070353406886));
#49926=CARTESIAN_POINT('Ctrl Pts',(86.4528737656282,-4.65080033845505,129.198727286169));
#49927=CARTESIAN_POINT('Ctrl Pts',(86.4451207219862,-4.6937651104652,129.329056902511));
#49928=CARTESIAN_POINT('Ctrl Pts',(86.4373676783443,-4.73118920099771,129.460845896075));
#49929=CARTESIAN_POINT('Ctrl Pts',(86.4349900511002,-4.74266605335986,129.501261649687));
#49930=CARTESIAN_POINT('Ctrl Pts',(86.4326124238561,-4.75362218332535,129.541814564842));
#49931=CARTESIAN_POINT('Ctrl Pts',(86.4302347966119,-4.76405452823404,129.582490119308));
#49932=CARTESIAN_POINT('Origin',(213.235140564004,0.,130.804360617566));
#49933=CARTESIAN_POINT('',(84.3346156335084,-4.75804253168638,129.583987249709));
#49934=CARTESIAN_POINT('',(84.6799609333917,-4.76405452823403,129.582490119308));
#49935=CARTESIAN_POINT('',(213.235140564004,-4.76405452823405,129.582490119308));
#49936=CARTESIAN_POINT('',(86.014859435991,-4.91323682400955,130.800674691398));
#49937=CARTESIAN_POINT('Ctrl Pts',(86.014859435991,-4.91323682400955,130.800674691398));
#49938=CARTESIAN_POINT('Ctrl Pts',(85.9538892158643,-4.90576278147865,131.879764980307));
#49939=CARTESIAN_POINT('Ctrl Pts',(85.8001031211331,-4.02348310616932,134.61268188659));
#49940=CARTESIAN_POINT('Ctrl Pts',(85.5535011517979,0.497709270771224,136.600390751394));
#49941=CARTESIAN_POINT('Ctrl Pts',(85.2750535279847,5.14538832177028,133.518519575448));
#49942=CARTESIAN_POINT('Ctrl Pts',(84.9966059041722,5.06470687125616,127.942468911244));
#49943=CARTESIAN_POINT('Ctrl Pts',(84.7181582803589,0.329807230743486,124.996356913967));
#49944=CARTESIAN_POINT('Ctrl Pts',(84.4974948568047,-3.66267472747781,126.891296693768));
#49945=CARTESIAN_POINT('Ctrl Pts',(84.3696473078543,-4.60768184021397,128.982085784445));
#49946=CARTESIAN_POINT('Ctrl Pts',(84.3346156335084,-4.75804253168638,129.583987249709));
#49947=CARTESIAN_POINT('Ctrl Pts',(86.0846345799591,-4.77024925041304,129.580946905184));
#49948=CARTESIAN_POINT('Ctrl Pts',(86.0613761986364,-4.86912523137873,129.978032068211));
#49949=CARTESIAN_POINT('Ctrl Pts',(86.0381178173137,-4.91608795577263,130.389032854305));
#49950=CARTESIAN_POINT('Ctrl Pts',(86.014859435991,-4.91323682400955,130.800674691398));
#49951=CARTESIAN_POINT('',(86.3601405639686,-4.91824989921154,130.803364924019));
#49952=CARTESIAN_POINT('Ctrl Pts',(86.4302347966119,-4.76405452823404,129.582490119308));
#49953=CARTESIAN_POINT('Ctrl Pts',(86.4224725614478,-4.79811298491391,129.715283524994));
#49954=CARTESIAN_POINT('Ctrl Pts',(86.4147103262837,-4.8265848866449,129.849384456535));
#49955=CARTESIAN_POINT('Ctrl Pts',(86.4069480911196,-4.84939749013098,129.984283154633));
#49956=CARTESIAN_POINT('Ctrl Pts',(86.3991741738781,-4.87224442633088,130.119384873766));
#49957=CARTESIAN_POINT('Ctrl Pts',(86.3914002566367,-4.88941500410759,130.255286370261));
#49958=CARTESIAN_POINT('Ctrl Pts',(86.3836263393952,-4.90088841095131,130.391473410325));
#49959=CARTESIAN_POINT('Ctrl Pts',(86.3788359019558,-4.90795854509265,130.47539448579));
#49960=CARTESIAN_POINT('Ctrl Pts',(86.3740454645165,-4.91286634404094,130.559423971005));
#49961=CARTESIAN_POINT('Ctrl Pts',(86.3692550270772,-4.91561677684126,130.643442111058));
#49962=CARTESIAN_POINT('Ctrl Pts',(86.3662168727209,-4.91736113515921,130.696727449076));
#49963=CARTESIAN_POINT('Ctrl Pts',(86.3631787183647,-4.91823910390381,130.750041304561));
#49964=CARTESIAN_POINT('Ctrl Pts',(86.3601405640085,-4.9182498992114,130.803364923318));
#49965=CARTESIAN_POINT('Ctrl Pts',(86.3601405639686,-4.91824989921154,130.803364924019));
#49966=CARTESIAN_POINT('Ctrl Pts',(86.3524082609104,-4.91827737396147,130.93907704791));
#49967=CARTESIAN_POINT('Ctrl Pts',(86.3446759578523,-4.91268341904247,131.075014422619));
#49968=CARTESIAN_POINT('Ctrl Pts',(86.3369436547941,-4.90143815997771,131.210669645788));
#49969=CARTESIAN_POINT('Ctrl Pts',(86.3292207938126,-4.89020663273363,131.34615921753));
#49970=CARTESIAN_POINT('Ctrl Pts',(86.3214979328312,-4.87333756169104,131.481366932733));
#49971=CARTESIAN_POINT('Ctrl Pts',(86.3137750718497,-4.85085304816715,131.615783914981));
#49972=CARTESIAN_POINT('Ctrl Pts',(86.3060597424904,-4.82839046237952,131.750069808774));
#49973=CARTESIAN_POINT('Ctrl Pts',(86.2983444131311,-4.80032339511772,131.883566116271));
#49974=CARTESIAN_POINT('Ctrl Pts',(86.2906290837717,-4.76672582936199,132.015768034661));
#49975=CARTESIAN_POINT('Ctrl Pts',(86.2829193826055,-4.73315277242225,132.147873514145));
#49976=CARTESIAN_POINT('Ctrl Pts',(86.2752096814392,-4.69405734287461,132.278686101701));
#49977=CARTESIAN_POINT('Ctrl Pts',(86.267499980273,-4.64956470873308,132.40771057369));
#49978=CARTESIAN_POINT('Ctrl Pts',(86.2597932472713,-4.60508920384931,132.536685372436));
#49979=CARTESIAN_POINT('Ctrl Pts',(86.2520865142695,-4.55522075419097,132.663873050959));
#49980=CARTESIAN_POINT('Ctrl Pts',(86.2443797812678,-4.50013447636924,132.788793220879));
#49981=CARTESIAN_POINT('Ctrl Pts',(86.236674393087,-4.44505781107418,132.913691592295));
#49982=CARTESIAN_POINT('Ctrl Pts',(86.2289690049061,-4.38476528788441,133.036322880162));
#49983=CARTESIAN_POINT('Ctrl Pts',(86.2212636167253,-4.31948011112654,133.15622681956));
#49984=CARTESIAN_POINT('Ctrl Pts',(86.2135578585224,-4.25419179929563,133.27613651689));
#49985=CARTESIAN_POINT('Ctrl Pts',(86.2058521003194,-4.18391054613569,133.393318257734));
#49986=CARTESIAN_POINT('Ctrl Pts',(86.1981463421165,-4.10890521767763,133.507336935376));
#49987=CARTESIAN_POINT('Ctrl Pts',(86.1904384991179,-4.03387959650045,133.621386460813));
#49988=CARTESIAN_POINT('Ctrl Pts',(86.1827306561194,-3.95412757487608,133.732270890298));
#49989=CARTESIAN_POINT('Ctrl Pts',(86.1750228131208,-3.86996071508352,133.839585012271));
#49990=CARTESIAN_POINT('Ctrl Pts',(86.1673066825565,-3.78570335806874,133.947014519681));
#49991=CARTESIAN_POINT('Ctrl Pts',(86.1595905519922,-3.69702192855418,134.05086574247));
#49992=CARTESIAN_POINT('Ctrl Pts',(86.1518744214279,-3.60426784015897,134.150767107952));
#49993=CARTESIAN_POINT('Ctrl Pts',(86.1441537660352,-3.5114593596916,134.250727056752));
#49994=CARTESIAN_POINT('Ctrl Pts',(86.1364331106425,-3.41457374424503,134.346732257083));
#49995=CARTESIAN_POINT('Ctrl Pts',(86.1287124552499,-3.31399763511203,134.43844960065));
#49996=CARTESIAN_POINT('Ctrl Pts',(86.1209801595676,-3.21326988923563,134.530305224763));
#49997=CARTESIAN_POINT('Ctrl Pts',(86.1132478638852,-3.1088408402803,134.61785982786));
#49998=CARTESIAN_POINT('Ctrl Pts',(86.1055155682029,-3.00112886320961,134.700821654059));
#49999=CARTESIAN_POINT('Ctrl Pts',(86.1006128465567,-2.9328332543458,134.75342423909));
#50000=CARTESIAN_POINT('Ctrl Pts',(86.0957101249105,-2.8632183992832,134.804181267004));
#50001=CARTESIAN_POINT('Ctrl Pts',(86.0908074032643,-2.79239623547075,134.853027846004));
#50002=CARTESIAN_POINT('Ctrl Pts',(86.0830330691453,-2.6800922532648,134.930484747114));
#50003=CARTESIAN_POINT('Ctrl Pts',(86.0752587350262,-2.5643851390634,135.003388076089));
#50004=CARTESIAN_POINT('Ctrl Pts',(86.0674844009071,-2.44568050828408,135.071424000491));
#50005=CARTESIAN_POINT('Ctrl Pts',(86.05971964796,-2.32712217035335,135.139376076697));
#50006=CARTESIAN_POINT('Ctrl Pts',(86.0519548950129,-2.20557400208879,135.202472491291));
#50007=CARTESIAN_POINT('Ctrl Pts',(86.0441901420659,-2.08147216534957,135.260441483908));
#50008=CARTESIAN_POINT('Ctrl Pts',(86.0364331011809,-1.95749358830405,135.318352900904));
#50009=CARTESIAN_POINT('Ctrl Pts',(86.0286760602958,-1.83096674214791,135.371146866091));
#50010=CARTESIAN_POINT('Ctrl Pts',(86.0209190194108,-1.70235375663139,135.418596713583));
#50011=CARTESIAN_POINT('Ctrl Pts',(86.0131678281707,-1.5738377591677,135.466010778775));
#50012=CARTESIAN_POINT('Ctrl Pts',(86.0054166369305,-1.44323911896507,135.508088613046));
#50013=CARTESIAN_POINT('Ctrl Pts',(85.9976654456904,-1.31104105636989,135.544651158346));
#50014=CARTESIAN_POINT('Ctrl Pts',(85.9899175489133,-1.17889918147782,135.58119816359));
#50015=CARTESIAN_POINT('Ctrl Pts',(85.9821696521363,-1.0451596122878,135.612234438188));
#50016=CARTESIAN_POINT('Ctrl Pts',(85.9744217553592,-0.910321676117569,
135.637630474349));
#50017=CARTESIAN_POINT('Ctrl Pts',(85.9666754792751,-0.775511945136911,
135.663021198207));
#50018=CARTESIAN_POINT('Ctrl Pts',(85.958929203191,-0.639604688137216,135.682773958028));
#50019=CARTESIAN_POINT('Ctrl Pts',(85.9511829271069,-0.503110008515032,
135.69681024754));
#50020=CARTESIAN_POINT('Ctrl Pts',(85.9434365938415,-0.366614321319944,
135.710846640664));
#50021=CARTESIAN_POINT('Ctrl Pts',(85.9356902605761,-0.229531591764014,
135.719166439283));
#50022=CARTESIAN_POINT('Ctrl Pts',(85.9279439273108,-0.0923772421223119,
135.721743001278));
#50023=CARTESIAN_POINT('Ctrl Pts',(85.9201958593078,0.0448078222849374,
135.724320140276));
#50024=CARTESIAN_POINT('Ctrl Pts',(85.9124477913048,0.182064147871934,135.721151476003));
#50025=CARTESIAN_POINT('Ctrl Pts',(85.9046997233018,0.318876512293178,135.712262494377));
#50026=CARTESIAN_POINT('Ctrl Pts',(85.89694342056,0.455834282523323,135.703364065436));
#50027=CARTESIAN_POINT('Ctrl Pts',(85.8891871178182,0.592346758257384,135.688733199831));
#50028=CARTESIAN_POINT('Ctrl Pts',(85.8814308150763,0.727903482690584,135.668447333732));
#50029=CARTESIAN_POINT('Ctrl Pts',(85.8736703725621,0.863532557829333,135.648150640456));
#50030=CARTESIAN_POINT('Ctrl Pts',(85.865909930048,0.998204481512188,135.622193006538));
#50031=CARTESIAN_POINT('Ctrl Pts',(85.8581494875338,1.13142016893736,135.590702797542));
#50032=CARTESIAN_POINT('Ctrl Pts',(85.8503765872684,1.26484970601023,135.559162037668));
#50033=CARTESIAN_POINT('Ctrl Pts',(85.8426036870029,1.39681795879816,135.522071060734));
#50034=CARTESIAN_POINT('Ctrl Pts',(85.8348307867375,1.52684129285869,135.479608068656));
#50035=CARTESIAN_POINT('Ctrl Pts',(85.8273404509754,1.65213795121718,135.438688713298));
#50036=CARTESIAN_POINT('Ctrl Pts',(85.8198501152134,1.77562835251854,135.392781241775));
#50037=CARTESIAN_POINT('Ctrl Pts',(85.8123597794514,1.89690003015802,135.342086186404));
#50038=CARTESIAN_POINT('Ctrl Pts',(85.8045854453323,2.02276976031493,135.2894690126));
#50039=CARTESIAN_POINT('Ctrl Pts',(85.7968111112132,2.14664791724025,135.2315273705));
#50040=CARTESIAN_POINT('Ctrl Pts',(85.7890367770941,2.26805121977541,135.168432881745));
#50041=CARTESIAN_POINT('Ctrl Pts',(85.781272024147,2.38930490359008,135.105416151308));
#50042=CARTESIAN_POINT('Ctrl Pts',(85.7735072712,2.50808945809706,135.037259388228));
#50043=CARTESIAN_POINT('Ctrl Pts',(85.7657425182529,2.62394048746622,134.964182654713));
#50044=CARTESIAN_POINT('Ctrl Pts',(85.7579854773679,2.73967645195987,134.891178502041));
#50045=CARTESIAN_POINT('Ctrl Pts',(85.7502284364829,2.85248436101213,134.813264310691));
#50046=CARTESIAN_POINT('Ctrl Pts',(85.7424713955979,2.96192372177463,134.730706365063));
#50047=CARTESIAN_POINT('Ctrl Pts',(85.7347202043578,3.07128055346372,134.648210677024));
#50048=CARTESIAN_POINT('Ctrl Pts',(85.7269690131177,3.17727358222047,134.561078439508));
#50049=CARTESIAN_POINT('Ctrl Pts',(85.7192178218775,3.27949096903656,134.469619414228));
#50050=CARTESIAN_POINT('Ctrl Pts',(85.7114699251005,3.38166491073673,134.378199261473));
#50051=CARTESIAN_POINT('Ctrl Pts',(85.7037220283234,3.48006611146722,134.282456238736));
#50052=CARTESIAN_POINT('Ctrl Pts',(85.6959741315463,3.57431571404229,134.182740442105));
#50053=CARTESIAN_POINT('Ctrl Pts',(85.6882278554622,3.66854560163235,134.083045503869));
#50054=CARTESIAN_POINT('Ctrl Pts',(85.6804815793781,3.75862535002504,133.979379728633));
#50055=CARTESIAN_POINT('Ctrl Pts',(85.672735303294,3.84421318632328,133.872129846272));
#50056=CARTESIAN_POINT('Ctrl Pts',(85.6649889700287,3.92980165441137,133.764879172218));
#50057=CARTESIAN_POINT('Ctrl Pts',(85.6572426367633,4.01089790037469,133.654044643834));
#50058=CARTESIAN_POINT('Ctrl Pts',(85.6494963034979,4.08720091111563,133.540045499762));
#50059=CARTESIAN_POINT('Ctrl Pts',(85.641748235495,4.16352100938694,133.426020826372));
#50060=CARTESIAN_POINT('Ctrl Pts',(85.634000167492,4.23504551904515,133.308830451916));
#50061=CARTESIAN_POINT('Ctrl Pts',(85.626252099489,4.3015173918517,133.188921623306));
#50062=CARTESIAN_POINT('Ctrl Pts',(85.6184957967472,4.3680599117556,133.068885354167));
#50063=CARTESIAN_POINT('Ctrl Pts',(85.6107394940053,4.42953887779171,132.94612520186));
#50064=CARTESIAN_POINT('Ctrl Pts',(85.6029831912635,4.48574352483045,132.821112484292));
#50065=CARTESIAN_POINT('Ctrl Pts',(85.5952227487493,4.54197816998169,132.696033043672));
#50066=CARTESIAN_POINT('Ctrl Pts',(85.5874623062351,4.59293274170323,132.568699004988));
#50067=CARTESIAN_POINT('Ctrl Pts',(85.579701863721,4.63844547005359,132.439599647139));
#50068=CARTESIAN_POINT('Ctrl Pts',(85.5719289634555,4.68403125947587,132.310293047541));
#50069=CARTESIAN_POINT('Ctrl Pts',(85.5641560631901,4.7241576342459,132.179215839905));
#50070=CARTESIAN_POINT('Ctrl Pts',(85.5563831629247,4.75871310445237,132.046871242073));
#50071=CARTESIAN_POINT('Ctrl Pts',(85.5488928271626,4.7920123962769,131.919337703728));
#50072=CARTESIAN_POINT('Ctrl Pts',(85.5414024914006,4.82013871864219,131.790627621974));
#50073=CARTESIAN_POINT('Ctrl Pts',(85.5339121556386,4.84303783678936,131.661196409259));
#50074=CARTESIAN_POINT('Ctrl Pts',(85.5261378215195,4.86680518196106,131.526857772775));
#50075=CARTESIAN_POINT('Ctrl Pts',(85.5183634874004,4.88501640718023,131.391316698084));
#50076=CARTESIAN_POINT('Ctrl Pts',(85.5105891532813,4.89755467732237,131.255072549001));
#50077=CARTESIAN_POINT('Ctrl Pts',(85.5028244003342,4.91007749516717,131.118996308654));
#50078=CARTESIAN_POINT('Ctrl Pts',(85.4950596473871,4.91694123327284,130.982219103527));
#50079=CARTESIAN_POINT('Ctrl Pts',(85.48729489444,4.91808001891918,130.845250591984));
#50080=CARTESIAN_POINT('Ctrl Pts',(85.479537853555,4.91921767350756,130.708418119497));
#50081=CARTESIAN_POINT('Ctrl Pts',(85.47178081267,4.91464168800971,130.571395107141));
#50082=CARTESIAN_POINT('Ctrl Pts',(85.464023771785,4.90433799788751,130.434696087246));
#50083=CARTESIAN_POINT('Ctrl Pts',(85.4562725805448,4.89404207785817,130.298100153145));
#50084=CARTESIAN_POINT('Ctrl Pts',(85.4485213893047,4.87802707978905,130.161828113472));
#50085=CARTESIAN_POINT('Ctrl Pts',(85.4407701980646,4.85633100593914,130.026393893821));
#50086=CARTESIAN_POINT('Ctrl Pts',(85.4330223012875,4.83464415349942,129.891017237327));
#50087=CARTESIAN_POINT('Ctrl Pts',(85.4252744045104,4.80728108946488,129.756478077843));
#50088=CARTESIAN_POINT('Ctrl Pts',(85.4175265077333,4.77433157802729,129.623284394136));
#50089=CARTESIAN_POINT('Ctrl Pts',(85.4097802316492,4.74138895891712,129.490118571676));
#50090=CARTESIAN_POINT('Ctrl Pts',(85.4020339555651,4.70286231056995,129.35829804447));
#50091=CARTESIAN_POINT('Ctrl Pts',(85.394287679481,4.65889226318408,129.228319392679));
#50092=CARTESIAN_POINT('Ctrl Pts',(85.3865413462156,4.61492189122137,129.098339781415));
#50093=CARTESIAN_POINT('Ctrl Pts',(85.3787950129502,4.56550816532366,128.970202443046));
#50094=CARTESIAN_POINT('Ctrl Pts',(85.3710486796848,4.51084109790222,128.844387237141));
#50095=CARTESIAN_POINT('Ctrl Pts',(85.3633006116819,4.45616178817026,128.718543855793));
#50096=CARTESIAN_POINT('Ctrl Pts',(85.3555525436789,4.39622695169032,128.595024000211));
#50097=CARTESIAN_POINT('Ctrl Pts',(85.347804475676,4.33127392910448,128.474285680239));
#50098=CARTESIAN_POINT('Ctrl Pts',(85.3400481729341,4.26625187367311,128.353419038143));
#50099=CARTESIAN_POINT('Ctrl Pts',(85.3322918701923,4.19620116363837,128.235340181936));
#50100=CARTESIAN_POINT('Ctrl Pts',(85.3245355674504,4.12140440840354,128.120481193134));
#50101=CARTESIAN_POINT('Ctrl Pts',(85.3167751249362,4.04656773188832,128.00556090063));
#50102=CARTESIAN_POINT('Ctrl Pts',(85.3090146824221,3.96698018950555,127.893864218116));
#50103=CARTESIAN_POINT('Ctrl Pts',(85.3012542399079,3.88296598484741,127.785791714424));
#50104=CARTESIAN_POINT('Ctrl Pts',(85.2934813396425,3.79881691312958,127.677545723154));
#50105=CARTESIAN_POINT('Ctrl Pts',(85.285708439377,3.71022723175037,127.572935835156));
#50106=CARTESIAN_POINT('Ctrl Pts',(85.2779355391116,3.61756004911154,127.472327851585));
#50107=CARTESIAN_POINT('Ctrl Pts',(85.2704452033496,3.52826155197713,127.375377221634));
#50108=CARTESIAN_POINT('Ctrl Pts',(85.2629548675877,3.43517707920089,127.282142806943));
#50109=CARTESIAN_POINT('Ctrl Pts',(85.2554645318257,3.3386604669637,127.192916398305));
#50110=CARTESIAN_POINT('Ctrl Pts',(85.2476901977066,3.23848439803689,127.100306943263));
#50111=CARTESIAN_POINT('Ctrl Pts',(85.2399158635876,3.1342934652414,127.011722062072));
#50112=CARTESIAN_POINT('Ctrl Pts',(85.2321415294685,3.02644464525853,126.927529969771));
#50113=CARTESIAN_POINT('Ctrl Pts',(85.2243767765214,2.91872873930756,126.843441636699));
#50114=CARTESIAN_POINT('Ctrl Pts',(85.2166120235743,2.8073642210049,126.763735559099));
#50115=CARTESIAN_POINT('Ctrl Pts',(85.2088472706272,2.69274427455205,126.688742640352));
#50116=CARTESIAN_POINT('Ctrl Pts',(85.2010902297421,2.57823817024588,126.613824205629));
#50117=CARTESIAN_POINT('Ctrl Pts',(85.1933331888572,2.46048339732106,126.543609826675));
#50118=CARTESIAN_POINT('Ctrl Pts',(85.1855761479721,2.33990524417316,126.478389453678));
#50119=CARTESIAN_POINT('Ctrl Pts',(85.177824956732,2.21941801994792,126.413218263871));
#50120=CARTESIAN_POINT('Ctrl Pts',(85.1700737654918,2.09611199590156,126.353033769242));
#50121=CARTESIAN_POINT('Ctrl Pts',(85.1623225742516,1.97044009334086,126.298081786751));
#50122=CARTESIAN_POINT('Ctrl Pts',(85.1545746774746,1.84482160469167,126.243153160318));
#50123=CARTESIAN_POINT('Ctrl Pts',(85.1468267806974,1.71683959497981,126.19345277905));
#50124=CARTESIAN_POINT('Ctrl Pts',(85.1390788839203,1.58696996086753,126.14917969672));
#50125=CARTESIAN_POINT('Ctrl Pts',(85.1313326078362,1.45712749268314,126.104915875366));
#50126=CARTESIAN_POINT('Ctrl Pts',(85.1235863317522,1.32539855529597,126.066077220901));
#50127=CARTESIAN_POINT('Ctrl Pts',(85.1158400556681,1.19227694971759,126.032813830865));
#50128=CARTESIAN_POINT('Ctrl Pts',(85.1080937224027,1.05915436146558,125.999550195287));
#50129=CARTESIAN_POINT('Ctrl Pts',(85.1003473891373,0.924639463812012,125.971862001037));
#50130=CARTESIAN_POINT('Ctrl Pts',(85.0926010558719,0.789238682553677,125.949848761111));
#50131=CARTESIAN_POINT('Ctrl Pts',(85.084852987869,0.653807579229459,125.927830591473));
#50132=CARTESIAN_POINT('Ctrl Pts',(85.077104919866,0.517490583356969,125.911489967764));
#50133=CARTESIAN_POINT('Ctrl Pts',(85.069356851863,0.380801320003617,125.900874774089));
#50134=CARTESIAN_POINT('Ctrl Pts',(85.0616005491212,0.243966781674364,125.890248298459));
#50135=CARTESIAN_POINT('Ctrl Pts',(85.0538442463793,0.106759575923239,125.885359438734));
#50136=CARTESIAN_POINT('Ctrl Pts',(85.0460879436374,-0.0303040175490168,
125.886203978232));
#50137=CARTESIAN_POINT('Ctrl Pts',(85.0383275011232,-0.1674407659882,125.887048968487));
#50138=CARTESIAN_POINT('Ctrl Pts',(85.0305670586091,-0.304433359093195,
125.893633436688));
#50139=CARTESIAN_POINT('Ctrl Pts',(85.0228066160949,-0.44076954700117,125.90590113841));
#50140=CARTESIAN_POINT('Ctrl Pts',(85.0150337158295,-0.577324593861055,
125.918188533335));
#50141=CARTESIAN_POINT('Ctrl Pts',(85.007260815564,-0.713220742048475,125.936177341568));
#50142=CARTESIAN_POINT('Ctrl Pts',(84.9994879152986,-0.847953963730991,
125.959759794186));
#50143=CARTESIAN_POINT('Ctrl Pts',(84.9919975795366,-0.977789293432203,
125.982484965251));
#50144=CARTESIAN_POINT('Ctrl Pts',(84.9845072437746,-1.10654447829828,126.01040408997));
#50145=CARTESIAN_POINT('Ctrl Pts',(84.9770169080126,-1.23378276937296,126.043377195992));
#50146=CARTESIAN_POINT('Ctrl Pts',(84.9692425738935,-1.36584533892763,126.077600487352));
#50147=CARTESIAN_POINT('Ctrl Pts',(84.9614682397744,-1.49669205250879,126.117376977864));
#50148=CARTESIAN_POINT('Ctrl Pts',(84.9536939056553,-1.62582016576019,126.162605362158));
#50149=CARTESIAN_POINT('Ctrl Pts',(84.9459291527082,-1.75478914015226,126.207778006511));
#50150=CARTESIAN_POINT('Ctrl Pts',(84.9381643997612,-1.88204336300204,126.258389047894));
#50151=CARTESIAN_POINT('Ctrl Pts',(84.9303996468141,-2.00709191025934,126.314286550663));
#50152=CARTESIAN_POINT('Ctrl Pts',(84.9226426059291,-2.13201625753672,126.370128535245));
#50153=CARTESIAN_POINT('Ctrl Pts',(84.9148855650441,-2.25473893421092,126.431246373789));
#50154=CARTESIAN_POINT('Ctrl Pts',(84.9071285241591,-2.37478611821173,126.497438984282));
#50155=CARTESIAN_POINT('Ctrl Pts',(84.899377332919,-2.49474277369709,126.563581678412));
#50156=CARTESIAN_POINT('Ctrl Pts',(84.8916261416789,-2.61202761145537,126.634791339215));
#50157=CARTESIAN_POINT('Ctrl Pts',(84.8838749504388,-2.72618900368645,126.710819781239));
#50158=CARTESIAN_POINT('Ctrl Pts',(84.8761270536617,-2.84030187428096,126.786815909147));
#50159=CARTESIAN_POINT('Ctrl Pts',(84.8683791568846,-2.9512936150138,126.867626528481));
#50160=CARTESIAN_POINT('Ctrl Pts',(84.8606312601075,-3.05873952253601,126.95295884733));
#50161=CARTESIAN_POINT('Ctrl Pts',(84.8528849840234,-3.16616295469033,127.038273316497));
#50162=CARTESIAN_POINT('Ctrl Pts',(84.8451387079393,-3.27004172297506,127.128107360853));
#50163=CARTESIAN_POINT('Ctrl Pts',(84.8373924318552,-3.36998263457143,127.222126663008));
#50164=CARTESIAN_POINT('Ctrl Pts',(84.8296460985898,-3.46992428390917,127.316146659192));
#50165=CARTESIAN_POINT('Ctrl Pts',(84.8218997653245,-3.5659277337931,127.414351706934));
#50166=CARTESIAN_POINT('Ctrl Pts',(84.8141534320591,-3.65763552560786,127.516369525073));
#50167=CARTESIAN_POINT('Ctrl Pts',(84.8064053640561,-3.74936385474624,127.618410189395));
#50168=CARTESIAN_POINT('Ctrl Pts',(84.7986572960532,-3.83679435025959,127.724265032463));
#50169=CARTESIAN_POINT('Ctrl Pts',(84.7909092280503,-3.91960909900015,127.833527809491));
#50170=CARTESIAN_POINT('Ctrl Pts',(84.7831529253084,-4.00251186424158,127.942906712299));
#50171=CARTESIAN_POINT('Ctrl Pts',(84.7753966225665,-4.08078884656849,128.055700472309));
#50172=CARTESIAN_POINT('Ctrl Pts',(84.7676403198246,-4.15416453180601,128.171472449568));
#50173=CARTESIAN_POINT('Ctrl Pts',(84.7598798773105,-4.22757937985613,128.287306217817));
#50174=CARTESIAN_POINT('Ctrl Pts',(84.7521194347963,-4.29608752308006,128.406121032125));
#50175=CARTESIAN_POINT('Ctrl Pts',(84.7443589922821,-4.35945939794346,128.527455520689));
#50176=CARTESIAN_POINT('Ctrl Pts',(84.7365860920167,-4.42293300296619,128.648984786146));
#50177=CARTESIAN_POINT('Ctrl Pts',(84.7288131917512,-4.48125369667361,128.773041454646));
#50178=CARTESIAN_POINT('Ctrl Pts',(84.7210402914858,-4.53423970875748,128.899143221564));
#50179=CARTESIAN_POINT('Ctrl Pts',(84.7135499557238,-4.58529954583825,129.020660871624));
#50180=CARTESIAN_POINT('Ctrl Pts',(84.7060596199618,-4.63140571794234,129.144077224061));
#50181=CARTESIAN_POINT('Ctrl Pts',(84.6985692841997,-4.67243991429253,129.268949171137));
#50182=CARTESIAN_POINT('Ctrl Pts',(84.6923665005971,-4.7064205325662,129.372356239974));
#50183=CARTESIAN_POINT('Ctrl Pts',(84.6861637169944,-4.73698299476726,129.476938621189));
#50184=CARTESIAN_POINT('Ctrl Pts',(84.6799609333917,-4.76405452823403,129.582490119308));
#50185=CARTESIAN_POINT('Origin',(213.235140564004,0.,130.804360617566));
#50186=CARTESIAN_POINT('',(82.5850015336781,-4.76405452823407,129.582490119308));
#50187=CARTESIAN_POINT('',(82.9299460717117,-4.76405452823408,129.582490119308));
#50188=CARTESIAN_POINT('',(213.235140564004,-4.76405452823405,129.582490119308));
#50189=CARTESIAN_POINT('',(84.2648594359911,-4.91520650470561,130.80752635475));
#50190=CARTESIAN_POINT('Ctrl Pts',(84.2648594359911,-4.91824897989084,130.807528314317));
#50191=CARTESIAN_POINT('Ctrl Pts',(84.2561178632596,-4.91814915973146,130.962511709407));
#50192=CARTESIAN_POINT('Ctrl Pts',(84.2473762905281,-4.9107195796762,131.117215891758));
#50193=CARTESIAN_POINT('Ctrl Pts',(84.2386347177967,-4.89606346316109,131.270992835913));
#50194=CARTESIAN_POINT('Ctrl Pts',(84.2298585400784,-4.8813493279422,131.425378531981));
#50195=CARTESIAN_POINT('Ctrl Pts',(84.22108236236,-4.85935143879908,131.578829450587));
#50196=CARTESIAN_POINT('Ctrl Pts',(84.2123061846417,-4.83022408257366,131.730707407178));
#50197=CARTESIAN_POINT('Ctrl Pts',(84.203481116158,-4.80093446223002,131.883431453011));
#50198=CARTESIAN_POINT('Ctrl Pts',(84.1946560476744,-4.76443581593382,132.034564780633));
#50199=CARTESIAN_POINT('Ctrl Pts',(84.1858309791907,-4.720933766625,132.183478971312));
#50200=CARTESIAN_POINT('Ctrl Pts',(84.1776416637049,-4.68056558061833,132.321665466981));
#50201=CARTESIAN_POINT('Ctrl Pts',(84.1694523482191,-4.63416726118915,132.45794114906));
#50202=CARTESIAN_POINT('Ctrl Pts',(84.1612630327332,-4.58193918638087,132.591821485615));
#50203=CARTESIAN_POINT('Ctrl Pts',(84.1534886986142,-4.53235769148566,132.718917635489));
#50204=CARTESIAN_POINT('Ctrl Pts',(84.1457143644951,-4.47740546934383,132.844150558214));
#50205=CARTESIAN_POINT('Ctrl Pts',(84.137940030376,-4.41724249475759,132.967032993357));
#50206=CARTESIAN_POINT('Ctrl Pts',(84.1301752774289,-4.35715366566061,133.08976398688));
#50207=CARTESIAN_POINT('Ctrl Pts',(84.1224105244818,-4.29186703182705,133.210149908756));
#50208=CARTESIAN_POINT('Ctrl Pts',(84.1146457715348,-4.22159144787465,133.327721216));
#50209=CARTESIAN_POINT('Ctrl Pts',(84.1068887306498,-4.151385662623,133.445175749765));
#50210=CARTESIAN_POINT('Ctrl Pts',(84.0991316897647,-4.0762009874072,133.559820898686));
#50211=CARTESIAN_POINT('Ctrl Pts',(84.0913746488797,-3.99629305932868,133.671209906674));
#50212=CARTESIAN_POINT('Ctrl Pts',(84.0836234576396,-3.9164453904402,133.782514915345));
#50213=CARTESIAN_POINT('Ctrl Pts',(84.0758722663995,-3.83188178529054,133.890568354179));
#50214=CARTESIAN_POINT('Ctrl Pts',(84.0681210751594,-3.74290203338909,133.99495106934));
#50215=CARTESIAN_POINT('Ctrl Pts',(84.0603731783823,-3.65396010025588,134.099289419062));
#50216=CARTESIAN_POINT('Ctrl Pts',(84.0526252816052,-3.56060600663916,134.199959851231));
#50217=CARTESIAN_POINT('Ctrl Pts',(84.0448773848282,-3.4631806562809,134.296575216422));
#50218=CARTESIAN_POINT('Ctrl Pts',(84.0371311087441,-3.36577568520561,134.393170371761));
#50219=CARTESIAN_POINT('Ctrl Pts',(84.0293848326599,-3.26430142873579,134.485711872179));
#50220=CARTESIAN_POINT('Ctrl Pts',(84.0216385565758,-3.15913630377159,134.573848762751));
#50221=CARTESIAN_POINT('Ctrl Pts',(84.0138922233105,-3.0539704025024,134.66198630393));
#50222=CARTESIAN_POINT('Ctrl Pts',(84.0061458900452,-2.94511387802007,134.745718919255));
#50223=CARTESIAN_POINT('Ctrl Pts',(83.9983995567798,-2.83297862475211,134.824735621741));
#50224=CARTESIAN_POINT('Ctrl Pts',(83.9906514887768,-2.72081825957183,134.90377001947));
#50225=CARTESIAN_POINT('Ctrl Pts',(83.9829034207739,-2.60537802406574,134.978086177694));
#50226=CARTESIAN_POINT('Ctrl Pts',(83.9751553527709,-2.48709886790086,135.047416389505));
#50227=CARTESIAN_POINT('Ctrl Pts',(83.9673990500291,-2.36869400324111,135.11682028629));
#50228=CARTESIAN_POINT('Ctrl Pts',(83.9596427472872,-2.24744452849331,135.181227453072));
#50229=CARTESIAN_POINT('Ctrl Pts',(83.9518864445454,-2.12381656805513,135.240415875084));
#50230=CARTESIAN_POINT('Ctrl Pts',(83.9441260020312,-2.00012262365202,135.29963588774));
#50231=CARTESIAN_POINT('Ctrl Pts',(83.9363655595171,-1.87404802324866,135.353631451633));
#50232=CARTESIAN_POINT('Ctrl Pts',(83.9286051170029,-1.74607802281383,135.402229102065));
#50233=CARTESIAN_POINT('Ctrl Pts',(83.9208322167375,-1.61790259357365,135.450904765759));
#50234=CARTESIAN_POINT('Ctrl Pts',(83.913059316472,-1.48782605528891,135.494165076688));
#50235=CARTESIAN_POINT('Ctrl Pts',(83.9052864162066,-1.35634880543654,135.531886501207));
#50236=CARTESIAN_POINT('Ctrl Pts',(83.8977960804446,-1.22965108478769,135.568236656929));
#50237=CARTESIAN_POINT('Ctrl Pts',(83.8903057446826,-1.10165302254058,135.599443566678));
#50238=CARTESIAN_POINT('Ctrl Pts',(83.8828154089205,-0.972808598513784,
135.625442082669));
#50239=CARTESIAN_POINT('Ctrl Pts',(83.8750410748015,-0.839078998988413,
135.652426340296));
#50240=CARTESIAN_POINT('Ctrl Pts',(83.8672667406823,-0.704013975969372,
135.673884933197));
#50241=CARTESIAN_POINT('Ctrl Pts',(83.8594924065632,-0.568109945745981,
135.689689076538));
#50242=CARTESIAN_POINT('Ctrl Pts',(83.8517276536162,-0.43237340509384,135.705473742686));
#50243=CARTESIAN_POINT('Ctrl Pts',(83.8439629006691,-0.295800299212012,
135.715617779991));
#50244=CARTESIAN_POINT('Ctrl Pts',(83.836198147722,-0.158898558931744,135.720043104309));
#50245=CARTESIAN_POINT('Ctrl Pts',(83.828441106837,-0.0221327913898985,
135.724464033332));
#50246=CARTESIAN_POINT('Ctrl Pts',(83.820684065952,0.114960572758557,135.723177540087));
#50247=CARTESIAN_POINT('Ctrl Pts',(83.812927025067,0.251867486865856,135.71615721673));
#50248=CARTESIAN_POINT('Ctrl Pts',(83.8051758338269,0.388671158404247,135.709142187453));
#50249=CARTESIAN_POINT('Ctrl Pts',(83.7974246425867,0.525288270891732,135.696401954517));
#50250=CARTESIAN_POINT('Ctrl Pts',(83.7896734513466,0.661204134782529,135.677962176439));
#50251=CARTESIAN_POINT('Ctrl Pts',(83.7819255545695,0.797062230805592,135.659530235758));
#50252=CARTESIAN_POINT('Ctrl Pts',(83.7741776577924,0.932219284424532,135.635403620472));
#50253=CARTESIAN_POINT('Ctrl Pts',(83.7664297610153,1.06616530906384,135.605659878834));
#50254=CARTESIAN_POINT('Ctrl Pts',(83.7586834849312,1.20008331508235,135.575922358944));
#50255=CARTESIAN_POINT('Ctrl Pts',(83.7509372088471,1.33279041456422,135.540570134504));
#50256=CARTESIAN_POINT('Ctrl Pts',(83.743190932763,1.46378679561312,135.499731878658));
#50257=CARTESIAN_POINT('Ctrl Pts',(83.7354445994976,1.59478414364745,135.458893321353));
#50258=CARTESIAN_POINT('Ctrl Pts',(83.7276982662323,1.72407037480231,135.412568768195));
#50259=CARTESIAN_POINT('Ctrl Pts',(83.719951932967,1.85116120792071,135.36093666157));
#50260=CARTESIAN_POINT('Ctrl Pts',(83.712203864964,1.97828050214999,135.309292992292));
#50261=CARTESIAN_POINT('Ctrl Pts',(83.704455796961,2.10320305788241,135.252339551516));
#50262=CARTESIAN_POINT('Ctrl Pts',(83.696707728958,2.22546530164882,135.190302620563));
#50263=CARTESIAN_POINT('Ctrl Pts',(83.6889514262161,2.34785748718283,135.128199756022));
#50264=CARTESIAN_POINT('Ctrl Pts',(83.6811951234743,2.46758336348586,135.061002785831));
#50265=CARTESIAN_POINT('Ctrl Pts',(83.6734388207324,2.58420419162596,134.988983869244));
#50266=CARTESIAN_POINT('Ctrl Pts',(83.6656783782182,2.70088726381351,134.916926513993));
#50267=CARTESIAN_POINT('Ctrl Pts',(83.6579179357041,2.81446166201237,134.840042303254));
#50268=CARTESIAN_POINT('Ctrl Pts',(83.6501574931899,2.92451915275325,134.758645734712));
#50269=CARTESIAN_POINT('Ctrl Pts',(83.6423845929245,3.03475331754872,134.677118501171));
#50270=CARTESIAN_POINT('Ctrl Pts',(83.634611692659,3.14145898856807,134.591064680302));
#50271=CARTESIAN_POINT('Ctrl Pts',(83.6268387923936,3.24426175639737,134.500838497721));
#50272=CARTESIAN_POINT('Ctrl Pts',(83.6193484566316,3.34332738467118,134.413892264144));
#50273=CARTESIAN_POINT('Ctrl Pts',(83.6118581208696,3.43876872083921,134.323071966272));
#50274=CARTESIAN_POINT('Ctrl Pts',(83.6043677851076,3.5302855670449,134.228724336217));
#50275=CARTESIAN_POINT('Ctrl Pts',(83.5965934509885,3.62527230229075,134.130799487092));
#50276=CARTESIAN_POINT('Ctrl Pts',(83.5888191168694,3.71633196832571,134.028764351604));
#50277=CARTESIAN_POINT('Ctrl Pts',(83.5810447827503,3.80308788969193,133.922966967489));
#50278=CARTESIAN_POINT('Ctrl Pts',(83.5732800298032,3.88973689213861,133.817299969194));
#50279=CARTESIAN_POINT('Ctrl Pts',(83.5655152768561,3.97209245773049,133.70788024721));
#50280=CARTESIAN_POINT('Ctrl Pts',(83.557750523909,4.04981434304294,133.595092931742));
#50281=CARTESIAN_POINT('Ctrl Pts',(83.5499934830241,4.1274590338832,133.482417638225));
#50282=CARTESIAN_POINT('Ctrl Pts',(83.5422364421391,4.20047898269506,133.366381727258));
#50283=CARTESIAN_POINT('Ctrl Pts',(83.5344794012541,4.26857411704109,133.247403406759));
#50284=CARTESIAN_POINT('Ctrl Pts',(83.5267282100139,4.33661790031661,133.128514808737));
#50285=CARTESIAN_POINT('Ctrl Pts',(83.5189770187738,4.39974406788301,133.006688555704));
#50286=CARTESIAN_POINT('Ctrl Pts',(83.5112258275337,4.45769600470672,132.882371539607));
#50287=CARTESIAN_POINT('Ctrl Pts',(83.5034779307566,4.51562331041136,132.758107361559));
#50288=CARTESIAN_POINT('Ctrl Pts',(83.4957300339795,4.56838059454582,132.631354879615));
#50289=CARTESIAN_POINT('Ctrl Pts',(83.4879821372024,4.6157574404497,132.502585076651));
#50290=CARTESIAN_POINT('Ctrl Pts',(83.4802358611183,4.66312437613874,132.373842209553));
#50291=CARTESIAN_POINT('Ctrl Pts',(83.4724895850343,4.70511297731109,132.243083227462));
#50292=CARTESIAN_POINT('Ctrl Pts',(83.4647433089502,4.74156133978977,132.110798187261));
#50293=CARTESIAN_POINT('Ctrl Pts',(83.4569969756849,4.77800997132198,131.978512170562));
#50294=CARTESIAN_POINT('Ctrl Pts',(83.4492506424195,4.80891817870165,131.844700450193));
#50295=CARTESIAN_POINT('Ctrl Pts',(83.4415043091542,4.83417432476711,131.709866918076));
#50296=CARTESIAN_POINT('Ctrl Pts',(83.4337562411512,4.85943612677136,131.575003190924));
#50297=CARTESIAN_POINT('Ctrl Pts',(83.4260081731482,4.87904327681805,131.439117580891));
#50298=CARTESIAN_POINT('Ctrl Pts',(83.4182601051453,4.89293557900721,131.302722416047));
#50299=CARTESIAN_POINT('Ctrl Pts',(83.4105038024034,4.90684264610045,131.166182288799));
#50300=CARTESIAN_POINT('Ctrl Pts',(83.4027474996616,4.9150226925705,131.029131914487));
#50301=CARTESIAN_POINT('Ctrl Pts',(83.3949911969197,4.91746754459602,130.892087525324));
#50302=CARTESIAN_POINT('Ctrl Pts',(83.3872307544056,4.91991370151268,130.754969991444));
#50303=CARTESIAN_POINT('Ctrl Pts',(83.3794703118914,4.91661857398014,130.61785883974));
#50304=CARTESIAN_POINT('Ctrl Pts',(83.3717098693772,4.90762609764359,130.481267522271));
#50305=CARTESIAN_POINT('Ctrl Pts',(83.3639369691118,4.89861918578571,130.344456936292));
#50306=CARTESIAN_POINT('Ctrl Pts',(83.3561640688464,4.88389669073476,130.208168241041));
#50307=CARTESIAN_POINT('Ctrl Pts',(83.3483911685809,4.86355425510033,130.072907905359));
#50308=CARTESIAN_POINT('Ctrl Pts',(83.3409008328188,4.84395131824052,129.942564623577));
#50309=CARTESIAN_POINT('Ctrl Pts',(83.3334104970567,4.81913000295944,129.81317653501));
#50310=CARTESIAN_POINT('Ctrl Pts',(83.3259201612946,4.78921976052727,129.68518362179));
#50311=CARTESIAN_POINT('Ctrl Pts',(83.3181458271755,4.75817546216255,129.552337818363));
#50312=CARTESIAN_POINT('Ctrl Pts',(83.3103714930564,4.72155038663917,129.420574259306));
#50313=CARTESIAN_POINT('Ctrl Pts',(83.3025971589373,4.67943374567492,129.290397975247));
#50314=CARTESIAN_POINT('Ctrl Pts',(83.2948324059902,4.63736900970662,129.160382121823));
#50315=CARTESIAN_POINT('Ctrl Pts',(83.2870676530432,4.58982629352253,129.031950019602));
#50316=CARTESIAN_POINT('Ctrl Pts',(83.2793029000961,4.53694570819007,128.905596097296));
#50317=CARTESIAN_POINT('Ctrl Pts',(83.2715458592111,4.4841176446004,128.779367671487));
#50318=CARTESIAN_POINT('Ctrl Pts',(83.263788818326,4.42596241234019,128.655213676307));
#50319=CARTESIAN_POINT('Ctrl Pts',(83.256031777441,4.36266966509301,128.53361262279));
#50320=CARTESIAN_POINT('Ctrl Pts',(83.2482805862009,4.29942464739888,128.412103269574));
#50321=CARTESIAN_POINT('Ctrl Pts',(83.2405293949608,4.2310500059352,128.293143371438));
#50322=CARTESIAN_POINT('Ctrl Pts',(83.2327782037206,4.15778301686013,128.177190381892));
#50323=CARTESIAN_POINT('Ctrl Pts',(83.2250303069435,4.08454716820992,128.06128667546));
#50324=CARTESIAN_POINT('Ctrl Pts',(83.2172824101664,4.00642331607687,127.948387665562));
#50325=CARTESIAN_POINT('Ctrl Pts',(83.2095345133893,3.92369397634716,127.838924959441));
#50326=CARTESIAN_POINT('Ctrl Pts',(83.2017882373052,3.84098194181183,127.729485150559));
#50327=CARTESIAN_POINT('Ctrl Pts',(83.1940419612211,3.75366657145433,127.623480527428));
#50328=CARTESIAN_POINT('Ctrl Pts',(83.186295685137,3.66207265084623,127.521312192333));
#50329=CARTESIAN_POINT('Ctrl Pts',(83.1785493518716,3.57047805411269,127.419143103055));
#50330=CARTESIAN_POINT('Ctrl Pts',(83.1708030186063,3.47460510508494,127.320810649428));
#50331=CARTESIAN_POINT('Ctrl Pts',(83.1630566853409,3.37481739969444,127.22668112085));
#50332=CARTESIAN_POINT('Ctrl Pts',(83.155308617338,3.27500734753928,127.132530512618));
#50333=CARTESIAN_POINT('Ctrl Pts',(83.147560549335,3.17128107886975,127.042584970567));
#50334=CARTESIAN_POINT('Ctrl Pts',(83.139812481332,3.06403709244642,126.95717206505));
#50335=CARTESIAN_POINT('Ctrl Pts',(83.1320561785901,2.95667912583795,126.87166838168));
#50336=CARTESIAN_POINT('Ctrl Pts',(83.1242998758483,2.84579627938628,126.790707201957));
#50337=CARTESIAN_POINT('Ctrl Pts',(83.1165435731064,2.73181845572317,126.714574438868));
#50338=CARTESIAN_POINT('Ctrl Pts',(83.1087831305922,2.61777979866376,126.638401041431));
#50339=CARTESIAN_POINT('Ctrl Pts',(83.101022688078,2.50064320662612,126.567061398925));
#50340=CARTESIAN_POINT('Ctrl Pts',(83.0932622455639,2.38086440965835,126.500796080427));
#50341=CARTESIAN_POINT('Ctrl Pts',(83.0854893452984,2.26089333313223,126.434424386956));
#50342=CARTESIAN_POINT('Ctrl Pts',(83.077716445033,2.13827192572876,126.373143470186));
#50343=CARTESIAN_POINT('Ctrl Pts',(83.0699435447675,2.01347799119524,126.317146622059));
#50344=CARTESIAN_POINT('Ctrl Pts',(83.0624532090056,1.89322063052057,126.26318540041));
#50345=CARTESIAN_POINT('Ctrl Pts',(83.0549628732436,1.77094623994652,126.214130853583));
#50346=CARTESIAN_POINT('Ctrl Pts',(83.0474725374817,1.64709496047675,126.170111891648));
#50347=CARTESIAN_POINT('Ctrl Pts',(83.0396982033626,1.51854782210056,126.124423937392));
#50348=CARTESIAN_POINT('Ctrl Pts',(83.0319238692435,1.38789466019064,126.084016228531));
#50349=CARTESIAN_POINT('Ctrl Pts',(83.0241495351245,1.25560859243,126.049086690113));
#50350=CARTESIAN_POINT('Ctrl Pts',(83.0163847821774,1.12348555542521,126.014200199229));
#50351=CARTESIAN_POINT('Ctrl Pts',(83.0086200292303,0.989733991047752,125.984778544455));
#50352=CARTESIAN_POINT('Ctrl Pts',(83.0008552762832,0.854845609630931,125.960971097179));
#50353=CARTESIAN_POINT('Ctrl Pts',(82.9930982353982,0.720091201256126,125.937187295795));
#50354=CARTESIAN_POINT('Ctrl Pts',(82.9853411945132,0.584202605330228,125.919006672712));
#50355=CARTESIAN_POINT('Ctrl Pts',(82.9775841536282,0.447684919187686,125.906528313819));
#50356=CARTESIAN_POINT('Ctrl Pts',(82.9698329623881,0.311270182094217,125.894059364952));
#50357=CARTESIAN_POINT('Ctrl Pts',(82.962081771148,0.174227686818944,125.887284156587));
#50358=CARTESIAN_POINT('Ctrl Pts',(82.9543305799078,0.0370705555139816,
125.886250326365));
#50359=CARTESIAN_POINT('Ctrl Pts',(82.9465826831307,-0.100028280351483,
125.88521693555));
#50360=CARTESIAN_POINT('Ctrl Pts',(82.9388347863537,-0.237241265203965,
125.88992007237));
#50361=CARTESIAN_POINT('Ctrl Pts',(82.9310868895766,-0.374052568908428,
125.900355342468));
#50362=CARTESIAN_POINT('Ctrl Pts',(82.9233406134925,-0.510835254637467,
125.910788429732));
#50363=CARTESIAN_POINT('Ctrl Pts',(82.9155943374084,-0.647216036759036,
125.926951235604));
#50364=CARTESIAN_POINT('Ctrl Pts',(82.9078480613243,-0.782681902026623,
125.948787314367));
#50365=CARTESIAN_POINT('Ctrl Pts',(82.9001017280589,-0.918148767272268,
125.970623554319));
#50366=CARTESIAN_POINT('Ctrl Pts',(82.8923553947936,-1.05270031620454,125.99813308851));
#50367=CARTESIAN_POINT('Ctrl Pts',(82.8846090615282,-1.1858318466972,126.031208001751));
#50368=CARTESIAN_POINT('Ctrl Pts',(82.8768609935253,-1.31899319107304,126.064290321891));
#50369=CARTESIAN_POINT('Ctrl Pts',(82.8691129255224,-1.45073350486117,126.102940406882));
#50370=CARTESIAN_POINT('Ctrl Pts',(82.8613648575194,-1.58056179553372,126.147000048209));
#50371=CARTESIAN_POINT('Ctrl Pts',(82.8536085547776,-1.71052806925866,126.191106516647));
#50372=CARTESIAN_POINT('Ctrl Pts',(82.8458522520357,-1.83857788967085,126.240633900505));
#50373=CARTESIAN_POINT('Ctrl Pts',(82.8380959492938,-1.96423833720213,126.295375053477));
#50374=CARTESIAN_POINT('Ctrl Pts',(82.8303355067796,-2.0899658534979,126.35014542345));
#50375=CARTESIAN_POINT('Ctrl Pts',(82.8225750642655,-2.21330110439849,126.41013493647));
#50376=CARTESIAN_POINT('Ctrl Pts',(82.8148146217513,-2.33379535910342,126.475090207401));
#50377=CARTESIAN_POINT('Ctrl Pts',(82.8070417214859,-2.45448304188299,126.5401497503));
#50378=CARTESIAN_POINT('Ctrl Pts',(82.7992688212205,-2.57232027862376,126.610190780783));
#50379=CARTESIAN_POINT('Ctrl Pts',(82.791495920955,-2.68688618274251,126.684915788043));
#50380=CARTESIAN_POINT('Ctrl Pts',(82.784005585193,-2.79728732767313,126.756924353067));
#50381=CARTESIAN_POINT('Ctrl Pts',(82.7765152494309,-2.90465060204122,126.833282080065));
#50382=CARTESIAN_POINT('Ctrl Pts',(82.7690249136688,-3.00862964318992,126.913688344987));
#50383=CARTESIAN_POINT('Ctrl Pts',(82.7613420431602,-3.11528140542439,126.996161406421));
#50384=CARTESIAN_POINT('Ctrl Pts',(82.7536591726516,-3.21872733800515,127.083168532652));
#50385=CARTESIAN_POINT('Ctrl Pts',(82.745976302143,-3.31855067135844,127.174428868328));
#50386=CARTESIAN_POINT('Ctrl Pts',(82.7383022090127,-3.41825996046872,127.26558494265));
#50387=CARTESIAN_POINT('Ctrl Pts',(82.7306281158823,-3.51435458540387,127.360984299332));
#50388=CARTESIAN_POINT('Ctrl Pts',(82.7229540227519,-3.6064479870395,127.460303802965));
#50389=CARTESIAN_POINT('Ctrl Pts',(82.7152869408815,-3.69845724964197,127.559532565602));
#50390=CARTESIAN_POINT('Ctrl Pts',(82.707619859011,-3.78647228722919,127.662674061862));
#50391=CARTESIAN_POINT('Ctrl Pts',(82.6999527771406,-3.87014120156489,127.769366360166));
#50392=CARTESIAN_POINT('Ctrl Pts',(82.6922909466049,-3.95375280941995,127.875985582822));
#50393=CARTESIAN_POINT('Ctrl Pts',(82.6846291160692,-4.03302396835301,127.986150456225));
#50394=CARTESIAN_POINT('Ctrl Pts',(82.6769672855335,-4.1076414774153,128.099464213724));
#50395=CARTESIAN_POINT('Ctrl Pts',(82.6693034728789,-4.18227829006,128.212807285542));
#50396=CARTESIAN_POINT('Ctrl Pts',(82.6616396602243,-4.25225879858586,128.329300553625));
#50397=CARTESIAN_POINT('Ctrl Pts',(82.6539758475697,-4.31731150377491,128.448515876953));
#50398=CARTESIAN_POINT('Ctrl Pts',(82.6463181977752,-4.38231189678708,128.567635333199));
#50399=CARTESIAN_POINT('Ctrl Pts',(82.6386605479807,-4.44239221228738,128.689472118773));
#50400=CARTESIAN_POINT('Ctrl Pts',(82.6310028981862,-4.49732678689444,128.813573126551));
#50401=CARTESIAN_POINT('Ctrl Pts',(82.6233360041015,-4.55232767834325,128.937823948666));
#50402=CARTESIAN_POINT('Ctrl Pts',(82.6156691100169,-4.60217022978223,129.064344097086));
#50403=CARTESIAN_POINT('Ctrl Pts',(82.6080022159322,-4.64667602726679,129.192658113962));
#50404=CARTESIAN_POINT('Ctrl Pts',(82.6003353218475,-4.69118182475133,129.320972130837));
#50405=CARTESIAN_POINT('Ctrl Pts',(82.5926684277628,-4.73035075754575,129.451079628921));
#50406=CARTESIAN_POINT('Ctrl Pts',(82.5850015336782,-4.76405452823407,129.582490119308));
#50407=CARTESIAN_POINT('Ctrl Pts',(84.3346156335084,-4.75804253168638,129.583987249709));
#50408=CARTESIAN_POINT('Ctrl Pts',(84.3113635676693,-4.85784354785265,129.98349577336));
#50409=CARTESIAN_POINT('Ctrl Pts',(84.2881115018302,-4.90980811696373,130.395781134632));
#50410=CARTESIAN_POINT('Ctrl Pts',(84.2648594359911,-4.91222318036076,130.80752443328));
#50411=CARTESIAN_POINT('',(84.6101405640561,-4.91824832607103,130.800302834979));
#50412=CARTESIAN_POINT('Ctrl Pts',(84.6799609333917,-4.76405452823403,129.582490119308));
#50413=CARTESIAN_POINT('Ctrl Pts',(84.6707042004072,-4.80445476993726,129.74001004855));
#50414=CARTESIAN_POINT('Ctrl Pts',(84.6614474674228,-4.83707811757595,129.89968928916));
#50415=CARTESIAN_POINT('Ctrl Pts',(84.6521907344383,-4.86172162268382,130.060824521584));
#50416=CARTESIAN_POINT('Ctrl Pts',(84.6430287442445,-4.88611290117459,130.220310532665));
#50417=CARTESIAN_POINT('Ctrl Pts',(84.6338667540507,-4.90268679106901,130.381222826308));
#50418=CARTESIAN_POINT('Ctrl Pts',(84.624704763857,-4.91129310170885,130.542858931898));
#50419=CARTESIAN_POINT('Ctrl Pts',(84.61985003059,-4.91585339283395,130.628506281694));
#50420=CARTESIAN_POINT('Ctrl Pts',(84.6149952973231,-4.91817741637721,130.71435651443));
#50421=CARTESIAN_POINT('Ctrl Pts',(84.6101405640561,-4.91824832607103,130.800302834979));
#50422=CARTESIAN_POINT('Ctrl Pts',(84.6101405640085,-4.91824832607172,130.800302835822));
#50423=CARTESIAN_POINT('Ctrl Pts',(84.6022231096909,-4.91836397076609,130.940470385572));
#50424=CARTESIAN_POINT('Ctrl Pts',(84.5943056553734,-4.91248282886161,131.080726137906));
#50425=CARTESIAN_POINT('Ctrl Pts',(84.5863882010559,-4.90061189985685,131.220516921713));
#50426=CARTESIAN_POINT('Ctrl Pts',(84.578667859878,-4.88903650979596,131.356827470689));
#50427=CARTESIAN_POINT('Ctrl Pts',(84.5709475187001,-4.87176610452158,131.492695517939));
#50428=CARTESIAN_POINT('Ctrl Pts',(84.5632271775222,-4.8488598733744,131.627610877742));
#50429=CARTESIAN_POINT('Ctrl Pts',(84.5555069731711,-4.82595404819188,131.762523846455));
#50430=CARTESIAN_POINT('Ctrl Pts',(84.54778676882,-4.79741266131601,131.896483773269));
#50431=CARTESIAN_POINT('Ctrl Pts',(84.5400665644689,-4.76334632654458,132.028989065665));
#50432=CARTESIAN_POINT('Ctrl Pts',(84.5323447993181,-4.72927310455587,132.161521146759));
#50433=CARTESIAN_POINT('Ctrl Pts',(84.5246230341673,-4.68967281016804,132.292597627195));
#50434=CARTESIAN_POINT('Ctrl Pts',(84.5169012690165,-4.64470626867822,132.421730933913));
#50435=CARTESIAN_POINT('Ctrl Pts',(84.5088363016307,-4.59774114043548,132.556603710638));
#50436=CARTESIAN_POINT('Ctrl Pts',(84.5007713342449,-4.54492193281031,132.68935615759));
#50437=CARTESIAN_POINT('Ctrl Pts',(84.4927063668591,-4.48648790788609,132.819455978806));
#50438=CARTESIAN_POINT('Ctrl Pts',(84.4849719812259,-4.43044908451035,132.944223028686));
#50439=CARTESIAN_POINT('Ctrl Pts',(84.4772375955927,-4.36924685834616,133.066550280504));
#50440=CARTESIAN_POINT('Ctrl Pts',(84.4695032099595,-4.30313890311398,133.185994225619));
#50441=CARTESIAN_POINT('Ctrl Pts',(84.4617632195596,-4.23698304237429,133.305524726472));
#50442=CARTESIAN_POINT('Ctrl Pts',(84.4540232291596,-4.16591457714448,133.422167425126));
#50443=CARTESIAN_POINT('Ctrl Pts',(84.4462832387597,-4.09023414508859,133.535508306881));
#50444=CARTESIAN_POINT('Ctrl Pts',(84.438532281005,-4.01444647593027,133.649009789566));
#50445=CARTESIAN_POINT('Ctrl Pts',(84.4307813232504,-3.93403403030331,133.759199803597));
#50446=CARTESIAN_POINT('Ctrl Pts',(84.4230303654957,-3.84933743120659,133.865697646253));
#50447=CARTESIAN_POINT('Ctrl Pts',(84.4220607971261,-3.83874272199816,133.879019476012));
#50448=CARTESIAN_POINT('Ctrl Pts',(84.4210912287565,-3.82808102276651,133.892283580521));
#50449=CARTESIAN_POINT('Ctrl Pts',(84.4201216603869,-3.81735303935774,133.905489256531));
#50450=CARTESIAN_POINT('Ctrl Pts',(84.4123473262678,-3.73133236246876,134.011376928601));
#50451=CARTESIAN_POINT('Ctrl Pts',(84.4045729921487,-3.6407663472809,134.113850479068));
#50452=CARTESIAN_POINT('Ctrl Pts',(84.3967986580296,-3.54595610683364,134.212494762653));
#50453=CARTESIAN_POINT('Ctrl Pts',(84.3890339050825,-3.45126271153431,134.311017475975));
#50454=CARTESIAN_POINT('Ctrl Pts',(84.3812691521355,-3.35233576668802,134.405720033102));
#50455=CARTESIAN_POINT('Ctrl Pts',(84.3735043991884,-3.24951752112357,134.496219084844));
#50456=CARTESIAN_POINT('Ctrl Pts',(84.3657473583034,-3.14680139608996,134.586628251652));
#50457=CARTESIAN_POINT('Ctrl Pts',(84.3579903174183,-3.04020195322999,134.672841964832));
#50458=CARTESIAN_POINT('Ctrl Pts',(84.3502332765333,-2.93009903210777,134.754512858245));
#50459=CARTESIAN_POINT('Ctrl Pts',(84.3424820852932,-2.82007914045499,134.836122163002));
#50460=CARTESIAN_POINT('Ctrl Pts',(84.3347308940531,-2.70656134201906,134.91319523481));
#50461=CARTESIAN_POINT('Ctrl Pts',(84.326979702813,-2.58995909232361,134.985424472925));
#50462=CARTESIAN_POINT('Ctrl Pts',(84.3192318060359,-2.47340640169484,135.057623011687));
#50463=CARTESIAN_POINT('Ctrl Pts',(84.3114839092588,-2.35377219890244,135.124981606019));
#50464=CARTESIAN_POINT('Ctrl Pts',(84.3037360124817,-2.23149931820796,135.187235684841));
#50465=CARTESIAN_POINT('Ctrl Pts',(84.2959897363977,-2.10925201436422,135.249476741451));
#50466=CARTESIAN_POINT('Ctrl Pts',(84.2882434603135,-1.98436747867226,135.3066152291));
#50467=CARTESIAN_POINT('Ctrl Pts',(84.2804971842294,-1.85731321564461,135.358432496829));
#50468=CARTESIAN_POINT('Ctrl Pts',(84.2727508509641,-1.73025801473109,135.410250147061));
#50469=CARTESIAN_POINT('Ctrl Pts',(84.2650045176987,-1.6010334165379,135.456746351351));
#50470=CARTESIAN_POINT('Ctrl Pts',(84.2572581844333,-1.47012660075453,135.497750739882));
#50471=CARTESIAN_POINT('Ctrl Pts',(84.2495101164304,-1.3391904692975,135.538764311062));
#50472=CARTESIAN_POINT('Ctrl Pts',(84.2417620484274,-1.20657174363826,135.574283502373));
#50473=CARTESIAN_POINT('Ctrl Pts',(84.2340139804244,-1.07277205622993,135.604188028825));
#50474=CARTESIAN_POINT('Ctrl Pts',(84.2262576776826,-0.938830164921678,
135.634124338163));
#50475=CARTESIAN_POINT('Ctrl Pts',(84.2185013749408,-0.803705186746459,
135.658433976839));
#50476=CARTESIAN_POINT('Ctrl Pts',(84.2107450721989,-0.667908775237267,
135.677047856704));
#50477=CARTESIAN_POINT('Ctrl Pts',(84.2029846296847,-0.532039885094409,
135.695671671358));
#50478=CARTESIAN_POINT('Ctrl Pts',(84.1952241871706,-0.395499236582211,
135.708593632932));
#50479=CARTESIAN_POINT('Ctrl Pts',(84.1874637446564,-0.258801877121319,
135.715796726374));
#50480=CARTESIAN_POINT('Ctrl Pts',(84.179690844391,-0.121885078923599,135.723011382861));
#50481=CARTESIAN_POINT('Ctrl Pts',(84.1719179441256,0.0151885417650007,
135.724488821566));
#50482=CARTESIAN_POINT('Ctrl Pts',(84.1641450438601,0.151904764818353,135.720264197268));
#50483=CARTESIAN_POINT('Ctrl Pts',(84.1566547080981,0.28365100879633,135.716193148704));
#50484=CARTESIAN_POINT('Ctrl Pts',(84.149164372336,0.415065081377441,135.706827430218));
#50485=CARTESIAN_POINT('Ctrl Pts',(84.141674036574,0.545694790682726,135.692243621272));
#50486=CARTESIAN_POINT('Ctrl Pts',(84.1338997024549,0.681277365120273,135.677106862778));
#50487=CARTESIAN_POINT('Ctrl Pts',(84.1261253683358,0.816444408737128,135.65630056632));
#50488=CARTESIAN_POINT('Ctrl Pts',(84.1183510342168,0.950683889099185,135.629853670665));
#50489=CARTESIAN_POINT('Ctrl Pts',(84.1105862812697,1.08475793129884,135.603439368445));
#50490=CARTESIAN_POINT('Ctrl Pts',(84.1028215283226,1.21790630483996,135.571398373355));
#50491=CARTESIAN_POINT('Ctrl Pts',(84.0950567753756,1.34962149333913,135.533811419426));
#50492=CARTESIAN_POINT('Ctrl Pts',(84.0872997344906,1.48120586045632,135.49626179739));
#50493=CARTESIAN_POINT('Ctrl Pts',(84.0795426936056,1.61135950175615,135.45317728492));
#50494=CARTESIAN_POINT('Ctrl Pts',(84.0717856527206,1.73958485570378,135.404689691916));
#50495=CARTESIAN_POINT('Ctrl Pts',(84.0640344614805,1.86771351391429,135.356238663782));
#50496=CARTESIAN_POINT('Ctrl Pts',(84.0562832702404,1.99391641493001,135.302392802894));
#50497=CARTESIAN_POINT('Ctrl Pts',(84.0485320790003,2.11771128272307,135.243333695377));
#50498=CARTESIAN_POINT('Ctrl Pts',(84.0407841822232,2.24145353439541,135.184299689555));
#50499=CARTESIAN_POINT('Ctrl Pts',(84.0330362854461,2.3627894363381,135.120057012091));
#50500=CARTESIAN_POINT('Ctrl Pts',(84.025288388669,2.48125703467484,135.050835224858));
#50501=CARTESIAN_POINT('Ctrl Pts',(84.0175421125849,2.59969985214396,134.981627917331));
#50502=CARTESIAN_POINT('Ctrl Pts',(84.0097958365008,2.71527522206464,134.907443768799));
#50503=CARTESIAN_POINT('Ctrl Pts',(84.0020495604167,2.82754648958596,134.828557917865));
#50504=CARTESIAN_POINT('Ctrl Pts',(83.9943032271513,2.93981858586836,134.749671484613));
#50505=CARTESIAN_POINT('Ctrl Pts',(83.986556893886,3.04878621118814,134.666083504474));
#50506=CARTESIAN_POINT('Ctrl Pts',(83.9788105606206,3.15404269607171,134.57811176647));
#50507=CARTESIAN_POINT('Ctrl Pts',(83.9710624926177,3.25932275241521,134.490120327806));
#50508=CARTESIAN_POINT('Ctrl Pts',(83.9633144246147,3.36088971463278,134.39774342846));
#50509=CARTESIAN_POINT('Ctrl Pts',(83.9555663566117,3.45837123896024,134.301338089045));
#50510=CARTESIAN_POINT('Ctrl Pts',(83.9478100538699,3.55595636781174,134.204830288888));
#50511=CARTESIAN_POINT('Ctrl Pts',(83.940053751128,3.64944710662891,134.104285771311));
#50512=CARTESIAN_POINT('Ctrl Pts',(83.9322974483862,3.73850876836502,134.000097661091));
#50513=CARTESIAN_POINT('Ctrl Pts',(83.924537005872,3.82761796499148,133.895853942539));
#50514=CARTESIAN_POINT('Ctrl Pts',(83.9167765633578,3.91229313294367,133.787963063781));
#50515=CARTESIAN_POINT('Ctrl Pts',(83.9090161208437,3.99224156126581,133.676849151747));
#50516=CARTESIAN_POINT('Ctrl Pts',(83.9012432205782,4.07231832990279,133.565556869797));
#50517=CARTESIAN_POINT('Ctrl Pts',(83.8934703203128,4.14765298112051,133.451031542294));
#50518=CARTESIAN_POINT('Ctrl Pts',(83.8856974200474,4.21799714309085,133.333724799209));
#50519=CARTESIAN_POINT('Ctrl Pts',(83.8782070842853,4.28578411758761,133.220682451712));
#50520=CARTESIAN_POINT('Ctrl Pts',(83.8707167485232,4.34893698957217,133.105057670997));
#50521=CARTESIAN_POINT('Ctrl Pts',(83.8632264127612,4.40727576675886,132.987272291968));
#50522=CARTESIAN_POINT('Ctrl Pts',(83.8554520786421,4.46782647641402,132.865021044493));
#50523=CARTESIAN_POINT('Ctrl Pts',(83.847677744523,4.52338263865331,132.740054871111));
#50524=CARTESIAN_POINT('Ctrl Pts',(83.8399034104039,4.57369183444076,132.61282020132));
#50525=CARTESIAN_POINT('Ctrl Pts',(83.8321386574568,4.62393902864056,132.485742336887));
#50526=CARTESIAN_POINT('Ctrl Pts',(83.8243739045097,4.66895198025211,132.356401898778));
#50527=CARTESIAN_POINT('Ctrl Pts',(83.8166091515626,4.70852428810017,132.225269513615));
#50528=CARTESIAN_POINT('Ctrl Pts',(83.8088521106776,4.74805729217426,132.094267370985));
#50529=CARTESIAN_POINT('Ctrl Pts',(83.8010950697926,4.78216029391859,131.961477195029));
#50530=CARTESIAN_POINT('Ctrl Pts',(83.7933380289076,4.81067524457085,131.827388844827));
#50531=CARTESIAN_POINT('Ctrl Pts',(83.7855868376674,4.83916869187696,131.693401611694));
#50532=CARTESIAN_POINT('Ctrl Pts',(83.7778356464273,4.86208239479386,131.558118533749));
#50533=CARTESIAN_POINT('Ctrl Pts',(83.7700844551872,4.8793084448986,131.422043515209));
#50534=CARTESIAN_POINT('Ctrl Pts',(83.7623365584102,4.89652717347253,131.286026332183));
#50535=CARTESIAN_POINT('Ctrl Pts',(83.7545886616331,4.90806300826837,131.149218265083));
#50536=CARTESIAN_POINT('Ctrl Pts',(83.746840764856,4.91385938883968,131.01213205259));
#50537=CARTESIAN_POINT('Ctrl Pts',(83.7390944887719,4.91965455693313,130.875074515578));
#50538=CARTESIAN_POINT('Ctrl Pts',(83.7313482126878,4.91971264229594,130.73773933927));
#50539=CARTESIAN_POINT('Ctrl Pts',(83.7236019366037,4.91402910421499,130.600642612893));
#50540=CARTESIAN_POINT('Ctrl Pts',(83.7158556033384,4.90834552417944,130.463544874499));
#50541=CARTESIAN_POINT('Ctrl Pts',(83.7081092700731,4.89692025232132,130.326685980179));
#50542=CARTESIAN_POINT('Ctrl Pts',(83.7003629368077,4.87980083876222,130.190579845209));
#50543=CARTESIAN_POINT('Ctrl Pts',(83.6926148688048,4.86267759142913,130.054443230213));
#50544=CARTESIAN_POINT('Ctrl Pts',(83.6848668008018,4.839857713749,129.919060097846));
#50545=CARTESIAN_POINT('Ctrl Pts',(83.6771187327988,4.81144031637585,129.784936689824));
#50546=CARTESIAN_POINT('Ctrl Pts',(83.669362430057,4.78299271665458,129.650670733848));
#50547=CARTESIAN_POINT('Ctrl Pts',(83.6616061273151,4.74893579441718,129.517667559799));
#50548=CARTESIAN_POINT('Ctrl Pts',(83.6538498245733,4.70941939014874,129.386421242913));
#50549=CARTESIAN_POINT('Ctrl Pts',(83.6460893820591,4.66988189478548,129.255104875916));
#50550=CARTESIAN_POINT('Ctrl Pts',(83.6383289395449,4.62487923944162,129.125547603642));
#50551=CARTESIAN_POINT('Ctrl Pts',(83.6305684970308,4.57461003669489,128.998224943075));
#50552=CARTESIAN_POINT('Ctrl Pts',(83.6227955967653,4.52426013736125,128.870697892869));
#50553=CARTESIAN_POINT('Ctrl Pts',(83.6150226964999,4.46862695494123,128.74541298026));
#50554=CARTESIAN_POINT('Ctrl Pts',(83.6072497962345,4.40795620748108,128.62282328453));
#50555=CARTESIAN_POINT('Ctrl Pts',(83.5997594604724,4.34949099451108,128.504690033024));
#50556=CARTESIAN_POINT('Ctrl Pts',(83.5922691247103,4.28634826173377,128.389059714973));
#50557=CARTESIAN_POINT('Ctrl Pts',(83.5847787889482,4.21878562057418,128.276311775052));
#50558=CARTESIAN_POINT('Ctrl Pts',(83.5770044548292,4.1486613213403,128.159288962721));
#50559=CARTESIAN_POINT('Ctrl Pts',(83.5692301207101,4.07355320317336,128.045000720816));
#50560=CARTESIAN_POINT('Ctrl Pts',(83.561455786591,3.99370042119825,127.933900722667));
#50561=CARTESIAN_POINT('Ctrl Pts',(83.5536910336439,3.91394605064022,127.822937645338));
#50562=CARTESIAN_POINT('Ctrl Pts',(83.5459262806968,3.82945887679586,127.7151553082));
#50563=CARTESIAN_POINT('Ctrl Pts',(83.5381615277497,3.74052328629487,127.610981747594));
#50564=CARTESIAN_POINT('Ctrl Pts',(83.5304044868647,3.65167602787645,127.506911653637));
#50565=CARTESIAN_POINT('Ctrl Pts',(83.5226474459798,3.55838939748659,127.406443498738));
#50566=CARTESIAN_POINT('Ctrl Pts',(83.5148904050948,3.46099009822698,127.309975034595));
#50567=CARTESIAN_POINT('Ctrl Pts',(83.5071392138547,3.36366424853672,127.213579318072));
#50568=CARTESIAN_POINT('Ctrl Pts',(83.4993880226145,3.26223217977089,127.121177562756));
#50569=CARTESIAN_POINT('Ctrl Pts',(83.4916368313744,3.15705951368052,127.033132927598));
#50570=CARTESIAN_POINT('Ctrl Pts',(83.4838889345974,3.05193154877831,126.945125713759));
#50571=CARTESIAN_POINT('Ctrl Pts',(83.4761410378203,2.94306644780682,126.861472187243));
#50572=CARTESIAN_POINT('Ctrl Pts',(83.4683931410432,2.83086502003662,126.782497081737));
#50573=CARTESIAN_POINT('Ctrl Pts',(83.4606468649591,2.71868706238611,126.70353849612));
#50574=CARTESIAN_POINT('Ctrl Pts',(83.452900588875,2.60317448558009,126.629256609866));
#50575=CARTESIAN_POINT('Ctrl Pts',(83.4451543127909,2.48475903573677,126.559934202039));
#50576=CARTESIAN_POINT('Ctrl Pts',(83.4374079795255,2.36634271177799,126.49061128249));
#50577=CARTESIAN_POINT('Ctrl Pts',(83.4296616462602,2.24502380942433,126.42624811194));
#50578=CARTESIAN_POINT('Ctrl Pts',(83.4219153129948,2.12126040215382,126.367082468886));
#50579=CARTESIAN_POINT('Ctrl Pts',(83.4141672449918,1.99746927892603,126.307903576096));
#50580=CARTESIAN_POINT('Ctrl Pts',(83.4064191769888,1.87123291412311,126.253924695519));
#50581=CARTESIAN_POINT('Ctrl Pts',(83.3986711089859,1.74303079496808,126.205336078569));
#50582=CARTESIAN_POINT('Ctrl Pts',(83.390914806244,1.61469242107529,126.156695821059));
#50583=CARTESIAN_POINT('Ctrl Pts',(83.3831585035021,1.48438448554622,126.113457409923));
#50584=CARTESIAN_POINT('Ctrl Pts',(83.3754022007603,1.35260366031213,126.075761839851));
#50585=CARTESIAN_POINT('Ctrl Pts',(83.3676417582461,1.22075249968341,126.038046150517));
#50586=CARTESIAN_POINT('Ctrl Pts',(83.3598813157319,1.08742726280206,126.005879288723));
#50587=CARTESIAN_POINT('Ctrl Pts',(83.3521208732177,0.953135370523119,125.979351184626));
#50588=CARTESIAN_POINT('Ctrl Pts',(83.3443479729523,0.818627900977277,125.952780495262));
#50589=CARTESIAN_POINT('Ctrl Pts',(83.3365750726869,0.683151061731547,125.931866711726));
#50590=CARTESIAN_POINT('Ctrl Pts',(83.3288021724214,0.547218857826103,125.916648004887));
#50591=CARTESIAN_POINT('Ctrl Pts',(83.3213118366594,0.416228131925276,125.901982536376));
#50592=CARTESIAN_POINT('Ctrl Pts',(83.3138215008974,0.284814881115421,125.892605294422));
#50593=CARTESIAN_POINT('Ctrl Pts',(83.3063311651354,0.153437588217663,125.888504642355));
#50594=CARTESIAN_POINT('Ctrl Pts',(83.2985568310163,0.0170790853282307,
125.884248512817));
#50595=CARTESIAN_POINT('Ctrl Pts',(83.2907824968972,-0.119672621885078,
125.885663513408));
#50596=CARTESIAN_POINT('Ctrl Pts',(83.2830081627781,-0.256306576012906,
125.892793657665));
#50597=CARTESIAN_POINT('Ctrl Pts',(83.275243409831,-0.392772141003785,125.899915014656));
#50598=CARTESIAN_POINT('Ctrl Pts',(83.2674786568839,-0.529119854969217,
125.912737480859));
#50599=CARTESIAN_POINT('Ctrl Pts',(83.2597139039368,-0.664835880894192,
125.931253157846));
#50600=CARTESIAN_POINT('Ctrl Pts',(83.2519568630518,-0.800417111748958,
125.949750444802));
#50601=CARTESIAN_POINT('Ctrl Pts',(83.2441998221668,-0.935367518250482,
125.97392963717));
#50602=CARTESIAN_POINT('Ctrl Pts',(83.2364427812818,-1.06917586962323,126.003730864886));
#50603=CARTESIAN_POINT('Ctrl Pts',(83.2286915900417,-1.2028833150766,126.033509619265));
#50604=CARTESIAN_POINT('Ctrl Pts',(83.2209403988015,-1.33545003956144,126.068901885636));
#50605=CARTESIAN_POINT('Ctrl Pts',(83.2131892075614,-1.46637287968032,126.109796352351));
#50606=CARTESIAN_POINT('Ctrl Pts',(83.2054413107844,-1.59724007410003,126.150673437826));
#50607=CARTESIAN_POINT('Ctrl Pts',(83.1976934140073,-1.72646440140175,126.19704795606));
#50608=CARTESIAN_POINT('Ctrl Pts',(83.1899455172302,-1.85355600673697,126.248758221352));
#50609=CARTESIAN_POINT('Ctrl Pts',(83.1821992411461,-1.98062102724805,126.300457669972));
#50610=CARTESIAN_POINT('Ctrl Pts',(83.174452965062,-2.10555385124076,126.357490498368));
#50611=CARTESIAN_POINT('Ctrl Pts',(83.1667066889779,-2.22788319935621,126.419646315297));
#50612=CARTESIAN_POINT('Ctrl Pts',(83.1589603557126,-2.35021345047912,126.481802591045));
#50613=CARTESIAN_POINT('Ctrl Pts',(83.1512140224473,-2.46993983882313,126.549081753685));
#50614=CARTESIAN_POINT('Ctrl Pts',(83.1434676891819,-2.58661471470199,126.621226938111));
#50615=CARTESIAN_POINT('Ctrl Pts',(83.135719621179,-2.70331571911033,126.693388278952));
#50616=CARTESIAN_POINT('Ctrl Pts',(83.127971553176,-2.81696351877103,126.770417604401));
#50617=CARTESIAN_POINT('Ctrl Pts',(83.120223485173,-2.92713887522575,126.852014343814));
#50618=CARTESIAN_POINT('Ctrl Pts',(83.1124671824312,-3.03743132736064,126.933697805213));
#50619=CARTESIAN_POINT('Ctrl Pts',(83.1047108796893,-3.14424364932664,127.01995814451));
#50620=CARTESIAN_POINT('Ctrl Pts',(83.0969545769474,-3.24718875498737,127.110453708617));
#50621=CARTESIAN_POINT('Ctrl Pts',(83.0891941344333,-3.35018880555083,127.200997572931));
#50622=CARTESIAN_POINT('Ctrl Pts',(83.0814336919191,-3.4493172445754,127.295780896167));
#50623=CARTESIAN_POINT('Ctrl Pts',(83.0736732494049,-3.54422413790561,127.394425380236));
#50624=CARTESIAN_POINT('Ctrl Pts',(83.0659003491395,-3.63928338420618,127.493228217187));
#50625=CARTESIAN_POINT('Ctrl Pts',(83.058127448874,-3.73010728342227,127.595904308099));
#50626=CARTESIAN_POINT('Ctrl Pts',(83.0503545486086,-3.81638588904121,127.702041838261));
#50627=CARTESIAN_POINT('Ctrl Pts',(83.0428642128466,-3.89952805002321,127.804321001857));
#50628=CARTESIAN_POINT('Ctrl Pts',(83.0353738770846,-3.97844946126611,127.909814063253));
#50629=CARTESIAN_POINT('Ctrl Pts',(83.0278835413225,-4.05291209186718,128.018128997959));
#50630=CARTESIAN_POINT('Ctrl Pts',(83.0197220855216,-4.13404643454255,128.13614874771));
#50631=CARTESIAN_POINT('Ctrl Pts',(83.0115606297207,-4.21014831198426,128.257899455109));
#50632=CARTESIAN_POINT('Ctrl Pts',(83.0033991739198,-4.28086393652291,128.382917448818));
#50633=CARTESIAN_POINT('Ctrl Pts',(82.9955264872026,-4.34907749689586,128.50351204891));
#50634=CARTESIAN_POINT('Ctrl Pts',(82.9876538004853,-4.41227920792827,128.627146321197));
#50635=CARTESIAN_POINT('Ctrl Pts',(82.9797811137681,-4.47019316825711,128.753371563239));
#50636=CARTESIAN_POINT('Ctrl Pts',(82.971916466424,-4.52804798842798,128.879467907505));
#50637=CARTESIAN_POINT('Ctrl Pts',(82.9640518190799,-4.58062564658625,129.008149616813));
#50638=CARTESIAN_POINT('Ctrl Pts',(82.9561871717358,-4.62769532321257,129.138942034141));
#50639=CARTESIAN_POINT('Ctrl Pts',(82.9483306012287,-4.67471666021335,129.269600130247));
#50640=CARTESIAN_POINT('Ctrl Pts',(82.9404740307217,-4.71624115631711,129.402364263728));
#50641=CARTESIAN_POINT('Ctrl Pts',(82.9326174602146,-4.7520856600064,129.536738851241));
#50642=CARTESIAN_POINT('Ctrl Pts',(82.9317269973803,-4.75614827209916,129.551968852161));
#50643=CARTESIAN_POINT('Ctrl Pts',(82.930836534546,-4.76013797056555,129.567219520401));
#50644=CARTESIAN_POINT('Ctrl Pts',(82.9299460717117,-4.76405452823408,129.582490119308));
#50645=CARTESIAN_POINT('Origin',(213.235140564004,0.,130.804360617566));
#50646=CARTESIAN_POINT('',(80.8348654436249,-4.76405452823406,129.582490119308));
#50647=CARTESIAN_POINT('',(81.1802785703833,-4.76405452823402,129.582490119308));
#50648=CARTESIAN_POINT('',(213.235140564004,-4.76405452823405,129.582490119308));
#50649=CARTESIAN_POINT('',(82.5148594360284,-4.91824936146013,130.806866809299));
#50650=CARTESIAN_POINT('Ctrl Pts',(82.5148594359911,-4.9182493614598,130.806866809955));
#50651=CARTESIAN_POINT('Ctrl Pts',(82.5067653872794,-4.91817690027791,130.949067449884));
#50652=CARTESIAN_POINT('Ctrl Pts',(82.4986713385677,-4.91193788385077,131.091106696134));
#50653=CARTESIAN_POINT('Ctrl Pts',(82.490577289856,-4.89957058449461,131.232602546918));
#50654=CARTESIAN_POINT('Ctrl Pts',(82.4828029557369,-4.88769179295649,131.368509317391));
#50655=CARTESIAN_POINT('Ctrl Pts',(82.4750286216178,-4.87013512454896,131.504136729985));
#50656=CARTESIAN_POINT('Ctrl Pts',(82.4672542874987,-4.84691722233577,131.638972205267));
#50657=CARTESIAN_POINT('Ctrl Pts',(82.4594895345516,-4.82372793411203,131.773641507876));
#50658=CARTESIAN_POINT('Ctrl Pts',(82.4517247816046,-4.79489135987155,131.907520433511));
#50659=CARTESIAN_POINT('Ctrl Pts',(82.4439600286575,-4.76047603140207,132.040099674546));
#50660=CARTESIAN_POINT('Ctrl Pts',(82.4362029877725,-4.726094884722,132.17254723601));
#50661=CARTESIAN_POINT('Ctrl Pts',(82.4284459468875,-4.68614610804533,132.303697305779));
#50662=CARTESIAN_POINT('Ctrl Pts',(82.4206889060025,-4.64074953320795,132.43304930253));
#50663=CARTESIAN_POINT('Ctrl Pts',(82.4129377147623,-4.59538719228079,132.562303753934));
#50664=CARTESIAN_POINT('Ctrl Pts',(82.4051865235222,-4.54458535931464,132.689762463825));
#50665=CARTESIAN_POINT('Ctrl Pts',(82.3974353322821,-4.48851399484798,132.814938937491));
#50666=CARTESIAN_POINT('Ctrl Pts',(82.389687435505,-4.43246646220698,132.940062207817));
#50667=CARTESIAN_POINT('Ctrl Pts',(82.3819395387279,-4.37115401213281,133.062904815141));
#50668=CARTESIAN_POINT('Ctrl Pts',(82.3741916419508,-4.30479505477375,133.182999429764));
#50669=CARTESIAN_POINT('Ctrl Pts',(82.3664453658667,-4.23844997827803,133.303068923183));
#50670=CARTESIAN_POINT('Ctrl Pts',(82.3586990897826,-4.16706068314926,133.420391225269));
#50671=CARTESIAN_POINT('Ctrl Pts',(82.3509528136985,-4.09089175024567,133.534523204349));
#50672=CARTESIAN_POINT('Ctrl Pts',(82.3432064804331,-4.01472225508037,133.648656025926));
#50673=CARTESIAN_POINT('Ctrl Pts',(82.3354601471678,-3.93377326876532,133.759598152307));
#50674=CARTESIAN_POINT('Ctrl Pts',(82.3277138139024,-3.84835272986233,133.866935405071));
#50675=CARTESIAN_POINT('Ctrl Pts',(82.3199657458995,-3.76291306162192,133.974296695268));
#50676=CARTESIAN_POINT('Ctrl Pts',(82.3122176778965,-3.67300009158274,134.078051199583));
#50677=CARTESIAN_POINT('Ctrl Pts',(82.3044696098935,-3.57896180232162,134.177818113967));
#50678=CARTESIAN_POINT('Ctrl Pts',(82.2967133071516,-3.48482356804753,134.277691061815));
#50679=CARTESIAN_POINT('Ctrl Pts',(82.2889570044098,-3.38655152475659,134.373567668799));
#50680=CARTESIAN_POINT('Ctrl Pts',(82.2812007016679,-3.28453065244961,134.465103910344));
#50681=CARTESIAN_POINT('Ctrl Pts',(82.2734402591538,-3.18245532853136,134.556689007537));
#50682=CARTESIAN_POINT('Ctrl Pts',(82.2656798166396,-3.07662749023608,134.643928874735));
#50683=CARTESIAN_POINT('Ctrl Pts',(82.2579193741255,-2.96746411810112,134.726520707399));
#50684=CARTESIAN_POINT('Ctrl Pts',(82.25014647386,-2.85812550723007,134.809245123806));
#50685=CARTESIAN_POINT('Ctrl Pts',(82.2423735735946,-2.74544098410032,134.887306372584));
#50686=CARTESIAN_POINT('Ctrl Pts',(82.2346006733291,-2.62985608838645,134.960445315557));
#50687=CARTESIAN_POINT('Ctrl Pts',(82.2271103375671,-2.51847299477234,135.030925473728));
#50688=CARTESIAN_POINT('Ctrl Pts',(82.2196200018051,-2.40439700593382,135.09683483517));
#50689=CARTESIAN_POINT('Ctrl Pts',(82.212129666043,-2.28804551597863,135.157983336556));
#50690=CARTESIAN_POINT('Ctrl Pts',(82.2043553319239,-2.16728252391777,135.221450301959));
#50691=CARTESIAN_POINT('Ctrl Pts',(82.1965809978048,-2.04368553241509,135.279989308987));
#50692=CARTESIAN_POINT('Ctrl Pts',(82.1888066636858,-1.91769478504621,135.33333729822));
#50693=CARTESIAN_POINT('Ctrl Pts',(82.1810419107387,-1.79185931001342,135.386619540823));
#50694=CARTESIAN_POINT('Ctrl Pts',(82.1732771577916,-1.66363630547921,135.434723343701));
#50695=CARTESIAN_POINT('Ctrl Pts',(82.1655124048445,-1.53349130947839,135.477431071374));
#50696=CARTESIAN_POINT('Ctrl Pts',(82.1577553639595,-1.40347557532224,135.52009638113));
#50697=CARTESIAN_POINT('Ctrl Pts',(82.1499983230745,-1.27154201766559,135.557376160133));
#50698=CARTESIAN_POINT('Ctrl Pts',(82.1422412821895,-1.13817656178746,135.589100649866));
#50699=CARTESIAN_POINT('Ctrl Pts',(82.1344900909494,-1.00491167783714,135.620801215915));
#50700=CARTESIAN_POINT('Ctrl Pts',(82.1267388997092,-0.870217423766029,
135.646954741106));
#50701=CARTESIAN_POINT('Ctrl Pts',(82.1189877084691,-0.734594969174971,
135.667441255779));
#50702=CARTESIAN_POINT('Ctrl Pts',(82.111239811692,-0.599030157744871,135.687919063137));
#50703=CARTESIAN_POINT('Ctrl Pts',(82.103491914915,-0.4625383162154,135.702734592286));
#50704=CARTESIAN_POINT('Ctrl Pts',(82.0957440181379,-0.325630678316247,
135.711818994755));
#50705=CARTESIAN_POINT('Ctrl Pts',(82.0879977420538,-0.188751678543555,
135.720901496962));
#50706=CARTESIAN_POINT('Ctrl Pts',(82.0802514659697,-0.0514574452606876,
135.724255231154));
#50707=CARTESIAN_POINT('Ctrl Pts',(82.0725051898856,0.0857361898891255,
135.721863273208));
#50708=CARTESIAN_POINT('Ctrl Pts',(82.0647588566203,0.222930837771094,135.719471297604));
#50709=CARTESIAN_POINT('Ctrl Pts',(82.0570125233549,0.360024495132422,135.711333552044));
#50710=CARTESIAN_POINT('Ctrl Pts',(82.0492661900896,0.496502253621075,135.697485240407));
#50711=CARTESIAN_POINT('Ctrl Pts',(82.0415181220866,0.633010575357471,135.683633827536));
#50712=CARTESIAN_POINT('Ctrl Pts',(82.0337700540836,0.768902334870384,135.664069343301));
#50713=CARTESIAN_POINT('Ctrl Pts',(82.0260219860807,0.903669057845986,135.63887872141));
#50714=CARTESIAN_POINT('Ctrl Pts',(82.0182656833388,1.0385790124986,135.613661326626));
#50715=CARTESIAN_POINT('Ctrl Pts',(82.0105093805969,1.172361157148,135.582805921387));
#50716=CARTESIAN_POINT('Ctrl Pts',(82.0027530778551,1.30451796308115,135.546450446586));
#50717=CARTESIAN_POINT('Ctrl Pts',(81.9949926353409,1.43674530508087,135.510075567774));
#50718=CARTESIAN_POINT('Ctrl Pts',(81.9872321928268,1.56734520770359,135.468194889389));
#50719=CARTESIAN_POINT('Ctrl Pts',(81.9794717503126,1.69583752474888,135.420995555717));
#50720=CARTESIAN_POINT('Ctrl Pts',(81.9716988500472,1.82453610906841,135.373720453484));
#50721=CARTESIAN_POINT('Ctrl Pts',(81.9639259497818,1.9511199856992,135.3211097845));
#50722=CARTESIAN_POINT('Ctrl Pts',(81.9561530495163,2.07513030927651,135.263398323397));
#50723=CARTESIAN_POINT('Ctrl Pts',(81.9486627137543,2.19463254522889,135.207784819271));
#50724=CARTESIAN_POINT('Ctrl Pts',(81.9411723779922,2.31174481608836,135.147435078846));
#50725=CARTESIAN_POINT('Ctrl Pts',(81.9336820422302,2.42608160448446,135.082597533736));
#50726=CARTESIAN_POINT('Ctrl Pts',(81.9259077081111,2.54475350696426,135.015301653397));
#50727=CARTESIAN_POINT('Ctrl Pts',(81.918133373992,2.66081122441982,134.94295776719));
#50728=CARTESIAN_POINT('Ctrl Pts',(81.910359039873,2.77379547510258,134.865794074463));
#50729=CARTESIAN_POINT('Ctrl Pts',(81.9025942869259,2.886640482794,134.78872547909));
#50730=CARTESIAN_POINT('Ctrl Pts',(81.8948295339788,2.99641924049701,134.706849114367));
#50731=CARTESIAN_POINT('Ctrl Pts',(81.8870647810317,3.10269701064094,134.620439013336));
#50732=CARTESIAN_POINT('Ctrl Pts',(81.8793077401467,3.2088692242053,134.534114736034));
#50733=CARTESIAN_POINT('Ctrl Pts',(81.8715506992617,3.31154706866801,134.443265928586));
#50734=CARTESIAN_POINT('Ctrl Pts',(81.8637936583767,3.41032506689953,134.348209655064));
#50735=CARTESIAN_POINT('Ctrl Pts',(81.8560424671366,3.50902857587426,134.253225064218));
#50736=CARTESIAN_POINT('Ctrl Pts',(81.8482912758964,3.60383781173919,134.154039592729));
#50737=CARTESIAN_POINT('Ctrl Pts',(81.8405400846563,3.6943809462108,134.051010042246));
#50738=CARTESIAN_POINT('Ctrl Pts',(81.8327921878792,3.78488559743488,133.94802428207));
#50739=CARTESIAN_POINT('Ctrl Pts',(81.8250442911022,3.87112749605116,133.841197985536));
#50740=CARTESIAN_POINT('Ctrl Pts',(81.8172963943251,3.95277238357095,133.730924053779));
#50741=CARTESIAN_POINT('Ctrl Pts',(81.809550118241,4.0344001927404,133.620673188951));
#50742=CARTESIAN_POINT('Ctrl Pts',(81.8018038421569,4.11143267098657,133.506976437366));
#50743=CARTESIAN_POINT('Ctrl Pts',(81.7940575660728,4.18357675996161,133.390258634892));
#50744=CARTESIAN_POINT('Ctrl Pts',(81.7863112328074,4.25572138148787,133.273539970833));
#50745=CARTESIAN_POINT('Ctrl Pts',(81.7785648995421,4.32297733617789,133.15380054395));
#50746=CARTESIAN_POINT('Ctrl Pts',(81.7708185662767,4.3850959215103,133.031492589779));
#50747=CARTESIAN_POINT('Ctrl Pts',(81.7630704982737,4.44722841786919,132.909157245589));
#50748=CARTESIAN_POINT('Ctrl Pts',(81.7553224302708,4.50422107854499,132.784252578039));
#50749=CARTESIAN_POINT('Ctrl Pts',(81.7475743622678,4.55587220054092,132.65725337076));
#50750=CARTESIAN_POINT('Ctrl Pts',(81.739818059526,4.60757821796396,132.530119187212));
#50751=CARTESIAN_POINT('Ctrl Pts',(81.7320617567842,4.6539312086601,132.400886379795));
#50752=CARTESIAN_POINT('Ctrl Pts',(81.7243054540423,4.69477829978572,132.270048093927));
#50753=CARTESIAN_POINT('Ctrl Pts',(81.7165450115281,4.7356471922338,132.139139975726));
#50754=CARTESIAN_POINT('Ctrl Pts',(81.7087845690139,4.77100422883346,132.006625049208));
#50755=CARTESIAN_POINT('Ctrl Pts',(81.7010241264998,4.80074732862297,131.873008431029));
#50756=CARTESIAN_POINT('Ctrl Pts',(81.6932512262343,4.83053817467672,131.739177319593));
#50757=CARTESIAN_POINT('Ctrl Pts',(81.6854783259689,4.85469700615102,131.604241367469));
#50758=CARTESIAN_POINT('Ctrl Pts',(81.6777054257035,4.87317332846537,131.468713515681));
#50759=CARTESIAN_POINT('Ctrl Pts',(81.6702150899414,4.89097798992463,131.338112442679));
#50760=CARTESIAN_POINT('Ctrl Pts',(81.6627247541794,4.90350608713774,131.206962063589));
#50761=CARTESIAN_POINT('Ctrl Pts',(81.6552344184173,4.91075825110139,131.075721008448));
#50762=CARTESIAN_POINT('Ctrl Pts',(81.6474600842982,4.91828538306595,130.939503908812));
#50763=CARTESIAN_POINT('Ctrl Pts',(81.6396857501791,4.92015245386743,130.802757626599));
#50764=CARTESIAN_POINT('Ctrl Pts',(81.63191141606,4.91630320107411,130.665991915872));
#50765=CARTESIAN_POINT('Ctrl Pts',(81.6241466631129,4.91245869214083,130.52939475666));
#50766=CARTESIAN_POINT('Ctrl Pts',(81.6163819101659,4.90291188767403,130.392778603635));
#50767=CARTESIAN_POINT('Ctrl Pts',(81.6086171572188,4.8876583531565,130.256657335378));
#50768=CARTESIAN_POINT('Ctrl Pts',(81.6008601163338,4.87241996866449,130.120671264684));
#50769=CARTESIAN_POINT('Ctrl Pts',(81.5931030754487,4.85148617696365,129.985179486618));
#50770=CARTESIAN_POINT('Ctrl Pts',(81.5853460345637,4.82490456274736,129.850694521451));
#50771=CARTESIAN_POINT('Ctrl Pts',(81.5775948433236,4.79834299393312,129.716310972442));
#50772=CARTESIAN_POINT('Ctrl Pts',(81.5698436520835,4.76614215552057,129.582933107092));
#50773=CARTESIAN_POINT('Ctrl Pts',(81.5620924608434,4.72840125257126,129.451066615073));
#50774=CARTESIAN_POINT('Ctrl Pts',(81.5543445640663,4.69067639051244,129.319256169831));
#50775=CARTESIAN_POINT('Ctrl Pts',(81.5465966672892,4.64741625453818,129.188956195374));
#50776=CARTESIAN_POINT('Ctrl Pts',(81.5388487705121,4.59877072862245,129.060660285495));
#50777=CARTESIAN_POINT('Ctrl Pts',(81.531102494428,4.55013537830209,128.932391212354));
#50778=CARTESIAN_POINT('Ctrl Pts',(81.5233562183439,4.49611701724912,128.806125735303));
#50779=CARTESIAN_POINT('Ctrl Pts',(81.5156099422598,4.43691466671601,128.682340046794));
#50780=CARTESIAN_POINT('Ctrl Pts',(81.5078636089945,4.37771187916459,128.558553444526));
#50781=CARTESIAN_POINT('Ctrl Pts',(81.5001172757291,4.31332519445919,128.43724702003));
#50782=CARTESIAN_POINT('Ctrl Pts',(81.4923709424638,4.24400066137644,128.318874458132));
#50783=CARTESIAN_POINT('Ctrl Pts',(81.4846228744608,4.1746606035452,128.20047538752));
#50784=CARTESIAN_POINT('Ctrl Pts',(81.4768748064578,4.1003806944691,128.085011824201));
#50785=CARTESIAN_POINT('Ctrl Pts',(81.4691267384549,4.0214513576687,127.972910098767));
#50786=CARTESIAN_POINT('Ctrl Pts',(81.461370435713,3.94243813382978,127.860689230286));
#50787=CARTESIAN_POINT('Ctrl Pts',(81.4536141329712,3.85876583659238,127.751837657333));
#50788=CARTESIAN_POINT('Ctrl Pts',(81.4458578302293,3.77076673165735,127.646750553304));
#50789=CARTESIAN_POINT('Ctrl Pts',(81.4380973877152,3.68272065895036,127.541607361124));
#50790=CARTESIAN_POINT('Ctrl Pts',(81.4303369452009,3.59034344017912,127.44023293023));
#50791=CARTESIAN_POINT('Ctrl Pts',(81.4225765026868,3.49400486703745,127.342986172115));
#50792=CARTESIAN_POINT('Ctrl Pts',(81.4148036024213,3.3975116426657,127.245583304872));
#50793=CARTESIAN_POINT('Ctrl Pts',(81.407030702156,3.2970446430831,127.152321617622));
#50794=CARTESIAN_POINT('Ctrl Pts',(81.3992578018905,3.19300812654605,127.063520850039));
#50795=CARTESIAN_POINT('Ctrl Pts',(81.3917674661285,3.09275359943771,126.977948214034));
#50796=CARTESIAN_POINT('Ctrl Pts',(81.3842771303665,2.98918481369777,126.896517987611));
#50797=CARTESIAN_POINT('Ctrl Pts',(81.3767867946045,2.88268796883494,126.819477540632));
#50798=CARTESIAN_POINT('Ctrl Pts',(81.3690124604854,2.77215326372966,126.73951608169));
#50799=CARTESIAN_POINT('Ctrl Pts',(81.3612381263663,2.65811394102197,126.664030556397));
#50800=CARTESIAN_POINT('Ctrl Pts',(81.3534637922472,2.54096846002318,126.593343834452));
#50801=CARTESIAN_POINT('Ctrl Pts',(81.3456990393001,2.42396735036012,126.522744227575));
#50802=CARTESIAN_POINT('Ctrl Pts',(81.337934286353,2.30386803064109,126.456931856807));
#50803=CARTESIAN_POINT('Ctrl Pts',(81.3301695334059,2.18110044450705,126.396188216959));
#50804=CARTESIAN_POINT('Ctrl Pts',(81.3224124925209,2.0584547928702,126.335504908551));
#50805=CARTESIAN_POINT('Ctrl Pts',(81.3146554516359,1.93314649690615,126.27988048477));
#50806=CARTESIAN_POINT('Ctrl Pts',(81.3068984107509,1.80563247512261,126.229551940989));
#50807=CARTESIAN_POINT('Ctrl Pts',(81.2991472195108,1.67821461265507,126.179261350355));
#50808=CARTESIAN_POINT('Ctrl Pts',(81.2913960282707,1.54859469736793,126.13425883353));
#50809=CARTESIAN_POINT('Ctrl Pts',(81.2836448370306,1.41725180306267,126.094734264105));
#50810=CARTESIAN_POINT('Ctrl Pts',(81.2758969402535,1.28596473299101,126.055226493676));
#50811=CARTESIAN_POINT('Ctrl Pts',(81.2681490434763,1.15295651401138,126.021192152314));
#50812=CARTESIAN_POINT('Ctrl Pts',(81.2604011466993,1.01872343651059,125.992771937888));
#50813=CARTESIAN_POINT('Ctrl Pts',(81.2526548706151,0.884518437675891,125.964357668359));
#50814=CARTESIAN_POINT('Ctrl Pts',(81.244908594531,0.749089472187793,125.94155527084));
#50815=CARTESIAN_POINT('Ctrl Pts',(81.2371623184469,0.61294475009084,125.924454696768));
#50816=CARTESIAN_POINT('Ctrl Pts',(81.2294159851816,0.476799023004475,125.907353996464));
#50817=CARTESIAN_POINT('Ctrl Pts',(81.2216696519163,0.339937916683439,125.895955252318));
#50818=CARTESIAN_POINT('Ctrl Pts',(81.2139233186509,0.202876124396793,125.890296684257));
#50819=CARTESIAN_POINT('Ctrl Pts',(81.2061752506479,0.0657836380721764,
125.884636848999));
#50820=CARTESIAN_POINT('Ctrl Pts',(81.1984271826449,-0.0715092330902062,
125.884719763892));
#50821=CARTESIAN_POINT('Ctrl Pts',(81.1906791146419,-0.208486824079857,
125.890531529504));
#50822=CARTESIAN_POINT('Ctrl Pts',(81.1829228119001,-0.345609996483358,
125.896349471929));
#50823=CARTESIAN_POINT('Ctrl Pts',(81.1751665091582,-0.482416828112082,
125.907908411289));
#50824=CARTESIAN_POINT('Ctrl Pts',(81.1674102064163,-0.618395250667723,
125.925142403912));
#50825=CARTESIAN_POINT('Ctrl Pts',(81.1596497639022,-0.754446249001807,
125.942385594836));
#50826=CARTESIAN_POINT('Ctrl Pts',(81.151889321388,-0.889667571971185,125.965309809141));
#50827=CARTESIAN_POINT('Ctrl Pts',(81.1441288788739,-1.02355737572774,125.99379793103));
#50828=CARTESIAN_POINT('Ctrl Pts',(81.1363559786084,-1.15766211128347,126.022331784581));
#50829=CARTESIAN_POINT('Ctrl Pts',(81.128583078343,-1.29043067739237,126.056447296702));
#50830=CARTESIAN_POINT('Ctrl Pts',(81.1208101780776,-1.42137555654968,126.095977180574));
#50831=CARTESIAN_POINT('Ctrl Pts',(81.1133198423155,-1.54756025951983,126.134070053597));
#50832=CARTESIAN_POINT('Ctrl Pts',(81.1058295065534,-1.67205127373518,126.177190379836));
#50833=CARTESIAN_POINT('Ctrl Pts',(81.0983391707913,-1.79443172965663,126.225146948157));
#50834=CARTESIAN_POINT('Ctrl Pts',(81.0905645511766,-1.92145694231566,126.274923632216));
#50835=CARTESIAN_POINT('Ctrl Pts',(81.082789931562,-2.04661061911688,126.330068596351));
#50836=CARTESIAN_POINT('Ctrl Pts',(81.0750153119473,-2.16940569024455,126.390421105788));
#50837=CARTESIAN_POINT('Ctrl Pts',(81.0672503393391,-2.29204839316452,126.450698727824));
#50838=CARTESIAN_POINT('Ctrl Pts',(81.059485366731,-2.41233796615942,126.516170867084));
#50839=CARTESIAN_POINT('Ctrl Pts',(81.0517203941228,-2.52980514577362,126.586627934368));
#50840=CARTESIAN_POINT('Ctrl Pts',(81.0439631991324,-2.64715466691435,126.657014429847));
#50841=CARTESIAN_POINT('Ctrl Pts',(81.0362060041421,-2.76168708758237,126.732375716743));
#50842=CARTESIAN_POINT('Ctrl Pts',(81.0284488091517,-2.87295601645599,126.812455459623));
#50843=CARTESIAN_POINT('Ctrl Pts',(81.0203828355881,-2.98865405419512,126.895722812044));
#50844=CARTESIAN_POINT('Ctrl Pts',(81.0123168620245,-3.1008230318001,126.984091844958));
#50845=CARTESIAN_POINT('Ctrl Pts',(81.0042508884609,-3.20899182468354,127.077223038724));
#50846=CARTESIAN_POINT('Ctrl Pts',(80.9965033315683,-3.31289048865175,127.166677735852));
#50847=CARTESIAN_POINT('Ctrl Pts',(80.9887557746757,-3.41309844799211,127.260525492969));
#50848=CARTESIAN_POINT('Ctrl Pts',(80.9810082177832,-3.50923050459839,127.3584232519));
#50849=CARTESIAN_POINT('Ctrl Pts',(80.9732623064951,-3.60534214246561,127.45630021705));
#50850=CARTESIAN_POINT('Ctrl Pts',(80.9655163952071,-3.69737932647029,127.558225193637));
#50851=CARTESIAN_POINT('Ctrl Pts',(80.957770483919,-3.78499327957319,127.66381784026));
#50852=CARTESIAN_POINT('Ctrl Pts',(80.950024540456,-3.8726075966066,127.769410925495));
#50853=CARTESIAN_POINT('Ctrl Pts',(80.942278596993,-3.9557983970433,127.878671409902));
#50854=CARTESIAN_POINT('Ctrl Pts',(80.93453265353,-4.03425707023025,127.991185728975));
#50855=CARTESIAN_POINT('Ctrl Pts',(80.9267850004671,-4.11273305995673,128.103724880978));
#50856=CARTESIAN_POINT('Ctrl Pts',(80.9190373474043,-4.18647462132941,128.219518975694));
#50857=CARTESIAN_POINT('Ctrl Pts',(80.9112896943415,-4.25521659140841,128.338125668762));
#50858=CARTESIAN_POINT('Ctrl Pts',(80.9035350182762,-4.32402087390902,128.456839875046));
#50859=CARTESIAN_POINT('Ctrl Pts',(80.8957803422108,-4.38781632098078,128.578371431358));
#50860=CARTESIAN_POINT('Ctrl Pts',(80.8880256661455,-4.4463836983863,128.702253325056));
#50861=CARTESIAN_POINT('Ctrl Pts',(80.880266827541,-4.50498251346924,128.826201715824));
#50862=CARTESIAN_POINT('Ctrl Pts',(80.8725079889365,-4.55834751555681,128.952502598175));
#50863=CARTESIAN_POINT('Ctrl Pts',(80.864749150332,-4.60630808629086,129.080670135875));
#50864=CARTESIAN_POINT('Ctrl Pts',(80.8569807784024,-4.65432758642592,129.208995153691));
#50865=CARTESIAN_POINT('Ctrl Pts',(80.8492124064728,-4.69692927701624,129.339191035204));
#50866=CARTESIAN_POINT('Ctrl Pts',(80.8414440345432,-4.7339926362512,129.470757684749));
#50867=CARTESIAN_POINT('Ctrl Pts',(80.8392511709038,-4.74445491760923,129.507896447486));
#50868=CARTESIAN_POINT('Ctrl Pts',(80.8370583072644,-4.75447620437195,129.545144379941));
#50869=CARTESIAN_POINT('Ctrl Pts',(80.834865443625,-4.76405452823406,129.582490119308));
#50870=CARTESIAN_POINT('Ctrl Pts',(82.5850015336782,-4.76405452823407,129.582490119308));
#50871=CARTESIAN_POINT('Ctrl Pts',(82.5773335909647,-4.79776290870888,129.713918583184));
#50872=CARTESIAN_POINT('Ctrl Pts',(82.5696656482512,-4.82600456944424,129.846649998683));
#50873=CARTESIAN_POINT('Ctrl Pts',(82.5619977055377,-4.8487025933768,129.9801845299));
#50874=CARTESIAN_POINT('Ctrl Pts',(82.5541413272862,-4.87195840895081,130.117000599878));
#50875=CARTESIAN_POINT('Ctrl Pts',(82.5462849490346,-4.88939453811731,130.254659320202));
#50876=CARTESIAN_POINT('Ctrl Pts',(82.5384285707831,-4.90098484835512,130.39261970547));
#50877=CARTESIAN_POINT('Ctrl Pts',(82.5305721925315,-4.91257515859294,130.530580090738));
#50878=CARTESIAN_POINT('Ctrl Pts',(82.52271581428,-4.91831969490199,130.668841692983));
#50879=CARTESIAN_POINT('Ctrl Pts',(82.5148594360285,-4.91824936146013,130.806866809299));
#50880=CARTESIAN_POINT('',(82.8601405639574,-4.91824929785569,130.806988666655));
#50881=CARTESIAN_POINT('Ctrl Pts',(82.9299460717117,-4.76405452823408,129.582490119308));
#50882=CARTESIAN_POINT('Ctrl Pts',(82.922096320366,-4.79858039797789,129.717105961436));
#50883=CARTESIAN_POINT('Ctrl Pts',(82.9142465690203,-4.82741833376636,129.853271812892));
#50884=CARTESIAN_POINT('Ctrl Pts',(82.9063968176746,-4.8504404544737,129.99047459354));
#50885=CARTESIAN_POINT('Ctrl Pts',(82.8985501336065,-4.87345357932459,130.127623762423));
#50886=CARTESIAN_POINT('Ctrl Pts',(82.8907034495385,-4.89065534906821,130.265808683398));
#50887=CARTESIAN_POINT('Ctrl Pts',(82.8828567654704,-4.90196890338083,130.404505727903));
#50888=CARTESIAN_POINT('Ctrl Pts',(82.8752846983164,-4.91288650784435,130.538348676841));
#50889=CARTESIAN_POINT('Ctrl Pts',(82.8677126311625,-4.91832107151274,130.672668169506));
#50890=CARTESIAN_POINT('Ctrl Pts',(82.8601405640085,-4.91824929785617,130.806988665748));
#50891=CARTESIAN_POINT('Ctrl Pts',(82.8601405639574,-4.91824929785569,130.806988666655));
#50892=CARTESIAN_POINT('Ctrl Pts',(82.851577185383,-4.9181681277878,130.958893983424));
#50893=CARTESIAN_POINT('Ctrl Pts',(82.8430138068086,-4.91104525378221,131.110552142097));
#50894=CARTESIAN_POINT('Ctrl Pts',(82.8344504282341,-4.89697364043576,131.261342266407));
#50895=CARTESIAN_POINT('Ctrl Pts',(82.8258400492867,-4.88282479459631,131.412960007063));
#50896=CARTESIAN_POINT('Ctrl Pts',(82.8172296703393,-4.86165081058521,131.563699927854));
#50897=CARTESIAN_POINT('Ctrl Pts',(82.8086192913919,-4.83359637437726,131.71294696575));
#50898=CARTESIAN_POINT('Ctrl Pts',(82.7999845646764,-4.80546260799013,131.862616032954));
#50899=CARTESIAN_POINT('Ctrl Pts',(82.791349837961,-4.7704095404838,132.010783547129));
#50900=CARTESIAN_POINT('Ctrl Pts',(82.7827151112456,-4.72863183602382,132.156848703222));
#50901=CARTESIAN_POINT('Ctrl Pts',(82.774048941806,-4.68670200111655,132.30344574487));
#50902=CARTESIAN_POINT('Ctrl Pts',(82.7653827723665,-4.63799858526797,132.447924879106));
#50903=CARTESIAN_POINT('Ctrl Pts',(82.7567166029269,-4.5827656387525,132.589701526964));
#50904=CARTESIAN_POINT('Ctrl Pts',(82.7542897077878,-4.56729807025514,132.629405003791));
#50905=CARTESIAN_POINT('Ctrl Pts',(82.7518628126487,-4.55131870898378,132.668896688921));
#50906=CARTESIAN_POINT('Ctrl Pts',(82.7494359175096,-4.53483355529004,132.708164097003));
#50907=CARTESIAN_POINT('Ctrl Pts',(82.7416615833905,-4.4820248901134,132.833953607023));
#50908=CARTESIAN_POINT('Ctrl Pts',(82.7338872492714,-4.42389479364209,132.957743443183));
#50909=CARTESIAN_POINT('Ctrl Pts',(82.7261129151523,-4.36061562278928,133.079050586064));
#50910=CARTESIAN_POINT('Ctrl Pts',(82.7183481622052,-4.29741443785907,133.200208228733));
#50911=CARTESIAN_POINT('Ctrl Pts',(82.7105834092581,-4.22907698383168,133.318888922698));
#50912=CARTESIAN_POINT('Ctrl Pts',(82.702818656311,-4.15582402939334,133.434628607566));
#50913=CARTESIAN_POINT('Ctrl Pts',(82.695061615426,-4.08264383082204,133.550253338146));
#50914=CARTESIAN_POINT('Ctrl Pts',(82.687304574541,-4.00455805526149,133.662942544433));
#50915=CARTESIAN_POINT('Ctrl Pts',(82.679547533656,-3.921833657157,133.772256139327));
#50916=CARTESIAN_POINT('Ctrl Pts',(82.6717963424159,-3.83917164216473,133.881487299989));
#50917=CARTESIAN_POINT('Ctrl Pts',(82.6640451511758,-3.75187820219944,133.987347605575));
#50918=CARTESIAN_POINT('Ctrl Pts',(82.6562939599357,-3.66026372536504,134.089425688958));
#50919=CARTESIAN_POINT('Ctrl Pts',(82.6485460631586,-3.56868818712707,134.191460386432));
#50920=CARTESIAN_POINT('Ctrl Pts',(82.6407981663814,-3.47279552538185,134.289715768633));
#50921=CARTESIAN_POINT('Ctrl Pts',(82.6330502696044,-3.37293641236893,134.383813511601));
#50922=CARTESIAN_POINT('Ctrl Pts',(82.6253039935202,-3.27309818772981,134.477891571349));
#50923=CARTESIAN_POINT('Ctrl Pts',(82.6175577174362,-3.1692954464943,134.567813453768));
#50924=CARTESIAN_POINT('Ctrl Pts',(82.6098114413521,-3.06191543821069,134.653237974893));
#50925=CARTESIAN_POINT('Ctrl Pts',(82.6020651080867,-2.95453463727226,134.738663126603));
#50926=CARTESIAN_POINT('Ctrl Pts',(82.5943187748213,-2.84357682255117,134.819590607373));
#50927=CARTESIAN_POINT('Ctrl Pts',(82.586572441556,-2.72946169029487,134.895720042465));
#50928=CARTESIAN_POINT('Ctrl Pts',(82.578824373553,-2.61532100274585,134.971866526217));
#50929=CARTESIAN_POINT('Ctrl Pts',(82.57107630555,-2.49802191586648,135.04321260925));
#50930=CARTESIAN_POINT('Ctrl Pts',(82.563328237547,-2.37801206723457,135.109501924258));
#50931=CARTESIAN_POINT('Ctrl Pts',(82.5555719348052,-2.25787467070748,135.175861692339));
#50932=CARTESIAN_POINT('Ctrl Pts',(82.5478156320633,-2.13502110003358,135.237153767129));
#50933=CARTESIAN_POINT('Ctrl Pts',(82.5400593293215,-2.00992299332331,135.293168101009));
#50934=CARTESIAN_POINT('Ctrl Pts',(82.5322988868073,-1.88475811798676,135.349212331425));
#50935=CARTESIAN_POINT('Ctrl Pts',(82.5245384442931,-1.75734668256869,135.399973063411));
#50936=CARTESIAN_POINT('Ctrl Pts',(82.516778001779,-1.62817821159039,135.445289271812));
#50937=CARTESIAN_POINT('Ctrl Pts',(82.5090051015135,-1.49880238791544,135.490678225814));
#50938=CARTESIAN_POINT('Ctrl Pts',(82.5012322012481,-1.36766426655302,135.530605076922));
#50939=CARTESIAN_POINT('Ctrl Pts',(82.4934593009826,-1.23526723443079,135.564959101165));
#50940=CARTESIAN_POINT('Ctrl Pts',(82.4859689652206,-1.10768316791465,135.598064270094));
#50941=CARTESIAN_POINT('Ctrl Pts',(82.4784786294586,-0.97893043172973,135.625994685055));
#50942=CARTESIAN_POINT('Ctrl Pts',(82.4709882936966,-0.849464520335529,
135.648696804413));
#50943=CARTESIAN_POINT('Ctrl Pts',(82.4632139595775,-0.715089869560122,
135.672259681526));
#50944=CARTESIAN_POINT('Ctrl Pts',(82.4554396254585,-0.579521237438656,
135.690264615214));
#50945=CARTESIAN_POINT('Ctrl Pts',(82.4476652913394,-0.443258165010642,
135.702595530435));
#50946=CARTESIAN_POINT('Ctrl Pts',(82.4399005383923,-0.307163024641307,
135.714911248905));
#50947=CARTESIAN_POINT('Ctrl Pts',(82.4321357854452,-0.170375532459404,
135.72156682744));
#50948=CARTESIAN_POINT('Ctrl Pts',(82.4243710324981,-0.0334054464857481,
135.72249716901));
#50949=CARTESIAN_POINT('Ctrl Pts',(82.4166139916131,0.103428598867672,135.72342658655));
#50950=CARTESIAN_POINT('Ctrl Pts',(82.4088569507281,0.240444488682426,135.718642080652));
#50951=CARTESIAN_POINT('Ctrl Pts',(82.4010999098431,0.377127669820007,135.708130369824));
#50952=CARTESIAN_POINT('Ctrl Pts',(82.393348718603,0.513707777107358,135.697626585958));
#50953=CARTESIAN_POINT('Ctrl Pts',(82.3855975273628,0.64995528687834,135.681404223587));
#50954=CARTESIAN_POINT('Ctrl Pts',(82.3778463361227,0.785356331966813,135.659502067034));
#50955=CARTESIAN_POINT('Ctrl Pts',(82.3700984393456,0.920699827999275,135.637609219481));
#50956=CARTESIAN_POINT('Ctrl Pts',(82.3623505425686,1.05519718976395,135.610041441435));
#50957=CARTESIAN_POINT('Ctrl Pts',(82.3546026457915,1.18834057568716,135.576889270039));
#50958=CARTESIAN_POINT('Ctrl Pts',(82.3468563697074,1.32145611088417,135.543744033363));
#50959=CARTESIAN_POINT('Ctrl Pts',(82.3391100936233,1.45321785444385,135.505016821227));
#50960=CARTESIAN_POINT('Ctrl Pts',(82.3313638175392,1.58312944079426,135.460849019376));
#50961=CARTESIAN_POINT('Ctrl Pts',(82.3236174842739,1.71304198612249,135.416680891488));
#50962=CARTESIAN_POINT('Ctrl Pts',(82.3158711510085,1.84110397683198,135.367072219595));
#50963=CARTESIAN_POINT('Ctrl Pts',(82.3081248177432,1.96683584307418,135.312213746152));
#50964=CARTESIAN_POINT('Ctrl Pts',(82.3003767497402,2.09259586609605,135.257342987533));
#50965=CARTESIAN_POINT('Ctrl Pts',(82.2926286817372,2.21602436802573,135.197220244264));
#50966=CARTESIAN_POINT('Ctrl Pts',(82.2848806137343,2.33666370074194,135.132083553723));
#50967=CARTESIAN_POINT('Ctrl Pts',(82.2771243109924,2.45743125037659,135.066877635132));
#50968=CARTESIAN_POINT('Ctrl Pts',(82.2693680082506,2.57540336459376,134.996647310296));
#50969=CARTESIAN_POINT('Ctrl Pts',(82.2616117055087,2.69014839246293,134.921675845846));
#50970=CARTESIAN_POINT('Ctrl Pts',(82.2538512629946,2.80495466320845,134.846664366869));
#50971=CARTESIAN_POINT('Ctrl Pts',(82.2460908204804,2.91653009768779,134.76690693331));
#50972=CARTESIAN_POINT('Ctrl Pts',(82.2383303779662,3.02447462091655,134.682728357986));
#50973=CARTESIAN_POINT('Ctrl Pts',(82.2305574777008,3.13259242627686,134.59841465174));
#50974=CARTESIAN_POINT('Ctrl Pts',(82.2227845774354,3.23706737472395,134.509665874504));
#50975=CARTESIAN_POINT('Ctrl Pts',(82.21501167717,3.33753421811541,134.416845690948));
#50976=CARTESIAN_POINT('Ctrl Pts',(82.2075213414079,3.4343488386893,134.327399754864));
#50977=CARTESIAN_POINT('Ctrl Pts',(82.2000310056458,3.52744148669571,134.234173502969));
#50978=CARTESIAN_POINT('Ctrl Pts',(82.1925406698838,3.6165209101586,134.13752121509));
#50979=CARTESIAN_POINT('Ctrl Pts',(82.1847663357647,3.70897780703686,134.03720432634));
#50980=CARTESIAN_POINT('Ctrl Pts',(82.1769920016456,3.79740402478476,133.932878703086));
#50981=CARTESIAN_POINT('Ctrl Pts',(82.1692176675265,3.88143189204782,133.824901881958));
#50982=CARTESIAN_POINT('Ctrl Pts',(82.1614529145794,3.96535620247422,133.717058132612));
#50983=CARTESIAN_POINT('Ctrl Pts',(82.1536881616323,4.04489270993608,133.605572444186));
#50984=CARTESIAN_POINT('Ctrl Pts',(82.1459234086852,4.11971110979609,133.490838504004));
#50985=CARTESIAN_POINT('Ctrl Pts',(82.1381663678002,4.1944551989666,133.37621851919));
#50986=CARTESIAN_POINT('Ctrl Pts',(82.1304093269152,4.26449029389417,133.258357028291));
#50987=CARTESIAN_POINT('Ctrl Pts',(82.1226522860302,4.32952709194406,133.137679760466));
#50988=CARTESIAN_POINT('Ctrl Pts',(82.1149010947901,4.39451484523863,133.017093496307));
#50989=CARTESIAN_POINT('Ctrl Pts',(82.10714990355,4.45451161939667,132.893696024492));
#50990=CARTESIAN_POINT('Ctrl Pts',(82.0993987123099,4.50927228701171,132.767940639895));
#50991=CARTESIAN_POINT('Ctrl Pts',(82.0916508155328,4.56400967988226,132.642238704691));
#50992=CARTESIAN_POINT('Ctrl Pts',(82.0839029187557,4.61351523676614,132.51418120766));
#50993=CARTESIAN_POINT('Ctrl Pts',(82.0761550219786,4.65759062835227,132.38424434784));
#50994=CARTESIAN_POINT('Ctrl Pts',(82.0684087458945,4.70165680031662,132.25433466801));
#50995=CARTESIAN_POINT('Ctrl Pts',(82.0606624698104,4.7402949407882,132.122546777342));
#50996=CARTESIAN_POINT('Ctrl Pts',(82.0529161937263,4.77335570388328,131.9893747047));
#50997=CARTESIAN_POINT('Ctrl Pts',(82.045169860461,4.80641671102539,131.856201649011));
#50998=CARTESIAN_POINT('Ctrl Pts',(82.0374235271956,4.83390016443737,131.721644770405));
#50999=CARTESIAN_POINT('Ctrl Pts',(82.0296771939302,4.85570732193208,131.586210645535));
#51000=CARTESIAN_POINT('Ctrl Pts',(82.0219291259273,4.87751936298852,131.450746191132));
#51001=CARTESIAN_POINT('Ctrl Pts',(82.0141810579243,4.8936525165128,131.314404485464));
#51002=CARTESIAN_POINT('Ctrl Pts',(82.0064329899213,4.9040596801063,131.177699225877));
#51003=CARTESIAN_POINT('Ctrl Pts',(81.9986766871794,4.9144779045571,131.040848674313));
#51004=CARTESIAN_POINT('Ctrl Pts',(81.9909203844376,4.9191579526102,130.903634187434));
#51005=CARTESIAN_POINT('Ctrl Pts',(81.9831640816957,4.91810482663278,130.766572037924));
#51006=CARTESIAN_POINT('Ctrl Pts',(81.9754036391816,4.91705113857032,130.629436734219));
#51007=CARTESIAN_POINT('Ctrl Pts',(81.9676431966674,4.91025819858745,130.492454320189));
#51008=CARTESIAN_POINT('Ctrl Pts',(81.9598827541533,4.8977830306026,130.35613695951));
#51009=CARTESIAN_POINT('Ctrl Pts',(81.9521098538878,4.88528783637061,130.219600770102));
#51010=CARTESIAN_POINT('Ctrl Pts',(81.9443369536223,4.86709223816449,130.083732155184));
#51011=CARTESIAN_POINT('Ctrl Pts',(81.9365640533569,4.84330477182661,129.949034977998));
#51012=CARTESIAN_POINT('Ctrl Pts',(81.9290737175949,4.82038203980718,129.819234382486));
#51013=CARTESIAN_POINT('Ctrl Pts',(81.9215833818329,4.79226700394512,129.690521834871));
#51014=CARTESIAN_POINT('Ctrl Pts',(81.9140930460709,4.75910030108536,129.56333387059));
#51015=CARTESIAN_POINT('Ctrl Pts',(81.9063187119518,4.7246760726058,129.431323535986));
#51016=CARTESIAN_POINT('Ctrl Pts',(81.8985443778327,4.68470050173065,129.30053750697));
#51017=CARTESIAN_POINT('Ctrl Pts',(81.8907700437136,4.63927565880348,129.171478373149));
#51018=CARTESIAN_POINT('Ctrl Pts',(81.8830052907665,4.59390679793552,129.042578293175));
#51019=CARTESIAN_POINT('Ctrl Pts',(81.8752405378195,4.54310215589425,128.915401239073));
#51020=CARTESIAN_POINT('Ctrl Pts',(81.8674757848724,4.48701441525125,128.790437903104));
#51021=CARTESIAN_POINT('Ctrl Pts',(81.8597187439874,4.43098238174296,128.665598682481));
#51022=CARTESIAN_POINT('Ctrl Pts',(81.8519617031024,4.36967785094957,128.542969158864));
#51023=CARTESIAN_POINT('Ctrl Pts',(81.8442046622174,4.30330262572821,128.423022847761));
#51024=CARTESIAN_POINT('Ctrl Pts',(81.8364534709772,4.23697745458051,128.303166989104));
#51025=CARTESIAN_POINT('Ctrl Pts',(81.8287022797371,4.16558938867971,128.185990656141));
#51026=CARTESIAN_POINT('Ctrl Pts',(81.820951088497,4.08938730049043,128.071945098453));
#51027=CARTESIAN_POINT('Ctrl Pts',(81.8132031917199,4.01321760022133,127.95794801317));
#51028=CARTESIAN_POINT('Ctrl Pts',(81.8054552949428,3.93223816392902,127.84707938097));
#51029=CARTESIAN_POINT('Ctrl Pts',(81.7977073981658,3.84674242951302,127.739763459132));
#51030=CARTESIAN_POINT('Ctrl Pts',(81.7899611220817,3.76126457896165,127.632469985471));
#51031=CARTESIAN_POINT('Ctrl Pts',(81.7822148459976,3.67127255282988,127.528728049599));
#51032=CARTESIAN_POINT('Ctrl Pts',(81.7744685699135,3.57710126649333,127.428930335105));
#51033=CARTESIAN_POINT('Ctrl Pts',(81.7667222366481,3.48292928500574,127.329131883928));
#51034=CARTESIAN_POINT('Ctrl Pts',(81.7589759033827,3.38457825007597,127.23327799658));
#51035=CARTESIAN_POINT('Ctrl Pts',(81.7512295701174,3.28242098642447,127.141725564714));
#51036=CARTESIAN_POINT('Ctrl Pts',(81.7434815021144,3.18024084536216,127.050152630316));
#51037=CARTESIAN_POINT('Ctrl Pts',(81.7357334341115,3.07425307054073,126.962883329097));
#51038=CARTESIAN_POINT('Ctrl Pts',(81.7279853661085,2.96486439008743,126.880234955601));
#51039=CARTESIAN_POINT('Ctrl Pts',(81.7202290633667,2.85535945004272,126.79749874243));
#51040=CARTESIAN_POINT('Ctrl Pts',(81.7124727606248,2.74244669640408,126.719393503649));
#51041=CARTESIAN_POINT('Ctrl Pts',(81.7047164578829,2.62656318790534,126.646194088621));
#51042=CARTESIAN_POINT('Ctrl Pts',(81.6969560153688,2.51061782888877,126.572955604861));
#51043=CARTESIAN_POINT('Ctrl Pts',(81.6891955728546,2.3916988944344,126.50462835689));
#51044=CARTESIAN_POINT('Ctrl Pts',(81.6814351303404,2.27026810516819,126.441441205847));
#51045=CARTESIAN_POINT('Ctrl Pts',(81.673662230075,2.14864238441902,126.37815262118));
#51046=CARTESIAN_POINT('Ctrl Pts',(81.6658893298096,2.02449710540683,126.320020788138));
#51047=CARTESIAN_POINT('Ctrl Pts',(81.6581164295442,1.8983148488219,126.267226742834));
#51048=CARTESIAN_POINT('Ctrl Pts',(81.6506260937821,1.77671963509715,126.216351894057));
#51049=CARTESIAN_POINT('Ctrl Pts',(81.6431357580201,1.65323325982777,126.170433594022));
#51050=CARTESIAN_POINT('Ctrl Pts',(81.635645422258,1.52829901028968,126.129589479034));
#51051=CARTESIAN_POINT('Ctrl Pts',(81.6278710881389,1.39862784070796,126.087196747014));
#51052=CARTESIAN_POINT('Ctrl Pts',(81.6200967540198,1.26698607792881,126.050136283649));
#51053=CARTESIAN_POINT('Ctrl Pts',(81.6123224199007,1.13385173633451,126.018593876227));
#51054=CARTESIAN_POINT('Ctrl Pts',(81.6045576669536,1.00088147091768,125.987090342003));
#51055=CARTESIAN_POINT('Ctrl Pts',(81.5967929140065,0.866422663464341,125.961091422));
#51056=CARTESIAN_POINT('Ctrl Pts',(81.5890281610594,0.730970675930676,125.940733891199));
#51057=CARTESIAN_POINT('Ctrl Pts',(81.5812711201744,0.59565322122066,125.920396579785));
#51058=CARTESIAN_POINT('Ctrl Pts',(81.5735140792894,0.459344933612567,125.905689564869));
#51059=CARTESIAN_POINT('Ctrl Pts',(81.5657570384044,0.322553274488322,125.896699010689));
#51060=CARTESIAN_POINT('Ctrl Pts',(81.5580058471643,0.185864771018213,125.887715236356));
#51061=CARTESIAN_POINT('Ctrl Pts',(81.5502546559242,0.0486940101203715,
125.884439367856));
#51062=CARTESIAN_POINT('Ctrl Pts',(81.542503464684,-0.0884448375064001,
125.886905933157));
#51063=CARTESIAN_POINT('Ctrl Pts',(81.534755567907,-0.225525397464632,125.889371450102));
#51064=CARTESIAN_POINT('Ctrl Pts',(81.5270076711299,-0.362573681045943,
125.89757453949));
#51065=CARTESIAN_POINT('Ctrl Pts',(81.5192597743528,-0.499074138234663,
125.911497645129));
#51066=CARTESIAN_POINT('Ctrl Pts',(81.5115134982687,-0.635546042470348,
125.925417838354));
#51067=CARTESIAN_POINT('Ctrl Pts',(81.5037672221846,-0.771469959545438,
125.945055628269));
#51068=CARTESIAN_POINT('Ctrl Pts',(81.4960209461005,-0.906334483693587,
125.970341496155));
#51069=CARTESIAN_POINT('Ctrl Pts',(81.4882746128351,-1.04120000338102,125.995627550695));
#51070=CARTESIAN_POINT('Ctrl Pts',(81.4805282795698,-1.17500573026741,126.026561694355));
#51071=CARTESIAN_POINT('Ctrl Pts',(81.4727819463044,-1.30724988042935,126.063023167793));
#51072=CARTESIAN_POINT('Ctrl Pts',(81.4650338783015,-1.43952364575162,126.099492806526));
#51073=CARTESIAN_POINT('Ctrl Pts',(81.4572858102985,-1.5702347616486,126.141492134233));
#51074=CARTESIAN_POINT('Ctrl Pts',(81.4495377422955,-1.69889643274634,126.188850464473));
#51075=CARTESIAN_POINT('Ctrl Pts',(81.4417814395537,-1.8276948469993,126.236259127711));
#51076=CARTESIAN_POINT('Ctrl Pts',(81.4340251368118,-1.95443909783057,126.289038035815));
#51077=CARTESIAN_POINT('Ctrl Pts',(81.4262688340699,-2.07866170576452,126.346968041688));
#51078=CARTESIAN_POINT('Ctrl Pts',(81.4185083915558,-2.20295061504476,126.404928966551));
#51079=CARTESIAN_POINT('Ctrl Pts',(81.4107479490416,-2.3247148527201,126.468046287552));
#51080=CARTESIAN_POINT('Ctrl Pts',(81.4029875065274,-2.44351230015598,126.53605525109));
#51081=CARTESIAN_POINT('Ctrl Pts',(81.395214606262,-2.56250045180074,126.604173388654));
#51082=CARTESIAN_POINT('Ctrl Pts',(81.3874417059966,-2.67851196504096,126.677198652156));
#51083=CARTESIAN_POINT('Ctrl Pts',(81.3796688057311,-2.79113368241745,126.754822887235));
#51084=CARTESIAN_POINT('Ctrl Pts',(81.3721784699691,-2.8996613166897,126.829625285845));
#51085=CARTESIAN_POINT('Ctrl Pts',(81.3646881342072,-3.00504108513744,126.908697907888));
#51086=CARTESIAN_POINT('Ctrl Pts',(81.3571977984452,-3.10693440940455,126.991731388522));
#51087=CARTESIAN_POINT('Ctrl Pts',(81.3495289385518,-3.21125625193625,127.076743883245));
#51088=CARTESIAN_POINT('Ctrl Pts',(81.3418600786585,-3.31227284385009,127.166193516741));
#51089=CARTESIAN_POINT('Ctrl Pts',(81.3341912187651,-3.40957549528741,127.259790403219));
#51090=CARTESIAN_POINT('Ctrl Pts',(81.326531144205,-3.50676667823614,127.353280066479));
#51091=CARTESIAN_POINT('Ctrl Pts',(81.318871069645,-3.60025209160735,127.450907262715));
#51092=CARTESIAN_POINT('Ctrl Pts',(81.3112109950849,-3.68965426932632,127.552340562993));
#51093=CARTESIAN_POINT('Ctrl Pts',(81.3035579300338,-3.77897463774127,127.653681044642));
#51094=CARTESIAN_POINT('Ctrl Pts',(81.2959048649828,-3.86421893559665,127.758820405727));
#51095=CARTESIAN_POINT('Ctrl Pts',(81.2882517999317,-3.94504530048864,127.867389279675));
#51096=CARTESIAN_POINT('Ctrl Pts',(81.2806039750461,-4.02581632238755,127.975883814929));
#51097=CARTESIAN_POINT('Ctrl Pts',(81.2729561501605,-4.10217518854663,128.08780287122));
#51098=CARTESIAN_POINT('Ctrl Pts',(81.2653083252748,-4.17381959123836,128.202743220197));
#51099=CARTESIAN_POINT('Ctrl Pts',(81.2576631539417,-4.24543913559636,128.31764368852));
#51100=CARTESIAN_POINT('Ctrl Pts',(81.2500179826086,-4.31234725350306,128.435563026244));
#51101=CARTESIAN_POINT('Ctrl Pts',(81.2423728112755,-4.37428458156263,128.556068496421));
#51102=CARTESIAN_POINT('Ctrl Pts',(81.2347293281183,-4.43620823287052,128.676547357065));
#51103=CARTESIAN_POINT('Ctrl Pts',(81.2270858449612,-4.49316309720848,128.799610854807));
#51104=CARTESIAN_POINT('Ctrl Pts',(81.2194423618041,-4.54493580077072,128.924801725333));
#51105=CARTESIAN_POINT('Ctrl Pts',(81.2117965489251,-4.59672428457306,129.050030753842));
#51106=CARTESIAN_POINT('Ctrl Pts',(81.204150736046,-4.64332729735608,129.177388078851));
#51107=CARTESIAN_POINT('Ctrl Pts',(81.196504923167,-4.68457970185101,129.306396639526));
#51108=CARTESIAN_POINT('Ctrl Pts',(81.1910961389058,-4.71376238781293,129.397659593981));
#51109=CARTESIAN_POINT('Ctrl Pts',(81.1856873546445,-4.74026842832691,129.489748476775));
#51110=CARTESIAN_POINT('Ctrl Pts',(81.1802785703833,-4.76405452823402,129.582490119308));
#51111=CARTESIAN_POINT('Origin',(213.235140564004,0.,130.804360617566));
#51112=CARTESIAN_POINT('',(79.0845758390371,-4.76405452823407,129.582490119308));
#51113=CARTESIAN_POINT('',(79.4301745447722,-4.76405452823408,129.582490119308));
#51114=CARTESIAN_POINT('',(213.235140564004,-4.76405452823405,129.582490119308));
#51115=CARTESIAN_POINT('',(80.7648594359615,-4.91824805085141,130.799981942384));
#51116=CARTESIAN_POINT('Ctrl Pts',(80.7648594359614,-4.91824805085141,130.799981942385));
#51117=CARTESIAN_POINT('Ctrl Pts',(80.7572118377638,-4.91836808905016,130.934812139328));
#51118=CARTESIAN_POINT('Ctrl Pts',(80.7495642395661,-4.91293955423797,131.069824535811));
#51119=CARTESIAN_POINT('Ctrl Pts',(80.7419166413684,-4.90194425981586,131.204517506996));
#51120=CARTESIAN_POINT('Ctrl Pts',(80.7342755102555,-4.89095826341109,131.339096576949));
#51121=CARTESIAN_POINT('Ctrl Pts',(80.7266343791426,-4.87441490385902,131.473356359034));
#51122=CARTESIAN_POINT('Ctrl Pts',(80.7189932480296,-4.85234805594347,131.606795291843));
#51123=CARTESIAN_POINT('Ctrl Pts',(80.7113561437386,-4.83029283710029,131.74016390328));
#51124=CARTESIAN_POINT('Ctrl Pts',(80.7037190394476,-4.80271998351891,131.872712128746));
#51125=CARTESIAN_POINT('Ctrl Pts',(80.6960819351566,-4.76971516029594,132.003944025313));
#51126=CARTESIAN_POINT('Ctrl Pts',(80.6884468335639,-4.73671899201585,132.13514150859));
#51127=CARTESIAN_POINT('Ctrl Pts',(80.6808117319711,-4.69829378405131,132.26502295834));
#51128=CARTESIAN_POINT('Ctrl Pts',(80.6731766303783,-4.65457610529979,132.393103624623));
#51129=CARTESIAN_POINT('Ctrl Pts',(80.6655417659445,-4.61085978449238,132.521180312506));
#51130=CARTESIAN_POINT('Ctrl Pts',(80.6579069015108,-4.56185145022658,132.64745594647));
#51131=CARTESIAN_POINT('Ctrl Pts',(80.650272037077,-4.50773705983245,132.771462460866));
#51132=CARTESIAN_POINT('Ctrl Pts',(80.6426356446608,-4.45361183940423,132.895493792963));
#51133=CARTESIAN_POINT('Ctrl Pts',(80.6349992522445,-4.39437869263396,133.017254733084));
#51134=CARTESIAN_POINT('Ctrl Pts',(80.6273628598282,-4.33027084295917,133.136299186465));
#51135=CARTESIAN_POINT('Ctrl Pts',(80.6197186820037,-4.26609763444075,133.25546500732));
#51136=CARTESIAN_POINT('Ctrl Pts',(80.6120745041792,-4.19703999081989,133.371908455793));
#51137=CARTESIAN_POINT('Ctrl Pts',(80.6044303263548,-4.12337620251523,133.485209691093));
#51138=CARTESIAN_POINT('Ctrl Pts',(80.5967820282655,-4.04967270891822,133.598571996544));
#51139=CARTESIAN_POINT('Ctrl Pts',(80.5891337301762,-3.97135836115872,133.708788388718));
#51140=CARTESIAN_POINT('Ctrl Pts',(80.5814854320869,-3.88875274177736,133.815470907114));
#51141=CARTESIAN_POINT('Ctrl Pts',(80.5738254851517,-3.80602130876754,133.922315909791));
#51142=CARTESIAN_POINT('Ctrl Pts',(80.5661655382165,-3.71898581138502,134.025615982294));
#51143=CARTESIAN_POINT('Ctrl Pts',(80.5585055912813,-3.62800415247761,134.125018524082));
#51144=CARTESIAN_POINT('Ctrl Pts',(80.5528183685761,-3.56045369022636,134.198821175378));
#51145=CARTESIAN_POINT('Ctrl Pts',(80.5471311458709,-3.49072869504952,134.270476063957));
#51146=CARTESIAN_POINT('Ctrl Pts',(80.5414439231657,-3.41898725962216,134.339853395248));
#51147=CARTESIAN_POINT('Ctrl Pts',(80.5336695890466,-3.32091797025072,134.43469099555));
#51148=CARTESIAN_POINT('Ctrl Pts',(80.5258952549275,-3.21874437560722,134.525595276033));
#51149=CARTESIAN_POINT('Ctrl Pts',(80.5181209208084,-3.11281508625975,134.612190091328));
#51150=CARTESIAN_POINT('Ctrl Pts',(80.5103561678613,-3.00701634529437,134.698678186253));
#51151=CARTESIAN_POINT('Ctrl Pts',(80.5025914149143,-2.89747141886499,134.780867138288));
#51152=CARTESIAN_POINT('Ctrl Pts',(80.4948266619672,-2.78456595452368,134.858417290506));
#51153=CARTESIAN_POINT('Ctrl Pts',(80.4870696210822,-2.67177262948109,134.935890418819));
#51154=CARTESIAN_POINT('Ctrl Pts',(80.4793125801972,-2.55562572894983,135.008733696171));
#51155=CARTESIAN_POINT('Ctrl Pts',(80.4715555393122,-2.43654391702278,135.076647686914));
#51156=CARTESIAN_POINT('Ctrl Pts',(80.4638043480721,-2.31755190561634,135.144510463188));
#51157=CARTESIAN_POINT('Ctrl Pts',(80.4560531568319,-2.19562972637481,135.207451158837));
#51158=CARTESIAN_POINT('Ctrl Pts',(80.4483019655918,-2.07122466125247,135.265213839218));
#51159=CARTESIAN_POINT('Ctrl Pts',(80.4405540688147,-1.9468724716016,135.322951968918));
#51160=CARTESIAN_POINT('Ctrl Pts',(80.4328061720376,-1.82003984882979,135.37551629626));
#51161=CARTESIAN_POINT('Ctrl Pts',(80.4250582752605,-1.69119809548402,135.422697121583));
#51162=CARTESIAN_POINT('Ctrl Pts',(80.4173119991764,-1.56238329305555,135.469868077694));
#51163=CARTESIAN_POINT('Ctrl Pts',(80.4095657230923,-1.43156056287851,135.511657637332));
#51164=CARTESIAN_POINT('Ctrl Pts',(80.4018194470082,-1.29922020765802,135.547904642292));
#51165=CARTESIAN_POINT('Ctrl Pts',(80.3940731137429,-1.16687887553118,135.584151914819));
#51166=CARTESIAN_POINT('Ctrl Pts',(80.3863267804775,-1.03302027308394,135.614856447748));
#51167=CARTESIAN_POINT('Ctrl Pts',(80.3785804472122,-0.898148461546721,
135.639907370884));
#51168=CARTESIAN_POINT('Ctrl Pts',(80.3708323792092,-0.763246446402719,
135.664963904));
#51169=CARTESIAN_POINT('Ctrl Pts',(80.3630843112063,-0.627331154979045,
135.684364236575));
#51170=CARTESIAN_POINT('Ctrl Pts',(80.3553362432033,-0.490915006359956,
135.698048952455));
#51171=CARTESIAN_POINT('Ctrl Pts',(80.3475799404615,-0.35435387303437,135.711748212614));
#51172=CARTESIAN_POINT('Ctrl Pts',(80.3398236377196,-0.217291208785866,
135.719719682272));
#51173=CARTESIAN_POINT('Ctrl Pts',(80.3320673349778,-0.0802432576695204,
135.721955973235));
#51174=CARTESIAN_POINT('Ctrl Pts',(80.3243068924636,0.0568778400650496,
135.724193457774));
#51175=CARTESIAN_POINT('Ctrl Pts',(80.3165464499494,0.193983818373639,135.720689674225));
#51176=CARTESIAN_POINT('Ctrl Pts',(80.3087860074352,0.330561292654718,135.711489339568));
#51177=CARTESIAN_POINT('Ctrl Pts',(80.3010131071698,0.467358013222105,135.702274235718));
#51178=CARTESIAN_POINT('Ctrl Pts',(80.2932402069044,0.60362414552211,135.687344349521));
#51179=CARTESIAN_POINT('Ctrl Pts',(80.2854673066389,0.738853366851134,135.666796094237));
#51180=CARTESIAN_POINT('Ctrl Pts',(80.2779769708769,0.869166665362811,135.646994819791));
#51181=CARTESIAN_POINT('Ctrl Pts',(80.2704866351149,0.998516830283219,135.621976626608));
#51182=CARTESIAN_POINT('Ctrl Pts',(80.2629962993529,1.12646407699086,135.591871635386));
#51183=CARTESIAN_POINT('Ctrl Pts',(80.2552219652338,1.25926248244623,135.560625204272));
#51184=CARTESIAN_POINT('Ctrl Pts',(80.2474476311147,1.39097015179278,135.523799649453));
#51185=CARTESIAN_POINT('Ctrl Pts',(80.2396732969956,1.52108219075252,135.481484951115));
#51186=CARTESIAN_POINT('Ctrl Pts',(80.2319085440485,1.65103387825269,135.439222401861));
#51187=CARTESIAN_POINT('Ctrl Pts',(80.2241437911015,1.77939347983067,135.391484288934));
#51188=CARTESIAN_POINT('Ctrl Pts',(80.2163790381544,1.90566678057145,135.338411475676));
#51189=CARTESIAN_POINT('Ctrl Pts',(80.2086219972694,2.03181466488979,135.285391375084));
#51190=CARTESIAN_POINT('Ctrl Pts',(80.2008649563843,2.15588001393795,135.227047268921));
#51191=CARTESIAN_POINT('Ctrl Pts',(80.1931079154993,2.2773846058556,135.163569538863));
#51192=CARTESIAN_POINT('Ctrl Pts',(80.1853567242592,2.39879757021539,135.100139677854));
#51193=CARTESIAN_POINT('Ctrl Pts',(80.1776055330191,2.5176532760326,135.031584078853));
#51194=CARTESIAN_POINT('Ctrl Pts',(80.1698543417789,2.63349463142193,134.958140713909));
#51195=CARTESIAN_POINT('Ctrl Pts',(80.1621064450019,2.74928675114489,134.884728564354));
#51196=CARTESIAN_POINT('Ctrl Pts',(80.1543585482248,2.86206673910389,134.806432989613));
#51197=CARTESIAN_POINT('Ctrl Pts',(80.1466106514477,2.97140341849634,134.723537162077));
#51198=CARTESIAN_POINT('Ctrl Pts',(80.1388643753636,3.0807172270124,134.640658674562));
#51199=CARTESIAN_POINT('Ctrl Pts',(80.1311180992795,3.18658884826157,134.553182084324));
#51200=CARTESIAN_POINT('Ctrl Pts',(80.1233718231954,3.28861767469218,134.461432786966));
#51201=CARTESIAN_POINT('Ctrl Pts',(80.1156254899301,3.39064725427655,134.369682812336));
#51202=CARTESIAN_POINT('Ctrl Pts',(80.1078791566648,3.48883369172806,134.273660329073));
#51203=CARTESIAN_POINT('Ctrl Pts',(80.1001328233994,3.58281125140452,134.173729490116));
#51204=CARTESIAN_POINT('Ctrl Pts',(80.0923847553964,3.67680985670381,134.073776272341));
#51205=CARTESIAN_POINT('Ctrl Pts',(80.0846366873934,3.76659744087556,133.969913241981));
#51206=CARTESIAN_POINT('Ctrl Pts',(80.0768886193904,3.85184704039493,133.862539395843));
#51207=CARTESIAN_POINT('Ctrl Pts',(80.0691323166486,3.93718724420322,133.755051431502));
#51208=CARTESIAN_POINT('Ctrl Pts',(80.0613760139068,4.01797958535831,133.644045504318));
#51209=CARTESIAN_POINT('Ctrl Pts',(80.0536197111649,4.09393880544138,133.529951951534));
#51210=CARTESIAN_POINT('Ctrl Pts',(80.0458592686507,4.1699385672473,133.415797503586));
#51211=CARTESIAN_POINT('Ctrl Pts',(80.0380988261366,4.24109986519031,133.298552480399));
#51212=CARTESIAN_POINT('Ctrl Pts',(80.0303383836224,4.3071828240157,133.178672977599));
#51213=CARTESIAN_POINT('Ctrl Pts',(80.022565483357,4.37337186507316,133.058601033578));
#51214=CARTESIAN_POINT('Ctrl Pts',(80.0147925830915,4.43446610197331,132.935886509045));
#51215=CARTESIAN_POINT('Ctrl Pts',(80.0070196828261,4.49027297013191,132.811007501351));
#51216=CARTESIAN_POINT('Ctrl Pts',(79.9995293470641,4.54405111806405,132.690668160137));
#51217=CARTESIAN_POINT('Ctrl Pts',(79.992039011302,4.59291952728006,132.568319258483));
#51218=CARTESIAN_POINT('Ctrl Pts',(79.98454867554,4.6367499576783,132.444401133063));
#51219=CARTESIAN_POINT('Ctrl Pts',(79.9767743414209,4.68224223216699,132.315784614253));
#51220=CARTESIAN_POINT('Ctrl Pts',(79.9690000073018,4.72245106236455,132.185070109983));
#51221=CARTESIAN_POINT('Ctrl Pts',(79.9612256731827,4.75717924345912,132.052731038596));
#51222=CARTESIAN_POINT('Ctrl Pts',(79.9534609202356,4.79186462517414,131.920555063287));
#51223=CARTESIAN_POINT('Ctrl Pts',(79.9456961672886,4.82108269876557,131.786758879042));
#51224=CARTESIAN_POINT('Ctrl Pts',(79.9379314143415,4.84468484131862,131.651834422942));
#51225=CARTESIAN_POINT('Ctrl Pts',(79.9301743734566,4.8682635418909,131.517043975714));
#51226=CARTESIAN_POINT('Ctrl Pts',(79.9224173325716,4.88623734460999,131.381127869331));
#51227=CARTESIAN_POINT('Ctrl Pts',(79.9146602916866,4.89850793237532,131.244591351336));
#51228=CARTESIAN_POINT('Ctrl Pts',(79.9069091004465,4.91076926679497,131.108157796592));
#51229=CARTESIAN_POINT('Ctrl Pts',(79.8991579092064,4.91733591196603,130.971105149296));
#51230=CARTESIAN_POINT('Ctrl Pts',(79.8914067179663,4.91816101118458,130.833946603504));
#51231=CARTESIAN_POINT('Ctrl Pts',(79.8836588211892,4.91898575971395,130.696846353751));
#51232=CARTESIAN_POINT('Ctrl Pts',(79.8759109244121,4.91407381353474,130.559640685163));
#51233=CARTESIAN_POINT('Ctrl Pts',(79.868163027635,4.90343035200612,130.422845420588));
#51234=CARTESIAN_POINT('Ctrl Pts',(79.8604167515509,4.89278911686022,130.286078770634));
#51235=CARTESIAN_POINT('Ctrl Pts',(79.8526704754668,4.87641878137003,130.149722743478));
#51236=CARTESIAN_POINT('Ctrl Pts',(79.8449241993827,4.85437657190657,130.014290265873));
#51237=CARTESIAN_POINT('Ctrl Pts',(79.8371778661174,4.83233419973252,129.878856788535));
#51238=CARTESIAN_POINT('Ctrl Pts',(79.829431532852,4.80461993284453,129.74434726024));
#51239=CARTESIAN_POINT('Ctrl Pts',(79.8216851995867,4.77134245437662,129.611266218299));
#51240=CARTESIAN_POINT('Ctrl Pts',(79.8139371315837,4.73805752364807,129.478155373781));
#51241=CARTESIAN_POINT('Ctrl Pts',(79.8061890635807,4.69920699708112,129.346474031395));
#51242=CARTESIAN_POINT('Ctrl Pts',(79.7984409955777,4.65494983021665,129.216712942335));
#51243=CARTESIAN_POINT('Ctrl Pts',(79.7906846928359,4.61064562630863,129.086813941646));
#51244=CARTESIAN_POINT('Ctrl Pts',(79.782928390094,4.56092342977415,128.95883964176));
#51245=CARTESIAN_POINT('Ctrl Pts',(79.7751720873522,4.50599110638188,128.833262646458));
#51246=CARTESIAN_POINT('Ctrl Pts',(79.767411644838,4.45102946395463,128.707618626932));
#51247=CARTESIAN_POINT('Ctrl Pts',(79.7596512023238,4.39085232514546,128.584374812678));
#51248=CARTESIAN_POINT('Ctrl Pts',(79.7518907598097,4.32571375768699,128.463979548369));
#51249=CARTESIAN_POINT('Ctrl Pts',(79.7441178595442,4.26047062401726,128.343391014893));
#51250=CARTESIAN_POINT('Ctrl Pts',(79.7363449592788,4.19025034642582,128.225660505131));
#51251=CARTESIAN_POINT('Ctrl Pts',(79.7285720590133,4.11535107589342,128.111208452418));
#51252=CARTESIAN_POINT('Ctrl Pts',(79.7210817232513,4.04317458250418,128.000917020107));
#51253=CARTESIAN_POINT('Ctrl Pts',(79.7135913874892,3.96665355529998,127.893670073526));
#51254=CARTESIAN_POINT('Ctrl Pts',(79.7061010517271,3.88608914508753,127.789813517431));
#51255=CARTESIAN_POINT('Ctrl Pts',(79.698326717608,3.80247011077556,127.682019208446));
#51256=CARTESIAN_POINT('Ctrl Pts',(79.6905523834889,3.71423015118311,127.57753599839));
#51257=CARTESIAN_POINT('Ctrl Pts',(79.6827780493698,3.62166097255255,127.476785695436));
#51258=CARTESIAN_POINT('Ctrl Pts',(79.6750132964227,3.52920587716163,127.376159558226));
#51259=CARTESIAN_POINT('Ctrl Pts',(79.6672485434757,3.43243244051844,127.279257459676));
#51260=CARTESIAN_POINT('Ctrl Pts',(79.6594837905286,3.33167420890646,127.186470344464));
#51261=CARTESIAN_POINT('Ctrl Pts',(79.6517267496436,3.23101605179008,127.093775386722));
#51262=CARTESIAN_POINT('Ctrl Pts',(79.6439697087586,3.12638126155002,127.005187542014));
#51263=CARTESIAN_POINT('Ctrl Pts',(79.6362126678735,3.01814177445785,126.921062625939));
#51264=CARTESIAN_POINT('Ctrl Pts',(79.6284614766334,2.90998391160531,126.837001149118));
#51265=CARTESIAN_POINT('Ctrl Pts',(79.6207102853933,2.79822707001655,126.757396140999));
#51266=CARTESIAN_POINT('Ctrl Pts',(79.6129590941532,2.68327768719087,126.682564417373));
#51267=CARTESIAN_POINT('Ctrl Pts',(79.6052111973761,2.56837716091925,126.607764499227));
#51268=CARTESIAN_POINT('Ctrl Pts',(79.597463300599,2.4502871191785,126.537734043354));
#51269=CARTESIAN_POINT('Ctrl Pts',(79.5897154038219,2.32944433791154,126.472747507064));
#51270=CARTESIAN_POINT('Ctrl Pts',(79.5819691277378,2.20862683434936,126.407774564557));
#51271=CARTESIAN_POINT('Ctrl Pts',(79.5742228516537,2.08505808069978,126.347843628078));
#51272=CARTESIAN_POINT('Ctrl Pts',(79.5664765755696,1.95920054901721,126.293183800899));
#51273=CARTESIAN_POINT('Ctrl Pts',(79.5587302423043,1.83334208828294,126.238523570234));
#51274=CARTESIAN_POINT('Ctrl Pts',(79.5509839090389,1.70519517440829,126.189134682254));
#51275=CARTESIAN_POINT('Ctrl Pts',(79.5432375757736,1.5752430348128,126.145198413503));
#51276=CARTESIAN_POINT('Ctrl Pts',(79.5354895077706,1.44526179333632,126.101252305528));
#51277=CARTESIAN_POINT('Ctrl Pts',(79.5277414397676,1.31347489199163,126.062761371778));
#51278=CARTESIAN_POINT('Ctrl Pts',(79.5199933717646,1.18038113300863,126.029857141461));
#51279=CARTESIAN_POINT('Ctrl Pts',(79.5122370690227,1.04714592039503,125.996917940137));
#51280=CARTESIAN_POINT('Ctrl Pts',(79.5044807662809,0.912601455721774,125.969577397253));
#51281=CARTESIAN_POINT('Ctrl Pts',(79.4967244635391,0.777257710458418,125.947916083338));
#51282=CARTESIAN_POINT('Ctrl Pts',(79.4889640210249,0.641841728163002,125.926243208127));
#51283=CARTESIAN_POINT('Ctrl Pts',(79.4812035785107,0.505626003350469,125.910255647311));
#51284=CARTESIAN_POINT('Ctrl Pts',(79.4734431359965,0.36912507090641,125.899981987757));
#51285=CARTESIAN_POINT('Ctrl Pts',(79.4656702357311,0.232405015047702,125.889691836012));
#51286=CARTESIAN_POINT('Ctrl Pts',(79.4578973354657,0.0953992276199499,
125.885133928038));
#51287=CARTESIAN_POINT('Ctrl Pts',(79.4501244352002,-0.041377411016928,
125.886284675456));
#51288=CARTESIAN_POINT('Ctrl Pts',(79.4426340994382,-0.173181874319512,
125.887393590308));
#51289=CARTESIAN_POINT('Ctrl Pts',(79.4351437636762,-0.304773252202186,
125.893803303403));
#51290=CARTESIAN_POINT('Ctrl Pts',(79.4276534279142,-0.435697745829174,
125.90544741801));
#51291=CARTESIAN_POINT('Ctrl Pts',(79.4198790937951,-0.571586281426142,
125.917533022762));
#51292=CARTESIAN_POINT('Ctrl Pts',(79.412104759676,-0.707186818704931,125.935296072674));
#51293=CARTESIAN_POINT('Ctrl Pts',(79.4043304255569,-0.841986804155042,
125.958719144641));
#51294=CARTESIAN_POINT('Ctrl Pts',(79.3965656726098,-0.976620660670781,
125.982113349766));
#51295=CARTESIAN_POINT('Ctrl Pts',(79.3888009196627,-1.11045554691931,126.011153631549));
#51296=CARTESIAN_POINT('Ctrl Pts',(79.3810361667156,-1.24298226015877,126.045770683202));
#51297=CARTESIAN_POINT('Ctrl Pts',(79.3732791258306,-1.37537734599815,126.080353352711));
#51298=CARTESIAN_POINT('Ctrl Pts',(79.3655220849456,-1.50646646866026,126.120501671209));
#51299=CARTESIAN_POINT('Ctrl Pts',(79.3577650440606,-1.63574922976492,126.166095045197));
#51300=CARTESIAN_POINT('Ctrl Pts',(79.3500138528205,-1.76493449773253,126.211654036867));
#51301=CARTESIAN_POINT('Ctrl Pts',(79.3422626615804,-1.89231574828529,126.262649781464));
#51302=CARTESIAN_POINT('Ctrl Pts',(79.3345114703403,-2.01740674592696,126.318911578285));
#51303=CARTESIAN_POINT('Ctrl Pts',(79.3267635735633,-2.14244457655867,126.375149462341));
#51304=CARTESIAN_POINT('Ctrl Pts',(79.3190156767862,-2.26519373452042,126.436648786953));
#51305=CARTESIAN_POINT('Ctrl Pts',(79.3112677800091,-2.38518722303943,126.50319043103));
#51306=CARTESIAN_POINT('Ctrl Pts',(79.303521503925,-2.5051556115074,126.569718156028));
#51307=CARTESIAN_POINT('Ctrl Pts',(79.2957752278409,-2.62236913538159,126.641285913061));
#51308=CARTESIAN_POINT('Ctrl Pts',(79.2880289517568,-2.73638506614919,126.717628447206));
#51309=CARTESIAN_POINT('Ctrl Pts',(79.2802826184915,-2.8504018385561,126.793971544894));
#51310=CARTESIAN_POINT('Ctrl Pts',(79.2725362852262,-2.961220645891,126.875089272501));
#51311=CARTESIAN_POINT('Ctrl Pts',(79.2647899519608,-3.06842777884041,126.960673061515));
#51312=CARTESIAN_POINT('Ctrl Pts',(79.2570418839579,-3.17565892008443,127.046276016425));
#51313=CARTESIAN_POINT('Ctrl Pts',(79.2492938159548,-3.27927647201899,127.13634677904));
#51314=CARTESIAN_POINT('Ctrl Pts',(79.2415457479518,-3.37890016060658,127.230536787667));
#51315=CARTESIAN_POINT('Ctrl Pts',(79.23378944521,-3.47862973043593,127.324826902556));
#51316=CARTESIAN_POINT('Ctrl Pts',(79.2260331424681,-3.57435667307585,127.423244739924));
#51317=CARTESIAN_POINT('Ctrl Pts',(79.2182768397263,-3.66573755022288,127.52540479667));
#51318=CARTESIAN_POINT('Ctrl Pts',(79.2105163972121,-3.75716720009572,127.627619379315));
#51319=CARTESIAN_POINT('Ctrl Pts',(79.2027559546979,-3.8442459143172,127.733579859291));
#51320=CARTESIAN_POINT('Ctrl Pts',(79.1949955121837,-3.9266715232722,127.842868795726));
#51321=CARTESIAN_POINT('Ctrl Pts',(79.1872226119182,-4.00922944913182,127.952333172465));
#51322=CARTESIAN_POINT('Ctrl Pts',(79.1794497116528,-4.08711912085463,128.06513636104));
#51323=CARTESIAN_POINT('Ctrl Pts',(79.1716768113874,-4.16008207859903,128.180832427929));
#51324=CARTESIAN_POINT('Ctrl Pts',(79.1641864756254,-4.23039264904657,128.292322651366));
#51325=CARTESIAN_POINT('Ctrl Pts',(79.1566961398633,-4.29612832993051,128.406498810934));
#51326=CARTESIAN_POINT('Ctrl Pts',(79.1492058041013,-4.35709969334681,128.522943223765));
#51327=CARTESIAN_POINT('Ctrl Pts',(79.1409632472063,-4.42419413983025,128.65108163149));
#51328=CARTESIAN_POINT('Ctrl Pts',(79.1327206903113,-4.48571150014336,128.782333424784));
#51329=CARTESIAN_POINT('Ctrl Pts',(79.1244781334162,-4.54136974383764,128.916201749182));
#51330=CARTESIAN_POINT('Ctrl Pts',(79.1162547834092,-4.59689829213924,129.049758132281));
#51331=CARTESIAN_POINT('Ctrl Pts',(79.1080314334022,-4.6465948238171,129.185918594868));
#51332=CARTESIAN_POINT('Ctrl Pts',(79.0998080833951,-4.69022365273293,129.324162945009));
#51333=CARTESIAN_POINT('Ctrl Pts',(79.0947306686091,-4.71716178145714,129.409520361011));
#51334=CARTESIAN_POINT('Ctrl Pts',(79.0896532538231,-4.74178760065504,129.495671706625));
#51335=CARTESIAN_POINT('Ctrl Pts',(79.0845758390371,-4.76405452823407,129.582490119308));
#51336=CARTESIAN_POINT('Ctrl Pts',(80.834865443625,-4.76405452823406,129.582490119308));
#51337=CARTESIAN_POINT('Ctrl Pts',(80.8298741447429,-4.78585628385885,129.667494833602));
#51338=CARTESIAN_POINT('Ctrl Pts',(80.8248828458608,-4.80536250632687,129.753006308476));
#51339=CARTESIAN_POINT('Ctrl Pts',(80.8198915469787,-4.82255633145487,129.838890010844));
#51340=CARTESIAN_POINT('Ctrl Pts',(80.8086626854037,-4.86123706103406,130.032101483092));
#51341=CARTESIAN_POINT('Ctrl Pts',(80.7974338238288,-4.88831646052915,130.22770670874));
#51342=CARTESIAN_POINT('Ctrl Pts',(80.7862049622537,-4.90356361051494,130.424562012864));
#51343=CARTESIAN_POINT('Ctrl Pts',(80.7790897868329,-4.91322497699388,130.549299504017));
#51344=CARTESIAN_POINT('Ctrl Pts',(80.771974611412,-4.91813636965101,130.674538570167));
#51345=CARTESIAN_POINT('Ctrl Pts',(80.7648594359911,-4.91824805085094,130.799981941862));
#51346=CARTESIAN_POINT('',(81.1101405640462,-4.91824902053953,130.807464560535));
#51347=CARTESIAN_POINT('Ctrl Pts',(81.1802785703833,-4.76405452823402,129.582490119308));
#51348=CARTESIAN_POINT('Ctrl Pts',(81.1726260494128,-4.7977078631708,129.713703961466));
#51349=CARTESIAN_POINT('Ctrl Pts',(81.1649735284423,-4.8259143747193,129.846224591726));
#51350=CARTESIAN_POINT('Ctrl Pts',(81.1573210074718,-4.84859535890923,129.979553908049));
#51351=CARTESIAN_POINT('Ctrl Pts',(81.1494576002342,-4.871901380013,130.116557480468));
#51352=CARTESIAN_POINT('Ctrl Pts',(81.1415941929966,-4.88937286395555,130.254414499012));
#51353=CARTESIAN_POINT('Ctrl Pts',(81.133730785759,-4.90098157502492,130.392580744617));
#51354=CARTESIAN_POINT('Ctrl Pts',(81.1258673785213,-4.9125902860943,130.530746990221));
#51355=CARTESIAN_POINT('Ctrl Pts',(81.1180039712838,-4.9183362664278,130.669222006222));
#51356=CARTESIAN_POINT('Ctrl Pts',(81.1101405640462,-4.91824902053953,130.807464560535));
#51357=CARTESIAN_POINT('Ctrl Pts',(81.1101405640085,-4.91824902053911,130.807464561198));
#51358=CARTESIAN_POINT('Ctrl Pts',(81.0996771008831,-4.91813292654806,130.991417372709));
#51359=CARTESIAN_POINT('Ctrl Pts',(81.0892136377577,-4.90769710711438,131.175044159719));
#51360=CARTESIAN_POINT('Ctrl Pts',(81.0787501746323,-4.88704688904051,131.357493302208));
#51361=CARTESIAN_POINT('Ctrl Pts',(81.0709758405132,-4.87170381447581,131.493052684074));
#51362=CARTESIAN_POINT('Ctrl Pts',(81.0632015063941,-4.85069184088119,131.628187907528));
#51363=CARTESIAN_POINT('Ctrl Pts',(81.055427172275,-4.82404068621336,131.76238698477));
#51364=CARTESIAN_POINT('Ctrl Pts',(81.0476624193279,-4.79742237671175,131.896420673643));
#51365=CARTESIAN_POINT('Ctrl Pts',(81.0398976663808,-4.76517878956605,132.029520132061));
#51366=CARTESIAN_POINT('Ctrl Pts',(81.0321329134337,-4.72739143106729,132.161177967091));
#51367=CARTESIAN_POINT('Ctrl Pts',(81.0243758725487,-4.68964160350576,132.292705037703));
#51368=CARTESIAN_POINT('Ctrl Pts',(81.0166188316638,-4.64635906924106,132.422792960993));
#51369=CARTESIAN_POINT('Ctrl Pts',(81.0088617907788,-4.59767639522331,132.550944376596));
#51370=CARTESIAN_POINT('Ctrl Pts',(81.0011105995387,-4.54903043318877,132.678999152219));
#51371=CARTESIAN_POINT('Ctrl Pts',(80.9933594082985,-4.49499257532123,132.80511996286));
#51372=CARTESIAN_POINT('Ctrl Pts',(80.9856082170584,-4.43574514147814,132.928824809393));
#51373=CARTESIAN_POINT('Ctrl Pts',(80.9778603202813,-4.37652288937483,133.052477078066));
#51374=CARTESIAN_POINT('Ctrl Pts',(80.9701124235042,-4.3120956337143,133.173715073085));
#51375=CARTESIAN_POINT('Ctrl Pts',(80.9623645267272,-4.24269363912157,133.292077190461));
#51376=CARTESIAN_POINT('Ctrl Pts',(80.9546182506431,-4.17330616192998,133.410414549034));
#51377=CARTESIAN_POINT('Ctrl Pts',(80.9468719745589,-4.09894621326297,133.525876889475));
#51378=CARTESIAN_POINT('Ctrl Pts',(80.9391256984748,-4.01988959592007,133.638027976152));
#51379=CARTESIAN_POINT('Ctrl Pts',(80.9313793652095,-3.94083239499918,133.750179890702));
#51380=CARTESIAN_POINT('Ctrl Pts',(80.9236330319441,-3.85707868147744,133.859020183162));
#51381=CARTESIAN_POINT('Ctrl Pts',(80.9158866986788,-3.76894686289186,133.964142668151));
#51382=CARTESIAN_POINT('Ctrl Pts',(80.9081386306758,-3.68079530779669,134.069288694591));
#51383=CARTESIAN_POINT('Ctrl Pts',(80.9003905626729,-3.58826394779479,134.17071495728));
#51384=CARTESIAN_POINT('Ctrl Pts',(80.8926424946699,-3.49171036973018,134.268049656209));
#51385=CARTESIAN_POINT('Ctrl Pts',(80.884886191928,-3.39505417337366,134.365487803616));
#51386=CARTESIAN_POINT('Ctrl Pts',(80.8771298891862,-3.29436749523585,134.458825422532));
#51387=CARTESIAN_POINT('Ctrl Pts',(80.8693735864444,-3.19004396897555,134.547728424569));
#51388=CARTESIAN_POINT('Ctrl Pts',(80.8616131439302,-3.0856647621081,134.636678876814));
#51389=CARTESIAN_POINT('Ctrl Pts',(80.853852701416,-2.97764514709398,134.721189755163));
#51390=CARTESIAN_POINT('Ctrl Pts',(80.8460922589018,-2.86640969582959,134.800968994447));
#51391=CARTESIAN_POINT('Ctrl Pts',(80.8383193586364,-2.75499567954388,134.880876302448));
#51392=CARTESIAN_POINT('Ctrl Pts',(80.8305464583709,-2.64035583814411,134.956036578377));
#51393=CARTESIAN_POINT('Ctrl Pts',(80.8227735581055,-2.52294217905883,135.026202137996));
#51394=CARTESIAN_POINT('Ctrl Pts',(80.8152832223434,-2.40979680222775,135.093817002787));
#51395=CARTESIAN_POINT('Ctrl Pts',(80.8077928865814,-2.29407604748352,135.156793840408));
#51396=CARTESIAN_POINT('Ctrl Pts',(80.8003025508193,-2.17620202315962,135.214953300743));
#51397=CARTESIAN_POINT('Ctrl Pts',(80.7925282167002,-2.05385876937729,135.275317894694));
#51398=CARTESIAN_POINT('Ctrl Pts',(80.7847538825811,-1.92880819368285,135.330683815357));
#51399=CARTESIAN_POINT('Ctrl Pts',(80.7769795484621,-1.80149710919527,135.380799323379));
#51400=CARTESIAN_POINT('Ctrl Pts',(80.769214795515,-1.67434292424121,135.430853068516));
#51401=CARTESIAN_POINT('Ctrl Pts',(80.7614500425679,-1.54493413385633,135.475669133874));
#51402=CARTESIAN_POINT('Ctrl Pts',(80.7536852896208,-1.41374167822589,135.515041834731));
#51403=CARTESIAN_POINT('Ctrl Pts',(80.7459282487358,-1.28267952479186,135.554375430065));
#51404=CARTESIAN_POINT('Ctrl Pts',(80.7381712078508,-1.14983760364137,135.588276308276));
#51405=CARTESIAN_POINT('Ctrl Pts',(80.7304141669658,-1.01570601381134,135.616587166265));
#51406=CARTESIAN_POINT('Ctrl Pts',(80.7226629757257,-0.881675573656675,
135.644876674816));
#51407=CARTESIAN_POINT('Ctrl Pts',(80.7149117844855,-0.746357781611912,
135.667584473384));
#51408=CARTESIAN_POINT('Ctrl Pts',(80.7071605932454,-0.610256705529213,
135.684603420527));
#51409=CARTESIAN_POINT('Ctrl Pts',(80.6994126964683,-0.474213476034372,
135.701615134164));
#51410=CARTESIAN_POINT('Ctrl Pts',(80.6916647996913,-0.337388011779061,
135.712942757012));
#51411=CARTESIAN_POINT('Ctrl Pts',(80.6839169029142,-0.200293136925427,
135.718530508992));
#51412=CARTESIAN_POINT('Ctrl Pts',(80.6761706268301,-0.0632269393641897,
135.724117092135));
#51413=CARTESIAN_POINT('Ctrl Pts',(80.668424350746,0.0741081663090297,135.723966176671));
#51414=CARTESIAN_POINT('Ctrl Pts',(80.6606780746619,0.211196084552891,135.718074007292));
#51415=CARTESIAN_POINT('Ctrl Pts',(80.6529317413966,0.34828501474853,135.712181794418));
#51416=CARTESIAN_POINT('Ctrl Pts',(80.6451854081312,0.485126363269211,135.70054825985));
#51417=CARTESIAN_POINT('Ctrl Pts',(80.6374390748658,0.621206287798106,135.683221735747));
#51418=CARTESIAN_POINT('Ctrl Pts',(80.6296910068629,0.757316686482588,135.665891331489));
#51419=CARTESIAN_POINT('Ctrl Pts',(80.6219429388599,0.892664934109089,135.642865450153));
#51420=CARTESIAN_POINT('Ctrl Pts',(80.614194870857,1.02674494037685,135.614243972691));
#51421=CARTESIAN_POINT('Ctrl Pts',(80.6064385681151,1.16096744847094,135.585592075983));
#51422=CARTESIAN_POINT('Ctrl Pts',(80.5986822653732,1.29391863966632,135.551332784993));
#51423=CARTESIAN_POINT('Ctrl Pts',(80.5909259626314,1.42510466733082,135.511616691932));
#51424=CARTESIAN_POINT('Ctrl Pts',(80.5831655201172,1.55636071292831,135.471879401196));
#51425=CARTESIAN_POINT('Ctrl Pts',(80.5754050776031,1.68584934879639,135.42667963385));
#51426=CARTESIAN_POINT('Ctrl Pts',(80.5676446350889,1.8130953607569,135.376216725899));
#51427=CARTESIAN_POINT('Ctrl Pts',(80.5598717348235,1.9405456393121,135.325672810408));
#51428=CARTESIAN_POINT('Ctrl Pts',(80.552098834558,2.06574574261073,135.269849030101));
#51429=CARTESIAN_POINT('Ctrl Pts',(80.5443259342926,2.18824296583373,135.208991792248));
#51430=CARTESIAN_POINT('Ctrl Pts',(80.5368355985305,2.30628710644093,135.150346868281));
#51431=CARTESIAN_POINT('Ctrl Pts',(80.5293452627685,2.42182119810366,135.087028238962));
#51432=CARTESIAN_POINT('Ctrl Pts',(80.5218549270065,2.53446618862478,135.019294092868));
#51433=CARTESIAN_POINT('Ctrl Pts',(80.5140805928874,2.65138214819897,134.948991786037));
#51434=CARTESIAN_POINT('Ctrl Pts',(80.5063062587683,2.76555595599027,134.873709827595));
#51435=CARTESIAN_POINT('Ctrl Pts',(80.4985319246492,2.87653430314573,134.793688062804));
#51436=CARTESIAN_POINT('Ctrl Pts',(80.4907671717021,2.98737587940666,134.713764917685));
#51437=CARTESIAN_POINT('Ctrl Pts',(80.483002418755,3.09502951663782,134.629113815307));
#51438=CARTESIAN_POINT('Ctrl Pts',(80.475237665808,3.1990676117833,134.540019793366));
#51439=CARTESIAN_POINT('Ctrl Pts',(80.467480624923,3.30300237482599,134.451014260864));
#51440=CARTESIAN_POINT('Ctrl Pts',(80.459723584038,3.40332844701351,134.357574843069));
#51441=CARTESIAN_POINT('Ctrl Pts',(80.451966543153,3.49964857429439,134.260028848016));
#51442=CARTESIAN_POINT('Ctrl Pts',(80.4442153519128,3.59589606581808,134.162556413156));
#51443=CARTESIAN_POINT('Ctrl Pts',(80.4364641606727,3.6881433517926,134.060983842104));
#51444=CARTESIAN_POINT('Ctrl Pts',(80.4287129694326,3.77602783010214,133.955677308855));
#51445=CARTESIAN_POINT('Ctrl Pts',(80.4209650726555,3.86387495516399,133.850415533691));
#51446=CARTESIAN_POINT('Ctrl Pts',(80.4132171758784,3.94736271065898,133.741423252356));
#51447=CARTESIAN_POINT('Ctrl Pts',(80.4054692791013,4.02616697324001,133.629101767847));
#51448=CARTESIAN_POINT('Ctrl Pts',(80.3977230030172,4.10495475166813,133.516803778571));
#51449=CARTESIAN_POINT('Ctrl Pts',(80.3899767269331,4.17906076142679,133.401178291141));
#51450=CARTESIAN_POINT('Ctrl Pts',(80.382230450849,4.24820288082263,133.282657481517));
#51451=CARTESIAN_POINT('Ctrl Pts',(80.3744841175837,4.3173455106099,133.164135797));
#51452=CARTESIAN_POINT('Ctrl Pts',(80.3667377843183,4.38152397991067,133.042719085342));
#51453=CARTESIAN_POINT('Ctrl Pts',(80.3589914510529,4.44050120761483,132.91886578135));
#51454=CARTESIAN_POINT('Ctrl Pts',(80.35124338305,4.49949164286018,132.79498474127));
#51455=CARTESIAN_POINT('Ctrl Pts',(80.343495315047,4.55327835067198,132.66866637598));
#51456=CARTESIAN_POINT('Ctrl Pts',(80.335747247044,4.60167180955522,132.540390461677));
#51457=CARTESIAN_POINT('Ctrl Pts',(80.3279909443021,4.6501167015825,132.411978214206));
#51458=CARTESIAN_POINT('Ctrl Pts',(80.3202346415603,4.69315675615369,132.281604628071));
#51459=CARTESIAN_POINT('Ctrl Pts',(80.3124783388184,4.73065173459248,132.149766589196));
#51460=CARTESIAN_POINT('Ctrl Pts',(80.3047178963043,4.76816672523025,132.01785818439));
#51461=CARTESIAN_POINT('Ctrl Pts',(80.2969574537901,4.8001306514611,131.88448414941));
#51462=CARTESIAN_POINT('Ctrl Pts',(80.289197011276,4.82645435543933,131.75015204138));
#51463=CARTESIAN_POINT('Ctrl Pts',(80.2814241110105,4.8528203165641,131.615604291526));
#51464=CARTESIAN_POINT('Ctrl Pts',(80.2736512107451,4.87352790319527,131.480095781941));
#51465=CARTESIAN_POINT('Ctrl Pts',(80.2658783104796,4.88853972673615,131.344140575162));
#51466=CARTESIAN_POINT('Ctrl Pts',(80.2583879747176,4.90300583267882,131.2131276826));
#51467=CARTESIAN_POINT('Ctrl Pts',(80.2508976389555,4.9121830751767,131.081700313398));
#51468=CARTESIAN_POINT('Ctrl Pts',(80.2434073031935,4.91608378862042,130.950316932138));
#51469=CARTESIAN_POINT('Ctrl Pts',(80.2356329690744,4.92013239879994,130.813952110045));
#51470=CARTESIAN_POINT('Ctrl Pts',(80.2278586349554,4.91850928702849,130.677202714578));
#51471=CARTESIAN_POINT('Ctrl Pts',(80.2200843008363,4.91117121740962,130.540579769536));
#51472=CARTESIAN_POINT('Ctrl Pts',(80.2123195478892,4.90384219130573,130.404125200064));
#51473=CARTESIAN_POINT('Ctrl Pts',(80.2045547949421,4.89081224194038,130.267797157598));
#51474=CARTESIAN_POINT('Ctrl Pts',(80.1967900419951,4.87209004970578,130.132109466538));
#51475=CARTESIAN_POINT('Ctrl Pts',(80.1890330011101,4.85338645261645,129.996556542407));
#51476=CARTESIAN_POINT('Ctrl Pts',(80.1812759602251,4.82900191670185,129.861643088791));
#51477=CARTESIAN_POINT('Ctrl Pts',(80.1735189193401,4.79899708996234,129.727880244762));
#51478=CARTESIAN_POINT('Ctrl Pts',(80.1657677280999,4.76901489009605,129.594218272334));
#51479=CARTESIAN_POINT('Ctrl Pts',(80.1580165368598,4.73342092072011,129.461705562363));
#51480=CARTESIAN_POINT('Ctrl Pts',(80.1502653456197,4.69232725908536,129.330845108267));
#51481=CARTESIAN_POINT('Ctrl Pts',(80.1425174488426,4.65125106335302,129.200040273355));
#51482=CARTESIAN_POINT('Ctrl Pts',(80.1347695520655,4.60467994139138,129.070886669815));
#51483=CARTESIAN_POINT('Ctrl Pts',(80.1270216552884,4.55277632419008,128.943873905871));
#51484=CARTESIAN_POINT('Ctrl Pts',(80.1192753792044,4.50088356410662,128.816887710259));
#51485=CARTESIAN_POINT('Ctrl Pts',(80.1115291031202,4.44366067526238,128.692041825192));
#51486=CARTESIAN_POINT('Ctrl Pts',(80.1037828270361,4.38131876586578,128.569807209305));
#51487=CARTESIAN_POINT('Ctrl Pts',(80.0960364937708,4.31897639627537,128.447571691109));
#51488=CARTESIAN_POINT('Ctrl Pts',(80.0882901605054,4.25151510836129,128.327947828839));
#51489=CARTESIAN_POINT('Ctrl Pts',(80.0805438272401,4.1791924481783,128.211382880757));
#51490=CARTESIAN_POINT('Ctrl Pts',(80.0727957592371,4.10685359183697,128.094791828763));
#51491=CARTESIAN_POINT('Ctrl Pts',(80.0650476912341,4.02965140298172,127.981261386225));
#51492=CARTESIAN_POINT('Ctrl Pts',(80.0572996232312,3.94788708991859,127.871210333698));
#51493=CARTESIAN_POINT('Ctrl Pts',(80.0495433204893,3.86603587677058,127.761042317603));
#51494=CARTESIAN_POINT('Ctrl Pts',(80.0417870177475,3.77961308719027,127.654361392877));
#51495=CARTESIAN_POINT('Ctrl Pts',(80.0340307150056,3.6889609629497,127.551554125268));
#51496=CARTESIAN_POINT('Ctrl Pts',(80.0262702724915,3.59826045494081,127.448691986326));
#51497=CARTESIAN_POINT('Ctrl Pts',(80.0185098299773,3.50332638485288,127.349707906173));
#51498=CARTESIAN_POINT('Ctrl Pts',(80.0107493874631,3.40453758287727,127.254951242856));
#51499=CARTESIAN_POINT('Ctrl Pts',(80.0029764871977,3.30559019634674,127.160042467731));
#51500=CARTESIAN_POINT('Ctrl Pts',(79.9952035869322,3.20277600581824,127.06937492922));
#51501=CARTESIAN_POINT('Ctrl Pts',(79.9874306866668,3.09650729721128,126.983257946763));
#51502=CARTESIAN_POINT('Ctrl Pts',(79.9799403509048,2.99410172383655,126.900271533534));
#51503=CARTESIAN_POINT('Ctrl Pts',(79.9724500151427,2.8884886796471,126.821510756162));
#51504=CARTESIAN_POINT('Ctrl Pts',(79.9649596793807,2.78006055091892,126.747213048679));
#51505=CARTESIAN_POINT('Ctrl Pts',(79.9571853452616,2.66752133673431,126.670098321035));
#51506=CARTESIAN_POINT('Ctrl Pts',(79.9494110111425,2.55159286582454,126.597547502398));
#51507=CARTESIAN_POINT('Ctrl Pts',(79.9416366770234,2.43268170692635,126.529873189197));
#51508=CARTESIAN_POINT('Ctrl Pts',(79.9338719240763,2.31391709540427,126.462282278539));
#51509=CARTESIAN_POINT('Ctrl Pts',(79.9261071711292,2.19217744636074,126.399556107017));
#51510=CARTESIAN_POINT('Ctrl Pts',(79.9183424181822,2.06789974677971,126.34196510621));
#51511=CARTESIAN_POINT('Ctrl Pts',(79.9105853772972,1.94374548156191,126.284431305597));
#51512=CARTESIAN_POINT('Ctrl Pts',(79.9028283364122,1.81705853479989,126.232022689145));
#51513=CARTESIAN_POINT('Ctrl Pts',(79.8950712955272,1.68830172399631,126.184964515125));
#51514=CARTESIAN_POINT('Ctrl Pts',(79.887320104287,1.55964200970525,126.13794182804));
#51515=CARTESIAN_POINT('Ctrl Pts',(79.8795689130469,1.42891590397324,126.096261686007));
#51516=CARTESIAN_POINT('Ctrl Pts',(79.8718177218068,1.29660716989956,126.06010167549));
#51517=CARTESIAN_POINT('Ctrl Pts',(79.8640698250297,1.16435467056731,126.023957033943));
#51518=CARTESIAN_POINT('Ctrl Pts',(79.8563219282526,1.030521257106,125.993327960346));
#51519=CARTESIAN_POINT('Ctrl Pts',(79.8485740314756,0.895606648697689,125.968342442113));
#51520=CARTESIAN_POINT('Ctrl Pts',(79.8408277553915,0.760720261517129,125.943362150312));
#51521=CARTESIAN_POINT('Ctrl Pts',(79.8330814793073,0.624753513424354,125.924023136925));
#51522=CARTESIAN_POINT('Ctrl Pts',(79.8253352032232,0.488216744399233,125.910402355281));
#51523=CARTESIAN_POINT('Ctrl Pts',(79.8175888699579,0.351678967490605,125.896781473092));
#51524=CARTESIAN_POINT('Ctrl Pts',(79.8098425366925,0.214571550287528,125.888878945684));
#51525=CARTESIAN_POINT('Ctrl Pts',(79.8020962034272,0.0774099937671157,
125.886719846285));
#51526=CARTESIAN_POINT('Ctrl Pts',(79.7943481354242,-0.0597822791327743,
125.88456026337));
#51527=CARTESIAN_POINT('Ctrl Pts',(79.7866000674212,-0.197028324633647,
125.888146674007));
#51528=CARTESIAN_POINT('Ctrl Pts',(79.7788519994183,-0.333813000346846,
125.897452024236));
#51529=CARTESIAN_POINT('Ctrl Pts',(79.7710956966764,-0.470743052441243,
125.906767264301));
#51530=CARTESIAN_POINT('Ctrl Pts',(79.7633393939345,-0.607210364536801,
125.921813559155));
#51531=CARTESIAN_POINT('Ctrl Pts',(79.7555830911927,-0.742704717882201,
125.94251191933));
#51532=CARTESIAN_POINT('Ctrl Pts',(79.7478226486785,-0.878271388643729,
125.963221326844));
#51533=CARTESIAN_POINT('Ctrl Pts',(79.7400622061644,-1.01286368242679,125.989588735539));
#51534=CARTESIAN_POINT('Ctrl Pts',(79.7323017636502,-1.14598290744194,126.021484261402));
#51535=CARTESIAN_POINT('Ctrl Pts',(79.7245288633847,-1.27931582725477,126.053430988795));
#51536=CARTESIAN_POINT('Ctrl Pts',(79.7167559631193,-1.41117057659969,126.090923459893));
#51537=CARTESIAN_POINT('Ctrl Pts',(79.7089830628539,-1.54106406565972,126.133782001588));
#51538=CARTESIAN_POINT('Ctrl Pts',(79.7014927270918,-1.66623559921065,126.175082527338));
#51539=CARTESIAN_POINT('Ctrl Pts',(79.6940023913298,-1.78958570196112,126.221365648523));
#51540=CARTESIAN_POINT('Ctrl Pts',(79.6865120555678,-1.91070251956831,126.272429578349));
#51541=CARTESIAN_POINT('Ctrl Pts',(79.6787372956776,-2.03641840273769,126.325432515208));
#51542=CARTESIAN_POINT('Ctrl Pts',(79.6709625357874,-2.16012629599077,126.383754417044));
#51543=CARTESIAN_POINT('Ctrl Pts',(79.6631877758972,-2.2813433638567,126.447222162262));
#51544=CARTESIAN_POINT('Ctrl Pts',(79.6554226943927,-2.40240953503272,126.510610899855));
#51545=CARTESIAN_POINT('Ctrl Pts',(79.6476576128882,-2.52099070744273,126.579132554978));
#51546=CARTESIAN_POINT('Ctrl Pts',(79.6398925313837,-2.63662309986672,126.652565621212));
#51547=CARTESIAN_POINT('Ctrl Pts',(79.6321352587413,-2.75213920794696,126.725924840354));
#51548=CARTESIAN_POINT('Ctrl Pts',(79.6243779860988,-2.86471210971172,126.804185432721));
#51549=CARTESIAN_POINT('Ctrl Pts',(79.6166207134564,-2.97390208826842,126.887079745342));
#51550=CARTESIAN_POINT('Ctrl Pts',(79.6088521230946,-3.08325137301405,126.970094999255));
#51551=CARTESIAN_POINT('Ctrl Pts',(79.6010835327327,-3.18920751056089,127.057757314326));
#51552=CARTESIAN_POINT('Ctrl Pts',(79.5933149423708,-3.29135687202745,127.149753524668));
#51553=CARTESIAN_POINT('Ctrl Pts',(79.5855673853042,-3.39322966624365,127.241500657204));
#51554=CARTESIAN_POINT('Ctrl Pts',(79.5778198282376,-3.49131597439789,127.337557991071));
#51555=CARTESIAN_POINT('Ctrl Pts',(79.570072271171,-3.58523813826385,127.437574233722));
#51556=CARTESIAN_POINT('Ctrl Pts',(79.5623264684862,-3.6791390340918,127.537567828372));
#51557=CARTESIAN_POINT('Ctrl Pts',(79.5545806658014,-3.76887739469223,127.64151826309));
#51558=CARTESIAN_POINT('Ctrl Pts',(79.5468348631166,-3.85411277790421,127.749037761026));
#51559=CARTESIAN_POINT('Ctrl Pts',(79.5390891370196,-3.93934731833801,127.856556195846));
#51560=CARTESIAN_POINT('Ctrl Pts',(79.5313434109227,-4.02007872793979,127.967643316808));
#51561=CARTESIAN_POINT('Ctrl Pts',(79.5235976848257,-4.09600743652683,128.081879002859));
#51562=CARTESIAN_POINT('Ctrl Pts',(79.5158124231546,-4.17232369885024,128.196697768325));
#51563=CARTESIAN_POINT('Ctrl Pts',(79.5080271614835,-4.2437878623242,128.314697006798));
#51564=CARTESIAN_POINT('Ctrl Pts',(79.5002418998124,-4.3101407549323,128.435422092578));
#51565=CARTESIAN_POINT('Ctrl Pts',(79.49248811021,-4.37622541470655,128.555659144897));
#51566=CARTESIAN_POINT('Ctrl Pts',(79.4847343206076,-4.43723991423492,128.678599676034));
#51567=CARTESIAN_POINT('Ctrl Pts',(79.4769805310053,-4.49297545682033,128.803772052441));
#51568=CARTESIAN_POINT('Ctrl Pts',(79.4691795332998,-4.54905033918414,128.929706527223));
#51569=CARTESIAN_POINT('Ctrl Pts',(79.4613785355943,-4.59978161849782,129.057899743097));
#51570=CARTESIAN_POINT('Ctrl Pts',(79.4535775378887,-4.64500696200414,129.187854080173));
#51571=CARTESIAN_POINT('Ctrl Pts',(79.4457765401832,-4.69023230551044,129.317808417249));
#51572=CARTESIAN_POINT('Ctrl Pts',(79.4379755424777,-4.72995164131195,129.449523480783));
#51573=CARTESIAN_POINT('Ctrl Pts',(79.4301745447722,-4.76405452823407,129.582490119308));
#51574=CARTESIAN_POINT('Origin',(213.235140564004,0.,130.804360617566));
#51575=CARTESIAN_POINT('',(77.3348925457121,-4.76405452823405,129.582490119308));
#51576=CARTESIAN_POINT('',(77.6798548998299,-4.76405452823404,129.582490119308));
#51577=CARTESIAN_POINT('',(213.235140564004,-4.76405452823405,129.582490119308));
#51578=CARTESIAN_POINT('',(79.0148594360372,-4.91824997683007,130.803883217332));
#51579=CARTESIAN_POINT('Ctrl Pts',(79.0148594359911,-4.91824997683015,130.803883218151));
#51580=CARTESIAN_POINT('Ctrl Pts',(79.006801254778,-4.91826386524818,130.946964062875));
#51581=CARTESIAN_POINT('Ctrl Pts',(78.9987430735649,-4.91202970327439,131.089943852501));
#51582=CARTESIAN_POINT('Ctrl Pts',(78.9906848923518,-4.89959985564133,131.23226751994));
#51583=CARTESIAN_POINT('Ctrl Pts',(78.982618049138,-4.88715664676137,131.374744175712));
#51584=CARTESIAN_POINT('Ctrl Pts',(78.9745512059242,-4.86850449730708,131.516562960778));
#51585=CARTESIAN_POINT('Ctrl Pts',(78.9664843627104,-4.84374728067055,131.657176742822));
#51586=CARTESIAN_POINT('Ctrl Pts',(78.958400333963,-4.81893732147206,131.798090087261));
#51587=CARTESIAN_POINT('Ctrl Pts',(78.9503163052157,-4.78799635360567,131.937792957518));
#51588=CARTESIAN_POINT('Ctrl Pts',(78.9422322764683,-4.7510791765238,132.075749512005));
#51589=CARTESIAN_POINT('Ctrl Pts',(78.9341394529842,-4.71412183668822,132.213856151508));
#51590=CARTESIAN_POINT('Ctrl Pts',(78.9260466295,-4.67117541861149,132.350212357506));
#51591=CARTESIAN_POINT('Ctrl Pts',(78.9179538060158,-4.62244372778178,132.484300213501));
#51592=CARTESIAN_POINT('Ctrl Pts',(78.9098426664952,-4.5736017452318,132.618691543069));
#51593=CARTESIAN_POINT('Ctrl Pts',(78.9017315269746,-4.51894843833848,132.750803938434));
#51594=CARTESIAN_POINT('Ctrl Pts',(78.893620387454,-4.45873540362251,132.88014038984));
#51595=CARTESIAN_POINT('Ctrl Pts',(78.8859996517321,-4.40216288093094,133.001657090777));
#51596=CARTESIAN_POINT('Ctrl Pts',(78.8783789160102,-4.34068314080648,133.120723396886));
#51597=CARTESIAN_POINT('Ctrl Pts',(78.8707581802883,-4.27453987883232,133.236950160989));
#51598=CARTESIAN_POINT('Ctrl Pts',(78.8629838461692,-4.20706347798609,133.355519513175));
#51599=CARTESIAN_POINT('Ctrl Pts',(78.8552095120502,-4.13454305546345,133.471467001158));
#51600=CARTESIAN_POINT('Ctrl Pts',(78.8474351779311,-4.05720750929386,133.584333691002));
#51601=CARTESIAN_POINT('Ctrl Pts',(78.839670424984,-3.97996727227313,133.697061282738));
#51602=CARTESIAN_POINT('Ctrl Pts',(78.8319056720369,-3.89792393777996,133.80671531143));
#51603=CARTESIAN_POINT('Ctrl Pts',(78.8241409190898,-3.81135220013507,133.912861457042));
#51604=CARTESIAN_POINT('Ctrl Pts',(78.8163838782047,-3.72486644676045,134.018902176806));
#51605=CARTESIAN_POINT('Ctrl Pts',(78.8086268373198,-3.63386148631231,134.12144164595));
#51606=CARTESIAN_POINT('Ctrl Pts',(78.8008697964347,-3.53865499956588,134.220074870332));
#51607=CARTESIAN_POINT('Ctrl Pts',(78.7931186051946,-3.44352030877209,134.318633714631));
#51608=CARTESIAN_POINT('Ctrl Pts',(78.7853674139545,-3.34419066862125,134.413291897305));
#51609=CARTESIAN_POINT('Ctrl Pts',(78.7776162227144,-3.24102344620704,134.503678133492));
#51610=CARTESIAN_POINT('Ctrl Pts',(78.7698683259373,-3.13790007261416,134.594025953117));
#51611=CARTESIAN_POINT('Ctrl Pts',(78.7621204291602,-3.03094265429462,134.680105180429));
#51612=CARTESIAN_POINT('Ctrl Pts',(78.7543725323831,-2.9205446006123,134.761582155253));
#51613=CARTESIAN_POINT('Ctrl Pts',(78.746626256299,-2.81016963982283,134.843042086851));
#51614=CARTESIAN_POINT('Ctrl Pts',(78.7388799802149,-2.69635578957786,134.919901448793));
#51615=CARTESIAN_POINT('Ctrl Pts',(78.7311337041308,-2.5795283312385,134.9918678296));
#51616=CARTESIAN_POINT('Ctrl Pts',(78.7233873708655,-2.46270001050554,135.063834741646));
#51617=CARTESIAN_POINT('Ctrl Pts',(78.7156410376001,-2.34285837016483,135.130908395431));
#51618=CARTESIAN_POINT('Ctrl Pts',(78.7078947043347,-2.22045602371151,135.192840776945));
#51619=CARTESIAN_POINT('Ctrl Pts',(78.7001466363318,-2.09802626610153,135.254787027787));
#51620=CARTESIAN_POINT('Ctrl Pts',(78.6923985683288,-1.97303501006068,135.311589538824));
#51621=CARTESIAN_POINT('Ctrl Pts',(78.6846505003258,-1.84595734562999,135.363047329835));
#51622=CARTESIAN_POINT('Ctrl Pts',(78.676894197584,-1.71874462154513,135.414559810798));
#51623=CARTESIAN_POINT('Ctrl Pts',(78.6691378948421,-1.58944142241624,135.460716077484));
#51624=CARTESIAN_POINT('Ctrl Pts',(78.6613815921003,-1.45854112573695,135.501364007711));
#51625=CARTESIAN_POINT('Ctrl Pts',(78.6536211495861,-1.32757096362773,135.542033632962));
#51626=CARTESIAN_POINT('Ctrl Pts',(78.6458607070719,-1.19500238316923,135.577188963459));
#51627=CARTESIAN_POINT('Ctrl Pts',(78.6381002645577,-1.06134065578097,135.606728687059));
#51628=CARTESIAN_POINT('Ctrl Pts',(78.6303273642923,-0.927464362722071,
135.636315830446));
#51629=CARTESIAN_POINT('Ctrl Pts',(78.6225544640269,-0.792491801222578,
135.660269284396));
#51630=CARTESIAN_POINT('Ctrl Pts',(78.6147815637614,-0.656935988556452,
135.678539334995));
#51631=CARTESIAN_POINT('Ctrl Pts',(78.6072912279995,-0.526307971126326,
135.696145223236));
#51632=CARTESIAN_POINT('Ctrl Pts',(78.5998008922375,-0.395138678276404,
135.70847371739));
#51633=CARTESIAN_POINT('Ctrl Pts',(78.5923105564755,-0.263886738552775,
135.715526146411));
#51634=CARTESIAN_POINT('Ctrl Pts',(78.5845362223564,-0.127658341640397,
135.722845970422));
#51635=CARTESIAN_POINT('Ctrl Pts',(78.5767618882373,0.00909062358639984,
135.724504934498));
#51636=CARTESIAN_POINT('Ctrl Pts',(78.5689875541183,0.145850318033386,135.720447552032));
#51637=CARTESIAN_POINT('Ctrl Pts',(78.5612228011712,0.282441468379067,135.716395169928));
#51638=CARTESIAN_POINT('Ctrl Pts',(78.5534580482241,0.419042934593818,135.706640469987));
#51639=CARTESIAN_POINT('Ctrl Pts',(78.545693295277,0.555140831940946,135.691179799735));
#51640=CARTESIAN_POINT('Ctrl Pts',(78.537936254392,0.691103554938062,135.675734485238));
#51641=CARTESIAN_POINT('Ctrl Pts',(78.5301792135071,0.826563318439076,135.654594522357));
#51642=CARTESIAN_POINT('Ctrl Pts',(78.5224221726221,0.961007675183125,135.627808275698));
#51643=CARTESIAN_POINT('Ctrl Pts',(78.514670981382,1.09535064639166,135.601042228756));
#51644=CARTESIAN_POINT('Ctrl Pts',(78.5069197901419,1.228679353097,135.568638449226));
#51645=CARTESIAN_POINT('Ctrl Pts',(78.4991685989018,1.36048825718647,135.530696911627));
#51646=CARTESIAN_POINT('Ctrl Pts',(78.4914207021247,1.49224113897594,135.492771500193));
#51647=CARTESIAN_POINT('Ctrl Pts',(78.4836728053476,1.62247512798519,135.449313119934));
#51648=CARTESIAN_POINT('Ctrl Pts',(78.4759249085705,1.75069685909023,135.400472405814));
#51649=CARTESIAN_POINT('Ctrl Pts',(78.4681786324864,1.87889176897335,135.351641908119));
#51650=CARTESIAN_POINT('Ctrl Pts',(78.4604323564024,2.00507489306106,135.297431455056));
#51651=CARTESIAN_POINT('Ctrl Pts',(78.4526860803182,2.12877034232941,135.238040792333));
#51652=CARTESIAN_POINT('Ctrl Pts',(78.4449397470529,2.25246670468938,135.178649691201));
#51653=CARTESIAN_POINT('Ctrl Pts',(78.4371934137875,2.37367500314165,135.114078473326));
#51654=CARTESIAN_POINT('Ctrl Pts',(78.4294470805222,2.49194192782743,135.044573877632));
#51655=CARTESIAN_POINT('Ctrl Pts',(78.4216990125192,2.61023533757091,134.975053716865));
#51656=CARTESIAN_POINT('Ctrl Pts',(78.4139509445162,2.72558572580896,134.900598177916));
#51657=CARTESIAN_POINT('Ctrl Pts',(78.4062028765132,2.83756720441572,134.821498332771));
#51658=CARTESIAN_POINT('Ctrl Pts',(78.3984465737714,2.94966769827062,134.74231441937));
#51659=CARTESIAN_POINT('Ctrl Pts',(78.3906902710296,3.05839181018284,134.65847656546));
#51660=CARTESIAN_POINT('Ctrl Pts',(78.3829339682877,3.16334487286462,134.570317637743));
#51661=CARTESIAN_POINT('Ctrl Pts',(78.3751735257736,3.26835395215603,134.482111656952));
#51662=CARTESIAN_POINT('Ctrl Pts',(78.3674130832594,3.36958768325885,134.389580270526));
#51663=CARTESIAN_POINT('Ctrl Pts',(78.3596526407453,3.46668771785457,134.293093815931));
#51664=CARTESIAN_POINT('Ctrl Pts',(78.3518797404799,3.56394362604601,134.196452472714));
#51665=CARTESIAN_POINT('Ctrl Pts',(78.3441068402144,3.65705231162963,134.095843661059));
#51666=CARTESIAN_POINT('Ctrl Pts',(78.336333939949,3.7456946505146,133.991672125343));
#51667=CARTESIAN_POINT('Ctrl Pts',(78.3288436041869,3.83111461710567,133.891287487341));
#51668=CARTESIAN_POINT('Ctrl Pts',(78.3213532684247,3.91238713517407,133.787594898587));
#51669=CARTESIAN_POINT('Ctrl Pts',(78.3138629326626,3.98926542287362,133.680980934599));
#51670=CARTESIAN_POINT('Ctrl Pts',(78.3060885985435,4.06905857421684,133.570324669762));
#51671=CARTESIAN_POINT('Ctrl Pts',(78.2983142644245,4.14437046366273,133.456170602991));
#51672=CARTESIAN_POINT('Ctrl Pts',(78.2905399303054,4.21487882827283,133.338917684487));
#51673=CARTESIAN_POINT('Ctrl Pts',(78.2827751773583,4.28530029762511,133.221809269725));
#51674=CARTESIAN_POINT('Ctrl Pts',(78.2750104244112,4.35092982146337,133.101609933854));
#51675=CARTESIAN_POINT('Ctrl Pts',(78.2672456714641,4.41148655960332,132.978750048404));
#51676=CARTESIAN_POINT('Ctrl Pts',(78.2594886305791,4.47198315193708,132.856012189124));
#51677=CARTESIAN_POINT('Ctrl Pts',(78.2517315896942,4.52741681341114,132.730619387361));
#51678=CARTESIAN_POINT('Ctrl Pts',(78.2439745488092,4.57755124427728,132.603028921761));
#51679=CARTESIAN_POINT('Ctrl Pts',(78.236223357569,4.62764786837942,132.475534673123));
#51680=CARTESIAN_POINT('Ctrl Pts',(78.2284721663289,4.67245307364692,132.345846421763));
#51681=CARTESIAN_POINT('Ctrl Pts',(78.2207209750887,4.71177771577674,132.214443529883));
#51682=CARTESIAN_POINT('Ctrl Pts',(78.2129730783116,4.75108564388447,132.083096487739));
#51683=CARTESIAN_POINT('Ctrl Pts',(78.2052251815346,4.7849175299681,131.950036628307));
#51684=CARTESIAN_POINT('Ctrl Pts',(78.1974772847575,4.81313343159022,131.815760455518));
#51685=CARTESIAN_POINT('Ctrl Pts',(78.1897310086734,4.84134343105397,131.681512370409));
#51686=CARTESIAN_POINT('Ctrl Pts',(78.1819847325893,4.86393970233621,131.546048860378));
#51687=CARTESIAN_POINT('Ctrl Pts',(78.1742384565052,4.88083306751467,131.409878271772));
#51688=CARTESIAN_POINT('Ctrl Pts',(78.1664921232399,4.89772655739614,131.273706677986));
#51689=CARTESIAN_POINT('Ctrl Pts',(78.1587457899745,4.90891700903694,131.136828383199));
#51690=CARTESIAN_POINT('Ctrl Pts',(78.1509994567091,4.91436698582944,130.999758138251));
#51691=CARTESIAN_POINT('Ctrl Pts',(78.1432513887062,4.91981818310644,130.862657197371));
#51692=CARTESIAN_POINT('Ctrl Pts',(78.1355033207032,4.9195263319306,130.725364611374));
#51693=CARTESIAN_POINT('Ctrl Pts',(78.1277552527003,4.91350611647311,130.58839602352));
#51694=CARTESIAN_POINT('Ctrl Pts',(78.1199989499584,4.90747950265899,130.451281863821));
#51695=CARTESIAN_POINT('Ctrl Pts',(78.1122426472166,4.89571237997539,130.314492781351));
#51696=CARTESIAN_POINT('Ctrl Pts',(78.1044863444747,4.87827147129727,130.178540743459));
#51697=CARTESIAN_POINT('Ctrl Pts',(78.0967259019605,4.86082125388104,130.042516143871));
#51698=CARTESIAN_POINT('Ctrl Pts',(78.0889654594464,4.83769128228768,129.907329864238));
#51699=CARTESIAN_POINT('Ctrl Pts',(78.0812050169322,4.80899943589805,129.773483569596));
#51700=CARTESIAN_POINT('Ctrl Pts',(78.0734321166668,4.78026153080945,129.639422412999));
#51701=CARTESIAN_POINT('Ctrl Pts',(78.0656592164013,4.7459440070381,129.506705918636));
#51702=CARTESIAN_POINT('Ctrl Pts',(78.0578863161359,4.70621489312572,129.375821348865));
#51703=CARTESIAN_POINT('Ctrl Pts',(78.0503959803739,4.6679300325755,129.249694762883));
#51704=CARTESIAN_POINT('Ctrl Pts',(78.0429056446118,4.62462030213842,129.125269514622));
#51705=CARTESIAN_POINT('Ctrl Pts',(78.0354153088498,4.57647754712891,129.002962182148));
#51706=CARTESIAN_POINT('Ctrl Pts',(78.0276409747307,4.52650944493073,128.87601752999));
#51707=CARTESIAN_POINT('Ctrl Pts',(78.0198666406116,4.47117631138528,128.750952442997));
#51708=CARTESIAN_POINT('Ctrl Pts',(78.0120923064925,4.41063960360692,128.628253692437));
#51709=CARTESIAN_POINT('Ctrl Pts',(78.0043275535454,4.35017750191063,128.505706157121));
#51710=CARTESIAN_POINT('Ctrl Pts',(77.9965628005983,4.28452475714507,128.385519502921));
#51711=CARTESIAN_POINT('Ctrl Pts',(77.9887980476512,4.21389165208789,128.268162634962));
#51712=CARTESIAN_POINT('Ctrl Pts',(77.9810410067662,4.1433287008267,128.1509223275));
#51713=CARTESIAN_POINT('Ctrl Pts',(77.9732839658813,4.06779543346437,128.036506545897));
#51714=CARTESIAN_POINT('Ctrl Pts',(77.9655269249963,3.98754884569005,127.925361266101));
#51715=CARTESIAN_POINT('Ctrl Pts',(77.9577757337562,3.90736277249174,127.814299801825));
#51716=CARTESIAN_POINT('Ctrl Pts',(77.9500245425161,3.82247068153627,127.706504246014));
#51717=CARTESIAN_POINT('Ctrl Pts',(77.942273351276,3.73317363670454,127.602392838104));
#51718=CARTESIAN_POINT('Ctrl Pts',(77.9345254544989,3.64391454549869,127.498325680319));
#51719=CARTESIAN_POINT('Ctrl Pts',(77.9267775577219,3.5502544781255,127.397939852198));
#51720=CARTESIAN_POINT('Ctrl Pts',(77.9190296609448,3.45253551509754,127.301621463776));
#51721=CARTESIAN_POINT('Ctrl Pts',(77.9112833848607,3.35483699277,127.205323223086));
#51722=CARTESIAN_POINT('Ctrl Pts',(77.9035371087766,3.25308154182775,127.113091004044));
#51723=CARTESIAN_POINT('Ctrl Pts',(77.8957908326925,3.14764864560424,127.025274608181));
#51724=CARTESIAN_POINT('Ctrl Pts',(77.8880444994271,3.04221497109896,126.937457564078));
#51725=CARTESIAN_POINT('Ctrl Pts',(77.8802981661618,2.93310409755433,126.854056658412));
#51726=CARTESIAN_POINT('Ctrl Pts',(77.8725518328964,2.82072886402738,126.775381623063));
#51727=CARTESIAN_POINT('Ctrl Pts',(77.8648037648934,2.70832846484634,126.696688968986));
#51728=CARTESIAN_POINT('Ctrl Pts',(77.8570556968905,2.59266257122968,126.622724515357));
#51729=CARTESIAN_POINT('Ctrl Pts',(77.8493076288875,2.47417294560971,126.553754625744));
#51730=CARTESIAN_POINT('Ctrl Pts',(77.8415513261456,2.35555738780526,126.484711434111));
#51731=CARTESIAN_POINT('Ctrl Pts',(77.8337950234038,2.23411244141613,126.420673607353));
#51732=CARTESIAN_POINT('Ctrl Pts',(77.8260387206619,2.11030490441751,126.361861740482));
#51733=CARTESIAN_POINT('Ctrl Pts',(77.8182782781477,1.98643128760853,126.303018483947));
#51734=CARTESIAN_POINT('Ctrl Pts',(77.8105178356336,1.86019292725123,126.249406897873));
#51735=CARTESIAN_POINT('Ctrl Pts',(77.8027573931194,1.73207560503359,126.201198969204));
#51736=CARTESIAN_POINT('Ctrl Pts',(77.794984492854,1.60375261751669,126.152913652889));
#51737=CARTESIAN_POINT('Ctrl Pts',(77.7872115925885,1.47354501223205,126.110049450576));
#51738=CARTESIAN_POINT('Ctrl Pts',(77.7794386923231,1.34195356033271,126.072728372303));
#51739=CARTESIAN_POINT('Ctrl Pts',(77.771948356561,1.21514578916798,126.036764009231));
#51740=CARTESIAN_POINT('Ctrl Pts',(77.7644580207989,1.08705333669959,126.005946826103));
#51741=CARTESIAN_POINT('Ctrl Pts',(77.7569676850368,0.958130378930791,125.980340588641));
#51742=CARTESIAN_POINT('Ctrl Pts',(77.7491933509177,0.824319268033662,125.953763482903));
#51743=CARTESIAN_POINT('Ctrl Pts',(77.7414190167986,0.689189558051129,125.932716080867));
#51744=CARTESIAN_POINT('Ctrl Pts',(77.7336446826795,0.553238054949885,125.917325655848));
#51745=CARTESIAN_POINT('Ctrl Pts',(77.7258799297324,0.417454099926246,125.901954198152));
#51746=CARTESIAN_POINT('Ctrl Pts',(77.7181151767854,0.280850751681747,125.892225889389));
#51747=CARTESIAN_POINT('Ctrl Pts',(77.7103504238383,0.143936176356196,125.888217267374));
#51748=CARTESIAN_POINT('Ctrl Pts',(77.7025933829533,0.00715758651664383,
125.88421262678));
#51749=CARTESIAN_POINT('Ctrl Pts',(77.6948363420683,-0.129931226982009,
125.885916379108));
#51750=CARTESIAN_POINT('Ctrl Pts',(77.6870793011833,-0.266816139496606,
125.8933533675));
#51751=CARTESIAN_POINT('Ctrl Pts',(77.6793281099431,-0.403597826033775,
125.900784747601));
#51752=CARTESIAN_POINT('Ctrl Pts',(77.671576918703,-0.540175528833602,125.913940737022));
#51753=CARTESIAN_POINT('Ctrl Pts',(77.6638257274629,-0.67603463883003,125.932794110825));
#51754=CARTESIAN_POINT('Ctrl Pts',(77.6560778306858,-0.811836005080364,
125.951639471441));
#51755=CARTESIAN_POINT('Ctrl Pts',(77.6483299339087,-0.946918999543146,
125.976177346553));
#51756=CARTESIAN_POINT('Ctrl Pts',(77.6405820371317,-1.08077387403529,126.006328636045));
#51757=CARTESIAN_POINT('Ctrl Pts',(77.6328357610475,-1.21460074897345,126.036473618536));
#51758=CARTESIAN_POINT('Ctrl Pts',(77.6250894849635,-1.34719963375454,126.072229593989));
#51759=CARTESIAN_POINT('Ctrl Pts',(77.6173432088794,-1.47807111043409,126.113466368598));
#51760=CARTESIAN_POINT('Ctrl Pts',(77.609596875614,-1.60894355317689,126.154703447608));
#51761=CARTESIAN_POINT('Ctrl Pts',(77.6018505423486,-1.73808818948174,126.201421289009));
#51762=CARTESIAN_POINT('Ctrl Pts',(77.5941042090833,-1.86502128355201,126.253439977256));
#51763=CARTESIAN_POINT('Ctrl Pts',(77.5863561410803,-1.99198280340921,126.305470314729));
#51764=CARTESIAN_POINT('Ctrl Pts',(77.5786080730773,-2.11673143382669,126.362803712988));
#51765=CARTESIAN_POINT('Ctrl Pts',(77.5708600050743,-2.23880429220509,126.425212480804));
#51766=CARTESIAN_POINT('Ctrl Pts',(77.5631037023325,-2.36100689106963,126.487687577401));
#51767=CARTESIAN_POINT('Ctrl Pts',(77.5553473995906,-2.48052768834805,126.555248640724));
#51768=CARTESIAN_POINT('Ctrl Pts',(77.5475910968488,-2.59692877549976,126.627622177409));
#51769=CARTESIAN_POINT('Ctrl Pts',(77.5398306543346,-2.71339198941677,126.700034342031));
#51770=CARTESIAN_POINT('Ctrl Pts',(77.5320702118204,-2.8267318524565,126.777263878047));
#51771=CARTESIAN_POINT('Ctrl Pts',(77.5243097693062,-2.93654109026335,126.85899504671));
#51772=CARTESIAN_POINT('Ctrl Pts',(77.5165368690408,-3.04652660360691,126.940857417501));
#51773=CARTESIAN_POINT('Ctrl Pts',(77.5087639687753,-3.15296986214332,127.027235615132));
#51774=CARTESIAN_POINT('Ctrl Pts',(77.5009910685099,-3.25549753633386,127.117774276054));
#51775=CARTESIAN_POINT('Ctrl Pts',(77.4935007327479,-3.35429807131511,127.205021628597));
#51776=CARTESIAN_POINT('Ctrl Pts',(77.486010396986,-3.44946253965899,127.296131996392));
#51777=CARTESIAN_POINT('Ctrl Pts',(77.478520061224,-3.54069180023272,127.390757735234));
#51778=CARTESIAN_POINT('Ctrl Pts',(77.470846416256,-3.63415369280847,127.487699227283));
#51779=CARTESIAN_POINT('Ctrl Pts',(77.4631727712879,-3.72379809036211,127.5886551613));
#51780=CARTESIAN_POINT('Ctrl Pts',(77.4554991263198,-3.80925352721912,127.693288354203));
#51781=CARTESIAN_POINT('Ctrl Pts',(77.447834521834,-3.89460828723173,127.797798276544));
#51782=CARTESIAN_POINT('Ctrl Pts',(77.4401699173482,-3.97578364684764,127.905976536633));
#51783=CARTESIAN_POINT('Ctrl Pts',(77.4325053128624,-4.05244416295984,128.017448460968));
#51784=CARTESIAN_POINT('Ctrl Pts',(77.4248479741973,-4.12903200714726,128.128814713183));
#51785=CARTESIAN_POINT('Ctrl Pts',(77.4171906355321,-4.20111329310754,128.243468091448));
#51786=CARTESIAN_POINT('Ctrl Pts',(77.409533296867,-4.26839250749628,128.361000540858));
#51787=CARTESIAN_POINT('Ctrl Pts',(77.4018819124277,-4.33561940662809,128.478441598888));
#51788=CARTESIAN_POINT('Ctrl Pts',(77.3942305279885,-4.39805146679596,128.598756925088));
#51789=CARTESIAN_POINT('Ctrl Pts',(77.3865791435492,-4.45543657273441,128.721509684628));
#51790=CARTESIAN_POINT('Ctrl Pts',(77.3789311472552,-4.51279626770592,128.844208087445));
#51791=CARTESIAN_POINT('Ctrl Pts',(77.3712831509613,-4.56511328486775,128.969341412917));
#51792=CARTESIAN_POINT('Ctrl Pts',(77.3636351546673,-4.61218172281993,129.09644878782));
#51793=CARTESIAN_POINT('Ctrl Pts',(77.355988294649,-4.65924316773515,129.223537278167));
#51794=CARTESIAN_POINT('Ctrl Pts',(77.3483414346307,-4.70105744378289,129.352598858408));
#51795=CARTESIAN_POINT('Ctrl Pts',(77.3406945746124,-4.73746718313463,129.483153687815));
#51796=CARTESIAN_POINT('Ctrl Pts',(77.3387605649789,-4.74667577156033,129.516173031331));
#51797=CARTESIAN_POINT('Ctrl Pts',(77.3368265553455,-4.75553889964443,129.54928781268));
#51798=CARTESIAN_POINT('Ctrl Pts',(77.3348925457121,-4.76405452823405,129.582490119308));
#51799=CARTESIAN_POINT('Ctrl Pts',(79.0845758390371,-4.76405452823407,129.582490119308));
#51800=CARTESIAN_POINT('Ctrl Pts',(79.0763773866997,-4.80000871991458,129.72267496699));
#51801=CARTESIAN_POINT('Ctrl Pts',(79.0681789343622,-4.82981020052689,129.86459984855));
#51802=CARTESIAN_POINT('Ctrl Pts',(79.0599804820248,-4.85330185278545,130.007715032472));
#51803=CARTESIAN_POINT('Ctrl Pts',(79.0518001104447,-4.87674169686777,130.150514592079));
#51804=CARTESIAN_POINT('Ctrl Pts',(79.0436197388646,-4.89389941114362,130.294498904072));
#51805=CARTESIAN_POINT('Ctrl Pts',(79.0354393672845,-4.90466844418986,130.439106575743));
#51806=CARTESIAN_POINT('Ctrl Pts',(79.028579390202,-4.91369924666305,130.560373110385));
#51807=CARTESIAN_POINT('Ctrl Pts',(79.0217194131196,-4.91823815351782,130.682077652307));
#51808=CARTESIAN_POINT('Ctrl Pts',(79.0148594360371,-4.91824997683007,130.803883217332));
#51809=CARTESIAN_POINT('',(79.3601405639593,-4.91824827266494,130.800238612192));
#51810=CARTESIAN_POINT('Ctrl Pts',(79.4301745447722,-4.76405452823407,129.582490119308));
#51811=CARTESIAN_POINT('Ctrl Pts',(79.4228045070997,-4.79627342777008,129.708111119609));
#51812=CARTESIAN_POINT('Ctrl Pts',(79.4154344694273,-4.82347969088767,129.834848857671));
#51813=CARTESIAN_POINT('Ctrl Pts',(79.4080644317549,-4.84562331757989,129.962269335919));
#51814=CARTESIAN_POINT('Ctrl Pts',(79.395942616872,-4.88204388359722,130.171843223904));
#51815=CARTESIAN_POINT('Ctrl Pts',(79.3838208019891,-4.90487565833682,130.383842954193));
#51816=CARTESIAN_POINT('Ctrl Pts',(79.3716989871062,-4.9138708413202,130.596860214378));
#51817=CARTESIAN_POINT('Ctrl Pts',(79.367846179407,-4.91672987774251,130.664565797086));
#51818=CARTESIAN_POINT('Ctrl Pts',(79.3639933717077,-4.91819139497684,130.73237394268));
#51819=CARTESIAN_POINT('Ctrl Pts',(79.3601405640085,-4.91824827266422,130.800238611325));
#51820=CARTESIAN_POINT('Ctrl Pts',(79.3601405639593,-4.91824827266494,130.800238612192));
#51821=CARTESIAN_POINT('Ctrl Pts',(79.3524935954593,-4.91836116223177,130.934934923014));
#51822=CARTESIAN_POINT('Ctrl Pts',(79.3448466269593,-4.91293649359095,131.069828220389));
#51823=CARTESIAN_POINT('Ctrl Pts',(79.3371996584593,-4.90195240701566,131.204417690811));
#51824=CARTESIAN_POINT('Ctrl Pts',(79.3295598048268,-4.89097854021836,131.338881936937));
#51825=CARTESIAN_POINT('Ctrl Pts',(79.3219199511942,-4.87445557616604,131.473042518561));
#51826=CARTESIAN_POINT('Ctrl Pts',(79.3142800975617,-4.8524137038026,131.606398216216));
#51827=CARTESIAN_POINT('Ctrl Pts',(79.3065857938276,-4.83021473651977,131.740704355024));
#51828=CARTESIAN_POINT('Ctrl Pts',(79.2988914900934,-4.80241787379798,131.874193677035));
#51829=CARTESIAN_POINT('Ctrl Pts',(79.2911971863593,-4.76910726066446,132.006358537189));
#51830=CARTESIAN_POINT('Ctrl Pts',(79.2835648230416,-4.73606480347094,132.137459448379));
#51831=CARTESIAN_POINT('Ctrl Pts',(79.275932459724,-4.69759715576904,132.267256748717));
#51832=CARTESIAN_POINT('Ctrl Pts',(79.2683000964063,-4.65383771736922,132.395265254209));
#51833=CARTESIAN_POINT('Ctrl Pts',(79.2606685338525,-4.61008287007373,132.523260329446));
#51834=CARTESIAN_POINT('Ctrl Pts',(79.2530369712986,-4.56103746654411,132.649466601059));
#51835=CARTESIAN_POINT('Ctrl Pts',(79.2454054087448,-4.50688442699455,132.773415168414));
#51836=CARTESIAN_POINT('Ctrl Pts',(79.237772879891,-4.45272453064732,132.897379429998));
#51837=CARTESIAN_POINT('Ctrl Pts',(79.2301403510372,-4.39345587438817,133.019085049171));
#51838=CARTESIAN_POINT('Ctrl Pts',(79.2225078221834,-4.32930882260372,133.138084718874));
#51839=CARTESIAN_POINT('Ctrl Pts',(79.2147669043299,-4.26425082309718,133.258774294427));
#51840=CARTESIAN_POINT('Ctrl Pts',(79.2070259864765,-4.1941750058629,133.376680096048));
#51841=CARTESIAN_POINT('Ctrl Pts',(79.199285068623,-4.11936840775755,133.491363963985));
#51842=CARTESIAN_POINT('Ctrl Pts',(79.1916413917208,-4.04550152570298,133.604607179972));
#51843=CARTESIAN_POINT('Ctrl Pts',(79.1839977148185,-3.96702232233983,133.714708651486));
#51844=CARTESIAN_POINT('Ctrl Pts',(79.1763540379162,-3.88424856211802,133.821278940985));
#51845=CARTESIAN_POINT('Ctrl Pts',(79.1685644995872,-3.79989526119619,133.929882871451));
#51846=CARTESIAN_POINT('Ctrl Pts',(79.1607749612582,-3.71108212784948,134.034819148194));
#51847=CARTESIAN_POINT('Ctrl Pts',(79.1529854229292,-3.61818496038963,134.13571479491));
#51848=CARTESIAN_POINT('Ctrl Pts',(79.1451958846001,-3.52528779292972,134.236610441627));
#51849=CARTESIAN_POINT('Ctrl Pts',(79.1374063462711,-3.42830694881053,134.333465199769));
#51850=CARTESIAN_POINT('Ctrl Pts',(79.1296168079421,-3.32765300859565,134.425949842876));
#51851=CARTESIAN_POINT('Ctrl Pts',(79.121842473823,-3.22719553235255,134.518253967463));
#51852=CARTESIAN_POINT('Ctrl Pts',(79.1140681397039,-3.12273546025575,134.606521316976));
#51853=CARTESIAN_POINT('Ctrl Pts',(79.1062938055848,-3.01463088805298,134.690384764596));
#51854=CARTESIAN_POINT('Ctrl Pts',(79.0985290526377,-2.90665954507379,134.774144858011));
#51855=CARTESIAN_POINT('Ctrl Pts',(79.0907642996906,-2.79505294472124,134.853511611131));
#51856=CARTESIAN_POINT('Ctrl Pts',(79.0829995467435,-2.6802052765317,134.928155318827));
#51857=CARTESIAN_POINT('Ctrl Pts',(79.0752425058584,-2.56547167666536,135.00272488934));
#51858=CARTESIAN_POINT('Ctrl Pts',(79.0674854649735,-2.44750374075563,135.072580538043));
#51859=CARTESIAN_POINT('Ctrl Pts',(79.0597284240885,-2.32672763773676,135.137433610523));
#51860=CARTESIAN_POINT('Ctrl Pts',(79.0519772328483,-2.20604261291718,135.202237776796));
#51861=CARTESIAN_POINT('Ctrl Pts',(79.0442260416083,-2.08255397911777,135.262046691532));
#51862=CARTESIAN_POINT('Ctrl Pts',(79.0364748503681,-1.9567154037297,135.316615917447));
#51863=CARTESIAN_POINT('Ctrl Pts',(79.028726953591,-1.83093031309267,135.371161949986));
#51864=CARTESIAN_POINT('Ctrl Pts',(79.020979056814,-1.70279762532049,135.420472567832));
#51865=CARTESIAN_POINT('Ctrl Pts',(79.0132311600369,-1.5727938407223,135.464350166598));
#51866=CARTESIAN_POINT('Ctrl Pts',(79.0054848839528,-1.4428172501133,135.508218587116));
#51867=CARTESIAN_POINT('Ctrl Pts',(78.9977386078687,-1.31097071138136,135.54665612411));
#51868=CARTESIAN_POINT('Ctrl Pts',(78.9899923317845,-1.17774848009606,135.579514183697));
#51869=CARTESIAN_POINT('Ctrl Pts',(78.9822459985192,-1.04452526539461,135.612372485834));
#51870=CARTESIAN_POINT('Ctrl Pts',(78.9744996652539,-0.909926717466218,
135.639651134757));
#51871=CARTESIAN_POINT('Ctrl Pts',(78.9667533319885,-0.774459562645285,
135.661252159316));
#51872=CARTESIAN_POINT('Ctrl Pts',(78.9590052639855,-0.638962070894385,
135.682858021275));
#51873=CARTESIAN_POINT('Ctrl Pts',(78.9512571959825,-0.502595971195422,
135.698783667251));
#51874=CARTESIAN_POINT('Ctrl Pts',(78.9435091279796,-0.365875031979472,
135.70898277666));
#51875=CARTESIAN_POINT('Ctrl Pts',(78.9357528252377,-0.229008784122138,
135.719192725803));
#51876=CARTESIAN_POINT('Ctrl Pts',(78.9279965224959,-0.0917873338982612,
135.723663951346));
#51877=CARTESIAN_POINT('Ctrl Pts',(78.920240219754,0.0452730542169191,135.722402241329));
#51878=CARTESIAN_POINT('Ctrl Pts',(78.9124797772398,0.182406595588418,135.721139857899));
#51879=CARTESIAN_POINT('Ctrl Pts',(78.9047193347257,0.319378513296868,135.714138461866));
#51880=CARTESIAN_POINT('Ctrl Pts',(78.8969588922115,0.455676731040842,135.70145585651));
#51881=CARTESIAN_POINT('Ctrl Pts',(78.8891859919461,0.592193746783647,135.68875289191));
#51882=CARTESIAN_POINT('Ctrl Pts',(78.8814130916806,0.728034513765061,135.670350545871));
#51883=CARTESIAN_POINT('Ctrl Pts',(78.8736401914151,0.862695334498785,135.646358120904));
#51884=CARTESIAN_POINT('Ctrl Pts',(78.8661498556531,0.992460895208244,135.623237881019));
#51885=CARTESIAN_POINT('Ctrl Pts',(78.8586595198912,1.12113050747743,135.594926999127));
#51886=CARTESIAN_POINT('Ctrl Pts',(78.8511691841292,1.24826785040078,135.561566776243));
#51887=CARTESIAN_POINT('Ctrl Pts',(78.8433948500101,1.3802256443241,135.526941690369));
#51888=CARTESIAN_POINT('Ctrl Pts',(78.835620515891,1.51095068587766,135.486767131713));
#51889=CARTESIAN_POINT('Ctrl Pts',(78.8278461817719,1.6399405413726,135.441145935355));
#51890=CARTESIAN_POINT('Ctrl Pts',(78.8200814288248,1.76877142839854,135.395580963044));
#51891=CARTESIAN_POINT('Ctrl Pts',(78.8123166758778,1.89587101921497,135.344582838007));
#51892=CARTESIAN_POINT('Ctrl Pts',(78.8045519229307,2.02074885448547,135.288304989388));
#51893=CARTESIAN_POINT('Ctrl Pts',(78.7967948820457,2.14550265932984,135.232083036722));
#51894=CARTESIAN_POINT('Ctrl Pts',(78.7890378411607,2.26803874588437,135.170591955658));
#51895=CARTESIAN_POINT('Ctrl Pts',(78.7812808002757,2.38788390629803,135.104034269431));
#51896=CARTESIAN_POINT('Ctrl Pts',(78.7735296090355,2.50763869054421,135.037526774873));
#51897=CARTESIAN_POINT('Ctrl Pts',(78.7657784177953,2.62470624733536,134.965960469206));
#51898=CARTESIAN_POINT('Ctrl Pts',(78.7580272265552,2.73863570635442,134.889584911333));
#51899=CARTESIAN_POINT('Ctrl Pts',(78.7502793297781,2.85251674231392,134.813241815109));
#51900=CARTESIAN_POINT('Ctrl Pts',(78.742531433001,2.96326200921285,134.732093749404));
#51901=CARTESIAN_POINT('Ctrl Pts',(78.7347835362239,3.07044769682727,134.646434797426));
#51902=CARTESIAN_POINT('Ctrl Pts',(78.7270372601399,3.17761096350643,134.560793763454));
#51903=CARTESIAN_POINT('Ctrl Pts',(78.7192909840557,3.28121582670241,134.470643963965));
#51904=CARTESIAN_POINT('Ctrl Pts',(78.7115447079716,3.38087011296483,134.376320911545));
#51905=CARTESIAN_POINT('Ctrl Pts',(78.7037983747063,3.48052513485256,134.281997162853));
#51906=CARTESIAN_POINT('Ctrl Pts',(78.696052041441,3.57622923767062,134.183500368513));
#51907=CARTESIAN_POINT('Ctrl Pts',(78.6883057081756,3.66762609755516,134.081203895941));
#51908=CARTESIAN_POINT('Ctrl Pts',(78.6805576401727,3.75904342513277,133.978884514784));
#51909=CARTESIAN_POINT('Ctrl Pts',(78.6728095721697,3.84615132994452,133.872764053674));
#51910=CARTESIAN_POINT('Ctrl Pts',(78.6650615041667,3.92863313678456,133.763249723136));
#51911=CARTESIAN_POINT('Ctrl Pts',(78.6573052014248,4.01120260627058,133.653618999463));
#51912=CARTESIAN_POINT('Ctrl Pts',(78.649548898683,4.08913592061772,133.540587513698));
#51913=CARTESIAN_POINT('Ctrl Pts',(78.6417925959411,4.16215889590909,133.424592742341));
#51914=CARTESIAN_POINT('Ctrl Pts',(78.634032153427,4.23522084576107,133.308536061083));
#51915=CARTESIAN_POINT('Ctrl Pts',(78.6262717109127,4.30336704023561,133.189513281894));
#51916=CARTESIAN_POINT('Ctrl Pts',(78.6185112683986,4.36636932111877,133.067986473155));
#51917=CARTESIAN_POINT('Ctrl Pts',(78.6107383681331,4.42947273885629,132.946264578794));
#51918=CARTESIAN_POINT('Ctrl Pts',(78.6029654678677,4.48741557660095,132.822030976786));
#51919=CARTESIAN_POINT('Ctrl Pts',(78.5951925676023,4.54001753285584,132.695768522768));
#51920=CARTESIAN_POINT('Ctrl Pts',(78.5877022318403,4.59070727550465,132.57409602699));
#51921=CARTESIAN_POINT('Ctrl Pts',(78.5802118960782,4.63643759712486,132.45053991488));
#51922=CARTESIAN_POINT('Ctrl Pts',(78.5727215603162,4.67709153615477,132.325543652223));
#51923=CARTESIAN_POINT('Ctrl Pts',(78.5649472261971,4.71928688163942,132.195808118277));
#51924=CARTESIAN_POINT('Ctrl Pts',(78.557172892078,4.75614696573537,132.06411010822));
#51925=CARTESIAN_POINT('Ctrl Pts',(78.5493985579589,4.78748672882742,131.930927918619));
#51926=CARTESIAN_POINT('Ctrl Pts',(78.5416338050118,4.81878786846238,131.797909864163));
#51927=CARTESIAN_POINT('Ctrl Pts',(78.5338690520647,4.84458213494296,131.66341164648));
#51928=CARTESIAN_POINT('Ctrl Pts',(78.5261042991176,4.86473350730262,131.527928835101));
#51929=CARTESIAN_POINT('Ctrl Pts',(78.5183472582326,4.88486486503517,131.39258058716));
#51930=CARTESIAN_POINT('Ctrl Pts',(78.5105902173476,4.89936442491144,131.256250075822));
#51931=CARTESIAN_POINT('Ctrl Pts',(78.5028331764626,4.90814679506125,131.119444893007));
#51932=CARTESIAN_POINT('Ctrl Pts',(78.4950819852225,4.91692254235735,130.982742876045));
#51933=CARTESIAN_POINT('Ctrl Pts',(78.4873307939824,4.91998965651643,130.845567288675));
#51934=CARTESIAN_POINT('Ctrl Pts',(78.4795796027423,4.91731439209068,130.708432353546));
#51935=CARTESIAN_POINT('Ctrl Pts',(78.4718317059652,4.91464026472366,130.571355704422));
#51936=CARTESIAN_POINT('Ctrl Pts',(78.4640838091881,4.90622862067617,130.434320063246));
#51937=CARTESIAN_POINT('Ctrl Pts',(78.456335912411,4.89209780070101,130.297840952719));
#51938=CARTESIAN_POINT('Ctrl Pts',(78.4485896363269,4.87796993658877,130.16139039068));
#51939=CARTESIAN_POINT('Ctrl Pts',(78.4408433602428,4.85812531635059,130.025496516376));
#51940=CARTESIAN_POINT('Ctrl Pts',(78.4330970841587,4.83263423689746,129.890670629186));
#51941=CARTESIAN_POINT('Ctrl Pts',(78.4253507508934,4.80714296927496,129.755843746741));
#51942=CARTESIAN_POINT('Ctrl Pts',(78.417604417628,4.77600523189807,129.6220852513));
#51943=CARTESIAN_POINT('Ctrl Pts',(78.4098580843626,4.73934254759697,129.48989674243));
#51944=CARTESIAN_POINT('Ctrl Pts',(78.4021100163596,4.70267165294192,129.35767863086));
#51945=CARTESIAN_POINT('Ctrl Pts',(78.3943619483567,4.66047345380189,129.227031582152));
#51946=CARTESIAN_POINT('Ctrl Pts',(78.3866138803537,4.61291937724,129.098442131359));
#51947=CARTESIAN_POINT('Ctrl Pts',(78.3788575776118,4.56531475963967,128.969716014167));
#51948=CARTESIAN_POINT('Ctrl Pts',(78.37110127487,4.51234302947892,128.843052230617));
#51949=CARTESIAN_POINT('Ctrl Pts',(78.3633449721281,4.45422404502419,128.718917926139));
#51950=CARTESIAN_POINT('Ctrl Pts',(78.3555845296139,4.39607404071757,128.594717367444));
#51951=CARTESIAN_POINT('Ctrl Pts',(78.3478240870998,4.332771488363,128.473049324588));
#51952=CARTESIAN_POINT('Ctrl Pts',(78.3400636445856,4.2645818140865,128.354355512783));
#51953=CARTESIAN_POINT('Ctrl Pts',(78.3322907443201,4.19628267569111,128.235471163134));
#51954=CARTESIAN_POINT('Ctrl Pts',(78.3245178440547,4.12308094697651,128.119570916253));
#51955=CARTESIAN_POINT('Ctrl Pts',(78.3167449437893,4.04528541070257,128.007067460162));
#51956=CARTESIAN_POINT('Ctrl Pts',(78.3092546080273,3.97031793812805,127.898653788081));
#51957=CARTESIAN_POINT('Ctrl Pts',(78.3017642722653,3.8910850375808,127.793394476732));
#51958=CARTESIAN_POINT('Ctrl Pts',(78.2942739365033,3.80789658880433,127.691627633278));
#51959=CARTESIAN_POINT('Ctrl Pts',(78.2864996023843,3.72155402470724,127.586002269023));
#51960=CARTESIAN_POINT('Ctrl Pts',(78.2787252682652,3.63067653477672,127.483804845003));
#51961=CARTESIAN_POINT('Ctrl Pts',(78.2709509341461,3.53556649421695,127.38544958809));
#51962=CARTESIAN_POINT('Ctrl Pts',(78.263186181199,3.440573668282,127.287215545241));
#51963=CARTESIAN_POINT('Ctrl Pts',(78.2554214282519,3.341358939651,127.192814526361));
#51964=CARTESIAN_POINT('Ctrl Pts',(78.2476566753049,3.23826572235054,127.102628837176));
#51965=CARTESIAN_POINT('Ctrl Pts',(78.2398996344199,3.13527489868692,127.012532721689));
#51966=CARTESIAN_POINT('Ctrl Pts',(78.2321425935349,3.02841354470191,126.92664385988));
#51967=CARTESIAN_POINT('Ctrl Pts',(78.2243855526499,2.91806255546323,126.84530846018));
#51968=CARTESIAN_POINT('Ctrl Pts',(78.2166343614098,2.80779478276455,126.764034396138));
#51969=CARTESIAN_POINT('Ctrl Pts',(78.2088831701697,2.69404292621752,126.687307190457));
#51970=CARTESIAN_POINT('Ctrl Pts',(78.2011319789296,2.57722137566154,126.615433184042));
#51971=CARTESIAN_POINT('Ctrl Pts',(78.1933840821525,2.46044947738031,126.543589725996));
#51972=CARTESIAN_POINT('Ctrl Pts',(78.1856361853755,2.34061081233478,126.476595569026));
#51973=CARTESIAN_POINT('Ctrl Pts',(78.1778882885984,2.2181490179987,126.414713935149));
#51974=CARTESIAN_POINT('Ctrl Pts',(78.1701420125143,2.09571284002993,126.352845245577));
#51975=CARTESIAN_POINT('Ctrl Pts',(78.1623957364302,1.97065497289314,126.296087128158));
#51976=CARTESIAN_POINT('Ctrl Pts',(78.1546494603461,1.8434435844337,126.244656809915));
#51977=CARTESIAN_POINT('Ctrl Pts',(78.1469031270808,1.71623125692876,126.193226112025));
#51978=CARTESIAN_POINT('Ctrl Pts',(78.1391567938154,1.58686573884364,126.147123438327));
#51979=CARTESIAN_POINT('Ctrl Pts',(78.1314104605501,1.45583472615832,126.106517675043));
#51980=CARTESIAN_POINT('Ctrl Pts',(78.1236623925471,1.32477436998648,126.06590281838));
#51981=CARTESIAN_POINT('Ctrl Pts',(78.1159143245442,1.19204815040842,126.030787437373));
#51982=CARTESIAN_POINT('Ctrl Pts',(78.1081662565412,1.05815806365989,126.00129028966));
#51983=CARTESIAN_POINT('Ctrl Pts',(78.1004099537994,0.924125676933488,125.971761792027));
#51984=CARTESIAN_POINT('Ctrl Pts',(78.0926536510576,0.788927334470095,125.947863539905));
#51985=CARTESIAN_POINT('Ctrl Pts',(78.0848973483157,0.653074897713318,125.929663063822));
#51986=CARTESIAN_POINT('Ctrl Pts',(78.0771369058016,0.517149952420606,125.911452873597));
#51987=CARTESIAN_POINT('Ctrl Pts',(78.0693764632874,0.38057060634952,125.898946554643));
#51988=CARTESIAN_POINT('Ctrl Pts',(78.0616160207733,0.243851956322985,125.892159554306));
#51989=CARTESIAN_POINT('Ctrl Pts',(78.0538431205078,0.106913833382116,125.885361658872));
#51990=CARTESIAN_POINT('Ctrl Pts',(78.0460702202424,-0.0301636492058501,
125.88430143196));
#51991=CARTESIAN_POINT('Ctrl Pts',(78.038297319977,-0.166866380695651,125.888942153845));
#51992=CARTESIAN_POINT('Ctrl Pts',(78.0308069842148,-0.298599623565729,
125.893414173799));
#51993=CARTESIAN_POINT('Ctrl Pts',(78.0233166484526,-0.429984581423569,
125.903179828136));
#51994=CARTESIAN_POINT('Ctrl Pts',(78.0158263126904,-0.560569297566246,
125.918161161432));
#51995=CARTESIAN_POINT('Ctrl Pts',(78.0080519785713,-0.696105172908503,
125.933710516532));
#51996=CARTESIAN_POINT('Ctrl Pts',(78.0002776444522,-0.831208263231464,
125.954928118601));
#51997=CARTESIAN_POINT('Ctrl Pts',(77.9925033103331,-0.965366626552349,
125.981783470559));
#51998=CARTESIAN_POINT('Ctrl Pts',(77.984738557386,-1.09935965168088,126.008605725694));
#51999=CARTESIAN_POINT('Ctrl Pts',(77.976973804439,-1.2324098867209,126.041051830221));
#52000=CARTESIAN_POINT('Ctrl Pts',(77.9692090514919,-1.36401006336641,126.079039505775));
#52001=CARTESIAN_POINT('Ctrl Pts',(77.9614520106069,-1.49547953286105,126.116989451435));
#52002=CARTESIAN_POINT('Ctrl Pts',(77.9536949697219,-1.62550143686279,126.160469907253));
#52003=CARTESIAN_POINT('Ctrl Pts',(77.9459379288369,-1.75357861732545,126.209347549537));
#52004=CARTESIAN_POINT('Ctrl Pts',(77.9381867375968,-1.88155921378855,126.258188332809));
#52005=CARTESIAN_POINT('Ctrl Pts',(77.9304355463568,-2.00759764196169,126.312418062506));
#52006=CARTESIAN_POINT('Ctrl Pts',(77.9226843551168,-2.13121218073661,126.371853685459));
#52007=CARTESIAN_POINT('Ctrl Pts',(77.9149364583397,-2.25477418003645,126.431264046687));
#52008=CARTESIAN_POINT('Ctrl Pts',(77.9071885615626,-2.3759139873479,126.495875731332));
#52009=CARTESIAN_POINT('Ctrl Pts',(77.8994406647855,-2.4941703496418,126.565457772552));
#52010=CARTESIAN_POINT('Ctrl Pts',(77.8916943887014,-2.61240197525402,126.635025258709));
#52011=CARTESIAN_POINT('Ctrl Pts',(77.8839481126173,-2.72775101880756,126.709560835295));
#52012=CARTESIAN_POINT('Ctrl Pts',(77.8762018365332,-2.83978166490133,126.788788035954));
#52013=CARTESIAN_POINT('Ctrl Pts',(77.8684555032679,-2.95181313797966,126.868015821451));
#52014=CARTESIAN_POINT('Ctrl Pts',(77.8607091700025,-3.06052584551001,126.951935074384));
#52015=CARTESIAN_POINT('Ctrl Pts',(77.8529628367372,-3.16551408714294,127.040226769441));
#52016=CARTESIAN_POINT('Ctrl Pts',(77.8452147687342,-3.27052584016485,127.128538236811));
#52017=CARTESIAN_POINT('Ctrl Pts',(77.8374667007312,-3.37181116842586,127.22122384317));
#52018=CARTESIAN_POINT('Ctrl Pts',(77.8297186327283,-3.46899881653439,127.317925436269));
#52019=CARTESIAN_POINT('Ctrl Pts',(77.8219623299864,-3.56628975683167,127.414729804973));
#52020=CARTESIAN_POINT('Ctrl Pts',(77.8142060272446,-3.65947403968033,127.515558410484));
#52021=CARTESIAN_POINT('Ctrl Pts',(77.8064497245028,-3.74821817612046,127.620017111174));
#52022=CARTESIAN_POINT('Ctrl Pts',(77.7986892819886,-3.83700967797842,127.724531564618));
#52023=CARTESIAN_POINT('Ctrl Pts',(77.7909288394744,-3.92135607099913,127.832679665718));
#52024=CARTESIAN_POINT('Ctrl Pts',(77.7831683969602,-4.00096593647908,127.944036398595));
#52025=CARTESIAN_POINT('Ctrl Pts',(77.7753954966948,-4.08070359878254,128.055571891185));
#52026=CARTESIAN_POINT('Ctrl Pts',(77.7676225964294,-4.15568932535336,128.170325980979));
#52027=CARTESIAN_POINT('Ctrl Pts',(77.7598496961639,-4.22567612012016,128.287846284138));
#52028=CARTESIAN_POINT('Ctrl Pts',(77.7523593604019,-4.2931187186116,128.401094428263));
#52029=CARTESIAN_POINT('Ctrl Pts',(77.7448690246398,-4.35591937601727,128.516910889031));
#52030=CARTESIAN_POINT('Ctrl Pts',(77.7373786888777,-4.41389938480556,128.634873285657));
#52031=CARTESIAN_POINT('Ctrl Pts',(77.7290264058955,-4.47855141858496,128.766410155188));
#52032=CARTESIAN_POINT('Ctrl Pts',(77.7206741229133,-4.53739134454764,128.900984554709));
#52033=CARTESIAN_POINT('Ctrl Pts',(77.7123218399311,-4.59014481042747,129.038078170785));
#52034=CARTESIAN_POINT('Ctrl Pts',(77.703990322518,-4.64276711986235,129.174830942691));
#52035=CARTESIAN_POINT('Ctrl Pts',(77.695658805105,-4.68933303616603,129.314090161865));
#52036=CARTESIAN_POINT('Ctrl Pts',(77.687327287692,-4.72961527939854,129.45531563263));
#52037=CARTESIAN_POINT('Ctrl Pts',(77.684836491738,-4.7416580854671,129.497536492739));
#52038=CARTESIAN_POINT('Ctrl Pts',(77.6823456957839,-4.75313958750526,129.539932931064));
#52039=CARTESIAN_POINT('Ctrl Pts',(77.6798548998299,-4.76405452823404,129.582490119308));
#52040=CARTESIAN_POINT('Origin',(213.235140564004,0.,130.804360617566));
#52041=CARTESIAN_POINT('',(75.5849534216701,-4.76405452823407,129.582490119308));
#52042=CARTESIAN_POINT('',(75.9301393004801,-4.76405452823408,129.582490119308));
#52043=CARTESIAN_POINT('',(213.235140564004,-4.76405452823405,129.582490119308));
#52044=CARTESIAN_POINT('',(77.2648594359911,-4.91824790196687,130.808903446917));
#52045=CARTESIAN_POINT('Ctrl Pts',(77.2648594359911,-4.91824790196687,130.808903446917));
#52046=CARTESIAN_POINT('Ctrl Pts',(77.2546216692904,-4.91808097156089,130.98962894981));
#52047=CARTESIAN_POINT('Ctrl Pts',(77.2443839025897,-4.90794932828341,131.169911861407));
#52048=CARTESIAN_POINT('Ctrl Pts',(77.2341461358891,-4.88801892813298,131.348836531371));
#52049=CARTESIAN_POINT('Ctrl Pts',(77.2236182800186,-4.86752379610282,131.532831067691));
#52050=CARTESIAN_POINT('Ctrl Pts',(77.2130904241482,-4.83666667707839,131.715389732876));
#52051=CARTESIAN_POINT('Ctrl Pts',(77.2025625682778,-4.79567552321711,131.895543158902));
#52052=CARTESIAN_POINT('Ctrl Pts',(77.2017325246556,-4.79244367370771,131.909746924999));
#52053=CARTESIAN_POINT('Ctrl Pts',(77.2009024810333,-4.78914885370999,131.923935750888));
#52054=CARTESIAN_POINT('Ctrl Pts',(77.2000724374111,-4.78579118739459,131.938109166917));
#52055=CARTESIAN_POINT('Ctrl Pts',(77.192298103292,-4.75434269589643,132.070859866845));
#52056=CARTESIAN_POINT('Ctrl Pts',(77.1845237691729,-4.71731674706899,132.202511341451));
#52057=CARTESIAN_POINT('Ctrl Pts',(77.1767494350539,-4.67480408935632,132.332558833976));
#52058=CARTESIAN_POINT('Ctrl Pts',(77.1689846821068,-4.6323438246948,132.462446054588));
#52059=CARTESIAN_POINT('Ctrl Pts',(77.1612199291597,-4.58441042558499,132.590732858247));
#52060=CARTESIAN_POINT('Ctrl Pts',(77.1534551762126,-4.53114550731624,132.716925244978));
#52061=CARTESIAN_POINT('Ctrl Pts',(77.1456981353276,-4.47793349251521,132.842992295652));
#52062=CARTESIAN_POINT('Ctrl Pts',(77.1379410944426,-4.41940064757198,132.966968711237));
#52063=CARTESIAN_POINT('Ctrl Pts',(77.1301840535576,-4.35573808171466,133.088376560155));
#52064=CARTESIAN_POINT('Ctrl Pts',(77.1224328623175,-4.29212352429368,133.209692854469));
#52065=CARTESIAN_POINT('Ctrl Pts',(77.1146816710773,-4.22338712652755,133.328444092702));
#52066=CARTESIAN_POINT('Ctrl Pts',(77.1069304798372,-4.14976755580649,133.444173545649));
#52067=CARTESIAN_POINT('Ctrl Pts',(77.0991825830602,-4.07617927536665,133.559853810492));
#52068=CARTESIAN_POINT('Ctrl Pts',(77.0914346862831,-3.99771215934754,133.672514515318));
#52069=CARTESIAN_POINT('Ctrl Pts',(77.083686789506,-3.91465003599075,133.781724914762));
#52070=CARTESIAN_POINT('Ctrl Pts',(77.0759405134219,-3.83160528743949,133.890912469745));
#52071=CARTESIAN_POINT('Ctrl Pts',(77.0681942373378,-3.74396767991217,133.996650843918));
#52072=CARTESIAN_POINT('Ctrl Pts',(77.0604479612537,-3.65206321829336,134.098539925389));
#52073=CARTESIAN_POINT('Ctrl Pts',(77.0527016279884,-3.56015807825664,134.200429758982));
#52074=CARTESIAN_POINT('Ctrl Pts',(77.044955294723,-3.46398628314191,134.298469952862));
#52075=CARTESIAN_POINT('Ctrl Pts',(77.0372089614576,-3.36391254205541,134.392295325988));
#52076=CARTESIAN_POINT('Ctrl Pts',(77.0294608934546,-3.26381639014854,134.486141710657));
#52077=CARTESIAN_POINT('Ctrl Pts',(77.0217128254516,-3.15981683864191,134.575771129004));
#52078=CARTESIAN_POINT('Ctrl Pts',(77.0139647574487,-3.05231338146174,134.660857225091));
#52079=CARTESIAN_POINT('Ctrl Pts',(77.0062084547068,-2.94469566832798,134.746033751692));
#52080=CARTESIAN_POINT('Ctrl Pts',(76.9984521519649,-2.83356691749657,134.826657067167));
#52081=CARTESIAN_POINT('Ctrl Pts',(76.990695849223,-2.71935789982876,134.902442568325));
#52082=CARTESIAN_POINT('Ctrl Pts',(76.9829354067089,-2.60508792536938,134.978268518488));
#52083=CARTESIAN_POINT('Ctrl Pts',(76.9751749641947,-2.48773474256846,135.04925130706));
#52084=CARTESIAN_POINT('Ctrl Pts',(76.9674145216806,-2.36775481157271,135.115151753167));
#52085=CARTESIAN_POINT('Ctrl Pts',(76.9596416214151,-2.24758227814048,135.18115798852));
#52086=CARTESIAN_POINT('Ctrl Pts',(76.9518687211497,-2.12477492068018,135.242065404057));
#52087=CARTESIAN_POINT('Ctrl Pts',(76.9440958208843,-1.99981112904014,135.297682163001));
#52088=CARTESIAN_POINT('Ctrl Pts',(76.9366054851223,-1.87939008599151,135.351277112666));
#52089=CARTESIAN_POINT('Ctrl Pts',(76.9291151493603,-1.75696695661656,135.399959271092));
#52090=CARTESIAN_POINT('Ctrl Pts',(76.9216248135983,-1.63298227223813,135.443601068443));
#52091=CARTESIAN_POINT('Ctrl Pts',(76.9138504794792,-1.50429667086663,135.488897557806));
#52092=CARTESIAN_POINT('Ctrl Pts',(76.9060761453601,-1.37352112696702,135.528907416218));
#52093=CARTESIAN_POINT('Ctrl Pts',(76.898301811241,-1.2411293584466,135.563434159559));
#52094=CARTESIAN_POINT('Ctrl Pts',(76.8905370582939,-1.1089007509487,135.597918351775));
#52095=CARTESIAN_POINT('Ctrl Pts',(76.8827723053468,-0.975060256702649,
135.626932776517));
#52096=CARTESIAN_POINT('Ctrl Pts',(76.8750075523997,-0.840100038399312,
135.650329559685));
#52097=CARTESIAN_POINT('Ctrl Pts',(76.8672505115147,-0.705273864487582,
135.673703104838));
#52098=CARTESIAN_POINT('Ctrl Pts',(76.8594934706297,-0.569330562425579,
135.691470045567));
#52099=CARTESIAN_POINT('Ctrl Pts',(76.8517364297447,-0.432775528791537,
135.703532833786));
#52100=CARTESIAN_POINT('Ctrl Pts',(76.8439852385046,-0.296323472370509,
135.715586525362));
#52101=CARTESIAN_POINT('Ctrl Pts',(76.8362340472645,-0.159260990462933,
135.72194459213));
#52102=CARTESIAN_POINT('Ctrl Pts',(76.8284828560244,-0.0221013478367807,
135.722560958435));
#52103=CARTESIAN_POINT('Ctrl Pts',(76.8207349592473,0.114999998282496,135.723177062768));
#52104=CARTESIAN_POINT('Ctrl Pts',(76.8129870624702,0.252198032843212,135.718056318605));
#52105=CARTESIAN_POINT('Ctrl Pts',(76.8052391656931,0.388976941474538,135.707204690296));
#52106=CARTESIAN_POINT('Ctrl Pts',(76.797492889609,0.525727238906792,135.696355331913));
#52107=CARTESIAN_POINT('Ctrl Pts',(76.7897466135248,0.66205819530066,135.679777504718));
#52108=CARTESIAN_POINT('Ctrl Pts',(76.7820003374407,0.797456971587216,135.657529215602));
#52109=CARTESIAN_POINT('Ctrl Pts',(76.7742540041754,0.932856747356688,135.635280762255));
#52110=CARTESIAN_POINT('Ctrl Pts',(76.7665076709101,1.06732394349632,135.607361826856));
#52111=CARTESIAN_POINT('Ctrl Pts',(76.7587613376447,1.20035418867435,135.573881860231));
#52112=CARTESIAN_POINT('Ctrl Pts',(76.7510132696417,1.33341422505343,135.540394396));
#52113=CARTESIAN_POINT('Ctrl Pts',(76.7432652016387,1.46503629106591,135.501343517834));
#52114=CARTESIAN_POINT('Ctrl Pts',(76.7355171336358,1.59472987799049,135.456888927931));
#52115=CARTESIAN_POINT('Ctrl Pts',(76.7277608308939,1.72456130480271,135.41238709116));
#52116=CARTESIAN_POINT('Ctrl Pts',(76.720004528152,1.85245978777724,135.362470197103));
#52117=CARTESIAN_POINT('Ctrl Pts',(76.7122482254102,1.97795304001854,135.307346830512));
#52118=CARTESIAN_POINT('Ctrl Pts',(76.704487782896,2.10351327178717,135.25219404292));
#52119=CARTESIAN_POINT('Ctrl Pts',(76.6967273403818,2.22666536396528,135.191829417689));
#52120=CARTESIAN_POINT('Ctrl Pts',(76.6889668978677,2.34696135904811,135.126507704563));
#52121=CARTESIAN_POINT('Ctrl Pts',(76.6811939976022,2.46745046394154,135.061081131223));
#52122=CARTESIAN_POINT('Ctrl Pts',(76.6734210973368,2.58507397406459,134.990681769151));
#52123=CARTESIAN_POINT('Ctrl Pts',(76.6656481970713,2.69941191030411,134.91560840881));
#52124=CARTESIAN_POINT('Ctrl Pts',(76.6581578613092,2.80959337456222,134.843264154215));
#52125=CARTESIAN_POINT('Ctrl Pts',(76.6506675255472,2.91672374497599,134.766580004025));
#52126=CARTESIAN_POINT('Ctrl Pts',(76.6431771897851,3.0204575754891,134.685857635106));
#52127=CARTESIAN_POINT('Ctrl Pts',(76.635402855666,3.12812450571457,134.602074653035));
#52128=CARTESIAN_POINT('Ctrl Pts',(76.6276285215469,3.23247330858299,134.513675789963));
#52129=CARTESIAN_POINT('Ctrl Pts',(76.6198541874278,3.33308262033824,134.420953393716));
#52130=CARTESIAN_POINT('Ctrl Pts',(76.6120894344808,3.43356794010847,134.328345269535));
#52131=CARTESIAN_POINT('Ctrl Pts',(76.6043246815337,3.53032265375021,134.231424476455));
#52132=CARTESIAN_POINT('Ctrl Pts',(76.5965599285866,3.62295632464049,134.130525155325));
#52133=CARTESIAN_POINT('Ctrl Pts',(76.5888028877016,3.71549799046288,134.029726048824));
#52134=CARTESIAN_POINT('Ctrl Pts',(76.5810458468166,3.80392649624825,133.92495656413));
#52135=CARTESIAN_POINT('Ctrl Pts',(76.5732888059316,3.88788659283367,133.816589178576));
#52136=CARTESIAN_POINT('Ctrl Pts',(76.5655376146915,3.97178337445719,133.70830351371));
#52137=CARTESIAN_POINT('Ctrl Pts',(76.5577864234513,4.05121821550742,133.596425656263));
#52138=CARTESIAN_POINT('Ctrl Pts',(76.5500352322112,4.12587491908604,133.481362525402));
#52139=CARTESIAN_POINT('Ctrl Pts',(76.5422873354341,4.20049989157411,133.366348299441));
#52140=CARTESIAN_POINT('Ctrl Pts',(76.534539438657,4.27035055341159,133.248151820014));
#52141=CARTESIAN_POINT('Ctrl Pts',(76.5267915418799,4.33515311230626,133.127210280235));
#52142=CARTESIAN_POINT('Ctrl Pts',(76.5190452657958,4.3999421159026,133.006294038819));
#52143=CARTESIAN_POINT('Ctrl Pts',(76.5112989897117,4.45968493237443,132.882634223577));
#52144=CARTESIAN_POINT('Ctrl Pts',(76.5035527136276,4.51415316251924,132.756693654683));
#52145=CARTESIAN_POINT('Ctrl Pts',(76.4958063803623,4.56862179473611,132.630752156124));
#52146=CARTESIAN_POINT('Ctrl Pts',(76.488060047097,4.61781560773609,132.502530229161));
#52147=CARTESIAN_POINT('Ctrl Pts',(76.4803137138316,4.66155406057587,132.372511376527));
#52148=CARTESIAN_POINT('Ctrl Pts',(76.4725656458286,4.70530230833894,132.242463407071));
#52149=CARTESIAN_POINT('Ctrl Pts',(76.4648175778257,4.74359264028721,132.110618081685));
#52150=CARTESIAN_POINT('Ctrl Pts',(76.4570695098227,4.77629428645647,131.977474402185));
#52151=CARTESIAN_POINT('Ctrl Pts',(76.4493132070808,4.80903068832443,131.844189215998));
#52152=CARTESIAN_POINT('Ctrl Pts',(76.441556904339,4.83616644577664,131.709603299473));
#52153=CARTESIAN_POINT('Ctrl Pts',(76.4338006015971,4.85762176446778,131.574226746103));
#52154=CARTESIAN_POINT('Ctrl Pts',(76.4260401590829,4.87908853450852,131.438777938191));
#52155=CARTESIAN_POINT('Ctrl Pts',(76.4182797165687,4.89486877966622,131.302538040768));
#52156=CARTESIAN_POINT('Ctrl Pts',(76.4105192740546,4.90493469614097,131.166021631628));
#52157=CARTESIAN_POINT('Ctrl Pts',(76.4027463737891,4.91501677131845,131.02928607423));
#52158=CARTESIAN_POINT('Ctrl Pts',(76.3949734735236,4.91936617452899,130.892273509092));
#52159=CARTESIAN_POINT('Ctrl Pts',(76.3872005732582,4.91800727768246,130.755498780082));
#52160=CARTESIAN_POINT('Ctrl Pts',(76.3797102374962,4.91669778015917,130.623696156987));
#52161=CARTESIAN_POINT('Ctrl Pts',(76.3722199017344,4.91008781480973,130.492114685978));
#52162=CARTESIAN_POINT('Ctrl Pts',(76.3647295659724,4.89824446889413,130.36120806432));
#52163=CARTESIAN_POINT('Ctrl Pts',(76.3569552318533,4.88595207891834,130.225338078313));
#52164=CARTESIAN_POINT('Ctrl Pts',(76.3491808977342,4.86798268864196,130.089764730396));
#52165=CARTESIAN_POINT('Ctrl Pts',(76.3414065636152,4.84435450116717,129.955000546971));
#52166=CARTESIAN_POINT('Ctrl Pts',(76.3336418106681,4.82075543332172,129.820402448357));
#52167=CARTESIAN_POINT('Ctrl Pts',(76.325877057721,4.79151151125301,129.686611911453));
#52168=CARTESIAN_POINT('Ctrl Pts',(76.3181123047739,4.75669281658857,129.554138032938));
#52169=CARTESIAN_POINT('Ctrl Pts',(76.3103552638889,4.72190870434256,129.421795729346));
#52170=CARTESIAN_POINT('Ctrl Pts',(76.3025982230039,4.68156093700724,129.29076785739));
#52171=CARTESIAN_POINT('Ctrl Pts',(76.2948411821189,4.63577086946081,129.161554631347));
#52172=CARTESIAN_POINT('Ctrl Pts',(76.2870899908788,4.59001533256052,129.032438846002));
#52173=CARTESIAN_POINT('Ctrl Pts',(76.2793387996387,4.53882579443605,128.905135349796));
#52174=CARTESIAN_POINT('Ctrl Pts',(76.2715876083986,4.48237369556122,128.780130117885));
#52175=CARTESIAN_POINT('Ctrl Pts',(76.2638397116215,4.42594559033429,128.655178016531));
#52176=CARTESIAN_POINT('Ctrl Pts',(76.2560918148444,4.3642595336146,128.532522592214));
#52177=CARTESIAN_POINT('Ctrl Pts',(76.2483439180673,4.29753535692961,128.4126305077));
#52178=CARTESIAN_POINT('Ctrl Pts',(76.2405976419832,4.23082513750398,128.292763502026));
#52179=CARTESIAN_POINT('Ctrl Pts',(76.2328513658992,4.1590790843152,128.175659027826));
#52180=CARTESIAN_POINT('Ctrl Pts',(76.2251050898151,4.08256312573636,128.061759409428));
#52181=CARTESIAN_POINT('Ctrl Pts',(76.2173587565497,4.00604660233411,127.947858950249));
#52182=CARTESIAN_POINT('Ctrl Pts',(76.2096124232844,3.92476032129899,127.837163718613));
#52183=CARTESIAN_POINT('Ctrl Pts',(76.2018660900191,3.83901348038315,127.730086953766));
#52184=CARTESIAN_POINT('Ctrl Pts',(76.1941180220161,3.75324743705686,127.622986209819));
#52185=CARTESIAN_POINT('Ctrl Pts',(76.1863699540131,3.66301909046738,127.51950585024));
#52186=CARTESIAN_POINT('Ctrl Pts',(76.1786218860101,3.56867758061624,127.420025618174));
#52187=CARTESIAN_POINT('Ctrl Pts',(76.1708655832682,3.47423580348568,127.320439657334));
#52188=CARTESIAN_POINT('Ctrl Pts',(76.1631092805264,3.37567239997271,127.224862600739));
#52189=CARTESIAN_POINT('Ctrl Pts',(76.1553529777846,3.2733733953874,127.133637299626));
#52190=CARTESIAN_POINT('Ctrl Pts',(76.1475925352704,3.1710197907431,127.042363308822));
#52191=CARTESIAN_POINT('Ctrl Pts',(76.1398320927562,3.06492691448858,126.955445949249));
#52192=CARTESIAN_POINT('Ctrl Pts',(76.1320716502421,2.95551266686261,126.873186754899));
#52193=CARTESIAN_POINT('Ctrl Pts',(76.1242987499766,2.84592277777308,126.790795510788));
#52194=CARTESIAN_POINT('Ctrl Pts',(76.1165258497112,2.73300118500108,126.71307759651));
#52195=CARTESIAN_POINT('Ctrl Pts',(76.1087529494458,2.61719421488499,126.640290792975));
#52196=CARTESIAN_POINT('Ctrl Pts',(76.1012626136837,2.50559711983159,126.570149973086));
#52197=CARTESIAN_POINT('Ctrl Pts',(76.0937722779216,2.39132105396002,126.504588125));
#52198=CARTESIAN_POINT('Ctrl Pts',(76.0862819421595,2.27478398793205,126.443794040761));
#52199=CARTESIAN_POINT('Ctrl Pts',(76.0785076080404,2.15382838362607,126.380694930341));
#52200=CARTESIAN_POINT('Ctrl Pts',(76.0707332739213,2.0300537920153,126.322532381187));
#52201=CARTESIAN_POINT('Ctrl Pts',(76.0629589398022,1.90390125529857,126.269568111555));
#52202=CARTESIAN_POINT('Ctrl Pts',(76.0551941868551,1.77790419030886,126.216669115652));
#52203=CARTESIAN_POINT('Ctrl Pts',(76.0474294339081,1.64953536826582,126.168955802307));
#52204=CARTESIAN_POINT('Ctrl Pts',(76.039664680961,1.51926098745546,126.126644389053));
#52205=CARTESIAN_POINT('Ctrl Pts',(76.0319076400759,1.38911599699667,126.084375000091));
#52206=CARTESIAN_POINT('Ctrl Pts',(76.0241505991909,1.25706958362367,126.047496954132));
#52207=CARTESIAN_POINT('Ctrl Pts',(76.0163935583059,1.12360818705126,126.016178529916));
#52208=CARTESIAN_POINT('Ctrl Pts',(76.0086423670658,0.990247434756191,125.984883723168));
#52209=CARTESIAN_POINT('Ctrl Pts',(76.0008911758257,0.855474202245346,125.959140282095));
#52210=CARTESIAN_POINT('Ctrl Pts',(75.9931399845856,0.719790021944568,125.939066650414));
#52211=CARTESIAN_POINT('Ctrl Pts',(75.9853920878085,0.58416351103982,125.919001550562));
#52212=CARTESIAN_POINT('Ctrl Pts',(75.9776441910314,0.44762720835677,125.904601524251));
#52213=CARTESIAN_POINT('Ctrl Pts',(75.9698962942543,0.310692554808173,125.895933863617));
#52214=CARTESIAN_POINT('Ctrl Pts',(75.9621500181702,0.173786545037129,125.88726801607));
#52215=CARTESIAN_POINT('Ctrl Pts',(75.954403742086,0.0364827400784687,125.884332173831));
#52216=CARTESIAN_POINT('Ctrl Pts',(75.9466574660019,-0.100702979302659,
125.887141690931));
#52217=CARTESIAN_POINT('Ctrl Pts',(75.9389111327366,-0.237889711357603,
125.88995122877));
#52218=CARTESIAN_POINT('Ctrl Pts',(75.9311647994712,-0.374957965212396,
125.898506202571));
#52219=CARTESIAN_POINT('Ctrl Pts',(75.9234184662059,-0.511392942048524,
125.912769841415));
#52220=CARTESIAN_POINT('Ctrl Pts',(75.9156703982029,-0.647858472551647,
125.927036674502));
#52221=CARTESIAN_POINT('Ctrl Pts',(75.9079223301999,-0.78369005506314,125.947014675887));
#52222=CARTESIAN_POINT('Ctrl Pts',(75.900174262197,-0.918379482220692,125.972615364644));
#52223=CARTESIAN_POINT('Ctrl Pts',(75.8924179594551,-1.05321205890425,125.998243262118));
#52224=CARTESIAN_POINT('Ctrl Pts',(75.8846616567132,-1.1868996706441,126.029505711265));
#52225=CARTESIAN_POINT('Ctrl Pts',(75.8769053539714,-1.31894521087635,126.066263257527));
#52226=CARTESIAN_POINT('Ctrl Pts',(75.8691449114572,-1.45106122778941,126.103040422399));
#52227=CARTESIAN_POINT('Ctrl Pts',(75.8613844689431,-1.58153305510366,126.145318407975));
#52228=CARTESIAN_POINT('Ctrl Pts',(75.8536240264289,-1.70988111844552,126.192908609436));
#52229=CARTESIAN_POINT('Ctrl Pts',(75.8458511261635,-1.83843521749277,126.240575206914));
#52230=CARTESIAN_POINT('Ctrl Pts',(75.838078225898,-1.96485837901661,126.293570909987));
#52231=CARTESIAN_POINT('Ctrl Pts',(75.8303053256325,-2.0886924743509,126.351659548542));
#52232=CARTESIAN_POINT('Ctrl Pts',(75.8228149898706,-2.20802488839984,126.407636518769));
#52233=CARTESIAN_POINT('Ctrl Pts',(75.8153246541086,-2.32495293295197,126.468342429125));
#52234=CARTESIAN_POINT('Ctrl Pts',(75.8078343183466,-2.43909184856289,126.533527675765));
#52235=CARTESIAN_POINT('Ctrl Pts',(75.8000588645336,-2.55757543792452,126.601194185071));
#52236=CARTESIAN_POINT('Ctrl Pts',(75.7922834107205,-2.67342873198506,126.673902173205));
#52237=CARTESIAN_POINT('Ctrl Pts',(75.7845079569074,-2.78619294902018,126.75142194133));
#52238=CARTESIAN_POINT('Ctrl Pts',(75.7767423286274,-2.89881467038056,126.828843750794));
#52239=CARTESIAN_POINT('Ctrl Pts',(75.7689767003473,-3.00835476318595,126.911065021064));
#52240=CARTESIAN_POINT('Ctrl Pts',(75.7612110720673,-3.11437918435546,126.997810294957));
#52241=CARTESIAN_POINT('Ctrl Pts',(75.7534548404659,-3.2202753123113,127.084450604071));
#52242=CARTESIAN_POINT('Ctrl Pts',(75.7456986088644,-3.32266394081346,127.175603767778));
#52243=CARTESIAN_POINT('Ctrl Pts',(75.737942377263,-3.42114069247982,127.270951580282));
#52244=CARTESIAN_POINT('Ctrl Pts',(75.7301914739738,-3.51954979339658,127.36623389153));
#52245=CARTESIAN_POINT('Ctrl Pts',(75.7224405706846,-3.61405208432284,127.465704847871));
#52246=CARTESIAN_POINT('Ctrl Pts',(75.7146896673954,-3.70427687070828,127.5690065523));
#52247=CARTESIAN_POINT('Ctrl Pts',(75.7069424101299,-3.79445921536855,127.672259663623));
#52248=CARTESIAN_POINT('Ctrl Pts',(75.6991951528643,-3.88036780317911,127.77933964323));
#52249=CARTESIAN_POINT('Ctrl Pts',(75.6914478955988,-3.96166965843234,127.889852669394));
#52250=CARTESIAN_POINT('Ctrl Pts',(75.6837026048881,-4.04295087611694,128.00033764306));
#52251=CARTESIAN_POINT('Ctrl Pts',(75.6759573141774,-4.11962745824334,128.114253613544));
#52252=CARTESIAN_POINT('Ctrl Pts',(75.6682120234667,-4.19140775088568,128.231175018291));
#52253=CARTESIAN_POINT('Ctrl Pts',(75.6604647800918,-4.26320614004766,128.348125900077));
#52254=CARTESIAN_POINT('Ctrl Pts',(75.6527175367169,-4.33010556436869,128.468083399465));
#52255=CARTESIAN_POINT('Ctrl Pts',(75.644970293342,-4.39185861014737,128.590594367264));
#52256=CARTESIAN_POINT('Ctrl Pts',(75.6372220623902,-4.45361952787191,128.713120952102));
#52257=CARTESIAN_POINT('Ctrl Pts',(75.6294738314384,-4.51023259159163,128.83820130099));
#52258=CARTESIAN_POINT('Ctrl Pts',(75.6217256004867,-4.56149753334166,128.965359987926));
#52259=CARTESIAN_POINT('Ctrl Pts',(75.613971480313,-4.61280144019459,129.092615324758));
#52260=CARTESIAN_POINT('Ctrl Pts',(75.6062173601394,-4.65874896788764,129.221951788917));
#52261=CARTESIAN_POINT('Ctrl Pts',(75.5984632399657,-4.69918886814165,129.352876189805));
#52262=CARTESIAN_POINT('Ctrl Pts',(75.5939599672005,-4.72267469211181,129.428911674891));
#52263=CARTESIAN_POINT('Ctrl Pts',(75.5894566944353,-4.74430383295107,129.505482458159));
#52264=CARTESIAN_POINT('Ctrl Pts',(75.5849534216701,-4.76405452823408,129.582490119308));
#52265=CARTESIAN_POINT('Ctrl Pts',(77.3348925457121,-4.76405452823405,129.582490119308));
#52266=CARTESIAN_POINT('Ctrl Pts',(77.3272431990384,-4.79773533007694,129.713811054516));
#52267=CARTESIAN_POINT('Ctrl Pts',(77.3195938523647,-4.82597605115416,129.846501919531));
#52268=CARTESIAN_POINT('Ctrl Pts',(77.311944505691,-4.84868252185261,129.980066456007));
#52269=CARTESIAN_POINT('Ctrl Pts',(77.3040969940744,-4.87197722925453,130.117091132267));
#52270=CARTESIAN_POINT('Ctrl Pts',(77.2962494824577,-4.88944694813033,130.255034923563));
#52271=CARTESIAN_POINT('Ctrl Pts',(77.2884019708411,-4.90104660224639,130.393355428902));
#52272=CARTESIAN_POINT('Ctrl Pts',(77.2805544592244,-4.91264625636247,130.53167593424));
#52273=CARTESIAN_POINT('Ctrl Pts',(77.2727069476077,-4.91837585841854,130.670372698479));
#52274=CARTESIAN_POINT('Ctrl Pts',(77.2648594359911,-4.91824790196687,130.808903446917));
#52275=CARTESIAN_POINT('',(77.610140564059,-4.91824986258823,130.803198012381));
#52276=CARTESIAN_POINT('Ctrl Pts',(77.6798548998299,-4.76405452823404,129.582490119308));
#52277=CARTESIAN_POINT('Ctrl Pts',(77.6715497968428,-4.8004483993194,129.724389270316));
#52278=CARTESIAN_POINT('Ctrl Pts',(77.6632446938558,-4.83053974511505,129.868076996986));
#52279=CARTESIAN_POINT('Ctrl Pts',(77.6549395908687,-4.85416491434517,130.012990889285));
#52280=CARTESIAN_POINT('Ctrl Pts',(77.6466578611242,-4.8777235947174,130.157496947078));
#52281=CARTESIAN_POINT('Ctrl Pts',(77.6383761313797,-4.89485234025123,130.30322199338));
#52282=CARTESIAN_POINT('Ctrl Pts',(77.6300944016353,-4.90543804606879,130.44959218791));
#52283=CARTESIAN_POINT('Ctrl Pts',(77.6234431224431,-4.91393971021512,130.567146015342));
#52284=CARTESIAN_POINT('Ctrl Pts',(77.6167918432511,-4.91822194956528,130.685115603136));
#52285=CARTESIAN_POINT('Ctrl Pts',(77.610140564059,-4.91824986258823,130.803198012381));
#52286=CARTESIAN_POINT('Ctrl Pts',(77.6101405640085,-4.91824986258845,130.803198013277));
#52287=CARTESIAN_POINT('Ctrl Pts',(77.6021562717305,-4.91828336976134,130.944945854718));
#52288=CARTESIAN_POINT('Ctrl Pts',(77.5941719794525,-4.9121846040386,131.086623373462));
#52289=CARTESIAN_POINT('Ctrl Pts',(77.5861876871745,-4.89999794552716,131.227684602629));
#52290=CARTESIAN_POINT('Ctrl Pts',(77.578197210792,-4.88780184803631,131.368855088492));
#52291=CARTESIAN_POINT('Ctrl Pts',(77.5702067344094,-4.86950848728427,131.509407978856));
#52292=CARTESIAN_POINT('Ctrl Pts',(77.5622162580269,-4.84521387953863,131.648804531646));
#52293=CARTESIAN_POINT('Ctrl Pts',(77.5542183824385,-4.82089677491125,131.788330166074));
#52294=CARTESIAN_POINT('Ctrl Pts',(77.5462205068502,-4.79056740431481,131.926696978207));
#52295=CARTESIAN_POINT('Ctrl Pts',(77.5382226312619,-4.75437242730818,132.063378443076));
#52296=CARTESIAN_POINT('Ctrl Pts',(77.5302103941641,-4.71811245622919,132.20030534214));
#52297=CARTESIAN_POINT('Ctrl Pts',(77.5221981570663,-4.67596592520096,132.335540503171));
#52298=CARTESIAN_POINT('Ctrl Pts',(77.5141859199685,-4.62812909180166,132.468573396065));
#52299=CARTESIAN_POINT('Ctrl Pts',(77.506165460645,-4.58024316783804,132.601742808442));
#52300=CARTESIAN_POINT('Ctrl Pts',(77.4981450013216,-4.5266554290561,132.732705116981));
#52301=CARTESIAN_POINT('Ctrl Pts',(77.4901245419981,-4.46760931258675,132.860971930524));
#52302=CARTESIAN_POINT('Ctrl Pts',(77.4820894853217,-4.40845573132449,132.989472191539));
#52303=CARTESIAN_POINT('Ctrl Pts',(77.4740544286453,-4.34382408587754,133.115266840236));
#52304=CARTESIAN_POINT('Ctrl Pts',(77.4660193719689,-4.27400307237721,133.237893193845));
#52305=CARTESIAN_POINT('Ctrl Pts',(77.4636566030008,-4.2534716771846,133.273952397239));
#52306=CARTESIAN_POINT('Ctrl Pts',(77.4612938340328,-4.23249183570568,133.309737841135));
#52307=CARTESIAN_POINT('Ctrl Pts',(77.4589310650647,-4.21107156838282,133.345238282559));
#52308=CARTESIAN_POINT('Ctrl Pts',(77.4511567309456,-4.14059141677328,133.462047118603));
#52309=CARTESIAN_POINT('Ctrl Pts',(77.4433823968265,-4.06513579240713,133.576106227857));
#52310=CARTESIAN_POINT('Ctrl Pts',(77.4356080627074,-3.98494523012703,133.686962666998));
#52311=CARTESIAN_POINT('Ctrl Pts',(77.4278433097603,-3.90485349554822,133.797682485484));
#52312=CARTESIAN_POINT('Ctrl Pts',(77.4200785568133,-3.82003866068413,133.905207173487));
#52313=CARTESIAN_POINT('Ctrl Pts',(77.4123138038662,-3.73078641364259,134.009109562223));
#52314=CARTESIAN_POINT('Ctrl Pts',(77.4045567629812,-3.64162281319116,134.112908753642));
#52315=CARTESIAN_POINT('Ctrl Pts',(77.3967997220962,-3.54803082439464,134.213092510766));
#52316=CARTESIAN_POINT('Ctrl Pts',(77.3890426812112,-3.45033835946079,134.30926407811));
#52317=CARTESIAN_POINT('Ctrl Pts',(77.3812914899711,-3.35271956517468,134.405363121727));
#52318=CARTESIAN_POINT('Ctrl Pts',(77.373540298731,-3.25100672707678,134.497455724719));
#52319=CARTESIAN_POINT('Ctrl Pts',(77.3657891074909,-3.14556657055547,134.585179842642));
#52320=CARTESIAN_POINT('Ctrl Pts',(77.3580412107138,-3.04017122891317,134.672866675475));
#52321=CARTESIAN_POINT('Ctrl Pts',(77.3502933139367,-2.93105201963838,134.756188466594));
#52322=CARTESIAN_POINT('Ctrl Pts',(77.3425454171597,-2.81861073852276,134.834821703743));
#52323=CARTESIAN_POINT('Ctrl Pts',(77.3347991410756,-2.7061929776992,134.913438492513));
#52324=CARTESIAN_POINT('Ctrl Pts',(77.3270528649915,-2.59045484743002,134.987368454149));
#52325=CARTESIAN_POINT('Ctrl Pts',(77.3193065889074,-2.47182895251582,135.056330124983));
#52326=CARTESIAN_POINT('Ctrl Pts',(77.311560255642,-2.35320218193213,135.125292304877));
#52327=CARTESIAN_POINT('Ctrl Pts',(77.3038139223767,-2.23168794216799,135.189285924294));
#52328=CARTESIAN_POINT('Ctrl Pts',(77.2960675891113,-2.10774502829557,135.248074600058));
#52329=CARTESIAN_POINT('Ctrl Pts',(77.2883195211084,-1.9837743582672,135.306876441139));
#52330=CARTESIAN_POINT('Ctrl Pts',(77.2805714531054,-1.85737428503835,135.360470851618));
#52331=CARTESIAN_POINT('Ctrl Pts',(77.2728233851024,-1.72902487267096,135.408669040357));
#52332=CARTESIAN_POINT('Ctrl Pts',(77.2650670823606,-1.60053904902064,135.456918454705));
#52333=CARTESIAN_POINT('Ctrl Pts',(77.2573107796187,-1.47010011421914,135.499760053032));
#52334=CARTESIAN_POINT('Ctrl Pts',(77.2495544768769,-1.33820516703648,135.537054353));
#52335=CARTESIAN_POINT('Ctrl Pts',(77.2417940343627,-1.20623982354905,135.574368558059));
#52336=CARTESIAN_POINT('Ctrl Pts',(77.2340335918486,-1.07281729935912,135.606129474699));
#52337=CARTESIAN_POINT('Ctrl Pts',(77.2262731493344,-0.938445286687876,
135.632248717594));
#52338=CARTESIAN_POINT('Ctrl Pts',(77.218500249069,-0.803857568132993,135.658409889416));
#52339=CARTESIAN_POINT('Ctrl Pts',(77.2107273488036,-0.668317702043727,
135.678911231185));
#52340=CARTESIAN_POINT('Ctrl Pts',(77.2029544485382,-0.532339807258399,
135.693716136661));
#52341=CARTESIAN_POINT('Ctrl Pts',(77.195464112776,-0.401305051454326,135.707982846533));
#52342=CARTESIAN_POINT('Ctrl Pts',(77.1879737770139,-0.26986386824087,135.716960068321));
#52343=CARTESIAN_POINT('Ctrl Pts',(77.1804834412518,-0.138474702897517,
135.720660834107));
#52344=CARTESIAN_POINT('Ctrl Pts',(77.1727091071327,-0.00210387741711957,
135.724501915552));
#52345=CARTESIAN_POINT('Ctrl Pts',(77.1649347730136,0.134642889596524,135.722670696359));
#52346=CARTESIAN_POINT('Ctrl Pts',(77.1571604388945,0.271254509138723,135.715124718373));
#52347=CARTESIAN_POINT('Ctrl Pts',(77.1493956859474,0.407697767069261,135.70758804013));
#52348=CARTESIAN_POINT('Ctrl Pts',(77.1416309330004,0.544005822304882,135.694350637779));
#52349=CARTESIAN_POINT('Ctrl Pts',(77.1338661800533,0.679664864250737,135.675421973657));
#52350=CARTESIAN_POINT('Ctrl Pts',(77.1261091391683,0.815189167723767,135.656512109751));
#52351=CARTESIAN_POINT('Ctrl Pts',(77.1183520982832,0.950065355999913,135.631922286763));
#52352=CARTESIAN_POINT('Ctrl Pts',(77.1105950573982,1.08378238289549,135.60171393049));
#52353=CARTESIAN_POINT('Ctrl Pts',(77.1028438661581,1.21739857274074,135.571528354574));
#52354=CARTESIAN_POINT('Ctrl Pts',(77.095092674918,1.34985696130164,135.535732764628));
#52355=CARTESIAN_POINT('Ctrl Pts',(77.0873414836778,1.48065472630576,135.494440003245));
#52356=CARTESIAN_POINT('Ctrl Pts',(77.0795935869007,1.61139689877062,135.453164792386));
#52357=CARTESIAN_POINT('Ctrl Pts',(77.0718456901237,1.74047947943285,135.406397174554));
#52358=CARTESIAN_POINT('Ctrl Pts',(77.0640977933466,1.86741310782857,135.354300325651));
#52359=CARTESIAN_POINT('Ctrl Pts',(77.0563515172625,1.9943201844455,135.302214374286));
#52360=CARTESIAN_POINT('Ctrl Pts',(77.0486052411784,2.11907884144682,135.24480155752));
#52361=CARTESIAN_POINT('Ctrl Pts',(77.0408589650943,2.24121844201513,135.182273700037));
#52362=CARTESIAN_POINT('Ctrl Pts',(77.0331126318289,2.36335894419048,135.119745380987));
#52363=CARTESIAN_POINT('Ctrl Pts',(77.0253662985636,2.48288000334231,135.052102124037));
#52364=CARTESIAN_POINT('Ctrl Pts',(77.0176199652982,2.5993347536669,134.979602155595));
#52365=CARTESIAN_POINT('Ctrl Pts',(77.0098718972953,2.71581558322506,134.907085951287));
#52366=CARTESIAN_POINT('Ctrl Pts',(77.0021238292923,2.82922840570717,134.829711077823));
#52367=CARTESIAN_POINT('Ctrl Pts',(76.9943757612893,2.93915489943044,134.747779380474));
#52368=CARTESIAN_POINT('Ctrl Pts',(76.9866194585474,3.04919822433953,134.665760605142));
#52369=CARTESIAN_POINT('Ctrl Pts',(76.9788631558056,3.15574750475749,134.57917556543));
#52370=CARTESIAN_POINT('Ctrl Pts',(76.9711068530638,3.25841669621541,134.488367091003));
#52371=CARTESIAN_POINT('Ctrl Pts',(76.9633464105496,3.36114068531206,134.397510149359));
#52372=CARTESIAN_POINT('Ctrl Pts',(76.9555859680354,3.45998017734825,134.302425552283));
#52373=CARTESIAN_POINT('Ctrl Pts',(76.9478255255212,3.55458639119861,134.203492661192));
#52374=CARTESIAN_POINT('Ctrl Pts',(76.9400526252558,3.64934447534232,134.104400954242));
#52375=CARTESIAN_POINT('Ctrl Pts',(76.9322797249904,3.73985544316665,134.001448902211));
#52376=CARTESIAN_POINT('Ctrl Pts',(76.924506824725,3.82581060301693,133.895049261274));
#52377=CARTESIAN_POINT('Ctrl Pts',(76.917016488963,3.90864107629849,133.792517515289));
#52378=CARTESIAN_POINT('Ctrl Pts',(76.9095261532009,3.98724103739184,133.686784732903));
#52379=CARTESIAN_POINT('Ctrl Pts',(76.9020358174389,4.06137364968444,133.57824366127));
#52380=CARTESIAN_POINT('Ctrl Pts',(76.8942614833198,4.13831702250445,133.465587221916));
#52381=CARTESIAN_POINT('Ctrl Pts',(76.8864871492007,4.21069133373102,133.349548475254));
#52382=CARTESIAN_POINT('Ctrl Pts',(76.8787128150816,4.27818460602471,133.230534465268));
#52383=CARTESIAN_POINT('Ctrl Pts',(76.8709480621345,4.34559469889244,133.111667129413));
#52384=CARTESIAN_POINT('Ctrl Pts',(76.8631833091874,4.40813553075663,132.989832162786));
#52385=CARTESIAN_POINT('Ctrl Pts',(76.8554185562403,4.46553733537104,132.865466963417));
#52386=CARTESIAN_POINT('Ctrl Pts',(76.8476615153553,4.5228821277038,132.741225285317));
#52387=CARTESIAN_POINT('Ctrl Pts',(76.8399044744703,4.57509788750142,132.614458728263));
#52388=CARTESIAN_POINT('Ctrl Pts',(76.8321474335853,4.62196006108111,132.485630452028));
#52389=CARTESIAN_POINT('Ctrl Pts',(76.8243962423451,4.66878689553123,132.356899326197));
#52390=CARTESIAN_POINT('Ctrl Pts',(76.816645051105,4.7102680464194,132.226109941763));
#52391=CARTESIAN_POINT('Ctrl Pts',(76.8088938598648,4.74622666369328,132.093746331519));
#52392=CARTESIAN_POINT('Ctrl Pts',(76.8011459630877,4.78216999759554,131.961438979342));
#52393=CARTESIAN_POINT('Ctrl Pts',(76.7933980663107,4.8125953640511,131.827559108621));
#52394=CARTESIAN_POINT('Ctrl Pts',(76.7856501695336,4.83737553628356,131.692606632736));
#52395=CARTESIAN_POINT('Ctrl Pts',(76.7779038934495,4.86215052503818,131.557682386));
#52396=CARTESIAN_POINT('Ctrl Pts',(76.7701576173653,4.88128259778654,131.421686364668));
#52397=CARTESIAN_POINT('Ctrl Pts',(76.7624113412812,4.89469557793779,131.285129025239));
#52398=CARTESIAN_POINT('Ctrl Pts',(76.7546650080159,4.90810865710057,131.148570677775));
#52399=CARTESIAN_POINT('Ctrl Pts',(76.7469186747505,4.91580252120763,131.011451393039));
#52400=CARTESIAN_POINT('Ctrl Pts',(76.7391723414852,4.91775288156668,130.874286709568));
#52401=CARTESIAN_POINT('Ctrl Pts',(76.7314242734822,4.91970367869542,130.737091309016));
#52402=CARTESIAN_POINT('Ctrl Pts',(76.7236762054792,4.91590840709392,130.599850880349));
#52403=CARTESIAN_POINT('Ctrl Pts',(76.7159281374762,4.90639490464888,130.463080524189));
#52404=CARTESIAN_POINT('Ctrl Pts',(76.7081718347343,4.89687129114028,130.326164806867));
#52405=CARTESIAN_POINT('Ctrl Pts',(76.7004155319925,4.88161733369204,130.189720550698));
#52406=CARTESIAN_POINT('Ctrl Pts',(76.6926592292506,4.86071279814397,130.054257853633));
#52407=CARTESIAN_POINT('Ctrl Pts',(76.6848987867364,4.83979710521585,129.918722856049));
#52408=CARTESIAN_POINT('Ctrl Pts',(76.6771383442223,4.81322490049464,129.784170844829));
#52409=CARTESIAN_POINT('Ctrl Pts',(76.6693779017082,4.78112682676611,129.651100313525));
#52410=CARTESIAN_POINT('Ctrl Pts',(76.6616050014428,4.7489772263601,129.51781616559));
#52411=CARTESIAN_POINT('Ctrl Pts',(76.6538321011773,4.71128413819533,129.38601862609));
#52412=CARTESIAN_POINT('Ctrl Pts',(76.6460592009119,4.66822797035095,129.256190510849));
#52413=CARTESIAN_POINT('Ctrl Pts',(76.6385688651499,4.62673700266022,129.131081974616));
#52414=CARTESIAN_POINT('Ctrl Pts',(76.631078529388,4.58026621721277,129.007802449736));
#52415=CARTESIAN_POINT('Ctrl Pts',(76.6235881936261,4.5290180273398,128.886763482991));
#52416=CARTESIAN_POINT('Ctrl Pts',(76.615813859507,4.47582674677051,128.76113528703));
#52417=CARTESIAN_POINT('Ctrl Pts',(76.6080395253879,4.41732014587441,128.637522952274));
#52418=CARTESIAN_POINT('Ctrl Pts',(76.6002651912688,4.3536720509113,128.516408971308));
#52419=CARTESIAN_POINT('Ctrl Pts',(76.5925004383217,4.29010239653689,128.3954442525));
#52420=CARTESIAN_POINT('Ctrl Pts',(76.5847356853746,4.22140403583596,128.276972103959));
#52421=CARTESIAN_POINT('Ctrl Pts',(76.5769709324275,4.14779914891238,128.161455911985));
#52422=CARTESIAN_POINT('Ctrl Pts',(76.5692138915425,4.0742673674002,128.046054452322));
#52423=CARTESIAN_POINT('Ctrl Pts',(76.5614568506576,3.99583896634726,127.933603434245));
#52424=CARTESIAN_POINT('Ctrl Pts',(76.5536998097726,3.91278223843609,127.824542130295));
#52425=CARTESIAN_POINT('Ctrl Pts',(76.5459486185324,3.82978814424896,127.715563070323));
#52426=CARTESIAN_POINT('Ctrl Pts',(76.5381974272922,3.74217290626452,127.609968946278));
#52427=CARTESIAN_POINT('Ctrl Pts',(76.530446236052,3.65024816320902,127.508170178667));
#52428=CARTESIAN_POINT('Ctrl Pts',(76.5226983392749,3.55836249062194,127.406414678248));
#52429=CARTESIAN_POINT('Ctrl Pts',(76.5149504424979,3.46217121745989,127.308451615436));
#52430=CARTESIAN_POINT('Ctrl Pts',(76.5072025457208,3.36202616582613,127.214658245112));
#52431=CARTESIAN_POINT('Ctrl Pts',(76.4994562696367,3.2619020623783,127.12088449434));
#52432=CARTESIAN_POINT('Ctrl Pts',(76.4917099935526,3.15782611067157,127.031278968271));
#52433=CARTESIAN_POINT('Ctrl Pts',(76.4839637174685,3.05018659690714,126.946181670634));
#52434=CARTESIAN_POINT('Ctrl Pts',(76.4762173842031,2.9425462885725,126.861083744829));
#52435=CARTESIAN_POINT('Ctrl Pts',(76.4684710509378,2.8313426723869,126.780494356329));
#52436=CARTESIAN_POINT('Ctrl Pts',(76.4607247176724,2.71699635689118,126.704712601072));
#52437=CARTESIAN_POINT('Ctrl Pts',(76.4529766496694,2.60262443433084,126.628913875017));
#52438=CARTESIAN_POINT('Ctrl Pts',(76.4452285816665,2.48510873783818,126.557925140525));
#52439=CARTESIAN_POINT('Ctrl Pts',(76.4374805136635,2.36489768321145,126.492001401262));
#52440=CARTESIAN_POINT('Ctrl Pts',(76.4297242109216,2.24455886684518,126.426007597465));
#52441=CARTESIAN_POINT('Ctrl Pts',(76.4219679081798,2.12151931322841,126.365089730585));
#52442=CARTESIAN_POINT('Ctrl Pts',(76.4142116054379,1.99625129759965,126.309456411765));
#52443=CARTESIAN_POINT('Ctrl Pts',(76.4064511629237,1.87091642265929,126.253793399767));
#52444=CARTESIAN_POINT('Ctrl Pts',(76.3986907204095,1.7433510791951,126.203420699483));
#52445=CARTESIAN_POINT('Ctrl Pts',(76.3909302778954,1.61404527956611,126.158497845377));
#52446=CARTESIAN_POINT('Ctrl Pts',(76.3831573776299,1.48453190678832,126.113502877118));
#52447=CARTESIAN_POINT('Ctrl Pts',(76.3753844773645,1.35327286924824,126.07397535028));
#52448=CARTESIAN_POINT('Ctrl Pts',(76.3676115770991,1.22077188854755,126.040024456186));
#52449=CARTESIAN_POINT('Ctrl Pts',(76.3601212413371,1.09308765224506,126.007307762609));
#52450=CARTESIAN_POINT('Ctrl Pts',(76.352630905575,0.964250501858037,125.97976935606));
#52451=CARTESIAN_POINT('Ctrl Pts',(76.345140569813,0.834716092698463,125.957461391557));
#52452=CARTESIAN_POINT('Ctrl Pts',(76.3373662356939,0.700270347044384,125.934307613799));
#52453=CARTESIAN_POINT('Ctrl Pts',(76.3295919015748,0.564647542042625,125.916715387791));
#52454=CARTESIAN_POINT('Ctrl Pts',(76.3218175674557,0.428347569711353,125.904799267606));
#52455=CARTESIAN_POINT('Ctrl Pts',(76.3140528145086,0.292215574914962,125.892897832974));
#52456=CARTESIAN_POINT('Ctrl Pts',(76.3062880615616,0.155408459031892,125.886658619341));
#52457=CARTESIAN_POINT('Ctrl Pts',(76.2985233086145,0.0184361758547634,
125.886145171907));
#52458=CARTESIAN_POINT('Ctrl Pts',(76.2907662677295,-0.118400064520302,
125.885632234436));
#52459=CARTESIAN_POINT('Ctrl Pts',(76.2830092268444,-0.255400757296971,
125.89083374741));
#52460=CARTESIAN_POINT('Ctrl Pts',(76.2752521859594,-0.392051311295803,
125.901761426136));
#52461=CARTESIAN_POINT('Ctrl Pts',(76.2675009947193,-0.528598816048227,
125.912680864214));
#52462=CARTESIAN_POINT('Ctrl Pts',(76.2597498034792,-0.664796319438987,
125.929317841996));
#52463=CARTESIAN_POINT('Ctrl Pts',(76.2519986122391,-0.800130074728278,
125.951632011306));
#52464=CARTESIAN_POINT('Ctrl Pts',(76.244250715462,-0.935406309561701,125.973936696498));
#52465=CARTESIAN_POINT('Ctrl Pts',(76.2365028186849,-1.06981914151023,126.001913710557));
#52466=CARTESIAN_POINT('Ctrl Pts',(76.2287549219078,-1.20286100691642,126.035470971061));
#52467=CARTESIAN_POINT('Ctrl Pts',(76.2210086458237,-1.33587504283241,126.06902121211));
#52468=CARTESIAN_POINT('Ctrl Pts',(76.2132623697396,-1.46751830376856,126.108149282288));
#52469=CARTESIAN_POINT('Ctrl Pts',(76.2055160936555,-1.59729485678162,126.152712285738));
#52470=CARTESIAN_POINT('Ctrl Pts',(76.1977697603901,-1.72707236777616,126.197275618142));
#52471=CARTESIAN_POINT('Ctrl Pts',(76.1900234271248,-1.85498277357909,126.2472738369));
#52472=CARTESIAN_POINT('Ctrl Pts',(76.1822770938594,-1.98054708711762,126.302514740794));
#52473=CARTESIAN_POINT('Ctrl Pts',(76.1745290258565,-2.10613951991306,126.357768015505));
#52474=CARTESIAN_POINT('Ctrl Pts',(76.1667809578535,-2.22938445718106,126.418266154193));
#52475=CARTESIAN_POINT('Ctrl Pts',(76.1590328898505,-2.34982497742408,126.483769727656));
#52476=CARTESIAN_POINT('Ctrl Pts',(76.1512765871086,-2.47039350328543,126.549342919096));
#52477=CARTESIAN_POINT('Ctrl Pts',(76.1435202843668,-2.58815131411329,126.619931985165));
#52478=CARTESIAN_POINT('Ctrl Pts',(76.1357639816249,-2.70266762314266,126.695252346747));
#52479=CARTESIAN_POINT('Ctrl Pts',(76.1280035391108,-2.81724505297434,126.770612909073));
#52480=CARTESIAN_POINT('Ctrl Pts',(76.1202430965966,-2.92857721645162,126.850709570443));
#52481=CARTESIAN_POINT('Ctrl Pts',(76.1124826540824,-3.03626502906172,126.935216301855));
#52482=CARTESIAN_POINT('Ctrl Pts',(76.1047097538169,-3.14412571170862,127.019858690975));
#52483=CARTESIAN_POINT('Ctrl Pts',(76.0969368535515,-3.24833005548526,127.108925042938));
#52484=CARTESIAN_POINT('Ctrl Pts',(76.089163953286,-3.34851392081119,127.20205058307));
#52485=CARTESIAN_POINT('Ctrl Pts',(76.0816736175241,-3.44505585028365,127.291790775248));
#52486=CARTESIAN_POINT('Ctrl Pts',(76.0741832817621,-3.5378643184477,127.385299937322));
#52487=CARTESIAN_POINT('Ctrl Pts',(76.0666929460002,-3.62664915298228,127.482222904636));
#52488=CARTESIAN_POINT('Ctrl Pts',(76.0590029828683,-3.71780022096293,127.581728997414));
#52489=CARTESIAN_POINT('Ctrl Pts',(76.0513130197365,-3.80501329057441,127.685164594423));
#52490=CARTESIAN_POINT('Ctrl Pts',(76.0436230566047,-3.88792480186614,127.792181373641));
#52491=CARTESIAN_POINT('Ctrl Pts',(76.035942259654,-3.9707374853851,127.899070592405));
#52492=CARTESIAN_POINT('Ctrl Pts',(76.0282614627032,-4.04925856324953,128.009532192583));
#52493=CARTESIAN_POINT('Ctrl Pts',(76.0205806657525,-4.12316150282434,128.123181346401));
#52494=CARTESIAN_POINT('Ctrl Pts',(76.0129084811636,-4.19698157614698,128.236703067135));
#52495=CARTESIAN_POINT('Ctrl Pts',(76.0052362965747,-4.26619360138958,128.353404894275));
#52496=CARTESIAN_POINT('Ctrl Pts',(75.9975641119859,-4.33051198459884,128.472869889781));
#52497=CARTESIAN_POINT('Ctrl Pts',(75.9898969959661,-4.39478787636778,128.592255961666));
#52498=CARTESIAN_POINT('Ctrl Pts',(75.9822298799464,-4.45417636577332,128.714401221262));
#52499=CARTESIAN_POINT('Ctrl Pts',(75.9745627639267,-4.50843587467326,128.83886092882));
#52500=CARTESIAN_POINT('Ctrl Pts',(75.9668982869073,-4.56267670759917,128.963277797689));
#52501=CARTESIAN_POINT('Ctrl Pts',(75.9592338098879,-4.61179190649494,129.09000716624));
#52502=CARTESIAN_POINT('Ctrl Pts',(75.9515693328685,-4.6555866404337,129.218581283637));
#52503=CARTESIAN_POINT('Ctrl Pts',(75.9444259887391,-4.69640362700555,129.338413225775));
#52504=CARTESIAN_POINT('Ctrl Pts',(75.9372826446096,-4.73259941719584,129.459847118768));
#52505=CARTESIAN_POINT('Ctrl Pts',(75.9301393004801,-4.76405452823408,129.582490119308));
#52506=CARTESIAN_POINT('Origin',(213.235140564004,0.,130.804360617566));
#52507=CARTESIAN_POINT('',(73.8346539883595,-4.76405452823405,129.582490119308));
#52508=CARTESIAN_POINT('',(74.1802344108983,-4.76405452823402,129.582490119308));
#52509=CARTESIAN_POINT('',(213.235140564004,-4.76405452823405,129.582490119308));
#52510=CARTESIAN_POINT('',(75.5148594359626,-4.91824975138238,130.802796799436));
#52511=CARTESIAN_POINT('Ctrl Pts',(75.5148594359626,-4.91824975138238,130.802796799436));
#52512=CARTESIAN_POINT('Ctrl Pts',(75.5071480679706,-4.91829279726256,130.93817724134));
#52513=CARTESIAN_POINT('Ctrl Pts',(75.4994366999785,-4.91274186277529,131.073785176132));
#52514=CARTESIAN_POINT('Ctrl Pts',(75.4917253319864,-4.9015667560916,131.209115355744));
#52515=CARTESIAN_POINT('Ctrl Pts',(75.484023229282,-4.89040507641316,131.344282934758));
#52516=CARTESIAN_POINT('Ctrl Pts',(75.4763211265776,-4.87363269840611,131.479173029789));
#52517=CARTESIAN_POINT('Ctrl Pts',(75.4686190238732,-4.85127141023658,131.61327888706));
#52518=CARTESIAN_POINT('Ctrl Pts',(75.4609242586911,-4.82893142487945,131.7472569864));
#52519=CARTESIAN_POINT('Ctrl Pts',(75.453229493509,-4.80101318715482,131.880451944431));
#52520=CARTESIAN_POINT('Ctrl Pts',(75.4455347283269,-4.76759037113984,132.012361079286));
#52521=CARTESIAN_POINT('Ctrl Pts',(75.4378453800766,-4.73419108399346,132.144177353242));
#52522=CARTESIAN_POINT('Ctrl Pts',(75.4301560318263,-4.69529502713937,132.274709221102));
#52523=CARTESIAN_POINT('Ctrl Pts',(75.4224666835761,-4.65102705737138,132.403463608026));
#52524=CARTESIAN_POINT('Ctrl Pts',(75.4147800166523,-4.60677452413606,132.532173097448));
#52525=CARTESIAN_POINT('Ctrl Pts',(75.4070933497284,-4.55715393016955,132.659105962261));
#52526=CARTESIAN_POINT('Ctrl Pts',(75.3994066828046,-4.50234006970444,132.783784008161));
#52527=CARTESIAN_POINT('Ctrl Pts',(75.3917211385253,-4.44753421485211,132.908443844722));
#52528=CARTESIAN_POINT('Ctrl Pts',(75.3840355942459,-4.38753676183005,133.030849153161));
#52529=CARTESIAN_POINT('Ctrl Pts',(75.3763500499666,-4.32257055738247,133.150541948783));
#52530=CARTESIAN_POINT('Ctrl Pts',(75.3686638977918,-4.25759921437067,133.270244211621));
#52531=CARTESIAN_POINT('Ctrl Pts',(75.3609777456169,-4.18765852810816,133.387233185288));
#52532=CARTESIAN_POINT('Ctrl Pts',(75.3532915934421,-4.11301694566277,133.501076150801));
#52533=CARTESIAN_POINT('Ctrl Pts',(75.3456031026954,-4.03835265293261,133.614953753926));
#52534=CARTESIAN_POINT('Ctrl Pts',(75.3379146119487,-3.95898483720637,133.725683112525));
#52535=CARTESIAN_POINT('Ctrl Pts',(75.330226121202,-3.87522454920135,133.832861526558));
#52536=CARTESIAN_POINT('Ctrl Pts',(75.3225292817413,-3.79137330827571,133.940156322591));
#52537=CARTESIAN_POINT('Ctrl Pts',(75.3148324422806,-3.70312031831821,134.043892162812));
#52538=CARTESIAN_POINT('Ctrl Pts',(75.3071356028199,-3.61081632476517,134.14370015276));
#52539=CARTESIAN_POINT('Ctrl Pts',(75.2994339805125,-3.51845497314282,134.243570163791));
#52540=CARTESIAN_POINT('Ctrl Pts',(75.2917323582051,-3.42203788672323,134.339507184623));
#52541=CARTESIAN_POINT('Ctrl Pts',(75.2840307358977,-3.32195086392682,134.431180921931));
#52542=CARTESIAN_POINT('Ctrl Pts',(75.2763179510522,-3.22171877751165,134.522987528853));
#52543=CARTESIAN_POINT('Ctrl Pts',(75.2686051662068,-3.11780643955999,134.610518261872));
#52544=CARTESIAN_POINT('Ctrl Pts',(75.2608923813613,-3.01063104336579,134.693484398474));
#52545=CARTESIAN_POINT('Ctrl Pts',(75.2575746111478,-2.96452793738835,134.72917352792));
#52546=CARTESIAN_POINT('Ctrl Pts',(75.2542568409344,-2.91782137235664,134.764018575186));
#52547=CARTESIAN_POINT('Ctrl Pts',(75.2509390707209,-2.87054600307479,134.79799914737));
#52548=CARTESIAN_POINT('Ctrl Pts',(75.2431647366018,-2.75976843478319,134.877623806316));
#52549=CARTESIAN_POINT('Ctrl Pts',(75.2353904024827,-2.64549988832472,134.952761885495));
#52550=CARTESIAN_POINT('Ctrl Pts',(75.2276160683636,-2.52813980386932,135.023091729475));
#52551=CARTESIAN_POINT('Ctrl Pts',(75.2198513154165,-2.41092435522924,135.093334898209));
#52552=CARTESIAN_POINT('Ctrl Pts',(75.2120865624694,-2.29062528158387,135.158781423122));
#52553=CARTESIAN_POINT('Ctrl Pts',(75.2043218095223,-2.16767338135606,135.219151119307));
#52554=CARTESIAN_POINT('Ctrl Pts',(75.1965647686373,-2.0448435986892,135.279460855458));
#52555=CARTESIAN_POINT('Ctrl Pts',(75.1888077277524,-1.91936658153298,135.334703626243));
#52556=CARTESIAN_POINT('Ctrl Pts',(75.1810506868674,-1.79169996761107,135.384643828085));
#52557=CARTESIAN_POINT('Ctrl Pts',(75.1732994956272,-1.66412962807539,135.434546369633));
#52558=CARTESIAN_POINT('Ctrl Pts',(75.1655483043871,-1.53437334099751,135.479154159575));
#52559=CARTESIAN_POINT('Ctrl Pts',(75.157797113147,-1.40291075586978,135.518278783335));
#52560=CARTESIAN_POINT('Ctrl Pts',(75.1500492163699,-1.27150404584779,135.557386778086));
#52561=CARTESIAN_POINT('Ctrl Pts',(75.1423013195928,-1.13839285412539,135.591016130537));
#52562=CARTESIAN_POINT('Ctrl Pts',(75.1345534228157,-1.00407389702651,135.619027654009));
#52563=CARTESIAN_POINT('Ctrl Pts',(75.1268071467316,-0.86978303655796,135.647033318074));
#52564=CARTESIAN_POINT('Ctrl Pts',(75.1190608706475,-0.734285295713348,
135.669423410787));
#52565=CARTESIAN_POINT('Ctrl Pts',(75.1113145945635,-0.59808915596445,135.686109527948));
#52566=CARTESIAN_POINT('Ctrl Pts',(75.1035682612981,-0.461892010846495,
135.702795768282));
#52567=CARTESIAN_POINT('Ctrl Pts',(75.0958219280327,-0.324996844600614,
135.713777901501));
#52568=CARTESIAN_POINT('Ctrl Pts',(75.0880755947673,-0.187918464440154,
135.719019274403));
#52569=CARTESIAN_POINT('Ctrl Pts',(75.0803275267644,-0.0508093865270786,
135.724261821074));
#52570=CARTESIAN_POINT('Ctrl Pts',(75.0725794587615,0.0864825963395565,
135.723761034292));
#52571=CARTESIAN_POINT('Ctrl Pts',(75.0648313907585,0.223441863842868,135.717532382931));
#52572=CARTESIAN_POINT('Ctrl Pts',(75.0570750880166,0.360546693285705,135.711297111686));
#52573=CARTESIAN_POINT('Ctrl Pts',(75.0493187852747,0.497317709799175,135.69932183293));
#52574=CARTESIAN_POINT('Ctrl Pts',(75.0415624825329,0.633243048166705,135.68167404859));
#52575=CARTESIAN_POINT('Ctrl Pts',(75.0338020400187,0.769240933980048,135.664016845096));
#52576=CARTESIAN_POINT('Ctrl Pts',(75.0260415975046,0.904391857190708,135.640681169782));
#52577=CARTESIAN_POINT('Ctrl Pts',(75.0182811549904,1.03819433273526,135.611785665341));
#52578=CARTESIAN_POINT('Ctrl Pts',(75.010508254725,1.17221159989199,135.582843775272));
#52579=CARTESIAN_POINT('Ctrl Pts',(75.0027353544596,1.30487571514227,135.548324319327));
#52580=CARTESIAN_POINT('Ctrl Pts',(74.9949624541941,1.435699672403,135.508396067386));
#52581=CARTESIAN_POINT('Ctrl Pts',(74.9874721184321,1.56176784929163,135.469919307976));
#52582=CARTESIAN_POINT('Ctrl Pts',(74.97998178267,1.68612704343233,135.426420273644));
#52583=CARTESIAN_POINT('Ctrl Pts',(74.972491446908,1.80836096919779,135.378091443444));
#52584=CARTESIAN_POINT('Ctrl Pts',(74.9647171127889,1.93522943141076,135.327930210957));
#52585=CARTESIAN_POINT('Ctrl Pts',(74.9569427786698,2.0602101659701,135.272406813714));
#52586=CARTESIAN_POINT('Ctrl Pts',(74.9491684445508,2.18281664788325,135.211683449425));
#52587=CARTESIAN_POINT('Ctrl Pts',(74.9414036916037,2.3052720282651,135.151034921255));
#52588=CARTESIAN_POINT('Ctrl Pts',(74.9336389386566,2.4253586309896,135.085199348886));
#52589=CARTESIAN_POINT('Ctrl Pts',(74.9258741857095,2.54260787148895,135.014387728446));
#52590=CARTESIAN_POINT('Ctrl Pts',(74.9181171448245,2.65974065839003,134.943646439105));
#52591=CARTESIAN_POINT('Ctrl Pts',(74.9103601039395,2.77404135872734,134.867939137866));
#52592=CARTESIAN_POINT('Ctrl Pts',(74.9026030630545,2.88506438817311,134.787523498819));
#52593=CARTESIAN_POINT('Ctrl Pts',(74.8948518718144,2.99600369428821,134.707168501833));
#52594=CARTESIAN_POINT('Ctrl Pts',(74.8871006805742,3.10366993396344,134.622112462695));
#52595=CARTESIAN_POINT('Ctrl Pts',(74.8793494893341,3.20764532641281,134.532657081427));
#52596=CARTESIAN_POINT('Ctrl Pts',(74.871601592557,3.31157652654705,134.443239721083));
#52597=CARTESIAN_POINT('Ctrl Pts',(74.8638536957799,3.41181970374504,134.349426992025));
#52598=CARTESIAN_POINT('Ctrl Pts',(74.8561057990028,3.50798926900413,134.251561561963));
#52599=CARTESIAN_POINT('Ctrl Pts',(74.8483595229187,3.60413871766346,134.153716603239));
#52600=CARTESIAN_POINT('Ctrl Pts',(74.8406132468346,3.69621597542709,134.051820908391));
#52601=CARTESIAN_POINT('Ctrl Pts',(74.8328669707504,3.78387181867998,133.946254492651));
#52602=CARTESIAN_POINT('Ctrl Pts',(74.8251206374851,3.87152830898816,133.840687297645));
#52603=CARTESIAN_POINT('Ctrl Pts',(74.8173743042198,3.95476306990133,133.731449628468));
#52604=CARTESIAN_POINT('Ctrl Pts',(74.8096279709545,4.03326699816961,133.618954795059));
#52605=CARTESIAN_POINT('Ctrl Pts',(74.8018799029515,4.11178850684843,133.506434769212));
#52606=CARTESIAN_POINT('Ctrl Pts',(74.7941318349485,4.18557685102805,133.390656448226));
#52607=CARTESIAN_POINT('Ctrl Pts',(74.7863837669455,4.25436633973549,133.272061999384));
#52608=CARTESIAN_POINT('Ctrl Pts',(74.7786274642037,4.32322893873014,133.15334150695));
#52609=CARTESIAN_POINT('Ctrl Pts',(74.7708711614618,4.38708187279911,133.031799246521));
#52610=CARTESIAN_POINT('Ctrl Pts',(74.7631148587199,4.44570525757098,132.907902351239));
#52611=CARTESIAN_POINT('Ctrl Pts',(74.7553544162057,4.50435993140837,132.783939328455));
#52612=CARTESIAN_POINT('Ctrl Pts',(74.7475939736916,4.55777934210613,132.657619526572));
#52613=CARTESIAN_POINT('Ctrl Pts',(74.7398335311775,4.60579224219589,132.529428988451));
#52614=CARTESIAN_POINT('Ctrl Pts',(74.732060630912,4.65388221685529,132.401032667498));
#52615=CARTESIAN_POINT('Ctrl Pts',(74.7242877306466,4.69654821572148,132.270759980973));
#52616=CARTESIAN_POINT('Ctrl Pts',(74.7165148303811,4.73366899098852,132.139111885126));
#52617=CARTESIAN_POINT('Ctrl Pts',(74.709024494619,4.76944033257327,132.012249529164));
#52618=CARTESIAN_POINT('Ctrl Pts',(74.701534158857,4.80006254510861,131.884110326518));
#52619=CARTESIAN_POINT('Ctrl Pts',(74.6940438230949,4.82547255412337,131.755148549705));
#52620=CARTESIAN_POINT('Ctrl Pts',(74.6862694889758,4.85184599135294,131.621297147929));
#52621=CARTESIAN_POINT('Ctrl Pts',(74.6784951548567,4.87268772460145,131.486135563861));
#52622=CARTESIAN_POINT('Ctrl Pts',(74.6707208207376,4.8878712367538,131.350160796583));
#52623=CARTESIAN_POINT('Ctrl Pts',(74.6629560677905,4.90303603658441,131.214353606053));
#52624=CARTESIAN_POINT('Ctrl Pts',(74.6551913148435,4.91255644704091,131.077735611162));
#52625=CARTESIAN_POINT('Ctrl Pts',(74.6474265618964,4.91635670373674,130.940815093941));
#52626=CARTESIAN_POINT('Ctrl Pts',(74.6396695210114,4.92015318596405,130.804030568107));
#52627=CARTESIAN_POINT('Ctrl Pts',(74.6319124801263,4.91824080977142,130.666944506176));
#52628=CARTESIAN_POINT('Ctrl Pts',(74.6241554392413,4.91059551445619,130.530071070002));
#52629=CARTESIAN_POINT('Ctrl Pts',(74.6164042480012,4.90295598451768,130.393300851152));
#52630=CARTESIAN_POINT('Ctrl Pts',(74.6086530567611,4.88959216231733,130.256743327684));
#52631=CARTESIAN_POINT('Ctrl Pts',(74.600901865521,4.87053205590813,130.120913066637));
#52632=CARTESIAN_POINT('Ctrl Pts',(74.5931539687439,4.85148005055249,129.985140537073));
#52633=CARTESIAN_POINT('Ctrl Pts',(74.5854060719669,4.82673663053243,129.850095041502));
#52634=CARTESIAN_POINT('Ctrl Pts',(74.5776581751898,4.79638167162292,129.716286207142));
#52635=CARTESIAN_POINT('Ctrl Pts',(74.5699118991057,4.76603306231643,129.582505362705));
#52636=CARTESIAN_POINT('Ctrl Pts',(74.5621656230216,4.73007533533806,129.449961045979));
#52637=CARTESIAN_POINT('Ctrl Pts',(74.5544193469375,4.68863944437119,129.319152476198));
#52638=CARTESIAN_POINT('Ctrl Pts',(74.5466730136721,4.64720324753399,129.188342940817));
#52639=CARTESIAN_POINT('Ctrl Pts',(74.5389266804068,4.60028892407935,129.059269550661));
#52640=CARTESIAN_POINT('Ctrl Pts',(74.5311803471414,4.54807712550698,128.932415767166));
#52641=CARTESIAN_POINT('Ctrl Pts',(74.5234322791384,4.49585363446423,128.805533575644));
#52642=CARTESIAN_POINT('Ctrl Pts',(74.5156842111354,4.43833045641633,128.680872341356));
#52643=CARTESIAN_POINT('Ctrl Pts',(74.5079361431324,4.37573598675864,128.558894599857));
#52644=CARTESIAN_POINT('Ctrl Pts',(74.5001798403906,4.31307499095384,128.436787218963));
#52645=CARTESIAN_POINT('Ctrl Pts',(74.4924235376487,4.24533211555801,128.317369376525));
#52646=CARTESIAN_POINT('Ctrl Pts',(74.4846672349069,4.17278152004028,128.201078564367));
#52647=CARTESIAN_POINT('Ctrl Pts',(74.4769067923927,4.10019220208532,128.0847256843));
#52648=CARTESIAN_POINT('Ctrl Pts',(74.4691463498785,4.02279027152226,127.971503482714));
#52649=CARTESIAN_POINT('Ctrl Pts',(74.4613859073644,3.94089208653534,127.86181875299));
#52650=CARTESIAN_POINT('Ctrl Pts',(74.4536130070989,3.8588624313112,127.751957947601));
#52651=CARTESIAN_POINT('Ctrl Pts',(74.4458401068335,3.77232234518507,127.645646265236));
#52652=CARTESIAN_POINT('Ctrl Pts',(74.4380672065681,3.68162775943859,127.543256494201));
#52653=CARTESIAN_POINT('Ctrl Pts',(74.4305768708061,3.59423015033061,127.444588849247));
#52654=CARTESIAN_POINT('Ctrl Pts',(74.4230865350441,3.50297506391935,127.349563145572));
#52655=CARTESIAN_POINT('Ctrl Pts',(74.4155961992822,3.40821059924742,127.258477994907));
#52656=CARTESIAN_POINT('Ctrl Pts',(74.4078218651631,3.30985311109372,127.163939323068));
#52657=CARTESIAN_POINT('Ctrl Pts',(74.400047531044,3.20740330835137,127.073346444924));
#52658=CARTESIAN_POINT('Ctrl Pts',(74.3922731969249,3.10121094483079,126.987074443049));
#52659=CARTESIAN_POINT('Ctrl Pts',(74.3845084439778,2.99514945390779,126.900908763705));
#52660=CARTESIAN_POINT('Ctrl Pts',(74.3767436910308,2.88535487998499,126.819053609438));
#52661=CARTESIAN_POINT('Ctrl Pts',(74.3689789380837,2.77221390262702,126.741847461823));
#52662=CARTESIAN_POINT('Ctrl Pts',(74.3612218971987,2.65918529848254,126.664717996443));
#52663=CARTESIAN_POINT('Ctrl Pts',(74.3534648563137,2.54281722605666,126.592228567708));
#52664=CARTESIAN_POINT('Ctrl Pts',(74.3457078154287,2.42352925888212,126.524677335611));
#52665=CARTESIAN_POINT('Ctrl Pts',(74.3379566241886,2.30433124769205,126.457177044424));
#52666=CARTESIAN_POINT('Ctrl Pts',(74.3302054329485,2.18221806335954,126.394607729487));
#52667=CARTESIAN_POINT('Ctrl Pts',(74.3224542417084,2.05763776474414,126.337223962885));
#52668=CARTESIAN_POINT('Ctrl Pts',(74.3147063449313,1.93311041607842,126.279864585913));
#52669=CARTESIAN_POINT('Ctrl Pts',(74.3069584481542,1.80611839305563,126.227686536921));
#52670=CARTESIAN_POINT('Ctrl Pts',(74.2992105513771,1.67713363429334,126.180898080114));
#52671=CARTESIAN_POINT('Ctrl Pts',(74.291464275293,1.54817585636173,126.134119410444));
#52672=CARTESIAN_POINT('Ctrl Pts',(74.2837179992089,1.41722653910186,126.092728223761));
#52673=CARTESIAN_POINT('Ctrl Pts',(74.2759717231248,1.28477647345796,126.056884185213));
#52674=CARTESIAN_POINT('Ctrl Pts',(74.2682253898594,1.15232543009793,126.021039882072));
#52675=CARTESIAN_POINT('Ctrl Pts',(74.260479056594,1.01837399363812,125.990742910905));
#52676=CARTESIAN_POINT('Ctrl Pts',(74.2527327233287,0.883426560424877,125.966102607204));
#52677=CARTESIAN_POINT('Ctrl Pts',(74.2449846553257,0.748448906669721,125.941456785477));
#52678=CARTESIAN_POINT('Ctrl Pts',(74.2372365873228,0.612475196857113,125.922470222157));
#52679=CARTESIAN_POINT('Ctrl Pts',(74.2294885193198,0.476018028540152,125.909200773495));
#52680=CARTESIAN_POINT('Ctrl Pts',(74.2217322165779,0.339415831920844,125.895917221905));
#52681=CARTESIAN_POINT('Ctrl Pts',(74.2139759138361,0.202329540125689,125.888362960773));
#52682=CARTESIAN_POINT('Ctrl Pts',(74.2062196110942,0.0652754173056658,
125.886543806989));
#52683=CARTESIAN_POINT('Ctrl Pts',(74.1984591685801,-0.0718518554262336,
125.884723682268));
#52684=CARTESIAN_POINT('Ctrl Pts',(74.1906987260658,-0.20894653435704,125.888644753023));
#52685=CARTESIAN_POINT('Ctrl Pts',(74.1829382835517,-0.34549537336629,125.898260739915));
#52686=CARTESIAN_POINT('Ctrl Pts',(74.1751653832863,-0.482263412694153,
125.907892163244));
#52687=CARTESIAN_POINT('Ctrl Pts',(74.1673924830209,-0.618483472380627,
125.923236727519));
#52688=CARTESIAN_POINT('Ctrl Pts',(74.1596195827555,-0.753649525516159,
125.944196478857));
#52689=CARTESIAN_POINT('Ctrl Pts',(74.1521292469934,-0.883901952158292,
125.96439429044));
#52690=CARTESIAN_POINT('Ctrl Pts',(74.1446389112313,-1.01317537116423,125.989806065149));
#52691=CARTESIAN_POINT('Ctrl Pts',(74.1371485754692,-1.14103039599215,126.020300344333));
#52692=CARTESIAN_POINT('Ctrl Pts',(74.1293742413502,-1.27373308294637,126.051950823382));
#52693=CARTESIAN_POINT('Ctrl Pts',(74.1215999072311,-1.40532805791054,126.089177080467));
#52694=CARTESIAN_POINT('Ctrl Pts',(74.113825573112,-1.53531070281407,126.131887599097));
#52695=CARTESIAN_POINT('Ctrl Pts',(74.1060608201649,-1.66513315572456,126.174545480829));
#52696=CARTESIAN_POINT('Ctrl Pts',(74.0982960672179,-1.79334686435497,126.222674055109));
#52697=CARTESIAN_POINT('Ctrl Pts',(74.0905313142708,-1.91945804481905,126.276130955029));
#52698=CARTESIAN_POINT('Ctrl Pts',(74.0827742733858,-2.04544396988066,126.329534760802));
#52699=CARTESIAN_POINT('Ctrl Pts',(74.0750172325008,-2.16933116487668,126.388256208965));
#52700=CARTESIAN_POINT('Ctrl Pts',(74.0672601916158,-2.2906419896182,126.452103463181));
#52701=CARTESIAN_POINT('Ctrl Pts',(74.0595090003757,-2.41186133292386,126.515902569686));
#52702=CARTESIAN_POINT('Ctrl Pts',(74.0517578091355,-2.53050782854871,126.584819607026));
#52703=CARTESIAN_POINT('Ctrl Pts',(74.0440066178953,-2.6461251110297,126.658615213024));
#52704=CARTESIAN_POINT('Ctrl Pts',(74.0362587211182,-2.76169325308097,126.732379453921));
#52705=CARTESIAN_POINT('Ctrl Pts',(74.0285108243412,-2.87423441385383,126.811017929491));
#52706=CARTESIAN_POINT('Ctrl Pts',(74.0207629275641,-2.9833182804222,126.8942461563));
#52707=CARTESIAN_POINT('Ctrl Pts',(74.01301665148,-3.09237932899719,126.977456973559));
#52708=CARTESIAN_POINT('Ctrl Pts',(74.0052703753959,-3.19798421120625,127.065255395409));
#52709=CARTESIAN_POINT('Ctrl Pts',(73.9975240993118,-3.29973331174558,127.157314808441));
#52710=CARTESIAN_POINT('Ctrl Pts',(73.9897777660465,-3.40148316337352,127.249374901035));
#52711=CARTESIAN_POINT('Ctrl Pts',(73.9820314327811,-3.49937688662317,127.345695785269));
#52712=CARTESIAN_POINT('Ctrl Pts',(73.9742850995158,-3.59304985590273,127.445912196718));
#52713=CARTESIAN_POINT('Ctrl Pts',(73.9665370315129,-3.68674380259395,127.546151050936));
#52714=CARTESIAN_POINT('Ctrl Pts',(73.95878896351,-3.77621484753823,127.65028688273));
#52715=CARTESIAN_POINT('Ctrl Pts',(73.951040895507,-3.86113724313427,127.757919701976));
#52716=CARTESIAN_POINT('Ctrl Pts',(73.9432845927652,-3.94614989526328,127.865666914664));
#52717=CARTESIAN_POINT('Ctrl Pts',(73.9355282900234,-4.02660399833575,127.976918231771));
#52718=CARTESIAN_POINT('Ctrl Pts',(73.9277719872815,-4.10221560505266,128.091242449818));
#52719=CARTESIAN_POINT('Ctrl Pts',(73.9200115447674,-4.17786756796064,128.205627686143));
#52720=CARTESIAN_POINT('Ctrl Pts',(73.9122511022532,-4.24867168276926,128.323088756771));
#52721=CARTESIAN_POINT('Ctrl Pts',(73.9044906597391,-4.31438946353308,128.443168838092));
#52722=CARTESIAN_POINT('Ctrl Pts',(73.8967177594737,-4.38021274031282,128.56344168262));
#52723=CARTESIAN_POINT('Ctrl Pts',(73.8889448592082,-4.44093319342798,128.68634158859));
#52724=CARTESIAN_POINT('Ctrl Pts',(73.8811719589428,-4.49635971435013,128.811389874763));
#52725=CARTESIAN_POINT('Ctrl Pts',(73.8736816231807,-4.54977134162642,128.931892340758));
#52726=CARTESIAN_POINT('Ctrl Pts',(73.8661912874185,-4.59826713651736,129.054389414328));
#52727=CARTESIAN_POINT('Ctrl Pts',(73.8587009516564,-4.64172019974865,129.178440370523));
#52728=CARTESIAN_POINT('Ctrl Pts',(73.8506852972241,-4.68822075058504,129.311191375075));
#52729=CARTESIAN_POINT('Ctrl Pts',(73.8426696427918,-4.72905423412978,129.446024503799));
#52730=CARTESIAN_POINT('Ctrl Pts',(73.8346539883595,-4.76405452823405,129.582490119308));
#52731=CARTESIAN_POINT('Ctrl Pts',(75.5849534216701,-4.76405452823408,129.582490119308));
#52732=CARTESIAN_POINT('Ctrl Pts',(75.5771898855308,-4.79810426152783,129.715249512644));
#52733=CARTESIAN_POINT('Ctrl Pts',(75.5694263493916,-4.82656819574603,129.849307539283));
#52734=CARTESIAN_POINT('Ctrl Pts',(75.5616628132524,-4.84937572042938,129.98415443336));
#52735=CARTESIAN_POINT('Ctrl Pts',(75.5538880904119,-4.87221610912731,130.119195632182));
#52736=CARTESIAN_POINT('Ctrl Pts',(75.5461133675714,-4.88938376665781,130.255027581356));
#52737=CARTESIAN_POINT('Ctrl Pts',(75.5383386447309,-4.90086001478842,130.391136492002));
#52738=CARTESIAN_POINT('Ctrl Pts',(75.5353546613319,-4.90526466491014,130.443375875729));
#52739=CARTESIAN_POINT('Ctrl Pts',(75.5323706779328,-4.90883147788219,130.495656069877));
#52740=CARTESIAN_POINT('Ctrl Pts',(75.5293866945337,-4.91156143249047,130.547948142495));
#52741=CARTESIAN_POINT('Ctrl Pts',(75.5245442750195,-4.91599161312486,130.632807915159));
#52742=CARTESIAN_POINT('Ctrl Pts',(75.5197018555053,-4.91822272034478,130.717783492037));
#52743=CARTESIAN_POINT('Ctrl Pts',(75.5148594359911,-4.91824975138222,130.802796798936));
#52744=CARTESIAN_POINT('',(75.8601405639734,-4.91824791822853,130.808885807146));
#52745=CARTESIAN_POINT('Ctrl Pts',(75.9301393004801,-4.76405452823408,129.582490119308));
#52746=CARTESIAN_POINT('Ctrl Pts',(75.9224754798333,-4.79780151354726,129.714069102862));
#52747=CARTESIAN_POINT('Ctrl Pts',(75.9148116591865,-4.82609118446505,129.847039594704));
#52748=CARTESIAN_POINT('Ctrl Pts',(75.9071478385396,-4.84882489549495,129.98090436777));
#52749=CARTESIAN_POINT('Ctrl Pts',(75.8993132927844,-4.87206503999421,130.117751214522));
#52750=CARTESIAN_POINT('Ctrl Pts',(75.8914787470293,-4.88949867655914,130.255532226787));
#52751=CARTESIAN_POINT('Ctrl Pts',(75.8836442012741,-4.90107623634819,130.393708954958));
#52752=CARTESIAN_POINT('Ctrl Pts',(75.8758096555189,-4.91265379613726,130.531885683128));
#52753=CARTESIAN_POINT('Ctrl Pts',(75.8679751097637,-4.91837528338702,130.670457681576));
#52754=CARTESIAN_POINT('Ctrl Pts',(75.8601405640085,-4.9182479182291,130.808885806526));
#52755=CARTESIAN_POINT('Ctrl Pts',(75.8601405639734,-4.91824791822853,130.808885807146));
#52756=CARTESIAN_POINT('Ctrl Pts',(75.8503022766471,-4.91808797849113,130.982717923244));
#52757=CARTESIAN_POINT('Ctrl Pts',(75.8404639893208,-4.90870856374795,131.15613754042));
#52758=CARTESIAN_POINT('Ctrl Pts',(75.8306257019945,-4.89026174281333,131.328310185059));
#52759=CARTESIAN_POINT('Ctrl Pts',(75.8205861445655,-4.87143753977756,131.504005110022));
#52760=CARTESIAN_POINT('Ctrl Pts',(75.8105465871366,-4.8431711433919,131.678401729631));
#52761=CARTESIAN_POINT('Ctrl Pts',(75.8005070297076,-4.8056723255412,131.850638096071));
#52762=CARTESIAN_POINT('Ctrl Pts',(75.7964197938675,-4.79040606371979,131.920757785596));
#52763=CARTESIAN_POINT('Ctrl Pts',(75.7923325580274,-4.77361015724972,131.990519695717));
#52764=CARTESIAN_POINT('Ctrl Pts',(75.7882453221872,-4.75530099873472,132.059866680448));
#52765=CARTESIAN_POINT('Ctrl Pts',(75.7804709880682,-4.72047513565686,132.19177162808));
#52766=CARTESIAN_POINT('Ctrl Pts',(75.7726966539491,-4.68010168226192,132.322435379416));
#52767=CARTESIAN_POINT('Ctrl Pts',(75.76492231983,-4.63428423813055,132.451355657848));
#52768=CARTESIAN_POINT('Ctrl Pts',(75.7571575668829,-4.58852325990428,132.580117053559));
#52769=CARTESIAN_POINT('Ctrl Pts',(75.7493928139358,-4.53733176998093,132.707138886732));
#52770=CARTESIAN_POINT('Ctrl Pts',(75.7416280609887,-4.4808639437233,132.83193093209));
#52771=CARTESIAN_POINT('Ctrl Pts',(75.7338710201037,-4.42445220210681,132.95659903223));
#52772=CARTESIAN_POINT('Ctrl Pts',(75.7261139792187,-4.36277471318464,133.079041397932));
#52773=CARTESIAN_POINT('Ctrl Pts',(75.7183569383337,-4.29603472009752,133.198785130099));
#52774=CARTESIAN_POINT('Ctrl Pts',(75.7106057470936,-4.22934505615845,133.318438562585));
#52775=CARTESIAN_POINT('Ctrl Pts',(75.7028545558535,-4.15760067647177,133.435397072079));
#52776=CARTESIAN_POINT('Ctrl Pts',(75.6951033646134,-4.08105182579783,133.549210168571));
#52777=CARTESIAN_POINT('Ctrl Pts',(75.6873554678363,-4.00453551042728,133.662974891462));
#52778=CARTESIAN_POINT('Ctrl Pts',(75.6796075710593,-3.92321900324693,133.773596536577));
#52779=CARTESIAN_POINT('Ctrl Pts',(75.6718596742822,-3.83739703209034,133.880651741729));
#52780=CARTESIAN_POINT('Ctrl Pts',(75.6641133981981,-3.75159301304001,133.98768455324));
#52781=CARTESIAN_POINT('Ctrl Pts',(75.656367122114,-3.66128564897798,134.091152103815));
#52782=CARTESIAN_POINT('Ctrl Pts',(75.6486208460299,-3.56681104892234,134.19066273105));
#52783=CARTESIAN_POINT('Ctrl Pts',(75.6408745127645,-3.47233575147679,134.29017409285));
#52784=CARTESIAN_POINT('Ctrl Pts',(75.6331281794992,-3.37369342584159,134.38572818949));
#52785=CARTESIAN_POINT('Ctrl Pts',(75.6253818462338,-3.2712579812657,134.476969265721));
#52786=CARTESIAN_POINT('Ctrl Pts',(75.6176337782309,-3.1687995969821,134.568230774759));
#52787=CARTESIAN_POINT('Ctrl Pts',(75.6098857102279,-3.06254669535508,134.655177081424));
#52788=CARTESIAN_POINT('Ctrl Pts',(75.6021376422249,-2.9529069683634,134.737492130583));
#52789=CARTESIAN_POINT('Ctrl Pts',(75.594381339483,-2.84315071496514,134.819894665156));
#52790=CARTESIAN_POINT('Ctrl Pts',(75.5866250367412,-2.73000075885075,134.897655874578));
#52791=CARTESIAN_POINT('Ctrl Pts',(75.5788687339993,-2.61389499327657,134.970502241014));
#52792=CARTESIAN_POINT('Ctrl Pts',(75.5711082914851,-2.49772725855935,135.043387487749));
#52793=CARTESIAN_POINT('Ctrl Pts',(75.563347848971,-2.37860091029006,135.111352470902));
#52794=CARTESIAN_POINT('Ctrl Pts',(75.5555874064568,-2.25697836353062,135.174169735715));
#52795=CARTESIAN_POINT('Ctrl Pts',(75.5478145061914,-2.13516057746198,135.237087840377));
#52796=CARTESIAN_POINT('Ctrl Pts',(75.540041605926,-2.01083894017883,135.294841548631));
#52797=CARTESIAN_POINT('Ctrl Pts',(75.5322687056605,-1.88449658114783,135.347251294012));
#52798=CARTESIAN_POINT('Ctrl Pts',(75.5247783698985,-1.76274708510464,135.397755813137));
#52799=CARTESIAN_POINT('Ctrl Pts',(75.5172880341364,-1.63912152230594,135.443298050433));
#52800=CARTESIAN_POINT('Ctrl Pts',(75.5097976983744,-1.51406353601884,135.483761719352));
#52801=CARTESIAN_POINT('Ctrl Pts',(75.5020233642553,-1.38426393817138,135.525759580578));
#52802=CARTESIAN_POINT('Ctrl Pts',(75.4942490301362,-1.25250998584571,135.562419200038));
#52803=CARTESIAN_POINT('Ctrl Pts',(75.4864746960171,-1.11928025668258,135.593556246218));
#52804=CARTESIAN_POINT('Ctrl Pts',(75.47870994307,-0.986214721253562,135.624654918772));
#52805=CARTESIAN_POINT('Ctrl Pts',(75.470945190123,-0.851677404835057,135.650244471991));
#52806=CARTESIAN_POINT('Ctrl Pts',(75.4631804371759,-0.716164083384742,
135.670189639241));
#52807=CARTESIAN_POINT('Ctrl Pts',(75.4554233962909,-0.580785355675603,
135.690114996668));
#52808=CARTESIAN_POINT('Ctrl Pts',(75.4476663554059,-0.444432936343657,
135.704407067924));
#52809=CARTESIAN_POINT('Ctrl Pts',(75.4399093145209,-0.307614546674604,
135.712981233704));
#52810=CARTESIAN_POINT('Ctrl Pts',(75.4321581232807,-0.170899332817772,
135.721548933639));
#52811=CARTESIAN_POINT('Ctrl Pts',(75.4244069320406,-0.033719236668912,
135.724407286354));
#52812=CARTESIAN_POINT('Ctrl Pts',(75.4166557408005,0.103411468363519,135.721523328999));
#52813=CARTESIAN_POINT('Ctrl Pts',(75.4089078440234,0.240483889188416,135.718640597404));
#52814=CARTESIAN_POINT('Ctrl Pts',(75.4011599472464,0.377506570589019,135.710020418178));
#52815=CARTESIAN_POINT('Ctrl Pts',(75.3934120504693,0.513964018372659,135.695681916593));
#52816=CARTESIAN_POINT('Ctrl Pts',(75.3856657743852,0.650392922199905,135.681346414314));
#52817=CARTESIAN_POINT('Ctrl Pts',(75.3779194983011,0.786256439007236,135.661295009712));
#52818=CARTESIAN_POINT('Ctrl Pts',(75.3701732222169,0.921043376988179,135.635598777728));
#52819=CARTESIAN_POINT('Ctrl Pts',(75.3624268889516,1.05583130993568,135.609902356061));
#52820=CARTESIAN_POINT('Ctrl Pts',(75.3546805556862,1.18954226415061,135.578561097081));
#52821=CARTESIAN_POINT('Ctrl Pts',(75.3469342224209,1.32167482558368,135.541697286826));
#52822=CARTESIAN_POINT('Ctrl Pts',(75.3391861544179,1.45383697718765,135.504825221177));
#52823=CARTESIAN_POINT('Ctrl Pts',(75.3314380864149,1.58441965613331,135.462428248334));
#52824=CARTESIAN_POINT('Ctrl Pts',(75.323690018412,1.71293658881232,135.414678535585));
#52825=CARTESIAN_POINT('Ctrl Pts',(75.3159337156701,1.84159011081684,135.366878073873));
#52826=CARTESIAN_POINT('Ctrl Pts',(75.3081774129282,1.96817313373631,135.313713644336));
#52827=CARTESIAN_POINT('Ctrl Pts',(75.3004211101864,2.09221884726884,135.255405815902));
#52828=CARTESIAN_POINT('Ctrl Pts',(75.2926606676722,2.21633076773362,135.197066866825));
#52829=CARTESIAN_POINT('Ctrl Pts',(75.2849002251581,2.33790233399149,135.133579229724));
#52830=CARTESIAN_POINT('Ctrl Pts',(75.2771397826439,2.45649223527464,135.065209002634));
#52831=CARTESIAN_POINT('Ctrl Pts',(75.2693668823785,2.57527250759533,134.996729021585));
#52832=CARTESIAN_POINT('Ctrl Pts',(75.261593982113,2.69106121969569,134.923350997191));
#52833=CARTESIAN_POINT('Ctrl Pts',(75.2538210818476,2.80344615394611,134.845384339895));
#52834=CARTESIAN_POINT('Ctrl Pts',(75.2463307460856,2.91174561275604,134.770251966977));
#52835=CARTESIAN_POINT('Ctrl Pts',(75.2388404103235,3.01688422323087,134.690858971426));
#52836=CARTESIAN_POINT('Ctrl Pts',(75.2313500745615,3.11852435018292,134.607515747168));
#52837=CARTESIAN_POINT('Ctrl Pts',(75.2235757404424,3.22401819344106,134.52101253923));
#52838=CARTESIAN_POINT('Ctrl Pts',(75.2158014063233,3.3260771990486,134.429979627452));
#52839=CARTESIAN_POINT('Ctrl Pts',(75.2080270722042,3.42428760077671,134.33472001707));
#52840=CARTESIAN_POINT('Ctrl Pts',(75.2002623192571,3.52237696696193,134.239577805644));
#52841=CARTESIAN_POINT('Ctrl Pts',(75.1924975663101,3.61662688860021,134.140219529622));
#52842=CARTESIAN_POINT('Ctrl Pts',(75.184732813363,3.70665558302411,134.036989184435));
#52843=CARTESIAN_POINT('Ctrl Pts',(75.176975772478,3.79659485967952,133.933861369082));
#52844=CARTESIAN_POINT('Ctrl Pts',(75.169218731593,3.882320997241,133.826869430614));
#52845=CARTESIAN_POINT('Ctrl Pts',(75.161461690708,3.96348836733584,133.716394790527));
#52846=CARTESIAN_POINT('Ctrl Pts',(75.1537104994679,4.04459452848551,133.606003460226));
#52847=CARTESIAN_POINT('Ctrl Pts',(75.1459593082277,4.121148534356,133.492134969655));
#52848=CARTESIAN_POINT('Ctrl Pts',(75.1382081169876,4.19284467502947,133.375204174373));
#52849=CARTESIAN_POINT('Ctrl Pts',(75.1304602202105,4.2645103429306,133.258323077798));
#52850=CARTESIAN_POINT('Ctrl Pts',(75.1227123234335,4.33132204827438,133.138382597821));
#52851=CARTESIAN_POINT('Ctrl Pts',(75.1149644266564,4.39301724448878,133.015826771981));
#52852=CARTESIAN_POINT('Ctrl Pts',(75.1072181505723,4.45469953539814,132.893296582178));
#52853=CARTESIAN_POINT('Ctrl Pts',(75.0994718744882,4.51126727030657,132.768152483663));
#52854=CARTESIAN_POINT('Ctrl Pts',(75.0917255984041,4.56250393491628,132.640862974323));
#52855=CARTESIAN_POINT('Ctrl Pts',(75.0839792651388,4.61374097774341,132.51357252536));
#52856=CARTESIAN_POINT('Ctrl Pts',(75.0762329318734,4.65964672575764,132.384136996657));
#52857=CARTESIAN_POINT('Ctrl Pts',(75.0684865986081,4.70005303512522,132.253044340644));
#52858=CARTESIAN_POINT('Ctrl Pts',(75.0607385306051,4.74046839320559,132.121922327339));
#52859=CARTESIAN_POINT('Ctrl Pts',(75.0529904626021,4.77538174683741,131.989142821823));
#52860=CARTESIAN_POINT('Ctrl Pts',(75.0452423945991,4.804675102473,131.855208000479));
#52861=CARTESIAN_POINT('Ctrl Pts',(75.0374860918573,4.83399959143558,131.721130831613));
#52862=CARTESIAN_POINT('Ctrl Pts',(75.0297297891155,4.8576920670216,131.585896276636));
#52863=CARTESIAN_POINT('Ctrl Pts',(75.0219734863736,4.8756857777461,131.450016299168));
#52864=CARTESIAN_POINT('Ctrl Pts',(75.0142130438595,4.89368909225581,131.314063798464));
#52865=CARTESIAN_POINT('Ctrl Pts',(75.0064526013453,4.90598754621258,131.177465578061));
#52866=CARTESIAN_POINT('Ctrl Pts',(74.9986921588311,4.9125664761791,131.040736757693));
#52867=CARTESIAN_POINT('Ctrl Pts',(74.9909192585657,4.91915596722805,130.903788448084));
#52868=CARTESIAN_POINT('Ctrl Pts',(74.9831463583002,4.9200075843185,130.766709510745));
#52869=CARTESIAN_POINT('Ctrl Pts',(74.9753734580348,4.91515882952152,130.630013999943));
#52870=CARTESIAN_POINT('Ctrl Pts',(74.9678831222728,4.91048633917467,130.498287715273));
#52871=CARTESIAN_POINT('Ctrl Pts',(74.9603927865107,4.900520750606,130.366917771223));
#52872=CARTESIAN_POINT('Ctrl Pts',(74.9529024507486,4.88534070695033,130.236356005336));
#52873=CARTESIAN_POINT('Ctrl Pts',(74.9451281166295,4.86958510732567,130.100843950414));
#52874=CARTESIAN_POINT('Ctrl Pts',(74.9373537825105,4.84816192592134,129.965773306116));
#52875=CARTESIAN_POINT('Ctrl Pts',(74.9295794483914,4.82110243887114,129.831655967423));
#52876=CARTESIAN_POINT('Ctrl Pts',(74.9218146954443,4.79407630022036,129.697703916362));
#52877=CARTESIAN_POINT('Ctrl Pts',(74.9140499424972,4.76142775345753,129.56470321284));
#52878=CARTESIAN_POINT('Ctrl Pts',(74.9062851895501,4.72323984882572,129.433160999361));
#52879=CARTESIAN_POINT('Ctrl Pts',(74.8985281486651,4.68508987295917,129.301749435463));
#52880=CARTESIAN_POINT('Ctrl Pts',(74.8907711077801,4.64141159628598,129.171793851877));
#52881=CARTESIAN_POINT('Ctrl Pts',(74.8830140668951,4.59233909893608,129.043791203177));
#52882=CARTESIAN_POINT('Ctrl Pts',(74.8752628756549,4.54330360753817,128.91588508227));
#52883=CARTESIAN_POINT('Ctrl Pts',(74.8675116844148,4.48888213160629,128.789929328463));
#52884=CARTESIAN_POINT('Ctrl Pts',(74.8597604931747,4.42925845719295,128.66640538373));
#52885=CARTESIAN_POINT('Ctrl Pts',(74.8520125963976,4.3696601244317,128.54293393997));
#52886=CARTESIAN_POINT('Ctrl Pts',(74.8442646996205,4.30486416044099,128.421892600921));
#52887=CARTESIAN_POINT('Ctrl Pts',(74.8365168028434,4.23510223374301,128.303742267588));
#52888=CARTESIAN_POINT('Ctrl Pts',(74.8287705267593,4.16535489973621,128.185616648758));
#52889=CARTESIAN_POINT('Ctrl Pts',(74.8210242506752,4.09064386785236,128.070381169236));
#52890=CARTESIAN_POINT('Ctrl Pts',(74.8132779745911,4.01124626736472,127.958471223185));
#52891=CARTESIAN_POINT('Ctrl Pts',(74.8055316413258,3.93184808078202,127.846560451039));
#52892=CARTESIAN_POINT('Ctrl Pts',(74.7977853080604,3.8477634827909,127.737975580214));
#52893=CARTESIAN_POINT('Ctrl Pts',(74.7900389747951,3.75931211574209,127.633121825085));
#52894=CARTESIAN_POINT('Ctrl Pts',(74.7822909067921,3.67084094062291,127.528244588685));
#52895=CARTESIAN_POINT('Ctrl Pts',(74.7745428387891,3.57800130256527,127.427100429426));
#52896=CARTESIAN_POINT('Ctrl Pts',(74.7667947707861,3.48115191838819,127.330060057223));
#52897=CARTESIAN_POINT('Ctrl Pts',(74.7590384680443,3.38419960153308,127.232916549357));
#52898=CARTESIAN_POINT('Ctrl Pts',(74.7512821653024,3.2832293021638,127.139885818387));
#52899=CARTESIAN_POINT('Ctrl Pts',(74.7435258625605,3.178635668966,127.051300753072));
#52900=CARTESIAN_POINT('Ctrl Pts',(74.7357654200464,3.07398621099685,126.96266840724));
#52901=CARTESIAN_POINT('Ctrl Pts',(74.7280049775322,2.96570987427895,126.878486694891));
#52902=CARTESIAN_POINT('Ctrl Pts',(74.720244535018,2.85423211768801,126.799046387589));
#52903=CARTESIAN_POINT('Ctrl Pts',(74.7124716347526,2.74257540710567,126.719478555653));
#52904=CARTESIAN_POINT('Ctrl Pts',(74.7046987344872,2.62770733468377,126.644667552105));
#52905=CARTESIAN_POINT('Ctrl Pts',(74.6969258342217,2.51008065962286,126.574859684278));
#52906=CARTESIAN_POINT('Ctrl Pts',(74.6894354984598,2.39673001048507,126.507589508282));
#52907=CARTESIAN_POINT('Ctrl Pts',(74.6819451626978,2.28081811192248,126.444965176537));
#52908=CARTESIAN_POINT('Ctrl Pts',(74.6744548269358,2.16276761619343,126.387164753577));
#52909=CARTESIAN_POINT('Ctrl Pts',(74.6666804928167,2.04024120003718,126.327172810011));
#52910=CARTESIAN_POINT('Ctrl Pts',(74.6589061586976,1.91502268875096,126.272187756736));
#52911=CARTESIAN_POINT('Ctrl Pts',(74.6511318245785,1.78755965959214,126.222459971993));
#52912=CARTESIAN_POINT('Ctrl Pts',(74.6433670716314,1.66025371722515,126.172793472301));
#52913=CARTESIAN_POINT('Ctrl Pts',(74.6356023186843,1.53070912156609,126.128371490371));
#52914=CARTESIAN_POINT('Ctrl Pts',(74.6278375657373,1.39939743665238,126.089398276593));
#52915=CARTESIAN_POINT('Ctrl Pts',(74.6200805248523,1.2682161723553,126.05046377156));
#52916=CARTESIAN_POINT('Ctrl Pts',(74.6123234839673,1.13527168390767,126.016967375489));
#52917=CARTESIAN_POINT('Ctrl Pts',(74.6045664430823,1.00105454685282,125.989064899053));
#52918=CARTESIAN_POINT('Ctrl Pts',(74.5968152518422,0.866938623984995,125.961183464093));
#52919=CARTESIAN_POINT('Ctrl Pts',(74.589064060602,0.731552343995152,125.938887631517));
#52920=CARTESIAN_POINT('Ctrl Pts',(74.5813128693619,0.595400098502344,125.922283008064));
#52921=CARTESIAN_POINT('Ctrl Pts',(74.5735649725848,0.459305721345851,125.905685442018));
#52922=CARTESIAN_POINT('Ctrl Pts',(74.5658170758077,0.322446413469263,125.894774321286));
#52923=CARTESIAN_POINT('Ctrl Pts',(74.5580691790306,0.185335166434737,125.889603864828));
#52924=CARTESIAN_POINT('Ctrl Pts',(74.5503229029465,0.048252600117314,125.884434489919));
#52925=CARTESIAN_POINT('Ctrl Pts',(74.5425766268624,-0.0890814100943838,
125.885003405504));
#52926=CARTESIAN_POINT('Ctrl Pts',(74.5348303507783,-0.226150759619665,
125.891312796058));
#52927=CARTESIAN_POINT('Ctrl Pts',(74.5270840175129,-0.363221120959654,
125.897622233186));
#52928=CARTESIAN_POINT('Ctrl Pts',(74.5193376842476,-0.500026427163158,
125.909672211862));
#52929=CARTESIAN_POINT('Ctrl Pts',(74.5115913509823,-0.636052985399898,
125.92741283619));
#52930=CARTESIAN_POINT('Ctrl Pts',(74.5038432829793,-0.772110005841306,
125.945157433409));
#52931=CARTESIAN_POINT('Ctrl Pts',(74.4960952149763,-0.907387543681894,
125.968595161599));
#52932=CARTESIAN_POINT('Ctrl Pts',(74.4883471469734,-1.04137981496835,125.997624599905));
#52933=CARTESIAN_POINT('Ctrl Pts',(74.4805908442315,-1.17551449483525,126.026684891044));
#52934=CARTESIAN_POINT('Ctrl Pts',(74.4728345414896,-1.30836079671276,126.06134868104));
#52935=CARTESIAN_POINT('Ctrl Pts',(74.4650782387478,-1.43942533460707,126.101463875281));
#52936=CARTESIAN_POINT('Ctrl Pts',(74.4573177962336,-1.57055982559161,126.14160048021));
#52937=CARTESIAN_POINT('Ctrl Pts',(74.4495573537194,-1.69991028913348,126.187194157058));
#52938=CARTESIAN_POINT('Ctrl Pts',(74.4417969112052,-1.8270021199659,126.238044124358));
#52939=CARTESIAN_POINT('Ctrl Pts',(74.4340240109398,-1.95429796988785,126.28897572054));
#52940=CARTESIAN_POINT('Ctrl Pts',(74.4262511106744,-2.07932758488358,126.345180308323));
#52941=CARTESIAN_POINT('Ctrl Pts',(74.4184782104089,-2.2016390122099,126.4064101037));
#52942=CARTESIAN_POINT('Ctrl Pts',(74.4109878746469,-2.31950411106951,126.465414041786));
#52943=CARTESIAN_POINT('Ctrl Pts',(74.4034975388848,-2.4348449474596,126.529084023851));
#52944=CARTESIAN_POINT('Ctrl Pts',(74.3960072031228,-2.54728325677598,126.597160708809));
#52945=CARTESIAN_POINT('Ctrl Pts',(74.3882315941812,-2.66400383527471,126.667830128322));
#52946=CARTESIAN_POINT('Ctrl Pts',(74.3804559852396,-2.77796621339256,126.743472462004));
#52947=CARTESIAN_POINT('Ctrl Pts',(74.372680376298,-2.8887175935236,126.823846363432));
#52948=CARTESIAN_POINT('Ctrl Pts',(74.3646617944063,-3.00292974306261,126.906731795992));
#52949=CARTESIAN_POINT('Ctrl Pts',(74.3566432125147,-3.11372655075258,126.994649195824));
#52950=CARTESIAN_POINT('Ctrl Pts',(74.348624630623,-3.22063854773003,127.087282409164));
#52951=CARTESIAN_POINT('Ctrl Pts',(74.3408685462443,-3.32405065735999,127.176883167583));
#52952=CARTESIAN_POINT('Ctrl Pts',(74.3331124618656,-3.42382796139808,127.270895573751));
#52953=CARTESIAN_POINT('Ctrl Pts',(74.3253563774869,-3.5195753913396,127.368989876703));
#52954=CARTESIAN_POINT('Ctrl Pts',(74.3176056108797,-3.61525717437204,127.467016923669));
#52955=CARTESIAN_POINT('Ctrl Pts',(74.3098548442726,-3.70691430864919,127.569120020638));
#52956=CARTESIAN_POINT('Ctrl Pts',(74.3021040776655,-3.79418655244898,127.674930722567));
#52957=CARTESIAN_POINT('Ctrl Pts',(74.2943569465692,-3.8814178610486,127.780691793799));
#52958=CARTESIAN_POINT('Ctrl Pts',(74.2866098154728,-3.96426812432516,127.890156708005));
#52959=CARTESIAN_POINT('Ctrl Pts',(74.2788626843765,-4.04241585072074,128.002922209829));
#52960=CARTESIAN_POINT('Ctrl Pts',(74.2711175093536,-4.12054384559356,128.115659239488));
#52961=CARTESIAN_POINT('Ctrl Pts',(74.2633723343307,-4.19397144569641,128.231694876198));
#52962=CARTESIAN_POINT('Ctrl Pts',(74.2556271593079,-4.26241938771938,128.350595342383));
#52963=CARTESIAN_POINT('Ctrl Pts',(74.2478803958074,-4.33088136790436,128.469520194166));
#52964=CARTESIAN_POINT('Ctrl Pts',(74.240133632307,-4.39436145126947,128.591310712345));
#52965=CARTESIAN_POINT('Ctrl Pts',(74.2323868688065,-4.45262543002663,128.715506902635));
#52966=CARTESIAN_POINT('Ctrl Pts',(74.2246390865264,-4.51089707110035,128.839719426011));
#52967=CARTESIAN_POINT('Ctrl Pts',(74.2168913042463,-4.56395108278894,128.966337894346));
#52968=CARTESIAN_POINT('Ctrl Pts',(74.2091435219662,-4.61160101714329,129.094881421675));
#52969=CARTESIAN_POINT('Ctrl Pts',(74.2013908164532,-4.65928123006226,129.223506630407));
#52970=CARTESIAN_POINT('Ctrl Pts',(74.1936381109402,-4.70155038350649,129.354058970607));
#52971=CARTESIAN_POINT('Ctrl Pts',(74.1858854054271,-4.73827157912007,129.486041420633));
#52972=CARTESIAN_POINT('Ctrl Pts',(74.1840017405842,-4.74719368057893,129.51810902601));
#52973=CARTESIAN_POINT('Ctrl Pts',(74.1821180757413,-4.7557885000028,129.550261000689));
#52974=CARTESIAN_POINT('Ctrl Pts',(74.1802344108984,-4.76405452823402,129.582490119308));
#52975=CARTESIAN_POINT('Origin',(213.235140564004,0.,130.804360617566));
#52976=CARTESIAN_POINT('',(72.0846889553802,-4.76405452823408,129.582490119308));
#52977=CARTESIAN_POINT('',(72.4299696197722,-4.76405452823407,129.582490119308));
#52978=CARTESIAN_POINT('',(213.235140564004,-4.76405452823405,129.582490119308));
#52979=CARTESIAN_POINT('',(73.764859436044,-4.91824854295789,130.800574829328));
#52980=CARTESIAN_POINT('Ctrl Pts',(73.7648594359911,-4.91824854295861,130.800574830266));
#52981=CARTESIAN_POINT('Ctrl Pts',(73.7571129956196,-4.91835416522511,130.937792406713));
#52982=CARTESIAN_POINT('Ctrl Pts',(73.7493665552481,-4.91271299733684,131.075074362928));
#52983=CARTESIAN_POINT('Ctrl Pts',(73.7416201148767,-4.90133565926305,131.211904256624));
#52984=CARTESIAN_POINT('Ctrl Pts',(73.7338747671406,-4.8899599259627,131.348714850464));
#52985=CARTESIAN_POINT('Ctrl Pts',(73.7261294194045,-4.87284966382949,131.485073119667));
#52986=CARTESIAN_POINT('Ctrl Pts',(73.7183840716684,-4.85006751003875,131.620466131925));
#52987=CARTESIAN_POINT('Ctrl Pts',(73.7106381452548,-4.82728365412693,131.755869259789));
#52988=CARTESIAN_POINT('Ctrl Pts',(73.7028922188412,-4.79882712764685,131.89030660211));
#52989=CARTESIAN_POINT('Ctrl Pts',(73.6951462924276,-4.76481192753374,132.023274214886));
#52990=CARTESIAN_POINT('Ctrl Pts',(73.6873981159975,-4.73078684677441,132.156280451747));
#52991=CARTESIAN_POINT('Ctrl Pts',(73.6796499395675,-4.69119997565195,132.287815731318));
#52992=CARTESIAN_POINT('Ctrl Pts',(73.6719017631375,-4.64621542224321,132.417390472407));
#52993=CARTESIAN_POINT('Ctrl Pts',(73.6641446191071,-4.60117880451946,132.547115180977));
#52994=CARTESIAN_POINT('Ctrl Pts',(73.6563874750767,-4.55073215402375,132.674874449209));
#52995=CARTESIAN_POINT('Ctrl Pts',(73.6486303310463,-4.49508829535229,132.800197354247));
#52996=CARTESIAN_POINT('Ctrl Pts',(73.6408686127013,-4.43941162402268,132.925594161019));
#52997=CARTESIAN_POINT('Ctrl Pts',(73.6331068943563,-4.3785318114894,133.048551392652));
#52998=CARTESIAN_POINT('Ctrl Pts',(73.6253451760113,-4.31270760178373,133.168622913509));
#52999=CARTESIAN_POINT('Ctrl Pts',(73.6175704459995,-4.24677304503256,133.28889572106));
#53000=CARTESIAN_POINT('Ctrl Pts',(73.6097957159876,-4.17587773049316,133.406272817251));
#53001=CARTESIAN_POINT('Ctrl Pts',(73.6020209859758,-4.10032417432361,133.520336451029));
#53002=CARTESIAN_POINT('Ctrl Pts',(73.5947650999316,-4.02981265907372,133.626788086933));
#53003=CARTESIAN_POINT('Ctrl Pts',(73.5875092138875,-3.95524446899847,133.730353859054));
#53004=CARTESIAN_POINT('Ctrl Pts',(73.5802533278434,-3.87689590057486,133.830721673125));
#53005=CARTESIAN_POINT('Ctrl Pts',(73.5724789937243,-3.79294916478359,133.938260975238));
#53006=CARTESIAN_POINT('Ctrl Pts',(73.5647046596052,-3.70439160296181,134.042475129251));
#53007=CARTESIAN_POINT('Ctrl Pts',(73.5569303254861,-3.61151620383971,134.142943216799));
#53008=CARTESIAN_POINT('Ctrl Pts',(73.5491655725391,-3.51875526534665,134.243287486409));
#53009=CARTESIAN_POINT('Ctrl Pts',(73.541400819592,-3.42168734029623,134.339894591062));
#53010=CARTESIAN_POINT('Ctrl Pts',(73.5336360666449,-3.3206471633281,134.432374603093));
#53011=CARTESIAN_POINT('Ctrl Pts',(73.5258790257599,-3.21970734088822,134.524762762673));
#53012=CARTESIAN_POINT('Ctrl Pts',(73.5181219848749,-3.11480340438348,134.613031724739));
#53013=CARTESIAN_POINT('Ctrl Pts',(73.5103649439899,-3.00630837134294,134.696826807386));
#53014=CARTESIAN_POINT('Ctrl Pts',(73.5026137527498,-2.89789515525086,134.78055869951));
#53015=CARTESIAN_POINT('Ctrl Pts',(73.4948625615097,-2.78589654105055,134.859823189522));
#53016=CARTESIAN_POINT('Ctrl Pts',(73.4871113702696,-2.67071992863701,134.934304700151));
#53017=CARTESIAN_POINT('Ctrl Pts',(73.4793634734925,-2.55559226935603,135.008754554152));
#53018=CARTESIAN_POINT('Ctrl Pts',(73.4716155767154,-2.43728962598206,135.078425260182));
#53019=CARTESIAN_POINT('Ctrl Pts',(73.4638676799383,-2.31624960778856,135.143043691601));
#53020=CARTESIAN_POINT('Ctrl Pts',(73.4561214038542,-2.19523490855745,135.207648606237));
#53021=CARTESIAN_POINT('Ctrl Pts',(73.4483751277702,-2.07148431811454,135.26720316434));
#53022=CARTESIAN_POINT('Ctrl Pts',(73.4406288516861,-1.94546100368361,135.321479671304));
#53023=CARTESIAN_POINT('Ctrl Pts',(73.4328825184207,-1.81943675897737,135.375756578926));
#53024=CARTESIAN_POINT('Ctrl Pts',(73.4251361851554,-1.69114011588459,135.424755203015));
#53025=CARTESIAN_POINT('Ctrl Pts',(73.41738985189,-1.56105485132995,135.468295738646));
#53026=CARTESIAN_POINT('Ctrl Pts',(73.4096417838871,-1.43094045508253,135.511846024877));
#53027=CARTESIAN_POINT('Ctrl Pts',(73.4018937158842,-1.29903701100444,135.549935666345));
#53028=CARTESIAN_POINT('Ctrl Pts',(73.3941456478812,-1.16584371934485,135.582434652631));
#53029=CARTESIAN_POINT('Ctrl Pts',(73.3863893451393,-1.0325088682695,135.614968179227));
#53030=CARTESIAN_POINT('Ctrl Pts',(73.3786330423975,-0.897881811589283,
135.641899088402));
#53031=CARTESIAN_POINT('Ctrl Pts',(73.3708767396557,-0.76247276364059,135.663148362179));
#53032=CARTESIAN_POINT('Ctrl Pts',(73.3631162971415,-0.626991443805735,
135.684408977334));
#53033=CARTESIAN_POINT('Ctrl Pts',(73.3553558546273,-0.490727689299462,
135.699981870287));
#53034=CARTESIAN_POINT('Ctrl Pts',(73.3475954121132,-0.35419611963266,135.70984002037));
#53035=CARTESIAN_POINT('Ctrl Pts',(73.3398225118477,-0.217445377369619,
135.719713995631));
#53036=CARTESIAN_POINT('Ctrl Pts',(73.3320496115823,-0.0804263518392551,
135.723854884005));
#53037=CARTESIAN_POINT('Ctrl Pts',(73.3242767113169,0.0563461507783298,
135.722287840878));
#53038=CARTESIAN_POINT('Ctrl Pts',(73.3167863755548,0.188146628417826,135.720777763716));
#53039=CARTESIAN_POINT('Ctrl Pts',(73.3092960397927,0.319717887817951,135.713967561421));
#53040=CARTESIAN_POINT('Ctrl Pts',(73.3018057040306,0.450606334333693,135.701925011625));
#53041=CARTESIAN_POINT('Ctrl Pts',(73.2940313699115,0.586457456080612,135.689425864894));
#53042=CARTESIAN_POINT('Ctrl Pts',(73.2862570357924,0.722003300653231,135.67125017587));
#53043=CARTESIAN_POINT('Ctrl Pts',(73.2784827016733,0.856731369945098,135.647416927609));
#53044=CARTESIAN_POINT('Ctrl Pts',(73.2707179487262,0.991293398932373,135.623613051698));
#53045=CARTESIAN_POINT('Ctrl Pts',(73.2629531957792,1.12503927663804,135.594165557071));
#53046=CARTESIAN_POINT('Ctrl Pts',(73.2551884428321,1.25746001362484,135.559145300034));
#53047=CARTESIAN_POINT('Ctrl Pts',(73.2474314019471,1.38974922846869,135.52415982561));
#53048=CARTESIAN_POINT('Ctrl Pts',(73.2396743610621,1.52071554626341,135.483612702881));
#53049=CARTESIAN_POINT('Ctrl Pts',(73.2319173201771,1.64985893799172,135.437626047825));
#53050=CARTESIAN_POINT('Ctrl Pts',(73.224166128937,1.77890494168338,135.391674071663));
#53051=CARTESIAN_POINT('Ctrl Pts',(73.2164149376969,1.90613038871053,135.340290858565));
#53052=CARTESIAN_POINT('Ctrl Pts',(73.2086637464568,2.03104956538335,135.283648588377));
#53053=CARTESIAN_POINT('Ctrl Pts',(73.2009158496797,2.15591564807444,135.227030392666));
#53054=CARTESIAN_POINT('Ctrl Pts',(73.1931679529027,2.27847705468136,135.165157746701));
#53055=CARTESIAN_POINT('Ctrl Pts',(73.1854200561256,2.39826745752363,135.098251191938));
#53056=CARTESIAN_POINT('Ctrl Pts',(73.1776737800415,2.51803280279601,135.031358632584));
#53057=CARTESIAN_POINT('Ctrl Pts',(73.1699275039574,2.63502795611112,134.959434449401));
#53058=CARTESIAN_POINT('Ctrl Pts',(73.1621812278732,2.7488109983516,134.882745243596));
#53059=CARTESIAN_POINT('Ctrl Pts',(73.1544348946079,2.8625948805128,134.806055471689));
#53060=CARTESIAN_POINT('Ctrl Pts',(73.1466885613425,2.97316628008363,134.724600825483));
#53061=CARTESIAN_POINT('Ctrl Pts',(73.1389422280772,3.0801124288433,134.638691131252));
#53062=CARTESIAN_POINT('Ctrl Pts',(73.1311941600742,3.18708252745132,134.552762198141));
#53063=CARTESIAN_POINT('Ctrl Pts',(73.1234460920712,3.29042545501798,134.462376476542));
#53064=CARTESIAN_POINT('Ctrl Pts',(73.1156980240682,3.38976200016907,134.367883683958));
#53065=CARTESIAN_POINT('Ctrl Pts',(73.1079417213264,3.4892041213824,134.27329046331));
#53066=CARTESIAN_POINT('Ctrl Pts',(73.1001854185845,3.58463107057883,134.174581721921));
#53067=CARTESIAN_POINT('Ctrl Pts',(73.0924291158427,3.67570058438456,134.072144006418));
#53068=CARTESIAN_POINT('Ctrl Pts',(73.0846686733285,3.76681870473185,133.969651616821));
#53069=CARTESIAN_POINT('Ctrl Pts',(73.0769082308143,3.85357450835811,133.863426589995));
#53070=CARTESIAN_POINT('Ctrl Pts',(73.0691477883001,3.93566709759427,133.753887284578));
#53071=CARTESIAN_POINT('Ctrl Pts',(73.0613748880347,4.0178914691425,133.644172136943));
#53072=CARTESIAN_POINT('Ctrl Pts',(73.0536019877693,4.09543744598224,133.531132401497));
#53073=CARTESIAN_POINT('Ctrl Pts',(73.0458290875039,4.16804792673728,133.415214796359));
#53074=CARTESIAN_POINT('Ctrl Pts',(73.0383387517418,4.23801883362236,133.303511088146));
#53075=CARTESIAN_POINT('Ctrl Pts',(73.0308484159798,4.3034066970687,133.189135380633));
#53076=CARTESIAN_POINT('Ctrl Pts',(73.0233580802177,4.36402336133263,133.072505931307));
#53077=CARTESIAN_POINT('Ctrl Pts',(73.0155837460986,4.42693832484599,132.95145444096));
#53078=CARTESIAN_POINT('Ctrl Pts',(73.0078094119796,4.48491244278982,132.82759147918));
#53079=CARTESIAN_POINT('Ctrl Pts',(73.0000350778605,4.53768466840429,132.701358485943));
#53080=CARTESIAN_POINT('Ctrl Pts',(72.9922703249134,4.59039185696704,132.57528106359));
#53081=CARTESIAN_POINT('Ctrl Pts',(72.9845055719663,4.63790975956583,132.446839778655));
#53082=CARTESIAN_POINT('Ctrl Pts',(72.9767408190192,4.68002286839308,132.316501157932));
#53083=CARTESIAN_POINT('Ctrl Pts',(72.9689837781342,4.72209414988702,132.186291991364));
#53084=CARTESIAN_POINT('Ctrl Pts',(72.9612267372492,4.75877120097884,132.05418960879));
#53085=CARTESIAN_POINT('Ctrl Pts',(72.9534696963642,4.78988648340216,131.920680705454));
#53086=CARTESIAN_POINT('Ctrl Pts',(72.9457185051241,4.82097830154879,131.78727248222));
#53087=CARTESIAN_POINT('Ctrl Pts',(72.9379673138839,4.84651661089373,131.65246022864));
#53088=CARTESIAN_POINT('Ctrl Pts',(72.9302161226439,4.86638373110485,131.51674565681));
#53089=CARTESIAN_POINT('Ctrl Pts',(72.9224682258668,4.88624240726,131.381088767292));
#53090=CARTESIAN_POINT('Ctrl Pts',(72.9147203290897,4.9004346318855,131.244530708327));
#53091=CARTESIAN_POINT('Ctrl Pts',(72.9069724323126,4.90889389125081,131.107583022643));
#53092=CARTESIAN_POINT('Ctrl Pts',(72.8992261562285,4.91735138112142,130.970663983462));
#53093=CARTESIAN_POINT('Ctrl Pts',(72.8914798801445,4.92007826694303,130.833355869647));
#53094=CARTESIAN_POINT('Ctrl Pts',(72.8837336040604,4.91705997978462,130.696174584731));
#53095=CARTESIAN_POINT('Ctrl Pts',(72.875987270795,4.9140416703459,130.558992287175));
#53096=CARTESIAN_POINT('Ctrl Pts',(72.8682409375297,4.90527811190195,130.421937211257));
#53097=CARTESIAN_POINT('Ctrl Pts',(72.8604946042643,4.89080685876596,130.285524099241));
#53098=CARTESIAN_POINT('Ctrl Pts',(72.8527465362614,4.8763323648932,130.149080438454));
#53099=CARTESIAN_POINT('Ctrl Pts',(72.8449984682585,4.85614767409693,130.013279416351));
#53100=CARTESIAN_POINT('Ctrl Pts',(72.8372504002555,4.8303420406053,129.878629105052));
#53101=CARTESIAN_POINT('Ctrl Pts',(72.8294940975137,4.80450898057928,129.7438356858));
#53102=CARTESIAN_POINT('Ctrl Pts',(72.8217377947718,4.77304311784609,129.610195804994));
#53103=CARTESIAN_POINT('Ctrl Pts',(72.81398149203,4.73608466331452,129.478206356397));
#53104=CARTESIAN_POINT('Ctrl Pts',(72.8062210495158,4.69910648294285,129.346146461056));
#53105=CARTESIAN_POINT('Ctrl Pts',(72.7984606070016,4.6566299904133,129.215739124723));
#53106=CARTESIAN_POINT('Ctrl Pts',(72.7907001644874,4.60884452015681,129.087463634191));
#53107=CARTESIAN_POINT('Ctrl Pts',(72.782927264222,4.56098234042133,128.958982224455));
#53108=CARTESIAN_POINT('Ctrl Pts',(72.7751543639566,4.50779430418635,128.832639859765));
#53109=CARTESIAN_POINT('Ctrl Pts',(72.7673814636911,4.44951727848421,128.708894308848));
#53110=CARTESIAN_POINT('Ctrl Pts',(72.7598911279291,4.39335876945708,128.589647220403));
#53111=CARTESIAN_POINT('Ctrl Pts',(72.752400792167,4.3324749848179,128.472811695312));
#53112=CARTESIAN_POINT('Ctrl Pts',(72.7449104564049,4.26711611366088,128.35877211272));
#53113=CARTESIAN_POINT('Ctrl Pts',(72.7371361222858,4.19927914103882,128.240408684693));
#53114=CARTESIAN_POINT('Ctrl Pts',(72.7293617881668,4.12640615015668,128.124682460991));
#53115=CARTESIAN_POINT('Ctrl Pts',(72.7215874540477,4.04872743482068,128.012051676738));
#53116=CARTESIAN_POINT('Ctrl Pts',(72.7138227011006,3.9711444515591,127.89955969986));
#53117=CARTESIAN_POINT('Ctrl Pts',(72.7060579481535,3.88876774794136,127.790155890767));
#53118=CARTESIAN_POINT('Ctrl Pts',(72.6982931952064,3.80187333893661,127.684273731407));
#53119=CARTESIAN_POINT('Ctrl Pts',(72.6905361543214,3.71506523468359,127.5784967357));
#53120=CARTESIAN_POINT('Ctrl Pts',(72.6827791134364,3.62374860089221,127.476234729307));
#53121=CARTESIAN_POINT('Ctrl Pts',(72.6750220725514,3.52824234952909,127.377891737583));
#53122=CARTESIAN_POINT('Ctrl Pts',(72.6672708813112,3.43280812017318,127.279622907075));
#53123=CARTESIAN_POINT('Ctrl Pts',(72.6595196900711,3.33319083316311,127.185267488108));
#53124=CARTESIAN_POINT('Ctrl Pts',(72.6517684988309,3.22974898400071,127.095195676121));
#53125=CARTESIAN_POINT('Ctrl Pts',(72.6440206020538,3.12635110038367,127.005162147056));
#53126=CARTESIAN_POINT('Ctrl Pts',(72.6362727052768,3.01913218192569,126.919408860048));
#53127=CARTESIAN_POINT('Ctrl Pts',(72.6285248084997,2.90848665171518,126.838268276319));
#53128=CARTESIAN_POINT('Ctrl Pts',(72.6207785324156,2.79786426616427,126.757144665452));
#53129=CARTESIAN_POINT('Ctrl Pts',(72.6130322563314,2.68381700963804,126.680632069727));
#53130=CARTESIAN_POINT('Ctrl Pts',(72.6052859802473,2.56677105152774,126.609021604859));
#53131=CARTESIAN_POINT('Ctrl Pts',(72.597539646982,2.44972422941076,126.53741061138));
#53132=CARTESIAN_POINT('Ctrl Pts',(72.5897933137166,2.32967899503847,126.470702025005));
#53133=CARTESIAN_POINT('Ctrl Pts',(72.5820469804513,2.20708871467882,126.409142480996));
#53134=CARTESIAN_POINT('Ctrl Pts',(72.5742989124483,2.08447098107628,126.347569151153));
#53135=CARTESIAN_POINT('Ctrl Pts',(72.5665508444453,1.95930741668214,126.291147333609));
#53136=CARTESIAN_POINT('Ctrl Pts',(72.5588027764423,1.83207372105153,126.240076561645));
#53137=CARTESIAN_POINT('Ctrl Pts',(72.5510464737005,1.70470479993467,126.188951511057));
#53138=CARTESIAN_POINT('Ctrl Pts',(72.5432901709586,1.57526171593054,126.143189012623));
#53139=CARTESIAN_POINT('Ctrl Pts',(72.5355338682168,1.44423830725503,126.10293968615));
#53140=CARTESIAN_POINT('Ctrl Pts',(72.5277734257026,1.31314496744117,126.062668877399));
#53141=CARTESIAN_POINT('Ctrl Pts',(72.5200129831884,1.18047000029822,126.027917202897));
#53142=CARTESIAN_POINT('Ctrl Pts',(72.5122525406742,1.04671898326458,125.998784436443));
#53143=CARTESIAN_POINT('Ctrl Pts',(72.5044796404088,0.912753257224633,125.969604903487));
#53144=CARTESIAN_POINT('Ctrl Pts',(72.4967067401434,0.777708414834669,125.946062370536));
#53145=CARTESIAN_POINT('Ctrl Pts',(72.4889338398779,0.642097622304449,125.928204989827));
#53146=CARTESIAN_POINT('Ctrl Pts',(72.4814435041159,0.511416623665579,125.910996769886));
#53147=CARTESIAN_POINT('Ctrl Pts',(72.4739531683538,0.380210414686311,125.899067567044));
#53148=CARTESIAN_POINT('Ctrl Pts',(72.4664628325918,0.248937617743522,125.892414656445));
#53149=CARTESIAN_POINT('Ctrl Pts',(72.4586884984727,0.112687572805058,125.885509498719));
#53150=CARTESIAN_POINT('Ctrl Pts',(72.4509141643536,-0.024065808326198,
125.884266759137));
#53151=CARTESIAN_POINT('Ctrl Pts',(72.4431398302345,-0.160812520035402,
125.888740372277));
#53152=CARTESIAN_POINT('Ctrl Pts',(72.4353750772874,-0.29739070364355,125.893208472087));
#53153=CARTESIAN_POINT('Ctrl Pts',(72.4276103243403,-0.433961847179008,
125.903378894719));
#53154=CARTESIAN_POINT('Ctrl Pts',(72.4198455713932,-0.570012057168461,
125.919253728543));
#53155=CARTESIAN_POINT('Ctrl Pts',(72.4120885305081,-0.705927140171936,
125.935112795258));
#53156=CARTESIAN_POINT('Ctrl Pts',(72.4043314896231,-0.841321933458148,
125.956664953144));
#53157=CARTESIAN_POINT('Ctrl Pts',(72.3965744487381,-0.975684139345104,
125.983860278106));
#53158=CARTESIAN_POINT('Ctrl Pts',(72.388823257498,-1.10994502164659,126.011035094862));
#53159=CARTESIAN_POINT('Ctrl Pts',(72.3810720662579,-1.24317448482418,126.043844531021));
#53160=CARTESIAN_POINT('Ctrl Pts',(72.3733208750178,-1.37486729739485,126.082187073841));
#53161=CARTESIAN_POINT('Ctrl Pts',(72.3655729782407,-1.50650413700743,126.120513320058));
#53162=CARTESIAN_POINT('Ctrl Pts',(72.3578250814636,-1.63660525042133,126.164367886486));
#53163=CARTESIAN_POINT('Ctrl Pts',(72.3500771846865,-1.76467773327882,126.213598637222));
#53164=CARTESIAN_POINT('Ctrl Pts',(72.3423309086024,-1.89272342613399,126.262819089947));
#53165=CARTESIAN_POINT('Ctrl Pts',(72.3345846325183,-2.01874096777867,126.317413349935));
#53166=CARTESIAN_POINT('Ctrl Pts',(72.3268383564342,-2.14225507935043,126.377180223964));
#53167=CARTESIAN_POINT('Ctrl Pts',(72.3190920231689,-2.26577010267488,126.436947539177));
#53168=CARTESIAN_POINT('Ctrl Pts',(72.3113456899035,-2.38678130712269,126.501887374329));
#53169=CARTESIAN_POINT('Ctrl Pts',(72.3035993566381,-2.50483613592317,126.57175161192));
#53170=CARTESIAN_POINT('Ctrl Pts',(72.2958512886351,-2.62291740228515,126.641631495123));
#53171=CARTESIAN_POINT('Ctrl Pts',(72.288103220632,-2.73804063918003,126.716437776103));
#53172=CARTESIAN_POINT('Ctrl Pts',(72.280355152629,-2.84978084637762,126.795878087965));
#53173=CARTESIAN_POINT('Ctrl Pts',(72.2725988498871,-2.96163981239646,126.875402829934));
#53174=CARTESIAN_POINT('Ctrl Pts',(72.2648425471453,-3.07010824711773,126.959571214311));
#53175=CARTESIAN_POINT('Ctrl Pts',(72.2570862444034,-3.1747924982135,127.048049174703));
#53176=CARTESIAN_POINT('Ctrl Pts',(72.2493258018892,-3.27953262244607,127.136574358446));
#53177=CARTESIAN_POINT('Ctrl Pts',(72.241565359375,-3.3804842509303,127.229413436928));
#53178=CARTESIAN_POINT('Ctrl Pts',(72.2338049168609,-3.47729016418737,127.326194983709));
#53179=CARTESIAN_POINT('Ctrl Pts',(72.2260320165954,-3.57425147889035,127.42313189282));
#53180=CARTESIAN_POINT('Ctrl Pts',(72.21825911633,-3.66705351458595,127.524023629274));
#53181=CARTESIAN_POINT('Ctrl Pts',(72.2104862160645,-3.7553783805642,127.628464479263));
#53182=CARTESIAN_POINT('Ctrl Pts',(72.2029958803027,-3.84049241518525,127.729108641281));
#53183=CARTESIAN_POINT('Ctrl Pts',(72.1955055445408,-3.92144895223041,127.833048115323));
#53184=CARTESIAN_POINT('Ctrl Pts',(72.188015208779,-3.99800238759951,127.939895576542));
#53185=CARTESIAN_POINT('Ctrl Pts',(72.1801680009989,-4.07820315999718,128.051833713311));
#53186=CARTESIAN_POINT('Ctrl Pts',(72.1723207932188,-4.1538238619774,128.167316490552));
#53187=CARTESIAN_POINT('Ctrl Pts',(72.1644735854388,-4.22453841970315,128.285936863915));
#53188=CARTESIAN_POINT('Ctrl Pts',(72.15663976097,-4.29513237466587,128.404354931767));
#53189=CARTESIAN_POINT('Ctrl Pts',(72.1488059365013,-4.36083665984594,128.525899611086));
#53190=CARTESIAN_POINT('Ctrl Pts',(72.1409721120325,-4.42136704575762,128.650133027642));
#53191=CARTESIAN_POINT('Ctrl Pts',(72.1331460284686,-4.48183761925449,128.774243684356));
#53192=CARTESIAN_POINT('Ctrl Pts',(72.1253199449047,-4.53714429870375,128.90103745197));
#53193=CARTESIAN_POINT('Ctrl Pts',(72.1174938613408,-4.58704729095068,129.030049423586));
#53194=CARTESIAN_POINT('Ctrl Pts',(72.1096754184713,-4.63690156233876,129.158935439348));
#53195=CARTESIAN_POINT('Ctrl Pts',(72.1018569756018,-4.68136251686823,129.290034991461));
#53196=CARTESIAN_POINT('Ctrl Pts',(72.0940385327322,-4.72023752319487,129.422861147018));
#53197=CARTESIAN_POINT('Ctrl Pts',(72.0909220069482,-4.73573357037371,129.475807257324));
#53198=CARTESIAN_POINT('Ctrl Pts',(72.0878054811642,-4.75034258938988,129.529027477863));
#53199=CARTESIAN_POINT('Ctrl Pts',(72.0846889553802,-4.76405452823408,129.582490119308));
#53200=CARTESIAN_POINT('Ctrl Pts',(73.8346539883595,-4.76405452823405,129.582490119308));
#53201=CARTESIAN_POINT('Ctrl Pts',(73.8255849805719,-4.80365428175128,129.736888957262));
#53202=CARTESIAN_POINT('Ctrl Pts',(73.8165159727843,-4.83578606109947,129.893377862653));
#53203=CARTESIAN_POINT('Ctrl Pts',(73.8074469649967,-4.86025312007588,130.051285142403));
#53204=CARTESIAN_POINT('Ctrl Pts',(73.7984546414948,-4.88451329435409,130.207857214682));
#53205=CARTESIAN_POINT('Ctrl Pts',(73.7894623179928,-4.9012377478513,130.365823666452));
#53206=CARTESIAN_POINT('Ctrl Pts',(73.7804699944909,-4.91028171654727,130.524509716832));
#53207=CARTESIAN_POINT('Ctrl Pts',(73.7752664750086,-4.91551512116138,130.616335367293));
#53208=CARTESIAN_POINT('Ctrl Pts',(73.7700629555264,-4.91817759325308,130.708401611938));
#53209=CARTESIAN_POINT('Ctrl Pts',(73.7648594360441,-4.91824854295789,130.800574829327));
#53210=CARTESIAN_POINT('',(74.1101405639752,-4.91824993278002,130.803547469765));
#53211=CARTESIAN_POINT('Ctrl Pts',(74.1802344108984,-4.76405452823402,129.582490119308));
#53212=CARTESIAN_POINT('Ctrl Pts',(74.1724725663659,-4.79811559078052,129.715293685228));
#53213=CARTESIAN_POINT('Ctrl Pts',(74.1647107218333,-4.82658990219488,129.849407549553));
#53214=CARTESIAN_POINT('Ctrl Pts',(74.1569488773009,-4.84940405230466,129.984321959946));
#53215=CARTESIAN_POINT('Ctrl Pts',(74.1491751916872,-4.87225300653901,130.119442189005));
#53216=CARTESIAN_POINT('Ctrl Pts',(74.1414015060735,-4.8894245022994,130.255365016246));
#53217=CARTESIAN_POINT('Ctrl Pts',(74.1336278204598,-4.90089705890828,130.391576072695));
#53218=CARTESIAN_POINT('Ctrl Pts',(74.1282717400766,-4.90880166663911,130.485425683252));
#53219=CARTESIAN_POINT('Ctrl Pts',(74.1229156596932,-4.91400195047625,130.579412074753));
#53220=CARTESIAN_POINT('Ctrl Pts',(74.1175595793099,-4.91650525847084,130.673367847046));
#53221=CARTESIAN_POINT('Ctrl Pts',(74.1150865742095,-4.91766108381245,130.716749030201));
#53222=CARTESIAN_POINT('Ctrl Pts',(74.112613569109,-4.91824275702076,130.760145578916));
#53223=CARTESIAN_POINT('Ctrl Pts',(74.1101405640085,-4.91824993277992,130.80354746918));
#53224=CARTESIAN_POINT('Ctrl Pts',(74.1101405639751,-4.91824993278002,130.803547469765));
#53225=CARTESIAN_POINT('Ctrl Pts',(74.1024010897476,-4.9182723898963,130.939377279035));
#53226=CARTESIAN_POINT('Ctrl Pts',(74.0946616155201,-4.91266366247495,131.075431159965));
#53227=CARTESIAN_POINT('Ctrl Pts',(74.0869221412926,-4.90139408870185,131.211200942188));
#53228=CARTESIAN_POINT('Ctrl Pts',(74.0791921512183,-4.89013832495776,131.346804348587));
#53229=CARTESIAN_POINT('Ctrl Pts',(74.071462161144,-4.87323554730515,131.482123959232));
#53230=CARTESIAN_POINT('Ctrl Pts',(74.0637321710696,-4.85070806910426,131.616650153893));
#53231=CARTESIAN_POINT('Ctrl Pts',(74.0560097611196,-4.82820268162847,131.751044430497));
#53232=CARTESIAN_POINT('Ctrl Pts',(74.0482873511696,-4.80008363301125,131.884646452297));
#53233=CARTESIAN_POINT('Ctrl Pts',(74.0405649412196,-4.76642511610775,132.016950686401));
#53234=CARTESIAN_POINT('Ctrl Pts',(74.0328482143336,-4.73279136912823,132.149157555377));
#53235=CARTESIAN_POINT('Ctrl Pts',(74.0251314874476,-4.69362636385047,132.280068156235));
#53236=CARTESIAN_POINT('Ctrl Pts',(74.0174147605616,-4.64905547675876,132.409186538506));
#53237=CARTESIAN_POINT('Ctrl Pts',(74.0097010786887,-4.60450217729633,132.538253970786));
#53238=CARTESIAN_POINT('Ctrl Pts',(74.0019873968157,-4.55454736596363,132.665530218108));
#53239=CARTESIAN_POINT('Ctrl Pts',(73.9942737149428,-4.49936636838801,132.790534161222));
#53240=CARTESIAN_POINT('Ctrl Pts',(73.986561439136,-4.44419542932082,132.915515318354));
#53241=CARTESIAN_POINT('Ctrl Pts',(73.9788491633293,-4.38380035794345,133.038224633974));
#53242=CARTESIAN_POINT('Ctrl Pts',(73.9711368875225,-4.31840457467215,133.158201094733));
#53243=CARTESIAN_POINT('Ctrl Pts',(73.9634243087146,-4.25300622212107,133.278182269147));
#53244=CARTESIAN_POINT('Ctrl Pts',(73.9557117299068,-4.18260695575512,133.395430028371));
#53245=CARTESIAN_POINT('Ctrl Pts',(73.9479991510989,-4.10747587241486,133.509508491533));
#53246=CARTESIAN_POINT('Ctrl Pts',(73.9402845603475,-4.03232518998874,133.623616713798));
#53247=CARTESIAN_POINT('Ctrl Pts',(73.9325699695962,-3.95244045207264,133.734553665618));
#53248=CARTESIAN_POINT('Ctrl Pts',(73.9248553788449,-3.86813347597635,133.841913328966));
#53249=CARTESIAN_POINT('Ctrl Pts',(73.9171325154805,-3.78373609469729,133.949388117661));
#53250=CARTESIAN_POINT('Ctrl Pts',(73.9094096521162,-3.69490724946674,134.05327764649));
#53251=CARTESIAN_POINT('Ctrl Pts',(73.9016867887518,-3.60199865307248,134.153209489307));
#53252=CARTESIAN_POINT('Ctrl Pts',(73.8939594770243,-3.50903654140076,134.253198892787));
#53253=CARTESIAN_POINT('Ctrl Pts',(73.8862321652968,-3.41199027813661,134.349225792332));
#53254=CARTESIAN_POINT('Ctrl Pts',(73.8785048535693,-3.31124685375613,134.44095618705));
#53255=CARTESIAN_POINT('Ctrl Pts',(73.8707657502589,-3.21034969875357,134.53282655885));
#53256=CARTESIAN_POINT('Ctrl Pts',(73.8630266469485,-3.10574441657411,134.620387077677));
#53257=CARTESIAN_POINT('Ctrl Pts',(73.8552875436381,-2.99784983306095,134.70334502904));
#53258=CARTESIAN_POINT('Ctrl Pts',(73.8498956809244,-2.9226792663274,134.761142149303));
#53259=CARTESIAN_POINT('Ctrl Pts',(73.8445038182107,-2.84591271882602,134.816706096356));
#53260=CARTESIAN_POINT('Ctrl Pts',(73.8391119554971,-2.76769911226722,134.86995094204));
#53261=CARTESIAN_POINT('Ctrl Pts',(73.831337621378,-2.65492570865199,134.946722781837));
#53262=CARTESIAN_POINT('Ctrl Pts',(73.8235632872589,-2.53877695497952,135.018920418037));
#53263=CARTESIAN_POINT('Ctrl Pts',(73.8157889531398,-2.41966036953933,135.086232493111));
#53264=CARTESIAN_POINT('Ctrl Pts',(73.8080242001927,-2.30069058464511,135.153461612068));
#53265=CARTESIAN_POINT('Ctrl Pts',(73.8002594472457,-2.17876058260213,135.215816959432));
#53266=CARTESIAN_POINT('Ctrl Pts',(73.7924946942986,-2.05430817147097,135.273029434913));
#53267=CARTESIAN_POINT('Ctrl Pts',(73.7847376534136,-1.92997936822893,135.330185086157));
#53268=CARTESIAN_POINT('Ctrl Pts',(73.7769806125286,-1.80313349447147,135.382207868369));
#53269=CARTESIAN_POINT('Ctrl Pts',(73.7692235716436,-1.67423405116622,135.428873932977));
#53270=CARTESIAN_POINT('Ctrl Pts',(73.7614723804034,-1.54543181193333,135.475504806343));
#53271=CARTESIAN_POINT('Ctrl Pts',(73.7537211891633,-1.41457945170024,135.516786870018));
#53272=CARTESIAN_POINT('Ctrl Pts',(73.7459699979231,-1.28216127183758,135.55254401077));
#53273=CARTESIAN_POINT('Ctrl Pts',(73.7382221011461,-1.14979937323427,135.588285953783));
#53274=CARTESIAN_POINT('Ctrl Pts',(73.730474204369,-1.01587335531616,135.618507542634));
#53275=CARTESIAN_POINT('Ctrl Pts',(73.7227263075919,-0.880883324500299,
135.643082311476));
#53276=CARTESIAN_POINT('Ctrl Pts',(73.7149800315078,-0.745921530688839,
135.667651939807));
#53277=CARTESIAN_POINT('Ctrl Pts',(73.7072337554237,-0.609896551080293,
135.686577027607));
#53278=CARTESIAN_POINT('Ctrl Pts',(73.6994874793396,-0.473318957510143,
135.699782175201));
#53279=CARTESIAN_POINT('Ctrl Pts',(73.6917411460742,-0.336740355755131,
135.712987420274));
#53280=CARTESIAN_POINT('Ctrl Pts',(73.6839948128089,-0.199609521049129,
135.720472603262));
#53281=CARTESIAN_POINT('Ctrl Pts',(73.6762484795435,-0.0624420282957672,
135.722214220064));
#53282=CARTESIAN_POINT('Ctrl Pts',(73.6685004115405,0.0747561821669182,
135.723956226889));
#53283=CARTESIAN_POINT('Ctrl Pts',(73.6607523435376,0.211990676153668,135.719952103112));
#53284=CARTESIAN_POINT('Ctrl Pts',(73.6530042755346,0.348746396004895,135.710230470484));
#53285=CARTESIAN_POINT('Ctrl Pts',(73.6452479727927,0.485647461462126,135.70049850559));
#53286=CARTESIAN_POINT('Ctrl Pts',(73.6374916700509,0.622068345704522,135.685036920874));
#53287=CARTESIAN_POINT('Ctrl Pts',(73.629735367309,0.757499072760819,135.663926258368));
#53288=CARTESIAN_POINT('Ctrl Pts',(73.6219749247949,0.893002083273795,135.642804328466));
#53289=CARTESIAN_POINT('Ctrl Pts',(73.6142144822807,1.02751350031223,135.616027389259));
#53290=CARTESIAN_POINT('Ctrl Pts',(73.6064540397665,1.16053502971884,135.583726842004));
#53291=CARTESIAN_POINT('Ctrl Pts',(73.5986811395011,1.29377009709373,135.551374443042));
#53292=CARTESIAN_POINT('Ctrl Pts',(73.5909082392357,1.42551012151131,135.513480825106));
#53293=CARTESIAN_POINT('Ctrl Pts',(73.5831353389702,1.55527256225537,135.47022713083));
#53294=CARTESIAN_POINT('Ctrl Pts',(73.5756450032082,1.68031781142644,135.428545817289));
#53295=CARTESIAN_POINT('Ctrl Pts',(73.5681546674462,1.80352647292725,135.381887475203));
#53296=CARTESIAN_POINT('Ctrl Pts',(73.5606643316842,1.92448730849223,135.330455143971));
#53297=CARTESIAN_POINT('Ctrl Pts',(73.5528899975651,2.05003441090299,135.277072740268));
#53298=CARTESIAN_POINT('Ctrl Pts',(73.545115663446,2.17355756543163,135.21837809019));
#53299=CARTESIAN_POINT('Ctrl Pts',(73.5373413293269,2.29457454458329,135.154545754069));
#53300=CARTESIAN_POINT('Ctrl Pts',(73.5295765763798,2.41544238112357,135.090792085597));
#53301=CARTESIAN_POINT('Ctrl Pts',(73.5218118234328,2.53380984526579,135.021913510005));
#53302=CARTESIAN_POINT('Ctrl Pts',(73.5140470704857,2.64921388936514,134.948132912335));
#53303=CARTESIAN_POINT('Ctrl Pts',(73.5062900296007,2.76450331254058,134.874425594595));
#53304=CARTESIAN_POINT('Ctrl Pts',(73.4985329887158,2.87683484572569,134.795826153054));
#53305=CARTESIAN_POINT('Ctrl Pts',(73.4907759478308,2.98576962518211,134.712603548582));
#53306=CARTESIAN_POINT('Ctrl Pts',(73.4830247565907,3.09462225607425,134.629443702924));
#53307=CARTESIAN_POINT('Ctrl Pts',(73.4752735653506,3.20008292236485,134.541667870116));
#53308=CARTESIAN_POINT('Ctrl Pts',(73.4675223741105,3.30174167828348,134.449588313113));
#53309=CARTESIAN_POINT('Ctrl Pts',(73.4597744773334,3.40335722651923,134.357547892379));
#53310=CARTESIAN_POINT('Ctrl Pts',(73.4520265805563,3.50117378914889,134.2612076475));
#53311=CARTESIAN_POINT('Ctrl Pts',(73.4442786837792,3.59481464714033,134.160919974289));
#53312=CARTESIAN_POINT('Ctrl Pts',(73.4365324076951,3.68843591748294,134.060653279098));
#53313=CARTESIAN_POINT('Ctrl Pts',(73.428786131611,3.77788295390878,133.956441083553));
#53314=CARTESIAN_POINT('Ctrl Pts',(73.4210398555269,3.86281634398755,133.848672190832));
#53315=CARTESIAN_POINT('Ctrl Pts',(73.4132935222616,3.94775036102526,133.740902502586));
#53316=CARTESIAN_POINT('Ctrl Pts',(73.4055471889962,4.02817042323014,133.629576371842));
#53317=CARTESIAN_POINT('Ctrl Pts',(73.3978008557308,4.10377807510627,133.515114861827));
#53318=CARTESIAN_POINT('Ctrl Pts',(73.3900527877279,4.17940265879176,133.400627718949));
#53319=CARTESIAN_POINT('Ctrl Pts',(73.3823047197249,4.25021247219443,133.283004125769));
#53320=CARTESIAN_POINT('Ctrl Pts',(73.3745566517219,4.3159531943571,133.162692885636));
#53321=CARTESIAN_POINT('Ctrl Pts',(73.3668003489801,4.38176378654169,133.042253777285));
#53322=CARTESIAN_POINT('Ctrl Pts',(73.3590440462383,4.44249433762443,132.919121659523));
#53323=CARTESIAN_POINT('Ctrl Pts',(73.3512877434964,4.49793695542664,132.793769124512));
#53324=CARTESIAN_POINT('Ctrl Pts',(73.3435273009823,4.55340916462324,132.668349685078));
#53325=CARTESIAN_POINT('Ctrl Pts',(73.3357668584681,4.60358767383935,132.540707830658));
#53326=CARTESIAN_POINT('Ctrl Pts',(73.328006415954,4.64831369451026,132.411333815827));
#53327=CARTESIAN_POINT('Ctrl Pts',(73.3202335156885,4.6931115133602,132.281752118341));
#53328=CARTESIAN_POINT('Ctrl Pts',(73.3124606154231,4.73243924051452,132.15043307863));
#53329=CARTESIAN_POINT('Ctrl Pts',(73.3046877151577,4.76618845135738,132.017880583882));
#53330=CARTESIAN_POINT('Ctrl Pts',(73.2971973793955,4.79871079337739,131.890146706196));
#53331=CARTESIAN_POINT('Ctrl Pts',(73.2897070436334,4.8260530998275,131.761267796232));
#53332=CARTESIAN_POINT('Ctrl Pts',(73.2822167078713,4.84816390917852,131.631699588145));
#53333=CARTESIAN_POINT('Ctrl Pts',(73.2744423737522,4.87111305658625,131.497218762069));
#53334=CARTESIAN_POINT('Ctrl Pts',(73.2666680396331,4.8884988674008,131.361569341743));
#53335=CARTESIAN_POINT('Ctrl Pts',(73.258893705514,4.90020754843163,131.225251392938));
#53336=CARTESIAN_POINT('Ctrl Pts',(73.2511289525669,4.91190179955954,131.089101443823));
#53337=CARTESIAN_POINT('Ctrl Pts',(73.2433641996198,4.91793280882639,130.952284991339));
#53338=CARTESIAN_POINT('Ctrl Pts',(73.2355994466727,4.91823780716757,130.815312085393));
#53339=CARTESIAN_POINT('Ctrl Pts',(73.2278424057877,4.91854250258009,130.678475222869));
#53340=CARTESIAN_POINT('Ctrl Pts',(73.2200853649027,4.91313250389666,130.541482604555));
#53341=CARTESIAN_POINT('Ctrl Pts',(73.2123283240177,4.90199687894406,130.404848838863));
#53342=CARTESIAN_POINT('Ctrl Pts',(73.2045771327776,4.89086965145283,130.268318109755));
#53343=CARTESIAN_POINT('Ctrl Pts',(73.1968259415375,4.87402542352043,130.132146082727));
#53344=CARTESIAN_POINT('Ctrl Pts',(73.1890747502973,4.85150532511271,129.996846442518));
#53345=CARTESIAN_POINT('Ctrl Pts',(73.1813268535202,4.8289947983476,129.861604308266));
#53346=CARTESIAN_POINT('Ctrl Pts',(73.1735789567432,4.80081326323675,129.727234208219));
#53347=CARTESIAN_POINT('Ctrl Pts',(73.1658310599661,4.76705357451973,129.594243565311));
#53348=CARTESIAN_POINT('Ctrl Pts',(73.158084783882,4.73330094760181,129.461280741179));
#53349=CARTESIAN_POINT('Ctrl Pts',(73.1503385077979,4.69397258410012,129.329697178945));
#53350=CARTESIAN_POINT('Ctrl Pts',(73.1425922317138,4.64921213443177,129.199988593517));
#53351=CARTESIAN_POINT('Ctrl Pts',(73.1348458984484,4.60445135435186,129.070279050608));
#53352=CARTESIAN_POINT('Ctrl Pts',(73.1270995651831,4.5542585356277,128.942444881702));
#53353=CARTESIAN_POINT('Ctrl Pts',(73.1193532319178,4.49882660819147,128.816964780817));
#53354=CARTESIAN_POINT('Ctrl Pts',(73.1116051639148,4.44338226715946,128.691456579533));
#53355=CARTESIAN_POINT('Ctrl Pts',(73.1038570959118,4.38269664071301,128.568303852849));
#53356=CARTESIAN_POINT('Ctrl Pts',(73.0961090279088,4.31700985313275,128.447963157362));
#53357=CARTESIAN_POINT('Ctrl Pts',(73.0883527251669,4.25125325285301,128.327494562352));
#53358=CARTESIAN_POINT('Ctrl Pts',(73.0805964224251,4.18048506118321,128.209844312428));
#53359=CARTESIAN_POINT('Ctrl Pts',(73.0728401196832,4.10499051249334,128.095442760775));
#53360=CARTESIAN_POINT('Ctrl Pts',(73.0650796771691,4.02945567008975,127.98098014957));
#53361=CARTESIAN_POINT('Ctrl Pts',(73.0573192346549,3.94918967287014,127.869770008497));
#53362=CARTESIAN_POINT('Ctrl Pts',(73.0495587921407,3.86451915679611,127.762210925448));
#53363=CARTESIAN_POINT('Ctrl Pts',(73.0417858918753,3.77971272009299,127.654479179009));
#53364=CARTESIAN_POINT('Ctrl Pts',(73.0340129916099,3.69048788999537,127.550410499726));
#53365=CARTESIAN_POINT('Ctrl Pts',(73.0262400913444,3.59720999491291,127.45036847163));
#53366=CARTESIAN_POINT('Ctrl Pts',(73.0187497555824,3.50732298626972,127.353963223247));
#53367=CARTESIAN_POINT('Ctrl Pts',(73.0112594198204,3.4136726937871,127.26129716758));
#53368=CARTESIAN_POINT('Ctrl Pts',(73.0037690840584,3.31661472330351,127.172659936113));
#53369=CARTESIAN_POINT('Ctrl Pts',(72.9959947499393,3.21587677036862,127.080661997074));
#53370=CARTESIAN_POINT('Ctrl Pts',(72.9882204158202,3.11114852667453,126.992712996937));
#53371=CARTESIAN_POINT('Ctrl Pts',(72.9804460817011,3.00278920371803,126.909178970899));
#53372=CARTESIAN_POINT('Ctrl Pts',(72.972681328754,2.89456342394287,126.825747893082));
#53373=CARTESIAN_POINT('Ctrl Pts',(72.9649165758069,2.78271577544925,126.746721199684));
#53374=CARTESIAN_POINT('Ctrl Pts',(72.9571518228599,2.66764144945669,126.672427394529));
#53375=CARTESIAN_POINT('Ctrl Pts',(72.9493947819749,2.55268141690743,126.598207379028));
#53376=CARTESIAN_POINT('Ctrl Pts',(72.9416377410899,2.43450141085251,126.528711107711));
#53377=CARTESIAN_POINT('Ctrl Pts',(72.933880700205,2.31352847681695,126.464225936539));
#53378=CARTESIAN_POINT('Ctrl Pts',(72.9261295089649,2.19264676941173,126.399789394136));
#53379=CARTESIAN_POINT('Ctrl Pts',(72.9183783177248,2.0689766698402,126.340356613353));
#53380=CARTESIAN_POINT('Ctrl Pts',(72.9106271264847,1.94297258737516,126.286170649536));
#53381=CARTESIAN_POINT('Ctrl Pts',(72.9028792297076,1.81702206000609,126.232007716199));
#53382=CARTESIAN_POINT('Ctrl Pts',(72.8951313329305,1.68873988117719,126.183087318582));
#53383=CARTESIAN_POINT('Ctrl Pts',(72.8873834361534,1.55860315043029,126.139605609855));
#53384=CARTESIAN_POINT('Ctrl Pts',(72.8796371600693,1.42849364148203,126.096132996564));
#53385=CARTESIAN_POINT('Ctrl Pts',(72.8718908839852,1.29653072281361,126.05809693312));
#53386=CARTESIAN_POINT('Ctrl Pts',(72.8641446079011,1.16320909997391,126.025644508375));
#53387=CARTESIAN_POINT('Ctrl Pts',(72.8563982746357,1.0298864929841,125.993191844074));
#53388=CARTESIAN_POINT('Ctrl Pts',(72.8486519413703,0.895205541682873,125.966322993184));
#53389=CARTESIAN_POINT('Ctrl Pts',(72.840905608105,0.75967326824796,125.945134384099));
#53390=CARTESIAN_POINT('Ctrl Pts',(72.833157540102,0.624110643300587,125.923941029973));
#53391=CARTESIAN_POINT('Ctrl Pts',(72.8254094720991,0.487696703052019,125.908430509263));
#53392=CARTESIAN_POINT('Ctrl Pts',(72.8176614040961,0.35094535453753,125.898647578605));
#53393=CARTESIAN_POINT('Ctrl Pts',(72.8099051013542,0.214048665062105,125.888854250532));
#53394=CARTESIAN_POINT('Ctrl Pts',(72.8021487986123,0.0768142415660106,
125.884800700592));
#53395=CARTESIAN_POINT('Ctrl Pts',(72.7943924958705,-0.0602416714836149,
125.88647956944));
#53396=CARTESIAN_POINT('Ctrl Pts',(72.7866320533563,-0.197370735400709,
125.888159334351));
#53397=CARTESIAN_POINT('Ctrl Pts',(72.7788716108422,-0.334320708823159,
125.895577593354));
#53398=CARTESIAN_POINT('Ctrl Pts',(72.771111168328,-0.47057969375474,125.908674984856));
#53399=CARTESIAN_POINT('Ctrl Pts',(72.7633382680626,-0.607057413705437,
125.921793401453));
#53400=CARTESIAN_POINT('Ctrl Pts',(72.7555653677971,-0.742841541070479,
125.940609114821));
#53401=CARTESIAN_POINT('Ctrl Pts',(72.7477924675317,-0.87742871337592,125.965011289873));
#53402=CARTESIAN_POINT('Ctrl Pts',(72.7403021317696,-1.00712330296425,125.988526384397));
#53403=CARTESIAN_POINT('Ctrl Pts',(72.7328117960075,-1.13570615065991,126.017228761194));
#53404=CARTESIAN_POINT('Ctrl Pts',(72.7253214602454,-1.26274136764996,126.050975791894));
#53405=CARTESIAN_POINT('Ctrl Pts',(72.7175471261263,-1.39459316350288,126.086002351521));
#53406=CARTESIAN_POINT('Ctrl Pts',(72.7097727920073,-1.52519532200987,126.12657460615));
#53407=CARTESIAN_POINT('Ctrl Pts',(72.7019984578882,-1.65404572480389,126.172588191943));
#53408=CARTESIAN_POINT('Ctrl Pts',(72.6942337049411,-1.78273733099207,126.218545070104));
#53409=CARTESIAN_POINT('Ctrl Pts',(72.686468951994,-1.90968111234199,126.269929806356));
#53410=CARTESIAN_POINT('Ctrl Pts',(72.6787041990469,-2.03438707877458,126.326587479474));
#53411=CARTESIAN_POINT('Ctrl Pts',(72.670947158162,-2.15896918548292,126.383188879393));
#53412=CARTESIAN_POINT('Ctrl Pts',(72.663190117277,-2.28131754675942,126.445052633331));
#53413=CARTESIAN_POINT('Ctrl Pts',(72.655433076392,-2.40095957335598,126.51197477871));
#53414=CARTESIAN_POINT('Ctrl Pts',(72.6476818851518,-2.52051137697057,126.57884645758));
#53415=CARTESIAN_POINT('Ctrl Pts',(72.6399306939117,-2.63736056829631,126.65076874513));
#53416=CARTESIAN_POINT('Ctrl Pts',(72.6321795026715,-2.751057038676,126.72749071132));
#53417=CARTESIAN_POINT('Ctrl Pts',(72.6244316058945,-2.86470518502214,126.804180068628));
#53418=CARTESIAN_POINT('Ctrl Pts',(72.6166837091173,-2.97520295215812,126.885664828958));
#53419=CARTESIAN_POINT('Ctrl Pts',(72.6089358123402,-3.08212742691119,126.971649620532));
#53420=CARTESIAN_POINT('Ctrl Pts',(72.6011895362561,-3.18902953536932,127.057616425942));
#53421=CARTESIAN_POINT('Ctrl Pts',(72.5934432601721,-3.29235953369525,127.148081145428));
#53422=CARTESIAN_POINT('Ctrl Pts',(72.5856969840879,-3.39172627144004,127.242707074319));
#53423=CARTESIAN_POINT('Ctrl Pts',(72.5779506508226,-3.49109374268744,127.337333701717));
#53424=CARTESIAN_POINT('Ctrl Pts',(72.5702043175573,-3.58649761185007,127.436121330195));
#53425=CARTESIAN_POINT('Ctrl Pts',(72.5624579842919,-3.67758269311653,127.538695509538));
#53426=CARTESIAN_POINT('Ctrl Pts',(72.554709916289,-3.76868817225541,127.641292659658));
#53427=CARTESIAN_POINT('Ctrl Pts',(72.546961848286,-3.85547267940951,127.747677755724));
#53428=CARTESIAN_POINT('Ctrl Pts',(72.539213780283,-3.93762078024857,127.857442625247));
#53429=CARTESIAN_POINT('Ctrl Pts',(72.5314574775412,-4.01985618906673,127.967324154179));
#53430=CARTESIAN_POINT('Ctrl Pts',(72.5237011747993,-4.0974451134704,128.080592318591));
#53431=CARTESIAN_POINT('Ctrl Pts',(72.5159448720574,-4.17011470234065,128.196808809486));
#53432=CARTESIAN_POINT('Ctrl Pts',(72.5081844295432,-4.24282307715867,128.313087328621));
#53433=CARTESIAN_POINT('Ctrl Pts',(72.5004239870291,-4.3106066915869,128.432316970079));
#53434=CARTESIAN_POINT('Ctrl Pts',(72.4926635445149,-4.3732387948454,128.554034973185));
#53435=CARTESIAN_POINT('Ctrl Pts',(72.4848906442495,-4.43597144071613,128.675948368835));
#53436=CARTESIAN_POINT('Ctrl Pts',(72.4771177439841,-4.49353588572341,128.800357753468));
#53437=CARTESIAN_POINT('Ctrl Pts',(72.4693448437187,-4.54575329885191,128.926779724907));
#53438=CARTESIAN_POINT('Ctrl Pts',(72.4618545079567,-4.59607247748532,129.048605939247));
#53439=CARTESIAN_POINT('Ctrl Pts',(72.4543641721947,-4.64142652498172,129.172300666421));
#53440=CARTESIAN_POINT('Ctrl Pts',(72.4468738364327,-4.68169983007849,129.297420086708));
#53441=CARTESIAN_POINT('Ctrl Pts',(72.4412390975458,-4.7119961432934,129.391543405794));
#53442=CARTESIAN_POINT('Ctrl Pts',(72.435604358659,-4.73946555878566,129.486618100619));
#53443=CARTESIAN_POINT('Ctrl Pts',(72.4299696197722,-4.76405452823407,129.582490119308));
#53444=CARTESIAN_POINT('Origin',(213.235140564004,0.,130.804360617566));
#53445=CARTESIAN_POINT('',(70.3350012833218,-4.76405452823407,129.582490119308));
#53446=CARTESIAN_POINT('',(70.6799389637606,-4.76405452823405,129.582490119308));
#53447=CARTESIAN_POINT('',(213.235140564004,-4.76405452823405,129.582490119308));
#53448=CARTESIAN_POINT('',(72.0148594359372,-4.91824905725685,130.807405825623));
#53449=CARTESIAN_POINT('Ctrl Pts',(72.0148594359372,-4.91824905725685,130.807405825623));
#53450=CARTESIAN_POINT('Ctrl Pts',(72.006085115023,-4.91815272426633,130.962991135701));
#53451=CARTESIAN_POINT('Ctrl Pts',(71.9973107941087,-4.91066945928422,131.118299997196));
#53452=CARTESIAN_POINT('Ctrl Pts',(71.9885364731944,-4.8959029357732,131.272674087357));
#53453=CARTESIAN_POINT('Ctrl Pts',(71.9798018354719,-4.88120319609536,131.426349997375));
#53454=CARTESIAN_POINT('Ctrl Pts',(71.9710671977494,-4.8592861090345,131.579099399438));
#53455=CARTESIAN_POINT('Ctrl Pts',(71.9623325600269,-4.83030408212401,131.730290170349));
#53456=CARTESIAN_POINT('Ctrl Pts',(71.9535383975168,-4.80112454856788,131.882511275752));
#53457=CARTESIAN_POINT('Ctrl Pts',(71.9447442350066,-4.76478354229904,132.033152235707));
#53458=CARTESIAN_POINT('Ctrl Pts',(71.9359500724964,-4.72148566284163,132.181588339506));
#53459=CARTESIAN_POINT('Ctrl Pts',(71.9271559099863,-4.67818778338425,132.330024443306));
#53460=CARTESIAN_POINT('Ctrl Pts',(71.9183617474761,-4.62793317195716,132.476255525112));
#53461=CARTESIAN_POINT('Ctrl Pts',(71.909567584966,-4.57097351201412,132.619679932443));
#53462=CARTESIAN_POINT('Ctrl Pts',(71.9017932508469,-4.52061926541078,132.746471910887));
#53463=CARTESIAN_POINT('Ctrl Pts',(71.8940189167278,-4.46490573306048,132.871368003562));
#53464=CARTESIAN_POINT('Ctrl Pts',(71.8862445826088,-4.40399585289402,132.993881932875));
#53465=CARTESIAN_POINT('Ctrl Pts',(71.8784798296617,-4.34316103871114,133.11624487472));
#53466=CARTESIAN_POINT('Ctrl Pts',(71.8707150767146,-4.27714279121172,133.236231147852));
#53467=CARTESIAN_POINT('Ctrl Pts',(71.8629503237675,-4.2061528193853,133.353372489346));
#53468=CARTESIAN_POINT('Ctrl Pts',(71.8551932828825,-4.13523335579972,133.470397484409));
#53469=CARTESIAN_POINT('Ctrl Pts',(71.8474362419976,-4.05935219602026,133.584582838763));
#53470=CARTESIAN_POINT('Ctrl Pts',(71.8396792011126,-3.97876769194306,133.695483360732));
#53471=CARTESIAN_POINT('Ctrl Pts',(71.8319280098725,-3.89824395726725,133.806300251754));
#53472=CARTESIAN_POINT('Ctrl Pts',(71.8241768186323,-3.81302416693415,133.913836925942));
#53473=CARTESIAN_POINT('Ctrl Pts',(71.8164256273922,-3.72341065640713,134.017676062127));
#53474=CARTESIAN_POINT('Ctrl Pts',(71.8086777306151,-3.6338352340126,134.121471063909));
#53475=CARTESIAN_POINT('Ctrl Pts',(71.800929833838,-3.53987006053692,134.221571358023));
#53476=CARTESIAN_POINT('Ctrl Pts',(71.793181937061,-3.44185839009431,134.317591877395));
#53477=CARTESIAN_POINT('Ctrl Pts',(71.7854356609769,-3.34386722158028,134.413592311343));
#53478=CARTESIAN_POINT('Ctrl Pts',(71.7776893848929,-3.24183151881422,134.505514394581));
#53479=CARTESIAN_POINT('Ctrl Pts',(71.7699431088088,-3.13613182804734,134.593009482215));
#53480=CARTESIAN_POINT('Ctrl Pts',(71.7621967755434,-3.03043135702936,134.680505215719));
#53481=CARTESIAN_POINT('Ctrl Pts',(71.7544504422781,-2.92106714521088,134.76357363911));
#53482=CARTESIAN_POINT('Ctrl Pts',(71.7467041090128,-2.80845297245401,134.841906278486));
#53483=CARTESIAN_POINT('Ctrl Pts',(71.7389560410098,-2.69581358053396,134.920256459913));
#53484=CARTESIAN_POINT('Ctrl Pts',(71.7312079730068,-2.57992310031957,134.993868523751));
#53485=CARTESIAN_POINT('Ctrl Pts',(71.7234599050039,-2.461224102916,135.062477452239));
#53486=CARTESIAN_POINT('Ctrl Pts',(71.715703602262,-2.34239895080545,135.131159299112));
#53487=CARTESIAN_POINT('Ctrl Pts',(71.7079472995202,-2.22075965782467,135.19482719261));
#53488=CARTESIAN_POINT('Ctrl Pts',(71.7001909967784,-2.096773691202,135.253261959514));
#53489=CARTESIAN_POINT('Ctrl Pts',(71.6924305542642,-1.97272154953571,135.311727914812));
#53490=CARTESIAN_POINT('Ctrl Pts',(71.6846701117501,-1.84632059867971,135.364955026416));
#53491=CARTESIAN_POINT('Ctrl Pts',(71.6769096692359,-1.71805714154095,135.41277278673));
#53492=CARTESIAN_POINT('Ctrl Pts',(71.6691367689705,-1.58958778451411,135.460667308359));
#53493=CARTESIAN_POINT('Ctrl Pts',(71.6613638687051,-1.45925031845517,135.503135004966));
#53494=CARTESIAN_POINT('Ctrl Pts',(71.6535909684396,-1.32754588355426,135.540055391256));
#53495=CARTESIAN_POINT('Ctrl Pts',(71.6461006326775,-1.20062923660357,135.575633628509));
#53496=CARTESIAN_POINT('Ctrl Pts',(71.6386102969154,-1.07244358054496,135.606060799531));
#53497=CARTESIAN_POINT('Ctrl Pts',(71.6311199611533,-0.943443283358898,
135.631274521251));
#53498=CARTESIAN_POINT('Ctrl Pts',(71.6233456270342,-0.809551900698114,
135.657444228892));
#53499=CARTESIAN_POINT('Ctrl Pts',(71.6155712929151,-0.674358755575522,
135.678080245084));
#53500=CARTESIAN_POINT('Ctrl Pts',(71.607796958796,-0.538361039032828,135.693056809206));
#53501=CARTESIAN_POINT('Ctrl Pts',(71.6000322058489,-0.402530927521401,
135.70801491605));
#53502=CARTESIAN_POINT('Ctrl Pts',(71.5922674529019,-0.265898602388661,
135.717327406151));
#53503=CARTESIAN_POINT('Ctrl Pts',(71.5845026999548,-0.128972460375438,
135.720919288727));
#53504=CARTESIAN_POINT('Ctrl Pts',(71.5767456590698,0.00781768466321653,
135.724507603794));
#53505=CARTESIAN_POINT('Ctrl Pts',(71.5689886181848,0.144900677539574,135.722386608166));
#53506=CARTESIAN_POINT('Ctrl Pts',(71.5612315772998,0.281762320377915,135.714533023634));
#53507=CARTESIAN_POINT('Ctrl Pts',(71.5534803860597,0.418520754786671,135.706685361552));
#53508=CARTESIAN_POINT('Ctrl Pts',(71.5457291948195,0.555057782661346,135.693113737522));
#53509=CARTESIAN_POINT('Ctrl Pts',(71.5379780035794,0.690858880182849,135.673846942649));
#53510=CARTESIAN_POINT('Ctrl Pts',(71.5302301068023,0.826602258615478,135.654588336678));
#53511=CARTESIAN_POINT('Ctrl Pts',(71.5224822100252,0.961609942532017,135.629639429055));
#53512=CARTESIAN_POINT('Ctrl Pts',(71.5147343132482,1.09537242686405,135.599080871029));
#53513=CARTESIAN_POINT('Ctrl Pts',(71.5069880371641,1.22910693096795,135.568528705194));
#53514=CARTESIAN_POINT('Ctrl Pts',(71.49924176108,1.36159637267027,135.532369309967));
#53515=CARTESIAN_POINT('Ctrl Pts',(71.4914954849959,1.49234173260498,135.490734398607));
#53516=CARTESIAN_POINT('Ctrl Pts',(71.4837491517305,1.62308805767215,135.449099179907));
#53517=CARTESIAN_POINT('Ctrl Pts',(71.4760028184652,1.75208990274901,135.401988483051));
#53518=CARTESIAN_POINT('Ctrl Pts',(71.4682564851998,1.87886408188063,135.349583695075));
#53519=CARTESIAN_POINT('Ctrl Pts',(71.4605084171968,2.00566665121076,135.29716717141));
#53520=CARTESIAN_POINT('Ctrl Pts',(71.4527603491939,2.1302402006583,135.239454346796));
#53521=CARTESIAN_POINT('Ctrl Pts',(71.4450122811909,2.25212254278166,135.176674320263));
#53522=CARTESIAN_POINT('Ctrl Pts',(71.4372559784491,2.37413442290857,135.113827570372));
#53523=CARTESIAN_POINT('Ctrl Pts',(71.4294996757072,2.49344903393805,135.045903039794));
#53524=CARTESIAN_POINT('Ctrl Pts',(71.4217433729654,2.60962930177763,134.973175553468));
#53525=CARTESIAN_POINT('Ctrl Pts',(71.4139829304512,2.72587157852443,134.900409250294));
#53526=CARTESIAN_POINT('Ctrl Pts',(71.406222487937,2.83897585643969,134.822835104444));
#53527=CARTESIAN_POINT('Ctrl Pts',(71.3984620454228,2.94853582405441,134.740770092807));
#53528=CARTESIAN_POINT('Ctrl Pts',(71.3906891451574,3.05827166705535,134.658573343128));
#53529=CARTESIAN_POINT('Ctrl Pts',(71.382916244892,3.16445152703313,134.571871568931));
#53530=CARTESIAN_POINT('Ctrl Pts',(71.3751433446266,3.26670315778261,134.481021268406));
#53531=CARTESIAN_POINT('Ctrl Pts',(71.3676530088645,3.36523768419839,134.393473605142));
#53532=CARTESIAN_POINT('Ctrl Pts',(71.3601626731024,3.46012440312911,134.302074011457));
#53533=CARTESIAN_POINT('Ctrl Pts',(71.3526723373404,3.55106523293699,134.207171040426));
#53534=CARTESIAN_POINT('Ctrl Pts',(71.3448980032213,3.64545411194756,134.108669794404));
#53535=CARTESIAN_POINT('Ctrl Pts',(71.3371236691022,3.735890974027,134.006082243358));
#53536=CARTESIAN_POINT('Ctrl Pts',(71.3293493349831,3.82200126930088,133.899758711505));
#53537=CARTESIAN_POINT('Ctrl Pts',(71.321584582036,3.90800544133174,133.793566213903));
#53538=CARTESIAN_POINT('Ctrl Pts',(71.313819829089,3.98969341216099,133.68364719751));
#53539=CARTESIAN_POINT('Ctrl Pts',(71.3060550761419,4.06672728906478,133.570388856553));
#53540=CARTESIAN_POINT('Ctrl Pts',(71.2982980352569,4.14368465483599,133.457243005378));
#53541=CARTESIAN_POINT('Ctrl Pts',(71.2905409943719,4.21599690723227,133.340764751133));
#53542=CARTESIAN_POINT('Ctrl Pts',(71.2827839534869,4.28336652512617,133.221374120617));
#53543=CARTESIAN_POINT('Ctrl Pts',(71.2750327622468,4.35068533906715,133.102073523503));
#53544=CARTESIAN_POINT('Ctrl Pts',(71.2672815710066,4.41306874607118,132.979865260729));
#53545=CARTESIAN_POINT('Ctrl Pts',(71.2595303797665,4.4702628562173,132.85519777805));
#53546=CARTESIAN_POINT('Ctrl Pts',(71.2517824829894,4.52743265734095,132.730583282378));
#53547=CARTESIAN_POINT('Ctrl Pts',(71.2440345862124,4.57941738567087,132.603512000301));
#53548=CARTESIAN_POINT('Ctrl Pts',(71.2362866894353,4.62600949545162,132.474456186835));
#53549=CARTESIAN_POINT('Ctrl Pts',(71.2285404133512,4.67259185916741,132.345427369062));
#53550=CARTESIAN_POINT('Ctrl Pts',(71.2207941372671,4.71378371535038,132.2144152131));
#53551=CARTESIAN_POINT('Ctrl Pts',(71.213047861183,4.74942614593861,132.081910752306));
#53552=CARTESIAN_POINT('Ctrl Pts',(71.2053015279176,4.78506883963114,131.949405313395));
#53553=CARTESIAN_POINT('Ctrl Pts',(71.1975551946522,4.81516192443107,131.815407925216));
#53554=CARTESIAN_POINT('Ctrl Pts',(71.1898088613869,4.83959683257826,131.680423149922));
#53555=CARTESIAN_POINT('Ctrl Pts',(71.1820607933839,4.86403721275371,131.545408145724));
#53556=CARTESIAN_POINT('Ctrl Pts',(71.174312725381,4.88281682524807,131.409405699049));
#53557=CARTESIAN_POINT('Ctrl Pts',(71.166564657378,4.89587859396303,131.272928494906));
#53558=CARTESIAN_POINT('Ctrl Pts',(71.1588083546361,4.90895424488122,131.136306241165));
#53559=CARTESIAN_POINT('Ctrl Pts',(71.1510520518943,4.91629987526594,130.999208611814));
#53560=CARTESIAN_POINT('Ctrl Pts',(71.1432957491525,4.9179104538993,130.862151879258));
#53561=CARTESIAN_POINT('Ctrl Pts',(71.1355353066383,4.91952189214697,130.725021995397));
#53562=CARTESIAN_POINT('Ctrl Pts',(71.1277748641241,4.91539219116826,130.587933442422));
#53563=CARTESIAN_POINT('Ctrl Pts',(71.1200144216099,4.90556841132274,130.451399395429));
#53564=CARTESIAN_POINT('Ctrl Pts',(71.1122415213445,4.8957288614737,130.314646171863));
#53565=CARTESIAN_POINT('Ctrl Pts',(71.104468621079,4.88017701122511,130.178449621732));
#53566=CARTESIAN_POINT('Ctrl Pts',(71.0966957208136,4.8590115844341,130.04331562229));
#53567=CARTESIAN_POINT('Ctrl Pts',(71.0892053850515,4.83861557421938,129.913094084109));
#53568=CARTESIAN_POINT('Ctrl Pts',(71.0817150492895,4.81300709680015,129.783859487195));
#53569=CARTESIAN_POINT('Ctrl Pts',(71.0742247135275,4.78231827934427,129.656051017524));
#53570=CARTESIAN_POINT('Ctrl Pts',(71.0664503794084,4.75046588604696,129.523396650878));
#53571=CARTESIAN_POINT('Ctrl Pts',(71.0586760452893,4.71303940691852,129.391858480325));
#53572=CARTESIAN_POINT('Ctrl Pts',(71.0509017111702,4.67013112628863,129.261940984078));
#53573=CARTESIAN_POINT('Ctrl Pts',(71.0431369582231,4.62727572627983,129.132183599534));
#53574=CARTESIAN_POINT('Ctrl Pts',(71.0353722052761,4.57895208829263,129.00404328287));
#53575=CARTESIAN_POINT('Ctrl Pts',(71.027607452329,4.52530333052641,128.878013600742));
#53576=CARTESIAN_POINT('Ctrl Pts',(71.019850411444,4.47170785746271,128.752109093071));
#53577=CARTESIAN_POINT('Ctrl Pts',(71.0120933705589,4.41279794207661,128.628311405582));
#53578=CARTESIAN_POINT('Ctrl Pts',(71.0043363296739,4.34876614737032,128.507097885969));
#53579=CARTESIAN_POINT('Ctrl Pts',(70.9965851384338,4.28478263953856,128.385975774413));
#53580=CARTESIAN_POINT('Ctrl Pts',(70.9888339471937,4.21568512223401,128.267434296179));
#53581=CARTESIAN_POINT('Ctrl Pts',(70.9810827559535,4.141713651868,128.151929451931));
#53582=CARTESIAN_POINT('Ctrl Pts',(70.9733348591764,4.06777362135009,128.036473700324));
#53583=CARTESIAN_POINT('Ctrl Pts',(70.9655869623994,3.98896396835337,127.924052344245));
#53584=CARTESIAN_POINT('Ctrl Pts',(70.9578390656223,3.90556983084545,127.815095263187));
#53585=CARTESIAN_POINT('Ctrl Pts',(70.9500927895382,3.82219313759333,127.706160973602));
#53586=CARTESIAN_POINT('Ctrl Pts',(70.9423465134541,3.73423410475888,127.600689827934));
#53587=CARTESIAN_POINT('Ctrl Pts',(70.9346002373699,3.64201995351961,127.499080943973));
#53588=CARTESIAN_POINT('Ctrl Pts',(70.9268539041046,3.54980512157643,127.397471309959));
#53589=CARTESIAN_POINT('Ctrl Pts',(70.9191075708392,3.45333537129719,127.299724284058));
#53590=CARTESIAN_POINT('Ctrl Pts',(70.9113612375739,3.35297652158428,127.206203935568));
#53591=CARTESIAN_POINT('Ctrl Pts',(70.9036131695709,3.25259519720282,127.112662643845));
#53592=CARTESIAN_POINT('Ctrl Pts',(70.895865101568,3.1483233262968,127.023350179515));
#53593=CARTESIAN_POINT('Ctrl Pts',(70.888117033565,3.04056139425724,126.938591681086));
#53594=CARTESIAN_POINT('Ctrl Pts',(70.8803607308231,2.93268493155391,126.853743100316));
#53595=CARTESIAN_POINT('Ctrl Pts',(70.8726044280813,2.82131130582427,126.773458395975));
#53596=CARTESIAN_POINT('Ctrl Pts',(70.8648481253394,2.70687215216847,126.698020858813));
#53597=CARTESIAN_POINT('Ctrl Pts',(70.8570876828253,2.5923719188905,126.622543058367));
#53598=CARTESIAN_POINT('Ctrl Pts',(70.849327240311,2.47480323247012,126.551917781302));
#53599=CARTESIAN_POINT('Ctrl Pts',(70.8415667977969,2.35462327892404,126.486382818081));
#53600=CARTESIAN_POINT('Ctrl Pts',(70.8337938975314,2.23425040184753,126.420742652318));
#53601=CARTESIAN_POINT('Ctrl Pts',(70.826020997266,2.11125823200087,126.360209302252));
#53602=CARTESIAN_POINT('Ctrl Pts',(70.8182480970006,1.98612574090169,126.304973147718));
#53603=CARTESIAN_POINT('Ctrl Pts',(70.8107577612386,1.86554213104403,126.251744966532));
#53604=CARTESIAN_POINT('Ctrl Pts',(70.8032674254765,1.74297139698017,126.203435647493));
#53605=CARTESIAN_POINT('Ctrl Pts',(70.7957770897145,1.61885445627116,126.160171419018));
#53606=CARTESIAN_POINT('Ctrl Pts',(70.7880027555954,1.49003158403027,126.115266814171));
#53607=CARTESIAN_POINT('Ctrl Pts',(70.7802284214764,1.35913486962784,126.075655176852));
#53608=CARTESIAN_POINT('Ctrl Pts',(70.7724540873573,1.22663862680702,126.041531548439));
#53609=CARTESIAN_POINT('Ctrl Pts',(70.7646893344102,1.09430567376403,126.007449974348));
#53610=CARTESIAN_POINT('Ctrl Pts',(70.7569245814631,0.960377489529723,125.978843048425));
#53611=CARTESIAN_POINT('Ctrl Pts',(70.749159828516,0.82534668459318,125.955857146109));
#53612=CARTESIAN_POINT('Ctrl Pts',(70.741402787631,0.690449994155701,125.932894073715));
#53613=CARTESIAN_POINT('Ctrl Pts',(70.733645746746,0.554453245317691,125.915540979931));
#53614=CARTESIAN_POINT('Ctrl Pts',(70.725888705861,0.417862129219237,125.903893874136));
#53615=CARTESIAN_POINT('Ctrl Pts',(70.7181375146209,0.281374017543864,125.892255551514));
#53616=CARTESIAN_POINT('Ctrl Pts',(70.7103863233807,0.144292818732098,125.886314685243));
#53617=CARTESIAN_POINT('Ctrl Pts',(70.7026351321406,0.00713193541294979,
125.886115788565));
#53618=CARTESIAN_POINT('Ctrl Pts',(70.6948872353635,-0.129970650871808,
125.885916976423));
#53619=CARTESIAN_POINT('Ctrl Pts',(70.6871393385865,-0.267152464156722,
125.891455280489));
#53620=CARTESIAN_POINT('Ctrl Pts',(70.6793914418094,-0.403897710613602,
125.902723166483));
#53621=CARTESIAN_POINT('Ctrl Pts',(70.6716451657253,-0.540614352912809,
125.913988695478));
#53622=CARTESIAN_POINT('Ctrl Pts',(70.6638988896412,-0.676894220627435,
125.930981390421));
#53623=CARTESIAN_POINT('Ctrl Pts',(70.6561526135571,-0.812224653617011,
125.953641683783));
#53624=CARTESIAN_POINT('Ctrl Pts',(70.6484062802917,-0.9475560855851,125.976302144419));
#53625=CARTESIAN_POINT('Ctrl Pts',(70.6406599470264,-1.08193768324619,126.004630222391));
#53626=CARTESIAN_POINT('Ctrl Pts',(70.6329136137611,-1.21486541073539,126.038514932244));
#53627=CARTESIAN_POINT('Ctrl Pts',(70.6251655457581,-1.34782290646742,126.072407230344));
#53628=CARTESIAN_POINT('Ctrl Pts',(70.6174174777551,-1.47932550537516,126.111858539921));
#53629=CARTESIAN_POINT('Ctrl Pts',(70.6096694097522,-1.60888318708784,126.15670766658));
#53630=CARTESIAN_POINT('Ctrl Pts',(70.6019131070103,-1.73857856424649,126.201604459425));
#53631=CARTESIAN_POINT('Ctrl Pts',(70.5941568042685,-1.86632452494904,126.251910401257));
#53632=CARTESIAN_POINT('Ctrl Pts',(70.5864005015266,-1.99164941934777,126.307415470812));
#53633=CARTESIAN_POINT('Ctrl Pts',(70.5786400590125,-2.1170412034161,126.362950165095));
#53634=CARTESIAN_POINT('Ctrl Pts',(70.5708796164983,-2.24000899600728,126.423689343327));
#53635=CARTESIAN_POINT('Ctrl Pts',(70.5631191739841,-2.36010561706203,126.489376893516));
#53636=CARTESIAN_POINT('Ctrl Pts',(70.5553462737187,-2.48039502787466,126.555169891193));
#53637=CARTESIAN_POINT('Ctrl Pts',(70.5475733734533,-2.59780372173181,126.625926932684));
#53638=CARTESIAN_POINT('Ctrl Pts',(70.5398004731878,-2.71191263088104,126.701347950638));
#53639=CARTESIAN_POINT('Ctrl Pts',(70.5323101374258,-2.82187339375954,126.774027224616));
#53640=CARTESIAN_POINT('Ctrl Pts',(70.5248198016638,-2.92876986777689,126.851037087606));
#53641=CARTESIAN_POINT('Ctrl Pts',(70.5173294659018,-3.03225752667745,126.932074812721));
#53642=CARTESIAN_POINT('Ctrl Pts',(70.5096504214894,-3.13835241401994,127.015154171244));
#53643=CARTESIAN_POINT('Ctrl Pts',(70.5019713770771,-3.24121802712842,127.102744192016));
#53644=CARTESIAN_POINT('Ctrl Pts',(70.4942923326647,-3.34043953367328,127.19456189958));
#53645=CARTESIAN_POINT('Ctrl Pts',(70.4866220665762,-3.43954761484029,127.286274645442));
#53646=CARTESIAN_POINT('Ctrl Pts',(70.4789518004876,-3.53501957954672,127.382205201285));
#53647=CARTESIAN_POINT('Ctrl Pts',(70.4712815343991,-3.62647104661938,127.482028483277));
#53648=CARTESIAN_POINT('Ctrl Pts',(70.463618277831,-3.71783894019916,127.58176054114));
#53649=CARTESIAN_POINT('Ctrl Pts',(70.4559550212629,-3.80519337265196,127.685377958043));
#53650=CARTESIAN_POINT('Ctrl Pts',(70.4482917646948,-3.88818484862489,127.792517054991));
#53651=CARTESIAN_POINT('Ctrl Pts',(70.4406337551094,-3.9711195008654,127.899582794485));
#53652=CARTESIAN_POINT('Ctrl Pts',(70.432975745524,-4.04969689349164,128.010165102239));
#53653=CARTESIAN_POINT('Ctrl Pts',(70.4253177359387,-4.12360643396907,128.123865693074));
#53654=CARTESIAN_POINT('Ctrl Pts',(70.4176622211966,-4.19749189603343,128.237529242279));
#53655=CARTESIAN_POINT('Ctrl Pts',(70.4100067064544,-4.26671230702162,128.354308721683));
#53656=CARTESIAN_POINT('Ctrl Pts',(70.4023511917123,-4.33099942319238,128.473775485285));
#53657=CARTESIAN_POINT('Ctrl Pts',(70.3946973965434,-4.39527209926215,128.593215414396));
#53658=CARTESIAN_POINT('Ctrl Pts',(70.3870436013745,-4.45461349788046,128.715341072046));
#53659=CARTESIAN_POINT('Ctrl Pts',(70.3793898062057,-4.50880088122335,128.839698388077));
#53660=CARTESIAN_POINT('Ctrl Pts',(70.3717331260633,-4.56300868961845,128.964102578575));
#53661=CARTESIAN_POINT('Ctrl Pts',(70.3640764459209,-4.61205843806267,129.090739741065));
#53662=CARTESIAN_POINT('Ctrl Pts',(70.3564197657785,-4.65577518997623,129.219134941865));
#53663=CARTESIAN_POINT('Ctrl Pts',(70.3492802716263,-4.69653900521189,129.338857428406));
#53664=CARTESIAN_POINT('Ctrl Pts',(70.342140777474,-4.7326663351914,129.460108031017));
#53665=CARTESIAN_POINT('Ctrl Pts',(70.3350012833217,-4.76405452823407,129.582490119308));
#53666=CARTESIAN_POINT('Ctrl Pts',(72.0846889553802,-4.76405452823408,129.582490119308));
#53667=CARTESIAN_POINT('Ctrl Pts',(72.0768771839665,-4.79842438085585,129.716497653045));
#53668=CARTESIAN_POINT('Ctrl Pts',(72.0690654125529,-4.8271544673346,129.852029213444));
#53669=CARTESIAN_POINT('Ctrl Pts',(72.0612536411393,-4.85012136542963,129.988575227219));
#53670=CARTESIAN_POINT('Ctrl Pts',(72.0534433806316,-4.873083821405,130.125094831084));
#53671=CARTESIAN_POINT('Ctrl Pts',(72.0456331201239,-4.89028523801872,130.262628122795));
#53672=CARTESIAN_POINT('Ctrl Pts',(72.0378228596163,-4.90165330297286,130.400655329075));
#53673=CARTESIAN_POINT('Ctrl Pts',(72.0301683850745,-4.91279461685024,130.535929400343));
#53674=CARTESIAN_POINT('Ctrl Pts',(72.0225139105328,-4.91833309546384,130.671677509427));
#53675=CARTESIAN_POINT('Ctrl Pts',(72.0148594359911,-4.91824905725744,130.807405824667));
#53676=CARTESIAN_POINT('',(72.3601405640541,-4.91824826462081,130.80022902533));
#53677=CARTESIAN_POINT('Ctrl Pts',(72.4299696197722,-4.76405452823407,129.582490119308));
#53678=CARTESIAN_POINT('Ctrl Pts',(72.420648395519,-4.804730645262,129.741085682254));
#53679=CARTESIAN_POINT('Ctrl Pts',(72.4113271712659,-4.83752185098372,129.901864273602));
#53680=CARTESIAN_POINT('Ctrl Pts',(72.4020059470127,-4.86222315289459,130.064111285276));
#53681=CARTESIAN_POINT('Ctrl Pts',(72.3927861825788,-4.88665558565701,130.224592267936));
#53682=CARTESIAN_POINT('Ctrl Pts',(72.3835664181449,-4.90317321832964,130.386509839184));
#53683=CARTESIAN_POINT('Ctrl Pts',(72.374346653711,-4.91162412170554,130.549151782334));
#53684=CARTESIAN_POINT('Ctrl Pts',(72.369611290492,-4.91596459019584,130.632686310898));
#53685=CARTESIAN_POINT('Ctrl Pts',(72.364875927273,-4.91817785348301,130.716411592138));
#53686=CARTESIAN_POINT('Ctrl Pts',(72.3601405640541,-4.91824826462081,130.800229025329));
#53687=CARTESIAN_POINT('Ctrl Pts',(72.3601405640086,-4.91824826462148,130.800229026135));
#53688=CARTESIAN_POINT('Ctrl Pts',(72.3521524660341,-4.91836704135129,130.941620897751));
#53689=CARTESIAN_POINT('Ctrl Pts',(72.3441643680595,-4.91238371391025,131.083109084369));
#53690=CARTESIAN_POINT('Ctrl Pts',(72.336176270085,-4.90030416846064,131.224124978925));
#53691=CARTESIAN_POINT('Ctrl Pts',(72.328463029565,-4.88864026051642,131.360288745984));
#53692=CARTESIAN_POINT('Ctrl Pts',(72.3207497890451,-4.87129276819467,131.496011763084));
#53693=CARTESIAN_POINT('Ctrl Pts',(72.3130365485251,-4.84831995643009,131.630784638624));
#53694=CARTESIAN_POINT('Ctrl Pts',(72.3053236522739,-4.82534817002179,131.765551498783));
#53695=CARTESIAN_POINT('Ctrl Pts',(72.2976107560226,-4.79675162952417,131.899367912903));
#53696=CARTESIAN_POINT('Ctrl Pts',(72.2898978597713,-4.76264004127198,132.031732973362));
#53697=CARTESIAN_POINT('Ctrl Pts',(72.2821836032061,-4.7285224368013,132.164121378883));
#53698=CARTESIAN_POINT('Ctrl Pts',(72.2744693466409,-4.68888794776022,132.295057539556));
#53699=CARTESIAN_POINT('Ctrl Pts',(72.2667550900757,-4.64389651894893,132.424054472526));
#53700=CARTESIAN_POINT('Ctrl Pts',(72.2590377680226,-4.59888721146346,132.55310266624));
#53701=CARTESIAN_POINT('Ctrl Pts',(72.2513204459696,-4.54851685859578,132.68020972698));
#53702=CARTESIAN_POINT('Ctrl Pts',(72.2436031239165,-4.49299385105062,132.804907871925));
#53703=CARTESIAN_POINT('Ctrl Pts',(72.2358767886456,-4.43740599705268,132.929751654375));
#53704=CARTESIAN_POINT('Ctrl Pts',(72.2281504533747,-4.37665363631315,133.052180544785));
#53705=CARTESIAN_POINT('Ctrl Pts',(72.2204241181038,-4.31099167701347,133.17175028199));
#53706=CARTESIAN_POINT('Ctrl Pts',(72.2126924048926,-4.24528401349726,133.291403246093));
#53707=CARTESIAN_POINT('Ctrl Pts',(72.2049606916814,-4.17466014955658,133.408192757649));
#53708=CARTESIAN_POINT('Ctrl Pts',(72.1972289784701,-4.09941814286994,133.521703796557));
#53709=CARTESIAN_POINT('Ctrl Pts',(72.1894861168925,-4.02406764464513,133.635378507166));
#53710=CARTESIAN_POINT('Ctrl Pts',(72.1817432553149,-3.9440859441397,133.745764992871));
#53711=CARTESIAN_POINT('Ctrl Pts',(72.1740003937372,-3.85981134077771,133.852481264145));
#53712=CARTESIAN_POINT('Ctrl Pts',(72.1721423333647,-3.83958790021258,133.878090048801));
#53713=CARTESIAN_POINT('Ctrl Pts',(72.1702842729921,-3.81911741400135,133.90348764891));
#53714=CARTESIAN_POINT('Ctrl Pts',(72.1684262126196,-3.7984048624164,133.928669111244));
#53715=CARTESIAN_POINT('Ctrl Pts',(72.1606518785005,-3.71174121097692,134.034031189185));
#53716=CARTESIAN_POINT('Ctrl Pts',(72.1528775443814,-3.6205530881804,134.135951540015));
#53717=CARTESIAN_POINT('Ctrl Pts',(72.1451032102623,-3.52514412859453,134.234016859106));
#53718=CARTESIAN_POINT('Ctrl Pts',(72.1373384573153,-3.42985275202453,134.331961321456));
#53719=CARTESIAN_POINT('Ctrl Pts',(72.1295737043682,-3.33035115872052,134.426059927572));
#53720=CARTESIAN_POINT('Ctrl Pts',(72.1218089514211,-3.22698392472551,134.515931418731));
#53721=CARTESIAN_POINT('Ctrl Pts',(72.1140519105361,-3.12371935652432,134.605713648259));
#53722=CARTESIAN_POINT('Ctrl Pts',(72.1062948696511,-3.01659708136271,134.691276863034));
#53723=CARTESIAN_POINT('Ctrl Pts',(72.0985378287661,-2.90599904628351,134.772276015543));
#53724=CARTESIAN_POINT('Ctrl Pts',(72.090786637526,-2.79548441404283,134.85321408596));
#53725=CARTESIAN_POINT('Ctrl Pts',(72.0830354462858,-2.68149955316458,134.929594714724));
#53726=CARTESIAN_POINT('Ctrl Pts',(72.0752842550457,-2.56445978396509,135.001112823609));
#53727=CARTESIAN_POINT('Ctrl Pts',(72.0675363582686,-2.44746975978988,135.07260053539));
#53728=CARTESIAN_POINT('Ctrl Pts',(72.0597884614916,-2.32742774265982,135.139229634374));
#53729=CARTESIAN_POINT('Ctrl Pts',(72.0520405647145,-2.20477816915101,135.200738250042));
#53730=CARTESIAN_POINT('Ctrl Pts',(72.0442942886304,-2.08215425128896,135.262233999434));
#53731=CARTESIAN_POINT('Ctrl Pts',(72.0365480125463,-1.95692421122605,135.318611220823));
#53732=CARTESIAN_POINT('Ctrl Pts',(72.0288017364622,-1.82955687580346,135.369654113137));
#53733=CARTESIAN_POINT('Ctrl Pts',(72.0210554031969,-1.70218860018439,135.420697382237));
#53734=CARTESIAN_POINT('Ctrl Pts',(72.0133090699315,-1.57268336063143,135.466406098253));
#53735=CARTESIAN_POINT('Ctrl Pts',(72.0055627366662,-1.4415293648972,135.506612860124));
#53736=CARTESIAN_POINT('Ctrl Pts',(71.9978146686632,-1.31034599813435,135.546828626021));
#53737=CARTESIAN_POINT('Ctrl Pts',(71.9900666006602,-1.1775135141936,135.581539871419));
#53738=CARTESIAN_POINT('Ctrl Pts',(71.9823185326572,-1.04353426844288,135.610629367135));
#53739=CARTESIAN_POINT('Ctrl Pts',(71.9745622299154,-0.909412627955762,
135.639749779513));
#53740=CARTESIAN_POINT('Ctrl Pts',(71.9668059271736,-0.774142173662908,
135.663236423692));
#53741=CARTESIAN_POINT('Ctrl Pts',(71.9590496244317,-0.638234970176708,
135.681023327385));
#53742=CARTESIAN_POINT('Ctrl Pts',(71.9512891819175,-0.50225522892355,135.698819724485));
#53743=CARTESIAN_POINT('Ctrl Pts',(71.9435287394034,-0.365638450545266,
135.710910284962));
#53744=CARTESIAN_POINT('Ctrl Pts',(71.9357682968892,-0.228899776495294,
135.717281129321));
#53745=CARTESIAN_POINT('Ctrl Pts',(71.9279953966238,-0.0919415973870206,
135.723662200725));
#53746=CARTESIAN_POINT('Ctrl Pts',(71.9202224963584,0.0451384772335222,
135.724305206021));
#53747=CARTESIAN_POINT('Ctrl Pts',(71.912449596093,0.181826450764625,135.719248429541));
#53748=CARTESIAN_POINT('Ctrl Pts',(71.9049592603309,0.313545472161917,135.714375479623));
#53749=CARTESIAN_POINT('Ctrl Pts',(71.8974689245689,0.44490009815809,135.704209979903));
#53750=CARTESIAN_POINT('Ctrl Pts',(71.8899785888068,0.575438611413163,135.688831261044));
#53751=CARTESIAN_POINT('Ctrl Pts',(71.8822042546877,0.710926532074436,135.672869453384));
#53752=CARTESIAN_POINT('Ctrl Pts',(71.8744299205686,0.845964417527061,135.65124074226));
#53753=CARTESIAN_POINT('Ctrl Pts',(71.8666555864496,0.980040420982166,135.623977182786));
#53754=CARTESIAN_POINT('Ctrl Pts',(71.8588908335025,1.11395118774573,135.596747223212));
#53755=CARTESIAN_POINT('Ctrl Pts',(71.8511260805554,1.24690205172469,135.563896309825));
#53756=CARTESIAN_POINT('Ctrl Pts',(71.8433613276083,1.37838599738973,135.525508264558));
#53757=CARTESIAN_POINT('Ctrl Pts',(71.8356042867233,1.50973935134625,135.487158346839));
#53758=CARTESIAN_POINT('Ctrl Pts',(71.8278472458383,1.63962831354438,135.443282350468));
#53759=CARTESIAN_POINT('Ctrl Pts',(71.8200902049533,1.76755613403222,135.394015111702));
#53760=CARTESIAN_POINT('Ctrl Pts',(71.8123390137131,1.89538748315593,135.344785025744));
#53761=CARTESIAN_POINT('Ctrl Pts',(71.804587822473,2.02126027088641,135.290171929615));
#53762=CARTESIAN_POINT('Ctrl Pts',(71.7968366312328,2.14469333549757,135.230360341829));
#53763=CARTESIAN_POINT('Ctrl Pts',(71.7890887344558,2.26807393776324,135.170574175562));
#53764=CARTESIAN_POINT('Ctrl Pts',(71.7813408376787,2.38901652822067,135.105594082291));
#53765=CARTESIAN_POINT('Ctrl Pts',(71.7735929409016,2.50706055896076,135.035652431682));
#53766=CARTESIAN_POINT('Ctrl Pts',(71.7658466648175,2.62507989743435,134.965725411358));
#53767=CARTESIAN_POINT('Ctrl Pts',(71.7581003887334,2.74020154604287,134.890839097205));
#53768=CARTESIAN_POINT('Ctrl Pts',(71.7503541126493,2.85199053287238,134.811271280771));
#53769=CARTESIAN_POINT('Ctrl Pts',(71.7426077793839,2.96378034490288,134.731702876986));
#53770=CARTESIAN_POINT('Ctrl Pts',(71.7348614461186,3.07223712754459,134.647453128674));
#53771=CARTESIAN_POINT('Ctrl Pts',(71.7271151128532,3.17695615333055,134.558842294484));
#53772=CARTESIAN_POINT('Ctrl Pts',(71.7193670448502,3.28169863021613,134.470211616513));
#53773=CARTESIAN_POINT('Ctrl Pts',(71.7116189768472,3.38270138622691,134.377218161769));
#53774=CARTESIAN_POINT('Ctrl Pts',(71.7038709088443,3.47959425778319,134.280221210815));
#53775=CARTESIAN_POINT('Ctrl Pts',(71.6961146061024,3.57659010823639,134.183121170347));
#53776=CARTESIAN_POINT('Ctrl Pts',(71.6883583033606,3.66946707187015,134.082009410964));
#53777=CARTESIAN_POINT('Ctrl Pts',(71.6806020006187,3.75789286090079,133.977281087494));
#53778=CARTESIAN_POINT('Ctrl Pts',(71.6728415581046,3.84636584543755,133.872496867365));
#53779=CARTESIAN_POINT('Ctrl Pts',(71.6650811155904,3.93038268215294,133.764092545794));
#53780=CARTESIAN_POINT('Ctrl Pts',(71.6573206730762,4.00965324729545,133.652494023668));
#53781=CARTESIAN_POINT('Ctrl Pts',(71.6495477728108,4.08905106458643,133.540716353687));
#53782=CARTESIAN_POINT('Ctrl Pts',(71.6417748725454,4.16368717185269,133.425734564668));
#53783=CARTESIAN_POINT('Ctrl Pts',(71.6340019722799,4.23331595106767,133.308001790126));
#53784=CARTESIAN_POINT('Ctrl Pts',(71.6265116365179,4.30041354877379,133.194548898489));
#53785=CARTESIAN_POINT('Ctrl Pts',(71.6190213007559,4.36286140982298,133.078541830577));
#53786=CARTESIAN_POINT('Ctrl Pts',(71.6115309649939,4.4204821130932,132.960403509144));
#53787=CARTESIAN_POINT('Ctrl Pts',(71.6037566308748,4.48028752284144,132.837785937345));
#53788=CARTESIAN_POINT('Ctrl Pts',(71.5959822967557,4.53508195118663,132.712483893169));
#53789=CARTESIAN_POINT('Ctrl Pts',(71.5882079626366,4.58461570131261,132.584945334387));
#53790=CARTESIAN_POINT('Ctrl Pts',(71.5804432096895,4.63408840551846,132.457563955481));
#53791=CARTESIAN_POINT('Ctrl Pts',(71.5726784567425,4.67831319118628,132.327951907138));
#53792=CARTESIAN_POINT('Ctrl Pts',(71.5649137037954,4.71708652580282,132.196581063684));
#53793=CARTESIAN_POINT('Ctrl Pts',(71.5571566629104,4.75582135019678,132.065340699604));
#53794=CARTESIAN_POINT('Ctrl Pts',(71.5493996220255,4.78911538860001,131.932345389292));
#53795=CARTESIAN_POINT('Ctrl Pts',(71.5416425811405,4.81681357708976,131.798085944839));
#53796=CARTESIAN_POINT('Ctrl Pts',(71.5338913899004,4.84449087816003,131.663927746478));
#53797=CARTESIAN_POINT('Ctrl Pts',(71.5261401986602,4.86658065004571,131.528507692802));
#53798=CARTESIAN_POINT('Ctrl Pts',(71.5183890074202,4.88297805373112,131.392330335562));
#53799=CARTESIAN_POINT('Ctrl Pts',(71.5106411106431,4.89936848808262,131.256210857331));
#53800=CARTESIAN_POINT('Ctrl Pts',(71.502893213866,4.91007131961105,131.119335103067));
#53801=CARTESIAN_POINT('Ctrl Pts',(71.4951453170889,4.91503311010378,130.98221614625));
#53802=CARTESIAN_POINT('Ctrl Pts',(71.4873990410048,4.91999386269691,130.845125871764));
#53803=CARTESIAN_POINT('Ctrl Pts',(71.4796527649208,4.91921594878504,130.707792886375));
#53804=CARTESIAN_POINT('Ctrl Pts',(71.4719064888367,4.91269796932078,130.570733297393));
#53805=CARTESIAN_POINT('Ctrl Pts',(71.4641601555713,4.9061799417423,130.433672696667));
#53806=CARTESIAN_POINT('Ctrl Pts',(71.456413822306,4.89392178263315,130.296885886899));
#53807=CARTESIAN_POINT('Ctrl Pts',(71.4486674890406,4.87597416958209,130.160886484389));
#53808=CARTESIAN_POINT('Ctrl Pts',(71.4409194210377,4.85802253728749,130.024856625755));
#53809=CARTESIAN_POINT('Ctrl Pts',(71.4331713530347,4.8343789668538,129.889614912796));
#53810=CARTESIAN_POINT('Ctrl Pts',(71.4254232850317,4.80514564873579,129.755666974534));
#53811=CARTESIAN_POINT('Ctrl Pts',(71.4176669822898,4.77588126109942,129.621576674809));
#53812=CARTESIAN_POINT('Ctrl Pts',(71.409910679548,4.74101534178669,129.488783279153));
#53813=CARTESIAN_POINT('Ctrl Pts',(71.4021543768062,4.70070073608266,129.357779941526));
#53814=CARTESIAN_POINT('Ctrl Pts',(71.394393934292,4.66036461325975,129.226706683474));
#53815=CARTESIAN_POINT('Ctrl Pts',(71.3866334917779,4.61457413982189,129.097425755532));
#53816=CARTESIAN_POINT('Ctrl Pts',(71.3788730492637,4.56353081927382,128.970411456864));
#53817=CARTESIAN_POINT('Ctrl Pts',(71.3711001489983,4.51240555945615,128.843193263568));
#53818=CARTESIAN_POINT('Ctrl Pts',(71.3633272487328,4.45601076296702,128.71824932717));
#53819=CARTESIAN_POINT('Ctrl Pts',(71.3555543484674,4.39459490132233,128.596031222804));
#53820=CARTESIAN_POINT('Ctrl Pts',(71.3480640127053,4.3354116609449,128.478256054378));
#53821=CARTESIAN_POINT('Ctrl Pts',(71.3405736769432,4.27156622349005,128.363012246424));
#53822=CARTESIAN_POINT('Ctrl Pts',(71.333083341181,4.20331850539734,128.250677668435));
#53823=CARTESIAN_POINT('Ctrl Pts',(71.3253090070619,4.13248315433055,128.134083890778));
#53824=CARTESIAN_POINT('Ctrl Pts',(71.3175346729429,4.05668072277566,128.020254970803));
#53825=CARTESIAN_POINT('Ctrl Pts',(71.3097603388238,3.97615312306491,127.909643117629));
#53826=CARTESIAN_POINT('Ctrl Pts',(71.3019955858767,3.8957247664239,127.799167583679));
#53827=CARTESIAN_POINT('Ctrl Pts',(71.2942308329296,3.81058305625279,127.691901540906));
#53828=CARTESIAN_POINT('Ctrl Pts',(71.2864660799825,3.72101497949097,127.588271286577));
#53829=CARTESIAN_POINT('Ctrl Pts',(71.2787090390975,3.63153586300561,127.484743959277));
#53830=CARTESIAN_POINT('Ctrl Pts',(71.2709519982125,3.53763938282546,127.384845528017));
#53831=CARTESIAN_POINT('Ctrl Pts',(71.2631949573274,3.43965465722664,127.288971748391));
#53832=CARTESIAN_POINT('Ctrl Pts',(71.2554437660873,3.34174382267147,127.193170267928));
#53833=CARTESIAN_POINT('Ctrl Pts',(71.2476925748472,3.23975115749493,127.101387670395));
#53834=CARTESIAN_POINT('Ctrl Pts',(71.2399413836071,3.13404448732548,127.01398488237));
#53835=CARTESIAN_POINT('Ctrl Pts',(71.23219348683,3.02838274531089,126.926619242861));
#53836=CARTESIAN_POINT('Ctrl Pts',(71.2244455900528,2.91901043859797,126.843629959021));
#53837=CARTESIAN_POINT('Ctrl Pts',(71.2166976932758,2.80633034577734,126.765339318678));
#53838=CARTESIAN_POINT('Ctrl Pts',(71.2089514171917,2.69367382320295,126.68706505505));
#53839=CARTESIAN_POINT('Ctrl Pts',(71.2012051411076,2.57771121165227,126.613487702908));
#53840=CARTESIAN_POINT('Ctrl Pts',(71.1934588650235,2.45887597060068,126.544887407919));
#53841=CARTESIAN_POINT('Ctrl Pts',(71.1857125317581,2.34003985233441,126.476286606537));
#53842=CARTESIAN_POINT('Ctrl Pts',(71.1779661984928,2.21833140085124,126.412663131081));
#53843=CARTESIAN_POINT('Ctrl Pts',(71.1702198652274,2.09421012856732,126.354251967218));
#53844=CARTESIAN_POINT('Ctrl Pts',(71.1624717972245,1.97006106018539,126.295827722579));
#53845=CARTESIAN_POINT('Ctrl Pts',(71.1547237292215,1.8434984494833,126.242618278689));
#53846=CARTESIAN_POINT('Ctrl Pts',(71.1469756612185,1.71500293291465,126.194810964661));
#53847=CARTESIAN_POINT('Ctrl Pts',(71.1392193584767,1.58637084978152,126.146952840451));
#53848=CARTESIAN_POINT('Ctrl Pts',(71.1314630557349,1.45580212407566,126.104508451812));
#53849=CARTESIAN_POINT('Ctrl Pts',(71.123706752993,1.32379427680081,126.067615767438));
#53850=CARTESIAN_POINT('Ctrl Pts',(71.1159463104788,1.19171597296336,126.030703392328));
#53851=CARTESIAN_POINT('Ctrl Pts',(71.1081858679647,1.05819739747268,125.999348715071));
#53852=CARTESIAN_POINT('Ctrl Pts',(71.1004254254505,0.923746509212891,125.973638575343));
#53853=CARTESIAN_POINT('Ctrl Pts',(71.0926525251851,0.789079788451096,125.947887163417));
#53854=CARTESIAN_POINT('Ctrl Pts',(71.0848796249197,0.653478151141005,125.927798453338));
#53855=CARTESIAN_POINT('Ctrl Pts',(71.0771067246542,0.517455825156352,125.913407486375));
#53856=CARTESIAN_POINT('Ctrl Pts',(71.0696163888922,0.386378253340808,125.899539667309));
#53857=CARTESIAN_POINT('Ctrl Pts',(71.0621260531302,0.254910355380659,125.890962548851));
#53858=CARTESIAN_POINT('Ctrl Pts',(71.0546357173681,0.123510534766719,125.88766170363));
#53859=CARTESIAN_POINT('Ctrl Pts',(71.0468613832491,-0.0128713499838206,
125.884235705859));
#53860=CARTESIAN_POINT('Ctrl Pts',(71.03908704913,-0.14961190999431,125.88648312669));
#53861=CARTESIAN_POINT('Ctrl Pts',(71.0313127150109,-0.286199929399382,
125.894444868501));
#53862=CARTESIAN_POINT('Ctrl Pts',(71.0235479620638,-0.422619616277758,
125.902396798178));
#53863=CARTESIAN_POINT('Ctrl Pts',(71.0157832091168,-0.558886750044252,
125.916049014046));
#53864=CARTESIAN_POINT('Ctrl Pts',(71.0080184561697,-0.694487551284044,
125.935390489951));
#53865=CARTESIAN_POINT('Ctrl Pts',(71.0002614152847,-0.82995367189604,125.954712755629));
#53866=CARTESIAN_POINT('Ctrl Pts',(70.9925043743997,-0.964754392471565,
125.97971298144));
#53867=CARTESIAN_POINT('Ctrl Pts',(70.9847473335147,-1.09837885615307,126.010328186422));
#53868=CARTESIAN_POINT('Ctrl Pts',(70.9769961422746,-1.23190255258751,126.040920304241));
#53869=CARTESIAN_POINT('Ctrl Pts',(70.9692449510345,-1.36425137814753,126.077118886155));
#53870=CARTESIAN_POINT('Ctrl Pts',(70.9614937597943,-1.49492285634377,126.118809559677));
#53871=CARTESIAN_POINT('Ctrl Pts',(70.9537458630172,-1.62553879567608,126.160482513552));
#53872=CARTESIAN_POINT('Ctrl Pts',(70.9459979662401,-1.75447843389537,126.207642797732));
#53873=CARTESIAN_POINT('Ctrl Pts',(70.9382500694631,-1.88125290945574,126.260125747628));
#53874=CARTESIAN_POINT('Ctrl Pts',(70.930503793379,-2.00800086652884,126.312597719221));
#53875=CARTESIAN_POINT('Ctrl Pts',(70.9227575172949,-2.13258420079174,126.370389992492));
#53876=CARTESIAN_POINT('Ctrl Pts',(70.9150112412108,-2.25453292232848,126.43328931128));
#53877=CARTESIAN_POINT('Ctrl Pts',(70.9072649079454,-2.37648254406289,126.496189094377));
#53878=CARTESIAN_POINT('Ctrl Pts',(70.89951857468,-2.49579716679538,126.564195818998));
#53879=CARTESIAN_POINT('Ctrl Pts',(70.8917722414147,-2.61203071274441,126.637049899827));
#53880=CARTESIAN_POINT('Ctrl Pts',(70.8840241734117,-2.72829028839078,126.709920295823));
#53881=CARTESIAN_POINT('Ctrl Pts',(70.8762761054087,-2.84146708305424,126.787640000511));
#53882=CARTESIAN_POINT('Ctrl Pts',(70.8685280374057,-2.95114369570283,126.869905896793));
#53883=CARTESIAN_POINT('Ctrl Pts',(70.8607717346638,-3.06093687395969,126.952259226248));
#53884=CARTESIAN_POINT('Ctrl Pts',(70.8530154319219,-3.16722212577158,127.039168164261));
#53885=CARTESIAN_POINT('Ctrl Pts',(70.8452591291801,-3.26961445191326,127.130288707772));
#53886=CARTESIAN_POINT('Ctrl Pts',(70.8374986866659,-3.37206142792266,127.22145788506));
#53887=CARTESIAN_POINT('Ctrl Pts',(70.8297382441518,-3.47061105733544,127.316842875125));
#53888=CARTESIAN_POINT('Ctrl Pts',(70.8219778016376,-3.5649157152874,127.416063256738));
#53889=CARTESIAN_POINT('Ctrl Pts',(70.8142049013722,-3.65937175944821,127.515442915715));
#53890=CARTESIAN_POINT('Ctrl Pts',(70.8064320011067,-3.74956895739949,127.61866997513));
#53891=CARTESIAN_POINT('Ctrl Pts',(70.7986591008413,-3.83519987520419,127.725330741171));
#53892=CARTESIAN_POINT('Ctrl Pts',(70.7911687650793,-3.91771789345501,127.828114119703));
#53893=CARTESIAN_POINT('Ctrl Pts',(70.7836784293173,-3.99599567625939,127.934085643587));
#53894=CARTESIAN_POINT('Ctrl Pts',(70.7761880935553,-4.06979758348905,128.042851846635));
#53895=CARTESIAN_POINT('Ctrl Pts',(70.7681673327391,-4.14882574250351,128.159320283734));
#53896=CARTESIAN_POINT('Ctrl Pts',(70.7601465719229,-4.22297037620041,128.279360341728));
#53897=CARTESIAN_POINT('Ctrl Pts',(70.7521258111067,-4.29189898167231,128.402530858066));
#53898=CARTESIAN_POINT('Ctrl Pts',(70.744239767767,-4.35966985560124,128.523632590465));
#53899=CARTESIAN_POINT('Ctrl Pts',(70.7363537244274,-4.42239831387511,128.647760124096));
#53900=CARTESIAN_POINT('Ctrl Pts',(70.7284676810877,-4.47980973293724,128.774462142474));
#53901=CARTESIAN_POINT('Ctrl Pts',(70.7203795615332,-4.53869229307202,128.9044108415));
#53902=CARTESIAN_POINT('Ctrl Pts',(70.7122914419787,-4.59198139575677,129.037067438954));
#53903=CARTESIAN_POINT('Ctrl Pts',(70.7042033224242,-4.63942941463817,129.171915283385));
#53904=CARTESIAN_POINT('Ctrl Pts',(70.6961152028696,-4.68687743351954,129.306763127815));
#53905=CARTESIAN_POINT('Ctrl Pts',(70.6880270833151,-4.72848417136962,129.443801837749));
#53906=CARTESIAN_POINT('Ctrl Pts',(70.6799389637605,-4.76405452823405,129.582490119308));
#53907=CARTESIAN_POINT('Origin',(213.235140564004,0.,130.804360617566));
#53908=CARTESIAN_POINT('',(68.5848726604778,-4.764054528234,129.582490119308));
#53909=CARTESIAN_POINT('',(68.9302764532207,-4.76405452823407,129.582490119308));
#53910=CARTESIAN_POINT('',(213.235140564004,-4.76405452823405,129.582490119308));
#53911=CARTESIAN_POINT('',(70.2648594360286,-4.9182492826405,130.80701698844));
#53912=CARTESIAN_POINT('Ctrl Pts',(70.2648594359911,-4.91824928264014,130.807016989099));
#53913=CARTESIAN_POINT('Ctrl Pts',(70.2562002380237,-4.91816710427662,130.959169529675));
#53914=CARTESIAN_POINT('Ctrl Pts',(70.2475410400562,-4.91102501605397,131.111127544565));
#53915=CARTESIAN_POINT('Ctrl Pts',(70.2388818420887,-4.89687297662618,131.262419689399));
#53916=CARTESIAN_POINT('Ctrl Pts',(70.2311075079696,-4.88416710208777,131.398251632258));
#53917=CARTESIAN_POINT('Ctrl Pts',(70.2233331738506,-4.86578515640856,131.533769659566));
#53918=CARTESIAN_POINT('Ctrl Pts',(70.2155588397315,-4.84174690256046,131.668461302698));
#53919=CARTESIAN_POINT('Ctrl Pts',(70.2077940867844,-4.8177382737119,131.802986950418));
#53920=CARTESIAN_POINT('Ctrl Pts',(70.2000293338373,-4.78808727472672,131.936687859174));
#53921=CARTESIAN_POINT('Ctrl Pts',(70.1922645808903,-4.75286553642302,132.06905514795));
#53922=CARTESIAN_POINT('Ctrl Pts',(70.1845075400053,-4.71767878084629,132.201290967668));
#53923=CARTESIAN_POINT('Ctrl Pts',(70.1767504991203,-4.67693239662847,132.332195427988));
#53924=CARTESIAN_POINT('Ctrl Pts',(70.1689934582353,-4.63074926056585,132.46126868631));
#53925=CARTESIAN_POINT('Ctrl Pts',(70.1612422669952,-4.58460095156539,132.590244609484));
#53926=CARTESIAN_POINT('Ctrl Pts',(70.153491075755,-4.5330241824954,132.717391712683));
#53927=CARTESIAN_POINT('Ctrl Pts',(70.1457398845149,-4.47619187217681,132.842224544809));
#53928=CARTESIAN_POINT('Ctrl Pts',(70.1379919877378,-4.41938371710624,132.967004319651));
#53929=CARTESIAN_POINT('Ctrl Pts',(70.1302440909608,-4.35732462519227,133.089471424699));
#53930=CARTESIAN_POINT('Ctrl Pts',(70.1224961941837,-4.29023584730505,133.209159868439));
#53931=CARTESIAN_POINT('Ctrl Pts',(70.1147499180996,-4.2231611029439,133.328823275936));
#53932=CARTESIAN_POINT('Ctrl Pts',(70.1070036420156,-4.15105895634079,133.44570883741));
#53933=CARTESIAN_POINT('Ctrl Pts',(70.0992573659315,-4.07419668092015,133.559375039975));
#53934=CARTESIAN_POINT('Ctrl Pts',(70.0915110326661,-3.99733383811966,133.673042081598));
#53935=CARTESIAN_POINT('Ctrl Pts',(70.0837646994008,-3.9157110153896,133.783489393023));
#53936=CARTESIAN_POINT('Ctrl Pts',(70.0760183661355,-3.82963866680803,133.89030467801));
#53937=CARTESIAN_POINT('Ctrl Pts',(70.0682702981325,-3.7435470429209,133.997143883539));
#53938=CARTESIAN_POINT('Ctrl Pts',(70.0605222301296,-3.65300415564433,134.100349139754));
#53939=CARTESIAN_POINT('Ctrl Pts',(70.0527741621266,-3.55836029917016,134.19954176793));
#53940=CARTESIAN_POINT('Ctrl Pts',(70.0450178593848,-3.46361585407893,134.298839819212));
#53941=CARTESIAN_POINT('Ctrl Pts',(70.0372615566429,-3.36476200342189,134.394116440004));
#53942=CARTESIAN_POINT('Ctrl Pts',(70.0295052539011,-3.26218581424232,134.485029955588));
#53943=CARTESIAN_POINT('Ctrl Pts',(70.021744811387,-3.15955487706193,134.575991994453));
#53944=CARTESIAN_POINT('Ctrl Pts',(70.0139843688728,-3.05319794567822,134.662586041209));
#53945=CARTESIAN_POINT('Ctrl Pts',(70.0062239263586,-2.94353383616001,134.744511835207));
#53946=CARTESIAN_POINT('Ctrl Pts',(69.9984510260932,-2.83369368407769,134.826569143763));
#53947=CARTESIAN_POINT('Ctrl Pts',(69.9906781258278,-2.72053606775357,134.903943003572));
#53948=CARTESIAN_POINT('Ctrl Pts',(69.9829052255624,-2.60450809605509,134.976376993383));
#53949=CARTESIAN_POINT('Ctrl Pts',(69.9754148898002,-2.49269803338263,135.046177825215));
#53950=CARTESIAN_POINT('Ctrl Pts',(69.9679245540381,-2.37822294911583,135.111391552588));
#53951=CARTESIAN_POINT('Ctrl Pts',(69.9604342182759,-2.2615013865985,135.171830656492));
#53952=CARTESIAN_POINT('Ctrl Pts',(69.9526598841568,-2.1403542905638,135.234561327389));
#53953=CARTESIAN_POINT('Ctrl Pts',(69.9448855500377,-2.01640324547606,135.292346879857));
#53954=CARTESIAN_POINT('Ctrl Pts',(69.9371112159187,-1.89009008807158,135.344926939235));
#53955=CARTESIAN_POINT('Ctrl Pts',(69.9293464629716,-1.76393260034467,135.397442198389));
#53956=CARTESIAN_POINT('Ctrl Pts',(69.9215817100245,-1.63541914998415,135.444764580192));
#53957=CARTESIAN_POINT('Ctrl Pts',(69.9138169570774,-1.50501659120844,135.48667928706));
#53958=CARTESIAN_POINT('Ctrl Pts',(69.9060599161924,-1.37474355009245,135.52855236365));
#53959=CARTESIAN_POINT('Ctrl Pts',(69.8983028753074,-1.24258550426309,135.565028334931));
#53960=CARTESIAN_POINT('Ctrl Pts',(69.8905458344224,-1.10902940336458,135.5959404035));
#53961=CARTESIAN_POINT('Ctrl Pts',(69.8827946431823,-0.975574018160483,
135.626829161038));
#53962=CARTESIAN_POINT('Ctrl Pts',(69.8750434519422,-0.840723055730653,
135.652162279509));
#53963=CARTESIAN_POINT('Ctrl Pts',(69.867292260702,-0.704978406679796,135.671822842239));
#53964=CARTESIAN_POINT('Ctrl Pts',(69.859544363925,-0.569291452726078,135.691475048705));
#53965=CARTESIAN_POINT('Ctrl Pts',(69.8517964671478,-0.432711953743312,
135.705459438777));
#53966=CARTESIAN_POINT('Ctrl Pts',(69.8440485703708,-0.295751553089399,
135.713710277281));
#53967=CARTESIAN_POINT('Ctrl Pts',(69.8363022942867,-0.158819801598778,
135.721959389888));
#53968=CARTESIAN_POINT('Ctrl Pts',(69.8285560182026,-0.0215076969282203,
135.724477312977));
#53969=CARTESIAN_POINT('Ctrl Pts',(69.8208097421185,0.115668835814261,135.72125026275));
#53970=CARTESIAN_POINT('Ctrl Pts',(69.8130634088532,0.252846381162745,135.718023188702));
#53971=CARTESIAN_POINT('Ctrl Pts',(69.8053170755878,0.389887961729139,135.709051065912));
#53972=CARTESIAN_POINT('Ctrl Pts',(69.7975707423224,0.526278892997474,135.694372231999));
#53973=CARTESIAN_POINT('Ctrl Pts',(69.7898226743195,0.662700368069012,135.679690110862));
#53974=CARTESIAN_POINT('Ctrl Pts',(69.7820746063165,0.798470515253588,135.659298777401));
#53975=CARTESIAN_POINT('Ctrl Pts',(69.7743265383136,0.933081398848373,135.63328825894));
#53976=CARTESIAN_POINT('Ctrl Pts',(69.7665702355717,1.06783534849232,135.60725009619));
#53977=CARTESIAN_POINT('Ctrl Pts',(69.7588139328299,1.20142718885886,135.575580892744));
#53978=CARTESIAN_POINT('Ctrl Pts',(69.751057630088,1.33336024013838,135.538421615538));
#53979=CARTESIAN_POINT('Ctrl Pts',(69.7432971875738,1.46536370805997,135.501242505306));
#53980=CARTESIAN_POINT('Ctrl Pts',(69.7355367450596,1.59570625139251,135.458567604197));
#53981=CARTESIAN_POINT('Ctrl Pts',(69.7277763025455,1.72390887203196,135.410586975815));
#53982=CARTESIAN_POINT('Ctrl Pts',(69.72000340228,1.85231729489918,135.362529324669));
#53983=CARTESIAN_POINT('Ctrl Pts',(69.7122305020147,1.97857857014905,135.309149078453));
#53984=CARTESIAN_POINT('Ctrl Pts',(69.7044576017493,2.10223529005804,135.250683800572));
#53985=CARTESIAN_POINT('Ctrl Pts',(69.6969672659872,2.22139677672685,135.194343882806));
#53986=CARTESIAN_POINT('Ctrl Pts',(69.6894769302251,2.33813951176859,135.133282364889));
#53987=CARTESIAN_POINT('Ctrl Pts',(69.681986594463,2.45207949722928,135.067750020584));
#53988=CARTESIAN_POINT('Ctrl Pts',(69.6742122603439,2.57033955186919,134.999732997528));
#53989=CARTESIAN_POINT('Ctrl Pts',(69.6664379262248,2.68595474127514,134.926683975419));
#53990=CARTESIAN_POINT('Ctrl Pts',(69.6586635921057,2.79846718132218,134.848833945153));
#53991=CARTESIAN_POINT('Ctrl Pts',(69.6508988391586,2.91084095984239,134.771079858092));
#53992=CARTESIAN_POINT('Ctrl Pts',(69.6431340862115,3.02011927892806,134.688536755891));
#53993=CARTESIAN_POINT('Ctrl Pts',(69.6353693332644,3.12586907718008,134.601481312886));
#53994=CARTESIAN_POINT('Ctrl Pts',(69.6276122923794,3.23151384324152,134.514512334575));
#53995=CARTESIAN_POINT('Ctrl Pts',(69.6198552514944,3.33363676284464,134.423040181161));
#53996=CARTESIAN_POINT('Ctrl Pts',(69.6120982106094,3.43183429643148,134.3273843791));
#53997=CARTESIAN_POINT('Ctrl Pts',(69.6043470193693,3.52995777849452,134.231800711824));
#53998=CARTESIAN_POINT('Ctrl Pts',(69.5965958281292,3.62416148764677,134.132039947284));
#53999=CARTESIAN_POINT('Ctrl Pts',(69.5888446368891,3.71407577444676,134.02846114394));
#54000=CARTESIAN_POINT('Ctrl Pts',(69.581096740112,3.80395184527631,133.924926364352));
#54001=CARTESIAN_POINT('Ctrl Pts',(69.5733488433349,3.8895418640421,133.817577068146));
#54002=CARTESIAN_POINT('Ctrl Pts',(69.5656009465578,3.9705139701492,133.706808183906));
#54003=CARTESIAN_POINT('Ctrl Pts',(69.5578546704737,4.05146913863726,133.596062470127));
#54004=CARTESIAN_POINT('Ctrl Pts',(69.5501083943896,4.12780808525213,133.48189890652));
#54005=CARTESIAN_POINT('Ctrl Pts',(69.5423621183054,4.19924034317215,133.36474410501));
#54006=CARTESIAN_POINT('Ctrl Pts',(69.5346157850401,4.27067312838887,133.24758843869));
#54007=CARTESIAN_POINT('Ctrl Pts',(69.5268694517747,4.3371989491043,133.127441824215));
#54008=CARTESIAN_POINT('Ctrl Pts',(69.5191231185094,4.39857186029102,133.004758002666));
#54009=CARTESIAN_POINT('Ctrl Pts',(69.5113750505064,4.45995851551567,132.882046706926));
#54010=CARTESIAN_POINT('Ctrl Pts',(69.5036269825035,4.5161897900859,132.756797423067));
#54011=CARTESIAN_POINT('Ctrl Pts',(69.4958789145005,4.56706687488476,132.62948615375));
#54012=CARTESIAN_POINT('Ctrl Pts',(69.4881226117586,4.61799803245479,132.5020395765));
#54013=CARTESIAN_POINT('Ctrl Pts',(69.4803663090167,4.66356348755793,132.372526999657));
#54014=CARTESIAN_POINT('Ctrl Pts',(69.4726100062749,4.70361337209909,132.241442490081));
#54015=CARTESIAN_POINT('Ctrl Pts',(69.4648495637607,4.74368463246956,132.110288016755));
#54016=CARTESIAN_POINT('Ctrl Pts',(69.4570891212465,4.77823435801524,131.977560317115));
#54017=CARTESIAN_POINT('Ctrl Pts',(69.4493286787323,4.80716354445415,131.843765119851));
#54018=CARTESIAN_POINT('Ctrl Pts',(69.4415557784669,4.83613917059129,131.70975514266));
#54019=CARTESIAN_POINT('Ctrl Pts',(69.4337828782014,4.8594761610183,131.574674628922));
#54020=CARTESIAN_POINT('Ctrl Pts',(69.426009977936,4.87712714450783,131.439036817533));
#54021=CARTESIAN_POINT('Ctrl Pts',(69.418519642174,4.89413647028723,131.308329782241));
#54022=CARTESIAN_POINT('Ctrl Pts',(69.4110293064121,4.90586598580105,131.177105570981));
#54023=CARTESIAN_POINT('Ctrl Pts',(69.4035389706501,4.91231911384552,131.045822801454));
#54024=CARTESIAN_POINT('Ctrl Pts',(69.395764636531,4.91901691420122,130.909562405817));
#54025=CARTESIAN_POINT('Ctrl Pts',(69.3879903024119,4.92005153697714,130.772807291806));
#54026=CARTESIAN_POINT('Ctrl Pts',(69.3802159682929,4.91536982380163,130.636067546525));
#54027=CARTESIAN_POINT('Ctrl Pts',(69.3724512153458,4.91069388041919,130.49949632076));
#54028=CARTESIAN_POINT('Ctrl Pts',(69.3646864623987,4.90031563153282,130.362940813024));
#54029=CARTESIAN_POINT('Ctrl Pts',(69.3569217094516,4.88423377083227,130.226914919373));
#54030=CARTESIAN_POINT('Ctrl Pts',(69.3491646685666,4.86816788286248,130.091024128558));
#54031=CARTESIAN_POINT('Ctrl Pts',(69.3414076276816,4.8464097021061,129.955662290772));
#54032=CARTESIAN_POINT('Ctrl Pts',(69.3336505867966,4.81900993223122,129.82134162713));
#54033=CARTESIAN_POINT('Ctrl Pts',(69.3258993955565,4.79163082473589,129.687122255746));
#54034=CARTESIAN_POINT('Ctrl Pts',(69.3181482043163,4.75861867400674,129.553942877222));
#54035=CARTESIAN_POINT('Ctrl Pts',(69.3103970130762,4.72007576154382,129.422308567972));
#54036=CARTESIAN_POINT('Ctrl Pts',(69.3026491162991,4.68154923084692,129.290730206815));
#54037=CARTESIAN_POINT('Ctrl Pts',(69.2949012195221,4.63749672345477,129.160695983241));
#54038=CARTESIAN_POINT('Ctrl Pts',(69.287153322745,4.58807112520987,129.032698569512));
#54039=CARTESIAN_POINT('Ctrl Pts',(69.2794070466609,4.53865586573464,128.904727930082));
#54040=CARTESIAN_POINT('Ctrl Pts',(69.2716607705768,4.48386989171959,128.778793617534));
#54041=CARTESIAN_POINT('Ctrl Pts',(69.2639144944927,4.42391511944843,128.655370603998));
#54042=CARTESIAN_POINT('Ctrl Pts',(69.2561681612274,4.36395990460476,128.531946679381));
#54043=CARTESIAN_POINT('Ctrl Pts',(69.248421827962,4.29883598619877,128.411034442437));
#54044=CARTESIAN_POINT('Ctrl Pts',(69.2406754946966,4.22879217015668,128.293086071818));
#54045=CARTESIAN_POINT('Ctrl Pts',(69.2329274266936,4.15873266828765,128.17511128748));
#54046=CARTESIAN_POINT('Ctrl Pts',(69.2251793586907,4.08375127596382,128.060102026322));
#54047=CARTESIAN_POINT('Ctrl Pts',(69.2174312906877,4.00414100652024,127.94848284315));
#54048=CARTESIAN_POINT('Ctrl Pts',(69.2096749879459,3.92444612633492,127.836745029782));
#54049=CARTESIAN_POINT('Ctrl Pts',(69.201918685204,3.84011276893118,127.728404810618));
#54050=CARTESIAN_POINT('Ctrl Pts',(69.1941623824622,3.75147559938637,127.62385532914));
#54051=CARTESIAN_POINT('Ctrl Pts',(69.186401939948,3.66279112151537,127.519250046454));
#54052=CARTESIAN_POINT('Ctrl Pts',(69.1786414974338,3.56979851934587,127.418439820144));
#54053=CARTESIAN_POINT('Ctrl Pts',(69.1708810549196,3.47286976251647,127.321781304026));
#54054=CARTESIAN_POINT('Ctrl Pts',(69.1631081546542,3.37578540704155,127.224967623076));
#54055=CARTESIAN_POINT('Ctrl Pts',(69.1553352543888,3.27475255851865,127.132319234892));
#54056=CARTESIAN_POINT('Ctrl Pts',(69.1475623541234,3.17017741406035,127.044153412387));
#54057=CARTESIAN_POINT('Ctrl Pts',(69.1400720183613,3.06940383951158,126.959192639606));
#54058=CARTESIAN_POINT('Ctrl Pts',(69.1325816825992,2.96534128375956,126.878394374491));
#54059=CARTESIAN_POINT('Ctrl Pts',(69.1250913468372,2.8583774449682,126.802003631414));
#54060=CARTESIAN_POINT('Ctrl Pts',(69.1173170127181,2.74735803971859,126.722716510096));
#54061=CARTESIAN_POINT('Ctrl Pts',(69.109542678599,2.63286132807756,126.647926573101));
#54062=CARTESIAN_POINT('Ctrl Pts',(69.1017683444799,2.51528772737339,126.57795425861));
#54063=CARTESIAN_POINT('Ctrl Pts',(69.0940035915328,2.39785902562423,126.508068178743));
#54064=CARTESIAN_POINT('Ctrl Pts',(69.0862388385857,2.27736131248673,126.442988105973));
#54065=CARTESIAN_POINT('Ctrl Pts',(69.0784740856386,2.1542262371748,126.382992912707));
#54066=CARTESIAN_POINT('Ctrl Pts',(69.0707170447536,2.03121346135574,126.323057307513));
#54067=CARTESIAN_POINT('Ctrl Pts',(69.0629600038686,1.90556888540873,126.268196701488));
#54068=CARTESIAN_POINT('Ctrl Pts',(69.0552029629836,1.77775086203394,126.218645304222));
#54069=CARTESIAN_POINT('Ctrl Pts',(69.0474517717435,1.65002922722469,126.169131274051));
#54070=CARTESIAN_POINT('Ctrl Pts',(69.0397005805034,1.52013777040098,126.124918624232));
#54071=CARTESIAN_POINT('Ctrl Pts',(69.0319493892632,1.3885567123026,126.086194308583));
#54072=CARTESIAN_POINT('Ctrl Pts',(69.0242014924861,1.25703157966414,126.047486451801));
#54073=CARTESIAN_POINT('Ctrl Pts',(69.0164535957091,1.1238186483229,126.014262399798));
#54074=CARTESIAN_POINT('Ctrl Pts',(69.008705698932,0.989415055938439,125.986659826776));
#54075=CARTESIAN_POINT('Ctrl Pts',(69.0009594228479,0.855039577887912,125.959063027617));
#54076=CARTESIAN_POINT('Ctrl Pts',(68.9932131467637,0.719474316919027,125.937085447126));
#54077=CARTESIAN_POINT('Ctrl Pts',(68.9854668706796,0.58322802122029,125.920813941454));
#54078=CARTESIAN_POINT('Ctrl Pts',(68.9777205374143,0.446980719782534,125.90454231567));
#54079=CARTESIAN_POINT('Ctrl Pts',(68.969974204149,0.310052761789971,125.893976895116));
#54080=CARTESIAN_POINT('Ctrl Pts',(68.9622278708836,0.172959063631132,125.889152765928));
#54081=CARTESIAN_POINT('Ctrl Pts',(68.9544798028806,0.0358346642889456,
125.884327556409));
#54082=CARTESIAN_POINT('Ctrl Pts',(68.9467317348777,-0.10145515842818,125.885246210441));
#54083=CARTESIAN_POINT('Ctrl Pts',(68.9389836668747,-0.238394833673622,
125.89189168985));
#54084=CARTESIAN_POINT('Ctrl Pts',(68.9312273641329,-0.37548005003533,125.898544232153));
#54085=CARTESIAN_POINT('Ctrl Pts',(68.923471061391,-0.512213984405493,125.910935739367));
#54086=CARTESIAN_POINT('Ctrl Pts',(68.9157147586492,-0.648084979391088,
125.928997151937));
#54087=CARTESIAN_POINT('Ctrl Pts',(68.907954316135,-0.784028492817888,125.947068204428));
#54088=CARTESIAN_POINT('Ctrl Pts',(68.9001938736208,-0.919107764250167,
125.970815124573));
#54089=CARTESIAN_POINT('Ctrl Pts',(68.8924334311066,-1.05282167205489,126.000117743881));
#54090=CARTESIAN_POINT('Ctrl Pts',(68.8846605308412,-1.18675022929499,126.029467402355));
#54091=CARTESIAN_POINT('Ctrl Pts',(68.8768876305758,-1.31930866470442,126.06439048234));
#54092=CARTESIAN_POINT('Ctrl Pts',(68.8691147303103,-1.45001048813332,126.104716732461));
#54093=CARTESIAN_POINT('Ctrl Pts',(68.8616243945483,-1.57596097106219,126.143577021814));
#54094=CARTESIAN_POINT('Ctrl Pts',(68.8541340587863,-1.70018719308175,126.187454361271));
#54095=CARTESIAN_POINT('Ctrl Pts',(68.8466437230243,-1.82227345633294,126.236155005639));
#54096=CARTESIAN_POINT('Ctrl Pts',(68.8388690701877,-1.94899385219394,126.286704221977));
#54097=CARTESIAN_POINT('Ctrl Pts',(68.8310944173512,-2.07381005234418,126.342610272175));
#54098=CARTESIAN_POINT('Ctrl Pts',(68.8233197645146,-2.19623596822923,126.403709457299));
#54099=CARTESIAN_POINT('Ctrl Pts',(68.8155547661712,-2.31850985672469,126.464732770011));
#54100=CARTESIAN_POINT('Ctrl Pts',(68.8077897678278,-2.43839902053174,126.530936213092));
#54101=CARTESIAN_POINT('Ctrl Pts',(68.8000247694845,-2.55543547617925,126.602107342288));
#54102=CARTESIAN_POINT('Ctrl Pts',(68.7922675562135,-2.67235459280879,126.673207116363));
#54103=CARTESIAN_POINT('Ctrl Pts',(68.7845103429426,-2.7864263612898,126.749264462785));
#54104=CARTESIAN_POINT('Ctrl Pts',(68.7767531296716,-2.89720595602794,126.830020331323));
#54105=CARTESIAN_POINT('Ctrl Pts',(68.7687581101219,-3.01138162642746,126.913251863726));
#54106=CARTESIAN_POINT('Ctrl Pts',(68.7607630905721,-3.12205965059716,127.001474441783));
#54107=CARTESIAN_POINT('Ctrl Pts',(68.7527680710223,-3.22878309858132,127.094354854118));
#54108=CARTESIAN_POINT('Ctrl Pts',(68.7450205156125,-3.33220321177032,127.184360405271));
#54109=CARTESIAN_POINT('Ctrl Pts',(68.7372729602028,-3.43190961048867,127.27873944472));
#54110=CARTESIAN_POINT('Ctrl Pts',(68.729525404793,-3.52751887892082,127.377146935673));
#54111=CARTESIAN_POINT('Ctrl Pts',(68.721779520941,-3.62310751937272,127.47553319492));
#54112=CARTESIAN_POINT('Ctrl Pts',(68.714033637089,-3.71460051624365,127.577945896049));
#54113=CARTESIAN_POINT('Ctrl Pts',(68.706287753237,-3.80165106594283,127.684002908053));
#54114=CARTESIAN_POINT('Ctrl Pts',(68.6985418631607,-3.88870168559236,127.79006000528));
#54115=CARTESIAN_POINT('Ctrl Pts',(68.6907959730844,-3.9713096035126,127.899761116662));
#54116=CARTESIAN_POINT('Ctrl Pts',(68.6830500830082,-4.04916835248726,128.012691096345));
#54117=CARTESIAN_POINT('Ctrl Pts',(68.6753025092992,-4.12704402469869,128.125645622284));
#54118=CARTESIAN_POINT('Ctrl Pts',(68.6675549355903,-4.2001682528382,128.24183009085));
#54119=CARTESIAN_POINT('Ctrl Pts',(68.6598073618814,-4.26827816424066,128.360800801403));
#54120=CARTESIAN_POINT('Ctrl Pts',(68.6520529055,-4.33644858209741,128.479877201359));
#54121=CARTESIAN_POINT('Ctrl Pts',(68.6442984491186,-4.39959559598578,128.601744445292));
#54122=CARTESIAN_POINT('Ctrl Pts',(68.6365439927371,-4.4575023965855,128.725934422837));
#54123=CARTESIAN_POINT('Ctrl Pts',(68.6287853919948,-4.51544014541292,128.850190773583));
#54124=CARTESIAN_POINT('Ctrl Pts',(68.6210267912524,-4.56813195087572,128.976771971067));
#54125=CARTESIAN_POINT('Ctrl Pts',(68.6132681905101,-4.61540971117823,129.105191332162));
#54126=CARTESIAN_POINT('Ctrl Pts',(68.6055003269813,-4.6627439151376,129.233764009706));
#54127=CARTESIAN_POINT('Ctrl Pts',(68.5977324634524,-4.70465105193333,129.364178860521));
#54128=CARTESIAN_POINT('Ctrl Pts',(68.5899645999236,-4.74101319515054,129.495935248694));
#54129=CARTESIAN_POINT('Ctrl Pts',(68.588267286775,-4.74895848713026,129.52472461262));
#54130=CARTESIAN_POINT('Ctrl Pts',(68.5865699736264,-4.75663923244104,129.553577993554));
#54131=CARTESIAN_POINT('Ctrl Pts',(68.5848726604777,-4.764054528234,129.582490119308));
#54132=CARTESIAN_POINT('Ctrl Pts',(70.3350012833217,-4.76405452823407,129.582490119308));
#54133=CARTESIAN_POINT('Ctrl Pts',(70.3273374882257,-4.79774776682839,129.713859545221));
#54134=CARTESIAN_POINT('Ctrl Pts',(70.3196736931296,-4.82597963576157,129.846532485872));
#54135=CARTESIAN_POINT('Ctrl Pts',(70.3120098980335,-4.84867284953609,129.980009563299));
#54136=CARTESIAN_POINT('Ctrl Pts',(70.3041514876994,-4.87194233722539,130.116876172006));
#54137=CARTESIAN_POINT('Ctrl Pts',(70.2962930773652,-4.88938805275968,130.254587853234));
#54138=CARTESIAN_POINT('Ctrl Pts',(70.2884346670311,-4.90098342265885,130.392602735646));
#54139=CARTESIAN_POINT('Ctrl Pts',(70.2805762566969,-4.91257879255801,130.530617618058));
#54140=CARTESIAN_POINT('Ctrl Pts',(70.2727178463627,-4.91832386127279,130.668935251341));
#54141=CARTESIAN_POINT('Ctrl Pts',(70.2648594360285,-4.9182492826405,130.807016988441));
#54142=CARTESIAN_POINT('',(70.610140563959,-4.91824936975562,130.806850476685));
#54143=CARTESIAN_POINT('Ctrl Pts',(70.6799389637605,-4.76405452823405,129.582490119308));
#54144=CARTESIAN_POINT('Ctrl Pts',(70.6720764007095,-4.79863292086401,129.717310747372));
#54145=CARTESIAN_POINT('Ctrl Pts',(70.6642138376585,-4.82750701748767,129.853689778277));
#54146=CARTESIAN_POINT('Ctrl Pts',(70.6563512746074,-4.85054752096174,129.991112925044));
#54147=CARTESIAN_POINT('Ctrl Pts',(70.6484922998902,-4.87357750916011,130.128473354334));
#54148=CARTESIAN_POINT('Ctrl Pts',(70.640633325173,-4.89077914228013,130.266876581894));
#54149=CARTESIAN_POINT('Ctrl Pts',(70.6327743504558,-4.9020741159162,130.405797668254));
#54150=CARTESIAN_POINT('Ctrl Pts',(70.6252297549734,-4.91291726150903,130.539161553275));
#54151=CARTESIAN_POINT('Ctrl Pts',(70.6176851594909,-4.91831713022705,130.673002336079));
#54152=CARTESIAN_POINT('Ctrl Pts',(70.6101405640085,-4.91824936975607,130.806850475807));
#54153=CARTESIAN_POINT('Ctrl Pts',(70.610140563959,-4.91824936975562,130.806850476685));
#54154=CARTESIAN_POINT('Ctrl Pts',(70.6016108271431,-4.91817276138222,130.958175939769));
#54155=CARTESIAN_POINT('Ctrl Pts',(70.5930810903272,-4.91110805520333,131.109261575527));
#54156=CARTESIAN_POINT('Ctrl Pts',(70.5845513535113,-4.89714603271158,131.259491144775));
#54157=CARTESIAN_POINT('Ctrl Pts',(70.5759770590162,-4.8831110753411,131.410505483953));
#54158=CARTESIAN_POINT('Ctrl Pts',(70.567402764521,-4.86210663986195,131.560654550213));
#54159=CARTESIAN_POINT('Ctrl Pts',(70.5588284700258,-4.83427521236157,131.709328149385));
#54160=CARTESIAN_POINT('Ctrl Pts',(70.5502311723227,-4.80636911841312,131.858400611662));
#54161=CARTESIAN_POINT('Ctrl Pts',(70.5416338746195,-4.77159947113251,132.005989455552));
#54162=CARTESIAN_POINT('Ctrl Pts',(70.5330365769164,-4.73015873715347,132.151498837583));
#54163=CARTESIAN_POINT('Ctrl Pts',(70.5244085520494,-4.68856989195753,132.297528277286));
#54164=CARTESIAN_POINT('Ctrl Pts',(70.5157805271824,-4.64026231123063,132.44146314563));
#54165=CARTESIAN_POINT('Ctrl Pts',(70.5071525023153,-4.58547784383415,132.58272391178));
#54166=CARTESIAN_POINT('Ctrl Pts',(70.5040151581244,-4.56555697744916,132.634089508301));
#54167=CARTESIAN_POINT('Ctrl Pts',(70.5008778139334,-4.54478017037869,132.685101764255));
#54168=CARTESIAN_POINT('Ctrl Pts',(70.4977404697424,-4.5231605431846,132.735733642923));
#54169=CARTESIAN_POINT('Ctrl Pts',(70.4899661356233,-4.46958713997907,132.861199361022));
#54170=CARTESIAN_POINT('Ctrl Pts',(70.4821918015042,-4.41070457665497,132.984633049248));
#54171=CARTESIAN_POINT('Ctrl Pts',(70.4744174673851,-4.3466881472084,133.105552746315));
#54172=CARTESIAN_POINT('Ctrl Pts',(70.4666527144379,-4.28275061228981,133.226323420663));
#54173=CARTESIAN_POINT('Ctrl Pts',(70.4588879614908,-4.21369198132697,133.344585926272));
#54174=CARTESIAN_POINT('Ctrl Pts',(70.4511232085436,-4.1397358437831,133.459877555226));
#54175=CARTESIAN_POINT('Ctrl Pts',(70.4433661676586,-4.06585316051765,133.575054674909));
#54176=CARTESIAN_POINT('Ctrl Pts',(70.4356091267735,-3.98708286052146,133.687266463047));
#54177=CARTESIAN_POINT('Ctrl Pts',(70.4278520858885,-3.9036945722289,133.796074465722));
#54178=CARTESIAN_POINT('Ctrl Pts',(70.4201008946483,-3.82036916769308,133.904800415437));
#54179=CARTESIAN_POINT('Ctrl Pts',(70.4123497034081,-3.73243294334538,134.010127379731));
#54180=CARTESIAN_POINT('Ctrl Pts',(70.404598512168,-3.64019878564739,134.11164588852));
#54181=CARTESIAN_POINT('Ctrl Pts',(70.3968506153908,-3.54800382992697,134.213121249235));
#54182=CARTESIAN_POINT('Ctrl Pts',(70.3891027186137,-3.45151483645035,134.310791085142));
#54183=CARTESIAN_POINT('Ctrl Pts',(70.3813548218366,-3.35108477392525,134.404279213933));
#54184=CARTESIAN_POINT('Ctrl Pts',(70.3736085457524,-3.25067571920421,134.497747787022));
#54185=CARTESIAN_POINT('Ctrl Pts',(70.3658622696683,-3.14632752117113,134.587036126648));
#54186=CARTESIAN_POINT('Ctrl Pts',(70.3581159935842,-3.03842949908311,134.671805412466));
#54187=CARTESIAN_POINT('Ctrl Pts',(70.3503696603188,-2.9305306805164,134.756575324032));
#54188=CARTESIAN_POINT('Ctrl Pts',(70.3426233270534,-2.81908229304039,134.836825873692));
#54189=CARTESIAN_POINT('Ctrl Pts',(70.334876993788,-2.70450585359283,134.912259247082));
#54190=CARTESIAN_POINT('Ctrl Pts',(70.3271289257849,-2.58990375554607,134.987709513254));
#54191=CARTESIAN_POINT('Ctrl Pts',(70.319380857782,-2.47217253808847,135.058340241574));
#54192=CARTESIAN_POINT('Ctrl Pts',(70.3116327897789,-2.35176139108469,135.123897794383));
#54193=CARTESIAN_POINT('Ctrl Pts',(70.303876487037,-2.23122226968098,135.189525022539));
#54194=CARTESIAN_POINT('Ctrl Pts',(70.2961201842951,-2.10799787294231,135.250068117174));
#54195=CARTESIAN_POINT('Ctrl Pts',(70.2883638815532,-1.98256110886023,135.305319905555));
#54196=CARTESIAN_POINT('Ctrl Pts',(70.280603439039,-1.85705739540033,135.360601183479));
#54197=CARTESIAN_POINT('Ctrl Pts',(70.2728429965248,-1.72933932563703,135.410585385415));
#54198=CARTESIAN_POINT('Ctrl Pts',(70.2650825540106,-1.59989739522771,135.455114469066));
#54199=CARTESIAN_POINT('Ctrl Pts',(70.2573096537452,-1.47024767314038,135.499715034756));
#54200=CARTESIAN_POINT('Ctrl Pts',(70.2495367534797,-1.33886893538751,135.538842871145));
#54201=CARTESIAN_POINT('Ctrl Pts',(70.2417638532142,-1.20626523357843,135.572390320573));
#54202=CARTESIAN_POINT('Ctrl Pts',(70.2342735174526,-1.07848201034693,135.604718235712));
#54203=CARTESIAN_POINT('Ctrl Pts',(70.226783181691,-0.949561639295706,135.631864378736));
#54204=CARTESIAN_POINT('Ctrl Pts',(70.2192928459294,-0.819959932368054,
135.653777981725));
#54205=CARTESIAN_POINT('Ctrl Pts',(70.2115185118103,-0.685444337322694,
135.676522445634));
#54206=CARTESIAN_POINT('Ctrl Pts',(70.2037441776912,-0.549768615832144,
135.69370180099));
#54207=CARTESIAN_POINT('Ctrl Pts',(70.1959698435722,-0.413433006262309,
135.70520301575));
#54208=CARTESIAN_POINT('Ctrl Pts',(70.1882050906251,-0.277265418146605,
135.71669005629));
#54209=CARTESIAN_POINT('Ctrl Pts',(70.180440337678,-0.140439945924335,135.722512847223));
#54210=CARTESIAN_POINT('Ctrl Pts',(70.1726755847309,-0.00346673443578061,
135.722609395765));
#54211=CARTESIAN_POINT('Ctrl Pts',(70.1649185438459,0.133370433327954,135.722705848413));
#54212=CARTESIAN_POINT('Ctrl Pts',(70.1571615029609,0.270354659910084,135.71708737655));
#54213=CARTESIAN_POINT('Ctrl Pts',(70.1494044620759,0.406971320857371,135.70574383116));
#54214=CARTESIAN_POINT('Ctrl Pts',(70.1416532708358,0.543484958117916,135.694408840026));
#54215=CARTESIAN_POINT('Ctrl Pts',(70.1339020795956,0.679631193413864,135.677357400954));
#54216=CARTESIAN_POINT('Ctrl Pts',(70.1261508883555,0.814896405191022,135.654631425604));
#54217=CARTESIAN_POINT('Ctrl Pts',(70.1184029915784,0.950104125644858,135.6319151094));
#54218=CARTESIAN_POINT('Ctrl Pts',(70.1106550948013,1.08443118259516,135.603529118504));
#54219=CARTESIAN_POINT('Ctrl Pts',(70.1029071980243,1.21737029500267,135.569567079761));
#54220=CARTESIAN_POINT('Ctrl Pts',(70.0951609219402,1.35028159941389,135.535612145144));
#54221=CARTESIAN_POINT('Ctrl Pts',(70.087414645856,1.48180515820139,135.496083579402));
#54222=CARTESIAN_POINT('Ctrl Pts',(70.0796683697719,1.61144547564495,135.451125787178));
#54223=CARTESIAN_POINT('Ctrl Pts',(70.0719220365066,1.7410867500637,135.406167663087));
#54224=CARTESIAN_POINT('Ctrl Pts',(70.0641757032412,1.86884438601461,135.355780360642));
#54225=CARTESIAN_POINT('Ctrl Pts',(70.0564293699759,1.99423998363794,135.300157538042));
#54226=CARTESIAN_POINT('Ctrl Pts',(70.0486813019729,2.11966366273593,135.244522259096));
#54227=CARTESIAN_POINT('Ctrl Pts',(70.04093323397,2.24272389361813,135.183649285437));
#54228=CARTESIAN_POINT('Ctrl Pts',(70.033185165967,2.36296448564355,135.117779435869));
#54229=CARTESIAN_POINT('Ctrl Pts',(70.0254288632251,2.48333287080122,135.05183957904));
#54230=CARTESIAN_POINT('Ctrl Pts',(70.0176725604833,2.60087528734744,134.980892425666));
#54231=CARTESIAN_POINT('Ctrl Pts',(70.0099162577414,2.71516181667355,134.90522386471));
#54232=CARTESIAN_POINT('Ctrl Pts',(70.0021558152273,2.82950934416146,134.829514917165));
#54233=CARTESIAN_POINT('Ctrl Pts',(69.9943953727131,2.9405972052705,134.749079769989));
#54234=CARTESIAN_POINT('Ctrl Pts',(69.9866349301989,3.04802730965653,134.664245665348));
#54235=CARTESIAN_POINT('Ctrl Pts',(69.9788620299335,3.15562987038333,134.57927537747));
#54236=CARTESIAN_POINT('Ctrl Pts',(69.971089129668,3.25956264415466,134.489892275879));
#54237=CARTESIAN_POINT('Ctrl Pts',(69.9633162294026,3.35946260332538,134.396462241874));
#54238=CARTESIAN_POINT('Ctrl Pts',(69.9558258936406,3.4557309473473,134.306428624942));
#54239=CARTESIAN_POINT('Ctrl Pts',(69.9483355578786,3.548254375906,134.212637418942));
#54240=CARTESIAN_POINT('Ctrl Pts',(69.9408452221165,3.63674379902352,134.115444670073));
#54241=CARTESIAN_POINT('Ctrl Pts',(69.9330708879975,3.72858832551419,134.014566828589));
#54242=CARTESIAN_POINT('Ctrl Pts',(69.9252965538784,3.81637784524895,133.909704862762));
#54243=CARTESIAN_POINT('Ctrl Pts',(69.9175222197593,3.89974687011235,133.801218540716));
#54244=CARTESIAN_POINT('Ctrl Pts',(69.9097574668123,3.9830131501034,133.692865918367));
#54245=CARTESIAN_POINT('Ctrl Pts',(69.9019927138652,4.0618695389089,133.580898134217));
#54246=CARTESIAN_POINT('Ctrl Pts',(69.8942279609181,4.13598813449779,133.465710878955));
#54247=CARTESIAN_POINT('Ctrl Pts',(69.8864709200331,4.21003311445275,133.350638029298));
#54248=CARTESIAN_POINT('Ctrl Pts',(69.8787138791482,4.27934945544398,133.232352398599));
#54249=CARTESIAN_POINT('Ctrl Pts',(69.8709568382632,4.34365045173104,133.111281469194));
#54250=CARTESIAN_POINT('Ctrl Pts',(69.8632056470231,4.40790295813652,132.99030184032));
#54251=CARTESIAN_POINT('Ctrl Pts',(69.855454455783,4.46714746525789,132.866541437381));
#54252=CARTESIAN_POINT('Ctrl Pts',(69.8477032645429,4.52114160956485,132.740455039014));
#54253=CARTESIAN_POINT('Ctrl Pts',(69.8399553677659,4.57511280492015,132.614422230729));
#54254=CARTESIAN_POINT('Ctrl Pts',(69.8322074709888,4.62383792224919,132.486065751932));
#54255=CARTESIAN_POINT('Ctrl Pts',(69.8244595742118,4.6671215346742,132.355863000123));
#54256=CARTESIAN_POINT('Ctrl Pts',(69.8167132981277,4.71039609310064,132.225687483923));
#54257=CARTESIAN_POINT('Ctrl Pts',(69.8089670220436,4.74823128740072,132.093666833652));
#54258=CARTESIAN_POINT('Ctrl Pts',(69.8012207459595,4.78048078175164,131.96029597813));
#54259=CARTESIAN_POINT('Ctrl Pts',(69.7934744126942,4.81273051416095,131.826924138096));
#54260=CARTESIAN_POINT('Ctrl Pts',(69.7857280794288,4.83939437245644,131.692202452937));
#54261=CARTESIAN_POINT('Ctrl Pts',(69.7779817461635,4.86037669995633,131.55663809099));
#54262=CARTESIAN_POINT('Ctrl Pts',(69.7702336781606,4.88136372630301,131.421043370345));
#54263=CARTESIAN_POINT('Ctrl Pts',(69.7624856101576,4.89666663025674,131.284605983689));
#54264=CARTESIAN_POINT('Ctrl Pts',(69.7547375421547,4.90624143731314,131.147839905575));
#54265=CARTESIAN_POINT('Ctrl Pts',(69.7469812394128,4.91582642058842,131.010928470846));
#54266=CARTESIAN_POINT('Ctrl Pts',(69.739224936671,4.91967111840357,130.873688037453));
#54267=CARTESIAN_POINT('Ctrl Pts',(69.7314686339292,4.91778367573147,130.736634838064));
#54268=CARTESIAN_POINT('Ctrl Pts',(69.723708191415,4.91589522567438,130.599508489257));
#54269=CARTESIAN_POINT('Ctrl Pts',(69.7159477489009,4.90826856071481,130.462569963748));
#54270=CARTESIAN_POINT('Ctrl Pts',(69.7081873063868,4.89496382140032,130.326331068603));
#54271=CARTESIAN_POINT('Ctrl Pts',(69.7004144061214,4.88163772413715,130.189873470688));
#54272=CARTESIAN_POINT('Ctrl Pts',(69.6926415058559,4.86261539223056,130.054118134872));
#54273=CARTESIAN_POINT('Ctrl Pts',(69.6848686055905,4.83800842667057,129.919568254373));
#54274=CARTESIAN_POINT('Ctrl Pts',(69.6773782698283,4.81429598628915,129.789909600937));
#54275=CARTESIAN_POINT('Ctrl Pts',(69.6698879340661,4.78539796152252,129.661370582267));
#54276=CARTESIAN_POINT('Ctrl Pts',(69.6623975983038,4.75145764392505,129.534386869614));
#54277=CARTESIAN_POINT('Ctrl Pts',(69.6546232641847,4.71623046887089,129.402588530905));
#54278=CARTESIAN_POINT('Ctrl Pts',(69.6468489300656,4.67545950697025,129.272048267698));
#54279=CARTESIAN_POINT('Ctrl Pts',(69.6390745959465,4.62924988608115,129.143268038955));
#54280=CARTESIAN_POINT('Ctrl Pts',(69.6313098429994,4.58309721441994,129.014646520334));
#54281=CARTESIAN_POINT('Ctrl Pts',(69.6235450900523,4.53151935084535,128.887781084804));
#54282=CARTESIAN_POINT('Ctrl Pts',(69.6157803371052,4.4746719620832,128.763161486113));
#54283=CARTESIAN_POINT('Ctrl Pts',(69.6080232962202,4.41788103494906,128.638665661363));
#54284=CARTESIAN_POINT('Ctrl Pts',(69.6002662553352,4.35583115926982,128.516411587866));
#54285=CARTESIAN_POINT('Ctrl Pts',(69.5925092144502,4.28872701658698,128.396871543926));
#54286=CARTESIAN_POINT('Ctrl Pts',(69.58475802321,4.22167347766014,128.277421646063));
#54287=CARTESIAN_POINT('Ctrl Pts',(69.5770068319699,4.14957344881735,128.160682043525));
#54288=CARTESIAN_POINT('Ctrl Pts',(69.5692556407298,4.07267854479646,128.047102462577));
#54289=CARTESIAN_POINT('Ctrl Pts',(69.5615077439527,3.99581632316091,127.93357115598));
#54290=CARTESIAN_POINT('Ctrl Pts',(69.5537598471755,3.9141634983973,127.823197522732));
#54291=CARTESIAN_POINT('Ctrl Pts',(69.5460119503984,3.82801608554287,127.716404026011));
#54292=CARTESIAN_POINT('Ctrl Pts',(69.5382656743143,3.7418866928701,127.609632868188));
#54293=CARTESIAN_POINT('Ctrl Pts',(69.5305193982302,3.65126482747268,127.50644066142));
#54294=CARTESIAN_POINT('Ctrl Pts',(69.522773122146,3.55648778889753,127.407218043295));
#54295=CARTESIAN_POINT('Ctrl Pts',(69.5150267888807,3.46171005069981,127.307994692732));
#54296=CARTESIAN_POINT('Ctrl Pts',(69.5072804556154,3.3627773481677,127.212741271999));
#54297=CARTESIAN_POINT('Ctrl Pts',(69.49953412235,3.26006467161488,127.121812396648));
#54298=CARTESIAN_POINT('Ctrl Pts',(69.491786054347,3.15732899327044,127.030863158405));
#54299=CARTESIAN_POINT('Ctrl Pts',(69.484037986344,3.05081194915019,126.944240651752));
#54300=CARTESIAN_POINT('Ctrl Pts',(69.476289918341,2.94092219130759,126.862259689485));
#54301=CARTESIAN_POINT('Ctrl Pts',(69.4685336155991,2.8309156413225,126.780191596876));
#54302=CARTESIAN_POINT('Ctrl Pts',(69.4607773128572,2.71752953093789,126.702775137184));
#54303=CARTESIAN_POINT('Ctrl Pts',(69.4530210101154,2.601202583876,126.630282494179));
#54304=CARTESIAN_POINT('Ctrl Pts',(69.4452605676012,2.48481354961978,126.557751159668));
#54305=CARTESIAN_POINT('Ctrl Pts',(69.4375001250869,2.36548089110542,126.49014907095));
#54306=CARTESIAN_POINT('Ctrl Pts',(69.4297396825727,2.24366771354702,126.427702274299));
#54307=CARTESIAN_POINT('Ctrl Pts',(69.4219667823073,2.12165899066209,126.365155232507));
#54308=CARTESIAN_POINT('Ctrl Pts',(69.4141938820418,1.99716214680654,126.307780184063));
#54309=CARTESIAN_POINT('Ctrl Pts',(69.4064209817764,1.87066085574772,126.255755224121));
#54310=CARTESIAN_POINT('Ctrl Pts',(69.3989306460145,1.74875820525897,126.205621502517));
#54311=CARTESIAN_POINT('Ctrl Pts',(69.3914403102526,1.62499460018356,126.160455749859));
#54312=CARTESIAN_POINT('Ctrl Pts',(69.3839499744907,1.49981403566988,126.120372901858));
#54313=CARTESIAN_POINT('Ctrl Pts',(69.3761756403717,1.36988721200246,126.07877030049));
#54314=CARTESIAN_POINT('Ctrl Pts',(69.3684013062526,1.23802229068093,126.042511864544));
#54315=CARTESIAN_POINT('Ctrl Pts',(69.3606269721335,1.10469840817102,126.011780468055));
#54316=CARTESIAN_POINT('Ctrl Pts',(69.3528622191864,0.971538835430809,125.981086945266));
#54317=CARTESIAN_POINT('Ctrl Pts',(69.3450974662393,0.836924256382496,125.955906995888));
#54318=CARTESIAN_POINT('Ctrl Pts',(69.3373327132923,0.701350856392471,125.936374376959));
#54319=CARTESIAN_POINT('Ctrl Pts',(69.3295756724073,0.565912109814567,125.916861158103));
#54320=CARTESIAN_POINT('Ctrl Pts',(69.3218186315223,0.42951682190927,125.902984162909));
#54321=CARTESIAN_POINT('Ctrl Pts',(69.3140615906373,0.292672969162603,125.894826464958));
#54322=CARTESIAN_POINT('Ctrl Pts',(69.3063103993971,0.155932311429783,125.886674918791));
#54323=CARTESIAN_POINT('Ctrl Pts',(69.298559208157,0.0187441508472424,125.884234108341));
#54324=CARTESIAN_POINT('Ctrl Pts',(69.2908080169169,-0.118377141231064,
125.887535431032));
#54325=CARTESIAN_POINT('Ctrl Pts',(69.2830601201398,-0.255440153102407,
125.890835350573));
#54326=CARTESIAN_POINT('Ctrl Pts',(69.2753122233627,-0.392435962962857,
125.899872539779));
#54327=CARTESIAN_POINT('Ctrl Pts',(69.2675643265857,-0.528849137218226,
125.914626304481));
#54328=CARTESIAN_POINT('Ctrl Pts',(69.2598180505016,-0.66523377677827,125.929376983013));
#54329=CARTESIAN_POINT('Ctrl Pts',(69.2520717744175,-0.801035634696752,
125.949841816548));
#54330=CARTESIAN_POINT('Ctrl Pts',(69.2443254983334,-0.935743737862675,
125.975948174583));
#54331=CARTESIAN_POINT('Ctrl Pts',(69.2365791650681,-1.07045283541321,126.002054725329));
#54332=CARTESIAN_POINT('Ctrl Pts',(69.2288328318027,-1.20406777827664,126.033802809289));
#54333=CARTESIAN_POINT('Ctrl Pts',(69.2210864985373,-1.33608752692281,126.071068614858));
#54334=CARTESIAN_POINT('Ctrl Pts',(69.2133384305344,-1.46813684047616,126.108342765845));
#54335=CARTESIAN_POINT('Ctrl Pts',(69.2055903625315,-1.5985898727702,126.151136991065));
#54336=CARTESIAN_POINT('Ctrl Pts',(69.1978422945285,-1.72696087646697,126.199277643976));
#54337=CARTESIAN_POINT('Ctrl Pts',(69.1900859917867,-1.85546831439429,126.247469461345));
#54338=CARTESIAN_POINT('Ctrl Pts',(69.1823296890448,-1.98188893675404,126.301018919807));
#54339=CARTESIAN_POINT('Ctrl Pts',(69.1745733863029,-2.1057566067425,126.359704030645));
#54340=CARTESIAN_POINT('Ctrl Pts',(69.1668129437887,-2.22969038863619,126.418420463494));
#54341=CARTESIAN_POINT('Ctrl Pts',(69.1590525012746,-2.35106815725444,126.482277828553));
#54342=CARTESIAN_POINT('Ctrl Pts',(69.1512920587604,-2.46944941378446,126.551008685823));
#54343=CARTESIAN_POINT('Ctrl Pts',(69.143519158495,-2.58802070641685,126.619849875967));
#54344=CARTESIAN_POINT('Ctrl Pts',(69.1357462582296,-2.70358554472652,126.693579981489));
#54345=CARTESIAN_POINT('Ctrl Pts',(69.1279733579642,-2.81573265473219,126.771888338731));
#54346=CARTESIAN_POINT('Ctrl Pts',(69.1204830222021,-2.92380293480823,126.84734998994));
#54347=CARTESIAN_POINT('Ctrl Pts',(69.11299268644,-3.02869941332029,126.927062623513));
#54348=CARTESIAN_POINT('Ctrl Pts',(69.1055023506779,-3.13008540137689,127.010714819315));
#54349=CARTESIAN_POINT('Ctrl Pts',(69.0978360489836,-3.23385318919103,127.096332205609));
#54350=CARTESIAN_POINT('Ctrl Pts',(69.0901697472893,-3.33429156583331,127.186364052398));
#54351=CARTESIAN_POINT('Ctrl Pts',(69.0825034455951,-3.43099375406175,127.280518265518));
#54352=CARTESIAN_POINT('Ctrl Pts',(69.0748459328249,-3.5275850794212,127.374564536859));
#54353=CARTESIAN_POINT('Ctrl Pts',(69.0671884200548,-3.62044844565388,127.472723502388));
#54354=CARTESIAN_POINT('Ctrl Pts',(69.0595309072847,-3.70920854237395,127.574661707191));
#54355=CARTESIAN_POINT('Ctrl Pts',(69.0518804058702,-3.79788736876317,127.676506575551));
#54356=CARTESIAN_POINT('Ctrl Pts',(69.0442299044556,-3.88247013323087,127.782123501593));
#54357=CARTESIAN_POINT('Ctrl Pts',(69.036579403041,-3.96261735362609,127.891141303604));
#54358=CARTESIAN_POINT('Ctrl Pts',(69.0289341419549,-4.04270967595161,128.000084432197));
#54359=CARTESIAN_POINT('Ctrl Pts',(69.0212888808688,-4.11837225937918,128.11242348059));
#54360=CARTESIAN_POINT('Ctrl Pts',(69.0136436197827,-4.18930537909567,128.227753642651));
#54361=CARTESIAN_POINT('Ctrl Pts',(69.006001064684,-4.26021339252376,128.343042984397));
#54362=CARTESIAN_POINT('Ctrl Pts',(68.9983585095853,-4.32639505752586,128.46132099407));
#54363=CARTESIAN_POINT('Ctrl Pts',(68.9907159544867,-4.38759377732882,128.582153627287));
#54364=CARTESIAN_POINT('Ctrl Pts',(68.9830750803242,-4.44877903682396,128.702959684058));
#54365=CARTESIAN_POINT('Ctrl Pts',(68.9754342061618,-4.50498335275461,128.826318885969));
#54366=CARTESIAN_POINT('Ctrl Pts',(68.9677933319993,-4.5559962659104,128.951772944199));
#54367=CARTESIAN_POINT('Ctrl Pts',(68.9601502965188,-4.60702360871435,129.077262488698));
#54368=CARTESIAN_POINT('Ctrl Pts',(68.9525072610383,-4.65285646314337,129.204847700251));
#54369=CARTESIAN_POINT('Ctrl Pts',(68.9448642255579,-4.69333273727326,129.334050827168));
#54370=CARTESIAN_POINT('Ctrl Pts',(68.9400016347788,-4.71908422800734,129.416251405091));
#54371=CARTESIAN_POINT('Ctrl Pts',(68.9351390439998,-4.74266854441486,129.499106492975));
#54372=CARTESIAN_POINT('Ctrl Pts',(68.9302764532207,-4.76405452823407,129.582490119308));
#54373=CARTESIAN_POINT('Origin',(213.235140564004,0.,130.804360617566));
#54374=CARTESIAN_POINT('',(66.8345747415593,-4.7640545282341,129.582490119308));
#54375=CARTESIAN_POINT('',(67.1801803489693,-4.76405452823408,129.582490119308));
#54376=CARTESIAN_POINT('',(213.235140564004,-4.76405452823405,129.582490119308));
#54377=CARTESIAN_POINT('',(68.5148594359566,-4.91824809583631,130.800032765609));
#54378=CARTESIAN_POINT('Ctrl Pts',(68.5148594359566,-4.9182480958363,130.800032765609));
#54379=CARTESIAN_POINT('Ctrl Pts',(68.5072124510153,-4.91836670518795,130.934822546704));
#54380=CARTESIAN_POINT('Ctrl Pts',(68.4995654660739,-4.91294006782637,131.069798280582));
#54381=CARTESIAN_POINT('Ctrl Pts',(68.4919184811327,-4.90194906913478,131.204458588204));
#54382=CARTESIAN_POINT('Ctrl Pts',(68.4842781235352,-4.89096759591342,131.339002190985));
#54383=CARTESIAN_POINT('Ctrl Pts',(68.4766377659378,-4.87443138624882,131.47323051136));
#54384=CARTESIAN_POINT('Ctrl Pts',(68.4689974083404,-4.85237338428922,131.606642115509));
#54385=CARTESIAN_POINT('Ctrl Pts',(68.4613612904117,-4.83032762241411,131.739979688958));
#54386=CARTESIAN_POINT('Ctrl Pts',(68.4537251724831,-4.80276622695132,131.872501050486));
#54387=CARTESIAN_POINT('Ctrl Pts',(68.4460890545544,-4.76977394128991,132.003710279463));
#54388=CARTESIAN_POINT('Ctrl Pts',(68.4384550823034,-4.7367909261517,132.134882639876));
#54389=CARTESIAN_POINT('Ctrl Pts',(68.4308211100523,-4.69838015266099,132.264743209749));
#54390=CARTESIAN_POINT('Ctrl Pts',(68.4231871378013,-4.65467729142473,132.392807146472));
#54391=CARTESIAN_POINT('Ctrl Pts',(68.4155535448375,-4.61097660152694,132.520864720451));
#54392=CARTESIAN_POINT('Ctrl Pts',(68.4079199518736,-4.56198447712011,132.647125456961));
#54393=CARTESIAN_POINT('Ctrl Pts',(68.4002863589098,-4.5078860138274,132.771121088198));
#54394=CARTESIAN_POINT('Ctrl Pts',(68.3926513793562,-4.45377772392009,132.89513924239));
#54395=CARTESIAN_POINT('Ctrl Pts',(68.3850163998027,-4.39456141258378,133.016891103625));
#54396=CARTESIAN_POINT('Ctrl Pts',(68.3773814202491,-4.33046949035708,133.135930272452));
#54397=CARTESIAN_POINT('Ctrl Pts',(68.3697387349083,-4.26631288181285,133.25508958443));
#54398=CARTESIAN_POINT('Ctrl Pts',(68.3620960495676,-4.19727102724456,133.371530380898));
#54399=CARTESIAN_POINT('Ctrl Pts',(68.3544533642268,-4.12362146972974,133.484832411278));
#54400=CARTESIAN_POINT('Ctrl Pts',(68.3468066842611,-4.04993341758311,133.598193661565));
#54401=CARTESIAN_POINT('Ctrl Pts',(68.3391600042954,-3.97163310107924,133.708412551059));
#54402=CARTESIAN_POINT('Ctrl Pts',(68.3315133243297,-3.88903942880687,133.815100623559));
#54403=CARTESIAN_POINT('Ctrl Pts',(68.3238548412143,-3.80631826780864,133.921953376064));
#54404=CARTESIAN_POINT('Ctrl Pts',(68.3161963580988,-3.71929077470398,134.025264118247));
#54405=CARTESIAN_POINT('Ctrl Pts',(68.3085378749833,-3.62831429920305,134.124679639693));
#54406=CARTESIAN_POINT('Ctrl Pts',(68.3022747417884,-3.55391343220651,134.205981986786));
#54407=CARTESIAN_POINT('Ctrl Pts',(68.2960116085934,-3.47687224182813,134.284679833575));
#54408=CARTESIAN_POINT('Ctrl Pts',(68.2897484753985,-3.39740236567618,134.36060023663));
#54409=CARTESIAN_POINT('Ctrl Pts',(68.2819741412794,-3.29875758991056,134.454839104211));
#54410=CARTESIAN_POINT('Ctrl Pts',(68.2741998071603,-3.1960325281503,134.545119740777));
#54411=CARTESIAN_POINT('Ctrl Pts',(68.2664254730413,-3.08957807420817,134.63106813002));
#54412=CARTESIAN_POINT('Ctrl Pts',(68.2586607200942,-2.98325481586642,134.716910595555));
#54413=CARTESIAN_POINT('Ctrl Pts',(68.2508959671471,-2.87321161157181,134.79843119376));
#54414=CARTESIAN_POINT('Ctrl Pts',(68.2431312142,-2.7598361693194,134.875292621545));
#54415=CARTESIAN_POINT('Ctrl Pts',(68.235374173315,-2.64657333315455,134.952077709476));
#54416=CARTESIAN_POINT('Ctrl Pts',(68.22761713243,-2.52998516685193,135.024212618061));
#54417=CARTESIAN_POINT('Ctrl Pts',(68.2198600915451,-2.41049214949732,135.091400465726));
#54418=CARTESIAN_POINT('Ctrl Pts',(68.2121089003049,-2.2910892427563,135.158537646513));
#54419=CARTESIAN_POINT('Ctrl Pts',(68.2043577090648,-2.16878618457121,135.220735001106));
#54420=CARTESIAN_POINT('Ctrl Pts',(68.1966065178246,-2.04403180655608,135.277739322336));
#54421=CARTESIAN_POINT('Ctrl Pts',(68.1888586210476,-1.91933045248004,135.334719415208));
#54422=CARTESIAN_POINT('Ctrl Pts',(68.1811107242705,-1.79218020564322,135.386510702481));
#54423=CARTESIAN_POINT('Ctrl Pts',(68.1733628274934,-1.66305363636179,135.43290635733));
#54424=CARTESIAN_POINT('Ctrl Pts',(68.1656165514094,-1.53395407757501,135.479292307208));
#54425=CARTESIAN_POINT('Ctrl Pts',(68.1578702753253,-1.40287938632966,135.520284737492));
#54426=CARTESIAN_POINT('Ctrl Pts',(68.1501239992412,-1.27032083726244,135.555725477574));
#54427=CARTESIAN_POINT('Ctrl Pts',(68.1423776659759,-1.1377613096783,135.591166479271));
#54428=CARTESIAN_POINT('Ctrl Pts',(68.1346313327106,-1.00371828011441,135.621055608009));
#54429=CARTESIAN_POINT('Ctrl Pts',(68.1268849994452,-0.868696475360461,
135.645285064012));
#54430=CARTESIAN_POINT('Ctrl Pts',(68.1191369314423,-0.733644433409144,
135.669519946033));
#54431=CARTESIAN_POINT('Ctrl Pts',(68.1113888634393,-0.597613564849928,
135.688092564209));
#54432=CARTESIAN_POINT('Ctrl Pts',(68.1036407954363,-0.461116640956121,
135.700946622726));
#54433=CARTESIAN_POINT('Ctrl Pts',(68.0958844926945,-0.324474646507265,
135.71381434269));
#54434=CARTESIAN_POINT('Ctrl Pts',(68.0881281899526,-0.187365997114212,
135.720951325315));
#54435=CARTESIAN_POINT('Ctrl Pts',(68.0803718872108,-0.0503069722412662,
135.722353325068));
#54436=CARTESIAN_POINT('Ctrl Pts',(68.0726114446966,0.0868252051600223,
135.72375607311));
#54437=CARTESIAN_POINT('Ctrl Pts',(68.0648510021825,0.22390731468705,135.719417751473));
#54438=CARTESIAN_POINT('Ctrl Pts',(68.0570905596683,0.36042625345506,135.709386201426));
#54439=CARTESIAN_POINT('Ctrl Pts',(68.0493176594029,0.497164344543161,135.699338547844));
#54440=CARTESIAN_POINT('Ctrl Pts',(68.0415447591375,0.63333706969227,135.68357944764));
#54441=CARTESIAN_POINT('Ctrl Pts',(68.033771858872,0.768438702474648,135.662208394415));
#54442=CARTESIAN_POINT('Ctrl Pts',(68.0262815231099,0.898629050606371,135.641614232805));
#54443=CARTESIAN_POINT('Ctrl Pts',(68.0187911873478,1.02782452612636,135.615809111983));
#54444=CARTESIAN_POINT('Ctrl Pts',(68.0113008515857,1.15558614464289,135.58492582733));
#54445=CARTESIAN_POINT('Ctrl Pts',(68.0035265174666,1.28819188375612,135.552871593553));
#54446=CARTESIAN_POINT('Ctrl Pts',(67.9957521833476,1.4196729452598,135.515244979061));
#54447=CARTESIAN_POINT('Ctrl Pts',(67.9879778492285,1.54952499196543,135.472139035805));
#54448=CARTESIAN_POINT('Ctrl Pts',(67.9802130962814,1.6792170076287,135.429086216771));
#54449=CARTESIAN_POINT('Ctrl Pts',(67.9724483433343,1.80728363555723,135.380567626994));
#54450=CARTESIAN_POINT('Ctrl Pts',(67.9646835903873,1.93323152746781,135.32672713563));
#54451=CARTESIAN_POINT('Ctrl Pts',(67.9569265495023,2.05905432615643,135.272940119401));
#54452=CARTESIAN_POINT('Ctrl Pts',(67.9491695086173,2.18276221942639,135.213841873226));
#54453=CARTESIAN_POINT('Ctrl Pts',(67.9414124677324,2.30387815318501,135.149625686325));
#54454=CARTESIAN_POINT('Ctrl Pts',(67.9336612764923,2.42490275247552,135.08545792535));
#54455=CARTESIAN_POINT('Ctrl Pts',(67.9259100852522,2.54333893878154,135.01618008811));
#54456=CARTESIAN_POINT('Ctrl Pts',(67.9181588940121,2.65873107729005,134.942032924691));
#54457=CARTESIAN_POINT('Ctrl Pts',(67.910410997235,2.77407417106214,134.867917275795));
#54458=CARTESIAN_POINT('Ctrl Pts',(67.902663100458,2.88637546208292,134.788936627892));
#54459=CARTESIAN_POINT('Ctrl Pts',(67.8949152036809,2.99520550528921,134.705376772824));
#54460=CARTESIAN_POINT('Ctrl Pts',(67.8871689275968,3.10401278359656,134.621834396676));
#54461=CARTESIAN_POINT('Ctrl Pts',(67.8794226515127,3.2093499484564,134.533714956568));
#54462=CARTESIAN_POINT('Ctrl Pts',(67.8716763754286,3.3108183805148,134.441346280687));
#54463=CARTESIAN_POINT('Ctrl Pts',(67.8639300421633,3.41228756158984,134.348976922961));
#54464=CARTESIAN_POINT('Ctrl Pts',(67.8561837088979,3.50988766376385,134.252358530059));
#54465=CARTESIAN_POINT('Ctrl Pts',(67.8484373756326,3.60325517487317,134.15185747451));
#54466=CARTESIAN_POINT('Ctrl Pts',(67.8406893076297,3.69664359498936,134.051333912446));
#54467=CARTESIAN_POINT('Ctrl Pts',(67.8329412396267,3.78579727185954,133.946926243919));
#54468=CARTESIAN_POINT('Ctrl Pts',(67.8251931716237,3.87039167682359,133.83903544866));
#54469=CARTESIAN_POINT('Ctrl Pts',(67.8174368688819,3.95507598972792,133.73102998578));
#54470=CARTESIAN_POINT('Ctrl Pts',(67.80968056614,4.0351911094021,133.619534309366));
#54471=CARTESIAN_POINT('Ctrl Pts',(67.8019242633982,4.11045440229741,133.50498048514));
#54472=CARTESIAN_POINT('Ctrl Pts',(67.794163820884,4.18575786547838,133.390365520088));
#54473=CARTESIAN_POINT('Ctrl Pts',(67.7864033783699,4.25620414123331,133.272689490161));
#54474=CARTESIAN_POINT('Ctrl Pts',(67.7786429358557,4.32155613513531,133.152409942724));
#54475=CARTESIAN_POINT('Ctrl Pts',(67.7708700355903,4.3870130378596,133.031937311879));
#54476=CARTESIAN_POINT('Ctrl Pts',(67.7630971353249,4.44735914468388,132.908853163001));
#54477=CARTESIAN_POINT('Ctrl Pts',(67.7553242350594,4.50240480490596,132.783636756779));
#54478=CARTESIAN_POINT('Ctrl Pts',(67.7478338992972,4.55544941672865,132.662972282322));
#54479=CARTESIAN_POINT('Ctrl Pts',(67.740343563535,4.60357214803633,132.54032817163));
#54480=CARTESIAN_POINT('Ctrl Pts',(67.7328532277728,4.64664744155759,132.416145533852));
#54481=CARTESIAN_POINT('Ctrl Pts',(67.7250788936537,4.6913559479241,132.287254473621));
#54482=CARTESIAN_POINT('Ctrl Pts',(67.7173045595346,4.73076833685649,132.156297628626));
#54483=CARTESIAN_POINT('Ctrl Pts',(67.7095302254155,4.76469028902847,132.02374960888));
#54484=CARTESIAN_POINT('Ctrl Pts',(67.7017654724684,4.79857043542609,131.891364942722));
#54485=CARTESIAN_POINT('Ctrl Pts',(67.6940007195214,4.82697351232497,131.757393378703));
#54486=CARTESIAN_POINT('Ctrl Pts',(67.6862359665743,4.84975389412462,131.622327749499));
#54487=CARTESIAN_POINT('Ctrl Pts',(67.6784789256893,4.87251165012791,131.487396269383));
#54488=CARTESIAN_POINT('Ctrl Pts',(67.6707218848042,4.88965775991696,131.351373269572));
#54489=CARTESIAN_POINT('Ctrl Pts',(67.6629648439192,4.90109698379797,131.214764586731));
#54490=CARTESIAN_POINT('Ctrl Pts',(67.6552136526791,4.91252758127122,131.078258921561));
#54491=CARTESIAN_POINT('Ctrl Pts',(67.647462461439,4.91825982641321,130.941168840501));
#54492=CARTESIAN_POINT('Ctrl Pts',(67.6397112701989,4.91824998734602,130.804007813325));
#54493=CARTESIAN_POINT('Ctrl Pts',(67.6319633734218,4.91824015246071,130.666905083245));
#54494=CARTESIAN_POINT('Ctrl Pts',(67.6242154766447,4.9124930874401,130.52973185717));
#54495=CARTESIAN_POINT('Ctrl Pts',(67.6164675798677,4.90101711150753,130.393003916867));
#54496=CARTESIAN_POINT('Ctrl Pts',(67.6087213037836,4.88954353610172,130.2563045771));
#54497=CARTESIAN_POINT('Ctrl Pts',(67.6009750276995,4.87234346607608,130.120050727184));
#54498=CARTESIAN_POINT('Ctrl Pts',(67.5932287516154,4.84947724907209,129.984754936014));
#54499=CARTESIAN_POINT('Ctrl Pts',(67.58548241835,4.82661086327484,129.849458146121));
#54500=CARTESIAN_POINT('Ctrl Pts',(67.5777360850846,4.79807831219077,129.715119814583));
#54501=CARTESIAN_POINT('Ctrl Pts',(67.5699897518192,4.76399134820206,129.582243807782));
#54502=CARTESIAN_POINT('Ctrl Pts',(67.5622416838162,4.72989675067411,129.449338044321));
#54503=CARTESIAN_POINT('Ctrl Pts',(67.5544936158133,4.69024536221057,129.317895635868));
#54504=CARTESIAN_POINT('Ctrl Pts',(67.5467455478103,4.64519912274906,129.188406356916));
#54505=CARTESIAN_POINT('Ctrl Pts',(67.5389892450684,4.60010500760831,129.058779455219));
#54506=CARTESIAN_POINT('Ctrl Pts',(67.5312329423266,4.54960471642406,128.931110199524));
#54507=CARTESIAN_POINT('Ctrl Pts',(67.5234766395847,4.49390898798704,128.805869919517));
#54508=CARTESIAN_POINT('Ctrl Pts',(67.5157161970706,4.43818353306278,128.680562795001));
#54509=CARTESIAN_POINT('Ctrl Pts',(67.5079557545564,4.37725728911844,128.557687579494));
#54510=CARTESIAN_POINT('Ctrl Pts',(67.5001953120422,4.3113870483806,128.437691062779));
#54511=CARTESIAN_POINT('Ctrl Pts',(67.4924224117768,4.24541106688456,128.317501917002));
#54512=CARTESIAN_POINT('Ctrl Pts',(67.4846495115113,4.17447543128331,128.200201039274));
#54513=CARTESIAN_POINT('Ctrl Pts',(67.4768766112459,4.0988808463306,128.086207040212));
#54514=CARTESIAN_POINT('Ctrl Pts',(67.4693862754839,4.0260343149524,127.976357010149));
#54515=CARTESIAN_POINT('Ctrl Pts',(67.4618959397219,3.94886186290223,127.869577855818));
#54516=CARTESIAN_POINT('Ctrl Pts',(67.4544056039599,3.86766674102762,127.766213642377));
#54517=CARTESIAN_POINT('Ctrl Pts',(67.4466312698408,3.78339308142829,127.658930343367));
#54518=CARTESIAN_POINT('Ctrl Pts',(67.4388569357217,3.69451873776251,127.554986210823));
#54519=CARTESIAN_POINT('Ctrl Pts',(67.4310826016027,3.60133797853409,127.454801269403));
#54520=CARTESIAN_POINT('Ctrl Pts',(67.4233178486556,3.50827205626348,127.354739796969));
#54521=CARTESIAN_POINT('Ctrl Pts',(67.4155530957085,3.41091054202979,127.258428581168));
#54522=CARTESIAN_POINT('Ctrl Pts',(67.4077883427614,3.30958935572785,127.16625652904));
#54523=CARTESIAN_POINT('Ctrl Pts',(67.4000313018764,3.20836880305625,127.074176023493));
#54524=CARTESIAN_POINT('Ctrl Pts',(67.3922742609913,3.10319669210154,126.98622676178));
#54525=CARTESIAN_POINT('Ctrl Pts',(67.3845172201063,2.99444711819473,126.902762288825));
#54526=CARTESIAN_POINT('Ctrl Pts',(67.3767660288661,2.88577955318754,126.819360757078));
#54527=CARTESIAN_POINT('Ctrl Pts',(67.369014837626,2.77354020391473,126.74043751947));
#54528=CARTESIAN_POINT('Ctrl Pts',(67.3612636463859,2.65813742889289,126.666306911822));
#54529=CARTESIAN_POINT('Ctrl Pts',(67.3535157496088,2.54278370312938,126.592207811661));
#54530=CARTESIAN_POINT('Ctrl Pts',(67.3457678528317,2.42426955406166,126.522897500893));
#54531=CARTESIAN_POINT('Ctrl Pts',(67.3380199560546,2.30303342023976,126.458647772962));
#54532=CARTESIAN_POINT('Ctrl Pts',(67.3302736799705,2.18182264640334,126.394411484689));
#54533=CARTESIAN_POINT('Ctrl Pts',(67.3225274038864,2.05789136557562,126.335233856668));
#54534=CARTESIAN_POINT('Ctrl Pts',(67.3147811278023,1.93170343585908,126.281341172727));
#54535=CARTESIAN_POINT('Ctrl Pts',(67.3070347945369,1.80551457465208,126.227448090963));
#54536=CARTESIAN_POINT('Ctrl Pts',(67.2992884612715,1.67706939086354,126.178840184682));
#54537=CARTESIAN_POINT('Ctrl Pts',(67.2915421280062,1.5468522064417,126.135695785526));
#54538=CARTESIAN_POINT('Ctrl Pts',(67.2837940600032,1.4166058607841,126.092541724481));
#54539=CARTESIAN_POINT('Ctrl Pts',(67.2760459920003,1.28458709590686,126.054853728153));
#54540=CARTESIAN_POINT('Ctrl Pts',(67.2682979239973,1.15129550545385,126.022760286963));
#54541=CARTESIAN_POINT('Ctrl Pts',(67.2605416212554,1.01786225111233,125.990632736482));
#54542=CARTESIAN_POINT('Ctrl Pts',(67.2527853185135,0.883153849591547,125.9641117105));
#54543=CARTESIAN_POINT('Ctrl Pts',(67.2450290157717,0.747680753368192,125.943274673711));
#54544=CARTESIAN_POINT('Ctrl Pts',(67.2372685732575,0.612135351074182,125.922426515568));
#54545=CARTESIAN_POINT('Ctrl Pts',(67.2295081307434,0.475824829202853,125.907268434744));
#54546=CARTESIAN_POINT('Ctrl Pts',(67.2217476882292,0.339263887122995,125.897825885457));
#54547=CARTESIAN_POINT('Ctrl Pts',(67.2139747879637,0.202483725295785,125.888368178151));
#54548=CARTESIAN_POINT('Ctrl Pts',(67.2062018876983,0.0654527309883036,
125.884644347739));
#54549=CARTESIAN_POINT('Ctrl Pts',(67.1984289874328,-0.0713143685682095,
125.886627672058));
#54550=CARTESIAN_POINT('Ctrl Pts',(67.1909386516709,-0.203109639559009,
125.888538897542));
#54551=CARTESIAN_POINT('Ctrl Pts',(67.1834483159089,-0.334659561614416,
125.895749525948));
#54552=CARTESIAN_POINT('Ctrl Pts',(67.175957980147,-0.465510748482276,125.90819039937));
#54553=CARTESIAN_POINT('Ctrl Pts',(67.1681836460279,-0.60132319787256,125.92110297229));
#54554=CARTESIAN_POINT('Ctrl Pts',(67.1604093119089,-0.736813094060469,
125.939691132051));
#54555=CARTESIAN_POINT('Ctrl Pts',(67.1526349777898,-0.871467999091324,
125.963934335816));
#54556=CARTESIAN_POINT('Ctrl Pts',(67.1448702248427,-1.00595695398618,125.988147661998));
#54557=CARTESIAN_POINT('Ctrl Pts',(67.1371054718956,-1.13961258414576,126.018002096671));
#54558=CARTESIAN_POINT('Ctrl Pts',(67.1293407189486,-1.27192611815261,126.053425234669));
#54559=CARTESIAN_POINT('Ctrl Pts',(67.1215836780636,-1.404108236492,126.088813189907));
#54560=CARTESIAN_POINT('Ctrl Pts',(67.1138266371786,-1.53495053616552,126.129758741246));
#54561=CARTESIAN_POINT('Ctrl Pts',(67.1060695962936,-1.66395336215103,126.176138251356));
#54562=CARTESIAN_POINT('Ctrl Pts',(67.0983184050535,-1.79285890610162,126.222482786317));
#54563=CARTESIAN_POINT('Ctrl Pts',(67.0905672138135,-1.91992737100342,126.274252991908));
#54564=CARTESIAN_POINT('Ctrl Pts',(67.0828160225734,-2.04467356947265,126.331275210736));
#54565=CARTESIAN_POINT('Ctrl Pts',(67.0750681257963,-2.16936674748033,126.388273193599));
#54566=CARTESIAN_POINT('Ctrl Pts',(67.0673202290192,-2.29173926733986,126.450518587736));
#54567=CARTESIAN_POINT('Ctrl Pts',(67.0595723322422,-2.41132547478305,126.517789433372));
#54568=CARTESIAN_POINT('Ctrl Pts',(67.0518260561581,-2.53088666736995,126.585046207398));
#54569=CARTESIAN_POINT('Ctrl Pts',(67.044079780074,-2.64766236629879,126.657326150435));
#54570=CARTESIAN_POINT('Ctrl Pts',(67.0363335039899,-2.76121146594152,126.734361317461));
#54571=CARTESIAN_POINT('Ctrl Pts',(67.0285871707245,-2.87476140377776,126.811397053144));
#54572=CARTESIAN_POINT('Ctrl Pts',(67.0208408374592,-2.98508437126533,126.893187863362));
#54573=CARTESIAN_POINT('Ctrl Pts',(67.0130945041938,-3.09176854509996,126.979422666954));
#54574=CARTESIAN_POINT('Ctrl Pts',(67.0053464361909,-3.19847661011503,127.065676782232));
#54575=CARTESIAN_POINT('Ctrl Pts',(66.9975983681879,-3.30154395595853,127.156376625492));
#54576=CARTESIAN_POINT('Ctrl Pts',(66.989850300185,-3.4005924374325,127.251171326665));
#54577=CARTESIAN_POINT('Ctrl Pts',(66.9820939974431,-3.49974618881181,127.346066776774));
#54578=CARTESIAN_POINT('Ctrl Pts',(66.9743376947013,-3.59487226054278,127.445065507758));
#54579=CARTESIAN_POINT('Ctrl Pts',(66.9665813919595,-3.68562956735191,127.54777993305));
#54580=CARTESIAN_POINT('Ctrl Pts',(66.9588209494453,-3.77643531406844,127.650549180124));
#54581=CARTESIAN_POINT('Ctrl Pts',(66.9510605069311,-3.86286740340615,127.757037769747));
#54582=CARTESIAN_POINT('Ctrl Pts',(66.943300064417,-3.94462621242947,127.866826429388));
#54583=CARTESIAN_POINT('Ctrl Pts',(66.9355271641516,-4.02651626795113,127.976791331532));
#54584=CARTESIAN_POINT('Ctrl Pts',(66.9277542638861,-4.10371783153262,128.090066566665));
#54585=CARTESIAN_POINT('Ctrl Pts',(66.9199813636206,-4.17597516264491,128.206204636207));
#54586=CARTESIAN_POINT('Ctrl Pts',(66.9124910278585,-4.2456057577677,128.318120794389));
#54587=CARTESIAN_POINT('Ctrl Pts',(66.9050006920963,-4.31064519803317,128.432694990288));
#54588=CARTESIAN_POINT('Ctrl Pts',(66.8975103563341,-4.37090660160109,128.549508395672));
#54589=CARTESIAN_POINT('Ctrl Pts',(66.8892429190004,-4.43741995873967,128.678440868048));
#54590=CARTESIAN_POINT('Ctrl Pts',(66.8809754816667,-4.498302134916,128.810468544938));
#54591=CARTESIAN_POINT('Ctrl Pts',(66.8727080443329,-4.55327294673881,128.945089648881));
#54592=CARTESIAN_POINT('Ctrl Pts',(66.8644601753659,-4.6081136470217,129.079392115376));
#54593=CARTESIAN_POINT('Ctrl Pts',(66.8562123063989,-4.65707076253721,129.216275477697));
#54594=CARTESIAN_POINT('Ctrl Pts',(66.8479644374318,-4.69991063187567,129.355214967577));
#54595=CARTESIAN_POINT('Ctrl Pts',(66.8435012054743,-4.72309289564009,129.430400348659));
#54596=CARTESIAN_POINT('Ctrl Pts',(66.8390379735168,-4.74448463186782,129.506187390391));
#54597=CARTESIAN_POINT('Ctrl Pts',(66.8345747415593,-4.76405452823409,129.582490119308));
#54598=CARTESIAN_POINT('Ctrl Pts',(68.5848726604777,-4.764054528234,129.582490119308));
#54599=CARTESIAN_POINT('Ctrl Pts',(68.5793138067223,-4.78834029123518,129.677179940662));
#54600=CARTESIAN_POINT('Ctrl Pts',(68.5737549529669,-4.80977775907463,129.772499935554));
#54601=CARTESIAN_POINT('Ctrl Pts',(68.5681960992114,-4.82834407427217,129.868264167973));
#54602=CARTESIAN_POINT('Ctrl Pts',(68.5567818981128,-4.86646697957742,130.064900426987));
#54603=CARTESIAN_POINT('Ctrl Pts',(68.5453676970142,-4.89258700281412,130.263933162505));
#54604=CARTESIAN_POINT('Ctrl Pts',(68.5339534959156,-4.90647035960978,130.464167036247));
#54605=CARTESIAN_POINT('Ctrl Pts',(68.5275888092741,-4.91421187518088,130.575819691599));
#54606=CARTESIAN_POINT('Ctrl Pts',(68.5212241226326,-4.91814937569076,130.687845448596));
#54607=CARTESIAN_POINT('Ctrl Pts',(68.5148594359911,-4.91824809583577,130.800032765));
#54608=CARTESIAN_POINT('',(68.8601405640458,-4.91824893709338,130.807594080086));
#54609=CARTESIAN_POINT('Ctrl Pts',(68.9302764532207,-4.76405452823407,129.582490119308));
#54610=CARTESIAN_POINT('Ctrl Pts',(68.9226268490548,-4.79769797436187,129.71366540515));
#54611=CARTESIAN_POINT('Ctrl Pts',(68.9149772448887,-4.82589836869319,129.846148951193));
#54612=CARTESIAN_POINT('Ctrl Pts',(68.9073276407228,-4.84857649036195,129.979442997673));
#54613=CARTESIAN_POINT('Ctrl Pts',(68.8994631279433,-4.87189173306073,130.116481818145));
#54614=CARTESIAN_POINT('Ctrl Pts',(68.8915986151638,-4.88936978039464,130.254376893832));
#54615=CARTESIAN_POINT('Ctrl Pts',(68.8837341023843,-4.90098179994194,130.392583421575));
#54616=CARTESIAN_POINT('Ctrl Pts',(68.8758695896048,-4.91259381948925,130.530789949319));
#54617=CARTESIAN_POINT('Ctrl Pts',(68.8680050768253,-4.9183398524931,130.669307470833));
#54618=CARTESIAN_POINT('Ctrl Pts',(68.8601405640458,-4.91824893709338,130.807594080086));
#54619=CARTESIAN_POINT('Ctrl Pts',(68.8601405640086,-4.91824893709295,130.80759408074));
#54620=CARTESIAN_POINT('Ctrl Pts',(68.8491119516274,-4.91812144401943,131.001517017064));
#54621=CARTESIAN_POINT('Ctrl Pts',(68.8380833392462,-4.9065250417326,131.195064423835));
#54622=CARTESIAN_POINT('Ctrl Pts',(68.827054726865,-4.88358926773127,131.387231895465));
#54623=CARTESIAN_POINT('Ctrl Pts',(68.8192803927459,-4.86742128900431,131.52269536808));
#54624=CARTESIAN_POINT('Ctrl Pts',(68.8115060586268,-4.84558709825159,131.657700181946));
#54625=CARTESIAN_POINT('Ctrl Pts',(68.8037317245076,-4.81811952949426,131.791734539647));
#54626=CARTESIAN_POINT('Ctrl Pts',(68.7959669715605,-4.79068581206062,131.925603711982));
#54627=CARTESIAN_POINT('Ctrl Pts',(68.7882022186133,-4.75763260813217,132.058504428508));
#54628=CARTESIAN_POINT('Ctrl Pts',(68.7804374656662,-4.71904451113463,132.189929801847));
#54629=CARTESIAN_POINT('Ctrl Pts',(68.7726804247812,-4.68049474037897,132.321224641653));
#54630=CARTESIAN_POINT('Ctrl Pts',(68.7649233838962,-4.63642112592656,132.451046681645));
#54631=CARTESIAN_POINT('Ctrl Pts',(68.7571663430111,-4.58695925984507,132.578899377645));
#54632=CARTESIAN_POINT('Ctrl Pts',(68.749415151771,-4.53753469334155,132.706655658932));
#54633=CARTESIAN_POINT('Ctrl Pts',(68.7416639605307,-4.48273010349809,132.832445189068));
#54634=CARTESIAN_POINT('Ctrl Pts',(68.7339127692906,-4.42273074085967,132.955787087691));
#54635=CARTESIAN_POINT('Ctrl Pts',(68.7261648725135,-4.36275687955099,133.079076562717));
#54636=CARTESIAN_POINT('Ctrl Pts',(68.7184169757364,-4.29759280749071,133.199920124484));
#54637=CARTESIAN_POINT('Ctrl Pts',(68.7106690789593,-4.22747159495209,133.317857579246));
#54638=CARTESIAN_POINT('Ctrl Pts',(68.7029228028752,-4.1573650502595,133.435770364034));
#54639=CARTESIAN_POINT('Ctrl Pts',(68.6951765267911,-4.08230362727125,133.550777915111));
#54640=CARTESIAN_POINT('Ctrl Pts',(68.6874302507069,-4.00256577916699,133.662445683819));
#54641=CARTESIAN_POINT('Ctrl Pts',(68.6796839174416,-3.92282734245606,133.774114276834));
#54642=CARTESIAN_POINT('Ctrl Pts',(68.6719375841762,-3.83841263894339,133.882442720109));
#54643=CARTESIAN_POINT('Ctrl Pts',(68.6641912509108,-3.74964254283232,133.987026774027));
#54644=CARTESIAN_POINT('Ctrl Pts',(68.6564431829078,-3.6608525672736,134.091634248819));
#54645=CARTESIAN_POINT('Ctrl Pts',(68.6486951149048,-3.56770551121351,134.192495367662));
#54646=CARTESIAN_POINT('Ctrl Pts',(68.6409470469018,-3.47056121812299,134.289240514171));
#54647=CARTESIAN_POINT('Ctrl Pts',(68.6331907441599,-3.37331367892187,134.386088482572));
#54648=CARTESIAN_POINT('Ctrl Pts',(68.625434441418,-3.27206069369573,134.478811463771));
#54649=CARTESIAN_POINT('Ctrl Pts',(68.6176781386761,-3.16719792250111,134.567077771725));
#54650=CARTESIAN_POINT('Ctrl Pts',(68.6099176961619,-3.06227918288801,134.655391190066));
#54651=CARTESIAN_POINT('Ctrl Pts',(68.6021572536477,-2.95374712752299,134.739242956568));
#54652=CARTESIAN_POINT('Ctrl Pts',(68.5943968111335,-2.84202809831967,134.818343595963));
#54653=CARTESIAN_POINT('Ctrl Pts',(68.5866239108681,-2.73012972781272,134.897571214727));
#54654=CARTESIAN_POINT('Ctrl Pts',(68.5788510106026,-2.61503448849036,134.972032252856));
#54655=CARTESIAN_POINT('Ctrl Pts',(68.5710781103372,-2.49719588713077,135.041481782201));
#54656=CARTESIAN_POINT('Ctrl Pts',(68.5635877745755,-2.38364101575402,135.108406646218));
#54657=CARTESIAN_POINT('Ctrl Pts',(68.5560974388139,-2.26753904716802,135.170677891941));
#54658=CARTESIAN_POINT('Ctrl Pts',(68.5486071030522,-2.14931317364053,135.22811874207));
#54659=CARTESIAN_POINT('Ctrl Pts',(68.5408327689331,-2.02660473017823,135.287737479494));
#54660=CARTESIAN_POINT('Ctrl Pts',(68.533058434814,-1.9012194433073,135.342341156007));
#54661=CARTESIAN_POINT('Ctrl Pts',(68.5252841006949,-1.77360565027721,135.391680756798));
#54662=CARTESIAN_POINT('Ctrl Pts',(68.5175193477478,-1.64614912984187,135.440959550941));
#54663=CARTESIAN_POINT('Ctrl Pts',(68.5097545948007,-1.51646992899177,135.484987037924));
#54664=CARTESIAN_POINT('Ctrl Pts',(68.5019898418536,-1.38504023124802,135.523560403581));
#54665=CARTESIAN_POINT('Ctrl Pts',(68.4942328009686,-1.25374107133307,135.562095457628));
#54666=CARTESIAN_POINT('Ctrl Pts',(68.4864757600836,-1.12069524716776,135.595187061255));
#54667=CARTESIAN_POINT('Ctrl Pts',(68.4787187191986,-0.986393806257207,
135.622680897651));
#54668=CARTESIAN_POINT('Ctrl Pts',(68.4709675279585,-0.852193643107774,
135.650154000731));
#54669=CARTESIAN_POINT('Ctrl Pts',(68.4632163367183,-0.716740129372833,
135.672037660768));
#54670=CARTESIAN_POINT('Ctrl Pts',(68.4554651454781,-0.580537975765703,
135.68822780671));
#54671=CARTESIAN_POINT('Ctrl Pts',(68.4477172487011,-0.444393711707353,
135.704411071407));
#54672=CARTESIAN_POINT('Ctrl Pts',(68.439969351924,-0.307501828055501,135.714905588944));
#54673=CARTESIAN_POINT('Ctrl Pts',(68.4322214551469,-0.170375479020028,
135.71965870198));
#54674=CARTESIAN_POINT('Ctrl Pts',(68.4244751790628,-0.0332778138606709,
135.724410820768));
#54675=CARTESIAN_POINT('Ctrl Pts',(68.4167289029787,0.104053828645908,135.723423910331));
#54676=CARTESIAN_POINT('Ctrl Pts',(68.4089826268946,0.24110333966079,135.716697357052));
#54677=CARTESIAN_POINT('Ctrl Pts',(68.4012362936293,0.378153862344217,135.709970754119));
#54678=CARTESIAN_POINT('Ctrl Pts',(68.3934899603639,0.514921858885063,135.697504442965));
#54679=CARTESIAN_POINT('Ctrl Pts',(68.3857436270985,0.650893790698375,135.679349882757));
#54680=CARTESIAN_POINT('Ctrl Pts',(68.3779955590955,0.78689617248287,135.661191256962));
#54681=CARTESIAN_POINT('Ctrl Pts',(68.3702474910926,0.922101747344729,135.637341899042));
#54682=CARTESIAN_POINT('Ctrl Pts',(68.3624994230896,1.05600504236359,135.607904768815));
#54683=CARTESIAN_POINT('Ctrl Pts',(68.3547431203477,1.19005065139804,135.578436352457));
#54684=CARTESIAN_POINT('Ctrl Pts',(68.3469868176058,1.32279083328778,135.543368384575));
#54685=CARTESIAN_POINT('Ctrl Pts',(68.339230514864,1.45373266724798,135.502854460775));
#54686=CARTESIAN_POINT('Ctrl Pts',(68.3314700723498,1.58474438880756,135.462318913475));
#54687=CARTESIAN_POINT('Ctrl Pts',(68.3237096298356,1.71395548173818,135.416331749496));
#54688=CARTESIAN_POINT('Ctrl Pts',(68.3159491873214,1.84089195408112,135.365095193914));
#54689=CARTESIAN_POINT('Ctrl Pts',(68.308176287056,1.96803219611835,135.313776388865));
#54690=CARTESIAN_POINT('Ctrl Pts',(68.3004033867905,2.09289016455381,135.257191514278));
#54691=CARTESIAN_POINT('Ctrl Pts',(68.2926304865251,2.21501466290698,135.195589728602));
#54692=CARTESIAN_POINT('Ctrl Pts',(68.2851401507631,2.33269962813115,135.136227323001));
#54693=CARTESIAN_POINT('Ctrl Pts',(68.2776498150011,2.44784614074524,135.072206578021));
#54694=CARTESIAN_POINT('Ctrl Pts',(68.2701594792391,2.56007672724223,135.003787984855));
#54695=CARTESIAN_POINT('Ctrl Pts',(68.2623851451201,2.6765625705385,134.932775279932));
#54696=CARTESIAN_POINT('Ctrl Pts',(68.254610811001,2.79027600030487,134.856799707916));
#54697=CARTESIAN_POINT('Ctrl Pts',(68.2468364768819,2.90076517609331,134.776103869044));
#54698=CARTESIAN_POINT('Ctrl Pts',(68.2390717239349,3.01111818384715,134.695507480582));
#54699=CARTESIAN_POINT('Ctrl Pts',(68.2313069709878,3.11825453121856,134.610202628347));
#54700=CARTESIAN_POINT('Ctrl Pts',(68.2235422180407,3.22174835817949,134.520476947697));
#54701=CARTESIAN_POINT('Ctrl Pts',(68.2157851771557,3.32513939361262,134.430840383859));
#54702=CARTESIAN_POINT('Ctrl Pts',(68.2080281362707,3.42489481473299,134.336791984003));
#54703=CARTESIAN_POINT('Ctrl Pts',(68.2002710953857,3.52061936726625,134.238661468297));
#54704=CARTESIAN_POINT('Ctrl Pts',(68.1925199041456,3.61627173316981,134.140604953576));
#54705=CARTESIAN_POINT('Ctrl Pts',(68.1847687129055,3.70789900894599,134.038472729016));
#54706=CARTESIAN_POINT('Ctrl Pts',(68.1770175216654,3.79514082820219,133.932633169089));
#54707=CARTESIAN_POINT('Ctrl Pts',(68.1692696248883,3.88234556735784,133.826838593798));
#54708=CARTESIAN_POINT('Ctrl Pts',(68.1615217281112,3.96516830906575,133.717340118174));
#54709=CARTESIAN_POINT('Ctrl Pts',(68.1537738313341,4.04328737882934,133.604541010808));
#54710=CARTESIAN_POINT('Ctrl Pts',(68.1460275552501,4.12139010776759,133.491765498584));
#54711=CARTESIAN_POINT('Ctrl Pts',(68.138281279166,4.19479089935299,133.375691049112));
#54712=CARTESIAN_POINT('Ctrl Pts',(68.1305350030819,4.26321026789703,133.256751547699));
#54713=CARTESIAN_POINT('Ctrl Pts',(68.1227886698166,4.3316301414973,133.137811168301));
#54714=CARTESIAN_POINT('Ctrl Pts',(68.1150423365513,4.39506832373357,133.016006033656));
#54715=CARTESIAN_POINT('Ctrl Pts',(68.1072960032859,4.45329052851111,132.891796013255));
#54716=CARTESIAN_POINT('Ctrl Pts',(68.099547935283,4.51152577174772,132.76755817688));
#54717=CARTESIAN_POINT('Ctrl Pts',(68.09179986728,4.56454254727345,132.64091473702));
#54718=CARTESIAN_POINT('Ctrl Pts',(68.084051799277,4.61215425763861,132.512346614653));
#54719=CARTESIAN_POINT('Ctrl Pts',(68.0762954965352,4.65981657029614,132.383641848556));
#54720=CARTESIAN_POINT('Ctrl Pts',(68.0685391937934,4.70206220641158,132.253008680913));
#54721=CARTESIAN_POINT('Ctrl Pts',(68.0607828910515,4.73875395459257,132.120944842116));
#54722=CARTESIAN_POINT('Ctrl Pts',(68.0530224485374,4.77546528626439,131.988810516871));
#54723=CARTESIAN_POINT('Ctrl Pts',(68.0452620060232,4.80661673467081,131.855244379512));
#54724=CARTESIAN_POINT('Ctrl Pts',(68.037501563509,4.8321222332623,131.720754520488));
#54725=CARTESIAN_POINT('Ctrl Pts',(68.0297286632436,4.8576686755444,131.586048766403));
#54726=CARTESIAN_POINT('Ctrl Pts',(68.0219557629782,4.87755099975233,131.45041671452));
#54727=CARTESIAN_POINT('Ctrl Pts',(68.0141828627128,4.89173494722666,131.314372645445));
#54728=CARTESIAN_POINT('Ctrl Pts',(68.0066925269506,4.90540327248334,131.183274120953));
#54729=CARTESIAN_POINT('Ctrl Pts',(67.9992021911885,4.91378030924849,131.051793322314));
#54730=CARTESIAN_POINT('Ctrl Pts',(67.9917118554263,4.91688118248826,130.920388630532));
#54731=CARTESIAN_POINT('Ctrl Pts',(67.9839375213072,4.92009962627935,130.784001689924));
#54732=CARTESIAN_POINT('Ctrl Pts',(67.9761631871881,4.91764411219603,130.647264708449));
#54733=CARTESIAN_POINT('Ctrl Pts',(67.968388853069,4.90947451588986,130.510688963626));
#54734=CARTESIAN_POINT('Ctrl Pts',(67.9606241001219,4.90131498788099,130.374281536202));
#54735=CARTESIAN_POINT('Ctrl Pts',(67.9528593471749,4.88745541244134,130.238035336579));
#54736=CARTESIAN_POINT('Ctrl Pts',(67.9450945942278,4.86790759759728,130.102464126796));
#54737=CARTESIAN_POINT('Ctrl Pts',(67.9373375533428,4.8483791979185,129.967027568251));
#54738=CARTESIAN_POINT('Ctrl Pts',(67.9295805124577,4.82317385730762,129.832265049859));
#54739=CARTESIAN_POINT('Ctrl Pts',(67.9218234715727,4.79235533408991,129.698687332043));
#54740=CARTESIAN_POINT('Ctrl Pts',(67.9140722803326,4.76156005136029,129.565210346222));
#54741=CARTESIAN_POINT('Ctrl Pts',(67.9063210890925,4.72516009898088,129.432916761999));
#54742=CARTESIAN_POINT('Ctrl Pts',(67.8985698978524,4.6832706139897,129.302308881226));
#54743=CARTESIAN_POINT('Ctrl Pts',(67.8908220010753,4.64139893314707,129.171756512287));
#54744=CARTESIAN_POINT('Ctrl Pts',(67.8830741042981,4.59404247939745,129.042888793302));
#54745=CARTESIAN_POINT('Ctrl Pts',(67.875326207521,4.5413666611052,128.91619433466));
#54746=CARTESIAN_POINT('Ctrl Pts',(67.8675799314369,4.48870186145858,128.789526377768));
#54747=CARTESIAN_POINT('Ctrl Pts',(67.8598336553529,4.43072006048388,128.665031137772));
#54748=CARTESIAN_POINT('Ctrl Pts',(67.8520873792688,4.36763522933708,128.543178279506));
#54749=CARTESIAN_POINT('Ctrl Pts',(67.8443410460034,4.30454993251239,128.42132452175));
#54750=CARTESIAN_POINT('Ctrl Pts',(67.836594712738,4.23636171009661,128.30211353184));
#54751=CARTESIAN_POINT('Ctrl Pts',(67.8288483794727,4.16333082596077,128.185990991997));
#54752=CARTESIAN_POINT('Ctrl Pts',(67.8211003114697,4.09028358706489,128.069842447316));
#54753=CARTESIAN_POINT('Ctrl Pts',(67.8133522434667,4.01239173655985,127.95678405987));
#54754=CARTESIAN_POINT('Ctrl Pts',(67.8056041754637,3.92995902640709,127.847232768916));
#54755=CARTESIAN_POINT('Ctrl Pts',(67.7978478727219,3.84743870578892,127.737565045546));
#54756=CARTESIAN_POINT('Ctrl Pts',(67.79009156998,3.76036812035407,127.63141217742));
#54757=CARTESIAN_POINT('Ctrl Pts',(67.7823352672382,3.66909185866908,127.529158639802));
#54758=CARTESIAN_POINT('Ctrl Pts',(67.774574824724,3.57776688009496,127.426850526393));
#54759=CARTESIAN_POINT('Ctrl Pts',(67.7668143822098,3.48223202472447,127.328446170816));
#54760=CARTESIAN_POINT('Ctrl Pts',(67.7590539396956,3.38286824237172,127.234292618598));
#54761=CARTESIAN_POINT('Ctrl Pts',(67.7512810394302,3.28334495245443,127.13998792274));
#54762=CARTESIAN_POINT('Ctrl Pts',(67.7435081391648,3.17998074779317,127.049947923247));
#54763=CARTESIAN_POINT('Ctrl Pts',(67.7357352388993,3.07318978958398,126.964479424131));
#54764=CARTESIAN_POINT('Ctrl Pts',(67.7282449031374,2.9702809516966,126.88211792024));
#54765=CARTESIAN_POINT('Ctrl Pts',(67.7207545673754,2.86419042506642,126.8040014987));
#54766=CARTESIAN_POINT('Ctrl Pts',(67.7132642316134,2.75531203402774,126.730365200578));
#54767=CARTESIAN_POINT('Ctrl Pts',(67.7054898974943,2.64230548569932,126.65393695983));
#54768=CARTESIAN_POINT('Ctrl Pts',(67.6977155633752,2.52593752525034,126.582093174899));
#54769=CARTESIAN_POINT('Ctrl Pts',(67.6899412292562,2.40661661674796,126.515143961521));
#54770=CARTESIAN_POINT('Ctrl Pts',(67.6821764763091,2.28744276060129,126.448277257066));
#54771=CARTESIAN_POINT('Ctrl Pts',(67.674411723362,2.16532353510161,126.386293311512));
#54772=CARTESIAN_POINT('Ctrl Pts',(67.6666469704149,2.04069756533032,126.329459891365));
#54773=CARTESIAN_POINT('Ctrl Pts',(67.6588899295299,1.91619537582912,126.272682918972));
#54774=CARTESIAN_POINT('Ctrl Pts',(67.6511328886449,1.78919175015911,126.221046452932));
#54775=CARTESIAN_POINT('Ctrl Pts',(67.6433758477599,1.66015086845906,126.174772930044));
#54776=CARTESIAN_POINT('Ctrl Pts',(67.6356246565198,1.53120729749151,126.128534302379));
#54777=CARTESIAN_POINT('Ctrl Pts',(67.6278734652796,1.40022989495658,126.087650699494));
#54778=CARTESIAN_POINT('Ctrl Pts',(67.6201222740395,1.26770349600975,126.052296759756));
#54779=CARTESIAN_POINT('Ctrl Pts',(67.6123743772624,1.13523342431791,126.016957846386));
#54780=CARTESIAN_POINT('Ctrl Pts',(67.6046264804854,1.00121604261531,125.987144022249));
#54781=CARTESIAN_POINT('Ctrl Pts',(67.5968785837083,0.866151839921082,125.962980230455));
#54782=CARTESIAN_POINT('Ctrl Pts',(67.5891323076242,0.731115889746415,125.938821493205));
#54783=CARTESIAN_POINT('Ctrl Pts',(67.5813860315401,0.595033938739008,125.920310506312));
#54784=CARTESIAN_POINT('Ctrl Pts',(67.573639755456,0.458416785860073,125.907521115097));
#54785=CARTESIAN_POINT('Ctrl Pts',(67.5658934221907,0.321798624504351,125.894731629473));
#54786=CARTESIAN_POINT('Ctrl Pts',(67.5581470889253,0.184645642656913,125.887663860246));
#54787=CARTESIAN_POINT('Ctrl Pts',(67.5504007556599,0.0474734843716824,
125.886339742175));
#54788=CARTESIAN_POINT('Ctrl Pts',(67.542652687657,-0.0897293926673115,
125.885015327577));
#54789=CARTESIAN_POINT('Ctrl Pts',(67.534904619654,-0.226951063817352,125.8894371274));
#54790=CARTESIAN_POINT('Ctrl Pts',(67.527156551651,-0.363676560919306,125.899574952367));
#54791=CARTESIAN_POINT('Ctrl Pts',(67.5194002489092,-0.50054737150682,125.909723551936));
#54792=CARTESIAN_POINT('Ctrl Pts',(67.5116439461673,-0.636920564111838,
125.925600283279));
#54793=CARTESIAN_POINT('Ctrl Pts',(67.5038876434254,-0.7722864102675,125.947123052549));
#54794=CARTESIAN_POINT('Ctrl Pts',(67.4961272009113,-0.907724505251042,
125.968657309168));
#54795=CARTESIAN_POINT('Ctrl Pts',(67.4883667583971,-1.04215379944995,125.99584353083));
#54796=CARTESIAN_POINT('Ctrl Pts',(67.4806063158829,-1.17507640095522,126.02854880025));
#54797=CARTESIAN_POINT('Ctrl Pts',(67.4728334156175,-1.30821238162074,126.061306571071));
#54798=CARTESIAN_POINT('Ctrl Pts',(67.4650605153521,-1.43983646068943,126.099600984804));
#54799=CARTESIAN_POINT('Ctrl Pts',(67.4572876150866,-1.56946665101604,126.143249430966));
#54800=CARTESIAN_POINT('Ctrl Pts',(67.4497972793246,-1.69438445740572,126.185311146166));
#54801=CARTESIAN_POINT('Ctrl Pts',(67.4423069435626,-1.8174505362692,126.232344276918));
#54802=CARTESIAN_POINT('Ctrl Pts',(67.4348166078005,-1.93825426922783,126.284144533094));
#54803=CARTESIAN_POINT('Ctrl Pts',(67.4270418140675,-2.06364572506759,126.337911990239));
#54804=CARTESIAN_POINT('Ctrl Pts',(67.4192670203345,-2.18699683237101,126.396986136842));
#54805=CARTESIAN_POINT('Ctrl Pts',(67.4114922266015,-2.30782581219541,126.461190912953));
#54806=CARTESIAN_POINT('Ctrl Pts',(67.4037271187352,-2.42850426283095,126.525315702518));
#54807=CARTESIAN_POINT('Ctrl Pts',(67.3959620108689,-2.54666649606018,126.594558221521));
#54808=CARTESIAN_POINT('Ctrl Pts',(67.3881969030026,-2.66185008304264,126.668694141905));
#54809=CARTESIAN_POINT('Ctrl Pts',(67.3804396114472,-2.7769177269199,126.742755437518));
#54810=CARTESIAN_POINT('Ctrl Pts',(67.3726823198917,-2.88901236495634,126.821700121321));
#54811=CARTESIAN_POINT('Ctrl Pts',(67.3649250283362,-2.99769591471208,126.905257866237));
#54812=CARTESIAN_POINT('Ctrl Pts',(67.3571740386271,-3.1062911724367,126.988747730752));
#54813=CARTESIAN_POINT('Ctrl Pts',(67.3494230489179,-3.21148055074902,127.076842957219));
#54814=CARTESIAN_POINT('Ctrl Pts',(67.3416720592087,-3.3128550918911,127.169230055587));
#54815=CARTESIAN_POINT('Ctrl Pts',(67.3339245176007,-3.41418453560908,127.26157605468));
#54816=CARTESIAN_POINT('Ctrl Pts',(67.3261769759928,-3.51170223007268,127.358209864512));
#54817=CARTESIAN_POINT('Ctrl Pts',(67.3184294343847,-3.60503258532045,127.458777989491));
#54818=CARTESIAN_POINT('Ctrl Pts',(67.3106836615481,-3.69834163315655,127.559323154668));
#54819=CARTESIAN_POINT('Ctrl Pts',(67.3029378887114,-3.78746497852078,127.663800561191));
#54820=CARTESIAN_POINT('Ctrl Pts',(67.2951921158747,-3.87206446114142,127.771820449445));
#54821=CARTESIAN_POINT('Ctrl Pts',(67.2874464340175,-3.95666295008322,127.879839068932));
#54822=CARTESIAN_POINT('Ctrl Pts',(67.2797007521603,-4.03673744186551,127.99139977903));
#54823=CARTESIAN_POINT('Ctrl Pts',(67.271955070303,-4.11199083712506,128.106080717722));
#54824=CARTESIAN_POINT('Ctrl Pts',(67.2642040531959,-4.1872960671584,128.220840649004));
#54825=CARTESIAN_POINT('Ctrl Pts',(67.2564530360887,-4.25777334983864,128.338724776482));
#54826=CARTESIAN_POINT('Ctrl Pts',(67.2487020189816,-4.32316944740157,128.459283008711));
#54827=CARTESIAN_POINT('Ctrl Pts',(67.2409484295368,-4.38858724803102,128.579881250718));
#54828=CARTESIAN_POINT('Ctrl Pts',(67.2331948400921,-4.44892032817435,128.703155016199));
#54829=CARTESIAN_POINT('Ctrl Pts',(67.2254412506474,-4.50396245748309,128.828631576406));
#54830=CARTESIAN_POINT('Ctrl Pts',(67.217677895398,-4.55907391348107,128.954266176911));
#54831=CARTESIAN_POINT('Ctrl Pts',(67.2099145401486,-4.60888095666048,129.082108752829));
#54832=CARTESIAN_POINT('Ctrl Pts',(67.2021511848992,-4.65322612099232,129.211668014012));
#54833=CARTESIAN_POINT('Ctrl Pts',(67.1948275729225,-4.69505942195193,129.333888590863));
#54834=CARTESIAN_POINT('Ctrl Pts',(67.1875039609459,-4.73203243839533,129.45763647703));
#54835=CARTESIAN_POINT('Ctrl Pts',(67.1801803489693,-4.76405452823408,129.582490119308));
#54836=CARTESIAN_POINT('Origin',(213.235140564004,0.,130.804360617566));
#54837=CARTESIAN_POINT('',(65.0848845757186,-4.764054528234,129.582490119308));
#54838=CARTESIAN_POINT('',(65.4298554009981,-4.76405452823407,129.582490119308));
#54839=CARTESIAN_POINT('',(213.235140564004,-4.76405452823405,129.582490119308));
#54840=CARTESIAN_POINT('',(66.7648594360216,-4.91824995804488,130.803718206823));
#54841=CARTESIAN_POINT('Ctrl Pts',(66.7648594359911,-4.91824995804495,130.803718207364));
#54842=CARTESIAN_POINT('Ctrl Pts',(66.7568197494795,-4.91826860358419,130.946467220818));
#54843=CARTESIAN_POINT('Ctrl Pts',(66.7487800629679,-4.9120681202326,131.089122546079));
#54844=CARTESIAN_POINT('Ctrl Pts',(66.7407403764563,-4.89969894598051,131.231131400607));
#54845=CARTESIAN_POINT('Ctrl Pts',(66.7326926649578,-4.88731742516968,131.373282004344));
#54846=CARTESIAN_POINT('Ctrl Pts',(66.7246449534593,-4.86875496264839,131.514784505445));
#54847=CARTESIAN_POINT('Ctrl Pts',(66.7165972419608,-4.84411353660799,131.6550938936));
#54848=CARTESIAN_POINT('Ctrl Pts',(66.7084693661741,-4.81922665415721,131.796800921595));
#54849=CARTESIAN_POINT('Ctrl Pts',(66.7003414903875,-4.78813913118351,131.937290584989));
#54850=CARTESIAN_POINT('Ctrl Pts',(66.6922136146009,-4.75100775206522,132.076016389509));
#54851=CARTESIAN_POINT('Ctrl Pts',(66.6841409245608,-4.71412848345291,132.213800288999));
#54852=CARTESIAN_POINT('Ctrl Pts',(66.6760682345207,-4.67128735843842,132.349843902826));
#54853=CARTESIAN_POINT('Ctrl Pts',(66.6679955444806,-4.62268674879548,132.483631377453));
#54854=CARTESIAN_POINT('Ctrl Pts',(66.6598400758208,-4.5735877809387,132.618790729663));
#54855=CARTESIAN_POINT('Ctrl Pts',(66.6516846071609,-4.51861071253405,132.751647085802));
#54856=CARTESIAN_POINT('Ctrl Pts',(66.643529138501,-4.45801197923393,132.881693584499));
#54857=CARTESIAN_POINT('Ctrl Pts',(66.6353736698411,-4.39741324593388,133.011740083196));
#54858=CARTESIAN_POINT('Ctrl Pts',(66.6272182011812,-4.33119306907287,133.138976436277));
#54859=CARTESIAN_POINT('Ctrl Pts',(66.6190627325213,-4.2596528185075,133.262925428239));
#54860=CARTESIAN_POINT('Ctrl Pts',(66.6112883984022,-4.19145590254206,133.381081835605));
#54861=CARTESIAN_POINT('Ctrl Pts',(66.6035140642831,-4.11823101838583,133.496585722954));
#54862=CARTESIAN_POINT('Ctrl Pts',(66.595739730164,-4.04020985348845,133.60897955822));
#54863=CARTESIAN_POINT('Ctrl Pts',(66.5879749772169,-3.96228484270385,133.721234878129));
#54864=CARTESIAN_POINT('Ctrl Pts',(66.5802102242698,-3.87957553308772,133.830387454122));
#54865=CARTESIAN_POINT('Ctrl Pts',(66.5724454713227,-3.79235925770069,133.936004646352));
#54866=CARTESIAN_POINT('Ctrl Pts',(66.5646884304377,-3.70522960674778,134.041516938099));
#54867=CARTESIAN_POINT('Ctrl Pts',(66.5569313895527,-3.61360214555809,134.143500534399));
#54868=CARTESIAN_POINT('Ctrl Pts',(66.5491743486677,-3.51779701433527,134.241552382428));
#54869=CARTESIAN_POINT('Ctrl Pts',(66.5414231574276,-3.42206413050729,134.339530288795));
#54870=CARTESIAN_POINT('Ctrl Pts',(66.5336719661875,-3.32216011947938,134.43358206996));
#54871=CARTESIAN_POINT('Ctrl Pts',(66.5259207749473,-3.2184446018404,134.523338623334));
#54872=CARTESIAN_POINT('Ctrl Pts',(66.5181728781703,-3.11477316606312,134.613057027778));
#54873=CARTESIAN_POINT('Ctrl Pts',(66.5104249813932,-3.00729374072816,134.698483580078));
#54874=CARTESIAN_POINT('Ctrl Pts',(66.5026770846161,-2.89640175899458,134.779287021035));
#54875=CARTESIAN_POINT('Ctrl Pts',(66.494930808532,-2.78553297347302,134.860073559654));
#54876=CARTESIAN_POINT('Ctrl Pts',(66.4871845324479,-2.67125336718392,134.93623868036));
#54877=CARTESIAN_POINT('Ctrl Pts',(66.4794382563638,-2.55398999360058,135.007492565898));
#54878=CARTESIAN_POINT('Ctrl Pts',(66.4716919230985,-2.43672575440566,135.078746977416));
#54879=CARTESIAN_POINT('Ctrl Pts',(66.4639455898331,-2.31647803808475,135.145089878401));
#54880=CARTESIAN_POINT('Ctrl Pts',(66.4561992565678,-2.19370095947873,135.206276014627));
#54881=CARTESIAN_POINT('Ctrl Pts',(66.4484511885648,-2.07089638579707,135.267475853064));
#54882=CARTESIAN_POINT('Ctrl Pts',(66.4407031205618,-1.94556167254729,135.323516454431));
#54883=CARTESIAN_POINT('Ctrl Pts',(66.4329550525588,-1.81817312439181,135.374199734235));
#54884=CARTESIAN_POINT('Ctrl Pts',(66.4251987498169,-1.69064918617141,135.424936880833));
#54885=CARTESIAN_POINT('Ctrl Pts',(66.4174424470751,-1.56106741643523,135.470305187077));
#54886=CARTESIAN_POINT('Ctrl Pts',(66.4096861443333,-1.42992210954663,135.510155536932));
#54887=CARTESIAN_POINT('Ctrl Pts',(66.4019257018191,-1.29870680645904,135.550027156119));
#54888=CARTESIAN_POINT('Ctrl Pts',(66.3941652593049,-1.16592668171449,135.584374852692));
#54889=CARTESIAN_POINT('Ctrl Pts',(66.3864048167908,-1.03208761408673,135.613100392117));
#54890=CARTESIAN_POINT('Ctrl Pts',(66.3786319165253,-0.898033696106121,
135.641872044328));
#54891=CARTESIAN_POINT('Ctrl Pts',(66.3708590162599,-0.762917823862867,
135.665003438184));
#54892=CARTESIAN_POINT('Ctrl Pts',(66.3630861159945,-0.627253307748616,
135.682447983575));
#54893=CARTESIAN_POINT('Ctrl Pts',(66.3555957802324,-0.496520538513051,
135.699258375801));
#54894=CARTESIAN_POINT('Ctrl Pts',(66.3481054444704,-0.365278628881969,
135.710788176821));
#54895=CARTESIAN_POINT('Ctrl Pts',(66.3406151087084,-0.233986190814424,
135.717041507366));
#54896=CARTESIAN_POINT('Ctrl Pts',(66.3328407745893,-0.0977157600522679,
135.72353193484));
#54897=CARTESIAN_POINT('Ctrl Pts',(66.3250664404702,0.0390407701182173,
135.724358438414));
#54898=CARTESIAN_POINT('Ctrl Pts',(66.3172921063511,0.175773232286202,135.719468636044));
#54899=CARTESIAN_POINT('Ctrl Pts',(66.309527353404,0.312337183914696,135.71458485992));
#54900=CARTESIAN_POINT('Ctrl Pts',(66.3017626004569,0.448876739593951,135.703998808814));
#54901=CARTESIAN_POINT('Ctrl Pts',(66.2939978475098,0.584878001874702,135.687709958482));
#54902=CARTESIAN_POINT('Ctrl Pts',(66.2862408066248,0.720744185784659,135.671437286465));
#54903=CARTESIAN_POINT('Ctrl Pts',(66.2784837657398,0.856072754576127,135.64947313323));
#54904=CARTESIAN_POINT('Ctrl Pts',(66.2707267248547,0.990351564891798,135.621868981899));
#54905=CARTESIAN_POINT('Ctrl Pts',(66.2629755336146,1.12452911451226,135.594285647073));
#54906=CARTESIAN_POINT('Ctrl Pts',(66.2552243423745,1.25765809994303,135.561070858228));
#54907=CARTESIAN_POINT('Ctrl Pts',(66.2474731511343,1.38923360101116,135.522327665387));
#54908=CARTESIAN_POINT('Ctrl Pts',(66.2397252543573,1.52075317898091,135.483600939436));
#54909=CARTESIAN_POINT('Ctrl Pts',(66.2319773575801,1.65072021156031,135.439350593103));
#54910=CARTESIAN_POINT('Ctrl Pts',(66.2242294608031,1.77864225972406,135.389730261818));
#54911=CARTESIAN_POINT('Ctrl Pts',(66.216483184719,1.9065375493532,135.340120310036));
#54912=CARTESIAN_POINT('Ctrl Pts',(66.2087369086349,2.03238834114532,135.285142748876));
#54913=CARTESIAN_POINT('Ctrl Pts',(66.2009906325508,2.15571997080239,135.225000217215));
#54914=CARTESIAN_POINT('Ctrl Pts',(66.1932442992854,2.27905251086554,135.164857241595));
#54915=CARTESIAN_POINT('Ctrl Pts',(66.1854979660201,2.39986550027812,135.09954939076));
#54916=CARTESIAN_POINT('Ctrl Pts',(66.1777516327547,2.51770713954999,135.029326158486));
#54917=CARTESIAN_POINT('Ctrl Pts',(66.1700035647517,2.63557516863977,134.959087200205));
#54918=CARTESIAN_POINT('Ctrl Pts',(66.1622554967488,2.75047018770366,134.883930870191));
#54919=CARTESIAN_POINT('Ctrl Pts',(66.1545074287458,2.86196808834432,134.804150827539));
#54920=CARTESIAN_POINT('Ctrl Pts',(66.146751126004,2.97358449028078,134.724285993708));
#54921=CARTESIAN_POINT('Ctrl Pts',(66.1389948232621,3.08179624297426,134.63978785859));
#54922=CARTESIAN_POINT('Ctrl Pts',(66.1312385205202,3.18621071270336,134.550991685173));
#54923=CARTESIAN_POINT('Ctrl Pts',(66.123478078006,3.29068091157882,134.462148118563));
#54924=CARTESIAN_POINT('Ctrl Pts',(66.1157176354919,3.39134950224234,134.369002208074));
#54925=CARTESIAN_POINT('Ctrl Pts',(66.1079571929778,3.48786039736403,134.271926465679));
#54926=CARTESIAN_POINT('Ctrl Pts',(66.1001842927123,3.58452622034241,134.174694888684));
#54927=CARTESIAN_POINT('Ctrl Pts',(66.0924113924469,3.67702074644487,134.073521162081));
#54928=CARTESIAN_POINT('Ctrl Pts',(66.0846384921815,3.76502732128719,133.968811965345));
#54929=CARTESIAN_POINT('Ctrl Pts',(66.0771481564195,3.84983463545808,133.867909211658));
#54930=CARTESIAN_POINT('Ctrl Pts',(66.0696578206575,3.93047444151396,133.763723815205));
#54931=CARTESIAN_POINT('Ctrl Pts',(66.0621674848956,4.00670231537586,133.656643846571));
#54932=CARTESIAN_POINT('Ctrl Pts',(66.0543931507765,4.08582039224497,133.545503908378));
#54933=CARTESIAN_POINT('Ctrl Pts',(66.0466188166573,4.16043599813095,133.43089351177));
#54934=CARTESIAN_POINT('Ctrl Pts',(66.0388444825382,4.23022930458927,133.313213561262));
#54935=CARTESIAN_POINT('Ctrl Pts',(66.0310797295911,4.2999365970349,133.195678640777));
#54936=CARTESIAN_POINT('Ctrl Pts',(66.0233149766441,4.36483321743604,133.075082026382));
#54937=CARTESIAN_POINT('Ctrl Pts',(66.015550223697,4.4246409506054,132.951855791187));
#54938=CARTESIAN_POINT('Ctrl Pts',(66.007793182812,4.48438928189103,132.828751946026));
#54939=CARTESIAN_POINT('Ctrl Pts',(66.0000361419269,4.53905861473284,132.70302402707));
#54940=CARTESIAN_POINT('Ctrl Pts',(65.9922791010419,4.58841543734564,132.575130742915));
#54941=CARTESIAN_POINT('Ctrl Pts',(65.9845279098018,4.63773503959436,132.447333904081));
#54942=CARTESIAN_POINT('Ctrl Pts',(65.9767767185618,4.68174996552895,132.317375313543));
#54943=CARTESIAN_POINT('Ctrl Pts',(65.9690255273217,4.72027399236456,132.185735475998));
#54944=CARTESIAN_POINT('Ctrl Pts',(65.9612776305446,4.75878164546126,132.054151588894));
#54945=CARTESIAN_POINT('Ctrl Pts',(65.9535297337675,4.79180293158724,131.92088825046));
#54946=CARTESIAN_POINT('Ctrl Pts',(65.9457818369904,4.81920093325826,131.786442807295));
#54947=CARTESIAN_POINT('Ctrl Pts',(65.9380355609063,4.84659320385795,131.652025487219));
#54948=CARTESIAN_POINT('Ctrl Pts',(65.9302892848222,4.86836445164901,131.516426937096));
#54949=CARTESIAN_POINT('Ctrl Pts',(65.9225430087381,4.88442859480994,131.380156036706));
#54950=CARTESIAN_POINT('Ctrl Pts',(65.9147966754727,4.90049285655268,131.243884130396));
#54951=CARTESIAN_POINT('Ctrl Pts',(65.9070503422074,4.9108498838293,131.106940252193));
#54952=CARTESIAN_POINT('Ctrl Pts',(65.899304008942,4.91546537416024,130.969839371283));
#54953=CARTESIAN_POINT('Ctrl Pts',(65.8915559409391,4.92008189809823,130.832707787581));
#54954=CARTESIAN_POINT('Ctrl Pts',(65.8838078729361,4.91895431339053,130.695419521879));
#54955=CARTESIAN_POINT('Ctrl Pts',(65.8760598049332,4.91210044280317,130.558490118496));
#54956=CARTESIAN_POINT('Ctrl Pts',(65.8683035021913,4.90523928784057,130.421415184914));
#54957=CARTESIAN_POINT('Ctrl Pts',(65.8605471994494,4.89263970920417,130.284700266643));
#54958=CARTESIAN_POINT('Ctrl Pts',(65.8527908967076,4.87437154502329,130.148856915389));
#54959=CARTESIAN_POINT('Ctrl Pts',(65.8450304541934,4.85609363057314,130.012941060449));
#54960=CARTESIAN_POINT('Ctrl Pts',(65.8372700116793,4.83214117027004,129.877898084206));
#54961=CARTESIAN_POINT('Ctrl Pts',(65.8295095691651,4.8026350950883,129.744228924838));
#54962=CARTESIAN_POINT('Ctrl Pts',(65.8217366688996,4.77308165413526,129.610345187869));
#54963=CARTESIAN_POINT('Ctrl Pts',(65.8139637686342,4.73795688321754,129.477840052943));
#54964=CARTESIAN_POINT('Ctrl Pts',(65.8061908683688,4.69743177386798,129.347199750553));
#54965=CARTESIAN_POINT('Ctrl Pts',(65.7987005326067,4.65837985431943,129.221308552216));
#54966=CARTESIAN_POINT('Ctrl Pts',(65.7912101968445,4.61431351450875,129.097149247888));
#54967=CARTESIAN_POINT('Ctrl Pts',(65.7837198610824,4.56542713202485,128.975137240099));
#54968=CARTESIAN_POINT('Ctrl Pts',(65.7759455269633,4.51468720749096,128.848499109952));
#54969=CARTESIAN_POINT('Ctrl Pts',(65.7681711928443,4.45859379245806,128.723773168615));
#54970=CARTESIAN_POINT('Ctrl Pts',(65.7603968587252,4.39731130416395,128.601445195501));
#54971=CARTESIAN_POINT('Ctrl Pts',(65.7526321057781,4.33610434105961,128.479267980681));
#54972=CARTESIAN_POINT('Ctrl Pts',(65.744867352831,4.26972120241002,128.359483200153));
#54973=CARTESIAN_POINT('Ctrl Pts',(65.7371025998839,4.19837502145539,128.242558470303));
#54974=CARTESIAN_POINT('Ctrl Pts',(65.7293455589989,4.12709970253359,128.125749871744));
#54975=CARTESIAN_POINT('Ctrl Pts',(65.7215885181139,4.05087135328964,128.011796002438));
#54976=CARTESIAN_POINT('Ctrl Pts',(65.7138314772289,3.96994967943336,127.901141265663));
#54977=CARTESIAN_POINT('Ctrl Pts',(65.7060802859888,3.88908902924115,127.790569974486));
#54978=CARTESIAN_POINT('Ctrl Pts',(65.6983290947487,3.80354232899519,127.683293178129));
#54979=CARTESIAN_POINT('Ctrl Pts',(65.6905779035086,3.71361318294052,127.57972727562));
#54980=CARTESIAN_POINT('Ctrl Pts',(65.6828300067315,3.62372225917162,127.476205391382));
#54981=CARTESIAN_POINT('Ctrl Pts',(65.6750821099545,3.52945285007382,127.376391558591));
#54982=CARTESIAN_POINT('Ctrl Pts',(65.6673342131774,3.43114938018312,127.280669797791));
#54983=CARTESIAN_POINT('Ctrl Pts',(65.6595879370933,3.33286647325929,127.184968059919));
#54984=CARTESIAN_POINT('Ctrl Pts',(65.6518416610092,3.23055146391411,127.093356964039));
#54985=CARTESIAN_POINT('Ctrl Pts',(65.6440953849251,3.12458595779127,127.006183995176));
#54986=CARTESIAN_POINT('Ctrl Pts',(65.6363490516597,3.01861966945485,126.919010382821));
#54987=CARTESIAN_POINT('Ctrl Pts',(65.6286027183944,2.90900313249718,126.836275211237));
#54988=CARTESIAN_POINT('Ctrl Pts',(65.620856385129,2.79615106375221,126.758285693497));
#54989=CARTESIAN_POINT('Ctrl Pts',(65.613108317126,2.6832737225689,126.680278710546));
#54990=CARTESIAN_POINT('Ctrl Pts',(65.6053602491231,2.56715972935017,126.60701971843));
#54991=CARTESIAN_POINT('Ctrl Pts',(65.5976121811201,2.44825245977412,126.538772386652));
#54992=CARTESIAN_POINT('Ctrl Pts',(65.5898558783782,2.32921881413694,126.470452520798));
#54993=CARTESIAN_POINT('Ctrl Pts',(65.5820995756364,2.20738630141379,126.407155150371));
#54994=CARTESIAN_POINT('Ctrl Pts',(65.5743432728945,2.08322305375562,126.349098024766));
#54995=CARTESIAN_POINT('Ctrl Pts',(65.5665828303803,1.9589935364337,126.291009912326));
#54996=CARTESIAN_POINT('Ctrl Pts',(65.5588223878662,1.8324311660397,126.238167768281));
#54997=CARTESIAN_POINT('Ctrl Pts',(65.551061945352,1.70402276219455,126.190740619298));
#54998=CARTESIAN_POINT('Ctrl Pts',(65.5432890450866,1.57540822577998,126.143237336045));
#54999=CARTESIAN_POINT('Ctrl Pts',(65.5355161448212,1.4449421063749,126.101166538557));
#55000=CARTESIAN_POINT('Ctrl Pts',(65.5277432445557,1.31312590856396,126.064647186275));
#55001=CARTESIAN_POINT('Ctrl Pts',(65.5202529087937,1.1861015615686,126.029455404435));
#55002=CARTESIAN_POINT('Ctrl Pts',(65.5127625730317,1.05782388941703,125.999418527393));
#55003=CARTESIAN_POINT('Ctrl Pts',(65.5052722372697,0.928747447857728,125.974597554993));
#55004=CARTESIAN_POINT('Ctrl Pts',(65.4974979031506,0.794777033784942,125.94883548788));
#55005=CARTESIAN_POINT('Ctrl Pts',(65.4897235690315,0.659521705933291,125.928611048702));
#55006=CARTESIAN_POINT('Ctrl Pts',(65.4819492349125,0.523479035813597,125.914048484219));
#55007=CARTESIAN_POINT('Ctrl Pts',(65.4741844819654,0.38760402612616,125.899503866795));
#55008=CARTESIAN_POINT('Ctrl Pts',(65.4664197290183,0.250943989848566,125.890607281628));
#55009=CARTESIAN_POINT('Ctrl Pts',(65.4586549760712,0.114007549612928,125.887432171765));
#55010=CARTESIAN_POINT('Ctrl Pts',(65.4508979351862,-0.0227928834199881,
125.884260215465));
#55011=CARTESIAN_POINT('Ctrl Pts',(65.4431408943012,-0.159868785756313,
125.886798434745));
#55012=CARTESIAN_POINT('Ctrl Pts',(65.4353838534162,-0.296705891051209,
125.895068542662));
#55013=CARTESIAN_POINT('Ctrl Pts',(65.427632662176,-0.433439806420751,125.903332414026));
#55014=CARTESIAN_POINT('Ctrl Pts',(65.4198814709359,-0.569934894510545,
125.917319546939));
#55015=CARTESIAN_POINT('Ctrl Pts',(65.4121302796958,-0.705676721514948,
125.936999584397));
#55016=CARTESIAN_POINT('Ctrl Pts',(65.4043823829187,-0.841360854621289,
125.956671257314));
#55017=CARTESIAN_POINT('Ctrl Pts',(65.3966344861416,-0.976291977298376,
125.982030966324));
#55018=CARTESIAN_POINT('Ctrl Pts',(65.3888865893645,-1.10996083231246,126.012996509795));
#55019=CARTESIAN_POINT('Ctrl Pts',(65.3811403132805,-1.24360172668364,126.043955575942));
#55020=CARTESIAN_POINT('Ctrl Pts',(65.3733940371964,-1.37598049794283,126.080518055968));
#55021=CARTESIAN_POINT('Ctrl Pts',(65.3656477611123,-1.50659852992527,126.122550718379));
#55022=CARTESIAN_POINT('Ctrl Pts',(65.357901427847,-1.63721752610017,126.164583691066));
#55023=CARTESIAN_POINT('Ctrl Pts',(65.3501550945816,-1.76607538489307,126.21208680695));
#55024=CARTESIAN_POINT('Ctrl Pts',(65.3424087613163,-1.89268947466686,126.264877209183));
#55025=CARTESIAN_POINT('Ctrl Pts',(65.3346606933133,-2.01933191878851,126.317679433461));
#55026=CARTESIAN_POINT('Ctrl Pts',(65.3269126253104,-2.14372923323401,126.375771149786));
#55027=CARTESIAN_POINT('Ctrl Pts',(65.3191645573074,-2.26541993000123,126.438921853449));
#55028=CARTESIAN_POINT('Ctrl Pts',(65.3114082545656,-2.38723996108896,126.502139674432));
#55029=CARTESIAN_POINT('Ctrl Pts',(65.3036519518237,-2.50634728055511,126.570427043021));
#55030=CARTESIAN_POINT('Ctrl Pts',(65.2958956490819,-2.62230565280428,126.643507805248));
#55031=CARTESIAN_POINT('Ctrl Pts',(65.2881352065677,-2.73832591552831,126.716627572879));
#55032=CARTESIAN_POINT('Ctrl Pts',(65.2803747640536,-2.85119356053653,126.794545609926));
#55033=CARTESIAN_POINT('Ctrl Pts',(65.2726143215394,-2.96050324301058,126.876943704298));
#55034=CARTESIAN_POINT('Ctrl Pts',(65.264841421274,-3.06998839909099,126.959474071406));
#55035=CARTESIAN_POINT('Ctrl Pts',(65.2570685210085,-3.17590387687434,127.046498618975));
#55036=CARTESIAN_POINT('Ctrl Pts',(65.2492956207431,-3.2778785169376,127.137659717479));
#55037=CARTESIAN_POINT('Ctrl Pts',(65.241805284981,-3.37614612197718,127.225506880432));
#55038=CARTESIAN_POINT('Ctrl Pts',(65.2343149492189,-3.47075421247686,127.317194853294));
#55039=CARTESIAN_POINT('Ctrl Pts',(65.2268246134568,-3.56140576905517,127.412374177345));
#55040=CARTESIAN_POINT('Ctrl Pts',(65.2191475807491,-3.65431681963504,127.5099258502));
#55041=CARTESIAN_POINT('Ctrl Pts',(65.2114705480414,-3.74338205395473,127.611471582107));
#55042=CARTESIAN_POINT('Ctrl Pts',(65.2037935153337,-3.82823189034494,127.716671569711));
#55043=CARTESIAN_POINT('Ctrl Pts',(65.1961255500607,-3.91298150958423,127.821747304358));
#55044=CARTESIAN_POINT('Ctrl Pts',(65.1884575847876,-3.99352538054134,127.930468404211));
#55045=CARTESIAN_POINT('Ctrl Pts',(65.1807896195146,-4.06953018480535,128.042457806557));
#55046=CARTESIAN_POINT('Ctrl Pts',(65.1727975325316,-4.14874768060431,128.159180954466));
#55047=CARTESIAN_POINT('Ctrl Pts',(65.1648054455486,-4.22303364486602,128.279454471617));
#55048=CARTESIAN_POINT('Ctrl Pts',(65.1568133585656,-4.29205620188384,128.402811820983));
#55049=CARTESIAN_POINT('Ctrl Pts',(65.1491588987257,-4.35816288864318,128.520957917075));
#55050=CARTESIAN_POINT('Ctrl Pts',(65.1415044388858,-4.41944155453826,128.641932227695));
#55051=CARTESIAN_POINT('Ctrl Pts',(65.1338499790459,-4.47564455395244,128.765294927311));
#55052=CARTESIAN_POINT('Ctrl Pts',(65.1261988623244,-4.53182300646449,128.888603747736));
#55053=CARTESIAN_POINT('Ctrl Pts',(65.1185477456028,-4.5829300369661,129.014298517022));
#55054=CARTESIAN_POINT('Ctrl Pts',(65.1108966288812,-4.62876447172692,129.141915873288));
#55055=CARTESIAN_POINT('Ctrl Pts',(65.1032467506769,-4.67459148708259,129.269512571616));
#55056=CARTESIAN_POINT('Ctrl Pts',(65.0955968724725,-4.71514746886405,129.399030860214));
#55057=CARTESIAN_POINT('Ctrl Pts',(65.0879469942681,-4.75027998543829,129.529988959672));
#55058=CARTESIAN_POINT('Ctrl Pts',(65.086926188085,-4.75496809800567,129.547464118634));
#55059=CARTESIAN_POINT('Ctrl Pts',(65.0859053819018,-4.75955971051597,129.564964893244));
#55060=CARTESIAN_POINT('Ctrl Pts',(65.0848845757186,-4.764054528234,129.582490119308));
#55061=CARTESIAN_POINT('Ctrl Pts',(66.8345747415593,-4.76405452823409,129.582490119308));
#55062=CARTESIAN_POINT('Ctrl Pts',(66.8263521180634,-4.80010819768355,129.723062829301));
#55063=CARTESIAN_POINT('Ctrl Pts',(66.8181294945675,-4.82997550392153,129.865386831657));
#55064=CARTESIAN_POINT('Ctrl Pts',(66.8099068710717,-4.85349778080253,130.008909579321));
#55065=CARTESIAN_POINT('Ctrl Pts',(66.8017034909999,-4.87696500844651,130.152096440379));
#55066=CARTESIAN_POINT('Ctrl Pts',(66.7935001109281,-4.89411676822097,130.296476141404));
#55067=CARTESIAN_POINT('Ctrl Pts',(66.7852967308564,-4.90484495065059,130.44148450568));
#55068=CARTESIAN_POINT('Ctrl Pts',(66.7784842992448,-4.91375408426128,130.561905546288));
#55069=CARTESIAN_POINT('Ctrl Pts',(66.7716718676332,-4.91823415872638,130.682759772639));
#55070=CARTESIAN_POINT('Ctrl Pts',(66.7648594360216,-4.91824995804488,130.803718206823));
#55071=CARTESIAN_POINT('',(67.1101405639552,-4.91824833737017,130.800316553325));
#55072=CARTESIAN_POINT('Ctrl Pts',(67.1801803489693,-4.76405452823408,129.582490119308));
#55073=CARTESIAN_POINT('Ctrl Pts',(67.1722432273088,-4.79875915536151,129.717802933762));
#55074=CARTESIAN_POINT('Ctrl Pts',(67.1643061056482,-4.82764789875426,129.854414213236));
#55075=CARTESIAN_POINT('Ctrl Pts',(67.1563689839877,-4.85065958804843,129.991781622407));
#55076=CARTESIAN_POINT('Ctrl Pts',(67.1439813375631,-4.88657445527619,130.206174064384));
#55077=CARTESIAN_POINT('Ctrl Pts',(67.1315936911385,-4.90828242222668,130.423009367747));
#55078=CARTESIAN_POINT('Ctrl Pts',(67.1192060447139,-4.91552932682745,130.64079259013));
#55079=CARTESIAN_POINT('Ctrl Pts',(67.1161842178121,-4.9172971276289,130.69391835572));
#55080=CARTESIAN_POINT('Ctrl Pts',(67.1131623909104,-4.91820457997885,130.747100369239));
#55081=CARTESIAN_POINT('Ctrl Pts',(67.1101405640086,-4.91824833736939,130.800316552386));
#55082=CARTESIAN_POINT('Ctrl Pts',(67.1101405639552,-4.91824833737017,130.800316553325));
#55083=CARTESIAN_POINT('Ctrl Pts',(67.1024929960437,-4.91835907751146,130.934994808511));
#55084=CARTESIAN_POINT('Ctrl Pts',(67.0948454281322,-4.91293374377952,131.069873198528));
#55085=CARTESIAN_POINT('Ctrl Pts',(67.0871978602207,-4.90194968703462,131.204451017702));
#55086=CARTESIAN_POINT('Ctrl Pts',(67.0795575524082,-4.89097605783222,131.338901077529));
#55087=CARTESIAN_POINT('Ctrl Pts',(67.0719172445957,-4.87445423398753,131.473050734335));
#55088=CARTESIAN_POINT('Ctrl Pts',(67.0642769367832,-4.85241361143598,131.606398775044));
#55089=CARTESIAN_POINT('Ctrl Pts',(67.0565121210911,-4.83001381079315,131.741919880267));
#55090=CARTESIAN_POINT('Ctrl Pts',(67.0487473053991,-4.80191375142125,131.87661259095));
#55091=CARTESIAN_POINT('Ctrl Pts',(67.0409824897071,-4.76819932657029,132.009955178185));
#55092=CARTESIAN_POINT('Ctrl Pts',(67.0333500180552,-4.73505953264051,132.14102506541));
#55093=CARTESIAN_POINT('Ctrl Pts',(67.0257175464032,-4.69649534909657,132.270790082721));
#55094=CARTESIAN_POINT('Ctrl Pts',(67.0180850747513,-4.65263987246651,132.398764982724));
#55095=CARTESIAN_POINT('Ctrl Pts',(67.0104535181768,-4.60878965378661,132.526724539474));
#55096=CARTESIAN_POINT('Ctrl Pts',(67.0028219616023,-4.55964953417331,132.652894023819));
#55097=CARTESIAN_POINT('Ctrl Pts',(66.9951904050278,-4.50540214616269,132.776804422558));
#55098=CARTESIAN_POINT('Ctrl Pts',(66.987557996453,-4.45114870187897,132.900728654871));
#55099=CARTESIAN_POINT('Ctrl Pts',(66.9799255878781,-4.39178701776272,133.022392930459));
#55100=CARTESIAN_POINT('Ctrl Pts',(66.9722931793033,-4.32754719246508,133.141349783028));
#55101=CARTESIAN_POINT('Ctrl Pts',(66.9644288610426,-4.2613554489021,133.263921123218));
#55102=CARTESIAN_POINT('Ctrl Pts',(66.9565645427819,-4.18998461287187,133.383617484527));
#55103=CARTESIAN_POINT('Ctrl Pts',(66.9487002245212,-4.11373581287558,133.499979419319));
#55104=CARTESIAN_POINT('Ctrl Pts',(66.9410567650359,-4.03962835762559,133.613073486056));
#55105=CARTESIAN_POINT('Ctrl Pts',(66.9334133055505,-3.96091354320488,133.723017613029));
#55106=CARTESIAN_POINT('Ctrl Pts',(66.9257698460652,-3.87790958048365,133.829422657937));
#55107=CARTESIAN_POINT('Ctrl Pts',(66.9177950984168,-3.79130800199817,133.940439584668));
#55108=CARTESIAN_POINT('Ctrl Pts',(66.9098203507684,-3.70003745642511,134.047603378814));
#55109=CARTESIAN_POINT('Ctrl Pts',(66.90184560312,-3.60450218679224,134.150514685733));
#55110=CARTESIAN_POINT('Ctrl Pts',(66.8938708554716,-3.50896691715949,134.253425992652));
#55111=CARTESIAN_POINT('Ctrl Pts',(66.8858961078232,-3.40916732640844,134.352084522751));
#55112=CARTESIAN_POINT('Ctrl Pts',(66.8779213601748,-3.30554571334739,134.446139111581));
#55113=CARTESIAN_POINT('Ctrl Pts',(66.8701470260557,-3.20452821694329,134.537830012815));
#55114=CARTESIAN_POINT('Ctrl Pts',(66.8623726919366,-3.09953277183999,134.62545984883));
#55115=CARTESIAN_POINT('Ctrl Pts',(66.8545983578175,-2.99091970195566,134.708663679439));
#55116=CARTESIAN_POINT('Ctrl Pts',(66.8468336048704,-2.88244048797293,134.791764968763));
#55117=CARTESIAN_POINT('Ctrl Pts',(66.8390688519233,-2.7703528274791,134.870450870348));
#55118=CARTESIAN_POINT('Ctrl Pts',(66.8313040989762,-2.65505290971584,134.944394084714));
#55119=CARTESIAN_POINT('Ctrl Pts',(66.8235470580912,-2.5398675094565,135.018263857638));
#55120=CARTESIAN_POINT('Ctrl Pts',(66.8157900172062,-2.42147652805856,135.087400107768));
#55121=CARTESIAN_POINT('Ctrl Pts',(66.8080329763212,-2.30030788368171,135.151516780251));
#55122=CARTESIAN_POINT('Ctrl Pts',(66.8002817850811,-2.17923061352214,135.215585101853));
#55123=CARTESIAN_POINT('Ctrl Pts',(66.792530593841,-2.05538019384104,135.274641198104));
#55124=CARTESIAN_POINT('Ctrl Pts',(66.7847794026009,-1.92921177158329,135.328443397852));
#55125=CARTESIAN_POINT('Ctrl Pts',(66.7770315058238,-1.80309697427066,135.38222273023));
#55126=CARTESIAN_POINT('Ctrl Pts',(66.7692836090467,-1.67466649277362,135.430752454426));
#55127=CARTESIAN_POINT('Ctrl Pts',(66.7615357122696,-1.5443980214469,135.473837870305));
#55128=CARTESIAN_POINT('Ctrl Pts',(66.7537894361856,-1.41415679947611,135.516914273645));
#55129=CARTESIAN_POINT('Ctrl Pts',(66.7460431601014,-1.28207872335766,135.554548511176));
#55130=CARTESIAN_POINT('Ctrl Pts',(66.7382968840173,-1.14865894403689,135.586595000444));
#55131=CARTESIAN_POINT('Ctrl Pts',(66.730550550752,-1.01523817984162,135.618641726272));
#55132=CARTESIAN_POINT('Ctrl Pts',(66.7228042174866,-0.880476072833954,
135.64510053022));
#55133=CARTESIAN_POINT('Ctrl Pts',(66.7150578842213,-0.744879936338025,
135.665876527541));
#55134=CARTESIAN_POINT('Ctrl Pts',(66.7073098162183,-0.60925343402767,135.686657177502));
#55135=CARTESIAN_POINT('Ctrl Pts',(66.6995617482154,-0.472792916949479,
135.701752429259));
#55136=CARTESIAN_POINT('Ctrl Pts',(66.6918136802124,-0.336012425982121,
135.711119090538));
#55137=CARTESIAN_POINT('Ctrl Pts',(66.6840573774706,-0.199086563081068,
135.720495706817));
#55138=CARTESIAN_POINT('Ctrl Pts',(66.6763010747287,-0.0618404376339475,
135.724131543603));
#55139=CARTESIAN_POINT('Ctrl Pts',(66.6685447719869,0.0752097306826276,
135.722035531477));
#55140=CARTESIAN_POINT('Ctrl Pts',(66.6607843294727,0.212333046800534,135.719938400647));
#55141=CARTESIAN_POINT('Ctrl Pts',(66.6530238869585,0.349259807251273,135.712103347394));
#55142=CARTESIAN_POINT('Ctrl Pts',(66.6452634444443,0.485478297085964,135.698591291079));
#55143=CARTESIAN_POINT('Ctrl Pts',(66.6374905441789,0.621915456933632,135.685057544012));
#55144=CARTESIAN_POINT('Ctrl Pts',(66.6297176439135,0.757641686796736,135.665828637622));
#55145=CARTESIAN_POINT('Ctrl Pts',(66.6219447436481,0.892153963876741,135.641016938542));
#55146=CARTESIAN_POINT('Ctrl Pts',(66.614454407886,1.02177638086946,135.617107207221));
#55147=CARTESIAN_POINT('Ctrl Pts',(66.6069640721239,1.15027127281611,135.588013601413));
#55148=CARTESIAN_POINT('Ctrl Pts',(66.5994737363619,1.2772031870345,135.553880075525));
#55149=CARTESIAN_POINT('Ctrl Pts',(66.5916994022428,1.40894776336004,135.518452366628));
#55150=CARTESIAN_POINT('Ctrl Pts',(66.5839250681237,1.53942582893993,135.477482791881));
#55151=CARTESIAN_POINT('Ctrl Pts',(66.5761507340046,1.66813558538054,135.431077242916));
#55152=CARTESIAN_POINT('Ctrl Pts',(66.5683859810575,1.79668671854929,135.384728884643));
#55153=CARTESIAN_POINT('Ctrl Pts',(66.5606212281104,1.92347351444267,135.332958013198));
#55154=CARTESIAN_POINT('Ctrl Pts',(66.5528564751634,2.04800645677809,135.275921040449));
#55155=CARTESIAN_POINT('Ctrl Pts',(66.5450994342784,2.17241571123975,135.218940717626));
#55156=CARTESIAN_POINT('Ctrl Pts',(66.5373423933933,2.29457521382065,135.156704863911));
#55157=CARTESIAN_POINT('Ctrl Pts',(66.5295853525083,2.41401299825359,135.089418879336));
#55158=CARTESIAN_POINT('Ctrl Pts',(66.5218341612682,2.5333607137242,135.022183635645));
#55159=CARTESIAN_POINT('Ctrl Pts',(66.5140829700281,2.64999045710881,134.949906032491));
#55160=CARTESIAN_POINT('Ctrl Pts',(66.5063317787879,2.76345288557983,134.872838368726));
#55161=CARTESIAN_POINT('Ctrl Pts',(66.4985838820109,2.87686708949188,134.795803460773));
#55162=CARTESIAN_POINT('Ctrl Pts',(66.4908359852338,2.98711633322886,134.713982760682));
#55163=CARTESIAN_POINT('Ctrl Pts',(66.4830880884567,3.09377860458702,134.627672926062));
#55164=CARTESIAN_POINT('Ctrl Pts',(66.4753418123726,3.20041856449737,134.5413811456));
#55165=CARTESIAN_POINT('Ctrl Pts',(66.4675955362885,3.30347274071809,134.450602344169));
#55166=CARTESIAN_POINT('Ctrl Pts',(66.4598492602044,3.40255100942519,134.35567441541));
#55167=CARTESIAN_POINT('Ctrl Pts',(66.452102926939,3.50163000950569,134.260745785915));
#55168=CARTESIAN_POINT('Ctrl Pts',(66.4443565936737,3.59673276120459,134.161668238454));
#55169=CARTESIAN_POINT('Ctrl Pts',(66.4366102604083,3.68750522005332,134.058817302572));
#55170=CARTESIAN_POINT('Ctrl Pts',(66.4288621924053,3.77829800676484,133.955943333935));
#55171=CARTESIAN_POINT('Ctrl Pts',(66.4211141244024,3.86475831230156,133.849294588451));
#55172=CARTESIAN_POINT('Ctrl Pts',(66.4133660563994,3.94657194613094,133.73928019679));
#55173=CARTESIAN_POINT('Ctrl Pts',(66.4056097536576,4.02847253246385,133.629148880525));
#55174=CARTESIAN_POINT('Ctrl Pts',(66.3978534509157,4.10571634815101,133.515645086767));
#55175=CARTESIAN_POINT('Ctrl Pts',(66.3900971481739,4.17803187739915,133.399207952948));
#55176=CARTESIAN_POINT('Ctrl Pts',(66.3823367056597,4.25038600362273,133.282708673124));
#55177=CARTESIAN_POINT('Ctrl Pts',(66.3745762631455,4.31780641006646,133.163273273924));
#55178=CARTESIAN_POINT('Ctrl Pts',(66.3668158206313,4.38006775548502,133.04136520403));
#55179=CARTESIAN_POINT('Ctrl Pts',(66.3590429203659,4.44242904834255,132.919261436479));
#55180=CARTESIAN_POINT('Ctrl Pts',(66.3512700201005,4.49961456734348,132.794677421732));
#55181=CARTESIAN_POINT('Ctrl Pts',(66.3434971198351,4.55144695361076,132.668097104027));
#55182=CARTESIAN_POINT('Ctrl Pts',(66.336006784073,4.60139510207919,132.546118299708));
#55183=CARTESIAN_POINT('Ctrl Pts',(66.3285164483111,4.64637245529841,132.42228610336));
#55184=CARTESIAN_POINT('Ctrl Pts',(66.321026112549,4.68626475337587,132.29704468453));
#55185=CARTESIAN_POINT('Ctrl Pts',(66.31325177843,4.72766958006006,132.167054699238));
#55186=CARTESIAN_POINT('Ctrl Pts',(66.3054774443109,4.7637272980565,132.035134751446));
#55187=CARTESIAN_POINT('Ctrl Pts',(66.2977031101918,4.79425576270565,131.901764255369));
#55188=CARTESIAN_POINT('Ctrl Pts',(66.2899383572447,4.82474660375058,131.768558126509));
#55189=CARTESIAN_POINT('Ctrl Pts',(66.2821736042976,4.84972166349704,131.633905383745));
#55190=CARTESIAN_POINT('Ctrl Pts',(66.2744088513505,4.86904794017105,131.498302415425));
#55191=CARTESIAN_POINT('Ctrl Pts',(66.2666518104655,4.8883550217146,131.362834129885));
#55192=CARTESIAN_POINT('Ctrl Pts',(66.2588947695804,4.90202443042993,131.226417881499));
#55193=CARTESIAN_POINT('Ctrl Pts',(66.2511377286954,4.90997386588508,131.089561772587));
#55194=CARTESIAN_POINT('Ctrl Pts',(66.2433865374554,4.91791730660904,130.952808867933));
#55195=CARTESIAN_POINT('Ctrl Pts',(66.2356353462153,4.92014933720628,130.815617151715));
#55196=CARTESIAN_POINT('Ctrl Pts',(66.2278841549752,4.91663934307343,130.678501042473));
#55197=CARTESIAN_POINT('Ctrl Pts',(66.2201362581981,4.91313084078168,130.541443211234));
#55198=CARTESIAN_POINT('Ctrl Pts',(66.212388361421,4.90388517773935,130.404461313076));
#55199=CARTESIAN_POINT('Ctrl Pts',(66.2046404646439,4.88892383249246,130.268070749503));
#55200=CARTESIAN_POINT('Ctrl Pts',(66.1968941885598,4.87396561683648,130.131708715896));
#55201=CARTESIAN_POINT('Ctrl Pts',(66.1891479124757,4.85329413968906,129.995938159226));
#55202=CARTESIAN_POINT('Ctrl Pts',(66.1814016363916,4.8269828090832,129.861269941483));
#55203=CARTESIAN_POINT('Ctrl Pts',(66.1736553031263,4.80067128425308,129.726600729649));
#55204=CARTESIAN_POINT('Ctrl Pts',(66.165908969861,4.76871989785951,129.593034256689));
#55205=CARTESIAN_POINT('Ctrl Pts',(66.1581626365956,4.73125322386009,129.461071373131));
#55206=CARTESIAN_POINT('Ctrl Pts',(66.1504145685926,4.69377815945876,129.329078937401));
#55207=CARTESIAN_POINT('Ctrl Pts',(66.1426665005896,4.65078545648614,129.198691181695));
#55208=CARTESIAN_POINT('Ctrl Pts',(66.1349184325866,4.60244950050618,129.070393588528));
#55209=CARTESIAN_POINT('Ctrl Pts',(66.1271621298448,4.55406217249707,128.941959639153));
#55210=CARTESIAN_POINT('Ctrl Pts',(66.1194058271029,4.50032038537794,128.815620656346));
#55211=CARTESIAN_POINT('Ctrl Pts',(66.111649524361,4.44144683698859,128.691842438543));
#55212=CARTESIAN_POINT('Ctrl Pts',(66.1038890818469,4.38254186601374,128.567998156578));
#55213=CARTESIAN_POINT('Ctrl Pts',(66.0961286393327,4.31849985859843,128.446717708552));
#55214=CARTESIAN_POINT('Ctrl Pts',(66.0883681968185,4.2495889247968,128.32844118577));
#55215=CARTESIAN_POINT('Ctrl Pts',(66.0805952965531,4.18056736904661,128.209974795014));
#55216=CARTESIAN_POINT('Ctrl Pts',(66.0728223962876,4.10666147889138,128.094522295196));
#55217=CARTESIAN_POINT('Ctrl Pts',(66.0650494960222,4.0281825435191,127.982494487044));
#55218=CARTESIAN_POINT('Ctrl Pts',(66.0575591602601,3.9525565151239,127.874539171899));
#55219=CARTESIAN_POINT('Ctrl Pts',(66.0500688244981,3.87268433927344,127.769764123914));
#55220=CARTESIAN_POINT('Ctrl Pts',(66.042578488736,3.78887794812418,127.668505557663));
#55221=CARTESIAN_POINT('Ctrl Pts',(66.0348041546169,3.70189401218245,127.563407742096));
#55222=CARTESIAN_POINT('Ctrl Pts',(66.0270298204978,3.61039610127415,127.461765408633));
#55223=CARTESIAN_POINT('Ctrl Pts',(66.0192554863787,3.51468910651767,127.363990935827));
#55224=CARTESIAN_POINT('Ctrl Pts',(66.0114907334316,3.41910006207865,127.266336961321));
#55225=CARTESIAN_POINT('Ctrl Pts',(66.0037259804846,3.31931252587049,127.172541639686));
#55226=CARTESIAN_POINT('Ctrl Pts',(65.9959612275375,3.21567223276058,127.082985179109));
#55227=CARTESIAN_POINT('Ctrl Pts',(65.9882041866524,3.11213487665057,126.99351766727));
#55228=CARTESIAN_POINT('Ctrl Pts',(65.9804471457674,3.0047526726784,126.908280892175));
#55229=CARTESIAN_POINT('Ctrl Pts',(65.9726901048824,2.89390861632368,126.827618737224));
#55230=CARTESIAN_POINT('Ctrl Pts',(65.9649389136423,2.78314814833485,126.747017410232));
#55231=CARTESIAN_POINT('Ctrl Pts',(65.9571877224022,2.66893133906706,126.670984065966));
#55232=CARTESIAN_POINT('Ctrl Pts',(65.9494365311621,2.55167443546606,126.599822517145));
#55233=CARTESIAN_POINT('Ctrl Pts',(65.941688634385,2.43446736917655,126.528691213881));
#55234=CARTESIAN_POINT('Ctrl Pts',(65.9339407376079,2.31422311201487,126.462427790126));
#55235=CARTESIAN_POINT('Ctrl Pts',(65.9261928408308,2.1913868955423,126.401292762474));
#55236=CARTESIAN_POINT('Ctrl Pts',(65.9184465647467,2.06857637375801,126.340170522951));
#55237=CARTESIAN_POINT('Ctrl Pts',(65.9107002886626,1.94317532088278,126.284174719862));
#55238=CARTESIAN_POINT('Ctrl Pts',(65.9029540125785,1.81565321841043,126.233519726332));
#55239=CARTESIAN_POINT('Ctrl Pts',(65.8952076793131,1.68813017459889,126.182864358878));
#55240=CARTESIAN_POINT('Ctrl Pts',(65.8874613460478,1.55848641329632,126.137550023984));
#55241=CARTESIAN_POINT('Ctrl Pts',(65.8797150127824,1.4272106495052,126.097742635996));
#55242=CARTESIAN_POINT('Ctrl Pts',(65.8719669447794,1.29590548741734,126.057926333419));
#55243=CARTESIAN_POINT('Ctrl Pts',(65.8642188767764,1.1629679696571,126.02361954519));
#55244=CARTESIAN_POINT('Ctrl Pts',(65.8564708087735,1.02890080607087,125.994937970952));
#55245=CARTESIAN_POINT('Ctrl Pts',(65.8487145060316,0.894691154307397,125.966225913595));
#55246=CARTESIAN_POINT('Ctrl Pts',(65.8409582032897,0.759349841311873,125.943151094937));
#55247=CARTESIAN_POINT('Ctrl Pts',(65.8332019005479,0.623389130121796,125.925777928409));
#55248=CARTESIAN_POINT('Ctrl Pts',(65.8254414580337,0.487355852606459,125.908395489299));
#55249=CARTESIAN_POINT('Ctrl Pts',(65.8176810155195,0.350702907520669,125.896720799304));
#55250=CARTESIAN_POINT('Ctrl Pts',(65.8099205730053,0.213945476176173,125.890766169942));
#55251=CARTESIAN_POINT('Ctrl Pts',(65.8021476727399,0.0769685096623139,
125.88480198168));
#55252=CARTESIAN_POINT('Ctrl Pts',(65.7943747724745,-0.060112887099783,
125.884576203956));
#55253=CARTESIAN_POINT('Ctrl Pts',(65.786601872209,-0.196784836413529,125.890048988186));
#55254=CARTESIAN_POINT('Ctrl Pts',(65.7791115364471,-0.328488416112371,
125.895322822925));
#55255=CARTESIAN_POINT('Ctrl Pts',(65.7716212006851,-0.459811493396904,
125.905888073856));
#55256=CARTESIAN_POINT('Ctrl Pts',(65.7641308649232,-0.590302594474758,
125.921664035814));
#55257=CARTESIAN_POINT('Ctrl Pts',(65.7563565308041,-0.72574130531305,125.938038148164));
#55258=CARTESIAN_POINT('Ctrl Pts',(65.748582196685,-0.860712734922414,125.960077767977));
#55259=CARTESIAN_POINT('Ctrl Pts',(65.740807862566,-0.994705136449562,125.987749282403));
#55260=CARTESIAN_POINT('Ctrl Pts',(65.7330431096189,-1.12853240431671,126.01538669416));
#55261=CARTESIAN_POINT('Ctrl Pts',(65.7252783566719,-1.26138266559559,126.04864211208));
#55262=CARTESIAN_POINT('Ctrl Pts',(65.7175136037248,-1.39274916223049,126.087430171438));
#55263=CARTESIAN_POINT('Ctrl Pts',(65.7097565628398,-1.52398518380933,126.126179705949));
#55264=CARTESIAN_POINT('Ctrl Pts',(65.7019995219549,-1.65374000093024,126.17045083641));
#55265=CARTESIAN_POINT('Ctrl Pts',(65.6942424810699,-1.78151727633739,126.220107215254));
#55266=CARTESIAN_POINT('Ctrl Pts',(65.6864912898298,-1.90919819390755,126.269726147836));
#55267=CARTESIAN_POINT('Ctrl Pts',(65.6787400985896,-2.03490417512514,126.324722104468));
#55268=CARTESIAN_POINT('Ctrl Pts',(65.6709889073494,-2.15815462210365,126.384909103001));
#55269=CARTESIAN_POINT('Ctrl Pts',(65.6632410105723,-2.28135268435421,126.445070520454));
#55270=CARTESIAN_POINT('Ctrl Pts',(65.6554931137953,-2.40209693756204,126.510418420384));
#55271=CARTESIAN_POINT('Ctrl Pts',(65.6477452170182,-2.51992754320466,126.580719032453));
#55272=CARTESIAN_POINT('Ctrl Pts',(65.6399989409341,-2.63773350122471,126.651004939149));
#55273=CARTESIAN_POINT('Ctrl Pts',(65.63225266485,-2.75262668841713,126.726241297131));
#55274=CARTESIAN_POINT('Ctrl Pts',(65.6245063887659,-2.86417298038462,126.806148992235));
#55275=CARTESIAN_POINT('Ctrl Pts',(65.6167600555006,-2.97572009576164,126.886057277199));
#55276=CARTESIAN_POINT('Ctrl Pts',(65.6090137222352,-3.08391994878583,126.97063674041));
#55277=CARTESIAN_POINT('Ctrl Pts',(65.6012673889699,-3.18836878862205,127.059565892853));
#55278=CARTESIAN_POINT('Ctrl Pts',(65.5935193209669,-3.29284101905133,127.148514960362));
#55279=CARTESIAN_POINT('Ctrl Pts',(65.5857712529639,-3.39356026713621,127.241815402012));
#55280=CARTESIAN_POINT('Ctrl Pts',(65.578023184961,-3.49015746453798,127.339106812254));
#55281=CARTESIAN_POINT('Ctrl Pts',(65.5702668822191,-3.58685732659107,127.436501624965));
#55282=CARTESIAN_POINT('Ctrl Pts',(65.5625105794773,-3.67942611061071,127.537895601534));
#55283=CARTESIAN_POINT('Ctrl Pts',(65.5547542767354,-3.76753273306773,127.642892577594));
#55284=CARTESIAN_POINT('Ctrl Pts',(65.5469938342212,-3.85568638068187,127.747945593701));
#55285=CARTESIAN_POINT('Ctrl Pts',(65.5392333917071,-3.9393728827717,127.856605131502));
#55286=CARTESIAN_POINT('Ctrl Pts',(65.5314729491929,-4.01830341322532,127.968444409043));
#55287=CARTESIAN_POINT('Ctrl Pts',(65.5237000489275,-4.09736064997366,128.080463220922));
#55288=CARTESIAN_POINT('Ctrl Pts',(65.5159271486621,-4.171646446517,128.19567164399));
#55289=CARTESIAN_POINT('Ctrl Pts',(65.5081542483966,-4.24091656514903,128.313615799255));
#55290=CARTESIAN_POINT('Ctrl Pts',(65.5006639126345,-4.30766854048874,128.427272387394));
#55291=CARTESIAN_POINT('Ctrl Pts',(65.4931735768724,-4.36976302667466,128.543468987778));
#55292=CARTESIAN_POINT('Ctrl Pts',(65.4856832411102,-4.42702389063793,128.661782139605));
#55293=CARTESIAN_POINT('Ctrl Pts',(65.477302578159,-4.49109097873786,128.79415840145));
#55294=CARTESIAN_POINT('Ctrl Pts',(65.4689219152079,-4.54928649637606,128.929554254977));
#55295=CARTESIAN_POINT('Ctrl Pts',(65.4605412522567,-4.60133789404382,129.067445925551));
#55296=CARTESIAN_POINT('Ctrl Pts',(65.4521817467578,-4.65325788504737,129.204989480892));
#55297=CARTESIAN_POINT('Ctrl Pts',(65.4438222412588,-4.69906458275434,129.345016013224));
#55298=CARTESIAN_POINT('Ctrl Pts',(65.4354627357599,-4.73853267723818,129.486980213413));
#55299=CARTESIAN_POINT('Ctrl Pts',(65.4335936241726,-4.74735739453008,129.518722154559));
#55300=CARTESIAN_POINT('Ctrl Pts',(65.4317245125853,-4.75586541040771,129.550560873191));
#55301=CARTESIAN_POINT('Ctrl Pts',(65.429855400998,-4.76405452823407,129.582490119308));
#55302=CARTESIAN_POINT('Origin',(213.235140564004,0.,130.804360617566));
#55303=CARTESIAN_POINT('',(63.3349537467758,-4.76405452823404,129.582490119308));
#55304=CARTESIAN_POINT('',(63.6801307828278,-4.76405452823405,129.582490119308));
#55305=CARTESIAN_POINT('',(213.235140564004,-4.76405452823405,129.582490119308));
#55306=CARTESIAN_POINT('',(65.0148594359565,-4.91824789621477,130.808909670108));
#55307=CARTESIAN_POINT('Ctrl Pts',(65.0148594359565,-4.91824789621477,130.808909670108));
#55308=CARTESIAN_POINT('Ctrl Pts',(65.0047250992943,-4.91808238954424,130.987848652825));
#55309=CARTESIAN_POINT('Ctrl Pts',(64.9945907626321,-4.90814809073405,131.166352314953));
#55310=CARTESIAN_POINT('Ctrl Pts',(64.9844564259699,-4.8886074676266,131.343526723665));
#55311=CARTESIAN_POINT('Ctrl Pts',(64.9740577776672,-4.86855720937276,131.525321983268));
#55312=CARTESIAN_POINT('Ctrl Pts',(64.9636591293646,-4.83839296868917,131.705718119363));
#55313=CARTESIAN_POINT('Ctrl Pts',(64.953260481062,-4.79833791901245,131.883775402284));
#55314=CARTESIAN_POINT('Ctrl Pts',(64.9516326505893,-4.79206760112586,131.911648935707));
#55315=CARTESIAN_POINT('Ctrl Pts',(64.9500048201166,-4.78555499743603,131.939465198035));
#55316=CARTESIAN_POINT('Ctrl Pts',(64.9483769896439,-4.77880106855221,131.96722063051));
#55317=CARTESIAN_POINT('Ctrl Pts',(64.9406026555249,-4.74654506853212,132.099777434981));
#55318=CARTESIAN_POINT('Ctrl Pts',(64.9328283214058,-4.70871840581664,132.23120108293));
#55319=CARTESIAN_POINT('Ctrl Pts',(64.9250539872867,-4.66541489976612,132.360987379362));
#55320=CARTESIAN_POINT('Ctrl Pts',(64.9172892343396,-4.62216476141667,132.490613725783));
#55321=CARTESIAN_POINT('Ctrl Pts',(64.9095244813925,-4.5734513322157,132.618606368379));
#55322=CARTESIAN_POINT('Ctrl Pts',(64.9017597284454,-4.51941923194677,132.744472178381));
#55323=CARTESIAN_POINT('Ctrl Pts',(64.8940026875604,-4.46544079712163,132.870212976687));
#55324=CARTESIAN_POINT('Ctrl Pts',(64.8862456466754,-4.40615435702613,132.993830789235));
#55325=CARTESIAN_POINT('Ctrl Pts',(64.8784886057904,-4.34175392665275,133.114848856639));
#55326=CARTESIAN_POINT('Ctrl Pts',(64.8707374145503,-4.27740206114478,133.235775663377));
#55327=CARTESIAN_POINT('Ctrl Pts',(64.8629862233101,-4.20794406441188,133.354106283462));
#55328=CARTESIAN_POINT('Ctrl Pts',(64.85523503207,-4.13362137966262,133.469385448988));
#55329=CARTESIAN_POINT('Ctrl Pts',(64.8474871352929,-4.05933028403699,133.584615617794));
#55330=CARTESIAN_POINT('Ctrl Pts',(64.8397392385158,-3.9801788241445,133.696796583671));
#55331=CARTESIAN_POINT('Ctrl Pts',(64.8319913417387,-3.89645344503732,133.805499336978));
#55332=CARTESIAN_POINT('Ctrl Pts',(64.8242450656546,-3.81274557947455,133.914179352014));
#55333=CARTESIAN_POINT('Ctrl Pts',(64.8164987895705,-3.72446593617333,134.019382292108));
#55334=CARTESIAN_POINT('Ctrl Pts',(64.8087525134864,-3.63194294957278,134.120710037267));
#55335=CARTESIAN_POINT('Ctrl Pts',(64.8010061802211,-3.53941927998857,134.222038530404));
#55336=CARTESIAN_POINT('Ctrl Pts',(64.7932598469556,-3.44265246822719,134.319491482812));
#55337=CARTESIAN_POINT('Ctrl Pts',(64.7855135136903,-3.34200943959831,134.412705940305));
#55338=CARTESIAN_POINT('Ctrl Pts',(64.7777654456873,-3.24134387266084,134.50594127253));
#55339=CARTESIAN_POINT('Ctrl Pts',(64.7700173776844,-3.13680064831548,134.594935955464));
#55340=CARTESIAN_POINT('Ctrl Pts',(64.7622693096814,-3.02878123970798,134.679366071045));
#55341=CARTESIAN_POINT('Ctrl Pts',(64.7545130069395,-2.92064702678771,134.763885919958));
#55342=CARTESIAN_POINT('Ctrl Pts',(64.7467567041976,-2.80902955790968,134.84383126942));
#55343=CARTESIAN_POINT('Ctrl Pts',(64.7390004014557,-2.69436132841434,134.918920143742));
#55344=CARTESIAN_POINT('Ctrl Pts',(64.7312399589416,-2.57963189703217,134.994049095257));
#55345=CARTESIAN_POINT('Ctrl Pts',(64.7234795164274,-2.46184879613242,135.06431620655));
#55346=CARTESIAN_POINT('Ctrl Pts',(64.7157190739132,-2.34146993336652,135.12948507978));
#55347=CARTESIAN_POINT('Ctrl Pts',(64.7079461736478,-2.22089782776354,135.19475856787));
#55348=CARTESIAN_POINT('Ctrl Pts',(64.7001732733823,-2.09772198491311,135.254917291692));
#55349=CARTESIAN_POINT('Ctrl Pts',(64.6924003731169,-1.97242195356502,135.309772330117));
#55350=CARTESIAN_POINT('Ctrl Pts',(64.6849100373549,-1.85167689396918,135.362633249724));
#55351=CARTESIAN_POINT('Ctrl Pts',(64.6774197015929,-1.72895969069575,135.410569281846));
#55352=CARTESIAN_POINT('Ctrl Pts',(64.6699293658309,-1.60471164345935,135.45345554065));
#55353=CARTESIAN_POINT('Ctrl Pts',(64.6621550317118,-1.47575269374651,135.497967844992));
#55354=CARTESIAN_POINT('Ctrl Pts',(64.6543806975928,-1.34473602145048,135.537180894261));
#55355=CARTESIAN_POINT('Ctrl Pts',(64.6466063634737,-1.21213653175627,135.570901091629));
#55356=CARTESIAN_POINT('Ctrl Pts',(64.6388416105266,-1.07970045908236,135.604579731868));
#55357=CARTESIAN_POINT('Ctrl Pts',(64.6310768575795,-0.945685825551951,
135.632778893962));
#55358=CARTESIAN_POINT('Ctrl Pts',(64.6233121046324,-0.810585684888883,
135.655353702487));
#55359=CARTESIAN_POINT('Ctrl Pts',(64.6155550637474,-0.675619727590283,
135.677906089394));
#55360=CARTESIAN_POINT('Ctrl Pts',(64.6077980228624,-0.539570791831687,
135.694845175478));
#55361=CARTESIAN_POINT('Ctrl Pts',(64.6000409819774,-0.402944858630383,
135.706076490952));
#55362=CARTESIAN_POINT('Ctrl Pts',(64.5922897907373,-0.266421956108101,
135.717299336804));
#55363=CARTESIAN_POINT('Ctrl Pts',(64.5845385994971,-0.12932331029386,135.722822947541));
#55364=CARTESIAN_POINT('Ctrl Pts',(64.576787408257,0.00783754307838197,
135.722604372751));
#55365=CARTESIAN_POINT('Ctrl Pts',(64.5690395114799,0.144940099429055,135.722385890861));
#55366=CARTESIAN_POINT('Ctrl Pts',(64.5612916147029,0.282104420604652,135.716430078196));
#55367=CARTESIAN_POINT('Ctrl Pts',(64.5535437179258,0.418814738097866,135.704746038903));
#55368=CARTESIAN_POINT('Ctrl Pts',(64.5457974418417,0.55549645873998,135.693064443659));
#55369=CARTESIAN_POINT('Ctrl Pts',(64.5380511657576,0.691723975297531,135.675657038385));
#55370=CARTESIAN_POINT('Ctrl Pts',(64.5303048896735,0.826984811307728,135.652584950697));
#55371=CARTESIAN_POINT('Ctrl Pts',(64.5225585564081,0.962246645782506,135.629512692696));
#55372=CARTESIAN_POINT('Ctrl Pts',(64.5148122231428,1.09654140007225,135.60077573458));
#55373=CARTESIAN_POINT('Ctrl Pts',(64.5070658898774,1.2293653784483,135.566486595401));
#55374=CARTESIAN_POINT('Ctrl Pts',(64.4993178218745,1.36221910183318,135.532189777407));
#55375=CARTESIAN_POINT('Ctrl Pts',(64.4915697538715,1.49360101541403,135.492338401889));
#55376=CARTESIAN_POINT('Ctrl Pts',(64.4838216858685,1.62302159171013,135.447095153951));
#55377=CARTESIAN_POINT('Ctrl Pts',(64.4760653831267,1.75257971773501,135.401803820951));
#55378=CARTESIAN_POINT('Ctrl Pts',(64.4683090803848,1.8801719727445,135.351109297371));
#55379=CARTESIAN_POINT('Ctrl Pts',(64.460552777643,2.00532734830802,135.295223039042));
#55380=CARTESIAN_POINT('Ctrl Pts',(64.4527923351288,2.13054952306384,135.239306952535));
#55381=CARTESIAN_POINT('Ctrl Pts',(64.4450318926147,2.25333187691139,135.178193783981));
#55382=CARTESIAN_POINT('Ctrl Pts',(64.4372714501005,2.37322801137952,135.112141005249));
#55383=CARTESIAN_POINT('Ctrl Pts',(64.4294985498351,2.49331661376673,135.045982192732));
#55384=CARTESIAN_POINT('Ctrl Pts',(64.4217256495697,2.61050940369994,134.974868127305));
#55385=CARTESIAN_POINT('Ctrl Pts',(64.4139527493043,2.72438822866959,134.899100150428));
#55386=CARTESIAN_POINT('Ctrl Pts',(64.4064624135422,2.83412727150845,134.826086530359));
#55387=CARTESIAN_POINT('Ctrl Pts',(64.3989720777802,2.9407888588564,134.748751667977));
#55388=CARTESIAN_POINT('Ctrl Pts',(64.3914817420181,3.04402938745015,134.667399337387));
#55389=CARTESIAN_POINT('Ctrl Pts',(64.383707407899,3.1511843120645,134.582962508457));
#55390=CARTESIAN_POINT('Ctrl Pts',(64.3759330737799,3.25499307262124,134.493930082431));
#55391=CARTESIAN_POINT('Ctrl Pts',(64.3681587396608,3.35503609277531,134.400596966678));
#55392=CARTESIAN_POINT('Ctrl Pts',(64.3603939867137,3.45495581884814,134.307378875649));
#55393=CARTESIAN_POINT('Ctrl Pts',(64.3526292337666,3.5511187554723,134.209870904883));
#55394=CARTESIAN_POINT('Ctrl Pts',(64.3448644808195,3.64313650726891,134.108409565736));
#55395=CARTESIAN_POINT('Ctrl Pts',(64.3371074399345,3.73506286573708,134.007048999422));
#55396=CARTESIAN_POINT('Ctrl Pts',(64.3293503990496,3.8228519715566,133.901743166451));
#55397=CARTESIAN_POINT('Ctrl Pts',(64.3215933581646,3.9061508495217,133.792866699755));
#55398=CARTESIAN_POINT('Ctrl Pts',(64.3138421669244,3.98938691115495,133.68407233765));
#55399=CARTESIAN_POINT('Ctrl Pts',(64.3060909756843,4.06813924818851,133.571713010616));
#55400=CARTESIAN_POINT('Ctrl Pts',(64.2983397844442,4.14209414661494,133.456197555064));
#55401=CARTESIAN_POINT('Ctrl Pts',(64.2905918876671,4.21601761223683,133.340731196661));
#55402=CARTESIAN_POINT('Ctrl Pts',(64.2828439908901,4.28514748438497,133.222111706337));
#55403=CARTESIAN_POINT('Ctrl Pts',(64.275096094113,4.34921263715847,133.100777935756));
#55404=CARTESIAN_POINT('Ctrl Pts',(64.2673498180289,4.41326438888309,132.979469545584));
#55405=CARTESIAN_POINT('Ctrl Pts',(64.2596035419447,4.47225334606476,132.85544834999));
#55406=CARTESIAN_POINT('Ctrl Pts',(64.2518572658606,4.52595393105044,132.729178550906));
#55407=CARTESIAN_POINT('Ctrl Pts',(64.2441109325953,4.57965491244157,132.602907819728));
#55408=CARTESIAN_POINT('Ctrl Pts',(64.2363645993299,4.62806729073105,132.474388811718));
#55409=CARTESIAN_POINT('Ctrl Pts',(64.2286182660646,4.67101347153892,132.344106119655));
#55410=CARTESIAN_POINT('Ctrl Pts',(64.2208701980616,4.71396926984627,132.213794251685));
#55411=CARTESIAN_POINT('Ctrl Pts',(64.2131221300586,4.75145631244567,132.081718284969));
#55412=CARTESIAN_POINT('Ctrl Pts',(64.2053740620557,4.78334686936146,131.948378008111));
#55413=CARTESIAN_POINT('Ctrl Pts',(64.1976177593138,4.8152713199406,131.814896015621));
#55414=CARTESIAN_POINT('Ctrl Pts',(64.189861456572,4.8415873119562,131.680147409603));
#55415=CARTESIAN_POINT('Ctrl Pts',(64.1821051538301,4.86221815762524,131.544642759833));
#55416=CARTESIAN_POINT('Ctrl Pts',(64.174344711316,4.88286001459783,131.409065787151));
#55417=CARTESIAN_POINT('Ctrl Pts',(64.1665842688018,4.89781063645912,131.272732355106));
#55418=CARTESIAN_POINT('Ctrl Pts',(64.1588238262876,4.90704535230545,131.136157201209));
#55419=CARTESIAN_POINT('Ctrl Pts',(64.1510509260222,4.91629489253747,130.999362804751));
#55420=CARTESIAN_POINT('Ctrl Pts',(64.1432780257567,4.91981018079097,130.862326302087));
#55421=CARTESIAN_POINT('Ctrl Pts',(64.1355051254913,4.91761872252499,130.725562379187));
#55422=CARTESIAN_POINT('Ctrl Pts',(64.1280147897293,4.91550692928694,130.593770169372));
#55423=CARTESIAN_POINT('Ctrl Pts',(64.1205244539673,4.90809611264359,130.462231372997));
#55424=CARTESIAN_POINT('Ctrl Pts',(64.1130341182053,4.89545612039598,130.331399270543));
#55425=CARTESIAN_POINT('Ctrl Pts',(64.1052597840862,4.88233687900042,130.195606629159));
#55426=CARTESIAN_POINT('Ctrl Pts',(64.0974854499671,4.86354254820619,130.060145177881));
#55427=CARTESIAN_POINT('Ctrl Pts',(64.089711115848,4.83909445067185,129.925527322807));
#55428=CARTESIAN_POINT('Ctrl Pts',(64.081946362901,4.81467648323273,129.791075372208));
#55429=CARTESIAN_POINT('Ctrl Pts',(64.0741816099539,4.78461868201375,129.657465330187));
#55430=CARTESIAN_POINT('Ctrl Pts',(64.0664168570068,4.74899422635998,129.525205857383));
#55431=CARTESIAN_POINT('Ctrl Pts',(64.0586598161218,4.71340515341778,129.393077746551));
#55432=CARTESIAN_POINT('Ctrl Pts',(64.0509027752368,4.67226052978635,129.26229791055));
#55433=CARTESIAN_POINT('Ctrl Pts',(64.0431457343518,4.62568475304174,129.133365815666));
#55434=CARTESIAN_POINT('Ctrl Pts',(64.0353945431116,4.57914409945268,129.004530949478));
#55435=CARTESIAN_POINT('Ctrl Pts',(64.0276433518715,4.52718057723726,128.877541417159));
#55436=CARTESIAN_POINT('Ctrl Pts',(64.0198921606314,4.46996858196161,128.752882141253));
#55437=CARTESIAN_POINT('Ctrl Pts',(64.0121442638543,4.41278090331013,128.628275848865));
#55438=CARTESIAN_POINT('Ctrl Pts',(64.0043963670772,4.35034935110855,128.505998197604));
#55439=CARTESIAN_POINT('Ctrl Pts',(63.9966484703001,4.28289659352007,128.386514503415));
#55440=CARTESIAN_POINT('Ctrl Pts',(63.988902194216,4.21545794559435,128.267055802639));
#55441=CARTESIAN_POINT('Ctrl Pts',(63.9811559181319,4.14300037352101,128.150390236704));
#55442=CARTESIAN_POINT('Ctrl Pts',(63.9734096420478,4.06579249329982,128.03695850296));
#55443=CARTESIAN_POINT('Ctrl Pts',(63.9656633087824,3.9885840431477,127.923525931889));
#55444=CARTESIAN_POINT('Ctrl Pts',(63.9579169755171,3.90662543486509,127.813327563843));
#55445=CARTESIAN_POINT('Ctrl Pts',(63.9501706422517,3.82022837597998,127.706774748239));
#55446=CARTESIAN_POINT('Ctrl Pts',(63.9424225742488,3.73381196907245,127.600198070869));
#55447=CARTESIAN_POINT('Ctrl Pts',(63.9346745062458,3.6429553798851,127.497268874097));
#55448=CARTESIAN_POINT('Ctrl Pts',(63.9269264382428,3.548010053555,127.398364768718));
#55449=CARTESIAN_POINT('Ctrl Pts',(63.9191701355009,3.45296381820221,127.299355546878));
#55450=CARTESIAN_POINT('Ctrl Pts',(63.911413832759,3.35382043616919,127.204380244517));
#55451=CARTESIAN_POINT('Ctrl Pts',(63.9036575300172,3.25096801264665,127.113779356674));
#55452=CARTESIAN_POINT('Ctrl Pts',(63.895897087503,3.14806069368886,127.023130112409));
#55453=CARTESIAN_POINT('Ctrl Pts',(63.8881366449889,3.04144069245173,126.936860180664));
#55454=CARTESIAN_POINT('Ctrl Pts',(63.8803762024747,2.93152773695433,126.855268545967));
#55455=CARTESIAN_POINT('Ctrl Pts',(63.8726033022093,2.82143833942314,126.773545933134));
#55456=CARTESIAN_POINT('Ctrl Pts',(63.8648304019438,2.70804574782339,126.696516844576));
#55457=CARTESIAN_POINT('Ctrl Pts',(63.8570575016784,2.59179784940959,126.624436339508));
#55458=CARTESIAN_POINT('Ctrl Pts',(63.8495671659163,2.47977585491329,126.554976142359));
#55459=CARTESIAN_POINT('Ctrl Pts',(63.8420768301543,2.36510281273498,126.490111139832));
#55460=CARTESIAN_POINT('Ctrl Pts',(63.8345864943922,2.24819783502318,126.430027576164));
#55461=CARTESIAN_POINT('Ctrl Pts',(63.8268121602731,2.12686036954963,126.367665925919));
#55462=CARTESIAN_POINT('Ctrl Pts',(63.8190378261541,2.00273401925019,126.310257905454));
#55463=CARTESIAN_POINT('Ctrl Pts',(63.811263492035,1.87626141130551,126.258062543424));
#55464=CARTESIAN_POINT('Ctrl Pts',(63.8034987390879,1.74994466954694,126.205931507514));
#55465=CARTESIAN_POINT('Ctrl Pts',(63.7957339861408,1.6212877813998,126.159000495641));
#55466=CARTESIAN_POINT('Ctrl Pts',(63.7879692331937,1.49075825269003,126.117482883452));
#55467=CARTESIAN_POINT('Ctrl Pts',(63.7802121923087,1.36035836774831,126.07600650714));
#55468=CARTESIAN_POINT('Ctrl Pts',(63.7724551514237,1.22808991375647,126.039932948444));
#55469=CARTESIAN_POINT('Ctrl Pts',(63.7646981105387,1.09444034577713,126.009427521887));
#55470=CARTESIAN_POINT('Ctrl Pts',(63.7569469192985,0.960891563976645,125.978945099711));
#55471=CARTESIAN_POINT('Ctrl Pts',(63.7491957280584,0.825964120868906,125.954022538523));
#55472=CARTESIAN_POINT('Ctrl Pts',(63.7414445368182,0.690160260588042,125.934775226878));
#55473=CARTESIAN_POINT('Ctrl Pts',(63.7336966400412,0.554414120570484,125.915536095853));
#55474=CARTESIAN_POINT('Ctrl Pts',(63.7259487432641,0.417792690541549,125.90196747157));
#55475=CARTESIAN_POINT('Ctrl Pts',(63.718200846487,0.280807811564492,125.89413353163));
#55476=CARTESIAN_POINT('Ctrl Pts',(63.7104545704029,0.143851586871065,125.886301230381));
#55477=CARTESIAN_POINT('Ctrl Pts',(63.7027082943188,0.00653245452892467,
125.884201249768));
#55478=CARTESIAN_POINT('Ctrl Pts',(63.6949620182347,-0.130633620790511,
125.887845803227));
#55479=CARTESIAN_POINT('Ctrl Pts',(63.6872156849694,-0.267800708638755,
125.891490383588));
#55480=CARTESIAN_POINT('Ctrl Pts',(63.679469351704,-0.404814346382526,125.900879572251));
#55481=CARTESIAN_POINT('Ctrl Pts',(63.6717230184386,-0.541159968576361,
125.915973465252));
#55482=CARTESIAN_POINT('Ctrl Pts',(63.6639749504356,-0.677536124426932,
125.931070738425));
#55483=CARTESIAN_POINT('Ctrl Pts',(63.6562268824327,-0.813243578529007,
125.95187521506));
#55484=CARTESIAN_POINT('Ctrl Pts',(63.6484788144297,-0.94777467154469,125.978295322268));
#55485=CARTESIAN_POINT('Ctrl Pts',(63.6407225116878,-1.08244874580697,126.004743509081));
#55486=CARTESIAN_POINT('Ctrl Pts',(63.632966208946,-1.21594357722377,126.036819173445));
#55487=CARTESIAN_POINT('Ctrl Pts',(63.6252099062041,-1.34776291734092,126.074379837358));
#55488=CARTESIAN_POINT('Ctrl Pts',(63.6174494636899,-1.47965261340907,126.111960548527));
#55489=CARTESIAN_POINT('Ctrl Pts',(63.6096890211758,-1.60986466528448,126.155031969836));
#55490=CARTESIAN_POINT('Ctrl Pts',(63.6019285786616,-1.73792065557005,126.203402580652));
#55491=CARTESIAN_POINT('Ctrl Pts',(63.5941556783962,-1.86618221269932,126.251850840267));
#55492=CARTESIAN_POINT('Ctrl Pts',(63.5863827781307,-1.99228043200819,126.305615135119));
#55493=CARTESIAN_POINT('Ctrl Pts',(63.5786098778653,-2.11575863095306,126.364456510713));
#55494=CARTESIAN_POINT('Ctrl Pts',(63.5711195421033,-2.23474808634247,126.421158854091));
#55495=CARTESIAN_POINT('Ctrl Pts',(63.5636292063413,-2.35130443038167,126.482575413903));
#55496=CARTESIAN_POINT('Ctrl Pts',(63.5561388705794,-2.46504443016443,126.548454248787));
#55497=CARTESIAN_POINT('Ctrl Pts',(63.5483633800025,-2.5831144773057,126.616841070971));
#55498=CARTESIAN_POINT('Ctrl Pts',(63.5405878894257,-2.69852356378702,126.690253314783));
#55499=CARTESIAN_POINT('Ctrl Pts',(63.5328123988489,-2.81081430818872,126.768458489493));
#55500=CARTESIAN_POINT('Ctrl Pts',(63.5250467412648,-2.92296304816458,126.84656476486));
#55501=CARTESIAN_POINT('Ctrl Pts',(63.5172810836807,-3.03200097539874,126.929451688261));
#55502=CARTESIAN_POINT('Ctrl Pts',(63.5095154260966,-3.1374957269162,127.016841162028));
#55503=CARTESIAN_POINT('Ctrl Pts',(63.5017591825011,-3.24286259146789,127.104124697114));
#55504=CARTESIAN_POINT('Ctrl Pts',(63.4940029389056,-3.34469453602573,127.195899663385));
#55505=CARTESIAN_POINT('Ctrl Pts',(63.4862466953101,-3.44258912612857,127.291845397505));
#55506=CARTESIAN_POINT('Ctrl Pts',(63.478495790603,-3.54041633202876,127.387725088886));
#55507=CARTESIAN_POINT('Ctrl Pts',(63.4707448858959,-3.63431129752257,127.487769563984));
#55508=CARTESIAN_POINT('Ctrl Pts',(63.4629939811888,-3.72390551370555,127.591618675316));
#55509=CARTESIAN_POINT('Ctrl Pts',(63.455246733062,-3.81345746276433,127.695418794609));
#55510=CARTESIAN_POINT('Ctrl Pts',(63.4474994849352,-3.89871244547512,127.803019682853));
#55511=CARTESIAN_POINT('Ctrl Pts',(63.4397522368085,-3.97933989115521,127.914025499771));
#55512=CARTESIAN_POINT('Ctrl Pts',(63.4320069657834,-4.05994676067018,128.025002987947));
#55513=CARTESIAN_POINT('Ctrl Pts',(63.4242616947583,-4.1359282151993,128.139383358595));
#55514=CARTESIAN_POINT('Ctrl Pts',(63.4165164237332,-4.2069951992801,128.256739284688));
#55515=CARTESIAN_POINT('Ctrl Pts',(63.4087693006532,-4.27807917695116,128.374123273018));
#55516=CARTESIAN_POINT('Ctrl Pts',(63.401022177573,-4.3442461294841,128.494483906459));
#55517=CARTESIAN_POINT('Ctrl Pts',(63.3932750544929,-4.40525141754686,128.617366559343));
#55518=CARTESIAN_POINT('Ctrl Pts',(63.3855269480811,-4.46626444892787,128.740264809555));
#55519=CARTESIAN_POINT('Ctrl Pts',(63.3777788416692,-4.52211434429908,128.865685363115));
#55520=CARTESIAN_POINT('Ctrl Pts',(63.3700307352573,-4.57260374214846,128.993151607046));
#55521=CARTESIAN_POINT('Ctrl Pts',(63.3622769768212,-4.62312997058361,129.120710833991));
#55522=CARTESIAN_POINT('Ctrl Pts',(63.3545232183852,-4.668287756345,129.250318364881));
#55523=CARTESIAN_POINT('Ctrl Pts',(63.3467694599491,-4.70792887445211,129.381480167352));
#55524=CARTESIAN_POINT('Ctrl Pts',(63.3428308888913,-4.72806483326005,129.448104641582));
#55525=CARTESIAN_POINT('Ctrl Pts',(63.3388923178335,-4.74677818570645,129.515129921998));
#55526=CARTESIAN_POINT('Ctrl Pts',(63.3349537467757,-4.76405452823404,129.582490119308));
#55527=CARTESIAN_POINT('Ctrl Pts',(65.0848845757186,-4.764054528234,129.582490119308));
#55528=CARTESIAN_POINT('Ctrl Pts',(65.0772322777973,-4.7977491559196,129.713864961267));
#55529=CARTESIAN_POINT('Ctrl Pts',(65.0695799798758,-4.82600021089149,129.846614648772));
#55530=CARTESIAN_POINT('Ctrl Pts',(65.0619276819544,-4.84871248717968,129.980242738153));
#55531=CARTESIAN_POINT('Ctrl Pts',(65.0540829742939,-4.87199584201207,130.117230778505));
#55532=CARTESIAN_POINT('Ctrl Pts',(65.0462382666333,-4.88945810571101,130.255141541152));
#55533=CARTESIAN_POINT('Ctrl Pts',(65.0383935589728,-4.9010531451034,130.393433456901));
#55534=CARTESIAN_POINT('Ctrl Pts',(65.0305488513122,-4.9126481844958,130.53172537265));
#55535=CARTESIAN_POINT('Ctrl Pts',(65.0227041436517,-4.91837601030066,130.67039798834));
#55536=CARTESIAN_POINT('Ctrl Pts',(65.0148594359911,-4.91824789621533,130.808909669497));
#55537=CARTESIAN_POINT('',(65.3601405640372,-4.91824982213702,130.80303791232));
#55538=CARTESIAN_POINT('Ctrl Pts',(65.429855400998,-4.76405452823407,129.582490119308));
#55539=CARTESIAN_POINT('Ctrl Pts',(65.4215226915695,-4.8005625354538,129.724834285372));
#55540=CARTESIAN_POINT('Ctrl Pts',(65.4131899821409,-4.83072868413131,129.868979158078));
#55541=CARTESIAN_POINT('Ctrl Pts',(65.4048572727123,-4.85438774821024,130.014358938754));
#55542=CARTESIAN_POINT('Ctrl Pts',(65.3965493778483,-4.8779763562897,130.159305782703));
#55543=CARTESIAN_POINT('Ctrl Pts',(65.3882414829842,-4.89509647502741,130.305479910784));
#55544=CARTESIAN_POINT('Ctrl Pts',(65.3799335881201,-4.90563342858695,130.452304191932));
#55545=CARTESIAN_POINT('Ctrl Pts',(65.3733359134258,-4.91400129950882,130.568903987679));
#55546=CARTESIAN_POINT('Ctrl Pts',(65.3667382387315,-4.91821832289317,130.685913442699));
#55547=CARTESIAN_POINT('Ctrl Pts',(65.3601405640372,-4.91824982213702,130.80303791232));
#55548=CARTESIAN_POINT('Ctrl Pts',(65.3601405640086,-4.91824982213716,130.803037912827));
#55549=CARTESIAN_POINT('Ctrl Pts',(65.3521725263887,-4.91828786388298,130.944489594425));
#55550=CARTESIAN_POINT('Ctrl Pts',(65.3442044887688,-4.91221920987186,131.085878215402));
#55551=CARTESIAN_POINT('Ctrl Pts',(65.3362364511489,-4.90008637273233,131.22665980329));
#55552=CARTESIAN_POINT('Ctrl Pts',(65.3282627522565,-4.88794491523975,131.367541416174));
#55553=CARTESIAN_POINT('Ctrl Pts',(65.3202890533641,-4.86973071607465,131.507814779279));
#55554=CARTESIAN_POINT('Ctrl Pts',(65.3123153544717,-4.84553795241052,131.646942966212));
#55555=CARTESIAN_POINT('Ctrl Pts',(65.3043347342982,-4.82132418909227,131.786191918338));
#55556=CARTESIAN_POINT('Ctrl Pts',(65.2963541141246,-4.79112157690867,131.924293360148));
#55557=CARTESIAN_POINT('Ctrl Pts',(65.2883734939511,-4.75507497764448,132.060722436263));
#55558=CARTESIAN_POINT('Ctrl Pts',(65.2803789381551,-4.71896543442539,132.197389742496));
#55559=CARTESIAN_POINT('Ctrl Pts',(65.2723843823592,-4.67699160683641,132.332378501668));
#55560=CARTESIAN_POINT('Ctrl Pts',(65.2643898265632,-4.62934800013868,132.465179739599));
#55561=CARTESIAN_POINT('Ctrl Pts',(65.2563873827478,-4.5816573847383,132.598112009044));
#55562=CARTESIAN_POINT('Ctrl Pts',(65.2483849389324,-4.52828596843571,132.728852121924));
#55563=CARTESIAN_POINT('Ctrl Pts',(65.240382495117,-4.46947549004429,132.856913151947));
#55564=CARTESIAN_POINT('Ctrl Pts',(65.2323654589606,-4.41055777159297,132.985207699412));
#55565=CARTESIAN_POINT('Ctrl Pts',(65.2243484228043,-4.3461813371905,133.110813084765));
#55566=CARTESIAN_POINT('Ctrl Pts',(65.2163313866479,-4.27663326362702,133.233267983222));
#55567=CARTESIAN_POINT('Ctrl Pts',(65.2132994635311,-4.25033122284085,133.279578593548));
#55568=CARTESIAN_POINT('Ctrl Pts',(65.2102675404142,-4.22328994696924,133.325438920385));
#55569=CARTESIAN_POINT('Ctrl Pts',(65.2072356172974,-4.19552650344427,133.370825193865));
#55570=CARTESIAN_POINT('Ctrl Pts',(65.1994612831783,-4.12433660912941,133.487202833024));
#55571=CARTESIAN_POINT('Ctrl Pts',(65.1916869490592,-4.04818807260937,133.600800509225));
#55572=CARTESIAN_POINT('Ctrl Pts',(65.1839126149401,-3.96732418146484,133.711166751739));
#55573=CARTESIAN_POINT('Ctrl Pts',(65.176147861993,-3.88655994783903,133.821396977723));
#55574=CARTESIAN_POINT('Ctrl Pts',(65.1683831090459,-3.80109215110217,133.928403381569));
#55575=CARTESIAN_POINT('Ctrl Pts',(65.1606183560988,-3.71120907436658,134.031760541474));
#55576=CARTESIAN_POINT('Ctrl Pts',(65.1528613152139,-3.62141527077019,134.13501504559));
#55577=CARTESIAN_POINT('Ctrl Pts',(65.1451042743289,-3.52721516905121,134.234627225541));
#55578=CARTESIAN_POINT('Ctrl Pts',(65.1373472334439,-3.42893909050521,134.330202329286));
#55579=CARTESIAN_POINT('Ctrl Pts',(65.1295960422037,-3.33073712271412,134.425705359103));
#55580=CARTESIAN_POINT('Ctrl Pts',(65.1218448509636,-3.2284655753056,134.517177100917));
#55581=CARTESIAN_POINT('Ctrl Pts',(65.1140936597235,-3.12249337074076,134.604257749355));
#55582=CARTESIAN_POINT('Ctrl Pts',(65.1063457629464,-3.01656620719005,134.691301386195));
#55583=CARTESIAN_POINT('Ctrl Pts',(65.0985978661693,-2.90694181624934,134.773957393956));
#55584=CARTESIAN_POINT('Ctrl Pts',(65.0908499693923,-2.79402395557692,134.851904712219));
#55585=CARTESIAN_POINT('Ctrl Pts',(65.0831036933082,-2.68112971488672,134.929835725584));
#55586=CARTESIAN_POINT('Ctrl Pts',(65.0753574172241,-2.5649436963167,135.00305978662));
#55587=CARTESIAN_POINT('Ctrl Pts',(65.06761114114,-2.44590021000154,135.071298070261));
#55588=CARTESIAN_POINT('Ctrl Pts',(65.0598648078746,-2.32685584493441,135.139536857622));
#55589=CARTESIAN_POINT('Ctrl Pts',(65.0521184746093,-2.20495430922282,135.202789599718));
#55590=CARTESIAN_POINT('Ctrl Pts',(65.0443721413439,-2.08065582837002,135.260822710569));
#55591=CARTESIAN_POINT('Ctrl Pts',(65.036624073341,-1.95632951173442,135.318868817532));
#55592=CARTESIAN_POINT('Ctrl Pts',(65.028876005338,-1.82960553601768,135.371692801908));
#55593=CARTESIAN_POINT('Ctrl Pts',(65.021127937335,-1.70096510561251,135.419108798343));
#55594=CARTESIAN_POINT('Ctrl Pts',(65.0133716345932,-1.57218795462689,135.466575189064));
#55595=CARTESIAN_POINT('Ctrl Pts',(65.0056153318514,-1.44149064758776,135.508621974816));
#55596=CARTESIAN_POINT('Ctrl Pts',(64.9978590291095,-1.30937112312363,135.545112701828));
#55597=CARTESIAN_POINT('Ctrl Pts',(64.9900985865954,-1.17718108249107,135.581622905038));
#55598=CARTESIAN_POINT('Ctrl Pts',(64.9823381440812,-1.043567692597,135.612571052448));
#55599=CARTESIAN_POINT('Ctrl Pts',(64.974577701567,-0.909039174282838,135.637871850833));
#55600=CARTESIAN_POINT('Ctrl Pts',(64.9668048013016,-0.774294698848376,
135.663213264306));
#55601=CARTESIAN_POINT('Ctrl Pts',(64.9590319010362,-0.63863254651262,135.682889156596));
#55602=CARTESIAN_POINT('Ctrl Pts',(64.9512590007707,-0.502567049421009,
135.696866051731));
#55603=CARTESIAN_POINT('Ctrl Pts',(64.9437686650087,-0.371447875876249,
135.710334851523));
#55604=CARTESIAN_POINT('Ctrl Pts',(64.9362783292466,-0.239954481067576,
135.718511787194));
#55605=CARTESIAN_POINT('Ctrl Pts',(64.9287879934845,-0.108545222450552,
135.721412681271));
#55606=CARTESIAN_POINT('Ctrl Pts',(64.9210136593655,0.0278464581471533,
135.724423563629));
#55607=CARTESIAN_POINT('Ctrl Pts',(64.9132393252464,0.1645795444088,135.72175996198));
#55608=CARTESIAN_POINT('Ctrl Pts',(64.9054649911273,0.301142698344161,135.713382530099));
#55609=CARTESIAN_POINT('Ctrl Pts',(64.8977002381802,0.437537550397666,135.705015422655));
#55610=CARTESIAN_POINT('Ctrl Pts',(64.8899354852331,0.573762500335554,135.690948519742));
#55611=CARTESIAN_POINT('Ctrl Pts',(64.882170732286,0.709303804682606,135.671194411231));
#55612=CARTESIAN_POINT('Ctrl Pts',(64.874413691401,0.8447104874952,135.651459922779));
#55613=CARTESIAN_POINT('Ctrl Pts',(64.866656650516,0.979434491595894,135.626049525744));
#55614=CARTESIAN_POINT('Ctrl Pts',(64.858899609631,1.11296515418576,135.595027755666));
#55615=CARTESIAN_POINT('Ctrl Pts',(64.8511484183908,1.24639512026371,135.564029379346));
#55616=CARTESIAN_POINT('Ctrl Pts',(64.8433972271507,1.378633156761,135.527428140803));
#55617=CARTESIAN_POINT('Ctrl Pts',(64.8356460359106,1.5091771376262,135.485339941358));
#55618=CARTESIAN_POINT('Ctrl Pts',(64.8278981391335,1.63966563381769,135.44326963052));
#55619=CARTESIAN_POINT('Ctrl Pts',(64.8201502423564,1.76846113511477,135.395717116878));
#55620=CARTESIAN_POINT('Ctrl Pts',(64.8124023455794,1.8950752834183,135.342848552184));
#55621=CARTESIAN_POINT('Ctrl Pts',(64.8046560694953,2.02166294677132,135.289991046455));
#55622=CARTESIAN_POINT('Ctrl Pts',(64.7969097934112,2.14606980417232,135.23181985206));
#55623=CARTESIAN_POINT('Ctrl Pts',(64.7891635173271,2.26782651696071,135.168549654658));
#55624=CARTESIAN_POINT('Ctrl Pts',(64.7814171840617,2.38958412852948,135.105278990209));
#55625=CARTESIAN_POINT('Ctrl Pts',(64.7736708507963,2.50869120952819,135.03690942792));
#55626=CARTESIAN_POINT('Ctrl Pts',(64.765924517531,2.6247024743299,134.963701909615));
#55627=CARTESIAN_POINT('Ctrl Pts',(64.758176449528,2.74073971905016,134.890477996994));
#55628=CARTESIAN_POINT('Ctrl Pts',(64.750428381525,2.85367943743922,134.812414181067));
#55629=CARTESIAN_POINT('Ctrl Pts',(64.742680313522,2.96310515298264,134.729814847954));
#55630=CARTESIAN_POINT('Ctrl Pts',(64.7349240107801,3.07264716747873,134.647127727286));
#55631=CARTESIAN_POINT('Ctrl Pts',(64.7271677080384,3.17866740607291,134.559895696083));
#55632=CARTESIAN_POINT('Ctrl Pts',(64.7194114052965,3.28078191835024,134.468463927617));
#55633=CARTESIAN_POINT('Ctrl Pts',(64.7116509627823,3.38295093221738,134.376983359263));
#55634=CARTESIAN_POINT('Ctrl Pts',(64.7038905202681,3.48120978605622,134.281298859843));
#55635=CARTESIAN_POINT('Ctrl Pts',(64.696130077754,3.57521201448411,134.181791906873));
#55636=CARTESIAN_POINT('Ctrl Pts',(64.6883571774885,3.66936514363409,134.082125216508));
#55637=CARTESIAN_POINT('Ctrl Pts',(64.6805842772231,3.75924773613774,133.97862410599));
#55638=CARTESIAN_POINT('Ctrl Pts',(64.6728113769577,3.84455361862368,133.871703202937));
#55639=CARTESIAN_POINT('Ctrl Pts',(64.6653210411956,3.92675841740883,133.768669144027));
#55640=CARTESIAN_POINT('Ctrl Pts',(64.6578307054336,4.00471329677018,133.662459860351));
#55641=CARTESIAN_POINT('Ctrl Pts',(64.6503403696716,4.07818381524667,133.55346953348));
#55642=CARTESIAN_POINT('Ctrl Pts',(64.6425660355525,4.15443999076197,133.44034680524));
#55643=CARTESIAN_POINT('Ctrl Pts',(64.6347917014334,4.2261066002734,133.323869645532));
#55644=CARTESIAN_POINT('Ctrl Pts',(64.6270173673144,4.29287415001397,133.204446989896));
#55645=CARTESIAN_POINT('Ctrl Pts',(64.6192526143673,4.35955941471667,133.085171512009));
#55646=CARTESIAN_POINT('Ctrl Pts',(64.6114878614202,4.42135744382118,132.962958098908));
#55647=CARTESIAN_POINT('Ctrl Pts',(64.6037231084731,4.47800113864534,132.83824578266));
#55648=CARTESIAN_POINT('Ctrl Pts',(64.5959660675881,4.53458857415319,132.713657332444));
#55649=CARTESIAN_POINT('Ctrl Pts',(64.5882090267031,4.58603170250018,132.586575271931));
#55650=CARTESIAN_POINT('Ctrl Pts',(64.5804519858181,4.63210879354899,132.457464119234));
#55651=CARTESIAN_POINT('Ctrl Pts',(64.5727007945779,4.67815113750526,132.32845033026));
#55652=CARTESIAN_POINT('Ctrl Pts',(64.5649496033378,4.71883536773837,132.197410861511));
#55653=CARTESIAN_POINT('Ctrl Pts',(64.5571984120977,4.75398758391762,132.064830813349));
#55654=CARTESIAN_POINT('Ctrl Pts',(64.5494505153206,4.78912485946715,131.932307115245));
#55655=CARTESIAN_POINT('Ctrl Pts',(64.5417026185435,4.81873469743844,131.798244517167));
#55656=CARTESIAN_POINT('Ctrl Pts',(64.5339547217665,4.84269291652695,131.663143697697));
#55657=CARTESIAN_POINT('Ctrl Pts',(64.5262084456824,4.86664612407251,131.528071138406));
#55658=CARTESIAN_POINT('Ctrl Pts',(64.5184621695982,4.88494999596582,131.391961174409));
#55659=CARTESIAN_POINT('Ctrl Pts',(64.5107158935141,4.897531464321,131.255324716454));
#55660=CARTESIAN_POINT('Ctrl Pts',(64.5029695602488,4.91011302554975,131.118687249879));
#55661=CARTESIAN_POINT('Ctrl Pts',(64.4952232269835,4.91697206310214,130.981523670911));
#55662=CARTESIAN_POINT('Ctrl Pts',(64.4874768937181,4.91808742696531,130.844349656386));
#55663=CARTESIAN_POINT('Ctrl Pts',(64.4797288257152,4.91920304060647,130.707144922693));
#55664=CARTESIAN_POINT('Ctrl Pts',(64.4719807577122,4.91457241787994,130.56993013967));
#55665=CARTESIAN_POINT('Ctrl Pts',(64.4642326897093,4.90422653172033,130.433220228939));
#55666=CARTESIAN_POINT('Ctrl Pts',(64.4564763869675,4.89386964982974,130.296365021286));
#55667=CARTESIAN_POINT('Ctrl Pts',(64.4487200842256,4.87778540008737,130.160016148282));
#55668=CARTESIAN_POINT('Ctrl Pts',(64.4409637814837,4.85605665196616,130.024683212869));
#55669=CARTESIAN_POINT('Ctrl Pts',(64.4332033389696,4.83431630655784,129.889278046193));
#55670=CARTESIAN_POINT('Ctrl Pts',(64.4254428964554,4.80692553787551,129.754890280463));
#55671=CARTESIAN_POINT('Ctrl Pts',(64.4176824539413,4.77401802075615,129.622017604733));
#55672=CARTESIAN_POINT('Ctrl Pts',(64.4099095536758,4.74105767756888,129.488931629987));
#55673=CARTESIAN_POINT('Ctrl Pts',(64.4021366534104,4.70256299873831,129.357365980916));
#55674=CARTESIAN_POINT('Ctrl Pts',(64.3943637531449,4.65871732803803,129.227802366204));
#55675=CARTESIAN_POINT('Ctrl Pts',(64.3868734173829,4.61646555790804,129.102948715237));
#55676=CARTESIAN_POINT('Ctrl Pts',(64.3793830816208,4.56924519599688,128.9799543553));
#55677=CARTESIAN_POINT('Ctrl Pts',(64.3718927458588,4.51726115708756,128.859229593401));
#55678=CARTESIAN_POINT('Ctrl Pts',(64.3641184117397,4.46330612754309,128.733927515463));
#55679=CARTESIAN_POINT('Ctrl Pts',(64.3563440776206,4.40404814727171,128.610673617242));
#55680=CARTESIAN_POINT('Ctrl Pts',(64.3485697435015,4.33966397638195,128.489949324258));
#55681=CARTESIAN_POINT('Ctrl Pts',(64.3408049905544,4.27535915322854,128.369373813175));
#55682=CARTESIAN_POINT('Ctrl Pts',(64.3330402376073,4.20594089175434,128.251322046068));
#55683=CARTESIAN_POINT('Ctrl Pts',(64.3252754846602,4.13163418871067,128.13625604818));
#55684=CARTESIAN_POINT('Ctrl Pts',(64.3175184437752,4.0574012881322,128.021304335464));
#55685=CARTESIAN_POINT('Ctrl Pts',(64.3097614028902,3.97828981891137,127.909332816781));
#55686=CARTESIAN_POINT('Ctrl Pts',(64.3020043620052,3.89457074273651,127.800779123363));
#55687=CARTESIAN_POINT('Ctrl Pts',(64.2942531707651,3.81091479976834,127.692307291129));
#55688=CARTESIAN_POINT('Ctrl Pts',(64.286501979525,3.72265840368777,127.587248462321));
#55689=CARTESIAN_POINT('Ctrl Pts',(64.2787507882849,3.63011568579323,127.486011152808));
#55690=CARTESIAN_POINT('Ctrl Pts',(64.2710028915078,3.53761230102221,127.384816871852));
#55691=CARTESIAN_POINT('Ctrl Pts',(64.2632549947307,3.44082648109317,127.287441167651));
#55692=CARTESIAN_POINT('Ctrl Pts',(64.2555070979536,3.34011233804845,127.194259146455));
#55693=CARTESIAN_POINT('Ctrl Pts',(64.2477608218695,3.23941926223132,127.10109661693));
#55694=CARTESIAN_POINT('Ctrl Pts',(64.2400145457854,3.13479978454073,127.012126290902));
#55695=CARTESIAN_POINT('Ctrl Pts',(64.2322682697013,3.02664425368308,126.927685802193));
#55696=CARTESIAN_POINT('Ctrl Pts',(64.2245219364359,2.91848792444557,126.843244690164));
#55697=CARTESIAN_POINT('Ctrl Pts',(64.2167756031705,2.80679579812318,126.763333722774));
#55698=CARTESIAN_POINT('Ctrl Pts',(64.2090292699052,2.69199029614568,126.688249430054));
#55699=CARTESIAN_POINT('Ctrl Pts',(64.2012812019022,2.57715908427265,126.613148322729));
#55700=CARTESIAN_POINT('Ctrl Pts',(64.1935331338993,2.45921343649804,126.542876254894));
#55701=CARTESIAN_POINT('Ctrl Pts',(64.1857850658963,2.3386033125917,126.477685495855));
#55702=CARTESIAN_POINT('Ctrl Pts',(64.1780287631545,2.21786500281007,126.412425451301));
#55703=CARTESIAN_POINT('Ctrl Pts',(64.1702724604125,2.09445690448507,126.352257689774));
#55704=CARTESIAN_POINT('Ctrl Pts',(64.1625161576707,1.96885255398031,126.297387943677));
#55705=CARTESIAN_POINT('Ctrl Pts',(64.1547557151565,1.84318116465148,126.242488911944));
#55706=CARTESIAN_POINT('Ctrl Pts',(64.1469952726423,1.71531155175319,126.192893671402));
#55707=CARTESIAN_POINT('Ctrl Pts',(64.1392348301281,1.58573468969725,126.148758770716));
#55708=CARTESIAN_POINT('Ctrl Pts',(64.1314619298627,1.45594981935939,126.10455302077));
#55709=CARTESIAN_POINT('Ctrl Pts',(64.1236890295973,1.32445259847015,126.065825237303));
#55710=CARTESIAN_POINT('Ctrl Pts',(64.1159161293318,1.19174740397696,126.032681543318));
#55711=CARTESIAN_POINT('Ctrl Pts',(64.1084257935699,1.0638663775689,126.000742706094));
#55712=CARTESIAN_POINT('Ctrl Pts',(64.1009354578079,0.934863980140043,125.97398907807));
#55713=CARTESIAN_POINT('Ctrl Pts',(64.0934451220459,0.805196176042556,125.952470039597));
#55714=CARTESIAN_POINT('Ctrl Pts',(64.0856707879269,0.670611977739899,125.930135100239));
#55715=CARTESIAN_POINT('Ctrl Pts',(64.0778964538078,0.534884596641799,125.913368774682));
#55716=CARTESIAN_POINT('Ctrl Pts',(64.0701221196887,0.398514612827742,125.902282571894));
#55717=CARTESIAN_POINT('Ctrl Pts',(64.0623573667416,0.262312692831556,125.891210031859));
#55718=CARTESIAN_POINT('Ctrl Pts',(64.0545926137946,0.125470131803469,125.885803717569));
#55719=CARTESIAN_POINT('Ctrl Pts',(64.0468278608475,-0.0115027390944946,
125.886124068813));
#55720=CARTESIAN_POINT('Ctrl Pts',(64.0390708199626,-0.148339566605917,
125.886444101879));
#55721=CARTESIAN_POINT('Ctrl Pts',(64.0313137790776,-0.285306057990205,
125.892479480584));
#55722=CARTESIAN_POINT('Ctrl Pts',(64.0235567381926,-0.421887560287729,
125.904238787553));
#55723=CARTESIAN_POINT('Ctrl Pts',(64.0158055469525,-0.558366065412477,
125.915989226737));
#55724=CARTESIAN_POINT('Ctrl Pts',(64.0080543557124,-0.694459771373267,
125.933454969135));
#55725=CARTESIAN_POINT('Ctrl Pts',(64.0003031644723,-0.829655186559642,
125.956592539995));
#55726=CARTESIAN_POINT('Ctrl Pts',(63.9925552676952,-0.964793140088108,
125.979720276771));
#55727=CARTESIAN_POINT('Ctrl Pts',(63.9848073709181,-1.09903317765276,126.008514981539));
#55728=CARTESIAN_POINT('Ctrl Pts',(63.977059474141,-1.23186830553191,126.042881483901));
#55729=CARTESIAN_POINT('Ctrl Pts',(63.9693131980569,-1.36467564716625,126.077240797532));
#55730=CARTESIAN_POINT('Ctrl Pts',(63.9615669219728,-1.49607828538895,126.117169492652));
#55731=CARTESIAN_POINT('Ctrl Pts',(63.9538206458887,-1.62558116629291,126.162521657165));
#55732=CARTESIAN_POINT('Ctrl Pts',(63.9460743126233,-1.75508500315789,126.207874156458));
#55733=CARTESIAN_POINT('Ctrl Pts',(63.938327979358,-1.88268868572854,126.25865007581));
#55734=CARTESIAN_POINT('Ctrl Pts',(63.9305816460926,-2.00791440579,126.314654301834));
#55735=CARTESIAN_POINT('Ctrl Pts',(63.9228335780896,-2.13316816928287,126.370671069616));
#55736=CARTESIAN_POINT('Ctrl Pts',(63.9150855100866,-2.25604255376626,126.431918314328));
#55737=CARTESIAN_POINT('Ctrl Pts',(63.9073374420836,-2.37608210368182,126.498153829793));
#55738=CARTESIAN_POINT('Ctrl Pts',(63.8995811393418,-2.49624923305936,126.564459741152));
#55739=CARTESIAN_POINT('Ctrl Pts',(63.8918248366,-2.61357516642692,126.635764324587));
#55740=CARTESIAN_POINT('Ctrl Pts',(63.8840685338581,-2.72763085731484,126.711780383933));
#55741=CARTESIAN_POINT('Ctrl Pts',(63.8763080913439,-2.84174742315945,126.787837015339));
#55742=CARTESIAN_POINT('Ctrl Pts',(63.8685476488297,-2.95258995279779,126.868609903182));
#55743=CARTESIAN_POINT('Ctrl Pts',(63.8607872063156,-3.05976135374225,126.953770595161));
#55744=CARTESIAN_POINT('Ctrl Pts',(63.8530143060501,-3.1671047957336,127.039067994643));
#55745=CARTESIAN_POINT('Ctrl Pts',(63.8452414057847,-3.27076503668067,127.12876701783));
#55746=CARTESIAN_POINT('Ctrl Pts',(63.8374685055193,-3.3703801642367,127.222500680184));
#55747=CARTESIAN_POINT('Ctrl Pts',(63.8299781697572,-3.46637403099191,127.312826887813));
#55748=CARTESIAN_POINT('Ctrl Pts',(63.822487833995,-3.55861156282144,127.406899268869));
#55749=CARTESIAN_POINT('Ctrl Pts',(63.8149974982329,-3.64680475476847,127.504360898915));
#55750=CARTESIAN_POINT('Ctrl Pts',(63.8073028132597,-3.73740400830844,127.604481449447));
#55751=CARTESIAN_POINT('Ctrl Pts',(63.7996081282865,-3.82403581350862,127.7085114365));
#55752=CARTESIAN_POINT('Ctrl Pts',(63.7919134433133,-3.9063384991868,127.816099820334));
#55753=CARTESIAN_POINT('Ctrl Pts',(63.7842279597593,-3.98854276608501,127.923559548374));
#55754=CARTESIAN_POINT('Ctrl Pts',(63.7765424762052,-4.06642796712949,128.034568897793));
#55755=CARTESIAN_POINT('Ctrl Pts',(63.7688569926512,-4.13966969626655,128.148740564111));
#55756=CARTESIAN_POINT('Ctrl Pts',(63.7611802099884,-4.21282850696225,128.262782974379));
#55757=CARTESIAN_POINT('Ctrl Pts',(63.7535034273255,-4.28135409549743,128.379980241164));
#55758=CARTESIAN_POINT('Ctrl Pts',(63.7458266446627,-4.3449632047769,128.499913219244));
#55759=CARTESIAN_POINT('Ctrl Pts',(63.7381549607444,-4.40853006633148,128.619766540564));
#55760=CARTESIAN_POINT('Ctrl Pts',(63.7304832768262,-4.46718675547075,128.742351608546));
#55761=CARTESIAN_POINT('Ctrl Pts',(63.7228115929079,-4.52069420216972,128.867221749811));
#55762=CARTESIAN_POINT('Ctrl Pts',(63.7151427412837,-4.57418189455909,128.992045790511));
#55763=CARTESIAN_POINT('Ctrl Pts',(63.7074738896594,-4.62252396468919,129.119152861596));
#55764=CARTESIAN_POINT('Ctrl Pts',(63.6998050380352,-4.66552823982081,129.248073592003));
#55765=CARTESIAN_POINT('Ctrl Pts',(63.693246952966,-4.70230371918418,129.358321274265));
#55766=CARTESIAN_POINT('Ctrl Pts',(63.6866888678969,-4.73517640793081,129.469894766533));
#55767=CARTESIAN_POINT('Ctrl Pts',(63.6801307828278,-4.76405452823405,129.582490119308));
#55768=CARTESIAN_POINT('Origin',(213.235140564004,0.,130.804360617566));
#55769=CARTESIAN_POINT('',(61.5846617476392,-4.76405452823404,129.582490119308));
#55770=CARTESIAN_POINT('',(61.9302338125864,-4.76405452823398,129.582490119308));
#55771=CARTESIAN_POINT('',(213.235140564004,-4.76405452823405,129.582490119308));
#55772=CARTESIAN_POINT('',(63.264859435939,-4.91824980396436,130.802971983528));
#55773=CARTESIAN_POINT('Ctrl Pts',(63.264859435939,-4.91824980396436,130.802971983528));
#55774=CARTESIAN_POINT('Ctrl Pts',(63.2571418302039,-4.91828805502452,130.93844919633));
#55775=CARTESIAN_POINT('Ctrl Pts',(63.2494242244688,-4.91272432380155,131.074153444162));
#55776=CARTESIAN_POINT('Ctrl Pts',(63.2417066187337,-4.90152846008028,131.209578852006));
#55777=CARTESIAN_POINT('Ctrl Pts',(63.2339983402522,-4.89034612732488,131.344840588997));
#55778=CARTESIAN_POINT('Ctrl Pts',(63.2262900617706,-4.87354523437112,131.479823764385));
#55779=CARTESIAN_POINT('Ctrl Pts',(63.2185817832891,-4.85114760933017,131.614021000066));
#55780=CARTESIAN_POINT('Ctrl Pts',(63.210880909227,-4.82877149900356,131.748089328545));
#55781=CARTESIAN_POINT('Ctrl Pts',(63.2031800351649,-4.80080941755057,131.881372830076));
#55782=CARTESIAN_POINT('Ctrl Pts',(63.1954791611028,-4.76733507809624,132.013368192254));
#55783=CARTESIAN_POINT('Ctrl Pts',(63.1877837757607,-4.73388459713836,132.145269476074));
#55784=CARTESIAN_POINT('Ctrl Pts',(63.1800883904185,-4.69492977372091,132.275884064037));
#55785=CARTESIAN_POINT('Ctrl Pts',(63.1723930050764,-4.65059550550699,132.404718235931));
#55786=CARTESIAN_POINT('Ctrl Pts',(63.1647003972949,-4.60627723923585,132.533505906616));
#55787=CARTESIAN_POINT('Ctrl Pts',(63.1570077895134,-4.55658351663959,132.660514063682));
#55788=CARTESIAN_POINT('Ctrl Pts',(63.1493151817319,-4.50168917783681,132.785263848077));
#55789=CARTESIAN_POINT('Ctrl Pts',(63.1416237703605,-4.44680337659991,132.90999423048));
#55790=CARTESIAN_POINT('Ctrl Pts',(63.1339323589891,-4.3867187275044,133.032466575268));
#55791=CARTESIAN_POINT('Ctrl Pts',(63.1262409476178,-4.32165813623516,133.152222201223));
#55792=CARTESIAN_POINT('Ctrl Pts',(63.1185490066165,-4.25659306489875,133.271986073541));
#55793=CARTESIAN_POINT('Ctrl Pts',(63.1108570656151,-4.1865515595093,133.389032505933));
#55794=CARTESIAN_POINT('Ctrl Pts',(63.1031651246138,-4.11180214760816,133.502928045188));
#55795=CARTESIAN_POINT('Ctrl Pts',(63.0954709278749,-4.03703081470508,133.616856985434));
#55796=CARTESIAN_POINT('Ctrl Pts',(63.0877767311361,-3.95754904691294,133.727632862686));
#55797=CARTESIAN_POINT('Ctrl Pts',(63.0800825343972,-3.87366800687072,133.834852200634));
#55798=CARTESIAN_POINT('Ctrl Pts',(63.0723800101768,-3.78969618180665,133.942187582803));
#55799=CARTESIAN_POINT('Ctrl Pts',(63.0646774859563,-3.70131582336188,134.045958427595));
#55800=CARTESIAN_POINT('Ctrl Pts',(63.0569749617358,-3.60887784046913,134.145795009421));
#55801=CARTESIAN_POINT('Ctrl Pts',(63.0492677377164,-3.51638345529507,134.245692507883));
#55802=CARTESIAN_POINT('Ctrl Pts',(63.0415605136969,-3.41982679653603,134.341650683781));
#55803=CARTESIAN_POINT('Ctrl Pts',(63.0338532896774,-3.31959388321576,134.433338367982));
#55804=CARTESIAN_POINT('Ctrl Pts',(63.0261347544936,-3.21921386751972,134.525160613534));
#55805=CARTESIAN_POINT('Ctrl Pts',(63.0184162193096,-3.11514712843326,134.612699599544));
#55806=CARTESIAN_POINT('Ctrl Pts',(63.0106976841257,-3.00781118819578,134.695665658123));
#55807=CARTESIAN_POINT('Ctrl Pts',(63.006879663735,-2.95471681229151,134.736705323791));
#55808=CARTESIAN_POINT('Ctrl Pts',(63.0030616433443,-2.90082294085479,134.77662674693));
#55809=CARTESIAN_POINT('Ctrl Pts',(62.9992436229536,-2.84618240724453,134.815398982777));
#55810=CARTESIAN_POINT('Ctrl Pts',(62.9914692888345,-2.7349221935055,134.894347831962));
#55811=CARTESIAN_POINT('Ctrl Pts',(62.9836949547154,-2.62019837736383,134.96878893393));
#55812=CARTESIAN_POINT('Ctrl Pts',(62.9759206205964,-2.50241234959665,135.038403070717));
#55813=CARTESIAN_POINT('Ctrl Pts',(62.9681558676493,-2.38477148258202,135.107931414302));
#55814=CARTESIAN_POINT('Ctrl Pts',(62.9603911147022,-2.26407624622692,135.172644432036));
#55815=CARTESIAN_POINT('Ctrl Pts',(62.9526263617551,-2.14075913653756,135.232264566595));
#55816=CARTESIAN_POINT('Ctrl Pts',(62.9448693208701,-2.01756450713984,135.291825485597));
#55817=CARTESIAN_POINT('Ctrl Pts',(62.937112279985,-1.89175353635624,135.346303418643));
#55818=CARTESIAN_POINT('Ctrl Pts',(62.9293552391,-1.76378528761729,135.395465552294));
#55819=CARTESIAN_POINT('Ctrl Pts',(62.9216040478599,-1.63591354073033,135.444590612398));
#55820=CARTESIAN_POINT('Ctrl Pts',(62.9138528566198,-1.50588811745759,135.488407712512));
#55821=CARTESIAN_POINT('Ctrl Pts',(62.9061016653797,-1.37418980533761,135.526731361314));
#55822=CARTESIAN_POINT('Ctrl Pts',(62.8983537686026,-1.24254746851345,135.565038721543));
#55823=CARTESIAN_POINT('Ctrl Pts',(62.8906058718255,-1.10923403161969,135.597857165315));
#55824=CARTESIAN_POINT('Ctrl Pts',(62.8828579750485,-0.974747049046067,
135.625050532182));
#55825=CARTESIAN_POINT('Ctrl Pts',(62.8751116989644,-0.84028819825018,135.652238210782));
#55826=CARTESIAN_POINT('Ctrl Pts',(62.8673654228803,-0.704656673015628,
135.673803075452));
#55827=CARTESIAN_POINT('Ctrl Pts',(62.8596191467962,-0.568361483534681,
135.689659818898));
#55828=CARTESIAN_POINT('Ctrl Pts',(62.8518728135309,-0.432065287953422,
135.705516679395));
#55829=CARTESIAN_POINT('Ctrl Pts',(62.8441264802655,-0.295105806695978,
135.715665289407));
#55830=CARTESIAN_POINT('Ctrl Pts',(62.8363801470002,-0.157998060555954,
135.720072130192));
#55831=CARTESIAN_POINT('Ctrl Pts',(62.8286320789972,-0.0208596100868197,
135.724479957857));
#55832=CARTESIAN_POINT('Ctrl Pts',(62.8208840109942,0.116426780646181,135.723143445086));
#55833=CARTESIAN_POINT('Ctrl Pts',(62.8131359429913,0.253345595042856,135.716081199192));
#55834=CARTESIAN_POINT('Ctrl Pts',(62.8053796402494,0.390409928384827,135.70901144746));
#55835=CARTESIAN_POINT('Ctrl Pts',(62.7976233375076,0.527105513927296,135.696203826581));
#55836=CARTESIAN_POINT('Ctrl Pts',(62.7898670347657,0.662920906840735,135.677728953099));
#55837=CARTESIAN_POINT('Ctrl Pts',(62.7821065922515,0.798808788518695,135.65924421902));
#55838=CARTESIAN_POINT('Ctrl Pts',(62.7743461497374,0.933815156816525,135.635086274032));
#55839=CARTESIAN_POINT('Ctrl Pts',(62.7665857072232,1.0674392581739,135.605376811312));
#55840=CARTESIAN_POINT('Ctrl Pts',(62.7588128069578,1.20127786480155,135.575619656325));
#55841=CARTESIAN_POINT('Ctrl Pts',(62.7510399066924,1.33372939236694,135.540293275822));
#55842=CARTESIAN_POINT('Ctrl Pts',(62.7432670064269,1.46430787116021,135.499569401098));
#55843=CARTESIAN_POINT('Ctrl Pts',(62.7357766706649,1.59013949334254,135.460325941798));
#55844=CARTESIAN_POINT('Ctrl Pts',(62.7282863349028,1.71423159242746,135.41607070369));
#55845=CARTESIAN_POINT('Ctrl Pts',(62.7207959991407,1.83616906217512,135.366998696311));
#55846=CARTESIAN_POINT('Ctrl Pts',(62.7130216650216,1.96272982814982,135.316066108856));
#55847=CARTESIAN_POINT('Ctrl Pts',(62.7052473309026,2.08737026042727,135.259782947128));
#55848=CARTESIAN_POINT('Ctrl Pts',(62.6974729967835,2.2096048303726,135.198314367447));
#55849=CARTESIAN_POINT('Ctrl Pts',(62.6897082438364,2.33168875713472,135.136921542297));
#55850=CARTESIAN_POINT('Ctrl Pts',(62.6819434908893,2.45137237511715,135.070356188473));
#55851=CARTESIAN_POINT('Ctrl Pts',(62.6741787379422,2.56818839282721,134.998832150602));
#55852=CARTESIAN_POINT('Ctrl Pts',(62.6664216970572,2.68488838722183,134.927379151413));
#55853=CARTESIAN_POINT('Ctrl Pts',(62.6586646561722,2.79872611800074,134.85097747205));
#55854=CARTESIAN_POINT('Ctrl Pts',(62.6509076152872,2.90925757762716,134.769887494227));
#55855=CARTESIAN_POINT('Ctrl Pts',(62.6431564240471,3.01970568461976,134.688858666987));
#55856=CARTESIAN_POINT('Ctrl Pts',(62.6354052328069,3.12685216923693,134.603148808781));
#55857=CARTESIAN_POINT('Ctrl Pts',(62.6276540415668,3.23028109496689,134.513062157189));
#55858=CARTESIAN_POINT('Ctrl Pts',(62.6199061447897,3.33366606064463,134.423013794827));
#55859=CARTESIAN_POINT('Ctrl Pts',(62.6121582480127,3.43333631585974,134.328592595229));
#55860=CARTESIAN_POINT('Ctrl Pts',(62.6044103512356,3.52890836466922,134.230143566947));
#55861=CARTESIAN_POINT('Ctrl Pts',(62.5966640751515,3.62446042186626,134.131715132079));
#55862=CARTESIAN_POINT('Ctrl Pts',(62.5889177990674,3.71591570563536,134.02926082472));
#55863=CARTESIAN_POINT('Ctrl Pts',(62.5811715229833,3.80292731209237,133.923162778884));
#55864=CARTESIAN_POINT('Ctrl Pts',(62.5734251897179,3.88993956084953,133.817063949856));
#55865=CARTESIAN_POINT('Ctrl Pts',(62.5656788564526,3.97250781891797,133.707321630985));
#55866=CARTESIAN_POINT('Ctrl Pts',(62.5579325231872,4.0503255047097,133.594351006151));
#55867=CARTESIAN_POINT('Ctrl Pts',(62.5501844551843,4.12816061723252,133.481355082329));
#55868=CARTESIAN_POINT('Ctrl Pts',(62.5424363871812,4.20124281878338,133.365129735853));
#55869=CARTESIAN_POINT('Ctrl Pts',(62.5346883191783,4.2693091149097,133.246118743149));
#55870=CARTESIAN_POINT('Ctrl Pts',(62.5269320164364,4.33744775270554,133.126981264145));
#55871=CARTESIAN_POINT('Ctrl Pts',(62.5191757136946,4.40055964149048,133.005052564679));
#55872=CARTESIAN_POINT('Ctrl Pts',(62.5114194109527,4.45842774453909,132.880801107738));
#55873=CARTESIAN_POINT('Ctrl Pts',(62.5036589684385,4.51632673353659,132.756483334053));
#55874=CARTESIAN_POINT('Ctrl Pts',(62.4958985259244,4.56897621000845,132.629840693468));
#55875=CARTESIAN_POINT('Ctrl Pts',(62.4881380834102,4.61620788833998,132.501360262271));
#55876=CARTESIAN_POINT('Ctrl Pts',(62.4803651831448,4.66351538715467,132.372673582879));
#55877=CARTESIAN_POINT('Ctrl Pts',(62.4725922828793,4.70538758870002,132.242143589959));
#55878=CARTESIAN_POINT('Ctrl Pts',(62.4648193826139,4.74170629687945,132.110271968552));
#55879=CARTESIAN_POINT('Ctrl Pts',(62.4573290468519,4.77670472853521,131.983194212747));
#55880=CARTESIAN_POINT('Ctrl Pts',(62.4498387110899,4.80654635401489,131.854870978125));
#55881=CARTESIAN_POINT('Ctrl Pts',(62.4423483753279,4.83117086530171,131.72575691274));
#55882=CARTESIAN_POINT('Ctrl Pts',(62.4345740412088,4.85672902241847,131.591747448321));
#55883=CARTESIAN_POINT('Ctrl Pts',(62.4267997070897,4.87674760259234,131.456461498939));
#55884=CARTESIAN_POINT('Ctrl Pts',(62.4190253729706,4.89110311642676,131.32039682461));
#55885=CARTESIAN_POINT('Ctrl Pts',(62.4112606200235,4.90544093837332,131.184499837832));
#55886=CARTESIAN_POINT('Ctrl Pts',(62.4034958670765,4.914129539927,131.047826420717));
#55887=CARTESIAN_POINT('Ctrl Pts',(62.3957311141294,4.91709625216194,130.910885307075));
#55888=CARTESIAN_POINT('Ctrl Pts',(62.3879740732444,4.92006001781648,130.774080205277));
#55889=CARTESIAN_POINT('Ctrl Pts',(62.3802170323594,4.91731319528724,130.637008324411));
#55890=CARTESIAN_POINT('Ctrl Pts',(62.3724599914744,4.9088348541665,130.500183963268));
#55891=CARTESIAN_POINT('Ctrl Pts',(62.3647088002344,4.90036290662878,130.36346278244));
#55892=CARTESIAN_POINT('Ctrl Pts',(62.3569576089942,4.88616806762424,130.226989138446));
#55893=CARTESIAN_POINT('Ctrl Pts',(62.3492064177541,4.86628147700257,130.091277418296));
#55894=CARTESIAN_POINT('Ctrl Pts',(62.3414585209771,4.84640333871233,129.955623379247));
#55895=CARTESIAN_POINT('Ctrl Pts',(62.3337106242,4.82083831686868,129.820731005977));
#55896=CARTESIAN_POINT('Ctrl Pts',(62.3259627274229,4.78966938801219,129.687109430035));
#55897=CARTESIAN_POINT('Ctrl Pts',(62.3182164513388,4.7585069790237,129.553515804846));
#55898=CARTESIAN_POINT('Ctrl Pts',(62.3104701752547,4.72174308338244,129.42119282875));
#55899=CARTESIAN_POINT('Ctrl Pts',(62.3027238991706,4.67951169123469,129.290638914578));
#55900=CARTESIAN_POINT('Ctrl Pts',(62.2949775659052,4.63727998734435,129.160084036686));
#55901=CARTESIAN_POINT('Ctrl Pts',(62.2872312326399,4.58958082674231,129.031298618764));
#55902=CARTESIAN_POINT('Ctrl Pts',(62.2794848993745,4.53659780054823,128.904765013612));
#55903=CARTESIAN_POINT('Ctrl Pts',(62.2717368313715,4.48360290917272,128.778203072137));
#55904=CARTESIAN_POINT('Ctrl Pts',(62.2639887633686,4.42532194858005,128.653894307444));
#55905=CARTESIAN_POINT('Ctrl Pts',(62.2562406953656,4.36198612551915,128.532299856213));
#55906=CARTESIAN_POINT('Ctrl Pts',(62.2484843926238,4.29858298839197,128.410576172953));
#55907=CARTESIAN_POINT('Ctrl Pts',(62.2407280898819,4.2301144378132,128.291572913161));
#55908=CARTESIAN_POINT('Ctrl Pts',(62.2329717871401,4.15685729130931,128.17572589167));
#55909=CARTESIAN_POINT('Ctrl Pts',(62.2252113446259,4.08356104526051,128.059817039134));
#55910=CARTESIAN_POINT('Ctrl Pts',(62.2174509021117,4.00547133309866,127.947068102813));
#55911=CARTESIAN_POINT('Ctrl Pts',(62.2096904595975,3.92290698341341,127.837883942791));
#55912=CARTESIAN_POINT('Ctrl Pts',(62.2019175593321,3.84021009410445,127.728524510662));
#55913=CARTESIAN_POINT('Ctrl Pts',(62.1941446590667,3.75302446198057,127.622741592074));
#55914=CARTESIAN_POINT('Ctrl Pts',(62.1863717588013,3.66170828099704,127.520905801769));
#55915=CARTESIAN_POINT('Ctrl Pts',(62.1788814230392,3.57371167320297,127.42277199895));
#55916=CARTESIAN_POINT('Ctrl Pts',(62.1713910872771,3.48187982910589,127.328303551492));
#55917=CARTESIAN_POINT('Ctrl Pts',(62.163900751515,3.38656265903332,127.237796946616));
#55918=CARTESIAN_POINT('Ctrl Pts',(62.1561264173959,3.28763150948712,127.143858756308));
#55919=CARTESIAN_POINT('Ctrl Pts',(62.1483520832768,3.18463214033952,127.053891197667));
#55920=CARTESIAN_POINT('Ctrl Pts',(62.1405777491577,3.07791658215494,126.96826721727));
#55921=CARTESIAN_POINT('Ctrl Pts',(62.1328129962106,2.97133254135852,126.882748760776));
#55922=CARTESIAN_POINT('Ctrl Pts',(62.1250482432635,2.86104172611729,126.80156347383));
#55923=CARTESIAN_POINT('Ctrl Pts',(62.1172834903164,2.74743286926502,126.725047477909));
#55924=CARTESIAN_POINT('Ctrl Pts',(62.1095264494314,2.63393685033129,126.648607478753));
#55925=CARTESIAN_POINT('Ctrl Pts',(62.1017694085464,2.51712967020883,126.576827758566));
#55926=CARTESIAN_POINT('Ctrl Pts',(62.0940123676614,2.39743270964121,126.510003917751));
#55927=CARTESIAN_POINT('Ctrl Pts',(62.0862611764213,2.27782601348201,126.443230469315));
#55928=CARTESIAN_POINT('Ctrl Pts',(62.0785099851811,2.15533421444377,126.381405651254));
#55929=CARTESIAN_POINT('Ctrl Pts',(62.070758793941,2.03040691273705,126.324781303478));
#55930=CARTESIAN_POINT('Ctrl Pts',(62.0630108971639,1.90553270846643,126.268181022559));
#55931=CARTESIAN_POINT('Ctrl Pts',(62.0552630003868,1.77822541571749,126.216776976794));
#55932=CARTESIAN_POINT('Ctrl Pts',(62.0475151036097,1.64895823212723,126.170774553706));
#55933=CARTESIAN_POINT('Ctrl Pts',(62.0397688275256,1.51971808844474,126.124781753333));
#55934=CARTESIAN_POINT('Ctrl Pts',(62.0320225514415,1.3885192374707,126.084188459195));
#55935=CARTESIAN_POINT('Ctrl Pts',(62.0242762753573,1.25585343298319,126.049151345897));
#55936=CARTESIAN_POINT('Ctrl Pts',(62.016529942092,1.12318664918702,126.014113973964));
#55937=CARTESIAN_POINT('Ctrl Pts',(62.0087836088266,0.989053268274115,125.984632964543));
#55938=CARTESIAN_POINT('Ctrl Pts',(62.0010372755612,0.853958342801723,125.960814580698));
#55939=CARTESIAN_POINT('Ctrl Pts',(61.9932892075583,0.718833163757822,125.936990862891));
#55940=CARTESIAN_POINT('Ctrl Pts',(61.9855411395553,0.582746396623301,125.918832361914));
#55941=CARTESIAN_POINT('Ctrl Pts',(61.9777930715523,0.446210981641435,125.906393812619));
#55942=CARTESIAN_POINT('Ctrl Pts',(61.9700367688105,0.309530455195548,125.893942043486));
#55943=CARTESIAN_POINT('Ctrl Pts',(61.9622804660686,0.172400718360169,125.887222405485));
#55944=CARTESIAN_POINT('Ctrl Pts',(61.9545241633268,0.0353380611301516,
125.886237572751));
#55945=CARTESIAN_POINT('Ctrl Pts',(61.9467637208126,-0.101797750566906,
125.885252214384));
#55946=CARTESIAN_POINT('Ctrl Pts',(61.9390032782984,-0.238866020780342,
125.890007746714));
#55947=CARTESIAN_POINT('Ctrl Pts',(61.9312428357842,-0.375353794614429,
125.900454766984));
#55948=CARTESIAN_POINT('Ctrl Pts',(61.9234699355188,-0.512060670739889,
125.91091855774));
#55949=CARTESIAN_POINT('Ctrl Pts',(61.9156970352534,-0.648184799866215,
125.927092047883));
#55950=CARTESIAN_POINT('Ctrl Pts',(61.907924134988,-0.783220760732462,125.948874205016));
#55951=CARTESIAN_POINT('Ctrl Pts',(61.900433799226,-0.913347824284512,125.969864525871));
#55952=CARTESIAN_POINT('Ctrl Pts',(61.8929434634641,-1.04246415946571,125.996062753751));
#55953=CARTESIAN_POINT('Ctrl Pts',(61.8854531277022,-1.17013118810115,126.027334757773));
#55954=CARTESIAN_POINT('Ctrl Pts',(61.8776787935831,-1.30263875093255,126.059792449332));
#55955=CARTESIAN_POINT('Ctrl Pts',(61.869904459464,-1.43400468095375,126.097819072665));
#55956=CARTESIAN_POINT('Ctrl Pts',(61.8621301253449,-1.5637249265304,126.14132004122));
#55957=CARTESIAN_POINT('Ctrl Pts',(61.8543653723978,-1.69328530349746,126.184767398719));
#55958=CARTESIAN_POINT('Ctrl Pts',(61.8466006194507,-1.82120366433245,126.233675554525));
#55959=CARTESIAN_POINT('Ctrl Pts',(61.8388358665037,-1.94698710092558,126.287899138562));
#55960=CARTESIAN_POINT('Ctrl Pts',(61.8310788256187,-2.07264560763589,126.342068866971));
#55961=CARTESIAN_POINT('Ctrl Pts',(61.8233217847338,-2.19617305316668,126.40154336368));
#55962=CARTESIAN_POINT('Ctrl Pts',(61.8155647438488,-2.31709297394084,126.466127888376));
#55963=CARTESIAN_POINT('Ctrl Pts',(61.8078135526088,-2.43792170806164,126.530663709379));
#55964=CARTESIAN_POINT('Ctrl Pts',(61.8000623613687,-2.55614648787296,126.600301704741));
#55965=CARTESIAN_POINT('Ctrl Pts',(61.7923111701286,-2.6713124134327,126.67479973869));
#55966=CARTESIAN_POINT('Ctrl Pts',(61.7845632733515,-2.78642939040287,126.749266108989));
#55967=CARTESIAN_POINT('Ctrl Pts',(61.7768153765745,-2.89848977132767,126.828588197559));
#55968=CARTESIAN_POINT('Ctrl Pts',(61.7690674797974,-3.00706498298513,126.912478906799));
#55969=CARTESIAN_POINT('Ctrl Pts',(61.7613212037133,-3.11561748304877,126.996352067911));
#55970=CARTESIAN_POINT('Ctrl Pts',(61.7535749276292,-3.22068595473,127.084791709951));
#55971=CARTESIAN_POINT('Ctrl Pts',(61.7458286515451,-3.32187277831748,127.17746879299));
#55972=CARTESIAN_POINT('Ctrl Pts',(61.7380823182798,-3.42306034884379,127.270146560151));
#55973=CARTESIAN_POINT('Ctrl Pts',(61.7303359850143,-3.52036592578884,127.367061566662));
#55974=CARTESIAN_POINT('Ctrl Pts',(61.722589651749,-3.6134271137847,127.467846335285));
#55975=CARTESIAN_POINT('Ctrl Pts',(61.714841583746,-3.70650914218761,127.568653673957));
#55976=CARTESIAN_POINT('Ctrl Pts',(61.7070935157431,-3.79534462507557,127.673332212));
#55977=CARTESIAN_POINT('Ctrl Pts',(61.6993454477401,-3.87961025573602,127.781479983785));
#55978=CARTESIAN_POINT('Ctrl Pts',(61.6915891449983,-3.96396544491174,127.889742696309));
#55979=CARTESIAN_POINT('Ctrl Pts',(61.6838328422565,-4.04374083901207,128.001481699149));
#55980=CARTESIAN_POINT('Ctrl Pts',(61.6760765395146,-4.11865512085688,128.116264068344));
#55981=CARTESIAN_POINT('Ctrl Pts',(61.6683160970005,-4.19360938670953,128.231107700346));
#55982=CARTESIAN_POINT('Ctrl Pts',(61.6605556544863,-4.26369717080579,128.348997599436));
#55983=CARTESIAN_POINT('Ctrl Pts',(61.6527952119721,-4.32868277243377,128.469475498736));
#55984=CARTESIAN_POINT('Ctrl Pts',(61.6450223117067,-4.39377269471863,128.590146799855));
#55985=CARTESIAN_POINT('Ctrl Pts',(61.6372494114413,-4.45374389621378,128.713414051406));
#55986=CARTESIAN_POINT('Ctrl Pts',(61.6294765111759,-4.50840818580015,128.838797417689));
#55987=CARTESIAN_POINT('Ctrl Pts',(61.6219861754136,-4.56108529077072,128.95962278279));
#55988=CARTESIAN_POINT('Ctrl Pts',(61.6144958396513,-4.60883451269228,129.082412794444));
#55989=CARTESIAN_POINT('Ctrl Pts',(61.607005503889,-4.65153163745955,129.206725963394));
#55990=CARTESIAN_POINT('Ctrl Pts',(61.5995575851391,-4.69398697273639,129.330335159466));
#55991=CARTESIAN_POINT('Ctrl Pts',(61.5921096663892,-4.73153827174323,129.455709728754));
#55992=CARTESIAN_POINT('Ctrl Pts',(61.5846617476392,-4.76405452823404,129.582490119308));
#55993=CARTESIAN_POINT('Ctrl Pts',(63.3349537467757,-4.76405452823404,129.582490119308));
#55994=CARTESIAN_POINT('Ctrl Pts',(63.3271906269684,-4.7981070602073,129.715260424653));
#55995=CARTESIAN_POINT('Ctrl Pts',(63.319427507161,-4.82657353511072,129.849332155469));
#55996=CARTESIAN_POINT('Ctrl Pts',(63.3116643873537,-4.8493826737915,129.984195545382));
#55997=CARTESIAN_POINT('Ctrl Pts',(63.3038899276852,-4.87222513058033,130.119255934973));
#55998=CARTESIAN_POINT('Ctrl Pts',(63.2961154680168,-4.88939370113894,130.255109905985));
#55999=CARTESIAN_POINT('Ctrl Pts',(63.2883410083483,-4.90086903852806,130.391243527993));
#56000=CARTESIAN_POINT('Ctrl Pts',(63.284791087821,-4.90610882849322,130.453403930109));
#56001=CARTESIAN_POINT('Ctrl Pts',(63.2812411672937,-4.91016232332491,130.515622647955));
#56002=CARTESIAN_POINT('Ctrl Pts',(63.2776912467664,-4.91303128814727,130.577850961732));
#56003=CARTESIAN_POINT('Ctrl Pts',(63.273413976508,-4.91648808043679,130.652829348912));
#56004=CARTESIAN_POINT('Ctrl Pts',(63.2691367062496,-4.91822860435436,130.727887471573));
#56005=CARTESIAN_POINT('Ctrl Pts',(63.2648594359911,-4.91824980396411,130.802971982613));
#56006=CARTESIAN_POINT('',(63.6101405639656,-4.91824793751526,130.808864796387));
#56007=CARTESIAN_POINT('Ctrl Pts',(63.6801307828278,-4.76405452823405,129.582490119308));
#56008=CARTESIAN_POINT('Ctrl Pts',(63.6724626857052,-4.79782051767604,129.714143199672));
#56009=CARTESIAN_POINT('Ctrl Pts',(63.6647945885826,-4.82612406158235,129.84719330369));
#56010=CARTESIAN_POINT('Ctrl Pts',(63.65712649146,-4.84886539797774,129.981142897401));
#56011=CARTESIAN_POINT('Ctrl Pts',(63.6492955035514,-4.87208982086775,130.117937936891));
#56012=CARTESIAN_POINT('Ctrl Pts',(63.6414645156428,-4.88951296919464,130.255670685851));
#56013=CARTESIAN_POINT('Ctrl Pts',(63.6336335277342,-4.90108418362794,130.393803815781));
#56014=CARTESIAN_POINT('Ctrl Pts',(63.6258025398256,-4.91265539806124,130.53193694571));
#56015=CARTESIAN_POINT('Ctrl Pts',(63.6179715519171,-4.91837468076857,130.670470013715));
#56016=CARTESIAN_POINT('Ctrl Pts',(63.6101405640085,-4.91824793751596,130.808864795629));
#56017=CARTESIAN_POINT('Ctrl Pts',(63.6101405639656,-4.91824793751526,130.808864796387));
#56018=CARTESIAN_POINT('Ctrl Pts',(63.6003856693909,-4.9180900561228,130.98126022376));
#56019=CARTESIAN_POINT('Ctrl Pts',(63.5906307748162,-4.90886436956287,131.153250222946));
#56020=CARTESIAN_POINT('Ctrl Pts',(63.5808758802415,-4.89071988369391,131.324016351433));
#56021=CARTESIAN_POINT('Ctrl Pts',(63.5709349483462,-4.8722293611244,131.498039190973));
#56022=CARTESIAN_POINT('Ctrl Pts',(63.5609940164509,-4.84447662962381,131.670791202816));
#56023=CARTESIAN_POINT('Ctrl Pts',(63.5510530845557,-4.80766771366139,131.841430633292));
#56024=CARTESIAN_POINT('Ctrl Pts',(63.5462186811771,-4.78976706314237,131.924414788893));
#56025=CARTESIAN_POINT('Ctrl Pts',(63.5413842777985,-4.76972534017766,132.006899665763));
#56026=CARTESIAN_POINT('Ctrl Pts',(63.53654987442,-4.74757027226103,132.088790285724));
#56027=CARTESIAN_POINT('Ctrl Pts',(63.5287755403009,-4.71194211157042,132.220480794549));
#56028=CARTESIAN_POINT('Ctrl Pts',(63.5210012061818,-4.67077401886086,132.350896360319));
#56029=CARTESIAN_POINT('Ctrl Pts',(63.5132268720627,-4.62417264929384,132.47953534637));
#56030=CARTESIAN_POINT('Ctrl Pts',(63.5054621191156,-4.57762871175,132.608015796367));
#56031=CARTESIAN_POINT('Ctrl Pts',(63.4976973661685,-4.52566495233479,132.73472365899));
#56032=CARTESIAN_POINT('Ctrl Pts',(63.4899326132214,-4.46843852769493,132.859169656555));
#56033=CARTESIAN_POINT('Ctrl Pts',(63.4821755723364,-4.41126894114677,132.983492052601));
#56034=CARTESIAN_POINT('Ctrl Pts',(63.4744185314515,-4.3488472535323,133.105556701348));
#56035=CARTESIAN_POINT('Ctrl Pts',(63.4666614905665,-4.28137958289765,133.22489194966));
#56036=CARTESIAN_POINT('Ctrl Pts',(63.4589102993263,-4.21396279015807,133.344137206332));
#56037=CARTESIAN_POINT('Ctrl Pts',(63.4511591080862,-4.14150778008419,133.460656820454));
#56038=CARTESIAN_POINT('Ctrl Pts',(63.443407916846,-4.06426753506044,133.574001833672));
#56039=CARTESIAN_POINT('Ctrl Pts',(63.4356600200689,-3.98706011920139,133.687298672236));
#56040=CARTESIAN_POINT('Ctrl Pts',(63.4279121232919,-3.9050717332755,133.797423271129));
#56041=CARTESIAN_POINT('Ctrl Pts',(63.4201642265148,-3.81859967678151,133.903954070099));
#56042=CARTESIAN_POINT('Ctrl Pts',(63.4124179504307,-3.73214570837762,134.010462585122));
#56043=CARTESIAN_POINT('Ctrl Pts',(63.4046716743466,-3.64121018115383,134.113378492125));
#56044=CARTESIAN_POINT('Ctrl Pts',(63.3969253982625,-3.54613158206114,134.212312181953));
#56045=CARTESIAN_POINT('Ctrl Pts',(63.3891790649971,-3.45105228111983,134.311246602087));
#56046=CARTESIAN_POINT('Ctrl Pts',(63.3814327317318,-3.35183011819047,134.406198464498));
#56047=CARTESIAN_POINT('Ctrl Pts',(63.3736863984664,-3.24884116117753,134.496814296617));
#56048=CARTESIAN_POINT('Ctrl Pts',(63.3659383304635,-3.14582914050188,134.587450421524));
#56049=CARTESIAN_POINT('Ctrl Pts',(63.3581902624605,-3.03904894064808,134.673748325705));
#56050=CARTESIAN_POINT('Ctrl Pts',(63.3504421944575,-2.92891016995861,134.755394441619));
#56051=CARTESIAN_POINT('Ctrl Pts',(63.3426858917156,-2.81865434247283,134.837127331997));
#56052=CARTESIAN_POINT('Ctrl Pts',(63.3349295889738,-2.70503312821193,134.914198324785));
#56053=CARTESIAN_POINT('Ctrl Pts',(63.3271732862319,-2.58848607729979,134.986336572796));
#56054=CARTESIAN_POINT('Ctrl Pts',(63.3194128437178,-2.47187682171742,135.058513323163));
#56055=CARTESIAN_POINT('Ctrl Pts',(63.3116524012036,-2.3523389584402,135.125751891189));
#56056=CARTESIAN_POINT('Ctrl Pts',(63.3038919586894,-2.23033627854425,135.18782764118));
#56057=CARTESIAN_POINT('Ctrl Pts',(63.296119058424,-2.10813774911563,135.250003040675));
#56058=CARTESIAN_POINT('Ctrl Pts',(63.2883461581586,-1.98346685200986,135.306998897794));
#56059=CARTESIAN_POINT('Ctrl Pts',(63.2805732578931,-1.85680780081433,135.358638590344));
#56060=CARTESIAN_POINT('Ctrl Pts',(63.2730829221311,-1.73475312516517,135.408401049998));
#56061=CARTESIAN_POINT('Ctrl Pts',(63.2655925863692,-1.61085262433766,135.453189899611));
#56062=CARTESIAN_POINT('Ctrl Pts',(63.2581022506072,-1.48555064124843,135.492891555374));
#56063=CARTESIAN_POINT('Ctrl Pts',(63.2503279164881,-1.3554977953851,135.534098511483));
#56064=CARTESIAN_POINT('Ctrl Pts',(63.242553582369,-1.22352312664602,135.569955428021));
#56065=CARTESIAN_POINT('Ctrl Pts',(63.2347792482499,-1.09010632588325,135.600280890128));
#56066=CARTESIAN_POINT('Ctrl Pts',(63.2270144953028,-0.95685394940363,135.630568978812));
#56067=CARTESIAN_POINT('Ctrl Pts',(63.2192497423557,-0.82216335477627,135.655339091086));
#56068=CARTESIAN_POINT('Ctrl Pts',(63.2114849894086,-0.686531132179684,
135.674458980746));
#56069=CARTESIAN_POINT('Ctrl Pts',(63.2037279485236,-0.551033621418844,
135.693559880262));
#56070=CARTESIAN_POINT('Ctrl Pts',(63.1959709076386,-0.4145967284873,135.707021670841));
#56071=CARTESIAN_POINT('Ctrl Pts',(63.1882138667536,-0.277728680365565,
135.71476282539));
#56072=CARTESIAN_POINT('Ctrl Pts',(63.1804626755135,-0.140963845503597,
135.722498142274));
#56073=CARTESIAN_POINT('Ctrl Pts',(63.1727114842734,-0.00376889137982753,
135.724521387849));
#56074=CARTESIAN_POINT('Ctrl Pts',(63.1649602930333,0.133341717471359,135.720802730403));
#56075=CARTESIAN_POINT('Ctrl Pts',(63.1572123962562,0.270394050656239,135.717085653487));
#56076=CARTESIAN_POINT('Ctrl Pts',(63.1494644994791,0.407361719866178,135.70763153802));
#56077=CARTESIAN_POINT('Ctrl Pts',(63.141716602702,0.543729356880365,135.692462646878));
#56078=CARTESIAN_POINT('Ctrl Pts',(63.1339703266179,0.680068468724636,135.677296928741));
#56079=CARTESIAN_POINT('Ctrl Pts',(63.1262240505339,0.815807409704502,135.656418855856));
#56080=CARTESIAN_POINT('Ctrl Pts',(63.1184777744498,0.950435430138027,135.629902613616));
#56081=CARTESIAN_POINT('Ctrl Pts',(63.1107314411844,1.08506444436502,135.603386175638));
#56082=CARTESIAN_POINT('Ctrl Pts',(63.1029851079191,1.21858213808644,135.571231560809));
#56083=CARTESIAN_POINT('Ctrl Pts',(63.0952387746537,1.35048785093288,135.533564105151));
#56084=CARTESIAN_POINT('Ctrl Pts',(63.0874907066508,1.48242310314914,135.495888214127));
#56085=CARTESIAN_POINT('Ctrl Pts',(63.0797426386477,1.61274528029281,135.452697132971));
#56086=CARTESIAN_POINT('Ctrl Pts',(63.0719945706448,1.74096916579623,135.404165985867));
#56087=CARTESIAN_POINT('Ctrl Pts',(63.0642382679029,1.86932932917104,135.355583259282));
#56088=CARTESIAN_POINT('Ctrl Pts',(63.0564819651611,1.99558637982774,135.30164926797));
#56089=CARTESIAN_POINT('Ctrl Pts',(63.0487256624192,2.11927485877901,135.242587418378));
#56090=CARTESIAN_POINT('Ctrl Pts',(63.0409652199051,2.24302935399585,135.183494045699));
#56091=CARTESIAN_POINT('Ctrl Pts',(63.0332047773909,2.36421220054728,135.119267544247));
#56092=CARTESIAN_POINT('Ctrl Pts',(63.0254443348767,2.48238371565623,135.05017669351));
#56093=CARTESIAN_POINT('Ctrl Pts',(63.0176714346113,2.60074493017201,134.980974932006));
#56094=CARTESIAN_POINT('Ctrl Pts',(63.0098985343458,2.71608482411405,134.906893428381));
#56095=CARTESIAN_POINT('Ctrl Pts',(63.0021256340804,2.8279930709594,134.828244096633));
#56096=CARTESIAN_POINT('Ctrl Pts',(62.9946352983183,2.9358331711522,134.752453866199));
#56097=CARTESIAN_POINT('Ctrl Pts',(62.9871449625563,3.04048654595383,134.672422333052));
#56098=CARTESIAN_POINT('Ctrl Pts',(62.9796546267943,3.14161745588812,134.588461940649));
#56099=CARTESIAN_POINT('Ctrl Pts',(62.9718802926752,3.24658277501035,134.501318164449));
#56100=CARTESIAN_POINT('Ctrl Pts',(62.9641059585561,3.3480857465286,134.409665677165));
#56101=CARTESIAN_POINT('Ctrl Pts',(62.956331624437,3.44571445635907,134.313809997132));
#56102=CARTESIAN_POINT('Ctrl Pts',(62.94856687149,3.54322284753,134.218072450658));
#56103=CARTESIAN_POINT('Ctrl Pts',(62.9408021185429,3.63686620090813,134.11814228949));
#56104=CARTESIAN_POINT('Ctrl Pts',(62.9330373655958,3.72626483489741,134.014365826706));
#56105=CARTESIAN_POINT('Ctrl Pts',(62.9252803247108,3.81557467690312,133.910692436168));
#56106=CARTESIAN_POINT('Ctrl Pts',(62.9175232838258,3.90064793586042,133.803180640681));
#56107=CARTESIAN_POINT('Ctrl Pts',(62.9097662429408,3.98114131162124,133.692213958614));
#56108=CARTESIAN_POINT('Ctrl Pts',(62.9020150517007,4.06157398670125,133.581330957385));
#56109=CARTESIAN_POINT('Ctrl Pts',(62.8942638604605,4.13743342438148,133.466998570571));
#56110=CARTESIAN_POINT('Ctrl Pts',(62.8865126692204,4.20841644575172,133.349633506988));
#56111=CARTESIAN_POINT('Ctrl Pts',(62.8787647724433,4.27936929744435,133.232318326688));
#56112=CARTESIAN_POINT('Ctrl Pts',(62.8710168756663,4.34544965317717,133.111973367116));
#56113=CARTESIAN_POINT('Ctrl Pts',(62.8632689788892,4.40639767422509,132.989044255781));
#56114=CARTESIAN_POINT('Ctrl Pts',(62.8555227028051,4.46733294626091,132.866140858566));
#56115=CARTESIAN_POINT('Ctrl Pts',(62.847776426721,4.52313784545243,132.740654734823));
#56116=CARTESIAN_POINT('Ctrl Pts',(62.8400301506369,4.57359871339299,132.613055691742));
#56117=CARTESIAN_POINT('Ctrl Pts',(62.8322838173716,4.6240599538242,132.485455706755));
#56118=CARTESIAN_POINT('Ctrl Pts',(62.8245374841063,4.66917694050983,132.355743134874));
#56119=CARTESIAN_POINT('Ctrl Pts',(62.8167911508409,4.70878450303639,132.22440694303));
#56120=CARTESIAN_POINT('Ctrl Pts',(62.8090430828379,4.74840093540196,132.093041339357));
#56121=CARTESIAN_POINT('Ctrl Pts',(62.8012950148349,4.78250537563281,131.960051766445));
#56122=CARTESIAN_POINT('Ctrl Pts',(62.793546946832,4.81098288925761,131.825941109632));
#56123=CARTESIAN_POINT('Ctrl Pts',(62.7857906440901,4.83949066912279,131.691687918418));
#56124=CARTESIAN_POINT('Ctrl Pts',(62.7780343413482,4.8623594946218,131.5563116462));
#56125=CARTESIAN_POINT('Ctrl Pts',(62.7702780386064,4.8795257319743,131.420324653449));
#56126=CARTESIAN_POINT('Ctrl Pts',(62.7625175960922,4.89670113146455,131.284265080345));
#56127=CARTESIAN_POINT('Ctrl Pts',(62.7547571535781,4.90816784542063,131.14759452661));
#56128=CARTESIAN_POINT('Ctrl Pts',(62.7469967110639,4.91391434635695,131.010828191697));
#56129=CARTESIAN_POINT('Ctrl Pts',(62.7392238107985,4.91967007208672,130.873842307321));
#56130=CARTESIAN_POINT('Ctrl Pts',(62.7314509105331,4.91968723499943,130.736760725701));
#56131=CARTESIAN_POINT('Ctrl Pts',(62.7236780102676,4.91400646566557,130.600097263298));
#56132=CARTESIAN_POINT('Ctrl Pts',(62.7161876745055,4.90853220660595,130.468401861986));
#56133=CARTESIAN_POINT('Ctrl Pts',(62.7086973387435,4.89776711653985,130.337095015282));
#56134=CARTESIAN_POINT('Ctrl Pts',(62.7012070029814,4.88179258760838,130.206628073637));
#56135=CARTESIAN_POINT('Ctrl Pts',(62.6934326688623,4.86521237955723,130.071214438246));
#56136=CARTESIAN_POINT('Ctrl Pts',(62.6856583347432,4.84296738172533,129.93627670548));
#56137=CARTESIAN_POINT('Ctrl Pts',(62.6778840006241,4.81509198571704,129.802326570448));
#56138=CARTESIAN_POINT('Ctrl Pts',(62.670119247677,4.78725094364304,129.668541516986));
#56139=CARTESIAN_POINT('Ctrl Pts',(62.6623544947299,4.75379338874968,129.53574201863));
#56140=CARTESIAN_POINT('Ctrl Pts',(62.6545897417828,4.71480545686168,129.404434702938));
#56141=CARTESIAN_POINT('Ctrl Pts',(62.6468327008978,4.6758562483373,129.273257803523));
#56142=CARTESIAN_POINT('Ctrl Pts',(62.6390756600128,4.63138770439831,129.14357050978));
#56143=CARTESIAN_POINT('Ctrl Pts',(62.6313186191278,4.581536927794,129.015868950893));
#56144=CARTESIAN_POINT('Ctrl Pts',(62.6235674278877,4.53172374404811,128.888263692744));
#56145=CARTESIAN_POINT('Ctrl Pts',(62.6158162366476,4.4765365479962,128.762641551576));
#56146=CARTESIAN_POINT('Ctrl Pts',(62.6080650454075,4.41616205295959,128.639482841686));
#56147=CARTESIAN_POINT('Ctrl Pts',(62.6003171486304,4.35581321869391,128.516376477533));
#56148=CARTESIAN_POINT('Ctrl Pts',(62.5925692518533,4.29028164223597,128.395731812524));
#56149=CARTESIAN_POINT('Ctrl Pts',(62.5848213550763,4.21980179345092,128.278008328892));
#56150=CARTESIAN_POINT('Ctrl Pts',(62.5770750789922,4.14933668753086,128.160309470475));
#56151=CARTESIAN_POINT('Ctrl Pts',(62.5693288029081,4.0739255687979,128.045530913256));
#56152=CARTESIAN_POINT('Ctrl Pts',(62.561582526824,3.99384821175853,127.934106356367));
#56153=CARTESIAN_POINT('Ctrl Pts',(62.5538361935586,3.91377026360631,127.822680976966));
#56154=CARTESIAN_POINT('Ctrl Pts',(62.5460898602933,3.82902623657936,127.714609964781));
#56155=CARTESIAN_POINT('Ctrl Pts',(62.5383435270279,3.73993823376111,127.610296580927));
#56156=CARTESIAN_POINT('Ctrl Pts',(62.530595459025,3.65083028030233,127.505959836813));
#56157=CARTESIAN_POINT('Ctrl Pts',(62.5228473910219,3.55737666914271,127.405382692749));
#56158=CARTESIAN_POINT('Ctrl Pts',(62.515099323019,3.45993836707158,127.30893366817));
#56159=CARTESIAN_POINT('Ctrl Pts',(62.5073430202771,3.36239650641335,127.212382136419));
#56160=CARTESIAN_POINT('Ctrl Pts',(62.4995867175353,3.26086177332516,127.119967763965));
#56161=CARTESIAN_POINT('Ctrl Pts',(62.4918304147934,3.15573083556911,127.032021031058));
#56162=CARTESIAN_POINT('Ctrl Pts',(62.4840699722792,3.05054378626614,126.944027358331));
#56163=CARTESIAN_POINT('Ctrl Pts',(62.4763095297651,2.94175701768135,126.860506314468));
#56164=CARTESIAN_POINT('Ctrl Pts',(62.4685490872509,2.82979775081672,126.781746075757));
#56165=CARTESIAN_POINT('Ctrl Pts',(62.4607761869855,2.71765875699764,126.702859404119));
#56166=CARTESIAN_POINT('Ctrl Pts',(62.45300328672,2.60233741700265,126.628749021205));
#56167=CARTESIAN_POINT('Ctrl Pts',(62.4452303864546,2.48428798098635,126.559658473713));
#56168=CARTESIAN_POINT('Ctrl Pts',(62.4377400506926,2.37052993931783,126.493079541652));
#56169=CARTESIAN_POINT('Ctrl Pts',(62.4302497149306,2.25423897625108,126.431161958817));
#56170=CARTESIAN_POINT('Ctrl Pts',(62.4227593791685,2.13583882014304,126.374081213638));
#56171=CARTESIAN_POINT('Ctrl Pts',(62.4149850450494,2.01294948612922,126.314836234656));
#56172=CARTESIAN_POINT('Ctrl Pts',(62.4072107109304,1.88739858522604,126.260614440746));
#56173=CARTESIAN_POINT('Ctrl Pts',(62.3994363768113,1.75963521052172,126.211663480981));
#56174=CARTESIAN_POINT('Ctrl Pts',(62.3916716238642,1.63202929275819,126.1627728489));
#56175=CARTESIAN_POINT('Ctrl Pts',(62.383906870917,1.50221668804784,126.119140264729));
#56176=CARTESIAN_POINT('Ctrl Pts',(62.3761421179699,1.3706701950212,126.080967104531));
#56177=CARTESIAN_POINT('Ctrl Pts',(62.368385077085,1.23925435582608,126.042831858454));
#56178=CARTESIAN_POINT('Ctrl Pts',(62.3606280362,1.10610842846165,126.010145353828));
#56179=CARTESIAN_POINT('Ctrl Pts',(62.352870995315,0.971723927845806,125.98306041217));
#56180=CARTESIAN_POINT('Ctrl Pts',(62.3451198040749,0.837440767627235,125.955995895477));
#56181=CARTESIAN_POINT('Ctrl Pts',(62.3373686128347,0.701921274970532,125.934524610705));
#56182=CARTESIAN_POINT('Ctrl Pts',(62.3296174215946,0.565670475007717,125.91874909226));
#56183=CARTESIAN_POINT('Ctrl Pts',(62.3218695248175,0.42947758526931,125.90298027883));
#56184=CARTESIAN_POINT('Ctrl Pts',(62.3141216280404,0.292554393989836,125.892902461708));
#56185=CARTESIAN_POINT('Ctrl Pts',(62.3063737312633,0.155414213273108,125.888566736125));
#56186=CARTESIAN_POINT('Ctrl Pts',(62.2986274551792,0.0183027193259736,
125.884231917482));
#56187=CARTESIAN_POINT('Ctrl Pts',(62.2908811790951,-0.119025283253796,
125.885636813627));
#56188=CARTESIAN_POINT('Ctrl Pts',(62.283134903011,-0.256053686150223,125.892780467318));
#56189=CARTESIAN_POINT('Ctrl Pts',(62.2753885697457,-0.393083100559192,
125.899924173742));
#56190=CARTESIAN_POINT('Ctrl Pts',(62.2676422364804,-0.529812520436778,
125.912806701888));
#56191=CARTESIAN_POINT('Ctrl Pts',(62.259895903215,-0.665728566200701,125.931375029793));
#56192=CARTESIAN_POINT('Ctrl Pts',(62.252147835212,-0.801675049420699,125.949947515946));
#56193=CARTESIAN_POINT('Ctrl Pts',(62.2443997672091,-0.936807408777758,
125.974208282659));
#56194=CARTESIAN_POINT('Ctrl Pts',(62.2366516992061,-1.0706204870671,126.004052832103));
#56195=CARTESIAN_POINT('Ctrl Pts',(62.2288953964643,-1.20457578348844,126.033929100691));
#56196=CARTESIAN_POINT('Ctrl Pts',(62.2211390937224,-1.33720861570305,126.069400921593));
#56197=CARTESIAN_POINT('Ctrl Pts',(62.2133827909805,-1.46802653270147,126.110313199635));
#56198=CARTESIAN_POINT('Ctrl Pts',(62.2056223484664,-1.59891427116123,126.151247313792));
#56199=CARTESIAN_POINT('Ctrl Pts',(62.1978619059522,-1.72798479648652,126.197627538881));
#56200=CARTESIAN_POINT('Ctrl Pts',(62.1901014634381,-1.85476473441771,126.249250208096));
#56201=CARTESIAN_POINT('Ctrl Pts',(62.1823285631726,-1.98174819076026,126.300955746603));
#56202=CARTESIAN_POINT('Ctrl Pts',(62.1745556629072,-2.10643335596814,126.357920383799));
#56203=CARTESIAN_POINT('Ctrl Pts',(62.1667827626418,-2.22836979400339,126.419893589104));
#56204=CARTESIAN_POINT('Ctrl Pts',(62.1592924268797,-2.34587353537686,126.479613912294));
#56205=CARTESIAN_POINT('Ctrl Pts',(62.1518020911177,-2.46082465751549,126.54398482711));
#56206=CARTESIAN_POINT('Ctrl Pts',(62.1443117553556,-2.57284648150626,126.612744694667));
#56207=CARTESIAN_POINT('Ctrl Pts',(62.136536109027,-2.68913527177037,126.684123659337));
#56208=CARTESIAN_POINT('Ctrl Pts',(62.1287604626984,-2.80263561438379,126.760458703787));
#56209=CARTESIAN_POINT('Ctrl Pts',(62.1209848163697,-2.91289618281779,126.841505726124));
#56210=CARTESIAN_POINT('Ctrl Pts',(62.1130368578788,-3.02560017989628,126.924348790498));
#56211=CARTESIAN_POINT('Ctrl Pts',(62.1050888993877,-3.13491874251687,127.012114984055));
#56212=CARTESIAN_POINT('Ctrl Pts',(62.0971409408968,-3.24039644520109,127.104493871259));
#56213=CARTESIAN_POINT('Ctrl Pts',(62.0893847860394,-3.34332871352529,127.194643430485));
#56214=CARTESIAN_POINT('Ctrl Pts',(62.081628631182,-3.44260304548939,127.289185343095));
#56215=CARTESIAN_POINT('Ctrl Pts',(62.0738724763246,-3.53782608525522,127.387787824109));
#56216=CARTESIAN_POINT('Ctrl Pts',(62.0661216651445,-3.63298352019386,127.486322371998));
#56217=CARTESIAN_POINT('Ctrl Pts',(62.0583708539645,-3.7240949459022,127.588911642184));
#56218=CARTESIAN_POINT('Ctrl Pts',(62.0506200427844,-3.8108020325401,127.695185336034));
#56219=CARTESIAN_POINT('Ctrl Pts',(62.0428728929696,-3.8974681600686,127.801408827807));
#56220=CARTESIAN_POINT('Ctrl Pts',(62.0351257431549,-3.97973384270997,127.911312977104));
#56221=CARTESIAN_POINT('Ctrl Pts',(62.0273785933402,-4.05727967981009,128.024492875694));
#56222=CARTESIAN_POINT('Ctrl Pts',(62.0192831949441,-4.13831134439668,128.142760418137));
#56223=CARTESIAN_POINT('Ctrl Pts',(62.0111877965479,-4.21418867069417,128.264604719481));
#56224=CARTESIAN_POINT('Ctrl Pts',(62.0030923981517,-4.28459647969843,128.389528103983));
#56225=CARTESIAN_POINT('Ctrl Pts',(61.995345734245,-4.35197125312783,128.509070024772));
#56226=CARTESIAN_POINT('Ctrl Pts',(61.9875990703384,-4.41433773627809,128.631430899895));
#56227=CARTESIAN_POINT('Ctrl Pts',(61.9798524064317,-4.47146622546811,128.75614850526));
#56228=CARTESIAN_POINT('Ctrl Pts',(61.9721046736809,-4.52860259694843,128.880883318507));
#56229=CARTESIAN_POINT('Ctrl Pts',(61.96435694093,-4.58049937994932,129.007975150914));
#56230=CARTESIAN_POINT('Ctrl Pts',(61.9566092081791,-4.62697483225407,129.136941364892));
#56231=CARTESIAN_POINT('Ctrl Pts',(61.9488567769419,-4.67347846884025,129.265985788331));
#56232=CARTESIAN_POINT('Ctrl Pts',(61.9411043457046,-4.71455408953464,129.396906491452));
#56233=CARTESIAN_POINT('Ctrl Pts',(61.9333519144674,-4.75006966796013,129.529205249768));
#56234=CARTESIAN_POINT('Ctrl Pts',(61.9323125471737,-4.75483123623481,129.546942524459));
#56235=CARTESIAN_POINT('Ctrl Pts',(61.93127317988,-4.75949293913251,129.564704552633));
#56236=CARTESIAN_POINT('Ctrl Pts',(61.9302338125864,-4.76405452823398,129.582490119308));
#56237=CARTESIAN_POINT('Origin',(213.235140564004,0.,130.804360617566));
#56238=CARTESIAN_POINT('',(59.8346812321181,-4.76405452823407,129.582490119308));
#56239=CARTESIAN_POINT('',(60.1799785705036,-4.76405452823408,129.582490119308));
#56240=CARTESIAN_POINT('',(213.235140564004,-4.76405452823405,129.582490119308));
#56241=CARTESIAN_POINT('',(61.5148594360427,-4.91824847206951,130.800483829468));
#56242=CARTESIAN_POINT('Ctrl Pts',(61.5148594359911,-4.91824847207023,130.800483830382));
#56243=CARTESIAN_POINT('Ctrl Pts',(61.5070968711613,-4.91835683968032,130.937963348214));
#56244=CARTESIAN_POINT('Ctrl Pts',(61.4993343063315,-4.91269642418725,131.075513890078));
#56245=CARTESIAN_POINT('Ctrl Pts',(61.4915717415017,-4.90127649067233,131.21261522499));
#56246=CARTESIAN_POINT('Ctrl Pts',(61.4838346137862,-4.88989397908694,131.349267293145));
#56247=CARTESIAN_POINT('Ctrl Pts',(61.4760974860707,-4.87278968287947,131.48547270254));
#56248=CARTESIAN_POINT('Ctrl Pts',(61.4683603583553,-4.85002488767876,131.620719393716));
#56249=CARTESIAN_POINT('Ctrl Pts',(61.4606228913126,-4.82725909408254,131.755972016405));
#56250=CARTESIAN_POINT('Ctrl Pts',(61.45288542427,-4.7988323720717,131.890265451109));
#56251=CARTESIAN_POINT('Ctrl Pts',(61.4451479572273,-4.76485739254276,132.023096475425));
#56252=CARTESIAN_POINT('Ctrl Pts',(61.4374084705606,-4.73087354490682,132.15596217113));
#56253=CARTESIAN_POINT('Ctrl Pts',(61.4296689838938,-4.69133865478323,132.287364317687));
#56254=CARTESIAN_POINT('Ctrl Pts',(61.4219294972271,-4.64641554361799,132.416813921859));
#56255=CARTESIAN_POINT('Ctrl Pts',(61.4141485291312,-4.60125165745883,132.546957338789));
#56256=CARTESIAN_POINT('Ctrl Pts',(61.4063675610354,-4.55064175497602,132.675126844799));
#56257=CARTESIAN_POINT('Ctrl Pts',(61.3985865929395,-4.49480021507383,132.800846051791));
#56258=CARTESIAN_POINT('Ctrl Pts',(61.3908339172754,-4.43916172098069,132.926108130306));
#56259=CARTESIAN_POINT('Ctrl Pts',(61.3830812416113,-4.37832979695381,133.04893737307));
#56260=CARTESIAN_POINT('Ctrl Pts',(61.3753285659473,-4.31256219993804,133.168888125159));
#56261=CARTESIAN_POINT('Ctrl Pts',(61.3675334516354,-4.24643458684454,133.28949549542));
#56262=CARTESIAN_POINT('Ctrl Pts',(61.3597383373236,-4.17531732287121,133.407192432046));
#56263=CARTESIAN_POINT('Ctrl Pts',(61.3519432230118,-4.09951552627355,133.521556877011));
#56264=CARTESIAN_POINT('Ctrl Pts',(61.3441481087,-4.0237137296759,133.635921321976));
#56265=CARTESIAN_POINT('Ctrl Pts',(61.3363529943881,-3.94322768337033,133.746952992341));
#56266=CARTESIAN_POINT('Ctrl Pts',(61.3285578800763,-3.85840175194456,133.854265367405));
#56267=CARTESIAN_POINT('Ctrl Pts',(61.3207835459572,-3.77380194923675,133.961291669456));
#56268=CARTESIAN_POINT('Ctrl Pts',(61.3130092118382,-3.68461164704665,134.064964817607));
#56269=CARTESIAN_POINT('Ctrl Pts',(61.3052348777191,-3.5911263909256,134.164865684799));
#56270=CARTESIAN_POINT('Ctrl Pts',(61.297470124772,-3.49775634702795,134.2646434331));
#56271=CARTESIAN_POINT('Ctrl Pts',(61.289705371825,-3.40010214555527,134.360657867836));
#56272=CARTESIAN_POINT('Ctrl Pts',(61.2819406188779,-3.29850088854574,134.452521106191));
#56273=CARTESIAN_POINT('Ctrl Pts',(61.2741835779929,-3.19700054333671,134.544293104683));
#56274=CARTESIAN_POINT('Ctrl Pts',(61.2664265371079,-3.0915612322331,134.631921851292));
#56275=CARTESIAN_POINT('Ctrl Pts',(61.2586694962229,-2.98255812490224,134.71505494135));
#56276=CARTESIAN_POINT('Ctrl Pts',(61.2509183049828,-2.87363721766269,134.798125340099));
#56277=CARTESIAN_POINT('Ctrl Pts',(61.2431671137427,-2.76115817308868,134.876706594169));
#56278=CARTESIAN_POINT('Ctrl Pts',(61.2354159225026,-2.64553030453546,134.950485612098));
#56279=CARTESIAN_POINT('Ctrl Pts',(61.2276680257255,-2.5299515809107,135.024233271976));
#56280=CARTESIAN_POINT('Ctrl Pts',(61.2199201289484,-2.41122702404822,135.093182545402));
#56281=CARTESIAN_POINT('Ctrl Pts',(61.2121722321714,-2.28979589771299,135.157062974645));
#56282=CARTESIAN_POINT('Ctrl Pts',(61.2044259560873,-2.1683901721518,135.220930041479));
#56283=CARTESIAN_POINT('Ctrl Pts',(61.1966796800032,-2.04427934902221,135.279730191205));
#56284=CARTESIAN_POINT('Ctrl Pts',(61.1889334039191,-1.91792797300829,135.333238552867));
#56285=CARTESIAN_POINT('Ctrl Pts',(61.1811870706538,-1.79157566429721,135.386747309515));
#56286=CARTESIAN_POINT('Ctrl Pts',(61.1734407373884,-1.66298312971189,135.434964047692));
#56287=CARTESIAN_POINT('Ctrl Pts',(61.1656944041231,-1.53263523173735,135.477711910689));
#56288=CARTESIAN_POINT('Ctrl Pts',(61.1579463361201,-1.40225814325484,135.520469346775));
#56289=CARTESIAN_POINT('Ctrl Pts',(61.1501982681172,-1.27012528058317,135.557755348827));
#56290=CARTESIAN_POINT('Ctrl Pts',(61.1424502001142,-1.13673662613277,135.589442947611));
#56291=CARTESIAN_POINT('Ctrl Pts',(61.1346938973724,-1.00320620463307,135.621164224352));
#56292=CARTESIAN_POINT('Ctrl Pts',(61.1269375946305,-0.868417706192536,
135.647275121455));
#56293=CARTESIAN_POINT('Ctrl Pts',(61.1191812918887,-0.732881816699323,
135.667699728224));
#56294=CARTESIAN_POINT('Ctrl Pts',(61.1114208493745,-0.59727358762098,135.68813523622));
#56295=CARTESIAN_POINT('Ctrl Pts',(61.1036604068604,-0.460917561147342,
135.702878364494));
#56296=CARTESIAN_POINT('Ctrl Pts',(61.0958999643462,-0.324328511737044,
135.711905225511));
#56297=CARTESIAN_POINT('Ctrl Pts',(61.0881270640808,-0.18752019745864,135.720946577248));
#56298=CARTESIAN_POINT('Ctrl Pts',(61.0803541638153,-0.0504785038106941,
135.724253315202));
#56299=CARTESIAN_POINT('Ctrl Pts',(61.0725812635499,0.0862819256928151,
135.721853728064));
#56300=CARTESIAN_POINT('Ctrl Pts',(61.0650909277877,0.218070769107917,135.719541371964));
#56301=CARTESIAN_POINT('Ctrl Pts',(61.0576005920255,0.349598135164484,135.711930384246));
#56302=CARTESIAN_POINT('Ctrl Pts',(61.0501102562634,0.480410850203245,135.699091302446));
#56303=CARTESIAN_POINT('Ctrl Pts',(61.0423359221443,0.616183369089502,135.685765422958));
#56304=CARTESIAN_POINT('Ctrl Pts',(61.0345615880252,0.7516160617334,135.666764964658));
#56305=CARTESIAN_POINT('Ctrl Pts',(61.0267872539061,0.886196555079165,135.642112029975));
#56306=CARTESIAN_POINT('Ctrl Pts',(61.0190225009591,1.02061118999468,135.617489477831));
#56307=CARTESIAN_POINT('Ctrl Pts',(61.011257748012,1.15417533444104,135.587228379679));
#56308=CARTESIAN_POINT('Ctrl Pts',(61.0034929950649,1.28638043973377,135.551402688874));
#56309=CARTESIAN_POINT('Ctrl Pts',(60.9957359541799,1.41845423705217,135.515612580651));
#56310=CARTESIAN_POINT('Ctrl Pts',(60.9879789132949,1.54917130649983,135.474268980017));
#56311=CARTESIAN_POINT('Ctrl Pts',(60.9802218724099,1.67803237167848,135.427497044506));
#56312=CARTESIAN_POINT('Ctrl Pts',(60.9724706811697,1.80679626172584,135.380760380075));
#56313=CARTESIAN_POINT('Ctrl Pts',(60.9647194899296,1.93370656735855,135.328603661582));
#56314=CARTESIAN_POINT('Ctrl Pts',(60.9569682986895,2.05827863199355,135.27120202236));
#56315=CARTESIAN_POINT('Ctrl Pts',(60.9492204019124,2.18279775017768,135.213824780365));
#56316=CARTESIAN_POINT('Ctrl Pts',(60.9414725051353,2.30498024964787,135.151207214689));
#56317=CARTESIAN_POINT('Ctrl Pts',(60.9337246083583,2.42436115386205,135.083572701367));
#56318=CARTESIAN_POINT('Ctrl Pts',(60.9259783322742,2.54371708616446,135.015952335727));
#56319=CARTESIAN_POINT('Ctrl Pts',(60.9182320561901,2.66027224891248,134.943317302427));
#56320=CARTESIAN_POINT('Ctrl Pts',(60.910485780106,2.77358635405368,134.865936887822));
#56321=CARTESIAN_POINT('Ctrl Pts',(60.9027394468406,2.88690129565401,134.788555902013));
#56322=CARTESIAN_POINT('Ctrl Pts',(60.8949931135753,2.99697480904156,134.70642968548));
#56323=CARTESIAN_POINT('Ctrl Pts',(60.88724678031,3.10339601964365,134.619870571394));
#56324=CARTESIAN_POINT('Ctrl Pts',(60.879498712307,3.20984106253783,134.533292072995));
#56325=CARTESIAN_POINT('Ctrl Pts',(60.871750644304,3.31263187185724,134.442278948302));
#56326=CARTESIAN_POINT('Ctrl Pts',(60.8640025763011,3.41139137208327,134.347183216706));
#56327=CARTESIAN_POINT('Ctrl Pts',(60.8562462735592,3.51025583508154,134.251986416234));
#56328=CARTESIAN_POINT('Ctrl Pts',(60.8484899708174,3.60508014811188,134.152698612765));
#56329=CARTESIAN_POINT('Ctrl Pts',(60.8407336680755,3.69552440716086,134.049708429216));
#56330=CARTESIAN_POINT('Ctrl Pts',(60.8329732255614,3.78601693903398,133.946663276704));
#56331=CARTESIAN_POINT('Ctrl Pts',(60.8252127830472,3.87212451338747,133.839912110781));
#56332=CARTESIAN_POINT('Ctrl Pts',(60.8174523405331,3.95354878479494,133.729875113983));
#56333=CARTESIAN_POINT('Ctrl Pts',(60.8096794402677,4.03510376567149,133.619661476029));
#56334=CARTESIAN_POINT('Ctrl Pts',(60.8019065400022,4.11196020080972,133.506151790576));
#56335=CARTESIAN_POINT('Ctrl Pts',(60.7941336397368,4.18386371289693,133.389794332517));
#56336=CARTESIAN_POINT('Ctrl Pts',(60.7866433039747,4.25315335120643,133.277666761144));
#56337=CARTESIAN_POINT('Ctrl Pts',(60.7791529682126,4.31784376577217,133.162895138263));
#56338=CARTESIAN_POINT('Ctrl Pts',(60.7716626324505,4.37774935038862,133.045898858969));
#56339=CARTESIAN_POINT('Ctrl Pts',(60.7638882983314,4.43992627345327,132.924466630186));
#56340=CARTESIAN_POINT('Ctrl Pts',(60.7561139642124,4.49714532826618,132.800253058388));
#56341=CARTESIAN_POINT('Ctrl Pts',(60.7483396300933,4.54914816007457,132.673701164441));
#56342=CARTESIAN_POINT('Ctrl Pts',(60.7405748771462,4.60108690304031,132.547305234393));
#56343=CARTESIAN_POINT('Ctrl Pts',(60.7328101241991,4.64782206668505,132.418577074217));
#56344=CARTESIAN_POINT('Ctrl Pts',(60.725045371252,4.68914098707509,132.28798451392));
#56345=CARTESIAN_POINT('Ctrl Pts',(60.717288330367,4.73041886893084,132.157521659995));
#56346=CARTESIAN_POINT('Ctrl Pts',(60.709531289482,4.76629109578391,132.025198461353));
#56347=CARTESIAN_POINT('Ctrl Pts',(60.701774248597,4.79659309512409,131.891502624071));
#56348=CARTESIAN_POINT('Ctrl Pts',(60.6940230573568,4.82687224349089,131.75790760786));
#56349=CARTESIAN_POINT('Ctrl Pts',(60.6862718661168,4.85158943921836,131.622942393101));
#56350=CARTESIAN_POINT('Ctrl Pts',(60.6785206748766,4.87063005821867,131.487109398947));
#56351=CARTESIAN_POINT('Ctrl Pts',(60.6707727780995,4.88966258444798,131.351334137439));
#56352=CARTESIAN_POINT('Ctrl Pts',(60.6630248813224,4.90302327845965,131.214692216479));
#56353=CARTESIAN_POINT('Ctrl Pts',(60.6552769845453,4.91064874166126,131.077695574205));
#56354=CARTESIAN_POINT('Ctrl Pts',(60.6475307084612,4.91827260978037,130.940727588675));
#56355=CARTESIAN_POINT('Ctrl Pts',(60.6397844323771,4.92016361161753,130.803405419533));
#56356=CARTESIAN_POINT('Ctrl Pts',(60.632038156293,4.91631031896289,130.666245049439));
#56357=CARTESIAN_POINT('Ctrl Pts',(60.6242918230277,4.91245699786414,130.529083666859));
#56358=CARTESIAN_POINT('Ctrl Pts',(60.6165454897623,4.90285930864056,130.392084476522));
#56359=CARTESIAN_POINT('Ctrl Pts',(60.608799156497,4.8875579382918,130.255761982551));
#56360=CARTESIAN_POINT('Ctrl Pts',(60.601051088494,4.87225314130715,130.119408960101));
#56361=CARTESIAN_POINT('Ctrl Pts',(60.593303020491,4.85124216511973,129.983733324017));
#56362=CARTESIAN_POINT('Ctrl Pts',(60.585554952488,4.8246173550832,129.849242593691));
#56363=CARTESIAN_POINT('Ctrl Pts',(60.5777986497461,4.79796424788179,129.714608925018));
#56364=CARTESIAN_POINT('Ctrl Pts',(60.5700423470042,4.76568546425192,129.581163061886));
#56365=CARTESIAN_POINT('Ctrl Pts',(60.5622860442624,4.72792423723797,129.44940103535));
#56366=CARTESIAN_POINT('Ctrl Pts',(60.5545256017482,4.69014285592013,129.317568683453));
#56367=CARTESIAN_POINT('Ctrl Pts',(60.546765159234,4.64687332391115,129.187422329733));
#56368=CARTESIAN_POINT('Ctrl Pts',(60.5390047167199,4.59830788968875,129.059440099569));
#56369=CARTESIAN_POINT('Ctrl Pts',(60.5312318164544,4.54966449391998,128.931252420968));
#56370=CARTESIAN_POINT('Ctrl Pts',(60.523458916189,4.49570836130183,128.805236167784));
#56371=CARTESIAN_POINT('Ctrl Pts',(60.5156860159235,4.4366791410462,128.681847658382));
#56372=CARTESIAN_POINT('Ctrl Pts',(60.5081956801616,4.37979578163313,128.562944632095));
#56373=CARTESIAN_POINT('Ctrl Pts',(60.5007053443996,4.31820191402721,128.446481888575));
#56374=CARTESIAN_POINT('Ctrl Pts',(60.4932150086377,4.25215006251213,128.332842276874));
#56375=CARTESIAN_POINT('Ctrl Pts',(60.4854406745186,4.18359383497015,128.214893984754));
#56376=CARTESIAN_POINT('Ctrl Pts',(60.4776663403995,4.11001773588511,128.09961350377));
#56377=CARTESIAN_POINT('Ctrl Pts',(60.4698920062804,4.03165484420368,127.987457658693));
#56378=CARTESIAN_POINT('Ctrl Pts',(60.4621272533334,3.95338852778296,127.875440035671));
#56379=CARTESIAN_POINT('Ctrl Pts',(60.4543625003863,3.87034737837648,127.766539703954));
#56380=CARTESIAN_POINT('Ctrl Pts',(60.4465977474393,3.78281004456712,127.661188457276));
#56381=CARTESIAN_POINT('Ctrl Pts',(60.4388407065543,3.69535965407188,127.555941846942));
#56382=CARTESIAN_POINT('Ctrl Pts',(60.4310836656693,3.60342221430857,127.454237605496));
#56383=CARTESIAN_POINT('Ctrl Pts',(60.4233266247843,3.50731909075212,127.356477809502));
#56384=CARTESIAN_POINT('Ctrl Pts',(60.4155754335442,3.41128843930847,127.258791734929));
#56385=CARTESIAN_POINT('Ctrl Pts',(60.4078242423041,3.31109862975987,127.16504446285));
#56386=CARTESIAN_POINT('Ctrl Pts',(60.400073051064,3.20711040445073,127.075603999581));
#56387=CARTESIAN_POINT('Ctrl Pts',(60.3923251542869,3.10316637691119,126.986201550895));
#56388=CARTESIAN_POINT('Ctrl Pts',(60.3845772575098,2.99542744037391,126.901102524685));
#56389=CARTESIAN_POINT('Ctrl Pts',(60.3768293607328,2.88429003440538,126.820636975051));
#56390=CARTESIAN_POINT('Ctrl Pts',(60.3690830846487,2.77317587598648,126.740188257076));
#56391=CARTESIAN_POINT('Ctrl Pts',(60.3613368085646,2.65866497860516,126.664371316973));
#56392=CARTESIAN_POINT('Ctrl Pts',(60.3535905324805,2.54118527586067,126.59347467085));
#56393=CARTESIAN_POINT('Ctrl Pts',(60.3458441992152,2.42370470590771,126.522577501385));
#56394=CARTESIAN_POINT('Ctrl Pts',(60.3380978659498,2.3032556215966,126.456600900381));
#56395=CARTESIAN_POINT('Ctrl Pts',(60.3303515326845,2.18029288213429,126.395788738758));
#56396=CARTESIAN_POINT('Ctrl Pts',(60.3226034646816,2.05730260601972,126.334962958674));
#56397=CARTESIAN_POINT('Ctrl Pts',(60.3148553966786,1.93179790499943,126.279304092638));
#56398=CARTESIAN_POINT('Ctrl Pts',(60.3071073286756,1.80425568443069,126.229008774516));
#56399=CARTESIAN_POINT('Ctrl Pts',(60.2993510259338,1.67657791047129,126.178660001931));
#56400=CARTESIAN_POINT('Ctrl Pts',(60.291594723192,1.54685865543108,126.133686308163));
#56401=CARTESIAN_POINT('Ctrl Pts',(60.2838384204501,1.41559266524179,126.094235304094));
#56402=CARTESIAN_POINT('Ctrl Pts',(60.2760779779359,1.28425661444102,126.054763243836));
#56403=CARTESIAN_POINT('Ctrl Pts',(60.2683175354218,1.15137256215172,126.020819843384));
#56404=CARTESIAN_POINT('Ctrl Pts',(60.2605570929076,1.01744668379657,125.992501797096));
#56405=CARTESIAN_POINT('Ctrl Pts',(60.2527841926422,0.883305815732105,125.964138292167));
#56406=CARTESIAN_POINT('Ctrl Pts',(60.2450112923767,0.748120165330152,125.941418251691));
#56407=CARTESIAN_POINT('Ctrl Pts',(60.2372383921113,0.612403182409007,125.924386703222));
#56408=CARTESIAN_POINT('Ctrl Pts',(60.2297480563491,0.481619853664547,125.90797429444));
#56409=CARTESIAN_POINT('Ctrl Pts',(60.2222577205869,0.350343459186021,125.896844002052));
#56410=CARTESIAN_POINT('Ctrl Pts',(60.2147673848247,0.219032596266184,125.890990309491));
#56411=CARTESIAN_POINT('Ctrl Pts',(60.2069930507056,0.0827430420705576,
125.884914672397));
#56412=CARTESIAN_POINT('Ctrl Pts',(60.1992187165865,-0.0540153702457747,
125.884504412487));
#56413=CARTESIAN_POINT('Ctrl Pts',(60.1914443824674,-0.190732316202125,
125.889810358788));
#56414=CARTESIAN_POINT('Ctrl Pts',(60.1836796295203,-0.327280770740772,
125.895109765984));
#56415=CARTESIAN_POINT('Ctrl Pts',(60.1759148765733,-0.463787473679632,
125.906111347496));
#56416=CARTESIAN_POINT('Ctrl Pts',(60.1681501236262,-0.599738528354169,
125.922814063439));
#56417=CARTESIAN_POINT('Ctrl Pts',(60.1603930827412,-0.735554554524998,
125.93950019001));
#56418=CARTESIAN_POINT('Ctrl Pts',(60.1526360418562,-0.870815645156497,
125.961876135121));
#56419=CARTESIAN_POINT('Ctrl Pts',(60.1448790009712,-1.00500981596048,125.9898888571));
#56420=CARTESIAN_POINT('Ctrl Pts',(60.1371278097311,-1.13910278989602,126.017880454468));
#56421=CARTESIAN_POINT('Ctrl Pts',(60.129376618491,-1.27213006428987,126.051500288301));
#56422=CARTESIAN_POINT('Ctrl Pts',(60.1216254272508,-1.40358703495665,126.090643772252));
#56423=CARTESIAN_POINT('Ctrl Pts',(60.1138775304738,-1.53498813290453,126.129770619177));
#56424=CARTESIAN_POINT('Ctrl Pts',(60.1061296336967,-1.66481988065294,126.174416335486));
#56425=CARTESIAN_POINT('Ctrl Pts',(60.0983817369196,-1.79259030907093,126.224425787645));
#56426=CARTESIAN_POINT('Ctrl Pts',(60.0906354608355,-1.92033401066954,126.274424778904));
#56427=CARTESIAN_POINT('Ctrl Pts',(60.0828891847514,-2.04601688674455,126.329785131931));
#56428=CARTESIAN_POINT('Ctrl Pts',(60.0751429086673,-2.16916489195958,126.390302764072));
#56429=CARTESIAN_POINT('Ctrl Pts',(60.067396575402,-2.2923138062252,126.450820842941));
#56430=CARTESIAN_POINT('Ctrl Pts',(60.0596502421367,-2.41292746140714,126.516496104456));
#56431=CARTESIAN_POINT('Ctrl Pts',(60.0519039088713,-2.53055481948119,126.587077680876));
#56432=CARTESIAN_POINT('Ctrl Pts',(60.0441558408683,-2.64820851938684,126.65767506355));
#56433=CARTESIAN_POINT('Ctrl Pts',(60.0364077728653,-2.76287425624932,126.733180746361));
#56434=CARTESIAN_POINT('Ctrl Pts',(60.0286597048623,-2.87412881743299,126.813299780733));
#56435=CARTESIAN_POINT('Ctrl Pts',(60.0209034021204,-2.98550162128808,126.893503966569));
#56436=CARTESIAN_POINT('Ctrl Pts',(60.0131470993786,-3.09345568949495,126.978331069649));
#56437=CARTESIAN_POINT('Ctrl Pts',(60.0053907966368,-3.19759941057609,127.067444633498));
#56438=CARTESIAN_POINT('Ctrl Pts',(59.9976303541226,-3.30179871629688,127.156605759939));
#56439=CARTESIAN_POINT('Ctrl Pts',(59.9898699116084,-3.40218333655968,127.250057639544));
#56440=CARTESIAN_POINT('Ctrl Pts',(59.9821094690942,-3.49839831948231,127.347426678257));
#56441=CARTESIAN_POINT('Ctrl Pts',(59.9743365688288,-3.59476775523709,127.444952022396));
#56442=CARTESIAN_POINT('Ctrl Pts',(59.9665636685634,-3.68695391488976,127.54640680189));
#56443=CARTESIAN_POINT('Ctrl Pts',(59.9587907682979,-3.77464138331522,127.651383375361));
#56444=CARTESIAN_POINT('Ctrl Pts',(59.9513004325359,-3.8591411913919,127.752543785965));
#56445=CARTESIAN_POINT('Ctrl Pts',(59.9438100967739,-3.93946351942171,127.85697413967));
#56446=CARTESIAN_POINT('Ctrl Pts',(59.9363197610119,-4.01536512561121,127.964285623745));
#56447=CARTESIAN_POINT('Ctrl Pts',(59.9284606122327,-4.0950040142499,128.076880966044));
#56448=CARTESIAN_POINT('Ctrl Pts',(59.9206014634536,-4.17002604765882,128.193001885756));
#56449=CARTESIAN_POINT('Ctrl Pts',(59.9127423146745,-4.24010706841768,128.312238006045));
#56450=CARTESIAN_POINT('Ctrl Pts',(59.904896692256,-4.31006747291255,128.431268909355));
#56451=CARTESIAN_POINT('Ctrl Pts',(59.8970510698376,-4.37510361483341,128.553404007396));
#56452=CARTESIAN_POINT('Ctrl Pts',(59.8892054474192,-4.43493339828359,128.678202388438));
#56453=CARTESIAN_POINT('Ctrl Pts',(59.8813676673364,-4.49470337701437,128.80287602338));
#56454=CARTESIAN_POINT('Ctrl Pts',(59.8735298872537,-4.54927718823693,128.930207304384));
#56455=CARTESIAN_POINT('Ctrl Pts',(59.865692107171,-4.59841734646034,129.059728573187));
#56456=CARTESIAN_POINT('Ctrl Pts',(59.857862136672,-4.64750854130667,129.189120786673));
#56457=CARTESIAN_POINT('Ctrl Pts',(59.850032166173,-4.69117673258091,129.320698287841));
#56458=CARTESIAN_POINT('Ctrl Pts',(59.842202195674,-4.72923173486454,129.453971688239));
#56459=CARTESIAN_POINT('Ctrl Pts',(59.8396952078221,-4.74141612667611,129.496642959584));
#56460=CARTESIAN_POINT('Ctrl Pts',(59.83718821997,-4.7530254545675,129.539487928472));
#56461=CARTESIAN_POINT('Ctrl Pts',(59.834681232118,-4.76405452823407,129.582490119308));
#56462=CARTESIAN_POINT('Ctrl Pts',(61.5846617476392,-4.76405452823404,129.582490119308));
#56463=CARTESIAN_POINT('Ctrl Pts',(61.5755367020045,-4.80389281518532,129.737818995501));
#56464=CARTESIAN_POINT('Ctrl Pts',(61.5664116563698,-4.83617178160265,129.89525866267));
#56465=CARTESIAN_POINT('Ctrl Pts',(61.557286610735,-4.86069278516076,130.054128179727));
#56466=CARTESIAN_POINT('Ctrl Pts',(61.5482434123213,-4.88499384724346,130.211572714486));
#56467=CARTESIAN_POINT('Ctrl Pts',(61.5392002139076,-4.90167542415839,130.370421469466));
#56468=CARTESIAN_POINT('Ctrl Pts',(61.530157015494,-4.91059106967392,130.529991506807));
#56469=CARTESIAN_POINT('Ctrl Pts',(61.5250578223435,-4.91561833950312,130.619968349535));
#56470=CARTESIAN_POINT('Ctrl Pts',(61.5199586291931,-4.91817728586783,130.710174166229));
#56471=CARTESIAN_POINT('Ctrl Pts',(61.5148594360427,-4.91824847206951,130.800483829468));
#56472=CARTESIAN_POINT('',(61.8601405639556,-4.91824995978084,130.803731637669));
#56473=CARTESIAN_POINT('Ctrl Pts',(61.9302338125864,-4.76405452823398,129.582490119308));
#56474=CARTESIAN_POINT('Ctrl Pts',(61.9224723506434,-4.79811813637933,129.715303610479));
#56475=CARTESIAN_POINT('Ctrl Pts',(61.9147108887005,-4.82659481655101,129.849430166516));
#56476=CARTESIAN_POINT('Ctrl Pts',(61.9069494267576,-4.84941049226405,129.984360044384));
#56477=CARTESIAN_POINT('Ctrl Pts',(61.8991759628984,-4.87226144893715,130.119498570713));
#56478=CARTESIAN_POINT('Ctrl Pts',(61.8914024990392,-4.88943386429407,130.255442512898));
#56479=CARTESIAN_POINT('Ctrl Pts',(61.88362903518,-4.9009055896504,130.391677368774));
#56480=CARTESIAN_POINT('Ctrl Pts',(61.8777074006343,-4.90964446930554,130.495457748216));
#56481=CARTESIAN_POINT('Ctrl Pts',(61.8717857660886,-4.91507630026852,130.599406853097));
#56482=CARTESIAN_POINT('Ctrl Pts',(61.8658641315429,-4.91721155718995,130.703298437016));
#56483=CARTESIAN_POINT('Ctrl Pts',(61.8639562756981,-4.91789950278441,130.736770642042));
#56484=CARTESIAN_POINT('Ctrl Pts',(61.8620484198533,-4.91824567789724,130.770249895539));
#56485=CARTESIAN_POINT('Ctrl Pts',(61.8601405640086,-4.91824995978073,130.803731636738));
#56486=CARTESIAN_POINT('Ctrl Pts',(61.8601405639556,-4.91824995978084,130.803731637669));
#56487=CARTESIAN_POINT('Ctrl Pts',(61.8523936239596,-4.91826734654802,130.939685850747));
#56488=CARTESIAN_POINT('Ctrl Pts',(61.8446466839636,-4.91264322818731,131.07586272131));
#56489=CARTESIAN_POINT('Ctrl Pts',(61.8368997439676,-4.90134821179031,131.211753265119));
#56490=CARTESIAN_POINT('Ctrl Pts',(61.8291623232629,-4.89006707449273,131.347476829235));
#56491=CARTESIAN_POINT('Ctrl Pts',(61.8214249025581,-4.87312893442009,131.482914377715));
#56492=CARTESIAN_POINT('Ctrl Pts',(61.8136874818533,-4.85055637356318,131.617555507728));
#56493=CARTESIAN_POINT('Ctrl Pts',(61.805957683371,-4.82800604919633,131.752064001211));
#56494=CARTESIAN_POINT('Ctrl Pts',(61.7982278848885,-4.79983241316138,131.885777251261));
#56495=CARTESIAN_POINT('Ctrl Pts',(61.7904980864062,-4.76610992436556,132.018188962664));
#56496=CARTESIAN_POINT('Ctrl Pts',(61.7827740199854,-4.73241244261029,132.150502483656));
#56497=CARTESIAN_POINT('Ctrl Pts',(61.7750499535647,-4.69317439419713,132.281516006551));
#56498=CARTESIAN_POINT('Ctrl Pts',(61.767325887144,-4.6485214192105,132.410732827747));
#56499=CARTESIAN_POINT('Ctrl Pts',(61.7596049357203,-4.60388645208125,132.539897537788));
#56500=CARTESIAN_POINT('Ctrl Pts',(61.7518839842966,-4.55384102912814,132.667266615246));
#56501=CARTESIAN_POINT('Ctrl Pts',(61.744163032873,-4.49856073868545,132.792358188706));
#56502=CARTESIAN_POINT('Ctrl Pts',(61.7364435444671,-4.44329092312385,132.917426058974));
#56503=CARTESIAN_POINT('Ctrl Pts',(61.7287240560611,-4.38278837203244,133.040216923306));
#56504=CARTESIAN_POINT('Ctrl Pts',(61.7210045676553,-4.31727677366038,133.16026900333));
#56505=CARTESIAN_POINT('Ctrl Pts',(61.7132848394377,-4.25176314012163,133.280324812861));
#56506=CARTESIAN_POINT('Ctrl Pts',(61.7055651112202,-4.18124033838913,133.397641322872));
#56507=CARTESIAN_POINT('Ctrl Pts',(61.6978453830026,-4.10597774563099,133.511781865707));
#56508=CARTESIAN_POINT('Ctrl Pts',(61.6901237123201,-4.03069621503663,133.625951128982));
#56509=CARTESIAN_POINT('Ctrl Pts',(61.6824020416376,-3.95067273752078,133.736942506331));
#56510=CARTESIAN_POINT('Ctrl Pts',(61.6746803709551,-3.86621943257266,133.844349163876));
#56511=CARTESIAN_POINT('Ctrl Pts',(61.6669504404176,-3.78167578810138,133.951870714098));
#56512=CARTESIAN_POINT('Ctrl Pts',(61.6592205098801,-3.6926930965086,134.055799576265));
#56513=CARTESIAN_POINT('Ctrl Pts',(61.6514905793427,-3.59962341446769,134.155762464035));
#56514=CARTESIAN_POINT('Ctrl Pts',(61.6437562747536,-3.50650106809962,134.255781916716));
#56515=CARTESIAN_POINT('Ctrl Pts',(61.6360219701646,-3.40928740441371,134.351830648011));
#56516=CARTESIAN_POINT('Ctrl Pts',(61.6282876655756,-3.30836980543768,134.443573759575));
#56517=CARTESIAN_POINT('Ctrl Pts',(61.6205414175746,-3.20729636821523,134.535458542024));
#56518=CARTESIAN_POINT('Ctrl Pts',(61.6127951695735,-3.10250787234992,134.623024170925));
#56519=CARTESIAN_POINT('Ctrl Pts',(61.6050489215724,-2.99442363468164,134.705976969613));
#56520=CARTESIAN_POINT('Ctrl Pts',(61.5991714502916,-2.912414641073,134.768917465695));
#56521=CARTESIAN_POINT('Ctrl Pts',(61.5932939790107,-2.82850893532166,134.829203201345));
#56522=CARTESIAN_POINT('Ctrl Pts',(61.5874165077298,-2.74289943095491,134.886723386131));
#56523=CARTESIAN_POINT('Ctrl Pts',(61.5796421736108,-2.62966078479028,134.962807319808));
#56524=CARTESIAN_POINT('Ctrl Pts',(61.5718678394917,-2.51307469558143,135.034296587921));
#56525=CARTESIAN_POINT('Ctrl Pts',(61.5640935053726,-2.39355056938918,135.100882319394));
#56526=CARTESIAN_POINT('Ctrl Pts',(61.5563287524255,-2.27417374600044,135.167385989903));
#56527=CARTESIAN_POINT('Ctrl Pts',(61.5485639994784,-2.15186642833995,135.228997959436));
#56528=CARTESIAN_POINT('Ctrl Pts',(61.5407992465313,-2.02706805444654,135.285451797752));
#56529=CARTESIAN_POINT('Ctrl Pts',(61.5330422056464,-1.90239363205743,135.34184956532));
#56530=CARTESIAN_POINT('Ctrl Pts',(61.5252851647613,-1.77523343101907,135.393099236834));
#56531=CARTESIAN_POINT('Ctrl Pts',(61.5175281238763,-1.64605230634128,135.438979789331));
#56532=CARTESIAN_POINT('Ctrl Pts',(61.5097769326362,-1.51696859815449,135.484825742946));
#56533=CARTESIAN_POINT('Ctrl Pts',(61.5020257413961,-1.38586736667427,135.525310506302));
#56534=CARTESIAN_POINT('Ctrl Pts',(61.494274550156,-1.2532339763495,135.560260917512));
#56535=CARTESIAN_POINT('Ctrl Pts',(61.4865266533789,-1.12065695875356,135.595196473864));
#56536=CARTESIAN_POINT('Ctrl Pts',(61.4787787566018,-0.986549454784961,
135.624602257095));
#56537=CARTESIAN_POINT('Ctrl Pts',(61.4710308598247,-0.851412331428461,
135.648354847991));
#56538=CARTESIAN_POINT('Ctrl Pts',(61.4632845837406,-0.716303475845133,
135.672102470357));
#56539=CARTESIAN_POINT('Ctrl Pts',(61.4555383076565,-0.580165814083412,
135.69019918486));
#56540=CARTESIAN_POINT('Ctrl Pts',(61.4477920315724,-0.443510367498282,
135.702572701217));
#56541=CARTESIAN_POINT('Ctrl Pts',(61.440045698307,-0.306853912153503,135.714946308912));
#56542=CARTESIAN_POINT('Ctrl Pts',(61.4322993650417,-0.169680053730782,
135.721596598904));
#56543=CARTESIAN_POINT('Ctrl Pts',(61.4245530317763,-0.0325045006574862,
135.722503205976));
#56544=CARTESIAN_POINT('Ctrl Pts',(61.4168049637733,0.104701771929812,135.723410016078));
#56545=CARTESIAN_POINT('Ctrl Pts',(61.4090568957703,0.241909349041014,135.718570581171));
#56546=CARTESIAN_POINT('Ctrl Pts',(61.4013088277674,0.378603356788063,135.70801665778));
#56547=CARTESIAN_POINT('Ctrl Pts',(61.3935525250255,0.515442644553225,135.697451517553));
#56548=CARTESIAN_POINT('Ctrl Pts',(61.3857962222837,0.651766882178081,135.681159786662));
#56549=CARTESIAN_POINT('Ctrl Pts',(61.3780399195418,0.787066593422253,135.659225110013));
#56550=CARTESIAN_POINT('Ctrl Pts',(61.3702794770276,0.922438518195928,135.637278726166));
#56551=CARTESIAN_POINT('Ctrl Pts',(61.3625190345135,1.05678444422027,135.609683473899));
#56552=CARTESIAN_POINT('Ctrl Pts',(61.3547585919993,1.18960688644697,135.576573785292));
#56553=CARTESIAN_POINT('Ctrl Pts',(61.3469856917339,1.32264254704954,135.543410946074));
#56554=CARTESIAN_POINT('Ctrl Pts',(61.3392127914685,1.45414946142179,135.504716091298));
#56555=CARTESIAN_POINT('Ctrl Pts',(61.331439891203,1.58364620045453,135.460673297604));
#56556=CARTESIAN_POINT('Ctrl Pts',(61.323949555441,1.70843540684064,135.418231570399));
#56557=CARTESIAN_POINT('Ctrl Pts',(61.316459219679,1.8313577629988,135.37082408669));
#56558=CARTESIAN_POINT('Ctrl Pts',(61.3089688839169,1.9520032742412,135.318656385441));
#56559=CARTESIAN_POINT('Ctrl Pts',(61.3011945497979,2.07722309671176,135.264510729943));
#56560=CARTESIAN_POINT('Ctrl Pts',(61.2934202156788,2.2003866716478,135.20506524684));
#56561=CARTESIAN_POINT('Ctrl Pts',(61.2856458815597,2.32101284308728,135.140497428683));
#56562=CARTESIAN_POINT('Ctrl Pts',(61.2778811286126,2.44149035355097,135.076009184592));
#56563=CARTESIAN_POINT('Ctrl Pts',(61.2701163756656,2.55943634117847,135.006411348809));
#56564=CARTESIAN_POINT('Ctrl Pts',(61.2623516227185,2.67438912366864,134.931929620951));
#56565=CARTESIAN_POINT('Ctrl Pts',(61.2545945818335,2.789227733435,134.857521869394));
#56566=CARTESIAN_POINT('Ctrl Pts',(61.2468375409485,2.90107872826772,134.778240090193));
#56567=CARTESIAN_POINT('Ctrl Pts',(61.2390805000635,3.00950488980073,134.694355910721));
#56568=CARTESIAN_POINT('Ctrl Pts',(61.2313293088233,3.11784928632189,134.610534988961));
#56569=CARTESIAN_POINT('Ctrl Pts',(61.2235781175832,3.22277368226279,134.522118813426));
#56570=CARTESIAN_POINT('Ctrl Pts',(61.2158269263431,3.32387004028159,134.429422136743));
#56571=CARTESIAN_POINT('Ctrl Pts',(61.208079029566,3.42492342965125,134.33676485862));
#56572=CARTESIAN_POINT('Ctrl Pts',(61.2003311327889,3.52215172955124,134.239830961522));
#56573=CARTESIAN_POINT('Ctrl Pts',(61.1925832360118,3.61518037306248,134.138975127929));
#56574=CARTESIAN_POINT('Ctrl Pts',(61.1848369599277,3.70818955698696,134.038140391202));
#56575=CARTESIAN_POINT('Ctrl Pts',(61.1770906838437,3.79700056695303,133.933385636968));
#56576=CARTESIAN_POINT('Ctrl Pts',(61.1693444077596,3.88127636357424,133.825101727304));
#56577=CARTESIAN_POINT('Ctrl Pts',(61.1615980744942,3.96555278230024,133.716817018312));
#56578=CARTESIAN_POINT('Ctrl Pts',(61.1538517412289,4.04529368075161,133.605003410438));
#56579=CARTESIAN_POINT('Ctrl Pts',(61.1461054079635,4.1202031720935,133.490083775892));
#56580=CARTESIAN_POINT('Ctrl Pts',(61.1383573399606,4.19512943889628,133.375138405891));
#56581=CARTESIAN_POINT('Ctrl Pts',(61.1306092719576,4.26522193215958,133.257085952571));
#56582=CARTESIAN_POINT('Ctrl Pts',(61.1228612039547,4.33022906763158,133.136376759092));
#56583=CARTESIAN_POINT('Ctrl Pts',(61.1151049012129,4.39530529346102,133.015539274445));
#56584=CARTESIAN_POINT('Ctrl Pts',(61.107348598471,4.45528517919736,132.892039753934));
#56585=CARTESIAN_POINT('Ctrl Pts',(61.0995922957292,4.50996371331631,132.766352046464));
#56586=CARTESIAN_POINT('Ctrl Pts',(61.091831853215,4.56467143101526,132.64059725568));
#56587=CARTESIAN_POINT('Ctrl Pts',(61.0840714107008,4.61407201834288,132.51265231534));
#56588=CARTESIAN_POINT('Ctrl Pts',(61.0763109681867,4.65800967399521,132.383008437527));
#56589=CARTESIAN_POINT('Ctrl Pts',(61.0685380679212,4.70201786227305,132.253156443851));
#56590=CARTESIAN_POINT('Ctrl Pts',(61.0607651676558,4.74054548450815,132.12160043814));
#56591=CARTESIAN_POINT('Ctrl Pts',(61.0529922673904,4.77348718539787,131.988844958257));
#56592=CARTESIAN_POINT('Ctrl Pts',(61.0455019316283,4.80523137248538,131.860915474458));
#56593=CARTESIAN_POINT('Ctrl Pts',(61.0380115958661,4.83178864984061,131.731872511942));
#56594=CARTESIAN_POINT('Ctrl Pts',(61.0305212601041,4.853110331071,131.602172109682));
#56595=CARTESIAN_POINT('Ctrl Pts',(61.022746925985,4.87524043032563,131.46755407725));
#56596=CARTESIAN_POINT('Ctrl Pts',(61.0149725918659,4.89180018249795,131.331801337828));
#56597=CARTESIAN_POINT('Ctrl Pts',(61.0071982577468,4.90267884054802,131.195414640615));
#56598=CARTESIAN_POINT('Ctrl Pts',(60.9994335047997,4.91354409162429,131.059196027817));
#56599=CARTESIAN_POINT('Ctrl Pts',(60.9916687518526,4.9187421485711,130.922345397759));
#56600=CARTESIAN_POINT('Ctrl Pts',(60.9839039989055,4.91821334830532,130.785373172993));
#56601=CARTESIAN_POINT('Ctrl Pts',(60.9761469580205,4.91768507325141,130.648536990971));
#56602=CARTESIAN_POINT('Ctrl Pts',(60.9683899171354,4.91144126185184,130.51157984301));
#56603=CARTESIAN_POINT('Ctrl Pts',(60.9606328762504,4.89947411470341,130.375016394534));
#56604=CARTESIAN_POINT('Ctrl Pts',(60.9528816850103,4.88751599207375,130.238555929617));
#56605=CARTESIAN_POINT('Ctrl Pts',(60.9451304937702,4.86984315844706,130.102488961136));
#56606=CARTESIAN_POINT('Ctrl Pts',(60.93737930253,4.84649986997196,129.967328913948));
#56607=CARTESIAN_POINT('Ctrl Pts',(60.9296314057529,4.82316650301722,129.832226313385));
#56608=CARTESIAN_POINT('Ctrl Pts',(60.9218835089758,4.7941675411071,129.698030251907));
#56609=CARTESIAN_POINT('Ctrl Pts',(60.9141356121987,4.75959892608824,129.565247577816));
#56610=CARTESIAN_POINT('Ctrl Pts',(60.9063893361146,4.72503754207842,129.432492678997));
#56611=CARTESIAN_POINT('Ctrl Pts',(60.8986430600305,4.68490892074898,129.301150957613));
#56612=CARTESIAN_POINT('Ctrl Pts',(60.8908967839464,4.63935972741285,129.171717244946));
#56613=CARTESIAN_POINT('Ctrl Pts',(60.8831504506811,4.59381019784285,129.042282576828));
#56614=CARTESIAN_POINT('Ctrl Pts',(60.8754041174157,4.54284014620555,128.914756314327));
#56615=CARTESIAN_POINT('Ctrl Pts',(60.8676577841503,4.48664541280495,128.789615968173));
#56616=CARTESIAN_POINT('Ctrl Pts',(60.8599097161474,4.43043809498344,128.664447597707));
#56617=CARTESIAN_POINT('Ctrl Pts',(60.8521616481444,4.36900392729882,128.541666563391));
#56618=CARTESIAN_POINT('Ctrl Pts',(60.8444135801414,4.30258580877236,128.421727951658));
#56619=CARTESIAN_POINT('Ctrl Pts',(60.8366572773996,4.23609710027915,128.301661867742));
#56620=CARTESIAN_POINT('Ctrl Pts',(60.8289009746577,4.16461404931552,128.184444583674));
#56621=CARTESIAN_POINT('Ctrl Pts',(60.8211446719158,4.08842450464875,128.070504708362));
#56622=CARTESIAN_POINT('Ctrl Pts',(60.8133842294016,4.01219429532796,127.956504019909));
#56623=CARTESIAN_POINT('Ctrl Pts',(60.8056237868875,3.93125281755737,127.84578454121));
#56624=CARTESIAN_POINT('Ctrl Pts',(60.7978633443734,3.84592912756436,127.738742864445));
#56625=CARTESIAN_POINT('Ctrl Pts',(60.7900904441079,3.76046846840949,127.631529354877));
#56626=CARTESIAN_POINT('Ctrl Pts',(60.7823175438425,3.6706117958522,127.528005740611));
#56627=CARTESIAN_POINT('Ctrl Pts',(60.7745446435771,3.57672664477264,127.428533375086));
#56628=CARTESIAN_POINT('Ctrl Pts',(60.7670543078151,3.48625445541802,127.332677080604));
#56629=CARTESIAN_POINT('Ctrl Pts',(60.7595639720531,3.3920418134763,127.240582817736));
#56630=CARTESIAN_POINT('Ctrl Pts',(60.7520736362911,3.29444608126646,127.152538047927));
#56631=CARTESIAN_POINT('Ctrl Pts',(60.7442993021721,3.19314997720558,127.061155033909));
#56632=CARTESIAN_POINT('Ctrl Pts',(60.736524968053,3.08788830335667,126.973845173808));
#56633=CARTESIAN_POINT('Ctrl Pts',(60.7287506339339,2.97902249272132,126.890972309417));
#56634=CARTESIAN_POINT('Ctrl Pts',(60.7209858809868,2.87029084946766,126.808201578424));
#56635=CARTESIAN_POINT('Ctrl Pts',(60.7132211280397,2.75796421533843,126.72985719759));
#56636=CARTESIAN_POINT('Ctrl Pts',(60.7054563750926,2.64243977392719,126.656265259011));
#56637=CARTESIAN_POINT('Ctrl Pts',(60.6976993342075,2.52703007301992,126.582746412983));
#56638=CARTESIAN_POINT('Ctrl Pts',(60.6899422933226,2.40842921303719,126.51397082451));
#56639=CARTESIAN_POINT('Ctrl Pts',(60.6821852524376,2.2870659808092,126.450223244684));
#56640=CARTESIAN_POINT('Ctrl Pts',(60.6744340611974,2.16579426953886,126.386523737405));
#56641=CARTESIAN_POINT('Ctrl Pts',(60.6666828699573,2.04176467708187,126.327844872771));
#56642=CARTESIAN_POINT('Ctrl Pts',(60.6589316787172,1.91543308383876,126.274426935509));
#56643=CARTESIAN_POINT('Ctrl Pts',(60.6511837819401,1.78915518489278,126.221031702295));
#56644=CARTESIAN_POINT('Ctrl Pts',(60.6434358851631,1.66057759049002,126.172893101093));
#56645=CARTESIAN_POINT('Ctrl Pts',(60.635687988386,1.53017858537276,126.130204377198));
#56646=CARTESIAN_POINT('Ctrl Pts',(60.6279417123019,1.3998068569163,126.087524582865));
#56647=CARTESIAN_POINT('Ctrl Pts',(60.6201954362177,1.26761484690105,126.050292519883));
#56648=CARTESIAN_POINT('Ctrl Pts',(60.6124491601336,1.13409814708177,126.018652262966));
#56649=CARTESIAN_POINT('Ctrl Pts',(60.6047028268683,1.00058046167255,125.987011772488));
#56650=CARTESIAN_POINT('Ctrl Pts',(60.596956493603,0.865738447375988,125.960963260593));
#56651=CARTESIAN_POINT('Ctrl Pts',(60.5892101603376,0.730079703962902,125.940600067502));
#56652=CARTESIAN_POINT('Ctrl Pts',(60.5814620923347,0.59439058071519,125.920232314215));
#56653=CARTESIAN_POINT('Ctrl Pts',(60.5737140243317,0.457884750959189,125.905552471252));
#56654=CARTESIAN_POINT('Ctrl Pts',(60.5659659563288,0.321076384654983,125.896602166122));
#56655=CARTESIAN_POINT('Ctrl Pts',(60.5582096535869,0.184122616790654,125.887642348502));
#56656=CARTESIAN_POINT('Ctrl Pts',(60.5504533508451,0.0468660608217313,
125.884424258552));
#56657=CARTESIAN_POINT('Ctrl Pts',(60.5426970481032,-0.0901770931478938,
125.886937394538));
#56658=CARTESIAN_POINT('Ctrl Pts',(60.5349366055891,-0.227293391175082,
125.889451871861));
#56659=CARTESIAN_POINT('Ctrl Pts',(60.5271761630749,-0.364195670183447,
125.89770364678));
#56660=CARTESIAN_POINT('Ctrl Pts',(60.5194157205608,-0.500372403011901,
125.911630242734));
#56661=CARTESIAN_POINT('Ctrl Pts',(60.5116428202953,-0.636767738821279,
125.925579194896));
#56662=CARTESIAN_POINT('Ctrl Pts',(60.5038699200299,-0.77243481383313,125.945221116175));
#56663=CARTESIAN_POINT('Ctrl Pts',(60.4960970197645,-0.906870949584289,
125.97044210943));
#56664=CARTESIAN_POINT('Ctrl Pts',(60.4886066840024,-1.03641999317725,125.994746256052));
#56665=CARTESIAN_POINT('Ctrl Pts',(60.4811163482404,-1.16482573901601,126.024230821351));
#56666=CARTESIAN_POINT('Ctrl Pts',(60.4736260124783,-1.29165317458304,126.05875052622));
#56667=CARTESIAN_POINT('Ctrl Pts',(60.4658516783592,-1.4232893109174,126.09457905619));
#56668=CARTESIAN_POINT('Ctrl Pts',(60.4580773442401,-1.55364207483918,126.135945571518));
#56669=CARTESIAN_POINT('Ctrl Pts',(60.450303010121,-1.68220999257674,126.18274265376));
#56670=CARTESIAN_POINT('Ctrl Pts',(60.4425382571739,-1.81061946184613,126.22948206278));
#56671=CARTESIAN_POINT('Ctrl Pts',(60.4347735042268,-1.93724809774762,126.28163858982));
#56672=CARTESIAN_POINT('Ctrl Pts',(60.4270087512797,-2.06160686232993,126.339054333816));
#56673=CARTESIAN_POINT('Ctrl Pts',(60.4192517103947,-2.18584211203394,126.396413051686));
#56674=CARTESIAN_POINT('Ctrl Pts',(60.4114946695097,-2.30781162424967,126.459020428634));
#56675=CARTESIAN_POINT('Ctrl Pts',(60.4037376286247,-2.42704406006311,126.526669629076));
#56676=CARTESIAN_POINT('Ctrl Pts',(60.3959864373845,-2.5461865817697,126.594267814729));
#56677=CARTESIAN_POINT('Ctrl Pts',(60.3882352461444,-2.66259579677202,126.666900063919));
#56678=CARTESIAN_POINT('Ctrl Pts',(60.3804840549043,-2.77582313223473,126.744312711315));
#56679=CARTESIAN_POINT('Ctrl Pts',(60.3727361581272,-2.88900234305896,126.821692456271));
#56680=CARTESIAN_POINT('Ctrl Pts',(60.3649882613501,-2.99900204206298,126.903848338149));
#56681=CARTESIAN_POINT('Ctrl Pts',(60.357240364573,-3.10540112192147,126.990482416251));
#56682=CARTESIAN_POINT('Ctrl Pts',(60.3494940884889,-3.21177794538616,127.077098372371));
#56683=CARTESIAN_POINT('Ctrl Pts',(60.3417478124048,-3.31455534482194,127.168190414784));
#56684=CARTESIAN_POINT('Ctrl Pts',(60.3340015363208,-3.4133442266439,127.263419464011));
#56685=CARTESIAN_POINT('Ctrl Pts',(60.3262552030554,-3.51213383770307,127.358649216198));
#56686=CARTESIAN_POINT('Ctrl Pts',(60.31850886979,-3.60693459091922,127.458015764801));
#56687=CARTESIAN_POINT('Ctrl Pts',(60.3107625365247,-3.69739358644646,127.561142504425));
#56688=CARTESIAN_POINT('Ctrl Pts',(60.3030144685217,-3.78787283963893,127.664292338568));
#56689=CARTESIAN_POINT('Ctrl Pts',(60.2952664005186,-3.87400814260205,127.771203745493));
#56690=CARTESIAN_POINT('Ctrl Pts',(60.2875183325156,-3.95548655151164,127.881466640134));
#56691=CARTESIAN_POINT('Ctrl Pts',(60.2797620297737,-4.03705155664337,127.991846723491));
#56692=CARTESIAN_POINT('Ctrl Pts',(60.2720057270319,-4.1139495480378,128.105585095111));
#56693=CARTESIAN_POINT('Ctrl Pts',(60.2642494242901,-4.18591034774258,128.222241793197));
#56694=CARTESIAN_POINT('Ctrl Pts',(60.2564889817759,-4.25790955509305,128.338960754475));
#56695=CARTESIAN_POINT('Ctrl Pts',(60.2487285392617,-4.32496612897891,128.458600804984));
#56696=CARTESIAN_POINT('Ctrl Pts',(60.2409680967475,-4.38685613977697,128.580697812328));
#56697=CARTESIAN_POINT('Ctrl Pts',(60.2331951964821,-4.44884550191454,128.702990820626));
#56698=CARTESIAN_POINT('Ctrl Pts',(60.2254222962167,-4.50565156515005,128.827748311357));
#56699=CARTESIAN_POINT('Ctrl Pts',(60.2176493959513,-4.55709844438776,128.954485802705));
#56700=CARTESIAN_POINT('Ctrl Pts',(60.2101590601893,-4.6066750999779,129.076616067008));
#56701=CARTESIAN_POINT('Ctrl Pts',(60.2026687244273,-4.65127534225548,129.200584585365));
#56702=CARTESIAN_POINT('Ctrl Pts',(60.1951783886654,-4.69078626375652,129.325946842518));
#56703=CARTESIAN_POINT('Ctrl Pts',(60.1901117826114,-4.71751220508084,129.410744265652));
#56704=CARTESIAN_POINT('Ctrl Pts',(60.1850451765575,-4.74194769037687,129.496295894021));
#56705=CARTESIAN_POINT('Ctrl Pts',(60.1799785705036,-4.76405452823407,129.582490119308));
#56706=CARTESIAN_POINT('Origin',(213.235140564004,0.,130.804360617566));
#56707=CARTESIAN_POINT('',(58.0850005708557,-4.76405452823401,129.582490119308));
#56708=CARTESIAN_POINT('',(58.429932073253,-4.76405452823401,129.582490119308));
#56709=CARTESIAN_POINT('',(213.235140564004,-4.76405452823405,129.582490119308));
#56710=CARTESIAN_POINT('',(59.7648594359381,-4.91824913396613,130.80727930587));
#56711=CARTESIAN_POINT('Ctrl Pts',(59.7648594359381,-4.91824913396613,130.80727930587));
#56712=CARTESIAN_POINT('Ctrl Pts',(59.7559438277098,-4.91815530429253,130.965390643192));
#56713=CARTESIAN_POINT('Ctrl Pts',(59.7470282194816,-4.91043248621711,131.123221752801));
#56714=CARTESIAN_POINT('Ctrl Pts',(59.7381126112533,-4.8951889725416,131.280079006539));
#56715=CARTESIAN_POINT('Ctrl Pts',(59.7294177150926,-4.88032282262348,131.433053150129));
#56716=CARTESIAN_POINT('Ctrl Pts',(59.7207228189319,-4.85830408773118,131.585100927552));
#56717=CARTESIAN_POINT('Ctrl Pts',(59.7120279227713,-4.82928394905967,131.735596141939));
#56718=CARTESIAN_POINT('Ctrl Pts',(59.7030019585092,-4.79915883546559,131.891821633489));
#56719=CARTESIAN_POINT('Ctrl Pts',(59.6939759942471,-4.76148881981934,132.046373734296));
#56720=CARTESIAN_POINT('Ctrl Pts',(59.684950029985,-4.71649769137675,132.198574585986));
#56721=CARTESIAN_POINT('Ctrl Pts',(59.6759240657229,-4.67150656293416,132.350775437676));
#56722=CARTESIAN_POINT('Ctrl Pts',(59.6668981014609,-4.6191944896861,132.500624835296));
#56723=CARTESIAN_POINT('Ctrl Pts',(59.6578721371988,-4.55983845854355,132.647471111944));
#56724=CARTESIAN_POINT('Ctrl Pts',(59.6500978030798,-4.50871332612744,132.773954220635));
#56725=CARTESIAN_POINT('Ctrl Pts',(59.6423234689607,-4.45224054805438,132.898508855189));
#56726=CARTESIAN_POINT('Ctrl Pts',(59.6345491348417,-4.390586019346,133.020649738873));
#56727=CARTESIAN_POINT('Ctrl Pts',(59.6267843818947,-4.32900747433403,133.142640094834));
#56728=CARTESIAN_POINT('Ctrl Pts',(59.6190196289477,-4.26226005949961,133.262222273087));
#56729=CARTESIAN_POINT('Ctrl Pts',(59.6112548760006,-4.19055833035914,133.378929308115));
#56730=CARTESIAN_POINT('Ctrl Pts',(59.6034978351157,-4.11892781638696,133.495520428071));
#56731=CARTESIAN_POINT('Ctrl Pts',(59.5957407942307,-4.04235298384866,133.609241756677));
#56732=CARTESIAN_POINT('Ctrl Pts',(59.5879837533458,-3.96109488986182,133.719649683167));
#56733=CARTESIAN_POINT('Ctrl Pts',(59.5802325621057,-3.87989807323564,133.82997435018));
#56734=CARTESIAN_POINT('Ctrl Pts',(59.5724813708657,-3.79402525557015,133.93699027491));
#56735=CARTESIAN_POINT('Ctrl Pts',(59.5647301796256,-3.70378130707953,134.040281984322));
#56736=CARTESIAN_POINT('Ctrl Pts',(59.5569822828486,-3.61357571467447,134.143529792002));
#56737=CARTESIAN_POINT('Ctrl Pts',(59.5492343860716,-3.51900294325448,134.243056238808));
#56738=CARTESIAN_POINT('Ctrl Pts',(59.5414864892946,-3.42040858458665,134.338478354284));
#56739=CARTESIAN_POINT('Ctrl Pts',(59.5337402132105,-3.3218348497332,134.433880509511));
#56740=CARTESIAN_POINT('Ctrl Pts',(59.5259939371264,-3.21924148164196,134.525179769361));
#56741=CARTESIAN_POINT('Ctrl Pts',(59.5182476610424,-3.1130111418139,134.612029811895));
#56742=CARTESIAN_POINT('Ctrl Pts',(59.5105013277771,-3.00678001781775,134.698880495536));
#56743=CARTESIAN_POINT('Ctrl Pts',(59.5027549945118,-2.89691217119505,134.781281648864));
#56744=CARTESIAN_POINT('Ctrl Pts',(59.4950086612465,-2.7838232519097,134.858927322484));
#56745=CARTESIAN_POINT('Ctrl Pts',(59.4872605932436,-2.67070900714497,134.936590384314));
#56746=CARTESIAN_POINT('Ctrl Pts',(59.4795125252408,-2.55437257658767,135.009495626044));
#56747=CARTESIAN_POINT('Ctrl Pts',(59.4717644572379,-2.43525813638147,135.077380728879));
#56748=CARTESIAN_POINT('Ctrl Pts',(59.4640081544961,-2.31601709993057,135.14533798081));
#56749=CARTESIAN_POINT('Ctrl Pts',(59.4562518517543,-2.19399249610628,135.208264241788));
#56750=CARTESIAN_POINT('Ctrl Pts',(59.4484955490125,-2.06965311764546,135.26594318826));
#56751=CARTESIAN_POINT('Ctrl Pts',(59.4407351064984,-1.94524737551457,135.323652919723));
#56752=CARTESIAN_POINT('Ctrl Pts',(59.4329746639843,-1.81852475804048,135.376109606687));
#56753=CARTESIAN_POINT('Ctrl Pts',(59.4252142214702,-1.68997259704823,135.423145704981));
#56754=CARTESIAN_POINT('Ctrl Pts',(59.4174413212048,-1.56121407271484,135.470257309795));
#56755=CARTESIAN_POINT('Ctrl Pts',(59.4096684209395,-1.43062050858531,135.511930818425));
#56756=CARTESIAN_POINT('Ctrl Pts',(59.4018955206741,-1.29869376899297,135.548048798389));
#56757=CARTESIAN_POINT('Ctrl Pts',(59.3944051849114,-1.17156289867661,135.582853798809));
#56758=CARTESIAN_POINT('Ctrl Pts',(59.3869148491488,-1.04319439876613,135.612500103617));
#56759=CARTESIAN_POINT('Ctrl Pts',(59.3794245133861,-0.914043008567175,
135.636928096763));
#56760=CARTESIAN_POINT('Ctrl Pts',(59.371650179267,-0.77999480416525,135.662282284691));
#56761=CARTESIAN_POINT('Ctrl Pts',(59.3638758451479,-0.644678546570666,
135.682094959499));
#56762=CARTESIAN_POINT('Ctrl Pts',(59.3561015110288,-0.50859218315392,135.696243389438));
#56763=CARTESIAN_POINT('Ctrl Pts',(59.3483367580817,-0.372673534017698,
135.710374382701));
#56764=CARTESIAN_POINT('Ctrl Pts',(59.3405720051347,-0.235987052594861,
135.718854980519));
#56765=CARTESIAN_POINT('Ctrl Pts',(59.3328072521876,-0.0990415826969921,
135.721613288255));
#56766=CARTESIAN_POINT('Ctrl Pts',(59.3250502113026,0.037767871029396,135.724368856401));
#56767=CARTESIAN_POINT('Ctrl Pts',(59.3172931704176,0.174835412972991,135.721413436983));
#56768=CARTESIAN_POINT('Ctrl Pts',(59.3095361295326,0.311646713083914,135.712726882294));
#56769=CARTESIAN_POINT('Ctrl Pts',(59.3017849382925,0.448354842729186,135.704046878204));
#56770=CARTESIAN_POINT('Ctrl Pts',(59.2940337470523,0.584806726561502,135.689644365982));
#56771=CARTESIAN_POINT('Ctrl Pts',(59.2862825558122,0.720488025554324,135.669551268253));
#56772=CARTESIAN_POINT('Ctrl Pts',(59.2785346590351,0.856111656375657,135.649466710626));
#56773=CARTESIAN_POINT('Ctrl Pts',(59.2707867622581,0.990964967830361,135.623696435157));
#56774=CARTESIAN_POINT('Ctrl Pts',(59.263038865481,1.12453895523701,135.592324193101));
#56775=CARTESIAN_POINT('Ctrl Pts',(59.2552925893969,1.2580850018452,135.560958513443));
#56776=CARTESIAN_POINT('Ctrl Pts',(59.2475463133127,1.3903518763231,135.523993287329));
#56777=CARTESIAN_POINT('Ctrl Pts',(59.2398000372286,1.52084137032635,135.481563263251));
#56778=CARTESIAN_POINT('Ctrl Pts',(59.2320537039633,1.65133182757321,135.439132925965));
#56779=CARTESIAN_POINT('Ctrl Pts',(59.2243073706979,1.78004450636128,135.391237831114));
#56780=CARTESIAN_POINT('Ctrl Pts',(59.2165610374326,1.90649733384231,135.338062303667));
#56781=CARTESIAN_POINT('Ctrl Pts',(59.2088129694296,2.03297847955729,135.284874867928));
#56782=CARTESIAN_POINT('Ctrl Pts',(59.2010649014266,2.15719840660112,135.226404798045));
#56783=CARTESIAN_POINT('Ctrl Pts',(59.1933168334236,2.27869633068629,135.162884002271));
#56784=CARTESIAN_POINT('Ctrl Pts',(59.1855605306818,2.40032338421102,135.099295695838));
#56785=CARTESIAN_POINT('Ctrl Pts',(59.17780422794,2.51922230872019,135.030646121841));
#56786=CARTESIAN_POINT('Ctrl Pts',(59.1700479251981,2.63495771115671,134.957212760722));
#56787=CARTESIAN_POINT('Ctrl Pts',(59.162287482684,2.75075488506239,134.883740206007));
#56788=CARTESIAN_POINT('Ctrl Pts',(59.1545270401698,2.86338485157338,134.805478999584));
#56789=CARTESIAN_POINT('Ctrl Pts',(59.1467665976556,2.97244323627699,134.722748585801));
#56790=CARTESIAN_POINT('Ctrl Pts',(59.1389936973902,3.08167669118148,134.639885365814));
#56791=CARTESIAN_POINT('Ctrl Pts',(59.1312207971247,3.18732680558401,134.552538851055));
#56792=CARTESIAN_POINT('Ctrl Pts',(59.1234478968593,3.28902351028198,134.461067799077));
#56793=CARTESIAN_POINT('Ctrl Pts',(59.1159575610973,3.38702328360564,134.372921950239));
#56794=CARTESIAN_POINT('Ctrl Pts',(59.1084672253352,3.48135186923592,134.280946447587));
#56795=CARTESIAN_POINT('Ctrl Pts',(59.1009768895732,3.57171331279927,134.185491652245));
#56796=CARTESIAN_POINT('Ctrl Pts',(59.0932025554541,3.66550083796009,134.086417659325));
#56797=CARTESIAN_POINT('Ctrl Pts',(59.085428221335,3.75531154491298,133.98328149414));
#56798=CARTESIAN_POINT('Ctrl Pts',(59.0776538872159,3.840773023246,133.876435754409));
#56799=CARTESIAN_POINT('Ctrl Pts',(59.0698891342688,3.92612917794488,133.769721692502));
#56800=CARTESIAN_POINT('Ctrl Pts',(59.0621243813217,4.00714652703377,133.659307454789));
#56801=CARTESIAN_POINT('Ctrl Pts',(59.0543596283746,4.08348954101034,133.545582285173));
#56802=CARTESIAN_POINT('Ctrl Pts',(59.0466025874896,4.15975673002908,133.431970068999));
#56803=CARTESIAN_POINT('Ctrl Pts',(59.0388455466046,4.23135860645275,133.315053787623));
#56804=CARTESIAN_POINT('Ctrl Pts',(59.0310885057196,4.2980002114886,133.195255271152));
#56805=CARTESIAN_POINT('Ctrl Pts',(59.0233373144794,4.36459156157178,133.075547095674));
#56806=CARTESIAN_POINT('Ctrl Pts',(59.0155861232394,4.4262298963735,132.95296135163));
#56807=CARTESIAN_POINT('Ctrl Pts',(59.0078349319992,4.48266406049338,132.82794802197));
#56808=CARTESIAN_POINT('Ctrl Pts',(59.0000870352221,4.53907423858807,132.702987826309));
#56809=CARTESIAN_POINT('Ctrl Pts',(58.992339138445,4.59028448480026,132.575602452772));
#56810=CARTESIAN_POINT('Ctrl Pts',(58.9845912416679,4.63609013197015,132.446265411014));
#56811=CARTESIAN_POINT('Ctrl Pts',(58.9768449655838,4.68188619758612,132.316955423777));
#56812=CARTESIAN_POINT('Ctrl Pts',(58.9690986894997,4.72227978240038,132.185694948646));
#56813=CARTESIAN_POINT('Ctrl Pts',(58.9613524134156,4.75711496035481,132.052975977262));
#56814=CARTESIAN_POINT('Ctrl Pts',(58.9536060801503,4.79195039545456,131.920256026176));
#56815=CARTESIAN_POINT('Ctrl Pts',(58.9458597468849,4.82122724256446,131.78607793551));
#56816=CARTESIAN_POINT('Ctrl Pts',(58.9381134136195,4.8448400073489,131.65094691895));
#56817=CARTESIAN_POINT('Ctrl Pts',(58.9303653456165,4.86845806004833,131.515785640736));
#56818=CARTESIAN_POINT('Ctrl Pts',(58.9226172776136,4.88640943910494,131.37967139704));
#56819=CARTESIAN_POINT('Ctrl Pts',(58.9148692096106,4.89864019033708,131.243117210809));
#56820=CARTESIAN_POINT('Ctrl Pts',(58.9071129068688,4.91088394055718,131.106417893164));
#56821=CARTESIAN_POINT('Ctrl Pts',(58.8993566041269,4.91739488266153,130.969278088977));
#56822=CARTESIAN_POINT('Ctrl Pts',(58.891600301385,4.91817112822213,130.832214091716));
#56823=CARTESIAN_POINT('Ctrl Pts',(58.8838398588708,4.91894778808837,130.695076939272));
#56824=CARTESIAN_POINT('Ctrl Pts',(58.8760794163567,4.91398366669107,130.558016064892));
#56825=CARTESIAN_POINT('Ctrl Pts',(58.8683189738425,4.90332894736035,130.421544347695));
#56826=CARTESIAN_POINT('Ctrl Pts',(58.8605460735771,4.89265712412829,130.284853553982));
#56827=CARTESIAN_POINT('Ctrl Pts',(58.8527731733116,4.87627649496156,130.148754195784));
#56828=CARTESIAN_POINT('Ctrl Pts',(58.8450002730462,4.8542888613066,130.013751540022));
#56829=CARTESIAN_POINT('Ctrl Pts',(58.8375099372842,4.83310053351864,129.883656570849));
#56830=CARTESIAN_POINT('Ctrl Pts',(58.8300196015222,4.8067058428928,129.754580254425));
#56831=CARTESIAN_POINT('Ctrl Pts',(58.8225292657602,4.77523958759863,129.626960964292));
#56832=CARTESIAN_POINT('Ctrl Pts',(58.8147549316412,4.74258027967089,129.494502949983));
#56833=CARTESIAN_POINT('Ctrl Pts',(58.806980597522,4.70435378378937,129.363195042129));
#56834=CARTESIAN_POINT('Ctrl Pts',(58.799206263403,4.66065545347599,129.233541147835));
#56835=CARTESIAN_POINT('Ctrl Pts',(58.7914415104559,4.6170109774493,129.104047040379));
#56836=CARTESIAN_POINT('Ctrl Pts',(58.7836767575089,4.56790820830916,128.976203257559));
#56837=CARTESIAN_POINT('Ctrl Pts',(58.7759120045618,4.51349326608363,128.850502485685));
#56838=CARTESIAN_POINT('Ctrl Pts',(58.7681549636768,4.45913236954584,128.72492656159));
#56839=CARTESIAN_POINT('Ctrl Pts',(58.7603979227918,4.39946995396238,128.601489769161));
#56840=CARTESIAN_POINT('Ctrl Pts',(58.7526408819068,4.33470148451864,128.480668275062));
#56841=CARTESIAN_POINT('Ctrl Pts',(58.7448896906666,4.26998185748153,128.359937893391));
#56842=CARTESIAN_POINT('Ctrl Pts',(58.7371384994265,4.20016402476987,128.241819227656));
#56843=CARTESIAN_POINT('Ctrl Pts',(58.7293873081864,4.12549081415279,128.126766808782));
#56844=CARTESIAN_POINT('Ctrl Pts',(58.7216394114093,4.05084934164219,128.011763290254));
#56845=CARTESIAN_POINT('Ctrl Pts',(58.7138915146323,3.97135680810245,127.899823753809));
#56846=CARTESIAN_POINT('Ctrl Pts',(58.7061436178552,3.88730096301673,127.791376335259));
#56847=CARTESIAN_POINT('Ctrl Pts',(58.6983973417711,3.80326270060176,127.682951601571));
#56848=CARTESIAN_POINT('Ctrl Pts',(58.690651065687,3.71466326464459,127.578017841637));
#56849=CARTESIAN_POINT('Ctrl Pts',(58.6829047896029,3.62183229980335,127.476972173966));
#56850=CARTESIAN_POINT('Ctrl Pts',(58.6751584563375,3.52900064970502,127.375925760399));
#56851=CARTESIAN_POINT('Ctrl Pts',(58.6674121230722,3.43193767289633,127.278767784275));
#56852=CARTESIAN_POINT('Ctrl Pts',(58.6596657898068,3.33101139769506,127.185860081304));
#56853=CARTESIAN_POINT('Ctrl Pts',(58.6519177218038,3.23006252075423,127.092931572298));
#56854=CARTESIAN_POINT('Ctrl Pts',(58.6441696538009,3.12524891144429,127.004255495195));
#56855=CARTESIAN_POINT('Ctrl Pts',(58.636421585798,3.01697302694656,126.920154544611));
#56856=CARTESIAN_POINT('Ctrl Pts',(58.6286652830561,2.90858206555029,126.835964210537));
#56857=CARTESIAN_POINT('Ctrl Pts',(58.6209089803142,2.79672178753323,126.756358956556));
#56858=CARTESIAN_POINT('Ctrl Pts',(58.6131526775724,2.68182554446955,126.681619440687));
#56859=CARTESIAN_POINT('Ctrl Pts',(58.6053922350582,2.56686797782134,126.606840034089));
#56860=CARTESIAN_POINT('Ctrl Pts',(58.597631792544,2.44887155356918,126.536931739511));
#56861=CARTESIAN_POINT('Ctrl Pts',(58.5898713500299,2.32829489675721,126.472129559989));
#56862=CARTESIAN_POINT('Ctrl Pts',(58.5820984497645,2.20752467959159,126.407223354256));
#56863=CARTESIAN_POINT('Ctrl Pts',(58.5743255494991,2.0841663048219,126.34743981398));
#56864=CARTESIAN_POINT('Ctrl Pts',(58.5665526492336,1.9586998939876,126.292966399833));
#56865=CARTESIAN_POINT('Ctrl Pts',(58.5590623134716,1.83779450321693,126.240473231501));
#56866=CARTESIAN_POINT('Ctrl Pts',(58.5515719777095,1.71493196756685,126.192910930368));
#56867=CARTESIAN_POINT('Ctrl Pts',(58.5440816419474,1.59055396481745,126.150403038526));
#56868=CARTESIAN_POINT('Ctrl Pts',(58.5363073078283,1.46146013229102,126.106283447045));
#56869=CARTESIAN_POINT('Ctrl Pts',(58.5285329737093,1.33032471582221,126.067469349091));
#56870=CARTESIAN_POINT('Ctrl Pts',(58.5207586395902,1.19762320763845,126.034152895147));
#56871=CARTESIAN_POINT('Ctrl Pts',(58.5129938866431,1.06508524220348,126.000877500754));
#56872=CARTESIAN_POINT('Ctrl Pts',(58.505229133696,0.930985400870419,125.973086363722));
#56873=CARTESIAN_POINT('Ctrl Pts',(58.4974643807489,0.79581717603026,125.950922858118));
#56874=CARTESIAN_POINT('Ctrl Pts',(58.4897073398639,0.660783202176733,125.92878136562));
#56875=CARTESIAN_POINT('Ctrl Pts',(58.4819502989789,0.524683339836303,125.912256444159));
#56876=CARTESIAN_POINT('Ctrl Pts',(58.4741932580939,0.388023855216127,125.901441023051));
#56877=CARTESIAN_POINT('Ctrl Pts',(58.4664420668538,0.251467426576173,125.890633757936));
#56878=CARTESIAN_POINT('Ctrl Pts',(58.4586908756136,0.114352603822298,125.885527453901));
#56879=CARTESIAN_POINT('Ctrl Pts',(58.4509396843735,-0.0228069489639163,
125.886163498135));
#56880=CARTESIAN_POINT('Ctrl Pts',(58.4431917875964,-0.159908205281159,
125.886799272033));
#56881=CARTESIAN_POINT('Ctrl Pts',(58.4354438908193,-0.297053763675912,
125.893172538122));
#56882=CARTESIAN_POINT('Ctrl Pts',(58.4276959940423,-0.433727885739765,
125.905272622476));
#56883=CARTESIAN_POINT('Ctrl Pts',(58.4199497179582,-0.570373418523635,
125.917370175754));
#56884=CARTESIAN_POINT('Ctrl Pts',(58.412203441874,-0.706547321930654,125.935192130097));
#56885=CARTESIAN_POINT('Ctrl Pts',(58.4044571657899,-0.841737307923214,
125.958675798374));
#56886=CARTESIAN_POINT('Ctrl Pts',(58.3967108325246,-0.976928291857541,
125.982159640002));
#56887=CARTESIAN_POINT('Ctrl Pts',(58.3889644992593,-1.11113495868771,126.011305212047));
#56888=CARTESIAN_POINT('Ctrl Pts',(58.3812181659939,-1.24385395748742,126.045998462902));
#56889=CARTESIAN_POINT('Ctrl Pts',(58.3734700979909,-1.37660267778671,126.08069948307));
#56890=CARTESIAN_POINT('Ctrl Pts',(58.365722029988,-1.50786268893686,126.12095055535));
#56891=CARTESIAN_POINT('Ctrl Pts',(58.357973961985,-1.63714496088211,126.16658750544));
#56892=CARTESIAN_POINT('Ctrl Pts',(58.3502176592431,-1.76656463556447,126.212272959024));
#56893=CARTESIAN_POINT('Ctrl Pts',(58.3424613565013,-1.8940020028837,126.263355594724));
#56894=CARTESIAN_POINT('Ctrl Pts',(58.3347050537594,-2.01898670018973,126.319622524103));
#56895=CARTESIAN_POINT('Ctrl Pts',(58.3269446112453,-2.1440381055921,126.375919484837));
#56896=CARTESIAN_POINT('Ctrl Pts',(58.3191841687311,-2.26663388325725,126.437406077568));
#56897=CARTESIAN_POINT('Ctrl Pts',(58.311423726217,-2.38632842043751,126.50382347294));
#56898=CARTESIAN_POINT('Ctrl Pts',(58.3036508259515,-2.50621510191484,126.57034748741));
#56899=CARTESIAN_POINT('Ctrl Pts',(58.2958779256861,-2.62319090226604,126.641817917981));
#56900=CARTESIAN_POINT('Ctrl Pts',(58.2881050254206,-2.73683858809815,126.717932151877));
#56901=CARTESIAN_POINT('Ctrl Pts',(58.2806146896586,-2.84635489428918,126.79127944165));
#56902=CARTESIAN_POINT('Ctrl Pts',(58.2731243538965,-2.95278060686873,126.868938587004));
#56903=CARTESIAN_POINT('Ctrl Pts',(58.2656340181345,-3.05577304874891,126.95060476943));
#56904=CARTESIAN_POINT('Ctrl Pts',(58.2579584955031,-3.16131181812213,127.034290020847));
#56905=CARTESIAN_POINT('Ctrl Pts',(58.2502829728717,-3.26359770182087,127.12246271423));
#56906=CARTESIAN_POINT('Ctrl Pts',(58.2426074502402,-3.36221779805692,127.214837732707));
#56907=CARTESIAN_POINT('Ctrl Pts',(58.2349407074451,-3.46072508525823,127.307107085735));
#56908=CARTESIAN_POINT('Ctrl Pts',(58.2272739646499,-3.55557463086907,127.403568936786));
#56909=CARTESIAN_POINT('Ctrl Pts',(58.2196072218548,-3.6463842256354,127.503896234856));
#56910=CARTESIAN_POINT('Ctrl Pts',(58.2119474876462,-3.73711080641249,127.604131818286));
#56911=CARTESIAN_POINT('Ctrl Pts',(58.2042877534376,-3.82380451202177,127.708225527098));
#56912=CARTESIAN_POINT('Ctrl Pts',(58.196628019229,-3.906118243966,127.815811918506));
#56913=CARTESIAN_POINT('Ctrl Pts',(58.1889735286932,-3.98837562587644,127.923324658814));
#56914=CARTESIAN_POINT('Ctrl Pts',(58.1813190381574,-4.06625875475251,128.034325008515));
#56915=CARTESIAN_POINT('Ctrl Pts',(58.1736645476217,-4.13945963983709,128.148413149588));
#56916=CARTESIAN_POINT('Ctrl Pts',(58.1660126001096,-4.21263620565627,128.26246338757));
#56917=CARTESIAN_POINT('Ctrl Pts',(58.1583606525976,-4.28113340026512,128.379599042323));
#56918=CARTESIAN_POINT('Ctrl Pts',(58.1507087050855,-4.34468576966756,128.49939020011));
#56919=CARTESIAN_POINT('Ctrl Pts',(58.1430584659616,-4.40822395024907,128.619154613099));
#56920=CARTESIAN_POINT('Ctrl Pts',(58.1354082268377,-4.46681931675069,128.741572993394));
#56921=CARTESIAN_POINT('Ctrl Pts',(58.1277579877138,-4.52025207441814,128.86619028289));
#56922=CARTESIAN_POINT('Ctrl Pts',(58.1201050400426,-4.57370374981474,128.990851692813));
#56923=CARTESIAN_POINT('Ctrl Pts',(58.1124520923714,-4.62198900403304,129.117713198785));
#56924=CARTESIAN_POINT('Ctrl Pts',(58.1047991447002,-4.66493598282515,129.246299213563));
#56925=CARTESIAN_POINT('Ctrl Pts',(58.0981996200853,-4.70197133911506,129.35718545062));
#56926=CARTESIAN_POINT('Ctrl Pts',(58.0916000954705,-4.7350376245353,129.46935365218));
#56927=CARTESIAN_POINT('Ctrl Pts',(58.0850005708556,-4.76405452823401,129.582490119308));
#56928=CARTESIAN_POINT('Ctrl Pts',(59.834681232118,-4.76405452823407,129.582490119308));
#56929=CARTESIAN_POINT('Ctrl Pts',(59.826858033056,-4.79847138378228,129.716680916742));
#56930=CARTESIAN_POINT('Ctrl Pts',(59.8190348339941,-4.82723403352823,129.85240374661));
#56931=CARTESIAN_POINT('Ctrl Pts',(59.8112116349321,-4.85021766907435,129.989147991867));
#56932=CARTESIAN_POINT('Ctrl Pts',(59.8033904177206,-4.87319548217733,130.125857595712));
#56933=CARTESIAN_POINT('Ctrl Pts',(59.7955692005092,-4.89039712729127,130.263587726225));
#56934=CARTESIAN_POINT('Ctrl Pts',(59.7877479832978,-4.90174887817213,130.401817454864));
#56935=CARTESIAN_POINT('Ctrl Pts',(59.780118467529,-4.91282239269153,130.536659112609));
#56936=CARTESIAN_POINT('Ctrl Pts',(59.77248895176,-4.9183294285159,130.671975811274));
#56937=CARTESIAN_POINT('Ctrl Pts',(59.7648594359912,-4.91824913396669,130.807279304929));
#56938=CARTESIAN_POINT('',(60.1101405640517,-4.91824820688785,130.800160862287));
#56939=CARTESIAN_POINT('Ctrl Pts',(60.1799785705036,-4.76405452823407,129.582490119308));
#56940=CARTESIAN_POINT('Ctrl Pts',(60.1705897890123,-4.80502007161657,129.742214151218));
#56941=CARTESIAN_POINT('Ctrl Pts',(60.1612010075211,-4.83798653576062,129.904146054801));
#56942=CARTESIAN_POINT('Ctrl Pts',(60.1518122260298,-4.86274682488788,130.067559165652));
#56943=CARTESIAN_POINT('Ctrl Pts',(60.1425322321957,-4.88722021695095,130.229078811467));
#56944=CARTESIAN_POINT('Ctrl Pts',(60.1332522383617,-4.90367645610653,130.39204551948));
#56945=CARTESIAN_POINT('Ctrl Pts',(60.1239722445276,-4.91196185149144,130.555736741012));
#56946=CARTESIAN_POINT('Ctrl Pts',(60.119361684369,-4.91607826735803,130.637063112324));
#56947=CARTESIAN_POINT('Ctrl Pts',(60.1147511242104,-4.91817853369338,130.718567997687));
#56948=CARTESIAN_POINT('Ctrl Pts',(60.1101405640517,-4.91824820688785,130.800160862287));
#56949=CARTESIAN_POINT('Ctrl Pts',(60.1101405640086,-4.91824820688851,130.80016086305));
#56950=CARTESIAN_POINT('Ctrl Pts',(60.1020818223771,-4.91836998778967,130.942776031742));
#56951=CARTESIAN_POINT('Ctrl Pts',(60.0940230807456,-4.91228351706248,131.085495793871));
#56952=CARTESIAN_POINT('Ctrl Pts',(60.0859643391141,-4.89999351809681,131.227735847249));
#56953=CARTESIAN_POINT('Ctrl Pts',(60.0782578572168,-4.88824073349627,131.363758373662));
#56954=CARTESIAN_POINT('Ctrl Pts',(60.0705513753195,-4.87081531724437,131.499341807809));
#56955=CARTESIAN_POINT('Ctrl Pts',(60.0628448934223,-4.8477746302262,131.633977515318));
#56956=CARTESIAN_POINT('Ctrl Pts',(60.0551389575367,-4.82473557566313,131.768603683755));
#56957=CARTESIAN_POINT('Ctrl Pts',(60.0474330216512,-4.79608210801656,131.90228186953));
#56958=CARTESIAN_POINT('Ctrl Pts',(60.0397270857656,-4.76192304593058,132.034511814426));
#56959=CARTESIAN_POINT('Ctrl Pts',(60.0320199848852,-4.72775881962653,132.166761750042));
#56960=CARTESIAN_POINT('Ctrl Pts',(60.0243128840048,-4.68808744182136,132.297562626526));
#56961=CARTESIAN_POINT('Ctrl Pts',(60.0166057831243,-4.64306799604225,132.426428016483));
#56962=CARTESIAN_POINT('Ctrl Pts',(60.0088958057678,-4.598031747919,132.555341502114));
#56963=CARTESIAN_POINT('Ctrl Pts',(60.0011858284111,-4.54764359099658,132.68231769126));
#56964=CARTESIAN_POINT('Ctrl Pts',(59.9934758510546,-4.49211108833518,132.806889277175));
#56965=CARTESIAN_POINT('Ctrl Pts',(59.9857569937017,-4.43651462589887,132.931604338897));
#56966=CARTESIAN_POINT('Ctrl Pts',(59.9780381363489,-4.37576215104937,133.053908907796));
#56967=CARTESIAN_POINT('Ctrl Pts',(59.970319278996,-4.31010778649247,133.173359125653));
#56968=CARTESIAN_POINT('Ctrl Pts',(59.9625952002613,-4.24440901037383,133.292890145003));
#56969=CARTESIAN_POINT('Ctrl Pts',(59.9548711215266,-4.17380194550736,133.409562631417));
#56970=CARTESIAN_POINT('Ctrl Pts',(59.9471470427918,-4.09858390753986,133.522961915174));
#56971=CARTESIAN_POINT('Ctrl Pts',(59.9394117226403,-4.02325639925976,133.636526237204));
#56972=CARTESIAN_POINT('Ctrl Pts',(59.9316764024889,-3.9433047543799,133.746807529783));
#56973=CARTESIAN_POINT('Ctrl Pts',(59.9239410823374,-3.8590666051325,133.853424080279));
#56974=CARTESIAN_POINT('Ctrl Pts',(59.9215376431757,-3.83289299333098,133.886550878876));
#56975=CARTESIAN_POINT('Ctrl Pts',(59.9191342040141,-3.80630582714366,133.91932415076));
#56976=CARTESIAN_POINT('Ctrl Pts',(59.9167307648524,-3.77931593418707,133.951733193557));
#56977=CARTESIAN_POINT('Ctrl Pts',(59.9089564307333,-3.69201251955062,134.056565773138));
#56978=CARTESIAN_POINT('Ctrl Pts',(59.9011820966143,-3.60020566815491,134.157929147634));
#56979=CARTESIAN_POINT('Ctrl Pts',(59.8934077624952,-3.50420152484457,134.255411868385));
#56980=CARTESIAN_POINT('Ctrl Pts',(59.8856430095481,-3.40831569806085,134.352774450394));
#56981=CARTESIAN_POINT('Ctrl Pts',(59.8778782566011,-3.30824314336715,134.44626561864));
#56982=CARTESIAN_POINT('Ctrl Pts',(59.870113503654,-3.20433075125238,134.535506218997));
#56983=CARTESIAN_POINT('Ctrl Pts',(59.862356462769,-3.10052156639065,134.624658184331));
#56984=CARTESIAN_POINT('Ctrl Pts',(59.854599421884,-2.99288042838321,134.709567730124));
#56985=CARTESIAN_POINT('Ctrl Pts',(59.8468423809991,-2.88179137759845,134.789892140274));
#56986=CARTESIAN_POINT('Ctrl Pts',(59.839091189759,-2.77078609993059,134.870155977162));
#56987=CARTESIAN_POINT('Ctrl Pts',(59.8313399985188,-2.65633840036138,134.945841332569));
#56988=CARTESIAN_POINT('Ctrl Pts',(59.8235888072787,-2.53886544860995,135.016645662094));
#56989=CARTESIAN_POINT('Ctrl Pts',(59.8158409105016,-2.42144242599672,135.087419897891));
#56990=CARTESIAN_POINT('Ctrl Pts',(59.8080930137246,-2.30099704273012,135.153317032561));
#56991=CARTESIAN_POINT('Ctrl Pts',(59.8003451169475,-2.17797532123207,135.214077905851));
#56992=CARTESIAN_POINT('Ctrl Pts',(59.7925988408634,-2.05497933322628,135.274826069277));
#56993=CARTESIAN_POINT('Ctrl Pts',(59.7848525647793,-1.9294084292378,135.330439935328));
#56994=CARTESIAN_POINT('Ctrl Pts',(59.7771062886952,-1.80173274106393,135.380706560814));
#56995=CARTESIAN_POINT('Ctrl Pts',(59.7693599554299,-1.67405611041678,135.430973557356));
#56996=CARTESIAN_POINT('Ctrl Pts',(59.7616136221646,-1.5442750283675,135.475893091344));
#56997=CARTESIAN_POINT('Ctrl Pts',(59.7538672888992,-1.41287871264106,135.515300736679));
#56998=CARTESIAN_POINT('Ctrl Pts',(59.7461192208963,-1.28145297162128,135.554717207083));
#56999=CARTESIAN_POINT('Ctrl Pts',(59.7383711528933,-1.14841165155659,135.58861922033));
#57000=CARTESIAN_POINT('Ctrl Pts',(59.7306230848904,-1.01425781211474,135.616892607388));
#57001=CARTESIAN_POINT('Ctrl Pts',(59.7228667821486,-0.879961392375511,
135.645196043739));
#57002=CARTESIAN_POINT('Ctrl Pts',(59.7151104794067,-0.744550474461484,
135.667858823115));
#57003=CARTESIAN_POINT('Ctrl Pts',(59.7073541766648,-0.608537515089716,
135.684818091536));
#57004=CARTESIAN_POINT('Ctrl Pts',(59.6995937341507,-0.472451961506259,
135.701786411629));
#57005=CARTESIAN_POINT('Ctrl Pts',(59.6918332916365,-0.335764115647522,
135.713045122989));
#57006=CARTESIAN_POINT('Ctrl Pts',(59.6840728491224,-0.19898919391101,135.718583482191));
#57007=CARTESIAN_POINT('Ctrl Pts',(59.676299948857,-0.0619947089278186,
135.724130732059));
#57008=CARTESIAN_POINT('Ctrl Pts',(59.6685270485915,0.0750867400721471,
135.723939280121));
#57009=CARTESIAN_POINT('Ctrl Pts',(59.6607541483261,0.211741399057937,135.71805053884));
#57010=CARTESIAN_POINT('Ctrl Pts',(59.653263812564,0.343428316979685,135.712375868137));
#57011=CARTESIAN_POINT('Ctrl Pts',(59.6457734768018,0.474718628998842,135.701410963868));
#57012=CARTESIAN_POINT('Ctrl Pts',(59.6382831410397,0.605161109052965,135.685237904959));
#57013=CARTESIAN_POINT('Ctrl Pts',(59.6305088069206,0.740549355383369,135.668451639606));
#57014=CARTESIAN_POINT('Ctrl Pts',(59.6227344728015,0.875453078793381,135.646001315275));
#57015=CARTESIAN_POINT('Ctrl Pts',(59.6149601386824,1.00936063710604,135.617922102242));
#57016=CARTESIAN_POINT('Ctrl Pts',(59.6071953857353,1.14310316632074,135.589877494331));
#57017=CARTESIAN_POINT('Ctrl Pts',(59.5994306327882,1.27585159419434,135.556217879951));
#57018=CARTESIAN_POINT('Ctrl Pts',(59.5916658798411,1.40709942483922,135.517030165828));
#57019=CARTESIAN_POINT('Ctrl Pts',(59.5839088389561,1.53821689828878,135.477881373495));
#57020=CARTESIAN_POINT('Ctrl Pts',(59.576151798071,1.66783636830249,135.433215519066));
#57021=CARTESIAN_POINT('Ctrl Pts',(59.568394757186,1.79546191491862,135.383170460154));
#57022=CARTESIAN_POINT('Ctrl Pts',(59.5606435659458,1.92299121811709,135.33316314061));
#57023=CARTESIAN_POINT('Ctrl Pts',(59.5528923747057,2.04852922829915,135.277784832949));
#57024=CARTESIAN_POINT('Ctrl Pts',(59.5451411834655,2.17159591587006,135.217222981234));
#57025=CARTESIAN_POINT('Ctrl Pts',(59.5373932866884,2.29461029681568,135.156686869921));
#57026=CARTESIAN_POINT('Ctrl Pts',(59.5296453899114,2.41515509421585,135.090971768705));
#57027=CARTESIAN_POINT('Ctrl Pts',(59.5218974931343,2.53277118319451,135.020312846432));
#57028=CARTESIAN_POINT('Ctrl Pts',(59.5141512170502,2.65036266942285,134.949668704482));
#57029=CARTESIAN_POINT('Ctrl Pts',(59.506404940966,2.76502633084446,134.874082999649));
#57030=CARTESIAN_POINT('Ctrl Pts',(59.4986586648819,2.87632889460038,134.79383616613));
#57031=CARTESIAN_POINT('Ctrl Pts',(59.4909123316166,2.98763227996654,134.713588740247));
#57032=CARTESIAN_POINT('Ctrl Pts',(59.4831659983511,3.09557420102438,134.628680345668));
#57033=CARTESIAN_POINT('Ctrl Pts',(59.4754196650858,3.19975188731087,134.539433698799));
#57034=CARTESIAN_POINT('Ctrl Pts',(59.4676715970828,3.30395290346817,134.450167065762));
#57035=CARTESIAN_POINT('Ctrl Pts',(59.4599235290798,3.40438771057849,134.356560501527));
#57036=CARTESIAN_POINT('Ctrl Pts',(59.4521754610768,3.50068833896314,134.258975533291));
#57037=CARTESIAN_POINT('Ctrl Pts',(59.4444191583349,3.59709131680136,134.161286850589));
#57038=CARTESIAN_POINT('Ctrl Pts',(59.436662855593,3.68935106366185,134.059611596133));
#57039=CARTESIAN_POINT('Ctrl Pts',(59.4289065528512,3.77713770333707,133.95434694016));
#57040=CARTESIAN_POINT('Ctrl Pts',(59.421146110337,3.8649711973852,133.849026101271));
#57041=CARTESIAN_POINT('Ctrl Pts',(59.4133856678228,3.94832658958905,133.740112353848));
#57042=CARTESIAN_POINT('Ctrl Pts',(59.4056252253086,4.026916354152,133.628033356954));
#57043=CARTESIAN_POINT('Ctrl Pts',(59.3978523250431,4.10563227798191,133.515774440904));
#57044=CARTESIAN_POINT('Ctrl Pts',(59.3900794247777,4.1795670756285,133.400340451062));
#57045=CARTESIAN_POINT('Ctrl Pts',(59.3823065245122,4.24847789196826,133.282186007693));
#57046=CARTESIAN_POINT('Ctrl Pts',(59.3748161887503,4.31488362655663,133.168326775956));
#57047=CARTESIAN_POINT('Ctrl Pts',(59.3673258529885,4.37662416264115,133.051941719534));
#57048=CARTESIAN_POINT('Ctrl Pts',(59.3598355172267,4.43352465683783,132.933454833356));
#57049=CARTESIAN_POINT('Ctrl Pts',(59.3520611831075,4.49258255056777,132.810475480873));
#57050=CARTESIAN_POINT('Ctrl Pts',(59.3442868489884,4.54661321459122,132.684842209016));
#57051=CARTESIAN_POINT('Ctrl Pts',(59.3365125148694,4.59536968356444,132.557004487232));
#57052=CARTESIAN_POINT('Ctrl Pts',(59.3287477619223,4.64406606454714,132.429324314014));
#57053=CARTESIAN_POINT('Ctrl Pts',(59.3209830089752,4.68750104550558,132.299445458259));
#57054=CARTESIAN_POINT('Ctrl Pts',(59.3132182560281,4.72547397013043,132.16784102451));
#57055=CARTESIAN_POINT('Ctrl Pts',(59.3054612151431,4.76340917951127,132.036367302139));
#57056=CARTESIAN_POINT('Ctrl Pts',(59.297704174258,4.79589302085066,131.903171785659));
#57057=CARTESIAN_POINT('Ctrl Pts',(59.289947133373,4.82277342081136,131.768746221988));
#57058=CARTESIAN_POINT('Ctrl Pts',(59.2821959421329,4.84963355005316,131.63442202968));
#57059=CARTESIAN_POINT('Ctrl Pts',(59.2744447508928,4.87089857236288,131.498870018313));
#57060=CARTESIAN_POINT('Ctrl Pts',(59.2666935596527,4.886466722017,131.362595368473));
#57061=CARTESIAN_POINT('Ctrl Pts',(59.2589456628757,4.9020282547923,131.226378638994));
#57062=CARTESIAN_POINT('Ctrl Pts',(59.2511977660986,4.91189768645576,131.089440269548));
#57063=CARTESIAN_POINT('Ctrl Pts',(59.2434498693215,4.91602470300874,130.952293649401));
#57064=CARTESIAN_POINT('Ctrl Pts',(59.2357035932374,4.92015085627883,130.81517571737));
#57065=CARTESIAN_POINT('Ctrl Pts',(59.2279573171533,4.91853697191796,130.677850011827));
#57066=CARTESIAN_POINT('Ctrl Pts',(59.2202110410692,4.91118479259633,130.540832639031));
#57067=CARTESIAN_POINT('Ctrl Pts',(59.2124647078038,4.90383255900258,130.403814254805));
#57068=CARTESIAN_POINT('Ctrl Pts',(59.2047183745385,4.89074196687274,130.267104598272));
#57069=CARTESIAN_POINT('Ctrl Pts',(59.1969720412731,4.87196681938482,130.131216967731));
#57070=CARTESIAN_POINT('Ctrl Pts',(59.1892239732701,4.85318746733278,129.995298906097));
#57071=CARTESIAN_POINT('Ctrl Pts',(59.1814759052671,4.82872108026649,129.860203623977));
#57072=CARTESIAN_POINT('Ctrl Pts',(59.1737278372641,4.79867292465472,129.726436118964));
#57073=CARTESIAN_POINT('Ctrl Pts',(59.1659715345222,4.76859283350563,129.592526444256));
#57074=CARTESIAN_POINT('Ctrl Pts',(59.1582152317803,4.73291920908674,129.4599477477));
#57075=CARTESIAN_POINT('Ctrl Pts',(59.1504589290385,4.69180789581938,129.329192243709));
#57076=CARTESIAN_POINT('Ctrl Pts',(59.1426984865243,4.6506746402063,129.198366951569));
#57077=CARTESIAN_POINT('Ctrl Pts',(59.1349380440102,4.60409804545684,129.069367158512));
#57078=CARTESIAN_POINT('Ctrl Pts',(59.127177601496,4.55228249853596,128.942665928305));
#57079=CARTESIAN_POINT('Ctrl Pts',(59.1194047012306,4.50038377269927,128.815761306035));
#57080=CARTESIAN_POINT('Ctrl Pts',(59.1116318009651,4.44322945187069,128.691162975691));
#57081=CARTESIAN_POINT('Ctrl Pts',(59.1038589006997,4.3810707518285,128.569320991525));
#57082=CARTESIAN_POINT('Ctrl Pts',(59.0963685649377,4.32117167710184,128.451908270386));
#57083=CARTESIAN_POINT('Ctrl Pts',(59.0888782291758,4.25662590078738,128.337055242935));
#57084=CARTESIAN_POINT('Ctrl Pts',(59.0813878934138,4.18769563470786,128.225138189479));
#57085=CARTESIAN_POINT('Ctrl Pts',(59.0736135592947,4.11615185663832,128.108977766923));
#57086=CARTESIAN_POINT('Ctrl Pts',(59.0658392251757,4.03965792058266,127.99561238685));
#57087=CARTESIAN_POINT('Ctrl Pts',(59.0580648910566,3.9584584871163,127.885492777413));
#57088=CARTESIAN_POINT('Ctrl Pts',(59.0503001381095,3.87735912469468,127.775508880554));
#57089=CARTESIAN_POINT('Ctrl Pts',(59.0425353851624,3.79156603315425,127.668763106928));
#57090=CARTESIAN_POINT('Ctrl Pts',(59.0347706322153,3.70136878910965,127.565679998934));
#57091=CARTESIAN_POINT('Ctrl Pts',(59.0270135913303,3.61126113023965,127.462699274535));
#57092=CARTESIAN_POINT('Ctrl Pts',(59.0192565504454,3.51675827963859,127.363374268688));
#57093=CARTESIAN_POINT('Ctrl Pts',(59.0114995095604,3.41819175856144,127.268098726218));
#57094=CARTESIAN_POINT('Ctrl Pts',(59.0037483183203,3.31969956726484,127.172895031775));
#57095=CARTESIAN_POINT('Ctrl Pts',(58.9959971270802,3.21715008505486,127.081734993063));
#57096=CARTESIAN_POINT('Ctrl Pts',(58.9882459358401,3.11091332780757,126.994977290915));
#57097=CARTESIAN_POINT('Ctrl Pts',(58.980498039063,3.0047217240155,126.908256463103));
#57098=CARTESIAN_POINT('Ctrl Pts',(58.972750142286,2.89484626439237,126.825934497136));
#57099=CARTESIAN_POINT('Ctrl Pts',(58.9650022455089,2.78169168192374,126.748331223045));
#57100=CARTESIAN_POINT('Ctrl Pts',(58.9572559694248,2.66856076895459,126.670744181886));
#57101=CARTESIAN_POINT('Ctrl Pts',(58.9495096933407,2.55215241969669,126.597874090294));
#57102=CARTESIAN_POINT('Ctrl Pts',(58.9417634172567,2.43290179092059,126.52999845015));
#57103=CARTESIAN_POINT('Ctrl Pts',(58.9340170839913,2.31365028186361,126.462122308964));
#57104=CARTESIAN_POINT('Ctrl Pts',(58.926270750726,2.19155679120304,126.399240886193));
#57105=CARTESIAN_POINT('Ctrl Pts',(58.9185244174606,2.0670822532658,126.341586365967));
#57106=CARTESIAN_POINT('Ctrl Pts',(58.9107763494577,1.94257984011883,126.283918934411));
#57107=CARTESIAN_POINT('Ctrl Pts',(58.9030282814547,1.81569567334134,126.231480898903));
#57108=CARTESIAN_POINT('Ctrl Pts',(58.8952802134518,1.68691152080732,126.184456659315));
#57109=CARTESIAN_POINT('Ctrl Pts',(58.88752391071,1.55799049494325,126.137382441805));
#57110=CARTESIAN_POINT('Ctrl Pts',(58.8797676079681,1.42716581733296,126.095733648455));
#57111=CARTESIAN_POINT('Ctrl Pts',(58.8720113052263,1.2949358396169,126.059645216852));
#57112=CARTESIAN_POINT('Ctrl Pts',(58.8642508627121,1.16263528677999,126.023537523766));
#57113=CARTESIAN_POINT('Ctrl Pts',(58.8564904201979,1.02892832025904,125.992996192904));
#57114=CARTESIAN_POINT('Ctrl Pts',(58.8487299776838,0.894323418144604,125.968104970244));
#57115=CARTESIAN_POINT('Ctrl Pts',(58.8409570774184,0.759502436291817,125.943173789983));
#57116=CARTESIAN_POINT('Ctrl Pts',(58.8331841771529,0.623781025685959,125.923910897756));
#57117=CARTESIAN_POINT('Ctrl Pts',(58.8254112768875,0.487673617979483,125.91034820393));
#57118=CARTESIAN_POINT('Ctrl Pts',(58.8179209411253,0.356514057373872,125.897278548186));
#57119=CARTESIAN_POINT('Ctrl Pts',(58.8104306053631,0.224996383851764,125.889501871051));
#57120=CARTESIAN_POINT('Ctrl Pts',(58.8029402696009,0.0935789045873223,
125.887000954991));
#57121=CARTESIAN_POINT('Ctrl Pts',(58.7951659354818,-0.0428213083436484,
125.884405215939));
#57122=CARTESIAN_POINT('Ctrl Pts',(58.7873916013627,-0.179545654179816,
125.88748497373));
#57123=CARTESIAN_POINT('Ctrl Pts',(58.7796172672437,-0.31608267754306,125.896278018072));
#57124=CARTESIAN_POINT('Ctrl Pts',(58.7718525142966,-0.452451431227674,
125.905060225772));
#57125=CARTESIAN_POINT('Ctrl Pts',(58.7640877613495,-0.588632935366884,
125.919541685416));
#57126=CARTESIAN_POINT('Ctrl Pts',(58.7563230084024,-0.724113487184336,
125.939708243534));
#57127=CARTESIAN_POINT('Ctrl Pts',(58.7485659675174,-0.859459477807414,
125.959854771941));
#57128=CARTESIAN_POINT('Ctrl Pts',(58.7408089266324,-0.994105517367409,
125.985675104803));
#57129=CARTESIAN_POINT('Ctrl Pts',(58.7330518857475,-1.12754114185477,126.017103152595));
#57130=CARTESIAN_POINT('Ctrl Pts',(58.7253006945074,-1.26087614149972,126.048507500251));
#57131=CARTESIAN_POINT('Ctrl Pts',(58.7175495032673,-1.39300216389963,126.085511056355));
#57132=CARTESIAN_POINT('Ctrl Pts',(58.7097983120272,-1.52341743809267,126.127996391822));
#57133=CARTESIAN_POINT('Ctrl Pts',(58.7020504152501,-1.65377728231558,126.170463669889));
#57134=CARTESIAN_POINT('Ctrl Pts',(58.694302518473,-1.7824274535464,126.218407972474));
#57135=CARTESIAN_POINT('Ctrl Pts',(58.6865546216959,-1.90888010165679,126.271661662198));
#57136=CARTESIAN_POINT('Ctrl Pts',(58.6788083456118,-2.03530629859919,126.324904212397));
#57137=CARTESIAN_POINT('Ctrl Pts',(58.6710620695277,-2.15953552665045,126.383453789027));
#57138=CARTESIAN_POINT('Ctrl Pts',(58.6633157934436,-2.28109910275321,126.447094278918));
#57139=CARTESIAN_POINT('Ctrl Pts',(58.6555694601783,-2.40266357621084,126.510735238588));
#57140=CARTESIAN_POINT('Ctrl Pts',(58.6478231269129,-2.52156201208438,126.579467005176));
#57141=CARTESIAN_POINT('Ctrl Pts',(58.6400767936476,-2.6373499210266,126.653027282773));
#57142=CARTESIAN_POINT('Ctrl Pts',(58.6323287256445,-2.75316375986853,126.726604033685));
#57143=CARTESIAN_POINT('Ctrl Pts',(58.6245806576416,-2.86586535572596,126.805011237679));
#57144=CARTESIAN_POINT('Ctrl Pts',(58.6168325896386,-2.9750391604602,126.887943242435));
#57145=CARTESIAN_POINT('Ctrl Pts',(58.6090762868967,-3.0843289964127,126.970963388312));
#57146=CARTESIAN_POINT('Ctrl Pts',(58.6013199841549,-3.19008323963164,127.058517704599));
#57147=CARTESIAN_POINT('Ctrl Pts',(58.5935636814131,-3.29191899206923,127.150259851009));
#57148=CARTESIAN_POINT('Ctrl Pts',(58.5858032388989,-3.39380909731424,127.242050962964));
#57149=CARTESIAN_POINT('Ctrl Pts',(58.5780427963847,-3.4917762653225,127.338034085332));
#57150=CARTESIAN_POINT('Ctrl Pts',(58.5702823538706,-3.58547519340248,127.43782668784));
#57151=CARTESIAN_POINT('Ctrl Pts',(58.5625094536051,-3.67932453532001,127.537779486293));
#57152=CARTESIAN_POINT('Ctrl Pts',(58.5547365533398,-3.76889168971608,127.641553689095));
#57153=CARTESIAN_POINT('Ctrl Pts',(58.5469636530744,-3.85387174662136,127.74873373866));
#57154=CARTESIAN_POINT('Ctrl Pts',(58.5394733173123,-3.93576256440708,127.852017523454));
#57155=CARTESIAN_POINT('Ctrl Pts',(58.5319829815502,-4.01339381816233,127.958463583014));
#57156=CARTESIAN_POINT('Ctrl Pts',(58.5244926457881,-4.08653226726503,128.067677024035));
#57157=CARTESIAN_POINT('Ctrl Pts',(58.5165831192501,-4.16376385240355,128.183002509768));
#57158=CARTESIAN_POINT('Ctrl Pts',(58.5086735927121,-4.23622414022661,128.301770154107));
#57159=CARTESIAN_POINT('Ctrl Pts',(58.5007640661741,-4.30359753563025,128.423555855764));
#57160=CARTESIAN_POINT('Ctrl Pts',(58.4928642412395,-4.3708882927165,128.545192178496));
#57161=CARTESIAN_POINT('Ctrl Pts',(58.4849644163049,-4.43310439364135,128.669838869824));
#57162=CARTESIAN_POINT('Ctrl Pts',(58.4770645913703,-4.48997264878427,128.797041839776));
#57163=CARTESIAN_POINT('Ctrl Pts',(58.4691757325853,-4.54676196220404,128.924068232803));
#57164=CARTESIAN_POINT('Ctrl Pts',(58.4612868738004,-4.59821806827637,129.053643497022));
#57165=CARTESIAN_POINT('Ctrl Pts',(58.4533980150154,-4.6441133165706,129.185288486575));
#57166=CARTESIAN_POINT('Ctrl Pts',(58.445576034428,-4.689619485587,129.315817449102));
#57167=CARTESIAN_POINT('Ctrl Pts',(58.4377540538405,-4.72965858030162,129.448380840351));
#57168=CARTESIAN_POINT('Ctrl Pts',(58.429932073253,-4.76405452823401,129.582490119308));
#57169=CARTESIAN_POINT('Origin',(213.235140564004,0.,130.804360617566));
#57170=CARTESIAN_POINT('',(56.3348795324218,-4.7640545282341,129.582490119308));
#57171=CARTESIAN_POINT('',(56.6802739192585,-4.76405452823399,129.582490119308));
#57172=CARTESIAN_POINT('',(213.235140564004,-4.76405452823405,129.582490119308));
#57173=CARTESIAN_POINT('',(58.014859436029,-4.91824920186863,130.807162548786));
#57174=CARTESIAN_POINT('Ctrl Pts',(58.0148594359912,-4.91824920186825,130.807162549451));
#57175=CARTESIAN_POINT('Ctrl Pts',(58.005635088768,-4.91815684843496,130.969271129642));
#57176=CARTESIAN_POINT('Ctrl Pts',(57.9964107415448,-4.91005038252175,131.1311482706));
#57177=CARTESIAN_POINT('Ctrl Pts',(57.9871863943216,-4.89399391332884,131.292219858331));
#57178=CARTESIAN_POINT('Ctrl Pts',(57.9794120602026,-4.88046142661098,131.427971940275));
#57179=CARTESIAN_POINT('Ctrl Pts',(57.9716377260835,-4.86125488480983,131.563375560627));
#57180=CARTESIAN_POINT('Ctrl Pts',(57.9638633919644,-4.83639717007311,131.697918380561));
#57181=CARTESIAN_POINT('Ctrl Pts',(57.9560986390173,-4.81157009024821,131.832295388494));
#57182=CARTESIAN_POINT('Ctrl Pts',(57.9483338860702,-4.78110576524688,131.965813326035));
#57183=CARTESIAN_POINT('Ctrl Pts',(57.9405691331231,-4.74507892226327,132.097963757634));
#57184=CARTESIAN_POINT('Ctrl Pts',(57.9328120922381,-4.70908786164799,132.229982935561));
#57185=CARTESIAN_POINT('Ctrl Pts',(57.9250550513531,-4.66754537976121,132.360636935718));
#57186=CARTESIAN_POINT('Ctrl Pts',(57.9172980104681,-4.62057739380636,132.489426672754));
#57187=CARTESIAN_POINT('Ctrl Pts',(57.909546819228,-4.57364482677502,132.618119288447));
#57188=CARTESIAN_POINT('Ctrl Pts',(57.9017956279878,-4.5212950327972,132.744950073473));
#57189=CARTESIAN_POINT('Ctrl Pts',(57.8940444367477,-4.46370388256866,132.869434638332));
#57190=CARTESIAN_POINT('Ctrl Pts',(57.8862965399706,-4.40613721011535,132.99386629393));
#57191=CARTESIAN_POINT('Ctrl Pts',(57.8785486431936,-4.34333377598378,133.115953358639));
#57192=CARTESIAN_POINT('Ctrl Pts',(57.8708007464165,-4.27551766356744,133.235231196396));
#57193=CARTESIAN_POINT('Ctrl Pts',(57.8630544703324,-4.20771573681978,133.354484083801));
#57194=CARTESIAN_POINT('Ctrl Pts',(57.8553081942482,-4.13490341051346,133.470928573425));
#57195=CARTESIAN_POINT('Ctrl Pts',(57.8475619181641,-4.05735064073519,133.584124787532));
#57196=CARTESIAN_POINT('Ctrl Pts',(57.8398155848988,-3.9797972984801,133.697321837227));
#57197=CARTESIAN_POINT('Ctrl Pts',(57.8320692516335,-3.89750366389842,133.80727024103));
#57198=CARTESIAN_POINT('Ctrl Pts',(57.8243229183681,-3.81078269508045,133.913559600162));
#57199=CARTESIAN_POINT('Ctrl Pts',(57.8165748503652,-3.7240423057028,134.019872762058));
#57200=CARTESIAN_POINT('Ctrl Pts',(57.8088267823621,-3.63287285628821,134.122524945865));
#57201=CARTESIAN_POINT('Ctrl Pts',(57.8010787143592,-3.53762693966327,134.221139612214));
#57202=CARTESIAN_POINT('Ctrl Pts',(57.7933224116173,-3.4422797945447,134.319859087404));
#57203=CARTESIAN_POINT('Ctrl Pts',(57.7855661088755,-3.34284779958689,134.414532191494));
#57204=CARTESIAN_POINT('Ctrl Pts',(57.7778098061336,-3.23972009453267,134.504819612283));
#57205=CARTESIAN_POINT('Ctrl Pts',(57.7700493636195,-3.13653734711714,134.595155222187));
#57206=CARTESIAN_POINT('Ctrl Pts',(57.7622889211053,-3.02965526374008,134.681100239727));
#57207=CARTESIAN_POINT('Ctrl Pts',(57.7545284785912,-2.91949448048244,134.762356959269));
#57208=CARTESIAN_POINT('Ctrl Pts',(57.7467555783257,-2.80915685735589,134.843744119311));
#57209=CARTESIAN_POINT('Ctrl Pts',(57.7389826780604,-2.69553034093435,134.920427723032));
#57210=CARTESIAN_POINT('Ctrl Pts',(57.7312097777949,-2.57906359271026,134.992154075612));
#57211=CARTESIAN_POINT('Ctrl Pts',(57.7237194420329,-2.46683070414553,135.061272994609));
#57212=CARTESIAN_POINT('Ctrl Pts',(57.7162291062708,-2.35196076637003,135.125788671392));
#57213=CARTESIAN_POINT('Ctrl Pts',(57.7087387705087,-2.23487345645436,135.185516138218));
#57214=CARTESIAN_POINT('Ctrl Pts',(57.7009644363896,-2.11334674559567,135.247508190102));
#57215=CARTESIAN_POINT('Ctrl Pts',(57.6931901022706,-1.98904623997409,135.304538146744));
#57216=CARTESIAN_POINT('Ctrl Pts',(57.6854157681515,-1.86241535311417,135.356348327895));
#57217=CARTESIAN_POINT('Ctrl Pts',(57.6776510152044,-1.73594052750498,135.408094657627));
#57218=CARTESIAN_POINT('Ctrl Pts',(57.6698862622573,-1.60714139343105,135.454633864807));
#57219=CARTESIAN_POINT('Ctrl Pts',(57.6621215093102,-1.47648610399494,135.495753997705));
#57220=CARTESIAN_POINT('Ctrl Pts',(57.6543644684252,-1.34596058323421,135.536833289507));
#57221=CARTESIAN_POINT('Ctrl Pts',(57.6466074275401,-1.21358294639676,135.572504101437));
#57222=CARTESIAN_POINT('Ctrl Pts',(57.6388503866551,-1.07984114944792,135.602602603383));
#57223=CARTESIAN_POINT('Ctrl Pts',(57.631099195415,-0.9462002082287,135.632678407815));
#57224=CARTESIAN_POINT('Ctrl Pts',(57.6233480041749,-0.811197534392437,
135.657190180838));
#57225=CARTESIAN_POINT('Ctrl Pts',(57.6155968129347,-0.675335720949953,
135.676024063096));
#57226=CARTESIAN_POINT('Ctrl Pts',(57.6078489161576,-0.539531652402228,
135.694849940451));
#57227=CARTESIAN_POINT('Ctrl Pts',(57.6001010193805,-0.402869556969357,
135.708002673248));
#57228=CARTESIAN_POINT('Ctrl Pts',(57.5923531226034,-0.265861468678331,
135.715419642051));
#57229=CARTESIAN_POINT('Ctrl Pts',(57.5846068465193,-0.128882039525824,
135.722835059384));
#57230=CARTESIAN_POINT('Ctrl Pts',(57.5768605704352,0.00844284838225112,
135.724517078066));
#57231=CARTESIAN_POINT('Ctrl Pts',(57.5691142943511,0.145597195590896,135.720455055139));
#57232=CARTESIAN_POINT('Ctrl Pts',(57.5613679610858,0.282752555241587,135.716393002227));
#57233=CARTESIAN_POINT('Ctrl Pts',(57.5536216278204,0.419736980886966,135.706586834671));
#57234=CARTESIAN_POINT('Ctrl Pts',(57.5458752945551,0.556036030918943,135.691078022411));
#57235=CARTESIAN_POINT('Ctrl Pts',(57.5381272265521,0.69236560417833,135.675565737061));
#57236=CARTESIAN_POINT('Ctrl Pts',(57.5303791585491,0.828009108022459,135.654348309982));
#57237=CARTESIAN_POINT('Ctrl Pts',(57.5226310905462,0.962459164181244,135.627518858779));
#57238=CARTESIAN_POINT('Ctrl Pts',(57.5148747878043,1.09705211545969,135.600660892917));
#57239=CARTESIAN_POINT('Ctrl Pts',(57.5071184850624,1.23044870124893,135.568179064778));
#57240=CARTESIAN_POINT('Ctrl Pts',(57.4993621823205,1.3621531090474,135.530217362116));
#57241=CARTESIAN_POINT('Ctrl Pts',(57.4916017398063,1.49392781145386,135.492235398151));
#57242=CARTESIAN_POINT('Ctrl Pts',(57.4838412972922,1.62400816560539,135.448767855652));
#57243=CARTESIAN_POINT('Ctrl Pts',(57.476080854778,1.75191633924377,135.4000077105));
#57244=CARTESIAN_POINT('Ctrl Pts',(57.4683079545126,1.88002984243764,135.351169291234));
#57245=CARTESIAN_POINT('Ctrl Pts',(57.4605350542471,2.0059638376489,135.29702144581));
#57246=CARTESIAN_POINT('Ctrl Pts',(57.4527621539817,2.12926237174458,135.237804517603));
#57247=CARTESIAN_POINT('Ctrl Pts',(57.4452718182197,2.24807869355462,135.180740273894));
#57248=CARTESIAN_POINT('Ctrl Pts',(57.4377814824578,2.36444756683125,135.118969241143));
#57249=CARTESIAN_POINT('Ctrl Pts',(57.4302911466958,2.47798652726619,135.05274452597));
#57250=CARTESIAN_POINT('Ctrl Pts',(57.4225168125767,2.59583035189627,134.984008880593));
#57251=CARTESIAN_POINT('Ctrl Pts',(57.4147424784576,2.71099872908913,134.91025742944));
#57252=CARTESIAN_POINT('Ctrl Pts',(57.4069681443385,2.82303518931051,134.831723946397));
#57253=CARTESIAN_POINT('Ctrl Pts',(57.3992033913914,2.93493357460766,134.753287248854));
#57254=CARTESIAN_POINT('Ctrl Pts',(57.3914386384444,3.04370740572751,134.670080467841));
#57255=CARTESIAN_POINT('Ctrl Pts',(57.3836738854973,3.14892531348982,134.582382908734));
#57256=CARTESIAN_POINT('Ctrl Pts',(57.3759168446123,3.25403871734283,134.49477245208));
#57257=CARTESIAN_POINT('Ctrl Pts',(57.3681598037273,3.35560292788416,134.402680342236));
#57258=CARTESIAN_POINT('Ctrl Pts',(57.3604027628423,3.45321635808074,134.306428556196));
#57259=CARTESIAN_POINT('Ctrl Pts',(57.3526515716021,3.55075617723029,134.210249354378));
#57260=CARTESIAN_POINT('Ctrl Pts',(57.344900380362,3.64435086891673,134.109916993458));
#57261=CARTESIAN_POINT('Ctrl Pts',(57.3371491891219,3.73363297623808,134.005792775405));
#57262=CARTESIAN_POINT('Ctrl Pts',(57.3294012923448,3.82287713628215,133.901712812923));
#57263=CARTESIAN_POINT('Ctrl Pts',(57.3216533955677,3.90781210362773,133.793844494914));
#57264=CARTESIAN_POINT('Ctrl Pts',(57.3139054987906,3.98810842787089,133.682584762772));
#57265=CARTESIAN_POINT('Ctrl Pts',(57.3061592227065,4.068387955854,133.571348303767));
#57266=CARTESIAN_POINT('Ctrl Pts',(57.2984129466224,4.14403054206982,133.45672215851));
#57267=CARTESIAN_POINT('Ctrl Pts',(57.2906666705383,4.21474832198624,133.339134699178));
#57268=CARTESIAN_POINT('Ctrl Pts',(57.282920337273,4.28546662392524,133.221546371843));
#57269=CARTESIAN_POINT('Ctrl Pts',(57.2751740040076,4.3512598455273,133.100997021854));
#57270=CARTESIAN_POINT('Ctrl Pts',(57.2674276707423,4.41188480837251,132.977941879022));
#57271=CARTESIAN_POINT('Ctrl Pts',(57.2596796027393,4.47252334775781,132.854859178844));
#57272=CARTESIAN_POINT('Ctrl Pts',(57.2519315347363,4.52799115255192,132.729269919836));
#57273=CARTESIAN_POINT('Ctrl Pts',(57.2441834667333,4.57809231488464,132.601651306045));
#57274=CARTESIAN_POINT('Ctrl Pts',(57.2364271639914,4.6282467253289,132.473897057673));
#57275=CARTESIAN_POINT('Ctrl Pts',(57.2286708612496,4.67302295639439,132.34410951054));
#57276=CARTESIAN_POINT('Ctrl Pts',(57.2209145585077,4.71227415028793,132.212783634642));
#57277=CARTESIAN_POINT('Ctrl Pts',(57.2131541159935,4.75154629372549,132.081387666169));
#57278=CARTESIAN_POINT('Ctrl Pts',(57.2053936734793,4.78528742796441,131.94845211168));
#57279=CARTESIAN_POINT('Ctrl Pts',(57.1976332309652,4.81340162907112,131.814483293163));
#57280=CARTESIAN_POINT('Ctrl Pts',(57.1898603306997,4.84156096158931,131.680299416005));
#57281=CARTESIAN_POINT('Ctrl Pts',(57.1820874304343,4.86407524620841,131.545079346112));
#57282=CARTESIAN_POINT('Ctrl Pts',(57.1743145301689,4.88090023680959,131.409336601232));
#57283=CARTESIAN_POINT('Ctrl Pts',(57.1668241944069,4.89711359662268,131.278528447044));
#57284=CARTESIAN_POINT('Ctrl Pts',(57.159333858645,4.90804409579596,131.147235266175));
#57285=CARTESIAN_POINT('Ctrl Pts',(57.151843522883,4.91369794879832,131.015915646991));
#57286=CARTESIAN_POINT('Ctrl Pts',(57.1440691887639,4.91956616935576,130.879617004532));
#57287=CARTESIAN_POINT('Ctrl Pts',(57.1362948546449,4.91976830576783,130.742858126234));
#57288=CARTESIAN_POINT('Ctrl Pts',(57.1285205205258,4.91425430569275,130.606149413341));
#57289=CARTESIAN_POINT('Ctrl Pts',(57.1207557675787,4.90874710112997,130.469609181719));
#57290=CARTESIAN_POINT('Ctrl Pts',(57.1129910146315,4.89753779239387,130.333119379387));
#57291=CARTESIAN_POINT('Ctrl Pts',(57.1052262616844,4.88062820142956,130.197193900831));
#57292=CARTESIAN_POINT('Ctrl Pts',(57.0974692207994,4.86373540530941,130.061403425378));
#57293=CARTESIAN_POINT('Ctrl Pts',(57.0897121799145,4.84115364175492,129.926176543756));
#57294=CARTESIAN_POINT('Ctrl Pts',(57.0819551390295,4.81293673153005,129.792025158941));
#57295=CARTESIAN_POINT('Ctrl Pts',(57.0742039477894,4.78474109989663,129.657974938729));
#57296=CARTESIAN_POINT('Ctrl Pts',(57.0664527565493,4.75091886012837,129.524998982043));
#57297=CARTESIAN_POINT('Ctrl Pts',(57.0587015653091,4.71157536637377,129.39360173332));
#57298=CARTESIAN_POINT('Ctrl Pts',(57.0509536685321,4.67224859465355,129.262260331933));
#57299=CARTESIAN_POINT('Ctrl Pts',(57.0432057717549,4.62740534822537,129.132496677708));
#57300=CARTESIAN_POINT('Ctrl Pts',(57.0354578749779,4.57720150913501,129.004802503119));
#57301=CARTESIAN_POINT('Ctrl Pts',(57.0277115988938,4.52700817160558,128.877135039399));
#57302=CARTESIAN_POINT('Ctrl Pts',(57.0199653228097,4.47145661474297,128.751536557896));
#57303=CARTESIAN_POINT('Ctrl Pts',(57.0122190467256,4.41075164237998,128.628480792819));
#57304=CARTESIAN_POINT('Ctrl Pts',(57.0044727134603,4.35004622190669,128.505424119372));
#57305=CARTESIAN_POINT('Ctrl Pts',(56.9967263801949,4.28418748299094,128.384910550427));
#57306=CARTESIAN_POINT('Ctrl Pts',(56.9889800469296,4.213426979489,128.267390741707));
#57307=CARTESIAN_POINT('Ctrl Pts',(56.9812319789266,4.14265062966281,128.149844615242));
#57308=CARTESIAN_POINT('Ctrl Pts',(56.9734839109236,4.06697053255439,128.035293917956));
#57309=CARTESIAN_POINT('Ctrl Pts',(56.9657358429207,3.98668228045549,127.924161413135));
#57310=CARTESIAN_POINT('Ctrl Pts',(56.9579795401788,3.90630869704693,127.812910795366));
#57311=CARTESIAN_POINT('Ctrl Pts',(56.950223237437,3.82131740448047,127.705085944579));
#57312=CARTESIAN_POINT('Ctrl Pts',(56.9424669346951,3.73204545480885,127.601077959769));
#57313=CARTESIAN_POINT('Ctrl Pts',(56.934706492181,3.64272585800965,127.497014462766));
#57314=CARTESIAN_POINT('Ctrl Pts',(56.9269460496668,3.54912131831683,127.3967721766));
#57315=CARTESIAN_POINT('Ctrl Pts',(56.9191856071527,3.45160596953027,127.300705484194));
#57316=CARTESIAN_POINT('Ctrl Pts',(56.9114127068872,3.35393408044883,127.204484577006));
#57317=CARTESIAN_POINT('Ctrl Pts',(56.9036398066218,3.25233912679516,127.112452921007));
#57318=CARTESIAN_POINT('Ctrl Pts',(56.8958669063564,3.14722922948623,127.024925310597));
#57319=CARTESIAN_POINT('Ctrl Pts',(56.8883765705942,3.04594034169891,126.940579549292));
#57320=CARTESIAN_POINT('Ctrl Pts',(56.8808862348321,2.94138787201112,126.860416239494));
#57321=CARTESIAN_POINT('Ctrl Pts',(56.87339589907,2.83396100287565,126.784678031008));
#57322=CARTESIAN_POINT('Ctrl Pts',(56.8656215649509,2.72246101134678,126.706068185327));
#57323=CARTESIAN_POINT('Ctrl Pts',(56.8578472308319,2.60751115349037,126.631976607998));
#57324=CARTESIAN_POINT('Ctrl Pts',(56.8500728967128,2.48951378981403,126.562721293811));
#57325=CARTESIAN_POINT('Ctrl Pts',(56.8423081437657,2.3716618473427,126.493551330609));
#57326=CARTESIAN_POINT('Ctrl Pts',(56.8345433908186,2.25077020587402,126.429205967404));
#57327=CARTESIAN_POINT('Ctrl Pts',(56.8267786378715,2.12727220419992,126.369961443863));
#57328=CARTESIAN_POINT('Ctrl Pts',(56.8190215969865,2.00389686248211,126.310775762818));
#57329=CARTESIAN_POINT('Ctrl Pts',(56.8112645561015,1.87792066235791,126.256681007429));
#57330=CARTESIAN_POINT('Ctrl Pts',(56.8035075152166,1.74980337373552,126.207908592823));
#57331=CARTESIAN_POINT('Ctrl Pts',(56.7957563239764,1.62178269935692,126.159172957875));
#57332=CARTESIAN_POINT('Ctrl Pts',(56.7880051327362,1.49162451417256,126.11575181338));
#57333=CARTESIAN_POINT('Ctrl Pts',(56.7802539414961,1.3598101680658,126.07782918645));
#57334=CARTESIAN_POINT('Ctrl Pts',(56.772506044719,1.22805184657257,126.039922677649));
#57335=CARTESIAN_POINT('Ctrl Pts',(56.764758147942,1.09463913912374,126.007510146134));
#57336=CARTESIAN_POINT('Ctrl Pts',(56.7570102511649,0.960070012230005,125.980726237338));
#57337=CARTESIAN_POINT('Ctrl Pts',(56.7492639750808,0.825529034296639,125.953947931159));
#57338=CARTESIAN_POINT('Ctrl Pts',(56.7415176989967,0.689832501267799,125.932795982084));
#57339=CARTESIAN_POINT('Ctrl Pts',(56.7337714229126,0.553489680624103,125.917354147758));
#57340=CARTESIAN_POINT('Ctrl Pts',(56.7260250896473,0.417145853528676,125.901912199445));
#57341=CARTESIAN_POINT('Ctrl Pts',(56.7182787563819,0.280156117780283,125.892180493989));
#57342=CARTESIAN_POINT('Ctrl Pts',(56.7105324231166,0.143035593806511,125.888190982433));
#57343=CARTESIAN_POINT('Ctrl Pts',(56.7027843551136,0.00588436264212172,
125.884200577454));
#57344=CARTESIAN_POINT('Ctrl Pts',(56.6950362871106,-0.131397324304559,
125.885954936584));
#57345=CARTESIAN_POINT('Ctrl Pts',(56.6872882191077,-0.268294009455447,
125.893433883538));
#57346=CARTESIAN_POINT('Ctrl Pts',(56.6795319163658,-0.405336190032405,
125.900920779206));
#57347=CARTESIAN_POINT('Ctrl Pts',(56.671775613624,-0.541992160417936,125.914144395102));
#57348=CARTESIAN_POINT('Ctrl Pts',(56.6640193108822,-0.677750693083948,
125.933032558348));
#57349=CARTESIAN_POINT('Ctrl Pts',(56.656258868368,-0.81358168416664,125.951930802775));
#57350=CARTESIAN_POINT('Ctrl Pts',(56.6484984258538,-0.948513898649796,
125.97649954881));
#57351=CARTESIAN_POINT('Ctrl Pts',(56.6407379833396,-1.08204695568472,126.006615579718));
#57352=CARTESIAN_POINT('Ctrl Pts',(56.6329650830742,-1.21579437183731,126.036779955552));
#57353=CARTESIAN_POINT('Ctrl Pts',(56.6251921828088,-1.34813776454576,126.072509309314));
#57354=CARTESIAN_POINT('Ctrl Pts',(56.6174192825434,-1.47859168904217,126.11363043138));
#57355=CARTESIAN_POINT('Ctrl Pts',(56.6099289467813,-1.60430328478988,126.153256697081));
#57356=CARTESIAN_POINT('Ctrl Pts',(56.6024386110192,-1.72826011136683,126.197889423865));
#57357=CARTESIAN_POINT('Ctrl Pts',(56.5949482752572,-1.85004765799785,126.24733233966));
#57358=CARTESIAN_POINT('Ctrl Pts',(56.5871735890506,-1.9764585411689,126.298652222727));
#57359=CARTESIAN_POINT('Ctrl Pts',(56.579398902844,-2.10093263870519,126.355317294945));
#57360=CARTESIAN_POINT('Ctrl Pts',(56.5716242166374,-2.22298486132498,126.417160899201));
#57361=CARTESIAN_POINT('Ctrl Pts',(56.5638591924093,-2.34488540374524,126.47892764742));
#57362=CARTESIAN_POINT('Ctrl Pts',(56.5560941681812,-2.46436971456976,126.545859947179));
#57363=CARTESIAN_POINT('Ctrl Pts',(56.5483291439531,-2.58097110765602,126.617742506973));
#57364=CARTESIAN_POINT('Ctrl Pts',(56.5405719122506,-2.69745548638277,126.689552929621));
#57365=CARTESIAN_POINT('Ctrl Pts',(56.5328146805481,-2.81106237440224,126.766303521817));
#57366=CARTESIAN_POINT('Ctrl Pts',(56.5250574488456,-2.92134852833313,126.84773252808));
#57367=CARTESIAN_POINT('Ctrl Pts',(56.5171333689946,-3.03400679660734,126.93091296829));
#57368=CARTESIAN_POINT('Ctrl Pts',(56.5092092891436,-3.14319947597826,127.018975197812));
#57369=CARTESIAN_POINT('Ctrl Pts',(56.5012852092927,-3.24848352729114,127.111592301598));
#57370=CARTESIAN_POINT('Ctrl Pts',(56.4935376544102,-3.35142216258106,127.202146171337));
#57371=CARTESIAN_POINT('Ctrl Pts',(56.4857900995278,-3.45062417595126,127.297053837237));
#57372=CARTESIAN_POINT('Ctrl Pts',(56.4780425446454,-3.54570794400332,127.395968292975));
#57373=CARTESIAN_POINT('Ctrl Pts',(56.4702966872692,-3.64077087899478,127.49486107634));
#57374=CARTESIAN_POINT('Ctrl Pts',(56.4625508298929,-3.73171709344343,127.597758621025));
#57375=CARTESIAN_POINT('Ctrl Pts',(56.4548049725166,-3.81820176637489,127.704277016475));
#57376=CARTESIAN_POINT('Ctrl Pts',(56.4470591348612,-3.90468621911755,127.810795140732));
#57377=CARTESIAN_POINT('Ctrl Pts',(56.4393132972058,-3.98670890717965,127.920933793503));
#57378=CARTESIAN_POINT('Ctrl Pts',(56.4315674595503,-4.06396551489316,128.034276258515));
#57379=CARTESIAN_POINT('Ctrl Pts',(56.4235101322896,-4.14432890476678,128.152176655317));
#57380=CARTESIAN_POINT('Ctrl Pts',(56.4154528050289,-4.21953462021701,128.273543546488));
#57381=CARTESIAN_POINT('Ctrl Pts',(56.4073954777682,-4.28929058584831,128.397875767696));
#57382=CARTESIAN_POINT('Ctrl Pts',(56.3996411023675,-4.35642375872829,128.517533153633));
#57383=CARTESIAN_POINT('Ctrl Pts',(56.3918867269668,-4.41850943101319,128.639936542851));
#57384=CARTESIAN_POINT('Ctrl Pts',(56.3841323515661,-4.47533513597769,128.764615907269));
#57385=CARTESIAN_POINT('Ctrl Pts',(56.3763737897062,-4.53219152020112,128.889362584015));
#57386=CARTESIAN_POINT('Ctrl Pts',(56.3686152278464,-4.58378213233051,129.01638732268));
#57387=CARTESIAN_POINT('Ctrl Pts',(56.3608566659866,-4.62994337852036,129.145201983138));
#57388=CARTESIAN_POINT('Ctrl Pts',(56.3530891692021,-4.67615778498204,129.274164989297));
#57389=CARTESIAN_POINT('Ctrl Pts',(56.3453216724176,-4.71693023038613,129.404921659424));
#57390=CARTESIAN_POINT('Ctrl Pts',(56.3375541756331,-4.75214743207228,129.53697044625));
#57391=CARTESIAN_POINT('Ctrl Pts',(56.336662627896,-4.75618963734661,129.552126911756));
#57392=CARTESIAN_POINT('Ctrl Pts',(56.3357710801589,-4.76015871201734,129.567300391007));
#57393=CARTESIAN_POINT('Ctrl Pts',(56.3348795324218,-4.7640545282341,129.582490119308));
#57394=CARTESIAN_POINT('Ctrl Pts',(58.0850005708556,-4.76405452823401,129.582490119308));
#57395=CARTESIAN_POINT('Ctrl Pts',(58.0773406290219,-4.7977338926578,129.713805450041));
#57396=CARTESIAN_POINT('Ctrl Pts',(58.0696806871882,-4.82595685688633,129.846425082283));
#57397=CARTESIAN_POINT('Ctrl Pts',(58.0620207453545,-4.84864573011683,129.979850068016));
#57398=CARTESIAN_POINT('Ctrl Pts',(58.0541605271336,-4.87192782528797,130.116763575552));
#57399=CARTESIAN_POINT('Ctrl Pts',(58.0463003089126,-4.88938240304201,130.254524676396));
#57400=CARTESIAN_POINT('Ctrl Pts',(58.0384400906917,-4.90098241019879,130.392590684931));
#57401=CARTESIAN_POINT('Ctrl Pts',(58.0305798724708,-4.91258241735558,130.530656693466));
#57402=CARTESIAN_POINT('Ctrl Pts',(58.0227196542499,-4.91832789773181,130.669027157201));
#57403=CARTESIAN_POINT('Ctrl Pts',(58.014859436029,-4.91824920186863,130.807162548786));
#57404=CARTESIAN_POINT('',(58.360140563961,-4.91824943933405,130.80670901921));
#57405=CARTESIAN_POINT('Ctrl Pts',(58.429932073253,-4.76405452823401,129.582490119308));
#57406=CARTESIAN_POINT('Ctrl Pts',(58.4220562464825,-4.79868725641491,129.71752260086));
#57407=CARTESIAN_POINT('Ctrl Pts',(58.4141804197121,-4.82759868947349,129.854122001551));
#57408=CARTESIAN_POINT('Ctrl Pts',(58.4063045929416,-4.85065810554657,129.991772772718));
#57409=CARTESIAN_POINT('Ctrl Pts',(58.398432893145,-4.87370543836646,130.129351414169));
#57410=CARTESIAN_POINT('Ctrl Pts',(58.3905611933484,-4.89090679894885,130.267979961966));
#57411=CARTESIAN_POINT('Ctrl Pts',(58.3826894935518,-4.90218243012851,130.407132113756));
#57412=CARTESIAN_POINT('Ctrl Pts',(58.3751731837041,-4.91294899133708,130.54000185166));
#57413=CARTESIAN_POINT('Ctrl Pts',(58.3676568738563,-4.91831311720544,130.673348625442));
#57414=CARTESIAN_POINT('Ctrl Pts',(58.3601405640086,-4.91824943933446,130.806709018365));
#57415=CARTESIAN_POINT('Ctrl Pts',(58.360140563961,-4.91824943933405,130.80670901921));
#57416=CARTESIAN_POINT('Ctrl Pts',(58.3516434233677,-4.91817745187903,130.957472097261));
#57417=CARTESIAN_POINT('Ctrl Pts',(58.3431462827744,-4.91116916197694,131.108002699756));
#57418=CARTESIAN_POINT('Ctrl Pts',(58.3346491421812,-4.89731318198262,131.257689041646));
#57419=CARTESIAN_POINT('Ctrl Pts',(58.3261097318004,-4.88338827417381,131.408120011662));
#57420=CARTESIAN_POINT('Ctrl Pts',(58.3175703214197,-4.86254746430372,131.557698053368));
#57421=CARTESIAN_POINT('Ctrl Pts',(58.3090309110389,-4.83493105773902,131.705817621205));
#57422=CARTESIAN_POINT('Ctrl Pts',(58.3004697617653,-4.80724434771368,131.854314259035));
#57423=CARTESIAN_POINT('Ctrl Pts',(58.2919086124917,-4.77274761906352,132.001344755767));
#57424=CARTESIAN_POINT('Ctrl Pts',(58.2833474632182,-4.73163116557672,132.146317984789));
#57425=CARTESIAN_POINT('Ctrl Pts',(58.2747562731633,-4.69037043585458,132.291799919935));
#57426=CARTESIAN_POINT('Ctrl Pts',(58.2661650831084,-4.64244356693815,132.435209897501));
#57427=CARTESIAN_POINT('Ctrl Pts',(58.2575738930536,-4.58809023710242,132.57597317078));
#57428=CARTESIAN_POINT('Ctrl Pts',(58.2537309360275,-4.56377724792976,132.638938511625));
#57429=CARTESIAN_POINT('Ctrl Pts',(58.2498879790014,-4.53817901021214,132.701374596378));
#57430=CARTESIAN_POINT('Ctrl Pts',(58.2460450219752,-4.51131992370108,132.763231621108));
#57431=CARTESIAN_POINT('Ctrl Pts',(58.2382706878561,-4.45698376764921,132.888368898106));
#57432=CARTESIAN_POINT('Ctrl Pts',(58.2304963537371,-4.39735091938783,133.011441864516));
#57433=CARTESIAN_POINT('Ctrl Pts',(58.2227220196179,-4.33259960350039,133.131969635045));
#57434=CARTESIAN_POINT('Ctrl Pts',(58.2149572666708,-4.2679280878227,133.252348865869));
#57435=CARTESIAN_POINT('Ctrl Pts',(58.2071925137237,-4.19815083891782,133.370188800859));
#57436=CARTESIAN_POINT('Ctrl Pts',(58.1994277607765,-4.12349425874082,133.485028101726));
#57437=CARTESIAN_POINT('Ctrl Pts',(58.1916707198915,-4.04891182853172,133.59975334258));
#57438=CARTESIAN_POINT('Ctrl Pts',(58.1839136790064,-3.9694599229629,133.71148355452));
#57439=CARTESIAN_POINT('Ctrl Pts',(58.1761566381214,-3.88541083446654,133.819781933056));
#57440=CARTESIAN_POINT('Ctrl Pts',(58.1684054468812,-3.80142512804163,133.927998642942));
#57441=CARTESIAN_POINT('Ctrl Pts',(58.160654255641,-3.71284937782166,134.032788363015));
#57442=CARTESIAN_POINT('Ctrl Pts',(58.1529030644009,-3.6199989570318,134.133743535404));
#57443=CARTESIAN_POINT('Ctrl Pts',(58.1451551676238,-3.52718800014777,134.234655799151));
#57444=CARTESIAN_POINT('Ctrl Pts',(58.1374072708467,-3.43010625037576,134.331736469572));
#57445=CARTESIAN_POINT('Ctrl Pts',(58.1296593740695,-3.32910895981231,134.424611519948));
#57446=CARTESIAN_POINT('Ctrl Pts',(58.1219130979854,-3.2281327957048,134.517467142865));
#57447=CARTESIAN_POINT('Ctrl Pts',(58.1141668219013,-3.12324300753604,134.606118631086));
#57448=CARTESIAN_POINT('Ctrl Pts',(58.1064205458172,-3.01483096984557,134.69022954044));
#57449=CARTESIAN_POINT('Ctrl Pts',(58.0986742125518,-2.90641813188207,134.774341070682));
#57450=CARTESIAN_POINT('Ctrl Pts',(58.0909278792864,-2.79448330141324,134.853911715517));
#57451=CARTESIAN_POINT('Ctrl Pts',(58.083181546021,-2.67944980044767,134.928646231994));
#57452=CARTESIAN_POINT('Ctrl Pts',(58.075433478018,-2.56439053852699,135.003397484748));
#57453=CARTESIAN_POINT('Ctrl Pts',(58.067685410015,-2.44623155306565,135.073310241108));
#57454=CARTESIAN_POINT('Ctrl Pts',(58.0599373420119,-2.32542356957031,135.138133602459));
#57455=CARTESIAN_POINT('Ctrl Pts',(58.0521810392701,-2.20448718991249,135.20302585885));
#57456=CARTESIAN_POINT('Ctrl Pts',(58.0444247365281,-2.08089653323544,135.262817729883));
#57457=CARTESIAN_POINT('Ctrl Pts',(58.0366684337862,-1.95512575988806,135.31730492539));
#57458=CARTESIAN_POINT('Ctrl Pts',(58.028907991272,-1.82928785889206,135.371821202354));
#57459=CARTESIAN_POINT('Ctrl Pts',(58.0211475487578,-1.70126788742459,135.421027022057));
#57460=CARTESIAN_POINT('Ctrl Pts',(58.0133871062436,-1.57155729410359,135.464767330917));
#57461=CARTESIAN_POINT('Ctrl Pts',(58.0056142059781,-1.44163847782304,135.508577855604));
#57462=CARTESIAN_POINT('Ctrl Pts',(57.9978413057127,-1.31002399196821,135.546905227379));
#57463=CARTESIAN_POINT('Ctrl Pts',(57.9900684054472,-1.17721853415224,135.579644858881));
#57464=CARTESIAN_POINT('Ctrl Pts',(57.9825780696855,-1.04924088925148,135.61119432231));
#57465=CARTESIAN_POINT('Ctrl Pts',(57.9750877339239,-0.920157660517325,
135.637555187488));
#57466=CARTESIAN_POINT('Ctrl Pts',(57.9675973981622,-0.790424960486675,
135.658679462094));
#57467=CARTESIAN_POINT('Ctrl Pts',(57.9598230640431,-0.655773405696139,
135.680604669993));
#57468=CARTESIAN_POINT('Ctrl Pts',(57.952048729924,-0.519995622350196,135.696957810429));
#57469=CARTESIAN_POINT('Ctrl Pts',(57.9442743958049,-0.383592527604621,
135.707628898546));
#57470=CARTESIAN_POINT('Ctrl Pts',(57.9365096428578,-0.247357537482625,
135.718286835501));
#57471=CARTESIAN_POINT('Ctrl Pts',(57.9287448899108,-0.110499155338198,
135.723276623065));
#57472=CARTESIAN_POINT('Ctrl Pts',(57.9209801369637,0.0264721060725106,
135.722539375003));
#57473=CARTESIAN_POINT('Ctrl Pts',(57.9132230960787,0.163307325695244,135.721802859185));
#57474=CARTESIAN_POINT('Ctrl Pts',(57.9054660551937,0.300254813044118,135.715350629551));
#57475=CARTESIAN_POINT('Ctrl Pts',(57.8977090143087,0.436799891420765,135.703175669939));
#57476=CARTESIAN_POINT('Ctrl Pts',(57.8899578230685,0.573242000091827,135.691009891559));
#57477=CARTESIAN_POINT('Ctrl Pts',(57.8822066318283,0.709281915964279,135.673130007634));
#57478=CARTESIAN_POINT('Ctrl Pts',(57.8744554405882,0.844406282128312,135.649581055606));
#57479=CARTESIAN_POINT('Ctrl Pts',(57.8667075438111,0.979473216832164,135.626042112512));
#57480=CARTESIAN_POINT('Ctrl Pts',(57.8589596470341,1.11362499143005,135.59683896062));
#57481=CARTESIAN_POINT('Ctrl Pts',(57.851211750257,1.2463549042146,135.562068313005));
#57482=CARTESIAN_POINT('Ctrl Pts',(57.8434654741729,1.37905705276273,135.52730493866));
#57483=CARTESIAN_POINT('Ctrl Pts',(57.8357191980888,1.51033755312422,135.486976484057));
#57484=CARTESIAN_POINT('Ctrl Pts',(57.8279729220046,1.63970179779126,135.441230367389));
#57485=CARTESIAN_POINT('Ctrl Pts',(57.8202265887393,1.76906699739577,135.395483913033));
#57486=CARTESIAN_POINT('Ctrl Pts',(57.8124802554739,1.89651554448227,135.344319847155));
#57487=CARTESIAN_POINT('Ctrl Pts',(57.8047339222086,2.02157022690707,135.287934736523));
#57488=CARTESIAN_POINT('Ctrl Pts',(57.7969858542056,2.14665291446093,135.231536998836));
#57489=CARTESIAN_POINT('Ctrl Pts',(57.7892377862026,2.26934031425386,135.169916050458));
#57490=CARTESIAN_POINT('Ctrl Pts',(57.7814897181996,2.38917771002942,135.103315482693));
#57491=CARTESIAN_POINT('Ctrl Pts',(57.7737334154578,2.50914247041529,135.036644131052));
#57492=CARTESIAN_POINT('Ctrl Pts',(57.7659771127159,2.62625083371306,134.964982778112));
#57493=CARTESIAN_POINT('Ctrl Pts',(57.758220809974,2.74007462956671,134.888619924577));
#57494=CARTESIAN_POINT('Ctrl Pts',(57.7504603674599,2.85395917660753,134.812216313888));
#57495=CARTESIAN_POINT('Ctrl Pts',(57.7426999249457,2.96455534794491,134.731106433647));
#57496=CARTESIAN_POINT('Ctrl Pts',(57.7349394824315,3.07146705262637,134.645619943247));
#57497=CARTESIAN_POINT('Ctrl Pts',(57.727166582166,3.17855038146722,134.559996222343));
#57498=CARTESIAN_POINT('Ctrl Pts',(57.7193936819006,3.28193712929566,134.46998210852));
#57499=CARTESIAN_POINT('Ctrl Pts',(57.7116207816352,3.38126650241594,134.375945686151));
#57500=CARTESIAN_POINT('Ctrl Pts',(57.7041304458732,3.4769850026265,134.285327724599));
#57501=CARTESIAN_POINT('Ctrl Pts',(57.6966401101113,3.56893578324734,134.190975039964));
#57502=CARTESIAN_POINT('Ctrl Pts',(57.6891497743494,3.65683192701093,134.093245431617));
#57503=CARTESIAN_POINT('Ctrl Pts',(57.6813754402303,3.74806067978168,133.991810375464));
#57504=CARTESIAN_POINT('Ctrl Pts',(57.6736011061112,3.83521024843067,133.886415952762));
#57505=CARTESIAN_POINT('Ctrl Pts',(57.6658267719921,3.9179173416248,133.777424149799));
#57506=CARTESIAN_POINT('Ctrl Pts',(57.658062019045,4.00052250571843,133.668566669493));
#57507=CARTESIAN_POINT('Ctrl Pts',(57.650297266098,4.07869585381554,133.556120938625));
#57508=CARTESIAN_POINT('Ctrl Pts',(57.6425325131509,4.15211189864189,133.440484636586));
#57509=CARTESIAN_POINT('Ctrl Pts',(57.6347754722659,4.22545502561742,133.324963186153));
#57510=CARTESIAN_POINT('Ctrl Pts',(57.6270184313808,4.29405004412983,133.206257798771));
#57511=CARTESIAN_POINT('Ctrl Pts',(57.6192613904958,4.35761285595699,133.084797694115));
#57512=CARTESIAN_POINT('Ctrl Pts',(57.6115101992557,4.42112773457331,132.963429183469));
#57513=CARTESIAN_POINT('Ctrl Pts',(57.6037590080156,4.4796177793311,132.839310435393));
#57514=CARTESIAN_POINT('Ctrl Pts',(57.5960078167755,4.53284339955716,132.712897695432));
#57515=CARTESIAN_POINT('Ctrl Pts',(57.5882599199984,4.58604639747478,132.586538684259));
#57516=CARTESIAN_POINT('Ctrl Pts',(57.5805120232213,4.63398926972184,132.45788797999));
#57517=CARTESIAN_POINT('Ctrl Pts',(57.5727641264442,4.67647949909547,132.327424160902));
#57518=CARTESIAN_POINT('Ctrl Pts',(57.5650178503601,4.71896084042909,132.196987632032));
#57519=CARTESIAN_POINT('Ctrl Pts',(57.557271574276,4.75599168656037,132.064739114232));
#57520=CARTESIAN_POINT('Ctrl Pts',(57.5495252981919,4.78742871714996,131.931174417938));
#57521=CARTESIAN_POINT('Ctrl Pts',(57.5417789649266,4.81886597980057,131.797608735699));
#57522=CARTESIAN_POINT('Ctrl Pts',(57.5340326316612,4.84470925494023,131.662727236147));
#57523=CARTESIAN_POINT('Ctrl Pts',(57.5262862983959,4.86486597493708,131.527037660511));
#57524=CARTESIAN_POINT('Ctrl Pts',(57.5185382303929,4.88502720889162,131.391317698135));
#57525=CARTESIAN_POINT('Ctrl Pts',(57.5107901623899,4.89949929621964,131.254789686228));
#57526=CARTESIAN_POINT('Ctrl Pts',(57.5030420943869,4.90824139194049,131.117967857505));
#57527=CARTESIAN_POINT('Ctrl Pts',(57.4952857916451,4.9169927788647,130.981000612914));
#57528=CARTESIAN_POINT('Ctrl Pts',(57.4875294889032,4.92000198397472,130.8437393185));
#57529=CARTESIAN_POINT('Ctrl Pts',(57.4797731861614,4.91728029454729,130.70670014779));
#57530=CARTESIAN_POINT('Ctrl Pts',(57.4720127436472,4.91455715247226,130.569587835147));
#57531=CARTESIAN_POINT('Ctrl Pts',(57.464252301133,4.90609704514428,130.432698272466));
#57532=CARTESIAN_POINT('Ctrl Pts',(57.4564918586188,4.89196322751154,130.296542891236));
#57533=CARTESIAN_POINT('Ctrl Pts',(57.4487189583534,4.87780672101999,130.160168941301));
#57534=CARTESIAN_POINT('Ctrl Pts',(57.440946058088,4.85795836029175,130.02453191505));
#57535=CARTESIAN_POINT('Ctrl Pts',(57.4331731578226,4.83253280732908,129.890134317032));
#57536=CARTESIAN_POINT('Ctrl Pts',(57.4256828220605,4.80803153725963,129.760622410229));
#57537=CARTESIAN_POINT('Ctrl Pts',(57.4181924862984,4.77835159441672,129.632261683571));
#57538=CARTESIAN_POINT('Ctrl Pts',(57.4107021505364,4.74363891975441,129.505486927983));
#57539=CARTESIAN_POINT('Ctrl Pts',(57.4029278164173,4.70761010348175,129.373905469005));
#57540=CARTESIAN_POINT('Ctrl Pts',(57.3951534822982,4.66604526133884,129.243615808824));
#57541=CARTESIAN_POINT('Ctrl Pts',(57.3873791481791,4.61905257480261,129.115119257159));
#57542=CARTESIAN_POINT('Ctrl Pts',(57.379614395232,4.57211780255267,128.98678106601));
#57543=CARTESIAN_POINT('Ctrl Pts',(57.371849642285,4.51976862868185,128.860231950098));
#57544=CARTESIAN_POINT('Ctrl Pts',(57.3640848893379,4.46216369830185,128.73596070651));
#57545=CARTESIAN_POINT('Ctrl Pts',(57.3563278484529,4.4046159819508,128.611812890873));
#57546=CARTESIAN_POINT('Ctrl Pts',(57.3485708075679,4.34182306066696,128.489938797666));
#57547=CARTESIAN_POINT('Ctrl Pts',(57.3408137666829,4.27399248709164,128.370809450489));
#57548=CARTESIAN_POINT('Ctrl Pts',(57.3330625754428,4.2062130650795,128.251769939679));
#57549=CARTESIAN_POINT('Ctrl Pts',(57.3253113842027,4.13340374498811,128.135471393396));
#57550=CARTESIAN_POINT('Ctrl Pts',(57.3175601929626,4.0558188745049,128.02236199792));
#57551=CARTESIAN_POINT('Ctrl Pts',(57.3098122961855,3.97826697966128,127.909300676955));
#57552=CARTESIAN_POINT('Ctrl Pts',(57.3020643994084,3.89594379210233,127.799426132596));
#57553=CARTESIAN_POINT('Ctrl Pts',(57.2943165026313,3.80914789303409,127.693159018265));
#57554=CARTESIAN_POINT('Ctrl Pts',(57.2865702265472,3.72237014979684,127.586914132723));
#57555=CARTESIAN_POINT('Ctrl Pts',(57.2788239504631,3.63112180316098,127.484275478884));
#57556=CARTESIAN_POINT('Ctrl Pts',(57.271077674379,3.53574252434591,127.38563163386));
#57557=CARTESIAN_POINT('Ctrl Pts',(57.2633313411137,3.44036254146268,127.286987060669));
#57558=CARTESIAN_POINT('Ctrl Pts',(57.2555850078483,3.34085183731661,127.192337636203));
#57559=CARTESIAN_POINT('Ctrl Pts',(57.247838674583,3.23758755391919,127.102035686768));
#57560=CARTESIAN_POINT('Ctrl Pts',(57.24009060658,3.13430014520149,127.011713514838));
#57561=CARTESIAN_POINT('Ctrl Pts',(57.232342538577,3.02725777881118,126.92574101258));
#57562=CARTESIAN_POINT('Ctrl Pts',(57.2245944705741,2.91687101558521,126.844430499377));
#57563=CARTESIAN_POINT('Ctrl Pts',(57.2168381678322,2.80636693199382,126.763033568393));
#57564=CARTESIAN_POINT('Ctrl Pts',(57.2090818650904,2.6925116664282,126.686308756485));
#57565=CARTESIAN_POINT('Ctrl Pts',(57.2013255623486,2.57574559134194,126.614525571746));
#57566=CARTESIAN_POINT('Ctrl Pts',(57.1935651198344,2.45891719468549,126.542704074159));
#57567=CARTESIAN_POINT('Ctrl Pts',(57.1858046773202,2.33917523402769,126.475829649714));
#57568=CARTESIAN_POINT('Ctrl Pts',(57.1780442348061,2.21698418201019,126.414125521445));
#57569=CARTESIAN_POINT('Ctrl Pts',(57.1702713345407,2.09459697806837,126.35232234023));
#57570=CARTESIAN_POINT('Ctrl Pts',(57.1624984342752,1.96975318264655,126.295706202438));
#57571=CARTESIAN_POINT('Ctrl Pts',(57.1547255340098,1.84293754466647,126.244452255662));
#57572=CARTESIAN_POINT('Ctrl Pts',(57.1472351982477,1.72073197455491,126.195061518952));
#57573=CARTESIAN_POINT('Ctrl Pts',(57.1397448624856,1.5966957257728,126.150649987302));
#57574=CARTESIAN_POINT('Ctrl Pts',(57.1322545267235,1.47127348488866,126.111329891568));
#57575=CARTESIAN_POINT('Ctrl Pts',(57.1244801926044,1.34109582162124,126.070518962453));
#57576=CARTESIAN_POINT('Ctrl Pts',(57.1167058584853,1.20901262805993,126.035063897496));
#57577=CARTESIAN_POINT('Ctrl Pts',(57.1089315243663,1.07550414499935,126.005144650703));
#57578=CARTESIAN_POINT('Ctrl Pts',(57.1011667714192,0.942160199212331,125.975262276708));
#57579=CARTESIAN_POINT('Ctrl Pts',(57.093402018472,0.807394836761404,125.950902231007));
#57580=CARTESIAN_POINT('Ctrl Pts',(57.085637265525,0.671705048036853,125.932195247739));
#57581=CARTESIAN_POINT('Ctrl Pts',(57.0778802246399,0.536150028323353,125.91350684451));
#57582=CARTESIAN_POINT('Ctrl Pts',(57.070123183755,0.399672794298141,125.900460383256));
#57583=CARTESIAN_POINT('Ctrl Pts',(57.06236614287,0.262781818728084,125.893135843821));
#57584=CARTESIAN_POINT('Ctrl Pts',(57.0546149516299,0.125994073707748,125.885816827879));
#57585=CARTESIAN_POINT('Ctrl Pts',(57.0468637603897,-0.0112064030019008,
125.884211165923));
#57586=CARTESIAN_POINT('Ctrl Pts',(57.0391125691496,-0.148305058451984,
125.888347123673));
#57587=CARTESIAN_POINT('Ctrl Pts',(57.0313646723725,-0.285345443316461,
125.892481323531));
#57588=CARTESIAN_POINT('Ctrl Pts',(57.0236167755954,-0.422283703026263,
125.902352277677));
#57589=CARTESIAN_POINT('Ctrl Pts',(57.0158688788183,-0.558604539508258,
125.917936154736));
#57590=CARTESIAN_POINT('Ctrl Pts',(57.0081226027342,-0.694896860610184,
125.933516771985));
#57591=CARTESIAN_POINT('Ctrl Pts',(57.0003763266501,-0.830571627184759,
125.954807890808));
#57592=CARTESIAN_POINT('Ctrl Pts',(56.992630050566,-0.965118317710622,125.981733771612));
#57593=CARTESIAN_POINT('Ctrl Pts',(56.9848837173007,-1.09966600142941,126.008659851176));
#57594=CARTESIAN_POINT('Ctrl Pts',(56.9771373840353,-1.23308520911929,126.041220698999));
#57595=CARTESIAN_POINT('Ctrl Pts',(56.9693910507699,-1.36487566420962,126.0792894558));
#57596=CARTESIAN_POINT('Ctrl Pts',(56.9616429827669,-1.4966956328586,126.117366737836));
#57597=CARTESIAN_POINT('Ctrl Pts',(56.9538949147639,-1.62688574756502,126.160954274813));
#57598=CARTESIAN_POINT('Ctrl Pts',(56.9461468467609,-1.75496132702647,126.209875466524));
#57599=CARTESIAN_POINT('Ctrl Pts',(56.9383905440191,-1.88317302673807,126.258848652261));
#57600=CARTESIAN_POINT('Ctrl Pts',(56.9306342412772,-2.00926533606393,126.313166676787));
#57601=CARTESIAN_POINT('Ctrl Pts',(56.9228779385354,-2.1327734781451,126.372604717991));
#57602=CARTESIAN_POINT('Ctrl Pts',(56.9151174960212,-2.25634754024046,126.432074483067));
#57603=CARTESIAN_POINT('Ctrl Pts',(56.907357053507,-2.37733434210384,126.496669525926));
#57604=CARTESIAN_POINT('Ctrl Pts',(56.8995966109928,-2.49529502106704,126.566119730082));
#57605=CARTESIAN_POINT('Ctrl Pts',(56.8918237107274,-2.61344506098418,126.635681421872));
#57606=CARTESIAN_POINT('Ctrl Pts',(56.8840508104619,-2.72855894206567,126.710113637318));
#57607=CARTESIAN_POINT('Ctrl Pts',(56.8762779101965,-2.84022728904805,126.789103214977));
#57608=CARTESIAN_POINT('Ctrl Pts',(56.8687875744345,-2.94783621034038,126.865221322524));
#57609=CARTESIAN_POINT('Ctrl Pts',(56.8612972386726,-3.0522455119358,126.945571013843));
#57610=CARTESIAN_POINT('Ctrl Pts',(56.8538069029107,-3.1531204068837,127.029838825048));
#57611=CARTESIAN_POINT('Ctrl Pts',(56.8461428595284,-3.25633468133444,127.116060882554));
#57612=CARTESIAN_POINT('Ctrl Pts',(56.8384788161462,-3.35619520654422,127.206674880249));
#57613=CARTESIAN_POINT('Ctrl Pts',(56.830814772764,-3.45229711328055,127.30138649489));
#57614=CARTESIAN_POINT('Ctrl Pts',(56.8231595226317,-3.54828875862553,127.395989443276));
#57615=CARTESIAN_POINT('Ctrl Pts',(56.8155042724994,-3.64053007409822,127.49468038369));
#57616=CARTESIAN_POINT('Ctrl Pts',(56.8078490223671,-3.72864790079033,127.597123817074));
#57617=CARTESIAN_POINT('Ctrl Pts',(56.8002007863767,-3.81668498930518,127.699473386408));
#57618=CARTESIAN_POINT('Ctrl Pts',(56.7925525503864,-3.90060584027376,127.805568309344));
#57619=CARTESIAN_POINT('Ctrl Pts',(56.784904314396,-3.98007334735288,127.915035573167));
#57620=CARTESIAN_POINT('Ctrl Pts',(56.777261320038,-4.0594863922711,128.024427814834));
#57621=CARTESIAN_POINT('Ctrl Pts',(56.76961832568,-4.1344519278296,128.137187475971));
#57622=CARTESIAN_POINT('Ctrl Pts',(56.761975331322,-4.20467280688083,128.252908158754));
#57623=CARTESIAN_POINT('Ctrl Pts',(56.7543350965373,-4.27486833203923,128.368587059523));
#57624=CARTESIAN_POINT('Ctrl Pts',(56.7466948617526,-4.34032239617133,128.487224513723));
#57625=CARTESIAN_POINT('Ctrl Pts',(56.7390546269679,-4.40078116245027,128.608385157156));
#57626=CARTESIAN_POINT('Ctrl Pts',(56.7314160671341,-4.46122667449377,128.729519238821));
#57627=CARTESIAN_POINT('Ctrl Pts',(56.7237775073004,-4.51667889069151,128.853175047383));
#57628=CARTESIAN_POINT('Ctrl Pts',(56.7161389474666,-4.56693025803882,128.978893258036));
#57629=CARTESIAN_POINT('Ctrl Pts',(56.7084983915517,-4.61719475689396,129.104644320923));
#57630=CARTESIAN_POINT('Ctrl Pts',(56.7008578356368,-4.6622555425973,129.232458488203));
#57631=CARTESIAN_POINT('Ctrl Pts',(56.6932172797219,-4.70195355749686,129.361857305389));
#57632=CARTESIAN_POINT('Ctrl Pts',(56.6889028262341,-4.72437015136132,129.434925964835));
#57633=CARTESIAN_POINT('Ctrl Pts',(56.6845883727463,-4.7450776601896,129.508499598817));
#57634=CARTESIAN_POINT('Ctrl Pts',(56.6802739192584,-4.76405452823399,129.582490119308));
#57635=CARTESIAN_POINT('Origin',(213.235140564004,0.,130.804360617566));
#57636=CARTESIAN_POINT('',(54.5845740201626,-4.7640545282341,129.582490119308));
#57637=CARTESIAN_POINT('',(54.9301858291403,-4.76405452823401,129.582490119308));
#57638=CARTESIAN_POINT('',(213.235140564004,-4.76405452823405,129.582490119308));
#57639=CARTESIAN_POINT('',(56.2648594359518,-4.91824814598434,130.800090134965));
#57640=CARTESIAN_POINT('Ctrl Pts',(56.2648594359517,-4.91824814598434,130.800090134965));
#57641=CARTESIAN_POINT('Ctrl Pts',(56.2572127733997,-4.91836515257441,130.934844798205));
#57642=CARTESIAN_POINT('Ctrl Pts',(56.2495661108478,-4.912939801848,131.069789027858));
#57643=CARTESIAN_POINT('Ctrl Pts',(56.2419194482958,-4.90195208324078,131.204421658048));
#57644=CARTESIAN_POINT('Ctrl Pts',(56.2342795697229,-4.89097411273652,131.338934844631));
#57645=CARTESIAN_POINT('Ctrl Pts',(56.22663969115,-4.8744436226077,131.473136581709));
#57646=CARTESIAN_POINT('Ctrl Pts',(56.2189998125771,-4.85239265815541,131.606525534263));
#57647=CARTESIAN_POINT('Ctrl Pts',(56.2113643828619,-4.83035453443104,131.7398368117));
#57648=CARTESIAN_POINT('Ctrl Pts',(56.2037289531468,-4.80280239497657,131.872335848918));
#57649=CARTESIAN_POINT('Ctrl Pts',(56.1960935234316,-4.7698200926489,132.0035267221));
#57650=CARTESIAN_POINT('Ctrl Pts',(56.1884603794111,-4.73684766369814,132.134678322798));
#57651=CARTESIAN_POINT('Ctrl Pts',(56.1808272353906,-4.69844840147115,132.264522146939));
#57652=CARTESIAN_POINT('Ctrl Pts',(56.1731940913702,-4.65475710850639,132.392573236616));
#57653=CARTESIAN_POINT('Ctrl Pts',(56.1655614659798,-4.61106878412397,132.520615625927));
#57654=CARTESIAN_POINT('Ctrl Pts',(56.1579288405894,-4.56208927434166,132.646865141058));
#57655=CARTESIAN_POINT('Ctrl Pts',(56.1502962151989,-4.50800284216768,132.770853291722));
#57656=CARTESIAN_POINT('Ctrl Pts',(56.1426623420016,-4.4539075677641,132.894861712381));
#57657=CARTESIAN_POINT('Ctrl Pts',(56.1350284688042,-4.39470387265641,133.016607663781));
#57658=CARTESIAN_POINT('Ctrl Pts',(56.1273945956068,-4.33062338238191,133.135644423212));
#57659=CARTESIAN_POINT('Ctrl Pts',(56.1197530945517,-4.2664788621123,133.254800125602));
#57660=CARTESIAN_POINT('Ctrl Pts',(56.1121115934966,-4.19744800635254,133.371240873789));
#57661=CARTESIAN_POINT('Ctrl Pts',(56.1044700924415,-4.12380763749675,133.484545990152));
#57662=CARTESIAN_POINT('Ctrl Pts',(56.0968247204177,-4.05012996450993,133.597908503687));
#57663=CARTESIAN_POINT('Ctrl Pts',(56.089179348394,-3.97183836277016,133.708131894121));
#57664=CARTESIAN_POINT('Ctrl Pts',(56.0815339763703,-3.88925109250205,133.814827193028));
#57665=CARTESIAN_POINT('Ctrl Pts',(56.0738766440318,-3.80653462384529,133.921689404591));
#57666=CARTESIAN_POINT('Ctrl Pts',(56.0662193116933,-3.71950932307574,134.025012191351));
#57667=CARTESIAN_POINT('Ctrl Pts',(56.0585619793549,-3.62853201158557,134.124441716485));
#57668=CARTESIAN_POINT('Ctrl Pts',(56.0517256621137,-3.54730923900561,134.213210460861));
#57669=CARTESIAN_POINT('Ctrl Pts',(56.0448893448725,-3.46293714824102,134.298876441918));
#57670=CARTESIAN_POINT('Ctrl Pts',(56.0380530276313,-3.37569157973648,134.381215300244));
#57671=CARTESIAN_POINT('Ctrl Pts',(56.0302786935123,-3.27647497289476,134.474851943049));
#57672=CARTESIAN_POINT('Ctrl Pts',(56.0225043593932,-3.17320225053233,134.564505590316));
#57673=CARTESIAN_POINT('Ctrl Pts',(56.0147300252741,-3.06622657670409,134.649804368658));
#57674=CARTESIAN_POINT('Ctrl Pts',(56.006965272327,-2.95938274083331,134.73499802388));
#57675=CARTESIAN_POINT('Ctrl Pts',(55.9992005193799,-2.84884533636479,134.815847247478));
#57676=CARTESIAN_POINT('Ctrl Pts',(55.9914357664329,-2.7350041173699,134.892017102701));
#57677=CARTESIAN_POINT('Ctrl Pts',(55.9836787255479,-2.6212759670786,134.968111304951));
#57678=CARTESIAN_POINT('Ctrl Pts',(55.9759216846628,-2.50425085522174,135.039535171784));
#57679=CARTESIAN_POINT('Ctrl Pts',(55.9681646437778,-2.38435106029703,135.105994386701));
#57680=CARTESIAN_POINT('Ctrl Pts',(55.9604134525377,-2.26454168274003,135.172403484207));
#57681=CARTESIAN_POINT('Ctrl Pts',(55.9526622612976,-2.1418622775962,135.233855192998));
#57682=CARTESIAN_POINT('Ctrl Pts',(55.9449110700574,-2.01676320950764,135.290099042762));
#57683=CARTESIAN_POINT('Ctrl Pts',(55.9371631732803,-1.89171731186048,135.346318987388));
#57684=CARTESIAN_POINT('Ctrl Pts',(55.9294152765033,-1.76425415255729,135.397335315446));
#57685=CARTESIAN_POINT('Ctrl Pts',(55.9216673797262,-1.6348475521722,135.442944080613));
#57686=CARTESIAN_POINT('Ctrl Pts',(55.9139211036421,-1.50546802085839,135.48854330541));
#57687=CARTESIAN_POINT('Ctrl Pts',(55.906174827558,-1.37414622556528,135.52873708735));
#57688=CARTESIAN_POINT('Ctrl Pts',(55.8984285514739,-1.24137439465677,135.563370249285));
#57689=CARTESIAN_POINT('Ctrl Pts',(55.8906822182086,-1.10860158365659,135.598003666873));
#57690=CARTESIAN_POINT('Ctrl Pts',(55.8829358849432,-0.974379093989027,
135.627076283868));
#57691=CARTESIAN_POINT('Ctrl Pts',(55.8751895516779,-0.839212299300182,
135.650483374905));
#57692=CARTESIAN_POINT('Ctrl Pts',(55.8674414836749,-0.704015234944847,
135.673895707799));
#57693=CARTESIAN_POINT('Ctrl Pts',(55.8596934156719,-0.567873829924174,
135.69163992336));
#57694=CARTESIAN_POINT('Ctrl Pts',(55.8519453476689,-0.431301188699605,
135.703662848203));
#57695=CARTESIAN_POINT('Ctrl Pts',(55.8441890449271,-0.294583396446707,
135.715698551154));
#57696=CARTESIAN_POINT('Ctrl Pts',(55.8364327421852,-0.157433842520411,
135.722000782282));
#57697=CARTESIAN_POINT('Ctrl Pts',(55.8286764394434,-0.020368822663326,
135.722568438873));
#57698=CARTESIAN_POINT('Ctrl Pts',(55.8209159969292,0.116769352921991,135.723136398439));
#57699=CARTESIAN_POINT('Ctrl Pts',(55.8131555544151,0.253822514040031,135.717963699471));
#57700=CARTESIAN_POINT('Ctrl Pts',(55.8053951119009,0.390277858536041,135.707101305756));
#57701=CARTESIAN_POINT('Ctrl Pts',(55.7976222116355,0.526952253264972,135.696221474763));
#57702=CARTESIAN_POINT('Ctrl Pts',(55.78984931137,0.663026525333134,135.67963374451));
#57703=CARTESIAN_POINT('Ctrl Pts',(55.7820764111046,0.797995563328515,135.657440685256));
#57704=CARTESIAN_POINT('Ctrl Pts',(55.7745860753425,0.928058136826458,135.636054399607));
#57705=CARTESIAN_POINT('Ctrl Pts',(55.7670957395805,1.05709413555759,135.609463307364));
#57706=CARTESIAN_POINT('Ctrl Pts',(55.7596054038185,1.18466539162675,135.577802873672));
#57707=CARTESIAN_POINT('Ctrl Pts',(55.7518310696994,1.31707355064403,135.544942025014));
#57708=CARTESIAN_POINT('Ctrl Pts',(55.7440567355802,1.44832313222639,135.506515745115));
#57709=CARTESIAN_POINT('Ctrl Pts',(55.7362824014612,1.57791037496313,135.462620154247));
#57710=CARTESIAN_POINT('Ctrl Pts',(55.7285176485141,1.70733791300475,135.418778660773));
#57711=CARTESIAN_POINT('Ctrl Pts',(55.720752895567,1.83510682172838,135.369481392018));
#57712=CARTESIAN_POINT('Ctrl Pts',(55.7129881426199,1.96072463776384,135.314875217627));
#57713=CARTESIAN_POINT('Ctrl Pts',(55.7052311017349,2.08621768841351,135.260323278859));
#57714=CARTESIAN_POINT('Ctrl Pts',(55.6974740608499,2.2095635418646,135.200473082578));
#57715=CARTESIAN_POINT('Ctrl Pts',(55.6897170199649,2.3302863294695,135.135520818388));
#57716=CARTESIAN_POINT('Ctrl Pts',(55.6819658287249,2.45091807908036,135.070617535207));
#57717=CARTESIAN_POINT('Ctrl Pts',(55.6742146374847,2.56893035717939,135.000620026842));
#57718=CARTESIAN_POINT('Ctrl Pts',(55.6664634462446,2.68386900290952,134.925771812499));
#57719=CARTESIAN_POINT('Ctrl Pts',(55.6587155494676,2.79875879664992,134.850955410644));
#57720=CARTESIAN_POINT('Ctrl Pts',(55.6509676526906,2.91057722936676,134.771292616236));
#57721=CARTESIAN_POINT('Ctrl Pts',(55.6432197559135,3.01889660364952,134.687071829976));
#57722=CARTESIAN_POINT('Ctrl Pts',(55.6354734798294,3.12719331985427,134.602868660888));
#57723=CARTESIAN_POINT('Ctrl Pts',(55.6277272037452,3.23199212501721,134.514109636208));
#57724=CARTESIAN_POINT('Ctrl Pts',(55.6199809276611,3.33289640275313,134.421125004558));
#57725=CARTESIAN_POINT('Ctrl Pts',(55.6122345943957,3.43380142534151,134.328139686517));
#57726=CARTESIAN_POINT('Ctrl Pts',(55.6044882611304,3.53081157563075,134.230928964205));
#57727=CARTESIAN_POINT('Ctrl Pts',(55.5967419278651,3.62356557840581,134.129861416167));
#57728=CARTESIAN_POINT('Ctrl Pts',(55.5889938598621,3.71634035279655,134.028771234751));
#57729=CARTESIAN_POINT('Ctrl Pts',(55.5812457918591,3.80485681874277,133.92382279692));
#57730=CARTESIAN_POINT('Ctrl Pts',(55.5734977238561,3.88879289447455,133.815419050474));
#57731=CARTESIAN_POINT('Ctrl Pts',(55.5657414211143,3.97281817846658,133.706900091235));
#57732=CARTESIAN_POINT('Ctrl Pts',(55.5579851183724,4.05225310796458,133.594918797105));
#57733=CARTESIAN_POINT('Ctrl Pts',(55.5502288156305,4.12681768476306,133.479908946269));
#57734=CARTESIAN_POINT('Ctrl Pts',(55.5424683731164,4.20142205892128,133.364837711213));
#57735=CARTESIAN_POINT('Ctrl Pts',(55.5347079306022,4.27115070207514,133.246735035075));
#57736=CARTESIAN_POINT('Ctrl Pts',(55.5269474880881,4.33576930941126,133.126059900003));
#57737=CARTESIAN_POINT('Ctrl Pts',(55.5191745878226,4.40049164827245,133.005191046491));
#57738=CARTESIAN_POINT('Ctrl Pts',(55.5114016875572,4.46008738887331,132.881741834197));
#57739=CARTESIAN_POINT('Ctrl Pts',(55.5036287872917,4.5143698014213,132.756192669387));
#57740=CARTESIAN_POINT('Ctrl Pts',(55.4961384515297,4.56667891154403,132.635207532957));
#57741=CARTESIAN_POINT('Ctrl Pts',(55.4886481157677,4.61405418173537,132.512272757855));
#57742=CARTESIAN_POINT('Ctrl Pts',(55.4811577800057,4.65637274220682,132.387830209359));
#57743=CARTESIAN_POINT('Ctrl Pts',(55.4733834458866,4.70029582376101,132.258669383813));
#57744=CARTESIAN_POINT('Ctrl Pts',(55.4656091117675,4.73891031098766,132.127475050747));
#57745=CARTESIAN_POINT('Ctrl Pts',(55.4578347776484,4.77202477724665,131.994722994258));
#57746=CARTESIAN_POINT('Ctrl Pts',(55.4500700247014,4.80509843288537,131.862134542815));
#57747=CARTESIAN_POINT('Ctrl Pts',(55.4423052717543,4.83268546060512,131.727992563388));
#57748=CARTESIAN_POINT('Ctrl Pts',(55.4345405188072,4.85464323751589,131.592790765988));
#57749=CARTESIAN_POINT('Ctrl Pts',(55.4267834779222,4.87657920565311,131.45772325292));
#57750=CARTESIAN_POINT('Ctrl Pts',(55.4190264370373,4.89289698715673,131.321598400063));
#57751=CARTESIAN_POINT('Ctrl Pts',(55.4112693961523,4.9035044232689,131.184922614463));
#57752=CARTESIAN_POINT('Ctrl Pts',(55.4035182049122,4.91410386023096,131.048349897136));
#57753=CARTESIAN_POINT('Ctrl Pts',(55.3957670136721,4.91900149293363,130.911227462234));
#57754=CARTESIAN_POINT('Ctrl Pts',(55.388015822432,4.91815671594552,130.774069036228));
#57755=CARTESIAN_POINT('Ctrl Pts',(55.3802679256549,4.91731229801016,130.636968906211));
#57756=CARTESIAN_POINT('Ctrl Pts',(55.3725200288778,4.91073032710799,130.499833205655));
#57757=CARTESIAN_POINT('Ctrl Pts',(55.3647721321007,4.89842226201817,130.363177656126));
#57758=CARTESIAN_POINT('Ctrl Pts',(55.3570258560166,4.8861167715102,130.226550691992));
#57759=CARTESIAN_POINT('Ctrl Pts',(55.3492795799325,4.86808760430425,130.090404068252));
#57760=CARTESIAN_POINT('Ctrl Pts',(55.3415333038484,4.84439822707602,129.955249976953));
#57761=CARTESIAN_POINT('Ctrl Pts',(55.333786970583,4.82070867497819,129.820094887976));
#57762=CARTESIAN_POINT('Ctrl Pts',(55.3260406373177,4.79135889698251,129.685932731154));
#57763=CARTESIAN_POINT('Ctrl Pts',(55.3182943040523,4.75646371057833,129.553266683262));
#57764=CARTESIAN_POINT('Ctrl Pts',(55.3105462360494,4.72156070963934,129.42057092573));
#57765=CARTESIAN_POINT('Ctrl Pts',(55.3027981680464,4.68110992857659,129.289372321857));
#57766=CARTESIAN_POINT('Ctrl Pts',(55.2950501000435,4.63527628572367,129.160159651289));
#57767=CARTESIAN_POINT('Ctrl Pts',(55.2872937973016,4.58939393032945,129.030809651955));
#57768=CARTESIAN_POINT('Ctrl Pts',(55.2795374945597,4.5381174158025,128.903450171282));
#57769=CARTESIAN_POINT('Ctrl Pts',(55.2717811918179,4.48166034614662,128.778551247394));
#57770=CARTESIAN_POINT('Ctrl Pts',(55.2640207493037,4.42517314365262,128.653585661189));
#57771=CARTESIAN_POINT('Ctrl Pts',(55.2562603067895,4.36350005221747,128.531083597615));
#57772=CARTESIAN_POINT('Ctrl Pts',(55.2484998642753,4.2969005790462,128.411490275008));
#57773=CARTESIAN_POINT('Ctrl Pts',(55.2407269640099,4.23019419448835,128.291704970583));
#57774=CARTESIAN_POINT('Ctrl Pts',(55.2329540637445,4.15854582942361,128.174838071517));
#57775=CARTESIAN_POINT('Ctrl Pts',(55.225181163479,4.08225873123598,128.061306350194));
#57776=CARTESIAN_POINT('Ctrl Pts',(55.2176908277169,4.00874486122184,127.951901792908));
#57777=CARTESIAN_POINT('Ctrl Pts',(55.2102004919547,3.93092384397705,127.845594387566));
#57778=CARTESIAN_POINT('Ctrl Pts',(55.2027101561926,3.84910101915288,127.742726346975));
#57779=CARTESIAN_POINT('Ctrl Pts',(55.1949358220735,3.76417585705744,127.635958033361));
#57780=CARTESIAN_POINT('Ctrl Pts',(55.1871614879544,3.67467042258962,127.532556830017));
#57781=CARTESIAN_POINT('Ctrl Pts',(55.1793871538353,3.5808815356104,127.432940962521));
#57782=CARTESIAN_POINT('Ctrl Pts',(55.1716224008882,3.48720823505236,127.333447862679));
#57783=CARTESIAN_POINT('Ctrl Pts',(55.1638576479411,3.38926225099517,127.237731098473));
#57784=CARTESIAN_POINT('Ctrl Pts',(55.156092894994,3.28738186449743,127.146177524899));
#57785=CARTESIAN_POINT('Ctrl Pts',(55.148335854109,3.18560266703541,127.054714883625));
#57786=CARTESIAN_POINT('Ctrl Pts',(55.140578813224,3.07989713255731,126.967407463899));
#57787=CARTESIAN_POINT('Ctrl Pts',(55.1328217723389,2.97064150159132,126.884606526871));
#57788=CARTESIAN_POINT('Ctrl Pts',(55.1250705810988,2.86146826114637,126.801868030673));
#57789=CARTESIAN_POINT('Ctrl Pts',(55.1173193898586,2.74875056326018,126.723629488105));
#57790=CARTESIAN_POINT('Ctrl Pts',(55.1095681986185,2.6328986723348,126.650202743373));
#57791=CARTESIAN_POINT('Ctrl Pts',(55.1018203018414,2.51709602155398,126.576807206967));
#57792=CARTESIAN_POINT('Ctrl Pts',(55.0940724050643,2.39816215674454,126.508219609622));
#57793=CARTESIAN_POINT('Ctrl Pts',(55.0863245082872,2.27653716281707,126.444709070847));
#57794=CARTESIAN_POINT('Ctrl Pts',(55.0785782322031,2.15493761021641,126.381211817107));
#57795=CARTESIAN_POINT('Ctrl Pts',(55.070831956119,2.03064839452989,126.322789690393));
#57796=CARTESIAN_POINT('Ctrl Pts',(55.0630856800349,1.90413474271972,126.269666146704));
#57797=CARTESIAN_POINT('Ctrl Pts',(55.0553393467695,1.77762015701433,126.216542210869));
#57798=CARTESIAN_POINT('Ctrl Pts',(55.0475930135042,1.64888146289512,126.16871708747));
#57799=CARTESIAN_POINT('Ctrl Pts',(55.0398466802388,1.51840405889225,126.126366156642));
#57800=CARTESIAN_POINT('Ctrl Pts',(55.0320986122359,1.3878974353796,126.084005741616));
#57801=CARTESIAN_POINT('Ctrl Pts',(55.0243505442329,1.25565169897352,126.047122079252));
#57802=CARTESIAN_POINT('Ctrl Pts',(55.0166024762299,1.12216721621925,126.015840616423));
#57803=CARTESIAN_POINT('Ctrl Pts',(55.008846173488,0.988540864568406,125.984525907284));
#57804=CARTESIAN_POINT('Ctrl Pts',(55.0010898707462,0.853673517869801,125.95882538095));
#57805=CARTESIAN_POINT('Ctrl Pts',(54.9933335680043,0.71807609069216,125.938813393412));
#57806=CARTESIAN_POINT('Ctrl Pts',(54.9855731254902,0.582406291084875,125.918790724873));
#57807=CARTESIAN_POINT('Ctrl Pts',(54.977812682976,0.446006023191823,125.90446268573));
#57808=CARTESIAN_POINT('Ctrl Pts',(54.9700522404619,0.309390131792696,125.895851596606));
#57809=CARTESIAN_POINT('Ctrl Pts',(54.9622793401964,0.172554932436135,125.887226684197));
#57810=CARTESIAN_POINT('Ctrl Pts',(54.954506439931,0.0355038089827734,125.884337069335));
#57811=CARTESIAN_POINT('Ctrl Pts',(54.9467335396655,-0.10124868353825,125.887152897062));
#57812=CARTESIAN_POINT('Ctrl Pts',(54.9392432039036,-0.233029878495543,
125.889866362359));
#57813=CARTESIAN_POINT('Ctrl Pts',(54.9317528681417,-0.36453347009346,125.897877638882));
#57814=CARTESIAN_POINT('Ctrl Pts',(54.9242625323797,-0.495306501463842,
125.911114810118));
#57815=CARTESIAN_POINT('Ctrl Pts',(54.9164881982606,-0.631037832067771,
125.924853872725));
#57816=CARTESIAN_POINT('Ctrl Pts',(54.9087138641416,-0.766412066537457,
125.944266453546));
#57817=CARTESIAN_POINT('Ctrl Pts',(54.9009395300225,-0.900916901462603,
125.969328890766));
#57818=CARTESIAN_POINT('Ctrl Pts',(54.8931747770754,-1.03525597119956,125.994360440773));
#57819=CARTESIAN_POINT('Ctrl Pts',(54.8854100241284,-1.1687273926123,126.025027922069));
#57820=CARTESIAN_POINT('Ctrl Pts',(54.8776452711813,-1.30082284446051,126.061255833795));
#57821=CARTESIAN_POINT('Ctrl Pts',(54.8698882302963,-1.43278709724409,126.097447763449));
#57822=CARTESIAN_POINT('Ctrl Pts',(54.8621311894112,-1.56337772552062,126.139189030377));
#57823=CARTESIAN_POINT('Ctrl Pts',(54.8543741485262,-1.69209583614093,126.186352958));
#57824=CARTESIAN_POINT('Ctrl Pts',(54.8466229572861,-1.82071687943326,126.233481318938));
#57825=CARTESIAN_POINT('Ctrl Pts',(54.8388717660459,-1.94746785011645,126.28602406716));
#57826=CARTESIAN_POINT('Ctrl Pts',(54.8311205748058,-2.07186462689798,126.343804595016));
#57827=CARTESIAN_POINT('Ctrl Pts',(54.8233726780287,-2.19620853173031,126.401560564606));
#57828=CARTESIAN_POINT('Ctrl Pts',(54.8156247812516,-2.31819987892907,126.464549721742));
#57829=CARTESIAN_POINT('Ctrl Pts',(54.8078768844745,-2.43737437398574,126.532547276192));
#57830=CARTESIAN_POINT('Ctrl Pts',(54.8001306083904,-2.55652394030714,126.600530607021));
#57831=CARTESIAN_POINT('Ctrl Pts',(54.7923843323063,-2.67285748712374,126.673520057702));
#57832=CARTESIAN_POINT('Ctrl Pts',(54.7846380562222,-2.78593554803751,126.751245003044));
#57833=CARTESIAN_POINT('Ctrl Pts',(54.7768917229569,-2.8990144436683,126.828970522134));
#57834=CARTESIAN_POINT('Ctrl Pts',(54.7691453896915,-3.0088374832503,126.911431384176));
#57835=CARTESIAN_POINT('Ctrl Pts',(54.7613990564261,-3.11499474474874,126.998314006884));
#57836=CARTESIAN_POINT('Ctrl Pts',(54.7536509884232,-3.22117577942869,127.085216086351));
#57837=CARTESIAN_POINT('Ctrl Pts',(54.7459029204202,-3.32368909998309,127.176541649342));
#57838=CARTESIAN_POINT('Ctrl Pts',(54.7381548524173,-3.42215870406584,127.271937530408));
#57839=CARTESIAN_POINT('Ctrl Pts',(54.7303985496754,-3.52073296281641,127.367434799353));
#57840=CARTESIAN_POINT('Ctrl Pts',(54.7226422469336,-3.61525463870687,127.467010755518));
#57841=CARTESIAN_POINT('Ctrl Pts',(54.7148859441917,-3.70538501213266,127.570275743237));
#57842=CARTESIAN_POINT('Ctrl Pts',(54.7071255016775,-3.79556349085239,127.673595846589));
#57843=CARTESIAN_POINT('Ctrl Pts',(54.6993650591634,-3.88134575253328,127.780608599885));
#57844=CARTESIAN_POINT('Ctrl Pts',(54.6916046166493,-3.96243473202198,127.890892914473));
#57845=CARTESIAN_POINT('Ctrl Pts',(54.6838317163838,-4.04365388273929,128.001354267233));
#57846=CARTESIAN_POINT('Ctrl Pts',(54.6760588161184,-4.12016447744683,128.115097351468));
#57847=CARTESIAN_POINT('Ctrl Pts',(54.668285915853,-4.19171350440472,128.231673120125));
#57848=CARTESIAN_POINT('Ctrl Pts',(54.660795580091,-4.26066154401186,128.344011065954));
#57849=CARTESIAN_POINT('Ctrl Pts',(54.6533052443289,-4.32500233359532,128.458979052589));
#57850=CARTESIAN_POINT('Ctrl Pts',(54.6458149085668,-4.38455154430366,128.576157121957));
#57851=CARTESIAN_POINT('Ctrl Pts',(54.6375218026115,-4.45048288965953,128.705893648566));
#57852=CARTESIAN_POINT('Ctrl Pts',(54.6292286966562,-4.51072777099052,128.838707251713));
#57853=CARTESIAN_POINT('Ctrl Pts',(54.620935590701,-4.56500784274803,128.974091113327));
#57854=CARTESIAN_POINT('Ctrl Pts',(54.6126624204053,-4.61915743154251,129.109149527924));
#57855=CARTESIAN_POINT('Ctrl Pts',(54.6043892501097,-4.66737068634018,129.246765592799));
#57856=CARTESIAN_POINT('Ctrl Pts',(54.5961160798141,-4.70941595869355,129.386409846029));
#57857=CARTESIAN_POINT('Ctrl Pts',(54.592268726597,-4.72896868250741,129.45134997753));
#57858=CARTESIAN_POINT('Ctrl Pts',(54.5884213733797,-4.74718815391943,129.516728381839));
#57859=CARTESIAN_POINT('Ctrl Pts',(54.5845740201626,-4.76405452823409,129.582490119308));
#57860=CARTESIAN_POINT('Ctrl Pts',(56.3348795324218,-4.7640545282341,129.582490119308));
#57861=CARTESIAN_POINT('Ctrl Pts',(56.3287532387626,-4.79082473154765,129.686866735733));
#57862=CARTESIAN_POINT('Ctrl Pts',(56.3226269451034,-4.81413419198721,129.792010703334));
#57863=CARTESIAN_POINT('Ctrl Pts',(56.3165006514442,-4.83395290102421,129.8976730125));
#57864=CARTESIAN_POINT('Ctrl Pts',(56.3048853013623,-4.87152884113435,130.098006979447));
#57865=CARTESIAN_POINT('Ctrl Pts',(56.2932699512804,-4.89665970140022,130.300742953123));
#57866=CARTESIAN_POINT('Ctrl Pts',(56.2816546011985,-4.90910818688879,130.504627616511));
#57867=CARTESIAN_POINT('Ctrl Pts',(56.2760562127961,-4.91510813147043,130.602896332211));
#57868=CARTESIAN_POINT('Ctrl Pts',(56.2704578243936,-4.91816248136354,130.701431544498));
#57869=CARTESIAN_POINT('Ctrl Pts',(56.2648594359911,-4.91824814598373,130.800090134272));
#57870=CARTESIAN_POINT('',(56.6101405640451,-4.9182488539182,130.807718210793));
#57871=CARTESIAN_POINT('Ctrl Pts',(56.6802739192584,-4.76405452823399,129.582490119308));
#57872=CARTESIAN_POINT('Ctrl Pts',(56.6726269392178,-4.7976893168761,129.713631649744));
#57873=CARTESIAN_POINT('Ctrl Pts',(56.6649799591772,-4.82588445460891,129.846083118555));
#57874=CARTESIAN_POINT('Ctrl Pts',(56.6573329791366,-4.84856017054484,129.979347081249));
#57875=CARTESIAN_POINT('Ctrl Pts',(56.6494675766213,-4.87188357824431,130.116417493594));
#57876=CARTESIAN_POINT('Ctrl Pts',(56.6416021741061,-4.88936747251833,130.254347052025));
#57877=CARTESIAN_POINT('Ctrl Pts',(56.6337367715908,-4.90098238976537,130.392590441728));
#57878=CARTESIAN_POINT('Ctrl Pts',(56.6258713690756,-4.91259730701242,130.530833831431));
#57879=CARTESIAN_POINT('Ctrl Pts',(56.6180059665604,-4.91834328750372,130.669390592671));
#57880=CARTESIAN_POINT('Ctrl Pts',(56.6101405640451,-4.9182488539182,130.807718210793));
#57881=CARTESIAN_POINT('Ctrl Pts',(56.6101405640086,-4.91824885391776,130.807718211435));
#57882=CARTESIAN_POINT('Ctrl Pts',(56.5985468023716,-4.91810965688516,131.011615905063));
#57883=CARTESIAN_POINT('Ctrl Pts',(56.5869530407347,-4.90529105125989,131.215084519275));
#57884=CARTESIAN_POINT('Ctrl Pts',(56.5753592790977,-4.8799506832259,131.416948890212));
#57885=CARTESIAN_POINT('Ctrl Pts',(56.5675849449786,-4.86295839944731,131.552311433926));
#57886=CARTESIAN_POINT('Ctrl Pts',(56.5598106108596,-4.8403028006108,131.687180835548));
#57887=CARTESIAN_POINT('Ctrl Pts',(56.5520362767405,-4.81201983558532,131.821045507015));
#57888=CARTESIAN_POINT('Ctrl Pts',(56.5442715237934,-4.78377172678651,131.954745202238));
#57889=CARTESIAN_POINT('Ctrl Pts',(56.5365067708463,-4.74991013087439,132.087442252188));
#57890=CARTESIAN_POINT('Ctrl Pts',(56.5287420178992,-4.71052272527471,132.21863029382));
#57891=CARTESIAN_POINT('Ctrl Pts',(56.5209849770142,-4.67117443980159,132.349688037639));
#57892=CARTESIAN_POINT('Ctrl Pts',(56.5132279361292,-4.62631137832631,132.479239383728));
#57893=CARTESIAN_POINT('Ctrl Pts',(56.5054708952443,-4.5760721530097,132.606788622494));
#57894=CARTESIAN_POINT('Ctrl Pts',(56.4977197040041,-4.52587081348363,132.734241675388));
#57895=CARTESIAN_POINT('Ctrl Pts',(56.489968512764,-4.47030152246953,132.859695263841));
#57896=CARTESIAN_POINT('Ctrl Pts',(56.4822173215239,-4.40955245433536,132.982669644074));
#57897=CARTESIAN_POINT('Ctrl Pts',(56.4744694247468,-4.34882920617569,133.105591756914));
#57898=CARTESIAN_POINT('Ctrl Pts',(56.4667215279697,-4.28293073239527,133.226036407528));
#57899=CARTESIAN_POINT('Ctrl Pts',(56.4589736311926,-4.21209290027906,133.343544829457));
#57900=CARTESIAN_POINT('Ctrl Pts',(56.4512273551085,-4.14126988591024,133.461028671158));
#57901=CARTESIAN_POINT('Ctrl Pts',(56.4434810790245,-4.06550977003041,133.575577171225));
#57902=CARTESIAN_POINT('Ctrl Pts',(56.4357348029404,-3.98509364588115,133.686757484074));
#57903=CARTESIAN_POINT('Ctrl Pts',(56.4279884696751,-3.90467692811833,133.797938617631));
#57904=CARTESIAN_POINT('Ctrl Pts',(56.4202421364097,-3.81960436263369,133.905751197572));
#57905=CARTESIAN_POINT('Ctrl Pts',(56.4124958031444,-3.73019927840682,134.009792945018));
#57906=CARTESIAN_POINT('Ctrl Pts',(56.4047477351414,-3.64077417253122,134.113857991892));
#57907=CARTESIAN_POINT('Ctrl Pts',(56.3969996671385,-3.54701487201289,134.214150229444));
#57908=CARTESIAN_POINT('Ctrl Pts',(56.3892515991355,-3.44928346361555,134.310302238604));
#57909=CARTESIAN_POINT('Ctrl Pts',(56.3814952963936,-3.35144818511435,134.406556439264));
#57910=CARTESIAN_POINT('Ctrl Pts',(56.3737389936517,-3.2496326447677,134.49866134686));
#57911=CARTESIAN_POINT('Ctrl Pts',(56.3659826909099,-3.14423451436854,134.586287689993));
#57912=CARTESIAN_POINT('Ctrl Pts',(56.3582222483957,-3.0387801298137,134.673960801943));
#57913=CARTESIAN_POINT('Ctrl Pts',(56.3504618058816,-2.92973965579445,134.757150349439));
#57914=CARTESIAN_POINT('Ctrl Pts',(56.3427013633674,-2.81754118844338,134.835569457843));
#57915=CARTESIAN_POINT('Ctrl Pts',(56.334928463102,-2.70516261015201,134.914114451561));
#57916=CARTESIAN_POINT('Ctrl Pts',(56.3271555628366,-2.58961623780505,134.98787349271));
#57917=CARTESIAN_POINT('Ctrl Pts',(56.3193826625712,-2.47135706072542,135.056604418303));
#57918=CARTESIAN_POINT('Ctrl Pts',(56.3118923268091,-2.3573969026084,135.122836801628));
#57919=CARTESIAN_POINT('Ctrl Pts',(56.304401991047,-2.24091802236904,135.184400147977));
#57920=CARTESIAN_POINT('Ctrl Pts',(56.2969116552849,-2.12234468052803,135.241120259414));
#57921=CARTESIAN_POINT('Ctrl Pts',(56.2891373211658,-1.99927559439256,135.299990931117));
#57922=CARTESIAN_POINT('Ctrl Pts',(56.2813629870467,-1.87356024254338,135.35383034012));
#57923=CARTESIAN_POINT('Ctrl Pts',(56.2735886529277,-1.74564846974714,135.402392205384));
#57924=CARTESIAN_POINT('Ctrl Pts',(56.2658238999806,-1.61789433677907,135.450894222488));
#57925=CARTESIAN_POINT('Ctrl Pts',(56.2580591470334,-1.48794953077456,135.494131499641));
#57926=CARTESIAN_POINT('Ctrl Pts',(56.2502943940863,-1.35628746109362,135.531904100748));
#57927=CARTESIAN_POINT('Ctrl Pts',(56.2425373532013,-1.22475616003675,135.569639185576));
#57928=CARTESIAN_POINT('Ctrl Pts',(56.2347803123164,-1.09151136291889,135.601920288398));
#57929=CARTESIAN_POINT('Ctrl Pts',(56.2270232714314,-0.957045047517442,
135.628596084407));
#57930=CARTESIAN_POINT('Ctrl Pts',(56.2192720801913,-0.822680134210064,
135.65525176399));
#57931=CARTESIAN_POINT('Ctrl Pts',(56.2115208889511,-0.687095918065139,
135.676310474589));
#57932=CARTESIAN_POINT('Ctrl Pts',(56.203769697711,-0.550797733954898,135.691671219397));
#57933=CARTESIAN_POINT('Ctrl Pts',(56.1960218009339,-0.414557480208963,
135.707025435478));
#57934=CARTESIAN_POINT('Ctrl Pts',(56.1882739041568,-0.277604249739808,
135.716686458826));
#57935=CARTESIAN_POINT('Ctrl Pts',(56.1805260073798,-0.14045150778993,135.720604756791));
#57936=CARTESIAN_POINT('Ctrl Pts',(56.1727797312957,-0.00332745523699676,
135.724522235132));
#57937=CARTESIAN_POINT('Ctrl Pts',(56.1650334552115,0.133995635228279,135.722699366293));
#57938=CARTESIAN_POINT('Ctrl Pts',(56.1572871791274,0.271001660594019,135.715138678368));
#57939=CARTESIAN_POINT('Ctrl Pts',(56.1495408458621,0.408008697306929,135.707577934632));
#57940=CARTESIAN_POINT('Ctrl Pts',(56.1417945125968,0.544698273878758,135.694279308836));
#57941=CARTESIAN_POINT('Ctrl Pts',(56.1340481793314,0.680557174485788,135.675297385248));
#57942=CARTESIAN_POINT('Ctrl Pts',(56.1263001113285,0.816446499751629,135.65631121079));
#57943=CARTESIAN_POINT('Ctrl Pts',(56.1185520433255,0.951504391756165,135.631639260033));
#57944=CARTESIAN_POINT('Ctrl Pts',(56.1108039753225,1.08522601368991,135.601387567846));
#57945=CARTESIAN_POINT('Ctrl Pts',(56.1030476725807,1.21908975655493,135.5711037238));
#57946=CARTESIAN_POINT('Ctrl Pts',(56.0952913698389,1.35161401040232,135.535228378483));
#57947=CARTESIAN_POINT('Ctrl Pts',(56.087535067097,1.48230679856,135.493918125204));
#57948=CARTESIAN_POINT('Ctrl Pts',(56.0797746245828,1.61306934139398,135.452585823398));
#57949=CARTESIAN_POINT('Ctrl Pts',(56.0720141820686,1.74199810342242,135.405812966859));
#57950=CARTESIAN_POINT('Ctrl Pts',(56.0642537395545,1.86862033246999,135.353804662236));
#57951=CARTESIAN_POINT('Ctrl Pts',(56.056480839289,1.99544582676044,135.301712869265));
#57952=CARTESIAN_POINT('Ctrl Pts',(56.0487079390237,2.11995703367442,135.244368997172));
#57953=CARTESIAN_POINT('Ctrl Pts',(56.0409350387582,2.24170428178922,135.18202494635));
#57954=CARTESIAN_POINT('Ctrl Pts',(56.0334447029962,2.35902571077323,135.12194725881));
#57955=CARTESIAN_POINT('Ctrl Pts',(56.025954367234,2.47378037754475,135.057226770481));
#57956=CARTESIAN_POINT('Ctrl Pts',(56.018464031472,2.58559240127427,134.988126265517));
#57957=CARTESIAN_POINT('Ctrl Pts',(56.0106896973529,2.70164381186705,134.916405793905));
#57958=CARTESIAN_POINT('Ctrl Pts',(56.0029153632338,2.81489264991569,134.839739423617));
#57959=CARTESIAN_POINT('Ctrl Pts',(55.9951410291147,2.92488856012024,134.758372500879));
#57960=CARTESIAN_POINT('Ctrl Pts',(55.9873762761676,3.03474891019622,134.6771058556));
#57961=CARTESIAN_POINT('Ctrl Pts',(55.9796115232205,3.1413639977316,134.59115041451));
#57962=CARTESIAN_POINT('Ctrl Pts',(55.9718467702734,3.24430972150662,134.50079639997));
#57963=CARTESIAN_POINT('Ctrl Pts',(55.9640897293884,3.34715319813736,134.410532126311));
#57964=CARTESIAN_POINT('Ctrl Pts',(55.9563326885034,3.44633427171678,134.315878229392));
#57965=CARTESIAN_POINT('Ctrl Pts',(55.9485756476184,3.54145970239391,134.217166829296));
#57966=CARTESIAN_POINT('Ctrl Pts',(55.9408244563783,3.6365133982438,134.118529868234));
#57967=CARTESIAN_POINT('Ctrl Pts',(55.9330732651382,3.72751726853929,134.015841774714));
#57968=CARTESIAN_POINT('Ctrl Pts',(55.9253220738981,3.81411319596449,133.909473110032));
#57969=CARTESIAN_POINT('Ctrl Pts',(55.917574177121,3.90067231781051,133.803149654871));
#57970=CARTESIAN_POINT('Ctrl Pts',(55.9098262803439,3.98282697670444,133.693149042463));
#57971=CARTESIAN_POINT('Ctrl Pts',(55.9020783835668,4.06025795891991,133.579876492053));
#57972=CARTESIAN_POINT('Ctrl Pts',(55.8943321074827,4.13767274424313,133.466627635818));
#57973=CARTESIAN_POINT('Ctrl Pts',(55.8865858313987,4.21036559776212,133.350108525484));
#57974=CARTESIAN_POINT('Ctrl Pts',(55.8788395553146,4.27805968014959,133.230754739628));
#57975=CARTESIAN_POINT('Ctrl Pts',(55.8710932220492,4.34575426223939,133.11140007273));
#57976=CARTESIAN_POINT('Ctrl Pts',(55.8633468887839,4.40844980668608,132.98921102863));
#57977=CARTESIAN_POINT('Ctrl Pts',(55.8556005555185,4.46591483109181,132.864648894467));
#57978=CARTESIAN_POINT('Ctrl Pts',(55.8478524875156,4.52339272439132,132.740058865477));
#57979=CARTESIAN_POINT('Ctrl Pts',(55.8401044195126,4.57563760307485,132.613095043865));
#57980=CARTESIAN_POINT('Ctrl Pts',(55.8323563515096,4.62246580065241,132.484239477573));
#57981=CARTESIAN_POINT('Ctrl Pts',(55.8246000487677,4.66934376779563,132.355246962052));
#57982=CARTESIAN_POINT('Ctrl Pts',(55.8168437460259,4.71079342002766,132.22435905356));
#57983=CARTESIAN_POINT('Ctrl Pts',(55.809087443284,4.74668057832452,132.092074308515));
#57984=CARTESIAN_POINT('Ctrl Pts',(55.8013270007699,4.78258689067836,131.959718959117));
#57985=CARTESIAN_POINT('Ctrl Pts',(55.7935665582557,4.8129247069318,131.82596566872));
#57986=CARTESIAN_POINT('Ctrl Pts',(55.7858061157415,4.83761105502072,131.691323042273));
#57987=CARTESIAN_POINT('Ctrl Pts',(55.7780332154761,4.86233703182713,131.556464275528));
#57988=CARTESIAN_POINT('Ctrl Pts',(55.7702603152106,4.88139335686474,131.420713707242));
#57989=CARTESIAN_POINT('Ctrl Pts',(55.7624874149452,4.89474890268087,131.284585817034));
#57990=CARTESIAN_POINT('Ctrl Pts',(55.7549970791832,4.90761894076603,131.153406518521));
#57991=CARTESIAN_POINT('Ctrl Pts',(55.7475067434211,4.9151954613839,131.021877162518));
#57992=CARTESIAN_POINT('Ctrl Pts',(55.7400164076591,4.91749637951566,130.890456029467));
#57993=CARTESIAN_POINT('Ctrl Pts',(55.73224207354,4.91988453765773,130.754052024212));
#57994=CARTESIAN_POINT('Ctrl Pts',(55.7244677394209,4.91659671225258,130.617332523567));
#57995=CARTESIAN_POINT('Ctrl Pts',(55.7166934053018,4.90759589198655,130.480809039828));
#57996=CARTESIAN_POINT('Ctrl Pts',(55.7089286523547,4.89860616442708,130.344453809081));
#57997=CARTESIAN_POINT('Ctrl Pts',(55.7011638994076,4.88391747648488,130.208294500954));
#57998=CARTESIAN_POINT('Ctrl Pts',(55.6933991464605,4.86354476338292,130.072844796089));
#57999=CARTESIAN_POINT('Ctrl Pts',(55.6856421055755,4.84319228474684,129.937529621781));
#58000=CARTESIAN_POINT('Ctrl Pts',(55.6778850646906,4.81716707343298,129.80292303229));
#58001=CARTESIAN_POINT('Ctrl Pts',(55.6701280238056,4.78553599572897,129.669535390457));
#58002=CARTESIAN_POINT('Ctrl Pts',(55.6623768325655,4.75392877126671,129.536248337283));
#58003=CARTESIAN_POINT('Ctrl Pts',(55.6546256413253,4.71672418469763,129.404178780996));
#58004=CARTESIAN_POINT('Ctrl Pts',(55.6468744500852,4.67404042858048,129.273828313269));
#58005=CARTESIAN_POINT('Ctrl Pts',(55.6391265533081,4.63137481419825,129.143533247969));
#58006=CARTESIAN_POINT('Ctrl Pts',(55.6313786565311,4.58323478347159,129.01495618878));
#58007=CARTESIAN_POINT('Ctrl Pts',(55.623630759754,4.52978871601037,128.88858473015));
#58008=CARTESIAN_POINT('Ctrl Pts',(55.6158844836699,4.47635382831429,128.762239705705));
#58009=CARTESIAN_POINT('Ctrl Pts',(55.6081382075857,4.41761526374631,128.638099723998));
#58010=CARTESIAN_POINT('Ctrl Pts',(55.6003919315016,4.35378984848113,128.516633138655));
#58011=CARTESIAN_POINT('Ctrl Pts',(55.5926455982363,4.28996396207132,128.395165656675));
#58012=CARTESIAN_POINT('Ctrl Pts',(55.5848992649709,4.22105133189382,128.276371956532));
#58013=CARTESIAN_POINT('Ctrl Pts',(55.5771529317056,4.14731492999175,128.160696127891));
#58014=CARTESIAN_POINT('Ctrl Pts',(55.5694048637026,4.07356201533362,128.04499439445));
#58015=CARTESIAN_POINT('Ctrl Pts',(55.5616567956997,3.99498338948993,127.932412251517));
#58016=CARTESIAN_POINT('Ctrl Pts',(55.5539087276967,3.91188533682192,127.823364781598));
#58017=CARTESIAN_POINT('Ctrl Pts',(55.5461524249548,3.82869896655476,127.714201414731));
#58018=CARTESIAN_POINT('Ctrl Pts',(55.538396122213,3.74098381169831,127.608580536739));
#58019=CARTESIAN_POINT('Ctrl Pts',(55.5306398194711,3.64908679484475,127.506884518155));
#58020=CARTESIAN_POINT('Ctrl Pts',(55.522879376957,3.55714072978619,127.405134221343));
#58021=CARTESIAN_POINT('Ctrl Pts',(55.5151189344428,3.4610086292125,127.307313236752));
#58022=CARTESIAN_POINT('Ctrl Pts',(55.5073584919286,3.36107354844426,127.213766284527));
#58023=CARTESIAN_POINT('Ctrl Pts',(55.4995855916632,3.26097804301254,127.12006916243));
#58024=CARTESIAN_POINT('Ctrl Pts',(55.4918126913978,3.15706765441735,127.030660038422));
#58025=CARTESIAN_POINT('Ctrl Pts',(55.4840397911323,3.04975840378438,126.945843189713));
#58026=CARTESIAN_POINT('Ctrl Pts',(55.4765494553703,2.94635011470789,126.864109647095));
#58027=CARTESIAN_POINT('Ctrl Pts',(55.4690591196084,2.83978603685906,126.786640476018));
#58028=CARTESIAN_POINT('Ctrl Pts',(55.4615687838464,2.73046141803724,126.713668315875));
#58029=CARTESIAN_POINT('Ctrl Pts',(55.4537944497273,2.61699172306397,126.637929394101));
#58030=CARTESIAN_POINT('Ctrl Pts',(55.4460201156082,2.5001885851331,126.566795305073));
#58031=CARTESIAN_POINT('Ctrl Pts',(55.4382457814891,2.3804623485064,126.500573672346));
#58032=CARTESIAN_POINT('Ctrl Pts',(55.430481028542,2.26088366376594,126.434433651864));
#58033=CARTESIAN_POINT('Ctrl Pts',(55.4227162755949,2.13838938698267,126.373194229116));
#58034=CARTESIAN_POINT('Ctrl Pts',(55.4149515226478,2.01341976508197,126.317120495612));
#58035=CARTESIAN_POINT('Ctrl Pts',(55.4071944817628,1.88857426477168,126.26110245533));
#58036=CARTESIAN_POINT('Ctrl Pts',(55.3994374408778,1.76125866635961,126.210240053112));
#58037=CARTESIAN_POINT('Ctrl Pts',(55.3916803999928,1.63193849542028,126.164752896038));
#58038=CARTESIAN_POINT('Ctrl Pts',(55.3839292087527,1.50271584582782,126.119300041183));
#58039=CARTESIAN_POINT('Ctrl Pts',(55.3761780175125,1.37149199990593,126.0792144924));
#58040=CARTESIAN_POINT('Ctrl Pts',(55.3684268262724,1.23875284690055,126.044667933495));
#58041=CARTESIAN_POINT('Ctrl Pts',(55.3606789294953,1.10607011157614,126.010136057799));
#58042=CARTESIAN_POINT('Ctrl Pts',(55.3529310327182,0.971873727695399,125.981138587885));
#58043=CARTESIAN_POINT('Ctrl Pts',(55.3451831359411,0.836664935568744,125.957797417928));
#58044=CARTESIAN_POINT('Ctrl Pts',(55.337436859857,0.701484426206638,125.93446113044));
#58045=CARTESIAN_POINT('Ctrl Pts',(55.3296905837729,0.565292314851211,125.916778855973));
#58046=CARTESIAN_POINT('Ctrl Pts',(55.3219443076888,0.428599840517179,125.904821329101));
#58047=CARTESIAN_POINT('Ctrl Pts',(55.3141979744234,0.291906357150353,125.892863713962));
#58048=CARTESIAN_POINT('Ctrl Pts',(55.3064516411581,0.154712892912518,125.886630964813));
#58049=CARTESIAN_POINT('Ctrl Pts',(55.2987053078927,0.0175352158270222,
125.886141877137));
#58050=CARTESIAN_POINT('Ctrl Pts',(55.2909572398897,-0.119673181248134,
125.885652679933));
#58051=CARTESIAN_POINT('Ctrl Pts',(55.2832091718868,-0.256865393247976,
125.890909705091));
#58052=CARTESIAN_POINT('Ctrl Pts',(55.2754611038838,-0.39352664532523,125.901879629136));
#58053=CARTESIAN_POINT('Ctrl Pts',(55.2677048011419,-0.53033314260748,125.912861212147));
#58054=CARTESIAN_POINT('Ctrl Pts',(55.2599484984001,-0.66660716236299,125.929567791662));
#58055=CARTESIAN_POINT('Ctrl Pts',(55.2521921956582,-0.801839485297545,
125.951914172491));
#58056=CARTESIAN_POINT('Ctrl Pts',(55.244431753144,-0.937143985794801,125.974272480257));
#58057=CARTESIAN_POINT('Ctrl Pts',(55.2366713106299,-1.07140529908273,126.002276507491));
#58058=CARTESIAN_POINT('Ctrl Pts',(55.2289108681157,-1.20412635158235,126.035790308561));
#58059=CARTESIAN_POINT('Ctrl Pts',(55.2211379678503,-1.33706045969769,126.06935790896));
#58060=CARTESIAN_POINT('Ctrl Pts',(55.2133650675848,-1.46844899111134,126.108452846314));
#58061=CARTESIAN_POINT('Ctrl Pts',(55.2055921673193,-1.59781107921,126.152889579534));
#58062=CARTESIAN_POINT('Ctrl Pts',(55.1981018315573,-1.72247052956302,126.195710925571));
#58063=CARTESIAN_POINT('Ctrl Pts',(55.1906114957953,-1.84524802428055,126.243492323061));
#58064=CARTESIAN_POINT('Ctrl Pts',(55.1831211600332,-1.96573419616374,126.296026986108));
#58065=CARTESIAN_POINT('Ctrl Pts',(55.1753463323093,-2.09079657778077,126.35055697885));
#58066=CARTESIAN_POINT('Ctrl Pts',(55.1675715045853,-2.21378632720528,126.410381188876));
#58067=CARTESIAN_POINT('Ctrl Pts',(55.1597966768613,-2.3342227398772,126.475320624318));
#58068=CARTESIAN_POINT('Ctrl Pts',(55.1520315424838,-2.45450899721224,126.540179095851));
#58069=CARTESIAN_POINT('Ctrl Pts',(55.1442664081063,-2.57224791122007,126.61013991905));
#58070=CARTESIAN_POINT('Ctrl Pts',(55.1365012737288,-2.68697842258056,126.684975952463));
#58071=CARTESIAN_POINT('Ctrl Pts',(55.1287439631096,-2.80159333725745,126.759736584858));
#58072=CARTESIAN_POINT('Ctrl Pts',(55.1209866524904,-2.91320555633316,126.839362439414));
#58073=CARTESIAN_POINT('Ctrl Pts',(55.1132293418711,-3.02137864805867,126.92358052491));
#58074=CARTESIAN_POINT('Ctrl Pts',(55.1054783623063,-3.12946345535509,127.007729876625));
#58075=CARTESIAN_POINT('Ctrl Pts',(55.0977273827415,-3.2341144168565,127.096463757374));
#58076=CARTESIAN_POINT('Ctrl Pts',(55.0899764031767,-3.33492449257867,127.189466194308));
#58077=CARTESIAN_POINT('Ctrl Pts',(55.082228882296,-3.4356895842839,127.282427131193));
#58078=CARTESIAN_POINT('Ctrl Pts',(55.0744813614152,-3.53261691328355,127.379652570323));
#58079=CARTESIAN_POINT('Ctrl Pts',(55.0667338405344,-3.62533305166879,127.480786738896));
#58080=CARTESIAN_POINT('Ctrl Pts',(55.0589880990026,-3.71802789622737,127.5818976803));
#58081=CARTESIAN_POINT('Ctrl Pts',(55.0512423574709,-3.80651321101492,127.686915276679));
#58082=CARTESIAN_POINT('Ctrl Pts',(55.0434966159391,-3.89045321884099,127.795447721766));
#58083=CARTESIAN_POINT('Ctrl Pts',(55.0357509759684,-3.9743921260574,127.903978743792));
#58084=CARTESIAN_POINT('Ctrl Pts',(55.0280053359977,-4.05378560671355,128.016024212992));
#58085=CARTESIAN_POINT('Ctrl Pts',(55.020259696027,-4.1283391397021,128.131160473524));
#58086=CARTESIAN_POINT('Ctrl Pts',(55.0125088500431,-4.20294278174242,128.246374119643));
#58087=CARTESIAN_POINT('Ctrl Pts',(55.0047580040593,-4.27269976305797,128.36468237964));
#58088=CARTESIAN_POINT('Ctrl Pts',(54.9970071580754,-4.33735960634371,128.485633659134));
#58089=CARTESIAN_POINT('Ctrl Pts',(54.9892537440566,-4.40204087293446,128.606625012591));
#58090=CARTESIAN_POINT('Ctrl Pts',(54.9815003300378,-4.46162146331655,128.730260779794));
#58091=CARTESIAN_POINT('Ctrl Pts',(54.9737469160189,-4.51589804062317,128.856067018235));
#58092=CARTESIAN_POINT('Ctrl Pts',(54.9659840490561,-4.5702407918047,128.982026639345));
#58093=CARTESIAN_POINT('Ctrl Pts',(54.9582211820932,-4.61926646590382,129.110161654877));
#58094=CARTESIAN_POINT('Ctrl Pts',(54.9504583151303,-4.66282061557448,129.239979919183));
#58095=CARTESIAN_POINT('Ctrl Pts',(54.9437008198003,-4.70073405199019,129.352985374383));
#58096=CARTESIAN_POINT('Ctrl Pts',(54.9369433244703,-4.73450216614208,129.467265908031));
#58097=CARTESIAN_POINT('Ctrl Pts',(54.9301858291403,-4.76405452823401,129.582490119308));
#58098=CARTESIAN_POINT('Origin',(213.235140564004,0.,130.804360617566));
#58099=CARTESIAN_POINT('',(52.8348764518332,-4.76405452823407,129.582490119308));
#58100=CARTESIAN_POINT('',(53.1798562900863,-4.764054528234,129.582490119308));
#58101=CARTESIAN_POINT('',(213.235140564004,-4.76405452823405,129.582490119308));
#58102=CARTESIAN_POINT('',(54.5148594360289,-4.91824993385995,130.80355402808));
#58103=CARTESIAN_POINT('Ctrl Pts',(54.5148594359912,-4.91824993386006,130.803554028749));
#58104=CARTESIAN_POINT('Ctrl Pts',(54.5068376887833,-4.91827329161115,130.945980077076));
#58105=CARTESIAN_POINT('Ctrl Pts',(54.4988159415755,-4.91210560527091,131.088319782868));
#58106=CARTESIAN_POINT('Ctrl Pts',(54.4907941943676,-4.89979539987938,131.230022574782));
#58107=CARTESIAN_POINT('Ctrl Pts',(54.4827650289623,-4.8874738104923,131.371856407885));
#58108=CARTESIAN_POINT('Ctrl Pts',(54.474735863557,-4.86899840424747,131.513051804552));
#58109=CARTESIAN_POINT('Ctrl Pts',(54.4667066981516,-4.84446927726166,131.653065798514));
#58110=CARTESIAN_POINT('Ctrl Pts',(54.4584284137018,-4.81917909076744,131.797423974047));
#58111=CARTESIAN_POINT('Ctrl Pts',(54.4501501292521,-4.78745354683138,131.940525851146));
#58112=CARTESIAN_POINT('Ctrl Pts',(54.4418718448023,-4.74945803535454,132.08179219417));
#58113=CARTESIAN_POINT('Ctrl Pts',(54.4338185529847,-4.71249519075356,132.219219108077));
#58114=CARTESIAN_POINT('Ctrl Pts',(54.425765261167,-4.66959895055311,132.354908664619));
#58115=CARTESIAN_POINT('Ctrl Pts',(54.4177119693495,-4.62097090322452,132.488347248764));
#58116=CARTESIAN_POINT('Ctrl Pts',(54.4093211885835,-4.57030500244111,132.627377837824));
#58117=CARTESIAN_POINT('Ctrl Pts',(54.4009304078176,-4.51341667649597,132.763964305249));
#58118=CARTESIAN_POINT('Ctrl Pts',(54.3925396270517,-4.4505871748321,132.897553600002));
#58119=CARTESIAN_POINT('Ctrl Pts',(54.3841488462858,-4.38775767316832,133.031142894755));
#58120=CARTESIAN_POINT('Ctrl Pts',(54.3757580655199,-4.31898725652325,133.161734677998));
#58121=CARTESIAN_POINT('Ctrl Pts',(54.367367284754,-4.24460791517983,133.288809592468));
#58122=CARTESIAN_POINT('Ctrl Pts',(54.3595929506349,-4.17569301115675,133.406548676686));
#58123=CARTESIAN_POINT('Ctrl Pts',(54.3518186165158,-4.10176637874171,133.521604683362));
#58124=CARTESIAN_POINT('Ctrl Pts',(54.3440442823967,-4.02306248621924,133.633521499254));
#58125=CARTESIAN_POINT('Ctrl Pts',(54.3362795294496,-3.94445558921022,133.745300387674));
#58126=CARTESIAN_POINT('Ctrl Pts',(54.3285147765025,-3.86108336929452,133.853947466279));
#58127=CARTESIAN_POINT('Ctrl Pts',(54.3207500235554,-3.77322578799594,133.959031791445));
#58128=CARTESIAN_POINT('Ctrl Pts',(54.3129929826704,-3.68545546808591,134.064011745377));
#58129=CARTESIAN_POINT('Ctrl Pts',(54.3052359417854,-3.59320890144388,134.165435689794));
#58130=CARTESIAN_POINT('Ctrl Pts',(54.2974789009004,-3.49680867583896,134.262902528123));
#58131=CARTESIAN_POINT('Ctrl Pts',(54.2897277096603,-3.40048114639432,134.36029586595));
#58132=CARTESIAN_POINT('Ctrl Pts',(54.2819765184202,-3.30000646646958,134.453737760481));
#58133=CARTESIAN_POINT('Ctrl Pts',(54.2742253271801,-3.19574649682287,134.54286130508));
#58134=CARTESIAN_POINT('Ctrl Pts',(54.266477430403,-3.09153084044406,134.631946969796));
#58135=CARTESIAN_POINT('Ctrl Pts',(54.258729533626,-2.98353339078297,134.716717681571));
#58136=CARTESIAN_POINT('Ctrl Pts',(54.2509816368489,-2.87215159014095,134.796844594459));
#58137=CARTESIAN_POINT('Ctrl Pts',(54.2432353607648,-2.76079308817067,134.876954746525));
#58138=CARTESIAN_POINT('Ctrl Pts',(54.2354890846807,-2.64605196051,134.952422803668));
#58139=CARTESIAN_POINT('Ctrl Pts',(54.2277428085966,-2.52835701691984,135.022961553598));
#58140=CARTESIAN_POINT('Ctrl Pts',(54.2199964753312,-2.41066120453218,135.09350082423));
#58141=CARTESIAN_POINT('Ctrl Pts',(54.2122501420658,-2.29001186805411,135.159110514055));
#58142=CARTESIAN_POINT('Ctrl Pts',(54.2045038088004,-2.16686460684491,135.219548137718));
#58143=CARTESIAN_POINT('Ctrl Pts',(54.1967557407975,-2.0436897676604,135.279999295967));
#58144=CARTESIAN_POINT('Ctrl Pts',(54.1890076727945,-1.91801624152583,135.335275911058));
#58145=CARTESIAN_POINT('Ctrl Pts',(54.1812596047915,-1.79032153007529,135.385182801568));
#58146=CARTESIAN_POINT('Ctrl Pts',(54.1735033020497,-1.66249110316584,135.435142733716));
#58147=CARTESIAN_POINT('Ctrl Pts',(54.1657469993079,-1.53263556452254,135.479721398379));
#58148=CARTESIAN_POINT('Ctrl Pts',(54.157990696566,-1.40125010706227,135.518772691193));
#58149=CARTESIAN_POINT('Ctrl Pts',(54.1502302540518,-1.26979452522724,135.557844826858));
#58150=CARTESIAN_POINT('Ctrl Pts',(54.1424698115376,-1.1368077764126,135.591383616741));
#58151=CARTESIAN_POINT('Ctrl Pts',(54.1347093690234,-1.00279632800082,135.619293907555));
#58152=CARTESIAN_POINT('Ctrl Pts',(54.1269364687579,-0.868569752515257,
135.647249002447));
#58153=CARTESIAN_POINT('Ctrl Pts',(54.1191635684926,-0.733315576296101,
135.669557479067));
#58154=CARTESIAN_POINT('Ctrl Pts',(54.1113906682271,-0.597547383831778,
135.686175872835));
#58155=CARTESIAN_POINT('Ctrl Pts',(54.1039003324651,-0.466714707143525,
135.70219014613));
#58156=CARTESIAN_POINT('Ctrl Pts',(54.0964099967031,-0.335405043950435,
135.712920826775));
#58157=CARTESIAN_POINT('Ctrl Pts',(54.0889196609411,-0.204076972630477,
135.718374827124));
#58158=CARTESIAN_POINT('Ctrl Pts',(54.081145326822,-0.0677695575697286,
135.724035617555));
#58159=CARTESIAN_POINT('Ctrl Pts',(54.073370992703,0.0689894699806697,135.724029630001));
#58160=CARTESIAN_POINT('Ctrl Pts',(54.0655966585839,0.205689633197736,135.718307588922));
#58161=CARTESIAN_POINT('Ctrl Pts',(54.0578319056368,0.342221325680881,135.712592599747));
#58162=CARTESIAN_POINT('Ctrl Pts',(54.0500671526897,0.478693911300481,135.701175589746));
#58163=CARTESIAN_POINT('Ctrl Pts',(54.0423023997427,0.614593498937375,135.684059162923));
#58164=CARTESIAN_POINT('Ctrl Pts',(54.0345453588576,0.750358109188164,135.666959736377));
#58165=CARTESIAN_POINT('Ctrl Pts',(54.0267883179726,0.885550468619621,135.644172206678));
#58166=CARTESIAN_POINT('Ctrl Pts',(54.0190312770876,1.01965875675565,135.615751173556));
#58167=CARTESIAN_POINT('Ctrl Pts',(54.0112800858475,1.1536659127882,135.587351572957));
#58168=CARTESIAN_POINT('Ctrl Pts',(54.0035288946073,1.28659024379954,135.553327005585));
#58169=CARTESIAN_POINT('Ctrl Pts',(53.9957777033672,1.41792746626644,135.513783593145));
#58170=CARTESIAN_POINT('Ctrl Pts',(53.9880298065901,1.54920886691043,135.474256987709));
#58171=CARTESIAN_POINT('Ctrl Pts',(53.9802819098131,1.67890412708408,135.429216315017));
#58172=CARTESIAN_POINT('Ctrl Pts',(53.972534013036,1.80652175210833,135.378818205265));
#58173=CARTESIAN_POINT('Ctrl Pts',(53.9647877369519,1.93411268227637,135.328430637712));
#58174=CARTESIAN_POINT('Ctrl Pts',(53.9570414608677,2.05962647832543,135.272688005669));
#58175=CARTESIAN_POINT('Ctrl Pts',(53.9492951847836,2.18258971827225,135.211795833674));
#58176=CARTESIAN_POINT('Ctrl Pts',(53.9415488515183,2.30555386590577,135.150903212188));
#58177=CARTESIAN_POINT('Ctrl Pts',(53.933802518253,2.42596706950877,135.084861148398));
#58178=CARTESIAN_POINT('Ctrl Pts',(53.9260561849876,2.54337905670134,135.013921881692));
#58179=CARTESIAN_POINT('Ctrl Pts',(53.9183081169846,2.66081733749453,134.942966728629));
#58180=CARTESIAN_POINT('Ctrl Pts',(53.9105600489817,2.77525272990735,134.867112392496));
#58181=CARTESIAN_POINT('Ctrl Pts',(53.9028119809787,2.88626292098648,134.786655108615));
#58182=CARTESIAN_POINT('Ctrl Pts',(53.8950556782369,2.99739109501743,134.706112313776));
#58183=CARTESIAN_POINT('Ctrl Pts',(53.887299375495,3.10508647866565,134.62095702856));
#58184=CARTESIAN_POINT('Ctrl Pts',(53.8795430727532,3.20895848632532,134.531526899816));
#58185=CARTESIAN_POINT('Ctrl Pts',(53.871782630239,3.31288593360315,134.44204903952));
#58186=CARTESIAN_POINT('Ctrl Pts',(53.8640221877248,3.4129856535157,134.348292056524));
#58187=CARTESIAN_POINT('Ctrl Pts',(53.8562617452107,3.50890383291668,134.250630623506));
#58188=CARTESIAN_POINT('Ctrl Pts',(53.8484888449453,3.60497598869444,134.152812415686));
#58189=CARTESIAN_POINT('Ctrl Pts',(53.8407159446798,3.6968529278972,134.051077523164));
#58190=CARTESIAN_POINT('Ctrl Pts',(53.8329430444144,3.78422047758097,133.945834545447));
#58191=CARTESIAN_POINT('Ctrl Pts',(53.8254527086523,3.86841199676875,133.844417415061));
#58192=CARTESIAN_POINT('Ctrl Pts',(53.8179623728903,3.94841610267741,133.739743071533));
#58193=CARTESIAN_POINT('Ctrl Pts',(53.8104720371282,4.02399073805242,133.632201066136));
#58194=CARTESIAN_POINT('Ctrl Pts',(53.8026977030091,4.10243080869763,133.520581572919));
#58195=CARTESIAN_POINT('Ctrl Pts',(53.79492336889,4.17634736611468,133.405519093404));
#58196=CARTESIAN_POINT('Ctrl Pts',(53.7871490347709,4.24542302820429,133.287416471568));
#58197=CARTESIAN_POINT('Ctrl Pts',(53.7793842818238,4.31441356071384,133.169459400658));
#58198=CARTESIAN_POINT('Ctrl Pts',(53.7716195288767,4.37857487290968,133.04846997649));
#58199=CARTESIAN_POINT('Ctrl Pts',(53.7638547759296,4.43763138491084,132.924881957745));
#58200=CARTESIAN_POINT('Ctrl Pts',(53.7560977350447,4.49662924115157,132.801416688363));
#58201=CARTESIAN_POINT('Ctrl Pts',(53.7483406941597,4.55053221956859,132.675358311108));
#58202=CARTESIAN_POINT('Ctrl Pts',(53.7405836532747,4.59910960499256,132.547166947531));
#58203=CARTESIAN_POINT('Ctrl Pts',(53.7328324620346,4.64765035783256,132.419072254058));
#58204=CARTESIAN_POINT('Ctrl Pts',(53.7250812707944,4.69087337344552,132.288848140004));
#58205=CARTESIAN_POINT('Ctrl Pts',(53.7173300795542,4.72859535746534,132.156976234753));
#58206=CARTESIAN_POINT('Ctrl Pts',(53.7095821827772,4.76630130863558,132.02516037858));
#58207=CARTESIAN_POINT('Ctrl Pts',(53.701834286,4.79851077118784,131.891698499265));
#58208=CARTESIAN_POINT('Ctrl Pts',(53.6940863892229,4.82508985766454,131.75708876765));
#58209=CARTESIAN_POINT('Ctrl Pts',(53.6863401131388,4.85166338436933,131.622507193489));
#58210=CARTESIAN_POINT('Ctrl Pts',(53.6785938370548,4.87260880192745,131.486778627929));
#58211=CARTESIAN_POINT('Ctrl Pts',(53.6708475609707,4.88784312780795,131.350412465325));
#58212=CARTESIAN_POINT('Ctrl Pts',(53.6631012277053,4.90307756614477,131.214045296096));
#58213=CARTESIAN_POINT('Ctrl Pts',(53.65535489444,4.91260078527364,131.077040908981));
#58214=CARTESIAN_POINT('Ctrl Pts',(53.6476085611746,4.91638161811415,130.939914472433));
#58215=CARTESIAN_POINT('Ctrl Pts',(53.6398604931717,4.92016329764596,130.80275732737));
#58216=CARTESIAN_POINT('Ctrl Pts',(53.6321124251687,4.91820002118929,130.66547846923));
#58217=CARTESIAN_POINT('Ctrl Pts',(53.6243643571657,4.91051274944456,130.528593324287));
#58218=CARTESIAN_POINT('Ctrl Pts',(53.6166080544239,4.90281730757593,130.391562696183));
#58219=CARTESIAN_POINT('Ctrl Pts',(53.608851751682,4.88938573986858,130.254927008135));
#58220=CARTESIAN_POINT('Ctrl Pts',(53.6010954489401,4.87029099711833,130.119197377244));
#58221=CARTESIAN_POINT('Ctrl Pts',(53.5933350064259,4.8511860629289,129.983395303362));
#58222=CARTESIAN_POINT('Ctrl Pts',(53.5855745639118,4.8264120014831,129.848500634578));
#58223=CARTESIAN_POINT('Ctrl Pts',(53.5778141213976,4.79609279086751,129.715013563644));
#58224=CARTESIAN_POINT('Ctrl Pts',(53.5700412211322,4.76572490916348,129.581312207414));
#58225=CARTESIAN_POINT('Ctrl Pts',(53.5622683208667,4.72979419266053,129.449023341951));
#58226=CARTESIAN_POINT('Ctrl Pts',(53.5544954206013,4.68847458954646,129.318632147866));
#58227=CARTESIAN_POINT('Ctrl Pts',(53.5470050848393,4.64865705808367,129.192981002122));
#58228=CARTESIAN_POINT('Ctrl Pts',(53.5395147490773,4.60383574179493,129.069092242499));
#58229=CARTESIAN_POINT('Ctrl Pts',(53.5320244133154,4.55420754334088,128.947380080598));
#58230=CARTESIAN_POINT('Ctrl Pts',(53.5242500791963,4.502697676658,128.821053165085));
#58231=CARTESIAN_POINT('Ctrl Pts',(53.5164757450772,4.44584605869994,128.696670991169));
#58232=CARTESIAN_POINT('Ctrl Pts',(53.5087014109582,4.38382006073538,128.57471832841));
#58233=CARTESIAN_POINT('Ctrl Pts',(53.5009366580111,4.3218705042698,128.452915961408));
#58234=CARTESIAN_POINT('Ctrl Pts',(53.493171905064,4.25475943158813,128.333537493221));
#58235=CARTESIAN_POINT('Ctrl Pts',(53.4854071521169,4.18270281849537,128.21704923417));
#58236=CARTESIAN_POINT('Ctrl Pts',(53.4776501112319,4.11071777304664,128.1006766729));
#58237=CARTESIAN_POINT('Ctrl Pts',(53.4698930703468,4.03379716659119,127.987188938493));
#58238=CARTESIAN_POINT('Ctrl Pts',(53.4621360294618,3.95220340523599,127.877028845091));
#58239=CARTESIAN_POINT('Ctrl Pts',(53.4543848382217,3.87067117437092,127.766951824273));
#58240=CARTESIAN_POINT('Ctrl Pts',(53.4466336469816,3.78447303479879,127.660197762551));
#58241=CARTESIAN_POINT('Ctrl Pts',(53.4388824557415,3.69391511987863,127.557181203115));
#58242=CARTESIAN_POINT('Ctrl Pts',(53.4311345589644,3.6033956944879,127.454208428465));
#58243=CARTESIAN_POINT('Ctrl Pts',(53.4233866621873,3.50852043685308,127.354970289643));
#58244=CARTESIAN_POINT('Ctrl Pts',(53.4156387654103,3.40963610277082,127.259848703468));
#58245=CARTESIAN_POINT('Ctrl Pts',(53.4078924893262,3.31077245315983,127.164747014679));
#58246=CARTESIAN_POINT('Ctrl Pts',(53.400146213242,3.20790167673188,127.073760436642));
#58247=CARTESIAN_POINT('Ctrl Pts',(53.392399937158,3.10140748730035,126.987234125004));
#58248=CARTESIAN_POINT('Ctrl Pts',(53.3846536038926,2.99491251175262,126.900707174648));
#58249=CARTESIAN_POINT('Ctrl Pts',(53.3769072706272,2.88479437326305,126.818640802929));
#58250=CARTESIAN_POINT('Ctrl Pts',(53.3691609373619,2.77146965107501,126.741339692728));
#58251=CARTESIAN_POINT('Ctrl Pts',(53.3614128693589,2.65811955060102,126.664021271479));
#58252=CARTESIAN_POINT('Ctrl Pts',(53.3536648013559,2.54156176042712,126.591470455517));
#58253=CARTESIAN_POINT('Ctrl Pts',(53.3459167333529,2.42224125304778,126.523948210504));
#58254=CARTESIAN_POINT('Ctrl Pts',(53.3381604306111,2.30279393041359,126.456354202045));
#58255=CARTESIAN_POINT('Ctrl Pts',(53.3304041278693,2.18057836590518,126.393799633457));
#58256=CARTESIAN_POINT('Ctrl Pts',(53.3226478251274,2.05606400850246,126.336499400446));
#58257=CARTESIAN_POINT('Ctrl Pts',(53.3148873826132,1.93148319403798,126.279168584577));
#58258=CARTESIAN_POINT('Ctrl Pts',(53.3071269400991,1.80460150342239,126.227097840645));
#58259=CARTESIAN_POINT('Ctrl Pts',(53.2993664975849,1.67590677617028,126.180453228778));
#58260=CARTESIAN_POINT('Ctrl Pts',(53.2915935973195,1.54700545671699,126.133733738839));
#58261=CARTESIAN_POINT('Ctrl Pts',(53.283820697054,1.41628565766153,126.092457905126));
#58262=CARTESIAN_POINT('Ctrl Pts',(53.2760477967886,1.28424959843668,126.056741632073));
#58263=CARTESIAN_POINT('Ctrl Pts',(53.2685574610265,1.15701338254359,126.022323735509));
#58264=CARTESIAN_POINT('Ctrl Pts',(53.2610671252645,1.02855524408416,125.99306827758));
#58265=CARTESIAN_POINT('Ctrl Pts',(53.2535767895025,0.899330101708337,125.969033489991));
#58266=CARTESIAN_POINT('Ctrl Pts',(53.2458024553834,0.765205348782019,125.944087416125));
#58267=CARTESIAN_POINT('Ctrl Pts',(53.2380281212643,0.629829414996312,125.92468668923));
#58268=CARTESIAN_POINT('Ctrl Pts',(53.2302537871452,0.493700618968488,125.910952524904));
#58269=CARTESIAN_POINT('Ctrl Pts',(53.2224890341981,0.357739589515404,125.897235286708));
#58270=CARTESIAN_POINT('Ctrl Pts',(53.214724281251,0.221027929192346,125.889170754803));
#58271=CARTESIAN_POINT('Ctrl Pts',(53.2069595283039,0.0840746982764856,
125.886829274747));
#58272=CARTESIAN_POINT('Ctrl Pts',(53.199202487419,-0.0527425087593545,
125.884490120281));
#58273=CARTESIAN_POINT('Ctrl Pts',(53.191445446534,-0.189800420535316,125.887862712458));
#58274=CARTESIAN_POINT('Ctrl Pts',(53.183688405649,-0.32658464806115,125.896965633448));
#58275=CARTESIAN_POINT('Ctrl Pts',(53.1759372144088,-0.463265725537165,
125.906061689854));
#58276=CARTESIAN_POINT('Ctrl Pts',(53.1681860231687,-0.599673141040839,
125.920879447961));
#58277=CARTESIAN_POINT('Ctrl Pts',(53.1604348319286,-0.73529265508951,125.941385419822));
#58278=CARTESIAN_POINT('Ctrl Pts',(53.1526869351515,-0.870854527226942,
125.961882676098));
#58279=CARTESIAN_POINT('Ctrl Pts',(53.1449390383744,-1.0056287781965,125.988063279294));
#58280=CARTESIAN_POINT('Ctrl Pts',(53.1371911415973,-1.13910666058445,126.019841929306));
#58281=CARTESIAN_POINT('Ctrl Pts',(53.1294448655132,-1.27255662227703,126.051613931909));
#58282=CARTESIAN_POINT('Ctrl Pts',(53.1216985894291,-1.40471037467112,126.08898156167));
#58283=CARTESIAN_POINT('Ctrl Pts',(53.113952313345,-1.53507012185805,126.131808554348));
#58284=CARTESIAN_POINT('Ctrl Pts',(53.1062059800796,-1.66543083133103,126.174635863166));
#58285=CARTESIAN_POINT('Ctrl Pts',(53.0984596468143,-1.79399713773751,126.222922493288));
#58286=CARTESIAN_POINT('Ctrl Pts',(53.0907133135489,-1.92028753148398,126.27648265334));
#58287=CARTESIAN_POINT('Ctrl Pts',(53.0829652455459,-2.04660620708816,126.330054807817));
#58288=CARTESIAN_POINT('Ctrl Pts',(53.075217177543,-2.17064759597379,126.388902689599));
#58289=CARTESIAN_POINT('Ctrl Pts',(53.06746910954,-2.29195162183667,126.452792989037));
#58290=CARTESIAN_POINT('Ctrl Pts',(53.0597128067981,-2.41338457106194,126.516751191846));
#58291=CARTESIAN_POINT('Ctrl Pts',(53.0519565040563,-2.53207399915068,126.585762335289));
#58292=CARTESIAN_POINT('Ctrl Pts',(53.0442002013144,-2.64758535961753,126.659547615024));
#58293=CARTESIAN_POINT('Ctrl Pts',(53.0364397588002,-2.76315837197544,126.733372276185));
#58294=CARTESIAN_POINT('Ctrl Pts',(53.0286793162861,-2.87554961660038,126.811975926982));
#58295=CARTESIAN_POINT('Ctrl Pts',(53.0209188737719,-2.9843556932314,126.895037893771));
#58296=CARTESIAN_POINT('Ctrl Pts',(53.0131459735065,-3.09333643503599,126.978233199003));
#58297=CARTESIAN_POINT('Ctrl Pts',(53.0053730732411,-3.19872020732929,127.065900871786));
#58298=CARTESIAN_POINT('Ctrl Pts',(52.9976001729756,-3.30013803455746,127.157681029863));
#58299=CARTESIAN_POINT('Ctrl Pts',(52.9901098372136,-3.39786906831007,127.246124748015));
#58300=CARTESIAN_POINT('Ctrl Pts',(52.9826195014515,-3.4919172752251,127.33838692841));
#58301=CARTESIAN_POINT('Ctrl Pts',(52.9751291656895,-3.5819877686786,127.434116310763));
#58302=CARTESIAN_POINT('Ctrl Pts',(52.9674484309785,-3.67434778930741,127.532279065178));
#58303=CARTESIAN_POINT('Ctrl Pts',(52.9597676962676,-3.76283341313691,127.634415575219));
#58304=CARTESIAN_POINT('Ctrl Pts',(52.9520869615566,-3.84707694345011,127.740183394611));
#58305=CARTESIAN_POINT('Ctrl Pts',(52.9444153230666,-3.93122070495366,127.845825954183));
#58306=CARTESIAN_POINT('Ctrl Pts',(52.9367436845765,-4.01113211449058,127.955090962074));
#58307=CARTESIAN_POINT('Ctrl Pts',(52.9290720460865,-4.08647997867179,128.067598946098));
#58308=CARTESIAN_POINT('Ctrl Pts',(52.921222413232,-4.16357603461273,128.182717296491));
#58309=CARTESIAN_POINT('Ctrl Pts',(52.9133727803776,-4.2358938671708,128.301230672763));
#58310=CARTESIAN_POINT('Ctrl Pts',(52.9055231475232,-4.30312156478415,128.422695682864));
#58311=CARTESIAN_POINT('Ctrl Pts',(52.8978650440355,-4.36870892092036,128.541196972636));
#58312=CARTESIAN_POINT('Ctrl Pts',(52.8902069405478,-4.4294514484076,128.662507154076));
#58313=CARTESIAN_POINT('Ctrl Pts',(52.8825488370601,-4.48510316096557,128.786185031053));
#58314=CARTESIAN_POINT('Ctrl Pts',(52.8746034395223,-4.54284264968404,128.914502688394));
#58315=CARTESIAN_POINT('Ctrl Pts',(52.8666580419845,-4.59510166066938,129.045368783277));
#58316=CARTESIAN_POINT('Ctrl Pts',(52.8587126444467,-4.64165819593947,129.178263371222));
#58317=CARTESIAN_POINT('Ctrl Pts',(52.8507672469089,-4.68821473120951,129.311157959166));
#58318=CARTESIAN_POINT('Ctrl Pts',(52.8428218493711,-4.7290686185793,129.44608058855));
#58319=CARTESIAN_POINT('Ctrl Pts',(52.8348764518333,-4.76405452823406,129.582490119308));
#58320=CARTESIAN_POINT('Ctrl Pts',(54.5845740201626,-4.76405452823409,129.582490119308));
#58321=CARTESIAN_POINT('Ctrl Pts',(54.5763264523982,-4.80021096026599,129.72346349905));
#58322=CARTESIAN_POINT('Ctrl Pts',(54.5680788846337,-4.83014611411045,129.866199623673));
#58323=CARTESIAN_POINT('Ctrl Pts',(54.5598313168694,-4.85369976884236,130.010143004792));
#58324=CARTESIAN_POINT('Ctrl Pts',(54.5516042144782,-4.87719497793954,130.153729207276));
#58325=CARTESIAN_POINT('Ctrl Pts',(54.543377112087,-4.89434021591618,130.298516386051));
#58326=CARTESIAN_POINT('Ctrl Pts',(54.5351500096957,-4.90502581197444,130.443937468525));
#58327=CARTESIAN_POINT('Ctrl Pts',(54.5283864851401,-4.91381047124995,130.563488558988));
#58328=CARTESIAN_POINT('Ctrl Pts',(54.5216229605845,-4.91823023978955,130.683467711439));
#58329=CARTESIAN_POINT('Ctrl Pts',(54.5148594360288,-4.91824993385995,130.80355402808));
#58330=CARTESIAN_POINT('',(54.8601405639799,-4.91824840592091,130.800400799834));
#58331=CARTESIAN_POINT('Ctrl Pts',(54.9301858291403,-4.76405452823401,129.582490119308));
#58332=CARTESIAN_POINT('Ctrl Pts',(54.9224099595592,-4.79806051746806,129.715078955219));
#58333=CARTESIAN_POINT('Ctrl Pts',(54.9146340899781,-4.82648327833249,129.848917122839));
#58334=CARTESIAN_POINT('Ctrl Pts',(54.906858220397,-4.84926406211354,129.983494539333));
#58335=CARTESIAN_POINT('Ctrl Pts',(54.9061299923381,-4.85139753487553,129.996098023709));
#58336=CARTESIAN_POINT('Ctrl Pts',(54.9054017642793,-4.85348156097654,130.008707990245));
#58337=CARTESIAN_POINT('Ctrl Pts',(54.9046735362204,-4.85551611554211,130.021324019308));
#58338=CARTESIAN_POINT('Ctrl Pts',(54.8919953708024,-4.8909369140413,130.240964146374));
#58339=CARTESIAN_POINT('Ctrl Pts',(54.8793172053843,-4.91146097444499,130.463068264155));
#58340=CARTESIAN_POINT('Ctrl Pts',(54.8666390399663,-4.91682660785611,130.686042526058));
#58341=CARTESIAN_POINT('Ctrl Pts',(54.8644728813137,-4.9177433661454,130.724139333505));
#58342=CARTESIAN_POINT('Ctrl Pts',(54.8623067226612,-4.91821769887402,130.762261452176));
#58343=CARTESIAN_POINT('Ctrl Pts',(54.8601405640086,-4.9182484059205,130.80040079933));
#58344=CARTESIAN_POINT('Ctrl Pts',(54.86014056398,-4.91824840592091,130.800400799834));
#58345=CARTESIAN_POINT('Ctrl Pts',(54.852492109661,-4.91835682891756,130.935066399749));
#58346=CARTESIAN_POINT('Ctrl Pts',(54.8448436553421,-4.91293021809761,131.069935130745));
#58347=CARTESIAN_POINT('Ctrl Pts',(54.8371952010231,-4.90194516963234,131.204506361537));
#58348=CARTESIAN_POINT('Ctrl Pts',(54.82955414848,-4.89097075192503,131.338947361299));
#58349=CARTESIAN_POINT('Ctrl Pts',(54.8219130959369,-4.87444862781496,131.473091033895));
#58350=CARTESIAN_POINT('Ctrl Pts',(54.8142720433938,-4.85240743479849,131.606436143444));
#58351=CARTESIAN_POINT('Ctrl Pts',(54.8064367879361,-4.82980604881087,131.743170316056));
#58352=CARTESIAN_POINT('Ctrl Pts',(54.7986015324783,-4.8014012748303,131.879064358487));
#58353=CARTESIAN_POINT('Ctrl Pts',(54.7907662770205,-4.76728078796237,132.013582247882));
#58354=CARTESIAN_POINT('Ctrl Pts',(54.7831334019653,-4.73404161478038,132.14462561309));
#58355=CARTESIAN_POINT('Ctrl Pts',(54.77550052691,-4.69537848645466,132.27436263008));
#58356=CARTESIAN_POINT('Ctrl Pts',(54.7678676518548,-4.65142422714408,132.402307963894));
#58357=CARTESIAN_POINT('Ctrl Pts',(54.7602358035559,-4.60747588045612,132.530236086806));
#58358=CARTESIAN_POINT('Ctrl Pts',(54.7526039552569,-4.55823794898747,132.656372624051));
#58359=CARTESIAN_POINT('Ctrl Pts',(54.7449721069579,-4.50389280758113,132.780248428227));
#58360=CARTESIAN_POINT('Ctrl Pts',(54.7373395184934,-4.44954239557686,132.904136246348));
#58361=CARTESIAN_POINT('Ctrl Pts',(54.7297069300288,-4.39008395131953,133.025762525944));
#58362=CARTESIAN_POINT('Ctrl Pts',(54.7220743415642,-4.32574733667684,133.144679621833));
#58363=CARTESIAN_POINT('Ctrl Pts',(54.7140869724678,-4.25842020513429,133.269124263536));
#58364=CARTESIAN_POINT('Ctrl Pts',(54.7060996033714,-4.18575073073993,133.390601374145));
#58365=CARTESIAN_POINT('Ctrl Pts',(54.698112234275,-4.10805454349081,133.508629637136));
#58366=CARTESIAN_POINT('Ctrl Pts',(54.6904686914493,-4.03370288558408,133.621577226251));
#58367=CARTESIAN_POINT('Ctrl Pts',(54.6828251486237,-3.95474855325779,133.731366409381));
#58368=CARTESIAN_POINT('Ctrl Pts',(54.675181605798,-3.87151022752934,133.837608319393));
#58369=CARTESIAN_POINT('Ctrl Pts',(54.6675329846001,-3.7882165982317,133.943920816562));
#58370=CARTESIAN_POINT('Ctrl Pts',(54.6598843634022,-3.70063357168755,134.046681044275));
#58371=CARTESIAN_POINT('Ctrl Pts',(54.6522357422043,-3.60911751086314,134.145536137541));
#58372=CARTESIAN_POINT('Ctrl Pts',(54.6445767165599,-3.51747696041644,134.244525703742));
#58373=CARTESIAN_POINT('Ctrl Pts',(54.6369176909155,-3.42189298822956,134.339599256715));
#58374=CARTESIAN_POINT('Ctrl Pts',(54.6292586652711,-3.32275596349902,134.430443334429));
#58375=CARTESIAN_POINT('Ctrl Pts',(54.6282477476499,-3.30967083102071,134.44243387777));
#58376=CARTESIAN_POINT('Ctrl Pts',(54.6272368300286,-3.29652384142501,134.454350798694));
#58377=CARTESIAN_POINT('Ctrl Pts',(54.6262259124074,-3.28331592988795,134.466193432844));
#58378=CARTESIAN_POINT('Ctrl Pts',(54.6184515782884,-3.18174215656343,134.557267713085));
#58379=CARTESIAN_POINT('Ctrl Pts',(54.6106772441693,-3.07621522909855,134.644256788446));
#58380=CARTESIAN_POINT('Ctrl Pts',(54.6029029100503,-2.96709768623001,134.726797918896));
#58381=CARTESIAN_POINT('Ctrl Pts',(54.5951381571032,-2.8581146209808,134.809237324781));
#58382=CARTESIAN_POINT('Ctrl Pts',(54.5873734041561,-2.74555005379505,134.887239459094));
#58383=CARTESIAN_POINT('Ctrl Pts',(54.579608651209,-2.62980215893878,134.960479440138));
#58384=CARTESIAN_POINT('Ctrl Pts',(54.571851610324,-2.51416922652359,135.033646678202));
#58385=CARTESIAN_POINT('Ctrl Pts',(54.5640945694389,-2.39535958665857,135.10206096789));
#58386=CARTESIAN_POINT('Ctrl Pts',(54.5563375285539,-2.27380289087217,135.165438864509));
#58387=CARTESIAN_POINT('Ctrl Pts',(54.5485863373138,-2.15233786193547,135.228768967364));
#58388=CARTESIAN_POINT('Ctrl Pts',(54.5408351460737,-2.02813024569562,135.287070056785));
#58389=CARTESIAN_POINT('Ctrl Pts',(54.5330839548336,-1.90163665178557,135.340103236706));
#58390=CARTESIAN_POINT('Ctrl Pts',(54.5253360580565,-1.77519682102744,135.393113876111));
#58391=CARTESIAN_POINT('Ctrl Pts',(54.5175881612794,-1.64647330484419,135.440860908369));
#58392=CARTESIAN_POINT('Ctrl Pts',(54.5098402645023,-1.51594497393495,135.483152544816));
#58393=CARTESIAN_POINT('Ctrl Pts',(54.5020939884183,-1.38544394673884,135.525435334764));
#58394=CARTESIAN_POINT('Ctrl Pts',(54.4943477123341,-1.25313922743567,135.562264878283));
#58395=CARTESIAN_POINT('Ctrl Pts',(54.4866014362501,-1.11952684399851,135.593498609738));
#58396=CARTESIAN_POINT('Ctrl Pts',(54.4788551029847,-0.985913474264903,
135.624732571754));
#58397=CARTESIAN_POINT('Ctrl Pts',(54.4711087697194,-0.850992801837409,
135.650370550286));
#58398=CARTESIAN_POINT('Ctrl Pts',(54.463362436454,-0.715272708231192,135.670320750506));
#58399=CARTESIAN_POINT('Ctrl Pts',(54.4556143684511,-0.579522221051399,
135.690275418435));
#58400=CARTESIAN_POINT('Ctrl Pts',(54.4478663004481,-0.442972343188713,
135.704539716612));
#58401=CARTESIAN_POINT('Ctrl Pts',(54.4401182324452,-0.306137368921437,
135.713073582677));
#58402=CARTESIAN_POINT('Ctrl Pts',(54.4323619297034,-0.169156964814779,
135.721616518637));
#58403=CARTESIAN_POINT('Ctrl Pts',(54.4246056269615,-0.0318912498499723,
135.724416831938));
#58404=CARTESIAN_POINT('Ctrl Pts',(54.4168493242196,0.105143620223701,135.721486595373));
#58405=CARTESIAN_POINT('Ctrl Pts',(54.4090888817055,0.24225162993376,135.718554794852));
#58406=CARTESIAN_POINT('Ctrl Pts',(54.4013284391913,0.379128159255964,135.709886374709));
#58407=CARTESIAN_POINT('Ctrl Pts',(54.3935679966771,0.515261873555775,135.695545368131));
#58408=CARTESIAN_POINT('Ctrl Pts',(54.3857950964117,0.651614121778978,135.681181340096));
#58409=CARTESIAN_POINT('Ctrl Pts',(54.3780221961463,0.787220785138221,135.661126585887));
#58410=CARTESIAN_POINT('Ctrl Pts',(54.3702492958809,0.921579534162419,135.635496532101));
#58411=CARTESIAN_POINT('Ctrl Pts',(54.3627589601188,1.05105400423141,135.610798195329));
#58412=CARTESIAN_POINT('Ctrl Pts',(54.3552686243567,1.1793694144294,135.580922943679));
#58413=CARTESIAN_POINT('Ctrl Pts',(54.3477782885946,1.30609119643344,135.546017379617));
#58414=CARTESIAN_POINT('Ctrl Pts',(54.3400039544755,1.43761767331749,135.509788360483));
#58415=CARTESIAN_POINT('Ctrl Pts',(54.3322296203564,1.567843928011,135.468025287788));
#58416=CARTESIAN_POINT('Ctrl Pts',(54.3244552862373,1.69626881600993,135.420837105791));
#58417=CARTESIAN_POINT('Ctrl Pts',(54.3166905332902,1.82453543181206,135.373707079011));
#58418=CARTESIAN_POINT('Ctrl Pts',(54.3089257803432,1.95100473465113,135.321165379547));
#58419=CARTESIAN_POINT('Ctrl Pts',(54.3011610273961,2.07518816943759,135.263371396195));
#58420=CARTESIAN_POINT('Ctrl Pts',(54.2934039865111,2.1992482634861,135.205634814641));
#58421=CARTESIAN_POINT('Ctrl Pts',(54.285646945626,2.3210266554283,135.142656494447));
#58422=CARTESIAN_POINT('Ctrl Pts',(54.277889904741,2.44005263806973,135.074644704831));
#58423=CARTESIAN_POINT('Ctrl Pts',(54.2701387135009,2.55898886229112,135.006684203435));
#58424=CARTESIAN_POINT('Ctrl Pts',(54.2623875222608,2.67517647051101,134.933697981066));
#58425=CARTESIAN_POINT('Ctrl Pts',(54.2546363310207,2.78816766404181,134.85594106718));
#58426=CARTESIAN_POINT('Ctrl Pts',(54.2468884342436,2.90111083330153,134.778217202056));
#58427=CARTESIAN_POINT('Ctrl Pts',(54.2391405374666,3.01085996855044,134.695726899473));
#58428=CARTESIAN_POINT('Ctrl Pts',(54.2313926406895,3.11699487124277,134.608769380455));
#58429=CARTESIAN_POINT('Ctrl Pts',(54.2236463646054,3.22310757280147,134.521830051075));
#58430=CARTESIAN_POINT('Ctrl Pts',(54.2159000885213,3.32560724333658,134.430425611544));
#58431=CARTESIAN_POINT('Ctrl Pts',(54.2081538124372,3.42410582310673,134.334896324037));
#58432=CARTESIAN_POINT('Ctrl Pts',(54.2004074791719,3.52260512997115,134.239366331354));
#58433=CARTESIAN_POINT('Ctrl Pts',(54.1926611459065,3.61710300648337,134.139711702128));
#58434=CARTESIAN_POINT('Ctrl Pts',(54.1849148126411,3.70724770068939,134.036310114113));
#58435=CARTESIAN_POINT('Ctrl Pts',(54.1771667446381,3.79741258217466,133.932885370031));
#58436=CARTESIAN_POINT('Ctrl Pts',(54.1694186766352,3.88322208461788,133.82571229208));
#58437=CARTESIAN_POINT('Ctrl Pts',(54.1616706086322,3.96436451380227,133.71520191592));
#58438=CARTESIAN_POINT('Ctrl Pts',(54.1539143058903,4.04559318212589,133.604574088018));
#58439=CARTESIAN_POINT('Ctrl Pts',(54.1461580031485,4.12214463685522,133.490602192192));
#58440=CARTESIAN_POINT('Ctrl Pts',(54.1384017004066,4.19375004038174,133.373727010531));
#58441=CARTESIAN_POINT('Ctrl Pts',(54.1306412578924,4.2653936618683,133.256789449066));
#58442=CARTESIAN_POINT('Ctrl Pts',(54.1228808153783,4.3320857819934,133.136945855578));
#58443=CARTESIAN_POINT('Ctrl Pts',(54.1151203728641,4.39360388483041,133.014661041876));
#58444=CARTESIAN_POINT('Ctrl Pts',(54.1073474725987,4.45522074198733,132.892179925735));
#58445=CARTESIAN_POINT('Ctrl Pts',(54.0995745723332,4.51164682321409,132.767250114756));
#58446=CARTESIAN_POINT('Ctrl Pts',(54.0918016720678,4.56270771882563,132.640356623844));
#58447=CARTESIAN_POINT('Ctrl Pts',(54.0843113363058,4.61191242226692,132.518076030953));
#58448=CARTESIAN_POINT('Ctrl Pts',(54.0768210005438,4.65613514043298,132.393972339013));
#58449=CARTESIAN_POINT('Ctrl Pts',(54.0693306647818,4.69526431933435,132.268490404875));
#58450=CARTESIAN_POINT('Ctrl Pts',(54.0615563306627,4.73587709294693,132.138250785065));
#58451=CARTESIAN_POINT('Ctrl Pts',(54.0537819965436,4.77113110871178,132.00611378788));
#58452=CARTESIAN_POINT('Ctrl Pts',(54.0460076624245,4.80084714367447,131.87255992742));
#58453=CARTESIAN_POINT('Ctrl Pts',(54.0382429094774,4.83052655627995,131.739170660156));
#58454=CARTESIAN_POINT('Ctrl Pts',(54.0304781565302,4.85468148383218,131.604368381918));
#58455=CARTESIAN_POINT('Ctrl Pts',(54.0227134035831,4.87318194867812,131.468650281476));
#58456=CARTESIAN_POINT('Ctrl Pts',(54.0149563626981,4.89166403860154,131.333066978164));
#58457=CARTESIAN_POINT('Ctrl Pts',(54.0071993218131,4.90450278963085,131.196570047684));
#58458=CARTESIAN_POINT('Ctrl Pts',(53.9994422809281,4.91161899582196,131.059668083929));
#58459=CARTESIAN_POINT('Ctrl Pts',(53.991691089688,4.91872983562658,130.922869359011));
#58460=CARTESIAN_POINT('Ctrl Pts',(53.9839398984479,4.9201266999531,130.785666597634));
#58461=CARTESIAN_POINT('Ctrl Pts',(53.9761887072078,4.91578210617702,130.648574395165));
#58462=CARTESIAN_POINT('Ctrl Pts',(53.9684408104307,4.91143935896917,130.51154046054));
#58463=CARTESIAN_POINT('Ctrl Pts',(53.9606929136535,4.90136001953327,130.374617381314));
#58464=CARTESIAN_POINT('Ctrl Pts',(53.9529450168764,4.88556870341262,130.238320418697));
#58465=CARTESIAN_POINT('Ctrl Pts',(53.9451987407923,4.86978069049489,130.102051966467));
#58466=CARTESIAN_POINT('Ctrl Pts',(53.9374524647083,4.84828312242722,129.96640975846));
#58467=CARTESIAN_POINT('Ctrl Pts',(53.9297061886242,4.82115251564445,129.831904200345));
#58468=CARTESIAN_POINT('Ctrl Pts',(53.9219598553588,4.7940217085897,129.697397649339));
#58469=CARTESIAN_POINT('Ctrl Pts',(53.9142135220935,4.7612578571496,129.564028148214));
#58470=CARTESIAN_POINT('Ctrl Pts',(53.9064671888281,4.722988581793,129.432295779902));
#58471=CARTESIAN_POINT('Ctrl Pts',(53.8987191208252,4.68471073629768,129.300533911041));
#58472=CARTESIAN_POINT('Ctrl Pts',(53.8909710528222,4.64092512260295,129.170410279904));
#58473=CARTESIAN_POINT('Ctrl Pts',(53.8832229848192,4.59180907831169,129.042409298478));
#58474=CARTESIAN_POINT('Ctrl Pts',(53.8754666820774,4.54264083290387,128.914272276086));
#58475=CARTESIAN_POINT('Ctrl Pts',(53.8677103793355,4.48813098024788,128.78826277556));
#58476=CARTESIAN_POINT('Ctrl Pts',(53.8599540765937,4.42850504950473,128.66484523108));
#58477=CARTESIAN_POINT('Ctrl Pts',(53.8521936340795,4.36884729460704,128.54136181494));
#58478=CARTESIAN_POINT('Ctrl Pts',(53.8444331915653,4.30406820523118,128.420473455837));
#58479=CARTESIAN_POINT('Ctrl Pts',(53.8366727490511,4.23443856542452,128.302618604859));
#58480=CARTESIAN_POINT('Ctrl Pts',(53.8288998487857,4.16469714993862,128.184574562811));
#58481=CARTESIAN_POINT('Ctrl Pts',(53.8211269485202,4.09008983695267,128.069574088191));
#58482=CARTESIAN_POINT('Ctrl Pts',(53.8133540482548,4.01093041054784,127.958026079209));
#58483=CARTESIAN_POINT('Ctrl Pts',(53.8058637124928,3.93464862868371,127.850533121327));
#58484=CARTESIAN_POINT('Ctrl Pts',(53.7983733767309,3.85414013722455,127.746246219187));
#58485=CARTESIAN_POINT('Ctrl Pts',(53.7908830409689,3.76971890918094,127.645499682314));
#58486=CARTESIAN_POINT('Ctrl Pts',(53.7831087068498,3.68209682461642,127.540933309873));
#58487=CARTESIAN_POINT('Ctrl Pts',(53.7753343727307,3.58998188321917,127.43984983336));
#58488=CARTESIAN_POINT('Ctrl Pts',(53.7675600386116,3.49368148072396,127.342659767731));
#58489=CARTESIAN_POINT('Ctrl Pts',(53.7597952856645,3.3974997598686,127.245589480172));
#58490=CARTESIAN_POINT('Ctrl Pts',(53.7520305327175,3.2971431137477,127.152403331404));
#58491=CARTESIAN_POINT('Ctrl Pts',(53.7442657797704,3.19295958525813,127.063479417981));
#58492=CARTESIAN_POINT('Ctrl Pts',(53.7365087388854,3.08887953331793,126.974643825043));
#58493=CARTESIAN_POINT('Ctrl Pts',(53.7287516980005,2.98098045844711,126.890062295143));
#58494=CARTESIAN_POINT('Ctrl Pts',(53.7209946571155,2.86964744234516,126.810076373907));
#58495=CARTESIAN_POINT('Ctrl Pts',(53.7132434658753,2.75839838333549,126.730150770676));
#58496=CARTESIAN_POINT('Ctrl Pts',(53.7054922746351,2.64372085369219,126.654814105268));
#58497=CARTESIAN_POINT('Ctrl Pts',(53.697741083395,2.52603294204318,126.584367650959));
#58498=CARTESIAN_POINT('Ctrl Pts',(53.6899931866179,2.40839505089669,126.513951138273));
#58499=CARTESIAN_POINT('Ctrl Pts',(53.6822452898408,2.28774965731439,126.448420903148));
#58500=CARTESIAN_POINT('Ctrl Pts',(53.6744973930637,2.16454357044688,126.388034747101));
#58501=CARTESIAN_POINT('Ctrl Pts',(53.6667511169796,2.0413632556369,126.327661222536));
#58502=CARTESIAN_POINT('Ctrl Pts',(53.6590048408955,1.91562366380614,126.272429808721));
#58503=CARTESIAN_POINT('Ctrl Pts',(53.6512585648114,1.78779557270011,126.222552016944));
#58504=CARTESIAN_POINT('Ctrl Pts',(53.643512231546,1.65996653799563,126.17267385698));
#58505=CARTESIAN_POINT('Ctrl Pts',(53.6357658982807,1.53004933747325,126.128149540027));
#58506=CARTESIAN_POINT('Ctrl Pts',(53.6280195650153,1.39853368704842,126.089142002412));
#58507=CARTESIAN_POINT('Ctrl Pts',(53.6202714970123,1.26698858460625,126.05012572933));
#58508=CARTESIAN_POINT('Ctrl Pts',(53.6125234290093,1.1338446947131,126.016628805129));
#58509=CARTESIAN_POINT('Ctrl Pts',(53.6047753610064,0.999605422197866,125.988763867171));
#58510=CARTESIAN_POINT('Ctrl Pts',(53.5970190582645,0.865223478586152,125.960869314026));
#58511=CARTESIAN_POINT('Ctrl Pts',(53.5892627555227,0.729744210181454,125.938618783877));
#58512=CARTESIAN_POINT('Ctrl Pts',(53.5815064527808,0.593680262633053,125.922073570673));
#58513=CARTESIAN_POINT('Ctrl Pts',(53.5737460102667,0.457543693659038,125.90551952679));
#58514=CARTESIAN_POINT('Ctrl Pts',(53.5659855677526,0.320822213284483,125.894676898364));
#58515=CARTESIAN_POINT('Ctrl Pts',(53.5582251252384,0.184031068219737,125.889554860628));
#58516=CARTESIAN_POINT('Ctrl Pts',(53.550452224973,0.0470203338650006,125.884424600543));
#58517=CARTESIAN_POINT('Ctrl Pts',(53.5426793247075,-0.0900598974694271,
125.885033280372));
#58518=CARTESIAN_POINT('Ctrl Pts',(53.5349064244421,-0.226696000177562,
125.891337924152));
#58519=CARTESIAN_POINT('Ctrl Pts',(53.52741608868,-0.358365036386869,125.89741337825));
#58520=CARTESIAN_POINT('Ctrl Pts',(53.519925752918,-0.48962136687944,125.908777834277));
#58521=CARTESIAN_POINT('Ctrl Pts',(53.512435417156,-0.620014017502905,125.925347840313));
#58522=CARTESIAN_POINT('Ctrl Pts',(53.5046610830369,-0.755350545106557,
125.942546103163));
#58523=CARTESIAN_POINT('Ctrl Pts',(53.4968867489178,-0.890185312586909,
125.965406924036));
#58524=CARTESIAN_POINT('Ctrl Pts',(53.4891124147987,-1.02400678718314,125.993893575552));
#58525=CARTESIAN_POINT('Ctrl Pts',(53.4813476618516,-1.15766333877208,126.022345119816));
#58526=CARTESIAN_POINT('Ctrl Pts',(53.4735829089045,-1.29030870347633,126.056408618839));
#58527=CARTESIAN_POINT('Ctrl Pts',(53.4658181559574,-1.42143665226848,126.095995624696));
#58528=CARTESIAN_POINT('Ctrl Pts',(53.4580611150724,-1.55243436293331,126.13554331218));
#58529=CARTESIAN_POINT('Ctrl Pts',(53.4503040741874,-1.6819172850617,126.1806034768));
#58530=CARTESIAN_POINT('Ctrl Pts',(53.4425470333024,-1.80938992058016,126.23103675217));
#58531=CARTESIAN_POINT('Ctrl Pts',(53.4347958420622,-1.93676642799223,126.281431995414));
#58532=CARTESIAN_POINT('Ctrl Pts',(53.4270446508221,-2.06213530417115,126.337192141085));
#58533=CARTESIAN_POINT('Ctrl Pts',(53.419293459582,-2.18501709226091,126.398128284946));
#58534=CARTESIAN_POINT('Ctrl Pts',(53.4115455628049,-2.30784665231276,126.45903852932));
#58535=CARTESIAN_POINT('Ctrl Pts',(53.4037976660278,-2.42819087719435,126.525120223046));
#58536=CARTESIAN_POINT('Ctrl Pts',(53.3960497692507,-2.5455913599293,126.596136800948));
#58537=CARTESIAN_POINT('Ctrl Pts',(53.3883034931666,-2.66296728501429,126.667138523713));
#58538=CARTESIAN_POINT('Ctrl Pts',(53.3805572170825,-2.77740035843642,126.743072875181));
#58539=CARTESIAN_POINT('Ctrl Pts',(53.3728109409984,-2.8884581628889,126.82365810372));
#58540=CARTESIAN_POINT('Ctrl Pts',(53.365064607733,-2.99951678714487,126.904243927121));
#58541=CARTESIAN_POINT('Ctrl Pts',(53.3573182744677,-3.10719977627718,126.989480466486));
#58542=CARTESIAN_POINT('Ctrl Pts',(53.3495719412024,-3.21110534392616,127.079043781013));
#58543=CARTESIAN_POINT('Ctrl Pts',(53.3418238731994,-3.3150341805063,127.168627152622));
#58544=CARTESIAN_POINT('Ctrl Pts',(53.3340758051964,-3.41518361622664,127.262538972281));
#58545=CARTESIAN_POINT('Ctrl Pts',(53.3263277371935,-3.51118678347731,127.360416594497));
#58546=CARTESIAN_POINT('Ctrl Pts',(53.3185714344516,-3.60729198403673,127.458398242214));
#58547=CARTESIAN_POINT('Ctrl Pts',(53.3108151317097,-3.6992418390565,127.560353832651));
#58548=CARTESIAN_POINT('Ctrl Pts',(53.3030588289679,-3.78670768270662,127.665885193378));
#58549=CARTESIAN_POINT('Ctrl Pts',(53.2952983864537,-3.87422020951093,127.77147287937));
#58550=CARTESIAN_POINT('Ctrl Pts',(53.2875379439396,-3.9572437196356,127.880639827452));
#58551=CARTESIAN_POINT('Ctrl Pts',(53.2797775014255,-4.03549199026289,127.992957505413));
#58552=CARTESIAN_POINT('Ctrl Pts',(53.27200460116,-4.11386587196086,128.105455485681));
#58553=CARTESIAN_POINT('Ctrl Pts',(53.2642317008947,-4.18744898578896,128.221113972932));
#58554=CARTESIAN_POINT('Ctrl Pts',(53.2564588006292,-4.25599986145627,128.339477609838));
#58555=CARTESIAN_POINT('Ctrl Pts',(53.2489684648672,-4.32205874012393,128.453538430403));
#58556=CARTESIAN_POINT('Ctrl Pts',(53.2414781291051,-4.38344475415493,128.570110864694));
#58557=CARTESIAN_POINT('Ctrl Pts',(53.2339877933431,-4.43998435146986,128.688770387582));
#58558=CARTESIAN_POINT('Ctrl Pts',(53.2255778333685,-4.50346558455553,128.821998305502));
#58559=CARTESIAN_POINT('Ctrl Pts',(53.2171678733939,-4.56101434039324,128.958227943729));
#58560=CARTESIAN_POINT('Ctrl Pts',(53.2087579134193,-4.61235985925138,129.096929918748));
#58561=CARTESIAN_POINT('Ctrl Pts',(53.2003695126458,-4.66357375223106,129.235276326821));
#58562=CARTESIAN_POINT('Ctrl Pts',(53.1919811118724,-4.70861601874745,129.37608216204));
#58563=CARTESIAN_POINT('Ctrl Pts',(53.1835927110989,-4.74726330354813,129.518796854353));
#58564=CARTESIAN_POINT('Ctrl Pts',(53.1823472374281,-4.75300148618504,129.539986518095));
#58565=CARTESIAN_POINT('Ctrl Pts',(53.1811017637572,-4.75859877524437,129.561218221204));
#58566=CARTESIAN_POINT('Ctrl Pts',(53.1798562900863,-4.764054528234,129.582490119308));
#58567=CARTESIAN_POINT('Origin',(213.235140564004,0.,130.804360617566));
#58568=CARTESIAN_POINT('',(51.084953843968,-4.7640545282341,129.582490119308));
#58569=CARTESIAN_POINT('',(51.4301221724605,-4.76405452823404,129.582490119308));
#58570=CARTESIAN_POINT('',(213.235140564004,-4.76405452823405,129.582490119308));
#58571=CARTESIAN_POINT('',(52.7648594359568,-4.91824789652852,130.808909330876));
#58572=CARTESIAN_POINT('Ctrl Pts',(52.7648594359567,-4.91824789652852,130.808909330876));
#58573=CARTESIAN_POINT('Ctrl Pts',(52.7548231293723,-4.91808396720261,130.986156171337));
#58574=CARTESIAN_POINT('Ctrl Pts',(52.7447868227878,-4.90833502185388,131.16297489367));
#58575=CARTESIAN_POINT('Ctrl Pts',(52.7347505162034,-4.88916015830731,131.338491695973));
#58576=CARTESIAN_POINT('Ctrl Pts',(52.7244724401057,-4.86952338206541,131.518236608637));
#58577=CARTESIAN_POINT('Ctrl Pts',(52.7141943640081,-4.84000106204612,131.696616434439));
#58578=CARTESIAN_POINT('Ctrl Pts',(52.7039162879104,-4.80081190051794,131.872718309702));
#58579=CARTESIAN_POINT('Ctrl Pts',(52.7015047058992,-4.79161680640899,131.914037726925));
#58580=CARTESIAN_POINT('Ctrl Pts',(52.6990931238879,-4.78188972917596,131.95523183297));
#58581=CARTESIAN_POINT('Ctrl Pts',(52.6966815418767,-4.77163386947856,131.996289003898));
#58582=CARTESIAN_POINT('Ctrl Pts',(52.6889072077576,-4.7385715561945,132.128647000972));
#58583=CARTESIAN_POINT('Ctrl Pts',(52.6811328736385,-4.6999455812719,132.259837952312));
#58584=CARTESIAN_POINT('Ctrl Pts',(52.6733585395194,-4.65585283151093,132.389358243372));
#58585=CARTESIAN_POINT('Ctrl Pts',(52.6655937865723,-4.61181442212335,132.518718912249));
#58586=CARTESIAN_POINT('Ctrl Pts',(52.6578290336252,-4.56232276792526,132.646412650967));
#58587=CARTESIAN_POINT('Ctrl Pts',(52.6500642806781,-4.50752548783554,132.771947220238));
#58588=CARTESIAN_POINT('Ctrl Pts',(52.6423072397931,-4.45278263317699,132.897357106804));
#58589=CARTESIAN_POINT('Ctrl Pts',(52.6345501989081,-4.39274479481001,133.020611735612));
#58590=CARTESIAN_POINT('Ctrl Pts',(52.6267931580231,-4.32760888630213,133.141235537132));
#58591=CARTESIAN_POINT('Ctrl Pts',(52.619041966783,-4.26252209728937,133.261768375306));
#58592=CARTESIAN_POINT('Ctrl Pts',(52.6112907755428,-4.19234507538148,133.379673992458));
#58593=CARTESIAN_POINT('Ctrl Pts',(52.6035395843026,-4.11732203065863,133.494498598851));
#58594=CARTESIAN_POINT('Ctrl Pts',(52.5957916875256,-4.0423308727313,133.609274401723));
#58595=CARTESIAN_POINT('Ctrl Pts',(52.5880437907485,-3.96249800195209,133.720971471744));
#58596=CARTESIAN_POINT('Ctrl Pts',(52.5802958939715,-3.87811246956949,133.829162550895));
#58597=CARTESIAN_POINT('Ctrl Pts',(52.5725496178874,-3.793744588821,133.937330998804));
#58598=CARTESIAN_POINT('Ctrl Pts',(52.5648033418033,-3.70482618098061,134.041994606486));
#58599=CARTESIAN_POINT('Ctrl Pts',(52.5570570657192,-3.6116880978717,134.142757260596));
#58600=CARTESIAN_POINT('Ctrl Pts',(52.5493107324538,-3.51854932723861,134.243520658513));
#58601=CARTESIAN_POINT('Ctrl Pts',(52.5415643991884,-3.42119108456039,134.340382758294));
#58602=CARTESIAN_POINT('Ctrl Pts',(52.5338180659231,-3.31998249775356,134.432982846059));
#58603=CARTESIAN_POINT('Ctrl Pts',(52.5260699979201,-3.21875124598558,134.52560367097));
#58604=CARTESIAN_POINT('Ctrl Pts',(52.5183219299171,-3.11366822268962,134.613960320759));
#58605=CARTESIAN_POINT('Ctrl Pts',(52.5105738619142,-3.00513686535423,134.697731327245));
#58606=CARTESIAN_POINT('Ctrl Pts',(52.5028175591723,-2.89649015960073,134.781591366555));
#58607=CARTESIAN_POINT('Ctrl Pts',(52.4950612564305,-2.78438810870268,134.860855787601));
#58608=CARTESIAN_POINT('Ctrl Pts',(52.4873049536886,-2.66926491645348,134.93524525264));
#58609=CARTESIAN_POINT('Ctrl Pts',(52.4795445111745,-2.55408027949013,135.009674421576));
#58610=CARTESIAN_POINT('Ctrl Pts',(52.4717840686603,-2.43587162498801,135.079223251817));
#58611=CARTESIAN_POINT('Ctrl Pts',(52.4640236261461,-2.31509829113535,135.143658137313));
#58612=CARTESIAN_POINT('Ctrl Pts',(52.4562507258807,-2.19413108120543,135.208196459407));
#58613=CARTESIAN_POINT('Ctrl Pts',(52.4484778256153,-2.07059131729113,135.267604262311));
#58614=CARTESIAN_POINT('Ctrl Pts',(52.4407049253498,-1.94495968927383,135.321695547544));
#58615=CARTESIAN_POINT('Ctrl Pts',(52.4332145895878,-1.82389508738227,135.373820478311));
#58616=CARTESIAN_POINT('Ctrl Pts',(52.4257242538257,-1.70088835754032,135.421008607842));
#58617=CARTESIAN_POINT('Ctrl Pts',(52.4182339180637,-1.57638155150185,135.463137738934));
#58618=CARTESIAN_POINT('Ctrl Pts',(52.4104595839446,-1.44715403206905,135.506864208837));
#58619=CARTESIAN_POINT('Ctrl Pts',(52.4026852498255,-1.31590108624763,135.545278995907));
#58620=CARTESIAN_POINT('Ctrl Pts',(52.3949109157064,-1.18309878890254,135.578191397788));
#58621=CARTESIAN_POINT('Ctrl Pts',(52.3871461627594,-1.05046015852005,135.611063238076));
#58622=CARTESIAN_POINT('Ctrl Pts',(52.3793814098123,-0.91627635166687,135.638446092593));
#58623=CARTESIAN_POINT('Ctrl Pts',(52.3716166568652,-0.781041294829518,
135.660198089956));
#58624=CARTESIAN_POINT('Ctrl Pts',(52.3638596159802,-0.64594055535728,135.68192848293));
#58625=CARTESIAN_POINT('Ctrl Pts',(52.3561025750952,-0.509791027245484,
135.698039086684));
#58626=CARTESIAN_POINT('Ctrl Pts',(52.3483455342102,-0.37309925720116,135.708438513234));
#58627=CARTESIAN_POINT('Ctrl Pts',(52.34059434297,-0.236510567483933,135.718830097495));
#58628=CARTESIAN_POINT('Ctrl Pts',(52.3328431517299,-0.0993808380037102,
135.723519047522));
#58629=CARTESIAN_POINT('Ctrl Pts',(52.3250919604898,0.0377761435688174,
135.722465539736));
#58630=CARTESIAN_POINT('Ctrl Pts',(52.3173440637127,0.174874829765394,135.721412479719));
#58631=CARTESIAN_POINT('Ctrl Pts',(52.3095961669357,0.312000354881666,135.714621819247));
#58632=CARTESIAN_POINT('Ctrl Pts',(52.3018482701586,0.448637015385838,135.702105801926));
#58633=CARTESIAN_POINT('Ctrl Pts',(52.2941019940745,0.585245094446364,135.689592402686));
#58634=CARTESIAN_POINT('Ctrl Pts',(52.2863557179903,0.721364123206853,135.671356064373));
#58635=CARTESIAN_POINT('Ctrl Pts',(52.2786094419062,0.856482006800656,135.647461033057));
#58636=CARTESIAN_POINT('Ctrl Pts',(52.2708631086409,0.991600887803797,135.623565825353));
#58637=CARTESIAN_POINT('Ctrl Pts',(52.2631167753755,1.12571822390223,135.59401190938));
#58638=CARTESIAN_POINT('Ctrl Pts',(52.2553704421101,1.25833101363501,135.558914868242));
#58639=CARTESIAN_POINT('Ctrl Pts',(52.2476223741072,1.39097350108239,135.523809967366));
#58640=CARTESIAN_POINT('Ctrl Pts',(52.2398743061043,1.52211039382675,135.483159571203));
#58641=CARTESIAN_POINT('Ctrl Pts',(52.2321262381013,1.65125316376758,135.437129341736));
#58642=CARTESIAN_POINT('Ctrl Pts',(52.2243699353594,1.78053318818129,135.391050190793));
#58643=CARTESIAN_POINT('Ctrl Pts',(52.2166136326176,1.90781448724799,135.339579916194));
#58644=CARTESIAN_POINT('Ctrl Pts',(52.2088573298757,2.03262734845544,135.282932837014));
#58645=CARTESIAN_POINT('Ctrl Pts',(52.2010968873616,2.15750682604496,135.226255523582));
#58646=CARTESIAN_POINT('Ctrl Pts',(52.1933364448474,2.27991489181693,135.164396076276));
#58647=CARTESIAN_POINT('Ctrl Pts',(52.1855760023332,2.39940672287524,135.097614679548));
#58648=CARTESIAN_POINT('Ctrl Pts',(52.1778031020678,2.51909037282892,135.030726079392));
#58649=CARTESIAN_POINT('Ctrl Pts',(52.1700302018024,2.63584809995036,134.958899945769));
#58650=CARTESIAN_POINT('Ctrl Pts',(52.162257301537,2.7492635938284,134.882440159967));
#58651=CARTESIAN_POINT('Ctrl Pts',(52.1547669657749,2.85855614882788,134.808759879969));
#58652=CARTESIAN_POINT('Ctrl Pts',(52.1472766300128,2.96474500072612,134.730777171067));
#58653=CARTESIAN_POINT('Ctrl Pts',(52.1397862942508,3.06748840178517,134.648797893347));
#58654=CARTESIAN_POINT('Ctrl Pts',(52.1320119601317,3.17412735012311,134.563710346395));
#58655=CARTESIAN_POINT('Ctrl Pts',(52.1242376260127,3.27739222169619,134.474047656544));
#58656=CARTESIAN_POINT('Ctrl Pts',(52.1164632918936,3.37686524311802,134.380107279778));
#58657=CARTESIAN_POINT('Ctrl Pts',(52.1086985389465,3.4762156729311,134.286282676131));
#58658=CARTESIAN_POINT('Ctrl Pts',(52.1009337859995,3.57178326918456,134.188191140872));
#58659=CARTESIAN_POINT('Ctrl Pts',(52.0931690330524,3.66318169213571,134.086171543397));
#58660=CARTESIAN_POINT('Ctrl Pts',(52.0854119921674,3.7544893368847,133.984253273223));
#58661=CARTESIAN_POINT('Ctrl Pts',(52.0776549512823,3.84163578968079,133.878414994121));
#58662=CARTESIAN_POINT('Ctrl Pts',(52.0698979103973,3.92427036235503,133.76903348074));
#58663=CARTESIAN_POINT('Ctrl Pts',(52.0621467191572,4.00684261965522,133.65973445281));
#58664=CARTESIAN_POINT('Ctrl Pts',(52.0543955279171,4.08490953447537,133.546897819707));
#58665=CARTESIAN_POINT('Ctrl Pts',(52.0466443366769,4.1581598873237,133.43093431993));
#58666=CARTESIAN_POINT('Ctrl Pts',(52.0388964398999,4.23137910681805,133.315020107735));
#58667=CARTESIAN_POINT('Ctrl Pts',(52.0311485431228,4.29978562764388,133.195982002002));
#58668=CARTESIAN_POINT('Ctrl Pts',(52.0234006463457,4.36311100033826,133.074260496686));
#58669=CARTESIAN_POINT('Ctrl Pts',(52.0156543702616,4.42642312672981,132.952564452884));
#58670=CARTESIAN_POINT('Ctrl Pts',(52.0079080941776,4.48465603876369,132.828186472591));
#58671=CARTESIAN_POINT('Ctrl Pts',(52.0001618180935,4.53758698869521,132.701592122292));
#58672=CARTESIAN_POINT('Ctrl Pts',(51.9924154848281,4.59051832935098,132.574996837501));
#58673=CARTESIAN_POINT('Ctrl Pts',(51.9846691515628,4.63814747899145,132.446185510763));
#58674=CARTESIAN_POINT('Ctrl Pts',(51.9769228182975,4.68029979638086,132.315643806944));
#58675=CARTESIAN_POINT('Ctrl Pts',(51.9691747502945,4.72246155348949,132.185072869216));
#58676=CARTESIAN_POINT('Ctrl Pts',(51.9614266822915,4.75914391764377,132.052771155293));
#58677=CARTESIAN_POINT('Ctrl Pts',(51.9536786142885,4.79022220358968,131.91923922205));
#58678=CARTESIAN_POINT('Ctrl Pts',(51.9459223115466,4.82133351990773,131.78556536948));
#58679=CARTESIAN_POINT('Ctrl Pts',(51.9381660088048,4.84682877133794,131.650659067129));
#58680=CARTESIAN_POINT('Ctrl Pts',(51.930409706063,4.86663437950127,131.515031342133));
#58681=CARTESIAN_POINT('Ctrl Pts',(51.9226492635488,4.88645055851403,131.379331228536));
#58682=CARTESIAN_POINT('Ctrl Pts',(51.9148888210346,4.90057100307806,131.242909313755));
#58683=CARTESIAN_POINT('Ctrl Pts',(51.9071283785204,4.90897417610009,131.106280475943));
#58684=CARTESIAN_POINT('Ctrl Pts',(51.899355478255,4.91739083864145,130.969432309391));
#58685=CARTESIAN_POINT('Ctrl Pts',(51.8915825779896,4.92007188167751,130.832376947139));
#58686=CARTESIAN_POINT('Ctrl Pts',(51.8838096777242,4.91704794319729,130.695628898186));
#58687=CARTESIAN_POINT('Ctrl Pts',(51.8763193419621,4.91413393249765,130.563851985259));
#58688=CARTESIAN_POINT('Ctrl Pts',(51.8688290062,4.90592253917078,130.432360737737));
#58689=CARTESIAN_POINT('Ctrl Pts',(51.861338670438,4.89248636897057,130.301608002518));
#58690=CARTESIAN_POINT('Ctrl Pts',(51.8535643363189,4.87854076229345,130.165897737603));
#58691=CARTESIAN_POINT('Ctrl Pts',(51.8457900021997,4.85892218741209,130.030553202538));
#58692=CARTESIAN_POINT('Ctrl Pts',(51.8380156680807,4.83365508575137,129.89608666413));
#58693=CARTESIAN_POINT('Ctrl Pts',(51.8302509151336,4.80841912353526,129.761785843713));
#58694=CARTESIAN_POINT('Ctrl Pts',(51.8224861621865,4.77754855696881,129.628361247544));
#58695=CARTESIAN_POINT('Ctrl Pts',(51.8147214092394,4.74111966040295,129.496321081374));
#58696=CARTESIAN_POINT('Ctrl Pts',(51.8069643683544,4.70472694553076,129.364412059359));
#58697=CARTESIAN_POINT('Ctrl Pts',(51.7992073274694,4.66278699023241,129.233885105407));
#58698=CARTESIAN_POINT('Ctrl Pts',(51.7914502865844,4.61542723017222,129.10523891931));
#58699=CARTESIAN_POINT('Ctrl Pts',(51.7836990953443,4.56810318447544,128.976689746302));
#58700=CARTESIAN_POINT('Ctrl Pts',(51.7759479041042,4.51536760369651,128.850018883513));
#58701=CARTESIAN_POINT('Ctrl Pts',(51.7681967128641,4.4573978320316,128.725710182909));
#58702=CARTESIAN_POINT('Ctrl Pts',(51.760448816087,4.39945269906604,128.601454316819));
#58703=CARTESIAN_POINT('Ctrl Pts',(51.7527009193099,4.3362779648067,128.479558969658));
#58704=CARTESIAN_POINT('Ctrl Pts',(51.7449530225328,4.26809912580147,128.360488093306));
#58705=CARTESIAN_POINT('Ctrl Pts',(51.7372067464487,4.19993454833959,128.241442124014));
#58706=CARTESIAN_POINT('Ctrl Pts',(51.7294604703645,4.12676814232369,128.125219789429));
#58707=CARTESIAN_POINT('Ctrl Pts',(51.7217141942804,4.04887120142656,128.012260143593));
#58708=CARTESIAN_POINT('Ctrl Pts',(51.7139678610151,3.97097368551191,127.899299663915));
#58709=CARTESIAN_POINT('Ctrl Pts',(51.7062215277497,3.88834578698797,127.789602242901));
#58710=CARTESIAN_POINT('Ctrl Pts',(51.6984751944843,3.80130171160818,127.683577324893));
#58711=CARTESIAN_POINT('Ctrl Pts',(51.6907271264814,3.71423814331134,127.57752866334));
#58712=CARTESIAN_POINT('Ctrl Pts',(51.6829790584785,3.62275667825065,127.475154443454));
#58713=CARTESIAN_POINT('Ctrl Pts',(51.6752309904755,3.52721105367583,127.376830129689));
#58714=CARTESIAN_POINT('Ctrl Pts',(51.6674746877337,3.43156388207406,127.278401315673));
#58715=CARTESIAN_POINT('Ctrl Pts',(51.6597183849917,3.33184419531554,127.184031286891));
#58716=CARTESIAN_POINT('Ctrl Pts',(51.6519620822499,3.22844216409022,127.094058169567));
#58717=CARTESIAN_POINT('Ctrl Pts',(51.6442016397357,3.12498494408731,127.004037030882));
#58718=CARTESIAN_POINT('Ctrl Pts',(51.6364411972215,3.01784176871079,126.918417723729));
#58719=CARTESIAN_POINT('Ctrl Pts',(51.6286807547073,2.90743417820678,126.837496672093));
#58720=CARTESIAN_POINT('Ctrl Pts',(51.6209078544419,2.79684935163712,126.756445718801));
#58721=CARTESIAN_POINT('Ctrl Pts',(51.6131349541765,2.68298996301386,126.680108310303));
#58722=CARTESIAN_POINT('Ctrl Pts',(51.6053620539111,2.56630544391106,126.608736774673));
#58723=CARTESIAN_POINT('Ctrl Pts',(51.5978717181491,2.45386270098901,126.539959774138));
#58724=CARTESIAN_POINT('Ctrl Pts',(51.5903813823871,2.33879693175673,126.475794020765));
#58725=CARTESIAN_POINT('Ctrl Pts',(51.5828910466251,2.22152837431909,126.416423204089));
#58726=CARTESIAN_POINT('Ctrl Pts',(51.575116712506,2.09981354388233,126.354801324852));
#58727=CARTESIAN_POINT('Ctrl Pts',(51.567342378387,1.97534003444174,126.29814996035));
#58728=CARTESIAN_POINT('Ctrl Pts',(51.5595680442679,1.84855204175805,126.246725440041));
#58729=CARTESIAN_POINT('Ctrl Pts',(51.5518032913208,1.72192030394415,126.195364295858));
#58730=CARTESIAN_POINT('Ctrl Pts',(51.5440385383737,1.59298011712144,126.149217324504));
#58731=CARTESIAN_POINT('Ctrl Pts',(51.5362737854266,1.46220027733216,126.10849505183));
#58732=CARTESIAN_POINT('Ctrl Pts',(51.5285167445416,1.33155032992344,126.067813225091));
#58733=CARTESIAN_POINT('Ctrl Pts',(51.5207597036566,1.19906473656917,126.032545490375));
#58734=CARTESIAN_POINT('Ctrl Pts',(51.5130026627716,1.06523194961701,126.002854191868));
#58735=CARTESIAN_POINT('Ctrl Pts',(51.5052514715315,0.931500087010555,125.973185283801));
#58736=CARTESIAN_POINT('Ctrl Pts',(51.4975002802914,0.796423433092171,125.949084526014));
#58737=CARTESIAN_POINT('Ctrl Pts',(51.4897490890512,0.660504925093427,125.93066424762));
#58738=CARTESIAN_POINT('Ctrl Pts',(51.4820011922741,0.524644186086142,125.912251798335));
#58739=CARTESIAN_POINT('Ctrl Pts',(51.474253295497,0.38794269126859,125.899515078869));
#58740=CARTESIAN_POINT('Ctrl Pts',(51.4665053987199,0.250912662888079,125.892515149913));
#58741=CARTESIAN_POINT('Ctrl Pts',(51.4587591226358,0.113911298235665,125.885516685191));
#58742=CARTESIAN_POINT('Ctrl Pts',(51.4510128465517,-0.0234180730788876,
125.884252644021));
#58743=CARTESIAN_POINT('Ctrl Pts',(51.4432665704676,-0.160559421597148,
125.888732098787));
#58744=CARTESIAN_POINT('Ctrl Pts',(51.4355202372022,-0.297701782461875,
125.893211586619));
#58745=CARTESIAN_POINT('Ctrl Pts',(51.4277739039369,-0.434655727003954,
125.903434642224));
#58746=CARTESIAN_POINT('Ctrl Pts',(51.4200275706716,-0.570906942218394,
125.919358230072));
#58747=CARTESIAN_POINT('Ctrl Pts',(51.4122795026686,-0.707188669947411,
125.935285383896));
#58748=CARTESIAN_POINT('Ctrl Pts',(51.4045314346657,-0.842766966950066,
125.956915564863));
#58749=CARTESIAN_POINT('Ctrl Pts',(51.3967833666627,-0.977134740724373,
125.984154111516));
#58750=CARTESIAN_POINT('Ctrl Pts',(51.3890270639208,-1.11164532216801,126.01142160762));
#58751=CARTESIAN_POINT('Ctrl Pts',(51.381270761179,-1.24494242656168,126.044309298625));
#58752=CARTESIAN_POINT('Ctrl Pts',(51.3735144584371,-1.37653068194959,126.082671688364));
#58753=CARTESIAN_POINT('Ctrl Pts',(51.3657540159229,-1.50818916995145,126.121054553265));
#58754=CARTESIAN_POINT('Ctrl Pts',(51.3579935734088,-1.63813662133238,126.164917814277));
#58755=CARTESIAN_POINT('Ctrl Pts',(51.3502331308947,-1.76589579339966,126.214067042058));
#58756=CARTESIAN_POINT('Ctrl Pts',(51.3424602306292,-1.89386005583188,126.263295168542));
#58757=CARTESIAN_POINT('Ctrl Pts',(51.3346873303637,-2.01962866030996,126.317826062918));
#58758=CARTESIAN_POINT('Ctrl Pts',(51.3269144300983,-2.14274638733545,126.377417995162));
#58759=CARTESIAN_POINT('Ctrl Pts',(51.3194240943363,-2.26138847486888,126.434843610565));
#58760=CARTESIAN_POINT('Ctrl Pts',(51.3119337585742,-2.37756879935849,126.496968544019));
#58761=CARTESIAN_POINT('Ctrl Pts',(51.3044434228122,-2.49090566863703,126.563538525984));
#58762=CARTESIAN_POINT('Ctrl Pts',(51.2966678953229,-2.60855779674132,126.632643135065));
#58763=CARTESIAN_POINT('Ctrl Pts',(51.2888923678337,-2.72351839674755,126.706756922238));
#58764=CARTESIAN_POINT('Ctrl Pts',(51.2811168403445,-2.83533150450471,126.78564461341));
#58765=CARTESIAN_POINT('Ctrl Pts',(51.2729433821621,-2.95286690795564,126.868569565547));
#58766=CARTESIAN_POINT('Ctrl Pts',(51.2647699239798,-3.06692375881384,126.956769812886));
#58767=CARTESIAN_POINT('Ctrl Pts',(51.2565964657974,-3.17700074393878,127.049916672651));
#58768=CARTESIAN_POINT('Ctrl Pts',(51.2488405326635,-3.28145466260714,127.138305308141));
#58769=CARTESIAN_POINT('Ctrl Pts',(51.2410845995295,-3.38232484246005,127.231147469214));
#58770=CARTESIAN_POINT('Ctrl Pts',(51.2333286663955,-3.47921249652988,127.328117894957));
#58771=CARTESIAN_POINT('Ctrl Pts',(51.2255779942255,-3.57603443027332,127.425022544229));
#58772=CARTESIAN_POINT('Ctrl Pts',(51.2178273220555,-3.66887893771196,127.526049611477));
#58773=CARTESIAN_POINT('Ctrl Pts',(51.2100766498855,-3.75738161869157,127.630834749699));
#58774=CARTESIAN_POINT('Ctrl Pts',(51.202329556529,-3.84584343423647,127.735571504187));
#58775=CARTESIAN_POINT('Ctrl Pts',(51.1945824631724,-3.92996716150484,127.844062578221));
#58776=CARTESIAN_POINT('Ctrl Pts',(51.1868353698159,-4.00942675444775,127.955908377626));
#58777=CARTESIAN_POINT('Ctrl Pts',(51.1790901759024,-4.088866865378,128.067726754524));
#58778=CARTESIAN_POINT('Ctrl Pts',(51.171344981989,-4.16364489307399,128.182897900499));
#58779=CARTESIAN_POINT('Ctrl Pts',(51.1635997880755,-4.23347667225136,128.30099122253));
#58780=CARTESIAN_POINT('Ctrl Pts',(51.1558527688126,-4.30332490904099,128.419112376217));
#58781=CARTESIAN_POINT('Ctrl Pts',(51.1481057495497,-4.36822436574079,128.540156747432));
#58782=CARTESIAN_POINT('Ctrl Pts',(51.1403587302867,-4.42793561778904,128.663666985302));
#58783=CARTESIAN_POINT('Ctrl Pts',(51.1326106529049,-4.48765502543907,128.787194092694));
#58784=CARTESIAN_POINT('Ctrl Pts',(51.1248625755231,-4.54218465436355,128.913187382096));
#58785=CARTESIAN_POINT('Ctrl Pts',(51.1171144981413,-4.59133260736094,129.041168072469));
#58786=CARTESIAN_POINT('Ctrl Pts',(51.1093610395618,-4.6405146946135,129.169237648041));
#58787=CARTESIAN_POINT('Ctrl Pts',(51.1016075809823,-4.68430751131722,129.299297012578));
#58788=CARTESIAN_POINT('Ctrl Pts',(51.0938541224028,-4.72256850915155,129.430850610733));
#58789=CARTESIAN_POINT('Ctrl Pts',(51.0908873629246,-4.73720857936148,129.481187873805));
#58790=CARTESIAN_POINT('Ctrl Pts',(51.0879206034463,-4.75103925705807,129.531743774527));
#58791=CARTESIAN_POINT('Ctrl Pts',(51.084953843968,-4.7640545282341,129.582490119308));
#58792=CARTESIAN_POINT('Ctrl Pts',(52.8348764518333,-4.76405452823406,129.582490119308));
#58793=CARTESIAN_POINT('Ctrl Pts',(52.827220890531,-4.79776420415706,129.713923634116));
#58794=CARTESIAN_POINT('Ctrl Pts',(52.8195653292287,-4.82602643062361,129.846737056546));
#58795=CARTESIAN_POINT('Ctrl Pts',(52.8119097679264,-4.84874494536196,129.980433729228));
#58796=CARTESIAN_POINT('Ctrl Pts',(52.8040680459372,-4.87201590741839,130.117381510932));
#58797=CARTESIAN_POINT('Ctrl Pts',(52.796226323948,-4.88946999659759,130.255255614782));
#58798=CARTESIAN_POINT('Ctrl Pts',(52.7883846019588,-4.9010600126408,130.393515372987));
#58799=CARTESIAN_POINT('Ctrl Pts',(52.7805428799695,-4.912650028684,130.531775131192));
#58800=CARTESIAN_POINT('Ctrl Pts',(52.7727011579803,-4.9183759803035,130.670420092754));
#58801=CARTESIAN_POINT('Ctrl Pts',(52.7648594359911,-4.91824789652908,130.80890933027));
#58802=CARTESIAN_POINT('',(53.1101405640403,-4.91824977699176,130.802879529943));
#58803=CARTESIAN_POINT('Ctrl Pts',(53.1798562900863,-4.764054528234,129.582490119308));
#58804=CARTESIAN_POINT('Ctrl Pts',(53.1714950727012,-4.80068054274802,129.725294394021));
#58805=CARTESIAN_POINT('Ctrl Pts',(53.163133855316,-4.83092384607784,129.869911740266));
#58806=CARTESIAN_POINT('Ctrl Pts',(53.1547726379309,-4.85461763059599,130.015772814461));
#58807=CARTESIAN_POINT('Ctrl Pts',(53.1464377560349,-4.87823678633974,130.16117446719));
#58808=CARTESIAN_POINT('Ctrl Pts',(53.1381028741389,-4.89534751386974,130.307811751342));
#58809=CARTESIAN_POINT('Ctrl Pts',(53.1297679922429,-4.90583356353445,130.455104108108));
#58810=CARTESIAN_POINT('Ctrl Pts',(53.1232255161754,-4.91406460145802,130.570721429517));
#58811=CARTESIAN_POINT('Ctrl Pts',(53.1166830401079,-4.91821480319711,130.686742000312));
#58812=CARTESIAN_POINT('Ctrl Pts',(53.1101405640404,-4.91824977699175,130.802879529943));
#58813=CARTESIAN_POINT('Ctrl Pts',(53.1101405640086,-4.91824977699192,130.802879530507));
#58814=CARTESIAN_POINT('Ctrl Pts',(53.1021882788582,-4.91829228711791,130.944043020104));
#58815=CARTESIAN_POINT('Ctrl Pts',(53.0942359937077,-4.91225293971663,131.085150680015));
#58816=CARTESIAN_POINT('Ctrl Pts',(53.0862837085573,-4.90017239467302,131.225660469197));
#58817=CARTESIAN_POINT('Ctrl Pts',(53.0783262621069,-4.88808400895026,131.366261453948));
#58818=CARTESIAN_POINT('Ctrl Pts',(53.0703688156565,-4.86994664079856,131.50626343506));
#58819=CARTESIAN_POINT('Ctrl Pts',(53.0624113692061,-4.84585264216121,131.645131236082));
#58820=CARTESIAN_POINT('Ctrl Pts',(53.0544474601463,-4.82173907567583,131.784111818052));
#58821=CARTESIAN_POINT('Ctrl Pts',(53.0464835510865,-4.79165929709876,131.921956028801));
#58822=CARTESIAN_POINT('Ctrl Pts',(53.0385196420267,-4.7557563841171,132.058140613191));
#58823=CARTESIAN_POINT('Ctrl Pts',(53.0305422080014,-4.71979249785521,132.194556477445));
#58824=CARTESIAN_POINT('Ctrl Pts',(53.0225647739761,-4.67798581071775,132.329306734823));
#58825=CARTESIAN_POINT('Ctrl Pts',(53.0145873399508,-4.63052908993263,132.461883893357));
#58826=CARTESIAN_POINT('Ctrl Pts',(53.0066023422531,-4.58302737384138,132.594586752734));
#58827=CARTESIAN_POINT('Ctrl Pts',(52.9986173445555,-4.52986507690039,132.725112071137));
#58828=CARTESIAN_POINT('Ctrl Pts',(52.9906323468578,-4.47128225528688,132.852974308835));
#58829=CARTESIAN_POINT('Ctrl Pts',(52.9826327569507,-4.41259237630968,132.981070208787));
#58830=CARTESIAN_POINT('Ctrl Pts',(52.9746331670437,-4.348462343365,133.106492983004));
#58831=CARTESIAN_POINT('Ctrl Pts',(52.9666335771366,-4.27917763168596,133.228782581453));
#58832=CARTESIAN_POINT('Ctrl Pts',(52.9629357746011,-4.2471508421262,133.285310827584));
#58833=CARTESIAN_POINT('Ctrl Pts',(52.9592379720656,-4.21402322918207,133.341170016988));
#58834=CARTESIAN_POINT('Ctrl Pts',(52.9555401695301,-4.17982597172962,133.39631700388));
#58835=CARTESIAN_POINT('Ctrl Pts',(52.947765835411,-4.10792897267713,133.512259133738));
#58836=CARTESIAN_POINT('Ctrl Pts',(52.9399915012919,-4.03109034571519,133.625391167482));
#58837=CARTESIAN_POINT('Ctrl Pts',(52.9322171671729,-3.94955612214741,133.735263123708));
#58838=CARTESIAN_POINT('Ctrl Pts',(52.9244524142258,-3.86812238222315,133.844999672567));
#58839=CARTESIAN_POINT('Ctrl Pts',(52.9166876612787,-3.78200479065436,133.951483827095));
#58840=CARTESIAN_POINT('Ctrl Pts',(52.9089229083316,-3.6914942148754,134.054291928231));
#58841=CARTESIAN_POINT('Ctrl Pts',(52.9011658674466,-3.60107353547641,134.156997918912));
#58842=CARTESIAN_POINT('Ctrl Pts',(52.8934088265615,-3.50626881145433,134.256034830523));
#58843=CARTESIAN_POINT('Ctrl Pts',(52.8856517856765,-3.40741276095235,134.351009929099));
#58844=CARTESIAN_POINT('Ctrl Pts',(52.8779005944364,-3.30863125856704,134.445913406215));
#58845=CARTESIAN_POINT('Ctrl Pts',(52.8701494031963,-3.20580479155851,134.536760897331));
#58846=CARTESIAN_POINT('Ctrl Pts',(52.8623982119562,-3.09930446578999,134.623194849479));
#58847=CARTESIAN_POINT('Ctrl Pts',(52.8546503151791,-2.99284940550091,134.709592064892));
#58848=CARTESIAN_POINT('Ctrl Pts',(52.8469024184021,-2.88272389506647,134.791579226446));
#58849=CARTESIAN_POINT('Ctrl Pts',(52.839154521625,-2.76933363905012,134.868837737458));
#58850=CARTESIAN_POINT('Ctrl Pts',(52.8314082455409,-2.65596710183092,134.946080087655));
#58851=CARTESIAN_POINT('Ctrl Pts',(52.8236619694568,-2.53933750027575,135.018595534746));
#58852=CARTESIAN_POINT('Ctrl Pts',(52.8159156933727,-2.41988083375982,135.086107902601));
#58853=CARTESIAN_POINT('Ctrl Pts',(52.8081693601074,-2.30042328544208,135.153620768816));
#58854=CARTESIAN_POINT('Ctrl Pts',(52.8004230268421,-2.17813897088937,135.216130289737));
#58855=CARTESIAN_POINT('Ctrl Pts',(52.7926766935767,-2.05348952898221,135.273405685235));
#58856=CARTESIAN_POINT('Ctrl Pts',(52.7849286255738,-1.92881217269695,135.330693907161));
#58857=CARTESIAN_POINT('Ctrl Pts',(52.7771805575708,-1.80176899029603,135.382745508022));
#58858=CARTESIAN_POINT('Ctrl Pts',(52.7694324895679,-1.67284230867172,135.429377555137));
#58859=CARTESIAN_POINT('Ctrl Pts',(52.761676186826,-1.54377860223557,135.476059163346));
#58860=CARTESIAN_POINT('Ctrl Pts',(52.7539198840842,-1.41282776599566,135.517309578464));
#58861=CARTESIAN_POINT('Ctrl Pts',(52.7461635813424,-1.2804885599877,135.552995380342));
#58862=CARTESIAN_POINT('Ctrl Pts',(52.7384031388282,-1.14807872056084,135.588700228806));
#58863=CARTESIAN_POINT('Ctrl Pts',(52.730642696314,-1.0142794160562,135.618834460189));
#58864=CARTESIAN_POINT('Ctrl Pts',(52.7228822537998,-0.87959937710309,135.643315876535));
#58865=CARTESIAN_POINT('Ctrl Pts',(52.7151093535344,-0.74470313779512,135.667836592623));
#58866=CARTESIAN_POINT('Ctrl Pts',(52.707336453269,-0.608923726223788,135.686686306338));
#58867=CARTESIAN_POINT('Ctrl Pts',(52.6995635530036,-0.472775668782891,
135.699834673212));
#58868=CARTESIAN_POINT('Ctrl Pts',(52.6920732172415,-0.34157693616476,135.712505063833));
#58869=CARTESIAN_POINT('Ctrl Pts',(52.6845828814794,-0.210036202295073,
135.719881410388));
#58870=CARTESIAN_POINT('Ctrl Pts',(52.6770925457173,-0.0786117198208892,
135.721982325262));
#58871=CARTESIAN_POINT('Ctrl Pts',(52.6693182115982,0.057795761850565,135.724162896963));
#58872=CARTESIAN_POINT('Ctrl Pts',(52.6615438774791,0.194510100665746,135.720667011559));
#58873=CARTESIAN_POINT('Ctrl Pts',(52.65376954336,0.331019728596693,135.711458436214));
#58874=CARTESIAN_POINT('Ctrl Pts',(52.6460047904129,0.467361120611432,135.702261209615));
#58875=CARTESIAN_POINT('Ctrl Pts',(52.6382400374658,0.603497917385632,135.687365327394));
#58876=CARTESIAN_POINT('Ctrl Pts',(52.6304752845187,0.73891646160067,135.66678650649));
#58877=CARTESIAN_POINT('Ctrl Pts',(52.6227182436337,0.874200506208711,135.646228124761));
#58878=CARTESIAN_POINT('Ctrl Pts',(52.6149612027487,1.00876733388674,135.619998095269));
#58879=CARTESIAN_POINT('Ctrl Pts',(52.6072041618636,1.14210668414339,135.588164060908));
#58880=CARTESIAN_POINT('Ctrl Pts',(52.5994529706235,1.2753454821586,135.556354032841));
#58881=CARTESIAN_POINT('Ctrl Pts',(52.5917017793834,1.40735826646417,135.518948501972));
#58882=CARTESIAN_POINT('Ctrl Pts',(52.5839505881433,1.5376436258362,135.47606642406));
#58883=CARTESIAN_POINT('Ctrl Pts',(52.5762026913662,1.66787361045484,135.433202572174));
#58884=CARTESIAN_POINT('Ctrl Pts',(52.5684547945891,1.79637725982186,135.384866924796));
#58885=CARTESIAN_POINT('Ctrl Pts',(52.560706897812,1.9226672362991,135.331228603377));
#58886=CARTESIAN_POINT('Ctrl Pts',(52.5529606217279,2.04893079563594,135.277601501938));
#58887=CARTESIAN_POINT('Ctrl Pts',(52.5452143456438,2.1729812434949,135.218674085469));
#58888=CARTESIAN_POINT('Ctrl Pts',(52.5374680695597,2.29435055676372,135.154663892647));
#58889=CARTESIAN_POINT('Ctrl Pts',(52.5297217362944,2.41572076595306,135.090653227316));
#58890=CARTESIAN_POINT('Ctrl Pts',(52.521975403029,2.53440945524215,135.021559893149));
#58891=CARTESIAN_POINT('Ctrl Pts',(52.5142290697637,2.64997293568108,134.947647537713));
#58892=CARTESIAN_POINT('Ctrl Pts',(52.5064810017607,2.76556229576036,134.873718630117));
#58893=CARTESIAN_POINT('Ctrl Pts',(52.4987329337577,2.87802472503326,134.794968764409));
#58894=CARTESIAN_POINT('Ctrl Pts',(52.4909848657547,2.98694560758643,134.711704856281));
#58895=CARTESIAN_POINT('Ctrl Pts',(52.4832285630129,3.0959822525496,134.628352454281));
#58896=CARTESIAN_POINT('Ctrl Pts',(52.475472260271,3.20146952070079,134.540476664001));
#58897=CARTESIAN_POINT('Ctrl Pts',(52.4677159575292,3.30302556990645,134.448424989534));
#58898=CARTESIAN_POINT('Ctrl Pts',(52.459955515015,3.40463582263364,134.356324184316));
#58899=CARTESIAN_POINT('Ctrl Pts',(52.4521950725008,3.50231039725711,134.260043328175));
#58900=CARTESIAN_POINT('Ctrl Pts',(52.4444346299867,3.59570515697534,134.159966000593));
#58901=CARTESIAN_POINT('Ctrl Pts',(52.4366617297212,3.68924984225294,134.059728020001));
#58902=CARTESIAN_POINT('Ctrl Pts',(52.4288888294558,3.77850072880353,133.955681686265));
#58903=CARTESIAN_POINT('Ctrl Pts',(52.4211159291904,3.86315417288444,133.848243483089));
#58904=CARTESIAN_POINT('Ctrl Pts',(52.4136255934284,3.94473025104327,133.74471092922));
#58905=CARTESIAN_POINT('Ctrl Pts',(52.4061352576664,4.02203716002516,133.63802907988));
#58906=CARTESIAN_POINT('Ctrl Pts',(52.3986449219044,4.09484286220777,133.528593536449));
#58907=CARTESIAN_POINT('Ctrl Pts',(52.3908705877854,4.17040901471789,133.415008711126));
#58908=CARTESIAN_POINT('Ctrl Pts',(52.3830962536663,4.24136526688172,133.298097454477));
#58909=CARTESIAN_POINT('Ctrl Pts',(52.3753219195472,4.30740461997317,133.178270578439));
#58910=CARTESIAN_POINT('Ctrl Pts',(52.3675571666001,4.37336258546413,133.058591378317));
#58911=CARTESIAN_POINT('Ctrl Pts',(52.359792413653,4.4344155218605,132.936004047404));
#58912=CARTESIAN_POINT('Ctrl Pts',(52.3520276607059,4.49029900794166,132.810949235539));
#58913=CARTESIAN_POINT('Ctrl Pts',(52.3442706198209,4.54612698975663,132.686018629876));
#58914=CARTESIAN_POINT('Ctrl Pts',(52.3365135789359,4.59679558040917,132.558625774976));
#58915=CARTESIAN_POINT('Ctrl Pts',(52.3287565380509,4.64208588152368,132.429236530077));
#58916=CARTESIAN_POINT('Ctrl Pts',(52.3210053468108,4.68734202886951,132.299944858615));
#58917=CARTESIAN_POINT('Ctrl Pts',(52.3132541555707,4.72722783087796,132.168660161268));
#58918=CARTESIAN_POINT('Ctrl Pts',(52.3055029643306,4.76157234338392,132.035868587991));
#58919=CARTESIAN_POINT('Ctrl Pts',(52.2977550675536,4.79590225855609,131.903133454675));
#58920=CARTESIAN_POINT('Ctrl Pts',(52.2900071707765,4.82469547083971,131.768893096979));
#58921=CARTESIAN_POINT('Ctrl Pts',(52.2822592739994,4.84783084900366,131.633648940134));
#58922=CARTESIAN_POINT('Ctrl Pts',(52.2745129979153,4.87096138774524,131.498433073452));
#58923=CARTESIAN_POINT('Ctrl Pts',(52.2667667218312,4.88843638052679,131.362214210394));
#58924=CARTESIAN_POINT('Ctrl Pts',(52.2590204457472,4.90018587087492,131.225503697027));
#58925=CARTESIAN_POINT('Ctrl Pts',(52.2512741124818,4.91193544795512,131.088792174494));
#58926=CARTESIAN_POINT('Ctrl Pts',(52.2435277792164,4.91795940478863,130.951589383941));
#58927=CARTESIAN_POINT('Ctrl Pts',(52.2357814459511,4.91823973082573,130.814411121397));
#58928=CARTESIAN_POINT('Ctrl Pts',(52.2280333779481,4.9185201196399,130.677202138732));
#58929=CARTESIAN_POINT('Ctrl Pts',(52.2202853099451,4.91305431737767,130.540018085897));
#58930=CARTESIAN_POINT('Ctrl Pts',(52.2125372419422,4.90187643087385,130.403373686428));
#58931=CARTESIAN_POINT('Ctrl Pts',(52.2047809392003,4.89068666437921,130.266584059665));
#58932=CARTESIAN_POINT('Ctrl Pts',(52.1970246364585,4.87377271835034,130.130335622283));
#58933=CARTESIAN_POINT('Ctrl Pts',(52.1892683337167,4.85122056282258,129.995137463333));
#58934=CARTESIAN_POINT('Ctrl Pts',(52.1815078912025,4.82865637053038,129.859867145054));
#58935=CARTESIAN_POINT('Ctrl Pts',(52.1737474486883,4.80044805286173,129.725648604601));
#58936=CARTESIAN_POINT('Ctrl Pts',(52.1659870061741,4.76673231175148,129.592978708091));
#58937=CARTESIAN_POINT('Ctrl Pts',(52.1582141059087,4.73296244714045,129.460095838084));
#58938=CARTESIAN_POINT('Ctrl Pts',(52.1504412056432,4.69366760407845,129.328766954656));
#58939=CARTESIAN_POINT('Ctrl Pts',(52.1426683053778,4.6490340552396,129.1994726415));
#58940=CARTESIAN_POINT('Ctrl Pts',(52.1351779696157,4.6060230483258,129.074878502298));
#58941=CARTESIAN_POINT('Ctrl Pts',(52.1276876338536,4.55805485971953,128.952173864907));
#58942=CARTESIAN_POINT('Ctrl Pts',(52.1201972980915,4.50533689806242,128.831767781358));
#58943=CARTESIAN_POINT('Ctrl Pts',(52.1124229639725,4.45062011886634,128.706796464556));
#58944=CARTESIAN_POINT('Ctrl Pts',(52.1046486298534,4.39061295504604,128.58390557009));
#58945=CARTESIAN_POINT('Ctrl Pts',(52.0968742957344,4.32549509400887,128.46357543857));
#58946=CARTESIAN_POINT('Ctrl Pts',(52.0891095427873,4.26045748491567,128.343393603183));
#58947=CARTESIAN_POINT('Ctrl Pts',(52.0813447898402,4.19032189498778,128.225766591963));
#58948=CARTESIAN_POINT('Ctrl Pts',(52.0735800368931,4.11531612928665,128.111155051974));
#58949=CARTESIAN_POINT('Ctrl Pts',(52.0658229960081,4.0403848603692,127.996657345782));
#58950=CARTESIAN_POINT('Ctrl Pts',(52.058065955123,3.96059325448489,127.88516947564));
#58951=CARTESIAN_POINT('Ctrl Pts',(52.050308914238,3.87621493228729,127.777127415249));
#58952=CARTESIAN_POINT('Ctrl Pts',(52.0425577229978,3.79190024043905,127.669166830216));
#58953=CARTESIAN_POINT('Ctrl Pts',(52.0348065317577,3.70300595663472,127.564647189637));
#58954=CARTESIAN_POINT('Ctrl Pts',(52.0270553405176,3.60984869310465,127.463975089608));
#58955=CARTESIAN_POINT('Ctrl Pts',(52.0193074437405,3.51673102389662,127.363345777907));
#58956=CARTESIAN_POINT('Ctrl Pts',(52.0115595469635,3.41935424363475,127.266561040609));
#58957=CARTESIAN_POINT('Ctrl Pts',(52.0038116501864,3.3180747411787,127.173993821435));
#58958=CARTESIAN_POINT('Ctrl Pts',(51.9960653741023,3.21681642421138,127.081445965328));
#58959=CARTESIAN_POINT('Ctrl Pts',(51.9883190980182,3.11165729725033,126.99311413617));
#58960=CARTESIAN_POINT('Ctrl Pts',(51.9805728219341,3.00298975704259,126.909333585362));
#58961=CARTESIAN_POINT('Ctrl Pts',(51.9728264886688,2.89432141467575,126.825552416106));
#58962=CARTESIAN_POINT('Ctrl Pts',(51.9650801554035,2.78214491701042,126.746322830957));
#58963=CARTESIAN_POINT('Ctrl Pts',(51.9573338221382,2.66688448271236,126.671938783052));
#58964=CARTESIAN_POINT('Ctrl Pts',(51.9495857541352,2.55159823663935,126.597538077356));
#58965=CARTESIAN_POINT('Ctrl Pts',(51.9418376861322,2.43322700810209,126.527985280134));
#58966=CARTESIAN_POINT('Ctrl Pts',(51.9340896181293,2.31222228416855,126.463529916986));
#58967=CARTESIAN_POINT('Ctrl Pts',(51.9263333153874,2.19108895497411,126.399006049911));
#58968=CARTESIAN_POINT('Ctrl Pts',(51.9185770126456,2.06731688487346,126.339590623275));
#58969=CARTESIAN_POINT('Ctrl Pts',(51.9108207099037,1.94138085380819,126.28548648312));
#58970=CARTESIAN_POINT('Ctrl Pts',(51.9030602673896,1.81537760689129,126.231353465956));
#58971=CARTESIAN_POINT('Ctrl Pts',(51.8952998248753,1.6872084628153,126.182537522926));
#58972=CARTESIAN_POINT('Ctrl Pts',(51.8875393823612,1.55736533985158,126.139192211096));
#58973=CARTESIAN_POINT('Ctrl Pts',(51.8797664820957,1.42731378117977,126.095777317522));
#58974=CARTESIAN_POINT('Ctrl Pts',(51.8719935818304,1.29558324961926,126.057850712499));
#58975=CARTESIAN_POINT('Ctrl Pts',(51.8642206815649,1.16267875877338,126.025515446775));
#58976=CARTESIAN_POINT('Ctrl Pts',(51.8567303458029,1.03460568093487,125.994355649407));
#58977=CARTESIAN_POINT('Ctrl Pts',(51.8492400100407,0.905442816692088,125.968387791274));
#58978=CARTESIAN_POINT('Ctrl Pts',(51.8417496742786,0.775646422541445,125.947658476226));
#58979=CARTESIAN_POINT('Ctrl Pts',(51.8339753401595,0.640928758656959,125.926143202897));
#58980=CARTESIAN_POINT('Ctrl Pts',(51.8262010060404,0.505101830890329,125.910203399075));
#58981=CARTESIAN_POINT('Ctrl Pts',(51.8184266719213,0.368666888833184,125.899947524486));
#58982=CARTESIAN_POINT('Ctrl Pts',(51.8106619189742,0.232400090648583,125.889704289345));
#58983=CARTESIAN_POINT('Ctrl Pts',(51.8028971660272,0.0955271552260384,
125.885131074731));
#58984=CARTESIAN_POINT('Ctrl Pts',(51.7951324130801,-0.0414412278135017,
125.886285212782));
#58985=CARTESIAN_POINT('Ctrl Pts',(51.787375372195,-0.178273571924836,125.887438204528));
#58986=CARTESIAN_POINT('Ctrl Pts',(51.77961833131,-0.315200786575555,125.894307225319));
#58987=CARTESIAN_POINT('Ctrl Pts',(51.7718612904249,-0.451708176096456,
125.906897724787));
#58988=CARTESIAN_POINT('Ctrl Pts',(51.7641100991848,-0.588112624331933,
125.919478729661));
#58989=CARTESIAN_POINT('Ctrl Pts',(51.7563589079447,-0.724097489860024,
125.937772589476));
#58990=CARTESIAN_POINT('Ctrl Pts',(51.7486077167046,-0.859149555227231,
125.961732704516));
#58991=CARTESIAN_POINT('Ctrl Pts',(51.7408598199275,-0.994144219864393,
125.985682635868));
#58992=CARTESIAN_POINT('Ctrl Pts',(51.7331119231504,-1.12820648873137,126.015293964348));
#58993=CARTESIAN_POINT('Ctrl Pts',(51.7253640263733,-1.26082995682914,126.050468435105));
#58994=CARTESIAN_POINT('Ctrl Pts',(51.7176177502892,-1.39342568295641,126.085635548122));
#58995=CARTESIAN_POINT('Ctrl Pts',(51.7098714742051,-1.52458282929203,126.12636338861));
#58996=CARTESIAN_POINT('Ctrl Pts',(51.702125198121,-1.65380723930944,126.172503033647));
#58997=CARTESIAN_POINT('Ctrl Pts',(51.6943788648557,-1.78303260323173,126.218643019276));
#58998=CARTESIAN_POINT('Ctrl Pts',(51.6866325315904,-1.91032483416792,126.270194757702));
#58999=CARTESIAN_POINT('Ctrl Pts',(51.678886198325,-2.03520732046639,126.326960230598));
#59000=CARTESIAN_POINT('Ctrl Pts',(51.6711381303221,-2.16011777333162,126.383738415729));
#59001=CARTESIAN_POINT('Ctrl Pts',(51.6633900623191,-2.28261705187411,126.445732496925));
#59002=CARTESIAN_POINT('Ctrl Pts',(51.6556419943161,-2.40225118335179,126.512697500011));
#59003=CARTESIAN_POINT('Ctrl Pts',(51.6478856915743,-2.52201246340839,126.579733674299));
#59004=CARTESIAN_POINT('Ctrl Pts',(51.6401293888324,-2.63890217176005,126.651751132883));
#59005=CARTESIAN_POINT('Ctrl Pts',(51.6323730860906,-2.75249301813096,126.728460073191));
#59006=CARTESIAN_POINT('Ctrl Pts',(51.6246126435764,-2.86614449135657,126.805209955369));
#59007=CARTESIAN_POINT('Ctrl Pts',(51.6168522010623,-2.97649327984469,126.886656076616));
#59008=CARTESIAN_POINT('Ctrl Pts',(51.6090917585481,-3.08314429784728,126.972467573501));
#59009=CARTESIAN_POINT('Ctrl Pts',(51.6013188582827,-3.18996652153214,127.058416822619));
#59010=CARTESIAN_POINT('Ctrl Pts',(51.5935459580174,-3.29307881848113,127.148745193199));
#59011=CARTESIAN_POINT('Ctrl Pts',(51.5857730577519,-3.39212151699185,127.243083504442));
#59012=CARTESIAN_POINT('Ctrl Pts',(51.5782827219899,-3.48756376393847,127.333992380447));
#59013=CARTESIAN_POINT('Ctrl Pts',(51.5707923862278,-3.57922694153472,127.428624494595));
#59014=CARTESIAN_POINT('Ctrl Pts',(51.5633020504658,-3.66682522286025,127.526621175893));
#59015=CARTESIAN_POINT('Ctrl Pts',(51.5556023183827,-3.75687236074222,127.627357406551));
#59016=CARTESIAN_POINT('Ctrl Pts',(51.5479025862996,-3.84292231403989,127.731983074538));
#59017=CARTESIAN_POINT('Ctrl Pts',(51.5402028542165,-3.9246153017362,127.840144398078));
#59018=CARTESIAN_POINT('Ctrl Pts',(51.5325123610161,-4.00621026629049,127.948175939208));
#59019=CARTESIAN_POINT('Ctrl Pts',(51.5248218678156,-4.0834584230912,128.059734384513));
#59020=CARTESIAN_POINT('Ctrl Pts',(51.5171313746152,-4.15603749327386,128.174429930836));
#59021=CARTESIAN_POINT('Ctrl Pts',(51.5094496720891,-4.22853360142158,128.28899437358));
#59022=CARTESIAN_POINT('Ctrl Pts',(51.5017679695631,-4.29637103494933,128.406688444264));
#59023=CARTESIAN_POINT('Ctrl Pts',(51.4940862670369,-4.3592688727129,128.527090770162));
#59024=CARTESIAN_POINT('Ctrl Pts',(51.4864096958712,-4.42212469485984,128.647412667572));
#59025=CARTESIAN_POINT('Ctrl Pts',(51.4787331247054,-4.48004729878422,128.770438870475));
#59026=CARTESIAN_POINT('Ctrl Pts',(51.4710565535396,-4.53280012004181,128.895720752571));
#59027=CARTESIAN_POINT('Ctrl Pts',(51.4633830021108,-4.58553218989361,129.020953352465));
#59028=CARTESIAN_POINT('Ctrl Pts',(51.4557094506819,-4.63309836484631,129.148439500688));
#59029=CARTESIAN_POINT('Ctrl Pts',(51.448035899253,-4.67530912500759,129.27770818557));
#59030=CARTESIAN_POINT('Ctrl Pts',(51.4420646569889,-4.70815580329139,129.378299761941));
#59031=CARTESIAN_POINT('Ctrl Pts',(51.4360934147247,-4.73776052669814,129.479970206387));
#59032=CARTESIAN_POINT('Ctrl Pts',(51.4301221724605,-4.76405452823404,129.582490119308));
#59033=CARTESIAN_POINT('Origin',(213.235140564004,0.,130.804360617566));
#59034=CARTESIAN_POINT('',(49.3346698100615,-4.76405452823405,129.582490119308));
#59035=CARTESIAN_POINT('',(49.6802330064605,-4.76405452823399,129.582490119308));
#59036=CARTESIAN_POINT('',(213.235140564004,-4.76405452823405,129.582490119308));
#59037=CARTESIAN_POINT('',(51.0148594359441,-4.91824985095919,130.803149816199));
#59038=CARTESIAN_POINT('Ctrl Pts',(51.0148594359441,-4.91824985095919,130.803149816199));
#59039=CARTESIAN_POINT('Ctrl Pts',(51.0071353012034,-4.91828322888797,130.938730265459));
#59040=CARTESIAN_POINT('Ctrl Pts',(50.9994111664627,-4.91270608195937,131.074537070603));
#59041=CARTESIAN_POINT('Ctrl Pts',(50.991687031722,-4.90148835380578,131.210063686332));
#59042=CARTESIAN_POINT('Ctrl Pts',(50.9839722803074,-4.89028425301693,131.3454256635));
#59043=CARTESIAN_POINT('Ctrl Pts',(50.9762575288928,-4.8734532339703,131.480507737074));
#59044=CARTESIAN_POINT('Ctrl Pts',(50.9685427774782,-4.85101721727347,131.614801867884));
#59045=CARTESIAN_POINT('Ctrl Pts',(50.9608354919237,-4.82860291276832,131.748966037125));
#59046=CARTESIAN_POINT('Ctrl Pts',(50.9531282063692,-4.80059446742222,131.882343392155));
#59047=CARTESIAN_POINT('Ctrl Pts',(50.9454209208147,-4.76706568556513,132.014429959384));
#59048=CARTESIAN_POINT('Ctrl Pts',(50.9377191907425,-4.73356107156231,132.146421317401));
#59049=CARTESIAN_POINT('Ctrl Pts',(50.9300174606703,-4.69454413678102,132.277123356345));
#59050=CARTESIAN_POINT('Ctrl Pts',(50.9223157305981,-4.65013987091716,132.406041685509));
#59051=CARTESIAN_POINT('Ctrl Pts',(50.9146168686266,-4.60575214106635,132.53491200588));
#59052=CARTESIAN_POINT('Ctrl Pts',(50.9069180066552,-4.55598119723129,132.661999562747));
#59053=CARTESIAN_POINT('Ctrl Pts',(50.8992191446838,-4.50100197519907,132.786824811884));
#59054=CARTESIAN_POINT('Ctrl Pts',(50.8915215491434,-4.4460317970224,132.911629527782));
#59055=CARTESIAN_POINT('Ctrl Pts',(50.883823953603,-4.38585520413647,133.034172313289));
#59056=CARTESIAN_POINT('Ctrl Pts',(50.8761263580627,-4.32069520911287,133.153993774561));
#59057=CARTESIAN_POINT('Ctrl Pts',(50.8684283077829,-4.25553136472944,133.273822314346));
#59058=CARTESIAN_POINT('Ctrl Pts',(50.8607302575032,-4.18538372205302,133.390928861787));
#59059=CARTESIAN_POINT('Ctrl Pts',(50.8530322072234,-4.11052093495727,133.504879216979));
#59060=CARTESIAN_POINT('Ctrl Pts',(50.8453319810314,-4.03563698732653,133.618861781104));
#59061=CARTESIAN_POINT('Ctrl Pts',(50.8376317548393,-3.95603546178864,133.729686047173));
#59062=CARTESIAN_POINT('Ctrl Pts',(50.8299315286472,-3.87202767655376,133.836947753083));
#59063=CARTESIAN_POINT('Ctrl Pts',(50.8222229943479,-3.78792925168435,133.944325188288));
#59064=CARTESIAN_POINT('Ctrl Pts',(50.8145144600486,-3.69941531952466,134.048132076211));
#59065=CARTESIAN_POINT('Ctrl Pts',(50.8068059257493,-3.60683699387736,134.147997852988));
#59066=CARTESIAN_POINT('Ctrl Pts',(50.7990927726815,-3.51420319752235,134.247923466938));
#59067=CARTESIAN_POINT('Ctrl Pts',(50.7913796196137,-3.41750043865668,134.343902988288));
#59068=CARTESIAN_POINT('Ctrl Pts',(50.7836664665459,-3.31711499612581,134.435604366611));
#59069=CARTESIAN_POINT('Ctrl Pts',(50.7759418527052,-3.21658039348492,134.527442001619));
#59070=CARTESIAN_POINT('Ctrl Pts',(50.7682172388645,-3.11235248358655,134.614988546159));
#59071=CARTESIAN_POINT('Ctrl Pts',(50.7604926250238,-3.00484915483977,134.697953382502));
#59072=CARTESIAN_POINT('Ctrl Pts',(50.7561778084113,-2.94479992023208,134.744295900262));
#59073=CARTESIAN_POINT('Ctrl Pts',(50.7518629917988,-2.88372922305448,134.789209658533));
#59074=CARTESIAN_POINT('Ctrl Pts',(50.7475481751863,-2.82171334507904,134.832650187682));
#59075=CARTESIAN_POINT('Ctrl Pts',(50.7397738410673,-2.70997460868076,134.910920301627));
#59076=CARTESIAN_POINT('Ctrl Pts',(50.7319995069481,-2.5947997739891,134.984661667943));
#59077=CARTESIAN_POINT('Ctrl Pts',(50.7242251728291,-2.47659216751477,135.053557517958));
#59078=CARTESIAN_POINT('Ctrl Pts',(50.716460419882,-2.35853024135089,135.122368459996));
#59079=CARTESIAN_POINT('Ctrl Pts',(50.7086956669349,-2.23744331469214,135.186345572587));
#59080=CARTESIAN_POINT('Ctrl Pts',(50.7009309139878,-2.11376556510177,135.245213936275));
#59081=CARTESIAN_POINT('Ctrl Pts',(50.6931738731028,-1.99021065399618,135.304023831075));
#59082=CARTESIAN_POINT('Ctrl Pts',(50.6854168322178,-1.8640703915577,135.357734907682));
#59083=CARTESIAN_POINT('Ctrl Pts',(50.6776597913328,-1.73580524991296,135.406117151421));
#59084=CARTESIAN_POINT('Ctrl Pts',(50.6699086000927,-1.60763683400894,135.454462909733));
#59085=CARTESIAN_POINT('Ctrl Pts',(50.6621574088526,-1.4773470926808,135.497487696361));
#59086=CARTESIAN_POINT('Ctrl Pts',(50.6544062176125,-1.34541793369754,135.535008950108));
#59087=CARTESIAN_POINT('Ctrl Pts',(50.6466583208354,-1.21354484812635,135.572514256322));
#59088=CARTESIAN_POINT('Ctrl Pts',(50.6389104240584,-1.08003410603958,135.604520575315));
#59089=CARTESIAN_POINT('Ctrl Pts',(50.6311625272813,-0.945384081455753,
135.630894777916));
#59090=CARTESIAN_POINT('Ctrl Pts',(50.6234162511972,-0.810762222754529,
135.657263463604));
#59091=CARTESIAN_POINT('Ctrl Pts',(50.6156699751131,-0.675001939005924,
135.678002301136));
#59092=CARTESIAN_POINT('Ctrl Pts',(50.607923699029,-0.53861275026113,135.693029083289));
#59093=CARTESIAN_POINT('Ctrl Pts',(50.6001773657637,-0.402222554722327,
135.708055976367));
#59094=CARTESIAN_POINT('Ctrl Pts',(50.5924310324983,-0.265203833537383,
135.717370687113));
#59095=CARTESIAN_POINT('Ctrl Pts',(50.584684699233,-0.128071801995861,135.720942832483));
#59096=CARTESIAN_POINT('Ctrl Pts',(50.5769366312301,0.00909093931313087,
135.724515777809));
#59097=CARTESIAN_POINT('Ctrl Pts',(50.5691885632271,0.14636665071432,135.722343588573));
#59098=CARTESIAN_POINT('Ctrl Pts',(50.5614404952242,0.28323993842686,135.714448009841));
#59099=CARTESIAN_POINT('Ctrl Pts',(50.5536841924823,0.420258696698767,135.706544039595));
#59100=CARTESIAN_POINT('Ctrl Pts',(50.5459278897404,0.556873785965126,135.692904551183));
#59101=CARTESIAN_POINT('Ctrl Pts',(50.5381715869986,0.692574200735226,135.673603273152));
#59102=CARTESIAN_POINT('Ctrl Pts',(50.5304111444844,0.828347042902733,135.654291693447));
#59103=CARTESIAN_POINT('Ctrl Pts',(50.5226507019702,0.963203853577455,135.629312373967));
#59104=CARTESIAN_POINT('Ctrl Pts',(50.5148902594561,1.09664462925778,135.598790053862));
#59105=CARTESIAN_POINT('Ctrl Pts',(50.5071173591906,1.23029961591755,135.568218736619));
#59106=CARTESIAN_POINT('Ctrl Pts',(50.4993444589252,1.36253364775798,135.53208674059));
#59107=CARTESIAN_POINT('Ctrl Pts',(50.4915715586598,1.49286180945023,135.490568752123));
#59108=CARTESIAN_POINT('Ctrl Pts',(50.4840812228977,1.61845221418903,135.450560047113));
#59109=CARTESIAN_POINT('Ctrl Pts',(50.4765908871356,1.74227261993963,135.405550245124));
#59110=CARTESIAN_POINT('Ctrl Pts',(50.4691005513735,1.86390911523152,135.355736878946));
#59111=CARTESIAN_POINT('Ctrl Pts',(50.4613262172544,1.99015749521196,135.30403482385));
#59112=CARTESIAN_POINT('Ctrl Pts',(50.4535518831354,2.11445300661022,135.24699398323));
#59113=CARTESIAN_POINT('Ctrl Pts',(50.4457775490163,2.23631113514054,135.184782465898));
#59114=CARTESIAN_POINT('Ctrl Pts',(50.4380127960692,2.35801908441822,135.122647618701));
#59115=CARTESIAN_POINT('Ctrl Pts',(50.4302480431222,2.47729528273821,135.055354950026));
#59116=CARTESIAN_POINT('Ctrl Pts',(50.4224832901751,2.59367374899857,134.983121145074));
#59117=CARTESIAN_POINT('Ctrl Pts',(50.4147262492901,2.70993662652575,134.910959083754));
#59118=CARTESIAN_POINT('Ctrl Pts',(50.4069692084051,2.82330716944753,134.833865857359));
#59119=CARTESIAN_POINT('Ctrl Pts',(50.3992121675201,2.93334296347093,134.752104545578));
#59120=CARTESIAN_POINT('Ctrl Pts',(50.39146097628,3.04329577864551,134.670404890639));
#59121=CARTESIAN_POINT('Ctrl Pts',(50.3837097850398,3.14991853785197,134.584044389374));
#59122=CARTESIAN_POINT('Ctrl Pts',(50.3759585937998,3.25279716426536,134.493329805652));
#59123=CARTESIAN_POINT('Ctrl Pts',(50.3682106970227,3.35563206451844,134.402653778047));
#59124=CARTESIAN_POINT('Ctrl Pts',(50.3604628002456,3.45472570443246,134.307627606723));
#59125=CARTESIAN_POINT('Ctrl Pts',(50.3527149034686,3.54969669533472,134.208598628286));
#59126=CARTESIAN_POINT('Ctrl Pts',(50.3449686273845,3.64464782035316,134.109590364576));
#59127=CARTESIAN_POINT('Ctrl Pts',(50.3372223513004,3.73547774121884,134.006581241188));
#59128=CARTESIAN_POINT('Ctrl Pts',(50.3294760752163,3.82184188663316,133.899955496757));
#59129=CARTESIAN_POINT('Ctrl Pts',(50.321729741951,3.90820666956787,133.793328965241));
#59130=CARTESIAN_POINT('Ctrl Pts',(50.3139834086857,3.99010536519393,133.683086063219));
#59131=CARTESIAN_POINT('Ctrl Pts',(50.3062370754203,4.06723392494572,133.569643833128));
#59132=CARTESIAN_POINT('Ctrl Pts',(50.2984890074174,4.14437975710328,133.456176198438));
#59133=CARTESIAN_POINT('Ctrl Pts',(50.2907409394145,4.21675310793709,133.339508133245));
#59134=CARTESIAN_POINT('Ctrl Pts',(50.2829928714116,4.28409368926029,133.220085006676));
#59135=CARTESIAN_POINT('Ctrl Pts',(50.2752365686697,4.35150584095505,133.100534955786));
#59136=CARTESIAN_POINT('Ctrl Pts',(50.2674802659279,4.41387434582178,132.978224335396));
#59137=CARTESIAN_POINT('Ctrl Pts',(50.259723963186,4.47098502282337,132.853622920979));
#59138=CARTESIAN_POINT('Ctrl Pts',(50.2519635206719,4.52812618151293,132.728955003035));
#59139=CARTESIAN_POINT('Ctrl Pts',(50.2442030781577,4.58000377281345,132.601994216538));
#59140=CARTESIAN_POINT('Ctrl Pts',(50.2364426356436,4.62645247919981,132.473228653154));
#59141=CARTESIAN_POINT('Ctrl Pts',(50.2286697353782,4.67297574917319,132.344256383855));
#59142=CARTESIAN_POINT('Ctrl Pts',(50.2208968351127,4.71405260180808,132.213473921379));
#59143=CARTESIAN_POINT('Ctrl Pts',(50.2131239348473,4.74956789709703,132.081383660962));
#59144=CARTESIAN_POINT('Ctrl Pts',(50.2056335990851,4.78379212194542,131.954095214224));
#59145=CARTESIAN_POINT('Ctrl Pts',(50.1981432633229,4.8128520545781,131.825592702687));
#59146=CARTESIAN_POINT('Ctrl Pts',(50.1906529275607,4.83669015566738,131.696331133093));
#59147=CARTESIAN_POINT('Ctrl Pts',(50.1828785934416,4.86143208560437,131.562168571803));
#59148=CARTESIAN_POINT('Ctrl Pts',(50.1751042593225,4.8806267709077,131.426763270177));
#59149=CARTESIAN_POINT('Ctrl Pts',(50.1673299252034,4.89415375447531,131.290613730723));
#59150=CARTESIAN_POINT('Ctrl Pts',(50.1595651722563,4.90766406724457,131.15463198341));
#59151=CARTESIAN_POINT('Ctrl Pts',(50.1518004193092,4.91552053793604,131.017908208552));
#59152=CARTESIAN_POINT('Ctrl Pts',(50.1440356663622,4.91765359577738,130.880951572892));
#59153=CARTESIAN_POINT('Ctrl Pts',(50.1362786254772,4.91978453503561,130.744130964493));
#59154=CARTESIAN_POINT('Ctrl Pts',(50.1285215845921,4.91620336795408,130.607078343939));
#59155=CARTESIAN_POINT('Ctrl Pts',(50.1207645437071,4.9068922951956,130.470308127903));
#59156=CARTESIAN_POINT('Ctrl Pts',(50.113013352467,4.89758824398954,130.333641051351));
#59157=CARTESIAN_POINT('Ctrl Pts',(50.1052621612269,4.8825629141755,130.19725634391));
#59158=CARTESIAN_POINT('Ctrl Pts',(50.0975109699867,4.86185057624597,130.061668193506));
#59159=CARTESIAN_POINT('Ctrl Pts',(50.0897630732096,4.84114704161254,129.926137671681));
#59160=CARTESIAN_POINT('Ctrl Pts',(50.0820151764326,4.81476136526627,129.791403419199));
#59161=CARTESIAN_POINT('Ctrl Pts',(50.0742672796555,4.78277962143859,129.657974053072));
#59162=CARTESIAN_POINT('Ctrl Pts',(50.0665210035714,4.75080456750228,129.524572597492));
#59163=CARTESIAN_POINT('Ctrl Pts',(50.0587747274873,4.71323586549744,129.392475865301));
#59164=CARTESIAN_POINT('Ctrl Pts',(50.0510284514032,4.6702105370682,129.262181444462));
#59165=CARTESIAN_POINT('Ctrl Pts',(50.0432821181378,4.62718489103582,129.131886061818));
#59166=CARTESIAN_POINT('Ctrl Pts',(50.0355357848724,4.57870266079615,129.003393388321));
#59167=CARTESIAN_POINT('Ctrl Pts',(50.0277894516071,4.52495037028572,128.877184650263));
#59168=CARTESIAN_POINT('Ctrl Pts',(50.0200413836041,4.47118604232237,128.750947648633));
#59169=CARTESIAN_POINT('Ctrl Pts',(50.0122933156011,4.41214945880708,128.626995959843));
#59170=CARTESIAN_POINT('Ctrl Pts',(50.0045452475981,4.34807462927492,128.505789304608));
#59171=CARTESIAN_POINT('Ctrl Pts',(49.9967889448562,4.28393170025152,128.384453829497));
#59172=CARTESIAN_POINT('Ctrl Pts',(49.9890326421144,4.2147400116167,128.265869562061));
#59173=CARTESIAN_POINT('Ctrl Pts',(49.9812763393726,4.14077902869673,128.15047062399));
#59174=CARTESIAN_POINT('Ctrl Pts',(49.9735158968584,4.06677857057324,128.03501009403));
#59175=CARTESIAN_POINT('Ctrl Pts',(49.9657554543442,3.98800397045543,127.922738600928));
#59176=CARTESIAN_POINT('Ctrl Pts',(49.95799501183,3.90477651552403,127.814059056467));
#59177=CARTESIAN_POINT('Ctrl Pts',(49.9502221115645,3.82141545649326,127.705205049952));
#59178=CARTESIAN_POINT('Ctrl Pts',(49.9424492112991,3.73358750906663,127.599954814966));
#59179=CARTESIAN_POINT('Ctrl Pts',(49.9346763110337,3.64165311660002,127.498676778954));
#59180=CARTESIAN_POINT('Ctrl Pts',(49.9271859752717,3.55306077086919,127.401080454657));
#59181=CARTESIAN_POINT('Ctrl Pts',(49.9196956395097,3.46065557195196,127.307172763982));
#59182=CARTESIAN_POINT('Ctrl Pts',(49.9122053037477,3.36478922849466,127.217248058654));
#59183=CARTESIAN_POINT('Ctrl Pts',(49.9044309696286,3.26528808348653,127.12391383079));
#59184=CARTESIAN_POINT('Ctrl Pts',(49.8966566355097,3.16174296461367,127.034574925435));
#59185=CARTESIAN_POINT('Ctrl Pts',(49.8888823013906,3.05450816614984,126.949602139344));
#59186=CARTESIAN_POINT('Ctrl Pts',(49.8811175484435,2.9474055249914,126.864734074618));
#59187=CARTESIAN_POINT('Ctrl Pts',(49.8733527954964,2.83662255529905,126.784221663344));
#59188=CARTESIAN_POINT('Ctrl Pts',(49.8655880425493,2.72255002877106,126.708398654444));
#59189=CARTESIAN_POINT('Ctrl Pts',(49.8578310016643,2.60859080068472,126.632650954027));
#59190=CARTESIAN_POINT('Ctrl Pts',(49.8500739607794,2.49134884119863,126.561583602211));
#59191=CARTESIAN_POINT('Ctrl Pts',(49.8423169198944,2.3712473226527,126.49548962886));
#59192=CARTESIAN_POINT('Ctrl Pts',(49.8345657286543,2.25123637359583,126.429445497489));
#59193=CARTESIAN_POINT('Ctrl Pts',(49.8268145374142,2.12837049883189,126.368367467247));
#59194=CARTESIAN_POINT('Ctrl Pts',(49.819063346174,2.0031008232624,126.312504636533));
#59195=CARTESIAN_POINT('Ctrl Pts',(49.811315449397,1.87788439064671,126.256665549011));
#59196=CARTESIAN_POINT('Ctrl Pts',(49.8035675526198,1.75026654559043,126.206037411269));
#59197=CARTESIAN_POINT('Ctrl Pts',(49.7958196558428,1.62072172721546,126.160822726536));
#59198=CARTESIAN_POINT('Ctrl Pts',(49.7880733797587,1.49120400682364,126.11561749974));
#59199=CARTESIAN_POINT('Ctrl Pts',(49.7803271036746,1.3597604837576,126.075823602347));
#59200=CARTESIAN_POINT('Ctrl Pts',(49.7725808275904,1.22688385640715,126.041594712613));
#59201=CARTESIAN_POINT('Ctrl Pts',(49.7648344943251,1.09400624819162,126.007365570208));
#59202=CARTESIAN_POINT('Ctrl Pts',(49.7570881610598,0.9596958931877,125.978701614964));
#59203=CARTESIAN_POINT('Ctrl Pts',(49.7493418277944,0.824458481448597,125.955706033574));
#59204=CARTESIAN_POINT('Ctrl Pts',(49.7415937597915,0.689190784229912,125.932705302483));
#59205=CARTESIAN_POINT('Ctrl Pts',(49.7338456917885,0.552996002519423,125.915375536718));
#59206=CARTESIAN_POINT('Ctrl Pts',(49.7260976237856,0.416387400243408,125.903768347705));
#59207=CARTESIAN_POINT('Ctrl Pts',(49.7183413210438,0.279633608718113,125.892148822433));
#59208=CARTESIAN_POINT('Ctrl Pts',(49.7105850183019,0.142465508235302,125.886264056561));
#59209=CARTESIAN_POINT('Ctrl Pts',(49.7028287155601,0.00539939550242816,
125.886113581372));
#59210=CARTESIAN_POINT('Ctrl Pts',(49.6950682730459,-0.131739873541793,
125.88596302587));
#59211=CARTESIAN_POINT('Ctrl Pts',(49.6873078305317,-0.268776655922635,
125.891552843556));
#59212=CARTESIAN_POINT('Ctrl Pts',(49.6795473880175,-0.405198306976869,
125.902830510087));
#59213=CARTESIAN_POINT('Ctrl Pts',(49.6717744877521,-0.541838954176136,
125.914126280529));
#59214=CARTESIAN_POINT('Ctrl Pts',(49.6640015874867,-0.677862108612464,
125.931128097226));
#59215=CARTESIAN_POINT('Ctrl Pts',(49.6562286872213,-0.812762973402048,
125.953731853007));
#59216=CARTESIAN_POINT('Ctrl Pts',(49.6487383514591,-0.942759851963584,
125.975513905331));
#59217=CARTESIAN_POINT('Ctrl Pts',(49.641248015697,-1.07171431887242,126.002497615599));
#59218=CARTESIAN_POINT('Ctrl Pts',(49.6337576799349,-1.19918862057225,126.034546185663));
#59219=CARTESIAN_POINT('Ctrl Pts',(49.6259833458158,-1.33149614916414,126.067809887002));
#59220=CARTESIAN_POINT('Ctrl Pts',(49.6182090116968,-1.46262816642929,126.106635467491));
#59221=CARTESIAN_POINT('Ctrl Pts',(49.6104346775777,-1.59208120584745,126.150925274028));
#59222=CARTESIAN_POINT('Ctrl Pts',(49.6026699246306,-1.72137470596408,126.195160497337));
#59223=CARTESIAN_POINT('Ctrl Pts',(49.5949051716835,-1.84899297894216,126.244846422357));
#59224=CARTESIAN_POINT('Ctrl Pts',(49.5871404187364,-1.9744440107132,126.299834681237));
#59225=CARTESIAN_POINT('Ctrl Pts',(49.5793833778514,-2.09977044275076,126.354768325003));
#59226=CARTESIAN_POINT('Ctrl Pts',(49.5716263369664,-2.22293356146207,126.414993666411));
#59227=CARTESIAN_POINT('Ctrl Pts',(49.5638692960815,-2.3434580975374,126.480313068384));
#59228=CARTESIAN_POINT('Ctrl Pts',(49.5561181048414,-2.46389174512236,126.545583212488));
#59229=CARTESIAN_POINT('Ctrl Pts',(49.5483669136013,-2.58169042825956,126.61593958541));
#59230=CARTESIAN_POINT('Ctrl Pts',(49.5406157223612,-2.69640072938429,126.691137286761));
#59231=CARTESIAN_POINT('Ctrl Pts',(49.5328678255841,-2.8110622755712,126.766303027084));
#59232=CARTESIAN_POINT('Ctrl Pts',(49.525119928807,-2.92263772420907,126.846305789344));
#59233=CARTESIAN_POINT('Ctrl Pts',(49.5173720320299,-3.03070025766095,126.930855872414));
#59234=CARTESIAN_POINT('Ctrl Pts',(49.5096257559458,-3.13874018676054,127.01538826943));
#59235=CARTESIAN_POINT('Ctrl Pts',(49.5018794798617,-3.24326835456314,127.104465854498));
#59236=CARTESIAN_POINT('Ctrl Pts',(49.4941332037776,-3.34388915168383,127.197757173361));
#59237=CARTESIAN_POINT('Ctrl Pts',(49.4863868705123,-3.4445106915648,127.29104918088));
#59238=CARTESIAN_POINT('Ctrl Pts',(49.4786405372469,-3.54122451651026,127.388554718446));
#59239=CARTESIAN_POINT('Ctrl Pts',(49.4708942039816,-3.63367047480488,127.489904109625));
#59240=CARTESIAN_POINT('Ctrl Pts',(49.4631461359786,-3.72613713573001,127.591276197297));
#59241=CARTESIAN_POINT('Ctrl Pts',(49.4553980679757,-3.81433376472951,127.696493562688));
#59242=CARTESIAN_POINT('Ctrl Pts',(49.4476499999727,-3.89793950795982,127.805152279556));
#59243=CARTESIAN_POINT('Ctrl Pts',(49.4398936972309,-3.98163410836929,127.913926480203));
#59244=CARTESIAN_POINT('Ctrl Pts',(49.4321373944891,-4.06072783739054,128.026149028244));
#59245=CARTESIAN_POINT('Ctrl Pts',(49.4243810917473,-4.13494201838662,128.141385295284));
#59246=CARTESIAN_POINT('Ctrl Pts',(49.4166206492331,-4.20919580972574,128.256683067391));
#59247=CARTESIAN_POINT('Ctrl Pts',(49.4088602067189,-4.27856466598069,128.374997426489));
#59248=CARTESIAN_POINT('Ctrl Pts',(49.4010997642048,-4.34281568040714,128.495868679415));
#59249=CARTESIAN_POINT('Ctrl Pts',(49.3933268639394,-4.40716983626589,128.616933965606));
#59250=CARTESIAN_POINT('Ctrl Pts',(49.3855539636739,-4.46638956388585,128.740563995026));
#59251=CARTESIAN_POINT('Ctrl Pts',(49.3777810634085,-4.52028959653083,128.866277795292));
#59252=CARTESIAN_POINT('Ctrl Pts',(49.3702907276464,-4.57223022722405,128.987421582266));
#59253=CARTESIAN_POINT('Ctrl Pts',(49.3628003918843,-4.61923110680947,129.11049998197));
#59254=CARTESIAN_POINT('Ctrl Pts',(49.3553100561221,-4.66117071095364,129.2350707572));
#59255=CARTESIAN_POINT('Ctrl Pts',(49.3484299741019,-4.69969340547216,129.349492483824));
#59256=CARTESIAN_POINT('Ctrl Pts',(49.3415498920817,-4.73402183531188,129.465393105414));
#59257=CARTESIAN_POINT('Ctrl Pts',(49.3346698100615,-4.76405452823405,129.582490119308));
#59258=CARTESIAN_POINT('Ctrl Pts',(51.084953843968,-4.7640545282341,129.582490119308));
#59259=CARTESIAN_POINT('Ctrl Pts',(51.0771911324384,-4.79810979842364,129.715271100917));
#59260=CARTESIAN_POINT('Ctrl Pts',(51.0694284209086,-4.82657877292075,129.84935629399));
#59261=CARTESIAN_POINT('Ctrl Pts',(51.061665709379,-4.84938950445108,129.984235933984));
#59262=CARTESIAN_POINT('Ctrl Pts',(51.053891502998,-4.87223401360747,130.119315300763));
#59263=CARTESIAN_POINT('Ctrl Pts',(51.046117296617,-4.88940349871459,130.255191076787));
#59264=CARTESIAN_POINT('Ctrl Pts',(51.038343090236,-4.9008779442993,130.391349192082));
#59265=CARTESIAN_POINT('Ctrl Pts',(51.0342273264905,-4.90695266174609,130.463433030242));
#59266=CARTESIAN_POINT('Ctrl Pts',(51.0301115627449,-4.91143206568912,130.535596003573));
#59267=CARTESIAN_POINT('Ctrl Pts',(51.0259957989994,-4.91431908962279,130.607762174365));
#59268=CARTESIAN_POINT('Ctrl Pts',(51.0222836779967,-4.91692297625045,130.672850837089));
#59269=CARTESIAN_POINT('Ctrl Pts',(51.0185715569939,-4.91823380993961,130.737991574334));
#59270=CARTESIAN_POINT('Ctrl Pts',(51.0148594359912,-4.91824985095898,130.803149815373));
#59271=CARTESIAN_POINT('',(51.3601405639582,-4.9182479625051,130.808837426072));
#59272=CARTESIAN_POINT('Ctrl Pts',(51.4301221724605,-4.76405452823404,129.582490119308));
#59273=CARTESIAN_POINT('Ctrl Pts',(51.4224494757503,-4.79784078076855,129.714222205162));
#59274=CARTESIAN_POINT('Ctrl Pts',(51.4147767790401,-4.82615905439274,129.847356967975));
#59275=CARTESIAN_POINT('Ctrl Pts',(51.4071040823299,-4.84890845285665,129.981396536749));
#59276=CARTESIAN_POINT('Ctrl Pts',(51.3992768292764,-4.87211610791191,130.118136155636));
#59277=CARTESIAN_POINT('Ctrl Pts',(51.3914495762228,-4.88952803686276,130.255817000296));
#59278=CARTESIAN_POINT('Ctrl Pts',(51.3836223231693,-4.90109248538486,130.393902931313));
#59279=CARTESIAN_POINT('Ctrl Pts',(51.3757950701157,-4.91265693390694,130.53198886233));
#59280=CARTESIAN_POINT('Ctrl Pts',(51.3679678170622,-4.91837390208594,130.670479439719));
#59281=CARTESIAN_POINT('Ctrl Pts',(51.3601405640086,-4.91824796250591,130.808837425181));
#59282=CARTESIAN_POINT('Ctrl Pts',(51.3601405639582,-4.9182479625051,130.808837426072));
#59283=CARTESIAN_POINT('Ctrl Pts',(51.3504651616975,-4.91809228639094,130.979864113998));
#59284=CARTESIAN_POINT('Ctrl Pts',(51.3407897594369,-4.90901213047814,131.150492424705));
#59285=CARTESIAN_POINT('Ctrl Pts',(51.3311143571762,-4.89115351568566,131.319918905731));
#59286=CARTESIAN_POINT('Ctrl Pts',(51.3212665221831,-4.87297662888093,131.492364865461));
#59287=CARTESIAN_POINT('Ctrl Pts',(51.3114186871899,-4.84570562792725,131.663565909079));
#59288=CARTESIAN_POINT('Ctrl Pts',(51.3015708521968,-4.80954295808226,131.832698887233));
#59289=CARTESIAN_POINT('Ctrl Pts',(51.2959987103488,-4.78908124988764,131.928398393378));
#59290=CARTESIAN_POINT('Ctrl Pts',(51.2904265685008,-4.76577368212046,132.023436216678));
#59291=CARTESIAN_POINT('Ctrl Pts',(51.2848544266528,-4.73966362282522,132.117666295985));
#59292=CARTESIAN_POINT('Ctrl Pts',(51.2770800925336,-4.70323448473597,132.249137486165));
#59293=CARTESIAN_POINT('Ctrl Pts',(51.2693057584145,-4.66127327820999,132.379300033773));
#59294=CARTESIAN_POINT('Ctrl Pts',(51.2615314242953,-4.61388971003747,132.50765296068));
#59295=CARTESIAN_POINT('Ctrl Pts',(51.2537666713481,-4.566564537878,132.635847704075));
#59296=CARTESIAN_POINT('Ctrl Pts',(51.2460019184009,-4.51383043450627,132.762236900944));
#59297=CARTESIAN_POINT('Ctrl Pts',(51.2382371654537,-4.45584753202936,132.886332239325));
#59298=CARTESIAN_POINT('Ctrl Pts',(51.2304801245686,-4.39792221898846,133.010304324466));
#59299=CARTESIAN_POINT('Ctrl Pts',(51.2227230836835,-4.33475864573901,133.13198673311));
#59300=CARTESIAN_POINT('Ctrl Pts',(51.2149660427984,-4.26656579759478,133.250909075556));
#59301=CARTESIAN_POINT('Ctrl Pts',(51.2072148515582,-4.19842437420781,133.369741737739));
#59302=CARTESIAN_POINT('Ctrl Pts',(51.1994636603179,-4.12526141859278,133.485818138811));
#59303=CARTESIAN_POINT('Ctrl Pts',(51.1917124690777,-4.04733264138388,133.598690868715));
#59304=CARTESIAN_POINT('Ctrl Pts',(51.1839645723005,-3.96943698598421,133.711515624698));
#59305=CARTESIAN_POINT('Ctrl Pts',(51.1762166755233,-3.8867797594212,133.821139096662));
#59306=CARTESIAN_POINT('Ctrl Pts',(51.1684687787462,-3.79966082184224,133.927141541912));
#59307=CARTESIAN_POINT('Ctrl Pts',(51.160722502662,-3.71256010766695,134.033121813735));
#59308=CARTESIAN_POINT('Ctrl Pts',(51.1529762265778,-3.62099978692932,134.135482263581));
#59309=CARTESIAN_POINT('Ctrl Pts',(51.1452299504936,-3.52532071197048,134.233835349978));
#59310=CARTESIAN_POINT('Ctrl Pts',(51.1374836172282,-3.42964093073059,134.332189162395));
#59311=CARTESIAN_POINT('Ctrl Pts',(51.1297372839628,-3.32984260721947,134.426535272099));
#59312=CARTESIAN_POINT('Ctrl Pts',(51.1219909506973,-3.22630395406181,134.516522502304));
#59313=CARTESIAN_POINT('Ctrl Pts',(51.1142428826943,-3.12274211414066,134.606529884526));
#59314=CARTESIAN_POINT('Ctrl Pts',(51.1064948146912,-3.01543857283784,134.692176188423));
#59315=CARTESIAN_POINT('Ctrl Pts',(51.0987467466881,-2.90480483968136,134.773150345665));
#59316=CARTESIAN_POINT('Ctrl Pts',(51.0909904439462,-2.79405352367658,134.854210563205));
#59317=CARTESIAN_POINT('Ctrl Pts',(51.0832341412043,-2.6799652615433,134.930588483465));
#59318=CARTESIAN_POINT('Ctrl Pts',(51.0754778384623,-2.56298124398526,135.002015939943));
#59319=CARTESIAN_POINT('Ctrl Pts',(51.0677173959481,-2.44593478853458,135.073481519405));
#59320=CARTESIAN_POINT('Ctrl Pts',(51.0599569534338,-2.32598983976687,135.139991180753));
#59321=CARTESIAN_POINT('Ctrl Pts',(51.0521965109195,-2.2036115475865,135.201323115683));
#59322=CARTESIAN_POINT('Ctrl Pts',(51.044423610654,-2.08103680290745,135.262753506079));
#59323=CARTESIAN_POINT('Ctrl Pts',(51.0366507103885,-1.95602126570306,135.318989400059));
#59324=CARTESIAN_POINT('Ctrl Pts',(51.028877810123,-1.82905021573878,135.36985712625));
#59325=CARTESIAN_POINT('Ctrl Pts',(51.021387474362,-1.70669488327935,135.418875682459));
#59326=CARTESIAN_POINT('Ctrl Pts',(51.0138971386009,-1.58252403561694,135.462909484716));
#59327=CARTESIAN_POINT('Ctrl Pts',(51.0064068028399,-1.45698269885223,135.501847656159));
#59328=CARTESIAN_POINT('Ctrl Pts',(50.9986324687208,-1.32668142412954,135.542262180211));
#59329=CARTESIAN_POINT('Ctrl Pts',(50.9908581346018,-1.19449092934741,135.577315065137));
#59330=CARTESIAN_POINT('Ctrl Pts',(50.9830838004827,-1.06089200079412,135.606827819448));
#59331=CARTESIAN_POINT('Ctrl Pts',(50.9753190475356,-0.927457720980185,
135.636304201927));
#59332=CARTESIAN_POINT('Ctrl Pts',(50.9675542945886,-0.792618839153976,
135.660253955388));
#59333=CARTESIAN_POINT('Ctrl Pts',(50.9597895416415,-0.656872741313494,
135.678547858965));
#59334=CARTESIAN_POINT('Ctrl Pts',(50.9520325007565,-0.521261468410889,
135.696823592779));
#59335=CARTESIAN_POINT('Ctrl Pts',(50.9442754598715,-0.384745157598823,
135.70945460385));
#59336=CARTESIAN_POINT('Ctrl Pts',(50.9365184189865,-0.247832522720093,
135.716362460316));
#59337=CARTESIAN_POINT('Ctrl Pts',(50.9287672277464,-0.11102313472435,135.723265107515));
#59338=CARTESIAN_POINT('Ctrl Pts',(50.9210160365063,0.0261815935647434,
135.724453170977));
#59339=CARTESIAN_POINT('Ctrl Pts',(50.9132648452661,0.163267025550551,135.719899951237));
#59340=CARTESIAN_POINT('Ctrl Pts',(50.9055169484891,0.300294192570704,135.715348666737));
#59341=CARTESIAN_POINT('Ctrl Pts',(50.897769051712,0.437201774202527,135.705060965355));
#59342=CARTESIAN_POINT('Ctrl Pts',(50.8900211549349,0.573474547294229,135.689062246745));
#59343=CARTESIAN_POINT('Ctrl Pts',(50.8822748788509,0.709718815059501,135.673066874723));
#59344=CARTESIAN_POINT('Ctrl Pts',(50.8745286027667,0.845328150355438,135.651362907199));
#59345=CARTESIAN_POINT('Ctrl Pts',(50.8667823266827,0.979792264550653,135.62402763727));
#59346=CARTESIAN_POINT('Ctrl Pts',(50.8590359934173,1.11425737132923,135.596692165559));
#59347=CARTESIAN_POINT('Ctrl Pts',(50.851289660152,1.24757685700965,135.563725386382));
#59348=CARTESIAN_POINT('Ctrl Pts',(50.8435433268867,1.3792508334545,135.525255681102));
#59349=CARTESIAN_POINT('Ctrl Pts',(50.8357952588837,1.51095429737359,135.486777360797));
#59350=CARTESIAN_POINT('Ctrl Pts',(50.8280471908807,1.64101114357892,135.44279377179));
#59351=CARTESIAN_POINT('Ctrl Pts',(50.8202991228778,1.76893723052337,135.39348298867));
#59352=CARTESIAN_POINT('Ctrl Pts',(50.8125428201359,1.89699927883535,135.344119797463));
#59353=CARTESIAN_POINT('Ctrl Pts',(50.804786517394,2.02292567872778,135.28941824292));
#59354=CARTESIAN_POINT('Ctrl Pts',(50.7970302146522,2.14625233977566,135.22960456073));
#59355=CARTESIAN_POINT('Ctrl Pts',(50.789269772138,2.26964482397584,135.169758954176));
#59356=CARTESIAN_POINT('Ctrl Pts',(50.7815093296239,2.39043446034551,135.10479596831));
#59357=CARTESIAN_POINT('Ctrl Pts',(50.7737488871097,2.50818321039096,135.034987054113));
#59358=CARTESIAN_POINT('Ctrl Pts',(50.7659759868443,2.62612098118323,134.96506607645));
#59359=CARTESIAN_POINT('Ctrl Pts',(50.758203086579,2.74100778300454,134.890283838713));
#59360=CARTESIAN_POINT('Ctrl Pts',(50.7504301863135,2.85243519564335,134.810954746893));
#59361=CARTESIAN_POINT('Ctrl Pts',(50.7429398505513,2.95981194116658,134.734509467377));
#59362=CARTESIAN_POINT('Ctrl Pts',(50.7354495147891,3.06397620232771,134.653842362231));
#59363=CARTESIAN_POINT('Ctrl Pts',(50.727959179027,3.16459414780303,134.569267912864));
#59364=CARTESIAN_POINT('Ctrl Pts',(50.7201848449079,3.26902705326087,134.481486797546));
#59365=CARTESIAN_POINT('Ctrl Pts',(50.7124105107888,3.36997022945993,134.389218130973));
#59366=CARTESIAN_POINT('Ctrl Pts',(50.7046361766698,3.46701362972503,134.292769933257));
#59367=CARTESIAN_POINT('Ctrl Pts',(50.6968714237227,3.5639374326722,134.196440599325));
#59368=CARTESIAN_POINT('Ctrl Pts',(50.6891066707756,3.65697074780113,134.09594225596));
#59369=CARTESIAN_POINT('Ctrl Pts',(50.6813419178285,3.74573600865641,133.991623521055));
#59370=CARTESIAN_POINT('Ctrl Pts',(50.6735848769435,3.83441310660324,133.887408396987));
#59371=CARTESIAN_POINT('Ctrl Pts',(50.6658278360586,3.91883033453536,133.779380728371));
#59372=CARTESIAN_POINT('Ctrl Pts',(50.6580707951736,3.99864673325042,133.667926116235));
#59373=CARTESIAN_POINT('Ctrl Pts',(50.6503196039335,4.07840294179842,133.556555552888));
#59374=CARTESIAN_POINT('Ctrl Pts',(50.6425684126934,4.15356500028906,133.44176350646));
#59375=CARTESIAN_POINT('Ctrl Pts',(50.6348172214532,4.22383227205413,133.323968523581));
#59376=CARTESIAN_POINT('Ctrl Pts',(50.6270693246762,4.29406967835416,133.206223606712));
#59377=CARTESIAN_POINT('Ctrl Pts',(50.6193214278991,4.3594162358441,133.085478626973));
#59378=CARTESIAN_POINT('Ctrl Pts',(50.611573531122,4.41961482327418,132.962180785327));
#59379=CARTESIAN_POINT('Ctrl Pts',(50.6038272550379,4.4798008184575,132.838908734931));
#59380=CARTESIAN_POINT('Ctrl Pts',(50.5960809789538,4.53484081406104,132.713085235895));
#59381=CARTESIAN_POINT('Ctrl Pts',(50.5883347028697,4.58452401548642,132.585181387303));
#59382=CARTESIAN_POINT('Ctrl Pts',(50.5805883696044,4.63420758366191,132.457276594555));
#59383=CARTESIAN_POINT('Ctrl Pts',(50.5728420363391,4.67853413719242,132.327291786044));
#59384=CARTESIAN_POINT('Ctrl Pts',(50.5650957030738,4.7173414852052,132.195716925081));
#59385=CARTESIAN_POINT('Ctrl Pts',(50.5573476350708,4.75615752385449,132.06411259884));
#59386=CARTESIAN_POINT('Ctrl Pts',(50.5495995670679,4.78945178693184,131.930917886509));
#59387=CARTESIAN_POINT('Ctrl Pts',(50.5418514990649,4.81711240330117,131.796636363748));
#59388=CARTESIAN_POINT('Ctrl Pts',(50.5340951963231,4.84480241770275,131.662212124988));
#59389=CARTESIAN_POINT('Ctrl Pts',(50.5263388935813,4.8668467457021,131.526699151947));
#59390=CARTESIAN_POINT('Ctrl Pts',(50.5185825908394,4.88318487358148,131.39061018296));
#59391=CARTESIAN_POINT('Ctrl Pts',(50.5108221483253,4.89953172161167,131.254448579193));
#59392=CARTESIAN_POINT('Ctrl Pts',(50.5030617058111,4.9101662706639,131.117710756505));
#59393=CARTESIAN_POINT('Ctrl Pts',(50.495301263297,4.91508012963144,130.980911974973));
#59394=CARTESIAN_POINT('Ctrl Pts',(50.4875283630316,4.92000187676161,130.843893591892));
#59395=CARTESIAN_POINT('Ctrl Pts',(50.4797554627661,4.91918458486074,130.706814445602));
#59396=CARTESIAN_POINT('Ctrl Pts',(50.4719825625007,4.91267201149314,130.570188095711));
#59397=CARTESIAN_POINT('Ctrl Pts',(50.4644922267385,4.90639618657151,130.438528457777));
#59398=CARTESIAN_POINT('Ctrl Pts',(50.4570018909764,4.8948319939123,130.307289574042));
#59399=CARTESIAN_POINT('Ctrl Pts',(50.4495115552142,4.87806357164692,130.176922291138));
#59400=CARTESIAN_POINT('Ctrl Pts',(50.4417372210951,4.86065936955502,130.04161209308));
#59401=CARTESIAN_POINT('Ctrl Pts',(50.433962886976,4.83759337959216,129.906812272014));
#59402=CARTESIAN_POINT('Ctrl Pts',(50.4261885528569,4.80890310755886,129.773034304215));
#59403=CARTESIAN_POINT('Ctrl Pts',(50.4184237999098,4.78024819372172,129.639421205805));
#59404=CARTESIAN_POINT('Ctrl Pts',(50.4106590469627,4.74598287047987,129.506827833549));
#59405=CARTESIAN_POINT('Ctrl Pts',(50.4028942940157,4.70619635604785,129.375760281285));
#59406=CARTESIAN_POINT('Ctrl Pts',(50.3951372531306,4.66644935814285,129.244822907162));
#59407=CARTESIAN_POINT('Ctrl Pts',(50.3873802122456,4.62119219473625,129.115408708873));
#59408=CARTESIAN_POINT('Ctrl Pts',(50.3796231713606,4.5705649861163,128.988012971825));
#59409=CARTESIAN_POINT('Ctrl Pts',(50.3718719801204,4.51997595586819,128.860713304894));
#59410=CARTESIAN_POINT('Ctrl Pts',(50.3641207888804,4.46402508467799,128.73542943134));
#59411=CARTESIAN_POINT('Ctrl Pts',(50.3563695976402,4.4029020062171,128.612640519983));
#59412=CARTESIAN_POINT('Ctrl Pts',(50.3486217008631,4.34180490669507,128.489903797189));
#59413=CARTESIAN_POINT('Ctrl Pts',(50.340873804086,4.27554014606638,128.369660276752));
#59414=CARTESIAN_POINT('Ctrl Pts',(50.3331259073089,4.20434498685076,128.252368005107));
#59415=CARTESIAN_POINT('Ctrl Pts',(50.3253796312248,4.13316472012766,128.135100268477));
#59416=CARTESIAN_POINT('Ctrl Pts',(50.3176333551408,4.05705630893208,128.020782886723));
#59417=CARTESIAN_POINT('Ctrl Pts',(50.3098870790567,3.97630216263665,127.909847847874));
#59418=CARTESIAN_POINT('Ctrl Pts',(50.3021407457913,3.89554742023246,127.798911990127));
#59419=CARTESIAN_POINT('Ctrl Pts',(50.2943944125259,3.8101471043905,127.691358841193));
#59420=CARTESIAN_POINT('Ctrl Pts',(50.2866480792605,3.72042576699122,127.587589693983));
#59421=CARTESIAN_POINT('Ctrl Pts',(50.2789000112576,3.63068433712052,127.483797308392));
#59422=CARTESIAN_POINT('Ctrl Pts',(50.2711519432546,3.53662021581656,127.383790906446));
#59423=CARTESIAN_POINT('Ctrl Pts',(50.2634038752516,3.43859660646317,127.287936803445));
#59424=CARTESIAN_POINT('Ctrl Pts',(50.2556475725097,3.34046881645126,127.191980825562));
#59425=CARTESIAN_POINT('Ctrl Pts',(50.2478912697678,3.23837341205098,127.100186236071));
#59426=CARTESIAN_POINT('Ctrl Pts',(50.240134967026,3.13270906540218,127.012881094471));
#59427=CARTESIAN_POINT('Ctrl Pts',(50.2323745245118,3.02698832250993,126.925529355489));
#59428=CARTESIAN_POINT('Ctrl Pts',(50.2246140819976,2.91769515319169,126.842672075015));
#59429=CARTESIAN_POINT('Ctrl Pts',(50.2168536394834,2.80525852474488,126.764594823384));
#59430=CARTESIAN_POINT('Ctrl Pts',(50.209080739218,2.69264140304059,126.686392235217));
#59431=CARTESIAN_POINT('Ctrl Pts',(50.2013078389526,2.57687106874703,126.612985219126));
#59432=CARTESIAN_POINT('Ctrl Pts',(50.1935349386871,2.45840324614048,126.544614552145));
#59433=CARTESIAN_POINT('Ctrl Pts',(50.1860446029252,2.34424202728925,126.478729331126));
#59434=CARTESIAN_POINT('Ctrl Pts',(50.1785542671632,2.22757630892479,126.41752079158));
#59435=CARTESIAN_POINT('Ctrl Pts',(50.1710639314013,2.10883087980123,126.361161839332));
#59436=CARTESIAN_POINT('Ctrl Pts',(50.1632895972822,1.98558318163933,126.302666020279));
#59437=CARTESIAN_POINT('Ctrl Pts',(50.1555152631631,1.85970454345402,126.249209494943));
#59438=CARTESIAN_POINT('Ctrl Pts',(50.147740929044,1.73164555752309,126.201037174051));
#59439=CARTESIAN_POINT('Ctrl Pts',(50.1399761760969,1.60374439284735,126.15292422124));
#59440=CARTESIAN_POINT('Ctrl Pts',(50.1322114231498,1.47366858933964,126.11008265165));
#59441=CARTESIAN_POINT('Ctrl Pts',(50.1244466702027,1.34189216270387,126.072710959553));
#59442=CARTESIAN_POINT('Ctrl Pts',(50.1166896293177,1.21024661827275,126.035376385547));
#59443=CARTESIAN_POINT('Ctrl Pts',(50.1089325884327,1.07690418576258,126.003500983578));
#59444=CARTESIAN_POINT('Ctrl Pts',(50.1011755475477,0.94235730125259,125.977234580339));
#59445=CARTESIAN_POINT('Ctrl Pts',(50.0934243563075,0.807911879594832,125.950987984799));
#59446=CARTESIAN_POINT('Ctrl Pts',(50.0856731650674,0.672264195995571,125.930342043457));
#59447=CARTESIAN_POINT('Ctrl Pts',(50.0779219738273,0.535919890385907,125.915396214588));
#59448=CARTESIAN_POINT('Ctrl Pts',(50.0701740770502,0.399633534743231,125.900456738094));
#59449=CARTESIAN_POINT('Ctrl Pts',(50.0624261802731,0.262651533800107,125.891212598019));
#59450=CARTESIAN_POINT('Ctrl Pts',(50.054678283496,0.125487501181038,125.887711763972));
#59451=CARTESIAN_POINT('Ctrl Pts',(50.0469320074119,-0.0116478396793211,
125.884211662224));
#59452=CARTESIAN_POINT('Ctrl Pts',(50.0391857313278,-0.148964745887869,
125.886452486869));
#59453=CARTESIAN_POINT('Ctrl Pts',(50.0314394552437,-0.285947124517925,
125.894430138987));
#59454=CARTESIAN_POINT('Ctrl Pts',(50.0236931219784,-0.422930514320783,
125.902407849994));
#59455=CARTESIAN_POINT('Ctrl Pts',(50.015946788713,-0.559578981313767,125.916122450243));
#59456=CARTESIAN_POINT('Ctrl Pts',(50.0082004554476,-0.695379478186064,
125.935517793669));
#59457=CARTESIAN_POINT('Ctrl Pts',(50.0004523874446,-0.831210386638062,
125.954917480546));
#59458=CARTESIAN_POINT('Ctrl Pts',(49.9927043194417,-0.966192560132653,
125.98000038679));
#59459=CARTESIAN_POINT('Ctrl Pts',(49.9849562514387,-1.09982148693239,126.010658941472));
#59460=CARTESIAN_POINT('Ctrl Pts',(49.9771999486969,-1.23359243614573,126.041350080432));
#59461=CARTESIAN_POINT('Ctrl Pts',(49.969443645955,-1.36600688393938,126.077628617819));
#59462=CARTESIAN_POINT('Ctrl Pts',(49.9616873432131,-1.49657333253622,126.119336463643));
#59463=CARTESIAN_POINT('Ctrl Pts',(49.9539269006989,-1.62720946837813,126.1610665702));
#59464=CARTESIAN_POINT('Ctrl Pts',(49.9461664581847,-1.75599527273129,126.208231624894));
#59465=CARTESIAN_POINT('Ctrl Pts',(49.9384060156706,-1.88245861988423,126.260625083127));
#59466=CARTESIAN_POINT('Ctrl Pts',(49.9306331154051,-2.00912497722873,126.313102647991));
#59467=CARTESIAN_POINT('Ctrl Pts',(49.9228602151397,-2.13346107239415,126.370825223755));
#59468=CARTESIAN_POINT('Ctrl Pts',(49.9150873148743,-2.2550180027388,126.433539542548));
#59469=CARTESIAN_POINT('Ctrl Pts',(49.9075969791123,-2.372156032481,126.493974037884));
#59470=CARTESIAN_POINT('Ctrl Pts',(49.9001066433503,-2.4867131808113,126.559043500163));
#59471=CARTESIAN_POINT('Ctrl Pts',(49.8926163075884,-2.59831436846585,126.628484002396));
#59472=CARTESIAN_POINT('Ctrl Pts',(49.884840623724,-2.71416705940923,126.700569875434));
#59473=CARTESIAN_POINT('Ctrl Pts',(49.8770649398596,-2.82720115807032,126.777594810078));
#59474=CARTESIAN_POINT('Ctrl Pts',(49.8692892559952,-2.93696682574024,126.859311957917));
#59475=CARTESIAN_POINT('Ctrl Pts',(49.8614119122646,-3.04816757787158,126.942097481793));
#59476=CARTESIAN_POINT('Ctrl Pts',(49.8535345685339,-3.15601345051436,127.029698638517));
#59477=CARTESIAN_POINT('Ctrl Pts',(49.8456572248033,-3.26006276520945,127.121810708957));
#59478=CARTESIAN_POINT('Ctrl Pts',(49.8379009985295,-3.36251227814322,127.212506517763));
#59479=CARTESIAN_POINT('Ctrl Pts',(49.8301447722556,-3.46128082528066,127.307575264625));
#59480=CARTESIAN_POINT('Ctrl Pts',(49.8223885459818,-3.55597677385618,127.406683139303));
#59481=CARTESIAN_POINT('Ctrl Pts',(49.8146376892888,-3.6506071650933,127.505722402298));
#59482=CARTESIAN_POINT('Ctrl Pts',(49.8068868325958,-3.74117029849785,127.608794948126));
#59483=CARTESIAN_POINT('Ctrl Pts',(49.7991359759027,-3.82730976560157,127.715528634335));
#59484=CARTESIAN_POINT('Ctrl Pts',(49.7913888064269,-3.91340825466433,127.822211545475));
#59485=CARTESIAN_POINT('Ctrl Pts',(49.7836416369511,-3.99508702078494,127.932551827118));
#59486=CARTESIAN_POINT('Ctrl Pts',(49.7758944674753,-4.07202876268352,128.046142928844));
#59487=CARTESIAN_POINT('Ctrl Pts',(49.7679226790574,-4.15120132871993,128.163027454469));
#59488=CARTESIAN_POINT('Ctrl Pts',(49.7599508906395,-4.22535772592946,128.283353848185));
#59489=CARTESIAN_POINT('Ctrl Pts',(49.7519791022216,-4.2941990691015,128.406645576651));
#59490=CARTESIAN_POINT('Ctrl Pts',(49.744232553407,-4.36109532843337,128.526453748034));
#59491=CARTESIAN_POINT('Ctrl Pts',(49.7364860045924,-4.42297266520529,128.649061571292));
#59492=CARTESIAN_POINT('Ctrl Pts',(49.7287394557779,-4.47960302675391,128.77400602164));
#59493=CARTESIAN_POINT('Ctrl Pts',(49.7206550475583,-4.53870327530838,128.904399822229));
#59494=CARTESIAN_POINT('Ctrl Pts',(49.7125706393387,-4.59208832374198,129.037338255335));
#59495=CARTESIAN_POINT('Ctrl Pts',(49.7044862311191,-4.63955485263867,129.172271823457));
#59496=CARTESIAN_POINT('Ctrl Pts',(49.6964018228996,-4.68702138153536,129.307205391578));
#59497=CARTESIAN_POINT('Ctrl Pts',(49.6883174146801,-4.72856926789924,129.444133627827));
#59498=CARTESIAN_POINT('Ctrl Pts',(49.6802330064605,-4.76405452823399,129.582490119308));
#59499=CARTESIAN_POINT('Origin',(213.235140564004,0.,130.804360617566));
#59500=CARTESIAN_POINT('',(47.584673688373,-4.76405452823404,129.582490119308));
#59501=CARTESIAN_POINT('',(47.9299877718525,-4.76405452823408,129.582490119308));
#59502=CARTESIAN_POINT('',(213.235140564004,-4.76405452823405,129.582490119308));
#59503=CARTESIAN_POINT('',(49.2648594360413,-4.91824840372241,130.800398070159));
#59504=CARTESIAN_POINT('Ctrl Pts',(49.2648594359912,-4.91824840372313,130.800398071045));
#59505=CARTESIAN_POINT('Ctrl Pts',(49.2570262275045,-4.91836015682128,130.939104202001));
#59506=CARTESIAN_POINT('Ctrl Pts',(49.2491930190177,-4.91259963290899,131.077889086034));
#59507=CARTESIAN_POINT('Ctrl Pts',(49.241359810531,-4.90097509382102,131.216217622176));
#59508=CARTESIAN_POINT('Ctrl Pts',(49.2336305484484,-4.88950481196243,131.352710543454));
#59509=CARTESIAN_POINT('Ctrl Pts',(49.2259012863658,-4.87232524866436,131.488758754675));
#59510=CARTESIAN_POINT('Ctrl Pts',(49.2181720242833,-4.84949672177395,131.623851073889));
#59511=CARTESIAN_POINT('Ctrl Pts',(49.2104426438067,-4.82666784520474,131.758945462395));
#59512=CARTESIAN_POINT('Ctrl Pts',(49.2027132633302,-4.79818989785096,131.893083542743));
#59513=CARTESIAN_POINT('Ctrl Pts',(49.1949838828536,-4.76417460104857,132.025762858117));
#59514=CARTESIAN_POINT('Ctrl Pts',(49.1872526954078,-4.7301513521732,132.158473191172));
#59515=CARTESIAN_POINT('Ctrl Pts',(49.1795215079621,-4.6905882753529,132.289723700585));
#59516=CARTESIAN_POINT('Ctrl Pts',(49.1717903205162,-4.64564727057392,132.419026062762));
#59517=CARTESIAN_POINT('Ctrl Pts',(49.1638796631656,-4.5996630162419,132.551330018521));
#59518=CARTESIAN_POINT('Ctrl Pts',(49.155969005815,-4.54804822638849,132.681593858697));
#59519=CARTESIAN_POINT('Ctrl Pts',(49.1480583484644,-4.49102842017358,132.809316176099));
#59520=CARTESIAN_POINT('Ctrl Pts',(49.1403142332452,-4.43520904517906,132.934349570695));
#59521=CARTESIAN_POINT('Ctrl Pts',(49.1325701180259,-4.3742102145194,133.056947071731));
#59522=CARTESIAN_POINT('Ctrl Pts',(49.1248260028067,-4.30828963720264,133.176664026591));
#59523=CARTESIAN_POINT('Ctrl Pts',(49.1168320743904,-4.24024256386856,133.300242865525));
#59524=CARTESIAN_POINT('Ctrl Pts',(49.1088381459742,-4.16695111041679,133.420751794026));
#59525=CARTESIAN_POINT('Ctrl Pts',(49.1008442175579,-4.08874597150404,133.53773571861));
#59526=CARTESIAN_POINT('Ctrl Pts',(49.0928502891417,-4.01054083259129,133.654719643194));
#59527=CARTESIAN_POINT('Ctrl Pts',(49.0848563607253,-3.92742233257059,133.768178241303));
#59528=CARTESIAN_POINT('Ctrl Pts',(49.0768624323091,-3.83976462881858,133.877696046343));
#59529=CARTESIAN_POINT('Ctrl Pts',(49.06908809819,-3.75451489407085,133.984205382433));
#59530=CARTESIAN_POINT('Ctrl Pts',(49.0613137640709,-3.66469515649169,134.087333683076));
#59531=CARTESIAN_POINT('Ctrl Pts',(49.0535394299518,-3.57060350750201,134.186663628048));
#59532=CARTESIAN_POINT('Ctrl Pts',(49.0457746770047,-3.47662781806025,134.28587115774));
#59533=CARTESIAN_POINT('Ctrl Pts',(49.0380099240576,-3.37839095877677,134.38128936471));
#59534=CARTESIAN_POINT('Ctrl Pts',(49.0302451711105,-3.2762323865968,134.472532425363));
#59535=CARTESIAN_POINT('Ctrl Pts',(49.0224881302255,-3.17417527975104,134.563684862121));
#59536=CARTESIAN_POINT('Ctrl Pts',(49.0147310893405,-3.06820450114081,134.65067014616));
#59537=CARTESIAN_POINT('Ctrl Pts',(49.0069740484555,-2.95869735866967,134.733138163101));
#59538=CARTESIAN_POINT('Ctrl Pts',(48.9992228572154,-2.84927279638665,134.81554399027));
#59539=CARTESIAN_POINT('Ctrl Pts',(48.9914716659752,-2.73631748939105,134.893439096542));
#59540=CARTESIAN_POINT('Ctrl Pts',(48.9837204747351,-2.62024264933108,134.966512887862));
#59541=CARTESIAN_POINT('Ctrl Pts',(48.975972577958,-2.50421714417454,135.03955562087));
#59542=CARTESIAN_POINT('Ctrl Pts',(48.968224681181,-2.38507507320559,135.10778090675));
#59543=CARTESIAN_POINT('Ctrl Pts',(48.9604767844039,-2.2632573384036,135.170920966704));
#59544=CARTESIAN_POINT('Ctrl Pts',(48.9527305083198,-2.14146508524564,135.234047819119));
#59545=CARTESIAN_POINT('Ctrl Pts',(48.9449842322357,-2.01699862840108,135.292091381607));
#59546=CARTESIAN_POINT('Ctrl Pts',(48.9372379561516,-1.89032387280038,135.344829615194));
#59547=CARTESIAN_POINT('Ctrl Pts',(48.9294916228862,-1.76364818211542,135.397568238083));
#59548=CARTESIAN_POINT('Ctrl Pts',(48.9217452896209,-1.6347645210809,135.445001303658));
#59549=CARTESIAN_POINT('Ctrl Pts',(48.9139989563555,-1.50415881977546,135.486954909985));
#59550=CARTESIAN_POINT('Ctrl Pts',(48.9062508883526,-1.37352387022878,135.528917911531));
#59551=CARTESIAN_POINT('Ctrl Pts',(48.8985028203496,-1.2411664851953,135.56539889252));
#59552=CARTESIAN_POINT('Ctrl Pts',(48.8907547523466,-1.10758741071973,135.596273929607));
#59553=CARTESIAN_POINT('Ctrl Pts',(48.8829984496048,-0.973866366814014,
135.62718178105));
#59554=CARTESIAN_POINT('Ctrl Pts',(48.8752421468629,-0.838921421250006,
135.65247169853));
#59555=CARTESIAN_POINT('Ctrl Pts',(48.8674858441211,-0.703263712543963,
135.67207088145));
#59556=CARTESIAN_POINT('Ctrl Pts',(48.8597254016069,-0.567533599234209,
135.691680525043));
#59557=CARTESIAN_POINT('Ctrl Pts',(48.8519649590928,-0.431090353515187,
135.705593342325));
#59558=CARTESIAN_POINT('Ctrl Pts',(48.8442045165786,-0.294448885718147,
135.713788579783));
#59559=CARTESIAN_POINT('Ctrl Pts',(48.8364316163132,-0.157588068906726,
135.721996972964));
#59560=CARTESIAN_POINT('Ctrl Pts',(48.8286587160477,-0.0205287852715254,
135.724469437965));
#59561=CARTESIAN_POINT('Ctrl Pts',(48.8208858157823,0.11621450340992,135.721237395735));
#59562=CARTESIAN_POINT('Ctrl Pts',(48.8133954800203,0.247986829112416,135.718122846381));
#59563=CARTESIAN_POINT('Ctrl Pts',(48.8059051442583,0.379465428026367,135.709711355268));
#59564=CARTESIAN_POINT('Ctrl Pts',(48.7984148084963,0.510197564270782,135.696076217221));
#59565=CARTESIAN_POINT('Ctrl Pts',(48.7906404743772,0.645886449196257,135.681924098772));
#59566=CARTESIAN_POINT('Ctrl Pts',(48.7828661402581,0.781200971403702,135.662099575266));
#59567=CARTESIAN_POINT('Ctrl Pts',(48.775091806139,0.915628901874171,135.636627867683));
#59568=CARTESIAN_POINT('Ctrl Pts',(48.7673270531919,1.04989116193451,135.611187551703));
#59569=CARTESIAN_POINT('Ctrl Pts',(48.7595623002448,1.18326862385331,135.580113971362));
#59570=CARTESIAN_POINT('Ctrl Pts',(48.7517975472977,1.31525319854346,135.543484174324));
#59571=CARTESIAN_POINT('Ctrl Pts',(48.7440405064127,1.44710668429356,135.506890758518));
#59572=CARTESIAN_POINT('Ctrl Pts',(48.7362834655276,1.57756966162535,135.464752211981));
#59573=CARTESIAN_POINT('Ctrl Pts',(48.7285264246426,1.70614362526044,135.417196729166));
#59574=CARTESIAN_POINT('Ctrl Pts',(48.7207752334025,1.83462063026886,135.369677108312));
#59575=CARTESIAN_POINT('Ctrl Pts',(48.7130240421623,1.9612110917978,135.31674881711));
#59576=CARTESIAN_POINT('Ctrl Pts',(48.7052728509222,2.08543142833007,135.258589935892));
#59577=CARTESIAN_POINT('Ctrl Pts',(48.6975249541451,2.20959896790597,135.20045577375));
#59578=CARTESIAN_POINT('Ctrl Pts',(48.6897770573681,2.33139803272242,135.137095608677));
#59579=CARTESIAN_POINT('Ctrl Pts',(48.682029160591,2.45036501460562,135.068735643018));
#59580=CARTESIAN_POINT('Ctrl Pts',(48.6742828845069,2.56930711116083,135.000389976789));
#59581=CARTESIAN_POINT('Ctrl Pts',(48.6665366084228,2.68541796434803,134.92704678489));
#59582=CARTESIAN_POINT('Ctrl Pts',(48.6587903323386,2.79825893349477,134.848978028844));
#59583=CARTESIAN_POINT('Ctrl Pts',(48.6510439990733,2.91110073560791,134.770908696513));
#59584=CARTESIAN_POINT('Ctrl Pts',(48.6432976658079,3.02067228399814,134.68811395287));
#59585=CARTESIAN_POINT('Ctrl Pts',(48.6355513325425,3.12656461296599,134.600908626409));
#59586=CARTESIAN_POINT('Ctrl Pts',(48.6278032645395,3.23248065578671,134.51368377092));
#59587=CARTESIAN_POINT('Ctrl Pts',(48.6200551965365,3.33471553790816,134.422046615657));
#59588=CARTESIAN_POINT('Ctrl Pts',(48.6123071285336,3.43289433364003,134.326351468855));
#59589=CARTESIAN_POINT('Ctrl Pts',(48.6045508257917,3.53117747496434,134.230554616111));
#59590=CARTESIAN_POINT('Ctrl Pts',(48.5967945230498,3.62539563807892,134.130691429707));
#59591=CARTESIAN_POINT('Ctrl Pts',(48.5890382203079,3.71521129092596,134.027152594451));
#59592=CARTESIAN_POINT('Ctrl Pts',(48.5812777777938,3.80507488109122,133.923558497401));
#59593=CARTESIAN_POINT('Ctrl Pts',(48.5735173352796,3.89053103542438,133.816285148084));
#59594=CARTESIAN_POINT('Ctrl Pts',(48.5657568927654,3.97128397179708,133.705754537365));
#59595=CARTESIAN_POINT('Ctrl Pts',(48.5579839924999,4.05216653995226,133.595046493097));
#59596=CARTESIAN_POINT('Ctrl Pts',(48.5502110922345,4.1283305854456,133.48107106378));
#59597=CARTESIAN_POINT('Ctrl Pts',(48.5424381919691,4.19952446445392,133.364278064468));
#59598=CARTESIAN_POINT('Ctrl Pts',(48.5349478562071,4.26813026663278,133.251730784866));
#59599=CARTESIAN_POINT('Ctrl Pts',(48.5274575204452,4.33212083518902,133.136567499525));
#59600=CARTESIAN_POINT('Ctrl Pts',(48.5199671846832,4.39131312033296,133.019208725607));
#59601=CARTESIAN_POINT('Ctrl Pts',(48.5121928505641,4.45274969895984,132.897400258104));
#59602=CARTESIAN_POINT('Ctrl Pts',(48.5044185164451,4.50921157036847,132.772840679068));
#59603=CARTESIAN_POINT('Ctrl Pts',(48.496644182326,4.56044308138651,132.645974573837));
#59604=CARTESIAN_POINT('Ctrl Pts',(48.4888794293789,4.61161145414598,132.519264819743));
#59605=CARTESIAN_POINT('Ctrl Pts',(48.4811146764318,4.65756214704797,132.390254554396));
#59606=CARTESIAN_POINT('Ctrl Pts',(48.4733499234847,4.69808534791299,132.25941289368));
#59607=CARTESIAN_POINT('Ctrl Pts',(48.4655928825997,4.73856830056364,132.128701186747));
#59608=CARTESIAN_POINT('Ctrl Pts',(48.4578358417147,4.77363437391953,131.99616207532));
#59609=CARTESIAN_POINT('Ctrl Pts',(48.4500788008297,4.80312196732493,131.862284258242));
#59610=CARTESIAN_POINT('Ctrl Pts',(48.4423276095895,4.83258732390692,131.728507399466));
#59611=CARTESIAN_POINT('Ctrl Pts',(48.4345764183493,4.85648249011215,131.593394224713));
#59612=CARTESIAN_POINT('Ctrl Pts',(48.4268252271092,4.8746959023445,131.457447841577));
#59613=CARTESIAN_POINT('Ctrl Pts',(48.4190773303321,4.89290157339069,131.32155923928));
#59614=CARTESIAN_POINT('Ctrl Pts',(48.411329433555,4.90543024170309,131.184838519642));
#59615=CARTESIAN_POINT('Ctrl Pts',(48.4035815367779,4.91222162617665,131.04779799724));
#59616=CARTESIAN_POINT('Ctrl Pts',(48.3958352606938,4.919011590039,130.91078614076));
#59617=CARTESIAN_POINT('Ctrl Pts',(48.3880889846097,4.92006663781996,130.773455004815));
#59618=CARTESIAN_POINT('Ctrl Pts',(48.3803427085255,4.91537848245433,130.636320632072));
#59619=CARTESIAN_POINT('Ctrl Pts',(48.3725963752602,4.91069029248181,130.499185247033));
#59620=CARTESIAN_POINT('Ctrl Pts',(48.3648500419948,4.90025882812449,130.362247018832));
#59621=CARTESIAN_POINT('Ctrl Pts',(48.3571037087295,4.8841279075608,130.226020194384));
#59622=CARTESIAN_POINT('Ctrl Pts',(48.3493556407265,4.8679933745893,130.089762862884));
#59623=CARTESIAN_POINT('Ctrl Pts',(48.3416075727236,4.8461568915804,129.954217640332));
#59624=CARTESIAN_POINT('Ctrl Pts',(48.3338595047206,4.81871389159144,129.819891474584));
#59625=CARTESIAN_POINT('Ctrl Pts',(48.3261032019787,4.79124172485552,129.685422545389));
#59626=CARTESIAN_POINT('Ctrl Pts',(48.3183468992369,4.75815121643137,129.552175644818));
#59627=CARTESIAN_POINT('Ctrl Pts',(48.310590596495,4.7195886161914,129.420645922834));
#59628=CARTESIAN_POINT('Ctrl Pts',(48.3028301539808,4.68100543393058,129.289045999477));
#59629=CARTESIAN_POINT('Ctrl Pts',(48.2950697114666,4.63694446581079,129.15916545099));
#59630=CARTESIAN_POINT('Ctrl Pts',(48.2873092689524,4.58760086723276,129.031481223624));
#59631=CARTESIAN_POINT('Ctrl Pts',(48.279536368687,4.53817805792977,128.9035920262));
#59632=CARTESIAN_POINT('Ctrl Pts',(48.2717634684216,4.48345582829295,128.777906554099));
#59633=CARTESIAN_POINT('Ctrl Pts',(48.2639905681561,4.42367660083347,128.654879658418));
#59634=CARTESIAN_POINT('Ctrl Pts',(48.2565002323942,4.36607049886774,128.536325100283));
#59635=CARTESIAN_POINT('Ctrl Pts',(48.2490098966323,4.30376883067783,128.420239453904));
#59636=CARTESIAN_POINT('Ctrl Pts',(48.2415195608704,4.23702644637958,128.30700402405));
#59637=CARTESIAN_POINT('Ctrl Pts',(48.2337452267513,4.16775350429406,128.189475238454));
#59638=CARTESIAN_POINT('Ctrl Pts',(48.2259708926322,4.09347702339569,128.07464477195));
#59639=CARTESIAN_POINT('Ctrl Pts',(48.2181965585132,4.01443285913479,127.962968022024));
#59640=CARTESIAN_POINT('Ctrl Pts',(48.2104318055661,3.93548610974164,127.851428903712));
#59641=CARTESIAN_POINT('Ctrl Pts',(48.202667052619,3.85178359166624,127.743036084711));
#59642=CARTESIAN_POINT('Ctrl Pts',(48.1949022996719,3.76360657677979,127.638219654545));
#59643=CARTESIAN_POINT('Ctrl Pts',(48.1871452587869,3.67551714054784,127.533507329535));
#59644=CARTESIAN_POINT('Ctrl Pts',(48.179388217902,3.5829623015873,127.432364621724));
#59645=CARTESIAN_POINT('Ctrl Pts',(48.171631177017,3.4862658669731,127.335191643982));
#59646=CARTESIAN_POINT('Ctrl Pts',(48.1638799857769,3.38964235189244,127.238091945138));
#59647=CARTESIAN_POINT('Ctrl Pts',(48.1561287945368,3.28888373237513,127.144956293787));
#59648=CARTESIAN_POINT('Ctrl Pts',(48.1483776032966,3.18435298424078,127.056150493486));
#59649=CARTESIAN_POINT('Ctrl Pts',(48.1406297065196,3.07986666446284,126.967382438019));
#59650=CARTESIAN_POINT('Ctrl Pts',(48.1328818097425,2.97161170215211,126.882940825983));
#59651=CARTESIAN_POINT('Ctrl Pts',(48.1251339129655,2.85998653866297,126.803153292125));
#59652=CARTESIAN_POINT('Ctrl Pts',(48.1173876368814,2.74838472475152,126.723382448098));
#59653=CARTESIAN_POINT('Ctrl Pts',(48.1096413607972,2.63341442975789,126.648263973041));
#59654=CARTESIAN_POINT('Ctrl Pts',(48.1018950847131,2.5155053356322,126.578083772764));
#59655=CARTESIAN_POINT('Ctrl Pts',(48.0941487514478,2.39759537112803,126.507903054433));
#59656=CARTESIAN_POINT('Ctrl Pts',(48.0864024181824,2.27674690016223,126.442660883586));
#59657=CARTESIAN_POINT('Ctrl Pts',(48.078656084917,2.1534162580258,126.382598357768));
#59658=CARTESIAN_POINT('Ctrl Pts',(48.0709080169141,2.03005799684767,126.322522381365));
#59659=CARTESIAN_POINT('Ctrl Pts',(48.0631599489111,1.90421680982264,126.267628529296));
#59660=CARTESIAN_POINT('Ctrl Pts',(48.0554118809081,1.77637079043816,126.218110528727));
#59661=CARTESIAN_POINT('Ctrl Pts',(48.0476555781663,1.64838889478272,126.168539899837));
#59662=CARTESIAN_POINT('Ctrl Pts',(48.0398992754245,1.51839827550077,126.124356677252));
#59663=CARTESIAN_POINT('Ctrl Pts',(48.0321429726826,1.3868945679069,126.085705457458));
#59664=CARTESIAN_POINT('Ctrl Pts',(48.0243825301684,1.25532067282479,126.047033608345));
#59665=CARTESIAN_POINT('Ctrl Pts',(48.0166220876543,1.1222324594565,126.01389973973));
#59666=CARTESIAN_POINT('Ctrl Pts',(48.0088616451402,0.988136682452456,125.986397462944));
#59667=CARTESIAN_POINT('Ctrl Pts',(48.0010887448747,0.853825643002705,125.958851037063));
#59668=CARTESIAN_POINT('Ctrl Pts',(47.9933158446093,0.718504193942803,125.936954330961));
#59669=CARTESIAN_POINT('Ctrl Pts',(47.9855429443439,0.582686049673517,125.920749245844));
#59670=CARTESIAN_POINT('Ctrl Pts',(47.9780526085818,0.451805237052026,125.905133256388));
#59671=CARTESIAN_POINT('Ctrl Pts',(47.9705622728196,0.320463521573599,125.894802286893));
#59672=CARTESIAN_POINT('Ctrl Pts',(47.9630719370575,0.189119458453297,125.88974802928));
#59673=CARTESIAN_POINT('Ctrl Pts',(47.9552976029384,0.0527954452601593,
125.884502137954));
#59674=CARTESIAN_POINT('Ctrl Pts',(47.9475232688194,-0.0839629306078813,
125.884924372917));
#59675=CARTESIAN_POINT('Ctrl Pts',(47.9397489347003,-0.220645044714559,
125.891062455766));
#59676=CARTESIAN_POINT('Ctrl Pts',(47.9319841817532,-0.357158710331046,
125.897192973977));
#59677=CARTESIAN_POINT('Ctrl Pts',(47.924219428806,-0.493595914367787,125.909025306701));
#59678=CARTESIAN_POINT('Ctrl Pts',(47.9164546758589,-0.629442776011608,
125.926555285839));
#59679=CARTESIAN_POINT('Ctrl Pts',(47.9086976349739,-0.765154712637708,
125.944067853955));
#59680=CARTESIAN_POINT('Ctrl Pts',(47.9009405940889,-0.900277088465724,
125.967266757142));
#59681=CARTESIAN_POINT('Ctrl Pts',(47.8931835532039,-1.03429825157307,125.996095838117));
#59682=CARTESIAN_POINT('Ctrl Pts',(47.8854323619638,-1.16821834827861,126.024903178857));
#59683=CARTESIAN_POINT('Ctrl Pts',(47.8776811707236,-1.30103850451456,126.05933216457));
#59684=CARTESIAN_POINT('Ctrl Pts',(47.8699299794835,-1.43225476209144,126.099275139175));
#59685=CARTESIAN_POINT('Ctrl Pts',(47.8621820827064,-1.56341524925855,126.13920113695));
#59686=CARTESIAN_POINT('Ctrl Pts',(47.8544341859294,-1.69297282037823,126.184636348776));
#59687=CARTESIAN_POINT('Ctrl Pts',(47.8466862891523,-1.82043645977644,126.235422649239));
#59688=CARTESIAN_POINT('Ctrl Pts',(47.8389400130682,-1.94787343652891,126.286198326303));
#59689=CARTESIAN_POINT('Ctrl Pts',(47.8311937369841,-2.07321698980928,126.34232272097));
#59690=CARTESIAN_POINT('Ctrl Pts',(47.8234474609,-2.19599432537318,126.403588868721));
#59691=CARTESIAN_POINT('Ctrl Pts',(47.8157011276346,-2.31877256725115,126.464855468725));
#59692=CARTESIAN_POINT('Ctrl Pts',(47.8079547943694,-2.43898420378337,126.531263722983));
#59693=CARTESIAN_POINT('Ctrl Pts',(47.800208461104,-2.5561797324055,126.602560022804));
#59694=CARTESIAN_POINT('Ctrl Pts',(47.7924603931011,-2.673401506154,126.673872288938));
#59695=CARTESIAN_POINT('Ctrl Pts',(47.784712325098,-2.7876054940033,126.750074575689));
#59696=CARTESIAN_POINT('Ctrl Pts',(47.7769642570951,-2.89837028659462,126.830869363733));
#59697=CARTESIAN_POINT('Ctrl Pts',(47.7692079543532,-3.00925280132562,126.911750021439));
#59698=CARTESIAN_POINT('Ctrl Pts',(47.7614516516114,-3.11668850274028,126.997232699924));
#59699=CARTESIAN_POINT('Ctrl Pts',(47.7536953488695,-3.22028783472276,127.086978565095));
#59700=CARTESIAN_POINT('Ctrl Pts',(47.7459349063553,-3.32394246078833,127.176772330336));
#59701=CARTESIAN_POINT('Ctrl Pts',(47.7381744638411,-3.42375635304082,127.27083354817));
#59702=CARTESIAN_POINT('Ctrl Pts',(47.730414021327,-3.51937684034752,127.368786470771));
#59703=CARTESIAN_POINT('Ctrl Pts',(47.7226411210615,-3.61515082614912,127.466896636099));
#59704=CARTESIAN_POINT('Ctrl Pts',(47.7148682207961,-3.70671769376669,127.568910699191));
#59705=CARTESIAN_POINT('Ctrl Pts',(47.7070953205306,-3.79376451534785,127.674419106198));
#59706=CARTESIAN_POINT('Ctrl Pts',(47.6996049847686,-3.87764696570682,127.77609201685));
#59707=CARTESIAN_POINT('Ctrl Pts',(47.6921146490066,-3.95733210834618,127.881009380511));
#59708=CARTESIAN_POINT('Ctrl Pts',(47.6846243132446,-4.03257907279263,127.988780910974));
#59709=CARTESIAN_POINT('Ctrl Pts',(47.6767527933233,-4.1116553650274,128.102036948611));
#59710=CARTESIAN_POINT('Ctrl Pts',(47.6688812734021,-4.18607751906586,128.218799537863));
#59711=CARTESIAN_POINT('Ctrl Pts',(47.6610097534808,-4.25552329444847,128.338654926915));
#59712=CARTESIAN_POINT('Ctrl Pts',(47.6531519072033,-4.32484843534068,128.458302114768));
#59713=CARTESIAN_POINT('Ctrl Pts',(47.6452940609259,-4.38921423111591,128.581031074442));
#59714=CARTESIAN_POINT('Ctrl Pts',(47.6374362146484,-4.44834071839569,128.706397816284));
#59715=CARTESIAN_POINT('Ctrl Pts',(47.6295863185946,-4.50740738409309,128.831637717564));
#59716=CARTESIAN_POINT('Ctrl Pts',(47.6217364225407,-4.56124512815604,128.959509750956));
#59717=CARTESIAN_POINT('Ctrl Pts',(47.6138865264869,-4.60961876995572,129.089543467497));
#59718=CARTESIAN_POINT('Ctrl Pts',(47.6060446040402,-4.65794327576532,129.219445101044));
#59719=CARTESIAN_POINT('Ctrl Pts',(47.5982026815935,-4.70081460317361,129.351503690871));
#59720=CARTESIAN_POINT('Ctrl Pts',(47.5903607591468,-4.7380450070248,129.485227351399));
#59721=CARTESIAN_POINT('Ctrl Pts',(47.5884650688889,-4.74704500853698,129.517553434989));
#59722=CARTESIAN_POINT('Ctrl Pts',(47.5865693786309,-4.75571559087855,129.54997672912));
#59723=CARTESIAN_POINT('Ctrl Pts',(47.584673688373,-4.76405452823404,129.582490119308));
#59724=CARTESIAN_POINT('Ctrl Pts',(49.3346698100615,-4.76405452823405,129.582490119308));
#59725=CARTESIAN_POINT('Ctrl Pts',(49.3254862744199,-4.80414217617995,129.738791250234));
#59726=CARTESIAN_POINT('Ctrl Pts',(49.3163027387783,-4.83657436684548,129.897224746301));
#59727=CARTESIAN_POINT('Ctrl Pts',(49.3071192031367,-4.86115052127794,130.057099838467));
#59728=CARTESIAN_POINT('Ctrl Pts',(49.2980231085379,-4.8854926738339,130.2154526798));
#59729=CARTESIAN_POINT('Ctrl Pts',(49.2889270139392,-4.90212761659773,130.375219717216));
#59730=CARTESIAN_POINT('Ctrl Pts',(49.2798309193404,-4.91090720595042,130.535709399359));
#59731=CARTESIAN_POINT('Ctrl Pts',(49.2748404249074,-4.91572405248973,130.62376068957));
#59732=CARTESIAN_POINT('Ctrl Pts',(49.2698499304744,-4.91817720641674,130.712029150127));
#59733=CARTESIAN_POINT('Ctrl Pts',(49.2648594360413,-4.91824840372241,130.800398070159));
#59734=CARTESIAN_POINT('',(49.6101405639704,-4.91824998000026,130.803917077946));
#59735=CARTESIAN_POINT('Ctrl Pts',(49.6802330064605,-4.76405452823399,129.582490119308));
#59736=CARTESIAN_POINT('Ctrl Pts',(49.6724719190686,-4.79812062176887,129.715313300975));
#59737=CARTESIAN_POINT('Ctrl Pts',(49.6647108316767,-4.82659962982157,129.849452307907));
#59738=CARTESIAN_POINT('Ctrl Pts',(49.6569497442848,-4.84941681015589,129.98439740871));
#59739=CARTESIAN_POINT('Ctrl Pts',(49.6491764923101,-4.87226975371082,130.119554019933));
#59740=CARTESIAN_POINT('Ctrl Pts',(49.6414032403354,-4.88944309030547,130.25551886157));
#59741=CARTESIAN_POINT('Ctrl Pts',(49.6336299883607,-4.90091400340569,130.391777300257));
#59742=CARTESIAN_POINT('Ctrl Pts',(49.6271428868324,-4.91048695667491,130.505490624966));
#59743=CARTESIAN_POINT('Ctrl Pts',(49.620655785304,-4.91608934210965,130.619408272993));
#59744=CARTESIAN_POINT('Ctrl Pts',(49.6141686837756,-4.91773564682657,130.733232771885));
#59745=CARTESIAN_POINT('Ctrl Pts',(49.6128259771866,-4.91807640057942,130.756792277464));
#59746=CARTESIAN_POINT('Ctrl Pts',(49.6114832705976,-4.9182478550434,130.780354237637));
#59747=CARTESIAN_POINT('Ctrl Pts',(49.6101405640086,-4.9182499800002,130.803917077276));
#59748=CARTESIAN_POINT('Ctrl Pts',(49.6101405639704,-4.91824998000026,130.803917077946));
#59749=CARTESIAN_POINT('Ctrl Pts',(49.6023858624895,-4.91826225251079,130.940002495971));
#59750=CARTESIAN_POINT('Ctrl Pts',(49.5946311610085,-4.91262212522694,131.076308917794));
#59751=CARTESIAN_POINT('Ctrl Pts',(49.5868764595276,-4.90130053173813,131.212326498595));
#59752=CARTESIAN_POINT('Ctrl Pts',(49.5791313051447,-4.8899928766792,131.348176623152));
#59753=CARTESIAN_POINT('Ctrl Pts',(49.5713861507619,-4.87301770363844,131.483738226168));
#59754=CARTESIAN_POINT('Ctrl Pts',(49.563640996379,-4.85039792117699,131.618500082733));
#59755=CARTESIAN_POINT('Ctrl Pts',(49.5559034995563,-4.82780050267849,131.753128701537));
#59756=CARTESIAN_POINT('Ctrl Pts',(49.5481660027335,-4.79956964437166,131.886958762052));
#59757=CARTESIAN_POINT('Ctrl Pts',(49.5404285059108,-4.76578012873537,132.019483173957));
#59758=CARTESIAN_POINT('Ctrl Pts',(49.5326967839559,-4.73201583184741,132.15190867649));
#59759=CARTESIAN_POINT('Ctrl Pts',(49.524965062001,-4.69270123139867,132.283030090413));
#59760=CARTESIAN_POINT('Ctrl Pts',(49.5172333400461,-4.64796228752467,132.412349932284));
#59761=CARTESIAN_POINT('Ctrl Pts',(49.5095047957713,-4.60324173102356,132.541616624663));
#59762=CARTESIAN_POINT('Ctrl Pts',(49.5017762514966,-4.55310139271184,132.669082846602));
#59763=CARTESIAN_POINT('Ctrl Pts',(49.4940477072218,-4.49771717862265,132.794265952908));
#59764=CARTESIAN_POINT('Ctrl Pts',(49.4863206784171,-4.44234382467905,132.919424512387));
#59765=CARTESIAN_POINT('Ctrl Pts',(49.4785936496123,-4.38172879902203,133.042300487275));
#59766=CARTESIAN_POINT('Ctrl Pts',(49.4708666208076,-4.31609611074062,133.162431317386));
#59767=CARTESIAN_POINT('Ctrl Pts',(49.463139411378,-4.25046188824779,133.282564955641));
#59768=CARTESIAN_POINT('Ctrl Pts',(49.4554122019484,-4.17980995816366,133.399952976335));
#59769=CARTESIAN_POINT('Ctrl Pts',(49.4476849925188,-4.10441002871984,133.514157912318));
#59770=CARTESIAN_POINT('Ctrl Pts',(49.4399559065927,-4.02899178895314,133.628390582136));
#59771=CARTESIAN_POINT('Ctrl Pts',(49.4322268206667,-3.94882347236212,133.73943830128));
#59772=CARTESIAN_POINT('Ctrl Pts',(49.4244977347406,-3.8642175489307,133.846893410657));
#59773=CARTESIAN_POINT('Ctrl Pts',(49.4167603993979,-3.77952132381062,133.954463209142));
#59774=CARTESIAN_POINT('Ctrl Pts',(49.4090230640552,-3.69037827561775,134.05843243005));
#59775=CARTESIAN_POINT('Ctrl Pts',(49.4012857287126,-3.59714085074586,134.15842692019));
#59776=CARTESIAN_POINT('Ctrl Pts',(49.3935440914271,-3.50385158605436,134.258477007063));
#59777=CARTESIAN_POINT('Ctrl Pts',(49.3858024541417,-3.40646368920475,134.354547684766));
#59778=CARTESIAN_POINT('Ctrl Pts',(49.3780608168562,-3.3053649772015,134.446303152806));
#59779=CARTESIAN_POINT('Ctrl Pts',(49.3703070839518,-3.20410830746311,134.538201980594));
#59780=CARTESIAN_POINT('Ctrl Pts',(49.3625533510475,-3.0991295414686,134.625771877587));
#59781=CARTESIAN_POINT('Ctrl Pts',(49.3547996181431,-2.99084852814562,134.708718201624));
#59782=CARTESIAN_POINT('Ctrl Pts',(49.3484400987496,-2.90203773047353,134.776749788839));
#59783=CARTESIAN_POINT('Ctrl Pts',(49.3420805793561,-2.81100612753598,134.841671806076));
#59784=CARTESIAN_POINT('Ctrl Pts',(49.3357210599626,-2.71799811049721,134.903344556768));
#59785=CARTESIAN_POINT('Ctrl Pts',(49.3279467258435,-2.60429841788268,134.978737765005));
#59786=CARTESIAN_POINT('Ctrl Pts',(49.3201723917244,-2.48727931327768,135.049516015972));
#59787=CARTESIAN_POINT('Ctrl Pts',(49.3123980576053,-2.36735207534362,135.115372936484));
#59788=CARTESIAN_POINT('Ctrl Pts',(49.3046333046582,-2.24757263701227,135.181148694228));
#59789=CARTESIAN_POINT('Ctrl Pts',(49.2968685517111,-2.1248925358767,135.242015002876));
#59790=CARTESIAN_POINT('Ctrl Pts',(49.289103798764,-1.99975282367048,135.29770811211));
#59791=CARTESIAN_POINT('Ctrl Pts',(49.2813467578789,-1.87473740199042,135.353345906162));
#59792=CARTESIAN_POINT('Ctrl Pts',(49.2735897169939,-1.7472675856387,135.403820567902));
#59793=CARTESIAN_POINT('Ctrl Pts',(49.2658326761089,-1.61780956644197,135.448913908167));
#59794=CARTESIAN_POINT('Ctrl Pts',(49.2580814848688,-1.48844917254455,135.493973243192));
#59795=CARTESIAN_POINT('Ctrl Pts',(49.2503302936286,-1.35710392782053,135.533659206053));
#59796=CARTESIAN_POINT('Ctrl Pts',(49.2425791023885,-1.22426024181166,135.56780159262));
#59797=CARTESIAN_POINT('Ctrl Pts',(49.2348312056114,-1.09147301791324,135.601929467761));
#59798=CARTESIAN_POINT('Ctrl Pts',(49.2270833088343,-0.957188997297075,
135.63051835573));
#59799=CARTESIAN_POINT('Ctrl Pts',(49.2193354120572,-0.821909788955781,
135.653447888519));
#59800=CARTESIAN_POINT('Ctrl Pts',(49.2115891359731,-0.686658878108406,
135.676372624944));
#59801=CARTESIAN_POINT('Ctrl Pts',(49.203842859889,-0.550413578824121,135.693640295569));
#59802=CARTESIAN_POINT('Ctrl Pts',(49.1960965838049,-0.413685343041333,
135.705181722182));
#59803=CARTESIAN_POINT('Ctrl Pts',(49.1883502505395,-0.276956097961955,
135.716723233992));
#59804=CARTESIAN_POINT('Ctrl Pts',(49.1806039172741,-0.139744298850251,
135.722538384558));
#59805=CARTESIAN_POINT('Ctrl Pts',(49.1728575840087,-0.00256576854755872,
135.722609948307));
#59806=CARTESIAN_POINT('Ctrl Pts',(49.1651095160057,0.13464348193624,135.722681528081));
#59807=CARTESIAN_POINT('Ctrl Pts',(49.1573614480027,0.271819057895434,135.717006961373));
#59808=CARTESIAN_POINT('Ctrl Pts',(49.1496133799997,0.408446288292338,135.705621138297));
#59809=CARTESIAN_POINT('Ctrl Pts',(49.1418570772578,0.545218727735405,135.694223214234));
#59810=CARTESIAN_POINT('Ctrl Pts',(49.134100774516,0.681441267198078,135.677101940863));
#59811=CARTESIAN_POINT('Ctrl Pts',(49.1263444717741,0.816604949049659,135.654344062866));
#59812=CARTESIAN_POINT('Ctrl Pts',(49.1185840292599,0.951840771827943,135.631574038305));
#59813=CARTESIAN_POINT('Ctrl Pts',(49.1108235867457,1.08601622860084,135.603161495531));
#59814=CARTESIAN_POINT('Ctrl Pts',(49.1030631442315,1.21863466186354,135.569243892464));
#59815=CARTESIAN_POINT('Ctrl Pts',(49.0952902439661,1.35146598600862,135.53527184185));
#59816=CARTESIAN_POINT('Ctrl Pts',(49.0875173437006,1.48273491729863,135.495777184086));
#59817=CARTESIAN_POINT('Ctrl Pts',(49.0797444434352,1.61196115607087,135.450946922997));
#59818=CARTESIAN_POINT('Ctrl Pts',(49.0722541076733,1.73648969555917,135.40774635482));
#59819=CARTESIAN_POINT('Ctrl Pts',(49.0647637719115,1.85912119143873,135.359591486192));
#59820=CARTESIAN_POINT('Ctrl Pts',(49.0572734361496,1.97944690779201,135.30669034802));
#59821=CARTESIAN_POINT('Ctrl Pts',(49.0494991020305,2.1043348102562,135.251783447115));
#59822=CARTESIAN_POINT('Ctrl Pts',(49.0417247679115,2.22713424172844,135.19158933376));
#59823=CARTESIAN_POINT('Ctrl Pts',(49.0339504337924,2.34736513560895,135.126288426152));
#59824=CARTESIAN_POINT('Ctrl Pts',(49.0261856808453,2.46744785565794,135.061067996076));
#59825=CARTESIAN_POINT('Ctrl Pts',(49.0184209278982,2.58496799623908,134.990753479077));
#59826=CARTESIAN_POINT('Ctrl Pts',(49.0106561749511,2.69946525750274,134.915573380977));
#59827=CARTESIAN_POINT('Ctrl Pts',(49.0028991340661,2.81384879847238,134.840467952811));
#59828=CARTESIAN_POINT('Ctrl Pts',(48.9951420931811,2.92521511027227,134.760506773765));
#59829=CARTESIAN_POINT('Ctrl Pts',(48.9873850522961,3.03312863610992,134.675964127652));
#59830=CARTESIAN_POINT('Ctrl Pts',(48.9796338610559,3.14096078351843,134.591485235806));
#59831=CARTESIAN_POINT('Ctrl Pts',(48.9718826698158,3.24534502109734,134.502431993839));
#59832=CARTESIAN_POINT('Ctrl Pts',(48.9641314785756,3.34587523505336,134.409121632385));
#59833=CARTESIAN_POINT('Ctrl Pts',(48.9563835817986,3.44636272098658,134.315850930323));
#59834=CARTESIAN_POINT('Ctrl Pts',(48.9486356850215,3.54299915532662,134.218326972927));
#59835=CARTESIAN_POINT('Ctrl Pts',(48.9408877882444,3.63541213714717,134.116906716201));
#59836=CARTESIAN_POINT('Ctrl Pts',(48.9331415121603,3.72780578816425,134.015507674406));
#59837=CARTESIAN_POINT('Ctrl Pts',(48.9253952360761,3.81597748074614,133.91021424321));
#59838=CARTESIAN_POINT('Ctrl Pts',(48.917648959992,3.89959256103934,133.801419329101));
#59839=CARTESIAN_POINT('Ctrl Pts',(48.9099026267266,3.98320825856018,133.692623611892));
#59840=CARTESIAN_POINT('Ctrl Pts',(48.9021562934613,4.06226703842993,133.580326670183));
#59841=CARTESIAN_POINT('Ctrl Pts',(48.8944099601959,4.13647559343899,133.464953169496));
#59842=CARTESIAN_POINT('Ctrl Pts',(48.8866618921929,4.21070076693912,133.349553831713));
#59843=CARTESIAN_POINT('Ctrl Pts',(48.8789138241899,4.28007334276029,133.23107689273));
#59844=CARTESIAN_POINT('Ctrl Pts',(48.871165756187,4.34434448267861,133.109974218827));
#59845=CARTESIAN_POINT('Ctrl Pts',(48.8634094534451,4.40868393072945,132.988742835561));
#59846=CARTESIAN_POINT('Ctrl Pts',(48.8556531507032,4.46791092854265,132.864880488621));
#59847=CARTESIAN_POINT('Ctrl Pts',(48.8478968479613,4.52182335284511,132.738862266096));
#59848=CARTESIAN_POINT('Ctrl Pts',(48.8401364054471,4.57576455183176,132.612776783851));
#59849=CARTESIAN_POINT('Ctrl Pts',(48.8323759629329,4.62438538671388,132.484533498637));
#59850=CARTESIAN_POINT('Ctrl Pts',(48.8246155204187,4.66753304922153,132.354624561843));
#59851=CARTESIAN_POINT('Ctrl Pts',(48.8168426201533,4.71074997618745,132.224507083691));
#59852=CARTESIAN_POINT('Ctrl Pts',(48.8090697198879,4.74847606584788,132.092718986835));
#59853=CARTESIAN_POINT('Ctrl Pts',(48.8012968196225,4.78060903611737,131.95976544112));
#59854=CARTESIAN_POINT('Ctrl Pts',(48.7938064838606,4.81157389197885,131.831645091685));
#59855=CARTESIAN_POINT('Ctrl Pts',(48.7863161480987,4.83734515614878,131.702442858355));
#59856=CARTESIAN_POINT('Ctrl Pts',(48.7788258123368,4.85787691917531,131.572615068021));
#59857=CARTESIAN_POINT('Ctrl Pts',(48.7710514782177,4.87918715023787,131.437864817554));
#59858=CARTESIAN_POINT('Ctrl Pts',(48.7632771440986,4.89492023014025,131.302013789405));
#59859=CARTESIAN_POINT('Ctrl Pts',(48.7555028099796,4.9049684620969,131.165563397642));
#59860=CARTESIAN_POINT('Ctrl Pts',(48.7477380570325,4.91500431050568,131.029281168793));
#59861=CARTESIAN_POINT('Ctrl Pts',(48.7399733040854,4.91936922251657,130.892401432213));
#59862=CARTESIAN_POINT('Ctrl Pts',(48.7322085511383,4.91800664323881,130.755434964183));
#59863=CARTESIAN_POINT('Ctrl Pts',(48.7244515102534,4.91664541729399,130.618604533179));
#59864=CARTESIAN_POINT('Ctrl Pts',(48.7166944693684,4.90956802454522,130.48168793057));
#59865=CARTESIAN_POINT('Ctrl Pts',(48.7089374284834,4.89676979864831,130.34519985972));
#59866=CARTESIAN_POINT('Ctrl Pts',(48.7011862372433,4.88398122399307,130.208814715586));
#59867=CARTESIAN_POINT('Ctrl Pts',(48.6934350460031,4.86548043954567,130.072857847666));
#59868=CARTESIAN_POINT('Ctrl Pts',(48.685683854763,4.84131482599757,129.937842401903));
#59869=CARTESIAN_POINT('Ctrl Pts',(48.6779359579859,4.81715948347998,129.802884341306));
#59870=CARTESIAN_POINT('Ctrl Pts',(48.6701880612089,4.7873441693381,129.668867291083));
#59871=CARTESIAN_POINT('Ctrl Pts',(48.6624401644318,4.75196790897045,129.536297506118));
#59872=CARTESIAN_POINT('Ctrl Pts',(48.6546938883477,4.7165990485538,129.403755451894));
#59873=CARTESIAN_POINT('Ctrl Pts',(48.6469476122636,4.67567165637769,129.272660438277));
#59874=CARTESIAN_POINT('Ctrl Pts',(48.6392013361796,4.62933540721616,129.143506394585));
#59875=CARTESIAN_POINT('Ctrl Pts',(48.6314550029142,4.5829988160109,129.014351397507));
#59876=CARTESIAN_POINT('Ctrl Pts',(48.6237086696489,4.53125342017473,128.887137766943));
#59877=CARTESIAN_POINT('Ctrl Pts',(48.6159623363835,4.47429796312652,128.762341812642));
#59878=CARTESIAN_POINT('Ctrl Pts',(48.6082142683806,4.41732975129861,128.637517911153));
#59879=CARTESIAN_POINT('Ctrl Pts',(48.6004662003776,4.35514931884176,128.515113118901));
#59880=CARTESIAN_POINT('Ctrl Pts',(48.5927181323746,4.28800233051721,128.395581035292));
#59881=CARTESIAN_POINT('Ctrl Pts',(48.5849618296328,4.22078397757449,128.275921911563));
#59882=CARTESIAN_POINT('Ctrl Pts',(48.5772055268909,4.14858871614824,128.15914193688));
#59883=CARTESIAN_POINT('Ctrl Pts',(48.5694492241491,4.07170699873664,128.045667959994));
#59884=CARTESIAN_POINT('Ctrl Pts',(48.561688781635,3.99478424723779,127.932133418631));
#59885=CARTESIAN_POINT('Ctrl Pts',(48.5539283391208,3.91317028823315,127.821908705057));
#59886=CARTESIAN_POINT('Ctrl Pts',(48.5461678966067,3.82719658602265,127.715388401045));
#59887=CARTESIAN_POINT('Ctrl Pts',(48.5383949963413,3.74108487119274,127.608697101185));
#59888=CARTESIAN_POINT('Ctrl Pts',(48.5306220960759,3.65059968584837,127.505722388042));
#59889=CARTESIAN_POINT('Ctrl Pts',(48.5228491958105,3.5561107577211,127.406823371071));
#59890=CARTESIAN_POINT('Ctrl Pts',(48.5153588600483,3.46505674013221,127.311519582477));
#59891=CARTESIAN_POINT('Ctrl Pts',(48.5078685242861,3.37028523981213,127.220000524991));
#59892=CARTESIAN_POINT('Ctrl Pts',(48.5003781885239,3.27215536231819,127.132551479368));
#59893=CARTESIAN_POINT('Ctrl Pts',(48.4926038544048,3.17030486069543,127.041786776603));
#59894=CARTESIAN_POINT('Ctrl Pts',(48.4848295202857,3.06451365720145,126.955119291837));
#59895=CARTESIAN_POINT('Ctrl Pts',(48.4770551861666,2.95514539294957,126.872910659977));
#59896=CARTESIAN_POINT('Ctrl Pts',(48.4692904332195,2.84591191530886,126.790803342908));
#59897=CARTESIAN_POINT('Ctrl Pts',(48.4615256802724,2.7331104578492,126.713144177718));
#59898=CARTESIAN_POINT('Ctrl Pts',(48.4537609273253,2.61714018182043,126.640256832692));
#59899=CARTESIAN_POINT('Ctrl Pts',(48.4460038864403,2.50128508910469,126.567441880405));
#59900=CARTESIAN_POINT('Ctrl Pts',(48.4382468455553,2.38226776999332,126.499389523282));
#59901=CARTESIAN_POINT('Ctrl Pts',(48.4304898046703,2.26051873673281,126.436381896993));
#59902=CARTESIAN_POINT('Ctrl Pts',(48.4227386134302,2.1388615153655,126.373421785245));
#59903=CARTESIAN_POINT('Ctrl Pts',(48.4149874221901,2.01447702598552,126.315499011128));
#59904=CARTESIAN_POINT('Ctrl Pts',(48.40723623095,1.88782260322829,126.262851079842));
#59905=CARTESIAN_POINT('Ctrl Pts',(48.3994883341729,1.76122201197917,126.21022552533));
#59906=CARTESIAN_POINT('Ctrl Pts',(48.3917404373958,1.63235376649237,126.162870504337));
#59907=CARTESIAN_POINT('Ctrl Pts',(48.3839925406187,1.50169731898762,126.120976347122));
#59908=CARTESIAN_POINT('Ctrl Pts',(48.3762462645346,1.37106820199506,126.079090953261));
#59909=CARTESIAN_POINT('Ctrl Pts',(48.3684999884505,1.23865199905632,126.042664270389));
#59910=CARTESIAN_POINT('Ctrl Pts',(48.3607537123663,1.10494516976763,126.011837353741));
#59911=CARTESIAN_POINT('Ctrl Pts',(48.353007379101,0.971237353485504,125.981010209535));
#59912=CARTESIAN_POINT('Ctrl Pts',(48.3452610458356,0.836239272813611,125.955783001873));
#59913=CARTESIAN_POINT('Ctrl Pts',(48.3375147125703,0.700459086306537,125.93624597934));
#59914=CARTESIAN_POINT('Ctrl Pts',(48.3297666445673,0.564648492767759,125.916704581626));
#59915=CARTESIAN_POINT('Ctrl Pts',(48.3220185765643,0.428055831776927,125.902855960378));
#59916=CARTESIAN_POINT('Ctrl Pts',(48.3142705085613,0.291195517166221,125.894738612433));
#59917=CARTESIAN_POINT('Ctrl Pts',(48.3065142058194,0.154189745784861,125.886612637275));
#59918=CARTESIAN_POINT('Ctrl Pts',(48.2987579030776,0.0169161434348984,
125.884230126563));
#59919=CARTESIAN_POINT('Ctrl Pts',(48.2910016003357,-0.120109173270614,
125.887577436563));
#59920=CARTESIAN_POINT('Ctrl Pts',(48.2832411578215,-0.257207624513591,
125.890926533122));
#59921=CARTESIAN_POINT('Ctrl Pts',(48.2754807153074,-0.394057136144087,
125.900011518186));
#59922=CARTESIAN_POINT('Ctrl Pts',(48.2677202727932,-0.530146570791028,
125.914766802536));
#59923=CARTESIAN_POINT('Ctrl Pts',(48.2599473725277,-0.666454468279731,
125.929545773379));
#59924=CARTESIAN_POINT('Ctrl Pts',(48.2521744722623,-0.801999463745009,
125.950013174732));
#59925=CARTESIAN_POINT('Ctrl Pts',(48.2444015719969,-0.936279581361401,
125.976052051616));
#59926=CARTESIAN_POINT('Ctrl Pts',(48.2369112362349,-1.06567827846977,126.001144349737));
#59927=CARTESIAN_POINT('Ctrl Pts',(48.229420900473,-1.19390216432778,126.031410010976));
#59928=CARTESIAN_POINT('Ctrl Pts',(48.221930564711,-1.32051711883283,126.066701110872));
#59929=CARTESIAN_POINT('Ctrl Pts',(48.2141562305919,-1.45193271782338,126.103330283547));
#59930=CARTESIAN_POINT('Ctrl Pts',(48.2063818964729,-1.5820312568905,126.145489526722));
#59931=CARTESIAN_POINT('Ctrl Pts',(48.1986075623538,-1.7103119254403,126.19306837133));
#59932=CARTESIAN_POINT('Ctrl Pts',(48.1908428094067,-1.83843449953018,126.240588579264));
#59933=CARTESIAN_POINT('Ctrl Pts',(48.1830780564596,-1.96474329771196,126.293514964412));
#59934=CARTESIAN_POINT('Ctrl Pts',(48.1753133035125,-2.08875025228365,126.351686651724));
#59935=CARTESIAN_POINT('Ctrl Pts',(48.1675562626275,-2.21263404140089,126.409800562098));
#59936=CARTESIAN_POINT('Ctrl Pts',(48.1597992217425,-2.33422018493114,126.473149242116));
#59937=CARTESIAN_POINT('Ctrl Pts',(48.1520421808574,-2.45303861176011,126.541522990854));
#59938=CARTESIAN_POINT('Ctrl Pts',(48.1442909896173,-2.57176743668864,126.609845178416));
#59939=CARTESIAN_POINT('Ctrl Pts',(48.1365397983772,-2.68773236178119,126.683184697831));
#59940=CARTESIAN_POINT('Ctrl Pts',(48.128788607137,-2.80048636664627,126.761285157878));
#59941=CARTESIAN_POINT('Ctrl Pts',(48.1210407103599,-2.91319244805147,126.839352423147));
#59942=CARTESIAN_POINT('Ctrl Pts',(48.1132928135829,-3.02269000284436,126.922176382256));
#59943=CARTESIAN_POINT('Ctrl Pts',(48.1055449168058,-3.12855974515137,127.009456536628));
#59944=CARTESIAN_POINT('Ctrl Pts',(48.0977986407217,-3.23440734179072,127.096718433874));
#59945=CARTESIAN_POINT('Ctrl Pts',(48.0900523646376,-3.33662833388241,127.188434423764));
#59946=CARTESIAN_POINT('Ctrl Pts',(48.0823060885535,-3.43483569912353,127.284263064582));
#59947=CARTESIAN_POINT('Ctrl Pts',(48.0745597552881,-3.53304378930899,127.380092412784));
#59948=CARTESIAN_POINT('Ctrl Pts',(48.0668134220227,-3.62723791370176,127.480034199447));
#59949=CARTESIAN_POINT('Ctrl Pts',(48.0590670887573,-3.71706747149833,127.583709677953));
#59950=CARTESIAN_POINT('Ctrl Pts',(48.0513190207544,-3.80691714600129,127.687408373863));
#59951=CARTESIAN_POINT('Ctrl Pts',(48.0435709527514,-3.89240005299712,127.794842130003));
#59952=CARTESIAN_POINT('Ctrl Pts',(48.0358228847485,-3.97320575076395,127.905598963929));
#59953=CARTESIAN_POINT('Ctrl Pts',(48.0280665820066,-4.05409732978829,128.016473511536));
#59954=CARTESIAN_POINT('Ctrl Pts',(48.0203102792647,-4.1303015386904,128.130677875748));
#59955=CARTESIAN_POINT('Ctrl Pts',(48.0125539765228,-4.20155088269604,128.247770458269));
#59956=CARTESIAN_POINT('Ctrl Pts',(48.0047935340087,-4.27283825462176,128.364925536626));
#59957=CARTESIAN_POINT('Ctrl Pts',(47.9970330914945,-4.33916530315918,128.48497156288));
#59958=CARTESIAN_POINT('Ctrl Pts',(47.9892726489803,-4.40031092813965,128.60744305011));
#59959=CARTESIAN_POINT('Ctrl Pts',(47.9814997487149,-4.46155470950558,128.730111139445));
#59960=CARTESIAN_POINT('Ctrl Pts',(47.9737268484495,-4.5176002859999,128.855212113339));
#59961=CARTESIAN_POINT('Ctrl Pts',(47.965953948184,-4.56827472496393,128.982260428291));
#59962=CARTESIAN_POINT('Ctrl Pts',(47.9584636124221,-4.61710702042993,129.104690216978));
#59963=CARTESIAN_POINT('Ctrl Pts',(47.9509732766601,-4.66095180481061,129.228927932819));
#59964=CARTESIAN_POINT('Ctrl Pts',(47.9434829408981,-4.69969887862443,129.354528381493));
#59965=CARTESIAN_POINT('Ctrl Pts',(47.9389845512163,-4.72296878835696,129.429958880246));
#59966=CARTESIAN_POINT('Ctrl Pts',(47.9344861615344,-4.74442940765616,129.505972072028));
#59967=CARTESIAN_POINT('Ctrl Pts',(47.9299877718525,-4.76405452823408,129.582490119308));
#59968=CARTESIAN_POINT('Origin',(213.235140564004,0.,130.804360617566));
#59969=CARTESIAN_POINT('',(45.8349994066072,-4.76405452823404,129.582490119308));
#59970=CARTESIAN_POINT('',(46.1799254115191,-4.76405452823402,129.582490119308));
#59971=CARTESIAN_POINT('',(213.235140564004,-4.76405452823405,129.582490119308));
#59972=CARTESIAN_POINT('',(47.5148594359393,-4.91824920960731,130.807148931941));
#59973=CARTESIAN_POINT('Ctrl Pts',(47.5148594359393,-4.91824920960731,130.807148931941));
#59974=CARTESIAN_POINT('Ctrl Pts',(47.505802540397,-4.91815813926165,130.9677860034));
#59975=CARTESIAN_POINT('Ctrl Pts',(47.4967456448546,-4.9101921353692,131.128139470124));
#59976=CARTESIAN_POINT('Ctrl Pts',(47.4876887493124,-4.89446417761299,131.287479108791));
#59977=CARTESIAN_POINT('Ctrl Pts',(47.479032267672,-4.8794315677169,131.43977419161));
#59978=CARTESIAN_POINT('Ctrl Pts',(47.4703757860316,-4.85730870168485,131.591143020276));
#59979=CARTESIAN_POINT('Ctrl Pts',(47.4617193043913,-4.82824555908569,131.740965061112));
#59980=CARTESIAN_POINT('Ctrl Pts',(47.4530368824345,-4.79909532485441,131.891236063928));
#59981=CARTESIAN_POINT('Ctrl Pts',(47.4443544604778,-4.7629632741104,132.039950790789));
#59982=CARTESIAN_POINT('Ctrl Pts',(47.435672038521,-4.72004930543188,132.18650301862));
#59983=CARTESIAN_POINT('Ctrl Pts',(47.426957849973,-4.67697832635815,132.3335914407));
#59984=CARTESIAN_POINT('Ctrl Pts',(47.418243661425,-4.62707582962666,132.478501311877));
#59985=CARTESIAN_POINT('Ctrl Pts',(47.409529472877,-4.57059100507844,132.620642789145));
#59986=CARTESIAN_POINT('Ctrl Pts',(47.4084118783952,-4.56334682762346,132.63887243035));
#59987=CARTESIAN_POINT('Ctrl Pts',(47.4072942839134,-4.55599444550586,132.657056570192));
#59988=CARTESIAN_POINT('Ctrl Pts',(47.4061766894317,-4.54853443858162,132.675193994309));
#59989=CARTESIAN_POINT('Ctrl Pts',(47.3984023553126,-4.49664031481259,132.80136354637));
#59990=CARTESIAN_POINT('Ctrl Pts',(47.3906280211935,-4.43941038363547,132.925572107387));
#59991=CARTESIAN_POINT('Ctrl Pts',(47.3828536870744,-4.37701349101544,133.047335419468));
#59992=CARTESIAN_POINT('Ctrl Pts',(47.3750889341273,-4.314693496989,133.16894866915));
#59993=CARTESIAN_POINT('Ctrl Pts',(47.3673241811802,-4.24721938816846,133.288122321364));
#59994=CARTESIAN_POINT('Ctrl Pts',(47.3595594282331,-4.17480855864665,133.404390725305));
#59995=CARTESIAN_POINT('Ctrl Pts',(47.3518023873481,-4.10246964858174,133.520543649828));
#59996=CARTESIAN_POINT('Ctrl Pts',(47.3440453464632,-4.02520398079192,133.633796738702));
#59997=CARTESIAN_POINT('Ctrl Pts',(47.3362883055782,-3.94327530794265,133.743707978507));
#59998=CARTESIAN_POINT('Ctrl Pts',(47.3285371143381,-3.86140841814278,133.853536333391));
#59999=CARTESIAN_POINT('Ctrl Pts',(47.3207859230979,-3.77488575519245,133.960027543149));
#60000=CARTESIAN_POINT('Ctrl Pts',(47.3130347318578,-3.68401471275957,134.062767998277));
#60001=CARTESIAN_POINT('Ctrl Pts',(47.3052868350807,-3.5931822929438,134.165464785971));
#60002=CARTESIAN_POINT('Ctrl Pts',(47.2975389383037,-3.49800542800665,134.26441369748));
#60003=CARTESIAN_POINT('Ctrl Pts',(47.2897910415266,-3.39883203456208,134.35923387316));
#60004=CARTESIAN_POINT('Ctrl Pts',(47.2820447654425,-3.29967938605348,134.454034214503));
#60005=CARTESIAN_POINT('Ctrl Pts',(47.2742984893584,-3.19653215427026,134.544707267839));
#60006=CARTESIAN_POINT('Ctrl Pts',(47.2665522132743,-3.08977510178349,134.630909047012));
#60007=CARTESIAN_POINT('Ctrl Pts',(47.258805880009,-2.98301726124041,134.717111462508));
#60008=CARTESIAN_POINT('Ctrl Pts',(47.2510595467437,-2.87264985100474,134.798842292367));
#60009=CARTESIAN_POINT('Ctrl Pts',(47.2433132134783,-2.75909037574016,134.875798123042));
#60010=CARTESIAN_POINT('Ctrl Pts',(47.2355651454754,-2.64550546961845,134.952771187442));
#60011=CARTESIAN_POINT('Ctrl Pts',(47.2278170774723,-2.52872739960516,135.024966905534));
#60012=CARTESIAN_POINT('Ctrl Pts',(47.2200690094694,-2.40920193042337,135.09212566721));
#60013=CARTESIAN_POINT('Ctrl Pts',(47.2123127067275,-2.28954942815057,135.159355806016));
#60014=CARTESIAN_POINT('Ctrl Pts',(47.2045564039857,-2.16714403514731,135.221538102717));
#60015=CARTESIAN_POINT('Ctrl Pts',(47.1968001012438,-2.04245585228769,135.278459091444));
#60016=CARTESIAN_POINT('Ctrl Pts',(47.1890396587297,-1.91770111959041,135.335410460616));
#60017=CARTESIAN_POINT('Ctrl Pts',(47.1812792162155,-1.79066153124912,135.387094779138));
#60018=CARTESIAN_POINT('Ctrl Pts',(47.1735187737014,-1.66182542994866,135.43334747247));
#60019=CARTESIAN_POINT('Ctrl Pts',(47.165745873436,-1.53278250950103,135.479674414731));
#60020=CARTESIAN_POINT('Ctrl Pts',(47.1579729731705,-1.40193768649131,135.520552191155));
#60021=CARTESIAN_POINT('Ctrl Pts',(47.1502000729051,-1.26979353079927,135.555866426427));
#60022=CARTESIAN_POINT('Ctrl Pts',(47.1427097371431,-1.14245314801696,135.589896900296));
#60023=CARTESIAN_POINT('Ctrl Pts',(47.135219401381,-1.01390656101556,135.61876124033));
#60024=CARTESIAN_POINT('Ctrl Pts',(47.1277290656189,-0.884608863575147,
135.64240259971));
#60025=CARTESIAN_POINT('Ctrl Pts',(47.1199547314998,-0.750408804637845,
135.666940328416));
#60026=CARTESIAN_POINT('Ctrl Pts',(47.1121803973807,-0.614974448765209,
135.685928927673));
#60027=CARTESIAN_POINT('Ctrl Pts',(47.1044060632616,-0.478804481204911,
135.699248699155));
#60028=CARTESIAN_POINT('Ctrl Pts',(47.0966413103146,-0.342802330959771,
135.712552055208));
#60029=CARTESIAN_POINT('Ctrl Pts',(47.0888765573675,-0.206066758215026,
135.720200446491));
#60030=CARTESIAN_POINT('Ctrl Pts',(47.0811118044204,-0.0691070349976097,
135.722125077177));
#60031=CARTESIAN_POINT('Ctrl Pts',(47.0733547635354,0.0677166578917276,
135.724047796293));
#60032=CARTESIAN_POINT('Ctrl Pts',(47.0655977226504,0.204763669814227,135.7202580626));
#60033=CARTESIAN_POINT('Ctrl Pts',(47.0578406817654,0.341519557604534,135.710738859638));
#60034=CARTESIAN_POINT('Ctrl Pts',(47.0500894905253,0.478172316716238,135.70122683518));
#60035=CARTESIAN_POINT('Ctrl Pts',(47.0423382992852,0.614534000231392,135.685993968457));
#60036=CARTESIAN_POINT('Ctrl Pts',(47.034587108045,0.750090472975039,135.665075312428));
#60037=CARTESIAN_POINT('Ctrl Pts',(47.026839211268,0.885589330601681,135.644165547387));
#60038=CARTESIAN_POINT('Ctrl Pts',(47.0190913144908,1.02028327255562,135.617574858998));
#60039=CARTESIAN_POINT('Ctrl Pts',(47.0113434177137,1.15366381340378,135.585390095424));
#60040=CARTESIAN_POINT('Ctrl Pts',(47.0035971416296,1.28701645391815,135.553212064207));
#60041=CARTESIAN_POINT('Ctrl Pts',(46.9958508655456,1.41905585997372,135.515442376967));
#60042=CARTESIAN_POINT('Ctrl Pts',(46.9881045894615,1.54928465270907,135.472218812432));
#60043=CARTESIAN_POINT('Ctrl Pts',(46.9803582561962,1.67951440676379,135.428994928831));
#60044=CARTESIAN_POINT('Ctrl Pts',(46.9726119229308,1.80793314976746,135.380317210757));
#60045=CARTESIAN_POINT('Ctrl Pts',(46.9648655896655,1.9340599398419,135.326372914276));
#60046=CARTESIAN_POINT('Ctrl Pts',(46.9571175216625,2.06021497513649,135.272416537344));
#60047=CARTESIAN_POINT('Ctrl Pts',(46.9493694536595,2.18407667676163,135.213191388823));
#60048=CARTESIAN_POINT('Ctrl Pts',(46.9416213856566,2.30518568065845,135.148932177592));
#60049=CARTESIAN_POINT('Ctrl Pts',(46.9338650829147,2.42642340064584,135.084604670907));
#60050=CARTESIAN_POINT('Ctrl Pts',(46.9261087801728,2.54490223279135,135.015232597327));
#60051=CARTESIAN_POINT('Ctrl Pts',(46.918352477431,2.66018848120692,134.941096082513));
#60052=CARTESIAN_POINT('Ctrl Pts',(46.9105920349168,2.77553626136447,134.86691999881));
#60053=CARTESIAN_POINT('Ctrl Pts',(46.9028315924027,2.88768774292624,134.787974631811));
#60054=CARTESIAN_POINT('Ctrl Pts',(46.8950711498885,2.99624050352007,134.70458188149));
#60055=CARTESIAN_POINT('Ctrl Pts',(46.8872982496231,3.10496752264206,134.621055261723));
#60056=CARTESIAN_POINT('Ctrl Pts',(46.8795253493577,3.21008397656531,134.533067243059));
#60057=CARTESIAN_POINT('Ctrl Pts',(46.8717524490922,3.31122198680281,134.440978829121));
#60058=CARTESIAN_POINT('Ctrl Pts',(46.8642621133301,3.40868337561786,134.352238060986));
#60059=CARTESIAN_POINT('Ctrl Pts',(46.856771777568,3.50245033256831,134.259690057551));
#60060=CARTESIAN_POINT('Ctrl Pts',(46.8492814418059,3.59222904151158,134.16368697501));
#60061=CARTESIAN_POINT('Ctrl Pts',(46.8415071076869,3.68541173749129,134.064043906416));
#60062=CARTESIAN_POINT('Ctrl Pts',(46.8337327735678,3.77459296134874,133.960362948841));
#60063=CARTESIAN_POINT('Ctrl Pts',(46.8259584394487,3.85940245593429,133.852998960438));
#60064=CARTESIAN_POINT('Ctrl Pts',(46.8181936865016,3.94410743039741,133.745767288555));
#60065=CARTESIAN_POINT('Ctrl Pts',(46.8104289335545,4.02445115561818,133.634861920963));
#60066=CARTESIAN_POINT('Ctrl Pts',(46.8026641806074,4.100100477749,133.520674136816));
#60067=CARTESIAN_POINT('Ctrl Pts',(46.7949071397224,4.17567466390661,133.406599765587));
#60068=CARTESIAN_POINT('Ctrl Pts',(46.7871500988374,4.24656351112388,133.289249789453));
#60069=CARTESIAN_POINT('Ctrl Pts',(46.7793930579524,4.31247463387257,133.169047826206));
#60070=CARTESIAN_POINT('Ctrl Pts',(46.7716418667122,4.37833605253089,133.048936508194));
#60071=CARTESIAN_POINT('Ctrl Pts',(46.7638906754721,4.43922703109902,132.925977825342));
#60072=CARTESIAN_POINT('Ctrl Pts',(46.756139484232,4.49489915800388,132.800623281114));
#60073=CARTESIAN_POINT('Ctrl Pts',(46.7483915874549,4.55054762276969,132.675322015911));
#60074=CARTESIAN_POINT('Ctrl Pts',(46.7406436906778,4.60098148924961,132.547627271227));
#60075=CARTESIAN_POINT('Ctrl Pts',(46.7328957939008,4.64599897646354,132.418013793809));
#60076=CARTESIAN_POINT('Ctrl Pts',(46.7251495178166,4.6910070469896,132.288427428737));
#60077=CARTESIAN_POINT('Ctrl Pts',(46.7174032417325,4.730600863636,132.156923498343));
#60078=CARTESIAN_POINT('Ctrl Pts',(46.7096569656484,4.76462749812631,132.023994934318));
#60079=CARTESIAN_POINT('Ctrl Pts',(46.701910632383,4.79865438379351,131.891065389044));
#60080=CARTESIAN_POINT('Ctrl Pts',(46.6941642991177,4.82711390834911,131.756711567909));
#60081=CARTESIAN_POINT('Ctrl Pts',(46.6864179658523,4.84990365479118,131.621439317413));
#60082=CARTESIAN_POINT('Ctrl Pts',(46.6786698978494,4.87269850483896,131.486136773633));
#60083=CARTESIAN_POINT('Ctrl Pts',(46.6709218298464,4.88982098526288,131.34991577668));
#60084=CARTESIAN_POINT('Ctrl Pts',(46.6631737618434,4.90122026579724,131.213289668427));
#60085=CARTESIAN_POINT('Ctrl Pts',(46.6554174591016,4.91263166162261,131.076518352321));
#60086=CARTESIAN_POINT('Ctrl Pts',(46.6476611563597,4.91830767418128,130.939341455065));
#60087=CARTESIAN_POINT('Ctrl Pts',(46.6399048536178,4.91824955790514,130.802275272055));
#60088=CARTESIAN_POINT('Ctrl Pts',(46.6321444111037,4.91819141061059,130.665135932696));
#60089=CARTESIAN_POINT('Ctrl Pts',(46.6243839685895,4.91239305274211,130.528107815752));
#60090=CARTESIAN_POINT('Ctrl Pts',(46.6166235260754,4.90090778874081,130.391703485361));
#60091=CARTESIAN_POINT('Ctrl Pts',(46.6088506258099,4.88940408757413,130.255080186629));
#60092=CARTESIAN_POINT('Ctrl Pts',(46.6010777255445,4.87219528647958,130.119083063576));
#60093=CARTESIAN_POINT('Ctrl Pts',(46.5933048252791,4.84938626072064,129.984216754068));
#60094=CARTESIAN_POINT('Ctrl Pts',(46.5858144895171,4.82740640050065,129.854253174619));
#60095=CARTESIAN_POINT('Ctrl Pts',(46.5783241537551,4.80022647473307,129.725339921653));
#60096=CARTESIAN_POINT('Ctrl Pts',(46.5708338179931,4.76798394759412,129.597914540037));
#60097=CARTESIAN_POINT('Ctrl Pts',(46.563059483874,4.73451893523855,129.465657786346));
#60098=CARTESIAN_POINT('Ctrl Pts',(46.555285149755,4.69549383910071,129.334585006854));
#60099=CARTESIAN_POINT('Ctrl Pts',(46.5475108156359,4.65100707836144,129.205199518886));
#60100=CARTESIAN_POINT('Ctrl Pts',(46.5397460626888,4.60657514357895,129.075973486969));
#60101=CARTESIAN_POINT('Ctrl Pts',(46.5319813097417,4.55669506280702,128.94843097529));
#60102=CARTESIAN_POINT('Ctrl Pts',(46.5242165567946,4.50151595248786,128.823063771559));
#60103=CARTESIAN_POINT('Ctrl Pts',(46.5164595159096,4.44639164683888,128.697821084302));
#60104=CARTESIAN_POINT('Ctrl Pts',(46.5087024750246,4.38597894187071,128.574749760928));
#60105=CARTESIAN_POINT('Ctrl Pts',(46.5009454341396,4.32047619770884,128.454324769428));
#60106=CARTESIAN_POINT('Ctrl Pts',(46.4931942428995,4.25502284967587,128.333990591352));
#60107=CARTESIAN_POINT('Ctrl Pts',(46.4854430516594,4.18448728868249,128.216299115046));
#60108=CARTESIAN_POINT('Ctrl Pts',(46.4776918604193,4.10911510485752,128.101703384854));
#60109=CARTESIAN_POINT('Ctrl Pts',(46.4699439636422,4.0337749562213,127.987156360904));
#60110=CARTESIAN_POINT('Ctrl Pts',(46.4621960668651,3.95360248776345,127.875702792054));
#60111=CARTESIAN_POINT('Ctrl Pts',(46.454448170088,3.86888804982,127.76776905457));
#60112=CARTESIAN_POINT('Ctrl Pts',(46.4467018940039,3.78419133231074,127.659857894497));
#60113=CARTESIAN_POINT('Ctrl Pts',(46.4389556179198,3.69495477631535,127.555465408657));
#60114=CARTESIAN_POINT('Ctrl Pts',(46.4312093418357,3.60151043775749,127.45498670156));
#60115=CARTESIAN_POINT('Ctrl Pts',(46.4234630085703,3.50806540941487,127.354507252752));
#60116=CARTESIAN_POINT('Ctrl Pts',(46.415716675305,3.41041280278097,127.257941926629));
#60117=CARTESIAN_POINT('Ctrl Pts',(46.4079703420397,3.30892284195152,127.165650311907));
#60118=CARTESIAN_POINT('Ctrl Pts',(46.4002222740367,3.20741015314888,127.073338029117));
#60119=CARTESIAN_POINT('Ctrl Pts',(46.3924742060337,3.10205868934166,126.985301625166));
#60120=CARTESIAN_POINT('Ctrl Pts',(46.3847261380307,2.99327286458827,126.901861338819));
#60121=CARTESIAN_POINT('Ctrl Pts',(46.3769698352889,2.88437142096591,126.818332371143));
#60122=CARTESIAN_POINT('Ctrl Pts',(46.3692135325471,2.77202863568509,126.739409517326));
#60123=CARTESIAN_POINT('Ctrl Pts',(46.3614572298052,2.65667956073602,126.66537079225));
#60124=CARTESIAN_POINT('Ctrl Pts',(46.353696787291,2.5412689205124,126.591292550478));
#60125=CARTESIAN_POINT('Ctrl Pts',(46.3459363447769,2.42284913082927,126.522103828865));
#60126=CARTESIAN_POINT('Ctrl Pts',(46.3381759022627,2.30188023876371,126.458036834311));
#60127=CARTESIAN_POINT('Ctrl Pts',(46.3304030019973,2.18071715669349,126.39386699373));
#60128=CARTESIAN_POINT('Ctrl Pts',(46.3226301017319,2.05699714809038,126.334835478545));
#60129=CARTESIAN_POINT('Ctrl Pts',(46.3148572014664,1.93120146672462,126.281126823319));
#60130=CARTESIAN_POINT('Ctrl Pts',(46.3073668657043,1.80997877523568,126.229370612994));
#60131=CARTESIAN_POINT('Ctrl Pts',(46.2998765299422,1.68682899071688,126.182557092208));
#60132=CARTESIAN_POINT('Ctrl Pts',(46.2923861941801,1.56219453480081,126.140807112144));
#60133=CARTESIAN_POINT('Ctrl Pts',(46.284611860061,1.43283452560796,126.097474168896));
#60134=CARTESIAN_POINT('Ctrl Pts',(46.2768375259419,1.30146526634353,126.059459048579));
#60135=CARTESIAN_POINT('Ctrl Pts',(46.2690631918229,1.16856341009971,126.026951003656));
#60136=CARTESIAN_POINT('Ctrl Pts',(46.2612984388757,1.03582534351575,125.994483021994));
#60137=CARTESIAN_POINT('Ctrl Pts',(46.2535336859287,0.901558814202811,125.967508703664));
#60138=CARTESIAN_POINT('Ctrl Pts',(46.2457689329815,0.76625817816726,125.946168416048));
#60139=CARTESIAN_POINT('Ctrl Pts',(46.2380118920966,0.631091924631192,125.924849323907));
#60140=CARTESIAN_POINT('Ctrl Pts',(46.2302548512116,0.494893992018743,125.909153187106));
#60141=CARTESIAN_POINT('Ctrl Pts',(46.2224978103266,0.358171202844252,125.899169851454));
#60142=CARTESIAN_POINT('Ctrl Pts',(46.2147466190865,0.221551517388626,125.889194044313));
#60143=CARTESIAN_POINT('Ctrl Pts',(46.2069954278463,0.084408151533053,125.88492249173));
#60144=CARTESIAN_POINT('Ctrl Pts',(46.1992442366062,-0.0527449882223296,
125.886393453308));
#60145=CARTESIAN_POINT('Ctrl Pts',(46.1914963398291,-0.189839834234823,
125.887863789688));
#60146=CARTESIAN_POINT('Ctrl Pts',(46.183748443052,-0.326944055760556,125.895071781636));
#60147=CARTESIAN_POINT('Ctrl Pts',(46.1760005462749,-0.463541988921763,
125.908003615977));
#60148=CARTESIAN_POINT('Ctrl Pts',(46.1682542701908,-0.600111348740063,
125.920932745258));
#60149=CARTESIAN_POINT('Ctrl Pts',(46.1605079941067,-0.73617424186564,125.939583298602));
#60150=CARTESIAN_POINT('Ctrl Pts',(46.1527617180226,-0.871218771346769,
125.963889471598));
#60151=CARTESIAN_POINT('Ctrl Pts',(46.1450153847573,-1.00626429769594,125.988195824015));
#60152=CARTESIAN_POINT('Ctrl Pts',(46.1372690514919,-1.14029106061802,126.018157810134));
#60153=CARTESIAN_POINT('Ctrl Pts',(46.1295227182265,-1.27279641277715,126.053658316419));
#60154=CARTESIAN_POINT('Ctrl Pts',(46.1217746502235,-1.40533143859117,126.089166772797));
#60155=CARTESIAN_POINT('Ctrl Pts',(46.1140265822206,-1.53634399809588,126.130216116262));
#60156=CARTESIAN_POINT('Ctrl Pts',(46.1062785142176,-1.66534606967169,126.176639198689));
#60157=CARTESIAN_POINT('Ctrl Pts',(46.0985222114757,-1.79448524618432,126.223111620121));
#60158=CARTESIAN_POINT('Ctrl Pts',(46.0907659087339,-1.92160929788193,126.274969056805));
#60159=CARTESIAN_POINT('Ctrl Pts',(46.083009605992,-2.04624916674153,126.331995761015));
#60160=CARTESIAN_POINT('Ctrl Pts',(46.0752491634778,-2.17095555965215,126.389052902095));
#60161=CARTESIAN_POINT('Ctrl Pts',(46.0674887209636,-2.29317477955967,126.451284630918));
#60162=CARTESIAN_POINT('Ctrl Pts',(46.0597282784495,-2.41246279754036,126.51842941035));
#60163=CARTESIAN_POINT('Ctrl Pts',(46.051955378184,-2.53194230723723,126.585681976544));
#60164=CARTESIAN_POINT('Ctrl Pts',(46.0441824779185,-2.64848087950111,126.657863147832));
#60165=CARTESIAN_POINT('Ctrl Pts',(46.0364095776531,-2.76166313075925,126.734667777227));
#60166=CARTESIAN_POINT('Ctrl Pts',(46.0289192418911,-2.87073092209435,126.808680364884));
#60167=CARTESIAN_POINT('Ctrl Pts',(46.0214289061292,-2.97668192959079,126.886985914913));
#60168=CARTESIAN_POINT('Ctrl Pts',(46.0139385703672,-3.0791753380265,126.969277528481));
#60169=CARTESIAN_POINT('Ctrl Pts',(46.0062662665041,-3.18415869237542,127.053568311263));
#60170=CARTESIAN_POINT('Ctrl Pts',(45.9985939626409,-3.28586538037238,127.142323491893));
#60171=CARTESIAN_POINT('Ctrl Pts',(45.9909216587777,-3.38388442460361,127.235255790943));
#60172=CARTESIAN_POINT('Ctrl Pts',(45.9832581368705,-3.4817912732094,127.328081716813));
#60173=CARTESIAN_POINT('Ctrl Pts',(45.9755946149633,-3.5760185804573,127.425074983214));
#60174=CARTESIAN_POINT('Ctrl Pts',(45.9679310930561,-3.6661863034484,127.525906553391));
#60175=CARTESIAN_POINT('Ctrl Pts',(45.9602745796377,-3.75627156572728,127.626645910491));
#60176=CARTESIAN_POINT('Ctrl Pts',(45.9526180662192,-3.84230435958751,127.731216294445));
#60177=CARTESIAN_POINT('Ctrl Pts',(45.9449615528008,-3.92393997776921,127.839250482451));
#60178=CARTESIAN_POINT('Ctrl Pts',(45.9373102808078,-4.00551971059158,127.947210713407));
#60179=CARTESIAN_POINT('Ctrl Pts',(45.9296590088148,-4.08270801339723,128.058629712873));
#60180=CARTESIAN_POINT('Ctrl Pts',(45.9220077368217,-4.15519949093131,128.1731061158));
#60181=CARTESIAN_POINT('Ctrl Pts',(45.9143590574688,-4.22766640466617,128.287543728299));
#60182=CARTESIAN_POINT('Ctrl Pts',(45.9067103781159,-4.29543943944494,128.405036347591));
#60183=CARTESIAN_POINT('Ctrl Pts',(45.8990616987629,-4.35825592345803,128.52515277971));
#60184=CARTESIAN_POINT('Ctrl Pts',(45.8914147178437,-4.42105845870593,128.645242539278));
#60185=CARTESIAN_POINT('Ctrl Pts',(45.8837677369244,-4.47890644962051,128.767954594915));
#60186=CARTESIAN_POINT('Ctrl Pts',(45.8761207560051,-4.53158303530208,128.892832889108));
#60187=CARTESIAN_POINT('Ctrl Pts',(45.868471240813,-4.58427707844028,129.017752569002));
#60188=CARTESIAN_POINT('Ctrl Pts',(45.8608217256209,-4.63179613443582,129.144839551711));
#60189=CARTESIAN_POINT('Ctrl Pts',(45.8531722104289,-4.67397141950254,129.273617584862));
#60190=CARTESIAN_POINT('Ctrl Pts',(45.847114609155,-4.70736975313983,129.375596070828));
#60191=CARTESIAN_POINT('Ctrl Pts',(45.8410570078811,-4.73741796184024,129.478634551205));
#60192=CARTESIAN_POINT('Ctrl Pts',(45.8349994066072,-4.76405452823404,129.582490119308));
#60193=CARTESIAN_POINT('Ctrl Pts',(47.584673688373,-4.76405452823404,129.582490119308));
#60194=CARTESIAN_POINT('Ctrl Pts',(47.5768386373108,-4.79852007433907,129.716870760484));
#60195=CARTESIAN_POINT('Ctrl Pts',(47.5690035862485,-4.82731639010679,129.852791560815));
#60196=CARTESIAN_POINT('Ctrl Pts',(47.5611685351863,-4.85031727127793,129.989740810268));
#60197=CARTESIAN_POINT('Ctrl Pts',(47.5533359516971,-4.87331090854572,130.126646928889));
#60198=CARTESIAN_POINT('Ctrl Pts',(47.5455033682079,-4.89051267838828,130.264580479608));
#60199=CARTESIAN_POINT('Ctrl Pts',(47.5376707847186,-4.90184743077124,130.40301933145));
#60200=CARTESIAN_POINT('Ctrl Pts',(47.5300670018095,-4.91285107938441,130.537414193253));
#60201=CARTESIAN_POINT('Ctrl Pts',(47.5224632189003,-4.91832566835751,130.67228490252));
#60202=CARTESIAN_POINT('Ctrl Pts',(47.5148594359912,-4.91824920960783,130.80714893102));
#60203=CARTESIAN_POINT('',(47.8601405640491,-4.91824815320621,130.800098460401));
#60204=CARTESIAN_POINT('Ctrl Pts',(47.9299877718525,-4.76405452823408,129.582490119308));
#60205=CARTESIAN_POINT('Ctrl Pts',(47.9205281284413,-4.80532410594932,129.743399576467));
#60206=CARTESIAN_POINT('Ctrl Pts',(47.9110684850301,-4.83847374891171,129.90654298482));
#60207=CARTESIAN_POINT('Ctrl Pts',(47.9016088416188,-4.86329419106527,130.071180780384));
#60208=CARTESIAN_POINT('Ctrl Pts',(47.8922659995719,-4.88780816696217,130.233785738312));
#60209=CARTESIAN_POINT('Ctrl Pts',(47.8829231575249,-4.9041973201447,130.397848411231));
#60210=CARTESIAN_POINT('Ctrl Pts',(47.8735803154779,-4.91230617172183,130.562635282188));
#60211=CARTESIAN_POINT('Ctrl Pts',(47.869100398335,-4.91619438721422,130.641651016846));
#60212=CARTESIAN_POINT('Ctrl Pts',(47.864620481192,-4.91817946166017,130.72083294852));
#60213=CARTESIAN_POINT('Ctrl Pts',(47.8601405640491,-4.91824815320621,130.8000984604));
#60214=CARTESIAN_POINT('Ctrl Pts',(47.8601405640086,-4.91824815320683,130.800098461117));
#60215=CARTESIAN_POINT('Ctrl Pts',(47.8524381977585,-4.91836625524756,130.936380446706));
#60216=CARTESIAN_POINT('Ctrl Pts',(47.8447358315084,-4.91281565009925,131.07276389767));
#60217=CARTESIAN_POINT('Ctrl Pts',(47.8370334652582,-4.90159787939591,131.208738276694));
#60218=CARTESIAN_POINT('Ctrl Pts',(47.82933331255,-4.89038333250777,131.344673578767));
#60219=CARTESIAN_POINT('Ctrl Pts',(47.8216331598417,-4.87350488796626,131.480199648344));
#60220=CARTESIAN_POINT('Ctrl Pts',(47.8139330071335,-4.85101614673146,131.614808275747));
#60221=CARTESIAN_POINT('Ctrl Pts',(47.8062336919552,-4.82852985155125,131.749402262043));
#60222=CARTESIAN_POINT('Ctrl Pts',(47.7985343767769,-4.80043453830914,131.883078614066));
#60223=CARTESIAN_POINT('Ctrl Pts',(47.7908350615986,-4.76683532933868,132.015337085326));
#60224=CARTESIAN_POINT('Ctrl Pts',(47.7831348669977,-4.73323228263685,132.147610663266));
#60225=CARTESIAN_POINT('Ctrl Pts',(47.7754346723968,-4.69412418708643,132.278465654424));
#60226=CARTESIAN_POINT('Ctrl Pts',(47.7677344777959,-4.64966653709696,132.40741525054));
#60227=CARTESIAN_POINT('Ctrl Pts',(47.7600316865266,-4.605193895048,132.536408331186));
#60228=CARTESIAN_POINT('Ctrl Pts',(47.7523288952573,-4.55536823880411,132.663494364407));
#60229=CARTESIAN_POINT('Ctrl Pts',(47.744626103988,-4.50039368934766,132.788205294798));
#60230=CARTESIAN_POINT('Ctrl Pts',(47.7369146038724,-4.44535698516225,132.913057224508));
#60231=CARTESIAN_POINT('Ctrl Pts',(47.7292031037567,-4.38515992568094,133.035528327846));
#60232=CARTESIAN_POINT('Ctrl Pts',(47.7214916036411,-4.32005337966299,133.155173638494));
#60233=CARTESIAN_POINT('Ctrl Pts',(47.7137751213887,-4.25490477053053,133.274896247888));
#60234=CARTESIAN_POINT('Ctrl Pts',(47.7060586391363,-4.18484056161315,133.391789090369));
#60235=CARTESIAN_POINT('Ctrl Pts',(47.698342156884,-4.11015503604208,133.505436077859));
#60236=CARTESIAN_POINT('Ctrl Pts',(47.6906142195231,-4.03535863989877,133.619251774164));
#60237=CARTESIAN_POINT('Ctrl Pts',(47.6828862821622,-3.95592746153042,133.729811675631));
#60238=CARTESIAN_POINT('Ctrl Pts',(47.6751583448013,-3.87219640440636,133.836732307877));
#60239=CARTESIAN_POINT('Ctrl Pts',(47.6717840022293,-3.83563590223619,133.883418354149));
#60240=CARTESIAN_POINT('Ctrl Pts',(47.6684096596573,-3.79825608211373,133.929411020072));
#60241=CARTESIAN_POINT('Ctrl Pts',(47.6650353170852,-3.76008696201467,133.974680648823));
#60242=CARTESIAN_POINT('Ctrl Pts',(47.6572609829662,-3.67214701924133,134.078979845434));
#60243=CARTESIAN_POINT('Ctrl Pts',(47.6494866488471,-3.57972484118302,134.179782487539));
#60244=CARTESIAN_POINT('Ctrl Pts',(47.641712314728,-3.48312907161698,134.276678997691));
#60245=CARTESIAN_POINT('Ctrl Pts',(47.6339475617809,-3.38665234770393,134.373456091554));
#60246=CARTESIAN_POINT('Ctrl Pts',(47.6261828088339,-3.28601253984568,134.466336357582));
#60247=CARTESIAN_POINT('Ctrl Pts',(47.6184180558868,-3.18155884012283,134.554942760292));
#60248=CARTESIAN_POINT('Ctrl Pts',(47.6106610150018,-3.07720888528708,134.643461157874));
#60249=CARTESIAN_POINT('Ctrl Pts',(47.6029039741168,-2.9690528731147,134.727713888331));
#60250=CARTESIAN_POINT('Ctrl Pts',(47.5951469332318,-2.85747692306889,134.807360579673));
#60251=CARTESIAN_POINT('Ctrl Pts',(47.5873957419917,-2.7459851133151,134.886947208826));
#60252=CARTESIAN_POINT('Ctrl Pts',(47.5796445507515,-2.6310788159564,134.961934486326));
#60253=CARTESIAN_POINT('Ctrl Pts',(47.5718933595114,-2.51317703465633,135.032022412811));
#60254=CARTESIAN_POINT('Ctrl Pts',(47.5641454627343,-2.39532536475829,135.102080550058));
#60255=CARTESIAN_POINT('Ctrl Pts',(47.5563975659573,-2.27448107850308,135.167243278573));
#60256=CARTESIAN_POINT('Ctrl Pts',(47.5486496691802,-2.15109176763085,135.227254157968));
#60257=CARTESIAN_POINT('Ctrl Pts',(47.5409033930961,-2.02772826714266,135.287252484381));
#60258=CARTESIAN_POINT('Ctrl Pts',(47.5331571170121,-1.90182115230442,135.342100934302));
#60259=CARTESIAN_POINT('Ctrl Pts',(47.525410840928,-1.77384184244861,135.391589430311));
#60260=CARTESIAN_POINT('Ctrl Pts',(47.5176645076626,-1.64586158787843,135.441078291633));
#60261=CARTESIAN_POINT('Ctrl Pts',(47.5099181743973,-1.51580947241909,135.485206979082));
#60262=CARTESIAN_POINT('Ctrl Pts',(47.5021718411319,-1.38417570563983,135.523814047617));
#60263=CARTESIAN_POINT('Ctrl Pts',(47.494423773129,-1.25251246039118,135.562429761936));
#60264=CARTESIAN_POINT('Ctrl Pts',(47.486675705126,-1.11926723409643,135.595521286781));
#60265=CARTESIAN_POINT('Ctrl Pts',(47.478927637123,-0.984943772082143,135.622977517501));
#60266=CARTESIAN_POINT('Ctrl Pts',(47.4711713343811,-0.850477549493772,
135.650462929029));
#60267=CARTESIAN_POINT('Ctrl Pts',(47.4634150316393,-0.714931185659699,
135.672301003825));
#60268=CARTESIAN_POINT('Ctrl Pts',(47.4556587288974,-0.578817510412338,
135.688432008541));
#60269=CARTESIAN_POINT('Ctrl Pts',(47.4478982863833,-0.442631187198379,
135.70457162286));
#60270=CARTESIAN_POINT('Ctrl Pts',(47.4401378438691,-0.305877338877144,
135.714998067908));
#60271=CARTESIAN_POINT('Ctrl Pts',(47.432377401355,-0.169071237698675,135.719703736727));
#60272=CARTESIAN_POINT('Ctrl Pts',(47.4246045010896,-0.0320455232213341,
135.724416959503));
#60273=CARTESIAN_POINT('Ctrl Pts',(47.4168316008241,0.105032220554808,135.723391057423));
#60274=CARTESIAN_POINT('Ctrl Pts',(47.4090587005587,0.241648501206889,135.71667056955));
#60275=CARTESIAN_POINT('Ctrl Pts',(47.4015683647966,0.373298435942736,135.71019438834));
#60276=CARTESIAN_POINT('Ctrl Pts',(47.3940780290345,0.50451956897092,135.698430485831));
#60277=CARTESIAN_POINT('Ctrl Pts',(47.3865876932724,0.634861182226907,135.681463686172));
#60278=CARTESIAN_POINT('Ctrl Pts',(47.3788133591533,0.770144737364827,135.663853585146));
#60279=CARTESIAN_POINT('Ctrl Pts',(47.3710390250342,0.904909299824789,135.640582479512));
#60280=CARTESIAN_POINT('Ctrl Pts',(47.3632646909151,1.03864345100084,135.611688653408));
#60281=CARTESIAN_POINT('Ctrl Pts',(47.355499937968,1.17221278678756,135.582830436362));
#60282=CARTESIAN_POINT('Ctrl Pts',(47.347735185021,1.30475385951347,135.548363368258));
#60283=CARTESIAN_POINT('Ctrl Pts',(47.3399704320739,1.43576071170107,135.508377437395));
#60284=CARTESIAN_POINT('Ctrl Pts',(47.3322133911889,1.56663744603638,135.468431221123));
#60285=CARTESIAN_POINT('Ctrl Pts',(47.3244563503039,1.69598262076747,135.422977163744));
#60286=CARTESIAN_POINT('Ctrl Pts',(47.3166993094189,1.82330116429928,135.372156139124));
#60287=CARTESIAN_POINT('Ctrl Pts',(47.3089481181787,1.9505236959272,135.321373439034));
#60288=CARTESIAN_POINT('Ctrl Pts',(47.3011969269386,2.07572227670362,135.265231971906));
#60289=CARTESIAN_POINT('Ctrl Pts',(47.2934457356985,2.19841802695287,135.203922100404));
#60290=CARTESIAN_POINT('Ctrl Pts',(47.2856978389214,2.32106162823508,135.142638287233));
#60291=CARTESIAN_POINT('Ctrl Pts',(47.2779499421443,2.441204165746,135.076190613168));
#60292=CARTESIAN_POINT('Ctrl Pts',(47.2702020453672,2.55838795465559,135.004817037525));
#60293=CARTESIAN_POINT('Ctrl Pts',(47.2624557692831,2.67554723124274,134.933458391695));
#60294=CARTESIAN_POINT('Ctrl Pts',(47.254709493199,2.78974865657309,134.857176097037));
#60295=CARTESIAN_POINT('Ctrl Pts',(47.2469632171149,2.90056067289784,134.776253220009));
#60296=CARTESIAN_POINT('Ctrl Pts',(47.2392168838495,3.01137350721171,134.695329745626));
#60297=CARTESIAN_POINT('Ctrl Pts',(47.2314705505842,3.11879656685803,134.609765851093));
#60298=CARTESIAN_POINT('Ctrl Pts',(47.2237242173188,3.22242905330253,134.519886698612));
#60299=CARTESIAN_POINT('Ctrl Pts',(47.2159761493158,3.32608474752369,134.429987418318));
#60300=CARTESIAN_POINT('Ctrl Pts',(47.2082280813129,3.42594788408402,134.335771213219));
#60301=CARTESIAN_POINT('Ctrl Pts',(47.2004800133099,3.52165270084111,134.237601843748));
#60302=CARTESIAN_POINT('Ctrl Pts',(47.1927237105681,3.61745923381635,134.139328138703));
#60303=CARTESIAN_POINT('Ctrl Pts',(47.1849674078262,3.70909834518456,134.037093156789));
#60304=CARTESIAN_POINT('Ctrl Pts',(47.1772111050843,3.79624258253802,133.931296068935));
#60305=CARTESIAN_POINT('Ctrl Pts',(47.1694506625702,3.88343333139493,133.825442513989));
#60306=CARTESIAN_POINT('Ctrl Pts',(47.161690220056,3.96612419032239,133.716023376554));
#60307=CARTESIAN_POINT('Ctrl Pts',(47.1539297775419,4.0440302421331,133.603468058021));
#60308=CARTESIAN_POINT('Ctrl Pts',(47.1461568772764,4.12206135565435,133.490732055699));
#60309=CARTESIAN_POINT('Ctrl Pts',(47.138383977011,4.19529210400014,133.374850142483));
#60310=CARTESIAN_POINT('Ctrl Pts',(47.1306110767455,4.2634824039491,133.256278408544));
#60311=CARTESIAN_POINT('Ctrl Pts',(47.1231207409836,4.32919381473354,133.142017055799));
#60312=CARTESIAN_POINT('Ctrl Pts',(47.1156304052215,4.39022473803754,133.025258323553));
#60313=CARTESIAN_POINT('Ctrl Pts',(47.1081400694596,4.44640291469404,132.906427263203));
#60314=CARTESIAN_POINT('Ctrl Pts',(47.1003657353405,4.50471110399385,132.783090687081));
#60315=CARTESIAN_POINT('Ctrl Pts',(47.0925914012214,4.5579760015696,132.657130842929));
#60316=CARTESIAN_POINT('Ctrl Pts',(47.0848170671023,4.60595338270132,132.528998695217));
#60317=CARTESIAN_POINT('Ctrl Pts',(47.0770523141552,4.65387163599859,132.401024458924));
#60318=CARTESIAN_POINT('Ctrl Pts',(47.0692875612081,4.69651520274848,132.270883608466));
#60319=CARTESIAN_POINT('Ctrl Pts',(47.061522808261,4.73368631028101,132.139050461072));
#60320=CARTESIAN_POINT('Ctrl Pts',(47.053765767376,4.77082049894551,132.007348252218));
#60321=CARTESIAN_POINT('Ctrl Pts',(47.046008726491,4.80249293952037,131.873957465181));
#60322=CARTESIAN_POINT('Ctrl Pts',(47.038251685606,4.82855455488895,131.739370763479));
#60323=CARTESIAN_POINT('Ctrl Pts',(47.0305004943659,4.85459651699055,131.604885554657));
#60324=CARTESIAN_POINT('Ctrl Pts',(47.0227493031258,4.8750360017413,131.469206608528));
#60325=CARTESIAN_POINT('Ctrl Pts',(47.0149981118857,4.8897743204808,131.332839715796));
#60326=CARTESIAN_POINT('Ctrl Pts',(47.0072502151086,4.90450637504174,131.196530782631));
#60327=CARTESIAN_POINT('Ctrl Pts',(46.9995023183315,4.91354204112497,131.059534872303));
#60328=CARTESIAN_POINT('Ctrl Pts',(46.9917544215544,4.91683413081026,130.922365670845));
#60329=CARTESIAN_POINT('Ctrl Pts',(46.9840081454703,4.92012553186136,130.785225162226));
#60330=CARTESIAN_POINT('Ctrl Pts',(46.9762618693862,4.91767573685475,130.647911825182));
#60331=CARTESIAN_POINT('Ctrl Pts',(46.9685155933021,4.90948963011366,130.510941745803));
#60332=CARTESIAN_POINT('Ctrl Pts',(46.9607692600368,4.9013034629446,130.373970655343));
#60333=CARTESIAN_POINT('Ctrl Pts',(46.9530229267714,4.88738092287106,130.237343217874));
#60334=CARTESIAN_POINT('Ctrl Pts',(46.9452765935061,4.86777893666666,130.101572394668));
#60335=CARTESIAN_POINT('Ctrl Pts',(46.9375285255031,4.84817256073334,129.965771166527));
#60336=CARTESIAN_POINT('Ctrl Pts',(46.9297804575001,4.82288426364582,129.830827321253));
#60337=CARTESIAN_POINT('Ctrl Pts',(46.9220323894972,4.79202238398621,129.697245206294));
#60338=CARTESIAN_POINT('Ctrl Pts',(46.9142760867553,4.76112770395369,129.563521118675));
#60339=CARTESIAN_POINT('Ctrl Pts',(46.9065197840135,4.72464769632839,129.431162033973));
#60340=CARTESIAN_POINT('Ctrl Pts',(46.8987634812716,4.68274119889307,129.300659208812));
#60341=CARTESIAN_POINT('Ctrl Pts',(46.8910030387575,4.64081233469817,129.170086730363));
#60342=CARTESIAN_POINT('Ctrl Pts',(46.8832425962433,4.59345134455043,129.041372852326));
#60343=CARTESIAN_POINT('Ctrl Pts',(46.8754821537291,4.54086549130139,128.91498938554));
#60344=CARTESIAN_POINT('Ctrl Pts',(46.8677092534637,4.48819522257243,128.788403036793));
#60345=CARTESIAN_POINT('Ctrl Pts',(46.8599363531982,4.43028349527913,128.664154929541));
#60346=CARTESIAN_POINT('Ctrl Pts',(46.8521634529328,4.36738426015332,128.542693580475));
#60347=CARTESIAN_POINT('Ctrl Pts',(46.8446731171707,4.30677157065743,128.425647657389));
#60348=CARTESIAN_POINT('Ctrl Pts',(46.8371827814086,4.24152784724818,128.311189666356));
#60349=CARTESIAN_POINT('Ctrl Pts',(46.8296924456465,4.17191758741517,128.199694284556));
#60350=CARTESIAN_POINT('Ctrl Pts',(46.8219181115274,4.09966803342372,128.083971521467));
#60351=CARTESIAN_POINT('Ctrl Pts',(46.8141437774084,4.02248542737804,127.971073882093));
#60352=CARTESIAN_POINT('Ctrl Pts',(46.8063694432893,3.94061716903076,127.861450596916));
#60353=CARTESIAN_POINT('Ctrl Pts',(46.7986046903422,3.858849805995,127.751962412642));
#60354=CARTESIAN_POINT('Ctrl Pts',(46.7908399373951,3.77240851217956,127.645740863667));
#60355=CARTESIAN_POINT('Ctrl Pts',(46.7830751844481,3.68158544314398,127.543208721789));
#60356=CARTESIAN_POINT('Ctrl Pts',(46.775318143563,3.59085258086095,127.44077841628));
#60357=CARTESIAN_POINT('Ctrl Pts',(46.767561102678,3.495746861676,127.342030516369));
#60358=CARTESIAN_POINT('Ctrl Pts',(46.759804061793,3.39660219753829,127.247356741524));
#60359=CARTESIAN_POINT('Ctrl Pts',(46.7520528705528,3.2975322991629,127.152754360909));
#60360=CARTESIAN_POINT('Ctrl Pts',(46.7443016793127,3.19442979992645,127.062220258986));
#60361=CARTESIAN_POINT('Ctrl Pts',(46.7365504880726,3.08766689224149,126.976110857551));
#60362=CARTESIAN_POINT('Ctrl Pts',(46.7288025912955,2.98094936164044,126.890038054909));
#60363=CARTESIAN_POINT('Ctrl Pts',(46.7210546945184,2.87057482058224,126.808386457286));
#60364=CARTESIAN_POINT('Ctrl Pts',(46.7133067977413,2.75694994144988,126.731473425065));
#60365=CARTESIAN_POINT('Ctrl Pts',(46.7055605216572,2.64334883019276,126.654576481392));
#60366=CARTESIAN_POINT('Ctrl Pts',(46.6978142455731,2.52649905678103,126.582416350576));
#60367=CARTESIAN_POINT('Ctrl Pts',(46.690067969489,2.40683745915553,126.515267880435));
#60368=CARTESIAN_POINT('Ctrl Pts',(46.6823216362236,2.28717497821513,126.448118914621));
#60369=CARTESIAN_POINT('Ctrl Pts',(46.6745753029583,2.16470097259514,126.385981874628));
#60370=CARTESIAN_POINT('Ctrl Pts',(46.6668289696929,2.03987778145311,126.329086134449));
#60371=CARTESIAN_POINT('Ctrl Pts',(46.6590809016899,1.9150266370234,126.272177652864));
#60372=CARTESIAN_POINT('Ctrl Pts',(46.651332833687,1.78782561590957,126.220512968849));
#60373=CARTESIAN_POINT('Ctrl Pts',(46.643584765684,1.65875759955394,126.174273546201));
#60374=CARTESIAN_POINT('Ctrl Pts',(46.6358284629422,1.52955240817425,126.127984979744));
#60375=CARTESIAN_POINT('Ctrl Pts',(46.6280721602003,1.39847662641538,126.087133324995));
#60376=CARTESIAN_POINT('Ctrl Pts',(46.6203158574584,1.26602941808786,126.051850483433));
#60377=CARTESIAN_POINT('Ctrl Pts',(46.6125554149442,1.13351151869698,126.016548810356));
#60378=CARTESIAN_POINT('Ctrl Pts',(46.60479497243,0.999621115706425,125.98682195761));
#60379=CARTESIAN_POINT('Ctrl Pts',(46.5970345299158,0.864867187571389,125.962750574371));
#60380=CARTESIAN_POINT('Ctrl Pts',(46.5892616296504,0.729896940468386,125.938640549612));
#60381=CARTESIAN_POINT('Ctrl Pts',(46.5814887293849,0.594060785773303,125.920204189031));
#60382=CARTESIAN_POINT('Ctrl Pts',(46.5737158291195,0.457873339854812,125.907470270912));
#60383=CARTESIAN_POINT('Ctrl Pts',(46.5662254933575,0.326636650632228,125.895199262792));
#60384=CARTESIAN_POINT('Ctrl Pts',(46.5587351575956,0.195074074991304,125.88822331515));
#60385=CARTESIAN_POINT('Ctrl Pts',(46.5512448218336,0.0636438068067698,
125.886522420924));
#60386=CARTESIAN_POINT('Ctrl Pts',(46.5434704877146,-0.0727696799445072,
125.884757036775));
#60387=CARTESIAN_POINT('Ctrl Pts',(46.5356961535955,-0.209472745235359,
125.888669017406));
#60388=CARTESIAN_POINT('Ctrl Pts',(46.5279218194764,-0.345953713127084,
125.898293038448));
#60389=CARTESIAN_POINT('Ctrl Pts',(46.5201570665293,-0.482266480423721,
125.907905198744));
#60390=CARTESIAN_POINT('Ctrl Pts',(46.5123923135823,-0.618357308680023,
125.923215365549));
#60391=CARTESIAN_POINT('Ctrl Pts',(46.5046275606352,-0.753712590793564,
125.9442062586));
#60392=CARTESIAN_POINT('Ctrl Pts',(46.4968705197502,-0.88893343613255,125.9651763032));
#60393=CARTESIAN_POINT('Ctrl Pts',(46.4891134788651,-1.02341980531881,125.99181578633));
#60394=CARTESIAN_POINT('Ctrl Pts',(46.4813564379801,-1.15666164610616,126.024055512353));
#60395=CARTESIAN_POINT('Ctrl Pts',(46.47360524674,-1.28980300818526,126.056270926147));
#60396=CARTESIAN_POINT('Ctrl Pts',(46.4658540554999,-1.42170133144778,126.094078085262));
#60397=CARTESIAN_POINT('Ctrl Pts',(46.4581028642597,-1.55185556905271,126.137356508365));
#60398=CARTESIAN_POINT('Ctrl Pts',(46.4503549674827,-1.68195448763432,126.180616536984));
#60399=CARTESIAN_POINT('Ctrl Pts',(46.4426070707056,-1.81031042469731,126.229343081379));
#60400=CARTESIAN_POINT('Ctrl Pts',(46.4348591739285,-1.93643655960838,126.283365537596));
#60401=CARTESIAN_POINT('Ctrl Pts',(46.4271128978444,-2.06253631165116,126.33737669348));
#60402=CARTESIAN_POINT('Ctrl Pts',(46.4193666217602,-2.18640683013136,126.396681403893));
#60403=CARTESIAN_POINT('Ctrl Pts',(46.4116203456761,-2.3075807562174,126.461060706665));
#60404=CARTESIAN_POINT('Ctrl Pts',(46.4038740124107,-2.42875557678216,126.52544048467));
#60405=CARTESIAN_POINT('Ctrl Pts',(46.3961276791454,-2.54723341997167,126.594894746345));
#60406=CARTESIAN_POINT('Ctrl Pts',(46.38838134588,-2.6625714013437,126.669158494907));
#60407=CARTESIAN_POINT('Ctrl Pts',(46.3806332778771,-2.77793521185586,126.743438874319));
#60408=CARTESIAN_POINT('Ctrl Pts',(46.3728852098742,-2.89015743270729,126.822530672212));
#60409=CARTESIAN_POINT('Ctrl Pts',(46.3651371418712,-2.99882438405085,126.906125712366));
#60410=CARTESIAN_POINT('Ctrl Pts',(46.3573808391294,-3.10760682792435,126.989809598324));
#60411=CARTESIAN_POINT('Ctrl Pts',(46.3496245363875,-3.21282614378835,127.078006048528));
#60412=CARTESIAN_POINT('Ctrl Pts',(46.3418682336456,-3.31410154896094,127.170366398298));
#60413=CARTESIAN_POINT('Ctrl Pts',(46.3341077911315,-3.4154310078662,127.262776043567));
#60414=CARTESIAN_POINT('Ctrl Pts',(46.3263473486174,-3.51281208426044,127.359353741548));
#60415=CARTESIAN_POINT('Ctrl Pts',(46.3185869061032,-3.60590181042014,127.4597148671));
#60416=CARTESIAN_POINT('Ctrl Pts',(46.3108140058378,-3.69914097247252,127.560237101241));
#60417=CARTESIAN_POINT('Ctrl Pts',(46.3030411055723,-3.78807476436956,127.664554602038));
#60418=CARTESIAN_POINT('Ctrl Pts',(46.2952682053069,-3.87240081140812,127.772249963532));
#60419=CARTESIAN_POINT('Ctrl Pts',(46.2877778695449,-3.95366139423257,127.876030327368));
#60420=CARTESIAN_POINT('Ctrl Pts',(46.2802875337828,-4.0306432422824,127.982946978204));
#60421=CARTESIAN_POINT('Ctrl Pts',(46.2727971980208,-4.10311552308458,128.092603610251));
#60422=CARTESIAN_POINT('Ctrl Pts',(46.2648734482723,-4.17978127413056,128.208605314075));
#60423=CARTESIAN_POINT('Ctrl Pts',(46.2569496985237,-4.25163626346315,128.328030286094));
#60424=CARTESIAN_POINT('Ctrl Pts',(46.2490259487752,-4.31836681451101,128.450450866146));
#60425=CARTESIAN_POINT('Ctrl Pts',(46.241112019846,-4.38501465867017,128.572719716216));
#60426=CARTESIAN_POINT('Ctrl Pts',(46.2331980909168,-4.44655052719398,128.697976463837));
#60427=CARTESIAN_POINT('Ctrl Pts',(46.2252841619876,-4.50270335582552,128.825763753135));
#60428=CARTESIAN_POINT('Ctrl Pts',(46.2173814468959,-4.55877661731677,128.95336997107));
#60429=CARTESIAN_POINT('Ctrl Pts',(46.2094787318042,-4.60948188764378,129.083499249448));
#60430=CARTESIAN_POINT('Ctrl Pts',(46.2015760167124,-4.65459381296858,129.21566949001));
#60431=CARTESIAN_POINT('Ctrl Pts',(46.1943591483146,-4.69579064525495,129.336369176279));
#60432=CARTESIAN_POINT('Ctrl Pts',(46.1871422799169,-4.73232327563257,129.458770447004));
#60433=CARTESIAN_POINT('Ctrl Pts',(46.1799254115191,-4.76405452823402,129.582490119308));
#60434=CARTESIAN_POINT('Origin',(213.235140564004,0.,130.804360617566));
#60435=CARTESIAN_POINT('',(44.0848860644534,-4.76405452823407,129.582490119308));
#60436=CARTESIAN_POINT('',(44.4302709800425,-4.764054528234,129.582490119308));
#60437=CARTESIAN_POINT('',(213.235140564004,-4.76405452823405,129.582490119308));
#60438=CARTESIAN_POINT('',(45.764859436029,-4.91824911967543,130.807303288442));
#60439=CARTESIAN_POINT('Ctrl Pts',(45.7648594359911,-4.91824911967503,130.807303289108));
#60440=CARTESIAN_POINT('Ctrl Pts',(45.7550699395122,-4.91814616794528,130.979372188753));
#60441=CARTESIAN_POINT('Ctrl Pts',(45.7452804430333,-4.90901394869115,131.15116886393));
#60442=CARTESIAN_POINT('Ctrl Pts',(45.7354909465544,-4.89093350128723,131.322001949461));
#60443=CARTESIAN_POINT('Ctrl Pts',(45.7277166124353,-4.87657490384115,131.457669140146));
#60444=CARTESIAN_POINT('Ctrl Pts',(45.7199422783162,-4.85654447762349,131.592953336111));
#60445=CARTESIAN_POINT('Ctrl Pts',(45.7121679441971,-4.83086822310986,131.727342347313));
#60446=CARTESIAN_POINT('Ctrl Pts',(45.70440319125,-4.80522361228517,131.86156573607));
#60447=CARTESIAN_POINT('Ctrl Pts',(45.6966384383029,-4.77394709013444,131.99489575484));
#60448=CARTESIAN_POINT('Ctrl Pts',(45.6888736853558,-4.7371164774588,132.126824432378));
#60449=CARTESIAN_POINT('Ctrl Pts',(45.6811166444708,-4.70032244546698,132.258622076494));
#60450=CARTESIAN_POINT('Ctrl Pts',(45.6733596035858,-4.65798540528323,132.389020775057));
#60451=CARTESIAN_POINT('Ctrl Pts',(45.6656025627009,-4.6102343098522,132.517522218455));
#60452=CARTESIAN_POINT('Ctrl Pts',(45.6578513714607,-4.56251922389369,132.645926757916));
#60453=CARTESIAN_POINT('Ctrl Pts',(45.6501001802206,-4.50939834484913,132.772436525006));
#60454=CARTESIAN_POINT('Ctrl Pts',(45.6423489889805,-4.45105048877216,132.896568209776));
#60455=CARTESIAN_POINT('Ctrl Pts',(45.6346010922034,-4.39272743209042,133.020647135269));
#60456=CARTESIAN_POINT('Ctrl Pts',(45.6268531954264,-4.3291819829457,133.142349635659));
#60457=CARTESIAN_POINT('Ctrl Pts',(45.6191052986493,-4.26064104895134,133.261212447549));
#60458=CARTESIAN_POINT('Ctrl Pts',(45.6113590225652,-4.19211445224281,133.380050395902));
#60459=CARTESIAN_POINT('Ctrl Pts',(45.6036127464811,-4.11859464432113,133.496049498781));
#60460=CARTESIAN_POINT('Ctrl Pts',(45.595866470397,-4.04035425393199,133.608771529903));
#60461=CARTESIAN_POINT('Ctrl Pts',(45.5881201371317,-3.96211328599007,133.721494393113));
#60462=CARTESIAN_POINT('Ctrl Pts',(45.5803738038664,-3.87915188897781,133.830939815115));
#60463=CARTESIAN_POINT('Ctrl Pts',(45.572627470601,-3.79178551340098,133.936699309799));
#60464=CARTESIAN_POINT('Ctrl Pts',(45.5648794025981,-3.70439957272998,134.042482488589));
#60465=CARTESIAN_POINT('Ctrl Pts',(45.557131334595,-3.612606939495,134.144577796174));
#60466=CARTESIAN_POINT('Ctrl Pts',(45.5493832665921,-3.51676249209189,134.242610846493));
#60467=CARTESIAN_POINT('Ctrl Pts',(45.5416269638502,-3.42081618006964,134.340748087504));
#60468=CARTESIAN_POINT('Ctrl Pts',(45.5338706611084,-3.32080972530035,134.434814166746));
#60469=CARTESIAN_POINT('Ctrl Pts',(45.5261143583666,-3.21713432580663,134.524472147106));
#60470=CARTESIAN_POINT('Ctrl Pts',(45.5183539158524,-3.11340359163046,134.61417798063));
#60471=CARTESIAN_POINT('Ctrl Pts',(45.5105934733382,-3.00600031681478,134.69947078423));
#60472=CARTESIAN_POINT('Ctrl Pts',(45.502833030824,-2.89534694186584,134.780055418318));
#60473=CARTESIAN_POINT('Ctrl Pts',(45.4950601305586,-2.78451593629623,134.860769414015));
#60474=CARTESIAN_POINT('Ctrl Pts',(45.4872872302932,-2.67042473024954,134.93675992011));
#60475=CARTESIAN_POINT('Ctrl Pts',(45.4795143300277,-2.55352352121795,135.007775977614));
#60476=CARTESIAN_POINT('Ctrl Pts',(45.4720239942657,-2.4408719655904,135.076210422549));
#60477=CARTESIAN_POINT('Ctrl Pts',(45.4645336585036,-2.32561143085241,135.14002565809));
#60478=CARTESIAN_POINT('Ctrl Pts',(45.4570433227416,-2.20816271225007,135.199039274616));
#60479=CARTESIAN_POINT('Ctrl Pts',(45.4492689886225,-2.08626088978468,135.260290410348));
#60480=CARTESIAN_POINT('Ctrl Pts',(45.4414946545035,-1.96161552963054,135.3165626579));
#60481=CARTESIAN_POINT('Ctrl Pts',(45.4337203203844,-1.8346716056696,135.367601040977));
#60482=CARTESIAN_POINT('Ctrl Pts',(45.4259555674373,-1.7078841287498,135.418576523808));
#60483=CARTESIAN_POINT('Ctrl Pts',(45.4181908144901,-1.57880408366228,135.464330831838));
#60484=CARTESIAN_POINT('Ctrl Pts',(45.410426061543,-1.4479009050461,135.504654867043));
#60485=CARTESIAN_POINT('Ctrl Pts',(45.402669020658,-1.31712774131233,135.544938851848));
#60486=CARTESIAN_POINT('Ctrl Pts',(45.3949119797731,-1.18453541876935,135.579803182633));
#60487=CARTESIAN_POINT('Ctrl Pts',(45.3871549388881,-1.05061288162221,135.609087002645));
#60488=CARTESIAN_POINT('Ctrl Pts',(45.3794037476479,-0.916791336501912,
135.6383487395));
#60489=CARTESIAN_POINT('Ctrl Pts',(45.3716525564078,-0.781641953832756,
135.662038258783));
#60490=CARTESIAN_POINT('Ctrl Pts',(45.3639013651677,-0.645668010407917,
135.680044762672));
#60491=CARTESIAN_POINT('Ctrl Pts',(45.3561534683906,-0.509751859536257,
135.698043613316));
#60492=CARTESIAN_POINT('Ctrl Pts',(45.3484055716135,-0.373012231717856,
135.710364201459));
#60493=CARTESIAN_POINT('Ctrl Pts',(45.3406576748364,-0.235961532675184,
135.716947025722));
#60494=CARTESIAN_POINT('Ctrl Pts',(45.3329113987523,-0.09893950168428,135.723528473));
#60495=CARTESIAN_POINT('Ctrl Pts',(45.3251651226682,0.0383930808367228,
135.724374524948));
#60496=CARTESIAN_POINT('Ctrl Pts',(45.317418846584,0.175520160206388,135.71947767984));
#60497=CARTESIAN_POINT('Ctrl Pts',(45.3096725133187,0.312648251817003,135.714580798585));
#60498=CARTESIAN_POINT('Ctrl Pts',(45.3019261800533,0.4495704465331,135.703940949635));
#60499=CARTESIAN_POINT('Ctrl Pts',(45.294179846788,0.585772564717304,135.687602733714));
#60500=CARTESIAN_POINT('Ctrl Pts',(45.286431778785,0.72200518442133,135.671260858963));
#60501=CARTESIAN_POINT('Ctrl Pts',(45.278683710782,0.857517018604362,135.649218124486));
#60502=CARTESIAN_POINT('Ctrl Pts',(45.270935642779,0.991801265230155,135.621570734718));
#60503=CARTESIAN_POINT('Ctrl Pts',(45.2631793400371,1.12622823075127,135.593893960975));
#60504=CARTESIAN_POINT('Ctrl Pts',(45.2554230372953,1.25942461890314,135.560600711769));
#60505=CARTESIAN_POINT('Ctrl Pts',(45.2476667345535,1.3908955028648,135.521837990337));
#60506=CARTESIAN_POINT('Ctrl Pts',(45.2399062920393,1.52243655679592,135.483054580074));
#60507=CARTESIAN_POINT('Ctrl Pts',(45.2321458495251,1.65224990159093,135.438796006891));
#60508=CARTESIAN_POINT('Ctrl Pts',(45.2243854070109,1.7798588885437,135.389258151794));
#60509=CARTESIAN_POINT('Ctrl Pts',(45.2166125067455,1.90767272477092,135.339640774134));
#60510=CARTESIAN_POINT('Ctrl Pts',(45.2088396064801,2.03327477341276,135.284727335972));
#60511=CARTESIAN_POINT('Ctrl Pts',(45.2010667062146,2.15621055282234,135.224760951744));
#60512=CARTESIAN_POINT('Ctrl Pts',(45.1935763704526,2.27467730699366,135.166974496628));
#60513=CARTESIAN_POINT('Ctrl Pts',(45.1860860346906,2.39066800641625,135.104496237989));
#60514=CARTESIAN_POINT('Ctrl Pts',(45.1785956989285,2.50380173459983,135.037581605929));
#60515=CARTESIAN_POINT('Ctrl Pts',(45.1708213648095,2.62122496247376,134.968129885255));
#60516=CARTESIAN_POINT('Ctrl Pts',(45.1630470306905,2.73594225984691,134.893678737945));
#60517=CARTESIAN_POINT('Ctrl Pts',(45.1552726965714,2.84749858869034,134.814464712213));
#60518=CARTESIAN_POINT('Ctrl Pts',(45.1475079436243,2.95891743432839,134.735348310689));
#60519=CARTESIAN_POINT('Ctrl Pts',(45.1397431906772,3.06718274682794,134.651480934121));
#60520=CARTESIAN_POINT('Ctrl Pts',(45.1319784377301,3.17186486521209,134.563144508578));
#60521=CARTESIAN_POINT('Ctrl Pts',(45.1242213968451,3.27644301184065,134.474895820019));
#60522=CARTESIAN_POINT('Ctrl Pts',(45.1164643559601,3.37744474982086,134.382187166251));
#60523=CARTESIAN_POINT('Ctrl Pts',(45.1087073150751,3.47447045952549,134.28534296288));
#60524=CARTESIAN_POINT('Ctrl Pts',(45.100956123835,3.57142300138768,134.188571790475));
#60525=CARTESIAN_POINT('Ctrl Pts',(45.0932049325949,3.66440520742259,134.087671551027));
#60526=CARTESIAN_POINT('Ctrl Pts',(45.0854537413547,3.75305182688401,133.983005776627));
#60527=CARTESIAN_POINT('Ctrl Pts',(45.0777058445777,3.84166076916742,133.878384487973));
#60528=CARTESIAN_POINT('Ctrl Pts',(45.0699579478006,3.92593753779637,133.770001145261));
#60529=CARTESIAN_POINT('Ctrl Pts',(45.0622100510235,4.00555510476579,133.658254687987));
#60530=CARTESIAN_POINT('Ctrl Pts',(45.0544637749394,4.08515601745656,133.546531605663));
#60531=CARTESIAN_POINT('Ctrl Pts',(45.0467174988553,4.16009944030952,133.431447126272));
#60532=CARTESIAN_POINT('Ctrl Pts',(45.0389712227712,4.23010012174904,133.313431366365));
#60533=CARTESIAN_POINT('Ctrl Pts',(45.0312248895059,4.30010131991768,133.195414735293));
#60534=CARTESIAN_POINT('Ctrl Pts',(45.0234785562406,4.3651595044144,133.07446711679));
#60535=CARTESIAN_POINT('Ctrl Pts',(45.0157322229752,4.42503427243789,132.951045212529));
#60536=CARTESIAN_POINT('Ctrl Pts',(45.0079841549723,4.48492244900046,132.827595668788));
#60537=CARTESIAN_POINT('Ctrl Pts',(45.0002360869693,4.53962472863854,132.701671088387));
#60538=CARTESIAN_POINT('Ctrl Pts',(44.9924880189664,4.58894811198817,132.573749859079));
#60539=CARTESIAN_POINT('Ctrl Pts',(44.9847317162245,4.63832391681664,132.445692673565));
#60540=CARTESIAN_POINT('Ctrl Pts',(44.9769754134826,4.68230926464487,132.315634965467));
#60541=CARTESIAN_POINT('Ctrl Pts',(44.9692191107408,4.72076031342351,132.184072589575));
#60542=CARTESIAN_POINT('Ctrl Pts',(44.9614586682266,4.75923188468466,132.052439994882));
#60543=CARTESIAN_POINT('Ctrl Pts',(44.9536982257125,4.7921631773269,131.91930151152));
#60544=CARTESIAN_POINT('Ctrl Pts',(44.9459377831983,4.81946135131954,131.785164036013));
#60545=CARTESIAN_POINT('Ctrl Pts',(44.9381648829329,4.84680334676447,131.650811231122));
#60546=CARTESIAN_POINT('Ctrl Pts',(44.9303919826674,4.86849409130069,131.515456615703));
#60547=CARTESIAN_POINT('Ctrl Pts',(44.922619082402,4.88449246555745,131.379613967328));
#60548=CARTESIAN_POINT('Ctrl Pts',(44.9151287466399,4.89990925861265,131.248709541387));
#60549=CARTESIAN_POINT('Ctrl Pts',(44.9076384108779,4.91004033641195,131.117352256024));
#60550=CARTESIAN_POINT('Ctrl Pts',(44.9001480751158,4.91489470486667,130.986000653278));
#60551=CARTESIAN_POINT('Ctrl Pts',(44.8923737409967,4.91993312817675,130.849668814593));
#60552=CARTESIAN_POINT('Ctrl Pts',(44.8845994068775,4.91930277073469,130.712911239658));
#60553=CARTESIAN_POINT('Ctrl Pts',(44.8768250727585,4.9129566880833,130.576238624945));
#60554=CARTESIAN_POINT('Ctrl Pts',(44.8690603198114,4.90661842641161,130.439734447014));
#60555=CARTESIAN_POINT('Ctrl Pts',(44.8612955668643,4.89457847319077,130.303315407765));
#60556=CARTESIAN_POINT('Ctrl Pts',(44.8535308139172,4.87684177855376,130.167495381074));
#60557=CARTESIAN_POINT('Ctrl Pts',(44.8457737730322,4.8591227002519,130.031810252747));
#60558=CARTESIAN_POINT('Ctrl Pts',(44.8380167321472,4.83571819067468,129.896723338171));
#60559=CARTESIAN_POINT('Ctrl Pts',(44.8302596912622,4.8066851856876,129.762746203211));
#60560=CARTESIAN_POINT('Ctrl Pts',(44.8225085000221,4.77767407471542,129.628870101452));
#60561=CARTESIAN_POINT('Ctrl Pts',(44.8147573087819,4.7430429992034,129.496102494075));
#60562=CARTESIAN_POINT('Ctrl Pts',(44.8070061175418,4.70290038204455,129.364947174852));
#60563=CARTESIAN_POINT('Ctrl Pts',(44.7992582207647,4.66277482656883,129.233847600139));
#60564=CARTESIAN_POINT('Ctrl Pts',(44.7915103239876,4.61714250278745,129.104359323703));
#60565=CARTESIAN_POINT('Ctrl Pts',(44.7837624272105,4.56616228317317,128.976973120009));
#60566=CARTESIAN_POINT('Ctrl Pts',(44.7760161511264,4.51519272752183,128.849613562763));
#60567=CARTESIAN_POINT('Ctrl Pts',(44.7682698750424,4.45887764629468,128.724355566403));
#60568=CARTESIAN_POINT('Ctrl Pts',(44.7605235989583,4.39742472328459,128.601671609661));
#60569=CARTESIAN_POINT('Ctrl Pts',(44.7527772656929,4.33597134664297,128.478986747294));
#60570=CARTESIAN_POINT('Ctrl Pts',(44.7450309324275,4.26938022763687,128.358876312022));
#60571=CARTESIAN_POINT('Ctrl Pts',(44.7372845991622,4.19790565873112,128.241789419942));
#60572=CARTESIAN_POINT('Ctrl Pts',(44.7295365311592,4.12641508359124,128.124676307064));
#60573=CARTESIAN_POINT('Ctrl Pts',(44.7217884631562,4.05003908605181,128.010588418369));
#60574=CARTESIAN_POINT('Ctrl Pts',(44.7140403951532,3.96907582640807,127.899946709955));
#60575=CARTESIAN_POINT('Ctrl Pts',(44.7062840924113,3.88802651804852,127.789187410217));
#60576=CARTESIAN_POINT('Ctrl Pts',(44.6985277896695,3.80238043970247,127.681881923296));
#60577=CARTESIAN_POINT('Ctrl Pts',(44.6907714869276,3.71247701790846,127.578419289209));
#60578=CARTESIAN_POINT('Ctrl Pts',(44.6830110444135,3.62252561195119,127.474901433999));
#60579=CARTESIAN_POINT('Ctrl Pts',(44.6752506018993,3.5283126032853,127.375230802491));
#60580=CARTESIAN_POINT('Ctrl Pts',(44.6674901593851,3.4302142760083,127.279759493585));
#60581=CARTESIAN_POINT('Ctrl Pts',(44.6597172591197,3.33195847258772,127.184134925658));
#60582=CARTESIAN_POINT('Ctrl Pts',(44.6519443588542,3.22980517844126,127.092723412112));
#60583=CARTESIAN_POINT('Ctrl Pts',(44.6441714585888,3.1241644231672,127.005837257164));
#60584=CARTESIAN_POINT('Ctrl Pts',(44.6366811228268,3.02236397544136,126.922109632803));
#60585=CARTESIAN_POINT('Ctrl Pts',(44.6291907870649,2.91732546605125,126.842584248806));
#60586=CARTESIAN_POINT('Ctrl Pts',(44.621700451303,2.80943954731722,126.767501381418));
#60587=CARTESIAN_POINT('Ctrl Pts',(44.6139261171839,2.69746310118208,126.689571724292));
#60588=CARTESIAN_POINT('Ctrl Pts',(44.6061517830648,2.58206435661931,126.616181252119));
#60589=CARTESIAN_POINT('Ctrl Pts',(44.5983774489457,2.46364760240628,126.547645504517));
#60590=CARTESIAN_POINT('Ctrl Pts',(44.5906126959987,2.34537678625976,126.479194221099));
#60591=CARTESIAN_POINT('Ctrl Pts',(44.5828479430515,2.22409569614404,126.415585951799));
#60592=CARTESIAN_POINT('Ctrl Pts',(44.5750831901044,2.10023934437156,126.357094293311));
#60593=CARTESIAN_POINT('Ctrl Pts',(44.5673261492194,1.97650600847355,126.298660729563));
#60594=CARTESIAN_POINT('Ctrl Pts',(44.5595691083345,1.85020285226648,126.24533382931));
#60595=CARTESIAN_POINT('Ctrl Pts',(44.5518120674494,1.72179104582964,126.197342204644));
#60596=CARTESIAN_POINT('Ctrl Pts',(44.5440608762093,1.59347607573494,126.149386770836));
#60597=CARTESIAN_POINT('Ctrl Pts',(44.5363096849692,1.46305598524942,126.106758740651));
#60598=CARTESIAN_POINT('Ctrl Pts',(44.5285584937291,1.33101323556341,126.069639207678));
#60599=CARTESIAN_POINT('Ctrl Pts',(44.520810596952,1.19902660756837,126.032535451496));
#60600=CARTESIAN_POINT('Ctrl Pts',(44.5130627001749,1.06541906766878,126.000935641527));
#60601=CARTESIAN_POINT('Ctrl Pts',(44.5053148033978,0.930689392774144,125.974971389446));
#60602=CARTESIAN_POINT('Ctrl Pts',(44.4975685273137,0.795987900423058,125.949012568527));
#60603=CARTESIAN_POINT('Ctrl Pts',(44.4898222512295,0.660165123618893,125.92868703466));
#60604=CARTESIAN_POINT('Ctrl Pts',(44.4820759751454,0.52373083026329,125.914075443884));
#60605=CARTESIAN_POINT('Ctrl Pts',(44.4743296418801,0.387295529780727,125.899463745249));
#60606=CARTESIAN_POINT('Ctrl Pts',(44.4665833086147,0.250249092481418,125.890566115502));
#60607=CARTESIAN_POINT('Ctrl Pts',(44.4588369753494,0.113106823744031,125.887411369412));
#60608=CARTESIAN_POINT('Ctrl Pts',(44.4510889073464,-0.0240661570535617,
125.884255916838));
#60609=CARTESIAN_POINT('Ctrl Pts',(44.4433408393434,-0.161334621206717,
125.886845916057));
#60610=CARTESIAN_POINT('Ctrl Pts',(44.4355927713405,-0.29818324350635,125.895158053423));
#60611=CARTESIAN_POINT('Ctrl Pts',(44.4278364685986,-0.435177310150283,
125.903479025026));
#60612=CARTESIAN_POINT('Ctrl Pts',(44.4200801658567,-0.571750252714067,
125.917534259599));
#60613=CARTESIAN_POINT('Ctrl Pts',(44.4123238631148,-0.707391292478267,
125.937248473612));
#60614=CARTESIAN_POINT('Ctrl Pts',(44.4045634206007,-0.843104727949646,
125.956973209695));
#60615=CARTESIAN_POINT('Ctrl Pts',(44.3968029780865,-0.977884885520969,
125.982362871216));
#60616=CARTESIAN_POINT('Ctrl Pts',(44.3890425355723,-1.11123214366968,126.013291197763));
#60617=CARTESIAN_POINT('Ctrl Pts',(44.3812696353069,-1.24479346267501,126.044269173205));
#60618=CARTESIAN_POINT('Ctrl Pts',(44.3734967350414,-1.37691690864932,126.08080347678));
#60619=CARTESIAN_POINT('Ctrl Pts',(44.365723834776,-1.50711810019504,126.122717947032));
#60620=CARTESIAN_POINT('Ctrl Pts',(44.3582334990139,-1.63258615047159,126.163108720715));
#60621=CARTESIAN_POINT('Ctrl Pts',(44.3507431632519,-1.75626898833957,126.208495180944));
#60622=CARTESIAN_POINT('Ctrl Pts',(44.3432528274898,-1.87775330546755,126.25867853604));
#60623=CARTESIAN_POINT('Ctrl Pts',(44.3354781077651,-2.00384999146667,126.310767191757));
#60624=CARTESIAN_POINT('Ctrl Pts',(44.3277033880404,-2.12797737304117,126.368189193849));
#60625=CARTESIAN_POINT('Ctrl Pts',(44.3199286683157,-2.249651378157,126.430774933113));
#60626=CARTESIAN_POINT('Ctrl Pts',(44.3121636180535,-2.37117405663129,126.493282834142));
#60627=CARTESIAN_POINT('Ctrl Pts',(44.3043985677913,-2.49024908562383,126.560941516447));
#60628=CARTESIAN_POINT('Ctrl Pts',(44.296633517529,-2.60641109361732,126.633532849177));
#60629=CARTESIAN_POINT('Ctrl Pts',(44.2888762672442,-2.72245641710769,126.706051264058));
#60630=CARTESIAN_POINT('Ctrl Pts',(44.2811190169592,-2.83559421356403,126.783492262603));
#60631=CARTESIAN_POINT('Ctrl Pts',(44.2733617666743,-2.94538283824572,126.865591393726));
#60632=CARTESIAN_POINT('Ctrl Pts',(44.2655086124151,-3.05652879510756,126.948705527933));
#60633=CARTESIAN_POINT('Ctrl Pts',(44.2576554581559,-3.16424184388855,127.036593573022));
#60634=CARTESIAN_POINT('Ctrl Pts',(44.2498023038967,-3.26809253596495,127.128934895439));
#60635=CARTESIAN_POINT('Ctrl Pts',(44.242054748587,-3.37054677973221,127.220034532501));
#60636=CARTESIAN_POINT('Ctrl Pts',(44.2343071932773,-3.46924159716566,127.315468153682));
#60637=CARTESIAN_POINT('Ctrl Pts',(44.2265596379676,-3.5637971673641,127.414886792267));
#60638=CARTESIAN_POINT('Ctrl Pts',(44.2188138061074,-3.65833170360465,127.514283315101));
#60639=CARTESIAN_POINT('Ctrl Pts',(44.2110679742472,-3.74872855568951,127.617662808277));
#60640=CARTESIAN_POINT('Ctrl Pts',(44.203322142387,-3.83464489437725,127.724639591803));
#60641=CARTESIAN_POINT('Ctrl Pts',(44.1955763561873,-3.92056072660066,127.831615744716));
#60642=CARTESIAN_POINT('Ctrl Pts',(44.1878305699877,-4.00199585391208,127.942188840526));
#60643=CARTESIAN_POINT('Ctrl Pts',(44.1800847837881,-4.07864812024744,128.055940603503));
#60644=CARTESIAN_POINT('Ctrl Pts',(44.1721515571768,-4.15715529607555,128.172445047321));
#60645=CARTESIAN_POINT('Ctrl Pts',(44.1642183305656,-4.23064491744802,128.292283618335));
#60646=CARTESIAN_POINT('Ctrl Pts',(44.1562851039544,-4.29884027181409,128.414976726282));
#60647=CARTESIAN_POINT('Ctrl Pts',(44.1485309979343,-4.3654958753593,128.53489960427));
#60648=CARTESIAN_POINT('Ctrl Pts',(44.1407768919142,-4.42709360075255,128.657549114743));
#60649=CARTESIAN_POINT('Ctrl Pts',(44.1330227858941,-4.48342265354858,128.782454494091));
#60650=CARTESIAN_POINT('Ctrl Pts',(44.1249999989873,-4.54170351611003,128.911687862763));
#60651=CARTESIAN_POINT('Ctrl Pts',(44.1169772120806,-4.59434381810093,129.04333582851));
#60652=CARTESIAN_POINT('Ctrl Pts',(44.1089544251738,-4.64116551597762,129.176857709489));
#60653=CARTESIAN_POINT('Ctrl Pts',(44.100931638267,-4.68798721385437,129.310379590468));
#60654=CARTESIAN_POINT('Ctrl Pts',(44.0929088513602,-4.72899022487565,129.445774932689));
#60655=CARTESIAN_POINT('Ctrl Pts',(44.0848860644534,-4.76405452823407,129.582490119308));
#60656=CARTESIAN_POINT('Ctrl Pts',(45.8349994066072,-4.76405452823404,129.582490119308));
#60657=CARTESIAN_POINT('Ctrl Pts',(45.8273430242476,-4.79772127647897,129.713756259751));
#60658=CARTESIAN_POINT('Ctrl Pts',(45.819686641888,-4.8259362161401,129.84632770776));
#60659=CARTESIAN_POINT('Ctrl Pts',(45.8120302595285,-4.84862121517186,129.979705917534));
#60660=CARTESIAN_POINT('Ctrl Pts',(45.8041684556119,-4.87191485515217,130.116662678931));
#60661=CARTESIAN_POINT('Ctrl Pts',(45.7963066516953,-4.88937757302127,130.254469649115));
#60662=CARTESIAN_POINT('Ctrl Pts',(45.7884448477787,-4.90098179813617,130.392583400083));
#60663=CARTESIAN_POINT('Ctrl Pts',(45.7805830438621,-4.91258602325106,130.530697151051));
#60664=CARTESIAN_POINT('Ctrl Pts',(45.7727212399455,-4.91833179871113,130.669117228304));
#60665=CARTESIAN_POINT('Ctrl Pts',(45.7648594360289,-4.91824911967543,130.807303288442));
#60666=CARTESIAN_POINT('',(46.1101405639631,-4.91824950622351,130.80656448512));
#60667=CARTESIAN_POINT('Ctrl Pts',(46.1799254115191,-4.76405452823402,129.582490119308));
#60668=CARTESIAN_POINT('Ctrl Pts',(46.1720358594244,-4.79874344822382,129.717741691871));
#60669=CARTESIAN_POINT('Ctrl Pts',(46.1641463073297,-4.82769341870851,129.854568823594));
#60670=CARTESIAN_POINT('Ctrl Pts',(46.1562567552351,-4.85077228469552,129.992454647315));
#60671=CARTESIAN_POINT('Ctrl Pts',(46.1483718873479,-4.87383744823192,130.130258605068));
#60672=CARTESIAN_POINT('Ctrl Pts',(46.1404870194608,-4.89103838901357,130.269119637774));
#60673=CARTESIAN_POINT('Ctrl Pts',(46.1326021515737,-4.90229388879109,130.408510026532));
#60674=CARTESIAN_POINT('Ctrl Pts',(46.1251149557187,-4.91298171926418,130.540870283659));
#60675=CARTESIAN_POINT('Ctrl Pts',(46.1176277598636,-4.91830903941853,130.673707492938));
#60676=CARTESIAN_POINT('Ctrl Pts',(46.1101405640086,-4.91824950622387,130.806564484312));
#60677=CARTESIAN_POINT('Ctrl Pts',(46.1101405639631,-4.91824950622351,130.80656448512));
#60678=CARTESIAN_POINT('Ctrl Pts',(46.1016750146247,-4.9181821937889,130.956781927965));
#60679=CARTESIAN_POINT('Ctrl Pts',(46.0932094652862,-4.91122864733905,131.106774266232));
#60680=CARTESIAN_POINT('Ctrl Pts',(46.0847439159477,-4.89747532373009,131.255933995828));
#60681=CARTESIAN_POINT('Ctrl Pts',(46.0762382420686,-4.88365681288149,131.405800704428));
#60682=CARTESIAN_POINT('Ctrl Pts',(46.0677325681894,-4.86297399945099,131.554826638305));
#60683=CARTESIAN_POINT('Ctrl Pts',(46.0592268943102,-4.83556502632671,131.702410693378));
#60684=CARTESIAN_POINT('Ctrl Pts',(46.0507006717052,-4.80808983628866,131.850351294485));
#60685=CARTESIAN_POINT('Ctrl Pts',(46.0421744491002,-4.77385606786064,131.9968428017));
#60686=CARTESIAN_POINT('Ctrl Pts',(46.0336482264952,-4.73305186516659,132.141298575791));
#60687=CARTESIAN_POINT('Ctrl Pts',(46.0250926202755,-4.69210704041427,132.286252182629));
#60688=CARTESIAN_POINT('Ctrl Pts',(46.0165370140557,-4.64454654209171,132.429155766391));
#60689=CARTESIAN_POINT('Ctrl Pts',(46.007981407836,-4.59060790677837,132.569439116875));
#60690=CARTESIAN_POINT('Ctrl Pts',(46.0034374632933,-4.56196070618539,132.643944622212));
#60691=CARTESIAN_POINT('Ctrl Pts',(45.9988935187506,-4.53151518136126,132.717711426559));
#60692=CARTESIAN_POINT('Ctrl Pts',(45.9943495742079,-4.49931213559914,132.790657012606));
#60693=CARTESIAN_POINT('Ctrl Pts',(45.9865752400889,-4.4442152401473,132.915461211496));
#60694=CARTESIAN_POINT('Ctrl Pts',(45.9788009059698,-4.38383431666588,133.038168895575));
#60695=CARTESIAN_POINT('Ctrl Pts',(45.9710265718507,-4.31835051372151,133.158300273365));
#60696=CARTESIAN_POINT('Ctrl Pts',(45.9632618189036,-4.25294741371182,133.278283599968));
#60697=CARTESIAN_POINT('Ctrl Pts',(45.9554970659565,-4.18245413248686,133.395696597737));
#60698=CARTESIAN_POINT('Ctrl Pts',(45.9477323130094,-4.10709987610411,133.510079315104));
#60699=CARTESIAN_POINT('Ctrl Pts',(45.9399752721244,-4.03182046263121,133.624348425943));
#60700=CARTESIAN_POINT('Ctrl Pts',(45.9322182312394,-3.95168989560982,133.735592921479));
#60701=CARTESIAN_POINT('Ctrl Pts',(45.9244611903544,-3.86698312138009,133.843377662839));
#60702=CARTESIAN_POINT('Ctrl Pts',(45.9167099991143,-3.78234022518784,133.951081122887));
#60703=CARTESIAN_POINT('Ctrl Pts',(45.9089588078741,-3.69312823130316,134.055329715716));
#60704=CARTESIAN_POINT('Ctrl Pts',(45.901207616634,-3.5996649880285,134.155717810773));
#60705=CARTESIAN_POINT('Ctrl Pts',(45.8934597198569,-3.5062414691252,134.256063238213));
#60706=CARTESIAN_POINT('Ctrl Pts',(45.8857118230799,-3.40857056045793,134.352551145788));
#60707=CARTESIAN_POINT('Ctrl Pts',(45.8779639263028,-3.30700978434805,134.44480967623));
#60708=CARTESIAN_POINT('Ctrl Pts',(45.8702176502187,-3.20547025256313,134.537048908176));
#60709=CARTESIAN_POINT('Ctrl Pts',(45.8624713741346,-3.10004276098854,134.625060259979));
#60710=CARTESIAN_POINT('Ctrl Pts',(45.8547250980504,-2.99112072494369,134.708509676108));
#60711=CARTESIAN_POINT('Ctrl Pts',(45.8469787647851,-2.88219788486127,134.791959708242));
#60712=CARTESIAN_POINT('Ctrl Pts',(45.8392324315197,-2.76978075918621,134.870847499733));
#60713=CARTESIAN_POINT('Ctrl Pts',(45.8314860982544,-2.65429445931159,134.944880389982));
#60714=CARTESIAN_POINT('Ctrl Pts',(45.8237380302514,-2.53878229708083,135.018929859383));
#60715=CARTESIAN_POINT('Ctrl Pts',(45.8159899622484,-2.420199922041,135.088122053139));
#60716=CARTESIAN_POINT('Ctrl Pts',(45.8082418942454,-2.29899957863895,135.152208820979));
#60717=CARTESIAN_POINT('Ctrl Pts',(45.8004855915036,-2.17767042206963,135.216363700997));
#60718=CARTESIAN_POINT('Ctrl Pts',(45.7927292887618,-2.05371808515203,135.27540213282));
#60719=CARTESIAN_POINT('Ctrl Pts',(45.7849729860199,-1.92761796302219,135.32912271641));
#60720=CARTESIAN_POINT('Ctrl Pts',(45.7772125435057,-1.80145053746019,135.382871972293));
#60721=CARTESIAN_POINT('Ctrl Pts',(45.7694521009916,-1.67313340811606,135.431297586424));
#60722=CARTESIAN_POINT('Ctrl Pts',(45.7616916584774,-1.54315895835751,135.47424749968));
#60723=CARTESIAN_POINT('Ctrl Pts',(45.753918758212,-1.41297586207361,135.51726635995));
#60724=CARTESIAN_POINT('Ctrl Pts',(45.7461458579465,-1.28113050514035,135.554791846875));
#60725=CARTESIAN_POINT('Ctrl Pts',(45.7383729576811,-1.14812821247293,135.586722447271));
#60726=CARTESIAN_POINT('Ctrl Pts',(45.7308826219191,-1.01996088815652,135.617492289915));
#60727=CARTESIAN_POINT('Ctrl Pts',(45.723392286157,-0.890719584960743,135.643066900438));
#60728=CARTESIAN_POINT('Ctrl Pts',(45.715901950395,-0.760860699114758,135.663401063893));
#60729=CARTESIAN_POINT('Ctrl Pts',(45.7081276162759,-0.626078174142351,
135.684506203336));
#60730=CARTESIAN_POINT('Ctrl Pts',(45.7003532821568,-0.490203360237131,
135.700032522881));
#60731=CARTESIAN_POINT('Ctrl Pts',(45.6925789480377,-0.353737834783081,
135.709873088934));
#60732=CARTESIAN_POINT('Ctrl Pts',(45.6848141950907,-0.217440490892878,
135.719701527368));
#60733=CARTESIAN_POINT('Ctrl Pts',(45.6770494421436,-0.0805542701644052,
135.723858126666));
#60734=CARTESIAN_POINT('Ctrl Pts',(45.6692846891965,0.0564099656475737,
135.722287109318));
#60735=CARTESIAN_POINT('Ctrl Pts',(45.6615276483115,0.193238166649687,135.720717652326));
#60736=CARTESIAN_POINT('Ctrl Pts',(45.6537706074265,0.330143840125569,135.713431904011));
#60737=CARTESIAN_POINT('Ctrl Pts',(45.6460135665415,0.466612276203251,135.700425981325));
#60738=CARTESIAN_POINT('Ctrl Pts',(45.6382623753014,0.602977800371718,135.687429866506));
#60739=CARTESIAN_POINT('Ctrl Pts',(45.6305111840612,0.738906355810972,135.668722200273));
#60740=CARTESIAN_POINT('Ctrl Pts',(45.6227599928211,0.873884869278215,135.644351144183));
#60741=CARTESIAN_POINT('Ctrl Pts',(45.615012096044,1.00880601327656,135.619990446443));
#60742=CARTESIAN_POINT('Ctrl Pts',(45.607264199267,1.14277753447811,135.58997121569));
#60743=CARTESIAN_POINT('Ctrl Pts',(45.5995163024899,1.27529332928342,135.554393247642));
#60744=CARTESIAN_POINT('Ctrl Pts',(45.5917700264058,1.40778140464117,135.518822721738));
#60745=CARTESIAN_POINT('Ctrl Pts',(45.5840237503217,1.53881398192906,135.47769587266));
#60746=CARTESIAN_POINT('Ctrl Pts',(45.5762774742376,1.66789736017958,135.431163126687));
#60747=CARTESIAN_POINT('Ctrl Pts',(45.5685311409723,1.79698169129427,135.384630037219));
#60748=CARTESIAN_POINT('Ctrl Pts',(45.5607848077069,1.92411642686306,135.332691103813));
#60749=CARTESIAN_POINT('Ctrl Pts',(45.5530384744416,2.0488255601416,135.27554579452));
#60750=CARTESIAN_POINT('Ctrl Pts',(45.5452904064386,2.17356262116587,135.218387687931));
#60751=CARTESIAN_POINT('Ctrl Pts',(45.5375423384356,2.29587264364235,135.156021048221));
#60752=CARTESIAN_POINT('Ctrl Pts',(45.5297942704326,2.41530240254885,135.088692230168));
#60753=CARTESIAN_POINT('Ctrl Pts',(45.5220379676907,2.53485909282436,135.021291854246));
#60754=CARTESIAN_POINT('Ctrl Pts',(45.5142816649489,2.65152906337995,134.948918957179));
#60755=CARTESIAN_POINT('Ctrl Pts',(45.5065253622071,2.7648859079783,134.871864640719));
#60756=CARTESIAN_POINT('Ctrl Pts',(45.4987649196929,2.87830325453789,134.79476919805));
#60757=CARTESIAN_POINT('Ctrl Pts',(45.4910044771787,2.98840363792147,134.712987590302));
#60758=CARTESIAN_POINT('Ctrl Pts',(45.4832440346646,3.09479298124552,134.626851881877));
#60759=CARTESIAN_POINT('Ctrl Pts',(45.4754711343992,3.20135311018812,134.540577900766));
#60760=CARTESIAN_POINT('Ctrl Pts',(45.4676982341337,3.30419000103959,134.449936110218));
#60761=CARTESIAN_POINT('Ctrl Pts',(45.4599253338683,3.40294510742288,134.355296784039));
#60762=CARTESIAN_POINT('Ctrl Pts',(45.4524349981062,3.49811021694071,134.264097835748));
#60763=CARTESIAN_POINT('Ctrl Pts',(45.4449446623442,3.58948494235635,134.169187168747));
#60764=CARTESIAN_POINT('Ctrl Pts',(45.4374543265821,3.6767845497445,134.070924322327));
#60765=CARTESIAN_POINT('Ctrl Pts',(45.429679992463,3.76739414828029,133.968935810219));
#60766=CARTESIAN_POINT('Ctrl Pts',(45.421905658344,3.85390053648416,133.863012836071));
#60767=CARTESIAN_POINT('Ctrl Pts',(45.4141313242249,3.93594263326725,133.753519590923));
#60768=CARTESIAN_POINT('Ctrl Pts',(45.4063665712778,4.01788362049837,133.644161286413));
#60769=CARTESIAN_POINT('Ctrl Pts',(45.3986018183307,4.09537103114464,133.531241775546));
#60770=CARTESIAN_POINT('Ctrl Pts',(45.3908370653836,4.16808180474964,133.415160711678));
#60771=CARTESIAN_POINT('Ctrl Pts',(45.3830800244986,4.24072036098926,133.299194941159));
#60772=CARTESIAN_POINT('Ctrl Pts',(45.3753229836136,4.30859151520928,133.180074195765));
#60773=CARTESIAN_POINT('Ctrl Pts',(45.3675659427286,4.37141378723327,133.058229416606));
#60774=CARTESIAN_POINT('Ctrl Pts',(45.3598147514885,4.43418868449323,132.936476521544));
#60775=CARTESIAN_POINT('Ctrl Pts',(45.3520635602483,4.49192209951736,132.812004027597));
#60776=CARTESIAN_POINT('Ctrl Pts',(45.3443123690082,4.54437722336763,132.685269630314));
#60777=CARTESIAN_POINT('Ctrl Pts',(45.3365644722311,4.59681005239105,132.558589098531));
#60778=CARTESIAN_POINT('Ctrl Pts',(45.328816575454,4.64396890301551,132.429648935991));
#60779=CARTESIAN_POINT('Ctrl Pts',(45.321068678677,4.68566417484683,132.298928884009));
#60780=CARTESIAN_POINT('Ctrl Pts',(45.3133224025929,4.72735072492607,132.168236175843));
#60781=CARTESIAN_POINT('Ctrl Pts',(45.3055761265088,4.76357585069709,132.03576469103));
#60782=CARTESIAN_POINT('Ctrl Pts',(45.2978298504247,4.79419925261481,131.902011103252));
#60783=CARTESIAN_POINT('Ctrl Pts',(45.2900835171593,4.82482288058756,131.768256528136));
#60784=CARTESIAN_POINT('Ctrl Pts',(45.282337183894,4.84984461493951,131.633220212274));
#60785=CARTESIAN_POINT('Ctrl Pts',(45.2745908506286,4.86917498051886,131.497410450976));
#60786=CARTESIAN_POINT('Ctrl Pts',(45.2668427826256,4.88850967499952,131.361570276023));
#60787=CARTESIAN_POINT('Ctrl Pts',(45.2590947146227,4.90215040943353,131.224956697961));
#60788=CARTESIAN_POINT('Ctrl Pts',(45.2513466466197,4.91005946987748,131.088084188611));
#60789=CARTESIAN_POINT('Ctrl Pts',(45.2435903438778,4.91797693616498,130.951066209529));
#60790=CARTESIAN_POINT('Ctrl Pts',(45.235834041136,4.92015053706289,130.813789140364));
#60791=CARTESIAN_POINT('Ctrl Pts',(45.2280777383941,4.91659470173358,130.676769076368));
#60792=CARTESIAN_POINT('Ctrl Pts',(45.22031729588,4.91303696854789,130.539675880638));
#60793=CARTESIAN_POINT('Ctrl Pts',(45.2125568533658,4.90374373234417,130.402840353278));
#60794=CARTESIAN_POINT('Ctrl Pts',(45.2047964108516,4.88878136012727,130.266773531251));
#60795=CARTESIAN_POINT('Ctrl Pts',(45.1970235105862,4.87379496898219,130.130488282683));
#60796=CARTESIAN_POINT('Ctrl Pts',(45.1892506103208,4.85312131492092,129.994974592077));
#60797=CARTESIAN_POINT('Ctrl Pts',(45.1814777100554,4.82687811670912,129.860734256693));
#60798=CARTESIAN_POINT('Ctrl Pts',(45.1739873742933,4.80158892485491,129.731373895631));
#60799=CARTESIAN_POINT('Ctrl Pts',(45.1664970385313,4.77112816373635,129.603196217437));
#60800=CARTESIAN_POINT('Ctrl Pts',(45.1590067027693,4.73564441829933,129.476635116594));
#60801=CARTESIAN_POINT('Ctrl Pts',(45.1512323686502,4.69881529586907,129.345275413147));
#60802=CARTESIAN_POINT('Ctrl Pts',(45.1434580345311,4.65645811368422,129.215241183923));
#60803=CARTESIAN_POINT('Ctrl Pts',(45.135683700412,4.6086841028319,129.087033070822));
#60804=CARTESIAN_POINT('Ctrl Pts',(45.1279189474649,4.56096896917827,128.958982962763));
#60805=CARTESIAN_POINT('Ctrl Pts',(45.1201541945178,4.50785042482883,128.832754855793));
#60806=CARTESIAN_POINT('Ctrl Pts',(45.1123894415707,4.44949008740258,128.708836572224));
#60807=CARTESIAN_POINT('Ctrl Pts',(45.1046324006857,4.39118771428619,128.585041366042));
#60808=CARTESIAN_POINT('Ctrl Pts',(45.0968753598006,4.3276540742123,128.463551769214));
#60809=CARTESIAN_POINT('Ctrl Pts',(45.0891183189156,4.25909958323108,128.344837533181));
#60810=CARTESIAN_POINT('Ctrl Pts',(45.0813671276755,4.19059678972479,128.226212820478));
#60811=CARTESIAN_POINT('Ctrl Pts',(45.0736159364354,4.11708087636066,128.110359639935));
#60812=CARTESIAN_POINT('Ctrl Pts',(45.0658647451952,4.03880891435073,127.997724621242));
#60813=CARTESIAN_POINT('Ctrl Pts',(45.0581168484181,3.96057022001263,127.885137475437));
#60814=CARTESIAN_POINT('Ctrl Pts',(45.0503689516411,3.8775797201739,127.775766091407));
#60815=CARTESIAN_POINT('Ctrl Pts',(45.042621054864,3.79013855114537,127.670029297233));
#60816=CARTESIAN_POINT('Ctrl Pts',(45.0348747787799,3.70271567292438,127.564314620916));
#60817=CARTESIAN_POINT('Ctrl Pts',(45.0271285026958,3.61084422629065,127.462233323319));
#60818=CARTESIAN_POINT('Ctrl Pts',(45.0193822266117,3.51486624154943,127.364171906679));
#60819=CARTESIAN_POINT('Ctrl Pts',(45.0116358933464,3.41888754832052,127.266109766172));
#60820=CARTESIAN_POINT('Ctrl Pts',(45.0038895600809,3.31880252996573,127.17206784524));
#60821=CARTESIAN_POINT('Ctrl Pts',(44.9961432268156,3.21499046621918,127.082396167894));
#60822=CARTESIAN_POINT('Ctrl Pts',(44.9883951588126,3.11115515448074,126.992704409198));
#60823=CARTESIAN_POINT('Ctrl Pts',(44.9806470908096,3.00359143231425,126.907385097078));
#60824=CARTESIAN_POINT('Ctrl Pts',(44.9728990228066,2.89271175412661,126.82674804593));
#60825=CARTESIAN_POINT('Ctrl Pts',(44.9651427200648,2.78171423169752,126.746025292764));
#60826=CARTESIAN_POINT('Ctrl Pts',(44.957386417323,2.66739402989875,126.669994971707));
#60827=CARTESIAN_POINT('Ctrl Pts',(44.9496301145811,2.55019315359706,126.598923905184));
#60828=CARTESIAN_POINT('Ctrl Pts',(44.9418696720669,2.43292972365869,126.527814905894));
#60829=CARTESIAN_POINT('Ctrl Pts',(44.9341092295527,2.31278289793891,126.461670623779));
#60830=CARTESIAN_POINT('Ctrl Pts',(44.9263487870385,2.19021849929572,126.400711450359));
#60831=CARTESIAN_POINT('Ctrl Pts',(44.9185758867731,2.06745734939925,126.339654419863));
#60832=CARTESIAN_POINT('Ctrl Pts',(44.9108029865077,1.94227122854329,126.283799290654));
#60833=CARTESIAN_POINT('Ctrl Pts',(44.9030300862423,1.81514594284144,126.233318256278));
#60834=CARTESIAN_POINT('Ctrl Pts',(44.8955397504803,1.69264198148515,126.184672334656));
#60835=CARTESIAN_POINT('Ctrl Pts',(44.8880494147183,1.56833768521108,126.141016669702));
#60836=CARTESIAN_POINT('Ctrl Pts',(44.8805590789563,1.4426784155298,126.102460783258));
#60837=CARTESIAN_POINT('Ctrl Pts',(44.8727847448373,1.31225473644414,126.062443038661));
#60838=CARTESIAN_POINT('Ctrl Pts',(44.8650104107182,1.17995816503496,126.027792658493));
#60839=CARTESIAN_POINT('Ctrl Pts',(44.8572360765991,1.04627002863025,125.998686670065));
#60840=CARTESIAN_POINT('Ctrl Pts',(44.849471323652,0.912746650905595,125.969616552167));
#60841=CARTESIAN_POINT('Ctrl Pts',(44.8417065707049,0.777835498832337,125.946077312813));
#60842=CARTESIAN_POINT('Ctrl Pts',(44.8339418177578,0.642034349408489,125.928196658399));
#60843=CARTESIAN_POINT('Ctrl Pts',(44.8261847768728,0.50636807960071,125.910333763303));
#60844=CARTESIAN_POINT('Ctrl Pts',(44.8184277359879,0.369813956669882,125.89811831943));
#60845=CARTESIAN_POINT('Ctrl Pts',(44.8106706951029,0.232880930822069,125.891627209924));
#60846=CARTESIAN_POINT('Ctrl Pts',(44.8029195038627,0.0960511672342309,
125.885140995415));
#60847=CARTESIAN_POINT('Ctrl Pts',(44.7951683126226,-0.0411565415886018,
125.884370541452));
#60848=CARTESIAN_POINT('Ctrl Pts',(44.7874171213825,-0.178227480169567,
125.889340981002));
#60849=CARTESIAN_POINT('Ctrl Pts',(44.7796692246054,-0.315240159945149,
125.894309307982));
#60850=CARTESIAN_POINT('Ctrl Pts',(44.7719213278283,-0.452115795206562,
125.905013661296));
#60851=CARTESIAN_POINT('Ctrl Pts',(44.7641734310512,-0.588339242496301,
125.921427073247));
#60852=CARTESIAN_POINT('Ctrl Pts',(44.7564271549671,-0.724534194777504,
125.937837051865));
#60853=CARTESIAN_POINT('Ctrl Pts',(44.748680878883,-0.860076842529294,125.959953667027));
#60854=CARTESIAN_POINT('Ctrl Pts',(44.7409346027989,-0.994457134737505,
125.98769807285));
#60855=CARTESIAN_POINT('Ctrl Pts',(44.7331882695336,-1.12883841891032,126.015442683476));
#60856=CARTESIAN_POINT('Ctrl Pts',(44.7254419362682,-1.26205694752857,126.048815088608));
#60857=CARTESIAN_POINT('Ctrl Pts',(44.7176956030029,-1.39361322551899,126.08768538599));
#60858=CARTESIAN_POINT('Ctrl Pts',(44.7099475349999,-1.52519896462572,126.126564388106));
#60859=CARTESIAN_POINT('Ctrl Pts',(44.7021994669969,-1.6551213375015,126.170943621687));
#60860=CARTESIAN_POINT('Ctrl Pts',(44.6944513989939,-1.78289674683951,126.220643539407));
#60861=CARTESIAN_POINT('Ctrl Pts',(44.6866950962521,-1.91080795740329,126.27039627879));
#60862=CARTESIAN_POINT('Ctrl Pts',(44.6789387935102,-2.03656728129799,126.325480856605));
#60863=CARTESIAN_POINT('Ctrl Pts',(44.6711824907684,-2.15971131883188,126.385669625676));
#60864=CARTESIAN_POINT('Ctrl Pts',(44.6634220482542,-2.28292108204657,126.445890519306));
#60865=CARTESIAN_POINT('Ctrl Pts',(44.65566160574,-2.40351243394462,126.511220846371));
#60866=CARTESIAN_POINT('Ctrl Pts',(44.6479011632258,-2.52104816426468,126.58138782391));
#60867=CARTESIAN_POINT('Ctrl Pts',(44.6401282629604,-2.63877257337322,126.65166743971));
#60868=CARTESIAN_POINT('Ctrl Pts',(44.632355362695,-2.75343123163921,126.726799006967));
#60869=CARTESIAN_POINT('Ctrl Pts',(44.6245824624296,-2.86461667768654,126.806466878055));
#60870=CARTESIAN_POINT('Ctrl Pts',(44.6170921266675,-2.97176025271142,126.883238621358));
#60871=CARTESIAN_POINT('Ctrl Pts',(44.6096017909054,-3.07567850846933,126.964222393039));
#60872=CARTESIAN_POINT('Ctrl Pts',(44.6021114551433,-3.1760385723561,127.049102697076));
#60873=CARTESIAN_POINT('Ctrl Pts',(44.5944493708478,-3.27869982731611,127.135929251348));
#60874=CARTESIAN_POINT('Ctrl Pts',(44.5867872865522,-3.37798281463037,127.227125378155));
#60875=CARTESIAN_POINT('Ctrl Pts',(44.5791252022567,-3.47348456891262,127.322394504574));
#60876=CARTESIAN_POINT('Ctrl Pts',(44.5714719163122,-3.56887665878399,127.417554233707));
#60877=CARTESIAN_POINT('Ctrl Pts',(44.5638186303677,-3.6604958645176,127.516777384094));
#60878=CARTESIAN_POINT('Ctrl Pts',(44.5561653444232,-3.74797117485307,127.619726394461));
#60879=CARTESIAN_POINT('Ctrl Pts',(44.5485190763818,-3.83536627215974,127.72258100274));
#60880=CARTESIAN_POINT('Ctrl Pts',(44.5408728083403,-3.91862477014325,127.829154373051));
#60881=CARTESIAN_POINT('Ctrl Pts',(44.5332265402989,-3.99741193415087,127.93907164589));
#60882=CARTESIAN_POINT('Ctrl Pts',(44.5255855163638,-4.07614506287385,128.048913533211));
#60883=CARTESIAN_POINT('Ctrl Pts',(44.5179444924288,-4.15041272296012,128.162094435488));
#60884=CARTESIAN_POINT('Ctrl Pts',(44.5103034684937,-4.21992033996254,128.278206349341));
#60885=CARTESIAN_POINT('Ctrl Pts',(44.5026652587937,-4.28940235689147,128.394275498478));
#60886=CARTESIAN_POINT('Ctrl Pts',(44.4950270490937,-4.35412760826144,128.51327316857));
#60887=CARTESIAN_POINT('Ctrl Pts',(44.4873888393937,-4.41384501075719,128.634762663217));
#60888=CARTESIAN_POINT('Ctrl Pts',(44.47975229993,-4.47354935493497,128.756225591933));
#60889=CARTESIAN_POINT('Ctrl Pts',(44.4721157604663,-4.52824785426733,128.880178898073));
#60890=CARTESIAN_POINT('Ctrl Pts',(44.4644792210026,-4.57773585379053,129.006162209319));
#60891=CARTESIAN_POINT('Ctrl Pts',(44.4568408472416,-4.62723574033409,129.132175781765));
#60892=CARTESIAN_POINT('Ctrl Pts',(44.4492024734807,-4.67152248030369,129.260219957805));
#60893=CARTESIAN_POINT('Ctrl Pts',(44.4415640997197,-4.71044003946876,129.389815568064));
#60894=CARTESIAN_POINT('Ctrl Pts',(44.4377997264939,-4.72961954315858,129.453683383479));
#60895=CARTESIAN_POINT('Ctrl Pts',(44.4340353532682,-4.74749576595898,129.517927756512));
#60896=CARTESIAN_POINT('Ctrl Pts',(44.4302709800425,-4.764054528234,129.582490119308));
#60897=CARTESIAN_POINT('Origin',(213.235140564004,0.,130.804360617566));
#60898=CARTESIAN_POINT('',(42.3345736784939,-4.76405452823401,129.582490119308));
#60899=CARTESIAN_POINT('',(42.6801909902419,-4.76405452823402,129.582490119308));
#60900=CARTESIAN_POINT('',(213.235140564004,-4.76405452823405,129.582490119308));
#60901=CARTESIAN_POINT('',(44.0148594359472,-4.91824820103065,130.800154008622));
#60902=CARTESIAN_POINT('Ctrl Pts',(44.0148594359472,-4.91824820103065,130.800154008622));
#60903=CARTESIAN_POINT('Ctrl Pts',(44.0072128060144,-4.9183634320627,130.934878872191));
#60904=CARTESIAN_POINT('Ctrl Pts',(43.9995661760815,-4.91293875693969,131.06979677328));
#60905=CARTESIAN_POINT('Ctrl Pts',(43.9919195461486,-4.90195330182934,131.204406726389));
#60906=CARTESIAN_POINT('Ctrl Pts',(43.9842798532381,-4.89097781272339,131.338894561355));
#60907=CARTESIAN_POINT('Ctrl Pts',(43.9766401603276,-4.87445161028033,131.473074604134));
#60908=CARTESIAN_POINT('Ctrl Pts',(43.9690004674171,-4.85240587338236,131.606445589663));
#60909=CARTESIAN_POINT('Ctrl Pts',(43.9613654289013,-4.83037356759492,131.73973532046));
#60910=CARTESIAN_POINT('Ctrl Pts',(43.9537303903854,-4.80282848067744,131.872216577364));
#60911=CARTESIAN_POINT('Ctrl Pts',(43.9460953518696,-4.7698536067849,132.003393407919));
#60912=CARTESIAN_POINT('Ctrl Pts',(43.9384627361299,-4.73688919659057,132.134528612999));
#60913=CARTESIAN_POINT('Ctrl Pts',(43.9308301203903,-4.69849852268592,132.264359823546));
#60914=CARTESIAN_POINT('Ctrl Pts',(43.9231975046506,-4.65481555042062,132.392401943874));
#60915=CARTESIAN_POINT('Ctrl Pts',(43.9155655441217,-4.61113632805664,132.520433072612));
#60916=CARTESIAN_POINT('Ctrl Pts',(43.9079335835928,-4.56216584101016,132.646675034525));
#60917=CARTESIAN_POINT('Ctrl Pts',(43.900301623064,-4.50808754941105,132.770659096776));
#60918=CARTESIAN_POINT('Ctrl Pts',(43.8926685509213,-4.454001381176,132.894661217611));
#60919=CARTESIAN_POINT('Ctrl Pts',(43.8850354787787,-4.39480609090367,133.016404415087));
#60920=CARTESIAN_POINT('Ctrl Pts',(43.877402406636,-4.33073254764309,133.135441625014));
#60921=CARTESIAN_POINT('Ctrl Pts',(43.8697617828695,-4.26659561453228,133.254596601972));
#60922=CARTESIAN_POINT('Ctrl Pts',(43.862121159103,-4.19757098066915,133.371039888361));
#60923=CARTESIAN_POINT('Ctrl Pts',(43.8544805353364,-4.1239347749985,133.484350362706));
#60924=CARTESIAN_POINT('Ctrl Pts',(43.8468361622809,-4.05026243570526,133.59771643902));
#60925=CARTESIAN_POINT('Ctrl Pts',(43.8391917892253,-3.97197425240201,133.707946313502));
#60926=CARTESIAN_POINT('Ctrl Pts',(43.8315474161698,-3.88938786305494,133.814650489525));
#60927=CARTESIAN_POINT('Ctrl Pts',(43.8238909228139,-3.80667053140055,133.921523847071));
#60928=CARTESIAN_POINT('Ctrl Pts',(43.816234429458,-3.7196416392557,134.024860029935));
#60929=CARTESIAN_POINT('Ctrl Pts',(43.8085779361021,-3.62865750495909,134.124304558991));
#60930=CARTESIAN_POINT('Ctrl Pts',(43.8011711506894,-3.5406407161542,134.220505816269));
#60931=CARTESIAN_POINT('Ctrl Pts',(43.7937643652767,-3.4489229241383,134.313065116144));
#60932=CARTESIAN_POINT('Ctrl Pts',(43.786357579864,-3.35385570630374,134.401697822193));
#60933=CARTESIAN_POINT('Ctrl Pts',(43.7785832457449,-3.25407094489395,134.494728770481));
#60934=CARTESIAN_POINT('Ctrl Pts',(43.7708089116258,-3.15025438873821,134.5837521063));
#60935=CARTESIAN_POINT('Ctrl Pts',(43.7630345775067,-3.042761459047,134.668398112964));
#60936=CARTESIAN_POINT('Ctrl Pts',(43.7552698245596,-2.93540100478456,134.752939800989));
#60937=CARTESIAN_POINT('Ctrl Pts',(43.7475050716126,-2.82437349614604,134.833114654083));
#60938=CARTESIAN_POINT('Ctrl Pts',(43.7397403186655,-2.71007071883661,134.908590114244));
#60939=CARTESIAN_POINT('Ctrl Pts',(43.7319832777805,-2.5958814686573,134.983990611114));
#60940=CARTESIAN_POINT('Ctrl Pts',(43.7242262368954,-2.4784237476548,135.054700789556));
#60941=CARTESIAN_POINT('Ctrl Pts',(43.7164691960105,-2.358121618091,135.120428909054));
#60942=CARTESIAN_POINT('Ctrl Pts',(43.7087180047703,-2.23791020929892,135.186107462467));
#60943=CARTESIAN_POINT('Ctrl Pts',(43.7009668135302,-2.11485900312718,135.24681124834));
#60944=CARTESIAN_POINT('Ctrl Pts',(43.6932156222901,-1.98941988055753,135.3022925425));
#60945=CARTESIAN_POINT('Ctrl Pts',(43.685467725513,-1.86403407296118,135.35775025563));
#60946=CARTESIAN_POINT('Ctrl Pts',(43.677719828736,-1.73626272438607,135.407989734045));
#60947=CARTESIAN_POINT('Ctrl Pts',(43.6699719319589,-1.60658088810668,135.452809919481));
#60948=CARTESIAN_POINT('Ctrl Pts',(43.6622256558748,-1.47692617847183,135.4976207295));
#60949=CARTESIAN_POINT('Ctrl Pts',(43.6544793797907,-1.34536214530822,135.537014373701));
#60950=CARTESIAN_POINT('Ctrl Pts',(43.6467331037066,-1.21238195246728,135.570838674143));
#60951=CARTESIAN_POINT('Ctrl Pts',(43.6389867704412,-1.07940077799659,135.604663224269));
#60952=CARTESIAN_POINT('Ctrl Pts',(43.6312404371759,-0.945003801889273,
135.632918252224));
#60953=CARTESIAN_POINT('Ctrl Pts',(43.6234941039106,-0.809697025921017,
135.655502110938));
#60954=CARTESIAN_POINT('Ctrl Pts',(43.6157460359076,-0.674359948938434,
135.678091027151));
#60955=CARTESIAN_POINT('Ctrl Pts',(43.6079979679046,-0.538113052225963,
135.695006182579));
#60956=CARTESIAN_POINT('Ctrl Pts',(43.6002498999016,-0.401469754419894,
135.706197528234));
#60957=CARTESIAN_POINT('Ctrl Pts',(43.5924935971597,-0.264681230490841,
135.717400768185));
#60958=CARTESIAN_POINT('Ctrl Pts',(43.5847372944179,-0.127495854158278,
135.722868014285));
#60959=CARTESIAN_POINT('Ctrl Pts',(43.5769809916761,0.00957008168842241,
135.722601306678));
#60960=CARTESIAN_POINT('Ctrl Pts',(43.5692205491619,0.14670917375206,135.722334456722));
#60961=CARTESIAN_POINT('Ctrl Pts',(43.5614601066477,0.283728307905655,135.7163275721));
#60962=CARTESIAN_POINT('Ctrl Pts',(43.5536996641336,0.420115001726524,135.704634737228));
#60963=CARTESIAN_POINT('Ctrl Pts',(43.5459267638681,0.556720635576155,135.692923131979));
#60964=CARTESIAN_POINT('Ctrl Pts',(43.5381538636027,0.692691412281017,135.675507386341));
#60965=CARTESIAN_POINT('Ctrl Pts',(43.5303809633373,0.82752285416191,135.65249314343));
#60966=CARTESIAN_POINT('Ctrl Pts',(43.5228906275753,0.957452833509977,135.630315526218));
#60967=CARTESIAN_POINT('Ctrl Pts',(43.5154002918133,1.08632457397627,135.602939447898));
#60968=CARTESIAN_POINT('Ctrl Pts',(43.5079099560513,1.21370074039864,135.570503038356));
#60969=CARTESIAN_POINT('Ctrl Pts',(43.5001356219322,1.34590641288663,135.536836792488));
#60970=CARTESIAN_POINT('Ctrl Pts',(43.4923612878131,1.47691965104582,135.497612271082));
#60971=CARTESIAN_POINT('Ctrl Pts',(43.484586953694,1.60623728791046,135.45292865917));
#60972=CARTESIAN_POINT('Ctrl Pts',(43.4768222007469,1.73539555234493,135.408300115817));
#60973=CARTESIAN_POINT('Ctrl Pts',(43.4690574477999,1.86286200733933,135.358225994814));
#60974=CARTESIAN_POINT('Ctrl Pts',(43.4612926948528,1.98814509268487,135.302856160849));
#60975=CARTESIAN_POINT('Ctrl Pts',(43.4535356539678,2.11330374510369,135.247541320983));
#60976=CARTESIAN_POINT('Ctrl Pts',(43.4457786130828,2.23628298810924,135.186941392368));
#60977=CARTESIAN_POINT('Ctrl Pts',(43.4380215721978,2.35660815613244,135.12125545772));
#60978=CARTESIAN_POINT('Ctrl Pts',(43.4302703809576,2.47684258601109,135.055619057346));
#60979=CARTESIAN_POINT('Ctrl Pts',(43.4225191897175,2.594426582916,134.98490447164));
#60980=CARTESIAN_POINT('Ctrl Pts',(43.4147679984773,2.70890747677517,134.9093579799));
#60981=CARTESIAN_POINT('Ctrl Pts',(43.4070201017003,2.8233397132001,134.833843597436));
#60982=CARTESIAN_POINT('Ctrl Pts',(43.3992722049232,2.93467114413965,134.753501608457));
#60983=CARTESIAN_POINT('Ctrl Pts',(43.3915243081461,3.04247583568445,134.668623011837));
#60984=CARTESIAN_POINT('Ctrl Pts',(43.383778032062,3.15025797681178,134.583762169989));
#60985=CARTESIAN_POINT('Ctrl Pts',(43.3760317559779,3.25451453891941,134.494366849736));
#60986=CARTESIAN_POINT('Ctrl Pts',(43.3682854798938,3.35485092328759,134.400769707897));
#60987=CARTESIAN_POINT('Ctrl Pts',(43.3605391466285,3.45518804831616,134.307171875146));
#60988=CARTESIAN_POINT('Ctrl Pts',(43.3527928133631,3.55160465197346,134.209372425604));
#60989=CARTESIAN_POINT('Ctrl Pts',(43.3450464800978,3.64374170938024,134.107742130171));
#60990=CARTESIAN_POINT('Ctrl Pts',(43.3372984120948,3.73589940024208,134.006089075339));
#60991=CARTESIAN_POINT('Ctrl Pts',(43.3295503440918,3.82377537525408,133.900603757107));
#60992=CARTESIAN_POINT('Ctrl Pts',(43.3218022760889,3.9070500114714,133.791691076414));
#60993=CARTESIAN_POINT('Ctrl Pts',(43.314045973347,3.99041315296318,133.682662642028));
#60994=CARTESIAN_POINT('Ctrl Pts',(43.3062896706052,4.06916494879436,133.57019987969));
#60995=CARTESIAN_POINT('Ctrl Pts',(43.2985333678633,4.14302804647811,133.454738263977));
#60996=CARTESIAN_POINT('Ctrl Pts',(43.2907729253492,4.21693056712117,133.339215022923));
#60997=CARTESIAN_POINT('Ctrl Pts',(43.283012482835,4.28593899385358,133.220690076912));
#60998=CARTESIAN_POINT('Ctrl Pts',(43.2752520403209,4.3498218201577,133.099623825867));
#60999=CARTESIAN_POINT('Ctrl Pts',(43.2674791400554,4.41380719684576,132.978363228528));
#61000=CARTESIAN_POINT('Ctrl Pts',(43.25970623979,4.47265036288119,132.854553527274));
#61001=CARTESIAN_POINT('Ctrl Pts',(43.2519333395246,4.52616751630043,132.728676256147));
#61002=CARTESIAN_POINT('Ctrl Pts',(43.2444430037625,4.57773918639153,132.607374940891));
#61003=CARTESIAN_POINT('Ctrl Pts',(43.2369526680005,4.62436523995985,132.484154056768));
#61004=CARTESIAN_POINT('Ctrl Pts',(43.2294623322385,4.66592549925278,132.359456208815));
#61005=CARTESIAN_POINT('Ctrl Pts',(43.2216879981194,4.70906152840864,132.230030404056));
#61006=CARTESIAN_POINT('Ctrl Pts',(43.2139136640003,4.74687668305547,132.098603444373));
#61007=CARTESIAN_POINT('Ctrl Pts',(43.2061393298812,4.77918243633268,131.965652270317));
#61008=CARTESIAN_POINT('Ctrl Pts',(43.1983745769341,4.81144837565618,131.832864946701));
#61009=CARTESIAN_POINT('Ctrl Pts',(43.1906098239869,4.8382183319494,131.698557522546));
#61010=CARTESIAN_POINT('Ctrl Pts',(43.1828450710398,4.85935269031777,131.563224566902));
#61011=CARTESIAN_POINT('Ctrl Pts',(43.1750880301548,4.88046605774353,131.428026025856));
#61012=CARTESIAN_POINT('Ctrl Pts',(43.1673309892699,4.89595490630023,131.29180436411));
#61013=CARTESIAN_POINT('Ctrl Pts',(43.1595739483849,4.90573016158091,131.155066540321));
#61014=CARTESIAN_POINT('Ctrl Pts',(43.1518227571447,4.91549804526556,131.018431831588));
#61015=CARTESIAN_POINT('Ctrl Pts',(43.1440715659045,4.91956088404505,130.881282123965));
#61016=CARTESIAN_POINT('Ctrl Pts',(43.1363203746644,4.91788120043917,130.744131381584));
#61017=CARTESIAN_POINT('Ctrl Pts',(43.1285724778873,4.91620223074363,130.607038931927));
#61018=CARTESIAN_POINT('Ctrl Pts',(43.1208245811102,4.90878559785686,130.469945838502));
#61019=CARTESIAN_POINT('Ctrl Pts',(43.1130766843331,4.8956458996893,130.33336774357));
#61020=CARTESIAN_POINT('Ctrl Pts',(43.105330408249,4.88250895006333,130.19681821783));
#61021=CARTESIAN_POINT('Ctrl Pts',(43.0975841321649,4.86365135375417,130.060783865231));
#61022=CARTESIAN_POINT('Ctrl Pts',(43.0898378560808,4.83913969412001,129.925776481986));
#61023=CARTESIAN_POINT('Ctrl Pts',(43.0820915228155,4.81462785354638,129.790768102149));
#61024=CARTESIAN_POINT('Ctrl Pts',(43.0743451895501,4.78446193620564,129.65678709147));
#61025=CARTESIAN_POINT('Ctrl Pts',(43.0665988562847,4.74875982043973,129.524335918477));
#61026=CARTESIAN_POINT('Ctrl Pts',(43.0588507882818,4.71304970943258,129.391855083963));
#61027=CARTESIAN_POINT('Ctrl Pts',(43.0511027202788,4.67180103468843,129.260905146282));
#61028=CARTESIAN_POINT('Ctrl Pts',(43.0433546522759,4.62518168682574,129.131973872117));
#61029=CARTESIAN_POINT('Ctrl Pts',(43.035598349534,4.57851279136523,129.00290556826));
#61030=CARTESIAN_POINT('Ctrl Pts',(43.0278420467921,4.52646195356534,128.875860581961));
#61031=CARTESIAN_POINT('Ctrl Pts',(43.0200857440503,4.46924563472774,128.751307642369));
#61032=CARTESIAN_POINT('Ctrl Pts',(43.0123253015361,4.41199877781795,128.626688225122));
#61033=CARTESIAN_POINT('Ctrl Pts',(43.0045648590219,4.34958112421101,128.50456385284));
#61034=CARTESIAN_POINT('Ctrl Pts',(42.9968044165078,4.28225488647429,128.385378155917));
#61035=CARTESIAN_POINT('Ctrl Pts',(42.9890315162423,4.2148205706839,128.266001131532));
#61036=CARTESIAN_POINT('Ctrl Pts',(42.9812586159769,4.14246213111183,128.149572541674));
#61037=CARTESIAN_POINT('Ctrl Pts',(42.9734857157114,4.06548534653542,128.03650730505));
#61038=CARTESIAN_POINT('Ctrl Pts',(42.9659953799494,3.9913068619716,127.927552274573));
#61039=CARTESIAN_POINT('Ctrl Pts',(42.9585050441875,3.91284016322174,127.821720557482));
#61040=CARTESIAN_POINT('Ctrl Pts',(42.9510147084255,3.83039266742636,127.719352501559));
#61041=CARTESIAN_POINT('Ctrl Pts',(42.9432403743064,3.74481914976805,127.613103129681));
#61042=CARTESIAN_POINT('Ctrl Pts',(42.9354660401873,3.65468594115511,127.510248687106));
#61043=CARTESIAN_POINT('Ctrl Pts',(42.9276917060682,3.56029240180694,127.411205584837));
#61044=CARTESIAN_POINT('Ctrl Pts',(42.9199269531211,3.46601519405995,127.31228454434));
#61045=CARTESIAN_POINT('Ctrl Pts',(42.9121622001741,3.3674883696036,127.217165778549));
#61046=CARTESIAN_POINT('Ctrl Pts',(42.904397447227,3.2650525581251,127.12623407608));
#61047=CARTESIAN_POINT('Ctrl Pts',(42.896640406342,3.16271848733865,127.035392688261));
#61048=CARTESIAN_POINT('Ctrl Pts',(42.888883365457,3.05648344629503,126.94873034573));
#61049=CARTESIAN_POINT('Ctrl Pts',(42.881126324572,2.94672580677788,126.866596012848));
#61050=CARTESIAN_POINT('Ctrl Pts',(42.8733751333318,2.83705093635018,126.784523618105));
#61051=CARTESIAN_POINT('Ctrl Pts',(42.8656239420917,2.72385906664683,126.706972669736));
#61052=CARTESIAN_POINT('Ctrl Pts',(42.8578727508515,2.60756235275282,126.634252508775));
#61053=CARTESIAN_POINT('Ctrl Pts',(42.8501248540745,2.49131506806484,126.561563255822));
#61054=CARTESIAN_POINT('Ctrl Pts',(42.8423769572974,2.3719658946521,126.493700913438));
#61055=CARTESIAN_POINT('Ctrl Pts',(42.8346290605203,2.24995654747828,126.430931917226));
#61056=CARTESIAN_POINT('Ctrl Pts',(42.8268827844362,2.12797272202968,126.368176050934));
#61057=CARTESIAN_POINT('Ctrl Pts',(42.8191365083521,2.00333017706715,126.31051159038));
#61058=CARTESIAN_POINT('Ctrl Pts',(42.811390232268,1.87649549117341,126.258159155454));
#61059=CARTESIAN_POINT('Ctrl Pts',(42.8036438990026,1.74965986901465,126.205806334075));
#61060=CARTESIAN_POINT('Ctrl Pts',(42.7958975657373,1.62063243502493,126.158765765737));
#61061=CARTESIAN_POINT('Ctrl Pts',(42.7881512324719,1.48989964632975,126.117209872565));
#61062=CARTESIAN_POINT('Ctrl Pts',(42.780403164469,1.35913758093299,126.075644673238));
#61063=CARTESIAN_POINT('Ctrl Pts',(42.772655096466,1.22666977341246,126.039566711577));
#61064=CARTESIAN_POINT('Ctrl Pts',(42.764907028463,1.09299734467351,126.009098386255));
#61065=CARTESIAN_POINT('Ctrl Pts',(42.7571507257212,0.959182847286747,125.978597678834));
#61066=CARTESIAN_POINT('Ctrl Pts',(42.7493944229793,0.824161552969223,125.953718604491));
#61067=CARTESIAN_POINT('Ctrl Pts',(42.7416381202374,0.688444819449609,125.934532407755));
#61068=CARTESIAN_POINT('Ctrl Pts',(42.7338776777233,0.55265564982278,125.915335970768));
#61069=CARTESIAN_POINT('Ctrl Pts',(42.7261172352091,0.41617069026953,125.901838504235));
#61070=CARTESIAN_POINT('Ctrl Pts',(42.7183567926949,0.279504911902632,125.894059194362));
#61071=CARTESIAN_POINT('Ctrl Pts',(42.7105838924295,0.142619745495867,125.88626739645));
#61072=CARTESIAN_POINT('Ctrl Pts',(42.7028109921641,0.00555357137691959,
125.884212104214));
#61073=CARTESIAN_POINT('Ctrl Pts',(42.6950380918987,-0.131179246694201,
125.887860331007));
#61074=CARTESIAN_POINT('Ctrl Pts',(42.6875477561367,-0.262941482419246,
125.891375935567));
#61075=CARTESIAN_POINT('Ctrl Pts',(42.6800574203747,-0.394393870647627,
125.900187563347));
#61076=CARTESIAN_POINT('Ctrl Pts',(42.6725670846126,-0.52508390067963,125.914220541889));
#61077=CARTESIAN_POINT('Ctrl Pts',(42.6647927504936,-0.660729082922493,
125.928785585077));
#61078=CARTESIAN_POINT('Ctrl Pts',(42.6570184163745,-0.795982639331584,
125.949021867617));
#61079=CARTESIAN_POINT('Ctrl Pts',(42.6492440822554,-0.930332420024554,
125.974902609595));
#61080=CARTESIAN_POINT('Ctrl Pts',(42.6414793293083,-1.06451662662055,126.000751455873));
#61081=CARTESIAN_POINT('Ctrl Pts',(42.6337145763613,-1.19779889345439,126.032230847398));
#61082=CARTESIAN_POINT('Ctrl Pts',(42.6259498234141,-1.32967136829897,126.069262190413));
#61083=CARTESIAN_POINT('Ctrl Pts',(42.6181927825291,-1.46141286554227,126.106256753377));
#61084=CARTESIAN_POINT('Ctrl Pts',(42.6104357416441,-1.59174698333753,126.148792189156));
#61085=CARTESIAN_POINT('Ctrl Pts',(42.6026787007591,-1.72017560889519,126.196738786614));
#61086=CARTESIAN_POINT('Ctrl Pts',(42.594927509519,-1.84850738542694,126.24464922717));
#61087=CARTESIAN_POINT('Ctrl Pts',(42.5871763182789,-1.97493616508553,126.297962571032));
#61088=CARTESIAN_POINT('Ctrl Pts',(42.5794251270387,-2.09897891060893,126.356499266836));
#61089=CARTESIAN_POINT('Ctrl Pts',(42.5716772302617,-2.22296893465688,126.415011082983));
#61090=CARTESIAN_POINT('Ctrl Pts',(42.5639293334846,-2.34457458876074,126.478741669032));
#61091=CARTESIAN_POINT('Ctrl Pts',(42.5561814367075,-2.46333295537625,126.547463412622));
#61092=CARTESIAN_POINT('Ctrl Pts',(42.5484351606234,-2.58206648030144,126.616170781106));
#61093=CARTESIAN_POINT('Ctrl Pts',(42.5406888845393,-2.69795356422367,126.689867034781));
#61094=CARTESIAN_POINT('Ctrl Pts',(42.5329426084552,-2.81055639625962,126.768278878311));
#61095=CARTESIAN_POINT('Ctrl Pts',(42.5251962751899,-2.92316005950409,126.846691300661));
#61096=CARTESIAN_POINT('Ctrl Pts',(42.5174499419245,-3.03247910164669,126.929819158906));
#61097=CARTESIAN_POINT('Ctrl Pts',(42.5097036086592,-3.13810551711191,127.017346381262));
#61098=CARTESIAN_POINT('Ctrl Pts',(42.5019555406562,-3.24375558688036,127.104893204732));
#61099=CARTESIAN_POINT('Ctrl Pts',(42.4942074726533,-3.34571108347773,127.19684110335));
#61100=CARTESIAN_POINT('Ctrl Pts',(42.4864594046503,-3.44359816134269,127.292834629381));
#61101=CARTESIAN_POINT('Ctrl Pts',(42.4787031019085,-3.54158927475915,127.388930178474));
#61102=CARTESIAN_POINT('Ctrl Pts',(42.4709467991666,-3.63550305227369,127.489079669997));
#61103=CARTESIAN_POINT('Ctrl Pts',(42.4631904964247,-3.72500315250208,127.59289139362));
#61104=CARTESIAN_POINT('Ctrl Pts',(42.4554300539105,-3.81455102162901,127.696758524686));
#61105=CARTESIAN_POINT('Ctrl Pts',(42.4476696113964,-3.89968027696046,127.804291476259));
#61106=CARTESIAN_POINT('Ctrl Pts',(42.4399091688822,-3.98009642213317,127.915067359168));
#61107=CARTESIAN_POINT('Ctrl Pts',(42.4321362686167,-4.06064165844091,128.026021069359));
#61108=CARTESIAN_POINT('Ctrl Pts',(42.4243633683513,-4.13645844914655,128.140227787904));
#61109=CARTESIAN_POINT('Ctrl Pts',(42.4165904680858,-4.20729652067481,128.257236935917));
#61110=CARTESIAN_POINT('Ctrl Pts',(42.4091001323238,-4.27555944987259,128.369992506671));
#61111=CARTESIAN_POINT('Ctrl Pts',(42.4016097965618,-4.33919920460351,128.485350023863));
#61112=CARTESIAN_POINT('Ctrl Pts',(42.3941194607998,-4.39803401583533,128.60288841514));
#61113=CARTESIAN_POINT('Ctrl Pts',(42.3857998701641,-4.46338242745931,128.733439478599));
#61114=CARTESIAN_POINT('Ctrl Pts',(42.3774802795283,-4.52298784870698,128.867049546495));
#61115=CARTESIAN_POINT('Ctrl Pts',(42.3691606888926,-4.57657376185162,129.003206636133));
#61116=CARTESIAN_POINT('Ctrl Pts',(42.3608614078734,-4.63002886214853,129.139031341837));
#61117=CARTESIAN_POINT('Ctrl Pts',(42.3525621268542,-4.6774936438987,129.277390386455));
#61118=CARTESIAN_POINT('Ctrl Pts',(42.3442628458349,-4.71873845908369,129.417749490658));
#61119=CARTESIAN_POINT('Ctrl Pts',(42.3410331233879,-4.73478916336948,129.472371204085));
#61120=CARTESIAN_POINT('Ctrl Pts',(42.3378034009409,-4.74989839087753,129.527295554605));
#61121=CARTESIAN_POINT('Ctrl Pts',(42.3345736784939,-4.76405452823401,129.582490119308));
#61122=CARTESIAN_POINT('Ctrl Pts',(44.0848860644534,-4.76405452823407,129.582490119308));
#61123=CARTESIAN_POINT('Ctrl Pts',(44.0781924441946,-4.79330959060179,129.696555163473));
#61124=CARTESIAN_POINT('Ctrl Pts',(44.0714988239357,-4.81843174048182,129.811538591869));
#61125=CARTESIAN_POINT('Ctrl Pts',(44.0648052036769,-4.8393826038738,129.92711545467));
#61126=CARTESIAN_POINT('Ctrl Pts',(44.0529708853409,-4.87642372320972,130.131455308709));
#61127=CARTESIAN_POINT('Ctrl Pts',(44.0411365670048,-4.90053067147628,130.338205890149));
#61128=CARTESIAN_POINT('Ctrl Pts',(44.0293022486687,-4.91146188999161,130.546048469845));
#61129=CARTESIAN_POINT('Ctrl Pts',(44.0244879777762,-4.91590877452044,130.630600064051));
#61130=CARTESIAN_POINT('Ctrl Pts',(44.0196737068837,-4.91817565227183,130.715332067349));
#61131=CARTESIAN_POINT('Ctrl Pts',(44.0148594359912,-4.91824820102998,130.800154007847));
#61132=CARTESIAN_POINT('',(44.3601405640442,-4.91824877153122,130.807836798172));
#61133=CARTESIAN_POINT('Ctrl Pts',(44.4302709800425,-4.764054528234,129.582490119308));
#61134=CARTESIAN_POINT('Ctrl Pts',(44.4226263315709,-4.79768188373925,129.713602668057));
#61135=CARTESIAN_POINT('Ctrl Pts',(44.4149816830993,-4.82587262023684,129.846027035517));
#61136=CARTESIAN_POINT('Ctrl Pts',(44.4073370346278,-4.84854638452371,129.979266065638));
#61137=CARTESIAN_POINT('Ctrl Pts',(44.3994709561972,-4.87187690244891,130.116364411604));
#61138=CARTESIAN_POINT('Ctrl Pts',(44.3916048777666,-4.88936592869409,130.25432487215));
#61139=CARTESIAN_POINT('Ctrl Pts',(44.383738799336,-4.90098333508911,130.392601693341));
#61140=CARTESIAN_POINT('Ctrl Pts',(44.3758727209054,-4.91260074148413,130.530878514532));
#61141=CARTESIAN_POINT('Ctrl Pts',(44.3680066424748,-4.91834656725249,130.669471235366));
#61142=CARTESIAN_POINT('Ctrl Pts',(44.3601405640442,-4.91824877153122,130.807836798172));
#61143=CARTESIAN_POINT('Ctrl Pts',(44.3601405640086,-4.91824877153078,130.807836798798));
#61144=CARTESIAN_POINT('Ctrl Pts',(44.3479816531159,-4.91809760476005,131.021713963081));
#61145=CARTESIAN_POINT('Ctrl Pts',(44.3358227422232,-4.90399509209797,131.235104433717));
#61146=CARTESIAN_POINT('Ctrl Pts',(44.3236638313304,-4.87613127035324,131.446643185275));
#61147=CARTESIAN_POINT('Ctrl Pts',(44.3158894972113,-4.85831531117819,131.581899784181));
#61148=CARTESIAN_POINT('Ctrl Pts',(44.3081151630922,-4.83483914376921,131.716628775925));
#61149=CARTESIAN_POINT('Ctrl Pts',(44.3003408289731,-4.80574183051092,131.850318800754));
#61150=CARTESIAN_POINT('Ctrl Pts',(44.292576076026,-4.77668037709073,131.983844064576));
#61151=CARTESIAN_POINT('Ctrl Pts',(44.284811323079,-4.74201164394849,132.116332530811));
#61152=CARTESIAN_POINT('Ctrl Pts',(44.2770465701319,-4.70182638926108,132.247278379515));
#61153=CARTESIAN_POINT('Ctrl Pts',(44.269289529247,-4.66168104713524,132.378094170956));
#61154=CARTESIAN_POINT('Ctrl Pts',(44.2615324883619,-4.61603020105383,132.507370022569));
#61155=CARTESIAN_POINT('Ctrl Pts',(44.253775447477,-4.56501547813448,132.63461107772));
#61156=CARTESIAN_POINT('Ctrl Pts',(44.2460242562368,-4.51403922581445,132.761756179401));
#61157=CARTESIAN_POINT('Ctrl Pts',(44.2382730649967,-4.45770729276966,132.886869177443));
#61158=CARTESIAN_POINT('Ctrl Pts',(44.2305218737566,-4.39621077021821,133.009471482425));
#61159=CARTESIAN_POINT('Ctrl Pts',(44.2227739769795,-4.33474038532924,133.132021678156));
#61160=CARTESIAN_POINT('Ctrl Pts',(44.2150260802025,-4.26810995172021,133.252062954496));
#61161=CARTESIAN_POINT('Ctrl Pts',(44.2072781834254,-4.19655812494766,133.369137989276));
#61162=CARTESIAN_POINT('Ctrl Pts',(44.1995319073413,-4.12502126527479,133.486188534483));
#61163=CARTESIAN_POINT('Ctrl Pts',(44.1917856312571,-4.04856526382163,133.600273738903));
#61164=CARTESIAN_POINT('Ctrl Pts',(44.184039355173,-3.96747384347568,133.710962476066));
#61165=CARTESIAN_POINT('Ctrl Pts',(44.1762930219077,-3.8863818245314,133.821652030308));
#61166=CARTESIAN_POINT('Ctrl Pts',(44.1685466886423,-3.80065454946935,133.928944751878));
#61167=CARTESIAN_POINT('Ctrl Pts',(44.160800355377,-3.71061779006429,134.032440337548));
#61168=CARTESIAN_POINT('Ctrl Pts',(44.153052287374,-3.62056086755124,134.135959100336));
#61169=CARTESIAN_POINT('Ctrl Pts',(44.145304219371,-3.52619279685923,134.235678740231));
#61170=CARTESIAN_POINT('Ctrl Pts',(44.1375561513681,-3.42787789462754,134.331234049095));
#61171=CARTESIAN_POINT('Ctrl Pts',(44.1297998486262,-3.3294585021478,134.426890915278));
#61172=CARTESIAN_POINT('Ctrl Pts',(44.1220435458844,-3.22708417949222,134.51837433629));
#61173=CARTESIAN_POINT('Ctrl Pts',(44.1142872431426,-3.12115459545429,134.605357467575));
#61174=CARTESIAN_POINT('Ctrl Pts',(44.1065268006284,-3.01516847360774,134.692387024375));
#61175=CARTESIAN_POINT('Ctrl Pts',(44.0987663581142,-2.90562362146811,134.774911270247));
#61176=CARTESIAN_POINT('Ctrl Pts',(44.0910059156001,-2.79294987352374,134.852645941809));
#61177=CARTESIAN_POINT('Ctrl Pts',(44.0832330153346,-2.68009525167647,134.930505399967));
#61178=CARTESIAN_POINT('Ctrl Pts',(44.0754601150692,-2.56410202791718,135.003559710968));
#61179=CARTESIAN_POINT('Ctrl Pts',(44.0676872148038,-2.44542665725375,135.071569485959));
#61180=CARTESIAN_POINT('Ctrl Pts',(44.0601968790417,-2.33106543523915,135.137106934323));
#61181=CARTESIAN_POINT('Ctrl Pts',(44.0527065432797,-2.21421395952165,135.19796010004));
#61182=CARTESIAN_POINT('Ctrl Pts',(44.0452162075177,-2.09529754315362,135.253957370998));
#61183=CARTESIAN_POINT('Ctrl Pts',(44.0374418733986,-1.9718723747153,135.312077795505));
#61184=CARTESIAN_POINT('Ctrl Pts',(44.0296675392795,-1.84583161631654,135.36515094196));
#61185=CARTESIAN_POINT('Ctrl Pts',(44.0218932051605,-1.71762660357202,135.412933272218));
#61186=CARTESIAN_POINT('Ctrl Pts',(44.0141284522134,-1.58957959204769,135.460656715024));
#61187=CARTESIAN_POINT('Ctrl Pts',(44.0063636992663,-1.45937399604142,135.503102180172));
#61188=CARTESIAN_POINT('Ctrl Pts',(43.9985989463192,-1.32748443320978,135.540072617053));
#61189=CARTESIAN_POINT('Ctrl Pts',(43.9908419054342,-1.19572586495127,135.577006334375));
#61190=CARTESIAN_POINT('Ctrl Pts',(43.9830848645492,-1.06228703231538,135.608475740203));
#61191=CARTESIAN_POINT('Ctrl Pts',(43.9753278236642,-0.927660825121338,
135.634332507343));
#61192=CARTESIAN_POINT('Ctrl Pts',(43.967576632424,-0.793136140597192,135.660169775694));
#61193=CARTESIAN_POINT('Ctrl Pts',(43.959825441184,-0.657426246165173,135.680402756517));
#61194=CARTESIAN_POINT('Ctrl Pts',(43.9520742499438,-0.521037082131064,
135.694933530993));
#61195=CARTESIAN_POINT('Ctrl Pts',(43.9443263531667,-0.384705887130155,
135.709458129502));
#61196=CARTESIAN_POINT('Ctrl Pts',(43.9365784563896,-0.247696384695925,
135.718285300667));
#61197=CARTESIAN_POINT('Ctrl Pts',(43.9288305596125,-0.110522332076842,
135.721368638366));
#61198=CARTESIAN_POINT('Ctrl Pts',(43.9210842835285,0.0266230266875624,
135.724451331097));
#61199=CARTESIAN_POINT('Ctrl Pts',(43.9133380074443,0.163932476554009,135.721792571403));
#61200=CARTESIAN_POINT('Ctrl Pts',(43.9055917313602,0.300889939462038,135.713398028997));
#61201=CARTESIAN_POINT('Ctrl Pts',(43.8978453980949,0.437848413358758,135.705003424624));
#61202=CARTESIAN_POINT('Ctrl Pts',(43.8900990648296,0.574454504879496,135.690872976971));
#61203=CARTESIAN_POINT('Ctrl Pts',(43.8823527315642,0.710195339979163,135.671064393385));
#61204=CARTESIAN_POINT('Ctrl Pts',(43.8746046635613,0.845966573297689,135.651251373804));
#61205=CARTESIAN_POINT('Ctrl Pts',(43.8668565955583,0.980871777825297,135.625757744439));
#61206=CARTESIAN_POINT('Ctrl Pts',(43.8591085275553,1.11440677157029,135.594692611278));
#61207=CARTESIAN_POINT('Ctrl Pts',(43.8513522248135,1.24808368789591,135.563594461723));
#61208=CARTESIAN_POINT('Ctrl Pts',(43.8435959220716,1.38038710296623,135.526913068346));
#61209=CARTESIAN_POINT('Ctrl Pts',(43.8358396193298,1.51082600245228,135.484808016353));
#61210=CARTESIAN_POINT('Ctrl Pts',(43.8280791768156,1.64133452110641,135.442680491627));
#61211=CARTESIAN_POINT('Ctrl Pts',(43.8203187343015,1.76997617472984,135.395123675711));
#61212=CARTESIAN_POINT('Ctrl Pts',(43.8125582917873,1.89627946844864,135.342345549233));
#61213=CARTESIAN_POINT('Ctrl Pts',(43.8047853915219,2.0227855154272,135.289482698622));
#61214=CARTESIAN_POINT('Ctrl Pts',(43.7970124912565,2.14694534701132,135.231381953921));
#61215=CARTESIAN_POINT('Ctrl Pts',(43.789239590991,2.26831083349889,135.168297948135));
#61216=CARTESIAN_POINT('Ctrl Pts',(43.7817492552289,2.38526437885274,135.107507204857));
#61217=CARTESIAN_POINT('Ctrl Pts',(43.7742589194668,2.49962294750406,135.042089371421));
#61218=CARTESIAN_POINT('Ctrl Pts',(43.7667685837047,2.61101226522926,134.972309515204));
#61219=CARTESIAN_POINT('Ctrl Pts',(43.7589942495856,2.72662494279093,134.89988393453));
#61220=CARTESIAN_POINT('Ctrl Pts',(43.7512199154665,2.83940499264457,134.822529606872));
#61221=CARTESIAN_POINT('Ctrl Pts',(43.7434455813474,2.94890356132639,134.740494615348));
#61222=CARTESIAN_POINT('Ctrl Pts',(43.7356808284003,3.05826718280847,134.658560724619));
#61223=CARTESIAN_POINT('Ctrl Pts',(43.7279160754532,3.16435705984621,134.571957879786));
#61224=CARTESIAN_POINT('Ctrl Pts',(43.7201513225061,3.26675086574333,134.480978879456));
#61225=CARTESIAN_POINT('Ctrl Pts',(43.7123942816211,3.3690429726688,134.390090240752));
#61226=CARTESIAN_POINT('Ctrl Pts',(43.7046372407361,3.4676460235161,134.294834354205));
#61227=CARTESIAN_POINT('Ctrl Pts',(43.6968801998511,3.56216880742927,134.195545727506));
#61228=CARTESIAN_POINT('Ctrl Pts',(43.689129008611,3.65662031097582,134.096331975133));
#61229=CARTESIAN_POINT('Ctrl Pts',(43.6813778173709,3.74699740360873,133.993091817796));
#61230=CARTESIAN_POINT('Ctrl Pts',(43.6736266261308,3.832944230359,133.886197989891));
#61231=CARTESIAN_POINT('Ctrl Pts',(43.6658787293537,3.91885452741531,133.779349594713));
#61232=CARTESIAN_POINT('Ctrl Pts',(43.6581308325766,4.00033805922415,133.668850921635));
#61233=CARTESIAN_POINT('Ctrl Pts',(43.6503829357995,4.07707808465801,133.555109125536));
#61234=CARTESIAN_POINT('Ctrl Pts',(43.6426366597154,4.15380205773286,133.441391121769));
#61235=CARTESIAN_POINT('Ctrl Pts',(43.6348903836313,4.22578427952503,133.324431668233));
#61236=CARTESIAN_POINT('Ctrl Pts',(43.6271441075472,4.29275056732684,133.204668020632));
#61237=CARTESIAN_POINT('Ctrl Pts',(43.6193977742818,4.35971734945848,133.084903488964));
#61238=CARTESIAN_POINT('Ctrl Pts',(43.6116514410165,4.42166793290908,132.96233506317));
#61239=CARTESIAN_POINT('Ctrl Pts',(43.6039051077511,4.47837364755536,132.837425430941));
#61240=CARTESIAN_POINT('Ctrl Pts',(43.5961570397481,4.53509206105334,132.712487826065));
#61241=CARTESIAN_POINT('Ctrl Pts',(43.5884089717452,4.58656310694151,132.585208327393));
#61242=CARTESIAN_POINT('Ctrl Pts',(43.5806609037423,4.63260605649545,132.456070091966));
#61243=CARTESIAN_POINT('Ctrl Pts',(43.5729046010004,4.67869794104403,132.326794606885));
#61244=CARTESIAN_POINT('Ctrl Pts',(43.5651482982585,4.71935007346054,132.195656807646));
#61245=CARTESIAN_POINT('Ctrl Pts',(43.5573919955167,4.75443131206144,132.063156058211));
#61246=CARTESIAN_POINT('Ctrl Pts',(43.5496315530025,4.78953127457571,131.930584589137));
#61247=CARTESIAN_POINT('Ctrl Pts',(43.5418711104883,4.81905433449726,131.796649101981));
#61248=CARTESIAN_POINT('Ctrl Pts',(43.5341106679741,4.84292061732194,131.661858697341));
#61249=CARTESIAN_POINT('Ctrl Pts',(43.5263377677087,4.86682521242255,131.526851915178));
#61250=CARTESIAN_POINT('Ctrl Pts',(43.5185648674433,4.88505483215077,131.390987860777));
#61251=CARTESIAN_POINT('Ctrl Pts',(43.5107919671779,4.89758148141411,131.254781193705));
#61252=CARTESIAN_POINT('Ctrl Pts',(43.5033016314158,4.90965275542396,131.123525982066));
#61253=CARTESIAN_POINT('Ctrl Pts',(43.4958112956538,4.91642847914391,130.991952942567));
#61254=CARTESIAN_POINT('Ctrl Pts',(43.4883209598918,4.91792935690632,130.860520238104));
#61255=CARTESIAN_POINT('Ctrl Pts',(43.4805466257728,4.91948714090528,130.724104222703));
#61256=CARTESIAN_POINT('Ctrl Pts',(43.4727722916537,4.91536712600988,130.587407269081));
#61257=CARTESIAN_POINT('Ctrl Pts',(43.4649979575346,4.90553541531272,130.450941105353));
#61258=CARTESIAN_POINT('Ctrl Pts',(43.4572332045875,4.89571582132031,130.314643123976));
#61259=CARTESIAN_POINT('Ctrl Pts',(43.4494684516404,4.88019856517031,130.178575752779));
#61260=CARTESIAN_POINT('Ctrl Pts',(43.4417036986933,4.85900170872886,130.043252571971));
#61261=CARTESIAN_POINT('Ctrl Pts',(43.4339466578083,4.83782590530404,129.908063796053));
#61262=CARTESIAN_POINT('Ctrl Pts',(43.4261896169234,4.81098178766093,129.773618123358));
#61263=CARTESIAN_POINT('Ctrl Pts',(43.4184325760384,4.77853932757177,129.640425500238));
#61264=CARTESIAN_POINT('Ctrl Pts',(43.4106813847982,4.74612133259413,129.50733331871));
#61265=CARTESIAN_POINT('Ctrl Pts',(43.4029301935581,4.70811349046494,129.375492684244));
#61266=CARTESIAN_POINT('Ctrl Pts',(43.3951790023179,4.664637044884,129.245404459749));
#61267=CARTESIAN_POINT('Ctrl Pts',(43.3874311055409,4.6211790779522,129.115371526219));
#61268=CARTESIAN_POINT('Ctrl Pts',(43.3796832087638,4.57225725409508,128.987089891296));
#61269=CARTESIAN_POINT('Ctrl Pts',(43.3719353119867,4.5180429179286,128.861046115419));
#61270=CARTESIAN_POINT('Ctrl Pts',(43.3641890359026,4.46383992223251,128.735028705183));
#61271=CARTESIAN_POINT('Ctrl Pts',(43.3564427598186,4.40434677065039,128.611248581816));
#61272=CARTESIAN_POINT('Ctrl Pts',(43.3486964837345,4.33978313634112,128.490172770387));
#61273=CARTESIAN_POINT('Ctrl Pts',(43.3409501504692,4.27521902543786,128.369096065204));
#61274=CARTESIAN_POINT('Ctrl Pts',(43.3332038172038,4.20558454108145,128.250724056774));
#61275=CARTESIAN_POINT('Ctrl Pts',(43.3254574839385,4.13114535374258,128.135499225745));
#61276=CARTESIAN_POINT('Ctrl Pts',(43.3177094159355,4.05668949626383,128.020248590915));
#61277=CARTESIAN_POINT('Ctrl Pts',(43.3099613479325,3.97742700684167,127.908146864267));
#61278=CARTESIAN_POINT('Ctrl Pts',(43.3022132799296,3.8936666908876,127.799607256178));
#61279=CARTESIAN_POINT('Ctrl Pts',(43.2944569771877,3.80981735347287,127.690952290902));
#61280=CARTESIAN_POINT('Ctrl Pts',(43.2867006744459,3.72146087951199,127.585867316864));
#61281=CARTESIAN_POINT('Ctrl Pts',(43.278944371704,3.62894651276743,127.484732585697));
#61282=CARTESIAN_POINT('Ctrl Pts',(43.2711839291899,3.53638276831979,127.383543875878));
#61283=CARTESIAN_POINT('Ctrl Pts',(43.2634234866757,3.43965698475331,127.286309887065));
#61284=CARTESIAN_POINT('Ctrl Pts',(43.2556630441615,3.33915430870082,127.19337300125));
#61285=CARTESIAN_POINT('Ctrl Pts',(43.2478901438961,3.23849029683053,127.100286924896));
#61286=CARTESIAN_POINT('Ctrl Pts',(43.2401172436307,3.13403757473917,127.011511989461));
#61287=CARTESIAN_POINT('Ctrl Pts',(43.2323443433653,3.02621400806626,126.927349934078));
#61288=CARTESIAN_POINT('Ctrl Pts',(43.2248540076032,2.92231009963191,126.846247381398));
#61289=CARTESIAN_POINT('Ctrl Pts',(43.217363671841,2.81527641933454,126.769428331433));
#61290=CARTESIAN_POINT('Ctrl Pts',(43.2098733360789,2.7055096237925,126.697123013279));
#61291=CARTESIAN_POINT('Ctrl Pts',(43.2020990019599,2.5915809868357,126.622076217012));
#61292=CARTESIAN_POINT('Ctrl Pts',(43.1943246678407,2.47434699960622,126.551654459786));
#61293=CARTESIAN_POINT('Ctrl Pts',(43.1865503337216,2.35421987135499,126.486162861578));
#61294=CARTESIAN_POINT('Ctrl Pts',(43.1787855807746,2.23424078905326,126.420751975912));
#61295=CARTESIAN_POINT('Ctrl Pts',(43.1710208278275,2.11137600005726,126.36025934522));
#61296=CARTESIAN_POINT('Ctrl Pts',(43.1632560748804,1.98606735682288,126.304947376191));
#61297=CARTESIAN_POINT('Ctrl Pts',(43.1554990339954,1.8608831718995,126.249690343789));
#61298=CARTESIAN_POINT('Ctrl Pts',(43.1477419931104,1.73326031847178,126.199603890118));
#61299=CARTESIAN_POINT('Ctrl Pts',(43.1399849522253,1.60366565029975,126.154904784401));
#61300=CARTESIAN_POINT('Ctrl Pts',(43.1322337609852,1.47416871047527,126.110239386629));
#61301=CARTESIAN_POINT('Ctrl Pts',(43.1244825697451,1.34270328371439,126.070953377335));
#61302=CARTESIAN_POINT('Ctrl Pts',(43.116731378505,1.20975629534869,126.037215479397));
#61303=CARTESIAN_POINT('Ctrl Pts',(43.1089834817279,1.07686581299934,126.003491920967));
#61304=CARTESIAN_POINT('Ctrl Pts',(43.1012355849508,0.942495399636922,125.975311879787));
#61305=CARTESIAN_POINT('Ctrl Pts',(43.0934876881738,0.807147028289451,125.952794196582));
#61306=CARTESIAN_POINT('Ctrl Pts',(43.0857414120896,0.671826968903493,125.93028122359));
#61307=CARTESIAN_POINT('Ctrl Pts',(43.0779951360055,0.535529743848918,125.913428316773));
#61308=CARTESIAN_POINT('Ctrl Pts',(43.0702488599214,0.398767013249796,125.902303097336));
#61309=CARTESIAN_POINT('Ctrl Pts',(43.0625025266561,0.262003273099265,125.891177795775));
#61310=CARTESIAN_POINT('Ctrl Pts',(43.0547561933907,0.124774410225408,125.885780297662));
#61311=CARTESIAN_POINT('Ctrl Pts',(43.0470098601254,-0.0124037024909772,
125.886126258503));
#61312=CARTESIAN_POINT('Ctrl Pts',(43.0392617921224,-0.149612535294579,
125.886472296821));
#61313=CARTESIAN_POINT('Ctrl Pts',(43.0315137241194,-0.286770204436251,
125.892564352512));
#61314=CARTESIAN_POINT('Ctrl Pts',(43.0237656561165,-0.423362147455745,
125.90436596914));
#61315=CARTESIAN_POINT('Ctrl Pts',(43.0160093533746,-0.560099262017746,
125.916180128667));
#61316=CARTESIAN_POINT('Ctrl Pts',(43.0082530506327,-0.696269059239914,
125.933715937285));
#61317=CARTESIAN_POINT('Ctrl Pts',(43.0004967478909,-0.831362847869982,
125.956885101621));
#61318=CARTESIAN_POINT('Ctrl Pts',(42.9927363053767,-0.966528740122822,
125.980066632038));
#61319=CARTESIAN_POINT('Ctrl Pts',(42.9849758628625,-1.10061709739733,126.008887427144));
#61320=CARTESIAN_POINT('Ctrl Pts',(42.9772154203484,-1.23313168286379,126.043208517998));
#61321=CARTESIAN_POINT('Ctrl Pts',(42.9694425200829,-1.36585899250675,126.077584704114));
#61322=CARTESIAN_POINT('Ctrl Pts',(42.9616696198175,-1.49700710761508,126.117478716414));
#61323=CARTESIAN_POINT('Ctrl Pts',(42.953896719552,-1.62609629992612,126.162702090071));
#61324=CARTESIAN_POINT('Ctrl Pts',(42.9464063837901,-1.75049277493955,126.206281480185));
#61325=CARTESIAN_POINT('Ctrl Pts',(42.9389160480282,-1.87297713594478,126.254809373854));
#61326=CARTESIAN_POINT('Ctrl Pts',(42.9314257122662,-1.99314128209203,126.308076497082));
#61327=CARTESIAN_POINT('Ctrl Pts',(42.9236508504031,-2.11786995472762,126.3633670125));
#61328=CARTESIAN_POINT('Ctrl Pts',(42.9158759885401,-2.24049378767229,126.423939076832));
#61329=CARTESIAN_POINT('Ctrl Pts',(42.908101126677,-2.36053316856388,126.489610772835));
#61330=CARTESIAN_POINT('Ctrl Pts',(42.900335965639,-2.48042277431546,126.555200529165));
#61331=CARTESIAN_POINT('Ctrl Pts',(42.8925708046009,-2.5977340046897,126.625877070276));
#61332=CARTESIAN_POINT('Ctrl Pts',(42.8848056435628,-2.71200718697745,126.701410449665));
#61333=CARTESIAN_POINT('Ctrl Pts',(42.8770483137291,-2.82616512418129,126.776867653257));
#61334=CARTESIAN_POINT('Ctrl Pts',(42.8692909838953,-2.93729078688686,126.857171732654));
#61335=CARTESIAN_POINT('Ctrl Pts',(42.8615336540616,-3.04494941021352,126.942047042552));
#61336=CARTESIAN_POINT('Ctrl Pts',(42.8537826840201,-3.15251977037426,127.026852768023));
#61337=CARTESIAN_POINT('Ctrl Pts',(42.8460317139787,-3.25662844520335,127.116222020501));
#61338=CARTESIAN_POINT('Ctrl Pts',(42.8382807439373,-3.35687032746872,127.20983635599));
#61339=CARTESIAN_POINT('Ctrl Pts',(42.830533243161,-3.45706734236119,127.303408790537));
#61340=CARTESIAN_POINT('Ctrl Pts',(42.8227857423846,-3.55340072294593,127.401222261656));
#61341=CARTESIAN_POINT('Ctrl Pts',(42.8150382416083,-3.64549921708986,127.502918732465));
#61342=CARTESIAN_POINT('Ctrl Pts',(42.8072925307566,-3.73757643348692,127.604591708083));
#61343=CARTESIAN_POINT('Ctrl Pts',(42.7995468199049,-3.82542044845213,127.710145608475));
#61344=CARTESIAN_POINT('Ctrl Pts',(42.7918011090532,-3.90869788019213,127.819186595188));
#61345=CARTESIAN_POINT('Ctrl Pts',(42.784055510342,-3.99197410626239,127.928226003233));
#61346=CARTESIAN_POINT('Ctrl Pts',(42.7763099116306,-4.07068364444426,128.04075208582));
#61347=CARTESIAN_POINT('Ctrl Pts',(42.7685643129194,-4.14453456265979,128.156339408924));
#61348=CARTESIAN_POINT('Ctrl Pts',(42.7608136355511,-4.21843390366331,128.272002520665));
#61349=CARTESIAN_POINT('Ctrl Pts',(42.7530629581829,-4.2874680485546,128.390730553733));
#61350=CARTESIAN_POINT('Ctrl Pts',(42.7453122808146,-4.35138928918499,128.512070427283));
#61351=CARTESIAN_POINT('Ctrl Pts',(42.7375590397133,-4.41533167338616,128.633450437073));
#61352=CARTESIAN_POINT('Ctrl Pts',(42.729805798612,-4.47415761250167,128.757443657138));
#61353=CARTESIAN_POINT('Ctrl Pts',(42.7220525575107,-4.52766667012813,128.883574948442));
#61354=CARTESIAN_POINT('Ctrl Pts',(42.7142901688683,-4.58123885958533,129.009855053792));
#61355=CARTESIAN_POINT('Ctrl Pts',(42.7065277802259,-4.62948149385214,129.138277905235));
#61356=CARTESIAN_POINT('Ctrl Pts',(42.6987653915834,-4.67224314834394,129.268350518233));
#61357=CARTESIAN_POINT('Ctrl Pts',(42.6925739244696,-4.70635086823736,129.372099549992));
#61358=CARTESIAN_POINT('Ctrl Pts',(42.6863824573558,-4.73697251997796,129.476897780145));
#61359=CARTESIAN_POINT('Ctrl Pts',(42.6801909902419,-4.76405452823402,129.582490119308));
#61360=CARTESIAN_POINT('Origin',(213.235140564004,0.,130.804360617566));
#61361=CARTESIAN_POINT('',(40.5848681886094,-4.76405452823408,129.582490119308));
#61362=CARTESIAN_POINT('',(40.9298575685393,-4.7640545282341,129.582490119308));
#61363=CARTESIAN_POINT('',(213.235140564004,-4.76405452823405,129.582490119308));
#61364=CARTESIAN_POINT('',(42.264859436036,-4.9182499044007,130.80339089469));
#61365=CARTESIAN_POINT('Ctrl Pts',(42.2648594359912,-4.91824990440086,130.803390895484));
#61366=CARTESIAN_POINT('Ctrl Pts',(42.2568550863798,-4.91827792430065,130.945502611918));
#61367=CARTESIAN_POINT('Ctrl Pts',(42.2488507367685,-4.91214217362805,131.08753530788));
#61368=CARTESIAN_POINT('Ctrl Pts',(42.2408463871571,-4.89988927847153,131.228940552584));
#61369=CARTESIAN_POINT('Ctrl Pts',(42.2328351978916,-4.88762591331188,131.370466626964));
#61370=CARTESIAN_POINT('Ctrl Pts',(42.2248240086261,-4.86923501125477,131.511363830092));
#61371=CARTESIAN_POINT('Ctrl Pts',(42.2168128193606,-4.8448147996154,131.651091164982));
#61372=CARTESIAN_POINT('Ctrl Pts',(42.2083844041628,-4.81912277361354,131.798095555205));
#61373=CARTESIAN_POINT('Ctrl Pts',(42.1999559889649,-4.78675670518386,131.943804511185));
#61374=CARTESIAN_POINT('Ctrl Pts',(42.1915275737671,-4.74789083996242,132.087604800994));
#61375=CARTESIAN_POINT('Ctrl Pts',(42.1834930844567,-4.7108414811763,132.224684176438));
#61376=CARTESIAN_POINT('Ctrl Pts',(42.1754585951463,-4.66788626722541,132.36002894379));
#61377=CARTESIAN_POINT('Ctrl Pts',(42.1674241058359,-4.61922601848707,132.493127638985));
#61378=CARTESIAN_POINT('Ctrl Pts',(42.1593809267226,-4.57051314064548,132.626370288745));
#61379=CARTESIAN_POINT('Ctrl Pts',(42.1513377476093,-4.51608305489379,132.757361696482));
#61380=CARTESIAN_POINT('Ctrl Pts',(42.143294568496,-4.45618358258824,132.885612870603));
#61381=CARTESIAN_POINT('Ctrl Pts',(42.135236943681,-4.39617652969784,133.014094386257));
#61382=CARTESIAN_POINT('Ctrl Pts',(42.127179318866,-4.33068062810157,133.139825524779));
#61383=CARTESIAN_POINT('Ctrl Pts',(42.119121694051,-4.25998870793906,133.262343382097));
#61384=CARTESIAN_POINT('Ctrl Pts',(42.1179717416962,-4.24989983660076,133.279828646273));
#61385=CARTESIAN_POINT('Ctrl Pts',(42.1168217893414,-4.23970520285251,133.297248514659));
#61386=CARTESIAN_POINT('Ctrl Pts',(42.1156718369867,-4.22940572634524,133.314601694526));
#61387=CARTESIAN_POINT('Ctrl Pts',(42.1078975028676,-4.15977538793196,133.43191909273));
#61388=CARTESIAN_POINT('Ctrl Pts',(42.1001231687486,-4.085149746637,133.54652295529));
#61389=CARTESIAN_POINT('Ctrl Pts',(42.0923488346295,-4.00576604289151,133.65795860469));
#61390=CARTESIAN_POINT('Ctrl Pts',(42.0845840816824,-3.92648017246617,133.769256919612));
#61391=CARTESIAN_POINT('Ctrl Pts',(42.0768193287354,-3.84244813163981,133.877394474871));
#61392=CARTESIAN_POINT('Ctrl Pts',(42.0690545757883,-3.75395250002539,133.981942039033));
#61393=CARTESIAN_POINT('Ctrl Pts',(42.0612975349033,-3.66554476351985,134.08638576508));
#61394=CARTESIAN_POINT('Ctrl Pts',(42.0535404940183,-3.57268250965602,134.187246299313));
#61395=CARTESIAN_POINT('Ctrl Pts',(42.0457834531333,-3.47569076181493,134.284124516272));
#61396=CARTESIAN_POINT('Ctrl Pts',(42.0380322618932,-3.37877215620549,134.380929676613));
#61397=CARTESIAN_POINT('Ctrl Pts',(42.0302810706531,-3.27773053050994,134.473758221988));
#61398=CARTESIAN_POINT('Ctrl Pts',(42.022529879413,-3.1729299722468,134.562245455306));
#61399=CARTESIAN_POINT('Ctrl Pts',(42.0147819826359,-3.06817395701628,134.65069507919));
#61400=CARTESIAN_POINT('Ctrl Pts',(42.0070340858589,-2.95966248491463,134.734806809231));
#61401=CARTESIAN_POINT('Ctrl Pts',(41.9992861890819,-2.84779499265814,134.814254224919));
#61402=CARTESIAN_POINT('Ctrl Pts',(41.9915399129978,-2.73595090066944,134.893685021921));
#61403=CARTESIAN_POINT('Ctrl Pts',(41.9837936369136,-2.62075250341194,134.968453219004));
#61404=CARTESIAN_POINT('Ctrl Pts',(41.9760473608295,-2.50263035104442,135.038274219487));
#61405=CARTESIAN_POINT('Ctrl Pts',(41.9683010275642,-2.38450732672601,135.108095735373));
#61406=CARTESIAN_POINT('Ctrl Pts',(41.9605546942989,-2.2634608407967,135.172969782847));
#61407=CARTESIAN_POINT('Ctrl Pts',(41.9528083610335,-2.13994796025175,135.232656654408));
#61408=CARTESIAN_POINT('Ctrl Pts',(41.9450602930306,-2.01640741985358,135.292356892431));
#61409=CARTESIAN_POINT('Ctrl Pts',(41.9373122250276,-1.89039973771314,135.34686747295));
#61410=CARTESIAN_POINT('Ctrl Pts',(41.9295641570246,-1.76240359474225,135.395996124849));
#61411=CARTESIAN_POINT('Ctrl Pts',(41.9218078542828,-1.63427141594761,135.445176991264));
#61412=CARTESIAN_POINT('Ctrl Pts',(41.914051551541,-1.50414692024234,135.488964362466));
#61413=CARTESIAN_POINT('Ctrl Pts',(41.9062952487991,-1.37252618074724,135.527215151178));
#61414=CARTESIAN_POINT('Ctrl Pts',(41.898534806285,-1.24083519130045,135.565486355489));
#61415=CARTESIAN_POINT('Ctrl Pts',(41.8907743637708,-1.10764674628935,135.59821499589));
#61416=CARTESIAN_POINT('Ctrl Pts',(41.8830139212567,-0.973467882937817,
135.625309003868));
#61417=CARTESIAN_POINT('Ctrl Pts',(41.8752410209913,-0.839073623762808,
135.652446505553));
#61418=CARTESIAN_POINT('Ctrl Pts',(41.8674681207258,-0.703686155461381,
135.673931238289));
#61419=CARTESIAN_POINT('Ctrl Pts',(41.8596952204604,-0.567819317587671,
135.689722864634));
#61420=CARTESIAN_POINT('Ctrl Pts',(41.8522048846982,-0.43689158149619,135.704940425584));
#61421=CARTESIAN_POINT('Ctrl Pts',(41.8447145489361,-0.305519030465423,
135.714871588225));
#61422=CARTESIAN_POINT('Ctrl Pts',(41.8372242131739,-0.174160192299514,
135.719526056279));
#61423=CARTESIAN_POINT('Ctrl Pts',(41.8294498790548,-0.037820843861379,
135.724356999904));
#61424=CARTESIAN_POINT('Ctrl Pts',(41.8216755449358,0.0989356134130586,
135.723518521443));
#61425=CARTESIAN_POINT('Ctrl Pts',(41.8139012108167,0.235598412204566,135.716964453687));
#61426=CARTESIAN_POINT('Ctrl Pts',(41.8061364578697,0.372092786310282,135.710418463233));
#61427=CARTESIAN_POINT('Ctrl Pts',(41.7983717049226,0.50849334482837,135.698170917399));
#61428=CARTESIAN_POINT('Ctrl Pts',(41.7906069519755,0.644286222012198,135.680227548341));
#61429=CARTESIAN_POINT('Ctrl Pts',(41.7828499110905,0.779944227796062,135.66230200089));
#61430=CARTESIAN_POINT('Ctrl Pts',(41.7750928702055,0.914995368264727,135.638691939127));
#61431=CARTESIAN_POINT('Ctrl Pts',(41.7673358293205,1.04892816478898,135.609455077367));
#61432=CARTESIAN_POINT('Ctrl Pts',(41.7595846380803,1.18275996155007,135.580240263352));
#61433=CARTESIAN_POINT('Ctrl Pts',(41.7518334468403,1.31547471258287,135.545407178245));
#61434=CARTESIAN_POINT('Ctrl Pts',(41.7440822556001,1.44656878970031,135.505065011502));
#61435=CARTESIAN_POINT('Ctrl Pts',(41.7363343588231,1.57760714833758,135.464739991255));
#61436=CARTESIAN_POINT('Ctrl Pts',(41.7285864620459,1.70702583019955,135.418910661201));
#61437=CARTESIAN_POINT('Ctrl Pts',(41.7208385652688,1.83433430316589,135.367736640504));
#61438=CARTESIAN_POINT('Ctrl Pts',(41.7130922891848,1.96161614594413,135.316573324309));
#61439=CARTESIAN_POINT('Ctrl Pts',(41.7053460131007,2.08678829529036,135.260067686947));
#61440=CARTESIAN_POINT('Ctrl Pts',(41.6975997370166,2.20937858907897,135.198428131));
#61441=CARTESIAN_POINT('Ctrl Pts',(41.6898534037512,2.33196978780145,135.136788120045));
#61442=CARTESIAN_POINT('Ctrl Pts',(41.6821070704858,2.4519787436396,135.070014290514));
#61443=CARTESIAN_POINT('Ctrl Pts',(41.6743607372205,2.56895672800876,134.998361618057));
#61444=CARTESIAN_POINT('Ctrl Pts',(41.6666126692175,2.6859609087866,134.92669289948));
#61445=CARTESIAN_POINT('Ctrl Pts',(41.6588646012145,2.79993243410273,134.850143368037));
#61446=CARTESIAN_POINT('Ctrl Pts',(41.6511165332115,2.9104508020968,134.769011824302));
#61447=CARTESIAN_POINT('Ctrl Pts',(41.6433602304697,3.02108663032711,134.687794052997));
#61448=CARTESIAN_POINT('Ctrl Pts',(41.6356039277278,3.12826165423825,134.601984773143));
#61449=CARTESIAN_POINT('Ctrl Pts',(41.627847624986,3.23158735081323,134.51192400294));
#61450=CARTESIAN_POINT('Ctrl Pts',(41.6200871824718,3.3349681954237,134.421815164591));
#61451=CARTESIAN_POINT('Ctrl Pts',(41.6123267399576,3.43449533535338,134.327450583289));
#61452=CARTESIAN_POINT('Ctrl Pts',(41.6045662974435,3.52981724475025,134.229207078528));
#61453=CARTESIAN_POINT('Ctrl Pts',(41.5967933971781,3.62529217333835,134.130805864572));
#61454=CARTESIAN_POINT('Ctrl Pts',(41.5890204969126,3.71654812110762,134.028513575955));
#61455=CARTESIAN_POINT('Ctrl Pts',(41.5812475966472,3.80327340819616,133.922740717074));
#61456=CARTESIAN_POINT('Ctrl Pts',(41.5737572608851,3.88684601265181,133.820812968039));
#61457=CARTESIAN_POINT('Ctrl Pts',(41.5662669251231,3.9662114538305,133.715653556183));
#61458=CARTESIAN_POINT('Ctrl Pts',(41.558776589361,4.04113005027163,133.607653499034));
#61459=CARTESIAN_POINT('Ctrl Pts',(41.5510022552419,4.1188892080674,133.495558586894));
#61460=CARTESIAN_POINT('Ctrl Pts',(41.5432279211228,4.1921039780104,133.380048288156));
#61461=CARTESIAN_POINT('Ctrl Pts',(41.5354535870037,4.26045943610733,133.261527371326));
#61462=CARTESIAN_POINT('Ctrl Pts',(41.5276888340566,4.32873065221135,133.143152520934));
#61463=CARTESIAN_POINT('Ctrl Pts',(41.5199240811095,4.39215427868095,133.021774770302));
#61464=CARTESIAN_POINT('Ctrl Pts',(41.5121593281624,4.45045738115321,132.897829547605));
#61465=CARTESIAN_POINT('Ctrl Pts',(41.5044022872773,4.50870257616224,132.774007429051));
#61466=CARTESIAN_POINT('Ctrl Pts',(41.4966452463923,4.56183720276016,132.647623264636));
#61467=CARTESIAN_POINT('Ctrl Pts',(41.4888882055073,4.60963335094272,132.519138571814));
#61468=CARTESIAN_POINT('Ctrl Pts',(41.4811370142672,4.65739345567781,132.3907507703));
#61469=CARTESIAN_POINT('Ctrl Pts',(41.4733858230271,4.69982295932381,132.260265958234));
#61470=CARTESIAN_POINT('Ctrl Pts',(41.465634631787,4.7367415027254,132.128166871841));
#61471=CARTESIAN_POINT('Ctrl Pts',(41.4578867350099,4.77364435476136,131.996123931084));
#61472=CARTESIAN_POINT('Ctrl Pts',(41.4501388382328,4.80504080020648,131.862468456368));
#61473=CARTESIAN_POINT('Ctrl Pts',(41.4423909414557,4.83079998659112,131.727699424316));
#61474=CARTESIAN_POINT('Ctrl Pts',(41.4346446653716,4.85655378470931,131.592958583041));
#61475=CARTESIAN_POINT('Ctrl Pts',(41.4268983892875,4.87667259589443,131.457105031514));
#61476=CARTESIAN_POINT('Ctrl Pts',(41.4191521132034,4.89107653998105,131.320648659793));
#61477=CARTESIAN_POINT('Ctrl Pts',(41.411405779938,4.9054805903943,131.184191280783));
#61478=CARTESIAN_POINT('Ctrl Pts',(41.4036594466727,4.9141696484891,131.047131461503));
#61479=CARTESIAN_POINT('Ctrl Pts',(41.3959131134073,4.9171156837391,130.909984550588));
#61480=CARTESIAN_POINT('Ctrl Pts',(41.3881650454044,4.92006237873327,130.772806926573));
#61481=CARTESIAN_POINT('Ctrl Pts',(41.3804169774014,4.91726348327764,130.635542562912));
#61482=CARTESIAN_POINT('Ctrl Pts',(41.3726689093984,4.90874309523034,130.49870674874));
#61483=CARTESIAN_POINT('Ctrl Pts',(41.3649126066566,4.9002136516132,130.361725503835));
#61484=CARTESIAN_POINT('Ctrl Pts',(41.3571563039147,4.88595059254669,130.225174109095));
#61485=CARTESIAN_POINT('Ctrl Pts',(41.3494000011729,4.86602997878986,130.089563228078));
#61486=CARTESIAN_POINT('Ctrl Pts',(41.3416395586587,4.84609873280165,129.953879967451));
#61487=CARTESIAN_POINT('Ctrl Pts',(41.3338791161444,4.82050398822523,129.819138604696));
#61488=CARTESIAN_POINT('Ctrl Pts',(41.3261186736302,4.78937276566545,129.685838568609));
#61489=CARTESIAN_POINT('Ctrl Pts',(41.3183457733648,4.75819156850356,129.552324547471));
#61490=CARTESIAN_POINT('Ctrl Pts',(41.3105728730994,4.72145623784141,129.420256853484));
#61491=CARTESIAN_POINT('Ctrl Pts',(41.302799972834,4.67934367207602,129.290119599398));
#61492=CARTESIAN_POINT('Ctrl Pts',(41.295309637072,4.6387620041517,129.164713162295));
#61493=CARTESIAN_POINT('Ctrl Pts',(41.28781930131,4.59318737225453,129.041099538118));
#61494=CARTESIAN_POINT('Ctrl Pts',(41.2803289655481,4.54281919682059,128.919691732192));
#61495=CARTESIAN_POINT('Ctrl Pts',(41.272554631429,4.49054129670563,128.793680712402));
#61496=CARTESIAN_POINT('Ctrl Pts',(41.26478029731,4.43293358247985,128.669646914935));
#61497=CARTESIAN_POINT('Ctrl Pts',(41.2570059631909,4.37016637324084,128.548074081531));
#61498=CARTESIAN_POINT('Ctrl Pts',(41.2492412102438,4.30747651897746,128.426651075778));
#61499=CARTESIAN_POINT('Ctrl Pts',(41.2414764572967,4.239639999089,128.307683343545));
#61500=CARTESIAN_POINT('Ctrl Pts',(41.2337117043496,4.1668756239422,128.191635871808));
#61501=CARTESIAN_POINT('Ctrl Pts',(41.2259546634646,4.09418351939859,128.075703660056));
#61502=CARTESIAN_POINT('Ctrl Pts',(41.2181976225795,4.01657350605268,127.962686265877));
#61503=CARTESIAN_POINT('Ctrl Pts',(41.2104405816945,3.93431068068503,127.853024897871));
#61504=CARTESIAN_POINT('Ctrl Pts',(41.2026893904544,3.85210989035424,127.743446226356));
#61505=CARTESIAN_POINT('Ctrl Pts',(41.1949381992143,3.76526350556008,127.637218855082));
#61506=CARTESIAN_POINT('Ctrl Pts',(41.1871870079742,3.67408017743169,127.534755456036));
#61507=CARTESIAN_POINT('Ctrl Pts',(41.1794391111971,3.58293560464977,127.432335606667));
#61508=CARTESIAN_POINT('Ctrl Pts',(41.1716912144201,3.48745801411554,127.333676839121));
#61509=CARTESIAN_POINT('Ctrl Pts',(41.163943317643,3.38799648003716,127.239158952336));
#61510=CARTESIAN_POINT('Ctrl Pts',(41.1561970415589,3.2885557511677,127.144660836657));
#61511=CARTESIAN_POINT('Ctrl Pts',(41.1484507654748,3.18513301957122,127.054302148005));
#61512=CARTESIAN_POINT('Ctrl Pts',(41.1407044893907,3.07811409301214,126.968425699857));
#61513=CARTESIAN_POINT('Ctrl Pts',(41.1329581561253,2.9710943764638,126.882548617788));
#61514=CARTESIAN_POINT('Ctrl Pts',(41.12521182286,2.86047871691068,126.801154086934));
#61515=CARTESIAN_POINT('Ctrl Pts',(41.1174654895947,2.74668554056907,126.724544248692));
#61516=CARTESIAN_POINT('Ctrl Pts',(41.1097174215917,2.63286688103476,126.647917254209));
#61517=CARTESIAN_POINT('Ctrl Pts',(41.1019693535888,2.51586961299823,126.576077302798));
#61518=CARTESIAN_POINT('Ctrl Pts',(41.0942212855858,2.39614028928167,126.509282646611));
#61519=CARTESIAN_POINT('Ctrl Pts',(41.086464982844,2.27628371581475,126.442417000269));
#61520=CARTESIAN_POINT('Ctrl Pts',(41.0787086801021,2.15368962826356,126.380607551502));
#61521=CARTESIAN_POINT('Ctrl Pts',(41.0709523773603,2.02882877504139,126.324066334367));
#61522=CARTESIAN_POINT('Ctrl Pts',(41.0631919348461,1.90390127982238,126.267494939483));
#61523=CARTESIAN_POINT('Ctrl Pts',(41.0554314923319,1.77670497063303,126.216197525165));
#61524=CARTESIAN_POINT('Ctrl Pts',(41.0476710498178,1.64772868880453,126.170337178848));
#61525=CARTESIAN_POINT('Ctrl Pts',(41.0398981495523,1.51854536279828,126.124403213431));
#61526=CARTESIAN_POINT('Ctrl Pts',(41.0321252492869,1.38757672796261,126.083923872983));
#61527=CARTESIAN_POINT('Ctrl Pts',(41.0243523490215,1.25532569996852,126.049012002638));
#61528=CARTESIAN_POINT('Ctrl Pts',(41.0168620132594,1.12788232996117,126.015369266718));
#61529=CARTESIAN_POINT('Ctrl Pts',(41.0093716774973,0.999248485256093,125.986896311974));
#61530=CARTESIAN_POINT('Ctrl Pts',(41.0018813417352,0.869879430547576,125.963648599814));
#61531=CARTESIAN_POINT('Ctrl Pts',(40.9941070076161,0.735605308810048,125.939519443581));
#61532=CARTESIAN_POINT('Ctrl Pts',(40.9863326734969,0.600113785495589,125.92094314787));
#61533=CARTESIAN_POINT('Ctrl Pts',(40.9785583393779,0.463903907862529,125.908037892625));
#61534=CARTESIAN_POINT('Ctrl Pts',(40.9707935864308,0.327861896730224,125.895148541955));
#61535=CARTESIAN_POINT('Ctrl Pts',(40.9630288334837,0.191103678263022,125.887916362147));
#61536=CARTESIAN_POINT('Ctrl Pts',(40.9552640805366,0.0541387315197604,
125.886408598661));
#61537=CARTESIAN_POINT('Ctrl Pts',(40.9475070396516,-0.0826901797075282,
125.884902332707));
#61538=CARTESIAN_POINT('Ctrl Pts',(40.9397499987666,-0.219725022192236,
125.889109172808));
#61539=CARTESIAN_POINT('Ctrl Pts',(40.9319929578816,-0.3564513033596,125.899044569559));
#61540=CARTESIAN_POINT('Ctrl Pts',(40.9242417666415,-0.493074478174202,
125.90897247395));
#61541=CARTESIAN_POINT('Ctrl Pts',(40.9164905754014,-0.629389166464533,
125.924620308174));
#61542=CARTESIAN_POINT('Ctrl Pts',(40.9087393841613,-0.764881342126213,
125.945951454582));
#61543=CARTESIAN_POINT('Ctrl Pts',(40.9009914873842,-0.900315929999418,
125.967273534684));
#61544=CARTESIAN_POINT('Ctrl Pts',(40.8932435906071,-1.0349283151517,125.994274061933));
#61545=CARTESIAN_POINT('Ctrl Pts',(40.8854956938301,-1.16821027884121,126.026864640916));
#61546=CARTESIAN_POINT('Ctrl Pts',(40.877749417746,-1.30146436281679,126.059448402652));
#61547=CARTESIAN_POINT('Ctrl Pts',(40.8700031416618,-1.43338819933889,126.097619797478));
#61548=CARTESIAN_POINT('Ctrl Pts',(40.8622568655778,-1.56348483120099,126.141239533452));
#61549=CARTESIAN_POINT('Ctrl Pts',(40.8545105323124,-1.69358242340704,126.184859591418));
#61550=CARTESIAN_POINT('Ctrl Pts',(40.8467641990471,-1.82185241335442,126.2339279465));
#61551=CARTESIAN_POINT('Ctrl Pts',(40.8390178657817,-1.94781443133571,126.288255879677));
#61552=CARTESIAN_POINT('Ctrl Pts',(40.8312697977788,-2.07380465763723,126.342595979219));
#61553=CARTESIAN_POINT('Ctrl Pts',(40.8235217297759,-2.19748552456353,126.402197845827));
#61554=CARTESIAN_POINT('Ctrl Pts',(40.8157736617729,-2.31839838455661,126.466825373561));
#61555=CARTESIAN_POINT('Ctrl Pts',(40.8080173590311,-2.43943975217667,126.531521588201));
#61556=CARTESIAN_POINT('Ctrl Pts',(40.8002610562892,-2.55770689080747,126.601253949265));
#61557=CARTESIAN_POINT('Ctrl Pts',(40.7925047535473,-2.67276695917592,126.675741012367));
#61558=CARTESIAN_POINT('Ctrl Pts',(40.7847443110331,-2.78788843856741,126.750267831457));
#61559=CARTESIAN_POINT('Ctrl Pts',(40.776983868519,-2.89979911811035,126.829554183317));
#61560=CARTESIAN_POINT('Ctrl Pts',(40.7692234260048,-3.00809755704936,126.913276944632));
#61561=CARTESIAN_POINT('Ctrl Pts',(40.7614505257393,-3.11656984625669,126.997134105156));
#61562=CARTESIAN_POINT('Ctrl Pts',(40.7536776254739,-3.22141800802557,127.085441654592));
#61563=CARTESIAN_POINT('Ctrl Pts',(40.7459047252085,-3.32227526434383,127.177837471296));
#61564=CARTESIAN_POINT('Ctrl Pts',(40.7384143894464,-3.4194661053511,127.266874467333));
#61565=CARTESIAN_POINT('Ctrl Pts',(40.7309240536844,-3.51295094369156,127.359707436453));
#61566=CARTESIAN_POINT('Ctrl Pts',(40.7234337179223,-3.60243703642587,127.455983329821));
#61567=CARTESIAN_POINT('Ctrl Pts',(40.715748964601,-3.69424581111858,127.554758139766));
#61568=CARTESIAN_POINT('Ctrl Pts',(40.7080642112797,-3.78215134313305,127.657486478633));
#61569=CARTESIAN_POINT('Ctrl Pts',(40.7003794579584,-3.86578782177955,127.763823234227));
#61570=CARTESIAN_POINT('Ctrl Pts',(40.692703831564,-3.94932496815152,127.87003369718));
#61571=CARTESIAN_POINT('Ctrl Pts',(40.6850282051695,-4.0286028972979,127.979843744061));
#61572=CARTESIAN_POINT('Ctrl Pts',(40.6773525787751,-4.10329254126362,128.092871472592));
#61573=CARTESIAN_POINT('Ctrl Pts',(40.6696455462613,-4.17828779049929,128.20636167313));
#61574=CARTESIAN_POINT('Ctrl Pts',(40.6619385137475,-4.24865682752416,128.323095663254));
#61575=CARTESIAN_POINT('Ctrl Pts',(40.6542314812337,-4.31410685386605,128.442652524696));
#61576=CARTESIAN_POINT('Ctrl Pts',(40.6465694208885,-4.379174965429,128.561511746507));
#61577=CARTESIAN_POINT('Ctrl Pts',(40.6389073605433,-4.43938111500533,128.683160634019));
#61578=CARTESIAN_POINT('Ctrl Pts',(40.6312453001981,-4.49448096616251,128.807156595113));
#61579=CARTESIAN_POINT('Ctrl Pts',(40.6235157816,-4.55006592700635,128.932244240496));
#61580=CARTESIAN_POINT('Ctrl Pts',(40.6157862630018,-4.60045401555403,129.059720140441));
#61581=CARTESIAN_POINT('Ctrl Pts',(40.6080567444037,-4.64544223829743,129.189105382892));
#61582=CARTESIAN_POINT('Ctrl Pts',(40.6003272258056,-4.69043046104083,129.318490625343));
#61583=CARTESIAN_POINT('Ctrl Pts',(40.5925977072075,-4.73001866836183,129.449784818233));
#61584=CARTESIAN_POINT('Ctrl Pts',(40.5848681886094,-4.76405452823407,129.582490119308));
#61585=CARTESIAN_POINT('Ctrl Pts',(42.3345736784939,-4.76405452823401,129.582490119308));
#61586=CARTESIAN_POINT('Ctrl Pts',(42.3263003656675,-4.80031713428966,129.723877469957));
#61587=CARTESIAN_POINT('Ctrl Pts',(42.318027052841,-4.83032222928608,129.867039220305));
#61588=CARTESIAN_POINT('Ctrl Pts',(42.3097537400146,-4.85390803146789,130.011416808364));
#61589=CARTESIAN_POINT('Ctrl Pts',(42.3015021780208,-4.87743182573972,130.155414822626));
#61590=CARTESIAN_POINT('Ctrl Pts',(42.2932506160271,-4.89456993314338,130.300621998682));
#61591=CARTESIAN_POINT('Ctrl Pts',(42.2849990540334,-4.90521111842529,130.446468250817));
#61592=CARTESIAN_POINT('Ctrl Pts',(42.2782858480343,-4.91386844523521,130.565124080529));
#61593=CARTESIAN_POINT('Ctrl Pts',(42.271572642035,-4.91822640423858,130.684202544152));
#61594=CARTESIAN_POINT('Ctrl Pts',(42.2648594360359,-4.9182499044007,130.80339089469));
#61595=CARTESIAN_POINT('',(42.6101405639782,-4.91824847792861,130.800491269695));
#61596=CARTESIAN_POINT('Ctrl Pts',(42.6801909902419,-4.76405452823402,129.582490119308));
#61597=CARTESIAN_POINT('Ctrl Pts',(42.6724154236971,-4.79806552328429,129.71509847282));
#61598=CARTESIAN_POINT('Ctrl Pts',(42.6646398571522,-4.82649231743152,129.848959149606));
#61599=CARTESIAN_POINT('Ctrl Pts',(42.6568642906074,-4.84927547674462,129.983561974083));
#61600=CARTESIAN_POINT('Ctrl Pts',(42.6555688898893,-4.85307112568726,130.005986654584));
#61601=CARTESIAN_POINT('Ctrl Pts',(42.6542734891712,-4.85671025160539,130.028431928163));
#61602=CARTESIAN_POINT('Ctrl Pts',(42.6529780884531,-4.86019272010058,130.05089543192));
#61603=CARTESIAN_POINT('Ctrl Pts',(42.6399837889497,-4.89512572423288,130.276229177405));
#61604=CARTESIAN_POINT('Ctrl Pts',(42.6269894894463,-4.91439406463795,130.504051802434));
#61605=CARTESIAN_POINT('Ctrl Pts',(42.6139951899428,-4.91772728215714,130.732656776474));
#61606=CARTESIAN_POINT('Ctrl Pts',(42.6127103146314,-4.9180568704429,130.755261218301));
#61607=CARTESIAN_POINT('Ctrl Pts',(42.61142543932,-4.9182306836054,130.777873274665));
#61608=CARTESIAN_POINT('Ctrl Pts',(42.6101405640086,-4.91824847792818,130.80049126916));
#61609=CARTESIAN_POINT('Ctrl Pts',(42.6101405639782,-4.91824847792861,130.800491269695));
#61610=CARTESIAN_POINT('Ctrl Pts',(42.602490936903,-4.91835441810297,130.935149645914));
#61611=CARTESIAN_POINT('Ctrl Pts',(42.5948413098278,-4.91292591779319,131.070013994383));
#61612=CARTESIAN_POINT('Ctrl Pts',(42.5871916827525,-4.90193885387951,131.204583724503));
#61613=CARTESIAN_POINT('Ctrl Pts',(42.5795495955671,-4.89096261941543,131.339020815356));
#61614=CARTESIAN_POINT('Ctrl Pts',(42.5719075083817,-4.87443875066124,131.473163465993));
#61615=CARTESIAN_POINT('Ctrl Pts',(42.5642654211963,-4.85239516194762,131.606510388374));
#61616=CARTESIAN_POINT('Ctrl Pts',(42.5563597980065,-4.8295914040353,131.74445575543));
#61617=CARTESIAN_POINT('Ctrl Pts',(42.5484541748166,-4.80088036594323,131.881549087371));
#61618=CARTESIAN_POINT('Ctrl Pts',(42.5405485516268,-4.76635154074265,132.017239858282));
#61619=CARTESIAN_POINT('Ctrl Pts',(42.5329149785985,-4.73301092958273,132.148261206523));
#61620=CARTESIAN_POINT('Ctrl Pts',(42.5252814055703,-4.69424643173644,132.277974505326));
#61621=CARTESIAN_POINT('Ctrl Pts',(42.517647832542,-4.65019063055263,132.405894308133));
#61622=CARTESIAN_POINT('Ctrl Pts',(42.5100153953198,-4.60614138447046,132.533795077639));
#61623=CARTESIAN_POINT('Ctrl Pts',(42.5023829580976,-4.55680253169002,132.659902500209));
#61624=CARTESIAN_POINT('Ctrl Pts',(42.4947505208754,-4.50235621997596,132.783747272806));
#61625=CARTESIAN_POINT('Ctrl Pts',(42.4871174528635,-4.44790540849718,132.907602280667));
#61626=CARTESIAN_POINT('Ctrl Pts',(42.4794843848517,-4.38834646157192,133.029193897404));
#61627=CARTESIAN_POINT('Ctrl Pts',(42.4718513168399,-4.3239090338387,133.148074279596));
#61628=CARTESIAN_POINT('Ctrl Pts',(42.4642158511133,-4.25945136489127,133.266992004734));
#61629=CARTESIAN_POINT('Ctrl Pts',(42.4565803853868,-4.19011236062939,133.383196447527));
#61630=CARTESIAN_POINT('Ctrl Pts',(42.4489449196602,-4.11616654113823,133.496266274924));
#61631=CARTESIAN_POINT('Ctrl Pts',(42.4413012514732,-4.04214128475504,133.609457568493));
#61632=CARTESIAN_POINT('Ctrl Pts',(42.4336575832861,-3.96349955767633,133.719507188693));
#61633=CARTESIAN_POINT('Ctrl Pts',(42.426013915099,-3.88055806622757,133.826024423673));
#61634=CARTESIAN_POINT('Ctrl Pts',(42.4183653414255,-3.79756334531459,133.932610018352));
#61635=CARTESIAN_POINT('Ctrl Pts',(42.410716767752,-3.71026362787921,134.035658409125));
#61636=CARTESIAN_POINT('Ctrl Pts',(42.4030681940785,-3.61901352737722,134.134814663362));
#61637=CARTESIAN_POINT('Ctrl Pts',(42.395409002189,-3.52763674792596,134.234108572353));
#61638=CARTESIAN_POINT('Ctrl Pts',(42.3877498102996,-3.43229892749435,134.329499280756));
#61639=CARTESIAN_POINT('Ctrl Pts',(42.3800906184101,-3.33338899354607,134.420671013564));
#61640=CARTESIAN_POINT('Ctrl Pts',(42.3782372338201,-3.30945459550316,134.442732908221));
#61641=CARTESIAN_POINT('Ctrl Pts',(42.3763838492302,-3.28531116972019,134.464547956016));
#61642=CARTESIAN_POINT('Ctrl Pts',(42.3745304646402,-3.2609644819492,134.486112063545));
#61643=CARTESIAN_POINT('Ctrl Pts',(42.3667561305212,-3.15883819555765,134.576566348002));
#61644=CARTESIAN_POINT('Ctrl Pts',(42.3589817964021,-3.05278369607015,134.662911439298));
#61645=CARTESIAN_POINT('Ctrl Pts',(42.351207462283,-2.94316572360792,134.744786810997));
#61646=CARTESIAN_POINT('Ctrl Pts',(42.3434427093359,-2.83368284549992,134.826561278619));
#61647=CARTESIAN_POINT('Ctrl Pts',(42.3356779563888,-2.72064554274382,134.903876755263));
#61648=CARTESIAN_POINT('Ctrl Pts',(42.3279132034417,-2.6044539598755,134.976410789051));
#61649=CARTESIAN_POINT('Ctrl Pts',(42.3201561625567,-2.48837778012531,135.048872781015));
#61650=CARTESIAN_POINT('Ctrl Pts',(42.3123991216717,-2.36915388432812,135.116562575144));
#61651=CARTESIAN_POINT('Ctrl Pts',(42.3046420807867,-2.24721364146024,135.179199347409));
#61652=CARTESIAN_POINT('Ctrl Pts',(42.2968908895466,-2.12536535467789,135.241788884797));
#61653=CARTESIAN_POINT('Ctrl Pts',(42.2891396983065,-2.00080514443834,135.29933280702));
#61654=CARTESIAN_POINT('Ctrl Pts',(42.2813885070663,-1.87399106614283,135.351595001949));
#61655=CARTESIAN_POINT('Ctrl Pts',(42.2736406102893,-1.74723088721381,135.403834984052));
#61656=CARTESIAN_POINT('Ctrl Pts',(42.2658927135122,-1.61821910624177,135.450797555089));
#61657=CARTESIAN_POINT('Ctrl Pts',(42.2581448167352,-1.48743575252551,135.492293844971));
#61658=CARTESIAN_POINT('Ctrl Pts',(42.2503985406511,-1.35667975586748,135.533781454724));
#61659=CARTESIAN_POINT('Ctrl Pts',(42.242652264567,-1.22415329597946,135.569804939498));
#61660=CARTESIAN_POINT('Ctrl Pts',(42.234905988483,-1.09035325948175,135.600224755762));
#61661=CARTESIAN_POINT('Ctrl Pts',(42.2271596552176,-0.956552235302742,
135.630644796579));
#61662=CARTESIAN_POINT('Ctrl Pts',(42.2194133219523,-0.821477996990924,
135.655460999671));
#61663=CARTESIAN_POINT('Ctrl Pts',(42.211666988687,-0.685638975432793,135.674584663528));
#61664=CARTESIAN_POINT('Ctrl Pts',(42.203918920684,-0.549769533666885,135.693712609997));
#61665=CARTESIAN_POINT('Ctrl Pts',(42.196170852681,-0.413135354924745,135.707145426026));
#61666=CARTESIAN_POINT('Ctrl Pts',(42.188422784678,-0.276250967826932,135.714846180652));
#61667=CARTESIAN_POINT('Ctrl Pts',(42.1806664819362,-0.139221098374127,
135.722555119732));
#61668=CARTESIAN_POINT('Ctrl Pts',(42.1729101791943,-0.001940880323405,
135.724519805782));
#61669=CARTESIAN_POINT('Ctrl Pts',(42.1651538764525,0.135073613629645,135.720755453358));
#61670=CARTESIAN_POINT('Ctrl Pts',(42.1573934339384,0.272161236343732,135.716989091786));
#61671=CARTESIAN_POINT('Ctrl Pts',(42.1496329914242,0.408982462526884,135.707487625964));
#61672=CARTESIAN_POINT('Ctrl Pts',(42.14187254891,0.545026356806567,135.692318200533));
#61673=CARTESIAN_POINT('Ctrl Pts',(42.1340996486446,0.681288640822758,135.677124423794));
#61674=CARTESIAN_POINT('Ctrl Pts',(42.1263267483792,0.816770712723501,135.656244564904));
#61675=CARTESIAN_POINT('Ctrl Pts',(42.1185538481138,0.950970954979181,135.629797106143));
#61676=CARTESIAN_POINT('Ctrl Pts',(42.1110635123517,1.08029268040031,135.604311079124));
#61677=CARTESIAN_POINT('Ctrl Pts',(42.1035731765896,1.20842385407488,135.573655288672));
#61678=CARTESIAN_POINT('Ctrl Pts',(42.0960828408274,1.3349308081423,135.537978979873));
#61679=CARTESIAN_POINT('Ctrl Pts',(42.0883085067084,1.46623431182285,135.500949992983));
#61680=CARTESIAN_POINT('Ctrl Pts',(42.0805341725892,1.59620393004817,135.458394969886));
#61681=CARTESIAN_POINT('Ctrl Pts',(42.0727598384701,1.72433919077393,135.410425903432));
#61682=CARTESIAN_POINT('Ctrl Pts',(42.0649950855231,1.85231653624261,135.362515954565));
#61683=CARTESIAN_POINT('Ctrl Pts',(42.057230332576,1.97846365966066,135.309205374035));
#61684=CARTESIAN_POINT('Ctrl Pts',(42.0494655796289,2.10229298523511,135.250656521656));
#61685=CARTESIAN_POINT('Ctrl Pts',(42.0417085387439,2.22599932177772,135.192165820823));
#61686=CARTESIAN_POINT('Ctrl Pts',(42.0339514978589,2.3473920905378,135.128447367835));
#61687=CARTESIAN_POINT('Ctrl Pts',(42.0261944569739,2.46600186083584,135.05971229338));
#61688=CARTESIAN_POINT('Ctrl Pts',(42.0184432657337,2.58452218658345,134.99102905258));
#61689=CARTESIAN_POINT('Ctrl Pts',(42.0106920744936,2.70026335426499,134.917336915527));
#61690=CARTESIAN_POINT('Ctrl Pts',(42.0029408832534,2.81277912592624,134.83889363283));
#61691=CARTESIAN_POINT('Ctrl Pts',(41.9951929864764,2.92524707538293,134.760483690621));
#61692=CARTESIAN_POINT('Ctrl Pts',(41.9874450896993,3.03449203534917,134.677326842256));
#61693=CARTESIAN_POINT('Ctrl Pts',(41.9796971929222,3.1400956365078,134.589724861081));
#61694=CARTESIAN_POINT('Ctrl Pts',(41.9719509168381,3.24567714766962,134.502141204353));
#61695=CARTESIAN_POINT('Ctrl Pts',(41.964204640754,3.34761851435612,134.410114513748));
#61696=CARTESIAN_POINT('Ctrl Pts',(41.9564583646699,3.44553375528819,134.313987407364));
#61697=CARTESIAN_POINT('Ctrl Pts',(41.9487120314045,3.54344971900859,134.217859591392));
#61698=CARTESIAN_POINT('Ctrl Pts',(41.9409656981392,3.63733921868066,134.117631573139));
#61699=CARTESIAN_POINT('Ctrl Pts',(41.9332193648738,3.72685280789925,134.013683164577));
#61700=CARTESIAN_POINT('Ctrl Pts',(41.9254712968708,3.81638644306539,133.90971147749));
#61701=CARTESIAN_POINT('Ctrl Pts',(41.9177232288679,3.9015419627124,133.802018038411));
#61702=CARTESIAN_POINT('Ctrl Pts',(41.9099751608649,3.98201018048921,133.691015772755));
#61703=CARTESIAN_POINT('Ctrl Pts',(41.902218858123,4.06256392084534,133.579895532571));
#61704=CARTESIAN_POINT('Ctrl Pts',(41.8944625553811,4.1384201779745,133.465459757947));
#61705=CARTESIAN_POINT('Ctrl Pts',(41.8867062526393,4.2093128024148,133.348150859297));
#61706=CARTESIAN_POINT('Ctrl Pts',(41.8789458101251,4.28024326438338,133.230779349356));
#61707=CARTESIAN_POINT('Ctrl Pts',(41.8711853676109,4.3462046268886,133.110532002427));
#61708=CARTESIAN_POINT('Ctrl Pts',(41.8634249250968,4.40697720756797,132.987874976226));
#61709=CARTESIAN_POINT('Ctrl Pts',(41.8556520248314,4.46784734578889,132.865021050079));
#61710=CARTESIAN_POINT('Ctrl Pts',(41.8478791245659,4.52351189835222,132.739750072188));
#61711=CARTESIAN_POINT('Ctrl Pts',(41.8401062243005,4.5737994112277,132.612548110154));
#61712=CARTESIAN_POINT('Ctrl Pts',(41.8326158885385,4.62225884634341,132.489970259843));
#61713=CARTESIAN_POINT('Ctrl Pts',(41.8251255527765,4.66572529076719,132.365599671021));
#61714=CARTESIAN_POINT('Ctrl Pts',(41.8176352170145,4.70408990054633,132.239881871354));
#61715=CARTESIAN_POINT('Ctrl Pts',(41.8098608828954,4.74390911616609,132.109397443102));
#61716=CARTESIAN_POINT('Ctrl Pts',(41.8020865487763,4.77835812334886,131.97704829291));
#61717=CARTESIAN_POINT('Ctrl Pts',(41.7943122146572,4.80726062748651,131.843316016954));
#61718=CARTESIAN_POINT('Ctrl Pts',(41.7865474617101,4.83612751187087,131.709748554077));
#61719=CARTESIAN_POINT('Ctrl Pts',(41.7787827087631,4.85946141215908,131.574801735513));
#61720=CARTESIAN_POINT('Ctrl Pts',(41.771017955816,4.87713537963544,131.438973532033));
#61721=CARTESIAN_POINT('Ctrl Pts',(41.763260914931,4.89479179307817,131.303280235039));
#61722=CARTESIAN_POINT('Ctrl Pts',(41.755503874046,4.90679941067691,131.166707680409));
#61723=CARTESIAN_POINT('Ctrl Pts',(41.747746833161,4.91308212391046,131.029764934764));
#61724=CARTESIAN_POINT('Ctrl Pts',(41.7399956419208,4.91936009930108,130.892925458708));
#61725=CARTESIAN_POINT('Ctrl Pts',(41.7322444506807,4.91992174559568,130.75571673627));
#61726=CARTESIAN_POINT('Ctrl Pts',(41.7244932594406,4.91474271316701,130.618653520578));
#61727=CARTESIAN_POINT('Ctrl Pts',(41.7167453626635,4.90956588196528,130.481648560409));
#61728=CARTESIAN_POINT('Ctrl Pts',(41.7089974658864,4.89865323962955,130.344789373851));
#61729=CARTESIAN_POINT('Ctrl Pts',(41.7012495691094,4.88203253778829,130.208591062724));
#61730=CARTESIAN_POINT('Ctrl Pts',(41.6935032930253,4.86541531263955,130.072421241348));
#61731=CARTESIAN_POINT('Ctrl Pts',(41.6857570169412,4.84309245025204,129.936912408276));
#61732=CARTESIAN_POINT('Ctrl Pts',(41.6780107408571,4.8151435726271,129.802574493941));
#61733=CARTESIAN_POINT('Ctrl Pts',(41.6702644075917,4.78719448868986,129.668235587953));
#61734=CARTESIAN_POINT('Ctrl Pts',(41.6625180743263,4.75361938627987,129.535068000719));
#61735=CARTESIAN_POINT('Ctrl Pts',(41.654771741061,4.71454892764822,129.403571029044));
#61736=CARTESIAN_POINT('Ctrl Pts',(41.647023673058,4.67546971945842,129.272044609535));
#61737=CARTESIAN_POINT('Ctrl Pts',(41.639275605055,4.63089281753342,129.142189924746));
#61738=CARTESIAN_POINT('Ctrl Pts',(41.6315275370521,4.58099850494366,129.014490298184));
#61739=CARTESIAN_POINT('Ctrl Pts',(41.6237712343102,4.5310511640846,128.886654950939));
#61740=CARTESIAN_POINT('Ctrl Pts',(41.6160149315683,4.47577526577443,128.760979602022));
#61741=CARTESIAN_POINT('Ctrl Pts',(41.6082586288265,4.41539916213832,128.637927304148));
#61742=CARTESIAN_POINT('Ctrl Pts',(41.6004981863123,4.35499083395765,128.514809329557));
#61743=CARTESIAN_POINT('Ctrl Pts',(41.5927377437981,4.289477063034,128.394317538938));
#61744=CARTESIAN_POINT('Ctrl Pts',(41.5849773012839,4.21913129737396,128.276888726917));
#61745=CARTESIAN_POINT('Ctrl Pts',(41.5772044010185,4.14867260644606,128.159271407743));
#61746=CARTESIAN_POINT('Ctrl Pts',(41.5694315007531,4.07336663523073,128.044727219706));
#61747=CARTESIAN_POINT('Ctrl Pts',(41.5616586004876,3.99352965107491,127.933663143347));
#61748=CARTESIAN_POINT('Ctrl Pts',(41.5541682647256,3.91659494239102,127.826636525919));
#61749=CARTESIAN_POINT('Ctrl Pts',(41.5466779289637,3.83545311859458,127.722841634013));
#61750=CARTESIAN_POINT('Ctrl Pts',(41.5391875932017,3.75042018191592,127.622610859716));
#61751=CARTESIAN_POINT('Ctrl Pts',(41.5314132590827,3.66216319559726,127.518579805147));
#61752=CARTESIAN_POINT('Ctrl Pts',(41.5236389249636,3.5694346370642,127.418058931271));
#61753=CARTESIAN_POINT('Ctrl Pts',(41.5158645908445,3.47254439527722,127.321456874232));
#61754=CARTESIAN_POINT('Ctrl Pts',(41.5080998378974,3.37577356205404,127.224973870595));
#61755=CARTESIAN_POINT('Ctrl Pts',(41.5003350849504,3.27485152477227,127.13240034774));
#61756=CARTESIAN_POINT('Ctrl Pts',(41.4925703320033,3.17012862146141,127.04411227658));
#61757=CARTESIAN_POINT('Ctrl Pts',(41.4848132911183,3.06550973041472,126.955911894377));
#61758=CARTESIAN_POINT('Ctrl Pts',(41.4770562502333,2.95709778288425,126.871988743871));
#61759=CARTESIAN_POINT('Ctrl Pts',(41.4692992093484,2.84527993251994,126.792682020258));
#61760=CARTESIAN_POINT('Ctrl Pts',(41.4615480181082,2.73354640486565,126.713435102462));
#61761=CARTESIAN_POINT('Ctrl Pts',(41.4537968268681,2.6184124042664,126.63879790754));
#61762=CARTESIAN_POINT('Ctrl Pts',(41.446045635628,2.50029784553984,126.569069158163));
#61763=CARTESIAN_POINT('Ctrl Pts',(41.4382977388509,2.38223348865171,126.499370045365));
#61764=CARTESIAN_POINT('Ctrl Pts',(41.4305498420737,2.26119142920822,126.434575427118));
#61765=CARTESIAN_POINT('Ctrl Pts',(41.4228019452966,2.13762003739266,126.374940380307));
#61766=CARTESIAN_POINT('Ctrl Pts',(41.4150556692125,2.01407449404855,126.315317807863));
#61767=CARTESIAN_POINT('Ctrl Pts',(41.4073093931285,1.88800102258879,126.260852829943));
#61768=CARTESIAN_POINT('Ctrl Pts',(41.3995631170444,1.75987167956568,126.211754088158));
#61769=CARTESIAN_POINT('Ctrl Pts',(41.391816783779,1.63174139072086,126.162654983937));
#61770=CARTESIAN_POINT('Ctrl Pts',(41.3840704505137,1.50155556510905,126.118922334792));
#61771=CARTESIAN_POINT('Ctrl Pts',(41.3763241172483,1.36980490141204,126.080716092989));
#61772=CARTESIAN_POINT('Ctrl Pts',(41.3685760492453,1.23802473306704,126.042501295163));
#61773=CARTESIAN_POINT('Ctrl Pts',(41.3608279812424,1.1046794047361,126.00981547623));
#61774=CARTESIAN_POINT('Ctrl Pts',(41.3530799132394,0.970272997576767,125.982768207099));
#61775=CARTESIAN_POINT('Ctrl Pts',(41.3453236104975,0.835723741688818,125.955692191808));
#61776=CARTESIAN_POINT('Ctrl Pts',(41.3375673077556,0.700111538108701,125.93426677467));
#61777=CARTESIAN_POINT('Ctrl Pts',(41.3298110050138,0.563949396101245,125.918550127879));
#61778=CARTESIAN_POINT('Ctrl Pts',(41.3220505624996,0.427714580258837,125.90282509264));
#61779=CARTESIAN_POINT('Ctrl Pts',(41.3142901199854,0.290929630859906,125.892814927559));
#61780=CARTESIAN_POINT('Ctrl Pts',(41.3065296774712,0.154109840920753,125.888525671249));
#61781=CARTESIAN_POINT('Ctrl Pts',(41.2987567772058,0.0170704157083132,
125.884229529444));
#61782=CARTESIAN_POINT('Ctrl Pts',(41.2909838769404,-0.120003570640024,
125.885672644272));
#61783=CARTESIAN_POINT('Ctrl Pts',(41.283210976675,-0.256598763641481,125.89280891398));
#61784=CARTESIAN_POINT('Ctrl Pts',(41.2757206409129,-0.38822837731555,125.899685762309));
#61785=CARTESIAN_POINT('Ctrl Pts',(41.2682303051508,-0.519413097263414,
125.911849002319));
#61786=CARTESIAN_POINT('Ctrl Pts',(41.2607399693888,-0.649702465683745,
125.929212438425));
#61787=CARTESIAN_POINT('Ctrl Pts',(41.2529656352697,-0.784931795107384,
125.947234214488));
#61788=CARTESIAN_POINT('Ctrl Pts',(41.2451913011506,-0.919624904106275,
125.970915389302));
#61789=CARTESIAN_POINT('Ctrl Pts',(41.2374169670315,-1.05327049296709,126.000216122326));
#61790=CARTESIAN_POINT('Ctrl Pts',(41.2296522140844,-1.18675137558388,126.029480744815));
#61791=CARTESIAN_POINT('Ctrl Pts',(41.2218874611373,-1.31918692848946,126.064351062703));
#61792=CARTESIAN_POINT('Ctrl Pts',(41.2141227081902,-1.45007147044329,126.104735548148));
#61793=CARTESIAN_POINT('Ctrl Pts',(41.2063656673053,-1.58082601602474,126.145079923151));
#61794=CARTESIAN_POINT('Ctrl Pts',(41.1986086264202,-1.71003224512234,126.190927452209));
#61795=CARTESIAN_POINT('Ctrl Pts',(41.1908515855353,-1.83719551720577,126.24213575528));
#61796=CARTESIAN_POINT('Ctrl Pts',(41.1831003942951,-1.96426289447705,126.293305441771));
#61797=CARTESIAN_POINT('Ctrl Pts',(41.175349203055,-2.08929002002813,126.34982771027));
#61798=CARTESIAN_POINT('Ctrl Pts',(41.1675980118148,-2.21179859579991,126.411510741447));
#61799=CARTESIAN_POINT('Ctrl Pts',(41.1598501150377,-2.33425510215862,126.47316755569));
#61800=CARTESIAN_POINT('Ctrl Pts',(41.1521022182607,-2.45419483931453,126.53998059453));
#61801=CARTESIAN_POINT('Ctrl Pts',(41.1443543214836,-2.57116084882389,126.61171050672));
#61802=CARTESIAN_POINT('Ctrl Pts',(41.1366080453995,-2.68810239156556,126.683425414559));
#61803=CARTESIAN_POINT('Ctrl Pts',(41.1288617693154,-2.80207111085763,126.760054945737));
#61804=CARTESIAN_POINT('Ctrl Pts',(41.1211154932313,-2.91263631250718,126.841314721596));
#61805=CARTESIAN_POINT('Ctrl Pts',(41.113369159966,-3.02320233032363,126.922575097296));
#61806=CARTESIAN_POINT('Ctrl Pts',(41.1056228267007,-3.13036446533105,127.008465554344));
#61807=CARTESIAN_POINT('Ctrl Pts',(41.0978764934354,-3.23372291053355,127.098659712151));
#61808=CARTESIAN_POINT('Ctrl Pts',(41.0901284254324,-3.33710450214294,127.188874068314));
#61809=CARTESIAN_POINT('Ctrl Pts',(41.0823803574295,-3.43668041442428,127.283393786046));
#61810=CARTESIAN_POINT('Ctrl Pts',(41.0746322894265,-3.53208599409094,127.381853993344));
#61811=CARTESIAN_POINT('Ctrl Pts',(41.0668759866847,-3.62759297194367,127.480418845322));
#61812=CARTESIAN_POINT('Ctrl Pts',(41.0591196839428,-3.7189204907284,127.582932271623));
#61813=CARTESIAN_POINT('Ctrl Pts',(41.051363381201,-3.80574231449314,127.688994106515));
#61814=CARTESIAN_POINT('Ctrl Pts',(41.0436029386868,-3.89261047767926,127.795112549802));
#61815=CARTESIAN_POINT('Ctrl Pts',(41.0358424961727,-3.97496791937254,127.904782862944));
#61816=CARTESIAN_POINT('Ctrl Pts',(41.0280820536585,-4.05253103065552,128.017574779351));
#61817=CARTESIAN_POINT('Ctrl Pts',(41.0203091533931,-4.13021865313057,128.130547759356));
#61818=CARTESIAN_POINT('Ctrl Pts',(41.0125362531276,-4.2030963575945,128.246652025022));
#61819=CARTESIAN_POINT('Ctrl Pts',(41.0047633528622,-4.2709254501196,128.365430757562));
#61820=CARTESIAN_POINT('Ctrl Pts',(40.9972730171001,-4.33628878428097,128.479891583989));
#61821=CARTESIAN_POINT('Ctrl Pts',(40.989782681338,-4.39696405147731,128.596835532555));
#61822=CARTESIAN_POINT('Ctrl Pts',(40.9822923455758,-4.45278028704966,128.715837029535));
#61823=CARTESIAN_POINT('Ctrl Pts',(40.9735532160698,-4.51790224241996,128.854678534984));
#61824=CARTESIAN_POINT('Ctrl Pts',(40.9648140865637,-4.57659685686595,128.996719232411));
#61825=CARTESIAN_POINT('Ctrl Pts',(40.9560749570576,-4.62856642545606,129.141364553938));
#61826=CARTESIAN_POINT('Ctrl Pts',(40.9473358275515,-4.68053599404616,129.286009875465));
#61827=CARTESIAN_POINT('Ctrl Pts',(40.9385966980454,-4.72578031392211,129.433259538598));
#61828=CARTESIAN_POINT('Ctrl Pts',(40.9298575685393,-4.7640545282341,129.582490119308));
#61829=CARTESIAN_POINT('Origin',(213.235140564004,0.,130.804360617566));
#61830=CARTESIAN_POINT('',(38.8349537180509,-4.76405452823399,129.582490119308));
#61831=CARTESIAN_POINT('',(39.1801134839906,-4.76405452823399,129.582490119308));
#61832=CARTESIAN_POINT('',(213.235140564004,-4.76405452823405,129.582490119308));
#61833=CARTESIAN_POINT('',(40.5148594359403,-4.91824790287309,130.808902465697));
#61834=CARTESIAN_POINT('Ctrl Pts',(40.5148594359403,-4.91824790287309,130.808902465697));
#61835=CARTESIAN_POINT('Ctrl Pts',(40.5049161768737,-4.91808570323451,130.984544188899));
#61836=CARTESIAN_POINT('Ctrl Pts',(40.4949729178071,-4.90851119862581,131.159764942237));
#61837=CARTESIAN_POINT('Ctrl Pts',(40.4850296587406,-4.88968022370207,131.333709625723));
#61838=CARTESIAN_POINT('Ctrl Pts',(40.4748644570866,-4.87042892428828,131.511536912775));
#61839=CARTESIAN_POINT('Ctrl Pts',(40.4646992554327,-4.8415033080866,131.688030791579));
#61840=CARTESIAN_POINT('Ctrl Pts',(40.4545340537788,-4.80311786982472,131.862302861297));
#61841=CARTESIAN_POINT('Ctrl Pts',(40.4513514005557,-4.79109965877848,131.916866221992));
#61842=CARTESIAN_POINT('Ctrl Pts',(40.4481687473327,-4.77815447652257,131.971211951237));
#61843=CARTESIAN_POINT('Ctrl Pts',(40.4449860941096,-4.76428985575759,132.02531320994));
#61844=CARTESIAN_POINT('Ctrl Pts',(40.4372117599905,-4.73042245434591,132.15746749504));
#61845=CARTESIAN_POINT('Ctrl Pts',(40.4294374258714,-4.69099859851613,132.288420888444));
#61846=CARTESIAN_POINT('Ctrl Pts',(40.4216630917524,-4.646118238918,132.417670374709));
#61847=CARTESIAN_POINT('Ctrl Pts',(40.4138983388053,-4.60129319035206,132.546760572534));
#61848=CARTESIAN_POINT('Ctrl Pts',(40.4061335858583,-4.55102514508867,132.674150675636));
#61849=CARTESIAN_POINT('Ctrl Pts',(40.3983688329113,-4.49546471571193,132.799349352444));
#61850=CARTESIAN_POINT('Ctrl Pts',(40.3906117920263,-4.43995946973684,132.924423680161));
#61851=CARTESIAN_POINT('Ctrl Pts',(40.3828547511413,-4.37917245782283,133.047310557983));
#61852=CARTESIAN_POINT('Ctrl Pts',(40.3750977102563,-4.31330348481578,133.167535623861));
#61853=CARTESIAN_POINT('Ctrl Pts',(40.3673465190162,-4.24748418411366,133.287670027081));
#61854=CARTESIAN_POINT('Ctrl Pts',(40.3595953277762,-4.17659073746674,133.405146272263));
#61855=CARTESIAN_POINT('Ctrl Pts',(40.351844136536,-4.10087011277746,133.519512064655));
#61856=CARTESIAN_POINT('Ctrl Pts',(40.344096239759,-4.02518167137358,133.633829248534));
#61857=CARTESIAN_POINT('Ctrl Pts',(40.3363483429819,-3.94467034794428,133.745038283723));
#61858=CARTESIAN_POINT('Ctrl Pts',(40.3286004462048,-3.85962778922341,133.852713679656));
#61859=CARTESIAN_POINT('Ctrl Pts',(40.3208541701207,-3.77460301957251,133.960366552218));
#61860=CARTESIAN_POINT('Ctrl Pts',(40.3131078940367,-3.68504914209772,134.064486949139));
#61861=CARTESIAN_POINT('Ctrl Pts',(40.3053616179526,-3.59129941374683,134.164680778402));
#61862=CARTESIAN_POINT('Ctrl Pts',(40.2976152846872,-3.49754899335675,134.264875347274));
#61863=CARTESIAN_POINT('Ctrl Pts',(40.2898689514219,-3.39960292740766,134.361143005168));
#61864=CARTESIAN_POINT('Ctrl Pts',(40.2821226181566,-3.29783253274478,134.453125291873));
#61865=CARTESIAN_POINT('Ctrl Pts',(40.2743745501536,-3.19603934730779,134.545128177373));
#61866=CARTESIAN_POINT('Ctrl Pts',(40.2666264821506,-3.09042041895151,134.632843519928));
#61867=CARTESIAN_POINT('Ctrl Pts',(40.2588784141477,-2.9813811345578,134.715952313155));
#61868=CARTESIAN_POINT('Ctrl Pts',(40.2511221114058,-2.87222596191505,134.799149435397));
#61869=CARTESIAN_POINT('Ctrl Pts',(40.243365808664,-2.75964348298006,134.877729990855));
#61870=CARTESIAN_POINT('Ctrl Pts',(40.2356095059222,-2.64406959390957,134.951417290082));
#61871=CARTESIAN_POINT('Ctrl Pts',(40.227849063408,-2.52843401957462,135.02514391844));
#61872=CARTESIAN_POINT('Ctrl Pts',(40.2200886208939,-2.40980419173579,135.093971890471));
#61873=CARTESIAN_POINT('Ctrl Pts',(40.2123281783797,-2.28864086209718,135.157670400575));
#61874=CARTESIAN_POINT('Ctrl Pts',(40.2045552781143,-2.16728303032528,135.221471165182));
#61875=CARTESIAN_POINT('Ctrl Pts',(40.1967823778489,-2.04338392315899,135.280125845789));
#61876=CARTESIAN_POINT('Ctrl Pts',(40.1890094775835,-1.91742535379917,135.333451373458));
#61877=CARTESIAN_POINT('Ctrl Pts',(40.1815191418212,-1.79604569570078,135.38483838388));
#61878=CARTESIAN_POINT('Ctrl Pts',(40.1740288060588,-1.67275399734529,135.431276862248));
#61879=CARTESIAN_POINT('Ctrl Pts',(40.1665384702965,-1.54799304614553,135.472647304519));
#61880=CARTESIAN_POINT('Ctrl Pts',(40.1587641361774,-1.41850174556604,135.515586319682));
#61881=CARTESIAN_POINT('Ctrl Pts',(40.1509898020583,-1.28701738984544,135.553201421079));
#61882=CARTESIAN_POINT('Ctrl Pts',(40.1432154679392,-1.15401720588747,135.585304807892));
#61883=CARTESIAN_POINT('Ctrl Pts',(40.1354507149921,-1.02118093276966,135.61736863015));
#61884=CARTESIAN_POINT('Ctrl Pts',(40.127685962045,-0.88683292482405,135.643934162408));
#61885=CARTESIAN_POINT('Ctrl Pts',(40.1199212090979,-0.751467962997216,
135.664862542582));
#61886=CARTESIAN_POINT('Ctrl Pts',(40.1121641682129,-0.616237447558963,
135.685770136395));
#61887=CARTESIAN_POINT('Ctrl Pts',(40.1044071273279,-0.47999237216484,135.701051660835));
#61888=CARTESIAN_POINT('Ctrl Pts',(40.0966500864429,-0.343239830441347,
135.710618813106));
#61889=CARTESIAN_POINT('Ctrl Pts',(40.0888988952028,-0.206590414873348,
135.720178750712));
#61890=CARTESIAN_POINT('Ctrl Pts',(40.0811477039627,-0.069434683119747,
135.724032866279));
#61891=CARTESIAN_POINT('Ctrl Pts',(40.0733965127226,0.0677133442506273,
135.722144464535));
#61892=CARTESIAN_POINT('Ctrl Pts',(40.0656486159455,0.204803080051012,135.720256865413));
#61893=CARTESIAN_POINT('Ctrl Pts',(40.0579007191685,0.341884727871334,135.712631608764));
#61894=CARTESIAN_POINT('Ctrl Pts',(40.0501528223914,0.478442668264895,135.699284077201));
#61895=CARTESIAN_POINT('Ctrl Pts',(40.0424065463073,0.614972043681175,135.685939337654));
#61896=CARTESIAN_POINT('Ctrl Pts',(40.0346602702231,0.750977540703882,135.666874742054));
#61897=CARTESIAN_POINT('Ctrl Pts',(40.0269139941391,0.885947465038371,135.642157652549));
#61898=CARTESIAN_POINT('Ctrl Pts',(40.0191676608737,1.02091838569,135.617440380588));
#61899=CARTESIAN_POINT('Ctrl Pts',(40.0114213276084,1.15485333382986,135.587070601889));
#61900=CARTESIAN_POINT('Ctrl Pts',(40.003674994343,1.28725002090361,135.551166959327));
#61901=CARTESIAN_POINT('Ctrl Pts',(39.99592692634,1.41967635729765,135.515255276394));
#61902=CARTESIAN_POINT('Ctrl Pts',(39.988178858337,1.55056336988004,135.473807365901));
#61903=CARTESIAN_POINT('Ctrl Pts',(39.9804307903341,1.67942354803305,135.426991860572));
#61904=CARTESIAN_POINT('Ctrl Pts',(39.9726744875922,1.80842068031668,135.380126599166));
#61905=CARTESIAN_POINT('Ctrl Pts',(39.9649181848504,1.93538630698516,135.327882480798));
#61906=CARTESIAN_POINT('Ctrl Pts',(39.9571618821086,2.05985202885001,135.270476679845));
#61907=CARTESIAN_POINT('Ctrl Pts',(39.9494014395944,2.18438418181837,135.213040239687));
#61908=CARTESIAN_POINT('Ctrl Pts',(39.9416409970802,2.30641342363896,135.150436805853));
#61909=CARTESIAN_POINT('Ctrl Pts',(39.9338805545661,2.4254965234738,135.082929265738));
#61910=CARTESIAN_POINT('Ctrl Pts',(39.9261076543006,2.5447707860722,135.015313356525));
#61911=CARTESIAN_POINT('Ctrl Pts',(39.9183347540352,2.66108912388129,134.942777816249));
#61912=CARTESIAN_POINT('Ctrl Pts',(39.9105618537698,2.77403708401481,134.865629054768));
#61913=CARTESIAN_POINT('Ctrl Pts',(39.9030715180078,2.88287910129842,134.791284845092));
#61914=CARTESIAN_POINT('Ctrl Pts',(39.8955811822458,2.98859128287934,134.712657179348));
#61915=CARTESIAN_POINT('Ctrl Pts',(39.8880908464837,3.09083374920857,134.63005399227));
#61916=CARTESIAN_POINT('Ctrl Pts',(39.8803165123647,3.19695276972476,134.544318880247));
#61917=CARTESIAN_POINT('Ctrl Pts',(39.8725421782456,3.29966992579652,134.454029249055));
#61918=CARTESIAN_POINT('Ctrl Pts',(39.8647678441265,3.39856926247682,134.359485092271));
#61919=CARTESIAN_POINT('Ctrl Pts',(39.8570030911794,3.49734671456355,134.265057452711));
#61920=CARTESIAN_POINT('Ctrl Pts',(39.8492383382324,3.59231542915399,134.166385987778));
#61921=CARTESIAN_POINT('Ctrl Pts',(39.8414735852853,3.68309113645761,134.063811912347));
#61922=CARTESIAN_POINT('Ctrl Pts',(39.8337165444003,3.7737766840489,133.961339714933));
#61923=CARTESIAN_POINT('Ctrl Pts',(39.8259595035153,3.86027725457758,133.854972911575));
#61924=CARTESIAN_POINT('Ctrl Pts',(39.8182024626303,3.94224445990638,133.745090404683));
#61925=CARTESIAN_POINT('Ctrl Pts',(39.8104512713902,4.02414985312813,133.635290761044));
#61926=CARTESIAN_POINT('Ctrl Pts',(39.80270008015,4.10152845293663,133.521981003073));
#61927=CARTESIAN_POINT('Ctrl Pts',(39.7949488889099,4.17407154588811,133.405573756143));
#61928=CARTESIAN_POINT('Ctrl Pts',(39.7872009921328,4.24658380608992,133.289215985399));
#61929=CARTESIAN_POINT('Ctrl Pts',(39.7794530953558,4.31426444076474,133.169763675257));
#61930=CARTESIAN_POINT('Ctrl Pts',(39.7717051985787,4.37684768683512,133.047658945641));
#61931=CARTESIAN_POINT('Ctrl Pts',(39.7639589224946,4.43941784183948,132.925579757703));
#61932=CARTESIAN_POINT('Ctrl Pts',(39.7562126464105,4.49689255088361,132.800849601582));
#61933=CARTESIAN_POINT('Ctrl Pts',(39.7484663703264,4.54905190438516,132.673935391067));
#61934=CARTESIAN_POINT('Ctrl Pts',(39.7407200370611,4.60121164291528,132.547020243699));
#61935=CARTESIAN_POINT('Ctrl Pts',(39.7329737037957,4.64805579899109,132.417921371384));
#61936=CARTESIAN_POINT('Ctrl Pts',(39.7252273705303,4.68941269099244,132.28712549308));
#61937=CARTESIAN_POINT('Ctrl Pts',(39.7174793025274,4.73077884458294,132.156300323947));
#61938=CARTESIAN_POINT('Ctrl Pts',(39.7097312345245,4.76665517101362,132.023777765306));
#61939=CARTESIAN_POINT('Ctrl Pts',(39.7019831665215,4.79692003437235,131.890059123753));
#61940=CARTESIAN_POINT('Ctrl Pts',(39.6942268637797,4.82721706358803,131.756198364437));
#61941=CARTESIAN_POINT('Ctrl Pts',(39.6864705610378,4.85189062969693,131.621139364756));
#61942=CARTESIAN_POINT('Ctrl Pts',(39.6787142582959,4.87087026645046,131.485393590269));
#61943=CARTESIAN_POINT('Ctrl Pts',(39.6709538157817,4.88986003320762,131.349575364175));
#61944=CARTESIAN_POINT('Ctrl Pts',(39.6631933732676,4.90314977723614,131.213070021823));
#61945=CARTESIAN_POINT('Ctrl Pts',(39.6554329307534,4.91072109605126,131.076392562927));
#61946=CARTESIAN_POINT('Ctrl Pts',(39.647660030488,4.9183045690195,130.939495697241));
#61947=CARTESIAN_POINT('Ctrl Pts',(39.6398871302226,4.92015126749114,130.802426554038));
#61948=CARTESIAN_POINT('Ctrl Pts',(39.6321142299571,4.91629496084988,130.665699446281));
#61949=CARTESIAN_POINT('Ctrl Pts',(39.624623894195,4.91257884066842,130.533942713284));
#61950=CARTESIAN_POINT('Ctrl Pts',(39.6171335584329,4.9035671749343,130.402503887071));
#61951=CARTESIAN_POINT('Ctrl Pts',(39.6096432226708,4.88933532466376,130.271835364179));
#61952=CARTESIAN_POINT('Ctrl Pts',(39.6018688885517,4.87456386946474,130.136212504527));
#61953=CARTESIAN_POINT('Ctrl Pts',(39.5940945544325,4.85412177746983,130.000989900916));
#61954=CARTESIAN_POINT('Ctrl Pts',(39.5863202203134,4.82803660796453,129.866679661881));
#61955=CARTESIAN_POINT('Ctrl Pts',(39.5785554673663,4.80198358609935,129.732534948212));
#61956=CARTESIAN_POINT('Ctrl Pts',(39.5707907144193,4.7703013981057,129.599300741992));
#61957=CARTESIAN_POINT('Ctrl Pts',(39.5630259614722,4.73306941051397,129.467484775254));
#61958=CARTESIAN_POINT('Ctrl Pts',(39.5552689205872,4.6958744022572,129.335799729993));
#61959=CARTESIAN_POINT('Ctrl Pts',(39.5475118797022,4.65314066939234,129.205530494815));
#61960=CARTESIAN_POINT('Ctrl Pts',(39.5397548388172,4.60499868094981,129.077174984534));
#61961=CARTESIAN_POINT('Ctrl Pts',(39.5320036475771,4.55689299675532,128.948916268143));
#61962=CARTESIAN_POINT('Ctrl Pts',(39.5242524563369,4.50338731154936,128.822568768721));
#61963=CARTESIAN_POINT('Ctrl Pts',(39.5165012650968,4.44466191158653,128.698615249723));
#61964=CARTESIAN_POINT('Ctrl Pts',(39.5087533683197,4.38596147148516,128.574714414277));
#61965=CARTESIAN_POINT('Ctrl Pts',(39.5010054715426,4.32204589613112,128.453205888094));
#61966=CARTESIAN_POINT('Ctrl Pts',(39.4932575747656,4.25314350210117,128.334552241794));
#61967=CARTESIAN_POINT('Ctrl Pts',(39.4855112986814,4.18425552096667,128.215923415279));
#61968=CARTESIAN_POINT('Ctrl Pts',(39.4777650225973,4.11038299221635,128.100148618704));
#61969=CARTESIAN_POINT('Ctrl Pts',(39.4700187465132,4.03179987714314,127.987665246538));
#61970=CARTESIAN_POINT('Ctrl Pts',(39.4622724132479,3.95321618198722,127.875181044046));
#61971=CARTESIAN_POINT('Ctrl Pts',(39.4545260799825,3.86992205502932,127.765988634942));
#61972=CARTESIAN_POINT('Ctrl Pts',(39.4467797467172,3.78223418860525,127.660495543323));
#61973=CARTESIAN_POINT('Ctrl Pts',(39.4390316787142,3.69452668509149,127.554978827257));
#61974=CARTESIAN_POINT('Ctrl Pts',(39.4312836107112,3.60242373403662,127.453163377772));
#61975=CARTESIAN_POINT('Ctrl Pts',(39.4235355427082,3.50628135169511,127.355422499064));
#61976=CARTESIAN_POINT('Ctrl Pts',(39.4157792399664,3.41003678808554,127.257577740187));
#61977=CARTESIAN_POINT('Ctrl Pts',(39.4080229372245,3.30974449175124,127.163816481901));
#61978=CARTESIAN_POINT('Ctrl Pts',(39.4002666344827,3.20579668442348,127.074474469084));
#61979=CARTESIAN_POINT('Ctrl Pts',(39.3925061919685,3.10179339702101,126.985084771744));
#61980=CARTESIAN_POINT('Ctrl Pts',(39.3847457494543,2.99413101773505,126.900119261838));
#61981=CARTESIAN_POINT('Ctrl Pts',(39.3769853069401,2.88323288341853,126.819871791823));
#61982=CARTESIAN_POINT('Ctrl Pts',(39.3692124066747,2.77215672557187,126.739495501444));
#61983=CARTESIAN_POINT('Ctrl Pts',(39.3614395064092,2.6578347590267,126.663852601717));
#61984=CARTESIAN_POINT('Ctrl Pts',(39.3536666061438,2.54071794302273,126.593192680223));
#61985=CARTESIAN_POINT('Ctrl Pts',(39.3461762703818,2.42785861828093,126.525101424858));
#61986=CARTESIAN_POINT('Ctrl Pts',(39.3386859346199,2.31240438579782,126.461637298325));
#61987=CARTESIAN_POINT('Ctrl Pts',(39.3311955988579,2.19477659406254,126.402981428646));
#61988=CARTESIAN_POINT('Ctrl Pts',(39.3234212647388,2.07268890885039,126.34210160384));
#61989=CARTESIAN_POINT('Ctrl Pts',(39.3156469306198,1.94787285268034,126.286208994538));
#61990=CARTESIAN_POINT('Ctrl Pts',(39.3078725965007,1.82077417343337,126.235557221505));
#61991=CARTESIAN_POINT('Ctrl Pts',(39.3001078435536,1.6938321319496,126.184967872255));
#61992=CARTESIAN_POINT('Ctrl Pts',(39.2923430906065,1.56461342437721,126.139606651412));
#61993=CARTESIAN_POINT('Ctrl Pts',(39.2845783376594,1.43358811960335,126.099681227232));
#61994=CARTESIAN_POINT('Ctrl Pts',(39.2768212967744,1.30269295100914,126.059795457546));
#61995=CARTESIAN_POINT('Ctrl Pts',(39.2690642558894,1.16999512759449,126.025334853671));
#61996=CARTESIAN_POINT('Ctrl Pts',(39.2613072150044,1.03598408089232,125.996458783435));
#61997=CARTESIAN_POINT('Ctrl Pts',(39.2535560237643,0.902074092962925,125.967604488869));
#61998=CARTESIAN_POINT('Ctrl Pts',(39.2458048325241,0.766853233548651,125.944326427545));
#61999=CARTESIAN_POINT('Ctrl Pts',(39.238053641284,0.630825114341994,125.926733864973));
#62000=CARTESIAN_POINT('Ctrl Pts',(39.2303057445069,0.49485481071467,125.909148779708));
#62001=CARTESIAN_POINT('Ctrl Pts',(39.2225578477298,0.358078316632711,125.897244437024));
#62002=CARTESIAN_POINT('Ctrl Pts',(39.2148099509527,0.221008216546887,125.891078778437));
#62003=CARTESIAN_POINT('Ctrl Pts',(39.2070636748686,0.0839667885711129,
125.884914409572));
#62004=CARTESIAN_POINT('Ctrl Pts',(39.1993173987846,-0.0533677329258113,
125.884486354684));
#62005=CARTESIAN_POINT('Ctrl Pts',(39.1915711227005,-0.19047927282011,125.889800544769));
#62006=CARTESIAN_POINT('Ctrl Pts',(39.1838247894351,-0.327591824840462,
125.895114774083));
#62007=CARTESIAN_POINT('Ctrl Pts',(39.1760784561697,-0.464481001301833,
125.906171317812));
#62008=CARTESIAN_POINT('Ctrl Pts',(39.1683321229044,-0.600632760697747,
125.922924010452));
#62009=CARTESIAN_POINT('Ctrl Pts',(39.1605840549014,-0.736815010336169,
125.939680454741));
#62010=CARTESIAN_POINT('Ctrl Pts',(39.1528359868984,-0.872259126336232,
125.962135538527));
#62011=CARTESIAN_POINT('Ctrl Pts',(39.1450879188954,-1.00645860182237,125.990191515289));
#62012=CARTESIAN_POINT('Ctrl Pts',(39.1373316161535,-1.14080070610824,126.018277310277));
#62013=CARTESIAN_POINT('Ctrl Pts',(39.1295753134117,-1.27389514410548,126.051975809259));
#62014=CARTESIAN_POINT('Ctrl Pts',(39.1218190106699,-1.40524743871289,126.091138503291));
#62015=CARTESIAN_POINT('Ctrl Pts',(39.1140585681557,-1.53666983999487,126.130322099632));
#62016=CARTESIAN_POINT('Ctrl Pts',(39.1062981256415,-1.66634787563082,126.17497557498));
#62017=CARTESIAN_POINT('Ctrl Pts',(39.0985376831273,-1.79380549531682,126.224901598482));
#62018=CARTESIAN_POINT('Ctrl Pts',(39.0907647828619,-1.92146772128909,126.274907767669));
#62019=CARTESIAN_POINT('Ctrl Pts',(39.0829918825965,-2.04690205053444,126.330203240907));
#62020=CARTESIAN_POINT('Ctrl Pts',(39.0752189823311,-2.1696547434678,126.390543521599));
#62021=CARTESIAN_POINT('Ctrl Pts',(39.067728646569,-2.28794506681733,126.448690281101));
#62022=CARTESIAN_POINT('Ctrl Pts',(39.060238310807,-2.40374506665103,126.511521286134));
#62023=CARTESIAN_POINT('Ctrl Pts',(39.052747975045,-2.51667460568438,126.578779948403));
#62024=CARTESIAN_POINT('Ctrl Pts',(39.0449724104948,-2.63390445335527,126.648599791819));
#62025=CARTESIAN_POINT('Ctrl Pts',(39.0371968459445,-2.74841230454186,126.723412384054));
#62026=CARTESIAN_POINT('Ctrl Pts',(39.0294212813942,-2.85974362927395,126.802979676275));
#62027=CARTESIAN_POINT('Ctrl Pts',(39.0213184662549,-2.97576056125208,126.885895721256));
#62028=CARTESIAN_POINT('Ctrl Pts',(39.0132156511156,-3.08832735937844,126.97397528201));
#62029=CARTESIAN_POINT('Ctrl Pts',(39.0051128359763,-3.19695741531961,127.066895387342));
#62030=CARTESIAN_POINT('Ctrl Pts',(38.9973568344204,-3.30093792930302,127.155838361992));
#62031=CARTESIAN_POINT('Ctrl Pts',(38.9896008328644,-3.40131135378676,127.249215834932));
#62032=CARTESIAN_POINT('Ctrl Pts',(38.9818448313085,-3.49768059149839,127.346700492228));
#62033=CARTESIAN_POINT('Ctrl Pts',(38.9740941166275,-3.59398413916415,127.444118699152));
#62034=CARTESIAN_POINT('Ctrl Pts',(38.9663434019464,-3.68628865685686,127.54563824343));
#62035=CARTESIAN_POINT('Ctrl Pts',(38.9585926872654,-3.77423163532291,127.650892903219));
#62036=CARTESIAN_POINT('Ctrl Pts',(38.9508455772586,-3.86213371358698,127.756098611553));
#62037=CARTESIAN_POINT('Ctrl Pts',(38.9430984672518,-3.94567803950475,127.865035678907));
#62038=CARTESIAN_POINT('Ctrl Pts',(38.9353513572451,-4.02454063916857,127.977302834962));
#62039=CARTESIAN_POINT('Ctrl Pts',(38.927606172512,-4.10338364028701,128.089542090936));
#62040=CARTESIAN_POINT('Ctrl Pts',(38.919860987779,-4.17754700765423,128.205109468018));
#62041=CARTESIAN_POINT('Ctrl Pts',(38.9121158030459,-4.24674880726832,128.323572913939));
#62042=CARTESIAN_POINT('Ctrl Pts',(38.9043689020301,-4.31596594155246,128.442062610593));
#62043=CARTESIAN_POINT('Ctrl Pts',(38.8966220010143,-4.3802191108475,128.563449322638));
#62044=CARTESIAN_POINT('Ctrl Pts',(38.8888750999985,-4.43927126633542,128.687274486491));
#62045=CARTESIAN_POINT('Ctrl Pts',(38.8811271588079,-4.49833135074438,128.811116276325));
#62046=CARTESIAN_POINT('Ctrl Pts',(38.8733792176173,-4.5521888696628,128.937396813788));
#62047=CARTESIAN_POINT('Ctrl Pts',(38.8656312764266,-4.60065440837986,129.065636350422));
#62048=CARTESIAN_POINT('Ctrl Pts',(38.8578781666516,-4.64915227803773,129.19396143454));
#62049=CARTESIAN_POINT('Ctrl Pts',(38.8501250568766,-4.69225085665429,129.324247758232));
#62050=CARTESIAN_POINT('Ctrl Pts',(38.8423719471015,-4.72981017110029,129.455999090432));
#62051=CARTESIAN_POINT('Ctrl Pts',(38.8398992040847,-4.74178917503666,129.498019285697));
#62052=CARTESIAN_POINT('Ctrl Pts',(38.8374264610678,-4.7532051111186,129.540188406638));
#62053=CARTESIAN_POINT('Ctrl Pts',(38.8349537180509,-4.76405452823399,129.582490119308));
#62054=CARTESIAN_POINT('Ctrl Pts',(40.5848681886094,-4.76405452823407,129.582490119308));
#62055=CARTESIAN_POINT('Ctrl Pts',(40.5772090494279,-4.79778048213594,129.713987101709));
#62056=CARTESIAN_POINT('Ctrl Pts',(40.5695499102464,-4.82605472140716,129.846869198006));
#62057=CARTESIAN_POINT('Ctrl Pts',(40.5618907710649,-4.84877990805882,129.980639508388));
#62058=CARTESIAN_POINT('Ctrl Pts',(40.5540522152193,-4.87203743615042,130.1175434115));
#62059=CARTESIAN_POINT('Ctrl Pts',(40.5462136593737,-4.88948262910061,130.255377224386));
#62060=CARTESIAN_POINT('Ctrl Pts',(40.5383751035281,-4.9010672107594,130.393601249908));
#62061=CARTESIAN_POINT('Ctrl Pts',(40.5305365476825,-4.9126517924182,130.531825275429));
#62062=CARTESIAN_POINT('Ctrl Pts',(40.5226979918368,-4.91837576946825,130.670439064928));
#62063=CARTESIAN_POINT('Ctrl Pts',(40.5148594359912,-4.91824790287392,130.808902464798));
#62064=CARTESIAN_POINT('',(40.8601405640435,-4.91824972738764,130.802723073242));
#62065=CARTESIAN_POINT('Ctrl Pts',(40.9298575685393,-4.7640545282341,129.582490119308));
#62066=CARTESIAN_POINT('Ctrl Pts',(40.9214669057054,-4.80080258504007,129.725770235065));
#62067=CARTESIAN_POINT('Ctrl Pts',(40.9130762428715,-4.83112548624056,129.870876032944));
#62068=CARTESIAN_POINT('Ctrl Pts',(40.9046855800376,-4.85485483549579,130.017234459467));
#62069=CARTESIAN_POINT('Ctrl Pts',(40.8963228592268,-4.87850516286214,130.163105492966));
#62070=CARTESIAN_POINT('Ctrl Pts',(40.8879601384161,-4.89560567749403,130.310220558013));
#62071=CARTESIAN_POINT('Ctrl Pts',(40.8795974176054,-4.90603855309564,130.457995524003));
#62072=CARTESIAN_POINT('Ctrl Pts',(40.8731117997514,-4.91412965715151,130.572600803729));
#62073=CARTESIAN_POINT('Ctrl Pts',(40.8666261818975,-4.91821139772449,130.687602613548));
#62074=CARTESIAN_POINT('Ctrl Pts',(40.8601405640435,-4.91824972738764,130.802723073242));
#62075=CARTESIAN_POINT('Ctrl Pts',(40.8601405640087,-4.91824972738784,130.802723073859));
#62076=CARTESIAN_POINT('Ctrl Pts',(40.8522035403277,-4.91829663476603,130.94360615321));
#62077=CARTESIAN_POINT('Ctrl Pts',(40.8442665166468,-4.9122858041172,131.084440600289));
#62078=CARTESIAN_POINT('Ctrl Pts',(40.8363294929658,-4.90025605756969,131.224686244612));
#62079=CARTESIAN_POINT('Ctrl Pts',(40.8283877865347,-4.88821921361388,131.365014632208));
#62080=CARTESIAN_POINT('Ctrl Pts',(40.8204460801035,-4.87015640705927,131.504753162815));
#62081=CARTESIAN_POINT('Ctrl Pts',(40.8125043736724,-4.84615817870192,131.643368346673));
#62082=CARTESIAN_POINT('Ctrl Pts',(40.8045566451859,-4.82214175291309,131.782088639969));
#62083=CARTESIAN_POINT('Ctrl Pts',(40.7966089166995,-4.79218099659783,131.91968353129));
#62084=CARTESIAN_POINT('Ctrl Pts',(40.7886611882131,-4.75641721715871,132.05563129924));
#62085=CARTESIAN_POINT('Ctrl Pts',(40.7807003308895,-4.72059435960237,132.191803639041));
#62086=CARTESIAN_POINT('Ctrl Pts',(40.7727394735659,-4.67894941910968,132.326323067667));
#62087=CARTESIAN_POINT('Ctrl Pts',(40.7647786162423,-4.63167343917663,132.45868350483));
#62088=CARTESIAN_POINT('Ctrl Pts',(40.7568105101511,-4.58435441204664,132.591164462939));
#62089=CARTESIAN_POINT('Ctrl Pts',(40.7488424040599,-4.53139425756292,132.721482173791));
#62090=CARTESIAN_POINT('Ctrl Pts',(40.7408742979687,-4.47303136480114,132.849152409413));
#62091=CARTESIAN_POINT('Ctrl Pts',(40.7328915946058,-4.4145615534073,132.977056532122));
#62092=CARTESIAN_POINT('Ctrl Pts',(40.7249088912429,-4.35066939059248,133.102303164801));
#62093=CARTESIAN_POINT('Ctrl Pts',(40.71692618788,-4.28163876750627,133.224433452645));
#62094=CARTESIAN_POINT('Ctrl Pts',(40.7125656991743,-4.24393133449366,133.291146158424));
#62095=CARTESIAN_POINT('Ctrl Pts',(40.7082052104686,-4.20469143898111,133.35692952447));
#62096=CARTESIAN_POINT('Ctrl Pts',(40.7038447217628,-4.16397055502691,133.421712767998));
#62097=CARTESIAN_POINT('Ctrl Pts',(40.6960703876438,-4.09136911540656,133.537215092277));
#62098=CARTESIAN_POINT('Ctrl Pts',(40.6882960535247,-4.01384324528631,133.649877291414));
#62099=CARTESIAN_POINT('Ctrl Pts',(40.6805217194056,-3.93164171057593,133.759250890006));
#62100=CARTESIAN_POINT('Ctrl Pts',(40.6727569664586,-3.84954148191063,133.868489695412));
#62101=CARTESIAN_POINT('Ctrl Pts',(40.6649922135115,-3.76277728662918,133.974447654812));
#62102=CARTESIAN_POINT('Ctrl Pts',(40.6572274605645,-3.67164256570979,134.076702887587));
#62103=CARTESIAN_POINT('Ctrl Pts',(40.6494704196795,-3.58059836107999,134.178856559024));
#62104=CARTESIAN_POINT('Ctrl Pts',(40.6417133787945,-3.48519252777902,134.277314532446));
#62105=CARTESIAN_POINT('Ctrl Pts',(40.6339563379096,-3.38576016846868,134.371686106516));
#62106=CARTESIAN_POINT('Ctrl Pts',(40.6262051466694,-3.28640279187396,134.465986514247));
#62107=CARTESIAN_POINT('Ctrl Pts',(40.6184539554293,-3.18302521553785,134.55620638828));
#62108=CARTESIAN_POINT('Ctrl Pts',(40.6107027641892,-3.07600071497427,134.641990441295));
#62109=CARTESIAN_POINT('Ctrl Pts',(40.6029548674121,-2.9690217026784,134.7277380338));
#62110=CARTESIAN_POINT('Ctrl Pts',(40.595206970635,-2.85839915349167,134.809053311082));
#62111=CARTESIAN_POINT('Ctrl Pts',(40.587459073858,-2.74454070384922,134.885620152001));
#62112=CARTESIAN_POINT('Ctrl Pts',(40.5797127977739,-2.63070607093977,134.962170976787));
#62113=CARTESIAN_POINT('Ctrl Pts',(40.5719665216897,-2.51363720815222,135.033975122847));
#62114=CARTESIAN_POINT('Ctrl Pts',(40.5642202456056,-2.39377178794625,135.100759073218));
#62115=CARTESIAN_POINT('Ctrl Pts',(40.5564739123403,-2.27390548292081,135.167543516574));
#62116=CARTESIAN_POINT('Ctrl Pts',(40.5487275790749,-2.15124292081674,135.229307500008));
#62117=CARTESIAN_POINT('Ctrl Pts',(40.5409812458096,-2.0262471367856,135.285823057793));
#62118=CARTESIAN_POINT('Ctrl Pts',(40.5332331778066,-1.90122336081511,135.342351271846));
#62119=CARTESIAN_POINT('Ctrl Pts',(40.5254851098036,-1.77386567936097,135.393628560402));
#62120=CARTESIAN_POINT('Ctrl Pts',(40.5177370418006,-1.64465752394219,135.439474930228));
#62121=CARTESIAN_POINT('Ctrl Pts',(40.5099807390587,-1.51531204455876,135.485370026121));
#62122=CARTESIAN_POINT('Ctrl Pts',(40.502224436317,-1.38411253154962,135.525822542056));
#62123=CARTESIAN_POINT('Ctrl Pts',(40.4944681335751,-1.25155854787594,135.560702096449));
#62124=CARTESIAN_POINT('Ctrl Pts',(40.486707691061,-1.11893381614987,135.595600267109));
#62125=CARTESIAN_POINT('Ctrl Pts',(40.4789472485467,-0.984953555016894,
135.624919465832));
#62126=CARTESIAN_POINT('Ctrl Pts',(40.4711868060326,-0.850126986043015,
135.64858059297));
#62127=CARTESIAN_POINT('Ctrl Pts',(40.4634139057671,-0.715083981491278,
135.672279703049));
#62128=CARTESIAN_POINT('Ctrl Pts',(40.4556410055017,-0.579192342040389,
135.690302539705));
#62129=CARTESIAN_POINT('Ctrl Pts',(40.4478681052363,-0.44296676926654,135.702621891102));
#62130=CARTESIAN_POINT('Ctrl Pts',(40.4403777694742,-0.311693339193058,
135.714493403046));
#62131=CARTESIAN_POINT('Ctrl Pts',(40.4328874337121,-0.180110140553368,
135.721068887151));
#62132=CARTESIAN_POINT('Ctrl Pts',(40.42539709795,-0.0486753042053006,135.722369744973));
#62133=CARTESIAN_POINT('Ctrl Pts',(40.4176227638309,0.0877429239103127,
135.723719925215));
#62134=CARTESIAN_POINT('Ctrl Pts',(40.4098484297119,0.224433449278738,135.719391885597));
#62135=CARTESIAN_POINT('Ctrl Pts',(40.4020740955928,0.360884492790618,135.709352508014));
#62136=CARTESIAN_POINT('Ctrl Pts',(40.3943093426457,0.49716737258635,135.699325503067));
#62137=CARTESIAN_POINT('Ctrl Pts',(40.3865445896986,0.633210971597971,135.68360119351));
#62138=CARTESIAN_POINT('Ctrl Pts',(40.3787798367515,0.768501737697219,135.662198422769));
#62139=CARTESIAN_POINT('Ctrl Pts',(40.3710227958665,0.903658131100496,135.640816909561));
#62140=CARTESIAN_POINT('Ctrl Pts',(40.3632657549815,1.03806279593239,135.613768219576));
#62141=CARTESIAN_POINT('Ctrl Pts',(40.3555087140965,1.17120589291698,135.581123100556));
#62142=CARTESIAN_POINT('Ctrl Pts',(40.3477575228563,1.30424858565607,135.548502599473));
#62143=CARTESIAN_POINT('Ctrl Pts',(40.3400063316162,1.43603122598697,135.510294162354));
#62144=CARTESIAN_POINT('Ctrl Pts',(40.3322551403761,1.56605313609324,135.466619794986));
#62145=CARTESIAN_POINT('Ctrl Pts',(40.324507243599,1.69601978341925,135.422963990388));
#62146=CARTESIAN_POINT('Ctrl Pts',(40.316759346822,1.8242268191064,135.373847000371));
#62147=CARTESIAN_POINT('Ctrl Pts',(40.3090114500449,1.95018794403604,135.319440909813));
#62148=CARTESIAN_POINT('Ctrl Pts',(40.3012651739608,2.07612272061392,135.265046199836));
#62149=CARTESIAN_POINT('Ctrl Pts',(40.2935188978767,2.19981216219578,135.20536474487));
#62150=CARTESIAN_POINT('Ctrl Pts',(40.2857726217926,2.32078957856036,135.14061692855));
#62151=CARTESIAN_POINT('Ctrl Pts',(40.2780262885272,2.44176788795276,135.075868634276));
#62152=CARTESIAN_POINT('Ctrl Pts',(40.2702799552619,2.56003378747939,135.006054088509));
#62153=CARTESIAN_POINT('Ctrl Pts',(40.2625336219966,2.67514520130848,134.931439634791));
#62154=CARTESIAN_POINT('Ctrl Pts',(40.2547855539936,2.79028239354058,134.856808471683));
#62155=CARTESIAN_POINT('Ctrl Pts',(40.2470374859906,2.90226336636071,134.777375474301));
#62156=CARTESIAN_POINT('Ctrl Pts',(40.2392894179876,3.01067537982031,134.693450076532));
#62157=CARTESIAN_POINT('Ctrl Pts',(40.2315331152458,3.11920261485793,134.609435481853));
#62158=CARTESIAN_POINT('Ctrl Pts',(40.2237768125039,3.22415300369695,134.520919188765));
#62159=CARTESIAN_POINT('Ctrl Pts',(40.216020509762,3.32514682663451,134.428251019306));
#62160=CARTESIAN_POINT('Ctrl Pts',(40.2082600672478,3.42619455301623,134.335533390054));
#62161=CARTESIAN_POINT('Ctrl Pts',(40.2004996247337,3.52328122905683,134.238659744916));
#62162=CARTESIAN_POINT('Ctrl Pts',(40.1927391822195,3.61606505928803,134.138015751124));
#62163=CARTESIAN_POINT('Ctrl Pts',(40.1849662819541,3.70899783436048,134.037210194658));
#62164=CARTESIAN_POINT('Ctrl Pts',(40.1771933816887,3.79761370773354,133.932622493182));
#62165=CARTESIAN_POINT('Ctrl Pts',(40.1694204814232,3.88161157654487,133.824670971045));
#62166=CARTESIAN_POINT('Ctrl Pts',(40.1619301456613,3.96255591124648,133.720643758652));
#62167=CARTESIAN_POINT('Ctrl Pts',(40.1544398098993,4.03921198521355,133.613493296783));
#62168=CARTESIAN_POINT('Ctrl Pts',(40.1469494741373,4.11135017326076,133.503616591965));
#62169=CARTESIAN_POINT('Ctrl Pts',(40.1391751400182,4.18622350263413,133.389573878487));
#62170=CARTESIAN_POINT('Ctrl Pts',(40.1314008058991,4.25646676814036,133.272232857086));
#62171=CARTESIAN_POINT('Ctrl Pts',(40.1236264717801,4.32177547747018,133.152006200877));
#62172=CARTESIAN_POINT('Ctrl Pts',(40.115861718833,4.38700369965256,133.031927713276));
#62173=CARTESIAN_POINT('Ctrl Pts',(40.1080969658859,4.44730928100165,132.908971007069));
#62174=CARTESIAN_POINT('Ctrl Pts',(40.1003322129388,4.50243048755657,132.783578333539));
#62175=CARTESIAN_POINT('Ctrl Pts',(40.0925751720538,4.55749694695214,132.65831020178));
#62176=CARTESIAN_POINT('Ctrl Pts',(40.0848181311688,4.60738912236687,132.530611273081));
#62177=CARTESIAN_POINT('Ctrl Pts',(40.0770610902838,4.65189095529825,132.400948730548));
#62178=CARTESIAN_POINT('Ctrl Pts',(40.0693098990437,4.69635922905119,132.271383967546));
#62179=CARTESIAN_POINT('Ctrl Pts',(40.0615587078035,4.7354451248525,132.139858906402));
#62180=CARTESIAN_POINT('Ctrl Pts',(40.0538075165634,4.76898066103704,132.006860728649));
#62181=CARTESIAN_POINT('Ctrl Pts',(40.0460596197863,4.80250194372415,131.873919078669));
#62182=CARTESIAN_POINT('Ctrl Pts',(40.0383117230092,4.83047746337694,131.73950593568));
#62183=CARTESIAN_POINT('Ctrl Pts',(40.0305638262321,4.85278914332629,131.604123452983));
#62184=CARTESIAN_POINT('Ctrl Pts',(40.022817550148,4.87509615615314,131.468769289383));
#62185=CARTESIAN_POINT('Ctrl Pts',(40.0150712740638,4.8917416222805,131.332446574903));
#62186=CARTESIAN_POINT('Ctrl Pts',(40.0073249979797,4.90265869923977,131.195667071983));
#62187=CARTESIAN_POINT('Ctrl Pts',(39.9995786647144,4.91357585678645,131.058886559388));
#62188=CARTESIAN_POINT('Ctrl Pts',(39.991832331449,4.91876450968101,130.921649641349));
#62189=CARTESIAN_POINT('Ctrl Pts',(39.9840859981836,4.91820978750425,130.784472213976));
#62190=CARTESIAN_POINT('Ctrl Pts',(39.9763379301807,4.91765494110131,130.64726406667));
#62191=CARTESIAN_POINT('Ctrl Pts',(39.9685898621777,4.91135416184055,130.510115827427));
#62192=CARTESIAN_POINT('Ctrl Pts',(39.9608417941748,4.89934468919312,130.37354200263));
#62193=CARTESIAN_POINT('Ctrl Pts',(39.9530854914329,4.88732245273522,130.236823025547));
#62194=CARTESIAN_POINT('Ctrl Pts',(39.945329188691,4.86957943717226,130.100680072523));
#62195=CARTESIAN_POINT('Ctrl Pts',(39.9375728859492,4.84620470991631,129.965621699854));
#62196=CARTESIAN_POINT('Ctrl Pts',(39.929812443435,4.82281750686462,129.830491242464));
#62197=CARTESIAN_POINT('Ctrl Pts',(39.9220520009209,4.79379268547922,129.696446900806));
#62198=CARTESIAN_POINT('Ctrl Pts',(39.9142915584067,4.75926996972727,129.563984699648));
#62199=CARTESIAN_POINT('Ctrl Pts',(39.9065186581413,4.72469183504721,129.431309858404));
#62200=CARTESIAN_POINT('Ctrl Pts',(39.8987457578758,4.68459828383862,129.300222607059));
#62201=CARTESIAN_POINT('Ctrl Pts',(39.8909728576104,4.63917851077378,129.171202386507));
#62202=CARTESIAN_POINT('Ctrl Pts',(39.8834825218483,4.59540986086505,129.046872375954));
#62203=CARTESIAN_POINT('Ctrl Pts',(39.8759921860863,4.54669562304279,128.924462007975));
#62204=CARTESIAN_POINT('Ctrl Pts',(39.8685018503242,4.49324569212165,128.804379064469));
#62205=CARTESIAN_POINT('Ctrl Pts',(39.8607275162051,4.43776919082428,128.679743139661));
#62206=CARTESIAN_POINT('Ctrl Pts',(39.852953182086,4.37701506704252,128.557219802717));
#62207=CARTESIAN_POINT('Ctrl Pts',(39.8451788479669,4.31116592882415,128.437288291538));
#62208=CARTESIAN_POINT('Ctrl Pts',(39.8374140950198,4.24539794378352,128.317504585229));
#62209=CARTESIAN_POINT('Ctrl Pts',(39.8296493420727,4.17454762430183,128.200306688608));
#62210=CARTESIAN_POINT('Ctrl Pts',(39.8218845891257,4.09884557530925,128.08615385349));
#62211=CARTESIAN_POINT('Ctrl Pts',(39.8141275482407,4.02321871465893,127.972114396578));
#62212=CARTESIAN_POINT('Ctrl Pts',(39.8063705073557,3.9427499288189,127.8611143062));
#62213=CARTESIAN_POINT('Ctrl Pts',(39.7986134664707,3.85771548726882,127.753587882375));
#62214=CARTESIAN_POINT('Ctrl Pts',(39.7908622752305,3.77274517085235,127.646142545062));
#62215=CARTESIAN_POINT('Ctrl Pts',(39.7831110839904,3.68321629333454,127.542165965727));
#62216=CARTESIAN_POINT('Ctrl Pts',(39.7753598927503,3.58944793614549,127.442062805622));
#62217=CARTESIAN_POINT('Ctrl Pts',(39.7676119959732,3.49571943300985,127.342002192032));
#62218=CARTESIAN_POINT('Ctrl Pts',(39.7598640991961,3.39775530074743,127.245812008031));
#62219=CARTESIAN_POINT('Ctrl Pts',(39.752116202419,3.29591419182915,127.153863020991));
#62220=CARTESIAN_POINT('Ctrl Pts',(39.744369926335,3.19409438587555,127.061933267698));
#62221=CARTESIAN_POINT('Ctrl Pts',(39.7366236502509,3.0883995063539,126.974243208577));
#62222=CARTESIAN_POINT('Ctrl Pts',(39.7288773741668,2.97922398351145,126.89112570019));
#62223=CARTESIAN_POINT('Ctrl Pts',(39.7211310409015,2.87004765476009,126.808007578249));
#62224=CARTESIAN_POINT('Ctrl Pts',(39.7133847076362,2.75739094249258,126.729462311221));
#62225=CARTESIAN_POINT('Ctrl Pts',(39.7056383743708,2.64167984689107,126.655781264459));
#62226=CARTESIAN_POINT('Ctrl Pts',(39.6978903063679,2.52594283859184,126.582083717337));
#62227=CARTESIAN_POINT('Ctrl Pts',(39.6901422383649,2.40715041558078,126.513252768033));
#62228=CARTESIAN_POINT('Ctrl Pts',(39.6823941703619,2.28575557549405,126.449535189194));
#62229=CARTESIAN_POINT('Ctrl Pts',(39.6746378676201,2.16423171552666,126.385749890553));
#62230=CARTESIAN_POINT('Ctrl Pts',(39.6668815648782,2.04010026006971,126.327089000469));
#62231=CARTESIAN_POINT('Ctrl Pts',(39.6591252621364,1.91383721504967,126.273752471104));
#62232=CARTESIAN_POINT('Ctrl Pts',(39.6513648196222,1.7875067796408,126.220387474427));
#62233=CARTESIAN_POINT('Ctrl Pts',(39.643604377108,1.65904285374134,126.172352637803));
#62234=CARTESIAN_POINT('Ctrl Pts',(39.6358439345939,1.52893828125394,126.129798521004));
#62235=CARTESIAN_POINT('Ctrl Pts',(39.6280710343285,1.39862485335665,126.087176092559));
#62236=CARTESIAN_POINT('Ctrl Pts',(39.6202981340631,1.26666589244829,126.050052071362));
#62237=CARTESIAN_POINT('Ctrl Pts',(39.6125252337977,1.13356703007465,126.018526432094));
#62238=CARTESIAN_POINT('Ctrl Pts',(39.6050348980356,1.00530664660302,125.988146829222));
#62239=CARTESIAN_POINT('Ctrl Pts',(39.5975445622735,0.8759881017261,125.962965703229));
#62240=CARTESIAN_POINT('Ctrl Pts',(39.5900542265114,0.746067927177802,125.943026879739));
#62241=CARTESIAN_POINT('Ctrl Pts',(39.5822798923923,0.611221789724072,125.922332069696));
#62242=CARTESIAN_POINT('Ctrl Pts',(39.5745055582732,0.475300348405679,125.907219378263));
#62243=CARTESIAN_POINT('Ctrl Pts',(39.5667312241541,0.33880550375241,125.897794211908));
#62244=CARTESIAN_POINT('Ctrl Pts',(39.558966471207,0.202478876796096,125.888380661229));
#62245=CARTESIAN_POINT('Ctrl Pts',(39.5512017182599,0.0655806388564525,
125.884640715753));
#62246=CARTESIAN_POINT('Ctrl Pts',(39.5434369653128,-0.0713781809104709,
125.886628597845));
#62247=CARTESIAN_POINT('Ctrl Pts',(39.5356799244278,-0.208200971246262,
125.888614505544));
#62248=CARTESIAN_POINT('Ctrl Pts',(39.5279228835428,-0.345083835272505,
125.896316913889));
#62249=CARTESIAN_POINT('Ctrl Pts',(39.5201658426578,-0.481512053682665,
125.909738139309));
#62250=CARTESIAN_POINT('Ctrl Pts',(39.5124146514177,-0.617837390513364,
125.923149243679));
#62251=CARTESIAN_POINT('Ctrl Pts',(39.5046634601775,-0.75370837664104,125.942270543025));
#62252=CARTESIAN_POINT('Ctrl Pts',(39.4969122689373,-0.888612087786601,
125.967052314394));
#62253=CARTESIAN_POINT('Ctrl Pts',(39.4891643721602,-1.02345846125552,125.991823552849));
#62254=CARTESIAN_POINT('Ctrl Pts',(39.4814164753831,-1.15733799369815,126.022250407781));
#62255=CARTESIAN_POINT('Ctrl Pts',(39.473668578606,-1.28974488760317,126.058231543531));
#62256=CARTESIAN_POINT('Ctrl Pts',(39.4659223025219,-1.42212408483981,126.094205152802));
#62257=CARTESIAN_POINT('Ctrl Pts',(39.4581760264378,-1.5530308792119,126.135730629475));
#62258=CARTESIAN_POINT('Ctrl Pts',(39.4504297503537,-1.68197202988457,126.182656045313));
#62259=CARTESIAN_POINT('Ctrl Pts',(39.4426834170884,-1.81091413237188,126.229581807544));
#62260=CARTESIAN_POINT('Ctrl Pts',(39.434937083823,-1.93789019481426,126.281907454775));
#62261=CARTESIAN_POINT('Ctrl Pts',(39.4271907505576,-2.06242481978431,126.339432071079));
#62262=CARTESIAN_POINT('Ctrl Pts',(39.4194426825546,-2.18698733342016,126.396969569621));
#62263=CARTESIAN_POINT('Ctrl Pts',(39.4116946145517,-2.30910696676692,126.459708190089));
#62264=CARTESIAN_POINT('Ctrl Pts',(39.4039465465487,-2.42833124672092,126.527400199384));
#62265=CARTESIAN_POINT('Ctrl Pts',(39.3961902438068,-2.54768223965844,126.595164152551));
#62266=CARTESIAN_POINT('Ctrl Pts',(39.388433941065,-2.66413139160323,126.66789181765));
#62267=CARTESIAN_POINT('Ctrl Pts',(39.3806776383231,-2.77725318430666,126.745290796442));
#62268=CARTESIAN_POINT('Ctrl Pts',(39.372917195809,-2.89043535351673,126.822731085399));
#62269=CARTESIAN_POINT('Ctrl Pts',(39.3651567532948,-3.00028631184022,126.904847422035));
#62270=CARTESIAN_POINT('Ctrl Pts',(39.3573963107806,-3.10641299490876,126.991306544049));
#62271=CARTESIAN_POINT('Ctrl Pts',(39.3496234105152,-3.21271004195058,127.077904457922));
#62272=CARTESIAN_POINT('Ctrl Pts',(39.3418505102498,-3.31527057403758,127.168858828746));
#62273=CARTESIAN_POINT('Ctrl Pts',(39.3340776099843,-3.41373717343956,127.263798293135));
#62274=CARTESIAN_POINT('Ctrl Pts',(39.3265872742224,-3.50862426392981,127.355286468856));
#62275=CARTESIAN_POINT('Ctrl Pts',(39.3190969384604,-3.59970969067984,127.450474809468));
#62276=CARTESIAN_POINT('Ctrl Pts',(39.3116066026985,-3.68670981539713,127.549002910715));
#62277=CARTESIAN_POINT('Ctrl Pts',(39.3039014951383,-3.77620451096235,127.650356126637));
#62278=CARTESIAN_POINT('Ctrl Pts',(39.2961963875781,-3.86167199230871,127.755578846841));
#62279=CARTESIAN_POINT('Ctrl Pts',(39.2884912800179,-3.94275437005546,127.864314522705));
#62280=CARTESIAN_POINT('Ctrl Pts',(39.2807954511361,-4.0237391064261,127.972919256417));
#62281=CARTESIAN_POINT('Ctrl Pts',(39.2730996222543,-4.10034900457173,128.085028217023));
#62282=CARTESIAN_POINT('Ctrl Pts',(39.2654037933725,-4.1722639134616,128.200249080222));
#62283=CARTESIAN_POINT('Ctrl Pts',(39.2577168462748,-4.24409582509387,128.315336966605));
#62284=CARTESIAN_POINT('Ctrl Pts',(39.250029899177,-4.31124332455259,128.433529270244));
#62285=CARTESIAN_POINT('Ctrl Pts',(39.2423429520793,-4.37342782573868,128.554402370052));
#62286=CARTESIAN_POINT('Ctrl Pts',(39.2346611715276,-4.43557053151691,128.675194228709));
#62287=CARTESIAN_POINT('Ctrl Pts',(39.2269793909759,-4.49275669100498,128.798662947593));
#62288=CARTESIAN_POINT('Ctrl Pts',(39.2192976104242,-4.54475224278082,128.924357927611));
#62289=CARTESIAN_POINT('Ctrl Pts',(39.211619031124,-4.59672612629417,129.050000526382));
#62290=CARTESIAN_POINT('Ctrl Pts',(39.2039404518238,-4.6435135511543,129.177867174037));
#62291=CARTESIAN_POINT('Ctrl Pts',(39.1962618725236,-4.68492764495315,129.307485197214));
#62292=CARTESIAN_POINT('Ctrl Pts',(39.1908790763459,-4.71395952924944,129.398349323564));
#62293=CARTESIAN_POINT('Ctrl Pts',(39.1854962801682,-4.74035182336093,129.490073632747));
#62294=CARTESIAN_POINT('Ctrl Pts',(39.1801134839905,-4.76405452823399,129.582490119308));
#62295=CARTESIAN_POINT('Origin',(213.235140564004,0.,130.804360617566));
#62296=CARTESIAN_POINT('',(37.0846781642943,-4.76405452823403,129.582490119308));
#62297=CARTESIAN_POINT('',(37.4302319972992,-4.76405452823409,129.582490119308));
#62298=CARTESIAN_POINT('',(213.235140564004,-4.76405452823405,129.582490119308));
#62299=CARTESIAN_POINT('',(38.7648594359501,-4.91824989201514,130.803329990072));
#62300=CARTESIAN_POINT('Ctrl Pts',(38.7648594359501,-4.91824989201514,130.803329990072));
#62301=CARTESIAN_POINT('Ctrl Pts',(38.7571284799429,-4.91827832612957,130.939020218589));
#62302=CARTESIAN_POINT('Ctrl Pts',(38.7493975239357,-4.91268714457348,131.074935898356));
#62303=CARTESIAN_POINT('Ctrl Pts',(38.7416665679285,-4.90144643826978,131.210569769694));
#62304=CARTESIAN_POINT('Ctrl Pts',(38.7339450451304,-4.89021944772569,131.346038142394));
#62305=CARTESIAN_POINT('Ctrl Pts',(38.7262235223324,-4.87335667787914,131.481225000161));
#62306=CARTESIAN_POINT('Ctrl Pts',(38.7185019995344,-4.8508801956055,131.615621605401));
#62307=CARTESIAN_POINT('Ctrl Pts',(38.7107879983121,-4.82842560779075,131.749887294204));
#62308=CARTESIAN_POINT('Ctrl Pts',(38.7030739970898,-4.80036825250335,131.883363874273));
#62309=CARTESIAN_POINT('Ctrl Pts',(38.6953599958675,-4.76678207865275,132.015546679711));
#62310=CARTESIAN_POINT('Ctrl Pts',(38.6876516116237,-4.73322036069873,132.147633235751));
#62311=CARTESIAN_POINT('Ctrl Pts',(38.6799432273799,-4.69413793299307,132.278427509872));
#62312=CARTESIAN_POINT('Ctrl Pts',(38.6722348431361,-4.6496599296308,132.407434415395));
#62313=CARTESIAN_POINT('Ctrl Pts',(38.664529411506,-4.6051989630897,132.53639190621));
#62314=CARTESIAN_POINT('Ctrl Pts',(38.656823979876,-4.55534665848608,132.663563016094));
#62315=CARTESIAN_POINT('Ctrl Pts',(38.6491185482459,-4.50027809824341,132.788467494972));
#62316=CARTESIAN_POINT('Ctrl Pts',(38.6414144491673,-4.44521906137262,132.91335037329));
#62317=CARTESIAN_POINT('Ctrl Pts',(38.6337103500887,-4.38494572239737,133.035967038157));
#62318=CARTESIAN_POINT('Ctrl Pts',(38.6260062510101,-4.31968124987413,133.15585736687));
#62319=CARTESIAN_POINT('Ctrl Pts',(38.6183017685783,-4.25441352981426,133.275753661282));
#62320=CARTESIAN_POINT('Ctrl Pts',(38.6105972861466,-4.18415437138044,133.392923002053));
#62321=CARTESIAN_POINT('Ctrl Pts',(38.6028928037148,-4.10917260174733,133.506930430087));
#62322=CARTESIAN_POINT('Ctrl Pts',(38.5951862220833,-4.03417040222643,133.620968921124));
#62323=CARTESIAN_POINT('Ctrl Pts',(38.5874796404517,-3.95444324922921,133.731843455126));
#62324=CARTESIAN_POINT('Ctrl Pts',(38.5797730588201,-3.87030266124698,133.839148974741));
#62325=CARTESIAN_POINT('Ctrl Pts',(38.5720581865016,-3.78607155540491,133.946569932888));
#62326=CARTESIAN_POINT('Ctrl Pts',(38.5643433141832,-3.69741777832495,134.05041389815));
#62327=CARTESIAN_POINT('Ctrl Pts',(38.5566284418647,-3.6046926910649,134.150309461389));
#62328=CARTESIAN_POINT('Ctrl Pts',(38.5489090297513,-3.51191303998919,134.250263807891));
#62329=CARTESIAN_POINT('Ctrl Pts',(38.5411896176381,-3.41505758782715,134.346264846846));
#62330=CARTESIAN_POINT('Ctrl Pts',(38.5334702055248,-3.31451291341551,134.437979641253));
#62331=CARTESIAN_POINT('Ctrl Pts',(38.5257391821786,-3.21381700370119,134.529832389409));
#62332=CARTESIAN_POINT('Ctrl Pts',(38.5180081588324,-3.10942109242567,134.617385763959));
#62333=CARTESIAN_POINT('Ctrl Pts',(38.5102771354862,-3.00174347226363,134.700348193165));
#62334=CARTESIAN_POINT('Ctrl Pts',(38.5054689994639,-2.93477579914787,134.751944809357));
#62335=CARTESIAN_POINT('Ctrl Pts',(38.5006608634416,-2.86653935663988,134.801766539492));
#62336=CARTESIAN_POINT('Ctrl Pts',(38.4958527274192,-2.79713972328847,134.849752122835));
#62337=CARTESIAN_POINT('Ctrl Pts',(38.4880783933002,-2.68492660475101,134.927340601212));
#62338=CARTESIAN_POINT('Ctrl Pts',(38.4803040591811,-2.56930501935536,135.000379499363));
#62339=CARTESIAN_POINT('Ctrl Pts',(38.472529725062,-2.45068021440031,135.068554509645));
#62340=CARTESIAN_POINT('Ctrl Pts',(38.4647649721149,-2.33220160391541,135.136645500321));
#62341=CARTESIAN_POINT('Ctrl Pts',(38.4570002191679,-2.21072747387373,135.199884337073));
#62342=CARTESIAN_POINT('Ctrl Pts',(38.4492354662208,-2.08669366730699,135.257998748501));
#62343=CARTESIAN_POINT('Ctrl Pts',(38.4414784253358,-1.962783052866,135.316055439877));
#62344=CARTESIAN_POINT('Ctrl Pts',(38.4337213844507,-1.83631817294624,135.368997669762));
#62345=CARTESIAN_POINT('Ctrl Pts',(38.4259643435658,-1.70776089130751,135.416598230766));
#62346=CARTESIAN_POINT('Ctrl Pts',(38.4182131523256,-1.57930055571454,135.464162895818));
#62347=CARTESIAN_POINT('Ctrl Pts',(38.4104619610856,-1.44875132426562,135.50639377466));
#62348=CARTESIAN_POINT('Ctrl Pts',(38.4027107698455,-1.31659620710292,135.543111242989));
#62349=CARTESIAN_POINT('Ctrl Pts',(38.3949628730684,-1.18449725939038,135.579813105414));
#62350=CARTESIAN_POINT('Ctrl Pts',(38.3872149762913,-1.05079415940023,135.611006113622));
#62351=CARTESIAN_POINT('Ctrl Pts',(38.3794670795142,-0.915986082312354,
135.636560174653));
#62352=CARTESIAN_POINT('Ctrl Pts',(38.3717208034301,-0.781206204167893,
135.662108890325));
#62353=CARTESIAN_POINT('Ctrl Pts',(38.363974527346,-0.645322192552095,135.682020932234));
#62354=CARTESIAN_POINT('Ctrl Pts',(38.3562282512619,-0.508844058494613,
135.696217196273));
#62355=CARTESIAN_POINT('Ctrl Pts',(38.3484819179966,-0.372364916987106,
135.710413565105));
#62356=CARTESIAN_POINT('Ctrl Pts',(38.3407355847312,-0.235292033153742,
135.718894031424));
#62357=CARTESIAN_POINT('Ctrl Pts',(38.3329892514659,-0.0981407976885719,
135.721631349011));
#62358=CARTESIAN_POINT('Ctrl Pts',(38.3252411834629,0.0390411518450279,
135.724369279601));
#62359=CARTESIAN_POINT('Ctrl Pts',(38.31749311546,0.176301097113004,135.721361494392));
#62360=CARTESIAN_POINT('Ctrl Pts',(38.309745047457,0.313123786251959,135.712632875396));
#62361=CARTESIAN_POINT('Ctrl Pts',(38.3019887447152,0.450091892173327,135.70389497952));
#62362=CARTESIAN_POINT('Ctrl Pts',(38.2942324419733,0.586621422841188,135.689424128992));
#62363=CARTESIAN_POINT('Ctrl Pts',(38.2864761392314,0.722201831039167,135.669297161627));
#62364=CARTESIAN_POINT('Ctrl Pts',(38.2787156967173,0.857854602583064,135.649159451894));
#62365=CARTESIAN_POINT('Ctrl Pts',(38.2709552542032,0.99255685846541,135.623359683539));
#62366=CARTESIAN_POINT('Ctrl Pts',(38.263194811689,1.12580936377113,135.592025637066));
#62367=CARTESIAN_POINT('Ctrl Pts',(38.2554219114236,1.25927577782815,135.5606412904));
#62368=CARTESIAN_POINT('Ctrl Pts',(38.2476490111581,1.39128741396276,135.523705017729));
#62369=CARTESIAN_POINT('Ctrl Pts',(38.2398761108927,1.52136042919586,135.481394453982));
#62370=CARTESIAN_POINT('Ctrl Pts',(38.2323857751306,1.64670496269283,135.4406219858));
#62371=CARTESIAN_POINT('Ctrl Pts',(38.2248954393685,1.77024908689878,135.394859287784));
#62372=CARTESIAN_POINT('Ctrl Pts',(38.2174051036063,1.89158010045018,135.344306408661));
#62373=CARTESIAN_POINT('Ctrl Pts',(38.2096307694872,2.01751141625654,135.291836801762));
#62374=CARTESIAN_POINT('Ctrl Pts',(38.2018564353682,2.14145740096002,135.234040395919));
#62375=CARTESIAN_POINT('Ctrl Pts',(38.1940821012491,2.26293457257786,135.171088246206));
#62376=CARTESIAN_POINT('Ctrl Pts',(38.186317348302,2.38426203443824,135.108213679392));
#62377=CARTESIAN_POINT('Ctrl Pts',(38.1785525953548,2.50312639327234,135.040196189421));
#62378=CARTESIAN_POINT('Ctrl Pts',(38.1707878424077,2.61906299563609,134.967255294037));
#62379=CARTESIAN_POINT('Ctrl Pts',(38.1630308015227,2.73488444813212,134.894386844578));
#62380=CARTESIAN_POINT('Ctrl Pts',(38.1552737606378,2.84778360220955,134.816604927869));
#62381=CARTESIAN_POINT('Ctrl Pts',(38.1475167197528,2.95731965321308,134.734175311826));
#62382=CARTESIAN_POINT('Ctrl Pts',(38.1397655285127,3.06677310222863,134.651807856597));
#62383=CARTESIAN_POINT('Ctrl Pts',(38.1320143372725,3.17286818507974,134.564799912393));
#62384=CARTESIAN_POINT('Ctrl Pts',(38.1242631460323,3.2751926999721,134.473460758002));
#62385=CARTESIAN_POINT('Ctrl Pts',(38.1165152492553,3.37747372421589,134.382160425188));
#62386=CARTESIAN_POINT('Ctrl Pts',(38.1087673524782,3.47598707687795,134.286532803366));
#62387=CARTESIAN_POINT('Ctrl Pts',(38.1010194557011,3.57035349068835,134.186927544329));
#62388=CARTESIAN_POINT('Ctrl Pts',(38.093273179617,3.66470016507914,134.087343120564));
#62389=CARTESIAN_POINT('Ctrl Pts',(38.085526903533,3.75490135730511,133.983782998187));
#62390=CARTESIAN_POINT('Ctrl Pts',(38.0777806274489,3.8406148414214,133.876633506219));
#62391=CARTESIAN_POINT('Ctrl Pts',(38.0700342941836,3.92632895825492,133.769483223298));
#62392=CARTESIAN_POINT('Ctrl Pts',(38.0622879609182,4.00755505665235,133.658743823216));
#62393=CARTESIAN_POINT('Ctrl Pts',(38.0545416276528,4.08399163233707,133.544834191513));
#62394=CARTESIAN_POINT('Ctrl Pts',(38.0467935596499,4.16044532546293,133.430899050537));
#62395=CARTESIAN_POINT('Ctrl Pts',(38.039045491647,4.23210714375918,133.313792589805));
#62396=CARTESIAN_POINT('Ctrl Pts',(38.031297423644,4.29871951494976,133.193961754637));
#62397=CARTESIAN_POINT('Ctrl Pts',(38.0235411209022,4.36540268256133,133.074003561831));
#62398=CARTESIAN_POINT('Ctrl Pts',(38.0157848181603,4.42702549242186,132.951315552782));
#62399=CARTESIAN_POINT('Ctrl Pts',(38.0080285154185,4.48337662711915,132.826368798039));
#62400=CARTESIAN_POINT('Ctrl Pts',(38.0002680729043,4.53975783811389,132.701355355451));
#62401=CARTESIAN_POINT('Ctrl Pts',(37.9925076303902,4.5908616218996,132.574081127621));
#62402=CARTESIAN_POINT('Ctrl Pts',(37.984747187876,4.63652563516663,132.445035203504));
#62403=CARTESIAN_POINT('Ctrl Pts',(37.9769742876105,4.68226295236154,132.315782123414));
#62404=CARTESIAN_POINT('Ctrl Pts',(37.9692013873451,4.72254293396779,132.184752037572));
#62405=CARTESIAN_POINT('Ctrl Pts',(37.9614284870797,4.75725350033361,132.052448032799));
#62406=CARTESIAN_POINT('Ctrl Pts',(37.9539381513176,4.79070225018148,131.924953611853));
#62407=CARTESIAN_POINT('Ctrl Pts',(37.9464478155556,4.81897941313919,131.796276585114));
#62408=CARTESIAN_POINT('Ctrl Pts',(37.9389574797935,4.84203022070033,131.666872301153));
#62409=CARTESIAN_POINT('Ctrl Pts',(37.9311831456744,4.86595500663622,131.532561614435));
#62410=CARTESIAN_POINT('Ctrl Pts',(37.9234088115554,4.88432508580291,131.397041978058));
#62411=CARTESIAN_POINT('Ctrl Pts',(37.9156344774363,4.89702303785638,131.260812618552));
#62412=CARTESIAN_POINT('Ctrl Pts',(37.9078697244892,4.90970534081879,131.124751149556));
#62413=CARTESIAN_POINT('Ctrl Pts',(37.9001049715421,4.91672938952374,130.987982083306));
#62414=CARTESIAN_POINT('Ctrl Pts',(37.892340218595,4.91802871393031,130.851015000607));
#62415=CARTESIAN_POINT('Ctrl Pts',(37.88458317771,4.91932674782958,130.714183955545));
#62416=CARTESIAN_POINT('Ctrl Pts',(37.8768261368249,4.91491136889733,130.577155673838));
#62417=CARTESIAN_POINT('Ctrl Pts',(37.8690690959399,4.90476790952643,130.44044467098));
#62418=CARTESIAN_POINT('Ctrl Pts',(37.8613179046998,4.89463209941722,130.303836762953));
#62419=CARTESIAN_POINT('Ctrl Pts',(37.8535667134597,4.87877683556304,130.167546045853));
#62420=CARTESIAN_POINT('Ctrl Pts',(37.8458155222196,4.85723951782926,130.032086489463));
#62421=CARTESIAN_POINT('Ctrl Pts',(37.8380676254425,4.83571135402995,129.896684506997));
#62422=CARTESIAN_POINT('Ctrl Pts',(37.8303197286654,4.8085060009122,129.76211336793));
#62423=CARTESIAN_POINT('Ctrl Pts',(37.8225718318884,4.77571262720884,129.628881155892));
#62424=CARTESIAN_POINT('Ctrl Pts',(37.8148255558042,4.74292611317228,129.49567681316));
#62425=CARTESIAN_POINT('Ctrl Pts',(37.8070792797201,4.70455399692611,129.363811219768));
#62426=CARTESIAN_POINT('Ctrl Pts',(37.799333003636,4.66073632653493,129.233781120368));
#62427=CARTESIAN_POINT('Ctrl Pts',(37.7915866703707,4.61691833269178,129.103750061116));
#62428=CARTESIAN_POINT('Ctrl Pts',(37.7838403371053,4.56765482934145,128.975554893387));
#62429=CARTESIAN_POINT('Ctrl Pts',(37.77609400384,4.51313526632565,128.849675699133));
#62430=CARTESIAN_POINT('Ctrl Pts',(37.768345935837,4.45860349403173,128.723768315107));
#62431=CARTESIAN_POINT('Ctrl Pts',(37.7605978678341,4.39881347521647,128.600178295296));
#62432=CARTESIAN_POINT('Ctrl Pts',(37.7528497998311,4.3340020135298,128.479363927414));
#62433=CARTESIAN_POINT('Ctrl Pts',(37.7450934970892,4.26912166945028,128.358421156583));
#62434=CARTESIAN_POINT('Ctrl Pts',(37.7373371943474,4.19920940668318,128.240260275687));
#62435=CARTESIAN_POINT('Ctrl Pts',(37.7295808916055,4.12454732799884,128.125313697186));
#62436=CARTESIAN_POINT('Ctrl Pts',(37.7218204490913,4.04984539991507,128.010305768235));
#62437=CARTESIAN_POINT('Ctrl Pts',(37.7140600065772,3.97038883086328,127.898515878614));
#62438=CARTESIAN_POINT('Ctrl Pts',(37.706299564063,3.88650135470987,127.790344976874));
#62439=CARTESIAN_POINT('Ctrl Pts',(37.6985266637975,3.80247921493244,127.682000429599));
#62440=CARTESIAN_POINT('Ctrl Pts',(37.6907537635321,3.71401220670041,127.5772867783));
#62441=CARTESIAN_POINT('Ctrl Pts',(37.6829808632666,3.62146300941391,127.476570249477));
#62442=CARTESIAN_POINT('Ctrl Pts',(37.6754905275045,3.53227820856576,127.379515020166));
#62443=CARTESIAN_POINT('Ctrl Pts',(37.6680001917425,3.43930307893425,127.286171566055));
#62444=CARTESIAN_POINT('Ctrl Pts',(37.6605098559805,3.34289111445189,127.196832092465));
#62445=CARTESIAN_POINT('Ctrl Pts',(37.6527355218614,3.24282366103296,127.10410528558));
#62446=CARTESIAN_POINT('Ctrl Pts',(37.6449611877423,3.13873662933688,127.015398343996));
#62447=CARTESIAN_POINT('Ctrl Pts',(37.6371868536232,3.03098656421825,126.931079900909));
#62448=CARTESIAN_POINT('Ctrl Pts',(37.6294221006761,2.92336929142483,126.846865372767));
#62449=CARTESIAN_POINT('Ctrl Pts',(37.621657347729,2.81209827238428,126.767028820582));
#62450=CARTESIAN_POINT('Ctrl Pts',(37.6138925947819,2.69756630317921,126.691901608354));
#62451=CARTESIAN_POINT('Ctrl Pts',(37.6061355538969,2.58314808874105,126.616849013532));
#62452=CARTESIAN_POINT('Ctrl Pts',(37.5983785130119,2.46547569433492,126.546496663514));
#62453=CARTESIAN_POINT('Ctrl Pts',(37.5906214721269,2.34497406821629,126.481135006764));
#62454=CARTESIAN_POINT('Ctrl Pts',(37.5828702808868,2.22456331331063,126.415822639748));
#62455=CARTESIAN_POINT('Ctrl Pts',(37.5751190896467,2.10132791566018,126.355493660594));
#62456=CARTESIAN_POINT('Ctrl Pts',(37.5673678984065,1.97572050814078,126.300394416959));
#62457=CARTESIAN_POINT('Ctrl Pts',(37.5596200016294,1.85016648712079,126.245318591973));
#62458=CARTESIAN_POINT('Ctrl Pts',(37.5518721048523,1.72224281868317,126.195468238298));
#62459=CARTESIAN_POINT('Ctrl Pts',(37.5441242080752,1.59242516585422,126.151042967367));
#62460=CARTESIAN_POINT('Ctrl Pts',(37.5363779319911,1.46263466807933,126.106626989245));
#62461=CARTESIAN_POINT('Ctrl Pts',(37.528631655907,1.33095134360888,126.067633963173));
#62462=CARTESIAN_POINT('Ctrl Pts',(37.5208853798229,1.19786881718728,126.034214565367));
#62463=CARTESIAN_POINT('Ctrl Pts',(37.5131390465576,1.06478530838106,126.000794920866));
#62464=CARTESIAN_POINT('Ctrl Pts',(37.5053927132922,0.930302956205765,125.972949081951));
#62465=CARTESIAN_POINT('Ctrl Pts',(37.4976463800269,0.794928069472048,125.950777155127));
#62466=CARTESIAN_POINT('Ctrl Pts',(37.4898983120239,0.659522866471439,125.928600263053));
#62467=CARTESIAN_POINT('Ctrl Pts',(37.4821502440209,0.523225116931304,125.912099874661));
#62468=CARTESIAN_POINT('Ctrl Pts',(37.474402176018,0.386548389441731,125.901324476039));
#62469=CARTESIAN_POINT('Ctrl Pts',(37.4666458732761,0.249726400299151,125.890537625195));
#62470=CARTESIAN_POINT('Ctrl Pts',(37.4588895705342,0.112525018983439,125.885487949514));
#62471=CARTESIAN_POINT('Ctrl Pts',(37.4511332677924,-0.0245394702169603,
125.886171837446));
#62472=CARTESIAN_POINT('Ctrl Pts',(37.4433728252782,-0.161677114861992,
125.886856090389));
#62473=CARTESIAN_POINT('Ctrl Pts',(37.4356123827641,-0.298677331461582,
125.893279986299));
#62474=CARTESIAN_POINT('Ctrl Pts',(37.4278519402499,-0.435027804581187,
125.905387881191));
#62475=CARTESIAN_POINT('Ctrl Pts',(37.4200790399845,-0.571597159585056,
125.917515212752));
#62476=CARTESIAN_POINT('Ctrl Pts',(37.412306139719,-0.70751429894357,125.935344725993));
#62477=CARTESIAN_POINT('Ctrl Pts',(37.4045332394536,-0.842275068855532,
125.958769242833));
#62478=CARTESIAN_POINT('Ctrl Pts',(37.3970429036916,-0.972136945338934,
125.981342219483));
#62479=CARTESIAN_POINT('Ctrl Pts',(37.3895525679296,-1.10092476551482,126.009110412247));
#62480=CARTESIAN_POINT('Ctrl Pts',(37.3820622321676,-1.22820161666663,126.041934360781));
#62481=CARTESIAN_POINT('Ctrl Pts',(37.3742878980485,-1.36030420831501,126.0760028393));
#62482=CARTESIAN_POINT('Ctrl Pts',(37.3665135639294,-1.49119745367912,126.11562593825));
#62483=CARTESIAN_POINT('Ctrl Pts',(37.3587392298104,-1.62037849000892,126.160702941594));
#62484=CARTESIAN_POINT('Ctrl Pts',(37.3509744768633,-1.74940032225669,126.205724391559));
#62485=CARTESIAN_POINT('Ctrl Pts',(37.3432097239161,-1.87671377843557,126.256186244665));
#62486=CARTESIAN_POINT('Ctrl Pts',(37.335444970969,-2.0018277567502,126.311937140777));
#62487=CARTESIAN_POINT('Ctrl Pts',(37.327687930084,-2.12681747009793,126.367632664314));
#62488=CARTESIAN_POINT('Ctrl Pts',(37.319930889199,-2.2496116981351,126.428606618747));
#62489=CARTESIAN_POINT('Ctrl Pts',(37.312173848314,-2.36973638343055,126.494658477563));
#62490=CARTESIAN_POINT('Ctrl Pts',(37.3044226570739,-2.4897704817672,126.56066052616));
#62491=CARTESIAN_POINT('Ctrl Pts',(37.2966714658337,-2.60713870315736,126.631732669561));
#62492=CARTESIAN_POINT('Ctrl Pts',(37.2889202745936,-2.72138912921527,126.707627251836));
#62493=CARTESIAN_POINT('Ctrl Pts',(37.2811723778165,-2.83559099579344,126.783489576887));
#62494=CARTESIAN_POINT('Ctrl Pts',(37.2734244810394,-2.94667737767535,126.864170048307));
#62495=CARTESIAN_POINT('Ctrl Pts',(37.2656765842623,-3.05422322862498,126.949376372173));
#62496=CARTESIAN_POINT('Ctrl Pts',(37.2579303081782,-3.16174658330117,127.034564872713));
#62497=CARTESIAN_POINT('Ctrl Pts',(37.2501840320941,-3.26573057389539,127.124277100006));
#62498=CARTESIAN_POINT('Ctrl Pts',(37.24243775601,-3.36578161600863,127.218179197749));
#62499=CARTESIAN_POINT('Ctrl Pts',(37.2346914227446,-3.46583339667552,127.312081988656));
#62500=CARTESIAN_POINT('Ctrl Pts',(37.2269450894793,-3.56195188585453,127.410174444173));
#62501=CARTESIAN_POINT('Ctrl Pts',(37.219198756214,-3.65377918882848,127.512084702369));
#62502=CARTESIAN_POINT('Ctrl Pts',(37.211450688211,-3.74562705589024,127.614017782662));
#62503=CARTESIAN_POINT('Ctrl Pts',(37.2037026202081,-3.83318156284325,127.719770076533));
#62504=CARTESIAN_POINT('Ctrl Pts',(37.1959545522052,-3.91612432060231,127.828935712097));
#62505=CARTESIAN_POINT('Ctrl Pts',(37.1881982494633,-3.99915523091157,127.938217370197));
#62506=CARTESIAN_POINT('Ctrl Pts',(37.1804419467215,-4.07756436400675,128.050919304993));
#62507=CARTESIAN_POINT('Ctrl Pts',(37.1726856439796,-4.1510756941205,128.166605199757));
#62508=CARTESIAN_POINT('Ctrl Pts',(37.1649252014654,-4.22462625944472,128.282352839566));
#62509=CARTESIAN_POINT('Ctrl Pts',(37.1571647589513,-4.29327361737003,128.401087274491));
#62510=CARTESIAN_POINT('Ctrl Pts',(37.1494043164371,-4.35678766375012,128.522347402115));
#62511=CARTESIAN_POINT('Ctrl Pts',(37.1416314161717,-4.42040366851579,128.643802187259));
#62512=CARTESIAN_POINT('Ctrl Pts',(37.1338585159063,-4.47886972785175,128.767790413392));
#62513=CARTESIAN_POINT('Ctrl Pts',(37.1260856156408,-4.53200350626976,128.89382998927));
#62514=CARTESIAN_POINT('Ctrl Pts',(37.1185952798788,-4.58320573800636,129.01528770909));
#62515=CARTESIAN_POINT('Ctrl Pts',(37.1111049441168,-4.62945653362067,129.138649936129));
#62516=CARTESIAN_POINT('Ctrl Pts',(37.1036146083548,-4.6706370630542,129.263473701623));
#62517=CARTESIAN_POINT('Ctrl Pts',(37.0973024603346,-4.70534012652036,129.368663389944));
#62518=CARTESIAN_POINT('Ctrl Pts',(37.0909903123145,-4.73650493527999,129.475074674504));
#62519=CARTESIAN_POINT('Ctrl Pts',(37.0846781642943,-4.76405452823403,129.582490119308));
#62520=CARTESIAN_POINT('Ctrl Pts',(38.8349537180509,-4.76405452823399,129.582490119308));
#62521=CARTESIAN_POINT('Ctrl Pts',(38.8271914067485,-4.79811247623972,129.715281541681));
#62522=CARTESIAN_POINT('Ctrl Pts',(38.819429095446,-4.82658390929227,129.849379955364));
#62523=CARTESIAN_POINT('Ctrl Pts',(38.8116667841435,-4.84939621256512,129.984275599986));
#62524=CARTESIAN_POINT('Ctrl Pts',(38.8038928211692,-4.87224275840619,130.119373730664));
#62525=CARTESIAN_POINT('Ctrl Pts',(38.7961188581948,-4.88941315961131,130.2552710952));
#62526=CARTESIAN_POINT('Ctrl Pts',(38.7883448952204,-4.90088673234273,130.391453486062));
#62527=CARTESIAN_POINT('Ctrl Pts',(38.7836633805576,-4.90779616825762,130.473463120238));
#62528=CARTESIAN_POINT('Ctrl Pts',(38.7789818658948,-4.91264065855441,130.555576104893));
#62529=CARTESIAN_POINT('Ctrl Pts',(38.7743003512321,-4.91542478919734,130.637680672029));
#62530=CARTESIAN_POINT('Ctrl Pts',(38.7711533794851,-4.91729631606509,130.692872372085));
#62531=CARTESIAN_POINT('Ctrl Pts',(38.7680064077382,-4.91823831758393,130.748095770571));
#62532=CARTESIAN_POINT('Ctrl Pts',(38.7648594359912,-4.91824989201499,130.80332998935));
#62533=CARTESIAN_POINT('',(39.1101405639799,-4.91824799303067,130.808803763948));
#62534=CARTESIAN_POINT('Ctrl Pts',(39.1801134839905,-4.76405452823399,129.582490119308));
#62535=CARTESIAN_POINT('Ctrl Pts',(39.1724358615329,-4.79786231385947,129.714306162357));
#62536=CARTESIAN_POINT('Ctrl Pts',(39.1647582390752,-4.82619617992312,129.847530671823));
#62537=CARTESIAN_POINT('Ctrl Pts',(39.1570806166175,-4.84895407859681,129.981665409023));
#62538=CARTESIAN_POINT('Ctrl Pts',(39.149257274516,-4.87214391735433,130.11834599505));
#62539=CARTESIAN_POINT('Ctrl Pts',(39.1414339324146,-4.8895438922101,130.255971290643));
#62540=CARTESIAN_POINT('Ctrl Pts',(39.1336105903131,-4.9011011506914,130.394006413016));
#62541=CARTESIAN_POINT('Ctrl Pts',(39.1257872482116,-4.91265840917271,130.53204153539));
#62542=CARTESIAN_POINT('Ctrl Pts',(39.1179639061101,-4.91837294927344,130.670486047647));
#62543=CARTESIAN_POINT('Ctrl Pts',(39.1101405640087,-4.91824799303113,130.808803763438));
#62544=CARTESIAN_POINT('Ctrl Pts',(39.1101405639799,-4.91824799303067,130.808803763948));
#62545=CARTESIAN_POINT('Ctrl Pts',(39.1005410273949,-4.91809466697877,130.978524831473));
#62546=CARTESIAN_POINT('Ctrl Pts',(39.09094149081,-4.90915251206192,131.147854560965));
#62547=CARTESIAN_POINT('Ctrl Pts',(39.0813419542251,-4.891564635173,131.316003542295));
#62548=CARTESIAN_POINT('Ctrl Pts',(39.0715821838055,-4.87368318442951,131.486959237868));
#62549=CARTESIAN_POINT('Ctrl Pts',(39.061822413386,-4.84686501379065,131.656694537834));
#62550=CARTESIAN_POINT('Ctrl Pts',(39.0520626429664,-4.81130913710586,131.824403484166));
#62551=CARTESIAN_POINT('Ctrl Pts',(39.0457614216062,-4.78835312072256,131.932681768337));
#62552=CARTESIAN_POINT('Ctrl Pts',(39.0394602002459,-4.76175584959625,132.040115861972));
#62553=CARTESIAN_POINT('Ctrl Pts',(39.0331589788857,-4.73158134341099,132.146493641221));
#62554=CARTESIAN_POINT('Ctrl Pts',(39.0253846447666,-4.6943525778192,132.27774064104));
#62555=CARTESIAN_POINT('Ctrl Pts',(39.0176103106475,-4.65159981236601,132.407645347261));
#62556=CARTESIAN_POINT('Ctrl Pts',(39.0098359765284,-4.60343580140505,132.535707458855));
#62557=CARTESIAN_POINT('Ctrl Pts',(39.0020712235814,-4.55533114828305,132.663611745342));
#62558=CARTESIAN_POINT('Ctrl Pts',(38.9943064706342,-4.50182865503804,132.789677593055));
#62559=CARTESIAN_POINT('Ctrl Pts',(38.9865417176871,-4.44309142330373,132.913417673851));
#62560=CARTESIAN_POINT('Ctrl Pts',(38.9787846768021,-4.38441253021619,133.037034854253));
#62561=CARTESIAN_POINT('Ctrl Pts',(38.9710276359172,-4.32050941188381,133.158330513804));
#62562=CARTESIAN_POINT('Ctrl Pts',(38.9632705950322,-4.25159391314395,133.276835543671));
#62563=CARTESIAN_POINT('Ctrl Pts',(38.9555194037921,-4.18273038411758,133.395251207973));
#62564=CARTESIAN_POINT('Ctrl Pts',(38.9477682125519,-4.10886219404433,133.510880094741));
#62565=CARTESIAN_POINT('Ctrl Pts',(38.9400170213118,-4.03024777233264,133.623276358788));
#62566=CARTESIAN_POINT('Ctrl Pts',(38.9322691245347,-3.9516667638474,133.735624851424));
#62567=CARTESIAN_POINT('Ctrl Pts',(38.9245212277576,-3.86834375954424,133.844743134319));
#62568=CARTESIAN_POINT('Ctrl Pts',(38.9167733309805,-3.78058116910775,133.950213297888));
#62569=CARTESIAN_POINT('Ctrl Pts',(38.9090270548964,-3.69283693671324,134.055661399372));
#62570=CARTESIAN_POINT('Ctrl Pts',(38.9012807788123,-3.60065521526645,134.157462599055));
#62571=CARTESIAN_POINT('Ctrl Pts',(38.8935345027282,-3.50437920986823,134.25523143751));
#62572=CARTESIAN_POINT('Ctrl Pts',(38.8857881694628,-3.40810249378241,134.353000997673));
#62573=CARTESIAN_POINT('Ctrl Pts',(38.8780418361975,-3.30773170775642,134.446737858641));
#62574=CARTESIAN_POINT('Ctrl Pts',(38.8702955029322,-3.20364719512028,134.536093152421));
#62575=CARTESIAN_POINT('Ctrl Pts',(38.8625474349292,-3.0995393734792,134.6254684567));
#62576=CARTESIAN_POINT('Ctrl Pts',(38.8547993669262,-2.99171646690314,134.710459986657));
#62577=CARTESIAN_POINT('Ctrl Pts',(38.8470512989232,-2.88059187085699,134.790759184701));
#62578=CARTESIAN_POINT('Ctrl Pts',(38.8392949961814,-2.76934917026777,134.871143725687));
#62579=CARTESIAN_POINT('Ctrl Pts',(38.8315386934395,-2.65479808784851,134.946825743208));
#62580=CARTESIAN_POINT('Ctrl Pts',(38.8237823906977,-2.53738143853433,135.017539761381));
#62581=CARTESIAN_POINT('Ctrl Pts',(38.8160219481835,-2.4199021204189,135.088291521756));
#62582=CARTESIAN_POINT('Ctrl Pts',(38.8082615056694,-2.29955453076905,135.154069811887));
#62583=CARTESIAN_POINT('Ctrl Pts',(38.8005010631552,-2.17680516108111,135.214655659079));
#62584=CARTESIAN_POINT('Ctrl Pts',(38.7927281628898,-2.05385874320777,135.275338764051));
#62585=CARTESIAN_POINT('Ctrl Pts',(38.7849552626243,-1.92850319840539,135.330812611052));
#62586=CARTESIAN_POINT('Ctrl Pts',(38.7771823623589,-1.80122485463524,135.380906485963));
#62587=CARTESIAN_POINT('Ctrl Pts',(38.7696920265968,-1.6785733992556,135.429179322342));
#62588=CARTESIAN_POINT('Ctrl Pts',(38.7622016908348,-1.55413680592188,135.472456445569));
#62589=CARTESIAN_POINT('Ctrl Pts',(38.7547113550727,-1.4283607674286,135.510629689832));
#62590=CARTESIAN_POINT('Ctrl Pts',(38.7469370209536,-1.29781589220743,135.550250284255));
#62591=CARTESIAN_POINT('Ctrl Pts',(38.7391626868345,-1.16541446974887,135.584497838669));
#62592=CARTESIAN_POINT('Ctrl Pts',(38.7313883527154,-1.03163836396168,135.61319679158));
#62593=CARTESIAN_POINT('Ctrl Pts',(38.7236235997683,-0.89802712526896,135.641860375595));
#62594=CARTESIAN_POINT('Ctrl Pts',(38.7158588468212,-0.763044952747463,
135.664988882778));
#62595=CARTESIAN_POINT('Ctrl Pts',(38.7080940938741,-0.627190009783876,
135.682456122384));
#62596=CARTESIAN_POINT('Ctrl Pts',(38.7003370529891,-0.491469999865044,
135.699906013282));
#62597=CARTESIAN_POINT('Ctrl Pts',(38.6925800121042,-0.354879329834526,
135.711705776797));
#62598=CARTESIAN_POINT('Ctrl Pts',(38.6848229712192,-0.217927181546811,
135.717780079208));
#62599=CARTESIAN_POINT('Ctrl Pts',(38.6770717799791,-0.0810783099396389,
135.723849800941));
#62600=CARTESIAN_POINT('Ctrl Pts',(38.6693205887389,0.0561311083429407,
135.724202638266));
#62601=CARTESIAN_POINT('Ctrl Pts',(38.6615693974988,0.193186283712091,135.718815024953));
#62602=CARTESIAN_POINT('Ctrl Pts',(38.6538215007217,0.330183206976016,135.713429701519));
#62603=CARTESIAN_POINT('Ctrl Pts',(38.6460736039447,0.467025627869497,135.702308795436));
#62604=CARTESIAN_POINT('Ctrl Pts',(38.6383257071676,0.603198487401534,135.685480842196));
#62605=CARTESIAN_POINT('Ctrl Pts',(38.6305794310835,0.739342862506905,135.668656409002));
#62606=CARTESIAN_POINT('Ctrl Pts',(38.6228331549993,0.874817567065649,135.646127351088));
#62607=CARTESIAN_POINT('Ctrl Pts',(38.6150868789152,1.00911279240587,135.61797406639));
#62608=CARTESIAN_POINT('Ctrl Pts',(38.6073405456498,1.14340900908293,135.589820573871));
#62609=CARTESIAN_POINT('Ctrl Pts',(38.5995942123845,1.27652534652062,135.556042851942));
#62610=CARTESIAN_POINT('Ctrl Pts',(38.5918478791192,1.40796270733709,135.516772322548));
#62611=CARTESIAN_POINT('Ctrl Pts',(38.5840998111162,1.5394295026392,135.47749299879));
#62612=CARTESIAN_POINT('Ctrl Pts',(38.5763517431132,1.66921619860237,135.432718531759));
#62613=CARTESIAN_POINT('Ctrl Pts',(38.5686036751102,1.79683974664007,135.382629939853));
#62614=CARTESIAN_POINT('Ctrl Pts',(38.5608473723684,1.92459893450336,135.332488113195));
#62615=CARTESIAN_POINT('Ctrl Pts',(38.5530910696266,2.05019001738285,135.277021022406));
#62616=CARTESIAN_POINT('Ctrl Pts',(38.5453347668847,2.17315029061294,135.216457724035));
#62617=CARTESIAN_POINT('Ctrl Pts',(38.5375743243705,2.29617619144311,135.155862101207));
#62618=CARTESIAN_POINT('Ctrl Pts',(38.5298138818563,2.41656814172715,135.090165038154));
#62619=CARTESIAN_POINT('Ctrl Pts',(38.5220534393422,2.53388976348633,135.019640647291));
#62620=CARTESIAN_POINT('Ctrl Pts',(38.5142805390767,2.65139972032808,134.949003044416));
#62621=CARTESIAN_POINT('Ctrl Pts',(38.5065076388113,2.76582917285638,134.873522843648));
#62622=CARTESIAN_POINT('Ctrl Pts',(38.4987347385458,2.87677162230528,134.793516931324));
#62623=CARTESIAN_POINT('Ctrl Pts',(38.4912444027838,2.98368103426908,134.716419435437));
#62624=CARTESIAN_POINT('Ctrl Pts',(38.4837540670219,3.08735232193994,134.635119747445));
#62625=CARTESIAN_POINT('Ctrl Pts',(38.4762637312599,3.18745357451689,134.549934375056));
#62626=CARTESIAN_POINT('Ctrl Pts',(38.4684893971408,3.29135019651085,134.461519173382));
#62627=CARTESIAN_POINT('Ctrl Pts',(38.4607150630217,3.3917298369044,134.368637746568));
#62628=CARTESIAN_POINT('Ctrl Pts',(38.4529407289026,3.48818433162545,134.271600605092));
#62629=CARTESIAN_POINT('Ctrl Pts',(38.4451759759555,3.58451995480214,134.174683053221));
#62630=CARTESIAN_POINT('Ctrl Pts',(38.4374112230084,3.67693978429857,134.073620251662));
#62631=CARTESIAN_POINT('Ctrl Pts',(38.4296464700613,3.76506838279081,133.968763110203));
#62632=CARTESIAN_POINT('Ctrl Pts',(38.4218894291763,3.85310945071664,133.864010114336));
#62633=CARTESIAN_POINT('Ctrl Pts',(38.4141323882913,3.93686751951246,133.755470575595));
#62634=CARTESIAN_POINT('Ctrl Pts',(38.4063753474063,4.01600398355601,133.64353216338));
#62635=CARTESIAN_POINT('Ctrl Pts',(38.3986241561662,4.09508077017642,133.531678164793));
#62636=CARTESIAN_POINT('Ctrl Pts',(38.3908729649261,4.16954266431975,133.416430712412));
#62637=CARTESIAN_POINT('Ctrl Pts',(38.383121773686,4.23909158270006,133.298210175174));
#62638=CARTESIAN_POINT('Ctrl Pts',(38.3753738769089,4.30861094093478,133.180039884818));
#62639=CARTESIAN_POINT('Ctrl Pts',(38.3676259801318,4.37322127874126,133.05889935916));
#62640=CARTESIAN_POINT('Ctrl Pts',(38.3598780833547,4.4326682018728,132.935237356048));
#62641=CARTESIAN_POINT('Ctrl Pts',(38.3521318072706,4.49210268998955,132.811601220362));
#62642=CARTESIAN_POINT('Ctrl Pts',(38.3443855311865,4.54637574247788,132.685445008469));
#62643=CARTESIAN_POINT('Ctrl Pts',(38.3366392551024,4.5952794363588,132.55724109389));
#62644=CARTESIAN_POINT('Ctrl Pts',(38.3288929218371,4.64418349123561,132.42903623294));
#62645=CARTESIAN_POINT('Ctrl Pts',(38.3211465885717,4.68771796907419,132.298784004433));
#62646=CARTESIAN_POINT('Ctrl Pts',(38.3134002553064,4.72572366455252,132.166975349905));
#62647=CARTESIAN_POINT('Ctrl Pts',(38.3056521873034,4.7637378711429,132.035137177743));
#62648=CARTESIAN_POINT('Ctrl Pts',(38.2979041193004,4.79622072333547,131.901742261572));
#62649=CARTESIAN_POINT('Ctrl Pts',(38.2901560512974,4.82306341747488,131.767294848713));
#62650=CARTESIAN_POINT('Ctrl Pts',(38.2823997485555,4.84993464034905,131.632704543545));
#62651=CARTESIAN_POINT('Ctrl Pts',(38.2746434458137,4.87115365398788,131.497059891164));
#62652=CARTESIAN_POINT('Ctrl Pts',(38.2668871430718,4.88666306697858,131.360873988769));
#62653=CARTESIAN_POINT('Ctrl Pts',(38.2591267005577,4.90218075780997,131.224615399857));
#62654=CARTESIAN_POINT('Ctrl Pts',(38.2513662580435,4.91198274789094,131.087815375086));
#62655=CARTESIAN_POINT('Ctrl Pts',(38.2436058155293,4.91606378280456,130.950989216063));
#62656=CARTESIAN_POINT('Ctrl Pts',(38.2358329152639,4.92015136895772,130.813943411544));
#62657=CARTESIAN_POINT('Ctrl Pts',(38.2280600149985,4.918499652528,130.6768717801));
#62658=CARTESIAN_POINT('Ctrl Pts',(38.2202871147331,4.91115551645211,130.540287605461));
#62659=CARTESIAN_POINT('Ctrl Pts',(38.212796778971,4.9040783582213,130.408668609605));
#62660=CARTESIAN_POINT('Ctrl Pts',(38.2053064432089,4.8917154914845,130.277502551947));
#62661=CARTESIAN_POINT('Ctrl Pts',(38.1978161074468,4.87415379724563,130.147239758594));
#62662=CARTESIAN_POINT('Ctrl Pts',(38.1900417733277,4.85592624603203,130.012038011839));
#62663=CARTESIAN_POINT('Ctrl Pts',(38.1822674392087,4.83204011865691,129.877381097529));
#62664=CARTESIAN_POINT('Ctrl Pts',(38.1744931050896,4.80253603372715,129.743780254155));
#62665=CARTESIAN_POINT('Ctrl Pts',(38.1667283521425,4.77306830994521,129.610344061881));
#62666=CARTESIAN_POINT('Ctrl Pts',(38.1589635991954,4.73799648806898,129.477961729021));
#62667=CARTESIAN_POINT('Ctrl Pts',(38.1511988462483,4.69741286539684,129.347138796941));
#62668=CARTESIAN_POINT('Ctrl Pts',(38.1434418053633,4.65686955095092,129.216445800042));
#62669=CARTESIAN_POINT('Ctrl Pts',(38.1356847644783,4.61082544509765,129.087309492698));
#62670=CARTESIAN_POINT('Ctrl Pts',(38.1279277235933,4.55942368047204,128.960224298188));
#62671=CARTESIAN_POINT('Ctrl Pts',(38.1201765323532,4.50806067831697,128.833234939611));
#62672=CARTESIAN_POINT('Ctrl Pts',(38.1124253411131,4.45134820526876,128.70829397611));
#62673=CARTESIAN_POINT('Ctrl Pts',(38.1046741498729,4.38947880832195,128.585879413275));
#62674=CARTESIAN_POINT('Ctrl Pts',(38.0969262530959,4.32763570751926,128.463516879894));
#62675=CARTESIAN_POINT('Ctrl Pts',(38.0891783563188,4.26064021818513,128.343678959698));
#62676=CARTESIAN_POINT('Ctrl Pts',(38.0814304595417,4.18873238670201,128.226822246349));
#62677=CARTESIAN_POINT('Ctrl Pts',(38.0736841834576,4.11683959678708,128.109989976906));
#62678=CARTESIAN_POINT('Ctrl Pts',(38.0659379073735,4.04003671335433,127.99613800669));
#62679=CARTESIAN_POINT('Ctrl Pts',(38.0581916312894,3.95860877017774,127.885696596619));
#62680=CARTESIAN_POINT('Ctrl Pts',(38.0504452980241,3.87718022591847,127.775254371294));
#62681=CARTESIAN_POINT('Ctrl Pts',(38.0426989647587,3.7911267858018,127.668223071033));
#62682=CARTESIAN_POINT('Ctrl Pts',(38.0349526314934,3.70077543847887,127.565002005672));
#62683=CARTESIAN_POINT('Ctrl Pts',(38.0272045634904,3.61040385759816,127.461757824669));
#62684=CARTESIAN_POINT('Ctrl Pts',(38.0194564954874,3.51573271173069,127.362325870615));
#62685=CARTESIAN_POINT('Ctrl Pts',(38.0117084274845,3.41712742739617,127.2670702411));
#62686=CARTESIAN_POINT('Ctrl Pts',(38.0039521247426,3.31841734419204,127.171713372769));
#62687=CARTESIAN_POINT('Ctrl Pts',(37.9961958220007,3.21576505166253,127.080541967724));
#62688=CARTESIAN_POINT('Ctrl Pts',(37.9884395192589,3.10957121155231,126.993881652556));
#62689=CARTESIAN_POINT('Ctrl Pts',(37.9806790767447,3.00332069259218,126.907175084168));
#62690=CARTESIAN_POINT('Ctrl Pts',(37.9729186342305,2.89352517243947,126.824984637391));
#62691=CARTESIAN_POINT('Ctrl Pts',(37.9651581917163,2.78061534879152,126.747593266021));
#62692=CARTESIAN_POINT('Ctrl Pts',(37.9573852914509,2.66752427227099,126.670077659151));
#62693=CARTESIAN_POINT('Ctrl Pts',(37.9496123911855,2.5513092335913,126.597376730006));
#62694=CARTESIAN_POINT('Ctrl Pts',(37.94183949092,2.43242741426335,126.529728477037));
#62695=CARTESIAN_POINT('Ctrl Pts',(37.934349155158,2.31786724851352,126.46453940846));
#62696=CARTESIAN_POINT('Ctrl Pts',(37.926858819396,2.20083109794056,126.404042180308));
#62697=CARTESIAN_POINT('Ctrl Pts',(37.919368483634,2.08174479595503,126.348407109391));
#62698=CARTESIAN_POINT('Ctrl Pts',(37.9115941495149,1.95814330063388,126.290662617851));
#62699=CARTESIAN_POINT('Ctrl Pts',(37.9038198153958,1.83194158964571,126.237973341939));
#62700=CARTESIAN_POINT('Ctrl Pts',(37.8960454812768,1.703591737761,126.190581444964));
#62701=CARTESIAN_POINT('Ctrl Pts',(37.8882807283297,1.57540006559778,126.143247954267));
#62702=CARTESIAN_POINT('Ctrl Pts',(37.8805159753826,1.44506588329948,126.101198986768));
#62703=CARTESIAN_POINT('Ctrl Pts',(37.8727512224355,1.31306440607854,126.064630147593));
#62704=CARTESIAN_POINT('Ctrl Pts',(37.8649941815505,1.18119403458568,126.028097629105));
#62705=CARTESIAN_POINT('Ctrl Pts',(37.8572371406654,1.04766003798285,125.997034510947));
#62706=CARTESIAN_POINT('Ctrl Pts',(37.8494800997804,0.912955755263201,125.971587619438));
#62707=CARTESIAN_POINT('Ctrl Pts',(37.8417289085403,0.778353054091366,125.946159917629));
#62708=CARTESIAN_POINT('Ctrl Pts',(37.8339777173003,0.642582206024923,125.92634008476));
#62709=CARTESIAN_POINT('Ctrl Pts',(37.8262265260601,0.506149447057368,125.91222449929));
#62710=CARTESIAN_POINT('Ctrl Pts',(37.8184786292831,0.369774675651652,125.898114913319));
#62711=CARTESIAN_POINT('Ctrl Pts',(37.810730732506,0.232738940963491,125.889704792837));
#62712=CARTESIAN_POINT('Ctrl Pts',(37.8029828357289,0.0955561391059442,
125.88703898005));
#62713=CARTESIAN_POINT('Ctrl Pts',(37.7952365596448,-0.0415979670667733,
125.884373724894));
#62714=CARTESIAN_POINT('Ctrl Pts',(37.7874902835607,-0.178898688575267,
125.887450395006));
#62715=CARTESIAN_POINT('Ctrl Pts',(37.7797440074766,-0.315829967006171,
125.896261749935));
#62716=CARTESIAN_POINT('Ctrl Pts',(37.7719976742112,-0.452762256232666,
125.905073169907));
#62717=CARTESIAN_POINT('Ctrl Pts',(37.7642513409459,-0.589324706781487,
125.919619334061));
#62718=CARTESIAN_POINT('Ctrl Pts',(37.7565050076805,-0.725004622624458,
125.939840974305));
#62719=CARTESIAN_POINT('Ctrl Pts',(37.7487569396776,-0.860714923043844,
125.960067143045));
#62720=CARTESIAN_POINT('Ctrl Pts',(37.7410088716746,-0.995541908861559,
125.985971259362));
#62721=CARTESIAN_POINT('Ctrl Pts',(37.7332608036716,-1.12898173250234,126.017442683219));
#62722=CARTESIAN_POINT('Ctrl Pts',(37.7255045009298,-1.26256337757564,126.048947555279));
#62723=CARTESIAN_POINT('Ctrl Pts',(37.7177481981879,-1.39475453428196,126.086031464836));
#62724=CARTESIAN_POINT('Ctrl Pts',(37.7099918954461,-1.52506467628915,126.128533332942));
#62725=CARTESIAN_POINT('Ctrl Pts',(37.7022314529319,-1.65544436874287,126.171057885575));
#62726=CARTESIAN_POINT('Ctrl Pts',(37.6944710104177,-1.78394067991828,126.219006022153));
#62727=CARTESIAN_POINT('Ctrl Pts',(37.6867105679035,-1.91008275014688,126.272168327946));
#62728=CARTESIAN_POINT('Ctrl Pts',(37.6789376676381,-2.03642731482499,126.325415974591));
#62729=CARTESIAN_POINT('Ctrl Pts',(37.6711647673726,-2.1604097326283,126.383894349992));
#62730=CARTESIAN_POINT('Ctrl Pts',(37.6633918671072,-2.2815826509457,126.44734745837));
#62731=CARTESIAN_POINT('Ctrl Pts',(37.6559015313451,-2.39835062846626,126.508493886431));
#62732=CARTESIAN_POINT('Ctrl Pts',(37.6484111955832,-2.51250955803329,126.574259485001));
#62733=CARTESIAN_POINT('Ctrl Pts',(37.6409208598211,-2.62368597393076,126.644378048769));
#62734=CARTESIAN_POINT('Ctrl Pts',(37.633145138272,-2.73909827056281,126.717168167209));
#62735=CARTESIAN_POINT('Ctrl Pts',(37.625369416723,-2.85166193403462,126.794880145919));
#62736=CARTESIAN_POINT('Ctrl Pts',(37.6175936951739,-2.96092863014544,126.877264399024));
#62737=CARTESIAN_POINT('Ctrl Pts',(37.6097869577625,-3.07063117015674,126.959977267119));
#62738=CARTESIAN_POINT('Ctrl Pts',(37.601980220351,-3.17701001363012,127.047399613342));
#62739=CARTESIAN_POINT('Ctrl Pts',(37.5941734829396,-3.27963693609872,127.139232430193));
#62740=CARTESIAN_POINT('Ctrl Pts',(37.5864171843116,-3.38160079321118,127.230471921648));
#62741=CARTESIAN_POINT('Ctrl Pts',(37.5786608856836,-3.47986075706443,127.326064815401));
#62742=CARTESIAN_POINT('Ctrl Pts',(37.5709045870557,-3.57402692832669,127.425675284763));
#62743=CARTESIAN_POINT('Ctrl Pts',(37.5631536839099,-3.66812759516169,127.525216462504));
#62744=CARTESIAN_POINT('Ctrl Pts',(37.5554027807641,-3.75813986802794,127.628769372447));
#62745=CARTESIAN_POINT('Ctrl Pts',(37.5476518776184,-3.84370926926902,127.735960038138));
#62746=CARTESIAN_POINT('Ctrl Pts',(37.5399046875389,-3.92923767853069,127.843099354194));
#62747=CARTESIAN_POINT('Ctrl Pts',(37.5321574974594,-4.01032720884455,127.953872652802));
#62748=CARTESIAN_POINT('Ctrl Pts',(37.52441030738,-4.08666266672071,128.06787175208));
#62749=CARTESIAN_POINT('Ctrl Pts',(37.5165621148733,-4.16399333272432,128.183357091609));
#62750=CARTESIAN_POINT('Ctrl Pts',(37.5087139223665,-4.23644482229462,128.302152628001));
#62751=CARTESIAN_POINT('Ctrl Pts',(37.5008657298598,-4.30373392387507,128.423802410971));
#62752=CARTESIAN_POINT('Ctrl Pts',(37.4931192925096,-4.37015059361115,128.543874952723));
#62753=CARTESIAN_POINT('Ctrl Pts',(37.4853728551594,-4.43153778052614,128.666727803173));
#62754=CARTESIAN_POINT('Ctrl Pts',(37.4776264178092,-4.48766908577469,128.791897142349));
#62755=CARTESIAN_POINT('Ctrl Pts',(37.4697273477242,-4.54490638003987,128.91953276863));
#62756=CARTESIAN_POINT('Ctrl Pts',(37.4618282776392,-4.59667831078346,129.04957674941));
#62757=CARTESIAN_POINT('Ctrl Pts',(37.4539292075542,-4.6427964119176,129.181516034747));
#62758=CARTESIAN_POINT('Ctrl Pts',(37.4460301374693,-4.68891451305174,129.313455320084));
#62759=CARTESIAN_POINT('Ctrl Pts',(37.4381310673843,-4.72937867507802,129.447289494132));
#62760=CARTESIAN_POINT('Ctrl Pts',(37.4302319972993,-4.76405452823409,129.582490119308));
#62761=CARTESIAN_POINT('Origin',(213.235140564004,0.,130.804360617566));
#62762=CARTESIAN_POINT('',(35.3346663362986,-4.76405452823403,129.582490119308));
#62763=CARTESIAN_POINT('',(35.6799972093173,-4.76405452823406,129.582490119308));
#62764=CARTESIAN_POINT('',(213.235140564004,-4.76405452823405,129.582490119308));
#62765=CARTESIAN_POINT('',(37.0148594360394,-4.91824833830055,130.800317684988));
#62766=CARTESIAN_POINT('Ctrl Pts',(37.0148594359912,-4.91824833830126,130.800317685842));
#62767=CARTESIAN_POINT('Ctrl Pts',(37.0069555838475,-4.91836336589627,130.940249378149));
#62768=CARTESIAN_POINT('Ctrl Pts',(36.9990517317038,-4.91250179003222,131.080267730569));
#62769=CARTESIAN_POINT('Ctrl Pts',(36.99114787956,-4.90067081885339,131.219822514422));
#62770=CARTESIAN_POINT('Ctrl Pts',(36.9834261315574,-4.88911243233405,131.356161966865));
#62771=CARTESIAN_POINT('Ctrl Pts',(36.9757043835548,-4.8718567741881,131.492058569711));
#62772=CARTESIAN_POINT('Ctrl Pts',(36.9679826355522,-4.84896321405377,131.62700198004));
#62773=CARTESIAN_POINT('Ctrl Pts',(36.9602609837571,-4.82606993915677,131.761943709071));
#62774=CARTESIAN_POINT('Ctrl Pts',(36.952539331962,-4.79753896740725,131.89593188133));
#62775=CARTESIAN_POINT('Ctrl Pts',(36.9448176801668,-4.76348108957116,132.028464768281));
#62776=CARTESIAN_POINT('Ctrl Pts',(36.9370944283567,-4.72941615455136,132.16102511757));
#62777=CARTESIAN_POINT('Ctrl Pts',(36.9293711765465,-4.68982213260539,132.292129200606));
#62778=CARTESIAN_POINT('Ctrl Pts',(36.9216479247363,-4.64486002074495,132.421289326627));
#62779=CARTESIAN_POINT('Ctrl Pts',(36.9136078463868,-4.59805345389917,132.555747914586));
#62780=CARTESIAN_POINT('Ctrl Pts',(36.9055677680373,-4.54542915690043,132.688099216945));
#62781=CARTESIAN_POINT('Ctrl Pts',(36.8975276896877,-4.48722413897979,132.817816002981));
#62782=CARTESIAN_POINT('Ctrl Pts',(36.8897917680836,-4.43122102109632,132.942625593621));
#62783=CARTESIAN_POINT('Ctrl Pts',(36.8820558464795,-4.37005195295995,133.064996035608));
#62784=CARTESIAN_POINT('Ctrl Pts',(36.8743199248753,-4.30397461236673,133.184483639303));
#62785=CARTESIAN_POINT('Ctrl Pts',(36.8665783727035,-4.23784917757628,133.304058211697));
#62786=CARTESIAN_POINT('Ctrl Pts',(36.8588368205316,-4.16680855978427,133.420745432725));
#62787=CARTESIAN_POINT('Ctrl Pts',(36.8510952683598,-4.09115340355658,133.534131100788));
#62788=CARTESIAN_POINT('Ctrl Pts',(36.8433427586412,-4.01539116351749,133.647677257178));
#62789=CARTESIAN_POINT('Ctrl Pts',(36.8355902489226,-3.93500158236551,133.757912220027));
#62790=CARTESIAN_POINT('Ctrl Pts',(36.827837739204,-3.85032529005803,133.864455097029));
#62791=CARTESIAN_POINT('Ctrl Pts',(36.8269474876499,-3.84060157431263,133.876689839747));
#62792=CARTESIAN_POINT('Ctrl Pts',(36.8260572360959,-3.83082136961932,133.888875936193));
#62793=CARTESIAN_POINT('Ctrl Pts',(36.8251669845419,-3.82098522180156,133.901012841706));
#62794=CARTESIAN_POINT('Ctrl Pts',(36.8173926504228,-3.73508871397414,134.007001265093));
#62795=CARTESIAN_POINT('Ctrl Pts',(36.8096183163038,-3.64464286930925,134.109580896771));
#62796=CARTESIAN_POINT('Ctrl Pts',(36.8018439821847,-3.54994831405154,134.208336238816));
#62797=CARTESIAN_POINT('Ctrl Pts',(36.7940792292376,-3.45537046137022,134.306969873727));
#62798=CARTESIAN_POINT('Ctrl Pts',(36.7863144762904,-3.35655458447976,134.401788317172));
#62799=CARTESIAN_POINT('Ctrl Pts',(36.7785497233434,-3.25384248265377,134.492407819078));
#62800=CARTESIAN_POINT('Ctrl Pts',(36.7707926824583,-3.15123239593516,134.582937316416));
#62801=CARTESIAN_POINT('Ctrl Pts',(36.7630356415734,-3.04473407660474,134.669275914611));
#62802=CARTESIAN_POINT('Ctrl Pts',(36.7552786006884,-2.934726956821,134.751075802553));
#62803=CARTESIAN_POINT('Ctrl Pts',(36.7475274094482,-2.82480279426218,134.832814004563));
#62804=CARTESIAN_POINT('Ctrl Pts',(36.7397762182081,-2.71137541044566,134.910020076606));
#62805=CARTESIAN_POINT('Ctrl Pts',(36.732025026968,-2.59485790007508,134.98238593354));
#62806=CARTESIAN_POINT('Ctrl Pts',(36.7242771301909,-2.47838991275446,135.054721033054));
#62807=CARTESIAN_POINT('Ctrl Pts',(36.7165292334138,-2.35883474253219,135.122219803274));
#62808=CARTESIAN_POINT('Ctrl Pts',(36.7087813366367,-2.23663491326429,135.184617154262));
#62809=CARTESIAN_POINT('Ctrl Pts',(36.7010350605526,-2.11446064556651,135.247001453069));
#62810=CARTESIAN_POINT('Ctrl Pts',(36.6932887844685,-1.98964316715752,135.304286277493));
#62811=CARTESIAN_POINT('Ctrl Pts',(36.6855425083844,-1.86264972594991,135.356252428771));
#62812=CARTESIAN_POINT('Ctrl Pts',(36.677796175119,-1.73565534730556,135.408218963652));
#62813=CARTESIAN_POINT('Ctrl Pts',(36.6700498418537,-1.60648533565349,135.454866598976));
#62814=CARTESIAN_POINT('Ctrl Pts',(36.6623035085884,-1.47562667065963,135.496024394025));
#62815=CARTESIAN_POINT('Ctrl Pts',(36.6545554405854,-1.34473870077469,135.537191406077));
#62816=CARTESIAN_POINT('Ctrl Pts',(36.6468073725823,-1.21216169793079,135.572866014189));
#62817=CARTESIAN_POINT('Ctrl Pts',(36.6390593045793,-1.07839715325156,135.602927345492));
#62818=CARTESIAN_POINT('Ctrl Pts',(36.6313030018375,-0.944490442022615,
135.633020626336));
#62819=CARTESIAN_POINT('Ctrl Pts',(36.6235466990957,-0.809394049770029,
135.657488627067));
#62820=CARTESIAN_POINT('Ctrl Pts',(36.6157903963538,-0.673619548697748,
135.676261659881));
#62821=CARTESIAN_POINT('Ctrl Pts',(36.6080299538397,-0.537772580686338,
135.695044712429));
#62822=CARTESIAN_POINT('Ctrl Pts',(36.6002695113255,-0.401247171677058,
135.708126703174));
#62823=CARTESIAN_POINT('Ctrl Pts',(36.5925090688113,-0.264558348793582,
135.715490013396));
#62824=CARTESIAN_POINT('Ctrl Pts',(36.5847361685459,-0.127650100876764,
135.722865143857));
#62825=CARTESIAN_POINT('Ctrl Pts',(36.5769632682804,0.0094216939638202,
135.724503244287));
#62826=CARTESIAN_POINT('Ctrl Pts',(36.569190368015,0.146142774750661,135.720438866728));
#62827=CARTESIAN_POINT('Ctrl Pts',(36.561700032253,0.277893699871095,135.716522239531));
#62828=CARTESIAN_POINT('Ctrl Pts',(36.554209696491,0.409318659657122,135.707310556714));
#62829=CARTESIAN_POINT('Ctrl Pts',(36.546719360729,0.539965372782319,135.692879867676));
#62830=CARTESIAN_POINT('Ctrl Pts',(36.5389450266099,0.675565595744873,135.677902034677));
#62831=CARTESIAN_POINT('Ctrl Pts',(36.5311706924908,0.810756933385873,135.65725418057));
#62832=CARTESIAN_POINT('Ctrl Pts',(36.5233963583717,0.94502731970406,135.630964643951));
#62833=CARTESIAN_POINT('Ctrl Pts',(36.5156316054246,1.07913222977138,135.604707506836));
#62834=CARTESIAN_POINT('Ctrl Pts',(36.5078668524776,1.21231806681136,135.572822595748));
#62835=CARTESIAN_POINT('Ctrl Pts',(36.5001020995305,1.34407722016159,135.535390049808));
#62836=CARTESIAN_POINT('Ctrl Pts',(36.4923450586455,1.47570550846288,135.497994682401));
#62837=CARTESIAN_POINT('Ctrl Pts',(36.4845880177604,1.60590955932414,135.455062751421));
#62838=CARTESIAN_POINT('Ctrl Pts',(36.4768309768754,1.73419165705913,135.406725483489));
#62839=CARTESIAN_POINT('Ctrl Pts',(36.4690797856353,1.86237701626686,135.358424667068));
#62840=CARTESIAN_POINT('Ctrl Pts',(36.4613285943952,1.9886429428368,135.304726764434));
#62841=CARTESIAN_POINT('Ctrl Pts',(36.4535774031551,2.11250694823694,135.245812796319));
#62842=CARTESIAN_POINT('Ctrl Pts',(36.445829506378,2.23631830813009,135.186923868212));
#62843=CARTESIAN_POINT('Ctrl Pts',(36.4380816096009,2.35772942498303,135.122823451579));
#62844=CARTESIAN_POINT('Ctrl Pts',(36.4303337128239,2.47627807616937,135.053740566686));
#62845=CARTESIAN_POINT('Ctrl Pts',(36.4225874367398,2.59480192953367,134.984672132443));
#62846=CARTESIAN_POINT('Ctrl Pts',(36.4148411606557,2.7104641706291,134.910623499704));
#62847=CARTESIAN_POINT('Ctrl Pts',(36.4070948845716,2.82282782241725,134.831869295085));
#62848=CARTESIAN_POINT('Ctrl Pts',(36.3993485513062,2.9351923036482,134.75311450912));
#62849=CARTESIAN_POINT('Ctrl Pts',(36.3916022180409,3.04425782682659,134.669654306356));
#62850=CARTESIAN_POINT('Ctrl Pts',(36.3838558847756,3.14961735028056,134.581805998946));
#62851=CARTESIAN_POINT('Ctrl Pts',(36.3761078167726,3.25500046826902,134.493938018517));
#62852=CARTESIAN_POINT('Ctrl Pts',(36.3683597487697,3.35667563484056,134.401680228335));
#62853=CARTESIAN_POINT('Ctrl Pts',(36.3606116807667,3.45427008802615,134.305389212346));
#62854=CARTESIAN_POINT('Ctrl Pts',(36.3528553780249,3.55196826575824,134.20899585712));
#62855=CARTESIAN_POINT('Ctrl Pts',(36.3450990752831,3.64557678766811,134.108560988248));
#62856=CARTESIAN_POINT('Ctrl Pts',(36.3373427725412,3.73476050616096,134.004477337956));
#62857=CARTESIAN_POINT('Ctrl Pts',(36.3295823300271,3.82399182468987,133.900338135085));
#62858=CARTESIAN_POINT('Ctrl Pts',(36.3218218875129,3.90879339239342,133.792546577429));
#62859=CARTESIAN_POINT('Ctrl Pts',(36.3140614449988,3.98887200140158,133.681526448542));
#62860=CARTESIAN_POINT('Ctrl Pts',(36.3062885447334,4.06907915970186,133.570328100288));
#62861=CARTESIAN_POINT('Ctrl Pts',(36.2985156444679,4.14454799326345,133.45589115051));
#62862=CARTESIAN_POINT('Ctrl Pts',(36.2907427442025,4.21502960107745,133.338666937753));
#62863=CARTESIAN_POINT('Ctrl Pts',(36.2832524084404,4.28294902491581,133.225704120399));
#62864=CARTESIAN_POINT('Ctrl Pts',(36.2757620726782,4.34623737627149,133.110153440011));
#62865=CARTESIAN_POINT('Ctrl Pts',(36.2682717369161,4.40471416855361,132.992436520236));
#62866=CARTESIAN_POINT('Ctrl Pts',(36.260497402797,4.46540812618805,132.870256327669));
#62867=CARTESIAN_POINT('Ctrl Pts',(36.252723068678,4.52111072197726,132.745355356997));
#62868=CARTESIAN_POINT('Ctrl Pts',(36.2449487345589,4.57156901380272,132.618179741552));
#62869=CARTESIAN_POINT('Ctrl Pts',(36.2371839816118,4.62196512029315,132.491160858687));
#62870=CARTESIAN_POINT('Ctrl Pts',(36.2294192286647,4.66712963973266,132.361873268692));
#62871=CARTESIAN_POINT('Ctrl Pts',(36.2216544757175,4.70685561947062,132.230787355943));
#62872=CARTESIAN_POINT('Ctrl Pts',(36.2138974348325,4.74654214280535,132.099831639572));
#62873=CARTESIAN_POINT('Ctrl Pts',(36.2061403939475,4.78080076327774,131.967081526647));
#62874=CARTESIAN_POINT('Ctrl Pts',(36.1983833530626,4.8094728580747,131.833026690664));
#62875=CARTESIAN_POINT('Ctrl Pts',(36.1906321618224,4.83812333102186,131.699072946476));
#62876=CARTESIAN_POINT('Ctrl Pts',(36.1828809705823,4.86119558226044,131.563816818399));
#62877=CARTESIAN_POINT('Ctrl Pts',(36.1751297793422,4.87858111282007,131.427762083826));
#62878=CARTESIAN_POINT('Ctrl Pts',(36.1673818825651,4.89595925406551,131.291765176144));
#62879=CARTESIAN_POINT('Ctrl Pts',(36.1596339857881,4.90765543242442,131.154970724064));
#62880=CARTESIAN_POINT('Ctrl Pts',(36.151886089011,4.91361248651288,131.01789139962));
#62881=CARTESIAN_POINT('Ctrl Pts',(36.1441398129269,4.91956829451405,130.880840749216));
#62882=CARTESIAN_POINT('Ctrl Pts',(36.1363935368428,4.91978734914383,130.743505735324));
#62883=CARTESIAN_POINT('Ctrl Pts',(36.1286472607587,4.91426450478877,130.606402441496));
#62884=CARTESIAN_POINT('Ctrl Pts',(36.1209009274934,4.90874161966532,130.469298135601));
#62885=CARTESIAN_POINT('Ctrl Pts',(36.113154594228,4.89747676671626,130.332425943833));
#62886=CARTESIAN_POINT('Ctrl Pts',(36.1054082609626,4.88051689367513,130.196299836845));
#62887=CARTESIAN_POINT('Ctrl Pts',(36.0976601929596,4.86355322258803,130.060143245359));
#62888=CARTESIAN_POINT('Ctrl Pts',(36.0899121249567,4.84089204191675,129.924733459015));
#62889=CARTESIAN_POINT('Ctrl Pts',(36.0821640569537,4.81263186888596,129.79057683535));
#62890=CARTESIAN_POINT('Ctrl Pts',(36.0744077542119,4.78434166060696,129.656277628429));
#62891=CARTESIAN_POINT('Ctrl Pts',(36.06665145147,4.7504406535697,129.523234627932));
#62892=CARTESIAN_POINT('Ctrl Pts',(36.0588951487282,4.71107810905525,129.391942084382));
#62893=CARTESIAN_POINT('Ctrl Pts',(36.051134706214,4.6716945555656,129.260579466049));
#62894=CARTESIAN_POINT('Ctrl Pts',(36.0433742636998,4.62684378403051,129.130969535566));
#62895=CARTESIAN_POINT('Ctrl Pts',(36.0356138211856,4.57672384954214,129.003588042383));
#62896=CARTESIAN_POINT('Ctrl Pts',(36.0278409209202,4.5265234580855,128.876002065118));
#62897=CARTESIAN_POINT('Ctrl Pts',(36.0200680206547,4.47103715918253,128.750652031421));
#62898=CARTESIAN_POINT('Ctrl Pts',(36.0122951203893,4.41051013966063,128.627991308269));
#62899=CARTESIAN_POINT('Ctrl Pts',(36.0048047846273,4.35218342975687,128.509789611367));
#62900=CARTESIAN_POINT('Ctrl Pts',(35.9973144488653,4.2891762695934,128.394085363722));
#62901=CARTESIAN_POINT('Ctrl Pts',(35.9898241131033,4.22174582567467,128.281258311694));
#62902=CARTESIAN_POINT('Ctrl Pts',(35.9820497789842,4.15175873597951,128.164153387694));
#62903=CARTESIAN_POINT('Ctrl Pts',(35.9742754448651,4.07678462560965,128.049777190753));
#62904=CARTESIAN_POINT('Ctrl Pts',(35.966501110746,3.99706211777929,127.938583674203));
#62905=CARTESIAN_POINT('Ctrl Pts',(35.9587363577989,3.91743786081483,127.827527193723));
#62906=CARTESIAN_POINT('Ctrl Pts',(35.9509716048519,3.83307707569843,127.719645903975));
#62907=CARTESIAN_POINT('Ctrl Pts',(35.9432068519048,3.74426364716699,127.615368174332));
#62908=CARTESIAN_POINT('Ctrl Pts',(35.9354498110197,3.6555384293847,127.5111940148));
#62909=CARTESIAN_POINT('Ctrl Pts',(35.9276927701347,3.56236962088044,127.410616588503));
#62910=CARTESIAN_POINT('Ctrl Pts',(35.9199357292497,3.46508345833033,127.314034029794));
#62911=CARTESIAN_POINT('Ctrl Pts',(35.9121845380096,3.36787066003257,127.217524304745));
#62912=CARTESIAN_POINT('Ctrl Pts',(35.9044333467695,3.26654696419431,127.125003725297));
#62913=CARTESIAN_POINT('Ctrl Pts',(35.8966821555294,3.16147756666012,127.036835878695));
#62914=CARTESIAN_POINT('Ctrl Pts',(35.8889342587523,3.05645282642241,126.948705505779));
#62915=CARTESIAN_POINT('Ctrl Pts',(35.8811863619752,2.94768584976528,126.864924436933));
#62916=CARTESIAN_POINT('Ctrl Pts',(35.8734384651981,2.83557706506659,126.785817875406));
#62917=CARTESIAN_POINT('Ctrl Pts',(35.865692189114,2.72349173110873,126.706727861265));
#62918=CARTESIAN_POINT('Ctrl Pts',(35.8579459130299,2.60806629876926,126.632310634798));
#62919=CARTESIAN_POINT('Ctrl Pts',(35.8501996369458,2.48973218242708,126.562849480921));
#62920=CARTESIAN_POINT('Ctrl Pts',(35.8424533036804,2.37139719256966,126.493387814297));
#62921=CARTESIAN_POINT('Ctrl Pts',(35.8347069704151,2.25015381303461,126.42888249118));
#62922=CARTESIAN_POINT('Ctrl Pts',(35.8269606371497,2.12645983828727,126.369571826806));
#62923=CARTESIAN_POINT('Ctrl Pts',(35.8192125691467,2.00273816313141,126.31024788022));
#62924=CARTESIAN_POINT('Ctrl Pts',(35.8114645011437,1.87656515319319,126.25612107623));
#62925=CARTESIAN_POINT('Ctrl Pts',(35.8037164331407,1.74842007237432,126.207382228122));
#62926=CARTESIAN_POINT('Ctrl Pts',(35.7959601303989,1.62013879743897,126.158591579786));
#62927=CARTESIAN_POINT('Ctrl Pts',(35.788203827657,1.48988163076539,126.115200465608));
#62928=CARTESIAN_POINT('Ctrl Pts',(35.7804475249151,1.35814507868509,126.077350462326));
#62929=CARTESIAN_POINT('Ctrl Pts',(35.772687082401,1.22633821484043,126.039480257357));
#62930=CARTESIAN_POINT('Ctrl Pts',(35.7649266398868,1.09305077202556,126.007157148365));
#62931=CARTESIAN_POINT('Ctrl Pts',(35.7571661973727,0.958790065340662,125.980471660189));
#62932=CARTESIAN_POINT('Ctrl Pts',(35.7493932971072,0.824313831450109,125.953743334098));
#62933=CARTESIAN_POINT('Ctrl Pts',(35.7416203968418,0.688861598117829,125.932670773761));
#62934=CARTESIAN_POINT('Ctrl Pts',(35.7338474965763,0.552947325291186,125.91729275248));
#62935=CARTESIAN_POINT('Ctrl Pts',(35.7263571608143,0.421973878629179,125.902473761008));
#62936=CARTESIAN_POINT('Ctrl Pts',(35.7188668250523,0.290571709066281,125.892942497224));
#62937=CARTESIAN_POINT('Ctrl Pts',(35.7113764892902,0.159199312747926,125.888687861847));
#62938=CARTESIAN_POINT('Ctrl Pts',(35.7036021551711,0.0228458920933872,
125.884271910676));
#62939=CARTESIAN_POINT('Ctrl Pts',(35.695827821052,-0.113907379694791,125.885526624867));
#62940=CARTESIAN_POINT('Ctrl Pts',(35.6880534869329,-0.250549597146119,
125.892496616815));
#62941=CARTESIAN_POINT('Ctrl Pts',(35.6802887339859,-0.387023415275948,
125.899458018871));
#62942=CARTESIAN_POINT('Ctrl Pts',(35.6725239810387,-0.523386064679369,
125.912120664356));
#62943=CARTESIAN_POINT('Ctrl Pts',(35.6647592280917,-0.659123699436644,
125.930477257109));
#62944=CARTESIAN_POINT('Ctrl Pts',(35.6570021872067,-0.794726517661697,
125.948815617835));
#62945=CARTESIAN_POINT('Ctrl Pts',(35.6492451463217,-0.929705171676313,
125.972836619454));
#62946=CARTESIAN_POINT('Ctrl Pts',(35.6414881054367,-1.06354836088296,126.002480991153));
#62947=CARTESIAN_POINT('Ctrl Pts',(35.6337369141966,-1.19729061789893,126.0321030078));
#62948=CARTESIAN_POINT('Ctrl Pts',(35.6259857229566,-1.32989873427611,126.067339869612));
#62949=CARTESIAN_POINT('Ctrl Pts',(35.6182345317165,-1.46086941649534,126.10808085477));
#62950=CARTESIAN_POINT('Ctrl Pts',(35.6104866349394,-1.5917844326814,126.148804523922));
#62951=CARTESIAN_POINT('Ctrl Pts',(35.6027387381623,-1.72106302636876,126.195027547647));
#62952=CARTESIAN_POINT('Ctrl Pts',(35.5949908413852,-1.84821515353499,126.246588814509));
#62953=CARTESIAN_POINT('Ctrl Pts',(35.5872445653011,-1.97534068321765,126.298139295865));
#62954=CARTESIAN_POINT('Ctrl Pts',(35.579498289217,-2.10034026905229,126.355025652463));
#62955=CARTESIAN_POINT('Ctrl Pts',(35.5717520131329,-2.2227423854061,126.417038045584));
#62956=CARTESIAN_POINT('Ctrl Pts',(35.5640056798676,-2.34514540530436,126.479050896467));
#62957=CARTESIAN_POINT('Ctrl Pts',(35.5562593466021,-2.46495056870129,126.546189682686));
#62958=CARTESIAN_POINT('Ctrl Pts',(35.5485130133368,-2.58170992514885,126.618198063999));
#62959=CARTESIAN_POINT('Ctrl Pts',(35.5407649453338,-2.69849542904522,126.69022257109));
#62960=CARTESIAN_POINT('Ctrl Pts',(35.5330168773308,-2.81223343601147,126.767118638079));
#62961=CARTESIAN_POINT('Ctrl Pts',(35.5252688093278,-2.92250435558116,126.848586185914));
#62962=CARTESIAN_POINT('Ctrl Pts',(35.5175125065859,-3.03289247239596,126.930140318429));
#62963=CARTESIAN_POINT('Ctrl Pts',(35.5097562038441,-3.13980582594915,127.016275404726));
#62964=CARTESIAN_POINT('Ctrl Pts',(35.5019999011022,-3.24285692992184,127.106650245652));
#62965=CARTESIAN_POINT('Ctrl Pts',(35.494239458588,-3.34596303537152,127.197073322353));
#62966=CARTESIAN_POINT('Ctrl Pts',(35.4864790160739,-3.44520250097287,127.291740392943));
#62967=CARTESIAN_POINT('Ctrl Pts',(35.4787185735597,-3.54022494941101,127.39027356975));
#62968=CARTESIAN_POINT('Ctrl Pts',(35.4709456732943,-3.63539993631909,127.488964920759));
#62969=CARTESIAN_POINT('Ctrl Pts',(35.4631727730288,-3.72634411885754,127.591534487279));
#62970=CARTESIAN_POINT('Ctrl Pts',(35.4553998727634,-3.81274706804235,127.697570818169));
#62971=CARTESIAN_POINT('Ctrl Pts',(35.4479095370014,-3.89600905238817,127.799752461342));
#62972=CARTESIAN_POINT('Ctrl Pts',(35.4404192012393,-3.97505405687443,127.905152947208));
#62973=CARTESIAN_POINT('Ctrl Pts',(35.4329288654773,-4.04964359127354,128.013380530543));
#62974=CARTESIAN_POINT('Ctrl Pts',(35.4247403213791,-4.13118595614205,128.131696500207));
#62975=CARTESIAN_POINT('Ctrl Pts',(35.4165517772809,-4.20766704647845,128.253774597608));
#62976=CARTESIAN_POINT('Ctrl Pts',(35.4083632331827,-4.2787288669236,128.379146741254));
#62977=CARTESIAN_POINT('Ctrl Pts',(35.4004930663826,-4.34702774561443,128.499644313319));
#62978=CARTESIAN_POINT('Ctrl Pts',(35.3926228995825,-4.41032059105628,128.623184240247));
#62979=CARTESIAN_POINT('Ctrl Pts',(35.3847527327825,-4.46833125497048,128.749318316699));
#62980=CARTESIAN_POINT('Ctrl Pts',(35.376890577065,-4.5262828695363,128.875324000636));
#62981=CARTESIAN_POINT('Ctrl Pts',(35.3690284213476,-4.5789628450409,129.003918239692));
#62982=CARTESIAN_POINT('Ctrl Pts',(35.3611662656302,-4.62614009302874,129.13462683574));
#62983=CARTESIAN_POINT('Ctrl Pts',(35.3533121480127,-4.67326910800649,129.265201798112));
#62984=CARTESIAN_POINT('Ctrl Pts',(35.3454580303952,-4.71490647440109,129.397886458584));
#62985=CARTESIAN_POINT('Ctrl Pts',(35.3376039127777,-4.7508687549419,129.532185654828));
#62986=CARTESIAN_POINT('Ctrl Pts',(35.336624720618,-4.75535226090213,129.548929065918));
#62987=CARTESIAN_POINT('Ctrl Pts',(35.3356455284583,-4.75974761945892,129.565697547361));
#62988=CARTESIAN_POINT('Ctrl Pts',(35.3346663362986,-4.76405452823404,129.582490119308));
#62989=CARTESIAN_POINT('Ctrl Pts',(37.0846781642943,-4.76405452823403,129.582490119308));
#62990=CARTESIAN_POINT('Ctrl Pts',(37.0754335152278,-4.80440312556933,129.739808687943));
#62991=CARTESIAN_POINT('Ctrl Pts',(37.0661888661614,-4.8369949620545,129.899282122246));
#62992=CARTESIAN_POINT('Ctrl Pts',(37.0569442170948,-4.86162747657715,130.060209193802));
#62993=CARTESIAN_POINT('Ctrl Pts',(37.0477930819962,-4.88601082164451,130.219508412435));
#62994=CARTESIAN_POINT('Ctrl Pts',(37.0386419468975,-4.90259499612365,130.380231947554));
#62995=CARTESIAN_POINT('Ctrl Pts',(37.0294908117989,-4.91123014170045,130.541679141719));
#62996=CARTESIAN_POINT('Ctrl Pts',(37.0246136865457,-4.91583226877033,130.627722914348));
#62997=CARTESIAN_POINT('Ctrl Pts',(37.0197365612925,-4.91817735973255,130.713971890829));
#62998=CARTESIAN_POINT('Ctrl Pts',(37.0148594360393,-4.91824833830055,130.800317684988));
#62999=CARTESIAN_POINT('',(37.3601405639635,-4.9182499932755,130.804103429838));
#63000=CARTESIAN_POINT('Ctrl Pts',(37.4302319972993,-4.76405452823409,129.582490119308));
#63001=CARTESIAN_POINT('Ctrl Pts',(37.4224712764234,-4.79812304700691,129.715322756942));
#63002=CARTESIAN_POINT('Ctrl Pts',(37.4147105555475,-4.82660434211345,129.849473974204));
#63003=CARTESIAN_POINT('Ctrl Pts',(37.4069498346715,-4.84942300612506,129.984434053681));
#63004=CARTESIAN_POINT('Ctrl Pts',(37.3991767847143,-4.87227792104283,130.119608537698));
#63005=CARTESIAN_POINT('Ctrl Pts',(37.391403734757,-4.88945218054426,130.255594063599));
#63006=CARTESIAN_POINT('Ctrl Pts',(37.3836306847998,-4.90092230039882,130.391875868813));
#63007=CARTESIAN_POINT('Ctrl Pts',(37.3765782018693,-4.91132913232845,130.515524257838));
#63008=CARTESIAN_POINT('Ctrl Pts',(37.3695257189387,-4.91704102316591,130.639416300982));
#63009=CARTESIAN_POINT('Ctrl Pts',(37.3624732360082,-4.91807750796032,130.763169742425));
#63010=CARTESIAN_POINT('Ctrl Pts',(37.3616956786751,-4.91819178350845,130.776813929422));
#63011=CARTESIAN_POINT('Ctrl Pts',(37.3609181213419,-4.91824927975026,130.790458592636));
#63012=CARTESIAN_POINT('Ctrl Pts',(37.3601405640087,-4.91824999327546,130.804103429044));
#63013=CARTESIAN_POINT('Ctrl Pts',(37.3601405639634,-4.9182499932755,130.804103429838));
#63014=CARTESIAN_POINT('Ctrl Pts',(37.3523778041444,-4.9182571167472,130.940326938106));
#63015=CARTESIAN_POINT('Ctrl Pts',(37.3446150443255,-4.91260036309792,131.076769552372));
#63016=CARTESIAN_POINT('Ctrl Pts',(37.3368522845065,-4.90125105140445,131.212920519669));
#63017=CARTESIAN_POINT('Ctrl Pts',(37.3290990918319,-4.88991572706942,131.348903688916));
#63018=CARTESIAN_POINT('Ctrl Pts',(37.3213458991574,-4.87290183538294,131.484595539201));
#63019=CARTESIAN_POINT('Ctrl Pts',(37.3135927064828,-4.85023267081422,131.619483983362));
#63020=CARTESIAN_POINT('Ctrl Pts',(37.3058471995574,-4.82758597821549,131.754238712446));
#63021=CARTESIAN_POINT('Ctrl Pts',(37.298101692632,-4.79929523305588,131.888191235892));
#63022=CARTESIAN_POINT('Ctrl Pts',(37.2903561857066,-4.7654356002907,132.020833634933));
#63023=CARTESIAN_POINT('Ctrl Pts',(37.2826164899166,-4.73160137101562,132.153376517836));
#63024=CARTESIAN_POINT('Ctrl Pts',(37.2748767941265,-4.69220666661304,132.284610854149));
#63025=CARTESIAN_POINT('Ctrl Pts',(37.2671370983365,-4.64737782508226,132.41403835346));
#63026=CARTESIAN_POINT('Ctrl Pts',(37.2594006351337,-4.60256770691539,132.54341179565));
#63027=CARTESIAN_POINT('Ctrl Pts',(37.2516641719308,-4.55232809347918,132.670979531734));
#63028=CARTESIAN_POINT('Ctrl Pts',(37.243927708728,-4.49683526483856,132.796258120804));
#63029=CARTESIAN_POINT('Ctrl Pts',(37.2361928087239,-4.44135364885621,132.921511396584));
#63030=CARTESIAN_POINT('Ctrl Pts',(37.2284579087198,-4.38062108760279,133.044476086857));
#63031=CARTESIAN_POINT('Ctrl Pts',(37.2207230087157,-4.31486196531586,133.164688832618));
#63032=CARTESIAN_POINT('Ctrl Pts',(37.2129879830845,-4.24910177499682,133.284903530824));
#63033=CARTESIAN_POINT('Ctrl Pts',(37.2052529574535,-4.17831504931166,133.402365851346));
#63034=CARTESIAN_POINT('Ctrl Pts',(37.1975179318223,-4.10277187954645,133.516637514732));
#63035=CARTESIAN_POINT('Ctrl Pts',(37.1897810920046,-4.02721099175189,133.630935979598));
#63036=CARTESIAN_POINT('Ctrl Pts',(37.1820442521868,-3.94689165646444,133.742041971183));
#63037=CARTESIAN_POINT('Ctrl Pts',(37.174307412369,-3.86212674368066,133.849546995811));
#63038=CARTESIAN_POINT('Ctrl Pts',(37.1665623311173,-3.77727153764473,133.957166536904));
#63039=CARTESIAN_POINT('Ctrl Pts',(37.1588172498655,-3.68796153855184,134.061177140821));
#63040=CARTESIAN_POINT('Ctrl Pts',(37.1510721686138,-3.59454962950483,134.161203780945));
#63041=CARTESIAN_POINT('Ctrl Pts',(37.1433228552727,-3.5010866780555,134.261285077912));
#63042=CARTESIAN_POINT('Ctrl Pts',(37.1355735419316,-3.40351763033354,134.357377798867));
#63043=CARTESIAN_POINT('Ctrl Pts',(37.1278242285904,-3.302230782838,134.449145236632));
#63044=CARTESIAN_POINT('Ctrl Pts',(37.1200626672136,-3.2007838482657,134.541057715744));
#63045=CARTESIAN_POINT('Ctrl Pts',(37.1123011058368,-3.09560767478678,134.628631001705));
#63046=CARTESIAN_POINT('Ctrl Pts',(37.10453954446,-2.9871226855163,134.711569483774));
#63047=CARTESIAN_POINT('Ctrl Pts',(37.0977015670384,-2.89154682504207,134.784638733662));
#63048=CARTESIAN_POINT('Ctrl Pts',(37.0908635896169,-2.79340335410348,134.854111132265));
#63049=CARTESIAN_POINT('Ctrl Pts',(37.0840256121953,-2.69299607361674,134.919813838049));
#63050=CARTESIAN_POINT('Ctrl Pts',(37.0762512780763,-2.57883954773673,134.994513527124));
#63051=CARTESIAN_POINT('Ctrl Pts',(37.0684769439571,-2.46139176392207,135.06457813823));
#63052=CARTESIAN_POINT('Ctrl Pts',(37.060702609838,-2.34106585819466,135.129703807429));
#63053=CARTESIAN_POINT('Ctrl Pts',(37.0529378568909,-2.22088824339222,135.194749215061));
#63054=CARTESIAN_POINT('Ctrl Pts',(37.0451731039439,-2.09783990473823,135.254867607402));
#63055=CARTESIAN_POINT('Ctrl Pts',(37.0374083509968,-1.97236349131766,135.309797923824));
#63056=CARTESIAN_POINT('Ctrl Pts',(37.0296513101118,-1.84701170283981,135.364673682681));
#63057=CARTESIAN_POINT('Ctrl Pts',(37.0218942692268,-1.71923699461641,135.41437146429));
#63058=CARTESIAN_POINT('Ctrl Pts',(37.0141372283418,-1.58950687801603,135.458675921372));
#63059=CARTESIAN_POINT('Ctrl Pts',(37.0063860371016,-1.45987459190555,135.502946968118));
#63060=CARTESIAN_POINT('Ctrl Pts',(36.9986348458615,-1.32829020098468,135.541832659905));
#63061=CARTESIAN_POINT('Ctrl Pts',(36.9908836546213,-1.19524114186396,135.575165756669));
#63062=CARTESIAN_POINT('Ctrl Pts',(36.9831357578443,-1.06224863214274,135.608484685979));
#63063=CARTESIAN_POINT('Ctrl Pts',(36.9753878610671,-0.92779307082301,135.636255619314));
#63064=CARTESIAN_POINT('Ctrl Pts',(36.96763996429,-0.792376790317983,135.658361244334));
#63065=CARTESIAN_POINT('Ctrl Pts',(36.9598936882059,-0.656988835979415,
135.680462245334));
#63066=CARTESIAN_POINT('Ctrl Pts',(36.9521474121218,-0.52064094779285,135.696900232221));
#63067=CARTESIAN_POINT('Ctrl Pts',(36.9444011360377,-0.383844989328075,
135.707609141419));
#63068=CARTESIAN_POINT('Ctrl Pts',(36.9366548027723,-0.247048021066796,
135.718318129668));
#63069=CARTESIAN_POINT('Ctrl Pts',(36.928908469507,-0.109803365700026,135.723297925327));
#63070=CARTESIAN_POINT('Ctrl Pts',(36.9211621362416,0.0273730586309466,
135.722534443099));
#63071=CARTESIAN_POINT('Ctrl Pts',(36.9134140682387,0.164580202671034,135.721770789896));
#63072=CARTESIAN_POINT('Ctrl Pts',(36.9056660002356,0.301718694385837,135.715261301658));
#63073=CARTESIAN_POINT('Ctrl Pts',(36.8979179322326,0.438274084659371,135.703044000804));
#63074=CARTESIAN_POINT('Ctrl Pts',(36.8901616294908,0.574974607626718,135.690813715258));
#63075=CARTESIAN_POINT('Ctrl Pts',(36.882405326749,0.711090401150329,135.672863533843));
#63076=CARTESIAN_POINT('Ctrl Pts',(36.8746490240071,0.846113045068823,135.649283297802));
#63077=CARTESIAN_POINT('Ctrl Pts',(36.8668885814929,0.981207754637829,135.625690476279));
#63078=CARTESIAN_POINT('Ctrl Pts',(36.8591281389788,1.11520777023767,135.596461695834));
#63079=CARTESIAN_POINT('Ctrl Pts',(36.8513676964646,1.24761728031085,135.561737435138));
#63080=CARTESIAN_POINT('Ctrl Pts',(36.8435947961992,1.38023934588435,135.526957431975));
#63081=CARTESIAN_POINT('Ctrl Pts',(36.8358218959337,1.51126542987309,135.486664434713));
#63082=CARTESIAN_POINT('Ctrl Pts',(36.8280489956683,1.64021637985857,135.441048367431));
#63083=CARTESIAN_POINT('Ctrl Pts',(36.8205586599063,1.76447963800284,135.397090559094));
#63084=CARTESIAN_POINT('Ctrl Pts',(36.8130683241444,1.88681572945309,135.348190089941));
#63085=CARTESIAN_POINT('Ctrl Pts',(36.8055779883824,2.00681719220789,135.294557475117));
#63086=CARTESIAN_POINT('Ctrl Pts',(36.7978036542634,2.13136854689776,135.2388913634));
#63087=CARTESIAN_POINT('Ctrl Pts',(36.7900293201443,2.25379928452739,135.177950850309));
#63088=CARTESIAN_POINT('Ctrl Pts',(36.7822549860253,2.37363044564825,135.111919272999));
#63089=CARTESIAN_POINT('Ctrl Pts',(36.7744902330782,2.49331392557281,135.045969073706));
#63090=CARTESIAN_POINT('Ctrl Pts',(36.7667254801311,2.6104038643552,134.97494048102));
#63091=CARTESIAN_POINT('Ctrl Pts',(36.758960727184,2.72444136165393,134.899064798506));
#63092=CARTESIAN_POINT('Ctrl Pts',(36.751203686299,2.83836559530254,134.82326447679));
#63093=CARTESIAN_POINT('Ctrl Pts',(36.743446645414,2.94924309734985,134.74262686089));
#63094=CARTESIAN_POINT('Ctrl Pts',(36.735689604529,3.05663998871665,134.657428880896));
#63095=CARTESIAN_POINT('Ctrl Pts',(36.7279384132889,3.1639558912524,134.572295149361));
#63096=CARTESIAN_POINT('Ctrl Pts',(36.7201872220488,3.2677961024728,134.482608140862));
#63097=CARTESIAN_POINT('Ctrl Pts',(36.7124360308087,3.36775644718183,134.388687552287));
#63098=CARTESIAN_POINT('Ctrl Pts',(36.7046881340316,3.46767430607783,134.294806882467));
#63099=CARTESIAN_POINT('Ctrl Pts',(36.6969402372545,3.56371529395929,134.19669647856));
#63100=CARTESIAN_POINT('Ctrl Pts',(36.6891923404774,3.65550918969215,134.094715556866));
#63101=CARTESIAN_POINT('Ctrl Pts',(36.6814460643933,3.74728388412075,133.992755967383));
#63102=CARTESIAN_POINT('Ctrl Pts',(36.6736997883093,3.83481299208366,133.886927760912));
#63103=CARTESIAN_POINT('Ctrl Pts',(36.6659535122252,3.91776425766106,133.777625873794));
#63104=CARTESIAN_POINT('Ctrl Pts',(36.6582071789599,4.00071613556585,133.668323179835));
#63105=CARTESIAN_POINT('Ctrl Pts',(36.6504608456946,4.07908986730144,133.555547065496));
#63106=CARTESIAN_POINT('Ctrl Pts',(36.6427145124293,4.1525947361521,133.439723973876));
#63107=CARTESIAN_POINT('Ctrl Pts',(36.6349664444263,4.22611606590828,133.323874944478));
#63108=CARTESIAN_POINT('Ctrl Pts',(36.6272183764233,4.29476615366091,133.204977910039));
#63109=CARTESIAN_POINT('Ctrl Pts',(36.6194703084204,4.35829891643479,133.083486243218));
#63110=CARTESIAN_POINT('Ctrl Pts',(36.6117140056786,4.42189920258526,132.961865453607));
#63111=CARTESIAN_POINT('Ctrl Pts',(36.6039577029367,4.48037111779735,132.837644870003));
#63112=CARTESIAN_POINT('Ctrl Pts',(36.5962014001948,4.53351543453886,132.711300802076));
#63113=CARTESIAN_POINT('Ctrl Pts',(36.5884409576807,4.58668811600236,132.584889300515));
#63114=CARTESIAN_POINT('Ctrl Pts',(36.5806805151665,4.63452739677627,132.45635242253));
#63115=CARTESIAN_POINT('Ctrl Pts',(36.5729200726524,4.67688346728702,132.32618324058));
#63116=CARTESIAN_POINT('Ctrl Pts',(36.5651471723869,4.71930753152241,132.195805099503));
#63117=CARTESIAN_POINT('Ctrl Pts',(36.5573742721215,4.7562306906546,132.06378979496));
#63118=CARTESIAN_POINT('Ctrl Pts',(36.5496013718561,4.78755373960541,131.930643110056));
#63119=CARTESIAN_POINT('Ctrl Pts',(36.542111036094,4.81773811682938,131.802336642523));
#63120=CARTESIAN_POINT('Ctrl Pts',(36.5346207003317,4.84272241285229,131.672979926006));
#63121=CARTESIAN_POINT('Ctrl Pts',(36.5271303645696,4.86246349686421,131.543029558407));
#63122=CARTESIAN_POINT('Ctrl Pts',(36.5193560304505,4.88295307007626,131.408152083125));
#63123=CARTESIAN_POINT('Ctrl Pts',(36.5115816963315,4.89785889471362,131.272207800258));
#63124=CARTESIAN_POINT('Ctrl Pts',(36.5038073622124,4.90707632823586,131.135698770164));
#63125=CARTESIAN_POINT('Ctrl Pts',(36.4960426092653,4.91628240209508,130.99935797525));
#63126=CARTESIAN_POINT('Ctrl Pts',(36.4882778563181,4.91981400742653,130.862454204276));
#63127=CARTESIAN_POINT('Ctrl Pts',(36.480513103371,4.91761769962746,130.725498568324));
#63128=CARTESIAN_POINT('Ctrl Pts',(36.472756062486,4.91542357323227,130.588678958639));
#63129=CARTESIAN_POINT('Ctrl Pts',(36.464999021601,4.90751286138939,130.451807974875));
#63130=CARTESIAN_POINT('Ctrl Pts',(36.457241980716,4.89388403098659,130.315400339267));
#63131=CARTESIAN_POINT('Ctrl Pts',(36.4494907894759,4.88026547819087,130.179095569718));
#63132=CARTESIAN_POINT('Ctrl Pts',(36.4417395982358,4.86093742847594,130.043253840291));
#63133=CARTESIAN_POINT('Ctrl Pts',(36.4339884069957,4.83595038532041,129.908387999));
#63134=CARTESIAN_POINT('Ctrl Pts',(36.4262405102186,4.8109739623247,129.77357947929));
#63135=CARTESIAN_POINT('Ctrl Pts',(36.4184926134416,4.78034340076808,129.639746406371));
#63136=CARTESIAN_POINT('Ctrl Pts',(36.4107447166645,4.74416080593153,129.507394422955));
#63137=CARTESIAN_POINT('Ctrl Pts',(36.4029984405804,4.70798577971382,129.375070124721));
#63138=CARTESIAN_POINT('Ctrl Pts',(36.3952521644963,4.66626113327027,129.244226676643));
#63139=CARTESIAN_POINT('Ctrl Pts',(36.3875058884122,4.61913954528972,129.115357087777));
#63140=CARTESIAN_POINT('Ctrl Pts',(36.3797595551468,4.57201760946825,128.986486547624));
#63141=CARTESIAN_POINT('Ctrl Pts',(36.3720132218815,4.51949878687747,128.859590262946));
#63142=CARTESIAN_POINT('Ctrl Pts',(36.3642668886161,4.46178471668666,128.735143324858));
#63143=CARTESIAN_POINT('Ctrl Pts',(36.3565188206131,4.40405772182991,128.610668517742));
#63144=CARTESIAN_POINT('Ctrl Pts',(36.3487707526101,4.34113332871914,128.488644503307));
#63145=CARTESIAN_POINT('Ctrl Pts',(36.3410226846071,4.2732599587523,128.369523377128));
#63146=CARTESIAN_POINT('Ctrl Pts',(36.3332663818653,4.20531445216025,128.250275647598));
#63147=CARTESIAN_POINT('Ctrl Pts',(36.3255100791234,4.13240965549268,128.133937309625));
#63148=CARTESIAN_POINT('Ctrl Pts',(36.3177537763816,4.05483861421586,128.020933435985));
#63149=CARTESIAN_POINT('Ctrl Pts',(36.3099933338674,3.97722617093868,127.907869248775));
#63150=CARTESIAN_POINT('Ctrl Pts',(36.3022328913532,3.89494275493409,127.798143384742));
#63151=CARTESIAN_POINT('Ctrl Pts',(36.294472448839,3.80832222629196,127.692148400632));
#63152=CARTESIAN_POINT('Ctrl Pts',(36.2866995485736,3.72156264668746,127.585983263964));
#63153=CARTESIAN_POINT('Ctrl Pts',(36.2789266483081,3.630452301517,127.48356126771));
#63154=CARTESIAN_POINT('Ctrl Pts',(36.2711537480427,3.53536309766314,127.385239264034));
#63155=CARTESIAN_POINT('Ctrl Pts',(36.2636634122807,3.443730625885,127.29049151285));
#63156=CARTESIAN_POINT('Ctrl Pts',(36.2561730765187,3.34840377898473,127.199551052025));
#63157=CARTESIAN_POINT('Ctrl Pts',(36.2486827407567,3.24974339245113,127.112700971049));
#63158=CARTESIAN_POINT('Ctrl Pts',(36.2409084066377,3.14734226737451,127.022557942856));
#63159=CARTESIAN_POINT('Ctrl Pts',(36.2331340725186,3.04102545436761,126.93653604492));
#63160=CARTESIAN_POINT('Ctrl Pts',(36.2253597383995,2.9311587891807,126.854994691862));
#63161=CARTESIAN_POINT('Ctrl Pts',(36.2175949854524,2.82142752483986,126.773553831235));
#63162=CARTESIAN_POINT('Ctrl Pts',(36.2098302325054,2.70815542394951,126.696582759378));
#63163=CARTESIAN_POINT('Ctrl Pts',(36.2020654795583,2.59174361062467,126.624402708772));
#63164=CARTESIAN_POINT('Ctrl Pts',(36.1943084386733,2.47544741915411,126.552294348411));
#63165=CARTESIAN_POINT('Ctrl Pts',(36.1865513977883,2.35601805114521,126.484967744343));
#63166=CARTESIAN_POINT('Ctrl Pts',(36.1787943569034,2.23388772830796,126.422702406362));
#63167=CARTESIAN_POINT('Ctrl Pts',(36.1710431656632,2.11184950489721,126.360484023156));
#63168=CARTESIAN_POINT('Ctrl Pts',(36.1632919744232,1.98711472770768,126.303319485905));
#63169=CARTESIAN_POINT('Ctrl Pts',(36.1555407831831,1.86014216866299,126.251443511483));
#63170=CARTESIAN_POINT('Ctrl Pts',(36.147792886406,1.73322357634265,126.199589585734));
#63171=CARTESIAN_POINT('Ctrl Pts',(36.1400449896289,1.60406945503248,126.153019899707));
#63172=CARTESIAN_POINT('Ctrl Pts',(36.1322970928518,1.47316040666341,126.111921861574));
#63173=CARTESIAN_POINT('Ctrl Pts',(36.1245508167677,1.34227874164482,126.070832420264));
#63174=CARTESIAN_POINT('Ctrl Pts',(36.1168045406836,1.20964325251376,126.035212467305));
#63175=CARTESIAN_POINT('Ctrl Pts',(36.1090582645995,1.07575124831147,126.005200033229));
#63176=CARTESIAN_POINT('Ctrl Pts',(36.1013119313341,0.941858255748634,125.975187377607));
#63177=CARTESIAN_POINT('Ctrl Pts',(36.0935655980687,0.806709111104827,125.95078240898));
#63178=CARTESIAN_POINT('Ctrl Pts',(36.0858192648033,0.670812512888385,125.932072280957));
#63179=CARTESIAN_POINT('Ctrl Pts',(36.0780711968004,0.534885481571384,125.913357962931));
#63180=CARTESIAN_POINT('Ctrl Pts',(36.0703231287974,0.398211050838375,125.900341076563));
#63181=CARTESIAN_POINT('Ctrl Pts',(36.0625750607944,0.261303859331813,125.893056986594));
#63182=CARTESIAN_POINT('Ctrl Pts',(36.0548187580526,0.124251161232901,125.885765155008));
#63183=CARTESIAN_POINT('Ctrl Pts',(36.0470624553108,-0.0130344007740541,
125.884218311819));
#63184=CARTESIAN_POINT('Ctrl Pts',(36.0393061525689,-0.150036802691739,
125.888399671796));
#63185=CARTESIAN_POINT('Ctrl Pts',(36.0315457100547,-0.287112326916577,
125.89258326349));
#63186=CARTESIAN_POINT('Ctrl Pts',(36.0237852675405,-0.423904000159855,
125.902501122049));
#63187=CARTESIAN_POINT('Ctrl Pts',(36.0160248250264,-0.559901093780867,
125.918084548034));
#63188=CARTESIAN_POINT('Ctrl Pts',(36.0082519247609,-0.696116502009629,
125.933692989917));
#63189=CARTESIAN_POINT('Ctrl Pts',(36.0004790244955,-0.831534395258706,
125.954985112916));
#63190=CARTESIAN_POINT('Ctrl Pts',(35.99270612423,-0.965653518941221,125.981840908549));
#63191=CARTESIAN_POINT('Ctrl Pts',(35.9852157884679,-1.09489707465365,126.007720428365));
#63192=CARTESIAN_POINT('Ctrl Pts',(35.9777254527058,-1.2229343491525,126.03876606404));
#63193=CARTESIAN_POINT('Ctrl Pts',(35.9702351169437,-1.34933213083662,126.07482725124));
#63194=CARTESIAN_POINT('Ctrl Pts',(35.9624607828246,-1.48052232282976,126.112255709313));
#63195=CARTESIAN_POINT('Ctrl Pts',(35.9546864487055,-1.61036181619281,126.155206118109));
#63196=CARTESIAN_POINT('Ctrl Pts',(35.9469121145864,-1.73835048206726,126.20356496203));
#63197=CARTESIAN_POINT('Ctrl Pts',(35.9391473616393,-1.86618141334934,126.251864207999));
#63198=CARTESIAN_POINT('Ctrl Pts',(35.9313826086923,-1.99216569339321,126.305558490049));
#63199=CARTESIAN_POINT('Ctrl Pts',(35.9236178557452,-2.11581624283175,126.364483965105));
#63200=CARTESIAN_POINT('Ctrl Pts',(35.9158608148602,-2.23934398080176,126.423350914549));
#63201=CARTESIAN_POINT('Ctrl Pts',(35.9081037739752,-2.36054225022622,126.487438550228));
#63202=CARTESIAN_POINT('Ctrl Pts',(35.9003467330901,-2.47894226520921,126.556534313648));
#63203=CARTESIAN_POINT('Ctrl Pts',(35.89259554185,-2.59725299381955,126.625577971414));
#63204=CARTESIAN_POINT('Ctrl Pts',(35.8848443506099,-2.71276933187949,126.699622043432));
#63205=CARTESIAN_POINT('Ctrl Pts',(35.8770931593698,-2.82504582800595,126.77840742209));
#63206=CARTESIAN_POINT('Ctrl Pts',(35.8693452625927,-2.93727460362663,126.85715931486));
#63207=CARTESIAN_POINT('Ctrl Pts',(35.8615973658156,-3.04626595673606,126.940648282128));
#63208=CARTESIAN_POINT('Ctrl Pts',(35.8538494690385,-3.15160243844918,127.028571278572));
#63209=CARTESIAN_POINT('Ctrl Pts',(35.8461031929544,-3.25691688604112,127.11647588342));
#63210=CARTESIAN_POINT('Ctrl Pts',(35.8383569168703,-3.35857768295184,127.208812422219));
#63211=CARTESIAN_POINT('Ctrl Pts',(35.8306106407862,-3.45619989250171,127.30523710366));
#63212=CARTESIAN_POINT('Ctrl Pts',(35.8228643075208,-3.55382282267643,127.401662496886));
#63213=CARTESIAN_POINT('Ctrl Pts',(35.8151179742555,-3.64740682784782,127.50217581823));
#63214=CARTESIAN_POINT('Ctrl Pts',(35.8073716409901,-3.73660361924633,127.606396193884));
#63215=CARTESIAN_POINT('Ctrl Pts',(35.7996235729872,-3.82582038564783,127.710639908969));
#63216=CARTESIAN_POINT('Ctrl Pts',(35.7918755049842,-3.91064772907651,127.818592033328));
#63217=CARTESIAN_POINT('Ctrl Pts',(35.7841274369812,-3.99077772141636,127.929838702404));
#63218=CARTESIAN_POINT('Ctrl Pts',(35.7763711342394,-4.07099287686562,128.041203605763));
#63219=CARTESIAN_POINT('Ctrl Pts',(35.7686148314975,-4.1465004795,128.155869730682));
#63220=CARTESIAN_POINT('Ctrl Pts',(35.7608585287557,-4.21703572763549,128.273393858727));
#63221=CARTESIAN_POINT('Ctrl Pts',(35.7530980862415,-4.28760862255669,128.390980712939));
#63222=CARTESIAN_POINT('Ctrl Pts',(35.7453376437273,-4.35320368797253,128.511428266588));
#63223=CARTESIAN_POINT('Ctrl Pts',(35.7375772012132,-4.4136026613618,128.63426969548));
#63224=CARTESIAN_POINT('Ctrl Pts',(35.7298043009478,-4.47409859254521,128.757308320339));
#63225=CARTESIAN_POINT('Ctrl Pts',(35.7220314006823,-4.52938160550884,128.882748141734));
#63226=CARTESIAN_POINT('Ctrl Pts',(35.7142585004169,-4.5792817264392,129.010102572468));
#63227=CARTESIAN_POINT('Ctrl Pts',(35.7067681646548,-4.62736785228278,129.132827348858));
#63228=CARTESIAN_POINT('Ctrl Pts',(35.6992778288928,-4.67045555408226,129.25732965851));
#63229=CARTESIAN_POINT('Ctrl Pts',(35.6917874931308,-4.70843734442204,129.383163644535));
#63230=CARTESIAN_POINT('Ctrl Pts',(35.6878573985263,-4.72836596097904,129.449187316271));
#63231=CARTESIAN_POINT('Ctrl Pts',(35.6839273039218,-4.74691073125618,129.515646715085));
#63232=CARTESIAN_POINT('Ctrl Pts',(35.6799972093173,-4.76405452823406,129.582490119308));
#63233=CARTESIAN_POINT('Origin',(213.235140564004,0.,130.804360617566));
#63234=CARTESIAN_POINT('',(33.584997801213,-4.7640545282341,129.582490119308));
#63235=CARTESIAN_POINT('',(33.9299189896066,-4.764054528234,129.582490119308));
#63236=CARTESIAN_POINT('',(213.235140564004,-4.76405452823405,129.582490119308));
#63237=CARTESIAN_POINT('',(35.2648594359407,-4.91824928377686,130.80701488364));
#63238=CARTESIAN_POINT('Ctrl Pts',(35.2648594359407,-4.91824928377686,130.80701488364));
#63239=CARTESIAN_POINT('Ctrl Pts',(35.2562894561528,-4.91816724259869,130.959033918108));
#63240=CARTESIAN_POINT('Ctrl Pts',(35.2477194763649,-4.91103296049634,131.110804385526));
#63241=CARTESIAN_POINT('Ctrl Pts',(35.2391494965771,-4.89693982404999,131.261704494898));
#63242=CARTESIAN_POINT('Ctrl Pts',(35.2305320272072,-4.88276859206837,131.413440800305));
#63243=CARTESIAN_POINT('Ctrl Pts',(35.2219145578374,-4.8615612559285,131.56429684572));
#63244=CARTESIAN_POINT('Ctrl Pts',(35.2132970884676,-4.83346292747159,131.713656604172));
#63245=CARTESIAN_POINT('Ctrl Pts',(35.2046550026758,-4.80528433411579,131.863443019531));
#63246=CARTESIAN_POINT('Ctrl Pts',(35.1960129168841,-4.77017544093273,132.011724373643));
#63247=CARTESIAN_POINT('Ctrl Pts',(35.1873708310923,-4.72833133818723,132.157898876655));
#63248=CARTESIAN_POINT('Ctrl Pts',(35.1786971614629,-4.68633430970349,132.304607596971));
#63249=CARTESIAN_POINT('Ctrl Pts',(35.1700234918334,-4.63755287123151,132.449193829812));
#63250=CARTESIAN_POINT('Ctrl Pts',(35.161349822204,-4.58223150063536,132.591071992435));
#63251=CARTESIAN_POINT('Ctrl Pts',(35.1590602953575,-4.5676287121297,132.628522561356));
#63252=CARTESIAN_POINT('Ctrl Pts',(35.156770768511,-4.55257049352782,132.665784574027));
#63253=CARTESIAN_POINT('Ctrl Pts',(35.1544812416645,-4.53706187100313,132.702847552256));
#63254=CARTESIAN_POINT('Ctrl Pts',(35.1467069075454,-4.48440067883743,132.828698872426));
#63255=CARTESIAN_POINT('Ctrl Pts',(35.1389325734263,-4.42641571523285,132.952556757311));
#63256=CARTESIAN_POINT('Ctrl Pts',(35.1311582393072,-4.36327877084152,133.073937985805));
#63257=CARTESIAN_POINT('Ctrl Pts',(35.1233934863601,-4.30021963709144,133.195169622783));
#63258=CARTESIAN_POINT('Ctrl Pts',(35.115628733413,-4.2320213345633,133.313930332933));
#63259=CARTESIAN_POINT('Ctrl Pts',(35.1078639804659,-4.15890408787074,133.429755797418));
#63260=CARTESIAN_POINT('Ctrl Pts',(35.1001069395809,-4.08585946225846,133.545466222419));
#63261=CARTESIAN_POINT('Ctrl Pts',(35.0923498986959,-4.00790582232535,133.658246874925));
#63262=CARTESIAN_POINT('Ctrl Pts',(35.0845928578109,-3.92530960651127,133.767657355244));
#63263=CARTESIAN_POINT('Ctrl Pts',(35.0768416665708,-3.84277567714615,133.876985328268));
#63264=CARTESIAN_POINT('Ctrl Pts',(35.0690904753307,-3.75560637504087,133.982947876983));
#63265=CARTESIAN_POINT('Ctrl Pts',(35.0613392840906,-3.66411160592648,134.08513327074));
#63266=CARTESIAN_POINT('Ctrl Pts',(35.0535913873135,-3.57265572452953,134.18727523298));
#63267=CARTESIAN_POINT('Ctrl Pts',(35.0458434905364,-3.47687829288984,134.285642942603));
#63268=CARTESIAN_POINT('Ctrl Pts',(35.0380955937594,-3.377129539576,134.37985766489));
#63269=CARTESIAN_POINT('Ctrl Pts',(35.0303493176753,-3.27740165155103,134.474052679488));
#63270=CARTESIAN_POINT('Ctrl Pts',(35.0226030415912,-3.17370437823536,134.564096166386));
#63271=CARTESIAN_POINT('Ctrl Pts',(35.0148567655071,-3.0664245690127,134.64964648796));
#63272=CARTESIAN_POINT('Ctrl Pts',(35.0071104322417,-2.95914396787486,134.735197441048));
#63273=CARTESIAN_POINT('Ctrl Pts',(34.9993640989764,-2.84828108373235,134.816254918872));
#63274=CARTESIAN_POINT('Ctrl Pts',(34.9916177657111,-2.73425526047784,134.892518054976));
#63275=CARTESIAN_POINT('Ctrl Pts',(34.9838696977081,-2.62020390193065,134.968798269681));
#63276=CARTESIAN_POINT('Ctrl Pts',(34.976121629705,-2.50298851971675,135.040281788896));
#63277=CARTESIAN_POINT('Ctrl Pts',(34.9683735617021,-2.38305645062066,135.106711720818));
#63278=CARTESIAN_POINT('Ctrl Pts',(34.9606172589602,-2.26299691629449,135.173212255263));
#63279=CARTESIAN_POINT('Ctrl Pts',(34.9528609562184,-2.1402152698902,135.2346482835));
#63280=CARTESIAN_POINT('Ctrl Pts',(34.9451046534766,-2.01518290299934,135.290809205253));
#63281=CARTESIAN_POINT('Ctrl Pts',(34.9373442109624,-1.89008380256962,135.347000101781));
#63282=CARTESIAN_POINT('Ctrl Pts',(34.9295837684482,-1.76273195086124,135.39791013668));
#63283=CARTESIAN_POINT('Ctrl Pts',(34.921823325934,-1.63361668332313,135.44337771114));
#63284=CARTESIAN_POINT('Ctrl Pts',(34.9140504256686,-1.50429414849508,135.488918274186));
#63285=CARTESIAN_POINT('Ctrl Pts',(34.9062775254032,-1.37320291510912,135.528998803664));
#63286=CARTESIAN_POINT('Ctrl Pts',(34.8985046251378,-1.24084623996858,135.563507985662));
#63287=CARTESIAN_POINT('Ctrl Pts',(34.8910142893758,-1.11330106335539,135.596762671972));
#63288=CARTESIAN_POINT('Ctrl Pts',(34.8835239536137,-0.984581152594259,
135.624843977655));
#63289=CARTESIAN_POINT('Ctrl Pts',(34.8760336178516,-0.855141939076149,
135.647697827232));
#63290=CARTESIAN_POINT('Ctrl Pts',(34.8682592837326,-0.720794998435681,
135.671418187462));
#63291=CARTESIAN_POINT('Ctrl Pts',(34.8604849496135,-0.585247562854529,
135.689582007539));
#63292=CARTESIAN_POINT('Ctrl Pts',(34.8527106154944,-0.44899903697857,135.702072626994));
#63293=CARTESIAN_POINT('Ctrl Pts',(34.8449458625473,-0.312918425234057,
135.714547852876));
#63294=CARTESIAN_POINT('Ctrl Pts',(34.8371811096002,-0.176138827954184,
135.721363754211));
#63295=CARTESIAN_POINT('Ctrl Pts',(34.8294163566532,-0.0391699265099815,
135.722454636529));
#63296=CARTESIAN_POINT('Ctrl Pts',(34.8216593157682,0.0976629354903832,
135.723544435367));
#63297=CARTESIAN_POINT('Ctrl Pts',(34.8139022748831,0.234684339064692,135.718920527829));
#63298=CARTESIAN_POINT('Ctrl Pts',(34.8061452339981,0.371379746995001,135.708569029331));
#63299=CARTESIAN_POINT('Ctrl Pts',(34.798394042758,0.507972071854669,135.698225336977));
#63300=CARTESIAN_POINT('Ctrl Pts',(34.7906428515179,0.64423850212011,135.682162680213));
#63301=CARTESIAN_POINT('Ctrl Pts',(34.7828916602778,0.779665125519412,135.660419241033));
#63302=CARTESIAN_POINT('Ctrl Pts',(34.7751437635007,0.91503418899133,135.638685043395));
#63303=CARTESIAN_POINT('Ctrl Pts',(34.7673958667237,1.04956377031092,135.611274927415));
#63304=CARTESIAN_POINT('Ctrl Pts',(34.7596479699466,1.18274592213557,135.57827883494));
#63305=CARTESIAN_POINT('Ctrl Pts',(34.7519016938625,1.31590021512531,135.545289644535));
#63306=CARTESIAN_POINT('Ctrl Pts',(34.7441554177784,1.44770725999012,135.506716895738));
#63307=CARTESIAN_POINT('Ctrl Pts',(34.7364091416943,1.5776705257821,135.46270139241));
#63308=CARTESIAN_POINT('Ctrl Pts',(34.7286628084289,1.7076347509332,135.418685564171));
#63309=CARTESIAN_POINT('Ctrl Pts',(34.7209164751636,1.83575479954868,135.369227026644));
#63310=CARTESIAN_POINT('Ctrl Pts',(34.7131701418982,1.96155087854192,135.314515960056));
#63311=CARTESIAN_POINT('Ctrl Pts',(34.7054220738953,2.08737512869485,135.259792641304));
#63312=CARTESIAN_POINT('Ctrl Pts',(34.6976740058923,2.21087401516037,135.199814608753));
#63313=CARTESIAN_POINT('Ctrl Pts',(34.6899259378893,2.33158961113015,135.134819363215));
#63314=CARTESIAN_POINT('Ctrl Pts',(34.6821696351475,2.45243350507186,135.069755039957));
#63315=CARTESIAN_POINT('Ctrl Pts',(34.6744133324057,2.57048785457699,134.999663037401));
#63316=CARTESIAN_POINT('Ctrl Pts',(34.6666570296638,2.68532067699727,134.924826116049));
#63317=CARTESIAN_POINT('Ctrl Pts',(34.6588965871496,2.80021478915258,134.849949251979));
#63318=CARTESIAN_POINT('Ctrl Pts',(34.6511361446354,2.911883629951,134.770322649755));
#63319=CARTESIAN_POINT('Ctrl Pts',(34.6433757021212,3.01992674397284,134.686270653043));
#63320=CARTESIAN_POINT('Ctrl Pts',(34.6356028018558,3.12814329839277,134.602083728605));
#63321=CARTESIAN_POINT('Ctrl Pts',(34.6278299015904,3.232722196708,134.513457466464));
#63322=CARTESIAN_POINT('Ctrl Pts',(34.620057001325,3.33329776477895,134.420755102937));
#63323=CARTESIAN_POINT('Ctrl Pts',(34.6125666655629,3.4302171576165,134.331422703826));
#63324=CARTESIAN_POINT('Ctrl Pts',(34.6050763298009,3.52341901131686,134.238305629011));
#63325=CARTESIAN_POINT('Ctrl Pts',(34.5975859940388,3.61261165885588,134.141757816702));
#63326=CARTESIAN_POINT('Ctrl Pts',(34.5898116599197,3.70518607273547,134.041549364744));
#63327=CARTESIAN_POINT('Ctrl Pts',(34.5820373258007,3.7937345088545,133.937327456715));
#63328=CARTESIAN_POINT('Ctrl Pts',(34.5742629916816,3.87788887704562,133.829449198052));
#63329=CARTESIAN_POINT('Ctrl Pts',(34.5664982387345,3.96193953249892,133.721703889702));
#63330=CARTESIAN_POINT('Ctrl Pts',(34.5587334857874,4.04160665668523,133.61031150187));
#63331=CARTESIAN_POINT('Ctrl Pts',(34.5509687328403,4.11655948375679,133.495665334463));
#63332=CARTESIAN_POINT('Ctrl Pts',(34.5432116919553,4.19143786662386,133.381133035246));
#63333=CARTESIAN_POINT('Ctrl Pts',(34.5354546510703,4.2616110578223,133.263353712802));
#63334=CARTESIAN_POINT('Ctrl Pts',(34.5276976101853,4.32678925592282,133.142752756907));
#63335=CARTESIAN_POINT('Ctrl Pts',(34.5199464189452,4.39191830263723,133.022242747131));
#63336=CARTESIAN_POINT('Ctrl Pts',(34.512195227705,4.45205966863424,132.898915681749));
#63337=CARTESIAN_POINT('Ctrl Pts',(34.5044440364649,4.50696769537298,132.773224568012));
#63338=CARTESIAN_POINT('Ctrl Pts',(34.4966961396878,4.56185238473563,132.647586876351));
#63339=CARTESIAN_POINT('Ctrl Pts',(34.4889482429108,4.61150800263786,132.519587492294));
#63340=CARTESIAN_POINT('Ctrl Pts',(34.4812003461337,4.6557356617563,132.389702382092));
#63341=CARTESIAN_POINT('Ctrl Pts',(34.4734540700496,4.69995406940184,132.259844441055));
#63342=CARTESIAN_POINT('Ctrl Pts',(34.4657077939654,4.73874665071692,132.128101928324));
#63343=CARTESIAN_POINT('Ctrl Pts',(34.4579615178813,4.77196348087364,131.994968697376));
#63344=CARTESIAN_POINT('Ctrl Pts',(34.450215184616,4.80518055622947,131.861834483668));
#63345=CARTESIAN_POINT('Ctrl Pts',(34.4424688513506,4.83282170365258,131.727309910595));
#63346=CARTESIAN_POINT('Ctrl Pts',(34.4347225180853,4.85478758726982,131.591901438724));
#63347=CARTESIAN_POINT('Ctrl Pts',(34.4269744500823,4.87675838999441,131.456462643066));
#63348=CARTESIAN_POINT('Ctrl Pts',(34.4192263820794,4.89305133730586,131.320139940574));
#63349=CARTESIAN_POINT('Ctrl Pts',(34.4114783140764,4.90361872473794,131.183446973031));
#63350=CARTESIAN_POINT('Ctrl Pts',(34.4037220113346,4.91419734331514,131.046608726575));
#63351=CARTESIAN_POINT('Ctrl Pts',(34.3959657085927,4.91903821600145,130.90939981939));
#63352=CARTESIAN_POINT('Ctrl Pts',(34.3882094058508,4.91814574004211,130.772336529669));
#63353=CARTESIAN_POINT('Ctrl Pts',(34.3804489633367,4.91725278774148,130.635200085143));
#63354=CARTESIAN_POINT('Ctrl Pts',(34.3726885208225,4.91062040826214,130.498209803263));
#63355=CARTESIAN_POINT('Ctrl Pts',(34.3649280783083,4.89830502518097,130.36187791419));
#63356=CARTESIAN_POINT('Ctrl Pts',(34.3571551780429,4.88596987235357,130.225327173065));
#63357=CARTESIAN_POINT('Ctrl Pts',(34.3493822777775,4.86793353700968,130.089437324581));
#63358=CARTESIAN_POINT('Ctrl Pts',(34.341609377512,4.84430396434359,129.954712358847));
#63359=CARTESIAN_POINT('Ctrl Pts',(34.33411904175,4.82153338616318,129.824884984968));
#63360=CARTESIAN_POINT('Ctrl Pts',(34.3266287059879,4.79356923241567,129.696139572388));
#63361=CARTESIAN_POINT('Ctrl Pts',(34.3191383702259,4.7605516281902,129.568912821083));
#63362=CARTESIAN_POINT('Ctrl Pts',(34.3113640361068,4.72628215146513,129.436862228832));
#63363=CARTESIAN_POINT('Ctrl Pts',(34.3035897019877,4.68645990116027,129.306029434651));
#63364=CARTESIAN_POINT('Ctrl Pts',(34.2958153678686,4.64118635846841,129.176917147437));
#63365=CARTESIAN_POINT('Ctrl Pts',(34.2880506149216,4.5959686113717,129.047963979577));
#63366=CARTESIAN_POINT('Ctrl Pts',(34.2802858619744,4.54531306729262,128.920727465175));
#63367=CARTESIAN_POINT('Ctrl Pts',(34.2725211090273,4.48937183356195,128.795698475114));
#63368=CARTESIAN_POINT('Ctrl Pts',(34.2647640681423,4.43348616145325,128.670793665608));
#63369=CARTESIAN_POINT('Ctrl Pts',(34.2570070272574,4.37232540571543,128.548092371744));
#63370=CARTESIAN_POINT('Ctrl Pts',(34.2492499863724,4.30609081406378,128.428068345236));
#63371=CARTESIAN_POINT('Ctrl Pts',(34.2414987951323,4.23990617043293,128.30813482978));
#63372=CARTESIAN_POINT('Ctrl Pts',(34.2337476038921,4.16865549487908,128.190874904005));
#63373=CARTESIAN_POINT('Ctrl Pts',(34.225996412652,4.09258713079035,128.076740108883));
#63374=CARTESIAN_POINT('Ctrl Pts',(34.2182485158749,4.01655109778554,127.962653824093));
#63375=CARTESIAN_POINT('Ctrl Pts',(34.2105006190979,3.93570166523003,127.851690352791));
#63376=CARTESIAN_POINT('Ctrl Pts',(34.2027527223208,3.85033177355368,127.744274295897));
#63377=CARTESIAN_POINT('Ctrl Pts',(34.1950064462367,3.7649797394183,127.636880708128));
#63378=CARTESIAN_POINT('Ctrl Pts',(34.1872601701526,3.67510937007827,127.533033364684));
#63379=CARTESIAN_POINT('Ctrl Pts',(34.1795138940685,3.58105512041832,127.433125341436));
#63380=CARTESIAN_POINT('Ctrl Pts',(34.1717675608031,3.48700017647126,127.333216580689));
#63381=CARTESIAN_POINT('Ctrl Pts',(34.1640212275378,3.38876155856534,127.237247482833));
#63382=CARTESIAN_POINT('Ctrl Pts',(34.1562748942724,3.28671167285548,127.145575376258));
#63383=CARTESIAN_POINT('Ctrl Pts',(34.1485268262695,3.18463893378127,127.05388274035));
#63384=CARTESIAN_POINT('Ctrl Pts',(34.1407787582665,3.07875351931422,126.966489271772));
#63385=CARTESIAN_POINT('Ctrl Pts',(34.1330306902635,2.96946178540415,126.883712741574));
#63386=CARTESIAN_POINT('Ctrl Pts',(34.1252743875216,2.8600538949387,126.800848235493));
#63387=CARTESIAN_POINT('Ctrl Pts',(34.1175180847798,2.74723276529731,126.722610706354));
#63388=CARTESIAN_POINT('Ctrl Pts',(34.1097617820379,2.63143513276518,126.649275515604));
#63389=CARTESIAN_POINT('Ctrl Pts',(34.1020013395238,2.51557569554997,126.575901183654));
#63390=CARTESIAN_POINT('Ctrl Pts',(34.0942408970096,2.39673692852486,126.507434598819));
#63391=CARTESIAN_POINT('Ctrl Pts',(34.0864804544955,2.27538028375261,126.444105163259));
#63392=CARTESIAN_POINT('Ctrl Pts',(34.07870755423,2.15382882652046,126.380674065668));
#63393=CARTESIAN_POINT('Ctrl Pts',(34.0709346539645,2.02975176857446,126.322396763008));
#63394=CARTESIAN_POINT('Ctrl Pts',(34.0631617536991,1.90363147808261,126.269454856897));
#63395=CARTESIAN_POINT('Ctrl Pts',(34.055671417937,1.78209597782729,126.218437522425));
#63396=CARTESIAN_POINT('Ctrl Pts',(34.048181082175,1.65866350780082,126.172374516677));
#63397=CARTESIAN_POINT('Ctrl Pts',(34.0406907464129,1.53377721709419,126.131383995452));
#63398=CARTESIAN_POINT('Ctrl Pts',(34.0329164122938,1.40415582471778,126.088839306156));
#63399=CARTESIAN_POINT('Ctrl Pts',(34.0251420781747,1.27255759059411,126.051624572139));
#63400=CARTESIAN_POINT('Ctrl Pts',(34.0173677440556,1.13946031101753,126.019926140837));
#63401=CARTESIAN_POINT('Ctrl Pts',(34.0096029911085,1.00652706194278,125.988266775018));
#63402=CARTESIAN_POINT('Ctrl Pts',(34.0018382381615,0.872098819945926,125.962110274932));
#63403=CARTESIAN_POINT('Ctrl Pts',(33.9940734852144,0.736670786330147,125.941593996077));
#63404=CARTESIAN_POINT('Ctrl Pts',(33.9863164443294,0.601377261746741,125.921098094279));
#63405=CARTESIAN_POINT('Ctrl Pts',(33.9785594034443,0.465086305726717,125.906231323765));
#63406=CARTESIAN_POINT('Ctrl Pts',(33.9708023625593,0.328305278311106,125.897080443505));
#63407=CARTESIAN_POINT('Ctrl Pts',(33.9630511713192,0.191627398532086,125.887936463995));
#63408=CARTESIAN_POINT('Ctrl Pts',(33.9552999800791,0.0544605714722569,
125.884499821148));
#63409=CARTESIAN_POINT('Ctrl Pts',(33.947548788839,-0.0826810729926777,
125.886805645563));
#63410=CARTESIAN_POINT('Ctrl Pts',(33.9398008920619,-0.219764428600342,
125.889110489941));
#63411=CARTESIAN_POINT('Ctrl Pts',(33.9320529952848,-0.356822232809559,
125.897152940653));
#63412=CARTESIAN_POINT('Ctrl Pts',(33.9243050985077,-0.493338915381331,
125.910916045787));
#63413=CARTESIAN_POINT('Ctrl Pts',(33.9165588224236,-0.629827041606068,
125.924676271977));
#63414=CARTESIAN_POINT('Ctrl Pts',(33.9088125463395,-0.76577388258952,125.94415473322));
#63415=CARTESIAN_POINT('Ctrl Pts',(33.9010662702554,-0.900667951434378,
125.969282510259));
#63416=CARTESIAN_POINT('Ctrl Pts',(33.8933199369901,-1.03556301603643,125.994410472786));
#63417=CARTESIAN_POINT('Ctrl Pts',(33.8855736037247,-1.16940490863912,126.025187762725));
#63418=CARTESIAN_POINT('Ctrl Pts',(33.8778272704594,-1.30169170412281,126.061494208956));
#63419=CARTESIAN_POINT('Ctrl Pts',(33.8700792024564,-1.43400812431731,126.097808785765));
#63420=CARTESIAN_POINT('Ctrl Pts',(33.8623311344534,-1.56476837745789,126.139654879316));
#63421=CARTESIAN_POINT('Ctrl Pts',(33.8545830664505,-1.69348546844494,126.186862373856));
#63422=CARTESIAN_POINT('Ctrl Pts',(33.8468267637086,-1.82233936148805,126.234120041083));
#63423=CARTESIAN_POINT('Ctrl Pts',(33.8390704609667,-1.94914538693545,126.286750357153));
#63424=CARTESIAN_POINT('Ctrl Pts',(33.8313141582249,-2.07343580877234,126.344534723049));
#63425=CARTESIAN_POINT('Ctrl Pts',(33.8235537157107,-2.19779256814968,126.402349930202));
#63426=CARTESIAN_POINT('Ctrl Pts',(33.8157932731965,-2.31963070142117,126.465324489097));
#63427=CARTESIAN_POINT('Ctrl Pts',(33.8080328306824,-2.43850777994066,126.533194164515));
#63428=CARTESIAN_POINT('Ctrl Pts',(33.8002599304169,-2.55757569050001,126.601172790361));
#63429=CARTESIAN_POINT('Ctrl Pts',(33.7924870301515,-2.673672716297,126.674062027667));
#63430=CARTESIAN_POINT('Ctrl Pts',(33.7847141298861,-2.78638533897131,126.751554206538));
#63431=CARTESIAN_POINT('Ctrl Pts',(33.7772237941241,-2.89500057390483,126.826229349517));
#63432=CARTESIAN_POINT('Ctrl Pts',(33.7697334583621,-3.00047295026603,126.905178402581));
#63433=CARTESIAN_POINT('Ctrl Pts',(33.7622431226001,-3.10246352732764,126.988092397943));
#63434=CARTESIAN_POINT('Ctrl Pts',(33.7545737356394,-3.20689211727199,127.072988393945));
#63435=CARTESIAN_POINT('Ctrl Pts',(33.7469043486787,-3.30802008847212,127.162325913931));
#63436=CARTESIAN_POINT('Ctrl Pts',(33.739234961718,-3.40543838223453,127.255815494941));
#63437=CARTESIAN_POINT('Ctrl Pts',(33.7315743594801,-3.50274509045334,127.349197990462));
#63438=CARTESIAN_POINT('Ctrl Pts',(33.7239137572423,-3.59635028099301,127.446722817711));
#63439=CARTESIAN_POINT('Ctrl Pts',(33.7162531550044,-3.68587607219211,127.548058935759));
#63440=CARTESIAN_POINT('Ctrl Pts',(33.708599562025,-3.77531994954259,127.649302333805));
#63441=CARTESIAN_POINT('Ctrl Pts',(33.7009459690456,-3.8606915845894,127.754349789671));
#63442=CARTESIAN_POINT('Ctrl Pts',(33.6932923760662,-3.94164865608082,127.862832284451));
#63443=CARTESIAN_POINT('Ctrl Pts',(33.6856440233496,-4.02255029787662,127.971240503427));
#63444=CARTESIAN_POINT('Ctrl Pts',(33.6779956706331,-4.09904314811599,128.083078762522));
#63445=CARTESIAN_POINT('Ctrl Pts',(33.6703473179165,-4.17082440111321,128.197944135578));
#63446=CARTESIAN_POINT('Ctrl Pts',(33.6627016087951,-4.24258084346383,128.312769806288));
#63447=CARTESIAN_POINT('Ctrl Pts',(33.6550558996738,-4.30962871074624,128.430620171986));
#63448=CARTESIAN_POINT('Ctrl Pts',(33.6474101905524,-4.37170810607383,128.551062746048));
#63449=CARTESIAN_POINT('Ctrl Pts',(33.639766171144,-4.4337737817638,128.671478702124));
#63450=CARTESIAN_POINT('Ctrl Pts',(33.6321221517355,-4.49087298879841,128.794485367841));
#63451=CARTESIAN_POINT('Ctrl Pts',(33.6244781323271,-4.54279179119425,128.919625674833));
#63452=CARTESIAN_POINT('Ctrl Pts',(33.6168317504326,-4.59472663978789,129.044804658105));
#63453=CARTESIAN_POINT('Ctrl Pts',(33.6091853685381,-4.64147772989695,129.172118228636));
#63454=CARTESIAN_POINT('Ctrl Pts',(33.6015389866436,-4.68287933659217,129.301089457257));
#63455=CARTESIAN_POINT('Ctrl Pts',(33.5960252581668,-4.71273361551444,129.394089302903));
#63456=CARTESIAN_POINT('Ctrl Pts',(33.5905115296898,-4.73980732912571,129.487950657987));
#63457=CARTESIAN_POINT('Ctrl Pts',(33.5849978012129,-4.7640545282341,129.582490119308));
#63458=CARTESIAN_POINT('Ctrl Pts',(35.3346663362986,-4.76405452823404,129.582490119308));
#63459=CARTESIAN_POINT('Ctrl Pts',(35.3268190006772,-4.79857048949325,129.717067328405));
#63460=CARTESIAN_POINT('Ctrl Pts',(35.3189716650557,-4.82740159557297,129.853192944721));
#63461=CARTESIAN_POINT('Ctrl Pts',(35.3111243294342,-4.85042023697192,129.990354114353));
#63462=CARTESIAN_POINT('Ctrl Pts',(35.3032799627014,-4.87343016971004,130.127463391691));
#63463=CARTESIAN_POINT('Ctrl Pts',(35.2954355959687,-4.89063195106467,130.265607071631));
#63464=CARTESIAN_POINT('Ctrl Pts',(35.2875912292359,-4.90194899773832,130.404261772189));
#63465=CARTESIAN_POINT('Ctrl Pts',(35.280013964821,-4.91288069662027,130.53819525137));
#63466=CARTESIAN_POINT('Ctrl Pts',(35.2724367004061,-4.91832182157851,130.672605181811));
#63467=CARTESIAN_POINT('Ctrl Pts',(35.2648594359912,-4.91824928377735,130.807014882743));
#63468=CARTESIAN_POINT('',(35.6101405640464,-4.91824810389018,130.800041927872));
#63469=CARTESIAN_POINT('Ctrl Pts',(35.6799972093173,-4.76405452823406,129.582490119308));
#63470=CARTESIAN_POINT('Ctrl Pts',(35.6704631326066,-4.80564392796807,129.744646557664));
#63471=CARTESIAN_POINT('Ctrl Pts',(35.6609290558958,-4.83898524524807,129.909064387513));
#63472=CARTESIAN_POINT('Ctrl Pts',(35.6513949791851,-4.86386696777967,130.074990216301));
#63473=CARTESIAN_POINT('Ctrl Pts',(35.641986490425,-4.88842093497294,130.238730381452));
#63474=CARTESIAN_POINT('Ctrl Pts',(35.6325780016649,-4.90473667682801,130.403939105789));
#63475=CARTESIAN_POINT('Ctrl Pts',(35.6231695129047,-4.91265689632296,130.5698712116));
#63476=CARTESIAN_POINT('Ctrl Pts',(35.618826529952,-4.9163128903009,130.646465904459));
#63477=CARTESIAN_POINT('Ctrl Pts',(35.6144835469992,-4.91818064204093,130.723214432572));
#63478=CARTESIAN_POINT('Ctrl Pts',(35.6101405640464,-4.91824810389018,130.800041927872));
#63479=CARTESIAN_POINT('Ctrl Pts',(35.6101405640087,-4.91824810389076,130.800041928539));
#63480=CARTESIAN_POINT('Ctrl Pts',(35.60244394154,-4.91836765957639,130.936195404843));
#63481=CARTESIAN_POINT('Ctrl Pts',(35.5947473190712,-4.91282919250016,131.072456023416));
#63482=CARTESIAN_POINT('Ctrl Pts',(35.5870506966025,-4.90163285999156,131.208314041058));
#63483=CARTESIAN_POINT('Ctrl Pts',(35.5793566006028,-4.8904402027558,131.344127462376));
#63484=CARTESIAN_POINT('Ctrl Pts',(35.5716625046031,-4.8735934032755,131.479538150618));
#63485=CARTESIAN_POINT('Ctrl Pts',(35.5639684086034,-4.85114468232059,131.614038537293));
#63486=CARTESIAN_POINT('Ctrl Pts',(35.5562753587172,-4.82869901356424,131.748520636873));
#63487=CARTESIAN_POINT('Ctrl Pts',(35.5485823088309,-4.80065300315192,131.882092289763));
#63488=CARTESIAN_POINT('Ctrl Pts',(35.5408892589447,-4.76711041607429,132.014253729976));
#63489=CARTESIAN_POINT('Ctrl Pts',(35.5331955327345,-4.733564880146,132.146426788981));
#63490=CARTESIAN_POINT('Ctrl Pts',(35.5255018065243,-4.69452190390324,132.277189004101));
#63491=CARTESIAN_POINT('Ctrl Pts',(35.517808080314,-4.65013566353249,132.406053900702));
#63492=CARTESIAN_POINT('Ctrl Pts',(35.5101119551761,-4.60573558339437,132.534958977778));
#63493=CARTESIAN_POINT('Ctrl Pts',(35.5024158300383,-4.55598905413414,132.661965184604));
#63494=CARTESIAN_POINT('Ctrl Pts',(35.4947197049004,-4.5010989311345,132.786604667788));
#63495=CARTESIAN_POINT('Ctrl Pts',(35.4870150064303,-4.44614766161606,132.911382996907));
#63496=CARTESIAN_POINT('Ctrl Pts',(35.4793103079601,-4.38604151849413,133.033788975197));
#63497=CARTESIAN_POINT('Ctrl Pts',(35.47160560949,-4.32103017225646,133.15337771264));
#63498=CARTESIAN_POINT('Ctrl Pts',(35.4638960953197,-4.25597819170293,133.273041197136));
#63499=CARTESIAN_POINT('Ctrl Pts',(35.4561865811494,-4.18601510605575,133.389883594735));
#63500=CARTESIAN_POINT('Ctrl Pts',(35.4484770669791,-4.11143407551822,133.503488792582));
#63501=CARTESIAN_POINT('Ctrl Pts',(35.4407559761704,-4.03674105379598,133.617264580466));
#63502=CARTESIAN_POINT('Ctrl Pts',(35.4330348853616,-3.9574164727118,133.727793141836));
#63503=CARTESIAN_POINT('Ctrl Pts',(35.4253137945529,-3.87379422963091,133.834690851877));
#63504=CARTESIAN_POINT('Ctrl Pts',(35.4213224861412,-3.83056689679963,133.889950107316));
#63505=CARTESIAN_POINT('Ctrl Pts',(35.4173311777296,-3.78619174998896,133.944239705668));
#63506=CARTESIAN_POINT('Ctrl Pts',(35.413339869318,-3.74071865843683,133.997510626714));
#63507=CARTESIAN_POINT('Ctrl Pts',(35.4055655351989,-3.6521454461734,134.101272575511));
#63508=CARTESIAN_POINT('Ctrl Pts',(35.3977912010798,-3.55911136619014,134.201510749947));
#63509=CARTESIAN_POINT('Ctrl Pts',(35.3900168669607,-3.46192754976004,134.297817458964));
#63510=CARTESIAN_POINT('Ctrl Pts',(35.3822521140136,-3.36486350369824,134.39400547857));
#63511=CARTESIAN_POINT('Ctrl Pts',(35.3744873610665,-3.26366017192064,134.486271400666));
#63512=CARTESIAN_POINT('Ctrl Pts',(35.3667226081194,-3.15866903516011,134.574240322387));
#63513=CARTESIAN_POINT('Ctrl Pts',(35.3589655672344,-3.05378217707659,134.662121872135));
#63514=CARTESIAN_POINT('Ctrl Pts',(35.3512085263495,-2.94511529850038,134.745714665239));
#63515=CARTESIAN_POINT('Ctrl Pts',(35.3434514854645,-2.83305658368171,134.824680686436));
#63516=CARTESIAN_POINT('Ctrl Pts',(35.3357002942244,-2.72108237321172,134.903587158742));
#63517=CARTESIAN_POINT('Ctrl Pts',(35.3279491029842,-2.60572173595831,134.977873579655));
#63518=CARTESIAN_POINT('Ctrl Pts',(35.3201979117441,-2.48739549400316,135.047242505966));
#63519=CARTESIAN_POINT('Ctrl Pts',(35.312450014967,-2.36911954385729,135.116581948633));
#63520=CARTESIAN_POINT('Ctrl Pts',(35.30470211819,-2.24788083254293,135.181007856363));
#63521=CARTESIAN_POINT('Ctrl Pts',(35.2969542214129,-2.12412850453284,135.240266518138));
#63522=CARTESIAN_POINT('Ctrl Pts',(35.2892079453288,-2.0004020628418,135.299512784279));
#63523=CARTESIAN_POINT('Ctrl Pts',(35.2814616692447,-1.87416340268791,135.353593785641));
#63524=CARTESIAN_POINT('Ctrl Pts',(35.2737153931606,-1.7458852134702,135.402302318358));
#63525=CARTESIAN_POINT('Ctrl Pts',(35.2659690598952,-1.61760607733222,135.451011210631));
#63526=CARTESIAN_POINT('Ctrl Pts',(35.2582227266299,-1.48728774759163,135.494347416339));
#63527=CARTESIAN_POINT('Ctrl Pts',(35.2504763933645,-1.35542140749701,135.532152477473));
#63528=CARTESIAN_POINT('Ctrl Pts',(35.2427283253615,-1.22352553684964,135.569966004788));
#63529=CARTESIAN_POINT('Ctrl Pts',(35.2349802573585,-1.09008134177591,135.602245815011));
#63530=CARTESIAN_POINT('Ctrl Pts',(35.2272321893556,-0.955593234594663,
135.628883871992));
#63531=CARTESIAN_POINT('Ctrl Pts',(35.2194758866137,-0.820962191852861,
135.655550240217));
#63532=CARTESIAN_POINT('Ctrl Pts',(35.2117195838719,-0.685285404819466,
135.676562801214));
#63533=CARTESIAN_POINT('Ctrl Pts',(35.20396328113,-0.549076057439199,135.691864944485));
#63534=CARTESIAN_POINT('Ctrl Pts',(35.1962028386159,-0.412794011028866,
135.70717525497));
#63535=CARTESIAN_POINT('Ctrl Pts',(35.1884423961017,-0.275979227709126,
135.71676904735));
#63536=CARTESIAN_POINT('Ctrl Pts',(35.1806819535875,-0.139147016488932,
135.720641851416));
#63537=CARTESIAN_POINT('Ctrl Pts',(35.1729090533221,-0.002095150055894,
135.72452087245));
#63538=CARTESIAN_POINT('Ctrl Pts',(35.1651361530567,0.134973809029991,135.722660558244));
#63539=CARTESIAN_POINT('Ctrl Pts',(35.1573632527912,0.271546648981629,135.715108572809));
#63540=CARTESIAN_POINT('Ctrl Pts',(35.1498729170292,0.403154722194802,135.707831121068));
#63541=CARTESIAN_POINT('Ctrl Pts',(35.1423825812672,0.534301813784657,135.695268656236));
#63542=CARTESIAN_POINT('Ctrl Pts',(35.1348922455051,0.66453773038607,135.677508744536));
#63543=CARTESIAN_POINT('Ctrl Pts',(35.1271179113861,0.799711581349775,135.659075460387));
#63544=CARTESIAN_POINT('Ctrl Pts',(35.119343577267,0.934331989109421,135.634984435771));
#63545=CARTESIAN_POINT('Ctrl Pts',(35.1115692431479,1.06788777758088,135.605277067265));
#63546=CARTESIAN_POINT('Ctrl Pts',(35.1038044902008,1.20127897047926,135.575606310437));
#63547=CARTESIAN_POINT('Ctrl Pts',(35.0960397372537,1.33360777669981,135.540333065798));
#63548=CARTESIAN_POINT('Ctrl Pts',(35.0882749843066,1.46436879592354,135.499550399888));
#63549=CARTESIAN_POINT('Ctrl Pts',(35.0805179434216,1.59499994145957,135.458808239898));
#63550=CARTESIAN_POINT('Ctrl Pts',(35.0727609025366,1.72406602797549,135.412567663886));
#63551=CARTESIAN_POINT('Ctrl Pts',(35.0650038616516,1.85107285058801,135.36097255675));
#63552=CARTESIAN_POINT('Ctrl Pts',(35.0572526704115,1.97798389636694,135.309416357887));
#63553=CARTESIAN_POINT('Ctrl Pts',(35.0495014791713,2.10283840845757,135.252513811633));
#63554=CARTESIAN_POINT('Ctrl Pts',(35.0417502879313,2.22515867484831,135.190458192204));
#63555=CARTESIAN_POINT('Ctrl Pts',(35.0340023911542,2.34742695186333,135.128428948069));
#63556=CARTESIAN_POINT('Ctrl Pts',(35.0262544943771,2.46716277755906,135.0612511634));
#63557=CARTESIAN_POINT('Ctrl Pts',(35.0185065976001,2.58390992411118,134.98916557916));
#63558=CARTESIAN_POINT('Ctrl Pts',(35.010760321516,2.70063264967702,134.91709507367));
#63559=CARTESIAN_POINT('Ctrl Pts',(35.0030140454319,2.81436760714029,134.840119015856));
#63560=CARTESIAN_POINT('Ctrl Pts',(34.9952677693478,2.92468496985382,134.758523093946));
#63561=CARTESIAN_POINT('Ctrl Pts',(34.9875214360825,3.03500314690477,134.676926569714));
#63562=CARTESIAN_POINT('Ctrl Pts',(34.9797751028171,3.14190336453829,134.590710345827));
#63563=CARTESIAN_POINT('Ctrl Pts',(34.9720287695517,3.24498681100062,134.500202018239));
#63564=CARTESIAN_POINT('Ctrl Pts',(34.9642807015488,3.3480933422862,134.40967342194));
#63565=CARTESIAN_POINT('Ctrl Pts',(34.9565326335458,3.4473811078317,134.314851067192));
#63566=CARTESIAN_POINT('Ctrl Pts',(34.9487845655429,3.54248656658443,134.216100934189));
#63567=CARTESIAN_POINT('Ctrl Pts',(34.941028262801,3.63769310455074,134.117245848368));
#63568=CARTESIAN_POINT('Ctrl Pts',(34.9332719600592,3.72870818470604,134.01445492735));
#63569=CARTESIAN_POINT('Ctrl Pts',(34.9255156573173,3.81520679057626,133.908129327963));
#63570=CARTESIAN_POINT('Ctrl Pts',(34.9177552148031,3.90175156335674,133.801746979403));
#63571=CARTESIAN_POINT('Ctrl Pts',(34.9099947722889,3.98377482486769,133.691826506523));
#63572=CARTESIAN_POINT('Ctrl Pts',(34.9022343297748,4.06099427708879,133.57879903713));
#63573=CARTESIAN_POINT('Ctrl Pts',(34.8944614295094,4.13833768882981,133.465590126009));
#63574=CARTESIAN_POINT('Ctrl Pts',(34.886688529244,4.21086167428251,133.349264583466));
#63575=CARTESIAN_POINT('Ctrl Pts',(34.8789156289786,4.27832893102401,133.230279952676));
#63576=CARTESIAN_POINT('Ctrl Pts',(34.8714252932165,4.34334358304393,133.115620712919));
#63577=CARTESIAN_POINT('Ctrl Pts',(34.8639349574543,4.40366263204399,132.998492631387));
#63578=CARTESIAN_POINT('Ctrl Pts',(34.8564446216922,4.45911640945718,132.879321800193));
#63579=CARTESIAN_POINT('Ctrl Pts',(34.8486702875731,4.51667273369515,132.755632570714));
#63580=CARTESIAN_POINT('Ctrl Pts',(34.8408959534541,4.56916989107253,132.629350821757));
#63581=CARTESIAN_POINT('Ctrl Pts',(34.833121619335,4.61636640654297,132.5009289961));
#63582=CARTESIAN_POINT('Ctrl Pts',(34.8253568663879,4.66350475652624,132.372665438865));
#63583=CARTESIAN_POINT('Ctrl Pts',(34.8175921134408,4.70535532889446,132.242267416121));
#63584=CARTESIAN_POINT('Ctrl Pts',(34.8098273604937,4.74172324194553,132.110210440208));
#63585=CARTESIAN_POINT('Ctrl Pts',(34.8020703196087,4.77805503387275,131.978284625144));
#63586=CARTESIAN_POINT('Ctrl Pts',(34.7943132787236,4.80891490004916,131.844703510393));
#63587=CARTESIAN_POINT('Ctrl Pts',(34.7865562378386,4.83415676510285,131.709960657821));
#63588=CARTESIAN_POINT('Ctrl Pts',(34.7788050465985,4.85937959506961,131.575319415884));
#63589=CARTESIAN_POINT('Ctrl Pts',(34.7710538553584,4.87899278486863,131.439518562626));
#63590=CARTESIAN_POINT('Ctrl Pts',(34.7633026641183,4.89290072655954,131.303064480127));
#63591=CARTESIAN_POINT('Ctrl Pts',(34.7555547673412,4.90680275700424,131.166668394253));
#63592=CARTESIAN_POINT('Ctrl Pts',(34.7478068705642,4.91500432268716,131.029620019478));
#63593=CARTESIAN_POINT('Ctrl Pts',(34.7400589737871,4.91746136351502,130.892433319563));
#63594=CARTESIAN_POINT('Ctrl Pts',(34.732312697703,4.9199178903829,130.755275316148));
#63595=CARTESIAN_POINT('Ctrl Pts',(34.7245664216189,4.91663227550848,130.6179794358));
#63596=CARTESIAN_POINT('Ctrl Pts',(34.7168201455348,4.90761254468703,130.481061725315));
#63597=CARTESIAN_POINT('Ctrl Pts',(34.7090738122694,4.89859274728394,130.344143004135));
#63598=CARTESIAN_POINT('Ctrl Pts',(34.7013274790041,4.88383877517136,130.207602848509));
#63599=CARTESIAN_POINT('Ctrl Pts',(34.6935811457387,4.86341067660904,130.071953863675));
#63600=CARTESIAN_POINT('Ctrl Pts',(34.6858330777357,4.84297800331568,129.936274501191));
#63601=CARTESIAN_POINT('Ctrl Pts',(34.6780850097328,4.81686873327383,129.801487093156));
#63602=CARTESIAN_POINT('Ctrl Pts',(34.6703369417298,4.78519427316441,129.668095318186));
#63603=CARTESIAN_POINT('Ctrl Pts',(34.6625806389879,4.75348614906189,129.534561772851));
#63604=CARTESIAN_POINT('Ctrl Pts',(34.6548243362461,4.71620111000998,129.402427204617));
#63605=CARTESIAN_POINT('Ctrl Pts',(34.6470680335042,4.67350098126703,129.272181894115));
#63606=CARTESIAN_POINT('Ctrl Pts',(34.6393075909901,4.63077806217969,129.141867067769));
#63607=CARTESIAN_POINT('Ctrl Pts',(34.6315471484759,4.58263443161248,129.013443874292));
#63608=CARTESIAN_POINT('Ctrl Pts',(34.6237867059617,4.52928022062335,128.887382854114));
#63609=CARTESIAN_POINT('Ctrl Pts',(34.6160138056963,4.47584036071818,128.761119469595));
#63610=CARTESIAN_POINT('Ctrl Pts',(34.6082409054309,4.41717337290042,128.637226189494));
#63611=CARTESIAN_POINT('Ctrl Pts',(34.6004680051655,4.35353593344518,128.516149976322));
#63612=CARTESIAN_POINT('Ctrl Pts',(34.5929776694034,4.292211875207,128.399475188472));
#63613=CARTESIAN_POINT('Ctrl Pts',(34.5854873336414,4.22627262233482,128.285416475144));
#63614=CARTESIAN_POINT('Ctrl Pts',(34.5779969978794,4.15598494818403,128.174346896505));
#63615=CARTESIAN_POINT('Ctrl Pts',(34.5702226637603,4.08303229550444,128.059066081033));
#63616=CARTESIAN_POINT('Ctrl Pts',(34.5624483296412,4.00516387949855,127.94664036582));
#63617=CARTESIAN_POINT('Ctrl Pts',(34.5546739955221,3.9226298299287,127.837517467035));
#63618=CARTESIAN_POINT('Ctrl Pts',(34.546909242575,3.84019749619866,127.72852905247));
#63619=CARTESIAN_POINT('Ctrl Pts',(34.5391444896279,3.75311120322232,127.622835664225));
#63620=CARTESIAN_POINT('Ctrl Pts',(34.5313797366808,3.66166567467816,127.52085828783));
#63621=CARTESIAN_POINT('Ctrl Pts',(34.5236226957958,3.57031097112198,127.418982196803));
#63622=CARTESIAN_POINT('Ctrl Pts',(34.5158656549108,3.47460590753085,127.320815061969));
#63623=CARTESIAN_POINT('Ctrl Pts',(34.5081086140258,3.37488677417489,127.22674656292));
#63624=CARTESIAN_POINT('Ctrl Pts',(34.5003574227857,3.27524283979377,127.132749001659));
#63625=CARTESIAN_POINT('Ctrl Pts',(34.4926062315456,3.17159114403351,127.042844191301));
#63626=CARTESIAN_POINT('Ctrl Pts',(34.4848550403055,3.06430604205144,126.957386281396));
#63627=CARTESIAN_POINT('Ctrl Pts',(34.4771071435284,2.95706653909905,126.871964693383));
#63628=CARTESIAN_POINT('Ctrl Pts',(34.4693592467513,2.84619700657529,126.790986489735));
#63629=CARTESIAN_POINT('Ctrl Pts',(34.4616113499742,2.73210604119116,126.714766549423));
#63630=CARTESIAN_POINT('Ctrl Pts',(34.4538650738901,2.61803894117763,126.638562552681));
#63631=CARTESIAN_POINT('Ctrl Pts',(34.4461187978061,2.500752073524,126.567115056561));
#63632=CARTESIAN_POINT('Ctrl Pts',(34.438372521722,2.38068394115421,126.500696244636));
#63633=CARTESIAN_POINT('Ctrl Pts',(34.4306261884566,2.26061492246842,126.434276942421));
#63634=CARTESIAN_POINT('Ctrl Pts',(34.4228798551912,2.13776494020911,126.372886587719));
#63635=CARTESIAN_POINT('Ctrl Pts',(34.4151335219258,2.01259772123235,126.31675173588));
#63636=CARTESIAN_POINT('Ctrl Pts',(34.4073854539228,1.88740247192457,126.26060431303));
#63637=CARTESIAN_POINT('Ctrl Pts',(34.3996373859199,1.7598893099546,126.20971489496));
#63638=CARTESIAN_POINT('Ctrl Pts',(34.3918893179168,1.63054221243973,126.164262002671));
#63639=CARTESIAN_POINT('Ctrl Pts',(34.384133015175,1.50105764329072,126.118760802507));
#63640=CARTESIAN_POINT('Ctrl Pts',(34.3763767124331,1.36973561444498,126.078707800132));
#63641=CARTESIAN_POINT('Ctrl Pts',(34.3686204096912,1.23707608338644,126.044231856029));
#63642=CARTESIAN_POINT('Ctrl Pts',(34.3608599671771,1.10434574794187,126.009737511076));
#63643=CARTESIAN_POINT('Ctrl Pts',(34.3530995246629,0.970276869840605,125.980826237986));
#63644=CARTESIAN_POINT('Ctrl Pts',(34.3453390821487,0.835378909042103,125.957575586143));
#63645=CARTESIAN_POINT('Ctrl Pts',(34.3375661818832,0.700264398061065,125.934287610289));
#63646=CARTESIAN_POINT('Ctrl Pts',(34.3297932816179,0.564318532735446,125.91667846452));
#63647=CARTESIAN_POINT('Ctrl Pts',(34.3220203813524,0.428056095080841,125.904773793969));
#63648=CARTESIAN_POINT('Ctrl Pts',(34.3145300455905,0.296747140260636,125.893301888179));
#63649=CARTESIAN_POINT('Ctrl Pts',(34.3070397098285,0.165144537596052,125.887126928525));
#63650=CARTESIAN_POINT('Ctrl Pts',(34.2995493740665,0.0337063506838879,
125.886226119159));
#63651=CARTESIAN_POINT('Ctrl Pts',(34.2917750399474,-0.102715355035972,
125.885291155331));
#63652=CARTESIAN_POINT('Ctrl Pts',(34.2840007058283,-0.239392074199353,
125.890035213842));
#63653=CARTESIAN_POINT('Ctrl Pts',(34.2762263717092,-0.375811929267305,
125.900489854962));
#63654=CARTESIAN_POINT('Ctrl Pts',(34.2684616187622,-0.512063659055707,
125.910931611672));
#63655=CARTESIAN_POINT('Ctrl Pts',(34.2606968658152,-0.648058768532885,
125.927069918314));
#63656=CARTESIAN_POINT('Ctrl Pts',(34.2529321128681,-0.783283765302231,
125.948884368472));
#63657=CARTESIAN_POINT('Ctrl Pts',(34.2451750719831,-0.918374454698078,
125.970677152211));
#63658=CARTESIAN_POINT('Ctrl Pts',(34.2374180310982,-1.05269617006782,125.998134798475));
#63659=CARTESIAN_POINT('Ctrl Pts',(34.2296609902132,-1.18573928982888,126.031185008073));
#63660=CARTESIAN_POINT('Ctrl Pts',(34.2219097989731,-1.31868208073877,126.064210294251));
#63661=CARTESIAN_POINT('Ctrl Pts',(34.214158607733,-1.45034781732185,126.102819655417));
#63662=CARTESIAN_POINT('Ctrl Pts',(34.2064074164929,-1.58023619542438,126.146889562458));
#63663=CARTESIAN_POINT('Ctrl Pts',(34.1986595197158,-1.71006936750168,126.190940738612));
#63664=CARTESIAN_POINT('Ctrl Pts',(34.1909116229387,-1.83812631412066,126.240447719238));
#63665=CARTESIAN_POINT('Ctrl Pts',(34.1831637261616,-1.96392126218237,126.295236940126));
#63666=CARTESIAN_POINT('Ctrl Pts',(34.1754174500775,-2.08968989665294,126.35001470029));
#63667=CARTESIAN_POINT('Ctrl Pts',(34.1676711739934,-2.21319711549453,126.410072346929));
#63668=CARTESIAN_POINT('Ctrl Pts',(34.1599248979092,-2.33397690141957,126.475188076983));
#63669=CARTESIAN_POINT('Ctrl Pts',(34.1521785646439,-2.45475757891338,126.540304287706));
#63670=CARTESIAN_POINT('Ctrl Pts',(34.1444322313786,-2.57281043917829,126.610478470813));
#63671=CARTESIAN_POINT('Ctrl Pts',(34.1366858981132,-2.68769421908834,126.685442938469));
#63672=CARTESIAN_POINT('Ctrl Pts',(34.1289378301103,-2.80260372642357,126.760424193897));
#63673=CARTESIAN_POINT('Ctrl Pts',(34.1211897621073,-2.91434241383451,126.840197654912));
#63674=CARTESIAN_POINT('Ctrl Pts',(34.1134416941044,-3.0224984850947,126.924452632819));
#63675=CARTESIAN_POINT('Ctrl Pts',(34.1056853913625,-3.13076950591523,127.008797157921));
#63676=CARTESIAN_POINT('Ctrl Pts',(34.0979290886207,-3.23544999548343,127.097632473889));
#63677=CARTESIAN_POINT('Ctrl Pts',(34.0901727858788,-3.33616130059324,127.190607604572));
#63678=CARTESIAN_POINT('Ctrl Pts',(34.0824123433647,-3.43692635835894,127.283632358882));
#63679=CARTESIAN_POINT('Ctrl Pts',(34.0746519008506,-3.53371773464809,127.380801053753));
#63680=CARTESIAN_POINT('Ctrl Pts',(34.0668914583364,-3.62619480941399,127.481726983432));
#63681=CARTESIAN_POINT('Ctrl Pts',(34.059118558071,-3.71882033659002,127.582814928372));
#63682=CARTESIAN_POINT('Ctrl Pts',(34.0513456578055,-3.80711747051388,127.687671861642));
#63683=CARTESIAN_POINT('Ctrl Pts',(34.0435727575401,-3.8907863829533,127.795878544373));
#63684=CARTESIAN_POINT('Ctrl Pts',(34.0360824217779,-3.97141371967799,127.900151641632));
#63685=CARTESIAN_POINT('Ctrl Pts',(34.0285920860157,-4.04774330943377,128.007534921912));
#63686=CARTESIAN_POINT('Ctrl Pts',(34.0211017502535,-4.11954673645024,128.117630681621));
#63687=CARTESIAN_POINT('Ctrl Pts',(34.0131632968525,-4.1956458830708,128.234313042179));
#63688=CARTESIAN_POINT('Ctrl Pts',(34.0052248434515,-4.26689421093774,128.354399816872));
#63689=CARTESIAN_POINT('Ctrl Pts',(33.9972863900504,-4.33297996118468,128.477459734745));
#63690=CARTESIAN_POINT('Ctrl Pts',(33.9893578838863,-4.39898290303297,128.600365453042));
#63691=CARTESIAN_POINT('Ctrl Pts',(33.9814293777222,-4.45983596784123,128.726236578905));
#63692=CARTESIAN_POINT('Ctrl Pts',(33.9735008715581,-4.51527021446301,128.854612440779));
#63693=CARTESIAN_POINT('Ctrl Pts',(33.9655838239637,-4.57062434546535,128.982802769119));
#63694=CARTESIAN_POINT('Ctrl Pts',(33.9576667763694,-4.62057511695177,129.113490284522));
#63695=CARTESIAN_POINT('Ctrl Pts',(33.9497497287751,-4.66489946646814,129.246189885507));
#63696=CARTESIAN_POINT('Ctrl Pts',(33.9431394823856,-4.70190756423015,129.356985866944));
#63697=CARTESIAN_POINT('Ctrl Pts',(33.9365292359961,-4.73499410125762,129.469183955581));
#63698=CARTESIAN_POINT('Ctrl Pts',(33.9299189896066,-4.764054528234,129.582490119308));
#63699=CARTESIAN_POINT('Origin',(213.235140564004,0.,130.804360617566));
#63700=CARTESIAN_POINT('',(31.8348922615591,-4.76405452823409,129.582490119308));
#63701=CARTESIAN_POINT('',(32.1802676473795,-4.76405452823406,129.582490119308));
#63702=CARTESIAN_POINT('',(213.235140564004,-4.76405452823405,129.582490119308));
#63703=CARTESIAN_POINT('',(33.5148594360289,-4.9182490365939,130.807439017015));
#63704=CARTESIAN_POINT('Ctrl Pts',(33.5148594359912,-4.91824903659349,130.807439017678));
#63705=CARTESIAN_POINT('Ctrl Pts',(33.5045047902566,-4.91813509922922,130.989472642819));
#63706=CARTESIAN_POINT('Ctrl Pts',(33.4941501445219,-4.90791567783689,131.171189313812));
#63707=CARTESIAN_POINT('Ctrl Pts',(33.4837954987872,-4.88769185390603,131.351764859202));
#63708=CARTESIAN_POINT('Ctrl Pts',(33.4760211646682,-4.87250767779513,131.487342131427));
#63709=CARTESIAN_POINT('Ctrl Pts',(33.4682468305493,-4.85165410939625,131.622501889997));
#63710=CARTESIAN_POINT('Ctrl Pts',(33.4604724964303,-4.82516026654944,131.756732112631));
#63711=CARTESIAN_POINT('Ctrl Pts',(33.4527077434833,-4.79869907499611,131.890796908512));
#63712=CARTESIAN_POINT('Ctrl Pts',(33.4449429905363,-4.76661151465987,132.023934067916));
#63713=CARTESIAN_POINT('Ctrl Pts',(33.4371782375894,-4.72897849706514,132.155636102726));
#63714=CARTESIAN_POINT('Ctrl Pts',(33.4294211967045,-4.69138285711401,132.287207329219));
#63715=CARTESIAN_POINT('Ctrl Pts',(33.4216641558196,-4.64825282744883,132.417345894214));
#63716=CARTESIAN_POINT('Ctrl Pts',(33.4139071149347,-4.59972039197709,132.545554282306));
#63717=CARTESIAN_POINT('Ctrl Pts',(33.4061559236947,-4.55122455519253,132.673665987455));
#63718=CARTESIAN_POINT('Ctrl Pts',(33.3984047324547,-4.49733455949609,132.799850048742));
#63719=CARTESIAN_POINT('Ctrl Pts',(33.3906535412146,-4.43823215967319,132.923624253677));
#63720=CARTESIAN_POINT('Ctrl Pts',(33.3829056444377,-4.37915487994675,133.047345851274));
#63721=CARTESIAN_POINT('Ctrl Pts',(33.3751577476607,-4.31486977049039,133.168659277611));
#63722=CARTESIAN_POINT('Ctrl Pts',(33.3674098508837,-4.24560655472915,133.287102659128));
#63723=CARTESIAN_POINT('Ctrl Pts',(33.3596635747997,-4.17635782733951,133.405521264843));
#63724=CARTESIAN_POINT('Ctrl Pts',(33.3519172987157,-4.10213326210762,133.521070682589));
#63725=CARTESIAN_POINT('Ctrl Pts',(33.3441710226317,-4.02320815033575,133.633314353768));
#63726=CARTESIAN_POINT('Ctrl Pts',(33.3364246893665,-3.94428245595663,133.745558853504));
#63727=CARTESIAN_POINT('Ctrl Pts',(33.3286783561012,-3.86065637068076,133.854497238165));
#63728=CARTESIAN_POINT('Ctrl Pts',(33.320932022836,-3.77264782574022,133.959722949444));
#63729=CARTESIAN_POINT('Ctrl Pts',(33.3131839548331,-3.68461957189626,134.064972225292));
#63730=CARTESIAN_POINT('Ctrl Pts',(33.3054358868302,-3.59220715625296,134.166506873474));
#63731=CARTESIAN_POINT('Ctrl Pts',(33.2976878188274,-3.49576772962533,134.263954675112));
#63732=CARTESIAN_POINT('Ctrl Pts',(33.2899315160856,-3.39922580602742,134.361506045434));
#63733=CARTESIAN_POINT('Ctrl Pts',(33.2821752133439,-3.2986485972248,134.454961614173));
#63734=CARTESIAN_POINT('Ctrl Pts',(33.2744189106021,-3.19442934502391,134.543986831795));
#63735=CARTESIAN_POINT('Ctrl Pts',(33.2666584680881,-3.09015446787014,134.633059564856));
#63736=CARTESIAN_POINT('Ctrl Pts',(33.258898025574,-2.9822339814863,134.71769699396));
#63737=CARTESIAN_POINT('Ctrl Pts',(33.2511375830599,-2.87109211515023,134.797606556501));
#63738=CARTESIAN_POINT('Ctrl Pts',(33.2433646827946,-2.7597718340236,134.877644396966));
#63739=CARTESIAN_POINT('Ctrl Pts',(33.2355917825293,-2.64522016604579,134.95293898958));
#63740=CARTESIAN_POINT('Ctrl Pts',(33.227818882264,-2.52788882802643,135.023242120481));
#63741=CARTESIAN_POINT('Ctrl Pts',(33.2203285465007,-2.41482277966371,135.090989555503));
#63742=CARTESIAN_POINT('Ctrl Pts',(33.2128382107374,-2.29917591896668,135.154101985117));
#63743=CARTESIAN_POINT('Ctrl Pts',(33.2053478749742,-2.18137014376445,135.21239956458));
#63744=CARTESIAN_POINT('Ctrl Pts',(33.1975735408551,-2.05909772680879,135.272907514478));
#63745=CARTESIAN_POINT('Ctrl Pts',(33.189799206736,-1.93411213090131,135.328419967749));
#63746=CARTESIAN_POINT('Ctrl Pts',(33.1820248726169,-1.80685987379269,135.378684661507));
#63747=CARTESIAN_POINT('Ctrl Pts',(33.1742601196698,-1.67976444371827,135.428887408522));
#63748=CARTESIAN_POINT('Ctrl Pts',(33.1664953667226,-1.55040827072505,135.473855121959));
#63749=CARTESIAN_POINT('Ctrl Pts',(33.1587306137755,-1.4192620535936,135.51338156525));
#63750=CARTESIAN_POINT('Ctrl Pts',(33.1509735728905,-1.28824609273366,135.552868750321));
#63751=CARTESIAN_POINT('Ctrl Pts',(33.1432165320055,-1.15544399774161,135.586925308049));
#63752=CARTESIAN_POINT('Ctrl Pts',(33.1354594911205,-1.0213456829442,135.615393361004));
#63753=CARTESIAN_POINT('Ctrl Pts',(33.1277082998803,-0.887348492729106,
135.643839945979));
#63754=CARTESIAN_POINT('Ctrl Pts',(33.1199571086401,-0.752057409236861,
135.666706333698));
#63755=CARTESIAN_POINT('Ctrl Pts',(33.1122059174,-0.615976374393877,135.68388479198));
#63756=CARTESIAN_POINT('Ctrl Pts',(33.1044580206229,-0.479953177620966,
135.701055948959));
#63757=CARTESIAN_POINT('Ctrl Pts',(33.0967101238458,-0.343141084353969,
135.712543935904));
#63758=CARTESIAN_POINT('Ctrl Pts',(33.0889622270687,-0.206052853023449,
135.718292371697));
#63759=CARTESIAN_POINT('Ctrl Pts',(33.0812159509846,-0.0689932975954562,
135.724039605042));
#63760=CARTESIAN_POINT('Ctrl Pts',(33.0734696749004,0.0683418906295579,
135.724049658905));
#63761=CARTESIAN_POINT('Ctrl Pts',(33.0657233988163,0.205436620866316,135.718318173071));
#63762=CARTESIAN_POINT('Ctrl Pts',(33.057977065551,0.342532363105043,135.712586644929));
#63763=CARTESIAN_POINT('Ctrl Pts',(33.0502307322857,0.479387253189631,135.701113508848));
#63764=CARTESIAN_POINT('Ctrl Pts',(33.0424843990203,0.615487392506522,135.683946494684));
#63765=CARTESIAN_POINT('Ctrl Pts',(33.0347363310173,0.751618010506147,135.666775636086));
#63766=CARTESIAN_POINT('Ctrl Pts',(33.0269882630143,0.886993153588004,135.643908411011));
#63767=CARTESIAN_POINT('Ctrl Pts',(33.0192401950113,1.02110661472941,135.615444107161));
#63768=CARTESIAN_POINT('Ctrl Pts',(33.0114838922694,1.15536261325329,135.58694955111));
#63769=CARTESIAN_POINT('Ctrl Pts',(33.0037275895275,1.28835386812738,135.552846114531));
#63770=CARTESIAN_POINT('Ctrl Pts',(32.9959712867856,1.41958635655096,135.513283810696));
#63771=CARTESIAN_POINT('Ctrl Pts',(32.9882108442715,1.55088888770496,135.473700391268));
#63772=CARTESIAN_POINT('Ctrl Pts',(32.9804504017573,1.68043041286254,135.428652427418));
#63773=CARTESIAN_POINT('Ctrl Pts',(32.9726899592431,1.80773548453207,135.378338698019));
#63774=CARTESIAN_POINT('Ctrl Pts',(32.9649170589776,1.93524491760425,135.327944200555));
#63775=CARTESIAN_POINT('Ctrl Pts',(32.9571441587122,2.06051036544685,135.27226720449));
#63776=CARTESIAN_POINT('Ctrl Pts',(32.9493712584467,2.18307883474006,135.211553586317));
#63777=CARTESIAN_POINT('Ctrl Pts',(32.9418809226849,2.3011916314388,135.153047061095));
#63778=CARTESIAN_POINT('Ctrl Pts',(32.9343905869232,2.41679985892478,135.089863891726));
#63779=CARTESIAN_POINT('Ctrl Pts',(32.9269002511614,2.5295241626408,135.022261822326));
#63780=CARTESIAN_POINT('Ctrl Pts',(32.9191259170424,2.64652244259797,134.952096599915));
#63781=CARTESIAN_POINT('Ctrl Pts',(32.9113515829233,2.76078440926004,134.876948515263));
#63782=CARTESIAN_POINT('Ctrl Pts',(32.9035772488042,2.87185647296498,134.797056882146));
#63783=CARTESIAN_POINT('Ctrl Pts',(32.8958124958571,2.9827916502782,134.717263708327));
#63784=CARTESIAN_POINT('Ctrl Pts',(32.88804774291,3.09054443234698,134.63273884394));
#63785=CARTESIAN_POINT('Ctrl Pts',(32.8802829899629,3.19468688231904,134.5437668253));
#63786=CARTESIAN_POINT('Ctrl Pts',(32.8725259490779,3.29872589654164,134.454883174923));
#63787=CARTESIAN_POINT('Ctrl Pts',(32.8647689081929,3.39916141930434,134.361561412585));
#63788=CARTESIAN_POINT('Ctrl Pts',(32.8570118673078,3.49559581319379,134.264128380478));
#63789=CARTESIAN_POINT('Ctrl Pts',(32.8492606760677,3.59195748515665,134.166768823378));
#63790=CARTESIAN_POINT('Ctrl Pts',(32.8415094848276,3.68432376005028,134.065304444298));
#63791=CARTESIAN_POINT('Ctrl Pts',(32.8337582935875,3.77233160681873,133.960100991978));
#63792=CARTESIAN_POINT('Ctrl Pts',(32.8260103968104,3.86030204790462,133.854942253932));
#63793=CARTESIAN_POINT('Ctrl Pts',(32.8182625000333,3.94391749491032,133.746047902701));
#63794=CARTESIAN_POINT('Ctrl Pts',(32.8105146032562,4.02285335434779,133.633818861102));
#63795=CARTESIAN_POINT('Ctrl Pts',(32.8027683271721,4.10177270210512,133.521613295399));
#63796=CARTESIAN_POINT('Ctrl Pts',(32.795022051088,4.1760141845391,133.40607474637));
#63797=CARTESIAN_POINT('Ctrl Pts',(32.7872757750039,4.24529517360068,133.287635059005));
#63798=CARTESIAN_POINT('Ctrl Pts',(32.7795294417385,4.31457667407878,133.169194497345));
#63799=CARTESIAN_POINT('Ctrl Pts',(32.7717831084732,4.37889741071513,133.047853092086));
#63800=CARTESIAN_POINT('Ctrl Pts',(32.7640367752078,4.43801976523524,132.92406899984));
#63801=CARTESIAN_POINT('Ctrl Pts',(32.7562887072048,4.49715535979672,132.800257187004));
#63802=CARTESIAN_POINT('Ctrl Pts',(32.7485406392018,4.55109008726569,132.67400195139));
#63803=CARTESIAN_POINT('Ctrl Pts',(32.7407925711988,4.59963386393606,132.545782846732));
#63804=CARTESIAN_POINT('Ctrl Pts',(32.733036268457,4.64822923350994,132.417427469283));
#63805=CARTESIAN_POINT('Ctrl Pts',(32.725279965715,4.69142206820747,132.287104419556));
#63806=CARTESIAN_POINT('Ctrl Pts',(32.7175236629732,4.72907154705318,132.155310418762));
#63807=CARTESIAN_POINT('Ctrl Pts',(32.709763220459,4.76674112055941,132.023446075542));
#63808=CARTESIAN_POINT('Ctrl Pts',(32.7020027779448,4.79886135132349,131.890109596802));
#63809=CARTESIAN_POINT('Ctrl Pts',(32.6942423354307,4.82534248665787,131.755808434818));
#63810=CARTESIAN_POINT('Ctrl Pts',(32.6864694351652,4.85186613186153,131.621291680687));
#63811=CARTESIAN_POINT('Ctrl Pts',(32.6786965348997,4.87273253255604,131.485807535357));
#63812=CARTESIAN_POINT('Ctrl Pts',(32.6709236346343,4.88790369764239,131.349870017186));
#63813=CARTESIAN_POINT('Ctrl Pts',(32.6634332988723,4.90252335266384,131.218874170208));
#63814=CARTESIAN_POINT('Ctrl Pts',(32.6559429631104,4.9118546336778,131.087457647847));
#63815=CARTESIAN_POINT('Ctrl Pts',(32.6484526273485,4.91590933770428,130.956078928827));
#63816=CARTESIAN_POINT('Ctrl Pts',(32.6406782932294,4.92011777706637,130.819718945742));
#63817=CARTESIAN_POINT('Ctrl Pts',(32.6329039591103,4.91865494912831,130.682967741773));
#63818=CARTESIAN_POINT('Ctrl Pts',(32.6251296249912,4.91147701905707,130.546336289693));
#63819=CARTESIAN_POINT('Ctrl Pts',(32.6173648720441,4.90430793514313,130.409873223667));
#63820=CARTESIAN_POINT('Ctrl Pts',(32.609600119097,4.89143778358255,130.27353000256));
#63821=CARTESIAN_POINT('Ctrl Pts',(32.60183536615,4.87287464251269,130.137820460594));
#63822=CARTESIAN_POINT('Ctrl Pts',(32.594078325265,4.85432993861621,130.002245707258));
#63823=CARTESIAN_POINT('Ctrl Pts',(32.58632128438,4.83010355027915,129.867303765421));
#63824=CARTESIAN_POINT('Ctrl Pts',(32.578564243495,4.80025552635874,129.73350584489));
#63825=CARTESIAN_POINT('Ctrl Pts',(32.5708130522549,4.77043001106535,129.599808822412));
#63826=CARTESIAN_POINT('Ctrl Pts',(32.5630618610147,4.73499138307699,129.467254484097));
#63827=CARTESIAN_POINT('Ctrl Pts',(32.5553106697746,4.69405113001353,129.336345954384));
#63828=CARTESIAN_POINT('Ctrl Pts',(32.5475627729976,4.6531282776498,129.205493064287));
#63829=CARTESIAN_POINT('Ctrl Pts',(32.5398148762205,4.60670856743803,129.076284963876));
#63830=CARTESIAN_POINT('Ctrl Pts',(32.5320669794434,4.55495385639095,128.949211451421));
#63831=CARTESIAN_POINT('Ctrl Pts',(32.5243207033594,4.50320997131365,128.822164520005));
#63832=CARTESIAN_POINT('Ctrl Pts',(32.5165744272753,4.44613345249836,128.697251650269));
#63833=CARTESIAN_POINT('Ctrl Pts',(32.5088281511912,4.38393485600219,128.574944047961));
#63834=CARTESIAN_POINT('Ctrl Pts',(32.5010818179258,4.32173580037011,128.452635542806));
#63835=CARTESIAN_POINT('Ctrl Pts',(32.4933354846604,4.25441476883246,128.332932691945));
#63836=CARTESIAN_POINT('Ctrl Pts',(32.4855891513951,4.18222878303977,128.216283055202));
#63837=CARTESIAN_POINT('Ctrl Pts',(32.4778410833921,4.11002663169616,128.099607295581));
#63838=CARTESIAN_POINT('Ctrl Pts',(32.4700930153892,4.03295756386686,127.985986443046));
#63839=CARTESIAN_POINT('Ctrl Pts',(32.4623449473862,3.95132229680212,127.875839630908));
#63840=CARTESIAN_POINT('Ctrl Pts',(32.4545886446444,3.86960026680397,127.765575753428));
#63841=CARTESIAN_POINT('Ctrl Pts',(32.4468323419026,3.78330257632576,127.658793606617));
#63842=CARTESIAN_POINT('Ctrl Pts',(32.4390760391607,3.69277101381425,127.555880157099));
#63843=CARTESIAN_POINT('Ctrl Pts',(32.4313155966466,3.60219113188197,127.452911779575));
#63844=CARTESIAN_POINT('Ctrl Pts',(32.4235551541324,3.50737314534137,127.353816496058));
#63845=CARTESIAN_POINT('Ctrl Pts',(32.4157947116182,3.40869547464421,127.258944108376));
#63846=CARTESIAN_POINT('Ctrl Pts',(32.4080218113528,3.30985939778986,127.163919423115));
#63847=CARTESIAN_POINT('Ctrl Pts',(32.4002489110874,3.20715154847891,127.073131439308));
#63848=CARTESIAN_POINT('Ctrl Pts',(32.392476010822,3.10098384979719,126.986889959421));
#63849=CARTESIAN_POINT('Ctrl Pts',(32.3849856750599,2.99867561438155,126.903783574557));
#63850=CARTESIAN_POINT('Ctrl Pts',(32.3774953392977,2.89315495752513,126.824899063199));
#63851=CARTESIAN_POINT('Ctrl Pts',(32.3700050035356,2.78481398694011,126.750474319131));
#63852=CARTESIAN_POINT('Ctrl Pts',(32.3622306694165,2.6723652355271,126.673227738271));
#63853=CARTESIAN_POINT('Ctrl Pts',(32.3544563352975,2.55652188040092,126.600541090766));
#63854=CARTESIAN_POINT('Ctrl Pts',(32.3466820011784,2.4376901236276,126.532727449366));
#63855=CARTESIAN_POINT('Ctrl Pts',(32.3389172482313,2.31900481637421,126.464997382218));
#63856=CARTESIAN_POINT('Ctrl Pts',(32.3311524952842,2.19733877172655,126.402128563851));
#63857=CARTESIAN_POINT('Ctrl Pts',(32.3233877423371,2.07312865939804,126.344391937846));
#63858=CARTESIAN_POINT('Ctrl Pts',(32.3156307014521,1.94904191430415,126.286712656672));
#63859=CARTESIAN_POINT('Ctrl Pts',(32.307873660567,1.82241648222416,126.234155587604));
#63860=CARTESIAN_POINT('Ctrl Pts',(32.300116619682,1.69371491631963,126.186946531225));
#63861=CARTESIAN_POINT('Ctrl Pts',(32.2923654284419,1.56511040526729,126.139773075563));
#63862=CARTESIAN_POINT('Ctrl Pts',(32.2846142372018,1.43443324224509,126.097939739285));
#63863=CARTESIAN_POINT('Ctrl Pts',(32.2768630459616,1.30216698187255,126.061624675747));
#63864=CARTESIAN_POINT('Ctrl Pts',(32.2691151491846,1.16995693818882,126.025325047079));
#63865=CARTESIAN_POINT('Ctrl Pts',(32.2613672524075,1.03615951671507,125.9945391296));
#63866=CARTESIAN_POINT('Ctrl Pts',(32.2536193556304,0.901274286277271,125.969395496348));
#63867=CARTESIAN_POINT('Ctrl Pts',(32.2458730795463,0.766417270921887,125.944257122602));
#63868=CARTESIAN_POINT('Ctrl Pts',(32.2381268034622,0.630473283305439,125.924758757114));
#63869=CARTESIAN_POINT('Ctrl Pts',(32.2303805273781,0.493952572860944,125.910977951325));
#63870=CARTESIAN_POINT('Ctrl Pts',(32.2226341941127,0.357430854651577,125.89719704381));
#63871=CARTESIAN_POINT('Ctrl Pts',(32.2148878608474,0.220332794107589,125.889133819478));
#63872=CARTESIAN_POINT('Ctrl Pts',(32.207141527582,0.0831738624639008,125.886813955754));
#63873=CARTESIAN_POINT('Ctrl Pts',(32.199393459579,-0.0540157849715361,
125.884493572511));
#63874=CARTESIAN_POINT('Ctrl Pts',(32.1916453915761,-0.191265939797621,
125.887919115847));
#63875=CARTESIAN_POINT('Ctrl Pts',(32.1838973235731,-0.328061428269853,
125.897064135614));
#63876=CARTESIAN_POINT('Ctrl Pts',(32.1761410208312,-0.46500230461512,125.906218874816));
#63877=CARTESIAN_POINT('Ctrl Pts',(32.1683847180894,-0.601487158596418,
125.921105207243));
#63878=CARTESIAN_POINT('Ctrl Pts',(32.1606284153475,-0.737005679230065,
125.941644741506));
#63879=CARTESIAN_POINT('Ctrl Pts',(32.1528679728333,-0.872596530178557,
125.962195238337));
#63880=CARTESIAN_POINT('Ctrl Pts',(32.1451075303191,-1.00721963650943,125.988404874521));
#63881=CARTESIAN_POINT('Ctrl Pts',(32.1373470878049,-1.14037615453993,126.020144350647));
#63882=CARTESIAN_POINT('Ctrl Pts',(32.1295741875395,-1.27374642723425,126.051934777797));
#63883=CARTESIAN_POINT('Ctrl Pts',(32.1218012872741,-1.4056450305916,126.089272677393));
#63884=CARTESIAN_POINT('Ctrl Pts',(32.1140283870087,-1.53558866453363,126.131978942675));
#63885=CARTESIAN_POINT('Ctrl Pts',(32.1065380512467,-1.66080852007273,126.173132727644));
#63886=CARTESIAN_POINT('Ctrl Pts',(32.0990477154847,-1.78421278611718,126.219271239507));
#63887=CARTESIAN_POINT('Ctrl Pts',(32.0915573797228,-1.90538937209461,126.27019317434));
#63888=CARTESIAN_POINT('Ctrl Pts',(32.0837826263318,-2.03116718802486,126.323048680168));
#63889=CARTESIAN_POINT('Ctrl Pts',(32.0760078729409,-2.15494325307723,126.381225491961));
#63890=CARTESIAN_POINT('Ctrl Pts',(32.06823311955,-2.27623453040337,126.444551054626));
#63891=CARTESIAN_POINT('Ctrl Pts',(32.0604680431041,-2.39737484100826,126.50779779833));
#63892=CARTESIAN_POINT('Ctrl Pts',(32.0527029666583,-2.51603617442874,126.576180362149));
#63893=CARTESIAN_POINT('Ctrl Pts',(32.0449378902125,-2.63175449102122,126.6494777839));
#63894=CARTESIAN_POINT('Ctrl Pts',(32.0371806211944,-2.74735645816118,126.72270150846));
#63895=CARTESIAN_POINT('Ctrl Pts',(32.0294233521763,-2.86002096928335,126.80083004836));
#63896=CARTESIAN_POINT('Ctrl Pts',(32.0216660831582,-2.96930799465667,126.883596266656));
#63897=CARTESIAN_POINT('Ctrl Pts',(32.0138838405916,-3.07894685581445,126.966628940345));
#63898=CARTESIAN_POINT('Ctrl Pts',(32.0061015980249,-3.1851860933382,127.054329023599));
#63899=CARTESIAN_POINT('Ctrl Pts',(31.9983193554583,-3.28760955243346,127.14638214671));
#63900=CARTESIAN_POINT('Ctrl Pts',(31.9905717987671,-3.38957650463929,127.238024984079));
#63901=CARTESIAN_POINT('Ctrl Pts',(31.982824242076,-3.48776132977043,127.333981874158));
#63902=CARTESIAN_POINT('Ctrl Pts',(31.9750766853848,-3.58178601945645,127.433901899034));
#63903=CARTESIAN_POINT('Ctrl Pts',(31.9673308780817,-3.67578947849214,127.533799362102));
#63904=CARTESIAN_POINT('Ctrl Pts',(31.9595850707785,-3.76563440369733,127.637657894713));
#63905=CARTESIAN_POINT('Ctrl Pts',(31.9518392634754,-3.85097996662846,127.745090057592));
#63906=CARTESIAN_POINT('Ctrl Pts',(31.9440935277672,-3.93632474070641,127.852521227469));
#63907=CARTESIAN_POINT('Ctrl Pts',(31.9363477920589,-4.01716999289573,127.963525655289));
#63908=CARTESIAN_POINT('Ctrl Pts',(31.9286020563507,-4.09321573473597,128.077683516879));
#63909=CARTESIAN_POINT('Ctrl Pts',(31.9207929067847,-4.16988405834689,128.1927759818));
#63910=CARTESIAN_POINT('Ctrl Pts',(31.9129837572187,-4.24167369234902,128.311073421181));
#63911=CARTESIAN_POINT('Ctrl Pts',(31.9051746076528,-4.30832268917191,128.432117234507));
#63912=CARTESIAN_POINT('Ctrl Pts',(31.8974207673178,-4.37449963654455,128.552303740623));
#63913=CARTESIAN_POINT('Ctrl Pts',(31.8896669269828,-4.43560839980911,128.675197467796));
#63914=CARTESIAN_POINT('Ctrl Pts',(31.8819130866478,-4.49143985946111,128.800326922404));
#63915=CARTESIAN_POINT('Ctrl Pts',(31.8740762824664,-4.54786869956544,128.926795225946));
#63916=CARTESIAN_POINT('Ctrl Pts',(31.8662394782849,-4.59890648942169,129.05554700006));
#63917=CARTESIAN_POINT('Ctrl Pts',(31.8584026741034,-4.64438842963329,129.186077831033));
#63918=CARTESIAN_POINT('Ctrl Pts',(31.850565869922,-4.68987036984483,129.316608662006));
#63919=CARTESIAN_POINT('Ctrl Pts',(31.8427290657405,-4.72979638684535,129.448918145974));
#63920=CARTESIAN_POINT('Ctrl Pts',(31.8348922615591,-4.76405452823408,129.582490119308));
#63921=CARTESIAN_POINT('Ctrl Pts',(33.5849978012129,-4.7640545282341,129.582490119308));
#63922=CARTESIAN_POINT('Ctrl Pts',(33.5773446850024,-4.79770990922239,129.71371193899));
#63923=CARTESIAN_POINT('Ctrl Pts',(33.5696915687919,-4.82591769789479,129.846240287322));
#63924=CARTESIAN_POINT('Ctrl Pts',(33.5620384525814,-4.8485992859329,129.979576993243));
#63925=CARTESIAN_POINT('Ctrl Pts',(33.554175283156,-4.87190340998842,130.116573359227));
#63926=CARTESIAN_POINT('Ctrl Pts',(33.5463121137306,-4.88937354778417,130.254422640192));
#63927=CARTESIAN_POINT('Ctrl Pts',(33.5384489443052,-4.90098157445576,130.392580737842));
#63928=CARTESIAN_POINT('Ctrl Pts',(33.5305857748798,-4.91258960112736,130.530738835493));
#63929=CARTESIAN_POINT('Ctrl Pts',(33.5227226054543,-4.91833555897516,130.669205293498));
#63930=CARTESIAN_POINT('Ctrl Pts',(33.5148594360289,-4.9182490365939,130.807439017015));
#63931=CARTESIAN_POINT('',(33.8601405639655,-4.91824957007167,130.806417068353));
#63932=CARTESIAN_POINT('Ctrl Pts',(33.9299189896066,-4.764054528234,129.582490119308));
#63933=CARTESIAN_POINT('Ctrl Pts',(33.9220152405073,-4.79880154218852,129.717968199357));
#63934=CARTESIAN_POINT('Ctrl Pts',(33.914111491408,-4.82779127781455,129.855030603445));
#63935=CARTESIAN_POINT('Ctrl Pts',(33.9062077423087,-4.85089013886288,129.993159087006));
#63936=CARTESIAN_POINT('Ctrl Pts',(33.8983092543243,-4.87397362420029,130.131195625616));
#63937=CARTESIAN_POINT('Ctrl Pts',(33.8904107663399,-4.89117398588149,130.270296467006));
#63938=CARTESIAN_POINT('Ctrl Pts',(33.8825122783555,-4.90240853659577,130.409932420282));
#63939=CARTESIAN_POINT('Ctrl Pts',(33.8750550402399,-4.91301546794307,130.54176759622));
#63940=CARTESIAN_POINT('Ctrl Pts',(33.8675978021243,-4.91830490393996,130.674079413037));
#63941=CARTESIAN_POINT('Ctrl Pts',(33.8601405640087,-4.91824957007199,130.806417067586));
#63942=CARTESIAN_POINT('Ctrl Pts',(33.8601405639655,-4.91824957007167,130.806417068353));
#63943=CARTESIAN_POINT('Ctrl Pts',(33.8517056390285,-4.91818698159191,130.956104950805));
#63944=CARTESIAN_POINT('Ctrl Pts',(33.8432707140914,-4.91128657896475,131.105575117));
#63945=CARTESIAN_POINT('Ctrl Pts',(33.8348357891543,-4.89763267691119,131.254224179718));
#63946=CARTESIAN_POINT('Ctrl Pts',(33.8263627532913,-4.88391708339587,131.403544873002));
#63947=CARTESIAN_POINT('Ctrl Pts',(33.8178897174284,-4.86338690985431,131.552036764359));
#63948=CARTESIAN_POINT('Ctrl Pts',(33.8094166815654,-4.83617815412594,131.699102996162));
#63949=CARTESIAN_POINT('Ctrl Pts',(33.8009242185549,-4.80890701361357,131.846506424388));
#63950=CARTESIAN_POINT('Ctrl Pts',(33.7924317555444,-4.77492675024485,131.992477400738));
#63951=CARTESIAN_POINT('Ctrl Pts',(33.7839392925339,-4.73442338032173,132.136433557897));
#63952=CARTESIAN_POINT('Ctrl Pts',(33.7754180739657,-4.69378286561634,132.280877151926));
#63953=CARTESIAN_POINT('Ctrl Pts',(33.7668968553975,-4.6465751220737,132.423292017553));
#63954=CARTESIAN_POINT('Ctrl Pts',(33.7583756368293,-4.59303557172602,132.563112248513));
#63955=CARTESIAN_POINT('Ctrl Pts',(33.7531351333664,-4.56010903701138,132.649100936476));
#63956=CARTESIAN_POINT('Ctrl Pts',(33.7478946299035,-4.52478862071199,132.734108740538));
#63957=CARTESIAN_POINT('Ctrl Pts',(33.7426541264407,-4.48713762383094,132.818008801162));
#63958=CARTESIAN_POINT('Ctrl Pts',(33.7348797923216,-4.43128203061448,132.942475297279));
#63959=CARTESIAN_POINT('Ctrl Pts',(33.7271054582025,-4.37015526934994,133.064813152049));
#63960=CARTESIAN_POINT('Ctrl Pts',(33.7193311240834,-4.30394140587459,133.184543685588));
#63961=CARTESIAN_POINT('Ctrl Pts',(33.7115663711363,-4.23780914506827,133.304126661945));
#63962=CARTESIAN_POINT('Ctrl Pts',(33.7038016181891,-4.16660244367708,133.421108371713));
#63963=CARTESIAN_POINT('Ctrl Pts',(33.696036865242,-4.09055330336761,133.535030267086));
#63964=CARTESIAN_POINT('Ctrl Pts',(33.688279824357,-4.01457969613639,133.648839013626));
#63965=CARTESIAN_POINT('Ctrl Pts',(33.680522783472,-3.93377343692912,133.759593670555));
#63966=CARTESIAN_POINT('Ctrl Pts',(33.6727657425869,-3.84841211580568,133.866860780737));
#63967=CARTESIAN_POINT('Ctrl Pts',(33.6650145513468,-3.76311516631873,133.974046999955));
#63968=CARTESIAN_POINT('Ctrl Pts',(33.6572633601067,-3.6732702345515,134.077750602571));
#63969=CARTESIAN_POINT('Ctrl Pts',(33.6495121688666,-3.57919763210577,134.17756790038));
#63970=CARTESIAN_POINT('Ctrl Pts',(33.6417642720895,-3.48516501302541,134.277342773175));
#63971=CARTESIAN_POINT('Ctrl Pts',(33.6340163753123,-3.38690856469369,134.373234342509));
#63972=CARTESIAN_POINT('Ctrl Pts',(33.6262684785352,-3.28478806640864,134.464872934343));
#63973=CARTESIAN_POINT('Ctrl Pts',(33.6185222024511,-3.18268892953023,134.55649235736));
#63974=CARTESIAN_POINT('Ctrl Pts',(33.610775926367,-3.07672764120346,134.643860311451));
#63975=CARTESIAN_POINT('Ctrl Pts',(33.6030296502828,-2.96729964294952,134.726645142107));
#63976=CARTESIAN_POINT('Ctrl Pts',(33.5952833170175,-2.85787083692296,134.809430583861));
#63977=CARTESIAN_POINT('Ctrl Pts',(33.587536983752,-2.74497558169847,134.887632598793));
#63978=CARTESIAN_POINT('Ctrl Pts',(33.5797906504866,-2.62904076230094,134.960961119498));
#63979=CARTESIAN_POINT('Ctrl Pts',(33.5720425824836,-2.51307998010459,135.034306061616));
#63980=CARTESIAN_POINT('Ctrl Pts',(33.5642945144807,-2.39407860959861,135.102775128827));
#63981=CARTESIAN_POINT('Ctrl Pts',(33.5565464464777,-2.27249039741194,135.166122928395));
#63982=CARTESIAN_POINT('Ctrl Pts',(33.5487901437358,-2.15077295982644,135.229538054759));
#63983=CARTESIAN_POINT('Ctrl Pts',(33.541033840994,-2.02646353576651,135.287820859679));
#63984=CARTESIAN_POINT('Ctrl Pts',(33.5332775382521,-1.90003873753938,135.340772840717));
#63985=CARTESIAN_POINT('Ctrl Pts',(33.5255170957379,-1.77354646259069,135.39375308382));
#63986=CARTESIAN_POINT('Ctrl Pts',(33.5177566532237,-1.64493693020729,135.44139669795));
#63987=CARTESIAN_POINT('Ctrl Pts',(33.5099962107095,-1.51470344026117,135.483554624076));
#63988=CARTESIAN_POINT('Ctrl Pts',(33.5022233104441,-1.38426088795541,135.525780225848));
#63989=CARTESIAN_POINT('Ctrl Pts',(33.4944504101786,-1.25218954552087,135.562502437403));
#63990=CARTESIAN_POINT('Ctrl Pts',(33.4866775099131,-1.11899534644983,135.593622823493));
#63991=CARTESIAN_POINT('Ctrl Pts',(33.4791871741513,-0.99064309201547,135.62361190516));
#63992=CARTESIAN_POINT('Ctrl Pts',(33.4716968383895,-0.86124850345266,135.648399313348));
#63993=CARTESIAN_POINT('Ctrl Pts',(33.4642065026277,-0.731268243770763,
135.667942612161));
#63994=CARTESIAN_POINT('Ctrl Pts',(33.4564321685087,-0.596359743032192,
135.68822690109));
#63995=CARTESIAN_POINT('Ctrl Pts',(33.4486578343896,-0.460392933458573,
135.70292582441));
#63996=CARTESIAN_POINT('Ctrl Pts',(33.4408835002705,-0.323870034075956,
135.711935503752));
#63997=CARTESIAN_POINT('Ctrl Pts',(33.4331187473235,-0.187515386965612,
135.720934079471));
#63998=CARTESIAN_POINT('Ctrl Pts',(33.4253539943764,-0.0506064000222067,
135.724257336478));
#63999=CARTESIAN_POINT('Ctrl Pts',(33.4175892414293,0.0863457349310442,
135.721852608059));
#64000=CARTESIAN_POINT('Ctrl Pts',(33.4098322005443,0.223161847093359,135.719450268049));
#64001=CARTESIAN_POINT('Ctrl Pts',(33.4020751596593,0.360020633606295,135.711331271029));
#64002=CARTESIAN_POINT('Ctrl Pts',(33.3943181187743,0.496407370497047,135.697494867208));
#64003=CARTESIAN_POINT('Ctrl Pts',(33.3865669275341,0.632691257088577,135.683668897526));
#64004=CARTESIAN_POINT('Ctrl Pts',(33.378815736294,0.768503415212321,135.664134142205));
#64005=CARTESIAN_POINT('Ctrl Pts',(33.3710645450539,0.903331074304611,135.638941885132));
#64006=CARTESIAN_POINT('Ctrl Pts',(33.3633166482768,1.03810142804496,135.61376033544));
#64007=CARTESIAN_POINT('Ctrl Pts',(33.3555687514997,1.17188773148628,135.582926138198));
#64008=CARTESIAN_POINT('Ctrl Pts',(33.3478208547227,1.30418449789093,135.546542168072));
#64009=CARTESIAN_POINT('Ctrl Pts',(33.3400745786386,1.43645359066405,135.510165808688));
#64010=CARTESIAN_POINT('Ctrl Pts',(33.3323283025546,1.56723338941808,135.468242089107));
#64011=CARTESIAN_POINT('Ctrl Pts',(33.3245820264705,1.69603111802011,135.420924438116));
#64012=CARTESIAN_POINT('Ctrl Pts',(33.3168356932051,1.82482979737771,135.373606437836));
#64013=CARTESIAN_POINT('Ctrl Pts',(33.3090893599397,1.95164601040449,135.320894561518));
#64014=CARTESIAN_POINT('Ctrl Pts',(33.3013430266744,2.07600497339404,135.262991171104));
#64015=CARTESIAN_POINT('Ctrl Pts',(33.2935949586714,2.20039178571112,135.205074813627));
#64016=CARTESIAN_POINT('Ctrl Pts',(33.2858468906685,2.32231989862834,135.141964793605));
#64017=CARTESIAN_POINT('Ctrl Pts',(33.2780988226656,2.44133759515221,135.073910220158));
#64018=CARTESIAN_POINT('Ctrl Pts',(33.2703425199237,2.56048178510027,135.005783317502));
#64019=CARTESIAN_POINT('Ctrl Pts',(33.2625862171819,2.67670903966507,134.932701558111));
#64020=CARTESIAN_POINT('Ctrl Pts',(33.2548299144401,2.78959473252861,134.854958634001));
#64021=CARTESIAN_POINT('Ctrl Pts',(33.2470694719259,2.90254067588566,134.777174216152));
#64022=CARTESIAN_POINT('Ctrl Pts',(33.2393090294117,3.01214119150543,134.694723911344));
#64023=CARTESIAN_POINT('Ctrl Pts',(33.2315485868975,3.11800423117598,134.607942176685));
#64024=CARTESIAN_POINT('Ctrl Pts',(33.2237756866321,3.22403721159574,134.521021132281));
#64025=CARTESIAN_POINT('Ctrl Pts',(33.2160027863666,3.32632043481156,134.429755023772));
#64026=CARTESIAN_POINT('Ctrl Pts',(33.2082298861012,3.42449761505119,134.334516300678));
#64027=CARTESIAN_POINT('Ctrl Pts',(33.2007395503391,3.51910580749719,134.242739745059));
#64028=CARTESIAN_POINT('Ctrl Pts',(33.193249214577,3.60990109178267,134.147274612643));
#64029=CARTESIAN_POINT('Ctrl Pts',(33.1857588788148,3.69660092787551,134.048482169316));
#64030=CARTESIAN_POINT('Ctrl Pts',(33.1779845446957,3.78658801460439,133.945943980474));
#64031=CARTESIAN_POINT('Ctrl Pts',(33.1702102105766,3.87244801683716,133.839496379896));
#64032=CARTESIAN_POINT('Ctrl Pts',(33.1624358764576,3.95382207710918,133.729505749874));
#64033=CARTESIAN_POINT('Ctrl Pts',(33.1546711235105,4.0350958511244,133.619650673474));
#64034=CARTESIAN_POINT('Ctrl Pts',(33.1469063705634,4.11189445299536,133.506261566882));
#64035=CARTESIAN_POINT('Ctrl Pts',(33.1391416176163,4.18389726105459,133.38974004261));
#64036=CARTESIAN_POINT('Ctrl Pts',(33.1313845767313,4.2558285549098,133.273334249158));
#64037=CARTESIAN_POINT('Ctrl Pts',(33.1236275358463,4.32297332984678,133.153802559816));
#64038=CARTESIAN_POINT('Ctrl Pts',(33.1158704949613,4.38505273416512,133.031577621158));
#64039=CARTESIAN_POINT('Ctrl Pts',(33.1081193037212,4.44708532392176,132.909444853278));
#64040=CARTESIAN_POINT('Ctrl Pts',(33.1003681124811,4.50405996987923,132.784623225834));
#64041=CARTESIAN_POINT('Ctrl Pts',(33.0926169212409,4.55574265360974,132.657571867419));
#64042=CARTESIAN_POINT('Ctrl Pts',(33.0848690244639,4.60740337082099,132.53057450922));
#64043=CARTESIAN_POINT('Ctrl Pts',(33.0771211276868,4.65377645233411,132.401349666334));
#64044=CARTESIAN_POINT('Ctrl Pts',(33.0693732309097,4.69467522158936,132.270378225337));
#64045=CARTESIAN_POINT('Ctrl Pts',(33.0616269548256,4.73556543570374,132.139434180743));
#64046=CARTESIAN_POINT('Ctrl Pts',(33.0538806787415,4.77098349877912,132.006744637697));
#64047=CARTESIAN_POINT('Ctrl Pts',(33.0461344026575,4.80079213726351,131.872807114724));
#64048=CARTESIAN_POINT('Ctrl Pts',(33.0383880693921,4.83060099578849,131.738868603055));
#64049=CARTESIAN_POINT('Ctrl Pts',(33.0306417361267,4.85480026216309,131.603682474704));
#64050=CARTESIAN_POINT('Ctrl Pts',(33.0228954028614,4.87330355703107,131.467757560224));
#64051=CARTESIAN_POINT('Ctrl Pts',(33.0151473348584,4.89181099558365,131.331802206302));
#64052=CARTESIAN_POINT('Ctrl Pts',(33.0073992668555,4.90461987166122,131.195108124351));
#64053=CARTESIAN_POINT('Ctrl Pts',(32.9996511988525,4.91169560375513,131.058190006236));
#64054=CARTESIAN_POINT('Ctrl Pts',(32.9918948961106,4.91877885602131,130.921126369916));
#64055=CARTESIAN_POINT('Ctrl Pts',(32.9841385933688,4.92011677216353,130.783838612851));
#64056=CARTESIAN_POINT('Ctrl Pts',(32.976382290627,4.91572692269514,130.646842732898));
#64057=CARTESIAN_POINT('Ctrl Pts',(32.9686218481128,4.91133473023189,130.509773734119));
#64058=CARTESIAN_POINT('Ctrl Pts',(32.9608614055987,4.90120870951671,130.372997312571));
#64059=CARTESIAN_POINT('Ctrl Pts',(32.9531009630845,4.88541833715185,130.237024091754));
#64060=CARTESIAN_POINT('Ctrl Pts',(32.9453280628191,4.86960261667947,130.100832594652));
#64061=CARTESIAN_POINT('Ctrl Pts',(32.9375551625536,4.84810443535503,129.965447261201));
#64062=CARTESIAN_POINT('Ctrl Pts',(32.9297822622882,4.82104456434546,129.831369162776));
#64063=CARTESIAN_POINT('Ctrl Pts',(32.9222919265261,4.79496838780672,129.70216514095));
#64064=CARTESIAN_POINT('Ctrl Pts',(32.9148015907641,4.76372793714712,129.57417526089));
#64065=CARTESIAN_POINT('Ctrl Pts',(32.907311255002,4.72747443579848,129.447832504561));
#64066=CARTESIAN_POINT('Ctrl Pts',(32.8995369208829,4.6898463719273,129.316699424226));
#64067=CARTESIAN_POINT('Ctrl Pts',(32.8917625867639,4.6466984192615,129.186925444426));
#64068=CARTESIAN_POINT('Ctrl Pts',(32.8839882526448,4.59814485437666,129.059010520689));
#64069=CARTESIAN_POINT('Ctrl Pts',(32.8762234996977,4.54965112742119,128.931253240663));
#64070=CARTESIAN_POINT('Ctrl Pts',(32.8684587467506,4.49576518092037,128.805350820063));
#64071=CARTESIAN_POINT('Ctrl Pts',(32.8606939938035,4.43665159901168,128.681790088352));
#64072=CARTESIAN_POINT('Ctrl Pts',(32.8529369529185,4.37759672954589,128.558352078901));
#64073=CARTESIAN_POINT('Ctrl Pts',(32.8451799120334,4.3133247249444,128.437251480295));
#64074=CARTESIAN_POINT('Ctrl Pts',(32.8374228711484,4.24404885686923,128.318956754407));
#64075=CARTESIAN_POINT('Ctrl Pts',(32.8296716799083,4.17482523026507,128.200751235492));
#64076=CARTESIAN_POINT('Ctrl Pts',(32.8219204886682,4.10060544778748,128.085347713671));
#64077=CARTESIAN_POINT('Ctrl Pts',(32.814169297428,4.02164929464727,127.973191245493));
#64078=CARTESIAN_POINT('Ctrl Pts',(32.8064214006509,3.94272669997837,127.861082446806));
#64079=CARTESIAN_POINT('Ctrl Pts',(32.7986735038739,3.85907196310345,127.752218275903));
#64080=CARTESIAN_POINT('Ctrl Pts',(32.7909256070968,3.77098876427939,127.647015720001));
#64081=CARTESIAN_POINT('Ctrl Pts',(32.7831793310127,3.68292399056167,127.541835170206));
#64082=CARTESIAN_POINT('Ctrl Pts',(32.7754330549286,3.59043284826041,127.440315011511));
#64083=CARTESIAN_POINT('Ctrl Pts',(32.7676867788445,3.49385971409267,127.342839656956));
#64084=CARTESIAN_POINT('Ctrl Pts',(32.7599404455792,3.397285867044,127.245363582861));
#64085=CARTESIAN_POINT('Ctrl Pts',(32.7521941123137,3.29663024316775,127.151932650223));
#64086=CARTESIAN_POINT('Ctrl Pts',(32.7444477790484,3.19227424586641,127.062894567783));
#64087=CARTESIAN_POINT('Ctrl Pts',(32.7366997110454,3.08789487876302,126.973836545882));
#64088=CARTESIAN_POINT('Ctrl Pts',(32.7289516430425,2.97981378663374,126.889173585438));
#64089=CARTESIAN_POINT('Ctrl Pts',(32.7212035750395,2.86844530217183,126.80921298438));
#64090=CARTESIAN_POINT('Ctrl Pts',(32.7134472722976,2.75695845395933,126.729167400244));
#64091=CARTESIAN_POINT('Ctrl Pts',(32.7056909695557,2.64217755210482,126.653834387369));
#64092=CARTESIAN_POINT('Ctrl Pts',(32.6979346668139,2.52454621750959,126.583478072629));
#64093=CARTESIAN_POINT('Ctrl Pts',(32.6901742242997,2.40685209952911,126.513084206605));
#64094=CARTESIAN_POINT('Ctrl Pts',(32.6824137817855,2.28630486083248,126.44767251782));
#64095=CARTESIAN_POINT('Ctrl Pts',(32.6746533392713,2.16337165723281,126.387460558115));
#64096=CARTESIAN_POINT('Ctrl Pts',(32.6668804390058,2.04024111034122,126.327151940827));
#64097=CARTESIAN_POINT('Ctrl Pts',(32.6591075387404,1.91471730286885,126.272059889934));
#64098=CARTESIAN_POINT('Ctrl Pts',(32.651334638475,1.78728708011941,126.222353638551));
#64099=CARTESIAN_POINT('Ctrl Pts',(32.643844302713,1.66448926694566,126.174454334609));
#64100=CARTESIAN_POINT('Ctrl Pts',(32.6363539669511,1.5399215293189,126.131556154026));
#64101=CARTESIAN_POINT('Ctrl Pts',(32.6288636311891,1.41402988718873,126.093765905575));
#64102=CARTESIAN_POINT('Ctrl Pts',(32.6210892970701,1.28336502518216,126.054542828367));
#64103=CARTESIAN_POINT('Ctrl Pts',(32.613314962951,1.15085997822314,126.020698416971));
#64104=CARTESIAN_POINT('Ctrl Pts',(32.6055406288319,1.01699714233727,125.992406765441));
#64105=CARTESIAN_POINT('Ctrl Pts',(32.5977758758848,0.883299280432971,125.964149980844));
#64106=CARTESIAN_POINT('Ctrl Pts',(32.5900111229377,0.748247337919862,125.941432420093));
#64107=CARTESIAN_POINT('Ctrl Pts',(32.5822463699906,0.612339859958383,125.924378757107));
#64108=CARTESIAN_POINT('Ctrl Pts',(32.5744893291056,0.476567367219976,125.907342032061));
#64109=CARTESIAN_POINT('Ctrl Pts',(32.5667322882206,0.339941415446912,125.895958058216));
#64110=CARTESIAN_POINT('Ctrl Pts',(32.5589752473356,0.202971413425118,125.89030061917));
#64111=CARTESIAN_POINT('Ctrl Pts',(32.5512240560955,0.0661047015473196,
125.884647446444));
#64112=CARTESIAN_POINT('Ctrl Pts',(32.5434728648554,-0.0711051551062505,
125.884712229023));
#64113=CARTESIAN_POINT('Ctrl Pts',(32.5357216736152,-0.208143297603718,
125.890516966191));
#64114=CARTESIAN_POINT('Ctrl Pts',(32.5279737768382,-0.345123195235013,
125.89631923619));
#64115=CARTESIAN_POINT('Ctrl Pts',(32.5202258800611,-0.481931134070877,
125.907856592019));
#64116=CARTESIAN_POINT('Ctrl Pts',(32.512477983284,-0.618052144358261,125.925098930655));
#64117=CARTESIAN_POINT('Ctrl Pts',(32.5047317071999,-0.754144681064723,
125.942337662566));
#64118=CARTESIAN_POINT('Ctrl Pts',(32.4969854311159,-0.889550187411085,
125.965278954526));
#64119=CARTESIAN_POINT('Ctrl Pts',(32.4892391550318,-1.02375910179051,125.993840857291));
#64120=CARTESIAN_POINT('Ctrl Pts',(32.4814928217665,-1.15796900686948,126.022402970892));
#64121=CARTESIAN_POINT('Ctrl Pts',(32.473746488501,-1.29098191995453,126.056585696706));
#64122=CARTESIAN_POINT('Ctrl Pts',(32.4660001552357,-1.42229914597879,126.096256094316));
#64123=CARTESIAN_POINT('Ctrl Pts',(32.4582520872327,-1.55364577958533,126.135935375836));
#64124=CARTESIAN_POINT('Ctrl Pts',(32.4505040192298,-1.68329559630917,126.181104661533));
#64125=CARTESIAN_POINT('Ctrl Pts',(32.4427559512268,-1.81076610075897,126.231581463611));
#64126=CARTESIAN_POINT('Ctrl Pts',(32.434999648485,-1.93837208237799,126.282111913036));
#64127=CARTESIAN_POINT('Ctrl Pts',(32.4272433457431,-2.06379376078352,126.33796100296));
#64128=CARTESIAN_POINT('Ctrl Pts',(32.4194870430013,-2.18656913062253,126.398898269582));
#64129=CARTESIAN_POINT('Ctrl Pts',(32.4117266004871,-2.30941002937312,126.459868060257));
#64130=CARTESIAN_POINT('Ctrl Pts',(32.403966157973,-2.42960146274863,126.52593125069));
#64131=CARTESIAN_POINT('Ctrl Pts',(32.3962057154588,-2.54670788909553,126.596812401548));
#64132=CARTESIAN_POINT('Ctrl Pts',(32.3884328151934,-2.66400230507421,126.667807337122));
#64133=CARTESIAN_POINT('Ctrl Pts',(32.380659914928,-2.77820149180594,126.743635472161));
#64134=CARTESIAN_POINT('Ctrl Pts',(32.3728870146626,-2.88889991690063,126.823978684556));
#64135=CARTESIAN_POINT('Ctrl Pts',(32.3653966789004,-2.99557417541182,126.901401218809));
#64136=CARTESIAN_POINT('Ctrl Pts',(32.3579063431383,-3.09899753460147,126.983016069966));
#64137=CARTESIAN_POINT('Ctrl Pts',(32.3504160073762,-3.19883904854657,127.068505721562));
#64138=CARTESIAN_POINT('Ctrl Pts',(32.3427555834548,-3.30094773179821,127.155936644945));
#64139=CARTESIAN_POINT('Ctrl Pts',(32.3350951595333,-3.39965344572871,127.247714920717));
#64140=CARTESIAN_POINT('Ctrl Pts',(32.3274347356118,-3.49455512505835,127.343541705743));
#64141=CARTESIAN_POINT('Ctrl Pts',(32.3197831159588,-3.58934773211337,127.439258355254));
#64142=CARTESIAN_POINT('Ctrl Pts',(32.3121314963058,-3.68034471478857,127.539013981536));
#64143=CARTESIAN_POINT('Ctrl Pts',(32.3044798766527,-3.76717720600479,127.6424689431));
#64144=CARTESIAN_POINT('Ctrl Pts',(32.2968352796751,-3.85393000214713,127.745828953446));
#64145=CARTESIAN_POINT('Ctrl Pts',(32.2891906826974,-3.93652564899884,127.852881241732));
#64146=CARTESIAN_POINT('Ctrl Pts',(32.2815460857197,-4.0146317797902,127.963249085929));
#64147=CARTESIAN_POINT('Ctrl Pts',(32.2739067365241,-4.09268429311149,128.073541165977));
#64148=CARTESIAN_POINT('Ctrl Pts',(32.2662673873284,-4.16625318802899,128.187143947303));
#64149=CARTESIAN_POINT('Ctrl Pts',(32.2586280381327,-4.23504645809728,128.303647807134));
#64150=CARTESIAN_POINT('Ctrl Pts',(32.2509915588414,-4.30381388432724,128.420107899502));
#64151=CARTESIAN_POINT('Ctrl Pts',(32.2433550795501,-4.36780904705292,128.539466557496));
#64152=CARTESIAN_POINT('Ctrl Pts',(32.2357186002588,-4.42678361026189,128.661285740102));
#64153=CARTESIAN_POINT('Ctrl Pts',(32.2280837877793,-4.48574530111247,128.783078333275));
#64154=CARTESIAN_POINT('Ctrl Pts',(32.2204489752998,-4.53968840018407,128.907330018292));
#64155=CARTESIAN_POINT('Ctrl Pts',(32.2128141628203,-4.58841114259887,129.033579363719));
#64156=CARTESIAN_POINT('Ctrl Pts',(32.2051776741029,-4.63714458218635,129.159856427436));
#64157=CARTESIAN_POINT('Ctrl Pts',(32.1975411853855,-4.68065523172521,129.288131650922));
#64158=CARTESIAN_POINT('Ctrl Pts',(32.1899046966682,-4.7187900697642,129.417925137641));
#64159=CARTESIAN_POINT('Ctrl Pts',(32.1866923469053,-4.73483179292596,129.472523800943));
#64160=CARTESIAN_POINT('Ctrl Pts',(32.1834799971424,-4.74992285459696,129.527390938275));
#64161=CARTESIAN_POINT('Ctrl Pts',(32.1802676473795,-4.76405452823406,129.582490119308));
#64162=CARTESIAN_POINT('Origin',(213.235140564004,0.,130.804360617566));
#64163=CARTESIAN_POINT('',(30.0845737196929,-4.764054528234,129.582490119308));
#64164=CARTESIAN_POINT('',(30.4301958372212,-4.76405452823406,129.582490119308));
#64165=CARTESIAN_POINT('',(213.235140564004,-4.76405452823405,129.582490119308));
#64166=CARTESIAN_POINT('',(31.7648594359428,-4.91824826067858,130.800224335163));
#64167=CARTESIAN_POINT('Ctrl Pts',(31.7648594359429,-4.91824826067858,130.800224335163));
#64168=CARTESIAN_POINT('Ctrl Pts',(31.757212549846,-4.91836154469456,130.934924740103));
#64169=CARTESIAN_POINT('Ctrl Pts',(31.7495656637491,-4.91293693387984,131.069821508205));
#64170=CARTESIAN_POINT('Ctrl Pts',(31.7419187776522,-4.90195272443736,131.204413801382));
#64171=CARTESIAN_POINT('Ctrl Pts',(31.7342789780509,-4.89097869424312,131.338881365658));
#64172=CARTESIAN_POINT('Ctrl Pts',(31.7266391784498,-4.87445534555453,131.473044616405));
#64173=CARTESIAN_POINT('Ctrl Pts',(31.7189993788485,-4.85241302391724,131.606402329585));
#64174=CARTESIAN_POINT('Ctrl Pts',(31.7113186602338,-4.83025264289347,131.740474310984));
#64175=CARTESIAN_POINT('Ctrl Pts',(31.7036379416192,-4.8025139878959,131.873731687635));
#64176=CARTESIAN_POINT('Ctrl Pts',(31.6959572230045,-4.76928087100165,132.005669502074));
#64177=CARTESIAN_POINT('Ctrl Pts',(31.6883248466186,-4.73625692241787,132.13677690359));
#64178=CARTESIAN_POINT('Ctrl Pts',(31.6806924702326,-4.69780758699693,132.26658091181));
#64179=CARTESIAN_POINT('Ctrl Pts',(31.6730600938466,-4.65406632644129,132.394596352162));
#64180=CARTESIAN_POINT('Ctrl Pts',(31.6654284959104,-4.61032952719301,132.522598735821));
#64181=CARTESIAN_POINT('Ctrl Pts',(31.6577968979742,-4.56130200649142,132.648812532375));
#64182=CARTESIAN_POINT('Ctrl Pts',(31.6501653000381,-4.50716674333285,132.772768860359));
#64183=CARTESIAN_POINT('Ctrl Pts',(31.6425327135101,-4.45302446753059,132.896741245558));
#64184=CARTESIAN_POINT('Ctrl Pts',(31.6349001269821,-4.39377329563917,133.018455210967));
#64185=CARTESIAN_POINT('Ctrl Pts',(31.6272675404542,-4.3296436464861,133.137463477909));
#64186=CARTESIAN_POINT('Ctrl Pts',(31.6195504230911,-4.26480376197823,133.257789760462));
#64187=CARTESIAN_POINT('Ctrl Pts',(31.611833305728,-4.19497688306446,133.375349675669));
#64188=CARTESIAN_POINT('Ctrl Pts',(31.6041161883649,-4.12044738007431,133.489709095983));
#64189=CARTESIAN_POINT('Ctrl Pts',(31.5964724350254,-4.04662640385107,133.602981339984));
#64190=CARTESIAN_POINT('Ctrl Pts',(31.5888286816858,-3.96819211872463,133.713113386612));
#64191=CARTESIAN_POINT('Ctrl Pts',(31.5811849283463,-3.88546220587877,133.819715739138));
#64192=CARTESIAN_POINT('Ctrl Pts',(31.5734311289714,-3.80154124218248,133.92785283065));
#64193=CARTESIAN_POINT('Ctrl Pts',(31.5656773295965,-3.71320029065335,134.032357481853));
#64194=CARTESIAN_POINT('Ctrl Pts',(31.5579235302216,-3.62080982167619,134.132861676264));
#64195=CARTESIAN_POINT('Ctrl Pts',(31.5501697308467,-3.52841935269891,134.233365870675));
#64196=CARTESIAN_POINT('Ctrl Pts',(31.5424159314718,-3.43197971543658,134.329869355433));
#64197=CARTESIAN_POINT('Ctrl Pts',(31.5346621320969,-3.33189555451496,134.422047043488));
#64198=CARTESIAN_POINT('Ctrl Pts',(31.5268877979779,-3.23154633609829,134.514468849963));
#64199=CARTESIAN_POINT('Ctrl Pts',(31.5191134638588,-3.12718979311009,134.602858575542));
#64200=CARTESIAN_POINT('Ctrl Pts',(31.5113391297397,-3.01918359074611,134.686848673938));
#64201=CARTESIAN_POINT('Ctrl Pts',(31.5035743767926,-2.91131049637376,134.770735262044));
#64202=CARTESIAN_POINT('Ctrl Pts',(31.4958096238455,-2.79979699773103,134.850232773725));
#64203=CARTESIAN_POINT('Ctrl Pts',(31.4880448708984,-2.6850368976392,134.925011042052));
#64204=CARTESIAN_POINT('Ctrl Pts',(31.4802878300134,-2.57039077889661,134.999715039548));
#64205=CARTESIAN_POINT('Ctrl Pts',(31.4725307891284,-2.45250480118755,135.069708909408));
#64206=CARTESIAN_POINT('Ctrl Pts',(31.4647737482434,-2.33180479482437,135.134703497909));
#64207=CARTESIAN_POINT('Ctrl Pts',(31.4570225570033,-2.21119580927489,135.199649073484));
#64208=CARTESIAN_POINT('Ctrl Pts',(31.4492713657632,-2.08777736178262,135.259602687039));
#64209=CARTESIAN_POINT('Ctrl Pts',(31.441520174523,-1.9620028329244,135.314319369716));
#64210=CARTESIAN_POINT('Ctrl Pts',(31.433772277746,-1.83628176159591,135.369012796344));
#64211=CARTESIAN_POINT('Ctrl Pts',(31.4260243809689,-1.70820695836303,135.418473563473));
#64212=CARTESIAN_POINT('Ctrl Pts',(31.4182764841918,-1.57825469159732,135.462503508349));
#64213=CARTESIAN_POINT('Ctrl Pts',(31.4105302081077,-1.44832960804454,135.50652424311));
#64214=CARTESIAN_POINT('Ctrl Pts',(31.4027839320236,-1.31652821216427,135.545116289826));
#64215=CARTESIAN_POINT('Ctrl Pts',(31.3950376559395,-1.18334458502106,135.578130475404));
#64216=CARTESIAN_POINT('Ctrl Pts',(31.3872913226741,-1.05015997474638,135.611144904685));
#64217=CARTESIAN_POINT('Ctrl Pts',(31.3795449894088,-0.915593492328854,
135.6385812966));
#64218=CARTESIAN_POINT('Ctrl Pts',(31.3717986561434,-0.780151748923722,
135.660341086138));
#64219=CARTESIAN_POINT('Ctrl Pts',(31.3640505881404,-0.644679674279241,
135.682105748629));
#64220=CARTESIAN_POINT('Ctrl Pts',(31.3563025201375,-0.508332334554018,
135.698191217127));
#64221=CARTESIAN_POINT('Ctrl Pts',(31.3485544521345,-0.371623443534293,
135.708550568895));
#64222=CARTESIAN_POINT('Ctrl Pts',(31.3407981493926,-0.234769256678522,
135.718920930705));
#64223=CARTESIAN_POINT('Ctrl Pts',(31.3330418466508,-0.0975531413946325,
135.723552989186));
#64224=CARTESIAN_POINT('Ctrl Pts',(31.3252855439089,0.0395086314126486,
135.722451927266));
#64225=CARTESIAN_POINT('Ctrl Pts',(31.3175251013948,0.176643558214927,135.721350277675));
#64226=CARTESIAN_POINT('Ctrl Pts',(31.3097646588806,0.313623588109476,135.714509429987));
#64227=CARTESIAN_POINT('Ctrl Pts',(31.3020042163665,0.449936577395924,135.70198658724));
#64228=CARTESIAN_POINT('Ctrl Pts',(31.294231316101,0.586468388394074,135.689443641713));
#64229=CARTESIAN_POINT('Ctrl Pts',(31.2864584158357,0.722330631288314,135.671200526038));
#64230=CARTESIAN_POINT('Ctrl Pts',(31.2786855155702,0.85701948082588,135.647365952271));
#64231=CARTESIAN_POINT('Ctrl Pts',(31.2711951798082,0.98681205142256,135.624397825296));
#64232=CARTESIAN_POINT('Ctrl Pts',(31.2637048440461,1.11551475823591,135.596237775329));
#64233=CARTESIAN_POINT('Ctrl Pts',(31.256214508284,1.24269111504239,135.56302659188));
#64234=CARTESIAN_POINT('Ctrl Pts',(31.2484401741649,1.37468940207106,135.528556196316));
#64235=CARTESIAN_POINT('Ctrl Pts',(31.2406658400458,1.50546144206318,135.488534886884));
#64236=CARTESIAN_POINT('Ctrl Pts',(31.2328915059268,1.63450468114292,135.443064909696));
#64237=CARTESIAN_POINT('Ctrl Pts',(31.2251267529797,1.76338888596324,135.397650970191));
#64238=CARTESIAN_POINT('Ctrl Pts',(31.2173620000326,1.89054816391202,135.346801852455));
#64239=CARTESIAN_POINT('Ctrl Pts',(31.2095972470856,2.01549187615683,135.290670410664));
#64240=CARTESIAN_POINT('Ctrl Pts',(31.2018402062006,2.14031149254523,135.234594719412));
#64241=CARTESIAN_POINT('Ctrl Pts',(31.1940831653156,2.26291956806447,135.173247304016));
#64242=CARTESIAN_POINT('Ctrl Pts',(31.1863261244306,2.38284265781293,135.106830132927));
#64243=CARTESIAN_POINT('Ctrl Pts',(31.1785749331905,2.50267531262654,135.040463047542));
#64244=CARTESIAN_POINT('Ctrl Pts',(31.1708237419504,2.61982667121735,134.96903400485));
#64245=CARTESIAN_POINT('Ctrl Pts',(31.1630725507103,2.73384557107229,134.892792035118));
#64246=CARTESIAN_POINT('Ctrl Pts',(31.1553246539332,2.84781600985339,134.816582470257));
#64247=CARTESIAN_POINT('Ctrl Pts',(31.1475767571561,2.95865631358876,134.73556426381));
#64248=CARTESIAN_POINT('Ctrl Pts',(31.139828860379,3.06594232765335,134.650031002038));
#64249=CARTESIAN_POINT('Ctrl Pts',(31.1320825842949,3.17320589979662,134.56451563198));
#64250=CARTESIAN_POINT('Ctrl Pts',(31.1243363082109,3.27691635558389,134.474487328729));
#64251=CARTESIAN_POINT('Ctrl Pts',(31.1165900321268,3.37668112858294,134.380281144979));
#64252=CARTESIAN_POINT('Ctrl Pts',(31.1088436988615,3.47644663802261,134.28607426582));
#64253=CARTESIAN_POINT('Ctrl Pts',(31.1010973655961,3.57226612229523,134.187689713043));
#64254=CARTESIAN_POINT('Ctrl Pts',(31.0933510323308,3.6637828201612,134.085500436164));
#64255=CARTESIAN_POINT('Ctrl Pts',(31.0856029643278,3.75532001255724,133.983288274706));
#64256=CARTESIAN_POINT('Ctrl Pts',(31.0778548963249,3.8425522403587,133.87726998487));
#64257=CARTESIAN_POINT('Ctrl Pts',(31.0701068283219,3.92516235128952,133.767852405731));
#64258=CARTESIAN_POINT('Ctrl Pts',(31.0623505255801,4.00786026122942,133.658318536286));
#64259=CARTESIAN_POINT('Ctrl Pts',(31.0545942228383,4.08592600521726,133.545378473088));
#64260=CARTESIAN_POINT('Ctrl Pts',(31.0468379200964,4.15908488676225,133.429469370971));
#64261=CARTESIAN_POINT('Ctrl Pts',(31.0390774775823,4.2322828154051,133.313498404677));
#64262=CARTESIAN_POINT('Ctrl Pts',(31.031317035068,4.30056846858348,133.194555580778));
#64263=CARTESIAN_POINT('Ctrl Pts',(31.0235565925539,4.36371314665402,133.073102699914));
#64264=CARTESIAN_POINT('Ctrl Pts',(31.0157836922884,4.42695919016753,132.951454852104));
#64265=CARTESIAN_POINT('Ctrl Pts',(31.0080107920231,4.48504760118261,132.827289249704));
#64266=CARTESIAN_POINT('Ctrl Pts',(31.0002378917576,4.53779751237551,132.701088536688));
#64267=CARTESIAN_POINT('Ctrl Pts',(30.9927475559955,4.5886298314284,132.57947553747));
#64268=CARTESIAN_POINT('Ctrl Pts',(30.9852572202334,4.63450494062869,132.455973110321));
#64269=CARTESIAN_POINT('Ctrl Pts',(30.9777668844712,4.67530535871284,132.331024583634));
#64270=CARTESIAN_POINT('Ctrl Pts',(30.9699925503521,4.717652737049,132.201338595582));
#64271=CARTESIAN_POINT('Ctrl Pts',(30.962218216233,4.7546671578616,132.069683879357));
#64272=CARTESIAN_POINT('Ctrl Pts',(30.9544438821139,4.78616300105551,131.936538514289));
#64273=CARTESIAN_POINT('Ctrl Pts',(30.9466791291668,4.81762002843762,131.803557238983));
#64274=CARTESIAN_POINT('Ctrl Pts',(30.9389143762197,4.84357192133382,131.669089346911));
#64275=CARTESIAN_POINT('Ctrl Pts',(30.9311496232725,4.86388207801844,131.533630247834));
#64276=CARTESIAN_POINT('Ctrl Pts',(30.9233925823875,4.88417206236906,131.398305688644));
#64277=CARTESIAN_POINT('Ctrl Pts',(30.9156355415026,4.89883140403384,131.261992265753));
#64278=CARTESIAN_POINT('Ctrl Pts',(30.9078785006176,4.90777411625741,131.125197470645));
#64279=CARTESIAN_POINT('Ctrl Pts',(30.9001273093775,4.91671008471207,130.988505833557));
#64280=CARTESIAN_POINT('Ctrl Pts',(30.8923761181374,4.91993797901853,130.85133393535));
#64281=CARTESIAN_POINT('Ctrl Pts',(30.8846249268973,4.91742345103647,130.714195958766));
#64282=CARTESIAN_POINT('Ctrl Pts',(30.8768770301202,4.91490999179586,130.577116269479));
#64283=CARTESIAN_POINT('Ctrl Pts',(30.8691291333431,4.90665897175083,130.440070863221));
#64284=CARTESIAN_POINT('Ctrl Pts',(30.861381236566,4.89268812740213,130.303575283837));
#64285=CARTESIAN_POINT('Ctrl Pts',(30.8536349604819,4.87872020545289,130.167108256385));
#64286=CARTESIAN_POINT('Ctrl Pts',(30.8458886843978,4.85903487881592,130.031191215728));
#64287=CARTESIAN_POINT('Ctrl Pts',(30.8381424083137,4.83370184506461,129.896335543287));
#64288=CARTESIAN_POINT('Ctrl Pts',(30.8303960750483,4.80836862431053,129.761478875372));
#64289=CARTESIAN_POINT('Ctrl Pts',(30.822649741783,4.77738768543392,129.627683975552));
#64290=CARTESIAN_POINT('Ctrl Pts',(30.8149034085176,4.74087996326124,129.495452585484));
#64291=CARTESIAN_POINT('Ctrl Pts',(30.8071553405146,4.70436406543749,129.363191583114));
#64292=CARTESIAN_POINT('Ctrl Pts',(30.7994072725117,4.66231902549706,129.232495164023));
#64293=CARTESIAN_POINT('Ctrl Pts',(30.7916592045087,4.614915700122,129.103850063859));
#64294=CARTESIAN_POINT('Ctrl Pts',(30.7839029017669,4.5674619939285,128.975068238152));
#64295=CARTESIAN_POINT('Ctrl Pts',(30.7761465990249,4.51463876161879,128.848342453926));
#64296=CARTESIAN_POINT('Ctrl Pts',(30.7683902962831,4.45666531377142,128.724140113983));
#64297=CARTESIAN_POINT('Ctrl Pts',(30.7606298537689,4.3986609237493,128.599871483512));
#64298=CARTESIAN_POINT('Ctrl Pts',(30.7528694112547,4.3355010208798,128.478129327885));
#64299=CARTESIAN_POINT('Ctrl Pts',(30.7451089687405,4.26745051337621,128.359355673116));
#64300=CARTESIAN_POINT('Ctrl Pts',(30.7373360684751,4.19929076515675,128.240391352332));
#64301=CARTESIAN_POINT('Ctrl Pts',(30.7295631682096,4.12622493234602,128.124405385984));
#64302=CARTESIAN_POINT('Ctrl Pts',(30.7217902679442,4.04856131378395,128.011810823734));
#64303=CARTESIAN_POINT('Ctrl Pts',(30.7142999321822,3.9737209633802,127.903309357431));
#64304=CARTESIAN_POINT('Ctrl Pts',(30.7068095964203,3.8946114907362,127.797957250225));
#64305=CARTESIAN_POINT('Ctrl Pts',(30.6993192606583,3.81154237909028,127.696092972253));
#64306=CARTESIAN_POINT('Ctrl Pts',(30.6915449265392,3.72532367682728,127.590366479221));
#64307=CARTESIAN_POINT('Ctrl Pts',(30.6837705924202,3.63456603398841,127.488062608723));
#64308=CARTESIAN_POINT('Ctrl Pts',(30.6759962583011,3.53957134005861,127.38959594176));
#64309=CARTESIAN_POINT('Ctrl Pts',(30.668231505354,3.44469371859928,127.291250626163));
#64310=CARTESIAN_POINT('Ctrl Pts',(30.6604667524068,3.34558970469151,127.196733383448));
#64311=CARTESIAN_POINT('Ctrl Pts',(30.6527019994597,3.24260226402893,127.106426921593));
#64312=CARTESIAN_POINT('Ctrl Pts',(30.6449449585747,3.13971711194414,127.016210153388));
#64313=CARTESIAN_POINT('Ctrl Pts',(30.6371879176898,3.03295650091295,126.930196099358));
#64314=CARTESIAN_POINT('Ctrl Pts',(30.6294308768048,2.92270091995374,126.848731414139));
#64315=CARTESIAN_POINT('Ctrl Pts',(30.6216796855647,2.8125284835864,126.767328162074));
#64316=CARTESIAN_POINT('Ctrl Pts',(30.6139284943246,2.69886663643271,126.690467681584));
#64317=CARTESIAN_POINT('Ctrl Pts',(30.6061773030845,2.58212940898807,126.618456799065));
#64318=CARTESIAN_POINT('Ctrl Pts',(30.5984294063074,2.46544179797868,126.546476523092));
#64319=CARTESIAN_POINT('Ctrl Pts',(30.5906815095303,2.34568173849001,126.479341950335));
#64320=CARTESIAN_POINT('Ctrl Pts',(30.5829336127532,2.22329255917093,126.417316822613));
#64321=CARTESIAN_POINT('Ctrl Pts',(30.5751873366691,2.1009289810296,126.355304669211));
#64322=CARTESIAN_POINT('Ctrl Pts',(30.5674410605851,1.97593772546609,126.298400011594));
#64323=CARTESIAN_POINT('Ctrl Pts',(30.5596947845009,1.84878670539437,126.246820625371));
#64324=CARTESIAN_POINT('Ctrl Pts',(30.5519484512356,1.72163474672271,126.1952408584));
#64325=CARTESIAN_POINT('Ctrl Pts',(30.5442021179702,1.59232335402133,126.148986588228));
#64326=CARTESIAN_POINT('Ctrl Pts',(30.5364557847048,1.46134002498524,126.108227272581));
#64327=CARTESIAN_POINT('Ctrl Pts',(30.5287077167018,1.33032736314044,126.067458829169));
#64328=CARTESIAN_POINT('Ctrl Pts',(30.5209596486988,1.19764239314845,126.032187905091));
#64329=CARTESIAN_POINT('Ctrl Pts',(30.5132115806958,1.06378697170545,126.002533846291));
#64330=CARTESIAN_POINT('Ctrl Pts',(30.505455277954,0.9297892871282,125.972848270805));
#64331=CARTESIAN_POINT('Ctrl Pts',(30.4976989752121,0.794619048455475,125.948791570355));
#64332=CARTESIAN_POINT('Ctrl Pts',(30.4899426724703,0.658788037627371,125.930431875373));
#64333=CARTESIAN_POINT('Ctrl Pts',(30.4821822299561,0.522884529698626,125.912062381268));
#64334=CARTESIAN_POINT('Ctrl Pts',(30.4744217874419,0.386319935985556,125.8993959875));
#64335=CARTESIAN_POINT('Ctrl Pts',(30.4666613449278,0.249609334851573,125.892448745143));
#64336=CARTESIAN_POINT('Ctrl Pts',(30.4588884446623,0.112679273724425,125.885490350455));
#64337=CARTESIAN_POINT('Ctrl Pts',(30.4511155443969,-0.0243968720229893,
125.884269457005));
#64338=CARTESIAN_POINT('Ctrl Pts',(30.4433426441315,-0.161104948959712,
125.888749947678));
#64339=CARTESIAN_POINT('Ctrl Pts',(30.4358523083695,-0.292843342953098,
125.893067561229));
#64340=CARTESIAN_POINT('Ctrl Pts',(30.4283619726074,-0.424239656794046,
125.902679213748));
#64341=CARTESIAN_POINT('Ctrl Pts',(30.4208716368454,-0.554841842719261,
125.917507479598));
#64342=CARTESIAN_POINT('Ctrl Pts',(30.4130973027263,-0.690395850219506,
125.932897963655));
#64343=CARTESIAN_POINT('Ctrl Pts',(30.4053229686072,-0.825523716698272,
125.953957198051));
#64344=CARTESIAN_POINT('Ctrl Pts',(30.3975486344881,-0.959713464779091,
125.980655285767));
#64345=CARTESIAN_POINT('Ctrl Pts',(30.389783881541,-1.09373783598828,126.007320470477));
#64346=CARTESIAN_POINT('Ctrl Pts',(30.3820191285939,-1.22682600941911,126.03961060575));
#64347=CARTESIAN_POINT('Ctrl Pts',(30.3742543756468,-1.35847062067631,126.077444007845));
#64348=CARTESIAN_POINT('Ctrl Pts',(30.3664973347618,-1.48998448064956,126.115239833271));
#64349=CARTESIAN_POINT('Ctrl Pts',(30.3587402938768,-1.62005725838474,126.158567861736));
#64350=CARTESIAN_POINT('Ctrl Pts',(30.3509832529918,-1.74819163990967,126.207295352351));
#64351=CARTESIAN_POINT('Ctrl Pts',(30.3432320617517,-1.87622939430109,126.255986097186));
#64352=CARTESIAN_POINT('Ctrl Pts',(30.3354808705116,-2.00233129807149,126.310068061141));
#64353=CARTESIAN_POINT('Ctrl Pts',(30.3277296792714,-2.12601541588856,126.369358755796));
#64354=CARTESIAN_POINT('Ctrl Pts',(30.3199817824944,-2.24964696465584,126.428624250324));
#64355=CARTESIAN_POINT('Ctrl Pts',(30.3122338857172,-2.37086241952226,126.493093903724));
#64356=CARTESIAN_POINT('Ctrl Pts',(30.3044859889402,-2.48920025706133,126.562537289945));
#64357=CARTESIAN_POINT('Ctrl Pts',(30.2967397128561,-2.60751334087601,126.631966150107));
#64358=CARTESIAN_POINT('Ctrl Pts',(30.288993436772,-2.72294966766552,126.706366475934));
#64359=CARTESIAN_POINT('Ctrl Pts',(30.2812471606879,-2.83507309828441,126.785462312074));
#64360=CARTESIAN_POINT('Ctrl Pts',(30.2735008274225,-2.94719735657299,126.864558732082));
#64361=CARTESIAN_POINT('Ctrl Pts',(30.2657544941571,-3.05600835041942,126.948350506199));
#64362=CARTESIAN_POINT('Ctrl Pts',(30.2580081608918,-3.16110000582624,127.036519084849));
#64363=CARTESIAN_POINT('Ctrl Pts',(30.2502600928888,-3.26621519578077,127.124707408241));
#64364=CARTESIAN_POINT('Ctrl Pts',(30.2425120248858,-3.36760909042246,127.217274235325));
#64365=CARTESIAN_POINT('Ctrl Pts',(30.2347639568828,-3.46491001482774,127.313861849246));
#64366=CARTESIAN_POINT('Ctrl Pts',(30.227007654141,-3.56231435181325,127.410552117631));
#64367=CARTESIAN_POINT('Ctrl Pts',(30.2192513513991,-3.65561675094221,127.511271433436));
#64368=CARTESIAN_POINT('Ctrl Pts',(30.2114950486572,-3.74448326151398,127.615626046182));
#64369=CARTESIAN_POINT('Ctrl Pts',(30.203734606143,-3.83339720281852,127.720036356127));
#64370=CARTESIAN_POINT('Ctrl Pts',(30.1959741636288,-3.91787029730434,127.828085521302));
#64371=CARTESIAN_POINT('Ctrl Pts',(30.1882137211146,-3.99761062831091,127.939348867692));
#64372=CARTESIAN_POINT('Ctrl Pts',(30.1804408208492,-4.07747896557551,128.050790823882));
#64373=CARTESIAN_POINT('Ctrl Pts',(30.1726679205837,-4.15259914285998,128.165456944766));
#64374=CARTESIAN_POINT('Ctrl Pts',(30.1648950203183,-4.22272363402761,128.282895136318));
#64375=CARTESIAN_POINT('Ctrl Pts',(30.1574046845564,-4.29029892330751,128.396064153797));
#64376=CARTESIAN_POINT('Ctrl Pts',(30.1499143487945,-4.35323528499088,128.51180692693));
#64377=CARTESIAN_POINT('Ctrl Pts',(30.1424240130325,-4.41135351660019,128.629701284687));
#64378=CARTESIAN_POINT('Ctrl Pts',(30.1340770920882,-4.47611807457019,128.761077889855));
#64379=CARTESIAN_POINT('Ctrl Pts',(30.1257301711438,-4.53508181396193,128.895495486326));
#64380=CARTESIAN_POINT('Ctrl Pts',(30.1173832501995,-4.58797003398941,129.03243679592));
#64381=CARTESIAN_POINT('Ctrl Pts',(30.1090570204088,-4.64072714959,129.169038642173));
#64382=CARTESIAN_POINT('Ctrl Pts',(30.100730790618,-4.68743866908584,129.308151446056));
#64383=CARTESIAN_POINT('Ctrl Pts',(30.0924045608273,-4.72787693153724,129.449235980222));
#64384=CARTESIAN_POINT('Ctrl Pts',(30.0897942804491,-4.74055436245833,129.493466106035));
#64385=CARTESIAN_POINT('Ctrl Pts',(30.087184000071,-4.75261558259996,129.537889843891));
#64386=CARTESIAN_POINT('Ctrl Pts',(30.0845737196928,-4.764054528234,129.582490119308));
#64387=CARTESIAN_POINT('Ctrl Pts',(31.8348922615591,-4.76405452823408,129.582490119308));
#64388=CARTESIAN_POINT('Ctrl Pts',(31.8276314263427,-4.79579485422486,129.70624516862));
#64389=CARTESIAN_POINT('Ctrl Pts',(31.8203705911263,-4.82267033838414,129.83108358097));
#64390=CARTESIAN_POINT('Ctrl Pts',(31.8131097559098,-4.84463298162091,129.95659040348));
#64391=CARTESIAN_POINT('Ctrl Pts',(31.8010364482278,-4.88115243722137,130.165282990379));
#64392=CARTESIAN_POINT('Ctrl Pts',(31.7889631405457,-4.90419455431079,130.376398608338));
#64393=CARTESIAN_POINT('Ctrl Pts',(31.7768898328637,-4.91351263397855,130.588544357212));
#64394=CARTESIAN_POINT('Ctrl Pts',(31.7728797005729,-4.91660762113103,130.659008271519));
#64395=CARTESIAN_POINT('Ctrl Pts',(31.7688695682821,-4.91818885296885,130.729585588476));
#64396=CARTESIAN_POINT('Ctrl Pts',(31.7648594359912,-4.91824826067786,130.800224334311));
#64397=CARTESIAN_POINT('',(32.1101405640431,-4.91824869043815,130.80794969871));
#64398=CARTESIAN_POINT('Ctrl Pts',(32.1802676473795,-4.76405452823406,129.582490119308));
#64399=CARTESIAN_POINT('Ctrl Pts',(32.1726250379345,-4.79767566864033,129.71357843548));
#64400=CARTESIAN_POINT('Ctrl Pts',(32.1649824284896,-4.82586285442501,129.845980649058));
#64401=CARTESIAN_POINT('Ctrl Pts',(32.1573398190446,-4.84853511858555,129.979199865747));
#64402=CARTESIAN_POINT('Ctrl Pts',(32.1494732765444,-4.87187169372778,130.116322485643));
#64403=CARTESIAN_POINT('Ctrl Pts',(32.1416067340441,-4.88936513831279,130.254310262019));
#64404=CARTESIAN_POINT('Ctrl Pts',(32.1337401915439,-4.90098462731627,130.392617074436));
#64405=CARTESIAN_POINT('Ctrl Pts',(32.1258736490436,-4.91260411631975,130.530923886852));
#64406=CARTESIAN_POINT('Ctrl Pts',(32.1180071065434,-4.91834968784368,130.669549273215));
#64407=CARTESIAN_POINT('Ctrl Pts',(32.1101405640432,-4.91824869043815,130.80794969871));
#64408=CARTESIAN_POINT('Ctrl Pts',(32.1101405640087,-4.9182486904377,130.807949699317));
#64409=CARTESIAN_POINT('Ctrl Pts',(32.0974165038603,-4.91808532803547,131.031811114739));
#64410=CARTESIAN_POINT('Ctrl Pts',(32.0846924437118,-4.90263711850592,131.255124154281));
#64411=CARTESIAN_POINT('Ctrl Pts',(32.0719683835633,-4.87213117064359,131.476313680319));
#64412=CARTESIAN_POINT('Ctrl Pts',(32.0641940494444,-4.85349219624961,131.611459322429));
#64413=CARTESIAN_POINT('Ctrl Pts',(32.0564197153255,-4.8291963301871,131.746042911859));
#64414=CARTESIAN_POINT('Ctrl Pts',(32.0486453812066,-4.79928574690886,131.879553336113));
#64415=CARTESIAN_POINT('Ctrl Pts',(32.0408806282597,-4.76941202575137,132.012899220702));
#64416=CARTESIAN_POINT('Ctrl Pts',(32.0331158753128,-4.73393744004321,132.145174193811));
#64417=CARTESIAN_POINT('Ctrl Pts',(32.0253511223659,-4.69295582534925,132.275872997337));
#64418=CARTESIAN_POINT('Ctrl Pts',(32.0175940814811,-4.65201491417275,132.40644198897));
#64419=CARTESIAN_POINT('Ctrl Pts',(32.0098370405962,-4.60557797509594,132.535437555741));
#64420=CARTESIAN_POINT('Ctrl Pts',(32.0020799997114,-4.55378964494523,132.662365712309));
#64421=CARTESIAN_POINT('Ctrl Pts',(31.9943288084715,-4.50204036877727,132.789198151366));
#64422=CARTESIAN_POINT('Ctrl Pts',(31.9865776172316,-4.44494788110479,132.913965922886));
#64423=CARTESIAN_POINT('Ctrl Pts',(31.9788264259917,-4.38270618291501,133.036191609541));
#64424=CARTESIAN_POINT('Ctrl Pts',(31.9710785292148,-4.32049093910715,133.158365347018));
#64425=CARTESIAN_POINT('Ctrl Pts',(31.9633306324379,-4.25313101468764,133.277998800907));
#64426=CARTESIAN_POINT('Ctrl Pts',(31.955582735661,-4.18086784464108,133.394636110278));
#64427=CARTESIAN_POINT('Ctrl Pts',(31.9478364595771,-4.10861979049199,133.511249021638));
#64428=CARTESIAN_POINT('Ctrl Pts',(31.9400901834931,-4.03147073657413,133.62486670294));
#64429=CARTESIAN_POINT('Ctrl Pts',(31.9323439074092,-3.94970702490744,133.735059762804));
#64430=CARTESIAN_POINT('Ctrl Pts',(31.924597574144,-3.8679427096796,133.845253636087));
#64431=CARTESIAN_POINT('Ctrl Pts',(31.9168512408789,-3.78156390169932,133.952022523515));
#64432=CARTESIAN_POINT('Ctrl Pts',(31.9091049076137,-3.69089880346489,134.05496811234));
#64433=CARTESIAN_POINT('Ctrl Pts',(31.901356839611,-3.60021340141046,134.157936755116));
#64434=CARTESIAN_POINT('Ctrl Pts',(31.8936087716082,-3.50524005739219,134.257080102205));
#64435=CARTESIAN_POINT('Ctrl Pts',(31.8858607036055,-3.40634530442495,134.352035169934));
#64436=CARTESIAN_POINT('Ctrl Pts',(31.8781044008638,-3.30734544493726,134.44709115704));
#64437=CARTESIAN_POINT('Ctrl Pts',(31.8703480981221,-3.20441613349485,134.537949701517));
#64438=CARTESIAN_POINT('Ctrl Pts',(31.8625917953804,-3.09795902108185,134.624286397761));
#64439=CARTESIAN_POINT('Ctrl Pts',(31.8548313528664,-2.99144508930259,134.710669174499));
#64440=CARTESIAN_POINT('Ctrl Pts',(31.8470709103525,-2.88139991827175,134.792525060781));
#64441=CARTESIAN_POINT('Ctrl Pts',(31.8393104678385,-2.76825506490569,134.869572415016));
#64442=CARTESIAN_POINT('Ctrl Pts',(31.8315375675733,-2.65492858137648,134.946743452504));
#64443=CARTESIAN_POINT('Ctrl Pts',(31.823764667308,-2.53849280438096,135.019090326302));
#64444=CARTESIAN_POINT('Ctrl Pts',(31.8159917670428,-2.41940563769781,135.086376430565));
#64445=CARTESIAN_POINT('Ctrl Pts',(31.8085014312786,-2.30464758945076,135.151216515475));
#64446=CARTESIAN_POINT('Ctrl Pts',(31.8010110955145,-2.187427848196,135.211357245643));
#64447=CARTESIAN_POINT('Ctrl Pts',(31.7935207597504,-2.06817276375785,135.266629601138));
#64448=CARTESIAN_POINT('Ctrl Pts',(31.7857464256313,-1.94439608658098,135.323997624775));
#64449=CARTESIAN_POINT('Ctrl Pts',(31.7779720915122,-1.81803459211856,135.376302542037));
#64450=CARTESIAN_POINT('Ctrl Pts',(31.770197757393,-1.6895410901089,135.423303566698));
#64451=CARTESIAN_POINT('Ctrl Pts',(31.7624330044459,-1.5612059448565,135.470246666796));
#64452=CARTESIAN_POINT('Ctrl Pts',(31.7546682514988,-1.43074438366379,135.511898747109));
#64453=CARTESIAN_POINT('Ctrl Pts',(31.7469034985517,-1.29863221489678,135.54806564981));
#64454=CARTESIAN_POINT('Ctrl Pts',(31.7391464576666,-1.16665126179825,135.584196631032));
#64455=CARTESIAN_POINT('Ctrl Pts',(31.7313894167816,-1.03302333826876,135.614853173756));
#64456=CARTESIAN_POINT('Ctrl Pts',(31.7236323758966,-0.898242227905167,
135.639889953896));
#64457=CARTESIAN_POINT('Ctrl Pts',(31.7158811846564,-0.763562757025524,
135.664907853605));
#64458=CARTESIAN_POINT('Ctrl Pts',(31.7081299934163,-0.627732213086083,
135.684314354911));
#64459=CARTESIAN_POINT('Ctrl Pts',(31.7003788021761,-0.491257123078367,
135.698014620612));
#64460=CARTESIAN_POINT('Ctrl Pts',(31.692630905399,-0.354840038624496,135.711709063334));
#64461=CARTESIAN_POINT('Ctrl Pts',(31.6848830086219,-0.21777934116214,135.719702055223));
#64462=CARTESIAN_POINT('Ctrl Pts',(31.6771351118448,-0.0805890609082852,
135.721950318401));
#64463=CARTESIAN_POINT('Ctrl Pts',(31.6693888357607,0.0565725220964206,
135.724198111292));
#64464=CARTESIAN_POINT('Ctrl Pts',(31.6616425596766,0.193863243312399,135.720703559264));
#64465=CARTESIAN_POINT('Ctrl Pts',(31.6538962835924,0.330767068754069,135.711475473439));
#64466=CARTESIAN_POINT('Ctrl Pts',(31.6461499503271,0.467671904788678,135.702247319494));
#64467=CARTESIAN_POINT('Ctrl Pts',(31.6384036170617,0.604189449270041,135.687285573593));
#64468=CARTESIAN_POINT('Ctrl Pts',(31.6306572837963,0.739807188936438,135.666651064022));
#64469=CARTESIAN_POINT('Ctrl Pts',(31.6229092157933,0.875455299255326,135.646011933496));
#64470=CARTESIAN_POINT('Ctrl Pts',(31.6151611477903,1.01020281734468,135.619697570198));
#64471=CARTESIAN_POINT('Ctrl Pts',(31.6074130797873,1.14354623471323,135.587820147192));
#64472=CARTESIAN_POINT('Ctrl Pts',(31.5996567770454,1.27703137105257,135.555908844482));
#64473=CARTESIAN_POINT('Ctrl Pts',(31.5919004743035,1.40910904479453,135.518422762286));
#64474=CARTESIAN_POINT('Ctrl Pts',(31.5841441715616,1.53928922214793,135.475524471798));
#64475=CARTESIAN_POINT('Ctrl Pts',(31.5763837290474,1.66953888058163,135.4326032852));
#64476=CARTESIAN_POINT('Ctrl Pts',(31.5686232865333,1.7978886589368,135.384264272143));
#64477=CARTESIAN_POINT('Ctrl Pts',(31.5608628440191,1.92386833711233,135.330718279523));
#64478=CARTESIAN_POINT('Ctrl Pts',(31.5530899437537,2.05005024905121,135.277086330122));
#64479=CARTESIAN_POINT('Ctrl Pts',(31.5453170434882,2.17385410451755,135.218230865757));
#64480=CARTESIAN_POINT('Ctrl Pts',(31.5375441432227,2.29483333213541,135.154409242607));
#64481=CARTESIAN_POINT('Ctrl Pts',(31.530053807461,2.41141466009582,135.092907696218));
#64482=CARTESIAN_POINT('Ctrl Pts',(31.5225634716993,2.52537289302176,135.026794941759));
#64483=CARTESIAN_POINT('Ctrl Pts',(31.5150731359376,2.63633537716449,134.956338320012));
#64484=CARTESIAN_POINT('Ctrl Pts',(31.5072988018185,2.751505037625,134.883210314034));
#64485=CARTESIAN_POINT('Ctrl Pts',(31.4995244676994,2.86381212017765,134.805170895397));
#64486=CARTESIAN_POINT('Ctrl Pts',(31.4917501335803,2.97280928982719,134.722470874924));
#64487=CARTESIAN_POINT('Ctrl Pts',(31.4839853806332,3.0816721302065,134.639872774836));
#64488=CARTESIAN_POINT('Ctrl Pts',(31.4762206276861,3.1872328655475,134.552625735359));
#64489=CARTESIAN_POINT('Ctrl Pts',(31.468455874739,3.28907095932687,134.461025120499));
#64490=CARTESIAN_POINT('Ctrl Pts',(31.4606988338539,3.39080790607584,134.369515484662));
#64491=CARTESIAN_POINT('Ctrl Pts',(31.452941792969,3.48882928041906,134.273661138227));
#64492=CARTESIAN_POINT('Ctrl Pts',(31.4451847520839,3.58274591499209,134.173798964102));
#64493=CARTESIAN_POINT('Ctrl Pts',(31.4374335608438,3.67659172630042,134.074012096819));
#64494=CARTESIAN_POINT('Ctrl Pts',(31.4296823696036,3.76633869231463,133.970223701268));
#64495=CARTESIAN_POINT('Ctrl Pts',(31.4219311783634,3.85163323359892,133.862808671128));
#64496=CARTESIAN_POINT('Ctrl Pts',(31.4141832815863,3.93689152242786,133.755439295241));
#64497=CARTESIAN_POINT('Ctrl Pts',(31.4064353848092,4.01770090774935,133.644446656061));
#64498=CARTESIAN_POINT('Ctrl Pts',(31.3986874880321,4.09374713277167,133.530239829018));
#64499=CARTESIAN_POINT('Ctrl Pts',(31.3909412119479,4.16977745056309,133.41605689158));
#64500=CARTESIAN_POINT('Ctrl Pts',(31.3831949358638,4.24104637330068,133.298661428816));
#64501=CARTESIAN_POINT('Ctrl Pts',(31.3754486597797,4.30728238505632,133.178492357357));
#64502=CARTESIAN_POINT('Ctrl Pts',(31.3677023265143,4.37351888575106,133.058322398838));
#64503=CARTESIAN_POINT('Ctrl Pts',(31.3599559932489,4.43472221260389,132.935379133167));
#64504=CARTESIAN_POINT('Ctrl Pts',(31.3522096599836,4.49066651623954,132.810126631443));
#64505=CARTESIAN_POINT('Ctrl Pts',(31.3444615919806,4.54662334821411,132.68484608029));
#64506=CARTESIAN_POINT('Ctrl Pts',(31.3367135239776,4.59731865402818,132.557255620947));
#64507=CARTESIAN_POINT('Ctrl Pts',(31.3289654559746,4.64257464941985,132.427839501649));
#64508=CARTESIAN_POINT('Ctrl Pts',(31.3212091532327,4.68787874342203,132.29828583736));
#64509=CARTESIAN_POINT('Ctrl Pts',(31.3134528504908,4.72773184964324,132.166903006731));
#64510=CARTESIAN_POINT('Ctrl Pts',(31.3056965477489,4.76200586859986,132.034191162772));
#64511=CARTESIAN_POINT('Ctrl Pts',(31.2979361052347,4.79629818063242,131.901408486505));
#64512=CARTESIAN_POINT('Ctrl Pts',(31.2901756627205,4.82500539023408,131.767295765616));
#64513=CARTESIAN_POINT('Ctrl Pts',(31.2824152202063,4.84805072342043,131.632362577493));
#64514=CARTESIAN_POINT('Ctrl Pts',(31.2746423199408,4.87113305102145,131.497212782637));
#64515=CARTESIAN_POINT('Ctrl Pts',(31.2668694196754,4.88853528993475,131.361240276612));
#64516=CARTESIAN_POINT('Ctrl Pts',(31.25909651941,4.90023257846541,131.224959879865));
#64517=CARTESIAN_POINT('Ctrl Pts',(31.2516061836482,4.91150464109385,131.093633618814));
#64518=CARTESIAN_POINT('Ctrl Pts',(31.2441158478864,4.91747931683862,130.962021771309));
#64519=CARTESIAN_POINT('Ctrl Pts',(31.2366255121246,4.9181800986161,130.830582365726));
#64520=CARTESIAN_POINT('Ctrl Pts',(31.2288511780056,4.91890745074769,130.694159395125));
#64521=CARTESIAN_POINT('Ctrl Pts',(31.2210768438865,4.91395539903072,130.557490053881));
#64522=CARTESIAN_POINT('Ctrl Pts',(31.2133025097675,4.90329316222011,130.421086266969));
#64523=CARTESIAN_POINT('Ctrl Pts',(31.2055377568204,4.89264406566346,130.284850585534));
#64524=CARTESIAN_POINT('Ctrl Pts',(31.1977730038733,4.87629881630337,130.148880193293));
#64525=CARTESIAN_POINT('Ctrl Pts',(31.1900082509262,4.8542786019798,130.013688550992));
#64526=CARTESIAN_POINT('Ctrl Pts',(31.1822512100413,4.83228025844352,129.878631182935));
#64527=CARTESIAN_POINT('Ctrl Pts',(31.1744941691563,4.80461822918996,129.744351408971));
#64528=CARTESIAN_POINT('Ctrl Pts',(31.1667371282713,4.77136558888309,129.611358740064));
#64529=CARTESIAN_POINT('Ctrl Pts',(31.1589859370312,4.73813802465096,129.478466361964));
#64530=CARTESIAN_POINT('Ctrl Pts',(31.1512347457912,4.69932833535641,129.346859534723));
#64531=CARTESIAN_POINT('Ctrl Pts',(31.1434835545511,4.65506081134759,129.217038373926));
#64532=CARTESIAN_POINT('Ctrl Pts',(31.135735657774,4.61081210221734,129.087272390585));
#64533=CARTESIAN_POINT('Ctrl Pts',(31.1279877609969,4.5611102980461,128.959290933451));
#64534=CARTESIAN_POINT('Ctrl Pts',(31.1202398642199,4.50612970210671,128.833579510925));
#64535=CARTESIAN_POINT('Ctrl Pts',(31.1124935881358,4.45116060692274,128.70789438452));
#64536=CARTESIAN_POINT('Ctrl Pts',(31.1047473120517,4.39091507286729,128.584478706212));
#64537=CARTESIAN_POINT('Ctrl Pts',(31.0970010359676,4.32561561194335,128.463798155205));
#64538=CARTESIAN_POINT('Ctrl Pts',(31.0892547027023,4.26031566899363,128.343116713362));
#64539=CARTESIAN_POINT('Ctrl Pts',(31.081508369437,4.18996191078986,128.225170782961));
#64540=CARTESIAN_POINT('Ctrl Pts',(31.0737620361716,4.11482269638577,128.110401219244));
#64541=CARTESIAN_POINT('Ctrl Pts',(31.0660139681687,4.0396666550756,127.995605953678));
#64542=CARTESIAN_POINT('Ctrl Pts',(31.0582659001658,3.95972323917565,127.883988797286));
#64543=CARTESIAN_POINT('Ctrl Pts',(31.0505178321628,3.87530376370483,127.775961073002));
#64544=CARTESIAN_POINT('Ctrl Pts',(31.042761529421,3.79079456621087,127.667818535567));
#64545=CARTESIAN_POINT('Ctrl Pts',(31.0350052266791,3.70180004722754,127.563273359446));
#64546=CARTESIAN_POINT('Ctrl Pts',(31.0272489239373,3.60867175874623,127.46270366328));
#64547=CARTESIAN_POINT('Ctrl Pts',(31.0194884814232,3.51549376489332,127.362080290039));
#64548=CARTESIAN_POINT('Ctrl Pts',(31.011728038909,3.41817788254379,127.265436900046));
#64549=CARTESIAN_POINT('Ctrl Pts',(31.0039675963948,3.31711133537094,127.173113524451));
#64550=CARTESIAN_POINT('Ctrl Pts',(30.9961946961294,3.21588254720417,127.080641943178));
#64551=CARTESIAN_POINT('Ctrl Pts',(30.9884217958641,3.11089136215078,126.992504485904));
#64552=CARTESIAN_POINT('Ctrl Pts',(30.9806488955987,3.00255747487995,126.909000342503));
#64553=CARTESIAN_POINT('Ctrl Pts',(30.9731585598364,2.89816179728389,126.828531785045));
#64554=CARTESIAN_POINT('Ctrl Pts',(30.965668224074,2.7906624807089,126.752365702749));
#64555=CARTESIAN_POINT('Ctrl Pts',(30.9581778883117,2.68045757589407,126.680729905883));
#64556=CARTESIAN_POINT('Ctrl Pts',(30.9504035541926,2.56607421862117,126.606378016009));
#64557=CARTESIAN_POINT('Ctrl Pts',(30.9426292200736,2.44841372624144,126.536671200091));
#64558=CARTESIAN_POINT('Ctrl Pts',(30.9348548859545,2.32789015772045,126.471912063216));
#64559=CARTESIAN_POINT('Ctrl Pts',(30.9270901330074,2.20751512372633,126.40723273619));
#64560=CARTESIAN_POINT('Ctrl Pts',(30.9193253800602,2.08428437531739,126.34748913913));
#64561=CARTESIAN_POINT('Ctrl Pts',(30.9115606271131,1.95864135410702,126.292940984182));
#64562=CARTESIAN_POINT('Ctrl Pts',(30.9038035862281,1.83312312331657,126.238447007231));
#64563=CARTESIAN_POINT('Ctrl Pts',(30.8960465453431,1.70519774398497,126.189138358077));
#64564=CARTESIAN_POINT('Ctrl Pts',(30.8882895044581,1.57533338075835,126.145228960061));
#64565=CARTESIAN_POINT('Ctrl Pts',(30.880538313218,1.44556694925841,126.101352674463));
#64566=CARTESIAN_POINT('Ctrl Pts',(30.8727871219779,1.3138648131581,126.062867660414));
#64567=CARTESIAN_POINT('Ctrl Pts',(30.8650359307378,1.18071491583145,126.029939673616));
#64568=CARTESIAN_POINT('Ctrl Pts',(30.8572880339607,1.04762161076286,125.997025682089));
#64569=CARTESIAN_POINT('Ctrl Pts',(30.8495401371836,0.913082147063845,125.969664113865));
#64570=CARTESIAN_POINT('Ctrl Pts',(30.8417922404065,0.777599211879236,125.947970751813));
#64571=CARTESIAN_POINT('Ctrl Pts',(30.8340459643224,0.642144616803992,125.926281927545));
#64572=CARTESIAN_POINT('Ctrl Pts',(30.8262996882383,0.505747328594069,125.910259012868));
#64573=CARTESIAN_POINT('Ctrl Pts',(30.8185534121542,0.368919409523134,125.899966513115));
#64574=CARTESIAN_POINT('Ctrl Pts',(30.8108070788889,0.232090480419583,125.889673937385));
#64575=CARTESIAN_POINT('Ctrl Pts',(30.8030607456235,0.0948313039756817,
125.885111890313));
#64576=CARTESIAN_POINT('Ctrl Pts',(30.7953144123581,-0.0423421611861836,
125.886292886852));
#64577=CARTESIAN_POINT('Ctrl Pts',(30.7875663443551,-0.179546345394478,
125.887474147868));
#64578=CARTESIAN_POINT('Ctrl Pts',(30.7798182763522,-0.316664389250117,
125.89440100835));
#64579=CARTESIAN_POINT('Ctrl Pts',(30.7720702083492,-0.453181961747182,
125.907033880248));
#64580=CARTESIAN_POINT('Ctrl Pts',(30.7643139056073,-0.589844626744877,
125.919680178513));
#64581=CARTESIAN_POINT('Ctrl Pts',(30.7565576028654,-0.7259051556118,125.938044566439));
#64582=CARTESIAN_POINT('Ctrl Pts',(30.7488013001236,-0.860855403987377,
125.96203565574));
#64583=CARTESIAN_POINT('Ctrl Pts',(30.7410408576094,-0.99587767937397,125.986039549807));
#64584=CARTESIAN_POINT('Ctrl Pts',(30.7332804150953,-1.12978811194168,126.01567604482));
#64585=CARTESIAN_POINT('Ctrl Pts',(30.7255199725811,-1.2620913199983,126.050803153678));
#64586=CARTESIAN_POINT('Ctrl Pts',(30.7177470723156,-1.39460691290965,126.085986651689));
#64587=CARTESIAN_POINT('Ctrl Pts',(30.7099741720502,-1.52550975197105,126.126678260646));
#64588=CARTESIAN_POINT('Ctrl Pts',(30.7022012717848,-1.65432126504699,126.172686598973));
#64589=CARTESIAN_POINT('Ctrl Pts',(30.6947109360228,-1.77845015516478,126.217022418312));
#64590=CARTESIAN_POINT('Ctrl Pts',(30.6872206002609,-1.90063684375572,126.266295009943));
#64591=CARTESIAN_POINT('Ctrl Pts',(30.6797302644989,-2.02047451144142,126.320292619518));
#64592=CARTESIAN_POINT('Ctrl Pts',(30.6719553683487,-2.14486485264301,126.37634161654));
#64593=CARTESIAN_POINT('Ctrl Pts',(30.6641804721984,-2.26711822400421,126.43765929837));
#64594=CARTESIAN_POINT('Ctrl Pts',(30.6564055760482,-2.38675612313621,126.504060829043));
#64595=CARTESIAN_POINT('Ctrl Pts',(30.6486403882002,-2.50624463366379,126.570379445923));
#64596=CARTESIAN_POINT('Ctrl Pts',(30.6408752003522,-2.62312383178251,126.641769092157));
#64597=CARTESIAN_POINT('Ctrl Pts',(30.6331100125042,-2.73693544843405,126.717997024638));
#64598=CARTESIAN_POINT('Ctrl Pts',(30.6253526633053,-2.85063217677376,126.794148008046));
#64599=CARTESIAN_POINT('Ctrl Pts',(30.6175953141063,-2.96126716367557,126.875127341253));
#64600=CARTESIAN_POINT('Ctrl Pts',(30.6098379649074,-3.0684073272435,126.960656735031));
#64601=CARTESIAN_POINT('Ctrl Pts',(30.6020870037687,-3.17545926250074,127.046115696641));
#64602=CARTESIAN_POINT('Ctrl Pts',(30.5943360426299,-3.27902180075424,127.136117014887));
#64603=CARTESIAN_POINT('Ctrl Pts',(30.5865850814912,-3.37869178243243,127.23033978637));
#64604=CARTESIAN_POINT('Ctrl Pts',(30.578837600197,-3.47831701662366,127.324520255926));
#64605=CARTESIAN_POINT('Ctrl Pts',(30.5710901189027,-3.57405288770035,127.422918140061));
#64606=CARTESIAN_POINT('Ctrl Pts',(30.5633426376084,-3.66553033294913,127.525173151023));
#64607=CARTESIAN_POINT('Ctrl Pts',(30.5555969568124,-3.75698651903374,127.627404398139));
#64608=CARTESIAN_POINT('Ctrl Pts',(30.5478512760163,-3.84418598852938,127.733490696938));
#64609=CARTESIAN_POINT('Ctrl Pts',(30.5401055952202,-3.92679776726853,127.843036191321));
#64610=CARTESIAN_POINT('Ctrl Pts',(30.5323600371418,-4.00940823715925,127.952579950136));
#64611=CARTESIAN_POINT('Ctrl Pts',(30.5246144790634,-4.08743092668292,128.06558248268));
#64612=CARTESIAN_POINT('Ctrl Pts',(30.5168689209849,-4.16057650347028,128.181616592452));
#64613=CARTESIAN_POINT('Ctrl Pts',(30.5091184097264,-4.23376885586907,128.297724904475));
#64614=CARTESIAN_POINT('Ctrl Pts',(30.5013678984679,-4.30207765539265,128.416868336089));
#64615=CARTESIAN_POINT('Ctrl Pts',(30.4936173872094,-4.36525797165065,128.53859233651));
#64616=CARTESIAN_POINT('Ctrl Pts',(30.485864316519,-4.42845915178563,128.660356533541));
#64617=CARTESIAN_POINT('Ctrl Pts',(30.4781112458286,-4.48652830534811,128.784702644735));
#64618=CARTESIAN_POINT('Ctrl Pts',(30.4703581751383,-4.53926790328042,128.911154351797));
#64619=CARTESIAN_POINT('Ctrl Pts',(30.4625962548564,-4.59206769979935,129.037750394696));
#64620=CARTESIAN_POINT('Ctrl Pts',(30.4548343345745,-4.63952564950778,129.166456468992));
#64621=CARTESIAN_POINT('Ctrl Pts',(30.4470724142927,-4.68149335458289,129.296778767882));
#64622=CARTESIAN_POINT('Ctrl Pts',(30.4414468886022,-4.71190984876183,129.391231095892));
#64623=CARTESIAN_POINT('Ctrl Pts',(30.4358213629117,-4.73944348570093,129.486532037996));
#64624=CARTESIAN_POINT('Ctrl Pts',(30.4301958372212,-4.76405452823406,129.582490119308));
#64625=CARTESIAN_POINT('Origin',(213.235140564004,0.,130.804360617566));
#64626=CARTESIAN_POINT('',(28.3348598006328,-4.76405452823408,129.582490119308));
#64627=CARTESIAN_POINT('',(28.6798592372483,-4.76405452823403,129.582490119308));
#64628=CARTESIAN_POINT('',(213.235140564004,-4.76405452823405,129.582490119308));
#64629=CARTESIAN_POINT('',(30.0148594360429,-4.91824986981998,130.803229018815));
#64630=CARTESIAN_POINT('Ctrl Pts',(30.0148594359913,-4.91824986982019,130.803229019732));
#64631=CARTESIAN_POINT('Ctrl Pts',(30.006871955308,-4.91828249669703,130.945034816734));
#64632=CARTESIAN_POINT('Ctrl Pts',(29.9988844746248,-4.91217783929229,131.086768889376));
#64633=CARTESIAN_POINT('Ctrl Pts',(29.9908969939415,-4.89998063896011,131.227884879346));
#64634=CARTESIAN_POINT('Ctrl Pts',(29.9829032257318,-4.88777383732535,131.369111951964));
#64635=CARTESIAN_POINT('Ctrl Pts',(29.9749094575221,-4.86946496135127,131.509719618149));
#64636=CARTESIAN_POINT('Ctrl Pts',(29.9669156893125,-4.84515038299053,131.649168778456));
#64637=CARTESIAN_POINT('Ctrl Pts',(29.9589144275633,-4.82081301159287,131.788748661567));
#64638=CARTESIAN_POINT('Ctrl Pts',(29.9509131658141,-4.79045877355497,131.927167524177));
#64639=CARTESIAN_POINT('Ctrl Pts',(29.9429119040649,-4.75423467615063,132.063898511631));
#64640=CARTESIAN_POINT('Ctrl Pts',(29.9348961969934,-4.71794518046554,132.200876350551));
#64641=CARTESIAN_POINT('Ctrl Pts',(29.9268804899219,-4.67576474248506,132.336159882206));
#64642=CARTESIAN_POINT('Ctrl Pts',(29.9188647828504,-4.62788995883001,132.469238268164));
#64643=CARTESIAN_POINT('Ctrl Pts',(29.9108407880352,-4.57996567561917,132.602454248915));
#64644=CARTESIAN_POINT('Ctrl Pts',(29.90281679322,-4.5263354379027,132.733460208831));
#64645=CARTESIAN_POINT('Ctrl Pts',(29.8947927984047,-4.46724301163168,132.861767465403));
#64646=CARTESIAN_POINT('Ctrl Pts',(29.8867542047405,-4.40804307265357,132.990308164083));
#64647=CARTESIAN_POINT('Ctrl Pts',(29.8787156110763,-4.34336125144675,133.116140034342));
#64648=CARTESIAN_POINT('Ctrl Pts',(29.8706770174121,-4.27348655801177,133.23880012205));
#64649=CARTESIAN_POINT('Ctrl Pts',(29.8684434746813,-4.2540717051022,133.272881524682));
#64650=CARTESIAN_POINT('Ctrl Pts',(29.8662099319505,-4.2342562022846,133.306718242284));
#64651=CARTESIAN_POINT('Ctrl Pts',(29.8639763892196,-4.21404681532671,133.340300778677));
#64652=CARTESIAN_POINT('Ctrl Pts',(29.8562020551005,-4.14370362270071,133.457192143628));
#64653=CARTESIAN_POINT('Ctrl Pts',(29.8484277209815,-4.06838173780606,133.571339615384));
#64654=CARTESIAN_POINT('Ctrl Pts',(29.8406533868624,-3.9883211644295,133.682289969003));
#64655=CARTESIAN_POINT('Ctrl Pts',(29.8328886339153,-3.90835925855429,133.793103586228));
#64656=CARTESIAN_POINT('Ctrl Pts',(29.8251238809683,-3.82367051065479,133.900727611066));
#64657=CARTESIAN_POINT('Ctrl Pts',(29.8173591280212,-3.73454010796197,134.004734540176));
#64658=CARTESIAN_POINT('Ctrl Pts',(29.8096020871362,-3.64549823084174,134.108638168138));
#64659=CARTESIAN_POINT('Ctrl Pts',(29.8018450462511,-3.55202373080071,134.208931554762));
#64660=CARTESIAN_POINT('Ctrl Pts',(29.7940880053661,-3.45444405478792,134.305217560493));
#64661=CARTESIAN_POINT('Ctrl Pts',(29.786336814126,-3.35693796436774,134.401430956198));
#64662=CARTESIAN_POINT('Ctrl Pts',(29.7785856228859,-3.25533313703544,134.493642712621));
#64663=CARTESIAN_POINT('Ctrl Pts',(29.7708344316457,-3.14999587357852,134.581490355732));
#64664=CARTESIAN_POINT('Ctrl Pts',(29.7630865348687,-3.04470338126868,134.669300661251));
#64665=CARTESIAN_POINT('Ctrl Pts',(29.7553386380916,-2.9356819076587,134.752750292766));
#64666=CARTESIAN_POINT('Ctrl Pts',(29.7475907413145,-2.82333286907851,134.831515267301));
#64667=CARTESIAN_POINT('Ctrl Pts',(29.7398444652304,-2.71100733149522,134.910263765901));
#64668=CARTESIAN_POINT('Ctrl Pts',(29.7320981891463,-2.59535593335977,134.984329332361));
#64669=CARTESIAN_POINT('Ctrl Pts',(29.7243519130622,-2.4768109492746,135.053429996154));
#64670=CARTESIAN_POINT('Ctrl Pts',(29.7166055797968,-2.35826509011744,135.122531170032));
#64671=CARTESIAN_POINT('Ctrl Pts',(29.7088592465315,-2.23682594015884,135.186667171224));
#64672=CARTESIAN_POINT('Ctrl Pts',(29.7011129132662,-2.11295201709328,135.245601078964));
#64673=CARTESIAN_POINT('Ctrl Pts',(29.6933648452632,-1.98905035332137,135.304548184545));
#64674=CARTESIAN_POINT('Ctrl Pts',(29.6856167772602,-1.86271318443584,135.358290710583));
#64675=CARTESIAN_POINT('Ctrl Pts',(29.6778687092572,-1.73442035288852,135.40663930339));
#64676=CARTESIAN_POINT('Ctrl Pts',(29.6701124065154,-1.60599117019312,135.455039281656));
#64677=CARTESIAN_POINT('Ctrl Pts',(29.6623561037736,-1.47560253923632,135.498033736841));
#64678=CARTESIAN_POINT('Ctrl Pts',(29.6545998010317,-1.34375139496071,135.535482604055));
#64679=CARTESIAN_POINT('Ctrl Pts',(29.6468393585175,-1.21182987775927,135.572951458858));
#64680=CARTESIAN_POINT('Ctrl Pts',(29.6390789160033,-1.07844467189758,135.604868737004));
#64681=CARTESIAN_POINT('Ctrl Pts',(29.6313184734891,-0.944103365652468,
135.631145458168));
#64682=CARTESIAN_POINT('Ctrl Pts',(29.6235455732237,-0.809546402816311,
135.657464361057));
#64683=CARTESIAN_POINT('Ctrl Pts',(29.6157726729584,-0.674030659264654,
135.678124553783));
#64684=CARTESIAN_POINT('Ctrl Pts',(29.6079997726929,-0.538070210576818,
135.693088827539));
#64685=CARTESIAN_POINT('Ctrl Pts',(29.6005094369309,-0.407052266662118,
135.707509112252));
#64686=CARTESIAN_POINT('Ctrl Pts',(29.5930191011688,-0.275621695856512,
135.716640388885));
#64687=CARTESIAN_POINT('Ctrl Pts',(29.5855287654067,-0.144236958399345,
135.720495152171));
#64688=CARTESIAN_POINT('Ctrl Pts',(29.5777544312876,-0.00787072868834712,
135.724496069978));
#64689=CARTESIAN_POINT('Ctrl Pts',(29.5699800971686,0.128878090749471,135.72282513168));
#64690=CARTESIAN_POINT('Ctrl Pts',(29.5622057630495,0.265498461025315,135.71543928011));
#64691=CARTESIAN_POINT('Ctrl Pts',(29.5544410101024,0.401950458904537,135.708062530941));
#64692=CARTESIAN_POINT('Ctrl Pts',(29.5466762571553,0.538273935948422,135.694984903111));
#64693=CARTESIAN_POINT('Ctrl Pts',(29.5389115042083,0.673955070824333,135.676215256716));
#64694=CARTESIAN_POINT('Ctrl Pts',(29.5311544633233,0.809501445284316,135.657464252599));
#64695=CARTESIAN_POINT('Ctrl Pts',(29.5233974224382,0.944406362420823,135.633032533651));
#64696=CARTESIAN_POINT('Ctrl Pts',(29.5156403815533,1.07815870440459,135.602980926636));
#64697=CARTESIAN_POINT('Ctrl Pts',(29.5078891903131,1.21181018270755,135.572951981771));
#64698=CARTESIAN_POINT('Ctrl Pts',(29.500137999073,1.34431043596769,135.537311669681));
#64699=CARTESIAN_POINT('Ctrl Pts',(29.4923868078328,1.47515650999621,135.496172243528));
#64700=CARTESIAN_POINT('Ctrl Pts',(29.4846389110557,1.60594697095248,135.455050302729));
#64701=CARTESIAN_POINT('Ctrl Pts',(29.4768910142787,1.7350842788462,135.408434013537));
#64702=CARTESIAN_POINT('Ctrl Pts',(29.4691431175016,1.86207888229262,135.356485978166));
#64703=CARTESIAN_POINT('Ctrl Pts',(29.4613968414175,1.9890469212055,135.304548809205));
#64704=CARTESIAN_POINT('Ctrl Pts',(29.4536505653334,2.11387278554884,135.24728226036));
#64705=CARTESIAN_POINT('Ctrl Pts',(29.4459042892493,2.23608559055076,135.184897604538));
#64706=CARTESIAN_POINT('Ctrl Pts',(29.438157955984,2.3582992977,135.122512488207));
#64707=CARTESIAN_POINT('Ctrl Pts',(29.4304116227186,2.47789955879707,135.055009367264));
#64708=CARTESIAN_POINT('Ctrl Pts',(29.4226652894533,2.59443920568036,134.982645944172));
#64709=CARTESIAN_POINT('Ctrl Pts',(29.4149172214503,2.71100495080923,134.910266315793));
#64710=CARTESIAN_POINT('Ctrl Pts',(29.4071691534473,2.82450838577123,134.833024425612));
#64711=CARTESIAN_POINT('Ctrl Pts',(29.3994210854444,2.93453083538086,134.751221628382));
#64712=CARTESIAN_POINT('Ctrl Pts',(29.3916647827025,3.04467021815951,134.669331890165));
#64713=CARTESIAN_POINT('Ctrl Pts',(29.3839084799606,3.1513209109239,134.582871795368));
#64714=CARTESIAN_POINT('Ctrl Pts',(29.3761521772187,3.25409646764277,134.492183720939));
#64715=CARTESIAN_POINT('Ctrl Pts',(29.3683917347046,3.35692687877077,134.401447243555));
#64716=CARTESIAN_POINT('Ctrl Pts',(29.3606312921904,3.45587775070292,134.306478560659));
#64717=CARTESIAN_POINT('Ctrl Pts',(29.3528708496763,3.55059985790736,134.207656624605));
#64718=CARTESIAN_POINT('Ctrl Pts',(29.3450979494108,3.64547402144733,134.108676050806));
#64719=CARTESIAN_POINT('Ctrl Pts',(29.3373250491454,3.73610559626051,134.005830156573));
#64720=CARTESIAN_POINT('Ctrl Pts',(29.3295521488799,3.8221854071165,133.89953133598));
#64721=CARTESIAN_POINT('Ctrl Pts',(29.3220618131179,3.90513600002592,133.797096745266));
#64722=CARTESIAN_POINT('Ctrl Pts',(29.314571477356,3.98385983555859,133.691456161804));
#64723=CARTESIAN_POINT('Ctrl Pts',(29.3070811415939,4.05811961692932,133.583002054886));
#64724=CARTESIAN_POINT('Ctrl Pts',(29.2993068074748,4.13519498048149,133.470435877541));
#64725=CARTESIAN_POINT('Ctrl Pts',(29.2915324733557,4.20770524995025,133.354482039855));
#64726=CARTESIAN_POINT('Ctrl Pts',(29.2837581392366,4.27533797111791,133.235547219869));
#64727=CARTESIAN_POINT('Ctrl Pts',(29.2759933862895,4.34288734100114,133.116758976419));
#64728=CARTESIAN_POINT('Ctrl Pts',(29.2682286333425,4.4055709315585,132.994997397019));
#64729=CARTESIAN_POINT('Ctrl Pts',(29.2604638803954,4.46311846405882,132.870699563208));
#64730=CARTESIAN_POINT('Ctrl Pts',(29.2527068395104,4.52060883953867,132.746525183757));
#64731=CARTESIAN_POINT('Ctrl Pts',(29.2449497986254,4.57297314539408,132.619819915395));
#64732=CARTESIAN_POINT('Ctrl Pts',(29.2371927577404,4.61998628523119,132.491046654378));
#64733=CARTESIAN_POINT('Ctrl Pts',(29.2294415665002,4.66696397209396,132.362370502278));
#64734=CARTESIAN_POINT('Ctrl Pts',(29.2216903752601,4.70859839153284,132.23162982736));
#64735=CARTESIAN_POINT('Ctrl Pts',(29.2139391840199,4.74471212628655,132.099308454805));
#64736=CARTESIAN_POINT('Ctrl Pts',(29.2061912872428,4.78081051173948,131.967043322363));
#64737=CARTESIAN_POINT('Ctrl Pts',(29.1984433904658,4.81139277667065,131.833199204899));
#64738=CARTESIAN_POINT('Ctrl Pts',(29.1906954936887,4.83633110844715,131.698275866326));
#64739=CARTESIAN_POINT('Ctrl Pts',(29.1829492176046,4.86126422366228,131.563380750808));
#64740=CARTESIAN_POINT('Ctrl Pts',(29.1752029415205,4.8805556829645,131.427407247419));
#64741=CARTESIAN_POINT('Ctrl Pts',(29.1674566654364,4.89412871151387,131.290865723023));
#64742=CARTESIAN_POINT('Ctrl Pts',(29.1597103321711,4.90770184025621,131.154323190709));
#64743=CARTESIAN_POINT('Ctrl Pts',(29.1519639989057,4.91555641534079,131.017213018067));
#64744=CARTESIAN_POINT('Ctrl Pts',(29.1442176656404,4.91766754383402,130.880050714814));
#64745=CARTESIAN_POINT('Ctrl Pts',(29.1364695976374,4.91977914509984,130.742857695014));
#64746=CARTESIAN_POINT('Ctrl Pts',(29.1287215296345,4.91614473435951,130.605612912215));
#64747=CARTESIAN_POINT('Ctrl Pts',(29.1209734616315,4.90679154573585,130.468831499314));
#64748=CARTESIAN_POINT('Ctrl Pts',(29.1132171588896,4.89742841643201,130.331904713499));
#64749=CARTESIAN_POINT('Ctrl Pts',(29.1054608561478,4.8823343945294,130.195442672028));
#64750=CARTESIAN_POINT('Ctrl Pts',(29.097704553406,4.86158864793186,130.059955565998));
#64751=CARTESIAN_POINT('Ctrl Pts',(29.0899441108918,4.84083182870469,129.924396146419));
#64752=CARTESIAN_POINT('Ctrl Pts',(29.0821836683776,4.81441734942052,129.789813082584));
#64753=CARTESIAN_POINT('Ctrl Pts',(29.0744232258635,4.78247526849565,129.656705020827));
#64754=CARTESIAN_POINT('Ctrl Pts',(29.066650325598,4.7504819113068,129.523383282191));
#64755=CARTESIAN_POINT('Ctrl Pts',(29.0588774253325,4.71294332772681,129.391541653497));
#64756=CARTESIAN_POINT('Ctrl Pts',(29.0511045250671,4.67003935980689,129.261663161694));
#64757=CARTESIAN_POINT('Ctrl Pts',(29.043614189305,4.62869505918903,129.13650608021));
#64758=CARTESIAN_POINT('Ctrl Pts',(29.036123853543,4.58236880046733,129.013172172025));
#64759=CARTESIAN_POINT('Ctrl Pts',(29.0286335177809,4.53126251446374,128.892073220882));
#64760=CARTESIAN_POINT('Ctrl Pts',(29.0208591836617,4.47821851809335,128.766382766201));
#64761=CARTESIAN_POINT('Ctrl Pts',(29.0130848495427,4.41985684227472,128.6427019413));
#64762=CARTESIAN_POINT('Ctrl Pts',(29.0053105154236,4.35635074762307,128.521513442176));
#64763=CARTESIAN_POINT('Ctrl Pts',(28.9975457624765,4.29292291855755,128.400474297047));
#64764=CARTESIAN_POINT('Ctrl Pts',(28.9897810095294,4.22436346516957,128.281921709163));
#64765=CARTESIAN_POINT('Ctrl Pts',(28.9820162565823,4.15089402427952,128.166319324921));
#64766=CARTESIAN_POINT('Ctrl Pts',(28.9742592156973,4.0774975542738,128.050831758597));
#64767=CARTESIAN_POINT('Ctrl Pts',(28.9665021748123,3.99920100990512,127.938288892549));
#64768=CARTESIAN_POINT('Ctrl Pts',(28.9587451339273,3.91627216880442,127.829130313481));
#64769=CARTESIAN_POINT('Ctrl Pts',(28.9509939426872,3.83340586498799,127.720054051746));
#64770=CARTESIAN_POINT('Ctrl Pts',(28.9432427514471,3.74591445309607,127.614357307214));
#64771=CARTESIAN_POINT('Ctrl Pts',(28.9354915602069,3.6541090905907,127.512450865376));
#64772=CARTESIAN_POINT('Ctrl Pts',(28.9277436634299,3.56234274781325,127.410587736495));
#64773=CARTESIAN_POINT('Ctrl Pts',(28.9199957666528,3.46626636233686,127.31251199606));
#64774=CARTESIAN_POINT('Ctrl Pts',(28.9122478698757,3.36623131384609,127.218601311062));
#64775=CARTESIAN_POINT('Ctrl Pts',(28.9045015937916,3.26621719053096,127.124710270155));
#64776=CARTESIAN_POINT('Ctrl Pts',(28.8967553177075,3.16224633613331,127.034982819162));
#64777=CARTESIAN_POINT('Ctrl Pts',(28.8890090416234,3.05470663807239,126.949759416687));
#64778=CARTESIAN_POINT('Ctrl Pts',(28.881262708358,2.94716614617769,126.864535385112));
#64779=CARTESIAN_POINT('Ctrl Pts',(28.8735163750926,2.83605706446422,126.783815711226));
#64780=CARTESIAN_POINT('Ctrl Pts',(28.8657700418273,2.72179965061627,126.70789998375));
#64781=CARTESIAN_POINT('Ctrl Pts',(28.8580219738243,2.60751664961301,126.631967255474));
#64782=CARTESIAN_POINT('Ctrl Pts',(28.8502739058213,2.49008423908966,126.560840830669));
#64783=CARTESIAN_POINT('Ctrl Pts',(28.8425258378184,2.369950535649,126.494776238409));
#64784=CARTESIAN_POINT('Ctrl Pts',(28.8347695350765,2.24968915267839,126.428641431914));
#64785=CARTESIAN_POINT('Ctrl Pts',(28.8270132323346,2.12672108485306,126.36757939334));
#64786=CARTESIAN_POINT('Ctrl Pts',(28.8192569295927,2.00151836257592,126.311799287237));
#64787=CARTESIAN_POINT('Ctrl Pts',(28.8114964870785,1.87624881583596,126.255989409611));
#64788=CARTESIAN_POINT('Ctrl Pts',(28.8037360445644,1.74874260137819,126.205467225753));
#64789=CARTESIAN_POINT('Ctrl Pts',(28.7959756020502,1.61948954423614,126.160392844356));
#64790=CARTESIAN_POINT('Ctrl Pts',(28.7882027017848,1.49002899861257,126.115246105562));
#64791=CARTESIAN_POINT('Ctrl Pts',(28.7804298015193,1.3588163810876,126.075564758356));
#64792=CARTESIAN_POINT('Ctrl Pts',(28.7726569012539,1.22635528493476,126.041458584392));
#64793=CARTESIAN_POINT('Ctrl Pts',(28.7651665654919,1.09870948327789,126.008592255761));
#64794=CARTESIAN_POINT('Ctrl Pts',(28.75767622973,0.969904698905462,125.980902859279));
#64795=CARTESIAN_POINT('Ctrl Pts',(28.750185893968,0.840396525686057,125.958443084001));
#64796=CARTESIAN_POINT('Ctrl Pts',(28.7424115598489,0.705978010714365,125.935131739516));
#64797=CARTESIAN_POINT('Ctrl Pts',(28.7346372257298,0.57037591855945,125.91738056334));
#64798=CARTESIAN_POINT('Ctrl Pts',(28.7268628916108,0.434090006628336,125.905304695386));
#64799=CARTESIAN_POINT('Ctrl Pts',(28.7190981386637,0.297972054903456,125.893243709861));
#64800=CARTESIAN_POINT('Ctrl Pts',(28.7113333857166,0.161172345918071,125.886844150141));
#64801=CARTESIAN_POINT('Ctrl Pts',(28.7035686327695,0.0242007586337614,
125.886170159096));
#64802=CARTESIAN_POINT('Ctrl Pts',(28.6958115918845,-0.112634786539282,
125.885496837469));
#64803=CARTESIAN_POINT('Ctrl Pts',(28.6880545509994,-0.249641481856184,
125.890537769609));
#64804=CARTESIAN_POINT('Ctrl Pts',(28.6802975101144,-0.386304750222389,
125.901305273961));
#64805=CARTESIAN_POINT('Ctrl Pts',(28.6725463188743,-0.522864959754461,
125.912064658454));
#64806=CARTESIAN_POINT('Ctrl Pts',(28.6647951276342,-0.659081869641387,
125.928541988958));
#64807=CARTESIAN_POINT('Ctrl Pts',(28.6570439363941,-0.79444168620454,125.95069751948));
#64808=CARTESIAN_POINT('Ctrl Pts',(28.649296039617,-0.929743971234814,125.972843633311));
#64809=CARTESIAN_POINT('Ctrl Pts',(28.6415481428399,-1.06418950245819,126.000663084099));
#64810=CARTESIAN_POINT('Ctrl Pts',(28.6338002460628,-1.19727060863685,126.034064384396));
#64811=CARTESIAN_POINT('Ctrl Pts',(28.6260539699787,-1.33032387711717,126.067458697862));
#64812=CARTESIAN_POINT('Ctrl Pts',(28.6183076938946,-1.46201290928184,126.106432443298));
#64813=CARTESIAN_POINT('Ctrl Pts',(28.6105614178105,-1.59184160504136,126.150843306224));
#64814=CARTESIAN_POINT('Ctrl Pts',(28.6028150845451,-1.72167125916683,126.195254496981));
#64815=CARTESIAN_POINT('Ctrl Pts',(28.5950687512798,-1.84964017956391,126.245102758776));
#64816=CARTESIAN_POINT('Ctrl Pts',(28.5873224180144,-1.97526915421154,126.300196451939));
#64817=CARTESIAN_POINT('Ctrl Pts',(28.5795743500114,-2.10092626259682,126.355302482952));
#64818=CARTESIAN_POINT('Ctrl Pts',(28.5718262820084,-2.22424202452435,126.415656125818));
#64819=CARTESIAN_POINT('Ctrl Pts',(28.5640782140055,-2.34475923817768,126.481018487052));
#64820=CARTESIAN_POINT('Ctrl Pts',(28.5563219112636,-2.46540453895984,126.546450316181));
#64821=CARTESIAN_POINT('Ctrl Pts',(28.5485656085218,-2.58324500570006,126.616901310907));
#64822=CARTESIAN_POINT('Ctrl Pts',(28.5408093057799,-2.69784951837669,126.69208739723));
#64823=CARTESIAN_POINT('Ctrl Pts',(28.5330488632658,-2.81251519893226,126.767313612631));
#64824=CARTESIAN_POINT('Ctrl Pts',(28.5252884207516,-2.9239411665011,126.847279727569));
#64825=CARTESIAN_POINT('Ctrl Pts',(28.5175279782374,-3.03172795470893,126.931660181031));
#64826=CARTESIAN_POINT('Ctrl Pts',(28.509755077972,-3.1396877718382,127.016176089488));
#64827=CARTESIAN_POINT('Ctrl Pts',(28.5019821777066,-3.24399643789525,127.105120243311));
#64828=CARTESIAN_POINT('Ctrl Pts',(28.4942092774412,-3.34428938600066,127.19812829488));
#64829=CARTESIAN_POINT('Ctrl Pts',(28.4867189416792,-3.44093643281988,127.287755269502));
#64830=CARTESIAN_POINT('Ctrl Pts',(28.4792286059171,-3.53385443847036,127.381155587387));
#64831=CARTESIAN_POINT('Ctrl Pts',(28.471738270155,-3.62275281454509,127.477974424232));
#64832=CARTESIAN_POINT('Ctrl Pts',(28.4640491790996,-3.71401009993794,127.57736233901));
#64833=CARTESIAN_POINT('Ctrl Pts',(28.456360088044,-3.80133502515556,127.680683630055));
#64834=CARTESIAN_POINT('Ctrl Pts',(28.4486709969885,-3.88436366672537,127.787590495876));
#64835=CARTESIAN_POINT('Ctrl Pts',(28.4409910655761,-3.96729340028223,127.894370008707));
#64836=CARTESIAN_POINT('Ctrl Pts',(28.4333111341636,-4.04593678375962,128.004726290477));
#64837=CARTESIAN_POINT('Ctrl Pts',(28.4256312027512,-4.11996687512301,128.118274987809));
#64838=CARTESIAN_POINT('Ctrl Pts',(28.4179598667928,-4.19391411128604,128.23169660033));
#64839=CARTESIAN_POINT('Ctrl Pts',(28.4102885308345,-4.26325811512867,128.348303183766));
#64840=CARTESIAN_POINT('Ctrl Pts',(28.4026171948762,-4.32771284263925,128.467678222769));
#64841=CARTESIAN_POINT('Ctrl Pts',(28.3949509219467,-4.39212503047414,128.586974475069));
#64842=CARTESIAN_POINT('Ctrl Pts',(28.3872846490172,-4.45165416910228,128.709035199073));
#64843=CARTESIAN_POINT('Ctrl Pts',(28.3796183760877,-4.5060581971628,128.833416025173));
#64844=CARTESIAN_POINT('Ctrl Pts',(28.3719547042758,-4.56044376628301,128.957754649652));
#64845=CARTESIAN_POINT('Ctrl Pts',(28.3642910324639,-4.60970751792294,129.084411446939));
#64846=CARTESIAN_POINT('Ctrl Pts',(28.356627360652,-4.65365410871967,129.212918975879));
#64847=CARTESIAN_POINT('Ctrl Pts',(28.3493715073123,-4.69526210361161,129.334588040777));
#64848=CARTESIAN_POINT('Ctrl Pts',(28.3421156539726,-4.73210404157072,129.457915656724));
#64849=CARTESIAN_POINT('Ctrl Pts',(28.3348598006328,-4.76405452823408,129.582490119308));
#64850=CARTESIAN_POINT('Ctrl Pts',(30.0845737196928,-4.764054528234,129.582490119308));
#64851=CARTESIAN_POINT('Ctrl Pts',(30.0762738315874,-4.80042685421111,129.724305266266));
#64852=CARTESIAN_POINT('Ctrl Pts',(30.0679739434819,-4.83050405968412,129.867906679042));
#64853=CARTESIAN_POINT('Ctrl Pts',(30.0596740553765,-4.85412279584103,130.01273258282));
#64854=CARTESIAN_POINT('Ctrl Pts',(30.0513972716616,-4.87767578454456,130.157155334867));
#64855=CARTESIAN_POINT('Ctrl Pts',(30.0431204879468,-4.89480610788418,130.302795483977));
#64856=CARTESIAN_POINT('Ctrl Pts',(30.034843704232,-4.90540096313198,130.449079808341));
#64857=CARTESIAN_POINT('Ctrl Pts',(30.0281822815023,-4.91392804466475,130.566814155025));
#64858=CARTESIAN_POINT('Ctrl Pts',(30.0215208587727,-4.91822265953884,130.684965401437));
#64859=CARTESIAN_POINT('Ctrl Pts',(30.014859436043,-4.91824986981998,130.803229018816));
#64860=CARTESIAN_POINT('',(30.3601405639767,-4.91824855297799,130.800587869246));
#64861=CARTESIAN_POINT('Ctrl Pts',(30.4301958372212,-4.76405452823406,129.582490119308));
#64862=CARTESIAN_POINT('Ctrl Pts',(30.4224205637759,-4.79807047554281,129.715117781601));
#64863=CARTESIAN_POINT('Ctrl Pts',(30.4146452903305,-4.82650126630627,129.849000753027));
#64864=CARTESIAN_POINT('Ctrl Pts',(30.4068700168851,-4.84928678182263,129.98362876724));
#64865=CARTESIAN_POINT('Ctrl Pts',(30.4050075581521,-4.85474473550842,130.015877037675));
#64866=CARTESIAN_POINT('Ctrl Pts',(30.4031450994191,-4.85987901195573,130.048168045123));
#64867=CARTESIAN_POINT('Ctrl Pts',(30.4012826406861,-4.86468922843001,130.080494764457));
#64868=CARTESIAN_POINT('Ctrl Pts',(30.3875686151269,-4.90010876847374,130.31852927622));
#64869=CARTESIAN_POINT('Ctrl Pts',(30.3738545895678,-4.91806340583222,130.559225480776));
#64870=CARTESIAN_POINT('Ctrl Pts',(30.3601405640087,-4.91824855297756,130.800587868682));
#64871=CARTESIAN_POINT('Ctrl Pts',(30.3601405639766,-4.91824855297799,130.800587869246));
#64872=CARTESIAN_POINT('Ctrl Pts',(30.3524894783402,-4.91835184697044,130.935244487123));
#64873=CARTESIAN_POINT('Ctrl Pts',(30.3448383927039,-4.91292084437805,131.070109760254));
#64874=CARTESIAN_POINT('Ctrl Pts',(30.3371873070675,-4.90193073887906,131.204683104734));
#64875=CARTESIAN_POINT('Ctrl Pts',(30.3295438958543,-4.89095165700789,131.339121465391));
#64876=CARTESIAN_POINT('Ctrl Pts',(30.3219004846411,-4.87442459481917,131.473268080537));
#64877=CARTESIAN_POINT('Ctrl Pts',(30.3142570734279,-4.85237677947207,131.606621580433));
#64878=CARTESIAN_POINT('Ctrl Pts',(30.3062811544048,-4.82936982813323,131.74577629643));
#64879=CARTESIAN_POINT('Ctrl Pts',(30.2983052353817,-4.80035094440838,131.884066891241));
#64880=CARTESIAN_POINT('Ctrl Pts',(30.2903293163586,-4.76541147807761,132.020928127861));
#64881=CARTESIAN_POINT('Ctrl Pts',(30.2826947511554,-4.73196735294386,132.151931969767));
#64882=CARTESIAN_POINT('Ctrl Pts',(30.2750601859522,-4.69309904374229,132.281625834324));
#64883=CARTESIAN_POINT('Ctrl Pts',(30.2674256207491,-4.64893892523314,132.409524139439));
#64884=CARTESIAN_POINT('Ctrl Pts',(30.2597922977726,-4.60478599205496,132.537401634111));
#64885=CARTESIAN_POINT('Ctrl Pts',(30.2521589747961,-4.55534309303943,132.663483768904));
#64886=CARTESIAN_POINT('Ctrl Pts',(30.2445256518197,-4.50079218013342,132.787301063911));
#64887=CARTESIAN_POINT('Ctrl Pts',(30.2368918049718,-4.44623752342343,132.911126856442));
#64888=CARTESIAN_POINT('Ctrl Pts',(30.2292579581239,-4.3865743188075,133.032687130993));
#64889=CARTESIAN_POINT('Ctrl Pts',(30.221624111276,-4.32203204386775,133.151533826829));
#64890=CARTESIAN_POINT('Ctrl Pts',(30.2139879742221,-4.25747040580612,133.270416177482));
#64891=CARTESIAN_POINT('Ctrl Pts',(30.2063518371682,-4.18802697972943,133.386582976516));
#64892=CARTESIAN_POINT('Ctrl Pts',(30.1987157001143,-4.11397613336882,133.499612634831));
#64893=CARTESIAN_POINT('Ctrl Pts',(30.1910714077416,-4.03984620143695,133.612763007703));
#64894=CARTESIAN_POINT('Ctrl Pts',(30.1834271153688,-3.96109924965702,133.722769215435));
#64895=CARTESIAN_POINT('Ctrl Pts',(30.1757828229961,-3.87805187000201,133.829240244274));
#64896=CARTESIAN_POINT('Ctrl Pts',(30.1681337229086,-3.79495225946831,133.935778235797));
#64897=CARTESIAN_POINT('Ctrl Pts',(30.1604846228212,-3.70754709806342,134.038776316573));
#64898=CARTESIAN_POINT('Ctrl Pts',(30.1528355227338,-3.61619092374368,134.137879218914));
#64899=CARTESIAN_POINT('Ctrl Pts',(30.1451756766574,-3.52470640590252,134.237121347921));
#64900=CARTESIAN_POINT('Ctrl Pts',(30.137515830581,-3.42926008346147,134.332457095685));
#64901=CARTESIAN_POINT('Ctrl Pts',(30.1298559845046,-3.33024088731945,134.423570295787));
#64902=CARTESIAN_POINT('Ctrl Pts',(30.1275156619608,-3.29998742599787,134.451408228052));
#64903=CARTESIAN_POINT('Ctrl Pts',(30.125175339417,-3.26940065230052,134.478852288305));
#64904=CARTESIAN_POINT('Ctrl Pts',(30.1228350168732,-3.23849219777335,134.505894265591));
#64905=CARTESIAN_POINT('Ctrl Pts',(30.1150606827541,-3.13581718264174,134.595725202448));
#64906=CARTESIAN_POINT('Ctrl Pts',(30.1072863486349,-3.02923904101996,134.681423110129));
#64907=CARTESIAN_POINT('Ctrl Pts',(30.0995120145159,-2.9191247008982,134.762629689156));
#64908=CARTESIAN_POINT('Ctrl Pts',(30.0917472615688,-2.80914606685958,134.843736188332));
#64909=CARTESIAN_POINT('Ctrl Pts',(30.0839825086217,-2.69564021717182,134.920362142353));
#64910=CARTESIAN_POINT('Ctrl Pts',(30.0762177556747,-2.57900925181315,134.99218754111));
#64911=CARTESIAN_POINT('Ctrl Pts',(30.0684607147897,-2.46249412597348,135.063941601868));
#64912=CARTESIAN_POINT('Ctrl Pts',(30.0607036739046,-2.34286039212943,135.13090439217));
#64913=CARTESIAN_POINT('Ctrl Pts',(30.0529466330196,-2.22054112072062,135.192797719051));
#64914=CARTESIAN_POINT('Ctrl Pts',(30.0451954417795,-2.09831409122572,135.254644371693));
#64915=CARTESIAN_POINT('Ctrl Pts',(30.0374442505394,-1.97340590261091,135.311428994406));
#64916=CARTESIAN_POINT('Ctrl Pts',(30.0296930592992,-1.84627603907225,135.36291826775));
#64917=CARTESIAN_POINT('Ctrl Pts',(30.0219451625222,-1.71920020911707,135.414385656778));
#64918=CARTESIAN_POINT('Ctrl Pts',(30.0141972657451,-1.5899049439349,135.460562026379));
#64919=CARTESIAN_POINT('Ctrl Pts',(30.006449368968,-1.45887141363654,135.501261432037));
#64920=CARTESIAN_POINT('Ctrl Pts',(29.9987030928839,-1.32786529272796,135.541952324256));
#64921=CARTESIAN_POINT('Ctrl Pts',(29.9909568167999,-1.19512200307163,135.577168415421));
#64922=CARTESIAN_POINT('Ctrl Pts',(29.9832105407158,-1.06113927152275,135.606773189277));
#64923=CARTESIAN_POINT('Ctrl Pts',(29.9754642074504,-0.927155550943786,
135.63637818167));
#64924=CARTESIAN_POINT('Ctrl Pts',(29.967717874185,-0.791932751972515,135.660371689748));
#64925=CARTESIAN_POINT('Ctrl Pts',(29.9599715409197,-0.655979836026633,
135.678668108608));
#64926=CARTESIAN_POINT('Ctrl Pts',(29.9522234729167,-0.519996474367857,
135.696968624824));
#64927=CARTESIAN_POINT('Ctrl Pts',(29.9444754049137,-0.383283057777108,
135.709569460946));
#64928=CARTESIAN_POINT('Ctrl Pts',(29.9367273369108,-0.246354330151193,
135.716436818778));
#64929=CARTESIAN_POINT('Ctrl Pts',(29.9289710341689,-0.109280073043898,
135.72331147532));
#64930=CARTESIAN_POINT('Ctrl Pts',(29.9212147314271,0.0280095611243244,
135.724440461317));
#64931=CARTESIAN_POINT('Ctrl Pts',(29.9134584286852,0.164998601834844,135.719842132524));
#64932=CARTESIAN_POINT('Ctrl Pts',(29.905697986171,0.302060757721051,135.715241349464));
#64933=CARTESIAN_POINT('Ctrl Pts',(29.8979375436569,0.438821610804647,135.704907190044));
#64934=CARTESIAN_POINT('Ctrl Pts',(29.8901771011427,0.574770643908035,135.688909907869));
#64935=CARTESIAN_POINT('Ctrl Pts',(29.8824042008773,0.710937914468348,135.672886945437));
#64936=CARTESIAN_POINT('Ctrl Pts',(29.8746313006118,0.846290374572785,135.651182755576));
#64937=CARTESIAN_POINT('Ctrl Pts',(29.8668584003463,0.980327137220798,135.62391887186));
#64938=CARTESIAN_POINT('Ctrl Pts',(29.8593680645843,1.10949132592833,135.59764609899));
#64939=CARTESIAN_POINT('Ctrl Pts',(29.8518777288223,1.23743351513012,135.566210905697));
#64940=CARTESIAN_POINT('Ctrl Pts',(29.8443873930603,1.36372095349765,135.529765174161));
#64941=CARTESIAN_POINT('Ctrl Pts',(29.8366130589412,1.49479661847512,135.491937591637));
#64942=CARTESIAN_POINT('Ctrl Pts',(29.8288387248222,1.62450478416031,135.44859219503));
#64943=CARTESIAN_POINT('Ctrl Pts',(29.8210643907031,1.75234566951372,135.399844021631));
#64944=CARTESIAN_POINT('Ctrl Pts',(29.813299637756,1.88002900240139,135.351155925998));
#64945=CARTESIAN_POINT('Ctrl Pts',(29.8055348848088,2.00584927197037,135.297078439845));
#64946=CARTESIAN_POINT('Ctrl Pts',(29.7977701318617,2.12931989979165,135.237776887989));
#64947=CARTESIAN_POINT('Ctrl Pts',(29.7900130909767,2.25266789484475,135.17853423527));
#64948=CARTESIAN_POINT('Ctrl Pts',(29.7822560500918,2.37367054216918,135.114078010599));
#64949=CARTESIAN_POINT('Ctrl Pts',(29.7744990092067,2.49185970499534,135.044622198308));
#64950=CARTESIAN_POINT('Ctrl Pts',(29.7667478179666,2.60995974045491,134.975218763186));
#64951=CARTESIAN_POINT('Ctrl Pts',(29.7589966267264,2.72525017876658,134.900823442139));
#64952=CARTESIAN_POINT('Ctrl Pts',(29.7512454354862,2.83728635924497,134.821696697376));
#64953=CARTESIAN_POINT('Ctrl Pts',(29.7434975387091,2.94927492135753,134.742603583591));
#64954=CARTESIAN_POINT('Ctrl Pts',(29.7357496419321,3.05801165792907,134.658783270851));
#64955=CARTESIAN_POINT('Ctrl Pts',(29.728001745155,3.16308004437384,134.570540073644));
#64956=CARTESIAN_POINT('Ctrl Pts',(29.7202554690709,3.26812645277718,134.482315335012));
#64957=CARTESIAN_POINT('Ctrl Pts',(29.7125091929868,3.36950573814034,134.389669803414));
#64958=CARTESIAN_POINT('Ctrl Pts',(29.7047629169027,3.46683401194917,134.29294844018));
#64959=CARTESIAN_POINT('Ctrl Pts',(29.6970165836373,3.56416300421321,134.196226362971));
#64960=CARTESIAN_POINT('Ctrl Pts',(29.689270250372,3.65744064793493,134.095428669678));
#64961=CARTESIAN_POINT('Ctrl Pts',(29.6815239171066,3.74631981520688,133.990937292414));
#64962=CARTESIAN_POINT('Ctrl Pts',(29.6737758491036,3.83521888635222,133.886422515032));
#64963=CARTESIAN_POINT('Ctrl Pts',(29.6660277811006,3.91971726773403,133.778212705445));
#64964=CARTESIAN_POINT('Ctrl Pts',(29.6582797130976,3.99950829232395,133.666722663522));
#64965=CARTESIAN_POINT('Ctrl Pts',(29.6505234103558,4.07938411976421,133.555114128657));
#64966=CARTESIAN_POINT('Ctrl Pts',(29.6427671076139,4.15454236841179,133.440218715695));
#64967=CARTESIAN_POINT('Ctrl Pts',(29.6350108048721,4.22471958681367,133.322480446981));
#64968=CARTESIAN_POINT('Ctrl Pts',(29.6272503623579,4.2949342609101,133.204679337807));
#64969=CARTESIAN_POINT('Ctrl Pts',(29.6194899198437,4.36016242157305,133.084032693247));
#64970=CARTESIAN_POINT('Ctrl Pts',(29.6117294773295,4.42018722814457,132.961007999649));
#64971=CARTESIAN_POINT('Ctrl Pts',(29.6039565770641,4.48030839186435,132.837785815892));
#64972=CARTESIAN_POINT('Ctrl Pts',(29.5961836767987,4.53520935309395,132.712178313051));
#64973=CARTESIAN_POINT('Ctrl Pts',(29.5884107765332,4.58472161981121,132.584672593411));
#64974=CARTESIAN_POINT('Ctrl Pts',(29.5809204407712,4.63243399091916,132.461802027847));
#64975=CARTESIAN_POINT('Ctrl Pts',(29.5734301050092,4.67514255093558,132.337169150739));
#64976=CARTESIAN_POINT('Ctrl Pts',(29.5659397692473,4.71274116997774,132.211220144064));
#64977=CARTESIAN_POINT('Ctrl Pts',(29.5581654351282,4.75176535208891,132.080495742518));
#64978=CARTESIAN_POINT('Ctrl Pts',(29.5503911010091,4.78540807416891,131.947939343565));
#64979=CARTESIAN_POINT('Ctrl Pts',(29.54261676689,4.81349597648854,131.814033607612));
#64980=CARTESIAN_POINT('Ctrl Pts',(29.5348520139429,4.84154926297886,131.680292898512));
#64981=CARTESIAN_POINT('Ctrl Pts',(29.5270872609958,4.86406127135682,131.545206540126));
#64982=CARTESIAN_POINT('Ctrl Pts',(29.5193225080487,4.88090808654822,131.409273266771));
#64983=CARTESIAN_POINT('Ctrl Pts',(29.5115654671637,4.89773816924527,131.273475004259));
#64984=CARTESIAN_POINT('Ctrl Pts',(29.5038084262787,4.90891420846665,131.136831886226));
#64985=CARTESIAN_POINT('Ctrl Pts',(29.4960513853937,4.91436319593427,130.999853433154));
#64986=CARTESIAN_POINT('Ctrl Pts',(29.4883001941536,4.91980807427803,130.8629782766));
#64987=CARTESIAN_POINT('Ctrl Pts',(29.4805490029135,4.91953448172863,130.725768677422));
#64988=CARTESIAN_POINT('Ctrl Pts',(29.4727978116734,4.91352120255837,130.588739527435));
#64989=CARTESIAN_POINT('Ctrl Pts',(29.4650499148963,4.90751047919213,130.451768618491));
#64990=CARTESIAN_POINT('Ctrl Pts',(29.4573020181192,4.89576493832854,130.314978395968));
#64991=CARTESIAN_POINT('Ctrl Pts',(29.4495541213421,4.87831546665287,130.178883783211));
#64992=CARTESIAN_POINT('Ctrl Pts',(29.441807845258,4.86086964503051,130.042817638512));
#64993=CARTESIAN_POINT('Ctrl Pts',(29.4340615691739,4.83772231550504,129.907447201704));
#64994=CARTESIAN_POINT('Ctrl Pts',(29.4263152930898,4.80895620269387,129.77328190909));
#64995=CARTESIAN_POINT('Ctrl Pts',(29.4185689598245,4.78018987753779,129.639115626099));
#64996=CARTESIAN_POINT('Ctrl Pts',(29.4108226265591,4.74580476829578,129.50615488733));
#64997=CARTESIAN_POINT('Ctrl Pts',(29.4030762932938,4.70593457415945,129.37489818496));
#64998=CARTESIAN_POINT('Ctrl Pts',(29.3953282252908,4.66605545136963,129.243612088563));
#64999=CARTESIAN_POINT('Ctrl Pts',(29.3875801572878,4.62068891302786,129.114031161935));
#65000=CARTESIAN_POINT('Ctrl Pts',(29.3798320892848,4.57001818099174,128.986637622194));
#65001=CARTESIAN_POINT('Ctrl Pts',(29.372075786543,4.51929359549856,128.859108687083));
#65002=CARTESIAN_POINT('Ctrl Pts',(29.3643194838012,4.46325369980301,128.733772146721));
#65003=CARTESIAN_POINT('Ctrl Pts',(29.3565631810593,4.40212966053271,128.6110896552));
#65004=CARTESIAN_POINT('Ctrl Pts',(29.3488027385451,4.34097299752225,128.48834168434));
#65005=CARTESIAN_POINT('Ctrl Pts',(29.3410422960309,4.2747269726881,128.368250927073));
#65006=CARTESIAN_POINT('Ctrl Pts',(29.3332818535168,4.20366768786337,128.251252505379));
#65007=CARTESIAN_POINT('Ctrl Pts',(29.3255089532513,4.13249433236628,128.134066267432));
#65008=CARTESIAN_POINT('Ctrl Pts',(29.3177360529859,4.05649249341213,128.019982610454));
#65009=CARTESIAN_POINT('Ctrl Pts',(29.3099631527205,3.97598090989422,127.909406582239));
#65010=CARTESIAN_POINT('Ctrl Pts',(29.3024728169585,3.89839612523374,127.802850271174));
#65011=CARTESIAN_POINT('Ctrl Pts',(29.2949824811964,3.81662397583925,127.699551235658));
#65012=CARTESIAN_POINT('Ctrl Pts',(29.2874921454344,3.73098248145132,127.599839938025));
#65013=CARTESIAN_POINT('Ctrl Pts',(29.2797178113153,3.64209386377338,127.496348056237));
#65014=CARTESIAN_POINT('Ctrl Pts',(29.2719434771962,3.54875512419509,127.396393509835));
#65015=CARTESIAN_POINT('Ctrl Pts',(29.2641691430771,3.4512786334196,127.300383041011));
#65016=CARTESIAN_POINT('Ctrl Pts',(29.2564043901301,3.35392227370753,127.204490896509));
#65017=CARTESIAN_POINT('Ctrl Pts',(29.248639637183,3.25243858496823,127.112533429913));
#65018=CARTESIAN_POINT('Ctrl Pts',(29.240874884236,3.14718018738191,127.024884472562));
#65019=CARTESIAN_POINT('Ctrl Pts',(29.233117843351,3.0420263339198,126.937322569392));
#65020=CARTESIAN_POINT('Ctrl Pts',(29.2253608024659,2.93310553097379,126.854060908083));
#65021=CARTESIAN_POINT('Ctrl Pts',(29.2176037615809,2.82080698979821,126.775436320833));
#65022=CARTESIAN_POINT('Ctrl Pts',(29.2098525703408,2.70859313382654,126.696871024996));
#65023=CARTESIAN_POINT('Ctrl Pts',(29.2021013791007,2.59300692860439,126.62293606627));
#65024=CARTESIAN_POINT('Ctrl Pts',(29.1943501878606,2.47447009957901,126.55392760565));
#65025=CARTESIAN_POINT('Ctrl Pts',(29.1866022910835,2.35598365186756,126.484948475466));
#65026=CARTESIAN_POINT('Ctrl Pts',(29.1788543943065,2.23454941182109,126.420891875084));
#65027=CARTESIAN_POINT('Ctrl Pts',(29.1711064975294,2.11061729404101,126.362010147309));
#65028=CARTESIAN_POINT('Ctrl Pts',(29.1633602214453,1.98671110018831,126.303140736321));
#65029=CARTESIAN_POINT('Ctrl Pts',(29.1556139453612,1.86030842079838,126.249444212516));
#65030=CARTESIAN_POINT('Ctrl Pts',(29.1478676692771,1.73188257373812,126.201126340095));
#65031=CARTESIAN_POINT('Ctrl Pts',(29.1401213360118,1.60345577866778,126.152808111003));
#65032=CARTESIAN_POINT('Ctrl Pts',(29.1323750027464,1.47300615205,126.109868750194));
#65033=CARTESIAN_POINT('Ctrl Pts',(29.1246286694811,1.34102535714994,126.07246521995));
#65034=CARTESIAN_POINT('Ctrl Pts',(29.1168806014782,1.2090150060656,126.035053313444));
#65035=CARTESIAN_POINT('Ctrl Pts',(29.1091325334752,1.07547318045794,126.003179810966));
#65036=CARTESIAN_POINT('Ctrl Pts',(29.1013844654722,0.940904619134276,125.976951212907));
#65037=CARTESIAN_POINT('Ctrl Pts',(29.0936281627304,0.806193036742072,125.950694738782));
#65038=CARTESIAN_POINT('Ctrl Pts',(29.0858718599885,0.670452923146452,125.930095228582));
#65039=CARTESIAN_POINT('Ctrl Pts',(29.0781155572466,0.534197632218005,125.915207730589));
#65040=CARTESIAN_POINT('Ctrl Pts',(29.0703551147325,0.397869617738221,125.900312286691));
#65041=CARTESIAN_POINT('Ctrl Pts',(29.0625946722183,0.261026267931343,125.891134955886));
#65042=CARTESIAN_POINT('Ctrl Pts',(29.0548342297042,0.124182903025224,125.887678639942));
#65043=CARTESIAN_POINT('Ctrl Pts',(29.0470613294387,-0.0128801349986252,
125.884216775612));
#65044=CARTESIAN_POINT('Ctrl Pts',(29.0392884291733,-0.149942797033939,
125.886494271963));
#65045=CARTESIAN_POINT('Ctrl Pts',(29.0315155289078,-0.28649201874362,125.894461903163));
#65046=CARTESIAN_POINT('Ctrl Pts',(29.0240251931457,-0.418077332298904,
125.9021398909));
#65047=CARTESIAN_POINT('Ctrl Pts',(29.0165348573836,-0.549185580604208,
125.915101464177));
#65048=CARTESIAN_POINT('Ctrl Pts',(29.0090445216215,-0.679366838901137,
125.933257686945));
#65049=CARTESIAN_POINT('Ctrl Pts',(29.0012701875024,-0.814483959172609,
125.952102308418));
#65050=CARTESIAN_POINT('Ctrl Pts',(28.9934958533833,-0.949030418587731,
125.97660295966));
#65051=CARTESIAN_POINT('Ctrl Pts',(28.9857215192642,-1.08249516942704,126.006716688441));
#65052=CARTESIAN_POINT('Ctrl Pts',(28.9779567663171,-1.21579543688921,126.036793304744));
#65053=CARTESIAN_POINT('Ctrl Pts',(28.97019201337,-1.34801627054872,126.072469149366));
#65054=CARTESIAN_POINT('Ctrl Pts',(28.9624272604229,-1.47865255569009,126.113649617936));
#65055=CARTESIAN_POINT('Ctrl Pts',(28.9546702195379,-1.60915909103123,126.154789185484));
#65056=CARTESIAN_POINT('Ctrl Pts',(28.9469131786529,-1.73808383931453,126.201422380083));
#65057=CARTESIAN_POINT('Ctrl Pts',(28.9391561377679,-1.86493303588192,126.253403813313));
#65058=CARTESIAN_POINT('Ctrl Pts',(28.9314049465277,-1.99168657448327,126.30534604694));
#65059=CARTESIAN_POINT('Ctrl Pts',(28.9236537552877,-2.11636731647962,126.362628343812));
#65060=CARTESIAN_POINT('Ctrl Pts',(28.9159025640475,-2.23849814033236,126.425055976618));
#65061=CARTESIAN_POINT('Ctrl Pts',(28.9081546672705,-2.36057705532702,126.487457076015));
#65062=CARTESIAN_POINT('Ctrl Pts',(28.9004067704934,-2.48010786034616,126.554998984187));
#65063=CARTESIAN_POINT('Ctrl Pts',(28.8926588737163,-2.59663506241136,126.627439572687));
#65064=CARTESIAN_POINT('Ctrl Pts',(28.8849125976322,-2.71313788949824,126.699865008177));
#65065=CARTESIAN_POINT('Ctrl Pts',(28.877166321548,-2.82663803150784,126.777186879531));
#65066=CARTESIAN_POINT('Ctrl Pts',(28.8694200454639,-2.9367065333206,126.859118191599));
#65067=CARTESIAN_POINT('Ctrl Pts',(28.8616737121986,-3.04677584763359,126.941050108465));
#65068=CARTESIAN_POINT('Ctrl Pts',(28.8539273789333,-3.15341315758425,127.027591300495));
#65069=CARTESIAN_POINT('Ctrl Pts',(28.8461810456679,-3.2562206503555,127.118412959406));
#65070=CARTESIAN_POINT('Ctrl Pts',(28.838432977665,-3.35905116615221,127.209254957198));
#65071=CARTESIAN_POINT('Ctrl Pts',(28.830684909662,-3.45804986517336,127.304379070539));
#65072=CARTESIAN_POINT('Ctrl Pts',(28.822936841659,-3.55285432196795,127.403418214441));
#65073=CARTESIAN_POINT('Ctrl Pts',(28.8151805389171,-3.64775953806741,127.502562618323));
#65074=CARTESIAN_POINT('Ctrl Pts',(28.8074242361753,-3.73846133644194,127.605630081817));
#65075=CARTESIAN_POINT('Ctrl Pts',(28.7996679334334,-3.8246359231063,127.712218460713));
#65076=CARTESIAN_POINT('Ctrl Pts',(28.7919074909192,-3.91085650374247,127.818863729037));
#65077=CARTESIAN_POINT('Ctrl Pts',(28.784147048405,-3.99254482521903,127.929033343366));
#65078=CARTESIAN_POINT('Ctrl Pts',(28.7763866058908,-4.06941990302799,128.042295318675));
#65079=CARTESIAN_POINT('Ctrl Pts',(28.7686137056254,-4.14641838753629,128.15573911216));
#65080=CARTESIAN_POINT('Ctrl Pts',(28.7608408053599,-4.21858798212553,128.272284853956));
#65081=CARTESIAN_POINT('Ctrl Pts',(28.7530679050945,-4.28569277807604,128.391474280739));
#65082=CARTESIAN_POINT('Ctrl Pts',(28.7455775693325,-4.35035814566643,128.506330871638));
#65083=CARTESIAN_POINT('Ctrl Pts',(28.7380872335705,-4.41032041768173,128.623642001074));
#65084=CARTESIAN_POINT('Ctrl Pts',(28.7305968978086,-4.46541122321864,128.742981062498));
#65085=CARTESIAN_POINT('Ctrl Pts',(28.7221355457944,-4.52764377369516,128.877790747917));
#65086=CARTESIAN_POINT('Ctrl Pts',(28.7136741937802,-4.58383185446041,129.015559555786));
#65087=CARTESIAN_POINT('Ctrl Pts',(28.705212841766,-4.63370916988232,129.155748355253));
#65088=CARTESIAN_POINT('Ctrl Pts',(28.69676164026,-4.68352665088257,129.295768979755));
#65089=CARTESIAN_POINT('Ctrl Pts',(28.6883104387542,-4.72704834146951,129.438203558761));
#65090=CARTESIAN_POINT('Ctrl Pts',(28.6798592372483,-4.76405452823403,129.582490119308));
#65091=CARTESIAN_POINT('Origin',(213.235140564004,0.,130.804360617566));
#65092=CARTESIAN_POINT('',(26.5849533738221,-4.764054528234,129.582490119308));
#65093=CARTESIAN_POINT('',(26.9301047320142,-4.76405452823399,129.582490119308));
#65094=CARTESIAN_POINT('',(213.235140564004,-4.76405452823405,129.582490119308));
#65095=CARTESIAN_POINT('',(28.2648594359576,-4.9182479151818,130.808889117301));
#65096=CARTESIAN_POINT('Ctrl Pts',(28.2648594359576,-4.9182479151818,130.808889117301));
#65097=CARTESIAN_POINT('Ctrl Pts',(28.2550046190053,-4.918087596155,130.983006102042));
#65098=CARTESIAN_POINT('Ctrl Pts',(28.2451498020529,-4.90867757925288,131.156709223396));
#65099=CARTESIAN_POINT('Ctrl Pts',(28.2352949851005,-4.89017053265966,131.329160792878));
#65100=CARTESIAN_POINT('Ctrl Pts',(28.2252357564318,-4.87127960707866,131.505189407114));
#65101=CARTESIAN_POINT('Ctrl Pts',(28.2151765277632,-4.84291035541841,131.679914228869));
#65102=CARTESIAN_POINT('Ctrl Pts',(28.2051172990946,-4.80527329238343,131.852469222629));
#65103=CARTESIAN_POINT('Ctrl Pts',(28.2011750815104,-4.79052330542128,131.920093625357));
#65104=CARTESIAN_POINT('Ctrl Pts',(28.1972328639263,-4.77435042589291,131.987385019867));
#65105=CARTESIAN_POINT('Ctrl Pts',(28.1932906463422,-4.75676929952319,132.054292173138));
#65106=CARTESIAN_POINT('Ctrl Pts',(28.1855163122231,-4.72209806495262,132.18623784924));
#65107=CARTESIAN_POINT('Ctrl Pts',(28.177741978104,-4.68187778908076,132.31694883218));
#65108=CARTESIAN_POINT('Ctrl Pts',(28.1699676439849,-4.63621148270328,132.445922724265));
#65109=CARTESIAN_POINT('Ctrl Pts',(28.1622028910378,-4.59060145596709,132.574737667555));
#65110=CARTESIAN_POINT('Ctrl Pts',(28.1544381380908,-4.53955888233867,132.701819414554));
#65111=CARTESIAN_POINT('Ctrl Pts',(28.1466733851437,-4.48323736248634,132.826677559617));
#65112=CARTESIAN_POINT('Ctrl Pts',(28.1389163442587,-4.42697178196153,132.95141169381));
#65113=CARTESIAN_POINT('Ctrl Pts',(28.1311593033737,-4.36543784898505,133.073926267028));
#65114=CARTESIAN_POINT('Ctrl Pts',(28.1234022624887,-4.29883825227731,133.19374814228));
#65115=CARTESIAN_POINT('Ctrl Pts',(28.1156510712486,-4.23228887884352,133.313479658923));
#65116=CARTESIAN_POINT('Ctrl Pts',(28.1078998800085,-4.16068163443954,133.430522179011));
#65117=CARTESIAN_POINT('Ctrl Pts',(28.1001486887683,-4.08426623563861,133.544424919535));
#65118=CARTESIAN_POINT('Ctrl Pts',(28.0924007919913,-4.00788331542061,133.658279248355));
#65119=CARTESIAN_POINT('Ctrl Pts',(28.0846528952142,-3.92669652271729,133.768996127821));
#65120=CARTESIAN_POINT('Ctrl Pts',(28.0769049984372,-3.8410000889408,133.876151850586));
#65121=CARTESIAN_POINT('Ctrl Pts',(28.0691587223531,-3.75532158101085,133.983285158684));
#65122=CARTESIAN_POINT('Ctrl Pts',(28.061412446269,-3.66513555235274,134.086858486624));
#65123=CARTESIAN_POINT('Ctrl Pts',(28.0536661701849,-3.57077765268976,134.186479778322));
#65124=CARTESIAN_POINT('Ctrl Pts',(28.0459198369196,-3.4764190564982,134.286101805402));
#65125=CARTESIAN_POINT('Ctrl Pts',(28.0381735036542,-3.37788879670492,134.381771454176));
#65126=CARTESIAN_POINT('Ctrl Pts',(28.0304271703889,-3.27556036532457,134.473132531383));
#65127=CARTESIAN_POINT('Ctrl Pts',(28.0226791023859,-3.17320901820138,134.564514068271));
#65128=CARTESIAN_POINT('Ctrl Pts',(28.0149310343829,-3.06705809853189,134.651584853269));
#65129=CARTESIAN_POINT('Ctrl Pts',(28.0071829663799,-2.95751492756948,134.73402835361));
#65130=CARTESIAN_POINT('Ctrl Pts',(27.9994266636381,-2.84785533282154,134.816559475883));
#65131=CARTESIAN_POINT('Ctrl Pts',(27.9916703608962,-2.73479659763375,134.894453253922));
#65132=CARTESIAN_POINT('Ctrl Pts',(27.9839140581544,-2.6187762943739,134.967435656828));
#65133=CARTESIAN_POINT('Ctrl Pts',(27.9761536156402,-2.50269406758489,135.04045701264));
#65134=CARTESIAN_POINT('Ctrl Pts',(27.968393173126,-2.38364746228006,135.108561576014));
#65135=CARTESIAN_POINT('Ctrl Pts',(27.9606327306118,-2.26209862660601,135.171521350354));
#65136=CARTESIAN_POINT('Ctrl Pts',(27.9528598303464,-2.14035466995034,135.234582193313));
#65137=CARTESIAN_POINT('Ctrl Pts',(27.945086930081,-2.01610081065817,135.292481578153));
#65138=CARTESIAN_POINT('Ctrl Pts',(27.9373140298156,-1.88981996739606,135.34503937226));
#65139=CARTESIAN_POINT('Ctrl Pts',(27.9298236940535,-1.76812975086793,135.395686558167));
#65140=CARTESIAN_POINT('Ctrl Pts',(27.9223333582914,-1.6445576526277,135.441373664574));
#65141=CARTESIAN_POINT('Ctrl Pts',(27.9148430225294,-1.51954717933933,135.481983885024));
#65142=CARTESIAN_POINT('Ctrl Pts',(27.9070686884103,-1.38979689596103,135.524133854325));
#65143=CARTESIAN_POINT('Ctrl Pts',(27.8992943542913,-1.2580860025425,135.560947876209));
#65144=CARTESIAN_POINT('Ctrl Pts',(27.8915200201722,-1.12489286034248,135.592241058351));
#65145=CARTESIAN_POINT('Ctrl Pts',(27.8837552672251,-0.991863866786592,
135.623495674443));
#65146=CARTESIAN_POINT('Ctrl Pts',(27.875990514278,-0.857356636063686,135.649242900046));
#65147=CARTESIAN_POINT('Ctrl Pts',(27.8682257613309,-0.721866785246101,
135.669346887522));
#65148=CARTESIAN_POINT('Ctrl Pts',(27.8604687204459,-0.586511504858237,
135.689430907434));
#65149=CARTESIAN_POINT('Ctrl Pts',(27.8527116795609,-0.450175930793075,
135.703882786299));
#65150=CARTESIAN_POINT('Ctrl Pts',(27.8449546386759,-0.313367684806054,
135.712617309776));
#65151=CARTESIAN_POINT('Ctrl Pts',(27.8372034474358,-0.176662606981544,
135.72134524648));
#65152=CARTESIAN_POINT('Ctrl Pts',(27.8294522561957,-0.0394859553105575,
135.72436438477));
#65153=CARTESIAN_POINT('Ctrl Pts',(27.8217010649556,0.0976480357871611,
135.721641159045));
#65154=CARTESIAN_POINT('Ctrl Pts',(27.8139531681785,0.234723741280308,135.718919090763));
#65155=CARTESIAN_POINT('Ctrl Pts',(27.8062052714014,0.371756432193335,135.710459520493));
#65156=CARTESIAN_POINT('Ctrl Pts',(27.7984573746243,0.508230592271119,135.696280969287));
#65157=CARTESIAN_POINT('Ctrl Pts',(27.7907110985402,0.644676204896843,135.682105383927));
#65158=CARTESIAN_POINT('Ctrl Pts',(27.7829648224562,0.780563130447971,135.662213237487));
#65159=CARTESIAN_POINT('Ctrl Pts',(27.7752185463721,0.915380094162875,135.636675005694));
#65160=CARTESIAN_POINT('Ctrl Pts',(27.7674722131067,1.05019805306598,135.611136585384));
#65161=CARTESIAN_POINT('Ctrl Pts',(27.7597258798414,1.1839456502386,135.579952069321));
#65162=CARTESIAN_POINT('Ctrl Pts',(27.7519795465761,1.3161213286455,135.543243155758));
#65163=CARTESIAN_POINT('Ctrl Pts',(27.7442314785731,1.44832660687915,135.506526021489));
#65164=CARTESIAN_POINT('Ctrl Pts',(27.7364834105701,1.57895888923273,135.464282132534));
#65165=CARTESIAN_POINT('Ctrl Pts',(27.7287353425671,1.70753170063621,135.416683086109));
#65166=CARTESIAN_POINT('Ctrl Pts',(27.7209790398253,1.83624116075369,135.36903345085));
#65167=CARTESIAN_POINT('Ctrl Pts',(27.7132227370835,1.96288641026609,135.316017424638));
#65168=CARTESIAN_POINT('Ctrl Pts',(27.7054664343416,2.08700038066533,135.257855029104));
#65169=CARTESIAN_POINT('Ctrl Pts',(27.6977059918274,2.21118059442774,135.199661590549));
#65170=CARTESIAN_POINT('Ctrl Pts',(27.6899455493133,2.33282649045845,135.136316489981));
#65171=CARTESIAN_POINT('Ctrl Pts',(27.6821851067991,2.45149644640171,135.068085307996));
#65172=CARTESIAN_POINT('Ctrl Pts',(27.6744122065337,2.57035690189312,134.99974459526));
#65173=CARTESIAN_POINT('Ctrl Pts',(27.6666393062682,2.68623154017101,134.926502336162));
#65174=CARTESIAN_POINT('Ctrl Pts',(27.6588664060028,2.79870778123177,134.848667457776));
#65175=CARTESIAN_POINT('Ctrl Pts',(27.6513760702407,2.90709522762048,134.773662073274));
#65176=CARTESIAN_POINT('Ctrl Pts',(27.6438857344786,3.01232682168215,134.694392364263));
#65177=CARTESIAN_POINT('Ctrl Pts',(27.6363953987165,3.11406456465109,134.611168328718));
#65178=CARTESIAN_POINT('Ctrl Pts',(27.6286210645974,3.21965972506633,134.52478882857));
#65179=CARTESIAN_POINT('Ctrl Pts',(27.6208467304783,3.32182535941488,134.433875601751));
#65180=CARTESIAN_POINT('Ctrl Pts',(27.6130723963593,3.42014734660246,134.338731168319));
#65181=CARTESIAN_POINT('Ctrl Pts',(27.6053076434122,3.51834816072812,134.243703991897));
#65182=CARTESIAN_POINT('Ctrl Pts',(27.597542890465,3.61271447455497,134.144456253596));
#65183=CARTESIAN_POINT('Ctrl Pts',(27.589778137518,3.70286410248391,134.041331501129));
#65184=CARTESIAN_POINT('Ctrl Pts',(27.5820210966329,3.79292419253151,133.93830917362));
#65185=CARTESIAN_POINT('Ctrl Pts',(27.5742640557479,3.87877567548259,133.831417787468));
#65186=CARTESIAN_POINT('Ctrl Pts',(27.5665070148629,3.96007247614123,133.7210383588));
#65187=CARTESIAN_POINT('Ctrl Pts',(27.5587558236228,4.0413079702501,133.610742168117));
#65188=CARTESIAN_POINT('Ctrl Pts',(27.5510046323827,4.11799538775448,133.496963484014));
#65189=CARTESIAN_POINT('Ctrl Pts',(27.5432534411426,4.18982853269809,133.380116803444));
#65190=CARTESIAN_POINT('Ctrl Pts',(27.5355055443655,4.26163114663889,133.26331978583));
#65191=CARTESIAN_POINT('Ctrl Pts',(27.5277576475883,4.32858338723187,133.14345769763));
#65192=CARTESIAN_POINT('Ctrl Pts',(27.5200097508112,4.39042218763301,133.02097426835));
#65193=CARTESIAN_POINT('Ctrl Pts',(27.5122634747271,4.4522480526902,132.898516459962));
#65194=CARTESIAN_POINT('Ctrl Pts',(27.5045171986431,4.50896242899818,132.773438749934));
#65195=CARTESIAN_POINT('Ctrl Pts',(27.496770922559,4.56034825328579,132.646209382056));
#65196=CARTESIAN_POINT('Ctrl Pts',(27.4890245892936,4.61173445689188,132.518979074999));
#65197=CARTESIAN_POINT('Ctrl Pts',(27.4812782560283,4.6577918835755,132.389597440913));
#65198=CARTESIAN_POINT('Ctrl Pts',(27.4735319227629,4.69835181769382,132.258552234814));
#65199=CARTESIAN_POINT('Ctrl Pts',(27.4657838547599,4.73892083492816,132.127477682049));
#65200=CARTESIAN_POINT('Ctrl Pts',(27.4580357867569,4.77398979422473,131.994739189362));
#65201=CARTESIAN_POINT('Ctrl Pts',(27.4502877187539,4.80344011352057,131.860838794492));
#65202=CARTESIAN_POINT('Ctrl Pts',(27.4425314160121,4.83292173296623,131.726796088689));
#65203=CARTESIAN_POINT('Ctrl Pts',(27.4347751132702,4.85677269946563,131.591589396339));
#65204=CARTESIAN_POINT('Ctrl Pts',(27.4270188105283,4.87492566151178,131.45573060247));
#65205=CARTESIAN_POINT('Ctrl Pts',(27.4192583680141,4.89308831234036,131.319799296673));
#65206=CARTESIAN_POINT('Ctrl Pts',(27.4114979255,4.90554686337682,131.183215585004));
#65207=CARTESIAN_POINT('Ctrl Pts',(27.4037374829858,4.91228604742679,131.046494569659));
#65208=CARTESIAN_POINT('Ctrl Pts',(27.3959645827204,4.91903604981327,130.909554077602));
#65209=CARTESIAN_POINT('Ctrl Pts',(27.388191682455,4.92004833529016,130.772476232594));
#65210=CARTESIAN_POINT('Ctrl Pts',(27.3804187821895,4.91535980338444,130.635775132507));
#65211=CARTESIAN_POINT('Ctrl Pts',(27.3729284464276,4.91084171142324,130.504043461739));
#65212=CARTESIAN_POINT('Ctrl Pts',(27.3654381106656,4.90103010721261,130.372661927353));
#65213=CARTESIAN_POINT('Ctrl Pts',(27.3579477749036,4.88600310423868,130.24208245876));
#65214=CARTESIAN_POINT('Ctrl Pts',(27.3501734407846,4.87040634787951,130.106552029926));
#65215=CARTESIAN_POINT('Ctrl Pts',(27.3423991066654,4.84914149626035,129.971456368493));
#65216=CARTESIAN_POINT('Ctrl Pts',(27.3346247725464,4.8222392255061,129.837307405747));
#65217=CARTESIAN_POINT('Ctrl Pts',(27.3268600195993,4.79537010939626,129.703323769607));
#65218=CARTESIAN_POINT('Ctrl Pts',(27.3190952666522,4.76287747397065,129.57028489038));
#65219=CARTESIAN_POINT('Ctrl Pts',(27.3113305137051,4.72484377499819,129.438698007563));
#65220=CARTESIAN_POINT('Ctrl Pts',(27.3035734728201,4.68684785163173,129.307241818693));
#65221=CARTESIAN_POINT('Ctrl Pts',(27.2958164319351,4.64332192471477,129.177235129463));
#65222=CARTESIAN_POINT('Ctrl Pts',(27.2880593910501,4.59439949180924,129.049175051262));
#65223=CARTESIAN_POINT('Ctrl Pts',(27.28030819981,4.54551395169086,128.921211544161));
#65224=CARTESIAN_POINT('Ctrl Pts',(27.2725570085698,4.49124014473066,128.795192089957));
#65225=CARTESIAN_POINT('Ctrl Pts',(27.2648058173297,4.43176129256114,128.671598345709));
#65226=CARTESIAN_POINT('Ctrl Pts',(27.2570579205526,4.37230772049045,128.548057132099));
#65227=CARTESIAN_POINT('Ctrl Pts',(27.2493100237755,4.30765367245697,128.426939929435));
#65228=CARTESIAN_POINT('Ctrl Pts',(27.2415621269984,4.23803027660593,128.308707909942));
#65229=CARTESIAN_POINT('Ctrl Pts',(27.2338158509143,4.1684214444684,128.190500622038));
#65230=CARTESIAN_POINT('Ctrl Pts',(27.2260695748303,4.09384553035747,128.075177653553));
#65231=CARTESIAN_POINT('Ctrl Pts',(27.2183232987462,4.0145791530345,127.963174723169));
#65232=CARTESIAN_POINT('Ctrl Pts',(27.2105769654808,3.93531219058525,127.851170966005));
#65233=CARTESIAN_POINT('Ctrl Pts',(27.2028306322155,3.8513549216881,127.742487614977));
#65234=CARTESIAN_POINT('Ctrl Pts',(27.1950842989501,3.76302651352613,127.637530258832));
#65235=CARTESIAN_POINT('Ctrl Pts',(27.1873362309472,3.67467832482958,127.532549398215));
#65236=CARTESIAN_POINT('Ctrl Pts',(27.1795881629443,3.58195730068962,127.431296491939));
#65237=CARTESIAN_POINT('Ctrl Pts',(27.1718400949413,3.48522172317316,127.334142670113));
#65238=CARTESIAN_POINT('Ctrl Pts',(27.1640837921995,3.38838333393362,127.236885592049));
#65239=CARTESIAN_POINT('Ctrl Pts',(27.1563274894576,3.28752214439158,127.143736578616));
#65240=CARTESIAN_POINT('Ctrl Pts',(27.1485711867157,3.18303241278574,127.055028980907));
#65241=CARTESIAN_POINT('Ctrl Pts',(27.1408107442015,3.07848691186388,126.966274037281));
#65242=CARTESIAN_POINT('Ctrl Pts',(27.1330503016873,2.97030931813767,126.88196547305));
#65243=CARTESIAN_POINT('Ctrl Pts',(27.1252898591732,2.85892474937989,126.802394558254));
#65244=CARTESIAN_POINT('Ctrl Pts',(27.1175169589077,2.74736137622423,126.722695909162));
#65245=CARTESIAN_POINT('Ctrl Pts',(27.1097440586423,2.63258106799976,126.647750321182));
#65246=CARTESIAN_POINT('Ctrl Pts',(27.1019711583768,2.51503629490142,126.577804632153));
#65247=CARTESIAN_POINT('Ctrl Pts',(27.0944808226147,2.40176457038167,126.510401645103));
#65248=CARTESIAN_POINT('Ctrl Pts',(27.0869904868527,2.2859261528447,126.447641497095));
#65249=CARTESIAN_POINT('Ctrl Pts',(27.0795001510906,2.16794348555073,126.389702747928));
#65250=CARTESIAN_POINT('Ctrl Pts',(27.0717258169715,2.04548746956728,126.329567233476));
#65251=CARTESIAN_POINT('Ctrl Pts',(27.0639514828524,1.92033349177264,126.274435450496));
#65252=CARTESIAN_POINT('Ctrl Pts',(27.0561771487333,1.7929288356507,126.224558301658));
#65253=CARTESIAN_POINT('Ctrl Pts',(27.0484123957862,1.66568119438094,126.174742621949));
#65254=CARTESIAN_POINT('Ctrl Pts',(27.0406476428391,1.53618875430544,126.130168832494));
#65255=CARTESIAN_POINT('Ctrl Pts',(27.0328828898921,1.40492283973767,126.091041736259));
#65256=CARTESIAN_POINT('Ctrl Pts',(27.025125849007,1.27378730032678,126.051953501608));
#65257=CARTESIAN_POINT('Ctrl Pts',(27.017368808122,1.1408821640186,126.018301305523));
#65258=CARTESIAN_POINT('Ctrl Pts',(27.009611767237,1.00669782339524,125.990241533572));
#65259=CARTESIAN_POINT('Ctrl Pts',(27.0018605759969,0.872614672226939,125.962202921714));
#65260=CARTESIAN_POINT('Ctrl Pts',(26.9941093847568,0.73725461797565,125.939748419431));
#65261=CARTESIAN_POINT('Ctrl Pts',(26.9863581935166,0.601121928133267,125.922984224578));
#65262=CARTESIAN_POINT('Ctrl Pts',(26.9786102967395,0.46504709831534,125.906227154956));
#65263=CARTESIAN_POINT('Ctrl Pts',(26.9708623999624,0.328200673272089,125.895155630173));
#65264=CARTESIAN_POINT('Ctrl Pts',(26.9631145031854,0.191095580663751,125.889824470425));
#65265=CARTESIAN_POINT('Ctrl Pts',(26.9553682271012,0.0540191674853299,
125.884494425842));
#65266=CARTESIAN_POINT('Ctrl Pts',(26.9476219510171,-0.0833154152125675,
125.884902373097));
#65267=CARTESIAN_POINT('Ctrl Pts',(26.939875674933,-0.220392065764167,125.891051101583));
#65268=CARTESIAN_POINT('Ctrl Pts',(26.9321293416677,-0.357469728184462,
125.897199875458));
#65269=CARTESIAN_POINT('Ctrl Pts',(26.9243830084023,-0.494289064086698,
125.909089497605));
#65270=CARTESIAN_POINT('Ctrl Pts',(26.9166366751369,-0.630336322510923,
125.926670674261));
#65271=CARTESIAN_POINT('Ctrl Pts',(26.908888607134,-0.766414047775387,125.944255788098));
#65272=CARTESIAN_POINT('Ctrl Pts',(26.901140539131,-0.901718963841309,125.967534942622));
#65273=CARTESIAN_POINT('Ctrl Pts',(26.893392471128,-1.03574516822834,125.996407309869));
#65274=CARTESIAN_POINT('Ctrl Pts',(26.8856361683862,-1.16991381726033,126.025310363013));
#65275=CARTESIAN_POINT('Ctrl Pts',(26.8778798656443,-1.30280065699779,126.05981842126));
#65276=CARTESIAN_POINT('Ctrl Pts',(26.8701235629024,-1.43391212351709,126.099779968397));
#65277=CARTESIAN_POINT('Ctrl Pts',(26.8623631203883,-1.56509356817394,126.139762844216));
#65278=CARTESIAN_POINT('Ctrl Pts',(26.8546026778741,-1.69449738279775,126.185204879249));
#65279=CARTESIAN_POINT('Ctrl Pts',(26.8468422353599,-1.82164872711363,126.235905848445));
#65280=CARTESIAN_POINT('Ctrl Pts',(26.8390693350945,-1.9490041860552,126.286688207338));
#65281=CARTESIAN_POINT('Ctrl Pts',(26.831296434829,-2.07409959205256,126.342746210443));
#65282=CARTESIAN_POINT('Ctrl Pts',(26.8235235345636,-2.19648270224759,126.403832603654));
#65283=CARTESIAN_POINT('Ctrl Pts',(26.8160331988016,-2.31441687812141,126.462698352603));
#65284=CARTESIAN_POINT('Ctrl Pts',(26.8085428630397,-2.42983226228726,126.52623310099));
#65285=CARTESIAN_POINT('Ctrl Pts',(26.8010525272777,-2.54235028642948,126.594177951269));
#65286=CARTESIAN_POINT('Ctrl Pts',(26.7932769255178,-2.65915350785349,126.66471044997));
#65287=CARTESIAN_POINT('Ctrl Pts',(26.7855013237579,-2.7732043645862,126.740219083085));
#65288=CARTESIAN_POINT('Ctrl Pts',(26.777725721998,-2.88404977769799,126.820463035767));
#65289=CARTESIAN_POINT('Ctrl Pts',(26.769693540824,-2.99855286927972,126.903354879506));
#65290=CARTESIAN_POINT('Ctrl Pts',(26.76166135965,-3.10963493645122,126.991299800931));
#65291=CARTESIAN_POINT('Ctrl Pts',(26.753629178476,-3.21682377204222,127.083980545299));
#65292=CARTESIAN_POINT('Ctrl Pts',(26.74587310756,-3.32032793762808,127.173475342576));
#65293=CARTESIAN_POINT('Ctrl Pts',(26.738117036644,-3.42020176294556,127.267385488728));
#65294=CARTESIAN_POINT('Ctrl Pts',(26.730360965728,-3.51604985092081,127.365381625432));
#65295=CARTESIAN_POINT('Ctrl Pts',(26.7226102075952,-3.61183228450382,127.463310636365));
#65296=CARTESIAN_POINT('Ctrl Pts',(26.7148594494626,-3.70359419500579,127.565319790991));
#65297=CARTESIAN_POINT('Ctrl Pts',(26.7071086913299,-3.79097497367265,127.671041002288));
#65298=CARTESIAN_POINT('Ctrl Pts',(26.6993615637294,-3.87831482231281,127.776712692716));
#65299=CARTESIAN_POINT('Ctrl Pts',(26.6916144361289,-3.96127737484887,127.886092678676));
#65300=CARTESIAN_POINT('Ctrl Pts',(26.6838673085285,-4.03954073810423,127.998778024289));
#65301=CARTESIAN_POINT('Ctrl Pts',(26.676122132029,-4.1177843908648,128.111434990291));
#65302=CARTESIAN_POINT('Ctrl Pts',(26.6683769555294,-4.19133098842976,128.227395337436));
#65303=CARTESIAN_POINT('Ctrl Pts',(26.6606317790299,-4.25990083556751,128.346225565615));
#65304=CARTESIAN_POINT('Ctrl Pts',(26.6528849935841,-4.32848492708036,128.465080479022));
#65305=CARTESIAN_POINT('Ctrl Pts',(26.6451382081383,-4.39209000396303,128.586806127822));
#65306=CARTESIAN_POINT('Ctrl Pts',(26.6373914226925,-4.45048139914605,128.710942747585));
#65307=CARTESIAN_POINT('Ctrl Pts',(26.629643615013,-4.50888049941597,128.835095747904));
#65308=CARTESIAN_POINT('Ctrl Pts',(26.6218958073334,-4.5620643888499,128.961659995719));
#65309=CARTESIAN_POINT('Ctrl Pts',(26.6141479996539,-4.60984614003261,129.090154787531));
#65310=CARTESIAN_POINT('Ctrl Pts',(26.606395229731,-4.65765849402371,129.218731876484));
#65311=CARTESIAN_POINT('Ctrl Pts',(26.5986424598082,-4.70006167527236,129.349241608434));
#65312=CARTESIAN_POINT('Ctrl Pts',(26.5908896898854,-4.73691828870304,129.481187088262));
#65313=CARTESIAN_POINT('Ctrl Pts',(26.5889109178643,-4.74632535690903,129.514864087115));
#65314=CARTESIAN_POINT('Ctrl Pts',(26.5869321458431,-4.75537135427362,129.548634555822));
#65315=CARTESIAN_POINT('Ctrl Pts',(26.584953373822,-4.764054528234,129.582490119308));
#65316=CARTESIAN_POINT('Ctrl Pts',(28.3348598006328,-4.76405452823408,129.582490119308));
#65317=CARTESIAN_POINT('Ctrl Pts',(28.3271967665533,-4.79779799805008,129.714055395992));
#65318=CARTESIAN_POINT('Ctrl Pts',(28.3195337324737,-4.82608509567171,129.847011134992));
#65319=CARTESIAN_POINT('Ctrl Pts',(28.3118706983942,-4.84881738849676,129.980860164918));
#65320=CARTESIAN_POINT('Ctrl Pts',(28.3040354879937,-4.8720604401812,130.117716571987));
#65321=CARTESIAN_POINT('Ctrl Pts',(28.2962002775933,-4.88949601255481,130.255506459426));
#65322=CARTESIAN_POINT('Ctrl Pts',(28.2883650671927,-4.90107474611519,130.393691169601));
#65323=CARTESIAN_POINT('Ctrl Pts',(28.2805298567922,-4.91265347967555,130.531875879776));
#65324=CARTESIAN_POINT('Ctrl Pts',(28.2726946463917,-4.91837537905588,130.670454966552));
#65325=CARTESIAN_POINT('Ctrl Pts',(28.2648594359912,-4.91824791518235,130.808889116708));
#65326=CARTESIAN_POINT('',(28.6101405640463,-4.91824967358338,130.802568747881));
#65327=CARTESIAN_POINT('Ctrl Pts',(28.6798592372483,-4.76405452823403,129.582490119308));
#65328=CARTESIAN_POINT('Ctrl Pts',(28.6714381530766,-4.80092883698196,129.726262489471));
#65329=CARTESIAN_POINT('Ctrl Pts',(28.6630170689048,-4.83133387643135,129.871873410875));
#65330=CARTESIAN_POINT('Ctrl Pts',(28.6545959847331,-4.85509965397195,130.018745945795));
#65331=CARTESIAN_POINT('Ctrl Pts',(28.6462045412791,-4.87878178020488,130.16510151553));
#65332=CARTESIAN_POINT('Ctrl Pts',(28.6378130978251,-4.89587119819743,130.312709571153));
#65333=CARTESIAN_POINT('Ctrl Pts',(28.6294216543711,-4.90624850217443,130.460982258593));
#65334=CARTESIAN_POINT('Ctrl Pts',(28.6229946242628,-4.91419650843435,130.574544726317));
#65335=CARTESIAN_POINT('Ctrl Pts',(28.6165675941545,-4.91820811362474,130.688496695248));
#65336=CARTESIAN_POINT('Ctrl Pts',(28.6101405640463,-4.91824967358338,130.802568747881));
#65337=CARTESIAN_POINT('Ctrl Pts',(28.6101405640087,-4.91824967358362,130.802568748549));
#65338=CARTESIAN_POINT('Ctrl Pts',(28.6022183214708,-4.91830090221393,130.943179023052));
#65339=CARTESIAN_POINT('Ctrl Pts',(28.594296078933,-4.91231781269187,131.083747826792));
#65340=CARTESIAN_POINT('Ctrl Pts',(28.5863738363952,-4.90033740463775,131.223736800972));
#65341=CARTESIAN_POINT('Ctrl Pts',(28.5784473695675,-4.88835060840305,131.363800419925));
#65342=CARTESIAN_POINT('Ctrl Pts',(28.5705209027398,-4.87036015166487,131.50328322899));
#65343=CARTESIAN_POINT('Ctrl Pts',(28.5625944359122,-4.84645477838846,131.641653364182));
#65344=CARTESIAN_POINT('Ctrl Pts',(28.5546623705243,-4.82253252045522,131.780121231889));
#65345=CARTESIAN_POINT('Ctrl Pts',(28.5467303051364,-4.7926870820956,131.917474499724));
#65346=CARTESIAN_POINT('Ctrl Pts',(28.5387982397485,-4.75705801439906,132.053192916212));
#65347=CARTESIAN_POINT('Ctrl Pts',(28.5308534277911,-4.72137169195654,132.189129427755));
#65348=CARTESIAN_POINT('Ctrl Pts',(28.5229086158336,-4.67988326406572,132.323425485124));
#65349=CARTESIAN_POINT('Ctrl Pts',(28.5149638038762,-4.63278206483875,132.455576352171));
#65350=CARTESIAN_POINT('Ctrl Pts',(28.5070120490144,-4.58563970427,132.58784270475));
#65351=CARTESIAN_POINT('Ctrl Pts',(28.4990602941526,-4.53287492916211,132.717959791013));
#65352=CARTESIAN_POINT('Ctrl Pts',(28.4911085392909,-4.47472447691595,132.845444623233));
#65353=CARTESIAN_POINT('Ctrl Pts',(28.4831421766297,-4.41646719917555,132.973163651916));
#65354=CARTESIAN_POINT('Ctrl Pts',(28.4751758139685,-4.35280463859669,133.09824043786));
#65355=CARTESIAN_POINT('Ctrl Pts',(28.4672094513074,-4.28401911945446,133.220217245483));
#65356=CARTESIAN_POINT('Ctrl Pts',(28.4621893922034,-4.24067344385904,133.297081783241));
#65357=CARTESIAN_POINT('Ctrl Pts',(28.4571693330995,-4.19529432823964,133.372715901334));
#65358=CARTESIAN_POINT('Ctrl Pts',(28.4521492739956,-4.14796084086393,133.447011545169));
#65359=CARTESIAN_POINT('Ctrl Pts',(28.4443749398765,-4.0746576509486,133.562069783888));
#65360=CARTESIAN_POINT('Ctrl Pts',(28.4366006057574,-3.99644741041953,133.67425797368));
#65361=CARTESIAN_POINT('Ctrl Pts',(28.4288262716383,-3.91358161057447,133.783129161759));
#65362=CARTESIAN_POINT('Ctrl Pts',(28.4210615186912,-3.8308179354218,133.891866175829));
#65363=CARTESIAN_POINT('Ctrl Pts',(28.4132967657442,-3.74341035150631,133.99729401379));
#65364=CARTESIAN_POINT('Ctrl Pts',(28.4055320127971,-3.6516548624765,134.0989925891));
#65365=CARTESIAN_POINT('Ctrl Pts',(28.3977749719121,-3.55999050629192,134.200590155951));
#65366=CARTESIAN_POINT('Ctrl Pts',(28.3900179310271,-3.46398709900981,134.298465542789));
#65367=CARTESIAN_POINT('Ctrl Pts',(28.382260890142,-3.36398211539322,134.392230095378));
#65368=CARTESIAN_POINT('Ctrl Pts',(28.3745096989019,-3.26405254631271,134.485923939389));
#65369=CARTESIAN_POINT('Ctrl Pts',(28.3667585076618,-3.16012769134259,134.575512853207));
#65370=CARTESIAN_POINT('Ctrl Pts',(28.3590073164217,-3.05258298181562,134.660643828331));
#65371=CARTESIAN_POINT('Ctrl Pts',(28.3512594196446,-2.94508398165919,134.74573862052));
#65372=CARTESIAN_POINT('Ctrl Pts',(28.3435115228675,-2.833968492879,134.826379000362));
#65373=CARTESIAN_POINT('Ctrl Pts',(28.3357636260904,-2.71964606867674,134.902251333975));
#65374=CARTESIAN_POINT('Ctrl Pts',(28.3280173500063,-2.60534755826111,134.978107796731));
#65375=CARTESIAN_POINT('Ctrl Pts',(28.3202710739223,-2.48784377227086,135.04919798103));
#65376=CARTESIAN_POINT('Ctrl Pts',(28.3125247978382,-2.36757404003198,135.115251039215));
#65377=CARTESIAN_POINT('Ctrl Pts',(28.3047784645728,-2.24730341998926,135.181304584989));
#65378=CARTESIAN_POINT('Ctrl Pts',(28.2970321313075,-2.1242671556406,135.242320742248));
#65379=CARTESIAN_POINT('Ctrl Pts',(28.2892857980421,-1.99892966125069,135.298074368115));
#65380=CARTESIAN_POINT('Ctrl Pts',(28.2815377300391,-1.8735640983976,135.35384047962));
#65381=CARTESIAN_POINT('Ctrl Pts',(28.2737896620362,-1.74589663717662,135.404341555771));
#65382=CARTESIAN_POINT('Ctrl Pts',(28.2660415940332,-1.61641179581979,135.449400549454));
#65383=CARTESIAN_POINT('Ctrl Pts',(28.2582852912913,-1.48678933643303,135.494507432372));
#65384=CARTESIAN_POINT('Ctrl Pts',(28.2505289885495,-1.35534600830051,135.534160550141));
#65385=CARTESIAN_POINT('Ctrl Pts',(28.2427726858077,-1.22258215879735,135.568232564574));
#65386=CARTESIAN_POINT('Ctrl Pts',(28.2350122432935,-1.08974744922992,135.602322764267));
#65387=CARTESIAN_POINT('Ctrl Pts',(28.2272518007793,-0.955591196156083,
135.630825843896));
#65388=CARTESIAN_POINT('Ctrl Pts',(28.2194913582651,-0.820623093209166,
135.653665805053));
#65389=CARTESIAN_POINT('Ctrl Pts',(28.2117184579997,-0.685438327481676,
135.676542430944));
#65390=CARTESIAN_POINT('Ctrl Pts',(28.2039455577342,-0.549439495665727,
135.693737722699));
#65391=CARTESIAN_POINT('Ctrl Pts',(28.1961726574688,-0.41314145544745,135.70522760212));
#65392=CARTESIAN_POINT('Ctrl Pts',(28.1886823217068,-0.281798192305892,
135.716299795483));
#65393=CARTESIAN_POINT('Ctrl Pts',(28.1811919859448,-0.150177404762075,
135.722074173482));
#65394=CARTESIAN_POINT('Ctrl Pts',(28.1737016501829,-0.0187370849083707,
135.722574926047));
#65395=CARTESIAN_POINT('Ctrl Pts',(28.1659273160638,0.117686834623777,135.723094664799));
#65396=CARTESIAN_POINT('Ctrl Pts',(28.1581529819447,0.254348481427725,135.717934631344));
#65397=CARTESIAN_POINT('Ctrl Pts',(28.1503786478256,0.390735884276925,135.707064823536));
#65398=CARTESIAN_POINT('Ctrl Pts',(28.1426138948785,0.526955201841035,135.696208411795));
#65399=CARTESIAN_POINT('Ctrl Pts',(28.1348491419315,0.662900561944117,135.679656257572));
#65400=CARTESIAN_POINT('Ctrl Pts',(28.1270843889844,0.798058536678102,135.657430330081));
#65401=CARTESIAN_POINT('Ctrl Pts',(28.1193273480994,0.933082270606188,135.635226477696));
#65402=CARTESIAN_POINT('Ctrl Pts',(28.1115703072144,1.0673197921771,135.607360129517));
#65403=CARTESIAN_POINT('Ctrl Pts',(28.1038132663294,1.20026170222267,135.573905135513));
#65404=CARTESIAN_POINT('Ctrl Pts',(28.0960620750893,1.33310335974009,135.54047537018));
#65405=CARTESIAN_POINT('Ctrl Pts',(28.0883108838492,1.46465097284247,135.501465442639));
#65406=CARTESIAN_POINT('Ctrl Pts',(28.0805596926091,1.59440461567362,135.457000404184));
#65407=CARTESIAN_POINT('Ctrl Pts',(28.072811795832,1.7241031097451,135.412554264556));
#65408=CARTESIAN_POINT('Ctrl Pts',(28.0650638990549,1.85200878099351,135.362657751947));
#65409=CARTESIAN_POINT('Ctrl Pts',(28.0573160022778,1.97763638683973,135.307485908289));
#65410=CARTESIAN_POINT('Ctrl Pts',(28.0495697261937,2.10323771409902,135.252325605391));
#65411=CARTESIAN_POINT('Ctrl Pts',(28.0418234501096,2.22656156604584,135.191892323445));
#65412=CARTESIAN_POINT('Ctrl Pts',(28.0340771740255,2.34714260264339,135.126409282882));
#65413=CARTESIAN_POINT('Ctrl Pts',(28.0263308407602,2.46772452934292,135.060925758937));
#65414=CARTESIAN_POINT('Ctrl Pts',(28.0185845074948,2.58556325672055,134.990392588573));
#65415=CARTESIAN_POINT('Ctrl Pts',(28.0108381742294,2.70021833844389,134.91507880144));
#65416=CARTESIAN_POINT('Ctrl Pts',(28.0030901062264,2.81489909637797,134.839748148306));
#65417=CARTESIAN_POINT('Ctrl Pts',(27.9953420382235,2.92639446324936,134.759634962667));
#65418=CARTESIAN_POINT('Ctrl Pts',(27.9875939702205,3.03429359036853,134.675051185145));
#65419=CARTESIAN_POINT('Ctrl Pts',(27.9798376674786,3.14230739396372,134.590377510978));
#65420=CARTESIAN_POINT('Ctrl Pts',(27.9720813647368,3.24671701451504,134.501223995088));
#65421=CARTESIAN_POINT('Ctrl Pts',(27.9643250619949,3.347144868821,134.407942764489));
#65422=CARTESIAN_POINT('Ctrl Pts',(27.9565646194808,3.44762632449677,134.31461174689));
#65423=CARTESIAN_POINT('Ctrl Pts',(27.9488041769666,3.54412150437218,134.217148902442));
#65424=CARTESIAN_POINT('Ctrl Pts',(27.9410437344524,3.63629096697756,134.11594197184));
#65425=CARTESIAN_POINT('Ctrl Pts',(27.933270834187,3.72860838818661,134.014572574889));
#65426=CARTESIAN_POINT('Ctrl Pts',(27.9254979339216,3.81658596468831,133.909447381207));
#65427=CARTESIAN_POINT('Ctrl Pts',(27.9177250336562,3.89992514565808,133.800986540294));
#65428=CARTESIAN_POINT('Ctrl Pts',(27.9102346978941,3.98023473748121,133.696468524143));
#65429=CARTESIAN_POINT('Ctrl Pts',(27.9027443621321,4.05623713591522,133.588853420243));
#65430=CARTESIAN_POINT('Ctrl Pts',(27.89525402637,4.12770513672061,133.478539625559));
#65431=CARTESIAN_POINT('Ctrl Pts',(27.8874796922509,4.20188286849857,133.364043249821));
#65432=CARTESIAN_POINT('Ctrl Pts',(27.8797053581318,4.27141054445722,133.246276811783));
#65433=CARTESIAN_POINT('Ctrl Pts',(27.8719310240127,4.33598618998724,133.125654830444));
#65434=CARTESIAN_POINT('Ctrl Pts',(27.8641662710656,4.40048225180552,133.005181504917));
#65435=CARTESIAN_POINT('Ctrl Pts',(27.8564015181186,4.46003824346202,132.881859979622));
#65436=CARTESIAN_POINT('Ctrl Pts',(27.8486367651714,4.51439512795429,132.756134090898));
#65437=CARTESIAN_POINT('Ctrl Pts',(27.8408797242864,4.56869802442259,132.630533074899));
#65438=CARTESIAN_POINT('Ctrl Pts',(27.8331226834014,4.61781193582661,132.502532804333));
#65439=CARTESIAN_POINT('Ctrl Pts',(27.8253656425164,4.66152365154309,132.372601768858));
#65440=CARTESIAN_POINT('Ctrl Pts',(27.8176144512763,4.70520240391442,132.242768715388));
#65441=CARTESIAN_POINT('Ctrl Pts',(27.8098632600362,4.74348694516597,132.111008164157));
#65442=CARTESIAN_POINT('Ctrl Pts',(27.8021120687961,4.7762122623572,131.977808310226));
#65443=CARTESIAN_POINT('Ctrl Pts',(27.7943641720191,4.80892367041582,131.844665069785));
#65444=CARTESIAN_POINT('Ctrl Pts',(27.7866162752419,4.83608046079466,131.710084122231));
#65445=CARTESIAN_POINT('Ctrl Pts',(27.7788683784649,4.85756761576195,131.57456833033));
#65446=CARTESIAN_POINT('Ctrl Pts',(27.7711221023808,4.87905027607967,131.43908088541));
#65447=CARTESIAN_POINT('Ctrl Pts',(27.7633758262966,4.89486559874909,131.302659370997));
#65448=CARTESIAN_POINT('Ctrl Pts',(27.7556295502125,4.90494985778331,131.165815946938));
#65449=CARTESIAN_POINT('Ctrl Pts',(27.7478832169472,4.91503419125721,131.028971512732));
#65450=CARTESIAN_POINT('Ctrl Pts',(27.7401368836819,4.91938734794547,130.891705552573));
#65451=CARTESIAN_POINT('Ctrl Pts',(27.7323905504165,4.91799759811043,130.754534043532));
#65452=CARTESIAN_POINT('Ctrl Pts',(27.7246424824135,4.91660753705056,130.617331815881));
#65453=CARTESIAN_POINT('Ctrl Pts',(27.7168944144105,4.90947201426901,130.480224472309));
#65454=CARTESIAN_POINT('Ctrl Pts',(27.7091463464075,4.89663140049338,130.343726282977));
#65455=CARTESIAN_POINT('Ctrl Pts',(27.7013900436656,4.88377713956064,130.207083021746));
#65456=CARTESIAN_POINT('Ctrl Pts',(27.6936337409238,4.86520571193757,130.071050597907));
#65457=CARTESIAN_POINT('Ctrl Pts',(27.685877438182,4.84100927911253,129.936137016155));
#65458=CARTESIAN_POINT('Ctrl Pts',(27.6781169956678,4.81679993192274,129.801151426963));
#65459=CARTESIAN_POINT('Ctrl Pts',(27.6703565531536,4.78695968234598,129.667286251162));
#65460=CARTESIAN_POINT('Ctrl Pts',(27.6625961106394,4.75163127120419,129.535036653791));
#65461=CARTESIAN_POINT('Ctrl Pts',(27.654823210374,4.71624614776048,129.402574757625));
#65462=CARTESIAN_POINT('Ctrl Pts',(27.6470503101086,4.67535537408643,129.271733995848));
#65463=CARTESIAN_POINT('Ctrl Pts',(27.6392774098431,4.62915105984179,129.142992648793));
#65464=CARTESIAN_POINT('Ctrl Pts',(27.6317870740811,4.58462638880153,129.018931373982));
#65465=CARTESIAN_POINT('Ctrl Pts',(27.624296738319,4.53516790688726,128.896819811377));
#65466=CARTESIAN_POINT('Ctrl Pts',(27.616806402557,4.48098798730894,128.77706445763));
#65467=CARTESIAN_POINT('Ctrl Pts',(27.6090320684379,4.42475381961234,128.652768543246));
#65468=CARTESIAN_POINT('Ctrl Pts',(27.6012577343187,4.36325498713541,128.530617303972));
#65469=CARTESIAN_POINT('Ctrl Pts',(27.5934834001997,4.29667701179976,128.411088857241));
#65470=CARTESIAN_POINT('Ctrl Pts',(27.5857186472526,4.23018108786846,128.291707718638));
#65471=CARTESIAN_POINT('Ctrl Pts',(27.5779538943055,4.15861866421749,128.174943279426));
#65472=CARTESIAN_POINT('Ctrl Pts',(27.5701891413584,4.0822231371006,128.061253379155));
#65473=CARTESIAN_POINT('Ctrl Pts',(27.5624321004734,4.00590348709822,127.947676397296));
#65474=CARTESIAN_POINT('Ctrl Pts',(27.5546750595884,3.92476050310255,127.837168199832));
#65475=CARTESIAN_POINT('Ctrl Pts',(27.5469180187034,3.8390730931821,127.730161397004));
#65476=CARTESIAN_POINT('Ctrl Pts',(27.5391668274633,3.75345030080436,127.623235288838));
#65477=CARTESIAN_POINT('Ctrl Pts',(27.5314156362232,3.66329014709929,127.519805623638));
#65478=CARTESIAN_POINT('Ctrl Pts',(27.5236644449831,3.56891417087302,127.420275112819));
#65479=CARTESIAN_POINT('Ctrl Pts',(27.515916548206,3.47457830695383,127.320786905121));
#65480=CARTESIAN_POINT('Ctrl Pts',(27.508168651429,3.37603045278773,127.22519483878));
#65481=CARTESIAN_POINT('Ctrl Pts',(27.5004207546519,3.27363151116684,127.133867491078));
#65482=CARTESIAN_POINT('Ctrl Pts',(27.4926744785678,3.17125398919736,127.042559247089));
#65483=CARTESIAN_POINT('Ctrl Pts',(27.4849282024837,3.06502727367775,126.955514207393));
#65484=CARTESIAN_POINT('Ctrl Pts',(27.4771819263996,2.95534781373978,126.873062821377));
#65485=CARTESIAN_POINT('Ctrl Pts',(27.4694355931343,2.84566754417265,126.790610826722));
#65486=CARTESIAN_POINT('Ctrl Pts',(27.4616892598689,2.73253479183859,126.712752788339));
#65487=CARTESIAN_POINT('Ctrl Pts',(27.4539429266035,2.61637732265057,126.639777472998));
#65488=CARTESIAN_POINT('Ctrl Pts',(27.4461948586006,2.50019384080285,126.566785815341));
#65489=CARTESIAN_POINT('Ctrl Pts',(27.4384467905975,2.3809846252153,126.498679264512));
#65490=CARTESIAN_POINT('Ctrl Pts',(27.4306987225946,2.25920416730621,126.435701831059));
#65491=CARTESIAN_POINT('Ctrl Pts',(27.4229424198527,2.13729427967708,126.37265746444));
#65492=CARTESIAN_POINT('Ctrl Pts',(27.4151861171109,2.01280803860045,126.314753284608));
#65493=CARTESIAN_POINT('Ctrl Pts',(27.407429814369,1.88622265834908,126.262186342438));
#65494=CARTESIAN_POINT('Ctrl Pts',(27.3996693718548,1.75956971566852,126.209591343709));
#65495=CARTESIAN_POINT('Ctrl Pts',(27.3919089293407,1.6308157682231,126.162339393438));
#65496=CARTESIAN_POINT('Ctrl Pts',(27.3841484868265,1.50045456728431,126.120578048529));
#65497=CARTESIAN_POINT('Ctrl Pts',(27.376375586561,1.36988409897321,126.078749664602));
#65498=CARTESIAN_POINT('Ctrl Pts',(27.3686026862956,1.23770159850452,126.042429602877));
#65499=CARTESIAN_POINT('Ctrl Pts',(27.3608297860301,1.1044132966301,126.01171475826));
#65500=CARTESIAN_POINT('Ctrl Pts',(27.3533394502681,0.975970360262141,125.98211647561));
#65501=CARTESIAN_POINT('Ctrl Pts',(27.3458491145061,0.84650092669847,125.957723014853));
#65502=CARTESIAN_POINT('Ctrl Pts',(27.3383587787441,0.716461785993515,125.938575421761));
#65503=CARTESIAN_POINT('Ctrl Pts',(27.330584444625,0.581492171743992,125.918701841858));
#65504=CARTESIAN_POINT('Ctrl Pts',(27.322810110506,0.445481253493059,125.904416822821));
#65505=CARTESIAN_POINT('Ctrl Pts',(27.3150357763869,0.308931564110554,125.895822713954));
#65506=CARTESIAN_POINT('Ctrl Pts',(27.3072710234398,0.172550160016417,125.887239196558));
#65507=CARTESIAN_POINT('Ctrl Pts',(27.2995062704927,0.0356316923748154,
125.884332658805));
#65508=CARTESIAN_POINT('Ctrl Pts',(27.2917415175457,-0.101312489059482,
125.887154211276));
#65509=CARTESIAN_POINT('Ctrl Pts',(27.2839844766607,-0.238120655601647,
125.889972961341));
#65510=CARTESIAN_POINT('Ctrl Pts',(27.2762274357757,-0.37495409675927,125.898508471823));
#65511=CARTESIAN_POINT('Ctrl Pts',(27.2684703948908,-0.511298088661625,
125.912759925867));
#65512=CARTESIAN_POINT('Ctrl Pts',(27.2607192036507,-0.647539262499085,
125.927000632779));
#65513=CARTESIAN_POINT('Ctrl Pts',(27.2529680124105,-0.783291334474043,
125.946948663108));
#65514=CARTESIAN_POINT('Ctrl Pts',(27.2452168211705,-0.918041692488448,
125.972551172508));
#65515=CARTESIAN_POINT('Ctrl Pts',(27.2374689243934,-1.05273477800685,125.998142800158));
#65516=CARTESIAN_POINT('Ctrl Pts',(27.2297210276163,-1.18642661306955,126.029384054065));
#65517=CARTESIAN_POINT('Ctrl Pts',(27.2219731308392,-1.31861202639542,126.066170521512));
#65518=CARTESIAN_POINT('Ctrl Pts',(27.2142268547551,-1.4507697893824,126.102949294023));
#65519=CARTESIAN_POINT('Ctrl Pts',(27.206480578671,-1.58142138099239,126.145270868138));
#65520=CARTESIAN_POINT('Ctrl Pts',(27.1987343025869,-1.7100744943594,126.192980315938));
#65521=CARTESIAN_POINT('Ctrl Pts',(27.1909879693215,-1.83872855741499,126.240690115919));
#65522=CARTESIAN_POINT('Ctrl Pts',(27.1832416360561,-1.96538374621911,126.29378773301));
#65523=CARTESIAN_POINT('Ctrl Pts',(27.1754953027908,-2.08956589518471,126.352069361125));
#65524=CARTESIAN_POINT('Ctrl Pts',(27.1677472347878,-2.2137758538802,126.410364041006));
#65525=CARTESIAN_POINT('Ctrl Pts',(27.1599991667849,-2.33551131684215,126.473844875942));
#65526=CARTESIAN_POINT('Ctrl Pts',(27.1522510987819,-2.45432132737185,126.542261383092));
#65527=CARTESIAN_POINT('Ctrl Pts',(27.1444947960401,-2.57325761059524,126.61075060412));
#65528=CARTESIAN_POINT('Ctrl Pts',(27.1367384932982,-2.68926189106693,126.684185780783));
#65529=CARTESIAN_POINT('Ctrl Pts',(27.1289821905564,-2.80191043833319,126.762271930011));
#65530=CARTESIAN_POINT('Ctrl Pts',(27.1212217480422,-2.91461910952122,126.840399756168));
#65531=CARTESIAN_POINT('Ctrl Pts',(27.1134613055281,-3.02396816711284,126.923183265341));
#65532=CARTESIAN_POINT('Ctrl Pts',(27.1057008630139,-3.12956658268446,127.01028680871));
#65533=CARTESIAN_POINT('Ctrl Pts',(27.0979279627485,-3.23533451420719,127.09753017842));
#65534=CARTESIAN_POINT('Ctrl Pts',(27.090155062483,-3.3373394810141,127.189107179139));
#65535=CARTESIAN_POINT('Ctrl Pts',(27.0823821622176,-3.43522633259145,127.284644278659));
#65536=CARTESIAN_POINT('Ctrl Pts',(27.0748918264555,-3.52955475055266,127.376708363969));
#65537=CARTESIAN_POINT('Ctrl Pts',(27.0674014906934,-3.62005905125558,127.472449403809));
#65538=CARTESIAN_POINT('Ctrl Pts',(27.0599111549313,-3.70645779554588,127.571505274013));
#65539=CARTESIAN_POINT('Ctrl Pts',(27.0522003402356,-3.79539969726117,127.673476865666));
#65540=CARTESIAN_POINT('Ctrl Pts',(27.0444895255398,-3.88028405432929,127.779298092409));
#65541=CARTESIAN_POINT('Ctrl Pts',(27.0367787108441,-3.96075487053853,127.88860961345));
#65542=CARTESIAN_POINT('Ctrl Pts',(27.0290772170675,-4.04112841272462,127.997788997501));
#65543=CARTESIAN_POINT('Ctrl Pts',(27.0213757232908,-4.11709879048239,128.110449968231));
#65544=CARTESIAN_POINT('Ctrl Pts',(27.0136742295142,-4.1883479812841,128.226197657206));
#65545=CARTESIAN_POINT('Ctrl Pts',(27.0059817100385,-4.25951414771428,128.341810469152));
#65546=CARTESIAN_POINT('Ctrl Pts',(26.9982891905628,-4.32596987231821,128.460502502148));
#65547=CARTESIAN_POINT('Ctrl Pts',(26.9905966710871,-4.38743890312703,128.581847865335));
#65548=CARTESIAN_POINT('Ctrl Pts',(26.9829093560516,-4.44886634653436,128.703111131274));
#65549=CARTESIAN_POINT('Ctrl Pts',(26.9752220410162,-4.50531362653266,128.827023804066));
#65550=CARTESIAN_POINT('Ctrl Pts',(26.9675347259807,-4.55654918213162,128.953133291354));
#65551=CARTESIAN_POINT('Ctrl Pts',(26.9598507877126,-4.60776223175137,129.079187383174));
#65552=CARTESIAN_POINT('Ctrl Pts',(26.9521668494444,-4.65376796085912,129.207436002332));
#65553=CARTESIAN_POINT('Ctrl Pts',(26.9444829111763,-4.69438213913888,129.337404791976));
#65554=CARTESIAN_POINT('Ctrl Pts',(26.9396901847889,-4.71971454514624,129.418470623835));
#65555=CARTESIAN_POINT('Ctrl Pts',(26.9348974584015,-4.74295035070058,129.500205251406));
#65556=CARTESIAN_POINT('Ctrl Pts',(26.9301047320141,-4.76405452823399,129.582490119308));
#65557=CARTESIAN_POINT('Origin',(213.235140564004,0.,130.804360617566));
#65558=CARTESIAN_POINT('',(24.8346867982621,-4.76405452823407,129.582490119308));
#65559=CARTESIAN_POINT('',(25.1802307898757,-4.7640545282341,129.582490119308));
#65560=CARTESIAN_POINT('',(213.235140564004,-4.76405452823405,129.582490119308));
#65561=CARTESIAN_POINT('',(26.5148594359565,-4.91824992681965,130.803512184618));
#65562=CARTESIAN_POINT('Ctrl Pts',(26.5148594359565,-4.91824992681965,130.803512184618));
#65563=CARTESIAN_POINT('Ctrl Pts',(26.5071213653779,-4.91827335442518,130.93931881427));
#65564=CARTESIAN_POINT('Ctrl Pts',(26.4993832947993,-4.91266751947957,131.075349760757));
#65565=CARTESIAN_POINT('Ctrl Pts',(26.4916452242207,-4.90140271489009,131.211097005129));
#65566=CARTESIAN_POINT('Ctrl Pts',(26.4839166302215,-4.89015170596362,131.346678003987));
#65567=CARTESIAN_POINT('Ctrl Pts',(26.4761880362222,-4.87325554665902,131.481975602133));
#65568=CARTESIAN_POINT('Ctrl Pts',(26.468459442223,-4.85073650515059,131.616480325552));
#65569=CARTESIAN_POINT('Ctrl Pts',(26.4607384194964,-4.82823952429199,131.750853282191));
#65570=CARTESIAN_POINT('Ctrl Pts',(26.4530173967699,-4.80013068620106,131.884434522536));
#65571=CARTESIAN_POINT('Ctrl Pts',(26.4452963740434,-4.76648413899611,132.01671865676));
#65572=CARTESIAN_POINT('Ctrl Pts',(26.4375810242629,-4.73286231326318,132.148905596508));
#65573=CARTESIAN_POINT('Ctrl Pts',(26.4298656744825,-4.69371097281804,132.279796945508));
#65574=CARTESIAN_POINT('Ctrl Pts',(26.422150324702,-4.64915544975939,132.408896895271));
#65575=CARTESIAN_POINT('Ctrl Pts',(26.4144380056585,-4.60461742896188,132.537946132107));
#65576=CARTESIAN_POINT('Ctrl Pts',(26.4067256866149,-4.55467957499654,132.665204996173));
#65577=CARTESIAN_POINT('Ctrl Pts',(26.3990133675713,-4.49951716911133,132.790192510595));
#65578=CARTESIAN_POINT('Ctrl Pts',(26.3913024431291,-4.44436473812009,132.915157423806));
#65579=CARTESIAN_POINT('Ctrl Pts',(26.3835915186868,-4.38398979346227,133.037851442993));
#65580=CARTESIAN_POINT('Ctrl Pts',(26.3758805942445,-4.31861570996299,133.1578137002));
#65581=CARTESIAN_POINT('Ctrl Pts',(26.3681693541893,-4.25323895066184,133.277780867537));
#65582=CARTESIAN_POINT('Ctrl Pts',(26.3604581141342,-4.18286283443898,133.39501570358));
#65583=CARTESIAN_POINT('Ctrl Pts',(26.352746874079,-4.10775640988115,133.509082477495));
#65584=CARTESIAN_POINT('Ctrl Pts',(26.3450336083111,-4.03263025515848,133.623179216308));
#65585=CARTESIAN_POINT('Ctrl Pts',(26.3373203425433,-3.95277153721105,133.734105907581));
#65586=CARTESIAN_POINT('Ctrl Pts',(26.3296070767754,-3.86849202061374,133.841456689301));
#65587=CARTESIAN_POINT('Ctrl Pts',(26.3218855356824,-3.78412208312014,133.948922644366));
#65588=CARTESIAN_POINT('Ctrl Pts',(26.3141639945894,-3.69532211974546,134.052804717578));
#65589=CARTESIAN_POINT('Ctrl Pts',(26.3064424534963,-3.60244378223147,134.15273064765));
#65590=CARTESIAN_POINT('Ctrl Pts',(26.298716449483,-3.50951176260749,134.252714333221));
#65591=CARTESIAN_POINT('Ctrl Pts',(26.2909904454696,-3.41249695400789,134.348737043806));
#65592=CARTESIAN_POINT('Ctrl Pts',(26.2832644414563,-3.31178627641337,134.440464950758));
#65593=CARTESIAN_POINT('Ctrl Pts',(26.2755266750374,-3.21092227249013,134.532332508278));
#65594=CARTESIAN_POINT('Ctrl Pts',(26.2677889086186,-3.10635146373076,134.61989194957));
#65595=CARTESIAN_POINT('Ctrl Pts',(26.2600511421997,-2.99849258607423,134.702850745007));
#65596=CARTESIAN_POINT('Ctrl Pts',(26.2547531880171,-2.92464292958739,134.759651619249));
#65597=CARTESIAN_POINT('Ctrl Pts',(26.2494552338345,-2.849252461346,134.81429661822));
#65598=CARTESIAN_POINT('Ctrl Pts',(26.244157279652,-2.77246245245571,134.866704154519));
#65599=CARTESIAN_POINT('Ctrl Pts',(26.2363829455329,-2.65977910987732,134.943608122259));
#65600=CARTESIAN_POINT('Ctrl Pts',(26.2286086114138,-2.54371505817791,135.01594184576));
#65601=CARTESIAN_POINT('Ctrl Pts',(26.2208342772947,-2.42467745042779,135.08339349006));
#65602=CARTESIAN_POINT('Ctrl Pts',(26.2130695243476,-2.30578654589053,135.150762006237));
#65603=CARTESIAN_POINT('Ctrl Pts',(26.2053047714005,-2.18392971373467,135.213260223812));
#65604=CARTESIAN_POINT('Ctrl Pts',(26.1975400184535,-2.05954444631006,135.270618529529));
#65605=CARTESIAN_POINT('Ctrl Pts',(26.1897829775685,-1.93528272008642,135.327919866169));
#65606=CARTESIAN_POINT('Ctrl Pts',(26.1820259366835,-1.80849790888738,135.380091287538));
#65607=CARTESIAN_POINT('Ctrl Pts',(26.1742688957985,-1.6796532509913,135.426908401952));
#65608=CARTESIAN_POINT('Ctrl Pts',(26.1665177045584,-1.55090575585419,135.473690211217));
#65609=CARTESIAN_POINT('Ctrl Pts',(26.1587665133182,-1.42010187183409,135.515125617392));
#65610=CARTESIAN_POINT('Ctrl Pts',(26.1510153220781,-1.28772569354826,135.551037939723));
#65611=CARTESIAN_POINT('Ctrl Pts',(26.143267425301,-1.15540577866928,135.586934998358));
#65612=CARTESIAN_POINT('Ctrl Pts',(26.1355195285239,-1.02151527519313,135.617313539913));
#65613=CARTESIAN_POINT('Ctrl Pts',(26.1277716317469,-0.886554140963911,
135.642046512458));
#65614=CARTESIAN_POINT('Ctrl Pts',(26.1200253556628,-0.751621237694911,
135.666774311399));
#65615=CARTESIAN_POINT('Ctrl Pts',(26.1122790795787,-0.615618533444684,
135.685858819836));
#65616=CARTESIAN_POINT('Ctrl Pts',(26.1045328034946,-0.479056511322725,
135.699224039712));
#65617=CARTESIAN_POINT('Ctrl Pts',(26.0967864702293,-0.342493481130756,
135.712589358246));
#65618=CARTESIAN_POINT('Ctrl Pts',(26.0890401369639,-0.205371513934557,
135.720235265893));
#65619=CARTESIAN_POINT('Ctrl Pts',(26.0812938036986,-0.0682061567346617,
135.722137654265));
#65620=CARTESIAN_POINT('Ctrl Pts',(26.0735457356956,0.0689899176957541,
135.724040468664));
#65621=CARTESIAN_POINT('Ctrl Pts',(26.0657976676927,0.206229010612564,135.720197198936));
#65622=CARTESIAN_POINT('Ctrl Pts',(26.0580495996897,0.34299603116267,135.710635863117));
#65623=CARTESIAN_POINT('Ctrl Pts',(26.0502932969479,0.479908409329951,135.701064365397));
#65624=CARTESIAN_POINT('Ctrl Pts',(26.042536994206,0.616347322247349,135.685762688976));
#65625=CARTESIAN_POINT('Ctrl Pts',(26.0347806914642,0.751802699891313,135.66481077809));
#65626=CARTESIAN_POINT('Ctrl Pts',(26.02702024895,0.887330374148809,135.643847684538));
#65627=CARTESIAN_POINT('Ctrl Pts',(26.0192598064359,1.02187308379769,135.617228423329));
#65628=CARTESIAN_POINT('Ctrl Pts',(26.0114993639217,1.15493238100874,135.585083811581));
#65629=CARTESIAN_POINT('Ctrl Pts',(26.0037264636563,1.2882052768163,135.55288759845));
#65630=CARTESIAN_POINT('Ctrl Pts',(25.9959535633908,1.41998962550569,135.515148417823));
#65631=CARTESIAN_POINT('Ctrl Pts',(25.9881806631254,1.54980267437654,135.47204684663));
#65632=CARTESIAN_POINT('Ctrl Pts',(25.9806903273633,1.67489669194231,135.430512126116));
#65633=CARTESIAN_POINT('Ctrl Pts',(25.9731999916013,1.79815995662908,135.383998227827));
#65634=CARTESIAN_POINT('Ctrl Pts',(25.9657096558392,1.91918099247313,135.332707709014));
#65635=CARTESIAN_POINT('Ctrl Pts',(25.9579353217201,2.04479057767405,135.279472494593));
#65636=CARTESIAN_POINT('Ctrl Pts',(25.950160987601,2.16838244281859,135.220922665195));
#65637=CARTESIAN_POINT('Ctrl Pts',(25.9423866534819,2.28947415614256,135.157232215816));
#65638=CARTESIAN_POINT('Ctrl Pts',(25.9346219005349,2.41041663475197,135.093620259225));
#65639=CARTESIAN_POINT('Ctrl Pts',(25.9268571475877,2.5288647495377,135.02488046837));
#65640=CARTESIAN_POINT('Ctrl Pts',(25.9190923946406,2.64435519193146,134.951235185407));
#65641=CARTESIAN_POINT('Ctrl Pts',(25.9113353537556,2.75973092759032,134.877663047976));
#65642=CARTESIAN_POINT('Ctrl Pts',(25.9035783128706,2.87215450930422,134.79919532319));
#65643=CARTESIAN_POINT('Ctrl Pts',(25.8958212719855,2.98118675838969,134.716100457343));
#65644=CARTESIAN_POINT('Ctrl Pts',(25.8880700807454,3.09013678540752,134.633068253982));
#65645=CARTESIAN_POINT('Ctrl Pts',(25.8803188895053,3.19570026051014,134.545416090952));
#65646=CARTESIAN_POINT('Ctrl Pts',(25.8725676982652,3.29746687220816,134.453455750498));
#65647=CARTESIAN_POINT('Ctrl Pts',(25.8648198014881,3.39919023038121,134.361534495643));
#65648=CARTESIAN_POINT('Ctrl Pts',(25.857071904711,3.49711964534237,134.26530896684));
#65649=CARTESIAN_POINT('Ctrl Pts',(25.8493240079339,3.59087798527832,134.165131118112));
#65650=CARTESIAN_POINT('Ctrl Pts',(25.8415777318498,3.68461671299101,134.064974224431));
#65651=CARTESIAN_POINT('Ctrl Pts',(25.8338314557658,3.77418583413915,133.960866940524));
#65652=CARTESIAN_POINT('Ctrl Pts',(25.8260851796817,3.85924548081293,133.853197671481));
#65653=CARTESIAN_POINT('Ctrl Pts',(25.8183388464164,3.94430575537748,133.745527607648));
#65654=CARTESIAN_POINT('Ctrl Pts',(25.810592513151,4.02485624668364,133.634295812995));
#65655=CARTESIAN_POINT('Ctrl Pts',(25.8028461798856,4.10059800591613,133.519923000642));
#65656=CARTESIAN_POINT('Ctrl Pts',(25.7950981118826,4.17635672699065,133.40552457529));
#65657=CARTESIAN_POINT('Ctrl Pts',(25.7873500438797,4.24730435729436,133.28798405844));
#65658=CARTESIAN_POINT('Ctrl Pts',(25.7796019758767,4.31318605000646,133.167749955049));
#65659=CARTESIAN_POINT('Ctrl Pts',(25.7718456731348,4.37913776256549,133.047388065422));
#65660=CARTESIAN_POINT('Ctrl Pts',(25.764089370393,4.4400125939639,132.924327213964));
#65661=CARTESIAN_POINT('Ctrl Pts',(25.7563330676512,4.49560209824486,132.799039748844));
#65662=CARTESIAN_POINT('Ctrl Pts',(25.748572625137,4.55122127231809,132.673685414031));
#65663=CARTESIAN_POINT('Ctrl Pts',(25.7408121826228,4.60154935491937,132.546102461061));
#65664=CARTESIAN_POINT('Ctrl Pts',(25.7330517401086,4.64642698297014,132.416780958056));
#65665=CARTESIAN_POINT('Ctrl Pts',(25.7252788398432,4.69137665257352,132.287251856695));
#65666=CARTESIAN_POINT('Ctrl Pts',(25.7175059395777,4.73085827056162,132.155979002856));
#65667=CARTESIAN_POINT('Ctrl Pts',(25.7097330393123,4.76476282179153,132.023466156301));
#65668=CARTESIAN_POINT('Ctrl Pts',(25.7022427035503,4.79743485718374,131.895770485497));
#65669=CARTESIAN_POINT('Ctrl Pts',(25.6947523677883,4.82492820264624,131.766923711729));
#65670=CARTESIAN_POINT('Ctrl Pts',(25.6872620320263,4.84719086252336,131.637381508523));
#65671=CARTESIAN_POINT('Ctrl Pts',(25.6794876979072,4.87029761791637,131.502927673307));
#65672=CARTESIAN_POINT('Ctrl Pts',(25.6717133637881,4.88784241023631,131.367298723909));
#65673=CARTESIAN_POINT('Ctrl Pts',(25.663939029669,4.89971086024828,131.230994592379));
#65674=CARTESIAN_POINT('Ctrl Pts',(25.6561742767219,4.91156468345633,131.09485844351));
#65675=CARTESIAN_POINT('Ctrl Pts',(25.6484095237748,4.91775604989592,130.958049153896));
#65676=CARTESIAN_POINT('Ctrl Pts',(25.6406447708277,4.91822159272069,130.821076699523));
#65677=CARTESIAN_POINT('Ctrl Pts',(25.6328877299427,4.91868667316176,130.684240288123));
#65678=CARTESIAN_POINT('Ctrl Pts',(25.6251306890577,4.91343724599223,130.547241422898));
#65679=CARTESIAN_POINT('Ctrl Pts',(25.6173736481727,4.90246177587857,130.410594699095));
#65680=CARTESIAN_POINT('Ctrl Pts',(25.6096224569325,4.89149458245229,130.274051021649));
#65681=CARTESIAN_POINT('Ctrl Pts',(25.6018712656924,4.87480997208041,130.13785934519));
#65682=CARTESIAN_POINT('Ctrl Pts',(25.5941200744523,4.85244847261533,130.002533402318));
#65683=CARTESIAN_POINT('Ctrl Pts',(25.5863721776752,4.83009647738406,129.86726497658));
#65684=CARTESIAN_POINT('Ctrl Pts',(25.5786242808982,4.80207245559914,129.732861937511));
#65685=CARTESIAN_POINT('Ctrl Pts',(25.5708763841211,4.76846866719055,129.599831816531));
#65686=CARTESIAN_POINT('Ctrl Pts',(25.563130108037,4.73487190797012,129.466829522585));
#65687=CARTESIAN_POINT('Ctrl Pts',(25.5553838319529,4.69569779937562,129.335199954321));
#65688=CARTESIAN_POINT('Ctrl Pts',(25.5476375558688,4.65108941070256,129.205438994674));
#65689=CARTESIAN_POINT('Ctrl Pts',(25.5398912226034,4.60648069274045,129.075677077162));
#65690=CARTESIAN_POINT('Ctrl Pts',(25.5321448893381,4.55643774175662,128.94778416552));
#65691=CARTESIAN_POINT('Ctrl Pts',(25.5243985560727,4.50115292647783,128.822239179571));
#65692=CARTESIAN_POINT('Ctrl Pts',(25.5166504880698,4.44585573054797,128.696666078693));
#65693=CARTESIAN_POINT('Ctrl Pts',(25.5089024200668,4.38531449197364,128.573442307533));
#65694=CARTESIAN_POINT('Ctrl Pts',(25.5011543520638,4.3197687997447,128.453024703824));
#65695=CARTESIAN_POINT('Ctrl Pts',(25.493398049322,4.25415344477406,128.332479118853));
#65696=CARTESIAN_POINT('Ctrl Pts',(25.4856417465801,4.18352319849925,128.214746002991));
#65697=CARTESIAN_POINT('Ctrl Pts',(25.4778854438382,4.10816279068132,128.100256043449));
#65698=CARTESIAN_POINT('Ctrl Pts',(25.4701250013241,4.03276216074458,127.985704977168));
#65699=CARTESIAN_POINT('Ctrl Pts',(25.4623645588099,3.95262656705109,127.874400833443));
#65700=CARTESIAN_POINT('Ctrl Pts',(25.4546041162958,3.86808217815684,127.766742582736));
#65701=CARTESIAN_POINT('Ctrl Pts',(25.4468312160303,3.78340207110404,127.658911509448));
#65702=CARTESIAN_POINT('Ctrl Pts',(25.4390583157649,3.69429928024414,127.554738322039));
#65703=CARTESIAN_POINT('Ctrl Pts',(25.4312854154995,3.60113870758233,127.454587032493));
#65704=CARTESIAN_POINT('Ctrl Pts',(25.4237950797374,3.51136475639397,127.358076494588));
#65705=CARTESIAN_POINT('Ctrl Pts',(25.4163047439754,3.41782314127747,127.265300735919));
#65706=CARTESIAN_POINT('Ctrl Pts',(25.4088144082133,3.32086912835263,127.176549804575));
#65707=CARTESIAN_POINT('Ctrl Pts',(25.4010400740942,3.22023907455935,127.084433854694));
#65708=CARTESIAN_POINT('Ctrl Pts',(25.3932657399751,3.11561398702345,126.99636216395));
#65709=CARTESIAN_POINT('Ctrl Pts',(25.385491405856,3.00735264796848,126.912701188318));
#65710=CARTESIAN_POINT('Ctrl Pts',(25.3777266529089,2.89922473133816,126.829143317361));
#65711=CARTESIAN_POINT('Ctrl Pts',(25.3699618999619,2.78746978613843,126.749985582637));
#65712=CARTESIAN_POINT('Ctrl Pts',(25.3621971470148,2.67248261828102,126.675556950947));
#65713=CARTESIAN_POINT('Ctrl Pts',(25.3544401061298,2.55760965729992,126.601202242823));
#65714=CARTESIAN_POINT('Ctrl Pts',(25.3466830652447,2.43951118836747,126.531567501535));
#65715=CARTESIAN_POINT('Ctrl Pts',(25.3389260243597,2.31861391990805,126.466940583386));
#65716=CARTESIAN_POINT('Ctrl Pts',(25.3311748331196,2.19780782101939,126.402362400898));
#65717=CARTESIAN_POINT('Ctrl Pts',(25.3234236418795,2.07420746701642,126.342784708344));
#65718=CARTESIAN_POINT('Ctrl Pts',(25.3156724506394,1.94826698197686,126.288451093512));
#65719=CARTESIAN_POINT('Ctrl Pts',(25.3079245538623,1.82238002500284,126.234140571916));
#65720=CARTESIAN_POINT('Ctrl Pts',(25.3001766570852,1.69415527344232,126.185069849531));
#65721=CARTESIAN_POINT('Ctrl Pts',(25.2924287603081,1.56406959660007,126.141435638597));
#65722=CARTESIAN_POINT('Ctrl Pts',(25.284682484224,1.43401113087709,126.097810554999));
#65723=CARTESIAN_POINT('Ctrl Pts',(25.27693620814,1.30209288457659,126.05961984515));
#65724=CARTESIAN_POINT('Ctrl Pts',(25.2691899320559,1.16880939050615,126.02701117764));
#65725=CARTESIAN_POINT('Ctrl Pts',(25.2614435987905,1.03552491256723,125.994402269419));
#65726=CARTESIAN_POINT('Ctrl Pts',(25.2536972655251,0.900875546513192,125.967375578671));
#65727=CARTESIAN_POINT('Ctrl Pts',(25.2459509322598,0.765368201150668,125.946028128001));
#65728=CARTESIAN_POINT('Ctrl Pts',(25.2382028642568,0.62983050985806,125.924675896716));
#65729=CARTESIAN_POINT('Ctrl Pts',(25.2304547962539,0.493434843051849,125.909005497126));
#65730=CARTESIAN_POINT('Ctrl Pts',(25.2227067282509,0.356695054955446,125.899062288181));
#65731=CARTESIAN_POINT('Ctrl Pts',(25.214950425509,0.219809938184657,125.889108511474));
#65732=CARTESIAN_POINT('Ctrl Pts',(25.2071941227671,0.0825803600836163,
125.884894113103));
#65733=CARTESIAN_POINT('Ctrl Pts',(25.1994378200253,-0.0544774266093184,
125.886412338813));
#65734=CARTESIAN_POINT('Ctrl Pts',(25.1916773775111,-0.191608365169928,
125.887931374845));
#65735=CARTESIAN_POINT('Ctrl Pts',(25.1839169349969,-0.328566939395477,
125.895189110939));
#65736=CARTESIAN_POINT('Ctrl Pts',(25.1761564924828,-0.464841182064157,
125.908126785532));
#65737=CARTESIAN_POINT('Ctrl Pts',(25.1683835922173,-0.601334184245027,
125.921085228828));
#65738=CARTESIAN_POINT('Ctrl Pts',(25.1606106919519,-0.737140272066211,
125.939741777935));
#65739=CARTESIAN_POINT('Ctrl Pts',(25.1528377916865,-0.871755953490742,
125.963986187829));
#65740=CARTESIAN_POINT('Ctrl Pts',(25.1453474559245,-1.00147801581778,125.987349252355));
#65741=CARTESIAN_POINT('Ctrl Pts',(25.1378571201625,-1.13009441698203,126.015900898654));
#65742=CARTESIAN_POINT('Ctrl Pts',(25.1303667844006,-1.25716910129661,126.049499009354));
#65743=CARTESIAN_POINT('Ctrl Pts',(25.1225924502815,-1.38906186089178,126.084371002634));
#65744=CARTESIAN_POINT('Ctrl Pts',(25.1148181161623,-1.5197114840579,126.124790151797));
#65745=CARTESIAN_POINT('Ctrl Pts',(25.1070437820432,-1.64861573044893,126.170652681602));
#65746=CARTESIAN_POINT('Ctrl Pts',(25.0992790290961,-1.77736111387661,126.216458689938));
#65747=CARTESIAN_POINT('Ctrl Pts',(25.0915142761491,-1.90436503560955,126.267694601246));
#65748=CARTESIAN_POINT('Ctrl Pts',(25.083749523202,-2.02913732432348,126.324206068721));
#65749=CARTESIAN_POINT('Ctrl Pts',(25.075992482317,-2.15378568744161,126.38066140821));
#65750=CARTESIAN_POINT('Ctrl Pts',(25.0682354414319,-2.27620647461936,126.442381716256));
#65751=CARTESIAN_POINT('Ctrl Pts',(25.0604784005469,-2.39592685787054,126.50916358434));
#65752=CARTESIAN_POINT('Ctrl Pts',(25.0527272093068,-2.51555695904878,126.575895091697));
#65753=CARTESIAN_POINT('Ctrl Pts',(25.0449760180666,-2.63249036956697,126.647680371972));
#65754=CARTESIAN_POINT('Ctrl Pts',(25.0372248268265,-2.74627668696429,126.724269022867));
#65755=CARTESIAN_POINT('Ctrl Pts',(25.0294769300494,-2.86001464214169,126.800825121542));
#65756=CARTESIAN_POINT('Ctrl Pts',(25.0217290332724,-2.97060784092103,126.882180312475));
#65757=CARTESIAN_POINT('Ctrl Pts',(25.0139811364953,-3.0776330242175,126.968039719786));
#65758=CARTESIAN_POINT('Ctrl Pts',(25.0062348604112,-3.18463582015282,127.053881167159));
#65759=CARTESIAN_POINT('Ctrl Pts',(24.9984885843271,-3.28807178037368,127.144224712357));
#65760=CARTESIAN_POINT('Ctrl Pts',(24.9907423082429,-3.38754936005132,127.238734109403));
#65761=CARTESIAN_POINT('Ctrl Pts',(24.9829959749776,-3.48702767404986,127.333244204095));
#65762=CARTESIAN_POINT('Ctrl Pts',(24.9752496417122,-3.5825472657576,127.431919942712));
#65763=CARTESIAN_POINT('Ctrl Pts',(24.9675033084469,-3.67375251071746,127.534387291605));
#65764=CARTESIAN_POINT('Ctrl Pts',(24.9597552404439,-3.76497818045956,127.63687758735));
#65765=CARTESIAN_POINT('Ctrl Pts',(24.9520071724409,-3.85188732100181,127.743160891011));
#65766=CARTESIAN_POINT('Ctrl Pts',(24.9442591044379,-3.93416401981541,127.852829400098));
#65767=CARTESIAN_POINT('Ctrl Pts',(24.9365028016961,-4.0165281632836,127.962614466181));
#65768=CARTESIAN_POINT('Ctrl Pts',(24.9287464989542,-4.0942497949735,128.075791611519));
#65769=CARTESIAN_POINT('Ctrl Pts',(24.9209901962124,-4.16705555021563,128.191922847223));
#65770=CARTESIAN_POINT('Ctrl Pts',(24.9132297536982,-4.23990016408146,128.308116065664));
#65771=CARTESIAN_POINT('Ctrl Pts',(24.905469311184,-4.30782347992387,128.427266176667));
#65772=CARTESIAN_POINT('Ctrl Pts',(24.8977088686698,-4.37059820472111,128.548910685648));
#65773=CARTESIAN_POINT('Ctrl Pts',(24.8899359684044,-4.43347370107946,128.670750469195));
#65774=CARTESIAN_POINT('Ctrl Pts',(24.882163068139,-4.49118392565028,128.79509229761));
#65775=CARTESIAN_POINT('Ctrl Pts',(24.8743901678735,-4.54354948094981,128.921452978657));
#65776=CARTESIAN_POINT('Ctrl Pts',(24.8668998321115,-4.59401141641347,129.043220130665));
#65777=CARTESIAN_POINT('Ctrl Pts',(24.8594094963494,-4.63951041421743,129.166861613809));
#65778=CARTESIAN_POINT('Ctrl Pts',(24.8519191605873,-4.67993034298145,129.29193374418));
#65779=CARTESIAN_POINT('Ctrl Pts',(24.8461750398123,-4.71092721146841,129.387847925501));
#65780=CARTESIAN_POINT('Ctrl Pts',(24.8404309190372,-4.73898758443333,129.484754485873));
#65781=CARTESIAN_POINT('Ctrl Pts',(24.8346867982621,-4.76405452823407,129.582490119308));
#65782=CARTESIAN_POINT('Ctrl Pts',(26.584953373822,-4.764054528234,129.582490119308));
#65783=CARTESIAN_POINT('Ctrl Pts',(26.5771914547002,-4.79811509371724,129.715291747186));
#65784=CARTESIAN_POINT('Ctrl Pts',(26.5694295355783,-4.82658894433892,129.849403140099));
#65785=CARTESIAN_POINT('Ctrl Pts',(26.5616676164564,-4.84940279828725,129.984314544187));
#65786=CARTESIAN_POINT('Ctrl Pts',(26.5538938870113,-4.87225136517013,130.119431225769));
#65787=CARTESIAN_POINT('Ctrl Pts',(26.5461201575662,-4.88942268405172,130.255349962639));
#65788=CARTESIAN_POINT('Ctrl Pts',(26.5383464281211,-4.90089540289503,130.391556411698));
#65789=CARTESIAN_POINT('Ctrl Pts',(26.5330992532357,-4.90863935161451,130.48349414426));
#65790=CARTESIAN_POINT('Ctrl Pts',(26.5278520783502,-4.9137880539663,130.575562919708));
#65791=CARTESIAN_POINT('Ctrl Pts',(26.5226049034648,-4.91634834589865,130.667605346079));
#65792=CARTESIAN_POINT('Ctrl Pts',(26.5200230809736,-4.91760811319045,130.712893946466));
#65793=CARTESIAN_POINT('Ctrl Pts',(26.5174412584824,-4.91824211014721,130.758200034511));
#65794=CARTESIAN_POINT('Ctrl Pts',(26.5148594359912,-4.91824992681955,130.803512184009));
#65795=CARTESIAN_POINT('',(26.8601405639764,-4.91824802889422,130.808763886588));
#65796=CARTESIAN_POINT('Ctrl Pts',(26.9301047320141,-4.76405452823399,129.582490119308));
#65797=CARTESIAN_POINT('Ctrl Pts',(26.9224218544244,-4.79788512892272,129.714395117942));
#65798=CARTESIAN_POINT('Ctrl Pts',(26.9147389768347,-4.82623545671776,129.847714506907));
#65799=CARTESIAN_POINT('Ctrl Pts',(26.9070560992449,-4.84900229538889,129.981949648638));
#65800=CARTESIAN_POINT('Ctrl Pts',(26.8992368433722,-4.87217326679926,130.118567590032));
#65801=CARTESIAN_POINT('Ctrl Pts',(26.8914175874995,-4.88956054893843,130.256133687399));
#65802=CARTESIAN_POINT('Ctrl Pts',(26.8835983316268,-4.90111018938166,130.394114381704));
#65803=CARTESIAN_POINT('Ctrl Pts',(26.8757790757541,-4.91265982982489,130.532095076008));
#65804=CARTESIAN_POINT('Ctrl Pts',(26.8679598198814,-4.91837182446762,130.670489933609));
#65805=CARTESIAN_POINT('Ctrl Pts',(26.8601405640087,-4.91824802889473,130.808763886018));
#65806=CARTESIAN_POINT('Ctrl Pts',(26.8601405639765,-4.91824802889422,130.808763886588));
#65807=CARTESIAN_POINT('Ctrl Pts',(26.850613514715,-4.91809719527359,130.977238071039));
#65808=CARTESIAN_POINT('Ctrl Pts',(26.8410864654536,-4.90928611020261,131.145327951723));
#65809=CARTESIAN_POINT('Ctrl Pts',(26.8315594161922,-4.89195503112132,131.312257296022));
#65810=CARTESIAN_POINT('Ctrl Pts',(26.8218831116281,-4.87435243507981,131.481801835136));
#65811=CARTESIAN_POINT('Ctrl Pts',(26.8122068070639,-4.84796084158413,131.650149258514));
#65812=CARTESIAN_POINT('Ctrl Pts',(26.8025305024998,-4.81297596357176,131.816509537726));
#65813=CARTESIAN_POINT('Ctrl Pts',(26.795508178706,-4.78758660757745,131.937241139269));
#65814=CARTESIAN_POINT('Ctrl Pts',(26.7884858549122,-4.7576723990162,132.056926656006));
#65815=CARTESIAN_POINT('Ctrl Pts',(26.7814635311184,-4.7233237335095,132.175271253226));
#65816=CARTESIAN_POINT('Ctrl Pts',(26.7736891969994,-4.68529671994025,132.306289199279));
#65817=CARTESIAN_POINT('Ctrl Pts',(26.7659148628803,-4.64175397977864,132.435931250449));
#65818=CARTESIAN_POINT('Ctrl Pts',(26.7581405287612,-4.59281131076359,132.563697801343));
#65819=CARTESIAN_POINT('Ctrl Pts',(26.7503757758141,-4.54392895921404,132.691306891382));
#65820=CARTESIAN_POINT('Ctrl Pts',(26.742611022867,-4.48966005864959,132.817044718525));
#65821=CARTESIAN_POINT('Ctrl Pts',(26.7348462699199,-4.4301706741868,132.940424956502));
#65822=CARTESIAN_POINT('Ctrl Pts',(26.7270892290349,-4.37074037541939,133.063682651488));
#65823=CARTESIAN_POINT('Ctrl Pts',(26.7193321881499,-4.30610007995629,133.184587067291));
#65824=CARTESIAN_POINT('Ctrl Pts',(26.7115751472649,-4.23646448430847,133.302670393333));
#65825=CARTESIAN_POINT('Ctrl Pts',(26.7038239560248,-4.16688140140482,133.420664671821));
#65826=CARTESIAN_POINT('Ctrl Pts',(26.6960727647846,-4.0923107140849,133.535841759613));
#65827=CARTESIAN_POINT('Ctrl Pts',(26.6883215735445,-4.01301356095525,133.647757392919));
#65828=CARTESIAN_POINT('Ctrl Pts',(26.6805736767674,-3.9337501112311,133.759625459096));
#65829=CARTESIAN_POINT('Ctrl Pts',(26.6728257799903,-3.84976441675079,133.868234509505));
#65830=CARTESIAN_POINT('Ctrl Pts',(26.6650778832133,-3.76136142553019,133.973168483157));
#65831=CARTESIAN_POINT('Ctrl Pts',(26.6573316071292,-3.6729769263096,134.078080506885));
#65832=CARTESIAN_POINT('Ctrl Pts',(26.6495853310451,-3.58017721997951,134.179318684124));
#65833=CARTESIAN_POINT('Ctrl Pts',(26.641839054961,-3.4833078516829,134.276499651779));
#65834=CARTESIAN_POINT('Ctrl Pts',(26.6340927216956,-3.38643776831875,134.373681336801));
#65835=CARTESIAN_POINT('Ctrl Pts',(26.6263463884303,-3.28549823905269,134.466805475578));
#65836=CARTESIAN_POINT('Ctrl Pts',(26.618600055165,-3.18087172382634,134.555525521841));
#65837=CARTESIAN_POINT('Ctrl Pts',(26.610851987162,-3.07622177821734,134.644265436343));
#65838=CARTESIAN_POINT('Ctrl Pts',(26.6031039191591,-2.96788350178384,134.728599042967));
#65839=CARTESIAN_POINT('Ctrl Pts',(26.5953558511561,-2.85627216060912,134.808220306295));
#65840=CARTESIAN_POINT('Ctrl Pts',(26.5875995484142,-2.74454219757266,134.88792619205));
#65841=CARTESIAN_POINT('Ctrl Pts',(26.5798432456725,-2.62953253959788,134.962909502405));
#65842=CARTESIAN_POINT('Ctrl Pts',(26.5720869429306,-2.51168760944261,135.032907461941));
#65843=CARTESIAN_POINT('Ctrl Pts',(26.5643265004165,-2.39377978189987,135.102942781495));
#65844=CARTESIAN_POINT('Ctrl Pts',(26.5565660579022,-2.27303401089016,135.167987262969));
#65845=CARTESIAN_POINT('Ctrl Pts',(26.5488056153881,-2.14991811221573,135.227824777392));
#65846=CARTESIAN_POINT('Ctrl Pts',(26.5410327151227,-2.02660457697104,135.287758348305));
#65847=CARTESIAN_POINT('Ctrl Pts',(26.5332598148572,-1.90091366966469,135.342468092723));
#65848=CARTESIAN_POINT('Ctrl Pts',(26.5254869145918,-1.77333274843271,135.391786260106));
#65849=CARTESIAN_POINT('Ctrl Pts',(26.5179965788297,-1.65038971504309,135.43931158788));
#65850=CARTESIAN_POINT('Ctrl Pts',(26.5105062430676,-1.52569198709775,135.481830428419));
#65851=CARTESIAN_POINT('Ctrl Pts',(26.5030159073055,-1.39968590756955,135.519237330975));
#65852=CARTESIAN_POINT('Ctrl Pts',(26.4952415731864,-1.26890226923879,135.558062527611));
#65853=CARTESIAN_POINT('Ctrl Pts',(26.4874672390674,-1.13629482528775,135.59150348246));
#65854=CARTESIAN_POINT('Ctrl Pts',(26.4796929049483,-1.00234649939001,135.619387570519));
#65855=CARTESIAN_POINT('Ctrl Pts',(26.4719281520012,-0.868563252832645,
135.647237293931));
#65856=CARTESIAN_POINT('Ctrl Pts',(26.4641633990541,-0.73344279143046,135.669543697799));
#65857=CARTESIAN_POINT('Ctrl Pts',(26.456398646107,-0.597484037499191,135.68618362618));
#65858=CARTESIAN_POINT('Ctrl Pts',(26.448641605222,-0.461660319719009,135.70280702755));
#65859=CARTESIAN_POINT('Ctrl Pts',(26.440884564337,-0.325000351887533,135.713775106265));
#65860=CARTESIAN_POINT('Ctrl Pts',(26.433127523452,-0.188013765003033,135.719015629535));
#65861=CARTESIAN_POINT('Ctrl Pts',(26.4253763322119,-0.0511304807694892,
135.724252200886));
#65862=CARTESIAN_POINT('Ctrl Pts',(26.4176251409718,0.0860785431613368,
135.723769799));
#65863=CARTESIAN_POINT('Ctrl Pts',(26.4098739497317,0.223098383284125,135.717547991754));
#65864=CARTESIAN_POINT('Ctrl Pts',(26.4021260529546,0.36005998632011,135.711328828941));
#65865=CARTESIAN_POINT('Ctrl Pts',(26.3943781561775,0.496832175728681,135.699375130246));
#65866=CARTESIAN_POINT('Ctrl Pts',(26.3866302594004,0.632900075765341,135.681718565943));
#65867=CARTESIAN_POINT('Ctrl Pts',(26.3788839833163,0.768939513330597,135.664065695013));
#65868=CARTESIAN_POINT('Ctrl Pts',(26.3711377072322,0.904274567086835,135.640712381531));
#65869=CARTESIAN_POINT('Ctrl Pts',(26.3633914311481,1.03839592721278,135.611742125294));
#65870=CARTESIAN_POINT('Ctrl Pts',(26.3556450978827,1.17251827739196,135.582771655206));
#65871=CARTESIAN_POINT('Ctrl Pts',(26.3478987646174,1.30542653391143,135.548184242171));
#65872=CARTESIAN_POINT('Ctrl Pts',(26.340152431352,1.43662240863915,135.508114343846));
#65873=CARTESIAN_POINT('Ctrl Pts',(26.3324043633491,1.56784766377337,135.468035472146));
#65874=CARTESIAN_POINT('Ctrl Pts',(26.3246562953461,1.69735940020019,135.422471786226));
#65875=CARTESIAN_POINT('Ctrl Pts',(26.3169082273431,1.82467568019322,135.371607241585));
#65876=CARTESIAN_POINT('Ctrl Pts',(26.3091519246013,1.95212727344371,135.3206886375));
#65877=CARTESIAN_POINT('Ctrl Pts',(26.3013956218594,2.07737838548611,135.26445806582));
#65878=CARTESIAN_POINT('Ctrl Pts',(26.2936393191176,2.19996771455989,135.203147395462));
#65879=CARTESIAN_POINT('Ctrl Pts',(26.2858788766034,2.32262247324987,135.141804001754));
#65880=CARTESIAN_POINT('Ctrl Pts',(26.2781184340892,2.44261227628008,135.075375295942));
#65881=CARTESIAN_POINT('Ctrl Pts',(26.2703579915751,2.55950242235699,135.004138041722));
#65882=CARTESIAN_POINT('Ctrl Pts',(26.2625850913096,2.67658021087339,134.932786431137));
#65883=CARTESIAN_POINT('Ctrl Pts',(26.2548121910442,2.7905480738831,134.856611064286));
#65884=CARTESIAN_POINT('Ctrl Pts',(26.2470392907788,2.90100144912869,134.775931296108));
#65885=CARTESIAN_POINT('Ctrl Pts',(26.2395489550168,3.00743956596915,134.698184440723));
#65886=CARTESIAN_POINT('Ctrl Pts',(26.2320586192546,3.11061403857548,134.616255182471));
#65887=CARTESIAN_POINT('Ctrl Pts',(26.2245682834926,3.21019488896853,134.530462043633));
#65888=CARTESIAN_POINT('Ctrl Pts',(26.2167939493735,3.31355137757088,134.44141603186));
#65889=CARTESIAN_POINT('Ctrl Pts',(26.2090196152544,3.41336376255425,134.347925286562));
#65890=CARTESIAN_POINT('Ctrl Pts',(26.2012452811353,3.5092257775743,134.250302797073));
#65891=CARTESIAN_POINT('Ctrl Pts',(26.1934805281882,3.60496965122826,134.152800618578));
#65892=CARTESIAN_POINT('Ctrl Pts',(26.1857157752411,3.69677257044115,134.051177103745));
#65893=CARTESIAN_POINT('Ctrl Pts',(26.177951022294,3.78426124093248,133.945785441253));
#65894=CARTESIAN_POINT('Ctrl Pts',(26.170193981409,3.8716630164428,133.840498455246));
#65895=CARTESIAN_POINT('Ctrl Pts',(26.1624369405241,3.95475882241595,133.731451068354));
#65896=CARTESIAN_POINT('Ctrl Pts',(26.1546798996391,4.03321241935692,133.619033003981));
#65897=CARTESIAN_POINT('Ctrl Pts',(26.1469287083989,4.11160685383015,133.506699714944));
#65898=CARTESIAN_POINT('Ctrl Pts',(26.1391775171588,4.18536582441316,133.391001127147));
#65899=CARTESIAN_POINT('Ctrl Pts',(26.1314263259187,4.25419381224783,133.272359416255));
#65900=CARTESIAN_POINT('Ctrl Pts',(26.1236784291416,4.32299254635162,133.153768131255));
#65901=CARTESIAN_POINT('Ctrl Pts',(26.1159305323645,4.38686427031463,133.032236548586));
#65902=CARTESIAN_POINT('Ctrl Pts',(26.1081826355875,4.44555732631989,132.908214966351));
#65903=CARTESIAN_POINT('Ctrl Pts',(26.1004363595034,4.50423810500311,132.784219326758));
#65904=CARTESIAN_POINT('Ctrl Pts',(26.0926900834193,4.55774220326821,132.657735076772));
#65905=CARTESIAN_POINT('Ctrl Pts',(26.0849438073352,4.60586457746024,132.52923584685));
#65906=CARTESIAN_POINT('Ctrl Pts',(26.0771974740699,4.65398730688071,132.400735668376));
#65907=CARTESIAN_POINT('Ctrl Pts',(26.0694511408045,4.69672809584134,132.270220846419));
#65908=CARTESIAN_POINT('Ctrl Pts',(26.0617048075391,4.7339307304703,132.138183282544));
#65909=CARTESIAN_POINT('Ctrl Pts',(26.0539567395361,4.77114169637134,132.006116149772));
#65910=CARTESIAN_POINT('Ctrl Pts',(26.0462086715332,4.80281193401514,131.872525972759));
#65911=CARTESIAN_POINT('Ctrl Pts',(26.0384606035302,4.82883571125878,131.737917651802));
#65912=CARTESIAN_POINT('Ctrl Pts',(26.0307043007884,4.85488714688257,131.60316626752));
#65913=CARTESIAN_POINT('Ctrl Pts',(26.0229479980465,4.87528005988263,131.467394962162));
#65914=CARTESIAN_POINT('Ctrl Pts',(26.0151916953047,4.8899601832778,131.331117172777));
#65915=CARTESIAN_POINT('Ctrl Pts',(26.0074312527905,4.90464814189684,131.194766647833));
#65916=CARTESIAN_POINT('Ctrl Pts',(25.9996708102763,4.91361720979041,131.057909490153));
#65917=CARTESIAN_POINT('Ctrl Pts',(25.9919103677622,4.91686526942607,130.921061023785));
#65918=CARTESIAN_POINT('Ctrl Pts',(25.9841374674967,4.92011854313541,130.78399287611));
#65919=CARTESIAN_POINT('Ctrl Pts',(25.9763645672314,4.91763246338203,130.646933838752));
#65920=CARTESIAN_POINT('Ctrl Pts',(25.9685916669659,4.90945703673777,130.510396900543));
#65921=CARTESIAN_POINT('Ctrl Pts',(25.9611013312039,4.90157880744467,130.378823423953));
#65922=CARTESIAN_POINT('Ctrl Pts',(25.9536109954418,4.88841772474093,130.247735052778));
#65923=CARTESIAN_POINT('Ctrl Pts',(25.9461206596798,4.8700634092836,130.117581575911));
#65924=CARTESIAN_POINT('Ctrl Pts',(25.9383463255607,4.85101318437705,129.982493290409));
#65925=CARTESIAN_POINT('Ctrl Pts',(25.9305719914415,4.82630780469903,129.847984272616));
#65926=CARTESIAN_POINT('Ctrl Pts',(25.9227976573225,4.79599100015764,129.714565504296));
#65927=CARTESIAN_POINT('Ctrl Pts',(25.9150329043754,4.76571155836837,129.581311162684));
#65928=CARTESIAN_POINT('Ctrl Pts',(25.9072681514283,4.72983453745714,129.449144774696));
#65929=CARTESIAN_POINT('Ctrl Pts',(25.8995033984812,4.68845531038606,129.318571310493));
#65930=CARTESIAN_POINT('Ctrl Pts',(25.8917463575962,4.64711718174665,129.188127533695));
#65931=CARTESIAN_POINT('Ctrl Pts',(25.8839893167113,4.60028783962797,129.059273902488));
#65932=CARTESIAN_POINT('Ctrl Pts',(25.8762322758263,4.54811342370792,128.932503959703));
#65933=CARTESIAN_POINT('Ctrl Pts',(25.8684810845861,4.49597835292078,128.805829615117));
#65934=CARTESIAN_POINT('Ctrl Pts',(25.860729893346,4.43850637951602,128.681236191403));
#65935=CARTESIAN_POINT('Ctrl Pts',(25.8529787021059,4.37589295667642,128.559200513206));
#65936=CARTESIAN_POINT('Ctrl Pts',(25.8452308053288,4.3133061462118,128.437216703427));
#65937=CARTESIAN_POINT('Ctrl Pts',(25.8374829085517,4.24558241071458,128.317788824109));
#65938=CARTESIAN_POINT('Ctrl Pts',(25.8297350117746,4.17296457153491,128.201371999225));
#65939=CARTESIAN_POINT('Ctrl Pts',(25.8219887356905,4.10036192244175,128.08497952623));
#65940=CARTESIAN_POINT('Ctrl Pts',(25.8142424596063,4.02286741273072,127.971597186378));
#65941=CARTESIAN_POINT('Ctrl Pts',(25.8064961835222,3.94076869001512,127.861653497532));
#65942=CARTESIAN_POINT('Ctrl Pts',(25.7987498502569,3.8586693612654,127.751708997108));
#65943=CARTESIAN_POINT('Ctrl Pts',(25.7910035169916,3.7719659856159,127.645203511603));
#65944=CARTESIAN_POINT('Ctrl Pts',(25.7832571837262,3.68098797637171,127.542534352986));
#65945=CARTESIAN_POINT('Ctrl Pts',(25.7755091157233,3.58998959323315,127.439842202321));
#65946=CARTESIAN_POINT('Ctrl Pts',(25.7677610477202,3.49471493087628,127.340988380647));
#65947=CARTESIAN_POINT('Ctrl Pts',(25.7600129797173,3.39553162541569,127.246334754352));
#65948=CARTESIAN_POINT('Ctrl Pts',(25.7522566769754,3.29624290675776,127.151580529056));
#65949=CARTESIAN_POINT('Ctrl Pts',(25.7445003742336,3.19303752991747,127.061035686847));
#65950=CARTESIAN_POINT('Ctrl Pts',(25.7367440714917,3.0863181313976,126.97502340934));
#65951=CARTESIAN_POINT('Ctrl Pts',(25.7289836289776,2.97954177352148,126.88896522449));
#65952=CARTESIAN_POINT('Ctrl Pts',(25.7212231864633,2.86924797104752,126.807444657006));
#65953=CARTESIAN_POINT('Ctrl Pts',(25.7134627439492,2.75586913611329,126.730742033663));
#65954=CARTESIAN_POINT('Ctrl Pts',(25.7056898436837,2.64230829540793,126.65391628046));
#65955=CARTESIAN_POINT('Ctrl Pts',(25.6979169434184,2.52565285873307,126.581924132221));
#65956=CARTESIAN_POINT('Ctrl Pts',(25.690144043153,2.40636144789321,126.515000799995));
#65957=CARTESIAN_POINT('Ctrl Pts',(25.6826537073909,2.29140658031384,126.450510299464));
#65958=CARTESIAN_POINT('Ctrl Pts',(25.6751633716288,2.17400433434992,126.390726624453));
#65959=CARTESIAN_POINT('Ctrl Pts',(25.6676730358667,2.05458157228911,126.335817496446));
#65960=CARTESIAN_POINT('Ctrl Pts',(25.6598987017476,1.93063085990736,126.278826472161));
#65961=CARTESIAN_POINT('Ctrl Pts',(25.6521243676285,1.80411075256694,126.226906398095));
#65962=CARTESIAN_POINT('Ctrl Pts',(25.6443500335095,1.67547479077921,126.180296681161));
#65963=CARTESIAN_POINT('Ctrl Pts',(25.6365852805624,1.54699736131804,126.133744406537));
#65964=CARTESIAN_POINT('Ctrl Pts',(25.6288205276153,1.41640962981017,126.092489599269));
#65965=CARTESIAN_POINT('Ctrl Pts',(25.6210557746682,1.28418799336735,126.056724968088));
#65966=CARTESIAN_POINT('Ctrl Pts',(25.6132987337832,1.15209768131784,126.020995858844));
#65967=CARTESIAN_POINT('Ctrl Pts',(25.6055416928981,1.01837706877371,125.990746175552));
#65968=CARTESIAN_POINT('Ctrl Pts',(25.5977846520131,0.883520379361143,125.966119738718));
#65969=CARTESIAN_POINT('Ctrl Pts',(25.590033460773,0.748765386427281,125.941511872872));
#65970=CARTESIAN_POINT('Ctrl Pts',(25.5822822695329,0.612876404931816,125.922518882908));
#65971=CARTESIAN_POINT('Ctrl Pts',(25.5745310782928,0.476360248171889,125.909234063894));
#65972=CARTESIAN_POINT('Ctrl Pts',(25.5667831815157,0.339902114419901,125.895954891283));
#65973=CARTESIAN_POINT('Ctrl Pts',(25.5590352847386,0.202817723895715,125.888379102034));
#65974=CARTESIAN_POINT('Ctrl Pts',(25.5512873879615,0.0656212361583364,
125.88654840929));
#65975=CARTESIAN_POINT('Ctrl Pts',(25.5435411118774,-0.071546553031422,
125.884718099489));
#65976=CARTESIAN_POINT('Ctrl Pts',(25.5357948357933,-0.20882600211165,125.888630501059));
#65977=CARTESIAN_POINT('Ctrl Pts',(25.5280485597092,-0.345701106305024,
125.898275232292));
#65978=CARTESIAN_POINT('Ctrl Pts',(25.5203022264438,-0.482577220879138,
125.90792003472));
#65979=CARTESIAN_POINT('Ctrl Pts',(25.5125558931785,-0.619048594612275,
125.923297223765));
#65980=CARTESIAN_POINT('Ctrl Pts',(25.5048095599131,-0.75460290175703,125.944344411507));
#65981=CARTESIAN_POINT('Ctrl Pts',(25.4970614919101,-0.890187565349003,
125.96539631262));
#65982=CARTESIAN_POINT('Ctrl Pts',(25.4893134239071,-1.02485436742657,125.992120679126));
#65983=CARTESIAN_POINT('Ctrl Pts',(25.4815653559041,-1.15810014324691,126.024403805971));
#65984=CARTESIAN_POINT('Ctrl Pts',(25.4738090531623,-1.29148753426344,126.056721243708));
#65985=CARTESIAN_POINT('Ctrl Pts',(25.4660527504204,-1.42345050149076,126.094609151277));
#65986=CARTESIAN_POINT('Ctrl Pts',(25.4582964476785,-1.55349950821828,126.137903466743));
#65987=CARTESIAN_POINT('Ctrl Pts',(25.4505360051644,-1.68361792601657,126.181220889689));
#65988=CARTESIAN_POINT('Ctrl Pts',(25.4427755626502,-1.81181998253636,126.229950331418));
#65989=CARTESIAN_POINT('Ctrl Pts',(25.435015120136,-1.93763610160001,126.283879514821));
#65990=CARTESIAN_POINT('Ctrl Pts',(25.4272422198705,-2.06365419186741,126.337895270137));
#65991=CARTESIAN_POINT('Ctrl Pts',(25.4194693196051,-2.18727833809453,126.397127278236));
#65992=CARTESIAN_POINT('Ctrl Pts',(25.4116964193397,-2.3080627542776,126.461316824923));
#65993=CARTESIAN_POINT('Ctrl Pts',(25.4042060835778,-2.42445635269303,126.523172919903));
#65994=CARTESIAN_POINT('Ctrl Pts',(25.3967157478158,-2.53821283329266,126.589632217794));
#65995=CARTESIAN_POINT('Ctrl Pts',(25.3892254120539,-2.64896035774722,126.660426244825));
#65996=CARTESIAN_POINT('Ctrl Pts',(25.3814496526714,-2.763927981328,126.733917919619));
#65997=CARTESIAN_POINT('Ctrl Pts',(25.3736738932888,-2.87601703573611,126.812314070818));
#65998=CARTESIAN_POINT('Ctrl Pts',(25.3658981339063,-2.98478070791217,126.895362384236));
#65999=CARTESIAN_POINT('Ctrl Pts',(25.3581346820708,-3.09337222789739,126.978279247982));
#66000=CARTESIAN_POINT('Ctrl Pts',(25.3503712302353,-3.19864854090535,127.065833372998));
#66001=CARTESIAN_POINT('Ctrl Pts',(25.3426077783998,-3.30019022499862,127.157728261361));
#66002=CARTESIAN_POINT('Ctrl Pts',(25.3348514285176,-3.40163901944636,127.249539084902));
#66003=CARTESIAN_POINT('Ctrl Pts',(25.3270950786352,-3.49935969320959,127.345682512303));
#66004=CARTESIAN_POINT('Ctrl Pts',(25.319338728753,-3.59296420884819,127.445820569206));
#66005=CARTESIAN_POINT('Ctrl Pts',(25.3115877943238,-3.68650337018103,127.545888710111));
#66006=CARTESIAN_POINT('Ctrl Pts',(25.3038368598946,-3.7759318256622,127.649945646897));
#66007=CARTESIAN_POINT('Ctrl Pts',(25.2960859254653,-3.86089717024458,127.757615452099));
#66008=CARTESIAN_POINT('Ctrl Pts',(25.2883387240328,-3.94582159390907,127.865233401485));
#66009=CARTESIAN_POINT('Ctrl Pts',(25.2805915226004,-4.02628694324508,127.976460449943));
#66010=CARTESIAN_POINT('Ctrl Pts',(25.2728443211679,-4.1019802860687,128.090886682699));
#66011=CARTESIAN_POINT('Ctrl Pts',(25.2650974390395,-4.17767050915993,128.205308199331));
#66012=CARTESIAN_POINT('Ctrl Pts',(25.2573505569111,-4.24858889158202,128.322928318665));
#66013=CARTESIAN_POINT('Ctrl Pts',(25.2496036747827,-4.31446518421511,128.443307200827));
#66014=CARTESIAN_POINT('Ctrl Pts',(25.2418573440181,-4.38033678827769,128.56367751534));
#66015=CARTESIAN_POINT('Ctrl Pts',(25.2341110132535,-4.44116683329889,128.686805856572));
#66016=CARTESIAN_POINT('Ctrl Pts',(25.2263646824889,-4.49673087808077,128.812227471259));
#66017=CARTESIAN_POINT('Ctrl Pts',(25.218613615461,-4.5523288958436,128.937725771259));
#66018=CARTESIAN_POINT('Ctrl Pts',(25.210862548433,-4.60265432247078,129.065519787961));
#66019=CARTESIAN_POINT('Ctrl Pts',(25.2031114814051,-4.64753064735533,129.195124169932));
#66020=CARTESIAN_POINT('Ctrl Pts',(25.1954845842286,-4.69168806649772,129.322652327198));
#66021=CARTESIAN_POINT('Ctrl Pts',(25.1878576870521,-4.7305696063685,129.451932917159));
#66022=CARTESIAN_POINT('Ctrl Pts',(25.1802307898757,-4.7640545282341,129.582490119308));
#66023=CARTESIAN_POINT('Origin',(213.235140564004,0.,130.804360617566));
#66024=CARTESIAN_POINT('',(23.0846591878033,-4.76405452823398,129.582490119308));
#66025=CARTESIAN_POINT('',(23.4300068676217,-4.76405452823403,129.582490119308));
#66026=CARTESIAN_POINT('',(213.235140564004,-4.76405452823405,129.582490119308));
#66027=CARTESIAN_POINT('',(24.7648594360374,-4.91824827617447,130.800242801777));
#66028=CARTESIAN_POINT('Ctrl Pts',(24.7648594359913,-4.91824827617515,130.800242802593));
#66029=CARTESIAN_POINT('Ctrl Pts',(24.7568849401906,-4.91836645954758,130.941399015684));
#66030=CARTESIAN_POINT('Ctrl Pts',(24.7489104443899,-4.91240288179963,131.082649968674));
#66031=CARTESIAN_POINT('Ctrl Pts',(24.7409359485892,-4.90036364732372,131.223430046764));
#66032=CARTESIAN_POINT('Ctrl Pts',(24.7332213675798,-4.88871681071159,131.359621643583));
#66033=CARTESIAN_POINT('Ctrl Pts',(24.7255067865705,-4.87138422612501,131.495372160377));
#66034=CARTESIAN_POINT('Ctrl Pts',(24.7177922055612,-4.8484243349185,131.630172055529));
#66035=CARTESIAN_POINT('Ctrl Pts',(24.7100779293296,-4.82546535078202,131.764966625179));
#66036=CARTESIAN_POINT('Ctrl Pts',(24.7023636530981,-4.79687956809056,131.898810259205));
#66037=CARTESIAN_POINT('Ctrl Pts',(24.6946493768665,-4.76277686638179,132.031201920897));
#66038=CARTESIAN_POINT('Ctrl Pts',(24.6869337021269,-4.72866798225196,132.163617583648));
#66039=CARTESIAN_POINT('Ctrl Pts',(24.6792180273873,-4.68904028752408,132.294580368594));
#66040=CARTESIAN_POINT('Ctrl Pts',(24.6715023526477,-4.64405389505115,132.423603181965));
#66041=CARTESIAN_POINT('Ctrl Pts',(24.6637835755001,-4.59904941392792,132.552677874324));
#66042=CARTESIAN_POINT('Ctrl Pts',(24.6560647983525,-4.54868207766955,132.679810671195));
#66043=CARTESIAN_POINT('Ctrl Pts',(24.6483460212049,-4.49316043851339,132.804533694147));
#66044=CARTESIAN_POINT('Ctrl Pts',(24.6406182047815,-4.43757377928982,132.929402777256));
#66045=CARTESIAN_POINT('Ctrl Pts',(24.6328903883581,-4.37682092878727,133.051856093216));
#66046=CARTESIAN_POINT('Ctrl Pts',(24.6251625719347,-4.31115694857983,133.171449299304));
#66047=CARTESIAN_POINT('Ctrl Pts',(24.6174293470803,-4.24544701242726,133.291126204534));
#66048=CARTESIAN_POINT('Ctrl Pts',(24.6096961222258,-4.17481930515338,133.407938677641));
#66049=CARTESIAN_POINT('Ctrl Pts',(24.6019628973714,-4.09957202948641,133.521471626994));
#66050=CARTESIAN_POINT('Ctrl Pts',(24.5942185416995,-4.02421644665088,133.635167990001));
#66051=CARTESIAN_POINT('Ctrl Pts',(24.5864741860276,-3.94422825541909,133.745575091));
#66052=CARTESIAN_POINT('Ctrl Pts',(24.5787298303558,-3.85994588593471,133.852310882934));
#66053=CARTESIAN_POINT('Ctrl Pts',(24.5769770658287,-3.84087042585147,133.876468181203));
#66054=CARTESIAN_POINT('Ctrl Pts',(24.5752243013017,-3.82157514713822,133.900437569811));
#66055=CARTESIAN_POINT('Ctrl Pts',(24.5734715367746,-3.80206422677062,133.924214889485));
#66056=CARTESIAN_POINT('Ctrl Pts',(24.5656972026555,-3.7155241287903,134.029678472728));
#66057=CARTESIAN_POINT('Ctrl Pts',(24.5579228685364,-3.62445552854384,134.131705634315));
#66058=CARTESIAN_POINT('Ctrl Pts',(24.5501485344174,-3.5291615759598,134.229882714016));
#66059=CARTESIAN_POINT('Ctrl Pts',(24.5423837814703,-3.43398506465566,134.327938799241));
#66060=CARTESIAN_POINT('Ctrl Pts',(24.5346190285231,-3.33459383181647,134.42215396563));
#66061=CARTESIAN_POINT('Ctrl Pts',(24.526854275576,-3.23133200637872,134.512146550849));
#66062=CARTESIAN_POINT('Ctrl Pts',(24.519097234691,-3.1281727420416,134.602049754164));
#66063=CARTESIAN_POINT('Ctrl Pts',(24.5113401938061,-3.02115082832521,134.687738467207));
#66064=CARTESIAN_POINT('Ctrl Pts',(24.503583152921,-2.91064780758299,134.768867195025));
#66065=CARTESIAN_POINT('Ctrl Pts',(24.4958319616809,-2.80022811802831,134.849934743038));
#66066=CARTESIAN_POINT('Ctrl Pts',(24.4880807704408,-2.68633286048399,134.926448919951));
#66067=CARTESIAN_POINT('Ctrl Pts',(24.4803295792006,-2.56937699740166,134.998104160956));
#66068=CARTESIAN_POINT('Ctrl Pts',(24.4725816824235,-2.45247084368119,135.069728946572));
#66069=CARTESIAN_POINT('Ctrl Pts',(24.4648337856464,-2.33250700436656,135.136498699941));
#66070=CARTESIAN_POINT('Ctrl Pts',(24.4570858888693,-2.20992960879253,135.198151029805));
#66071=CARTESIAN_POINT('Ctrl Pts',(24.4493396127852,-2.08737785376737,135.25979046333));
#66072=CARTESIAN_POINT('Ctrl Pts',(24.4415933367011,-1.96221397895153,135.316314426981));
#66073=CARTESIAN_POINT('Ctrl Pts',(24.433847060617,-1.83490655792569,135.367506570325));
#66074=CARTESIAN_POINT('Ctrl Pts',(24.4261007273517,-1.70759819714538,135.418699091558));
#66075=CARTESIAN_POINT('Ctrl Pts',(24.4183543940863,-1.57814662131808,135.464559568085));
#66076=CARTESIAN_POINT('Ctrl Pts',(24.4106080608209,-1.44703984165177,135.50492002674));
#66077=CARTESIAN_POINT('Ctrl Pts',(24.402859992818,-1.31590370153101,135.545289523839));
#66078=CARTESIAN_POINT('Ctrl Pts',(24.3951119248151,-1.18311199356689,135.580156437137));
#66079=CARTESIAN_POINT('Ctrl Pts',(24.3873638568121,-1.04916693537901,135.609402948723));
#66080=CARTESIAN_POINT('Ctrl Pts',(24.3796075540703,-0.915079518789317,
135.638680543849));
#66081=CARTESIAN_POINT('Ctrl Pts',(24.3718512513283,-0.77983668589471,135.66232572116));
#66082=CARTESIAN_POINT('Ctrl Pts',(24.3640949485865,-0.643950423630331,
135.680271908228));
#66083=CARTESIAN_POINT('Ctrl Pts',(24.3563345060723,-0.507991634776325,
135.698227673717));
#66084=CARTESIAN_POINT('Ctrl Pts',(24.3485740635582,-0.371389121475727,
135.710478353168));
#66085=CARTESIAN_POINT('Ctrl Pts',(24.340813621044,-0.234658008560122,135.717009463303));
#66086=CARTESIAN_POINT('Ctrl Pts',(24.3330407207786,-0.0977074027236458,
135.723551057755));
#66087=CARTESIAN_POINT('Ctrl Pts',(24.3252678205131,0.039371824076289,135.724354732915));
#66088=CARTESIAN_POINT('Ctrl Pts',(24.3174949202477,0.176065630718323,135.719458170634));
#66089=CARTESIAN_POINT('Ctrl Pts',(24.3100045844857,0.30779027317707,135.714739610727));
#66090=CARTESIAN_POINT('Ctrl Pts',(24.3025142487238,0.439156723834318,135.704728077548));
#66091=CARTESIAN_POINT('Ctrl Pts',(24.2950239129618,0.56971317267766,135.689502372252));
#66092=CARTESIAN_POINT('Ctrl Pts',(24.2872495788427,0.705219708961442,135.673699379712));
#66093=CARTESIAN_POINT('Ctrl Pts',(24.2794752447236,0.84028285247154,135.652228960118));
#66094=CARTESIAN_POINT('Ctrl Pts',(24.2717009106046,0.974390719199168,135.625122568631));
#66095=CARTESIAN_POINT('Ctrl Pts',(24.2639361576575,1.10833330996662,135.598049583349));
#66096=CARTESIAN_POINT('Ctrl Pts',(24.2561714047104,1.24132258687751,135.565354523023));
#66097=CARTESIAN_POINT('Ctrl Pts',(24.2484066517633,1.37285143650384,135.527120615257));
#66098=CARTESIAN_POINT('Ctrl Pts',(24.2406496108783,1.50424964982285,135.488924681947));
#66099=CARTESIAN_POINT('Ctrl Pts',(24.2328925699932,1.63418994945571,135.445200957383));
#66100=CARTESIAN_POINT('Ctrl Pts',(24.2251355291082,1.76217542775139,135.396083695489));
#66101=CARTESIAN_POINT('Ctrl Pts',(24.217384337868,1.89006439120212,135.347003473304));
#66102=CARTESIAN_POINT('Ctrl Pts',(24.209633146628,2.01600110398207,135.292537949035));
#66103=CARTESIAN_POINT('Ctrl Pts',(24.2018819553878,2.13950418842319,135.232871077102));
#66104=CARTESIAN_POINT('Ctrl Pts',(24.1941340586107,2.26295478075869,135.173229565181));
#66105=CARTESIAN_POINT('Ctrl Pts',(24.1863861618337,2.38397345071505,135.108391272251));
#66106=CARTESIAN_POINT('Ctrl Pts',(24.1786382650566,2.50209937834119,135.038588028016));
#66107=CARTESIAN_POINT('Ctrl Pts',(24.1708919889725,2.6202005965696,134.968799385115));
#66108=CARTESIAN_POINT('Ctrl Pts',(24.1631457128884,2.73540993966643,134.894048055435));
#66109=CARTESIAN_POINT('Ctrl Pts',(24.1553994368043,2.84729211041955,134.814611320507));
#66110=CARTESIAN_POINT('Ctrl Pts',(24.147653103539,2.9591751070616,134.735173999196));
#66111=CARTESIAN_POINT('Ctrl Pts',(24.1399067702737,3.06773056356553,134.651051429961));
#66112=CARTESIAN_POINT('Ctrl Pts',(24.1321604370083,3.17255337737015,134.562563396853));
#66113=CARTESIAN_POINT('Ctrl Pts',(24.1244123690053,3.27739966551712,134.474055547463));
#66114=CARTESIAN_POINT('Ctrl Pts',(24.1166643010024,3.37851134892897,134.381180541005));
#66115=CARTESIAN_POINT('Ctrl Pts',(24.1089162329994,3.47551784317074,134.284297223929));
#66116=CARTESIAN_POINT('Ctrl Pts',(24.1011599302575,3.57262743706899,134.18731093811));
#66117=CARTESIAN_POINT('Ctrl Pts',(24.0934036275156,3.66562284907619,134.086308108422));
#66118=CARTESIAN_POINT('Ctrl Pts',(24.0856473247738,3.75417132847954,133.98168349995));
#66119=CARTESIAN_POINT('Ctrl Pts',(24.0778868822596,3.84276706887262,133.877003050175));
#66120=CARTESIAN_POINT('Ctrl Pts',(24.0701264397455,3.9269109075931,133.768697278434));
#66121=CARTESIAN_POINT('Ctrl Pts',(24.0623659972313,4.00631222189423,133.657191745271));
#66122=CARTESIAN_POINT('Ctrl Pts',(24.0545930969659,4.08584099823399,133.545507213527));
#66123=CARTESIAN_POINT('Ctrl Pts',(24.0468201967005,4.16061182333853,133.430612983789));
#66124=CARTESIAN_POINT('Ctrl Pts',(24.039047296435,4.23037854823634,133.312961901374));
#66125=CARTESIAN_POINT('Ctrl Pts',(24.031556960673,4.29760907695243,133.199587732149));
#66126=CARTESIAN_POINT('Ctrl Pts',(24.0240666249109,4.36019286593216,133.08365393849));
#66127=CARTESIAN_POINT('Ctrl Pts',(24.0165762891489,4.41795199847147,132.965583234906));
#66128=CARTESIAN_POINT('Ctrl Pts',(24.0088019550298,4.47790108607643,132.843035844708));
#66129=CARTESIAN_POINT('Ctrl Pts',(24.0010276209107,4.53284234216597,132.717798110651));
#66130=CARTESIAN_POINT('Ctrl Pts',(23.9932532867916,4.58252554504819,132.590317697532));
#66131=CARTESIAN_POINT('Ctrl Pts',(23.9854885338445,4.63214751782318,132.462994392629));
#66132=CARTESIAN_POINT('Ctrl Pts',(23.9777237808974,4.6765241902122,132.333434268783));
#66133=CARTESIAN_POINT('Ctrl Pts',(23.9699590279503,4.71545147676222,132.202108961439));
#66134=CARTESIAN_POINT('Ctrl Pts',(23.9622019870653,4.75434010018245,132.070914088242));
#66135=CARTESIAN_POINT('Ctrl Pts',(23.9544449461803,4.78778999830565,131.937957892922));
#66136=CARTESIAN_POINT('Ctrl Pts',(23.9466879052953,4.81564553203922,131.803731005486));
#66137=CARTESIAN_POINT('Ctrl Pts',(23.9389367140552,4.84348005969796,131.66960533959));
#66138=CARTESIAN_POINT('Ctrl Pts',(23.9311855228151,4.86572854101926,131.534211270154));
#66139=CARTESIAN_POINT('Ctrl Pts',(23.923434331575,4.88228554567899,131.398053225701));
#66140=CARTESIAN_POINT('Ctrl Pts',(23.9156864347979,4.89883551317014,131.261953052048));
#66141=CARTESIAN_POINT('Ctrl Pts',(23.9079385380209,4.90969876816926,131.125089936495));
#66142=CARTESIAN_POINT('Ctrl Pts',(23.9001906412438,4.91482127113167,130.987976889535));
#66143=CARTESIAN_POINT('Ctrl Pts',(23.8924443651597,4.91994270257689,130.850892523668));
#66144=CARTESIAN_POINT('Ctrl Pts',(23.8846980890756,4.91932575593822,130.713558720828));
#66145=CARTESIAN_POINT('Ctrl Pts',(23.8769518129915,4.91296842724458,130.576491586327));
#66146=CARTESIAN_POINT('Ctrl Pts',(23.8692054797262,4.90661105162259,130.439423440027));
#66147=CARTESIAN_POINT('Ctrl Pts',(23.8614591464608,4.89451322750493,130.302622356541));
#66148=CARTESIAN_POINT('Ctrl Pts',(23.8537128131954,4.87672503044056,130.166602011215));
#66149=CARTESIAN_POINT('Ctrl Pts',(23.8459647451925,4.85893284983277,130.030551205076));
#66150=CARTESIAN_POINT('Ctrl Pts',(23.8382166771894,4.83544781121733,129.895281872601));
#66151=CARTESIAN_POINT('Ctrl Pts',(23.8304686091865,4.80637151233564,129.761299762242));
#66152=CARTESIAN_POINT('Ctrl Pts',(23.8227123064446,4.7772643108175,129.627175254102));
#66153=CARTESIAN_POINT('Ctrl Pts',(23.8149560037028,4.74255406138123,129.494341083636));
#66154=CARTESIAN_POINT('Ctrl Pts',(23.8071997009609,4.70239303118569,129.363290583613));
#66155=CARTESIAN_POINT('Ctrl Pts',(23.7994392584467,4.66221056583905,129.232170137993));
#66156=CARTESIAN_POINT('Ctrl Pts',(23.7916788159326,4.61657165285026,129.102835628258));
#66157=CARTESIAN_POINT('Ctrl Pts',(23.7839183734184,4.5656772396639,128.975761589426));
#66158=CARTESIAN_POINT('Ctrl Pts',(23.776145473153,4.51470112624745,128.848483560065));
#66159=CARTESIAN_POINT('Ctrl Pts',(23.7683725728875,4.45845281414343,128.723473609665));
#66160=CARTESIAN_POINT('Ctrl Pts',(23.7605996726221,4.39718024540997,128.601183604279));
#66161=CARTESIAN_POINT('Ctrl Pts',(23.75310933686,4.33813508888617,128.483339148619));
#66162=CARTESIAN_POINT('Ctrl Pts',(23.745619001098,4.27442477150302,128.368020587173));
#66163=CARTESIAN_POINT('Ctrl Pts',(23.738128665336,4.20630876662415,128.255606093819));
#66164=CARTESIAN_POINT('Ctrl Pts',(23.7303543312169,4.13561012271688,128.138929370782));
#66165=CARTESIAN_POINT('Ctrl Pts',(23.7225799970978,4.05994116106895,128.025011681657));
#66166=CARTESIAN_POINT('Ctrl Pts',(23.7148056629787,3.97954326381621,127.914305518798));
#66167=CARTESIAN_POINT('Ctrl Pts',(23.7070409100316,3.89924444978648,127.80373579139));
#66168=CARTESIAN_POINT('Ctrl Pts',(23.6992761570846,3.81422852364892,127.696370028476));
#66169=CARTESIAN_POINT('Ctrl Pts',(23.6915114041375,3.72478197248664,127.592634863405));
#66170=CARTESIAN_POINT('Ctrl Pts',(23.6837543632525,3.63542426089996,127.489002729563));
#66171=CARTESIAN_POINT('Ctrl Pts',(23.6759973223674,3.54164493525683,127.388994311715));
#66172=CARTESIAN_POINT('Ctrl Pts',(23.6682402814824,3.44377264974579,127.293005750942));
#66173=CARTESIAN_POINT('Ctrl Pts',(23.6604890902423,3.34597417048686,127.19708957589));
#66174=CARTESIAN_POINT('Ctrl Pts',(23.6527378990022,3.24408915291436,127.10518749673));
#66175=CARTESIAN_POINT('Ctrl Pts',(23.6449867077621,3.1384849993654,127.017660870919));
#66176=CARTESIAN_POINT('Ctrl Pts',(23.637238810985,3.03292573039863,126.930171446258));
#66177=CARTESIAN_POINT('Ctrl Pts',(23.629490914208,2.92365076979577,126.84705402514));
#66178=CARTESIAN_POINT('Ctrl Pts',(23.6217430174309,2.81106251812016,126.768631367267));
#66179=CARTESIAN_POINT('Ctrl Pts',(23.6139967413468,2.69849781747983,126.690225113723));
#66180=CARTESIAN_POINT('Ctrl Pts',(23.6062504652627,2.58262152492707,126.616511893403));
#66181=CARTESIAN_POINT('Ctrl Pts',(23.5985041891786,2.46386677128336,126.547772359834));
#66182=CARTESIAN_POINT('Ctrl Pts',(23.5907578559133,2.34511114101887,126.479032318844));
#66183=CARTESIAN_POINT('Ctrl Pts',(23.5830115226479,2.22347734563218,126.415266233726));
#66184=CARTESIAN_POINT('Ctrl Pts',(23.5752651893826,2.09942462179924,126.356709628574));
#66185=CARTESIAN_POINT('Ctrl Pts',(23.5675171213796,1.97534411721892,126.298139910076));
#66186=CARTESIAN_POINT('Ctrl Pts',(23.5597690533766,1.84884395975591,126.244782159854));
#66187=CARTESIAN_POINT('Ctrl Pts',(23.5520209853736,1.72040456596692,126.196824270243));
#66188=CARTESIAN_POINT('Ctrl Pts',(23.5442646826318,1.59182866526177,126.148815410416));
#66189=CARTESIAN_POINT('Ctrl Pts',(23.53650837989,1.46130977792409,126.10621801252));
#66190=CARTESIAN_POINT('Ctrl Pts',(23.5287520771481,1.32934526290405,126.069170628295));
#66191=CARTESIAN_POINT('Ctrl Pts',(23.520991634634,1.19731031444896,126.032103470765));
#66192=CARTESIAN_POINT('Ctrl Pts',(23.5132311921198,1.06382858120302,126.000592319141));
#66193=CARTESIAN_POINT('Ctrl Pts',(23.5054707496056,0.929407919917445,125.974724608414));
#66194=CARTESIAN_POINT('Ctrl Pts',(23.4976978493402,0.794771474652884,125.948815372542));
#66195=CARTESIAN_POINT('Ctrl Pts',(23.4899249490748,0.659193476281055,125.928567738821));
#66196=CARTESIAN_POINT('Ctrl Pts',(23.4821520488094,0.52318811125092,125.914017351215));
#66197=CARTESIAN_POINT('Ctrl Pts',(23.4746617130473,0.392126883815917,125.899995906849));
#66198=CARTESIAN_POINT('Ctrl Pts',(23.4671713772852,0.260669129322521,125.891264701959));
#66199=CARTESIAN_POINT('Ctrl Pts',(23.4596810415231,0.129273267856855,125.887809846475));
#66200=CARTESIAN_POINT('Ctrl Pts',(23.4519067074041,-0.00710450763261369,
125.884223999095));
#66201=CARTESIAN_POINT('Ctrl Pts',(23.444132373285,-0.143847607897832,125.886311146019));
#66202=CARTESIAN_POINT('Ctrl Pts',(23.4363580391659,-0.280444865365881,
125.894112788791));
#66203=CARTESIAN_POINT('Ctrl Pts',(23.4285932862188,-0.416873778922149,
125.901904816735));
#66204=CARTESIAN_POINT('Ctrl Pts',(23.4208285332716,-0.553156820724757,
125.915397305761));
#66205=CARTESIAN_POINT('Ctrl Pts',(23.4130637803245,-0.688780198788125,
125.934579831919));
#66206=CARTESIAN_POINT('Ctrl Pts',(23.4053067394395,-0.824268873800814,
125.953743305721));
#66207=CARTESIAN_POINT('Ctrl Pts',(23.3975496985545,-0.959098804319341,
125.978585515665));
#66208=CARTESIAN_POINT('Ctrl Pts',(23.3897926576695,-1.09275906001764,126.009044079604));
#66209=CARTESIAN_POINT('Ctrl Pts',(23.3820414664293,-1.22631852147721,126.039479674503));
#66210=CARTESIAN_POINT('Ctrl Pts',(23.3742902751892,-1.35870968415475,126.075523106702));
#66211=CARTESIAN_POINT('Ctrl Pts',(23.3665390839491,-1.48942993785113,126.11706059274));
#66212=CARTESIAN_POINT('Ctrl Pts',(23.358791187172,-1.62009463195226,126.158580424239));
#66213=CARTESIAN_POINT('Ctrl Pts',(23.3510432903949,-1.7490894577416,126.205589547052));
#66214=CARTESIAN_POINT('Ctrl Pts',(23.3432953936178,-1.87592536100717,126.257923869691));
#66215=CARTESIAN_POINT('Ctrl Pts',(23.3355491175337,-2.00273473293604,126.310247245118));
#66216=CARTESIAN_POINT('Ctrl Pts',(23.3278028414496,-2.12738571941861,126.367893455701));
#66217=CARTESIAN_POINT('Ctrl Pts',(23.3200565653655,-2.2494080809062,126.430649796301));
#66218=CARTESIAN_POINT('Ctrl Pts',(23.3123102321002,-2.37143134313498,126.493406600153));
#66219=CARTESIAN_POINT('Ctrl Pts',(23.3045638988349,-2.49082559397138,126.56127343048));
#66220=CARTESIAN_POINT('Ctrl Pts',(23.2968175655695,-2.60714445168269,126.633991224987));
#66221=CARTESIAN_POINT('Ctrl Pts',(23.2890694975665,-2.72348935819601,126.70672530414));
#66222=CARTESIAN_POINT('Ctrl Pts',(23.2813214295635,-2.83675716967449,126.784312301954));
#66223=CARTESIAN_POINT('Ctrl Pts',(23.2735733615606,-2.94653013009208,126.86644959077));
#66224=CARTESIAN_POINT('Ctrl Pts',(23.2658170588187,-3.05641975851831,126.948674176074));
#66225=CARTESIAN_POINT('Ctrl Pts',(23.2580607560769,-3.16280680249636,127.035458478417));
#66226=CARTESIAN_POINT('Ctrl Pts',(23.250304453335,-3.26530585986261,127.126458946226));
#66227=CARTESIAN_POINT('Ctrl Pts',(23.2425440108208,-3.36785962406225,127.217507983725));
#66228=CARTESIAN_POINT('Ctrl Pts',(23.2347835683066,-3.466520985658,127.312777399149));
#66229=CARTESIAN_POINT('Ctrl Pts',(23.2270231257924,-3.56094187413623,127.411887178978));
#66230=CARTESIAN_POINT('Ctrl Pts',(23.219250225527,-3.65551433540667,127.511156058624));
#66231=CARTESIAN_POINT('Ctrl Pts',(23.2114773252616,-3.74583246289593,127.614277327821));
#66232=CARTESIAN_POINT('Ctrl Pts',(23.2037044249961,-3.83158833799136,127.720837653379));
#66233=CARTESIAN_POINT('Ctrl Pts',(23.1962140892342,-3.91422677102037,127.823524242693));
#66234=CARTESIAN_POINT('Ctrl Pts',(23.1887237534722,-3.99262870831164,127.92940394511));
#66235=CARTESIAN_POINT('Ctrl Pts',(23.1812334177102,-4.06655804872064,128.038083570905));
#66236=CARTESIAN_POINT('Ctrl Pts',(23.173185565218,-4.1459900588959,128.154852381424));
#66237=CARTESIAN_POINT('Ctrl Pts',(23.1651377127257,-4.22050995647638,128.275223161469));
#66238=CARTESIAN_POINT('Ctrl Pts',(23.1570898602335,-4.2897812136878,128.398750466026));
#66239=CARTESIAN_POINT('Ctrl Pts',(23.1492064240141,-4.35763727076484,128.519754128526));
#66240=CARTESIAN_POINT('Ctrl Pts',(23.1413229877948,-4.42045684504684,128.643786255033));
#66241=CARTESIAN_POINT('Ctrl Pts',(23.1334395515754,-4.47796506753759,128.770396036652));
#66242=CARTESIAN_POINT('Ctrl Pts',(23.1253094909467,-4.53727236989769,128.900966662468));
#66243=CARTESIAN_POINT('Ctrl Pts',(23.117179430318,-4.59093031649128,129.034278550125));
#66244=CARTESIAN_POINT('Ctrl Pts',(23.1090493696893,-4.63868701110859,129.169806893924));
#66245=CARTESIAN_POINT('Ctrl Pts',(23.1009193090606,-4.68644370572583,129.305335237722));
#66246=CARTESIAN_POINT('Ctrl Pts',(23.0927892484319,-4.72829894556715,129.443079645157));
#66247=CARTESIAN_POINT('Ctrl Pts',(23.0846591878033,-4.76405452823398,129.582490119308));
#66248=CARTESIAN_POINT('Ctrl Pts',(24.8346867982621,-4.76405452823407,129.582490119308));
#66249=CARTESIAN_POINT('Ctrl Pts',(24.8253782229543,-4.80467650385836,129.740874585743));
#66250=CARTESIAN_POINT('Ctrl Pts',(24.8160696476464,-4.83743482907301,129.901437429581));
#66251=CARTESIAN_POINT('Ctrl Pts',(24.8067610723386,-4.86212490932803,130.063466273822));
#66252=CARTESIAN_POINT('Ctrl Pts',(24.7975526181693,-4.88654942811261,130.223752368842));
#66253=CARTESIAN_POINT('Ctrl Pts',(24.788344164,-4.90307827616601,130.385473055383));
#66254=CARTESIAN_POINT('Ctrl Pts',(24.7791357098307,-4.91155986073502,130.547918037411));
#66255=CARTESIAN_POINT('Ctrl Pts',(24.7743769518996,-4.91594298596908,130.631866584299));
#66256=CARTESIAN_POINT('Ctrl Pts',(24.7696181939684,-4.91817775056553,130.716008228789));
#66257=CARTESIAN_POINT('Ctrl Pts',(24.7648594360373,-4.91824827617447,130.800242801777));
#66258=CARTESIAN_POINT('',(25.1101405639584,-4.91824999949758,130.804290318038));
#66259=CARTESIAN_POINT('Ctrl Pts',(25.1802307898757,-4.7640545282341,129.582490119308));
#66260=CARTESIAN_POINT('Ctrl Pts',(25.1724704274842,-4.79812541214831,129.715331978592));
#66261=CARTESIAN_POINT('Ctrl Pts',(25.1647100650928,-4.82660895352866,129.849495165861));
#66262=CARTESIAN_POINT('Ctrl Pts',(25.1569497027014,-4.84942908031038,129.984469980017));
#66263=CARTESIAN_POINT('Ctrl Pts',(25.1491768448978,-4.87228595110947,130.119662124996));
#66264=CARTESIAN_POINT('Ctrl Pts',(25.1414039870941,-4.88946113521461,130.255668120271));
#66265=CARTESIAN_POINT('Ctrl Pts',(25.1336311292905,-4.90093048084847,130.391973076059));
#66266=CARTESIAN_POINT('Ctrl Pts',(25.1260133489406,-4.9121709998446,130.525558591197));
#66267=CARTESIAN_POINT('Ctrl Pts',(25.1183955685907,-4.91793128908067,130.65943090316));
#66268=CARTESIAN_POINT('Ctrl Pts',(25.1107777882409,-4.91823712792333,130.793108239306));
#66269=CARTESIAN_POINT('Ctrl Pts',(25.1105653801635,-4.91824565568831,130.79683559093));
#66270=CARTESIAN_POINT('Ctrl Pts',(25.1103529720861,-4.91824994621942,130.800562952252));
#66271=CARTESIAN_POINT('Ctrl Pts',(25.1101405640087,-4.91824999949757,130.804290317156));
#66272=CARTESIAN_POINT('Ctrl Pts',(25.1101405639584,-4.91824999949758,130.804290318038));
#66273=CARTESIAN_POINT('Ctrl Pts',(25.1023694478026,-4.91825194869619,130.940658887285));
#66274=CARTESIAN_POINT('Ctrl Pts',(25.0945983316468,-4.91257795198346,131.07724441592));
#66275=CARTESIAN_POINT('Ctrl Pts',(25.086827215491,-4.9011997743606,131.213535194376));
#66276=CARTESIAN_POINT('Ctrl Pts',(25.0790656782968,-4.88983562189504,131.349657975841));
#66277=CARTESIAN_POINT('Ctrl Pts',(25.0713041411026,-4.87278131048978,131.485486343794));
#66278=CARTESIAN_POINT('Ctrl Pts',(25.0635426039084,-4.8500605813044,131.620507307921));
#66279=CARTESIAN_POINT('Ctrl Pts',(25.0557887730794,-4.82736241134048,131.755394210865));
#66280=CARTESIAN_POINT('Ctrl Pts',(25.0480349422505,-4.79900908420948,131.889474921901));
#66281=CARTESIAN_POINT('Ctrl Pts',(25.0402811114215,-4.76507620767709,132.022240659906));
#66282=CARTESIAN_POINT('Ctrl Pts',(25.0325331210781,-4.73116889070126,132.154906393616));
#66283=CARTESIAN_POINT('Ctrl Pts',(25.0247851307347,-4.69169048599964,132.286258748163));
#66284=CARTESIAN_POINT('Ctrl Pts',(25.0170371403913,-4.64676776865121,132.415798598602));
#66285=CARTESIAN_POINT('Ctrl Pts',(25.0092924292492,-4.6018640640566,132.545283623566));
#66286=CARTESIAN_POINT('Ctrl Pts',(25.0015477181072,-4.55152075755507,132.672957301151));
#66287=CARTESIAN_POINT('Ctrl Pts',(24.9938030069651,-4.49591456095806,132.798335372438));
#66288=CARTESIAN_POINT('Ctrl Pts',(24.9860599017827,-4.44031989497931,132.923687445063));
#66289=CARTESIAN_POINT('Ctrl Pts',(24.9783167966002,-4.37946466813168,133.046744500704));
#66290=CARTESIAN_POINT('Ctrl Pts',(24.9705736914178,-4.31357369545086,133.167042364314));
#66291=CARTESIAN_POINT('Ctrl Pts',(24.9628305112143,-4.24768208436868,133.28734139346));
#66292=CARTESIAN_POINT('Ctrl Pts',(24.9550873310108,-4.17675481816997,133.404880834054));
#66293=CARTESIAN_POINT('Ctrl Pts',(24.9473441508074,-4.10106242447939,133.519221581414));
#66294=CARTESIAN_POINT('Ctrl Pts',(24.9395992149067,-4.0253528682118,133.63358825452));
#66295=CARTESIAN_POINT('Ctrl Pts',(24.931854279006,-3.94487625050408,133.744754464969));
#66296=CARTESIAN_POINT('Ctrl Pts',(24.9241093431053,-3.85994589212343,133.852310875096));
#66297=CARTESIAN_POINT('Ctrl Pts',(24.9163561711497,-3.77492521781236,133.959981661961));
#66298=CARTESIAN_POINT('Ctrl Pts',(24.9086029991941,-3.68544158497976,134.064034672876));
#66299=CARTESIAN_POINT('Ctrl Pts',(24.9008498272385,-3.59184836161745,134.164094001281));
#66300=CARTESIAN_POINT('Ctrl Pts',(24.8930924907353,-3.49820486548413,134.264207075667));
#66301=CARTESIAN_POINT('Ctrl Pts',(24.8853351542321,-3.40044765936741,134.360321919051));
#66302=CARTESIAN_POINT('Ctrl Pts',(24.8775778177288,-3.29896556490838,134.452100913153));
#66303=CARTESIAN_POINT('Ctrl Pts',(24.8698080807413,-3.19732124632465,134.544026620496));
#66304=CARTESIAN_POINT('Ctrl Pts',(24.8620383437537,-3.09194044214155,134.631602378409));
#66305=CARTESIAN_POINT('Ctrl Pts',(24.8542686067661,-2.98324419280498,134.714531604696));
#66306=CARTESIAN_POINT('Ctrl Pts',(24.8469557926535,-2.88094015504777,134.7925839271));
#66307=CARTESIAN_POINT('Ctrl Pts',(24.8396429785408,-2.7756996540835,134.866520397982));
#66308=CARTESIAN_POINT('Ctrl Pts',(24.8323301644281,-2.66789424677801,134.936130619697));
#66309=CARTESIAN_POINT('Ctrl Pts',(24.8245558303091,-2.55328511774448,135.010134021585));
#66310=CARTESIAN_POINT('Ctrl Pts',(24.8167814961899,-2.43541300679089,135.07948239656));
#66311=CARTESIAN_POINT('Ctrl Pts',(24.8090071620709,-2.3146928919907,135.143874401191));
#66312=CARTESIAN_POINT('Ctrl Pts',(24.8012424091238,-2.19412155394278,135.20818704843));
#66313=CARTESIAN_POINT('Ctrl Pts',(24.7934776561767,-2.07070953737171,135.267555296753));
#66314=CARTESIAN_POINT('Ctrl Pts',(24.7857129032296,-1.94490107231132,135.321720784901));
#66315=CARTESIAN_POINT('Ctrl Pts',(24.7779558623446,-1.81921756199236,135.375832475122));
#66316=CARTESIAN_POINT('Ctrl Pts',(24.7701988214596,-1.69114269663616,135.42475153503));
#66317=CARTESIAN_POINT('Ctrl Pts',(24.7624417805746,-1.56114528982937,135.468265467211));
#66318=CARTESIAN_POINT('Ctrl Pts',(24.7546905893345,-1.43124591507793,135.511746585198));
#66319=CARTESIAN_POINT('Ctrl Pts',(24.7469393980943,-1.29942725386825,135.549830564987));
#66320=CARTESIAN_POINT('Ctrl Pts',(24.7391882068542,-1.16617775181755,135.58235313678));
#66321=CARTESIAN_POINT('Ctrl Pts',(24.7314403100771,-1.03298488435996,135.614861885612));
#66322=CARTESIAN_POINT('Ctrl Pts',(24.7236924133001,-0.898362764637024,
135.641813835252));
#66323=CARTESIAN_POINT('Ctrl Pts',(24.715944516523,-0.762814429868399,135.663094733371));
#66324=CARTESIAN_POINT('Ctrl Pts',(24.7081982404389,-0.627294448889324,
135.684371179985));
#66325=CARTESIAN_POINT('Ctrl Pts',(24.7004519643548,-0.490849024221865,
135.699978874018));
#66326=CARTESIAN_POINT('Ctrl Pts',(24.6927056882707,-0.353990412099897,
135.709854868979));
#66327=CARTESIAN_POINT('Ctrl Pts',(24.6849593550054,-0.21713078971893,135.719730936841));
#66328=CARTESIAN_POINT('Ctrl Pts',(24.67721302174,-0.0798583637485085,135.723875193064));
#66329=CARTESIAN_POINT('Ctrl Pts',(24.6694666884747,0.0573108714876579,
135.722276693152));
#66330=CARTESIAN_POINT('Ctrl Pts',(24.6617186204717,0.194510824822804,135.720677835268));
#66331=CARTESIAN_POINT('Ctrl Pts',(24.6539705524688,0.331607150575921,135.713333666712));
#66332=CARTESIAN_POINT('Ctrl Pts',(24.6462224844659,0.468085640615847,135.700285340797));
#66333=CARTESIAN_POINT('Ctrl Pts',(24.638466181724,0.604709181619474,135.687223146967));
#66334=CARTESIAN_POINT('Ctrl Pts',(24.6307098789822,0.740713185383398,135.668444722657));
#66335=CARTESIAN_POINT('Ctrl Pts',(24.6229535762403,0.875589788055244,135.644043002346));
#66336=CARTESIAN_POINT('Ctrl Pts',(24.6151931337262,1.01053837843099,135.619628258103));
#66337=CARTESIAN_POINT('Ctrl Pts',(24.6074326912119,1.14435798743811,135.589584323071));
#66338=CARTESIAN_POINT('Ctrl Pts',(24.5996722486978,1.27655366783885,135.554054691465));
#66339=CARTESIAN_POINT('Ctrl Pts',(24.5918993484323,1.40896156048173,135.518468024539));
#66340=CARTESIAN_POINT('Ctrl Pts',(24.5841264481669,1.53973994194982,135.47737818085));
#66341=CARTESIAN_POINT('Ctrl Pts',(24.5763535479015,1.66841082482402,135.430977997695));
#66342=CARTESIAN_POINT('Ctrl Pts',(24.5688632121394,1.79240419700439,135.386264578072));
#66343=CARTESIAN_POINT('Ctrl Pts',(24.5613728763773,1.91444035081732,135.336620320418));
#66344=CARTESIAN_POINT('Ctrl Pts',(24.5538825406152,2.03411311327613,135.282258216317));
#66345=CARTESIAN_POINT('Ctrl Pts',(24.5461082064961,2.15832330489626,135.225834956516));
#66346=CARTESIAN_POINT('Ctrl Pts',(24.538333872377,2.28038081196803,135.164150301861));
#66347=CARTESIAN_POINT('Ctrl Pts',(24.5305595382579,2.39980779994224,135.097390501673));
#66348=CARTESIAN_POINT('Ctrl Pts',(24.5227947853108,2.51908760482727,135.030712976972));
#66349=CARTESIAN_POINT('Ctrl Pts',(24.5150300323637,2.63574300300044,134.95897294059));
#66350=CARTESIAN_POINT('Ctrl Pts',(24.5072652794166,2.74931651063303,134.882404485263));
#66351=CARTESIAN_POINT('Ctrl Pts',(24.4995082385316,2.86277721545675,134.805912078805));
#66352=CARTESIAN_POINT('Ctrl Pts',(24.4917511976466,2.97316179914533,134.724601014107));
#66353=CARTESIAN_POINT('Ctrl Pts',(24.4839941567616,3.08003807641042,134.638750857273));
#66354=CARTESIAN_POINT('Ctrl Pts',(24.4762429655215,3.18683375744329,134.55296544071));
#66355=CARTESIAN_POINT('Ctrl Pts',(24.4684917742814,3.29012609446808,134.462647989066));
#66356=CARTESIAN_POINT('Ctrl Pts',(24.4607405830413,3.38951286586288,134.36812065363));
#66357=CARTESIAN_POINT('Ctrl Pts',(24.4529926862642,3.4888573952286,134.273633494835));
#66358=CARTESIAN_POINT('Ctrl Pts',(24.4452447894871,3.58429937781728,134.174940279933));
#66359=CARTESIAN_POINT('Ctrl Pts',(24.4374968927101,3.6754707860058,134.072402472212));
#66360=CARTESIAN_POINT('Ctrl Pts',(24.429750616626,3.76662312310115,133.96988611319));
#66361=CARTESIAN_POINT('Ctrl Pts',(24.4220043405419,3.85350640302204,133.863527052946));
#66362=CARTESIAN_POINT('Ctrl Pts',(24.4142580644578,3.93579078009416,133.753722243041));
#66363=CARTESIAN_POINT('Ctrl Pts',(24.4065117311924,4.01807576457098,133.643916622582));
#66364=CARTESIAN_POINT('Ctrl Pts',(24.398765397927,4.09576154400529,133.530665514573));
#66365=CARTESIAN_POINT('Ctrl Pts',(24.3910190646617,4.16856000294783,133.414397123886));
#66366=CARTESIAN_POINT('Ctrl Pts',(24.3832709966587,4.2413747646005,133.298102695699));
#66367=CARTESIAN_POINT('Ctrl Pts',(24.3755229286557,4.30929982043058,133.178789971577));
#66368=CARTESIAN_POINT('Ctrl Pts',(24.3677748606528,4.37209185183028,133.056913813755));
#66369=CARTESIAN_POINT('Ctrl Pts',(24.3600185579109,4.4349506193481,132.934908124501));
#66370=CARTESIAN_POINT('Ctrl Pts',(24.3522622551691,4.49266528526042,132.810333907273));
#66371=CARTESIAN_POINT('Ctrl Pts',(24.3445059524272,4.54503952515843,132.683668675668));
#66372=CARTESIAN_POINT('Ctrl Pts',(24.3367455099131,4.59744171876523,132.556935839015));
#66373=CARTESIAN_POINT('Ctrl Pts',(24.3289850673989,4.64449767272845,132.428110131241));
#66374=CARTESIAN_POINT('Ctrl Pts',(24.3212246248848,4.68606058172216,132.297685527601));
#66375=CARTESIAN_POINT('Ctrl Pts',(24.3134517246193,4.72769021118716,132.167051554808));
#66376=CARTESIAN_POINT('Ctrl Pts',(24.3056788243539,4.76380907158931,132.034813934454));
#66377=CARTESIAN_POINT('Ctrl Pts',(24.2979059240885,4.79432103853378,131.90147904416));
#66378=CARTESIAN_POINT('Ctrl Pts',(24.2904155883265,4.82372381862486,131.772991212979));
#66379=CARTESIAN_POINT('Ctrl Pts',(24.2829252525644,4.84792022069687,131.643484806644));
#66380=CARTESIAN_POINT('Ctrl Pts',(24.2754349168024,4.86686989417998,131.513416677144));
#66381=CARTESIAN_POINT('Ctrl Pts',(24.2676605826833,4.88653805029281,131.378416974982));
#66382=CARTESIAN_POINT('Ctrl Pts',(24.2598862485643,4.90061606732433,131.242384474862));
#66383=CARTESIAN_POINT('Ctrl Pts',(24.2521119144452,4.90900236085679,131.105821864831));
#66384=CARTESIAN_POINT('Ctrl Pts',(24.2443471614981,4.91737831903197,130.969427556012));
#66385=CARTESIAN_POINT('Ctrl Pts',(24.236582408551,4.9200764868191,130.832504823664));
#66386=CARTESIAN_POINT('Ctrl Pts',(24.2288176556039,4.91704653188386,130.695565094731));
#66387=CARTESIAN_POINT('Ctrl Pts',(24.2210606147189,4.91401958634258,130.558761376268));
#66388=CARTESIAN_POINT('Ctrl Pts',(24.2133035738339,4.9052758485401,130.421941083154));
#66389=CARTESIAN_POINT('Ctrl Pts',(24.2055465329489,4.89081691865295,130.285618937423));
#66390=CARTESIAN_POINT('Ctrl Pts',(24.1977953417088,4.87636889235729,130.149399593281));
#66391=CARTESIAN_POINT('Ctrl Pts',(24.1900441504686,4.85621429358276,130.013678036011));
#66392=CARTESIAN_POINT('Ctrl Pts',(24.1822929592285,4.8304067467237,129.878966796695));
#66393=CARTESIAN_POINT('Ctrl Pts',(24.1745450624514,4.80461016876053,129.74431281325));
#66394=CARTESIAN_POINT('Ctrl Pts',(24.1667971656743,4.77316549481603,129.610668676871));
#66395=CARTESIAN_POINT('Ctrl Pts',(24.1590492688973,4.7361779062701,129.478539399355));
#66396=CARTESIAN_POINT('Ctrl Pts',(24.1513029928132,4.69919805473034,129.346437760435));
#66397=CARTESIAN_POINT('Ctrl Pts',(24.1435567167291,4.65667770014155,129.215850726349));
#66398=CARTESIAN_POINT('Ctrl Pts',(24.135810440645,4.60877251944987,129.087270367619));
#66399=CARTESIAN_POINT('Ctrl Pts',(24.1280641073797,4.56086698513295,128.958689059737));
#66400=CARTESIAN_POINT('Ctrl Pts',(24.1203177741143,4.50757668189198,128.832114823132));
#66401=CARTESIAN_POINT('Ctrl Pts',(24.112571440849,4.44910613717478,128.708021512685));
#66402=CARTESIAN_POINT('Ctrl Pts',(24.104823372846,4.39062249838434,128.583900412401));
#66403=CARTESIAN_POINT('Ctrl Pts',(24.0970753048429,4.32695647630629,128.46226169743));
#66404=CARTESIAN_POINT('Ctrl Pts',(24.0893272368399,4.25835923976998,128.343555942756));
#66405=CARTESIAN_POINT('Ctrl Pts',(24.0815709340981,4.18968909727455,128.224724026195));
#66406=CARTESIAN_POINT('Ctrl Pts',(24.0738146313562,4.11607746687996,128.108831635892));
#66407=CARTESIAN_POINT('Ctrl Pts',(24.0660583286144,4.03781997616164,127.996302052897));
#66408=CARTESIAN_POINT('Ctrl Pts',(24.0582978861002,3.95952071706434,127.883712409476));
#66409=CARTESIAN_POINT('Ctrl Pts',(24.050537443586,3.87657089310265,127.774489460918));
#66410=CARTESIAN_POINT('Ctrl Pts',(24.0427770010718,3.78930674778514,127.669023724393));
#66411=CARTESIAN_POINT('Ctrl Pts',(24.0350041008064,3.70190251831451,127.563388684905));
#66412=CARTESIAN_POINT('Ctrl Pts',(24.027231200541,3.61017038944566,127.461523200825));
#66413=CARTESIAN_POINT('Ctrl Pts',(24.0194583002756,3.514484433431,127.363781853801));
#66414=CARTESIAN_POINT('Ctrl Pts',(24.0119679645136,3.42227690293597,127.269593650937));
#66415=CARTESIAN_POINT('Ctrl Pts',(24.0044776287515,3.32639824182405,127.179235156602));
#66416=CARTESIAN_POINT('Ctrl Pts',(23.9969872929895,3.2272110021447,127.092987258533));
#66417=CARTESIAN_POINT('Ctrl Pts',(23.9892129588704,3.12426304812545,127.003469245195));
#66418=CARTESIAN_POINT('Ctrl Pts',(23.9814386247513,3.01742456521416,126.918096121663));
#66419=CARTESIAN_POINT('Ctrl Pts',(23.9736642906322,2.9070635702418,126.837225068952));
#66420=CARTESIAN_POINT('Ctrl Pts',(23.9658995376851,2.7968385853322,126.756453682587));
#66421=CARTESIAN_POINT('Ctrl Pts',(23.958134784738,2.68310003834946,126.680173556254));
#66422=CARTESIAN_POINT('Ctrl Pts',(23.9503700317909,2.56625100141003,126.608703474726));
#66423=CARTESIAN_POINT('Ctrl Pts',(23.9426129909059,2.44951802058136,126.537304378291));
#66424=CARTESIAN_POINT('Ctrl Pts',(23.9348559500208,2.32968102917263,126.470706022091));
#66425=CARTESIAN_POINT('Ctrl Pts',(23.9270989091358,2.20717394234117,126.409185279681));
#66426=CARTESIAN_POINT('Ctrl Pts',(23.9193477178957,2.08475923905703,126.347710930542));
#66427=CARTESIAN_POINT('Ctrl Pts',(23.9115965266555,1.95967879614976,126.291306748411));
#66428=CARTESIAN_POINT('Ctrl Pts',(23.9038453354154,1.83239280583126,126.240204653136));
#66429=CARTESIAN_POINT('Ctrl Pts',(23.8960974386383,1.7051609154541,126.189124277615));
#66430=CARTESIAN_POINT('Ctrl Pts',(23.8883495418612,1.57572570417334,126.143341652212));
#66431=CARTESIAN_POINT('Ctrl Pts',(23.8806016450841,1.44456890582217,126.103041256064));
#66432=CARTESIAN_POINT('Ctrl Pts',(23.872855369,1.31343954264597,126.062749289891));
#66433=CARTESIAN_POINT('Ctrl Pts',(23.8651090929159,1.18058968217964,126.027937386756));
#66434=CARTESIAN_POINT('Ctrl Pts',(23.8573628168318,1.04651746448144,125.998740547374));
#66435=CARTESIAN_POINT('Ctrl Pts',(23.8496164835664,0.912444257092589,125.969543492467));
#66436=CARTESIAN_POINT('Ctrl Pts',(23.8418701503011,0.777149056478749,125.945961667211));
#66437=CARTESIAN_POINT('Ctrl Pts',(23.8341238170357,0.641141082252026,125.928079127009));
#66438=CARTESIAN_POINT('Ctrl Pts',(23.8263757490328,0.505102649982488,125.910192582136));
#66439=CARTESIAN_POINT('Ctrl Pts',(23.8186276810298,0.36835151402817,125.898007912993));
#66440=CARTESIAN_POINT('Ctrl Pts',(23.8108796130268,0.231402518771666,125.891557350916));
#66441=CARTESIAN_POINT('Ctrl Pts',(23.8031233102849,0.0943079724932895,
125.885099933105));
#66442=CARTESIAN_POINT('Ctrl Pts',(23.7953670075431,-0.0429844620036973,
125.884388814758));
#66443=CARTESIAN_POINT('Ctrl Pts',(23.7876107048012,-0.179958872459176,
125.88940406977));
#66444=CARTESIAN_POINT('Ctrl Pts',(23.779850262287,-0.317006390281922,125.894422001575));
#66445=CARTESIAN_POINT('Ctrl Pts',(23.7720898197728,-0.453735156272228,
125.905172366121));
#66446=CARTESIAN_POINT('Ctrl Pts',(23.7643293772587,-0.589634869444966,
125.92158335629));
#66447=CARTESIAN_POINT('Ctrl Pts',(23.7565564769932,-0.725752740901897,
125.938020690838));
#66448=CARTESIAN_POINT('Ctrl Pts',(23.7487835767278,-0.861038513975048,
125.960136746496));
#66449=CARTESIAN_POINT('Ctrl Pts',(23.7410106764623,-0.99499167389035,125.987808465727));
#66450=CARTESIAN_POINT('Ctrl Pts',(23.7335203407004,-1.12407529903236,126.014474248262));
#66451=CARTESIAN_POINT('Ctrl Pts',(23.7260300049386,-1.25192121769692,126.046298707963));
#66452=CARTESIAN_POINT('Ctrl Pts',(23.7185396691767,-1.37809714283713,126.083128646205));
#66453=CARTESIAN_POINT('Ctrl Pts',(23.7107653350576,-1.50905706653195,126.12135500275));
#66454=CARTESIAN_POINT('Ctrl Pts',(23.7029910009386,-1.63863270294063,126.165094985623));
#66455=CARTESIAN_POINT('Ctrl Pts',(23.6952166668195,-1.76632462347257,126.214232036904));
#66456=CARTESIAN_POINT('Ctrl Pts',(23.6874519138724,-1.89385917512443,126.26330853116));
#66457=CARTESIAN_POINT('Ctrl Pts',(23.6796871609253,-2.01951426863631,126.317768720451));
#66458=CARTESIAN_POINT('Ctrl Pts',(23.6719224079782,-2.14280383102489,126.377445799745));
#66459=CARTESIAN_POINT('Ctrl Pts',(23.6641653670932,-2.26597094048202,126.437063606922));
#66460=CARTESIAN_POINT('Ctrl Pts',(23.6564083262082,-2.38677684475436,126.501887823473));
#66461=CARTESIAN_POINT('Ctrl Pts',(23.6486512853232,-2.50475406053538,126.571703041204));
#66462=CARTESIAN_POINT('Ctrl Pts',(23.640900094083,-2.62264230878137,126.641465610738));
#66463=CARTESIAN_POINT('Ctrl Pts',(23.6331489028428,-2.73770577930966,126.716211491628));
#66464=CARTESIAN_POINT('Ctrl Pts',(23.6253977116026,-2.84950060625191,126.795678869476));
#66465=CARTESIAN_POINT('Ctrl Pts',(23.6176498148255,-2.96124791740973,126.875112471568));
#66466=CARTESIAN_POINT('Ctrl Pts',(23.6099019180484,-3.06972903012121,126.959263353281));
#66467=CARTESIAN_POINT('Ctrl Pts',(23.6021540212713,-3.17452834795856,127.047825933777));
#66468=CARTESIAN_POINT('Ctrl Pts',(23.5944077451872,-3.27930574403782,127.136369988891));
#66469=CARTESIAN_POINT('Ctrl Pts',(23.5866614691031,-3.38040257868966,127.229323655033));
#66470=CARTESIAN_POINT('Ctrl Pts',(23.578915193019,-3.4774360151217,127.326340804046));
#66471=CARTESIAN_POINT('Ctrl Pts',(23.5711688597536,-3.57447016783252,127.423358669218));
#66472=CARTESIAN_POINT('Ctrl Pts',(23.5634225264883,-3.66744058599315,127.524439800685));
#66473=CARTESIAN_POINT('Ctrl Pts',(23.5556761932229,-3.75600130577403,127.629201211564));
#66474=CARTESIAN_POINT('Ctrl Pts',(23.5479281252199,-3.84458185811382,127.733986083034));
#66475=CARTESIAN_POINT('Ctrl Pts',(23.5401800572169,-3.92875049466683,127.842452575407));
#66476=CARTESIAN_POINT('Ctrl Pts',(23.532431989214,-4.00820181233323,127.954184957346));
#66477=CARTESIAN_POINT('Ctrl Pts',(23.5246756864721,-4.08773757180564,128.066036089791));
#66478=CARTESIAN_POINT('Ctrl Pts',(23.5169193837303,-4.16254577021058,128.181159726421));
#66479=CARTESIAN_POINT('Ctrl Pts',(23.5091630809884,-4.23236430876659,128.299111045093));
#66480=CARTESIAN_POINT('Ctrl Pts',(23.5014026384742,-4.30222011157883,128.417125317934));
#66481=CARTESIAN_POINT('Ctrl Pts',(23.49364219596,-4.3670807632239,128.537969935751));
#66482=CARTESIAN_POINT('Ctrl Pts',(23.4858817534459,-4.42673084691588,128.66117675437));
#66483=CARTESIAN_POINT('Ctrl Pts',(23.4781088531804,-4.48647668621777,128.784581355513));
#66484=CARTESIAN_POINT('Ctrl Pts',(23.470335952915,-4.54099508711831,128.910355376189));
#66485=CARTESIAN_POINT('Ctrl Pts',(23.4625630526495,-4.59011904094761,129.03801120354));
#66486=CARTESIAN_POINT('Ctrl Pts',(23.4550727168875,-4.63745721531911,129.16102642002));
#66487=CARTESIAN_POINT('Ctrl Pts',(23.4475823811255,-4.67978623790627,129.285788710003));
#66488=CARTESIAN_POINT('Ctrl Pts',(23.4400920453635,-4.71700133734242,129.411851570554));
#66489=CARTESIAN_POINT('Ctrl Pts',(23.4367303194496,-4.73370378809248,129.468429646434));
#66490=CARTESIAN_POINT('Ctrl Pts',(23.4333685935357,-4.74939168437933,129.525319913658));
#66491=CARTESIAN_POINT('Ctrl Pts',(23.4300068676217,-4.76405452823403,129.582490119308));
#66492=CARTESIAN_POINT('Origin',(213.235140564004,0.,130.804360617566));
#66493=CARTESIAN_POINT('',(21.3349957656066,-4.76405452823399,129.582490119308));
#66494=CARTESIAN_POINT('',(21.6799128182693,-4.76405452823405,129.582490119308));
#66495=CARTESIAN_POINT('',(213.235140564004,-4.76405452823405,129.582490119308));
#66496=CARTESIAN_POINT('',(23.0148594359424,-4.91824935608045,130.80687734446));
#66497=CARTESIAN_POINT('Ctrl Pts',(23.0148594359423,-4.91824935608045,130.80687734446));
#66498=CARTESIAN_POINT('Ctrl Pts',(23.0063233041041,-4.91817186460964,130.958313075279));
#66499=CARTESIAN_POINT('Ctrl Pts',(22.9977871722658,-4.91109609712324,131.109507565572));
#66500=CARTESIAN_POINT('Ctrl Pts',(22.9892510404275,-4.89711325436575,131.259843697839));
#66501=CARTESIAN_POINT('Ctrl Pts',(22.9806698930086,-4.88305667261293,131.410972632797));
#66502=CARTESIAN_POINT('Ctrl Pts',(22.9720887455896,-4.86202006107709,131.561233895066));
#66503=CARTESIAN_POINT('Ctrl Pts',(22.9635075981707,-4.83414632790528,131.710016370543));
#66504=CARTESIAN_POINT('Ctrl Pts',(22.9549031950898,-4.80619705447221,131.859202059575));
#66505=CARTESIAN_POINT('Ctrl Pts',(22.9462987920088,-4.77137366953818,132.006900713411));
#66506=CARTESIAN_POINT('Ctrl Pts',(22.9376943889279,-4.72986906089499,132.15251555276));
#66507=CARTESIAN_POINT('Ctrl Pts',(22.9290591231688,-4.688215581567,132.298652690272));
#66508=CARTESIAN_POINT('Ctrl Pts',(22.9204238574096,-4.63983298507327,132.442690820695));
#66509=CARTESIAN_POINT('Ctrl Pts',(22.9117885916505,-4.58496354168943,132.584049462246));
#66510=CARTESIAN_POINT('Ctrl Pts',(22.9087876590661,-4.56589528077753,132.633174499662));
#66511=CARTESIAN_POINT('Ctrl Pts',(22.9057867264817,-4.54604400850942,132.681976149457));
#66512=CARTESIAN_POINT('Ctrl Pts',(22.9027857938973,-4.52542118092908,132.73043076107));
#66513=CARTESIAN_POINT('Ctrl Pts',(22.8950114597781,-4.4719948717462,132.855959185884));
#66514=CARTESIAN_POINT('Ctrl Pts',(22.887237125659,-4.41325702436792,132.979461805039));
#66515=CARTESIAN_POINT('Ctrl Pts',(22.8794627915399,-4.3493823677675,133.100456452119));
#66516=CARTESIAN_POINT('Ctrl Pts',(22.8716980385927,-4.28558643097271,133.221301984111));
#66517=CARTESIAN_POINT('Ctrl Pts',(22.8639332856456,-4.21666646184963,133.339645351477));
#66518=CARTESIAN_POINT('Ctrl Pts',(22.8561685326984,-4.1428455073722,133.455023584551));
#66519=CARTESIAN_POINT('Ctrl Pts',(22.8484114918134,-4.06909787290755,133.570287222338));
#66520=CARTESIAN_POINT('Ctrl Pts',(22.8406544509283,-3.99045914943143,133.682591259347));
#66521=CARTESIAN_POINT('Ctrl Pts',(22.8328974100433,-3.90719845128515,133.791496925935));
#66522=CARTESIAN_POINT('Ctrl Pts',(22.8251462188031,-3.8240005406789,133.900320465912));
#66523=CARTESIAN_POINT('Ctrl Pts',(22.817395027563,-3.73618782950813,134.005750427103));
#66524=CARTESIAN_POINT('Ctrl Pts',(22.8096438363228,-3.64407272408339,134.107376972974));
#66525=CARTESIAN_POINT('Ctrl Pts',(22.8018959395456,-3.55199677003571,134.208960324851));
#66526=CARTESIAN_POINT('Ctrl Pts',(22.7941480427685,-3.45562232076047,134.306743187538));
#66527=CARTESIAN_POINT('Ctrl Pts',(22.7864001459914,-3.35530190380313,134.400348965272));
#66528=CARTESIAN_POINT('Ctrl Pts',(22.7786538699072,-3.25500247171422,134.493935162694));
#66529=CARTESIAN_POINT('Ctrl Pts',(22.7709075938231,-3.15075899940555,134.583345746559));
#66530=CARTESIAN_POINT('Ctrl Pts',(22.7631613177389,-3.04296040873856,134.668241440437));
#66531=CARTESIAN_POINT('Ctrl Pts',(22.7554149844735,-2.93516102232701,134.753137760995));
#66532=CARTESIAN_POINT('Ctrl Pts',(22.7476686512081,-2.82380677234151,134.833518883169));
#66533=CARTESIAN_POINT('Ctrl Pts',(22.7399223179427,-2.70931882636476,134.909086498743));
#66534=CARTESIAN_POINT('Ctrl Pts',(22.7321742499397,-2.59480524160632,134.984671037161));
#66535=CARTESIAN_POINT('Ctrl Pts',(22.7244261819366,-2.47715689065008,135.055439708651));
#66536=CARTESIAN_POINT('Ctrl Pts',(22.7166781139336,-2.35682266576578,135.121138349235));
#66537=CARTESIAN_POINT('Ctrl Pts',(22.7089218111917,-2.23636054823513,135.186906815116));
#66538=CARTESIAN_POINT('Ctrl Pts',(22.7011655084498,-2.11320719814752,135.247594298355));
#66539=CARTESIAN_POINT('Ctrl Pts',(22.6934092057078,-1.98783528034439,135.30299307207));
#66540=CARTESIAN_POINT('Ctrl Pts',(22.6856487631936,-1.86239644777402,135.358421413779));
#66541=CARTESIAN_POINT('Ctrl Pts',(22.6778883206794,-1.73473705176687,135.408555278564));
#66542=CARTESIAN_POINT('Ctrl Pts',(22.6701278781652,-1.60534740240345,135.453236049334));
#66543=CARTESIAN_POINT('Ctrl Pts',(22.6623549778997,-1.47575004528803,135.497988545644));
#66544=CARTESIAN_POINT('Ctrl Pts',(22.6545820776342,-1.34441725915866,135.537270342975));
#66545=CARTESIAN_POINT('Ctrl Pts',(22.6468091773687,-1.21185296909385,135.570973192949));
#66546=CARTESIAN_POINT('Ctrl Pts',(22.6393188416073,-1.08410772489296,135.603450859431));
#66547=CARTESIAN_POINT('Ctrl Pts',(22.6318285058459,-0.955219260145688,
135.630748090198));
#66548=CARTESIAN_POINT('Ctrl Pts',(22.6243381700844,-0.825643326977589,
135.652813583113));
#66549=CARTESIAN_POINT('Ctrl Pts',(22.6165638359653,-0.691154482909617,
135.675715695899));
#66550=CARTESIAN_POINT('Ctrl Pts',(22.6087895018463,-0.555498990380398,
135.69305406373));
#66551=CARTESIAN_POINT('Ctrl Pts',(22.6010151677272,-0.419176954928391,
135.704715068313));
#66552=CARTESIAN_POINT('Ctrl Pts',(22.5932504147801,-0.283022924201629,
135.716361701751));
#66553=CARTESIAN_POINT('Ctrl Pts',(22.585485661833,-0.146204370804925,135.722344860571));
#66554=CARTESIAN_POINT('Ctrl Pts',(22.5777209088859,-0.00923136656696278,
135.722601954098));
#66555=CARTESIAN_POINT('Ctrl Pts',(22.5699638680009,0.127605594152209,135.722858792276));
#66556=CARTESIAN_POINT('Ctrl Pts',(22.5622068271159,0.264596311999639,135.717400882234));
#66557=CARTESIAN_POINT('Ctrl Pts',(22.5544497862309,0.401226174771141,135.706217471777));
#66558=CARTESIAN_POINT('Ctrl Pts',(22.5466985949908,0.537753003900302,135.695042494818));
#66559=CARTESIAN_POINT('Ctrl Pts',(22.5389474037507,0.673919131513696,135.678150643219));
#66560=CARTESIAN_POINT('Ctrl Pts',(22.5311962125106,0.80921088728567,135.6555832266));
#66561=CARTESIAN_POINT('Ctrl Pts',(22.5234483157335,0.944445140452415,135.633025401734));
#66562=CARTESIAN_POINT('Ctrl Pts',(22.5157004189564,1.07880537609453,135.604796873855));
#66563=CARTESIAN_POINT('Ctrl Pts',(22.5079525221793,1.21178420378202,135.570990675161));
#66564=CARTESIAN_POINT('Ctrl Pts',(22.5002062460952,1.34473521516545,135.537191547994));
#66565=CARTESIAN_POINT('Ctrl Pts',(22.4924599700112,1.47630501468061,135.497817166967));
#66566=CARTESIAN_POINT('Ctrl Pts',(22.4847136939271,1.60599793769223,135.453011355859));
#66567=CARTESIAN_POINT('Ctrl Pts',(22.4769673606617,1.73569181806755,135.408205214004));
#66568=CARTESIAN_POINT('Ctrl Pts',(22.4692210273963,1.8635084247593,135.357967689728));
#66569=CARTESIAN_POINT('Ctrl Pts',(22.461474694131,1.98896913125135,135.302491880372));
#66570=CARTESIAN_POINT('Ctrl Pts',(22.453726626128,2.11445793379874,135.247003647592));
#66571=CARTESIAN_POINT('Ctrl Pts',(22.445978558125,2.23758942880797,135.18627495352));
#66572=CARTESIAN_POINT('Ctrl Pts',(22.438230490122,2.35790714368988,135.120546082098));
#66573=CARTESIAN_POINT('Ctrl Pts',(22.4304741873802,2.47835273367096,135.054747353249));
#66574=CARTESIAN_POINT('Ctrl Pts',(22.4227178846384,2.59597822598835,134.983938019002));
#66575=CARTESIAN_POINT('Ctrl Pts',(22.4149615818965,2.71035336724085,134.908403464222));
#66576=CARTESIAN_POINT('Ctrl Pts',(22.4072011393823,2.82478955395015,134.832828594375));
#66577=CARTESIAN_POINT('Ctrl Pts',(22.3994406968681,2.9359716160551,134.752523707518));
#66578=CARTESIAN_POINT('Ctrl Pts',(22.391680254354,3.04350107992747,134.667815578994));
#66579=CARTESIAN_POINT('Ctrl Pts',(22.3839073540885,3.15120315964111,134.582971469462));
#66580=CARTESIAN_POINT('Ctrl Pts',(22.3761344538231,3.25524062713876,134.493710247924));
#66581=CARTESIAN_POINT('Ctrl Pts',(22.3683615535577,3.3552500261785,134.400397369927));
#66582=CARTESIAN_POINT('Ctrl Pts',(22.3608712177957,3.45162383165535,134.310476650085));
#66583=CARTESIAN_POINT('Ctrl Pts',(22.3533808820336,3.54425712847715,134.216793954376));
#66584=CARTESIAN_POINT('Ctrl Pts',(22.3458905462715,3.63286040954603,134.119704989913));
#66585=CARTESIAN_POINT('Ctrl Pts',(22.3381162121525,3.72482311094637,134.018934867853));
#66586=CARTESIAN_POINT('Ctrl Pts',(22.3303418780333,3.81273547813195,133.914175871351));
#66587=CARTESIAN_POINT('Ctrl Pts',(22.3225675439143,3.89623160155745,133.805787339897));
#66588=CARTESIAN_POINT('Ctrl Pts',(22.3148027909672,3.97962482347297,133.697532387622));
#66589=CARTESIAN_POINT('Ctrl Pts',(22.3070380380201,4.05861239453024,133.585657107236));
#66590=CARTESIAN_POINT('Ctrl Pts',(22.2992732850731,4.13286594913798,133.470556804825));
#66591=CARTESIAN_POINT('Ctrl Pts',(22.2915162441881,4.2070457540686,133.355570821657));
#66592=CARTESIAN_POINT('Ctrl Pts',(22.283759203303,4.2765006889549,133.237366517259));
#66593=CARTESIAN_POINT('Ctrl Pts',(22.2760021624181,4.34094354720525,133.116371037628));
#66594=CARTESIAN_POINT('Ctrl Pts',(22.2682509711779,4.4053378085949,132.995466801631));
#66595=CARTESIAN_POINT('Ctrl Pts',(22.2604997799379,4.4647273334603,132.871775923649));
#66596=CARTESIAN_POINT('Ctrl Pts',(22.2527485886978,4.51886922539576,132.745752897934));
#66597=CARTESIAN_POINT('Ctrl Pts',(22.2450006919207,4.5729881055828,132.619783435366));
#66598=CARTESIAN_POINT('Ctrl Pts',(22.2372527951435,4.62186363490008,132.491484155002));
#66599=CARTESIAN_POINT('Ctrl Pts',(22.2295048983665,4.66529982705084,132.361332224956));
#66600=CARTESIAN_POINT('Ctrl Pts',(22.2217586222824,4.70872693328657,132.231207519888));
#66601=CARTESIAN_POINT('Ctrl Pts',(22.2140123461983,4.74671684179706,132.099231306588));
#66602=CARTESIAN_POINT('Ctrl Pts',(22.2062660701143,4.77912263675844,131.965898342017));
#66603=CARTESIAN_POINT('Ctrl Pts',(22.1985197368489,4.81152867093203,131.832564393213));
#66604=CARTESIAN_POINT('Ctrl Pts',(22.1907734035836,4.83835041696987,131.697874053058));
#66605=CARTESIAN_POINT('Ctrl Pts',(22.1830270703183,4.8594916238085,131.562334377425));
#66606=CARTESIAN_POINT('Ctrl Pts',(22.1752790023153,4.88063756507382,131.426764348622));
#66607=CARTESIAN_POINT('Ctrl Pts',(22.1675309343124,4.89610037553176,131.290344992079));
#66608=CARTESIAN_POINT('Ctrl Pts',(22.1597828663094,4.90583547828324,131.153590230453));
#66609=CARTESIAN_POINT('Ctrl Pts',(22.1520265635676,4.91558092761777,131.01669012424));
#66610=CARTESIAN_POINT('Ctrl Pts',(22.1442702608258,4.9195864810515,130.879454291452));
#66611=CARTESIAN_POINT('Ctrl Pts',(22.1365139580839,4.91785967848011,130.742398973951));
#66612=CARTESIAN_POINT('Ctrl Pts',(22.1287535155698,4.9161319542622,130.6052705059));
#66613=CARTESIAN_POINT('Ctrl Pts',(22.1209930730556,4.90866579893738,130.46832313531));
#66614=CARTESIAN_POINT('Ctrl Pts',(22.1132326305414,4.89552075312753,130.332068739383));
#66615=CARTESIAN_POINT('Ctrl Pts',(22.105459730276,4.88235460572318,130.195595615804));
#66616=CARTESIAN_POINT('Ctrl Pts',(22.0976868300106,4.86349140447315,130.059818077336));
#66617=CARTESIAN_POINT('Ctrl Pts',(22.0899139297452,4.83904216050259,129.925239447659));
#66618=CARTESIAN_POINT('Ctrl Pts',(22.082423593983,4.81548170813386,129.795553090152));
#66619=CARTESIAN_POINT('Ctrl Pts',(22.0749332582209,4.78673436262831,129.666980288665));
#66620=CARTESIAN_POINT('Ctrl Pts',(22.0674429224587,4.7529429047956,129.539956882103));
#66621=CARTESIAN_POINT('Ctrl Pts',(22.0596685883396,4.71787023356905,129.408117344475));
#66622=CARTESIAN_POINT('Ctrl Pts',(22.0518942542205,4.67725230472525,129.277529383664));
#66623=CARTESIAN_POINT('Ctrl Pts',(22.0441199201015,4.63119365770849,129.148695081505));
#66624=CARTESIAN_POINT('Ctrl Pts',(22.0363551671544,4.58519177385779,129.020019556109));
#66625=CARTESIAN_POINT('Ctrl Pts',(22.0285904142072,4.53376264353133,128.89309375378));
#66626=CARTESIAN_POINT('Ctrl Pts',(22.0208256612601,4.47706135931208,128.768407610384));
#66627=CARTESIAN_POINT('Ctrl Pts',(22.0130686203751,4.42041639160767,128.643845307023));
#66628=CARTESIAN_POINT('Ctrl Pts',(22.0053115794901,4.35850985143435,128.521518589409));
#66629=CARTESIAN_POINT('Ctrl Pts',(21.9975545386051,4.29154586663991,128.401899975427));
#66630=CARTESIAN_POINT('Ctrl Pts',(21.989803347365,4.22463237990732,128.282371566773));
#66631=CARTESIAN_POINT('Ctrl Pts',(21.9820521561249,4.15266923001278,128.165547536638));
#66632=CARTESIAN_POINT('Ctrl Pts',(21.9743009648848,4.07590750440126,128.051877905892));
#66633=CARTESIAN_POINT('Ctrl Pts',(21.9665530681077,3.99917840457082,127.938256587771));
#66634=CARTESIAN_POINT('Ctrl Pts',(21.9588051713305,3.91765500382286,127.827787325808));
#66635=CARTESIAN_POINT('Ctrl Pts',(21.9510572745534,3.83163282182608,127.720892929847));
#66636=CARTESIAN_POINT('Ctrl Pts',(21.9433109984693,3.74562863381534,127.61402089389));
#66637=CARTESIAN_POINT('Ctrl Pts',(21.9355647223852,3.65512778130999,127.510722540942));
#66638=CARTESIAN_POINT('Ctrl Pts',(21.9278184463011,3.56046710576245,127.411388903672));
#66639=CARTESIAN_POINT('Ctrl Pts',(21.9200721130358,3.46580573145132,127.312054533144));
#66640=CARTESIAN_POINT('Ctrl Pts',(21.9123257797705,3.36698474254132,127.216685219723));
#66641=CARTESIAN_POINT('Ctrl Pts',(21.9045794465051,3.26437871344689,127.125636018239));
#66642=CARTESIAN_POINT('Ctrl Pts',(21.8968313785021,3.16174970644381,127.034566426918));
#66643=CARTESIAN_POINT('Ctrl Pts',(21.8890833104992,3.05533426493972,126.947819132111));
#66644=CARTESIAN_POINT('Ctrl Pts',(21.8813352424962,2.94554067171819,126.865709425374));
#66645=CARTESIAN_POINT('Ctrl Pts',(21.8735789397544,2.83563038855907,126.783512451464));
#66646=CARTESIAN_POINT('Ctrl Pts',(21.8658226370124,2.72233509518536,126.705963146124));
#66647=CARTESIAN_POINT('Ctrl Pts',(21.8580663342706,2.60609319599383,126.633334207161));
#66648=CARTESIAN_POINT('Ctrl Pts',(21.8503058917564,2.48978925500072,126.560666503947));
#66649=CARTESIAN_POINT('Ctrl Pts',(21.8425454492422,2.37053591424746,126.492924592945));
#66650=CARTESIAN_POINT('Ctrl Pts',(21.834785006728,2.24879601368324,126.430335063075));
#66651=CARTESIAN_POINT('Ctrl Pts',(21.8270121064626,2.12686068542307,126.367645058935));
#66652=CARTESIAN_POINT('Ctrl Pts',(21.8192392061972,2.00243117585515,126.310124128288));
#66653=CARTESIAN_POINT('Ctrl Pts',(21.8114663059318,1.8759909496709,126.257950933073));
#66654=CARTESIAN_POINT('Ctrl Pts',(21.8039759701698,1.75414714419302,126.207674364921));
#66655=CARTESIAN_POINT('Ctrl Pts',(21.7964856344078,1.63043656249565,126.162363581094));
#66656=CARTESIAN_POINT('Ctrl Pts',(21.7889952986458,1.50530306470711,126.122134037627));
#66657=CARTESIAN_POINT('Ctrl Pts',(21.7812209645267,1.37542509231568,126.080379178792));
#66658=CARTESIAN_POINT('Ctrl Pts',(21.7734466304077,1.24360275975388,126.043966210081));
#66659=CARTESIAN_POINT('Ctrl Pts',(21.7656722962886,1.11031498881336,126.013078566996));
#66660=CARTESIAN_POINT('Ctrl Pts',(21.7579075433415,0.977191483138436,125.98222899017));
#66661=CARTESIAN_POINT('Ctrl Pts',(21.7501427903944,0.842606509745777,125.956891277568));
#66662=CARTESIAN_POINT('Ctrl Pts',(21.7423780374473,0.707056096885537,125.937199767711));
#66663=CARTESIAN_POINT('Ctrl Pts',(21.7346209965623,0.571640314606091,125.91752781574));
#66664=CARTESIAN_POINT('Ctrl Pts',(21.7268639556773,0.435261385489979,125.903490962406));
#66665=CARTESIAN_POINT('Ctrl Pts',(21.7191069147923,0.29842718830451,125.895172876628));
#66666=CARTESIAN_POINT('Ctrl Pts',(21.7113557235522,0.161696178851553,125.886861063583));
#66667=CARTESIAN_POINT('Ctrl Pts',(21.7036045323121,0.0245109733550467,
125.884259457818));
#66668=CARTESIAN_POINT('Ctrl Pts',(21.695853341072,-0.112614093985012,125.887400059626));
#66669=CARTESIAN_POINT('Ctrl Pts',(21.6881054442949,-0.24968087951352,125.890539326595));
#66670=CARTESIAN_POINT('Ctrl Pts',(21.6803575475178,-0.386687187678713,
125.899415938054));
#66671=CARTESIAN_POINT('Ctrl Pts',(21.6726096507407,-0.523117560985009,
125.914009803985));
#66672=CARTESIAN_POINT('Ctrl Pts',(21.6648633746566,-0.659519395998308,
125.928600617194));
#66673=CARTESIAN_POINT('Ctrl Pts',(21.6571170985726,-0.795345147279287,
125.948906264554));
#66674=CARTESIAN_POINT('Ctrl Pts',(21.6493708224885,-0.930083756938391,
125.974854714518));
#66675=CARTESIAN_POINT('Ctrl Pts',(21.6416244892231,-1.06482336120712,126.000803356027));
#66676=CARTESIAN_POINT('Ctrl Pts',(21.6338781559577,-1.19847542392991,126.032394809324));
#66677=CARTESIAN_POINT('Ctrl Pts',(21.6261318226924,-1.33053876080233,126.069505850152));
#66678=CARTESIAN_POINT('Ctrl Pts',(21.6183837546894,-1.46263167234339,126.106625201741));
#66679=CARTESIAN_POINT('Ctrl Pts',(21.6106356866865,-1.59313477375025,126.149266494756));
#66680=CARTESIAN_POINT('Ctrl Pts',(21.6028876186836,-1.7215621144891,126.197256652117));
#66681=CARTESIAN_POINT('Ctrl Pts',(21.5951313159417,-1.85012594933417,126.245297813988));
#66682=CARTESIAN_POINT('Ctrl Pts',(21.5873750131999,-1.97660924968733,126.298699059209));
#66683=CARTESIAN_POINT('Ctrl Pts',(21.579618710458,-2.10054561887412,126.357238945571));
#66684=CARTESIAN_POINT('Ctrl Pts',(21.5718582679439,-2.22454813663279,126.415810076432));
#66685=CARTESIAN_POINT('Ctrl Pts',(21.5640978254297,-2.34600066851148,126.479525131853));
#66686=CARTESIAN_POINT('Ctrl Pts',(21.5563373829155,-2.46446240253599,126.548117188322));
#66687=CARTESIAN_POINT('Ctrl Pts',(21.5485644826501,-2.5831143018525,126.616819354848));
#66688=CARTESIAN_POINT('Ctrl Pts',(21.5407915823847,-2.69876547916453,126.690413957233));
#66689=CARTESIAN_POINT('Ctrl Pts',(21.5330186821193,-2.81100429664725,126.76859081408));
#66690=CARTESIAN_POINT('Ctrl Pts',(21.5255283463571,-2.91916295040333,126.843925745266));
#66691=CARTESIAN_POINT('Ctrl Pts',(21.518038010595,-3.02415278731309,126.923515375879));
#66692=CARTESIAN_POINT('Ctrl Pts',(21.5105476748329,-3.12563675370366,127.00704868063));
#66693=CARTESIAN_POINT('Ctrl Pts',(21.5028809039019,-3.22951117912261,127.092549615831));
#66694=CARTESIAN_POINT('Ctrl Pts',(21.4952141329709,-3.33006085910876,127.182469365699));
#66695=CARTESIAN_POINT('Ctrl Pts',(21.4875473620399,-3.4268786485251,127.276516262895));
#66696=CARTESIAN_POINT('Ctrl Pts',(21.4798893792858,-3.52358545877347,127.37045535711));
#66697=CARTESIAN_POINT('Ctrl Pts',(21.4722313965317,-3.6165685964263,127.468511917343));
#66698=CARTESIAN_POINT('Ctrl Pts',(21.4645734137776,-3.70545233636739,127.57035288019));
#66699=CARTESIAN_POINT('Ctrl Pts',(21.4569224419515,-3.79425470272478,127.67210060704));
#66700=CARTESIAN_POINT('Ctrl Pts',(21.4492714701254,-3.87896487069117,127.777625546692));
#66701=CARTESIAN_POINT('Ctrl Pts',(21.4416204982993,-3.95924290016274,127.886556868166));
#66702=CARTESIAN_POINT('Ctrl Pts',(21.4339747666824,-4.03946594659654,127.995413581743));
#66703=CARTESIAN_POINT('Ctrl Pts',(21.4263290350655,-4.11526265422054,128.10767171418));
#66704=CARTESIAN_POINT('Ctrl Pts',(21.4186833034487,-4.18633280130811,128.222926764222));
#66705=CARTESIAN_POINT('Ctrl Pts',(21.4110402676312,-4.25737788985743,128.338141176623));
#66706=CARTESIAN_POINT('Ctrl Pts',(21.4033972318137,-4.32369951793267,128.456350065217));
#66707=CARTESIAN_POINT('Ctrl Pts',(21.3957541959962,-4.38504055658446,128.577119638325));
#66708=CARTESIAN_POINT('Ctrl Pts',(21.3881128424118,-4.44636809406644,128.697862630036));
#66709=CARTESIAN_POINT('Ctrl Pts',(21.3804714888275,-4.50271704387422,128.821164824662));
#66710=CARTESIAN_POINT('Ctrl Pts',(21.3728301352431,-4.5538763862623,128.946568131538));
#66711=CARTESIAN_POINT('Ctrl Pts',(21.3651865881523,-4.60505041431342,129.07200743635));
#66712=CARTESIAN_POINT('Ctrl Pts',(21.3575430410616,-4.65103170633734,129.199548685551));
#66713=CARTESIAN_POINT('Ctrl Pts',(21.3498994939708,-4.69165758490788,129.328714261396));
#66714=CARTESIAN_POINT('Ctrl Pts',(21.3449315845161,-4.71806230039657,129.412665191226));
#66715=CARTESIAN_POINT('Ctrl Pts',(21.3399636750613,-4.74220571102834,129.497301912625));
#66716=CARTESIAN_POINT('Ctrl Pts',(21.3349957656066,-4.76405452823399,129.582490119308));
#66717=CARTESIAN_POINT('Ctrl Pts',(23.0846591878033,-4.76405452823398,129.582490119308));
#66718=CARTESIAN_POINT('Ctrl Pts',(23.0767991264479,-4.79862266817693,129.717270772301));
#66719=CARTESIAN_POINT('Ctrl Pts',(23.0689390650927,-4.82748971154215,129.853608202476));
#66720=CARTESIAN_POINT('Ctrl Pts',(23.0610790037373,-4.85052663452102,129.990988359432));
#66721=CARTESIAN_POINT('Ctrl Pts',(23.0532224290515,-4.87355333847808,130.128307575488));
#66722=CARTESIAN_POINT('Ctrl Pts',(23.0453658543657,-4.8907550081303,130.266668228245));
#66723=CARTESIAN_POINT('Ctrl Pts',(23.0375092796799,-4.90205361781031,130.405545634632));
#66724=CARTESIAN_POINT('Ctrl Pts',(23.0299593317837,-4.91291126478697,130.53900292666));
#66725=CARTESIAN_POINT('Ctrl Pts',(23.0224093838875,-4.91831789489641,130.672937064906));
#66726=CARTESIAN_POINT('Ctrl Pts',(23.0148594359913,-4.91824935608089,130.806877343592));
#66727=CARTESIAN_POINT('',(23.3601405640434,-4.91824805923248,130.79999136638));
#66728=CARTESIAN_POINT('Ctrl Pts',(23.4300068676217,-4.76405452823403,129.582490119308));
#66729=CARTESIAN_POINT('Ctrl Pts',(23.4203944872076,-4.80598085913958,129.745960247188));
#66730=CARTESIAN_POINT('Ctrl Pts',(23.4107821067936,-4.83952298414148,129.911720709109));
#66731=CARTESIAN_POINT('Ctrl Pts',(23.4011697263795,-4.86446705838591,130.079003257103));
#66732=CARTESIAN_POINT('Ctrl Pts',(23.3916925947081,-4.8890601628878,130.243932095264));
#66733=CARTESIAN_POINT('Ctrl Pts',(23.3822154630367,-4.90529544518096,130.410340540976));
#66734=CARTESIAN_POINT('Ctrl Pts',(23.3727383313653,-4.913013755741,130.577471000352));
#66735=CARTESIAN_POINT('Ctrl Pts',(23.3685390755913,-4.91643368925132,130.651525426403));
#66736=CARTESIAN_POINT('Ctrl Pts',(23.3643398198173,-4.91818207954048,130.725721319109));
#66737=CARTESIAN_POINT('Ctrl Pts',(23.3601405640433,-4.91824805923248,130.79999136638));
#66738=CARTESIAN_POINT('Ctrl Pts',(23.3601405640087,-4.91824805923302,130.799991366992));
#66739=CARTESIAN_POINT('Ctrl Pts',(23.3524493576804,-4.91836890525452,130.936021722922));
#66740=CARTESIAN_POINT('Ctrl Pts',(23.3447581513522,-4.91284195572749,131.072164803608));
#66741=CARTESIAN_POINT('Ctrl Pts',(23.3370669450239,-4.90166600722439,131.207911625644));
#66742=CARTESIAN_POINT('Ctrl Pts',(23.3293785715744,-4.89049417512461,131.343608448464));
#66743=CARTESIAN_POINT('Ctrl Pts',(23.321690198125,-4.87367751226833,131.478908907352));
#66744=CARTESIAN_POINT('Ctrl Pts',(23.3140018246755,-4.85126688212405,131.613306042738));
#66745=CARTESIAN_POINT('Ctrl Pts',(23.3063147009714,-4.82885989482867,131.747681331863));
#66746=CARTESIAN_POINT('Ctrl Pts',(23.2986275772674,-4.8008608136778,131.88115319757));
#66747=CARTESIAN_POINT('Ctrl Pts',(23.2909404535633,-4.7673720683186,132.013222323766));
#66748=CARTESIAN_POINT('Ctrl Pts',(23.2832528521044,-4.73388124163343,132.145299658059));
#66749=CARTESIAN_POINT('Ctrl Pts',(23.2755652506455,-4.69490016976641,132.275973694137));
#66750=CARTESIAN_POINT('Ctrl Pts',(23.2678776491866,-4.65058173179877,132.404758261391));
#66751=CARTESIAN_POINT('Ctrl Pts',(23.2601878424331,-4.60625058047556,132.533579772275));
#66752=CARTESIAN_POINT('Ctrl Pts',(23.2524980356797,-4.55657914682727,132.660510360545));
#66753=CARTESIAN_POINT('Ctrl Pts',(23.2448082289262,-4.50176904100897,132.785082345602));
#66754=CARTESIAN_POINT('Ctrl Pts',(23.2371099815117,-4.44689877327234,132.909791066202));
#66755=CARTESIAN_POINT('Ctrl Pts',(23.2294117340971,-4.38687873152101,133.032135650302));
#66756=CARTESIAN_POINT('Ctrl Pts',(23.2217134866826,-4.32195740773694,133.151671254914));
#66757=CARTESIAN_POINT('Ctrl Pts',(23.2140105872283,-4.25699685209071,133.27127909472));
#66758=CARTESIAN_POINT('Ctrl Pts',(23.2063076877739,-4.1871293199716,133.388074234461));
#66759=CARTESIAN_POINT('Ctrl Pts',(23.1986047883196,-4.11264686820347,133.501640506631));
#66760=CARTESIAN_POINT('Ctrl Pts',(23.1908901871356,-4.03805126767569,133.615379301087));
#66761=CARTESIAN_POINT('Ctrl Pts',(23.1831755859515,-3.9588269793492,133.725879111192));
#66762=CARTESIAN_POINT('Ctrl Pts',(23.1754609847674,-3.87530691427489,133.832756130486));
#66763=CARTESIAN_POINT('Ctrl Pts',(23.1708554636952,-3.82544647295366,133.896560383324));
#66764=CARTESIAN_POINT('Ctrl Pts',(23.166249942623,-3.77405578018836,133.959074172579));
#66765=CARTESIAN_POINT('Ctrl Pts',(23.1616444215508,-3.72121174115413,134.020222281257));
#66766=CARTESIAN_POINT('Ctrl Pts',(23.1538700874317,-3.63200854151381,134.123443137302));
#66767=CARTESIAN_POINT('Ctrl Pts',(23.1460957533127,-3.53836600701794,134.223113129705));
#66768=CARTESIAN_POINT('Ctrl Pts',(23.1383214191936,-3.44059774490611,134.318826468908));
#66769=CARTESIAN_POINT('Ctrl Pts',(23.1305566662465,-3.34294997343953,134.414421849974));
#66770=CARTESIAN_POINT('Ctrl Pts',(23.1227919132994,-3.24118686786929,134.50607000919));
#66771=CARTESIAN_POINT('Ctrl Pts',(23.1150271603523,-3.13566218455629,134.593398190202));
#66772=CARTESIAN_POINT('Ctrl Pts',(23.1072701194673,-3.03024230984653,134.680639635632));
#66773=CARTESIAN_POINT('Ctrl Pts',(23.0995130785823,-2.92106859155812,134.763569393822));
#66774=CARTESIAN_POINT('Ctrl Pts',(23.0917560376973,-2.80853126434396,134.841851818758));
#66775=CARTESIAN_POINT('Ctrl Pts',(23.0840048464572,-2.69607880240321,134.920075210309));
#66776=CARTESIAN_POINT('Ctrl Pts',(23.0762536552171,-2.58026809998581,134.993658021925));
#66777=CARTESIAN_POINT('Ctrl Pts',(23.068502463977,-2.46152178199783,135.062305377571));
#66778=CARTESIAN_POINT('Ctrl Pts',(23.0607545671999,-2.34282593436282,135.130923556259));
#66779=CARTESIAN_POINT('Ctrl Pts',(23.0530066704227,-2.2211972905342,135.194610255879));
#66780=CARTESIAN_POINT('Ctrl Pts',(23.0452587736456,-2.0970865310741,135.253114504183));
#66781=CARTESIAN_POINT('Ctrl Pts',(23.0375124975615,-1.97300173290936,135.311606514659));
#66782=CARTESIAN_POINT('Ctrl Pts',(23.0297662214774,-1.84643620526013,135.36491806347));
#66783=CARTESIAN_POINT('Ctrl Pts',(23.0220199453933,-1.71786389007637,135.412844827984));
#66784=CARTESIAN_POINT('Ctrl Pts',(23.014273612128,-1.58929062580134,135.460771946282));
#66785=CARTESIAN_POINT('Ctrl Pts',(23.0065272788626,-1.4587109107733,135.503314064408));
#66786=CARTESIAN_POINT('Ctrl Pts',(22.9987809455973,-1.32661688371923,135.540315717261));
#66787=CARTESIAN_POINT('Ctrl Pts',(22.9910328775943,-1.19449327512332,135.577325656379));
#66788=CARTESIAN_POINT('Ctrl Pts',(22.9832848095914,-1.06085505609451,135.60879255584));
#66789=CARTESIAN_POINT('Ctrl Pts',(22.9755367415884,-0.926207287252766,
135.634611451999));
#66790=CARTESIAN_POINT('Ctrl Pts',(22.9677804388465,-0.791416413160151,
135.660457788787));
#66791=CARTESIAN_POINT('Ctrl Pts',(22.9600241361046,-0.655614230480491,
135.680644057358));
#66792=CARTESIAN_POINT('Ctrl Pts',(22.9522678333628,-0.519314258254587,
135.695116772157));
#66793=CARTESIAN_POINT('Ctrl Pts',(22.9445073908486,-0.382941538629593,
135.70959721148));
#66794=CARTESIAN_POINT('Ctrl Pts',(22.9367469483345,-0.246070890033827,
135.718357995691));
#66795=CARTESIAN_POINT('Ctrl Pts',(22.9289865058203,-0.10921763914018,135.721397791495));
#66796=CARTESIAN_POINT('Ctrl Pts',(22.9212136055549,0.0278553007410634,
135.72444246705));
#66797=CARTESIAN_POINT('Ctrl Pts',(22.9134407052895,0.16491039599584,135.721747809652));
#66798=CARTESIAN_POINT('Ctrl Pts',(22.9056678050241,0.301434734490052,135.713364606497));
#66799=CARTESIAN_POINT('Ctrl Pts',(22.898177469262,0.432996069396678,135.705286153893));
#66800=CARTESIAN_POINT('Ctrl Pts',(22.8906871334999,0.56406425984617,135.691925592244));
#66801=CARTESIAN_POINT('Ctrl Pts',(22.8831967977378,0.694189653854869,135.673373226605));
#66802=CARTESIAN_POINT('Ctrl Pts',(22.8754224636188,0.829248791727227,135.654117442384));
#66803=CARTESIAN_POINT('Ctrl Pts',(22.8676481294997,0.963720056377465,135.629207391487));
#66804=CARTESIAN_POINT('Ctrl Pts',(22.8598737953807,1.0970925331851,135.598687581398));
#66805=CARTESIAN_POINT('Ctrl Pts',(22.8521090424336,1.23030064033491,135.568205384248));
#66806=CARTESIAN_POINT('Ctrl Pts',(22.8443442894865,1.36241227655698,135.532127270138));
#66807=CARTESIAN_POINT('Ctrl Pts',(22.8365795365395,1.49292261741866,135.490549380399));
#66808=CARTESIAN_POINT('Ctrl Pts',(22.8288224956545,1.62330333356975,135.449012786406));
#66809=CARTESIAN_POINT('Ctrl Pts',(22.8210654547694,1.75208554927871,135.401987405223));
#66810=CARTESIAN_POINT('Ctrl Pts',(22.8133084138845,1.87877594468694,135.349620127447));
#66811=CARTESIAN_POINT('Ctrl Pts',(22.8055572226444,2.00537080188213,135.297292340243));
#66812=CARTESIAN_POINT('Ctrl Pts',(22.7978060314044,2.1298766187578,135.239630823409));
#66813=CARTESIAN_POINT('Ctrl Pts',(22.7900548401643,2.25181686866827,135.176831755547));
#66814=CARTESIAN_POINT('Ctrl Pts',(22.7823069433872,2.37370529072016,135.114059378964));
#66815=CARTESIAN_POINT('Ctrl Pts',(22.7745590466101,2.49302996774566,135.046153972988));
#66816=CARTESIAN_POINT('Ctrl Pts',(22.7668111498331,2.60933614583188,134.973359051309));
#66817=CARTESIAN_POINT('Ctrl Pts',(22.759064873749,2.72561799517307,134.900579356759));
#66818=CARTESIAN_POINT('Ctrl Pts',(22.7513185976649,2.83888227027877,134.822912388165));
#66819=CARTESIAN_POINT('Ctrl Pts',(22.7435723215808,2.94870089153081,134.74064644494));
#66820=CARTESIAN_POINT('Ctrl Pts',(22.7358259883155,3.05852032343868,134.658379894447));
#66821=CARTESIAN_POINT('Ctrl Pts',(22.7280796550501,3.16489373783297,134.57151453598));
#66822=CARTESIAN_POINT('Ctrl Pts',(22.7203333217848,3.26742432451853,134.480380387105));
#66823=CARTESIAN_POINT('Ctrl Pts',(22.7125852537818,3.36997787221837,134.38922582937));
#66824=CARTESIAN_POINT('Ctrl Pts',(22.7048371857788,3.46868658760461,134.293800838651));
#66825=CARTESIAN_POINT('Ctrl Pts',(22.6970891177759,3.56318916418544,134.194473601337));
#66826=CARTESIAN_POINT('Ctrl Pts',(22.689332815034,3.65779217922913,134.095040797853));
#66827=CARTESIAN_POINT('Ctrl Pts',(22.6815765122922,3.74817985557386,133.991697746687));
#66828=CARTESIAN_POINT('Ctrl Pts',(22.6738202095504,3.83402962472286,133.884847575702));
#66829=CARTESIAN_POINT('Ctrl Pts',(22.6660597670362,3.91992521447854,133.777940375564));
#66830=CARTESIAN_POINT('Ctrl Pts',(22.6582993245221,4.00127783917086,133.667522640383));
#66831=CARTESIAN_POINT('Ctrl Pts',(22.650538882008,4.07780783040716,133.554027208404));
#66832=CARTESIAN_POINT('Ctrl Pts',(22.6427659817426,4.1544606743794,133.440349583482));
#66833=CARTESIAN_POINT('Ctrl Pts',(22.6349930814771,4.22627520953607,133.323584722098));
#66834=CARTESIAN_POINT('Ctrl Pts',(22.6272201812117,4.29301692304613,133.204191603477));
#66835=CARTESIAN_POINT('Ctrl Pts',(22.6197298454494,4.35733240715977,133.089138725448));
#66836=CARTESIAN_POINT('Ctrl Pts',(22.6122395096872,4.41693734671143,132.971645634855));
#66837=CARTESIAN_POINT('Ctrl Pts',(22.604749173925,4.47166467002125,132.852139448735));
#66838=CARTESIAN_POINT('Ctrl Pts',(22.5969748398059,4.52846699642694,132.728102149249));
#66839=CARTESIAN_POINT('Ctrl Pts',(22.5892005056868,4.58019446830472,132.601503174902));
#66840=CARTESIAN_POINT('Ctrl Pts',(22.5814261715677,4.62660836922988,132.472796430018));
#66841=CARTESIAN_POINT('Ctrl Pts',(22.5736614186206,4.67296506917014,132.344248304694));
#66842=CARTESIAN_POINT('Ctrl Pts',(22.5658966656736,4.71402109636827,132.213597941611));
#66843=CARTESIAN_POINT('Ctrl Pts',(22.5581319127265,4.74958446731142,132.081322030599));
#66844=CARTESIAN_POINT('Ctrl Pts',(22.5503748718415,4.78511251621329,131.949177497885));
#66845=CARTESIAN_POINT('Ctrl Pts',(22.5426178309564,4.81515866446744,131.815411005319));
#66846=CARTESIAN_POINT('Ctrl Pts',(22.5348607900714,4.83957984385959,131.680516994823));
#66847=CARTESIAN_POINT('Ctrl Pts',(22.5271095988313,4.86398260705025,131.545724708951));
#66848=CARTESIAN_POINT('Ctrl Pts',(22.5193584075912,4.8827687751236,131.409806980715));
#66849=CARTESIAN_POINT('Ctrl Pts',(22.5116072163511,4.89584582440208,131.273270764806));
#66850=CARTESIAN_POINT('Ctrl Pts',(22.503859319574,4.90891731558585,131.13679258043));
#66851=CARTESIAN_POINT('Ctrl Pts',(22.4961114227969,4.91628447695654,130.999696819586));
#66852=CARTESIAN_POINT('Ctrl Pts',(22.4883635260198,4.91790637788049,130.862497704717));
#66853=CARTESIAN_POINT('Ctrl Pts',(22.4806172499357,4.91952793953773,130.725327288945));
#66854=CARTESIAN_POINT('Ctrl Pts',(22.4728709738516,4.91540662654518,130.588053952842));
#66855=CARTESIAN_POINT('Ctrl Pts',(22.4651246977675,4.90555360587275,130.451193684786));
#66856=CARTESIAN_POINT('Ctrl Pts',(22.4573783645021,4.89570051246756,130.31433240646));
#66857=CARTESIAN_POINT('Ctrl Pts',(22.4496320312368,4.88011565502983,130.177884592223));
#66858=CARTESIAN_POINT('Ctrl Pts',(22.4418856979714,4.85886220108035,130.042362472284));
#66859=CARTESIAN_POINT('Ctrl Pts',(22.4341376299685,4.83760398756724,129.906810003107));
#66860=CARTESIAN_POINT('Ctrl Pts',(22.4263895619654,4.81067471205974,129.772184026908));
#66861=CARTESIAN_POINT('Ctrl Pts',(22.4186414939625,4.77818884520936,129.638987534808));
#66862=CARTESIAN_POINT('Ctrl Pts',(22.4108851912206,4.74566845199301,129.505649479891));
#66863=CARTESIAN_POINT('Ctrl Pts',(22.4031288884787,4.70757976312526,129.37374432442));
#66864=CARTESIAN_POINT('Ctrl Pts',(22.3953725857368,4.66408758534354,129.243761354865));
#66865=CARTESIAN_POINT('Ctrl Pts',(22.3876121432226,4.62057219447691,129.113709009485));
#66866=CARTESIAN_POINT('Ctrl Pts',(22.3798517007084,4.57164770746976,128.985581259335));
#66867=CARTESIAN_POINT('Ctrl Pts',(22.3720912581942,4.51752711579995,128.859847357001));
#66868=CARTESIAN_POINT('Ctrl Pts',(22.3643183579287,4.46331964495186,128.733911615445));
#66869=CARTESIAN_POINT('Ctrl Pts',(22.3565454576633,4.40389957053603,128.610377753406));
#66870=CARTESIAN_POINT('Ctrl Pts',(22.3487725573979,4.3395262848596,128.489691162652));
#66871=CARTESIAN_POINT('Ctrl Pts',(22.341282221636,4.27749313026517,128.373391833465));
#66872=CARTESIAN_POINT('Ctrl Pts',(22.333791885874,4.2108607913339,128.259736624332));
#66873=CARTESIAN_POINT('Ctrl Pts',(22.3263015501121,4.1398983074016,128.149096964579));
#66874=CARTESIAN_POINT('Ctrl Pts',(22.3185272159931,4.06624525932138,128.034262368497));
#66875=CARTESIAN_POINT('Ctrl Pts',(22.310752881874,3.98769391879824,127.922312743422));
#66876=CARTESIAN_POINT('Ctrl Pts',(22.3029785477549,3.90449713633556,127.813694274617));
#66877=CARTESIAN_POINT('Ctrl Pts',(22.2952137948078,3.82140288647188,127.705209668368));
#66878=CARTESIAN_POINT('Ctrl Pts',(22.2874490418607,3.73367482134943,127.60004835736));
#66879=CARTESIAN_POINT('Ctrl Pts',(22.2796842889136,3.64161022184459,127.498629525257));
#66880=CARTESIAN_POINT('Ctrl Pts',(22.2719272480287,3.54963706219798,127.397311423769));
#66881=CARTESIAN_POINT('Ctrl Pts',(22.2641702071437,3.45333620058764,127.299728691631));
#66882=CARTESIAN_POINT('Ctrl Pts',(22.2564131662588,3.35304629314327,127.206268954123));
#66883=CARTESIAN_POINT('Ctrl Pts',(22.2486619750187,3.25283201509825,127.11287969533));
#66884=CARTESIAN_POINT('Ctrl Pts',(22.2409107837785,3.14863496366501,127.023607507991));
#66885=CARTESIAN_POINT('Ctrl Pts',(22.2331595925384,3.04083164287378,126.93880425629));
#66886=CARTESIAN_POINT('Ctrl Pts',(22.2254116957613,2.93307414136934,126.854037048234));
#66887=CARTESIAN_POINT('Ctrl Pts',(22.2176637989843,2.8217137256914,126.773735239237));
#66888=CARTESIAN_POINT('Ctrl Pts',(22.2099159022072,2.70716090173826,126.698211215194));
#66889=CARTESIAN_POINT('Ctrl Pts',(22.2021696261231,2.59263203976657,126.622702989149));
#66890=CARTESIAN_POINT('Ctrl Pts',(22.194423350039,2.47491242397898,126.551970775239));
#66891=CARTESIAN_POINT('Ctrl Pts',(22.1866770739549,2.35444220603363,126.486284082701));
#66892=CARTESIAN_POINT('Ctrl Pts',(22.1789307406896,2.23397109880465,126.420596905279));
#66893=CARTESIAN_POINT('Ctrl Pts',(22.1711844074243,2.1107496921579,126.359955510709));
#66894=CARTESIAN_POINT('Ctrl Pts',(22.1634380741589,1.98524308346435,126.304583627308));
#66895=CARTESIAN_POINT('Ctrl Pts',(22.155690006156,1.85970836843616,126.249199343757));
#66896=CARTESIAN_POINT('Ctrl Pts',(22.1479419381531,1.73188779065886,126.19908707736));
#66897=CARTESIAN_POINT('Ctrl Pts',(22.1401938701501,1.60226640499075,126.154422399704));
#66898=CARTESIAN_POINT('Ctrl Pts',(22.1324375674083,1.47250725617108,126.109710251896));
#66899=CARTESIAN_POINT('Ctrl Pts',(22.1246812646664,1.34094384642488,126.070457386073));
#66900=CARTESIAN_POINT('Ctrl Pts',(22.1169249619246,1.20807690838336,126.036789616948));
#66901=CARTESIAN_POINT('Ctrl Pts',(22.1091645194104,1.07513905525627,126.003103878321));
#66902=CARTESIAN_POINT('Ctrl Pts',(22.1014040768963,0.940896670015681,125.975009256204));
#66903=CARTESIAN_POINT('Ctrl Pts',(22.0936436343821,0.805859675247033,125.952580197317));
#66904=CARTESIAN_POINT('Ctrl Pts',(22.0858707341167,0.67060590710636,125.930115133314));
#66905=CARTESIAN_POINT('Ctrl Pts',(22.0780978338512,0.534555368674742,125.913333854869));
#66906=CARTESIAN_POINT('Ctrl Pts',(22.0703249335858,0.398222988539267,125.902258873018));
#66907=CARTESIAN_POINT('Ctrl Pts',(22.0628345978236,0.266846633818932,125.891586494653));
#66908=CARTESIAN_POINT('Ctrl Pts',(22.0553442620614,0.135208880709391,125.886212751802));
#66909=CARTESIAN_POINT('Ctrl Pts',(22.0478539262992,0.00376764555583718,
125.886112060676));
#66910=CARTESIAN_POINT('Ctrl Pts',(22.0400795921801,-0.13265722397581,125.886007551816));
#66911=CARTESIAN_POINT('Ctrl Pts',(22.032305258061,-0.269302532405295,125.891583512413));
#66912=CARTESIAN_POINT('Ctrl Pts',(22.0245309239419,-0.405656219561243,
125.902868386211));
#66913=CARTESIAN_POINT('Ctrl Pts',(22.0167661709948,-0.541841862984792,
125.914139352411));
#66914=CARTESIAN_POINT('Ctrl Pts',(22.0090014180477,-0.677736214335374,
125.931105200879));
#66915=CARTESIAN_POINT('Ctrl Pts',(22.0012366651005,-0.812825914949846,
125.953742399804));
#66916=CARTESIAN_POINT('Ctrl Pts',(21.9934796242156,-0.947781442568135,
125.976357115143));
#66917=CARTESIAN_POINT('Ctrl Pts',(21.9857225833306,-1.08193352678154,126.004631907087));
#66918=CARTESIAN_POINT('Ctrl Pts',(21.9779655424457,-1.21477299555531,126.038491375574));
#66919=CARTESIAN_POINT('Ctrl Pts',(21.9702143512055,-1.3475122890527,126.072325310372));
#66920=CARTESIAN_POINT('Ctrl Pts',(21.9624631599654,-1.47894056003473,126.111735442906));
#66921=CARTESIAN_POINT('Ctrl Pts',(21.9547119687253,-1.6085582655739,126.156595200857));
#66922=CARTESIAN_POINT('Ctrl Pts',(21.9469640719482,-1.73812088013073,126.201435892215));
#66923=CARTESIAN_POINT('Ctrl Pts',(21.9392161751711,-1.8658740911082,126.251721474573));
#66924=CARTESIAN_POINT('Ctrl Pts',(21.931468278394,-1.99133319094225,126.307275429897));
#66925=CARTESIAN_POINT('Ctrl Pts',(21.92372200231,-2.11676604743703,126.362817764531));
#66926=CARTESIAN_POINT('Ctrl Pts',(21.9159757262259,-2.23990539003404,126.423626121938));
#66927=CARTESIAN_POINT('Ctrl Pts',(21.9082294501418,-2.36028656025812,126.489475866386));
#66928=CARTESIAN_POINT('Ctrl Pts',(21.9004831168765,-2.48066861910864,126.555326096922));
#66929=CARTESIAN_POINT('Ctrl Pts',(21.8927367836111,-2.59829212195689,126.626217601132));
#66930=CARTESIAN_POINT('Ctrl Pts',(21.8849904503458,-2.71271744334429,126.701880010046));
#66931=CARTESIAN_POINT('Ctrl Pts',(21.8772423823428,-2.8271683894892,126.777559363032));
#66932=CARTESIAN_POINT('Ctrl Pts',(21.8694943143397,-2.93841940294213,126.858011531136));
#66933=CARTESIAN_POINT('Ctrl Pts',(21.8617462463367,-3.04606058635649,126.942923324699));
#66934=CARTESIAN_POINT('Ctrl Pts',(21.8539899435949,-3.15381617210139,127.027925363526));
#66935=CARTESIAN_POINT('Ctrl Pts',(21.8462336408531,-3.25795395639954,127.117396253433));
#66936=CARTESIAN_POINT('Ctrl Pts',(21.8384773381113,-3.3580974295519,127.210982719802));
#66937=CARTESIAN_POINT('Ctrl Pts',(21.8307168955971,-3.45829435229115,127.304619136086));
#66938=CARTESIAN_POINT('Ctrl Pts',(21.8229564530829,-3.55449244183456,127.402375227227));
#66939=CARTESIAN_POINT('Ctrl Pts',(21.8151960105688,-3.64635343843405,127.503862221184));
#66940=CARTESIAN_POINT('Ctrl Pts',(21.8074231103034,-3.73836189846031,127.605512131073));
#66941=CARTESIAN_POINT('Ctrl Pts',(21.7996502100379,-3.82601910252778,127.710904611302));
#66942=CARTESIAN_POINT('Ctrl Pts',(21.7918773097725,-3.9090277799853,127.819618605632));
#66943=CARTESIAN_POINT('Ctrl Pts',(21.7843869740105,-3.98901888293133,127.924380572434));
#66944=CARTESIAN_POINT('Ctrl Pts',(21.7768966382484,-4.0646933859691,128.032226503026));
#66945=CARTESIAN_POINT('Ctrl Pts',(21.7694063024863,-4.13582529849485,128.142757310754));
#66946=CARTESIAN_POINT('Ctrl Pts',(21.7614526540249,-4.21135705629471,128.260124971799));
#66947=CARTESIAN_POINT('Ctrl Pts',(21.7534990055635,-4.28199732470296,128.380878229055));
#66948=CARTESIAN_POINT('Ctrl Pts',(21.7455453571021,-4.34743626146344,128.50458214671));
#66949=CARTESIAN_POINT('Ctrl Pts',(21.7376017899302,-4.41279225404161,128.628129269026));
#66950=CARTESIAN_POINT('Ctrl Pts',(21.7296582227582,-4.47295986578013,128.754619287473));
#66951=CARTESIAN_POINT('Ctrl Pts',(21.7217146555863,-4.52767227611354,128.883588162898));
#66952=CARTESIAN_POINT('Ctrl Pts',(21.713782789,-4.58230409705596,129.012367071859));
#66953=CARTESIAN_POINT('Ctrl Pts',(21.7058509224138,-4.63149658517907,129.143617227038));
#66954=CARTESIAN_POINT('Ctrl Pts',(21.6979190558275,-4.6750289639352,129.276850470671));
#66955=CARTESIAN_POINT('Ctrl Pts',(21.6919169766414,-4.7079701110927,129.377668666465));
#66956=CARTESIAN_POINT('Ctrl Pts',(21.6859148974553,-4.73767117147266,129.479621811719));
#66957=CARTESIAN_POINT('Ctrl Pts',(21.6799128182693,-4.76405452823405,129.582490119308));
#66958=CARTESIAN_POINT('Origin',(213.235140564004,0.,130.804360617566));
#66959=CARTESIAN_POINT('',(19.584898128716,-4.76405452823411,129.582490119308));
#66960=CARTESIAN_POINT('',(19.9302639333258,-4.76405452823407,129.582490119308));
#66961=CARTESIAN_POINT('',(213.235140564004,-4.76405452823405,129.582490119308));
#66962=CARTESIAN_POINT('',(21.2648594360286,-4.91824895315572,130.807569555502));
#66963=CARTESIAN_POINT('Ctrl Pts',(21.2648594359913,-4.91824895315529,130.807569556159));
#66964=CARTESIAN_POINT('Ctrl Pts',(21.2539396410009,-4.91812367982727,130.99957242459));
#66965=CARTESIAN_POINT('Ctrl Pts',(21.2430198460104,-4.90675553107628,131.191209609033));
#66966=CARTESIAN_POINT('Ctrl Pts',(21.2321000510199,-4.88426909130594,131.381507484675));
#66967=CARTESIAN_POINT('Ctrl Pts',(21.2243257169006,-4.8682598991846,131.516989814583));
#66968=CARTESIAN_POINT('Ctrl Pts',(21.2165513827813,-4.84658396133967,131.652020127371));
#66969=CARTESIAN_POINT('Ctrl Pts',(21.2087770486621,-4.81927351189672,131.786086587494));
#66970=CARTESIAN_POINT('Ctrl Pts',(21.2010122957148,-4.7919967201419,131.919987822686));
#66971=CARTESIAN_POINT('Ctrl Pts',(21.1932475427675,-4.75909931063389,132.052927189284));
#66972=CARTESIAN_POINT('Ctrl Pts',(21.1854827898202,-4.72066528262224,132.184397701106));
#66973=CARTESIAN_POINT('Ctrl Pts',(21.1777257489351,-4.68226942782904,132.315737634562));
#66974=CARTESIAN_POINT('Ctrl Pts',(21.1699687080499,-4.63834800687803,132.445611243662));
#66975=CARTESIAN_POINT('Ctrl Pts',(21.1622116671647,-4.58903602974887,132.573521825644));
#66976=CARTESIAN_POINT('Ctrl Pts',(21.1544604759244,-4.53976123916531,132.70133594926));
#66977=CARTESIAN_POINT('Ctrl Pts',(21.1467092846841,-4.48510412372615,132.827189628953));
#66978=CARTESIAN_POINT('Ctrl Pts',(21.1389580934439,-4.42524937021364,132.950601767559));
#66979=CARTESIAN_POINT('Ctrl Pts',(21.1312101966667,-4.36542005656797,133.073961452715));
#66980=CARTESIAN_POINT('Ctrl Pts',(21.1234622998895,-4.30039766890311,133.194881309691));
#66981=CARTESIAN_POINT('Ctrl Pts',(21.1157144031123,-4.23041473794333,133.312900871876));
#66982=CARTESIAN_POINT('Ctrl Pts',(21.1079681270281,-4.16044644590405,133.430895746912));
#66983=CARTESIAN_POINT('Ctrl Pts',(21.1002218509438,-4.08551987377458,133.545991197801));
#66984=CARTESIAN_POINT('Ctrl Pts',(21.0924755748595,-4.00591296521278,133.65775234981));
#66985=CARTESIAN_POINT('Ctrl Pts',(21.0847292415941,-3.92630546901098,133.769514326814));
#66986=CARTESIAN_POINT('Ctrl Pts',(21.0769829083287,-3.84201779426044,133.877941637384));
#66987=CARTESIAN_POINT('Ctrl Pts',(21.0692365750632,-3.75337034113855,133.982629666083));
#66988=CARTESIAN_POINT('Ctrl Pts',(21.0614885070601,-3.66470303603405,134.087341138941));
#66989=CARTESIAN_POINT('Ctrl Pts',(21.053740439057,-3.57167426235135,134.188311365318));
#66990=CARTESIAN_POINT('Ctrl Pts',(21.0459923710539,-3.47464343009023,134.285170307312));
#66991=CARTESIAN_POINT('Ctrl Pts',(21.038236068312,-3.37750947230591,134.382132192143));
#66992=CARTESIAN_POINT('Ctrl Pts',(21.03047976557,-3.27636523638796,134.47497378735));
#66993=CARTESIAN_POINT('Ctrl Pts',(21.0227234628281,-3.17160599335499,134.563362943372));
#66994=CARTESIAN_POINT('Ctrl Pts',(21.0149630203138,-3.06679083715964,134.651799275348));
#66995=CARTESIAN_POINT('Ctrl Pts',(21.0072025777995,-2.95835713823287,134.735778193684));
#66996=CARTESIAN_POINT('Ctrl Pts',(20.9994421352852,-2.84673089890415,134.815009723599));
#66997=CARTESIAN_POINT('Ctrl Pts',(20.9916692350196,-2.73492546722636,134.894368443));
#66998=CARTESIAN_POINT('Ctrl Pts',(20.9838963347541,-2.61991758206336,134.968964332062));
#66999=CARTESIAN_POINT('Ctrl Pts',(20.9761234344885,-2.50216046280378,135.038551931251));
#67000=CARTESIAN_POINT('Ctrl Pts',(20.9686330987281,-2.38868411146803,135.105609845913));
#67001=CARTESIAN_POINT('Ctrl Pts',(20.9611427629677,-2.27265521020997,135.168017130908));
#67002=CARTESIAN_POINT('Ctrl Pts',(20.9536524272073,-2.15449674380741,135.22559651304));
#67003=CARTESIAN_POINT('Ctrl Pts',(20.9458780930882,-2.03185826321195,135.285359034958));
#67004=CARTESIAN_POINT('Ctrl Pts',(20.9381037589692,-1.90653706293946,135.340109636914));
#67005=CARTESIAN_POINT('Ctrl Pts',(20.9303294248502,-1.77898118806346,135.389598778776));
#67006=CARTESIAN_POINT('Ctrl Pts',(20.9225646719031,-1.65158251440343,135.439026929694));
#67007=CARTESIAN_POINT('Ctrl Pts',(20.914799918956,-1.52195500684621,135.483206382242));
#67008=CARTESIAN_POINT('Ctrl Pts',(20.907035166009,-1.39057061087192,135.521933768952));
#67009=CARTESIAN_POINT('Ctrl Pts',(20.899278125124,-1.25931670773173,135.560622691076));
#67010=CARTESIAN_POINT('Ctrl Pts',(20.891521084239,-1.12630976132239,135.593870213769));
#67011=CARTESIAN_POINT('Ctrl Pts',(20.883764043354,-0.992040637938393,135.621521444773));
#67012=CARTESIAN_POINT('Ctrl Pts',(20.8760128521139,-0.857872767944983,
135.649151823769));
#67013=CARTESIAN_POINT('Ctrl Pts',(20.8682616608739,-0.722444996891805,
135.671194232601));
#67014=CARTESIAN_POINT('Ctrl Pts',(20.8605104696337,-0.586261913164761,
135.687544008723));
#67015=CARTESIAN_POINT('Ctrl Pts',(20.8527625728567,-0.450136710881104,
135.703886835754));
#67016=CARTESIAN_POINT('Ctrl Pts',(20.8450146760796,-0.313257221788848,
135.71454179581));
#67017=CARTESIAN_POINT('Ctrl Pts',(20.8372667793025,-0.17613653802619,135.719455630124));
#67018=CARTESIAN_POINT('Ctrl Pts',(20.8295205032184,-0.0390445369545952,
135.72436843657));
#67019=CARTESIAN_POINT('Ctrl Pts',(20.8217742271344,0.0982881679672947,
135.723542491976));
#67020=CARTESIAN_POINT('Ctrl Pts',(20.8140279510503,0.235345468974294,135.716976577799));
#67021=CARTESIAN_POINT('Ctrl Pts',(20.8062816177849,0.372403781707155,135.710410615153));
#67022=CARTESIAN_POINT('Ctrl Pts',(20.7985352845196,0.509186295951143,135.698104617083));
#67023=CARTESIAN_POINT('Ctrl Pts',(20.7907889512542,0.645179413159238,135.680109440807));
#67024=CARTESIAN_POINT('Ctrl Pts',(20.7830408832513,0.781202985083022,135.662110234636));
#67025=CARTESIAN_POINT('Ctrl Pts',(20.7752928152483,0.916436420686703,135.638419366319));
#67026=CARTESIAN_POINT('Ctrl Pts',(20.7675447472453,1.05037412671886,135.609139203143));
#67027=CARTESIAN_POINT('Ctrl Pts',(20.7597884445035,1.18445418333906,135.579827920662));
#67028=CARTESIAN_POINT('Ctrl Pts',(20.7520321417616,1.31723537689449,135.544915560424));
#67029=CARTESIAN_POINT('Ctrl Pts',(20.7442758390197,1.44822460691093,135.504555140183));
#67030=CARTESIAN_POINT('Ctrl Pts',(20.7365153965055,1.57928374982344,135.46417317837));
#67031=CARTESIAN_POINT('Ctrl Pts',(20.7287549539914,1.70854865513402,135.418337493123));
#67032=CARTESIAN_POINT('Ctrl Pts',(20.7209945114772,1.83554509418338,135.367249753817));
#67033=CARTESIAN_POINT('Ctrl Pts',(20.7132216112118,1.96274539919092,135.316080003937));
#67034=CARTESIAN_POINT('Ctrl Pts',(20.7054487109463,2.08766960447644,135.259641513104));
#67035=CARTESIAN_POINT('Ctrl Pts',(20.6976758106809,2.20986622183303,135.198182910752));
#67036=CARTESIAN_POINT('Ctrl Pts',(20.6901854749186,2.32762068435814,135.138958483399));
#67037=CARTESIAN_POINT('Ctrl Pts',(20.6826951391563,2.44284215601372,135.07507274457));
#67038=CARTESIAN_POINT('Ctrl Pts',(20.6752048033941,2.55515285823264,135.006785742844));
#67039=CARTESIAN_POINT('Ctrl Pts',(20.667430469275,2.67172185485804,134.935909618694));
#67040=CARTESIAN_POINT('Ctrl Pts',(20.6596561351559,2.78552425678915,134.860067381339));
#67041=CARTESIAN_POINT('Ctrl Pts',(20.6518818010368,2.89610793953882,134.779501101252));
#67042=CARTESIAN_POINT('Ctrl Pts',(20.6441170480897,3.00655533778249,134.699034111905));
#67043=CARTESIAN_POINT('Ctrl Pts',(20.6363522951427,3.1137915966007,134.613854891801));
#67044=CARTESIAN_POINT('Ctrl Pts',(20.6285875421956,3.21739051912314,134.524250576954));
#67045=CARTESIAN_POINT('Ctrl Pts',(20.6208305013107,3.32088654573525,134.434735258376));
#67046=CARTESIAN_POINT('Ctrl Pts',(20.6130734604258,3.42075213160468,134.340803845541));
#67047=CARTESIAN_POINT('Ctrl Pts',(20.6053164195408,3.51659163626656,134.242785595116));
#67048=CARTESIAN_POINT('Ctrl Pts',(20.5975652283007,3.61235886761257,134.144841261016));
#67049=CARTESIAN_POINT('Ctrl Pts',(20.5898140370606,3.70410578869839,134.042816502105));
#67050=CARTESIAN_POINT('Ctrl Pts',(20.5820628458205,3.79147160161056,133.937079270219));
#67051=CARTESIAN_POINT('Ctrl Pts',(20.5743149490435,3.87880028172168,133.831386979478));
#67052=CARTESIAN_POINT('Ctrl Pts',(20.5665670522664,3.96175130870287,133.721985654848));
#67053=CARTESIAN_POINT('Ctrl Pts',(20.5588191554894,4.04000253561102,133.609278187613));
#67054=CARTESIAN_POINT('Ctrl Pts',(20.5510728794053,4.11823739404941,133.49659429635));
#67055=CARTESIAN_POINT('Ctrl Pts',(20.5433266033212,4.19177418501898,133.380605959007));
#67056=CARTESIAN_POINT('Ctrl Pts',(20.5355803272371,4.26033291447015,133.261746733011));
#67057=CARTESIAN_POINT('Ctrl Pts',(20.5278339939718,4.32889215000629,133.142886629623));
#67058=CARTESIAN_POINT('Ctrl Pts',(20.5200876607065,4.39247305535386,133.02115593396));
#67059=CARTESIAN_POINT('Ctrl Pts',(20.5123413274412,4.45084080557019,132.897014240594));
#67060=CARTESIAN_POINT('Ctrl Pts',(20.5045932594382,4.50922162683949,132.772844746556));
#67061=CARTESIAN_POINT('Ctrl Pts',(20.4968451914353,4.56238680356838,132.646263534166));
#67062=CARTESIAN_POINT('Ctrl Pts',(20.4890971234323,4.61014917475224,132.517751305364));
#67063=CARTESIAN_POINT('Ctrl Pts',(20.4813408206905,4.65796230835257,132.389102492235));
#67064=CARTESIAN_POINT('Ctrl Pts',(20.4735845179487,4.70036102939339,132.258518930049));
#67065=CARTESIAN_POINT('Ctrl Pts',(20.4658282152069,4.73720754319135,132.126498188029));
#67066=CARTESIAN_POINT('Ctrl Pts',(20.4580677726928,4.77407372308315,131.994406982565));
#67067=CARTESIAN_POINT('Ctrl Pts',(20.4503073301787,4.80538170174257,131.860877449281));
#67068=CARTESIAN_POINT('Ctrl Pts',(20.4425468876646,4.831044817151,131.7264175774));
#67069=CARTESIAN_POINT('Ctrl Pts',(20.4347739873992,4.85674912927056,131.591741858596));
#67070=CARTESIAN_POINT('Ctrl Pts',(20.4270010871338,4.87679041291184,131.45613320377));
#67071=CARTESIAN_POINT('Ctrl Pts',(20.4192281868684,4.89113380665535,131.32010585302));
#67072=CARTESIAN_POINT('Ctrl Pts',(20.411737851106,4.90495578190807,131.189023439095));
#67073=CARTESIAN_POINT('Ctrl Pts',(20.4042475153437,4.91348692036363,131.057552549415));
#67074=CARTESIAN_POINT('Ctrl Pts',(20.3967571795814,4.91674180971358,130.926151582397));
#67075=CARTESIAN_POINT('Ctrl Pts',(20.3889828454623,4.92012010918239,130.789768507781));
#67076=CARTESIAN_POINT('Ctrl Pts',(20.3812085113432,4.91782486495393,130.653028742144));
#67077=CARTESIAN_POINT('Ctrl Pts',(20.3734341772241,4.90981535344358,130.516443515626));
#67078=CARTESIAN_POINT('Ctrl Pts',(20.365669424277,4.90181571294033,130.380026618192));
#67079=CARTESIAN_POINT('Ctrl Pts',(20.3579046713298,4.888115839948,130.243764267474));
#67080=CARTESIAN_POINT('Ctrl Pts',(20.3501399183827,4.86872694030906,130.108170238999));
#67081=CARTESIAN_POINT('Ctrl Pts',(20.3423828774977,4.8493572979986,129.972710884426));
#67082=CARTESIAN_POINT('Ctrl Pts',(20.3346258366128,4.8243099286192,129.837918915653));
#67083=CARTESIAN_POINT('Ctrl Pts',(20.3268687957278,4.79364799179473,129.704305167481));
#67084=CARTESIAN_POINT('Ctrl Pts',(20.3191176044876,4.76300917737529,129.570792178475));
#67085=CARTESIAN_POINT('Ctrl Pts',(20.3113664132474,4.72676431010166,129.438456021073));
#67086=CARTESIAN_POINT('Ctrl Pts',(20.3036152220073,4.68502793818937,129.307799131731));
#67087=CARTESIAN_POINT('Ctrl Pts',(20.2958673252302,4.6433093053485,129.177197775053));
#67088=CARTESIAN_POINT('Ctrl Pts',(20.2881194284531,4.59610392880527,129.048274638519));
#67089=CARTESIAN_POINT('Ctrl Pts',(20.280371531676,4.54357664411465,128.921518526058));
#67090=CARTESIAN_POINT('Ctrl Pts',(20.2726252555918,4.49106034699962,128.794788928242));
#67091=CARTESIAN_POINT('Ctrl Pts',(20.2648789795077,4.43322450558711,128.670225813822));
#67092=CARTESIAN_POINT('Ctrl Pts',(20.2571327034235,4.37028254039623,128.548299098102));
#67093=CARTESIAN_POINT('Ctrl Pts',(20.2493863701582,4.30734011058206,128.426371482346));
#67094=CARTESIAN_POINT('Ctrl Pts',(20.2416400368929,4.23929166111792,128.307080651528));
#67095=CARTESIAN_POINT('Ctrl Pts',(20.2338937036275,4.16639693331599,128.190872592616));
#67096=CARTESIAN_POINT('Ctrl Pts',(20.2261456356245,4.09348588124518,128.074638509715));
#67097=CARTESIAN_POINT('Ctrl Pts',(20.2183975676215,4.01572659894786,127.961488903602));
#67098=CARTESIAN_POINT('Ctrl Pts',(20.2106494996185,3.93342234948612,127.851841069271));
#67099=CARTESIAN_POINT('Ctrl Pts',(20.2028931968766,3.85103062608863,127.742076699917));
#67100=CARTESIAN_POINT('Ctrl Pts',(20.1951368941347,3.76408452127027,127.635821850068));
#67101=CARTESIAN_POINT('Ctrl Pts',(20.1873805913928,3.67292817272093,127.533461398615));
#67102=CARTESIAN_POINT('Ctrl Pts',(20.1796201488786,3.58172317128358,127.431046314307));
#67103=CARTESIAN_POINT('Ctrl Pts',(20.1718597063645,3.48630372038269,127.332530050792));
#67104=CARTESIAN_POINT('Ctrl Pts',(20.1640992638503,3.38705036280178,127.238260099865));
#67105=CARTESIAN_POINT('Ctrl Pts',(20.1563263635848,3.28763767492011,127.143838818445));
#67106=CARTESIAN_POINT('Ctrl Pts',(20.1485534633193,3.18437907632109,127.05367772856));
#67107=CARTESIAN_POINT('Ctrl Pts',(20.1407805630539,3.07768836831409,126.968084119444));
#67108=CARTESIAN_POINT('Ctrl Pts',(20.133290227292,2.97487613628343,126.885602053619));
#67109=CARTESIAN_POINT('Ctrl Pts',(20.1257998915302,2.86887724207329,126.807361338));
#67110=CARTESIAN_POINT('Ctrl Pts',(20.1183095557683,2.76008523425795,126.733597475091));
#67111=CARTESIAN_POINT('Ctrl Pts',(20.1105352216493,2.64716834439697,126.657036832898));
#67112=CARTESIAN_POINT('Ctrl Pts',(20.1027608875302,2.53088467132556,126.585056703491));
#67113=CARTESIAN_POINT('Ctrl Pts',(20.0949865534111,2.41164231534645,126.517967681153));
#67114=CARTESIAN_POINT('Ctrl Pts',(20.087221800464,2.2925469149141,126.450961340039));
#67115=CARTESIAN_POINT('Ctrl Pts',(20.0794570475169,2.17050042411475,126.388834302232));
#67116=CARTESIAN_POINT('Ctrl Pts',(20.0716922945698,2.04594115388183,126.331854848162));
#67117=CARTESIAN_POINT('Ctrl Pts',(20.0639352536848,1.92150559767225,126.274931986889));
#67118=CARTESIAN_POINT('Ctrl Pts',(20.0561782127998,1.7945625818715,126.223146696527));
#67119=CARTESIAN_POINT('Ctrl Pts',(20.0484211719148,1.66557602558337,126.176721957785));
#67120=CARTESIAN_POINT('Ctrl Pts',(20.0406699806747,1.53668673906053,126.130332228299));
#67121=CARTESIAN_POINT('Ctrl Pts',(20.0329187894345,1.40575734579168,126.089295136077));
#67122=CARTESIAN_POINT('Ctrl Pts',(20.0251675981944,1.27327247590721,126.053785887642));
#67123=CARTESIAN_POINT('Ctrl Pts',(20.0174197014173,1.14084391562659,126.018291731583));
#67124=CARTESIAN_POINT('Ctrl Pts',(20.0096718046402,1.00686157049138,125.988320847376));
#67125=CARTESIAN_POINT('Ctrl Pts',(20.0019239078631,0.871825782732259,125.96399876466));
#67126=CARTESIAN_POINT('Ctrl Pts',(19.994177631779,0.736818241548902,125.9396817696));
#67127=CARTESIAN_POINT('Ctrl Pts',(19.986431355695,0.600758080574644,125.92101129501));
#67128=CARTESIAN_POINT('Ctrl Pts',(19.9786850796108,0.464156011866409,125.908061784861));
#67129=CARTESIAN_POINT('Ctrl Pts',(19.9709387463455,0.327552934792919,125.895112179122));
#67130=CARTESIAN_POINT('Ctrl Pts',(19.9631924130801,0.190408331223513,125.887883658991));
#67131=CARTESIAN_POINT('Ctrl Pts',(19.9554460798148,0.0532378191483778,
125.886398763595));
#67132=CARTESIAN_POINT('Ctrl Pts',(19.9476980118118,-0.0839634113118627,
125.884913535667));
#67133=CARTESIAN_POINT('Ctrl Pts',(19.9399499438089,-0.221190170955723,
125.889174496184));
#67134=CARTESIAN_POINT('Ctrl Pts',(19.9322018758059,-0.357927456593226,
125.89915205948));
#67135=CARTESIAN_POINT('Ctrl Pts',(19.9244455730641,-0.4948100682451,125.90914022705));
#67136=CARTESIAN_POINT('Ctrl Pts',(19.9166892703222,-0.631201776147267,
125.924857105712));
#67137=CARTESIAN_POINT('Ctrl Pts',(19.9089329675803,-0.766592755961558,
125.946221199125));
#67138=CARTESIAN_POINT('Ctrl Pts',(19.9011725250662,-0.902055998018503,
125.967596695198));
#67139=CARTESIAN_POINT('Ctrl Pts',(19.893412082552,-1.0365170646004,125.994625334837));
#67140=CARTESIAN_POINT('Ctrl Pts',(19.8856516400378,-1.16947790834913,126.027174784423));
#67141=CARTESIAN_POINT('Ctrl Pts',(19.8778787397724,-1.30265219264795,126.059776485275));
#67142=CARTESIAN_POINT('Ctrl Pts',(19.870105839507,-1.43432106583708,126.097916597322));
#67143=CARTESIAN_POINT('Ctrl Pts',(19.8623329392416,-1.5640023270663,126.141413075138));
#67144=CARTESIAN_POINT('Ctrl Pts',(19.8548426034795,-1.68896934780209,126.183328346425));
#67145=CARTESIAN_POINT('Ctrl Pts',(19.8473522677175,-1.81209046923445,126.230217200242));
#67146=CARTESIAN_POINT('Ctrl Pts',(19.8398619319555,-1.93295483382021,126.281875827883));
#67147=CARTESIAN_POINT('Ctrl Pts',(19.8320871447504,-2.05840911854133,126.335496232894));
#67148=CARTESIAN_POINT('Ctrl Pts',(19.8243123575451,-2.18182927946781,126.394425706269));
#67149=CARTESIAN_POINT('Ctrl Pts',(19.81653757034,-2.30273333283727,126.458488753332));
#67150=CARTESIAN_POINT('Ctrl Pts',(19.8087724675611,-2.42348678576311,126.522472002216));
#67151=CARTESIAN_POINT('Ctrl Pts',(19.8010073647823,-2.54173002514391,126.591575919711));
#67152=CARTESIAN_POINT('Ctrl Pts',(19.7932422620035,-2.65700036040956,126.665576720419));
#67153=CARTESIAN_POINT('Ctrl Pts',(19.7854849741014,-2.77215468646279,126.739503045985));
#67154=CARTESIAN_POINT('Ctrl Pts',(19.7777276861993,-2.88434173596447,126.818316236782));
#67155=CARTESIAN_POINT('Ctrl Pts',(19.7699703982972,-2.99312311050278,126.901746479853));
#67156=CARTESIAN_POINT('Ctrl Pts',(19.7622194065634,-3.10181619312028,126.985109007137));
#67157=CARTESIAN_POINT('Ctrl Pts',(19.7544684148297,-3.20710879562608,127.073080888195));
#67158=CARTESIAN_POINT('Ctrl Pts',(19.746717423096,-3.30859159272759,127.165349112359));
#67159=CARTESIAN_POINT('Ctrl Pts',(19.7389698774254,-3.41002927094018,127.257576314399));
#67160=CARTESIAN_POINT('Ctrl Pts',(19.7312223317549,-3.50766022489781,127.354095797025));
#67161=CARTESIAN_POINT('Ctrl Pts',(19.7234747860844,-3.60110844992599,127.454554504614));
#67162=CARTESIAN_POINT('Ctrl Pts',(19.7157290071483,-3.69453536521233,127.554990303805));
#67163=CARTESIAN_POINT('Ctrl Pts',(19.7079832282122,-3.78378118368068,127.659363254309));
#67164=CARTESIAN_POINT('Ctrl Pts',(19.7002374492761,-3.86850728762713,127.767283992244));
#67165=CARTESIAN_POINT('Ctrl Pts',(19.6924917592817,-3.95323241869766,127.875203490968));
#67166=CARTESIAN_POINT('Ctrl Pts',(19.6847460692873,-4.03343769799112,127.986670388027));
#67167=CARTESIAN_POINT('Ctrl Pts',(19.6770003792929,-4.10882553095543,128.101263168588));
#67168=CARTESIAN_POINT('Ctrl Pts',(19.6692493289486,-4.184265535536,128.215935252273));
#67169=CARTESIAN_POINT('Ctrl Pts',(19.6614982786043,-4.25488121633397,128.333737215375));
#67170=CARTESIAN_POINT('Ctrl Pts',(19.6537472282599,-4.32041880507549,128.454219257722));
#67171=CARTESIAN_POINT('Ctrl Pts',(19.6459936047494,-4.38597815075279,128.574741297269));
#67172=CARTESIAN_POINT('Ctrl Pts',(19.6382399812389,-4.44645586956471,128.697944839499));
#67173=CARTESIAN_POINT('Ctrl Pts',(19.6304863577284,-4.50164517484358,128.823357391343));
#67174=CARTESIAN_POINT('Ctrl Pts',(19.6227229073165,-4.55690442675623,128.948928890392));
#67175=CARTESIAN_POINT('Ctrl Pts',(19.6149594569045,-4.60686172565171,129.07671463039));
#67176=CARTESIAN_POINT('Ctrl Pts',(19.6071960064926,-4.65135902473962,129.20622348782));
#67177=CARTESIAN_POINT('Ctrl Pts',(19.5997633805671,-4.69396015713153,129.330213574732));
#67178=CARTESIAN_POINT('Ctrl Pts',(19.5923307546415,-4.73155697456111,129.455782650757));
#67179=CARTESIAN_POINT('Ctrl Pts',(19.584898128716,-4.76405452823411,129.582490119308));
#67180=CARTESIAN_POINT('Ctrl Pts',(21.3349957656066,-4.76405452823399,129.582490119308));
#67181=CARTESIAN_POINT('Ctrl Pts',(21.3273456225782,-4.79769978247013,129.713672454937));
#67182=CARTESIAN_POINT('Ctrl Pts',(21.3196954795498,-4.82590128757831,129.846162751177));
#67183=CARTESIAN_POINT('Ctrl Pts',(21.3120453365213,-4.84857992481995,129.979463184467));
#67184=CARTESIAN_POINT('Ctrl Pts',(21.3041810197725,-4.8718934741269,130.116495502196));
#67185=CARTESIAN_POINT('Ctrl Pts',(21.2963167030238,-4.88937031344629,130.254383527775));
#67186=CARTESIAN_POINT('Ctrl Pts',(21.288452386275,-4.90098172796321,130.392582564884));
#67187=CARTESIAN_POINT('Ctrl Pts',(21.2805880695262,-4.91259314248012,130.530781601993));
#67188=CARTESIAN_POINT('Ctrl Pts',(21.2727237527774,-4.918339173616,130.669291192643));
#67189=CARTESIAN_POINT('Ctrl Pts',(21.2648594360286,-4.91824895315572,130.807569555502));
#67190=CARTESIAN_POINT('',(21.610140563968,-4.91824963054304,130.806266965701));
#67191=CARTESIAN_POINT('Ctrl Pts',(21.6799128182693,-4.76405452823405,129.582490119308));
#67192=CARTESIAN_POINT('Ctrl Pts',(21.6719943898972,-4.79886158663048,129.718202311725));
#67193=CARTESIAN_POINT('Ctrl Pts',(21.6640759615251,-4.82789234323369,129.855507719247));
#67194=CARTESIAN_POINT('Ctrl Pts',(21.6561575331531,-4.85101175268147,129.993886658795));
#67195=CARTESIAN_POINT('Ctrl Pts',(21.6482449636327,-4.87411405605911,130.132163211651));
#67196=CARTESIAN_POINT('Ctrl Pts',(21.6403323941123,-4.8913136665669,130.271511353085));
#67197=CARTESIAN_POINT('Ctrl Pts',(21.6324198245919,-4.90252642019679,130.411400362868));
#67198=CARTESIAN_POINT('Ctrl Pts',(21.6249934043975,-4.91305026074918,130.542694573245));
#67199=CARTESIAN_POINT('Ctrl Pts',(21.6175669842031,-4.9183007179387,130.674464880059));
#67200=CARTESIAN_POINT('Ctrl Pts',(21.6101405640087,-4.91824963054332,130.806266964978));
#67201=CARTESIAN_POINT('Ctrl Pts',(21.610140563968,-4.91824963054304,130.8062669657));
#67202=CARTESIAN_POINT('Ctrl Pts',(21.6017353324186,-4.91819180974393,130.955440728217));
#67203=CARTESIAN_POINT('Ctrl Pts',(21.593330100869,-4.91134301940546,131.104404178229));
#67204=CARTESIAN_POINT('Ctrl Pts',(21.5849248693196,-4.89778544524941,131.252557889761));
#67205=CARTESIAN_POINT('Ctrl Pts',(21.5764834188236,-4.88416945020985,131.401350009804));
#67206=CARTESIAN_POINT('Ctrl Pts',(21.5680419683276,-4.86378681331425,131.549325129188));
#67207=CARTESIAN_POINT('Ctrl Pts',(21.5596005178316,-4.83677140407179,131.695890452879));
#67208=CARTESIAN_POINT('Ctrl Pts',(21.5511406982542,-4.80969720774602,131.842774711139));
#67209=CARTESIAN_POINT('Ctrl Pts',(21.5426808786767,-4.77596146114176,131.988242777102));
#67210=CARTESIAN_POINT('Ctrl Pts',(21.5342210590993,-4.73574807339157,132.131716352804));
#67211=CARTESIAN_POINT('Ctrl Pts',(21.5257330831344,-4.69540084546728,132.275667444313));
#67212=CARTESIAN_POINT('Ctrl Pts',(21.5172451071696,-4.64853291458363,132.417610498472));
#67213=CARTESIAN_POINT('Ctrl Pts',(21.5087571312047,-4.59537761380565,132.556983694281));
#67214=CARTESIAN_POINT('Ctrl Pts',(21.5028243136943,-4.5582237975681,132.654400998477));
#67215=CARTESIAN_POINT('Ctrl Pts',(21.4968914961838,-4.51799925047187,132.750563247881));
#67216=CARTESIAN_POINT('Ctrl Pts',(21.4909586786734,-4.47479683952839,132.845285973243));
#67217=CARTESIAN_POINT('Ctrl Pts',(21.4831843445544,-4.4181846182973,132.969410154433));
#67218=CARTESIAN_POINT('Ctrl Pts',(21.4754100104353,-4.35631428432474,133.091373646621));
#67219=CARTESIAN_POINT('Ctrl Pts',(21.4676356763162,-4.28937281389802,133.210698899249));
#67220=CARTESIAN_POINT('Ctrl Pts',(21.4598709233691,-4.22251384285087,133.329877094168));
#67221=CARTESIAN_POINT('Ctrl Pts',(21.452106170422,-4.15059635988457,133.446423181133));
#67222=CARTESIAN_POINT('Ctrl Pts',(21.4443414174749,-4.0738551536779,133.559880033094));
#67223=CARTESIAN_POINT('Ctrl Pts',(21.4365843765899,-3.9971901679192,133.673224198111));
#67224=CARTESIAN_POINT('Ctrl Pts',(21.428827335705,-3.91571121083265,133.783484912376));
#67225=CARTESIAN_POINT('Ctrl Pts',(21.42107029482,-3.82969850591166,133.890230416556));
#67226=CARTESIAN_POINT('Ctrl Pts',(21.4133191035799,-3.74375066384029,133.996895423121));
#67227=CARTESIAN_POINT('Ctrl Pts',(21.4055679123397,-3.65327612342795,134.100050192748));
#67228=CARTESIAN_POINT('Ctrl Pts',(21.3978167210996,-3.55859764770646,134.199292994542));
#67229=CARTESIAN_POINT('Ctrl Pts',(21.3900688243225,-3.46395941286292,134.298493615497));
#67230=CARTESIAN_POINT('Ctrl Pts',(21.3823209275455,-3.36512106579618,134.393785293293));
#67231=CARTESIAN_POINT('Ctrl Pts',(21.3745730307684,-3.26244462944918,134.484800550818));
#67232=CARTESIAN_POINT('Ctrl Pts',(21.3668267546843,-3.15978967079923,134.575796769914));
#67233=CARTESIAN_POINT('Ctrl Pts',(21.3590804786002,-3.05329851215573,134.662518088841));
#67234=CARTESIAN_POINT('Ctrl Pts',(21.3513342025161,-2.94336860658837,134.744635266401));
#67235=CARTESIAN_POINT('Ctrl Pts',(21.3435878692507,-2.83343788954342,134.826753050131));
#67236=CARTESIAN_POINT('Ctrl Pts',(21.3358415359854,-2.72006868814584,134.904266390699));
#67237=CARTESIAN_POINT('Ctrl Pts',(21.3280952027201,-2.60368964523393,134.976887824643));
#67238=CARTESIAN_POINT('Ctrl Pts',(21.3203471347171,-2.48728454004212,135.049525521655));
#67239=CARTESIAN_POINT('Ctrl Pts',(21.312599066714,-2.36786858371024,135.117268925174));
#67240=CARTESIAN_POINT('Ctrl Pts',(21.304850998711,-2.24589700823557,135.179875409096));
#67241=CARTESIAN_POINT('Ctrl Pts',(21.2970946959692,-2.12379579991917,135.242548431935));
#67242=CARTESIAN_POINT('Ctrl Pts',(21.2893383932273,-1.9991338950492,135.300073450262));
#67243=CARTESIAN_POINT('Ctrl Pts',(21.2815820904855,-1.87238910544307,135.352254866591));
#67244=CARTESIAN_POINT('Ctrl Pts',(21.2738216479713,-1.74557666832651,135.404464133714));
#67245=CARTESIAN_POINT('Ctrl Pts',(21.2660612054571,-1.61667949857841,135.45132398239));
#67246=CARTESIAN_POINT('Ctrl Pts',(21.258300762943,-1.48619179429567,135.49268835921));
#67247=CARTESIAN_POINT('Ctrl Pts',(21.2505278626775,-1.35549461956586,135.5341191378));
#67248=CARTESIAN_POINT('Ctrl Pts',(21.2427549624122,-1.22320218558329,135.57003671323));
#67249=CARTESIAN_POINT('Ctrl Pts',(21.2349820621467,-1.08982101566974,135.600345731837));
#67250=CARTESIAN_POINT('Ctrl Pts',(21.2274917263847,-0.961288587248536,
135.629552941273));
#67251=CARTESIAN_POINT('Ctrl Pts',(21.2200013906225,-0.831745508073716,
135.653552228622));
#67252=CARTESIAN_POINT('Ctrl Pts',(21.2125110548605,-0.701648691013128,
135.67230393861));
#67253=CARTESIAN_POINT('Ctrl Pts',(21.2047367207414,-0.56661921359256,135.691766625382));
#67254=CARTESIAN_POINT('Ctrl Pts',(21.1969623866224,-0.43056544665073,135.705637607803));
#67255=CARTESIAN_POINT('Ctrl Pts',(21.1891880525033,-0.293990232245845,
135.713816066579));
#67256=CARTESIAN_POINT('Ctrl Pts',(21.1814232995562,-0.157583334586822,
135.721984446135));
#67257=CARTESIAN_POINT('Ctrl Pts',(21.1736585466091,-0.0206566546412068,
135.724474237708));
#67258=CARTESIAN_POINT('Ctrl Pts',(21.165893793662,0.116278304641728,135.721235887325));
#67259=CARTESIAN_POINT('Ctrl Pts',(21.158136752777,0.253077258192844,135.718000753318));
#67260=CARTESIAN_POINT('Ctrl Pts',(21.150379711892,0.38988408639012,135.709048808445));
#67261=CARTESIAN_POINT('Ctrl Pts',(21.142622671007,0.52618407023321,135.694382436202));
#67262=CARTESIAN_POINT('Ctrl Pts',(21.1348714797669,0.662381269198224,135.679727123983));
#67263=CARTESIAN_POINT('Ctrl Pts',(21.1271202885268,0.798071997436957,135.659366003441));
#67264=CARTESIAN_POINT('Ctrl Pts',(21.1193690972867,0.932743806065768,135.633353478893));
#67265=CARTESIAN_POINT('Ctrl Pts',(21.1116212005096,1.06735837558342,135.607352010361));
#67266=CARTESIAN_POINT('Ctrl Pts',(21.1038733037326,1.20095450376418,135.575703989204));
#67267=CARTESIAN_POINT('Ctrl Pts',(21.0961254069555,1.33302733946318,135.538515365221));
#67268=CARTESIAN_POINT('Ctrl Pts',(21.0883791308714,1.46507254837211,135.501334520297));
#67269=CARTESIAN_POINT('Ctrl Pts',(21.0806328547873,1.59559472249907,135.45861548371));
#67270=CARTESIAN_POINT('Ctrl Pts',(21.0728865787032,1.72410202880573,135.410514681074));
#67271=CARTESIAN_POINT('Ctrl Pts',(21.0651402454379,1.85261028372413,135.362413523368));
#67272=CARTESIAN_POINT('Ctrl Pts',(21.0573939121725,1.97910327498779,135.308930657396));
#67273=CARTESIAN_POINT('Ctrl Pts',(21.0496475789072,2.10310745952155,135.250271331492));
#67274=CARTESIAN_POINT('Ctrl Pts',(21.0418995109042,2.22713941393265,135.19159886924));
#67275=CARTESIAN_POINT('Ctrl Pts',(21.0341514429013,2.34868109919985,135.127747807469));
#67276=CARTESIAN_POINT('Ctrl Pts',(21.0264033748983,2.46728232309684,135.058970000416));
#67277=CARTESIAN_POINT('Ctrl Pts',(21.0186470721565,2.58600959778595,134.990119095491));
#67278=CARTESIAN_POINT('Ctrl Pts',(21.0108907694145,2.70178982951656,134.916331181848));
#67279=CARTESIAN_POINT('Ctrl Pts',(21.0031344666727,2.81420018762465,134.837902530882));
#67280=CARTESIAN_POINT('Ctrl Pts',(20.9953740241585,2.92667054252564,134.759432020182));
#67281=CARTESIAN_POINT('Ctrl Pts',(20.9876135816444,3.03576712909411,134.67631607354));
#67282=CARTESIAN_POINT('Ctrl Pts',(20.9798531391302,3.14109994231722,134.588891528376));
#67283=CARTESIAN_POINT('Ctrl Pts',(20.9720802388648,3.24660184512298,134.50132664157));
#67284=CARTESIAN_POINT('Ctrl Pts',(20.9643073385994,3.34832761056063,134.409439597));
#67285=CARTESIAN_POINT('Ctrl Pts',(20.956534438334,3.44592322666501,134.313605006096));
#67286=CARTESIAN_POINT('Ctrl Pts',(20.9490441025719,3.53997099629627,134.221254243964));
#67287=CARTESIAN_POINT('Ctrl Pts',(20.9415537668098,3.63018347499754,134.125238183631));
#67288=CARTESIAN_POINT('Ctrl Pts',(20.9340634310477,3.71628032709946,134.025919804189));
#67289=CARTESIAN_POINT('Ctrl Pts',(20.9262890969286,3.80564156751676,133.922835738204));
#67290=CARTESIAN_POINT('Ctrl Pts',(20.9185147628095,3.89085200220441,133.815867455649));
#67291=CARTESIAN_POINT('Ctrl Pts',(20.9107404286904,3.97155501061956,133.705383516497));
#67292=CARTESIAN_POINT('Ctrl Pts',(20.9029756757433,4.05215855978947,133.595035738926));
#67293=CARTESIAN_POINT('Ctrl Pts',(20.8952109227963,4.12826550708481,133.481181238284));
#67294=CARTESIAN_POINT('Ctrl Pts',(20.8874461698492,4.19955768150787,133.364223571356));
#67295=CARTESIAN_POINT('Ctrl Pts',(20.8796891289642,4.27077904753815,133.247382068433));
#67296=CARTESIAN_POINT('Ctrl Pts',(20.8719320880791,4.33719495511777,133.127443864432));
#67297=CARTESIAN_POINT('Ctrl Pts',(20.8641750471941,4.39852919135532,133.004843295365));
#67298=CARTESIAN_POINT('Ctrl Pts',(20.856423855954,4.45981717496822,132.882335180341));
#67299=CARTESIAN_POINT('Ctrl Pts',(20.8486726647139,4.51603094064258,132.757169044712));
#67300=CARTESIAN_POINT('Ctrl Pts',(20.8409214734738,4.56693926913249,132.629805433099));
#67301=CARTESIAN_POINT('Ctrl Pts',(20.8331735766967,4.61782596022483,132.502495954418));
#67302=CARTESIAN_POINT('Ctrl Pts',(20.8254256799196,4.66341155425515,132.372991219659));
#67303=CARTESIAN_POINT('Ctrl Pts',(20.8176777831425,4.70351230541546,132.241773242843));
#67304=CARTESIAN_POINT('Ctrl Pts',(20.8099315070584,4.74360466836304,132.110582713999));
#67305=CARTESIAN_POINT('Ctrl Pts',(20.8021852309742,4.77821435631338,131.97768002958));
#67306=CARTESIAN_POINT('Ctrl Pts',(20.7944389548901,4.80720712679434,131.843563534516));
#67307=CARTESIAN_POINT('Ctrl Pts',(20.7866926216248,4.83620011129336,131.709446049435));
#67308=CARTESIAN_POINT('Ctrl Pts',(20.7789462883595,4.85957601297787,131.574115117967));
#67309=CARTESIAN_POINT('Ctrl Pts',(20.7711999550941,4.87725155148807,131.438080087053));
#67310=CARTESIAN_POINT('Ctrl Pts',(20.7634518870911,4.89493104831257,131.302014592038));
#67311=CARTESIAN_POINT('Ctrl Pts',(20.7557038190881,4.90690759139603,131.165245071447));
#67312=CARTESIAN_POINT('Ctrl Pts',(20.7479557510852,4.91314973294599,131.028286418118));
#67313=CARTESIAN_POINT('Ctrl Pts',(20.7401994483433,4.91939850871827,130.891182203502));
#67314=CARTESIAN_POINT('Ctrl Pts',(20.7324431456015,4.91990069052779,130.753888845786));
#67315=CARTESIAN_POINT('Ctrl Pts',(20.7246868428596,4.91467698958774,130.61692222631));
#67316=CARTESIAN_POINT('Ctrl Pts',(20.7169264003455,4.90945050060121,130.479882503624));
#67317=CARTESIAN_POINT('Ctrl Pts',(20.7091659578313,4.89849207059793,130.343170256188));
#67318=CARTESIAN_POINT('Ctrl Pts',(20.7014055153171,4.88187428320314,130.207295675118));
#67319=CARTESIAN_POINT('Ctrl Pts',(20.6936326150516,4.86522981946075,130.071202976109));
#67320=CARTESIAN_POINT('Ctrl Pts',(20.6858597147862,4.84290790749611,129.935951016566));
#67321=CARTESIAN_POINT('Ctrl Pts',(20.6780868145208,4.8150323664022,129.802040123413));
#67322=CARTESIAN_POINT('Ctrl Pts',(20.6705964787587,4.78817017144131,129.672997228527));
#67323=CARTESIAN_POINT('Ctrl Pts',(20.6631061429967,4.75615118886716,129.545199889313));
#67324=CARTESIAN_POINT('Ctrl Pts',(20.6556158072347,4.7191292749939,129.419080159177));
#67325=CARTESIAN_POINT('Ctrl Pts',(20.6478414731156,4.68070366400356,129.288178561139));
#67326=CARTESIAN_POINT('Ctrl Pts',(20.6400671389966,4.63676653972007,129.158669639584));
#67327=CARTESIAN_POINT('Ctrl Pts',(20.6322928048775,4.58743521997294,129.031052645145));
#67328=CARTESIAN_POINT('Ctrl Pts',(20.6245280519304,4.53816469666853,128.903592927246));
#67329=CARTESIAN_POINT('Ctrl Pts',(20.6167632989832,4.48351334477991,128.778020858378));
#67330=CARTESIAN_POINT('Ctrl Pts',(20.6089985460361,4.4236487088643,128.654822257112));
#67331=CARTESIAN_POINT('Ctrl Pts',(20.6012415051511,4.36384353134911,128.531746018434));
#67332=CARTESIAN_POINT('Ctrl Pts',(20.5934844642662,4.29883554384291,128.411038905476));
#67333=CARTESIAN_POINT('Ctrl Pts',(20.5857274233812,4.22884086571668,128.293168073187));
#67334=CARTESIAN_POINT('Ctrl Pts',(20.5779762321411,4.15889897112161,128.17538612821));
#67335=CARTESIAN_POINT('Ctrl Pts',(20.5702250409009,4.08397806977192,128.060436541431));
#67336=CARTESIAN_POINT('Ctrl Pts',(20.5624738496608,4.00434065125074,127.948762779767));
#67337=CARTESIAN_POINT('Ctrl Pts',(20.5547259528837,3.92473708075683,127.837136482432));
#67338=CARTESIAN_POINT('Ctrl Pts',(20.5469780561066,3.84042120670279,127.728783558656));
#67339=CARTESIAN_POINT('Ctrl Pts',(20.5392301593295,3.75169924203856,127.624119139347));
#67340=CARTESIAN_POINT('Ctrl Pts',(20.5314838832454,3.66299583609671,127.519476613577));
#67341=CARTESIAN_POINT('Ctrl Pts',(20.5237376071613,3.56988842542124,127.41852135565));
#67342=CARTESIAN_POINT('Ctrl Pts',(20.5159913310772,3.47272372038001,127.321635675167));
#67343=CARTESIAN_POINT('Ctrl Pts',(20.5082449978119,3.37555829809113,127.224749279496));
#67344=CARTESIAN_POINT('Ctrl Pts',(20.5004986645465,3.27433579852477,127.131932797268));
#67345=CARTESIAN_POINT('Ctrl Pts',(20.4927523312812,3.16943973461865,127.043531609073));
#67346=CARTESIAN_POINT('Ctrl Pts',(20.4850042632782,3.06452017996618,126.955110624045));
#67347=CARTESIAN_POINT('Ctrl Pts',(20.4772561952752,2.95592572285877,126.871107152495));
#67348=CARTESIAN_POINT('Ctrl Pts',(20.4695081272723,2.84407255892277,126.791825964497));
#67349=CARTESIAN_POINT('Ctrl Pts',(20.4617518245304,2.73210051611321,126.712460515509));
#67350=CARTESIAN_POINT('Ctrl Pts',(20.4539955217886,2.6168631674517,126.637827602308));
#67351=CARTESIAN_POINT('Ctrl Pts',(20.4462392190467,2.49880573343549,126.568188646429));
#67352=CARTESIAN_POINT('Ctrl Pts',(20.4384787765326,2.38068528861194,126.498512522142));
#67353=CARTESIAN_POINT('Ctrl Pts',(20.4307183340184,2.25974210386092,126.433835850541));
#67354=CARTESIAN_POINT('Ctrl Pts',(20.4229578915042,2.13644465064005,126.374373335727));
#67355=CARTESIAN_POINT('Ctrl Pts',(20.4151849912388,2.01294926940144,126.314815366406));
#67356=CARTESIAN_POINT('Ctrl Pts',(20.4074120909734,1.88709242664392,126.260488435286));
#67357=CARTESIAN_POINT('Ctrl Pts',(20.399639190708,1.75936198882108,126.21155880878));
#67358=CARTESIAN_POINT('Ctrl Pts',(20.392148854946,1.636274874147,126.164407897443));
#67359=CARTESIAN_POINT('Ctrl Pts',(20.3846585191839,1.51144831106987,126.122268790839));
#67360=CARTESIAN_POINT('Ctrl Pts',(20.3771681834219,1.3853289614509,126.085245580712));
#67361=CARTESIAN_POINT('Ctrl Pts',(20.3693938493029,1.25442775835778,126.046818624319));
#67362=CARTESIAN_POINT('Ctrl Pts',(20.3616195151838,1.12171914587204,126.013781435811));
#67363=CARTESIAN_POINT('Ctrl Pts',(20.3538451810647,0.987686570841499,125.986305169537));
#67364=CARTESIAN_POINT('Ctrl Pts',(20.3460804281176,0.853819178980851,125.958862765306));
#67365=CARTESIAN_POINT('Ctrl Pts',(20.3383156751706,0.718631450427147,125.936967724965));
#67366=CARTESIAN_POINT('Ctrl Pts',(20.3305509222235,0.58262268002947,125.920741685338));
#67367=CARTESIAN_POINT('Ctrl Pts',(20.3227938813385,0.446748995459941,125.904531761643));
#67368=CARTESIAN_POINT('Ctrl Pts',(20.3150368404535,0.310056277569384,125.893979679664));
#67369=CARTESIAN_POINT('Ctrl Pts',(20.3072797995685,0.173054374847257,125.889156120717));
#67370=CARTESIAN_POINT('Ctrl Pts',(20.2995286083284,0.0361557863255061,
125.884336199253));
#67371=CARTESIAN_POINT('Ctrl Pts',(20.2917774170882,-0.10105113379744,125.885236215975));
#67372=CARTESIAN_POINT('Ctrl Pts',(20.2840262258481,-0.23805140221298,125.891875035663));
#67373=CARTESIAN_POINT('Ctrl Pts',(20.276278329071,-0.374993441859656,125.898511033676));
#67374=CARTESIAN_POINT('Ctrl Pts',(20.2685304322939,-0.511728614801637,
125.910880964499));
#67375=CARTESIAN_POINT('Ctrl Pts',(20.2607825355168,-0.647742144072723,
125.9289515909));
#67376=CARTESIAN_POINT('Ctrl Pts',(20.2530362594327,-0.783727222245598,
125.947018437316));
#67377=CARTESIAN_POINT('Ctrl Pts',(20.2452899833486,-0.918990569685856,
125.970783555977));
#67378=CARTESIAN_POINT('Ctrl Pts',(20.2375437072645,-1.05302313307597,126.00016189731));
#67379=CARTESIAN_POINT('Ctrl Pts',(20.2297973739992,-1.18705668586403,126.029540455508));
#67380=CARTESIAN_POINT('Ctrl Pts',(20.2220510407339,-1.31985905457379,126.06453223535));
#67381=CARTESIAN_POINT('Ctrl Pts',(20.2143047074685,-1.45093236262411,126.105001263187));
#67382=CARTESIAN_POINT('Ctrl Pts',(20.2065566394656,-1.58203502363297,126.145479353782));
#67383=CARTESIAN_POINT('Ctrl Pts',(20.1988085714625,-1.71140747998354,126.191437017829));
#67384=CARTESIAN_POINT('Ctrl Pts',(20.1910605034595,-1.838568356079,126.242688833831));
#67385=CARTESIAN_POINT('Ctrl Pts',(20.1833042007177,-1.96586438026681,126.293995120873));
#67386=CARTESIAN_POINT('Ctrl Pts',(20.1755478979759,-2.09094376563688,126.350606653398));
#67387=CARTESIAN_POINT('Ctrl Pts',(20.167791595234,-2.21334591829464,126.412290159517));
#67388=CARTESIAN_POINT('Ctrl Pts',(20.1600311527199,-2.33581340066673,126.474006587981));
#67389=CARTESIAN_POINT('Ctrl Pts',(20.1522707102057,-2.45560046178221,126.540800193785));
#67390=CARTESIAN_POINT('Ctrl Pts',(20.1445102676915,-2.57227324473449,126.612392891435));
#67391=CARTESIAN_POINT('Ctrl Pts',(20.1367373674261,-2.68913332119584,126.684100516039));
#67392=CARTESIAN_POINT('Ctrl Pts',(20.1289644671607,-2.80286880470068,126.760622409023));
#67393=CARTESIAN_POINT('Ctrl Pts',(20.1211915668953,-2.91307610687209,126.841637985578));
#67394=CARTESIAN_POINT('Ctrl Pts',(20.1137012311332,-3.01927709601458,126.91970844186));
#67395=CARTESIAN_POINT('Ctrl Pts',(20.1062108953711,-3.12220172624427,127.001951348225));
#67396=CARTESIAN_POINT('Ctrl Pts',(20.098720559609,-3.22152099058269,127.088047179529));
#67397=CARTESIAN_POINT('Ctrl Pts',(20.0910614977135,-3.32307750515688,127.176082392082));
#67398=CARTESIAN_POINT('Ctrl Pts',(20.083402435818,-3.42120616241053,127.268442879405));
#67399=CARTESIAN_POINT('Ctrl Pts',(20.0757433739224,-3.51550779383497,127.364827507682));
#67400=CARTESIAN_POINT('Ctrl Pts',(20.0680931230708,-3.60970093993493,127.46110125434));
#67401=CARTESIAN_POINT('Ctrl Pts',(20.0604428722193,-3.70007553284389,127.561389654635));
#67402=CARTESIAN_POINT('Ctrl Pts',(20.0527926213676,-3.78626484654163,127.665350968912));
#67403=CARTESIAN_POINT('Ctrl Pts',(20.0451493990129,-3.87237497573554,127.769216771057));
#67404=CARTESIAN_POINT('Ctrl Pts',(20.0375061766581,-3.9543072152907,127.876748469623));
#67405=CARTESIAN_POINT('Ctrl Pts',(20.0298629543033,-4.03173156280554,127.987567464355));
#67406=CARTESIAN_POINT('Ctrl Pts',(20.0222249846418,-4.1091027015647,128.098310300345));
#67407=CARTESIAN_POINT('Ctrl Pts',(20.0145870149802,-4.18197187982267,128.212335609902));
#67408=CARTESIAN_POINT('Ctrl Pts',(20.0069490453187,-4.25004965468716,128.329232137023));
#67409=CARTESIAN_POINT('Ctrl Pts',(19.9993140021762,-4.31810134527726,128.446083874768));
#67410=CARTESIAN_POINT('Ctrl Pts',(19.9916789590337,-4.38136507934984,128.565804295163));
#67411=CARTESIAN_POINT('Ctrl Pts',(19.9840439158911,-4.43959526219746,128.687954000119));
#67412=CARTESIAN_POINT('Ctrl Pts',(19.97641053745,-4.49781274886634,128.810077072246));
#67413=CARTESIAN_POINT('Ctrl Pts',(19.9687771590089,-4.55099869748895,128.934628009698));
#67414=CARTESIAN_POINT('Ctrl Pts',(19.9611437805678,-4.59895422551359,129.061144310239));
#67415=CARTESIAN_POINT('Ctrl Pts',(19.9535088799648,-4.64691931628697,129.187685839229));
#67416=CARTESIAN_POINT('Ctrl Pts',(19.9458739793618,-4.68965176189308,129.316193136262));
#67417=CARTESIAN_POINT('Ctrl Pts',(19.9382390787587,-4.72700154321437,129.446185565171));
#67418=CARTESIAN_POINT('Ctrl Pts',(19.9355806969477,-4.74000629395983,129.491447386712));
#67419=CARTESIAN_POINT('Ctrl Pts',(19.9329223151368,-4.7523589215535,129.536889126366));
#67420=CARTESIAN_POINT('Ctrl Pts',(19.9302639333258,-4.76405452823407,129.582490119308));
#67421=CARTESIAN_POINT('Origin',(213.235140564004,0.,130.804360617566));
#67422=CARTESIAN_POINT('',(17.8345741463799,-4.76405452823412,129.582490119309));
#67423=CARTESIAN_POINT('',(18.1802003750168,-4.76405452823408,129.582490119308));
#67424=CARTESIAN_POINT('',(213.235140564004,-4.76405452823405,129.582490119308));
#67425=CARTESIAN_POINT('',(19.5148594359387,-4.91824832460085,130.800301053439));
#67426=CARTESIAN_POINT('Ctrl Pts',(19.5148594359387,-4.91824832460085,130.800301053439));
#67427=CARTESIAN_POINT('Ctrl Pts',(19.5072120057733,-4.9183594917055,130.934982366288));
#67428=CARTESIAN_POINT('Ctrl Pts',(19.499564575608,-4.91293433359908,131.069863219504));
#67429=CARTESIAN_POINT('Ctrl Pts',(19.4919171454426,-4.90195035046161,131.204442889242));
#67430=CARTESIAN_POINT('Ctrl Pts',(19.4842769476887,-4.8909767552171,131.338895282819));
#67431=CARTESIAN_POINT('Ctrl Pts',(19.4766367499348,-4.87445482369759,131.47304665972));
#67432=CARTESIAN_POINT('Ctrl Pts',(19.468996552181,-4.85241410186351,131.606395807901));
#67433=CARTESIAN_POINT('Ctrl Pts',(19.4612453076872,-4.83005302833382,131.741683124263));
#67434=CARTESIAN_POINT('Ctrl Pts',(19.4534940631934,-4.80201146538665,131.876144287265));
#67435=CARTESIAN_POINT('Ctrl Pts',(19.4457428186996,-4.76837496711769,132.009260296156));
#67436=CARTESIAN_POINT('Ctrl Pts',(19.4381103908622,-4.73525407331205,132.14033580702));
#67437=CARTESIAN_POINT('Ctrl Pts',(19.4304779630248,-4.69670866418405,132.270106707331));
#67438=CARTESIAN_POINT('Ctrl Pts',(19.4228455351874,-4.65287189227426,132.398087763781));
#67439=CARTESIAN_POINT('Ctrl Pts',(19.4152140006218,-4.6090402508622,132.526053841791));
#67440=CARTESIAN_POINT('Ctrl Pts',(19.4075824660562,-4.55991860874222,132.652230110592));
#67441=CARTESIAN_POINT('Ctrl Pts',(19.3999509314906,-4.50568965152999,132.776147580348));
#67442=CARTESIAN_POINT('Ctrl Pts',(19.3923185231087,-4.4514544850618,132.900079238745));
#67443=CARTESIAN_POINT('Ctrl Pts',(19.3846861147267,-4.3921110029713,133.02175121418));
#67444=CARTESIAN_POINT('Ctrl Pts',(19.3770537063447,-4.32788935284373,133.140716072552));
#67445=CARTESIAN_POINT('Ctrl Pts',(19.3692131211768,-4.2619160332504,133.262925741817));
#67446=CARTESIAN_POINT('Ctrl Pts',(19.3613725360089,-4.19079482862168,133.382278098069));
#67447=CARTESIAN_POINT('Ctrl Pts',(19.353531950841,-4.1148241224104,133.49831783774));
#67448=CARTESIAN_POINT('Ctrl Pts',(19.3458884728877,-4.04076327037145,133.611440413783));
#67449=CARTESIAN_POINT('Ctrl Pts',(19.3382449949344,-3.96209412539492,133.72141464901));
#67450=CARTESIAN_POINT('Ctrl Pts',(19.3306015169811,-3.87913481056252,133.827851345844));
#67451=CARTESIAN_POINT('Ctrl Pts',(19.3226623782059,-3.79296650901433,133.938405168608));
#67452=CARTESIAN_POINT('Ctrl Pts',(19.3147232394306,-3.70216979308598,134.045141910077));
#67453=CARTESIAN_POINT('Ctrl Pts',(19.3067841006554,-3.60714332747181,134.147667375489));
#67454=CARTESIAN_POINT('Ctrl Pts',(19.2988449618802,-3.51211686185776,134.250192840902));
#67455=CARTESIAN_POINT('Ctrl Pts',(19.2909058231049,-3.41286104041815,134.348506746843));
#67456=CARTESIAN_POINT('Ctrl Pts',(19.2829666843296,-3.30981193811156,134.442262210083));
#67457=CARTESIAN_POINT('Ctrl Pts',(19.2751923502106,-3.208901981165,134.53407145002));
#67458=CARTESIAN_POINT('Ctrl Pts',(19.2674180160915,-3.10400931831421,134.621824290045));
#67459=CARTESIAN_POINT('Ctrl Pts',(19.2596436819724,-2.9954938454868,134.705155367889));
#67460=CARTESIAN_POINT('Ctrl Pts',(19.2518789290254,-2.8871121082812,134.788383747628));
#67461=CARTESIAN_POINT('Ctrl Pts',(19.2441141760783,-2.77511675180746,134.867200972087));
#67462=CARTESIAN_POINT('Ctrl Pts',(19.2363494231312,-2.65990358141037,134.941279277644));
#67463=CARTESIAN_POINT('Ctrl Pts',(19.2285923822462,-2.5448048423585,135.015284007583));
#67464=CARTESIAN_POINT('Ctrl Pts',(19.2208353413611,-2.42649497625105,135.084558975212));
#67465=CARTESIAN_POINT('Ctrl Pts',(19.2130783004762,-2.30540156567152,135.148817624316));
#67466=CARTESIAN_POINT('Ctrl Pts',(19.205327109236,-2.18439947257454,135.213027815473));
#67467=CARTESIAN_POINT('Ctrl Pts',(19.1975759179959,-2.06061835707731,135.272229035106));
#67468=CARTESIAN_POINT('Ctrl Pts',(19.1898247267557,-1.93451308255149,135.326179078754));
#67469=CARTESIAN_POINT('Ctrl Pts',(19.1820768299787,-1.80846140613166,135.380106192194));
#67470=CARTESIAN_POINT('Ctrl Pts',(19.1743289332016,-1.68008789410022,135.42878641525));
#67471=CARTESIAN_POINT('Ctrl Pts',(19.1665810364245,-1.54987001227751,135.47202448802));
#67472=CARTESIAN_POINT('Ctrl Pts',(19.1588347603404,-1.41967936922851,135.515253516318));
#67473=CARTESIAN_POINT('Ctrl Pts',(19.1510884842563,-1.2876454945807,135.553042535506));
#67474=CARTESIAN_POINT('Ctrl Pts',(19.1433422081722,-1.15426336830343,135.585245382868));
#67475=CARTESIAN_POINT('Ctrl Pts',(19.1355958749068,-1.0208802574296,135.617448467943));
#67476=CARTESIAN_POINT('Ctrl Pts',(19.1278495416415,-0.886149255112507,
135.644065207152));
#67477=CARTESIAN_POINT('Ctrl Pts',(19.1201032083762,-0.750577563114254,
135.665000121196));
#67478=CARTESIAN_POINT('Ctrl Pts',(19.1123551403732,-0.614975510775381,
135.685939723469));
#67479=CARTESIAN_POINT('Ctrl Pts',(19.1046070723703,-0.478532780438202,
135.701194908983));
#67480=CARTESIAN_POINT('Ctrl Pts',(19.0968590043673,-0.34176336200302,135.710721882994));
#67481=CARTESIAN_POINT('Ctrl Pts',(19.0891027016254,-0.204848583402535,
135.720258982386));
#67482=CARTESIAN_POINT('Ctrl Pts',(19.0813463988835,-0.0676068137607187,
135.724055681606));
#67483=CARTESIAN_POINT('Ctrl Pts',(19.0735900961417,0.069445717132957,135.722120306171));
#67484=CARTESIAN_POINT('Ctrl Pts',(19.0658296536275,0.206571397089129,135.720183897769));
#67485=CARTESIAN_POINT('Ctrl Pts',(19.0580692111134,0.34350724687965,135.712509340504));
#67486=CARTESIAN_POINT('Ctrl Pts',(19.0503087685992,0.479741480504115,135.69915695392));
#67487=CARTESIAN_POINT('Ctrl Pts',(19.0425358683338,0.616194409414515,135.685783132899));
#67488=CARTESIAN_POINT('Ctrl Pts',(19.0347629680683,0.75194308407296,135.666713323192));
#67489=CARTESIAN_POINT('Ctrl Pts',(19.0269900678029,0.886484350322532,135.642059301768));
#67490=CARTESIAN_POINT('Ctrl Pts',(19.0194997320409,1.01613470265511,135.618301516123));
#67491=CARTESIAN_POINT('Ctrl Pts',(19.0120093962789,1.14466360668811,135.58935853799));
#67492=CARTESIAN_POINT('Ctrl Pts',(19.0045190605169,1.2716354413108,135.555373811286));
#67493=CARTESIAN_POINT('Ctrl Pts',(18.9967447263978,1.40342145163528,135.52010054334));
#67494=CARTESIAN_POINT('Ctrl Pts',(18.9889703922787,1.53394744765447,135.479283928885));
#67495=CARTESIAN_POINT('Ctrl Pts',(18.9811960581596,1.66271150720481,135.433029271327));
#67496=CARTESIAN_POINT('Ctrl Pts',(18.9734313052125,1.7913168765599,135.3868316185));
#67497=CARTESIAN_POINT('Ctrl Pts',(18.9656665522655,1.91816426552975,135.335209388264));
#67498=CARTESIAN_POINT('Ctrl Pts',(18.9579017993184,2.04276397483909,135.278318418619));
#67499=CARTESIAN_POINT('Ctrl Pts',(18.9501447584334,2.16723992995991,135.221483953887));
#67500=CARTESIAN_POINT('Ctrl Pts',(18.9423877175484,2.28947229470515,135.15939132496));
#67501=CARTESIAN_POINT('Ctrl Pts',(18.9346306766635,2.4089888623843,135.092245378542));
#67502=CARTESIAN_POINT('Ctrl Pts',(18.9268794854233,2.5284153016904,135.025150067404));
#67503=CARTESIAN_POINT('Ctrl Pts',(18.9191282941832,2.64512968088099,134.953009214555));
#67504=CARTESIAN_POINT('Ctrl Pts',(18.9113771029431,2.75868236171997,134.876074592004));
#67505=CARTESIAN_POINT('Ctrl Pts',(18.903629206166,2.87218677964077,134.79917266872));
#67506=CARTESIAN_POINT('Ctrl Pts',(18.8958813093888,2.98253184894381,134.717481246964));
#67507=CARTESIAN_POINT('Ctrl Pts',(18.8881334126118,3.08929521000551,134.631296489505));
#67508=CARTESIAN_POINT('Ctrl Pts',(18.8803871365277,3.19603623847348,134.545129760041));
#67509=CARTESIAN_POINT('Ctrl Pts',(18.8726408604436,3.29919674491121,134.454471809825));
#67510=CARTESIAN_POINT('Ctrl Pts',(18.8648945843595,3.39838620972065,134.359660075007));
#67511=CARTESIAN_POINT('Ctrl Pts',(18.8571482510942,3.49757640672432,134.26484764031));
#67512=CARTESIAN_POINT('Ctrl Pts',(18.8494019178289,3.59279522098654,134.165881629973));
#67513=CARTESIAN_POINT('Ctrl Pts',(18.8416555845635,3.68368816812722,134.063137158309));
#67514=CARTESIAN_POINT('Ctrl Pts',(18.8339075165606,3.77460147011271,133.960369677734));
#67515=CARTESIAN_POINT('Ctrl Pts',(18.8261594485576,3.86118671828092,133.853822344842));
#67516=CARTESIAN_POINT('Ctrl Pts',(18.8184113805547,3.94312924277681,133.743903921765));
#67517=CARTESIAN_POINT('Ctrl Pts',(18.8106550778128,4.02515885676319,133.633868676078));
#67518=CARTESIAN_POINT('Ctrl Pts',(18.802898775071,4.10253565615266,133.520455497057));
#67519=CARTESIAN_POINT('Ctrl Pts',(18.7951424723291,4.17498761062946,133.404103203591));
#67520=CARTESIAN_POINT('Ctrl Pts',(18.787382029815,4.24747823489596,133.287688809402));
#67521=CARTESIAN_POINT('Ctrl Pts',(18.7796215873008,4.31503858417031,133.168332515085));
#67522=CARTESIAN_POINT('Ctrl Pts',(18.7718611447866,4.37744277415799,133.046497504884));
#67523=CARTESIAN_POINT('Ctrl Pts',(18.7640882445212,4.43994714089134,132.924466914309));
#67524=CARTESIAN_POINT('Ctrl Pts',(18.7563153442557,4.49727864439844,132.799950011764));
#67525=CARTESIAN_POINT('Ctrl Pts',(18.7485424439903,4.54925935869746,132.673430533274));
#67526=CARTESIAN_POINT('Ctrl Pts',(18.7410521082282,4.59935044310082,132.551510356509));
#67527=CARTESIAN_POINT('Ctrl Pts',(18.7335617724661,4.64447290801315,132.427730962764));
#67528=CARTESIAN_POINT('Ctrl Pts',(18.726071436704,4.68451197301331,132.302536387359));
#67529=CARTESIAN_POINT('Ctrl Pts',(18.7182971025849,4.72606913133215,132.172595021577));
#67530=CARTESIAN_POINT('Ctrl Pts',(18.7105227684658,4.76228144672758,132.040717427323));
#67531=CARTESIAN_POINT('Ctrl Pts',(18.7027484343467,4.79296621274816,131.907382804992));
#67532=CARTESIAN_POINT('Ctrl Pts',(18.6949836813996,4.82361316253692,131.774212505668));
#67533=CARTESIAN_POINT('Ctrl Pts',(18.6872189284525,4.84874603037898,131.639589128437));
#67534=CARTESIAN_POINT('Ctrl Pts',(18.6794541755054,4.86823123277945,131.504008905415));
#67535=CARTESIAN_POINT('Ctrl Pts',(18.6716971346204,4.88769708220229,131.368563342583));
#67536=CARTESIAN_POINT('Ctrl Pts',(18.6639400937354,4.90152637376799,131.232163209689));
#67537=CARTESIAN_POINT('Ctrl Pts',(18.6561830528503,4.90963621155905,131.095316512244));
#67538=CARTESIAN_POINT('Ctrl Pts',(18.6484318616102,4.91773993365834,130.958573011959));
#67539=CARTESIAN_POINT('Ctrl Pts',(18.6406806703701,4.92013276388098,130.821384006119));
#67540=CARTESIAN_POINT('Ctrl Pts',(18.6329294791299,4.91678348469934,130.684263877028));
#67541=CARTESIAN_POINT('Ctrl Pts',(18.6251815823528,4.91343562905071,130.547202027651));
#67542=CARTESIAN_POINT('Ctrl Pts',(18.6174336855758,4.90435052759191,130.410209386828));
#67543=CARTESIAN_POINT('Ctrl Pts',(18.6096857887987,4.8895490547568,130.273801380886));
#67544=CARTESIAN_POINT('Ctrl Pts',(18.6019395127146,4.87475067807071,130.137421908557));
#67545=CARTESIAN_POINT('Ctrl Pts',(18.5941932366305,4.85423835055292,130.001627216299));
#67546=CARTESIAN_POINT('Ctrl Pts',(18.5864469605464,4.82808488140931,129.866928251789));
#67547=CARTESIAN_POINT('Ctrl Pts',(18.578700627281,4.80193121920673,129.732228292961));
#67548=CARTESIAN_POINT('Ctrl Pts',(18.5709542940157,4.77013640680457,129.598624461819));
#67549=CARTESIAN_POINT('Ctrl Pts',(18.5632079607503,4.73282443103251,129.466617754561));
#67550=CARTESIAN_POINT('Ctrl Pts',(18.5554598927473,4.69550409950208,129.334581485315));
#67551=CARTESIAN_POINT('Ctrl Pts',(18.5477118247444,4.6526642523596,129.204143427817));
#67552=CARTESIAN_POINT('Ctrl Pts',(18.5399637567414,4.60447870601963,129.075789268645));
#67553=CARTESIAN_POINT('Ctrl Pts',(18.5322074539995,4.55624194750766,128.947298693145));
#67554=CARTESIAN_POINT('Ctrl Pts',(18.5244511512577,4.50264827807244,128.820896806862));
#67555=CARTESIAN_POINT('Ctrl Pts',(18.5166948485158,4.44391984944271,128.697049668933));
#67556=CARTESIAN_POINT('Ctrl Pts',(18.5089344060016,4.38516007568227,128.573136430057));
#67557=CARTESIAN_POINT('Ctrl Pts',(18.5011739634874,4.32126026396362,128.451781002287));
#67558=CARTESIAN_POINT('Ctrl Pts',(18.4934135209733,4.25248800832976,128.333423790872));
#67559=CARTESIAN_POINT('Ctrl Pts',(18.4856406207078,4.18360535336593,128.214876581955));
#67560=CARTESIAN_POINT('Ctrl Pts',(18.4778677204424,4.10983483479806,128.099337537022));
#67561=CARTESIAN_POINT('Ctrl Pts',(18.4700948201769,4.03148726010452,127.987217821378));
#67562=CARTESIAN_POINT('Ctrl Pts',(18.462604484415,3.95598781709757,127.879173939811));
#67563=CARTESIAN_POINT('Ctrl Pts',(18.4551141486531,3.87623850199006,127.77430534635));
#67564=CARTESIAN_POINT('Ctrl Pts',(18.4476238128911,3.79255085265012,127.672948620948));
#67565=CARTESIAN_POINT('Ctrl Pts',(18.439849478772,3.70569016064817,127.567748924495));
#67566=CARTESIAN_POINT('Ctrl Pts',(18.4320751446529,3.61431144664124,127.465999416983));
#67567=CARTESIAN_POINT('Ctrl Pts',(18.4243008105339,3.51871911819316,127.368112834044));
#67568=CARTESIAN_POINT('Ctrl Pts',(18.4165360575868,3.42324459874682,127.270346887569));
#67569=CARTESIAN_POINT('Ctrl Pts',(18.4087713046398,3.32356706772349,127.176434670302));
#67570=CARTESIAN_POINT('Ctrl Pts',(18.4010065516927,3.22003181411451,127.086756795399));
#67571=CARTESIAN_POINT('Ctrl Pts',(18.3932495108077,3.11659939317901,126.997167989826));
#67572=CARTESIAN_POINT('Ctrl Pts',(18.3854924699227,3.00931716821446,126.911805411579));
#67573=CARTESIAN_POINT('Ctrl Pts',(18.3777354290377,2.89856773137483,126.831013392727));
#67574=CARTESIAN_POINT('Ctrl Pts',(18.3699842377976,2.78790181154732,126.750282299766));
#67575=CARTESIAN_POINT('Ctrl Pts',(18.3622330465575,2.67377419872415,126.674115135248));
#67576=CARTESIAN_POINT('Ctrl Pts',(18.3544818553175,2.55660078346902,126.602816199561));
#67577=CARTESIAN_POINT('Ctrl Pts',(18.3467339585404,2.43947717004044,126.531547567824));
#67578=CARTESIAN_POINT('Ctrl Pts',(18.3389860617633,2.31931066222879,126.465143252389));
#67579=CARTESIAN_POINT('Ctrl Pts',(18.3312381649862,2.19654618594038,126.403864291522));
#67580=CARTESIAN_POINT('Ctrl Pts',(18.3234918889021,2.07380738933391,126.342598148892));
#67581=CARTESIAN_POINT('Ctrl Pts',(18.315745612818,1.94847205476656,126.286455402836));
#67582=CARTESIAN_POINT('Ctrl Pts',(18.3079993367339,1.82100941214491,126.235650976608));
#67583=CARTESIAN_POINT('Ctrl Pts',(18.3002530034685,1.69354582862264,126.184846175354));
#67584=CARTESIAN_POINT('Ctrl Pts',(18.2925066702032,1.56395526889053,126.139379917316));
#67585=CARTESIAN_POINT('Ctrl Pts',(18.2847603369378,1.43272625314865,126.099418689546));
#67586=CARTESIAN_POINT('Ctrl Pts',(18.2770122689348,1.30146784957912,126.059448512737));
#67587=CARTESIAN_POINT('Ctrl Pts',(18.2692642009318,1.16857063380698,126.024985933221));
#67588=CARTESIAN_POINT('Ctrl Pts',(18.2615161329288,1.0345371797228,125.996147239785));
#67589=CARTESIAN_POINT('Ctrl Pts',(18.253759830187,0.900361273288428,125.967277896242));
#67590=CARTESIAN_POINT('Ctrl Pts',(18.2460035274452,0.765047099043303,125.944044461116));
#67591=CARTESIAN_POINT('Ctrl Pts',(18.2382472247033,0.629106844174649,125.926511948213));
#67592=CARTESIAN_POINT('Ctrl Pts',(18.2304867821891,0.493094033898705,125.908970077679));
#67593=CARTESIAN_POINT('Ctrl Pts',(18.2227263396749,0.356454866477291,125.897135226033));
#67594=CARTESIAN_POINT('Ctrl Pts',(18.2149658971608,0.219704508438073,125.891020308624));
#67595=CARTESIAN_POINT('Ctrl Pts',(18.2071929968953,0.0827346265840056,
125.884895575007));
#67596=CARTESIAN_POINT('Ctrl Pts',(18.1994200966299,-0.0543464113851937,
125.884509125583));
#67597=CARTESIAN_POINT('Ctrl Pts',(18.1916471963644,-0.191024681419766,
125.889821714109));
#67598=CARTESIAN_POINT('Ctrl Pts',(18.1841568606023,-0.322734352068102,
125.894941176661));
#67599=CARTESIAN_POINT('Ctrl Pts',(18.1766665248402,-0.454069722584113,
125.905352497755));
#67600=CARTESIAN_POINT('Ctrl Pts',(18.1691761890781,-0.584579224891734,
125.920975501448));
#67601=CARTESIAN_POINT('Ctrl Pts',(18.161401854959,-0.720037034645514,125.937190856073));
#67602=CARTESIAN_POINT('Ctrl Pts',(18.1536275208399,-0.855034203980925,
125.959072261967));
#67603=CARTESIAN_POINT('Ctrl Pts',(18.1458531867208,-0.989058946998879,
125.986586706115));
#67604=CARTESIAN_POINT('Ctrl Pts',(18.1380884337737,-1.12291851649902,126.014067241169));
#67605=CARTESIAN_POINT('Ctrl Pts',(18.1303236808266,-1.25580766489575,126.047166923667));
#67606=CARTESIAN_POINT('Ctrl Pts',(18.1225589278795,-1.38721953442619,126.08580098291));
#67607=CARTESIAN_POINT('Ctrl Pts',(18.1148018869945,-1.51850088383524,126.124396670261));
#67608=CARTESIAN_POINT('Ctrl Pts',(18.1070448461095,-1.64830750161597,126.168515685875));
#67609=CARTESIAN_POINT('Ctrl Pts',(18.0992878052245,-1.77614289104181,126.218022264031));
#67610=CARTESIAN_POINT('Ctrl Pts',(18.0915366139844,-1.90388187880537,126.267491508892));
#67611=CARTESIAN_POINT('Ctrl Pts',(18.0837854227443,-2.02965223393379,126.322340088914));
#67612=CARTESIAN_POINT('Ctrl Pts',(18.0760342315042,-2.15297314088268,126.38238258538));
#67613=CARTESIAN_POINT('Ctrl Pts',(18.0682863347271,-2.27624163315727,126.442399562183));
#67614=CARTESIAN_POINT('Ctrl Pts',(18.0605384379501,-2.39706239710342,126.50760589399));
#67615=CARTESIAN_POINT('Ctrl Pts',(18.052790541173,-2.51497532051442,126.577768349591));
#67616=CARTESIAN_POINT('Ctrl Pts',(18.0450442650889,-2.63286357908359,126.64791612872));
#67617=CARTESIAN_POINT('Ctrl Pts',(18.0372979890047,-2.74784487120467,126.723017769767));
#67618=CARTESIAN_POINT('Ctrl Pts',(18.0295517129206,-2.8594847456314,126.802794667591));
#67619=CARTESIAN_POINT('Ctrl Pts',(18.0218053796552,-2.97112544415847,126.88257215431));
#67620=CARTESIAN_POINT('Ctrl Pts',(18.0140590463899,-3.07942435767732,126.967024739363));
#67621=CARTESIAN_POINT('Ctrl Pts',(18.0063127131245,-3.18397735881582,127.055831407189));
#67622=CARTESIAN_POINT('Ctrl Pts',(17.9985646451215,-3.28855377387414,127.144657962653));
#67623=CARTESIAN_POINT('Ctrl Pts',(17.9908165771185,-3.38938230937185,127.237840288103));
#67624=CARTESIAN_POINT('Ctrl Pts',(17.9830685091155,-3.4860934747957,127.335018410823));
#67625=CARTESIAN_POINT('Ctrl Pts',(17.9753122063736,-3.58290742599678,127.432299815608));
#67626=CARTESIAN_POINT('Ctrl Pts',(17.9675559036318,-3.67559498938548,127.533585223503));
#67627=CARTESIAN_POINT('Ctrl Pts',(17.9597996008899,-3.76382461731946,127.638478858473));
#67628=CARTESIAN_POINT('Ctrl Pts',(17.9520391583757,-3.8521013360624,127.743428478333));
#67629=CARTESIAN_POINT('Ctrl Pts',(17.9442787158616,-3.93591513952066,127.85198985331));
#67630=CARTESIAN_POINT('Ctrl Pts',(17.9365182733474,-4.0149767015535,127.963736540275));
#67631=CARTESIAN_POINT('Ctrl Pts',(17.928745373082,-4.09416518022448,128.075662612943));
#67632=CARTESIAN_POINT('Ctrl Pts',(17.9209724728166,-4.16858596048213,128.19078388717));
#67633=CARTESIAN_POINT('Ctrl Pts',(17.9131995725511,-4.23799427280047,128.308646770545));
#67634=CARTESIAN_POINT('Ctrl Pts',(17.9057092367892,-4.3048794181364,128.42222504123));
#67635=CARTESIAN_POINT('Ctrl Pts',(17.8982189010272,-4.36711005464315,128.538348781416));
#67636=CARTESIAN_POINT('Ctrl Pts',(17.8907285652652,-4.42450955303831,128.656594737035));
#67637=CARTESIAN_POINT('Ctrl Pts',(17.8823534369874,-4.48868934115728,128.78880844255));
#67638=CARTESIAN_POINT('Ctrl Pts',(17.8739783087096,-4.54700911824314,128.924045188624));
#67639=CARTESIAN_POINT('Ctrl Pts',(17.8656031804317,-4.59919598865022,129.061782263378));
#67640=CARTESIAN_POINT('Ctrl Pts',(17.8572491334189,-4.65125149805542,129.199172636367));
#67641=CARTESIAN_POINT('Ctrl Pts',(17.848895086406,-4.69720477936736,129.339050511504));
#67642=CARTESIAN_POINT('Ctrl Pts',(17.8405410393931,-4.73683014450314,129.48087157544));
#67643=CARTESIAN_POINT('Ctrl Pts',(17.8385520750553,-4.7462643071315,129.514636891589));
#67644=CARTESIAN_POINT('Ctrl Pts',(17.8365631107176,-4.75533998593173,129.548512251133));
#67645=CARTESIAN_POINT('Ctrl Pts',(17.8345741463799,-4.76405452823412,129.582490119309));
#67646=CARTESIAN_POINT('Ctrl Pts',(19.584898128716,-4.76405452823411,129.582490119308));
#67647=CARTESIAN_POINT('Ctrl Pts',(19.5770701885249,-4.79828050826579,129.715936696));
#67648=CARTESIAN_POINT('Ctrl Pts',(19.5692422483337,-4.8268499179298,129.850645650192));
#67649=CARTESIAN_POINT('Ctrl Pts',(19.5614143081426,-4.84970383971167,129.986096766729));
#67650=CARTESIAN_POINT('Ctrl Pts',(19.549079713458,-4.88571508344255,130.199528982776));
#67651=CARTESIAN_POINT('Ctrl Pts',(19.5367451187733,-4.90764377638311,130.415400463251));
#67652=CARTESIAN_POINT('Ctrl Pts',(19.5244105240887,-4.91523706832655,130.632233848443));
#67653=CARTESIAN_POINT('Ctrl Pts',(19.5212268280562,-4.9171969814045,130.688200956062));
#67654=CARTESIAN_POINT('Ctrl Pts',(19.5180431320238,-4.91820204469388,130.744231974131));
#67655=CARTESIAN_POINT('Ctrl Pts',(19.5148594359913,-4.91824832460009,130.800301052513));
#67656=CARTESIAN_POINT('',(19.8601405640419,-4.9182486111303,130.808056779749));
#67657=CARTESIAN_POINT('Ctrl Pts',(19.9302639333258,-4.76405452823407,129.582490119308));
#67658=CARTESIAN_POINT('Ctrl Pts',(19.9226230702679,-4.79767066593726,129.713558930017));
#67659=CARTESIAN_POINT('Ctrl Pts',(19.9149822072099,-4.82585514710882,129.845943911475));
#67660=CARTESIAN_POINT('Ctrl Pts',(19.907341344152,-4.84852636025179,129.979148404591));
#67661=CARTESIAN_POINT('Ctrl Pts',(19.8994745474669,-4.87186794130703,130.116291637879));
#67662=CARTESIAN_POINT('Ctrl Pts',(19.891607750782,-4.88936509178852,130.254303138695));
#67663=CARTESIAN_POINT('Ctrl Pts',(19.8837409540969,-4.90098625865664,130.392636492746));
#67664=CARTESIAN_POINT('Ctrl Pts',(19.8758741574119,-4.91260742552476,130.530969846797));
#67665=CARTESIAN_POINT('Ctrl Pts',(19.8680073607269,-4.91835264568835,130.669624591082));
#67666=CARTESIAN_POINT('Ctrl Pts',(19.8601405640419,-4.9182486111303,130.808056779749));
#67667=CARTESIAN_POINT('Ctrl Pts',(19.8601405640087,-4.91824861112986,130.808056780332));
#67668=CARTESIAN_POINT('Ctrl Pts',(19.8468513546045,-4.9180728677745,131.041907281002));
#67669=CARTESIAN_POINT('Ctrl Pts',(19.8335621452003,-4.90121708260459,131.275143667519));
#67670=CARTESIAN_POINT('Ctrl Pts',(19.8202729357961,-4.86795053232145,131.505959275897));
#67671=CARTESIAN_POINT('Ctrl Pts',(19.812498601677,-4.84848923338151,131.640988953347));
#67672=CARTESIAN_POINT('Ctrl Pts',(19.8047242675579,-4.82337456895603,131.775422153426));
#67673=CARTESIAN_POINT('Ctrl Pts',(19.7969499334388,-4.79265182400327,131.908748029835));
#67674=CARTESIAN_POINT('Ctrl Pts',(19.7891851804917,-4.7619669420879,132.041909594017));
#67675=CARTESIAN_POINT('Ctrl Pts',(19.7814204275447,-4.72568781833477,132.173966172509));
#67676=CARTESIAN_POINT('Ctrl Pts',(19.7736556745976,-4.68391136221968,132.304413087771));
#67677=CARTESIAN_POINT('Ctrl Pts',(19.7658986337126,-4.64217639906987,132.434730441319));
#67678=CARTESIAN_POINT('Ctrl Pts',(19.7581415928275,-4.59495508773192,132.563440943275));
#67679=CARTESIAN_POINT('Ctrl Pts',(19.7503845519425,-4.54239506938144,132.690051497896));
#67680=CARTESIAN_POINT('Ctrl Pts',(19.7426333607024,-4.48987468694967,132.816566574512));
#67681=CARTESIAN_POINT('Ctrl Pts',(19.7348821694623,-4.43202376022778,132.9409844962));
#67682=CARTESIAN_POINT('Ctrl Pts',(19.7271309782222,-4.36903919278346,133.062829035415));
#67683=CARTESIAN_POINT('Ctrl Pts',(19.7193830814451,-4.3060813954603,133.184621787451));
#67684=CARTESIAN_POINT('Ctrl Pts',(19.711635184668,-4.23799447627153,133.303842985833));
#67685=CARTESIAN_POINT('Ctrl Pts',(19.703887287891,-4.16502264068342,133.420038247759));
#67686=CARTESIAN_POINT('Ctrl Pts',(19.6961410118068,-4.09206606923021,133.536209204142));
#67687=CARTESIAN_POINT('Ctrl Pts',(19.6883947357228,-4.01422682162775,133.649355152185));
#67688=CARTESIAN_POINT('Ctrl Pts',(19.6806484596387,-3.93179384841794,133.759048451508));
#67689=CARTESIAN_POINT('Ctrl Pts',(19.6729021263734,-3.84936026670676,133.868742560561));
#67690=CARTESIAN_POINT('Ctrl Pts',(19.6651557931079,-3.76233312659987,133.974983657488));
#67691=CARTESIAN_POINT('Ctrl Pts',(19.6574094598426,-3.67104304915753,134.077375434785));
#67692=CARTESIAN_POINT('Ctrl Pts',(19.6496613918396,-3.57973252793531,134.179790142009));
#67693=CARTESIAN_POINT('Ctrl Pts',(19.6419133238367,-3.48415742985533,134.278353522501));
#67694=CARTESIAN_POINT('Ctrl Pts',(19.6341652558337,-3.38468649072615,134.372704830502));
#67695=CARTESIAN_POINT('Ctrl Pts',(19.6264089530918,-3.28510983269901,134.467156416197));
#67696=CARTESIAN_POINT('Ctrl Pts',(19.61865265035,-3.18162934654533,134.557386717343));
#67697=CARTESIAN_POINT('Ctrl Pts',(19.6108963476081,-3.07464865055661,134.643073779308));
#67698=CARTESIAN_POINT('Ctrl Pts',(19.6031359050939,-2.96761085574931,134.728806575038));
#67699=CARTESIAN_POINT('Ctrl Pts',(19.5953754625798,-2.85706944358312,134.809991068529));
#67700=CARTESIAN_POINT('Ctrl Pts',(19.5876150200656,-2.74345767741099,134.886348250418));
#67701=CARTESIAN_POINT('Ctrl Pts',(19.5798421198002,-2.62966353154581,134.962828007634));
#67702=CARTESIAN_POINT('Ctrl Pts',(19.5720692195348,-2.51278951587592,135.034464763388));
#67703=CARTESIAN_POINT('Ctrl Pts',(19.5642963192693,-2.39329496598304,135.10102470361));
#67704=CARTESIAN_POINT('Ctrl Pts',(19.5568059835073,-2.27814434396737,135.165165022351));
#67705=CARTESIAN_POINT('Ctrl Pts',(19.5493156477453,-2.16056068086108,135.224591088396));
#67706=CARTESIAN_POINT('Ctrl Pts',(19.5418253119832,-2.04097134746111,135.279136480259));
#67707=CARTESIAN_POINT('Ctrl Pts',(19.5340509778642,-1.91684774813689,135.335749977234));
#67708=CARTESIAN_POINT('Ctrl Pts',(19.5262766437451,-1.7901701999834,135.387284727124));
#67709=CARTESIAN_POINT('Ctrl Pts',(19.518502309626,-1.66139297008352,135.433502704547));
#67710=CARTESIAN_POINT('Ctrl Pts',(19.5107375566789,-1.53277444661052,135.479663722443));
#67711=CARTESIAN_POINT('Ctrl Pts',(19.5029728037318,-1.40206175453398,135.520520874487));
#67712=CARTESIAN_POINT('Ctrl Pts',(19.4952080507848,-1.2697318752981,135.555882902829));
#67713=CARTESIAN_POINT('Ctrl Pts',(19.4874510098998,-1.1375334279638,135.591209809106));
#67714=CARTESIAN_POINT('Ctrl Pts',(19.4796939690148,-1.00372136517407,135.621052352737));
#67715=CARTESIAN_POINT('Ctrl Pts',(19.4719369281298,-0.868790346006051,
135.645268218129));
#67716=CARTESIAN_POINT('Ctrl Pts',(19.4641857368896,-0.733961079369011,
135.669465822148));
#67717=CARTESIAN_POINT('Ctrl Pts',(19.4564345456495,-0.598014919173669,
135.688045124823));
#67718=CARTESIAN_POINT('Ctrl Pts',(19.4486833544094,-0.461458960327743,
135.70091437408));
#67719=CARTESIAN_POINT('Ctrl Pts',(19.4409354576323,-0.324961041407075,
135.713778153564));
#67720=CARTESIAN_POINT('Ctrl Pts',(19.4331875608552,-0.187854227752063,
135.720936669993));
#67721=CARTESIAN_POINT('Ctrl Pts',(19.4254396640781,-0.0506528035006185,
135.722349775342));
#67722=CARTESIAN_POINT('Ctrl Pts',(19.417693387994,0.0865199211705932,135.723762585099));
#67723=CARTESIAN_POINT('Ctrl Pts',(19.4099471119099,0.223786826377065,135.719432370229));
#67724=CARTESIAN_POINT('Ctrl Pts',(19.4022008358258,0.36063194132993,135.709371082936));
#67725=CARTESIAN_POINT('Ctrl Pts',(19.3944545025604,0.497478066442161,135.699309721373));
#67726=CARTESIAN_POINT('Ctrl Pts',(19.3867081692951,0.633902005175143,135.683517231637));
#67727=CARTESIAN_POINT('Ctrl Pts',(19.3789618360298,0.769391624041899,135.662057560702));
#67728=CARTESIAN_POINT('Ctrl Pts',(19.3712137680268,0.904911584869381,135.640593084023));
#67729=CARTESIAN_POINT('Ctrl Pts',(19.3634657000238,1.03949642340052,135.613458961881));
#67730=CARTESIAN_POINT('Ctrl Pts',(19.3557176320208,1.1726433233022,135.580770430262));
#67731=CARTESIAN_POINT('Ctrl Pts',(19.3479613292789,1.30593173331356,135.548047156882));
#67732=CARTESIAN_POINT('Ctrl Pts',(19.3402050265371,1.43777877153954,135.509757774928));
#67733=CARTESIAN_POINT('Ctrl Pts',(19.3324487237952,1.56769540288516,135.466067835557));
#67734=CARTESIAN_POINT('Ctrl Pts',(19.3246882812811,1.69768137464881,135.42235457755));
#67735=CARTESIAN_POINT('Ctrl Pts',(19.316927838767,1.8257345216869,135.373235158573));
#67736=CARTESIAN_POINT('Ctrl Pts',(19.3091673962528,1.95138591609533,135.318923283978));
#67737=CARTESIAN_POINT('Ctrl Pts',(19.3013944959874,2.07723901727688,135.264524223141));
#67738=CARTESIAN_POINT('Ctrl Pts',(19.2936215957219,2.20068230902758,135.204916220025));
#67739=CARTESIAN_POINT('Ctrl Pts',(19.2858486954565,2.32127079484554,135.140359344445));
#67740=CARTESIAN_POINT('Ctrl Pts',(19.2783583596944,2.43747558545995,135.078149273902));
#67741=CARTESIAN_POINT('Ctrl Pts',(19.2708680239325,2.5510292599072,135.011344048248));
#67742=CARTESIAN_POINT('Ctrl Pts',(19.2633776881704,2.66156079872216,134.94021327176));
#67743=CARTESIAN_POINT('Ctrl Pts',(19.2556033540513,2.77628317442661,134.866385550262));
#67744=CARTESIAN_POINT('Ctrl Pts',(19.2478290199323,2.88811312809731,134.787663932428));
#67745=CARTESIAN_POINT('Ctrl Pts',(19.2400546858132,2.99660485978374,134.704301947486));
#67746=CARTESIAN_POINT('Ctrl Pts',(19.2322899328661,3.10496288510706,134.621042698741));
#67747=CARTESIAN_POINT('Ctrl Pts',(19.2245251799189,3.20999056715886,134.533154697592));
#67748=CARTESIAN_POINT('Ctrl Pts',(19.2167604269718,3.31126917517196,134.440935862499));
#67749=CARTESIAN_POINT('Ctrl Pts',(19.2090033860868,3.41244719184381,134.348808620452));
#67750=CARTESIAN_POINT('Ctrl Pts',(19.2012463452018,3.50988325746431,134.252359366049));
#67751=CARTESIAN_POINT('Ctrl Pts',(19.1934893043168,3.60319026258126,134.151927344928));
#67752=CARTESIAN_POINT('Ctrl Pts',(19.1857381130767,3.69642690415983,134.051571060375));
#67753=CARTESIAN_POINT('Ctrl Pts',(19.1779869218366,3.78554041794808,133.947238272527));
#67754=CARTESIAN_POINT('Ctrl Pts',(19.1702357305965,3.87017951314547,133.839306020457));
#67755=CARTESIAN_POINT('Ctrl Pts',(19.1624878338194,3.95478263446958,133.731419642473));
#67756=CARTESIAN_POINT('Ctrl Pts',(19.1547399370423,4.03491487888207,133.619937150065));
#67757=CARTESIAN_POINT('Ctrl Pts',(19.1469920402652,4.11026448557195,133.505269524054));
#67758=CARTESIAN_POINT('Ctrl Pts',(19.1392457641811,4.18559833074846,133.390625884038));
#67759=CARTESIAN_POINT('Ctrl Pts',(19.1314994880969,4.2561513135353,133.272798762179));
#67760=CARTESIAN_POINT('Ctrl Pts',(19.1237532120128,4.32165459484505,133.152228719772));
#67761=CARTESIAN_POINT('Ctrl Pts',(19.1160068787475,4.38715835968523,133.031657787344));
#67762=CARTESIAN_POINT('Ctrl Pts',(19.1082605454821,4.44761216202877,132.908344237505));
#67763=CARTESIAN_POINT('Ctrl Pts',(19.1005142122168,4.50279298161737,132.782753507565));
#67764=CARTESIAN_POINT('Ctrl Pts',(19.0927661442138,4.55798615856785,132.657134652451));
#67765=CARTESIAN_POINT('Ctrl Pts',(19.0850180762108,4.60790384577495,132.529237960349));
#67766=CARTESIAN_POINT('Ctrl Pts',(19.0772700082078,4.65237121002717,132.399548752743));
#67767=CARTESIAN_POINT('Ctrl Pts',(19.069513705466,4.69688583472329,132.269721709905));
#67768=CARTESIAN_POINT('Ctrl Pts',(19.0617574027241,4.73593843797796,132.138098716327));
#67769=CARTESIAN_POINT('Ctrl Pts',(19.0540010999823,4.76940396725428,132.005180695529));
#67770=CARTESIAN_POINT('Ctrl Pts',(19.0462406574681,4.80288735809124,131.872191732382));
#67771=CARTESIAN_POINT('Ctrl Pts',(19.0384802149539,4.83077765361724,131.737906747359));
#67772=CARTESIAN_POINT('Ctrl Pts',(19.0307197724397,4.85300118321247,131.602835775751));
#67773=CARTESIAN_POINT('Ctrl Pts',(19.0229468721743,4.87526038799032,131.467547976228));
#67774=CARTESIAN_POINT('Ctrl Pts',(19.0151739719089,4.89183460124296,131.331472057091));
#67775=CARTESIAN_POINT('Ctrl Pts',(19.0074010716434,4.90270209559428,131.195122980589));
#67776=CARTESIAN_POINT('Ctrl Pts',(18.9999107358814,4.91317452915234,131.063730536461));
#67777=CARTESIAN_POINT('Ctrl Pts',(18.9924204001193,4.91834793552886,130.932084757867));
#67778=CARTESIAN_POINT('Ctrl Pts',(18.9849300643573,4.91824859535366,130.800643521688));
#67779=CARTESIAN_POINT('Ctrl Pts',(18.9771557302382,4.91814548866552,130.66421865109));
#67780=CARTESIAN_POINT('Ctrl Pts',(18.9693813961192,4.91236158362694,130.527581986556));
#67781=CARTESIAN_POINT('Ctrl Pts',(18.9616070620001,4.90086921579578,130.391245630952));
#67782=CARTESIAN_POINT('Ctrl Pts',(18.953842309053,4.88939101128088,130.255077297721));
#67783=CARTESIAN_POINT('Ctrl Pts',(18.9460775561058,4.87221837438962,130.119208922868));
#67784=CARTESIAN_POINT('Ctrl Pts',(18.9383128031587,4.84937561815072,129.984153828649));
#67785=CARTESIAN_POINT('Ctrl Pts',(18.9305557622737,4.82655554965938,129.849232873054));
#67786=CARTESIAN_POINT('Ctrl Pts',(18.9227987213888,4.79807663382164,129.715123973606));
#67787=CARTESIAN_POINT('Ctrl Pts',(18.9150416805038,4.76401504548548,129.582336187005));
#67788=CARTESIAN_POINT('Ctrl Pts',(18.9072904892636,4.72997914325799,129.449648536707));
#67789=CARTESIAN_POINT('Ctrl Pts',(18.8995392980235,4.69036904490487,129.318280393429));
#67790=CARTESIAN_POINT('Ctrl Pts',(18.8917881067834,4.64531208281695,129.1887311069));
#67791=CARTESIAN_POINT('Ctrl Pts',(18.8840402100063,4.60027427113991,129.059236882274));
#67792=CARTESIAN_POINT('Ctrl Pts',(18.8762923132292,4.5497943283726,128.931560345329));
#67793=CARTESIAN_POINT('Ctrl Pts',(18.8685444164522,4.49404950998589,128.806185934438));
#67794=CARTESIAN_POINT('Ctrl Pts',(18.860798140368,4.4383163522134,128.68083774917));
#67795=CARTESIAN_POINT('Ctrl Pts',(18.8530518642839,4.37732066810429,128.557791089135));
#67796=CARTESIAN_POINT('Ctrl Pts',(18.8453055881998,4.31128780026043,128.437510270411));
#67797=CARTESIAN_POINT('Ctrl Pts',(18.8375592549345,4.24525444497703,128.317228563803));
#67798=CARTESIAN_POINT('Ctrl Pts',(18.8298129216691,4.17418401990964,128.199713081962));
#67799=CARTESIAN_POINT('Ctrl Pts',(18.8220665884038,4.0983475627509,128.085403038384));
#67800=CARTESIAN_POINT('Ctrl Pts',(18.8143185204008,4.02249412254329,127.971067395863));
#67801=CARTESIAN_POINT('Ctrl Pts',(18.8065704523978,3.94187274249744,127.859938945742));
#67802=CARTESIAN_POINT('Ctrl Pts',(18.7988223843948,3.85679723570375,127.752427108269));
#67803=CARTESIAN_POINT('Ctrl Pts',(18.791066081653,3.77163130964914,127.644801005937));
#67804=CARTESIAN_POINT('Ctrl Pts',(18.7833097789112,3.68200204336714,127.540799501692));
#67805=CARTESIAN_POINT('Ctrl Pts',(18.7755534761693,3.58826328405119,127.440798567175));
#67806=CARTESIAN_POINT('Ctrl Pts',(18.7677930336552,3.49447449353685,127.340744259148));
#67807=CARTESIAN_POINT('Ctrl Pts',(18.7600325911409,3.39657211847902,127.24469504913));
#67808=CARTESIAN_POINT('Ctrl Pts',(18.7522721486268,3.29494544524281,127.152988604832));
#67809=CARTESIAN_POINT('Ctrl Pts',(18.7444992483613,3.19315563184874,127.061134945209));
#67810=CARTESIAN_POINT('Ctrl Pts',(18.7367263480959,3.08762987431949,126.973638232061));
#67811=CARTESIAN_POINT('Ctrl Pts',(18.7289534478305,2.97878968080195,126.890795094919));
#67812=CARTESIAN_POINT('Ctrl Pts',(18.7214631120685,2.87390610247098,126.810963514482));
#67813=CARTESIAN_POINT('Ctrl Pts',(18.7139727763065,2.76594513305206,126.735453222222));
#67814=CARTESIAN_POINT('Ctrl Pts',(18.7064824405445,2.65530620265505,126.66448960114));
#67815=CARTESIAN_POINT('Ctrl Pts',(18.6987081064254,2.54047236358374,126.590835372796));
#67816=CARTESIAN_POINT('Ctrl Pts',(18.6909337723063,2.42238972600694,126.521846081197));
#67817=CARTESIAN_POINT('Ctrl Pts',(18.6831594381872,2.30147418326171,126.457821805329));
#67818=CARTESIAN_POINT('Ctrl Pts',(18.6753946852401,2.18070765811654,126.39387643366));
#67819=CARTESIAN_POINT('Ctrl Pts',(18.6676299322931,2.05711551665556,126.334884084053));
#67820=CARTESIAN_POINT('Ctrl Pts',(18.659865179346,1.93114277321776,126.281101764488));
#67821=CARTESIAN_POINT('Ctrl Pts',(18.652108138461,1.80529514768465,126.227372862281));
#67822=CARTESIAN_POINT('Ctrl Pts',(18.644351097576,1.67707198277137,126.178843844796));
#67823=CARTESIAN_POINT('Ctrl Pts',(18.636594056691,1.5469427366621,126.135725781558));
#67824=CARTESIAN_POINT('Ctrl Pts',(18.6288428654508,1.41691162202958,126.092640233986));
#67825=CARTESIAN_POINT('Ctrl Pts',(18.6210916742107,1.28497765686095,126.05495764126));
#67826=CARTESIAN_POINT('Ctrl Pts',(18.6133404829706,1.15162978449178,126.022840785758));
#67827=CARTESIAN_POINT('Ctrl Pts',(18.6055925861935,1.01833858852554,125.990737580776));
#67828=CARTESIAN_POINT('Ctrl Pts',(18.5978446894165,0.883635059899439,125.964195499401));
#67829=CARTESIAN_POINT('Ctrl Pts',(18.5900967926394,0.748022581247887,125.943327262358));
#67830=CARTESIAN_POINT('Ctrl Pts',(18.5823505165553,0.612438469803402,125.9224633905));
#67831=CARTESIAN_POINT('Ctrl Pts',(18.5746042404711,0.475946172690013,125.907271061698));
#67832=CARTESIAN_POINT('Ctrl Pts',(18.5668579643871,0.339058135356334,125.897811663021));
#67833=CARTESIAN_POINT('Ctrl Pts',(18.5591116311217,0.202169087546445,125.888352194516));
#67834=CARTESIAN_POINT('Ctrl Pts',(18.5513652978564,0.0648846837221543,
125.884625767534));
#67835=CARTESIAN_POINT('Ctrl Pts',(18.5436189645911,-0.0722790508716011,
125.88664175601));
#67836=CARTESIAN_POINT('Ctrl Pts',(18.5358708965881,-0.209473502332692,
125.888658195952));
#67837=CARTESIAN_POINT('Ctrl Pts',(18.5281228285852,-0.346546839942367,
125.896419604547));
#67838=CARTESIAN_POINT('Ctrl Pts',(18.5203747605823,-0.482984983207766,
125.909883263599));
#67839=CARTESIAN_POINT('Ctrl Pts',(18.5126184578404,-0.619568134555649,
125.923361231989));
#67840=CARTESIAN_POINT('Ctrl Pts',(18.5048621550985,-0.755514353294202,
125.942553518722));
#67841=CARTESIAN_POINT('Ctrl Pts',(18.4971058523566,-0.890316060784019,
125.967365643989));
#67842=CARTESIAN_POINT('Ctrl Pts',(18.4893454098425,-1.02518971600411,125.992191012234));
#67843=CARTESIAN_POINT('Ctrl Pts',(18.4815849673283,-1.15891726176452,126.022642108962));
#67844=CARTESIAN_POINT('Ctrl Pts',(18.4738245248142,-1.2910041898671,126.058573934176));
#67845=CARTESIAN_POINT('Ctrl Pts',(18.4660516245487,-1.4233031556328,126.094563440345));
#67846=CARTESIAN_POINT('Ctrl Pts',(18.4582787242832,-1.55395586799444,126.136051138116));
#67847=CARTESIAN_POINT('Ctrl Pts',(18.4505058240178,-1.68248492867731,126.182842736255));
#67848=CARTESIAN_POINT('Ctrl Pts',(18.4430154882557,-1.80634163425989,126.227933341942));
#67849=CARTESIAN_POINT('Ctrl Pts',(18.4355251524937,-1.9282261227659,126.27794880572));
#67850=CARTESIAN_POINT('Ctrl Pts',(18.4280348167316,-2.04773287136316,126.332674900743));
#67851=CARTESIAN_POINT('Ctrl Pts',(18.420259886146,-2.1717802711554,126.389480310212));
#67852=CARTESIAN_POINT('Ctrl Pts',(18.4124849555604,-2.293658649495,126.451541345122));
#67853=CARTESIAN_POINT('Ctrl Pts',(18.4047100249748,-2.41289063170151,126.518670257548));
#67854=CARTESIAN_POINT('Ctrl Pts',(18.3969448101675,-2.5319736181719,126.585715283743));
#67855=CARTESIAN_POINT('Ctrl Pts',(18.3891795953601,-2.64841645136489,126.6578153959));
#67856=CARTESIAN_POINT('Ctrl Pts',(18.3814143805528,-2.76176228286144,126.734735062866));
#67857=CARTESIAN_POINT('Ctrl Pts',(18.3736570118381,-2.8749935879856,126.811577009018));
#67858=CARTESIAN_POINT('Ctrl Pts',(18.3658996431232,-2.98513379777967,126.893228599994));
#67859=CARTESIAN_POINT('Ctrl Pts',(18.3581422744085,-3.09175152938691,126.979408912899));
#67860=CARTESIAN_POINT('Ctrl Pts',(18.3503913215521,-3.19828108105846,127.06551794897));
#67861=CARTESIAN_POINT('Ctrl Pts',(18.3426403686959,-3.30129365293273,127.15614800374));
#67862=CARTESIAN_POINT('Ctrl Pts',(18.3348894158395,-3.40038804793612,127.250975726233));
#67863=CARTESIAN_POINT('Ctrl Pts',(18.3271419534053,-3.49943781858518,127.345760745747));
#67864=CARTESIAN_POINT('Ctrl Pts',(18.3193944909712,-3.59457264104929,127.44473940239));
#67865=CARTESIAN_POINT('Ctrl Pts',(18.311647028537,-3.68542565559922,127.547549170836));
#67866=CARTESIAN_POINT('Ctrl Pts',(18.3039013771726,-3.77625743207812,127.650334906165));
#67867=CARTESIAN_POINT('Ctrl Pts',(18.2961557258082,-3.8628091341744,127.756949678145));
#67868=CARTESIAN_POINT('Ctrl Pts',(18.2884100744438,-3.94475220748754,127.866995627644));
#67869=CARTESIAN_POINT('Ctrl Pts',(18.2806645563721,-4.02669387066683,127.977039683394));
#67870=CARTESIAN_POINT('Ctrl Pts',(18.2729190383004,-4.10402683062057,128.090514484904));
#67871=CARTESIAN_POINT('Ctrl Pts',(18.2651735202287,-4.17646436527294,128.206991088965));
#67872=CARTESIAN_POINT('Ctrl Pts',(18.257423172576,-4.24894706707074,128.323540319956));
#67873=CARTESIAN_POINT('Ctrl Pts',(18.2496728249232,-4.31652803848912,128.44309476067));
#67874=CARTESIAN_POINT('Ctrl Pts',(18.2419224772704,-4.37896513540232,128.565198406954));
#67875=CARTESIAN_POINT('Ctrl Pts',(18.2341695744863,-4.44142281655195,128.687342308319));
#67876=CARTESIAN_POINT('Ctrl Pts',(18.2264166717022,-4.4987330775707,128.812036736195));
#67877=CARTESIAN_POINT('Ctrl Pts',(18.218663768918,-4.55070130352922,128.938804210336));
#67878=CARTESIAN_POINT('Ctrl Pts',(18.2109023070429,-4.60272690164677,129.065711633908));
#67879=CARTESIAN_POINT('Ctrl Pts',(18.2031408451677,-4.6493985481491,129.194696308785));
#67880=CARTESIAN_POINT('Ctrl Pts',(18.1953793832926,-4.69057087589728,129.325263622544));
#67881=CARTESIAN_POINT('Ctrl Pts',(18.1903197138673,-4.71741097009964,129.410379990568));
#67882=CARTESIAN_POINT('Ctrl Pts',(18.185260044442,-4.74191504912875,129.49616862629));
#67883=CARTESIAN_POINT('Ctrl Pts',(18.1802003750167,-4.76405452823408,129.582490119308));
#67884=CARTESIAN_POINT('Origin',(213.235140564004,0.,130.804360617566));
#67885=CARTESIAN_POINT('',(16.0848513025106,-4.76405452823409,129.582490119308));
#67886=CARTESIAN_POINT('',(16.4298612965399,-4.76405452823409,129.582490119308));
#67887=CARTESIAN_POINT('',(213.235140564004,-4.76405452823405,129.582490119308));
#67888=CARTESIAN_POINT('',(17.7648594360204,-4.9182498302975,130.803068611917));
#67889=CARTESIAN_POINT('Ctrl Pts',(17.7648594359913,-4.91824983029764,130.803068612434));
#67890=CARTESIAN_POINT('Ctrl Pts',(17.7568883079903,-4.91828700392096,130.944576693201));
#67891=CARTESIAN_POINT('Ctrl Pts',(17.7489171799893,-4.91221261508659,131.086020317408));
#67892=CARTESIAN_POINT('Ctrl Pts',(17.7409460519883,-4.9000695348613,131.226855133535));
#67893=CARTESIAN_POINT('Ctrl Pts',(17.7329691638686,-4.88791767976969,131.367791720108));
#67894=CARTESIAN_POINT('Ctrl Pts',(17.724992275749,-4.86968842145711,131.508118265165));
#67895=CARTESIAN_POINT('Ctrl Pts',(17.7170153876293,-4.84547629013657,131.647297497898));
#67896=CARTESIAN_POINT('Ctrl Pts',(17.7090314877391,-4.82124287609155,131.786599070678));
#67897=CARTESIAN_POINT('Ctrl Pts',(17.7010475878487,-4.79101616576517,131.924750968601));
#67898=CARTESIAN_POINT('Ctrl Pts',(17.6930636879584,-4.75494136603763,132.061228020296));
#67899=CARTESIAN_POINT('Ctrl Pts',(17.685065771649,-4.71880323391348,132.197944669128));
#67900=CARTESIAN_POINT('Ctrl Pts',(17.6770678553396,-4.67679659075788,132.332980250728));
#67901=CARTESIAN_POINT('Ctrl Pts',(17.6690699390301,-4.62911627812375,132.465825497156));
#67902=CARTESIAN_POINT('Ctrl Pts',(17.6610640711306,-4.58138856135538,132.598802819351));
#67903=CARTESIAN_POINT('Ctrl Pts',(17.6530582032311,-4.52797606011424,132.72958513304));
#67904=CARTESIAN_POINT('Ctrl Pts',(17.6450523353316,-4.46912083899419,132.857685236073));
#67905=CARTESIAN_POINT('Ctrl Pts',(17.637031874495,-4.41015833774535,132.986018837431));
#67906=CARTESIAN_POINT('Ctrl Pts',(17.6290114136584,-4.34573345708694,133.111660141843));
#67907=CARTESIAN_POINT('Ctrl Pts',(17.6209909528218,-4.27613358421434,133.234147569637));
#67908=CARTESIAN_POINT('Ctrl Pts',(17.6180876156986,-4.2509390350735,133.278486954054));
#67909=CARTESIAN_POINT('Ctrl Pts',(17.6151842785755,-4.22506676861061,133.322413351635));
#67910=CARTESIAN_POINT('Ctrl Pts',(17.6122809414523,-4.19853175125283,133.365905892634));
#67911=CARTESIAN_POINT('Ctrl Pts',(17.6045066073332,-4.12747831100699,133.482366892879));
#67912=CARTESIAN_POINT('Ctrl Pts',(17.5967322732141,-4.05146297359281,133.596053744055));
#67913=CARTESIAN_POINT('Ctrl Pts',(17.5889579390951,-3.97072849725918,133.706514690587));
#67914=CARTESIAN_POINT('Ctrl Pts',(17.581193186148,-3.89009351895228,133.816839503875));
#67915=CARTESIAN_POINT('Ctrl Pts',(17.5734284332009,-3.80475120215271,133.923946010243));
#67916=CARTESIAN_POINT('Ctrl Pts',(17.5656636802538,-3.71498933114176,134.027408450286));
#67917=CARTESIAN_POINT('Ctrl Pts',(17.5579066393688,-3.62531661288664,134.130768129975));
#67918=CARTESIAN_POINT('Ctrl Pts',(17.5501495984839,-3.53123333040069,134.230490652582));
#67919=CARTESIAN_POINT('Ctrl Pts',(17.5423925575989,-3.43306934206733,134.326180879172));
#67920=CARTESIAN_POINT('Ctrl Pts',(17.5346413663587,-3.3349793799609,134.421798945018));
#67921=CARTESIAN_POINT('Ctrl Pts',(17.5268901751186,-3.23281511599657,134.513390495547));
#67922=CARTESIAN_POINT('Ctrl Pts',(17.5191389838785,-3.12694505065742,134.600595293224));
#67923=CARTESIAN_POINT('Ctrl Pts',(17.5113910871014,-3.02111998292037,134.687763026536));
#67924=CARTESIAN_POINT('Ctrl Pts',(17.5036431903243,-2.91159254763293,134.770547467268));
#67925=CARTESIAN_POINT('Ctrl Pts',(17.4958952935472,-2.79876612586406,134.848627081984));
#67926=CARTESIAN_POINT('Ctrl Pts',(17.4881490174631,-2.68596330495037,134.926690364127));
#67927=CARTESIAN_POINT('Ctrl Pts',(17.480402741379,-2.56986319144211,135.000050555438));
#67928=CARTESIAN_POINT('Ctrl Pts',(17.4726564652949,-2.45089976836731,135.068428321991));
#67929=CARTESIAN_POINT('Ctrl Pts',(17.4649101320296,-2.33193546713171,135.136806593292));
#67930=CARTESIAN_POINT('Ctrl Pts',(17.4571637987643,-2.21010815311608,135.200202171618));
#67931=CARTESIAN_POINT('Ctrl Pts',(17.449417465499,-2.08587777772356,135.25838093172));
#67932=CARTESIAN_POINT('Ctrl Pts',(17.441669397496,-1.96161958180016,135.316572720553));
#67933=CARTESIAN_POINT('Ctrl Pts',(17.433921329493,-1.83495760764034,135.36954520066));
#67934=CARTESIAN_POINT('Ctrl Pts',(17.4261732614901,-1.7063728414552,135.4171119428));
#67935=CARTESIAN_POINT('Ctrl Pts',(17.4184169587483,-1.57765141384985,135.464729239439));
#67936=CARTESIAN_POINT('Ctrl Pts',(17.4106606560064,-1.4470034792404,135.506929185431));
#67937=CARTESIAN_POINT('Ctrl Pts',(17.4029043532646,-1.31492681597713,135.543574743465));
#67938=CARTESIAN_POINT('Ctrl Pts',(17.3951439107504,-1.18277965942175,135.580239860338));
#67939=CARTESIAN_POINT('Ctrl Pts',(17.3873834682363,-1.0492026353477,135.611344593524));
#67940=CARTESIAN_POINT('Ctrl Pts',(17.3796230257221,-0.914703864275895,
135.636803054179));
#67941=CARTESIAN_POINT('Ctrl Pts',(17.3718501254566,-0.779989183836526,
135.662302383015));
#67942=CARTESIAN_POINT('Ctrl Pts',(17.3640772251912,-0.644350186620545,
135.682137270161));
#67943=CARTESIAN_POINT('Ctrl Pts',(17.3563043249258,-0.508301165183191,
135.696273636823));
#67944=CARTESIAN_POINT('Ctrl Pts',(17.3488139891637,-0.37719786836078,135.709896110949));
#67945=CARTESIAN_POINT('Ctrl Pts',(17.3413236534016,-0.245714147985853,
135.718227163212));
#67946=CARTESIAN_POINT('Ctrl Pts',(17.3338333176395,-0.114308379744584,
135.721282078889));
#67947=CARTESIAN_POINT('Ctrl Pts',(17.3260589835204,0.0220796781381341,
135.724452822623));
#67948=CARTESIAN_POINT('Ctrl Pts',(17.3182846494013,0.158815792461206,135.721949486406));
#67949=CARTESIAN_POINT('Ctrl Pts',(17.3105103152822,0.295388671702986,135.713732124707));
#67950=CARTESIAN_POINT('Ctrl Pts',(17.3027455623352,0.431793237076968,135.705524890172));
#67951=CARTESIAN_POINT('Ctrl Pts',(17.2949808093881,0.568034581130291,135.691617664942));
#67952=CARTESIAN_POINT('Ctrl Pts',(17.287216056441,0.703598945984164,135.672022436726));
#67953=CARTESIAN_POINT('Ctrl Pts',(17.279459015556,0.839028666399557,135.652446670767));
#67954=CARTESIAN_POINT('Ctrl Pts',(17.271701974671,0.973782361252646,135.627194199962));
#67955=CARTESIAN_POINT('Ctrl Pts',(17.263944933786,1.10734929245375,135.596328961264));
#67956=CARTESIAN_POINT('Ctrl Pts',(17.2561937425459,1.24081549979359,135.565486998282));
#67957=CARTESIAN_POINT('Ctrl Pts',(17.2484425513058,1.37309634543516,135.529040779876));
#67958=CARTESIAN_POINT('Ctrl Pts',(17.2406913600656,1.50368956782508,135.48710561875));
#67959=CARTESIAN_POINT('Ctrl Pts',(17.2329434632885,1.63422728461162,135.445188281186));
#67960=CARTESIAN_POINT('Ctrl Pts',(17.2251955665115,1.76307843330656,135.397786760239));
#67961=CARTESIAN_POINT('Ctrl Pts',(17.2174476697344,1.88975446140122,135.345066635149));
#67962=CARTESIAN_POINT('Ctrl Pts',(17.2097013936503,2.01640399160146,135.292357537973));
#67963=CARTESIAN_POINT('Ctrl Pts',(17.2019551175661,2.14087894547366,135.234332199678));
#67964=CARTESIAN_POINT('Ctrl Pts',(17.194208841482,2.26270973304852,135.171204755667));
#67965=CARTESIAN_POINT('Ctrl Pts',(17.1864625082166,2.38454141995092,135.108076845664));
#67966=CARTESIAN_POINT('Ctrl Pts',(17.1787161749513,2.50372855447549,135.039846934661));
#67967=CARTESIAN_POINT('Ctrl Pts',(17.170969841686,2.61982554545366,134.966775442387));
#67968=CARTESIAN_POINT('Ctrl Pts',(17.163221773683,2.73594853554753,134.893687586259));
#67969=CARTESIAN_POINT('Ctrl Pts',(17.15547370568,2.84897967424441,134.815756199567));
#67970=CARTESIAN_POINT('Ctrl Pts',(17.1477256376771,2.95850212854773,134.733285180074));
#67971=CARTESIAN_POINT('Ctrl Pts',(17.1399693349352,3.06814098461898,134.6507265094));
#67972=CARTESIAN_POINT('Ctrl Pts',(17.1322130321934,3.17426339425559,134.563618803471));
#67973=CARTESIAN_POINT('Ctrl Pts',(17.1244567294515,3.27648500273192,134.472306785297));
#67974=CARTESIAN_POINT('Ctrl Pts',(17.1166962869373,3.37876116995867,134.38094603115));
#67975=CARTESIAN_POINT('Ctrl Pts',(17.1089358444232,3.47713210723224,134.285376765761));
#67976=CARTESIAN_POINT('Ctrl Pts',(17.101175401909,3.57125090228166,134.185980060296));
#67977=CARTESIAN_POINT('Ctrl Pts',(17.0934025016436,3.66552078517624,134.086423794416));
#67978=CARTESIAN_POINT('Ctrl Pts',(17.0856296013781,3.75552462864681,133.983028105559));
#67979=CARTESIAN_POINT('Ctrl Pts',(17.0778567011127,3.84095577355102,133.876207262196));
#67980=CARTESIAN_POINT('Ctrl Pts',(17.0703663653507,3.92328128115025,133.773269625554));
#67981=CARTESIAN_POINT('Ctrl Pts',(17.0628760295886,4.00136059389691,133.667151785036));
#67982=CARTESIAN_POINT('Ctrl Pts',(17.0553856938266,4.07495880847432,133.558247647155));
#67983=CARTESIAN_POINT('Ctrl Pts',(17.0476113597075,4.1513475217268,133.445214375785));
#67984=CARTESIAN_POINT('Ctrl Pts',(17.0398370255884,4.22315060382649,133.328821295865));
#67985=CARTESIAN_POINT('Ctrl Pts',(17.0320626914693,4.29005808190938,133.209476979895));
#67986=CARTESIAN_POINT('Ctrl Pts',(17.0242979385222,4.35688310250523,133.090279745129));
#67987=CARTESIAN_POINT('Ctrl Pts',(17.0165331855752,4.41882433438697,132.968138848882));
#67988=CARTESIAN_POINT('Ctrl Pts',(17.0087684326281,4.47561416447044,132.843493009857));
#67989=CARTESIAN_POINT('Ctrl Pts',(17.0010113917431,4.53234759009423,132.718970970837));
#67990=CARTESIAN_POINT('Ctrl Pts',(16.993254350858,4.58393963482862,132.591949293637));
#67991=CARTESIAN_POINT('Ctrl Pts',(16.985497309973,4.63016802423113,132.462892236163));
#67992=CARTESIAN_POINT('Ctrl Pts',(16.9777461187329,4.67636155244552,132.333932501621));
#67993=CARTESIAN_POINT('Ctrl Pts',(16.9699949274927,4.71719934489805,132.202940808498));
#67994=CARTESIAN_POINT('Ctrl Pts',(16.9622437362526,4.75250693279576,132.070402052997));
#67995=CARTESIAN_POINT('Ctrl Pts',(16.9544958394755,4.7877995140267,131.937919630003));
#67996=CARTESIAN_POINT('Ctrl Pts',(16.9467479426985,4.81756646520682,131.803891829434));
#67997=CARTESIAN_POINT('Ctrl Pts',(16.9390000459214,4.84168301827607,131.668819183975));
#67998=CARTESIAN_POINT('Ctrl Pts',(16.9312537698373,4.8657945266823,131.533774792801));
#67999=CARTESIAN_POINT('Ctrl Pts',(16.9235074937532,4.88425791924941,131.397686376098));
#68000=CARTESIAN_POINT('Ctrl Pts',(16.9157612176691,4.89699952930785,131.261064758623));
#68001=CARTESIAN_POINT('Ctrl Pts',(16.9080148844038,4.90974123342197,131.124442132638));
#68002=CARTESIAN_POINT('Ctrl Pts',(16.9002685511384,4.91676103444208,130.987286687303));
#68003=CARTESIAN_POINT('Ctrl Pts',(16.8925222178731,4.91803717794974,130.850114074311));
#68004=CARTESIAN_POINT('Ctrl Pts',(16.8847741498701,4.9193136072409,130.712910742463));
#68005=CARTESIAN_POINT('Ctrl Pts',(16.8770260818671,4.91484381589012,130.575690626182));
#68006=CARTESIAN_POINT('Ctrl Pts',(16.8692780138641,4.90465817327578,130.438968683037));
#68007=CARTESIAN_POINT('Ctrl Pts',(16.8615217111223,4.89446170523928,130.302101430183));
#68008=CARTESIAN_POINT('Ctrl Pts',(16.8537654083804,4.87853727981489,130.165733798634));
#68009=CARTESIAN_POINT('Ctrl Pts',(16.8460091056386,4.85696716911769,130.030375488114));
#68010=CARTESIAN_POINT('Ctrl Pts',(16.8382486631244,4.83538554580289,129.894944932787));
#68011=CARTESIAN_POINT('Ctrl Pts',(16.8304882206102,4.80815231060895,129.760525154897));
#68012=CARTESIAN_POINT('Ctrl Pts',(16.822727778096,4.77540055494424,129.627613999836));
#68013=CARTESIAN_POINT('Ctrl Pts',(16.8149548778305,4.74259622325382,129.49448948399));
#68014=CARTESIAN_POINT('Ctrl Pts',(16.8071819775651,4.70425577776178,129.362878806029));
#68015=CARTESIAN_POINT('Ctrl Pts',(16.7994090772997,4.66056199750942,129.233263889204));
#68016=CARTESIAN_POINT('Ctrl Pts',(16.7919187415377,4.61845659622734,129.108360801085));
#68017=CARTESIAN_POINT('Ctrl Pts',(16.7844284057757,4.57138042731904,128.985311179079));
#68018=CARTESIAN_POINT('Ctrl Pts',(16.7769380700137,4.51953792450967,128.864525570089));
#68019=CARTESIAN_POINT('Ctrl Pts',(16.7691637358946,4.46572979744902,128.739160338023));
#68020=CARTESIAN_POINT('Ctrl Pts',(16.7613894017756,4.40661632265131,128.615837068728));
#68021=CARTESIAN_POINT('Ctrl Pts',(16.7536150676565,4.34237369582919,128.49503739457));
#68022=CARTESIAN_POINT('Ctrl Pts',(16.7458503147094,4.27821024230318,128.374386595214));
#68023=CARTESIAN_POINT('Ctrl Pts',(16.7380855617624,4.20893039591155,128.256253544686));
#68024=CARTESIAN_POINT('Ctrl Pts',(16.7303208088153,4.1347586117155,128.141100531629));
#68025=CARTESIAN_POINT('Ctrl Pts',(16.7225637679303,4.06066049598095,128.026061890167));
#68026=CARTESIAN_POINT('Ctrl Pts',(16.7148067270453,3.98168032189687,127.913997722567));
#68027=CARTESIAN_POINT('Ctrl Pts',(16.7070496861603,3.8980885380219,127.805345977348));
#68028=CARTESIAN_POINT('Ctrl Pts',(16.6992984949201,3.81455979136117,127.696776167255));
#68029=CARTESIAN_POINT('Ctrl Pts',(16.69154730368,3.72642659439786,127.591613966095));
#68030=CARTESIAN_POINT('Ctrl Pts',(16.6837961124398,3.63400259939691,127.490268257647));
#68031=CARTESIAN_POINT('Ctrl Pts',(16.6760482156627,3.54161788705958,127.388965623828));
#68032=CARTESIAN_POINT('Ctrl Pts',(16.6683003188856,3.44494626678687,127.291476544737));
#68033=CARTESIAN_POINT('Ctrl Pts',(16.6605524221085,3.34434141071926,127.19817654142));
#68034=CARTESIAN_POINT('Ctrl Pts',(16.6528061460244,3.24375759901876,127.104896054452));
#68035=CARTESIAN_POINT('Ctrl Pts',(16.6450598699404,3.13924247449838,127.015803166003));
#68036=CARTESIAN_POINT('Ctrl Pts',(16.6373135938562,3.03118598985885,126.931235967186));
#68037=CARTESIAN_POINT('Ctrl Pts',(16.6295672605909,2.92312870757075,126.846668144112));
#68038=CARTESIAN_POINT('Ctrl Pts',(16.6218209273255,2.81153032088532,126.766626318291));
#68039=CARTESIAN_POINT('Ctrl Pts',(16.6140745940602,2.69681290338204,126.691407514666));
#68040=CARTESIAN_POINT('Ctrl Pts',(16.6063265260572,2.58206979570897,126.616171866312));
#68041=CARTESIAN_POINT('Ctrl Pts',(16.5985784580542,2.46420659420051,126.545761603729));
#68042=CARTESIAN_POINT('Ctrl Pts',(16.5908303900513,2.34367296263487,126.480429523444));
#68043=CARTESIAN_POINT('Ctrl Pts',(16.5830740873094,2.22301122649107,126.415028007446));
#68044=CARTESIAN_POINT('Ctrl Pts',(16.5753177845676,2.09967373501934,126.354715641742));
#68045=CARTESIAN_POINT('Ctrl Pts',(16.5675614818258,1.97413378312091,126.299698713622));
#68046=CARTESIAN_POINT('Ctrl Pts',(16.5598010393116,1.84852682677004,126.244652421311));
#68047=CARTESIAN_POINT('Ctrl Pts',(16.5520405967974,1.72071543183442,126.19490734003));
#68048=CARTESIAN_POINT('Ctrl Pts',(16.5442801542832,1.59119038889936,126.150620593803));
#68049=CARTESIAN_POINT('Ctrl Pts',(16.5365072540178,1.46145742086669,126.106262754559));
#68050=CARTESIAN_POINT('Ctrl Pts',(16.5287343537524,1.3300056827843,126.067380871002));
#68051=CARTESIAN_POINT('Ctrl Pts',(16.520961453487,1.19733942686742,126.034081657236));
#68052=CARTESIAN_POINT('Ctrl Pts',(16.513471117725,1.06949592351978,126.001992953766));
#68053=CARTESIAN_POINT('Ctrl Pts',(16.505980781963,0.940524972385241,125.975088141586));
#68054=CARTESIAN_POINT('Ctrl Pts',(16.498490446201,0.810882479624476,125.953417135444));
#68055=CARTESIAN_POINT('Ctrl Pts',(16.4907161120819,0.676324552346135,125.930924466518));
#68056=CARTESIAN_POINT('Ctrl Pts',(16.4829417779627,0.540616916136176,125.913999067653));
#68057=CARTESIAN_POINT('Ctrl Pts',(16.4751674438436,0.404260020031606,125.902753034466));
#68058=CARTESIAN_POINT('Ctrl Pts',(16.4674026908966,0.268071171615288,125.891520861009));
#68059=CARTESIAN_POINT('Ctrl Pts',(16.4596379379496,0.131235041275635,125.885954158516));
#68060=CARTESIAN_POINT('Ctrl Pts',(16.4518731850025,-0.00573811101679774,
125.886113964888));
#68061=CARTESIAN_POINT('Ctrl Pts',(16.4441161441175,-0.14257521964339,125.886273612538));
#68062=CARTESIAN_POINT('Ctrl Pts',(16.4363591032325,-0.279548690958253,
125.892148449922));
#68063=CARTESIAN_POINT('Ctrl Pts',(16.4286020623475,-0.416143882414879,
125.903747662881));
#68064=CARTESIAN_POINT('Ctrl Pts',(16.4208508711074,-0.552636066374886,
125.915338128783));
#68065=CARTESIAN_POINT('Ctrl Pts',(16.4130996798673,-0.688750150289997,
125.932644344993));
#68066=CARTESIAN_POINT('Ctrl Pts',(16.4053484886272,-0.823972591946111,
125.955623438648));
#68067=CARTESIAN_POINT('Ctrl Pts',(16.3976005918501,-0.959137560457898,
125.978592765575));
#68068=CARTESIAN_POINT('Ctrl Pts',(16.3898526950731,-1.0934112558241,126.007230109041));
#68069=CARTESIAN_POINT('Ctrl Pts',(16.382104798296,-1.22628657312295,126.041440892956));
#68070=CARTESIAN_POINT('Ctrl Pts',(16.3743585222119,-1.3591340957697,126.075644520713));
#68071=CARTESIAN_POINT('Ctrl Pts',(16.3666122461277,-1.49058344379092,126.115419172572));
#68072=CARTESIAN_POINT('Ctrl Pts',(16.3588659700436,-1.62013939259733,126.160619516788));
#68073=CARTESIAN_POINT('Ctrl Pts',(16.3511196367782,-1.74969629775649,126.205820194663));
#68074=CARTESIAN_POINT('Ctrl Pts',(16.3433733035129,-1.87735940666773,126.256446516025));
#68075=CARTESIAN_POINT('Ctrl Pts',(16.3356269702476,-2.00265068275373,126.312303927656));
#68076=CARTESIAN_POINT('Ctrl Pts',(16.3278789022447,-2.12797001695128,126.368173848166));
#68077=CARTESIAN_POINT('Ctrl Pts',(16.3201308342417,-2.25091610436807,126.429277030862));
#68078=CARTESIAN_POINT('Ctrl Pts',(16.3123827662388,-2.37103320587095,126.495371803568));
#68079=CARTESIAN_POINT('Ctrl Pts',(16.3046264634969,-2.49127796925954,126.561536822586));
#68080=CARTESIAN_POINT('Ctrl Pts',(16.2968701607551,-2.60868739748767,126.632703840386));
#68081=CARTESIAN_POINT('Ctrl Pts',(16.2891138580132,-2.72283210776043,126.708586163882));
#68082=CARTESIAN_POINT('Ctrl Pts',(16.2813534154991,-2.83703774050189,126.784508988059));
#68083=CARTESIAN_POINT('Ctrl Pts',(16.2735929729849,-2.94797486716718,126.865151902901));
#68084=CARTESIAN_POINT('Ctrl Pts',(16.2658325304708,-3.05524601056549,126.950186921762));
#68085=CARTESIAN_POINT('Ctrl Pts',(16.2580596302054,-3.16268935512641,127.035358446385));
#68086=CARTESIAN_POINT('Ctrl Pts',(16.2502867299399,-3.26645466027605,127.124935908735));
#68087=CARTESIAN_POINT('Ctrl Pts',(16.2425138296744,-3.36617958377696,127.218552748722));
#68088=CARTESIAN_POINT('Ctrl Pts',(16.2350234939122,-3.46227925511926,127.308766380772));
#68089=CARTESIAN_POINT('Ctrl Pts',(16.22753315815,-3.55462698497167,127.402730586441));
#68090=CARTESIAN_POINT('Ctrl Pts',(16.2200428223877,-3.64293435022734,127.500088779107));
#68091=CARTESIAN_POINT('Ctrl Pts',(16.2123490717802,-3.73363987620862,127.600090925573));
#68092=CARTESIAN_POINT('Ctrl Pts',(16.2046553211726,-3.8203836463713,127.70400636712));
#68093=CARTESIAN_POINT('Ctrl Pts',(16.196961570565,-3.90280362575176,127.811484589175));
#68094=CARTESIAN_POINT('Ctrl Pts',(16.1892770144218,-3.98512510862497,127.918834368714));
#68095=CARTESIAN_POINT('Ctrl Pts',(16.1815924582786,-4.06313283469464,128.029738148571));
#68096=CARTESIAN_POINT('Ctrl Pts',(16.1739079021353,-4.13650198839578,128.143809102842));
#68097=CARTESIAN_POINT('Ctrl Pts',(16.166232029742,-4.20978823303011,128.257751153945));
#68098=CARTESIAN_POINT('Ctrl Pts',(16.1585561573487,-4.278446124117,128.374852921575));
#68099=CARTESIAN_POINT('Ctrl Pts',(16.1508802849553,-4.34219195467867,128.494695687057));
#68100=CARTESIAN_POINT('Ctrl Pts',(16.1432095053106,-4.40589549148183,128.614458939872));
#68101=CARTESIAN_POINT('Ctrl Pts',(16.1355387256659,-4.46469326139856,128.736959222908));
#68102=CARTESIAN_POINT('Ctrl Pts',(16.1278679460212,-4.51834571167189,128.86175023658));
#68103=CARTESIAN_POINT('Ctrl Pts',(16.1201999619047,-4.57197860892104,128.986495771589));
#68104=CARTESIAN_POINT('Ctrl Pts',(16.1125319777883,-4.62046975447682,129.113530012034));
#68105=CARTESIAN_POINT('Ctrl Pts',(16.1048639936718,-4.66362646419048,129.242383900389));
#68106=CARTESIAN_POINT('Ctrl Pts',(16.0981930966181,-4.70117139950928,129.354482596883));
#68107=CARTESIAN_POINT('Ctrl Pts',(16.0915221995643,-4.73467966531899,129.467957974628));
#68108=CARTESIAN_POINT('Ctrl Pts',(16.0848513025106,-4.7640545282341,129.582490119308));
#68109=CARTESIAN_POINT('Ctrl Pts',(17.8345741463799,-4.76405452823412,129.582490119309));
#68110=CARTESIAN_POINT('Ctrl Pts',(17.826246821477,-4.8005402629227,129.724747445111));
#68111=CARTESIAN_POINT('Ctrl Pts',(17.8179194965742,-4.83069182849782,129.868803123946));
#68112=CARTESIAN_POINT('Ctrl Pts',(17.8095921716714,-4.8543443026394,130.014092021497));
#68113=CARTESIAN_POINT('Ctrl Pts',(17.8012893778004,-4.87792710019173,130.158952920068));
#68114=CARTESIAN_POINT('Ctrl Pts',(17.7929865839295,-4.89504893771605,130.305039501495));
#68115=CARTESIAN_POINT('Ctrl Pts',(17.7846837900586,-4.90559544208159,130.451775278778));
#68116=CARTESIAN_POINT('Ctrl Pts',(17.7780756720458,-4.91398930883925,130.568560947318));
#68117=CARTESIAN_POINT('Ctrl Pts',(17.7714675540331,-4.91821901310473,130.685757473852));
#68118=CARTESIAN_POINT('Ctrl Pts',(17.7648594360204,-4.9182498302975,130.803068611917));
#68119=CARTESIAN_POINT('',(18.1101405639752,-4.91824863063063,130.80069049496));
#68120=CARTESIAN_POINT('Ctrl Pts',(18.1802003750167,-4.76405452823408,129.582490119308));
#68121=CARTESIAN_POINT('Ctrl Pts',(18.1724253847387,-4.79807537432806,129.71513688189));
#68122=CARTESIAN_POINT('Ctrl Pts',(18.1646503944607,-4.82651012511269,129.849041933792));
#68123=CARTESIAN_POINT('Ctrl Pts',(18.1568754041827,-4.84929797755833,129.983694919886));
#68124=CARTESIAN_POINT('Ctrl Pts',(18.1544460004281,-4.85641835871787,130.025769116546));
#68125=CARTESIAN_POINT('Ctrl Pts',(18.1520165966734,-4.86298779495552,130.067916315731));
#68126=CARTESIAN_POINT('Ctrl Pts',(18.1495871929188,-4.86900547391144,130.110120920112));
#68127=CARTESIAN_POINT('Ctrl Pts',(18.1364383166155,-4.90157548870386,130.338548624393));
#68128=CARTESIAN_POINT('Ctrl Pts',(18.1232894403121,-4.91807597667301,130.569320852748));
#68129=CARTESIAN_POINT('Ctrl Pts',(18.1101405640087,-4.91824863063019,130.80069049437));
#68130=CARTESIAN_POINT('Ctrl Pts',(18.1101405639752,-4.91824863063063,130.80069049496));
#68131=CARTESIAN_POINT('Ctrl Pts',(18.1024877344152,-4.91834911762773,130.935350856185));
#68132=CARTESIAN_POINT('Ctrl Pts',(18.0948349048551,-4.91291499953517,131.070222394372));
#68133=CARTESIAN_POINT('Ctrl Pts',(18.087182075295,-4.90192082362746,131.204804498013));
#68134=CARTESIAN_POINT('Ctrl Pts',(18.0795370510837,-4.89093786100716,131.339249337359));
#68135=CARTESIAN_POINT('Ctrl Pts',(18.0718920268724,-4.87440615162998,131.473404930247));
#68136=CARTESIAN_POINT('Ctrl Pts',(18.0642470026611,-4.85235227221648,131.606769795489));
#68137=CARTESIAN_POINT('Ctrl Pts',(18.0566078217135,-4.83031524907821,131.740032726971));
#68138=CARTESIAN_POINT('Ctrl Pts',(18.0489686407659,-4.80276451771623,131.872505736876));
#68139=CARTESIAN_POINT('Ctrl Pts',(18.0413294598183,-4.76977850556778,132.003692127335));
#68140=CARTESIAN_POINT('Ctrl Pts',(18.0336934871889,-4.73680634694948,132.134823421876));
#68141=CARTESIAN_POINT('Ctrl Pts',(18.0260575145595,-4.69840354306254,132.26466878065));
#68142=CARTESIAN_POINT('Ctrl Pts',(18.0184215419301,-4.65469960475385,132.392741759485));
#68143=CARTESIAN_POINT('Ctrl Pts',(18.0107870094105,-4.61100390880987,132.520790584337));
#68144=CARTESIAN_POINT('Ctrl Pts',(18.0031524768908,-4.56200919624942,132.647067312195));
#68145=CARTESIAN_POINT('Ctrl Pts',(17.9955179443712,-4.50789465898002,132.771101273077));
#68146=CARTESIAN_POINT('Ctrl Pts',(17.9878830865016,-4.45377781558775,132.895140519739));
#68147=CARTESIAN_POINT('Ctrl Pts',(17.9802482286319,-4.39454087526188,133.016936439758));
#68148=CARTESIAN_POINT('Ctrl Pts',(17.9726133707622,-4.33041069719544,133.136039466832));
#68149=CARTESIAN_POINT('Ctrl Pts',(17.9649764220151,-4.26626295647827,133.255175111387));
#68150=CARTESIAN_POINT('Ctrl Pts',(17.957339473268,-4.19721950497333,133.371616041812));
#68151=CARTESIAN_POINT('Ctrl Pts',(17.9497025245208,-4.12355226990168,133.484938864864));
#68152=CARTESIAN_POINT('Ctrl Pts',(17.942057511435,-4.04980724492238,133.598381352676));
#68153=CARTESIAN_POINT('Ctrl Pts',(17.9344124983492,-3.97142891044997,133.708698822479));
#68154=CARTESIAN_POINT('Ctrl Pts',(17.9267674852633,-3.88873164018912,133.815498158943));
#68155=CARTESIAN_POINT('Ctrl Pts',(17.9191178451733,-3.80598431892015,133.922362133749));
#68156=CARTESIAN_POINT('Ctrl Pts',(17.9114682050834,-3.71891311803668,134.025703429375));
#68157=CARTESIAN_POINT('Ctrl Pts',(17.9038185649934,-3.62787060720634,134.125164423856));
#68158=CARTESIAN_POINT('Ctrl Pts',(17.8961579427078,-3.53669739131641,134.22476820938));
#68159=CARTESIAN_POINT('Ctrl Pts',(17.8884973204221,-3.44154176957863,134.32048029062));
#68160=CARTESIAN_POINT('Ctrl Pts',(17.8808366981365,-3.34279104476289,134.411981868966));
#68161=CARTESIAN_POINT('Ctrl Pts',(17.8776043217929,-3.30112347587621,134.450590682482));
#68162=CARTESIAN_POINT('Ctrl Pts',(17.8743719454494,-3.25881621449291,134.488450374975));
#68163=CARTESIAN_POINT('Ctrl Pts',(17.8711395691059,-3.21589991007689,134.525539305948));
#68164=CARTESIAN_POINT('Ctrl Pts',(17.8633652349868,-3.11267997086588,134.614743566486));
#68165=CARTESIAN_POINT('Ctrl Pts',(17.8555909008677,-3.0055821364023,134.699791114984));
#68166=CARTESIAN_POINT('Ctrl Pts',(17.8478165667486,-2.89497550894862,134.780325892199));
#68167=CARTESIAN_POINT('Ctrl Pts',(17.8400518138015,-2.78450519427823,134.860761417498));
#68168=CARTESIAN_POINT('Ctrl Pts',(17.8322870608545,-2.67053500365993,134.936695009494));
#68169=CARTESIAN_POINT('Ctrl Pts',(17.8245223079074,-2.55346897761433,135.007809111703));
#68170=CARTESIAN_POINT('Ctrl Pts',(17.8167652670224,-2.43651922319598,135.078852582383));
#68171=CARTESIAN_POINT('Ctrl Pts',(17.8090082261374,-2.31648008437703,135.145085887524));
#68172=CARTESIAN_POINT('Ctrl Pts',(17.8012511852524,-2.19378631701284,135.206233475542));
#68173=CARTESIAN_POINT('Ctrl Pts',(17.7934999940123,-2.07118507397319,135.267334951688));
#68174=CARTESIAN_POINT('Ctrl Pts',(17.7857488027722,-1.94593353550228,135.323358170717));
#68175=CARTESIAN_POINT('Ctrl Pts',(17.7779976115321,-1.81849259756462,135.37407261452));
#68176=CARTESIAN_POINT('Ctrl Pts',(17.770249714755,-1.69110582542519,135.424765503331));
#68177=CARTESIAN_POINT('Ctrl Pts',(17.762501817978,-1.56153186711679,135.470153960414));
#68178=CARTESIAN_POINT('Ctrl Pts',(17.7547539212009,-1.43025301573231,135.510054973715));
#68179=CARTESIAN_POINT('Ctrl Pts',(17.7470076451168,-1.29900162505332,135.549947640584));
#68180=CARTESIAN_POINT('Ctrl Pts',(17.7392613690326,-1.16604642448024,135.584355033195));
#68181=CARTESIAN_POINT('Ctrl Pts',(17.7315150929485,-1.03188596265973,135.613143667628));
#68182=CARTESIAN_POINT('Ctrl Pts',(17.7237687596832,-0.897724510497346,
135.641932514572));
#68183=CARTESIAN_POINT('Ctrl Pts',(17.7160224264178,-0.762358161597664,
135.665102438548));
#68184=CARTESIAN_POINT('Ctrl Pts',(17.7082760931525,-0.626296389049847,
135.68257093443));
#68185=CARTESIAN_POINT('Ctrl Pts',(17.7005280251495,-0.490204146411083,
135.700043342262));
#68186=CARTESIAN_POINT('Ctrl Pts',(17.6927799571466,-0.353416557937074,
135.711811731549));
#68187=CARTESIAN_POINT('Ctrl Pts',(17.6850318891436,-0.216448563726812,
135.717845438115));
#68188=CARTESIAN_POINT('Ctrl Pts',(17.6772755864018,-0.079334998302549,
135.723885557376));
#68189=CARTESIAN_POINT('Ctrl Pts',(17.6695192836599,0.0579589646647878,
135.724178801485));
#68190=CARTESIAN_POINT('Ctrl Pts',(17.6617629809181,0.194917475952982,135.718746666715));
#68191=CARTESIAN_POINT('Ctrl Pts',(17.6540025384039,0.331949086122393,135.713311632651));
#68192=CARTESIAN_POINT('Ctrl Pts',(17.6462420958897,0.468644498382405,135.702145162569));
#68193=CARTESIAN_POINT('Ctrl Pts',(17.6384816533755,0.604493632667761,135.685320616435));
#68194=CARTESIAN_POINT('Ctrl Pts',(17.6307087531101,0.740560844043591,135.668469062046));
#68195=CARTESIAN_POINT('Ctrl Pts',(17.6229358528448,0.875778676816222,135.645941345472));
#68196=CARTESIAN_POINT('Ctrl Pts',(17.6151629525793,1.00964699307473,135.617862047074));
#68197=CARTESIAN_POINT('Ctrl Pts',(17.6076726168172,1.13864885884493,135.5908035019));
#68198=CARTESIAN_POINT('Ctrl Pts',(17.6001822810551,1.26639732263179,135.558590070608));
#68199=CARTESIAN_POINT('Ctrl Pts',(17.592691945293,1.39246056567462,135.521376266845));
#68200=CARTESIAN_POINT('Ctrl Pts',(17.5849176111739,1.52330353489222,135.482751490402));
#68201=CARTESIAN_POINT('Ctrl Pts',(17.5771432770548,1.65274544165364,135.438617326465));
#68202=CARTESIAN_POINT('Ctrl Pts',(17.5693689429357,1.78028721444383,135.389091852501));
#68203=CARTESIAN_POINT('Ctrl Pts',(17.5616041899886,1.90767180339761,135.339627414258));
#68204=CARTESIAN_POINT('Ctrl Pts',(17.5538394370415,2.03316055680117,135.284785026342));
#68205=CARTESIAN_POINT('Ctrl Pts',(17.5460746840944,2.15626791161973,135.22473297245));
#68206=CARTESIAN_POINT('Ctrl Pts',(17.5383176432094,2.27925299447797,135.164740563104));
#68207=CARTESIAN_POINT('Ctrl Pts',(17.5305606023244,2.39986103656915,135.099548955198));
#68208=CARTESIAN_POINT('Ctrl Pts',(17.5228035614394,2.51762521238051,135.029374978783));
#68209=CARTESIAN_POINT('Ctrl Pts',(17.5150523701992,2.63530058131066,134.959253921109));
#68210=CARTESIAN_POINT('Ctrl Pts',(17.5073011789592,2.75013601812175,134.884158172813));
#68211=CARTESIAN_POINT('Ctrl Pts',(17.499549987719,2.86168845587438,134.804350898056));
#68212=CARTESIAN_POINT('Ctrl Pts',(17.4918020909419,2.97319348086536,134.724577543519));
#68213=CARTESIAN_POINT('Ctrl Pts',(17.4840541941648,3.08141796476232,134.640096872397));
#68214=CARTESIAN_POINT('Ctrl Pts',(17.4763062973877,3.18594724314544,134.551215729042));
#68215=CARTESIAN_POINT('Ctrl Pts',(17.4685600213036,3.29045465625706,134.462353177706));
#68216=CARTESIAN_POINT('Ctrl Pts',(17.4608137452195,3.39126810365021,134.369092238131));
#68217=CARTESIAN_POINT('Ctrl Pts',(17.4530674691354,3.48800580380087,134.271780202092));
#68218=CARTESIAN_POINT('Ctrl Pts',(17.4453211358701,3.58474421804698,134.174467447717));
#68219=CARTESIAN_POINT('Ctrl Pts',(17.4375748026047,3.67740654938099,134.073103814479));
#68220=CARTESIAN_POINT('Ctrl Pts',(17.4298284693394,3.76564800125611,133.968073340481));
#68221=CARTESIAN_POINT('Ctrl Pts',(17.4220804013364,3.85390921419255,133.863019345637));
#68222=CARTESIAN_POINT('Ctrl Pts',(17.4143323333335,3.93774732619028,133.754297175296));
#68223=CARTESIAN_POINT('Ctrl Pts',(17.4065842653305,4.01685820090729,133.642323488413));
#68224=CARTESIAN_POINT('Ctrl Pts',(17.3988279625886,4.09605315560337,133.530230794562));
#68225=CARTESIAN_POINT('Ctrl Pts',(17.3910716598467,4.1705106107527,133.414880000754));
#68226=CARTESIAN_POINT('Ctrl Pts',(17.3833153571049,4.23996982267342,133.29671672481));
#68227=CARTESIAN_POINT('Ctrl Pts',(17.3755549145907,4.3094661070672,133.178490381568));
#68228=CARTESIAN_POINT('Ctrl Pts',(17.3677944720766,4.37395864883448,133.057448909983));
#68229=CARTESIAN_POINT('Ctrl Pts',(17.3600340295624,4.43323345705695,132.934061107713));
#68230=CARTESIAN_POINT('Ctrl Pts',(17.3522611292969,4.49260341846359,132.810475232389));
#68231=CARTESIAN_POINT('Ctrl Pts',(17.3444882290315,4.54673875398404,132.684535859031));
#68232=CARTESIAN_POINT('Ctrl Pts',(17.336715328766,4.59547393984774,132.556731106555));
#68233=CARTESIAN_POINT('Ctrl Pts',(17.3292249930041,4.64243747894838,132.433572378754));
#68234=CARTESIAN_POINT('Ctrl Pts',(17.3217346572422,4.68438657197599,132.308681831678));
#68235=CARTESIAN_POINT('Ctrl Pts',(17.3142443214802,4.72121780705052,132.182506285081));
#68236=CARTESIAN_POINT('Ctrl Pts',(17.3064699873611,4.75944550959783,132.051546754283));
#68237=CARTESIAN_POINT('Ctrl Pts',(17.298695653242,4.79228069993176,131.918788018494));
#68238=CARTESIAN_POINT('Ctrl Pts',(17.2909213191229,4.81955295962598,131.784713784471));
#68239=CARTESIAN_POINT('Ctrl Pts',(17.2831565661759,4.84679160869744,131.650804784959));
#68240=CARTESIAN_POINT('Ctrl Pts',(17.2753918132288,4.86848089097449,131.515583892426));
#68241=CARTESIAN_POINT('Ctrl Pts',(17.2676270602817,4.88449992961611,131.379550586255));
#68242=CARTESIAN_POINT('Ctrl Pts',(17.2598700193967,4.90050305792272,131.243652390281));
#68243=CARTESIAN_POINT('Ctrl Pts',(17.2521129785118,4.91084710463466,131.106943772206));
#68244=CARTESIAN_POINT('Ctrl Pts',(17.2443559376268,4.91546216442233,130.969934687494));
#68245=CARTESIAN_POINT('Ctrl Pts',(17.2366047463867,4.9200737439575,130.833028922399));
#68246=CARTESIAN_POINT('Ctrl Pts',(17.2288535551466,4.91896492270234,130.695823530833));
#68247=CARTESIAN_POINT('Ctrl Pts',(17.2211023639065,4.91211761961487,130.558833524216));
#68248=CARTESIAN_POINT('Ctrl Pts',(17.2133544671294,4.90527322681385,130.421901742005));
#68249=CARTESIAN_POINT('Ctrl Pts',(17.2056065703523,4.8926952226579,130.285185552329));
#68250=CARTESIAN_POINT('Ctrl Pts',(17.1978586735752,4.8744176277446,130.149199680977));
#68251=CARTESIAN_POINT('Ctrl Pts',(17.1901123974911,4.85614385611008,130.013242254937));
#68252=CARTESIAN_POINT('Ctrl Pts',(17.182366121407,4.83217291717957,129.878015230594));
#68253=CARTESIAN_POINT('Ctrl Pts',(17.1746198453229,4.80259063512115,129.744027531245));
#68254=CARTESIAN_POINT('Ctrl Pts',(17.1668735120575,4.77300813469308,129.61003884283));
#68255=CARTESIAN_POINT('Ctrl Pts',(17.1591271787923,4.737814292772,129.477289879435));
#68256=CARTESIAN_POINT('Ctrl Pts',(17.1513808455269,4.69714584053573,129.346278310137));
#68257=CARTESIAN_POINT('Ctrl Pts',(17.143632777524,4.65646828088173,129.215237401706));
#68258=CARTESIAN_POINT('Ctrl Pts',(17.135884709521,4.61031378719728,129.085935034909));
#68259=CARTESIAN_POINT('Ctrl Pts',(17.128136641518,4.55886851333777,128.958852302603));
#68260=CARTESIAN_POINT('Ctrl Pts',(17.1203803387762,4.50736856282885,128.831634505257));
#68261=CARTESIAN_POINT('Ctrl Pts',(17.1126240360344,4.45056674632708,128.706641417842));
#68262=CARTESIAN_POINT('Ctrl Pts',(17.1048677332925,4.38869703639658,128.58433327872));
#68263=CARTESIAN_POINT('Ctrl Pts',(17.0971072907783,4.32679430473895,128.461959860061));
#68264=CARTESIAN_POINT('Ctrl Pts',(17.0893468482642,4.25981848076507,128.342274586155));
#68265=CARTESIAN_POINT('Ctrl Pts',(17.08158640575,4.1880483099035,128.225710890206));
#68266=CARTESIAN_POINT('Ctrl Pts',(17.0738135054846,4.1161629271922,128.108960075864));
#68267=CARTESIAN_POINT('Ctrl Pts',(17.0660406052191,4.03946803677542,127.995341177358));
#68268=CARTESIAN_POINT('Ctrl Pts',(17.0582677049537,3.95828483728186,127.885257294721));
#68269=CARTESIAN_POINT('Ctrl Pts',(17.0507773691915,3.88005285157638,127.7791752385));
#68270=CARTESIAN_POINT('Ctrl Pts',(17.0432870334293,3.79765340667968,127.676375887157));
#68271=CARTESIAN_POINT('Ctrl Pts',(17.0357966976671,3.71140652805818,127.577187761026));
#68272=CARTESIAN_POINT('Ctrl Pts',(17.028022363548,3.62188957282146,127.474238886948));
#68273=CARTESIAN_POINT('Ctrl Pts',(17.020248029429,3.52794411089937,127.374854371873));
#68274=CARTESIAN_POINT('Ctrl Pts',(17.0124736953099,3.4298849831627,127.279439048967));
#68275=CARTESIAN_POINT('Ctrl Pts',(17.0047089423628,3.33194670453718,127.184141316919));
#68276=CARTESIAN_POINT('Ctrl Pts',(16.9969441894157,3.22990512485546,127.092803314099));
#68277=CARTESIAN_POINT('Ctrl Pts',(16.9891794364686,3.12411513338199,127.005796718423));
#68278=CARTESIAN_POINT('Ctrl Pts',(16.9814223955835,3.01843021401929,126.918876538924));
#68279=CARTESIAN_POINT('Ctrl Pts',(16.9736653546985,2.90900459175828,126.836279452103));
#68280=CARTESIAN_POINT('Ctrl Pts',(16.9659083138135,2.79622952103531,126.758339914679));
#68281=CARTESIAN_POINT('Ctrl Pts',(16.9581571225733,2.68353949486998,126.680459152066));
#68282=CARTESIAN_POINT('Ctrl Pts',(16.9504059313332,2.56750536811216,126.607229169221));
#68283=CARTESIAN_POINT('Ctrl Pts',(16.942654740093,2.44855066121156,126.53894355449));
#68284=CARTESIAN_POINT('Ctrl Pts',(16.9349068433159,2.3296465132351,126.470686962967));
#68285=CARTESIAN_POINT('Ctrl Pts',(16.9271589465388,2.20782459237548,126.407370754093));
#68286=CARTESIAN_POINT('Ctrl Pts',(16.9194110497617,2.08353634098049,126.349244527236));
#68287=CARTESIAN_POINT('Ctrl Pts',(16.9116647736776,1.95927408800835,126.291130459134));
#68288=CARTESIAN_POINT('Ctrl Pts',(16.9039184975935,1.8325468845856,126.238204379187));
#68289=CARTESIAN_POINT('Ctrl Pts',(16.8961722215094,1.70382929235474,126.190669166568));
#68290=CARTESIAN_POINT('Ctrl Pts',(16.8884258882441,1.57511074996057,126.143133603054));
#68291=CARTESIAN_POINT('Ctrl Pts',(16.8806795549787,1.4444021561953,126.100989121716));
#68292=CARTESIAN_POINT('Ctrl Pts',(16.8729332217134,1.31219612068867,126.064389689032));
#68293=CARTESIAN_POINT('Ctrl Pts',(16.8651851537104,1.17996047855685,126.027782060158));
#68294=CARTESIAN_POINT('Ctrl Pts',(16.8574370857075,1.0462271041137,125.996722055219));
#68295=CARTESIAN_POINT('Ctrl Pts',(16.8496890177045,0.911501375113033,125.971313100143));
#68296=CARTESIAN_POINT('Ctrl Pts',(16.8419327149626,0.776632458003775,125.945877140128));
#68297=CARTESIAN_POINT('Ctrl Pts',(16.8341764122207,0.640769464292466,125.926104300189));
#68298=CARTESIAN_POINT('Ctrl Pts',(16.8264201094789,0.504426073432944,125.912046502657));
#68299=CARTESIAN_POINT('Ctrl Pts',(16.8186596669647,0.368009912000501,125.897981202055));
#68300=CARTESIAN_POINT('Ctrl Pts',(16.8108992244505,0.23111323256635,125.889637045597));
#68301=CARTESIAN_POINT('Ctrl Pts',(16.8031387819363,0.0942513634745103,
125.887013798093));
#68302=CARTESIAN_POINT('Ctrl Pts',(16.7953658816709,-0.042830208439435,
125.884386339519));
#68303=CARTESIAN_POINT('Ctrl Pts',(16.7875929814055,-0.179876467254304,
125.887498133001));
#68304=CARTESIAN_POINT('Ctrl Pts',(16.77982008114,-0.316374657790517,125.896296830449));
#68305=CARTESIAN_POINT('Ctrl Pts',(16.7723297453781,-0.447910795280879,
125.904775673083));
#68306=CARTESIAN_POINT('Ctrl Pts',(16.7648394096162,-0.578937713675355,
125.918535099333));
#68307=CARTESIAN_POINT('Ctrl Pts',(16.7573490738542,-0.709006037930606,
125.937483435976));
#68308=CARTESIAN_POINT('Ctrl Pts',(16.7495747397352,-0.844005942235119,
125.957150204563));
#68309=CARTESIAN_POINT('Ctrl Pts',(16.7418004056161,-0.978400766397726,
125.982469424352));
#68310=CARTESIAN_POINT('Ctrl Pts',(16.734026071497,-1.11167973362992,126.013395033017));
#68311=CARTESIAN_POINT('Ctrl Pts',(16.7262613185499,-1.24479444644594,126.044282528632));
#68312=CARTESIAN_POINT('Ctrl Pts',(16.7184965656028,-1.37679566136668,126.080762578007));
#68313=CARTESIAN_POINT('Ctrl Pts',(16.7107318126558,-1.50717884891897,126.122737503744));
#68314=CARTESIAN_POINT('Ctrl Pts',(16.7029747717708,-1.63743253805147,126.164670739394));
#68315=CARTESIAN_POINT('Ctrl Pts',(16.6952177308858,-1.76607102816584,126.212087871524));
#68316=CARTESIAN_POINT('Ctrl Pts',(16.6874606900008,-1.89260144877294,126.264840508722));
#68317=CARTESIAN_POINT('Ctrl Pts',(16.6797094987607,-2.01903645180526,126.317553364745));
#68318=CARTESIAN_POINT('Ctrl Pts',(16.6719583075206,-2.14336619015607,126.375593567374));
#68319=CARTESIAN_POINT('Ctrl Pts',(16.6642071162805,-2.26511473648712,126.43876348853));
#68320=CARTESIAN_POINT('Ctrl Pts',(16.6564592195034,-2.38681153643872,126.501906560785));
#68321=CARTESIAN_POINT('Ctrl Pts',(16.6487113227264,-2.50592898006322,126.570174835499));
#68322=CARTESIAN_POINT('Ctrl Pts',(16.6409634259493,-2.62201305672604,126.643323415995));
#68323=CARTESIAN_POINT('Ctrl Pts',(16.6332171498652,-2.73807285110251,126.716456695385));
#68324=CARTESIAN_POINT('Ctrl Pts',(16.6254708737811,-2.85110021003967,126.794468041723));
#68325=CARTESIAN_POINT('Ctrl Pts',(16.617724597697,-2.96066793338639,126.877067854005));
#68326=CARTESIAN_POINT('Ctrl Pts',(16.6099782644316,-3.0702364655376,126.959668276021));
#68327=CARTESIAN_POINT('Ctrl Pts',(16.6022319311663,-3.17634499894735,127.046856996216));
#68328=CARTESIAN_POINT('Ctrl Pts',(16.5944855979009,-3.27859772971845,127.138302790801));
#68329=CARTESIAN_POINT('Ctrl Pts',(16.5867375298979,-3.38087335927908,127.229769064037));
#68330=CARTESIAN_POINT('Ctrl Pts',(16.578989461895,-3.47929117660609,127.325494048129));
#68331=CARTESIAN_POINT('Ctrl Pts',(16.571241393892,-3.57349099751393,127.425108458702));
#68332=CARTESIAN_POINT('Ctrl Pts',(16.5634850911501,-3.66779093511267,127.524828740656));
#68333=CARTESIAN_POINT('Ctrl Pts',(16.5557287884083,-3.75786365208871,127.628446422139));
#68334=CARTESIAN_POINT('Ctrl Pts',(16.5479724856665,-3.84338780842195,127.735557395368));
#68335=CARTESIAN_POINT('Ctrl Pts',(16.5402120431523,-3.92895761157227,127.842725536948));
#68336=CARTESIAN_POINT('Ctrl Pts',(16.5324516006381,-4.00997378584083,127.953390370087));
#68337=CARTESIAN_POINT('Ctrl Pts',(16.524691158124,-4.0861579815411,128.067118207331));
#68338=CARTESIAN_POINT('Ctrl Pts',(16.5169182578585,-4.16246447487574,128.181028610596));
#68339=CARTESIAN_POINT('Ctrl Pts',(16.5091453575931,-4.23392328531967,128.298011509875));
#68340=CARTESIAN_POINT('Ctrl Pts',(16.5013724573277,-4.300301298103,128.417607214293));
#68341=CARTESIAN_POINT('Ctrl Pts',(16.4938821215656,-4.36426630292633,128.532855313614));
#68342=CARTESIAN_POINT('Ctrl Pts',(16.4863917858034,-4.42351335783911,128.650529276918));
#68343=CARTESIAN_POINT('Ctrl Pts',(16.4789014500413,-4.47787669193268,128.770201480638));
#68344=CARTESIAN_POINT('Ctrl Pts',(16.4704079154249,-4.5395210393493,128.905901673153));
#68345=CARTESIAN_POINT('Ctrl Pts',(16.4619143808085,-4.59505545712627,129.044543350627));
#68346=CARTESIAN_POINT('Ctrl Pts',(16.4534208461921,-4.64421539216793,129.185581307823));
#68347=CARTESIAN_POINT('Ctrl Pts',(16.4455676629748,-4.68966902181364,129.315986017817));
#68348=CARTESIAN_POINT('Ctrl Pts',(16.4377144797573,-4.72967346533817,129.448438876883));
#68349=CARTESIAN_POINT('Ctrl Pts',(16.4298612965399,-4.76405452823409,129.582490119308));
#68350=CARTESIAN_POINT('Origin',(213.235140564004,0.,130.804360617566));
#68351=CARTESIAN_POINT('',(14.334952816073,-4.76405452823406,129.582490119308));
#68352=CARTESIAN_POINT('',(14.6800959310997,-4.76405452823407,129.582490119308));
#68353=CARTESIAN_POINT('',(213.235140564004,-4.76405452823405,129.582490119308));
#68354=CARTESIAN_POINT('',(16.0148594359499,-4.91824793335368,130.808869338258));
#68355=CARTESIAN_POINT('Ctrl Pts',(16.0148594359499,-4.91824793335368,130.808869338258));
#68356=CARTESIAN_POINT('Ctrl Pts',(16.0050887965409,-4.91808964415007,130.981535955167));
#68357=CARTESIAN_POINT('Ctrl Pts',(15.9953181571318,-4.90883501695725,131.153795784248));
#68358=CARTESIAN_POINT('Ctrl Pts',(15.9855475177229,-4.89063364109632,131.324827380267));
#68359=CARTESIAN_POINT('Ctrl Pts',(15.9755880421458,-4.87208048906916,131.499164486794));
#68360=CARTESIAN_POINT('Ctrl Pts',(15.9656285665686,-4.84423143683517,131.672225602518));
#68361=CARTESIAN_POINT('Ctrl Pts',(15.9556690909914,-4.80729321664908,131.843165215005));
#68362=CARTESIAN_POINT('Ctrl Pts',(15.9509777935192,-4.78989388897932,131.923684371434));
#68363=CARTESIAN_POINT('Ctrl Pts',(15.9462864960471,-4.77047856592294,132.003733145737));
#68364=CARTESIAN_POINT('Ctrl Pts',(15.9415951985749,-4.74907247945354,132.08322481966));
#68365=CARTESIAN_POINT('Ctrl Pts',(15.9338208644558,-4.71359869647948,132.214956997469));
#68366=CARTESIAN_POINT('Ctrl Pts',(15.9260465303367,-4.67258349094273,132.345420726402));
#68367=CARTESIAN_POINT('Ctrl Pts',(15.9182721962176,-4.62613292996776,132.474114245131));
#68368=CARTESIAN_POINT('Ctrl Pts',(15.9105074432705,-4.57973961515778,132.6026491606));
#68369=CARTESIAN_POINT('Ctrl Pts',(15.9027426903235,-4.52792440456582,132.729417842436));
#68370=CARTESIAN_POINT('Ctrl Pts',(15.8949779373764,-4.47084388125271,132.85393082909));
#68371=CARTESIAN_POINT('Ctrl Pts',(15.8872208964914,-4.41382005112021,132.978320147689));
#68372=CARTESIAN_POINT('Ctrl Pts',(15.8794638556063,-4.35154147724408,133.100457876481));
#68373=CARTESIAN_POINT('Ctrl Pts',(15.8717068147214,-4.28421372470851,133.219872121062));
#68374=CARTESIAN_POINT('Ctrl Pts',(15.8639556234813,-4.21693674455496,133.339196314432));
#68375=CARTESIAN_POINT('Ctrl Pts',(15.8562044322412,-4.14461835582714,133.455800772371));
#68376=CARTESIAN_POINT('Ctrl Pts',(15.8484532410011,-4.06751101451575,133.569236240319));
#68377=CARTESIAN_POINT('Ctrl Pts',(15.840705344224,-3.9904364458811,133.682623495167));
#68378=CARTESIAN_POINT('Ctrl Pts',(15.832957447447,-3.90857719231051,133.792844116254));
#68379=CARTESIAN_POINT('Ctrl Pts',(15.8252095506699,-3.82223005899156,133.899476195156));
#68380=CARTESIAN_POINT('Ctrl Pts',(15.8174632745858,-3.73590098763136,134.006085968926));
#68381=CARTESIAN_POINT('Ctrl Pts',(15.8097169985016,-3.64508614966657,134.109108389938));
#68382=CARTESIAN_POINT('Ctrl Pts',(15.8019707224175,-3.55012357515833,134.208153452567));
#68383=CARTESIAN_POINT('Ctrl Pts',(15.7942243891522,-3.45516029965794,134.307199246324));
#68384=CARTESIAN_POINT('Ctrl Pts',(15.7864780558868,-3.35604949709565,134.402267340904));
#68385=CARTESIAN_POINT('Ctrl Pts',(15.7787317226215,-3.25316682081566,134.493003823197));
#68386=CARTESIAN_POINT('Ctrl Pts',(15.7709836546185,-3.15026110467366,134.583760625295));
#68387=CARTESIAN_POINT('Ctrl Pts',(15.7632355866155,-3.04358212715293,134.670183626296));
#68388=CARTESIAN_POINT('Ctrl Pts',(15.7554875186125,-2.93353912878493,134.751958778776));
#68389=CARTESIAN_POINT('Ctrl Pts',(15.7477312158707,-2.82337917540874,134.833820842861));
#68390=CARTESIAN_POINT('Ctrl Pts',(15.7399749131288,-2.70984837340149,134.911024957097));
#68391=CARTESIAN_POINT('Ctrl Pts',(15.732218610387,-2.59338595512761,134.983299759292));
#68392=CARTESIAN_POINT('Ctrl Pts',(15.7244581678728,-2.47686137735449,135.055613136724));
#68393=CARTESIAN_POINT('Ctrl Pts',(15.7166977253586,-2.35740240589971,135.122991767803));
#68394=CARTESIAN_POINT('Ctrl Pts',(15.7089372828445,-2.23547256822738,135.185210473382));
#68395=CARTESIAN_POINT('Ctrl Pts',(15.701164382579,-2.11334699795519,135.247529057951));
#68396=CARTESIAN_POINT('Ctrl Pts',(15.6933914823136,-1.98874299080975,135.30467100154));
#68397=CARTESIAN_POINT('Ctrl Pts',(15.6856185820482,-1.8621445530286,135.356459114537));
#68398=CARTESIAN_POINT('Ctrl Pts',(15.6781282462862,-1.74014828734301,135.406364599181));
#68399=CARTESIAN_POINT('Ctrl Pts',(15.6706379105241,-1.61630036822402,135.451298640675));
#68400=CARTESIAN_POINT('Ctrl Pts',(15.6631475747621,-1.49104500515247,135.491147134478));
#68401=CARTESIAN_POINT('Ctrl Pts',(15.655373240643,-1.3610405469197,135.532506496036));
#68402=CARTESIAN_POINT('Ctrl Pts',(15.647598906524,-1.22910799639871,135.568518074249));
#68403=CARTESIAN_POINT('Ctrl Pts',(15.6398245724049,-1.09572683147738,135.598999892139));
#68404=CARTESIAN_POINT('Ctrl Pts',(15.6320598194578,-0.962510046921385,
135.629444143913));
#68405=CARTESIAN_POINT('Ctrl Pts',(15.6242950665107,-0.827848577635766,
135.654372108789));
#68406=CARTESIAN_POINT('Ctrl Pts',(15.6165303135637,-0.692238858453363,
135.673650958606));
#68407=CARTESIAN_POINT('Ctrl Pts',(15.6087732726787,-0.55676382875563,135.692910660398));
#68408=CARTESIAN_POINT('Ctrl Pts',(15.6010162317937,-0.42034280798432,135.706532358167));
#68409=CARTESIAN_POINT('Ctrl Pts',(15.5932591909087,-0.283483927213691,
135.714433929189));
#68410=CARTESIAN_POINT('Ctrl Pts',(15.5855079996685,-0.146728252789657,
135.722329541575));
#68411=CARTESIAN_POINT('Ctrl Pts',(15.5777568084284,-0.0095357643326108,
135.724513590713));
#68412=CARTESIAN_POINT('Ctrl Pts',(15.5700056171883,0.127579108941926,135.720955641916));
#68413=CARTESIAN_POINT('Ctrl Pts',(15.5622577204112,0.264635704737663,135.717399205341));
#68414=CARTESIAN_POINT('Ctrl Pts',(15.5545098236341,0.401614360947145,135.708105634924));
#68415=CARTESIAN_POINT('Ctrl Pts',(15.5467619268571,0.537999683609464,135.693096589465));
#68416=CARTESIAN_POINT('Ctrl Pts',(15.539015650773,0.674356477402409,135.678090683574));
#68417=CARTESIAN_POINT('Ctrl Pts',(15.5312693746889,0.810119796142087,135.657371723404));
#68418=CARTESIAN_POINT('Ctrl Pts',(15.5235230986048,0.944778803545363,135.631013295652));
#68419=CARTESIAN_POINT('Ctrl Pts',(15.5157767653395,1.07943880497084,135.604654673327));
#68420=CARTESIAN_POINT('Ctrl Pts',(15.5080304320742,1.21299409510976,135.572656575456));
#68421=CARTESIAN_POINT('Ctrl Pts',(15.5002840988088,1.34494386703139,135.535143751153));
#68422=CARTESIAN_POINT('Ctrl Pts',(15.4925360308058,1.47692318818957,135.497622526114));
#68423=CARTESIAN_POINT('Ctrl Pts',(15.4847879628029,1.60729589968721,135.454584224061));
#68424=CARTESIAN_POINT('Ctrl Pts',(15.4770398947999,1.73557658002847,135.406203400339));
#68425=CARTESIAN_POINT('Ctrl Pts',(15.4692835920581,1.86399359860336,135.357771156901));
#68426=CARTESIAN_POINT('Ctrl Pts',(15.4615272893162,1.99031377807332,135.303985187373));
#68427=CARTESIAN_POINT('Ctrl Pts',(15.4537709865743,2.11407139791809,135.245068352489));
#68428=CARTESIAN_POINT('Ctrl Pts',(15.4460105440602,2.23789507093084,135.186120071916));
#68429=CARTESIAN_POINT('Ctrl Pts',(15.438250101546,2.35915311353804,135.12203565189));
#68430=CARTESIAN_POINT('Ctrl Pts',(15.4304896590318,2.47740552823067,135.053083356366));
#68431=CARTESIAN_POINT('Ctrl Pts',(15.4227167587664,2.59584777219731,134.984020372495));
#68432=CARTESIAN_POINT('Ctrl Pts',(15.414943858501,2.71127441716679,134.910074108594));
#68433=CARTESIAN_POINT('Ctrl Pts',(15.4071709582356,2.82327477130643,134.831555997505));
#68434=CARTESIAN_POINT('Ctrl Pts',(15.3996806224735,2.93120363046228,134.755892217529));
#68435=CARTESIAN_POINT('Ctrl Pts',(15.3921902867114,3.03595073760808,134.675983402621));
#68436=CARTESIAN_POINT('Ctrl Pts',(15.3846999509493,3.13717998728614,134.592141602506));
#68437=CARTESIAN_POINT('Ctrl Pts',(15.3769256168302,3.24224737473282,134.505120915057));
#68438=CARTESIAN_POINT('Ctrl Pts',(15.3691512827111,3.34385770157291,134.413587461436));
#68439=CARTESIAN_POINT('Ctrl Pts',(15.361376948592,3.4415986959103,134.317846276966));
#68440=CARTESIAN_POINT('Ctrl Pts',(15.3536121956449,3.53921923320752,134.222223084949));
#68441=CARTESIAN_POINT('Ctrl Pts',(15.3458474426978,3.63297964949225,134.122402750943));
#68442=CARTESIAN_POINT('Ctrl Pts',(15.3380826897507,3.72249985751884,134.018731142766));
#68443=CARTESIAN_POINT('Ctrl Pts',(15.3303256488657,3.81193115281268,133.915162502692));
#68444=CARTESIAN_POINT('Ctrl Pts',(15.3225686079807,3.89713036692762,133.807750494645));
#68445=CARTESIAN_POINT('Ctrl Pts',(15.3148115670957,3.97775375043304,133.696878234352));
#68446=CARTESIAN_POINT('Ctrl Pts',(15.3070603758556,4.05831633521779,133.586089583692));
#68447=CARTESIAN_POINT('Ctrl Pts',(15.2993091846155,4.13430972873748,133.471846189568));
#68448=CARTESIAN_POINT('Ctrl Pts',(15.2915579933754,4.20543026386955,133.354564405154));
#68449=CARTESIAN_POINT('Ctrl Pts',(15.2838100965983,4.27652057087708,133.237332468627));
#68450=CARTESIAN_POINT('Ctrl Pts',(15.2760621998212,4.34274193644835,133.117065043902));
#68451=CARTESIAN_POINT('Ctrl Pts',(15.2683143030441,4.40383399972079,132.994207453626));
#68452=CARTESIAN_POINT('Ctrl Pts',(15.26056802696,4.4649132838506,132.871375562509));
#68453=CARTESIAN_POINT('Ctrl Pts',(15.2528217508759,4.52086522585035,132.745954933376));
#68454=CARTESIAN_POINT('Ctrl Pts',(15.2450754747918,4.57147561680339,132.618415122666));
#68455=CARTESIAN_POINT('Ctrl Pts',(15.2373291415264,4.62208638135077,132.490874370485));
#68456=CARTESIAN_POINT('Ctrl Pts',(15.229582808261,4.66735537196735,132.361214768913));
#68457=CARTESIAN_POINT('Ctrl Pts',(15.2218364749957,4.70711684523941,132.229925090946));
#68458=CARTESIAN_POINT('Ctrl Pts',(15.2140884069927,4.74688722281772,132.098606011567));
#68459=CARTESIAN_POINT('Ctrl Pts',(15.2063403389898,4.78114751548703,131.965656503508));
#68460=CARTESIAN_POINT('Ctrl Pts',(15.1985922709868,4.80978219942763,131.83157931705));
#68461=CARTESIAN_POINT('Ctrl Pts',(15.190835968245,4.83844731665112,131.697359631762));
#68462=CARTESIAN_POINT('Ctrl Pts',(15.1830796655031,4.86147479973481,131.562010256876));
#68463=CARTESIAN_POINT('Ctrl Pts',(15.1753233627613,4.87880041440905,131.426043477923));
#68464=CARTESIAN_POINT('Ctrl Pts',(15.1675629202471,4.89613527628551,131.290004129407));
#68465=CARTESIAN_POINT('Ctrl Pts',(15.1598024777329,4.9077621726739,131.153347109582));
#68466=CARTESIAN_POINT('Ctrl Pts',(15.1520420352187,4.91366897223597,131.016587604035));
#68467=CARTESIAN_POINT('Ctrl Pts',(15.1442691349533,4.91958525391707,130.879608559988));
#68468=CARTESIAN_POINT('Ctrl Pts',(15.1364962346879,4.91976308888877,130.742527092646));
#68469=CARTESIAN_POINT('Ctrl Pts',(15.1287233344224,4.91424250545409,130.605857065738));
#68470=CARTESIAN_POINT('Ctrl Pts',(15.1212329986604,4.90892260913278,130.47415533856));
#68471=CARTESIAN_POINT('Ctrl Pts',(15.1137426628984,4.89831143001804,130.342835964388));
#68472=CARTESIAN_POINT('Ctrl Pts',(15.1062523271364,4.88248983117134,130.212350388762));
#68473=CARTESIAN_POINT('Ctrl Pts',(15.0984779930173,4.86606835159545,130.076917412876));
#68474=CARTESIAN_POINT('Ctrl Pts',(15.0907036588982,4.84398152832882,129.94195369964));
#68475=CARTESIAN_POINT('Ctrl Pts',(15.0829293247791,4.81626315319903,129.807970984121));
#68476=CARTESIAN_POINT('Ctrl Pts',(15.075164571832,4.78857893848932,129.674153390324));
#68477=CARTESIAN_POINT('Ctrl Pts',(15.0673998188849,4.75527705965809,129.541314767893));
#68478=CARTESIAN_POINT('Ctrl Pts',(15.0596350659378,4.71644305865732,129.409961844997));
#68479=CARTESIAN_POINT('Ctrl Pts',(15.0518780250528,4.67764762813387,129.278739383675));
#68480=CARTESIAN_POINT('Ctrl Pts',(15.0441209841679,4.63333112003381,129.14900005784));
#68481=CARTESIAN_POINT('Ctrl Pts',(15.0363639432829,4.58363005550378,129.02124015703));
#68482=CARTESIAN_POINT('Ctrl Pts',(15.0286127520428,4.53396647093312,128.893576600955));
#68483=CARTESIAN_POINT('Ctrl Pts',(15.0208615608026,4.47892655335453,128.767889861668));
#68484=CARTESIAN_POINT('Ctrl Pts',(15.0131103695625,4.41869645298907,128.644660471981));
#68485=CARTESIAN_POINT('Ctrl Pts',(15.0053624727854,4.35849195202295,128.521483458071));
#68486=CARTESIAN_POINT('Ctrl Pts',(14.9976145760083,4.29310182708948,128.400762066971));
#68487=CARTESIAN_POINT('Ctrl Pts',(14.9898666792312,4.22276000933783,128.282956055415));
#68488=CARTESIAN_POINT('Ctrl Pts',(14.9821204031471,4.15243290557807,128.165174686337));
#68489=CARTESIAN_POINT('Ctrl Pts',(14.974374127063,4.07715636954441,128.050307819276));
#68490=CARTESIAN_POINT('Ctrl Pts',(14.9666278509789,3.99720966721641,127.938789480984));
#68491=CARTESIAN_POINT('Ctrl Pts',(14.9588815177135,3.91726237474002,127.82727031949));
#68492=CARTESIAN_POINT('Ctrl Pts',(14.9511351844482,3.83264507497081,127.719100053837));
#68493=CARTESIAN_POINT('Ctrl Pts',(14.9433888511829,3.74367939811231,127.614682322401));
#68494=CARTESIAN_POINT('Ctrl Pts',(14.9356407831799,3.65469379800732,127.510241207337));
#68495=CARTESIAN_POINT('Ctrl Pts',(14.927892715177,3.56135813659362,127.409554596234));
#68496=CARTESIAN_POINT('Ctrl Pts',(14.920144647174,3.4640329484743,127.312991431361));
#68497=CARTESIAN_POINT('Ctrl Pts',(14.9123883444322,3.36660432198686,127.216325638006));
#68498=CARTESIAN_POINT('Ctrl Pts',(14.9046320416903,3.26517797668552,127.123792321097));
#68499=CARTESIAN_POINT('Ctrl Pts',(14.8968757389485,3.16015019270701,127.035722425588));
#68500=CARTESIAN_POINT('Ctrl Pts',(14.8891152964343,3.05506635223773,126.947605524524));
#68501=CARTESIAN_POINT('Ctrl Pts',(14.8813548539201,2.94637755263178,126.863957030053));
#68502=CARTESIAN_POINT('Ctrl Pts',(14.8735944114059,2.8345106768289,126.785065619007));
#68503=CARTESIAN_POINT('Ctrl Pts',(14.8658215111405,2.72246422238591,126.706047564464));
#68504=CARTESIAN_POINT('Ctrl Pts',(14.8580486108751,2.60722982570853,126.631802065367));
#68505=CARTESIAN_POINT('Ctrl Pts',(14.8502757106096,2.48926145118047,126.562573200667));
#68506=CARTESIAN_POINT('Ctrl Pts',(14.8427853748476,2.3755815242106,126.495860979575));
#68507=CARTESIAN_POINT('Ctrl Pts',(14.8352950390855,2.25936321405745,126.433807135694));
#68508=CARTESIAN_POINT('Ctrl Pts',(14.8278047033235,2.14103004309853,126.376587653982));
#68509=CARTESIAN_POINT('Ctrl Pts',(14.8200303692044,2.01821023399662,126.317198678228));
#68510=CARTESIAN_POINT('Ctrl Pts',(14.8122560350853,1.8927229722042,126.262829764498));
#68511=CARTESIAN_POINT('Ctrl Pts',(14.8044817009662,1.7650170602338,126.213729088072));
#68512=CARTESIAN_POINT('Ctrl Pts',(14.7967169480191,1.63746853438632,126.164688923842));
#68513=CARTESIAN_POINT('Ctrl Pts',(14.788952195072,1.50770716019783,126.120904217473));
#68514=CARTESIAN_POINT('Ctrl Pts',(14.7811874421249,1.37620549994302,126.082576899052));
#68515=CARTESIAN_POINT('Ctrl Pts',(14.7734304012399,1.24483444899121,126.044287647864));
#68516=CARTESIAN_POINT('Ctrl Pts',(14.7656733603549,1.11172692463833,126.011445106564));
#68517=CARTESIAN_POINT('Ctrl Pts',(14.7579163194699,0.977374262343983,125.984202672663));
#68518=CARTESIAN_POINT('Ctrl Pts',(14.7501651282298,0.8431229164372,125.956980782494));
#68519=CARTESIAN_POINT('Ctrl Pts',(14.7424139369897,0.707628683165423,125.935350671311));
#68520=CARTESIAN_POINT('Ctrl Pts',(14.7346627457496,0.571396467134131,125.919415465382));
#68521=CARTESIAN_POINT('Ctrl Pts',(14.7269148489725,0.435222153428951,125.903487032341));
#68522=CARTESIAN_POINT('Ctrl Pts',(14.7191669521954,0.29831086831951,125.893248735718));
#68523=CARTESIAN_POINT('Ctrl Pts',(14.7114190554183,0.161175863668773,125.888752272359));
#68524=CARTESIAN_POINT('Ctrl Pts',(14.7036727793342,0.0240695447047199,
125.884256749563));
#68525=CARTESIAN_POINT('Ctrl Pts',(14.6959265032501,-0.113260010210574,
125.885500683844));
#68526=CARTESIAN_POINT('Ctrl Pts',(14.688180227166,-0.250296691993672,125.892483722887));
#68527=CARTESIAN_POINT('Ctrl Pts',(14.6804338939007,-0.387334385350425,
125.899466813478));
#68528=CARTESIAN_POINT('Ctrl Pts',(14.6726875606354,-0.524078810802432,
125.91218907347));
#68529=CARTESIAN_POINT('Ctrl Pts',(14.66494122737,-0.660016526973496,125.930598082663));
#68530=CARTESIAN_POINT('Ctrl Pts',(14.657193159367,-0.79598468545357,125.949011214427));
#68531=CARTESIAN_POINT('Ctrl Pts',(14.649445091364,-0.931145387811661,125.973113577069));
#68532=CARTESIAN_POINT('Ctrl Pts',(14.641697023361,-1.06499335470903,126.002801264926));
#68533=CARTESIAN_POINT('Ctrl Pts',(14.6339407206192,-1.19898357681844,126.032520505211));
#68534=CARTESIAN_POINT('Ctrl Pts',(14.6261844178773,-1.33165789412531,126.067836844015));
#68535=CARTESIAN_POINT('Ctrl Pts',(14.6184281151355,-1.46252367417283,126.108595763468));
#68536=CARTESIAN_POINT('Ctrl Pts',(14.6106676726213,-1.59345930122745,126.149376437183));
#68537=CARTESIAN_POINT('Ctrl Pts',(14.6029072301072,-1.72258409973279,126.195605348029));
#68538=CARTESIAN_POINT('Ctrl Pts',(14.5951467875931,-1.84942445703835,126.247079384176));
#68539=CARTESIAN_POINT('Ctrl Pts',(14.5873738873276,-1.97646842974598,126.298636051016));
#68540=CARTESIAN_POINT('Ctrl Pts',(14.5796009870622,-2.10122027703923,126.355454506739));
#68541=CARTESIAN_POINT('Ctrl Pts',(14.5718280867967,-2.22322926954491,126.417284748888));
#68542=CARTESIAN_POINT('Ctrl Pts',(14.5643377510347,-2.34080292785123,126.476867305994));
#68543=CARTESIAN_POINT('Ctrl Pts',(14.5568474152726,-2.4558294195921,126.541103443432));
#68544=CARTESIAN_POINT('Ctrl Pts',(14.5493570795106,-2.56793175944869,126.609731964));
#68545=CARTESIAN_POINT('Ctrl Pts',(14.5415814403922,-2.68430402455614,126.680974512547));
#68546=CARTESIAN_POINT('Ctrl Pts',(14.5338058012739,-2.79789365806825,126.757176396579));
#68547=CARTESIAN_POINT('Ctrl Pts',(14.5260301621556,-2.90824904890265,126.838094044067));
#68548=CARTESIAN_POINT('Ctrl Pts',(14.5180686060688,-3.02124305752823,126.920946447461));
#68549=CARTESIAN_POINT('Ctrl Pts',(14.510107049982,-3.13084582219223,127.008742832104));
#68550=CARTESIAN_POINT('Ctrl Pts',(14.5021454938952,-3.23659923655579,127.101171661487));
#68551=CARTESIAN_POINT('Ctrl Pts',(14.4943893526811,-3.33962412349214,127.191215748991));
#68552=CARTESIAN_POINT('Ctrl Pts',(14.486633211467,-3.43899551995466,127.285655914357));
#68553=CARTESIAN_POINT('Ctrl Pts',(14.4788770702529,-3.53431973952729,127.384160763568));
#68554=CARTESIAN_POINT('Ctrl Pts',(14.4711262677283,-3.62957834575012,127.482597810146));
#68555=CARTESIAN_POINT('Ctrl Pts',(14.4633754652037,-3.72079504694466,127.585093694297));
#68556=CARTESIAN_POINT('Ctrl Pts',(14.455624662679,-3.80761114440574,127.691278473533));
#68557=CARTESIAN_POINT('Ctrl Pts',(14.4478775165418,-3.89438628697464,127.797413160835));
#68558=CARTESIAN_POINT('Ctrl Pts',(14.4401303704045,-3.97676471054156,127.907232977849));
#68559=CARTESIAN_POINT('Ctrl Pts',(14.4323832242672,-4.05442661119648,128.02033333377));
#68560=CARTESIAN_POINT('Ctrl Pts',(14.4242640235843,-4.13581820310089,128.13886530293));
#68561=CARTESIAN_POINT('Ctrl Pts',(14.4161448229015,-4.21202872068971,128.261000375865));
#68562=CARTESIAN_POINT('Ctrl Pts',(14.4080256222186,-4.28273977518678,128.38623674139));
#68563=CARTESIAN_POINT('Ctrl Pts',(14.4002789357348,-4.35020656059208,128.50572718115));
#68564=CARTESIAN_POINT('Ctrl Pts',(14.3925322492509,-4.41266711117819,128.628040287164));
#68565=CARTESIAN_POINT('Ctrl Pts',(14.3847855627671,-4.46989140568988,128.752713990137));
#68566=CARTESIAN_POINT('Ctrl Pts',(14.3770377993638,-4.52712365533874,128.877405024847));
#68567=CARTESIAN_POINT('Ctrl Pts',(14.3692900359605,-4.57911804373872,129.004456951509));
#68568=CARTESIAN_POINT('Ctrl Pts',(14.3615422725572,-4.62569249797559,129.133387255518));
#68569=CARTESIAN_POINT('Ctrl Pts',(14.3537897751549,-4.67229540989897,129.262396337868));
#68570=CARTESIAN_POINT('Ctrl Pts',(14.3460372777525,-4.71347165420832,129.393285717809));
#68571=CARTESIAN_POINT('Ctrl Pts',(14.3382847803502,-4.749088862512,129.525557255643));
#68572=CARTESIAN_POINT('Ctrl Pts',(14.3371741255911,-4.75419153070459,129.544507021811));
#68573=CARTESIAN_POINT('Ctrl Pts',(14.336063470832,-4.75918018708975,129.563485137165));
#68574=CARTESIAN_POINT('Ctrl Pts',(14.334952816073,-4.76405452823406,129.582490119308));
#68575=CARTESIAN_POINT('Ctrl Pts',(16.0848513025106,-4.7640545282341,129.582490119308));
#68576=CARTESIAN_POINT('Ctrl Pts',(16.0771840538337,-4.79781676096018,129.714128552294));
#68577=CARTESIAN_POINT('Ctrl Pts',(16.0695168051568,-4.82611756725086,129.847162936191));
#68578=CARTESIAN_POINT('Ctrl Pts',(16.0618495564799,-4.84885740150383,129.981095798458));
#68579=CARTESIAN_POINT('Ctrl Pts',(16.0540178697318,-4.87208493279666,130.11790109417));
#68580=CARTESIAN_POINT('Ctrl Pts',(16.0461861829837,-4.88951015732492,130.255643418976));
#68581=CARTESIAN_POINT('Ctrl Pts',(16.0383544962356,-4.90108262611967,130.393785223213));
#68582=CARTESIAN_POINT('Ctrl Pts',(16.0305228094875,-4.91265509491442,130.53192702745));
#68583=CARTESIAN_POINT('Ctrl Pts',(16.0226911227394,-4.91837481054274,130.670467867685));
#68584=CARTESIAN_POINT('Ctrl Pts',(16.0148594359913,-4.91824793335435,130.808869337526));
#68585=CARTESIAN_POINT('',(16.360140564049,-4.91824961586008,130.802416757441));
#68586=CARTESIAN_POINT('Ctrl Pts',(16.4298612965399,-4.76405452823409,129.582490119308));
#68587=CARTESIAN_POINT('Ctrl Pts',(16.4214087741111,-4.80105948497718,129.726771884021));
#68588=CARTESIAN_POINT('Ctrl Pts',(16.4129562516822,-4.83154930639298,129.872905341603));
#68589=CARTESIAN_POINT('Ctrl Pts',(16.4045037292534,-4.85535239555172,130.020309485617));
#68590=CARTESIAN_POINT('Ctrl Pts',(16.3960826455574,-4.87906695031521,130.167165367317));
#68591=CARTESIAN_POINT('Ctrl Pts',(16.3876615618615,-4.89614432061384,130.31528224506));
#68592=CARTESIAN_POINT('Ctrl Pts',(16.3792404781655,-4.90646351831546,130.464068381481));
#68593=CARTESIAN_POINT('Ctrl Pts',(16.3728738401267,-4.91426519788417,130.576555979276));
#68594=CARTESIAN_POINT('Ctrl Pts',(16.3665072020878,-4.91820495795325,130.689425740071));
#68595=CARTESIAN_POINT('Ctrl Pts',(16.3601405640489,-4.91824961586008,130.802416757442));
#68596=CARTESIAN_POINT('Ctrl Pts',(16.3601405640087,-4.91824961586036,130.802416758157));
#68597=CARTESIAN_POINT('Ctrl Pts',(16.3522326324733,-4.91830508493801,130.942761666103));
#68598=CARTESIAN_POINT('Ctrl Pts',(16.3443247009378,-4.91234897419799,131.083072226503));
#68599=CARTESIAN_POINT('Ctrl Pts',(16.3364167694024,-4.90041647627177,131.222811835254));
#68600=CARTESIAN_POINT('Ctrl Pts',(16.3285050531866,-4.88847826753609,131.362618322396));
#68601=CARTESIAN_POINT('Ctrl Pts',(16.3205933369708,-4.87055800315575,131.501852946995));
#68602=CARTESIAN_POINT('Ctrl Pts',(16.3126816207551,-4.84674264482889,131.639985412134));
#68603=CARTESIAN_POINT('Ctrl Pts',(16.3047647134023,-4.82291166046301,131.778208510521));
#68604=CARTESIAN_POINT('Ctrl Pts',(16.2968478060496,-4.79317793675304,131.915327646397));
#68605=CARTESIAN_POINT('Ctrl Pts',(16.2889308986969,-4.75767928262551,132.050823976906));
#68606=CARTESIAN_POINT('Ctrl Pts',(16.2810016138169,-4.72212512885164,132.186532146387));
#68607=CARTESIAN_POINT('Ctrl Pts',(16.273072328937,-4.68078813042954,132.320612085298));
#68608=CARTESIAN_POINT('Ctrl Pts',(16.2651430440571,-4.63385592650999,132.452560336911));
#68609=CARTESIAN_POINT('Ctrl Pts',(16.2572071134798,-4.58688438774137,132.584619177078));
#68610=CARTESIAN_POINT('Ctrl Pts',(16.2492711829025,-4.53430843109388,132.714542427513));
#68611=CARTESIAN_POINT('Ctrl Pts',(16.2413352523251,-4.47636315764902,132.841848272337));
#68612=CARTESIAN_POINT('Ctrl Pts',(16.2333846977217,-4.41831110489378,132.969388711451));
#68613=CARTESIAN_POINT('Ctrl Pts',(16.2254341431182,-4.3548701281287,133.094301778135));
#68614=CARTESIAN_POINT('Ctrl Pts',(16.2174835885147,-4.28632100174241,133.216130783341));
#68615=CARTESIAN_POINT('Ctrl Pts',(16.2118070010859,-4.2373778614832,133.303115029585));
#68616=CARTESIAN_POINT('Ctrl Pts',(16.2061304136572,-4.18583164427882,133.388527667036));
#68617=CARTESIAN_POINT('Ctrl Pts',(16.2004538262285,-4.13179742248621,133.472212397938));
#68618=CARTESIAN_POINT('Ctrl Pts',(16.1926794921094,-4.05779519855281,133.586822287572));
#68619=CARTESIAN_POINT('Ctrl Pts',(16.1849051579903,-3.97890348572438,133.698532310843));
#68620=CARTESIAN_POINT('Ctrl Pts',(16.1771308238712,-3.89537649136763,133.806897054148));
#68621=CARTESIAN_POINT('Ctrl Pts',(16.1693660709242,-3.8119524365664,133.915128247591));
#68622=CARTESIAN_POINT('Ctrl Pts',(16.161601317977,-3.72390470293747,134.020022057445));
#68623=CARTESIAN_POINT('Ctrl Pts',(16.1538365650299,-3.6315318458311,134.121160206811));
#68624=CARTESIAN_POINT('Ctrl Pts',(16.1460795241449,-3.53925073474864,134.222197904341));
#68625=CARTESIAN_POINT('Ctrl Pts',(16.13832248326,-3.44265331092744,134.319487077785));
#68626=CARTESIAN_POINT('Ctrl Pts',(16.130565442375,-3.34207940872658,134.412641134414));
#68627=CARTESIAN_POINT('Ctrl Pts',(16.1228142511349,-3.24158135008772,134.505724942845));
#68628=CARTESIAN_POINT('Ctrl Pts',(16.1150630598947,-3.13711306745785,134.594679576698));
#68629=CARTESIAN_POINT('Ctrl Pts',(16.1073118686546,-3.02905213407681,134.679154319371));
#68630=CARTESIAN_POINT('Ctrl Pts',(16.0995639718775,-2.92103712947493,134.763593158024));
#68631=CARTESIAN_POINT('Ctrl Pts',(16.0918160751005,-2.8094328185267,134.843555652269));
#68632=CARTESIAN_POINT('Ctrl Pts',(16.0840681783234,-2.6946506560242,134.918730667098));
#68633=CARTESIAN_POINT('Ctrl Pts',(16.0763219022393,-2.57989250347584,134.993889956935));
#68634=CARTESIAN_POINT('Ctrl Pts',(16.0685756261552,-2.46195814842898,135.064263545201));
#68635=CARTESIAN_POINT('Ctrl Pts',(16.0608293500711,-2.34128856079642,135.129583263579));
#68636=CARTESIAN_POINT('Ctrl Pts',(16.0530830168058,-2.22061808240855,135.194903464132));
#68637=CARTESIAN_POINT('Ctrl Pts',(16.0453366835404,-2.09721267496941,135.25516953424));
#68638=CARTESIAN_POINT('Ctrl Pts',(16.0375903502751,-1.97153811464774,135.310159162218));
#68639=CARTESIAN_POINT('Ctrl Pts',(16.0298422822721,-1.84583541038,135.365161104742));
#68640=CARTESIAN_POINT('Ctrl Pts',(16.0220942142692,-1.71786290015782,135.414884097152));
#68641=CARTESIAN_POINT('Ctrl Pts',(16.0143461462662,-1.58810617097229,135.459154045015));
#68642=CARTESIAN_POINT('Ctrl Pts',(16.0065898435243,-1.45821153479016,135.503471043505));
#68643=CARTESIAN_POINT('Ctrl Pts',(15.9988335407825,-1.32652926221515,135.542323293748));
#68644=CARTESIAN_POINT('Ctrl Pts',(15.9910772380407,-1.19356046649581,135.57558650567));
#68645=CARTESIAN_POINT('Ctrl Pts',(15.9833167955265,-1.06052070132659,135.608867471171));
#68646=CARTESIAN_POINT('Ctrl Pts',(15.9755563530123,-0.92619342752175,135.636553375513));
#68647=CARTESIAN_POINT('Ctrl Pts',(15.9677959104981,-0.791088791895037,
135.658571324348));
#68648=CARTESIAN_POINT('Ctrl Pts',(15.9600230102327,-0.65576727431319,135.680624618349));
#68649=CARTESIAN_POINT('Ctrl Pts',(15.9522501099673,-0.519666289619082,
135.696991728025));
#68650=CARTESIAN_POINT('Ctrl Pts',(15.9444772097018,-0.383300832530537,
135.707651709708));
#68651=CARTESIAN_POINT('Ctrl Pts',(15.9369868739397,-0.251892603290093,
135.717924174207));
#68652=CARTESIAN_POINT('Ctrl Pts',(15.9294965381777,-0.120239104095079,
135.722897232128));
#68653=CARTESIAN_POINT('Ctrl Pts',(15.9220062024156,0.0112018286986203,
135.722597860881));
#68654=CARTESIAN_POINT('Ctrl Pts',(15.9142318682965,0.147626384408839,135.722287138883));
#68655=CARTESIAN_POINT('Ctrl Pts',(15.9064575341774,0.284254088600799,135.716295302799));
#68656=CARTESIAN_POINT('Ctrl Pts',(15.8986832000583,0.420572796901996,135.704595467551));
#68657=CARTESIAN_POINT('Ctrl Pts',(15.8909184471112,0.556723504578179,135.692910051304));
#68658=CARTESIAN_POINT('Ctrl Pts',(15.8831536941642,0.692565588267988,135.675530665761));
#68659=CARTESIAN_POINT('Ctrl Pts',(15.8753889412171,0.827585763308846,135.652482405111));
#68660=CARTESIAN_POINT('Ctrl Pts',(15.8676319003321,0.962471834408769,135.629457036318));
#68661=CARTESIAN_POINT('Ctrl Pts',(15.859874859447,1.0965372384991,135.600774062543));
#68662=CARTESIAN_POINT('Ctrl Pts',(15.852117818562,1.22927303539538,135.566510433243));
#68663=CARTESIAN_POINT('Ctrl Pts',(15.8443666273218,1.36190873519467,135.532272642412));
#68664=CARTESIAN_POINT('Ctrl Pts',(15.8366154360817,1.49321644652337,135.492462669975));
#68665=CARTESIAN_POINT('Ctrl Pts',(15.8288642448416,1.62269701401046,135.447208608102));
#68666=CARTESIAN_POINT('Ctrl Pts',(15.8211163480645,1.752122548802,135.401973780412));
#68667=CARTESIAN_POINT('Ctrl Pts',(15.8133684512874,1.87972211601999,135.351299594145));
#68668=CARTESIAN_POINT('Ctrl Pts',(15.8056205545103,2.00501154760564,135.295364041799));
#68669=CARTESIAN_POINT('Ctrl Pts',(15.7978742784262,2.13027477134314,135.239440189964));
#68670=CARTESIAN_POINT('Ctrl Pts',(15.7901280023422,2.25322846384438,135.178257320417));
#68671=CARTESIAN_POINT('Ctrl Pts',(15.7823817262581,2.37340865250036,135.112041482107));
#68672=CARTESIAN_POINT('Ctrl Pts',(15.7746353929927,2.49358972829903,135.045825155008));
#68673=CARTESIAN_POINT('Ctrl Pts',(15.7668890597274,2.61099691696992,134.97457597368));
#68674=CARTESIAN_POINT('Ctrl Pts',(15.7591427264621,2.72519141800093,134.898565643912));
#68675=CARTESIAN_POINT('Ctrl Pts',(15.7513946584591,2.83941149209853,134.822538292157));
#68676=CARTESIAN_POINT('Ctrl Pts',(15.7436465904561,2.95041712151859,134.741747886886));
#68677=CARTESIAN_POINT('Ctrl Pts',(15.7358985224532,3.05779936405475,134.656508863894));
#68678=CARTESIAN_POINT('Ctrl Pts',(15.7281422197114,3.16529573371629,134.571179247854));
#68679=CARTESIAN_POINT('Ctrl Pts',(15.7203859169695,3.26916071704303,134.481391812776));
#68680=CARTESIAN_POINT('Ctrl Pts',(15.7126296142276,3.36901888132632,134.387500977609));
#68681=CARTESIAN_POINT('Ctrl Pts',(15.7048691717135,3.46893034291883,134.293560030076));
#68682=CARTESIAN_POINT('Ctrl Pts',(15.6971087291993,3.56483045096466,134.19551159784));
#68683=CARTESIAN_POINT('Ctrl Pts',(15.6893482866851,3.65638213057086,134.093745480689));
#68684=CARTESIAN_POINT('Ctrl Pts',(15.6815753864197,3.74808077706075,133.991815999532));
#68685=CARTESIAN_POINT('Ctrl Pts',(15.6738024861543,3.83541679664981,133.886157209097));
#68686=CARTESIAN_POINT('Ctrl Pts',(15.6660295858888,3.91809420161419,133.777191068462));
#68687=CARTESIAN_POINT('Ctrl Pts',(15.6585392501268,3.99776607465664,133.672186121509));
#68688=CARTESIAN_POINT('Ctrl Pts',(15.6510489143647,4.07311198126007,133.564110363295));
#68689=CARTESIAN_POINT('Ctrl Pts',(15.6435585786027,4.14390714654999,133.453363566464));
#68690=CARTESIAN_POINT('Ctrl Pts',(15.6357842444836,4.21738653204919,133.338417771171));
#68691=CARTESIAN_POINT('Ctrl Pts',(15.6280099103645,4.28619604208648,133.220230280375));
#68692=CARTESIAN_POINT('Ctrl Pts',(15.6202355762454,4.35003623094224,133.099217443599));
#68693=CARTESIAN_POINT('Ctrl Pts',(15.6124708232983,4.4137977424708,132.978353744329));
#68694=CARTESIAN_POINT('Ctrl Pts',(15.6047060703512,4.47260193756526,132.854671969672));
#68695=CARTESIAN_POINT('Ctrl Pts',(15.5969413174041,4.52619248578029,132.728617524574));
#68696=CARTESIAN_POINT('Ctrl Pts',(15.5891842765191,4.57972980710733,132.602688278527));
#68697=CARTESIAN_POINT('Ctrl Pts',(15.5814272356342,4.62806363456646,132.47439140919));
#68698=CARTESIAN_POINT('Ctrl Pts',(15.5736701947492,4.67098361331424,132.344196695416));
#68699=CARTESIAN_POINT('Ctrl Pts',(15.565919003509,4.71387122577234,132.214100162488));
#68700=CARTESIAN_POINT('Ctrl Pts',(15.5581678122689,4.75135299382685,132.082109003605));
#68701=CARTESIAN_POINT('Ctrl Pts',(15.5504166210287,4.78326687937643,131.948712409263));
#68702=CARTESIAN_POINT('Ctrl Pts',(15.5426687242516,4.81516720067318,131.815372512033));
#68703=CARTESIAN_POINT('Ctrl Pts',(15.5349208274745,4.84150425547309,131.680628746862));
#68704=CARTESIAN_POINT('Ctrl Pts',(15.5271729306975,4.86216608924381,131.544984667343));
#68705=CARTESIAN_POINT('Ctrl Pts',(15.5194266546134,4.88282360100431,131.409368961641));
#68706=CARTESIAN_POINT('Ctrl Pts',(15.5116803785293,4.89780819417306,131.272853702445));
#68707=CARTESIAN_POINT('Ctrl Pts',(15.5039341024452,4.90705926160619,131.135951428031));
#68708=CARTESIAN_POINT('Ctrl Pts',(15.4961877691798,4.91631039732861,130.999048143035));
#68709=CARTESIAN_POINT('Ctrl Pts',(15.4884414359145,4.91982789650269,130.861758227196));
#68710=CARTESIAN_POINT('Ctrl Pts',(15.4806951026491,4.91760317050699,130.724597719427));
#68711=CARTESIAN_POINT('Ctrl Pts',(15.4729470346461,4.91537794629932,130.587406495512));
#68712=CARTESIAN_POINT('Ctrl Pts',(15.4651989666432,4.90740794440638,130.450345128173));
#68713=CARTESIAN_POINT('Ctrl Pts',(15.4574508986402,4.89373666531621,130.313927632297));
#68714=CARTESIAN_POINT('Ctrl Pts',(15.4496945958983,4.88005085622802,130.177365150284));
#68715=CARTESIAN_POINT('Ctrl Pts',(15.4419382931565,4.86065170471596,130.041448296362));
#68716=CARTESIAN_POINT('Ctrl Pts',(15.4341819904146,4.83563446292962,129.906684504802));
#68717=CARTESIAN_POINT('Ctrl Pts',(15.4264215479005,4.81060386868809,129.771848785748));
#68718=CARTESIAN_POINT('Ctrl Pts',(15.4186611053863,4.77994929666152,129.638167736228));
#68719=CARTESIAN_POINT('Ctrl Pts',(15.4109006628722,4.74381649923732,129.506135643201));
#68720=CARTESIAN_POINT('Ctrl Pts',(15.4031277626068,4.70762569823893,129.373891600538));
#68721=CARTESIAN_POINT('Ctrl Pts',(15.3953548623413,4.66593921732234,129.243302176684));
#68722=CARTESIAN_POINT('Ctrl Pts',(15.3875819620759,4.61895207401608,129.114844473683));
#68723=CARTESIAN_POINT('Ctrl Pts',(15.3800916263139,4.57367303172241,128.991056531751));
#68724=CARTESIAN_POINT('Ctrl Pts',(15.3726012905519,4.52347213841844,128.869248299408));
#68725=CARTESIAN_POINT('Ctrl Pts',(15.3651109547898,4.46856423783985,128.749824972998));
#68726=CARTESIAN_POINT('Ctrl Pts',(15.3573366206708,4.41157448752199,128.625873674871));
#68727=CARTESIAN_POINT('Ctrl Pts',(15.3495622865517,4.34933322521199,128.504099059624));
#68728=CARTESIAN_POINT('Ctrl Pts',(15.3417879524326,4.28202887983068,128.384978106512));
#68729=CARTESIAN_POINT('Ctrl Pts',(15.3340231994855,4.21480748103971,128.266003959327));
#68730=CARTESIAN_POINT('Ctrl Pts',(15.3262584465384,4.14253560499146,128.149677304275));
#68731=CARTESIAN_POINT('Ctrl Pts',(15.3184936935913,4.06544943061467,128.036454551672));
#68732=CARTESIAN_POINT('Ctrl Pts',(15.3107366527063,3.988439819313,127.923344253502));
#68733=CARTESIAN_POINT('Ctrl Pts',(15.3029796118212,3.90662564394487,127.813332043874));
#68734=CARTESIAN_POINT('Ctrl Pts',(15.2952225709362,3.82028844083258,127.706848827219));
#68735=CARTESIAN_POINT('Ctrl Pts',(15.2874713796961,3.73401634527724,127.600445910386));
#68736=CARTESIAN_POINT('Ctrl Pts',(15.2797201884561,3.6432282563021,127.497566991944));
#68737=CARTESIAN_POINT('Ctrl Pts',(15.271968997216,3.54824815817462,127.398612818549));
#68738=CARTESIAN_POINT('Ctrl Pts',(15.2642211004389,3.45330842912226,127.299700703317));
#68739=CARTESIAN_POINT('Ctrl Pts',(15.2564732036618,3.35418050477971,127.204710296835));
#68740=CARTESIAN_POINT('Ctrl Pts',(15.2487253068848,3.25122752488696,127.114007972639));
#68741=CARTESIAN_POINT('Ctrl Pts',(15.2409790308007,3.1482960805382,127.023324621415));
#68742=CARTESIAN_POINT('Ctrl Pts',(15.2332327547166,3.04154146529052,126.93692782663));
#68743=CARTESIAN_POINT('Ctrl Pts',(15.2254864786325,2.93136213246959,126.85514561825));
#68744=CARTESIAN_POINT('Ctrl Pts',(15.2177401453671,2.82118198632957,126.773362806172));
#68745=CARTESIAN_POINT('Ctrl Pts',(15.2099938121017,2.70757738610485,126.696194881492));
#68746=CARTESIAN_POINT('Ctrl Pts',(15.2022474788363,2.5909778475882,126.623928001699));
#68747=CARTESIAN_POINT('Ctrl Pts',(15.1944994108333,2.47435219741349,126.551644938239));
#68748=CARTESIAN_POINT('Ctrl Pts',(15.1867513428304,2.35473060659061,126.484265309597));
#68749=CARTESIAN_POINT('Ctrl Pts',(15.1790032748274,2.23256904347863,126.422030355183));
#68750=CARTESIAN_POINT('Ctrl Pts',(15.1712469720855,2.11027764560363,126.359729256718));
#68751=CARTESIAN_POINT('Ctrl Pts',(15.1634906693437,1.98544123179093,126.3025839328));
#68752=CARTESIAN_POINT('Ctrl Pts',(15.1557343666019,1.85853820697621,126.250788525712));
#68753=CARTESIAN_POINT('Ctrl Pts',(15.1479739240877,1.73156745019634,126.198965473857));
#68754=CARTESIAN_POINT('Ctrl Pts',(15.1402134815735,1.60252825223089,126.152498160878));
#68755=CARTESIAN_POINT('Ctrl Pts',(15.1324530390594,1.47191525342404,126.111531135341));
#68756=CARTESIAN_POINT('Ctrl Pts',(15.1246801387939,1.34109258303586,126.070498345898));
#68757=CARTESIAN_POINT('Ctrl Pts',(15.1169072385284,1.20869144107801,126.034983589498));
#68758=CARTESIAN_POINT('Ctrl Pts',(15.109134338263,1.07521863874984,126.005080677681));
#68759=CARTESIAN_POINT('Ctrl Pts',(15.101644002501,0.946597908984719,125.976264812029));
#68760=CARTESIAN_POINT('Ctrl Pts',(15.094153666739,0.816982384270664,125.952659920416));
#68761=CARTESIAN_POINT('Ctrl Pts',(15.086663330977,0.686829096056115,125.934304267244));
#68762=CARTESIAN_POINT('Ctrl Pts',(15.078888996858,0.551741006359105,125.915252653903));
#68763=CARTESIAN_POINT('Ctrl Pts',(15.0711146627388,0.415645651109847,125.901795836598));
#68764=CARTESIAN_POINT('Ctrl Pts',(15.0633403286197,0.279046176896683,125.894033103677));
#68765=CARTESIAN_POINT('Ctrl Pts',(15.0555755756726,0.142615049327056,125.88627993763));
#68766=CARTESIAN_POINT('Ctrl Pts',(15.0478108227256,0.0056814255469059,
125.884206915303));
#68767=CARTESIAN_POINT('Ctrl Pts',(15.0400460697785,-0.131243043038496,
125.887862033599));
#68768=CARTESIAN_POINT('Ctrl Pts',(15.0322890288935,-0.268031516311589,
125.891513521579));
#68769=CARTESIAN_POINT('Ctrl Pts',(15.0245319880084,-0.404810464188582,
125.900881817912));
#68770=CARTESIAN_POINT('Ctrl Pts',(15.0167749471234,-0.541065177307815,
125.915962972488));
#68771=CARTESIAN_POINT('Ctrl Pts',(15.0090237558833,-0.677217139686495,
125.931032754247));
#68772=CARTESIAN_POINT('Ctrl Pts',(15.0012725646433,-0.812845267167011,
125.951806776379));
#68773=CARTESIAN_POINT('Ctrl Pts',(14.9935213734032,-0.947437278827389,
125.9782290751));
#68774=CARTESIAN_POINT('Ctrl Pts',(14.9857734766262,-1.08197208529355,126.004640143639));
#68775=CARTESIAN_POINT('Ctrl Pts',(14.978025579849,-1.21547126897631,126.036694638864));
#68776=CARTESIAN_POINT('Ctrl Pts',(14.9702776830719,-1.34743030354397,126.074285074872));
#68777=CARTESIAN_POINT('Ctrl Pts',(14.9625314069878,-1.47936173512649,126.111867647772));
#68778=CARTESIAN_POINT('Ctrl Pts',(14.9547851309037,-1.60975328263125,126.154983751087));
#68779=CARTESIAN_POINT('Ctrl Pts',(14.9470388548196,-1.73811359140382,126.20347546296));
#68780=CARTESIAN_POINT('Ctrl Pts',(14.9392925215543,-1.86647484770234,126.251967532786));
#68781=CARTESIAN_POINT('Ctrl Pts',(14.9315461882889,-1.99280446961197,126.305835152184));
#68782=CARTESIAN_POINT('Ctrl Pts',(14.9237998550236,-2.11662954095628,126.364871632463));
#68783=CARTESIAN_POINT('Ctrl Pts',(14.9160517870206,-2.24048234206729,126.423921333553));
#68784=CARTESIAN_POINT('Ctrl Pts',(14.9083037190177,-2.36182912369358,126.488142030652));
#68785=CARTESIAN_POINT('Ctrl Pts',(14.9005556510147,-2.48022046225175,126.557280500459));
#68786=CARTESIAN_POINT('Ctrl Pts',(14.8927993482729,-2.59873762853342,126.626492451454));
#68787=CARTESIAN_POINT('Ctrl Pts',(14.885043045531,-2.71429273895081,126.700632418516));
#68788=CARTESIAN_POINT('Ctrl Pts',(14.8772867427891,-2.82646386654663,126.779402844669));
#68789=CARTESIAN_POINT('Ctrl Pts',(14.8695263002749,-2.93869486325066,126.85821531297));
#68790=CARTESIAN_POINT('Ctrl Pts',(14.8617658577607,-3.0475379681402,126.941662927106));
#68791=CARTESIAN_POINT('Ctrl Pts',(14.8540054152466,-3.15260420322612,127.029407664177));
#68792=CARTESIAN_POINT('Ctrl Pts',(14.8462325149811,-3.25783909995994,127.117293256889));
#68793=CARTESIAN_POINT('Ctrl Pts',(14.8384596147157,-3.35928472165498,127.209489494083));
#68794=CARTESIAN_POINT('Ctrl Pts',(14.8306867144503,-3.45658819817418,127.305620688571));
#68795=CARTESIAN_POINT('Ctrl Pts',(14.8231963786882,-3.5503544482303,127.398257272001));
#68796=CARTESIAN_POINT('Ctrl Pts',(14.8157060429261,-3.64027426921428,127.494547463348));
#68797=CARTESIAN_POINT('Ctrl Pts',(14.808215707164,-3.72606843153878,127.594127431956));
#68798=CARTESIAN_POINT('Ctrl Pts',(14.8004988501849,-3.81445716354266,127.696718877805));
#68799=CARTESIAN_POINT('Ctrl Pts',(14.7927819932059,-3.8987577119728,127.803140151212));
#68800=CARTESIAN_POINT('Ctrl Pts',(14.7850651362268,-3.97861597536864,127.91302909333));
#68801=CARTESIAN_POINT('Ctrl Pts',(14.777357644971,-4.05837731712915,128.022784666458));
#68802=CARTESIAN_POINT('Ctrl Pts',(14.7696501537153,-4.13370686506258,128.135999220308));
#68803=CARTESIAN_POINT('Ctrl Pts',(14.7619426624595,-4.20428872582697,128.25227531876));
#68804=CARTESIAN_POINT('Ctrl Pts',(14.7542442395176,-4.27478754290774,128.368414611586));
#68805=CARTESIAN_POINT('Ctrl Pts',(14.7465458165756,-4.34054958910387,128.487607940334));
#68806=CARTESIAN_POINT('Ctrl Pts',(14.7388473936337,-4.40130094564209,128.609427122357));
#68807=CARTESIAN_POINT('Ctrl Pts',(14.731154215882,-4.46201091027164,128.731163304942));
#68808=CARTESIAN_POINT('Ctrl Pts',(14.7234610381303,-4.51771679823394,128.855521428867));
#68809=CARTESIAN_POINT('Ctrl Pts',(14.7157678603785,-4.56818954633877,128.982046887381));
#68810=CARTESIAN_POINT('Ctrl Pts',(14.7080782288489,-4.61863902869028,129.108514023132));
#68811=CARTESIAN_POINT('Ctrl Pts',(14.7003885973193,-4.66386002327873,129.237146137795));
#68812=CARTESIAN_POINT('Ctrl Pts',(14.6926989657897,-4.70367093645055,129.367467168458));
#68813=CARTESIAN_POINT('Ctrl Pts',(14.6884979542264,-4.72542049700328,129.43866435842));
#68814=CARTESIAN_POINT('Ctrl Pts',(14.6842969426631,-4.7455561645854,129.510365280194));
#68815=CARTESIAN_POINT('Ctrl Pts',(14.6800959310998,-4.76405452823407,129.582490119308));
#68816=CARTESIAN_POINT('Origin',(213.235140564004,0.,130.804360617566));
#68817=CARTESIAN_POINT('',(12.5846956991378,-4.76405452823411,129.582490119308));
#68818=CARTESIAN_POINT('',(12.9302349012324,-4.7640545282341,129.582490119308));
#68819=CARTESIAN_POINT('',(213.235140564004,-4.76405452823405,129.582490119308));
#68820=CARTESIAN_POINT('',(14.2648594359355,-4.91824995510319,130.803696067003));
#68821=CARTESIAN_POINT('Ctrl Pts',(14.2648594359355,-4.91824995510319,130.803696067003));
#68822=CARTESIAN_POINT('Ctrl Pts',(14.2571139563985,-4.91826832183562,130.939625800473));
#68823=CARTESIAN_POINT('Ctrl Pts',(14.2493684768615,-4.91264721499648,131.0757784822));
#68824=CARTESIAN_POINT('Ctrl Pts',(14.2416229973244,-4.90135718546593,131.211645288259));
#68825=CARTESIAN_POINT('Ctrl Pts',(14.2338870308702,-4.8900810224733,131.347345221218));
#68826=CARTESIAN_POINT('Ctrl Pts',(14.226151064416,-4.8731498207027,131.482759588039));
#68827=CARTESIAN_POINT('Ctrl Pts',(14.2184150979618,-4.85058610595946,131.617378139624));
#68828=CARTESIAN_POINT('Ctrl Pts',(14.2106867461381,-4.82804460102725,131.7518641841));
#68829=CARTESIAN_POINT('Ctrl Pts',(14.2029583943145,-4.79988167951563,131.885555585763));
#68830=CARTESIAN_POINT('Ctrl Pts',(14.1952300424909,-4.76617174467524,132.017946198709));
#68831=CARTESIAN_POINT('Ctrl Pts',(14.1875074137658,-4.73248677314925,132.150238772057));
#68832=CARTESIAN_POINT('Ctrl Pts',(14.1797847850407,-4.69326306038384,132.281232093317));
#68833=CARTESIAN_POINT('Ctrl Pts',(14.1720621563155,-4.64862619136131,132.410429605963));
#68834=CARTESIAN_POINT('Ctrl Pts',(14.1643426296658,-4.60400725236479,132.539575221717));
#68835=CARTESIAN_POINT('Ctrl Pts',(14.156623103016,-4.55397960920367,132.666926091366));
#68836=CARTESIAN_POINT('Ctrl Pts',(14.1489035763663,-4.49871879539489,132.792000489993));
#68837=CARTESIAN_POINT('Ctrl Pts',(14.1411855021117,-4.44346837866608,132.91705135642));
#68838=CARTESIAN_POINT('Ctrl Pts',(14.1334674278571,-4.38298690867677,133.039826243258));
#68839=CARTESIAN_POINT('Ctrl Pts',(14.1257493536025,-4.31749801802492,133.159863520738));
#68840=CARTESIAN_POINT('Ctrl Pts',(14.118031027675,-4.25200699189477,133.279904712423));
#68841=CARTESIAN_POINT('Ctrl Pts',(14.1103127017474,-4.1815084089773,133.397207771056));
#68842=CARTESIAN_POINT('Ctrl Pts',(14.1025943758199,-4.10627158855874,133.511336181456));
#68843=CARTESIAN_POINT('Ctrl Pts',(14.094874094318,-4.0310157055618,133.625493508306));
#68844=CARTESIAN_POINT('Ctrl Pts',(14.0871538128162,-3.95101941357975,133.736474257679));
#68845=CARTESIAN_POINT('Ctrl Pts',(14.0794335313144,-3.86659477019901,133.843871753517));
#68846=CARTESIAN_POINT('Ctrl Pts',(14.0717049876774,-3.78207977676924,133.951384184623));
#68847=CARTESIAN_POINT('Ctrl Pts',(14.0639764440405,-3.69312721127982,134.055305393542));
#68848=CARTESIAN_POINT('Ctrl Pts',(14.0562479004035,-3.60008906066226,134.15526226008));
#68849=CARTESIAN_POINT('Ctrl Pts',(14.0485149685762,-3.50699808390658,134.255275881134));
#68850=CARTESIAN_POINT('Ctrl Pts',(14.0407820367489,-3.40981718115627,134.351320399342));
#68851=CARTESIAN_POINT('Ctrl Pts',(14.0330491049216,-3.30893365570468,134.443061089526));
#68852=CARTESIAN_POINT('Ctrl Pts',(14.0253042589508,-3.20789469880424,134.534943124775));
#68853=CARTESIAN_POINT('Ctrl Pts',(14.01755941298,-3.10314202617667,134.622507834068));
#68854=CARTESIAN_POINT('Ctrl Pts',(14.0098145670092,-2.99509485695859,134.705461726269));
#68855=CARTESIAN_POINT('Ctrl Pts',(14.0040303219677,-2.91439973336894,134.767415913794));
#68856=CARTESIAN_POINT('Ctrl Pts',(13.9982460769262,-2.83186763822481,134.826799121679));
#68857=CARTESIAN_POINT('Ctrl Pts',(13.9924618318848,-2.74768244700801,134.883505654569));
#68858=CARTESIAN_POINT('Ctrl Pts',(13.9846874977657,-2.63453305591139,134.959722261967));
#68859=CARTESIAN_POINT('Ctrl Pts',(13.9769131636466,-2.51803083870433,135.031348130466));
#68860=CARTESIAN_POINT('Ctrl Pts',(13.9691388295275,-2.39858483914146,135.098073909338));
#68861=CARTESIAN_POINT('Ctrl Pts',(13.9613740765804,-2.27928604609785,135.164717454651));
#68862=CARTESIAN_POINT('Ctrl Pts',(13.9536093236333,-2.15705102727736,135.226472737154));
#68863=CARTESIAN_POINT('Ctrl Pts',(13.9458445706862,-2.03231890813653,135.283072811727));
#68864=CARTESIAN_POINT('Ctrl Pts',(13.9380875298012,-1.90771067469467,135.339616670309));
#68865=CARTESIAN_POINT('Ctrl Pts',(13.9303304889162,-1.78061063027463,135.391015349931));
#68866=CARTESIAN_POINT('Ctrl Pts',(13.9225734480312,-1.65148337050791,135.437047282929));
#68867=CARTESIAN_POINT('Ctrl Pts',(13.9148222567911,-1.52245348661242,135.483044502889));
#68868=CARTESIAN_POINT('Ctrl Pts',(13.907071065551,-1.39139979700716,135.523682900994));
#68869=CARTESIAN_POINT('Ctrl Pts',(13.8993198743108,-1.25880746284614,135.558788746582));
#68870=CARTESIAN_POINT('Ctrl Pts',(13.8915719775338,-1.12627148396433,135.59387967125));
#68871=CARTESIAN_POINT('Ctrl Pts',(13.8838240807567,-0.992198538364546,
135.623442620463));
#68872=CARTESIAN_POINT('Ctrl Pts',(13.8760761839796,-0.857089348028968,
135.647353588033));
#68873=CARTESIAN_POINT('Ctrl Pts',(13.8683299078956,-0.722008419623206,
135.671259553944));
#68874=CARTESIAN_POINT('Ctrl Pts',(13.8605836318115,-0.585892062368198,
135.689515821727));
#68875=CARTESIAN_POINT('Ctrl Pts',(13.8528373557274,-0.449251212537125,
135.702049502186));
#68876=CARTESIAN_POINT('Ctrl Pts',(13.8450910224621,-0.312609354054525,
135.714583275166));
#68877=CARTESIAN_POINT('Ctrl Pts',(13.8373446891967,-0.175443384600942,
135.721394340818));
#68878=CARTESIAN_POINT('Ctrl Pts',(13.8295983559314,-0.0382689883796058,
135.722461729482));
#68879=CARTESIAN_POINT('Ctrl Pts',(13.8218502879285,0.0989361270964765,
135.72352935718));
#68880=CARTESIAN_POINT('Ctrl Pts',(13.8141022199255,0.236149282216913,135.718850745347));
#68881=CARTESIAN_POINT('Ctrl Pts',(13.8063541519226,0.372855566225771,135.708457047005));
#68882=CARTESIAN_POINT('Ctrl Pts',(13.7985978491807,0.509707143300472,135.698052302116));
#68883=CARTESIAN_POINT('Ctrl Pts',(13.7908415464389,0.646050382673326,135.681920366811));
#68884=CARTESIAN_POINT('Ctrl Pts',(13.783085243697,0.781375710414469,135.660144288785));
#68885=CARTESIAN_POINT('Ctrl Pts',(13.7753248011829,0.916773265357595,135.63835658821));
#68886=CARTESIAN_POINT('Ctrl Pts',(13.7675643586687,1.05115144324327,135.610918820533));
#68887=CARTESIAN_POINT('Ctrl Pts',(13.7598039161545,1.1840126017983,135.577964834642));
#68888=CARTESIAN_POINT('Ctrl Pts',(13.7520310158891,1.31708704087991,135.544957948087));
#68889=CARTESIAN_POINT('Ctrl Pts',(13.7442581156237,1.44863921880625,135.506417257945));
#68890=CARTESIAN_POINT('Ctrl Pts',(13.7364852153583,1.57818749104427,135.462526276451));
#68891=CARTESIAN_POINT('Ctrl Pts',(13.7289948795962,1.70302635727561,135.420230842688));
#68892=CARTESIAN_POINT('Ctrl Pts',(13.7215045438341,1.82600419487917,135.372967467714));
#68893=CARTESIAN_POINT('Ctrl Pts',(13.7140142080719,1.9467107685384,135.320941209801));
#68894=CARTESIAN_POINT('Ctrl Pts',(13.7062398739529,2.0719939686243,135.266942360507));
#68895=CARTESIAN_POINT('Ctrl Pts',(13.6984655398337,2.19522713446769,135.20764127714));
#68896=CARTESIAN_POINT('Ctrl Pts',(13.6906912057147,2.31592890239964,135.143214888169));
#68897=CARTESIAN_POINT('Ctrl Pts',(13.6829264527676,2.43648191619019,135.078867898965));
#68898=CARTESIAN_POINT('Ctrl Pts',(13.6751616998205,2.55450939778924,135.009408354405));
#68899=CARTESIAN_POINT('Ctrl Pts',(13.6673969468734,2.66954940067231,134.935061412815));
#68900=CARTESIAN_POINT('Ctrl Pts',(13.6596399059884,2.78447514420273,134.860788313656));
#68901=CARTESIAN_POINT('Ctrl Pts',(13.6518828651034,2.89641898765502,134.781637688443));
#68902=CARTESIAN_POINT('Ctrl Pts',(13.6441258242184,3.00494339459148,134.697880651905));
#68903=CARTESIAN_POINT('Ctrl Pts',(13.6363746329783,3.11338596242833,134.614186777201));
#68904=CARTESIAN_POINT('Ctrl Pts',(13.6286234417381,3.21841391808913,134.525893643326));
#68905=CARTESIAN_POINT('Ctrl Pts',(13.620872250498,3.31961885559364,134.433315524435));
#68906=CARTESIAN_POINT('Ctrl Pts',(13.6131243537209,3.42078077829998,134.340776753714));
#68907=CARTESIAN_POINT('Ctrl Pts',(13.6053764569439,3.51812262675017,134.243956883602));
#68908=CARTESIAN_POINT('Ctrl Pts',(13.5976285601668,3.61126941856233,134.143210157311));
#68909=CARTESIAN_POINT('Ctrl Pts',(13.5898822840827,3.70439672607366,134.042484505063));
#68910=CARTESIAN_POINT('Ctrl Pts',(13.5821360079986,3.79333045712705,133.93783391736));
#68911=CARTESIAN_POINT('Ctrl Pts',(13.5743897319145,3.87773311444168,133.829648860967));
#68912=CARTESIAN_POINT('Ctrl Pts',(13.5666433986491,3.96213639479755,133.721463005977));
#68913=CARTESIAN_POINT('Ctrl Pts',(13.5588970653838,4.04200829418442,133.609742938488));
#68914=CARTESIAN_POINT('Ctrl Pts',(13.5511507321184,4.11705243032601,133.494911183611));
#68915=CARTESIAN_POINT('Ctrl Pts',(13.5434026641154,4.19211337208167,133.380053712959));
#68916=CARTESIAN_POINT('Ctrl Pts',(13.5356545961125,4.26234418540212,133.2620834955));
#68917=CARTESIAN_POINT('Ctrl Pts',(13.5279065281095,4.32749275836524,133.141450579206));
#68918=CARTESIAN_POINT('Ctrl Pts',(13.5201502253676,4.3927105720068,133.020689452812));
#68919=CARTESIAN_POINT('Ctrl Pts',(13.5123939226258,4.45283516920389,132.89726031901));
#68920=CARTESIAN_POINT('Ctrl Pts',(13.504637619884,4.50766098317906,132.771636786086));
#68921=CARTESIAN_POINT('Ctrl Pts',(13.4968771773698,4.56251605934192,132.6459462041));
#68922=CARTESIAN_POINT('Ctrl Pts',(13.4891167348557,4.61206657583323,132.518059253622));
#68923=CARTESIAN_POINT('Ctrl Pts',(13.4813562923415,4.65615615571087,132.388466963786));
#68924=CARTESIAN_POINT('Ctrl Pts',(13.4735833920761,4.70031651209633,132.258666640902));
#68925=CARTESIAN_POINT('Ctrl Pts',(13.4658104918106,4.73899830346059,132.127155883431));
#68926=CARTESIAN_POINT('Ctrl Pts',(13.4580375915452,4.77209558320917,131.994439105404));
#68927=CARTESIAN_POINT('Ctrl Pts',(13.4505472557831,4.80398969347205,131.866546916552));
#68928=CARTESIAN_POINT('Ctrl Pts',(13.4430569200211,4.83069820266381,131.737535170218));
#68929=CARTESIAN_POINT('Ctrl Pts',(13.435566584259,4.85217188990619,131.607859847998));
#68930=CARTESIAN_POINT('Ctrl Pts',(13.4277922501399,4.87445975852701,131.473267846522));
#68931=CARTESIAN_POINT('Ctrl Pts',(13.4200179160209,4.89117861387149,131.337534609884));
#68932=CARTESIAN_POINT('Ctrl Pts',(13.4122435819018,4.90221712205221,131.20116075713));
#68933=CARTESIAN_POINT('Ctrl Pts',(13.4044788289547,4.91324202625818,131.064954972962));
#68934=CARTESIAN_POINT('Ctrl Pts',(13.3967140760076,4.91860048100911,130.928110529502));
#68935=CARTESIAN_POINT('Ctrl Pts',(13.3889493230604,4.91823222500125,130.79113777902));
#68936=CARTESIAN_POINT('Ctrl Pts',(13.3811922821754,4.91786433475046,130.654301071804));
#68937=CARTESIAN_POINT('Ctrl Pts',(13.3734352412904,4.91178105386311,130.517336699605));
#68938=CARTESIAN_POINT('Ctrl Pts',(13.3656782004054,4.89997397970673,130.380759318351));
#68939=CARTESIAN_POINT('Ctrl Pts',(13.3579270091653,4.88817580935676,130.244284931161));
#68940=CARTESIAN_POINT('Ctrl Pts',(13.3501758179252,4.8706624707216,130.108197341978));
#68941=CARTESIAN_POINT('Ctrl Pts',(13.342424626685,4.84747761813886,129.973010027175));
#68942=CARTESIAN_POINT('Ctrl Pts',(13.3346767299079,4.824302619737,129.837880170588));
#68943=CARTESIAN_POINT('Ctrl Pts',(13.3269288331308,4.79546096772526,129.70365021187));
#68944=CARTESIAN_POINT('Ctrl Pts',(13.3191809363537,4.76104800981208,129.570827111428));
#68945=CARTESIAN_POINT('Ctrl Pts',(13.3114346602696,4.72664225034779,129.438031794715));
#68946=CARTESIAN_POINT('Ctrl Pts',(13.3036883841855,4.6866676010156,129.306643129159));
#68947=CARTESIAN_POINT('Ctrl Pts',(13.2959421081013,4.64127014704047,129.177156117606));
#68948=CARTESIAN_POINT('Ctrl Pts',(13.288195774836,4.59587235795176,129.047668150209));
#68949=CARTESIAN_POINT('Ctrl Pts',(13.2804494415707,4.54505181369432,128.920082233773));
#68950=CARTESIAN_POINT('Ctrl Pts',(13.2727031083054,4.48900379475163,128.794876108244));
#68951=CARTESIAN_POINT('Ctrl Pts',(13.2649550403024,4.43294322424386,128.669641943672));
#68952=CARTESIAN_POINT('Ctrl Pts',(13.2572069722994,4.37165300928843,128.546788987267));
#68953=CARTESIAN_POINT('Ctrl Pts',(13.2494589042965,4.30537551533711,128.42677260985));
#68954=CARTESIAN_POINT('Ctrl Pts',(13.2417026015546,4.23902758087623,128.306628677598));
#68955=CARTESIAN_POINT('Ctrl Pts',(13.2339462988128,4.16768196832323,128.189327689415));
#68956=CARTESIAN_POINT('Ctrl Pts',(13.2261899960709,4.09162602387908,128.075298591298));
#68957=CARTESIAN_POINT('Ctrl Pts',(13.2184295535567,4.01552948608718,127.961208632419));
#68958=CARTESIAN_POINT('Ctrl Pts',(13.2106691110425,3.93471783720559,127.850394359005));
#68959=CARTESIAN_POINT('Ctrl Pts',(13.2029086685283,3.84951966839361,127.743252748648));
#68960=CARTESIAN_POINT('Ctrl Pts',(13.1951357682629,3.76418473191775,127.635939145067));
#68961=CARTESIAN_POINT('Ctrl Pts',(13.1873628679975,3.67444946016647,127.532310281725));
#68962=CARTESIAN_POINT('Ctrl Pts',(13.179589967732,3.58068096422841,127.432727942598));
#68963=CARTESIAN_POINT('Ctrl Pts',(13.1720996319701,3.49032118930705,127.336765672332));
#68964=CARTESIAN_POINT('Ctrl Pts',(13.1646092962081,3.39621655492498,127.244561046946));
#68965=CARTESIAN_POINT('Ctrl Pts',(13.1571189604461,3.29872408622477,127.156401946547));
#68966=CARTESIAN_POINT('Ctrl Pts',(13.149344626327,3.19753516094088,127.064900267061));
#68967=CARTESIAN_POINT('Ctrl Pts',(13.141570292208,3.09237589448637,126.977467090686));
#68968=CARTESIAN_POINT('Ctrl Pts',(13.1337959580889,2.9836072931589,126.894466682597));
#68969=CARTESIAN_POINT('Ctrl Pts',(13.1260312051418,2.8749727394115,126.811568565093));
#68970=CARTESIAN_POINT('Ctrl Pts',(13.1182664521946,2.76273800917329,126.73309258105));
#68971=CARTESIAN_POINT('Ctrl Pts',(13.1105016992475,2.64729990355545,126.659365287878));
#68972=CARTESIAN_POINT('Ctrl Pts',(13.1027446583625,2.53197645269135,126.585711221693));
#68973=CARTESIAN_POINT('Ctrl Pts',(13.0949876174775,2.41345628541489,126.516796669476));
#68974=CARTESIAN_POINT('Ctrl Pts',(13.0872305765925,2.29216785450756,126.452906884701));
#68975=CARTESIAN_POINT('Ctrl Pts',(13.0794793853524,2.1709708881503,126.389065279711));
#68976=CARTESIAN_POINT('Ctrl Pts',(13.0717281941123,2.04701015785136,126.330241081431));
#68977=CARTESIAN_POINT('Ctrl Pts',(13.0639770028722,1.92074126206259,126.276675108754));
#68978=CARTESIAN_POINT('Ctrl Pts',(13.0562291060951,1.79452603392217,126.223131903043));
#68979=CARTESIAN_POINT('Ctrl Pts',(13.048481209318,1.66600495065421,126.174842630283));
#68980=CARTESIAN_POINT('Ctrl Pts',(13.040733312541,1.53565607017141,126.132001096227));
#68981=CARTESIAN_POINT('Ctrl Pts',(13.0329870364569,1.40533445586477,126.089168523697));
#68982=CARTESIAN_POINT('Ctrl Pts',(13.0252407603729,1.2731861760135,126.051781545242));
#68983=CARTESIAN_POINT('Ctrl Pts',(13.0174944842888,1.13970665316326,126.019984816353));
#68984=CARTESIAN_POINT('Ctrl Pts',(13.0097481510234,1.00622614499769,125.988187852748));
#68985=CARTESIAN_POINT('Ctrl Pts',(13.002001817758,0.871414754547387,125.961981311651));
#68986=CARTESIAN_POINT('Ctrl Pts',(12.9942554844927,0.735779971831289,125.941459128172));
#68987=CARTESIAN_POINT('Ctrl Pts',(12.9865074164897,0.600114814645843,125.920932348892));
#68988=CARTESIAN_POINT('Ctrl Pts',(12.9787593484868,0.463626284765305,125.906092518776));
#68989=CARTESIAN_POINT('Ctrl Pts',(12.9710112804839,0.326828503005363,125.896981867956));
#68990=CARTESIAN_POINT('Ctrl Pts',(12.963254977742,0.189885330934866,125.887861534228));
#68991=CARTESIAN_POINT('Ctrl Pts',(12.9554986750001,0.0526326411411423,
125.884482569333));
#68992=CARTESIAN_POINT('Ctrl Pts',(12.9477423722583,-0.0844133643174855,
125.886835076562));
#68993=CARTESIAN_POINT('Ctrl Pts',(12.9399819297441,-0.221532515355789,
125.889188839396));
#68994=CARTESIAN_POINT('Ctrl Pts',(12.9322214872299,-0.358444372156434,
125.897280146735));
#68995=CARTESIAN_POINT('Ctrl Pts',(12.9244610447157,-0.494637334681499,
125.911047121617));
#68996=CARTESIAN_POINT('Ctrl Pts',(12.9166881444503,-0.631048926240653,
125.924836196468));
#68997=CARTESIAN_POINT('Ctrl Pts',(12.9089152441849,-0.766738930179669,
125.944319090115));
#68998=CARTESIAN_POINT('Ctrl Pts',(12.9011423439194,-0.901204534882882,
125.969382494678));
#68999=CARTESIAN_POINT('Ctrl Pts',(12.8936520081573,-1.03078197615781,125.993534781354));
#69000=CARTESIAN_POINT('Ctrl Pts',(12.8861616723953,-1.15922219238532,126.022868823197));
#69001=CARTESIAN_POINT('Ctrl Pts',(12.8786713366332,-1.28609000106636,126.057239851074));
#69002=CARTESIAN_POINT('Ctrl Pts',(12.8708970025141,-1.41776804127254,126.09291406692));
#69003=CARTESIAN_POINT('Ctrl Pts',(12.863122668395,-1.54816920096978,126.134127768548));
#69004=CARTESIAN_POINT('Ctrl Pts',(12.855348334276,-1.67679188082675,126.180774125362));
#69005=CARTESIAN_POINT('Ctrl Pts',(12.8475835813289,-1.80525604472684,126.22736299471));
#69006=CARTESIAN_POINT('Ctrl Pts',(12.8398188283817,-1.93194572583687,126.279371065655));
#69007=CARTESIAN_POINT('Ctrl Pts',(12.8320540754346,-2.05637170146708,126.336641010439));
#69008=CARTESIAN_POINT('Ctrl Pts',(12.8242970345496,-2.18067409546403,126.393854073907));
#69009=CARTESIAN_POINT('Ctrl Pts',(12.8165399936646,-2.30271690543444,126.456318448498));
#69010=CARTESIAN_POINT('Ctrl Pts',(12.8087829527796,-2.42202855035795,126.523827851221));
#69011=CARTESIAN_POINT('Ctrl Pts',(12.8010317615395,-2.54125022144256,126.59128634458));
#69012=CARTESIAN_POINT('Ctrl Pts',(12.7932805702993,-2.65774448808031,126.6637821017));
#69013=CARTESIAN_POINT('Ctrl Pts',(12.7855293790591,-2.77106248042518,126.741061983195));
#69014=CARTESIAN_POINT('Ctrl Pts',(12.777781482282,-2.88433230959951,126.818309018679));
#69015=CARTESIAN_POINT('Ctrl Pts',(12.7700335855049,-2.99442822720415,126.90033591448));
#69016=CARTESIAN_POINT('Ctrl Pts',(12.7622856887279,-3.10092877698945,126.986845223682));
#69017=CARTESIAN_POINT('Ctrl Pts',(12.7545394126438,-3.20740704915576,127.073336437002));
#69018=CARTESIAN_POINT('Ctrl Pts',(12.7467931365598,-3.3102911461455,127.164307952392));
#69019=CARTESIAN_POINT('Ctrl Pts',(12.7390468604757,-3.40919157720906,127.25942114666));
#69020=CARTESIAN_POINT('Ctrl Pts',(12.7313005272103,-3.50809273833326,127.354535043032));
#69021=CARTESIAN_POINT('Ctrl Pts',(12.723554193945,-3.6030098930557,127.453790408282));
#69022=CARTESIAN_POINT('Ctrl Pts',(12.7158078606796,-3.69358970035717,127.556811050906));
#69023=CARTESIAN_POINT('Ctrl Pts',(12.7080597926766,-3.78418979237833,127.659854764288));
#69024=CARTESIAN_POINT('Ctrl Pts',(12.7003117246737,-3.87045034605917,127.766665139372));
#69025=CARTESIAN_POINT('Ctrl Pts',(12.6925636566707,-3.95205793713351,127.876832458173));
#69026=CARTESIAN_POINT('Ctrl Pts',(12.6848073539289,-4.03375226172667,127.987116864111));
#69027=CARTESIAN_POINT('Ctrl Pts',(12.6770510511871,-4.11078351200734,128.100765026171));
#69028=CARTESIAN_POINT('Ctrl Pts',(12.6692947484452,-4.18288099453353,128.217337299528));
#69029=CARTESIAN_POINT('Ctrl Pts',(12.6615343059311,-4.25501695765696,128.333971791018));
#69030=CARTESIAN_POINT('Ctrl Pts',(12.6537738634169,-4.32221371449295,128.453533162948));
#69031=CARTESIAN_POINT('Ctrl Pts',(12.6460134209027,-4.38424679156678,128.575557545705));
#69032=CARTESIAN_POINT('Ctrl Pts',(12.6382405206373,-4.44637944964296,128.697777812835));
#69033=CARTESIAN_POINT('Ctrl Pts',(12.630467620372,-4.50333170097486,128.822468636001));
#69034=CARTESIAN_POINT('Ctrl Pts',(12.6226947201066,-4.55492709273088,128.949145739875));
#69035=CARTESIAN_POINT('Ctrl Pts',(12.6152043843445,-4.60464686203589,129.071217811943));
#69036=CARTESIAN_POINT('Ctrl Pts',(12.6077140485824,-4.64939237604732,129.195133969611));
#69037=CARTESIAN_POINT('Ctrl Pts',(12.6002237128204,-4.68905020636647,129.320449830263));
#69038=CARTESIAN_POINT('Ctrl Pts',(12.5950477082595,-4.71645473363021,129.407046144085));
#69039=CARTESIAN_POINT('Ctrl Pts',(12.5898717036987,-4.74146979795504,129.494432598722));
#69040=CARTESIAN_POINT('Ctrl Pts',(12.5846956991378,-4.76405452823411,129.582490119308));
#69041=CARTESIAN_POINT('Ctrl Pts',(14.334952816073,-4.76405452823406,129.582490119308));
#69042=CARTESIAN_POINT('Ctrl Pts',(14.3271912810888,-4.7981176509159,129.715301717665));
#69043=CARTESIAN_POINT('Ctrl Pts',(14.3194297461047,-4.82659387817116,129.849425848687));
#69044=CARTESIAN_POINT('Ctrl Pts',(14.3116682111206,-4.84940926176714,129.984352767368));
#69045=CARTESIAN_POINT('Ctrl Pts',(14.3038947053308,-4.87225983408868,130.119487787143));
#69046=CARTESIAN_POINT('Ctrl Pts',(14.296121199541,-4.88943207225405,130.255427680485));
#69047=CARTESIAN_POINT('Ctrl Pts',(14.2883476937511,-4.90090395618872,130.39165797072));
#69048=CARTESIAN_POINT('Ctrl Pts',(14.2825349477333,-4.90948221540155,130.493526046524));
#69049=CARTESIAN_POINT('Ctrl Pts',(14.2767222017155,-4.91487420243906,130.595556415439));
#69050=CARTESIAN_POINT('Ctrl Pts',(14.2709094556978,-4.91708972550395,130.697535087642));
#69051=CARTESIAN_POINT('Ctrl Pts',(14.2688927824623,-4.91785837874528,130.73291555295));
#69052=CARTESIAN_POINT('Ctrl Pts',(14.2668761092268,-4.91824517299084,130.768304344428));
#69053=CARTESIAN_POINT('Ctrl Pts',(14.2648594359913,-4.91824995510306,130.803696066023));
#69054=CARTESIAN_POINT('',(14.6101405639733,-4.91824806987161,130.808717876352));
#69055=CARTESIAN_POINT('Ctrl Pts',(14.6800959310998,-4.76405452823407,129.582490119308));
#69056=CARTESIAN_POINT('Ctrl Pts',(14.6724074655865,-4.79790923889645,129.714489122364));
#69057=CARTESIAN_POINT('Ctrl Pts',(14.6647190000732,-4.8262769048776,129.847908572509));
#69058=CARTESIAN_POINT('Ctrl Pts',(14.6570305345599,-4.84905312519189,129.982249401509));
#69059=CARTESIAN_POINT('Ctrl Pts',(14.649215539468,-4.87220417524972,130.118801086295));
#69060=CARTESIAN_POINT('Ctrl Pts',(14.6414005443761,-4.88957802181369,130.256304331193));
#69061=CARTESIAN_POINT('Ctrl Pts',(14.6335855492843,-4.90111961205373,130.39422696759));
#69062=CARTESIAN_POINT('Ctrl Pts',(14.6257705541924,-4.91266120229374,130.532149603987));
#69063=CARTESIAN_POINT('Ctrl Pts',(14.6179555591006,-4.91837053000324,130.670491201671));
#69064=CARTESIAN_POINT('Ctrl Pts',(14.6101405640088,-4.91824806987217,130.808717875725));
#69065=CARTESIAN_POINT('Ctrl Pts',(14.6101405639733,-4.91824806987162,130.808717876352));
#69066=CARTESIAN_POINT('Ctrl Pts',(14.6006828491783,-4.91809986847844,130.9759999341));
#69067=CARTESIAN_POINT('Ctrl Pts',(14.5912251343833,-4.90941345961392,131.142904723301));
#69068=CARTESIAN_POINT('Ctrl Pts',(14.5817674195883,-4.89232631017948,131.308668397821));
#69069=CARTESIAN_POINT('Ctrl Pts',(14.5721703630257,-4.87498741350398,131.476874290564));
#69070=CARTESIAN_POINT('Ctrl Pts',(14.5625733064631,-4.84899846510879,131.643905236848));
#69071=CARTESIAN_POINT('Ctrl Pts',(14.5529762499004,-4.81455199274701,131.808986006274));
#69072=CARTESIAN_POINT('Ctrl Pts',(14.545240194384,-4.78678516436619,131.942055347757));
#69073=CARTESIAN_POINT('Ctrl Pts',(14.5375041388675,-4.7535237939816,132.073857971543));
#69074=CARTESIAN_POINT('Ctrl Pts',(14.5297680833511,-4.71489109911027,132.203998065633));
#69075=CARTESIAN_POINT('Ctrl Pts',(14.5219937492321,-4.67606724666873,132.334782103001));
#69076=CARTESIAN_POINT('Ctrl Pts',(14.514219415113,-4.63173614529118,132.464156695185));
#69077=CARTESIAN_POINT('Ctrl Pts',(14.506445080994,-4.58201663181093,132.591622950943));
#69078=CARTESIAN_POINT('Ctrl Pts',(14.4986803280469,-4.53235839318747,132.718932115932));
#69079=CARTESIAN_POINT('Ctrl Pts',(14.4909155750999,-4.47732509625781,132.844337263243));
#69080=CARTESIAN_POINT('Ctrl Pts',(14.4831508221528,-4.41708576346771,132.967353086501));
#69081=CARTESIAN_POINT('Ctrl Pts',(14.4753937812678,-4.35690626123224,133.09024672871));
#69082=CARTESIAN_POINT('Ctrl Pts',(14.4676367403828,-4.29153118390861,133.210755420609));
#69083=CARTESIAN_POINT('Ctrl Pts',(14.4598796994979,-4.22117807172571,133.328412667204));
#69084=CARTESIAN_POINT('Ctrl Pts',(14.4521285082578,-4.15087801337197,133.445981187555));
#69085=CARTESIAN_POINT('Ctrl Pts',(14.4443773170177,-4.07560759205015,133.560702208443));
#69086=CARTESIAN_POINT('Ctrl Pts',(14.4366261257776,-3.99563064588826,133.672133063932));
#69087=CARTESIAN_POINT('Ctrl Pts',(14.4288782290005,-3.91568769206196,133.783516558336));
#69088=CARTESIAN_POINT('Ctrl Pts',(14.4211303322236,-3.83104241952575,133.89161235171));
#69089=CARTESIAN_POINT('Ctrl Pts',(14.4133824354465,-3.74200230332689,133.99600624708));
#69090=CARTESIAN_POINT('Ctrl Pts',(14.4056361593625,-3.65298081240086,134.100378305497));
#69091=CARTESIAN_POINT('Ctrl Pts',(14.3978898832784,-3.55956655991525,134.201049708876));
#69092=CARTESIAN_POINT('Ctrl Pts',(14.3901436071943,-3.46210741825086,134.297639204652));
#69093=CARTESIAN_POINT('Ctrl Pts',(14.382397273929,-3.36464755716523,134.39422941343));
#69094=CARTESIAN_POINT('Ctrl Pts',(14.3746509406637,-3.26314302501076,134.486737379268));
#69095=CARTESIAN_POINT('Ctrl Pts',(14.3669046073984,-3.1579783841685,134.574818890459));
#69096=CARTESIAN_POINT('Ctrl Pts',(14.3591565393954,-3.05279019243393,134.662920126893));
#69097=CARTESIAN_POINT('Ctrl Pts',(14.3514084713925,-2.9439405606578,134.746592685173));
#69098=CARTESIAN_POINT('Ctrl Pts',(14.3436604033895,-2.83184661015392,134.825533063391));
#69099=CARTESIAN_POINT('Ctrl Pts',(14.3359041006477,-2.71963352486567,134.904557340382));
#69100=CARTESIAN_POINT('Ctrl Pts',(14.3281477979059,-2.60416955306115,134.978839165039));
#69101=CARTESIAN_POINT('Ctrl Pts',(14.3203914951641,-2.48590070885261,135.048118472136));
#69102=CARTESIAN_POINT('Ctrl Pts',(14.31263105265,-2.36756874100076,135.117434755686));
#69103=CARTESIAN_POINT('Ctrl Pts',(14.3048706101358,-2.24642926291042,135.181743018257));
#69104=CARTESIAN_POINT('Ctrl Pts',(14.2971101676216,-2.1229513973547,135.24082998261));
#69105=CARTESIAN_POINT('Ctrl Pts',(14.2893372673562,-1.99927531416751,135.300011798603));
#69106=CARTESIAN_POINT('Ctrl Pts',(14.2815643670909,-1.87325370188042,135.353955413148));
#69107=CARTESIAN_POINT('Ctrl Pts',(14.2737914668255,-1.74537493074503,135.402496045501));
#69108=CARTESIAN_POINT('Ctrl Pts',(14.2663011310631,-1.62214487504086,135.449272103603));
#69109=CARTESIAN_POINT('Ctrl Pts',(14.2588107953007,-1.49719063320006,135.491031085904));
#69110=CARTESIAN_POINT('Ctrl Pts',(14.2513204595383,-1.37095918183447,135.527670260628));
#69111=CARTESIAN_POINT('Ctrl Pts',(14.2435461254192,-1.2399416266296,135.565698620796));
#69112=CARTESIAN_POINT('Ctrl Pts',(14.2357717913002,-1.10713307500333,135.598331736911));
#69113=CARTESIAN_POINT('Ctrl Pts',(14.2279974571811,-0.973017492499181,
135.625399926863));
#69114=CARTESIAN_POINT('Ctrl Pts',(14.220232704234,-0.839067195464393,135.652434757691));
#69115=CARTESIAN_POINT('Ctrl Pts',(14.2124679512869,-0.703813452119732,
135.673918231672));
#69116=CARTESIAN_POINT('Ctrl Pts',(14.2047031983398,-0.567755925222235,
135.689730232229));
#69117=CARTESIAN_POINT('Ctrl Pts',(14.1969461574548,-0.431833532578712,
135.705526528084));
#69118=CARTESIAN_POINT('Ctrl Pts',(14.1891891165698,-0.295109330931846,
135.715662515573));
#69119=CARTESIAN_POINT('Ctrl Pts',(14.1814320756848,-0.158093381539117,
135.720069065513));
#69120=CARTESIAN_POINT('Ctrl Pts',(14.1736808844447,-0.021180756939468,
135.724472292439));
#69121=CARTESIAN_POINT('Ctrl Pts',(14.1659296932045,0.116022788308936,135.723154669218));
#69122=CARTESIAN_POINT('Ctrl Pts',(14.1581785019644,0.253002215864965,135.716098898589));
#69123=CARTESIAN_POINT('Ctrl Pts',(14.1504306051873,0.389923423510236,135.709046126851));
#69124=CARTESIAN_POINT('Ctrl Pts',(14.1426827084102,0.526620313289917,135.696260078493));
#69125=CARTESIAN_POINT('Ctrl Pts',(14.1349348116331,0.66257821178492,135.677775557397));
#69126=CARTESIAN_POINT('Ctrl Pts',(14.127188535549,0.798507670818471,135.659294902865));
#69127=CARTESIAN_POINT('Ctrl Pts',(14.119442259465,0.933698058881814,135.635118199181));
#69128=CARTESIAN_POINT('Ctrl Pts',(14.1116959833809,1.06764058387698,135.605332044908));
#69129=CARTESIAN_POINT('Ctrl Pts',(14.1039496501156,1.20158409760543,135.575545670762));
#69130=CARTESIAN_POINT('Ctrl Pts',(14.0962033168502,1.33427934824253,135.54014984827));
#69131=CARTESIAN_POINT('Ctrl Pts',(14.0884569835848,1.46522887537027,135.499282065821));
#69132=CARTESIAN_POINT('Ctrl Pts',(14.0807089155818,1.59620772773667,135.458405131315));
#69133=CARTESIAN_POINT('Ctrl Pts',(14.0729608475789,1.72543970552228,135.412053914885));
#69134=CARTESIAN_POINT('Ctrl Pts',(14.0652127795759,1.85244399971922,135.360415302313));
#69135=CARTESIAN_POINT('Ctrl Pts',(14.057456476834,1.9795832755914,135.308721807609));
#69136=CARTESIAN_POINT('Ctrl Pts',(14.0497001740922,2.10448977557084,135.251729838681));
#69137=CARTESIAN_POINT('Ctrl Pts',(14.0419438713504,2.22670361789578,135.189674068227));
#69138=CARTESIAN_POINT('Ctrl Pts',(14.0341834288362,2.34898268942833,135.12758517674));
#69139=CARTESIAN_POINT('Ctrl Pts',(14.026422986322,2.46856589893843,135.06042728971));
#69140=CARTESIAN_POINT('Ctrl Pts',(14.0186625438078,2.58502023792568,134.988479811855));
#69141=CARTESIAN_POINT('Ctrl Pts',(14.0108896435423,2.70166151975621,134.91641683752));
#69142=CARTESIAN_POINT('Ctrl Pts',(14.003116743277,2.81516357012621,134.839549127293));
#69143=CARTESIAN_POINT('Ctrl Pts',(13.9953438430115,2.92512377827804,134.758198492878));
#69144=CARTESIAN_POINT('Ctrl Pts',(13.9878535072495,3.03108665589094,134.679805158934));
#69145=CARTESIAN_POINT('Ctrl Pts',(13.9803631714874,3.13376049026414,134.597249366343));
#69146=CARTESIAN_POINT('Ctrl Pts',(13.9728728357253,3.23281724846769,134.510851640152));
#69147=CARTESIAN_POINT('Ctrl Pts',(13.9650985016062,3.33562977376589,134.421178117913));
#69148=CARTESIAN_POINT('Ctrl Pts',(13.9573241674871,3.4348712047546,134.327081518464));
#69149=CARTESIAN_POINT('Ctrl Pts',(13.949549833368,3.53013718787154,134.228877298399));
#69150=CARTESIAN_POINT('Ctrl Pts',(13.9417850804209,3.62528576417846,134.130794106259));
#69151=CARTESIAN_POINT('Ctrl Pts',(13.9340203274738,3.71646837131698,134.028613643848));
#69152=CARTESIAN_POINT('Ctrl Pts',(13.9262555745267,3.80331387188264,133.92269136565));
#69153=CARTESIAN_POINT('Ctrl Pts',(13.9184985336417,3.89007311627284,133.816874290952));
#69154=CARTESIAN_POINT('Ctrl Pts',(13.9107414927567,3.97250358027798,133.707323096698));
#69155=CARTESIAN_POINT('Ctrl Pts',(13.9029844518717,4.05027140298973,133.594429545859));
#69156=CARTESIAN_POINT('Ctrl Pts',(13.8952332606315,4.12798058038143,133.481621128924));
#69157=CARTESIAN_POINT('Ctrl Pts',(13.8874820693913,4.20103389423856,133.365475692964));
#69158=CARTESIAN_POINT('Ctrl Pts',(13.8797308781512,4.26913840108136,133.24641720473));
#69159=CARTESIAN_POINT('Ctrl Pts',(13.8719829813741,4.33721396169201,133.12740931953));
#69160=CARTESIAN_POINT('Ctrl Pts',(13.8642350845971,4.40034470502147,133.005491183247));
#69161=CARTESIAN_POINT('Ctrl Pts',(13.85648718782,4.45828171900775,132.881114617553));
#69162=CARTESIAN_POINT('Ctrl Pts',(13.8487409117359,4.51620661381969,132.756764068755));
#69163=CARTESIAN_POINT('Ctrl Pts',(13.8409946356517,4.56893977524758,132.629956467597));
#69164=CARTESIAN_POINT('Ctrl Pts',(13.8332483595676,4.61627904655845,132.501166683917));
#69165=CARTESIAN_POINT('Ctrl Pts',(13.8255020263022,4.663618667317,132.372375949541));
#69166=CARTESIAN_POINT('Ctrl Pts',(13.8177556930369,4.70556418362389,132.241603370407));
#69167=CARTESIAN_POINT('Ctrl Pts',(13.8100093597715,4.74196237884601,132.109341789886));
#69168=CARTESIAN_POINT('Ctrl Pts',(13.8022612917685,4.77836872519158,131.977050590301));
#69169=CARTESIAN_POINT('Ctrl Pts',(13.7945132237656,4.80922517473416,131.843270102678));
#69170=CARTESIAN_POINT('Ctrl Pts',(13.7867651557626,4.83442907076123,131.708505861583));
#69171=CARTESIAN_POINT('Ctrl Pts',(13.7790088530207,4.85965975378897,131.573598391449));
#69172=CARTESIAN_POINT('Ctrl Pts',(13.7712525502789,4.87922581048319,131.437705464168));
#69173=CARTESIAN_POINT('Ctrl Pts',(13.763496247537,4.89307610030521,131.301340837617));
#69174=CARTESIAN_POINT('Ctrl Pts',(13.7557358050229,4.90693378244394,131.164903429159));
#69175=CARTESIAN_POINT('Ctrl Pts',(13.7479753625086,4.91506959579771,131.027994209863));
#69176=CARTESIAN_POINT('Ctrl Pts',(13.7402149199945,4.91748455979706,130.891128507119));
#69177=CARTESIAN_POINT('Ctrl Pts',(13.732442019729,4.91990340051102,130.754043095398));
#69178=CARTESIAN_POINT('Ctrl Pts',(13.7246691194636,4.91658304955627,130.617001730901));
#69179=CARTESIAN_POINT('Ctrl Pts',(13.7168962191981,4.90757663528673,130.480517088546));
#69180=CARTESIAN_POINT('Ctrl Pts',(13.7094058834363,4.89889762686187,130.348994006729));
#69181=CARTESIAN_POINT('Ctrl Pts',(13.7019155476744,4.88493881588,130.217988179567));
#69182=CARTESIAN_POINT('Ctrl Pts',(13.6944252119125,4.86579255933035,130.087948842073));
#69183=CARTESIAN_POINT('Ctrl Pts',(13.6866508777935,4.84592036664384,129.95297902357));
#69184=CARTESIAN_POINT('Ctrl Pts',(13.6788765436744,4.82039665012975,129.818622886577));
#69185=CARTESIAN_POINT('Ctrl Pts',(13.6711022095553,4.789268249377,129.685391137192));
#69186=CARTESIAN_POINT('Ctrl Pts',(13.6633374566082,4.75817821159616,129.55232358403));
#69187=CARTESIAN_POINT('Ctrl Pts',(13.6555727036611,4.72149732108605,129.420378038389));
#69188=CARTESIAN_POINT('Ctrl Pts',(13.6478079507141,4.67932402293845,129.29005888051));
#69189=CARTESIAN_POINT('Ctrl Pts',(13.6400509098291,4.63719261190517,129.159869157455));
#69190=CARTESIAN_POINT('Ctrl Pts',(13.6322938689441,4.58957976879964,129.031302977105));
#69191=CARTESIAN_POINT('Ctrl Pts',(13.6245368280591,4.53663463492747,128.904852983552));
#69192=CARTESIAN_POINT('Ctrl Pts',(13.6167856368189,4.48372942739252,128.778498346923));
#69193=CARTESIAN_POINT('Ctrl Pts',(13.6090344455789,4.42550008327639,128.654257079851));
#69194=CARTESIAN_POINT('Ctrl Pts',(13.6012832543387,4.36214495470752,128.532604808369));
#69195=CARTESIAN_POINT('Ctrl Pts',(13.5935353575617,4.29881675375834,128.411004242348));
#69196=CARTESIAN_POINT('Ctrl Pts',(13.5857874607845,4.23036728162606,128.291990829352));
#69197=CARTESIAN_POINT('Ctrl Pts',(13.5780395640075,4.15704212563074,128.1760182068));
#69198=CARTESIAN_POINT('Ctrl Pts',(13.5702932879234,4.08373230767745,128.060069843221));
#69199=CARTESIAN_POINT('Ctrl Pts',(13.5625470118393,4.00554904327596,127.947161335157));
#69200=CARTESIAN_POINT('Ctrl Pts',(13.5548007357552,3.92278258322002,127.837719441541));
#69201=CARTESIAN_POINT('Ctrl Pts',(13.5470544024899,3.84001551220088,127.72827674005));
#69202=CARTESIAN_POINT('Ctrl Pts',(13.5393080692245,3.75266541384422,127.622301015903));
#69203=CARTESIAN_POINT('Ctrl Pts',(13.5315617359591,3.6610641139026,127.520187568472));
#69204=CARTESIAN_POINT('Ctrl Pts',(13.5238136679562,3.56944230048484,127.418051253442));
#69205=CARTESIAN_POINT('Ctrl Pts',(13.5160655999532,3.47356765207634,127.319779227212));
#69206=CARTESIAN_POINT('Ctrl Pts',(13.5083175319503,3.37381000076367,127.225731111561));
#69207=CARTESIAN_POINT('Ctrl Pts',(13.5005612292084,3.27394632583218,127.131583040454));
#69208=CARTESIAN_POINT('Ctrl Pts',(13.4928049264665,3.17019168899456,127.041668116254));
#69209=CARTESIAN_POINT('Ctrl Pts',(13.4850486237247,3.0629506865919,126.956307063624));
#69210=CARTESIAN_POINT('Ctrl Pts',(13.4772881812105,2.95565244643715,126.87090045123));
#69211=CARTESIAN_POINT('Ctrl Pts',(13.4695277386964,2.8448644486195,126.790052783814));
#69212=CARTESIAN_POINT('Ctrl Pts',(13.4617672961822,2.73102080369358,126.714041750742));
#69213=CARTESIAN_POINT('Ctrl Pts',(13.4539943959168,2.61699440684225,126.637908698012));
#69214=CARTESIAN_POINT('Ctrl Pts',(13.4462214956514,2.49990289488248,126.566627998375));
#69215=CARTESIAN_POINT('Ctrl Pts',(13.4384485953859,2.380206312918,126.50043206676));
#69216=CARTESIAN_POINT('Ctrl Pts',(13.4309582596238,2.26486100320381,126.436642523995));
#69217=CARTESIAN_POINT('Ctrl Pts',(13.4234679238617,2.14709701223217,126.37757461743));
#69218=CARTESIAN_POINT('Ctrl Pts',(13.4159775880996,2.02734221535028,126.32339346701));
#69219=CARTESIAN_POINT('Ctrl Pts',(13.4082032539805,1.9030468789475,126.267158021805));
#69220=CARTESIAN_POINT('Ctrl Pts',(13.4004289198614,1.77621306350427,126.216009073502));
#69221=CARTESIAN_POINT('Ctrl Pts',(13.3926545857423,1.64729575846675,126.170183263748));
#69222=CARTESIAN_POINT('Ctrl Pts',(13.3848898327953,1.51853733248636,126.12441393021));
#69223=CARTESIAN_POINT('Ctrl Pts',(13.3771250798482,1.38770089074569,126.083954811885));
#69224=CARTESIAN_POINT('Ctrl Pts',(13.3693603269011,1.25526399460268,126.04899571397));
#69225=CARTESIAN_POINT('Ctrl Pts',(13.3616032860161,1.12295863665178,126.014071337924));
#69226=CARTESIAN_POINT('Ctrl Pts',(13.3538462451311,0.989056363232963,125.984636210412));
#69227=CARTESIAN_POINT('Ctrl Pts',(13.3460892042461,0.854052264291844,125.960831140794));
#69228=CARTESIAN_POINT('Ctrl Pts',(13.338338013006,0.719149972991915,125.937044022765));
#69229=CARTESIAN_POINT('Ctrl Pts',(13.3305868217659,0.583147893483745,125.918878579497));
#69230=CARTESIAN_POINT('Ctrl Pts',(13.3228356305258,0.446553397587962,125.906425019214));
#69231=CARTESIAN_POINT('Ctrl Pts',(13.3150877337487,0.310016957996711,125.893976752027));
#69232=CARTESIAN_POINT('Ctrl Pts',(13.3073398369715,0.172888991349683,125.887235574733));
#69233=CARTESIAN_POINT('Ctrl Pts',(13.2995919401945,0.0356839015994468,
125.88624006987));
#69234=CARTESIAN_POINT('Ctrl Pts',(13.2918456641104,-0.101492487804,125.885244773246));
#69235=CARTESIAN_POINT('Ctrl Pts',(13.2840993880262,-0.238745577515022,
125.889992761299));
#69236=CARTESIAN_POINT('Ctrl Pts',(13.2763531119421,-0.37555943551309,125.900470511446));
#69237=CARTESIAN_POINT('Ctrl Pts',(13.2686067786768,-0.512374303439792,
125.910948338938));
#69238=CARTESIAN_POINT('Ctrl Pts',(13.2608604454115,-0.648749543360048,
125.927155983066));
#69239=CARTESIAN_POINT('Ctrl Pts',(13.2531141121461,-0.784173218791643,
125.949027938395));
#69240=CARTESIAN_POINT('Ctrl Pts',(13.2453660441432,-0.91962722141639,125.970904791796));
#69241=CARTESIAN_POINT('Ctrl Pts',(13.2376179761402,-1.05412884962571,125.998448418208));
#69242=CARTESIAN_POINT('Ctrl Pts',(13.2298699081372,-1.18717564015418,126.031542051779));
#69243=CARTESIAN_POINT('Ctrl Pts',(13.2221136053954,-1.3203638343949,126.064670857657));
#69244=CARTESIAN_POINT('Ctrl Pts',(13.2143573026535,-1.45209372220673,126.103361359288));
#69245=CARTESIAN_POINT('Ctrl Pts',(13.2066009999117,-1.58187677464065,126.147446517827));
#69246=CARTESIAN_POINT('Ctrl Pts',(13.1988405573975,-1.71172909619735,126.191555205941));
#69247=CARTESIAN_POINT('Ctrl Pts',(13.1910801148834,-1.83963214748684,126.241064147132));
#69248=CARTESIAN_POINT('Ctrl Pts',(13.1833196723692,-1.96511765322266,126.29575820978));
#69249=CARTESIAN_POINT('Ctrl Pts',(13.1755467721038,-2.09080459943255,126.350540072193));
#69250=CARTESIAN_POINT('Ctrl Pts',(13.1677738718383,-2.21406589314516,126.410523518127));
#69251=CARTESIAN_POINT('Ctrl Pts',(13.1600009715729,-2.33445733148285,126.475447124553));
#69252=CARTESIAN_POINT('Ctrl Pts',(13.1525106358108,-2.4504722377899,126.538010594354));
#69253=CARTESIAN_POINT('Ctrl Pts',(13.1450203000487,-2.56382205413805,126.605161128895));
#69254=CARTESIAN_POINT('Ctrl Pts',(13.1375299642867,-2.67413658336338,126.676627995894));
#69255=CARTESIAN_POINT('Ctrl Pts',(13.1297595003965,-2.7885767223821,126.750767624209));
#69256=CARTESIAN_POINT('Ctrl Pts',(13.1219890365063,-2.90011380735081,126.829788347022));
#69257=CARTESIAN_POINT('Ctrl Pts',(13.1142185726161,-3.00830292214689,126.91343571581));
#69258=CARTESIAN_POINT('Ctrl Pts',(13.1064604100668,-3.11632076387646,126.996950663316));
#69259=CARTESIAN_POINT('Ctrl Pts',(13.0987022475175,-3.22100088449626,127.085077431815));
#69260=CARTESIAN_POINT('Ctrl Pts',(13.0909440849681,-3.32192599673668,127.177517536496));
#69261=CARTESIAN_POINT('Ctrl Pts',(13.0831930221195,-3.42275874972563,127.269873046781));
#69262=CARTESIAN_POINT('Ctrl Pts',(13.0754419592708,-3.51984304309827,127.366533778881));
#69263=CARTESIAN_POINT('Ctrl Pts',(13.0676908964221,-3.61279320540572,127.467159946723));
#69264=CARTESIAN_POINT('Ctrl Pts',(13.0599452416455,-3.70567851452026,127.567715905669));
#69265=CARTESIAN_POINT('Ctrl Pts',(13.0521995868689,-3.79443516705613,127.672231509142));
#69266=CARTESIAN_POINT('Ctrl Pts',(13.0444539320923,-3.87871334140427,127.780329222605));
#69267=CARTESIAN_POINT('Ctrl Pts',(13.0367119978187,-3.96295103406133,127.888375013036));
#69268=CARTESIAN_POINT('Ctrl Pts',(13.0289700635451,-4.04271428975083,127.999999180904));
#69269=CARTESIAN_POINT('Ctrl Pts',(13.0212281292715,-4.11769295949528,128.11479043744));
#69270=CARTESIAN_POINT('Ctrl Pts',(13.0134865487772,-4.19266820297759,128.229576448419));
#69271=CARTESIAN_POINT('Ctrl Pts',(13.0057449682828,-4.26285907196028,128.347528938801));
#69272=CARTESIAN_POINT('Ctrl Pts',(12.9980033877885,-4.32799828600891,128.468206962773));
#69273=CARTESIAN_POINT('Ctrl Pts',(12.9902623349182,-4.39313306052229,128.588876761985));
#69274=CARTESIAN_POINT('Ctrl Pts',(12.982521282048,-4.4532166836464,128.712271378145));
#69275=CARTESIAN_POINT('Ctrl Pts',(12.9747802291778,-4.50802783479095,128.837925237684));
#69276=CARTESIAN_POINT('Ctrl Pts',(12.9670346006886,-4.56287138397525,128.963653369313));
#69277=CARTESIAN_POINT('Ctrl Pts',(12.9592889721994,-4.61243607931077,129.09164305243));
#69278=CARTESIAN_POINT('Ctrl Pts',(12.9515433437103,-4.65654867068509,129.221408457821));
#69279=CARTESIAN_POINT('Ctrl Pts',(12.944440529551,-4.69700033178115,129.340404554794));
#69280=CARTESIAN_POINT('Ctrl Pts',(12.9373377153916,-4.73286777220424,129.460893430873));
#69281=CARTESIAN_POINT('Ctrl Pts',(12.9302349012323,-4.7640545282341,129.582490119308));
#69282=CARTESIAN_POINT('Origin',(213.235140564004,0.,130.804360617566));
#69283=CARTESIAN_POINT('',(10.8346522545384,-4.76405452823402,129.582490119308));
#69284=CARTESIAN_POINT('',(11.1800167307073,-4.76405452823405,129.582490119308));
#69285=CARTESIAN_POINT('',(213.235140564004,-4.76405452823405,129.582490119308));
#69286=CARTESIAN_POINT('',(12.5148594360351,-4.91824821769922,130.800173542404));
#69287=CARTESIAN_POINT('Ctrl Pts',(12.5148594359913,-4.91824821769988,130.800173543179));
#69288=CARTESIAN_POINT('Ctrl Pts',(12.5068142965337,-4.91836943045601,130.942553249534));
#69289=CARTESIAN_POINT('Ctrl Pts',(12.498769157076,-4.91230289435018,131.085035942718));
#69290=CARTESIAN_POINT('Ctrl Pts',(12.4907240176183,-4.90005356047322,131.227040362756));
#69291=CARTESIAN_POINT('Ctrl Pts',(12.4830162607711,-4.88831791716201,131.363089656449));
#69292=CARTESIAN_POINT('Ctrl Pts',(12.4753085039239,-4.87090757015808,131.498699546133));
#69293=CARTESIAN_POINT('Ctrl Pts',(12.4676007470767,-4.84788005281825,131.63336125447));
#69294=CARTESIAN_POINT('Ctrl Pts',(12.459893497827,-4.82485405196521,131.768014094603));
#69295=CARTESIAN_POINT('Ctrl Pts',(12.4521862485774,-4.79621168283912,131.901718488149));
#69296=CARTESIAN_POINT('Ctrl Pts',(12.4444789993277,-4.76206193345132,132.033974054575));
#69297=CARTESIAN_POINT('Ctrl Pts',(12.4367705478664,-4.7279068572309,132.166250250824));
#69298=CARTESIAN_POINT('Ctrl Pts',(12.429062096405,-4.68824279042093,132.297076787814));
#69299=CARTESIAN_POINT('Ctrl Pts',(12.4213536449437,-4.64322898087268,132.425967133859));
#69300=CARTESIAN_POINT('Ctrl Pts',(12.4136422809646,-4.59819816356065,132.554906179105));
#69301=CARTESIAN_POINT('Ctrl Pts',(12.4059309169855,-4.54781371223153,132.681907205291));
#69302=CARTESIAN_POINT('Ctrl Pts',(12.3982195530064,-4.49228334782613,132.806502816648));
#69303=CARTESIAN_POINT('Ctrl Pts',(12.3904992836522,-4.43668885485341,132.931242315734));
#69304=CARTESIAN_POINT('Ctrl Pts',(12.3827790142979,-4.37593674684958,133.053570493914));
#69305=CARTESIAN_POINT('Ctrl Pts',(12.3750587449437,-4.31028129629677,133.173043418047));
#69306=CARTESIAN_POINT('Ctrl Pts',(12.3673332242949,-4.24458118718358,133.292597607159));
#69307=CARTESIAN_POINT('Ctrl Pts',(12.359607703646,-4.17397129776218,133.409292337912));
#69308=CARTESIAN_POINT('Ctrl Pts',(12.3518821829972,-4.09874908507779,133.522712875842));
#69309=CARTESIAN_POINT('Ctrl Pts',(12.3441454390979,-4.02341759332118,133.636298185463));
#69310=CARTESIAN_POINT('Ctrl Pts',(12.3364086951987,-3.94346063515098,133.746599490057));
#69311=CARTESIAN_POINT('Ctrl Pts',(12.3286719512995,-3.85921596973571,133.853235026497));
#69312=CARTESIAN_POINT('Ctrl Pts',(12.3263733305355,-3.83418650776852,133.884916915084));
#69313=CARTESIAN_POINT('Ctrl Pts',(12.3240747097715,-3.80877881157106,133.916275471344));
#69314=CARTESIAN_POINT('Ctrl Pts',(12.3217760890076,-3.78300234485484,133.947301329912));
#69315=CARTESIAN_POINT('Ctrl Pts',(12.3140017548885,-3.69582186349672,134.05223616502));
#69316=CARTESIAN_POINT('Ctrl Pts',(12.3062274207694,-3.60413388224911,134.153707075862));
#69317=CARTESIAN_POINT('Ctrl Pts',(12.2984530866503,-3.50824406349114,134.251302255233));
#69318=CARTESIAN_POINT('Ctrl Pts',(12.2906883337032,-3.41247242036487,134.348777157267));
#69319=CARTESIAN_POINT('Ctrl Pts',(12.2829235807562,-3.31250951455571,134.442385555422));
#69320=CARTESIAN_POINT('Ctrl Pts',(12.2751588278091,-3.20870179191121,134.531747889247));
#69321=CARTESIAN_POINT('Ctrl Pts',(12.2674017869241,-3.10499717256027,134.621021467141));
#69322=CARTESIAN_POINT('Ctrl Pts',(12.259644746039,-2.99745563019451,134.706057119805));
#69323=CARTESIAN_POINT('Ctrl Pts',(12.251887705154,-2.88646080322414,134.786511681244));
#69324=CARTESIAN_POINT('Ctrl Pts',(12.2441365139139,-2.77554967831635,134.866905571272));
#69325=CARTESIAN_POINT('Ctrl Pts',(12.2363853226737,-2.66119076747546,134.942725017794));
#69326=CARTESIAN_POINT('Ctrl Pts',(12.2286341314336,-2.5438008855245,135.013666987659));
#69327=CARTESIAN_POINT('Ctrl Pts',(12.2208862346565,-2.42646089740469,135.084578805294));
#69328=CARTESIAN_POINT('Ctrl Pts',(12.2131383378794,-2.30609283430186,135.150617067635));
#69329=CARTESIAN_POINT('Ctrl Pts',(12.2053904411023,-2.18314241457215,135.211522091825));
#69330=CARTESIAN_POINT('Ctrl Pts',(12.1976441650182,-2.06021771341975,135.272414375998));
#69331=CARTESIAN_POINT('Ctrl Pts',(12.1898978889341,-1.93471208019027,135.328175384359));
#69332=CARTESIAN_POINT('Ctrl Pts',(12.18215161285,-1.80709539676928,135.378591622825));
#69333=CARTESIAN_POINT('Ctrl Pts',(12.1744052795846,-1.67947777131093,135.429008233453));
#69334=CARTESIAN_POINT('Ctrl Pts',(12.1666589463192,-1.54974942818394,135.474079851807));
#69335=CARTESIAN_POINT('Ctrl Pts',(12.1589126130539,-1.4183993920549,135.513641478496));
#69336=CARTESIAN_POINT('Ctrl Pts',(12.1511645450509,-1.28701994099618,135.553211964736));
#69337=CARTESIAN_POINT('Ctrl Pts',(12.143416477048,-1.15401844855735,135.587269891213));
#69338=CARTESIAN_POINT('Ctrl Pts',(12.135668409045,-1.01989784024417,135.615700499342));
#69339=CARTESIAN_POINT('Ctrl Pts',(12.1279121063031,-0.88563468695223,135.644161323859));
#69340=CARTESIAN_POINT('Ctrl Pts',(12.1201558035612,-0.750250424888485,
135.666982801569));
#69341=CARTESIAN_POINT('Ctrl Pts',(12.1123995008194,-0.614257436747398,
135.684101477888));
#69342=CARTESIAN_POINT('Ctrl Pts',(12.1046390583052,-0.478191865053869,
135.701229290961));
#69343=CARTESIAN_POINT('Ctrl Pts',(12.0968786157911,-0.341517309318485,
135.712648205165));
#69344=CARTESIAN_POINT('Ctrl Pts',(12.0891181732769,-0.204748972992584,
135.7183468732));
#69345=CARTESIAN_POINT('Ctrl Pts',(12.0813452730115,-0.0677610839914891,
135.724054689243));
#69346=CARTESIAN_POINT('Ctrl Pts',(12.073572372746,0.0693204952466555,135.724023909351));
#69347=CARTESIAN_POINT('Ctrl Pts',(12.0657994724806,0.205981962504627,135.718295343793));
#69348=CARTESIAN_POINT('Ctrl Pts',(12.0583091367186,0.337675441197567,135.712775026023));
#69349=CARTESIAN_POINT('Ctrl Pts',(12.0508188009566,0.468978514894847,135.701964013463));
#69350=CARTESIAN_POINT('Ctrl Pts',(12.0433284651946,0.599439861640033,135.685943856104));
#69351=CARTESIAN_POINT('Ctrl Pts',(12.0355541310755,0.73484769000088,135.66931628961));
#69352=CARTESIAN_POINT('Ctrl Pts',(12.0277797969564,0.869777634565994,135.647024100123));
#69353=CARTESIAN_POINT('Ctrl Pts',(12.0200054628373,1.00371801228709,135.619101858205));
#69354=CARTESIAN_POINT('Ctrl Pts',(12.0122407098902,1.13749332046325,135.591214027955));
#69355=CARTESIAN_POINT('Ctrl Pts',(12.0044759569431,1.27028110927898,135.557710029917));
#69356=CARTESIAN_POINT('Ctrl Pts',(11.996711203996,1.40157478133202,135.518676177097));
#69357=CARTESIAN_POINT('Ctrl Pts',(11.988954163111,1.53273805065924,135.47968109325));
#69358=CARTESIAN_POINT('Ctrl Pts',(11.981197122226,1.66240978407772,135.435167195299));
#69359=CARTESIAN_POINT('Ctrl Pts',(11.973440081341,1.79009390038473,135.385271759501));
#69360=CARTESIAN_POINT('Ctrl Pts',(11.9656888901008,1.91768172910639,135.33541395024));
#69361=CARTESIAN_POINT('Ctrl Pts',(11.9579376988606,2.04328456146562,135.280182822575));
#69362=CARTESIAN_POINT('Ctrl Pts',(11.9501865076205,2.16642214849594,135.219765257801));
#69363=CARTESIAN_POINT('Ctrl Pts',(11.9424386108434,2.28950739876697,135.159373372103));
#69364=CARTESIAN_POINT('Ctrl Pts',(11.9346907140663,2.41012913743569,135.093799605484));
#69365=CARTESIAN_POINT('Ctrl Pts',(11.9269428172892,2.52782796430217,135.023278588491));
#69366=CARTESIAN_POINT('Ctrl Pts',(11.9191965412051,2.6455021711112,134.952772322975));
#69367=CARTESIAN_POINT('Ctrl Pts',(11.911450265121,2.76025434708535,134.877321066292));
#69368=CARTESIAN_POINT('Ctrl Pts',(11.9037039890369,2.87165089096896,134.797204744613));
#69369=CARTESIAN_POINT('Ctrl Pts',(11.8959576557715,2.9830482571564,134.717087831535));
#69370=CARTESIAN_POINT('Ctrl Pts',(11.8882113225061,3.09108962442339,134.63230601302));
#69371=CARTESIAN_POINT('Ctrl Pts',(11.8804649892408,3.19537184433061,134.54318153317));
#69372=CARTESIAN_POINT('Ctrl Pts',(11.8727169212378,3.29967741751793,134.454037094511));
#69373=CARTESIAN_POINT('Ctrl Pts',(11.8649688532349,3.40022187103907,134.360548313296));
#69374=CARTESIAN_POINT('Ctrl Pts',(11.8572207852319,3.49663681172535,134.263076285178));
#69375=CARTESIAN_POINT('Ctrl Pts',(11.84946448249,3.59315422335808,134.165500662629));
#69376=CARTESIAN_POINT('Ctrl Pts',(11.8417081797482,3.68553307948342,134.063933614821));
#69377=CARTESIAN_POINT('Ctrl Pts',(11.8339518770063,3.77344303860083,133.958771925074));
#69378=CARTESIAN_POINT('Ctrl Pts',(11.8261914344921,3.86139991791058,133.853554107366));
#69379=CARTESIAN_POINT('Ctrl Pts',(11.8184309919779,3.94488290966734,133.744738134851));
#69380=CARTESIAN_POINT('Ctrl Pts',(11.8106705494637,4.02360398701671,133.632751329289));
#69381=CARTESIAN_POINT('Ctrl Pts',(11.8028976491983,4.10245143442787,133.520584752566));
#69382=CARTESIAN_POINT('Ctrl Pts',(11.7951247489328,4.17652148041489,133.405237500317));
#69383=CARTESIAN_POINT('Ctrl Pts',(11.7873518486673,4.24557073716481,133.287163907847));
#69384=CARTESIAN_POINT('Ctrl Pts',(11.7798615129054,4.31210987950598,133.173382587875));
#69385=CARTESIAN_POINT('Ctrl Pts',(11.7723711771436,4.37398678704385,133.057069976916));
#69386=CARTESIAN_POINT('Ctrl Pts',(11.7648808413817,4.43102611955394,132.938649864676));
#69387=CARTESIAN_POINT('Ctrl Pts',(11.7571065072626,4.4902281156938,132.815739817886));
#69388=CARTESIAN_POINT('Ctrl Pts',(11.7493321731435,4.54440599621508,132.690169961175));
#69389=CARTESIAN_POINT('Ctrl Pts',(11.7415578390244,4.59331226912462,132.562389474215));
#69390=CARTESIAN_POINT('Ctrl Pts',(11.7337930860773,4.64215826942374,132.434766465284));
#69391=CARTESIAN_POINT('Ctrl Pts',(11.7260283331303,4.68574545036839,132.304938608488));
#69392=CARTESIAN_POINT('Ctrl Pts',(11.7182635801832,4.72387260126554,132.173378772856));
#69393=CARTESIAN_POINT('Ctrl Pts',(11.7105065392982,4.76196188373883,132.041949604307));
#69394=CARTESIAN_POINT('Ctrl Pts',(11.7027494984132,4.79460182001442,131.908792253334));
#69395=CARTESIAN_POINT('Ctrl Pts',(11.6949924575282,4.82163976048743,131.774398288271));
#69396=CARTESIAN_POINT('Ctrl Pts',(11.6872412662881,4.84865731143925,131.640105670742));
#69397=CARTESIAN_POINT('Ctrl Pts',(11.6794900750479,4.87008119841774,131.504578677024));
#69398=CARTESIAN_POINT('Ctrl Pts',(11.6717388838078,4.88580906365169,131.368322368077));
#69399=CARTESIAN_POINT('Ctrl Pts',(11.6639909870307,4.90153024412339,131.232123971695));
#69400=CARTESIAN_POINT('Ctrl Pts',(11.6562430902537,4.91156017322077,131.095197264182));
#69401=CARTESIAN_POINT('Ctrl Pts',(11.6484951934766,4.91584793524088,130.958055575479));
#69402=CARTESIAN_POINT('Ctrl Pts',(11.6407489173925,4.9201348003536,130.820942573862));
#69403=CARTESIAN_POINT('Ctrl Pts',(11.6330026413083,4.91868187530762,130.683615071028));
#69404=CARTESIAN_POINT('Ctrl Pts',(11.6252563652242,4.91149029784851,130.546589174927));
#69405=CARTESIAN_POINT('Ctrl Pts',(11.6175100319589,4.90429866730282,130.409562267333));
#69406=CARTESIAN_POINT('Ctrl Pts',(11.6097636986935,4.89136832030583,130.272837361343));
#69407=CARTESIAN_POINT('Ctrl Pts',(11.6020173654282,4.87275245836635,130.136927817964));
#69408=CARTESIAN_POINT('Ctrl Pts',(11.5942692974252,4.85413242753369,130.000987838585));
#69409=CARTESIAN_POINT('Ctrl Pts',(11.5865212294223,4.82982440122089,129.865863972434));
#69410=CARTESIAN_POINT('Ctrl Pts',(11.5787731614193,4.79993305392135,129.732061340138));
#69411=CARTESIAN_POINT('Ctrl Pts',(11.5710168586775,4.77000993774212,129.598116500811));
#69412=CARTESIAN_POINT('Ctrl Pts',(11.5632605559356,4.73449173210793,129.465496082595));
#69413=CARTESIAN_POINT('Ctrl Pts',(11.5555042531937,4.69353370441307,129.334692482224));
#69414=CARTESIAN_POINT('Ctrl Pts',(11.5477438106795,4.6525538161856,129.203819068034));
#69415=CARTESIAN_POINT('Ctrl Pts',(11.5399833681654,4.60612845290998,129.074764771586));
#69416=CARTESIAN_POINT('Ctrl Pts',(11.5322229256512,4.55446144693704,128.94800289588));
#69417=CARTESIAN_POINT('Ctrl Pts',(11.5244500253858,4.50271150049933,128.821037530757));
#69418=CARTESIAN_POINT('Ctrl Pts',(11.5166771251204,4.44570325949606,128.696372295942));
#69419=CARTESIAN_POINT('Ctrl Pts',(11.5089042248549,4.38368741202849,128.574457539824));
#69420=CARTESIAN_POINT('Ctrl Pts',(11.5014138890929,4.32392599682478,128.456974692175));
#69421=CARTESIAN_POINT('Ctrl Pts',(11.4939235533308,4.25951488303135,128.3420460901));
#69422=CARTESIAN_POINT('Ctrl Pts',(11.4864332175688,4.19071584125612,128.230048320982));
#69423=CARTESIAN_POINT('Ctrl Pts',(11.4786588834497,4.11930826290116,128.113804122407));
#69424=CARTESIAN_POINT('Ctrl Pts',(11.4708845493307,4.04294725391655,128.00034916236));
#69425=CARTESIAN_POINT('Ctrl Pts',(11.4631102152116,3.96187694641529,127.89013445545));
#69426=CARTESIAN_POINT('Ctrl Pts',(11.4553454622645,3.88090655082245,127.780055578315));
#69427=CARTESIAN_POINT('Ctrl Pts',(11.4475807093174,3.79523863396022,127.673209320713));
#69428=CARTESIAN_POINT('Ctrl Pts',(11.4398159563703,3.70516227464205,127.57002056416));
#69429=CARTESIAN_POINT('Ctrl Pts',(11.4320589154853,3.61517538043418,127.466934296134));
#69430=CARTESIAN_POINT('Ctrl Pts',(11.4243018746003,3.52078901267995,127.367498592584));
#69431=CARTESIAN_POINT('Ctrl Pts',(11.4165448337153,3.42233423090189,127.272107586638));
#69432=CARTESIAN_POINT('Ctrl Pts',(11.4087936424752,3.32395369464051,127.176788515792));
#69433=CARTESIAN_POINT('Ctrl Pts',(11.4010424512351,3.22151113072069,127.085508342385));
#69434=CARTESIAN_POINT('Ctrl Pts',(11.393291259995,3.1153761343578,126.998626180697));
#69435=CARTESIAN_POINT('Ctrl Pts',(11.3855433632179,3.0092862481996,126.911780946244));
#69436=CARTESIAN_POINT('Ctrl Pts',(11.3777954664409,2.89950735287498,126.829330252801));
#69437=CARTESIAN_POINT('Ctrl Pts',(11.3700475696638,2.7864438062216,126.751594404562));
#69438=CARTESIAN_POINT('Ctrl Pts',(11.3623012935797,2.67340391002482,126.673874816986));
#69439=CARTESIAN_POINT('Ctrl Pts',(11.3545550174956,2.55708105109701,126.600868334284));
#69440=CARTESIAN_POINT('Ctrl Pts',(11.3468087414115,2.4379100606524,126.532852968191));
#69441=CARTESIAN_POINT('Ctrl Pts',(11.3390624081462,2.3187381905143,126.464837100023));
#69442=CARTESIAN_POINT('Ctrl Pts',(11.3313160748808,2.19671848646086,126.401812615779));
#69443=CARTESIAN_POINT('Ctrl Pts',(11.3235697416154,2.0723116103615,126.344012239686));
#69444=CARTESIAN_POINT('Ctrl Pts',(11.3158216736124,1.94787687420431,126.286198919598));
#69445=CARTESIAN_POINT('Ctrl Pts',(11.3080736056094,1.8210542567252,126.233612200335));
#69446=CARTESIAN_POINT('Ctrl Pts',(11.3003255376064,1.69232530933384,126.186437046318));
#69447=CARTESIAN_POINT('Ctrl Pts',(11.2925692348646,1.56345954728617,126.139211753986));
#69448=CARTESIAN_POINT('Ctrl Pts',(11.2848129321227,1.43268377570976,126.097409650834));
#69449=CARTESIAN_POINT('Ctrl Pts',(11.2770566293809,1.30049618774361,126.06116625847));
#69450=CARTESIAN_POINT('Ctrl Pts',(11.2692961868667,1.16823804728131,126.024903521915));
#69451=CARTESIAN_POINT('Ctrl Pts',(11.2615357443525,1.03456696981866,125.994205495317));
#69452=CARTESIAN_POINT('Ctrl Pts',(11.2537753018383,0.899991334939068,125.969156520577));
#69453=CARTESIAN_POINT('Ctrl Pts',(11.2460024015729,0.765199667303492,125.944067335));
#69454=CARTESIAN_POINT('Ctrl Pts',(11.2382295013076,0.629500927784692,125.924645378178));
#69455=CARTESIAN_POINT('Ctrl Pts',(11.2304566010421,0.493409510279886,125.910923163417));
#69456=CARTESIAN_POINT('Ctrl Pts',(11.2229662652801,0.362265358594056,125.897699785727));
#69457=CARTESIAN_POINT('Ctrl Pts',(11.215475929518,0.230756890385802,125.88976896327));
#69458=CARTESIAN_POINT('Ctrl Pts',(11.2079855937559,0.0993424326949853,
125.8871140157));
#69459=CARTESIAN_POINT('Ctrl Pts',(11.2002112596368,-0.0370546441009691,
125.884358404985));
#69460=CARTESIAN_POINT('Ctrl Pts',(11.1924369255177,-0.173782505777523,
125.887277907303));
#69461=CARTESIAN_POINT('Ctrl Pts',(11.1846625913986,-0.310329741600855,
125.895910911806));
#69462=CARTESIAN_POINT('Ctrl Pts',(11.1768978384515,-0.446708695159241,
125.904533276902));
#69463=CARTESIAN_POINT('Ctrl Pts',(11.1691330855045,-0.582907079342031,
125.9188551095));
#69464=CARTESIAN_POINT('Ctrl Pts',(11.1613683325574,-0.718411175136592,
125.938862858247));
#69465=CARTESIAN_POINT('Ctrl Pts',(11.1536112916725,-0.853780686352752,
125.958850735015));
#69466=CARTESIAN_POINT('Ctrl Pts',(11.1458542507874,-0.988456897201061,
125.984513232747));
#69467=CARTESIAN_POINT('Ctrl Pts',(11.1380972099025,-1.12192926655965,126.015784860273));
#69468=CARTESIAN_POINT('Ctrl Pts',(11.1303460186623,-1.25530098336678,126.047032905621));
#69469=CARTESIAN_POINT('Ctrl Pts',(11.1225948274222,-1.38747028654043,126.083881572602));
#69470=CARTESIAN_POINT('Ctrl Pts',(11.1148436361821,-1.51793526782587,126.126214020334));
#69471=CARTESIAN_POINT('Ctrl Pts',(11.107095739405,-1.64834479801399,126.168528475647));
#69472=CARTESIAN_POINT('Ctrl Pts',(11.0993478426279,-1.77705107595486,126.216321955607));
#69473=CARTESIAN_POINT('Ctrl Pts',(11.0915999458508,-1.90356605536896,126.269427394756));
#69474=CARTESIAN_POINT('Ctrl Pts',(11.0838536697667,-2.03005457057688,126.322521725392));
#69475=CARTESIAN_POINT('Ctrl Pts',(11.0761073936825,-2.15435233872,126.38092565386));
#69476=CARTESIAN_POINT('Ctrl Pts',(11.0683611175984,-2.27599042375861,126.444423616478));
#69477=CARTESIAN_POINT('Ctrl Pts',(11.060614784333,-2.39762940670193,126.507922047823));
#69478=CARTESIAN_POINT('Ctrl Pts',(11.0528684510678,-2.51660832078079,126.576514407428));
#69479=CARTESIAN_POINT('Ctrl Pts',(11.0451221178024,-2.63248236951863,126.649938920546));
#69480=CARTESIAN_POINT('Ctrl Pts',(11.0373740497994,-2.74838236744611,126.723379876573));
#69481=CARTESIAN_POINT('Ctrl Pts',(11.0296259817964,-2.86117578625689,126.801654930198));
#69482=CARTESIAN_POINT('Ctrl Pts',(11.0218779137934,-2.97044671984541,126.884458916367));
#69483=CARTESIAN_POINT('Ctrl Pts',(11.0141216110516,-3.07983378788249,126.967350907599));
#69484=CARTESIAN_POINT('Ctrl Pts',(11.0063653083097,-3.18569058007435,127.054781210162));
#69485=CARTESIAN_POINT('Ctrl Pts',(10.9986090055679,-3.28763379269392,127.146403932798));
#69486=CARTESIAN_POINT('Ctrl Pts',(10.9908485630537,-3.38963141547551,127.23807555724));
#69487=CARTESIAN_POINT('Ctrl Pts',(10.9830881205395,-3.48771101713213,127.333943787254));
#69488=CARTESIAN_POINT('Ctrl Pts',(10.9753276780253,-3.58152684684924,127.433626497556));
#69489=CARTESIAN_POINT('Ctrl Pts',(10.9675547777599,-3.67549327806491,127.533469227395));
#69490=CARTESIAN_POINT('Ctrl Pts',(10.9597818774944,-3.76518200373369,127.63713837807));
#69491=CARTESIAN_POINT('Ctrl Pts',(10.952008977229,-3.85028762702443,127.744218749665));
#69492=CARTESIAN_POINT('Ctrl Pts',(10.944518641467,-3.93229944653996,127.847406480032));
#69493=CARTESIAN_POINT('Ctrl Pts',(10.937028305705,-4.01005541142441,127.953761475589));
#69494=CARTESIAN_POINT('Ctrl Pts',(10.929537969943,-4.08332181836509,128.062889116681));
#69495=CARTESIAN_POINT('Ctrl Pts',(10.9216308269926,-4.16066520743983,128.178089273974));
#69496=CARTESIAN_POINT('Ctrl Pts',(10.9137236840423,-4.2332444689001,128.296735493713));
#69497=CARTESIAN_POINT('Ctrl Pts',(10.9058165410919,-4.30074360286296,128.418404305113));
#69498=CARTESIAN_POINT('Ctrl Pts',(10.8979193786894,-4.36815753812039,128.539919543799));
#69499=CARTESIAN_POINT('Ctrl Pts',(10.8900222162869,-4.43050392698758,128.664449458864));
#69500=CARTESIAN_POINT('Ctrl Pts',(10.8821250538845,-4.48750917204769,128.791540582568));
#69501=CARTESIAN_POINT('Ctrl Pts',(10.8742129206602,-4.54462248318634,128.91887263567));
#69502=CARTESIAN_POINT('Ctrl Pts',(10.8663007874359,-4.5963741548825,129.0487753131));
#69503=CARTESIAN_POINT('Ctrl Pts',(10.8583886542115,-4.64253391849751,129.180765262159));
#69504=CARTESIAN_POINT('Ctrl Pts',(10.8504765209872,-4.68869368211251,129.312755211218));
#69505=CARTESIAN_POINT('Ctrl Pts',(10.8425643877628,-4.7292613624623,129.446832094024));
#69506=CARTESIAN_POINT('Ctrl Pts',(10.8346522545385,-4.76405452823403,129.582490119308));
#69507=CARTESIAN_POINT('Ctrl Pts',(12.5846956991378,-4.76405452823411,129.582490119308));
#69508=CARTESIAN_POINT('Ctrl Pts',(12.5753201746923,-4.80496324234701,129.741992574758));
#69509=CARTESIAN_POINT('Ctrl Pts',(12.5659446502468,-4.83789536222626,129.903698025889));
#69510=CARTESIAN_POINT('Ctrl Pts',(12.5565691258012,-4.86264420202425,130.066882192783));
#69511=CARTESIAN_POINT('Ctrl Pts',(12.5473009272211,-4.8871097306683,130.228198316771));
#69512=CARTESIAN_POINT('Ctrl Pts',(12.5380327286411,-4.9035782152433,130.390959472741));
#69513=CARTESIAN_POINT('Ctrl Pts',(12.528764530061,-4.9118963060295,130.55444514923));
#69514=CARTESIAN_POINT('Ctrl Pts',(12.5241294987191,-4.91605618792739,130.636204428332));
#69515=CARTESIAN_POINT('Ctrl Pts',(12.519494467377,-4.91817838360492,130.718144585058));
#69516=CARTESIAN_POINT('Ctrl Pts',(12.514859436035,-4.91824821769922,130.800173542404));
#69517=CARTESIAN_POINT('',(12.8601405640505,-4.91824999861463,130.804477352914));
#69518=CARTESIAN_POINT('Ctrl Pts',(12.9302349012323,-4.7640545282341,129.582490119308));
#69519=CARTESIAN_POINT('Ctrl Pts',(12.9224800024765,-4.79810443156944,129.715250175634));
#69520=CARTESIAN_POINT('Ctrl Pts',(12.9147251037206,-4.82657402661124,129.849330561244));
#69521=CARTESIAN_POINT('Ctrl Pts',(12.9069702049648,-4.84938717326976,129.984222149851));
#69522=CARTESIAN_POINT('Ctrl Pts',(12.8991652648124,-4.87234753032454,130.119984177091));
#69523=CARTESIAN_POINT('Ctrl Pts',(12.89136032466,-4.88957814010849,130.256567512834));
#69524=CARTESIAN_POINT('Ctrl Pts',(12.8835553845076,-4.90105455902557,130.393450320841));
#69525=CARTESIAN_POINT('Ctrl Pts',(12.8757504443553,-4.91253097794264,130.530333128848));
#69526=CARTESIAN_POINT('Ctrl Pts',(12.8679455042029,-4.91825324943492,130.667515009186));
#69527=CARTESIAN_POINT('Ctrl Pts',(12.8601405640505,-4.91824999861463,130.804477352914));
#69528=CARTESIAN_POINT('Ctrl Pts',(12.8601405640088,-4.91824999861462,130.804477353645));
#69529=CARTESIAN_POINT('Ctrl Pts',(12.8597878228304,-4.91824985169416,130.810667312513));
#69530=CARTESIAN_POINT('Ctrl Pts',(12.8594350816521,-4.91823801904131,130.816857255042));
#69531=CARTESIAN_POINT('Ctrl Pts',(12.8590823404737,-4.91821450080088,130.823047153146));
#69532=CARTESIAN_POINT('Ctrl Pts',(12.8513080063546,-4.91769616421236,130.959471078012));
#69533=CARTESIAN_POINT('Ctrl Pts',(12.8435336722355,-4.91149641095859,131.096089505437));
#69534=CARTESIAN_POINT('Ctrl Pts',(12.8357593381164,-4.89958913539054,131.232390250726));
#69535=CARTESIAN_POINT('Ctrl Pts',(12.8279945851693,-4.88769653447546,131.368523017527));
#69536=CARTESIAN_POINT('Ctrl Pts',(12.8202298322223,-4.87011044053039,131.504338495448));
#69537=CARTESIAN_POINT('Ctrl Pts',(12.8124650792752,-4.84685672884779,131.639323438608));
#69538=CARTESIAN_POINT('Ctrl Pts',(12.8047080383902,-4.8236261130795,131.77417431282));
#69539=CARTESIAN_POINT('Ctrl Pts',(12.7969509975053,-4.7947391477958,131.908195911061));
#69540=CARTESIAN_POINT('Ctrl Pts',(12.7891939566203,-4.7602735568853,132.04087941084));
#69541=CARTESIAN_POINT('Ctrl Pts',(12.7814427653802,-4.72583395674501,132.173462852959));
#69542=CARTESIAN_POINT('Ctrl Pts',(12.77369157414,-4.6858242024239,132.304709828234));
#69543=CARTESIAN_POINT('Ctrl Pts',(12.7659403828999,-4.64037314557179,132.434121376805));
#69544=CARTESIAN_POINT('Ctrl Pts',(12.7581924861228,-4.59494140663123,132.563477922017));
#69545=CARTESIAN_POINT('Ctrl Pts',(12.7504445893458,-4.54407309422403,132.691000223991));
#69546=CARTESIAN_POINT('Ctrl Pts',(12.7426966925687,-4.48794693746378,132.816204386105));
#69547=CARTESIAN_POINT('Ctrl Pts',(12.7349504164846,-4.43183252108565,132.941382358207));
#69548=CARTESIAN_POINT('Ctrl Pts',(12.7272041404005,-4.37046260779772,133.064242798418));
#69549=CARTESIAN_POINT('Ctrl Pts',(12.7194578643164,-4.3040639523765,133.184322078673));
#69550=CARTESIAN_POINT('Ctrl Pts',(12.7117115310511,-4.23766480681539,133.304402245326));
#69551=CARTESIAN_POINT('Ctrl Pts',(12.7039651977858,-4.16623703423832,133.421700868916));
#69552=CARTESIAN_POINT('Ctrl Pts',(12.6962188645204,-4.09005300789726,133.535779562929));
#69553=CARTESIAN_POINT('Ctrl Pts',(12.6884707965174,-4.01385192067183,133.649883804075));
#69554=CARTESIAN_POINT('Ctrl Pts',(12.6807227285145,-3.93289267728338,133.760766355709));
#69555=CARTESIAN_POINT('Ctrl Pts',(12.6729746605115,-3.84749033550317,133.868018754616));
#69556=CARTESIAN_POINT('Ctrl Pts',(12.6652183577697,-3.76199722709781,133.975385142648));
#69557=CARTESIAN_POINT('Ctrl Pts',(12.6574620550279,-3.67205183116872,134.079113364509));
#69558=CARTESIAN_POINT('Ctrl Pts',(12.649705752286,-3.57800913759869,134.17882852729));
#69559=CARTESIAN_POINT('Ctrl Pts',(12.6419453097719,-3.4839162506114,134.278596911057));
#69560=CARTESIAN_POINT('Ctrl Pts',(12.6341848672577,-3.38572198827512,134.374347695028));
#69561=CARTESIAN_POINT('Ctrl Pts',(12.6264244247436,-3.28381666289617,134.465744397913));
#69562=CARTESIAN_POINT('Ctrl Pts',(12.6186515244781,-3.18174775004218,134.557287818898));
#69563=CARTESIAN_POINT('Ctrl Pts',(12.6108786242127,-3.07595617140401,134.644462942661));
#69564=CARTESIAN_POINT('Ctrl Pts',(12.6031057239473,-2.96686433601439,134.726974423969));
#69565=CARTESIAN_POINT('Ctrl Pts',(12.5956153881851,-2.86173826362546,134.8064864051));
#69566=CARTESIAN_POINT('Ctrl Pts',(12.588125052423,-2.7535479669175,134.881667751548));
#69567=CARTESIAN_POINT('Ctrl Pts',(12.5806347166609,-2.64269356013857,134.952294297087));
#69568=CARTESIAN_POINT('Ctrl Pts',(12.5728603825418,-2.52763607483477,135.025598669565));
#69569=CARTESIAN_POINT('Ctrl Pts',(12.5650860484227,-2.40934400453649,135.09422823868));
#69570=CARTESIAN_POINT('Ctrl Pts',(12.5573117143037,-2.28823415399159,135.157884192672));
#69571=CARTESIAN_POINT('Ctrl Pts',(12.5495469613566,-2.1672735605136,135.22146169639));
#69572=CARTESIAN_POINT('Ctrl Pts',(12.5417822084094,-2.04350243910324,135.280077600784));
#69573=CARTESIAN_POINT('Ctrl Pts',(12.5340174554623,-1.91736658428213,135.333476253535));
#69574=CARTESIAN_POINT('Ctrl Pts',(12.5262604145773,-1.79135600937023,135.386821869991));
#69575=CARTESIAN_POINT('Ctrl Pts',(12.5185033736924,-1.6629857327419,135.434960395485));
#69576=CARTESIAN_POINT('Ctrl Pts',(12.5107463328074,-1.53272585282985,135.477682190341));
#69577=CARTESIAN_POINT('Ctrl Pts',(12.5029951415673,-1.4025642029067,135.520371768359));
#69578=CARTESIAN_POINT('Ctrl Pts',(12.4952439503272,-1.27051615599734,135.557652624935));
#69579=CARTESIAN_POINT('Ctrl Pts',(12.487492759087,-1.13707114862613,135.589363466621));
#69580=CARTESIAN_POINT('Ctrl Pts',(12.47974486231,-1.00368285894246,135.621060830352));
#69581=CARTESIAN_POINT('Ctrl Pts',(12.4719969655329,-0.868899169288064,
135.647192797582));
#69582=CARTESIAN_POINT('Ctrl Pts',(12.4642490687558,-0.733223803048837,
135.667648180228));
#69583=CARTESIAN_POINT('Ctrl Pts',(12.4565027926717,-0.597576817171404,
135.688099284049));
#69584=CARTESIAN_POINT('Ctrl Pts',(12.4487565165876,-0.461038912057853,
135.702876106881));
#69585=CARTESIAN_POINT('Ctrl Pts',(12.4410102405035,-0.324122717624308,
135.711918821645));
#69586=CARTESIAN_POINT('Ctrl Pts',(12.4332639072381,-0.187205512506706,
135.72096160316));
#69587=CARTESIAN_POINT('Ctrl Pts',(12.4255175739728,-0.0499104026122739,
135.72427016638));
#69588=CARTESIAN_POINT('Ctrl Pts',(12.4177712407074,0.087246560673206,135.721836708016));
#69589=CARTESIAN_POINT('Ctrl Pts',(12.4100231727045,0.224434239309634,135.719402704697));
#69590=CARTESIAN_POINT('Ctrl Pts',(12.4022751047015,0.361483318947243,135.711224127964));
#69591=CARTESIAN_POINT('Ctrl Pts',(12.3945270366985,0.497879851493844,135.697345260499));
#69592=CARTESIAN_POINT('Ctrl Pts',(12.3867707339567,0.634421347898376,135.683451642408));
#69593=CARTESIAN_POINT('Ctrl Pts',(12.3790144312148,0.770308522224405,135.663845671046));
#69594=CARTESIAN_POINT('Ctrl Pts',(12.371258128473,0.905034085747642,135.638623370679));
#69595=CARTESIAN_POINT('Ctrl Pts',(12.3634976859588,1.03983155636082,135.613387608411));
#69596=CARTESIAN_POINT('Ctrl Pts',(12.3557372434446,1.17346580004069,135.582529632081));
#69597=CARTESIAN_POINT('Ctrl Pts',(12.3479768009304,1.30544275220973,135.546195946128));
#69598=CARTESIAN_POINT('Ctrl Pts',(12.340203900665,1.43763156549876,135.509803934117));
#69599=CARTESIAN_POINT('Ctrl Pts',(12.3324310003996,1.56815739840512,135.4679187666));
#69600=CARTESIAN_POINT('Ctrl Pts',(12.3246581001342,1.69654344622106,135.420736186948));
#69601=CARTESIAN_POINT('Ctrl Pts',(12.3171677643721,1.82026233781431,135.375268812911));
#69602=CARTESIAN_POINT('Ctrl Pts',(12.30967742861,1.94199403189221,135.324882606345));
#69603=CARTESIAN_POINT('Ctrl Pts',(12.302187092848,2.06133365953379,135.269793027375));
#69604=CARTESIAN_POINT('Ctrl Pts',(12.2944127587289,2.18519808542954,135.212614710275));
#69605=CARTESIAN_POINT('Ctrl Pts',(12.2866384246098,2.30687783905734,135.150188199804));
#69606=CARTESIAN_POINT('Ctrl Pts',(12.2788640904907,2.42589622847365,135.082702650548));
#69607=CARTESIAN_POINT('Ctrl Pts',(12.2710993375436,2.54476793836198,135.015300271199));
#69608=CARTESIAN_POINT('Ctrl Pts',(12.2633345845965,2.6609844732171,134.942851449474));
#69609=CARTESIAN_POINT('Ctrl Pts',(12.2555698316494,2.77408978267536,134.865593058606));
#69610=CARTESIAN_POINT('Ctrl Pts',(12.2478127907644,2.88708275434562,134.788411401861));
#69611=CARTESIAN_POINT('Ctrl Pts',(12.2400557498794,2.99697032933374,134.706429901377));
#69612=CARTESIAN_POINT('Ctrl Pts',(12.2322987089944,3.10332203215698,134.619930748913));
#69613=CARTESIAN_POINT('Ctrl Pts',(12.2245475177543,3.20959353433398,134.533496826133));
#69614=CARTESIAN_POINT('Ctrl Pts',(12.2167963265141,3.31233416962784,134.442552278088));
#69615=CARTESIAN_POINT('Ctrl Pts',(12.209045135274,3.41114368489523,134.347421698538));
#69616=CARTESIAN_POINT('Ctrl Pts',(12.2012972384969,3.50991120348281,134.252331552023));
#69617=CARTESIAN_POINT('Ctrl Pts',(12.1935493417199,3.60475064414116,134.15305918324));
#69618=CARTESIAN_POINT('Ctrl Pts',(12.1858014449428,3.69529618639546,134.049968289068));
#69619=CARTESIAN_POINT('Ctrl Pts',(12.1780551688587,3.78582278847425,133.946898959288));
#69620=CARTESIAN_POINT('Ctrl Pts',(12.1703088927746,3.87205702086128,133.840012986446));
#69621=CARTESIAN_POINT('Ctrl Pts',(12.1625626166905,3.95367146035036,133.729709322611));
#69622=CARTESIAN_POINT('Ctrl Pts',(12.1548162834251,4.03528650229868,133.61940484454));
#69623=CARTESIAN_POINT('Ctrl Pts',(12.1470699501597,4.11228145075645,133.505682939423));
#69624=CARTESIAN_POINT('Ctrl Pts',(12.1393236168944,4.18437080221711,133.388973558038));
#69625=CARTESIAN_POINT('Ctrl Pts',(12.1315755488914,4.2564762975882,133.272238040396));
#69626=CARTESIAN_POINT('Ctrl Pts',(12.1238274808884,4.32367380450758,133.152514047768));
#69627=CARTESIAN_POINT('Ctrl Pts',(12.1160794128855,4.38572277775109,133.03025791511));
#69628=CARTESIAN_POINT('Ctrl Pts',(12.1083231101436,4.44783769738176,132.90787184718));
#69629=CARTESIAN_POINT('Ctrl Pts',(12.1005668074017,4.5047929753564,132.782948612471));
#69630=CARTESIAN_POINT('Ctrl Pts',(12.0928105046599,4.55639519766442,132.655966910815));
#69631=CARTESIAN_POINT('Ctrl Pts',(12.0850500621457,4.60802496163226,132.528917435202));
#69632=CARTESIAN_POINT('Ctrl Pts',(12.0772896196315,4.65429584510939,132.399807671321));
#69633=CARTESIAN_POINT('Ctrl Pts',(12.0695291771173,4.69506405245742,132.269132478923));
#69634=CARTESIAN_POINT('Ctrl Pts',(12.0617562768519,4.73589770455106,132.138247515105));
#69635=CARTESIAN_POINT('Ctrl Pts',(12.0539833765864,4.77121092782574,132.005792479052));
#69636=CARTESIAN_POINT('Ctrl Pts',(12.046210476321,4.80091068213192,131.872274324141));
#69637=CARTESIAN_POINT('Ctrl Pts',(12.038720140559,4.82953077555965,131.743609890475));
#69638=CARTESIAN_POINT('Ctrl Pts',(12.031229804797,4.85293838707447,131.613958593228));
#69639=CARTESIAN_POINT('Ctrl Pts',(12.0237394690351,4.87109594784187,131.483777521549));
#69640=CARTESIAN_POINT('Ctrl Pts',(12.015965134916,4.88994195804478,131.34866059497));
#69641=CARTESIAN_POINT('Ctrl Pts',(12.008190800797,4.90319164580439,131.212544918332));
#69642=CARTESIAN_POINT('Ctrl Pts',(12.0004164666779,4.91074648858991,131.075933788741));
#69643=CARTESIAN_POINT('Ctrl Pts',(11.9926517137308,4.91829202070688,130.939491020158));
#69644=CARTESIAN_POINT('Ctrl Pts',(11.9848869607837,4.92015665096811,130.802554400158));
#69645=CARTESIAN_POINT('Ctrl Pts',(11.9771222078367,4.91629316117279,130.665635652597));
#69646=CARTESIAN_POINT('Ctrl Pts',(11.9693651669517,4.91243350865,130.528852894666));
#69647=CARTESIAN_POINT('Ctrl Pts',(11.9616081260666,4.90285706889034,130.39208836213));
#69648=CARTESIAN_POINT('Ctrl Pts',(11.9538510851816,4.88756857529978,130.255856757742));
#69649=CARTESIAN_POINT('Ctrl Pts',(11.9460998939415,4.87229161088117,130.119727886666));
#69650=CARTESIAN_POINT('Ctrl Pts',(11.9383487027014,4.85131120988324,129.984131530765));
#69651=CARTESIAN_POINT('Ctrl Pts',(11.9305975114613,4.82468411562899,129.8495798852));
#69652=CARTESIAN_POINT('Ctrl Pts',(11.9228496146842,4.7980683386001,129.715085427673));
#69653=CARTESIAN_POINT('Ctrl Pts',(11.9151017179071,4.76581071746173,129.581635180066));
#69654=CARTESIAN_POINT('Ctrl Pts',(11.90735382113,4.72801950579517,129.449733504549));
#69655=CARTESIAN_POINT('Ctrl Pts',(11.8996075450459,4.69023619923541,129.31785942002));
#69656=CARTESIAN_POINT('Ctrl Pts',(11.8918612689619,4.64692171210883,129.187533638876));
#69657=CARTESIAN_POINT('Ctrl Pts',(11.8841149928778,4.59823471385015,129.059247274874));
#69658=CARTESIAN_POINT('Ctrl Pts',(11.8763686596124,4.54954735619512,128.93095996389));
#69659=CARTESIAN_POINT('Ctrl Pts',(11.868622326347,4.49548754699586,128.804712465615));
#69660=CARTESIAN_POINT('Ctrl Pts',(11.8608759930817,4.43626269439996,128.680977381131));
#69661=CARTESIAN_POINT('Ctrl Pts',(11.8531279250787,4.37702457880896,128.557214587032));
#69662=CARTESIAN_POINT('Ctrl Pts',(11.8453798570758,4.31261928693193,128.435965678892));
#69663=CARTESIAN_POINT('Ctrl Pts',(11.8376317890728,4.24330072572247,128.317679694411));
#69664=CARTESIAN_POINT('Ctrl Pts',(11.8298754863309,4.17390849192125,128.199267994178));
#69665=CARTESIAN_POINT('Ctrl Pts',(11.8221191835891,4.09959275550587,128.08382584598));
#69666=CARTESIAN_POINT('Ctrl Pts',(11.8143628808473,4.02065171520637,127.971774723457));
#69667=CARTESIAN_POINT('Ctrl Pts',(11.8066024383331,3.94166854169669,127.859663795875));
#69668=CARTESIAN_POINT('Ctrl Pts',(11.7988419958189,3.85805538351401,127.750947810087));
#69669=CARTESIAN_POINT('Ctrl Pts',(11.7910815533047,3.77015085512594,127.646015229219));
#69670=CARTESIAN_POINT('Ctrl Pts',(11.7833086530393,3.68210521458523,127.540914201257));
#69671=CARTESIAN_POINT('Ctrl Pts',(11.7755357527739,3.58975470118596,127.439609004013));
#69672=CARTESIAN_POINT('Ctrl Pts',(11.7677628525084,3.49347553868896,127.342451935483));
#69673=CARTESIAN_POINT('Ctrl Pts',(11.7602725167463,3.40069636626039,127.248826771117));
#69674=CARTESIAN_POINT('Ctrl Pts',(11.7527821809843,3.30426944375523,127.159053591539));
#69675=CARTESIAN_POINT('Ctrl Pts',(11.7452918452222,3.20455902634905,127.073411072324));
#69676=CARTESIAN_POINT('Ctrl Pts',(11.7375175111031,3.10106805816147,126.984521390962));
#69677=CARTESIAN_POINT('Ctrl Pts',(11.729743176984,2.99371186428505,126.899800205366));
#69678=CARTESIAN_POINT('Ctrl Pts',(11.7219688428649,2.88286062899448,126.81960244971));
#69679=CARTESIAN_POINT('Ctrl Pts',(11.7142040899178,2.77214600794435,126.73950353062));
#69680=CARTESIAN_POINT('Ctrl Pts',(11.7064393369708,2.65794522949385,126.6639171764));
#69681=CARTESIAN_POINT('Ctrl Pts',(11.6986745840237,2.54066329882483,126.593159712301));
#69682=CARTESIAN_POINT('Ctrl Pts',(11.6909175431387,2.4234978542229,126.522472525513));
#69683=CARTESIAN_POINT('Ctrl Pts',(11.6831605022536,2.30325768001945,126.456604885007));
#69684=CARTESIAN_POINT('Ctrl Pts',(11.6754034613686,2.18037836874034,126.395831017844));
#69685=CARTESIAN_POINT('Ctrl Pts',(11.6676522701284,2.05759172170556,126.335102980726));
#69686=CARTESIAN_POINT('Ctrl Pts',(11.6599010788884,1.93217024798331,126.279461243792));
#69687=CARTESIAN_POINT('Ctrl Pts',(11.6521498876482,1.8045755430211,126.229134921272));
#69688=CARTESIAN_POINT('Ctrl Pts',(11.6444019908711,1.67703506921221,126.178829988781));
#69689=CARTESIAN_POINT('Ctrl Pts',(11.636654094094,1.54732356423078,126.133836120493));
#69690=CARTESIAN_POINT('Ctrl Pts',(11.628906197317,1.41592387596149,126.094334859677));
#69691=CARTESIAN_POINT('Ctrl Pts',(11.6211599212328,1.28455167367433,126.054841861672));
#69692=CARTESIAN_POINT('Ctrl Pts',(11.6134136451487,1.15149236467301,126.02083929833));
#69693=CARTESIAN_POINT('Ctrl Pts',(11.6056673690646,1.01724490157407,125.99245913554));
#69694=CARTESIAN_POINT('Ctrl Pts',(11.5979210357993,0.882996447491034,125.964078763255));
#69695=CARTESIAN_POINT('Ctrl Pts',(11.590174702534,0.747560204320396,125.941320955203));
#69696=CARTESIAN_POINT('Ctrl Pts',(11.5824283692686,0.611445893908689,125.924266665466));
#69697=CARTESIAN_POINT('Ctrl Pts',(11.5746803012656,0.475301101640729,125.907208556539));
#69698=CARTESIAN_POINT('Ctrl Pts',(11.5669322332626,0.338478327828677,125.895856556129));
#69699=CARTESIAN_POINT('Ctrl Pts',(11.5591841652597,0.201492603517559,125.89023976097));
#69700=CARTESIAN_POINT('Ctrl Pts',(11.5514278625178,0.0643612891484933,
125.884616996215));
#69701=CARTESIAN_POINT('Ctrl Pts',(11.5436715597759,-0.0729329304169342,
125.884741629061));
#69702=CARTESIAN_POINT('Ctrl Pts',(11.5359152570341,-0.209874273773137,
125.890590593266));
#69703=CARTESIAN_POINT('Ctrl Pts',(11.5281548145199,-0.346888706847513,
125.89644267924));
#69704=CARTESIAN_POINT('Ctrl Pts',(11.5203943720057,-0.483549499050023,
125.908025151413));
#69705=CARTESIAN_POINT('Ctrl Pts',(11.5126339294916,-0.61934679596056,125.925263097652));
#69706=CARTESIAN_POINT('Ctrl Pts',(11.5048610292261,-0.755362086747616,
125.942528715772));
#69707=CARTESIAN_POINT('Ctrl Pts',(11.4970881289607,-0.890510726580555,
125.96546788457));
#69708=CARTESIAN_POINT('Ctrl Pts',(11.4893152286953,-1.02429295904482,125.993954502013));
#69709=CARTESIAN_POINT('Ctrl Pts',(11.4818248929333,-1.15321187038117,126.021405559158));
#69710=CARTESIAN_POINT('Ctrl Pts',(11.4743345571713,-1.28086169583977,126.05400766362));
#69711=CARTESIAN_POINT('Ctrl Pts',(11.4668442214093,-1.40681108894646,126.091604988158));
#69712=CARTESIAN_POINT('Ctrl Pts',(11.4590698872902,-1.53753589157485,126.130627826684));
#69713=CARTESIAN_POINT('Ctrl Pts',(11.4512955531711,-1.66684286955632,126.175155762833));
#69714=CARTESIAN_POINT('Ctrl Pts',(11.443521219052,-1.79423331307467,126.225069200681));
#69715=CARTESIAN_POINT('Ctrl Pts',(11.4357564661049,-1.92146675925659,126.274921124679));
#69716=CARTESIAN_POINT('Ctrl Pts',(11.4279917131579,-2.04678801004079,126.330145203168));
#69717=CARTESIAN_POINT('Ctrl Pts',(11.4202269602108,-2.16971201683931,126.390571675344));
#69718=CARTESIAN_POINT('Ctrl Pts',(11.4124699193258,-2.29251393378151,126.450938131096));
#69719=CARTESIAN_POINT('Ctrl Pts',(11.4047128784407,-2.41292299639496,126.516496526432));
#69720=CARTESIAN_POINT('Ctrl Pts',(11.3969558375557,-2.53047304128532,126.587028611448));
#69721=CARTESIAN_POINT('Ctrl Pts',(11.3892046463156,-2.64793444077242,126.65750750767));
#69722=CARTESIAN_POINT('Ctrl Pts',(11.3814534550755,-2.7625407800478,126.732952427695));
#69723=CARTESIAN_POINT('Ctrl Pts',(11.3737022638354,-2.87384979520548,126.813098860039));
#69724=CARTESIAN_POINT('Ctrl Pts',(11.3659543670583,-2.98511150106229,126.893211228011));
#69725=CARTESIAN_POINT('Ctrl Pts',(11.3582064702812,-3.0930783535679,126.978020905926));
#69726=CARTESIAN_POINT('Ctrl Pts',(11.3504585735042,-3.19733662415185,127.067219788756));
#69727=CARTESIAN_POINT('Ctrl Pts',(11.3427122974201,-3.30157308615313,127.156400013103));
#69728=CARTESIAN_POINT('Ctrl Pts',(11.334966021336,-3.40210221236536,127.249967362156));
#69729=CARTESIAN_POINT('Ctrl Pts',(11.3272197452519,-3.49854328006957,127.347573383735));
#69730=CARTESIAN_POINT('Ctrl Pts',(11.3194734119865,-3.59498505967983,127.445180125819));
#69731=CARTESIAN_POINT('Ctrl Pts',(11.3117270787212,-3.6873384457763,127.54682532181));
#69732=CARTESIAN_POINT('Ctrl Pts',(11.3039807454558,-3.77525981228915,127.65212388594));
#69733=CARTESIAN_POINT('Ctrl Pts',(11.2962326774528,-3.86320086818244,127.757446030953));
#69734=CARTESIAN_POINT('Ctrl Pts',(11.2884846094499,-3.9467076789601,127.866422872073));
#69735=CARTESIAN_POINT('Ctrl Pts',(11.2807365414469,-4.0254773778554,127.978636826592));
#69736=CARTESIAN_POINT('Ctrl Pts',(11.2729802387051,-4.10433079412415,128.090970043438));
#69737=CARTESIAN_POINT('Ctrl Pts',(11.2652239359632,-4.17843681625437,128.20654692583));
#69738=CARTESIAN_POINT('Ctrl Pts',(11.2574676332213,-4.24753605807933,128.324921064398));
#69739=CARTESIAN_POINT('Ctrl Pts',(11.2497071907071,-4.31667218025019,128.443358382807));
#69740=CARTESIAN_POINT('Ctrl Pts',(11.241946748193,-4.38079601468925,128.564595586849));
#69741=CARTESIAN_POINT('Ctrl Pts',(11.2341863056788,-4.43969499832822,128.688163229722));
#69742=CARTESIAN_POINT('Ctrl Pts',(11.2264134054134,-4.49868853184453,128.811929234344));
#69743=CARTESIAN_POINT('Ctrl Pts',(11.2186405051479,-4.55244030048262,128.9380327937));
#69744=CARTESIAN_POINT('Ctrl Pts',(11.2108676048825,-4.60078626690473,129.065985287334));
#69745=CARTESIAN_POINT('Ctrl Pts',(11.2033772691205,-4.64737473567126,129.189286385531));
#69746=CARTESIAN_POINT('Ctrl Pts',(11.1958869333585,-4.68894351052908,129.314304032733));
#69747=CARTESIAN_POINT('Ctrl Pts',(11.1883965975965,-4.72539054004279,129.440591096505));
#69748=CARTESIAN_POINT('Ctrl Pts',(11.1856033086334,-4.73898233198792,129.487685949476));
#69749=CARTESIAN_POINT('Ctrl Pts',(11.1828100196703,-4.75187229284884,129.534991768433));
#69750=CARTESIAN_POINT('Ctrl Pts',(11.1800167307073,-4.76405452823405,129.582490119308));
#69751=CARTESIAN_POINT('Origin',(213.235140564004,0.,130.804360617566));
#69752=CARTESIAN_POINT('',(9.08499331100838,-4.76405452823401,129.582490119308));
#69753=CARTESIAN_POINT('',(9.4299069079559,-4.76405452823399,129.582490119308));
#69754=CARTESIAN_POINT('',(213.235140564004,-4.76405452823405,129.582490119308));
#69755=CARTESIAN_POINT('',(10.7648594359442,-4.91824942613488,130.806736501389));
#69756=CARTESIAN_POINT('Ctrl Pts',(10.7648594359442,-4.91824942613488,130.80673650139));
#69757=CARTESIAN_POINT('Ctrl Pts',(10.7563560984096,-4.91817654457573,130.957606540948));
#69758=CARTESIAN_POINT('Ctrl Pts',(10.747852760875,-4.91115752432135,131.108242687845));
#69759=CARTESIAN_POINT('Ctrl Pts',(10.7393494233403,-4.89728139431641,131.258032313159));
#69760=CARTESIAN_POINT('Ctrl Pts',(10.7308033869406,-4.88333558637619,131.408574095725));
#69761=CARTESIAN_POINT('Ctrl Pts',(10.7222573505409,-4.86246371736281,131.558260588257));
#69762=CARTESIAN_POINT('Ctrl Pts',(10.7137113141411,-4.83480651108763,131.706485366614));
#69763=CARTESIAN_POINT('Ctrl Pts',(10.705143301354,-4.80707818348182,131.855091309408));
#69764=CARTESIAN_POINT('Ctrl Pts',(10.6965752885669,-4.77252969569435,132.002227780159));
#69765=CARTESIAN_POINT('Ctrl Pts',(10.6880072757797,-4.73135175804063,132.147302762331));
#69766=CARTESIAN_POINT('Ctrl Pts',(10.679409092323,-4.69002881990874,132.292888599174));
#69767=CARTESIAN_POINT('Ctrl Pts',(10.6708109088663,-4.64202978451954,132.436398178318));
#69768=CARTESIAN_POINT('Ctrl Pts',(10.6622127254095,-4.58759474578353,132.577255851628));
#69769=CARTESIAN_POINT('Ctrl Pts',(10.6585052656497,-4.56412284422976,132.637992419798));
#69770=CARTESIAN_POINT('Ctrl Pts',(10.6547978058899,-4.53945490902743,132.698236235402));
#69771=CARTESIAN_POINT('Ctrl Pts',(10.6510903461301,-4.51361279970871,132.757942598647));
#69772=CARTESIAN_POINT('Ctrl Pts',(10.643316012011,-4.45942335324091,132.883143476601));
#69773=CARTESIAN_POINT('Ctrl Pts',(10.6355416778919,-4.39993479864231,133.006286253589));
#69774=CARTESIAN_POINT('Ctrl Pts',(10.6277673437729,-4.33532479673268,133.126889835754));
#69775=CARTESIAN_POINT('Ctrl Pts',(10.6200025908258,-4.27079442087604,133.247344784782));
#69776=CARTESIAN_POINT('Ctrl Pts',(10.6122378378787,-4.2011553390139,133.365266424104));
#69777=CARTESIAN_POINT('Ctrl Pts',(10.6044730849316,-4.1266334122154,133.480193150384));
#69778=CARTESIAN_POINT('Ctrl Pts',(10.5967160440466,-4.05218550164527,133.595005729819));
#69779=CARTESIAN_POINT('Ctrl Pts',(10.5889590031616,-3.97286460861424,133.706828989864));
#69780=CARTESIAN_POINT('Ctrl Pts',(10.5812019622766,-3.8889425133929,133.815225807179));
#69781=CARTESIAN_POINT('Ctrl Pts',(10.5734507710364,-3.80508370447638,133.923540881611));
#69782=CARTESIAN_POINT('Ctrl Pts',(10.5656995797963,-3.71663083817425,134.028434348532));
#69783=CARTESIAN_POINT('Ctrl Pts',(10.5579483885562,-3.62389880980018,134.129498280706));
#69784=CARTESIAN_POINT('Ctrl Pts',(10.5502004917791,-3.53120619501176,134.230519258012));
#69785=CARTESIAN_POINT('Ctrl Pts',(10.542452595002,-3.43423829929339,134.327713650381));
#69786=CARTESIAN_POINT('Ctrl Pts',(10.5347046982249,-3.33334993610429,134.420707014964));
#69787=CARTESIAN_POINT('Ctrl Pts',(10.5269584221408,-3.23248267658601,134.513680927339));
#69788=CARTESIAN_POINT('Ctrl Pts',(10.5192121460567,-3.12769686806685,134.602455295029));
#69789=CARTESIAN_POINT('Ctrl Pts',(10.5114658699726,-3.01938349047435,134.686693215367));
#69790=CARTESIAN_POINT('Ctrl Pts',(10.5037195367072,-2.91106931333711,134.770931757531));
#69791=CARTESIAN_POINT('Ctrl Pts',(10.4959732034419,-2.79922782378346,134.850633545503));
#69792=CARTESIAN_POINT('Ctrl Pts',(10.4882268701766,-2.68428199747963,134.925502840361));
#69793=CARTESIAN_POINT('Ctrl Pts',(10.4804788021736,-2.56931042985481,135.00038890168));
#69794=CARTESIAN_POINT('Ctrl Pts',(10.4727307341707,-2.45123346966108,135.070440103085));
#69795=CARTESIAN_POINT('Ctrl Pts',(10.4649826661677,-2.3305015480195,135.135405017844));
#69796=CARTESIAN_POINT('Ctrl Pts',(10.4572263634258,-2.20964131105503,135.200438978087));
#69797=CARTESIAN_POINT('Ctrl Pts',(10.4494700606839,-2.08612082077943,135.260375667531));
#69798=CARTESIAN_POINT('Ctrl Pts',(10.4417137579421,-1.96041399776924,135.315010240386));
#69799=CARTESIAN_POINT('Ctrl Pts',(10.4339533154279,-1.83464008124248,135.369673973359));
#69800=CARTESIAN_POINT('Ctrl Pts',(10.4261928729138,-1.70667787140462,135.419029810303));
#69801=CARTESIAN_POINT('Ctrl Pts',(10.4184324303996,-1.57701863479912,135.462922121721));
#69802=CARTESIAN_POINT('Ctrl Pts',(10.4106595301341,-1.44715125767642,135.506884892974));
#69803=CARTESIAN_POINT('Ctrl Pts',(10.4028866298687,-1.3155817853907,135.54536650256));
#69804=CARTESIAN_POINT('Ctrl Pts',(10.3951137296033,-1.18281479262253,135.578261771638));
#69805=CARTESIAN_POINT('Ctrl Pts',(10.3876233938413,-1.05487421446154,135.609961214828));
#69806=CARTESIAN_POINT('Ctrl Pts',(10.3801330580792,-0.925821971717786,
135.636473359175));
#69807=CARTESIAN_POINT('Ctrl Pts',(10.3726427223172,-0.796114120363577,
135.657749677785));
#69808=CARTESIAN_POINT('Ctrl Pts',(10.3648683881981,-0.661488356401419,
135.679832694483));
#69809=CARTESIAN_POINT('Ctrl Pts',(10.3570940540791,-0.525729833688034,
135.696344967587));
#69810=CARTESIAN_POINT('Ctrl Pts',(10.34931971996,-0.389339340122872,135.707175925196));
#69811=CARTESIAN_POINT('Ctrl Pts',(10.3415549670129,-0.253116935651461,
135.717993534618));
#69812=CARTESIAN_POINT('Ctrl Pts',(10.3337902140658,-0.116264495999656,
135.723143729216));
#69813=CARTESIAN_POINT('Ctrl Pts',(10.3260254611187,0.0207075354470989,
135.722567024426));
#69814=CARTESIAN_POINT('Ctrl Pts',(10.3182684202337,0.157543524341253,135.721990892426));
#69815=CARTESIAN_POINT('Ctrl Pts',(10.3105113793487,0.294498480220442,135.715699182124));
#69816=CARTESIAN_POINT('Ctrl Pts',(10.3027543384637,0.431057734963402,135.703684274116));
#69817=CARTESIAN_POINT('Ctrl Pts',(10.2950031472236,0.567514009310084,135.691678426643));
#69818=CARTESIAN_POINT('Ctrl Pts',(10.2872519559834,0.703574788585392,135.673958006143));
#69819=CARTESIAN_POINT('Ctrl Pts',(10.2795007647433,0.838726663444165,135.650567448328));
#69820=CARTESIAN_POINT('Ctrl Pts',(10.2717528679662,0.973821095150829,135.627186832124));
#69821=CARTESIAN_POINT('Ctrl Pts',(10.2640049711892,1.10800700634759,135.598140938364));
#69822=CARTESIAN_POINT('Ctrl Pts',(10.2562570744121,1.24077758231864,135.563525886152));
#69823=CARTESIAN_POINT('Ctrl Pts',(10.248510798328,1.37352038554759,135.528918074663));
#69824=CARTESIAN_POINT('Ctrl Pts',(10.2407645222439,1.50484806434621,135.488743520438));
#69825=CARTESIAN_POINT('Ctrl Pts',(10.2330182461598,1.63426583875893,135.443149061844));
#69826=CARTESIAN_POINT('Ctrl Pts',(10.2252719128944,1.76368456850426,135.397554266681));
#69827=CARTESIAN_POINT('Ctrl Pts',(10.2175255796291,1.89119299698116,135.346539617228));
#69828=CARTESIAN_POINT('Ctrl Pts',(10.2097792463637,2.01631368197962,135.290301120778));
#69829=CARTESIAN_POINT('Ctrl Pts',(10.2020311783608,2.1414623868878,135.234050030108));
#69830=CARTESIAN_POINT('Ctrl Pts',(10.1942831103577,2.26422192775795,135.172572924839));
#69831=CARTESIAN_POINT('Ctrl Pts',(10.1865350423548,2.38413730313486,135.10611286314));
#69832=CARTESIAN_POINT('Ctrl Pts',(10.1787787396129,2.50418012599973,135.039582166896));
#69833=CARTESIAN_POINT('Ctrl Pts',(10.1710224368711,2.62137240247355,134.968058124825));
#69834=CARTESIAN_POINT('Ctrl Pts',(10.1632661341292,2.73528562434537,134.891828735576));
#69835=CARTESIAN_POINT('Ctrl Pts',(10.155505691615,2.84925964513373,134.815558660407));
#69836=CARTESIAN_POINT('Ctrl Pts',(10.1477452491009,2.95995080865304,134.734578464644));
#69837=CARTESIAN_POINT('Ctrl Pts',(10.1399848065868,3.06696263783213,134.649217343199));
#69838=CARTESIAN_POINT('Ctrl Pts',(10.1322119063213,3.17414625189949,134.563719192503));
#69839=CARTESIAN_POINT('Ctrl Pts',(10.1244390060559,3.2776384334331,134.473826319174));
#69840=CARTESIAN_POINT('Ctrl Pts',(10.1166661057904,3.37707795755671,134.37990638445));
#69841=CARTESIAN_POINT('Ctrl Pts',(10.1091757700284,3.47290260450552,134.289400675924));
#69842=CARTESIAN_POINT('Ctrl Pts',(10.1016854342664,3.5649639118874,134.195155830769));
#69843=CARTESIAN_POINT('Ctrl Pts',(10.0941950985043,3.65297454325851,134.097529311819));
#69844=CARTESIAN_POINT('Ctrl Pts',(10.0864207643853,3.74432212446818,133.99620125373));
#69845=CARTESIAN_POINT('Ctrl Pts',(10.0786464302662,3.83159516509547,133.890909050637));
#69846=CARTESIAN_POINT('Ctrl Pts',(10.0708720961471,3.91442994977599,133.78201426277));
#69847=CARTESIAN_POINT('Ctrl Pts',(10.0631073432,3.99716264798756,133.673253677997));
#69848=CARTESIAN_POINT('Ctrl Pts',(10.0553425902529,4.07546773900256,133.560899650636));
#69849=CARTESIAN_POINT('Ctrl Pts',(10.0475778373058,4.14901926965393,133.445349478304));
#69850=CARTESIAN_POINT('Ctrl Pts',(10.0398207964208,4.22249774788806,133.329914072032));
#69851=CARTESIAN_POINT('Ctrl Pts',(10.0320637555358,4.29123185278397,133.211289165783));
#69852=CARTESIAN_POINT('Ctrl Pts',(10.0243067146508,4.35493698323023,133.08990364595));
#69853=CARTESIAN_POINT('Ctrl Pts',(10.0165555234107,4.41859407314216,132.968609663881));
#69854=CARTESIAN_POINT('Ctrl Pts',(10.0088043321705,4.4772295561753,132.84455955671));
#69855=CARTESIAN_POINT('Ctrl Pts',(10.0010531409304,4.53060330705976,132.718209288846));
#69856=CARTESIAN_POINT('Ctrl Pts',(9.99330524415329,4.58395437267624,132.591912723216));
#69857=CARTESIAN_POINT('Ctrl Pts',(9.98555734737628,4.63204800230789,132.463318300721));
#69858=CARTESIAN_POINT('Ctrl Pts',(9.97780945059921,4.67469111794686,132.332904373658));
#69859=CARTESIAN_POINT('Ctrl Pts',(9.97006317451511,4.71732531356538,132.202517726378));
#69860=CARTESIAN_POINT('Ctrl Pts',(9.96231689843095,4.75451114154116,132.070312702935));
#69861=CARTESIAN_POINT('Ctrl Pts',(9.95457062234684,4.78610470049843,131.936784945443));
#69862=CARTESIAN_POINT('Ctrl Pts',(9.94682428908149,4.81769849267213,131.803256202279));
#69863=CARTESIAN_POINT('Ctrl Pts',(9.93907795581623,4.84369984343484,131.668405086043));
#69864=CARTESIAN_POINT('Ctrl Pts',(9.93133162255089,4.86401559009945,131.53273922912));
#69865=CARTESIAN_POINT('Ctrl Pts',(9.92358355454792,4.88433588633465,131.397042990769));
#69866=CARTESIAN_POINT('Ctrl Pts',(9.91583548654487,4.8989679869587,131.260532035244));
#69867=CARTESIAN_POINT('Ctrl Pts',(9.9080874185419,4.9078704442915,131.123720547034));
#69868=CARTESIAN_POINT('Ctrl Pts',(9.90033111580004,4.91678236326191,130.986763653946));
#69869=CARTESIAN_POINT('Ctrl Pts',(9.89257481305825,4.91995244901552,130.849505980879));
#69870=CARTESIAN_POINT('Ctrl Pts',(9.88481851031639,4.91739138381905,130.712463714233));
#69871=CARTESIAN_POINT('Ctrl Pts',(9.87705806780222,4.91482895170497,130.575348304003));
#69872=CARTESIAN_POINT('Ctrl Pts',(9.86929762528801,4.90652929719546,130.438448919336));
#69873=CARTESIAN_POINT('Ctrl Pts',(9.86153718277384,4.89255507575106,130.302277065513));
#69874=CARTESIAN_POINT('Ctrl Pts',(9.85376428250841,4.87855842164584,130.165886616541));
#69875=CARTESIAN_POINT('Ctrl Pts',(9.84599138224295,4.85886905347212,130.030226419376));
#69876=CARTESIAN_POINT('Ctrl Pts',(9.83821848197752,4.83360104417242,129.895799112617));
#69877=CARTESIAN_POINT('Ctrl Pts',(9.8307281462155,4.80925159065707,129.766258577061));
#69878=CARTESIAN_POINT('Ctrl Pts',(9.82323781045352,4.77972211863777,129.637863150984));
#69879=CARTESIAN_POINT('Ctrl Pts',(9.81574747469151,4.74515805935389,129.511047796069));
#69880=CARTESIAN_POINT('Ctrl Pts',(9.80797314057242,4.70928349325669,129.379424198427));
#69881=CARTESIAN_POINT('Ctrl Pts',(9.80019880645332,4.66787139098634,129.24908590997));
#69882=CARTESIAN_POINT('Ctrl Pts',(9.79242447233423,4.6210293463649,129.12053436687));
#69883=CARTESIAN_POINT('Ctrl Pts',(9.78465971938714,4.57424503037706,128.992141252057));
#69884=CARTESIAN_POINT('Ctrl Pts',(9.77689496644005,4.52204421952871,128.865530865083));
#69885=CARTESIAN_POINT('Ctrl Pts',(9.76913021349296,4.464584985908,128.741192188643));
#69886=CARTESIAN_POINT('Ctrl Pts',(9.76137317260795,4.40718282160814,128.616977007129));
#69887=CARTESIAN_POINT('Ctrl Pts',(9.75361613172297,4.3445327909691,128.495029398627));
#69888=CARTESIAN_POINT('Ctrl Pts',(9.74585909083797,4.27684189440716,128.375820629684));
#69889=CARTESIAN_POINT('Ctrl Pts',(9.73810789959784,4.20920204407687,128.256701757));
#69890=CARTESIAN_POINT('Ctrl Pts',(9.73035670835775,4.13652908646285,128.140317951463));
#69891=CARTESIAN_POINT('Ctrl Pts',(9.72260551711761,4.05907684376275,128.027117697163));
#69892=CARTESIAN_POINT('Ctrl Pts',(9.71485762034053,3.98165752033191,127.913965555991));
#69893=CARTESIAN_POINT('Ctrl Pts',(9.7071097235634,3.89946317227134,127.803994596847));
#69894=CARTESIAN_POINT('Ctrl Pts',(9.69936182678632,3.81279188753796,127.69762582283));
#69895=CARTESIAN_POINT('Ctrl Pts',(9.69161555070221,3.72613873256894,127.591279298867));
#69896=CARTESIAN_POINT('Ctrl Pts',(9.6838692746181,3.63501075044088,127.488533764175));
#69897=CARTESIAN_POINT('Ctrl Pts',(9.676122998534,3.53974715669219,127.389778193727));
#69898=CARTESIAN_POINT('Ctrl Pts',(9.66837666526864,3.44448285972928,127.291021894288));
#69899=CARTESIAN_POINT('Ctrl Pts',(9.66063033200331,3.34508316166357,127.196255899248));
#69900=CARTESIAN_POINT('Ctrl Pts',(9.65288399873796,3.24192479128902,127.105832976717));
#69901=CARTESIAN_POINT('Ctrl Pts',(9.64513593073498,3.13874331931268,127.0153898046));
#69902=CARTESIAN_POINT('Ctrl Pts',(9.63738786273201,3.03180179403487,126.929291898015));
#69903=CARTESIAN_POINT('Ctrl Pts',(9.62963979472903,2.92151040994382,126.847852057347));
#69904=CARTESIAN_POINT('Ctrl Pts',(9.62188349198717,2.81110180685728,126.766325661446));
#69905=CARTESIAN_POINT('Ctrl Pts',(9.61412718924527,2.69733654795029,126.689467453522));
#69906=CARTESIAN_POINT('Ctrl Pts',(9.60637088650341,2.58065468948598,126.617547457639));
#69907=CARTESIAN_POINT('Ctrl Pts',(9.59861044398924,2.46391055440042,126.545589075889));
#69908=CARTESIAN_POINT('Ctrl Pts',(9.59085000147507,2.34424705889555,126.478574348921));
#69909=CARTESIAN_POINT('Ctrl Pts',(9.58308955896089,2.22212841365627,126.416727044018));
#69910=CARTESIAN_POINT('Ctrl Pts',(9.57531665869545,2.09981373272648,126.354780456332));
#69911=CARTESIAN_POINT('Ctrl Pts',(9.56754375842999,1.97503638231783,126.298018029156));
#69912=CARTESIAN_POINT('Ctrl Pts',(9.55977085816454,1.84828090573022,126.246615478134));
#69913=CARTESIAN_POINT('Ctrl Pts',(9.5522805224025,1.72613330999434,126.197081539317));
#69914=CARTESIAN_POINT('Ctrl Pts',(9.54479018664053,1.60214920076463,126.152524656418));
#69915=CARTESIAN_POINT('Ctrl Pts',(9.5372998508785,1.47677313275936,126.11305758143));
#69916=CARTESIAN_POINT('Ctrl Pts',(9.52952551675939,1.34664339302863,126.072094100297));
#69917=CARTESIAN_POINT('Ctrl Pts',(9.52175118264028,1.21460184675343,126.036484246188));
#69918=CARTESIAN_POINT('Ctrl Pts',(9.5139768485212,1.08112852347603,126.006408535873));
#69919=CARTESIAN_POINT('Ctrl Pts',(9.5062120955741,0.947819694140715,125.976369891182));
#69920=CARTESIAN_POINT('Ctrl Pts',(9.49844734262707,0.813082976447265,125.951851904962));
#69921=CARTESIAN_POINT('Ctrl Pts',(9.49068258967998,0.677415207212283,125.93298589378));
#69922=CARTESIAN_POINT('Ctrl Pts',(9.48292554879497,0.541882185118286,125.914138620587));
#69923=CARTESIAN_POINT('Ctrl Pts',(9.47516850790994,0.40542033647734,125.900932204574));
#69924=CARTESIAN_POINT('Ctrl Pts',(9.46741146702493,0.268538039963397,125.893447221507));
#69925=CARTESIAN_POINT('Ctrl Pts',(9.45966027578481,0.131758967454229,125.885967882924));
#69926=CARTESIAN_POINT('Ctrl Pts',(9.45190908454467,-0.00543953303081873,
125.884201410645));
#69927=CARTESIAN_POINT('Ctrl Pts',(9.44415789330455,-0.142542942026305,
125.888176673471));
#69928=CARTESIAN_POINT('Ctrl Pts',(9.43640999652746,-0.279588078415802,
125.892150246704));
#69929=CARTESIAN_POINT('Ctrl Pts',(9.4286620997504,-0.416537813718125,125.901860689986));
#69930=CARTESIAN_POINT('Ctrl Pts',(9.42091420297331,-0.552876822281564,
125.917284775932));
#69931=CARTESIAN_POINT('Ctrl Pts',(9.4131679268892,-0.689187311663541,125.932705635492));
#69932=CARTESIAN_POINT('Ctrl Pts',(9.40542165080507,-0.824886940169155,
125.953837716535));
#69933=CARTESIAN_POINT('Ctrl Pts',(9.39767537472096,-0.959465097854031,
125.980605877895));
#69934=CARTESIAN_POINT('Ctrl Pts',(9.3899290414556,-1.09404424896429,126.007374236851));
#69935=CARTESIAN_POINT('Ctrl Pts',(9.38218270819028,-1.22750152928127,126.039778682872));
#69936=CARTESIAN_POINT('Ctrl Pts',(9.37443637492493,-1.35933651388733,126.077692943135));
#69937=CARTESIAN_POINT('Ctrl Pts',(9.36668830692195,-1.4912010220241,126.115615694033));
#69938=CARTESIAN_POINT('Ctrl Pts',(9.35894023891897,-1.62144213585741,126.159050606424));
#69939=CARTESIAN_POINT('Ctrl Pts',(9.35119217091599,-1.74957496742626,126.207821648314));
#69940=CARTESIAN_POINT('Ctrl Pts',(9.34343586817414,-1.8778439800933,126.256644524647));
#69941=CARTESIAN_POINT('Ctrl Pts',(9.33567956543229,-2.00399986846719,126.310814720217));
#69942=CARTESIAN_POINT('Ctrl Pts',(9.32792326269043,-2.12757759249629,126.370107957826));
#69943=CARTESIAN_POINT('Ctrl Pts',(9.32016282017626,-2.25122127367756,126.429432842022));
#69944=CARTESIAN_POINT('Ctrl Pts',(9.31240237766206,-2.37228370369536,126.493886032985));
#69945=CARTESIAN_POINT('Ctrl Pts',(9.30464193514788,-2.49032570358189,126.5631979288));
#69946=CARTESIAN_POINT('Ctrl Pts',(9.29686903488245,-2.60855719496591,126.632621090224));
#69947=CARTESIAN_POINT('Ctrl Pts',(9.28909613461702,-2.72375823829617,126.706918330613));
#69948=CARTESIAN_POINT('Ctrl Pts',(9.28132323435159,-2.83551909153673,126.785776968563));
#69949=CARTESIAN_POINT('Ctrl Pts',(9.27383289858961,-2.94321715625263,126.861768896391));
#69950=CARTESIAN_POINT('Ctrl Pts',(9.26634256282764,-3.04772056327013,126.941996155328));
#69951=CARTESIAN_POINT('Ctrl Pts',(9.25885222706566,-3.14869415846041,127.026145674107));
#69952=CARTESIAN_POINT('Ctrl Pts',(9.25118777213279,-3.25201497001521,127.112251319407));
#69953=CARTESIAN_POINT('Ctrl Pts',(9.24352331719991,-3.35198673246377,127.202753229069));
#69954=CARTESIAN_POINT('Ctrl Pts',(9.23585886226704,-3.44820420953052,127.297357510656));
#69955=CARTESIAN_POINT('Ctrl Pts',(9.2282031996922,-3.54431130973226,127.391853265972));
#69956=CARTESIAN_POINT('Ctrl Pts',(9.22054753711735,-3.63667240165821,127.490441759251));
#69957=CARTESIAN_POINT('Ctrl Pts',(9.21289187454252,-3.72491391245029,127.592787886437));
#69958=CARTESIAN_POINT('Ctrl Pts',(9.20524322549842,-3.81307458313985,127.695040251952));
#69959=CARTESIAN_POINT('Ctrl Pts',(9.19759457645428,-3.89712291543507,127.801043103937));
#69960=CARTESIAN_POINT('Ctrl Pts',(9.18994592741018,-3.97672134586974,127.910423783459));
#69961=CARTESIAN_POINT('Ctrl Pts',(9.18230251965738,-4.0562652309123,128.019729509089));
#69962=CARTESIAN_POINT('Ctrl Pts',(9.17465911190463,-4.13136504286035,128.13240813422));
#69963=CARTESIAN_POINT('Ctrl Pts',(9.16701570415182,-4.20172313864092,128.248053568577));
#69964=CARTESIAN_POINT('Ctrl Pts',(9.15937504556866,-4.27205592812527,128.363657407756));
#69965=CARTESIAN_POINT('Ctrl Pts',(9.15173438698547,-4.33765018133567,128.482225592273));
#69966=CARTESIAN_POINT('Ctrl Pts',(9.14409372840231,-4.39825153053533,128.603323013016));
#69967=CARTESIAN_POINT('Ctrl Pts',(9.13645474582435,-4.45883958661697,128.724393870616));
#69968=CARTESIAN_POINT('Ctrl Pts',(9.12881576324646,-4.5144367404964,128.847992499081));
#69969=CARTESIAN_POINT('Ctrl Pts',(9.12117678066849,-4.5648348802313,128.973659773975));
#69970=CARTESIAN_POINT('Ctrl Pts',(9.11353577045341,-4.61524639728936,129.099360405096));
#69971=CARTESIAN_POINT('Ctrl Pts',(9.10589476023829,-4.66045599357105,129.227130405468));
#69972=CARTESIAN_POINT('Ctrl Pts',(9.09825375002322,-4.70030402803673,129.356491456861));
#69973=CARTESIAN_POINT('Ctrl Pts',(9.09383360368492,-4.72335518733032,129.431323810376));
#69974=CARTESIAN_POINT('Ctrl Pts',(9.08941345734662,-4.74461309477974,129.506688265335));
#69975=CARTESIAN_POINT('Ctrl Pts',(9.08499331100833,-4.76405452823402,129.582490119308));
#69976=CARTESIAN_POINT('Ctrl Pts',(10.8346522545385,-4.76405452823403,129.582490119308));
#69977=CARTESIAN_POINT('Ctrl Pts',(10.8267790172283,-4.79867665138673,129.717481252017));
#69978=CARTESIAN_POINT('Ctrl Pts',(10.818905779918,-4.82758080289594,129.854037654495));
#69979=CARTESIAN_POINT('Ctrl Pts',(10.8110325426078,-4.85063653588562,129.991644025369));
#69980=CARTESIAN_POINT('Ctrl Pts',(10.8031633271452,-4.87368049142725,130.12918010345));
#69981=CARTESIAN_POINT('Ctrl Pts',(10.7952941116825,-4.89088191557338,130.267764714496));
#69982=CARTESIAN_POINT('Ctrl Pts',(10.7874248962198,-4.9021613315402,130.40687182269));
#69983=CARTESIAN_POINT('Ctrl Pts',(10.7799030761437,-4.91294280497544,130.539837890797));
#69984=CARTESIAN_POINT('Ctrl Pts',(10.7723812560675,-4.91831389514874,130.673280985255));
#69985=CARTESIAN_POINT('Ctrl Pts',(10.7648594359913,-4.91824942613528,130.806736500554));
#69986=CARTESIAN_POINT('',(11.1101405640401,-4.91824801950251,130.799946870896));
#69987=CARTESIAN_POINT('Ctrl Pts',(11.1800167307073,-4.76405452823405,129.582490119308));
#69988=CARTESIAN_POINT('Ctrl Pts',(11.1703218396064,-4.8063363855668,129.747346439332));
#69989=CARTESIAN_POINT('Ctrl Pts',(11.1606269485055,-4.840089161629,129.914523699574));
#69990=CARTESIAN_POINT('Ctrl Pts',(11.1509320574046,-4.86509658065642,130.083237657603));
#69991=CARTESIAN_POINT('Ctrl Pts',(11.1413830686639,-4.88972765286176,130.249412570645));
#69992=CARTESIAN_POINT('Ctrl Pts',(11.1318340799231,-4.9058745984055,130.417078356921));
#69993=CARTESIAN_POINT('Ctrl Pts',(11.1222850911824,-4.91337637600288,130.585464180325));
#69994=CARTESIAN_POINT('Ctrl Pts',(11.1182369154683,-4.91655666186421,130.656849268255));
#69995=CARTESIAN_POINT('Ctrl Pts',(11.1141887397541,-4.91818377896244,130.728363490022));
#69996=CARTESIAN_POINT('Ctrl Pts',(11.11014056404,-4.91824801950251,130.799946870896));
#69997=CARTESIAN_POINT('Ctrl Pts',(11.1101405640087,-4.918248019503,130.799946871451));
#69998=CARTESIAN_POINT('Ctrl Pts',(11.1024544495004,-4.91836999051411,130.935859465454));
#69999=CARTESIAN_POINT('Ctrl Pts',(11.0947683349922,-4.91285393968429,131.071890269725));
#70000=CARTESIAN_POINT('Ctrl Pts',(11.0870822204839,-4.90169732681665,131.207531026672));
#70001=CARTESIAN_POINT('Ctrl Pts',(11.0793992390307,-4.89054526166714,131.343116493009));
#70002=CARTESIAN_POINT('Ctrl Pts',(11.0717162575775,-4.87375723796405,131.478311832142));
#70003=CARTESIAN_POINT('Ctrl Pts',(11.0640332761243,-4.85138278522514,131.612610661625));
#70004=CARTESIAN_POINT('Ctrl Pts',(11.0563517432926,-4.82901255117571,131.746884169145));
#70005=CARTESIAN_POINT('Ctrl Pts',(11.0486702104609,-4.80105804789083,131.880261110623));
#70006=CARTESIAN_POINT('Ctrl Pts',(11.0409886776292,-4.76762039214223,132.012242589834));
#70007=CARTESIAN_POINT('Ctrl Pts',(11.0333068612482,-4.73418150210544,132.144228940893));
#70008=CARTESIAN_POINT('Ctrl Pts',(11.0256250448671,-4.69525915478474,132.274819341283));
#70009=CARTESIAN_POINT('Ctrl Pts',(11.0179432284861,-4.65100495372822,132.403527895525));
#70010=CARTESIAN_POINT('Ctrl Pts',(11.0102593964723,-4.60673914080644,132.532270221621));
#70011=CARTESIAN_POINT('Ctrl Pts',(11.0025755644586,-4.55713882092296,132.659129343108));
#70012=CARTESIAN_POINT('Ctrl Pts',(10.9948917324448,-4.50240437979523,132.78363772381));
#70013=CARTESIAN_POINT('Ctrl Pts',(10.9871995896671,-4.44761073838575,132.908280771662));
#70014=CARTESIAN_POINT('Ctrl Pts',(10.9795074468893,-4.38767204782599,133.03056763695));
#70015=CARTESIAN_POINT('Ctrl Pts',(10.9718153041116,-4.32283564172309,133.150053495406));
#70016=CARTESIAN_POINT('Ctrl Pts',(10.9641186702404,-4.25796138058213,133.269609116238));
#70017=CARTESIAN_POINT('Ctrl Pts',(10.9564220363693,-4.18818391336705,133.386360132513));
#70018=CARTESIAN_POINT('Ctrl Pts',(10.9487254024982,-4.11379421335629,133.49989029328));
#70019=CARTESIAN_POINT('Ctrl Pts',(10.9410169382095,-4.03929016969578,133.613594960101));
#70020=CARTESIAN_POINT('Ctrl Pts',(10.9333084739209,-3.96015996659395,133.724068561489));
#70021=CARTESIAN_POINT('Ctrl Pts',(10.9256000096322,-3.87673554877064,133.830927079317));
#70022=CARTESIAN_POINT('Ctrl Pts',(10.9203829976827,-3.82027473266398,133.903247861193));
#70023=CARTESIAN_POINT('Ctrl Pts',(10.9151659857332,-3.7618477954338,133.973913487563));
#70024=CARTESIAN_POINT('Ctrl Pts',(10.9099489737837,-3.70156693300311,134.042814770862));
#70025=CARTESIAN_POINT('Ctrl Pts',(10.9021746396646,-3.61173705144308,134.145490709269));
#70026=CARTESIAN_POINT('Ctrl Pts',(10.8944003055455,-3.51748953239293,134.244588826331));
#70027=CARTESIAN_POINT('Ctrl Pts',(10.8866259714264,-3.41914044743804,134.339705249026));
#70028=CARTESIAN_POINT('Ctrl Pts',(10.8788612184793,-3.32091256894066,134.434704449231));
#70029=CARTESIAN_POINT('Ctrl Pts',(10.8710964655323,-3.21859346044696,134.525731449512));
#70030=CARTESIAN_POINT('Ctrl Pts',(10.8633317125852,-3.1125391408373,134.612415653835));
#70031=CARTESIAN_POINT('Ctrl Pts',(10.8555746717002,-3.00659015587313,134.699013762185));
#70032=CARTESIAN_POINT('Ctrl Pts',(10.8478176308151,-2.89691364334437,134.781277412468));
#70033=CARTESIAN_POINT('Ctrl Pts',(10.8400605899301,-2.78390187384632,134.85887334036));
#70034=CARTESIAN_POINT('Ctrl Pts',(10.83230939869,-2.67097532740261,134.936410752558));
#70035=CARTESIAN_POINT('Ctrl Pts',(10.8245582074499,-2.55471885122989,135.009287228239));
#70036=CARTESIAN_POINT('Ctrl Pts',(10.8168070162097,-2.4355568573981,135.077210469466));
#70037=CARTESIAN_POINT('Ctrl Pts',(10.8090591194327,-2.31644551059244,135.145104841504));
#70038=CARTESIAN_POINT('Ctrl Pts',(10.8013112226556,-2.19443144124389,135.20804997308));
#70039=CARTESIAN_POINT('Ctrl Pts',(10.7935633258785,-2.06996684930385,135.265797640016));
#70040=CARTESIAN_POINT('Ctrl Pts',(10.7858170497944,-1.94552829267329,135.323533227384));
#70041=CARTESIAN_POINT('Ctrl Pts',(10.7780707737103,-1.81864058746095,135.376073348166));
#70042=CARTESIAN_POINT('Ctrl Pts',(10.7703244976262,-1.68977891060562,135.423216568532));
#70043=CARTESIAN_POINT('Ctrl Pts',(10.7625781643609,-1.56091628252266,135.470360136898));
#70044=CARTESIAN_POINT('Ctrl Pts',(10.7548318310955,-1.43008002088606,135.512106591029));
#70045=CARTESIAN_POINT('Ctrl Pts',(10.7470854978302,-1.29776320166481,135.548303464492));
#70046=CARTESIAN_POINT('Ctrl Pts',(10.7393374298272,-1.16541675100968,135.584508443994));
#70047=CARTESIAN_POINT('Ctrl Pts',(10.7315893618243,-1.03158946003955,135.615161266677));
#70048=CARTESIAN_POINT('Ctrl Pts',(10.7238412938213,-0.896787018960324,
135.640160045285));
#70049=CARTESIAN_POINT('Ctrl Pts',(10.7160849910794,-0.76184130824218,135.665185392892));
#70050=CARTESIAN_POINT('Ctrl Pts',(10.7083286883375,-0.625918762115954,
135.684544621027));
#70051=CARTESIAN_POINT('Ctrl Pts',(10.7005723855956,-0.489533215689875,
135.698187371062));
#70052=CARTESIAN_POINT('Ctrl Pts',(10.6928119430815,-0.353074876191179,
135.711837402644));
#70053=CARTESIAN_POINT('Ctrl Pts',(10.6850515005674,-0.216153434111273,
135.719764854052));
#70054=CARTESIAN_POINT('Ctrl Pts',(10.6772910580532,-0.0792842146913874,
135.721971528954));
#70055=CARTESIAN_POINT('Ctrl Pts',(10.6695181577878,0.0578047193501897,
135.724181746207));
#70056=CARTESIAN_POINT('Ctrl Pts',(10.6617452575223,0.194840872147232,135.720652845469));
#70057=CARTESIAN_POINT('Ctrl Pts',(10.6539723572569,0.331311650224775,135.711438735237));
#70058=CARTESIAN_POINT('Ctrl Pts',(10.6464820214948,0.462821371771351,135.702559581121));
#70059=CARTESIAN_POINT('Ctrl Pts',(10.6389916857327,0.593805804300594,135.688401417735));
#70060=CARTESIAN_POINT('Ctrl Pts',(10.6315013499706,0.723815853872389,135.669057285621));
#70061=CARTESIAN_POINT('Ctrl Pts',(10.6237270158515,0.858755273988071,135.648979714858));
#70062=CARTESIAN_POINT('Ctrl Pts',(10.6159526817324,0.993072412647427,135.623251560731));
#70063=CARTESIAN_POINT('Ctrl Pts',(10.6081783476133,1.12625663562571,135.591920439982));
#70064=CARTESIAN_POINT('Ctrl Pts',(10.6004135946663,1.25927672095201,135.560627932039));
#70065=CARTESIAN_POINT('Ctrl Pts',(10.5926488417192,1.39116629173078,135.523746285345));
#70066=CARTESIAN_POINT('Ctrl Pts',(10.5848840887721,1.52142111812217,135.481374712459));
#70067=CARTESIAN_POINT('Ctrl Pts',(10.5771270478871,1.65154657358389,135.439045223617));
#70068=CARTESIAN_POINT('Ctrl Pts',(10.5693700070021,1.78004014641446,135.391236779806));
#70069=CARTESIAN_POINT('Ctrl Pts',(10.5616129661171,1.90640942006008,135.338099271878));
#70070=CARTESIAN_POINT('Ctrl Pts',(10.5538617748769,2.03268339765342,135.285001835359));
#70071=CARTESIAN_POINT('Ctrl Pts',(10.5461105836368,2.15683590570613,135.226583484613));
#70072=CARTESIAN_POINT('Ctrl Pts',(10.5383593923967,2.2783916205963,135.163043295359));
#70073=CARTESIAN_POINT('Ctrl Pts',(10.5306114956196,2.39989567106504,135.099530112382));
#70074=CARTESIAN_POINT('Ctrl Pts',(10.5228635988425,2.51880477780077,135.030899601358));
#70075=CARTESIAN_POINT('Ctrl Pts',(10.5151157020654,2.63466567765311,134.957398039682));
#70076=CARTESIAN_POINT('Ctrl Pts',(10.5073694259813,2.75050234190286,134.883911852949));
#70077=CARTESIAN_POINT('Ctrl Pts',(10.4996231498972,2.86329173760149,134.805556851553));
#70078=CARTESIAN_POINT('Ctrl Pts',(10.4918768738131,2.97260754802252,134.722623935407));
#70079=CARTESIAN_POINT('Ctrl Pts',(10.4841305405477,3.08192416538788,134.639690407069));
#70080=CARTESIAN_POINT('Ctrl Pts',(10.4763842072824,3.18776683483693,134.552179132851));
#70081=CARTESIAN_POINT('Ctrl Pts',(10.468637874017,3.28974076243709,134.460422539698));
#70082=CARTESIAN_POINT('Ctrl Pts',(10.4608898060141,3.39173752639143,134.368645398291));
#70083=CARTESIAN_POINT('Ctrl Pts',(10.4531417380112,3.48986353393035,134.272621307609));
#70084=CARTESIAN_POINT('Ctrl Pts',(10.4453936700082,3.58375972651124,134.172720646591));
#70085=CARTESIAN_POINT('Ctrl Pts',(10.4376373672663,3.67775571308298,134.072713809963));
#70086=CARTESIAN_POINT('Ctrl Pts',(10.4298810645244,3.76751263626869,133.968822458062));
#70087=CARTESIAN_POINT('Ctrl Pts',(10.4221247617825,3.85271038750178,133.861451674852));
#70088=CARTESIAN_POINT('Ctrl Pts',(10.4143643192683,3.93795361134007,133.754023584621));
#70089=CARTESIAN_POINT('Ctrl Pts',(10.4066038767542,4.01863258466237,133.643112678706));
#70090=CARTESIAN_POINT('Ctrl Pts',(10.39884343424,4.09447027906687,133.529153489756));
#70091=CARTESIAN_POINT('Ctrl Pts',(10.3910705339746,4.17042971487088,133.415011363399));
#70092=CARTESIAN_POINT('Ctrl Pts',(10.3832976337091,4.24153213861732,133.297811509938));
#70093=CARTESIAN_POINT('Ctrl Pts',(10.3755247334437,4.30754583575698,133.178014327641));
#70094=CARTESIAN_POINT('Ctrl Pts',(10.3680343976817,4.3711597687267,133.062572074672));
#70095=CARTESIAN_POINT('Ctrl Pts',(10.3605440619197,4.43004839014375,132.944718328772));
#70096=CARTESIAN_POINT('Ctrl Pts',(10.3530537261578,4.48404723140638,132.824881216079));
#70097=CARTESIAN_POINT('Ctrl Pts',(10.3452793920387,4.54009345514839,132.700500442834));
#70098=CARTESIAN_POINT('Ctrl Pts',(10.3375050579196,4.59104932474587,132.57358893427));
#70099=CARTESIAN_POINT('Ctrl Pts',(10.3297307238005,4.6366788912414,132.444602039435));
#70100=CARTESIAN_POINT('Ctrl Pts',(10.3219659708534,4.6822522233743,132.315774109421));
#70101=CARTESIAN_POINT('Ctrl Pts',(10.3142012179064,4.72251218405631,132.184876247295));
#70102=CARTESIAN_POINT('Ctrl Pts',(10.3064364649593,4.75726969507791,132.052386302716));
#70103=CARTESIAN_POINT('Ctrl Pts',(10.2986794240743,4.79199268444946,131.920027949017));
#70104=CARTESIAN_POINT('Ctrl Pts',(10.2909223831893,4.82122400141028,131.786081035402));
#70105=CARTESIAN_POINT('Ctrl Pts',(10.2831653423043,4.84482359020511,131.65104086553));
#70106=CARTESIAN_POINT('Ctrl Pts',(10.2754141510642,4.86840538236648,131.5161025305));
#70107=CARTESIAN_POINT('Ctrl Pts',(10.267662959824,4.8863638325859,131.380072963768));
#70108=CARTESIAN_POINT('Ctrl Pts',(10.2599117685838,4.89860950487715,131.243459673847));
#70109=CARTESIAN_POINT('Ctrl Pts',(10.2521638718067,4.91084997243103,131.106904448219));
#70110=CARTESIAN_POINT('Ctrl Pts',(10.2444159750297,4.91738245649662,130.96976638144));
#70111=CARTESIAN_POINT('Ctrl Pts',(10.2366680782526,4.91816915741655,130.832559935582));
#70112=CARTESIAN_POINT('Ctrl Pts',(10.2289218021686,4.91895569377562,130.695382190354));
#70113=CARTESIAN_POINT('Ctrl Pts',(10.2211755260845,4.91399883538182,130.55813648521));
#70114=CARTESIAN_POINT('Ctrl Pts',(10.2134292500004,4.90331288996588,130.421338730992));
#70115=CARTESIAN_POINT('Ctrl Pts',(10.205682916735,4.89262686566873,130.284539966965));
#70116=CARTESIAN_POINT('Ctrl Pts',(10.1979365834697,4.87621170040865,130.148189550241));
#70117=CARTESIAN_POINT('Ctrl Pts',(10.1901902502044,4.85413367862674,130.01279931702));
#70118=CARTESIAN_POINT('Ctrl Pts',(10.1824421822014,4.83205071262496,129.877378764096));
#70119=CARTESIAN_POINT('Ctrl Pts',(10.1746941141985,4.80430242952618,129.742919208349));
#70120=CARTESIAN_POINT('Ctrl Pts',(10.1669460461955,4.77100635971077,129.609922934763));
#70121=CARTESIAN_POINT('Ctrl Pts',(10.1591897434537,4.73767490243609,129.476785311155));
#70122=CARTESIAN_POINT('Ctrl Pts',(10.1514334407118,4.6987839751433,129.345114456242));
#70123=CARTESIAN_POINT('Ctrl Pts',(10.14367713797,4.65450135994198,129.215398644202));
#70124=CARTESIAN_POINT('Ctrl Pts',(10.1359166954558,4.61019510977554,129.085613598926));
#70125=CARTESIAN_POINT('Ctrl Pts',(10.1281562529416,4.5604915792441,128.957786039927));
#70126=CARTESIAN_POINT('Ctrl Pts',(10.1203958104275,4.50560661235295,128.832383914554));
#70127=CARTESIAN_POINT('Ctrl Pts',(10.112622910162,4.45063353924048,128.706780482557));
#70128=CARTESIAN_POINT('Ctrl Pts',(10.1048500098967,4.39046258006013,128.583610616173));
#70129=CARTESIAN_POINT('Ctrl Pts',(10.0970771096312,4.32535583353923,128.463318119924));
#70130=CARTESIAN_POINT('Ctrl Pts',(10.0895867738691,4.26261588124758,128.34739855891));
#70131=CARTESIAN_POINT('Ctrl Pts',(10.082096438107,4.19529292534033,128.234151065501));
#70132=CARTESIAN_POINT('Ctrl Pts',(10.0746061023449,4.12365826116438,128.123945424423));
#70133=CARTESIAN_POINT('Ctrl Pts',(10.0668317682258,4.04930754692415,128.009561302969));
#70134=CARTESIAN_POINT('Ctrl Pts',(10.0590574341066,3.97007619263236,127.898091916367));
#70135=CARTESIAN_POINT('Ctrl Pts',(10.0512830999876,3.88621976016404,127.789981902439));
#70136=CARTESIAN_POINT('Ctrl Pts',(10.0435183470405,3.80246667325427,127.682005124442));
#70137=CARTESIAN_POINT('Ctrl Pts',(10.0357535940935,3.71410008678098,127.577379787462));
#70138=CARTESIAN_POINT('Ctrl Pts',(10.0279888411464,3.62141982780256,127.476523257763));
#70139=CARTESIAN_POINT('Ctrl Pts',(10.0202318002614,3.52883162016379,127.375766900192));
#70140=CARTESIAN_POINT('Ctrl Pts',(10.0124747593763,3.43193852899701,127.278772186714));
#70141=CARTESIAN_POINT('Ctrl Pts',(10.0047177184913,3.3310815637425,127.18592467393));
#70142=CARTESIAN_POINT('Ctrl Pts',(9.99696652725117,3.23030065551072,127.093147178179));
#70143=CARTESIAN_POINT('Ctrl Pts',(9.98921533601106,3.12556210946481,127.004510921874));
#70144=CARTESIAN_POINT('Ctrl Pts',(9.98146414477097,3.01724456455642,126.920365470793));
#70145=CARTESIAN_POINT('Ctrl Pts',(9.97371624799389,2.90897305749364,126.836255783773));
#70146=CARTESIAN_POINT('Ctrl Pts',(9.96596835121683,2.79712588516252,126.756633345042));
#70147=CARTESIAN_POINT('Ctrl Pts',(9.95822045443975,2.68211544743726,126.681808035837));
#70148=CARTESIAN_POINT('Ctrl Pts',(9.95047417835566,2.56712906741623,126.606998378474));
#70149=CARTESIAN_POINT('Ctrl Pts',(9.94272790227159,2.44898106563803,126.536984067783));
#70150=CARTESIAN_POINT('Ctrl Pts',(9.93498162618749,2.32811322618503,126.472031928678));
#70151=CARTESIAN_POINT('Ctrl Pts',(9.92723529292215,2.2072444945131,126.407079310111));
#70152=CARTESIAN_POINT('Ctrl Pts',(9.91948895965675,2.08365622949244,126.347189122762));
#70153=CARTESIAN_POINT('Ctrl Pts',(9.9117426263914,1.95781488177463,126.292582259623));
#70154=CARTESIAN_POINT('Ctrl Pts',(9.90399455838842,1.83194535275952,126.237963167656));
#70155=CARTESIAN_POINT('Ctrl Pts',(9.8962464903855,1.70382209561181,126.18862990986));
#70156=CARTESIAN_POINT('Ctrl Pts',(9.88849842238253,1.57393122495696,126.144755101902));
#70157=CARTESIAN_POINT('Ctrl Pts',(9.88074211964067,1.44390230473888,126.100833663276));
#70158=CARTESIAN_POINT('Ctrl Pts',(9.87298581689877,1.31210238922202,126.062382388535));
#70159=CARTESIAN_POINT('Ctrl Pts',(9.86522951415691,1.17903296763002,126.02952404196));
#70160=CARTESIAN_POINT('Ctrl Pts',(9.85746907164274,1.04589252288108,125.996648157896));
#70161=CARTESIAN_POINT('Ctrl Pts',(9.84970862912859,0.911481604901739,125.969371227809));
#70162=CARTESIAN_POINT('Ctrl Pts',(9.84194818661442,0.776310580008076,125.947764592996));
#70163=CARTESIAN_POINT('Ctrl Pts',(9.83417528634898,0.640922566585333,125.926123273295));
#70164=CARTESIAN_POINT('Ctrl Pts',(9.82640238608358,0.504772396449882,125.910170484012));
#70165=CARTESIAN_POINT('Ctrl Pts',(9.81862948581815,0.368375125679472,125.899925601249));
#70166=CARTESIAN_POINT('Ctrl Pts',(9.81113915005611,0.236936239265373,125.890053145779));
#70167=CARTESIAN_POINT('Ctrl Pts',(9.80364881429403,0.105268213603494,125.885480818858));
#70168=CARTESIAN_POINT('Ctrl Pts',(9.79615847853199,-0.0261711991809226,
125.886180249703));
#70169=CARTESIAN_POINT('Ctrl Pts',(9.78838414441291,-0.162594177251013,
125.886906199681));
#70170=CARTESIAN_POINT('Ctrl Pts',(9.78060981029386,-0.299203011504808,
125.893313855746));
#70171=CARTESIAN_POINT('Ctrl Pts',(9.77283547617478,-0.435485478113105,
125.905428544057));
#70172=CARTESIAN_POINT('Ctrl Pts',(9.76507072322768,-0.57159998876122,125.917528302098));
#70173=CARTESIAN_POINT('Ctrl Pts',(9.75730597028051,-0.707388546368588,
125.935321063716));
#70174=CARTESIAN_POINT('Ctrl Pts',(9.74954121733342,-0.842337945028206,
125.958780172576));
#70175=CARTESIAN_POINT('Ctrl Pts',(9.7417841764484,-0.977153310042805,125.982215981519));
#70176=CARTESIAN_POINT('Ctrl Pts',(9.73402713556341,-1.11113079204565,126.01130687141));
#70177=CARTESIAN_POINT('Ctrl Pts',(9.7262700946784,-1.24376168741733,126.04597434411));
#70178=CARTESIAN_POINT('Ctrl Pts',(9.71851890343822,-1.37629256479963,126.080615673799));
#70179=CARTESIAN_POINT('Ctrl Pts',(9.71076771219805,-1.50747850005841,126.120825117345));
#70180=CARTESIAN_POINT('Ctrl Pts',(9.70301652095787,-1.6368207300032,126.166473063913));
#70181=CARTESIAN_POINT('Ctrl Pts',(9.69526862418079,-1.76610798604925,126.212101608886));
#70182=CARTESIAN_POINT('Ctrl Pts',(9.68752072740372,-1.89355272744303,126.263163929624));
#70183=CARTESIAN_POINT('Ctrl Pts',(9.67977283062663,-2.01867133011636,126.319480560812));
#70184=CARTESIAN_POINT('Ctrl Pts',(9.67202655454253,-2.14376376067508,126.375785411776));
#70185=CARTESIAN_POINT('Ctrl Pts',(9.66428027845839,-2.26653066405425,126.437342226674));
#70186=CARTESIAN_POINT('Ctrl Pts',(9.65653400237429,-2.38650875780919,126.50392354543));
#70187=CARTESIAN_POINT('Ctrl Pts',(9.64878766910891,-2.50648773721548,126.570505355675));
#70188=CARTESIAN_POINT('Ctrl Pts',(9.64104133584361,-2.62367752406538,126.642111554077));
#70189=CARTESIAN_POINT('Ctrl Pts',(9.63329500257825,-2.73764014685824,126.718469100552));
#70190=CARTESIAN_POINT('Ctrl Pts',(9.62554693457525,-2.85162829079047,126.794843746769));
#70191=CARTESIAN_POINT('Ctrl Pts',(9.61779886657223,-2.9623875078377,126.875971640777));
#70192=CARTESIAN_POINT('Ctrl Pts',(9.61005079856923,-3.06950981472219,126.961537103557));
#70193=CARTESIAN_POINT('Ctrl Pts',(9.60229449582738,-3.17674597246892,127.047193506328));
#70194=CARTESIAN_POINT('Ctrl Pts',(9.59453819308545,-3.28033719263344,127.137296654798));
#70195=CARTESIAN_POINT('Ctrl Pts',(9.58678189034359,-3.37990912297542,127.231490988972));
#70196=CARTESIAN_POINT('Ctrl Pts',(9.57902144782944,-3.4795341978544,127.325735597498));
#70197=CARTESIAN_POINT('Ctrl Pts',(9.5712610053153,-3.57513543599653,127.424075462521));
#70198=CARTESIAN_POINT('Ctrl Pts',(9.56350056280115,-3.66637695048661,127.526119760118));
#70199=CARTESIAN_POINT('Ctrl Pts',(9.55572766253572,-3.75776493395605,127.628327868282));
#70200=CARTESIAN_POINT('Ctrl Pts',(9.54795476227035,-3.84477895999743,127.734251990114));
#70201=CARTESIAN_POINT('Ctrl Pts',(9.54018186200491,-3.92712432655619,127.843469267606));
#70202=CARTESIAN_POINT('Ctrl Pts',(9.53269152624299,-4.00647623162396,127.948716221957));
#70203=CARTESIAN_POINT('Ctrl Pts',(9.52520119048102,-4.08149284379729,128.057020806591));
#70204=CARTESIAN_POINT('Ctrl Pts',(9.5177108547191,-4.15195060601324,128.167982566579));
#70205=CARTESIAN_POINT('Ctrl Pts',(9.50974150827459,-4.22691417702676,128.286040386087));
#70206=CARTESIAN_POINT('Ctrl Pts',(9.50177216183008,-4.29694495240893,128.40746501991));
#70207=CARTESIAN_POINT('Ctrl Pts',(9.49380281538558,-4.36173500513333,128.53181781104));
#70208=CARTESIAN_POINT('Ctrl Pts',(9.48584369238272,-4.42644194221854,128.656011076728));
#70209=CARTESIAN_POINT('Ctrl Pts',(9.47788456937984,-4.48592137079548,128.783124703114));
#70210=CARTESIAN_POINT('Ctrl Pts',(9.46992544637698,-4.5399085880573,128.912691229279));
#70211=CARTESIAN_POINT('Ctrl Pts',(9.46197826351917,-4.59381481458623,129.042063381878));
#70212=CARTESIAN_POINT('Ctrl Pts',(9.45403108066137,-4.642245108635,129.173880767391));
#70213=CARTESIAN_POINT('Ctrl Pts',(9.44608389780356,-4.68498097380139,129.307652116348));
#70214=CARTESIAN_POINT('Ctrl Pts',(9.44069156785431,-4.71397815302414,129.398418777219));
#70215=CARTESIAN_POINT('Ctrl Pts',(9.4352992379051,-4.74035460762676,129.490084488557));
#70216=CARTESIAN_POINT('Ctrl Pts',(9.42990690795585,-4.76405452823399,129.582490119308));
#70217=CARTESIAN_POINT('Origin',(213.235140564004,0.,130.804360617566));
#70218=CARTESIAN_POINT('',(7.33490367089153,-4.76405452823399,129.582490119308));
#70219=CARTESIAN_POINT('',(7.68025985017537,-4.76405452823403,129.582490119308));
#70220=CARTESIAN_POINT('',(213.235140564004,-4.76405452823405,129.582490119308));
#70221=CARTESIAN_POINT('',(9.01485943602795,-4.91824886988786,130.807694736162));
#70222=CARTESIAN_POINT('Ctrl Pts',(9.0148594359913,-4.91824886988742,130.807694736807));
#70223=CARTESIAN_POINT('Ctrl Pts',(9.00337449174511,-4.91811194828998,131.009671463859));
#70224=CARTESIAN_POINT('Ctrl Pts',(8.99188954749892,-4.90553346737286,131.211229737893));
#70225=CARTESIAN_POINT('Ctrl Pts',(8.98040460325277,-4.88066534031835,131.41122872376));
#70226=CARTESIAN_POINT('Ctrl Pts',(8.97263026913369,-4.86383172541402,131.546611090995));
#70227=CARTESIAN_POINT('Ctrl Pts',(8.96485593501466,-4.84133422133454,131.681506954395));
#70228=CARTESIAN_POINT('Ctrl Pts',(8.95708160089558,-4.81320817729648,131.815404684116));
#70229=CARTESIAN_POINT('Ctrl Pts',(8.9493168479485,-4.78511679609403,131.949137396852));
#70230=CARTESIAN_POINT('Ctrl Pts',(8.94155209500138,-4.7514107564428,132.08187404452));
#70231=CARTESIAN_POINT('Ctrl Pts',(8.9337873420543,-4.71217714220482,132.213108161657));
#70232=CARTESIAN_POINT('Ctrl Pts',(8.9260303011693,-4.67298249534548,132.34421193522));
#70233=CARTESIAN_POINT('Ctrl Pts',(8.91827326028429,-4.62827131063702,132.473815775905));
#70234=CARTESIAN_POINT('Ctrl Pts',(8.91051621939928,-4.57818161912834,132.601423811996));
#70235=CARTESIAN_POINT('Ctrl Pts',(8.90276502815916,-4.52812970064574,132.728935617874));
#70236=CARTESIAN_POINT('Ctrl Pts',(8.89501383691906,-4.47270749080831,132.854454252413));
#70237=CARTESIAN_POINT('Ctrl Pts',(8.88726264567893,-4.41210260155147,132.977499751603));
#70238=CARTESIAN_POINT('Ctrl Pts',(8.87951474890185,-4.35152347098925,133.100492953173));
#70239=CARTESIAN_POINT('Ctrl Pts',(8.87176685212476,-4.28576621455026,133.221014760054));
#70240=CARTESIAN_POINT('Ctrl Pts',(8.86401895534769,-4.21506616164149,133.338606129643));
#70241=CARTESIAN_POINT('Ctrl Pts',(8.8562726792636,-4.14438089765976,133.456172901654));
#70242=CARTESIAN_POINT('Ctrl Pts',(8.84852640317951,-4.06875509507117,133.570810120778));
#70243=CARTESIAN_POINT('Ctrl Pts',(8.84078012709543,-3.98846933958987,133.682084612262));
#70244=CARTESIAN_POINT('Ctrl Pts',(8.83303379383008,-3.90818299145725,133.79335992515));
#70245=CARTESIAN_POINT('Ctrl Pts',(8.82528746056474,-3.82323685054995,133.901272143812));
#70246=CARTESIAN_POINT('Ctrl Pts',(8.81754112729939,-3.73395377411807,134.005418610675));
#70247=CARTESIAN_POINT('Ctrl Pts',(8.80979305929643,-3.64465070336038,134.109588400418));
#70248=CARTESIAN_POINT('Ctrl Pts',(8.80204499129345,-3.55100901886174,134.2099904635));
#70249=CARTESIAN_POINT('Ctrl Pts',(8.79429692329049,-3.45339037648862,134.306256956705));
#70250=CARTESIAN_POINT('Ctrl Pts',(8.78654062054865,-3.35566798386071,134.402625763085));
#70251=CARTESIAN_POINT('Ctrl Pts',(8.77878431780682,-3.25396046877286,134.49484994448));
#70252=CARTESIAN_POINT('Ctrl Pts',(8.77102801506499,-3.14866511680885,134.582599763609));
#70253=CARTESIAN_POINT('Ctrl Pts',(8.76326757255081,-3.04331356554482,134.670396417459));
#70254=CARTESIAN_POINT('Ctrl Pts',(8.75550713003664,-2.93437067213466,134.753713713157));
#70255=CARTESIAN_POINT('Ctrl Pts',(8.74774668752246,-2.82226419617377,134.832264274494));
#70256=CARTESIAN_POINT('Ctrl Pts',(8.73997378725704,-2.70997775694548,134.910940932166));
#70257=CARTESIAN_POINT('Ctrl Pts',(8.73220088699162,-2.59451791626622,134.984835353499));
#70258=CARTESIAN_POINT('Ctrl Pts',(8.7244279867262,-2.47633937930935,135.053704842383));
#70259=CARTESIAN_POINT('Ctrl Pts',(8.71693765096409,-2.36245692984319,135.120070751875));
#70260=CARTESIAN_POINT('Ctrl Pts',(8.70944731520199,-2.24605028744914,135.181770579768));
#70261=CARTESIAN_POINT('Ctrl Pts',(8.70195697943987,-2.12754350818067,135.238629630977));
#70262=CARTESIAN_POINT('Ctrl Pts',(8.69418264532078,-2.00454350835826,135.297644510394));
#70263=CARTESIAN_POINT('Ctrl Pts',(8.68640831120169,-1.87889134754276,135.351631232232));
#70264=CARTESIAN_POINT('Ctrl Pts',(8.6786339770826,-1.75103658152808,135.40034298836));
#70265=CARTESIAN_POINT('Ctrl Pts',(8.6708692241355,-1.62333938508579,135.448994711602));
#70266=CARTESIAN_POINT('Ctrl Pts',(8.66310447118845,-1.49344534635818,135.492384266176));
#70267=CARTESIAN_POINT('Ctrl Pts',(8.65533971824135,-1.3618276400368,135.530311161248));
#70268=CARTESIAN_POINT('Ctrl Pts',(8.64758267735635,-1.23034065827701,135.568200386794));
#70269=CARTESIAN_POINT('Ctrl Pts',(8.6398256364713,-1.09713378907069,135.600637642452));
#70270=CARTESIAN_POINT('Ctrl Pts',(8.6320685955863,-0.962698832490867,135.627471026879));
#70271=CARTESIAN_POINT('Ctrl Pts',(8.62431740434618,-0.82836525435755,135.654284176041));
#70272=CARTESIAN_POINT('Ctrl Pts',(8.61656621310607,-0.692805814067956,
135.675501789198));
#70273=CARTESIAN_POINT('Ctrl Pts',(8.60881502186595,-0.556525727769769,
135.691022277312));
#70274=CARTESIAN_POINT('Ctrl Pts',(8.60106712508886,-0.420303564143464,
135.706536168805));
#70275=CARTESIAN_POINT('Ctrl Pts',(8.5933192283118,-0.28336175134443,135.716357707148));
#70276=CARTESIAN_POINT('Ctrl Pts',(8.58557133153471,-0.146213696205706,
135.720436757898));
#70277=CARTESIAN_POINT('Ctrl Pts',(8.5778250554506,-0.00909432948354663,
135.724514955399));
#70278=CARTESIAN_POINT('Ctrl Pts',(8.57007877936647,0.128230803222779,135.722853042953));
#70279=CARTESIAN_POINT('Ctrl Pts',(8.56233250328236,0.265245596292749,135.715452943734));
#70280=CARTESIAN_POINT('Ctrl Pts',(8.55458617001701,0.402261400774609,135.708052789889));
#70281=CARTESIAN_POINT('Ctrl Pts',(8.54683983675167,0.538966470652652,135.694914385833));
#70282=CARTESIAN_POINT('Ctrl Pts',(8.53909350348633,0.674847526477958,135.676091714261));
#70283=CARTESIAN_POINT('Ctrl Pts',(8.53134543548336,0.810759011923582,135.657264827483));
#70284=CARTESIAN_POINT('Ctrl Pts',(8.5235973674804,0.94584572892552,135.632751193796));
#70285=CARTESIAN_POINT('Ctrl Pts',(8.51584929947742,1.07960271673855,135.602656256281));
#70286=CARTESIAN_POINT('Ctrl Pts',(8.50809299673556,1.21350186307015,135.572529333508));
#70287=CARTESIAN_POINT('Ctrl Pts',(8.50033669399372,1.34606807505181,135.536809343303));
#70288=CARTESIAN_POINT('Ctrl Pts',(8.49258039125186,1.47680919280781,135.495652302224));
#70289=CARTESIAN_POINT('Ctrl Pts',(8.48481994873769,1.60762009103489,135.454473294392));
#70290=CARTESIAN_POINT('Ctrl Pts',(8.47705950622351,1.7366035865406,135.407851586206));
#70291=CARTESIAN_POINT('Ctrl Pts',(8.46929906370934,1.86328668707073,135.355991730067));
#70292=CARTESIAN_POINT('Ctrl Pts',(8.46152616344391,1.99017315056022,135.304048623882));
#70293=CARTESIAN_POINT('Ctrl Pts',(8.4537532631784,2.1147514841769,135.246850729628));
#70294=CARTESIAN_POINT('Ctrl Pts',(8.44598036291296,2.23657172155684,135.184649420468));
#70295=CARTESIAN_POINT('Ctrl Pts',(8.43849002715095,2.35396348646102,135.124709285573));
#70296=CARTESIAN_POINT('Ctrl Pts',(8.43099969138902,2.4687939327003,135.060123344598));
#70297=CARTESIAN_POINT('Ctrl Pts',(8.423509355627,2.58068687169647,134.991153940952));
#70298=CARTESIAN_POINT('Ctrl Pts',(8.41573502150793,2.69682226548398,134.919569541404));
#70299=CARTESIAN_POINT('Ctrl Pts',(8.40796068738887,2.81016088569513,134.843035961709));
#70300=CARTESIAN_POINT('Ctrl Pts',(8.40018635326979,2.92025208977126,134.761798020064));
#70301=CARTESIAN_POINT('Ctrl Pts',(8.3924216003227,3.0302076162775,134.680660196921));
#70302=CARTESIAN_POINT('Ctrl Pts',(8.38465684737557,3.13692337816709,134.594829777445));
#70303=CARTESIAN_POINT('Ctrl Pts',(8.37689209442848,3.23997493434462,134.504596486713));
#70304=CARTESIAN_POINT('Ctrl Pts',(8.36913505354349,3.34292413826377,134.414452816956));
#70305=CARTESIAN_POINT('Ctrl Pts',(8.36137801265849,3.44221608668468,134.319915234286));
#70306=CARTESIAN_POINT('Ctrl Pts',(8.35362097177349,3.53745715075157,134.221315397644));
#70307=CARTESIAN_POINT('Ctrl Pts',(8.34586978053337,3.63262639279117,134.122789915906));
#70308=CARTESIAN_POINT('Ctrl Pts',(8.33811858929324,3.72375056035358,134.020208557727));
#70309=CARTESIAN_POINT('Ctrl Pts',(8.33036739805311,3.81047110203739,133.913941464407));
#70310=CARTESIAN_POINT('Ctrl Pts',(8.32261950127603,3.89715478517763,133.807719537435));
#70311=CARTESIAN_POINT('Ctrl Pts',(8.31487160449895,3.97943831835365,133.697815293313));
#70312=CARTESIAN_POINT('Ctrl Pts',(8.30712370772187,4.05700201310458,133.584633576857));
#70313=CARTESIAN_POINT('Ctrl Pts',(8.29937743163777,4.13454948320265,133.471475535576));
#70314=CARTESIAN_POINT('Ctrl Pts',(8.29163115555376,4.20737885777497,133.35504170791));
#70315=CARTESIAN_POINT('Ctrl Pts',(8.28388487946967,4.27521278714674,133.235767347654));
#70316=CARTESIAN_POINT('Ctrl Pts',(8.27613854620433,4.34304721725306,133.116492106942));
#70317=CARTESIAN_POINT('Ctrl Pts',(8.26839221293897,4.40588593529777,132.99437663165));
#70318=CARTESIAN_POINT('Ctrl Pts',(8.26064587967363,4.46349691837158,132.869881937279));
#70319=CARTESIAN_POINT('Ctrl Pts',(8.25289781167067,4.5211208030256,132.745359363184));
#70320=CARTESIAN_POINT('Ctrl Pts',(8.24514974366772,4.57351445895888,132.618456864529));
#70321=CARTESIAN_POINT('Ctrl Pts',(8.23740167566476,4.62049365480359,132.489656273651));
#70322=CARTESIAN_POINT('Ctrl Pts',(8.22964537292291,4.66752278069678,132.360718791972));
#70323=CARTESIAN_POINT('Ctrl Pts',(8.22188907018102,4.70912581698028,132.229879556147));
#70324=CARTESIAN_POINT('Ctrl Pts',(8.21413276743917,4.74516800036887,132.097636964978));
#70325=CARTESIAN_POINT('Ctrl Pts',(8.20637232492501,4.78122942055595,131.965323791957));
#70326=CARTESIAN_POINT('Ctrl Pts',(8.19861188241084,4.81172398698152,131.831606152112));
#70327=CARTESIAN_POINT('Ctrl Pts',(8.19085143989668,4.83656813150723,131.696992552794));
#70328=CARTESIAN_POINT('Ctrl Pts',(8.18307853963125,4.8614521580593,131.562162859775));
#70329=CARTESIAN_POINT('Ctrl Pts',(8.17530563936583,4.8806675820095,131.426434720481));
#70330=CARTESIAN_POINT('Ctrl Pts',(8.16753273910041,4.89418267290967,131.290322577693));
#70331=CARTESIAN_POINT('Ctrl Pts',(8.16004240333831,4.90720645621331,131.15915845414));
#70332=CARTESIAN_POINT('Ctrl Pts',(8.15255206757619,4.91493713598488,131.027638068854));
#70333=CARTESIAN_POINT('Ctrl Pts',(8.14506173181408,4.91739209004694,130.89621972296));
#70334=CARTESIAN_POINT('Ctrl Pts',(8.13728739769499,4.9199401244384,130.759818610539));
#70335=CARTESIAN_POINT('Ctrl Pts',(8.12951306357587,4.91681254897074,130.623095350177));
#70336=CARTESIAN_POINT('Ctrl Pts',(8.12173872945678,4.90797175281682,130.486561410436));
#70337=CARTESIAN_POINT('Ctrl Pts',(8.11397397650968,4.89914185215404,130.350195736574));
#70338=CARTESIAN_POINT('Ctrl Pts',(8.10620922356266,4.88461276538403,130.214019305498));
#70339=CARTESIAN_POINT('Ctrl Pts',(8.09844447061556,4.86439882563909,130.078545815002));
#70340=CARTESIAN_POINT('Ctrl Pts',(8.09068742973055,4.84420496266407,129.943206878687));
#70341=CARTESIAN_POINT('Ctrl Pts',(8.08293038884552,4.81833754038205,129.808569877744));
#70342=CARTESIAN_POINT('Ctrl Pts',(8.07517334796052,4.7868628268431,129.675145253037));
#70343=CARTESIAN_POINT('Ctrl Pts',(8.06742215672038,4.75541184863047,129.541821244878));
#70344=CARTESIAN_POINT('Ctrl Pts',(8.05967096548027,4.71836208513883,129.409708172153));
#70345=CARTESIAN_POINT('Ctrl Pts',(8.05191977424013,4.67583114093473,129.279307764723));
#70346=CARTESIAN_POINT('Ctrl Pts',(8.04417187746305,4.63331827351647,129.148962780945));
#70347=CARTESIAN_POINT('Ctrl Pts',(8.03642398068592,4.58532897985487,129.020329385584));
#70348=CARTESIAN_POINT('Ctrl Pts',(8.02867608390883,4.53203106793912,128.893895370111));
#70349=CARTESIAN_POINT('Ctrl Pts',(8.02092980782473,4.47874430479757,128.767487801908));
#70350=CARTESIAN_POINT('Ctrl Pts',(8.01318353174065,4.42015128391673,128.643279058536));
#70351=CARTESIAN_POINT('Ctrl Pts',(8.00543725565655,4.35646828236937,128.521737747443));
#70352=CARTESIAN_POINT('Ctrl Pts',(7.99769092239119,4.29278481072855,128.400195539159));
#70353=CARTESIAN_POINT('Ctrl Pts',(7.98994458912586,4.22401146489882,128.281321148751));
#70354=CARTESIAN_POINT('Ctrl Pts',(7.98219825586051,4.15041069622921,128.165558973803));
#70355=CARTESIAN_POINT('Ctrl Pts',(7.97445018785754,4.07679344517786,128.049770874719));
#70356=CARTESIAN_POINT('Ctrl Pts',(7.96670211985455,3.99834682981219,127.937096707828));
#70357=CARTESIAN_POINT('Ctrl Pts',(7.95895405185158,3.91537664776859,127.827951914345));
#70358=CARTESIAN_POINT('Ctrl Pts',(7.95119774910972,3.83231828402806,127.718691120477));
#70359=CARTESIAN_POINT('Ctrl Pts',(7.94344144636785,3.74472698669015,127.612967504902));
#70360=CARTESIAN_POINT('Ctrl Pts',(7.93568514362599,3.65294922993573,127.511163844518));
#70361=CARTESIAN_POINT('Ctrl Pts',(7.92792470111181,3.56112248862904,127.409305848455));
#70362=CARTESIAN_POINT('Ctrl Pts',(7.92016425859764,3.46510510917158,127.3113722555));
#70363=CARTESIAN_POINT('Ctrl Pts',(7.91240381608347,3.36527974257748,127.217708234536));
#70364=CARTESIAN_POINT('Ctrl Pts',(7.90463091581804,3.26529412744299,127.12389385577));
#70365=CARTESIAN_POINT('Ctrl Pts',(7.89685801555258,3.16148860584203,127.034363000759));
#70366=CARTESIAN_POINT('Ctrl Pts',(7.88908511528714,3.05427884197399,126.949420434117));
#70367=CARTESIAN_POINT('Ctrl Pts',(7.88159477952518,2.95096642306852,126.86756574373));
#70368=CARTESIAN_POINT('Ctrl Pts',(7.87410444376324,2.84449321932749,126.789971723085));
#70369=CARTESIAN_POINT('Ctrl Pts',(7.86661410800127,2.73525420560422,126.716871474678));
#70370=CARTESIAN_POINT('Ctrl Pts',(7.85883977388218,2.62187336147205,126.640999608135));
#70371=CARTESIAN_POINT('Ctrl Pts',(7.85106543976306,2.50515367938956,126.569728664076));
#70372=CARTESIAN_POINT('Ctrl Pts',(7.84329110564397,2.38550514277391,126.503366746808));
#70373=CARTESIAN_POINT('Ctrl Pts',(7.83552635269688,2.26600406228651,126.437086614672));
#70374=CARTESIAN_POINT('Ctrl Pts',(7.82776159974985,2.14358164781312,126.375703659566));
#70375=CARTESIAN_POINT('Ctrl Pts',(7.81999684680275,2.01867783526541,126.319483488825));
#70376=CARTESIAN_POINT('Ctrl Pts',(7.81223980591775,1.89389807894516,126.26331915675));
#70377=CARTESIAN_POINT('Ctrl Pts',(7.80448276503274,1.76664218334352,126.212307564018));
#70378=CARTESIAN_POINT('Ctrl Pts',(7.79672572414773,1.63737541631576,126.166668863197));
#70379=CARTESIAN_POINT('Ctrl Pts',(7.7889745329076,1.50820613036257,126.121064578875));
#70380=CARTESIAN_POINT('Ctrl Pts',(7.78122334166745,1.37702935848411,126.080825251355));
#70381=CARTESIAN_POINT('Ctrl Pts',(7.77347215042732,1.24433078836353,126.04612313383));
#70382=CARTESIAN_POINT('Ctrl Pts',(7.76572425365024,1.1116886186751,126.011435765631));
#70383=CARTESIAN_POINT('Ctrl Pts',(7.75797635687314,0.977526314643554,125.982281025278));
#70384=CARTESIAN_POINT('Ctrl Pts',(7.75022846009605,0.842344973363954,125.958781394362));
#70385=CARTESIAN_POINT('Ctrl Pts',(7.74248218401195,0.707191909106776,125.935286679062));
#70386=CARTESIAN_POINT('Ctrl Pts',(7.73473590792787,0.571020616534077,125.91744478721));
#70387=CARTESIAN_POINT('Ctrl Pts',(7.72698963184376,0.434342251402056,125.905327052551));
#70388=CARTESIAN_POINT('Ctrl Pts',(7.71924329857841,0.297662877341392,125.893209228441));
#70389=CARTESIAN_POINT('Ctrl Pts',(7.71149696531305,0.16047681268997,125.886815680366));
#70390=CARTESIAN_POINT('Ctrl Pts',(7.7037506320477,0.0232998030868416,125.886165808322));
#70391=CARTESIAN_POINT('Ctrl Pts',(7.69600256404473,-0.113907926356282,
125.885515790744));
#70392=CARTESIAN_POINT('Ctrl Pts',(7.68825449604176,-0.251106205830005,
125.890612010551));
#70393=CARTESIAN_POINT('Ctrl Pts',(7.6805064280388,-0.387780221782509,125.901421747654));
#70394=CARTESIAN_POINT('Ctrl Pts',(7.67275012529694,-0.524599496505796,
125.912242973475));
#70395=CARTESIAN_POINT('Ctrl Pts',(7.66499382255506,-0.660893004284258,
125.928789815979));
#70396=CARTESIAN_POINT('Ctrl Pts',(7.65723751981321,-0.796151426316966,
125.950977676887));
#70397=CARTESIAN_POINT('Ctrl Pts',(7.64947707729904,-0.931482039842065,
125.973177380125));
#70398=CARTESIAN_POINT('Ctrl Pts',(7.64171663478488,-1.06577608417067,126.001024021662));
#70399=CARTESIAN_POINT('Ctrl Pts',(7.63395619227072,-1.19853632672462,126.034382238577));
#70400=CARTESIAN_POINT('Ctrl Pts',(7.62618329200527,-1.331509687806,126.067794005063));
#70401=CARTESIAN_POINT('Ctrl Pts',(7.61841039173986,-1.46294395178855,126.106734916265));
#70402=CARTESIAN_POINT('Ctrl Pts',(7.61063749147442,-1.59235803491825,126.151019994838));
#70403=CARTESIAN_POINT('Ctrl Pts',(7.60314715571237,-1.71706759015198,126.193695199257));
#70404=CARTESIAN_POINT('Ctrl Pts',(7.59565681995031,-1.83990100467396,126.241332657545));
#70405=CARTESIAN_POINT('Ctrl Pts',(7.58816648418826,-1.9604486691947,126.293726063764));
#70406=CARTESIAN_POINT('Ctrl Pts',(7.58039166302064,-2.0855747734972,126.348109388712));
#70407=CARTESIAN_POINT('Ctrl Pts',(7.57261684185302,-2.20863445582198,126.407789347682));
#70408=CARTESIAN_POINT('Ctrl Pts',(7.5648420206854,-2.32914680335446,126.472587512829));
#70409=CARTESIAN_POINT('Ctrl Pts',(7.55707689142416,-2.4495089230728,126.537304902131));
#70410=CARTESIAN_POINT('Ctrl Pts',(7.5493117621629,-2.56732968538282,126.607127618751));
#70411=CARTESIAN_POINT('Ctrl Pts',(7.54154663290166,-2.68214776593824,126.681829062299));
#70412=CARTESIAN_POINT('Ctrl Pts',(7.53378932596478,-2.79685018270511,126.75645525418));
#70413=CARTESIAN_POINT('Ctrl Pts',(7.52603201902788,-2.90855561193974,126.835950180062));
#70414=CARTESIAN_POINT('Ctrl Pts',(7.518274712091,-3.01682730279926,126.920041360916));
#70415=CARTESIAN_POINT('Ctrl Pts',(7.51052373062126,-3.12501070670188,127.004063972096));
#70416=CARTESIAN_POINT('Ctrl Pts',(7.50277274915155,-3.22976563980371,127.092675136782));
#70417=CARTESIAN_POINT('Ctrl Pts',(7.49502176768181,-3.33068469169375,127.185559359274));
#70418=CARTESIAN_POINT('Ctrl Pts',(7.48727424285852,-3.43155873747922,127.278402158893));
#70419=CARTESIAN_POINT('Ctrl Pts',(7.4795267180353,-3.52860001835509,127.375513960967));
#70420=CARTESIAN_POINT('Ctrl Pts',(7.471779193212,-3.62143468904814,127.476539430143));
#70421=CARTESIAN_POINT('Ctrl Pts',(7.46403344570116,-3.71424806310507,127.577541723682));
#70422=CARTESIAN_POINT('Ctrl Pts',(7.4562876981903,-3.80285648317711,127.682455609967));
#70423=CARTESIAN_POINT('Ctrl Pts',(7.44854195067947,-3.88692371226027,127.790889675684));
#70424=CARTESIAN_POINT('Ctrl Pts',(7.44079630269244,-3.97098986117785,127.899322348149));
#70425=CARTESIAN_POINT('Ctrl Pts',(7.43305065470545,-4.05051469664554,128.011274800506));
#70426=CARTESIAN_POINT('Ctrl Pts',(7.42530500671842,-4.12520320028202,128.126323721091));
#70427=CARTESIAN_POINT('Ctrl Pts',(7.41755412798041,-4.19994214217289,128.241450335918));
#70428=CARTESIAN_POINT('Ctrl Pts',(7.40980324924236,-4.26983801271335,128.359677269191));
#70429=CARTESIAN_POINT('Ctrl Pts',(7.40205237050435,-4.33463980240314,128.480553214634));
#70430=CARTESIAN_POINT('Ctrl Pts',(7.39429892290299,-4.39946306926325,128.601469221829));
#70431=CARTESIAN_POINT('Ctrl Pts',(7.38654547530157,-4.45918871762214,128.725035640154));
#70432=CARTESIAN_POINT('Ctrl Pts',(7.3787920277002,-4.51361285293805,128.850778759467));
#70433=CARTESIAN_POINT('Ctrl Pts',(7.37102906749447,-4.56810376052012,128.976676151384));
#70434=CARTESIAN_POINT('Ctrl Pts',(7.36326610728878,-4.61728001501608,129.104755216337));
#70435=CARTESIAN_POINT('Ctrl Pts',(7.35550314708306,-4.66098658752424,129.234523972109));
#70436=CARTESIAN_POINT('Ctrl Pts',(7.34863665501921,-4.69964591660902,129.349307006935));
#70437=CARTESIAN_POINT('Ctrl Pts',(7.34177016295534,-4.73402658012365,129.465411605364));
#70438=CARTESIAN_POINT('Ctrl Pts',(7.33490367089149,-4.76405452823399,129.582490119308));
#70439=CARTESIAN_POINT('Ctrl Pts',(9.08499331100833,-4.76405452823402,129.582490119308));
#70440=CARTESIAN_POINT('Ctrl Pts',(9.07734584844658,-4.79769088846045,129.713637777328));
#70441=CARTESIAN_POINT('Ctrl Pts',(9.06969838588486,-4.82588697168254,129.846095034761));
#70442=CARTESIAN_POINT('Ctrl Pts',(9.06205092332311,-4.8485631154531,129.979364388503));
#70443=CARTESIAN_POINT('Ctrl Pts',(9.0541856754406,-4.87188503306103,130.11642900227));
#70444=CARTESIAN_POINT('Ctrl Pts',(9.04632042755805,-4.88936785715086,130.254352199333));
#70445=CARTESIAN_POINT('Ctrl Pts',(9.03845517967554,-4.90098224828163,130.39258875776));
#70446=CARTESIAN_POINT('Ctrl Pts',(9.03058993179303,-4.91259663941239,130.530825316186));
#70447=CARTESIAN_POINT('Ctrl Pts',(9.02272468391051,-4.91834263804842,130.669374776506));
#70448=CARTESIAN_POINT('Ctrl Pts',(9.01485943602799,-4.91824886988786,130.807694736162));
#70449=CARTESIAN_POINT('',(9.3601405639707,-4.91824968732061,130.806114376595));
#70450=CARTESIAN_POINT('Ctrl Pts',(9.42990690795585,-4.76405452823399,129.582490119308));
#70451=CARTESIAN_POINT('Ctrl Pts',(9.42197330691278,-4.79892363242829,129.718444227349));
#70452=CARTESIAN_POINT('Ctrl Pts',(9.41403970586967,-4.82799669543438,129.856000569293));
#70453=CARTESIAN_POINT('Ctrl Pts',(9.40610610482659,-4.85113721517965,129.994637960109));
#70454=CARTESIAN_POINT('Ctrl Pts',(9.39817898243846,-4.87425883815384,130.133162138298));
#70455=CARTESIAN_POINT('Ctrl Pts',(9.39025186005033,-4.89145751185162,130.272765247639));
#70456=CARTESIAN_POINT('Ctrl Pts',(9.3823247376622,-4.90264758826632,130.412914979238));
#70457=CARTESIAN_POINT('Ctrl Pts',(9.37493001311104,-4.91308612178979,130.543652037447));
#70458=CARTESIAN_POINT('Ctrl Pts',(9.36753528855989,-4.91829648867104,130.674864409002));
#70459=CARTESIAN_POINT('Ctrl Pts',(9.36014056400873,-4.91824968732085,130.80611437592));
#70460=CARTESIAN_POINT('Ctrl Pts',(9.36014056397079,-4.91824968732061,130.806114376595));
#70461=CARTESIAN_POINT('Ctrl Pts',(9.3517641285291,-4.9181966726834,130.95478886298));
#70462=CARTESIAN_POINT('Ctrl Pts',(9.3433876930874,-4.91139802649659,131.103260454074));
#70463=CARTESIAN_POINT('Ctrl Pts',(9.33501125764573,-4.89793381843472,131.250933537405));
#70464=CARTESIAN_POINT('Ctrl Pts',(9.32660038269188,-4.8844142526063,131.399213775055));
#70465=CARTESIAN_POINT('Ctrl Pts',(9.31818950773799,-4.86417428476807,131.54668865016));
#70466=CARTESIAN_POINT('Ctrl Pts',(9.30977863278414,-4.83734567219708,131.69276925675));
#70467=CARTESIAN_POINT('Ctrl Pts',(9.30135038794373,-4.81046165398046,131.839151544624));
#70468=CARTESIAN_POINT('Ctrl Pts',(9.29292214310327,-4.77696186955486,131.984133538149));
#70469=CARTESIAN_POINT('Ctrl Pts',(9.28449389826284,-4.73702814048069,132.127140818051));
#70470=CARTESIAN_POINT('Ctrl Pts',(9.27603806763434,-4.6969637076351,132.2706161632));
#70471=CARTESIAN_POINT('Ctrl Pts',(9.2675822370059,-4.65042327378475,132.412103591709));
#70472=CARTESIAN_POINT('Ctrl Pts',(9.25912640637742,-4.59763810719735,132.551045161995));
#70473=CARTESIAN_POINT('Ctrl Pts',(9.25250534788704,-4.55630642841202,132.659838763005));
#70474=CARTESIAN_POINT('Ctrl Pts',(9.24588428939664,-4.51114697948034,132.767071863098));
#70475=CARTESIAN_POINT('Ctrl Pts',(9.23926323090626,-4.46229023998372,132.872487518084));
#70476=CARTESIAN_POINT('Ctrl Pts',(9.23148889678717,-4.40492348852432,132.996264784882));
#70477=CARTESIAN_POINT('Ctrl Pts',(9.22371456266808,-4.34231187447133,133.117849395084));
#70478=CARTESIAN_POINT('Ctrl Pts',(9.21594022854899,-4.27464527763359,133.236764945161));
#70479=CARTESIAN_POINT('Ctrl Pts',(9.2081754756019,-4.207062073829,133.355533942451));
#70480=CARTESIAN_POINT('Ctrl Pts',(9.20041072265486,-4.13443647421598,133.471640087955));
#70481=CARTESIAN_POINT('Ctrl Pts',(9.19264596970777,-4.05700604578529,133.58462769232));
#70482=CARTESIAN_POINT('Ctrl Pts',(9.18488892882277,-3.9796525223477,133.697503075803));
#70483=CARTESIAN_POINT('Ctrl Pts',(9.17713188793769,-3.8975038866139,133.807265761656));
#70484=CARTESIAN_POINT('Ctrl Pts',(9.16937484705269,-3.81084298512702,133.91348570434));
#70485=CARTESIAN_POINT('Ctrl Pts',(9.16162365581257,-3.72424743530007,134.01962554574));
#70486=CARTESIAN_POINT('Ctrl Pts',(9.15387246457247,-3.63314663880996,134.122227659941));
#70487=CARTESIAN_POINT('Ctrl Pts',(9.14612127333234,-3.53786579815845,134.22089228824));
#70488=CARTESIAN_POINT('Ctrl Pts',(9.13837337655525,-3.44262545440579,134.319514981441));
#70489=CARTESIAN_POINT('Ctrl Pts',(9.13062547977819,-3.34320887109478,134.414203236631));
#70490=CARTESIAN_POINT('Ctrl Pts',(9.1228775830011,-3.23998030139839,134.504591787243));
#70491=CARTESIAN_POINT('Ctrl Pts',(9.11513130691699,-3.13677332489344,134.594961430519));
#70492=CARTESIAN_POINT('Ctrl Pts',(9.10738503083286,-3.02975624200152,134.681032900793));
#70493=CARTESIAN_POINT('Ctrl Pts',(9.09963875474875,-2.91932850261307,134.762479382375));
#70494=CARTESIAN_POINT('Ctrl Pts',(9.0918924214834,-2.80889994807228,134.843926465176));
#70495=CARTESIAN_POINT('Ctrl Pts',(9.08414608821806,-2.69506100143844,134.920748259094));
#70496=CARTESIAN_POINT('Ctrl Pts',(9.07639975495272,-2.57824204747977,134.992659915265));
#70497=CARTESIAN_POINT('Ctrl Pts',(9.06865168694975,-2.46139693272634,135.064587675553));
#70498=CARTESIAN_POINT('Ctrl Pts',(9.06090361894673,-2.34157081557059,135.131602905123));
#70499=CARTESIAN_POINT('Ctrl Pts',(9.05315555094376,-2.21922039650939,135.193465753493));
#70500=CARTESIAN_POINT('Ctrl Pts',(9.0453992482019,-2.09673994196665,135.255394350434));
#70501=CARTESIAN_POINT('Ctrl Pts',(9.03764294546011,-1.97173017567875,135.312159450558));
#70502=CARTESIAN_POINT('Ctrl Pts',(9.02988664271825,-1.84467009126778,135.363568368577));
#70503=CARTESIAN_POINT('Ctrl Pts',(9.02212620020407,-1.71754219106388,135.415004725085));
#70504=CARTESIAN_POINT('Ctrl Pts',(9.01436575768981,-1.58836216028212,135.461079071899));
#70505=CARTESIAN_POINT('Ctrl Pts',(9.00660531517562,-1.45762507693163,135.50164836664));
#70506=CARTESIAN_POINT('Ctrl Pts',(8.99883241491018,-1.32667812280883,135.542282786815));
#70507=CARTESIAN_POINT('Ctrl Pts',(8.99105951464476,-1.1941694994222,135.57739439518));
#70508=CARTESIAN_POINT('Ctrl Pts',(8.98328661437932,-1.06060630115362,135.606890923192));
#70509=CARTESIAN_POINT('Ctrl Pts',(8.97579627861731,-0.931898461567866,
135.635315178113));
#70510=CARTESIAN_POINT('Ctrl Pts',(8.96830594285535,-0.802211692053463,
135.658525455318));
#70511=CARTESIAN_POINT('Ctrl Pts',(8.96081560709334,-0.672003138405616,
135.676484881629));
#70512=CARTESIAN_POINT('Ctrl Pts',(8.95304127297425,-0.536857687869795,
135.695125245047));
#70513=CARTESIAN_POINT('Ctrl Pts',(8.94526693885518,-0.400722005081922,
135.708167772575));
#70514=CARTESIAN_POINT('Ctrl Pts',(8.93749260473609,-0.264099536499374,
135.715514707729));
#70515=CARTESIAN_POINT('Ctrl Pts',(8.92972785178899,-0.127645442899052,
135.722852588441));
#70516=CARTESIAN_POINT('Ctrl Pts',(8.92196309884195,0.00929385618066372,
135.724508822318));
#70517=CARTESIAN_POINT('Ctrl Pts',(8.91419834589485,0.146206565618375,135.72043696997));
#70518=CARTESIAN_POINT('Ctrl Pts',(8.90644130500985,0.282983291422756,135.716369161844));
#70519=CARTESIAN_POINT('Ctrl Pts',(8.89868426412476,0.419733091877031,135.706584600837));
#70520=CARTESIAN_POINT('Ctrl Pts',(8.89092722323977,0.555941272026413,135.691088803639));
#70521=CARTESIAN_POINT('Ctrl Pts',(8.88317603199965,0.692046736527599,135.675604691942));
#70522=CARTESIAN_POINT('Ctrl Pts',(8.87542484075957,0.82761100681146,135.654417960668));
#70523=CARTESIAN_POINT('Ctrl Pts',(8.86767364951945,0.962121974663368,135.627586132548));
#70524=CARTESIAN_POINT('Ctrl Pts',(8.85992575274236,1.09657577176592,135.60076570867));
#70525=CARTESIAN_POINT('Ctrl Pts',(8.8521778559653,1.22997677423242,135.568305036326));
#70526=CARTESIAN_POINT('Ctrl Pts',(8.8444299591882,1.36182078521822,135.530313136524));
#70527=CARTESIAN_POINT('Ctrl Pts',(8.83668368310409,1.49363721727915,135.492329183809));
#70528=CARTESIAN_POINT('Ctrl Pts',(8.82893740701994,1.62389693023184,135.448816413186));
#70529=CARTESIAN_POINT('Ctrl Pts',(8.82119113093583,1.75210905235757,135.399934241299));
#70530=CARTESIAN_POINT('Ctrl Pts',(8.81344479767048,1.8803221209159,135.351051708574));
#70531=CARTESIAN_POINT('Ctrl Pts',(8.80569846440514,2.00648720317191,135.296799834774));
#70532=CARTESIAN_POINT('Ctrl Pts',(8.79795213113979,2.13013201422899,135.237386747024));
#70533=CARTESIAN_POINT('Ctrl Pts',(8.79020406313683,2.25380451468422,135.177960354125));
#70534=CARTESIAN_POINT('Ctrl Pts',(8.78245599513389,2.37495526852933,135.11337061663));
#70535=CARTESIAN_POINT('Ctrl Pts',(8.77470792713092,2.49313562498726,135.043872124558));
#70536=CARTESIAN_POINT('Ctrl Pts',(8.76695162438906,2.61144158493456,134.974299768661));
#70537=CARTESIAN_POINT('Ctrl Pts',(8.75919532164722,2.72677050355186,134.899808435005));
#70538=CARTESIAN_POINT('Ctrl Pts',(8.75143901890536,2.8387013614973,134.820696963383));
#70539=CARTESIAN_POINT('Ctrl Pts',(8.74367857639119,2.95069196031181,134.741543267588));
#70540=CARTESIAN_POINT('Ctrl Pts',(8.73591813387695,3.0592805752148,134.657764759004));
#70541=CARTESIAN_POINT('Ctrl Pts',(8.72815769136278,3.1640792588443,134.569700642883));
#70542=CARTESIAN_POINT('Ctrl Pts',(8.72038479109735,3.26904617462435,134.481495158424));
#70543=CARTESIAN_POINT('Ctrl Pts',(8.71261189083194,3.37021071279827,134.3889905827));
#70544=CARTESIAN_POINT('Ctrl Pts',(8.70483899056651,3.46722114832605,134.292563675173));
#70545=CARTESIAN_POINT('Ctrl Pts',(8.69734865480451,3.56070501016758,134.19964212862));
#70546=CARTESIAN_POINT('Ctrl Pts',(8.68985831904251,3.65033134042777,134.10307869828));
#70547=CARTESIAN_POINT('Ctrl Pts',(8.6823679832805,3.735822018188,134.003238063002));
#70548=CARTESIAN_POINT('Ctrl Pts',(8.67459364916144,3.82455410098009,133.899611939692));
#70549=CARTESIAN_POINT('Ctrl Pts',(8.66681931504231,3.90911181061861,133.79212693891));
#70550=CARTESIAN_POINT('Ctrl Pts',(8.65904498092323,3.98914077669724,133.681153784652));
#70551=CARTESIAN_POINT('Ctrl Pts',(8.65128022797613,4.06907111422757,133.570317394888));
#70552=CARTESIAN_POINT('Ctrl Pts',(8.64351547502905,4.14448358677629,133.456001719116));
#70553=CARTESIAN_POINT('Ctrl Pts',(8.63575072208195,4.21506248580536,133.338612243442));
#70554=CARTESIAN_POINT('Ctrl Pts',(8.62799368119695,4.28557128487692,133.221339360651));
#70555=CARTESIAN_POINT('Ctrl Pts',(8.62023664031196,4.35125586403343,133.100999086347));
#70556=CARTESIAN_POINT('Ctrl Pts',(8.61247959942696,4.41184265942764,132.97802742988));
#70557=CARTESIAN_POINT('Ctrl Pts',(8.60472840818683,4.47238376584814,132.855148507295));
#70558=CARTESIAN_POINT('Ctrl Pts',(8.59697721694674,4.52783456821774,132.729642501557));
#70559=CARTESIAN_POINT('Ctrl Pts',(8.58922602570661,4.57796665504031,132.601971356252));
#70560=CARTESIAN_POINT('Ctrl Pts',(8.58147812892952,4.62807743438866,132.474354474589));
#70561=CARTESIAN_POINT('Ctrl Pts',(8.57373023215236,4.67287385174521,132.344574646803));
#70562=CARTESIAN_POINT('Ctrl Pts',(8.56598233537528,4.7121750988625,132.213114996498));
#70563=CARTESIAN_POINT('Ctrl Pts',(8.55823605929118,4.75146812500614,132.081682844718));
#70564=CARTESIAN_POINT('Ctrl Pts',(8.55048978320709,4.78526815535684,131.948571943684));
#70565=CARTESIAN_POINT('Ctrl Pts',(8.54274350712299,4.81344398349671,131.814281446265));
#70566=CARTESIAN_POINT('Ctrl Pts',(8.53499717385765,4.8416200196241,131.679989957544));
#70567=CARTESIAN_POINT('Ctrl Pts',(8.52725084059236,4.86417169041596,131.544519237696));
#70568=CARTESIAN_POINT('Ctrl Pts',(8.51950450732701,4.88101881759487,131.408379131177));
#70569=CARTESIAN_POINT('Ctrl Pts',(8.51175643932403,4.89786971757112,131.272208537024));
#70570=CARTESIAN_POINT('Ctrl Pts',(8.504008371321,4.90901348386535,131.135368645839));
#70571=CARTESIAN_POINT('Ctrl Pts',(8.49626030331802,4.91442180356658,130.998374532349));
#70572=CARTESIAN_POINT('Ctrl Pts',(8.48850400057617,4.91983587129435,130.861234819885));
#70573=CARTESIAN_POINT('Ctrl Pts',(8.48074769783432,4.91950230016269,130.723940948974));
#70574=CARTESIAN_POINT('Ctrl Pts',(8.47299139509246,4.91344494131719,130.587008665321));
#70575=CARTESIAN_POINT('Ctrl Pts',(8.4652309525783,4.90738434947689,130.450003296786));
#70576=CARTESIAN_POINT('Ctrl Pts',(8.45747051006412,4.89559391625424,130.313360289386));
#70577=CARTESIAN_POINT('Ctrl Pts',(8.44971006754994,4.87814932960778,130.177589382946));
#70578=CARTESIAN_POINT('Ctrl Pts',(8.44193716728451,4.86067673936218,130.041600524994));
#70579=CARTESIAN_POINT('Ctrl Pts',(8.43416426701909,4.83753192390406,129.906486951171));
#70580=CARTESIAN_POINT('Ctrl Pts',(8.42639136675365,4.80884174566431,129.772748225407));
#70581=CARTESIAN_POINT('Ctrl Pts',(8.41890103099157,4.78119452766961,129.643871239191));
#70582=CARTESIAN_POINT('Ctrl Pts',(8.41141069522956,4.74839819965585,129.516271176401));
#70583=CARTESIAN_POINT('Ctrl Pts',(8.40392035946749,4.71060924511826,129.390379145868));
#70584=CARTESIAN_POINT('Ctrl Pts',(8.39614602534841,4.6713875108839,129.259713880734));
#70585=CARTESIAN_POINT('Ctrl Pts',(8.38837169122933,4.62666284308901,129.130474816426));
#70586=CARTESIAN_POINT('Ctrl Pts',(8.38059735711025,4.57655559646977,129.003160480179));
#70587=CARTESIAN_POINT('Ctrl Pts',(8.37283260416315,4.52651010255378,128.876003047474));
#70588=CARTESIAN_POINT('Ctrl Pts',(8.36506785121598,4.4710953704033,128.750765983456));
#70589=CARTESIAN_POINT('Ctrl Pts',(8.35730309826889,4.41048189878688,128.627934077806));
#70590=CARTESIAN_POINT('Ctrl Pts',(8.34954605738388,4.34992862932497,128.505224170536));
#70591=CARTESIAN_POINT('Ctrl Pts',(8.3417890164989,4.28418706780876,128.384915016072));
#70592=CARTESIAN_POINT('Ctrl Pts',(8.3340319756139,4.2134761733098,128.267472445129));
#70593=CARTESIAN_POINT('Ctrl Pts',(8.32628078437376,4.14281860244644,128.150118438543));
#70594=CARTESIAN_POINT('Ctrl Pts',(8.31852959313362,4.06719935844619,128.035627046305));
#70595=CARTESIAN_POINT('Ctrl Pts',(8.31077840189349,3.98688362553787,127.924440129268));
#70596=CARTESIAN_POINT('Ctrl Pts',(8.3030305051164,3.90660202895852,127.813300469637));
#70597=CARTESIAN_POINT('Ctrl Pts',(8.29528260833936,3.82162814208108,127.705462808048));
#70598=CARTESIAN_POINT('Ctrl Pts',(8.28753471156227,3.73227069920171,127.601340403708));
#70599=CARTESIAN_POINT('Ctrl Pts',(8.27978843547817,3.64293194797306,127.497239779531));
#70600=CARTESIAN_POINT('Ctrl Pts',(8.27204215939406,3.54921171905273,127.396853163308));
#70601=CARTESIAN_POINT('Ctrl Pts',(8.26429588330996,3.4514590436119,127.30056074703));
#70602=CARTESIAN_POINT('Ctrl Pts',(8.2565495500446,3.35370564658301,127.204267619943));
#70603=CARTESIAN_POINT('Ctrl Pts',(8.24880321677919,3.2519200221632,127.112069027476));
#70604=CARTESIAN_POINT('Ctrl Pts',(8.24105688351383,3.14648777861424,127.024308009264));
#70605=CARTESIAN_POINT('Ctrl Pts',(8.23330881551085,3.04103192424536,126.936527337581));
#70606=CARTESIAN_POINT('Ctrl Pts',(8.22556074750791,2.93192812616736,126.853186467704));
#70607=CARTESIAN_POINT('Ctrl Pts',(8.21781267950493,2.81959442751738,126.774587630559));
#70608=CARTESIAN_POINT('Ctrl Pts',(8.21005637676307,2.70714133927568,126.695905257635));
#70609=CARTESIAN_POINT('Ctrl Pts',(8.20230007402117,2.59145181396916,126.621975209658));
#70610=CARTESIAN_POINT('Ctrl Pts',(8.19454377127931,2.47297265519326,126.553056193137));
#70611=CARTESIAN_POINT('Ctrl Pts',(8.18678332876513,2.35443026052283,126.484100392462));
#70612=CARTESIAN_POINT('Ctrl Pts',(8.179022886251,2.23309561131126,126.420161134664));
#70613=CARTESIAN_POINT('Ctrl Pts',(8.17126244373682,2.1094384773013,126.361450268146));
#70614=CARTESIAN_POINT('Ctrl Pts',(8.16348954347139,1.98558283788222,126.302645153734));
#70615=CARTESIAN_POINT('Ctrl Pts',(8.15571664320593,1.85939762351093,126.24908535549));
#70616=CARTESIAN_POINT('Ctrl Pts',(8.1479437429405,1.73137170371282,126.200934166966));
#70617=CARTESIAN_POINT('Ctrl Pts',(8.14045340717853,1.60799984857824,126.154533395431));
#70618=CARTESIAN_POINT('Ctrl Pts',(8.13296307141654,1.48291908554651,126.113154924286));
#70619=CARTESIAN_POINT('Ctrl Pts',(8.12547273565457,1.3565767018392,126.076900124391));
#70620=CARTESIAN_POINT('Ctrl Pts',(8.11769840153549,1.22544400825176,126.039270712739));
#70621=CARTESIAN_POINT('Ctrl Pts',(8.10992406741637,1.09253674780571,126.007041971325));
#70622=CARTESIAN_POINT('Ctrl Pts',(8.1021497332973,0.958339400256849,125.98038210845));
#70623=CARTESIAN_POINT('Ctrl Pts',(8.0943849803502,0.824307438945096,125.953755101473));
#70624=CARTESIAN_POINT('Ctrl Pts',(8.08662022740324,0.688988933781597,125.932683392871));
#70625=CARTESIAN_POINT('Ctrl Pts',(8.07885547445613,0.552883910802526,125.917285577864));
#70626=CARTESIAN_POINT('Ctrl Pts',(8.07109843357113,0.416914069251208,125.901903056185));
#70627=CARTESIAN_POINT('Ctrl Pts',(8.063341392686,0.280159650442069,125.892183257084));
#70628=CARTESIAN_POINT('Ctrl Pts',(8.055584351801,0.143130923675482,125.888193756974));
#70629=CARTESIAN_POINT('Ctrl Pts',(8.04783316056088,0.00620553133767746,
125.884207265376));
#70630=CARTESIAN_POINT('Ctrl Pts',(8.0400819693208,-0.1309933680014,125.88594248289));
#70631=CARTESIAN_POINT('Ctrl Pts',(8.03233077808068,-0.267950685739329,
125.893415139095));
#70632=CARTESIAN_POINT('Ctrl Pts',(8.0245828813036,-0.404849792963763,125.900884619223));
#70633=CARTESIAN_POINT('Ctrl Pts',(8.01683498452654,-0.541507133239762,
125.914086666668));
#70634=CARTESIAN_POINT('Ctrl Pts',(8.00908708774946,-0.67740814146322,125.93298491122));
#70635=CARTESIAN_POINT('Ctrl Pts',(8.00134081166537,-0.813280722125444,
125.951879202667));
#70636=CARTESIAN_POINT('Ctrl Pts',(7.99359453558127,-0.948396898426527,
125.976467267404));
#70637=CARTESIAN_POINT('Ctrl Pts',(7.98584825949717,-1.08224814420142,126.00666095868));
#70638=CARTESIAN_POINT('Ctrl Pts',(7.97810192623183,-1.21610037803581,126.03685487284));
#70639=CARTESIAN_POINT('Ctrl Pts',(7.97035559296646,-1.34868728132952,126.072654410078));
#70640=CARTESIAN_POINT('Ctrl Pts',(7.96260925970111,-1.4795118144361,126.113920568547));
#70641=CARTESIAN_POINT('Ctrl Pts',(7.95486119169814,-1.61036564478981,126.155195968285));
#70642=CARTESIAN_POINT('Ctrl Pts',(7.94711312369521,-1.73945594682301,126.201940307706));
#70643=CARTESIAN_POINT('Ctrl Pts',(7.93936505569224,-1.86630248257096,126.253965238475));
#70644=CARTESIAN_POINT('Ctrl Pts',(7.93160875295039,-1.99328383232659,126.306045461961));
#70645=CARTESIAN_POINT('Ctrl Pts',(7.92385245020855,-2.11801628979861,126.363417339325));
#70646=CARTESIAN_POINT('Ctrl Pts',(7.9160961474667,-2.24004068961837,126.425844799237));
#70647=CARTESIAN_POINT('Ctrl Pts',(7.90833570495254,-2.3621302175344,126.488305578564));
#70648=CARTESIAN_POINT('Ctrl Pts',(7.90057526243834,-2.48150846763626,126.555827124678));
#70649=CARTESIAN_POINT('Ctrl Pts',(7.89281481992418,-2.59774328384107,126.628128716227));
#70650=CARTESIAN_POINT('Ctrl Pts',(7.88504191965875,-2.71416469049186,126.70054637271));
#70651=CARTESIAN_POINT('Ctrl Pts',(7.87726901939337,-2.82743225625953,126.77775918809));
#70652=CARTESIAN_POINT('Ctrl Pts',(7.86949611912794,-2.93714435173543,126.859444126743));
#70653=CARTESIAN_POINT('Ctrl Pts',(7.86200578336589,-3.04286813619313,126.938159612124));
#70654=CARTESIAN_POINT('Ctrl Pts',(7.85451544760377,-3.14529022355345,127.021027526156));
#70655=CARTESIAN_POINT('Ctrl Pts',(7.8470251118417,-3.24408355797388,127.107726346857));
#70656=CARTESIAN_POINT('Ctrl Pts',(7.83936711384137,-3.34508826343304,127.196365817321));
#70657=CARTESIAN_POINT('Ctrl Pts',(7.83170911584105,-3.44264003407282,127.289308622642));
#70658=CARTESIAN_POINT('Ctrl Pts',(7.82405111784072,-3.53634159520523,127.386251317891));
#70659=CARTESIAN_POINT('Ctrl Pts',(7.81640193856051,-3.62993525243869,127.48308237685));
#70660=CARTESIAN_POINT('Ctrl Pts',(7.80875275928028,-3.7196872363694,127.583903882855));
#70661=CARTESIAN_POINT('Ctrl Pts',(7.80110358000007,-3.80523295924066,127.688371980166));
#70662=CARTESIAN_POINT('Ctrl Pts',(7.79346143612713,-3.89070000059879,127.792743991925));
#70663=CARTESIAN_POINT('Ctrl Pts',(7.78581929225413,-3.9719682192457,127.900755616373));
#70664=CARTESIAN_POINT('Ctrl Pts',(7.77817714838119,-4.04870997390888,128.012026359339));
#70665=CARTESIAN_POINT('Ctrl Pts',(7.77054026338514,-4.12539891938049,128.12322053228));
#70666=CARTESIAN_POINT('Ctrl Pts',(7.76290337838913,-4.19756736791663,128.237669032266));
#70667=CARTESIAN_POINT('Ctrl Pts',(7.75526649339307,-4.26492843596357,128.354958956219));
#70668=CARTESIAN_POINT('Ctrl Pts',(7.74763259241966,-4.33226318346841,128.472203050519));
#70669=CARTESIAN_POINT('Ctrl Pts',(7.73999869144624,-4.39479408454358,128.592286012124));
#70670=CARTESIAN_POINT('Ctrl Pts',(7.73236479047284,-4.45227827998498,128.714767073339));
#70671=CARTESIAN_POINT('Ctrl Pts',(7.72473255343253,-4.50974994580944,128.837221437812));
#70672=CARTESIAN_POINT('Ctrl Pts',(7.71710031639215,-4.56217692640189,128.962072495382));
#70673=CARTESIAN_POINT('Ctrl Pts',(7.70946807935184,-4.60936321395806,129.088856661199));
#70674=CARTESIAN_POINT('Ctrl Pts',(7.70183446999593,-4.65655798585214,129.215663623464));
#70675=CARTESIAN_POINT('Ctrl Pts',(7.69420086064008,-4.69851004404001,129.344404009283));
#70676=CARTESIAN_POINT('Ctrl Pts',(7.68656725128417,-4.7350723614769,129.474596430171));
#70677=CARTESIAN_POINT('Ctrl Pts',(7.68446478424792,-4.74514244282322,129.510454339651));
#70678=CARTESIAN_POINT('Ctrl Pts',(7.68236231721161,-4.75480396485171,129.546422313077));
#70679=CARTESIAN_POINT('Ctrl Pts',(7.68025985017536,-4.76405452823403,129.582490119308));
#70680=CARTESIAN_POINT('Origin',(213.235140564004,0.,130.804360617566));
#70681=CARTESIAN_POINT('',(5.58457496064637,-4.76405452823403,129.582490119308));
#70682=CARTESIAN_POINT('',(5.9302046085579,-4.76405452823401,129.582490119308));
#70683=CARTESIAN_POINT('',(213.235140564004,-4.76405452823405,129.582490119308));
#70684=CARTESIAN_POINT('',(7.26485943593479,-4.91824839244092,130.800384092418));
#70685=CARTESIAN_POINT('Ctrl Pts',(7.26485943593477,-4.91824839244093,130.800384092418));
#70686=CARTESIAN_POINT('Ctrl Pts',(7.2572111745685,-4.91835727452995,130.935051707829));
#70687=CARTESIAN_POINT('Ctrl Pts',(7.2495629132022,-4.91293095719067,131.069921889364));
#70688=CARTESIAN_POINT('Ctrl Pts',(7.24191465183594,-4.90194617917634,131.204493994027));
#70689=CARTESIAN_POINT('Ctrl Pts',(7.23427376524274,-4.89097199314379,131.338936338647));
#70690=CARTESIAN_POINT('Ctrl Pts',(7.22663287864958,-4.87445003899003,131.473080778438));
#70691=CARTESIAN_POINT('Ctrl Pts',(7.21899199205637,-4.85240909752608,131.606426084187));
#70692=CARTESIAN_POINT('Ctrl Pts',(7.21117029391079,-4.82984658611166,131.742926831578));
#70693=CARTESIAN_POINT('Ctrl Pts',(7.20334859576518,-4.80150060326161,131.878589721244));
#70694=CARTESIAN_POINT('Ctrl Pts',(7.1955268976196,-4.7674584782635,132.012881498864));
#70695=CARTESIAN_POINT('Ctrl Pts',(7.18789412315048,-4.73423859969954,132.143929620711));
#70696=CARTESIAN_POINT('Ctrl Pts',(7.18026134868138,-4.69559471079806,132.273671696196));
#70697=CARTESIAN_POINT('Ctrl Pts',(7.17262857421227,-4.65165968572856,132.401622409092));
#70698=CARTESIAN_POINT('Ctrl Pts',(7.16499680520051,-4.60773044817374,132.529556267175));
#70699=CARTESIAN_POINT('Ctrl Pts',(7.15736503618873,-4.55851159127469,132.655698850132));
#70700=CARTESIAN_POINT('Ctrl Pts',(7.14973326717697,-4.50418553713212,132.779581038074));
#70701=CARTESIAN_POINT('Ctrl Pts',(7.14210073665751,-4.44985406226613,132.903475587138));
#70702=CARTESIAN_POINT('Ctrl Pts',(7.13446820613806,-4.39041453938712,133.025108923194));
#70703=CARTESIAN_POINT('Ctrl Pts',(7.12683567561859,-4.32609687367602,133.144033437015));
#70704=CARTESIAN_POINT('Ctrl Pts',(7.11887197236391,-4.25898848774158,133.268118042425));
#70705=CARTESIAN_POINT('Ctrl Pts',(7.11090826910921,-4.1865693442687,133.38925304212));
#70706=CARTESIAN_POINT('Ctrl Pts',(7.10294456585453,-4.10915224902535,133.506961375508));
#70707=CARTESIAN_POINT('Ctrl Pts',(7.09530106243412,-4.03484789420867,133.61993696238));
#70708=CARTESIAN_POINT('Ctrl Pts',(7.08765755901373,-3.95593998433738,133.729755794599));
#70709=CARTESIAN_POINT('Ctrl Pts',(7.08001405559332,-3.87274710804022,133.836028953593));
#70710=CARTESIAN_POINT('Ctrl Pts',(7.07236545936534,-3.78949880096902,133.942372921575));
#70711=CARTESIAN_POINT('Ctrl Pts',(7.06471686313732,-3.70196010609965,134.045166208678));
#70712=CARTESIAN_POINT('Ctrl Pts',(7.05706826690934,-3.61048729867891,134.144055892374));
#70713=CARTESIAN_POINT('Ctrl Pts',(7.04940928413935,-3.5188902741955,134.243079865007));
#70714=CARTESIAN_POINT('Ctrl Pts',(7.04175030136939,-3.42334876518385,134.338189377904));
#70715=CARTESIAN_POINT('Ctrl Pts',(7.03409131859939,-3.32425305306113,134.429070909674));
#70716=CARTESIAN_POINT('Ctrl Pts',(7.03315129125375,-3.3120905137228,134.440225279339));
#70717=CARTESIAN_POINT('Ctrl Pts',(7.03221126390809,-3.29987447066042,134.451316011969));
#70718=CARTESIAN_POINT('Ctrl Pts',(7.03127123656245,-3.28760567540848,134.462342572896));
#70719=CARTESIAN_POINT('Ctrl Pts',(7.02349690244336,-3.18613871918751,134.553535844272));
#70720=CARTESIAN_POINT('Ctrl Pts',(7.01572256832429,-3.08071382331022,134.640648547029));
#70721=CARTESIAN_POINT('Ctrl Pts',(7.0079482342052,-2.97169310110002,134.723317516458));
#70722=CARTESIAN_POINT('Ctrl Pts',(7.00018348125811,-2.86280673718648,134.805884603771));
#70723=CARTESIAN_POINT('Ctrl Pts',(6.99241872831108,-2.75033367291102,134.884018620406));
#70724=CARTESIAN_POINT('Ctrl Pts',(6.98465397536398,-2.63467170147528,134.957394218194));
#70725=CARTESIAN_POINT('Ctrl Pts',(6.97689693447898,-2.51912460714011,135.030696938304));
#70726=CARTESIAN_POINT('Ctrl Pts',(6.96913989359391,-2.40039523664977,135.099250436693));
#70727=CARTESIAN_POINT('Ctrl Pts',(6.96138285270891,-2.27891290901463,135.162770765272));
#70728=CARTESIAN_POINT('Ctrl Pts',(6.95363166146881,-2.15752219214824,135.226243192677));
#70729=CARTESIAN_POINT('Ctrl Pts',(6.94588047022871,-2.03338299540185,135.284689824665));
#70730=CARTESIAN_POINT('Ctrl Pts',(6.93812927898861,-1.90695164808688,135.337871230144));
#70731=CARTESIAN_POINT('Ctrl Pts',(6.93038138221154,-1.78057403746684,135.391030032108));
#70732=CARTESIAN_POINT('Ctrl Pts',(6.92263348543447,-1.65190657356444,135.438927907227));
#70733=CARTESIAN_POINT('Ctrl Pts',(6.9148855886574,-1.52142790195612,135.48137250569));
#70734=CARTESIAN_POINT('Ctrl Pts',(6.90713931257332,-1.39097652367328,135.523808225657));
#70735=CARTESIAN_POINT('Ctrl Pts',(6.89939303648919,-1.25871506282197,135.560792817032));
#70736=CARTESIAN_POINT('Ctrl Pts',(6.89164676040511,-1.12513937993463,135.592183132888));
#70737=CARTESIAN_POINT('Ctrl Pts',(6.88390042713978,-0.99156271102194,135.62357368046));
#70738=CARTESIAN_POINT('Ctrl Pts',(6.87615409387449,-0.856672181312171,
135.64936978067));
#70739=CARTESIAN_POINT('Ctrl Pts',(6.86840776060916,-0.720975564379753,
135.66947904347));
#70740=CARTESIAN_POINT('Ctrl Pts',(6.86065969260619,-0.585248559130641,
135.689592809599));
#70741=CARTESIAN_POINT('Ctrl Pts',(6.8529116246032,-0.448715494117277,135.704017146844));
#70742=CARTESIAN_POINT('Ctrl Pts',(6.84516355660023,-0.311890616307963,
135.712711390072));
#70743=CARTESIAN_POINT('Ctrl Pts',(6.83740725385838,-0.174920319390276,
135.721414873645));
#70744=CARTESIAN_POINT('Ctrl Pts',(6.82965095111652,-0.0376579809348041,
135.724376072915));
#70745=CARTESIAN_POINT('Ctrl Pts',(6.82189464837467,0.0993802295133067,
135.721606455683));
#70746=CARTESIAN_POINT('Ctrl Pts',(6.8141342058605,0.236491581380661,135.718835360223));
#70747=CARTESIAN_POINT('Ctrl Pts',(6.80637376334631,0.373378176858677,135.710327377766));
#70748=CARTESIAN_POINT('Ctrl Pts',(6.79861332083215,0.509528606611335,135.696145942122));
#70749=CARTESIAN_POINT('Ctrl Pts',(6.79084042056672,0.645897597120513,135.68194174118));
#70750=CARTESIAN_POINT('Ctrl Pts',(6.78306752030125,0.781527673326089,135.662045944079));
#70751=CARTESIAN_POINT('Ctrl Pts',(6.77529462003582,0.915916370811572,135.636573388562));
#70752=CARTESIAN_POINT('Ctrl Pts',(6.76780428427374,1.04541970063984,135.6120268246));
#70753=CARTESIAN_POINT('Ctrl Pts',(6.76031394851172,1.17377003920796,135.582301990793));
#70754=CARTESIAN_POINT('Ctrl Pts',(6.75282361274964,1.30053264666007,135.547544980151));
#70755=CARTESIAN_POINT('Ctrl Pts',(6.74504927863056,1.43210149690128,135.511470146887));
#70756=CARTESIAN_POINT('Ctrl Pts',(6.73727494451147,1.56237661225875,135.469859739883));
#70757=CARTESIAN_POINT('Ctrl Pts',(6.72950061039239,1.6908567208801,135.422822115939));
#70758=CARTESIAN_POINT('Ctrl Pts',(6.7217358574453,1.81917848925018,135.375842461662));
#70759=CARTESIAN_POINT('Ctrl Pts',(6.71397110449823,1.94570928886396,135.323449031806));
#70760=CARTESIAN_POINT('Ctrl Pts',(6.70620635155115,2.0699603781493,135.265800642423));
#70761=CARTESIAN_POINT('Ctrl Pts',(6.69844931066616,2.19408805950096,135.208209510233));
#70762=CARTESIAN_POINT('Ctrl Pts',(6.69069226978117,2.31594018410765,135.14537396864));
#70763=CARTESIAN_POINT('Ctrl Pts',(6.68293522889618,2.4350458009878,135.07750173501));
#70764=CARTESIAN_POINT('Ctrl Pts',(6.67518403765605,2.55406159939608,135.009680684359));
#70765=CARTESIAN_POINT('Ctrl Pts',(6.66743284641591,2.67033467429255,134.936830694559));
#70766=CARTESIAN_POINT('Ctrl Pts',(6.65968165517577,2.78341692837952,134.859206270031));
#70767=CARTESIAN_POINT('Ctrl Pts',(6.65193375839868,2.89645111949194,134.781614837953));
#70768=CARTESIAN_POINT('Ctrl Pts',(6.64418586162162,3.00629686548536,134.699253227993));
#70769=CARTESIAN_POINT('Ctrl Pts',(6.63643796484453,3.11253361738844,134.612420168456));
#70770=CARTESIAN_POINT('Ctrl Pts',(6.62869168876044,3.21874814685306,134.525605272524));
#70771=CARTESIAN_POINT('Ctrl Pts',(6.62094541267632,3.32135488129076,134.434321034708));
#70772=CARTESIAN_POINT('Ctrl Pts',(6.61319913659221,3.41996536240851,134.338907262106));
#70773=CARTESIAN_POINT('Ctrl Pts',(6.60545280332685,3.51857657144656,134.243492785181));
#70774=CARTESIAN_POINT('Ctrl Pts',(6.59770647006154,3.61319118732984,134.143948984506));
#70775=CARTESIAN_POINT('Ctrl Pts',(6.58996013679618,3.70345701567332,134.040653125291));
#70776=CARTESIAN_POINT('Ctrl Pts',(6.58221206879322,3.79374305842295,133.937334133686));
#70777=CARTESIAN_POINT('Ctrl Pts',(6.57446400079024,3.87967811851019,133.830261705888));
#70778=CARTESIAN_POINT('Ctrl Pts',(6.56671593278728,3.96095002016121,133.719846511938));
#70779=CARTESIAN_POINT('Ctrl Pts',(6.55895963004543,4.04230829855656,133.609313967407));
#70780=CARTESIAN_POINT('Ctrl Pts',(6.55120332730362,4.11899328612188,133.49543187513));
#70781=CARTESIAN_POINT('Ctrl Pts',(6.54344702456177,4.19073562879666,133.37864070179));
#70782=CARTESIAN_POINT('Ctrl Pts',(6.53568658204762,4.26251626251975,133.261787193486));
#70783=CARTESIAN_POINT('Ctrl Pts',(6.52792613953346,4.3293488044162,133.142021851543));
#70784=CARTESIAN_POINT('Ctrl Pts',(6.52016569701931,4.39101019391058,133.019809226646));
#70785=CARTESIAN_POINT('Ctrl Pts',(6.51239279675388,4.45277056774158,132.897400415193));
#70786=CARTESIAN_POINT('Ctrl Pts',(6.5046198964884,4.50934303930082,132.772536826523));
#70787=CARTESIAN_POINT('Ctrl Pts',(6.49684699622296,4.56055263054152,132.645703270784));
#70788=CARTESIAN_POINT('Ctrl Pts',(6.48935666046088,4.60990062415172,132.52348043427));
#70789=CARTESIAN_POINT('Ctrl Pts',(6.48186632469884,4.6542687727465,132.39942866062));
#70790=CARTESIAN_POINT('Ctrl Pts',(6.47437598893677,4.69354500100034,132.273992675628));
#70791=CARTESIAN_POINT('Ctrl Pts',(6.46660165481768,4.73431039938595,132.143800747141));
#70792=CARTESIAN_POINT('Ctrl Pts',(6.45882732069861,4.76971926750344,132.011705161631));
#70793=CARTESIAN_POINT('Ctrl Pts',(6.45105298657953,4.79959181931533,131.878186222802));
#70794=CARTESIAN_POINT('Ctrl Pts',(6.44328823363245,4.82942755587681,131.744831834133));
#70795=CARTESIAN_POINT('Ctrl Pts',(6.43552348068539,4.85374046735714,131.610057960262));
#70796=CARTESIAN_POINT('Ctrl Pts',(6.42775872773831,4.87239999344214,131.474361637271));
#70797=CARTESIAN_POINT('Ctrl Pts',(6.42000168685332,4.89104098662277,131.33880008978));
#70798=CARTESIAN_POINT('Ctrl Pts',(6.41224464596833,4.90403971563981,131.202318301243));
#70799=CARTESIAN_POINT('Ctrl Pts',(6.40448760508335,4.9113163784853,131.065424772367));
#70800=CARTESIAN_POINT('Ctrl Pts',(6.3967364138432,4.91858755394277,130.928634475965));
#70801=CARTESIAN_POINT('Ctrl Pts',(6.38898522260302,4.92014523141444,130.791433446083));
#70802=CARTESIAN_POINT('Ctrl Pts',(6.38123403136288,4.91596132514216,130.654336245524));
#70803=CARTESIAN_POINT('Ctrl Pts',(6.37348613458579,4.91177919714166,130.517297314933));
#70804=CARTESIAN_POINT('Ctrl Pts',(6.36573823780875,4.90186035092097,130.380362515858));
#70805=CARTESIAN_POINT('Ctrl Pts',(6.35799034103167,4.88622879807351,130.244047138006));
#70806=CARTESIAN_POINT('Ctrl Pts',(6.35024406494757,4.87060051500995,130.107760274392));
#70807=CARTESIAN_POINT('Ctrl Pts',(6.34249778886339,4.84926194670322,129.972092962455));
#70808=CARTESIAN_POINT('Ctrl Pts',(6.33475151277929,4.82228901129376,129.837555697194));
#70809=CARTESIAN_POINT('Ctrl Pts',(6.3270051795139,4.79531587677608,129.703017438809));
#70810=CARTESIAN_POINT('Ctrl Pts',(6.31925884624859,4.76270836901654,129.569609627084));
#70811=CARTESIAN_POINT('Ctrl Pts',(6.3115125129832,4.72459352225369,129.43783249419));
#70812=CARTESIAN_POINT('Ctrl Pts',(6.30376444498021,4.68647013993534,129.306025850721));
#70813=CARTESIAN_POINT('Ctrl Pts',(6.29601637697722,4.64283707303733,129.175850988248));
#70814=CARTESIAN_POINT('Ctrl Pts',(6.28826830897424,4.59387109126585,129.047792526278));
#70815=CARTESIAN_POINT('Ctrl Pts',(6.28051200623239,4.5448530678663,128.919597962251));
#70816=CARTESIAN_POINT('Ctrl Pts',(6.27275570349055,4.49049094723878,128.79352465778));
#70817=CARTESIAN_POINT('Ctrl Pts',(6.26499940074871,4.43100971403031,128.670037311066));
#70818=CARTESIAN_POINT('Ctrl Pts',(6.25723895823452,4.3714967338965,128.546484055437));
#70819=CARTESIAN_POINT('Ctrl Pts',(6.24947851572029,4.30685938115965,128.425519852392));
#70820=CARTESIAN_POINT('Ctrl Pts',(6.2417180732061,4.23736792577663,128.307583470102));
#70821=CARTESIAN_POINT('Ctrl Pts',(6.23394517294067,4.16776491654045,128.189457765862));
#70822=CARTESIAN_POINT('Ctrl Pts',(6.22617227267524,4.093292445809,128.074369923685));
#70823=CARTESIAN_POINT('Ctrl Pts',(6.21839937240981,4.01426381818204,127.962729209284));
#70824=CARTESIAN_POINT('Ctrl Pts',(6.21090903664783,3.93810808023096,127.855146916059));
#70825=CARTESIAN_POINT('Ctrl Pts',(6.20341870088583,3.85772187779952,127.750765722285));
#70826=CARTESIAN_POINT('Ctrl Pts',(6.19592836512385,3.77341879184149,127.649920305264));
#70827=CARTESIAN_POINT('Ctrl Pts',(6.18815403100476,3.68591932875538,127.545251303604));
#70828=CARTESIAN_POINT('Ctrl Pts',(6.1803796968857,3.59392292965214,127.444059929443));
#70829=CARTESIAN_POINT('Ctrl Pts',(6.1726053627666,3.49773650889457,127.346757057751));
#70830=CARTESIAN_POINT('Ctrl Pts',(6.1648406098195,3.40166862930415,127.249574103152));
#70831=CARTESIAN_POINT('Ctrl Pts',(6.15707585687246,3.30142127475228,127.156270391283));
#70832=CARTESIAN_POINT('Ctrl Pts',(6.14931110392536,3.19734204473323,127.067224426379));
#70833=CARTESIAN_POINT('Ctrl Pts',(6.14155406304033,3.09336618767242,126.978266903182));
#70834=CARTESIAN_POINT('Ctrl Pts',(6.13379702215528,2.98556632415576,126.893558963859));
#70835=CARTESIAN_POINT('Ctrl Pts',(6.12603998127025,2.8743271352957,126.813442605153));
#70836=CARTESIAN_POINT('Ctrl Pts',(6.11828879003016,2.76317183277417,126.733386662817));
#70837=CARTESIAN_POINT('Ctrl Pts',(6.11053759879005,2.64858268332197,126.657915636672));
#70838=CARTESIAN_POINT('Ctrl Pts',(6.10278640754996,2.53097742216015,126.587331289826));
#70839=CARTESIAN_POINT('Ctrl Pts',(6.09503851077288,2.41342214637107,126.516776943211));
#70840=CARTESIAN_POINT('Ctrl Pts',(6.08729061399582,2.29285364305069,126.451105345734));
#70841=CARTESIAN_POINT('Ctrl Pts',(6.07954271721874,2.16971841887591,126.390574822436));
#70842=CARTESIAN_POINT('Ctrl Pts',(6.07179644113467,2.04660895193588,126.330056960819));
#70843=CARTESIAN_POINT('Ctrl Pts',(6.06405016505058,1.92093418271198,126.274678206715));
#70844=CARTESIAN_POINT('Ctrl Pts',(6.05630388896651,1.79316464071586,126.224650623059));
#70845=CARTESIAN_POINT('Ctrl Pts',(6.04855755570119,1.66539415555401,126.174622670111));
#70846=CARTESIAN_POINT('Ctrl Pts',(6.04081122243583,1.53552923081809,126.129946108978));
#70847=CARTESIAN_POINT('Ctrl Pts',(6.0330648891705,1.404059391111,126.090784449864));
#70848=CARTESIAN_POINT('Ctrl Pts',(6.02531682116754,1.27256010964468,126.051614020767));
#70849=CARTESIAN_POINT('Ctrl Pts',(6.01756875316456,1.13945557264713,126.017961062836));
#70850=CARTESIAN_POINT('Ctrl Pts',(6.0098206851616,1.00524905258022,125.989938803393));
#70851=CARTESIAN_POINT('Ctrl Pts',(6.00206438241975,0.87089989622652,125.961886761558));
#70852=CARTESIAN_POINT('Ctrl Pts',(5.99430807967794,0.735446800525724,125.939477452679));
#70853=CARTESIAN_POINT('Ctrl Pts',(5.9865517769361,0.599402338932921,125.922772771528));
#70854=CARTESIAN_POINT('Ctrl Pts',(5.97879133442193,0.463285266314561,125.906059174586));
#70855=CARTESIAN_POINT('Ctrl Pts',(5.97103089190775,0.326576588399491,125.895056303608));
#70856=CARTESIAN_POINT('Ctrl Pts',(5.96327044939358,0.189791540789937,125.889773937738));
#70857=CARTESIAN_POINT('Ctrl Pts',(5.95549754912814,0.052786913678754,125.884483092145));
#70858=CARTESIAN_POINT('Ctrl Pts',(5.94772464886272,-0.0842939369234755,
125.884931101068));
#70859=CARTESIAN_POINT('Ctrl Pts',(5.93995174859728,-0.220937335391866,
125.891075590588));
#70860=CARTESIAN_POINT('Ctrl Pts',(5.93246141283519,-0.352613402143094,
125.896996712436));
#70861=CARTESIAN_POINT('Ctrl Pts',(5.92497107707308,-0.483882962651974,
125.908207316311));
#70862=CARTESIAN_POINT('Ctrl Pts',(5.91748074131098,-0.61429494526265,125.924624478929));
#70863=CARTESIAN_POINT('Ctrl Pts',(5.90970640719189,-0.749651537830731,
125.941664103257));
#70864=CARTESIAN_POINT('Ctrl Pts',(5.9019320730728,-0.884513007652761,125.964366869825));
#70865=CARTESIAN_POINT('Ctrl Pts',(5.89415773895371,-1.01836777927145,125.992696650845));
#70866=CARTESIAN_POINT('Ctrl Pts',(5.8863929860066,-1.15205758684725,126.020991517942));
#70867=CARTESIAN_POINT('Ctrl Pts',(5.87862823305954,-1.28474278595388,126.054899521144));
#70868=CARTESIAN_POINT('Ctrl Pts',(5.87086348011243,-1.4159170442427,126.094332805937));
#70869=CARTESIAN_POINT('Ctrl Pts',(5.86310643922744,-1.54696101840859,126.133726925035));
#70870=CARTESIAN_POINT('Ctrl Pts',(5.85534939834241,-1.67649666620272,126.178635292951));
#70871=CARTESIAN_POINT('Ctrl Pts',(5.84759235745742,-1.80402832654186,126.228919124165));
#70872=CARTESIAN_POINT('Ctrl Pts',(5.83984116621732,-1.93146381426336,126.27916503595));
#70873=CARTESIAN_POINT('Ctrl Pts',(5.83208997497718,-2.05689796028396,126.334778199604));
#70874=CARTESIAN_POINT('Ctrl Pts',(5.82433878373709,-2.17985108666403,126.395570272985));
#70875=CARTESIAN_POINT('Ctrl Pts',(5.81659088696,-2.30275195468635,126.456336508113));
#70876=CARTESIAN_POINT('Ctrl Pts',(5.80884299018301,-2.42317355065415,126.52227710208));
#70877=CARTESIAN_POINT('Ctrl Pts',(5.80109509340591,-2.54065719063008,126.593156027167));
#70878=CARTESIAN_POINT('Ctrl Pts',(5.79334881732182,-2.65811625556071,126.66402012591));
#70879=CARTESIAN_POINT('Ctrl Pts',(5.7856025412377,-2.77263825233905,126.739820299258));
#70880=CARTESIAN_POINT('Ctrl Pts',(5.77785626515362,-2.88379043371678,126.820275302603));
#70881=CARTESIAN_POINT('Ctrl Pts',(5.77010993188827,-2.99494343559482,126.900730899849));
#70882=CARTESIAN_POINT('Ctrl Pts',(5.7623635986229,-3.10272625572969,126.985841166417));
#70883=CARTESIAN_POINT('Ctrl Pts',(5.75461726535755,-3.20673672834962,127.075282632654));
#70884=CARTESIAN_POINT('Ctrl Pts',(5.74686919735461,-3.31077049339332,127.164744128687));
#70885=CARTESIAN_POINT('Ctrl Pts',(5.7391211293517,-3.41102993350776,127.258538499599));
#70886=CARTESIAN_POINT('Ctrl Pts',(5.73137306134876,-3.50714775628163,127.356303530146));
#70887=CARTESIAN_POINT('Ctrl Pts',(5.72361675860691,-3.60336773422175,127.454172466531));
#70888=CARTESIAN_POINT('Ctrl Pts',(5.7158604558651,-3.69543702729854,127.556020213348));
#70889=CARTESIAN_POINT('Ctrl Pts',(5.70810415312326,-3.78302650321348,127.661448983669));
#70890=CARTESIAN_POINT('Ctrl Pts',(5.70034371060909,-3.87066272826922,127.766934024499));
#70891=CARTESIAN_POINT('Ctrl Pts',(5.69258326809486,-3.95381413494921,127.876003586496));
#70892=CARTESIAN_POINT('Ctrl Pts',(5.68482282558068,-4.03219399835365,127.988229473223));
#70893=CARTESIAN_POINT('Ctrl Pts',(5.67704992531526,-4.11069968407284,128.100635514905));
#70894=CARTESIAN_POINT('Ctrl Pts',(5.66927702504981,-4.18441830961435,128.216207676614));
#70895=CARTESIAN_POINT('Ctrl Pts',(5.66150412478439,-4.25310787113293,128.33449088436));
#70896=CARTESIAN_POINT('Ctrl Pts',(5.65401378902231,-4.31930039407231,128.448474199568));
#70897=CARTESIAN_POINT('Ctrl Pts',(5.64652345326028,-4.38082299942428,128.5649746038));
#70898=CARTESIAN_POINT('Ctrl Pts',(5.6390331174982,-4.4375016376466,128.683567775635));
#70899=CARTESIAN_POINT('Ctrl Pts',(5.63062887149623,-4.50109574528171,128.816630727941));
#70900=CARTESIAN_POINT('Ctrl Pts',(5.62222462549418,-4.55876921861174,128.952698836224));
#70901=CARTESIAN_POINT('Ctrl Pts',(5.61382037949224,-4.61025095434813,129.091243808813));
#70902=CARTESIAN_POINT('Ctrl Pts',(5.60543761451511,-4.66160110416448,129.22943466421));
#70903=CARTESIAN_POINT('Ctrl Pts',(5.59705484953792,-4.70679097399697,129.370089487592));
#70904=CARTESIAN_POINT('Ctrl Pts',(5.58867208456076,-4.74559683346664,129.512658733735));
#70905=CARTESIAN_POINT('Ctrl Pts',(5.58730637658928,-4.75191902808408,129.535885909551));
#70906=CARTESIAN_POINT('Ctrl Pts',(5.58594066861784,-4.75807187600522,129.559163849067));
#70907=CARTESIAN_POINT('Ctrl Pts',(5.58457496064636,-4.76405452823403,129.582490119308));
#70908=CARTESIAN_POINT('Ctrl Pts',(7.33490367089149,-4.76405452823399,129.582490119308));
#70909=CARTESIAN_POINT('Ctrl Pts',(7.32712774182063,-4.79805954746054,129.715075173174));
#70910=CARTESIAN_POINT('Ctrl Pts',(7.31935181274974,-4.82648152751553,129.848908982077));
#70911=CARTESIAN_POINT('Ctrl Pts',(7.31157588367887,-4.8492618516729,129.983481481268));
#70912=CARTESIAN_POINT('Ctrl Pts',(7.31095687591102,-4.85107529383255,129.994194210458));
#70913=CARTESIAN_POINT('Ctrl Pts',(7.31033786814316,-4.85285301182095,130.004911619619));
#70914=CARTESIAN_POINT('Ctrl Pts',(7.30971886037531,-4.85459499024321,130.015633451047));
#70915=CARTESIAN_POINT('Ctrl Pts',(7.29709861902769,-4.89011019579174,130.234228608222));
#70916=CARTESIAN_POINT('Ctrl Pts',(7.28447837768005,-4.91086740907761,130.455283374741));
#70917=CARTESIAN_POINT('Ctrl Pts',(7.27185813633238,-4.91660648592595,130.677223978273));
#70918=CARTESIAN_POINT('Ctrl Pts',(7.26952523621868,-4.9176673763371,130.718250551771));
#70919=CARTESIAN_POINT('Ctrl Pts',(7.26719233610501,-4.91821518082649,130.759307292362));
#70920=CARTESIAN_POINT('Ctrl Pts',(7.2648594359913,-4.91824839244012,130.800384091423));
#70921=CARTESIAN_POINT('',(7.6101405640404,-4.91824853408196,130.808157919327));
#70922=CARTESIAN_POINT('Ctrl Pts',(7.68025985017536,-4.76405452823403,129.582490119308));
#70923=CARTESIAN_POINT('Ctrl Pts',(7.67262044065622,-4.79766687065929,129.713544132286));
#70924=CARTESIAN_POINT('Ctrl Pts',(7.66498103113705,-4.82584948931522,129.845916780401));
#70925=CARTESIAN_POINT('Ctrl Pts',(7.65734162161792,-4.84852009828473,129.979111613308));
#70926=CARTESIAN_POINT('Ctrl Pts',(7.64947477868833,-4.87186563558502,130.116271799169));
#70927=CARTESIAN_POINT('Ctrl Pts',(7.64160793575874,-4.8893657805543,130.25430342844));
#70928=CARTESIAN_POINT('Ctrl Pts',(7.63374109282915,-4.90098822212115,130.392659865648));
#70929=CARTESIAN_POINT('Ctrl Pts',(7.62587424989955,-4.91261066368802,130.531016302857));
#70930=CARTESIAN_POINT('Ctrl Pts',(7.61800740696999,-4.91835543749873,130.669697084274));
#70931=CARTESIAN_POINT('Ctrl Pts',(7.61014056404039,-4.91824853408196,130.808157919327));
#70932=CARTESIAN_POINT('Ctrl Pts',(7.61014056400873,-4.91824853408153,130.808157919885));
#70933=CARTESIAN_POINT('Ctrl Pts',(7.59628620534876,-4.91806026560986,131.05200238028));
#70934=CARTESIAN_POINT('Ctrl Pts',(7.58243184668884,-4.8997349343828,131.295162959375));
#70935=CARTESIAN_POINT('Ctrl Pts',(7.56857748802884,-4.86358951030189,131.53557887348));
#70936=CARTESIAN_POINT('Ctrl Pts',(7.56080315390975,-4.84330660796207,131.670487582693));
#70937=CARTESIAN_POINT('Ctrl Pts',(7.55302881979068,-4.81737407580755,131.804765411944));
#70938=CARTESIAN_POINT('Ctrl Pts',(7.54525448567159,-4.78584030762398,131.937901800065));
#70939=CARTESIAN_POINT('Ctrl Pts',(7.5374897327245,-4.75434540199149,132.070874109486));
#70940=CARTESIAN_POINT('Ctrl Pts',(7.52972497977747,-4.71726308453112,132.202707399951));
#70941=CARTESIAN_POINT('Ctrl Pts',(7.52196022683037,-4.67469333503861,132.332897593189));
#70942=CARTESIAN_POINT('Ctrl Pts',(7.51420318594536,-4.63216586642137,132.462958479691));
#70943=CARTESIAN_POINT('Ctrl Pts',(7.50644614506031,-4.584161932627,132.591379147415));
#70944=CARTESIAN_POINT('Ctrl Pts',(7.4986891041753,-4.53083217370943,132.717667408486));
#70945=CARTESIAN_POINT('Ctrl Pts',(7.49093791293519,-4.47754263117812,132.843860434596));
#70946=CARTESIAN_POINT('Ctrl Pts',(7.48318672169511,-4.41893540909666,132.967923896096));
#70947=CARTESIAN_POINT('Ctrl Pts',(7.475435530455,-4.35521030631677,133.089382772875));
#70948=CARTESIAN_POINT('Ctrl Pts',(7.46768763367792,-4.2915122884053,133.210790026391));
#70949=CARTESIAN_POINT('Ctrl Pts',(7.45993973690087,-4.22270089743599,133.329594551477));
#70950=CARTESIAN_POINT('Ctrl Pts',(7.45219184012379,-4.14902310030759,133.4453434603));
#70951=CARTESIAN_POINT('Ctrl Pts',(7.44444556403969,-4.07536071498604,133.561068156946));
#70952=CARTESIAN_POINT('Ctrl Pts',(7.43669928795559,-3.99683415806429,133.673738179062));
#70953=CARTESIAN_POINT('Ctrl Pts',(7.4289530118715,-3.91373497789903,133.782927653117));
#70954=CARTESIAN_POINT('Ctrl Pts',(7.42120667860616,-3.83063518431451,133.892117933183));
#70955=CARTESIAN_POINT('Ctrl Pts',(7.41346034534081,-3.74296293690717,133.997827302806));
#70956=CARTESIAN_POINT('Ctrl Pts',(7.40571401207546,-3.65105126304789,134.099661474407));
#70957=CARTESIAN_POINT('Ctrl Pts',(7.39796594407249,-3.55911900620652,134.201518451065));
#70958=CARTESIAN_POINT('Ctrl Pts',(7.39021787606948,-3.46294569563908,134.299498212655));
#70959=CARTESIAN_POINT('Ctrl Pts',(7.3824698080665,-3.36290225628413,134.393242264706));
#70960=CARTESIAN_POINT('Ctrl Pts',(7.37471350532465,-3.26275248957129,134.487085949051));
#70961=CARTESIAN_POINT('Ctrl Pts',(7.36695720258282,-3.15872466321802,134.576684663347));
#70962=CARTESIAN_POINT('Ctrl Pts',(7.35920089984097,-3.0512243478669,134.661718915869));
#70963=CARTESIAN_POINT('Ctrl Pts',(7.3514404573268,-2.94366665636056,134.746798553731));
#70964=CARTESIAN_POINT('Ctrl Pts',(7.34368001481259,-2.83263309921594,134.82730864611));
#70965=CARTESIAN_POINT('Ctrl Pts',(7.33591957229842,-2.71855863016779,134.902972826209));
#70966=CARTESIAN_POINT('Ctrl Pts',(7.328146672033,-2.60430103865502,134.978758469168));
#70967=CARTESIAN_POINT('Ctrl Pts',(7.32037377176758,-2.48699311512489,135.049682452353));
#70968=CARTESIAN_POINT('Ctrl Pts',(7.31260087150216,-2.36709560994132,135.115513762131));
#70969=CARTESIAN_POINT('Ctrl Pts',(7.30511053574008,-2.25155668107396,135.178951937981));
#70970=CARTESIAN_POINT('Ctrl Pts',(7.29762019997802,-2.13361345318878,135.237661137868));
#70971=CARTESIAN_POINT('Ctrl Pts',(7.29012986421594,-2.01369430221937,135.291477544916));
#70972=CARTESIAN_POINT('Ctrl Pts',(7.28235553009686,-1.88922838019302,135.347334417394));
#70973=CARTESIAN_POINT('Ctrl Pts',(7.27458119597784,-1.76223947243117,135.398097090274));
#70974=CARTESIAN_POINT('Ctrl Pts',(7.26680686185875,-1.63318328652827,135.443530307834));
#70975=CARTESIAN_POINT('Ctrl Pts',(7.25904210891167,-1.50428615084059,135.488907533015));
#70976=CARTESIAN_POINT('Ctrl Pts',(7.25127735596448,-1.37332717148633,135.528968242813));
#70977=CARTESIAN_POINT('Ctrl Pts',(7.24351260301739,-1.24078448531313,135.563524086444));
#70978=CARTESIAN_POINT('Ctrl Pts',(7.2357555621324,-1.10837344240436,135.598045608724));
#70979=CARTESIAN_POINT('Ctrl Pts',(7.22799852124746,-0.974382198808795,
135.627073047435));
#70980=CARTESIAN_POINT('Ctrl Pts',(7.22024148036246,-0.83930627075409,135.650467100752));
#70981=CARTESIAN_POINT('Ctrl Pts',(7.21249028912233,-0.704332204507285,
135.67384351243));
#70982=CARTESIAN_POINT('Ctrl Pts',(7.20473909788218,-0.568275465590584,
135.69159492801));
#70983=CARTESIAN_POINT('Ctrl Pts',(7.19698790664205,-0.431643698037308,
135.703632683949));
#70984=CARTESIAN_POINT('Ctrl Pts',(7.18924000986497,-0.2950700026302,135.715665323521));
#70985=CARTESIAN_POINT('Ctrl Pts',(7.18149211308789,-0.157922153325711,
135.72198909923));
#70986=CARTESIAN_POINT('Ctrl Pts',(7.17374421631081,-0.0207146691257019,
135.722566994385));
#70987=CARTESIAN_POINT('Ctrl Pts',(7.16599794022671,0.116464114226464,135.723144768657));
#70988=CARTESIAN_POINT('Ctrl Pts',(7.15825166414256,0.253702116947971,135.717979051403));
#70989=CARTESIAN_POINT('Ctrl Pts',(7.15050538805846,0.390483450566157,135.707084935467));
#70990=CARTESIAN_POINT('Ctrl Pts',(7.14275905479311,0.527265793873075,135.696190739112));
#70991=CARTESIAN_POINT('Ctrl Pts',(7.13501272152783,0.663591071619001,135.679568090737));
#70992=CARTESIAN_POINT('Ctrl Pts',(7.12726638826248,0.79894754906899,135.657284053634));
#70993=CARTESIAN_POINT('Ctrl Pts',(7.11951832025951,0.934334338663608,135.634995026175));
#70994=CARTESIAN_POINT('Ctrl Pts',(7.11177025225655,1.06875151054637,135.607042150653));
#70995=CARTESIAN_POINT('Ctrl Pts',(7.10402218425358,1.20169695917431,135.573543721706));
#70996=CARTESIAN_POINT('Ctrl Pts',(7.09626588151172,1.33478370380732,135.540009690229));
#70997=CARTESIAN_POINT('Ctrl Pts',(7.08850957876982,1.46639522087747,135.500918427344));
#70998=CARTESIAN_POINT('Ctrl Pts',(7.08075327602796,1.59604349210736,135.456438458037));
#70999=CARTESIAN_POINT('Ctrl Pts',(7.07299283351379,1.72576096052324,135.411934748431));
#71000=CARTESIAN_POINT('Ctrl Pts',(7.06523239099967,1.85351273118804,135.36203674367));
#71001=CARTESIAN_POINT('Ctrl Pts',(7.0574719484855,1.97883118577096,135.306960999647));
#71002=CARTESIAN_POINT('Ctrl Pts',(7.04969904822006,2.10435081266243,135.251796843151));
#71003=CARTESIAN_POINT('Ctrl Pts',(7.04192614795461,2.2274289664611,135.191438510078));
#71004=CARTESIAN_POINT('Ctrl Pts',(7.03415324768918,2.34762224202864,135.126148774247));
#71005=CARTESIAN_POINT('Ctrl Pts',(7.02666291192713,2.46344618928086,135.063232484769));
#71006=CARTESIAN_POINT('Ctrl Pts',(7.01917257616506,2.57659109747155,134.995737263415));
#71007=CARTESIAN_POINT('Ctrl Pts',(7.01168224040302,2.68668759516743,134.923934967966));
#71008=CARTESIAN_POINT('Ctrl Pts',(7.00390790628395,2.80095843503624,134.849410266662));
#71009=CARTESIAN_POINT('Ctrl Pts',(6.99613357216491,2.91230711592514,134.770009366688));
#71010=CARTESIAN_POINT('Ctrl Pts',(6.98835923804583,3.02028938944762,134.685988506286));
#71011=CARTESIAN_POINT('Ctrl Pts',(6.98059448509874,3.12813858446863,134.602071194086));
#71012=CARTESIAN_POINT('Ctrl Pts',(6.97282973215161,3.23262932139203,134.513545487987));
#71013=CARTESIAN_POINT('Ctrl Pts',(6.96506497920453,3.33334469072293,134.420711849862));
#71014=CARTESIAN_POINT('Ctrl Pts',(6.95730793831954,3.43396002812917,134.327970415415));
#71015=CARTESIAN_POINT('Ctrl Pts',(6.94955089743459,3.53080717449782,134.230929827006));
#71016=CARTESIAN_POINT('Ctrl Pts',(6.94179385654959,3.62350109263339,134.129931680434));
#71017=CARTESIAN_POINT('Ctrl Pts',(6.93404266530948,3.71612510956425,134.029009697349));
#71018=CARTESIAN_POINT('Ctrl Pts',(6.92629147406933,3.80460186899259,133.924136383295));
#71019=CARTESIAN_POINT('Ctrl Pts',(6.91854028282921,3.88858238177032,133.815690908764));
#71020=CARTESIAN_POINT('Ctrl Pts',(6.91079238605214,3.97252720058986,133.707291526452));
#71021=CARTESIAN_POINT('Ctrl Pts',(6.9030444892751,4.05197933476359,133.595323311841));
#71022=CARTESIAN_POINT('Ctrl Pts',(6.89529659249803,4.12662953101364,133.480199135912));
#71023=CARTESIAN_POINT('Ctrl Pts',(6.88755031641393,4.20126411205189,133.36509904148));
#71024=CARTESIAN_POINT('Ctrl Pts',(6.87980404032983,4.27109854052124,133.246844626653));
#71025=CARTESIAN_POINT('Ctrl Pts',(6.87205776424574,4.33586666413687,133.125878081064));
#71026=CARTESIAN_POINT('Ctrl Pts',(6.8643114309804,4.40063526585608,133.004910642528));
#71027=CARTESIAN_POINT('Ctrl Pts',(6.85656509771505,4.46033730355215,132.88123137795));
#71028=CARTESIAN_POINT('Ctrl Pts',(6.8488187644497,4.51475259434785,132.755307073605));
#71029=CARTESIAN_POINT('Ctrl Pts',(6.84107069644674,4.56918007107063,132.629354569384));
#71030=CARTESIAN_POINT('Ctrl Pts',(6.83332262844376,4.61831828995238,132.501156383781));
#71031=CARTESIAN_POINT('Ctrl Pts',(6.8255745604408,4.66199537531048,132.371198893548));
#71032=CARTESIAN_POINT('Ctrl Pts',(6.81781825769896,4.70571888119466,132.241103282949));
#71033=CARTESIAN_POINT('Ctrl Pts',(6.81006195495711,4.7439695343741,132.10924500376));
#71034=CARTESIAN_POINT('Ctrl Pts',(6.80230565221527,4.77662533389249,131.97612573145));
#71035=CARTESIAN_POINT('Ctrl Pts',(6.79454520970111,4.80929856279434,131.842935409377));
#71036=CARTESIAN_POINT('Ctrl Pts',(6.78678476718693,4.83637091075933,131.708483136199));
#71037=CARTESIAN_POINT('Ctrl Pts',(6.77902432467278,4.8577718132622,131.573279386211));
#71038=CARTESIAN_POINT('Ctrl Pts',(6.77125142440736,4.87920707039365,131.437858595161));
#71039=CARTESIAN_POINT('Ctrl Pts',(6.76347852414195,4.89495264382186,131.301684305256));
#71040=CARTESIAN_POINT('Ctrl Pts',(6.75570562387654,4.90498994129464,131.165271601464));
#71041=CARTESIAN_POINT('Ctrl Pts',(6.74821528811446,4.91466235772195,131.033817843057));
#71042=CARTESIAN_POINT('Ctrl Pts',(6.74072495235235,4.91903430302753,130.90214301156));
#71043=CARTESIAN_POINT('Ctrl Pts',(6.73323461659027,4.91813484458084,130.770704815395));
#71044=CARTESIAN_POINT('Ctrl Pts',(6.72546028247117,4.91720128289376,130.634283100072));
#71045=CARTESIAN_POINT('Ctrl Pts',(6.71768594835209,4.91058573885847,130.497684175371));
#71046=CARTESIAN_POINT('Ctrl Pts',(6.70991161423299,4.89826366586087,130.361420303068));
#71047=CARTESIAN_POINT('Ctrl Pts',(6.70214686128589,4.88595677871698,130.225324363811));
#71048=CARTESIAN_POINT('Ctrl Pts',(6.69438210833877,4.86795739063315,130.089563040998));
#71049=CARTESIAN_POINT('Ctrl Pts',(6.68661735539166,4.84429293892591,129.954649499378));
#71050=CARTESIAN_POINT('Ctrl Pts',(6.67886031450665,4.82065199108574,129.819869955789));
#71051=CARTESIAN_POINT('Ctrl Pts',(6.67110327362168,4.79135724396076,129.685936900312));
#71052=CARTESIAN_POINT('Ctrl Pts',(6.66334623273667,4.7564879697602,129.553358916517));
#71053=CARTESIAN_POINT('Ctrl Pts',(6.65559504149654,4.72164499075055,129.420880910811));
#71054=CARTESIAN_POINT('Ctrl Pts',(6.64784385025639,4.68123595110599,129.289756319393));
#71055=CARTESIAN_POINT('Ctrl Pts',(6.64009265901626,4.63539122054166,129.160483707629));
#71056=CARTESIAN_POINT('Ctrl Pts',(6.63234476223918,4.58956597521078,129.031266040173));
#71057=CARTESIAN_POINT('Ctrl Pts',(6.62459686546214,4.53830976440054,128.903899154518));
#71058=CARTESIAN_POINT('Ctrl Pts',(6.61684896868505,4.48180278921155,128.778866401056));
#71059=CARTESIAN_POINT('Ctrl Pts',(6.60910269260094,4.42530763406361,128.65385980175));
#71060=CARTESIAN_POINT('Ctrl Pts',(6.6013564165168,4.36356406011884,128.531186719527));
#71061=CARTESIAN_POINT('Ctrl Pts',(6.5936101404327,4.29680023222776,128.411310090137));
#71062=CARTESIAN_POINT('Ctrl Pts',(6.58586380716735,4.23003591150127,128.291432575846));
#71063=CARTESIAN_POINT('Ctrl Pts',(6.57811747390196,4.15825145311134,128.174351897144));
#71064=CARTESIAN_POINT('Ctrl Pts',(6.57037114063661,4.0817205633461,128.060505609506));
#71065=CARTESIAN_POINT('Ctrl Pts',(6.56262307263363,4.00517253501872,127.94663382678));
#71066=CARTESIAN_POINT('Ctrl Pts',(6.55487500463068,3.92387617828241,127.835998200835));
#71067=CARTESIAN_POINT('Ctrl Pts',(6.54712693662771,3.83814779267064,127.729006234065));
#71068=CARTESIAN_POINT('Ctrl Pts',(6.53937063388585,3.75232829391047,127.62190055496));
#71069=CARTESIAN_POINT('Ctrl Pts',(6.53161433114397,3.66206760157558,127.518446576406));
#71070=CARTESIAN_POINT('Ctrl Pts',(6.52385802840212,3.56772184494956,127.419018109108));
#71071=CARTESIAN_POINT('Ctrl Pts',(6.51609758588795,3.47332573315253,127.319536573844));
#71072=CARTESIAN_POINT('Ctrl Pts',(6.50833714337374,3.37484049319558,127.224085102941));
#71073=CARTESIAN_POINT('Ctrl Pts',(6.50057670085957,3.27265745971043,127.132998988156));
#71074=CARTESIAN_POINT('Ctrl Pts',(6.49280380059412,3.17031039294841,127.041766653854));
#71075=CARTESIAN_POINT('Ctrl Pts',(6.48503090032871,3.06425397323944,126.954913927055));
#71076=CARTESIAN_POINT('Ctrl Pts',(6.47725800006327,2.954911506589,126.872734865955));
#71077=CARTESIAN_POINT('Ctrl Pts',(6.46976766430125,2.84954391401849,126.793543220723));
#71078=CARTESIAN_POINT('Ctrl Pts',(6.46227732853923,2.74112529228462,126.718691516558));
#71079=CARTESIAN_POINT('Ctrl Pts',(6.4547869927772,2.63005643606702,126.648402700839));
#71080=CARTESIAN_POINT('Ctrl Pts',(6.44701265865812,2.51477637040727,126.575448863309));
#71081=CARTESIAN_POINT('Ctrl Pts',(6.43923832453901,2.39627596322879,126.507179652453));
#71082=CARTESIAN_POINT('Ctrl Pts',(6.43146399041993,2.27497292682905,126.443892610036));
#71083=CARTESIAN_POINT('Ctrl Pts',(6.42369923747284,2.15381938558051,126.380683563242));
#71084=CARTESIAN_POINT('Ctrl Pts',(6.41593448452578,2.02987043081941,126.322444647072));
#71085=CARTESIAN_POINT('Ctrl Pts',(6.40816973157868,1.90357263312018,126.269430155813));
#71086=CARTESIAN_POINT('Ctrl Pts',(6.40041269069367,1.77740027617411,126.216468319294));
#71087=CARTESIAN_POINT('Ctrl Pts',(6.39265564980867,1.64888407703531,126.168720731739));
#71088=CARTESIAN_POINT('Ctrl Pts',(6.38489860892366,1.5184947700301,126.126395601035));
#71089=CARTESIAN_POINT('Ctrl Pts',(6.37714741768353,1.38820379061559,126.084102388041));
#71090=CARTESIAN_POINT('Ctrl Pts',(6.36939622644341,1.25604288524007,126.047223612979));
#71091=CARTESIAN_POINT('Ctrl Pts',(6.36164503520328,1.12250197908266,126.015919078876));
#71092=CARTESIAN_POINT('Ctrl Pts',(6.3538971384262,0.989017831372682,125.984627850034));
#71093=CARTESIAN_POINT('Ctrl Pts',(6.3461492416491,0.854155229307928,125.958906239035));
#71094=CARTESIAN_POINT('Ctrl Pts',(6.33840134487201,0.718418232359344,125.938863900281));
#71095=CARTESIAN_POINT('Ctrl Pts',(6.33065506878791,0.582709628664371,125.918825753952));
#71096=CARTESIAN_POINT('Ctrl Pts',(6.32290879270382,0.446127380419428,125.904464573982));
#71097=CARTESIAN_POINT('Ctrl Pts',(6.31516251661972,0.309184297259216,125.895838626902));
#71098=CARTESIAN_POINT('Ctrl Pts',(6.30741618335437,0.172240203216272,125.887212616148));
#71099=CARTESIAN_POINT('Ctrl Pts',(6.29966985008901,0.0349356591349389,
125.88432194734));
#71100=CARTESIAN_POINT('Ctrl Pts',(6.29192351682366,-0.102213262238794,
125.887172853048));
#71101=CARTESIAN_POINT('Ctrl Pts',(6.28417544882069,-0.239392897162357,
125.890024397197));
#71102=CARTESIAN_POINT('Ctrl Pts',(6.27642738081769,-0.376416449223656,
125.898620066303));
#71103=CARTESIAN_POINT('Ctrl Pts',(6.26867931281473,-0.512770107492321,
125.912914013609));
#71104=CARTESIAN_POINT('Ctrl Pts',(6.26092301007287,-0.649268684051809,
125.927223152692));
#71105=CARTESIAN_POINT('Ctrl Pts',(6.25316670733099,-0.78509555512517,125.947242627057));
#71106=CARTESIAN_POINT('Ctrl Pts',(6.24541040458914,-0.919743726602677,
125.972874868868));
#71107=CARTESIAN_POINT('Ctrl Pts',(6.23764996207496,-1.05446376386366,125.998520791378));
#71108=CARTESIAN_POINT('Ctrl Pts',(6.22988951956077,-1.18800346749367,126.029785361445));
#71109=CARTESIAN_POINT('Ctrl Pts',(6.22212907704659,-1.31986922111277,126.066520571547));
#71110=CARTESIAN_POINT('Ctrl Pts',(6.21435617678116,-1.4519466573459,126.10331475227));
#71111=CARTESIAN_POINT('Ctrl Pts',(6.20658327651567,-1.58234440162337,126.145597001514));
#71112=CARTESIAN_POINT('Ctrl Pts',(6.19881037625024,-1.71058624722145,126.193170125587));
#71113=CARTESIAN_POINT('Ctrl Pts',(6.19132004048827,-1.83416617870927,126.23901384677));
#71114=CARTESIAN_POINT('Ctrl Pts',(6.18382970472636,-1.95574395065215,126.289770329353));
#71115=CARTESIAN_POINT('Ctrl Pts',(6.17633936896439,-2.07491535179094,126.345222881927));
#71116=CARTESIAN_POINT('Ctrl Pts',(6.16856440379526,-2.19861521284597,126.402782606684));
#71117=CARTESIAN_POINT('Ctrl Pts',(6.16078943862611,-2.32011408055876,126.465584702731));
#71118=CARTESIAN_POINT('Ctrl Pts',(6.15301447345698,-2.43893572565106,126.533438517054));
#71119=CARTESIAN_POINT('Ctrl Pts',(6.14524923154099,-2.55760877420193,126.601207474429));
#71120=CARTESIAN_POINT('Ctrl Pts',(6.13748398962503,-2.67361092591063,126.674015386999));
#71121=CARTESIAN_POINT('Ctrl Pts',(6.12971874770903,-2.78648676993388,126.75162394422));
#71122=CARTESIAN_POINT('Ctrl Pts',(6.1219613593278,-2.89924845468501,126.829154010454));
#71123=CARTESIAN_POINT('Ctrl Pts',(6.1142039709465,-3.0088898043473,126.911474838259));
#71124=CARTESIAN_POINT('Ctrl Pts',(6.10644658256527,-3.1149811510953,126.998302881427));
#71125=CARTESIAN_POINT('Ctrl Pts',(6.09869563737146,-3.22098437972965,127.085058806335));
#71126=CARTESIAN_POINT('Ctrl Pts',(6.09094469217766,-3.32344317566096,127.176314245219));
#71127=CARTESIAN_POINT('Ctrl Pts',(6.08319374698385,-3.42195831907986,127.271743411445));
#71128=CARTESIAN_POINT('Ctrl Pts',(6.0754463027881,-3.52042896452899,127.367129473597));
#71129=CARTESIAN_POINT('Ctrl Pts',(6.06769885859239,-3.61495922139504,127.46668524084));
#71130=CARTESIAN_POINT('Ctrl Pts',(6.05995141439664,-3.70518444641721,127.570045963651));
#71131=CARTESIAN_POINT('Ctrl Pts',(6.05220579184048,-3.79538845697965,127.673382383482));
#71132=CARTESIAN_POINT('Ctrl Pts',(6.04446016928433,-3.88128919358331,127.780521683941));
#71133=CARTESIAN_POINT('Ctrl Pts',(6.03671454672818,-3.96256053364781,127.891064017548));
#71134=CARTESIAN_POINT('Ctrl Pts',(6.02896906803743,-4.04383036419728,128.001604297968));
#71135=CARTESIAN_POINT('Ctrl Pts',(6.02122358934664,-4.1204707390474,128.115547170041));
#71136=CARTESIAN_POINT('Ctrl Pts',(6.01347811065588,-4.19219755690558,128.232461959692));
#71137=CARTESIAN_POINT('Ctrl Pts',(6.00572792410674,-4.26396797177231,128.349447812514));
#71138=CARTESIAN_POINT('Ctrl Pts',(5.99797773755759,-4.33081865864229,128.469408858115));
#71139=CARTESIAN_POINT('Ctrl Pts',(5.99022755100845,-4.39251026806489,128.591887655597));
#71140=CARTESIAN_POINT('Ctrl Pts',(5.98247481362753,-4.45422218214933,128.714406764728));
#71141=CARTESIAN_POINT('Ctrl Pts',(5.97472207624662,-4.51077147100497,128.839444922287));
#71142=CARTESIAN_POINT('Ctrl Pts',(5.96696933886571,-4.56196644051339,128.966523503421));
#71143=CARTESIAN_POINT('Ctrl Pts',(5.95920832544955,-4.61321606057314,129.093737740745));
#71144=CARTESIAN_POINT('Ctrl Pts',(5.95144731203336,-4.65909981135122,129.222996384858));
#71145=CARTESIAN_POINT('Ctrl Pts',(5.94368629861719,-4.69947536023651,129.353804034378));
#71146=CARTESIAN_POINT('Ctrl Pts',(5.93919240193076,-4.72285420725288,129.429546212779));
#71147=CARTESIAN_POINT('Ctrl Pts',(5.93469850524435,-4.74438719609991,129.505807489811));
#71148=CARTESIAN_POINT('Ctrl Pts',(5.93020460855791,-4.76405452823401,129.582490119308));
#71149=CARTESIAN_POINT('Origin',(213.235140564004,0.,130.804360617566));
#71150=CARTESIAN_POINT('',(3.83484270885905,-4.76405452823401,129.582490119308));
#71151=CARTESIAN_POINT('',(4.17986374616532,-4.76405452823409,129.582490119308));
#71152=CARTESIAN_POINT('',(213.235140564004,-4.76405452823405,129.582490119308));
#71153=CARTESIAN_POINT('',(5.51485943602369,-4.91824978603851,130.802909882532));
#71154=CARTESIAN_POINT('Ctrl Pts',(5.51485943599135,-4.91824978603868,130.802909883106));
#71155=CARTESIAN_POINT('Ctrl Pts',(5.50690415626822,-4.91829144117287,130.944128252468));
#71156=CARTESIAN_POINT('Ctrl Pts',(5.49894887654507,-4.91224651275032,131.085289402386));
#71157=CARTESIAN_POINT('Ctrl Pts',(5.49099359682194,-4.90015601623778,131.225850924725));
#71158=CARTESIAN_POINT('Ctrl Pts',(5.4830330612392,-4.8880575318286,131.366505312638));
#71159=CARTESIAN_POINT('Ctrl Pts',(5.47507252565646,-4.8699055484061,131.506558924337));
#71160=CARTESIAN_POINT('Ctrl Pts',(5.46711199007373,-4.84579276826709,131.645476251418));
#71161=CARTESIAN_POINT('Ctrl Pts',(5.45914490500839,-4.82166014948372,131.784507871891));
#71162=CARTESIAN_POINT('Ctrl Pts',(5.45117781994306,-4.79155701944537,131.922400989644));
#71163=CARTESIAN_POINT('Ctrl Pts',(5.44321073487771,-4.75562679829129,132.058632046673));
#71164=CARTESIAN_POINT('Ctrl Pts',(5.43523004692704,-4.71963523039948,132.19509570263));
#71165=CARTESIAN_POINT('Ctrl Pts',(5.42724935897631,-4.67779678537567,132.329891279319));
#71166=CARTESIAN_POINT('Ctrl Pts',(5.41926867102563,-4.63030456398885,132.462511004957));
#71167=CARTESIAN_POINT('Ctrl Pts',(5.41128035769744,-4.58276696479505,132.59525744592));
#71168=CARTESIAN_POINT('Ctrl Pts',(5.4032920443693,-4.52956495186786,132.725823557045));
#71169=CARTESIAN_POINT('Ctrl Pts',(5.39530373104111,-4.47093890415826,132.853723537545));
#71170=CARTESIAN_POINT('Ctrl Pts',(5.38730082587285,-4.41220576727016,132.981857146344));
#71171=CARTESIAN_POINT('Ctrl Pts',(5.37929792070464,-4.3480289622186,133.107314573205));
#71172=CARTESIAN_POINT('Ctrl Pts',(5.37129501553639,-4.2786942712433,133.229635528938));
#71173=CARTESIAN_POINT('Ctrl Pts',(5.36772517491932,-4.2477662781193,133.28419900394));
#71174=CARTESIAN_POINT('Ctrl Pts',(5.36415533430224,-4.21581255218363,133.338138795468));
#71175=CARTESIAN_POINT('Ctrl Pts',(5.36058549368516,-4.18286110904065,133.391416087589));
#71176=CARTESIAN_POINT('Ctrl Pts',(5.35281115956605,-4.1111000540864,133.507442407623));
#71177=CARTESIAN_POINT('Ctrl Pts',(5.34503682544701,-4.03439408092906,133.62066442551));
#71178=CARTESIAN_POINT('Ctrl Pts',(5.33726249132792,-3.95298869328417,133.730631871785));
#71179=CARTESIAN_POINT('Ctrl Pts',(5.32949773838082,-3.87168363050414,133.84046379301));
#71180=CARTESIAN_POINT('Ctrl Pts',(5.32173298543377,-3.78569090719519,133.947048812037));
#71181=CARTESIAN_POINT('Ctrl Pts',(5.31396823248667,-3.69530089402499,134.049962929174));
#71182=CARTESIAN_POINT('Ctrl Pts',(5.30621119160166,-3.60500065749014,134.15277483056));
#71183=CARTESIAN_POINT('Ctrl Pts',(5.29845415071655,-3.5103120788495,134.251922793895));
#71184=CARTESIAN_POINT('Ctrl Pts',(5.29069710983154,-3.4115674156978,134.347013695508));
#71185=CARTESIAN_POINT('Ctrl Pts',(5.28294591859142,-3.31289721666484,134.442032888332));
#71186=CARTESIAN_POINT('Ctrl Pts',(5.27519472735137,-3.21017730180296,134.533000839009));
#71187=CARTESIAN_POINT('Ctrl Pts',(5.26744353611124,-3.10377835763593,134.619559559846));
#71188=CARTESIAN_POINT('Ctrl Pts',(5.25969563933416,-2.9974246358583,134.706081490917));
#71189=CARTESIAN_POINT('Ctrl Pts',(5.25194774255703,-2.88739529747263,134.788197673259));
#71190=CARTESIAN_POINT('Ctrl Pts',(5.24419984577995,-2.77409567333946,134.865589034887));
#71191=CARTESIAN_POINT('Ctrl Pts',(5.23645356969584,-2.6608197490452,134.942964207911));
#71192=CARTESIAN_POINT('Ctrl Pts',(5.22870729361176,-2.54427522229636,135.015616305683));
#71193=CARTESIAN_POINT('Ctrl Pts',(5.22096101752766,-2.42489776846515,135.083268641232));
#71194=CARTESIAN_POINT('Ctrl Pts',(5.21321468426229,-2.30551943341654,135.150921476175));
#71195=CARTESIAN_POINT('Ctrl Pts',(5.2054683509969,-2.18330846969928,135.213574282488));
#71196=CARTESIAN_POINT('Ctrl Pts',(5.19772201773154,-2.0587262453815,135.270995739117));
#71197=CARTESIAN_POINT('Ctrl Pts',(5.18997394972856,-1.93411612173872,135.328430054884));
#71198=CARTESIAN_POINT('Ctrl Pts',(5.1822258817256,-1.80713403580959,135.380630526146));
#71199=CARTESIAN_POINT('Ctrl Pts',(5.17447781372263,-1.67826209974133,135.427413655016));
#71200=CARTESIAN_POINT('Ctrl Pts',(5.16672151098077,-1.54925319704565,135.474246505552));
#71201=CARTESIAN_POINT('Ctrl Pts',(5.15896520823893,-1.41835079999062,135.515650378615));
#71202=CARTESIAN_POINT('Ctrl Pts',(5.15120890549707,-1.2860535118888,135.551491269556));
#71203=CARTESIAN_POINT('Ctrl Pts',(5.14344846298289,-1.15368561274076,135.587351289858));
#71204=CARTESIAN_POINT('Ctrl Pts',(5.1356880204687,-1.01992172019991,135.617642325487));
#71205=CARTESIAN_POINT('Ctrl Pts',(5.12792757795452,-0.885270468202647,
135.64228158226));
#71206=CARTESIAN_POINT('Ctrl Pts',(5.12015467768909,-0.750403062062084,
135.666960392156));
#71207=CARTESIAN_POINT('Ctrl Pts',(5.11238177742363,-0.614645837334676,
135.685969238732));
#71208=CARTESIAN_POINT('Ctrl Pts',(5.1046088771582,-0.478513284494333,135.699277174471));
#71209=CARTESIAN_POINT('Ctrl Pts',(5.09711854139623,-0.347329492848052,
135.712101333225));
#71210=CARTESIAN_POINT('Ctrl Pts',(5.08962820563424,-0.215797495084421,
135.719631852407));
#71211=CARTESIAN_POINT('Ctrl Pts',(5.08213786987227,-0.084375565351097,
135.721886807275));
#71212=CARTESIAN_POINT('Ctrl Pts',(5.07436353575318,0.0520292667940507,
135.724227259442));
#71213=CARTESIAN_POINT('Ctrl Pts',(5.06658920163414,0.188747609195711,135.720891618068));
#71214=CARTESIAN_POINT('Ctrl Pts',(5.05881486751505,0.325267936645508,135.711843050738));
#71215=CARTESIAN_POINT('Ctrl Pts',(5.05105011456797,0.461620014992709,135.702805634958));
#71216=CARTESIAN_POINT('Ctrl Pts',(5.0432853616209,0.597774177582164,135.688069327666));
#71217=CARTESIAN_POINT('Ctrl Pts',(5.03552060867381,0.73321674902639,135.667649243737));
#71218=CARTESIAN_POINT('Ctrl Pts',(5.02776356778882,0.868524796999067,135.647249441324));
#71219=CARTESIAN_POINT('Ctrl Pts',(5.02000652690377,1.00312227622098,135.6211771544));
#71220=CARTESIAN_POINT('Ctrl Pts',(5.01224948601879,1.13649884726764,135.589499427743));
#71221=CARTESIAN_POINT('Ctrl Pts',(5.00449829477867,1.26977483800474,135.557845589505));
#71222=CARTESIAN_POINT('Ctrl Pts',(4.99674710353862,1.40183137431215,135.52059481531));
#71223=CARTESIAN_POINT('Ctrl Pts',(4.98899591229849,1.53216690588338,135.477865473134));
#71224=CARTESIAN_POINT('Ctrl Pts',(4.98124801552141,1.66244704137687,135.435154292068));
#71225=CARTESIAN_POINT('Ctrl Pts',(4.97350011874427,1.79100725624612,135.386969295847));
#71226=CARTESIAN_POINT('Ctrl Pts',(4.96575222196719,1.91736001496204,135.333479034601));
#71227=CARTESIAN_POINT('Ctrl Pts',(4.95800594588309,2.04368634340485,135.279999962364));
#71228=CARTESIAN_POINT('Ctrl Pts',(4.95025966979898,2.16780577434087,135.22121798477));
#71229=CARTESIAN_POINT('Ctrl Pts',(4.94251339371488,2.28925003000418,135.157350091781));
#71230=CARTESIAN_POINT('Ctrl Pts',(4.93476706044952,2.4106951821414,135.093481727334));
#71231=CARTESIAN_POINT('Ctrl Pts',(4.9270207271842,2.52946477357003,135.024527554556));
#71232=CARTESIAN_POINT('Ctrl Pts',(4.91927439391884,2.64511480662607,134.950750700791));
#71233=CARTESIAN_POINT('Ctrl Pts',(4.91152632591586,2.76079073870515,134.876957325211));
#71234=CARTESIAN_POINT('Ctrl Pts',(4.90377825791289,2.87334539272677,134.798339329784));
#71235=CARTESIAN_POINT('Ctrl Pts',(4.89603018990991,2.98236379332925,134.715203144022));
#71236=CARTESIAN_POINT('Ctrl Pts',(4.88827388716806,3.09149805998509,134.631978600133));
#71237=CARTESIAN_POINT('Ctrl Pts',(4.88051758442617,3.19708825408913,134.544226510879));
#71238=CARTESIAN_POINT('Ctrl Pts',(4.87276128168432,3.29875212646374,134.452293932561));
#71239=CARTESIAN_POINT('Ctrl Pts',(4.86500083917015,3.40047025990822,134.360312287058));
#71240=CARTESIAN_POINT('Ctrl Pts',(4.85724039665602,3.49825761735194,134.26414598053));
#71241=CARTESIAN_POINT('Ctrl Pts',(4.84947995414186,3.59176961263977,134.164178188836));
#71242=CARTESIAN_POINT('Ctrl Pts',(4.84170705387644,3.68543172168391,134.064049919969));
#71243=CARTESIAN_POINT('Ctrl Pts',(4.83393415361098,3.77480449868644,133.960108267853));
#71244=CARTESIAN_POINT('Ctrl Pts',(4.82616125334556,3.85958381195648,133.852769360006));
#71245=CARTESIAN_POINT('Ctrl Pts',(4.81867091758351,3.94128118364331,133.749332491829));
#71246=CARTESIAN_POINT('Ctrl Pts',(4.81118058182146,4.01871308034606,133.64274132649));
#71247=CARTESIAN_POINT('Ctrl Pts',(4.8036902460594,4.09164700092106,133.533391193128));
#71248=CARTESIAN_POINT('Ctrl Pts',(4.79591591194033,4.16734623326212,133.419895016224));
#71249=CARTESIAN_POINT('Ctrl Pts',(4.78814157782123,4.23843946730323,133.303067007057));
#71250=CARTESIAN_POINT('Ctrl Pts',(4.78036724370216,4.30461922302025,133.183317617452));
#71251=CARTESIAN_POINT('Ctrl Pts',(4.77260249075509,4.37071741810292,133.063715808266));
#71252=CARTESIAN_POINT('Ctrl Pts',(4.76483773780799,4.43191399605386,132.941200121148));
#71253=CARTESIAN_POINT('Ctrl Pts',(4.75707298486091,4.4879440193524,132.816210895708));
#71254=CARTESIAN_POINT('Ctrl Pts',(4.74931594397591,4.54391839284207,132.691345811328));
#71255=CARTESIAN_POINT('Ctrl Pts',(4.7415589030909,4.59473626469316,132.564012432126));
#71256=CARTESIAN_POINT('Ctrl Pts',(4.73380186220589,4.64017819065105,132.434676360453));
#71257=CARTESIAN_POINT('Ctrl Pts',(4.72605067096575,4.68558584849916,132.305437822118));
#71258=CARTESIAN_POINT('Ctrl Pts',(4.71829947972566,4.72562550070614,132.174199964734));
#71259=CARTESIAN_POINT('Ctrl Pts',(4.71054828848551,4.76012563341238,132.04144873756));
#71260=CARTESIAN_POINT('Ctrl Pts',(4.70280039170845,4.79461110264175,131.9087539332));
#71261=CARTESIAN_POINT('Ctrl Pts',(4.69505249493136,4.82356163704551,131.774547415974));
#71262=CARTESIAN_POINT('Ctrl Pts',(4.6873045981543,4.84685551775979,131.639330468795));
#71263=CARTESIAN_POINT('Ctrl Pts',(4.67955832207022,4.87014452589638,131.504141806086));
#71264=CARTESIAN_POINT('Ctrl Pts',(4.67181204598612,4.88777916756064,131.367943518876));
#71265=CARTESIAN_POINT('Ctrl Pts',(4.66406576990204,4.89968888698319,131.231246870886));
#71266=CARTESIAN_POINT('Ctrl Pts',(4.65631943663671,4.91159869432056,131.094549213833));
#71267=CARTESIAN_POINT('Ctrl Pts',(4.64857310337144,4.91778346115495,130.957353578149));
#71268=CARTESIAN_POINT('Ctrl Pts',(4.64082677010612,4.91822457238921,130.820175738401));
#71269=CARTESIAN_POINT('Ctrl Pts',(4.63307870210316,4.91866578240726,130.682967178626));
#71270=CARTESIAN_POINT('Ctrl Pts',(4.62533063410015,4.91336077607595,130.545776813605));
#71271=CARTESIAN_POINT('Ctrl Pts',(4.61758256609718,4.90234305690388,130.409119406498));
#71272=CARTESIAN_POINT('Ctrl Pts',(4.60982626335533,4.89131362796874,130.272316758273));
#71273=CARTESIAN_POINT('Ctrl Pts',(4.60206996061352,4.8745593891082,130.136048589798));
#71274=CARTESIAN_POINT('Ctrl Pts',(4.59431365787168,4.85216571359989,130.00082409054));
#71275=CARTESIAN_POINT('Ctrl Pts',(4.58655321535754,4.82976008591273,129.865527417895));
#71276=CARTESIAN_POINT('Ctrl Pts',(4.57879277284337,4.8017091039469,129.731275906925));
#71277=CARTESIAN_POINT('Ctrl Pts',(4.57103233032922,4.76814888717111,129.598566583633));
#71278=CARTESIAN_POINT('Ctrl Pts',(4.56325943006379,4.73453479655596,129.465644223554));
#71279=CARTESIAN_POINT('Ctrl Pts',(4.55548652979832,4.69539390987147,129.334269373208));
#71280=CARTESIAN_POINT('Ctrl Pts',(4.54771362953289,4.65091193637605,129.204922834289));
#71281=CARTESIAN_POINT('Ctrl Pts',(4.54022329377076,4.60804699465992,129.080278367862));
#71282=CARTESIAN_POINT('Ctrl Pts',(4.53273295800869,4.56022265998851,128.95751759168));
#71283=CARTESIAN_POINT('Ctrl Pts',(4.52524262224657,4.50764586141486,128.837049800595));
#71284=CARTESIAN_POINT('Ctrl Pts',(4.51746828812748,4.45307559754362,128.712014436598));
#71285=CARTESIAN_POINT('Ctrl Pts',(4.50969395400838,4.39321251423806,128.589053292697));
#71286=CARTESIAN_POINT('Ctrl Pts',(4.50191961988929,4.32823573577927,128.46864691978));
#71287=CARTESIAN_POINT('Ctrl Pts',(4.4941548669422,4.26333903539278,128.348388936958));
#71288=CARTESIAN_POINT('Ctrl Pts',(4.48639011399515,4.1933413631873,128.230679801251));
#71289=CARTESIAN_POINT('Ctrl Pts',(4.47862536104805,4.11846998414756,128.115980426415));
#71290=CARTESIAN_POINT('Ctrl Pts',(4.47086832016304,4.04367296841699,128.001394972614));
#71291=CARTESIAN_POINT('Ctrl Pts',(4.46311127927798,3.96401209125675,127.88981365604));
#71292=CARTESIAN_POINT('Ctrl Pts',(4.45535423839297,3.87976046213168,127.781672770801));
#71293=CARTESIAN_POINT('Ctrl Pts',(4.44760304715284,3.79557236781552,127.673613435445));
#71294=CARTESIAN_POINT('Ctrl Pts',(4.43985185591273,3.70680065158938,127.568989674482));
#71295=CARTESIAN_POINT('Ctrl Pts',(4.43210066467259,3.61376144889855,127.468208454826));
#71296=CARTESIAN_POINT('Ctrl Pts',(4.4243527678955,3.52076179035076,127.367470069876));
#71297=CARTESIAN_POINT('Ctrl Pts',(4.41660487111835,3.4234985174841,127.270571264624));
#71298=CARTESIAN_POINT('Ctrl Pts',(4.40885697434126,3.32232758178954,127.177885400254));
#71299=CARTESIAN_POINT('Ctrl Pts',(4.40111069825715,3.22117780887359,127.085218923768));
#71300=CARTESIAN_POINT('Ctrl Pts',(4.39336442217312,3.11612228707666,126.996763899231));
#71301=CARTESIAN_POINT('Ctrl Pts',(4.385618146089,3.00755301993109,126.91285603774));
#71302=CARTESIAN_POINT('Ctrl Pts',(4.37787181282366,2.89898295135216,126.828947556861));
#71303=CARTESIAN_POINT('Ctrl Pts',(4.37012547955831,2.78689939501427,126.749586545085));
#71304=CARTESIAN_POINT('Ctrl Pts',(4.36237914629297,2.67172622475201,126.675067452571));
#71305=CARTESIAN_POINT('Ctrl Pts',(4.35463107829,2.55652726225698,126.600531672024));
#71306=CARTESIAN_POINT('Ctrl Pts',(4.346883010287,2.43823763722746,126.530840180741));
#71307=CARTESIAN_POINT('Ctrl Pts',(4.33913494228403,2.31730854395466,126.466243033335));
#71308=CARTESIAN_POINT('Ctrl Pts',(4.33137863954217,2.19625092580212,126.401577231312));
#71309=CARTESIAN_POINT('Ctrl Pts',(4.32362233680031,2.07254858099949,126.342016773374));
#71310=CARTESIAN_POINT('Ctrl Pts',(4.31586603405844,1.94667605140826,126.28776506191));
#71311=CARTESIAN_POINT('Ctrl Pts',(4.30810559154425,1.82073633985768,126.233484394674));
#71312=CARTESIAN_POINT('Ctrl Pts',(4.30034514903001,1.6926245005417,126.184518259292));
#71313=CARTESIAN_POINT('Ctrl Pts',(4.29258470651581,1.56283227141091,126.141020789295));
#71314=CARTESIAN_POINT('Ctrl Pts',(4.28481180625037,1.43283168827187,126.097453493298));
#71315=CARTESIAN_POINT('Ctrl Pts',(4.27703890598492,1.30114570062448,126.059372514173));
#71316=CARTESIAN_POINT('Ctrl Pts',(4.26926600571949,1.16827920094035,126.026881494519));
#71317=CARTESIAN_POINT('Ctrl Pts',(4.26177566995752,1.04024273319134,125.99557160527));
#71318=CARTESIAN_POINT('Ctrl Pts',(4.25428533419559,0.911110394362069,125.96945237436));
#71319=CARTESIAN_POINT('Ctrl Pts',(4.24679499843361,0.781338386011577,125.948570940382));
#71320=CARTESIAN_POINT('Ctrl Pts',(4.23902066431451,0.646646032519807,125.926897780488));
#71321=CARTESIAN_POINT('Ctrl Pts',(4.23124633019544,0.510837880950911,125.910798786112));
#71322=CARTESIAN_POINT('Ctrl Pts',(4.22347199607634,0.374415053427558,125.900383004417));
#71323=CARTESIAN_POINT('Ctrl Pts',(4.21570724312925,0.238160354847039,125.889980059242));
#71324=CARTESIAN_POINT('Ctrl Pts',(4.20794249018212,0.101292873665626,125.88524642025));
#71325=CARTESIAN_POINT('Ctrl Pts',(4.20017773723504,-0.035676768045025,
125.886240018117));
#71326=CARTESIAN_POINT('Ctrl Pts',(4.19242069635003,-0.172510369576782,
125.887232629129));
#71327=CARTESIAN_POINT('Ctrl Pts',(4.18466365546503,-0.309445541288254,
125.893941154063));
#71328=CARTESIAN_POINT('Ctrl Pts',(4.17690661458002,-0.445967594251223,
125.906371645817));
#71329=CARTESIAN_POINT('Ctrl Pts',(4.16915542333994,-0.582386694871138,
125.91879276364));
#71330=CARTESIAN_POINT('Ctrl Pts',(4.16140423209989,-0.718392909057021,
125.936927224268));
#71331=CARTESIAN_POINT('Ctrl Pts',(4.15365304085981,-0.85347296508882,125.960729029557));
#71332=CARTESIAN_POINT('Ctrl Pts',(4.14590514408274,-0.988495608493979,
125.984520718443));
#71333=CARTESIAN_POINT('Ctrl Pts',(4.1381572473056,-1.12259249244134,126.01397489342));
#71334=CARTESIAN_POINT('Ctrl Pts',(4.13040935052854,-1.25525709711611,126.04899389326));
#71335=CARTESIAN_POINT('Ctrl Pts',(4.12266307444444,-1.38789395121568,126.084005567879));
#71336=CARTESIAN_POINT('Ctrl Pts',(4.1149167983604,-1.51909874418968,126.124579652297));
#71337=CARTESIAN_POINT('Ctrl Pts',(4.10717052227631,-1.6483771452998,126.170567802889));
#71338=CARTESIAN_POINT('Ctrl Pts',(4.09942418901096,-1.77765650071371,126.216556292954));
#71339=CARTESIAN_POINT('Ctrl Pts',(4.09167785574562,-1.90500906753548,126.267958797907));
#71340=CARTESIAN_POINT('Ctrl Pts',(4.08393152248027,-2.02995800234534,126.324577858189));
#71341=CARTESIAN_POINT('Ctrl Pts',(4.07618345447731,-2.15493491860266,126.381209597916));
#71342=CARTESIAN_POINT('Ctrl Pts',(4.0684353864743,-2.27750677569764,126.443060056242));
#71343=CARTESIAN_POINT('Ctrl Pts',(4.06068731847134,-2.39721931406806,126.509884791256));
#71344=CARTESIAN_POINT('Ctrl Pts',(4.05293101572949,-2.51705908434902,126.576780548394));
#71345=CARTESIAN_POINT('Ctrl Pts',(4.04517471298766,-2.6340331234154,126.648660952148));
#71346=CARTESIAN_POINT('Ctrl Pts',(4.03741841024581,-2.74771380160992,126.72523670097));
#71347=CARTESIAN_POINT('Ctrl Pts',(4.02965796773162,-2.86145515460555,126.801853320575));
#71348=CARTESIAN_POINT('Ctrl Pts',(4.02189752521747,-2.97189932955123,126.883170047069));
#71349=CARTESIAN_POINT('Ctrl Pts',(4.01413708270329,-3.0786508531683,126.968856480326));
#71350=CARTESIAN_POINT('Ctrl Pts',(4.00636418243785,-3.18557374380789,127.054680465052));
#71351=CARTESIAN_POINT('Ctrl Pts',(3.99859128217245,-3.28879184298823,127.144887916603));
#71352=CARTESIAN_POINT('Ctrl Pts',(3.99081838190702,-3.38794504654056,127.239110076002));
#71353=CARTESIAN_POINT('Ctrl Pts',(3.98332804614494,-3.48349378139259,127.329907022576));
#71354=CARTESIAN_POINT('Ctrl Pts',(3.9758377103828,-3.5752678134635,127.424431634148));
#71355=CARTESIAN_POINT('Ctrl Pts',(3.96834737462072,-3.66298089563425,127.522325574987));
#71356=CARTESIAN_POINT('Ctrl Pts',(3.96064863976751,-3.75313436595113,127.622943159858));
#71357=CARTESIAN_POINT('Ctrl Pts',(3.95294990491429,-3.83929639987039,127.727454027614));
#71358=CARTESIAN_POINT('Ctrl Pts',(3.94525117006108,-3.92110685231847,127.835504926361));
#71359=CARTESIAN_POINT('Ctrl Pts',(3.9375616666992,-4.00281920650799,127.94342626214));
#71360=CARTESIAN_POINT('Ctrl Pts',(3.92987216333736,-4.08019011675992,128.054878873016));
#71361=CARTESIAN_POINT('Ctrl Pts',(3.92218265997548,-4.15289689457832,128.169473438672));
#71362=CARTESIAN_POINT('Ctrl Pts',(3.91450192989967,-4.22552071809771,128.283937258444));
#71363=CARTESIAN_POINT('Ctrl Pts',(3.90682119982385,-4.29349078972434,128.401535562331));
#71364=CARTESIAN_POINT('Ctrl Pts',(3.89914046974803,-4.35652573860561,128.521847408104));
#71365=CARTESIAN_POINT('Ctrl Pts',(3.89146486455688,-4.41951862809418,128.642078977091));
#71366=CARTESIAN_POINT('Ctrl Pts',(3.88378925936576,-4.47758275848176,128.765020135462));
#71367=CARTESIAN_POINT('Ctrl Pts',(3.87611365417462,-4.53048108308191,128.890222634468));
#71368=CARTESIAN_POINT('Ctrl Pts',(3.86844103308747,-4.58335884199401,129.015376457538));
#71369=CARTESIAN_POINT('Ctrl Pts',(3.86076841200032,-4.63107463184753,129.142789506805));
#71370=CARTESIAN_POINT('Ctrl Pts',(3.85309579091319,-4.6734384223704,129.271991088108));
#71371=CARTESIAN_POINT('Ctrl Pts',(3.84701143022851,-4.70703275455286,129.374447473319));
#71372=CARTESIAN_POINT('Ctrl Pts',(3.84092706954373,-4.73726240782115,129.478028048446));
#71373=CARTESIAN_POINT('Ctrl Pts',(3.83484270885904,-4.76405452823401,129.582490119308));
#71374=CARTESIAN_POINT('Ctrl Pts',(5.58457496064636,-4.76405452823403,129.582490119308));
#71375=CARTESIAN_POINT('Ctrl Pts',(5.57621930409528,-4.80065751242433,129.725204599138));
#71376=CARTESIAN_POINT('Ctrl Pts',(5.56786364754414,-4.83088577288846,129.869729750966));
#71377=CARTESIAN_POINT('Ctrl Pts',(5.55950799099307,-4.85457280706801,130.015496926314));
#71378=CARTESIAN_POINT('Ctrl Pts',(5.55117837062054,-4.87818603258305,130.160809891968));
#71379=CARTESIAN_POINT('Ctrl Pts',(5.542848750248,-4.89529863039668,130.307356877737));
#71380=CARTESIAN_POINT('Ctrl Pts',(5.53451912987546,-4.90579465410995,130.454557995783));
#71381=CARTESIAN_POINT('Ctrl Pts',(5.52796589859152,-4.9140522778525,130.570366751605));
#71382=CARTESIAN_POINT('Ctrl Pts',(5.52141266730759,-4.91821547224366,130.686580015051));
#71383=CARTESIAN_POINT('Ctrl Pts',(5.51485943602364,-4.91824978603851,130.802909882533));
#71384=CARTESIAN_POINT('',(5.86014056397397,-4.91824871042674,130.800799032843));
#71385=CARTESIAN_POINT('Ctrl Pts',(5.93020460855791,-4.76405452823401,129.582490119308));
#71386=CARTESIAN_POINT('Ctrl Pts',(5.92242989152009,-4.79808021972201,129.715155774008));
#71387=CARTESIAN_POINT('Ctrl Pts',(5.9146551744823,-4.82651889400264,129.849082692573));
#71388=CARTESIAN_POINT('Ctrl Pts',(5.90688045744446,-4.84930906415737,129.983760433078));
#71389=CARTESIAN_POINT('Ctrl Pts',(5.90388422001347,-4.85809198970231,130.035662834833));
#71390=CARTESIAN_POINT('Ctrl Pts',(5.90088798258247,-4.86603655196502,130.08767671438));
#71391=CARTESIAN_POINT('Ctrl Pts',(5.8978917451515,-4.87314129660454,130.139772801076));
#71392=CARTESIAN_POINT('Ctrl Pts',(5.88530801810389,-4.9029801092307,130.358568190401));
#71393=CARTESIAN_POINT('Ctrl Pts',(5.87272429105628,-4.91808839522474,130.579417271214));
#71394=CARTESIAN_POINT('Ctrl Pts',(5.8601405640087,-4.91824871042629,130.800799032232));
#71395=CARTESIAN_POINT('Ctrl Pts',(5.86014056397391,-4.91824871042674,130.800799032843));
#71396=CARTESIAN_POINT('Ctrl Pts',(5.85248570547013,-4.91834623240639,130.935468677974));
#71397=CARTESIAN_POINT('Ctrl Pts',(5.84483084696644,-4.91290838515486,131.070351857313));
#71398=CARTESIAN_POINT('Ctrl Pts',(5.83717598846266,-4.90190910706921,131.204947897109));
#71399=CARTESIAN_POINT('Ctrl Pts',(5.82952906258834,-4.89092122739117,131.339404456795));
#71400=CARTESIAN_POINT('Ctrl Pts',(5.82188213671392,-4.8743834115758,131.47357406995));
#71401=CARTESIAN_POINT('Ctrl Pts',(5.8142352108396,-4.85232162339504,131.606955113954));
#71402=CARTESIAN_POINT('Ctrl Pts',(5.806594256031,-4.83027706205674,131.740232008004));
#71403=CARTESIAN_POINT('Ctrl Pts',(5.79895330122243,-4.80271717437201,131.872721161818));
#71404=CARTESIAN_POINT('Ctrl Pts',(5.79131234641383,-4.76971978040956,132.003925654932));
#71405=CARTESIAN_POINT('Ctrl Pts',(5.78367476668045,-4.73673696167879,132.135072193896));
#71406=CARTESIAN_POINT('Ctrl Pts',(5.77603718694707,-4.69832150930007,132.264934809998));
#71407=CARTESIAN_POINT('Ctrl Pts',(5.76839960721369,-4.6546023401456,132.393026761729));
#71408=CARTESIAN_POINT('Ctrl Pts',(5.76076358446485,-4.61089208350954,132.521092600845));
#71409=CARTESIAN_POINT('Ctrl Pts',(5.75312756171603,-4.5618803897466,132.647388111796));
#71410=CARTESIAN_POINT('Ctrl Pts',(5.74549153896717,-4.5077458825195,132.771442243002));
#71411=CARTESIAN_POINT('Ctrl Pts',(5.7378553085799,-4.45360990326912,132.895499747483));
#71412=CARTESIAN_POINT('Ctrl Pts',(5.73021907819258,-4.39435099511473,133.01731538155));
#71413=CARTESIAN_POINT('Ctrl Pts',(5.72258284780531,-4.33019548578804,133.136439114821));
#71414=CARTESIAN_POINT('Ctrl Pts',(5.71494464519093,-4.26602340686762,133.255593614458));
#71415=CARTESIAN_POINT('Ctrl Pts',(5.70730644257658,-4.19695240360804,133.372054476202));
#71416=CARTESIAN_POINT('Ctrl Pts',(5.69966823996219,-4.12325391951159,133.485397763473));
#71417=CARTESIAN_POINT('Ctrl Pts',(5.6920220253493,-4.04947813029839,133.598859940788));
#71418=CARTESIAN_POINT('Ctrl Pts',(5.68437581073642,-3.97106539061897,133.7091976774));
#71419=CARTESIAN_POINT('Ctrl Pts',(5.67672959612352,-3.88832965658374,133.81601722884));
#71420=CARTESIAN_POINT('Ctrl Pts',(5.66907886296699,-3.80554502972464,133.922899905477));
#71421=CARTESIAN_POINT('Ctrl Pts',(5.66142812981041,-3.71843258245316,134.026259950901));
#71422=CARTESIAN_POINT('Ctrl Pts',(5.65377739665388,-3.62734453879843,134.125739045169));
#71423=CARTESIAN_POINT('Ctrl Pts',(5.64611553015503,-3.53612394387705,134.225362901356));
#71424=CARTESIAN_POINT('Ctrl Pts',(5.63845366365625,-3.44091648774859,134.321094248362));
#71425=CARTESIAN_POINT('Ctrl Pts',(5.6307917971574,-3.34210924864982,134.412613495704));
#71426=CARTESIAN_POINT('Ctrl Pts',(5.62700923855114,-3.293329467291,134.457795295298));
#71427=CARTESIAN_POINT('Ctrl Pts',(5.62322667994486,-3.24367280657356,134.501951138766));
#71428=CARTESIAN_POINT('Ctrl Pts',(5.6194441213386,-3.19318845602654,134.54504645666));
#71429=CARTESIAN_POINT('Ctrl Pts',(5.61166978721953,-3.08942741758886,134.633620735382));
#71430=CARTESIAN_POINT('Ctrl Pts',(5.60389545310043,-2.98181385883301,134.71801477323));
#71431=CARTESIAN_POINT('Ctrl Pts',(5.59612111898136,-2.87071904261656,134.797874764387));
#71432=CARTESIAN_POINT('Ctrl Pts',(5.58835636603427,-2.75976114083226,134.877636335242));
#71433=CARTESIAN_POINT('Ctrl Pts',(5.58059161308717,-2.64533083249046,134.952874751465));
#71434=CARTESIAN_POINT('Ctrl Pts',(5.57282686014008,-2.52783408368228,135.023274921966));
#71435=CARTESIAN_POINT('Ctrl Pts',(5.56506981925508,-2.41045403430128,135.093605170026));
#71436=CARTESIAN_POINT('Ctrl Pts',(5.55731277837004,-2.29001393860172,135.159106535709));
#71437=CARTESIAN_POINT('Ctrl Pts',(5.54955573748504,-2.16695022174466,135.219506119017));
#71438=CARTESIAN_POINT('Ctrl Pts',(5.54180454624488,-2.04397930819344,135.279860154529));
#71439=CARTESIAN_POINT('Ctrl Pts',(5.53405335500481,-1.91838906110722,135.335119893912));
#71440=CARTESIAN_POINT('Ctrl Pts',(5.52630216376465,-1.79064177114034,135.385057628933));
#71441=CARTESIAN_POINT('Ctrl Pts',(5.51855426698758,-1.66294877717999,135.434974139084));
#71442=CARTESIAN_POINT('Ctrl Pts',(5.5108063702105,-1.53310092715568,135.479573001762));
#71443=CARTESIAN_POINT('Ctrl Pts',(5.50305847343341,-1.40158161927083,135.518674144159));
#71444=CARTESIAN_POINT('Ctrl Pts',(5.49531219734931,-1.27008982238996,135.557767107441));
#71445=CARTESIAN_POINT('Ctrl Pts',(5.48756592126517,-1.13692763760397,135.59136452652));
#71446=CARTESIAN_POINT('Ctrl Pts',(5.47981964518107,-1.00259441687707,135.619335954756));
#71447=CARTESIAN_POINT('Ctrl Pts',(5.47207331191571,-0.868260204532673,
135.647307589471));
#71448=CARTESIAN_POINT('Ctrl Pts',(5.46432697865039,-0.732755321753876,
135.669653070774));
#71449=CARTESIAN_POINT('Ctrl Pts',(5.45658064538503,-0.59658973442259,135.686292996377));
#71450=CARTESIAN_POINT('Ctrl Pts',(5.44883257738204,-0.460393653752126,
135.702936648376));
#71451=CARTESIAN_POINT('Ctrl Pts',(5.44108450937911,-0.323536962109448,
135.713872154746));
#71452=CARTESIAN_POINT('Ctrl Pts',(5.43333644137613,-0.186534776714436,
135.719071986464));
#71453=CARTESIAN_POINT('Ctrl Pts',(5.42558013863428,-0.0493869837666271,
135.724277344625));
#71454=CARTESIAN_POINT('Ctrl Pts',(5.41782383589241,0.0879062205216979,
135.72373483598));
#71455=CARTESIAN_POINT('Ctrl Pts',(5.41006753315057,0.224829127339722,135.717469096523));
#71456=CARTESIAN_POINT('Ctrl Pts',(5.40230709063641,0.361825114035785,135.711200012852));
#71457=CARTESIAN_POINT('Ctrl Pts',(5.39454664812223,0.498450020173607,135.699201645886));
#71458=CARTESIAN_POINT('Ctrl Pts',(5.38678620560808,0.634194221701444,135.681550459233));
#71459=CARTESIAN_POINT('Ctrl Pts',(5.37901330534265,0.770156331872563,135.663870937328));
#71460=CARTESIAN_POINT('Ctrl Pts',(5.37124040507721,0.905234526767185,135.640520528812));
#71461=CARTESIAN_POINT('Ctrl Pts',(5.36346750481178,1.0389294360968,135.611626856221));
#71462=CARTESIAN_POINT('Ctrl Pts',(5.35597716904977,1.16776419871477,135.583783541407));
#71463=CARTESIAN_POINT('Ctrl Pts',(5.34848683328775,1.29531420331714,135.550793065797));
#71464=CARTESIAN_POINT('Ctrl Pts',(5.34099649752574,1.42114857971225,135.512812568779));
#71465=CARTESIAN_POINT('Ctrl Pts',(5.33322216340665,1.55175400473529,135.473392029672));
#71466=CARTESIAN_POINT('Ctrl Pts',(5.32544782928758,1.68092485605517,135.428470733813));
#71467=CARTESIAN_POINT('Ctrl Pts',(5.31767349516849,1.80816279017454,135.37816979447));
#71468=CARTESIAN_POINT('Ctrl Pts',(5.3099087422214,1.93524391491152,135.327930846539));
#71469=CARTESIAN_POINT('Ctrl Pts',(5.30214398927434,2.0603965021176,135.272325589066));
#71470=CARTESIAN_POINT('Ctrl Pts',(5.29437923632725,2.18313602214503,135.211525258388));
#71471=CARTESIAN_POINT('Ctrl Pts',(5.28662219544225,2.30575363555067,135.150785315456));
#71472=CARTESIAN_POINT('Ctrl Pts',(5.27886515455721,2.42596260323298,135.084860740015));
#71473=CARTESIAN_POINT('Ctrl Pts',(5.27110811367223,2.54329742823446,135.013971199798));
#71474=CARTESIAN_POINT('Ctrl Pts',(5.26335692243209,2.660543770132,134.943135117934));
#71475=CARTESIAN_POINT('Ctrl Pts',(5.25560573119195,2.77491995017405,134.86734172509));
#71476=CARTESIAN_POINT('Ctrl Pts',(5.24785453995182,2.88598451158511,134.786856877626));
#71477=CARTESIAN_POINT('Ctrl Pts',(5.24010664317474,2.99700186759469,134.706406238369));
#71478=CARTESIAN_POINT('Ctrl Pts',(5.23235874639765,3.10471008851892,134.621268339326));
#71479=CARTESIAN_POINT('Ctrl Pts',(5.22461084962057,3.20869638546944,134.531752543347));
#71480=CARTESIAN_POINT('Ctrl Pts',(5.21686457353648,3.31266093072833,134.442255472142));
#71481=CARTESIAN_POINT('Ctrl Pts',(5.20911829745239,3.41290480447179,134.348382580407));
#71482=CARTESIAN_POINT('Ctrl Pts',(5.20137202136829,3.50904834631291,134.250483477497));
#71483=CARTESIAN_POINT('Ctrl Pts',(5.19362568810293,3.60519259786381,134.152583651918));
#71484=CARTESIAN_POINT('Ctrl Pts',(5.18587935483762,3.69723618317356,134.050657834801));
#71485=CARTESIAN_POINT('Ctrl Pts',(5.17813302157228,3.78483664983259,133.945092156011));
#71486=CARTESIAN_POINT('Ctrl Pts',(5.17038495356932,3.87245673400862,133.839502836519));
#71487=CARTESIAN_POINT('Ctrl Pts',(5.16263688556637,3.95563146997038,133.730272334165));
#71488=CARTESIAN_POINT('Ctrl Pts',(5.1548888175634,4.0340592633321,133.617819151546));
#71489=CARTESIAN_POINT('Ctrl Pts',(5.14713251482155,4.11257041068601,133.505246452346));
#71490=CARTESIAN_POINT('Ctrl Pts',(5.13937621207964,4.18632431328884,133.389444552058));
#71491=CARTESIAN_POINT('Ctrl Pts',(5.13161990933779,4.2550629448919,133.270860647468));
#71492=CARTESIAN_POINT('Ctrl Pts',(5.12385946682361,4.32383826437243,133.152213451078));
#71493=CARTESIAN_POINT('Ctrl Pts',(5.11609902430944,4.38759279744898,133.030781637704));
#71494=CARTESIAN_POINT('Ctrl Pts',(5.10833858179527,4.44611541087243,132.907035298943));
#71495=CARTESIAN_POINT('Ctrl Pts',(5.10056568152983,4.50473196999033,132.783090311573));
#71496=CARTESIAN_POINT('Ctrl Pts',(5.09279278126444,4.55809967379698,132.656823734426));
#71497=CARTESIAN_POINT('Ctrl Pts',(5.085019880999,4.60605597290703,132.528724684968));
#71498=CARTESIAN_POINT('Ctrl Pts',(5.07752954523693,4.65226893974999,132.405282358619));
#71499=CARTESIAN_POINT('Ctrl Pts',(5.07003920947488,4.69345701135038,132.280138769438));
#71500=CARTESIAN_POINT('Ctrl Pts',(5.06254887371281,4.7295194976628,132.153741358398));
#71501=CARTESIAN_POINT('Ctrl Pts',(5.05477453959374,4.7669493041045,132.022551551101));
#71502=CARTESIAN_POINT('Ctrl Pts',(5.04700020547465,4.79897574597213,131.889595397901));
#71503=CARTESIAN_POINT('Ctrl Pts',(5.03922587135557,4.82543135245714,131.755357633978));
#71504=CARTESIAN_POINT('Ctrl Pts',(5.03146111840848,4.85185435477157,131.621285306101));
#71505=CARTESIAN_POINT('Ctrl Pts',(5.02369636546141,4.8727201072433,131.485934890081));
#71506=CARTESIAN_POINT('Ctrl Pts',(5.01593161251432,4.88791077574366,131.349806591856));
#71507=CARTESIAN_POINT('Ctrl Pts',(5.00817457162931,4.90308635665793,131.213813498176));
#71508=CARTESIAN_POINT('Ctrl Pts',(5.00041753074428,4.91259802755782,131.077044445846));
#71509=CARTESIAN_POINT('Ctrl Pts',(4.99266048985928,4.91637898865255,130.940009806416));
#71510=CARTESIAN_POINT('Ctrl Pts',(4.98490929861917,4.9201570984951,130.803078505874));
#71511=CARTESIAN_POINT('Ctrl Pts',(4.97715810737907,4.91821308962169,130.665882406115));
#71512=CARTESIAN_POINT('Ctrl Pts',(4.96940691613895,4.91053201634603,130.528936619083));
#71513=CARTESIAN_POINT('Ctrl Pts',(4.96165901936186,4.90285420773139,130.392049037662));
#71514=CARTESIAN_POINT('Ctrl Pts',(4.95391112258479,4.8894442063653,130.255411946902));
#71515=CARTESIAN_POINT('Ctrl Pts',(4.94616322580771,4.87033916549697,130.11953985596));
#71516=CARTESIAN_POINT('Ctrl Pts',(4.93841694972362,4.85123812099136,129.983696186531));
#71517=CARTESIAN_POINT('Ctrl Pts',(4.9306706736395,4.82644446090755,129.848617585542));
#71518=CARTESIAN_POINT('Ctrl Pts',(4.92292439755539,4.79604710578405,129.714812444422));
#71519=CARTESIAN_POINT('Ctrl Pts',(4.91517806429004,4.76564952627418,129.581006315584));
#71520=CARTESIAN_POINT('Ctrl Pts',(4.90743173102474,4.72964825579454,129.448474046625));
#71521=CARTESIAN_POINT('Ctrl Pts',(4.89968539775938,4.68818305244258,129.31771246508));
#71522=CARTESIAN_POINT('Ctrl Pts',(4.89193732975641,4.64670856324583,129.186921600385));
#71523=CARTESIAN_POINT('Ctrl Pts',(4.88418926175342,4.59976782448988,129.057902584763));
#71524=CARTESIAN_POINT('Ctrl Pts',(4.87644119375045,4.5475499151299,128.93113536899));
#71525=CARTESIAN_POINT('Ctrl Pts',(4.8686848910086,4.49527650795445,128.804233423511));
#71526=CARTESIAN_POINT('Ctrl Pts',(4.86092858826677,4.43771487545824,128.679588420708));
#71527=CARTESIAN_POINT('Ctrl Pts',(4.85317228552492,4.37510178747198,128.557659166158));
#71528=CARTESIAN_POINT('Ctrl Pts',(4.84541184301076,4.31245528099541,128.435664834293));
#71529=CARTESIAN_POINT('Ctrl Pts',(4.83765140049659,4.24475213969536,128.316389478728));
#71530=CARTESIAN_POINT('Ctrl Pts',(4.82989095798243,4.17227374226681,128.200264827836));
#71531=CARTESIAN_POINT('Ctrl Pts',(4.82211805771699,4.09967899608028,128.083953763345));
#71532=CARTESIAN_POINT('Ctrl Pts',(4.81434515745157,4.02229389615795,127.9708038335));
#71533=CARTESIAN_POINT('Ctrl Pts',(4.80657225718613,3.94044208896177,127.86121617564));
#71534=CARTESIAN_POINT('Ctrl Pts',(4.79908192142407,3.86156580112909,127.755612305178));
#71535=CARTESIAN_POINT('Ctrl Pts',(4.79159158566201,3.77854211407504,127.653316447279));
#71536=CARTESIAN_POINT('Ctrl Pts',(4.78410124989995,3.69169304713321,127.554655168106));
#71537=CARTESIAN_POINT('Ctrl Pts',(4.77632691578087,3.60155107142158,127.452253116547));
#71538=CARTESIAN_POINT('Ctrl Pts',(4.76855258166181,3.50700236833949,127.353442315528));
#71539=CARTESIAN_POINT('Ctrl Pts',(4.76077824754273,3.40836423725886,127.25862567419));
#71540=CARTESIAN_POINT('Ctrl Pts',(4.75301349459563,3.30984766885912,127.163925885889));
#71541=CARTESIAN_POINT('Ctrl Pts',(4.74524874164859,3.20725197942357,127.073210731409));
#71542=CARTESIAN_POINT('Ctrl Pts',(4.73748398870148,3.10093431415033,126.986849721468));
#71543=CARTESIAN_POINT('Ctrl Pts',(4.72972694781647,2.99472224508107,126.9005744865));
#71544=CARTESIAN_POINT('Ctrl Pts',(4.72196990693145,2.88479585831222,126.818645034834));
#71545=CARTESIAN_POINT('Ctrl Pts',(4.71421286604644,2.77154843696411,126.741393435313));
#71546=CARTESIAN_POINT('Ctrl Pts',(4.70646167480635,2.65838641637798,126.664200091826));
#71547=CARTESIAN_POINT('Ctrl Pts',(4.69871048356626,2.54190866777437,126.591677798427));
#71548=CARTESIAN_POINT('Ctrl Pts',(4.69095929232617,2.42254049091172,126.524117559936));
#71549=CARTESIAN_POINT('Ctrl Pts',(4.68321139554909,2.303223048708,126.456586036347));
#71550=CARTESIAN_POINT('Ctrl Pts',(4.67546349877192,2.18101796119212,126.394012565185));
#71551=CARTESIAN_POINT('Ctrl Pts',(4.66771560199484,2.05637818172992,126.336643993136));
#71552=CARTESIAN_POINT('Ctrl Pts',(4.65996932591073,1.93176447422232,126.279287421356));
#71553=CARTESIAN_POINT('Ctrl Pts',(4.65222304982664,1.80471744269036,126.227133746464));
#71554=CARTESIAN_POINT('Ctrl Pts',(4.64447677374253,1.67571287496711,126.18038295508));
#71555=CARTESIAN_POINT('Ctrl Pts',(4.63673044047714,1.54670735496128,126.133631818592));
#71556=CARTESIAN_POINT('Ctrl Pts',(4.62898410721181,1.41574463750276,126.092283778403));
#71557=CARTESIAN_POINT('Ctrl Pts',(4.62123777394643,1.283318260332,126.056489799484));
#71558=CARTESIAN_POINT('Ctrl Pts',(4.61348970594347,1.15086222719296,126.020687804751));
#71559=CARTESIAN_POINT('Ctrl Pts',(4.60574163794052,1.01694225945359,125.99044244829));
#71560=CARTESIAN_POINT('Ctrl Pts',(4.59799356993756,0.882064355087217,125.965854077735));
#71561=CARTESIAN_POINT('Ctrl Pts',(4.59023726719571,0.747043100878831,125.941239574368));
#71562=CARTESIAN_POINT('Ctrl Pts',(4.58248096445379,0.61106226150561,125.922294137379));
#71563=CARTESIAN_POINT('Ctrl Pts',(4.57472466171194,0.474635822970092,125.909066561224));
#71564=CARTESIAN_POINT('Ctrl Pts',(4.56696421919776,0.338136569536235,125.895831925114));
#71565=CARTESIAN_POINT('Ctrl Pts',(4.55920377668363,0.20119163323181,125.888321252197));
#71566=CARTESIAN_POINT('Ctrl Pts',(4.55144333416945,0.0643163314213354,
125.886531170339));
#71567=CARTESIAN_POINT('Ctrl Pts',(4.54367043390401,-0.0727786947746378,
125.884738214883));
#71568=CARTESIAN_POINT('Ctrl Pts',(4.53589753363858,-0.209803472069553,
125.888684190186));
#71569=CARTESIAN_POINT('Ctrl Pts',(4.52812463337315,-0.346245573441667,
125.898313627843));
#71570=CARTESIAN_POINT('Ctrl Pts',(4.52063429761112,-0.477727660751992,
125.907593011186));
#71571=CARTESIAN_POINT('Ctrl Pts',(4.51314396184914,-0.608668393989772,
125.922149780548));
#71572=CARTESIAN_POINT('Ctrl Pts',(4.50565362608711,-0.738618964478486,
125.941889528931));
#71573=CARTESIAN_POINT('Ctrl Pts',(4.497879291968,-0.873496650345266,125.962377715873));
#71574=CARTESIAN_POINT('Ctrl Pts',(4.49010495784889,-1.00773485920604,125.988514565996));
#71575=CARTESIAN_POINT('Ctrl Pts',(4.48233062372978,-1.14082310413027,126.020250908583));
#71576=CARTESIAN_POINT('Ctrl Pts',(4.47456587078265,-1.27374732968725,126.051948138964));
#71577=CARTESIAN_POINT('Ctrl Pts',(4.46680111783557,-1.40552403451739,126.08923104131));
#71578=CARTESIAN_POINT('Ctrl Pts',(4.45903636488845,-1.53564929308527,126.13199886882));
#71579=CARTESIAN_POINT('Ctrl Pts',(4.45127932400344,-1.66564530941155,126.17472421872));
#71580=CARTESIAN_POINT('Ctrl Pts',(4.44352228311836,-1.79399277461118,126.222923531322));
#71581=CARTESIAN_POINT('Ctrl Pts',(4.43576524223334,-1.92019973062742,126.27644541772));
#71582=CARTESIAN_POINT('Ctrl Pts',(4.42801405099323,-2.04631151299604,126.329926942847));
#71583=CARTESIAN_POINT('Ctrl Pts',(4.42026285975314,-2.17028564061794,126.388722900531));
#71584=CARTESIAN_POINT('Ctrl Pts',(4.41251166851302,-2.2916473979909,126.452632769253));
#71585=CARTESIAN_POINT('Ctrl Pts',(4.40476377173592,-2.41295757338004,126.516515474576));
#71586=CARTESIAN_POINT('Ctrl Pts',(4.39701587495879,-2.53165724166949,126.585507586127));
#71587=CARTESIAN_POINT('Ctrl Pts',(4.38926797818169,-2.647293891392,126.659361448073));
#71588=CARTESIAN_POINT('Ctrl Pts',(4.38152170209758,-2.76290635242006,126.733199861383));
#71589=CARTESIAN_POINT('Ctrl Pts',(4.37377542601346,-2.8754567400147,126.811897791967));
#71590=CARTESIAN_POINT('Ctrl Pts',(4.36602914992935,-2.98451962482338,126.895163043697));
#71591=CARTESIAN_POINT('Ctrl Pts',(4.35828281666399,-3.09358331470935,126.978428910072));
#71592=CARTESIAN_POINT('Ctrl Pts',(4.35053648339867,-3.19915913968632,127.066261927622));
#71593=CARTESIAN_POINT('Ctrl Pts',(4.34279015013331,-3.30085331944363,127.158328469323));
#71594=CARTESIAN_POINT('Ctrl Pts',(4.3350420821303,-3.40257027290781,127.250415628689));
#71595=CARTESIAN_POINT('Ctrl Pts',(4.32729401412733,-3.50040356163289,127.346737936408));
#71596=CARTESIAN_POINT('Ctrl Pts',(4.31954594612432,-3.59399525604552,127.446923922404));
#71597=CARTESIAN_POINT('Ctrl Pts',(4.31178964338246,-3.68768642082447,127.547216387258));
#71598=CARTESIAN_POINT('Ctrl Pts',(4.3040333406406,-3.77712671872418,127.65138044714));
#71599=CARTESIAN_POINT('Ctrl Pts',(4.29627703789873,-3.86199727559698,127.759010045664));
#71600=CARTESIAN_POINT('Ctrl Pts',(4.28851659538457,-3.94691313044127,127.866697089346));
#71601=CARTESIAN_POINT('Ctrl Pts',(4.28075615287032,-4.02725415541798,127.977853040572));
#71602=CARTESIAN_POINT('Ctrl Pts',(4.27299571035616,-4.10274464597638,128.092042525525));
#71603=CARTESIAN_POINT('Ctrl Pts',(4.26522281009071,-4.17835632057217,128.206415317578));
#71604=CARTESIAN_POINT('Ctrl Pts',(4.25744990982529,-4.24910169893824,128.323831039497));
#71605=CARTESIAN_POINT('Ctrl Pts',(4.24967700955983,-4.31475046889258,128.443828589889));
#71606=CARTESIAN_POINT('Ctrl Pts',(4.24218667379792,-4.37801274069866,128.559463927066));
#71607=CARTESIAN_POINT('Ctrl Pts',(4.23469633803604,-4.4365423830845,128.67749636378));
#71608=CARTESIAN_POINT('Ctrl Pts',(4.22720600227413,-4.49017623127887,128.797497275293));
#71609=CARTESIAN_POINT('Ctrl Pts',(4.21867919408695,-4.55123164326934,128.934103268305));
#71610=CARTESIAN_POINT('Ctrl Pts',(4.21015238589982,-4.60610988282734,129.073633207333));
#71611=CARTESIAN_POINT('Ctrl Pts',(4.20162557771272,-4.65454812012595,129.215535624078));
#71612=CARTESIAN_POINT('Ctrl Pts',(4.1943716338636,-4.69575559727382,129.336255140752));
#71613=CARTESIAN_POINT('Ctrl Pts',(4.18711769001443,-4.73230293808678,129.458691151222));
#71614=CARTESIAN_POINT('Ctrl Pts',(4.1798637461653,-4.76405452823409,129.582490119308));
#71615=CARTESIAN_POINT('Origin',(213.235140564004,0.,130.804360617566));
#71616=CARTESIAN_POINT('',(2.08495204958918,-4.764054528234,129.582490119308));
#71617=CARTESIAN_POINT('',(2.43008709577655,-4.76405452823407,129.582490119308));
#71618=CARTESIAN_POINT('',(213.235140564004,-4.76405452823405,129.582490119308));
#71619=CARTESIAN_POINT('',(3.76485943594234,-4.91824795725753,130.808843187376));
#71620=CARTESIAN_POINT('Ctrl Pts',(3.76485943594241,-4.91824795725753,130.808843187376));
#71621=CARTESIAN_POINT('Ctrl Pts',(3.75516901773868,-4.91809184520243,130.980128371696));
#71622=CARTESIAN_POINT('Ctrl Pts',(3.74547859953493,-4.90898427284577,131.151013822307));
#71623=CARTESIAN_POINT('Ctrl Pts',(3.7357881813312,-4.8910718301247,131.320693276867));
#71624=CARTESIAN_POINT('Ctrl Pts',(3.7259228264609,-4.8728360223069,131.493435876643));
#71625=CARTESIAN_POINT('Ctrl Pts',(3.71605747159059,-4.84547460045101,131.664928684303));
#71626=CARTESIAN_POINT('Ctrl Pts',(3.70619211672027,-4.80919068690557,131.834345083216));
#71627=CARTESIAN_POINT('Ctrl Pts',(3.7007613280828,-4.78921672063713,131.927607278679));
#71628=CARTESIAN_POINT('Ctrl Pts',(3.69533053944535,-4.76653972229635,132.020240647857));
#71629=CARTESIAN_POINT('Ctrl Pts',(3.68989975080788,-4.74119968075756,132.112110077395));
#71630=CARTESIAN_POINT('Ctrl Pts',(3.68212541668877,-4.70492466387409,132.243623875528));
#71631=CARTESIAN_POINT('Ctrl Pts',(3.67435108256961,-4.66311604850594,132.373835516073));
#71632=CARTESIAN_POINT('Ctrl Pts',(3.6665767484505,-4.61588295417604,132.502243892661));
#71633=CARTESIAN_POINT('Ctrl Pts',(3.65881199550337,-4.56870807041356,132.630494017401));
#71634=CARTESIAN_POINT('Ctrl Pts',(3.65104724255629,-4.51612214288966,132.756944936613));
#71635=CARTESIAN_POINT('Ctrl Pts',(3.64328248960916,-4.45828473125545,132.881108150983));
#71636=CARTESIAN_POINT('Ctrl Pts',(3.63552544872412,-4.40050476455383,133.005148044698));
#71637=CARTESIAN_POINT('Ctrl Pts',(3.62776840783913,-4.33748385753299,133.126904403205));
#71638=CARTESIAN_POINT('Ctrl Pts',(3.62001136695409,-4.26943044402365,133.245906592178));
#71639=CARTESIAN_POINT('Ctrl Pts',(3.61226017571392,-4.20142835012282,133.364819040674));
#71640=CARTESIAN_POINT('Ctrl Pts',(3.6045089844737,-4.1284014968548,133.480981115646));
#71641=CARTESIAN_POINT('Ctrl Pts',(3.59675779323354,-4.05060507027287,133.593945107625));
#71642=CARTESIAN_POINT('Ctrl Pts',(3.58900989645643,-3.97284170924763,133.706861086895));
#71643=CARTESIAN_POINT('Ctrl Pts',(3.58126199967937,-3.89031302813405,133.816581365339));
#71644=CARTESIAN_POINT('Ctrl Pts',(3.57351410290227,-3.80331839489694,133.922685849087));
#71645=CARTESIAN_POINT('Ctrl Pts',(3.56576782681814,-3.71634195906172,134.028768138064));
#71646=CARTESIAN_POINT('Ctrl Pts',(3.55802155073404,-3.6249016769672,134.131235834614));
#71647=CARTESIAN_POINT('Ctrl Pts',(3.55027527464992,-3.52933794648657,134.229700998023));
#71648=CARTESIAN_POINT('Ctrl Pts',(3.54252894138455,-3.43377351057619,134.32816688828));
#71649=CARTESIAN_POINT('Ctrl Pts',(3.53478260811909,-3.33408583783187,134.422629905881));
#71650=CARTESIAN_POINT('Ctrl Pts',(3.52703627485371,-3.23065272900738,134.512738430985));
#71651=CARTESIAN_POINT('Ctrl Pts',(3.51928820685072,-3.12719645705546,134.602867135268));
#71652=CARTESIAN_POINT('Ctrl Pts',(3.51154013884777,-3.01999337471197,134.688639149835));
#71653=CARTESIAN_POINT('Ctrl Pts',(3.50379207084478,-2.9094546266219,134.769742924246));
#71654=CARTESIAN_POINT('Ctrl Pts',(3.4960357681029,-2.79879839663478,134.850932896713));
#71655=CARTESIAN_POINT('Ctrl Pts',(3.48827946536104,-2.68479973473342,134.92744448632));
#71656=CARTESIAN_POINT('Ctrl Pts',(3.48052316261916,-2.56789951700299,134.999009009634));
#71657=CARTESIAN_POINT('Ctrl Pts',(3.47276272010497,-2.45093690610641,135.070611729088));
#71658=CARTESIAN_POINT('Ctrl Pts',(3.46500227759081,-2.33106999509739,135.137261931131));
#71659=CARTESIAN_POINT('Ctrl Pts',(3.45724183507662,-2.20876367358131,135.198737262412));
#71660=CARTESIAN_POINT('Ctrl Pts',(3.44946893481116,-2.08626101510008,135.260311279352));
#71661=CARTESIAN_POINT('Ctrl Pts',(3.44169603454567,-1.96131147734824,135.316693664275));
#71662=CARTESIAN_POINT('Ctrl Pts',(3.43392313428021,-1.83440013619927,135.367710177134));
#71663=CARTESIAN_POINT('Ctrl Pts',(3.42643279851843,-1.71210234197607,135.416872111247));
#71664=CARTESIAN_POINT('Ctrl Pts',(3.41894246275668,-1.58798319121196,135.46105142278));
#71665=CARTESIAN_POINT('Ctrl Pts',(3.4114521269949,-1.46248757974431,135.500136713335));
#71666=CARTESIAN_POINT('Ctrl Pts',(3.40367779287583,-1.33223376402007,135.540703934562));
#71667=CARTESIAN_POINT('Ctrl Pts',(3.3959034587567,-1.2000844452058,135.575911734682));
#71668=CARTESIAN_POINT('Ctrl Pts',(3.38812912463763,-1.06652020005127,135.605581058806));
#71669=CARTESIAN_POINT('Ctrl Pts',(3.38036437169055,-0.933120560891917,
135.63521381814));
#71670=CARTESIAN_POINT('Ctrl Pts',(3.37259961874353,-0.798309842973666,
135.659321598573));
#71671=CARTESIAN_POINT('Ctrl Pts',(3.36483486579644,-0.662585280494269,
135.677774596346));
#71672=CARTESIAN_POINT('Ctrl Pts',(3.35707782491145,-0.526995521563893,
135.696209266342));
#71673=CARTESIAN_POINT('Ctrl Pts',(3.3493207840264,-0.390494109217712,135.709000278258));
#71674=CARTESIAN_POINT('Ctrl Pts',(3.34156374314142,-0.253589665019819,
135.71606860403));
#71675=CARTESIAN_POINT('Ctrl Pts',(3.3338125519013,-0.116788461528071,135.723131599522));
#71676=CARTESIAN_POINT('Ctrl Pts',(3.32606136066122,0.0204147799969158,
135.724480478579));
#71677=CARTESIAN_POINT('Ctrl Pts',(3.3183101694211,0.157505454606213,135.72008793855));
#71678=CARTESIAN_POINT('Ctrl Pts',(3.31056227264402,0.294537862021787,135.715697265468));
#71679=CARTESIAN_POINT('Ctrl Pts',(3.30281437586693,0.431457407733053,135.70557003928));
#71680=CARTESIAN_POINT('Ctrl Pts',(3.29506647908985,0.567748839171424,135.689731055733));
#71681=CARTESIAN_POINT('Ctrl Pts',(3.28732020300576,0.704011761380442,135.673895385361));
#71682=CARTESIAN_POINT('Ctrl Pts',(3.27957392692169,0.839646442548953,135.65235037921));
#71683=CARTESIAN_POINT('Ctrl Pts',(3.27182765083759,0.974142503801548,135.625172732219));
#71684=CARTESIAN_POINT('Ctrl Pts',(3.26408131757225,1.10863955787352,135.597994884609));
#71685=CARTESIAN_POINT('Ctrl Pts',(3.25633498430693,1.24199759203833,135.56518439063));
#71686=CARTESIAN_POINT('Ctrl Pts',(3.24858865104159,1.37371656802735,135.52686904564));
#71687=CARTESIAN_POINT('Ctrl Pts',(3.24084058303862,1.50546504156776,135.488545120194));
#71688=CARTESIAN_POINT('Ctrl Pts',(3.23309251503565,1.63557335120067,135.444713999841));
#71689=CARTESIAN_POINT('Ctrl Pts',(3.22534444703268,1.76355714699191,135.395553191592));
#71690=CARTESIAN_POINT('Ctrl Pts',(3.21758814429084,1.89167696548434,135.346340134651));
#71691=CARTESIAN_POINT('Ctrl Pts',(3.20983184154892,2.01766739407113,135.291786214866));
#71692=CARTESIAN_POINT('Ctrl Pts',(3.20207553880707,2.14106407747729,135.232117123816));
#71693=CARTESIAN_POINT('Ctrl Pts',(3.1943150962929,2.26452662140879,135.172416185575));
#71694=CARTESIAN_POINT('Ctrl Pts',(3.18655465377879,2.38539231733127,135.107594820762));
#71695=CARTESIAN_POINT('Ctrl Pts',(3.17879421126463,2.50322280888666,135.037923966752));
#71696=CARTESIAN_POINT('Ctrl Pts',(3.17102131099921,2.6212424524076,134.968141270902));
#71697=CARTESIAN_POINT('Ctrl Pts',(3.16324841073373,2.73621682689186,134.893493742304));
#71698=CARTESIAN_POINT('Ctrl Pts',(3.15547551046831,2.84773714389602,134.814295308029));
#71699=CARTESIAN_POINT('Ctrl Pts',(3.14798517470621,2.95520341647541,134.737975936327));
#71700=CARTESIAN_POINT('Ctrl Pts',(3.14049483894416,3.05946215526273,134.657430976572));
#71701=CARTESIAN_POINT('Ctrl Pts',(3.13300450318206,3.1601791605628,134.572974518677));
#71702=CARTESIAN_POINT('Ctrl Pts',(3.12523016906299,3.26471488173007,134.485315868511));
#71703=CARTESIAN_POINT('Ctrl Pts',(3.11745583494393,3.36576613585352,134.393165579892));
#71704=CARTESIAN_POINT('Ctrl Pts',(3.10968150082485,3.46292251551207,134.296831192111));
#71705=CARTESIAN_POINT('Ctrl Pts',(3.10191674787777,3.55995915861568,134.200615527852));
#71706=CARTESIAN_POINT('Ctrl Pts',(3.09415199493068,3.65311020303134,134.100226297019));
#71707=CARTESIAN_POINT('Ctrl Pts',(3.0863872419836,3.74199767395112,133.996011674722));
#71708=CARTESIAN_POINT('Ctrl Pts',(3.07863020109861,3.83079686058169,133.891900559857));
#71709=CARTESIAN_POINT('Ctrl Pts',(3.07087316021368,3.91534064877232,133.783971910108));
#71710=CARTESIAN_POINT('Ctrl Pts',(3.0631161193287,3.99528762759541,133.672610926602));
#71711=CARTESIAN_POINT('Ctrl Pts',(3.05536492808856,4.07517431778009,133.561333921279));
#71712=CARTESIAN_POINT('Ctrl Pts',(3.04761373684839,4.15047087135219,133.446630050465));
#71713=CARTESIAN_POINT('Ctrl Pts',(3.03986254560826,4.22087616127534,133.328917508127));
#71714=CARTESIAN_POINT('Ctrl Pts',(3.03211464883119,4.29125152707197,133.21125499676));
#71715=CARTESIAN_POINT('Ctrl Pts',(3.02436675205405,4.35673956376432,133.090586692064));
#71716=CARTESIAN_POINT('Ctrl Pts',(3.01661885527699,4.4170826261191,132.967359493325));
#71717=CARTESIAN_POINT('Ctrl Pts',(3.0088725791929,4.47741306600616,132.84415807106));
#71718=CARTESIAN_POINT('Ctrl Pts',(3.00112630310885,4.53260050037787,132.718399170329));
#71719=CARTESIAN_POINT('Ctrl Pts',(2.99338002702476,4.5824335826097,132.590553642821));
#71720=CARTESIAN_POINT('Ctrl Pts',(2.98563369375941,4.63226703269803,132.462707171587));
#71721=CARTESIAN_POINT('Ctrl Pts',(2.97788736049404,4.6767459097886,132.332774407112));
#71722=CARTESIAN_POINT('Ctrl Pts',(2.97014102722869,4.71570744883851,132.201245122265));
#71723=CARTESIAN_POINT('Ctrl Pts',(2.96239295922573,4.7546777130549,132.069686382348));
#71724=CARTESIAN_POINT('Ctrl Pts',(2.95464489122278,4.78812806956927,131.93653078541));
#71725=CARTESIAN_POINT('Ctrl Pts',(2.94689682321982,4.81594605708595,131.802281775643));
#71726=CARTESIAN_POINT('Ctrl Pts',(2.93914052047796,4.84379360989085,131.667890084431));
#71727=CARTESIAN_POINT('Ctrl Pts',(2.93138421773616,4.86599675626703,131.53240304243));
#71728=CARTESIAN_POINT('Ctrl Pts',(2.92362791499431,4.8824943815624,131.396333316693));
#71729=CARTESIAN_POINT('Ctrl Pts',(2.91586747248016,4.89900081213713,131.260190966447));
#71730=CARTESIAN_POINT('Ctrl Pts',(2.90810702996598,4.90979562303861,131.123465702341));
#71731=CARTESIAN_POINT('Ctrl Pts',(2.90034658745182,4.91486981923424,130.986672774265));
#71732=CARTESIAN_POINT('Ctrl Pts',(2.8925736871864,4.91995216098007,130.849660254037));
#71733=CARTESIAN_POINT('Ctrl Pts',(2.88480078692092,4.91929553885698,130.712580243966));
#71734=CARTESIAN_POINT('Ctrl Pts',(2.8770278866555,4.91294310846071,130.575946354595));
#71735=CARTESIAN_POINT('Ctrl Pts',(2.86953755089338,4.90682160491007,130.444279451262));
#71736=CARTESIAN_POINT('Ctrl Pts',(2.86204721513129,4.89541124409234,130.313027103391));
#71737=CARTESIAN_POINT('Ctrl Pts',(2.85455687936917,4.87879563564792,130.182640255922));
#71738=CARTESIAN_POINT('Ctrl Pts',(2.84678254525008,4.86155004135932,130.047309751502));
#71739=CARTESIAN_POINT('Ctrl Pts',(2.83900821113101,4.83864206488063,129.912482987593));
#71740=CARTESIAN_POINT('Ctrl Pts',(2.83123387701193,4.81010861248993,129.77867148408));
#71741=CARTESIAN_POINT('Ctrl Pts',(2.82346912406483,4.78161032502918,129.645024891287));
#71742=CARTESIAN_POINT('Ctrl Pts',(2.81570437111772,4.74750043680579,129.512391448036));
#71743=CARTESIAN_POINT('Ctrl Pts',(2.80793961817062,4.70786757278504,129.381277352392));
#71744=CARTESIAN_POINT('Ctrl Pts',(2.80018257728562,4.66827407268356,129.250293481116));
#71745=CARTESIAN_POINT('Ctrl Pts',(2.79242553640064,4.62316862556491,129.120826326213));
#71746=CARTESIAN_POINT('Ctrl Pts',(2.78466849551563,4.57269077110158,128.993371336984));
#71747=CARTESIAN_POINT('Ctrl Pts',(2.7769173042755,4.52225098238097,128.866012462554));
#71748=CARTESIAN_POINT('Ctrl Pts',(2.76916611303533,4.46644699370828,128.740663095552));
#71749=CARTESIAN_POINT('Ctrl Pts',(2.76141492179519,4.40546787699527,128.617802626736));
#71750=CARTESIAN_POINT('Ctrl Pts',(2.7536670250181,4.34451467803353,128.494994376897));
#71751=CARTESIAN_POINT('Ctrl Pts',(2.74591912824104,4.27839089925505,128.374673270734));
#71752=CARTESIAN_POINT('Ctrl Pts',(2.73817123146395,4.20733326614456,128.257297632461));
#71753=CARTESIAN_POINT('Ctrl Pts',(2.73042495537984,4.13629049675909,128.139946546641));
#71754=CARTESIAN_POINT('Ctrl Pts',(2.72267867929577,4.06031612820225,128.025540037437));
#71755=CARTESIAN_POINT('Ctrl Pts',(2.71493240321166,3.97969206332346,127.91451042359));
#71756=CARTESIAN_POINT('Ctrl Pts',(2.70718606994631,3.89906740329614,127.803479990149));
#71757=CARTESIAN_POINT('Ctrl Pts',(2.69943973668084,3.81379320817995,127.695826818162));
#71758=CARTESIAN_POINT('Ctrl Pts',(2.69169340341548,3.72419355928067,127.59195258067));
#71759=CARTESIAN_POINT('Ctrl Pts',(2.68394533541251,3.63457384516137,127.488055081263));
#71760=CARTESIAN_POINT('Ctrl Pts',(2.67619726740958,3.5406270050612,127.387938496313));
#71761=CARTESIAN_POINT('Ctrl Pts',(2.66844919940661,3.44271581275968,127.291969566576));
#71762=CARTESIAN_POINT('Ctrl Pts',(2.66069289666475,3.34470055927768,127.195898639918));
#71763=CARTESIAN_POINT('Ctrl Pts',(2.65293659392291,3.24271281660731,127.103984448389));
#71764=CARTESIAN_POINT('Ctrl Pts',(2.64518029118105,3.13715087209901,127.016555518543));
#71765=CARTESIAN_POINT('Ctrl Pts',(2.63741984866688,3.03153258600251,126.929079925244));
#71766=CARTESIAN_POINT('Ctrl Pts',(2.6296594061527,2.92233660802012,126.846094600158));
#71767=CARTESIAN_POINT('Ctrl Pts',(2.62189896363853,2.80999157044021,126.767885616212));
#71768=CARTESIAN_POINT('Ctrl Pts',(2.6141260633731,2.69746618663247,126.689551084262));
#71769=CARTESIAN_POINT('Ctrl Pts',(2.60635316310764,2.58178197155513,126.616008425242));
#71770=CARTESIAN_POINT('Ctrl Pts',(2.59858026284221,2.46339436695886,126.547498950171));
#71771=CARTESIAN_POINT('Ctrl Pts',(2.59108992708022,2.34931044999069,126.481479967085));
#71772=CARTESIAN_POINT('Ctrl Pts',(2.58359959131826,2.23271655373394,126.420134726759));
#71773=CARTESIAN_POINT('Ctrl Pts',(2.57610925555628,2.1140372639896,126.36363663279));
#71774=CARTESIAN_POINT('Ctrl Pts',(2.56833492143719,1.99085821290211,126.304996396416));
#71775=CARTESIAN_POINT('Ctrl Pts',(2.56056058731809,1.86504231708822,126.251392366595));
#71776=CARTESIAN_POINT('Ctrl Pts',(2.552786253199,1.73703988145857,126.203069982024));
#71777=CARTESIAN_POINT('Ctrl Pts',(2.5450215002519,1.60919519739092,126.154807150474));
#71778=CARTESIAN_POINT('Ctrl Pts',(2.5372567473048,1.47916969744489,126.11181314965));
#71779=CARTESIAN_POINT('Ctrl Pts',(2.5294919943577,1.34743716434546,126.074287029276));
#71780=CARTESIAN_POINT('Ctrl Pts',(2.5217349534727,1.21583546985517,126.036798180374));
#71781=CARTESIAN_POINT('Ctrl Pts',(2.51397791258765,1.08253048980571,126.004766510851));
#71782=CARTESIAN_POINT('Ctrl Pts',(2.50622087170265,0.948014484327536,125.978342424479));
#71783=CARTESIAN_POINT('Ctrl Pts',(2.49846968046252,0.813599918415293,125.951938264716));
#71784=CARTESIAN_POINT('Ctrl Pts',(2.49071848922249,0.677976526911703,125.931133346144));
#71785=CARTESIAN_POINT('Ctrl Pts',(2.48296729798236,0.541649832826402,125.916027719624));
#71786=CARTESIAN_POINT('Ctrl Pts',(2.47521940120528,0.405381081222907,125.900928513399));
#71787=CARTESIAN_POINT('Ctrl Pts',(2.46747150442819,0.268410009344956,125.891523824321));
#71788=CARTESIAN_POINT('Ctrl Pts',(2.45972360765111,0.131250174239513,125.887862223967));
#71789=CARTESIAN_POINT('Ctrl Pts',(2.45197733156701,-0.00588096998543594,
125.884201389541));
#71790=CARTESIAN_POINT('Ctrl Pts',(2.44423105548288,-0.143200408321297,
125.886281264755));
#71791=CARTESIAN_POINT('Ctrl Pts',(2.43648477939877,-0.280192043391584,
125.894098355597));
#71792=CARTESIAN_POINT('Ctrl Pts',(2.42873844613342,-0.417184689702813,
125.901915504142));
#71793=CARTESIAN_POINT('Ctrl Pts',(2.42099211286805,-0.553849137589757,
125.91546993055));
#71794=CARTESIAN_POINT('Ctrl Pts',(2.4132457796027,-0.689672274285727,125.93470609013));
#71795=CARTESIAN_POINT('Ctrl Pts',(2.40549771159972,-0.825525827631614,
125.953946557514));
#71796=CARTESIAN_POINT('Ctrl Pts',(2.39774964359676,-0.96053730785265,125.978871235153));
#71797=CARTESIAN_POINT('Ctrl Pts',(2.39000157559377,-1.09420207747503,126.009373143531));
#71798=CARTESIAN_POINT('Ctrl Pts',(2.38224527285192,-1.22800890760501,126.0399074697));
#71799=CARTESIAN_POINT('Ctrl Pts',(2.37448897011011,-1.36046578618579,126.076030780401));
#71800=CARTESIAN_POINT('Ctrl Pts',(2.36673266736827,-1.49108103048203,126.117585561833));
#71801=CARTESIAN_POINT('Ctrl Pts',(2.3589722248541,-1.62176598806707,126.159162522304));
#71802=CARTESIAN_POINT('Ctrl Pts',(2.35121178233986,-1.75060698568748,126.206176595933));
#71803=CARTESIAN_POINT('Ctrl Pts',(2.34345133982569,-1.87713165586705,126.258421791642));
#71804=CARTESIAN_POINT('Ctrl Pts',(2.33567843956026,-2.00385943467953,126.310750855978));
#71805=CARTESIAN_POINT('Ctrl Pts',(2.3279055392948,-2.12826310054298,126.36832765889));
#71806=CARTESIAN_POINT('Ctrl Pts',(2.32013263902937,-2.24989345427112,126.430899458835));
#71807=CARTESIAN_POINT('Ctrl Pts',(2.31264230326736,-2.36710223827254,126.491196616244));
#71808=CARTESIAN_POINT('Ctrl Pts',(2.30515196750539,-2.4817355752373,126.556131762438));
#71809=CARTESIAN_POINT('Ctrl Pts',(2.29766163174338,-2.59341807681275,126.62544141024));
#71810=CARTESIAN_POINT('Ctrl Pts',(2.28988595511789,-2.70935507143737,126.697391376897));
#71811=CARTESIAN_POINT('Ctrl Pts',(2.2821102784924,-2.82247926998559,126.774283696204));
#71812=CARTESIAN_POINT('Ctrl Pts',(2.27433460186691,-2.93234054597536,126.855872047882));
#71813=CARTESIAN_POINT('Ctrl Pts',(2.26644366218868,-3.04383035497371,126.938669827746));
#71814=CARTESIAN_POINT('Ctrl Pts',(2.25855272251043,-3.15195935181584,127.026303834178));
#71815=CARTESIAN_POINT('Ctrl Pts',(2.2506617828322,-3.2562832339872,127.118468247657));
#71816=CARTESIAN_POINT('Ctrl Pts',(2.24290557038219,-3.35882592557094,127.209059077193));
#71817=CARTESIAN_POINT('Ctrl Pts',(2.23514935793222,-3.45769207768353,127.304026592513));
#71818=CARTESIAN_POINT('Ctrl Pts',(2.22739314548221,-3.55248972498134,127.403037372651));
#71819=CARTESIAN_POINT('Ctrl Pts',(2.21964229762557,-3.64722180537598,127.501979671866));
#71820=CARTESIAN_POINT('Ctrl Pts',(2.2118914497689,-3.73789071055311,127.604959390666));
#71821=CARTESIAN_POINT('Ctrl Pts',(2.20414060191226,-3.82413966135607,127.711604740853));
#71822=CARTESIAN_POINT('Ctrl Pts',(2.19639343629534,-3.91034763737561,127.818199426422));
#71823=CARTESIAN_POINT('Ctrl Pts',(2.18864627067844,-3.99213959289988,127.92845597419));
#71824=CARTESIAN_POINT('Ctrl Pts',(2.18089910506151,-4.06919782176642,128.041968149101));
#71825=CARTESIAN_POINT('Ctrl Pts',(2.17290351710548,-4.14872701697201,128.159120230709));
#71826=CARTESIAN_POINT('Ctrl Pts',(2.16490792914947,-4.2232135296843,128.279739901928));
#71827=CARTESIAN_POINT('Ctrl Pts',(2.15691234119345,-4.29235538605496,128.403346602133));
#71828=CARTESIAN_POINT('Ctrl Pts',(2.14916577050034,-4.35934386534797,128.523103653966));
#71829=CARTESIAN_POINT('Ctrl Pts',(2.14141919980721,-4.42131546369412,128.645664077464));
#71830=CARTESIAN_POINT('Ctrl Pts',(2.1336726291141,-4.47804181031442,128.770565001587));
#71831=CARTESIAN_POINT('Ctrl Pts',(2.12555253252662,-4.53750340072136,128.901488426664));
#71832=CARTESIAN_POINT('Ctrl Pts',(2.11743243593913,-4.59120110308603,129.034983256854));
#71833=CARTESIAN_POINT('Ctrl Pts',(2.10931233935165,-4.63892864520064,129.17049278716));
#71834=CARTESIAN_POINT('Ctrl Pts',(2.10119224276415,-4.68665618731532,129.306002317466));
#71835=CARTESIAN_POINT('Ctrl Pts',(2.09307214617668,-4.72841344343846,129.443526070619));
#71836=CARTESIAN_POINT('Ctrl Pts',(2.08495204958919,-4.764054528234,129.582490119308));
#71837=CARTESIAN_POINT('Ctrl Pts',(3.83484270885904,-4.76405452823401,129.582490119308));
#71838=CARTESIAN_POINT('Ctrl Pts',(3.82717092304017,-4.79783678081443,129.714206609402));
#71839=CARTESIAN_POINT('Ctrl Pts',(3.81949913722131,-4.82615215141464,129.847324677294));
#71840=CARTESIAN_POINT('Ctrl Pts',(3.81182735140243,-4.8488999635451,129.981346519247));
#71841=CARTESIAN_POINT('Ctrl Pts',(3.80399936550057,-4.87211092861365,130.11809708999));
#71842=CARTESIAN_POINT('Ctrl Pts',(3.79617137959876,-4.88952507481256,130.255788211832));
#71843=CARTESIAN_POINT('Ctrl Pts',(3.78834339369692,-4.90109085894145,130.393883511139));
#71844=CARTESIAN_POINT('Ctrl Pts',(3.78051540779509,-4.91265664307031,130.531978810446));
#71845=CARTESIAN_POINT('Ctrl Pts',(3.77268742189319,-4.91837406561657,130.670477846659));
#71846=CARTESIAN_POINT('Ctrl Pts',(3.76485943599135,-4.91824795725832,130.80884318651));
#71847=CARTESIAN_POINT('',(4.11014056405159,-4.91824955451988,130.80226730321));
#71848=CARTESIAN_POINT('Ctrl Pts',(4.1798637461653,-4.76405452823409,129.582490119308));
#71849=CARTESIAN_POINT('Ctrl Pts',(4.17137872466698,-4.80119472818719,129.727299195244));
#71850=CARTESIAN_POINT('Ctrl Pts',(4.16289370316864,-4.8317720853013,129.873973393409));
#71851=CARTESIAN_POINT('Ctrl Pts',(4.15440868167033,-4.85561338970576,130.021927443288));
#71852=CARTESIAN_POINT('Ctrl Pts',(4.1459570040762,-4.87936100405068,130.169300072642));
#71853=CARTESIAN_POINT('Ctrl Pts',(4.13750532648211,-4.89642530248433,130.317942265847));
#71854=CARTESIAN_POINT('Ctrl Pts',(4.12905364888798,-4.90668371155702,130.467258233651));
#71855=CARTESIAN_POINT('Ctrl Pts',(4.12274928727587,-4.91433576875379,130.578637524332));
#71856=CARTESIAN_POINT('Ctrl Pts',(4.11644492566373,-4.91820193766441,130.69039133125));
#71857=CARTESIAN_POINT('Ctrl Pts',(4.11014056405165,-4.91824955451988,130.80226730321));
#71858=CARTESIAN_POINT('Ctrl Pts',(4.11014056400876,-4.9182495545202,130.80226730397));
#71859=CARTESIAN_POINT('Ctrl Pts',(4.10224648305787,-4.91830917850728,130.942354125357));
#71860=CARTESIAN_POINT('Ctrl Pts',(4.09435240210698,-4.91237929659228,131.082413681721));
#71861=CARTESIAN_POINT('Ctrl Pts',(4.0864583211561,-4.90049331021611,131.221911068442));
#71862=CARTESIAN_POINT('Ctrl Pts',(4.07856087743446,-4.88860226057195,131.361467879147));
#71863=CARTESIAN_POINT('Ctrl Pts',(4.07066343371281,-4.87075008229045,131.500461674559));
#71864=CARTESIAN_POINT('Ctrl Pts',(4.06276598999116,-4.84702196962627,131.638363668196));
#71865=CARTESIAN_POINT('Ctrl Pts',(4.05486374740559,-4.82327943862775,131.776349457669));
#71866=CARTESIAN_POINT('Ctrl Pts',(4.04696150482002,-4.79365392157798,131.913241759357));
#71867=CARTESIAN_POINT('Ctrl Pts',(4.03905926223445,-4.75828149958854,132.048523080098));
#71868=CARTESIAN_POINT('Ctrl Pts',(4.03114499854317,-4.72285526811161,132.184010194453));
#71869=CARTESIAN_POINT('Ctrl Pts',(4.02323073485189,-4.68166475859979,132.317881073285));
#71870=CARTESIAN_POINT('Ctrl Pts',(4.01531647116062,-4.63489592976505,132.44963347723));
#71871=CARTESIAN_POINT('Ctrl Pts',(4.00739585069181,-4.5880895359651,132.581491705387));
#71872=CARTESIAN_POINT('Ctrl Pts',(3.999475230223,-4.5356960280495,132.711227723832));
#71873=CARTESIAN_POINT('Ctrl Pts',(3.99155460975419,-4.47794888609887,132.838360823069));
#71874=CARTESIAN_POINT('Ctrl Pts',(3.98361934313438,-4.42009496294793,132.965729006233));
#71875=CARTESIAN_POINT('Ctrl Pts',(3.97568407651458,-4.35686778787975,133.090484320939));
#71876=CARTESIAN_POINT('Ctrl Pts',(3.96774880989477,-4.28854660220437,133.212171055126));
#71877=CARTESIAN_POINT('Ctrl Pts',(3.96141866608358,-4.23404522860254,133.309243348247));
#71878=CARTESIAN_POINT('Ctrl Pts',(3.9550885222724,-4.17630313004901,133.404363398253));
#71879=CARTESIAN_POINT('Ctrl Pts',(3.94875837846121,-4.11548089883579,133.497314392479));
#71880=CARTESIAN_POINT('Ctrl Pts',(3.94098404434212,-4.04078238306371,133.611471686115));
#71881=CARTESIAN_POINT('Ctrl Pts',(3.93320971022298,-3.96121212129713,133.722699403411));
#71882=CARTESIAN_POINT('Ctrl Pts',(3.92543537610391,-3.8770270275519,133.830553686445));
#71883=CARTESIAN_POINT('Ctrl Pts',(3.91767062315682,-3.79294568441088,133.938275048715));
#71884=CARTESIAN_POINT('Ctrl Pts',(3.90990587020978,-3.70426106370937,134.042630943585));
#71885=CARTESIAN_POINT('Ctrl Pts',(3.90214111726269,-3.61127426143631,134.143204919295));
#71886=CARTESIAN_POINT('Ctrl Pts',(3.89438407637769,-3.51837981496627,134.243679003514));
#71887=CARTESIAN_POINT('Ctrl Pts',(3.88662703549263,-3.42119195405883,134.340378358479));
#71888=CARTESIAN_POINT('Ctrl Pts',(3.87886999460764,-3.32005286007642,134.432918467291));
#71889=CARTESIAN_POINT('Ctrl Pts',(3.87111880336752,-3.21899003587152,134.525388790886));
#71890=CARTESIAN_POINT('Ctrl Pts',(3.86336761212747,-3.11398219669232,134.613705848528));
#71891=CARTESIAN_POINT('Ctrl Pts',(3.85561642088734,-3.00540904369461,134.697521228507));
#71892=CARTESIAN_POINT('Ctrl Pts',(3.84786852411027,-2.89688203718321,134.781300984712));
#71893=CARTESIAN_POINT('Ctrl Pts',(3.84012062733318,-2.78479303960595,134.860582630319));
#71894=CARTESIAN_POINT('Ctrl Pts',(3.8323727305561,-2.66955539209871,134.935057540728));
#71895=CARTESIAN_POINT('Ctrl Pts',(3.82462645447201,-2.55434184982325,135.00951687259));
#71896=CARTESIAN_POINT('Ctrl Pts',(3.81688017838791,-2.43598129582079,135.079171257103));
#71897=CARTESIAN_POINT('Ctrl Pts',(3.80913390230381,-2.31491632425063,135.143755215228));
#71898=CARTESIAN_POINT('Ctrl Pts',(3.80138756903846,-2.19385045900619,135.208339650097));
#71899=CARTESIAN_POINT('Ctrl Pts',(3.79364123577312,-2.07008048130893,135.267853399872));
#71900=CARTESIAN_POINT('Ctrl Pts',(3.78589490250778,-1.94407351197216,135.322076992301));
#71901=CARTESIAN_POINT('Ctrl Pts',(3.77814683450482,-1.81803832424844,135.376312727727));
#71902=CARTESIAN_POINT('Ctrl Pts',(3.77039876650186,-1.68976550709223,135.425255793892));
#71903=CARTESIAN_POINT('Ctrl Pts',(3.7626506984989,-1.55974169826002,135.468735055495));
#71904=CARTESIAN_POINT('Ctrl Pts',(3.75489439575706,-1.42957969857648,135.512260527375));
#71905=CARTESIAN_POINT('Ctrl Pts',(3.74713809301523,-1.2976633610945,135.550310470406));
#71906=CARTESIAN_POINT('Ctrl Pts',(3.7393817902734,-1.16449454636711,135.582763647238));
#71907=CARTESIAN_POINT('Ctrl Pts',(3.73162134775923,-1.0312546554333,135.615234145308));
#71908=CARTESIAN_POINT('Ctrl Pts',(3.72386090524503,-0.896761338443784,
135.642101848452));
#71909=CARTESIAN_POINT('Ctrl Pts',(3.71610046273085,-0.761525176489029,
135.663296969081));
#71910=CARTESIAN_POINT('Ctrl Pts',(3.70832756246542,-0.626071921441587,
135.684526113999));
#71911=CARTESIAN_POINT('Ctrl Pts',(3.70055466219995,-0.489873827141526,
135.700064435106));
#71912=CARTESIAN_POINT('Ctrl Pts',(3.69278176193453,-0.353446006255062,
135.709894124042));
#71913=CARTESIAN_POINT('Ctrl Pts',(3.68529142617244,-0.221977680297659,
135.719366479026));
#71914=CARTESIAN_POINT('Ctrl Pts',(3.67780109041043,-0.0902963479219616,
135.723538032591));
#71915=CARTESIAN_POINT('Ctrl Pts',(3.67031075464834,0.0411403272179479,
135.722438548626));
#71916=CARTESIAN_POINT('Ctrl Pts',(3.66253642052925,0.177560463844138,135.721297377392));
#71917=CARTESIAN_POINT('Ctrl Pts',(3.65476208641021,0.31414916263425,135.714473960707));
#71918=CARTESIAN_POINT('Ctrl Pts',(3.64698775229112,0.45039412504755,135.701944531561));
#71919=CARTESIAN_POINT('Ctrl Pts',(3.63922299934403,0.586471177721238,135.689430543816));
#71920=CARTESIAN_POINT('Ctrl Pts',(3.63145824639686,0.722204951319387,135.671224570953));
#71921=CARTESIAN_POINT('Ctrl Pts',(3.62369349344976,0.857082323444843,135.647354831205));
#71922=CARTESIAN_POINT('Ctrl Pts',(3.61593645256475,0.991825733463049,135.623508799219));
#71923=CARTESIAN_POINT('Ctrl Pts',(3.60817941167973,1.12571405222937,135.594010262705));
#71924=CARTESIAN_POINT('Ctrl Pts',(3.60042237079472,1.25823881740201,135.55893926776));
#71925=CARTESIAN_POINT('Ctrl Pts',(3.59267117955457,1.39066364461834,135.523894720125));
#71926=CARTESIAN_POINT('Ctrl Pts',(3.58491998831445,1.52172658851761,135.483286177967));
#71927=CARTESIAN_POINT('Ctrl Pts',(3.57716879707431,1.65092928271038,135.437244769581));
#71928=CARTESIAN_POINT('Ctrl Pts',(3.56942090029723,1.78007706231118,135.391222930022));
#71929=CARTESIAN_POINT('Ctrl Pts',(3.56167300352011,1.90736579724985,135.339772947847));
#71930=CARTESIAN_POINT('Ctrl Pts',(3.55392510674304,2.03231241192895,135.283075759526));
#71931=CARTESIAN_POINT('Ctrl Pts',(3.54617883065893,2.15723289046998,135.226390431034));
#71932=CARTESIAN_POINT('Ctrl Pts',(3.53843255457485,2.27981186743149,135.164460241039));
#71933=CARTESIAN_POINT('Ctrl Pts',(3.53068627849075,2.39958675482496,135.097514058636));
#71934=CARTESIAN_POINT('Ctrl Pts',(3.52293994522539,2.51936252636945,135.030567382051));
#71935=CARTESIAN_POINT('Ctrl Pts',(3.51519361196002,2.63633382576766,134.958604829924));
#71936=CARTESIAN_POINT('Ctrl Pts',(3.50744727869466,2.7500635145877,134.881900774111));
#71937=CARTESIAN_POINT('Ctrl Pts',(3.49969921069166,2.86381867238316,134.805179540956));
#71938=CARTESIAN_POINT('Ctrl Pts',(3.49195114268869,2.97433045099858,134.72371490977));
#71939=CARTESIAN_POINT('Ctrl Pts',(3.48420307468569,3.0811918298643,134.63782379987));
#71940=CARTESIAN_POINT('Ctrl Pts',(3.47644677194383,3.188166782275,134.551841403876));
#71941=CARTESIAN_POINT('Ctrl Pts',(3.468690469202,3.29148327962229,134.461423376717));
#71942=CARTESIAN_POINT('Ctrl Pts',(3.46093416646013,3.39076805360215,134.36692641614));
#71943=CARTESIAN_POINT('Ctrl Pts',(3.45317372394595,3.49010581885543,134.27237901969));
#71944=CARTESIAN_POINT('Ctrl Pts',(3.44541328143177,3.58540730145787,134.173748632887));
#71945=CARTESIAN_POINT('Ctrl Pts',(3.43765283891759,3.6763378055837,134.071427100167));
#71946=CARTESIAN_POINT('Ctrl Pts',(3.42987993865215,3.76741427942705,133.968941311839));
#71947=CARTESIAN_POINT('Ctrl Pts',(3.4221070383867,3.85410550583488,133.862752839877));
#71948=CARTESIAN_POINT('Ctrl Pts',(3.41433413812126,3.93611807115195,133.753285437301));
#71949=CARTESIAN_POINT('Ctrl Pts',(3.40684380235932,4.01514927314168,133.647797450543));
#71950=CARTESIAN_POINT('Ctrl Pts',(3.39935346659739,4.08983589594292,133.539265042805));
#71951=CARTESIAN_POINT('Ctrl Pts',(3.39186313083545,4.15995560237529,133.428089347593));
#71952=CARTESIAN_POINT('Ctrl Pts',(3.38408879671637,4.23273391879019,133.312698392104));
#71953=CARTESIAN_POINT('Ctrl Pts',(3.37631446259734,4.30082271314453,133.194094228029));
#71954=CARTESIAN_POINT('Ctrl Pts',(3.36854012847826,4.36392507970444,133.072695019991));
#71955=CARTESIAN_POINT('Ctrl Pts',(3.36077537553116,4.42694967823727,132.951445425628));
#71956=CARTESIAN_POINT('Ctrl Pts',(3.35301062258409,4.48499989775883,132.827407984681));
#71957=CARTESIAN_POINT('Ctrl Pts',(3.34524586963698,4.53782212387933,132.701029654201));
#71958=CARTESIAN_POINT('Ctrl Pts',(3.33748882875198,4.59059188622012,132.574776844461));
#71959=CARTESIAN_POINT('Ctrl Pts',(3.32973178786687,4.6381438387067,132.446188130442));
#71960=CARTESIAN_POINT('Ctrl Pts',(3.32197474698188,4.68027049007024,132.315734562782));
#71961=CARTESIAN_POINT('Ctrl Pts',(3.31422355574176,4.72236537339829,132.185379371172));
#71962=CARTESIAN_POINT('Ctrl Pts',(3.30647236450168,4.75904297935461,132.053162495619));
#71963=CARTESIAN_POINT('Ctrl Pts',(3.29872117326155,4.79014425068146,131.919574103928));
#71964=CARTESIAN_POINT('Ctrl Pts',(3.29097327648448,4.82123230313835,131.786042490867));
#71965=CARTESIAN_POINT('Ctrl Pts',(3.28322537970742,4.84674864643022,131.651140901058));
#71966=CARTESIAN_POINT('Ctrl Pts',(3.27547748293034,4.86658439337261,131.515373560263));
#71967=CARTESIAN_POINT('Ctrl Pts',(3.26773120684624,4.88641599110435,131.379634619069));
#71968=CARTESIAN_POINT('Ctrl Pts',(3.25998493076212,4.90056929951295,131.243030673713));
#71969=CARTESIAN_POINT('Ctrl Pts',(3.25223865467802,4.90898683254339,131.106074621907));
#71970=CARTESIAN_POINT('Ctrl Pts',(3.24449232141269,4.91740442771014,130.969117559124));
#71971=CARTESIAN_POINT('Ctrl Pts',(3.23674598814735,4.92008613902789,130.831808774933));
#71972=CARTESIAN_POINT('Ctrl Pts',(3.22899965488202,4.91702651930969,130.694664350969));
#71973=CARTESIAN_POINT('Ctrl Pts',(3.22125158687905,4.91396621441086,130.557489214462));
#71974=CARTESIAN_POINT('Ctrl Pts',(3.21350351887613,4.90516202873807,130.420478902217));
#71975=CARTESIAN_POINT('Ctrl Pts',(3.20575545087317,4.89066059092794,130.284147154799));
#71976=CARTESIAN_POINT('Ctrl Pts',(3.19799914813132,4.87614374081711,130.147670512376));
#71977=CARTESIAN_POINT('Ctrl Pts',(3.19024284538943,4.85591758425885,130.01187426482));
#71978=CARTESIAN_POINT('Ctrl Pts',(3.18248654264758,4.83008046053437,129.877265257172));
#71979=CARTESIAN_POINT('Ctrl Pts',(3.1747261001334,4.80422954675894,129.742584404643));
#71980=CARTESIAN_POINT('Ctrl Pts',(3.16696565761921,4.7727617881989,129.609092435003));
#71981=CARTESIAN_POINT('Ctrl Pts',(3.15920521510503,4.73582594340621,129.477282738819));
#71982=CARTESIAN_POINT('Ctrl Pts',(3.1514323148396,4.69883080591651,129.345261450009));
#71983=CARTESIAN_POINT('Ctrl Pts',(3.1436594145742,4.65635016246514,129.214928203115));
#71984=CARTESIAN_POINT('Ctrl Pts',(3.13588651430877,4.60858193122296,129.086758904215));
#71985=CARTESIAN_POINT('Ctrl Pts',(3.1283961785467,4.56255019550716,128.963248882169));
#71986=CARTESIAN_POINT('Ctrl Pts',(3.12090584278461,4.51160875102569,128.841748493736));
#71987=CARTESIAN_POINT('Ctrl Pts',(3.11341550702255,4.45597490407882,128.722661619939));
#71988=CARTESIAN_POINT('Ctrl Pts',(3.10564117290348,4.39823168291575,128.599059531128));
#71989=CARTESIAN_POINT('Ctrl Pts',(3.09786683878435,4.33525029714539,128.477666052313));
#71990=CARTESIAN_POINT('Ctrl Pts',(3.09009250466528,4.26722207570553,128.358957006889));
#71991=CARTESIAN_POINT('Ctrl Pts',(3.0823277517182,4.19927769296874,128.240394259755));
#71992=CARTESIAN_POINT('Ctrl Pts',(3.07456299877111,4.1262990425844,128.124509699389));
#71993=CARTESIAN_POINT('Ctrl Pts',(3.06679824582403,4.04852507740453,128.011758289964));
#71994=CARTESIAN_POINT('Ctrl Pts',(3.05904120493902,3.9708283584231,127.899118866829));
#71995=CARTESIAN_POINT('Ctrl Pts',(3.05128416405397,3.88834602333693,127.789606721579));
#71996=CARTESIAN_POINT('Ctrl Pts',(3.04352712316896,3.80136222628971,127.683651036872));
#71997=CARTESIAN_POINT('Ctrl Pts',(3.03577593192882,3.71444402440048,127.577775254171));
#71998=CARTESIAN_POINT('Ctrl Pts',(3.02802474068875,3.62303136434073,127.475450894702));
#71999=CARTESIAN_POINT('Ctrl Pts',(3.0202735494486,3.52745066383389,127.377076725514));
#72000=CARTESIAN_POINT('Ctrl Pts',(3.01252565267152,3.43191058767473,127.278744367972));
#72001=CARTESIAN_POINT('Ctrl Pts',(3.00477775589443,3.3322062663772,127.184359141254));
#72002=CARTESIAN_POINT('Ctrl Pts',(2.99702985911736,3.22870306317286,127.094285201573));
#72003=CARTESIAN_POINT('Ctrl Pts',(2.98928358303327,3.12522151060737,127.004230103418));
#72004=CARTESIAN_POINT('Ctrl Pts',(2.98153730694914,3.01794295146319,126.918484755009));
#72005=CARTESIAN_POINT('Ctrl Pts',(2.97379103086504,2.90726782849507,126.837374754735));
#72006=CARTESIAN_POINT('Ctrl Pts',(2.96604469759967,2.79659188854803,126.756264155726));
#72007=CARTESIAN_POINT('Ctrl Pts',(2.95829836433435,2.68251965009295,126.679789204236));
#72008=CARTESIAN_POINT('Ctrl Pts',(2.95055203106898,2.56548236288651,126.608233437866));
#72009=CARTESIAN_POINT('Ctrl Pts',(2.94280396306597,2.44841886599092,126.536661647078));
#72010=CARTESIAN_POINT('Ctrl Pts',(2.93505589506296,2.32838933255448,126.470011437401));
#72011=CARTESIAN_POINT('Ctrl Pts',(2.92730782705996,2.20585119098098,126.408521268164));
#72012=CARTESIAN_POINT('Ctrl Pts',(2.91955152431812,2.0831828144129,126.346965746445));
#72013=CARTESIAN_POINT('Ctrl Pts',(2.91179522157622,1.95800085372341,126.29058139598));
#72014=CARTESIAN_POINT('Ctrl Pts',(2.90403891883437,1.83078488678367,126.239559443273));
#72015=CARTESIAN_POINT('Ctrl Pts',(2.89627847632019,1.70350102085163,126.188510258614));
#72016=CARTESIAN_POINT('Ctrl Pts',(2.88851803380606,1.57418135396013,126.142829304791));
#72017=CARTESIAN_POINT('Ctrl Pts',(2.88075759129188,1.4433213971969,126.102658116674));
#72018=CARTESIAN_POINT('Ctrl Pts',(2.87298469102646,1.31225137241423,126.0624224422));
#72019=CARTESIAN_POINT('Ctrl Pts',(2.86521179076101,1.17963649514066,126.027714307138));
#72020=CARTESIAN_POINT('Ctrl Pts',(2.85743889049559,1.04598413824297,125.998624436184));
#72021=CARTESIAN_POINT('Ctrl Pts',(2.84994855473362,0.917190381169401,125.970592055313));
#72022=CARTESIAN_POINT('Ctrl Pts',(2.84245821897168,0.787433568256173,125.947776607532));
#72023=CARTESIAN_POINT('Ctrl Pts',(2.83496788320971,0.657170955410278,125.930213574455));
#72024=CARTESIAN_POINT('Ctrl Pts',(2.82719354909065,0.521969396005091,125.911984633641));
#72025=CARTESIAN_POINT('Ctrl Pts',(2.81941921497166,0.385794646821428,125.899356516715));
#72026=CARTESIAN_POINT('Ctrl Pts',(2.81164488085258,0.249150449521832,125.892425447391));
#72027=CARTESIAN_POINT('Ctrl Pts',(2.80388012790551,0.11267465398335,125.88550291999));
#72028=CARTESIAN_POINT('Ctrl Pts',(2.79611537495831,-0.0242690518085328,
125.884263489906));
#72029=CARTESIAN_POINT('Ctrl Pts',(2.78835062201125,-0.161168733757474,
125.888752038584));
#72030=CARTESIAN_POINT('Ctrl Pts',(2.78059358112626,-0.297932445012727,
125.893236129173));
#72031=CARTESIAN_POINT('Ctrl Pts',(2.77283654024134,-0.434651831213299,
125.903436864212));
#72032=CARTESIAN_POINT('Ctrl Pts',(2.76507949935635,-0.570812216579347,
125.919347160481));
#72033=CARTESIAN_POINT('Ctrl Pts',(2.75732830811624,-0.706869922339248,
125.935245458672));
#72034=CARTESIAN_POINT('Ctrl Pts',(2.74957711687613,-0.842369079576227,
125.956844702817));
#72035=CARTESIAN_POINT('Ctrl Pts',(2.74182592563602,-0.976797757527117,
125.98408581177));
#72036=CARTESIAN_POINT('Ctrl Pts',(2.73407802885894,-1.11116929970424,126.011315342526));
#72037=CARTESIAN_POINT('Ctrl Pts',(2.72633013208189,-1.2444708851456,126.044181891278));
#72038=CARTESIAN_POINT('Ctrl Pts',(2.71858223530481,-1.37619865116445,126.08257490292));
#72039=CARTESIAN_POINT('Ctrl Pts',(2.71083595922072,-1.50789886257419,126.120959883572));
#72040=CARTESIAN_POINT('Ctrl Pts',(2.7030896831366,-1.63802553426643,126.164868918405));
#72041=CARTESIAN_POINT('Ctrl Pts',(2.69534340705252,-1.76608828200558,126.214141097471));
#72042=CARTESIAN_POINT('Ctrl Pts',(2.68759707378719,-1.89415197507484,126.263413640252));
#72043=CARTESIAN_POINT('Ctrl Pts',(2.67985074052184,-2.02015134890067,126.318049265873));
#72044=CARTESIAN_POINT('Ctrl Pts',(2.67210440725651,-2.14361475424143,126.377838410698));
#72045=CARTESIAN_POINT('Ctrl Pts',(2.66435633925359,-2.26710580835527,126.437640944887));
#72046=CARTESIAN_POINT('Ctrl Pts',(2.65660827125068,-2.38805941209476,126.502599124426));
#72047=CARTESIAN_POINT('Ctrl Pts',(2.64886020324775,-2.50602769164538,126.572456994939));
#72048=CARTESIAN_POINT('Ctrl Pts',(2.6411039005059,-2.624121349288,126.642389111227));
#72049=CARTESIAN_POINT('Ctrl Pts',(2.63334759776401,-2.73922300771383,126.717231121402));
#72050=CARTESIAN_POINT('Ctrl Pts',(2.62559129502216,-2.8509125590967,126.796682905613));
#72051=CARTESIAN_POINT('Ctrl Pts',(2.61783085250802,-2.96266172255591,126.876177095633));
#72052=CARTESIAN_POINT('Ctrl Pts',(2.61007040999388,-3.07099484152213,126.960285722551));
#72053=CARTESIAN_POINT('Ctrl Pts',(2.60230996747973,-3.17552500285442,127.048668401909));
#72054=CARTESIAN_POINT('Ctrl Pts',(2.59453706721429,-3.28022296528172,127.13719296099));
#72055=CARTESIAN_POINT('Ctrl Pts',(2.58676416694883,-3.38110548276027,127.230005018294));
#72056=CARTESIAN_POINT('Ctrl Pts',(2.5789912666834,-3.4778219786054,127.326726745574));
#72057=CARTESIAN_POINT('Ctrl Pts',(2.5715009309212,-3.57102258621452,127.419932394441));
#72058=CARTESIAN_POINT('Ctrl Pts',(2.56401059515899,-3.66035459546841,127.516768169228));
#72059=CARTESIAN_POINT('Ctrl Pts',(2.55652025939679,-3.74554099669369,127.616868546268));
#72060=CARTESIAN_POINT('Ctrl Pts',(2.54879702129302,-3.83337615932911,127.720081415585));
#72061=CARTESIAN_POINT('Ctrl Pts',(2.54107378318923,-3.91709218294665,127.827104364471));
#72062=CARTESIAN_POINT('Ctrl Pts',(2.53335054508545,-3.99633686245575,127.937572389552));
#72063=CARTESIAN_POINT('Ctrl Pts',(2.52563672019846,-4.07548495717279,128.047905774286));
#72064=CARTESIAN_POINT('Ctrl Pts',(2.51792289531153,-4.15017231769003,128.161675565284));
#72065=CARTESIAN_POINT('Ctrl Pts',(2.51020907042454,-4.22008518053593,128.278481734579));
#72066=CARTESIAN_POINT('Ctrl Pts',(2.50250440945722,-4.28991498784599,128.395149139724));
#72067=CARTESIAN_POINT('Ctrl Pts',(2.49479974848987,-4.35498138818687,128.514845403344));
#72068=CARTESIAN_POINT('Ctrl Pts',(2.48709508752256,-4.41501279501639,128.637140028345));
#72069=CARTESIAN_POINT('Ctrl Pts',(2.47939571550868,-4.47500299259391,128.759350702791));
#72070=CARTESIAN_POINT('Ctrl Pts',(2.47169634349475,-4.5299648967112,128.88415583685));
#72071=CARTESIAN_POINT('Ctrl Pts',(2.46399697148087,-4.57967193929555,129.011098787568));
#72072=CARTESIAN_POINT('Ctrl Pts',(2.45630130902744,-4.62935503300729,129.137980577122));
#72073=CARTESIAN_POINT('Ctrl Pts',(2.44860564657397,-4.67378815871689,129.266997765422));
#72074=CARTESIAN_POINT('Ctrl Pts',(2.44090998412054,-4.71279235395851,129.397672560117));
#72075=CARTESIAN_POINT('Ctrl Pts',(2.43730235467253,-4.73107702850097,129.458931254908));
#72076=CARTESIAN_POINT('Ctrl Pts',(2.43369472522455,-4.74816932413074,129.520553949601));
#72077=CARTESIAN_POINT('Ctrl Pts',(2.43008709577654,-4.76405452823407,129.582490119308));
#72078=CARTESIAN_POINT('Origin',(213.235140564004,0.,130.804360617566));
#72079=CARTESIAN_POINT('',(0.334704853334813,-4.76405452823404,129.582490119308));
#72080=CARTESIAN_POINT('',(0.68024183266882,-4.76405452823404,129.582490119308));
#72081=CARTESIAN_POINT('',(213.235140564004,-4.76405452823405,129.582490119308));
#72082=CARTESIAN_POINT('',(2.01485943595022,-4.9182499766426,130.803881289891));
#72083=CARTESIAN_POINT('Ctrl Pts',(2.01485943595023,-4.9182499766426,130.803881289891));
#72084=CARTESIAN_POINT('Ctrl Pts',(2.00710625195527,-4.91826323687598,130.939940912275));
#72085=CARTESIAN_POINT('Ctrl Pts',(1.99935306796029,-4.91262624006787,131.0762218757));
#72086=CARTESIAN_POINT('Ctrl Pts',(1.99159988396534,-4.90130985239998,131.21221450472));
#72087=CARTESIAN_POINT('Ctrl Pts',(1.98385624230379,-4.8900073925254,131.34803975902));
#72088=CARTESIAN_POINT('Ctrl Pts',(1.97611260064231,-4.87303948061168,131.483576996769));
#72089=CARTESIAN_POINT('Ctrl Pts',(1.96836895898076,-4.85042895777124,131.61831515445));
#72090=CARTESIAN_POINT('Ctrl Pts',(1.96063296861848,-4.82784077582469,131.752920180717));
#72091=CARTESIAN_POINT('Ctrl Pts',(1.95289697825616,-4.79962114165776,131.886727312609));
#72092=CARTESIAN_POINT('Ctrl Pts',(1.94516098789387,-4.76584477091121,132.019229615474));
#72093=CARTESIAN_POINT('Ctrl Pts',(1.93743076465436,-4.73209358019562,132.151633138867));
#72094=CARTESIAN_POINT('Ctrl Pts',(1.92970054141488,-4.69279399432024,132.282733389611));
#72095=CARTESIAN_POINT('Ctrl Pts',(1.92197031817537,-4.64807190734446,132.412033036517));
#72096=CARTESIAN_POINT('Ctrl Pts',(1.91424326113583,-4.60336813796008,132.541279723951));
#72097=CARTESIAN_POINT('Ctrl Pts',(1.90651620409623,-4.55324641239797,132.668726903142));
#72098=CARTESIAN_POINT('Ctrl Pts',(1.8987891470567,-4.49788257118241,132.793892079583));
#72099=CARTESIAN_POINT('Ctrl Pts',(1.89106359574771,-4.44252951842434,132.91903286575));
#72100=CARTESIAN_POINT('Ctrl Pts',(1.88333804443871,-4.38193654066813,133.041892174051));
#72101=CARTESIAN_POINT('Ctrl Pts',(1.87561249312972,-4.31632758104529,133.162007596146));
#72102=CARTESIAN_POINT('Ctrl Pts',(1.86788675011931,-4.25071699340516,133.282125998779));
#72103=CARTESIAN_POINT('Ctrl Pts',(1.86016100710894,-4.18009036471323,133.399500034469));
#72104=CARTESIAN_POINT('Ctrl Pts',(1.85243526409852,-4.10471733545377,133.513692390997));
#72105=CARTESIAN_POINT('Ctrl Pts',(1.8447076321693,-4.02932587773619,133.627912667183));
#72106=CARTESIAN_POINT('Ctrl Pts',(1.83698000024012,-3.94918592721915,133.738949388305));
#72107=CARTESIAN_POINT('Ctrl Pts',(1.8292523683109,-3.86460988258845,133.846395054896));
#72108=CARTESIAN_POINT('Ctrl Pts',(1.82151648514175,-3.77994353121904,133.953955447444));
#72109=CARTESIAN_POINT('Ctrl Pts',(1.81378060197253,-3.69083186904937,134.05791681778));
#72110=CARTESIAN_POINT('Ctrl Pts',(1.80604471880338,-3.59762726381741,134.157905180135));
#72111=CARTESIAN_POINT('Ctrl Pts',(1.79830451998079,-3.5043706620951,134.257949323467));
#72112=CARTESIAN_POINT('Ctrl Pts',(1.79056432115822,-3.40701684825682,134.354015767394));
#72113=CARTESIAN_POINT('Ctrl Pts',(1.78282412233563,-3.30595355212749,134.445768885486));
#72114=CARTESIAN_POINT('Ctrl Pts',(1.77507185722264,-3.20473270719266,134.537665038634));
#72115=CARTESIAN_POINT('Ctrl Pts',(1.76731959210972,-3.09979112926588,134.625234181002));
#72116=CARTESIAN_POINT('Ctrl Pts',(1.75956732699674,-2.99154856158227,134.708181856582));
#72117=CARTESIAN_POINT('Ctrl Pts',(1.75330034603704,-2.90404457393256,134.775237290825));
#72118=CARTESIAN_POINT('Ctrl Pts',(1.7470333650773,-2.81438396977513,134.839273274428));
#72119=CARTESIAN_POINT('Ctrl Pts',(1.74076638411759,-2.72280062517734,134.900156000399));
#72120=CARTESIAN_POINT('Ctrl Pts',(1.73299204999852,-2.60918937835477,134.975682423221));
#72121=CARTESIAN_POINT('Ctrl Pts',(1.72521771587948,-2.49225331267256,135.046597782595));
#72122=CARTESIAN_POINT('Ctrl Pts',(1.7174433817604,-2.37240334741237,135.112595223491));
#72123=CARTESIAN_POINT('Ctrl Pts',(1.70967862881333,-2.25270108652323,135.178511328439));
#72124=CARTESIAN_POINT('Ctrl Pts',(1.70191387586626,-2.13009241050186,135.239521387505));
#72125=CARTESIAN_POINT('Ctrl Pts',(1.69414912291919,-2.00501806163953,135.295361133598));
#72126=CARTESIAN_POINT('Ctrl Pts',(1.68639208203421,-1.88006793838389,135.351145418867));
#72127=CARTESIAN_POINT('Ctrl Pts',(1.67863504114923,-1.75265737048228,135.401769452145));
#72128=CARTESIAN_POINT('Ctrl Pts',(1.67087800026425,-1.62325229370357,135.447014497998));
#72129=CARTESIAN_POINT('Ctrl Pts',(1.66312680902413,-1.49394480229954,135.492225424209));
#72130=CARTESIAN_POINT('Ctrl Pts',(1.65537561778396,-1.36264616335181,135.532065308373));
#72131=CARTESIAN_POINT('Ctrl Pts',(1.64762442654384,-1.22984258657333,135.566363376359));
#72132=CARTESIAN_POINT('Ctrl Pts',(1.63987652976678,-1.09709545485781,135.600646866751));
#72133=CARTESIAN_POINT('Ctrl Pts',(1.63212863298972,-0.962845035256375,
135.629393128158));
#72134=CARTESIAN_POINT('Ctrl Pts',(1.62438073621266,-0.827592795334841,
135.652481204722));
#72135=CARTESIAN_POINT('Ctrl Pts',(1.61663446012857,-0.692368847266199,
135.675564451759));
#72136=CARTESIAN_POINT('Ctrl Pts',(1.60888818404446,-0.556143880848485,
135.692991802395));
#72137=CARTESIAN_POINT('Ctrl Pts',(1.60114190796037,-0.419429266585645,
135.704693478998));
#72138=CARTESIAN_POINT('Ctrl Pts',(1.59339557469502,-0.282713643126394,
135.71639524198));
#72139=CARTESIAN_POINT('Ctrl Pts',(1.58564924142971,-0.145508754150531,
135.72237121325));
#72140=CARTESIAN_POINT('Ctrl Pts',(1.57790290816436,-0.00833040195511292,
135.722603562654));
#72141=CARTESIAN_POINT('Ctrl Pts',(1.5701548401614,0.128878670380965,135.72283596409));
#72142=CARTESIAN_POINT('Ctrl Pts',(1.5624067721585,0.266060803221432,135.71732218352));
#72143=CARTESIAN_POINT('Ctrl Pts',(1.55465870415554,0.402701284987753,135.706096507796));
#72144=CARTESIAN_POINT('Ctrl Pts',(1.5469024014137,0.539486989884324,135.69485890129));
#72145=CARTESIAN_POINT('Ctrl Pts',(1.5391460986718,0.675729503463738,135.677897304875));
#72146=CARTESIAN_POINT('Ctrl Pts',(1.53138979592995,0.810919766772243,135.65529786663));
#72147=CARTESIAN_POINT('Ctrl Pts',(1.5236293534158,0.946182185194777,135.632686366384));
#72148=CARTESIAN_POINT('Ctrl Pts',(1.51586891090162,1.08039085188442,135.604431108955));
#72149=CARTESIAN_POINT('Ctrl Pts',(1.50810846838746,1.21304894856432,135.570668970042));
#72150=CARTESIAN_POINT('Ctrl Pts',(1.50033556812204,1.34591999979785,135.536852633147));
#72151=CARTESIAN_POINT('Ctrl Pts',(1.4925626678567,1.47723513224696,135.497511861629));
#72152=CARTESIAN_POINT('Ctrl Pts',(1.48478976759128,1.60651382739343,135.45283309623));
#72153=CARTESIAN_POINT('Ctrl Pts',(1.47729943182913,1.73109291634022,135.409778516491));
#72154=CARTESIAN_POINT('Ctrl Pts',(1.46980909606688,1.85378076987155,135.361767416195));
#72155=CARTESIAN_POINT('Ctrl Pts',(1.46231876030473,1.97416840851945,135.309007347034));
#72156=CARTESIAN_POINT('Ctrl Pts',(1.45454442618565,2.09912058107595,135.254246863815));
#72157=CARTESIAN_POINT('Ctrl Pts',(1.44677009206656,2.22199048116853,135.1941967239));
#72158=CARTESIAN_POINT('Ctrl Pts',(1.43899575794745,2.34229783106064,135.12903678268));
#72159=CARTESIAN_POINT('Ctrl Pts',(1.43123100500034,2.46245691289618,135.063957145265));
#72160=CARTESIAN_POINT('Ctrl Pts',(1.42346625205327,2.58005938775689,134.993780420848));
#72161=CARTESIAN_POINT('Ctrl Pts',(1.41570149910615,2.69464468827973,134.918734575585));
#72162=CARTESIAN_POINT('Ctrl Pts',(1.40794445822112,2.80911618106672,134.843763266913));
#72163=CARTESIAN_POINT('Ctrl Pts',(1.40018741733604,2.92057613813777,134.76393267423));
#72164=CARTESIAN_POINT('Ctrl Pts',(1.39243037645102,3.02858868151402,134.679516570648));
#72165=CARTESIAN_POINT('Ctrl Pts',(1.38467918521086,3.13651977179123,134.595164125906));
#72166=CARTESIAN_POINT('Ctrl Pts',(1.37692799397074,3.24100831616122,134.506233292922));
#72167=CARTESIAN_POINT('Ctrl Pts',(1.36917680273058,3.34164782928653,134.413040826108));
#72168=CARTESIAN_POINT('Ctrl Pts',(1.36142890595346,3.44224456793411,134.319887968579));
#72169=CARTESIAN_POINT('Ctrl Pts',(1.35368100917628,3.53899524283554,134.222477344855));
#72170=CARTESIAN_POINT('Ctrl Pts',(1.34593311239917,3.63152703493542,134.121165474206));
#72171=CARTESIAN_POINT('Ctrl Pts',(1.33818683631503,3.72403947137914,134.019874795817));
#72172=CARTESIAN_POINT('Ctrl Pts',(1.3304405602309,3.81233451686599,133.914684782183));
#72173=CARTESIAN_POINT('Ctrl Pts',(1.32269428414676,3.89607705725023,133.805987947277));
#72174=CARTESIAN_POINT('Ctrl Pts',(1.31494795088138,3.97982021580288,133.697290309996));
#72175=CARTESIAN_POINT('Ctrl Pts',(1.30720161761605,4.05901056358786,133.585086109498));
#72176=CARTESIAN_POINT('Ctrl Pts',(1.29945528435067,4.13335429585045,133.46979966723));
#72177=CARTESIAN_POINT('Ctrl Pts',(1.29170721634764,4.20771467687662,133.354487407363));
#72178=CARTESIAN_POINT('Ctrl Pts',(1.2839591483446,4.27722607078529,133.236091860723));
#72179=CARTESIAN_POINT('Ctrl Pts',(1.27621108034157,4.34163910989512,133.115064601621));
#72180=CARTESIAN_POINT('Ctrl Pts',(1.26845477759969,4.40612060794919,132.993908713309));
#72181=CARTESIAN_POINT('Ctrl Pts',(1.2606984748578,4.46549274300586,132.870115870873));
#72182=CARTESIAN_POINT('Ctrl Pts',(1.25294217211592,4.51955283508444,132.74416092517));
#72183=CARTESIAN_POINT('Ctrl Pts',(1.24518172960173,4.57364178066188,132.61813875352));
#72184=CARTESIAN_POINT('Ctrl Pts',(1.23742128708753,4.62241289493052,132.489952544433));
#72185=CARTESIAN_POINT('Ctrl Pts',(1.22966084457335,4.66571279287922,132.360094269855));
#72186=CARTESIAN_POINT('Ctrl Pts',(1.22188794430788,4.70908219966814,132.230027535246));
#72187=CARTESIAN_POINT('Ctrl Pts',(1.21411504404248,4.74696273104014,132.09828374732));
#72188=CARTESIAN_POINT('Ctrl Pts',(1.20634214377702,4.77925151287505,131.965367955692));
#72189=CARTESIAN_POINT('Ctrl Pts',(1.19885180801528,4.81036651615842,131.837283987889));
#72190=CARTESIAN_POINT('Ctrl Pts',(1.19136147225349,4.83628919938415,131.708112049573));
#72191=CARTESIAN_POINT('Ctrl Pts',(1.18387113649175,4.85697311827532,131.578308413513));
#72192=CARTESIAN_POINT('Ctrl Pts',(1.17609680237268,4.87844127423875,131.443583233133));
#72193=CARTESIAN_POINT('Ctrl Pts',(1.16832246825362,4.89433357308443,131.3077507389));
#72194=CARTESIAN_POINT('Ctrl Pts',(1.16054813413456,4.90454173039793,131.171312218306));
#72195=CARTESIAN_POINT('Ctrl Pts',(1.1527833811875,4.91473730706985,131.035041845994));
#72196=CARTESIAN_POINT('Ctrl Pts',(1.14501862824037,4.91926265157261,130.898167319511));
#72197=CARTESIAN_POINT('Ctrl Pts',(1.13725387529331,4.91806061037807,130.761199348496));
#72198=CARTESIAN_POINT('Ctrl Pts',(1.12949683440831,4.91685976306778,130.624367416));
#72199=CARTESIAN_POINT('Ctrl Pts',(1.12173979352335,4.90994285388088,130.487442612091));
#72200=CARTESIAN_POINT('Ctrl Pts',(1.11398275263835,4.89730461319729,130.35093963431));
#72201=CARTESIAN_POINT('Ctrl Pts',(1.10623156139825,4.88467590310936,130.214539594488));
#72202=CARTESIAN_POINT('Ctrl Pts',(1.09848037015815,4.86633448517438,130.078561135357));
#72203=CARTESIAN_POINT('Ctrl Pts',(1.09072917891805,4.84232713859761,129.943517458041));
#72204=CARTESIAN_POINT('Ctrl Pts',(1.08298128214098,4.81832999578348,129.80853117789));
#72205=CARTESIAN_POINT('Ctrl Pts',(1.07523338536392,4.7886717822832,129.674479273465));
#72206=CARTESIAN_POINT('Ctrl Pts',(1.06748548858684,4.75345093005052,129.54186811537));
#72207=CARTESIAN_POINT('Ctrl Pts',(1.05973921250273,4.71823744526082,129.40928469667));
#72208=CARTESIAN_POINT('Ctrl Pts',(1.0519929364186,4.67746373646669,129.278141802478));
#72209=CARTESIAN_POINT('Ctrl Pts',(1.04424666033449,4.63127889940931,129.148933537207));
#72210=CARTESIAN_POINT('Ctrl Pts',(1.03650032706913,4.58509372142596,129.01972431815));
#72211=CARTESIAN_POINT('Ctrl Pts',(1.02875399380379,4.533497467069,128.892450124662));
#72212=CARTESIAN_POINT('Ctrl Pts',(1.02100766053843,4.4766883213425,128.767587499112));
#72213=CARTESIAN_POINT('Ctrl Pts',(1.01325959253549,4.41986645360201,128.642696911444));
#72214=CARTESIAN_POINT('Ctrl Pts',(1.00551152453253,4.35782953339704,128.520219322154));
#72215=CARTESIAN_POINT('Ctrl Pts',(0.997763456529583,4.29082269366034,128.40060861828));
#72216=CARTESIAN_POINT('Ctrl Pts',(0.99000715378772,4.22374463825661,128.280870790726));
#72217=CARTESIAN_POINT('Ctrl Pts',(0.982250851045878,4.15168630316364,128.164006276852));
#72218=CARTESIAN_POINT('Ctrl Pts',(0.974494548304023,4.07493764037456,128.050442265552));
#72219=CARTESIAN_POINT('Ctrl Pts',(0.966734105789877,3.99814801451349,127.93681764172));
#72220=CARTESIAN_POINT('Ctrl Pts',(0.958973663275737,3.91666330495005,127.826497344883));
#72221=CARTESIAN_POINT('Ctrl Pts',(0.951213220761588,3.83081451327079,127.719876345048));
#72222=CARTESIAN_POINT('Ctrl Pts',(0.943440320496165,3.7448279094897,127.613084187718));
#72223=CARTESIAN_POINT('Ctrl Pts',(0.935667420230746,3.65446348202092,127.510003488448));
#72224=CARTESIAN_POINT('Ctrl Pts',(0.927894519965321,3.5600905374331,127.410993789801));
#72225=CARTESIAN_POINT('Ctrl Pts',(0.920404184203183,3.46914828709074,127.315583343088));
#72226=CARTESIAN_POINT('Ctrl Pts',(0.912913848441045,3.374484120522,127.223953267657));
#72227=CARTESIAN_POINT('Ctrl Pts',(0.905423512678908,3.27645680866257,127.136389264969));
#72228=CARTESIAN_POINT('Ctrl Pts',(0.897649178559821,3.17471276148065,127.045505246507));
#72229=CARTESIAN_POINT('Ctrl Pts',(0.889874844440721,3.06902321282255,126.958713824368));
#72230=CARTESIAN_POINT('Ctrl Pts',(0.882100510321635,2.95975137968282,126.876377059433));
#72231=CARTESIAN_POINT('Ctrl Pts',(0.874335757374518,2.85061421431125,126.794141767201));
#72232=CARTESIAN_POINT('Ctrl Pts',(0.866571004427363,2.73790385793331,126.716350441796));
#72233=CARTESIAN_POINT('Ctrl Pts',(0.858806251480246,2.62201909215602,126.643327219134));
#72234=CARTESIAN_POINT('Ctrl Pts',(0.851049210595241,2.5062494247621,126.570376524166));
#72235=CARTESIAN_POINT('Ctrl Pts',(0.843292169710317,2.38731195095036,126.502184714675));
#72236=CARTESIAN_POINT('Ctrl Pts',(0.835535128825313,2.26563685198288,126.439034430734));
#72237=CARTESIAN_POINT('Ctrl Pts',(0.827783937585192,2.1440535091542,126.375931768915));
#72238=CARTESIAN_POINT('Ctrl Pts',(0.820032746345022,2.01973699596873,126.317863244661));
#72239=CARTESIAN_POINT('Ctrl Pts',(0.812281555104903,1.89314436837007,126.265066899045));
#72240=CARTESIAN_POINT('Ctrl Pts',(0.804533658327831,1.76660554601511,126.212292993284));
#72241=CARTESIAN_POINT('Ctrl Pts',(0.79678576155074,1.63779289343586,126.164786959524));
#72242=CARTESIAN_POINT('Ctrl Pts',(0.789037864773661,1.5071856394384,126.122739689856));
#72243=CARTESIAN_POINT('Ctrl Pts',(0.781291588689562,1.3766057056629,126.08070121557));
#72244=CARTESIAN_POINT('Ctrl Pts',(0.773545312605469,1.24423228906344,126.044119353897));
#72245=CARTESIAN_POINT('Ctrl Pts',(0.765799036521372,1.11056168356567,126.013135741869));
#72246=CARTESIAN_POINT('Ctrl Pts',(0.758052703256014,0.976890091341672,
125.982151901128));
#72247=CARTESIAN_POINT('Ctrl Pts',(0.750306369990696,0.841921671979665,
125.956766480775));
#72248=CARTESIAN_POINT('Ctrl Pts',(0.742560036725337,0.706164477905643,
125.937070324945));
#72249=CARTESIAN_POINT('Ctrl Pts',(0.734811968722331,0.570376881948912,
125.917369758297));
#72250=CARTESIAN_POINT('Ctrl Pts',(0.727063900719244,0.433800546625983,
125.90336104755));
#72251=CARTESIAN_POINT('Ctrl Pts',(0.719315832716234,0.296949840293891,
125.895083292455));
#72252=CARTESIAN_POINT('Ctrl Pts',(0.711559529974378,0.159953687403126,
125.886796739664));
#72253=CARTESIAN_POINT('Ctrl Pts',(0.703803227232551,0.0226829718654649,
125.884253333452));
#72254=CARTESIAN_POINT('Ctrl Pts',(0.696046924490702,-0.114346174068859,
125.887440035029));
#72255=CARTESIAN_POINT('Ctrl Pts',(0.68828648197651,-0.251448456584796,
125.890628437444));
#72256=CARTESIAN_POINT('Ctrl Pts',(0.680526039462401,-0.388308522641809,
125.899553016204));
#72257=CARTESIAN_POINT('Ctrl Pts',(0.67276559694821,-0.524415158343417,
125.914148781234));
#72258=CARTESIAN_POINT('Ctrl Pts',(0.664992696682787,-0.660740284499077,
125.928767976683));
#72259=CARTESIAN_POINT('Ctrl Pts',(0.657219796417314,-0.796309176512856,
125.949076492924));
#72260=CARTESIAN_POINT('Ctrl Pts',(0.649446896151886,-0.930619721822204,
125.974957963422));
#72261=CARTESIAN_POINT('Ctrl Pts',(0.641956560389925,-1.06004774050061,
125.999898577275));
#72262=CARTESIAN_POINT('Ctrl Pts',(0.634466224627999,-1.1883070123873,126.030013927678));
#72263=CARTESIAN_POINT('Ctrl Pts',(0.626975888866042,-1.31496324429701,
126.0651565991));
#72264=CARTESIAN_POINT('Ctrl Pts',(0.619201554746944,-1.44642168573738,
126.10163171559));
#72265=CARTESIAN_POINT('Ctrl Pts',(0.611427220627866,-1.57656954990418,
126.143638442496));
#72266=CARTESIAN_POINT('Ctrl Pts',(0.603652886508769,-1.70490589706772,
126.19106689782));
#72267=CARTESIAN_POINT('Ctrl Pts',(0.595888133561661,-1.83308408115312,
126.238436901813));
#72268=CARTESIAN_POINT('Ctrl Pts',(0.588123380614518,-1.95945482710724,
126.291215205216));
#72269=CARTESIAN_POINT('Ctrl Pts',(0.580358627667408,-2.08352987900321,
126.349241505152));
#72270=CARTESIAN_POINT('Ctrl Pts',(0.572601586782389,-2.20748169780848,
126.407210172548));
#72271=CARTESIAN_POINT('Ctrl Pts',(0.564844545897377,-2.32914200823075,
126.470416299042));
#72272=CARTESIAN_POINT('Ctrl Pts',(0.557087505012362,-2.44804049369009,
126.53865073482));
#72273=CARTESIAN_POINT('Ctrl Pts',(0.549336313772261,-2.566849316876,126.606833714479));
#72274=CARTESIAN_POINT('Ctrl Pts',(0.541585122532171,-2.68290012289334,
126.680037262087));
#72275=CARTESIAN_POINT('Ctrl Pts',(0.533833931292065,-2.79574559114389,
126.758005510547));
#72276=CARTESIAN_POINT('Ctrl Pts',(0.526086034514964,-2.9085430970608,126.835940620422));
#72277=CARTESIAN_POINT('Ctrl Pts',(0.518338137737806,-3.01813765384677,
126.918636181555));
#72278=CARTESIAN_POINT('Ctrl Pts',(0.51059024096071,-3.12410962370458,127.005792187015));
#72279=CARTESIAN_POINT('Ctrl Pts',(0.502843964876572,-3.23005942651108,
127.092929961319));
#72280=CARTESIAN_POINT('Ctrl Pts',(0.495097688792449,-3.33238784786237,
127.184526075918));
#72281=CARTESIAN_POINT('Ctrl Pts',(0.487351412708307,-3.43070746552064,
127.280239542954));
#72282=CARTESIAN_POINT('Ctrl Pts',(0.479605079442925,-3.52902780895186,
127.375953716526));
#72283=CARTESIAN_POINT('Ctrl Pts',(0.471858746177595,-3.62333900949916,
127.475785030466));
#72284=CARTESIAN_POINT('Ctrl Pts',(0.464112412912215,-3.71329002267438,
127.579355149353));
#72285=CARTESIAN_POINT('Ctrl Pts',(0.456364344909199,-3.80326117975546,
127.682948462049));
#72286=CARTESIAN_POINT('Ctrl Pts',(0.448616276906127,-3.88886995015889,
127.790281950659));
#72287=CARTESIAN_POINT('Ctrl Pts',(0.440868208903112,-3.96980540949516,
127.900943996886));
#72288=CARTESIAN_POINT('Ctrl Pts',(0.433111906161231,-4.05082688800065,
128.011723656052));
#72289=CARTESIAN_POINT('Ctrl Pts',(0.425355603419435,-4.12716490245128,
128.125838623559));
#72290=CARTESIAN_POINT('Ctrl Pts',(0.417599300677551,-4.19855144066325,
128.242847614943));
#72291=CARTESIAN_POINT('Ctrl Pts',(0.409838858163378,-4.26997608001989,
128.359919057549));
#72292=CARTESIAN_POINT('Ctrl Pts',(0.402078415649149,-4.33644378784913,
128.479887260015));
#72293=CARTESIAN_POINT('Ctrl Pts',(0.394317973134974,-4.39773291854118,
128.602286994891));
#72294=CARTESIAN_POINT('Ctrl Pts',(0.386545072869516,-4.45912043598699,
128.724883216689));
#72295=CARTESIAN_POINT('Ctrl Pts',(0.378772172604079,-4.51531260369357,
128.849918414143));
#72296=CARTESIAN_POINT('Ctrl Pts',(0.370999272338622,-4.56613592001995,
128.976907246778));
#72297=CARTESIAN_POINT('Ctrl Pts',(0.363508936576789,-4.61511168078021,
129.099279715478));
#72298=CARTESIAN_POINT('Ctrl Pts',(0.35601860081495,-4.65910205293616,129.223465955907));
#72299=CARTESIAN_POINT('Ctrl Pts',(0.348528265053119,-4.69799631527375,
129.349020903213));
#72300=CARTESIAN_POINT('Ctrl Pts',(0.343920461147,-4.72192276391672,129.426258105258));
#72301=CARTESIAN_POINT('Ctrl Pts',(0.339312657240903,-4.74395159348324,
129.504109081819));
#72302=CARTESIAN_POINT('Ctrl Pts',(0.334704853334813,-4.76405452823404,
129.582490119308));
#72303=CARTESIAN_POINT('Ctrl Pts',(2.08495204958919,-4.764054528234,129.582490119308));
#72304=CARTESIAN_POINT('Ctrl Pts',(2.07719089070358,-4.79812014789423,129.715311453345));
#72305=CARTESIAN_POINT('Ctrl Pts',(2.06942973181799,-4.82659871089745,129.849448081613));
#72306=CARTESIAN_POINT('Ctrl Pts',(2.06166857293238,-4.84941560315185,129.984390270293));
#72307=CARTESIAN_POINT('Ctrl Pts',(2.05389528092719,-4.87226816534756,130.119543415833));
#72308=CARTESIAN_POINT('Ctrl Pts',(2.04612198892198,-4.88944132443237,130.255504250095));
#72309=CARTESIAN_POINT('Ctrl Pts',(2.03834869691681,-4.90091239245207,130.391758164823));
#72310=CARTESIAN_POINT('Ctrl Pts',(2.03197046725472,-4.91032476320187,130.503558771298));
#72311=CARTESIAN_POINT('Ctrl Pts',(2.0255922375926,-4.9158990529586,130.615556559118));
#72312=CARTESIAN_POINT('Ctrl Pts',(2.01921400793049,-4.91764890054129,130.727468787668));
#72313=CARTESIAN_POINT('Ctrl Pts',(2.01776248395077,-4.9180471216562,130.752937184382));
#72314=CARTESIAN_POINT('Ctrl Pts',(2.01631095997105,-4.9182474941043,130.77840868273));
#72315=CARTESIAN_POINT('Ctrl Pts',(2.01485943599133,-4.91824997664253,130.80388128917));
#72316=CARTESIAN_POINT('',(2.36014056397027,-4.91824811571211,130.808665823057));
#72317=CARTESIAN_POINT('Ctrl Pts',(2.43008709577654,-4.76405452823407,129.582490119308));
#72318=CARTESIAN_POINT('Ctrl Pts',(2.42239270595295,-4.79793465770959,129.714588229931));
#72319=CARTESIAN_POINT('Ctrl Pts',(2.41469831612934,-4.82632054610165,129.848112975725));
#72320=CARTESIAN_POINT('Ctrl Pts',(2.40700392630575,-4.84910659177793,129.982564825367));
#72321=CARTESIAN_POINT('Ctrl Pts',(2.39919336592291,-4.87223666313133,130.119046640598));
#72322=CARTESIAN_POINT('Ctrl Pts',(2.3913828055401,-4.8895963266762,130.25648337292));
#72323=CARTESIAN_POINT('Ctrl Pts',(2.38357224515727,-4.90112943007293,130.394344310362));
#72324=CARTESIAN_POINT('Ctrl Pts',(2.37576168477445,-4.91266253346964,130.532205247804));
#72325=CARTESIAN_POINT('Ctrl Pts',(2.36795112439161,-4.91836906840909,130.670489963754));
#72326=CARTESIAN_POINT('Ctrl Pts',(2.36014056400879,-4.9182481157127,130.808665822376));
#72327=CARTESIAN_POINT('Ctrl Pts',(2.3601405639703,-4.91824811571211,130.808665823057));
#72328=CARTESIAN_POINT('Ctrl Pts',(2.35074923592333,-4.91810268355692,130.974806887574));
#72329=CARTESIAN_POINT('Ctrl Pts',(2.34135790787636,-4.90953504095496,131.140577724705));
#72330=CARTESIAN_POINT('Ctrl Pts',(2.33196657982938,-4.89267991813134,131.305226149635));
#72331=CARTESIAN_POINT('Ctrl Pts',(2.32244488961019,-4.87559082728814,131.472160079471));
#72332=CARTESIAN_POINT('Ctrl Pts',(2.31292319939097,-4.84998263677548,131.637940234447));
#72333=CARTESIAN_POINT('Ctrl Pts',(2.30340150917178,-4.81604479222058,131.801805163305));
#72334=CARTESIAN_POINT('Ctrl Pts',(2.29495855130915,-4.78595183761593,131.947105488948));
#72335=CARTESIAN_POINT('Ctrl Pts',(2.28651559344653,-4.74931041912839,132.090900316533));
#72336=CARTESIAN_POINT('Ctrl Pts',(2.2780726355839,-4.70628375268726,132.23267301396));
#72337=CARTESIAN_POINT('Ctrl Pts',(2.27029830146482,-4.66666450000524,132.363218296394));
#72338=CARTESIAN_POINT('Ctrl Pts',(2.26252396734575,-4.62154668011665,132.49232063557));
#72339=CARTESIAN_POINT('Ctrl Pts',(2.25474963322668,-4.57105216454559,132.619481872883));
#72340=CARTESIAN_POINT('Ctrl Pts',(2.24698488027961,-4.52061987895223,132.746486395335));
#72341=CARTESIAN_POINT('Ctrl Pts',(2.23922012733254,-4.46482422493605,132.87155421588));
#72342=CARTESIAN_POINT('Ctrl Pts',(2.23145537438546,-4.4038371760089,132.994201066024));
#72343=CARTESIAN_POINT('Ctrl Pts',(2.22369833350046,-4.34291070027834,133.116726101587));
#72344=CARTESIAN_POINT('Ctrl Pts',(2.21594129261542,-4.276803263591,133.236834604088));
#72345=CARTESIAN_POINT('Ctrl Pts',(2.20818425173042,-4.2057352418327,133.354061411406));
#72346=CARTESIAN_POINT('Ctrl Pts',(2.20043306049029,-4.13472081302254,133.471199817076));
#72347=CARTESIAN_POINT('Ctrl Pts',(2.19268186925021,-4.05875344687101,133.58546052003));
#72348=CARTESIAN_POINT('Ctrl Pts',(2.18493067801009,-3.97809967125104,133.696402468593));
#72349=CARTESIAN_POINT('Ctrl Pts',(2.17718278123302,-3.89748017563722,133.807297263869));
#72350=CARTESIAN_POINT('Ctrl Pts',(2.16943488445592,-3.81217846160588,133.914875794679));
#72351=CARTESIAN_POINT('Ctrl Pts',(2.16168698767885,-3.72250451984202,134.018725743412));
#72352=CARTESIAN_POINT('Ctrl Pts',(2.15394071159476,-3.63284933593374,134.122553968974));
#72353=CARTESIAN_POINT('Ctrl Pts',(2.14619443551064,-3.53882399879116,134.222654868076));
#72354=CARTESIAN_POINT('Ctrl Pts',(2.13844815942656,-3.44077869514239,134.318649312815));
#72355=CARTESIAN_POINT('Ctrl Pts',(2.13070182616122,-3.34273266774545,134.414644466163));
#72356=CARTESIAN_POINT('Ctrl Pts',(2.12295549289591,-3.24066689398952,134.506532831145));
#72357=CARTESIAN_POINT('Ctrl Pts',(2.11520915963058,-3.13496802444492,134.593972543372));
#72358=CARTESIAN_POINT('Ctrl Pts',(2.10746109162761,-3.02924548437122,134.681431837115));
#72359=CARTESIAN_POINT('Ctrl Pts',(2.09971302362462,-2.91988853071488,134.764440246532));
#72360=CARTESIAN_POINT('Ctrl Pts',(2.09196495562165,-2.80731612456369,134.842696814475));
#72361=CARTESIAN_POINT('Ctrl Pts',(2.08420865287981,-2.69462407511977,134.921036554429));
#72362=CARTESIAN_POINT('Ctrl Pts',(2.07645235013801,-2.5787100680444,134.994614140847));
#72363=CARTESIAN_POINT('Ctrl Pts',(2.06869604739617,-2.46002169227708,135.063172228336));
#72364=CARTESIAN_POINT('Ctrl Pts',(2.06093560488201,-2.34126996894981,135.13176690734));
#72365=CARTESIAN_POINT('Ctrl Pts',(2.05317516236787,-2.21974127264585,135.195336568041));
#72366=CARTESIAN_POINT('Ctrl Pts',(2.04541471985371,-2.09590601572565,135.253670792834));
#72367=CARTESIAN_POINT('Ctrl Pts',(2.0376418195883,-1.97187196745764,135.312098660903));
#72368=CARTESIAN_POINT('Ctrl Pts',(2.02986891932286,-1.84552431996595,135.365274146675));
#72369=CARTESIAN_POINT('Ctrl Pts',(2.02209601905744,-1.71735243752097,135.413035445306));
#72370=CARTESIAN_POINT('Ctrl Pts',(2.01460568329531,-1.59383992584627,135.459060500428));
#72371=CARTESIAN_POINT('Ctrl Pts',(2.00711534753319,-1.46863380034468,135.500058077094));
#72372=CARTESIAN_POINT('Ctrl Pts',(1.99962501177106,-1.34218165470401,135.535928166305));
#72373=CARTESIAN_POINT('Ctrl Pts',(1.99185067765198,-1.21093503752911,135.573158280849));
#72374=CARTESIAN_POINT('Ctrl Pts',(1.98407634353283,-1.07793029949773,135.604982348999));
#72375=CARTESIAN_POINT('Ctrl Pts',(1.97630200941376,-0.943652430089781,
135.631233637823));
#72376=CARTESIAN_POINT('Ctrl Pts',(1.96853725646667,-0.809540046155123,
135.65745257428));
#72377=CARTESIAN_POINT('Ctrl Pts',(1.96077250351963,-0.674158032745218,
135.678112322297));
#72378=CARTESIAN_POINT('Ctrl Pts',(1.95300775057254,-0.53800677454321,135.693095809111));
#72379=CARTESIAN_POINT('Ctrl Pts',(1.94525070968754,-0.401990743690245,
135.708064414113));
#72380=CARTESIAN_POINT('Ctrl Pts',(1.93749366880255,-0.265207374593207,
135.717367934783));
#72381=CARTESIAN_POINT('Ctrl Pts',(1.92973662791755,-0.128167139868283,
135.720940348106));
#72382=CARTESIAN_POINT('Ctrl Pts',(1.92198543667743,0.00876975174943034,
135.724510067444));
#72383=CARTESIAN_POINT('Ctrl Pts',(1.91423424543737,0.145962734187203,135.722357271713));
#72384=CARTESIAN_POINT('Ctrl Pts',(1.90648305419725,0.28289667335303,135.714467799156));
#72385=CARTESIAN_POINT('Ctrl Pts',(1.89873515742017,0.419772411942066,135.706581679836));
#72386=CARTESIAN_POINT('Ctrl Pts',(1.89098726064303,0.556388936739516,135.692963755606));
#72387=CARTESIAN_POINT('Ctrl Pts',(1.88323936386595,0.69223179572312,135.673651962668));
#72388=CARTESIAN_POINT('Ctrl Pts',(1.87549308778186,0.828046239309058,135.654344209341));
#72389=CARTESIAN_POINT('Ctrl Pts',(1.86774681169782,0.963086952150149,135.629345011332));
#72390=CARTESIAN_POINT('Ctrl Pts',(1.86000053561372,1.09684567872519,135.598744062761));
#72391=CARTESIAN_POINT('Ctrl Pts',(1.85225420234838,1.23060539267676,135.568142888301));
#72392=CARTESIAN_POINT('Ctrl Pts',(1.84450786908304,1.36308272036018,135.531939967958));
#72393=CARTESIAN_POINT('Ctrl Pts',(1.83676153581769,1.49378104750507,135.490275815755));
#72394=CARTESIAN_POINT('Ctrl Pts',(1.82901346781471,1.62450864363412,135.448602333153));
#72395=CARTESIAN_POINT('Ctrl Pts',(1.8212653998117,1.75345607404007,135.401465303775));
#72396=CARTESIAN_POINT('Ctrl Pts',(1.81351733180873,1.8801436762501,135.34905453676));
#72397=CARTESIAN_POINT('Ctrl Pts',(1.80576102906687,2.00696592355136,135.296588066958));
#72398=CARTESIAN_POINT('Ctrl Pts',(1.79800472632501,2.13152318301157,135.238836812641));
#72399=CARTESIAN_POINT('Ctrl Pts',(1.79024842358317,2.25335700990883,135.17603824159));
#72400=CARTESIAN_POINT('Ctrl Pts',(1.78248798106899,2.37525586318801,135.113206153051));
#72401=CARTESIAN_POINT('Ctrl Pts',(1.77472753855485,2.4944280479782,135.045321573363));
#72402=CARTESIAN_POINT('Ctrl Pts',(1.76696709604067,2.61044226461746,134.972666537913));
#72403=CARTESIAN_POINT('Ctrl Pts',(1.75919419577525,2.72664271757638,134.899894870149));
#72404=CARTESIAN_POINT('Ctrl Pts',(1.75142129550978,2.83967474944634,134.822337664906));
#72405=CARTESIAN_POINT('Ctrl Pts',(1.74364839524435,2.94913771588834,134.740319178733));
#72406=CARTESIAN_POINT('Ctrl Pts',(1.73615805948226,3.05462142778048,134.661282271124));
#72407=CARTESIAN_POINT('Ctrl Pts',(1.72866772372022,3.15679081930401,134.578103003328));
#72408=CARTESIAN_POINT('Ctrl Pts',(1.72117738795814,3.25531981473364,134.491103891284));
#72409=CARTESIAN_POINT('Ctrl Pts',(1.71340305383905,3.35758456697151,134.400806181464));
#72410=CARTESIAN_POINT('Ctrl Pts',(1.70562871971992,3.45625136653761,134.306107214649));
#72411=CARTESIAN_POINT('Ctrl Pts',(1.69785438560083,3.55091778763522,134.207324903002));
#72412=CARTESIAN_POINT('Ctrl Pts',(1.69008963265374,3.64546754082941,134.108664331726));
#72413=CARTESIAN_POINT('Ctrl Pts',(1.68232487970668,3.73602645708835,134.005930708072));
#72414=CARTESIAN_POINT('Ctrl Pts',(1.67456012675959,3.82222556963625,133.899481739157));
#72415=CARTESIAN_POINT('Ctrl Pts',(1.66680308587459,3.90833906801025,133.793138496859));
#72416=CARTESIAN_POINT('Ctrl Pts',(1.65904604498957,3.99010113555588,133.683087554704));
#72417=CARTESIAN_POINT('Ctrl Pts',(1.65128900410457,4.06718030232289,133.569722700711));
#72418=CARTESIAN_POINT('Ctrl Pts',(1.64353781286444,4.14420134309065,133.456443336036));
#72419=CARTESIAN_POINT('Ctrl Pts',(1.63578662162434,4.21654629320427,133.339855355726));
#72420=CARTESIAN_POINT('Ctrl Pts',(1.62803543038422,4.2839247954175,133.220384501907));
#72421=CARTESIAN_POINT('Ctrl Pts',(1.62028753360714,4.35127465996991,133.100964426388));
#72422=CARTESIAN_POINT('Ctrl Pts',(1.61253963683011,4.4136620833328,132.978664254212));
#72423=CARTESIAN_POINT('Ctrl Pts',(1.60479174005303,4.47084090842272,132.85393731388));
#72424=CARTESIAN_POINT('Ctrl Pts',(1.59704546396892,4.52800777293514,132.729236463735));
#72425=CARTESIAN_POINT('Ctrl Pts',(1.58929918788476,4.57996804347919,132.602110210306));
#72426=CARTESIAN_POINT('Ctrl Pts',(1.58155291180066,4.62652245773492,132.473034645222));
#72427=CARTESIAN_POINT('Ctrl Pts',(1.57380657853531,4.6730772156447,132.343958127332));
#72428=CARTESIAN_POINT('Ctrl Pts',(1.56606024526992,4.71422590499153,132.212932636848));
#72429=CARTESIAN_POINT('Ctrl Pts',(1.55831391200456,4.74981831205854,132.080451940683));
#72430=CARTESIAN_POINT('Ctrl Pts',(1.55056584400159,4.78541868979834,131.947941576384));
#72431=CARTESIAN_POINT('Ctrl Pts',(1.54281777599861,4.8154602078429,131.813975735437));
#72432=CARTESIAN_POINT('Ctrl Pts',(1.53506970799563,4.83984328871408,131.679060567943));
#72433=CARTESIAN_POINT('Ctrl Pts',(1.52731340525377,4.8642522842138,131.544002011003));
#72434=CARTESIAN_POINT('Ctrl Pts',(1.51955710251191,4.88299075957508,131.407992497363));
#72435=CARTESIAN_POINT('Ctrl Pts',(1.51180079977004,4.89601070259675,131.271546086687));
#72436=CARTESIAN_POINT('Ctrl Pts',(1.50404035725587,4.90903759475403,131.135026850454));
#72437=CARTESIAN_POINT('Ctrl Pts',(1.49627991474181,4.91633985209286,130.998070642764));
#72438=CARTESIAN_POINT('Ctrl Pts',(1.48851947222764,4.91792163096898,130.861192775253));
#72439=CARTESIAN_POINT('Ctrl Pts',(1.4807465719622,4.91950594905698,130.724095179238));
#72440=CARTESIAN_POINT('Ctrl Pts',(1.47297367169672,4.91535144993815,130.587076565718));
#72441=CARTESIAN_POINT('Ctrl Pts',(1.46520077143128,4.90551438177984,130.450649276709));
#72442=CARTESIAN_POINT('Ctrl Pts',(1.45771043566926,4.89603491582718,130.319181463294));
#72443=CARTESIAN_POINT('Ctrl Pts',(1.45022009990723,4.88127889381572,130.188263034609));
#72444=CARTESIAN_POINT('Ctrl Pts',(1.44272976414521,4.86134140564454,130.058342655138));
#72445=CARTESIAN_POINT('Ctrl Pts',(1.43495543002614,4.84064798154949,129.92349630499));
#72446=CARTESIAN_POINT('Ctrl Pts',(1.42718109590707,4.81430687399003,129.789298027412));
#72447=CARTESIAN_POINT('Ctrl Pts',(1.419406761788,4.78236803050024,129.656258233913));
#72448=CARTESIAN_POINT('Ctrl Pts',(1.4116420088409,4.75046854878055,129.52338240007));
#72449=CARTESIAN_POINT('Ctrl Pts',(1.40387725589379,4.71298514789539,129.391662586066));
#72450=CARTESIAN_POINT('Ctrl Pts',(1.39611250294669,4.67001934141824,129.261602563534));
#72451=CARTESIAN_POINT('Ctrl Pts',(1.3883554620617,4.62709620918584,129.131671718451));
#72452=CARTESIAN_POINT('Ctrl Pts',(1.3805984211767,4.5787016294047,129.003397753025));
#72453=CARTESIAN_POINT('Ctrl Pts',(1.3728413802917,4.52498773948156,128.877272394354));
#72454=CARTESIAN_POINT('Ctrl Pts',(1.36509018905158,4.47131435562065,128.751242147798));
#72455=CARTESIAN_POINT('Ctrl Pts',(1.35733899781144,4.41232979850282,128.627357641175));
#72456=CARTESIAN_POINT('Ctrl Pts',(1.34958780657132,4.34823531185216,128.506093284277));
#72457=CARTESIAN_POINT('Ctrl Pts',(1.34183990979425,4.2841680670681,128.384880467966));
#72458=CARTESIAN_POINT('Ctrl Pts',(1.33409201301719,4.21499539472103,128.266285931379));
#72459=CARTESIAN_POINT('Ctrl Pts',(1.32634411624011,4.14096563900055,128.150761808568));
#72460=CARTESIAN_POINT('Ctrl Pts',(1.31859784015601,4.06695136870908,128.035261850913));
#72461=CARTESIAN_POINT('Ctrl Pts',(1.31085156407191,3.98808224672641,127.922831358503));
#72462=CARTESIAN_POINT('Ctrl Pts',(1.30310528798782,3.90465111627138,127.813895315527));
#72463=CARTESIAN_POINT('Ctrl Pts',(1.29535895472248,3.82121936994669,127.704958468409));
#72464=CARTESIAN_POINT('Ctrl Pts',(1.28761262145711,3.73322578567249,127.599516432588));
#72465=CARTESIAN_POINT('Ctrl Pts',(1.27986628819176,3.64100458935285,127.497962480195));
#72466=CARTESIAN_POINT('Ctrl Pts',(1.27211822018878,3.54876274073572,127.396385785498));
#72467=CARTESIAN_POINT('Ctrl Pts',(1.26437015218585,3.45229165894575,127.298699196218));
#72468=CARTESIAN_POINT('Ctrl Pts',(1.25662208418288,3.35196335833726,127.2052600762));
#72469=CARTESIAN_POINT('Ctrl Pts',(1.24886578144103,3.25152842761696,127.111721647972));
#72470=CARTESIAN_POINT('Ctrl Pts',(1.24110947869914,3.14722837544775,127.02243997361));
#72471=CARTESIAN_POINT('Ctrl Pts',(1.23335317595729,3.03946974301657,126.937733308943));
#72472=CARTESIAN_POINT('Ctrl Pts',(1.22559273344312,2.93165359655857,126.852981433779));
#72473=CARTESIAN_POINT('Ctrl Pts',(1.21783229092897,2.82037550868685,126.772809662271));
#72474=CARTESIAN_POINT('Ctrl Pts',(1.2100718484148,2.70607127228697,126.697493036087));
#72475=CARTESIAN_POINT('Ctrl Pts',(1.20229894814937,2.59158354457936,126.622055504968));
#72476=CARTESIAN_POINT('Ctrl Pts',(1.19452604788397,2.47406029620333,126.551488895265));
#72477=CARTESIAN_POINT('Ctrl Pts',(1.18675314761853,2.35396297851468,126.486022817175));
#72478=CARTESIAN_POINT('Ctrl Pts',(1.17926281185648,2.23823150083056,126.422936595923));
#72479=CARTESIAN_POINT('Ctrl Pts',(1.1717724760944,2.12011012864133,126.364586646589));
#72480=CARTESIAN_POINT('Ctrl Pts',(1.16428214033235,2.00002773449857,126.31113548146));
#72481=CARTESIAN_POINT('Ctrl Pts',(1.15650780621326,1.875392379884,126.255657699159));
#72482=CARTESIAN_POINT('Ctrl Pts',(1.14873347209425,1.74824955621147,126.205281771962));
#72483=CARTESIAN_POINT('Ctrl Pts',(1.14095913797516,1.61905568500213,126.160241567481));
#72484=CARTESIAN_POINT('Ctrl Pts',(1.13319438502807,1.49002103369284,126.115256871027));
#72485=CARTESIAN_POINT('Ctrl Pts',(1.12542963208091,1.35894072991131,126.075594940872));
#72486=CARTESIAN_POINT('Ctrl Pts',(1.11766487913383,1.22629348156548,126.041442671646));
#72487=CARTESIAN_POINT('Ctrl Pts',(1.10990783824882,1.09377798033653,126.007324322934));
#72488=CARTESIAN_POINT('Ctrl Pts',(1.10215079736381,0.959699007840664,125.978704841931));
#72489=CARTESIAN_POINT('Ctrl Pts',(1.09439375647881,0.824552501997182,125.955722021635));
#72490=CARTESIAN_POINT('Ctrl Pts',(1.08664256523868,0.689507911185042,125.932756532863));
#72491=CARTESIAN_POINT('Ctrl Pts',(1.0788913739985,0.553397773271081,125.915419309418));
#72492=CARTESIAN_POINT('Ctrl Pts',(1.07114018275837,0.416729999798574,125.903797469338));
#72493=CARTESIAN_POINT('Ctrl Pts',(1.06339228598128,0.280120313775526,125.89218056885));
#72494=CARTESIAN_POINT('Ctrl Pts',(1.05564438920424,0.142953852332378,125.886274253309));
#72495=CARTESIAN_POINT('Ctrl Pts',(1.04789649242716,0.00574524475383868,
125.886113973216));
#72496=CARTESIAN_POINT('Ctrl Pts',(1.04015021634305,-0.131434661741871,
125.885953726649));
#72497=CARTESIAN_POINT('Ctrl Pts',(1.03240394025895,-0.268656306120095,
125.891537125248));
#72498=CARTESIAN_POINT('Ctrl Pts',(1.02465766417484,-0.405403848235146,
125.902847506053));
#72499=CARTESIAN_POINT('Ctrl Pts',(1.01691133090949,-0.542152399789303,
125.914157970348));
#72500=CARTESIAN_POINT('Ctrl Pts',(1.00916499764412,-0.678426452462115,
125.93119546898));
#72501=CARTESIAN_POINT('Ctrl Pts',(1.00141866437878,-0.813714478006551,
125.953891381422));
#72502=CARTESIAN_POINT('Ctrl Pts',(0.993670596375804,-0.949032800366286,
125.976592376456));
#72503=CARTESIAN_POINT('Ctrl Pts',(0.98592252837279,-1.08336427070014,126.004954242135));
#72504=CARTESIAN_POINT('Ctrl Pts',(0.978174460369814,-1.21620714583907,
126.038857156135));
#72505=CARTESIAN_POINT('Ctrl Pts',(0.970418157627952,-1.34919120796672,
126.072796102555));
#72506=CARTESIAN_POINT('Ctrl Pts',(0.96266185488617,-1.48068313506388,126.112287764557));
#72507=CARTESIAN_POINT('Ctrl Pts',(0.954905552144311,-1.61019542404568,
126.157162132577));
#72508=CARTESIAN_POINT('Ctrl Pts',(0.94714510963014,-1.73977683763565,126.202060451398));
#72509=CARTESIAN_POINT('Ctrl Pts',(0.939384667115962,-1.86737614420063,
126.25234705748));
#72510=CARTESIAN_POINT('Ctrl Pts',(0.931624224601791,-1.99252638669743,
126.307803972664));
#72511=CARTESIAN_POINT('Ctrl Pts',(0.923851324336356,-2.1178775314738,126.363349912211));
#72512=CARTESIAN_POINT('Ctrl Pts',(0.916078424070928,-2.24077140517934,
126.424082573272));
#72513=CARTESIAN_POINT('Ctrl Pts',(0.908305523805495,-2.36076540452264,
126.489737833671));
#72514=CARTESIAN_POINT('Ctrl Pts',(0.900815188043487,-2.47639731974284,
126.553006359978));
#72515=CARTESIAN_POINT('Ctrl Pts',(0.893324852281462,-2.58933627161709,
126.62084564288));
#72516=CARTESIAN_POINT('Ctrl Pts',(0.885834516519452,-2.69921371786463,
126.692982701612));
#72517=CARTESIAN_POINT('Ctrl Pts',(0.878072281176324,-2.81307972117533,
126.767738339361));
#72518=CARTESIAN_POINT('Ctrl Pts',(0.870310045833136,-2.92402130880819,
126.847348396706));
#72519=CARTESIAN_POINT('Ctrl Pts',(0.862547810490014,-3.03159566656667,
126.931556623435));
#72520=CARTESIAN_POINT('Ctrl Pts',(0.854797860068331,-3.13899977149519,
127.015631577801));
#72521=CARTESIAN_POINT('Ctrl Pts',(0.847047909646632,-3.243046953757,127.10428996848));
#72522=CARTESIAN_POINT('Ctrl Pts',(0.83929795922495,-3.34332224722529,127.197231646527));
#72523=CARTESIAN_POINT('Ctrl Pts',(0.831555098781407,-3.4435058046695,127.290088297647));
#72524=CARTESIAN_POINT('Ctrl Pts',(0.823812238337883,-3.53992405127584,
127.387220176904));
#72525=CARTESIAN_POINT('Ctrl Pts',(0.816069377894337,-3.63219385504037,
127.48828600111));
#72526=CARTESIAN_POINT('Ctrl Pts',(0.808331908080964,-3.72439941996296,
127.589281462626));
#72527=CARTESIAN_POINT('Ctrl Pts',(0.800594438267576,-3.81246202473909,
127.694205131415));
#72528=CARTESIAN_POINT('Ctrl Pts',(0.792856968454203,-3.89603459572387,
127.802678174098));
#72529=CARTESIAN_POINT('Ctrl Pts',(0.785123194005817,-3.97956725299522,
127.911099410765));
#72530=CARTESIAN_POINT('Ctrl Pts',(0.777389419557418,-4.05861390533243,
128.023066337404));
#72531=CARTESIAN_POINT('Ctrl Pts',(0.769655645109026,-4.13286734607665,
128.1381665957));
#72532=CARTESIAN_POINT('Ctrl Pts',(0.761922227772828,-4.20711735811871,
128.253261539166));
#72533=CARTESIAN_POINT('Ctrl Pts',(0.754188810436655,-4.27657437691257,
128.371489202907));
#72534=CARTESIAN_POINT('Ctrl Pts',(0.746455393100462,-4.34097424555394,
128.492407836487));
#72535=CARTESIAN_POINT('Ctrl Pts',(0.738722464723643,-4.40537004239649,
128.613318824767));
#72536=CARTESIAN_POINT('Ctrl Pts',(0.730989536346873,-4.46470914538319,
128.736920095446));
#72537=CARTESIAN_POINT('Ctrl Pts',(0.723256607970058,-4.51877350937329,
128.862745559557));
#72538=CARTESIAN_POINT('Ctrl Pts',(0.715519219511834,-4.57286905578911,
128.988643595376));
#72539=CARTESIAN_POINT('Ctrl Pts',(0.707781831053554,-4.62168363215477,
129.116768025651));
#72540=CARTESIAN_POINT('Ctrl Pts',(0.700044442595328,-4.66504740260424,
129.246632851249));
#72541=CARTESIAN_POINT('Ctrl Pts',(0.693443572619805,-4.7020416173746,129.357422277526));
#72542=CARTESIAN_POINT('Ctrl Pts',(0.686842702644294,-4.73506949653453,
129.469477920621));
#72543=CARTESIAN_POINT('Ctrl Pts',(0.68024183266877,-4.76405452823404,129.582490119308));
#72544=CARTESIAN_POINT('Origin',(213.235140564004,0.,130.804360617566));
#72545=CARTESIAN_POINT('',(-1.41535445211275,-4.764054528234,129.582490119308));
#72546=CARTESIAN_POINT('',(-1.06997321827187,-4.76405452823403,129.582490119308));
#72547=CARTESIAN_POINT('',(213.235140564004,-4.76405452823405,129.582490119308));
#72548=CARTESIAN_POINT('',(0.264859436032587,-4.91824816321245,130.80011002262));
#72549=CARTESIAN_POINT('Ctrl Pts',(0.264859435991383,-4.91824816321308,
130.800110023348));
#72550=CARTESIAN_POINT('Ctrl Pts',(0.257155925891214,-4.91836596679253,
130.936417374421));
#72551=CARTESIAN_POINT('Ctrl Pts',(0.249452415791054,-4.91281295310806,
131.07282508718));
#72552=CARTESIAN_POINT('Ctrl Pts',(0.241748905690883,-4.9015909330034,131.208822467434));
#72553=CARTESIAN_POINT('Ctrl Pts',(0.234047548106026,-4.89037204855636,
131.344781847292));
#72554=CARTESIAN_POINT('Ctrl Pts',(0.226346190521118,-4.87348733670645,
131.480330728431));
#72555=CARTESIAN_POINT('Ctrl Pts',(0.218644832936263,-4.85099066675386,
131.614960773973));
#72556=CARTESIAN_POINT('Ctrl Pts',(0.210944272133467,-4.82849632430558,
131.749576890697));
#72557=CARTESIAN_POINT('Ctrl Pts',(0.203243711330728,-4.80039124349492,
131.883273970466));
#72558=CARTESIAN_POINT('Ctrl Pts',(0.195543150527925,-4.76678081049386,
132.015551670706));
#72559=CARTESIAN_POINT('Ctrl Pts',(0.187841670661972,-4.7331663660823,132.147845158312));
#72560=CARTESIAN_POINT('Ctrl Pts',(0.18014019079599,-4.69404535981923,132.278718545692));
#72561=CARTESIAN_POINT('Ctrl Pts',(0.172438710930038,-4.6495735423203,132.407684956886));
#72562=CARTESIAN_POINT('Ctrl Pts',(0.164734595837766,-4.60508650783633,
132.5366954967));
#72563=CARTESIAN_POINT('Ctrl Pts',(0.157030480745469,-4.55524514874875,
132.663797388243));
#72564=CARTESIAN_POINT('Ctrl Pts',(0.149326365653195,-4.50025383203119,
132.788522533789));
#72565=CARTESIAN_POINT('Ctrl Pts',(0.141613515289472,-4.44520016369075,
132.913389098302));
#72566=CARTESIAN_POINT('Ctrl Pts',(0.13390066492578,-4.38498504005876,133.035873174433));
#72567=CARTESIAN_POINT('Ctrl Pts',(0.126187814562059,-4.31985956285699,
133.155529777727));
#72568=CARTESIAN_POINT('Ctrl Pts',(0.118469949690756,-4.2546917443438,133.27526417573));
#72569=CARTESIAN_POINT('Ctrl Pts',(0.110752084819423,-4.18460741789559,
133.392167101679));
#72570=CARTESIAN_POINT('Ctrl Pts',(0.103034219948114,-4.1099010850809,133.50582246874));
#72571=CARTESIAN_POINT('Ctrl Pts',(0.0953049229631315,-4.03508409325585,
133.619646188202));
#72572=CARTESIAN_POINT('Ctrl Pts',(0.0875756259781753,-3.95563165761873,
133.730212425312));
#72573=CARTESIAN_POINT('Ctrl Pts',(0.0798463289931988,-3.87187887761787,
133.837137730965));
#72574=CARTESIAN_POINT('Ctrl Pts',(0.0765910997421861,-3.83660600612097,
133.882169819046));
#72575=CARTESIAN_POINT('Ctrl Pts',(0.0733358704911794,-3.80057083114038,
133.926556555174));
#72576=CARTESIAN_POINT('Ctrl Pts',(0.0700806412401676,-3.76380028239309,
133.970271307519));
#72577=CARTESIAN_POINT('Ctrl Pts',(0.0623063071210835,-3.67598264816203,
134.074673506092));
#72578=CARTESIAN_POINT('Ctrl Pts',(0.0545319730019769,-3.58367868344521,
134.175584406148));
#72579=CARTESIAN_POINT('Ctrl Pts',(0.0467576388828945,-3.48719655174587,
134.272594068762));
#72580=CARTESIAN_POINT('Ctrl Pts',(0.0389928859358018,-3.39083332565099,
134.369484175636));
#72581=CARTESIAN_POINT('Ctrl Pts',(0.0312281329887449,-3.29030245103418,
134.462482336865));
#72582=CARTESIAN_POINT('Ctrl Pts',(0.0234633800416475,-3.18595267781633,
134.55121110794));
#72583=CARTESIAN_POINT('Ctrl Pts',(0.015706339156641,-3.08170654626431,
134.639851752349));
#72584=CARTESIAN_POINT('Ctrl Pts',(0.00794929827169961,-2.97364936024052,
134.724231193607));
#72585=CARTESIAN_POINT('Ctrl Pts',(0.000192257386686379,-2.86216683999603,
134.804008607393));
#72586=CARTESIAN_POINT('Ctrl Pts',(-0.00755893385344394,-2.75076838958742,
134.883725860411));
#72587=CARTESIAN_POINT('Ctrl Pts',(-0.0153101250936031,-2.63595006306119,
134.958847767025));
#72588=CARTESIAN_POINT('Ctrl Pts',(-0.0230613163337239,-2.51813051216657,
135.029073836969));
#72589=CARTESIAN_POINT('Ctrl Pts',(-0.0308092131108083,-2.40036103772387,
135.099270058959));
#72590=CARTESIAN_POINT('Ctrl Pts',(-0.0385571098879394,-2.27959321111571,
135.164574383199));
#72591=CARTESIAN_POINT('Ctrl Pts',(-0.0463050066650226,-2.15627432320337,
135.224729844858));
#72592=CARTESIAN_POINT('Ctrl Pts',(-0.0540512827491253,-2.03298123094393,
135.284872723292));
#72593=CARTESIAN_POINT('Ctrl Pts',(-0.0617975588331814,-1.90713848995841,
135.339868710118));
#72594=CARTESIAN_POINT('Ctrl Pts',(-0.0695438349172832,-1.77921727302561,
135.389507175515));
#72595=CARTESIAN_POINT('Ctrl Pts',(-0.0772901681826248,-1.65129511180763,
135.439146007331));
#72596=CARTESIAN_POINT('Ctrl Pts',(-0.0850365014479683,-1.52129480851277,
135.483427097366));
#72597=CARTESIAN_POINT('Ctrl Pts',(-0.0927828347133186,-1.38970638314527,
135.522188426118));
#72598=CARTESIAN_POINT('Ctrl Pts',(-0.100530902716305,-1.25808848946211,
135.5609584352));
#72599=CARTESIAN_POINT('Ctrl Pts',(-0.108278970719271,-1.12488214096745,
135.594206112828));
#72600=CARTESIAN_POINT('Ctrl Pts',(-0.116027038722251,-0.990590952417051,
135.621819763993));
#72601=CARTESIAN_POINT('Ctrl Pts',(-0.123783341464108,-0.856157037593378,
135.649462763274));
#72602=CARTESIAN_POINT('Ctrl Pts',(-0.131539644205981,-0.720636363074086,
135.671459695725));
#72603=CARTESIAN_POINT('Ctrl Pts',(-0.13929594694784,-0.58454168832645,
135.687750226957));
#72604=CARTESIAN_POINT('Ctrl Pts',(-0.14705638946202,-0.448374375752984,
135.704049452936));
#72605=CARTESIAN_POINT('Ctrl Pts',(-0.154816831976237,-0.311632842108518,
135.71463617876));
#72606=CARTESIAN_POINT('Ctrl Pts',(-0.162577274490417,-0.17483235037309,
135.719502193529));
#72607=CARTESIAN_POINT('Ctrl Pts',(-0.17035017475585,-0.0378122543439376,
135.724376019658));
#72608=CARTESIAN_POINT('Ctrl Pts',(-0.178123075021275,0.099266597724136,
135.723510785855));
#72609=CARTESIAN_POINT('Ctrl Pts',(-0.185895975286712,0.235890661557176,
135.716950429294));
#72610=CARTESIAN_POINT('Ctrl Pts',(-0.193386311048693,0.367548096533708,
135.710628558218));
#72611=CARTESIAN_POINT('Ctrl Pts',(-0.200876646810635,0.498782927787022,
135.699018466883));
#72612=CARTESIAN_POINT('Ctrl Pts',(-0.208366982572613,0.629144338140574,
135.682204451094));
#72613=CARTESIAN_POINT('Ctrl Pts',(-0.2161413166917,0.764448440991128,135.664752926785));
#72614=CARTESIAN_POINT('Ctrl Pts',(-0.223915650810826,0.899240186732062,
135.64163979345));
#72615=CARTESIAN_POINT('Ctrl Pts',(-0.231689984929915,1.03300811223624,
135.612902735771));
#72616=CARTESIAN_POINT('Ctrl Pts',(-0.239454737877014,1.16661118072741,
135.584201093948));
#72617=CARTESIAN_POINT('Ctrl Pts',(-0.247219490824093,1.29919256094725,
135.5498893997));
#72618=CARTESIAN_POINT('Ctrl Pts',(-0.25498424377119,1.43024619029129,135.51005704824));
#72619=CARTESIAN_POINT('Ctrl Pts',(-0.262741284656176,1.56116965532278,
135.470264258833));
#72620=CARTESIAN_POINT('Ctrl Pts',(-0.270498325541162,1.69056801749238,
135.424961836975));
#72621=CARTESIAN_POINT('Ctrl Pts',(-0.278255366426151,1.81794604042814,
135.374290076167));
#72622=CARTESIAN_POINT('Ctrl Pts',(-0.286006557666269,1.94522800660595,
135.323656527329));
#72623=CARTESIAN_POINT('Ctrl Pts',(-0.29375774890639,2.07049230428448,135.267661842878));
#72624=CARTESIAN_POINT('Ctrl Pts',(-0.301508940146505,2.19325983099465,
135.206495824059));
#72625=CARTESIAN_POINT('Ctrl Pts',(-0.309256836923583,2.3159751782312,135.14535580243));
#72626=CARTESIAN_POINT('Ctrl Pts',(-0.317004733700642,2.43619551592867,
135.07904899198));
#72627=CARTESIAN_POINT('Ctrl Pts',(-0.324752630477718,2.55346288066148,
135.007812815413));
#72628=CARTESIAN_POINT('Ctrl Pts',(-0.332498906561814,2.67070571558959,
134.936591539918));
#72629=CARTESIAN_POINT('Ctrl Pts',(-0.340245182645885,2.78499647225651,
134.860443152107));
#72630=CARTESIAN_POINT('Ctrl Pts',(-0.347991458729979,2.89590326143027,
134.779650212418));
#72631=CARTESIAN_POINT('Ctrl Pts',(-0.355737791995302,3.00681086929244,
134.698856676334));
#72632=CARTESIAN_POINT('Ctrl Pts',(-0.363484125260661,3.11433414380964,
134.613418750162));
#72633=CARTESIAN_POINT('Ctrl Pts',(-0.371230458525986,3.21807190560325,
134.523661126112));
#72634=CARTESIAN_POINT('Ctrl Pts',(-0.378978526528957,3.32183289874962,
134.433883401463));
#72635=CARTESIAN_POINT('Ctrl Pts',(-0.386726594531866,3.42180639666844,
134.339784309752));
#72636=CARTESIAN_POINT('Ctrl Pts',(-0.394474662534833,3.51762621110825,
134.241727182456));
#72637=CARTESIAN_POINT('Ctrl Pts',(-0.402230965276666,3.61354786398699,
134.143565838878));
#72638=CARTESIAN_POINT('Ctrl Pts',(-0.409987268018584,3.70530674109778,
134.041438336555));
#72639=CARTESIAN_POINT('Ctrl Pts',(-0.417743570760422,3.7925749223932,133.935743462338));
#72640=CARTESIAN_POINT('Ctrl Pts',(-0.42550401327457,3.87988968134458,133.829992175584));
#72641=CARTESIAN_POINT('Ctrl Pts',(-0.433264455788733,3.96270873264421,
133.720670034511));
#72642=CARTESIAN_POINT('Ctrl Pts',(-0.441024898302885,4.04074665600303,
133.608206106265));
#72643=CARTESIAN_POINT('Ctrl Pts',(-0.448797798568311,4.11890985276441,
133.495561640938));
#72644=CARTESIAN_POINT('Ctrl Pts',(-0.456570698833782,4.19227637494115,
133.379765640413));
#72645=CARTESIAN_POINT('Ctrl Pts',(-0.464343599099209,4.26060560489768,
133.261273913149));
#72646=CARTESIAN_POINT('Ctrl Pts',(-0.471833934861339,4.32645089523526,
133.147089658633));
#72647=CARTESIAN_POINT('Ctrl Pts',(-0.47932427062341,4.38761862846298,133.030402540375));
#72648=CARTESIAN_POINT('Ctrl Pts',(-0.486814606385536,4.44393604733321,
132.911637407575));
#72649=CARTESIAN_POINT('Ctrl Pts',(-0.494588940504623,4.50238875825648,
132.78836925867));
#72650=CARTESIAN_POINT('Ctrl Pts',(-0.502363274623689,4.55580125562843,
132.66247193234));
#72651=CARTESIAN_POINT('Ctrl Pts',(-0.510137608742781,4.60392878632553,
132.534396106492));
#72652=CARTESIAN_POINT('Ctrl Pts',(-0.517902361689883,4.65199700414232,
132.406478122652));
#72653=CARTESIAN_POINT('Ctrl Pts',(-0.525667114636987,4.6947930785036,132.276387343723));
#72654=CARTESIAN_POINT('Ctrl Pts',(-0.533431867584085,4.73211868093234,
132.144597854801));
#72655=CARTESIAN_POINT('Ctrl Pts',(-0.541188908469091,4.76940721104654,
132.012939261057));
#72656=CARTESIAN_POINT('Ctrl Pts',(-0.548945949354093,4.80123597598984,
131.879585688624));
#72657=CARTESIAN_POINT('Ctrl Pts',(-0.556702990239103,4.82745532130159,
131.745029625952));
#72658=CARTESIAN_POINT('Ctrl Pts',(-0.564454181479197,4.85365489440094,
131.610575033053));
#72659=CARTESIAN_POINT('Ctrl Pts',(-0.57220537271931,4.8742533931664,131.474920137056));
#72660=CARTESIAN_POINT('Ctrl Pts',(-0.579956563959399,4.88915153617268,
131.338570612643));
#72661=CARTESIAN_POINT('Ctrl Pts',(-0.587704460736484,4.90404334707083,
131.202279040415));
#72662=CARTESIAN_POINT('Ctrl Pts',(-0.595452357513553,4.91323957860379,
131.065293814811));
#72663=CARTESIAN_POINT('Ctrl Pts',(-0.603200254290641,4.91669244079701,
130.928128566202));
#72664=CARTESIAN_POINT('Ctrl Pts',(-0.610946530374749,4.92014458072589,
130.790992009606));
#72665=CARTESIAN_POINT('Ctrl Pts',(-0.618692806458852,4.9178557311113,130.6536758955));
#72666=CARTESIAN_POINT('Ctrl Pts',(-0.626439082542959,4.90983017137331,
130.516696315345));
#72667=CARTESIAN_POINT('Ctrl Pts',(-0.634185415808306,4.90180455239248,
130.379715724038));
#72668=CARTESIAN_POINT('Ctrl Pts',(-0.641931749073644,4.88804216165495,
130.243072061936));
#72669=CARTESIAN_POINT('Ctrl Pts',(-0.649678082338994,4.86859932465799,
130.107278356682));
#72670=CARTESIAN_POINT('Ctrl Pts',(-0.65742615034198,4.84915213357247,129.971454241368));
#72671=CARTESIAN_POINT('Ctrl Pts',(-0.665174218344999,4.82402202030502,
129.836480848604));
#72672=CARTESIAN_POINT('Ctrl Pts',(-0.672922286347983,4.79331673222229,
129.702862652476));
#72673=CARTESIAN_POINT('Ctrl Pts',(-0.680678589089834,4.76257881019404,
129.569102445339));
#72674=CARTESIAN_POINT('Ctrl Pts',(-0.688434891831638,4.72625396450211,
129.43670069367));
#72675=CARTESIAN_POINT('Ctrl Pts',(-0.696191194573487,4.68450045702273,
129.306148839928));
#72676=CARTESIAN_POINT('Ctrl Pts',(-0.703951637087657,4.64272466443918,
129.17552730673));
#72677=CARTESIAN_POINT('Ctrl Pts',(-0.711712079601864,4.59551457118554,
129.046758005722));
#72678=CARTESIAN_POINT('Ctrl Pts',(-0.719472522116035,4.5430768869658,128.92031299035));
#72679=CARTESIAN_POINT('Ctrl Pts',(-0.72724542238147,4.49055502512016,128.793664994214));
#72680=CARTESIAN_POINT('Ctrl Pts',(-0.735018322646873,4.43278896767901,
128.669349094501));
#72681=CARTESIAN_POINT('Ctrl Pts',(-0.742791222912302,4.37003213949743,
128.547814105247));
#72682=CARTESIAN_POINT('Ctrl Pts',(-0.750281558674329,4.30955668009515,
128.43069721898));
#72683=CARTESIAN_POINT('Ctrl Pts',(-0.757771894436371,4.24444715666911,
128.316162834997));
#72684=CARTESIAN_POINT('Ctrl Pts',(-0.765262230198402,4.1749676273715,128.204585940233));
#72685=CARTESIAN_POINT('Ctrl Pts',(-0.773036564317499,4.10285376060263,
128.088778573591));
#72686=CARTESIAN_POINT('Ctrl Pts',(-0.780810898436576,4.02580353386628,
127.975790546737));
#72687=CARTESIAN_POINT('Ctrl Pts',(-0.788585232555675,3.9440638202062,127.866071379822));
#72688=CARTESIAN_POINT('Ctrl Pts',(-0.796349985502775,3.86242484343802,
127.756487431975));
#72689=CARTESIAN_POINT('Ctrl Pts',(-0.80411473844991,3.77610811030726,127.650164638912));
#72690=CARTESIAN_POINT('Ctrl Pts',(-0.811879491397008,3.6854052806458,127.547526114573));
#72691=CARTESIAN_POINT('Ctrl Pts',(-0.819636532282004,3.59479253831357,
127.444989532263));
#72692=CARTESIAN_POINT('Ctrl Pts',(-0.827393573166975,3.49980262596916,
127.346130227637));
#72693=CARTESIAN_POINT('Ctrl Pts',(-0.835150614051969,3.40076899620152,
127.251340311267));
#72694=CARTESIAN_POINT('Ctrl Pts',(-0.842901805292132,3.30181004846391,
127.15662187671));
#72695=CARTESIAN_POINT('Ctrl Pts',(-0.850652996532273,3.19881373424288,
127.065966991476));
#72696=CARTESIAN_POINT('Ctrl Pts',(-0.858404187772436,3.09215182793659,
126.979732513359));
#72697=CARTESIAN_POINT('Ctrl Pts',(-0.86615208454952,2.98553525578622,126.893534687197));
#72698=CARTESIAN_POINT('Ctrl Pts',(-0.873899981326623,2.87525649363664,
126.811753776668));
#72699=CARTESIAN_POINT('Ctrl Pts',(-0.881647878103706,2.76172184161628,
126.734707618594));
#72700=CARTESIAN_POINT('Ctrl Pts',(-0.889394154187809,2.6482109385976,126.657677576916));
#72701=CARTESIAN_POINT('Ctrl Pts',(-0.897140430271968,2.53144582368067,
126.585380537113));
#72702=CARTESIAN_POINT('Ctrl Pts',(-0.904886706356081,2.41186301235968,
126.518091858831));
#72703=CARTESIAN_POINT('Ctrl Pts',(-0.912633039621454,2.29227931830538,
126.450802683838));
#72704=CARTESIAN_POINT('Ctrl Pts',(-0.920379372886749,2.1698782270702,126.388522135864));
#72705=CARTESIAN_POINT('Ctrl Pts',(-0.928125706152116,2.04512180864695,
126.331480130643));
#72706=CARTESIAN_POINT('Ctrl Pts',(-0.935873774155067,1.92033745188947,
126.274425351261));
#72707=CARTESIAN_POINT('Ctrl Pts',(-0.94362184215799,1.79319707385472,126.222611611578));
#72708=CARTESIAN_POINT('Ctrl Pts',(-0.951369910160935,1.66418334296127,
126.176220941248));
#72709=CARTESIAN_POINT('Ctrl Pts',(-0.959126212902788,1.53503249473883,
126.129780966361));
#72710=CARTESIAN_POINT('Ctrl Pts',(-0.966882515644722,1.4040046848675,126.088775706945));
#72711=CARTESIAN_POINT('Ctrl Pts',(-0.97463881838658,1.27159892221444,126.053337649455));
#72712=CARTESIAN_POINT('Ctrl Pts',(-0.982399260900771,1.13912249061884,
126.017880677605));
#72713=CARTESIAN_POINT('Ctrl Pts',(-0.990159703414939,1.00526702217028,
125.987996913559));
#72714=CARTESIAN_POINT('Ctrl Pts',(-0.997920145929129,0.870541400446195,
125.963767603006));
#72715=CARTESIAN_POINT('Ctrl Pts',(-1.00569304619457,0.735599505193924,
125.939499397412));
#72716=CARTESIAN_POINT('Ctrl Pts',(-1.01346594646001,0.599785052894364,
125.920903837178));
#72717=CARTESIAN_POINT('Ctrl Pts',(-1.02123884672545,0.46361262583191,125.908010303744));
#72718=CARTESIAN_POINT('Ctrl Pts',(-1.02872918248739,0.332390409492662,
125.895585482727));
#72719=CARTESIAN_POINT('Ctrl Pts',(-1.0362195182493,0.200836100666851,125.888455336582));
#72720=CARTESIAN_POINT('Ctrl Pts',(-1.04370985401124,0.0694079163645821,
125.886600395306));
#72721=CARTESIAN_POINT('Ctrl Pts',(-1.0514841881303,-0.0670034074939693,
125.884675123367));
#72722=CARTESIAN_POINT('Ctrl Pts',(-1.0592585222494,-0.203710964080631,
125.888426872895));
#72723=CARTESIAN_POINT('Ctrl Pts',(-1.06703285636848,-0.340203118451164,
125.897890919229));
#72724=CARTESIAN_POINT('Ctrl Pts',(-1.07479760931557,-0.476527058439906,
125.907343301972));
#72725=CARTESIAN_POINT('Ctrl Pts',(-1.08256236226268,-0.612635738122209,
125.922493947443));
#72726=CARTESIAN_POINT('Ctrl Pts',(-1.09032711520976,-0.748015530494374,
125.943326177384));
#72727=CARTESIAN_POINT('Ctrl Pts',(-1.09808415609477,-0.883260861748602,
125.96413771646));
#72728=CARTESIAN_POINT('Ctrl Pts',(-1.10584119697979,-1.01777836245176,
125.990619551047));
#72729=CARTESIAN_POINT('Ctrl Pts',(-1.11359823786481,-1.15105789960446,
126.022703083378));
#72730=CARTESIAN_POINT('Ctrl Pts',(-1.12134942910496,-1.28423692962162,
126.054762421268));
#72731=CARTESIAN_POINT('Ctrl Pts',(-1.12910062034512,-1.41617947570971,
126.092414957592));
#72732=CARTESIAN_POINT('Ctrl Pts',(-1.13685181158527,-1.5463843501568,126.135540798373));
#72733=CARTESIAN_POINT('Ctrl Pts',(-1.14459970836237,-1.67653388405874,
126.178648309521));
#72734=CARTESIAN_POINT('Ctrl Pts',(-1.15234760513948,-1.80494684489254,
126.227224375624));
#72735=CARTESIAN_POINT('Ctrl Pts',(-1.16009550191657,-1.93113621239599,
126.281098963442));
#72736=CARTESIAN_POINT('Ctrl Pts',(-1.16784177800068,-2.05729918380391,
126.334962281856));
#72737=CARTESIAN_POINT('Ctrl Pts',(-1.17558805408473,-2.18123912770745,
126.394121764029));
#72738=CARTESIAN_POINT('Ctrl Pts',(-1.18333433016883,-2.30248842895252,
126.458358995726));
#72739=CARTESIAN_POINT('Ctrl Pts',(-1.1910806634342,-2.42373862523256,126.522596701607));
#72740=CARTESIAN_POINT('Ctrl Pts',(-1.19882699669964,-2.54229779374591,
126.591912048775));
#72741=CARTESIAN_POINT('Ctrl Pts',(-1.20657332996501,-2.65772273975424,
126.666040559729));
#72742=CARTESIAN_POINT('Ctrl Pts',(-1.214321397968,-2.77317353437893,126.74018567125));
#72743=CARTESIAN_POINT('Ctrl Pts',(-1.22206946597092,-2.88548838092046,
126.819145880174));
#72744=CARTESIAN_POINT('Ctrl Pts',(-1.22981753397391,-2.99425323860536,
126.902613495365));
#72745=CARTESIAN_POINT('Ctrl Pts',(-1.23757383671577,-3.10313369287517,
126.986169820931));
#72746=CARTESIAN_POINT('Ctrl Pts',(-1.24533013945765,-3.20845631071841,
127.074242883953));
#72747=CARTESIAN_POINT('Ctrl Pts',(-1.2530864421995,-3.30983990104797,127.166484466303));
#72748=CARTESIAN_POINT('Ctrl Pts',(-1.2608468847137,-3.41127760285271,127.258775280762));
#72749=CARTESIAN_POINT('Ctrl Pts',(-1.26860732722794,-3.50877181019504,
127.355238772934));
#72750=CARTESIAN_POINT('Ctrl Pts',(-1.27636776974214,-3.60197910477145,
127.45549071993));
#72751=CARTESIAN_POINT('Ctrl Pts',(-1.28414067000757,-3.69533602397128,
127.555903600252));
#72752=CARTESIAN_POINT('Ctrl Pts',(-1.29191357027294,-3.78439202437051,
127.660116790908));
#72753=CARTESIAN_POINT('Ctrl Pts',(-1.29968647053838,-3.86884424223603,
127.767713240636));
#72754=CARTESIAN_POINT('Ctrl Pts',(-1.30717680630035,-3.95022640925926,
127.871398288396));
#72755=CARTESIAN_POINT('Ctrl Pts',(-1.31466714206236,-4.02733352046038,
127.978224636069));
#72756=CARTESIAN_POINT('Ctrl Pts',(-1.32215747782433,-4.09993427901852,
128.087796248693));
#72757=CARTESIAN_POINT('Ctrl Pts',(-1.33007845192884,-4.1767090387597,128.203667410383));
#72758=CARTESIAN_POINT('Ctrl Pts',(-1.33799942603336,-4.24868068094989,
128.322965474712));
#72759=CARTESIAN_POINT('Ctrl Pts',(-1.34592040013786,-4.31553515966779,
128.445263470738));
#72760=CARTESIAN_POINT('Ctrl Pts',(-1.3538315769244,-4.38230694721971,128.567410198456));
#72761=CARTESIAN_POINT('Ctrl Pts',(-1.36174275371097,-4.44397398948351,
128.692549151836));
#72762=CARTESIAN_POINT('Ctrl Pts',(-1.36965393049752,-4.50026481313829,
128.820223607647));
#72763=CARTESIAN_POINT('Ctrl Pts',(-1.37755394090117,-4.55647618402545,
128.947717854888));
#72764=CARTESIAN_POINT('Ctrl Pts',(-1.38545395130488,-4.60732630606783,
129.077740137057));
#72765=CARTESIAN_POINT('Ctrl Pts',(-1.39335396170856,-4.65258938362391,
129.209808928253));
#72766=CARTESIAN_POINT('Ctrl Pts',(-1.40068745851,-4.69460662379444,129.332407001967));
#72767=CARTESIAN_POINT('Ctrl Pts',(-1.40802095531133,-4.73180972531184,
129.456768122098));
#72768=CARTESIAN_POINT('Ctrl Pts',(-1.41535445211275,-4.764054528234,129.582490119308));
#72769=CARTESIAN_POINT('Ctrl Pts',(0.334704853334813,-4.76405452823404,
129.582490119308));
#72770=CARTESIAN_POINT('Ctrl Pts',(0.325259123083958,-4.80526437630398,
129.743166691486));
#72771=CARTESIAN_POINT('Ctrl Pts',(0.315813392833079,-4.83837810705644,
129.906072091631));
#72772=CARTESIAN_POINT('Ctrl Pts',(0.306367662582232,-4.86318687792424,
130.070469308934));
#72773=CARTESIAN_POINT('Ctrl Pts',(0.297037133478273,-4.8876930783416,130.232861520009));
#72774=CARTESIAN_POINT('Ctrl Pts',(0.287706604374324,-4.9040956196616,130.396709380425));
#72775=CARTESIAN_POINT('Ctrl Pts',(0.27837607527033,-4.91223936948906,130.561281537138));
#72776=CARTESIAN_POINT('Ctrl Pts',(0.273870528857723,-4.91617184131476,
130.640750502084));
#72777=CARTESIAN_POINT('Ctrl Pts',(0.269364982445099,-4.91817926350584,
130.720388040219));
#72778=CARTESIAN_POINT('Ctrl Pts',(0.264859436032481,-4.91824816321245,
130.80011002262));
#72779=CARTESIAN_POINT('',(0.610140564062025,-4.91824999063408,130.80466414335));
#72780=CARTESIAN_POINT('Ctrl Pts',(0.68024183266877,-4.76405452823404,129.582490119308));
#72781=CARTESIAN_POINT('Ctrl Pts',(0.672495220846975,-4.79807061854507,
129.715118339165));
#72782=CARTESIAN_POINT('Ctrl Pts',(0.664748609025191,-4.82651737018263,
129.849063881117));
#72783=CARTESIAN_POINT('Ctrl Pts',(0.657001997203395,-4.84931889002808,
129.983818500843));
#72784=CARTESIAN_POINT('Ctrl Pts',(0.649191758346509,-4.87230769085994,
130.119679931793));
#72785=CARTESIAN_POINT('Ctrl Pts',(0.641381519489651,-4.88955806601628,
130.256363385809));
#72786=CARTESIAN_POINT('Ctrl Pts',(0.633571280632765,-4.90104574451915,
130.393345201029));
#72787=CARTESIAN_POINT('Ctrl Pts',(0.625761041775879,-4.91253342302202,
130.53032701625));
#72788=CARTESIAN_POINT('Ctrl Pts',(0.617950802918943,-4.91825844901687,
130.66760678831));
#72789=CARTESIAN_POINT('Ctrl Pts',(0.610140564062078,-4.91824999063408,
130.80466414335));
#72790=CARTESIAN_POINT('Ctrl Pts',(0.610140564008816,-4.91824999063402,
130.804664144283));
#72791=CARTESIAN_POINT('Ctrl Pts',(0.609222673574721,-4.91824899656807,
130.820771671519));
#72792=CARTESIAN_POINT('Ctrl Pts',(0.608304783140653,-4.91816887329494,
130.836878914827));
#72793=CARTESIAN_POINT('Ctrl Pts',(0.607386892706558,-4.91800962743144,
130.852985374549));
#72794=CARTESIAN_POINT('Ctrl Pts',(0.599612558587471,-4.91666084929413,
130.989403616534));
#72795=CARTESIAN_POINT('Ctrl Pts',(0.591838224468402,-4.90962957576278,
131.125981773078));
#72796=CARTESIAN_POINT('Ctrl Pts',(0.584063890349313,-4.89689281948563,
131.262207510064));
#72797=CARTESIAN_POINT('Ctrl Pts',(0.576299137402214,-4.88417176012228,
131.398265361004));
#72798=CARTESIAN_POINT('Ctrl Pts',(0.568534384455138,-4.86575924464363,
131.533971271033));
#72799=CARTESIAN_POINT('Ctrl Pts',(0.560769631508037,-4.84168427213609,
131.668812161292));
#72800=CARTESIAN_POINT('Ctrl Pts',(0.553012590623038,-4.81763321123067,
131.803519125678));
#72801=CARTESIAN_POINT('Ctrl Pts',(0.545255549737985,-4.7879309536471,131.937362397652));
#72802=CARTESIAN_POINT('Ctrl Pts',(0.537498508852991,-4.75265831918086,
132.069833637279));
#72803=CARTESIAN_POINT('Ctrl Pts',(0.52974731761287,-4.71741228408266,132.202204979313));
#72804=CARTESIAN_POINT('Ctrl Pts',(0.521996126372786,-4.67660433345869,
132.333205972155));
#72805=CARTESIAN_POINT('Ctrl Pts',(0.514244935132666,-4.63036635388174,
132.462338449547));
#72806=CARTESIAN_POINT('Ctrl Pts',(0.506497038355583,-4.58414802667949,
132.591416042191));
#72807=CARTESIAN_POINT('Ctrl Pts',(0.498749141578544,-4.5325043922969,132.718626331617));
#72808=CARTESIAN_POINT('Ctrl Pts',(0.491001244801453,-4.47561712215223,
132.843486518142));
#72809=CARTESIAN_POINT('Ctrl Pts',(0.483254968717341,-4.41874175159812,
132.968320586606));
#72810=CARTESIAN_POINT('Ctrl Pts',(0.47550869263321,-4.35662508898079,133.090805174417));
#72811=CARTESIAN_POINT('Ctrl Pts',(0.467762416549107,-4.28949670711112,
133.210478042419));
#72812=CARTESIAN_POINT('Ctrl Pts',(0.460016083283763,-4.22236782971507,
133.33015179382));
#72813=CARTESIAN_POINT('Ctrl Pts',(0.452269750018361,-4.15022735051399,
133.447013443013));
#72814=CARTESIAN_POINT('Ctrl Pts',(0.444523416753015,-4.07335030629657,
133.56062626962));
#72815=CARTESIAN_POINT('Ctrl Pts',(0.436775348750042,-3.99645604599812,
133.674264539032));
#72816=CARTESIAN_POINT('Ctrl Pts',(0.429027280747135,-3.91482332903275,
133.784652214376));
#72817=CARTESIAN_POINT('Ctrl Pts',(0.421279212744167,-3.82876969376594,
133.891382757849));
#72818=CARTESIAN_POINT('Ctrl Pts',(0.413522910002312,-3.7426245996714,133.998226735815));
#72819=CARTESIAN_POINT('Ctrl Pts',(0.405766607260464,-3.6520494470938,134.101405512678));
#72820=CARTESIAN_POINT('Ctrl Pts',(0.398010304518607,-3.55740150141835,
134.2005463634));
#72821=CARTESIAN_POINT('Ctrl Pts',(0.390249862004428,-3.46270303928437,
134.299740128579));
#72822=CARTESIAN_POINT('Ctrl Pts',(0.382489419490209,-3.36392773406066,
134.394891402165));
#72823=CARTESIAN_POINT('Ctrl Pts',(0.37472897697603,-3.26146793907907,134.485666085041));
#72824=CARTESIAN_POINT('Ctrl Pts',(0.366956076710598,-3.15884366653876,
134.576586487495));
#72825=CARTESIAN_POINT('Ctrl Pts',(0.359183176445221,-3.05252338825171,
134.663116012738));
#72826=CARTESIAN_POINT('Ctrl Pts',(0.351410276179791,-2.94293130327465,
134.744961892334));
#72827=CARTESIAN_POINT('Ctrl Pts',(0.343919940417796,-2.83732316663275,
134.823832468049));
#72828=CARTESIAN_POINT('Ctrl Pts',(0.336429604655745,-2.7286772242474,134.898353836516));
#72829=CARTESIAN_POINT('Ctrl Pts',(0.328939268893748,-2.61739494751692,
134.968304271269));
#72830=CARTESIAN_POINT('Ctrl Pts',(0.321164934774717,-2.50189336944019,
135.040906898017));
#72831=CARTESIAN_POINT('Ctrl Pts',(0.313390600655622,-2.38318572315328,
135.108815118178));
#72832=CARTESIAN_POINT('Ctrl Pts',(0.305616266536532,-2.26169062463364,
135.171732662737));
#72833=CARTESIAN_POINT('Ctrl Pts',(0.297851513589432,-2.14034525796458,
135.234572667047));
#72834=CARTESIAN_POINT('Ctrl Pts',(0.290086760642295,-2.0162196180991,135.292434055477));
#72835=CARTESIAN_POINT('Ctrl Pts',(0.2823220076952,-1.88976104752747,135.345063894124));
#72836=CARTESIAN_POINT('Ctrl Pts',(0.274564966810206,-1.76342807739106,
135.397641460074));
#72837=CARTESIAN_POINT('Ctrl Pts',(0.26680792592523,-1.63476714629866,135.444997667363));
#72838=CARTESIAN_POINT('Ctrl Pts',(0.259050885040239,-1.50424962010937,
135.486925741822));
#72839=CARTESIAN_POINT('Ctrl Pts',(0.25129969380011,-1.37383051820168,135.528822197994));
#72840=CARTESIAN_POINT('Ctrl Pts',(0.243548502559989,-1.24155797868094,
135.565298549901));
#72841=CARTESIAN_POINT('Ctrl Pts',(0.235797311319857,-1.10792241084239,
135.596196486422));
#72842=CARTESIAN_POINT('Ctrl Pts',(0.228049414542771,-0.974343641685012,
135.627081290495));
#72843=CARTESIAN_POINT('Ctrl Pts',(0.220301517765705,-0.839403376558608,
135.652392306984));
#72844=CARTESIAN_POINT('Ctrl Pts',(0.212553620988615,-0.703606006349638,
135.672021416176));
#72845=CARTESIAN_POINT('Ctrl Pts',(0.204807344904506,-0.567837042023063,
135.691646419382));
#72846=CARTESIAN_POINT('Ctrl Pts',(0.197061068820377,-0.43121171592598,
135.705591823451));
#72847=CARTESIAN_POINT('Ctrl Pts',(0.189314792736269,-0.29424301266107,
135.713800922937));
#72848=CARTESIAN_POINT('Ctrl Pts',(0.181568459470911,-0.157273298324307,
135.722010083021));
#72849=CARTESIAN_POINT('Ctrl Pts',(0.173822126205588,-0.0199605920267424,
135.724482830638));
#72850=CARTESIAN_POINT('Ctrl Pts',(0.166075792940234,0.117179016906247,
135.721214503995));
#72851=CARTESIAN_POINT('Ctrl Pts',(0.158327724937254,0.254349337303797,
135.717945445434));
#72852=CARTESIAN_POINT('Ctrl Pts',(0.150579656934228,0.391346092421572,
135.708932763584));
#72853=CARTESIAN_POINT('Ctrl Pts',(0.142831588931244,0.527655613250902,
135.694223868855));
#72854=CARTESIAN_POINT('Ctrl Pts',(0.135075286189384,0.664110005461073,
135.679499341337));
#72855=CARTESIAN_POINT('Ctrl Pts',(0.127318983447537,0.799875315000086,
135.659066549428));
#72856=CARTESIAN_POINT('Ctrl Pts',(0.119562680705684,0.93444484706951,135.633024603627));
#72857=CARTESIAN_POINT('Ctrl Pts',(0.11180223819152,1.06908620295001,135.606968758456));
#72858=CARTESIAN_POINT('Ctrl Pts',(0.104041795677362,1.20253012943633,135.575297884282));
#72859=CARTESIAN_POINT('Ctrl Pts',(0.0962813531631923,1.33428346291893,
135.538161490341));
#72860=CARTESIAN_POINT('Ctrl Pts',(0.0885084528977593,1.46624829854894,
135.500965481763));
#72861=CARTESIAN_POINT('Ctrl Pts',(0.0807355526322801,1.59651674621076,
135.458286542488));
#72862=CARTESIAN_POINT('Ctrl Pts',(0.0729626523668401,1.72461320157617,
135.410323314706));
#72863=CARTESIAN_POINT('Ctrl Pts',(0.0654723166047607,1.84805302813424,
135.364103671066));
#72864=CARTESIAN_POINT('Ctrl Pts',(0.0579819808427547,1.9694757516654,135.312977382666));
#72865=CARTESIAN_POINT('Ctrl Pts',(0.0504916450806832,2.08847782231686,
135.257162370192));
#72866=CARTESIAN_POINT('Ctrl Pts',(0.0427173109615991,2.21199189264627,
135.199231114556));
#72867=CARTESIAN_POINT('Ctrl Pts',(0.0349429768424324,2.333289383942,135.136065061507));
#72868=CARTESIAN_POINT('Ctrl Pts',(0.0271686427233533,2.45189476453013,
135.067856263884));
#72869=CARTESIAN_POINT('Ctrl Pts',(0.0194038897762637,2.57035397458675,
134.999731527507));
#72870=CARTESIAN_POINT('Ctrl Pts',(0.0116391368293173,2.68612733967731,
134.926576605057));
#72871=CARTESIAN_POINT('Ctrl Pts',(0.00387438388221995,2.79876025980233,
134.848631141486));
#72872=CARTESIAN_POINT('Ctrl Pts',(-0.00388265700278655,2.91128131132324,
134.770763094449));
#72873=CARTESIAN_POINT('Ctrl Pts',(-0.0116396978878533,3.02066780568661,
134.688114196033));
#72874=CARTESIAN_POINT('Ctrl Pts',(-0.0193967387728549,3.12649099316675,
134.600969253197));
#72875=CARTESIAN_POINT('Ctrl Pts',(-0.0271479300129735,3.2322343785579,
134.51389002704));
#72876=CARTESIAN_POINT('Ctrl Pts',(-0.034899121253116,3.33441950502844,
134.422321752578));
#72877=CARTESIAN_POINT('Ctrl Pts',(-0.0426503124932367,3.43264810274518,
134.326591454013));
#72878=CARTESIAN_POINT('Ctrl Pts',(-0.0503982092703211,3.53083495068769,
134.230901843379));
#72879=CARTESIAN_POINT('Ctrl Pts',(-0.0581461060473619,3.62506833510517,
134.131053999289));
#72880=CARTESIAN_POINT('Ctrl Pts',(-0.0658940028244501,3.71498465622671,
134.027413838737));
#72881=CARTESIAN_POINT('Ctrl Pts',(-0.0736402789085579,3.80488216879225,
133.923795357472));
#72882=CARTESIAN_POINT('Ctrl Pts',(-0.0813865549926884,3.89046415820408,
133.816386432731));
#72883=CARTESIAN_POINT('Ctrl Pts',(-0.089132831076796,3.97140563585688,
133.705588002309));
#72884=CARTESIAN_POINT('Ctrl Pts',(-0.096879164342154,4.05234771100129,
133.594788753999));
#72885=CARTESIAN_POINT('Ctrl Pts',(-0.104625497607482,4.12864897540637,
133.48060026578));
#72886=CARTESIAN_POINT('Ctrl Pts',(-0.112371830872831,4.2000265480877,133.363454218406));
#72887=CARTESIAN_POINT('Ctrl Pts',(-0.120119898875796,4.27142010528143,
133.246281936986));
#72888=CARTESIAN_POINT('Ctrl Pts',(-0.127867966878742,4.33788757326167,
133.126151112269));
#72889=CARTESIAN_POINT('Ctrl Pts',(-0.135616034881707,4.39919118910139,
133.003519535023));
#72890=CARTESIAN_POINT('Ctrl Pts',(-0.14337233762356,4.46055995915363,132.880757623478));
#72891=CARTESIAN_POINT('Ctrl Pts',(-0.151128640365466,4.51675373869174,
132.755490000364));
#72892=CARTESIAN_POINT('Ctrl Pts',(-0.158884943107324,4.56758203127038,
132.628196534011));
#72893=CARTESIAN_POINT('Ctrl Pts',(-0.166645385621494,4.61843745243918,
132.500835127303));
#72894=CARTESIAN_POINT('Ctrl Pts',(-0.174405828135649,4.66392155084546,
132.371446091527));
#72895=CARTESIAN_POINT('Ctrl Pts',(-0.182166270649816,4.7038935458668,132.240525152587));
#72896=CARTESIAN_POINT('Ctrl Pts',(-0.189939170915246,4.74392970748309,
132.109394047734));
#72897=CARTESIAN_POINT('Ctrl Pts',(-0.197712071180702,4.77843598508584,
131.976726504153));
#72898=CARTESIAN_POINT('Ctrl Pts',(-0.20548497144614,4.80732242621845,131.843030032191));
#72899=CARTESIAN_POINT('Ctrl Pts',(-0.212975307208133,4.83515877245517,
131.714193763746));
#72900=CARTESIAN_POINT('Ctrl Pts',(-0.220465642970109,4.85777672603543,
131.584402379861));
#72901=CARTESIAN_POINT('Ctrl Pts',(-0.227955978732098,4.87514150125221,
131.454113189911));
#72902=CARTESIAN_POINT('Ctrl Pts',(-0.235730312851184,4.89316466719935,
131.318884045721));
#72903=CARTESIAN_POINT('Ctrl Pts',(-0.243504646970255,4.90558553471498,
131.182690236381));
#72904=CARTESIAN_POINT('Ctrl Pts',(-0.251278981089342,4.91230864680604,
131.046035649405));
#72905=CARTESIAN_POINT('Ctrl Pts',(-0.25904373403643,4.91902347326231,130.909549476995));
#72906=CARTESIAN_POINT('Ctrl Pts',(-0.26680848698353,4.92005449690303,130.77260404358));
#72907=CARTESIAN_POINT('Ctrl Pts',(-0.274573239930618,4.9153576154106,130.635711350965));
#72908=CARTESIAN_POINT('Ctrl Pts',(-0.282330280815615,4.91066539892708,
130.498954622103));
#72909=CARTESIAN_POINT('Ctrl Pts',(-0.290087321700616,4.90025661206867,
130.362250918003));
#72910=CARTESIAN_POINT('Ctrl Pts',(-0.297844362585607,4.88413912129539,
130.226114903071));
#72911=CARTESIAN_POINT('Ctrl Pts',(-0.305595553825726,4.86803378484729,
130.090081549367));
#72912=CARTESIAN_POINT('Ctrl Pts',(-0.313346745065835,4.84622835906235,
129.954615419408));
#72913=CARTESIAN_POINT('Ctrl Pts',(-0.321097936305961,4.81878270408958,
129.820228353454));
#72914=CARTESIAN_POINT('Ctrl Pts',(-0.32884583308305,4.79134871425227,129.685898405587));
#72915=CARTESIAN_POINT('Ctrl Pts',(-0.336593729860114,4.75827934123794,
129.552646991799));
#72916=CARTESIAN_POINT('Ctrl Pts',(-0.344341626637203,4.71968590681787,
129.420977805946));
#72917=CARTESIAN_POINT('Ctrl Pts',(-0.3520879027213,4.68110054531236,129.289336162449));
#72918=CARTESIAN_POINT('Ctrl Pts',(-0.359834178805475,4.63699353068218,
129.159276463518));
#72919=CARTESIAN_POINT('Ctrl Pts',(-0.367580454889577,4.58752651897107,
129.031288847942));
#72920=CARTESIAN_POINT('Ctrl Pts',(-0.37532678815494,4.53805914210566,128.903300287591));
#72921=CARTESIAN_POINT('Ctrl Pts',(-0.38307312142022,4.48323183015402,128.777384205791));
#72922=CARTESIAN_POINT('Ctrl Pts',(-0.390819454685584,4.42325486427788,
128.654011932319));
#72923=CARTESIAN_POINT('Ctrl Pts',(-0.398567522688563,4.36326446697616,
128.530612030482));
#72924=CARTESIAN_POINT('Ctrl Pts',(-0.406315590691543,4.29812229186158,
128.409757422096));
#72925=CARTESIAN_POINT('Ctrl Pts',(-0.414063658694516,4.22808497460335,
128.291895590937));
#72926=CARTESIAN_POINT('Ctrl Pts',(-0.421819961436367,4.15797322085088,
128.173908494822));
#72927=CARTESIAN_POINT('Ctrl Pts',(-0.4295762641782,4.08295613221147,128.058920866481));
#72928=CARTESIAN_POINT('Ctrl Pts',(-0.437332566920048,4.00333446751986,
127.947352356523));
#72929=CARTESIAN_POINT('Ctrl Pts',(-0.445093009434219,3.92367030634834,
127.835724299092));
#72930=CARTESIAN_POINT('Ctrl Pts',(-0.452853451948422,3.83939691226101,
127.727519304586));
#72931=CARTESIAN_POINT('Ctrl Pts',(-0.460613894462597,3.75085525813705,
127.623123767691));
#72932=CARTESIAN_POINT('Ctrl Pts',(-0.468386794728035,3.66217146908954,
127.518560645811));
#72933=CARTESIAN_POINT('Ctrl Pts',(-0.476159694993406,3.56920599324174,
127.417819489305));
#72934=CARTESIAN_POINT('Ctrl Pts',(-0.483932595258835,3.47233719192184,
127.32125029946));
#72935=CARTESIAN_POINT('Ctrl Pts',(-0.491422931020872,3.37898981552757,
127.228191642909));
#72936=CARTESIAN_POINT('Ctrl Pts',(-0.498913266782951,3.28201820476584,
127.139007104667));
#72937=CARTESIAN_POINT('Ctrl Pts',(-0.506403602544992,3.18178830444075,
127.053973137822));
#72938=CARTESIAN_POINT('Ctrl Pts',(-0.514177936664069,3.0777581569809,126.965715082278));
#72939=CARTESIAN_POINT('Ctrl Pts',(-0.521952270783131,2.96988823026279,
126.881648973993));
#72940=CARTESIAN_POINT('Ctrl Pts',(-0.529726604902208,2.8585508622875,126.802127487148));
#72941=CARTESIAN_POINT('Ctrl Pts',(-0.537491357849296,2.74735070766773,
126.722704003429));
#72942=CARTESIAN_POINT('Ctrl Pts',(-0.545256110796364,2.6326919295012,126.6478142222));
#72943=CARTESIAN_POINT('Ctrl Pts',(-0.553020863743455,2.51498145102755,
126.577771997474));
#72944=CARTESIAN_POINT('Ctrl Pts',(-0.560777904628456,2.39738788426055,
126.507799339673));
#72945=CARTESIAN_POINT('Ctrl Pts',(-0.568534945513503,2.27674898280582,
126.44266485561));
#72946=CARTESIAN_POINT('Ctrl Pts',(-0.576291986398502,2.15350200041664,
126.382640115691));
#72947=CARTESIAN_POINT('Ctrl Pts',(-0.584043177638639,2.03034795953544,
126.322660640895));
#72948=CARTESIAN_POINT('Ctrl Pts',(-0.591794368878808,1.90459010253687,
126.267783410983));
#72949=CARTESIAN_POINT('Ctrl Pts',(-0.599545560118941,1.77669141099953,
126.218234726078));
#72950=CARTESIAN_POINT('Ctrl Pts',(-0.607293456896016,1.64884707981808,
126.168707100685));
#72951=CARTESIAN_POINT('Ctrl Pts',(-0.615041353673047,1.51886408764353,
126.124503656776));
#72952=CARTESIAN_POINT('Ctrl Pts',(-0.622789250450126,1.38722637851992,
126.085802995025));
#72953=CARTESIAN_POINT('Ctrl Pts',(-0.630535526534223,1.25561620516728,
126.047110428618));
#72954=CARTESIAN_POINT('Ctrl Pts',(-0.638281802618316,1.12235237819281,
126.013918465045));
#72955=CARTESIAN_POINT('Ctrl Pts',(-0.646028078702415,0.987934644282463,
125.986356030486));
#72956=CARTESIAN_POINT('Ctrl Pts',(-0.653774411967763,0.853515918130939,
125.958793392467));
#72957=CARTESIAN_POINT('Ctrl Pts',(-0.661520745233132,0.717943651043157,
125.936860444918));
#72958=CARTESIAN_POINT('Ctrl Pts',(-0.669267078498478,0.58172804821215,
125.920635037599));
#72959=CARTESIAN_POINT('Ctrl Pts',(-0.67701514650145,0.445481940841341,
125.904405996712));
#72960=CARTESIAN_POINT('Ctrl Pts',(-0.684763214504406,0.308592599189997,
125.893887085688));
#72961=CARTESIAN_POINT('Ctrl Pts',(-0.692511282507382,0.171575221880894,
125.88910426558));
#72962=CARTESIAN_POINT('Ctrl Pts',(-0.700267585249236,0.0344122208726595,
125.884316362235));
#72963=CARTESIAN_POINT('Ctrl Pts',(-0.708023887991096,-0.102878696273177,
125.885276741654));
#72964=CARTESIAN_POINT('Ctrl Pts',(-0.715780190732943,-0.239781898118024,
125.891959198317));
#72965=CARTESIAN_POINT('Ctrl Pts',(-0.723540633247101,-0.376758169323772,
125.898645221609));
#72966=CARTESIAN_POINT('Ctrl Pts',(-0.731301075761299,-0.513345923722532,
125.911059372217));
#72967=CARTESIAN_POINT('Ctrl Pts',(-0.739061518275463,-0.649035772352037,
125.929123635766));
#72968=CARTESIAN_POINT('Ctrl Pts',(-0.746834418540901,-0.784943442372726,
125.947216897675));
#72969=CARTESIAN_POINT('Ctrl Pts',(-0.754607318806317,-0.91994994098301,
125.970978329594));
#72970=CARTESIAN_POINT('Ctrl Pts',(-0.762380219071758,-1.05355628864653,
126.000278789667));
#72971=CARTESIAN_POINT('Ctrl Pts',(-0.769870554833828,-1.18230570903895,
126.028514104212));
#72972=CARTESIAN_POINT('Ctrl Pts',(-0.777360890595852,-1.30975471117975,
126.061892645352));
#72973=CARTESIAN_POINT('Ctrl Pts',(-0.784851226357915,-1.43547290515126,
126.100255963004));
#72974=CARTESIAN_POINT('Ctrl Pts',(-0.792625560477002,-1.56595774265788,
126.140073837504));
#72975=CARTESIAN_POINT('Ctrl Pts',(-0.800399894596131,-1.69499127069482,
126.18538807693));
#72976=CARTESIAN_POINT('Ctrl Pts',(-0.808174228715217,-1.82207551670014,
126.236076051786));
#72977=CARTESIAN_POINT('Ctrl Pts',(-0.815938981662313,-1.94900314273009,
126.286701558243));
#72978=CARTESIAN_POINT('Ctrl Pts',(-0.823703734609309,-2.0739859069617,
126.342687479582));
#72979=CARTESIAN_POINT('Ctrl Pts',(-0.831468487556407,-2.19653980317599,
126.403861105515));
#72980=CARTESIAN_POINT('Ctrl Pts',(-0.839225528441424,-2.31897197713303,
126.46497397294));
#72981=CARTESIAN_POINT('Ctrl Pts',(-0.846982569326493,-2.43897973628546,
126.531264117771));
#72982=CARTESIAN_POINT('Ctrl Pts',(-0.85473961021151,-2.55609825442499,
126.602510456479));
#72983=CARTESIAN_POINT('Ctrl Pts',(-0.862490801451634,-2.67312845257861,
126.673703067769));
#72984=CARTESIAN_POINT('Ctrl Pts',(-0.870241992691742,-2.78727341382176,
126.749844231291));
#72985=CARTESIAN_POINT('Ctrl Pts',(-0.877993183931864,-2.89809249259907,
126.830666748275));
#72986=CARTESIAN_POINT('Ctrl Pts',(-0.885741080708949,-3.00886447031184,
126.911454913534));
#72987=CARTESIAN_POINT('Ctrl Pts',(-0.893488977486078,-3.11631306186053,
126.996920244998));
#72988=CARTESIAN_POINT('Ctrl Pts',(-0.901236874263162,-3.22002642186285,
127.086752124865));
#72989=CARTESIAN_POINT('Ctrl Pts',(-0.908983150347267,-3.32371808726606,
127.176565213839));
#72990=CARTESIAN_POINT('Ctrl Pts',(-0.916729426431294,-3.42367577989525,
127.27074277863));
#72991=CARTESIAN_POINT('Ctrl Pts',(-0.924475702515394,-3.51952090521268,
127.368934055948));
#72992=CARTESIAN_POINT('Ctrl Pts',(-0.932222035780745,-3.61536673803706,
127.467126058092));
#72993=CARTESIAN_POINT('Ctrl Pts',(-0.939968369046134,-3.70709966988091,
127.569331552107));
#72994=CARTESIAN_POINT('Ctrl Pts',(-0.947714702311487,-3.79437842516739,
127.675163367611));
#72995=CARTESIAN_POINT('Ctrl Pts',(-0.955462770314454,-3.88167672592585,
127.781018883417));
#72996=CARTESIAN_POINT('Ctrl Pts',(-0.963210838317446,-3.96451861655245,
127.890502035108));
#72997=CARTESIAN_POINT('Ctrl Pts',(-0.970958906320419,-4.04260377783632,
128.003193404077));
#72998=CARTESIAN_POINT('Ctrl Pts',(-0.978715209062279,-4.12077192895895,
128.116004542775));
#72999=CARTESIAN_POINT('Ctrl Pts',(-0.986471511804122,-4.1941730287884,
128.232030388185));
#73000=CARTESIAN_POINT('Ctrl Pts',(-0.99422781454598,-4.26255041338435,
128.350822960252));
#73001=CARTESIAN_POINT('Ctrl Pts',(-1.00198825706015,-4.33096429304925,
128.469678935492));
#73002=CARTESIAN_POINT('Ctrl Pts',(-1.00974869957436,-4.39434893414989,
128.59130423327));
#73003=CARTESIAN_POINT('Ctrl Pts',(-1.01750914208853,-4.4524946352122,128.715228121551));
#73004=CARTESIAN_POINT('Ctrl Pts',(-1.02528204235397,-4.51073367691587,
128.839350943459));
#73005=CARTESIAN_POINT('Ctrl Pts',(-1.03305494261941,-4.56371682149993,
128.96577936868));
#73006=CARTESIAN_POINT('Ctrl Pts',(-1.04082784288485,-4.61128300903725,
129.094023787271));
#73007=CARTESIAN_POINT('Ctrl Pts',(-1.04831817864682,-4.65712004584514,
129.217606198216));
#73008=CARTESIAN_POINT('Ctrl Pts',(-1.05580851440876,-4.6979270326267,129.342874570061));
#73009=CARTESIAN_POINT('Ctrl Pts',(-1.06329885017072,-4.73360464165935,
129.469381157439));
#73010=CARTESIAN_POINT('Ctrl Pts',(-1.06552363953777,-4.74420165195899,
129.506956310196));
#73011=CARTESIAN_POINT('Ctrl Pts',(-1.0677484289048,-4.75435258515985,129.544662390509));
#73012=CARTESIAN_POINT('Ctrl Pts',(-1.06997321827188,-4.76405452823403,
129.582490119308));
#73013=CARTESIAN_POINT('Origin',(213.235140564004,0.,130.804360617566));
#73014=CARTESIAN_POINT('',(-3.16500955108754,-4.76405452823408,129.582490119308));
#73015=CARTESIAN_POINT('',(-2.82009873120266,-4.76405452823402,129.582490119308));
#73016=CARTESIAN_POINT('',(213.235140564004,-4.76405452823405,129.582490119308));
#73017=CARTESIAN_POINT('',(-1.48514056405364,-4.91824949356997,130.806592544705));
#73018=CARTESIAN_POINT('Ctrl Pts',(-1.48514056405364,-4.91824949356997,
130.806592544705));
#73019=CARTESIAN_POINT('Ctrl Pts',(-1.49361211986651,-4.91818127701446,
130.956913777718));
#73020=CARTESIAN_POINT('Ctrl Pts',(-1.50208367567946,-4.91121731645437,
131.107008485491));
#73021=CARTESIAN_POINT('Ctrl Pts',(-1.51055523149233,-4.89744448273245,
131.256268352677));
#73022=CARTESIAN_POINT('Ctrl Pts',(-1.51906731434727,-4.88360576120622,
131.406242263547));
#73023=CARTESIAN_POINT('Ctrl Pts',(-1.52757939720221,-4.86289295069057,
131.55537307392));
#73024=CARTESIAN_POINT('Ctrl Pts',(-1.53609148005714,-4.83544460907228,
131.703058840049));
#73025=CARTESIAN_POINT('Ctrl Pts',(-1.54462433530355,-4.80792928411897,
131.851105009924));
#73026=CARTESIAN_POINT('Ctrl Pts',(-1.55315719054997,-4.77364563370778,
131.997698835767));
#73027=CARTESIAN_POINT('Ctrl Pts',(-1.56169004579638,-4.73278221413539,
132.142252831484));
#73028=CARTESIAN_POINT('Ctrl Pts',(-1.5702524089246,-4.691777482784,132.287306716406));
#73029=CARTESIAN_POINT('Ctrl Pts',(-1.57881477205279,-4.64414752127059,
132.430306405755));
#73030=CARTESIAN_POINT('Ctrl Pts',(-1.58737713518101,-4.59013027638844,
132.570680834368));
#73031=CARTESIAN_POINT('Ctrl Pts',(-1.59178645733306,-4.56231325544641,
132.64296883108));
#73032=CARTESIAN_POINT('Ctrl Pts',(-1.5961957794851,-4.53280315123714,132.714561023417));
#73033=CARTESIAN_POINT('Ctrl Pts',(-1.60060510163714,-4.50163716490563,
132.785382045527));
#73034=CARTESIAN_POINT('Ctrl Pts',(-1.6083794357562,-4.4466865891624,132.910250737257));
#73035=CARTESIAN_POINT('Ctrl Pts',(-1.6161537698753,-4.38644953171332,133.033029108977));
#73036=CARTESIAN_POINT('Ctrl Pts',(-1.62392810399439,-4.32110657864136,
133.153237157217));
#73037=CARTESIAN_POINT('Ctrl Pts',(-1.63169285694149,-4.25584415491919,
133.27329705978));
#73038=CARTESIAN_POINT('Ctrl Pts',(-1.63945760988856,-4.18548854081923,
133.390792601431));
#73039=CARTESIAN_POINT('Ctrl Pts',(-1.64722236283566,-4.11026840313648,
133.505263562264));
#73040=CARTESIAN_POINT('Ctrl Pts',(-1.65497940372067,-4.03512297515488,
133.619620828925));
#73041=CARTESIAN_POINT('Ctrl Pts',(-1.6627364446057,-3.95512285183305,133.730959168355));
#73042=CARTESIAN_POINT('Ctrl Pts',(-1.67049348549071,-3.87054246929996,
133.838843119715));
#73043=CARTESIAN_POINT('Ctrl Pts',(-1.67824467673084,-3.78602586949127,
133.946645714947));
#73044=CARTESIAN_POINT('Ctrl Pts',(-1.68599586797096,-3.69693612571028,
134.050998800732));
#73045=CARTESIAN_POINT('Ctrl Pts',(-1.69374705921109,-3.60359061060528,
134.151496374248));
#73046=CARTESIAN_POINT('Ctrl Pts',(-1.70149495598818,-3.51028476983427,
134.251951233614));
#73047=CARTESIAN_POINT('Ctrl Pts',(-1.70924285276531,-3.412727020853,134.348553554092));
#73048=CARTESIAN_POINT('Ctrl Pts',(-1.71699074954239,-3.31127444988671,
134.440931059621));
#73049=CARTESIAN_POINT('Ctrl Pts',(-1.72473702562649,-3.20984310061121,
134.533289241767));
#73050=CARTESIAN_POINT('Ctrl Pts',(-1.73248330171057,-3.10451883875693,
134.621424103715));
#73051=CARTESIAN_POINT('Ctrl Pts',(-1.74022957779468,-2.99569468782962,
134.705001129047));
#73052=CARTESIAN_POINT('Ctrl Pts',(-1.74797591106004,-2.88686973358715,
134.788578771326));
#73053=CARTESIAN_POINT('Ctrl Pts',(-1.75572224432536,-2.77454514879164,
134.867598271717));
#73054=CARTESIAN_POINT('Ctrl Pts',(-1.76346857759071,-2.65914570151932,
134.941766471551));
#73055=CARTESIAN_POINT('Ctrl Pts',(-1.77121664559369,-2.54372041134091,
135.015951280839));
#73056=CARTESIAN_POINT('Ctrl Pts',(-1.77896471359672,-2.42521921729389,
135.085282416387));
#73057=CARTESIAN_POINT('Ctrl Pts',(-1.7867127815997,-2.30409407265979,135.149511198022));
#73058=CARTESIAN_POINT('Ctrl Pts',(-1.79446908434156,-2.18284019478057,
135.21380824277));
#73059=CARTESIAN_POINT('Ctrl Pts',(-1.80222538708341,-2.05895714141268,
135.272991917442));
#73060=CARTESIAN_POINT('Ctrl Pts',(-1.80998168982526,-1.93292007130647,
135.326860264934));
#73061=CARTESIAN_POINT('Ctrl Pts',(-1.81774213233943,-1.80681573142104,
135.380757363585));
#73062=CARTESIAN_POINT('Ctrl Pts',(-1.82550257485362,-1.67855544943819,
135.429333343788));
#73063=CARTESIAN_POINT('Ctrl Pts',(-1.83326301736778,-1.54863143016031,
135.472435569409));
#73064=CARTESIAN_POINT('Ctrl Pts',(-1.84103591763322,-1.41849884531257,
135.515606986548));
#73065=CARTESIAN_POINT('Ctrl Pts',(-1.84880881789865,-1.2866975622245,135.553286982436));
#73066=CARTESIAN_POINT('Ctrl Pts',(-1.85658171816408,-1.15373278648152,
135.585373451673));
#73067=CARTESIAN_POINT('Ctrl Pts',(-1.86407205392605,-1.02560161525594,
135.616293496932));
#73068=CARTESIAN_POINT('Ctrl Pts',(-1.87156238968801,-0.896390376604573,
135.642019572439));
#73069=CARTESIAN_POINT('Ctrl Pts',(-1.87905272544998,-0.766555413447032,
135.662505928342));
#73070=CARTESIAN_POINT('Ctrl Pts',(-1.88682705956907,-0.63179771819775,
135.683769030656));
#73071=CARTESIAN_POINT('Ctrl Pts',(-1.89460139368816,-0.49594119588205,
135.699454597165));
#73072=CARTESIAN_POINT('Ctrl Pts',(-1.90237572780725,-0.359487298203495,
135.709455106455));
#73073=CARTESIAN_POINT('Ctrl Pts',(-1.91014048075434,-0.223201567758778,
135.719443291011));
#73074=CARTESIAN_POINT('Ctrl Pts',(-1.91790523370135,-0.0863203129693952,
135.723760330545));
#73075=CARTESIAN_POINT('Ctrl Pts',(-1.92566998664844,0.0506456701371081,
135.722349848806));
#73076=CARTESIAN_POINT('Ctrl Pts',(-1.93342702753344,0.187475616698308,
135.720940767978));
#73077=CARTESIAN_POINT('Ctrl Pts',(-1.94118406841856,0.324389735692955,
135.713815490558));
#73078=CARTESIAN_POINT('Ctrl Pts',(-1.94894110930355,0.460873322153924,
135.700969530214));
#73079=CARTESIAN_POINT('Ctrl Pts',(-1.95669230054366,0.597253985280655,
135.688133257109));
#73080=CARTESIAN_POINT('Ctrl Pts',(-1.96444349178378,0.733204374435617,
135.669584924346));
#73081=CARTESIAN_POINT('Ctrl Pts',(-1.9721946830239,0.868211360278723,135.645372092081));
#73082=CARTESIAN_POINT('Ctrl Pts',(-1.97994257980098,1.00316096455142,135.621169550915));
#73083=CARTESIAN_POINT('Ctrl Pts',(-1.98769047657804,1.13716757899451,135.59130736758));
#73084=CARTESIAN_POINT('Ctrl Pts',(-1.99543837335511,1.26972498338656,135.555884744524));
#73085=CARTESIAN_POINT('Ctrl Pts',(-2.00318464943921,1.40225465962722,135.520469531117));
#73086=CARTESIAN_POINT('Ctrl Pts',(-2.01093092552328,1.53333535131349,135.479496292378));
#73087=CARTESIAN_POINT('Ctrl Pts',(-2.01867720160737,1.66247318150371,135.433114875817));
#73088=CARTESIAN_POINT('Ctrl Pts',(-2.02642353487273,1.79161196496023,135.38673311688));
#73089=CARTESIAN_POINT('Ctrl Pts',(-2.03416986813814,1.91880749035037,135.334943232614));
#73090=CARTESIAN_POINT('Ctrl Pts',(-2.0419162014035,2.04358351746206,135.277944133011));
#73091=CARTESIAN_POINT('Ctrl Pts',(-2.04966426940647,2.16838748729972,135.220932268854));
#73092=CARTESIAN_POINT('Ctrl Pts',(-2.05741233740945,2.29077052513087,135.158709030445));
#73093=CARTESIAN_POINT('Ctrl Pts',(-2.06516040541243,2.41027911749444,135.091520241171));
#73094=CARTESIAN_POINT('Ctrl Pts',(-2.07291670815428,2.52991472501214,135.024260042852));
#73095=CARTESIAN_POINT('Ctrl Pts',(-2.08067301089608,2.64666944303948,134.952023943305));
#73096=CARTESIAN_POINT('Ctrl Pts',(-2.08842931363793,2.76011652443431,134.875102544297));
#73097=CARTESIAN_POINT('Ctrl Pts',(-2.0961897561521,2.87362415595247,134.798140090022));
#73098=CARTESIAN_POINT('Ctrl Pts',(-2.10395019866628,2.98382031918437,134.716487586104));
#73099=CARTESIAN_POINT('Ctrl Pts',(-2.11171064118045,3.09031054830751,134.630476634824));
#73100=CARTESIAN_POINT('Ctrl Pts',(-2.11948354144589,3.1969717250002,134.54432761113));
#73101=CARTESIAN_POINT('Ctrl Pts',(-2.12725644171136,3.29991478562881,134.453806417024));
#73102=CARTESIAN_POINT('Ctrl Pts',(-2.1350293419768,3.39878075006804,134.359282905812));
#73103=CARTESIAN_POINT('Ctrl Pts',(-2.14251967773885,3.4940526876717,134.268195562322));
#73104=CARTESIAN_POINT('Ctrl Pts',(-2.15001001350078,3.58553859424845,134.173392059997));
#73105=CARTESIAN_POINT('Ctrl Pts',(-2.15750034926282,3.67295331465585,134.075231604147));
#73106=CARTESIAN_POINT('Ctrl Pts',(-2.16527468338191,3.7636823907565,133.973349364778));
#73107=CARTESIAN_POINT('Ctrl Pts',(-2.173049017501,3.85031287089078,133.867527856737));
#73108=CARTESIAN_POINT('Ctrl Pts',(-2.18082335162009,3.93248324735283,133.758130847592));
#73109=CARTESIAN_POINT('Ctrl Pts',(-2.18858810456719,4.01455235616967,133.648868660484));
#73110=CARTESIAN_POINT('Ctrl Pts',(-2.19635285751436,4.09217206551828,133.536040049468));
#73111=CARTESIAN_POINT('Ctrl Pts',(-2.20411761046145,4.1650188467341,133.42004428897));
#73112=CARTESIAN_POINT('Ctrl Pts',(-2.21187465134644,4.23779327549977,133.304163737096));
#73113=CARTESIAN_POINT('Ctrl Pts',(-2.21963169223139,4.30580400343781,133.185122624687));
#73114=CARTESIAN_POINT('Ctrl Pts',(-2.22738873311638,4.36876904546301,133.063351562635));
#73115=CARTESIAN_POINT('Ctrl Pts',(-2.23513992435652,4.43168660506031,132.941672329089));
#73116=CARTESIAN_POINT('Ctrl Pts',(-2.24289111559669,4.48956587350178,132.81726758945));
#73117=CARTESIAN_POINT('Ctrl Pts',(-2.25064230683682,4.54216950555128,132.690594761393));
#73118=CARTESIAN_POINT('Ctrl Pts',(-2.2583902036139,4.59475077965385,132.563975772667));
#73119=CARTESIAN_POINT('Ctrl Pts',(-2.26613810039093,4.64206072747275,132.435090973155));
#73120=CARTESIAN_POINT('Ctrl Pts',(-2.27388599716801,4.68390918644363,132.304419881612));
#73121=CARTESIAN_POINT('Ctrl Pts',(-2.28163227325211,4.72574889161904,132.173776123644));
#73122=CARTESIAN_POINT('Ctrl Pts',(-2.2893785493362,4.76212926112554,132.041347188965));
#73123=CARTESIAN_POINT('Ctrl Pts',(-2.2971248254203,4.79290941336774,131.907629586472));
#73124=CARTESIAN_POINT('Ctrl Pts',(-2.30487115868564,4.82368979282204,131.773910996906));
#73125=CARTESIAN_POINT('Ctrl Pts',(-2.31261749195099,4.84886978482011,131.638904101547));
#73126=CARTESIAN_POINT('Ctrl Pts',(-2.32036382521633,4.86835931850332,131.503117090482));
#73127=CARTESIAN_POINT('Ctrl Pts',(-2.3281118932193,4.88785321673246,131.367299670857));
#73128=CARTESIAN_POINT('Ctrl Pts',(-2.33585996122227,4.90165406532486,131.230702174814));
#73129=CARTESIAN_POINT('Ctrl Pts',(-2.34360802922524,4.90972354735527,131.09383902962));
#73130=CARTESIAN_POINT('Ctrl Pts',(-2.35136433196708,4.91780160572721,130.956830424646));
#73131=CARTESIAN_POINT('Ctrl Pts',(-2.35912063470901,4.92013610633213,130.819555997434));
#73132=CARTESIAN_POINT('Ctrl Pts',(-2.36687693745085,4.91674087341196,130.682531859794));
#73133=CARTESIAN_POINT('Ctrl Pts',(-2.37463737996501,4.91334382835375,130.545434588247));
#73134=CARTESIAN_POINT('Ctrl Pts',(-2.3823978224791,4.90421098220649,130.408588262362));
#73135=CARTESIAN_POINT('Ctrl Pts',(-2.39015826499326,4.88940810294767,130.27250399654));
#73136=CARTESIAN_POINT('Ctrl Pts',(-2.39793116525869,4.87458146079291,130.136201276173));
#73137=CARTESIAN_POINT('Ctrl Pts',(-2.40570406552415,4.85406665529249,130.00066344725));
#73138=CARTESIAN_POINT('Ctrl Pts',(-2.41347696578958,4.82798081697922,129.866392444662));
#73139=CARTESIAN_POINT('Ctrl Pts',(-2.42096730155164,4.80284326459482,129.737002531226));
#73140=CARTESIAN_POINT('Ctrl Pts',(-2.42845763731369,4.7725327602866,129.608789238297));
#73141=CARTESIAN_POINT('Ctrl Pts',(-2.43594797307574,4.73719738033461,129.482186634215));
#73142=CARTESIAN_POINT('Ctrl Pts',(-2.44372230719482,4.70052224871195,129.35078385392));
#73143=CARTESIAN_POINT('Ctrl Pts',(-2.45149664131394,4.65831750755569,129.22070006755));
#73144=CARTESIAN_POINT('Ctrl Pts',(-2.45927097543301,4.61069380107874,129.092436047033));
#73145=CARTESIAN_POINT('Ctrl Pts',(-2.4670357283801,4.56312878656376,128.964330100459));
#73146=CARTESIAN_POINT('Ctrl Pts',(-2.47480048132721,4.51015822951373,128.838039820433));
#73147=CARTESIAN_POINT('Ctrl Pts',(-2.48256523427429,4.45194317566456,128.714053218365));
#73148=CARTESIAN_POINT('Ctrl Pts',(-2.49032227515928,4.39378594182755,128.590189761538));
#73149=CARTESIAN_POINT('Ctrl Pts',(-2.49807931604422,4.33039474224271,128.468625780962));
#73150=CARTESIAN_POINT('Ctrl Pts',(-2.50583635692922,4.26197944222431,128.349831274381));
#73151=CARTESIAN_POINT('Ctrl Pts',(-2.51358754816935,4.19361573471585,128.231126351661));
#73152=CARTESIAN_POINT('Ctrl Pts',(-2.52133873940951,4.12023566230551,128.115187083367));
#73153=CARTESIAN_POINT('Ctrl Pts',(-2.52908993064963,4.04209577253818,128.00246040019));
#73154=CARTESIAN_POINT('Ctrl Pts',(-2.53683782742671,3.96398909430844,127.889781628862));
#73155=CARTESIAN_POINT('Ctrl Pts',(-2.54458572420377,3.88112684467706,127.780313047552));
#73156=CARTESIAN_POINT('Ctrl Pts',(-2.55233362098085,3.79380966884344,127.674473837011));
#73157=CARTESIAN_POINT('Ctrl Pts',(-2.56007989706494,3.70651075788066,127.568656765753));
#73158=CARTESIAN_POINT('Ctrl Pts',(-2.56782617314904,3.61475902291083,127.46646785659));
#73159=CARTESIAN_POINT('Ctrl Pts',(-2.57557244923314,3.5188960409885,127.368294012389));
#73160=CARTESIAN_POINT('Ctrl Pts',(-2.58331878249848,3.42303235142755,127.27011944349));
#73161=CARTESIAN_POINT('Ctrl Pts',(-2.59106511576381,3.32305762749868,127.175960278419));
#73162=CARTESIAN_POINT('Ctrl Pts',(-2.59881144902914,3.21935073841554,127.086166985496));
#73163=CARTESIAN_POINT('Ctrl Pts',(-2.6065595170321,3.11562062489366,126.996353583988));
#73164=CARTESIAN_POINT('Ctrl Pts',(-2.61430758503506,3.00815697860004,126.910908256017));
#73165=CARTESIAN_POINT('Ctrl Pts',(-2.62205565303802,2.89737189052766,126.830141299199));
#73166=CARTESIAN_POINT('Ctrl Pts',(-2.62981195577987,2.78646905874518,126.749288502299));
#73167=CARTESIAN_POINT('Ctrl Pts',(-2.6375682585217,2.67223804991851,126.673124239801));
#73168=CARTESIAN_POINT('Ctrl Pts',(-2.64532456126355,2.55512055587069,126.60191585202));
#73169=CARTESIAN_POINT('Ctrl Pts',(-2.65308500377771,2.43794055268995,126.530669458178));
#73170=CARTESIAN_POINT('Ctrl Pts',(-2.66084544629194,2.31787133660872,126.464384398499));
#73171=CARTESIAN_POINT('Ctrl Pts',(-2.6686058888061,2.19537847184615,126.403281610339));
#73172=CARTESIAN_POINT('Ctrl Pts',(-2.67637878907153,2.07268897066249,126.342080734559));
#73173=CARTESIAN_POINT('Ctrl Pts',(-2.68415168933696,1.94756840308402,126.286078914207));
#73174=CARTESIAN_POINT('Ctrl Pts',(-2.69192458960239,1.82050237306414,126.235448912119));
#73175=CARTESIAN_POINT('Ctrl Pts',(-2.69941492536449,1.69805551329447,126.186659438136));
#73176=CARTESIAN_POINT('Ctrl Pts',(-2.70690526112654,1.5738024708093,126.142858107236));
#73177=CARTESIAN_POINT('Ctrl Pts',(-2.71439559688864,1.44818847844375,126.104154963193));
#73178=CARTESIAN_POINT('Ctrl Pts',(-2.72216993100772,1.31781179337922,126.06398437768));
#73179=CARTESIAN_POINT('Ctrl Pts',(-2.72994426512682,1.18555592623878,126.029178957709));
#73180=CARTESIAN_POINT('Ctrl Pts',(-2.73771859924591,1.05190199652772,125.999916294629));
#73181=CARTESIAN_POINT('Ctrl Pts',(-2.74548335219301,0.918412783340025,
125.970689695166));
#73182=CARTESIAN_POINT('Ctrl Pts',(-2.75324810514009,0.783529314064722,
125.946992343851));
#73183=CARTESIAN_POINT('Ctrl Pts',(-2.76101285808718,0.647749215674395,
125.928952530432));
#73184=CARTESIAN_POINT('Ctrl Pts',(-2.76876989897218,0.512103975992138,
125.910930634409));
#73185=CARTESIAN_POINT('Ctrl Pts',(-2.77652693985721,0.375564264470655,
125.898555145085));
#73186=CARTESIAN_POINT('Ctrl Pts',(-2.7842839807422,0.238638940852387,125.891903542089));
#73187=CARTESIAN_POINT('Ctrl Pts',(-2.79203517198233,0.101816873685596,
125.885256955117));
#73188=CARTESIAN_POINT('Ctrl Pts',(-2.79978636322245,-0.0353898378473538,
125.88432568178));
#73189=CARTESIAN_POINT('Ctrl Pts',(-2.80753755446258,-0.172466508081281,
125.889135458319));
#73190=CARTESIAN_POINT('Ctrl Pts',(-2.81528545123967,-0.309484917073719,
125.893943190575));
#73191=CARTESIAN_POINT('Ctrl Pts',(-2.82303334801674,-0.446373004790244,
125.904487105854));
#73192=CARTESIAN_POINT('Ctrl Pts',(-2.83078124479383,-0.582615596518611,
125.92074084027));
#73193=CARTESIAN_POINT('Ctrl Pts',(-2.83852752087793,-0.718829689233839,
125.936991174756));
#73194=CARTESIAN_POINT('Ctrl Pts',(-2.84627379696204,-0.854398166564337,
125.958948906425));
#73195=CARTESIAN_POINT('Ctrl Pts',(-2.85402007304614,-0.988810885431754,
125.986535787277));
#73196=CARTESIAN_POINT('Ctrl Pts',(-2.8617664063115,-1.12322459650333,126.014122871768));
#73197=CARTESIAN_POINT('Ctrl Pts',(-2.86951273957685,-1.2564821491056,126.047339109755));
#73198=CARTESIAN_POINT('Ctrl Pts',(-2.87725907284221,-1.38808389625118,
126.086055184525));
#73199=CARTESIAN_POINT('Ctrl Pts',(-2.88500714084518,-1.5197151146954,126.124779929491));
#73200=CARTESIAN_POINT('Ctrl Pts',(-2.89275520884814,-1.64968941482233,
126.16900685176));
#73201=CARTESIAN_POINT('Ctrl Pts',(-2.90050327685111,-1.77752298921157,
126.218556970949));
#73202=CARTESIAN_POINT('Ctrl Pts',(-2.90825957959297,-1.90549242664508,
126.268159752595));
#73203=CARTESIAN_POINT('Ctrl Pts',(-2.91601588233487,-2.03131622828681,
126.323096891216));
#73204=CARTESIAN_POINT('Ctrl Pts',(-2.92377218507673,-2.15453072794016,
126.383141282941));
#73205=CARTESIAN_POINT('Ctrl Pts',(-2.93153262759091,-2.27781099088207,
126.443217722166));
#73206=CARTESIAN_POINT('Ctrl Pts',(-2.93929307010507,-2.39847883302623,
126.508406660333));
#73207=CARTESIAN_POINT('Ctrl Pts',(-2.94705351261925,-2.51609672468518,
126.578435827117));
#73208=CARTESIAN_POINT('Ctrl Pts',(-2.95482641288468,-2.63390342702529,
126.648577410937));
#73209=CARTESIAN_POINT('Ctrl Pts',(-2.96259931315011,-2.74865006755672,
126.723574536219));
#73210=CARTESIAN_POINT('Ctrl Pts',(-2.97037221341554,-2.85992881521558,
126.803112033136));
#73211=CARTESIAN_POINT('Ctrl Pts',(-2.97786254917752,-2.96716230010203,
126.879758141698));
#73212=CARTESIAN_POINT('Ctrl Pts',(-2.9853528849395,-3.07117540481709,126.96062005611));
#73213=CARTESIAN_POINT('Ctrl Pts',(-2.99284322070147,-3.17163488719524,
127.045382670726));
#73214=CARTESIAN_POINT('Ctrl Pts',(-3.00050565897731,-3.27440258779098,
127.132092842772));
#73215=CARTESIAN_POINT('Ctrl Pts',(-3.00816809725319,-3.37379675582324,
127.223176882538));
#73216=CARTESIAN_POINT('Ctrl Pts',(-3.01583053552906,-3.46941405963075,
127.318338651867));
#73217=CARTESIAN_POINT('Ctrl Pts',(-3.02348417649824,-3.56492158444669,
127.413391165207));
#73218=CARTESIAN_POINT('Ctrl Pts',(-3.03113781746743,-3.6566605822443,127.512511820838));
#73219=CARTESIAN_POINT('Ctrl Pts',(-3.03879145843661,-3.74425962852201,
127.615363455962));
#73220=CARTESIAN_POINT('Ctrl Pts',(-3.04643808230441,-3.83177836120907,
127.718120793436));
#73221=CARTESIAN_POINT('Ctrl Pts',(-3.0540847061722,-3.91516442972166,127.824602004542));
#73222=CARTESIAN_POINT('Ctrl Pts',(-3.06173133004,-3.99408264305215,127.934432586592));
#73223=CARTESIAN_POINT('Ctrl Pts',(-3.06937271037017,-4.07294673960785,
128.044187854255));
#73224=CARTESIAN_POINT('Ctrl Pts',(-3.07701409070032,-4.14734884027291,
128.157287598844));
#73225=CARTESIAN_POINT('Ctrl Pts',(-3.08465547103049,-4.21699387560951,
128.273324127198));
#73226=CARTESIAN_POINT('Ctrl Pts',(-3.09229404773085,-4.28661335811553,
128.389318081639));
#73227=CARTESIAN_POINT('Ctrl Pts',(-3.09993262443121,-4.35147903688056,
128.508246333531));
#73228=CARTESIAN_POINT('Ctrl Pts',(-3.10757120113158,-4.41133929890028,
128.629672443947));
#73229=CARTESIAN_POINT('Ctrl Pts',(-3.11520810678753,-4.4711864656589,128.75107199072));
#73230=CARTESIAN_POINT('Ctrl Pts',(-3.12284501244348,-4.52603021918189,
128.874967946026));
#73231=CARTESIAN_POINT('Ctrl Pts',(-3.13048191809943,-4.57566534712315,
129.00090014014));
#73232=CARTESIAN_POINT('Ctrl Pts',(-3.13812068892218,-4.62531259748629,
129.126863090762));
#73233=CARTESIAN_POINT('Ctrl Pts',(-3.1457594597449,-4.66974853392853,129.254862898307));
#73234=CARTESIAN_POINT('Ctrl Pts',(-3.15339823056763,-4.70881654090428,
129.384420531997));
#73235=CARTESIAN_POINT('Ctrl Pts',(-3.15726867074093,-4.72861166072115,
129.450065264877));
#73236=CARTESIAN_POINT('Ctrl Pts',(-3.16113911091424,-4.74702947019134,
129.516109676391));
#73237=CARTESIAN_POINT('Ctrl Pts',(-3.16500955108754,-4.76405452823408,
129.582490119308));
#73238=CARTESIAN_POINT('Ctrl Pts',(-1.41535445211275,-4.764054528234,129.582490119308));
#73239=CARTESIAN_POINT('Ctrl Pts',(-1.42324132509898,-4.79873248228505,
129.717698935842));
#73240=CARTESIAN_POINT('Ctrl Pts',(-1.43112819808529,-4.82767493793869,
129.854481638264));
#73241=CARTESIAN_POINT('Ctrl Pts',(-1.43901507107151,-4.85075001678642,
129.992321617797));
